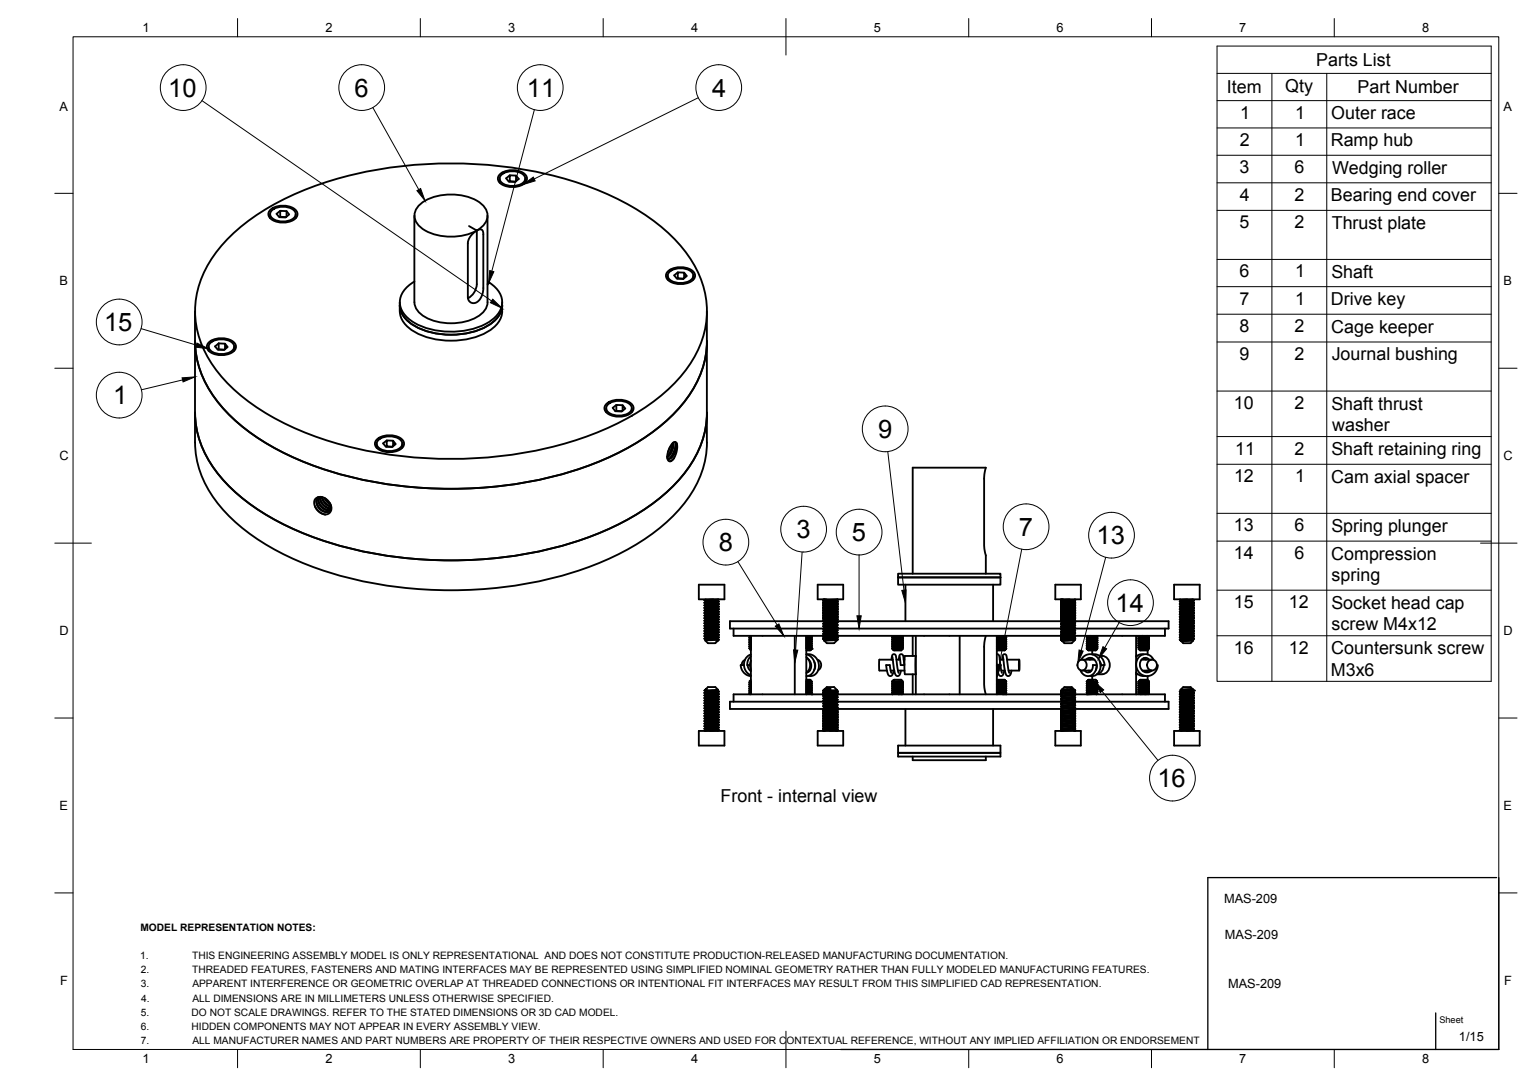
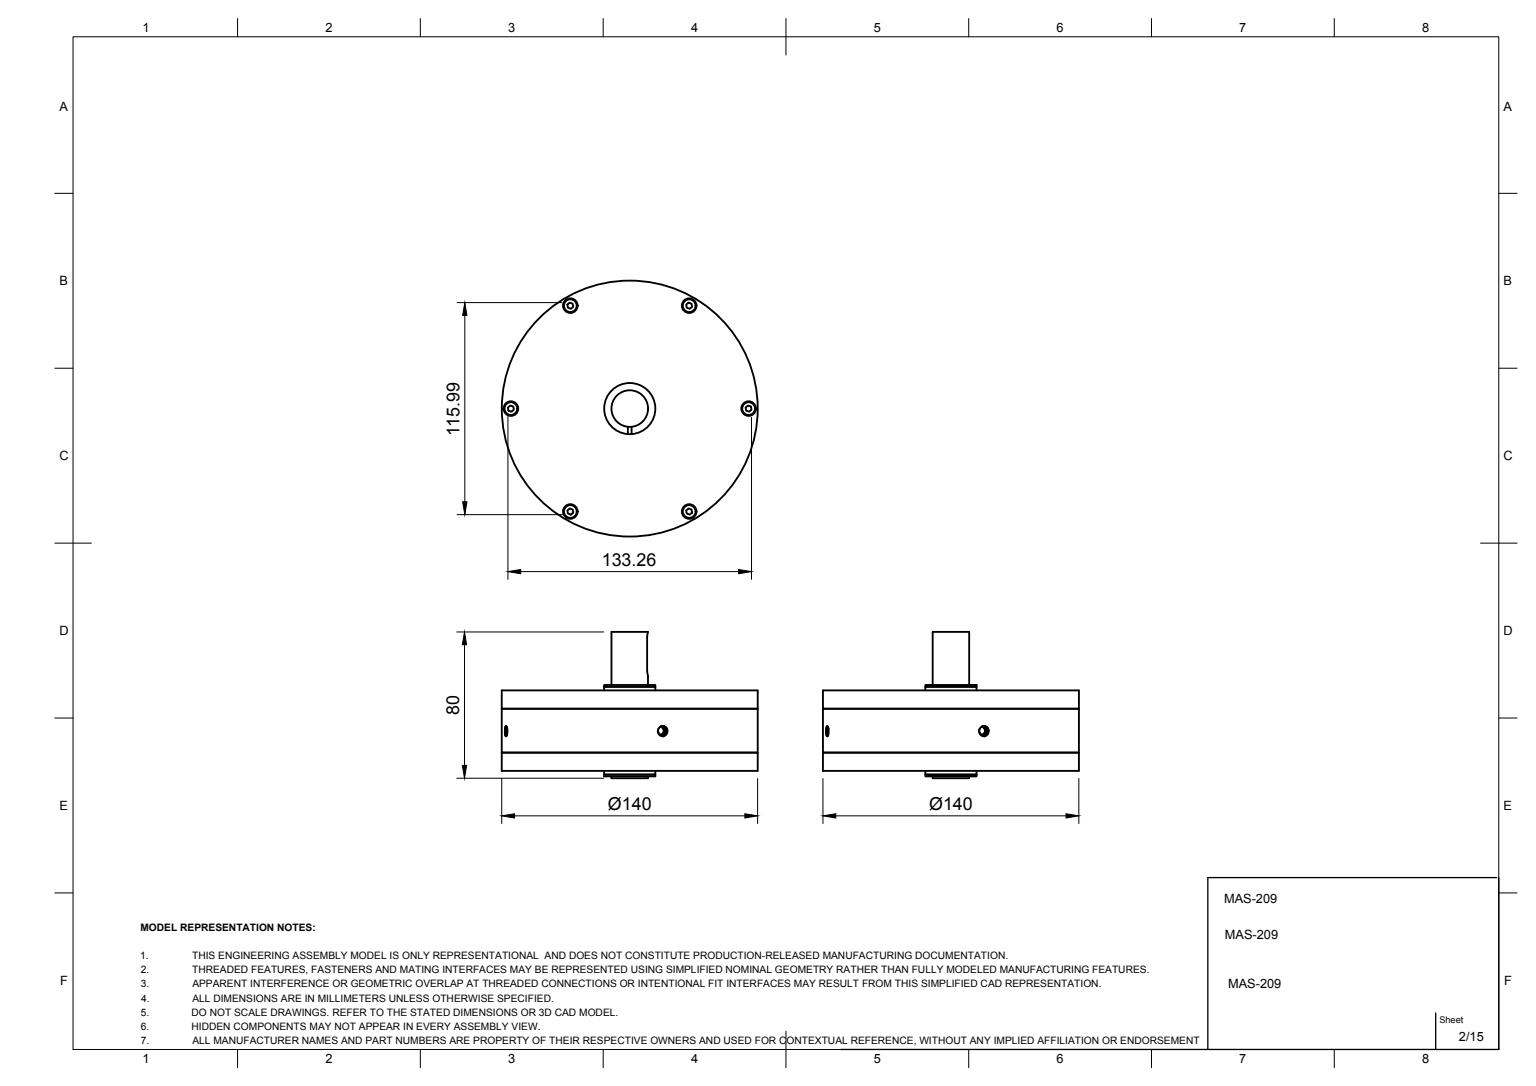
ISO-10303-21;
HEADER;
/* Generated by software containing ST-Developer
 * from STEP Tools, Inc. (www.steptools.com) 
 */

FILE_DESCRIPTION(
/* description */ ('Independent bearing-supported roller-ramp one-way clutch. Six logarit
hmic ramps with plain solid rollers, sprung guided plungers, native Co
il variants, removable shared keepers, rounded parallel key, shaft wit
h complete retaining lips, bronze journal/thrust support and bolted co
vers. Native rotor, roller planar/spin and plunger joints permit manua
l geometric engaged/released inspection. Automatic frictional torque s
witching/contact dynamics are not simulated; no capacity, hardness, fi
t, lubrication, speed, force or life rating. External input driver/cou
pling/anchors outside assembly.'),
/* implementation_level */ '2;1');

FILE_NAME(
/* name */ 'MAS-209.step',
/* time_stamp */ '2026-11-08T07:04:38-08:00',
/* author */ (''),
/* organization */ (''),
/* preprocessor_version */ 'ST-DEVELOPER v20.2',
/* originating_system */ 'Autodesk Translation Framework v15.17.0.0',
/* authorisation */ '');

FILE_SCHEMA (('AUTOMOTIVE_DESIGN { 1 0 10303 214 3 1 1 }'));
ENDSEC;

DATA;
#10=MECHANICAL_DESIGN_GEOMETRIC_PRESENTATION_REPRESENTATION('',(#300,#301,
#302,#303,#304,#305,#306,#307,#308,#309,#310,#311,#312,#313,#314,#315),
#99526);
#11=ITEM_DEFINED_TRANSFORMATION($,$,#18464,#19740);
#12=ITEM_DEFINED_TRANSFORMATION($,$,#18965,#19741);
#13=ITEM_DEFINED_TRANSFORMATION($,$,#19489,#19742);
#14=ITEM_DEFINED_TRANSFORMATION($,$,#19495,#19743);
#15=ITEM_DEFINED_TRANSFORMATION($,$,#19546,#19744);
#16=ITEM_DEFINED_TRANSFORMATION($,$,#19430,#19745);
#17=ITEM_DEFINED_TRANSFORMATION($,$,#19478,#19746);
#18=ITEM_DEFINED_TRANSFORMATION($,$,#19555,#19747);
#19=ITEM_DEFINED_TRANSFORMATION($,$,#19594,#19748);
#20=ITEM_DEFINED_TRANSFORMATION($,$,#19489,#19749);
#21=ITEM_DEFINED_TRANSFORMATION($,$,#19489,#19750);
#22=ITEM_DEFINED_TRANSFORMATION($,$,#19489,#19751);
#23=ITEM_DEFINED_TRANSFORMATION($,$,#19489,#19752);
#24=ITEM_DEFINED_TRANSFORMATION($,$,#19489,#19753);
#25=ITEM_DEFINED_TRANSFORMATION($,$,#19495,#19754);
#26=ITEM_DEFINED_TRANSFORMATION($,$,#19546,#19755);
#27=ITEM_DEFINED_TRANSFORMATION($,$,#19555,#19756);
#28=ITEM_DEFINED_TRANSFORMATION($,$,#19612,#19757);
#29=ITEM_DEFINED_TRANSFORMATION($,$,#19594,#19758);
#30=ITEM_DEFINED_TRANSFORMATION($,$,#19621,#19759);
#31=ITEM_DEFINED_TRANSFORMATION($,$,#19603,#19760);
#32=ITEM_DEFINED_TRANSFORMATION($,$,#19632,#19761);
#33=ITEM_DEFINED_TRANSFORMATION($,$,#19642,#19762);
#34=ITEM_DEFINED_TRANSFORMATION($,$,#19612,#19763);
#35=ITEM_DEFINED_TRANSFORMATION($,$,#19621,#19764);
#36=ITEM_DEFINED_TRANSFORMATION($,$,#19632,#19765);
#37=ITEM_DEFINED_TRANSFORMATION($,$,#19632,#19766);
#38=ITEM_DEFINED_TRANSFORMATION($,$,#19632,#19767);
#39=ITEM_DEFINED_TRANSFORMATION($,$,#19632,#19768);
#40=ITEM_DEFINED_TRANSFORMATION($,$,#19632,#19769);
#41=ITEM_DEFINED_TRANSFORMATION($,$,#19647,#19770);
#42=ITEM_DEFINED_TRANSFORMATION($,$,#19701,#19771);
#43=ITEM_DEFINED_TRANSFORMATION($,$,#19642,#19772);
#44=ITEM_DEFINED_TRANSFORMATION($,$,#19642,#19773);
#45=ITEM_DEFINED_TRANSFORMATION($,$,#19642,#19774);
#46=ITEM_DEFINED_TRANSFORMATION($,$,#19642,#19775);
#47=ITEM_DEFINED_TRANSFORMATION($,$,#19642,#19776);
#48=ITEM_DEFINED_TRANSFORMATION($,$,#19647,#19777);
#49=ITEM_DEFINED_TRANSFORMATION($,$,#19647,#19778);
#50=ITEM_DEFINED_TRANSFORMATION($,$,#19647,#19779);
#51=ITEM_DEFINED_TRANSFORMATION($,$,#19647,#19780);
#52=ITEM_DEFINED_TRANSFORMATION($,$,#19647,#19781);
#53=ITEM_DEFINED_TRANSFORMATION($,$,#19647,#19782);
#54=ITEM_DEFINED_TRANSFORMATION($,$,#19647,#19783);
#55=ITEM_DEFINED_TRANSFORMATION($,$,#19647,#19784);
#56=ITEM_DEFINED_TRANSFORMATION($,$,#19647,#19785);
#57=ITEM_DEFINED_TRANSFORMATION($,$,#19647,#19786);
#58=ITEM_DEFINED_TRANSFORMATION($,$,#19647,#19787);
#59=ITEM_DEFINED_TRANSFORMATION($,$,#19701,#19788);
#60=ITEM_DEFINED_TRANSFORMATION($,$,#19701,#19789);
#61=ITEM_DEFINED_TRANSFORMATION($,$,#19701,#19790);
#62=ITEM_DEFINED_TRANSFORMATION($,$,#19701,#19791);
#63=ITEM_DEFINED_TRANSFORMATION($,$,#19701,#19792);
#64=ITEM_DEFINED_TRANSFORMATION($,$,#19701,#19793);
#65=ITEM_DEFINED_TRANSFORMATION($,$,#19701,#19794);
#66=ITEM_DEFINED_TRANSFORMATION($,$,#19701,#19795);
#67=ITEM_DEFINED_TRANSFORMATION($,$,#19701,#19796);
#68=ITEM_DEFINED_TRANSFORMATION($,$,#19701,#19797);
#69=ITEM_DEFINED_TRANSFORMATION($,$,#19701,#19798);
#70=(
REPRESENTATION_RELATIONSHIP($,$,#99625,#99624)
REPRESENTATION_RELATIONSHIP_WITH_TRANSFORMATION(#11)
SHAPE_REPRESENTATION_RELATIONSHIP()
);
#71=(
REPRESENTATION_RELATIONSHIP($,$,#99626,#99624)
REPRESENTATION_RELATIONSHIP_WITH_TRANSFORMATION(#12)
SHAPE_REPRESENTATION_RELATIONSHIP()
);
#72=(
REPRESENTATION_RELATIONSHIP($,$,#99629,#99624)
REPRESENTATION_RELATIONSHIP_WITH_TRANSFORMATION(#13)
SHAPE_REPRESENTATION_RELATIONSHIP()
);
#73=(
REPRESENTATION_RELATIONSHIP($,$,#99630,#99624)
REPRESENTATION_RELATIONSHIP_WITH_TRANSFORMATION(#14)
SHAPE_REPRESENTATION_RELATIONSHIP()
);
#74=(
REPRESENTATION_RELATIONSHIP($,$,#99631,#99624)
REPRESENTATION_RELATIONSHIP_WITH_TRANSFORMATION(#15)
SHAPE_REPRESENTATION_RELATIONSHIP()
);
#75=(
REPRESENTATION_RELATIONSHIP($,$,#99627,#99624)
REPRESENTATION_RELATIONSHIP_WITH_TRANSFORMATION(#16)
SHAPE_REPRESENTATION_RELATIONSHIP()
);
#76=(
REPRESENTATION_RELATIONSHIP($,$,#99628,#99624)
REPRESENTATION_RELATIONSHIP_WITH_TRANSFORMATION(#17)
SHAPE_REPRESENTATION_RELATIONSHIP()
);
#77=(
REPRESENTATION_RELATIONSHIP($,$,#99632,#99624)
REPRESENTATION_RELATIONSHIP_WITH_TRANSFORMATION(#18)
SHAPE_REPRESENTATION_RELATIONSHIP()
);
#78=(
REPRESENTATION_RELATIONSHIP($,$,#99633,#99624)
REPRESENTATION_RELATIONSHIP_WITH_TRANSFORMATION(#19)
SHAPE_REPRESENTATION_RELATIONSHIP()
);
#79=(
REPRESENTATION_RELATIONSHIP($,$,#99629,#99624)
REPRESENTATION_RELATIONSHIP_WITH_TRANSFORMATION(#20)
SHAPE_REPRESENTATION_RELATIONSHIP()
);
#80=(
REPRESENTATION_RELATIONSHIP($,$,#99629,#99624)
REPRESENTATION_RELATIONSHIP_WITH_TRANSFORMATION(#21)
SHAPE_REPRESENTATION_RELATIONSHIP()
);
#81=(
REPRESENTATION_RELATIONSHIP($,$,#99629,#99624)
REPRESENTATION_RELATIONSHIP_WITH_TRANSFORMATION(#22)
SHAPE_REPRESENTATION_RELATIONSHIP()
);
#82=(
REPRESENTATION_RELATIONSHIP($,$,#99629,#99624)
REPRESENTATION_RELATIONSHIP_WITH_TRANSFORMATION(#23)
SHAPE_REPRESENTATION_RELATIONSHIP()
);
#83=(
REPRESENTATION_RELATIONSHIP($,$,#99629,#99624)
REPRESENTATION_RELATIONSHIP_WITH_TRANSFORMATION(#24)
SHAPE_REPRESENTATION_RELATIONSHIP()
);
#84=(
REPRESENTATION_RELATIONSHIP($,$,#99630,#99624)
REPRESENTATION_RELATIONSHIP_WITH_TRANSFORMATION(#25)
SHAPE_REPRESENTATION_RELATIONSHIP()
);
#85=(
REPRESENTATION_RELATIONSHIP($,$,#99631,#99624)
REPRESENTATION_RELATIONSHIP_WITH_TRANSFORMATION(#26)
SHAPE_REPRESENTATION_RELATIONSHIP()
);
#86=(
REPRESENTATION_RELATIONSHIP($,$,#99632,#99624)
REPRESENTATION_RELATIONSHIP_WITH_TRANSFORMATION(#27)
SHAPE_REPRESENTATION_RELATIONSHIP()
);
#87=(
REPRESENTATION_RELATIONSHIP($,$,#99635,#99624)
REPRESENTATION_RELATIONSHIP_WITH_TRANSFORMATION(#28)
SHAPE_REPRESENTATION_RELATIONSHIP()
);
#88=(
REPRESENTATION_RELATIONSHIP($,$,#99633,#99624)
REPRESENTATION_RELATIONSHIP_WITH_TRANSFORMATION(#29)
SHAPE_REPRESENTATION_RELATIONSHIP()
);
#89=(
REPRESENTATION_RELATIONSHIP($,$,#99636,#99624)
REPRESENTATION_RELATIONSHIP_WITH_TRANSFORMATION(#30)
SHAPE_REPRESENTATION_RELATIONSHIP()
);
#90=(
REPRESENTATION_RELATIONSHIP($,$,#99634,#99624)
REPRESENTATION_RELATIONSHIP_WITH_TRANSFORMATION(#31)
SHAPE_REPRESENTATION_RELATIONSHIP()
);
#91=(
REPRESENTATION_RELATIONSHIP($,$,#99637,#99624)
REPRESENTATION_RELATIONSHIP_WITH_TRANSFORMATION(#32)
SHAPE_REPRESENTATION_RELATIONSHIP()
);
#92=(
REPRESENTATION_RELATIONSHIP($,$,#99638,#99624)
REPRESENTATION_RELATIONSHIP_WITH_TRANSFORMATION(#33)
SHAPE_REPRESENTATION_RELATIONSHIP()
);
#93=(
REPRESENTATION_RELATIONSHIP($,$,#99635,#99624)
REPRESENTATION_RELATIONSHIP_WITH_TRANSFORMATION(#34)
SHAPE_REPRESENTATION_RELATIONSHIP()
);
#94=(
REPRESENTATION_RELATIONSHIP($,$,#99636,#99624)
REPRESENTATION_RELATIONSHIP_WITH_TRANSFORMATION(#35)
SHAPE_REPRESENTATION_RELATIONSHIP()
);
#95=(
REPRESENTATION_RELATIONSHIP($,$,#99637,#99624)
REPRESENTATION_RELATIONSHIP_WITH_TRANSFORMATION(#36)
SHAPE_REPRESENTATION_RELATIONSHIP()
);
#96=(
REPRESENTATION_RELATIONSHIP($,$,#99637,#99624)
REPRESENTATION_RELATIONSHIP_WITH_TRANSFORMATION(#37)
SHAPE_REPRESENTATION_RELATIONSHIP()
);
#97=(
REPRESENTATION_RELATIONSHIP($,$,#99637,#99624)
REPRESENTATION_RELATIONSHIP_WITH_TRANSFORMATION(#38)
SHAPE_REPRESENTATION_RELATIONSHIP()
);
#98=(
REPRESENTATION_RELATIONSHIP($,$,#99637,#99624)
REPRESENTATION_RELATIONSHIP_WITH_TRANSFORMATION(#39)
SHAPE_REPRESENTATION_RELATIONSHIP()
);
#99=(
REPRESENTATION_RELATIONSHIP($,$,#99637,#99624)
REPRESENTATION_RELATIONSHIP_WITH_TRANSFORMATION(#40)
SHAPE_REPRESENTATION_RELATIONSHIP()
);
#100=(
REPRESENTATION_RELATIONSHIP($,$,#99639,#99624)
REPRESENTATION_RELATIONSHIP_WITH_TRANSFORMATION(#41)
SHAPE_REPRESENTATION_RELATIONSHIP()
);
#101=(
REPRESENTATION_RELATIONSHIP($,$,#99640,#99624)
REPRESENTATION_RELATIONSHIP_WITH_TRANSFORMATION(#42)
SHAPE_REPRESENTATION_RELATIONSHIP()
);
#102=(
REPRESENTATION_RELATIONSHIP($,$,#99638,#99624)
REPRESENTATION_RELATIONSHIP_WITH_TRANSFORMATION(#43)
SHAPE_REPRESENTATION_RELATIONSHIP()
);
#103=(
REPRESENTATION_RELATIONSHIP($,$,#99638,#99624)
REPRESENTATION_RELATIONSHIP_WITH_TRANSFORMATION(#44)
SHAPE_REPRESENTATION_RELATIONSHIP()
);
#104=(
REPRESENTATION_RELATIONSHIP($,$,#99638,#99624)
REPRESENTATION_RELATIONSHIP_WITH_TRANSFORMATION(#45)
SHAPE_REPRESENTATION_RELATIONSHIP()
);
#105=(
REPRESENTATION_RELATIONSHIP($,$,#99638,#99624)
REPRESENTATION_RELATIONSHIP_WITH_TRANSFORMATION(#46)
SHAPE_REPRESENTATION_RELATIONSHIP()
);
#106=(
REPRESENTATION_RELATIONSHIP($,$,#99638,#99624)
REPRESENTATION_RELATIONSHIP_WITH_TRANSFORMATION(#47)
SHAPE_REPRESENTATION_RELATIONSHIP()
);
#107=(
REPRESENTATION_RELATIONSHIP($,$,#99639,#99624)
REPRESENTATION_RELATIONSHIP_WITH_TRANSFORMATION(#48)
SHAPE_REPRESENTATION_RELATIONSHIP()
);
#108=(
REPRESENTATION_RELATIONSHIP($,$,#99639,#99624)
REPRESENTATION_RELATIONSHIP_WITH_TRANSFORMATION(#49)
SHAPE_REPRESENTATION_RELATIONSHIP()
);
#109=(
REPRESENTATION_RELATIONSHIP($,$,#99639,#99624)
REPRESENTATION_RELATIONSHIP_WITH_TRANSFORMATION(#50)
SHAPE_REPRESENTATION_RELATIONSHIP()
);
#110=(
REPRESENTATION_RELATIONSHIP($,$,#99639,#99624)
REPRESENTATION_RELATIONSHIP_WITH_TRANSFORMATION(#51)
SHAPE_REPRESENTATION_RELATIONSHIP()
);
#111=(
REPRESENTATION_RELATIONSHIP($,$,#99639,#99624)
REPRESENTATION_RELATIONSHIP_WITH_TRANSFORMATION(#52)
SHAPE_REPRESENTATION_RELATIONSHIP()
);
#112=(
REPRESENTATION_RELATIONSHIP($,$,#99639,#99624)
REPRESENTATION_RELATIONSHIP_WITH_TRANSFORMATION(#53)
SHAPE_REPRESENTATION_RELATIONSHIP()
);
#113=(
REPRESENTATION_RELATIONSHIP($,$,#99639,#99624)
REPRESENTATION_RELATIONSHIP_WITH_TRANSFORMATION(#54)
SHAPE_REPRESENTATION_RELATIONSHIP()
);
#114=(
REPRESENTATION_RELATIONSHIP($,$,#99639,#99624)
REPRESENTATION_RELATIONSHIP_WITH_TRANSFORMATION(#55)
SHAPE_REPRESENTATION_RELATIONSHIP()
);
#115=(
REPRESENTATION_RELATIONSHIP($,$,#99639,#99624)
REPRESENTATION_RELATIONSHIP_WITH_TRANSFORMATION(#56)
SHAPE_REPRESENTATION_RELATIONSHIP()
);
#116=(
REPRESENTATION_RELATIONSHIP($,$,#99639,#99624)
REPRESENTATION_RELATIONSHIP_WITH_TRANSFORMATION(#57)
SHAPE_REPRESENTATION_RELATIONSHIP()
);
#117=(
REPRESENTATION_RELATIONSHIP($,$,#99639,#99624)
REPRESENTATION_RELATIONSHIP_WITH_TRANSFORMATION(#58)
SHAPE_REPRESENTATION_RELATIONSHIP()
);
#118=(
REPRESENTATION_RELATIONSHIP($,$,#99640,#99624)
REPRESENTATION_RELATIONSHIP_WITH_TRANSFORMATION(#59)
SHAPE_REPRESENTATION_RELATIONSHIP()
);
#119=(
REPRESENTATION_RELATIONSHIP($,$,#99640,#99624)
REPRESENTATION_RELATIONSHIP_WITH_TRANSFORMATION(#60)
SHAPE_REPRESENTATION_RELATIONSHIP()
);
#120=(
REPRESENTATION_RELATIONSHIP($,$,#99640,#99624)
REPRESENTATION_RELATIONSHIP_WITH_TRANSFORMATION(#61)
SHAPE_REPRESENTATION_RELATIONSHIP()
);
#121=(
REPRESENTATION_RELATIONSHIP($,$,#99640,#99624)
REPRESENTATION_RELATIONSHIP_WITH_TRANSFORMATION(#62)
SHAPE_REPRESENTATION_RELATIONSHIP()
);
#122=(
REPRESENTATION_RELATIONSHIP($,$,#99640,#99624)
REPRESENTATION_RELATIONSHIP_WITH_TRANSFORMATION(#63)
SHAPE_REPRESENTATION_RELATIONSHIP()
);
#123=(
REPRESENTATION_RELATIONSHIP($,$,#99640,#99624)
REPRESENTATION_RELATIONSHIP_WITH_TRANSFORMATION(#64)
SHAPE_REPRESENTATION_RELATIONSHIP()
);
#124=(
REPRESENTATION_RELATIONSHIP($,$,#99640,#99624)
REPRESENTATION_RELATIONSHIP_WITH_TRANSFORMATION(#65)
SHAPE_REPRESENTATION_RELATIONSHIP()
);
#125=(
REPRESENTATION_RELATIONSHIP($,$,#99640,#99624)
REPRESENTATION_RELATIONSHIP_WITH_TRANSFORMATION(#66)
SHAPE_REPRESENTATION_RELATIONSHIP()
);
#126=(
REPRESENTATION_RELATIONSHIP($,$,#99640,#99624)
REPRESENTATION_RELATIONSHIP_WITH_TRANSFORMATION(#67)
SHAPE_REPRESENTATION_RELATIONSHIP()
);
#127=(
REPRESENTATION_RELATIONSHIP($,$,#99640,#99624)
REPRESENTATION_RELATIONSHIP_WITH_TRANSFORMATION(#68)
SHAPE_REPRESENTATION_RELATIONSHIP()
);
#128=(
REPRESENTATION_RELATIONSHIP($,$,#99640,#99624)
REPRESENTATION_RELATIONSHIP_WITH_TRANSFORMATION(#69)
SHAPE_REPRESENTATION_RELATIONSHIP()
);
#129=CONTEXT_DEPENDENT_SHAPE_REPRESENTATION(#70,#99565);
#130=CONTEXT_DEPENDENT_SHAPE_REPRESENTATION(#71,#99566);
#131=CONTEXT_DEPENDENT_SHAPE_REPRESENTATION(#72,#99567);
#132=CONTEXT_DEPENDENT_SHAPE_REPRESENTATION(#73,#99568);
#133=CONTEXT_DEPENDENT_SHAPE_REPRESENTATION(#74,#99569);
#134=CONTEXT_DEPENDENT_SHAPE_REPRESENTATION(#75,#99570);
#135=CONTEXT_DEPENDENT_SHAPE_REPRESENTATION(#76,#99571);
#136=CONTEXT_DEPENDENT_SHAPE_REPRESENTATION(#77,#99572);
#137=CONTEXT_DEPENDENT_SHAPE_REPRESENTATION(#78,#99573);
#138=CONTEXT_DEPENDENT_SHAPE_REPRESENTATION(#79,#99574);
#139=CONTEXT_DEPENDENT_SHAPE_REPRESENTATION(#80,#99575);
#140=CONTEXT_DEPENDENT_SHAPE_REPRESENTATION(#81,#99576);
#141=CONTEXT_DEPENDENT_SHAPE_REPRESENTATION(#82,#99577);
#142=CONTEXT_DEPENDENT_SHAPE_REPRESENTATION(#83,#99578);
#143=CONTEXT_DEPENDENT_SHAPE_REPRESENTATION(#84,#99579);
#144=CONTEXT_DEPENDENT_SHAPE_REPRESENTATION(#85,#99580);
#145=CONTEXT_DEPENDENT_SHAPE_REPRESENTATION(#86,#99581);
#146=CONTEXT_DEPENDENT_SHAPE_REPRESENTATION(#87,#99582);
#147=CONTEXT_DEPENDENT_SHAPE_REPRESENTATION(#88,#99583);
#148=CONTEXT_DEPENDENT_SHAPE_REPRESENTATION(#89,#99584);
#149=CONTEXT_DEPENDENT_SHAPE_REPRESENTATION(#90,#99585);
#150=CONTEXT_DEPENDENT_SHAPE_REPRESENTATION(#91,#99586);
#151=CONTEXT_DEPENDENT_SHAPE_REPRESENTATION(#92,#99587);
#152=CONTEXT_DEPENDENT_SHAPE_REPRESENTATION(#93,#99588);
#153=CONTEXT_DEPENDENT_SHAPE_REPRESENTATION(#94,#99589);
#154=CONTEXT_DEPENDENT_SHAPE_REPRESENTATION(#95,#99590);
#155=CONTEXT_DEPENDENT_SHAPE_REPRESENTATION(#96,#99591);
#156=CONTEXT_DEPENDENT_SHAPE_REPRESENTATION(#97,#99592);
#157=CONTEXT_DEPENDENT_SHAPE_REPRESENTATION(#98,#99593);
#158=CONTEXT_DEPENDENT_SHAPE_REPRESENTATION(#99,#99594);
#159=CONTEXT_DEPENDENT_SHAPE_REPRESENTATION(#100,#99595);
#160=CONTEXT_DEPENDENT_SHAPE_REPRESENTATION(#101,#99596);
#161=CONTEXT_DEPENDENT_SHAPE_REPRESENTATION(#102,#99597);
#162=CONTEXT_DEPENDENT_SHAPE_REPRESENTATION(#103,#99598);
#163=CONTEXT_DEPENDENT_SHAPE_REPRESENTATION(#104,#99599);
#164=CONTEXT_DEPENDENT_SHAPE_REPRESENTATION(#105,#99600);
#165=CONTEXT_DEPENDENT_SHAPE_REPRESENTATION(#106,#99601);
#166=CONTEXT_DEPENDENT_SHAPE_REPRESENTATION(#107,#99602);
#167=CONTEXT_DEPENDENT_SHAPE_REPRESENTATION(#108,#99603);
#168=CONTEXT_DEPENDENT_SHAPE_REPRESENTATION(#109,#99604);
#169=CONTEXT_DEPENDENT_SHAPE_REPRESENTATION(#110,#99605);
#170=CONTEXT_DEPENDENT_SHAPE_REPRESENTATION(#111,#99606);
#171=CONTEXT_DEPENDENT_SHAPE_REPRESENTATION(#112,#99607);
#172=CONTEXT_DEPENDENT_SHAPE_REPRESENTATION(#113,#99608);
#173=CONTEXT_DEPENDENT_SHAPE_REPRESENTATION(#114,#99609);
#174=CONTEXT_DEPENDENT_SHAPE_REPRESENTATION(#115,#99610);
#175=CONTEXT_DEPENDENT_SHAPE_REPRESENTATION(#116,#99611);
#176=CONTEXT_DEPENDENT_SHAPE_REPRESENTATION(#117,#99612);
#177=CONTEXT_DEPENDENT_SHAPE_REPRESENTATION(#118,#99613);
#178=CONTEXT_DEPENDENT_SHAPE_REPRESENTATION(#119,#99614);
#179=CONTEXT_DEPENDENT_SHAPE_REPRESENTATION(#120,#99615);
#180=CONTEXT_DEPENDENT_SHAPE_REPRESENTATION(#121,#99616);
#181=CONTEXT_DEPENDENT_SHAPE_REPRESENTATION(#122,#99617);
#182=CONTEXT_DEPENDENT_SHAPE_REPRESENTATION(#123,#99618);
#183=CONTEXT_DEPENDENT_SHAPE_REPRESENTATION(#124,#99619);
#184=CONTEXT_DEPENDENT_SHAPE_REPRESENTATION(#125,#99620);
#185=CONTEXT_DEPENDENT_SHAPE_REPRESENTATION(#126,#99621);
#186=CONTEXT_DEPENDENT_SHAPE_REPRESENTATION(#127,#99622);
#187=CONTEXT_DEPENDENT_SHAPE_REPRESENTATION(#128,#99623);
#188=NEXT_ASSEMBLY_USAGE_OCCURRENCE('Outer race:1','Outer race:1',
'Outer race:1',#99642,#99643,'Outer race:1');
#189=NEXT_ASSEMBLY_USAGE_OCCURRENCE('Ramp hub:1','Ramp hub:1',
'Ramp hub:1',#99642,#99644,'Ramp hub:1');
#190=NEXT_ASSEMBLY_USAGE_OCCURRENCE('Wedging roller:1',
'Wedging roller:1','Wedging roller:1',#99642,#99647,'Wedging roller:1');
#191=NEXT_ASSEMBLY_USAGE_OCCURRENCE('Bearing end cover:1',
'Bearing end cover:1','Bearing end cover:1',#99642,#99648,
'Bearing end cover:1');
#192=NEXT_ASSEMBLY_USAGE_OCCURRENCE('Thrust plate:1','Thrust plate:1',
'Thrust plate:1',#99642,#99649,'Thrust plate:1');
#193=NEXT_ASSEMBLY_USAGE_OCCURRENCE('Shaft:1','Shaft:1','Shaft:1',#99642,
#99645,'Shaft:1');
#194=NEXT_ASSEMBLY_USAGE_OCCURRENCE('Drive key:1','Drive key:1',
'Drive key:1',#99642,#99646,'Drive key:1');
#195=NEXT_ASSEMBLY_USAGE_OCCURRENCE('Cage keeper:1','Cage keeper:1',
'Cage keeper:1',#99642,#99650,'Cage keeper:1');
#196=NEXT_ASSEMBLY_USAGE_OCCURRENCE('Journal bushing:1',
'Journal bushing:1','Journal bushing:1',#99642,#99651,
'Journal bushing:1');
#197=NEXT_ASSEMBLY_USAGE_OCCURRENCE('Wedging roller:2',
'Wedging roller:2','Wedging roller:2',#99642,#99647,'Wedging roller:2');
#198=NEXT_ASSEMBLY_USAGE_OCCURRENCE('Wedging roller:3',
'Wedging roller:3','Wedging roller:3',#99642,#99647,'Wedging roller:3');
#199=NEXT_ASSEMBLY_USAGE_OCCURRENCE('Wedging roller:4',
'Wedging roller:4','Wedging roller:4',#99642,#99647,'Wedging roller:4');
#200=NEXT_ASSEMBLY_USAGE_OCCURRENCE('Wedging roller:5',
'Wedging roller:5','Wedging roller:5',#99642,#99647,'Wedging roller:5');
#201=NEXT_ASSEMBLY_USAGE_OCCURRENCE('Wedging roller:6',
'Wedging roller:6','Wedging roller:6',#99642,#99647,'Wedging roller:6');
#202=NEXT_ASSEMBLY_USAGE_OCCURRENCE('Bearing end cover:2',
'Bearing end cover:2','Bearing end cover:2',#99642,#99648,
'Bearing end cover:2');
#203=NEXT_ASSEMBLY_USAGE_OCCURRENCE('Thrust plate:2','Thrust plate:2',
'Thrust plate:2',#99642,#99649,'Thrust plate:2');
#204=NEXT_ASSEMBLY_USAGE_OCCURRENCE('Cage keeper:2','Cage keeper:2',
'Cage keeper:2',#99642,#99650,'Cage keeper:2');
#205=NEXT_ASSEMBLY_USAGE_OCCURRENCE('Shaft thrust washer:1',
'Shaft thrust washer:1','Shaft thrust washer:1',#99642,#99653,
'Shaft thrust washer:1');
#206=NEXT_ASSEMBLY_USAGE_OCCURRENCE('Journal bushing:2',
'Journal bushing:2','Journal bushing:2',#99642,#99651,
'Journal bushing:2');
#207=NEXT_ASSEMBLY_USAGE_OCCURRENCE('Shaft retaining ring:1',
'Shaft retaining ring:1','Shaft retaining ring:1',#99642,#99654,
'Shaft retaining ring:1');
#208=NEXT_ASSEMBLY_USAGE_OCCURRENCE('Cam axial spacer:1',
'Cam axial spacer:1','Cam axial spacer:1',#99642,#99652,
'Cam axial spacer:1');
#209=NEXT_ASSEMBLY_USAGE_OCCURRENCE('Spring plunger:1',
'Spring plunger:1','Spring plunger:1',#99642,#99655,'Spring plunger:1');
#210=NEXT_ASSEMBLY_USAGE_OCCURRENCE('Compression spring:1',
'Compression spring:1','Compression spring:1',#99642,#99656,
'Compression spring:1');
#211=NEXT_ASSEMBLY_USAGE_OCCURRENCE('Shaft thrust washer:2',
'Shaft thrust washer:2','Shaft thrust washer:2',#99642,#99653,
'Shaft thrust washer:2');
#212=NEXT_ASSEMBLY_USAGE_OCCURRENCE('Shaft retaining ring:2',
'Shaft retaining ring:2','Shaft retaining ring:2',#99642,#99654,
'Shaft retaining ring:2');
#213=NEXT_ASSEMBLY_USAGE_OCCURRENCE('Spring plunger:2',
'Spring plunger:2','Spring plunger:2',#99642,#99655,'Spring plunger:2');
#214=NEXT_ASSEMBLY_USAGE_OCCURRENCE('Spring plunger:3',
'Spring plunger:3','Spring plunger:3',#99642,#99655,'Spring plunger:3');
#215=NEXT_ASSEMBLY_USAGE_OCCURRENCE('Spring plunger:4',
'Spring plunger:4','Spring plunger:4',#99642,#99655,'Spring plunger:4');
#216=NEXT_ASSEMBLY_USAGE_OCCURRENCE('Spring plunger:5',
'Spring plunger:5','Spring plunger:5',#99642,#99655,'Spring plunger:5');
#217=NEXT_ASSEMBLY_USAGE_OCCURRENCE('Spring plunger:6',
'Spring plunger:6','Spring plunger:6',#99642,#99655,'Spring plunger:6');
#218=NEXT_ASSEMBLY_USAGE_OCCURRENCE('Socket head cap screw M4x12:1',
'Socket head cap screw M4x12:1','Socket head cap screw M4x12:1',#99642,
#99657,'Socket head cap screw M4x12:1');
#219=NEXT_ASSEMBLY_USAGE_OCCURRENCE('Countersunk screw M3x6:1',
'Countersunk screw M3x6:1','Countersunk screw M3x6:1',#99642,#99658,
'Countersunk screw M3x6:1');
#220=NEXT_ASSEMBLY_USAGE_OCCURRENCE('Compression spring:2',
'Compression spring:2','Compression spring:2',#99642,#99656,
'Compression spring:2');
#221=NEXT_ASSEMBLY_USAGE_OCCURRENCE('Compression spring:3',
'Compression spring:3','Compression spring:3',#99642,#99656,
'Compression spring:3');
#222=NEXT_ASSEMBLY_USAGE_OCCURRENCE('Compression spring:4',
'Compression spring:4','Compression spring:4',#99642,#99656,
'Compression spring:4');
#223=NEXT_ASSEMBLY_USAGE_OCCURRENCE('Compression spring:5',
'Compression spring:5','Compression spring:5',#99642,#99656,
'Compression spring:5');
#224=NEXT_ASSEMBLY_USAGE_OCCURRENCE('Compression spring:6',
'Compression spring:6','Compression spring:6',#99642,#99656,
'Compression spring:6');
#225=NEXT_ASSEMBLY_USAGE_OCCURRENCE('Socket head cap screw M4x12:2',
'Socket head cap screw M4x12:2','Socket head cap screw M4x12:2',#99642,
#99657,'Socket head cap screw M4x12:2');
#226=NEXT_ASSEMBLY_USAGE_OCCURRENCE('Socket head cap screw M4x12:3',
'Socket head cap screw M4x12:3','Socket head cap screw M4x12:3',#99642,
#99657,'Socket head cap screw M4x12:3');
#227=NEXT_ASSEMBLY_USAGE_OCCURRENCE('Socket head cap screw M4x12:4',
'Socket head cap screw M4x12:4','Socket head cap screw M4x12:4',#99642,
#99657,'Socket head cap screw M4x12:4');
#228=NEXT_ASSEMBLY_USAGE_OCCURRENCE('Socket head cap screw M4x12:5',
'Socket head cap screw M4x12:5','Socket head cap screw M4x12:5',#99642,
#99657,'Socket head cap screw M4x12:5');
#229=NEXT_ASSEMBLY_USAGE_OCCURRENCE('Socket head cap screw M4x12:6',
'Socket head cap screw M4x12:6','Socket head cap screw M4x12:6',#99642,
#99657,'Socket head cap screw M4x12:6');
#230=NEXT_ASSEMBLY_USAGE_OCCURRENCE('Socket head cap screw M4x12:7',
'Socket head cap screw M4x12:7','Socket head cap screw M4x12:7',#99642,
#99657,'Socket head cap screw M4x12:7');
#231=NEXT_ASSEMBLY_USAGE_OCCURRENCE('Socket head cap screw M4x12:8',
'Socket head cap screw M4x12:8','Socket head cap screw M4x12:8',#99642,
#99657,'Socket head cap screw M4x12:8');
#232=NEXT_ASSEMBLY_USAGE_OCCURRENCE('Socket head cap screw M4x12:9',
'Socket head cap screw M4x12:9','Socket head cap screw M4x12:9',#99642,
#99657,'Socket head cap screw M4x12:9');
#233=NEXT_ASSEMBLY_USAGE_OCCURRENCE('Socket head cap screw M4x12:10',
'Socket head cap screw M4x12:10','Socket head cap screw M4x12:10',#99642,
#99657,'Socket head cap screw M4x12:10');
#234=NEXT_ASSEMBLY_USAGE_OCCURRENCE('Socket head cap screw M4x12:11',
'Socket head cap screw M4x12:11','Socket head cap screw M4x12:11',#99642,
#99657,'Socket head cap screw M4x12:11');
#235=NEXT_ASSEMBLY_USAGE_OCCURRENCE('Socket head cap screw M4x12:12',
'Socket head cap screw M4x12:12','Socket head cap screw M4x12:12',#99642,
#99657,'Socket head cap screw M4x12:12');
#236=NEXT_ASSEMBLY_USAGE_OCCURRENCE('Countersunk screw M3x6:2',
'Countersunk screw M3x6:2','Countersunk screw M3x6:2',#99642,#99658,
'Countersunk screw M3x6:2');
#237=NEXT_ASSEMBLY_USAGE_OCCURRENCE('Countersunk screw M3x6:3',
'Countersunk screw M3x6:3','Countersunk screw M3x6:3',#99642,#99658,
'Countersunk screw M3x6:3');
#238=NEXT_ASSEMBLY_USAGE_OCCURRENCE('Countersunk screw M3x6:4',
'Countersunk screw M3x6:4','Countersunk screw M3x6:4',#99642,#99658,
'Countersunk screw M3x6:4');
#239=NEXT_ASSEMBLY_USAGE_OCCURRENCE('Countersunk screw M3x6:5',
'Countersunk screw M3x6:5','Countersunk screw M3x6:5',#99642,#99658,
'Countersunk screw M3x6:5');
#240=NEXT_ASSEMBLY_USAGE_OCCURRENCE('Countersunk screw M3x6:6',
'Countersunk screw M3x6:6','Countersunk screw M3x6:6',#99642,#99658,
'Countersunk screw M3x6:6');
#241=NEXT_ASSEMBLY_USAGE_OCCURRENCE('Countersunk screw M3x6:7',
'Countersunk screw M3x6:7','Countersunk screw M3x6:7',#99642,#99658,
'Countersunk screw M3x6:7');
#242=NEXT_ASSEMBLY_USAGE_OCCURRENCE('Countersunk screw M3x6:8',
'Countersunk screw M3x6:8','Countersunk screw M3x6:8',#99642,#99658,
'Countersunk screw M3x6:8');
#243=NEXT_ASSEMBLY_USAGE_OCCURRENCE('Countersunk screw M3x6:9',
'Countersunk screw M3x6:9','Countersunk screw M3x6:9',#99642,#99658,
'Countersunk screw M3x6:9');
#244=NEXT_ASSEMBLY_USAGE_OCCURRENCE('Countersunk screw M3x6:10',
'Countersunk screw M3x6:10','Countersunk screw M3x6:10',#99642,#99658,
'Countersunk screw M3x6:10');
#245=NEXT_ASSEMBLY_USAGE_OCCURRENCE('Countersunk screw M3x6:11',
'Countersunk screw M3x6:11','Countersunk screw M3x6:11',#99642,#99658,
'Countersunk screw M3x6:11');
#246=NEXT_ASSEMBLY_USAGE_OCCURRENCE('Countersunk screw M3x6:12',
'Countersunk screw M3x6:12','Countersunk screw M3x6:12',#99642,#99658,
'Countersunk screw M3x6:12');
#247=CONICAL_SURFACE('',#19556,2.5,0.785398163397448);
#248=CONICAL_SURFACE('',#19561,2.5,0.785398163397448);
#249=CONICAL_SURFACE('',#19566,2.5,0.785398163397448);
#250=CONICAL_SURFACE('',#19571,2.5,0.785398163397448);
#251=CONICAL_SURFACE('',#19576,2.5,0.785398163397448);
#252=CONICAL_SURFACE('',#19581,2.5,0.785398163397448);
#253=CONICAL_SURFACE('',#19682,1.5,0.785398163397449);
#254=CONICAL_SURFACE('',#19720,1.25,0.785398163397449);
#255=CONICAL_SURFACE('',#19738,2.25,0.785398163397448);
#256=(
BOUNDED_SURFACE()
B_SPLINE_SURFACE(5,1,((#70021,#70022),(#70023,#70024),(#70025,#70026),(#70027,
#70028),(#70029,#70030),(#70031,#70032),(#70033,#70034),(#70035,#70036),
(#70037,#70038),(#70039,#70040),(#70041,#70042),(#70043,#70044),(#70045,
#70046),(#70047,#70048),(#70049,#70050),(#70051,#70052),(#70053,#70054),
(#70055,#70056),(#70057,#70058),(#70059,#70060),(#70061,#70062),(#70063,
#70064),(#70065,#70066),(#70067,#70068),(#70069,#70070),(#70071,#70072),
(#70073,#70074),(#70075,#70076),(#70077,#70078),(#70079,#70080),(#70081,
#70082),(#70083,#70084),(#70085,#70086),(#70087,#70088),(#70089,#70090),
(#70091,#70092),(#70093,#70094),(#70095,#70096),(#70097,#70098),(#70099,
#70100),(#70101,#70102),(#70103,#70104),(#70105,#70106),(#70107,#70108),
(#70109,#70110),(#70111,#70112),(#70113,#70114),(#70115,#70116),(#70117,
#70118),(#70119,#70120),(#70121,#70122),(#70123,#70124),(#70125,#70126),
(#70127,#70128),(#70129,#70130),(#70131,#70132),(#70133,#70134),(#70135,
#70136),(#70137,#70138),(#70139,#70140),(#70141,#70142),(#70143,#70144),
(#70145,#70146),(#70147,#70148),(#70149,#70150),(#70151,#70152),(#70153,
#70154),(#70155,#70156),(#70157,#70158),(#70159,#70160),(#70161,#70162),
(#70163,#70164),(#70165,#70166),(#70167,#70168),(#70169,#70170),(#70171,
#70172),(#70173,#70174),(#70175,#70176),(#70177,#70178),(#70179,#70180),
(#70181,#70182),(#70183,#70184),(#70185,#70186),(#70187,#70188),(#70189,
#70190),(#70191,#70192),(#70193,#70194),(#70195,#70196),(#70197,#70198),
(#70199,#70200),(#70201,#70202),(#70203,#70204),(#70205,#70206),(#70207,
#70208),(#70209,#70210),(#70211,#70212),(#70213,#70214),(#70215,#70216),
(#70217,#70218),(#70219,#70220),(#70221,#70222),(#70223,#70224),(#70225,
#70226),(#70227,#70228),(#70229,#70230),(#70231,#70232),(#70233,#70234),
(#70235,#70236),(#70237,#70238),(#70239,#70240),(#70241,#70242),(#70243,
#70244),(#70245,#70246),(#70247,#70248),(#70249,#70250),(#70251,#70252),
(#70253,#70254),(#70255,#70256),(#70257,#70258),(#70259,#70260),(#70261,
#70262),(#70263,#70264),(#70265,#70266),(#70267,#70268),(#70269,#70270),
(#70271,#70272),(#70273,#70274),(#70275,#70276),(#70277,#70278),(#70279,
#70280),(#70281,#70282),(#70283,#70284),(#70285,#70286),(#70287,#70288),
(#70289,#70290),(#70291,#70292),(#70293,#70294),(#70295,#70296),(#70297,
#70298),(#70299,#70300),(#70301,#70302),(#70303,#70304),(#70305,#70306),
(#70307,#70308),(#70309,#70310),(#70311,#70312),(#70313,#70314),(#70315,
#70316),(#70317,#70318),(#70319,#70320),(#70321,#70322),(#70323,#70324),
(#70325,#70326),(#70327,#70328),(#70329,#70330),(#70331,#70332),(#70333,
#70334),(#70335,#70336),(#70337,#70338),(#70339,#70340),(#70341,#70342),
(#70343,#70344),(#70345,#70346),(#70347,#70348),(#70349,#70350),(#70351,
#70352),(#70353,#70354),(#70355,#70356),(#70357,#70358),(#70359,#70360),
(#70361,#70362),(#70363,#70364),(#70365,#70366),(#70367,#70368),(#70369,
#70370),(#70371,#70372),(#70373,#70374),(#70375,#70376),(#70377,#70378),
(#70379,#70380),(#70381,#70382),(#70383,#70384),(#70385,#70386),(#70387,
#70388),(#70389,#70390),(#70391,#70392),(#70393,#70394),(#70395,#70396),
(#70397,#70398),(#70399,#70400),(#70401,#70402),(#70403,#70404),(#70405,
#70406),(#70407,#70408),(#70409,#70410),(#70411,#70412),(#70413,#70414),
(#70415,#70416),(#70417,#70418),(#70419,#70420),(#70421,#70422),(#70423,
#70424),(#70425,#70426),(#70427,#70428),(#70429,#70430),(#70431,#70432),
(#70433,#70434),(#70435,#70436),(#70437,#70438),(#70439,#70440),(#70441,
#70442),(#70443,#70444),(#70445,#70446),(#70447,#70448),(#70449,#70450),
(#70451,#70452),(#70453,#70454),(#70455,#70456),(#70457,#70458),(#70459,
#70460),(#70461,#70462),(#70463,#70464),(#70465,#70466),(#70467,#70468),
(#70469,#70470),(#70471,#70472),(#70473,#70474),(#70475,#70476),(#70477,
#70478),(#70479,#70480),(#70481,#70482),(#70483,#70484),(#70485,#70486),
(#70487,#70488),(#70489,#70490),(#70491,#70492),(#70493,#70494),(#70495,
#70496),(#70497,#70498),(#70499,#70500),(#70501,#70502),(#70503,#70504),
(#70505,#70506),(#70507,#70508),(#70509,#70510),(#70511,#70512),(#70513,
#70514),(#70515,#70516),(#70517,#70518),(#70519,#70520),(#70521,#70522),
(#70523,#70524),(#70525,#70526),(#70527,#70528),(#70529,#70530),(#70531,
#70532),(#70533,#70534),(#70535,#70536),(#70537,#70538),(#70539,#70540),
(#70541,#70542),(#70543,#70544),(#70545,#70546),(#70547,#70548),(#70549,
#70550),(#70551,#70552),(#70553,#70554),(#70555,#70556),(#70557,#70558),
(#70559,#70560),(#70561,#70562),(#70563,#70564),(#70565,#70566),(#70567,
#70568),(#70569,#70570),(#70571,#70572),(#70573,#70574),(#70575,#70576),
(#70577,#70578),(#70579,#70580),(#70581,#70582),(#70583,#70584),(#70585,
#70586),(#70587,#70588),(#70589,#70590),(#70591,#70592),(#70593,#70594),
(#70595,#70596),(#70597,#70598),(#70599,#70600),(#70601,#70602),(#70603,
#70604),(#70605,#70606),(#70607,#70608),(#70609,#70610),(#70611,#70612),
(#70613,#70614),(#70615,#70616),(#70617,#70618),(#70619,#70620),(#70621,
#70622),(#70623,#70624),(#70625,#70626),(#70627,#70628),(#70629,#70630),
(#70631,#70632),(#70633,#70634),(#70635,#70636),(#70637,#70638),(#70639,
#70640),(#70641,#70642),(#70643,#70644),(#70645,#70646),(#70647,#70648),
(#70649,#70650),(#70651,#70652),(#70653,#70654),(#70655,#70656),(#70657,
#70658),(#70659,#70660),(#70661,#70662),(#70663,#70664),(#70665,#70666),
(#70667,#70668),(#70669,#70670),(#70671,#70672),(#70673,#70674),(#70675,
#70676),(#70677,#70678),(#70679,#70680),(#70681,#70682),(#70683,#70684),
(#70685,#70686),(#70687,#70688),(#70689,#70690),(#70691,#70692),(#70693,
#70694),(#70695,#70696),(#70697,#70698),(#70699,#70700),(#70701,#70702),
(#70703,#70704),(#70705,#70706),(#70707,#70708),(#70709,#70710),(#70711,
#70712),(#70713,#70714),(#70715,#70716),(#70717,#70718),(#70719,#70720),
(#70721,#70722),(#70723,#70724),(#70725,#70726),(#70727,#70728),(#70729,
#70730),(#70731,#70732),(#70733,#70734),(#70735,#70736),(#70737,#70738),
(#70739,#70740),(#70741,#70742),(#70743,#70744),(#70745,#70746),(#70747,
#70748),(#70749,#70750),(#70751,#70752),(#70753,#70754),(#70755,#70756),
(#70757,#70758),(#70759,#70760),(#70761,#70762),(#70763,#70764),(#70765,
#70766),(#70767,#70768),(#70769,#70770),(#70771,#70772),(#70773,#70774),
(#70775,#70776),(#70777,#70778),(#70779,#70780),(#70781,#70782),(#70783,
#70784),(#70785,#70786),(#70787,#70788),(#70789,#70790),(#70791,#70792),
(#70793,#70794),(#70795,#70796),(#70797,#70798),(#70799,#70800),(#70801,
#70802),(#70803,#70804),(#70805,#70806),(#70807,#70808),(#70809,#70810),
(#70811,#70812),(#70813,#70814),(#70815,#70816),(#70817,#70818),(#70819,
#70820),(#70821,#70822),(#70823,#70824),(#70825,#70826),(#70827,#70828),
(#70829,#70830),(#70831,#70832),(#70833,#70834),(#70835,#70836),(#70837,
#70838),(#70839,#70840),(#70841,#70842),(#70843,#70844),(#70845,#70846),
(#70847,#70848),(#70849,#70850),(#70851,#70852),(#70853,#70854),(#70855,
#70856),(#70857,#70858),(#70859,#70860),(#70861,#70862),(#70863,#70864),
(#70865,#70866),(#70867,#70868),(#70869,#70870),(#70871,#70872),(#70873,
#70874),(#70875,#70876),(#70877,#70878),(#70879,#70880),(#70881,#70882),
(#70883,#70884),(#70885,#70886),(#70887,#70888),(#70889,#70890),(#70891,
#70892),(#70893,#70894),(#70895,#70896),(#70897,#70898),(#70899,#70900),
(#70901,#70902),(#70903,#70904),(#70905,#70906),(#70907,#70908),(#70909,
#70910),(#70911,#70912),(#70913,#70914),(#70915,#70916),(#70917,#70918),
(#70919,#70920),(#70921,#70922),(#70923,#70924),(#70925,#70926),(#70927,
#70928),(#70929,#70930),(#70931,#70932),(#70933,#70934),(#70935,#70936),
(#70937,#70938),(#70939,#70940),(#70941,#70942),(#70943,#70944),(#70945,
#70946),(#70947,#70948),(#70949,#70950),(#70951,#70952),(#70953,#70954),
(#70955,#70956),(#70957,#70958),(#70959,#70960),(#70961,#70962),(#70963,
#70964),(#70965,#70966),(#70967,#70968),(#70969,#70970),(#70971,#70972),
(#70973,#70974),(#70975,#70976),(#70977,#70978),(#70979,#70980),(#70981,
#70982),(#70983,#70984),(#70985,#70986),(#70987,#70988),(#70989,#70990),
(#70991,#70992),(#70993,#70994),(#70995,#70996),(#70997,#70998),(#70999,
#71000),(#71001,#71002),(#71003,#71004),(#71005,#71006),(#71007,#71008),
(#71009,#71010),(#71011,#71012),(#71013,#71014),(#71015,#71016),(#71017,
#71018),(#71019,#71020),(#71021,#71022),(#71023,#71024),(#71025,#71026),
(#71027,#71028),(#71029,#71030),(#71031,#71032),(#71033,#71034),(#71035,
#71036),(#71037,#71038),(#71039,#71040),(#71041,#71042),(#71043,#71044),
(#71045,#71046),(#71047,#71048),(#71049,#71050),(#71051,#71052),(#71053,
#71054),(#71055,#71056),(#71057,#71058),(#71059,#71060),(#71061,#71062),
(#71063,#71064),(#71065,#71066),(#71067,#71068),(#71069,#71070),(#71071,
#71072),(#71073,#71074),(#71075,#71076),(#71077,#71078),(#71079,#71080),
(#71081,#71082),(#71083,#71084),(#71085,#71086),(#71087,#71088),(#71089,
#71090),(#71091,#71092),(#71093,#71094),(#71095,#71096),(#71097,#71098),
(#71099,#71100),(#71101,#71102),(#71103,#71104),(#71105,#71106),(#71107,
#71108),(#71109,#71110),(#71111,#71112),(#71113,#71114),(#71115,#71116),
(#71117,#71118),(#71119,#71120),(#71121,#71122),(#71123,#71124),(#71125,
#71126),(#71127,#71128),(#71129,#71130),(#71131,#71132),(#71133,#71134),
(#71135,#71136),(#71137,#71138),(#71139,#71140),(#71141,#71142),(#71143,
#71144),(#71145,#71146),(#71147,#71148),(#71149,#71150),(#71151,#71152),
(#71153,#71154),(#71155,#71156),(#71157,#71158),(#71159,#71160),(#71161,
#71162),(#71163,#71164),(#71165,#71166),(#71167,#71168),(#71169,#71170),
(#71171,#71172),(#71173,#71174),(#71175,#71176),(#71177,#71178),(#71179,
#71180),(#71181,#71182),(#71183,#71184),(#71185,#71186),(#71187,#71188),
(#71189,#71190),(#71191,#71192),(#71193,#71194),(#71195,#71196),(#71197,
#71198),(#71199,#71200),(#71201,#71202),(#71203,#71204),(#71205,#71206),
(#71207,#71208),(#71209,#71210),(#71211,#71212),(#71213,#71214),(#71215,
#71216),(#71217,#71218),(#71219,#71220),(#71221,#71222),(#71223,#71224),
(#71225,#71226),(#71227,#71228),(#71229,#71230),(#71231,#71232),(#71233,
#71234),(#71235,#71236),(#71237,#71238),(#71239,#71240),(#71241,#71242),
(#71243,#71244),(#71245,#71246),(#71247,#71248),(#71249,#71250),(#71251,
#71252),(#71253,#71254),(#71255,#71256),(#71257,#71258),(#71259,#71260),
(#71261,#71262),(#71263,#71264),(#71265,#71266),(#71267,#71268),(#71269,
#71270),(#71271,#71272),(#71273,#71274),(#71275,#71276),(#71277,#71278),
(#71279,#71280),(#71281,#71282),(#71283,#71284),(#71285,#71286),(#71287,
#71288),(#71289,#71290),(#71291,#71292),(#71293,#71294),(#71295,#71296),
(#71297,#71298),(#71299,#71300),(#71301,#71302),(#71303,#71304),(#71305,
#71306),(#71307,#71308),(#71309,#71310),(#71311,#71312),(#71313,#71314),
(#71315,#71316),(#71317,#71318),(#71319,#71320),(#71321,#71322),(#71323,
#71324),(#71325,#71326),(#71327,#71328),(#71329,#71330),(#71331,#71332),
(#71333,#71334),(#71335,#71336),(#71337,#71338),(#71339,#71340),(#71341,
#71342),(#71343,#71344),(#71345,#71346),(#71347,#71348),(#71349,#71350),
(#71351,#71352),(#71353,#71354),(#71355,#71356),(#71357,#71358),(#71359,
#71360),(#71361,#71362),(#71363,#71364),(#71365,#71366),(#71367,#71368),
(#71369,#71370),(#71371,#71372),(#71373,#71374),(#71375,#71376),(#71377,
#71378),(#71379,#71380),(#71381,#71382),(#71383,#71384),(#71385,#71386),
(#71387,#71388),(#71389,#71390),(#71391,#71392),(#71393,#71394),(#71395,
#71396),(#71397,#71398),(#71399,#71400),(#71401,#71402),(#71403,#71404),
(#71405,#71406),(#71407,#71408),(#71409,#71410),(#71411,#71412),(#71413,
#71414),(#71415,#71416),(#71417,#71418),(#71419,#71420),(#71421,#71422),
(#71423,#71424),(#71425,#71426),(#71427,#71428),(#71429,#71430),(#71431,
#71432),(#71433,#71434),(#71435,#71436),(#71437,#71438),(#71439,#71440),
(#71441,#71442),(#71443,#71444),(#71445,#71446),(#71447,#71448),(#71449,
#71450),(#71451,#71452),(#71453,#71454),(#71455,#71456),(#71457,#71458),
(#71459,#71460),(#71461,#71462),(#71463,#71464),(#71465,#71466),(#71467,
#71468),(#71469,#71470),(#71471,#71472),(#71473,#71474),(#71475,#71476),
(#71477,#71478),(#71479,#71480),(#71481,#71482),(#71483,#71484),(#71485,
#71486),(#71487,#71488),(#71489,#71490),(#71491,#71492),(#71493,#71494),
(#71495,#71496),(#71497,#71498),(#71499,#71500),(#71501,#71502),(#71503,
#71504),(#71505,#71506),(#71507,#71508),(#71509,#71510),(#71511,#71512),
(#71513,#71514),(#71515,#71516),(#71517,#71518),(#71519,#71520),(#71521,
#71522),(#71523,#71524),(#71525,#71526),(#71527,#71528),(#71529,#71530),
(#71531,#71532),(#71533,#71534),(#71535,#71536),(#71537,#71538),(#71539,
#71540),(#71541,#71542),(#71543,#71544),(#71545,#71546),(#71547,#71548),
(#71549,#71550),(#71551,#71552),(#71553,#71554),(#71555,#71556),(#71557,
#71558),(#71559,#71560),(#71561,#71562),(#71563,#71564),(#71565,#71566),
(#71567,#71568),(#71569,#71570),(#71571,#71572),(#71573,#71574),(#71575,
#71576),(#71577,#71578),(#71579,#71580),(#71581,#71582),(#71583,#71584),
(#71585,#71586),(#71587,#71588),(#71589,#71590),(#71591,#71592),(#71593,
#71594),(#71595,#71596),(#71597,#71598),(#71599,#71600),(#71601,#71602),
(#71603,#71604),(#71605,#71606),(#71607,#71608),(#71609,#71610),(#71611,
#71612),(#71613,#71614),(#71615,#71616),(#71617,#71618),(#71619,#71620),
(#71621,#71622),(#71623,#71624),(#71625,#71626),(#71627,#71628),(#71629,
#71630),(#71631,#71632),(#71633,#71634),(#71635,#71636),(#71637,#71638),
(#71639,#71640),(#71641,#71642),(#71643,#71644),(#71645,#71646),(#71647,
#71648),(#71649,#71650),(#71651,#71652),(#71653,#71654),(#71655,#71656),
(#71657,#71658),(#71659,#71660),(#71661,#71662),(#71663,#71664),(#71665,
#71666),(#71667,#71668),(#71669,#71670),(#71671,#71672),(#71673,#71674),
(#71675,#71676),(#71677,#71678),(#71679,#71680),(#71681,#71682),(#71683,
#71684),(#71685,#71686),(#71687,#71688),(#71689,#71690),(#71691,#71692),
(#71693,#71694),(#71695,#71696),(#71697,#71698),(#71699,#71700),(#71701,
#71702),(#71703,#71704),(#71705,#71706),(#71707,#71708),(#71709,#71710),
(#71711,#71712),(#71713,#71714),(#71715,#71716),(#71717,#71718),(#71719,
#71720),(#71721,#71722),(#71723,#71724),(#71725,#71726),(#71727,#71728),
(#71729,#71730),(#71731,#71732),(#71733,#71734),(#71735,#71736),(#71737,
#71738),(#71739,#71740),(#71741,#71742),(#71743,#71744),(#71745,#71746),
(#71747,#71748),(#71749,#71750),(#71751,#71752),(#71753,#71754),(#71755,
#71756),(#71757,#71758),(#71759,#71760),(#71761,#71762),(#71763,#71764),
(#71765,#71766),(#71767,#71768),(#71769,#71770),(#71771,#71772),(#71773,
#71774),(#71775,#71776),(#71777,#71778),(#71779,#71780),(#71781,#71782),
(#71783,#71784),(#71785,#71786),(#71787,#71788),(#71789,#71790),(#71791,
#71792),(#71793,#71794),(#71795,#71796),(#71797,#71798),(#71799,#71800),
(#71801,#71802),(#71803,#71804),(#71805,#71806),(#71807,#71808),(#71809,
#71810),(#71811,#71812),(#71813,#71814),(#71815,#71816),(#71817,#71818),
(#71819,#71820),(#71821,#71822),(#71823,#71824),(#71825,#71826),(#71827,
#71828),(#71829,#71830),(#71831,#71832),(#71833,#71834),(#71835,#71836),
(#71837,#71838),(#71839,#71840),(#71841,#71842),(#71843,#71844),(#71845,
#71846),(#71847,#71848),(#71849,#71850),(#71851,#71852),(#71853,#71854),
(#71855,#71856),(#71857,#71858),(#71859,#71860),(#71861,#71862),(#71863,
#71864),(#71865,#71866),(#71867,#71868),(#71869,#71870),(#71871,#71872),
(#71873,#71874),(#71875,#71876),(#71877,#71878),(#71879,#71880),(#71881,
#71882),(#71883,#71884),(#71885,#71886),(#71887,#71888),(#71889,#71890),
(#71891,#71892),(#71893,#71894),(#71895,#71896),(#71897,#71898),(#71899,
#71900),(#71901,#71902),(#71903,#71904),(#71905,#71906),(#71907,#71908),
(#71909,#71910),(#71911,#71912),(#71913,#71914),(#71915,#71916),(#71917,
#71918),(#71919,#71920),(#71921,#71922),(#71923,#71924),(#71925,#71926),
(#71927,#71928),(#71929,#71930),(#71931,#71932),(#71933,#71934),(#71935,
#71936),(#71937,#71938),(#71939,#71940),(#71941,#71942),(#71943,#71944),
(#71945,#71946),(#71947,#71948),(#71949,#71950),(#71951,#71952),(#71953,
#71954),(#71955,#71956),(#71957,#71958),(#71959,#71960),(#71961,#71962),
(#71963,#71964),(#71965,#71966),(#71967,#71968),(#71969,#71970),(#71971,
#71972),(#71973,#71974),(#71975,#71976),(#71977,#71978),(#71979,#71980),
(#71981,#71982),(#71983,#71984),(#71985,#71986),(#71987,#71988),(#71989,
#71990),(#71991,#71992),(#71993,#71994),(#71995,#71996),(#71997,#71998),
(#71999,#72000),(#72001,#72002),(#72003,#72004),(#72005,#72006),(#72007,
#72008),(#72009,#72010),(#72011,#72012),(#72013,#72014),(#72015,#72016),
(#72017,#72018),(#72019,#72020),(#72021,#72022),(#72023,#72024),(#72025,
#72026),(#72027,#72028),(#72029,#72030)),.UNSPECIFIED.,.F.,.F.,.F.)
B_SPLINE_SURFACE_WITH_KNOTS((6,1,1,1,1,1,1,1,1,1,1,1,1,1,1,1,1,1,1,1,1,
1,1,1,1,1,1,1,1,1,1,1,1,1,1,1,1,1,1,1,1,1,1,1,1,1,1,1,1,1,1,1,1,1,1,1,1,
1,1,1,1,1,1,1,1,1,1,1,1,1,1,1,1,1,1,1,1,1,1,1,1,1,1,1,1,1,1,1,1,1,1,1,1,
1,1,1,1,1,1,1,1,1,1,1,1,1,1,1,1,1,1,1,1,1,1,1,1,1,1,1,1,1,1,1,1,1,1,1,1,
1,1,1,1,1,1,1,1,1,1,1,1,1,1,1,1,1,1,1,1,1,1,1,1,1,1,1,1,1,1,1,1,1,1,1,1,
1,1,1,1,1,1,1,1,1,1,1,1,1,1,1,1,1,1,1,1,1,1,1,1,1,1,1,1,1,1,1,1,1,1,1,1,
1,1,1,1,1,1,1,1,1,1,1,1,1,1,1,1,1,1,1,1,1,1,1,1,1,1,1,1,1,1,1,1,1,1,1,1,
1,1,1,1,1,1,1,1,1,1,1,1,1,1,1,1,1,1,1,1,1,1,1,1,1,1,1,1,1,1,1,1,1,1,1,1,
1,1,1,1,1,1,1,1,1,1,1,1,1,1,1,1,1,1,1,1,1,1,1,1,1,1,1,1,1,1,1,1,1,1,1,1,
1,1,1,1,1,1,1,1,1,1,1,1,1,1,1,1,1,1,1,1,1,1,1,1,1,1,1,1,1,1,1,1,1,1,1,1,
1,1,1,1,1,1,1,1,1,1,1,1,1,1,1,1,1,1,1,1,1,1,1,1,1,1,1,1,1,1,1,1,1,1,1,1,
1,1,1,1,1,1,1,1,1,1,1,1,1,1,1,1,1,1,1,1,1,1,1,1,1,1,1,1,1,1,1,1,1,1,1,1,
1,1,1,1,1,1,1,1,1,1,1,1,1,1,1,1,1,1,1,1,1,1,1,1,1,1,1,1,1,1,1,1,1,1,1,1,
1,1,1,1,1,1,1,1,1,1,1,1,1,1,1,1,1,1,1,1,1,1,1,1,1,1,1,1,1,1,1,1,1,1,1,1,
1,1,1,1,1,1,1,1,1,1,1,1,1,1,1,1,1,1,1,1,1,1,1,1,1,1,1,1,1,1,1,1,1,1,1,1,
1,1,1,1,1,1,1,1,1,1,1,1,1,1,1,1,1,1,1,1,1,1,1,1,1,1,1,1,1,1,1,1,1,1,1,1,
1,1,1,1,1,1,1,1,1,1,1,1,1,1,1,1,1,1,1,1,1,1,1,1,1,1,1,1,1,1,1,1,1,1,1,1,
1,1,1,1,1,1,1,1,1,1,1,1,1,1,1,1,1,1,1,1,1,1,1,1,1,1,1,1,1,1,1,1,1,1,1,1,
1,1,1,1,1,1,1,1,1,1,1,1,1,1,1,1,1,1,1,1,1,1,1,1,1,1,1,1,1,1,1,1,1,1,1,1,
1,1,1,1,1,1,1,1,1,1,1,1,1,1,1,1,1,1,1,1,1,1,1,1,1,1,1,1,1,1,1,1,1,1,1,1,
1,1,1,1,1,1,1,1,1,1,1,1,1,1,1,1,1,1,1,1,1,1,1,1,1,1,1,1,1,1,1,1,1,1,1,1,
1,1,1,1,1,1,1,1,1,1,1,1,1,1,1,1,1,1,1,1,1,1,1,1,1,1,1,1,1,1,1,1,1,1,1,1,
1,1,1,1,1,1,1,1,1,1,1,1,1,1,1,1,1,1,1,1,1,1,1,1,1,1,1,1,1,1,1,1,1,1,1,1,
1,1,1,1,1,1,1,1,1,1,1,1,1,1,1,1,1,1,1,1,1,1,1,1,1,1,1,1,1,1,1,1,1,1,1,1,
1,1,1,1,1,1,1,1,1,1,1,1,1,1,1,1,1,1,1,1,1,1,1,1,1,1,1,1,1,1,1,1,1,1,1,1,
1,1,1,1,1,1,1,1,1,1,1,1,1,1,1,1,1,1,1,1,1,1,1,1,1,1,1,1,1,1,1,1,1,1,1,1,
1,1,1,1,1,1,1,1,1,1,1,1,1,1,1,1,1,1,1,1,1,1,1,1,1,1,1,1,1,1,1,1,1,1,1,1,
1,1,1,1,1,1,1,1,1,1,1,1,1,1,1,1,1,1,1,1,1,1,1,1,1,1,1,1,1,1,1,1,1,1,1,1,
1,1,1,1,1,1,1,6),(2,2),(-1.,-0.999000000000001,-0.998000000000001,-0.997000000000001,
-0.996000000000001,-0.995000000000001,-0.994000000000001,-0.993000000000001,
-0.992000000000001,-0.991000000000001,-0.990000000000001,-0.989000000000001,
-0.988000000000001,-0.987000000000001,-0.986000000000001,-0.985000000000001,
-0.984000000000001,-0.983000000000001,-0.982000000000001,-0.981000000000001,
-0.980000000000001,-0.979000000000001,-0.978000000000001,-0.977000000000001,
-0.976000000000001,-0.975000000000001,-0.974000000000001,-0.973000000000001,
-0.972000000000001,-0.971000000000001,-0.970000000000001,-0.969000000000001,
-0.968000000000001,-0.967000000000001,-0.966000000000001,-0.965000000000001,
-0.964000000000001,-0.963000000000001,-0.962000000000001,-0.961000000000001,
-0.960000000000001,-0.959000000000001,-0.958000000000001,-0.957000000000001,
-0.956000000000001,-0.955000000000001,-0.954000000000001,-0.953000000000001,
-0.952000000000001,-0.951000000000001,-0.950000000000001,-0.949000000000001,
-0.948000000000001,-0.947000000000001,-0.946000000000001,-0.945000000000001,
-0.944000000000001,-0.943000000000001,-0.942000000000001,-0.941000000000001,
-0.940000000000001,-0.939000000000001,-0.938000000000001,-0.937000000000001,
-0.936000000000001,-0.935000000000001,-0.934000000000001,-0.933000000000001,
-0.932000000000001,-0.931000000000001,-0.930000000000001,-0.929000000000001,
-0.928000000000001,-0.927000000000001,-0.926000000000001,-0.925000000000001,
-0.924000000000001,-0.923000000000001,-0.922000000000001,-0.921000000000001,
-0.920000000000001,-0.919000000000001,-0.918000000000001,-0.917000000000001,
-0.916000000000001,-0.915000000000001,-0.914000000000001,-0.913000000000001,
-0.912000000000001,-0.911000000000001,-0.910000000000001,-0.909000000000001,
-0.908000000000001,-0.907000000000001,-0.906000000000001,-0.905000000000001,
-0.904000000000001,-0.903000000000001,-0.902000000000001,-0.901000000000001,
-0.900000000000001,-0.899000000000001,-0.898000000000001,-0.897000000000001,
-0.896000000000001,-0.895000000000001,-0.894000000000001,-0.893000000000001,
-0.892000000000001,-0.891000000000001,-0.890000000000001,-0.889000000000001,
-0.888000000000001,-0.887000000000001,-0.886000000000001,-0.885000000000001,
-0.884000000000001,-0.883000000000001,-0.882000000000001,-0.881000000000001,
-0.880000000000001,-0.879000000000001,-0.878000000000001,-0.877000000000001,
-0.876000000000001,-0.875000000000001,-0.874000000000001,-0.873000000000001,
-0.872000000000001,-0.871000000000001,-0.870000000000001,-0.869000000000001,
-0.868000000000001,-0.867000000000001,-0.866000000000001,-0.865000000000001,
-0.864000000000001,-0.863000000000001,-0.862000000000001,-0.861000000000001,
-0.860000000000001,-0.859000000000001,-0.858000000000001,-0.857000000000001,
-0.856000000000001,-0.855000000000001,-0.854000000000001,-0.853000000000001,
-0.852000000000001,-0.851000000000001,-0.850000000000001,-0.849000000000001,
-0.848000000000001,-0.847000000000001,-0.846000000000001,-0.845000000000001,
-0.844000000000001,-0.843000000000001,-0.842000000000001,-0.841000000000001,
-0.840000000000001,-0.839000000000001,-0.838000000000001,-0.837000000000001,
-0.836000000000001,-0.835000000000001,-0.834000000000001,-0.833000000000001,
-0.832000000000001,-0.831000000000001,-0.830000000000001,-0.829000000000001,
-0.828000000000001,-0.827000000000001,-0.826000000000001,-0.825000000000001,
-0.824000000000001,-0.823000000000001,-0.822000000000001,-0.821000000000001,
-0.820000000000001,-0.819000000000001,-0.818000000000001,-0.817000000000001,
-0.816000000000001,-0.815000000000001,-0.814000000000001,-0.813000000000001,
-0.812000000000001,-0.811000000000001,-0.810000000000001,-0.809000000000001,
-0.808000000000001,-0.807000000000001,-0.806000000000001,-0.805000000000001,
-0.804000000000001,-0.803000000000001,-0.802000000000001,-0.801000000000001,
-0.800000000000001,-0.799000000000001,-0.798000000000001,-0.797000000000001,
-0.796000000000001,-0.795000000000001,-0.794000000000001,-0.793000000000001,
-0.792000000000001,-0.791000000000001,-0.790000000000001,-0.789000000000001,
-0.788000000000001,-0.787000000000001,-0.786000000000001,-0.785000000000001,
-0.784000000000001,-0.783000000000001,-0.782000000000001,-0.781000000000001,
-0.780000000000001,-0.779000000000001,-0.778000000000001,-0.777000000000001,
-0.776000000000001,-0.775000000000001,-0.774000000000001,-0.773000000000001,
-0.772000000000001,-0.771000000000001,-0.770000000000001,-0.769000000000001,
-0.768000000000001,-0.767000000000001,-0.766000000000001,-0.765000000000001,
-0.764000000000001,-0.763000000000001,-0.762000000000001,-0.761000000000001,
-0.760000000000001,-0.759000000000001,-0.758000000000001,-0.757000000000001,
-0.756000000000001,-0.755000000000001,-0.754000000000001,-0.753000000000001,
-0.752000000000001,-0.751000000000001,-0.750000000000001,-0.749000000000001,
-0.748000000000001,-0.747000000000001,-0.746000000000001,-0.745000000000001,
-0.744000000000001,-0.743000000000001,-0.742000000000001,-0.741000000000001,
-0.740000000000001,-0.739000000000001,-0.738000000000001,-0.737000000000001,
-0.736000000000001,-0.735000000000001,-0.734000000000001,-0.733000000000001,
-0.732000000000001,-0.731000000000001,-0.730000000000001,-0.729000000000001,
-0.728000000000001,-0.727000000000001,-0.726000000000001,-0.725000000000001,
-0.724000000000001,-0.723000000000001,-0.722000000000001,-0.721000000000001,
-0.720000000000001,-0.719000000000001,-0.718000000000001,-0.717000000000001,
-0.716000000000001,-0.715000000000001,-0.714000000000001,-0.713000000000001,
-0.712000000000001,-0.711000000000001,-0.710000000000001,-0.709000000000001,
-0.708000000000001,-0.707000000000001,-0.706000000000001,-0.705000000000001,
-0.704000000000001,-0.703000000000001,-0.702000000000001,-0.701000000000001,
-0.700000000000001,-0.699000000000001,-0.698000000000001,-0.697000000000001,
-0.696000000000001,-0.695000000000001,-0.694000000000001,-0.693000000000001,
-0.692000000000001,-0.691000000000001,-0.690000000000001,-0.689000000000001,
-0.688000000000001,-0.687,-0.686,-0.685,-0.684,-0.683,-0.682,-0.681,-0.68,
-0.679,-0.678,-0.677,-0.676,-0.675,-0.674,-0.673,-0.672,-0.671,-0.67,-0.669,
-0.668,-0.667,-0.666,-0.665,-0.664,-0.663,-0.662,-0.661,-0.66,-0.659,-0.658,
-0.657,-0.656,-0.655,-0.654,-0.653,-0.652,-0.651,-0.65,-0.649,-0.648,-0.647,
-0.646,-0.645,-0.644,-0.643,-0.642,-0.641,-0.64,-0.639,-0.638,-0.637,-0.636,
-0.635,-0.634,-0.633,-0.632,-0.631,-0.63,-0.629,-0.628,-0.627,-0.626,-0.625,
-0.624,-0.623,-0.622,-0.621,-0.62,-0.619,-0.618,-0.617,-0.616,-0.615,-0.614,
-0.613,-0.612,-0.611,-0.61,-0.609,-0.608,-0.607,-0.606,-0.605,-0.604,-0.603,
-0.602,-0.601,-0.6,-0.599,-0.598,-0.597,-0.596,-0.595,-0.594,-0.593,-0.592,
-0.591,-0.59,-0.589,-0.588,-0.587,-0.586,-0.585,-0.584,-0.583,-0.582,-0.581,
-0.58,-0.579,-0.578,-0.577,-0.576,-0.575,-0.574,-0.573,-0.572,-0.571,-0.57,
-0.569,-0.568,-0.567,-0.566,-0.565,-0.564,-0.563,-0.562,-0.561,-0.56,-0.559,
-0.558,-0.557,-0.556,-0.555,-0.554,-0.553,-0.552,-0.551,-0.55,-0.549,-0.548,
-0.547,-0.546,-0.545,-0.544,-0.543,-0.542,-0.541,-0.54,-0.539,-0.538,-0.537,
-0.536,-0.535,-0.534,-0.533,-0.532,-0.531,-0.53,-0.529,-0.528,-0.527,-0.526,
-0.525,-0.524,-0.523,-0.522,-0.521,-0.52,-0.519,-0.518,-0.517,-0.516,-0.515,
-0.514,-0.513,-0.512,-0.511,-0.51,-0.509,-0.508,-0.507,-0.506,-0.505,-0.504,
-0.503,-0.502,-0.501,-0.5,-0.499,-0.498,-0.497,-0.496,-0.495,-0.494,-0.493,
-0.492,-0.491,-0.49,-0.489,-0.488,-0.487,-0.486,-0.485,-0.484,-0.483,-0.482,
-0.481,-0.48,-0.479,-0.478,-0.477,-0.476,-0.475,-0.474,-0.473,-0.472,-0.471,
-0.47,-0.469,-0.468,-0.467,-0.466,-0.465,-0.464,-0.463,-0.462,-0.461,-0.46,
-0.459,-0.458,-0.457,-0.456,-0.455,-0.454,-0.453,-0.452,-0.451,-0.45,-0.449,
-0.448,-0.447,-0.446,-0.445,-0.444,-0.443,-0.442,-0.441,-0.44,-0.439,-0.438,
-0.437,-0.436,-0.435,-0.434,-0.433,-0.432,-0.431,-0.43,-0.429,-0.428,-0.427,
-0.426,-0.425,-0.424,-0.423,-0.422,-0.421,-0.42,-0.419,-0.418,-0.417,-0.416,
-0.415,-0.414,-0.413,-0.412,-0.411,-0.41,-0.409,-0.408,-0.407,-0.406,-0.405,
-0.404,-0.403,-0.402,-0.401,-0.4,-0.399,-0.398,-0.397,-0.396,-0.395,-0.394,
-0.393,-0.392,-0.391,-0.39,-0.389,-0.388,-0.387,-0.386,-0.385,-0.384,-0.383,
-0.382,-0.381,-0.38,-0.379,-0.378,-0.377,-0.376,-0.375,-0.374,-0.373,-0.372,
-0.371,-0.37,-0.369,-0.368,-0.367,-0.366,-0.365,-0.364,-0.363,-0.362,-0.361,
-0.36,-0.359,-0.358,-0.357,-0.356,-0.355,-0.354,-0.353,-0.352,-0.351,-0.35,
-0.349,-0.348,-0.347,-0.346,-0.345,-0.344,-0.343,-0.342,-0.341,-0.34,-0.339,
-0.338,-0.337,-0.336,-0.335,-0.334,-0.333,-0.332,-0.331,-0.33,-0.329,-0.328,
-0.327,-0.326,-0.325,-0.324,-0.323,-0.322,-0.321,-0.32,-0.319,-0.318,-0.317,
-0.316,-0.315,-0.314,-0.313,-0.312,-0.311,-0.31,-0.309,-0.308,-0.307,-0.306,
-0.305,-0.304,-0.303,-0.302,-0.301,-0.3,-0.299,-0.298,-0.297,-0.296,-0.295,
-0.294,-0.293,-0.292,-0.291,-0.29,-0.289,-0.288,-0.287,-0.286,-0.285,-0.284,
-0.283,-0.282,-0.281,-0.28,-0.279,-0.278,-0.277,-0.276,-0.275,-0.274,-0.273,
-0.272,-0.271,-0.27,-0.269,-0.268,-0.267,-0.266,-0.265,-0.264,-0.263,-0.262,
-0.261,-0.26,-0.259,-0.258,-0.257,-0.256,-0.255,-0.254,-0.253,-0.252,-0.251,
-0.25,-0.249,-0.248,-0.247,-0.246,-0.245,-0.244,-0.243,-0.242,-0.241,-0.24,
-0.239,-0.238,-0.237,-0.236,-0.235,-0.234,-0.233,-0.232,-0.231,-0.23,-0.229,
-0.228,-0.227,-0.226,-0.225,-0.224,-0.223,-0.222,-0.221,-0.22,-0.219,-0.218,
-0.217,-0.216,-0.215,-0.214,-0.213,-0.212,-0.211,-0.21,-0.209,-0.208,-0.207,
-0.206,-0.205,-0.204,-0.203,-0.202,-0.201,-0.2,-0.199,-0.198,-0.197,-0.196,
-0.195,-0.194,-0.193,-0.192,-0.191,-0.19,-0.189,-0.188,-0.187,-0.186,-0.185,
-0.184,-0.183,-0.182,-0.181,-0.18,-0.179,-0.178,-0.177,-0.176,-0.175,-0.174,
-0.173,-0.172,-0.171,-0.17,-0.169,-0.168,-0.167,-0.166,-0.165,-0.164,-0.163,
-0.162,-0.161,-0.16,-0.159,-0.158,-0.157,-0.156,-0.155,-0.154,-0.153,-0.152,
-0.151,-0.15,-0.149,-0.148,-0.147,-0.146,-0.145,-0.144,-0.143,-0.142,-0.141,
-0.14,-0.139,-0.138,-0.137,-0.136,-0.135,-0.134,-0.133,-0.132,-0.131,-0.13,
-0.129,-0.128,-0.127,-0.126,-0.125,-0.124,-0.123,-0.122,-0.121,-0.12,-0.119,
-0.118,-0.117,-0.116,-0.115,-0.114,-0.113,-0.112,-0.111,-0.11,-0.109,-0.108,
-0.107,-0.106,-0.105,-0.104,-0.103,-0.102,-0.101,-0.1,-0.0990000000000001,
-0.0980000000000001,-0.0970000000000001,-0.0960000000000001,-0.0950000000000001,
-0.0940000000000001,-0.0930000000000001,-0.0920000000000001,-0.0910000000000001,
-0.0900000000000001,-0.0890000000000001,-0.0880000000000001,-0.0870000000000001,
-0.0860000000000001,-0.0850000000000001,-0.0840000000000001,-0.0830000000000001,
-0.0820000000000001,-0.0810000000000001,-0.0800000000000001,-0.0790000000000001,
-0.0780000000000001,-0.0770000000000001,-0.0760000000000001,-0.0750000000000001,
-0.0740000000000001,-0.0730000000000001,-0.0720000000000001,-0.071,-0.07,
-0.069,-0.068,-0.067,-0.066,-0.065,-0.064,-0.063,-0.062,-0.061,-0.06,-0.059,
-0.058,-0.057,-0.056,-0.055,-0.054,-0.053,-0.052,-0.051,-0.05,-0.049,-0.048,
-0.047,-0.046,-0.045,-0.044,-0.043,-0.042,-0.041,-0.04,-0.039,-0.038,-0.037,
-0.036,-0.035,-0.034,-0.033,-0.032,-0.031,-0.03,-0.029,-0.028,-0.027,-0.026,
-0.025,-0.024,-0.023,-0.022,-0.021,-0.02,-0.019,-0.018,-0.017,-0.016,-0.015,
-0.014,-0.013,-0.012,-0.011,-0.01,-0.009,-0.008,-0.007,-0.006,-0.005,-0.004,
-0.003,-0.002,-0.001,0.),(0.,2.),.UNSPECIFIED.)
GEOMETRIC_REPRESENTATION_ITEM()
RATIONAL_B_SPLINE_SURFACE(((1.,1.),(1.,1.),(1.,1.),(1.,1.),(1.,1.),(1.,
1.),(1.,1.),(1.,1.),(1.,1.),(1.,1.),(1.,1.),(1.,1.),(1.,1.),(1.,1.),(1.,
1.),(1.,1.),(1.,1.),(1.,1.),(1.,1.),(1.,1.),(1.,1.),(1.,1.),(1.,1.),(1.,
1.),(1.,1.),(1.,1.),(1.,1.),(1.,1.),(1.,1.),(1.,1.),(1.,1.),(1.,1.),(1.,
1.),(1.,1.),(1.,1.),(1.,1.),(1.,1.),(1.,1.),(1.,1.),(1.,1.),(1.,1.),(1.,
1.),(1.,1.),(1.,1.),(1.,1.),(1.,1.),(1.,1.),(1.,1.),(1.,1.),(1.,1.),(1.,
1.),(1.,1.),(1.,1.),(1.,1.),(1.,1.),(1.,1.),(1.,1.),(1.,1.),(1.,1.),(1.,
1.),(1.,1.),(1.,1.),(1.,1.),(1.,1.),(1.,1.),(1.,1.),(1.,1.),(1.,1.),(1.,
1.),(1.,1.),(1.,1.),(1.,1.),(1.,1.),(1.,1.),(1.,1.),(1.,1.),(1.,1.),(1.,
1.),(1.,1.),(1.,1.),(1.,1.),(1.,1.),(1.,1.),(1.,1.),(1.,1.),(1.,1.),(1.,
1.),(1.,1.),(1.,1.),(1.,1.),(1.,1.),(1.,1.),(1.,1.),(1.,1.),(1.,1.),(1.,
1.),(1.,1.),(1.,1.),(1.,1.),(1.,1.),(1.,1.),(1.,1.),(1.,1.),(1.,1.),(1.,
1.),(1.,1.),(1.,1.),(1.,1.),(1.,1.),(1.,1.),(1.,1.),(1.,1.),(1.,1.),(1.,
1.),(1.,1.),(1.,1.),(1.,1.),(1.,1.),(1.,1.),(1.,1.),(1.,1.),(1.,1.),(1.,
1.),(1.,1.),(1.,1.),(1.,1.),(1.,1.),(1.,1.),(1.,1.),(1.,1.),(1.,1.),(1.,
1.),(1.,1.),(1.,1.),(1.,1.),(1.,1.),(1.,1.),(1.,1.),(1.,1.),(1.,1.),(1.,
1.),(1.,1.),(1.,1.),(1.,1.),(1.,1.),(1.,1.),(1.,1.),(1.,1.),(1.,1.),(1.,
1.),(1.,1.),(1.,1.),(1.,1.),(1.,1.),(1.,1.),(1.,1.),(1.,1.),(1.,1.),(1.,
1.),(1.,1.),(1.,1.),(1.,1.),(1.,1.),(1.,1.),(1.,1.),(1.,1.),(1.,1.),(1.,
1.),(1.,1.),(1.,1.),(1.,1.),(1.,1.),(1.,1.),(1.,1.),(1.,1.),(1.,1.),(1.,
1.),(1.,1.),(1.,1.),(1.,1.),(1.,1.),(1.,1.),(1.,1.),(1.,1.),(1.,1.),(1.,
1.),(1.,1.),(1.,1.),(1.,1.),(1.,1.),(1.,1.),(1.,1.),(1.,1.),(1.,1.),(1.,
1.),(1.,1.),(1.,1.),(1.,1.),(1.,1.),(1.,1.),(1.,1.),(1.,1.),(1.,1.),(1.,
1.),(1.,1.),(1.,1.),(1.,1.),(1.,1.),(1.,1.),(1.,1.),(1.,1.),(1.,1.),(1.,
1.),(1.,1.),(1.,1.),(1.,1.),(1.,1.),(1.,1.),(1.,1.),(1.,1.),(1.,1.),(1.,
1.),(1.,1.),(1.,1.),(1.,1.),(1.,1.),(1.,1.),(1.,1.),(1.,1.),(1.,1.),(1.,
1.),(1.,1.),(1.,1.),(1.,1.),(1.,1.),(1.,1.),(1.,1.),(1.,1.),(1.,1.),(1.,
1.),(1.,1.),(1.,1.),(1.,1.),(1.,1.),(1.,1.),(1.,1.),(1.,1.),(1.,1.),(1.,
1.),(1.,1.),(1.,1.),(1.,1.),(1.,1.),(1.,1.),(1.,1.),(1.,1.),(1.,1.),(1.,
1.),(1.,1.),(1.,1.),(1.,1.),(1.,1.),(1.,1.),(1.,1.),(1.,1.),(1.,1.),(1.,
1.),(1.,1.),(1.,1.),(1.,1.),(1.,1.),(1.,1.),(1.,1.),(1.,1.),(1.,1.),(1.,
1.),(1.,1.),(1.,1.),(1.,1.),(1.,1.),(1.,1.),(1.,1.),(1.,1.),(1.,1.),(1.,
1.),(1.,1.),(1.,1.),(1.,1.),(1.,1.),(1.,1.),(1.,1.),(1.,1.),(1.,1.),(1.,
1.),(1.,1.),(1.,1.),(1.,1.),(1.,1.),(1.,1.),(1.,1.),(1.,1.),(1.,1.),(1.,
1.),(1.,1.),(1.,1.),(1.,1.),(1.,1.),(1.,1.),(1.,1.),(1.,1.),(1.,1.),(1.,
1.),(1.,1.),(1.,1.),(1.,1.),(1.,1.),(1.,1.),(1.,1.),(1.,1.),(1.,1.),(1.,
1.),(1.,1.),(1.,1.),(1.,1.),(1.,1.),(1.,1.),(1.,1.),(1.,1.),(1.,1.),(1.,
1.),(1.,1.),(1.,1.),(1.,1.),(1.,1.),(1.,1.),(1.,1.),(1.,1.),(1.,1.),(1.,
1.),(1.,1.),(1.,1.),(1.,1.),(1.,1.),(1.,1.),(1.,1.),(1.,1.),(1.,1.),(1.,
1.),(1.,1.),(1.,1.),(1.,1.),(1.,1.),(1.,1.),(1.,1.),(1.,1.),(1.,1.),(1.,
1.),(1.,1.),(1.,1.),(1.,1.),(1.,1.),(1.,1.),(1.,1.),(1.,1.),(1.,1.),(1.,
1.),(1.,1.),(1.,1.),(1.,1.),(1.,1.),(1.,1.),(1.,1.),(1.,1.),(1.,1.),(1.,
1.),(1.,1.),(1.,1.),(1.,1.),(1.,1.),(1.,1.),(1.,1.),(1.,1.),(1.,1.),(1.,
1.),(1.,1.),(1.,1.),(1.,1.),(1.,1.),(1.,1.),(1.,1.),(1.,1.),(1.,1.),(1.,
1.),(1.,1.),(1.,1.),(1.,1.),(1.,1.),(1.,1.),(1.,1.),(1.,1.),(1.,1.),(1.,
1.),(1.,1.),(1.,1.),(1.,1.),(1.,1.),(1.,1.),(1.,1.),(1.,1.),(1.,1.),(1.,
1.),(1.,1.),(1.,1.),(1.,1.),(1.,1.),(1.,1.),(1.,1.),(1.,1.),(1.,1.),(1.,
1.),(1.,1.),(1.,1.),(1.,1.),(1.,1.),(1.,1.),(1.,1.),(1.,1.),(1.,1.),(1.,
1.),(1.,1.),(1.,1.),(1.,1.),(1.,1.),(1.,1.),(1.,1.),(1.,1.),(1.,1.),(1.,
1.),(1.,1.),(1.,1.),(1.,1.),(1.,1.),(1.,1.),(1.,1.),(1.,1.),(1.,1.),(1.,
1.),(1.,1.),(1.,1.),(1.,1.),(1.,1.),(1.,1.),(1.,1.),(1.,1.),(1.,1.),(1.,
1.),(1.,1.),(1.,1.),(1.,1.),(1.,1.),(1.,1.),(1.,1.),(1.,1.),(1.,1.),(1.,
1.),(1.,1.),(1.,1.),(1.,1.),(1.,1.),(1.,1.),(1.,1.),(1.,1.),(1.,1.),(1.,
1.),(1.,1.),(1.,1.),(1.,1.),(1.,1.),(1.,1.),(1.,1.),(1.,1.),(1.,1.),(1.,
1.),(1.,1.),(1.,1.),(1.,1.),(1.,1.),(1.,1.),(1.,1.),(1.,1.),(1.,1.),(1.,
1.),(1.,1.),(1.,1.),(1.,1.),(1.,1.),(1.,1.),(1.,1.),(1.,1.),(1.,1.),(1.,
1.),(1.,1.),(1.,1.),(1.,1.),(1.,1.),(1.,1.),(1.,1.),(1.,1.),(1.,1.),(1.,
1.),(1.,1.),(1.,1.),(1.,1.),(1.,1.),(1.,1.),(1.,1.),(1.,1.),(1.,1.),(1.,
1.),(1.,1.),(1.,1.),(1.,1.),(1.,1.),(1.,1.),(1.,1.),(1.,1.),(1.,1.),(1.,
1.),(1.,1.),(1.,1.),(1.,1.),(1.,1.),(1.,1.),(1.,1.),(1.,1.),(1.,1.),(1.,
1.),(1.,1.),(1.,1.),(1.,1.),(1.,1.),(1.,1.),(1.,1.),(1.,1.),(1.,1.),(1.,
1.),(1.,1.),(1.,1.),(1.,1.),(1.,1.),(1.,1.),(1.,1.),(1.,1.),(1.,1.),(1.,
1.),(1.,1.),(1.,1.),(1.,1.),(1.,1.),(1.,1.),(1.,1.),(1.,1.),(1.,1.),(1.,
1.),(1.,1.),(1.,1.),(1.,1.),(1.,1.),(1.,1.),(1.,1.),(1.,1.),(1.,1.),(1.,
1.),(1.,1.),(1.,1.),(1.,1.),(1.,1.),(1.,1.),(1.,1.),(1.,1.),(1.,1.),(1.,
1.),(1.,1.),(1.,1.),(1.,1.),(1.,1.),(1.,1.),(1.,1.),(1.,1.),(1.,1.),(1.,
1.),(1.,1.),(1.,1.),(1.,1.),(1.,1.),(1.,1.),(1.,1.),(1.,1.),(1.,1.),(1.,
1.),(1.,1.),(1.,1.),(1.,1.),(1.,1.),(1.,1.),(1.,1.),(1.,1.),(1.,1.),(1.,
1.),(1.,1.),(1.,1.),(1.,1.),(1.,1.),(1.,1.),(1.,1.),(1.,1.),(1.,1.),(1.,
1.),(1.,1.),(1.,1.),(1.,1.),(1.,1.),(1.,1.),(1.,1.),(1.,1.),(1.,1.),(1.,
1.),(1.,1.),(1.,1.),(1.,1.),(1.,1.),(1.,1.),(1.,1.),(1.,1.),(1.,1.),(1.,
1.),(1.,1.),(1.,1.),(1.,1.),(1.,1.),(1.,1.),(1.,1.),(1.,1.),(1.,1.),(1.,
1.),(1.,1.),(1.,1.),(1.,1.),(1.,1.),(1.,1.),(1.,1.),(1.,1.),(1.,1.),(1.,
1.),(1.,1.),(1.,1.),(1.,1.),(1.,1.),(1.,1.),(1.,1.),(1.,1.),(1.,1.),(1.,
1.),(1.,1.),(1.,1.),(1.,1.),(1.,1.),(1.,1.),(1.,1.),(1.,1.),(1.,1.),(1.,
1.),(1.,1.),(1.,1.),(1.,1.),(1.,1.),(1.,1.),(1.,1.),(1.,1.),(1.,1.),(1.,
1.),(1.,1.),(1.,1.),(1.,1.),(1.,1.),(1.,1.),(1.,1.),(1.,1.),(1.,1.),(1.,
1.),(1.,1.),(1.,1.),(1.,1.),(1.,1.),(1.,1.),(1.,1.),(1.,1.),(1.,1.),(1.,
1.),(1.,1.),(1.,1.),(1.,1.),(1.,1.),(1.,1.),(1.,1.),(1.,1.),(1.,1.),(1.,
1.),(1.,1.),(1.,1.),(1.,1.),(1.,1.),(1.,1.),(1.,1.),(1.,1.),(1.,1.),(1.,
1.),(1.,1.),(1.,1.),(1.,1.),(1.,1.),(1.,1.),(1.,1.),(1.,1.),(1.,1.),(1.,
1.),(1.,1.),(1.,1.),(1.,1.),(1.,1.),(1.,1.),(1.,1.),(1.,1.),(1.,1.),(1.,
1.),(1.,1.),(1.,1.),(1.,1.),(1.,1.),(1.,1.),(1.,1.),(1.,1.),(1.,1.),(1.,
1.),(1.,1.),(1.,1.),(1.,1.),(1.,1.),(1.,1.),(1.,1.),(1.,1.),(1.,1.),(1.,
1.),(1.,1.),(1.,1.),(1.,1.),(1.,1.),(1.,1.),(1.,1.),(1.,1.),(1.,1.),(1.,
1.),(1.,1.),(1.,1.),(1.,1.),(1.,1.),(1.,1.),(1.,1.),(1.,1.),(1.,1.),(1.,
1.),(1.,1.),(1.,1.),(1.,1.),(1.,1.),(1.,1.),(1.,1.),(1.,1.),(1.,1.),(1.,
1.),(1.,1.),(1.,1.),(1.,1.),(1.,1.),(1.,1.),(1.,1.),(1.,1.),(1.,1.),(1.,
1.),(1.,1.),(1.,1.),(1.,1.),(1.,1.),(1.,1.),(1.,1.),(1.,1.),(1.,1.),(1.,
1.),(1.,1.),(1.,1.),(1.,1.),(1.,1.),(1.,1.),(1.,1.),(1.,1.),(1.,1.),(1.,
1.),(1.,1.),(1.,1.),(1.,1.),(1.,1.),(1.,1.),(1.,1.),(1.,1.),(1.,1.),(1.,
1.),(1.,1.),(1.,1.),(1.,1.),(1.,1.),(1.,1.),(1.,1.),(1.,1.),(1.,1.),(1.,
1.),(1.,1.),(1.,1.),(1.,1.),(1.,1.),(1.,1.),(1.,1.),(1.,1.),(1.,1.),(1.,
1.),(1.,1.),(1.,1.),(1.,1.),(1.,1.),(1.,1.),(1.,1.),(1.,1.),(1.,1.),(1.,
1.),(1.,1.),(1.,1.),(1.,1.),(1.,1.),(1.,1.),(1.,1.),(1.,1.),(1.,1.),(1.,
1.),(1.,1.),(1.,1.),(1.,1.),(1.,1.),(1.,1.),(1.,1.),(1.,1.),(1.,1.),(1.,
1.),(1.,1.),(1.,1.),(1.,1.),(1.,1.),(1.,1.),(1.,1.),(1.,1.),(1.,1.),(1.,
1.),(1.,1.),(1.,1.),(1.,1.),(1.,1.),(1.,1.),(1.,1.),(1.,1.),(1.,1.),(1.,
1.),(1.,1.),(1.,1.),(1.,1.),(1.,1.),(1.,1.),(1.,1.),(1.,1.),(1.,1.),(1.,
1.),(1.,1.),(1.,1.),(1.,1.),(1.,1.),(1.,1.),(1.,1.),(1.,1.),(1.,1.),(1.,
1.),(1.,1.),(1.,1.),(1.,1.),(1.,1.),(1.,1.),(1.,1.),(1.,1.),(1.,1.),(1.,
1.),(1.,1.),(1.,1.),(1.,1.),(1.,1.),(1.,1.),(1.,1.),(1.,1.),(1.,1.),(1.,
1.),(1.,1.),(1.,1.),(1.,1.),(1.,1.),(1.,1.),(1.,1.),(1.,1.),(1.,1.),(1.,
1.),(1.,1.),(1.,1.),(1.,1.),(1.,1.),(1.,1.),(1.,1.),(1.,1.),(1.,1.),(1.,
1.),(1.,1.),(1.,1.),(1.,1.),(1.,1.),(1.,1.),(1.,1.),(1.,1.),(1.,1.),(1.,
1.),(1.,1.),(1.,1.),(1.,1.),(1.,1.),(1.,1.),(1.,1.),(1.,1.),(1.,1.),(1.,
1.),(1.,1.),(1.,1.),(1.,1.),(1.,1.),(1.,1.),(1.,1.),(1.,1.),(1.,1.),(1.,
1.),(1.,1.),(1.,1.),(1.,1.),(1.,1.),(1.,1.),(1.,1.),(1.,1.),(1.,1.),(1.,
1.),(1.,1.),(1.,1.),(1.,1.),(1.,1.),(1.,1.),(1.,1.),(1.,1.),(1.,1.),(1.,
1.),(1.,1.),(1.,1.),(1.,1.),(1.,1.),(1.,1.),(1.,1.),(1.,1.),(1.,1.),(1.,
1.),(1.,1.),(1.,1.),(1.,1.),(1.,1.),(1.,1.),(1.,1.),(1.,1.),(1.,1.),(1.,
1.),(1.,1.),(1.,1.),(1.,1.),(1.,1.),(1.,1.),(1.,1.),(1.,1.),(1.,1.),(1.,
1.)))
REPRESENTATION_ITEM('')
SURFACE()
);
#257=(
BOUNDED_SURFACE()
B_SPLINE_SURFACE(5,1,((#72061,#72062),(#72063,#72064),(#72065,#72066),(#72067,
#72068),(#72069,#72070),(#72071,#72072),(#72073,#72074),(#72075,#72076),
(#72077,#72078),(#72079,#72080),(#72081,#72082),(#72083,#72084),(#72085,
#72086),(#72087,#72088),(#72089,#72090),(#72091,#72092),(#72093,#72094),
(#72095,#72096),(#72097,#72098),(#72099,#72100),(#72101,#72102),(#72103,
#72104),(#72105,#72106),(#72107,#72108),(#72109,#72110),(#72111,#72112),
(#72113,#72114),(#72115,#72116),(#72117,#72118),(#72119,#72120),(#72121,
#72122),(#72123,#72124),(#72125,#72126),(#72127,#72128),(#72129,#72130),
(#72131,#72132),(#72133,#72134),(#72135,#72136),(#72137,#72138),(#72139,
#72140),(#72141,#72142),(#72143,#72144),(#72145,#72146),(#72147,#72148),
(#72149,#72150),(#72151,#72152),(#72153,#72154),(#72155,#72156),(#72157,
#72158),(#72159,#72160),(#72161,#72162),(#72163,#72164),(#72165,#72166),
(#72167,#72168),(#72169,#72170),(#72171,#72172),(#72173,#72174),(#72175,
#72176),(#72177,#72178),(#72179,#72180),(#72181,#72182),(#72183,#72184),
(#72185,#72186),(#72187,#72188),(#72189,#72190),(#72191,#72192),(#72193,
#72194),(#72195,#72196),(#72197,#72198),(#72199,#72200),(#72201,#72202),
(#72203,#72204),(#72205,#72206),(#72207,#72208),(#72209,#72210),(#72211,
#72212),(#72213,#72214),(#72215,#72216),(#72217,#72218),(#72219,#72220),
(#72221,#72222),(#72223,#72224),(#72225,#72226),(#72227,#72228),(#72229,
#72230),(#72231,#72232),(#72233,#72234),(#72235,#72236),(#72237,#72238),
(#72239,#72240),(#72241,#72242),(#72243,#72244),(#72245,#72246),(#72247,
#72248),(#72249,#72250),(#72251,#72252),(#72253,#72254),(#72255,#72256),
(#72257,#72258),(#72259,#72260),(#72261,#72262),(#72263,#72264),(#72265,
#72266),(#72267,#72268),(#72269,#72270),(#72271,#72272),(#72273,#72274),
(#72275,#72276),(#72277,#72278),(#72279,#72280),(#72281,#72282),(#72283,
#72284),(#72285,#72286),(#72287,#72288),(#72289,#72290),(#72291,#72292),
(#72293,#72294),(#72295,#72296),(#72297,#72298),(#72299,#72300),(#72301,
#72302),(#72303,#72304),(#72305,#72306),(#72307,#72308),(#72309,#72310),
(#72311,#72312),(#72313,#72314),(#72315,#72316),(#72317,#72318),(#72319,
#72320),(#72321,#72322),(#72323,#72324),(#72325,#72326),(#72327,#72328),
(#72329,#72330),(#72331,#72332),(#72333,#72334),(#72335,#72336),(#72337,
#72338),(#72339,#72340),(#72341,#72342),(#72343,#72344),(#72345,#72346),
(#72347,#72348),(#72349,#72350),(#72351,#72352),(#72353,#72354),(#72355,
#72356),(#72357,#72358),(#72359,#72360),(#72361,#72362),(#72363,#72364),
(#72365,#72366),(#72367,#72368),(#72369,#72370),(#72371,#72372),(#72373,
#72374),(#72375,#72376),(#72377,#72378),(#72379,#72380),(#72381,#72382),
(#72383,#72384),(#72385,#72386),(#72387,#72388),(#72389,#72390),(#72391,
#72392),(#72393,#72394),(#72395,#72396),(#72397,#72398),(#72399,#72400),
(#72401,#72402),(#72403,#72404),(#72405,#72406),(#72407,#72408),(#72409,
#72410),(#72411,#72412),(#72413,#72414),(#72415,#72416),(#72417,#72418),
(#72419,#72420),(#72421,#72422),(#72423,#72424),(#72425,#72426),(#72427,
#72428),(#72429,#72430),(#72431,#72432),(#72433,#72434),(#72435,#72436),
(#72437,#72438),(#72439,#72440),(#72441,#72442),(#72443,#72444),(#72445,
#72446),(#72447,#72448),(#72449,#72450),(#72451,#72452),(#72453,#72454),
(#72455,#72456),(#72457,#72458),(#72459,#72460),(#72461,#72462),(#72463,
#72464),(#72465,#72466),(#72467,#72468),(#72469,#72470),(#72471,#72472),
(#72473,#72474),(#72475,#72476),(#72477,#72478),(#72479,#72480),(#72481,
#72482),(#72483,#72484),(#72485,#72486),(#72487,#72488),(#72489,#72490),
(#72491,#72492),(#72493,#72494),(#72495,#72496),(#72497,#72498),(#72499,
#72500),(#72501,#72502),(#72503,#72504),(#72505,#72506),(#72507,#72508),
(#72509,#72510),(#72511,#72512),(#72513,#72514),(#72515,#72516),(#72517,
#72518),(#72519,#72520),(#72521,#72522),(#72523,#72524),(#72525,#72526),
(#72527,#72528),(#72529,#72530),(#72531,#72532),(#72533,#72534),(#72535,
#72536),(#72537,#72538),(#72539,#72540),(#72541,#72542),(#72543,#72544),
(#72545,#72546),(#72547,#72548),(#72549,#72550),(#72551,#72552),(#72553,
#72554),(#72555,#72556),(#72557,#72558),(#72559,#72560),(#72561,#72562),
(#72563,#72564),(#72565,#72566),(#72567,#72568),(#72569,#72570),(#72571,
#72572),(#72573,#72574),(#72575,#72576),(#72577,#72578),(#72579,#72580),
(#72581,#72582),(#72583,#72584),(#72585,#72586),(#72587,#72588),(#72589,
#72590),(#72591,#72592),(#72593,#72594),(#72595,#72596),(#72597,#72598),
(#72599,#72600),(#72601,#72602),(#72603,#72604),(#72605,#72606),(#72607,
#72608),(#72609,#72610),(#72611,#72612),(#72613,#72614),(#72615,#72616),
(#72617,#72618),(#72619,#72620),(#72621,#72622),(#72623,#72624),(#72625,
#72626),(#72627,#72628),(#72629,#72630),(#72631,#72632),(#72633,#72634),
(#72635,#72636),(#72637,#72638),(#72639,#72640),(#72641,#72642),(#72643,
#72644),(#72645,#72646),(#72647,#72648),(#72649,#72650),(#72651,#72652),
(#72653,#72654),(#72655,#72656),(#72657,#72658),(#72659,#72660),(#72661,
#72662),(#72663,#72664),(#72665,#72666),(#72667,#72668),(#72669,#72670),
(#72671,#72672),(#72673,#72674),(#72675,#72676),(#72677,#72678),(#72679,
#72680),(#72681,#72682),(#72683,#72684),(#72685,#72686),(#72687,#72688),
(#72689,#72690),(#72691,#72692),(#72693,#72694),(#72695,#72696),(#72697,
#72698),(#72699,#72700),(#72701,#72702),(#72703,#72704),(#72705,#72706),
(#72707,#72708),(#72709,#72710),(#72711,#72712),(#72713,#72714),(#72715,
#72716),(#72717,#72718),(#72719,#72720),(#72721,#72722),(#72723,#72724),
(#72725,#72726),(#72727,#72728),(#72729,#72730),(#72731,#72732),(#72733,
#72734),(#72735,#72736),(#72737,#72738),(#72739,#72740),(#72741,#72742),
(#72743,#72744),(#72745,#72746),(#72747,#72748),(#72749,#72750),(#72751,
#72752),(#72753,#72754),(#72755,#72756),(#72757,#72758),(#72759,#72760),
(#72761,#72762),(#72763,#72764),(#72765,#72766),(#72767,#72768),(#72769,
#72770),(#72771,#72772),(#72773,#72774),(#72775,#72776),(#72777,#72778),
(#72779,#72780),(#72781,#72782),(#72783,#72784),(#72785,#72786),(#72787,
#72788),(#72789,#72790),(#72791,#72792),(#72793,#72794),(#72795,#72796),
(#72797,#72798),(#72799,#72800),(#72801,#72802),(#72803,#72804),(#72805,
#72806),(#72807,#72808),(#72809,#72810),(#72811,#72812),(#72813,#72814),
(#72815,#72816),(#72817,#72818),(#72819,#72820),(#72821,#72822),(#72823,
#72824),(#72825,#72826),(#72827,#72828),(#72829,#72830),(#72831,#72832),
(#72833,#72834),(#72835,#72836),(#72837,#72838),(#72839,#72840),(#72841,
#72842),(#72843,#72844),(#72845,#72846),(#72847,#72848),(#72849,#72850),
(#72851,#72852),(#72853,#72854),(#72855,#72856),(#72857,#72858),(#72859,
#72860),(#72861,#72862),(#72863,#72864),(#72865,#72866),(#72867,#72868),
(#72869,#72870),(#72871,#72872),(#72873,#72874),(#72875,#72876),(#72877,
#72878),(#72879,#72880),(#72881,#72882),(#72883,#72884),(#72885,#72886),
(#72887,#72888),(#72889,#72890),(#72891,#72892),(#72893,#72894),(#72895,
#72896),(#72897,#72898),(#72899,#72900),(#72901,#72902),(#72903,#72904),
(#72905,#72906),(#72907,#72908),(#72909,#72910),(#72911,#72912),(#72913,
#72914),(#72915,#72916),(#72917,#72918),(#72919,#72920),(#72921,#72922),
(#72923,#72924),(#72925,#72926),(#72927,#72928),(#72929,#72930),(#72931,
#72932),(#72933,#72934),(#72935,#72936),(#72937,#72938),(#72939,#72940),
(#72941,#72942),(#72943,#72944),(#72945,#72946),(#72947,#72948),(#72949,
#72950),(#72951,#72952),(#72953,#72954),(#72955,#72956),(#72957,#72958),
(#72959,#72960),(#72961,#72962),(#72963,#72964),(#72965,#72966),(#72967,
#72968),(#72969,#72970),(#72971,#72972),(#72973,#72974),(#72975,#72976),
(#72977,#72978),(#72979,#72980),(#72981,#72982),(#72983,#72984),(#72985,
#72986),(#72987,#72988),(#72989,#72990),(#72991,#72992),(#72993,#72994),
(#72995,#72996),(#72997,#72998),(#72999,#73000),(#73001,#73002),(#73003,
#73004),(#73005,#73006),(#73007,#73008),(#73009,#73010),(#73011,#73012),
(#73013,#73014),(#73015,#73016),(#73017,#73018),(#73019,#73020),(#73021,
#73022),(#73023,#73024),(#73025,#73026),(#73027,#73028),(#73029,#73030),
(#73031,#73032),(#73033,#73034),(#73035,#73036),(#73037,#73038),(#73039,
#73040),(#73041,#73042),(#73043,#73044),(#73045,#73046),(#73047,#73048),
(#73049,#73050),(#73051,#73052),(#73053,#73054),(#73055,#73056),(#73057,
#73058),(#73059,#73060),(#73061,#73062),(#73063,#73064),(#73065,#73066),
(#73067,#73068),(#73069,#73070),(#73071,#73072),(#73073,#73074),(#73075,
#73076),(#73077,#73078),(#73079,#73080),(#73081,#73082),(#73083,#73084),
(#73085,#73086),(#73087,#73088),(#73089,#73090),(#73091,#73092),(#73093,
#73094),(#73095,#73096),(#73097,#73098),(#73099,#73100),(#73101,#73102),
(#73103,#73104),(#73105,#73106),(#73107,#73108),(#73109,#73110),(#73111,
#73112),(#73113,#73114),(#73115,#73116),(#73117,#73118),(#73119,#73120),
(#73121,#73122),(#73123,#73124),(#73125,#73126),(#73127,#73128),(#73129,
#73130),(#73131,#73132),(#73133,#73134),(#73135,#73136),(#73137,#73138),
(#73139,#73140),(#73141,#73142),(#73143,#73144),(#73145,#73146),(#73147,
#73148),(#73149,#73150),(#73151,#73152),(#73153,#73154),(#73155,#73156),
(#73157,#73158),(#73159,#73160),(#73161,#73162),(#73163,#73164),(#73165,
#73166),(#73167,#73168),(#73169,#73170),(#73171,#73172),(#73173,#73174),
(#73175,#73176),(#73177,#73178),(#73179,#73180),(#73181,#73182),(#73183,
#73184),(#73185,#73186),(#73187,#73188),(#73189,#73190),(#73191,#73192),
(#73193,#73194),(#73195,#73196),(#73197,#73198),(#73199,#73200),(#73201,
#73202),(#73203,#73204),(#73205,#73206),(#73207,#73208),(#73209,#73210),
(#73211,#73212),(#73213,#73214),(#73215,#73216),(#73217,#73218),(#73219,
#73220),(#73221,#73222),(#73223,#73224),(#73225,#73226),(#73227,#73228),
(#73229,#73230),(#73231,#73232),(#73233,#73234),(#73235,#73236),(#73237,
#73238),(#73239,#73240),(#73241,#73242),(#73243,#73244),(#73245,#73246),
(#73247,#73248),(#73249,#73250),(#73251,#73252),(#73253,#73254),(#73255,
#73256),(#73257,#73258),(#73259,#73260),(#73261,#73262),(#73263,#73264),
(#73265,#73266),(#73267,#73268),(#73269,#73270),(#73271,#73272),(#73273,
#73274),(#73275,#73276),(#73277,#73278),(#73279,#73280),(#73281,#73282),
(#73283,#73284),(#73285,#73286),(#73287,#73288),(#73289,#73290),(#73291,
#73292),(#73293,#73294),(#73295,#73296),(#73297,#73298),(#73299,#73300),
(#73301,#73302),(#73303,#73304),(#73305,#73306),(#73307,#73308),(#73309,
#73310),(#73311,#73312),(#73313,#73314),(#73315,#73316),(#73317,#73318),
(#73319,#73320),(#73321,#73322),(#73323,#73324),(#73325,#73326),(#73327,
#73328),(#73329,#73330),(#73331,#73332),(#73333,#73334),(#73335,#73336),
(#73337,#73338),(#73339,#73340),(#73341,#73342),(#73343,#73344),(#73345,
#73346),(#73347,#73348),(#73349,#73350),(#73351,#73352),(#73353,#73354),
(#73355,#73356),(#73357,#73358),(#73359,#73360),(#73361,#73362),(#73363,
#73364),(#73365,#73366),(#73367,#73368),(#73369,#73370),(#73371,#73372),
(#73373,#73374),(#73375,#73376),(#73377,#73378),(#73379,#73380),(#73381,
#73382),(#73383,#73384),(#73385,#73386),(#73387,#73388),(#73389,#73390),
(#73391,#73392),(#73393,#73394),(#73395,#73396),(#73397,#73398),(#73399,
#73400),(#73401,#73402),(#73403,#73404),(#73405,#73406),(#73407,#73408),
(#73409,#73410),(#73411,#73412),(#73413,#73414),(#73415,#73416),(#73417,
#73418),(#73419,#73420),(#73421,#73422),(#73423,#73424),(#73425,#73426),
(#73427,#73428),(#73429,#73430),(#73431,#73432),(#73433,#73434),(#73435,
#73436),(#73437,#73438),(#73439,#73440),(#73441,#73442),(#73443,#73444),
(#73445,#73446),(#73447,#73448),(#73449,#73450),(#73451,#73452),(#73453,
#73454),(#73455,#73456),(#73457,#73458),(#73459,#73460),(#73461,#73462),
(#73463,#73464),(#73465,#73466),(#73467,#73468),(#73469,#73470),(#73471,
#73472),(#73473,#73474),(#73475,#73476),(#73477,#73478),(#73479,#73480),
(#73481,#73482),(#73483,#73484),(#73485,#73486),(#73487,#73488),(#73489,
#73490),(#73491,#73492),(#73493,#73494),(#73495,#73496),(#73497,#73498),
(#73499,#73500),(#73501,#73502),(#73503,#73504),(#73505,#73506),(#73507,
#73508),(#73509,#73510),(#73511,#73512),(#73513,#73514),(#73515,#73516),
(#73517,#73518),(#73519,#73520),(#73521,#73522),(#73523,#73524),(#73525,
#73526),(#73527,#73528),(#73529,#73530),(#73531,#73532),(#73533,#73534),
(#73535,#73536),(#73537,#73538),(#73539,#73540),(#73541,#73542),(#73543,
#73544),(#73545,#73546),(#73547,#73548),(#73549,#73550),(#73551,#73552),
(#73553,#73554),(#73555,#73556),(#73557,#73558),(#73559,#73560),(#73561,
#73562),(#73563,#73564),(#73565,#73566),(#73567,#73568),(#73569,#73570),
(#73571,#73572),(#73573,#73574),(#73575,#73576),(#73577,#73578),(#73579,
#73580),(#73581,#73582),(#73583,#73584),(#73585,#73586),(#73587,#73588),
(#73589,#73590),(#73591,#73592),(#73593,#73594),(#73595,#73596),(#73597,
#73598),(#73599,#73600),(#73601,#73602),(#73603,#73604),(#73605,#73606),
(#73607,#73608),(#73609,#73610),(#73611,#73612),(#73613,#73614),(#73615,
#73616),(#73617,#73618),(#73619,#73620),(#73621,#73622),(#73623,#73624),
(#73625,#73626),(#73627,#73628),(#73629,#73630),(#73631,#73632),(#73633,
#73634),(#73635,#73636),(#73637,#73638),(#73639,#73640),(#73641,#73642),
(#73643,#73644),(#73645,#73646),(#73647,#73648),(#73649,#73650),(#73651,
#73652),(#73653,#73654),(#73655,#73656),(#73657,#73658),(#73659,#73660),
(#73661,#73662),(#73663,#73664),(#73665,#73666),(#73667,#73668),(#73669,
#73670),(#73671,#73672),(#73673,#73674),(#73675,#73676),(#73677,#73678),
(#73679,#73680),(#73681,#73682),(#73683,#73684),(#73685,#73686),(#73687,
#73688),(#73689,#73690),(#73691,#73692),(#73693,#73694),(#73695,#73696),
(#73697,#73698),(#73699,#73700),(#73701,#73702),(#73703,#73704),(#73705,
#73706),(#73707,#73708),(#73709,#73710),(#73711,#73712),(#73713,#73714),
(#73715,#73716),(#73717,#73718),(#73719,#73720),(#73721,#73722),(#73723,
#73724),(#73725,#73726),(#73727,#73728),(#73729,#73730),(#73731,#73732),
(#73733,#73734),(#73735,#73736),(#73737,#73738),(#73739,#73740),(#73741,
#73742),(#73743,#73744),(#73745,#73746),(#73747,#73748),(#73749,#73750),
(#73751,#73752),(#73753,#73754),(#73755,#73756),(#73757,#73758),(#73759,
#73760),(#73761,#73762),(#73763,#73764),(#73765,#73766),(#73767,#73768),
(#73769,#73770),(#73771,#73772),(#73773,#73774),(#73775,#73776),(#73777,
#73778),(#73779,#73780),(#73781,#73782),(#73783,#73784),(#73785,#73786),
(#73787,#73788),(#73789,#73790),(#73791,#73792),(#73793,#73794),(#73795,
#73796),(#73797,#73798),(#73799,#73800),(#73801,#73802),(#73803,#73804),
(#73805,#73806),(#73807,#73808),(#73809,#73810),(#73811,#73812),(#73813,
#73814),(#73815,#73816),(#73817,#73818),(#73819,#73820),(#73821,#73822),
(#73823,#73824),(#73825,#73826),(#73827,#73828),(#73829,#73830),(#73831,
#73832),(#73833,#73834),(#73835,#73836),(#73837,#73838),(#73839,#73840),
(#73841,#73842),(#73843,#73844),(#73845,#73846),(#73847,#73848),(#73849,
#73850),(#73851,#73852),(#73853,#73854),(#73855,#73856),(#73857,#73858),
(#73859,#73860),(#73861,#73862),(#73863,#73864),(#73865,#73866),(#73867,
#73868),(#73869,#73870),(#73871,#73872),(#73873,#73874),(#73875,#73876),
(#73877,#73878),(#73879,#73880),(#73881,#73882),(#73883,#73884),(#73885,
#73886),(#73887,#73888),(#73889,#73890),(#73891,#73892),(#73893,#73894),
(#73895,#73896),(#73897,#73898),(#73899,#73900),(#73901,#73902),(#73903,
#73904),(#73905,#73906),(#73907,#73908),(#73909,#73910),(#73911,#73912),
(#73913,#73914),(#73915,#73916),(#73917,#73918),(#73919,#73920),(#73921,
#73922),(#73923,#73924),(#73925,#73926),(#73927,#73928),(#73929,#73930),
(#73931,#73932),(#73933,#73934),(#73935,#73936),(#73937,#73938),(#73939,
#73940),(#73941,#73942),(#73943,#73944),(#73945,#73946),(#73947,#73948),
(#73949,#73950),(#73951,#73952),(#73953,#73954),(#73955,#73956),(#73957,
#73958),(#73959,#73960),(#73961,#73962),(#73963,#73964),(#73965,#73966),
(#73967,#73968),(#73969,#73970),(#73971,#73972),(#73973,#73974),(#73975,
#73976),(#73977,#73978),(#73979,#73980),(#73981,#73982),(#73983,#73984),
(#73985,#73986),(#73987,#73988),(#73989,#73990),(#73991,#73992),(#73993,
#73994),(#73995,#73996),(#73997,#73998),(#73999,#74000),(#74001,#74002),
(#74003,#74004),(#74005,#74006),(#74007,#74008),(#74009,#74010),(#74011,
#74012),(#74013,#74014),(#74015,#74016),(#74017,#74018),(#74019,#74020),
(#74021,#74022),(#74023,#74024),(#74025,#74026),(#74027,#74028),(#74029,
#74030),(#74031,#74032),(#74033,#74034),(#74035,#74036),(#74037,#74038),
(#74039,#74040),(#74041,#74042),(#74043,#74044),(#74045,#74046),(#74047,
#74048),(#74049,#74050),(#74051,#74052),(#74053,#74054),(#74055,#74056),
(#74057,#74058),(#74059,#74060),(#74061,#74062),(#74063,#74064),(#74065,
#74066),(#74067,#74068),(#74069,#74070)),.UNSPECIFIED.,.F.,.F.,.F.)
B_SPLINE_SURFACE_WITH_KNOTS((6,1,1,1,1,1,1,1,1,1,1,1,1,1,1,1,1,1,1,1,1,
1,1,1,1,1,1,1,1,1,1,1,1,1,1,1,1,1,1,1,1,1,1,1,1,1,1,1,1,1,1,1,1,1,1,1,1,
1,1,1,1,1,1,1,1,1,1,1,1,1,1,1,1,1,1,1,1,1,1,1,1,1,1,1,1,1,1,1,1,1,1,1,1,
1,1,1,1,1,1,1,1,1,1,1,1,1,1,1,1,1,1,1,1,1,1,1,1,1,1,1,1,1,1,1,1,1,1,1,1,
1,1,1,1,1,1,1,1,1,1,1,1,1,1,1,1,1,1,1,1,1,1,1,1,1,1,1,1,1,1,1,1,1,1,1,1,
1,1,1,1,1,1,1,1,1,1,1,1,1,1,1,1,1,1,1,1,1,1,1,1,1,1,1,1,1,1,1,1,1,1,1,1,
1,1,1,1,1,1,1,1,1,1,1,1,1,1,1,1,1,1,1,1,1,1,1,1,1,1,1,1,1,1,1,1,1,1,1,1,
1,1,1,1,1,1,1,1,1,1,1,1,1,1,1,1,1,1,1,1,1,1,1,1,1,1,1,1,1,1,1,1,1,1,1,1,
1,1,1,1,1,1,1,1,1,1,1,1,1,1,1,1,1,1,1,1,1,1,1,1,1,1,1,1,1,1,1,1,1,1,1,1,
1,1,1,1,1,1,1,1,1,1,1,1,1,1,1,1,1,1,1,1,1,1,1,1,1,1,1,1,1,1,1,1,1,1,1,1,
1,1,1,1,1,1,1,1,1,1,1,1,1,1,1,1,1,1,1,1,1,1,1,1,1,1,1,1,1,1,1,1,1,1,1,1,
1,1,1,1,1,1,1,1,1,1,1,1,1,1,1,1,1,1,1,1,1,1,1,1,1,1,1,1,1,1,1,1,1,1,1,1,
1,1,1,1,1,1,1,1,1,1,1,1,1,1,1,1,1,1,1,1,1,1,1,1,1,1,1,1,1,1,1,1,1,1,1,1,
1,1,1,1,1,1,1,1,1,1,1,1,1,1,1,1,1,1,1,1,1,1,1,1,1,1,1,1,1,1,1,1,1,1,1,1,
1,1,1,1,1,1,1,1,1,1,1,1,1,1,1,1,1,1,1,1,1,1,1,1,1,1,1,1,1,1,1,1,1,1,1,1,
1,1,1,1,1,1,1,1,1,1,1,1,1,1,1,1,1,1,1,1,1,1,1,1,1,1,1,1,1,1,1,1,1,1,1,1,
1,1,1,1,1,1,1,1,1,1,1,1,1,1,1,1,1,1,1,1,1,1,1,1,1,1,1,1,1,1,1,1,1,1,1,1,
1,1,1,1,1,1,1,1,1,1,1,1,1,1,1,1,1,1,1,1,1,1,1,1,1,1,1,1,1,1,1,1,1,1,1,1,
1,1,1,1,1,1,1,1,1,1,1,1,1,1,1,1,1,1,1,1,1,1,1,1,1,1,1,1,1,1,1,1,1,1,1,1,
1,1,1,1,1,1,1,1,1,1,1,1,1,1,1,1,1,1,1,1,1,1,1,1,1,1,1,1,1,1,1,1,1,1,1,1,
1,1,1,1,1,1,1,1,1,1,1,1,1,1,1,1,1,1,1,1,1,1,1,1,1,1,1,1,1,1,1,1,1,1,1,1,
1,1,1,1,1,1,1,1,1,1,1,1,1,1,1,1,1,1,1,1,1,1,1,1,1,1,1,1,1,1,1,1,1,1,1,1,
1,1,1,1,1,1,1,1,1,1,1,1,1,1,1,1,1,1,1,1,1,1,1,1,1,1,1,1,1,1,1,1,1,1,1,1,
1,1,1,1,1,1,1,1,1,1,1,1,1,1,1,1,1,1,1,1,1,1,1,1,1,1,1,1,1,1,1,1,1,1,1,1,
1,1,1,1,1,1,1,1,1,1,1,1,1,1,1,1,1,1,1,1,1,1,1,1,1,1,1,1,1,1,1,1,1,1,1,1,
1,1,1,1,1,1,1,1,1,1,1,1,1,1,1,1,1,1,1,1,1,1,1,1,1,1,1,1,1,1,1,1,1,1,1,1,
1,1,1,1,1,1,1,1,1,1,1,1,1,1,1,1,1,1,1,1,1,1,1,1,1,1,1,1,1,1,1,1,1,1,1,1,
1,1,1,1,1,1,1,1,1,1,1,1,1,1,1,1,1,1,1,1,1,1,1,1,1,1,1,1,1,1,1,1,1,1,1,1,
1,1,1,1,1,1,1,6),(2,2),(-1.,-0.999000000000001,-0.998000000000001,-0.997000000000001,
-0.996000000000001,-0.995000000000001,-0.994000000000001,-0.993000000000001,
-0.992000000000001,-0.991000000000001,-0.990000000000001,-0.989000000000001,
-0.988000000000001,-0.987000000000001,-0.986000000000001,-0.985000000000001,
-0.984000000000001,-0.983000000000001,-0.982000000000001,-0.981000000000001,
-0.980000000000001,-0.979000000000001,-0.978000000000001,-0.977000000000001,
-0.976000000000001,-0.975000000000001,-0.974000000000001,-0.973000000000001,
-0.972000000000001,-0.971000000000001,-0.970000000000001,-0.969000000000001,
-0.968000000000001,-0.967000000000001,-0.966000000000001,-0.965000000000001,
-0.964000000000001,-0.963000000000001,-0.962000000000001,-0.961000000000001,
-0.960000000000001,-0.959000000000001,-0.958000000000001,-0.957000000000001,
-0.956000000000001,-0.955000000000001,-0.954000000000001,-0.953000000000001,
-0.952000000000001,-0.951000000000001,-0.950000000000001,-0.949000000000001,
-0.948000000000001,-0.947000000000001,-0.946000000000001,-0.945000000000001,
-0.944000000000001,-0.943000000000001,-0.942000000000001,-0.941000000000001,
-0.940000000000001,-0.939000000000001,-0.938000000000001,-0.937000000000001,
-0.936000000000001,-0.935000000000001,-0.934000000000001,-0.933000000000001,
-0.932000000000001,-0.931000000000001,-0.930000000000001,-0.929000000000001,
-0.928000000000001,-0.927000000000001,-0.926000000000001,-0.925000000000001,
-0.924000000000001,-0.923000000000001,-0.922000000000001,-0.921000000000001,
-0.920000000000001,-0.919000000000001,-0.918000000000001,-0.917000000000001,
-0.916000000000001,-0.915000000000001,-0.914000000000001,-0.913000000000001,
-0.912000000000001,-0.911000000000001,-0.910000000000001,-0.909000000000001,
-0.908000000000001,-0.907000000000001,-0.906000000000001,-0.905000000000001,
-0.904000000000001,-0.903000000000001,-0.902000000000001,-0.901000000000001,
-0.900000000000001,-0.899000000000001,-0.898000000000001,-0.897000000000001,
-0.896000000000001,-0.895000000000001,-0.894000000000001,-0.893000000000001,
-0.892000000000001,-0.891000000000001,-0.890000000000001,-0.889000000000001,
-0.888000000000001,-0.887000000000001,-0.886000000000001,-0.885000000000001,
-0.884000000000001,-0.883000000000001,-0.882000000000001,-0.881000000000001,
-0.880000000000001,-0.879000000000001,-0.878000000000001,-0.877000000000001,
-0.876000000000001,-0.875000000000001,-0.874000000000001,-0.873000000000001,
-0.872000000000001,-0.871000000000001,-0.870000000000001,-0.869000000000001,
-0.868000000000001,-0.867000000000001,-0.866000000000001,-0.865000000000001,
-0.864000000000001,-0.863000000000001,-0.862000000000001,-0.861000000000001,
-0.860000000000001,-0.859000000000001,-0.858000000000001,-0.857000000000001,
-0.856000000000001,-0.855000000000001,-0.854000000000001,-0.853000000000001,
-0.852000000000001,-0.851000000000001,-0.850000000000001,-0.849000000000001,
-0.848000000000001,-0.847000000000001,-0.846000000000001,-0.845000000000001,
-0.844000000000001,-0.843000000000001,-0.842000000000001,-0.841000000000001,
-0.840000000000001,-0.839000000000001,-0.838000000000001,-0.837000000000001,
-0.836000000000001,-0.835000000000001,-0.834000000000001,-0.833000000000001,
-0.832000000000001,-0.831000000000001,-0.830000000000001,-0.829000000000001,
-0.828000000000001,-0.827000000000001,-0.826000000000001,-0.825000000000001,
-0.824000000000001,-0.823000000000001,-0.822000000000001,-0.821000000000001,
-0.820000000000001,-0.819000000000001,-0.818000000000001,-0.817000000000001,
-0.816000000000001,-0.815000000000001,-0.814000000000001,-0.813000000000001,
-0.812000000000001,-0.811000000000001,-0.810000000000001,-0.809000000000001,
-0.808000000000001,-0.807000000000001,-0.806000000000001,-0.805000000000001,
-0.804000000000001,-0.803000000000001,-0.802000000000001,-0.801000000000001,
-0.800000000000001,-0.799000000000001,-0.798000000000001,-0.797000000000001,
-0.796000000000001,-0.795000000000001,-0.794000000000001,-0.793000000000001,
-0.792000000000001,-0.791000000000001,-0.790000000000001,-0.789000000000001,
-0.788000000000001,-0.787000000000001,-0.786000000000001,-0.785000000000001,
-0.784000000000001,-0.783000000000001,-0.782000000000001,-0.781000000000001,
-0.780000000000001,-0.779000000000001,-0.778000000000001,-0.777000000000001,
-0.776000000000001,-0.775000000000001,-0.774000000000001,-0.773000000000001,
-0.772000000000001,-0.771000000000001,-0.770000000000001,-0.769000000000001,
-0.768000000000001,-0.767000000000001,-0.766000000000001,-0.765000000000001,
-0.764000000000001,-0.763000000000001,-0.762000000000001,-0.761000000000001,
-0.760000000000001,-0.759000000000001,-0.758000000000001,-0.757000000000001,
-0.756000000000001,-0.755000000000001,-0.754000000000001,-0.753000000000001,
-0.752000000000001,-0.751000000000001,-0.750000000000001,-0.749000000000001,
-0.748000000000001,-0.747000000000001,-0.746000000000001,-0.745000000000001,
-0.744000000000001,-0.743000000000001,-0.742000000000001,-0.741000000000001,
-0.740000000000001,-0.739000000000001,-0.738000000000001,-0.737000000000001,
-0.736000000000001,-0.735000000000001,-0.734000000000001,-0.733000000000001,
-0.732000000000001,-0.731000000000001,-0.730000000000001,-0.729000000000001,
-0.728000000000001,-0.727000000000001,-0.726000000000001,-0.725000000000001,
-0.724000000000001,-0.723000000000001,-0.722000000000001,-0.721000000000001,
-0.720000000000001,-0.719000000000001,-0.718000000000001,-0.717000000000001,
-0.716000000000001,-0.715000000000001,-0.714000000000001,-0.713000000000001,
-0.712000000000001,-0.711000000000001,-0.710000000000001,-0.709000000000001,
-0.708000000000001,-0.707000000000001,-0.706000000000001,-0.705000000000001,
-0.704000000000001,-0.703000000000001,-0.702000000000001,-0.701000000000001,
-0.700000000000001,-0.699000000000001,-0.698000000000001,-0.697000000000001,
-0.696000000000001,-0.695000000000001,-0.694000000000001,-0.693000000000001,
-0.692000000000001,-0.691000000000001,-0.690000000000001,-0.689000000000001,
-0.688000000000001,-0.687,-0.686,-0.685,-0.684,-0.683,-0.682,-0.681,-0.68,
-0.679,-0.678,-0.677,-0.676,-0.675,-0.674,-0.673,-0.672,-0.671,-0.67,-0.669,
-0.668,-0.667,-0.666,-0.665,-0.664,-0.663,-0.662,-0.661,-0.66,-0.659,-0.658,
-0.657,-0.656,-0.655,-0.654,-0.653,-0.652,-0.651,-0.65,-0.649,-0.648,-0.647,
-0.646,-0.645,-0.644,-0.643,-0.642,-0.641,-0.64,-0.639,-0.638,-0.637,-0.636,
-0.635,-0.634,-0.633,-0.632,-0.631,-0.63,-0.629,-0.628,-0.627,-0.626,-0.625,
-0.624,-0.623,-0.622,-0.621,-0.62,-0.619,-0.618,-0.617,-0.616,-0.615,-0.614,
-0.613,-0.612,-0.611,-0.61,-0.609,-0.608,-0.607,-0.606,-0.605,-0.604,-0.603,
-0.602,-0.601,-0.6,-0.599,-0.598,-0.597,-0.596,-0.595,-0.594,-0.593,-0.592,
-0.591,-0.59,-0.589,-0.588,-0.587,-0.586,-0.585,-0.584,-0.583,-0.582,-0.581,
-0.58,-0.579,-0.578,-0.577,-0.576,-0.575,-0.574,-0.573,-0.572,-0.571,-0.57,
-0.569,-0.568,-0.567,-0.566,-0.565,-0.564,-0.563,-0.562,-0.561,-0.56,-0.559,
-0.558,-0.557,-0.556,-0.555,-0.554,-0.553,-0.552,-0.551,-0.55,-0.549,-0.548,
-0.547,-0.546,-0.545,-0.544,-0.543,-0.542,-0.541,-0.54,-0.539,-0.538,-0.537,
-0.536,-0.535,-0.534,-0.533,-0.532,-0.531,-0.53,-0.529,-0.528,-0.527,-0.526,
-0.525,-0.524,-0.523,-0.522,-0.521,-0.52,-0.519,-0.518,-0.517,-0.516,-0.515,
-0.514,-0.513,-0.512,-0.511,-0.51,-0.509,-0.508,-0.507,-0.506,-0.505,-0.504,
-0.503,-0.502,-0.501,-0.5,-0.499,-0.498,-0.497,-0.496,-0.495,-0.494,-0.493,
-0.492,-0.491,-0.49,-0.489,-0.488,-0.487,-0.486,-0.485,-0.484,-0.483,-0.482,
-0.481,-0.48,-0.479,-0.478,-0.477,-0.476,-0.475,-0.474,-0.473,-0.472,-0.471,
-0.47,-0.469,-0.468,-0.467,-0.466,-0.465,-0.464,-0.463,-0.462,-0.461,-0.46,
-0.459,-0.458,-0.457,-0.456,-0.455,-0.454,-0.453,-0.452,-0.451,-0.45,-0.449,
-0.448,-0.447,-0.446,-0.445,-0.444,-0.443,-0.442,-0.441,-0.44,-0.439,-0.438,
-0.437,-0.436,-0.435,-0.434,-0.433,-0.432,-0.431,-0.43,-0.429,-0.428,-0.427,
-0.426,-0.425,-0.424,-0.423,-0.422,-0.421,-0.42,-0.419,-0.418,-0.417,-0.416,
-0.415,-0.414,-0.413,-0.412,-0.411,-0.41,-0.409,-0.408,-0.407,-0.406,-0.405,
-0.404,-0.403,-0.402,-0.401,-0.4,-0.399,-0.398,-0.397,-0.396,-0.395,-0.394,
-0.393,-0.392,-0.391,-0.39,-0.389,-0.388,-0.387,-0.386,-0.385,-0.384,-0.383,
-0.382,-0.381,-0.38,-0.379,-0.378,-0.377,-0.376,-0.375,-0.374,-0.373,-0.372,
-0.371,-0.37,-0.369,-0.368,-0.367,-0.366,-0.365,-0.364,-0.363,-0.362,-0.361,
-0.36,-0.359,-0.358,-0.357,-0.356,-0.355,-0.354,-0.353,-0.352,-0.351,-0.35,
-0.349,-0.348,-0.347,-0.346,-0.345,-0.344,-0.343,-0.342,-0.341,-0.34,-0.339,
-0.338,-0.337,-0.336,-0.335,-0.334,-0.333,-0.332,-0.331,-0.33,-0.329,-0.328,
-0.327,-0.326,-0.325,-0.324,-0.323,-0.322,-0.321,-0.32,-0.319,-0.318,-0.317,
-0.316,-0.315,-0.314,-0.313,-0.312,-0.311,-0.31,-0.309,-0.308,-0.307,-0.306,
-0.305,-0.304,-0.303,-0.302,-0.301,-0.3,-0.299,-0.298,-0.297,-0.296,-0.295,
-0.294,-0.293,-0.292,-0.291,-0.29,-0.289,-0.288,-0.287,-0.286,-0.285,-0.284,
-0.283,-0.282,-0.281,-0.28,-0.279,-0.278,-0.277,-0.276,-0.275,-0.274,-0.273,
-0.272,-0.271,-0.27,-0.269,-0.268,-0.267,-0.266,-0.265,-0.264,-0.263,-0.262,
-0.261,-0.26,-0.259,-0.258,-0.257,-0.256,-0.255,-0.254,-0.253,-0.252,-0.251,
-0.25,-0.249,-0.248,-0.247,-0.246,-0.245,-0.244,-0.243,-0.242,-0.241,-0.24,
-0.239,-0.238,-0.237,-0.236,-0.235,-0.234,-0.233,-0.232,-0.231,-0.23,-0.229,
-0.228,-0.227,-0.226,-0.225,-0.224,-0.223,-0.222,-0.221,-0.22,-0.219,-0.218,
-0.217,-0.216,-0.215,-0.214,-0.213,-0.212,-0.211,-0.21,-0.209,-0.208,-0.207,
-0.206,-0.205,-0.204,-0.203,-0.202,-0.201,-0.2,-0.199,-0.198,-0.197,-0.196,
-0.195,-0.194,-0.193,-0.192,-0.191,-0.19,-0.189,-0.188,-0.187,-0.186,-0.185,
-0.184,-0.183,-0.182,-0.181,-0.18,-0.179,-0.178,-0.177,-0.176,-0.175,-0.174,
-0.173,-0.172,-0.171,-0.17,-0.169,-0.168,-0.167,-0.166,-0.165,-0.164,-0.163,
-0.162,-0.161,-0.16,-0.159,-0.158,-0.157,-0.156,-0.155,-0.154,-0.153,-0.152,
-0.151,-0.15,-0.149,-0.148,-0.147,-0.146,-0.145,-0.144,-0.143,-0.142,-0.141,
-0.14,-0.139,-0.138,-0.137,-0.136,-0.135,-0.134,-0.133,-0.132,-0.131,-0.13,
-0.129,-0.128,-0.127,-0.126,-0.125,-0.124,-0.123,-0.122,-0.121,-0.12,-0.119,
-0.118,-0.117,-0.116,-0.115,-0.114,-0.113,-0.112,-0.111,-0.11,-0.109,-0.108,
-0.107,-0.106,-0.105,-0.104,-0.103,-0.102,-0.101,-0.1,-0.0990000000000001,
-0.0980000000000001,-0.0970000000000001,-0.0960000000000001,-0.0950000000000001,
-0.0940000000000001,-0.0930000000000001,-0.0920000000000001,-0.0910000000000001,
-0.0900000000000001,-0.0890000000000001,-0.0880000000000001,-0.0870000000000001,
-0.0860000000000001,-0.0850000000000001,-0.0840000000000001,-0.0830000000000001,
-0.0820000000000001,-0.0810000000000001,-0.0800000000000001,-0.0790000000000001,
-0.0780000000000001,-0.0770000000000001,-0.0760000000000001,-0.0750000000000001,
-0.0740000000000001,-0.0730000000000001,-0.0720000000000001,-0.071,-0.07,
-0.069,-0.068,-0.067,-0.066,-0.065,-0.064,-0.063,-0.062,-0.061,-0.06,-0.059,
-0.058,-0.057,-0.056,-0.055,-0.054,-0.053,-0.052,-0.051,-0.05,-0.049,-0.048,
-0.047,-0.046,-0.045,-0.044,-0.043,-0.042,-0.041,-0.04,-0.039,-0.038,-0.037,
-0.036,-0.035,-0.034,-0.033,-0.032,-0.031,-0.03,-0.029,-0.028,-0.027,-0.026,
-0.025,-0.024,-0.023,-0.022,-0.021,-0.02,-0.019,-0.018,-0.017,-0.016,-0.015,
-0.014,-0.013,-0.012,-0.011,-0.01,-0.009,-0.008,-0.007,-0.006,-0.005,-0.004,
-0.003,-0.002,-0.001,0.),(0.,2.),.UNSPECIFIED.)
GEOMETRIC_REPRESENTATION_ITEM()
RATIONAL_B_SPLINE_SURFACE(((1.,1.),(1.,1.),(1.,1.),(1.,1.),(1.,1.),(1.,
1.),(1.,1.),(1.,1.),(1.,1.),(1.,1.),(1.,1.),(1.,1.),(1.,1.),(1.,1.),(1.,
1.),(1.,1.),(1.,1.),(1.,1.),(1.,1.),(1.,1.),(1.,1.),(1.,1.),(1.,1.),(1.,
1.),(1.,1.),(1.,1.),(1.,1.),(1.,1.),(1.,1.),(1.,1.),(1.,1.),(1.,1.),(1.,
1.),(1.,1.),(1.,1.),(1.,1.),(1.,1.),(1.,1.),(1.,1.),(1.,1.),(1.,1.),(1.,
1.),(1.,1.),(1.,1.),(1.,1.),(1.,1.),(1.,1.),(1.,1.),(1.,1.),(1.,1.),(1.,
1.),(1.,1.),(1.,1.),(1.,1.),(1.,1.),(1.,1.),(1.,1.),(1.,1.),(1.,1.),(1.,
1.),(1.,1.),(1.,1.),(1.,1.),(1.,1.),(1.,1.),(1.,1.),(1.,1.),(1.,1.),(1.,
1.),(1.,1.),(1.,1.),(1.,1.),(1.,1.),(1.,1.),(1.,1.),(1.,1.),(1.,1.),(1.,
1.),(1.,1.),(1.,1.),(1.,1.),(1.,1.),(1.,1.),(1.,1.),(1.,1.),(1.,1.),(1.,
1.),(1.,1.),(1.,1.),(1.,1.),(1.,1.),(1.,1.),(1.,1.),(1.,1.),(1.,1.),(1.,
1.),(1.,1.),(1.,1.),(1.,1.),(1.,1.),(1.,1.),(1.,1.),(1.,1.),(1.,1.),(1.,
1.),(1.,1.),(1.,1.),(1.,1.),(1.,1.),(1.,1.),(1.,1.),(1.,1.),(1.,1.),(1.,
1.),(1.,1.),(1.,1.),(1.,1.),(1.,1.),(1.,1.),(1.,1.),(1.,1.),(1.,1.),(1.,
1.),(1.,1.),(1.,1.),(1.,1.),(1.,1.),(1.,1.),(1.,1.),(1.,1.),(1.,1.),(1.,
1.),(1.,1.),(1.,1.),(1.,1.),(1.,1.),(1.,1.),(1.,1.),(1.,1.),(1.,1.),(1.,
1.),(1.,1.),(1.,1.),(1.,1.),(1.,1.),(1.,1.),(1.,1.),(1.,1.),(1.,1.),(1.,
1.),(1.,1.),(1.,1.),(1.,1.),(1.,1.),(1.,1.),(1.,1.),(1.,1.),(1.,1.),(1.,
1.),(1.,1.),(1.,1.),(1.,1.),(1.,1.),(1.,1.),(1.,1.),(1.,1.),(1.,1.),(1.,
1.),(1.,1.),(1.,1.),(1.,1.),(1.,1.),(1.,1.),(1.,1.),(1.,1.),(1.,1.),(1.,
1.),(1.,1.),(1.,1.),(1.,1.),(1.,1.),(1.,1.),(1.,1.),(1.,1.),(1.,1.),(1.,
1.),(1.,1.),(1.,1.),(1.,1.),(1.,1.),(1.,1.),(1.,1.),(1.,1.),(1.,1.),(1.,
1.),(1.,1.),(1.,1.),(1.,1.),(1.,1.),(1.,1.),(1.,1.),(1.,1.),(1.,1.),(1.,
1.),(1.,1.),(1.,1.),(1.,1.),(1.,1.),(1.,1.),(1.,1.),(1.,1.),(1.,1.),(1.,
1.),(1.,1.),(1.,1.),(1.,1.),(1.,1.),(1.,1.),(1.,1.),(1.,1.),(1.,1.),(1.,
1.),(1.,1.),(1.,1.),(1.,1.),(1.,1.),(1.,1.),(1.,1.),(1.,1.),(1.,1.),(1.,
1.),(1.,1.),(1.,1.),(1.,1.),(1.,1.),(1.,1.),(1.,1.),(1.,1.),(1.,1.),(1.,
1.),(1.,1.),(1.,1.),(1.,1.),(1.,1.),(1.,1.),(1.,1.),(1.,1.),(1.,1.),(1.,
1.),(1.,1.),(1.,1.),(1.,1.),(1.,1.),(1.,1.),(1.,1.),(1.,1.),(1.,1.),(1.,
1.),(1.,1.),(1.,1.),(1.,1.),(1.,1.),(1.,1.),(1.,1.),(1.,1.),(1.,1.),(1.,
1.),(1.,1.),(1.,1.),(1.,1.),(1.,1.),(1.,1.),(1.,1.),(1.,1.),(1.,1.),(1.,
1.),(1.,1.),(1.,1.),(1.,1.),(1.,1.),(1.,1.),(1.,1.),(1.,1.),(1.,1.),(1.,
1.),(1.,1.),(1.,1.),(1.,1.),(1.,1.),(1.,1.),(1.,1.),(1.,1.),(1.,1.),(1.,
1.),(1.,1.),(1.,1.),(1.,1.),(1.,1.),(1.,1.),(1.,1.),(1.,1.),(1.,1.),(1.,
1.),(1.,1.),(1.,1.),(1.,1.),(1.,1.),(1.,1.),(1.,1.),(1.,1.),(1.,1.),(1.,
1.),(1.,1.),(1.,1.),(1.,1.),(1.,1.),(1.,1.),(1.,1.),(1.,1.),(1.,1.),(1.,
1.),(1.,1.),(1.,1.),(1.,1.),(1.,1.),(1.,1.),(1.,1.),(1.,1.),(1.,1.),(1.,
1.),(1.,1.),(1.,1.),(1.,1.),(1.,1.),(1.,1.),(1.,1.),(1.,1.),(1.,1.),(1.,
1.),(1.,1.),(1.,1.),(1.,1.),(1.,1.),(1.,1.),(1.,1.),(1.,1.),(1.,1.),(1.,
1.),(1.,1.),(1.,1.),(1.,1.),(1.,1.),(1.,1.),(1.,1.),(1.,1.),(1.,1.),(1.,
1.),(1.,1.),(1.,1.),(1.,1.),(1.,1.),(1.,1.),(1.,1.),(1.,1.),(1.,1.),(1.,
1.),(1.,1.),(1.,1.),(1.,1.),(1.,1.),(1.,1.),(1.,1.),(1.,1.),(1.,1.),(1.,
1.),(1.,1.),(1.,1.),(1.,1.),(1.,1.),(1.,1.),(1.,1.),(1.,1.),(1.,1.),(1.,
1.),(1.,1.),(1.,1.),(1.,1.),(1.,1.),(1.,1.),(1.,1.),(1.,1.),(1.,1.),(1.,
1.),(1.,1.),(1.,1.),(1.,1.),(1.,1.),(1.,1.),(1.,1.),(1.,1.),(1.,1.),(1.,
1.),(1.,1.),(1.,1.),(1.,1.),(1.,1.),(1.,1.),(1.,1.),(1.,1.),(1.,1.),(1.,
1.),(1.,1.),(1.,1.),(1.,1.),(1.,1.),(1.,1.),(1.,1.),(1.,1.),(1.,1.),(1.,
1.),(1.,1.),(1.,1.),(1.,1.),(1.,1.),(1.,1.),(1.,1.),(1.,1.),(1.,1.),(1.,
1.),(1.,1.),(1.,1.),(1.,1.),(1.,1.),(1.,1.),(1.,1.),(1.,1.),(1.,1.),(1.,
1.),(1.,1.),(1.,1.),(1.,1.),(1.,1.),(1.,1.),(1.,1.),(1.,1.),(1.,1.),(1.,
1.),(1.,1.),(1.,1.),(1.,1.),(1.,1.),(1.,1.),(1.,1.),(1.,1.),(1.,1.),(1.,
1.),(1.,1.),(1.,1.),(1.,1.),(1.,1.),(1.,1.),(1.,1.),(1.,1.),(1.,1.),(1.,
1.),(1.,1.),(1.,1.),(1.,1.),(1.,1.),(1.,1.),(1.,1.),(1.,1.),(1.,1.),(1.,
1.),(1.,1.),(1.,1.),(1.,1.),(1.,1.),(1.,1.),(1.,1.),(1.,1.),(1.,1.),(1.,
1.),(1.,1.),(1.,1.),(1.,1.),(1.,1.),(1.,1.),(1.,1.),(1.,1.),(1.,1.),(1.,
1.),(1.,1.),(1.,1.),(1.,1.),(1.,1.),(1.,1.),(1.,1.),(1.,1.),(1.,1.),(1.,
1.),(1.,1.),(1.,1.),(1.,1.),(1.,1.),(1.,1.),(1.,1.),(1.,1.),(1.,1.),(1.,
1.),(1.,1.),(1.,1.),(1.,1.),(1.,1.),(1.,1.),(1.,1.),(1.,1.),(1.,1.),(1.,
1.),(1.,1.),(1.,1.),(1.,1.),(1.,1.),(1.,1.),(1.,1.),(1.,1.),(1.,1.),(1.,
1.),(1.,1.),(1.,1.),(1.,1.),(1.,1.),(1.,1.),(1.,1.),(1.,1.),(1.,1.),(1.,
1.),(1.,1.),(1.,1.),(1.,1.),(1.,1.),(1.,1.),(1.,1.),(1.,1.),(1.,1.),(1.,
1.),(1.,1.),(1.,1.),(1.,1.),(1.,1.),(1.,1.),(1.,1.),(1.,1.),(1.,1.),(1.,
1.),(1.,1.),(1.,1.),(1.,1.),(1.,1.),(1.,1.),(1.,1.),(1.,1.),(1.,1.),(1.,
1.),(1.,1.),(1.,1.),(1.,1.),(1.,1.),(1.,1.),(1.,1.),(1.,1.),(1.,1.),(1.,
1.),(1.,1.),(1.,1.),(1.,1.),(1.,1.),(1.,1.),(1.,1.),(1.,1.),(1.,1.),(1.,
1.),(1.,1.),(1.,1.),(1.,1.),(1.,1.),(1.,1.),(1.,1.),(1.,1.),(1.,1.),(1.,
1.),(1.,1.),(1.,1.),(1.,1.),(1.,1.),(1.,1.),(1.,1.),(1.,1.),(1.,1.),(1.,
1.),(1.,1.),(1.,1.),(1.,1.),(1.,1.),(1.,1.),(1.,1.),(1.,1.),(1.,1.),(1.,
1.),(1.,1.),(1.,1.),(1.,1.),(1.,1.),(1.,1.),(1.,1.),(1.,1.),(1.,1.),(1.,
1.),(1.,1.),(1.,1.),(1.,1.),(1.,1.),(1.,1.),(1.,1.),(1.,1.),(1.,1.),(1.,
1.),(1.,1.),(1.,1.),(1.,1.),(1.,1.),(1.,1.),(1.,1.),(1.,1.),(1.,1.),(1.,
1.),(1.,1.),(1.,1.),(1.,1.),(1.,1.),(1.,1.),(1.,1.),(1.,1.),(1.,1.),(1.,
1.),(1.,1.),(1.,1.),(1.,1.),(1.,1.),(1.,1.),(1.,1.),(1.,1.),(1.,1.),(1.,
1.),(1.,1.),(1.,1.),(1.,1.),(1.,1.),(1.,1.),(1.,1.),(1.,1.),(1.,1.),(1.,
1.),(1.,1.),(1.,1.),(1.,1.),(1.,1.),(1.,1.),(1.,1.),(1.,1.),(1.,1.),(1.,
1.),(1.,1.),(1.,1.),(1.,1.),(1.,1.),(1.,1.),(1.,1.),(1.,1.),(1.,1.),(1.,
1.),(1.,1.),(1.,1.),(1.,1.),(1.,1.),(1.,1.),(1.,1.),(1.,1.),(1.,1.),(1.,
1.),(1.,1.),(1.,1.),(1.,1.),(1.,1.),(1.,1.),(1.,1.),(1.,1.),(1.,1.),(1.,
1.),(1.,1.),(1.,1.),(1.,1.),(1.,1.),(1.,1.),(1.,1.),(1.,1.),(1.,1.),(1.,
1.),(1.,1.),(1.,1.),(1.,1.),(1.,1.),(1.,1.),(1.,1.),(1.,1.),(1.,1.),(1.,
1.),(1.,1.),(1.,1.),(1.,1.),(1.,1.),(1.,1.),(1.,1.),(1.,1.),(1.,1.),(1.,
1.),(1.,1.),(1.,1.),(1.,1.),(1.,1.),(1.,1.),(1.,1.),(1.,1.),(1.,1.),(1.,
1.),(1.,1.),(1.,1.),(1.,1.),(1.,1.),(1.,1.),(1.,1.),(1.,1.),(1.,1.),(1.,
1.),(1.,1.),(1.,1.),(1.,1.),(1.,1.),(1.,1.),(1.,1.),(1.,1.),(1.,1.),(1.,
1.),(1.,1.),(1.,1.),(1.,1.),(1.,1.),(1.,1.),(1.,1.),(1.,1.),(1.,1.),(1.,
1.),(1.,1.),(1.,1.),(1.,1.),(1.,1.),(1.,1.),(1.,1.),(1.,1.),(1.,1.),(1.,
1.),(1.,1.),(1.,1.),(1.,1.),(1.,1.),(1.,1.),(1.,1.),(1.,1.),(1.,1.),(1.,
1.),(1.,1.),(1.,1.),(1.,1.),(1.,1.),(1.,1.),(1.,1.),(1.,1.),(1.,1.),(1.,
1.),(1.,1.),(1.,1.),(1.,1.),(1.,1.),(1.,1.),(1.,1.),(1.,1.),(1.,1.),(1.,
1.),(1.,1.),(1.,1.),(1.,1.),(1.,1.),(1.,1.),(1.,1.),(1.,1.),(1.,1.),(1.,
1.),(1.,1.),(1.,1.),(1.,1.),(1.,1.),(1.,1.),(1.,1.),(1.,1.),(1.,1.),(1.,
1.),(1.,1.),(1.,1.),(1.,1.),(1.,1.),(1.,1.),(1.,1.),(1.,1.),(1.,1.),(1.,
1.),(1.,1.),(1.,1.),(1.,1.),(1.,1.),(1.,1.),(1.,1.),(1.,1.),(1.,1.),(1.,
1.),(1.,1.),(1.,1.),(1.,1.),(1.,1.),(1.,1.),(1.,1.),(1.,1.),(1.,1.),(1.,
1.),(1.,1.),(1.,1.),(1.,1.),(1.,1.),(1.,1.),(1.,1.),(1.,1.),(1.,1.),(1.,
1.),(1.,1.),(1.,1.),(1.,1.),(1.,1.),(1.,1.),(1.,1.),(1.,1.),(1.,1.),(1.,
1.),(1.,1.),(1.,1.),(1.,1.),(1.,1.),(1.,1.),(1.,1.),(1.,1.),(1.,1.),(1.,
1.),(1.,1.),(1.,1.),(1.,1.),(1.,1.),(1.,1.),(1.,1.),(1.,1.),(1.,1.),(1.,
1.),(1.,1.),(1.,1.),(1.,1.),(1.,1.),(1.,1.),(1.,1.),(1.,1.),(1.,1.),(1.,
1.),(1.,1.),(1.,1.),(1.,1.),(1.,1.),(1.,1.),(1.,1.),(1.,1.),(1.,1.),(1.,
1.),(1.,1.),(1.,1.),(1.,1.),(1.,1.),(1.,1.),(1.,1.),(1.,1.),(1.,1.),(1.,
1.),(1.,1.),(1.,1.),(1.,1.),(1.,1.),(1.,1.),(1.,1.),(1.,1.),(1.,1.),(1.,
1.),(1.,1.),(1.,1.),(1.,1.),(1.,1.),(1.,1.),(1.,1.),(1.,1.),(1.,1.),(1.,
1.),(1.,1.),(1.,1.),(1.,1.),(1.,1.),(1.,1.),(1.,1.),(1.,1.),(1.,1.),(1.,
1.),(1.,1.),(1.,1.),(1.,1.),(1.,1.),(1.,1.),(1.,1.),(1.,1.),(1.,1.),(1.,
1.),(1.,1.),(1.,1.),(1.,1.),(1.,1.),(1.,1.),(1.,1.),(1.,1.),(1.,1.),(1.,
1.),(1.,1.),(1.,1.),(1.,1.),(1.,1.),(1.,1.),(1.,1.),(1.,1.),(1.,1.),(1.,
1.),(1.,1.),(1.,1.),(1.,1.),(1.,1.),(1.,1.),(1.,1.),(1.,1.),(1.,1.),(1.,
1.),(1.,1.),(1.,1.),(1.,1.),(1.,1.),(1.,1.),(1.,1.),(1.,1.),(1.,1.),(1.,
1.),(1.,1.),(1.,1.),(1.,1.),(1.,1.),(1.,1.),(1.,1.),(1.,1.),(1.,1.),(1.,
1.),(1.,1.),(1.,1.),(1.,1.),(1.,1.),(1.,1.),(1.,1.),(1.,1.),(1.,1.),(1.,
1.),(1.,1.),(1.,1.),(1.,1.),(1.,1.),(1.,1.),(1.,1.),(1.,1.),(1.,1.),(1.,
1.)))
REPRESENTATION_ITEM('')
SURFACE()
);
#258=(
BOUNDED_SURFACE()
B_SPLINE_SURFACE(5,1,((#74101,#74102),(#74103,#74104),(#74105,#74106),(#74107,
#74108),(#74109,#74110),(#74111,#74112),(#74113,#74114),(#74115,#74116),
(#74117,#74118),(#74119,#74120),(#74121,#74122),(#74123,#74124),(#74125,
#74126),(#74127,#74128),(#74129,#74130),(#74131,#74132),(#74133,#74134),
(#74135,#74136),(#74137,#74138),(#74139,#74140),(#74141,#74142),(#74143,
#74144),(#74145,#74146),(#74147,#74148),(#74149,#74150),(#74151,#74152),
(#74153,#74154),(#74155,#74156),(#74157,#74158),(#74159,#74160),(#74161,
#74162),(#74163,#74164),(#74165,#74166),(#74167,#74168),(#74169,#74170),
(#74171,#74172),(#74173,#74174),(#74175,#74176),(#74177,#74178),(#74179,
#74180),(#74181,#74182),(#74183,#74184),(#74185,#74186),(#74187,#74188),
(#74189,#74190),(#74191,#74192),(#74193,#74194),(#74195,#74196),(#74197,
#74198),(#74199,#74200),(#74201,#74202),(#74203,#74204),(#74205,#74206),
(#74207,#74208),(#74209,#74210),(#74211,#74212),(#74213,#74214),(#74215,
#74216),(#74217,#74218),(#74219,#74220),(#74221,#74222),(#74223,#74224),
(#74225,#74226),(#74227,#74228),(#74229,#74230),(#74231,#74232),(#74233,
#74234),(#74235,#74236),(#74237,#74238),(#74239,#74240),(#74241,#74242),
(#74243,#74244),(#74245,#74246),(#74247,#74248),(#74249,#74250),(#74251,
#74252),(#74253,#74254),(#74255,#74256),(#74257,#74258),(#74259,#74260),
(#74261,#74262),(#74263,#74264),(#74265,#74266),(#74267,#74268),(#74269,
#74270),(#74271,#74272),(#74273,#74274),(#74275,#74276),(#74277,#74278),
(#74279,#74280),(#74281,#74282),(#74283,#74284),(#74285,#74286),(#74287,
#74288),(#74289,#74290),(#74291,#74292),(#74293,#74294),(#74295,#74296),
(#74297,#74298),(#74299,#74300),(#74301,#74302),(#74303,#74304),(#74305,
#74306),(#74307,#74308),(#74309,#74310),(#74311,#74312),(#74313,#74314),
(#74315,#74316),(#74317,#74318),(#74319,#74320),(#74321,#74322),(#74323,
#74324),(#74325,#74326),(#74327,#74328),(#74329,#74330),(#74331,#74332),
(#74333,#74334),(#74335,#74336),(#74337,#74338),(#74339,#74340),(#74341,
#74342),(#74343,#74344),(#74345,#74346),(#74347,#74348),(#74349,#74350),
(#74351,#74352),(#74353,#74354),(#74355,#74356),(#74357,#74358),(#74359,
#74360),(#74361,#74362),(#74363,#74364),(#74365,#74366),(#74367,#74368),
(#74369,#74370),(#74371,#74372),(#74373,#74374),(#74375,#74376),(#74377,
#74378),(#74379,#74380),(#74381,#74382),(#74383,#74384),(#74385,#74386),
(#74387,#74388),(#74389,#74390),(#74391,#74392),(#74393,#74394),(#74395,
#74396),(#74397,#74398),(#74399,#74400),(#74401,#74402),(#74403,#74404),
(#74405,#74406),(#74407,#74408),(#74409,#74410),(#74411,#74412),(#74413,
#74414),(#74415,#74416),(#74417,#74418),(#74419,#74420),(#74421,#74422),
(#74423,#74424),(#74425,#74426),(#74427,#74428),(#74429,#74430),(#74431,
#74432),(#74433,#74434),(#74435,#74436),(#74437,#74438),(#74439,#74440),
(#74441,#74442),(#74443,#74444),(#74445,#74446),(#74447,#74448),(#74449,
#74450),(#74451,#74452),(#74453,#74454),(#74455,#74456),(#74457,#74458),
(#74459,#74460),(#74461,#74462),(#74463,#74464),(#74465,#74466),(#74467,
#74468),(#74469,#74470),(#74471,#74472),(#74473,#74474),(#74475,#74476),
(#74477,#74478),(#74479,#74480),(#74481,#74482),(#74483,#74484),(#74485,
#74486),(#74487,#74488),(#74489,#74490),(#74491,#74492),(#74493,#74494),
(#74495,#74496),(#74497,#74498),(#74499,#74500),(#74501,#74502),(#74503,
#74504),(#74505,#74506),(#74507,#74508),(#74509,#74510),(#74511,#74512),
(#74513,#74514),(#74515,#74516),(#74517,#74518),(#74519,#74520),(#74521,
#74522),(#74523,#74524),(#74525,#74526),(#74527,#74528),(#74529,#74530),
(#74531,#74532),(#74533,#74534),(#74535,#74536),(#74537,#74538),(#74539,
#74540),(#74541,#74542),(#74543,#74544),(#74545,#74546),(#74547,#74548),
(#74549,#74550),(#74551,#74552),(#74553,#74554),(#74555,#74556),(#74557,
#74558),(#74559,#74560),(#74561,#74562),(#74563,#74564),(#74565,#74566),
(#74567,#74568),(#74569,#74570),(#74571,#74572),(#74573,#74574),(#74575,
#74576),(#74577,#74578),(#74579,#74580),(#74581,#74582),(#74583,#74584),
(#74585,#74586),(#74587,#74588),(#74589,#74590),(#74591,#74592),(#74593,
#74594),(#74595,#74596),(#74597,#74598),(#74599,#74600),(#74601,#74602),
(#74603,#74604),(#74605,#74606),(#74607,#74608),(#74609,#74610),(#74611,
#74612),(#74613,#74614),(#74615,#74616),(#74617,#74618),(#74619,#74620),
(#74621,#74622),(#74623,#74624),(#74625,#74626),(#74627,#74628),(#74629,
#74630),(#74631,#74632),(#74633,#74634),(#74635,#74636),(#74637,#74638),
(#74639,#74640),(#74641,#74642),(#74643,#74644),(#74645,#74646),(#74647,
#74648),(#74649,#74650),(#74651,#74652),(#74653,#74654),(#74655,#74656),
(#74657,#74658),(#74659,#74660),(#74661,#74662),(#74663,#74664),(#74665,
#74666),(#74667,#74668),(#74669,#74670),(#74671,#74672),(#74673,#74674),
(#74675,#74676),(#74677,#74678),(#74679,#74680),(#74681,#74682),(#74683,
#74684),(#74685,#74686),(#74687,#74688),(#74689,#74690),(#74691,#74692),
(#74693,#74694),(#74695,#74696),(#74697,#74698),(#74699,#74700),(#74701,
#74702),(#74703,#74704),(#74705,#74706),(#74707,#74708),(#74709,#74710),
(#74711,#74712),(#74713,#74714),(#74715,#74716),(#74717,#74718),(#74719,
#74720),(#74721,#74722),(#74723,#74724),(#74725,#74726),(#74727,#74728),
(#74729,#74730),(#74731,#74732),(#74733,#74734),(#74735,#74736),(#74737,
#74738),(#74739,#74740),(#74741,#74742),(#74743,#74744),(#74745,#74746),
(#74747,#74748),(#74749,#74750),(#74751,#74752),(#74753,#74754),(#74755,
#74756),(#74757,#74758),(#74759,#74760),(#74761,#74762),(#74763,#74764),
(#74765,#74766),(#74767,#74768),(#74769,#74770),(#74771,#74772),(#74773,
#74774),(#74775,#74776),(#74777,#74778),(#74779,#74780),(#74781,#74782),
(#74783,#74784),(#74785,#74786),(#74787,#74788),(#74789,#74790),(#74791,
#74792),(#74793,#74794),(#74795,#74796),(#74797,#74798),(#74799,#74800),
(#74801,#74802),(#74803,#74804),(#74805,#74806),(#74807,#74808),(#74809,
#74810),(#74811,#74812),(#74813,#74814),(#74815,#74816),(#74817,#74818),
(#74819,#74820),(#74821,#74822),(#74823,#74824),(#74825,#74826),(#74827,
#74828),(#74829,#74830),(#74831,#74832),(#74833,#74834),(#74835,#74836),
(#74837,#74838),(#74839,#74840),(#74841,#74842),(#74843,#74844),(#74845,
#74846),(#74847,#74848),(#74849,#74850),(#74851,#74852),(#74853,#74854),
(#74855,#74856),(#74857,#74858),(#74859,#74860),(#74861,#74862),(#74863,
#74864),(#74865,#74866),(#74867,#74868),(#74869,#74870),(#74871,#74872),
(#74873,#74874),(#74875,#74876),(#74877,#74878),(#74879,#74880),(#74881,
#74882),(#74883,#74884),(#74885,#74886),(#74887,#74888),(#74889,#74890),
(#74891,#74892),(#74893,#74894),(#74895,#74896),(#74897,#74898),(#74899,
#74900),(#74901,#74902),(#74903,#74904),(#74905,#74906),(#74907,#74908),
(#74909,#74910),(#74911,#74912),(#74913,#74914),(#74915,#74916),(#74917,
#74918),(#74919,#74920),(#74921,#74922),(#74923,#74924),(#74925,#74926),
(#74927,#74928),(#74929,#74930),(#74931,#74932),(#74933,#74934),(#74935,
#74936),(#74937,#74938),(#74939,#74940),(#74941,#74942),(#74943,#74944),
(#74945,#74946),(#74947,#74948),(#74949,#74950),(#74951,#74952),(#74953,
#74954),(#74955,#74956),(#74957,#74958),(#74959,#74960),(#74961,#74962),
(#74963,#74964),(#74965,#74966),(#74967,#74968),(#74969,#74970),(#74971,
#74972),(#74973,#74974),(#74975,#74976),(#74977,#74978),(#74979,#74980),
(#74981,#74982),(#74983,#74984),(#74985,#74986),(#74987,#74988),(#74989,
#74990),(#74991,#74992),(#74993,#74994),(#74995,#74996),(#74997,#74998),
(#74999,#75000),(#75001,#75002),(#75003,#75004),(#75005,#75006),(#75007,
#75008),(#75009,#75010),(#75011,#75012),(#75013,#75014),(#75015,#75016),
(#75017,#75018),(#75019,#75020),(#75021,#75022),(#75023,#75024),(#75025,
#75026),(#75027,#75028),(#75029,#75030),(#75031,#75032),(#75033,#75034),
(#75035,#75036),(#75037,#75038),(#75039,#75040),(#75041,#75042),(#75043,
#75044),(#75045,#75046),(#75047,#75048),(#75049,#75050),(#75051,#75052),
(#75053,#75054),(#75055,#75056),(#75057,#75058),(#75059,#75060),(#75061,
#75062),(#75063,#75064),(#75065,#75066),(#75067,#75068),(#75069,#75070),
(#75071,#75072),(#75073,#75074),(#75075,#75076),(#75077,#75078),(#75079,
#75080),(#75081,#75082),(#75083,#75084),(#75085,#75086),(#75087,#75088),
(#75089,#75090),(#75091,#75092),(#75093,#75094),(#75095,#75096),(#75097,
#75098),(#75099,#75100),(#75101,#75102),(#75103,#75104),(#75105,#75106),
(#75107,#75108),(#75109,#75110),(#75111,#75112),(#75113,#75114),(#75115,
#75116),(#75117,#75118),(#75119,#75120),(#75121,#75122),(#75123,#75124),
(#75125,#75126),(#75127,#75128),(#75129,#75130),(#75131,#75132),(#75133,
#75134),(#75135,#75136),(#75137,#75138),(#75139,#75140),(#75141,#75142),
(#75143,#75144),(#75145,#75146),(#75147,#75148),(#75149,#75150),(#75151,
#75152),(#75153,#75154),(#75155,#75156),(#75157,#75158),(#75159,#75160),
(#75161,#75162),(#75163,#75164),(#75165,#75166),(#75167,#75168),(#75169,
#75170),(#75171,#75172),(#75173,#75174),(#75175,#75176),(#75177,#75178),
(#75179,#75180),(#75181,#75182),(#75183,#75184),(#75185,#75186),(#75187,
#75188),(#75189,#75190),(#75191,#75192),(#75193,#75194),(#75195,#75196),
(#75197,#75198),(#75199,#75200),(#75201,#75202),(#75203,#75204),(#75205,
#75206),(#75207,#75208),(#75209,#75210),(#75211,#75212),(#75213,#75214),
(#75215,#75216),(#75217,#75218),(#75219,#75220),(#75221,#75222),(#75223,
#75224),(#75225,#75226),(#75227,#75228),(#75229,#75230),(#75231,#75232),
(#75233,#75234),(#75235,#75236),(#75237,#75238),(#75239,#75240),(#75241,
#75242),(#75243,#75244),(#75245,#75246),(#75247,#75248),(#75249,#75250),
(#75251,#75252),(#75253,#75254),(#75255,#75256),(#75257,#75258),(#75259,
#75260),(#75261,#75262),(#75263,#75264),(#75265,#75266),(#75267,#75268),
(#75269,#75270),(#75271,#75272),(#75273,#75274),(#75275,#75276),(#75277,
#75278),(#75279,#75280),(#75281,#75282),(#75283,#75284),(#75285,#75286),
(#75287,#75288),(#75289,#75290),(#75291,#75292),(#75293,#75294),(#75295,
#75296),(#75297,#75298),(#75299,#75300),(#75301,#75302),(#75303,#75304),
(#75305,#75306),(#75307,#75308),(#75309,#75310),(#75311,#75312),(#75313,
#75314),(#75315,#75316),(#75317,#75318),(#75319,#75320),(#75321,#75322),
(#75323,#75324),(#75325,#75326),(#75327,#75328),(#75329,#75330),(#75331,
#75332),(#75333,#75334),(#75335,#75336),(#75337,#75338),(#75339,#75340),
(#75341,#75342),(#75343,#75344),(#75345,#75346),(#75347,#75348),(#75349,
#75350),(#75351,#75352),(#75353,#75354),(#75355,#75356),(#75357,#75358),
(#75359,#75360),(#75361,#75362),(#75363,#75364),(#75365,#75366),(#75367,
#75368),(#75369,#75370),(#75371,#75372),(#75373,#75374),(#75375,#75376),
(#75377,#75378),(#75379,#75380),(#75381,#75382),(#75383,#75384),(#75385,
#75386),(#75387,#75388),(#75389,#75390),(#75391,#75392),(#75393,#75394),
(#75395,#75396),(#75397,#75398),(#75399,#75400),(#75401,#75402),(#75403,
#75404),(#75405,#75406),(#75407,#75408),(#75409,#75410),(#75411,#75412),
(#75413,#75414),(#75415,#75416),(#75417,#75418),(#75419,#75420),(#75421,
#75422),(#75423,#75424),(#75425,#75426),(#75427,#75428),(#75429,#75430),
(#75431,#75432),(#75433,#75434),(#75435,#75436),(#75437,#75438),(#75439,
#75440),(#75441,#75442),(#75443,#75444),(#75445,#75446),(#75447,#75448),
(#75449,#75450),(#75451,#75452),(#75453,#75454),(#75455,#75456),(#75457,
#75458),(#75459,#75460),(#75461,#75462),(#75463,#75464),(#75465,#75466),
(#75467,#75468),(#75469,#75470),(#75471,#75472),(#75473,#75474),(#75475,
#75476),(#75477,#75478),(#75479,#75480),(#75481,#75482),(#75483,#75484),
(#75485,#75486),(#75487,#75488),(#75489,#75490),(#75491,#75492),(#75493,
#75494),(#75495,#75496),(#75497,#75498),(#75499,#75500),(#75501,#75502),
(#75503,#75504),(#75505,#75506),(#75507,#75508),(#75509,#75510),(#75511,
#75512),(#75513,#75514),(#75515,#75516),(#75517,#75518),(#75519,#75520),
(#75521,#75522),(#75523,#75524),(#75525,#75526),(#75527,#75528),(#75529,
#75530),(#75531,#75532),(#75533,#75534),(#75535,#75536),(#75537,#75538),
(#75539,#75540),(#75541,#75542),(#75543,#75544),(#75545,#75546),(#75547,
#75548),(#75549,#75550),(#75551,#75552),(#75553,#75554),(#75555,#75556),
(#75557,#75558),(#75559,#75560),(#75561,#75562),(#75563,#75564),(#75565,
#75566),(#75567,#75568),(#75569,#75570),(#75571,#75572),(#75573,#75574),
(#75575,#75576),(#75577,#75578),(#75579,#75580),(#75581,#75582),(#75583,
#75584),(#75585,#75586),(#75587,#75588),(#75589,#75590),(#75591,#75592),
(#75593,#75594),(#75595,#75596),(#75597,#75598),(#75599,#75600),(#75601,
#75602),(#75603,#75604),(#75605,#75606),(#75607,#75608),(#75609,#75610),
(#75611,#75612),(#75613,#75614),(#75615,#75616),(#75617,#75618),(#75619,
#75620),(#75621,#75622),(#75623,#75624),(#75625,#75626),(#75627,#75628),
(#75629,#75630),(#75631,#75632),(#75633,#75634),(#75635,#75636),(#75637,
#75638),(#75639,#75640),(#75641,#75642),(#75643,#75644),(#75645,#75646),
(#75647,#75648),(#75649,#75650),(#75651,#75652),(#75653,#75654),(#75655,
#75656),(#75657,#75658),(#75659,#75660),(#75661,#75662),(#75663,#75664),
(#75665,#75666),(#75667,#75668),(#75669,#75670),(#75671,#75672),(#75673,
#75674),(#75675,#75676),(#75677,#75678),(#75679,#75680),(#75681,#75682),
(#75683,#75684),(#75685,#75686),(#75687,#75688),(#75689,#75690),(#75691,
#75692),(#75693,#75694),(#75695,#75696),(#75697,#75698),(#75699,#75700),
(#75701,#75702),(#75703,#75704),(#75705,#75706),(#75707,#75708),(#75709,
#75710),(#75711,#75712),(#75713,#75714),(#75715,#75716),(#75717,#75718),
(#75719,#75720),(#75721,#75722),(#75723,#75724),(#75725,#75726),(#75727,
#75728),(#75729,#75730),(#75731,#75732),(#75733,#75734),(#75735,#75736),
(#75737,#75738),(#75739,#75740),(#75741,#75742),(#75743,#75744),(#75745,
#75746),(#75747,#75748),(#75749,#75750),(#75751,#75752),(#75753,#75754),
(#75755,#75756),(#75757,#75758),(#75759,#75760),(#75761,#75762),(#75763,
#75764),(#75765,#75766),(#75767,#75768),(#75769,#75770),(#75771,#75772),
(#75773,#75774),(#75775,#75776),(#75777,#75778),(#75779,#75780),(#75781,
#75782),(#75783,#75784),(#75785,#75786),(#75787,#75788),(#75789,#75790),
(#75791,#75792),(#75793,#75794),(#75795,#75796),(#75797,#75798),(#75799,
#75800),(#75801,#75802),(#75803,#75804),(#75805,#75806),(#75807,#75808),
(#75809,#75810),(#75811,#75812),(#75813,#75814),(#75815,#75816),(#75817,
#75818),(#75819,#75820),(#75821,#75822),(#75823,#75824),(#75825,#75826),
(#75827,#75828),(#75829,#75830),(#75831,#75832),(#75833,#75834),(#75835,
#75836),(#75837,#75838),(#75839,#75840),(#75841,#75842),(#75843,#75844),
(#75845,#75846),(#75847,#75848),(#75849,#75850),(#75851,#75852),(#75853,
#75854),(#75855,#75856),(#75857,#75858),(#75859,#75860),(#75861,#75862),
(#75863,#75864),(#75865,#75866),(#75867,#75868),(#75869,#75870),(#75871,
#75872),(#75873,#75874),(#75875,#75876),(#75877,#75878),(#75879,#75880),
(#75881,#75882),(#75883,#75884),(#75885,#75886),(#75887,#75888),(#75889,
#75890),(#75891,#75892),(#75893,#75894),(#75895,#75896),(#75897,#75898),
(#75899,#75900),(#75901,#75902),(#75903,#75904),(#75905,#75906),(#75907,
#75908),(#75909,#75910),(#75911,#75912),(#75913,#75914),(#75915,#75916),
(#75917,#75918),(#75919,#75920),(#75921,#75922),(#75923,#75924),(#75925,
#75926),(#75927,#75928),(#75929,#75930),(#75931,#75932),(#75933,#75934),
(#75935,#75936),(#75937,#75938),(#75939,#75940),(#75941,#75942),(#75943,
#75944),(#75945,#75946),(#75947,#75948),(#75949,#75950),(#75951,#75952),
(#75953,#75954),(#75955,#75956),(#75957,#75958),(#75959,#75960),(#75961,
#75962),(#75963,#75964),(#75965,#75966),(#75967,#75968),(#75969,#75970),
(#75971,#75972),(#75973,#75974),(#75975,#75976),(#75977,#75978),(#75979,
#75980),(#75981,#75982),(#75983,#75984),(#75985,#75986),(#75987,#75988),
(#75989,#75990),(#75991,#75992),(#75993,#75994),(#75995,#75996),(#75997,
#75998),(#75999,#76000),(#76001,#76002),(#76003,#76004),(#76005,#76006),
(#76007,#76008),(#76009,#76010),(#76011,#76012),(#76013,#76014),(#76015,
#76016),(#76017,#76018),(#76019,#76020),(#76021,#76022),(#76023,#76024),
(#76025,#76026),(#76027,#76028),(#76029,#76030),(#76031,#76032),(#76033,
#76034),(#76035,#76036),(#76037,#76038),(#76039,#76040),(#76041,#76042),
(#76043,#76044),(#76045,#76046),(#76047,#76048),(#76049,#76050),(#76051,
#76052),(#76053,#76054),(#76055,#76056),(#76057,#76058),(#76059,#76060),
(#76061,#76062),(#76063,#76064),(#76065,#76066),(#76067,#76068),(#76069,
#76070),(#76071,#76072),(#76073,#76074),(#76075,#76076),(#76077,#76078),
(#76079,#76080),(#76081,#76082),(#76083,#76084),(#76085,#76086),(#76087,
#76088),(#76089,#76090),(#76091,#76092),(#76093,#76094),(#76095,#76096),
(#76097,#76098),(#76099,#76100),(#76101,#76102),(#76103,#76104),(#76105,
#76106),(#76107,#76108),(#76109,#76110)),.UNSPECIFIED.,.F.,.F.,.F.)
B_SPLINE_SURFACE_WITH_KNOTS((6,1,1,1,1,1,1,1,1,1,1,1,1,1,1,1,1,1,1,1,1,
1,1,1,1,1,1,1,1,1,1,1,1,1,1,1,1,1,1,1,1,1,1,1,1,1,1,1,1,1,1,1,1,1,1,1,1,
1,1,1,1,1,1,1,1,1,1,1,1,1,1,1,1,1,1,1,1,1,1,1,1,1,1,1,1,1,1,1,1,1,1,1,1,
1,1,1,1,1,1,1,1,1,1,1,1,1,1,1,1,1,1,1,1,1,1,1,1,1,1,1,1,1,1,1,1,1,1,1,1,
1,1,1,1,1,1,1,1,1,1,1,1,1,1,1,1,1,1,1,1,1,1,1,1,1,1,1,1,1,1,1,1,1,1,1,1,
1,1,1,1,1,1,1,1,1,1,1,1,1,1,1,1,1,1,1,1,1,1,1,1,1,1,1,1,1,1,1,1,1,1,1,1,
1,1,1,1,1,1,1,1,1,1,1,1,1,1,1,1,1,1,1,1,1,1,1,1,1,1,1,1,1,1,1,1,1,1,1,1,
1,1,1,1,1,1,1,1,1,1,1,1,1,1,1,1,1,1,1,1,1,1,1,1,1,1,1,1,1,1,1,1,1,1,1,1,
1,1,1,1,1,1,1,1,1,1,1,1,1,1,1,1,1,1,1,1,1,1,1,1,1,1,1,1,1,1,1,1,1,1,1,1,
1,1,1,1,1,1,1,1,1,1,1,1,1,1,1,1,1,1,1,1,1,1,1,1,1,1,1,1,1,1,1,1,1,1,1,1,
1,1,1,1,1,1,1,1,1,1,1,1,1,1,1,1,1,1,1,1,1,1,1,1,1,1,1,1,1,1,1,1,1,1,1,1,
1,1,1,1,1,1,1,1,1,1,1,1,1,1,1,1,1,1,1,1,1,1,1,1,1,1,1,1,1,1,1,1,1,1,1,1,
1,1,1,1,1,1,1,1,1,1,1,1,1,1,1,1,1,1,1,1,1,1,1,1,1,1,1,1,1,1,1,1,1,1,1,1,
1,1,1,1,1,1,1,1,1,1,1,1,1,1,1,1,1,1,1,1,1,1,1,1,1,1,1,1,1,1,1,1,1,1,1,1,
1,1,1,1,1,1,1,1,1,1,1,1,1,1,1,1,1,1,1,1,1,1,1,1,1,1,1,1,1,1,1,1,1,1,1,1,
1,1,1,1,1,1,1,1,1,1,1,1,1,1,1,1,1,1,1,1,1,1,1,1,1,1,1,1,1,1,1,1,1,1,1,1,
1,1,1,1,1,1,1,1,1,1,1,1,1,1,1,1,1,1,1,1,1,1,1,1,1,1,1,1,1,1,1,1,1,1,1,1,
1,1,1,1,1,1,1,1,1,1,1,1,1,1,1,1,1,1,1,1,1,1,1,1,1,1,1,1,1,1,1,1,1,1,1,1,
1,1,1,1,1,1,1,1,1,1,1,1,1,1,1,1,1,1,1,1,1,1,1,1,1,1,1,1,1,1,1,1,1,1,1,1,
1,1,1,1,1,1,1,1,1,1,1,1,1,1,1,1,1,1,1,1,1,1,1,1,1,1,1,1,1,1,1,1,1,1,1,1,
1,1,1,1,1,1,1,1,1,1,1,1,1,1,1,1,1,1,1,1,1,1,1,1,1,1,1,1,1,1,1,1,1,1,1,1,
1,1,1,1,1,1,1,1,1,1,1,1,1,1,1,1,1,1,1,1,1,1,1,1,1,1,1,1,1,1,1,1,1,1,1,1,
1,1,1,1,1,1,1,1,1,1,1,1,1,1,1,1,1,1,1,1,1,1,1,1,1,1,1,1,1,1,1,1,1,1,1,1,
1,1,1,1,1,1,1,1,1,1,1,1,1,1,1,1,1,1,1,1,1,1,1,1,1,1,1,1,1,1,1,1,1,1,1,1,
1,1,1,1,1,1,1,1,1,1,1,1,1,1,1,1,1,1,1,1,1,1,1,1,1,1,1,1,1,1,1,1,1,1,1,1,
1,1,1,1,1,1,1,1,1,1,1,1,1,1,1,1,1,1,1,1,1,1,1,1,1,1,1,1,1,1,1,1,1,1,1,1,
1,1,1,1,1,1,1,1,1,1,1,1,1,1,1,1,1,1,1,1,1,1,1,1,1,1,1,1,1,1,1,1,1,1,1,1,
1,1,1,1,1,1,1,1,1,1,1,1,1,1,1,1,1,1,1,1,1,1,1,1,1,1,1,1,1,1,1,1,1,1,1,1,
1,1,1,1,1,1,1,6),(2,2),(-1.,-0.999000000000001,-0.998000000000001,-0.997000000000001,
-0.996000000000001,-0.995000000000001,-0.994000000000001,-0.993000000000001,
-0.992000000000001,-0.991000000000001,-0.990000000000001,-0.989000000000001,
-0.988000000000001,-0.987000000000001,-0.986000000000001,-0.985000000000001,
-0.984000000000001,-0.983000000000001,-0.982000000000001,-0.981000000000001,
-0.980000000000001,-0.979000000000001,-0.978000000000001,-0.977000000000001,
-0.976000000000001,-0.975000000000001,-0.974000000000001,-0.973000000000001,
-0.972000000000001,-0.971000000000001,-0.970000000000001,-0.969000000000001,
-0.968000000000001,-0.967000000000001,-0.966000000000001,-0.965000000000001,
-0.964000000000001,-0.963000000000001,-0.962000000000001,-0.961000000000001,
-0.960000000000001,-0.959000000000001,-0.958000000000001,-0.957000000000001,
-0.956000000000001,-0.955000000000001,-0.954000000000001,-0.953000000000001,
-0.952000000000001,-0.951000000000001,-0.950000000000001,-0.949000000000001,
-0.948000000000001,-0.947000000000001,-0.946000000000001,-0.945000000000001,
-0.944000000000001,-0.943000000000001,-0.942000000000001,-0.941000000000001,
-0.940000000000001,-0.939000000000001,-0.938000000000001,-0.937000000000001,
-0.936000000000001,-0.935000000000001,-0.934000000000001,-0.933000000000001,
-0.932000000000001,-0.931000000000001,-0.930000000000001,-0.929000000000001,
-0.928000000000001,-0.927000000000001,-0.926000000000001,-0.925000000000001,
-0.924000000000001,-0.923000000000001,-0.922000000000001,-0.921000000000001,
-0.920000000000001,-0.919000000000001,-0.918000000000001,-0.917000000000001,
-0.916000000000001,-0.915000000000001,-0.914000000000001,-0.913000000000001,
-0.912000000000001,-0.911000000000001,-0.910000000000001,-0.909000000000001,
-0.908000000000001,-0.907000000000001,-0.906000000000001,-0.905000000000001,
-0.904000000000001,-0.903000000000001,-0.902000000000001,-0.901000000000001,
-0.900000000000001,-0.899000000000001,-0.898000000000001,-0.897000000000001,
-0.896000000000001,-0.895000000000001,-0.894000000000001,-0.893000000000001,
-0.892000000000001,-0.891000000000001,-0.890000000000001,-0.889000000000001,
-0.888000000000001,-0.887000000000001,-0.886000000000001,-0.885000000000001,
-0.884000000000001,-0.883000000000001,-0.882000000000001,-0.881000000000001,
-0.880000000000001,-0.879000000000001,-0.878000000000001,-0.877000000000001,
-0.876000000000001,-0.875000000000001,-0.874000000000001,-0.873000000000001,
-0.872000000000001,-0.871000000000001,-0.870000000000001,-0.869000000000001,
-0.868000000000001,-0.867000000000001,-0.866000000000001,-0.865000000000001,
-0.864000000000001,-0.863000000000001,-0.862000000000001,-0.861000000000001,
-0.860000000000001,-0.859000000000001,-0.858000000000001,-0.857000000000001,
-0.856000000000001,-0.855000000000001,-0.854000000000001,-0.853000000000001,
-0.852000000000001,-0.851000000000001,-0.850000000000001,-0.849000000000001,
-0.848000000000001,-0.847000000000001,-0.846000000000001,-0.845000000000001,
-0.844000000000001,-0.843000000000001,-0.842000000000001,-0.841000000000001,
-0.840000000000001,-0.839000000000001,-0.838000000000001,-0.837000000000001,
-0.836000000000001,-0.835000000000001,-0.834000000000001,-0.833000000000001,
-0.832000000000001,-0.831000000000001,-0.830000000000001,-0.829000000000001,
-0.828000000000001,-0.827000000000001,-0.826000000000001,-0.825000000000001,
-0.824000000000001,-0.823000000000001,-0.822000000000001,-0.821000000000001,
-0.820000000000001,-0.819000000000001,-0.818000000000001,-0.817000000000001,
-0.816000000000001,-0.815000000000001,-0.814000000000001,-0.813000000000001,
-0.812000000000001,-0.811000000000001,-0.810000000000001,-0.809000000000001,
-0.808000000000001,-0.807000000000001,-0.806000000000001,-0.805000000000001,
-0.804000000000001,-0.803000000000001,-0.802000000000001,-0.801000000000001,
-0.800000000000001,-0.799000000000001,-0.798000000000001,-0.797000000000001,
-0.796000000000001,-0.795000000000001,-0.794000000000001,-0.793000000000001,
-0.792000000000001,-0.791000000000001,-0.790000000000001,-0.789000000000001,
-0.788000000000001,-0.787000000000001,-0.786000000000001,-0.785000000000001,
-0.784000000000001,-0.783000000000001,-0.782000000000001,-0.781000000000001,
-0.780000000000001,-0.779000000000001,-0.778000000000001,-0.777000000000001,
-0.776000000000001,-0.775000000000001,-0.774000000000001,-0.773000000000001,
-0.772000000000001,-0.771000000000001,-0.770000000000001,-0.769000000000001,
-0.768000000000001,-0.767000000000001,-0.766000000000001,-0.765000000000001,
-0.764000000000001,-0.763000000000001,-0.762000000000001,-0.761000000000001,
-0.760000000000001,-0.759000000000001,-0.758000000000001,-0.757000000000001,
-0.756000000000001,-0.755000000000001,-0.754000000000001,-0.753000000000001,
-0.752000000000001,-0.751000000000001,-0.750000000000001,-0.749000000000001,
-0.748000000000001,-0.747000000000001,-0.746000000000001,-0.745000000000001,
-0.744000000000001,-0.743000000000001,-0.742000000000001,-0.741000000000001,
-0.740000000000001,-0.739000000000001,-0.738000000000001,-0.737000000000001,
-0.736000000000001,-0.735000000000001,-0.734000000000001,-0.733000000000001,
-0.732000000000001,-0.731000000000001,-0.730000000000001,-0.729000000000001,
-0.728000000000001,-0.727000000000001,-0.726000000000001,-0.725000000000001,
-0.724000000000001,-0.723000000000001,-0.722000000000001,-0.721000000000001,
-0.720000000000001,-0.719000000000001,-0.718000000000001,-0.717000000000001,
-0.716000000000001,-0.715000000000001,-0.714000000000001,-0.713000000000001,
-0.712000000000001,-0.711000000000001,-0.710000000000001,-0.709000000000001,
-0.708000000000001,-0.707000000000001,-0.706000000000001,-0.705000000000001,
-0.704000000000001,-0.703000000000001,-0.702000000000001,-0.701000000000001,
-0.700000000000001,-0.699000000000001,-0.698000000000001,-0.697000000000001,
-0.696000000000001,-0.695000000000001,-0.694000000000001,-0.693000000000001,
-0.692000000000001,-0.691000000000001,-0.690000000000001,-0.689000000000001,
-0.688000000000001,-0.687,-0.686,-0.685,-0.684,-0.683,-0.682,-0.681,-0.68,
-0.679,-0.678,-0.677,-0.676,-0.675,-0.674,-0.673,-0.672,-0.671,-0.67,-0.669,
-0.668,-0.667,-0.666,-0.665,-0.664,-0.663,-0.662,-0.661,-0.66,-0.659,-0.658,
-0.657,-0.656,-0.655,-0.654,-0.653,-0.652,-0.651,-0.65,-0.649,-0.648,-0.647,
-0.646,-0.645,-0.644,-0.643,-0.642,-0.641,-0.64,-0.639,-0.638,-0.637,-0.636,
-0.635,-0.634,-0.633,-0.632,-0.631,-0.63,-0.629,-0.628,-0.627,-0.626,-0.625,
-0.624,-0.623,-0.622,-0.621,-0.62,-0.619,-0.618,-0.617,-0.616,-0.615,-0.614,
-0.613,-0.612,-0.611,-0.61,-0.609,-0.608,-0.607,-0.606,-0.605,-0.604,-0.603,
-0.602,-0.601,-0.6,-0.599,-0.598,-0.597,-0.596,-0.595,-0.594,-0.593,-0.592,
-0.591,-0.59,-0.589,-0.588,-0.587,-0.586,-0.585,-0.584,-0.583,-0.582,-0.581,
-0.58,-0.579,-0.578,-0.577,-0.576,-0.575,-0.574,-0.573,-0.572,-0.571,-0.57,
-0.569,-0.568,-0.567,-0.566,-0.565,-0.564,-0.563,-0.562,-0.561,-0.56,-0.559,
-0.558,-0.557,-0.556,-0.555,-0.554,-0.553,-0.552,-0.551,-0.55,-0.549,-0.548,
-0.547,-0.546,-0.545,-0.544,-0.543,-0.542,-0.541,-0.54,-0.539,-0.538,-0.537,
-0.536,-0.535,-0.534,-0.533,-0.532,-0.531,-0.53,-0.529,-0.528,-0.527,-0.526,
-0.525,-0.524,-0.523,-0.522,-0.521,-0.52,-0.519,-0.518,-0.517,-0.516,-0.515,
-0.514,-0.513,-0.512,-0.511,-0.51,-0.509,-0.508,-0.507,-0.506,-0.505,-0.504,
-0.503,-0.502,-0.501,-0.5,-0.499,-0.498,-0.497,-0.496,-0.495,-0.494,-0.493,
-0.492,-0.491,-0.49,-0.489,-0.488,-0.487,-0.486,-0.485,-0.484,-0.483,-0.482,
-0.481,-0.48,-0.479,-0.478,-0.477,-0.476,-0.475,-0.474,-0.473,-0.472,-0.471,
-0.47,-0.469,-0.468,-0.467,-0.466,-0.465,-0.464,-0.463,-0.462,-0.461,-0.46,
-0.459,-0.458,-0.457,-0.456,-0.455,-0.454,-0.453,-0.452,-0.451,-0.45,-0.449,
-0.448,-0.447,-0.446,-0.445,-0.444,-0.443,-0.442,-0.441,-0.44,-0.439,-0.438,
-0.437,-0.436,-0.435,-0.434,-0.433,-0.432,-0.431,-0.43,-0.429,-0.428,-0.427,
-0.426,-0.425,-0.424,-0.423,-0.422,-0.421,-0.42,-0.419,-0.418,-0.417,-0.416,
-0.415,-0.414,-0.413,-0.412,-0.411,-0.41,-0.409,-0.408,-0.407,-0.406,-0.405,
-0.404,-0.403,-0.402,-0.401,-0.4,-0.399,-0.398,-0.397,-0.396,-0.395,-0.394,
-0.393,-0.392,-0.391,-0.39,-0.389,-0.388,-0.387,-0.386,-0.385,-0.384,-0.383,
-0.382,-0.381,-0.38,-0.379,-0.378,-0.377,-0.376,-0.375,-0.374,-0.373,-0.372,
-0.371,-0.37,-0.369,-0.368,-0.367,-0.366,-0.365,-0.364,-0.363,-0.362,-0.361,
-0.36,-0.359,-0.358,-0.357,-0.356,-0.355,-0.354,-0.353,-0.352,-0.351,-0.35,
-0.349,-0.348,-0.347,-0.346,-0.345,-0.344,-0.343,-0.342,-0.341,-0.34,-0.339,
-0.338,-0.337,-0.336,-0.335,-0.334,-0.333,-0.332,-0.331,-0.33,-0.329,-0.328,
-0.327,-0.326,-0.325,-0.324,-0.323,-0.322,-0.321,-0.32,-0.319,-0.318,-0.317,
-0.316,-0.315,-0.314,-0.313,-0.312,-0.311,-0.31,-0.309,-0.308,-0.307,-0.306,
-0.305,-0.304,-0.303,-0.302,-0.301,-0.3,-0.299,-0.298,-0.297,-0.296,-0.295,
-0.294,-0.293,-0.292,-0.291,-0.29,-0.289,-0.288,-0.287,-0.286,-0.285,-0.284,
-0.283,-0.282,-0.281,-0.28,-0.279,-0.278,-0.277,-0.276,-0.275,-0.274,-0.273,
-0.272,-0.271,-0.27,-0.269,-0.268,-0.267,-0.266,-0.265,-0.264,-0.263,-0.262,
-0.261,-0.26,-0.259,-0.258,-0.257,-0.256,-0.255,-0.254,-0.253,-0.252,-0.251,
-0.25,-0.249,-0.248,-0.247,-0.246,-0.245,-0.244,-0.243,-0.242,-0.241,-0.24,
-0.239,-0.238,-0.237,-0.236,-0.235,-0.234,-0.233,-0.232,-0.231,-0.23,-0.229,
-0.228,-0.227,-0.226,-0.225,-0.224,-0.223,-0.222,-0.221,-0.22,-0.219,-0.218,
-0.217,-0.216,-0.215,-0.214,-0.213,-0.212,-0.211,-0.21,-0.209,-0.208,-0.207,
-0.206,-0.205,-0.204,-0.203,-0.202,-0.201,-0.2,-0.199,-0.198,-0.197,-0.196,
-0.195,-0.194,-0.193,-0.192,-0.191,-0.19,-0.189,-0.188,-0.187,-0.186,-0.185,
-0.184,-0.183,-0.182,-0.181,-0.18,-0.179,-0.178,-0.177,-0.176,-0.175,-0.174,
-0.173,-0.172,-0.171,-0.17,-0.169,-0.168,-0.167,-0.166,-0.165,-0.164,-0.163,
-0.162,-0.161,-0.16,-0.159,-0.158,-0.157,-0.156,-0.155,-0.154,-0.153,-0.152,
-0.151,-0.15,-0.149,-0.148,-0.147,-0.146,-0.145,-0.144,-0.143,-0.142,-0.141,
-0.14,-0.139,-0.138,-0.137,-0.136,-0.135,-0.134,-0.133,-0.132,-0.131,-0.13,
-0.129,-0.128,-0.127,-0.126,-0.125,-0.124,-0.123,-0.122,-0.121,-0.12,-0.119,
-0.118,-0.117,-0.116,-0.115,-0.114,-0.113,-0.112,-0.111,-0.11,-0.109,-0.108,
-0.107,-0.106,-0.105,-0.104,-0.103,-0.102,-0.101,-0.1,-0.0990000000000001,
-0.0980000000000001,-0.0970000000000001,-0.0960000000000001,-0.0950000000000001,
-0.0940000000000001,-0.0930000000000001,-0.0920000000000001,-0.0910000000000001,
-0.0900000000000001,-0.0890000000000001,-0.0880000000000001,-0.0870000000000001,
-0.0860000000000001,-0.0850000000000001,-0.0840000000000001,-0.0830000000000001,
-0.0820000000000001,-0.0810000000000001,-0.0800000000000001,-0.0790000000000001,
-0.0780000000000001,-0.0770000000000001,-0.0760000000000001,-0.0750000000000001,
-0.0740000000000001,-0.0730000000000001,-0.0720000000000001,-0.071,-0.07,
-0.069,-0.068,-0.067,-0.066,-0.065,-0.064,-0.063,-0.062,-0.061,-0.06,-0.059,
-0.058,-0.057,-0.056,-0.055,-0.054,-0.053,-0.052,-0.051,-0.05,-0.049,-0.048,
-0.047,-0.046,-0.045,-0.044,-0.043,-0.042,-0.041,-0.04,-0.039,-0.038,-0.037,
-0.036,-0.035,-0.034,-0.033,-0.032,-0.031,-0.03,-0.029,-0.028,-0.027,-0.026,
-0.025,-0.024,-0.023,-0.022,-0.021,-0.02,-0.019,-0.018,-0.017,-0.016,-0.015,
-0.014,-0.013,-0.012,-0.011,-0.01,-0.009,-0.008,-0.007,-0.006,-0.005,-0.004,
-0.003,-0.002,-0.001,0.),(0.,2.),.UNSPECIFIED.)
GEOMETRIC_REPRESENTATION_ITEM()
RATIONAL_B_SPLINE_SURFACE(((1.,1.),(1.,1.),(1.,1.),(1.,1.),(1.,1.),(1.,
1.),(1.,1.),(1.,1.),(1.,1.),(1.,1.),(1.,1.),(1.,1.),(1.,1.),(1.,1.),(1.,
1.),(1.,1.),(1.,1.),(1.,1.),(1.,1.),(1.,1.),(1.,1.),(1.,1.),(1.,1.),(1.,
1.),(1.,1.),(1.,1.),(1.,1.),(1.,1.),(1.,1.),(1.,1.),(1.,1.),(1.,1.),(1.,
1.),(1.,1.),(1.,1.),(1.,1.),(1.,1.),(1.,1.),(1.,1.),(1.,1.),(1.,1.),(1.,
1.),(1.,1.),(1.,1.),(1.,1.),(1.,1.),(1.,1.),(1.,1.),(1.,1.),(1.,1.),(1.,
1.),(1.,1.),(1.,1.),(1.,1.),(1.,1.),(1.,1.),(1.,1.),(1.,1.),(1.,1.),(1.,
1.),(1.,1.),(1.,1.),(1.,1.),(1.,1.),(1.,1.),(1.,1.),(1.,1.),(1.,1.),(1.,
1.),(1.,1.),(1.,1.),(1.,1.),(1.,1.),(1.,1.),(1.,1.),(1.,1.),(1.,1.),(1.,
1.),(1.,1.),(1.,1.),(1.,1.),(1.,1.),(1.,1.),(1.,1.),(1.,1.),(1.,1.),(1.,
1.),(1.,1.),(1.,1.),(1.,1.),(1.,1.),(1.,1.),(1.,1.),(1.,1.),(1.,1.),(1.,
1.),(1.,1.),(1.,1.),(1.,1.),(1.,1.),(1.,1.),(1.,1.),(1.,1.),(1.,1.),(1.,
1.),(1.,1.),(1.,1.),(1.,1.),(1.,1.),(1.,1.),(1.,1.),(1.,1.),(1.,1.),(1.,
1.),(1.,1.),(1.,1.),(1.,1.),(1.,1.),(1.,1.),(1.,1.),(1.,1.),(1.,1.),(1.,
1.),(1.,1.),(1.,1.),(1.,1.),(1.,1.),(1.,1.),(1.,1.),(1.,1.),(1.,1.),(1.,
1.),(1.,1.),(1.,1.),(1.,1.),(1.,1.),(1.,1.),(1.,1.),(1.,1.),(1.,1.),(1.,
1.),(1.,1.),(1.,1.),(1.,1.),(1.,1.),(1.,1.),(1.,1.),(1.,1.),(1.,1.),(1.,
1.),(1.,1.),(1.,1.),(1.,1.),(1.,1.),(1.,1.),(1.,1.),(1.,1.),(1.,1.),(1.,
1.),(1.,1.),(1.,1.),(1.,1.),(1.,1.),(1.,1.),(1.,1.),(1.,1.),(1.,1.),(1.,
1.),(1.,1.),(1.,1.),(1.,1.),(1.,1.),(1.,1.),(1.,1.),(1.,1.),(1.,1.),(1.,
1.),(1.,1.),(1.,1.),(1.,1.),(1.,1.),(1.,1.),(1.,1.),(1.,1.),(1.,1.),(1.,
1.),(1.,1.),(1.,1.),(1.,1.),(1.,1.),(1.,1.),(1.,1.),(1.,1.),(1.,1.),(1.,
1.),(1.,1.),(1.,1.),(1.,1.),(1.,1.),(1.,1.),(1.,1.),(1.,1.),(1.,1.),(1.,
1.),(1.,1.),(1.,1.),(1.,1.),(1.,1.),(1.,1.),(1.,1.),(1.,1.),(1.,1.),(1.,
1.),(1.,1.),(1.,1.),(1.,1.),(1.,1.),(1.,1.),(1.,1.),(1.,1.),(1.,1.),(1.,
1.),(1.,1.),(1.,1.),(1.,1.),(1.,1.),(1.,1.),(1.,1.),(1.,1.),(1.,1.),(1.,
1.),(1.,1.),(1.,1.),(1.,1.),(1.,1.),(1.,1.),(1.,1.),(1.,1.),(1.,1.),(1.,
1.),(1.,1.),(1.,1.),(1.,1.),(1.,1.),(1.,1.),(1.,1.),(1.,1.),(1.,1.),(1.,
1.),(1.,1.),(1.,1.),(1.,1.),(1.,1.),(1.,1.),(1.,1.),(1.,1.),(1.,1.),(1.,
1.),(1.,1.),(1.,1.),(1.,1.),(1.,1.),(1.,1.),(1.,1.),(1.,1.),(1.,1.),(1.,
1.),(1.,1.),(1.,1.),(1.,1.),(1.,1.),(1.,1.),(1.,1.),(1.,1.),(1.,1.),(1.,
1.),(1.,1.),(1.,1.),(1.,1.),(1.,1.),(1.,1.),(1.,1.),(1.,1.),(1.,1.),(1.,
1.),(1.,1.),(1.,1.),(1.,1.),(1.,1.),(1.,1.),(1.,1.),(1.,1.),(1.,1.),(1.,
1.),(1.,1.),(1.,1.),(1.,1.),(1.,1.),(1.,1.),(1.,1.),(1.,1.),(1.,1.),(1.,
1.),(1.,1.),(1.,1.),(1.,1.),(1.,1.),(1.,1.),(1.,1.),(1.,1.),(1.,1.),(1.,
1.),(1.,1.),(1.,1.),(1.,1.),(1.,1.),(1.,1.),(1.,1.),(1.,1.),(1.,1.),(1.,
1.),(1.,1.),(1.,1.),(1.,1.),(1.,1.),(1.,1.),(1.,1.),(1.,1.),(1.,1.),(1.,
1.),(1.,1.),(1.,1.),(1.,1.),(1.,1.),(1.,1.),(1.,1.),(1.,1.),(1.,1.),(1.,
1.),(1.,1.),(1.,1.),(1.,1.),(1.,1.),(1.,1.),(1.,1.),(1.,1.),(1.,1.),(1.,
1.),(1.,1.),(1.,1.),(1.,1.),(1.,1.),(1.,1.),(1.,1.),(1.,1.),(1.,1.),(1.,
1.),(1.,1.),(1.,1.),(1.,1.),(1.,1.),(1.,1.),(1.,1.),(1.,1.),(1.,1.),(1.,
1.),(1.,1.),(1.,1.),(1.,1.),(1.,1.),(1.,1.),(1.,1.),(1.,1.),(1.,1.),(1.,
1.),(1.,1.),(1.,1.),(1.,1.),(1.,1.),(1.,1.),(1.,1.),(1.,1.),(1.,1.),(1.,
1.),(1.,1.),(1.,1.),(1.,1.),(1.,1.),(1.,1.),(1.,1.),(1.,1.),(1.,1.),(1.,
1.),(1.,1.),(1.,1.),(1.,1.),(1.,1.),(1.,1.),(1.,1.),(1.,1.),(1.,1.),(1.,
1.),(1.,1.),(1.,1.),(1.,1.),(1.,1.),(1.,1.),(1.,1.),(1.,1.),(1.,1.),(1.,
1.),(1.,1.),(1.,1.),(1.,1.),(1.,1.),(1.,1.),(1.,1.),(1.,1.),(1.,1.),(1.,
1.),(1.,1.),(1.,1.),(1.,1.),(1.,1.),(1.,1.),(1.,1.),(1.,1.),(1.,1.),(1.,
1.),(1.,1.),(1.,1.),(1.,1.),(1.,1.),(1.,1.),(1.,1.),(1.,1.),(1.,1.),(1.,
1.),(1.,1.),(1.,1.),(1.,1.),(1.,1.),(1.,1.),(1.,1.),(1.,1.),(1.,1.),(1.,
1.),(1.,1.),(1.,1.),(1.,1.),(1.,1.),(1.,1.),(1.,1.),(1.,1.),(1.,1.),(1.,
1.),(1.,1.),(1.,1.),(1.,1.),(1.,1.),(1.,1.),(1.,1.),(1.,1.),(1.,1.),(1.,
1.),(1.,1.),(1.,1.),(1.,1.),(1.,1.),(1.,1.),(1.,1.),(1.,1.),(1.,1.),(1.,
1.),(1.,1.),(1.,1.),(1.,1.),(1.,1.),(1.,1.),(1.,1.),(1.,1.),(1.,1.),(1.,
1.),(1.,1.),(1.,1.),(1.,1.),(1.,1.),(1.,1.),(1.,1.),(1.,1.),(1.,1.),(1.,
1.),(1.,1.),(1.,1.),(1.,1.),(1.,1.),(1.,1.),(1.,1.),(1.,1.),(1.,1.),(1.,
1.),(1.,1.),(1.,1.),(1.,1.),(1.,1.),(1.,1.),(1.,1.),(1.,1.),(1.,1.),(1.,
1.),(1.,1.),(1.,1.),(1.,1.),(1.,1.),(1.,1.),(1.,1.),(1.,1.),(1.,1.),(1.,
1.),(1.,1.),(1.,1.),(1.,1.),(1.,1.),(1.,1.),(1.,1.),(1.,1.),(1.,1.),(1.,
1.),(1.,1.),(1.,1.),(1.,1.),(1.,1.),(1.,1.),(1.,1.),(1.,1.),(1.,1.),(1.,
1.),(1.,1.),(1.,1.),(1.,1.),(1.,1.),(1.,1.),(1.,1.),(1.,1.),(1.,1.),(1.,
1.),(1.,1.),(1.,1.),(1.,1.),(1.,1.),(1.,1.),(1.,1.),(1.,1.),(1.,1.),(1.,
1.),(1.,1.),(1.,1.),(1.,1.),(1.,1.),(1.,1.),(1.,1.),(1.,1.),(1.,1.),(1.,
1.),(1.,1.),(1.,1.),(1.,1.),(1.,1.),(1.,1.),(1.,1.),(1.,1.),(1.,1.),(1.,
1.),(1.,1.),(1.,1.),(1.,1.),(1.,1.),(1.,1.),(1.,1.),(1.,1.),(1.,1.),(1.,
1.),(1.,1.),(1.,1.),(1.,1.),(1.,1.),(1.,1.),(1.,1.),(1.,1.),(1.,1.),(1.,
1.),(1.,1.),(1.,1.),(1.,1.),(1.,1.),(1.,1.),(1.,1.),(1.,1.),(1.,1.),(1.,
1.),(1.,1.),(1.,1.),(1.,1.),(1.,1.),(1.,1.),(1.,1.),(1.,1.),(1.,1.),(1.,
1.),(1.,1.),(1.,1.),(1.,1.),(1.,1.),(1.,1.),(1.,1.),(1.,1.),(1.,1.),(1.,
1.),(1.,1.),(1.,1.),(1.,1.),(1.,1.),(1.,1.),(1.,1.),(1.,1.),(1.,1.),(1.,
1.),(1.,1.),(1.,1.),(1.,1.),(1.,1.),(1.,1.),(1.,1.),(1.,1.),(1.,1.),(1.,
1.),(1.,1.),(1.,1.),(1.,1.),(1.,1.),(1.,1.),(1.,1.),(1.,1.),(1.,1.),(1.,
1.),(1.,1.),(1.,1.),(1.,1.),(1.,1.),(1.,1.),(1.,1.),(1.,1.),(1.,1.),(1.,
1.),(1.,1.),(1.,1.),(1.,1.),(1.,1.),(1.,1.),(1.,1.),(1.,1.),(1.,1.),(1.,
1.),(1.,1.),(1.,1.),(1.,1.),(1.,1.),(1.,1.),(1.,1.),(1.,1.),(1.,1.),(1.,
1.),(1.,1.),(1.,1.),(1.,1.),(1.,1.),(1.,1.),(1.,1.),(1.,1.),(1.,1.),(1.,
1.),(1.,1.),(1.,1.),(1.,1.),(1.,1.),(1.,1.),(1.,1.),(1.,1.),(1.,1.),(1.,
1.),(1.,1.),(1.,1.),(1.,1.),(1.,1.),(1.,1.),(1.,1.),(1.,1.),(1.,1.),(1.,
1.),(1.,1.),(1.,1.),(1.,1.),(1.,1.),(1.,1.),(1.,1.),(1.,1.),(1.,1.),(1.,
1.),(1.,1.),(1.,1.),(1.,1.),(1.,1.),(1.,1.),(1.,1.),(1.,1.),(1.,1.),(1.,
1.),(1.,1.),(1.,1.),(1.,1.),(1.,1.),(1.,1.),(1.,1.),(1.,1.),(1.,1.),(1.,
1.),(1.,1.),(1.,1.),(1.,1.),(1.,1.),(1.,1.),(1.,1.),(1.,1.),(1.,1.),(1.,
1.),(1.,1.),(1.,1.),(1.,1.),(1.,1.),(1.,1.),(1.,1.),(1.,1.),(1.,1.),(1.,
1.),(1.,1.),(1.,1.),(1.,1.),(1.,1.),(1.,1.),(1.,1.),(1.,1.),(1.,1.),(1.,
1.),(1.,1.),(1.,1.),(1.,1.),(1.,1.),(1.,1.),(1.,1.),(1.,1.),(1.,1.),(1.,
1.),(1.,1.),(1.,1.),(1.,1.),(1.,1.),(1.,1.),(1.,1.),(1.,1.),(1.,1.),(1.,
1.),(1.,1.),(1.,1.),(1.,1.),(1.,1.),(1.,1.),(1.,1.),(1.,1.),(1.,1.),(1.,
1.),(1.,1.),(1.,1.),(1.,1.),(1.,1.),(1.,1.),(1.,1.),(1.,1.),(1.,1.),(1.,
1.),(1.,1.),(1.,1.),(1.,1.),(1.,1.),(1.,1.),(1.,1.),(1.,1.),(1.,1.),(1.,
1.),(1.,1.),(1.,1.),(1.,1.),(1.,1.),(1.,1.),(1.,1.),(1.,1.),(1.,1.),(1.,
1.),(1.,1.),(1.,1.),(1.,1.),(1.,1.),(1.,1.),(1.,1.),(1.,1.),(1.,1.),(1.,
1.),(1.,1.),(1.,1.),(1.,1.),(1.,1.),(1.,1.),(1.,1.),(1.,1.),(1.,1.),(1.,
1.),(1.,1.),(1.,1.),(1.,1.),(1.,1.),(1.,1.),(1.,1.),(1.,1.),(1.,1.),(1.,
1.),(1.,1.),(1.,1.),(1.,1.),(1.,1.),(1.,1.),(1.,1.),(1.,1.),(1.,1.),(1.,
1.),(1.,1.),(1.,1.),(1.,1.),(1.,1.),(1.,1.),(1.,1.),(1.,1.),(1.,1.),(1.,
1.),(1.,1.),(1.,1.),(1.,1.),(1.,1.),(1.,1.),(1.,1.),(1.,1.),(1.,1.),(1.,
1.),(1.,1.),(1.,1.),(1.,1.),(1.,1.),(1.,1.),(1.,1.),(1.,1.),(1.,1.),(1.,
1.),(1.,1.),(1.,1.),(1.,1.),(1.,1.),(1.,1.),(1.,1.),(1.,1.),(1.,1.),(1.,
1.),(1.,1.),(1.,1.),(1.,1.),(1.,1.),(1.,1.),(1.,1.),(1.,1.),(1.,1.),(1.,
1.),(1.,1.),(1.,1.),(1.,1.),(1.,1.),(1.,1.),(1.,1.),(1.,1.),(1.,1.),(1.,
1.),(1.,1.),(1.,1.),(1.,1.),(1.,1.),(1.,1.),(1.,1.),(1.,1.),(1.,1.),(1.,
1.),(1.,1.),(1.,1.),(1.,1.),(1.,1.),(1.,1.),(1.,1.),(1.,1.),(1.,1.),(1.,
1.),(1.,1.),(1.,1.),(1.,1.),(1.,1.),(1.,1.),(1.,1.),(1.,1.),(1.,1.),(1.,
1.),(1.,1.),(1.,1.),(1.,1.),(1.,1.),(1.,1.),(1.,1.),(1.,1.),(1.,1.),(1.,
1.),(1.,1.),(1.,1.),(1.,1.),(1.,1.),(1.,1.),(1.,1.),(1.,1.),(1.,1.),(1.,
1.),(1.,1.),(1.,1.),(1.,1.),(1.,1.),(1.,1.),(1.,1.),(1.,1.),(1.,1.),(1.,
1.),(1.,1.),(1.,1.),(1.,1.),(1.,1.),(1.,1.),(1.,1.),(1.,1.),(1.,1.),(1.,
1.),(1.,1.),(1.,1.),(1.,1.),(1.,1.),(1.,1.),(1.,1.),(1.,1.),(1.,1.),(1.,
1.),(1.,1.),(1.,1.),(1.,1.),(1.,1.),(1.,1.),(1.,1.),(1.,1.),(1.,1.),(1.,
1.),(1.,1.),(1.,1.),(1.,1.),(1.,1.),(1.,1.),(1.,1.),(1.,1.),(1.,1.),(1.,
1.),(1.,1.),(1.,1.),(1.,1.),(1.,1.),(1.,1.),(1.,1.),(1.,1.),(1.,1.),(1.,
1.),(1.,1.),(1.,1.),(1.,1.),(1.,1.),(1.,1.),(1.,1.),(1.,1.),(1.,1.),(1.,
1.)))
REPRESENTATION_ITEM('')
SURFACE()
);
#259=(
BOUNDED_SURFACE()
B_SPLINE_SURFACE(5,1,((#76117,#76118),(#76119,#76120),(#76121,#76122),(#76123,
#76124),(#76125,#76126),(#76127,#76128),(#76129,#76130),(#76131,#76132),
(#76133,#76134),(#76135,#76136),(#76137,#76138),(#76139,#76140),(#76141,
#76142),(#76143,#76144),(#76145,#76146),(#76147,#76148),(#76149,#76150),
(#76151,#76152),(#76153,#76154),(#76155,#76156),(#76157,#76158),(#76159,
#76160),(#76161,#76162),(#76163,#76164),(#76165,#76166),(#76167,#76168),
(#76169,#76170),(#76171,#76172),(#76173,#76174),(#76175,#76176),(#76177,
#76178),(#76179,#76180),(#76181,#76182),(#76183,#76184),(#76185,#76186),
(#76187,#76188),(#76189,#76190),(#76191,#76192),(#76193,#76194),(#76195,
#76196),(#76197,#76198),(#76199,#76200),(#76201,#76202),(#76203,#76204),
(#76205,#76206),(#76207,#76208),(#76209,#76210),(#76211,#76212),(#76213,
#76214),(#76215,#76216),(#76217,#76218),(#76219,#76220),(#76221,#76222),
(#76223,#76224),(#76225,#76226),(#76227,#76228),(#76229,#76230),(#76231,
#76232),(#76233,#76234),(#76235,#76236),(#76237,#76238),(#76239,#76240),
(#76241,#76242),(#76243,#76244),(#76245,#76246),(#76247,#76248),(#76249,
#76250),(#76251,#76252),(#76253,#76254),(#76255,#76256),(#76257,#76258),
(#76259,#76260),(#76261,#76262),(#76263,#76264),(#76265,#76266),(#76267,
#76268),(#76269,#76270),(#76271,#76272),(#76273,#76274),(#76275,#76276),
(#76277,#76278),(#76279,#76280),(#76281,#76282),(#76283,#76284),(#76285,
#76286),(#76287,#76288),(#76289,#76290),(#76291,#76292),(#76293,#76294),
(#76295,#76296),(#76297,#76298),(#76299,#76300),(#76301,#76302),(#76303,
#76304),(#76305,#76306),(#76307,#76308),(#76309,#76310),(#76311,#76312),
(#76313,#76314),(#76315,#76316),(#76317,#76318),(#76319,#76320),(#76321,
#76322),(#76323,#76324),(#76325,#76326),(#76327,#76328),(#76329,#76330),
(#76331,#76332),(#76333,#76334),(#76335,#76336),(#76337,#76338),(#76339,
#76340),(#76341,#76342),(#76343,#76344),(#76345,#76346),(#76347,#76348),
(#76349,#76350),(#76351,#76352),(#76353,#76354),(#76355,#76356),(#76357,
#76358),(#76359,#76360),(#76361,#76362),(#76363,#76364),(#76365,#76366),
(#76367,#76368),(#76369,#76370),(#76371,#76372),(#76373,#76374),(#76375,
#76376),(#76377,#76378),(#76379,#76380),(#76381,#76382),(#76383,#76384),
(#76385,#76386),(#76387,#76388),(#76389,#76390),(#76391,#76392),(#76393,
#76394),(#76395,#76396),(#76397,#76398),(#76399,#76400),(#76401,#76402),
(#76403,#76404),(#76405,#76406),(#76407,#76408),(#76409,#76410),(#76411,
#76412),(#76413,#76414),(#76415,#76416),(#76417,#76418),(#76419,#76420),
(#76421,#76422),(#76423,#76424),(#76425,#76426),(#76427,#76428),(#76429,
#76430),(#76431,#76432),(#76433,#76434),(#76435,#76436),(#76437,#76438),
(#76439,#76440),(#76441,#76442),(#76443,#76444),(#76445,#76446),(#76447,
#76448),(#76449,#76450),(#76451,#76452),(#76453,#76454),(#76455,#76456),
(#76457,#76458),(#76459,#76460),(#76461,#76462),(#76463,#76464),(#76465,
#76466),(#76467,#76468),(#76469,#76470),(#76471,#76472),(#76473,#76474),
(#76475,#76476),(#76477,#76478),(#76479,#76480),(#76481,#76482),(#76483,
#76484),(#76485,#76486),(#76487,#76488),(#76489,#76490),(#76491,#76492),
(#76493,#76494),(#76495,#76496),(#76497,#76498),(#76499,#76500),(#76501,
#76502),(#76503,#76504),(#76505,#76506),(#76507,#76508),(#76509,#76510),
(#76511,#76512),(#76513,#76514),(#76515,#76516),(#76517,#76518),(#76519,
#76520),(#76521,#76522),(#76523,#76524),(#76525,#76526),(#76527,#76528),
(#76529,#76530),(#76531,#76532),(#76533,#76534),(#76535,#76536),(#76537,
#76538),(#76539,#76540),(#76541,#76542),(#76543,#76544),(#76545,#76546),
(#76547,#76548),(#76549,#76550),(#76551,#76552),(#76553,#76554),(#76555,
#76556),(#76557,#76558),(#76559,#76560),(#76561,#76562),(#76563,#76564),
(#76565,#76566),(#76567,#76568),(#76569,#76570),(#76571,#76572),(#76573,
#76574),(#76575,#76576),(#76577,#76578),(#76579,#76580),(#76581,#76582),
(#76583,#76584),(#76585,#76586),(#76587,#76588),(#76589,#76590),(#76591,
#76592),(#76593,#76594),(#76595,#76596),(#76597,#76598),(#76599,#76600),
(#76601,#76602),(#76603,#76604),(#76605,#76606),(#76607,#76608),(#76609,
#76610),(#76611,#76612),(#76613,#76614),(#76615,#76616),(#76617,#76618),
(#76619,#76620),(#76621,#76622),(#76623,#76624),(#76625,#76626),(#76627,
#76628),(#76629,#76630),(#76631,#76632),(#76633,#76634),(#76635,#76636),
(#76637,#76638),(#76639,#76640),(#76641,#76642),(#76643,#76644),(#76645,
#76646),(#76647,#76648),(#76649,#76650),(#76651,#76652),(#76653,#76654),
(#76655,#76656),(#76657,#76658),(#76659,#76660),(#76661,#76662),(#76663,
#76664),(#76665,#76666),(#76667,#76668),(#76669,#76670),(#76671,#76672),
(#76673,#76674),(#76675,#76676),(#76677,#76678),(#76679,#76680),(#76681,
#76682),(#76683,#76684),(#76685,#76686),(#76687,#76688),(#76689,#76690),
(#76691,#76692),(#76693,#76694),(#76695,#76696),(#76697,#76698),(#76699,
#76700),(#76701,#76702),(#76703,#76704),(#76705,#76706),(#76707,#76708),
(#76709,#76710),(#76711,#76712),(#76713,#76714),(#76715,#76716),(#76717,
#76718),(#76719,#76720),(#76721,#76722),(#76723,#76724),(#76725,#76726),
(#76727,#76728),(#76729,#76730),(#76731,#76732),(#76733,#76734),(#76735,
#76736),(#76737,#76738),(#76739,#76740),(#76741,#76742),(#76743,#76744),
(#76745,#76746),(#76747,#76748),(#76749,#76750),(#76751,#76752),(#76753,
#76754),(#76755,#76756),(#76757,#76758),(#76759,#76760),(#76761,#76762),
(#76763,#76764),(#76765,#76766),(#76767,#76768),(#76769,#76770),(#76771,
#76772),(#76773,#76774),(#76775,#76776),(#76777,#76778),(#76779,#76780),
(#76781,#76782),(#76783,#76784),(#76785,#76786),(#76787,#76788),(#76789,
#76790),(#76791,#76792),(#76793,#76794),(#76795,#76796),(#76797,#76798),
(#76799,#76800),(#76801,#76802),(#76803,#76804),(#76805,#76806),(#76807,
#76808),(#76809,#76810),(#76811,#76812),(#76813,#76814),(#76815,#76816),
(#76817,#76818),(#76819,#76820),(#76821,#76822),(#76823,#76824),(#76825,
#76826),(#76827,#76828),(#76829,#76830),(#76831,#76832),(#76833,#76834),
(#76835,#76836),(#76837,#76838),(#76839,#76840),(#76841,#76842),(#76843,
#76844),(#76845,#76846),(#76847,#76848),(#76849,#76850),(#76851,#76852),
(#76853,#76854),(#76855,#76856),(#76857,#76858),(#76859,#76860),(#76861,
#76862),(#76863,#76864),(#76865,#76866),(#76867,#76868),(#76869,#76870),
(#76871,#76872),(#76873,#76874),(#76875,#76876),(#76877,#76878),(#76879,
#76880),(#76881,#76882),(#76883,#76884),(#76885,#76886),(#76887,#76888),
(#76889,#76890),(#76891,#76892),(#76893,#76894),(#76895,#76896),(#76897,
#76898),(#76899,#76900),(#76901,#76902),(#76903,#76904),(#76905,#76906),
(#76907,#76908),(#76909,#76910),(#76911,#76912),(#76913,#76914),(#76915,
#76916),(#76917,#76918),(#76919,#76920),(#76921,#76922),(#76923,#76924),
(#76925,#76926),(#76927,#76928),(#76929,#76930),(#76931,#76932),(#76933,
#76934),(#76935,#76936),(#76937,#76938),(#76939,#76940),(#76941,#76942),
(#76943,#76944),(#76945,#76946),(#76947,#76948),(#76949,#76950),(#76951,
#76952),(#76953,#76954),(#76955,#76956),(#76957,#76958),(#76959,#76960),
(#76961,#76962),(#76963,#76964),(#76965,#76966),(#76967,#76968),(#76969,
#76970),(#76971,#76972),(#76973,#76974),(#76975,#76976),(#76977,#76978),
(#76979,#76980),(#76981,#76982),(#76983,#76984),(#76985,#76986),(#76987,
#76988),(#76989,#76990),(#76991,#76992),(#76993,#76994),(#76995,#76996),
(#76997,#76998),(#76999,#77000),(#77001,#77002),(#77003,#77004),(#77005,
#77006),(#77007,#77008),(#77009,#77010),(#77011,#77012),(#77013,#77014),
(#77015,#77016),(#77017,#77018),(#77019,#77020),(#77021,#77022),(#77023,
#77024),(#77025,#77026),(#77027,#77028),(#77029,#77030),(#77031,#77032),
(#77033,#77034),(#77035,#77036),(#77037,#77038),(#77039,#77040),(#77041,
#77042),(#77043,#77044),(#77045,#77046),(#77047,#77048),(#77049,#77050),
(#77051,#77052),(#77053,#77054),(#77055,#77056),(#77057,#77058),(#77059,
#77060),(#77061,#77062),(#77063,#77064),(#77065,#77066),(#77067,#77068),
(#77069,#77070),(#77071,#77072),(#77073,#77074),(#77075,#77076),(#77077,
#77078),(#77079,#77080),(#77081,#77082),(#77083,#77084),(#77085,#77086),
(#77087,#77088),(#77089,#77090),(#77091,#77092),(#77093,#77094),(#77095,
#77096),(#77097,#77098),(#77099,#77100),(#77101,#77102),(#77103,#77104),
(#77105,#77106),(#77107,#77108),(#77109,#77110),(#77111,#77112),(#77113,
#77114),(#77115,#77116),(#77117,#77118),(#77119,#77120),(#77121,#77122),
(#77123,#77124),(#77125,#77126),(#77127,#77128),(#77129,#77130),(#77131,
#77132),(#77133,#77134),(#77135,#77136),(#77137,#77138),(#77139,#77140),
(#77141,#77142),(#77143,#77144),(#77145,#77146),(#77147,#77148),(#77149,
#77150),(#77151,#77152),(#77153,#77154),(#77155,#77156),(#77157,#77158),
(#77159,#77160),(#77161,#77162),(#77163,#77164),(#77165,#77166),(#77167,
#77168),(#77169,#77170),(#77171,#77172),(#77173,#77174),(#77175,#77176),
(#77177,#77178),(#77179,#77180),(#77181,#77182),(#77183,#77184),(#77185,
#77186),(#77187,#77188),(#77189,#77190),(#77191,#77192),(#77193,#77194),
(#77195,#77196),(#77197,#77198),(#77199,#77200),(#77201,#77202),(#77203,
#77204),(#77205,#77206),(#77207,#77208),(#77209,#77210),(#77211,#77212),
(#77213,#77214),(#77215,#77216),(#77217,#77218),(#77219,#77220),(#77221,
#77222),(#77223,#77224),(#77225,#77226),(#77227,#77228),(#77229,#77230),
(#77231,#77232),(#77233,#77234),(#77235,#77236),(#77237,#77238),(#77239,
#77240),(#77241,#77242),(#77243,#77244),(#77245,#77246),(#77247,#77248),
(#77249,#77250),(#77251,#77252),(#77253,#77254),(#77255,#77256),(#77257,
#77258),(#77259,#77260),(#77261,#77262),(#77263,#77264),(#77265,#77266),
(#77267,#77268),(#77269,#77270),(#77271,#77272),(#77273,#77274),(#77275,
#77276),(#77277,#77278),(#77279,#77280),(#77281,#77282),(#77283,#77284),
(#77285,#77286),(#77287,#77288),(#77289,#77290),(#77291,#77292),(#77293,
#77294),(#77295,#77296),(#77297,#77298),(#77299,#77300),(#77301,#77302),
(#77303,#77304),(#77305,#77306),(#77307,#77308),(#77309,#77310),(#77311,
#77312),(#77313,#77314),(#77315,#77316),(#77317,#77318),(#77319,#77320),
(#77321,#77322),(#77323,#77324),(#77325,#77326),(#77327,#77328),(#77329,
#77330),(#77331,#77332),(#77333,#77334),(#77335,#77336),(#77337,#77338),
(#77339,#77340),(#77341,#77342),(#77343,#77344),(#77345,#77346),(#77347,
#77348),(#77349,#77350),(#77351,#77352),(#77353,#77354),(#77355,#77356),
(#77357,#77358),(#77359,#77360),(#77361,#77362),(#77363,#77364),(#77365,
#77366),(#77367,#77368),(#77369,#77370),(#77371,#77372),(#77373,#77374),
(#77375,#77376),(#77377,#77378),(#77379,#77380),(#77381,#77382),(#77383,
#77384),(#77385,#77386),(#77387,#77388),(#77389,#77390),(#77391,#77392),
(#77393,#77394),(#77395,#77396),(#77397,#77398),(#77399,#77400),(#77401,
#77402),(#77403,#77404),(#77405,#77406),(#77407,#77408),(#77409,#77410),
(#77411,#77412),(#77413,#77414),(#77415,#77416),(#77417,#77418),(#77419,
#77420),(#77421,#77422),(#77423,#77424),(#77425,#77426),(#77427,#77428),
(#77429,#77430),(#77431,#77432),(#77433,#77434),(#77435,#77436),(#77437,
#77438),(#77439,#77440),(#77441,#77442),(#77443,#77444),(#77445,#77446),
(#77447,#77448),(#77449,#77450),(#77451,#77452),(#77453,#77454),(#77455,
#77456),(#77457,#77458),(#77459,#77460),(#77461,#77462),(#77463,#77464),
(#77465,#77466),(#77467,#77468),(#77469,#77470),(#77471,#77472),(#77473,
#77474),(#77475,#77476),(#77477,#77478),(#77479,#77480),(#77481,#77482),
(#77483,#77484),(#77485,#77486),(#77487,#77488),(#77489,#77490),(#77491,
#77492),(#77493,#77494),(#77495,#77496),(#77497,#77498),(#77499,#77500),
(#77501,#77502),(#77503,#77504),(#77505,#77506),(#77507,#77508),(#77509,
#77510),(#77511,#77512),(#77513,#77514),(#77515,#77516),(#77517,#77518),
(#77519,#77520),(#77521,#77522),(#77523,#77524),(#77525,#77526),(#77527,
#77528),(#77529,#77530),(#77531,#77532),(#77533,#77534),(#77535,#77536),
(#77537,#77538),(#77539,#77540),(#77541,#77542),(#77543,#77544),(#77545,
#77546),(#77547,#77548),(#77549,#77550),(#77551,#77552),(#77553,#77554),
(#77555,#77556),(#77557,#77558),(#77559,#77560),(#77561,#77562),(#77563,
#77564),(#77565,#77566),(#77567,#77568),(#77569,#77570),(#77571,#77572),
(#77573,#77574),(#77575,#77576),(#77577,#77578),(#77579,#77580),(#77581,
#77582),(#77583,#77584),(#77585,#77586),(#77587,#77588),(#77589,#77590),
(#77591,#77592),(#77593,#77594),(#77595,#77596),(#77597,#77598),(#77599,
#77600),(#77601,#77602),(#77603,#77604),(#77605,#77606),(#77607,#77608),
(#77609,#77610),(#77611,#77612),(#77613,#77614),(#77615,#77616),(#77617,
#77618),(#77619,#77620),(#77621,#77622),(#77623,#77624),(#77625,#77626),
(#77627,#77628),(#77629,#77630),(#77631,#77632),(#77633,#77634),(#77635,
#77636),(#77637,#77638),(#77639,#77640),(#77641,#77642),(#77643,#77644),
(#77645,#77646),(#77647,#77648),(#77649,#77650),(#77651,#77652),(#77653,
#77654),(#77655,#77656),(#77657,#77658),(#77659,#77660),(#77661,#77662),
(#77663,#77664),(#77665,#77666),(#77667,#77668),(#77669,#77670),(#77671,
#77672),(#77673,#77674),(#77675,#77676),(#77677,#77678),(#77679,#77680),
(#77681,#77682),(#77683,#77684),(#77685,#77686),(#77687,#77688),(#77689,
#77690),(#77691,#77692),(#77693,#77694),(#77695,#77696),(#77697,#77698),
(#77699,#77700),(#77701,#77702),(#77703,#77704),(#77705,#77706),(#77707,
#77708),(#77709,#77710),(#77711,#77712),(#77713,#77714),(#77715,#77716),
(#77717,#77718),(#77719,#77720),(#77721,#77722),(#77723,#77724),(#77725,
#77726),(#77727,#77728),(#77729,#77730),(#77731,#77732),(#77733,#77734),
(#77735,#77736),(#77737,#77738),(#77739,#77740),(#77741,#77742),(#77743,
#77744),(#77745,#77746),(#77747,#77748),(#77749,#77750),(#77751,#77752),
(#77753,#77754),(#77755,#77756),(#77757,#77758),(#77759,#77760),(#77761,
#77762),(#77763,#77764),(#77765,#77766),(#77767,#77768),(#77769,#77770),
(#77771,#77772),(#77773,#77774),(#77775,#77776),(#77777,#77778),(#77779,
#77780),(#77781,#77782),(#77783,#77784),(#77785,#77786),(#77787,#77788),
(#77789,#77790),(#77791,#77792),(#77793,#77794),(#77795,#77796),(#77797,
#77798),(#77799,#77800),(#77801,#77802),(#77803,#77804),(#77805,#77806),
(#77807,#77808),(#77809,#77810),(#77811,#77812),(#77813,#77814),(#77815,
#77816),(#77817,#77818),(#77819,#77820),(#77821,#77822),(#77823,#77824),
(#77825,#77826),(#77827,#77828),(#77829,#77830),(#77831,#77832),(#77833,
#77834),(#77835,#77836),(#77837,#77838),(#77839,#77840),(#77841,#77842),
(#77843,#77844),(#77845,#77846),(#77847,#77848),(#77849,#77850),(#77851,
#77852),(#77853,#77854),(#77855,#77856),(#77857,#77858),(#77859,#77860),
(#77861,#77862),(#77863,#77864),(#77865,#77866),(#77867,#77868),(#77869,
#77870),(#77871,#77872),(#77873,#77874),(#77875,#77876),(#77877,#77878),
(#77879,#77880),(#77881,#77882),(#77883,#77884),(#77885,#77886),(#77887,
#77888),(#77889,#77890),(#77891,#77892),(#77893,#77894),(#77895,#77896),
(#77897,#77898),(#77899,#77900),(#77901,#77902),(#77903,#77904),(#77905,
#77906),(#77907,#77908),(#77909,#77910),(#77911,#77912),(#77913,#77914),
(#77915,#77916),(#77917,#77918),(#77919,#77920),(#77921,#77922),(#77923,
#77924),(#77925,#77926),(#77927,#77928),(#77929,#77930),(#77931,#77932),
(#77933,#77934),(#77935,#77936),(#77937,#77938),(#77939,#77940),(#77941,
#77942),(#77943,#77944),(#77945,#77946),(#77947,#77948),(#77949,#77950),
(#77951,#77952),(#77953,#77954),(#77955,#77956),(#77957,#77958),(#77959,
#77960),(#77961,#77962),(#77963,#77964),(#77965,#77966),(#77967,#77968),
(#77969,#77970),(#77971,#77972),(#77973,#77974),(#77975,#77976),(#77977,
#77978),(#77979,#77980),(#77981,#77982),(#77983,#77984),(#77985,#77986),
(#77987,#77988),(#77989,#77990),(#77991,#77992),(#77993,#77994),(#77995,
#77996),(#77997,#77998),(#77999,#78000),(#78001,#78002),(#78003,#78004),
(#78005,#78006),(#78007,#78008),(#78009,#78010),(#78011,#78012),(#78013,
#78014),(#78015,#78016),(#78017,#78018),(#78019,#78020),(#78021,#78022),
(#78023,#78024),(#78025,#78026),(#78027,#78028),(#78029,#78030),(#78031,
#78032),(#78033,#78034),(#78035,#78036),(#78037,#78038),(#78039,#78040),
(#78041,#78042),(#78043,#78044),(#78045,#78046),(#78047,#78048),(#78049,
#78050),(#78051,#78052),(#78053,#78054),(#78055,#78056),(#78057,#78058),
(#78059,#78060),(#78061,#78062),(#78063,#78064),(#78065,#78066),(#78067,
#78068),(#78069,#78070),(#78071,#78072),(#78073,#78074),(#78075,#78076),
(#78077,#78078),(#78079,#78080),(#78081,#78082),(#78083,#78084),(#78085,
#78086),(#78087,#78088),(#78089,#78090),(#78091,#78092),(#78093,#78094),
(#78095,#78096),(#78097,#78098),(#78099,#78100),(#78101,#78102),(#78103,
#78104),(#78105,#78106),(#78107,#78108),(#78109,#78110),(#78111,#78112),
(#78113,#78114),(#78115,#78116),(#78117,#78118),(#78119,#78120),(#78121,
#78122),(#78123,#78124),(#78125,#78126)),.UNSPECIFIED.,.F.,.F.,.F.)
B_SPLINE_SURFACE_WITH_KNOTS((6,1,1,1,1,1,1,1,1,1,1,1,1,1,1,1,1,1,1,1,1,
1,1,1,1,1,1,1,1,1,1,1,1,1,1,1,1,1,1,1,1,1,1,1,1,1,1,1,1,1,1,1,1,1,1,1,1,
1,1,1,1,1,1,1,1,1,1,1,1,1,1,1,1,1,1,1,1,1,1,1,1,1,1,1,1,1,1,1,1,1,1,1,1,
1,1,1,1,1,1,1,1,1,1,1,1,1,1,1,1,1,1,1,1,1,1,1,1,1,1,1,1,1,1,1,1,1,1,1,1,
1,1,1,1,1,1,1,1,1,1,1,1,1,1,1,1,1,1,1,1,1,1,1,1,1,1,1,1,1,1,1,1,1,1,1,1,
1,1,1,1,1,1,1,1,1,1,1,1,1,1,1,1,1,1,1,1,1,1,1,1,1,1,1,1,1,1,1,1,1,1,1,1,
1,1,1,1,1,1,1,1,1,1,1,1,1,1,1,1,1,1,1,1,1,1,1,1,1,1,1,1,1,1,1,1,1,1,1,1,
1,1,1,1,1,1,1,1,1,1,1,1,1,1,1,1,1,1,1,1,1,1,1,1,1,1,1,1,1,1,1,1,1,1,1,1,
1,1,1,1,1,1,1,1,1,1,1,1,1,1,1,1,1,1,1,1,1,1,1,1,1,1,1,1,1,1,1,1,1,1,1,1,
1,1,1,1,1,1,1,1,1,1,1,1,1,1,1,1,1,1,1,1,1,1,1,1,1,1,1,1,1,1,1,1,1,1,1,1,
1,1,1,1,1,1,1,1,1,1,1,1,1,1,1,1,1,1,1,1,1,1,1,1,1,1,1,1,1,1,1,1,1,1,1,1,
1,1,1,1,1,1,1,1,1,1,1,1,1,1,1,1,1,1,1,1,1,1,1,1,1,1,1,1,1,1,1,1,1,1,1,1,
1,1,1,1,1,1,1,1,1,1,1,1,1,1,1,1,1,1,1,1,1,1,1,1,1,1,1,1,1,1,1,1,1,1,1,1,
1,1,1,1,1,1,1,1,1,1,1,1,1,1,1,1,1,1,1,1,1,1,1,1,1,1,1,1,1,1,1,1,1,1,1,1,
1,1,1,1,1,1,1,1,1,1,1,1,1,1,1,1,1,1,1,1,1,1,1,1,1,1,1,1,1,1,1,1,1,1,1,1,
1,1,1,1,1,1,1,1,1,1,1,1,1,1,1,1,1,1,1,1,1,1,1,1,1,1,1,1,1,1,1,1,1,1,1,1,
1,1,1,1,1,1,1,1,1,1,1,1,1,1,1,1,1,1,1,1,1,1,1,1,1,1,1,1,1,1,1,1,1,1,1,1,
1,1,1,1,1,1,1,1,1,1,1,1,1,1,1,1,1,1,1,1,1,1,1,1,1,1,1,1,1,1,1,1,1,1,1,1,
1,1,1,1,1,1,1,1,1,1,1,1,1,1,1,1,1,1,1,1,1,1,1,1,1,1,1,1,1,1,1,1,1,1,1,1,
1,1,1,1,1,1,1,1,1,1,1,1,1,1,1,1,1,1,1,1,1,1,1,1,1,1,1,1,1,1,1,1,1,1,1,1,
1,1,1,1,1,1,1,1,1,1,1,1,1,1,1,1,1,1,1,1,1,1,1,1,1,1,1,1,1,1,1,1,1,1,1,1,
1,1,1,1,1,1,1,1,1,1,1,1,1,1,1,1,1,1,1,1,1,1,1,1,1,1,1,1,1,1,1,1,1,1,1,1,
1,1,1,1,1,1,1,1,1,1,1,1,1,1,1,1,1,1,1,1,1,1,1,1,1,1,1,1,1,1,1,1,1,1,1,1,
1,1,1,1,1,1,1,1,1,1,1,1,1,1,1,1,1,1,1,1,1,1,1,1,1,1,1,1,1,1,1,1,1,1,1,1,
1,1,1,1,1,1,1,1,1,1,1,1,1,1,1,1,1,1,1,1,1,1,1,1,1,1,1,1,1,1,1,1,1,1,1,1,
1,1,1,1,1,1,1,1,1,1,1,1,1,1,1,1,1,1,1,1,1,1,1,1,1,1,1,1,1,1,1,1,1,1,1,1,
1,1,1,1,1,1,1,1,1,1,1,1,1,1,1,1,1,1,1,1,1,1,1,1,1,1,1,1,1,1,1,1,1,1,1,1,
1,1,1,1,1,1,1,1,1,1,1,1,1,1,1,1,1,1,1,1,1,1,1,1,1,1,1,1,1,1,1,1,1,1,1,1,
1,1,1,1,1,1,1,6),(2,2),(-1.,-0.999000000000001,-0.998000000000001,-0.997000000000001,
-0.996000000000001,-0.995000000000001,-0.994000000000001,-0.993000000000001,
-0.992000000000001,-0.991000000000001,-0.990000000000001,-0.989000000000001,
-0.988000000000001,-0.987000000000001,-0.986000000000001,-0.985000000000001,
-0.984000000000001,-0.983000000000001,-0.982000000000001,-0.981000000000001,
-0.980000000000001,-0.979000000000001,-0.978000000000001,-0.977000000000001,
-0.976000000000001,-0.975000000000001,-0.974000000000001,-0.973000000000001,
-0.972000000000001,-0.971000000000001,-0.970000000000001,-0.969000000000001,
-0.968000000000001,-0.967000000000001,-0.966000000000001,-0.965000000000001,
-0.964000000000001,-0.963000000000001,-0.962000000000001,-0.961000000000001,
-0.960000000000001,-0.959000000000001,-0.958000000000001,-0.957000000000001,
-0.956000000000001,-0.955000000000001,-0.954000000000001,-0.953000000000001,
-0.952000000000001,-0.951000000000001,-0.950000000000001,-0.949000000000001,
-0.948000000000001,-0.947000000000001,-0.946000000000001,-0.945000000000001,
-0.944000000000001,-0.943000000000001,-0.942000000000001,-0.941000000000001,
-0.940000000000001,-0.939000000000001,-0.938000000000001,-0.937000000000001,
-0.936000000000001,-0.935000000000001,-0.934000000000001,-0.933000000000001,
-0.932000000000001,-0.931000000000001,-0.930000000000001,-0.929000000000001,
-0.928000000000001,-0.927000000000001,-0.926000000000001,-0.925000000000001,
-0.924000000000001,-0.923000000000001,-0.922000000000001,-0.921000000000001,
-0.920000000000001,-0.919000000000001,-0.918000000000001,-0.917000000000001,
-0.916000000000001,-0.915000000000001,-0.914000000000001,-0.913000000000001,
-0.912000000000001,-0.911000000000001,-0.910000000000001,-0.909000000000001,
-0.908000000000001,-0.907000000000001,-0.906000000000001,-0.905000000000001,
-0.904000000000001,-0.903000000000001,-0.902000000000001,-0.901000000000001,
-0.900000000000001,-0.899000000000001,-0.898000000000001,-0.897000000000001,
-0.896000000000001,-0.895000000000001,-0.894000000000001,-0.893000000000001,
-0.892000000000001,-0.891000000000001,-0.890000000000001,-0.889000000000001,
-0.888000000000001,-0.887000000000001,-0.886000000000001,-0.885000000000001,
-0.884000000000001,-0.883000000000001,-0.882000000000001,-0.881000000000001,
-0.880000000000001,-0.879000000000001,-0.878000000000001,-0.877000000000001,
-0.876000000000001,-0.875000000000001,-0.874000000000001,-0.873000000000001,
-0.872000000000001,-0.871000000000001,-0.870000000000001,-0.869000000000001,
-0.868000000000001,-0.867000000000001,-0.866000000000001,-0.865000000000001,
-0.864000000000001,-0.863000000000001,-0.862000000000001,-0.861000000000001,
-0.860000000000001,-0.859000000000001,-0.858000000000001,-0.857000000000001,
-0.856000000000001,-0.855000000000001,-0.854000000000001,-0.853000000000001,
-0.852000000000001,-0.851000000000001,-0.850000000000001,-0.849000000000001,
-0.848000000000001,-0.847000000000001,-0.846000000000001,-0.845000000000001,
-0.844000000000001,-0.843000000000001,-0.842000000000001,-0.841000000000001,
-0.840000000000001,-0.839000000000001,-0.838000000000001,-0.837000000000001,
-0.836000000000001,-0.835000000000001,-0.834000000000001,-0.833000000000001,
-0.832000000000001,-0.831000000000001,-0.830000000000001,-0.829000000000001,
-0.828000000000001,-0.827000000000001,-0.826000000000001,-0.825000000000001,
-0.824000000000001,-0.823000000000001,-0.822000000000001,-0.821000000000001,
-0.820000000000001,-0.819000000000001,-0.818000000000001,-0.817000000000001,
-0.816000000000001,-0.815000000000001,-0.814000000000001,-0.813000000000001,
-0.812000000000001,-0.811000000000001,-0.810000000000001,-0.809000000000001,
-0.808000000000001,-0.807000000000001,-0.806000000000001,-0.805000000000001,
-0.804000000000001,-0.803000000000001,-0.802000000000001,-0.801000000000001,
-0.800000000000001,-0.799000000000001,-0.798000000000001,-0.797000000000001,
-0.796000000000001,-0.795000000000001,-0.794000000000001,-0.793000000000001,
-0.792000000000001,-0.791000000000001,-0.790000000000001,-0.789000000000001,
-0.788000000000001,-0.787000000000001,-0.786000000000001,-0.785000000000001,
-0.784000000000001,-0.783000000000001,-0.782000000000001,-0.781000000000001,
-0.780000000000001,-0.779000000000001,-0.778000000000001,-0.777000000000001,
-0.776000000000001,-0.775000000000001,-0.774000000000001,-0.773000000000001,
-0.772000000000001,-0.771000000000001,-0.770000000000001,-0.769000000000001,
-0.768000000000001,-0.767000000000001,-0.766000000000001,-0.765000000000001,
-0.764000000000001,-0.763000000000001,-0.762000000000001,-0.761000000000001,
-0.760000000000001,-0.759000000000001,-0.758000000000001,-0.757000000000001,
-0.756000000000001,-0.755000000000001,-0.754000000000001,-0.753000000000001,
-0.752000000000001,-0.751000000000001,-0.750000000000001,-0.749000000000001,
-0.748000000000001,-0.747000000000001,-0.746000000000001,-0.745000000000001,
-0.744000000000001,-0.743000000000001,-0.742000000000001,-0.741000000000001,
-0.740000000000001,-0.739000000000001,-0.738000000000001,-0.737000000000001,
-0.736000000000001,-0.735000000000001,-0.734000000000001,-0.733000000000001,
-0.732000000000001,-0.731000000000001,-0.730000000000001,-0.729000000000001,
-0.728000000000001,-0.727000000000001,-0.726000000000001,-0.725000000000001,
-0.724000000000001,-0.723000000000001,-0.722000000000001,-0.721000000000001,
-0.720000000000001,-0.719000000000001,-0.718000000000001,-0.717000000000001,
-0.716000000000001,-0.715000000000001,-0.714000000000001,-0.713000000000001,
-0.712000000000001,-0.711000000000001,-0.710000000000001,-0.709000000000001,
-0.708000000000001,-0.707000000000001,-0.706000000000001,-0.705000000000001,
-0.704000000000001,-0.703000000000001,-0.702000000000001,-0.701000000000001,
-0.700000000000001,-0.699000000000001,-0.698000000000001,-0.697000000000001,
-0.696000000000001,-0.695000000000001,-0.694000000000001,-0.693000000000001,
-0.692000000000001,-0.691000000000001,-0.690000000000001,-0.689000000000001,
-0.688000000000001,-0.687,-0.686,-0.685,-0.684,-0.683,-0.682,-0.681,-0.68,
-0.679,-0.678,-0.677,-0.676,-0.675,-0.674,-0.673,-0.672,-0.671,-0.67,-0.669,
-0.668,-0.667,-0.666,-0.665,-0.664,-0.663,-0.662,-0.661,-0.66,-0.659,-0.658,
-0.657,-0.656,-0.655,-0.654,-0.653,-0.652,-0.651,-0.65,-0.649,-0.648,-0.647,
-0.646,-0.645,-0.644,-0.643,-0.642,-0.641,-0.64,-0.639,-0.638,-0.637,-0.636,
-0.635,-0.634,-0.633,-0.632,-0.631,-0.63,-0.629,-0.628,-0.627,-0.626,-0.625,
-0.624,-0.623,-0.622,-0.621,-0.62,-0.619,-0.618,-0.617,-0.616,-0.615,-0.614,
-0.613,-0.612,-0.611,-0.61,-0.609,-0.608,-0.607,-0.606,-0.605,-0.604,-0.603,
-0.602,-0.601,-0.6,-0.599,-0.598,-0.597,-0.596,-0.595,-0.594,-0.593,-0.592,
-0.591,-0.59,-0.589,-0.588,-0.587,-0.586,-0.585,-0.584,-0.583,-0.582,-0.581,
-0.58,-0.579,-0.578,-0.577,-0.576,-0.575,-0.574,-0.573,-0.572,-0.571,-0.57,
-0.569,-0.568,-0.567,-0.566,-0.565,-0.564,-0.563,-0.562,-0.561,-0.56,-0.559,
-0.558,-0.557,-0.556,-0.555,-0.554,-0.553,-0.552,-0.551,-0.55,-0.549,-0.548,
-0.547,-0.546,-0.545,-0.544,-0.543,-0.542,-0.541,-0.54,-0.539,-0.538,-0.537,
-0.536,-0.535,-0.534,-0.533,-0.532,-0.531,-0.53,-0.529,-0.528,-0.527,-0.526,
-0.525,-0.524,-0.523,-0.522,-0.521,-0.52,-0.519,-0.518,-0.517,-0.516,-0.515,
-0.514,-0.513,-0.512,-0.511,-0.51,-0.509,-0.508,-0.507,-0.506,-0.505,-0.504,
-0.503,-0.502,-0.501,-0.5,-0.499,-0.498,-0.497,-0.496,-0.495,-0.494,-0.493,
-0.492,-0.491,-0.49,-0.489,-0.488,-0.487,-0.486,-0.485,-0.484,-0.483,-0.482,
-0.481,-0.48,-0.479,-0.478,-0.477,-0.476,-0.475,-0.474,-0.473,-0.472,-0.471,
-0.47,-0.469,-0.468,-0.467,-0.466,-0.465,-0.464,-0.463,-0.462,-0.461,-0.46,
-0.459,-0.458,-0.457,-0.456,-0.455,-0.454,-0.453,-0.452,-0.451,-0.45,-0.449,
-0.448,-0.447,-0.446,-0.445,-0.444,-0.443,-0.442,-0.441,-0.44,-0.439,-0.438,
-0.437,-0.436,-0.435,-0.434,-0.433,-0.432,-0.431,-0.43,-0.429,-0.428,-0.427,
-0.426,-0.425,-0.424,-0.423,-0.422,-0.421,-0.42,-0.419,-0.418,-0.417,-0.416,
-0.415,-0.414,-0.413,-0.412,-0.411,-0.41,-0.409,-0.408,-0.407,-0.406,-0.405,
-0.404,-0.403,-0.402,-0.401,-0.4,-0.399,-0.398,-0.397,-0.396,-0.395,-0.394,
-0.393,-0.392,-0.391,-0.39,-0.389,-0.388,-0.387,-0.386,-0.385,-0.384,-0.383,
-0.382,-0.381,-0.38,-0.379,-0.378,-0.377,-0.376,-0.375,-0.374,-0.373,-0.372,
-0.371,-0.37,-0.369,-0.368,-0.367,-0.366,-0.365,-0.364,-0.363,-0.362,-0.361,
-0.36,-0.359,-0.358,-0.357,-0.356,-0.355,-0.354,-0.353,-0.352,-0.351,-0.35,
-0.349,-0.348,-0.347,-0.346,-0.345,-0.344,-0.343,-0.342,-0.341,-0.34,-0.339,
-0.338,-0.337,-0.336,-0.335,-0.334,-0.333,-0.332,-0.331,-0.33,-0.329,-0.328,
-0.327,-0.326,-0.325,-0.324,-0.323,-0.322,-0.321,-0.32,-0.319,-0.318,-0.317,
-0.316,-0.315,-0.314,-0.313,-0.312,-0.311,-0.31,-0.309,-0.308,-0.307,-0.306,
-0.305,-0.304,-0.303,-0.302,-0.301,-0.3,-0.299,-0.298,-0.297,-0.296,-0.295,
-0.294,-0.293,-0.292,-0.291,-0.29,-0.289,-0.288,-0.287,-0.286,-0.285,-0.284,
-0.283,-0.282,-0.281,-0.28,-0.279,-0.278,-0.277,-0.276,-0.275,-0.274,-0.273,
-0.272,-0.271,-0.27,-0.269,-0.268,-0.267,-0.266,-0.265,-0.264,-0.263,-0.262,
-0.261,-0.26,-0.259,-0.258,-0.257,-0.256,-0.255,-0.254,-0.253,-0.252,-0.251,
-0.25,-0.249,-0.248,-0.247,-0.246,-0.245,-0.244,-0.243,-0.242,-0.241,-0.24,
-0.239,-0.238,-0.237,-0.236,-0.235,-0.234,-0.233,-0.232,-0.231,-0.23,-0.229,
-0.228,-0.227,-0.226,-0.225,-0.224,-0.223,-0.222,-0.221,-0.22,-0.219,-0.218,
-0.217,-0.216,-0.215,-0.214,-0.213,-0.212,-0.211,-0.21,-0.209,-0.208,-0.207,
-0.206,-0.205,-0.204,-0.203,-0.202,-0.201,-0.2,-0.199,-0.198,-0.197,-0.196,
-0.195,-0.194,-0.193,-0.192,-0.191,-0.19,-0.189,-0.188,-0.187,-0.186,-0.185,
-0.184,-0.183,-0.182,-0.181,-0.18,-0.179,-0.178,-0.177,-0.176,-0.175,-0.174,
-0.173,-0.172,-0.171,-0.17,-0.169,-0.168,-0.167,-0.166,-0.165,-0.164,-0.163,
-0.162,-0.161,-0.16,-0.159,-0.158,-0.157,-0.156,-0.155,-0.154,-0.153,-0.152,
-0.151,-0.15,-0.149,-0.148,-0.147,-0.146,-0.145,-0.144,-0.143,-0.142,-0.141,
-0.14,-0.139,-0.138,-0.137,-0.136,-0.135,-0.134,-0.133,-0.132,-0.131,-0.13,
-0.129,-0.128,-0.127,-0.126,-0.125,-0.124,-0.123,-0.122,-0.121,-0.12,-0.119,
-0.118,-0.117,-0.116,-0.115,-0.114,-0.113,-0.112,-0.111,-0.11,-0.109,-0.108,
-0.107,-0.106,-0.105,-0.104,-0.103,-0.102,-0.101,-0.1,-0.0990000000000001,
-0.0980000000000001,-0.0970000000000001,-0.0960000000000001,-0.0950000000000001,
-0.0940000000000001,-0.0930000000000001,-0.0920000000000001,-0.0910000000000001,
-0.0900000000000001,-0.0890000000000001,-0.0880000000000001,-0.0870000000000001,
-0.0860000000000001,-0.0850000000000001,-0.0840000000000001,-0.0830000000000001,
-0.0820000000000001,-0.0810000000000001,-0.0800000000000001,-0.0790000000000001,
-0.0780000000000001,-0.0770000000000001,-0.0760000000000001,-0.0750000000000001,
-0.0740000000000001,-0.0730000000000001,-0.0720000000000001,-0.071,-0.07,
-0.069,-0.068,-0.067,-0.066,-0.065,-0.064,-0.063,-0.062,-0.061,-0.06,-0.059,
-0.058,-0.057,-0.056,-0.055,-0.054,-0.053,-0.052,-0.051,-0.05,-0.049,-0.048,
-0.047,-0.046,-0.045,-0.044,-0.043,-0.042,-0.041,-0.04,-0.039,-0.038,-0.037,
-0.036,-0.035,-0.034,-0.033,-0.032,-0.031,-0.03,-0.029,-0.028,-0.027,-0.026,
-0.025,-0.024,-0.023,-0.022,-0.021,-0.02,-0.019,-0.018,-0.017,-0.016,-0.015,
-0.014,-0.013,-0.012,-0.011,-0.01,-0.009,-0.008,-0.007,-0.006,-0.005,-0.004,
-0.003,-0.002,-0.001,0.),(0.,2.),.UNSPECIFIED.)
GEOMETRIC_REPRESENTATION_ITEM()
RATIONAL_B_SPLINE_SURFACE(((1.,1.),(1.,1.),(1.,1.),(1.,1.),(1.,1.),(1.,
1.),(1.,1.),(1.,1.),(1.,1.),(1.,1.),(1.,1.),(1.,1.),(1.,1.),(1.,1.),(1.,
1.),(1.,1.),(1.,1.),(1.,1.),(1.,1.),(1.,1.),(1.,1.),(1.,1.),(1.,1.),(1.,
1.),(1.,1.),(1.,1.),(1.,1.),(1.,1.),(1.,1.),(1.,1.),(1.,1.),(1.,1.),(1.,
1.),(1.,1.),(1.,1.),(1.,1.),(1.,1.),(1.,1.),(1.,1.),(1.,1.),(1.,1.),(1.,
1.),(1.,1.),(1.,1.),(1.,1.),(1.,1.),(1.,1.),(1.,1.),(1.,1.),(1.,1.),(1.,
1.),(1.,1.),(1.,1.),(1.,1.),(1.,1.),(1.,1.),(1.,1.),(1.,1.),(1.,1.),(1.,
1.),(1.,1.),(1.,1.),(1.,1.),(1.,1.),(1.,1.),(1.,1.),(1.,1.),(1.,1.),(1.,
1.),(1.,1.),(1.,1.),(1.,1.),(1.,1.),(1.,1.),(1.,1.),(1.,1.),(1.,1.),(1.,
1.),(1.,1.),(1.,1.),(1.,1.),(1.,1.),(1.,1.),(1.,1.),(1.,1.),(1.,1.),(1.,
1.),(1.,1.),(1.,1.),(1.,1.),(1.,1.),(1.,1.),(1.,1.),(1.,1.),(1.,1.),(1.,
1.),(1.,1.),(1.,1.),(1.,1.),(1.,1.),(1.,1.),(1.,1.),(1.,1.),(1.,1.),(1.,
1.),(1.,1.),(1.,1.),(1.,1.),(1.,1.),(1.,1.),(1.,1.),(1.,1.),(1.,1.),(1.,
1.),(1.,1.),(1.,1.),(1.,1.),(1.,1.),(1.,1.),(1.,1.),(1.,1.),(1.,1.),(1.,
1.),(1.,1.),(1.,1.),(1.,1.),(1.,1.),(1.,1.),(1.,1.),(1.,1.),(1.,1.),(1.,
1.),(1.,1.),(1.,1.),(1.,1.),(1.,1.),(1.,1.),(1.,1.),(1.,1.),(1.,1.),(1.,
1.),(1.,1.),(1.,1.),(1.,1.),(1.,1.),(1.,1.),(1.,1.),(1.,1.),(1.,1.),(1.,
1.),(1.,1.),(1.,1.),(1.,1.),(1.,1.),(1.,1.),(1.,1.),(1.,1.),(1.,1.),(1.,
1.),(1.,1.),(1.,1.),(1.,1.),(1.,1.),(1.,1.),(1.,1.),(1.,1.),(1.,1.),(1.,
1.),(1.,1.),(1.,1.),(1.,1.),(1.,1.),(1.,1.),(1.,1.),(1.,1.),(1.,1.),(1.,
1.),(1.,1.),(1.,1.),(1.,1.),(1.,1.),(1.,1.),(1.,1.),(1.,1.),(1.,1.),(1.,
1.),(1.,1.),(1.,1.),(1.,1.),(1.,1.),(1.,1.),(1.,1.),(1.,1.),(1.,1.),(1.,
1.),(1.,1.),(1.,1.),(1.,1.),(1.,1.),(1.,1.),(1.,1.),(1.,1.),(1.,1.),(1.,
1.),(1.,1.),(1.,1.),(1.,1.),(1.,1.),(1.,1.),(1.,1.),(1.,1.),(1.,1.),(1.,
1.),(1.,1.),(1.,1.),(1.,1.),(1.,1.),(1.,1.),(1.,1.),(1.,1.),(1.,1.),(1.,
1.),(1.,1.),(1.,1.),(1.,1.),(1.,1.),(1.,1.),(1.,1.),(1.,1.),(1.,1.),(1.,
1.),(1.,1.),(1.,1.),(1.,1.),(1.,1.),(1.,1.),(1.,1.),(1.,1.),(1.,1.),(1.,
1.),(1.,1.),(1.,1.),(1.,1.),(1.,1.),(1.,1.),(1.,1.),(1.,1.),(1.,1.),(1.,
1.),(1.,1.),(1.,1.),(1.,1.),(1.,1.),(1.,1.),(1.,1.),(1.,1.),(1.,1.),(1.,
1.),(1.,1.),(1.,1.),(1.,1.),(1.,1.),(1.,1.),(1.,1.),(1.,1.),(1.,1.),(1.,
1.),(1.,1.),(1.,1.),(1.,1.),(1.,1.),(1.,1.),(1.,1.),(1.,1.),(1.,1.),(1.,
1.),(1.,1.),(1.,1.),(1.,1.),(1.,1.),(1.,1.),(1.,1.),(1.,1.),(1.,1.),(1.,
1.),(1.,1.),(1.,1.),(1.,1.),(1.,1.),(1.,1.),(1.,1.),(1.,1.),(1.,1.),(1.,
1.),(1.,1.),(1.,1.),(1.,1.),(1.,1.),(1.,1.),(1.,1.),(1.,1.),(1.,1.),(1.,
1.),(1.,1.),(1.,1.),(1.,1.),(1.,1.),(1.,1.),(1.,1.),(1.,1.),(1.,1.),(1.,
1.),(1.,1.),(1.,1.),(1.,1.),(1.,1.),(1.,1.),(1.,1.),(1.,1.),(1.,1.),(1.,
1.),(1.,1.),(1.,1.),(1.,1.),(1.,1.),(1.,1.),(1.,1.),(1.,1.),(1.,1.),(1.,
1.),(1.,1.),(1.,1.),(1.,1.),(1.,1.),(1.,1.),(1.,1.),(1.,1.),(1.,1.),(1.,
1.),(1.,1.),(1.,1.),(1.,1.),(1.,1.),(1.,1.),(1.,1.),(1.,1.),(1.,1.),(1.,
1.),(1.,1.),(1.,1.),(1.,1.),(1.,1.),(1.,1.),(1.,1.),(1.,1.),(1.,1.),(1.,
1.),(1.,1.),(1.,1.),(1.,1.),(1.,1.),(1.,1.),(1.,1.),(1.,1.),(1.,1.),(1.,
1.),(1.,1.),(1.,1.),(1.,1.),(1.,1.),(1.,1.),(1.,1.),(1.,1.),(1.,1.),(1.,
1.),(1.,1.),(1.,1.),(1.,1.),(1.,1.),(1.,1.),(1.,1.),(1.,1.),(1.,1.),(1.,
1.),(1.,1.),(1.,1.),(1.,1.),(1.,1.),(1.,1.),(1.,1.),(1.,1.),(1.,1.),(1.,
1.),(1.,1.),(1.,1.),(1.,1.),(1.,1.),(1.,1.),(1.,1.),(1.,1.),(1.,1.),(1.,
1.),(1.,1.),(1.,1.),(1.,1.),(1.,1.),(1.,1.),(1.,1.),(1.,1.),(1.,1.),(1.,
1.),(1.,1.),(1.,1.),(1.,1.),(1.,1.),(1.,1.),(1.,1.),(1.,1.),(1.,1.),(1.,
1.),(1.,1.),(1.,1.),(1.,1.),(1.,1.),(1.,1.),(1.,1.),(1.,1.),(1.,1.),(1.,
1.),(1.,1.),(1.,1.),(1.,1.),(1.,1.),(1.,1.),(1.,1.),(1.,1.),(1.,1.),(1.,
1.),(1.,1.),(1.,1.),(1.,1.),(1.,1.),(1.,1.),(1.,1.),(1.,1.),(1.,1.),(1.,
1.),(1.,1.),(1.,1.),(1.,1.),(1.,1.),(1.,1.),(1.,1.),(1.,1.),(1.,1.),(1.,
1.),(1.,1.),(1.,1.),(1.,1.),(1.,1.),(1.,1.),(1.,1.),(1.,1.),(1.,1.),(1.,
1.),(1.,1.),(1.,1.),(1.,1.),(1.,1.),(1.,1.),(1.,1.),(1.,1.),(1.,1.),(1.,
1.),(1.,1.),(1.,1.),(1.,1.),(1.,1.),(1.,1.),(1.,1.),(1.,1.),(1.,1.),(1.,
1.),(1.,1.),(1.,1.),(1.,1.),(1.,1.),(1.,1.),(1.,1.),(1.,1.),(1.,1.),(1.,
1.),(1.,1.),(1.,1.),(1.,1.),(1.,1.),(1.,1.),(1.,1.),(1.,1.),(1.,1.),(1.,
1.),(1.,1.),(1.,1.),(1.,1.),(1.,1.),(1.,1.),(1.,1.),(1.,1.),(1.,1.),(1.,
1.),(1.,1.),(1.,1.),(1.,1.),(1.,1.),(1.,1.),(1.,1.),(1.,1.),(1.,1.),(1.,
1.),(1.,1.),(1.,1.),(1.,1.),(1.,1.),(1.,1.),(1.,1.),(1.,1.),(1.,1.),(1.,
1.),(1.,1.),(1.,1.),(1.,1.),(1.,1.),(1.,1.),(1.,1.),(1.,1.),(1.,1.),(1.,
1.),(1.,1.),(1.,1.),(1.,1.),(1.,1.),(1.,1.),(1.,1.),(1.,1.),(1.,1.),(1.,
1.),(1.,1.),(1.,1.),(1.,1.),(1.,1.),(1.,1.),(1.,1.),(1.,1.),(1.,1.),(1.,
1.),(1.,1.),(1.,1.),(1.,1.),(1.,1.),(1.,1.),(1.,1.),(1.,1.),(1.,1.),(1.,
1.),(1.,1.),(1.,1.),(1.,1.),(1.,1.),(1.,1.),(1.,1.),(1.,1.),(1.,1.),(1.,
1.),(1.,1.),(1.,1.),(1.,1.),(1.,1.),(1.,1.),(1.,1.),(1.,1.),(1.,1.),(1.,
1.),(1.,1.),(1.,1.),(1.,1.),(1.,1.),(1.,1.),(1.,1.),(1.,1.),(1.,1.),(1.,
1.),(1.,1.),(1.,1.),(1.,1.),(1.,1.),(1.,1.),(1.,1.),(1.,1.),(1.,1.),(1.,
1.),(1.,1.),(1.,1.),(1.,1.),(1.,1.),(1.,1.),(1.,1.),(1.,1.),(1.,1.),(1.,
1.),(1.,1.),(1.,1.),(1.,1.),(1.,1.),(1.,1.),(1.,1.),(1.,1.),(1.,1.),(1.,
1.),(1.,1.),(1.,1.),(1.,1.),(1.,1.),(1.,1.),(1.,1.),(1.,1.),(1.,1.),(1.,
1.),(1.,1.),(1.,1.),(1.,1.),(1.,1.),(1.,1.),(1.,1.),(1.,1.),(1.,1.),(1.,
1.),(1.,1.),(1.,1.),(1.,1.),(1.,1.),(1.,1.),(1.,1.),(1.,1.),(1.,1.),(1.,
1.),(1.,1.),(1.,1.),(1.,1.),(1.,1.),(1.,1.),(1.,1.),(1.,1.),(1.,1.),(1.,
1.),(1.,1.),(1.,1.),(1.,1.),(1.,1.),(1.,1.),(1.,1.),(1.,1.),(1.,1.),(1.,
1.),(1.,1.),(1.,1.),(1.,1.),(1.,1.),(1.,1.),(1.,1.),(1.,1.),(1.,1.),(1.,
1.),(1.,1.),(1.,1.),(1.,1.),(1.,1.),(1.,1.),(1.,1.),(1.,1.),(1.,1.),(1.,
1.),(1.,1.),(1.,1.),(1.,1.),(1.,1.),(1.,1.),(1.,1.),(1.,1.),(1.,1.),(1.,
1.),(1.,1.),(1.,1.),(1.,1.),(1.,1.),(1.,1.),(1.,1.),(1.,1.),(1.,1.),(1.,
1.),(1.,1.),(1.,1.),(1.,1.),(1.,1.),(1.,1.),(1.,1.),(1.,1.),(1.,1.),(1.,
1.),(1.,1.),(1.,1.),(1.,1.),(1.,1.),(1.,1.),(1.,1.),(1.,1.),(1.,1.),(1.,
1.),(1.,1.),(1.,1.),(1.,1.),(1.,1.),(1.,1.),(1.,1.),(1.,1.),(1.,1.),(1.,
1.),(1.,1.),(1.,1.),(1.,1.),(1.,1.),(1.,1.),(1.,1.),(1.,1.),(1.,1.),(1.,
1.),(1.,1.),(1.,1.),(1.,1.),(1.,1.),(1.,1.),(1.,1.),(1.,1.),(1.,1.),(1.,
1.),(1.,1.),(1.,1.),(1.,1.),(1.,1.),(1.,1.),(1.,1.),(1.,1.),(1.,1.),(1.,
1.),(1.,1.),(1.,1.),(1.,1.),(1.,1.),(1.,1.),(1.,1.),(1.,1.),(1.,1.),(1.,
1.),(1.,1.),(1.,1.),(1.,1.),(1.,1.),(1.,1.),(1.,1.),(1.,1.),(1.,1.),(1.,
1.),(1.,1.),(1.,1.),(1.,1.),(1.,1.),(1.,1.),(1.,1.),(1.,1.),(1.,1.),(1.,
1.),(1.,1.),(1.,1.),(1.,1.),(1.,1.),(1.,1.),(1.,1.),(1.,1.),(1.,1.),(1.,
1.),(1.,1.),(1.,1.),(1.,1.),(1.,1.),(1.,1.),(1.,1.),(1.,1.),(1.,1.),(1.,
1.),(1.,1.),(1.,1.),(1.,1.),(1.,1.),(1.,1.),(1.,1.),(1.,1.),(1.,1.),(1.,
1.),(1.,1.),(1.,1.),(1.,1.),(1.,1.),(1.,1.),(1.,1.),(1.,1.),(1.,1.),(1.,
1.),(1.,1.),(1.,1.),(1.,1.),(1.,1.),(1.,1.),(1.,1.),(1.,1.),(1.,1.),(1.,
1.),(1.,1.),(1.,1.),(1.,1.),(1.,1.),(1.,1.),(1.,1.),(1.,1.),(1.,1.),(1.,
1.),(1.,1.),(1.,1.),(1.,1.),(1.,1.),(1.,1.),(1.,1.),(1.,1.),(1.,1.),(1.,
1.),(1.,1.),(1.,1.),(1.,1.),(1.,1.),(1.,1.),(1.,1.),(1.,1.),(1.,1.),(1.,
1.),(1.,1.),(1.,1.),(1.,1.),(1.,1.),(1.,1.),(1.,1.),(1.,1.),(1.,1.),(1.,
1.),(1.,1.),(1.,1.),(1.,1.),(1.,1.),(1.,1.),(1.,1.),(1.,1.),(1.,1.),(1.,
1.),(1.,1.),(1.,1.),(1.,1.),(1.,1.),(1.,1.),(1.,1.),(1.,1.),(1.,1.),(1.,
1.),(1.,1.),(1.,1.),(1.,1.),(1.,1.),(1.,1.),(1.,1.),(1.,1.),(1.,1.),(1.,
1.),(1.,1.),(1.,1.),(1.,1.),(1.,1.),(1.,1.),(1.,1.),(1.,1.),(1.,1.),(1.,
1.),(1.,1.),(1.,1.),(1.,1.),(1.,1.),(1.,1.),(1.,1.),(1.,1.),(1.,1.),(1.,
1.),(1.,1.),(1.,1.),(1.,1.),(1.,1.),(1.,1.),(1.,1.),(1.,1.),(1.,1.),(1.,
1.),(1.,1.),(1.,1.),(1.,1.),(1.,1.),(1.,1.),(1.,1.),(1.,1.),(1.,1.),(1.,
1.),(1.,1.),(1.,1.),(1.,1.),(1.,1.),(1.,1.),(1.,1.),(1.,1.),(1.,1.),(1.,
1.),(1.,1.),(1.,1.),(1.,1.),(1.,1.),(1.,1.),(1.,1.),(1.,1.),(1.,1.),(1.,
1.),(1.,1.),(1.,1.),(1.,1.),(1.,1.),(1.,1.),(1.,1.),(1.,1.),(1.,1.),(1.,
1.),(1.,1.),(1.,1.),(1.,1.),(1.,1.),(1.,1.),(1.,1.),(1.,1.),(1.,1.),(1.,
1.),(1.,1.),(1.,1.),(1.,1.),(1.,1.),(1.,1.),(1.,1.),(1.,1.),(1.,1.),(1.,
1.),(1.,1.),(1.,1.),(1.,1.),(1.,1.),(1.,1.),(1.,1.),(1.,1.),(1.,1.),(1.,
1.),(1.,1.),(1.,1.),(1.,1.),(1.,1.),(1.,1.),(1.,1.),(1.,1.),(1.,1.),(1.,
1.),(1.,1.),(1.,1.),(1.,1.),(1.,1.),(1.,1.),(1.,1.),(1.,1.),(1.,1.),(1.,
1.),(1.,1.),(1.,1.),(1.,1.),(1.,1.),(1.,1.),(1.,1.),(1.,1.),(1.,1.),(1.,
1.)))
REPRESENTATION_ITEM('')
SURFACE()
);
#260=(
BOUNDED_SURFACE()
B_SPLINE_SURFACE(5,1,((#78157,#78158),(#78159,#78160),(#78161,#78162),(#78163,
#78164),(#78165,#78166),(#78167,#78168),(#78169,#78170),(#78171,#78172),
(#78173,#78174),(#78175,#78176),(#78177,#78178),(#78179,#78180),(#78181,
#78182),(#78183,#78184),(#78185,#78186),(#78187,#78188),(#78189,#78190),
(#78191,#78192),(#78193,#78194),(#78195,#78196),(#78197,#78198),(#78199,
#78200),(#78201,#78202),(#78203,#78204),(#78205,#78206),(#78207,#78208),
(#78209,#78210),(#78211,#78212),(#78213,#78214),(#78215,#78216),(#78217,
#78218),(#78219,#78220),(#78221,#78222),(#78223,#78224),(#78225,#78226),
(#78227,#78228),(#78229,#78230),(#78231,#78232),(#78233,#78234),(#78235,
#78236),(#78237,#78238),(#78239,#78240),(#78241,#78242),(#78243,#78244),
(#78245,#78246),(#78247,#78248),(#78249,#78250),(#78251,#78252),(#78253,
#78254),(#78255,#78256),(#78257,#78258),(#78259,#78260),(#78261,#78262),
(#78263,#78264),(#78265,#78266),(#78267,#78268),(#78269,#78270),(#78271,
#78272),(#78273,#78274),(#78275,#78276),(#78277,#78278),(#78279,#78280),
(#78281,#78282),(#78283,#78284),(#78285,#78286),(#78287,#78288),(#78289,
#78290),(#78291,#78292),(#78293,#78294),(#78295,#78296),(#78297,#78298),
(#78299,#78300),(#78301,#78302),(#78303,#78304),(#78305,#78306),(#78307,
#78308),(#78309,#78310),(#78311,#78312),(#78313,#78314),(#78315,#78316),
(#78317,#78318),(#78319,#78320),(#78321,#78322),(#78323,#78324),(#78325,
#78326),(#78327,#78328),(#78329,#78330),(#78331,#78332),(#78333,#78334),
(#78335,#78336),(#78337,#78338),(#78339,#78340),(#78341,#78342),(#78343,
#78344),(#78345,#78346),(#78347,#78348),(#78349,#78350),(#78351,#78352),
(#78353,#78354),(#78355,#78356),(#78357,#78358),(#78359,#78360),(#78361,
#78362),(#78363,#78364),(#78365,#78366),(#78367,#78368),(#78369,#78370),
(#78371,#78372),(#78373,#78374),(#78375,#78376),(#78377,#78378),(#78379,
#78380),(#78381,#78382),(#78383,#78384),(#78385,#78386),(#78387,#78388),
(#78389,#78390),(#78391,#78392),(#78393,#78394),(#78395,#78396),(#78397,
#78398),(#78399,#78400),(#78401,#78402),(#78403,#78404),(#78405,#78406),
(#78407,#78408),(#78409,#78410),(#78411,#78412),(#78413,#78414),(#78415,
#78416),(#78417,#78418),(#78419,#78420),(#78421,#78422),(#78423,#78424),
(#78425,#78426),(#78427,#78428),(#78429,#78430),(#78431,#78432),(#78433,
#78434),(#78435,#78436),(#78437,#78438),(#78439,#78440),(#78441,#78442),
(#78443,#78444),(#78445,#78446),(#78447,#78448),(#78449,#78450),(#78451,
#78452),(#78453,#78454),(#78455,#78456),(#78457,#78458),(#78459,#78460),
(#78461,#78462),(#78463,#78464),(#78465,#78466),(#78467,#78468),(#78469,
#78470),(#78471,#78472),(#78473,#78474),(#78475,#78476),(#78477,#78478),
(#78479,#78480),(#78481,#78482),(#78483,#78484),(#78485,#78486),(#78487,
#78488),(#78489,#78490),(#78491,#78492),(#78493,#78494),(#78495,#78496),
(#78497,#78498),(#78499,#78500),(#78501,#78502),(#78503,#78504),(#78505,
#78506),(#78507,#78508),(#78509,#78510),(#78511,#78512),(#78513,#78514),
(#78515,#78516),(#78517,#78518),(#78519,#78520),(#78521,#78522),(#78523,
#78524),(#78525,#78526),(#78527,#78528),(#78529,#78530),(#78531,#78532),
(#78533,#78534),(#78535,#78536),(#78537,#78538),(#78539,#78540),(#78541,
#78542),(#78543,#78544),(#78545,#78546),(#78547,#78548),(#78549,#78550),
(#78551,#78552),(#78553,#78554),(#78555,#78556),(#78557,#78558),(#78559,
#78560),(#78561,#78562),(#78563,#78564),(#78565,#78566),(#78567,#78568),
(#78569,#78570),(#78571,#78572),(#78573,#78574),(#78575,#78576),(#78577,
#78578),(#78579,#78580),(#78581,#78582),(#78583,#78584),(#78585,#78586),
(#78587,#78588),(#78589,#78590),(#78591,#78592),(#78593,#78594),(#78595,
#78596),(#78597,#78598),(#78599,#78600),(#78601,#78602),(#78603,#78604),
(#78605,#78606),(#78607,#78608),(#78609,#78610),(#78611,#78612),(#78613,
#78614),(#78615,#78616),(#78617,#78618),(#78619,#78620),(#78621,#78622),
(#78623,#78624),(#78625,#78626),(#78627,#78628),(#78629,#78630),(#78631,
#78632),(#78633,#78634),(#78635,#78636),(#78637,#78638),(#78639,#78640),
(#78641,#78642),(#78643,#78644),(#78645,#78646),(#78647,#78648),(#78649,
#78650),(#78651,#78652),(#78653,#78654),(#78655,#78656),(#78657,#78658),
(#78659,#78660),(#78661,#78662),(#78663,#78664),(#78665,#78666),(#78667,
#78668),(#78669,#78670),(#78671,#78672),(#78673,#78674),(#78675,#78676),
(#78677,#78678),(#78679,#78680),(#78681,#78682),(#78683,#78684),(#78685,
#78686),(#78687,#78688),(#78689,#78690),(#78691,#78692),(#78693,#78694),
(#78695,#78696),(#78697,#78698),(#78699,#78700),(#78701,#78702),(#78703,
#78704),(#78705,#78706),(#78707,#78708),(#78709,#78710),(#78711,#78712),
(#78713,#78714),(#78715,#78716),(#78717,#78718),(#78719,#78720),(#78721,
#78722),(#78723,#78724),(#78725,#78726),(#78727,#78728),(#78729,#78730),
(#78731,#78732),(#78733,#78734),(#78735,#78736),(#78737,#78738),(#78739,
#78740),(#78741,#78742),(#78743,#78744),(#78745,#78746),(#78747,#78748),
(#78749,#78750),(#78751,#78752),(#78753,#78754),(#78755,#78756),(#78757,
#78758),(#78759,#78760),(#78761,#78762),(#78763,#78764),(#78765,#78766),
(#78767,#78768),(#78769,#78770),(#78771,#78772),(#78773,#78774),(#78775,
#78776),(#78777,#78778),(#78779,#78780),(#78781,#78782),(#78783,#78784),
(#78785,#78786),(#78787,#78788),(#78789,#78790),(#78791,#78792),(#78793,
#78794),(#78795,#78796),(#78797,#78798),(#78799,#78800),(#78801,#78802),
(#78803,#78804),(#78805,#78806),(#78807,#78808),(#78809,#78810),(#78811,
#78812),(#78813,#78814),(#78815,#78816),(#78817,#78818),(#78819,#78820),
(#78821,#78822),(#78823,#78824),(#78825,#78826),(#78827,#78828),(#78829,
#78830),(#78831,#78832),(#78833,#78834),(#78835,#78836),(#78837,#78838),
(#78839,#78840),(#78841,#78842),(#78843,#78844),(#78845,#78846),(#78847,
#78848),(#78849,#78850),(#78851,#78852),(#78853,#78854),(#78855,#78856),
(#78857,#78858),(#78859,#78860),(#78861,#78862),(#78863,#78864),(#78865,
#78866),(#78867,#78868),(#78869,#78870),(#78871,#78872),(#78873,#78874),
(#78875,#78876),(#78877,#78878),(#78879,#78880),(#78881,#78882),(#78883,
#78884),(#78885,#78886),(#78887,#78888),(#78889,#78890),(#78891,#78892),
(#78893,#78894),(#78895,#78896),(#78897,#78898),(#78899,#78900),(#78901,
#78902),(#78903,#78904),(#78905,#78906),(#78907,#78908),(#78909,#78910),
(#78911,#78912),(#78913,#78914),(#78915,#78916),(#78917,#78918),(#78919,
#78920),(#78921,#78922),(#78923,#78924),(#78925,#78926),(#78927,#78928),
(#78929,#78930),(#78931,#78932),(#78933,#78934),(#78935,#78936),(#78937,
#78938),(#78939,#78940),(#78941,#78942),(#78943,#78944),(#78945,#78946),
(#78947,#78948),(#78949,#78950),(#78951,#78952),(#78953,#78954),(#78955,
#78956),(#78957,#78958),(#78959,#78960),(#78961,#78962),(#78963,#78964),
(#78965,#78966),(#78967,#78968),(#78969,#78970),(#78971,#78972),(#78973,
#78974),(#78975,#78976),(#78977,#78978),(#78979,#78980),(#78981,#78982),
(#78983,#78984),(#78985,#78986),(#78987,#78988),(#78989,#78990),(#78991,
#78992),(#78993,#78994),(#78995,#78996),(#78997,#78998),(#78999,#79000),
(#79001,#79002),(#79003,#79004),(#79005,#79006),(#79007,#79008),(#79009,
#79010),(#79011,#79012),(#79013,#79014),(#79015,#79016),(#79017,#79018),
(#79019,#79020),(#79021,#79022),(#79023,#79024),(#79025,#79026),(#79027,
#79028),(#79029,#79030),(#79031,#79032),(#79033,#79034),(#79035,#79036),
(#79037,#79038),(#79039,#79040),(#79041,#79042),(#79043,#79044),(#79045,
#79046),(#79047,#79048),(#79049,#79050),(#79051,#79052),(#79053,#79054),
(#79055,#79056),(#79057,#79058),(#79059,#79060),(#79061,#79062),(#79063,
#79064),(#79065,#79066),(#79067,#79068),(#79069,#79070),(#79071,#79072),
(#79073,#79074),(#79075,#79076),(#79077,#79078),(#79079,#79080),(#79081,
#79082),(#79083,#79084),(#79085,#79086),(#79087,#79088),(#79089,#79090),
(#79091,#79092),(#79093,#79094),(#79095,#79096),(#79097,#79098),(#79099,
#79100),(#79101,#79102),(#79103,#79104),(#79105,#79106),(#79107,#79108),
(#79109,#79110),(#79111,#79112),(#79113,#79114),(#79115,#79116),(#79117,
#79118),(#79119,#79120),(#79121,#79122),(#79123,#79124),(#79125,#79126),
(#79127,#79128),(#79129,#79130),(#79131,#79132),(#79133,#79134),(#79135,
#79136),(#79137,#79138),(#79139,#79140),(#79141,#79142),(#79143,#79144),
(#79145,#79146),(#79147,#79148),(#79149,#79150),(#79151,#79152),(#79153,
#79154),(#79155,#79156),(#79157,#79158),(#79159,#79160),(#79161,#79162),
(#79163,#79164),(#79165,#79166),(#79167,#79168),(#79169,#79170),(#79171,
#79172),(#79173,#79174),(#79175,#79176),(#79177,#79178),(#79179,#79180),
(#79181,#79182),(#79183,#79184),(#79185,#79186),(#79187,#79188),(#79189,
#79190),(#79191,#79192),(#79193,#79194),(#79195,#79196),(#79197,#79198),
(#79199,#79200),(#79201,#79202),(#79203,#79204),(#79205,#79206),(#79207,
#79208),(#79209,#79210),(#79211,#79212),(#79213,#79214),(#79215,#79216),
(#79217,#79218),(#79219,#79220),(#79221,#79222),(#79223,#79224),(#79225,
#79226),(#79227,#79228),(#79229,#79230),(#79231,#79232),(#79233,#79234),
(#79235,#79236),(#79237,#79238),(#79239,#79240),(#79241,#79242),(#79243,
#79244),(#79245,#79246),(#79247,#79248),(#79249,#79250),(#79251,#79252),
(#79253,#79254),(#79255,#79256),(#79257,#79258),(#79259,#79260),(#79261,
#79262),(#79263,#79264),(#79265,#79266),(#79267,#79268),(#79269,#79270),
(#79271,#79272),(#79273,#79274),(#79275,#79276),(#79277,#79278),(#79279,
#79280),(#79281,#79282),(#79283,#79284),(#79285,#79286),(#79287,#79288),
(#79289,#79290),(#79291,#79292),(#79293,#79294),(#79295,#79296),(#79297,
#79298),(#79299,#79300),(#79301,#79302),(#79303,#79304),(#79305,#79306),
(#79307,#79308),(#79309,#79310),(#79311,#79312),(#79313,#79314),(#79315,
#79316),(#79317,#79318),(#79319,#79320),(#79321,#79322),(#79323,#79324),
(#79325,#79326),(#79327,#79328),(#79329,#79330),(#79331,#79332),(#79333,
#79334),(#79335,#79336),(#79337,#79338),(#79339,#79340),(#79341,#79342),
(#79343,#79344),(#79345,#79346),(#79347,#79348),(#79349,#79350),(#79351,
#79352),(#79353,#79354),(#79355,#79356),(#79357,#79358),(#79359,#79360),
(#79361,#79362),(#79363,#79364),(#79365,#79366),(#79367,#79368),(#79369,
#79370),(#79371,#79372),(#79373,#79374),(#79375,#79376),(#79377,#79378),
(#79379,#79380),(#79381,#79382),(#79383,#79384),(#79385,#79386),(#79387,
#79388),(#79389,#79390),(#79391,#79392),(#79393,#79394),(#79395,#79396),
(#79397,#79398),(#79399,#79400),(#79401,#79402),(#79403,#79404),(#79405,
#79406),(#79407,#79408),(#79409,#79410),(#79411,#79412),(#79413,#79414),
(#79415,#79416),(#79417,#79418),(#79419,#79420),(#79421,#79422),(#79423,
#79424),(#79425,#79426),(#79427,#79428),(#79429,#79430),(#79431,#79432),
(#79433,#79434),(#79435,#79436),(#79437,#79438),(#79439,#79440),(#79441,
#79442),(#79443,#79444),(#79445,#79446),(#79447,#79448),(#79449,#79450),
(#79451,#79452),(#79453,#79454),(#79455,#79456),(#79457,#79458),(#79459,
#79460),(#79461,#79462),(#79463,#79464),(#79465,#79466),(#79467,#79468),
(#79469,#79470),(#79471,#79472),(#79473,#79474),(#79475,#79476),(#79477,
#79478),(#79479,#79480),(#79481,#79482),(#79483,#79484),(#79485,#79486),
(#79487,#79488),(#79489,#79490),(#79491,#79492),(#79493,#79494),(#79495,
#79496),(#79497,#79498),(#79499,#79500),(#79501,#79502),(#79503,#79504),
(#79505,#79506),(#79507,#79508),(#79509,#79510),(#79511,#79512),(#79513,
#79514),(#79515,#79516),(#79517,#79518),(#79519,#79520),(#79521,#79522),
(#79523,#79524),(#79525,#79526),(#79527,#79528),(#79529,#79530),(#79531,
#79532),(#79533,#79534),(#79535,#79536),(#79537,#79538),(#79539,#79540),
(#79541,#79542),(#79543,#79544),(#79545,#79546),(#79547,#79548),(#79549,
#79550),(#79551,#79552),(#79553,#79554),(#79555,#79556),(#79557,#79558),
(#79559,#79560),(#79561,#79562),(#79563,#79564),(#79565,#79566),(#79567,
#79568),(#79569,#79570),(#79571,#79572),(#79573,#79574),(#79575,#79576),
(#79577,#79578),(#79579,#79580),(#79581,#79582),(#79583,#79584),(#79585,
#79586),(#79587,#79588),(#79589,#79590),(#79591,#79592),(#79593,#79594),
(#79595,#79596),(#79597,#79598),(#79599,#79600),(#79601,#79602),(#79603,
#79604),(#79605,#79606),(#79607,#79608),(#79609,#79610),(#79611,#79612),
(#79613,#79614),(#79615,#79616),(#79617,#79618),(#79619,#79620),(#79621,
#79622),(#79623,#79624),(#79625,#79626),(#79627,#79628),(#79629,#79630),
(#79631,#79632),(#79633,#79634),(#79635,#79636),(#79637,#79638),(#79639,
#79640),(#79641,#79642),(#79643,#79644),(#79645,#79646),(#79647,#79648),
(#79649,#79650),(#79651,#79652),(#79653,#79654),(#79655,#79656),(#79657,
#79658),(#79659,#79660),(#79661,#79662),(#79663,#79664),(#79665,#79666),
(#79667,#79668),(#79669,#79670),(#79671,#79672),(#79673,#79674),(#79675,
#79676),(#79677,#79678),(#79679,#79680),(#79681,#79682),(#79683,#79684),
(#79685,#79686),(#79687,#79688),(#79689,#79690),(#79691,#79692),(#79693,
#79694),(#79695,#79696),(#79697,#79698),(#79699,#79700),(#79701,#79702),
(#79703,#79704),(#79705,#79706),(#79707,#79708),(#79709,#79710),(#79711,
#79712),(#79713,#79714),(#79715,#79716),(#79717,#79718),(#79719,#79720),
(#79721,#79722),(#79723,#79724),(#79725,#79726),(#79727,#79728),(#79729,
#79730),(#79731,#79732),(#79733,#79734),(#79735,#79736),(#79737,#79738),
(#79739,#79740),(#79741,#79742),(#79743,#79744),(#79745,#79746),(#79747,
#79748),(#79749,#79750),(#79751,#79752),(#79753,#79754),(#79755,#79756),
(#79757,#79758),(#79759,#79760),(#79761,#79762),(#79763,#79764),(#79765,
#79766),(#79767,#79768),(#79769,#79770),(#79771,#79772),(#79773,#79774),
(#79775,#79776),(#79777,#79778),(#79779,#79780),(#79781,#79782),(#79783,
#79784),(#79785,#79786),(#79787,#79788),(#79789,#79790),(#79791,#79792),
(#79793,#79794),(#79795,#79796),(#79797,#79798),(#79799,#79800),(#79801,
#79802),(#79803,#79804),(#79805,#79806),(#79807,#79808),(#79809,#79810),
(#79811,#79812),(#79813,#79814),(#79815,#79816),(#79817,#79818),(#79819,
#79820),(#79821,#79822),(#79823,#79824),(#79825,#79826),(#79827,#79828),
(#79829,#79830),(#79831,#79832),(#79833,#79834),(#79835,#79836),(#79837,
#79838),(#79839,#79840),(#79841,#79842),(#79843,#79844),(#79845,#79846),
(#79847,#79848),(#79849,#79850),(#79851,#79852),(#79853,#79854),(#79855,
#79856),(#79857,#79858),(#79859,#79860),(#79861,#79862),(#79863,#79864),
(#79865,#79866),(#79867,#79868),(#79869,#79870),(#79871,#79872),(#79873,
#79874),(#79875,#79876),(#79877,#79878),(#79879,#79880),(#79881,#79882),
(#79883,#79884),(#79885,#79886),(#79887,#79888),(#79889,#79890),(#79891,
#79892),(#79893,#79894),(#79895,#79896),(#79897,#79898),(#79899,#79900),
(#79901,#79902),(#79903,#79904),(#79905,#79906),(#79907,#79908),(#79909,
#79910),(#79911,#79912),(#79913,#79914),(#79915,#79916),(#79917,#79918),
(#79919,#79920),(#79921,#79922),(#79923,#79924),(#79925,#79926),(#79927,
#79928),(#79929,#79930),(#79931,#79932),(#79933,#79934),(#79935,#79936),
(#79937,#79938),(#79939,#79940),(#79941,#79942),(#79943,#79944),(#79945,
#79946),(#79947,#79948),(#79949,#79950),(#79951,#79952),(#79953,#79954),
(#79955,#79956),(#79957,#79958),(#79959,#79960),(#79961,#79962),(#79963,
#79964),(#79965,#79966),(#79967,#79968),(#79969,#79970),(#79971,#79972),
(#79973,#79974),(#79975,#79976),(#79977,#79978),(#79979,#79980),(#79981,
#79982),(#79983,#79984),(#79985,#79986),(#79987,#79988),(#79989,#79990),
(#79991,#79992),(#79993,#79994),(#79995,#79996),(#79997,#79998),(#79999,
#80000),(#80001,#80002),(#80003,#80004),(#80005,#80006),(#80007,#80008),
(#80009,#80010),(#80011,#80012),(#80013,#80014),(#80015,#80016),(#80017,
#80018),(#80019,#80020),(#80021,#80022),(#80023,#80024),(#80025,#80026),
(#80027,#80028),(#80029,#80030),(#80031,#80032),(#80033,#80034),(#80035,
#80036),(#80037,#80038),(#80039,#80040),(#80041,#80042),(#80043,#80044),
(#80045,#80046),(#80047,#80048),(#80049,#80050),(#80051,#80052),(#80053,
#80054),(#80055,#80056),(#80057,#80058),(#80059,#80060),(#80061,#80062),
(#80063,#80064),(#80065,#80066),(#80067,#80068),(#80069,#80070),(#80071,
#80072),(#80073,#80074),(#80075,#80076),(#80077,#80078),(#80079,#80080),
(#80081,#80082),(#80083,#80084),(#80085,#80086),(#80087,#80088),(#80089,
#80090),(#80091,#80092),(#80093,#80094),(#80095,#80096),(#80097,#80098),
(#80099,#80100),(#80101,#80102),(#80103,#80104),(#80105,#80106),(#80107,
#80108),(#80109,#80110),(#80111,#80112),(#80113,#80114),(#80115,#80116),
(#80117,#80118),(#80119,#80120),(#80121,#80122),(#80123,#80124),(#80125,
#80126),(#80127,#80128),(#80129,#80130),(#80131,#80132),(#80133,#80134),
(#80135,#80136),(#80137,#80138),(#80139,#80140),(#80141,#80142),(#80143,
#80144),(#80145,#80146),(#80147,#80148),(#80149,#80150),(#80151,#80152),
(#80153,#80154),(#80155,#80156),(#80157,#80158),(#80159,#80160),(#80161,
#80162),(#80163,#80164),(#80165,#80166)),.UNSPECIFIED.,.F.,.F.,.F.)
B_SPLINE_SURFACE_WITH_KNOTS((6,1,1,1,1,1,1,1,1,1,1,1,1,1,1,1,1,1,1,1,1,
1,1,1,1,1,1,1,1,1,1,1,1,1,1,1,1,1,1,1,1,1,1,1,1,1,1,1,1,1,1,1,1,1,1,1,1,
1,1,1,1,1,1,1,1,1,1,1,1,1,1,1,1,1,1,1,1,1,1,1,1,1,1,1,1,1,1,1,1,1,1,1,1,
1,1,1,1,1,1,1,1,1,1,1,1,1,1,1,1,1,1,1,1,1,1,1,1,1,1,1,1,1,1,1,1,1,1,1,1,
1,1,1,1,1,1,1,1,1,1,1,1,1,1,1,1,1,1,1,1,1,1,1,1,1,1,1,1,1,1,1,1,1,1,1,1,
1,1,1,1,1,1,1,1,1,1,1,1,1,1,1,1,1,1,1,1,1,1,1,1,1,1,1,1,1,1,1,1,1,1,1,1,
1,1,1,1,1,1,1,1,1,1,1,1,1,1,1,1,1,1,1,1,1,1,1,1,1,1,1,1,1,1,1,1,1,1,1,1,
1,1,1,1,1,1,1,1,1,1,1,1,1,1,1,1,1,1,1,1,1,1,1,1,1,1,1,1,1,1,1,1,1,1,1,1,
1,1,1,1,1,1,1,1,1,1,1,1,1,1,1,1,1,1,1,1,1,1,1,1,1,1,1,1,1,1,1,1,1,1,1,1,
1,1,1,1,1,1,1,1,1,1,1,1,1,1,1,1,1,1,1,1,1,1,1,1,1,1,1,1,1,1,1,1,1,1,1,1,
1,1,1,1,1,1,1,1,1,1,1,1,1,1,1,1,1,1,1,1,1,1,1,1,1,1,1,1,1,1,1,1,1,1,1,1,
1,1,1,1,1,1,1,1,1,1,1,1,1,1,1,1,1,1,1,1,1,1,1,1,1,1,1,1,1,1,1,1,1,1,1,1,
1,1,1,1,1,1,1,1,1,1,1,1,1,1,1,1,1,1,1,1,1,1,1,1,1,1,1,1,1,1,1,1,1,1,1,1,
1,1,1,1,1,1,1,1,1,1,1,1,1,1,1,1,1,1,1,1,1,1,1,1,1,1,1,1,1,1,1,1,1,1,1,1,
1,1,1,1,1,1,1,1,1,1,1,1,1,1,1,1,1,1,1,1,1,1,1,1,1,1,1,1,1,1,1,1,1,1,1,1,
1,1,1,1,1,1,1,1,1,1,1,1,1,1,1,1,1,1,1,1,1,1,1,1,1,1,1,1,1,1,1,1,1,1,1,1,
1,1,1,1,1,1,1,1,1,1,1,1,1,1,1,1,1,1,1,1,1,1,1,1,1,1,1,1,1,1,1,1,1,1,1,1,
1,1,1,1,1,1,1,1,1,1,1,1,1,1,1,1,1,1,1,1,1,1,1,1,1,1,1,1,1,1,1,1,1,1,1,1,
1,1,1,1,1,1,1,1,1,1,1,1,1,1,1,1,1,1,1,1,1,1,1,1,1,1,1,1,1,1,1,1,1,1,1,1,
1,1,1,1,1,1,1,1,1,1,1,1,1,1,1,1,1,1,1,1,1,1,1,1,1,1,1,1,1,1,1,1,1,1,1,1,
1,1,1,1,1,1,1,1,1,1,1,1,1,1,1,1,1,1,1,1,1,1,1,1,1,1,1,1,1,1,1,1,1,1,1,1,
1,1,1,1,1,1,1,1,1,1,1,1,1,1,1,1,1,1,1,1,1,1,1,1,1,1,1,1,1,1,1,1,1,1,1,1,
1,1,1,1,1,1,1,1,1,1,1,1,1,1,1,1,1,1,1,1,1,1,1,1,1,1,1,1,1,1,1,1,1,1,1,1,
1,1,1,1,1,1,1,1,1,1,1,1,1,1,1,1,1,1,1,1,1,1,1,1,1,1,1,1,1,1,1,1,1,1,1,1,
1,1,1,1,1,1,1,1,1,1,1,1,1,1,1,1,1,1,1,1,1,1,1,1,1,1,1,1,1,1,1,1,1,1,1,1,
1,1,1,1,1,1,1,1,1,1,1,1,1,1,1,1,1,1,1,1,1,1,1,1,1,1,1,1,1,1,1,1,1,1,1,1,
1,1,1,1,1,1,1,1,1,1,1,1,1,1,1,1,1,1,1,1,1,1,1,1,1,1,1,1,1,1,1,1,1,1,1,1,
1,1,1,1,1,1,1,1,1,1,1,1,1,1,1,1,1,1,1,1,1,1,1,1,1,1,1,1,1,1,1,1,1,1,1,1,
1,1,1,1,1,1,1,6),(2,2),(-1.,-0.999000000000001,-0.998000000000001,-0.997000000000001,
-0.996000000000001,-0.995000000000001,-0.994000000000001,-0.993000000000001,
-0.992000000000001,-0.991000000000001,-0.990000000000001,-0.989000000000001,
-0.988000000000001,-0.987000000000001,-0.986000000000001,-0.985000000000001,
-0.984000000000001,-0.983000000000001,-0.982000000000001,-0.981000000000001,
-0.980000000000001,-0.979000000000001,-0.978000000000001,-0.977000000000001,
-0.976000000000001,-0.975000000000001,-0.974000000000001,-0.973000000000001,
-0.972000000000001,-0.971000000000001,-0.970000000000001,-0.969000000000001,
-0.968000000000001,-0.967000000000001,-0.966000000000001,-0.965000000000001,
-0.964000000000001,-0.963000000000001,-0.962000000000001,-0.961000000000001,
-0.960000000000001,-0.959000000000001,-0.958000000000001,-0.957000000000001,
-0.956000000000001,-0.955000000000001,-0.954000000000001,-0.953000000000001,
-0.952000000000001,-0.951000000000001,-0.950000000000001,-0.949000000000001,
-0.948000000000001,-0.947000000000001,-0.946000000000001,-0.945000000000001,
-0.944000000000001,-0.943000000000001,-0.942000000000001,-0.941000000000001,
-0.940000000000001,-0.939000000000001,-0.938000000000001,-0.937000000000001,
-0.936000000000001,-0.935000000000001,-0.934000000000001,-0.933000000000001,
-0.932000000000001,-0.931000000000001,-0.930000000000001,-0.929000000000001,
-0.928000000000001,-0.927000000000001,-0.926000000000001,-0.925000000000001,
-0.924000000000001,-0.923000000000001,-0.922000000000001,-0.921000000000001,
-0.920000000000001,-0.919000000000001,-0.918000000000001,-0.917000000000001,
-0.916000000000001,-0.915000000000001,-0.914000000000001,-0.913000000000001,
-0.912000000000001,-0.911000000000001,-0.910000000000001,-0.909000000000001,
-0.908000000000001,-0.907000000000001,-0.906000000000001,-0.905000000000001,
-0.904000000000001,-0.903000000000001,-0.902000000000001,-0.901000000000001,
-0.900000000000001,-0.899000000000001,-0.898000000000001,-0.897000000000001,
-0.896000000000001,-0.895000000000001,-0.894000000000001,-0.893000000000001,
-0.892000000000001,-0.891000000000001,-0.890000000000001,-0.889000000000001,
-0.888000000000001,-0.887000000000001,-0.886000000000001,-0.885000000000001,
-0.884000000000001,-0.883000000000001,-0.882000000000001,-0.881000000000001,
-0.880000000000001,-0.879000000000001,-0.878000000000001,-0.877000000000001,
-0.876000000000001,-0.875000000000001,-0.874000000000001,-0.873000000000001,
-0.872000000000001,-0.871000000000001,-0.870000000000001,-0.869000000000001,
-0.868000000000001,-0.867000000000001,-0.866000000000001,-0.865000000000001,
-0.864000000000001,-0.863000000000001,-0.862000000000001,-0.861000000000001,
-0.860000000000001,-0.859000000000001,-0.858000000000001,-0.857000000000001,
-0.856000000000001,-0.855000000000001,-0.854000000000001,-0.853000000000001,
-0.852000000000001,-0.851000000000001,-0.850000000000001,-0.849000000000001,
-0.848000000000001,-0.847000000000001,-0.846000000000001,-0.845000000000001,
-0.844000000000001,-0.843000000000001,-0.842000000000001,-0.841000000000001,
-0.840000000000001,-0.839000000000001,-0.838000000000001,-0.837000000000001,
-0.836000000000001,-0.835000000000001,-0.834000000000001,-0.833000000000001,
-0.832000000000001,-0.831000000000001,-0.830000000000001,-0.829000000000001,
-0.828000000000001,-0.827000000000001,-0.826000000000001,-0.825000000000001,
-0.824000000000001,-0.823000000000001,-0.822000000000001,-0.821000000000001,
-0.820000000000001,-0.819000000000001,-0.818000000000001,-0.817000000000001,
-0.816000000000001,-0.815000000000001,-0.814000000000001,-0.813000000000001,
-0.812000000000001,-0.811000000000001,-0.810000000000001,-0.809000000000001,
-0.808000000000001,-0.807000000000001,-0.806000000000001,-0.805000000000001,
-0.804000000000001,-0.803000000000001,-0.802000000000001,-0.801000000000001,
-0.800000000000001,-0.799000000000001,-0.798000000000001,-0.797000000000001,
-0.796000000000001,-0.795000000000001,-0.794000000000001,-0.793000000000001,
-0.792000000000001,-0.791000000000001,-0.790000000000001,-0.789000000000001,
-0.788000000000001,-0.787000000000001,-0.786000000000001,-0.785000000000001,
-0.784000000000001,-0.783000000000001,-0.782000000000001,-0.781000000000001,
-0.780000000000001,-0.779000000000001,-0.778000000000001,-0.777000000000001,
-0.776000000000001,-0.775000000000001,-0.774000000000001,-0.773000000000001,
-0.772000000000001,-0.771000000000001,-0.770000000000001,-0.769000000000001,
-0.768000000000001,-0.767000000000001,-0.766000000000001,-0.765000000000001,
-0.764000000000001,-0.763000000000001,-0.762000000000001,-0.761000000000001,
-0.760000000000001,-0.759000000000001,-0.758000000000001,-0.757000000000001,
-0.756000000000001,-0.755000000000001,-0.754000000000001,-0.753000000000001,
-0.752000000000001,-0.751000000000001,-0.750000000000001,-0.749000000000001,
-0.748000000000001,-0.747000000000001,-0.746000000000001,-0.745000000000001,
-0.744000000000001,-0.743000000000001,-0.742000000000001,-0.741000000000001,
-0.740000000000001,-0.739000000000001,-0.738000000000001,-0.737000000000001,
-0.736000000000001,-0.735000000000001,-0.734000000000001,-0.733000000000001,
-0.732000000000001,-0.731000000000001,-0.730000000000001,-0.729000000000001,
-0.728000000000001,-0.727000000000001,-0.726000000000001,-0.725000000000001,
-0.724000000000001,-0.723000000000001,-0.722000000000001,-0.721000000000001,
-0.720000000000001,-0.719000000000001,-0.718000000000001,-0.717000000000001,
-0.716000000000001,-0.715000000000001,-0.714000000000001,-0.713000000000001,
-0.712000000000001,-0.711000000000001,-0.710000000000001,-0.709000000000001,
-0.708000000000001,-0.707000000000001,-0.706000000000001,-0.705000000000001,
-0.704000000000001,-0.703000000000001,-0.702000000000001,-0.701000000000001,
-0.700000000000001,-0.699000000000001,-0.698000000000001,-0.697000000000001,
-0.696000000000001,-0.695000000000001,-0.694000000000001,-0.693000000000001,
-0.692000000000001,-0.691000000000001,-0.690000000000001,-0.689000000000001,
-0.688000000000001,-0.687,-0.686,-0.685,-0.684,-0.683,-0.682,-0.681,-0.68,
-0.679,-0.678,-0.677,-0.676,-0.675,-0.674,-0.673,-0.672,-0.671,-0.67,-0.669,
-0.668,-0.667,-0.666,-0.665,-0.664,-0.663,-0.662,-0.661,-0.66,-0.659,-0.658,
-0.657,-0.656,-0.655,-0.654,-0.653,-0.652,-0.651,-0.65,-0.649,-0.648,-0.647,
-0.646,-0.645,-0.644,-0.643,-0.642,-0.641,-0.64,-0.639,-0.638,-0.637,-0.636,
-0.635,-0.634,-0.633,-0.632,-0.631,-0.63,-0.629,-0.628,-0.627,-0.626,-0.625,
-0.624,-0.623,-0.622,-0.621,-0.62,-0.619,-0.618,-0.617,-0.616,-0.615,-0.614,
-0.613,-0.612,-0.611,-0.61,-0.609,-0.608,-0.607,-0.606,-0.605,-0.604,-0.603,
-0.602,-0.601,-0.6,-0.599,-0.598,-0.597,-0.596,-0.595,-0.594,-0.593,-0.592,
-0.591,-0.59,-0.589,-0.588,-0.587,-0.586,-0.585,-0.584,-0.583,-0.582,-0.581,
-0.58,-0.579,-0.578,-0.577,-0.576,-0.575,-0.574,-0.573,-0.572,-0.571,-0.57,
-0.569,-0.568,-0.567,-0.566,-0.565,-0.564,-0.563,-0.562,-0.561,-0.56,-0.559,
-0.558,-0.557,-0.556,-0.555,-0.554,-0.553,-0.552,-0.551,-0.55,-0.549,-0.548,
-0.547,-0.546,-0.545,-0.544,-0.543,-0.542,-0.541,-0.54,-0.539,-0.538,-0.537,
-0.536,-0.535,-0.534,-0.533,-0.532,-0.531,-0.53,-0.529,-0.528,-0.527,-0.526,
-0.525,-0.524,-0.523,-0.522,-0.521,-0.52,-0.519,-0.518,-0.517,-0.516,-0.515,
-0.514,-0.513,-0.512,-0.511,-0.51,-0.509,-0.508,-0.507,-0.506,-0.505,-0.504,
-0.503,-0.502,-0.501,-0.5,-0.499,-0.498,-0.497,-0.496,-0.495,-0.494,-0.493,
-0.492,-0.491,-0.49,-0.489,-0.488,-0.487,-0.486,-0.485,-0.484,-0.483,-0.482,
-0.481,-0.48,-0.479,-0.478,-0.477,-0.476,-0.475,-0.474,-0.473,-0.472,-0.471,
-0.47,-0.469,-0.468,-0.467,-0.466,-0.465,-0.464,-0.463,-0.462,-0.461,-0.46,
-0.459,-0.458,-0.457,-0.456,-0.455,-0.454,-0.453,-0.452,-0.451,-0.45,-0.449,
-0.448,-0.447,-0.446,-0.445,-0.444,-0.443,-0.442,-0.441,-0.44,-0.439,-0.438,
-0.437,-0.436,-0.435,-0.434,-0.433,-0.432,-0.431,-0.43,-0.429,-0.428,-0.427,
-0.426,-0.425,-0.424,-0.423,-0.422,-0.421,-0.42,-0.419,-0.418,-0.417,-0.416,
-0.415,-0.414,-0.413,-0.412,-0.411,-0.41,-0.409,-0.408,-0.407,-0.406,-0.405,
-0.404,-0.403,-0.402,-0.401,-0.4,-0.399,-0.398,-0.397,-0.396,-0.395,-0.394,
-0.393,-0.392,-0.391,-0.39,-0.389,-0.388,-0.387,-0.386,-0.385,-0.384,-0.383,
-0.382,-0.381,-0.38,-0.379,-0.378,-0.377,-0.376,-0.375,-0.374,-0.373,-0.372,
-0.371,-0.37,-0.369,-0.368,-0.367,-0.366,-0.365,-0.364,-0.363,-0.362,-0.361,
-0.36,-0.359,-0.358,-0.357,-0.356,-0.355,-0.354,-0.353,-0.352,-0.351,-0.35,
-0.349,-0.348,-0.347,-0.346,-0.345,-0.344,-0.343,-0.342,-0.341,-0.34,-0.339,
-0.338,-0.337,-0.336,-0.335,-0.334,-0.333,-0.332,-0.331,-0.33,-0.329,-0.328,
-0.327,-0.326,-0.325,-0.324,-0.323,-0.322,-0.321,-0.32,-0.319,-0.318,-0.317,
-0.316,-0.315,-0.314,-0.313,-0.312,-0.311,-0.31,-0.309,-0.308,-0.307,-0.306,
-0.305,-0.304,-0.303,-0.302,-0.301,-0.3,-0.299,-0.298,-0.297,-0.296,-0.295,
-0.294,-0.293,-0.292,-0.291,-0.29,-0.289,-0.288,-0.287,-0.286,-0.285,-0.284,
-0.283,-0.282,-0.281,-0.28,-0.279,-0.278,-0.277,-0.276,-0.275,-0.274,-0.273,
-0.272,-0.271,-0.27,-0.269,-0.268,-0.267,-0.266,-0.265,-0.264,-0.263,-0.262,
-0.261,-0.26,-0.259,-0.258,-0.257,-0.256,-0.255,-0.254,-0.253,-0.252,-0.251,
-0.25,-0.249,-0.248,-0.247,-0.246,-0.245,-0.244,-0.243,-0.242,-0.241,-0.24,
-0.239,-0.238,-0.237,-0.236,-0.235,-0.234,-0.233,-0.232,-0.231,-0.23,-0.229,
-0.228,-0.227,-0.226,-0.225,-0.224,-0.223,-0.222,-0.221,-0.22,-0.219,-0.218,
-0.217,-0.216,-0.215,-0.214,-0.213,-0.212,-0.211,-0.21,-0.209,-0.208,-0.207,
-0.206,-0.205,-0.204,-0.203,-0.202,-0.201,-0.2,-0.199,-0.198,-0.197,-0.196,
-0.195,-0.194,-0.193,-0.192,-0.191,-0.19,-0.189,-0.188,-0.187,-0.186,-0.185,
-0.184,-0.183,-0.182,-0.181,-0.18,-0.179,-0.178,-0.177,-0.176,-0.175,-0.174,
-0.173,-0.172,-0.171,-0.17,-0.169,-0.168,-0.167,-0.166,-0.165,-0.164,-0.163,
-0.162,-0.161,-0.16,-0.159,-0.158,-0.157,-0.156,-0.155,-0.154,-0.153,-0.152,
-0.151,-0.15,-0.149,-0.148,-0.147,-0.146,-0.145,-0.144,-0.143,-0.142,-0.141,
-0.14,-0.139,-0.138,-0.137,-0.136,-0.135,-0.134,-0.133,-0.132,-0.131,-0.13,
-0.129,-0.128,-0.127,-0.126,-0.125,-0.124,-0.123,-0.122,-0.121,-0.12,-0.119,
-0.118,-0.117,-0.116,-0.115,-0.114,-0.113,-0.112,-0.111,-0.11,-0.109,-0.108,
-0.107,-0.106,-0.105,-0.104,-0.103,-0.102,-0.101,-0.1,-0.0990000000000001,
-0.0980000000000001,-0.0970000000000001,-0.0960000000000001,-0.0950000000000001,
-0.0940000000000001,-0.0930000000000001,-0.0920000000000001,-0.0910000000000001,
-0.0900000000000001,-0.0890000000000001,-0.0880000000000001,-0.0870000000000001,
-0.0860000000000001,-0.0850000000000001,-0.0840000000000001,-0.0830000000000001,
-0.0820000000000001,-0.0810000000000001,-0.0800000000000001,-0.0790000000000001,
-0.0780000000000001,-0.0770000000000001,-0.0760000000000001,-0.0750000000000001,
-0.0740000000000001,-0.0730000000000001,-0.0720000000000001,-0.071,-0.07,
-0.069,-0.068,-0.067,-0.066,-0.065,-0.064,-0.063,-0.062,-0.061,-0.06,-0.059,
-0.058,-0.057,-0.056,-0.055,-0.054,-0.053,-0.052,-0.051,-0.05,-0.049,-0.048,
-0.047,-0.046,-0.045,-0.044,-0.043,-0.042,-0.041,-0.04,-0.039,-0.038,-0.037,
-0.036,-0.035,-0.034,-0.033,-0.032,-0.031,-0.03,-0.029,-0.028,-0.027,-0.026,
-0.025,-0.024,-0.023,-0.022,-0.021,-0.02,-0.019,-0.018,-0.017,-0.016,-0.015,
-0.014,-0.013,-0.012,-0.011,-0.01,-0.009,-0.008,-0.007,-0.006,-0.005,-0.004,
-0.003,-0.002,-0.001,0.),(0.,2.),.UNSPECIFIED.)
GEOMETRIC_REPRESENTATION_ITEM()
RATIONAL_B_SPLINE_SURFACE(((1.,1.),(1.,1.),(1.,1.),(1.,1.),(1.,1.),(1.,
1.),(1.,1.),(1.,1.),(1.,1.),(1.,1.),(1.,1.),(1.,1.),(1.,1.),(1.,1.),(1.,
1.),(1.,1.),(1.,1.),(1.,1.),(1.,1.),(1.,1.),(1.,1.),(1.,1.),(1.,1.),(1.,
1.),(1.,1.),(1.,1.),(1.,1.),(1.,1.),(1.,1.),(1.,1.),(1.,1.),(1.,1.),(1.,
1.),(1.,1.),(1.,1.),(1.,1.),(1.,1.),(1.,1.),(1.,1.),(1.,1.),(1.,1.),(1.,
1.),(1.,1.),(1.,1.),(1.,1.),(1.,1.),(1.,1.),(1.,1.),(1.,1.),(1.,1.),(1.,
1.),(1.,1.),(1.,1.),(1.,1.),(1.,1.),(1.,1.),(1.,1.),(1.,1.),(1.,1.),(1.,
1.),(1.,1.),(1.,1.),(1.,1.),(1.,1.),(1.,1.),(1.,1.),(1.,1.),(1.,1.),(1.,
1.),(1.,1.),(1.,1.),(1.,1.),(1.,1.),(1.,1.),(1.,1.),(1.,1.),(1.,1.),(1.,
1.),(1.,1.),(1.,1.),(1.,1.),(1.,1.),(1.,1.),(1.,1.),(1.,1.),(1.,1.),(1.,
1.),(1.,1.),(1.,1.),(1.,1.),(1.,1.),(1.,1.),(1.,1.),(1.,1.),(1.,1.),(1.,
1.),(1.,1.),(1.,1.),(1.,1.),(1.,1.),(1.,1.),(1.,1.),(1.,1.),(1.,1.),(1.,
1.),(1.,1.),(1.,1.),(1.,1.),(1.,1.),(1.,1.),(1.,1.),(1.,1.),(1.,1.),(1.,
1.),(1.,1.),(1.,1.),(1.,1.),(1.,1.),(1.,1.),(1.,1.),(1.,1.),(1.,1.),(1.,
1.),(1.,1.),(1.,1.),(1.,1.),(1.,1.),(1.,1.),(1.,1.),(1.,1.),(1.,1.),(1.,
1.),(1.,1.),(1.,1.),(1.,1.),(1.,1.),(1.,1.),(1.,1.),(1.,1.),(1.,1.),(1.,
1.),(1.,1.),(1.,1.),(1.,1.),(1.,1.),(1.,1.),(1.,1.),(1.,1.),(1.,1.),(1.,
1.),(1.,1.),(1.,1.),(1.,1.),(1.,1.),(1.,1.),(1.,1.),(1.,1.),(1.,1.),(1.,
1.),(1.,1.),(1.,1.),(1.,1.),(1.,1.),(1.,1.),(1.,1.),(1.,1.),(1.,1.),(1.,
1.),(1.,1.),(1.,1.),(1.,1.),(1.,1.),(1.,1.),(1.,1.),(1.,1.),(1.,1.),(1.,
1.),(1.,1.),(1.,1.),(1.,1.),(1.,1.),(1.,1.),(1.,1.),(1.,1.),(1.,1.),(1.,
1.),(1.,1.),(1.,1.),(1.,1.),(1.,1.),(1.,1.),(1.,1.),(1.,1.),(1.,1.),(1.,
1.),(1.,1.),(1.,1.),(1.,1.),(1.,1.),(1.,1.),(1.,1.),(1.,1.),(1.,1.),(1.,
1.),(1.,1.),(1.,1.),(1.,1.),(1.,1.),(1.,1.),(1.,1.),(1.,1.),(1.,1.),(1.,
1.),(1.,1.),(1.,1.),(1.,1.),(1.,1.),(1.,1.),(1.,1.),(1.,1.),(1.,1.),(1.,
1.),(1.,1.),(1.,1.),(1.,1.),(1.,1.),(1.,1.),(1.,1.),(1.,1.),(1.,1.),(1.,
1.),(1.,1.),(1.,1.),(1.,1.),(1.,1.),(1.,1.),(1.,1.),(1.,1.),(1.,1.),(1.,
1.),(1.,1.),(1.,1.),(1.,1.),(1.,1.),(1.,1.),(1.,1.),(1.,1.),(1.,1.),(1.,
1.),(1.,1.),(1.,1.),(1.,1.),(1.,1.),(1.,1.),(1.,1.),(1.,1.),(1.,1.),(1.,
1.),(1.,1.),(1.,1.),(1.,1.),(1.,1.),(1.,1.),(1.,1.),(1.,1.),(1.,1.),(1.,
1.),(1.,1.),(1.,1.),(1.,1.),(1.,1.),(1.,1.),(1.,1.),(1.,1.),(1.,1.),(1.,
1.),(1.,1.),(1.,1.),(1.,1.),(1.,1.),(1.,1.),(1.,1.),(1.,1.),(1.,1.),(1.,
1.),(1.,1.),(1.,1.),(1.,1.),(1.,1.),(1.,1.),(1.,1.),(1.,1.),(1.,1.),(1.,
1.),(1.,1.),(1.,1.),(1.,1.),(1.,1.),(1.,1.),(1.,1.),(1.,1.),(1.,1.),(1.,
1.),(1.,1.),(1.,1.),(1.,1.),(1.,1.),(1.,1.),(1.,1.),(1.,1.),(1.,1.),(1.,
1.),(1.,1.),(1.,1.),(1.,1.),(1.,1.),(1.,1.),(1.,1.),(1.,1.),(1.,1.),(1.,
1.),(1.,1.),(1.,1.),(1.,1.),(1.,1.),(1.,1.),(1.,1.),(1.,1.),(1.,1.),(1.,
1.),(1.,1.),(1.,1.),(1.,1.),(1.,1.),(1.,1.),(1.,1.),(1.,1.),(1.,1.),(1.,
1.),(1.,1.),(1.,1.),(1.,1.),(1.,1.),(1.,1.),(1.,1.),(1.,1.),(1.,1.),(1.,
1.),(1.,1.),(1.,1.),(1.,1.),(1.,1.),(1.,1.),(1.,1.),(1.,1.),(1.,1.),(1.,
1.),(1.,1.),(1.,1.),(1.,1.),(1.,1.),(1.,1.),(1.,1.),(1.,1.),(1.,1.),(1.,
1.),(1.,1.),(1.,1.),(1.,1.),(1.,1.),(1.,1.),(1.,1.),(1.,1.),(1.,1.),(1.,
1.),(1.,1.),(1.,1.),(1.,1.),(1.,1.),(1.,1.),(1.,1.),(1.,1.),(1.,1.),(1.,
1.),(1.,1.),(1.,1.),(1.,1.),(1.,1.),(1.,1.),(1.,1.),(1.,1.),(1.,1.),(1.,
1.),(1.,1.),(1.,1.),(1.,1.),(1.,1.),(1.,1.),(1.,1.),(1.,1.),(1.,1.),(1.,
1.),(1.,1.),(1.,1.),(1.,1.),(1.,1.),(1.,1.),(1.,1.),(1.,1.),(1.,1.),(1.,
1.),(1.,1.),(1.,1.),(1.,1.),(1.,1.),(1.,1.),(1.,1.),(1.,1.),(1.,1.),(1.,
1.),(1.,1.),(1.,1.),(1.,1.),(1.,1.),(1.,1.),(1.,1.),(1.,1.),(1.,1.),(1.,
1.),(1.,1.),(1.,1.),(1.,1.),(1.,1.),(1.,1.),(1.,1.),(1.,1.),(1.,1.),(1.,
1.),(1.,1.),(1.,1.),(1.,1.),(1.,1.),(1.,1.),(1.,1.),(1.,1.),(1.,1.),(1.,
1.),(1.,1.),(1.,1.),(1.,1.),(1.,1.),(1.,1.),(1.,1.),(1.,1.),(1.,1.),(1.,
1.),(1.,1.),(1.,1.),(1.,1.),(1.,1.),(1.,1.),(1.,1.),(1.,1.),(1.,1.),(1.,
1.),(1.,1.),(1.,1.),(1.,1.),(1.,1.),(1.,1.),(1.,1.),(1.,1.),(1.,1.),(1.,
1.),(1.,1.),(1.,1.),(1.,1.),(1.,1.),(1.,1.),(1.,1.),(1.,1.),(1.,1.),(1.,
1.),(1.,1.),(1.,1.),(1.,1.),(1.,1.),(1.,1.),(1.,1.),(1.,1.),(1.,1.),(1.,
1.),(1.,1.),(1.,1.),(1.,1.),(1.,1.),(1.,1.),(1.,1.),(1.,1.),(1.,1.),(1.,
1.),(1.,1.),(1.,1.),(1.,1.),(1.,1.),(1.,1.),(1.,1.),(1.,1.),(1.,1.),(1.,
1.),(1.,1.),(1.,1.),(1.,1.),(1.,1.),(1.,1.),(1.,1.),(1.,1.),(1.,1.),(1.,
1.),(1.,1.),(1.,1.),(1.,1.),(1.,1.),(1.,1.),(1.,1.),(1.,1.),(1.,1.),(1.,
1.),(1.,1.),(1.,1.),(1.,1.),(1.,1.),(1.,1.),(1.,1.),(1.,1.),(1.,1.),(1.,
1.),(1.,1.),(1.,1.),(1.,1.),(1.,1.),(1.,1.),(1.,1.),(1.,1.),(1.,1.),(1.,
1.),(1.,1.),(1.,1.),(1.,1.),(1.,1.),(1.,1.),(1.,1.),(1.,1.),(1.,1.),(1.,
1.),(1.,1.),(1.,1.),(1.,1.),(1.,1.),(1.,1.),(1.,1.),(1.,1.),(1.,1.),(1.,
1.),(1.,1.),(1.,1.),(1.,1.),(1.,1.),(1.,1.),(1.,1.),(1.,1.),(1.,1.),(1.,
1.),(1.,1.),(1.,1.),(1.,1.),(1.,1.),(1.,1.),(1.,1.),(1.,1.),(1.,1.),(1.,
1.),(1.,1.),(1.,1.),(1.,1.),(1.,1.),(1.,1.),(1.,1.),(1.,1.),(1.,1.),(1.,
1.),(1.,1.),(1.,1.),(1.,1.),(1.,1.),(1.,1.),(1.,1.),(1.,1.),(1.,1.),(1.,
1.),(1.,1.),(1.,1.),(1.,1.),(1.,1.),(1.,1.),(1.,1.),(1.,1.),(1.,1.),(1.,
1.),(1.,1.),(1.,1.),(1.,1.),(1.,1.),(1.,1.),(1.,1.),(1.,1.),(1.,1.),(1.,
1.),(1.,1.),(1.,1.),(1.,1.),(1.,1.),(1.,1.),(1.,1.),(1.,1.),(1.,1.),(1.,
1.),(1.,1.),(1.,1.),(1.,1.),(1.,1.),(1.,1.),(1.,1.),(1.,1.),(1.,1.),(1.,
1.),(1.,1.),(1.,1.),(1.,1.),(1.,1.),(1.,1.),(1.,1.),(1.,1.),(1.,1.),(1.,
1.),(1.,1.),(1.,1.),(1.,1.),(1.,1.),(1.,1.),(1.,1.),(1.,1.),(1.,1.),(1.,
1.),(1.,1.),(1.,1.),(1.,1.),(1.,1.),(1.,1.),(1.,1.),(1.,1.),(1.,1.),(1.,
1.),(1.,1.),(1.,1.),(1.,1.),(1.,1.),(1.,1.),(1.,1.),(1.,1.),(1.,1.),(1.,
1.),(1.,1.),(1.,1.),(1.,1.),(1.,1.),(1.,1.),(1.,1.),(1.,1.),(1.,1.),(1.,
1.),(1.,1.),(1.,1.),(1.,1.),(1.,1.),(1.,1.),(1.,1.),(1.,1.),(1.,1.),(1.,
1.),(1.,1.),(1.,1.),(1.,1.),(1.,1.),(1.,1.),(1.,1.),(1.,1.),(1.,1.),(1.,
1.),(1.,1.),(1.,1.),(1.,1.),(1.,1.),(1.,1.),(1.,1.),(1.,1.),(1.,1.),(1.,
1.),(1.,1.),(1.,1.),(1.,1.),(1.,1.),(1.,1.),(1.,1.),(1.,1.),(1.,1.),(1.,
1.),(1.,1.),(1.,1.),(1.,1.),(1.,1.),(1.,1.),(1.,1.),(1.,1.),(1.,1.),(1.,
1.),(1.,1.),(1.,1.),(1.,1.),(1.,1.),(1.,1.),(1.,1.),(1.,1.),(1.,1.),(1.,
1.),(1.,1.),(1.,1.),(1.,1.),(1.,1.),(1.,1.),(1.,1.),(1.,1.),(1.,1.),(1.,
1.),(1.,1.),(1.,1.),(1.,1.),(1.,1.),(1.,1.),(1.,1.),(1.,1.),(1.,1.),(1.,
1.),(1.,1.),(1.,1.),(1.,1.),(1.,1.),(1.,1.),(1.,1.),(1.,1.),(1.,1.),(1.,
1.),(1.,1.),(1.,1.),(1.,1.),(1.,1.),(1.,1.),(1.,1.),(1.,1.),(1.,1.),(1.,
1.),(1.,1.),(1.,1.),(1.,1.),(1.,1.),(1.,1.),(1.,1.),(1.,1.),(1.,1.),(1.,
1.),(1.,1.),(1.,1.),(1.,1.),(1.,1.),(1.,1.),(1.,1.),(1.,1.),(1.,1.),(1.,
1.),(1.,1.),(1.,1.),(1.,1.),(1.,1.),(1.,1.),(1.,1.),(1.,1.),(1.,1.),(1.,
1.),(1.,1.),(1.,1.),(1.,1.),(1.,1.),(1.,1.),(1.,1.),(1.,1.),(1.,1.),(1.,
1.),(1.,1.),(1.,1.),(1.,1.),(1.,1.),(1.,1.),(1.,1.),(1.,1.),(1.,1.),(1.,
1.),(1.,1.),(1.,1.),(1.,1.),(1.,1.),(1.,1.),(1.,1.),(1.,1.),(1.,1.),(1.,
1.),(1.,1.),(1.,1.),(1.,1.),(1.,1.),(1.,1.),(1.,1.),(1.,1.),(1.,1.),(1.,
1.),(1.,1.),(1.,1.),(1.,1.),(1.,1.),(1.,1.),(1.,1.),(1.,1.),(1.,1.),(1.,
1.),(1.,1.),(1.,1.),(1.,1.),(1.,1.),(1.,1.),(1.,1.),(1.,1.),(1.,1.),(1.,
1.),(1.,1.),(1.,1.),(1.,1.),(1.,1.),(1.,1.),(1.,1.),(1.,1.),(1.,1.),(1.,
1.),(1.,1.),(1.,1.),(1.,1.),(1.,1.),(1.,1.),(1.,1.),(1.,1.),(1.,1.),(1.,
1.),(1.,1.),(1.,1.),(1.,1.),(1.,1.),(1.,1.),(1.,1.),(1.,1.),(1.,1.),(1.,
1.),(1.,1.),(1.,1.),(1.,1.),(1.,1.),(1.,1.),(1.,1.),(1.,1.),(1.,1.),(1.,
1.),(1.,1.),(1.,1.),(1.,1.),(1.,1.),(1.,1.),(1.,1.),(1.,1.),(1.,1.),(1.,
1.),(1.,1.),(1.,1.),(1.,1.),(1.,1.),(1.,1.),(1.,1.),(1.,1.),(1.,1.),(1.,
1.),(1.,1.),(1.,1.),(1.,1.),(1.,1.),(1.,1.),(1.,1.),(1.,1.),(1.,1.),(1.,
1.),(1.,1.),(1.,1.),(1.,1.),(1.,1.),(1.,1.),(1.,1.),(1.,1.),(1.,1.),(1.,
1.),(1.,1.),(1.,1.),(1.,1.),(1.,1.),(1.,1.),(1.,1.),(1.,1.),(1.,1.),(1.,
1.),(1.,1.),(1.,1.),(1.,1.),(1.,1.),(1.,1.),(1.,1.),(1.,1.),(1.,1.),(1.,
1.),(1.,1.),(1.,1.),(1.,1.),(1.,1.),(1.,1.),(1.,1.),(1.,1.),(1.,1.),(1.,
1.),(1.,1.),(1.,1.),(1.,1.),(1.,1.),(1.,1.),(1.,1.),(1.,1.),(1.,1.),(1.,
1.),(1.,1.),(1.,1.),(1.,1.),(1.,1.),(1.,1.),(1.,1.),(1.,1.),(1.,1.),(1.,
1.),(1.,1.),(1.,1.),(1.,1.),(1.,1.),(1.,1.),(1.,1.),(1.,1.),(1.,1.),(1.,
1.),(1.,1.),(1.,1.),(1.,1.),(1.,1.),(1.,1.),(1.,1.),(1.,1.),(1.,1.),(1.,
1.),(1.,1.),(1.,1.),(1.,1.),(1.,1.),(1.,1.),(1.,1.),(1.,1.),(1.,1.),(1.,
1.),(1.,1.),(1.,1.),(1.,1.),(1.,1.),(1.,1.),(1.,1.),(1.,1.),(1.,1.),(1.,
1.)))
REPRESENTATION_ITEM('')
SURFACE()
);
#261=(
BOUNDED_SURFACE()
B_SPLINE_SURFACE(5,1,((#80173,#80174),(#80175,#80176),(#80177,#80178),(#80179,
#80180),(#80181,#80182),(#80183,#80184),(#80185,#80186),(#80187,#80188),
(#80189,#80190),(#80191,#80192),(#80193,#80194),(#80195,#80196),(#80197,
#80198),(#80199,#80200),(#80201,#80202),(#80203,#80204),(#80205,#80206),
(#80207,#80208),(#80209,#80210),(#80211,#80212),(#80213,#80214),(#80215,
#80216),(#80217,#80218),(#80219,#80220),(#80221,#80222),(#80223,#80224),
(#80225,#80226),(#80227,#80228),(#80229,#80230),(#80231,#80232),(#80233,
#80234),(#80235,#80236),(#80237,#80238),(#80239,#80240),(#80241,#80242),
(#80243,#80244),(#80245,#80246),(#80247,#80248),(#80249,#80250),(#80251,
#80252),(#80253,#80254),(#80255,#80256),(#80257,#80258),(#80259,#80260),
(#80261,#80262),(#80263,#80264),(#80265,#80266),(#80267,#80268),(#80269,
#80270),(#80271,#80272),(#80273,#80274),(#80275,#80276),(#80277,#80278),
(#80279,#80280),(#80281,#80282),(#80283,#80284),(#80285,#80286),(#80287,
#80288),(#80289,#80290),(#80291,#80292),(#80293,#80294),(#80295,#80296),
(#80297,#80298),(#80299,#80300),(#80301,#80302),(#80303,#80304),(#80305,
#80306),(#80307,#80308),(#80309,#80310),(#80311,#80312),(#80313,#80314),
(#80315,#80316),(#80317,#80318),(#80319,#80320),(#80321,#80322),(#80323,
#80324),(#80325,#80326),(#80327,#80328),(#80329,#80330),(#80331,#80332),
(#80333,#80334),(#80335,#80336),(#80337,#80338),(#80339,#80340),(#80341,
#80342),(#80343,#80344),(#80345,#80346),(#80347,#80348),(#80349,#80350),
(#80351,#80352),(#80353,#80354),(#80355,#80356),(#80357,#80358),(#80359,
#80360),(#80361,#80362),(#80363,#80364),(#80365,#80366),(#80367,#80368),
(#80369,#80370),(#80371,#80372),(#80373,#80374),(#80375,#80376),(#80377,
#80378),(#80379,#80380),(#80381,#80382),(#80383,#80384),(#80385,#80386),
(#80387,#80388),(#80389,#80390),(#80391,#80392),(#80393,#80394),(#80395,
#80396),(#80397,#80398),(#80399,#80400),(#80401,#80402),(#80403,#80404),
(#80405,#80406),(#80407,#80408),(#80409,#80410),(#80411,#80412),(#80413,
#80414),(#80415,#80416),(#80417,#80418),(#80419,#80420),(#80421,#80422),
(#80423,#80424),(#80425,#80426),(#80427,#80428),(#80429,#80430),(#80431,
#80432),(#80433,#80434),(#80435,#80436),(#80437,#80438),(#80439,#80440),
(#80441,#80442),(#80443,#80444),(#80445,#80446),(#80447,#80448),(#80449,
#80450),(#80451,#80452),(#80453,#80454),(#80455,#80456),(#80457,#80458),
(#80459,#80460),(#80461,#80462),(#80463,#80464),(#80465,#80466),(#80467,
#80468),(#80469,#80470),(#80471,#80472),(#80473,#80474),(#80475,#80476),
(#80477,#80478),(#80479,#80480),(#80481,#80482),(#80483,#80484),(#80485,
#80486),(#80487,#80488),(#80489,#80490),(#80491,#80492),(#80493,#80494),
(#80495,#80496),(#80497,#80498),(#80499,#80500),(#80501,#80502),(#80503,
#80504),(#80505,#80506),(#80507,#80508),(#80509,#80510),(#80511,#80512),
(#80513,#80514),(#80515,#80516),(#80517,#80518),(#80519,#80520),(#80521,
#80522),(#80523,#80524),(#80525,#80526),(#80527,#80528),(#80529,#80530),
(#80531,#80532),(#80533,#80534),(#80535,#80536),(#80537,#80538),(#80539,
#80540),(#80541,#80542),(#80543,#80544),(#80545,#80546),(#80547,#80548),
(#80549,#80550),(#80551,#80552),(#80553,#80554),(#80555,#80556),(#80557,
#80558),(#80559,#80560),(#80561,#80562),(#80563,#80564),(#80565,#80566),
(#80567,#80568),(#80569,#80570),(#80571,#80572),(#80573,#80574),(#80575,
#80576),(#80577,#80578),(#80579,#80580),(#80581,#80582),(#80583,#80584),
(#80585,#80586),(#80587,#80588),(#80589,#80590),(#80591,#80592),(#80593,
#80594),(#80595,#80596),(#80597,#80598),(#80599,#80600),(#80601,#80602),
(#80603,#80604),(#80605,#80606),(#80607,#80608),(#80609,#80610),(#80611,
#80612),(#80613,#80614),(#80615,#80616),(#80617,#80618),(#80619,#80620),
(#80621,#80622),(#80623,#80624),(#80625,#80626),(#80627,#80628),(#80629,
#80630),(#80631,#80632),(#80633,#80634),(#80635,#80636),(#80637,#80638),
(#80639,#80640),(#80641,#80642),(#80643,#80644),(#80645,#80646),(#80647,
#80648),(#80649,#80650),(#80651,#80652),(#80653,#80654),(#80655,#80656),
(#80657,#80658),(#80659,#80660),(#80661,#80662),(#80663,#80664),(#80665,
#80666),(#80667,#80668),(#80669,#80670),(#80671,#80672),(#80673,#80674),
(#80675,#80676),(#80677,#80678),(#80679,#80680),(#80681,#80682),(#80683,
#80684),(#80685,#80686),(#80687,#80688),(#80689,#80690),(#80691,#80692),
(#80693,#80694),(#80695,#80696),(#80697,#80698),(#80699,#80700),(#80701,
#80702),(#80703,#80704),(#80705,#80706),(#80707,#80708),(#80709,#80710),
(#80711,#80712),(#80713,#80714),(#80715,#80716),(#80717,#80718),(#80719,
#80720),(#80721,#80722),(#80723,#80724),(#80725,#80726),(#80727,#80728),
(#80729,#80730),(#80731,#80732),(#80733,#80734),(#80735,#80736),(#80737,
#80738),(#80739,#80740),(#80741,#80742),(#80743,#80744),(#80745,#80746),
(#80747,#80748),(#80749,#80750),(#80751,#80752),(#80753,#80754),(#80755,
#80756),(#80757,#80758),(#80759,#80760),(#80761,#80762),(#80763,#80764),
(#80765,#80766),(#80767,#80768),(#80769,#80770),(#80771,#80772),(#80773,
#80774),(#80775,#80776),(#80777,#80778),(#80779,#80780),(#80781,#80782),
(#80783,#80784),(#80785,#80786),(#80787,#80788),(#80789,#80790),(#80791,
#80792),(#80793,#80794),(#80795,#80796),(#80797,#80798),(#80799,#80800),
(#80801,#80802),(#80803,#80804),(#80805,#80806),(#80807,#80808),(#80809,
#80810),(#80811,#80812),(#80813,#80814),(#80815,#80816),(#80817,#80818),
(#80819,#80820),(#80821,#80822),(#80823,#80824),(#80825,#80826),(#80827,
#80828),(#80829,#80830),(#80831,#80832),(#80833,#80834),(#80835,#80836),
(#80837,#80838),(#80839,#80840),(#80841,#80842),(#80843,#80844),(#80845,
#80846),(#80847,#80848),(#80849,#80850),(#80851,#80852),(#80853,#80854),
(#80855,#80856),(#80857,#80858),(#80859,#80860),(#80861,#80862),(#80863,
#80864),(#80865,#80866),(#80867,#80868),(#80869,#80870),(#80871,#80872),
(#80873,#80874),(#80875,#80876),(#80877,#80878),(#80879,#80880),(#80881,
#80882),(#80883,#80884),(#80885,#80886),(#80887,#80888),(#80889,#80890),
(#80891,#80892),(#80893,#80894),(#80895,#80896),(#80897,#80898),(#80899,
#80900),(#80901,#80902),(#80903,#80904),(#80905,#80906),(#80907,#80908),
(#80909,#80910),(#80911,#80912),(#80913,#80914),(#80915,#80916),(#80917,
#80918),(#80919,#80920),(#80921,#80922),(#80923,#80924),(#80925,#80926),
(#80927,#80928),(#80929,#80930),(#80931,#80932),(#80933,#80934),(#80935,
#80936),(#80937,#80938),(#80939,#80940),(#80941,#80942),(#80943,#80944),
(#80945,#80946),(#80947,#80948),(#80949,#80950),(#80951,#80952),(#80953,
#80954),(#80955,#80956),(#80957,#80958),(#80959,#80960),(#80961,#80962),
(#80963,#80964),(#80965,#80966),(#80967,#80968),(#80969,#80970),(#80971,
#80972),(#80973,#80974),(#80975,#80976),(#80977,#80978),(#80979,#80980),
(#80981,#80982),(#80983,#80984),(#80985,#80986),(#80987,#80988),(#80989,
#80990),(#80991,#80992),(#80993,#80994),(#80995,#80996),(#80997,#80998),
(#80999,#81000),(#81001,#81002),(#81003,#81004),(#81005,#81006),(#81007,
#81008),(#81009,#81010),(#81011,#81012),(#81013,#81014),(#81015,#81016),
(#81017,#81018),(#81019,#81020),(#81021,#81022),(#81023,#81024),(#81025,
#81026),(#81027,#81028),(#81029,#81030),(#81031,#81032),(#81033,#81034),
(#81035,#81036),(#81037,#81038),(#81039,#81040),(#81041,#81042),(#81043,
#81044),(#81045,#81046),(#81047,#81048),(#81049,#81050),(#81051,#81052),
(#81053,#81054),(#81055,#81056),(#81057,#81058),(#81059,#81060),(#81061,
#81062),(#81063,#81064),(#81065,#81066),(#81067,#81068),(#81069,#81070),
(#81071,#81072),(#81073,#81074),(#81075,#81076),(#81077,#81078),(#81079,
#81080),(#81081,#81082),(#81083,#81084),(#81085,#81086),(#81087,#81088),
(#81089,#81090),(#81091,#81092),(#81093,#81094),(#81095,#81096),(#81097,
#81098),(#81099,#81100),(#81101,#81102),(#81103,#81104),(#81105,#81106),
(#81107,#81108),(#81109,#81110),(#81111,#81112),(#81113,#81114),(#81115,
#81116),(#81117,#81118),(#81119,#81120),(#81121,#81122),(#81123,#81124),
(#81125,#81126),(#81127,#81128),(#81129,#81130),(#81131,#81132),(#81133,
#81134),(#81135,#81136),(#81137,#81138),(#81139,#81140),(#81141,#81142),
(#81143,#81144),(#81145,#81146),(#81147,#81148),(#81149,#81150),(#81151,
#81152),(#81153,#81154),(#81155,#81156),(#81157,#81158),(#81159,#81160),
(#81161,#81162),(#81163,#81164),(#81165,#81166),(#81167,#81168),(#81169,
#81170),(#81171,#81172),(#81173,#81174),(#81175,#81176),(#81177,#81178),
(#81179,#81180),(#81181,#81182),(#81183,#81184),(#81185,#81186),(#81187,
#81188),(#81189,#81190),(#81191,#81192),(#81193,#81194),(#81195,#81196),
(#81197,#81198),(#81199,#81200),(#81201,#81202),(#81203,#81204),(#81205,
#81206),(#81207,#81208),(#81209,#81210),(#81211,#81212),(#81213,#81214),
(#81215,#81216),(#81217,#81218),(#81219,#81220),(#81221,#81222),(#81223,
#81224),(#81225,#81226),(#81227,#81228),(#81229,#81230),(#81231,#81232),
(#81233,#81234),(#81235,#81236),(#81237,#81238),(#81239,#81240),(#81241,
#81242),(#81243,#81244),(#81245,#81246),(#81247,#81248),(#81249,#81250),
(#81251,#81252),(#81253,#81254),(#81255,#81256),(#81257,#81258),(#81259,
#81260),(#81261,#81262),(#81263,#81264),(#81265,#81266),(#81267,#81268),
(#81269,#81270),(#81271,#81272),(#81273,#81274),(#81275,#81276),(#81277,
#81278),(#81279,#81280),(#81281,#81282),(#81283,#81284),(#81285,#81286),
(#81287,#81288),(#81289,#81290),(#81291,#81292),(#81293,#81294),(#81295,
#81296),(#81297,#81298),(#81299,#81300),(#81301,#81302),(#81303,#81304),
(#81305,#81306),(#81307,#81308),(#81309,#81310),(#81311,#81312),(#81313,
#81314),(#81315,#81316),(#81317,#81318),(#81319,#81320),(#81321,#81322),
(#81323,#81324),(#81325,#81326),(#81327,#81328),(#81329,#81330),(#81331,
#81332),(#81333,#81334),(#81335,#81336),(#81337,#81338),(#81339,#81340),
(#81341,#81342),(#81343,#81344),(#81345,#81346),(#81347,#81348),(#81349,
#81350),(#81351,#81352),(#81353,#81354),(#81355,#81356),(#81357,#81358),
(#81359,#81360),(#81361,#81362),(#81363,#81364),(#81365,#81366),(#81367,
#81368),(#81369,#81370),(#81371,#81372),(#81373,#81374),(#81375,#81376),
(#81377,#81378),(#81379,#81380),(#81381,#81382),(#81383,#81384),(#81385,
#81386),(#81387,#81388),(#81389,#81390),(#81391,#81392),(#81393,#81394),
(#81395,#81396),(#81397,#81398),(#81399,#81400),(#81401,#81402),(#81403,
#81404),(#81405,#81406),(#81407,#81408),(#81409,#81410),(#81411,#81412),
(#81413,#81414),(#81415,#81416),(#81417,#81418),(#81419,#81420),(#81421,
#81422),(#81423,#81424),(#81425,#81426),(#81427,#81428),(#81429,#81430),
(#81431,#81432),(#81433,#81434),(#81435,#81436),(#81437,#81438),(#81439,
#81440),(#81441,#81442),(#81443,#81444),(#81445,#81446),(#81447,#81448),
(#81449,#81450),(#81451,#81452),(#81453,#81454),(#81455,#81456),(#81457,
#81458),(#81459,#81460),(#81461,#81462),(#81463,#81464),(#81465,#81466),
(#81467,#81468),(#81469,#81470),(#81471,#81472),(#81473,#81474),(#81475,
#81476),(#81477,#81478),(#81479,#81480),(#81481,#81482),(#81483,#81484),
(#81485,#81486),(#81487,#81488),(#81489,#81490),(#81491,#81492),(#81493,
#81494),(#81495,#81496),(#81497,#81498),(#81499,#81500),(#81501,#81502),
(#81503,#81504),(#81505,#81506),(#81507,#81508),(#81509,#81510),(#81511,
#81512),(#81513,#81514),(#81515,#81516),(#81517,#81518),(#81519,#81520),
(#81521,#81522),(#81523,#81524),(#81525,#81526),(#81527,#81528),(#81529,
#81530),(#81531,#81532),(#81533,#81534),(#81535,#81536),(#81537,#81538),
(#81539,#81540),(#81541,#81542),(#81543,#81544),(#81545,#81546),(#81547,
#81548),(#81549,#81550),(#81551,#81552),(#81553,#81554),(#81555,#81556),
(#81557,#81558),(#81559,#81560),(#81561,#81562),(#81563,#81564),(#81565,
#81566),(#81567,#81568),(#81569,#81570),(#81571,#81572),(#81573,#81574),
(#81575,#81576),(#81577,#81578),(#81579,#81580),(#81581,#81582),(#81583,
#81584),(#81585,#81586),(#81587,#81588),(#81589,#81590),(#81591,#81592),
(#81593,#81594),(#81595,#81596),(#81597,#81598),(#81599,#81600),(#81601,
#81602),(#81603,#81604),(#81605,#81606),(#81607,#81608),(#81609,#81610),
(#81611,#81612),(#81613,#81614),(#81615,#81616),(#81617,#81618),(#81619,
#81620),(#81621,#81622),(#81623,#81624),(#81625,#81626),(#81627,#81628),
(#81629,#81630),(#81631,#81632),(#81633,#81634),(#81635,#81636),(#81637,
#81638),(#81639,#81640),(#81641,#81642),(#81643,#81644),(#81645,#81646),
(#81647,#81648),(#81649,#81650),(#81651,#81652),(#81653,#81654),(#81655,
#81656),(#81657,#81658),(#81659,#81660),(#81661,#81662),(#81663,#81664),
(#81665,#81666),(#81667,#81668),(#81669,#81670),(#81671,#81672),(#81673,
#81674),(#81675,#81676),(#81677,#81678),(#81679,#81680),(#81681,#81682),
(#81683,#81684),(#81685,#81686),(#81687,#81688),(#81689,#81690),(#81691,
#81692),(#81693,#81694),(#81695,#81696),(#81697,#81698),(#81699,#81700),
(#81701,#81702),(#81703,#81704),(#81705,#81706),(#81707,#81708),(#81709,
#81710),(#81711,#81712),(#81713,#81714),(#81715,#81716),(#81717,#81718),
(#81719,#81720),(#81721,#81722),(#81723,#81724),(#81725,#81726),(#81727,
#81728),(#81729,#81730),(#81731,#81732),(#81733,#81734),(#81735,#81736),
(#81737,#81738),(#81739,#81740),(#81741,#81742),(#81743,#81744),(#81745,
#81746),(#81747,#81748),(#81749,#81750),(#81751,#81752),(#81753,#81754),
(#81755,#81756),(#81757,#81758),(#81759,#81760),(#81761,#81762),(#81763,
#81764),(#81765,#81766),(#81767,#81768),(#81769,#81770),(#81771,#81772),
(#81773,#81774),(#81775,#81776),(#81777,#81778),(#81779,#81780),(#81781,
#81782),(#81783,#81784),(#81785,#81786),(#81787,#81788),(#81789,#81790),
(#81791,#81792),(#81793,#81794),(#81795,#81796),(#81797,#81798),(#81799,
#81800),(#81801,#81802),(#81803,#81804),(#81805,#81806),(#81807,#81808),
(#81809,#81810),(#81811,#81812),(#81813,#81814),(#81815,#81816),(#81817,
#81818),(#81819,#81820),(#81821,#81822),(#81823,#81824),(#81825,#81826),
(#81827,#81828),(#81829,#81830),(#81831,#81832),(#81833,#81834),(#81835,
#81836),(#81837,#81838),(#81839,#81840),(#81841,#81842),(#81843,#81844),
(#81845,#81846),(#81847,#81848),(#81849,#81850),(#81851,#81852),(#81853,
#81854),(#81855,#81856),(#81857,#81858),(#81859,#81860),(#81861,#81862),
(#81863,#81864),(#81865,#81866),(#81867,#81868),(#81869,#81870),(#81871,
#81872),(#81873,#81874),(#81875,#81876),(#81877,#81878),(#81879,#81880),
(#81881,#81882),(#81883,#81884),(#81885,#81886),(#81887,#81888),(#81889,
#81890),(#81891,#81892),(#81893,#81894),(#81895,#81896),(#81897,#81898),
(#81899,#81900),(#81901,#81902),(#81903,#81904),(#81905,#81906),(#81907,
#81908),(#81909,#81910),(#81911,#81912),(#81913,#81914),(#81915,#81916),
(#81917,#81918),(#81919,#81920),(#81921,#81922),(#81923,#81924),(#81925,
#81926),(#81927,#81928),(#81929,#81930),(#81931,#81932),(#81933,#81934),
(#81935,#81936),(#81937,#81938),(#81939,#81940),(#81941,#81942),(#81943,
#81944),(#81945,#81946),(#81947,#81948),(#81949,#81950),(#81951,#81952),
(#81953,#81954),(#81955,#81956),(#81957,#81958),(#81959,#81960),(#81961,
#81962),(#81963,#81964),(#81965,#81966),(#81967,#81968),(#81969,#81970),
(#81971,#81972),(#81973,#81974),(#81975,#81976),(#81977,#81978),(#81979,
#81980),(#81981,#81982),(#81983,#81984),(#81985,#81986),(#81987,#81988),
(#81989,#81990),(#81991,#81992),(#81993,#81994),(#81995,#81996),(#81997,
#81998),(#81999,#82000),(#82001,#82002),(#82003,#82004),(#82005,#82006),
(#82007,#82008),(#82009,#82010),(#82011,#82012),(#82013,#82014),(#82015,
#82016),(#82017,#82018),(#82019,#82020),(#82021,#82022),(#82023,#82024),
(#82025,#82026),(#82027,#82028),(#82029,#82030),(#82031,#82032),(#82033,
#82034),(#82035,#82036),(#82037,#82038),(#82039,#82040),(#82041,#82042),
(#82043,#82044),(#82045,#82046),(#82047,#82048),(#82049,#82050),(#82051,
#82052),(#82053,#82054),(#82055,#82056),(#82057,#82058),(#82059,#82060),
(#82061,#82062),(#82063,#82064),(#82065,#82066),(#82067,#82068),(#82069,
#82070),(#82071,#82072),(#82073,#82074),(#82075,#82076),(#82077,#82078),
(#82079,#82080),(#82081,#82082),(#82083,#82084),(#82085,#82086),(#82087,
#82088),(#82089,#82090),(#82091,#82092),(#82093,#82094),(#82095,#82096),
(#82097,#82098),(#82099,#82100),(#82101,#82102),(#82103,#82104),(#82105,
#82106),(#82107,#82108),(#82109,#82110),(#82111,#82112),(#82113,#82114),
(#82115,#82116),(#82117,#82118),(#82119,#82120),(#82121,#82122),(#82123,
#82124),(#82125,#82126),(#82127,#82128),(#82129,#82130),(#82131,#82132),
(#82133,#82134),(#82135,#82136),(#82137,#82138),(#82139,#82140),(#82141,
#82142),(#82143,#82144),(#82145,#82146),(#82147,#82148),(#82149,#82150),
(#82151,#82152),(#82153,#82154),(#82155,#82156),(#82157,#82158),(#82159,
#82160),(#82161,#82162),(#82163,#82164),(#82165,#82166),(#82167,#82168),
(#82169,#82170),(#82171,#82172),(#82173,#82174),(#82175,#82176),(#82177,
#82178),(#82179,#82180),(#82181,#82182)),.UNSPECIFIED.,.F.,.F.,.F.)
B_SPLINE_SURFACE_WITH_KNOTS((6,1,1,1,1,1,1,1,1,1,1,1,1,1,1,1,1,1,1,1,1,
1,1,1,1,1,1,1,1,1,1,1,1,1,1,1,1,1,1,1,1,1,1,1,1,1,1,1,1,1,1,1,1,1,1,1,1,
1,1,1,1,1,1,1,1,1,1,1,1,1,1,1,1,1,1,1,1,1,1,1,1,1,1,1,1,1,1,1,1,1,1,1,1,
1,1,1,1,1,1,1,1,1,1,1,1,1,1,1,1,1,1,1,1,1,1,1,1,1,1,1,1,1,1,1,1,1,1,1,1,
1,1,1,1,1,1,1,1,1,1,1,1,1,1,1,1,1,1,1,1,1,1,1,1,1,1,1,1,1,1,1,1,1,1,1,1,
1,1,1,1,1,1,1,1,1,1,1,1,1,1,1,1,1,1,1,1,1,1,1,1,1,1,1,1,1,1,1,1,1,1,1,1,
1,1,1,1,1,1,1,1,1,1,1,1,1,1,1,1,1,1,1,1,1,1,1,1,1,1,1,1,1,1,1,1,1,1,1,1,
1,1,1,1,1,1,1,1,1,1,1,1,1,1,1,1,1,1,1,1,1,1,1,1,1,1,1,1,1,1,1,1,1,1,1,1,
1,1,1,1,1,1,1,1,1,1,1,1,1,1,1,1,1,1,1,1,1,1,1,1,1,1,1,1,1,1,1,1,1,1,1,1,
1,1,1,1,1,1,1,1,1,1,1,1,1,1,1,1,1,1,1,1,1,1,1,1,1,1,1,1,1,1,1,1,1,1,1,1,
1,1,1,1,1,1,1,1,1,1,1,1,1,1,1,1,1,1,1,1,1,1,1,1,1,1,1,1,1,1,1,1,1,1,1,1,
1,1,1,1,1,1,1,1,1,1,1,1,1,1,1,1,1,1,1,1,1,1,1,1,1,1,1,1,1,1,1,1,1,1,1,1,
1,1,1,1,1,1,1,1,1,1,1,1,1,1,1,1,1,1,1,1,1,1,1,1,1,1,1,1,1,1,1,1,1,1,1,1,
1,1,1,1,1,1,1,1,1,1,1,1,1,1,1,1,1,1,1,1,1,1,1,1,1,1,1,1,1,1,1,1,1,1,1,1,
1,1,1,1,1,1,1,1,1,1,1,1,1,1,1,1,1,1,1,1,1,1,1,1,1,1,1,1,1,1,1,1,1,1,1,1,
1,1,1,1,1,1,1,1,1,1,1,1,1,1,1,1,1,1,1,1,1,1,1,1,1,1,1,1,1,1,1,1,1,1,1,1,
1,1,1,1,1,1,1,1,1,1,1,1,1,1,1,1,1,1,1,1,1,1,1,1,1,1,1,1,1,1,1,1,1,1,1,1,
1,1,1,1,1,1,1,1,1,1,1,1,1,1,1,1,1,1,1,1,1,1,1,1,1,1,1,1,1,1,1,1,1,1,1,1,
1,1,1,1,1,1,1,1,1,1,1,1,1,1,1,1,1,1,1,1,1,1,1,1,1,1,1,1,1,1,1,1,1,1,1,1,
1,1,1,1,1,1,1,1,1,1,1,1,1,1,1,1,1,1,1,1,1,1,1,1,1,1,1,1,1,1,1,1,1,1,1,1,
1,1,1,1,1,1,1,1,1,1,1,1,1,1,1,1,1,1,1,1,1,1,1,1,1,1,1,1,1,1,1,1,1,1,1,1,
1,1,1,1,1,1,1,1,1,1,1,1,1,1,1,1,1,1,1,1,1,1,1,1,1,1,1,1,1,1,1,1,1,1,1,1,
1,1,1,1,1,1,1,1,1,1,1,1,1,1,1,1,1,1,1,1,1,1,1,1,1,1,1,1,1,1,1,1,1,1,1,1,
1,1,1,1,1,1,1,1,1,1,1,1,1,1,1,1,1,1,1,1,1,1,1,1,1,1,1,1,1,1,1,1,1,1,1,1,
1,1,1,1,1,1,1,1,1,1,1,1,1,1,1,1,1,1,1,1,1,1,1,1,1,1,1,1,1,1,1,1,1,1,1,1,
1,1,1,1,1,1,1,1,1,1,1,1,1,1,1,1,1,1,1,1,1,1,1,1,1,1,1,1,1,1,1,1,1,1,1,1,
1,1,1,1,1,1,1,1,1,1,1,1,1,1,1,1,1,1,1,1,1,1,1,1,1,1,1,1,1,1,1,1,1,1,1,1,
1,1,1,1,1,1,1,1,1,1,1,1,1,1,1,1,1,1,1,1,1,1,1,1,1,1,1,1,1,1,1,1,1,1,1,1,
1,1,1,1,1,1,1,6),(2,2),(-1.,-0.999000000000001,-0.998000000000001,-0.997000000000001,
-0.996000000000001,-0.995000000000001,-0.994000000000001,-0.993000000000001,
-0.992000000000001,-0.991000000000001,-0.990000000000001,-0.989000000000001,
-0.988000000000001,-0.987000000000001,-0.986000000000001,-0.985000000000001,
-0.984000000000001,-0.983000000000001,-0.982000000000001,-0.981000000000001,
-0.980000000000001,-0.979000000000001,-0.978000000000001,-0.977000000000001,
-0.976000000000001,-0.975000000000001,-0.974000000000001,-0.973000000000001,
-0.972000000000001,-0.971000000000001,-0.970000000000001,-0.969000000000001,
-0.968000000000001,-0.967000000000001,-0.966000000000001,-0.965000000000001,
-0.964000000000001,-0.963000000000001,-0.962000000000001,-0.961000000000001,
-0.960000000000001,-0.959000000000001,-0.958000000000001,-0.957000000000001,
-0.956000000000001,-0.955000000000001,-0.954000000000001,-0.953000000000001,
-0.952000000000001,-0.951000000000001,-0.950000000000001,-0.949000000000001,
-0.948000000000001,-0.947000000000001,-0.946000000000001,-0.945000000000001,
-0.944000000000001,-0.943000000000001,-0.942000000000001,-0.941000000000001,
-0.940000000000001,-0.939000000000001,-0.938000000000001,-0.937000000000001,
-0.936000000000001,-0.935000000000001,-0.934000000000001,-0.933000000000001,
-0.932000000000001,-0.931000000000001,-0.930000000000001,-0.929000000000001,
-0.928000000000001,-0.927000000000001,-0.926000000000001,-0.925000000000001,
-0.924000000000001,-0.923000000000001,-0.922000000000001,-0.921000000000001,
-0.920000000000001,-0.919000000000001,-0.918000000000001,-0.917000000000001,
-0.916000000000001,-0.915000000000001,-0.914000000000001,-0.913000000000001,
-0.912000000000001,-0.911000000000001,-0.910000000000001,-0.909000000000001,
-0.908000000000001,-0.907000000000001,-0.906000000000001,-0.905000000000001,
-0.904000000000001,-0.903000000000001,-0.902000000000001,-0.901000000000001,
-0.900000000000001,-0.899000000000001,-0.898000000000001,-0.897000000000001,
-0.896000000000001,-0.895000000000001,-0.894000000000001,-0.893000000000001,
-0.892000000000001,-0.891000000000001,-0.890000000000001,-0.889000000000001,
-0.888000000000001,-0.887000000000001,-0.886000000000001,-0.885000000000001,
-0.884000000000001,-0.883000000000001,-0.882000000000001,-0.881000000000001,
-0.880000000000001,-0.879000000000001,-0.878000000000001,-0.877000000000001,
-0.876000000000001,-0.875000000000001,-0.874000000000001,-0.873000000000001,
-0.872000000000001,-0.871000000000001,-0.870000000000001,-0.869000000000001,
-0.868000000000001,-0.867000000000001,-0.866000000000001,-0.865000000000001,
-0.864000000000001,-0.863000000000001,-0.862000000000001,-0.861000000000001,
-0.860000000000001,-0.859000000000001,-0.858000000000001,-0.857000000000001,
-0.856000000000001,-0.855000000000001,-0.854000000000001,-0.853000000000001,
-0.852000000000001,-0.851000000000001,-0.850000000000001,-0.849000000000001,
-0.848000000000001,-0.847000000000001,-0.846000000000001,-0.845000000000001,
-0.844000000000001,-0.843000000000001,-0.842000000000001,-0.841000000000001,
-0.840000000000001,-0.839000000000001,-0.838000000000001,-0.837000000000001,
-0.836000000000001,-0.835000000000001,-0.834000000000001,-0.833000000000001,
-0.832000000000001,-0.831000000000001,-0.830000000000001,-0.829000000000001,
-0.828000000000001,-0.827000000000001,-0.826000000000001,-0.825000000000001,
-0.824000000000001,-0.823000000000001,-0.822000000000001,-0.821000000000001,
-0.820000000000001,-0.819000000000001,-0.818000000000001,-0.817000000000001,
-0.816000000000001,-0.815000000000001,-0.814000000000001,-0.813000000000001,
-0.812000000000001,-0.811000000000001,-0.810000000000001,-0.809000000000001,
-0.808000000000001,-0.807000000000001,-0.806000000000001,-0.805000000000001,
-0.804000000000001,-0.803000000000001,-0.802000000000001,-0.801000000000001,
-0.800000000000001,-0.799000000000001,-0.798000000000001,-0.797000000000001,
-0.796000000000001,-0.795000000000001,-0.794000000000001,-0.793000000000001,
-0.792000000000001,-0.791000000000001,-0.790000000000001,-0.789000000000001,
-0.788000000000001,-0.787000000000001,-0.786000000000001,-0.785000000000001,
-0.784000000000001,-0.783000000000001,-0.782000000000001,-0.781000000000001,
-0.780000000000001,-0.779000000000001,-0.778000000000001,-0.777000000000001,
-0.776000000000001,-0.775000000000001,-0.774000000000001,-0.773000000000001,
-0.772000000000001,-0.771000000000001,-0.770000000000001,-0.769000000000001,
-0.768000000000001,-0.767000000000001,-0.766000000000001,-0.765000000000001,
-0.764000000000001,-0.763000000000001,-0.762000000000001,-0.761000000000001,
-0.760000000000001,-0.759000000000001,-0.758000000000001,-0.757000000000001,
-0.756000000000001,-0.755000000000001,-0.754000000000001,-0.753000000000001,
-0.752000000000001,-0.751000000000001,-0.750000000000001,-0.749000000000001,
-0.748000000000001,-0.747000000000001,-0.746000000000001,-0.745000000000001,
-0.744000000000001,-0.743000000000001,-0.742000000000001,-0.741000000000001,
-0.740000000000001,-0.739000000000001,-0.738000000000001,-0.737000000000001,
-0.736000000000001,-0.735000000000001,-0.734000000000001,-0.733000000000001,
-0.732000000000001,-0.731000000000001,-0.730000000000001,-0.729000000000001,
-0.728000000000001,-0.727000000000001,-0.726000000000001,-0.725000000000001,
-0.724000000000001,-0.723000000000001,-0.722000000000001,-0.721000000000001,
-0.720000000000001,-0.719000000000001,-0.718000000000001,-0.717000000000001,
-0.716000000000001,-0.715000000000001,-0.714000000000001,-0.713000000000001,
-0.712000000000001,-0.711000000000001,-0.710000000000001,-0.709000000000001,
-0.708000000000001,-0.707000000000001,-0.706000000000001,-0.705000000000001,
-0.704000000000001,-0.703000000000001,-0.702000000000001,-0.701000000000001,
-0.700000000000001,-0.699000000000001,-0.698000000000001,-0.697000000000001,
-0.696000000000001,-0.695000000000001,-0.694000000000001,-0.693000000000001,
-0.692000000000001,-0.691000000000001,-0.690000000000001,-0.689000000000001,
-0.688000000000001,-0.687,-0.686,-0.685,-0.684,-0.683,-0.682,-0.681,-0.68,
-0.679,-0.678,-0.677,-0.676,-0.675,-0.674,-0.673,-0.672,-0.671,-0.67,-0.669,
-0.668,-0.667,-0.666,-0.665,-0.664,-0.663,-0.662,-0.661,-0.66,-0.659,-0.658,
-0.657,-0.656,-0.655,-0.654,-0.653,-0.652,-0.651,-0.65,-0.649,-0.648,-0.647,
-0.646,-0.645,-0.644,-0.643,-0.642,-0.641,-0.64,-0.639,-0.638,-0.637,-0.636,
-0.635,-0.634,-0.633,-0.632,-0.631,-0.63,-0.629,-0.628,-0.627,-0.626,-0.625,
-0.624,-0.623,-0.622,-0.621,-0.62,-0.619,-0.618,-0.617,-0.616,-0.615,-0.614,
-0.613,-0.612,-0.611,-0.61,-0.609,-0.608,-0.607,-0.606,-0.605,-0.604,-0.603,
-0.602,-0.601,-0.6,-0.599,-0.598,-0.597,-0.596,-0.595,-0.594,-0.593,-0.592,
-0.591,-0.59,-0.589,-0.588,-0.587,-0.586,-0.585,-0.584,-0.583,-0.582,-0.581,
-0.58,-0.579,-0.578,-0.577,-0.576,-0.575,-0.574,-0.573,-0.572,-0.571,-0.57,
-0.569,-0.568,-0.567,-0.566,-0.565,-0.564,-0.563,-0.562,-0.561,-0.56,-0.559,
-0.558,-0.557,-0.556,-0.555,-0.554,-0.553,-0.552,-0.551,-0.55,-0.549,-0.548,
-0.547,-0.546,-0.545,-0.544,-0.543,-0.542,-0.541,-0.54,-0.539,-0.538,-0.537,
-0.536,-0.535,-0.534,-0.533,-0.532,-0.531,-0.53,-0.529,-0.528,-0.527,-0.526,
-0.525,-0.524,-0.523,-0.522,-0.521,-0.52,-0.519,-0.518,-0.517,-0.516,-0.515,
-0.514,-0.513,-0.512,-0.511,-0.51,-0.509,-0.508,-0.507,-0.506,-0.505,-0.504,
-0.503,-0.502,-0.501,-0.5,-0.499,-0.498,-0.497,-0.496,-0.495,-0.494,-0.493,
-0.492,-0.491,-0.49,-0.489,-0.488,-0.487,-0.486,-0.485,-0.484,-0.483,-0.482,
-0.481,-0.48,-0.479,-0.478,-0.477,-0.476,-0.475,-0.474,-0.473,-0.472,-0.471,
-0.47,-0.469,-0.468,-0.467,-0.466,-0.465,-0.464,-0.463,-0.462,-0.461,-0.46,
-0.459,-0.458,-0.457,-0.456,-0.455,-0.454,-0.453,-0.452,-0.451,-0.45,-0.449,
-0.448,-0.447,-0.446,-0.445,-0.444,-0.443,-0.442,-0.441,-0.44,-0.439,-0.438,
-0.437,-0.436,-0.435,-0.434,-0.433,-0.432,-0.431,-0.43,-0.429,-0.428,-0.427,
-0.426,-0.425,-0.424,-0.423,-0.422,-0.421,-0.42,-0.419,-0.418,-0.417,-0.416,
-0.415,-0.414,-0.413,-0.412,-0.411,-0.41,-0.409,-0.408,-0.407,-0.406,-0.405,
-0.404,-0.403,-0.402,-0.401,-0.4,-0.399,-0.398,-0.397,-0.396,-0.395,-0.394,
-0.393,-0.392,-0.391,-0.39,-0.389,-0.388,-0.387,-0.386,-0.385,-0.384,-0.383,
-0.382,-0.381,-0.38,-0.379,-0.378,-0.377,-0.376,-0.375,-0.374,-0.373,-0.372,
-0.371,-0.37,-0.369,-0.368,-0.367,-0.366,-0.365,-0.364,-0.363,-0.362,-0.361,
-0.36,-0.359,-0.358,-0.357,-0.356,-0.355,-0.354,-0.353,-0.352,-0.351,-0.35,
-0.349,-0.348,-0.347,-0.346,-0.345,-0.344,-0.343,-0.342,-0.341,-0.34,-0.339,
-0.338,-0.337,-0.336,-0.335,-0.334,-0.333,-0.332,-0.331,-0.33,-0.329,-0.328,
-0.327,-0.326,-0.325,-0.324,-0.323,-0.322,-0.321,-0.32,-0.319,-0.318,-0.317,
-0.316,-0.315,-0.314,-0.313,-0.312,-0.311,-0.31,-0.309,-0.308,-0.307,-0.306,
-0.305,-0.304,-0.303,-0.302,-0.301,-0.3,-0.299,-0.298,-0.297,-0.296,-0.295,
-0.294,-0.293,-0.292,-0.291,-0.29,-0.289,-0.288,-0.287,-0.286,-0.285,-0.284,
-0.283,-0.282,-0.281,-0.28,-0.279,-0.278,-0.277,-0.276,-0.275,-0.274,-0.273,
-0.272,-0.271,-0.27,-0.269,-0.268,-0.267,-0.266,-0.265,-0.264,-0.263,-0.262,
-0.261,-0.26,-0.259,-0.258,-0.257,-0.256,-0.255,-0.254,-0.253,-0.252,-0.251,
-0.25,-0.249,-0.248,-0.247,-0.246,-0.245,-0.244,-0.243,-0.242,-0.241,-0.24,
-0.239,-0.238,-0.237,-0.236,-0.235,-0.234,-0.233,-0.232,-0.231,-0.23,-0.229,
-0.228,-0.227,-0.226,-0.225,-0.224,-0.223,-0.222,-0.221,-0.22,-0.219,-0.218,
-0.217,-0.216,-0.215,-0.214,-0.213,-0.212,-0.211,-0.21,-0.209,-0.208,-0.207,
-0.206,-0.205,-0.204,-0.203,-0.202,-0.201,-0.2,-0.199,-0.198,-0.197,-0.196,
-0.195,-0.194,-0.193,-0.192,-0.191,-0.19,-0.189,-0.188,-0.187,-0.186,-0.185,
-0.184,-0.183,-0.182,-0.181,-0.18,-0.179,-0.178,-0.177,-0.176,-0.175,-0.174,
-0.173,-0.172,-0.171,-0.17,-0.169,-0.168,-0.167,-0.166,-0.165,-0.164,-0.163,
-0.162,-0.161,-0.16,-0.159,-0.158,-0.157,-0.156,-0.155,-0.154,-0.153,-0.152,
-0.151,-0.15,-0.149,-0.148,-0.147,-0.146,-0.145,-0.144,-0.143,-0.142,-0.141,
-0.14,-0.139,-0.138,-0.137,-0.136,-0.135,-0.134,-0.133,-0.132,-0.131,-0.13,
-0.129,-0.128,-0.127,-0.126,-0.125,-0.124,-0.123,-0.122,-0.121,-0.12,-0.119,
-0.118,-0.117,-0.116,-0.115,-0.114,-0.113,-0.112,-0.111,-0.11,-0.109,-0.108,
-0.107,-0.106,-0.105,-0.104,-0.103,-0.102,-0.101,-0.1,-0.0990000000000001,
-0.0980000000000001,-0.0970000000000001,-0.0960000000000001,-0.0950000000000001,
-0.0940000000000001,-0.0930000000000001,-0.0920000000000001,-0.0910000000000001,
-0.0900000000000001,-0.0890000000000001,-0.0880000000000001,-0.0870000000000001,
-0.0860000000000001,-0.0850000000000001,-0.0840000000000001,-0.0830000000000001,
-0.0820000000000001,-0.0810000000000001,-0.0800000000000001,-0.0790000000000001,
-0.0780000000000001,-0.0770000000000001,-0.0760000000000001,-0.0750000000000001,
-0.0740000000000001,-0.0730000000000001,-0.0720000000000001,-0.071,-0.07,
-0.069,-0.068,-0.067,-0.066,-0.065,-0.064,-0.063,-0.062,-0.061,-0.06,-0.059,
-0.058,-0.057,-0.056,-0.055,-0.054,-0.053,-0.052,-0.051,-0.05,-0.049,-0.048,
-0.047,-0.046,-0.045,-0.044,-0.043,-0.042,-0.041,-0.04,-0.039,-0.038,-0.037,
-0.036,-0.035,-0.034,-0.033,-0.032,-0.031,-0.03,-0.029,-0.028,-0.027,-0.026,
-0.025,-0.024,-0.023,-0.022,-0.021,-0.02,-0.019,-0.018,-0.017,-0.016,-0.015,
-0.014,-0.013,-0.012,-0.011,-0.01,-0.009,-0.008,-0.007,-0.006,-0.005,-0.004,
-0.003,-0.002,-0.001,0.),(0.,2.),.UNSPECIFIED.)
GEOMETRIC_REPRESENTATION_ITEM()
RATIONAL_B_SPLINE_SURFACE(((1.,1.),(1.,1.),(1.,1.),(1.,1.),(1.,1.),(1.,
1.),(1.,1.),(1.,1.),(1.,1.),(1.,1.),(1.,1.),(1.,1.),(1.,1.),(1.,1.),(1.,
1.),(1.,1.),(1.,1.),(1.,1.),(1.,1.),(1.,1.),(1.,1.),(1.,1.),(1.,1.),(1.,
1.),(1.,1.),(1.,1.),(1.,1.),(1.,1.),(1.,1.),(1.,1.),(1.,1.),(1.,1.),(1.,
1.),(1.,1.),(1.,1.),(1.,1.),(1.,1.),(1.,1.),(1.,1.),(1.,1.),(1.,1.),(1.,
1.),(1.,1.),(1.,1.),(1.,1.),(1.,1.),(1.,1.),(1.,1.),(1.,1.),(1.,1.),(1.,
1.),(1.,1.),(1.,1.),(1.,1.),(1.,1.),(1.,1.),(1.,1.),(1.,1.),(1.,1.),(1.,
1.),(1.,1.),(1.,1.),(1.,1.),(1.,1.),(1.,1.),(1.,1.),(1.,1.),(1.,1.),(1.,
1.),(1.,1.),(1.,1.),(1.,1.),(1.,1.),(1.,1.),(1.,1.),(1.,1.),(1.,1.),(1.,
1.),(1.,1.),(1.,1.),(1.,1.),(1.,1.),(1.,1.),(1.,1.),(1.,1.),(1.,1.),(1.,
1.),(1.,1.),(1.,1.),(1.,1.),(1.,1.),(1.,1.),(1.,1.),(1.,1.),(1.,1.),(1.,
1.),(1.,1.),(1.,1.),(1.,1.),(1.,1.),(1.,1.),(1.,1.),(1.,1.),(1.,1.),(1.,
1.),(1.,1.),(1.,1.),(1.,1.),(1.,1.),(1.,1.),(1.,1.),(1.,1.),(1.,1.),(1.,
1.),(1.,1.),(1.,1.),(1.,1.),(1.,1.),(1.,1.),(1.,1.),(1.,1.),(1.,1.),(1.,
1.),(1.,1.),(1.,1.),(1.,1.),(1.,1.),(1.,1.),(1.,1.),(1.,1.),(1.,1.),(1.,
1.),(1.,1.),(1.,1.),(1.,1.),(1.,1.),(1.,1.),(1.,1.),(1.,1.),(1.,1.),(1.,
1.),(1.,1.),(1.,1.),(1.,1.),(1.,1.),(1.,1.),(1.,1.),(1.,1.),(1.,1.),(1.,
1.),(1.,1.),(1.,1.),(1.,1.),(1.,1.),(1.,1.),(1.,1.),(1.,1.),(1.,1.),(1.,
1.),(1.,1.),(1.,1.),(1.,1.),(1.,1.),(1.,1.),(1.,1.),(1.,1.),(1.,1.),(1.,
1.),(1.,1.),(1.,1.),(1.,1.),(1.,1.),(1.,1.),(1.,1.),(1.,1.),(1.,1.),(1.,
1.),(1.,1.),(1.,1.),(1.,1.),(1.,1.),(1.,1.),(1.,1.),(1.,1.),(1.,1.),(1.,
1.),(1.,1.),(1.,1.),(1.,1.),(1.,1.),(1.,1.),(1.,1.),(1.,1.),(1.,1.),(1.,
1.),(1.,1.),(1.,1.),(1.,1.),(1.,1.),(1.,1.),(1.,1.),(1.,1.),(1.,1.),(1.,
1.),(1.,1.),(1.,1.),(1.,1.),(1.,1.),(1.,1.),(1.,1.),(1.,1.),(1.,1.),(1.,
1.),(1.,1.),(1.,1.),(1.,1.),(1.,1.),(1.,1.),(1.,1.),(1.,1.),(1.,1.),(1.,
1.),(1.,1.),(1.,1.),(1.,1.),(1.,1.),(1.,1.),(1.,1.),(1.,1.),(1.,1.),(1.,
1.),(1.,1.),(1.,1.),(1.,1.),(1.,1.),(1.,1.),(1.,1.),(1.,1.),(1.,1.),(1.,
1.),(1.,1.),(1.,1.),(1.,1.),(1.,1.),(1.,1.),(1.,1.),(1.,1.),(1.,1.),(1.,
1.),(1.,1.),(1.,1.),(1.,1.),(1.,1.),(1.,1.),(1.,1.),(1.,1.),(1.,1.),(1.,
1.),(1.,1.),(1.,1.),(1.,1.),(1.,1.),(1.,1.),(1.,1.),(1.,1.),(1.,1.),(1.,
1.),(1.,1.),(1.,1.),(1.,1.),(1.,1.),(1.,1.),(1.,1.),(1.,1.),(1.,1.),(1.,
1.),(1.,1.),(1.,1.),(1.,1.),(1.,1.),(1.,1.),(1.,1.),(1.,1.),(1.,1.),(1.,
1.),(1.,1.),(1.,1.),(1.,1.),(1.,1.),(1.,1.),(1.,1.),(1.,1.),(1.,1.),(1.,
1.),(1.,1.),(1.,1.),(1.,1.),(1.,1.),(1.,1.),(1.,1.),(1.,1.),(1.,1.),(1.,
1.),(1.,1.),(1.,1.),(1.,1.),(1.,1.),(1.,1.),(1.,1.),(1.,1.),(1.,1.),(1.,
1.),(1.,1.),(1.,1.),(1.,1.),(1.,1.),(1.,1.),(1.,1.),(1.,1.),(1.,1.),(1.,
1.),(1.,1.),(1.,1.),(1.,1.),(1.,1.),(1.,1.),(1.,1.),(1.,1.),(1.,1.),(1.,
1.),(1.,1.),(1.,1.),(1.,1.),(1.,1.),(1.,1.),(1.,1.),(1.,1.),(1.,1.),(1.,
1.),(1.,1.),(1.,1.),(1.,1.),(1.,1.),(1.,1.),(1.,1.),(1.,1.),(1.,1.),(1.,
1.),(1.,1.),(1.,1.),(1.,1.),(1.,1.),(1.,1.),(1.,1.),(1.,1.),(1.,1.),(1.,
1.),(1.,1.),(1.,1.),(1.,1.),(1.,1.),(1.,1.),(1.,1.),(1.,1.),(1.,1.),(1.,
1.),(1.,1.),(1.,1.),(1.,1.),(1.,1.),(1.,1.),(1.,1.),(1.,1.),(1.,1.),(1.,
1.),(1.,1.),(1.,1.),(1.,1.),(1.,1.),(1.,1.),(1.,1.),(1.,1.),(1.,1.),(1.,
1.),(1.,1.),(1.,1.),(1.,1.),(1.,1.),(1.,1.),(1.,1.),(1.,1.),(1.,1.),(1.,
1.),(1.,1.),(1.,1.),(1.,1.),(1.,1.),(1.,1.),(1.,1.),(1.,1.),(1.,1.),(1.,
1.),(1.,1.),(1.,1.),(1.,1.),(1.,1.),(1.,1.),(1.,1.),(1.,1.),(1.,1.),(1.,
1.),(1.,1.),(1.,1.),(1.,1.),(1.,1.),(1.,1.),(1.,1.),(1.,1.),(1.,1.),(1.,
1.),(1.,1.),(1.,1.),(1.,1.),(1.,1.),(1.,1.),(1.,1.),(1.,1.),(1.,1.),(1.,
1.),(1.,1.),(1.,1.),(1.,1.),(1.,1.),(1.,1.),(1.,1.),(1.,1.),(1.,1.),(1.,
1.),(1.,1.),(1.,1.),(1.,1.),(1.,1.),(1.,1.),(1.,1.),(1.,1.),(1.,1.),(1.,
1.),(1.,1.),(1.,1.),(1.,1.),(1.,1.),(1.,1.),(1.,1.),(1.,1.),(1.,1.),(1.,
1.),(1.,1.),(1.,1.),(1.,1.),(1.,1.),(1.,1.),(1.,1.),(1.,1.),(1.,1.),(1.,
1.),(1.,1.),(1.,1.),(1.,1.),(1.,1.),(1.,1.),(1.,1.),(1.,1.),(1.,1.),(1.,
1.),(1.,1.),(1.,1.),(1.,1.),(1.,1.),(1.,1.),(1.,1.),(1.,1.),(1.,1.),(1.,
1.),(1.,1.),(1.,1.),(1.,1.),(1.,1.),(1.,1.),(1.,1.),(1.,1.),(1.,1.),(1.,
1.),(1.,1.),(1.,1.),(1.,1.),(1.,1.),(1.,1.),(1.,1.),(1.,1.),(1.,1.),(1.,
1.),(1.,1.),(1.,1.),(1.,1.),(1.,1.),(1.,1.),(1.,1.),(1.,1.),(1.,1.),(1.,
1.),(1.,1.),(1.,1.),(1.,1.),(1.,1.),(1.,1.),(1.,1.),(1.,1.),(1.,1.),(1.,
1.),(1.,1.),(1.,1.),(1.,1.),(1.,1.),(1.,1.),(1.,1.),(1.,1.),(1.,1.),(1.,
1.),(1.,1.),(1.,1.),(1.,1.),(1.,1.),(1.,1.),(1.,1.),(1.,1.),(1.,1.),(1.,
1.),(1.,1.),(1.,1.),(1.,1.),(1.,1.),(1.,1.),(1.,1.),(1.,1.),(1.,1.),(1.,
1.),(1.,1.),(1.,1.),(1.,1.),(1.,1.),(1.,1.),(1.,1.),(1.,1.),(1.,1.),(1.,
1.),(1.,1.),(1.,1.),(1.,1.),(1.,1.),(1.,1.),(1.,1.),(1.,1.),(1.,1.),(1.,
1.),(1.,1.),(1.,1.),(1.,1.),(1.,1.),(1.,1.),(1.,1.),(1.,1.),(1.,1.),(1.,
1.),(1.,1.),(1.,1.),(1.,1.),(1.,1.),(1.,1.),(1.,1.),(1.,1.),(1.,1.),(1.,
1.),(1.,1.),(1.,1.),(1.,1.),(1.,1.),(1.,1.),(1.,1.),(1.,1.),(1.,1.),(1.,
1.),(1.,1.),(1.,1.),(1.,1.),(1.,1.),(1.,1.),(1.,1.),(1.,1.),(1.,1.),(1.,
1.),(1.,1.),(1.,1.),(1.,1.),(1.,1.),(1.,1.),(1.,1.),(1.,1.),(1.,1.),(1.,
1.),(1.,1.),(1.,1.),(1.,1.),(1.,1.),(1.,1.),(1.,1.),(1.,1.),(1.,1.),(1.,
1.),(1.,1.),(1.,1.),(1.,1.),(1.,1.),(1.,1.),(1.,1.),(1.,1.),(1.,1.),(1.,
1.),(1.,1.),(1.,1.),(1.,1.),(1.,1.),(1.,1.),(1.,1.),(1.,1.),(1.,1.),(1.,
1.),(1.,1.),(1.,1.),(1.,1.),(1.,1.),(1.,1.),(1.,1.),(1.,1.),(1.,1.),(1.,
1.),(1.,1.),(1.,1.),(1.,1.),(1.,1.),(1.,1.),(1.,1.),(1.,1.),(1.,1.),(1.,
1.),(1.,1.),(1.,1.),(1.,1.),(1.,1.),(1.,1.),(1.,1.),(1.,1.),(1.,1.),(1.,
1.),(1.,1.),(1.,1.),(1.,1.),(1.,1.),(1.,1.),(1.,1.),(1.,1.),(1.,1.),(1.,
1.),(1.,1.),(1.,1.),(1.,1.),(1.,1.),(1.,1.),(1.,1.),(1.,1.),(1.,1.),(1.,
1.),(1.,1.),(1.,1.),(1.,1.),(1.,1.),(1.,1.),(1.,1.),(1.,1.),(1.,1.),(1.,
1.),(1.,1.),(1.,1.),(1.,1.),(1.,1.),(1.,1.),(1.,1.),(1.,1.),(1.,1.),(1.,
1.),(1.,1.),(1.,1.),(1.,1.),(1.,1.),(1.,1.),(1.,1.),(1.,1.),(1.,1.),(1.,
1.),(1.,1.),(1.,1.),(1.,1.),(1.,1.),(1.,1.),(1.,1.),(1.,1.),(1.,1.),(1.,
1.),(1.,1.),(1.,1.),(1.,1.),(1.,1.),(1.,1.),(1.,1.),(1.,1.),(1.,1.),(1.,
1.),(1.,1.),(1.,1.),(1.,1.),(1.,1.),(1.,1.),(1.,1.),(1.,1.),(1.,1.),(1.,
1.),(1.,1.),(1.,1.),(1.,1.),(1.,1.),(1.,1.),(1.,1.),(1.,1.),(1.,1.),(1.,
1.),(1.,1.),(1.,1.),(1.,1.),(1.,1.),(1.,1.),(1.,1.),(1.,1.),(1.,1.),(1.,
1.),(1.,1.),(1.,1.),(1.,1.),(1.,1.),(1.,1.),(1.,1.),(1.,1.),(1.,1.),(1.,
1.),(1.,1.),(1.,1.),(1.,1.),(1.,1.),(1.,1.),(1.,1.),(1.,1.),(1.,1.),(1.,
1.),(1.,1.),(1.,1.),(1.,1.),(1.,1.),(1.,1.),(1.,1.),(1.,1.),(1.,1.),(1.,
1.),(1.,1.),(1.,1.),(1.,1.),(1.,1.),(1.,1.),(1.,1.),(1.,1.),(1.,1.),(1.,
1.),(1.,1.),(1.,1.),(1.,1.),(1.,1.),(1.,1.),(1.,1.),(1.,1.),(1.,1.),(1.,
1.),(1.,1.),(1.,1.),(1.,1.),(1.,1.),(1.,1.),(1.,1.),(1.,1.),(1.,1.),(1.,
1.),(1.,1.),(1.,1.),(1.,1.),(1.,1.),(1.,1.),(1.,1.),(1.,1.),(1.,1.),(1.,
1.),(1.,1.),(1.,1.),(1.,1.),(1.,1.),(1.,1.),(1.,1.),(1.,1.),(1.,1.),(1.,
1.),(1.,1.),(1.,1.),(1.,1.),(1.,1.),(1.,1.),(1.,1.),(1.,1.),(1.,1.),(1.,
1.),(1.,1.),(1.,1.),(1.,1.),(1.,1.),(1.,1.),(1.,1.),(1.,1.),(1.,1.),(1.,
1.),(1.,1.),(1.,1.),(1.,1.),(1.,1.),(1.,1.),(1.,1.),(1.,1.),(1.,1.),(1.,
1.),(1.,1.),(1.,1.),(1.,1.),(1.,1.),(1.,1.),(1.,1.),(1.,1.),(1.,1.),(1.,
1.),(1.,1.),(1.,1.),(1.,1.),(1.,1.),(1.,1.),(1.,1.),(1.,1.),(1.,1.),(1.,
1.),(1.,1.),(1.,1.),(1.,1.),(1.,1.),(1.,1.),(1.,1.),(1.,1.),(1.,1.),(1.,
1.),(1.,1.),(1.,1.),(1.,1.),(1.,1.),(1.,1.),(1.,1.),(1.,1.),(1.,1.),(1.,
1.),(1.,1.),(1.,1.),(1.,1.),(1.,1.),(1.,1.),(1.,1.),(1.,1.),(1.,1.),(1.,
1.),(1.,1.),(1.,1.),(1.,1.),(1.,1.),(1.,1.),(1.,1.),(1.,1.),(1.,1.),(1.,
1.),(1.,1.),(1.,1.),(1.,1.),(1.,1.),(1.,1.),(1.,1.),(1.,1.),(1.,1.),(1.,
1.),(1.,1.),(1.,1.),(1.,1.),(1.,1.),(1.,1.),(1.,1.),(1.,1.),(1.,1.),(1.,
1.),(1.,1.),(1.,1.),(1.,1.),(1.,1.),(1.,1.),(1.,1.),(1.,1.),(1.,1.),(1.,
1.),(1.,1.),(1.,1.),(1.,1.),(1.,1.),(1.,1.),(1.,1.),(1.,1.),(1.,1.),(1.,
1.),(1.,1.),(1.,1.),(1.,1.),(1.,1.),(1.,1.),(1.,1.),(1.,1.),(1.,1.),(1.,
1.),(1.,1.),(1.,1.),(1.,1.),(1.,1.),(1.,1.),(1.,1.),(1.,1.),(1.,1.),(1.,
1.),(1.,1.),(1.,1.),(1.,1.),(1.,1.),(1.,1.),(1.,1.),(1.,1.),(1.,1.),(1.,
1.),(1.,1.),(1.,1.),(1.,1.),(1.,1.),(1.,1.),(1.,1.),(1.,1.),(1.,1.),(1.,
1.),(1.,1.),(1.,1.),(1.,1.),(1.,1.),(1.,1.),(1.,1.),(1.,1.),(1.,1.),(1.,
1.),(1.,1.),(1.,1.),(1.,1.),(1.,1.),(1.,1.),(1.,1.),(1.,1.),(1.,1.),(1.,
1.),(1.,1.),(1.,1.),(1.,1.),(1.,1.),(1.,1.),(1.,1.),(1.,1.),(1.,1.),(1.,
1.)))
REPRESENTATION_ITEM('')
SURFACE()
);
#262=(
BOUNDED_SURFACE()
B_SPLINE_SURFACE(5,1,((#82213,#82214),(#82215,#82216),(#82217,#82218),(#82219,
#82220),(#82221,#82222),(#82223,#82224),(#82225,#82226),(#82227,#82228),
(#82229,#82230),(#82231,#82232),(#82233,#82234),(#82235,#82236),(#82237,
#82238),(#82239,#82240),(#82241,#82242),(#82243,#82244),(#82245,#82246),
(#82247,#82248),(#82249,#82250),(#82251,#82252),(#82253,#82254),(#82255,
#82256),(#82257,#82258),(#82259,#82260),(#82261,#82262),(#82263,#82264),
(#82265,#82266),(#82267,#82268),(#82269,#82270),(#82271,#82272),(#82273,
#82274),(#82275,#82276),(#82277,#82278),(#82279,#82280),(#82281,#82282),
(#82283,#82284),(#82285,#82286),(#82287,#82288),(#82289,#82290),(#82291,
#82292),(#82293,#82294),(#82295,#82296),(#82297,#82298),(#82299,#82300),
(#82301,#82302),(#82303,#82304),(#82305,#82306),(#82307,#82308),(#82309,
#82310),(#82311,#82312),(#82313,#82314),(#82315,#82316),(#82317,#82318),
(#82319,#82320),(#82321,#82322),(#82323,#82324),(#82325,#82326),(#82327,
#82328),(#82329,#82330),(#82331,#82332),(#82333,#82334),(#82335,#82336),
(#82337,#82338),(#82339,#82340),(#82341,#82342),(#82343,#82344),(#82345,
#82346),(#82347,#82348),(#82349,#82350),(#82351,#82352),(#82353,#82354),
(#82355,#82356),(#82357,#82358),(#82359,#82360),(#82361,#82362),(#82363,
#82364),(#82365,#82366),(#82367,#82368),(#82369,#82370),(#82371,#82372),
(#82373,#82374),(#82375,#82376),(#82377,#82378),(#82379,#82380),(#82381,
#82382),(#82383,#82384),(#82385,#82386),(#82387,#82388),(#82389,#82390),
(#82391,#82392),(#82393,#82394),(#82395,#82396),(#82397,#82398),(#82399,
#82400),(#82401,#82402),(#82403,#82404),(#82405,#82406),(#82407,#82408),
(#82409,#82410),(#82411,#82412),(#82413,#82414),(#82415,#82416),(#82417,
#82418),(#82419,#82420),(#82421,#82422),(#82423,#82424),(#82425,#82426),
(#82427,#82428),(#82429,#82430),(#82431,#82432),(#82433,#82434),(#82435,
#82436),(#82437,#82438),(#82439,#82440),(#82441,#82442),(#82443,#82444),
(#82445,#82446),(#82447,#82448),(#82449,#82450),(#82451,#82452),(#82453,
#82454),(#82455,#82456),(#82457,#82458),(#82459,#82460),(#82461,#82462),
(#82463,#82464),(#82465,#82466),(#82467,#82468),(#82469,#82470),(#82471,
#82472),(#82473,#82474),(#82475,#82476),(#82477,#82478),(#82479,#82480),
(#82481,#82482),(#82483,#82484),(#82485,#82486),(#82487,#82488),(#82489,
#82490),(#82491,#82492),(#82493,#82494),(#82495,#82496),(#82497,#82498),
(#82499,#82500),(#82501,#82502),(#82503,#82504),(#82505,#82506),(#82507,
#82508),(#82509,#82510),(#82511,#82512),(#82513,#82514),(#82515,#82516),
(#82517,#82518),(#82519,#82520),(#82521,#82522),(#82523,#82524),(#82525,
#82526),(#82527,#82528),(#82529,#82530),(#82531,#82532),(#82533,#82534),
(#82535,#82536),(#82537,#82538),(#82539,#82540),(#82541,#82542),(#82543,
#82544),(#82545,#82546),(#82547,#82548),(#82549,#82550),(#82551,#82552),
(#82553,#82554),(#82555,#82556),(#82557,#82558),(#82559,#82560),(#82561,
#82562),(#82563,#82564),(#82565,#82566),(#82567,#82568),(#82569,#82570),
(#82571,#82572),(#82573,#82574),(#82575,#82576),(#82577,#82578),(#82579,
#82580),(#82581,#82582),(#82583,#82584),(#82585,#82586),(#82587,#82588),
(#82589,#82590),(#82591,#82592),(#82593,#82594),(#82595,#82596),(#82597,
#82598),(#82599,#82600),(#82601,#82602),(#82603,#82604),(#82605,#82606),
(#82607,#82608),(#82609,#82610),(#82611,#82612),(#82613,#82614),(#82615,
#82616),(#82617,#82618),(#82619,#82620),(#82621,#82622),(#82623,#82624),
(#82625,#82626),(#82627,#82628),(#82629,#82630),(#82631,#82632),(#82633,
#82634),(#82635,#82636),(#82637,#82638),(#82639,#82640),(#82641,#82642),
(#82643,#82644),(#82645,#82646),(#82647,#82648),(#82649,#82650),(#82651,
#82652),(#82653,#82654),(#82655,#82656),(#82657,#82658),(#82659,#82660),
(#82661,#82662),(#82663,#82664),(#82665,#82666),(#82667,#82668),(#82669,
#82670),(#82671,#82672),(#82673,#82674),(#82675,#82676),(#82677,#82678),
(#82679,#82680),(#82681,#82682),(#82683,#82684),(#82685,#82686),(#82687,
#82688),(#82689,#82690),(#82691,#82692),(#82693,#82694),(#82695,#82696),
(#82697,#82698),(#82699,#82700),(#82701,#82702),(#82703,#82704),(#82705,
#82706),(#82707,#82708),(#82709,#82710),(#82711,#82712),(#82713,#82714),
(#82715,#82716),(#82717,#82718),(#82719,#82720),(#82721,#82722),(#82723,
#82724),(#82725,#82726),(#82727,#82728),(#82729,#82730),(#82731,#82732),
(#82733,#82734),(#82735,#82736),(#82737,#82738),(#82739,#82740),(#82741,
#82742),(#82743,#82744),(#82745,#82746),(#82747,#82748),(#82749,#82750),
(#82751,#82752),(#82753,#82754),(#82755,#82756),(#82757,#82758),(#82759,
#82760),(#82761,#82762),(#82763,#82764),(#82765,#82766),(#82767,#82768),
(#82769,#82770),(#82771,#82772),(#82773,#82774),(#82775,#82776),(#82777,
#82778),(#82779,#82780),(#82781,#82782),(#82783,#82784),(#82785,#82786),
(#82787,#82788),(#82789,#82790),(#82791,#82792),(#82793,#82794),(#82795,
#82796),(#82797,#82798),(#82799,#82800),(#82801,#82802),(#82803,#82804),
(#82805,#82806),(#82807,#82808),(#82809,#82810),(#82811,#82812),(#82813,
#82814),(#82815,#82816),(#82817,#82818),(#82819,#82820),(#82821,#82822),
(#82823,#82824),(#82825,#82826),(#82827,#82828),(#82829,#82830),(#82831,
#82832),(#82833,#82834),(#82835,#82836),(#82837,#82838),(#82839,#82840),
(#82841,#82842),(#82843,#82844),(#82845,#82846),(#82847,#82848),(#82849,
#82850),(#82851,#82852),(#82853,#82854),(#82855,#82856),(#82857,#82858),
(#82859,#82860),(#82861,#82862),(#82863,#82864),(#82865,#82866),(#82867,
#82868),(#82869,#82870),(#82871,#82872),(#82873,#82874),(#82875,#82876),
(#82877,#82878),(#82879,#82880),(#82881,#82882),(#82883,#82884),(#82885,
#82886),(#82887,#82888),(#82889,#82890),(#82891,#82892),(#82893,#82894),
(#82895,#82896),(#82897,#82898),(#82899,#82900),(#82901,#82902),(#82903,
#82904),(#82905,#82906),(#82907,#82908),(#82909,#82910),(#82911,#82912),
(#82913,#82914),(#82915,#82916),(#82917,#82918),(#82919,#82920),(#82921,
#82922),(#82923,#82924),(#82925,#82926),(#82927,#82928),(#82929,#82930),
(#82931,#82932),(#82933,#82934),(#82935,#82936),(#82937,#82938),(#82939,
#82940),(#82941,#82942),(#82943,#82944),(#82945,#82946),(#82947,#82948),
(#82949,#82950),(#82951,#82952),(#82953,#82954),(#82955,#82956),(#82957,
#82958),(#82959,#82960),(#82961,#82962),(#82963,#82964),(#82965,#82966),
(#82967,#82968),(#82969,#82970),(#82971,#82972),(#82973,#82974),(#82975,
#82976),(#82977,#82978),(#82979,#82980),(#82981,#82982),(#82983,#82984),
(#82985,#82986),(#82987,#82988),(#82989,#82990),(#82991,#82992),(#82993,
#82994),(#82995,#82996),(#82997,#82998),(#82999,#83000),(#83001,#83002),
(#83003,#83004),(#83005,#83006),(#83007,#83008),(#83009,#83010),(#83011,
#83012),(#83013,#83014),(#83015,#83016),(#83017,#83018),(#83019,#83020),
(#83021,#83022),(#83023,#83024),(#83025,#83026),(#83027,#83028),(#83029,
#83030),(#83031,#83032),(#83033,#83034),(#83035,#83036),(#83037,#83038),
(#83039,#83040),(#83041,#83042),(#83043,#83044),(#83045,#83046),(#83047,
#83048),(#83049,#83050),(#83051,#83052),(#83053,#83054),(#83055,#83056),
(#83057,#83058),(#83059,#83060),(#83061,#83062),(#83063,#83064),(#83065,
#83066),(#83067,#83068),(#83069,#83070),(#83071,#83072),(#83073,#83074),
(#83075,#83076),(#83077,#83078),(#83079,#83080),(#83081,#83082),(#83083,
#83084),(#83085,#83086),(#83087,#83088),(#83089,#83090),(#83091,#83092),
(#83093,#83094),(#83095,#83096),(#83097,#83098),(#83099,#83100),(#83101,
#83102),(#83103,#83104),(#83105,#83106),(#83107,#83108),(#83109,#83110),
(#83111,#83112),(#83113,#83114),(#83115,#83116),(#83117,#83118),(#83119,
#83120),(#83121,#83122),(#83123,#83124),(#83125,#83126),(#83127,#83128),
(#83129,#83130),(#83131,#83132),(#83133,#83134),(#83135,#83136),(#83137,
#83138),(#83139,#83140),(#83141,#83142),(#83143,#83144),(#83145,#83146),
(#83147,#83148),(#83149,#83150),(#83151,#83152),(#83153,#83154),(#83155,
#83156),(#83157,#83158),(#83159,#83160),(#83161,#83162),(#83163,#83164),
(#83165,#83166),(#83167,#83168),(#83169,#83170),(#83171,#83172),(#83173,
#83174),(#83175,#83176),(#83177,#83178),(#83179,#83180),(#83181,#83182),
(#83183,#83184),(#83185,#83186),(#83187,#83188),(#83189,#83190),(#83191,
#83192),(#83193,#83194),(#83195,#83196),(#83197,#83198),(#83199,#83200),
(#83201,#83202),(#83203,#83204),(#83205,#83206),(#83207,#83208),(#83209,
#83210),(#83211,#83212),(#83213,#83214),(#83215,#83216),(#83217,#83218),
(#83219,#83220),(#83221,#83222),(#83223,#83224),(#83225,#83226),(#83227,
#83228),(#83229,#83230),(#83231,#83232),(#83233,#83234),(#83235,#83236),
(#83237,#83238),(#83239,#83240),(#83241,#83242),(#83243,#83244),(#83245,
#83246),(#83247,#83248),(#83249,#83250),(#83251,#83252),(#83253,#83254),
(#83255,#83256),(#83257,#83258),(#83259,#83260),(#83261,#83262),(#83263,
#83264),(#83265,#83266),(#83267,#83268),(#83269,#83270),(#83271,#83272),
(#83273,#83274),(#83275,#83276),(#83277,#83278),(#83279,#83280),(#83281,
#83282),(#83283,#83284),(#83285,#83286),(#83287,#83288),(#83289,#83290),
(#83291,#83292),(#83293,#83294),(#83295,#83296),(#83297,#83298),(#83299,
#83300),(#83301,#83302),(#83303,#83304),(#83305,#83306),(#83307,#83308),
(#83309,#83310),(#83311,#83312),(#83313,#83314),(#83315,#83316),(#83317,
#83318),(#83319,#83320),(#83321,#83322),(#83323,#83324),(#83325,#83326),
(#83327,#83328),(#83329,#83330),(#83331,#83332),(#83333,#83334),(#83335,
#83336),(#83337,#83338),(#83339,#83340),(#83341,#83342),(#83343,#83344),
(#83345,#83346),(#83347,#83348),(#83349,#83350),(#83351,#83352),(#83353,
#83354),(#83355,#83356),(#83357,#83358),(#83359,#83360),(#83361,#83362),
(#83363,#83364),(#83365,#83366),(#83367,#83368),(#83369,#83370),(#83371,
#83372),(#83373,#83374),(#83375,#83376),(#83377,#83378),(#83379,#83380),
(#83381,#83382),(#83383,#83384),(#83385,#83386),(#83387,#83388),(#83389,
#83390),(#83391,#83392),(#83393,#83394),(#83395,#83396),(#83397,#83398),
(#83399,#83400),(#83401,#83402),(#83403,#83404),(#83405,#83406),(#83407,
#83408),(#83409,#83410),(#83411,#83412),(#83413,#83414),(#83415,#83416),
(#83417,#83418),(#83419,#83420),(#83421,#83422),(#83423,#83424),(#83425,
#83426),(#83427,#83428),(#83429,#83430),(#83431,#83432),(#83433,#83434),
(#83435,#83436),(#83437,#83438),(#83439,#83440),(#83441,#83442),(#83443,
#83444),(#83445,#83446),(#83447,#83448),(#83449,#83450),(#83451,#83452),
(#83453,#83454),(#83455,#83456),(#83457,#83458),(#83459,#83460),(#83461,
#83462),(#83463,#83464),(#83465,#83466),(#83467,#83468),(#83469,#83470),
(#83471,#83472),(#83473,#83474),(#83475,#83476),(#83477,#83478),(#83479,
#83480),(#83481,#83482),(#83483,#83484),(#83485,#83486),(#83487,#83488),
(#83489,#83490),(#83491,#83492),(#83493,#83494),(#83495,#83496),(#83497,
#83498),(#83499,#83500),(#83501,#83502),(#83503,#83504),(#83505,#83506),
(#83507,#83508),(#83509,#83510),(#83511,#83512),(#83513,#83514),(#83515,
#83516),(#83517,#83518),(#83519,#83520),(#83521,#83522),(#83523,#83524),
(#83525,#83526),(#83527,#83528),(#83529,#83530),(#83531,#83532),(#83533,
#83534),(#83535,#83536),(#83537,#83538),(#83539,#83540),(#83541,#83542),
(#83543,#83544),(#83545,#83546),(#83547,#83548),(#83549,#83550),(#83551,
#83552),(#83553,#83554),(#83555,#83556),(#83557,#83558),(#83559,#83560),
(#83561,#83562),(#83563,#83564),(#83565,#83566),(#83567,#83568),(#83569,
#83570),(#83571,#83572),(#83573,#83574),(#83575,#83576),(#83577,#83578),
(#83579,#83580),(#83581,#83582),(#83583,#83584),(#83585,#83586),(#83587,
#83588),(#83589,#83590),(#83591,#83592),(#83593,#83594),(#83595,#83596),
(#83597,#83598),(#83599,#83600),(#83601,#83602),(#83603,#83604),(#83605,
#83606),(#83607,#83608),(#83609,#83610),(#83611,#83612),(#83613,#83614),
(#83615,#83616),(#83617,#83618),(#83619,#83620),(#83621,#83622),(#83623,
#83624),(#83625,#83626),(#83627,#83628),(#83629,#83630),(#83631,#83632),
(#83633,#83634),(#83635,#83636),(#83637,#83638),(#83639,#83640),(#83641,
#83642),(#83643,#83644),(#83645,#83646),(#83647,#83648),(#83649,#83650),
(#83651,#83652),(#83653,#83654),(#83655,#83656),(#83657,#83658),(#83659,
#83660),(#83661,#83662),(#83663,#83664),(#83665,#83666),(#83667,#83668),
(#83669,#83670),(#83671,#83672),(#83673,#83674),(#83675,#83676),(#83677,
#83678),(#83679,#83680),(#83681,#83682),(#83683,#83684),(#83685,#83686),
(#83687,#83688),(#83689,#83690),(#83691,#83692),(#83693,#83694),(#83695,
#83696),(#83697,#83698),(#83699,#83700),(#83701,#83702),(#83703,#83704),
(#83705,#83706),(#83707,#83708),(#83709,#83710),(#83711,#83712),(#83713,
#83714),(#83715,#83716),(#83717,#83718),(#83719,#83720),(#83721,#83722),
(#83723,#83724),(#83725,#83726),(#83727,#83728),(#83729,#83730),(#83731,
#83732),(#83733,#83734),(#83735,#83736),(#83737,#83738),(#83739,#83740),
(#83741,#83742),(#83743,#83744),(#83745,#83746),(#83747,#83748),(#83749,
#83750),(#83751,#83752),(#83753,#83754),(#83755,#83756),(#83757,#83758),
(#83759,#83760),(#83761,#83762),(#83763,#83764),(#83765,#83766),(#83767,
#83768),(#83769,#83770),(#83771,#83772),(#83773,#83774),(#83775,#83776),
(#83777,#83778),(#83779,#83780),(#83781,#83782),(#83783,#83784),(#83785,
#83786),(#83787,#83788),(#83789,#83790),(#83791,#83792),(#83793,#83794),
(#83795,#83796),(#83797,#83798),(#83799,#83800),(#83801,#83802),(#83803,
#83804),(#83805,#83806),(#83807,#83808),(#83809,#83810),(#83811,#83812),
(#83813,#83814),(#83815,#83816),(#83817,#83818),(#83819,#83820),(#83821,
#83822),(#83823,#83824),(#83825,#83826),(#83827,#83828),(#83829,#83830),
(#83831,#83832),(#83833,#83834),(#83835,#83836),(#83837,#83838),(#83839,
#83840),(#83841,#83842),(#83843,#83844),(#83845,#83846),(#83847,#83848),
(#83849,#83850),(#83851,#83852),(#83853,#83854),(#83855,#83856),(#83857,
#83858),(#83859,#83860),(#83861,#83862),(#83863,#83864),(#83865,#83866),
(#83867,#83868),(#83869,#83870),(#83871,#83872),(#83873,#83874),(#83875,
#83876),(#83877,#83878),(#83879,#83880),(#83881,#83882),(#83883,#83884),
(#83885,#83886),(#83887,#83888),(#83889,#83890),(#83891,#83892),(#83893,
#83894),(#83895,#83896),(#83897,#83898),(#83899,#83900),(#83901,#83902),
(#83903,#83904),(#83905,#83906),(#83907,#83908),(#83909,#83910),(#83911,
#83912),(#83913,#83914),(#83915,#83916),(#83917,#83918),(#83919,#83920),
(#83921,#83922),(#83923,#83924),(#83925,#83926),(#83927,#83928),(#83929,
#83930),(#83931,#83932),(#83933,#83934),(#83935,#83936),(#83937,#83938),
(#83939,#83940),(#83941,#83942),(#83943,#83944),(#83945,#83946),(#83947,
#83948),(#83949,#83950),(#83951,#83952),(#83953,#83954),(#83955,#83956),
(#83957,#83958),(#83959,#83960),(#83961,#83962),(#83963,#83964),(#83965,
#83966),(#83967,#83968),(#83969,#83970),(#83971,#83972),(#83973,#83974),
(#83975,#83976),(#83977,#83978),(#83979,#83980),(#83981,#83982),(#83983,
#83984),(#83985,#83986),(#83987,#83988),(#83989,#83990),(#83991,#83992),
(#83993,#83994),(#83995,#83996),(#83997,#83998),(#83999,#84000),(#84001,
#84002),(#84003,#84004),(#84005,#84006),(#84007,#84008),(#84009,#84010),
(#84011,#84012),(#84013,#84014),(#84015,#84016),(#84017,#84018),(#84019,
#84020),(#84021,#84022),(#84023,#84024),(#84025,#84026),(#84027,#84028),
(#84029,#84030),(#84031,#84032),(#84033,#84034),(#84035,#84036),(#84037,
#84038),(#84039,#84040),(#84041,#84042),(#84043,#84044),(#84045,#84046),
(#84047,#84048),(#84049,#84050),(#84051,#84052),(#84053,#84054),(#84055,
#84056),(#84057,#84058),(#84059,#84060),(#84061,#84062),(#84063,#84064),
(#84065,#84066),(#84067,#84068),(#84069,#84070),(#84071,#84072),(#84073,
#84074),(#84075,#84076),(#84077,#84078),(#84079,#84080),(#84081,#84082),
(#84083,#84084),(#84085,#84086),(#84087,#84088),(#84089,#84090),(#84091,
#84092),(#84093,#84094),(#84095,#84096),(#84097,#84098),(#84099,#84100),
(#84101,#84102),(#84103,#84104),(#84105,#84106),(#84107,#84108),(#84109,
#84110),(#84111,#84112),(#84113,#84114),(#84115,#84116),(#84117,#84118),
(#84119,#84120),(#84121,#84122),(#84123,#84124),(#84125,#84126),(#84127,
#84128),(#84129,#84130),(#84131,#84132),(#84133,#84134),(#84135,#84136),
(#84137,#84138),(#84139,#84140),(#84141,#84142),(#84143,#84144),(#84145,
#84146),(#84147,#84148),(#84149,#84150),(#84151,#84152),(#84153,#84154),
(#84155,#84156),(#84157,#84158),(#84159,#84160),(#84161,#84162),(#84163,
#84164),(#84165,#84166),(#84167,#84168),(#84169,#84170),(#84171,#84172),
(#84173,#84174),(#84175,#84176),(#84177,#84178),(#84179,#84180),(#84181,
#84182),(#84183,#84184),(#84185,#84186),(#84187,#84188),(#84189,#84190),
(#84191,#84192),(#84193,#84194),(#84195,#84196),(#84197,#84198),(#84199,
#84200),(#84201,#84202),(#84203,#84204),(#84205,#84206),(#84207,#84208),
(#84209,#84210),(#84211,#84212),(#84213,#84214),(#84215,#84216),(#84217,
#84218),(#84219,#84220),(#84221,#84222)),.UNSPECIFIED.,.F.,.F.,.F.)
B_SPLINE_SURFACE_WITH_KNOTS((6,1,1,1,1,1,1,1,1,1,1,1,1,1,1,1,1,1,1,1,1,
1,1,1,1,1,1,1,1,1,1,1,1,1,1,1,1,1,1,1,1,1,1,1,1,1,1,1,1,1,1,1,1,1,1,1,1,
1,1,1,1,1,1,1,1,1,1,1,1,1,1,1,1,1,1,1,1,1,1,1,1,1,1,1,1,1,1,1,1,1,1,1,1,
1,1,1,1,1,1,1,1,1,1,1,1,1,1,1,1,1,1,1,1,1,1,1,1,1,1,1,1,1,1,1,1,1,1,1,1,
1,1,1,1,1,1,1,1,1,1,1,1,1,1,1,1,1,1,1,1,1,1,1,1,1,1,1,1,1,1,1,1,1,1,1,1,
1,1,1,1,1,1,1,1,1,1,1,1,1,1,1,1,1,1,1,1,1,1,1,1,1,1,1,1,1,1,1,1,1,1,1,1,
1,1,1,1,1,1,1,1,1,1,1,1,1,1,1,1,1,1,1,1,1,1,1,1,1,1,1,1,1,1,1,1,1,1,1,1,
1,1,1,1,1,1,1,1,1,1,1,1,1,1,1,1,1,1,1,1,1,1,1,1,1,1,1,1,1,1,1,1,1,1,1,1,
1,1,1,1,1,1,1,1,1,1,1,1,1,1,1,1,1,1,1,1,1,1,1,1,1,1,1,1,1,1,1,1,1,1,1,1,
1,1,1,1,1,1,1,1,1,1,1,1,1,1,1,1,1,1,1,1,1,1,1,1,1,1,1,1,1,1,1,1,1,1,1,1,
1,1,1,1,1,1,1,1,1,1,1,1,1,1,1,1,1,1,1,1,1,1,1,1,1,1,1,1,1,1,1,1,1,1,1,1,
1,1,1,1,1,1,1,1,1,1,1,1,1,1,1,1,1,1,1,1,1,1,1,1,1,1,1,1,1,1,1,1,1,1,1,1,
1,1,1,1,1,1,1,1,1,1,1,1,1,1,1,1,1,1,1,1,1,1,1,1,1,1,1,1,1,1,1,1,1,1,1,1,
1,1,1,1,1,1,1,1,1,1,1,1,1,1,1,1,1,1,1,1,1,1,1,1,1,1,1,1,1,1,1,1,1,1,1,1,
1,1,1,1,1,1,1,1,1,1,1,1,1,1,1,1,1,1,1,1,1,1,1,1,1,1,1,1,1,1,1,1,1,1,1,1,
1,1,1,1,1,1,1,1,1,1,1,1,1,1,1,1,1,1,1,1,1,1,1,1,1,1,1,1,1,1,1,1,1,1,1,1,
1,1,1,1,1,1,1,1,1,1,1,1,1,1,1,1,1,1,1,1,1,1,1,1,1,1,1,1,1,1,1,1,1,1,1,1,
1,1,1,1,1,1,1,1,1,1,1,1,1,1,1,1,1,1,1,1,1,1,1,1,1,1,1,1,1,1,1,1,1,1,1,1,
1,1,1,1,1,1,1,1,1,1,1,1,1,1,1,1,1,1,1,1,1,1,1,1,1,1,1,1,1,1,1,1,1,1,1,1,
1,1,1,1,1,1,1,1,1,1,1,1,1,1,1,1,1,1,1,1,1,1,1,1,1,1,1,1,1,1,1,1,1,1,1,1,
1,1,1,1,1,1,1,1,1,1,1,1,1,1,1,1,1,1,1,1,1,1,1,1,1,1,1,1,1,1,1,1,1,1,1,1,
1,1,1,1,1,1,1,1,1,1,1,1,1,1,1,1,1,1,1,1,1,1,1,1,1,1,1,1,1,1,1,1,1,1,1,1,
1,1,1,1,1,1,1,1,1,1,1,1,1,1,1,1,1,1,1,1,1,1,1,1,1,1,1,1,1,1,1,1,1,1,1,1,
1,1,1,1,1,1,1,1,1,1,1,1,1,1,1,1,1,1,1,1,1,1,1,1,1,1,1,1,1,1,1,1,1,1,1,1,
1,1,1,1,1,1,1,1,1,1,1,1,1,1,1,1,1,1,1,1,1,1,1,1,1,1,1,1,1,1,1,1,1,1,1,1,
1,1,1,1,1,1,1,1,1,1,1,1,1,1,1,1,1,1,1,1,1,1,1,1,1,1,1,1,1,1,1,1,1,1,1,1,
1,1,1,1,1,1,1,1,1,1,1,1,1,1,1,1,1,1,1,1,1,1,1,1,1,1,1,1,1,1,1,1,1,1,1,1,
1,1,1,1,1,1,1,1,1,1,1,1,1,1,1,1,1,1,1,1,1,1,1,1,1,1,1,1,1,1,1,1,1,1,1,1,
1,1,1,1,1,1,1,6),(2,2),(-1.,-0.999000000000001,-0.998000000000001,-0.997000000000001,
-0.996000000000001,-0.995000000000001,-0.994000000000001,-0.993000000000001,
-0.992000000000001,-0.991000000000001,-0.990000000000001,-0.989000000000001,
-0.988000000000001,-0.987000000000001,-0.986000000000001,-0.985000000000001,
-0.984000000000001,-0.983000000000001,-0.982000000000001,-0.981000000000001,
-0.980000000000001,-0.979000000000001,-0.978000000000001,-0.977000000000001,
-0.976000000000001,-0.975000000000001,-0.974000000000001,-0.973000000000001,
-0.972000000000001,-0.971000000000001,-0.970000000000001,-0.969000000000001,
-0.968000000000001,-0.967000000000001,-0.966000000000001,-0.965000000000001,
-0.964000000000001,-0.963000000000001,-0.962000000000001,-0.961000000000001,
-0.960000000000001,-0.959000000000001,-0.958000000000001,-0.957000000000001,
-0.956000000000001,-0.955000000000001,-0.954000000000001,-0.953000000000001,
-0.952000000000001,-0.951000000000001,-0.950000000000001,-0.949000000000001,
-0.948000000000001,-0.947000000000001,-0.946000000000001,-0.945000000000001,
-0.944000000000001,-0.943000000000001,-0.942000000000001,-0.941000000000001,
-0.940000000000001,-0.939000000000001,-0.938000000000001,-0.937000000000001,
-0.936000000000001,-0.935000000000001,-0.934000000000001,-0.933000000000001,
-0.932000000000001,-0.931000000000001,-0.930000000000001,-0.929000000000001,
-0.928000000000001,-0.927000000000001,-0.926000000000001,-0.925000000000001,
-0.924000000000001,-0.923000000000001,-0.922000000000001,-0.921000000000001,
-0.920000000000001,-0.919000000000001,-0.918000000000001,-0.917000000000001,
-0.916000000000001,-0.915000000000001,-0.914000000000001,-0.913000000000001,
-0.912000000000001,-0.911000000000001,-0.910000000000001,-0.909000000000001,
-0.908000000000001,-0.907000000000001,-0.906000000000001,-0.905000000000001,
-0.904000000000001,-0.903000000000001,-0.902000000000001,-0.901000000000001,
-0.900000000000001,-0.899000000000001,-0.898000000000001,-0.897000000000001,
-0.896000000000001,-0.895000000000001,-0.894000000000001,-0.893000000000001,
-0.892000000000001,-0.891000000000001,-0.890000000000001,-0.889000000000001,
-0.888000000000001,-0.887000000000001,-0.886000000000001,-0.885000000000001,
-0.884000000000001,-0.883000000000001,-0.882000000000001,-0.881000000000001,
-0.880000000000001,-0.879000000000001,-0.878000000000001,-0.877000000000001,
-0.876000000000001,-0.875000000000001,-0.874000000000001,-0.873000000000001,
-0.872000000000001,-0.871000000000001,-0.870000000000001,-0.869000000000001,
-0.868000000000001,-0.867000000000001,-0.866000000000001,-0.865000000000001,
-0.864000000000001,-0.863000000000001,-0.862000000000001,-0.861000000000001,
-0.860000000000001,-0.859000000000001,-0.858000000000001,-0.857000000000001,
-0.856000000000001,-0.855000000000001,-0.854000000000001,-0.853000000000001,
-0.852000000000001,-0.851000000000001,-0.850000000000001,-0.849000000000001,
-0.848000000000001,-0.847000000000001,-0.846000000000001,-0.845000000000001,
-0.844000000000001,-0.843000000000001,-0.842000000000001,-0.841000000000001,
-0.840000000000001,-0.839000000000001,-0.838000000000001,-0.837000000000001,
-0.836000000000001,-0.835000000000001,-0.834000000000001,-0.833000000000001,
-0.832000000000001,-0.831000000000001,-0.830000000000001,-0.829000000000001,
-0.828000000000001,-0.827000000000001,-0.826000000000001,-0.825000000000001,
-0.824000000000001,-0.823000000000001,-0.822000000000001,-0.821000000000001,
-0.820000000000001,-0.819000000000001,-0.818000000000001,-0.817000000000001,
-0.816000000000001,-0.815000000000001,-0.814000000000001,-0.813000000000001,
-0.812000000000001,-0.811000000000001,-0.810000000000001,-0.809000000000001,
-0.808000000000001,-0.807000000000001,-0.806000000000001,-0.805000000000001,
-0.804000000000001,-0.803000000000001,-0.802000000000001,-0.801000000000001,
-0.800000000000001,-0.799000000000001,-0.798000000000001,-0.797000000000001,
-0.796000000000001,-0.795000000000001,-0.794000000000001,-0.793000000000001,
-0.792000000000001,-0.791000000000001,-0.790000000000001,-0.789000000000001,
-0.788000000000001,-0.787000000000001,-0.786000000000001,-0.785000000000001,
-0.784000000000001,-0.783000000000001,-0.782000000000001,-0.781000000000001,
-0.780000000000001,-0.779000000000001,-0.778000000000001,-0.777000000000001,
-0.776000000000001,-0.775000000000001,-0.774000000000001,-0.773000000000001,
-0.772000000000001,-0.771000000000001,-0.770000000000001,-0.769000000000001,
-0.768000000000001,-0.767000000000001,-0.766000000000001,-0.765000000000001,
-0.764000000000001,-0.763000000000001,-0.762000000000001,-0.761000000000001,
-0.760000000000001,-0.759000000000001,-0.758000000000001,-0.757000000000001,
-0.756000000000001,-0.755000000000001,-0.754000000000001,-0.753000000000001,
-0.752000000000001,-0.751000000000001,-0.750000000000001,-0.749000000000001,
-0.748000000000001,-0.747000000000001,-0.746000000000001,-0.745000000000001,
-0.744000000000001,-0.743000000000001,-0.742000000000001,-0.741000000000001,
-0.740000000000001,-0.739000000000001,-0.738000000000001,-0.737000000000001,
-0.736000000000001,-0.735000000000001,-0.734000000000001,-0.733000000000001,
-0.732000000000001,-0.731000000000001,-0.730000000000001,-0.729000000000001,
-0.728000000000001,-0.727000000000001,-0.726000000000001,-0.725000000000001,
-0.724000000000001,-0.723000000000001,-0.722000000000001,-0.721000000000001,
-0.720000000000001,-0.719000000000001,-0.718000000000001,-0.717000000000001,
-0.716000000000001,-0.715000000000001,-0.714000000000001,-0.713000000000001,
-0.712000000000001,-0.711000000000001,-0.710000000000001,-0.709000000000001,
-0.708000000000001,-0.707000000000001,-0.706000000000001,-0.705000000000001,
-0.704000000000001,-0.703000000000001,-0.702000000000001,-0.701000000000001,
-0.700000000000001,-0.699000000000001,-0.698000000000001,-0.697000000000001,
-0.696000000000001,-0.695000000000001,-0.694000000000001,-0.693000000000001,
-0.692000000000001,-0.691000000000001,-0.690000000000001,-0.689000000000001,
-0.688000000000001,-0.687,-0.686,-0.685,-0.684,-0.683,-0.682,-0.681,-0.68,
-0.679,-0.678,-0.677,-0.676,-0.675,-0.674,-0.673,-0.672,-0.671,-0.67,-0.669,
-0.668,-0.667,-0.666,-0.665,-0.664,-0.663,-0.662,-0.661,-0.66,-0.659,-0.658,
-0.657,-0.656,-0.655,-0.654,-0.653,-0.652,-0.651,-0.65,-0.649,-0.648,-0.647,
-0.646,-0.645,-0.644,-0.643,-0.642,-0.641,-0.64,-0.639,-0.638,-0.637,-0.636,
-0.635,-0.634,-0.633,-0.632,-0.631,-0.63,-0.629,-0.628,-0.627,-0.626,-0.625,
-0.624,-0.623,-0.622,-0.621,-0.62,-0.619,-0.618,-0.617,-0.616,-0.615,-0.614,
-0.613,-0.612,-0.611,-0.61,-0.609,-0.608,-0.607,-0.606,-0.605,-0.604,-0.603,
-0.602,-0.601,-0.6,-0.599,-0.598,-0.597,-0.596,-0.595,-0.594,-0.593,-0.592,
-0.591,-0.59,-0.589,-0.588,-0.587,-0.586,-0.585,-0.584,-0.583,-0.582,-0.581,
-0.58,-0.579,-0.578,-0.577,-0.576,-0.575,-0.574,-0.573,-0.572,-0.571,-0.57,
-0.569,-0.568,-0.567,-0.566,-0.565,-0.564,-0.563,-0.562,-0.561,-0.56,-0.559,
-0.558,-0.557,-0.556,-0.555,-0.554,-0.553,-0.552,-0.551,-0.55,-0.549,-0.548,
-0.547,-0.546,-0.545,-0.544,-0.543,-0.542,-0.541,-0.54,-0.539,-0.538,-0.537,
-0.536,-0.535,-0.534,-0.533,-0.532,-0.531,-0.53,-0.529,-0.528,-0.527,-0.526,
-0.525,-0.524,-0.523,-0.522,-0.521,-0.52,-0.519,-0.518,-0.517,-0.516,-0.515,
-0.514,-0.513,-0.512,-0.511,-0.51,-0.509,-0.508,-0.507,-0.506,-0.505,-0.504,
-0.503,-0.502,-0.501,-0.5,-0.499,-0.498,-0.497,-0.496,-0.495,-0.494,-0.493,
-0.492,-0.491,-0.49,-0.489,-0.488,-0.487,-0.486,-0.485,-0.484,-0.483,-0.482,
-0.481,-0.48,-0.479,-0.478,-0.477,-0.476,-0.475,-0.474,-0.473,-0.472,-0.471,
-0.47,-0.469,-0.468,-0.467,-0.466,-0.465,-0.464,-0.463,-0.462,-0.461,-0.46,
-0.459,-0.458,-0.457,-0.456,-0.455,-0.454,-0.453,-0.452,-0.451,-0.45,-0.449,
-0.448,-0.447,-0.446,-0.445,-0.444,-0.443,-0.442,-0.441,-0.44,-0.439,-0.438,
-0.437,-0.436,-0.435,-0.434,-0.433,-0.432,-0.431,-0.43,-0.429,-0.428,-0.427,
-0.426,-0.425,-0.424,-0.423,-0.422,-0.421,-0.42,-0.419,-0.418,-0.417,-0.416,
-0.415,-0.414,-0.413,-0.412,-0.411,-0.41,-0.409,-0.408,-0.407,-0.406,-0.405,
-0.404,-0.403,-0.402,-0.401,-0.4,-0.399,-0.398,-0.397,-0.396,-0.395,-0.394,
-0.393,-0.392,-0.391,-0.39,-0.389,-0.388,-0.387,-0.386,-0.385,-0.384,-0.383,
-0.382,-0.381,-0.38,-0.379,-0.378,-0.377,-0.376,-0.375,-0.374,-0.373,-0.372,
-0.371,-0.37,-0.369,-0.368,-0.367,-0.366,-0.365,-0.364,-0.363,-0.362,-0.361,
-0.36,-0.359,-0.358,-0.357,-0.356,-0.355,-0.354,-0.353,-0.352,-0.351,-0.35,
-0.349,-0.348,-0.347,-0.346,-0.345,-0.344,-0.343,-0.342,-0.341,-0.34,-0.339,
-0.338,-0.337,-0.336,-0.335,-0.334,-0.333,-0.332,-0.331,-0.33,-0.329,-0.328,
-0.327,-0.326,-0.325,-0.324,-0.323,-0.322,-0.321,-0.32,-0.319,-0.318,-0.317,
-0.316,-0.315,-0.314,-0.313,-0.312,-0.311,-0.31,-0.309,-0.308,-0.307,-0.306,
-0.305,-0.304,-0.303,-0.302,-0.301,-0.3,-0.299,-0.298,-0.297,-0.296,-0.295,
-0.294,-0.293,-0.292,-0.291,-0.29,-0.289,-0.288,-0.287,-0.286,-0.285,-0.284,
-0.283,-0.282,-0.281,-0.28,-0.279,-0.278,-0.277,-0.276,-0.275,-0.274,-0.273,
-0.272,-0.271,-0.27,-0.269,-0.268,-0.267,-0.266,-0.265,-0.264,-0.263,-0.262,
-0.261,-0.26,-0.259,-0.258,-0.257,-0.256,-0.255,-0.254,-0.253,-0.252,-0.251,
-0.25,-0.249,-0.248,-0.247,-0.246,-0.245,-0.244,-0.243,-0.242,-0.241,-0.24,
-0.239,-0.238,-0.237,-0.236,-0.235,-0.234,-0.233,-0.232,-0.231,-0.23,-0.229,
-0.228,-0.227,-0.226,-0.225,-0.224,-0.223,-0.222,-0.221,-0.22,-0.219,-0.218,
-0.217,-0.216,-0.215,-0.214,-0.213,-0.212,-0.211,-0.21,-0.209,-0.208,-0.207,
-0.206,-0.205,-0.204,-0.203,-0.202,-0.201,-0.2,-0.199,-0.198,-0.197,-0.196,
-0.195,-0.194,-0.193,-0.192,-0.191,-0.19,-0.189,-0.188,-0.187,-0.186,-0.185,
-0.184,-0.183,-0.182,-0.181,-0.18,-0.179,-0.178,-0.177,-0.176,-0.175,-0.174,
-0.173,-0.172,-0.171,-0.17,-0.169,-0.168,-0.167,-0.166,-0.165,-0.164,-0.163,
-0.162,-0.161,-0.16,-0.159,-0.158,-0.157,-0.156,-0.155,-0.154,-0.153,-0.152,
-0.151,-0.15,-0.149,-0.148,-0.147,-0.146,-0.145,-0.144,-0.143,-0.142,-0.141,
-0.14,-0.139,-0.138,-0.137,-0.136,-0.135,-0.134,-0.133,-0.132,-0.131,-0.13,
-0.129,-0.128,-0.127,-0.126,-0.125,-0.124,-0.123,-0.122,-0.121,-0.12,-0.119,
-0.118,-0.117,-0.116,-0.115,-0.114,-0.113,-0.112,-0.111,-0.11,-0.109,-0.108,
-0.107,-0.106,-0.105,-0.104,-0.103,-0.102,-0.101,-0.1,-0.0990000000000001,
-0.0980000000000001,-0.0970000000000001,-0.0960000000000001,-0.0950000000000001,
-0.0940000000000001,-0.0930000000000001,-0.0920000000000001,-0.0910000000000001,
-0.0900000000000001,-0.0890000000000001,-0.0880000000000001,-0.0870000000000001,
-0.0860000000000001,-0.0850000000000001,-0.0840000000000001,-0.0830000000000001,
-0.0820000000000001,-0.0810000000000001,-0.0800000000000001,-0.0790000000000001,
-0.0780000000000001,-0.0770000000000001,-0.0760000000000001,-0.0750000000000001,
-0.0740000000000001,-0.0730000000000001,-0.0720000000000001,-0.071,-0.07,
-0.069,-0.068,-0.067,-0.066,-0.065,-0.064,-0.063,-0.062,-0.061,-0.06,-0.059,
-0.058,-0.057,-0.056,-0.055,-0.054,-0.053,-0.052,-0.051,-0.05,-0.049,-0.048,
-0.047,-0.046,-0.045,-0.044,-0.043,-0.042,-0.041,-0.04,-0.039,-0.038,-0.037,
-0.036,-0.035,-0.034,-0.033,-0.032,-0.031,-0.03,-0.029,-0.028,-0.027,-0.026,
-0.025,-0.024,-0.023,-0.022,-0.021,-0.02,-0.019,-0.018,-0.017,-0.016,-0.015,
-0.014,-0.013,-0.012,-0.011,-0.01,-0.009,-0.008,-0.007,-0.006,-0.005,-0.004,
-0.003,-0.002,-0.001,0.),(0.,2.),.UNSPECIFIED.)
GEOMETRIC_REPRESENTATION_ITEM()
RATIONAL_B_SPLINE_SURFACE(((1.,1.),(1.,1.),(1.,1.),(1.,1.),(1.,1.),(1.,
1.),(1.,1.),(1.,1.),(1.,1.),(1.,1.),(1.,1.),(1.,1.),(1.,1.),(1.,1.),(1.,
1.),(1.,1.),(1.,1.),(1.,1.),(1.,1.),(1.,1.),(1.,1.),(1.,1.),(1.,1.),(1.,
1.),(1.,1.),(1.,1.),(1.,1.),(1.,1.),(1.,1.),(1.,1.),(1.,1.),(1.,1.),(1.,
1.),(1.,1.),(1.,1.),(1.,1.),(1.,1.),(1.,1.),(1.,1.),(1.,1.),(1.,1.),(1.,
1.),(1.,1.),(1.,1.),(1.,1.),(1.,1.),(1.,1.),(1.,1.),(1.,1.),(1.,1.),(1.,
1.),(1.,1.),(1.,1.),(1.,1.),(1.,1.),(1.,1.),(1.,1.),(1.,1.),(1.,1.),(1.,
1.),(1.,1.),(1.,1.),(1.,1.),(1.,1.),(1.,1.),(1.,1.),(1.,1.),(1.,1.),(1.,
1.),(1.,1.),(1.,1.),(1.,1.),(1.,1.),(1.,1.),(1.,1.),(1.,1.),(1.,1.),(1.,
1.),(1.,1.),(1.,1.),(1.,1.),(1.,1.),(1.,1.),(1.,1.),(1.,1.),(1.,1.),(1.,
1.),(1.,1.),(1.,1.),(1.,1.),(1.,1.),(1.,1.),(1.,1.),(1.,1.),(1.,1.),(1.,
1.),(1.,1.),(1.,1.),(1.,1.),(1.,1.),(1.,1.),(1.,1.),(1.,1.),(1.,1.),(1.,
1.),(1.,1.),(1.,1.),(1.,1.),(1.,1.),(1.,1.),(1.,1.),(1.,1.),(1.,1.),(1.,
1.),(1.,1.),(1.,1.),(1.,1.),(1.,1.),(1.,1.),(1.,1.),(1.,1.),(1.,1.),(1.,
1.),(1.,1.),(1.,1.),(1.,1.),(1.,1.),(1.,1.),(1.,1.),(1.,1.),(1.,1.),(1.,
1.),(1.,1.),(1.,1.),(1.,1.),(1.,1.),(1.,1.),(1.,1.),(1.,1.),(1.,1.),(1.,
1.),(1.,1.),(1.,1.),(1.,1.),(1.,1.),(1.,1.),(1.,1.),(1.,1.),(1.,1.),(1.,
1.),(1.,1.),(1.,1.),(1.,1.),(1.,1.),(1.,1.),(1.,1.),(1.,1.),(1.,1.),(1.,
1.),(1.,1.),(1.,1.),(1.,1.),(1.,1.),(1.,1.),(1.,1.),(1.,1.),(1.,1.),(1.,
1.),(1.,1.),(1.,1.),(1.,1.),(1.,1.),(1.,1.),(1.,1.),(1.,1.),(1.,1.),(1.,
1.),(1.,1.),(1.,1.),(1.,1.),(1.,1.),(1.,1.),(1.,1.),(1.,1.),(1.,1.),(1.,
1.),(1.,1.),(1.,1.),(1.,1.),(1.,1.),(1.,1.),(1.,1.),(1.,1.),(1.,1.),(1.,
1.),(1.,1.),(1.,1.),(1.,1.),(1.,1.),(1.,1.),(1.,1.),(1.,1.),(1.,1.),(1.,
1.),(1.,1.),(1.,1.),(1.,1.),(1.,1.),(1.,1.),(1.,1.),(1.,1.),(1.,1.),(1.,
1.),(1.,1.),(1.,1.),(1.,1.),(1.,1.),(1.,1.),(1.,1.),(1.,1.),(1.,1.),(1.,
1.),(1.,1.),(1.,1.),(1.,1.),(1.,1.),(1.,1.),(1.,1.),(1.,1.),(1.,1.),(1.,
1.),(1.,1.),(1.,1.),(1.,1.),(1.,1.),(1.,1.),(1.,1.),(1.,1.),(1.,1.),(1.,
1.),(1.,1.),(1.,1.),(1.,1.),(1.,1.),(1.,1.),(1.,1.),(1.,1.),(1.,1.),(1.,
1.),(1.,1.),(1.,1.),(1.,1.),(1.,1.),(1.,1.),(1.,1.),(1.,1.),(1.,1.),(1.,
1.),(1.,1.),(1.,1.),(1.,1.),(1.,1.),(1.,1.),(1.,1.),(1.,1.),(1.,1.),(1.,
1.),(1.,1.),(1.,1.),(1.,1.),(1.,1.),(1.,1.),(1.,1.),(1.,1.),(1.,1.),(1.,
1.),(1.,1.),(1.,1.),(1.,1.),(1.,1.),(1.,1.),(1.,1.),(1.,1.),(1.,1.),(1.,
1.),(1.,1.),(1.,1.),(1.,1.),(1.,1.),(1.,1.),(1.,1.),(1.,1.),(1.,1.),(1.,
1.),(1.,1.),(1.,1.),(1.,1.),(1.,1.),(1.,1.),(1.,1.),(1.,1.),(1.,1.),(1.,
1.),(1.,1.),(1.,1.),(1.,1.),(1.,1.),(1.,1.),(1.,1.),(1.,1.),(1.,1.),(1.,
1.),(1.,1.),(1.,1.),(1.,1.),(1.,1.),(1.,1.),(1.,1.),(1.,1.),(1.,1.),(1.,
1.),(1.,1.),(1.,1.),(1.,1.),(1.,1.),(1.,1.),(1.,1.),(1.,1.),(1.,1.),(1.,
1.),(1.,1.),(1.,1.),(1.,1.),(1.,1.),(1.,1.),(1.,1.),(1.,1.),(1.,1.),(1.,
1.),(1.,1.),(1.,1.),(1.,1.),(1.,1.),(1.,1.),(1.,1.),(1.,1.),(1.,1.),(1.,
1.),(1.,1.),(1.,1.),(1.,1.),(1.,1.),(1.,1.),(1.,1.),(1.,1.),(1.,1.),(1.,
1.),(1.,1.),(1.,1.),(1.,1.),(1.,1.),(1.,1.),(1.,1.),(1.,1.),(1.,1.),(1.,
1.),(1.,1.),(1.,1.),(1.,1.),(1.,1.),(1.,1.),(1.,1.),(1.,1.),(1.,1.),(1.,
1.),(1.,1.),(1.,1.),(1.,1.),(1.,1.),(1.,1.),(1.,1.),(1.,1.),(1.,1.),(1.,
1.),(1.,1.),(1.,1.),(1.,1.),(1.,1.),(1.,1.),(1.,1.),(1.,1.),(1.,1.),(1.,
1.),(1.,1.),(1.,1.),(1.,1.),(1.,1.),(1.,1.),(1.,1.),(1.,1.),(1.,1.),(1.,
1.),(1.,1.),(1.,1.),(1.,1.),(1.,1.),(1.,1.),(1.,1.),(1.,1.),(1.,1.),(1.,
1.),(1.,1.),(1.,1.),(1.,1.),(1.,1.),(1.,1.),(1.,1.),(1.,1.),(1.,1.),(1.,
1.),(1.,1.),(1.,1.),(1.,1.),(1.,1.),(1.,1.),(1.,1.),(1.,1.),(1.,1.),(1.,
1.),(1.,1.),(1.,1.),(1.,1.),(1.,1.),(1.,1.),(1.,1.),(1.,1.),(1.,1.),(1.,
1.),(1.,1.),(1.,1.),(1.,1.),(1.,1.),(1.,1.),(1.,1.),(1.,1.),(1.,1.),(1.,
1.),(1.,1.),(1.,1.),(1.,1.),(1.,1.),(1.,1.),(1.,1.),(1.,1.),(1.,1.),(1.,
1.),(1.,1.),(1.,1.),(1.,1.),(1.,1.),(1.,1.),(1.,1.),(1.,1.),(1.,1.),(1.,
1.),(1.,1.),(1.,1.),(1.,1.),(1.,1.),(1.,1.),(1.,1.),(1.,1.),(1.,1.),(1.,
1.),(1.,1.),(1.,1.),(1.,1.),(1.,1.),(1.,1.),(1.,1.),(1.,1.),(1.,1.),(1.,
1.),(1.,1.),(1.,1.),(1.,1.),(1.,1.),(1.,1.),(1.,1.),(1.,1.),(1.,1.),(1.,
1.),(1.,1.),(1.,1.),(1.,1.),(1.,1.),(1.,1.),(1.,1.),(1.,1.),(1.,1.),(1.,
1.),(1.,1.),(1.,1.),(1.,1.),(1.,1.),(1.,1.),(1.,1.),(1.,1.),(1.,1.),(1.,
1.),(1.,1.),(1.,1.),(1.,1.),(1.,1.),(1.,1.),(1.,1.),(1.,1.),(1.,1.),(1.,
1.),(1.,1.),(1.,1.),(1.,1.),(1.,1.),(1.,1.),(1.,1.),(1.,1.),(1.,1.),(1.,
1.),(1.,1.),(1.,1.),(1.,1.),(1.,1.),(1.,1.),(1.,1.),(1.,1.),(1.,1.),(1.,
1.),(1.,1.),(1.,1.),(1.,1.),(1.,1.),(1.,1.),(1.,1.),(1.,1.),(1.,1.),(1.,
1.),(1.,1.),(1.,1.),(1.,1.),(1.,1.),(1.,1.),(1.,1.),(1.,1.),(1.,1.),(1.,
1.),(1.,1.),(1.,1.),(1.,1.),(1.,1.),(1.,1.),(1.,1.),(1.,1.),(1.,1.),(1.,
1.),(1.,1.),(1.,1.),(1.,1.),(1.,1.),(1.,1.),(1.,1.),(1.,1.),(1.,1.),(1.,
1.),(1.,1.),(1.,1.),(1.,1.),(1.,1.),(1.,1.),(1.,1.),(1.,1.),(1.,1.),(1.,
1.),(1.,1.),(1.,1.),(1.,1.),(1.,1.),(1.,1.),(1.,1.),(1.,1.),(1.,1.),(1.,
1.),(1.,1.),(1.,1.),(1.,1.),(1.,1.),(1.,1.),(1.,1.),(1.,1.),(1.,1.),(1.,
1.),(1.,1.),(1.,1.),(1.,1.),(1.,1.),(1.,1.),(1.,1.),(1.,1.),(1.,1.),(1.,
1.),(1.,1.),(1.,1.),(1.,1.),(1.,1.),(1.,1.),(1.,1.),(1.,1.),(1.,1.),(1.,
1.),(1.,1.),(1.,1.),(1.,1.),(1.,1.),(1.,1.),(1.,1.),(1.,1.),(1.,1.),(1.,
1.),(1.,1.),(1.,1.),(1.,1.),(1.,1.),(1.,1.),(1.,1.),(1.,1.),(1.,1.),(1.,
1.),(1.,1.),(1.,1.),(1.,1.),(1.,1.),(1.,1.),(1.,1.),(1.,1.),(1.,1.),(1.,
1.),(1.,1.),(1.,1.),(1.,1.),(1.,1.),(1.,1.),(1.,1.),(1.,1.),(1.,1.),(1.,
1.),(1.,1.),(1.,1.),(1.,1.),(1.,1.),(1.,1.),(1.,1.),(1.,1.),(1.,1.),(1.,
1.),(1.,1.),(1.,1.),(1.,1.),(1.,1.),(1.,1.),(1.,1.),(1.,1.),(1.,1.),(1.,
1.),(1.,1.),(1.,1.),(1.,1.),(1.,1.),(1.,1.),(1.,1.),(1.,1.),(1.,1.),(1.,
1.),(1.,1.),(1.,1.),(1.,1.),(1.,1.),(1.,1.),(1.,1.),(1.,1.),(1.,1.),(1.,
1.),(1.,1.),(1.,1.),(1.,1.),(1.,1.),(1.,1.),(1.,1.),(1.,1.),(1.,1.),(1.,
1.),(1.,1.),(1.,1.),(1.,1.),(1.,1.),(1.,1.),(1.,1.),(1.,1.),(1.,1.),(1.,
1.),(1.,1.),(1.,1.),(1.,1.),(1.,1.),(1.,1.),(1.,1.),(1.,1.),(1.,1.),(1.,
1.),(1.,1.),(1.,1.),(1.,1.),(1.,1.),(1.,1.),(1.,1.),(1.,1.),(1.,1.),(1.,
1.),(1.,1.),(1.,1.),(1.,1.),(1.,1.),(1.,1.),(1.,1.),(1.,1.),(1.,1.),(1.,
1.),(1.,1.),(1.,1.),(1.,1.),(1.,1.),(1.,1.),(1.,1.),(1.,1.),(1.,1.),(1.,
1.),(1.,1.),(1.,1.),(1.,1.),(1.,1.),(1.,1.),(1.,1.),(1.,1.),(1.,1.),(1.,
1.),(1.,1.),(1.,1.),(1.,1.),(1.,1.),(1.,1.),(1.,1.),(1.,1.),(1.,1.),(1.,
1.),(1.,1.),(1.,1.),(1.,1.),(1.,1.),(1.,1.),(1.,1.),(1.,1.),(1.,1.),(1.,
1.),(1.,1.),(1.,1.),(1.,1.),(1.,1.),(1.,1.),(1.,1.),(1.,1.),(1.,1.),(1.,
1.),(1.,1.),(1.,1.),(1.,1.),(1.,1.),(1.,1.),(1.,1.),(1.,1.),(1.,1.),(1.,
1.),(1.,1.),(1.,1.),(1.,1.),(1.,1.),(1.,1.),(1.,1.),(1.,1.),(1.,1.),(1.,
1.),(1.,1.),(1.,1.),(1.,1.),(1.,1.),(1.,1.),(1.,1.),(1.,1.),(1.,1.),(1.,
1.),(1.,1.),(1.,1.),(1.,1.),(1.,1.),(1.,1.),(1.,1.),(1.,1.),(1.,1.),(1.,
1.),(1.,1.),(1.,1.),(1.,1.),(1.,1.),(1.,1.),(1.,1.),(1.,1.),(1.,1.),(1.,
1.),(1.,1.),(1.,1.),(1.,1.),(1.,1.),(1.,1.),(1.,1.),(1.,1.),(1.,1.),(1.,
1.),(1.,1.),(1.,1.),(1.,1.),(1.,1.),(1.,1.),(1.,1.),(1.,1.),(1.,1.),(1.,
1.),(1.,1.),(1.,1.),(1.,1.),(1.,1.),(1.,1.),(1.,1.),(1.,1.),(1.,1.),(1.,
1.),(1.,1.),(1.,1.),(1.,1.),(1.,1.),(1.,1.),(1.,1.),(1.,1.),(1.,1.),(1.,
1.),(1.,1.),(1.,1.),(1.,1.),(1.,1.),(1.,1.),(1.,1.),(1.,1.),(1.,1.),(1.,
1.),(1.,1.),(1.,1.),(1.,1.),(1.,1.),(1.,1.),(1.,1.),(1.,1.),(1.,1.),(1.,
1.),(1.,1.),(1.,1.),(1.,1.),(1.,1.),(1.,1.),(1.,1.),(1.,1.),(1.,1.),(1.,
1.),(1.,1.),(1.,1.),(1.,1.),(1.,1.),(1.,1.),(1.,1.),(1.,1.),(1.,1.),(1.,
1.),(1.,1.),(1.,1.),(1.,1.),(1.,1.),(1.,1.),(1.,1.),(1.,1.),(1.,1.),(1.,
1.),(1.,1.),(1.,1.),(1.,1.),(1.,1.),(1.,1.),(1.,1.),(1.,1.),(1.,1.),(1.,
1.),(1.,1.),(1.,1.),(1.,1.),(1.,1.),(1.,1.),(1.,1.),(1.,1.),(1.,1.),(1.,
1.),(1.,1.),(1.,1.),(1.,1.),(1.,1.),(1.,1.),(1.,1.),(1.,1.),(1.,1.),(1.,
1.),(1.,1.),(1.,1.),(1.,1.),(1.,1.),(1.,1.),(1.,1.),(1.,1.),(1.,1.),(1.,
1.),(1.,1.),(1.,1.),(1.,1.),(1.,1.),(1.,1.),(1.,1.),(1.,1.),(1.,1.),(1.,
1.),(1.,1.),(1.,1.),(1.,1.),(1.,1.),(1.,1.),(1.,1.),(1.,1.),(1.,1.),(1.,
1.),(1.,1.),(1.,1.),(1.,1.),(1.,1.),(1.,1.),(1.,1.),(1.,1.),(1.,1.),(1.,
1.),(1.,1.),(1.,1.),(1.,1.),(1.,1.),(1.,1.),(1.,1.),(1.,1.),(1.,1.),(1.,
1.),(1.,1.),(1.,1.),(1.,1.),(1.,1.),(1.,1.),(1.,1.),(1.,1.),(1.,1.),(1.,
1.),(1.,1.),(1.,1.),(1.,1.),(1.,1.),(1.,1.),(1.,1.),(1.,1.),(1.,1.),(1.,
1.),(1.,1.),(1.,1.),(1.,1.),(1.,1.),(1.,1.),(1.,1.),(1.,1.),(1.,1.),(1.,
1.)))
REPRESENTATION_ITEM('')
SURFACE()
);
#263=(
BOUNDED_SURFACE()
B_SPLINE_SURFACE(5,1,((#84229,#84230),(#84231,#84232),(#84233,#84234),(#84235,
#84236),(#84237,#84238),(#84239,#84240),(#84241,#84242),(#84243,#84244),
(#84245,#84246),(#84247,#84248),(#84249,#84250),(#84251,#84252),(#84253,
#84254),(#84255,#84256),(#84257,#84258),(#84259,#84260),(#84261,#84262),
(#84263,#84264),(#84265,#84266),(#84267,#84268),(#84269,#84270),(#84271,
#84272),(#84273,#84274),(#84275,#84276),(#84277,#84278),(#84279,#84280),
(#84281,#84282),(#84283,#84284),(#84285,#84286),(#84287,#84288),(#84289,
#84290),(#84291,#84292),(#84293,#84294),(#84295,#84296),(#84297,#84298),
(#84299,#84300),(#84301,#84302),(#84303,#84304),(#84305,#84306),(#84307,
#84308),(#84309,#84310),(#84311,#84312),(#84313,#84314),(#84315,#84316),
(#84317,#84318),(#84319,#84320),(#84321,#84322),(#84323,#84324),(#84325,
#84326),(#84327,#84328),(#84329,#84330),(#84331,#84332),(#84333,#84334),
(#84335,#84336),(#84337,#84338),(#84339,#84340),(#84341,#84342),(#84343,
#84344),(#84345,#84346),(#84347,#84348),(#84349,#84350),(#84351,#84352),
(#84353,#84354),(#84355,#84356),(#84357,#84358),(#84359,#84360),(#84361,
#84362),(#84363,#84364),(#84365,#84366),(#84367,#84368),(#84369,#84370),
(#84371,#84372),(#84373,#84374),(#84375,#84376),(#84377,#84378),(#84379,
#84380),(#84381,#84382),(#84383,#84384),(#84385,#84386),(#84387,#84388),
(#84389,#84390),(#84391,#84392),(#84393,#84394),(#84395,#84396),(#84397,
#84398),(#84399,#84400),(#84401,#84402),(#84403,#84404),(#84405,#84406),
(#84407,#84408),(#84409,#84410),(#84411,#84412),(#84413,#84414),(#84415,
#84416),(#84417,#84418),(#84419,#84420),(#84421,#84422),(#84423,#84424),
(#84425,#84426),(#84427,#84428),(#84429,#84430),(#84431,#84432),(#84433,
#84434),(#84435,#84436),(#84437,#84438),(#84439,#84440),(#84441,#84442),
(#84443,#84444),(#84445,#84446),(#84447,#84448),(#84449,#84450),(#84451,
#84452),(#84453,#84454),(#84455,#84456),(#84457,#84458),(#84459,#84460),
(#84461,#84462),(#84463,#84464),(#84465,#84466),(#84467,#84468),(#84469,
#84470),(#84471,#84472),(#84473,#84474),(#84475,#84476),(#84477,#84478),
(#84479,#84480),(#84481,#84482),(#84483,#84484),(#84485,#84486),(#84487,
#84488),(#84489,#84490),(#84491,#84492),(#84493,#84494),(#84495,#84496),
(#84497,#84498),(#84499,#84500),(#84501,#84502),(#84503,#84504),(#84505,
#84506),(#84507,#84508),(#84509,#84510),(#84511,#84512),(#84513,#84514),
(#84515,#84516),(#84517,#84518),(#84519,#84520),(#84521,#84522),(#84523,
#84524),(#84525,#84526),(#84527,#84528),(#84529,#84530),(#84531,#84532),
(#84533,#84534),(#84535,#84536),(#84537,#84538),(#84539,#84540),(#84541,
#84542),(#84543,#84544),(#84545,#84546),(#84547,#84548),(#84549,#84550),
(#84551,#84552),(#84553,#84554),(#84555,#84556),(#84557,#84558),(#84559,
#84560),(#84561,#84562),(#84563,#84564),(#84565,#84566),(#84567,#84568),
(#84569,#84570),(#84571,#84572),(#84573,#84574),(#84575,#84576),(#84577,
#84578),(#84579,#84580),(#84581,#84582),(#84583,#84584),(#84585,#84586),
(#84587,#84588),(#84589,#84590),(#84591,#84592),(#84593,#84594),(#84595,
#84596),(#84597,#84598),(#84599,#84600),(#84601,#84602),(#84603,#84604),
(#84605,#84606),(#84607,#84608),(#84609,#84610),(#84611,#84612),(#84613,
#84614),(#84615,#84616),(#84617,#84618),(#84619,#84620),(#84621,#84622),
(#84623,#84624),(#84625,#84626),(#84627,#84628),(#84629,#84630),(#84631,
#84632),(#84633,#84634),(#84635,#84636),(#84637,#84638),(#84639,#84640),
(#84641,#84642),(#84643,#84644),(#84645,#84646),(#84647,#84648),(#84649,
#84650),(#84651,#84652),(#84653,#84654),(#84655,#84656),(#84657,#84658),
(#84659,#84660),(#84661,#84662),(#84663,#84664),(#84665,#84666),(#84667,
#84668),(#84669,#84670),(#84671,#84672),(#84673,#84674),(#84675,#84676),
(#84677,#84678),(#84679,#84680),(#84681,#84682),(#84683,#84684),(#84685,
#84686),(#84687,#84688),(#84689,#84690),(#84691,#84692),(#84693,#84694),
(#84695,#84696),(#84697,#84698),(#84699,#84700),(#84701,#84702),(#84703,
#84704),(#84705,#84706),(#84707,#84708),(#84709,#84710),(#84711,#84712),
(#84713,#84714),(#84715,#84716),(#84717,#84718),(#84719,#84720),(#84721,
#84722),(#84723,#84724),(#84725,#84726),(#84727,#84728),(#84729,#84730),
(#84731,#84732),(#84733,#84734),(#84735,#84736),(#84737,#84738),(#84739,
#84740),(#84741,#84742),(#84743,#84744),(#84745,#84746),(#84747,#84748),
(#84749,#84750),(#84751,#84752),(#84753,#84754),(#84755,#84756),(#84757,
#84758),(#84759,#84760),(#84761,#84762),(#84763,#84764),(#84765,#84766),
(#84767,#84768),(#84769,#84770),(#84771,#84772),(#84773,#84774),(#84775,
#84776),(#84777,#84778),(#84779,#84780),(#84781,#84782),(#84783,#84784),
(#84785,#84786),(#84787,#84788),(#84789,#84790),(#84791,#84792),(#84793,
#84794),(#84795,#84796),(#84797,#84798),(#84799,#84800),(#84801,#84802),
(#84803,#84804),(#84805,#84806),(#84807,#84808),(#84809,#84810),(#84811,
#84812),(#84813,#84814),(#84815,#84816),(#84817,#84818),(#84819,#84820),
(#84821,#84822),(#84823,#84824),(#84825,#84826),(#84827,#84828),(#84829,
#84830),(#84831,#84832),(#84833,#84834),(#84835,#84836),(#84837,#84838),
(#84839,#84840),(#84841,#84842),(#84843,#84844),(#84845,#84846),(#84847,
#84848),(#84849,#84850),(#84851,#84852),(#84853,#84854),(#84855,#84856),
(#84857,#84858),(#84859,#84860),(#84861,#84862),(#84863,#84864),(#84865,
#84866),(#84867,#84868),(#84869,#84870),(#84871,#84872),(#84873,#84874),
(#84875,#84876),(#84877,#84878),(#84879,#84880),(#84881,#84882),(#84883,
#84884),(#84885,#84886),(#84887,#84888),(#84889,#84890),(#84891,#84892),
(#84893,#84894),(#84895,#84896),(#84897,#84898),(#84899,#84900),(#84901,
#84902),(#84903,#84904),(#84905,#84906),(#84907,#84908),(#84909,#84910),
(#84911,#84912),(#84913,#84914),(#84915,#84916),(#84917,#84918),(#84919,
#84920),(#84921,#84922),(#84923,#84924),(#84925,#84926),(#84927,#84928),
(#84929,#84930),(#84931,#84932),(#84933,#84934),(#84935,#84936),(#84937,
#84938),(#84939,#84940),(#84941,#84942),(#84943,#84944),(#84945,#84946),
(#84947,#84948),(#84949,#84950),(#84951,#84952),(#84953,#84954),(#84955,
#84956),(#84957,#84958),(#84959,#84960),(#84961,#84962),(#84963,#84964),
(#84965,#84966),(#84967,#84968),(#84969,#84970),(#84971,#84972),(#84973,
#84974),(#84975,#84976),(#84977,#84978),(#84979,#84980),(#84981,#84982),
(#84983,#84984),(#84985,#84986),(#84987,#84988),(#84989,#84990),(#84991,
#84992),(#84993,#84994),(#84995,#84996),(#84997,#84998),(#84999,#85000),
(#85001,#85002),(#85003,#85004),(#85005,#85006),(#85007,#85008),(#85009,
#85010),(#85011,#85012),(#85013,#85014),(#85015,#85016),(#85017,#85018),
(#85019,#85020),(#85021,#85022),(#85023,#85024),(#85025,#85026),(#85027,
#85028),(#85029,#85030),(#85031,#85032),(#85033,#85034),(#85035,#85036),
(#85037,#85038),(#85039,#85040),(#85041,#85042),(#85043,#85044),(#85045,
#85046),(#85047,#85048),(#85049,#85050),(#85051,#85052),(#85053,#85054),
(#85055,#85056),(#85057,#85058),(#85059,#85060),(#85061,#85062),(#85063,
#85064),(#85065,#85066),(#85067,#85068),(#85069,#85070),(#85071,#85072),
(#85073,#85074),(#85075,#85076),(#85077,#85078),(#85079,#85080),(#85081,
#85082),(#85083,#85084),(#85085,#85086),(#85087,#85088),(#85089,#85090),
(#85091,#85092),(#85093,#85094),(#85095,#85096),(#85097,#85098),(#85099,
#85100),(#85101,#85102),(#85103,#85104),(#85105,#85106),(#85107,#85108),
(#85109,#85110),(#85111,#85112),(#85113,#85114),(#85115,#85116),(#85117,
#85118),(#85119,#85120),(#85121,#85122),(#85123,#85124),(#85125,#85126),
(#85127,#85128),(#85129,#85130),(#85131,#85132),(#85133,#85134),(#85135,
#85136),(#85137,#85138),(#85139,#85140),(#85141,#85142),(#85143,#85144),
(#85145,#85146),(#85147,#85148),(#85149,#85150),(#85151,#85152),(#85153,
#85154),(#85155,#85156),(#85157,#85158),(#85159,#85160),(#85161,#85162),
(#85163,#85164),(#85165,#85166),(#85167,#85168),(#85169,#85170),(#85171,
#85172),(#85173,#85174),(#85175,#85176),(#85177,#85178),(#85179,#85180),
(#85181,#85182),(#85183,#85184),(#85185,#85186),(#85187,#85188),(#85189,
#85190),(#85191,#85192),(#85193,#85194),(#85195,#85196),(#85197,#85198),
(#85199,#85200),(#85201,#85202),(#85203,#85204),(#85205,#85206),(#85207,
#85208),(#85209,#85210),(#85211,#85212),(#85213,#85214),(#85215,#85216),
(#85217,#85218),(#85219,#85220),(#85221,#85222),(#85223,#85224),(#85225,
#85226),(#85227,#85228),(#85229,#85230),(#85231,#85232),(#85233,#85234),
(#85235,#85236),(#85237,#85238),(#85239,#85240),(#85241,#85242),(#85243,
#85244),(#85245,#85246),(#85247,#85248),(#85249,#85250),(#85251,#85252),
(#85253,#85254),(#85255,#85256),(#85257,#85258),(#85259,#85260),(#85261,
#85262),(#85263,#85264),(#85265,#85266),(#85267,#85268),(#85269,#85270),
(#85271,#85272),(#85273,#85274),(#85275,#85276),(#85277,#85278),(#85279,
#85280),(#85281,#85282),(#85283,#85284),(#85285,#85286),(#85287,#85288),
(#85289,#85290),(#85291,#85292),(#85293,#85294),(#85295,#85296),(#85297,
#85298),(#85299,#85300),(#85301,#85302),(#85303,#85304),(#85305,#85306),
(#85307,#85308),(#85309,#85310),(#85311,#85312),(#85313,#85314),(#85315,
#85316),(#85317,#85318),(#85319,#85320),(#85321,#85322),(#85323,#85324),
(#85325,#85326),(#85327,#85328),(#85329,#85330),(#85331,#85332),(#85333,
#85334),(#85335,#85336),(#85337,#85338),(#85339,#85340),(#85341,#85342),
(#85343,#85344),(#85345,#85346),(#85347,#85348),(#85349,#85350),(#85351,
#85352),(#85353,#85354),(#85355,#85356),(#85357,#85358),(#85359,#85360),
(#85361,#85362),(#85363,#85364),(#85365,#85366),(#85367,#85368),(#85369,
#85370),(#85371,#85372),(#85373,#85374),(#85375,#85376),(#85377,#85378),
(#85379,#85380),(#85381,#85382),(#85383,#85384),(#85385,#85386),(#85387,
#85388),(#85389,#85390),(#85391,#85392),(#85393,#85394),(#85395,#85396),
(#85397,#85398),(#85399,#85400),(#85401,#85402),(#85403,#85404),(#85405,
#85406),(#85407,#85408),(#85409,#85410),(#85411,#85412),(#85413,#85414),
(#85415,#85416),(#85417,#85418),(#85419,#85420),(#85421,#85422),(#85423,
#85424),(#85425,#85426),(#85427,#85428),(#85429,#85430),(#85431,#85432),
(#85433,#85434),(#85435,#85436),(#85437,#85438),(#85439,#85440),(#85441,
#85442),(#85443,#85444),(#85445,#85446),(#85447,#85448),(#85449,#85450),
(#85451,#85452),(#85453,#85454),(#85455,#85456),(#85457,#85458),(#85459,
#85460),(#85461,#85462),(#85463,#85464),(#85465,#85466),(#85467,#85468),
(#85469,#85470),(#85471,#85472),(#85473,#85474),(#85475,#85476),(#85477,
#85478),(#85479,#85480),(#85481,#85482),(#85483,#85484),(#85485,#85486),
(#85487,#85488),(#85489,#85490),(#85491,#85492),(#85493,#85494),(#85495,
#85496),(#85497,#85498),(#85499,#85500),(#85501,#85502),(#85503,#85504),
(#85505,#85506),(#85507,#85508),(#85509,#85510),(#85511,#85512),(#85513,
#85514),(#85515,#85516),(#85517,#85518),(#85519,#85520),(#85521,#85522),
(#85523,#85524),(#85525,#85526),(#85527,#85528),(#85529,#85530),(#85531,
#85532),(#85533,#85534),(#85535,#85536),(#85537,#85538),(#85539,#85540),
(#85541,#85542),(#85543,#85544),(#85545,#85546),(#85547,#85548),(#85549,
#85550),(#85551,#85552),(#85553,#85554),(#85555,#85556),(#85557,#85558),
(#85559,#85560),(#85561,#85562),(#85563,#85564),(#85565,#85566),(#85567,
#85568),(#85569,#85570),(#85571,#85572),(#85573,#85574),(#85575,#85576),
(#85577,#85578),(#85579,#85580),(#85581,#85582),(#85583,#85584),(#85585,
#85586),(#85587,#85588),(#85589,#85590),(#85591,#85592),(#85593,#85594),
(#85595,#85596),(#85597,#85598),(#85599,#85600),(#85601,#85602),(#85603,
#85604),(#85605,#85606),(#85607,#85608),(#85609,#85610),(#85611,#85612),
(#85613,#85614),(#85615,#85616),(#85617,#85618),(#85619,#85620),(#85621,
#85622),(#85623,#85624),(#85625,#85626),(#85627,#85628),(#85629,#85630),
(#85631,#85632),(#85633,#85634),(#85635,#85636),(#85637,#85638),(#85639,
#85640),(#85641,#85642),(#85643,#85644),(#85645,#85646),(#85647,#85648),
(#85649,#85650),(#85651,#85652),(#85653,#85654),(#85655,#85656),(#85657,
#85658),(#85659,#85660),(#85661,#85662),(#85663,#85664),(#85665,#85666),
(#85667,#85668),(#85669,#85670),(#85671,#85672),(#85673,#85674),(#85675,
#85676),(#85677,#85678),(#85679,#85680),(#85681,#85682),(#85683,#85684),
(#85685,#85686),(#85687,#85688),(#85689,#85690),(#85691,#85692),(#85693,
#85694),(#85695,#85696),(#85697,#85698),(#85699,#85700),(#85701,#85702),
(#85703,#85704),(#85705,#85706),(#85707,#85708),(#85709,#85710),(#85711,
#85712),(#85713,#85714),(#85715,#85716),(#85717,#85718),(#85719,#85720),
(#85721,#85722),(#85723,#85724),(#85725,#85726),(#85727,#85728),(#85729,
#85730),(#85731,#85732),(#85733,#85734),(#85735,#85736),(#85737,#85738),
(#85739,#85740),(#85741,#85742),(#85743,#85744),(#85745,#85746),(#85747,
#85748),(#85749,#85750),(#85751,#85752),(#85753,#85754),(#85755,#85756),
(#85757,#85758),(#85759,#85760),(#85761,#85762),(#85763,#85764),(#85765,
#85766),(#85767,#85768),(#85769,#85770),(#85771,#85772),(#85773,#85774),
(#85775,#85776),(#85777,#85778),(#85779,#85780),(#85781,#85782),(#85783,
#85784),(#85785,#85786),(#85787,#85788),(#85789,#85790),(#85791,#85792),
(#85793,#85794),(#85795,#85796),(#85797,#85798),(#85799,#85800),(#85801,
#85802),(#85803,#85804),(#85805,#85806),(#85807,#85808),(#85809,#85810),
(#85811,#85812),(#85813,#85814),(#85815,#85816),(#85817,#85818),(#85819,
#85820),(#85821,#85822),(#85823,#85824),(#85825,#85826),(#85827,#85828),
(#85829,#85830),(#85831,#85832),(#85833,#85834),(#85835,#85836),(#85837,
#85838),(#85839,#85840),(#85841,#85842),(#85843,#85844),(#85845,#85846),
(#85847,#85848),(#85849,#85850),(#85851,#85852),(#85853,#85854),(#85855,
#85856),(#85857,#85858),(#85859,#85860),(#85861,#85862),(#85863,#85864),
(#85865,#85866),(#85867,#85868),(#85869,#85870),(#85871,#85872),(#85873,
#85874),(#85875,#85876),(#85877,#85878),(#85879,#85880),(#85881,#85882),
(#85883,#85884),(#85885,#85886),(#85887,#85888),(#85889,#85890),(#85891,
#85892),(#85893,#85894),(#85895,#85896),(#85897,#85898),(#85899,#85900),
(#85901,#85902),(#85903,#85904),(#85905,#85906),(#85907,#85908),(#85909,
#85910),(#85911,#85912),(#85913,#85914),(#85915,#85916),(#85917,#85918),
(#85919,#85920),(#85921,#85922),(#85923,#85924),(#85925,#85926),(#85927,
#85928),(#85929,#85930),(#85931,#85932),(#85933,#85934),(#85935,#85936),
(#85937,#85938),(#85939,#85940),(#85941,#85942),(#85943,#85944),(#85945,
#85946),(#85947,#85948),(#85949,#85950),(#85951,#85952),(#85953,#85954),
(#85955,#85956),(#85957,#85958),(#85959,#85960),(#85961,#85962),(#85963,
#85964),(#85965,#85966),(#85967,#85968),(#85969,#85970),(#85971,#85972),
(#85973,#85974),(#85975,#85976),(#85977,#85978),(#85979,#85980),(#85981,
#85982),(#85983,#85984),(#85985,#85986),(#85987,#85988),(#85989,#85990),
(#85991,#85992),(#85993,#85994),(#85995,#85996),(#85997,#85998),(#85999,
#86000),(#86001,#86002),(#86003,#86004),(#86005,#86006),(#86007,#86008),
(#86009,#86010),(#86011,#86012),(#86013,#86014),(#86015,#86016),(#86017,
#86018),(#86019,#86020),(#86021,#86022),(#86023,#86024),(#86025,#86026),
(#86027,#86028),(#86029,#86030),(#86031,#86032),(#86033,#86034),(#86035,
#86036),(#86037,#86038),(#86039,#86040),(#86041,#86042),(#86043,#86044),
(#86045,#86046),(#86047,#86048),(#86049,#86050),(#86051,#86052),(#86053,
#86054),(#86055,#86056),(#86057,#86058),(#86059,#86060),(#86061,#86062),
(#86063,#86064),(#86065,#86066),(#86067,#86068),(#86069,#86070),(#86071,
#86072),(#86073,#86074),(#86075,#86076),(#86077,#86078),(#86079,#86080),
(#86081,#86082),(#86083,#86084),(#86085,#86086),(#86087,#86088),(#86089,
#86090),(#86091,#86092),(#86093,#86094),(#86095,#86096),(#86097,#86098),
(#86099,#86100),(#86101,#86102),(#86103,#86104),(#86105,#86106),(#86107,
#86108),(#86109,#86110),(#86111,#86112),(#86113,#86114),(#86115,#86116),
(#86117,#86118),(#86119,#86120),(#86121,#86122),(#86123,#86124),(#86125,
#86126),(#86127,#86128),(#86129,#86130),(#86131,#86132),(#86133,#86134),
(#86135,#86136),(#86137,#86138),(#86139,#86140),(#86141,#86142),(#86143,
#86144),(#86145,#86146),(#86147,#86148),(#86149,#86150),(#86151,#86152),
(#86153,#86154),(#86155,#86156),(#86157,#86158),(#86159,#86160),(#86161,
#86162),(#86163,#86164),(#86165,#86166),(#86167,#86168),(#86169,#86170),
(#86171,#86172),(#86173,#86174),(#86175,#86176),(#86177,#86178),(#86179,
#86180),(#86181,#86182),(#86183,#86184),(#86185,#86186),(#86187,#86188),
(#86189,#86190),(#86191,#86192),(#86193,#86194),(#86195,#86196),(#86197,
#86198),(#86199,#86200),(#86201,#86202),(#86203,#86204),(#86205,#86206),
(#86207,#86208),(#86209,#86210),(#86211,#86212),(#86213,#86214),(#86215,
#86216),(#86217,#86218),(#86219,#86220),(#86221,#86222),(#86223,#86224),
(#86225,#86226),(#86227,#86228),(#86229,#86230),(#86231,#86232),(#86233,
#86234),(#86235,#86236),(#86237,#86238)),.UNSPECIFIED.,.F.,.F.,.F.)
B_SPLINE_SURFACE_WITH_KNOTS((6,1,1,1,1,1,1,1,1,1,1,1,1,1,1,1,1,1,1,1,1,
1,1,1,1,1,1,1,1,1,1,1,1,1,1,1,1,1,1,1,1,1,1,1,1,1,1,1,1,1,1,1,1,1,1,1,1,
1,1,1,1,1,1,1,1,1,1,1,1,1,1,1,1,1,1,1,1,1,1,1,1,1,1,1,1,1,1,1,1,1,1,1,1,
1,1,1,1,1,1,1,1,1,1,1,1,1,1,1,1,1,1,1,1,1,1,1,1,1,1,1,1,1,1,1,1,1,1,1,1,
1,1,1,1,1,1,1,1,1,1,1,1,1,1,1,1,1,1,1,1,1,1,1,1,1,1,1,1,1,1,1,1,1,1,1,1,
1,1,1,1,1,1,1,1,1,1,1,1,1,1,1,1,1,1,1,1,1,1,1,1,1,1,1,1,1,1,1,1,1,1,1,1,
1,1,1,1,1,1,1,1,1,1,1,1,1,1,1,1,1,1,1,1,1,1,1,1,1,1,1,1,1,1,1,1,1,1,1,1,
1,1,1,1,1,1,1,1,1,1,1,1,1,1,1,1,1,1,1,1,1,1,1,1,1,1,1,1,1,1,1,1,1,1,1,1,
1,1,1,1,1,1,1,1,1,1,1,1,1,1,1,1,1,1,1,1,1,1,1,1,1,1,1,1,1,1,1,1,1,1,1,1,
1,1,1,1,1,1,1,1,1,1,1,1,1,1,1,1,1,1,1,1,1,1,1,1,1,1,1,1,1,1,1,1,1,1,1,1,
1,1,1,1,1,1,1,1,1,1,1,1,1,1,1,1,1,1,1,1,1,1,1,1,1,1,1,1,1,1,1,1,1,1,1,1,
1,1,1,1,1,1,1,1,1,1,1,1,1,1,1,1,1,1,1,1,1,1,1,1,1,1,1,1,1,1,1,1,1,1,1,1,
1,1,1,1,1,1,1,1,1,1,1,1,1,1,1,1,1,1,1,1,1,1,1,1,1,1,1,1,1,1,1,1,1,1,1,1,
1,1,1,1,1,1,1,1,1,1,1,1,1,1,1,1,1,1,1,1,1,1,1,1,1,1,1,1,1,1,1,1,1,1,1,1,
1,1,1,1,1,1,1,1,1,1,1,1,1,1,1,1,1,1,1,1,1,1,1,1,1,1,1,1,1,1,1,1,1,1,1,1,
1,1,1,1,1,1,1,1,1,1,1,1,1,1,1,1,1,1,1,1,1,1,1,1,1,1,1,1,1,1,1,1,1,1,1,1,
1,1,1,1,1,1,1,1,1,1,1,1,1,1,1,1,1,1,1,1,1,1,1,1,1,1,1,1,1,1,1,1,1,1,1,1,
1,1,1,1,1,1,1,1,1,1,1,1,1,1,1,1,1,1,1,1,1,1,1,1,1,1,1,1,1,1,1,1,1,1,1,1,
1,1,1,1,1,1,1,1,1,1,1,1,1,1,1,1,1,1,1,1,1,1,1,1,1,1,1,1,1,1,1,1,1,1,1,1,
1,1,1,1,1,1,1,1,1,1,1,1,1,1,1,1,1,1,1,1,1,1,1,1,1,1,1,1,1,1,1,1,1,1,1,1,
1,1,1,1,1,1,1,1,1,1,1,1,1,1,1,1,1,1,1,1,1,1,1,1,1,1,1,1,1,1,1,1,1,1,1,1,
1,1,1,1,1,1,1,1,1,1,1,1,1,1,1,1,1,1,1,1,1,1,1,1,1,1,1,1,1,1,1,1,1,1,1,1,
1,1,1,1,1,1,1,1,1,1,1,1,1,1,1,1,1,1,1,1,1,1,1,1,1,1,1,1,1,1,1,1,1,1,1,1,
1,1,1,1,1,1,1,1,1,1,1,1,1,1,1,1,1,1,1,1,1,1,1,1,1,1,1,1,1,1,1,1,1,1,1,1,
1,1,1,1,1,1,1,1,1,1,1,1,1,1,1,1,1,1,1,1,1,1,1,1,1,1,1,1,1,1,1,1,1,1,1,1,
1,1,1,1,1,1,1,1,1,1,1,1,1,1,1,1,1,1,1,1,1,1,1,1,1,1,1,1,1,1,1,1,1,1,1,1,
1,1,1,1,1,1,1,1,1,1,1,1,1,1,1,1,1,1,1,1,1,1,1,1,1,1,1,1,1,1,1,1,1,1,1,1,
1,1,1,1,1,1,1,1,1,1,1,1,1,1,1,1,1,1,1,1,1,1,1,1,1,1,1,1,1,1,1,1,1,1,1,1,
1,1,1,1,1,1,1,6),(2,2),(-1.,-0.999000000000001,-0.998000000000001,-0.997000000000001,
-0.996000000000001,-0.995000000000001,-0.994000000000001,-0.993000000000001,
-0.992000000000001,-0.991000000000001,-0.990000000000001,-0.989000000000001,
-0.988000000000001,-0.987000000000001,-0.986000000000001,-0.985000000000001,
-0.984000000000001,-0.983000000000001,-0.982000000000001,-0.981000000000001,
-0.980000000000001,-0.979000000000001,-0.978000000000001,-0.977000000000001,
-0.976000000000001,-0.975000000000001,-0.974000000000001,-0.973000000000001,
-0.972000000000001,-0.971000000000001,-0.970000000000001,-0.969000000000001,
-0.968000000000001,-0.967000000000001,-0.966000000000001,-0.965000000000001,
-0.964000000000001,-0.963000000000001,-0.962000000000001,-0.961000000000001,
-0.960000000000001,-0.959000000000001,-0.958000000000001,-0.957000000000001,
-0.956000000000001,-0.955000000000001,-0.954000000000001,-0.953000000000001,
-0.952000000000001,-0.951000000000001,-0.950000000000001,-0.949000000000001,
-0.948000000000001,-0.947000000000001,-0.946000000000001,-0.945000000000001,
-0.944000000000001,-0.943000000000001,-0.942000000000001,-0.941000000000001,
-0.940000000000001,-0.939000000000001,-0.938000000000001,-0.937000000000001,
-0.936000000000001,-0.935000000000001,-0.934000000000001,-0.933000000000001,
-0.932000000000001,-0.931000000000001,-0.930000000000001,-0.929000000000001,
-0.928000000000001,-0.927000000000001,-0.926000000000001,-0.925000000000001,
-0.924000000000001,-0.923000000000001,-0.922000000000001,-0.921000000000001,
-0.920000000000001,-0.919000000000001,-0.918000000000001,-0.917000000000001,
-0.916000000000001,-0.915000000000001,-0.914000000000001,-0.913000000000001,
-0.912000000000001,-0.911000000000001,-0.910000000000001,-0.909000000000001,
-0.908000000000001,-0.907000000000001,-0.906000000000001,-0.905000000000001,
-0.904000000000001,-0.903000000000001,-0.902000000000001,-0.901000000000001,
-0.900000000000001,-0.899000000000001,-0.898000000000001,-0.897000000000001,
-0.896000000000001,-0.895000000000001,-0.894000000000001,-0.893000000000001,
-0.892000000000001,-0.891000000000001,-0.890000000000001,-0.889000000000001,
-0.888000000000001,-0.887000000000001,-0.886000000000001,-0.885000000000001,
-0.884000000000001,-0.883000000000001,-0.882000000000001,-0.881000000000001,
-0.880000000000001,-0.879000000000001,-0.878000000000001,-0.877000000000001,
-0.876000000000001,-0.875000000000001,-0.874000000000001,-0.873000000000001,
-0.872000000000001,-0.871000000000001,-0.870000000000001,-0.869000000000001,
-0.868000000000001,-0.867000000000001,-0.866000000000001,-0.865000000000001,
-0.864000000000001,-0.863000000000001,-0.862000000000001,-0.861000000000001,
-0.860000000000001,-0.859000000000001,-0.858000000000001,-0.857000000000001,
-0.856000000000001,-0.855000000000001,-0.854000000000001,-0.853000000000001,
-0.852000000000001,-0.851000000000001,-0.850000000000001,-0.849000000000001,
-0.848000000000001,-0.847000000000001,-0.846000000000001,-0.845000000000001,
-0.844000000000001,-0.843000000000001,-0.842000000000001,-0.841000000000001,
-0.840000000000001,-0.839000000000001,-0.838000000000001,-0.837000000000001,
-0.836000000000001,-0.835000000000001,-0.834000000000001,-0.833000000000001,
-0.832000000000001,-0.831000000000001,-0.830000000000001,-0.829000000000001,
-0.828000000000001,-0.827000000000001,-0.826000000000001,-0.825000000000001,
-0.824000000000001,-0.823000000000001,-0.822000000000001,-0.821000000000001,
-0.820000000000001,-0.819000000000001,-0.818000000000001,-0.817000000000001,
-0.816000000000001,-0.815000000000001,-0.814000000000001,-0.813000000000001,
-0.812000000000001,-0.811000000000001,-0.810000000000001,-0.809000000000001,
-0.808000000000001,-0.807000000000001,-0.806000000000001,-0.805000000000001,
-0.804000000000001,-0.803000000000001,-0.802000000000001,-0.801000000000001,
-0.800000000000001,-0.799000000000001,-0.798000000000001,-0.797000000000001,
-0.796000000000001,-0.795000000000001,-0.794000000000001,-0.793000000000001,
-0.792000000000001,-0.791000000000001,-0.790000000000001,-0.789000000000001,
-0.788000000000001,-0.787000000000001,-0.786000000000001,-0.785000000000001,
-0.784000000000001,-0.783000000000001,-0.782000000000001,-0.781000000000001,
-0.780000000000001,-0.779000000000001,-0.778000000000001,-0.777000000000001,
-0.776000000000001,-0.775000000000001,-0.774000000000001,-0.773000000000001,
-0.772000000000001,-0.771000000000001,-0.770000000000001,-0.769000000000001,
-0.768000000000001,-0.767000000000001,-0.766000000000001,-0.765000000000001,
-0.764000000000001,-0.763000000000001,-0.762000000000001,-0.761000000000001,
-0.760000000000001,-0.759000000000001,-0.758000000000001,-0.757000000000001,
-0.756000000000001,-0.755000000000001,-0.754000000000001,-0.753000000000001,
-0.752000000000001,-0.751000000000001,-0.750000000000001,-0.749000000000001,
-0.748000000000001,-0.747000000000001,-0.746000000000001,-0.745000000000001,
-0.744000000000001,-0.743000000000001,-0.742000000000001,-0.741000000000001,
-0.740000000000001,-0.739000000000001,-0.738000000000001,-0.737000000000001,
-0.736000000000001,-0.735000000000001,-0.734000000000001,-0.733000000000001,
-0.732000000000001,-0.731000000000001,-0.730000000000001,-0.729000000000001,
-0.728000000000001,-0.727000000000001,-0.726000000000001,-0.725000000000001,
-0.724000000000001,-0.723000000000001,-0.722000000000001,-0.721000000000001,
-0.720000000000001,-0.719000000000001,-0.718000000000001,-0.717000000000001,
-0.716000000000001,-0.715000000000001,-0.714000000000001,-0.713000000000001,
-0.712000000000001,-0.711000000000001,-0.710000000000001,-0.709000000000001,
-0.708000000000001,-0.707000000000001,-0.706000000000001,-0.705000000000001,
-0.704000000000001,-0.703000000000001,-0.702000000000001,-0.701000000000001,
-0.700000000000001,-0.699000000000001,-0.698000000000001,-0.697000000000001,
-0.696000000000001,-0.695000000000001,-0.694000000000001,-0.693000000000001,
-0.692000000000001,-0.691000000000001,-0.690000000000001,-0.689000000000001,
-0.688000000000001,-0.687,-0.686,-0.685,-0.684,-0.683,-0.682,-0.681,-0.68,
-0.679,-0.678,-0.677,-0.676,-0.675,-0.674,-0.673,-0.672,-0.671,-0.67,-0.669,
-0.668,-0.667,-0.666,-0.665,-0.664,-0.663,-0.662,-0.661,-0.66,-0.659,-0.658,
-0.657,-0.656,-0.655,-0.654,-0.653,-0.652,-0.651,-0.65,-0.649,-0.648,-0.647,
-0.646,-0.645,-0.644,-0.643,-0.642,-0.641,-0.64,-0.639,-0.638,-0.637,-0.636,
-0.635,-0.634,-0.633,-0.632,-0.631,-0.63,-0.629,-0.628,-0.627,-0.626,-0.625,
-0.624,-0.623,-0.622,-0.621,-0.62,-0.619,-0.618,-0.617,-0.616,-0.615,-0.614,
-0.613,-0.612,-0.611,-0.61,-0.609,-0.608,-0.607,-0.606,-0.605,-0.604,-0.603,
-0.602,-0.601,-0.6,-0.599,-0.598,-0.597,-0.596,-0.595,-0.594,-0.593,-0.592,
-0.591,-0.59,-0.589,-0.588,-0.587,-0.586,-0.585,-0.584,-0.583,-0.582,-0.581,
-0.58,-0.579,-0.578,-0.577,-0.576,-0.575,-0.574,-0.573,-0.572,-0.571,-0.57,
-0.569,-0.568,-0.567,-0.566,-0.565,-0.564,-0.563,-0.562,-0.561,-0.56,-0.559,
-0.558,-0.557,-0.556,-0.555,-0.554,-0.553,-0.552,-0.551,-0.55,-0.549,-0.548,
-0.547,-0.546,-0.545,-0.544,-0.543,-0.542,-0.541,-0.54,-0.539,-0.538,-0.537,
-0.536,-0.535,-0.534,-0.533,-0.532,-0.531,-0.53,-0.529,-0.528,-0.527,-0.526,
-0.525,-0.524,-0.523,-0.522,-0.521,-0.52,-0.519,-0.518,-0.517,-0.516,-0.515,
-0.514,-0.513,-0.512,-0.511,-0.51,-0.509,-0.508,-0.507,-0.506,-0.505,-0.504,
-0.503,-0.502,-0.501,-0.5,-0.499,-0.498,-0.497,-0.496,-0.495,-0.494,-0.493,
-0.492,-0.491,-0.49,-0.489,-0.488,-0.487,-0.486,-0.485,-0.484,-0.483,-0.482,
-0.481,-0.48,-0.479,-0.478,-0.477,-0.476,-0.475,-0.474,-0.473,-0.472,-0.471,
-0.47,-0.469,-0.468,-0.467,-0.466,-0.465,-0.464,-0.463,-0.462,-0.461,-0.46,
-0.459,-0.458,-0.457,-0.456,-0.455,-0.454,-0.453,-0.452,-0.451,-0.45,-0.449,
-0.448,-0.447,-0.446,-0.445,-0.444,-0.443,-0.442,-0.441,-0.44,-0.439,-0.438,
-0.437,-0.436,-0.435,-0.434,-0.433,-0.432,-0.431,-0.43,-0.429,-0.428,-0.427,
-0.426,-0.425,-0.424,-0.423,-0.422,-0.421,-0.42,-0.419,-0.418,-0.417,-0.416,
-0.415,-0.414,-0.413,-0.412,-0.411,-0.41,-0.409,-0.408,-0.407,-0.406,-0.405,
-0.404,-0.403,-0.402,-0.401,-0.4,-0.399,-0.398,-0.397,-0.396,-0.395,-0.394,
-0.393,-0.392,-0.391,-0.39,-0.389,-0.388,-0.387,-0.386,-0.385,-0.384,-0.383,
-0.382,-0.381,-0.38,-0.379,-0.378,-0.377,-0.376,-0.375,-0.374,-0.373,-0.372,
-0.371,-0.37,-0.369,-0.368,-0.367,-0.366,-0.365,-0.364,-0.363,-0.362,-0.361,
-0.36,-0.359,-0.358,-0.357,-0.356,-0.355,-0.354,-0.353,-0.352,-0.351,-0.35,
-0.349,-0.348,-0.347,-0.346,-0.345,-0.344,-0.343,-0.342,-0.341,-0.34,-0.339,
-0.338,-0.337,-0.336,-0.335,-0.334,-0.333,-0.332,-0.331,-0.33,-0.329,-0.328,
-0.327,-0.326,-0.325,-0.324,-0.323,-0.322,-0.321,-0.32,-0.319,-0.318,-0.317,
-0.316,-0.315,-0.314,-0.313,-0.312,-0.311,-0.31,-0.309,-0.308,-0.307,-0.306,
-0.305,-0.304,-0.303,-0.302,-0.301,-0.3,-0.299,-0.298,-0.297,-0.296,-0.295,
-0.294,-0.293,-0.292,-0.291,-0.29,-0.289,-0.288,-0.287,-0.286,-0.285,-0.284,
-0.283,-0.282,-0.281,-0.28,-0.279,-0.278,-0.277,-0.276,-0.275,-0.274,-0.273,
-0.272,-0.271,-0.27,-0.269,-0.268,-0.267,-0.266,-0.265,-0.264,-0.263,-0.262,
-0.261,-0.26,-0.259,-0.258,-0.257,-0.256,-0.255,-0.254,-0.253,-0.252,-0.251,
-0.25,-0.249,-0.248,-0.247,-0.246,-0.245,-0.244,-0.243,-0.242,-0.241,-0.24,
-0.239,-0.238,-0.237,-0.236,-0.235,-0.234,-0.233,-0.232,-0.231,-0.23,-0.229,
-0.228,-0.227,-0.226,-0.225,-0.224,-0.223,-0.222,-0.221,-0.22,-0.219,-0.218,
-0.217,-0.216,-0.215,-0.214,-0.213,-0.212,-0.211,-0.21,-0.209,-0.208,-0.207,
-0.206,-0.205,-0.204,-0.203,-0.202,-0.201,-0.2,-0.199,-0.198,-0.197,-0.196,
-0.195,-0.194,-0.193,-0.192,-0.191,-0.19,-0.189,-0.188,-0.187,-0.186,-0.185,
-0.184,-0.183,-0.182,-0.181,-0.18,-0.179,-0.178,-0.177,-0.176,-0.175,-0.174,
-0.173,-0.172,-0.171,-0.17,-0.169,-0.168,-0.167,-0.166,-0.165,-0.164,-0.163,
-0.162,-0.161,-0.16,-0.159,-0.158,-0.157,-0.156,-0.155,-0.154,-0.153,-0.152,
-0.151,-0.15,-0.149,-0.148,-0.147,-0.146,-0.145,-0.144,-0.143,-0.142,-0.141,
-0.14,-0.139,-0.138,-0.137,-0.136,-0.135,-0.134,-0.133,-0.132,-0.131,-0.13,
-0.129,-0.128,-0.127,-0.126,-0.125,-0.124,-0.123,-0.122,-0.121,-0.12,-0.119,
-0.118,-0.117,-0.116,-0.115,-0.114,-0.113,-0.112,-0.111,-0.11,-0.109,-0.108,
-0.107,-0.106,-0.105,-0.104,-0.103,-0.102,-0.101,-0.1,-0.0990000000000001,
-0.0980000000000001,-0.0970000000000001,-0.0960000000000001,-0.0950000000000001,
-0.0940000000000001,-0.0930000000000001,-0.0920000000000001,-0.0910000000000001,
-0.0900000000000001,-0.0890000000000001,-0.0880000000000001,-0.0870000000000001,
-0.0860000000000001,-0.0850000000000001,-0.0840000000000001,-0.0830000000000001,
-0.0820000000000001,-0.0810000000000001,-0.0800000000000001,-0.0790000000000001,
-0.0780000000000001,-0.0770000000000001,-0.0760000000000001,-0.0750000000000001,
-0.0740000000000001,-0.0730000000000001,-0.0720000000000001,-0.071,-0.07,
-0.069,-0.068,-0.067,-0.066,-0.065,-0.064,-0.063,-0.062,-0.061,-0.06,-0.059,
-0.058,-0.057,-0.056,-0.055,-0.054,-0.053,-0.052,-0.051,-0.05,-0.049,-0.048,
-0.047,-0.046,-0.045,-0.044,-0.043,-0.042,-0.041,-0.04,-0.039,-0.038,-0.037,
-0.036,-0.035,-0.034,-0.033,-0.032,-0.031,-0.03,-0.029,-0.028,-0.027,-0.026,
-0.025,-0.024,-0.023,-0.022,-0.021,-0.02,-0.019,-0.018,-0.017,-0.016,-0.015,
-0.014,-0.013,-0.012,-0.011,-0.01,-0.009,-0.008,-0.007,-0.006,-0.005,-0.004,
-0.003,-0.002,-0.001,0.),(0.,2.),.UNSPECIFIED.)
GEOMETRIC_REPRESENTATION_ITEM()
RATIONAL_B_SPLINE_SURFACE(((1.,1.),(1.,1.),(1.,1.),(1.,1.),(1.,1.),(1.,
1.),(1.,1.),(1.,1.),(1.,1.),(1.,1.),(1.,1.),(1.,1.),(1.,1.),(1.,1.),(1.,
1.),(1.,1.),(1.,1.),(1.,1.),(1.,1.),(1.,1.),(1.,1.),(1.,1.),(1.,1.),(1.,
1.),(1.,1.),(1.,1.),(1.,1.),(1.,1.),(1.,1.),(1.,1.),(1.,1.),(1.,1.),(1.,
1.),(1.,1.),(1.,1.),(1.,1.),(1.,1.),(1.,1.),(1.,1.),(1.,1.),(1.,1.),(1.,
1.),(1.,1.),(1.,1.),(1.,1.),(1.,1.),(1.,1.),(1.,1.),(1.,1.),(1.,1.),(1.,
1.),(1.,1.),(1.,1.),(1.,1.),(1.,1.),(1.,1.),(1.,1.),(1.,1.),(1.,1.),(1.,
1.),(1.,1.),(1.,1.),(1.,1.),(1.,1.),(1.,1.),(1.,1.),(1.,1.),(1.,1.),(1.,
1.),(1.,1.),(1.,1.),(1.,1.),(1.,1.),(1.,1.),(1.,1.),(1.,1.),(1.,1.),(1.,
1.),(1.,1.),(1.,1.),(1.,1.),(1.,1.),(1.,1.),(1.,1.),(1.,1.),(1.,1.),(1.,
1.),(1.,1.),(1.,1.),(1.,1.),(1.,1.),(1.,1.),(1.,1.),(1.,1.),(1.,1.),(1.,
1.),(1.,1.),(1.,1.),(1.,1.),(1.,1.),(1.,1.),(1.,1.),(1.,1.),(1.,1.),(1.,
1.),(1.,1.),(1.,1.),(1.,1.),(1.,1.),(1.,1.),(1.,1.),(1.,1.),(1.,1.),(1.,
1.),(1.,1.),(1.,1.),(1.,1.),(1.,1.),(1.,1.),(1.,1.),(1.,1.),(1.,1.),(1.,
1.),(1.,1.),(1.,1.),(1.,1.),(1.,1.),(1.,1.),(1.,1.),(1.,1.),(1.,1.),(1.,
1.),(1.,1.),(1.,1.),(1.,1.),(1.,1.),(1.,1.),(1.,1.),(1.,1.),(1.,1.),(1.,
1.),(1.,1.),(1.,1.),(1.,1.),(1.,1.),(1.,1.),(1.,1.),(1.,1.),(1.,1.),(1.,
1.),(1.,1.),(1.,1.),(1.,1.),(1.,1.),(1.,1.),(1.,1.),(1.,1.),(1.,1.),(1.,
1.),(1.,1.),(1.,1.),(1.,1.),(1.,1.),(1.,1.),(1.,1.),(1.,1.),(1.,1.),(1.,
1.),(1.,1.),(1.,1.),(1.,1.),(1.,1.),(1.,1.),(1.,1.),(1.,1.),(1.,1.),(1.,
1.),(1.,1.),(1.,1.),(1.,1.),(1.,1.),(1.,1.),(1.,1.),(1.,1.),(1.,1.),(1.,
1.),(1.,1.),(1.,1.),(1.,1.),(1.,1.),(1.,1.),(1.,1.),(1.,1.),(1.,1.),(1.,
1.),(1.,1.),(1.,1.),(1.,1.),(1.,1.),(1.,1.),(1.,1.),(1.,1.),(1.,1.),(1.,
1.),(1.,1.),(1.,1.),(1.,1.),(1.,1.),(1.,1.),(1.,1.),(1.,1.),(1.,1.),(1.,
1.),(1.,1.),(1.,1.),(1.,1.),(1.,1.),(1.,1.),(1.,1.),(1.,1.),(1.,1.),(1.,
1.),(1.,1.),(1.,1.),(1.,1.),(1.,1.),(1.,1.),(1.,1.),(1.,1.),(1.,1.),(1.,
1.),(1.,1.),(1.,1.),(1.,1.),(1.,1.),(1.,1.),(1.,1.),(1.,1.),(1.,1.),(1.,
1.),(1.,1.),(1.,1.),(1.,1.),(1.,1.),(1.,1.),(1.,1.),(1.,1.),(1.,1.),(1.,
1.),(1.,1.),(1.,1.),(1.,1.),(1.,1.),(1.,1.),(1.,1.),(1.,1.),(1.,1.),(1.,
1.),(1.,1.),(1.,1.),(1.,1.),(1.,1.),(1.,1.),(1.,1.),(1.,1.),(1.,1.),(1.,
1.),(1.,1.),(1.,1.),(1.,1.),(1.,1.),(1.,1.),(1.,1.),(1.,1.),(1.,1.),(1.,
1.),(1.,1.),(1.,1.),(1.,1.),(1.,1.),(1.,1.),(1.,1.),(1.,1.),(1.,1.),(1.,
1.),(1.,1.),(1.,1.),(1.,1.),(1.,1.),(1.,1.),(1.,1.),(1.,1.),(1.,1.),(1.,
1.),(1.,1.),(1.,1.),(1.,1.),(1.,1.),(1.,1.),(1.,1.),(1.,1.),(1.,1.),(1.,
1.),(1.,1.),(1.,1.),(1.,1.),(1.,1.),(1.,1.),(1.,1.),(1.,1.),(1.,1.),(1.,
1.),(1.,1.),(1.,1.),(1.,1.),(1.,1.),(1.,1.),(1.,1.),(1.,1.),(1.,1.),(1.,
1.),(1.,1.),(1.,1.),(1.,1.),(1.,1.),(1.,1.),(1.,1.),(1.,1.),(1.,1.),(1.,
1.),(1.,1.),(1.,1.),(1.,1.),(1.,1.),(1.,1.),(1.,1.),(1.,1.),(1.,1.),(1.,
1.),(1.,1.),(1.,1.),(1.,1.),(1.,1.),(1.,1.),(1.,1.),(1.,1.),(1.,1.),(1.,
1.),(1.,1.),(1.,1.),(1.,1.),(1.,1.),(1.,1.),(1.,1.),(1.,1.),(1.,1.),(1.,
1.),(1.,1.),(1.,1.),(1.,1.),(1.,1.),(1.,1.),(1.,1.),(1.,1.),(1.,1.),(1.,
1.),(1.,1.),(1.,1.),(1.,1.),(1.,1.),(1.,1.),(1.,1.),(1.,1.),(1.,1.),(1.,
1.),(1.,1.),(1.,1.),(1.,1.),(1.,1.),(1.,1.),(1.,1.),(1.,1.),(1.,1.),(1.,
1.),(1.,1.),(1.,1.),(1.,1.),(1.,1.),(1.,1.),(1.,1.),(1.,1.),(1.,1.),(1.,
1.),(1.,1.),(1.,1.),(1.,1.),(1.,1.),(1.,1.),(1.,1.),(1.,1.),(1.,1.),(1.,
1.),(1.,1.),(1.,1.),(1.,1.),(1.,1.),(1.,1.),(1.,1.),(1.,1.),(1.,1.),(1.,
1.),(1.,1.),(1.,1.),(1.,1.),(1.,1.),(1.,1.),(1.,1.),(1.,1.),(1.,1.),(1.,
1.),(1.,1.),(1.,1.),(1.,1.),(1.,1.),(1.,1.),(1.,1.),(1.,1.),(1.,1.),(1.,
1.),(1.,1.),(1.,1.),(1.,1.),(1.,1.),(1.,1.),(1.,1.),(1.,1.),(1.,1.),(1.,
1.),(1.,1.),(1.,1.),(1.,1.),(1.,1.),(1.,1.),(1.,1.),(1.,1.),(1.,1.),(1.,
1.),(1.,1.),(1.,1.),(1.,1.),(1.,1.),(1.,1.),(1.,1.),(1.,1.),(1.,1.),(1.,
1.),(1.,1.),(1.,1.),(1.,1.),(1.,1.),(1.,1.),(1.,1.),(1.,1.),(1.,1.),(1.,
1.),(1.,1.),(1.,1.),(1.,1.),(1.,1.),(1.,1.),(1.,1.),(1.,1.),(1.,1.),(1.,
1.),(1.,1.),(1.,1.),(1.,1.),(1.,1.),(1.,1.),(1.,1.),(1.,1.),(1.,1.),(1.,
1.),(1.,1.),(1.,1.),(1.,1.),(1.,1.),(1.,1.),(1.,1.),(1.,1.),(1.,1.),(1.,
1.),(1.,1.),(1.,1.),(1.,1.),(1.,1.),(1.,1.),(1.,1.),(1.,1.),(1.,1.),(1.,
1.),(1.,1.),(1.,1.),(1.,1.),(1.,1.),(1.,1.),(1.,1.),(1.,1.),(1.,1.),(1.,
1.),(1.,1.),(1.,1.),(1.,1.),(1.,1.),(1.,1.),(1.,1.),(1.,1.),(1.,1.),(1.,
1.),(1.,1.),(1.,1.),(1.,1.),(1.,1.),(1.,1.),(1.,1.),(1.,1.),(1.,1.),(1.,
1.),(1.,1.),(1.,1.),(1.,1.),(1.,1.),(1.,1.),(1.,1.),(1.,1.),(1.,1.),(1.,
1.),(1.,1.),(1.,1.),(1.,1.),(1.,1.),(1.,1.),(1.,1.),(1.,1.),(1.,1.),(1.,
1.),(1.,1.),(1.,1.),(1.,1.),(1.,1.),(1.,1.),(1.,1.),(1.,1.),(1.,1.),(1.,
1.),(1.,1.),(1.,1.),(1.,1.),(1.,1.),(1.,1.),(1.,1.),(1.,1.),(1.,1.),(1.,
1.),(1.,1.),(1.,1.),(1.,1.),(1.,1.),(1.,1.),(1.,1.),(1.,1.),(1.,1.),(1.,
1.),(1.,1.),(1.,1.),(1.,1.),(1.,1.),(1.,1.),(1.,1.),(1.,1.),(1.,1.),(1.,
1.),(1.,1.),(1.,1.),(1.,1.),(1.,1.),(1.,1.),(1.,1.),(1.,1.),(1.,1.),(1.,
1.),(1.,1.),(1.,1.),(1.,1.),(1.,1.),(1.,1.),(1.,1.),(1.,1.),(1.,1.),(1.,
1.),(1.,1.),(1.,1.),(1.,1.),(1.,1.),(1.,1.),(1.,1.),(1.,1.),(1.,1.),(1.,
1.),(1.,1.),(1.,1.),(1.,1.),(1.,1.),(1.,1.),(1.,1.),(1.,1.),(1.,1.),(1.,
1.),(1.,1.),(1.,1.),(1.,1.),(1.,1.),(1.,1.),(1.,1.),(1.,1.),(1.,1.),(1.,
1.),(1.,1.),(1.,1.),(1.,1.),(1.,1.),(1.,1.),(1.,1.),(1.,1.),(1.,1.),(1.,
1.),(1.,1.),(1.,1.),(1.,1.),(1.,1.),(1.,1.),(1.,1.),(1.,1.),(1.,1.),(1.,
1.),(1.,1.),(1.,1.),(1.,1.),(1.,1.),(1.,1.),(1.,1.),(1.,1.),(1.,1.),(1.,
1.),(1.,1.),(1.,1.),(1.,1.),(1.,1.),(1.,1.),(1.,1.),(1.,1.),(1.,1.),(1.,
1.),(1.,1.),(1.,1.),(1.,1.),(1.,1.),(1.,1.),(1.,1.),(1.,1.),(1.,1.),(1.,
1.),(1.,1.),(1.,1.),(1.,1.),(1.,1.),(1.,1.),(1.,1.),(1.,1.),(1.,1.),(1.,
1.),(1.,1.),(1.,1.),(1.,1.),(1.,1.),(1.,1.),(1.,1.),(1.,1.),(1.,1.),(1.,
1.),(1.,1.),(1.,1.),(1.,1.),(1.,1.),(1.,1.),(1.,1.),(1.,1.),(1.,1.),(1.,
1.),(1.,1.),(1.,1.),(1.,1.),(1.,1.),(1.,1.),(1.,1.),(1.,1.),(1.,1.),(1.,
1.),(1.,1.),(1.,1.),(1.,1.),(1.,1.),(1.,1.),(1.,1.),(1.,1.),(1.,1.),(1.,
1.),(1.,1.),(1.,1.),(1.,1.),(1.,1.),(1.,1.),(1.,1.),(1.,1.),(1.,1.),(1.,
1.),(1.,1.),(1.,1.),(1.,1.),(1.,1.),(1.,1.),(1.,1.),(1.,1.),(1.,1.),(1.,
1.),(1.,1.),(1.,1.),(1.,1.),(1.,1.),(1.,1.),(1.,1.),(1.,1.),(1.,1.),(1.,
1.),(1.,1.),(1.,1.),(1.,1.),(1.,1.),(1.,1.),(1.,1.),(1.,1.),(1.,1.),(1.,
1.),(1.,1.),(1.,1.),(1.,1.),(1.,1.),(1.,1.),(1.,1.),(1.,1.),(1.,1.),(1.,
1.),(1.,1.),(1.,1.),(1.,1.),(1.,1.),(1.,1.),(1.,1.),(1.,1.),(1.,1.),(1.,
1.),(1.,1.),(1.,1.),(1.,1.),(1.,1.),(1.,1.),(1.,1.),(1.,1.),(1.,1.),(1.,
1.),(1.,1.),(1.,1.),(1.,1.),(1.,1.),(1.,1.),(1.,1.),(1.,1.),(1.,1.),(1.,
1.),(1.,1.),(1.,1.),(1.,1.),(1.,1.),(1.,1.),(1.,1.),(1.,1.),(1.,1.),(1.,
1.),(1.,1.),(1.,1.),(1.,1.),(1.,1.),(1.,1.),(1.,1.),(1.,1.),(1.,1.),(1.,
1.),(1.,1.),(1.,1.),(1.,1.),(1.,1.),(1.,1.),(1.,1.),(1.,1.),(1.,1.),(1.,
1.),(1.,1.),(1.,1.),(1.,1.),(1.,1.),(1.,1.),(1.,1.),(1.,1.),(1.,1.),(1.,
1.),(1.,1.),(1.,1.),(1.,1.),(1.,1.),(1.,1.),(1.,1.),(1.,1.),(1.,1.),(1.,
1.),(1.,1.),(1.,1.),(1.,1.),(1.,1.),(1.,1.),(1.,1.),(1.,1.),(1.,1.),(1.,
1.),(1.,1.),(1.,1.),(1.,1.),(1.,1.),(1.,1.),(1.,1.),(1.,1.),(1.,1.),(1.,
1.),(1.,1.),(1.,1.),(1.,1.),(1.,1.),(1.,1.),(1.,1.),(1.,1.),(1.,1.),(1.,
1.),(1.,1.),(1.,1.),(1.,1.),(1.,1.),(1.,1.),(1.,1.),(1.,1.),(1.,1.),(1.,
1.),(1.,1.),(1.,1.),(1.,1.),(1.,1.),(1.,1.),(1.,1.),(1.,1.),(1.,1.),(1.,
1.),(1.,1.),(1.,1.),(1.,1.),(1.,1.),(1.,1.),(1.,1.),(1.,1.),(1.,1.),(1.,
1.),(1.,1.),(1.,1.),(1.,1.),(1.,1.),(1.,1.),(1.,1.),(1.,1.),(1.,1.),(1.,
1.),(1.,1.),(1.,1.),(1.,1.),(1.,1.),(1.,1.),(1.,1.),(1.,1.),(1.,1.),(1.,
1.),(1.,1.),(1.,1.),(1.,1.),(1.,1.),(1.,1.),(1.,1.),(1.,1.),(1.,1.),(1.,
1.),(1.,1.),(1.,1.),(1.,1.),(1.,1.),(1.,1.),(1.,1.),(1.,1.),(1.,1.),(1.,
1.),(1.,1.),(1.,1.),(1.,1.),(1.,1.),(1.,1.),(1.,1.),(1.,1.),(1.,1.),(1.,
1.),(1.,1.),(1.,1.),(1.,1.),(1.,1.),(1.,1.),(1.,1.),(1.,1.),(1.,1.),(1.,
1.),(1.,1.),(1.,1.),(1.,1.),(1.,1.),(1.,1.),(1.,1.),(1.,1.),(1.,1.),(1.,
1.),(1.,1.),(1.,1.),(1.,1.),(1.,1.),(1.,1.),(1.,1.),(1.,1.),(1.,1.),(1.,
1.),(1.,1.),(1.,1.),(1.,1.),(1.,1.),(1.,1.),(1.,1.),(1.,1.),(1.,1.),(1.,
1.),(1.,1.),(1.,1.),(1.,1.),(1.,1.),(1.,1.),(1.,1.),(1.,1.),(1.,1.),(1.,
1.),(1.,1.),(1.,1.),(1.,1.),(1.,1.),(1.,1.),(1.,1.),(1.,1.),(1.,1.),(1.,
1.),(1.,1.),(1.,1.),(1.,1.),(1.,1.),(1.,1.),(1.,1.),(1.,1.),(1.,1.),(1.,
1.),(1.,1.),(1.,1.),(1.,1.),(1.,1.),(1.,1.),(1.,1.),(1.,1.),(1.,1.),(1.,
1.)))
REPRESENTATION_ITEM('')
SURFACE()
);
#264=(
BOUNDED_SURFACE()
B_SPLINE_SURFACE(5,1,((#86297,#86298),(#86299,#86300),(#86301,#86302),(#86303,
#86304),(#86305,#86306),(#86307,#86308),(#86309,#86310),(#86311,#86312),
(#86313,#86314),(#86315,#86316),(#86317,#86318),(#86319,#86320),(#86321,
#86322),(#86323,#86324),(#86325,#86326),(#86327,#86328),(#86329,#86330),
(#86331,#86332),(#86333,#86334),(#86335,#86336),(#86337,#86338),(#86339,
#86340),(#86341,#86342),(#86343,#86344),(#86345,#86346),(#86347,#86348),
(#86349,#86350),(#86351,#86352),(#86353,#86354),(#86355,#86356),(#86357,
#86358),(#86359,#86360),(#86361,#86362),(#86363,#86364),(#86365,#86366),
(#86367,#86368),(#86369,#86370),(#86371,#86372),(#86373,#86374),(#86375,
#86376),(#86377,#86378),(#86379,#86380),(#86381,#86382),(#86383,#86384),
(#86385,#86386),(#86387,#86388),(#86389,#86390),(#86391,#86392),(#86393,
#86394),(#86395,#86396),(#86397,#86398),(#86399,#86400),(#86401,#86402),
(#86403,#86404),(#86405,#86406),(#86407,#86408),(#86409,#86410),(#86411,
#86412),(#86413,#86414),(#86415,#86416),(#86417,#86418),(#86419,#86420),
(#86421,#86422),(#86423,#86424),(#86425,#86426),(#86427,#86428),(#86429,
#86430),(#86431,#86432),(#86433,#86434),(#86435,#86436),(#86437,#86438),
(#86439,#86440),(#86441,#86442),(#86443,#86444),(#86445,#86446),(#86447,
#86448),(#86449,#86450),(#86451,#86452),(#86453,#86454),(#86455,#86456),
(#86457,#86458),(#86459,#86460),(#86461,#86462),(#86463,#86464),(#86465,
#86466),(#86467,#86468),(#86469,#86470),(#86471,#86472),(#86473,#86474),
(#86475,#86476),(#86477,#86478),(#86479,#86480),(#86481,#86482),(#86483,
#86484),(#86485,#86486),(#86487,#86488),(#86489,#86490),(#86491,#86492),
(#86493,#86494),(#86495,#86496),(#86497,#86498),(#86499,#86500),(#86501,
#86502),(#86503,#86504),(#86505,#86506),(#86507,#86508),(#86509,#86510),
(#86511,#86512),(#86513,#86514),(#86515,#86516),(#86517,#86518),(#86519,
#86520),(#86521,#86522),(#86523,#86524),(#86525,#86526),(#86527,#86528),
(#86529,#86530),(#86531,#86532),(#86533,#86534),(#86535,#86536),(#86537,
#86538),(#86539,#86540),(#86541,#86542),(#86543,#86544),(#86545,#86546),
(#86547,#86548),(#86549,#86550),(#86551,#86552),(#86553,#86554),(#86555,
#86556),(#86557,#86558),(#86559,#86560),(#86561,#86562),(#86563,#86564),
(#86565,#86566),(#86567,#86568),(#86569,#86570),(#86571,#86572),(#86573,
#86574),(#86575,#86576),(#86577,#86578),(#86579,#86580),(#86581,#86582),
(#86583,#86584),(#86585,#86586),(#86587,#86588),(#86589,#86590),(#86591,
#86592),(#86593,#86594),(#86595,#86596),(#86597,#86598),(#86599,#86600),
(#86601,#86602),(#86603,#86604),(#86605,#86606),(#86607,#86608),(#86609,
#86610),(#86611,#86612),(#86613,#86614),(#86615,#86616),(#86617,#86618),
(#86619,#86620),(#86621,#86622),(#86623,#86624),(#86625,#86626),(#86627,
#86628),(#86629,#86630),(#86631,#86632),(#86633,#86634),(#86635,#86636),
(#86637,#86638),(#86639,#86640),(#86641,#86642),(#86643,#86644),(#86645,
#86646),(#86647,#86648),(#86649,#86650),(#86651,#86652),(#86653,#86654),
(#86655,#86656),(#86657,#86658),(#86659,#86660),(#86661,#86662),(#86663,
#86664),(#86665,#86666),(#86667,#86668),(#86669,#86670),(#86671,#86672),
(#86673,#86674),(#86675,#86676),(#86677,#86678),(#86679,#86680),(#86681,
#86682),(#86683,#86684),(#86685,#86686),(#86687,#86688),(#86689,#86690),
(#86691,#86692),(#86693,#86694),(#86695,#86696),(#86697,#86698),(#86699,
#86700),(#86701,#86702),(#86703,#86704),(#86705,#86706),(#86707,#86708),
(#86709,#86710),(#86711,#86712),(#86713,#86714),(#86715,#86716),(#86717,
#86718),(#86719,#86720),(#86721,#86722),(#86723,#86724),(#86725,#86726),
(#86727,#86728),(#86729,#86730),(#86731,#86732),(#86733,#86734),(#86735,
#86736),(#86737,#86738),(#86739,#86740),(#86741,#86742),(#86743,#86744),
(#86745,#86746),(#86747,#86748),(#86749,#86750),(#86751,#86752),(#86753,
#86754),(#86755,#86756),(#86757,#86758),(#86759,#86760),(#86761,#86762),
(#86763,#86764),(#86765,#86766),(#86767,#86768),(#86769,#86770),(#86771,
#86772),(#86773,#86774),(#86775,#86776),(#86777,#86778),(#86779,#86780),
(#86781,#86782),(#86783,#86784),(#86785,#86786),(#86787,#86788),(#86789,
#86790),(#86791,#86792),(#86793,#86794),(#86795,#86796),(#86797,#86798),
(#86799,#86800),(#86801,#86802),(#86803,#86804),(#86805,#86806),(#86807,
#86808),(#86809,#86810),(#86811,#86812),(#86813,#86814),(#86815,#86816),
(#86817,#86818),(#86819,#86820),(#86821,#86822),(#86823,#86824),(#86825,
#86826),(#86827,#86828),(#86829,#86830),(#86831,#86832),(#86833,#86834),
(#86835,#86836),(#86837,#86838),(#86839,#86840),(#86841,#86842),(#86843,
#86844),(#86845,#86846),(#86847,#86848),(#86849,#86850),(#86851,#86852),
(#86853,#86854),(#86855,#86856),(#86857,#86858),(#86859,#86860),(#86861,
#86862),(#86863,#86864),(#86865,#86866),(#86867,#86868),(#86869,#86870),
(#86871,#86872),(#86873,#86874),(#86875,#86876),(#86877,#86878),(#86879,
#86880),(#86881,#86882),(#86883,#86884),(#86885,#86886),(#86887,#86888),
(#86889,#86890),(#86891,#86892),(#86893,#86894),(#86895,#86896),(#86897,
#86898),(#86899,#86900),(#86901,#86902),(#86903,#86904),(#86905,#86906),
(#86907,#86908),(#86909,#86910),(#86911,#86912),(#86913,#86914),(#86915,
#86916),(#86917,#86918),(#86919,#86920),(#86921,#86922),(#86923,#86924),
(#86925,#86926),(#86927,#86928),(#86929,#86930),(#86931,#86932),(#86933,
#86934),(#86935,#86936),(#86937,#86938),(#86939,#86940),(#86941,#86942),
(#86943,#86944),(#86945,#86946),(#86947,#86948),(#86949,#86950),(#86951,
#86952),(#86953,#86954),(#86955,#86956),(#86957,#86958),(#86959,#86960),
(#86961,#86962),(#86963,#86964),(#86965,#86966),(#86967,#86968),(#86969,
#86970),(#86971,#86972),(#86973,#86974),(#86975,#86976),(#86977,#86978),
(#86979,#86980),(#86981,#86982),(#86983,#86984),(#86985,#86986),(#86987,
#86988),(#86989,#86990),(#86991,#86992),(#86993,#86994),(#86995,#86996),
(#86997,#86998),(#86999,#87000),(#87001,#87002),(#87003,#87004),(#87005,
#87006),(#87007,#87008),(#87009,#87010),(#87011,#87012),(#87013,#87014),
(#87015,#87016),(#87017,#87018),(#87019,#87020),(#87021,#87022),(#87023,
#87024),(#87025,#87026),(#87027,#87028),(#87029,#87030),(#87031,#87032),
(#87033,#87034),(#87035,#87036),(#87037,#87038),(#87039,#87040),(#87041,
#87042),(#87043,#87044),(#87045,#87046),(#87047,#87048),(#87049,#87050),
(#87051,#87052),(#87053,#87054),(#87055,#87056),(#87057,#87058),(#87059,
#87060),(#87061,#87062),(#87063,#87064),(#87065,#87066),(#87067,#87068),
(#87069,#87070),(#87071,#87072),(#87073,#87074),(#87075,#87076),(#87077,
#87078),(#87079,#87080),(#87081,#87082),(#87083,#87084),(#87085,#87086),
(#87087,#87088),(#87089,#87090),(#87091,#87092),(#87093,#87094),(#87095,
#87096),(#87097,#87098),(#87099,#87100),(#87101,#87102),(#87103,#87104),
(#87105,#87106),(#87107,#87108),(#87109,#87110),(#87111,#87112),(#87113,
#87114),(#87115,#87116),(#87117,#87118),(#87119,#87120),(#87121,#87122),
(#87123,#87124),(#87125,#87126),(#87127,#87128),(#87129,#87130),(#87131,
#87132),(#87133,#87134),(#87135,#87136),(#87137,#87138),(#87139,#87140),
(#87141,#87142),(#87143,#87144),(#87145,#87146),(#87147,#87148),(#87149,
#87150),(#87151,#87152),(#87153,#87154),(#87155,#87156),(#87157,#87158),
(#87159,#87160),(#87161,#87162),(#87163,#87164),(#87165,#87166),(#87167,
#87168),(#87169,#87170),(#87171,#87172),(#87173,#87174),(#87175,#87176),
(#87177,#87178),(#87179,#87180),(#87181,#87182),(#87183,#87184),(#87185,
#87186),(#87187,#87188),(#87189,#87190),(#87191,#87192),(#87193,#87194),
(#87195,#87196),(#87197,#87198),(#87199,#87200),(#87201,#87202),(#87203,
#87204),(#87205,#87206),(#87207,#87208),(#87209,#87210),(#87211,#87212),
(#87213,#87214),(#87215,#87216),(#87217,#87218),(#87219,#87220),(#87221,
#87222),(#87223,#87224),(#87225,#87226),(#87227,#87228),(#87229,#87230),
(#87231,#87232),(#87233,#87234),(#87235,#87236),(#87237,#87238),(#87239,
#87240),(#87241,#87242),(#87243,#87244),(#87245,#87246),(#87247,#87248),
(#87249,#87250),(#87251,#87252),(#87253,#87254),(#87255,#87256),(#87257,
#87258),(#87259,#87260),(#87261,#87262),(#87263,#87264),(#87265,#87266),
(#87267,#87268),(#87269,#87270),(#87271,#87272),(#87273,#87274),(#87275,
#87276),(#87277,#87278),(#87279,#87280),(#87281,#87282),(#87283,#87284),
(#87285,#87286),(#87287,#87288),(#87289,#87290),(#87291,#87292),(#87293,
#87294),(#87295,#87296),(#87297,#87298),(#87299,#87300),(#87301,#87302),
(#87303,#87304),(#87305,#87306),(#87307,#87308),(#87309,#87310),(#87311,
#87312),(#87313,#87314),(#87315,#87316),(#87317,#87318),(#87319,#87320),
(#87321,#87322),(#87323,#87324),(#87325,#87326),(#87327,#87328),(#87329,
#87330),(#87331,#87332),(#87333,#87334),(#87335,#87336),(#87337,#87338),
(#87339,#87340),(#87341,#87342),(#87343,#87344),(#87345,#87346),(#87347,
#87348),(#87349,#87350),(#87351,#87352),(#87353,#87354),(#87355,#87356),
(#87357,#87358),(#87359,#87360),(#87361,#87362),(#87363,#87364),(#87365,
#87366),(#87367,#87368),(#87369,#87370),(#87371,#87372),(#87373,#87374),
(#87375,#87376),(#87377,#87378),(#87379,#87380),(#87381,#87382),(#87383,
#87384),(#87385,#87386),(#87387,#87388),(#87389,#87390),(#87391,#87392),
(#87393,#87394),(#87395,#87396),(#87397,#87398),(#87399,#87400),(#87401,
#87402),(#87403,#87404),(#87405,#87406),(#87407,#87408),(#87409,#87410),
(#87411,#87412),(#87413,#87414),(#87415,#87416),(#87417,#87418),(#87419,
#87420),(#87421,#87422),(#87423,#87424),(#87425,#87426),(#87427,#87428),
(#87429,#87430),(#87431,#87432),(#87433,#87434),(#87435,#87436),(#87437,
#87438),(#87439,#87440),(#87441,#87442),(#87443,#87444),(#87445,#87446),
(#87447,#87448),(#87449,#87450),(#87451,#87452),(#87453,#87454),(#87455,
#87456),(#87457,#87458),(#87459,#87460),(#87461,#87462),(#87463,#87464),
(#87465,#87466),(#87467,#87468),(#87469,#87470),(#87471,#87472),(#87473,
#87474),(#87475,#87476),(#87477,#87478),(#87479,#87480),(#87481,#87482),
(#87483,#87484),(#87485,#87486),(#87487,#87488),(#87489,#87490),(#87491,
#87492),(#87493,#87494),(#87495,#87496),(#87497,#87498),(#87499,#87500),
(#87501,#87502),(#87503,#87504),(#87505,#87506),(#87507,#87508),(#87509,
#87510),(#87511,#87512),(#87513,#87514),(#87515,#87516),(#87517,#87518),
(#87519,#87520),(#87521,#87522),(#87523,#87524),(#87525,#87526),(#87527,
#87528),(#87529,#87530),(#87531,#87532),(#87533,#87534),(#87535,#87536),
(#87537,#87538),(#87539,#87540),(#87541,#87542),(#87543,#87544),(#87545,
#87546),(#87547,#87548),(#87549,#87550),(#87551,#87552),(#87553,#87554),
(#87555,#87556),(#87557,#87558),(#87559,#87560),(#87561,#87562),(#87563,
#87564),(#87565,#87566),(#87567,#87568),(#87569,#87570),(#87571,#87572),
(#87573,#87574),(#87575,#87576),(#87577,#87578),(#87579,#87580),(#87581,
#87582),(#87583,#87584),(#87585,#87586),(#87587,#87588),(#87589,#87590),
(#87591,#87592),(#87593,#87594),(#87595,#87596),(#87597,#87598),(#87599,
#87600),(#87601,#87602),(#87603,#87604),(#87605,#87606),(#87607,#87608),
(#87609,#87610),(#87611,#87612),(#87613,#87614),(#87615,#87616),(#87617,
#87618),(#87619,#87620),(#87621,#87622),(#87623,#87624),(#87625,#87626),
(#87627,#87628),(#87629,#87630),(#87631,#87632),(#87633,#87634),(#87635,
#87636),(#87637,#87638),(#87639,#87640),(#87641,#87642),(#87643,#87644),
(#87645,#87646),(#87647,#87648),(#87649,#87650),(#87651,#87652),(#87653,
#87654),(#87655,#87656),(#87657,#87658),(#87659,#87660),(#87661,#87662),
(#87663,#87664),(#87665,#87666),(#87667,#87668),(#87669,#87670),(#87671,
#87672),(#87673,#87674),(#87675,#87676),(#87677,#87678),(#87679,#87680),
(#87681,#87682),(#87683,#87684),(#87685,#87686),(#87687,#87688),(#87689,
#87690),(#87691,#87692),(#87693,#87694),(#87695,#87696),(#87697,#87698),
(#87699,#87700),(#87701,#87702),(#87703,#87704),(#87705,#87706),(#87707,
#87708),(#87709,#87710),(#87711,#87712),(#87713,#87714),(#87715,#87716),
(#87717,#87718),(#87719,#87720),(#87721,#87722),(#87723,#87724),(#87725,
#87726),(#87727,#87728),(#87729,#87730),(#87731,#87732),(#87733,#87734),
(#87735,#87736),(#87737,#87738),(#87739,#87740),(#87741,#87742),(#87743,
#87744),(#87745,#87746),(#87747,#87748),(#87749,#87750),(#87751,#87752),
(#87753,#87754),(#87755,#87756),(#87757,#87758),(#87759,#87760),(#87761,
#87762),(#87763,#87764),(#87765,#87766),(#87767,#87768),(#87769,#87770),
(#87771,#87772),(#87773,#87774),(#87775,#87776),(#87777,#87778),(#87779,
#87780),(#87781,#87782),(#87783,#87784),(#87785,#87786),(#87787,#87788),
(#87789,#87790),(#87791,#87792),(#87793,#87794),(#87795,#87796),(#87797,
#87798),(#87799,#87800),(#87801,#87802),(#87803,#87804),(#87805,#87806),
(#87807,#87808),(#87809,#87810),(#87811,#87812),(#87813,#87814),(#87815,
#87816),(#87817,#87818),(#87819,#87820),(#87821,#87822),(#87823,#87824),
(#87825,#87826),(#87827,#87828),(#87829,#87830),(#87831,#87832),(#87833,
#87834),(#87835,#87836),(#87837,#87838),(#87839,#87840),(#87841,#87842),
(#87843,#87844),(#87845,#87846),(#87847,#87848),(#87849,#87850),(#87851,
#87852),(#87853,#87854),(#87855,#87856),(#87857,#87858),(#87859,#87860),
(#87861,#87862),(#87863,#87864),(#87865,#87866),(#87867,#87868),(#87869,
#87870),(#87871,#87872),(#87873,#87874),(#87875,#87876),(#87877,#87878),
(#87879,#87880),(#87881,#87882),(#87883,#87884),(#87885,#87886),(#87887,
#87888),(#87889,#87890),(#87891,#87892),(#87893,#87894),(#87895,#87896),
(#87897,#87898),(#87899,#87900),(#87901,#87902),(#87903,#87904),(#87905,
#87906),(#87907,#87908),(#87909,#87910),(#87911,#87912),(#87913,#87914),
(#87915,#87916),(#87917,#87918),(#87919,#87920),(#87921,#87922),(#87923,
#87924),(#87925,#87926),(#87927,#87928),(#87929,#87930),(#87931,#87932),
(#87933,#87934),(#87935,#87936),(#87937,#87938),(#87939,#87940),(#87941,
#87942),(#87943,#87944),(#87945,#87946),(#87947,#87948),(#87949,#87950),
(#87951,#87952),(#87953,#87954),(#87955,#87956),(#87957,#87958),(#87959,
#87960),(#87961,#87962),(#87963,#87964),(#87965,#87966),(#87967,#87968),
(#87969,#87970),(#87971,#87972),(#87973,#87974),(#87975,#87976),(#87977,
#87978),(#87979,#87980),(#87981,#87982),(#87983,#87984),(#87985,#87986),
(#87987,#87988),(#87989,#87990),(#87991,#87992),(#87993,#87994),(#87995,
#87996),(#87997,#87998),(#87999,#88000),(#88001,#88002),(#88003,#88004),
(#88005,#88006),(#88007,#88008),(#88009,#88010),(#88011,#88012),(#88013,
#88014),(#88015,#88016),(#88017,#88018),(#88019,#88020),(#88021,#88022),
(#88023,#88024),(#88025,#88026),(#88027,#88028),(#88029,#88030),(#88031,
#88032),(#88033,#88034),(#88035,#88036),(#88037,#88038),(#88039,#88040),
(#88041,#88042),(#88043,#88044),(#88045,#88046),(#88047,#88048),(#88049,
#88050),(#88051,#88052),(#88053,#88054),(#88055,#88056),(#88057,#88058),
(#88059,#88060),(#88061,#88062),(#88063,#88064),(#88065,#88066),(#88067,
#88068),(#88069,#88070),(#88071,#88072),(#88073,#88074),(#88075,#88076),
(#88077,#88078),(#88079,#88080),(#88081,#88082),(#88083,#88084),(#88085,
#88086),(#88087,#88088),(#88089,#88090),(#88091,#88092),(#88093,#88094),
(#88095,#88096),(#88097,#88098),(#88099,#88100),(#88101,#88102),(#88103,
#88104),(#88105,#88106),(#88107,#88108),(#88109,#88110),(#88111,#88112),
(#88113,#88114),(#88115,#88116),(#88117,#88118),(#88119,#88120),(#88121,
#88122),(#88123,#88124),(#88125,#88126),(#88127,#88128),(#88129,#88130),
(#88131,#88132),(#88133,#88134),(#88135,#88136),(#88137,#88138),(#88139,
#88140),(#88141,#88142),(#88143,#88144),(#88145,#88146),(#88147,#88148),
(#88149,#88150),(#88151,#88152),(#88153,#88154),(#88155,#88156),(#88157,
#88158),(#88159,#88160),(#88161,#88162),(#88163,#88164),(#88165,#88166),
(#88167,#88168),(#88169,#88170),(#88171,#88172),(#88173,#88174),(#88175,
#88176),(#88177,#88178),(#88179,#88180),(#88181,#88182),(#88183,#88184),
(#88185,#88186),(#88187,#88188),(#88189,#88190),(#88191,#88192),(#88193,
#88194),(#88195,#88196),(#88197,#88198),(#88199,#88200),(#88201,#88202),
(#88203,#88204),(#88205,#88206),(#88207,#88208),(#88209,#88210),(#88211,
#88212),(#88213,#88214),(#88215,#88216),(#88217,#88218),(#88219,#88220),
(#88221,#88222),(#88223,#88224),(#88225,#88226),(#88227,#88228),(#88229,
#88230),(#88231,#88232),(#88233,#88234),(#88235,#88236),(#88237,#88238),
(#88239,#88240),(#88241,#88242),(#88243,#88244),(#88245,#88246),(#88247,
#88248),(#88249,#88250),(#88251,#88252),(#88253,#88254),(#88255,#88256),
(#88257,#88258),(#88259,#88260),(#88261,#88262),(#88263,#88264),(#88265,
#88266),(#88267,#88268),(#88269,#88270),(#88271,#88272),(#88273,#88274),
(#88275,#88276),(#88277,#88278),(#88279,#88280),(#88281,#88282),(#88283,
#88284),(#88285,#88286),(#88287,#88288),(#88289,#88290),(#88291,#88292),
(#88293,#88294),(#88295,#88296),(#88297,#88298),(#88299,#88300),(#88301,
#88302),(#88303,#88304),(#88305,#88306)),.UNSPECIFIED.,.F.,.F.,.F.)
B_SPLINE_SURFACE_WITH_KNOTS((6,1,1,1,1,1,1,1,1,1,1,1,1,1,1,1,1,1,1,1,1,
1,1,1,1,1,1,1,1,1,1,1,1,1,1,1,1,1,1,1,1,1,1,1,1,1,1,1,1,1,1,1,1,1,1,1,1,
1,1,1,1,1,1,1,1,1,1,1,1,1,1,1,1,1,1,1,1,1,1,1,1,1,1,1,1,1,1,1,1,1,1,1,1,
1,1,1,1,1,1,1,1,1,1,1,1,1,1,1,1,1,1,1,1,1,1,1,1,1,1,1,1,1,1,1,1,1,1,1,1,
1,1,1,1,1,1,1,1,1,1,1,1,1,1,1,1,1,1,1,1,1,1,1,1,1,1,1,1,1,1,1,1,1,1,1,1,
1,1,1,1,1,1,1,1,1,1,1,1,1,1,1,1,1,1,1,1,1,1,1,1,1,1,1,1,1,1,1,1,1,1,1,1,
1,1,1,1,1,1,1,1,1,1,1,1,1,1,1,1,1,1,1,1,1,1,1,1,1,1,1,1,1,1,1,1,1,1,1,1,
1,1,1,1,1,1,1,1,1,1,1,1,1,1,1,1,1,1,1,1,1,1,1,1,1,1,1,1,1,1,1,1,1,1,1,1,
1,1,1,1,1,1,1,1,1,1,1,1,1,1,1,1,1,1,1,1,1,1,1,1,1,1,1,1,1,1,1,1,1,1,1,1,
1,1,1,1,1,1,1,1,1,1,1,1,1,1,1,1,1,1,1,1,1,1,1,1,1,1,1,1,1,1,1,1,1,1,1,1,
1,1,1,1,1,1,1,1,1,1,1,1,1,1,1,1,1,1,1,1,1,1,1,1,1,1,1,1,1,1,1,1,1,1,1,1,
1,1,1,1,1,1,1,1,1,1,1,1,1,1,1,1,1,1,1,1,1,1,1,1,1,1,1,1,1,1,1,1,1,1,1,1,
1,1,1,1,1,1,1,1,1,1,1,1,1,1,1,1,1,1,1,1,1,1,1,1,1,1,1,1,1,1,1,1,1,1,1,1,
1,1,1,1,1,1,1,1,1,1,1,1,1,1,1,1,1,1,1,1,1,1,1,1,1,1,1,1,1,1,1,1,1,1,1,1,
1,1,1,1,1,1,1,1,1,1,1,1,1,1,1,1,1,1,1,1,1,1,1,1,1,1,1,1,1,1,1,1,1,1,1,1,
1,1,1,1,1,1,1,1,1,1,1,1,1,1,1,1,1,1,1,1,1,1,1,1,1,1,1,1,1,1,1,1,1,1,1,1,
1,1,1,1,1,1,1,1,1,1,1,1,1,1,1,1,1,1,1,1,1,1,1,1,1,1,1,1,1,1,1,1,1,1,1,1,
1,1,1,1,1,1,1,1,1,1,1,1,1,1,1,1,1,1,1,1,1,1,1,1,1,1,1,1,1,1,1,1,1,1,1,1,
1,1,1,1,1,1,1,1,1,1,1,1,1,1,1,1,1,1,1,1,1,1,1,1,1,1,1,1,1,1,1,1,1,1,1,1,
1,1,1,1,1,1,1,1,1,1,1,1,1,1,1,1,1,1,1,1,1,1,1,1,1,1,1,1,1,1,1,1,1,1,1,1,
1,1,1,1,1,1,1,1,1,1,1,1,1,1,1,1,1,1,1,1,1,1,1,1,1,1,1,1,1,1,1,1,1,1,1,1,
1,1,1,1,1,1,1,1,1,1,1,1,1,1,1,1,1,1,1,1,1,1,1,1,1,1,1,1,1,1,1,1,1,1,1,1,
1,1,1,1,1,1,1,1,1,1,1,1,1,1,1,1,1,1,1,1,1,1,1,1,1,1,1,1,1,1,1,1,1,1,1,1,
1,1,1,1,1,1,1,1,1,1,1,1,1,1,1,1,1,1,1,1,1,1,1,1,1,1,1,1,1,1,1,1,1,1,1,1,
1,1,1,1,1,1,1,1,1,1,1,1,1,1,1,1,1,1,1,1,1,1,1,1,1,1,1,1,1,1,1,1,1,1,1,1,
1,1,1,1,1,1,1,1,1,1,1,1,1,1,1,1,1,1,1,1,1,1,1,1,1,1,1,1,1,1,1,1,1,1,1,1,
1,1,1,1,1,1,1,1,1,1,1,1,1,1,1,1,1,1,1,1,1,1,1,1,1,1,1,1,1,1,1,1,1,1,1,1,
1,1,1,1,1,1,1,1,1,1,1,1,1,1,1,1,1,1,1,1,1,1,1,1,1,1,1,1,1,1,1,1,1,1,1,1,
1,1,1,1,1,1,1,6),(2,2),(-1.,-0.999000000000001,-0.998000000000001,-0.997000000000001,
-0.996000000000001,-0.995000000000001,-0.994000000000001,-0.993000000000001,
-0.992000000000001,-0.991000000000001,-0.990000000000001,-0.989000000000001,
-0.988000000000001,-0.987000000000001,-0.986000000000001,-0.985000000000001,
-0.984000000000001,-0.983000000000001,-0.982000000000001,-0.981000000000001,
-0.980000000000001,-0.979000000000001,-0.978000000000001,-0.977000000000001,
-0.976000000000001,-0.975000000000001,-0.974000000000001,-0.973000000000001,
-0.972000000000001,-0.971000000000001,-0.970000000000001,-0.969000000000001,
-0.968000000000001,-0.967000000000001,-0.966000000000001,-0.965000000000001,
-0.964000000000001,-0.963000000000001,-0.962000000000001,-0.961000000000001,
-0.960000000000001,-0.959000000000001,-0.958000000000001,-0.957000000000001,
-0.956000000000001,-0.955000000000001,-0.954000000000001,-0.953000000000001,
-0.952000000000001,-0.951000000000001,-0.950000000000001,-0.949000000000001,
-0.948000000000001,-0.947000000000001,-0.946000000000001,-0.945000000000001,
-0.944000000000001,-0.943000000000001,-0.942000000000001,-0.941000000000001,
-0.940000000000001,-0.939000000000001,-0.938000000000001,-0.937000000000001,
-0.936000000000001,-0.935000000000001,-0.934000000000001,-0.933000000000001,
-0.932000000000001,-0.931000000000001,-0.930000000000001,-0.929000000000001,
-0.928000000000001,-0.927000000000001,-0.926000000000001,-0.925000000000001,
-0.924000000000001,-0.923000000000001,-0.922000000000001,-0.921000000000001,
-0.920000000000001,-0.919000000000001,-0.918000000000001,-0.917000000000001,
-0.916000000000001,-0.915000000000001,-0.914000000000001,-0.913000000000001,
-0.912000000000001,-0.911000000000001,-0.910000000000001,-0.909000000000001,
-0.908000000000001,-0.907000000000001,-0.906000000000001,-0.905000000000001,
-0.904000000000001,-0.903000000000001,-0.902000000000001,-0.901000000000001,
-0.900000000000001,-0.899000000000001,-0.898000000000001,-0.897000000000001,
-0.896000000000001,-0.895000000000001,-0.894000000000001,-0.893000000000001,
-0.892000000000001,-0.891000000000001,-0.890000000000001,-0.889000000000001,
-0.888000000000001,-0.887000000000001,-0.886000000000001,-0.885000000000001,
-0.884000000000001,-0.883000000000001,-0.882000000000001,-0.881000000000001,
-0.880000000000001,-0.879000000000001,-0.878000000000001,-0.877000000000001,
-0.876000000000001,-0.875000000000001,-0.874000000000001,-0.873000000000001,
-0.872000000000001,-0.871000000000001,-0.870000000000001,-0.869000000000001,
-0.868000000000001,-0.867000000000001,-0.866000000000001,-0.865000000000001,
-0.864000000000001,-0.863000000000001,-0.862000000000001,-0.861000000000001,
-0.860000000000001,-0.859000000000001,-0.858000000000001,-0.857000000000001,
-0.856000000000001,-0.855000000000001,-0.854000000000001,-0.853000000000001,
-0.852000000000001,-0.851000000000001,-0.850000000000001,-0.849000000000001,
-0.848000000000001,-0.847000000000001,-0.846000000000001,-0.845000000000001,
-0.844000000000001,-0.843000000000001,-0.842000000000001,-0.841000000000001,
-0.840000000000001,-0.839000000000001,-0.838000000000001,-0.837000000000001,
-0.836000000000001,-0.835000000000001,-0.834000000000001,-0.833000000000001,
-0.832000000000001,-0.831000000000001,-0.830000000000001,-0.829000000000001,
-0.828000000000001,-0.827000000000001,-0.826000000000001,-0.825000000000001,
-0.824000000000001,-0.823000000000001,-0.822000000000001,-0.821000000000001,
-0.820000000000001,-0.819000000000001,-0.818000000000001,-0.817000000000001,
-0.816000000000001,-0.815000000000001,-0.814000000000001,-0.813000000000001,
-0.812000000000001,-0.811000000000001,-0.810000000000001,-0.809000000000001,
-0.808000000000001,-0.807000000000001,-0.806000000000001,-0.805000000000001,
-0.804000000000001,-0.803000000000001,-0.802000000000001,-0.801000000000001,
-0.800000000000001,-0.799000000000001,-0.798000000000001,-0.797000000000001,
-0.796000000000001,-0.795000000000001,-0.794000000000001,-0.793000000000001,
-0.792000000000001,-0.791000000000001,-0.790000000000001,-0.789000000000001,
-0.788000000000001,-0.787000000000001,-0.786000000000001,-0.785000000000001,
-0.784000000000001,-0.783000000000001,-0.782000000000001,-0.781000000000001,
-0.780000000000001,-0.779000000000001,-0.778000000000001,-0.777000000000001,
-0.776000000000001,-0.775000000000001,-0.774000000000001,-0.773000000000001,
-0.772000000000001,-0.771000000000001,-0.770000000000001,-0.769000000000001,
-0.768000000000001,-0.767000000000001,-0.766000000000001,-0.765000000000001,
-0.764000000000001,-0.763000000000001,-0.762000000000001,-0.761000000000001,
-0.760000000000001,-0.759000000000001,-0.758000000000001,-0.757000000000001,
-0.756000000000001,-0.755000000000001,-0.754000000000001,-0.753000000000001,
-0.752000000000001,-0.751000000000001,-0.750000000000001,-0.749000000000001,
-0.748000000000001,-0.747000000000001,-0.746000000000001,-0.745000000000001,
-0.744000000000001,-0.743000000000001,-0.742000000000001,-0.741000000000001,
-0.740000000000001,-0.739000000000001,-0.738000000000001,-0.737000000000001,
-0.736000000000001,-0.735000000000001,-0.734000000000001,-0.733000000000001,
-0.732000000000001,-0.731000000000001,-0.730000000000001,-0.729000000000001,
-0.728000000000001,-0.727000000000001,-0.726000000000001,-0.725000000000001,
-0.724000000000001,-0.723000000000001,-0.722000000000001,-0.721000000000001,
-0.720000000000001,-0.719000000000001,-0.718000000000001,-0.717000000000001,
-0.716000000000001,-0.715000000000001,-0.714000000000001,-0.713000000000001,
-0.712000000000001,-0.711000000000001,-0.710000000000001,-0.709000000000001,
-0.708000000000001,-0.707000000000001,-0.706000000000001,-0.705000000000001,
-0.704000000000001,-0.703000000000001,-0.702000000000001,-0.701000000000001,
-0.700000000000001,-0.699000000000001,-0.698000000000001,-0.697000000000001,
-0.696000000000001,-0.695000000000001,-0.694000000000001,-0.693000000000001,
-0.692000000000001,-0.691000000000001,-0.690000000000001,-0.689000000000001,
-0.688000000000001,-0.687,-0.686,-0.685,-0.684,-0.683,-0.682,-0.681,-0.68,
-0.679,-0.678,-0.677,-0.676,-0.675,-0.674,-0.673,-0.672,-0.671,-0.67,-0.669,
-0.668,-0.667,-0.666,-0.665,-0.664,-0.663,-0.662,-0.661,-0.66,-0.659,-0.658,
-0.657,-0.656,-0.655,-0.654,-0.653,-0.652,-0.651,-0.65,-0.649,-0.648,-0.647,
-0.646,-0.645,-0.644,-0.643,-0.642,-0.641,-0.64,-0.639,-0.638,-0.637,-0.636,
-0.635,-0.634,-0.633,-0.632,-0.631,-0.63,-0.629,-0.628,-0.627,-0.626,-0.625,
-0.624,-0.623,-0.622,-0.621,-0.62,-0.619,-0.618,-0.617,-0.616,-0.615,-0.614,
-0.613,-0.612,-0.611,-0.61,-0.609,-0.608,-0.607,-0.606,-0.605,-0.604,-0.603,
-0.602,-0.601,-0.6,-0.599,-0.598,-0.597,-0.596,-0.595,-0.594,-0.593,-0.592,
-0.591,-0.59,-0.589,-0.588,-0.587,-0.586,-0.585,-0.584,-0.583,-0.582,-0.581,
-0.58,-0.579,-0.578,-0.577,-0.576,-0.575,-0.574,-0.573,-0.572,-0.571,-0.57,
-0.569,-0.568,-0.567,-0.566,-0.565,-0.564,-0.563,-0.562,-0.561,-0.56,-0.559,
-0.558,-0.557,-0.556,-0.555,-0.554,-0.553,-0.552,-0.551,-0.55,-0.549,-0.548,
-0.547,-0.546,-0.545,-0.544,-0.543,-0.542,-0.541,-0.54,-0.539,-0.538,-0.537,
-0.536,-0.535,-0.534,-0.533,-0.532,-0.531,-0.53,-0.529,-0.528,-0.527,-0.526,
-0.525,-0.524,-0.523,-0.522,-0.521,-0.52,-0.519,-0.518,-0.517,-0.516,-0.515,
-0.514,-0.513,-0.512,-0.511,-0.51,-0.509,-0.508,-0.507,-0.506,-0.505,-0.504,
-0.503,-0.502,-0.501,-0.5,-0.499,-0.498,-0.497,-0.496,-0.495,-0.494,-0.493,
-0.492,-0.491,-0.49,-0.489,-0.488,-0.487,-0.486,-0.485,-0.484,-0.483,-0.482,
-0.481,-0.48,-0.479,-0.478,-0.477,-0.476,-0.475,-0.474,-0.473,-0.472,-0.471,
-0.47,-0.469,-0.468,-0.467,-0.466,-0.465,-0.464,-0.463,-0.462,-0.461,-0.46,
-0.459,-0.458,-0.457,-0.456,-0.455,-0.454,-0.453,-0.452,-0.451,-0.45,-0.449,
-0.448,-0.447,-0.446,-0.445,-0.444,-0.443,-0.442,-0.441,-0.44,-0.439,-0.438,
-0.437,-0.436,-0.435,-0.434,-0.433,-0.432,-0.431,-0.43,-0.429,-0.428,-0.427,
-0.426,-0.425,-0.424,-0.423,-0.422,-0.421,-0.42,-0.419,-0.418,-0.417,-0.416,
-0.415,-0.414,-0.413,-0.412,-0.411,-0.41,-0.409,-0.408,-0.407,-0.406,-0.405,
-0.404,-0.403,-0.402,-0.401,-0.4,-0.399,-0.398,-0.397,-0.396,-0.395,-0.394,
-0.393,-0.392,-0.391,-0.39,-0.389,-0.388,-0.387,-0.386,-0.385,-0.384,-0.383,
-0.382,-0.381,-0.38,-0.379,-0.378,-0.377,-0.376,-0.375,-0.374,-0.373,-0.372,
-0.371,-0.37,-0.369,-0.368,-0.367,-0.366,-0.365,-0.364,-0.363,-0.362,-0.361,
-0.36,-0.359,-0.358,-0.357,-0.356,-0.355,-0.354,-0.353,-0.352,-0.351,-0.35,
-0.349,-0.348,-0.347,-0.346,-0.345,-0.344,-0.343,-0.342,-0.341,-0.34,-0.339,
-0.338,-0.337,-0.336,-0.335,-0.334,-0.333,-0.332,-0.331,-0.33,-0.329,-0.328,
-0.327,-0.326,-0.325,-0.324,-0.323,-0.322,-0.321,-0.32,-0.319,-0.318,-0.317,
-0.316,-0.315,-0.314,-0.313,-0.312,-0.311,-0.31,-0.309,-0.308,-0.307,-0.306,
-0.305,-0.304,-0.303,-0.302,-0.301,-0.3,-0.299,-0.298,-0.297,-0.296,-0.295,
-0.294,-0.293,-0.292,-0.291,-0.29,-0.289,-0.288,-0.287,-0.286,-0.285,-0.284,
-0.283,-0.282,-0.281,-0.28,-0.279,-0.278,-0.277,-0.276,-0.275,-0.274,-0.273,
-0.272,-0.271,-0.27,-0.269,-0.268,-0.267,-0.266,-0.265,-0.264,-0.263,-0.262,
-0.261,-0.26,-0.259,-0.258,-0.257,-0.256,-0.255,-0.254,-0.253,-0.252,-0.251,
-0.25,-0.249,-0.248,-0.247,-0.246,-0.245,-0.244,-0.243,-0.242,-0.241,-0.24,
-0.239,-0.238,-0.237,-0.236,-0.235,-0.234,-0.233,-0.232,-0.231,-0.23,-0.229,
-0.228,-0.227,-0.226,-0.225,-0.224,-0.223,-0.222,-0.221,-0.22,-0.219,-0.218,
-0.217,-0.216,-0.215,-0.214,-0.213,-0.212,-0.211,-0.21,-0.209,-0.208,-0.207,
-0.206,-0.205,-0.204,-0.203,-0.202,-0.201,-0.2,-0.199,-0.198,-0.197,-0.196,
-0.195,-0.194,-0.193,-0.192,-0.191,-0.19,-0.189,-0.188,-0.187,-0.186,-0.185,
-0.184,-0.183,-0.182,-0.181,-0.18,-0.179,-0.178,-0.177,-0.176,-0.175,-0.174,
-0.173,-0.172,-0.171,-0.17,-0.169,-0.168,-0.167,-0.166,-0.165,-0.164,-0.163,
-0.162,-0.161,-0.16,-0.159,-0.158,-0.157,-0.156,-0.155,-0.154,-0.153,-0.152,
-0.151,-0.15,-0.149,-0.148,-0.147,-0.146,-0.145,-0.144,-0.143,-0.142,-0.141,
-0.14,-0.139,-0.138,-0.137,-0.136,-0.135,-0.134,-0.133,-0.132,-0.131,-0.13,
-0.129,-0.128,-0.127,-0.126,-0.125,-0.124,-0.123,-0.122,-0.121,-0.12,-0.119,
-0.118,-0.117,-0.116,-0.115,-0.114,-0.113,-0.112,-0.111,-0.11,-0.109,-0.108,
-0.107,-0.106,-0.105,-0.104,-0.103,-0.102,-0.101,-0.1,-0.0990000000000001,
-0.0980000000000001,-0.0970000000000001,-0.0960000000000001,-0.0950000000000001,
-0.0940000000000001,-0.0930000000000001,-0.0920000000000001,-0.0910000000000001,
-0.0900000000000001,-0.0890000000000001,-0.0880000000000001,-0.0870000000000001,
-0.0860000000000001,-0.0850000000000001,-0.0840000000000001,-0.0830000000000001,
-0.0820000000000001,-0.0810000000000001,-0.0800000000000001,-0.0790000000000001,
-0.0780000000000001,-0.0770000000000001,-0.0760000000000001,-0.0750000000000001,
-0.0740000000000001,-0.0730000000000001,-0.0720000000000001,-0.071,-0.07,
-0.069,-0.068,-0.067,-0.066,-0.065,-0.064,-0.063,-0.062,-0.061,-0.06,-0.059,
-0.058,-0.057,-0.056,-0.055,-0.054,-0.053,-0.052,-0.051,-0.05,-0.049,-0.048,
-0.047,-0.046,-0.045,-0.044,-0.043,-0.042,-0.041,-0.04,-0.039,-0.038,-0.037,
-0.036,-0.035,-0.034,-0.033,-0.032,-0.031,-0.03,-0.029,-0.028,-0.027,-0.026,
-0.025,-0.024,-0.023,-0.022,-0.021,-0.02,-0.019,-0.018,-0.017,-0.016,-0.015,
-0.014,-0.013,-0.012,-0.011,-0.01,-0.009,-0.008,-0.007,-0.006,-0.005,-0.004,
-0.003,-0.002,-0.001,0.),(0.,2.),.UNSPECIFIED.)
GEOMETRIC_REPRESENTATION_ITEM()
RATIONAL_B_SPLINE_SURFACE(((1.,1.),(1.,1.),(1.,1.),(1.,1.),(1.,1.),(1.,
1.),(1.,1.),(1.,1.),(1.,1.),(1.,1.),(1.,1.),(1.,1.),(1.,1.),(1.,1.),(1.,
1.),(1.,1.),(1.,1.),(1.,1.),(1.,1.),(1.,1.),(1.,1.),(1.,1.),(1.,1.),(1.,
1.),(1.,1.),(1.,1.),(1.,1.),(1.,1.),(1.,1.),(1.,1.),(1.,1.),(1.,1.),(1.,
1.),(1.,1.),(1.,1.),(1.,1.),(1.,1.),(1.,1.),(1.,1.),(1.,1.),(1.,1.),(1.,
1.),(1.,1.),(1.,1.),(1.,1.),(1.,1.),(1.,1.),(1.,1.),(1.,1.),(1.,1.),(1.,
1.),(1.,1.),(1.,1.),(1.,1.),(1.,1.),(1.,1.),(1.,1.),(1.,1.),(1.,1.),(1.,
1.),(1.,1.),(1.,1.),(1.,1.),(1.,1.),(1.,1.),(1.,1.),(1.,1.),(1.,1.),(1.,
1.),(1.,1.),(1.,1.),(1.,1.),(1.,1.),(1.,1.),(1.,1.),(1.,1.),(1.,1.),(1.,
1.),(1.,1.),(1.,1.),(1.,1.),(1.,1.),(1.,1.),(1.,1.),(1.,1.),(1.,1.),(1.,
1.),(1.,1.),(1.,1.),(1.,1.),(1.,1.),(1.,1.),(1.,1.),(1.,1.),(1.,1.),(1.,
1.),(1.,1.),(1.,1.),(1.,1.),(1.,1.),(1.,1.),(1.,1.),(1.,1.),(1.,1.),(1.,
1.),(1.,1.),(1.,1.),(1.,1.),(1.,1.),(1.,1.),(1.,1.),(1.,1.),(1.,1.),(1.,
1.),(1.,1.),(1.,1.),(1.,1.),(1.,1.),(1.,1.),(1.,1.),(1.,1.),(1.,1.),(1.,
1.),(1.,1.),(1.,1.),(1.,1.),(1.,1.),(1.,1.),(1.,1.),(1.,1.),(1.,1.),(1.,
1.),(1.,1.),(1.,1.),(1.,1.),(1.,1.),(1.,1.),(1.,1.),(1.,1.),(1.,1.),(1.,
1.),(1.,1.),(1.,1.),(1.,1.),(1.,1.),(1.,1.),(1.,1.),(1.,1.),(1.,1.),(1.,
1.),(1.,1.),(1.,1.),(1.,1.),(1.,1.),(1.,1.),(1.,1.),(1.,1.),(1.,1.),(1.,
1.),(1.,1.),(1.,1.),(1.,1.),(1.,1.),(1.,1.),(1.,1.),(1.,1.),(1.,1.),(1.,
1.),(1.,1.),(1.,1.),(1.,1.),(1.,1.),(1.,1.),(1.,1.),(1.,1.),(1.,1.),(1.,
1.),(1.,1.),(1.,1.),(1.,1.),(1.,1.),(1.,1.),(1.,1.),(1.,1.),(1.,1.),(1.,
1.),(1.,1.),(1.,1.),(1.,1.),(1.,1.),(1.,1.),(1.,1.),(1.,1.),(1.,1.),(1.,
1.),(1.,1.),(1.,1.),(1.,1.),(1.,1.),(1.,1.),(1.,1.),(1.,1.),(1.,1.),(1.,
1.),(1.,1.),(1.,1.),(1.,1.),(1.,1.),(1.,1.),(1.,1.),(1.,1.),(1.,1.),(1.,
1.),(1.,1.),(1.,1.),(1.,1.),(1.,1.),(1.,1.),(1.,1.),(1.,1.),(1.,1.),(1.,
1.),(1.,1.),(1.,1.),(1.,1.),(1.,1.),(1.,1.),(1.,1.),(1.,1.),(1.,1.),(1.,
1.),(1.,1.),(1.,1.),(1.,1.),(1.,1.),(1.,1.),(1.,1.),(1.,1.),(1.,1.),(1.,
1.),(1.,1.),(1.,1.),(1.,1.),(1.,1.),(1.,1.),(1.,1.),(1.,1.),(1.,1.),(1.,
1.),(1.,1.),(1.,1.),(1.,1.),(1.,1.),(1.,1.),(1.,1.),(1.,1.),(1.,1.),(1.,
1.),(1.,1.),(1.,1.),(1.,1.),(1.,1.),(1.,1.),(1.,1.),(1.,1.),(1.,1.),(1.,
1.),(1.,1.),(1.,1.),(1.,1.),(1.,1.),(1.,1.),(1.,1.),(1.,1.),(1.,1.),(1.,
1.),(1.,1.),(1.,1.),(1.,1.),(1.,1.),(1.,1.),(1.,1.),(1.,1.),(1.,1.),(1.,
1.),(1.,1.),(1.,1.),(1.,1.),(1.,1.),(1.,1.),(1.,1.),(1.,1.),(1.,1.),(1.,
1.),(1.,1.),(1.,1.),(1.,1.),(1.,1.),(1.,1.),(1.,1.),(1.,1.),(1.,1.),(1.,
1.),(1.,1.),(1.,1.),(1.,1.),(1.,1.),(1.,1.),(1.,1.),(1.,1.),(1.,1.),(1.,
1.),(1.,1.),(1.,1.),(1.,1.),(1.,1.),(1.,1.),(1.,1.),(1.,1.),(1.,1.),(1.,
1.),(1.,1.),(1.,1.),(1.,1.),(1.,1.),(1.,1.),(1.,1.),(1.,1.),(1.,1.),(1.,
1.),(1.,1.),(1.,1.),(1.,1.),(1.,1.),(1.,1.),(1.,1.),(1.,1.),(1.,1.),(1.,
1.),(1.,1.),(1.,1.),(1.,1.),(1.,1.),(1.,1.),(1.,1.),(1.,1.),(1.,1.),(1.,
1.),(1.,1.),(1.,1.),(1.,1.),(1.,1.),(1.,1.),(1.,1.),(1.,1.),(1.,1.),(1.,
1.),(1.,1.),(1.,1.),(1.,1.),(1.,1.),(1.,1.),(1.,1.),(1.,1.),(1.,1.),(1.,
1.),(1.,1.),(1.,1.),(1.,1.),(1.,1.),(1.,1.),(1.,1.),(1.,1.),(1.,1.),(1.,
1.),(1.,1.),(1.,1.),(1.,1.),(1.,1.),(1.,1.),(1.,1.),(1.,1.),(1.,1.),(1.,
1.),(1.,1.),(1.,1.),(1.,1.),(1.,1.),(1.,1.),(1.,1.),(1.,1.),(1.,1.),(1.,
1.),(1.,1.),(1.,1.),(1.,1.),(1.,1.),(1.,1.),(1.,1.),(1.,1.),(1.,1.),(1.,
1.),(1.,1.),(1.,1.),(1.,1.),(1.,1.),(1.,1.),(1.,1.),(1.,1.),(1.,1.),(1.,
1.),(1.,1.),(1.,1.),(1.,1.),(1.,1.),(1.,1.),(1.,1.),(1.,1.),(1.,1.),(1.,
1.),(1.,1.),(1.,1.),(1.,1.),(1.,1.),(1.,1.),(1.,1.),(1.,1.),(1.,1.),(1.,
1.),(1.,1.),(1.,1.),(1.,1.),(1.,1.),(1.,1.),(1.,1.),(1.,1.),(1.,1.),(1.,
1.),(1.,1.),(1.,1.),(1.,1.),(1.,1.),(1.,1.),(1.,1.),(1.,1.),(1.,1.),(1.,
1.),(1.,1.),(1.,1.),(1.,1.),(1.,1.),(1.,1.),(1.,1.),(1.,1.),(1.,1.),(1.,
1.),(1.,1.),(1.,1.),(1.,1.),(1.,1.),(1.,1.),(1.,1.),(1.,1.),(1.,1.),(1.,
1.),(1.,1.),(1.,1.),(1.,1.),(1.,1.),(1.,1.),(1.,1.),(1.,1.),(1.,1.),(1.,
1.),(1.,1.),(1.,1.),(1.,1.),(1.,1.),(1.,1.),(1.,1.),(1.,1.),(1.,1.),(1.,
1.),(1.,1.),(1.,1.),(1.,1.),(1.,1.),(1.,1.),(1.,1.),(1.,1.),(1.,1.),(1.,
1.),(1.,1.),(1.,1.),(1.,1.),(1.,1.),(1.,1.),(1.,1.),(1.,1.),(1.,1.),(1.,
1.),(1.,1.),(1.,1.),(1.,1.),(1.,1.),(1.,1.),(1.,1.),(1.,1.),(1.,1.),(1.,
1.),(1.,1.),(1.,1.),(1.,1.),(1.,1.),(1.,1.),(1.,1.),(1.,1.),(1.,1.),(1.,
1.),(1.,1.),(1.,1.),(1.,1.),(1.,1.),(1.,1.),(1.,1.),(1.,1.),(1.,1.),(1.,
1.),(1.,1.),(1.,1.),(1.,1.),(1.,1.),(1.,1.),(1.,1.),(1.,1.),(1.,1.),(1.,
1.),(1.,1.),(1.,1.),(1.,1.),(1.,1.),(1.,1.),(1.,1.),(1.,1.),(1.,1.),(1.,
1.),(1.,1.),(1.,1.),(1.,1.),(1.,1.),(1.,1.),(1.,1.),(1.,1.),(1.,1.),(1.,
1.),(1.,1.),(1.,1.),(1.,1.),(1.,1.),(1.,1.),(1.,1.),(1.,1.),(1.,1.),(1.,
1.),(1.,1.),(1.,1.),(1.,1.),(1.,1.),(1.,1.),(1.,1.),(1.,1.),(1.,1.),(1.,
1.),(1.,1.),(1.,1.),(1.,1.),(1.,1.),(1.,1.),(1.,1.),(1.,1.),(1.,1.),(1.,
1.),(1.,1.),(1.,1.),(1.,1.),(1.,1.),(1.,1.),(1.,1.),(1.,1.),(1.,1.),(1.,
1.),(1.,1.),(1.,1.),(1.,1.),(1.,1.),(1.,1.),(1.,1.),(1.,1.),(1.,1.),(1.,
1.),(1.,1.),(1.,1.),(1.,1.),(1.,1.),(1.,1.),(1.,1.),(1.,1.),(1.,1.),(1.,
1.),(1.,1.),(1.,1.),(1.,1.),(1.,1.),(1.,1.),(1.,1.),(1.,1.),(1.,1.),(1.,
1.),(1.,1.),(1.,1.),(1.,1.),(1.,1.),(1.,1.),(1.,1.),(1.,1.),(1.,1.),(1.,
1.),(1.,1.),(1.,1.),(1.,1.),(1.,1.),(1.,1.),(1.,1.),(1.,1.),(1.,1.),(1.,
1.),(1.,1.),(1.,1.),(1.,1.),(1.,1.),(1.,1.),(1.,1.),(1.,1.),(1.,1.),(1.,
1.),(1.,1.),(1.,1.),(1.,1.),(1.,1.),(1.,1.),(1.,1.),(1.,1.),(1.,1.),(1.,
1.),(1.,1.),(1.,1.),(1.,1.),(1.,1.),(1.,1.),(1.,1.),(1.,1.),(1.,1.),(1.,
1.),(1.,1.),(1.,1.),(1.,1.),(1.,1.),(1.,1.),(1.,1.),(1.,1.),(1.,1.),(1.,
1.),(1.,1.),(1.,1.),(1.,1.),(1.,1.),(1.,1.),(1.,1.),(1.,1.),(1.,1.),(1.,
1.),(1.,1.),(1.,1.),(1.,1.),(1.,1.),(1.,1.),(1.,1.),(1.,1.),(1.,1.),(1.,
1.),(1.,1.),(1.,1.),(1.,1.),(1.,1.),(1.,1.),(1.,1.),(1.,1.),(1.,1.),(1.,
1.),(1.,1.),(1.,1.),(1.,1.),(1.,1.),(1.,1.),(1.,1.),(1.,1.),(1.,1.),(1.,
1.),(1.,1.),(1.,1.),(1.,1.),(1.,1.),(1.,1.),(1.,1.),(1.,1.),(1.,1.),(1.,
1.),(1.,1.),(1.,1.),(1.,1.),(1.,1.),(1.,1.),(1.,1.),(1.,1.),(1.,1.),(1.,
1.),(1.,1.),(1.,1.),(1.,1.),(1.,1.),(1.,1.),(1.,1.),(1.,1.),(1.,1.),(1.,
1.),(1.,1.),(1.,1.),(1.,1.),(1.,1.),(1.,1.),(1.,1.),(1.,1.),(1.,1.),(1.,
1.),(1.,1.),(1.,1.),(1.,1.),(1.,1.),(1.,1.),(1.,1.),(1.,1.),(1.,1.),(1.,
1.),(1.,1.),(1.,1.),(1.,1.),(1.,1.),(1.,1.),(1.,1.),(1.,1.),(1.,1.),(1.,
1.),(1.,1.),(1.,1.),(1.,1.),(1.,1.),(1.,1.),(1.,1.),(1.,1.),(1.,1.),(1.,
1.),(1.,1.),(1.,1.),(1.,1.),(1.,1.),(1.,1.),(1.,1.),(1.,1.),(1.,1.),(1.,
1.),(1.,1.),(1.,1.),(1.,1.),(1.,1.),(1.,1.),(1.,1.),(1.,1.),(1.,1.),(1.,
1.),(1.,1.),(1.,1.),(1.,1.),(1.,1.),(1.,1.),(1.,1.),(1.,1.),(1.,1.),(1.,
1.),(1.,1.),(1.,1.),(1.,1.),(1.,1.),(1.,1.),(1.,1.),(1.,1.),(1.,1.),(1.,
1.),(1.,1.),(1.,1.),(1.,1.),(1.,1.),(1.,1.),(1.,1.),(1.,1.),(1.,1.),(1.,
1.),(1.,1.),(1.,1.),(1.,1.),(1.,1.),(1.,1.),(1.,1.),(1.,1.),(1.,1.),(1.,
1.),(1.,1.),(1.,1.),(1.,1.),(1.,1.),(1.,1.),(1.,1.),(1.,1.),(1.,1.),(1.,
1.),(1.,1.),(1.,1.),(1.,1.),(1.,1.),(1.,1.),(1.,1.),(1.,1.),(1.,1.),(1.,
1.),(1.,1.),(1.,1.),(1.,1.),(1.,1.),(1.,1.),(1.,1.),(1.,1.),(1.,1.),(1.,
1.),(1.,1.),(1.,1.),(1.,1.),(1.,1.),(1.,1.),(1.,1.),(1.,1.),(1.,1.),(1.,
1.),(1.,1.),(1.,1.),(1.,1.),(1.,1.),(1.,1.),(1.,1.),(1.,1.),(1.,1.),(1.,
1.),(1.,1.),(1.,1.),(1.,1.),(1.,1.),(1.,1.),(1.,1.),(1.,1.),(1.,1.),(1.,
1.),(1.,1.),(1.,1.),(1.,1.),(1.,1.),(1.,1.),(1.,1.),(1.,1.),(1.,1.),(1.,
1.),(1.,1.),(1.,1.),(1.,1.),(1.,1.),(1.,1.),(1.,1.),(1.,1.),(1.,1.),(1.,
1.),(1.,1.),(1.,1.),(1.,1.),(1.,1.),(1.,1.),(1.,1.),(1.,1.),(1.,1.),(1.,
1.),(1.,1.),(1.,1.),(1.,1.),(1.,1.),(1.,1.),(1.,1.),(1.,1.),(1.,1.),(1.,
1.),(1.,1.),(1.,1.),(1.,1.),(1.,1.),(1.,1.),(1.,1.),(1.,1.),(1.,1.),(1.,
1.),(1.,1.),(1.,1.),(1.,1.),(1.,1.),(1.,1.),(1.,1.),(1.,1.),(1.,1.),(1.,
1.),(1.,1.),(1.,1.),(1.,1.),(1.,1.),(1.,1.),(1.,1.),(1.,1.),(1.,1.),(1.,
1.),(1.,1.),(1.,1.),(1.,1.),(1.,1.),(1.,1.),(1.,1.),(1.,1.),(1.,1.),(1.,
1.),(1.,1.),(1.,1.),(1.,1.),(1.,1.),(1.,1.),(1.,1.),(1.,1.),(1.,1.),(1.,
1.),(1.,1.),(1.,1.),(1.,1.),(1.,1.),(1.,1.),(1.,1.),(1.,1.),(1.,1.),(1.,
1.),(1.,1.),(1.,1.),(1.,1.),(1.,1.),(1.,1.),(1.,1.),(1.,1.),(1.,1.),(1.,
1.),(1.,1.),(1.,1.),(1.,1.),(1.,1.),(1.,1.),(1.,1.),(1.,1.),(1.,1.),(1.,
1.),(1.,1.),(1.,1.),(1.,1.),(1.,1.),(1.,1.),(1.,1.),(1.,1.),(1.,1.),(1.,
1.),(1.,1.),(1.,1.),(1.,1.),(1.,1.),(1.,1.),(1.,1.),(1.,1.),(1.,1.),(1.,
1.)))
REPRESENTATION_ITEM('')
SURFACE()
);
#265=(
BOUNDED_SURFACE()
B_SPLINE_SURFACE(5,1,((#88405,#88406),(#88407,#88408),(#88409,#88410),(#88411,
#88412),(#88413,#88414),(#88415,#88416),(#88417,#88418),(#88419,#88420),
(#88421,#88422),(#88423,#88424),(#88425,#88426),(#88427,#88428),(#88429,
#88430),(#88431,#88432),(#88433,#88434),(#88435,#88436),(#88437,#88438),
(#88439,#88440),(#88441,#88442),(#88443,#88444),(#88445,#88446),(#88447,
#88448),(#88449,#88450),(#88451,#88452),(#88453,#88454),(#88455,#88456),
(#88457,#88458),(#88459,#88460),(#88461,#88462),(#88463,#88464),(#88465,
#88466),(#88467,#88468),(#88469,#88470),(#88471,#88472),(#88473,#88474),
(#88475,#88476),(#88477,#88478),(#88479,#88480),(#88481,#88482),(#88483,
#88484),(#88485,#88486),(#88487,#88488),(#88489,#88490),(#88491,#88492),
(#88493,#88494),(#88495,#88496),(#88497,#88498),(#88499,#88500),(#88501,
#88502),(#88503,#88504),(#88505,#88506),(#88507,#88508),(#88509,#88510),
(#88511,#88512),(#88513,#88514),(#88515,#88516),(#88517,#88518),(#88519,
#88520),(#88521,#88522),(#88523,#88524),(#88525,#88526),(#88527,#88528),
(#88529,#88530),(#88531,#88532),(#88533,#88534),(#88535,#88536),(#88537,
#88538),(#88539,#88540),(#88541,#88542),(#88543,#88544),(#88545,#88546),
(#88547,#88548),(#88549,#88550),(#88551,#88552),(#88553,#88554),(#88555,
#88556),(#88557,#88558),(#88559,#88560),(#88561,#88562),(#88563,#88564),
(#88565,#88566),(#88567,#88568),(#88569,#88570),(#88571,#88572),(#88573,
#88574),(#88575,#88576),(#88577,#88578),(#88579,#88580),(#88581,#88582),
(#88583,#88584),(#88585,#88586),(#88587,#88588),(#88589,#88590),(#88591,
#88592),(#88593,#88594),(#88595,#88596),(#88597,#88598),(#88599,#88600),
(#88601,#88602),(#88603,#88604),(#88605,#88606),(#88607,#88608),(#88609,
#88610),(#88611,#88612),(#88613,#88614),(#88615,#88616),(#88617,#88618),
(#88619,#88620),(#88621,#88622),(#88623,#88624),(#88625,#88626),(#88627,
#88628),(#88629,#88630),(#88631,#88632),(#88633,#88634),(#88635,#88636),
(#88637,#88638),(#88639,#88640),(#88641,#88642),(#88643,#88644),(#88645,
#88646),(#88647,#88648),(#88649,#88650),(#88651,#88652),(#88653,#88654),
(#88655,#88656),(#88657,#88658),(#88659,#88660),(#88661,#88662),(#88663,
#88664),(#88665,#88666),(#88667,#88668),(#88669,#88670),(#88671,#88672),
(#88673,#88674),(#88675,#88676),(#88677,#88678),(#88679,#88680),(#88681,
#88682),(#88683,#88684),(#88685,#88686),(#88687,#88688),(#88689,#88690),
(#88691,#88692),(#88693,#88694),(#88695,#88696),(#88697,#88698),(#88699,
#88700),(#88701,#88702),(#88703,#88704),(#88705,#88706),(#88707,#88708),
(#88709,#88710),(#88711,#88712),(#88713,#88714),(#88715,#88716),(#88717,
#88718),(#88719,#88720),(#88721,#88722),(#88723,#88724),(#88725,#88726),
(#88727,#88728),(#88729,#88730),(#88731,#88732),(#88733,#88734),(#88735,
#88736),(#88737,#88738),(#88739,#88740),(#88741,#88742),(#88743,#88744),
(#88745,#88746),(#88747,#88748),(#88749,#88750),(#88751,#88752),(#88753,
#88754),(#88755,#88756),(#88757,#88758),(#88759,#88760),(#88761,#88762),
(#88763,#88764),(#88765,#88766),(#88767,#88768),(#88769,#88770),(#88771,
#88772),(#88773,#88774),(#88775,#88776),(#88777,#88778),(#88779,#88780),
(#88781,#88782),(#88783,#88784),(#88785,#88786),(#88787,#88788),(#88789,
#88790),(#88791,#88792),(#88793,#88794),(#88795,#88796),(#88797,#88798),
(#88799,#88800),(#88801,#88802),(#88803,#88804),(#88805,#88806),(#88807,
#88808),(#88809,#88810),(#88811,#88812),(#88813,#88814),(#88815,#88816),
(#88817,#88818),(#88819,#88820),(#88821,#88822),(#88823,#88824),(#88825,
#88826),(#88827,#88828),(#88829,#88830),(#88831,#88832),(#88833,#88834),
(#88835,#88836),(#88837,#88838),(#88839,#88840),(#88841,#88842),(#88843,
#88844),(#88845,#88846),(#88847,#88848),(#88849,#88850),(#88851,#88852),
(#88853,#88854),(#88855,#88856),(#88857,#88858),(#88859,#88860),(#88861,
#88862),(#88863,#88864),(#88865,#88866),(#88867,#88868),(#88869,#88870),
(#88871,#88872),(#88873,#88874),(#88875,#88876),(#88877,#88878),(#88879,
#88880),(#88881,#88882),(#88883,#88884),(#88885,#88886),(#88887,#88888),
(#88889,#88890),(#88891,#88892),(#88893,#88894),(#88895,#88896),(#88897,
#88898),(#88899,#88900),(#88901,#88902),(#88903,#88904),(#88905,#88906),
(#88907,#88908),(#88909,#88910),(#88911,#88912),(#88913,#88914),(#88915,
#88916),(#88917,#88918),(#88919,#88920),(#88921,#88922),(#88923,#88924),
(#88925,#88926),(#88927,#88928),(#88929,#88930),(#88931,#88932),(#88933,
#88934),(#88935,#88936),(#88937,#88938),(#88939,#88940),(#88941,#88942),
(#88943,#88944),(#88945,#88946),(#88947,#88948),(#88949,#88950),(#88951,
#88952),(#88953,#88954),(#88955,#88956),(#88957,#88958),(#88959,#88960),
(#88961,#88962),(#88963,#88964),(#88965,#88966),(#88967,#88968),(#88969,
#88970),(#88971,#88972),(#88973,#88974),(#88975,#88976),(#88977,#88978),
(#88979,#88980),(#88981,#88982),(#88983,#88984),(#88985,#88986),(#88987,
#88988),(#88989,#88990),(#88991,#88992),(#88993,#88994),(#88995,#88996),
(#88997,#88998),(#88999,#89000),(#89001,#89002),(#89003,#89004),(#89005,
#89006),(#89007,#89008),(#89009,#89010),(#89011,#89012),(#89013,#89014),
(#89015,#89016),(#89017,#89018),(#89019,#89020),(#89021,#89022),(#89023,
#89024),(#89025,#89026),(#89027,#89028),(#89029,#89030),(#89031,#89032),
(#89033,#89034),(#89035,#89036),(#89037,#89038),(#89039,#89040),(#89041,
#89042),(#89043,#89044),(#89045,#89046),(#89047,#89048),(#89049,#89050),
(#89051,#89052),(#89053,#89054),(#89055,#89056),(#89057,#89058),(#89059,
#89060),(#89061,#89062),(#89063,#89064),(#89065,#89066),(#89067,#89068),
(#89069,#89070),(#89071,#89072),(#89073,#89074),(#89075,#89076),(#89077,
#89078),(#89079,#89080),(#89081,#89082),(#89083,#89084),(#89085,#89086),
(#89087,#89088),(#89089,#89090),(#89091,#89092),(#89093,#89094),(#89095,
#89096),(#89097,#89098),(#89099,#89100),(#89101,#89102),(#89103,#89104),
(#89105,#89106),(#89107,#89108),(#89109,#89110),(#89111,#89112),(#89113,
#89114),(#89115,#89116),(#89117,#89118),(#89119,#89120),(#89121,#89122),
(#89123,#89124),(#89125,#89126),(#89127,#89128),(#89129,#89130),(#89131,
#89132),(#89133,#89134),(#89135,#89136),(#89137,#89138),(#89139,#89140),
(#89141,#89142),(#89143,#89144),(#89145,#89146),(#89147,#89148),(#89149,
#89150),(#89151,#89152),(#89153,#89154),(#89155,#89156),(#89157,#89158),
(#89159,#89160),(#89161,#89162),(#89163,#89164),(#89165,#89166),(#89167,
#89168),(#89169,#89170),(#89171,#89172),(#89173,#89174),(#89175,#89176),
(#89177,#89178),(#89179,#89180),(#89181,#89182),(#89183,#89184),(#89185,
#89186),(#89187,#89188),(#89189,#89190),(#89191,#89192),(#89193,#89194),
(#89195,#89196),(#89197,#89198),(#89199,#89200),(#89201,#89202),(#89203,
#89204),(#89205,#89206),(#89207,#89208),(#89209,#89210),(#89211,#89212),
(#89213,#89214),(#89215,#89216),(#89217,#89218),(#89219,#89220),(#89221,
#89222),(#89223,#89224),(#89225,#89226),(#89227,#89228),(#89229,#89230),
(#89231,#89232),(#89233,#89234),(#89235,#89236),(#89237,#89238),(#89239,
#89240),(#89241,#89242),(#89243,#89244),(#89245,#89246),(#89247,#89248),
(#89249,#89250),(#89251,#89252),(#89253,#89254),(#89255,#89256),(#89257,
#89258),(#89259,#89260),(#89261,#89262),(#89263,#89264),(#89265,#89266),
(#89267,#89268),(#89269,#89270),(#89271,#89272),(#89273,#89274),(#89275,
#89276),(#89277,#89278),(#89279,#89280),(#89281,#89282),(#89283,#89284),
(#89285,#89286),(#89287,#89288),(#89289,#89290),(#89291,#89292),(#89293,
#89294),(#89295,#89296),(#89297,#89298),(#89299,#89300),(#89301,#89302),
(#89303,#89304),(#89305,#89306),(#89307,#89308),(#89309,#89310),(#89311,
#89312),(#89313,#89314),(#89315,#89316),(#89317,#89318),(#89319,#89320),
(#89321,#89322),(#89323,#89324),(#89325,#89326),(#89327,#89328),(#89329,
#89330),(#89331,#89332),(#89333,#89334),(#89335,#89336),(#89337,#89338),
(#89339,#89340),(#89341,#89342),(#89343,#89344),(#89345,#89346),(#89347,
#89348),(#89349,#89350),(#89351,#89352),(#89353,#89354),(#89355,#89356),
(#89357,#89358),(#89359,#89360),(#89361,#89362),(#89363,#89364),(#89365,
#89366),(#89367,#89368),(#89369,#89370),(#89371,#89372),(#89373,#89374),
(#89375,#89376),(#89377,#89378),(#89379,#89380),(#89381,#89382),(#89383,
#89384),(#89385,#89386),(#89387,#89388),(#89389,#89390),(#89391,#89392),
(#89393,#89394),(#89395,#89396),(#89397,#89398),(#89399,#89400),(#89401,
#89402),(#89403,#89404),(#89405,#89406),(#89407,#89408),(#89409,#89410),
(#89411,#89412),(#89413,#89414),(#89415,#89416),(#89417,#89418),(#89419,
#89420),(#89421,#89422),(#89423,#89424),(#89425,#89426),(#89427,#89428),
(#89429,#89430),(#89431,#89432),(#89433,#89434),(#89435,#89436),(#89437,
#89438),(#89439,#89440),(#89441,#89442),(#89443,#89444),(#89445,#89446),
(#89447,#89448),(#89449,#89450),(#89451,#89452),(#89453,#89454),(#89455,
#89456),(#89457,#89458),(#89459,#89460),(#89461,#89462),(#89463,#89464),
(#89465,#89466),(#89467,#89468),(#89469,#89470),(#89471,#89472),(#89473,
#89474),(#89475,#89476),(#89477,#89478),(#89479,#89480),(#89481,#89482),
(#89483,#89484),(#89485,#89486),(#89487,#89488),(#89489,#89490),(#89491,
#89492),(#89493,#89494),(#89495,#89496),(#89497,#89498),(#89499,#89500),
(#89501,#89502),(#89503,#89504),(#89505,#89506),(#89507,#89508),(#89509,
#89510),(#89511,#89512),(#89513,#89514),(#89515,#89516),(#89517,#89518),
(#89519,#89520),(#89521,#89522),(#89523,#89524),(#89525,#89526),(#89527,
#89528),(#89529,#89530),(#89531,#89532),(#89533,#89534),(#89535,#89536),
(#89537,#89538),(#89539,#89540),(#89541,#89542),(#89543,#89544),(#89545,
#89546),(#89547,#89548),(#89549,#89550),(#89551,#89552),(#89553,#89554),
(#89555,#89556),(#89557,#89558),(#89559,#89560),(#89561,#89562),(#89563,
#89564),(#89565,#89566),(#89567,#89568),(#89569,#89570),(#89571,#89572),
(#89573,#89574),(#89575,#89576),(#89577,#89578),(#89579,#89580),(#89581,
#89582),(#89583,#89584),(#89585,#89586),(#89587,#89588),(#89589,#89590),
(#89591,#89592),(#89593,#89594),(#89595,#89596),(#89597,#89598),(#89599,
#89600),(#89601,#89602),(#89603,#89604),(#89605,#89606),(#89607,#89608),
(#89609,#89610),(#89611,#89612),(#89613,#89614),(#89615,#89616),(#89617,
#89618),(#89619,#89620),(#89621,#89622),(#89623,#89624),(#89625,#89626),
(#89627,#89628),(#89629,#89630),(#89631,#89632),(#89633,#89634),(#89635,
#89636),(#89637,#89638),(#89639,#89640),(#89641,#89642),(#89643,#89644),
(#89645,#89646),(#89647,#89648),(#89649,#89650),(#89651,#89652),(#89653,
#89654),(#89655,#89656),(#89657,#89658),(#89659,#89660),(#89661,#89662),
(#89663,#89664),(#89665,#89666),(#89667,#89668),(#89669,#89670),(#89671,
#89672),(#89673,#89674),(#89675,#89676),(#89677,#89678),(#89679,#89680),
(#89681,#89682),(#89683,#89684),(#89685,#89686),(#89687,#89688),(#89689,
#89690),(#89691,#89692),(#89693,#89694),(#89695,#89696),(#89697,#89698),
(#89699,#89700),(#89701,#89702),(#89703,#89704),(#89705,#89706),(#89707,
#89708),(#89709,#89710),(#89711,#89712),(#89713,#89714),(#89715,#89716),
(#89717,#89718),(#89719,#89720),(#89721,#89722),(#89723,#89724),(#89725,
#89726),(#89727,#89728),(#89729,#89730),(#89731,#89732),(#89733,#89734),
(#89735,#89736),(#89737,#89738),(#89739,#89740),(#89741,#89742),(#89743,
#89744),(#89745,#89746),(#89747,#89748),(#89749,#89750),(#89751,#89752),
(#89753,#89754),(#89755,#89756),(#89757,#89758),(#89759,#89760),(#89761,
#89762),(#89763,#89764),(#89765,#89766),(#89767,#89768),(#89769,#89770),
(#89771,#89772),(#89773,#89774),(#89775,#89776),(#89777,#89778),(#89779,
#89780),(#89781,#89782),(#89783,#89784),(#89785,#89786),(#89787,#89788),
(#89789,#89790),(#89791,#89792),(#89793,#89794),(#89795,#89796),(#89797,
#89798),(#89799,#89800),(#89801,#89802),(#89803,#89804),(#89805,#89806),
(#89807,#89808),(#89809,#89810),(#89811,#89812),(#89813,#89814),(#89815,
#89816),(#89817,#89818),(#89819,#89820),(#89821,#89822),(#89823,#89824),
(#89825,#89826),(#89827,#89828),(#89829,#89830),(#89831,#89832),(#89833,
#89834),(#89835,#89836),(#89837,#89838),(#89839,#89840),(#89841,#89842),
(#89843,#89844),(#89845,#89846),(#89847,#89848),(#89849,#89850),(#89851,
#89852),(#89853,#89854),(#89855,#89856),(#89857,#89858),(#89859,#89860),
(#89861,#89862),(#89863,#89864),(#89865,#89866),(#89867,#89868),(#89869,
#89870),(#89871,#89872),(#89873,#89874),(#89875,#89876),(#89877,#89878),
(#89879,#89880),(#89881,#89882),(#89883,#89884),(#89885,#89886),(#89887,
#89888),(#89889,#89890),(#89891,#89892),(#89893,#89894),(#89895,#89896),
(#89897,#89898),(#89899,#89900),(#89901,#89902),(#89903,#89904),(#89905,
#89906),(#89907,#89908),(#89909,#89910),(#89911,#89912),(#89913,#89914),
(#89915,#89916),(#89917,#89918),(#89919,#89920),(#89921,#89922),(#89923,
#89924),(#89925,#89926),(#89927,#89928),(#89929,#89930),(#89931,#89932),
(#89933,#89934),(#89935,#89936),(#89937,#89938),(#89939,#89940),(#89941,
#89942),(#89943,#89944),(#89945,#89946),(#89947,#89948),(#89949,#89950),
(#89951,#89952),(#89953,#89954),(#89955,#89956),(#89957,#89958),(#89959,
#89960),(#89961,#89962),(#89963,#89964),(#89965,#89966),(#89967,#89968),
(#89969,#89970),(#89971,#89972),(#89973,#89974),(#89975,#89976),(#89977,
#89978),(#89979,#89980),(#89981,#89982),(#89983,#89984),(#89985,#89986),
(#89987,#89988),(#89989,#89990),(#89991,#89992),(#89993,#89994),(#89995,
#89996),(#89997,#89998),(#89999,#90000),(#90001,#90002),(#90003,#90004),
(#90005,#90006),(#90007,#90008),(#90009,#90010),(#90011,#90012),(#90013,
#90014),(#90015,#90016),(#90017,#90018),(#90019,#90020),(#90021,#90022),
(#90023,#90024),(#90025,#90026),(#90027,#90028),(#90029,#90030),(#90031,
#90032),(#90033,#90034),(#90035,#90036),(#90037,#90038),(#90039,#90040),
(#90041,#90042),(#90043,#90044),(#90045,#90046),(#90047,#90048),(#90049,
#90050),(#90051,#90052),(#90053,#90054),(#90055,#90056),(#90057,#90058),
(#90059,#90060),(#90061,#90062),(#90063,#90064),(#90065,#90066),(#90067,
#90068),(#90069,#90070),(#90071,#90072),(#90073,#90074),(#90075,#90076),
(#90077,#90078),(#90079,#90080),(#90081,#90082),(#90083,#90084),(#90085,
#90086),(#90087,#90088),(#90089,#90090),(#90091,#90092),(#90093,#90094),
(#90095,#90096),(#90097,#90098),(#90099,#90100),(#90101,#90102),(#90103,
#90104),(#90105,#90106),(#90107,#90108),(#90109,#90110),(#90111,#90112),
(#90113,#90114),(#90115,#90116),(#90117,#90118),(#90119,#90120),(#90121,
#90122),(#90123,#90124),(#90125,#90126),(#90127,#90128),(#90129,#90130),
(#90131,#90132),(#90133,#90134),(#90135,#90136),(#90137,#90138),(#90139,
#90140),(#90141,#90142),(#90143,#90144),(#90145,#90146),(#90147,#90148),
(#90149,#90150),(#90151,#90152),(#90153,#90154),(#90155,#90156),(#90157,
#90158),(#90159,#90160),(#90161,#90162),(#90163,#90164),(#90165,#90166),
(#90167,#90168),(#90169,#90170),(#90171,#90172),(#90173,#90174),(#90175,
#90176),(#90177,#90178),(#90179,#90180),(#90181,#90182),(#90183,#90184),
(#90185,#90186),(#90187,#90188),(#90189,#90190),(#90191,#90192),(#90193,
#90194),(#90195,#90196),(#90197,#90198),(#90199,#90200),(#90201,#90202),
(#90203,#90204),(#90205,#90206),(#90207,#90208),(#90209,#90210),(#90211,
#90212),(#90213,#90214),(#90215,#90216),(#90217,#90218),(#90219,#90220),
(#90221,#90222),(#90223,#90224),(#90225,#90226),(#90227,#90228),(#90229,
#90230),(#90231,#90232),(#90233,#90234),(#90235,#90236),(#90237,#90238),
(#90239,#90240),(#90241,#90242),(#90243,#90244),(#90245,#90246),(#90247,
#90248),(#90249,#90250),(#90251,#90252),(#90253,#90254),(#90255,#90256),
(#90257,#90258),(#90259,#90260),(#90261,#90262),(#90263,#90264),(#90265,
#90266),(#90267,#90268),(#90269,#90270),(#90271,#90272),(#90273,#90274),
(#90275,#90276),(#90277,#90278),(#90279,#90280),(#90281,#90282),(#90283,
#90284),(#90285,#90286),(#90287,#90288),(#90289,#90290),(#90291,#90292),
(#90293,#90294),(#90295,#90296),(#90297,#90298),(#90299,#90300),(#90301,
#90302),(#90303,#90304),(#90305,#90306),(#90307,#90308),(#90309,#90310),
(#90311,#90312),(#90313,#90314),(#90315,#90316),(#90317,#90318),(#90319,
#90320),(#90321,#90322),(#90323,#90324),(#90325,#90326),(#90327,#90328),
(#90329,#90330),(#90331,#90332),(#90333,#90334),(#90335,#90336),(#90337,
#90338),(#90339,#90340),(#90341,#90342),(#90343,#90344),(#90345,#90346),
(#90347,#90348),(#90349,#90350),(#90351,#90352),(#90353,#90354),(#90355,
#90356),(#90357,#90358),(#90359,#90360),(#90361,#90362),(#90363,#90364),
(#90365,#90366),(#90367,#90368),(#90369,#90370),(#90371,#90372),(#90373,
#90374),(#90375,#90376),(#90377,#90378),(#90379,#90380),(#90381,#90382),
(#90383,#90384),(#90385,#90386),(#90387,#90388),(#90389,#90390),(#90391,
#90392),(#90393,#90394),(#90395,#90396),(#90397,#90398),(#90399,#90400),
(#90401,#90402),(#90403,#90404),(#90405,#90406),(#90407,#90408),(#90409,
#90410),(#90411,#90412),(#90413,#90414)),.UNSPECIFIED.,.F.,.F.,.F.)
B_SPLINE_SURFACE_WITH_KNOTS((6,1,1,1,1,1,1,1,1,1,1,1,1,1,1,1,1,1,1,1,1,
1,1,1,1,1,1,1,1,1,1,1,1,1,1,1,1,1,1,1,1,1,1,1,1,1,1,1,1,1,1,1,1,1,1,1,1,
1,1,1,1,1,1,1,1,1,1,1,1,1,1,1,1,1,1,1,1,1,1,1,1,1,1,1,1,1,1,1,1,1,1,1,1,
1,1,1,1,1,1,1,1,1,1,1,1,1,1,1,1,1,1,1,1,1,1,1,1,1,1,1,1,1,1,1,1,1,1,1,1,
1,1,1,1,1,1,1,1,1,1,1,1,1,1,1,1,1,1,1,1,1,1,1,1,1,1,1,1,1,1,1,1,1,1,1,1,
1,1,1,1,1,1,1,1,1,1,1,1,1,1,1,1,1,1,1,1,1,1,1,1,1,1,1,1,1,1,1,1,1,1,1,1,
1,1,1,1,1,1,1,1,1,1,1,1,1,1,1,1,1,1,1,1,1,1,1,1,1,1,1,1,1,1,1,1,1,1,1,1,
1,1,1,1,1,1,1,1,1,1,1,1,1,1,1,1,1,1,1,1,1,1,1,1,1,1,1,1,1,1,1,1,1,1,1,1,
1,1,1,1,1,1,1,1,1,1,1,1,1,1,1,1,1,1,1,1,1,1,1,1,1,1,1,1,1,1,1,1,1,1,1,1,
1,1,1,1,1,1,1,1,1,1,1,1,1,1,1,1,1,1,1,1,1,1,1,1,1,1,1,1,1,1,1,1,1,1,1,1,
1,1,1,1,1,1,1,1,1,1,1,1,1,1,1,1,1,1,1,1,1,1,1,1,1,1,1,1,1,1,1,1,1,1,1,1,
1,1,1,1,1,1,1,1,1,1,1,1,1,1,1,1,1,1,1,1,1,1,1,1,1,1,1,1,1,1,1,1,1,1,1,1,
1,1,1,1,1,1,1,1,1,1,1,1,1,1,1,1,1,1,1,1,1,1,1,1,1,1,1,1,1,1,1,1,1,1,1,1,
1,1,1,1,1,1,1,1,1,1,1,1,1,1,1,1,1,1,1,1,1,1,1,1,1,1,1,1,1,1,1,1,1,1,1,1,
1,1,1,1,1,1,1,1,1,1,1,1,1,1,1,1,1,1,1,1,1,1,1,1,1,1,1,1,1,1,1,1,1,1,1,1,
1,1,1,1,1,1,1,1,1,1,1,1,1,1,1,1,1,1,1,1,1,1,1,1,1,1,1,1,1,1,1,1,1,1,1,1,
1,1,1,1,1,1,1,1,1,1,1,1,1,1,1,1,1,1,1,1,1,1,1,1,1,1,1,1,1,1,1,1,1,1,1,1,
1,1,1,1,1,1,1,1,1,1,1,1,1,1,1,1,1,1,1,1,1,1,1,1,1,1,1,1,1,1,1,1,1,1,1,1,
1,1,1,1,1,1,1,1,1,1,1,1,1,1,1,1,1,1,1,1,1,1,1,1,1,1,1,1,1,1,1,1,1,1,1,1,
1,1,1,1,1,1,1,1,1,1,1,1,1,1,1,1,1,1,1,1,1,1,1,1,1,1,1,1,1,1,1,1,1,1,1,1,
1,1,1,1,1,1,1,1,1,1,1,1,1,1,1,1,1,1,1,1,1,1,1,1,1,1,1,1,1,1,1,1,1,1,1,1,
1,1,1,1,1,1,1,1,1,1,1,1,1,1,1,1,1,1,1,1,1,1,1,1,1,1,1,1,1,1,1,1,1,1,1,1,
1,1,1,1,1,1,1,1,1,1,1,1,1,1,1,1,1,1,1,1,1,1,1,1,1,1,1,1,1,1,1,1,1,1,1,1,
1,1,1,1,1,1,1,1,1,1,1,1,1,1,1,1,1,1,1,1,1,1,1,1,1,1,1,1,1,1,1,1,1,1,1,1,
1,1,1,1,1,1,1,1,1,1,1,1,1,1,1,1,1,1,1,1,1,1,1,1,1,1,1,1,1,1,1,1,1,1,1,1,
1,1,1,1,1,1,1,1,1,1,1,1,1,1,1,1,1,1,1,1,1,1,1,1,1,1,1,1,1,1,1,1,1,1,1,1,
1,1,1,1,1,1,1,1,1,1,1,1,1,1,1,1,1,1,1,1,1,1,1,1,1,1,1,1,1,1,1,1,1,1,1,1,
1,1,1,1,1,1,1,1,1,1,1,1,1,1,1,1,1,1,1,1,1,1,1,1,1,1,1,1,1,1,1,1,1,1,1,1,
1,1,1,1,1,1,1,6),(2,2),(-1.,-0.999000000000001,-0.998000000000001,-0.997000000000001,
-0.996000000000001,-0.995000000000001,-0.994000000000001,-0.993000000000001,
-0.992000000000001,-0.991000000000001,-0.990000000000001,-0.989000000000001,
-0.988000000000001,-0.987000000000001,-0.986000000000001,-0.985000000000001,
-0.984000000000001,-0.983000000000001,-0.982000000000001,-0.981000000000001,
-0.980000000000001,-0.979000000000001,-0.978000000000001,-0.977000000000001,
-0.976000000000001,-0.975000000000001,-0.974000000000001,-0.973000000000001,
-0.972000000000001,-0.971000000000001,-0.970000000000001,-0.969000000000001,
-0.968000000000001,-0.967000000000001,-0.966000000000001,-0.965000000000001,
-0.964000000000001,-0.963000000000001,-0.962000000000001,-0.961000000000001,
-0.960000000000001,-0.959000000000001,-0.958000000000001,-0.957000000000001,
-0.956000000000001,-0.955000000000001,-0.954000000000001,-0.953000000000001,
-0.952000000000001,-0.951000000000001,-0.950000000000001,-0.949000000000001,
-0.948000000000001,-0.947000000000001,-0.946000000000001,-0.945000000000001,
-0.944000000000001,-0.943000000000001,-0.942000000000001,-0.941000000000001,
-0.940000000000001,-0.939000000000001,-0.938000000000001,-0.937000000000001,
-0.936000000000001,-0.935000000000001,-0.934000000000001,-0.933000000000001,
-0.932000000000001,-0.931000000000001,-0.930000000000001,-0.929000000000001,
-0.928000000000001,-0.927000000000001,-0.926000000000001,-0.925000000000001,
-0.924000000000001,-0.923000000000001,-0.922000000000001,-0.921000000000001,
-0.920000000000001,-0.919000000000001,-0.918000000000001,-0.917000000000001,
-0.916000000000001,-0.915000000000001,-0.914000000000001,-0.913000000000001,
-0.912000000000001,-0.911000000000001,-0.910000000000001,-0.909000000000001,
-0.908000000000001,-0.907000000000001,-0.906000000000001,-0.905000000000001,
-0.904000000000001,-0.903000000000001,-0.902000000000001,-0.901000000000001,
-0.900000000000001,-0.899000000000001,-0.898000000000001,-0.897000000000001,
-0.896000000000001,-0.895000000000001,-0.894000000000001,-0.893000000000001,
-0.892000000000001,-0.891000000000001,-0.890000000000001,-0.889000000000001,
-0.888000000000001,-0.887000000000001,-0.886000000000001,-0.885000000000001,
-0.884000000000001,-0.883000000000001,-0.882000000000001,-0.881000000000001,
-0.880000000000001,-0.879000000000001,-0.878000000000001,-0.877000000000001,
-0.876000000000001,-0.875000000000001,-0.874000000000001,-0.873000000000001,
-0.872000000000001,-0.871000000000001,-0.870000000000001,-0.869000000000001,
-0.868000000000001,-0.867000000000001,-0.866000000000001,-0.865000000000001,
-0.864000000000001,-0.863000000000001,-0.862000000000001,-0.861000000000001,
-0.860000000000001,-0.859000000000001,-0.858000000000001,-0.857000000000001,
-0.856000000000001,-0.855000000000001,-0.854000000000001,-0.853000000000001,
-0.852000000000001,-0.851000000000001,-0.850000000000001,-0.849000000000001,
-0.848000000000001,-0.847000000000001,-0.846000000000001,-0.845000000000001,
-0.844000000000001,-0.843000000000001,-0.842000000000001,-0.841000000000001,
-0.840000000000001,-0.839000000000001,-0.838000000000001,-0.837000000000001,
-0.836000000000001,-0.835000000000001,-0.834000000000001,-0.833000000000001,
-0.832000000000001,-0.831000000000001,-0.830000000000001,-0.829000000000001,
-0.828000000000001,-0.827000000000001,-0.826000000000001,-0.825000000000001,
-0.824000000000001,-0.823000000000001,-0.822000000000001,-0.821000000000001,
-0.820000000000001,-0.819000000000001,-0.818000000000001,-0.817000000000001,
-0.816000000000001,-0.815000000000001,-0.814000000000001,-0.813000000000001,
-0.812000000000001,-0.811000000000001,-0.810000000000001,-0.809000000000001,
-0.808000000000001,-0.807000000000001,-0.806000000000001,-0.805000000000001,
-0.804000000000001,-0.803000000000001,-0.802000000000001,-0.801000000000001,
-0.800000000000001,-0.799000000000001,-0.798000000000001,-0.797000000000001,
-0.796000000000001,-0.795000000000001,-0.794000000000001,-0.793000000000001,
-0.792000000000001,-0.791000000000001,-0.790000000000001,-0.789000000000001,
-0.788000000000001,-0.787000000000001,-0.786000000000001,-0.785000000000001,
-0.784000000000001,-0.783000000000001,-0.782000000000001,-0.781000000000001,
-0.780000000000001,-0.779000000000001,-0.778000000000001,-0.777000000000001,
-0.776000000000001,-0.775000000000001,-0.774000000000001,-0.773000000000001,
-0.772000000000001,-0.771000000000001,-0.770000000000001,-0.769000000000001,
-0.768000000000001,-0.767000000000001,-0.766000000000001,-0.765000000000001,
-0.764000000000001,-0.763000000000001,-0.762000000000001,-0.761000000000001,
-0.760000000000001,-0.759000000000001,-0.758000000000001,-0.757000000000001,
-0.756000000000001,-0.755000000000001,-0.754000000000001,-0.753000000000001,
-0.752000000000001,-0.751000000000001,-0.750000000000001,-0.749000000000001,
-0.748000000000001,-0.747000000000001,-0.746000000000001,-0.745000000000001,
-0.744000000000001,-0.743000000000001,-0.742000000000001,-0.741000000000001,
-0.740000000000001,-0.739000000000001,-0.738000000000001,-0.737000000000001,
-0.736000000000001,-0.735000000000001,-0.734000000000001,-0.733000000000001,
-0.732000000000001,-0.731000000000001,-0.730000000000001,-0.729000000000001,
-0.728000000000001,-0.727000000000001,-0.726000000000001,-0.725000000000001,
-0.724000000000001,-0.723000000000001,-0.722000000000001,-0.721000000000001,
-0.720000000000001,-0.719000000000001,-0.718000000000001,-0.717000000000001,
-0.716000000000001,-0.715000000000001,-0.714000000000001,-0.713000000000001,
-0.712000000000001,-0.711000000000001,-0.710000000000001,-0.709000000000001,
-0.708000000000001,-0.707000000000001,-0.706000000000001,-0.705000000000001,
-0.704000000000001,-0.703000000000001,-0.702000000000001,-0.701000000000001,
-0.700000000000001,-0.699000000000001,-0.698000000000001,-0.697000000000001,
-0.696000000000001,-0.695000000000001,-0.694000000000001,-0.693000000000001,
-0.692000000000001,-0.691000000000001,-0.690000000000001,-0.689000000000001,
-0.688000000000001,-0.687,-0.686,-0.685,-0.684,-0.683,-0.682,-0.681,-0.68,
-0.679,-0.678,-0.677,-0.676,-0.675,-0.674,-0.673,-0.672,-0.671,-0.67,-0.669,
-0.668,-0.667,-0.666,-0.665,-0.664,-0.663,-0.662,-0.661,-0.66,-0.659,-0.658,
-0.657,-0.656,-0.655,-0.654,-0.653,-0.652,-0.651,-0.65,-0.649,-0.648,-0.647,
-0.646,-0.645,-0.644,-0.643,-0.642,-0.641,-0.64,-0.639,-0.638,-0.637,-0.636,
-0.635,-0.634,-0.633,-0.632,-0.631,-0.63,-0.629,-0.628,-0.627,-0.626,-0.625,
-0.624,-0.623,-0.622,-0.621,-0.62,-0.619,-0.618,-0.617,-0.616,-0.615,-0.614,
-0.613,-0.612,-0.611,-0.61,-0.609,-0.608,-0.607,-0.606,-0.605,-0.604,-0.603,
-0.602,-0.601,-0.6,-0.599,-0.598,-0.597,-0.596,-0.595,-0.594,-0.593,-0.592,
-0.591,-0.59,-0.589,-0.588,-0.587,-0.586,-0.585,-0.584,-0.583,-0.582,-0.581,
-0.58,-0.579,-0.578,-0.577,-0.576,-0.575,-0.574,-0.573,-0.572,-0.571,-0.57,
-0.569,-0.568,-0.567,-0.566,-0.565,-0.564,-0.563,-0.562,-0.561,-0.56,-0.559,
-0.558,-0.557,-0.556,-0.555,-0.554,-0.553,-0.552,-0.551,-0.55,-0.549,-0.548,
-0.547,-0.546,-0.545,-0.544,-0.543,-0.542,-0.541,-0.54,-0.539,-0.538,-0.537,
-0.536,-0.535,-0.534,-0.533,-0.532,-0.531,-0.53,-0.529,-0.528,-0.527,-0.526,
-0.525,-0.524,-0.523,-0.522,-0.521,-0.52,-0.519,-0.518,-0.517,-0.516,-0.515,
-0.514,-0.513,-0.512,-0.511,-0.51,-0.509,-0.508,-0.507,-0.506,-0.505,-0.504,
-0.503,-0.502,-0.501,-0.5,-0.499,-0.498,-0.497,-0.496,-0.495,-0.494,-0.493,
-0.492,-0.491,-0.49,-0.489,-0.488,-0.487,-0.486,-0.485,-0.484,-0.483,-0.482,
-0.481,-0.48,-0.479,-0.478,-0.477,-0.476,-0.475,-0.474,-0.473,-0.472,-0.471,
-0.47,-0.469,-0.468,-0.467,-0.466,-0.465,-0.464,-0.463,-0.462,-0.461,-0.46,
-0.459,-0.458,-0.457,-0.456,-0.455,-0.454,-0.453,-0.452,-0.451,-0.45,-0.449,
-0.448,-0.447,-0.446,-0.445,-0.444,-0.443,-0.442,-0.441,-0.44,-0.439,-0.438,
-0.437,-0.436,-0.435,-0.434,-0.433,-0.432,-0.431,-0.43,-0.429,-0.428,-0.427,
-0.426,-0.425,-0.424,-0.423,-0.422,-0.421,-0.42,-0.419,-0.418,-0.417,-0.416,
-0.415,-0.414,-0.413,-0.412,-0.411,-0.41,-0.409,-0.408,-0.407,-0.406,-0.405,
-0.404,-0.403,-0.402,-0.401,-0.4,-0.399,-0.398,-0.397,-0.396,-0.395,-0.394,
-0.393,-0.392,-0.391,-0.39,-0.389,-0.388,-0.387,-0.386,-0.385,-0.384,-0.383,
-0.382,-0.381,-0.38,-0.379,-0.378,-0.377,-0.376,-0.375,-0.374,-0.373,-0.372,
-0.371,-0.37,-0.369,-0.368,-0.367,-0.366,-0.365,-0.364,-0.363,-0.362,-0.361,
-0.36,-0.359,-0.358,-0.357,-0.356,-0.355,-0.354,-0.353,-0.352,-0.351,-0.35,
-0.349,-0.348,-0.347,-0.346,-0.345,-0.344,-0.343,-0.342,-0.341,-0.34,-0.339,
-0.338,-0.337,-0.336,-0.335,-0.334,-0.333,-0.332,-0.331,-0.33,-0.329,-0.328,
-0.327,-0.326,-0.325,-0.324,-0.323,-0.322,-0.321,-0.32,-0.319,-0.318,-0.317,
-0.316,-0.315,-0.314,-0.313,-0.312,-0.311,-0.31,-0.309,-0.308,-0.307,-0.306,
-0.305,-0.304,-0.303,-0.302,-0.301,-0.3,-0.299,-0.298,-0.297,-0.296,-0.295,
-0.294,-0.293,-0.292,-0.291,-0.29,-0.289,-0.288,-0.287,-0.286,-0.285,-0.284,
-0.283,-0.282,-0.281,-0.28,-0.279,-0.278,-0.277,-0.276,-0.275,-0.274,-0.273,
-0.272,-0.271,-0.27,-0.269,-0.268,-0.267,-0.266,-0.265,-0.264,-0.263,-0.262,
-0.261,-0.26,-0.259,-0.258,-0.257,-0.256,-0.255,-0.254,-0.253,-0.252,-0.251,
-0.25,-0.249,-0.248,-0.247,-0.246,-0.245,-0.244,-0.243,-0.242,-0.241,-0.24,
-0.239,-0.238,-0.237,-0.236,-0.235,-0.234,-0.233,-0.232,-0.231,-0.23,-0.229,
-0.228,-0.227,-0.226,-0.225,-0.224,-0.223,-0.222,-0.221,-0.22,-0.219,-0.218,
-0.217,-0.216,-0.215,-0.214,-0.213,-0.212,-0.211,-0.21,-0.209,-0.208,-0.207,
-0.206,-0.205,-0.204,-0.203,-0.202,-0.201,-0.2,-0.199,-0.198,-0.197,-0.196,
-0.195,-0.194,-0.193,-0.192,-0.191,-0.19,-0.189,-0.188,-0.187,-0.186,-0.185,
-0.184,-0.183,-0.182,-0.181,-0.18,-0.179,-0.178,-0.177,-0.176,-0.175,-0.174,
-0.173,-0.172,-0.171,-0.17,-0.169,-0.168,-0.167,-0.166,-0.165,-0.164,-0.163,
-0.162,-0.161,-0.16,-0.159,-0.158,-0.157,-0.156,-0.155,-0.154,-0.153,-0.152,
-0.151,-0.15,-0.149,-0.148,-0.147,-0.146,-0.145,-0.144,-0.143,-0.142,-0.141,
-0.14,-0.139,-0.138,-0.137,-0.136,-0.135,-0.134,-0.133,-0.132,-0.131,-0.13,
-0.129,-0.128,-0.127,-0.126,-0.125,-0.124,-0.123,-0.122,-0.121,-0.12,-0.119,
-0.118,-0.117,-0.116,-0.115,-0.114,-0.113,-0.112,-0.111,-0.11,-0.109,-0.108,
-0.107,-0.106,-0.105,-0.104,-0.103,-0.102,-0.101,-0.1,-0.0990000000000001,
-0.0980000000000001,-0.0970000000000001,-0.0960000000000001,-0.0950000000000001,
-0.0940000000000001,-0.0930000000000001,-0.0920000000000001,-0.0910000000000001,
-0.0900000000000001,-0.0890000000000001,-0.0880000000000001,-0.0870000000000001,
-0.0860000000000001,-0.0850000000000001,-0.0840000000000001,-0.0830000000000001,
-0.0820000000000001,-0.0810000000000001,-0.0800000000000001,-0.0790000000000001,
-0.0780000000000001,-0.0770000000000001,-0.0760000000000001,-0.0750000000000001,
-0.0740000000000001,-0.0730000000000001,-0.0720000000000001,-0.071,-0.07,
-0.069,-0.068,-0.067,-0.066,-0.065,-0.064,-0.063,-0.062,-0.061,-0.06,-0.059,
-0.058,-0.057,-0.056,-0.055,-0.054,-0.053,-0.052,-0.051,-0.05,-0.049,-0.048,
-0.047,-0.046,-0.045,-0.044,-0.043,-0.042,-0.041,-0.04,-0.039,-0.038,-0.037,
-0.036,-0.035,-0.034,-0.033,-0.032,-0.031,-0.03,-0.029,-0.028,-0.027,-0.026,
-0.025,-0.024,-0.023,-0.022,-0.021,-0.02,-0.019,-0.018,-0.017,-0.016,-0.015,
-0.014,-0.013,-0.012,-0.011,-0.01,-0.009,-0.008,-0.007,-0.006,-0.005,-0.004,
-0.003,-0.002,-0.001,0.),(0.,2.),.UNSPECIFIED.)
GEOMETRIC_REPRESENTATION_ITEM()
RATIONAL_B_SPLINE_SURFACE(((1.,1.),(1.,1.),(1.,1.),(1.,1.),(1.,1.),(1.,
1.),(1.,1.),(1.,1.),(1.,1.),(1.,1.),(1.,1.),(1.,1.),(1.,1.),(1.,1.),(1.,
1.),(1.,1.),(1.,1.),(1.,1.),(1.,1.),(1.,1.),(1.,1.),(1.,1.),(1.,1.),(1.,
1.),(1.,1.),(1.,1.),(1.,1.),(1.,1.),(1.,1.),(1.,1.),(1.,1.),(1.,1.),(1.,
1.),(1.,1.),(1.,1.),(1.,1.),(1.,1.),(1.,1.),(1.,1.),(1.,1.),(1.,1.),(1.,
1.),(1.,1.),(1.,1.),(1.,1.),(1.,1.),(1.,1.),(1.,1.),(1.,1.),(1.,1.),(1.,
1.),(1.,1.),(1.,1.),(1.,1.),(1.,1.),(1.,1.),(1.,1.),(1.,1.),(1.,1.),(1.,
1.),(1.,1.),(1.,1.),(1.,1.),(1.,1.),(1.,1.),(1.,1.),(1.,1.),(1.,1.),(1.,
1.),(1.,1.),(1.,1.),(1.,1.),(1.,1.),(1.,1.),(1.,1.),(1.,1.),(1.,1.),(1.,
1.),(1.,1.),(1.,1.),(1.,1.),(1.,1.),(1.,1.),(1.,1.),(1.,1.),(1.,1.),(1.,
1.),(1.,1.),(1.,1.),(1.,1.),(1.,1.),(1.,1.),(1.,1.),(1.,1.),(1.,1.),(1.,
1.),(1.,1.),(1.,1.),(1.,1.),(1.,1.),(1.,1.),(1.,1.),(1.,1.),(1.,1.),(1.,
1.),(1.,1.),(1.,1.),(1.,1.),(1.,1.),(1.,1.),(1.,1.),(1.,1.),(1.,1.),(1.,
1.),(1.,1.),(1.,1.),(1.,1.),(1.,1.),(1.,1.),(1.,1.),(1.,1.),(1.,1.),(1.,
1.),(1.,1.),(1.,1.),(1.,1.),(1.,1.),(1.,1.),(1.,1.),(1.,1.),(1.,1.),(1.,
1.),(1.,1.),(1.,1.),(1.,1.),(1.,1.),(1.,1.),(1.,1.),(1.,1.),(1.,1.),(1.,
1.),(1.,1.),(1.,1.),(1.,1.),(1.,1.),(1.,1.),(1.,1.),(1.,1.),(1.,1.),(1.,
1.),(1.,1.),(1.,1.),(1.,1.),(1.,1.),(1.,1.),(1.,1.),(1.,1.),(1.,1.),(1.,
1.),(1.,1.),(1.,1.),(1.,1.),(1.,1.),(1.,1.),(1.,1.),(1.,1.),(1.,1.),(1.,
1.),(1.,1.),(1.,1.),(1.,1.),(1.,1.),(1.,1.),(1.,1.),(1.,1.),(1.,1.),(1.,
1.),(1.,1.),(1.,1.),(1.,1.),(1.,1.),(1.,1.),(1.,1.),(1.,1.),(1.,1.),(1.,
1.),(1.,1.),(1.,1.),(1.,1.),(1.,1.),(1.,1.),(1.,1.),(1.,1.),(1.,1.),(1.,
1.),(1.,1.),(1.,1.),(1.,1.),(1.,1.),(1.,1.),(1.,1.),(1.,1.),(1.,1.),(1.,
1.),(1.,1.),(1.,1.),(1.,1.),(1.,1.),(1.,1.),(1.,1.),(1.,1.),(1.,1.),(1.,
1.),(1.,1.),(1.,1.),(1.,1.),(1.,1.),(1.,1.),(1.,1.),(1.,1.),(1.,1.),(1.,
1.),(1.,1.),(1.,1.),(1.,1.),(1.,1.),(1.,1.),(1.,1.),(1.,1.),(1.,1.),(1.,
1.),(1.,1.),(1.,1.),(1.,1.),(1.,1.),(1.,1.),(1.,1.),(1.,1.),(1.,1.),(1.,
1.),(1.,1.),(1.,1.),(1.,1.),(1.,1.),(1.,1.),(1.,1.),(1.,1.),(1.,1.),(1.,
1.),(1.,1.),(1.,1.),(1.,1.),(1.,1.),(1.,1.),(1.,1.),(1.,1.),(1.,1.),(1.,
1.),(1.,1.),(1.,1.),(1.,1.),(1.,1.),(1.,1.),(1.,1.),(1.,1.),(1.,1.),(1.,
1.),(1.,1.),(1.,1.),(1.,1.),(1.,1.),(1.,1.),(1.,1.),(1.,1.),(1.,1.),(1.,
1.),(1.,1.),(1.,1.),(1.,1.),(1.,1.),(1.,1.),(1.,1.),(1.,1.),(1.,1.),(1.,
1.),(1.,1.),(1.,1.),(1.,1.),(1.,1.),(1.,1.),(1.,1.),(1.,1.),(1.,1.),(1.,
1.),(1.,1.),(1.,1.),(1.,1.),(1.,1.),(1.,1.),(1.,1.),(1.,1.),(1.,1.),(1.,
1.),(1.,1.),(1.,1.),(1.,1.),(1.,1.),(1.,1.),(1.,1.),(1.,1.),(1.,1.),(1.,
1.),(1.,1.),(1.,1.),(1.,1.),(1.,1.),(1.,1.),(1.,1.),(1.,1.),(1.,1.),(1.,
1.),(1.,1.),(1.,1.),(1.,1.),(1.,1.),(1.,1.),(1.,1.),(1.,1.),(1.,1.),(1.,
1.),(1.,1.),(1.,1.),(1.,1.),(1.,1.),(1.,1.),(1.,1.),(1.,1.),(1.,1.),(1.,
1.),(1.,1.),(1.,1.),(1.,1.),(1.,1.),(1.,1.),(1.,1.),(1.,1.),(1.,1.),(1.,
1.),(1.,1.),(1.,1.),(1.,1.),(1.,1.),(1.,1.),(1.,1.),(1.,1.),(1.,1.),(1.,
1.),(1.,1.),(1.,1.),(1.,1.),(1.,1.),(1.,1.),(1.,1.),(1.,1.),(1.,1.),(1.,
1.),(1.,1.),(1.,1.),(1.,1.),(1.,1.),(1.,1.),(1.,1.),(1.,1.),(1.,1.),(1.,
1.),(1.,1.),(1.,1.),(1.,1.),(1.,1.),(1.,1.),(1.,1.),(1.,1.),(1.,1.),(1.,
1.),(1.,1.),(1.,1.),(1.,1.),(1.,1.),(1.,1.),(1.,1.),(1.,1.),(1.,1.),(1.,
1.),(1.,1.),(1.,1.),(1.,1.),(1.,1.),(1.,1.),(1.,1.),(1.,1.),(1.,1.),(1.,
1.),(1.,1.),(1.,1.),(1.,1.),(1.,1.),(1.,1.),(1.,1.),(1.,1.),(1.,1.),(1.,
1.),(1.,1.),(1.,1.),(1.,1.),(1.,1.),(1.,1.),(1.,1.),(1.,1.),(1.,1.),(1.,
1.),(1.,1.),(1.,1.),(1.,1.),(1.,1.),(1.,1.),(1.,1.),(1.,1.),(1.,1.),(1.,
1.),(1.,1.),(1.,1.),(1.,1.),(1.,1.),(1.,1.),(1.,1.),(1.,1.),(1.,1.),(1.,
1.),(1.,1.),(1.,1.),(1.,1.),(1.,1.),(1.,1.),(1.,1.),(1.,1.),(1.,1.),(1.,
1.),(1.,1.),(1.,1.),(1.,1.),(1.,1.),(1.,1.),(1.,1.),(1.,1.),(1.,1.),(1.,
1.),(1.,1.),(1.,1.),(1.,1.),(1.,1.),(1.,1.),(1.,1.),(1.,1.),(1.,1.),(1.,
1.),(1.,1.),(1.,1.),(1.,1.),(1.,1.),(1.,1.),(1.,1.),(1.,1.),(1.,1.),(1.,
1.),(1.,1.),(1.,1.),(1.,1.),(1.,1.),(1.,1.),(1.,1.),(1.,1.),(1.,1.),(1.,
1.),(1.,1.),(1.,1.),(1.,1.),(1.,1.),(1.,1.),(1.,1.),(1.,1.),(1.,1.),(1.,
1.),(1.,1.),(1.,1.),(1.,1.),(1.,1.),(1.,1.),(1.,1.),(1.,1.),(1.,1.),(1.,
1.),(1.,1.),(1.,1.),(1.,1.),(1.,1.),(1.,1.),(1.,1.),(1.,1.),(1.,1.),(1.,
1.),(1.,1.),(1.,1.),(1.,1.),(1.,1.),(1.,1.),(1.,1.),(1.,1.),(1.,1.),(1.,
1.),(1.,1.),(1.,1.),(1.,1.),(1.,1.),(1.,1.),(1.,1.),(1.,1.),(1.,1.),(1.,
1.),(1.,1.),(1.,1.),(1.,1.),(1.,1.),(1.,1.),(1.,1.),(1.,1.),(1.,1.),(1.,
1.),(1.,1.),(1.,1.),(1.,1.),(1.,1.),(1.,1.),(1.,1.),(1.,1.),(1.,1.),(1.,
1.),(1.,1.),(1.,1.),(1.,1.),(1.,1.),(1.,1.),(1.,1.),(1.,1.),(1.,1.),(1.,
1.),(1.,1.),(1.,1.),(1.,1.),(1.,1.),(1.,1.),(1.,1.),(1.,1.),(1.,1.),(1.,
1.),(1.,1.),(1.,1.),(1.,1.),(1.,1.),(1.,1.),(1.,1.),(1.,1.),(1.,1.),(1.,
1.),(1.,1.),(1.,1.),(1.,1.),(1.,1.),(1.,1.),(1.,1.),(1.,1.),(1.,1.),(1.,
1.),(1.,1.),(1.,1.),(1.,1.),(1.,1.),(1.,1.),(1.,1.),(1.,1.),(1.,1.),(1.,
1.),(1.,1.),(1.,1.),(1.,1.),(1.,1.),(1.,1.),(1.,1.),(1.,1.),(1.,1.),(1.,
1.),(1.,1.),(1.,1.),(1.,1.),(1.,1.),(1.,1.),(1.,1.),(1.,1.),(1.,1.),(1.,
1.),(1.,1.),(1.,1.),(1.,1.),(1.,1.),(1.,1.),(1.,1.),(1.,1.),(1.,1.),(1.,
1.),(1.,1.),(1.,1.),(1.,1.),(1.,1.),(1.,1.),(1.,1.),(1.,1.),(1.,1.),(1.,
1.),(1.,1.),(1.,1.),(1.,1.),(1.,1.),(1.,1.),(1.,1.),(1.,1.),(1.,1.),(1.,
1.),(1.,1.),(1.,1.),(1.,1.),(1.,1.),(1.,1.),(1.,1.),(1.,1.),(1.,1.),(1.,
1.),(1.,1.),(1.,1.),(1.,1.),(1.,1.),(1.,1.),(1.,1.),(1.,1.),(1.,1.),(1.,
1.),(1.,1.),(1.,1.),(1.,1.),(1.,1.),(1.,1.),(1.,1.),(1.,1.),(1.,1.),(1.,
1.),(1.,1.),(1.,1.),(1.,1.),(1.,1.),(1.,1.),(1.,1.),(1.,1.),(1.,1.),(1.,
1.),(1.,1.),(1.,1.),(1.,1.),(1.,1.),(1.,1.),(1.,1.),(1.,1.),(1.,1.),(1.,
1.),(1.,1.),(1.,1.),(1.,1.),(1.,1.),(1.,1.),(1.,1.),(1.,1.),(1.,1.),(1.,
1.),(1.,1.),(1.,1.),(1.,1.),(1.,1.),(1.,1.),(1.,1.),(1.,1.),(1.,1.),(1.,
1.),(1.,1.),(1.,1.),(1.,1.),(1.,1.),(1.,1.),(1.,1.),(1.,1.),(1.,1.),(1.,
1.),(1.,1.),(1.,1.),(1.,1.),(1.,1.),(1.,1.),(1.,1.),(1.,1.),(1.,1.),(1.,
1.),(1.,1.),(1.,1.),(1.,1.),(1.,1.),(1.,1.),(1.,1.),(1.,1.),(1.,1.),(1.,
1.),(1.,1.),(1.,1.),(1.,1.),(1.,1.),(1.,1.),(1.,1.),(1.,1.),(1.,1.),(1.,
1.),(1.,1.),(1.,1.),(1.,1.),(1.,1.),(1.,1.),(1.,1.),(1.,1.),(1.,1.),(1.,
1.),(1.,1.),(1.,1.),(1.,1.),(1.,1.),(1.,1.),(1.,1.),(1.,1.),(1.,1.),(1.,
1.),(1.,1.),(1.,1.),(1.,1.),(1.,1.),(1.,1.),(1.,1.),(1.,1.),(1.,1.),(1.,
1.),(1.,1.),(1.,1.),(1.,1.),(1.,1.),(1.,1.),(1.,1.),(1.,1.),(1.,1.),(1.,
1.),(1.,1.),(1.,1.),(1.,1.),(1.,1.),(1.,1.),(1.,1.),(1.,1.),(1.,1.),(1.,
1.),(1.,1.),(1.,1.),(1.,1.),(1.,1.),(1.,1.),(1.,1.),(1.,1.),(1.,1.),(1.,
1.),(1.,1.),(1.,1.),(1.,1.),(1.,1.),(1.,1.),(1.,1.),(1.,1.),(1.,1.),(1.,
1.),(1.,1.),(1.,1.),(1.,1.),(1.,1.),(1.,1.),(1.,1.),(1.,1.),(1.,1.),(1.,
1.),(1.,1.),(1.,1.),(1.,1.),(1.,1.),(1.,1.),(1.,1.),(1.,1.),(1.,1.),(1.,
1.),(1.,1.),(1.,1.),(1.,1.),(1.,1.),(1.,1.),(1.,1.),(1.,1.),(1.,1.),(1.,
1.),(1.,1.),(1.,1.),(1.,1.),(1.,1.),(1.,1.),(1.,1.),(1.,1.),(1.,1.),(1.,
1.),(1.,1.),(1.,1.),(1.,1.),(1.,1.),(1.,1.),(1.,1.),(1.,1.),(1.,1.),(1.,
1.),(1.,1.),(1.,1.),(1.,1.),(1.,1.),(1.,1.),(1.,1.),(1.,1.),(1.,1.),(1.,
1.),(1.,1.),(1.,1.),(1.,1.),(1.,1.),(1.,1.),(1.,1.),(1.,1.),(1.,1.),(1.,
1.),(1.,1.),(1.,1.),(1.,1.),(1.,1.),(1.,1.),(1.,1.),(1.,1.),(1.,1.),(1.,
1.),(1.,1.),(1.,1.),(1.,1.),(1.,1.),(1.,1.),(1.,1.),(1.,1.),(1.,1.),(1.,
1.),(1.,1.),(1.,1.),(1.,1.),(1.,1.),(1.,1.),(1.,1.),(1.,1.),(1.,1.),(1.,
1.),(1.,1.),(1.,1.),(1.,1.),(1.,1.),(1.,1.),(1.,1.),(1.,1.),(1.,1.),(1.,
1.),(1.,1.),(1.,1.),(1.,1.),(1.,1.),(1.,1.),(1.,1.),(1.,1.),(1.,1.),(1.,
1.),(1.,1.),(1.,1.),(1.,1.),(1.,1.),(1.,1.),(1.,1.),(1.,1.),(1.,1.),(1.,
1.),(1.,1.),(1.,1.),(1.,1.),(1.,1.),(1.,1.),(1.,1.),(1.,1.),(1.,1.),(1.,
1.),(1.,1.),(1.,1.),(1.,1.),(1.,1.),(1.,1.),(1.,1.),(1.,1.),(1.,1.),(1.,
1.),(1.,1.),(1.,1.),(1.,1.),(1.,1.),(1.,1.),(1.,1.),(1.,1.),(1.,1.),(1.,
1.),(1.,1.),(1.,1.),(1.,1.),(1.,1.),(1.,1.),(1.,1.),(1.,1.),(1.,1.),(1.,
1.),(1.,1.),(1.,1.),(1.,1.),(1.,1.),(1.,1.),(1.,1.),(1.,1.),(1.,1.),(1.,
1.),(1.,1.),(1.,1.),(1.,1.),(1.,1.),(1.,1.),(1.,1.),(1.,1.),(1.,1.),(1.,
1.),(1.,1.),(1.,1.),(1.,1.),(1.,1.),(1.,1.),(1.,1.),(1.,1.),(1.,1.),(1.,
1.),(1.,1.),(1.,1.),(1.,1.),(1.,1.),(1.,1.),(1.,1.),(1.,1.),(1.,1.),(1.,
1.),(1.,1.),(1.,1.),(1.,1.),(1.,1.),(1.,1.),(1.,1.),(1.,1.),(1.,1.),(1.,
1.),(1.,1.),(1.,1.),(1.,1.),(1.,1.),(1.,1.),(1.,1.),(1.,1.),(1.,1.),(1.,
1.)))
REPRESENTATION_ITEM('')
SURFACE()
);
#266=(
BOUNDED_SURFACE()
B_SPLINE_SURFACE(5,1,((#90421,#90422),(#90423,#90424),(#90425,#90426),(#90427,
#90428),(#90429,#90430),(#90431,#90432),(#90433,#90434),(#90435,#90436),
(#90437,#90438),(#90439,#90440),(#90441,#90442),(#90443,#90444),(#90445,
#90446),(#90447,#90448),(#90449,#90450),(#90451,#90452),(#90453,#90454),
(#90455,#90456),(#90457,#90458),(#90459,#90460),(#90461,#90462),(#90463,
#90464),(#90465,#90466),(#90467,#90468),(#90469,#90470),(#90471,#90472),
(#90473,#90474),(#90475,#90476),(#90477,#90478),(#90479,#90480),(#90481,
#90482),(#90483,#90484),(#90485,#90486),(#90487,#90488),(#90489,#90490),
(#90491,#90492),(#90493,#90494),(#90495,#90496),(#90497,#90498),(#90499,
#90500),(#90501,#90502),(#90503,#90504),(#90505,#90506),(#90507,#90508),
(#90509,#90510),(#90511,#90512),(#90513,#90514),(#90515,#90516),(#90517,
#90518),(#90519,#90520),(#90521,#90522),(#90523,#90524),(#90525,#90526),
(#90527,#90528),(#90529,#90530),(#90531,#90532),(#90533,#90534),(#90535,
#90536),(#90537,#90538),(#90539,#90540),(#90541,#90542),(#90543,#90544),
(#90545,#90546),(#90547,#90548),(#90549,#90550),(#90551,#90552),(#90553,
#90554),(#90555,#90556),(#90557,#90558),(#90559,#90560),(#90561,#90562),
(#90563,#90564),(#90565,#90566),(#90567,#90568),(#90569,#90570),(#90571,
#90572),(#90573,#90574),(#90575,#90576),(#90577,#90578),(#90579,#90580),
(#90581,#90582),(#90583,#90584),(#90585,#90586),(#90587,#90588),(#90589,
#90590),(#90591,#90592),(#90593,#90594),(#90595,#90596),(#90597,#90598),
(#90599,#90600),(#90601,#90602),(#90603,#90604),(#90605,#90606),(#90607,
#90608),(#90609,#90610),(#90611,#90612),(#90613,#90614),(#90615,#90616),
(#90617,#90618),(#90619,#90620),(#90621,#90622),(#90623,#90624),(#90625,
#90626),(#90627,#90628),(#90629,#90630),(#90631,#90632),(#90633,#90634),
(#90635,#90636),(#90637,#90638),(#90639,#90640),(#90641,#90642),(#90643,
#90644),(#90645,#90646),(#90647,#90648),(#90649,#90650),(#90651,#90652),
(#90653,#90654),(#90655,#90656),(#90657,#90658),(#90659,#90660),(#90661,
#90662),(#90663,#90664),(#90665,#90666),(#90667,#90668),(#90669,#90670),
(#90671,#90672),(#90673,#90674),(#90675,#90676),(#90677,#90678),(#90679,
#90680),(#90681,#90682),(#90683,#90684),(#90685,#90686),(#90687,#90688),
(#90689,#90690),(#90691,#90692),(#90693,#90694),(#90695,#90696),(#90697,
#90698),(#90699,#90700),(#90701,#90702),(#90703,#90704),(#90705,#90706),
(#90707,#90708),(#90709,#90710),(#90711,#90712),(#90713,#90714),(#90715,
#90716),(#90717,#90718),(#90719,#90720),(#90721,#90722),(#90723,#90724),
(#90725,#90726),(#90727,#90728),(#90729,#90730),(#90731,#90732),(#90733,
#90734),(#90735,#90736),(#90737,#90738),(#90739,#90740),(#90741,#90742),
(#90743,#90744),(#90745,#90746),(#90747,#90748),(#90749,#90750),(#90751,
#90752),(#90753,#90754),(#90755,#90756),(#90757,#90758),(#90759,#90760),
(#90761,#90762),(#90763,#90764),(#90765,#90766),(#90767,#90768),(#90769,
#90770),(#90771,#90772),(#90773,#90774),(#90775,#90776),(#90777,#90778),
(#90779,#90780),(#90781,#90782),(#90783,#90784),(#90785,#90786),(#90787,
#90788),(#90789,#90790),(#90791,#90792),(#90793,#90794),(#90795,#90796),
(#90797,#90798),(#90799,#90800),(#90801,#90802),(#90803,#90804),(#90805,
#90806),(#90807,#90808),(#90809,#90810),(#90811,#90812),(#90813,#90814),
(#90815,#90816),(#90817,#90818),(#90819,#90820),(#90821,#90822),(#90823,
#90824),(#90825,#90826),(#90827,#90828),(#90829,#90830),(#90831,#90832),
(#90833,#90834),(#90835,#90836),(#90837,#90838),(#90839,#90840),(#90841,
#90842),(#90843,#90844),(#90845,#90846),(#90847,#90848),(#90849,#90850),
(#90851,#90852),(#90853,#90854),(#90855,#90856),(#90857,#90858),(#90859,
#90860),(#90861,#90862),(#90863,#90864),(#90865,#90866),(#90867,#90868),
(#90869,#90870),(#90871,#90872),(#90873,#90874),(#90875,#90876),(#90877,
#90878),(#90879,#90880),(#90881,#90882),(#90883,#90884),(#90885,#90886),
(#90887,#90888),(#90889,#90890),(#90891,#90892),(#90893,#90894),(#90895,
#90896),(#90897,#90898),(#90899,#90900),(#90901,#90902),(#90903,#90904),
(#90905,#90906),(#90907,#90908),(#90909,#90910),(#90911,#90912),(#90913,
#90914),(#90915,#90916),(#90917,#90918),(#90919,#90920),(#90921,#90922),
(#90923,#90924),(#90925,#90926),(#90927,#90928),(#90929,#90930),(#90931,
#90932),(#90933,#90934),(#90935,#90936),(#90937,#90938),(#90939,#90940),
(#90941,#90942),(#90943,#90944),(#90945,#90946),(#90947,#90948),(#90949,
#90950),(#90951,#90952),(#90953,#90954),(#90955,#90956),(#90957,#90958),
(#90959,#90960),(#90961,#90962),(#90963,#90964),(#90965,#90966),(#90967,
#90968),(#90969,#90970),(#90971,#90972),(#90973,#90974),(#90975,#90976),
(#90977,#90978),(#90979,#90980),(#90981,#90982),(#90983,#90984),(#90985,
#90986),(#90987,#90988),(#90989,#90990),(#90991,#90992),(#90993,#90994),
(#90995,#90996),(#90997,#90998),(#90999,#91000),(#91001,#91002),(#91003,
#91004),(#91005,#91006),(#91007,#91008),(#91009,#91010),(#91011,#91012),
(#91013,#91014),(#91015,#91016),(#91017,#91018),(#91019,#91020),(#91021,
#91022),(#91023,#91024),(#91025,#91026),(#91027,#91028),(#91029,#91030),
(#91031,#91032),(#91033,#91034),(#91035,#91036),(#91037,#91038),(#91039,
#91040),(#91041,#91042),(#91043,#91044),(#91045,#91046),(#91047,#91048),
(#91049,#91050),(#91051,#91052),(#91053,#91054),(#91055,#91056),(#91057,
#91058),(#91059,#91060),(#91061,#91062),(#91063,#91064),(#91065,#91066),
(#91067,#91068),(#91069,#91070),(#91071,#91072),(#91073,#91074),(#91075,
#91076),(#91077,#91078),(#91079,#91080),(#91081,#91082),(#91083,#91084),
(#91085,#91086),(#91087,#91088),(#91089,#91090),(#91091,#91092),(#91093,
#91094),(#91095,#91096),(#91097,#91098),(#91099,#91100),(#91101,#91102),
(#91103,#91104),(#91105,#91106),(#91107,#91108),(#91109,#91110),(#91111,
#91112),(#91113,#91114),(#91115,#91116),(#91117,#91118),(#91119,#91120),
(#91121,#91122),(#91123,#91124),(#91125,#91126),(#91127,#91128),(#91129,
#91130),(#91131,#91132),(#91133,#91134),(#91135,#91136),(#91137,#91138),
(#91139,#91140),(#91141,#91142),(#91143,#91144),(#91145,#91146),(#91147,
#91148),(#91149,#91150),(#91151,#91152),(#91153,#91154),(#91155,#91156),
(#91157,#91158),(#91159,#91160),(#91161,#91162),(#91163,#91164),(#91165,
#91166),(#91167,#91168),(#91169,#91170),(#91171,#91172),(#91173,#91174),
(#91175,#91176),(#91177,#91178),(#91179,#91180),(#91181,#91182),(#91183,
#91184),(#91185,#91186),(#91187,#91188),(#91189,#91190),(#91191,#91192),
(#91193,#91194),(#91195,#91196),(#91197,#91198),(#91199,#91200),(#91201,
#91202),(#91203,#91204),(#91205,#91206),(#91207,#91208),(#91209,#91210),
(#91211,#91212),(#91213,#91214),(#91215,#91216),(#91217,#91218),(#91219,
#91220),(#91221,#91222),(#91223,#91224),(#91225,#91226),(#91227,#91228),
(#91229,#91230),(#91231,#91232),(#91233,#91234),(#91235,#91236),(#91237,
#91238),(#91239,#91240),(#91241,#91242),(#91243,#91244),(#91245,#91246),
(#91247,#91248),(#91249,#91250),(#91251,#91252),(#91253,#91254),(#91255,
#91256),(#91257,#91258),(#91259,#91260),(#91261,#91262),(#91263,#91264),
(#91265,#91266),(#91267,#91268),(#91269,#91270),(#91271,#91272),(#91273,
#91274),(#91275,#91276),(#91277,#91278),(#91279,#91280),(#91281,#91282),
(#91283,#91284),(#91285,#91286),(#91287,#91288),(#91289,#91290),(#91291,
#91292),(#91293,#91294),(#91295,#91296),(#91297,#91298),(#91299,#91300),
(#91301,#91302),(#91303,#91304),(#91305,#91306),(#91307,#91308),(#91309,
#91310),(#91311,#91312),(#91313,#91314),(#91315,#91316),(#91317,#91318),
(#91319,#91320),(#91321,#91322),(#91323,#91324),(#91325,#91326),(#91327,
#91328),(#91329,#91330),(#91331,#91332),(#91333,#91334),(#91335,#91336),
(#91337,#91338),(#91339,#91340),(#91341,#91342),(#91343,#91344),(#91345,
#91346),(#91347,#91348),(#91349,#91350),(#91351,#91352),(#91353,#91354),
(#91355,#91356),(#91357,#91358),(#91359,#91360),(#91361,#91362),(#91363,
#91364),(#91365,#91366),(#91367,#91368),(#91369,#91370),(#91371,#91372),
(#91373,#91374),(#91375,#91376),(#91377,#91378),(#91379,#91380),(#91381,
#91382),(#91383,#91384),(#91385,#91386),(#91387,#91388),(#91389,#91390),
(#91391,#91392),(#91393,#91394),(#91395,#91396),(#91397,#91398),(#91399,
#91400),(#91401,#91402),(#91403,#91404),(#91405,#91406),(#91407,#91408),
(#91409,#91410),(#91411,#91412),(#91413,#91414),(#91415,#91416),(#91417,
#91418),(#91419,#91420),(#91421,#91422),(#91423,#91424),(#91425,#91426),
(#91427,#91428),(#91429,#91430),(#91431,#91432),(#91433,#91434),(#91435,
#91436),(#91437,#91438),(#91439,#91440),(#91441,#91442),(#91443,#91444),
(#91445,#91446),(#91447,#91448),(#91449,#91450),(#91451,#91452),(#91453,
#91454),(#91455,#91456),(#91457,#91458),(#91459,#91460),(#91461,#91462),
(#91463,#91464),(#91465,#91466),(#91467,#91468),(#91469,#91470),(#91471,
#91472),(#91473,#91474),(#91475,#91476),(#91477,#91478),(#91479,#91480),
(#91481,#91482),(#91483,#91484),(#91485,#91486),(#91487,#91488),(#91489,
#91490),(#91491,#91492),(#91493,#91494),(#91495,#91496),(#91497,#91498),
(#91499,#91500),(#91501,#91502),(#91503,#91504),(#91505,#91506),(#91507,
#91508),(#91509,#91510),(#91511,#91512),(#91513,#91514),(#91515,#91516),
(#91517,#91518),(#91519,#91520),(#91521,#91522),(#91523,#91524),(#91525,
#91526),(#91527,#91528),(#91529,#91530),(#91531,#91532),(#91533,#91534),
(#91535,#91536),(#91537,#91538),(#91539,#91540),(#91541,#91542),(#91543,
#91544),(#91545,#91546),(#91547,#91548),(#91549,#91550),(#91551,#91552),
(#91553,#91554),(#91555,#91556),(#91557,#91558),(#91559,#91560),(#91561,
#91562),(#91563,#91564),(#91565,#91566),(#91567,#91568),(#91569,#91570),
(#91571,#91572),(#91573,#91574),(#91575,#91576),(#91577,#91578),(#91579,
#91580),(#91581,#91582),(#91583,#91584),(#91585,#91586),(#91587,#91588),
(#91589,#91590),(#91591,#91592),(#91593,#91594),(#91595,#91596),(#91597,
#91598),(#91599,#91600),(#91601,#91602),(#91603,#91604),(#91605,#91606),
(#91607,#91608),(#91609,#91610),(#91611,#91612),(#91613,#91614),(#91615,
#91616),(#91617,#91618),(#91619,#91620),(#91621,#91622),(#91623,#91624),
(#91625,#91626),(#91627,#91628),(#91629,#91630),(#91631,#91632),(#91633,
#91634),(#91635,#91636),(#91637,#91638),(#91639,#91640),(#91641,#91642),
(#91643,#91644),(#91645,#91646),(#91647,#91648),(#91649,#91650),(#91651,
#91652),(#91653,#91654),(#91655,#91656),(#91657,#91658),(#91659,#91660),
(#91661,#91662),(#91663,#91664),(#91665,#91666),(#91667,#91668),(#91669,
#91670),(#91671,#91672),(#91673,#91674),(#91675,#91676),(#91677,#91678),
(#91679,#91680),(#91681,#91682),(#91683,#91684),(#91685,#91686),(#91687,
#91688),(#91689,#91690),(#91691,#91692),(#91693,#91694),(#91695,#91696),
(#91697,#91698),(#91699,#91700),(#91701,#91702),(#91703,#91704),(#91705,
#91706),(#91707,#91708),(#91709,#91710),(#91711,#91712),(#91713,#91714),
(#91715,#91716),(#91717,#91718),(#91719,#91720),(#91721,#91722),(#91723,
#91724),(#91725,#91726),(#91727,#91728),(#91729,#91730),(#91731,#91732),
(#91733,#91734),(#91735,#91736),(#91737,#91738),(#91739,#91740),(#91741,
#91742),(#91743,#91744),(#91745,#91746),(#91747,#91748),(#91749,#91750),
(#91751,#91752),(#91753,#91754),(#91755,#91756),(#91757,#91758),(#91759,
#91760),(#91761,#91762),(#91763,#91764),(#91765,#91766),(#91767,#91768),
(#91769,#91770),(#91771,#91772),(#91773,#91774),(#91775,#91776),(#91777,
#91778),(#91779,#91780),(#91781,#91782),(#91783,#91784),(#91785,#91786),
(#91787,#91788),(#91789,#91790),(#91791,#91792),(#91793,#91794),(#91795,
#91796),(#91797,#91798),(#91799,#91800),(#91801,#91802),(#91803,#91804),
(#91805,#91806),(#91807,#91808),(#91809,#91810),(#91811,#91812),(#91813,
#91814),(#91815,#91816),(#91817,#91818),(#91819,#91820),(#91821,#91822),
(#91823,#91824),(#91825,#91826),(#91827,#91828),(#91829,#91830),(#91831,
#91832),(#91833,#91834),(#91835,#91836),(#91837,#91838),(#91839,#91840),
(#91841,#91842),(#91843,#91844),(#91845,#91846),(#91847,#91848),(#91849,
#91850),(#91851,#91852),(#91853,#91854),(#91855,#91856),(#91857,#91858),
(#91859,#91860),(#91861,#91862),(#91863,#91864),(#91865,#91866),(#91867,
#91868),(#91869,#91870),(#91871,#91872),(#91873,#91874),(#91875,#91876),
(#91877,#91878),(#91879,#91880),(#91881,#91882),(#91883,#91884),(#91885,
#91886),(#91887,#91888),(#91889,#91890),(#91891,#91892),(#91893,#91894),
(#91895,#91896),(#91897,#91898),(#91899,#91900),(#91901,#91902),(#91903,
#91904),(#91905,#91906),(#91907,#91908),(#91909,#91910),(#91911,#91912),
(#91913,#91914),(#91915,#91916),(#91917,#91918),(#91919,#91920),(#91921,
#91922),(#91923,#91924),(#91925,#91926),(#91927,#91928),(#91929,#91930),
(#91931,#91932),(#91933,#91934),(#91935,#91936),(#91937,#91938),(#91939,
#91940),(#91941,#91942),(#91943,#91944),(#91945,#91946),(#91947,#91948),
(#91949,#91950),(#91951,#91952),(#91953,#91954),(#91955,#91956),(#91957,
#91958),(#91959,#91960),(#91961,#91962),(#91963,#91964),(#91965,#91966),
(#91967,#91968),(#91969,#91970),(#91971,#91972),(#91973,#91974),(#91975,
#91976),(#91977,#91978),(#91979,#91980),(#91981,#91982),(#91983,#91984),
(#91985,#91986),(#91987,#91988),(#91989,#91990),(#91991,#91992),(#91993,
#91994),(#91995,#91996),(#91997,#91998),(#91999,#92000),(#92001,#92002),
(#92003,#92004),(#92005,#92006),(#92007,#92008),(#92009,#92010),(#92011,
#92012),(#92013,#92014),(#92015,#92016),(#92017,#92018),(#92019,#92020),
(#92021,#92022),(#92023,#92024),(#92025,#92026),(#92027,#92028),(#92029,
#92030),(#92031,#92032),(#92033,#92034),(#92035,#92036),(#92037,#92038),
(#92039,#92040),(#92041,#92042),(#92043,#92044),(#92045,#92046),(#92047,
#92048),(#92049,#92050),(#92051,#92052),(#92053,#92054),(#92055,#92056),
(#92057,#92058),(#92059,#92060),(#92061,#92062),(#92063,#92064),(#92065,
#92066),(#92067,#92068),(#92069,#92070),(#92071,#92072),(#92073,#92074),
(#92075,#92076),(#92077,#92078),(#92079,#92080),(#92081,#92082),(#92083,
#92084),(#92085,#92086),(#92087,#92088),(#92089,#92090),(#92091,#92092),
(#92093,#92094),(#92095,#92096),(#92097,#92098),(#92099,#92100),(#92101,
#92102),(#92103,#92104),(#92105,#92106),(#92107,#92108),(#92109,#92110),
(#92111,#92112),(#92113,#92114),(#92115,#92116),(#92117,#92118),(#92119,
#92120),(#92121,#92122),(#92123,#92124),(#92125,#92126),(#92127,#92128),
(#92129,#92130),(#92131,#92132),(#92133,#92134),(#92135,#92136),(#92137,
#92138),(#92139,#92140),(#92141,#92142),(#92143,#92144),(#92145,#92146),
(#92147,#92148),(#92149,#92150),(#92151,#92152),(#92153,#92154),(#92155,
#92156),(#92157,#92158),(#92159,#92160),(#92161,#92162),(#92163,#92164),
(#92165,#92166),(#92167,#92168),(#92169,#92170),(#92171,#92172),(#92173,
#92174),(#92175,#92176),(#92177,#92178),(#92179,#92180),(#92181,#92182),
(#92183,#92184),(#92185,#92186),(#92187,#92188),(#92189,#92190),(#92191,
#92192),(#92193,#92194),(#92195,#92196),(#92197,#92198),(#92199,#92200),
(#92201,#92202),(#92203,#92204),(#92205,#92206),(#92207,#92208),(#92209,
#92210),(#92211,#92212),(#92213,#92214),(#92215,#92216),(#92217,#92218),
(#92219,#92220),(#92221,#92222),(#92223,#92224),(#92225,#92226),(#92227,
#92228),(#92229,#92230),(#92231,#92232),(#92233,#92234),(#92235,#92236),
(#92237,#92238),(#92239,#92240),(#92241,#92242),(#92243,#92244),(#92245,
#92246),(#92247,#92248),(#92249,#92250),(#92251,#92252),(#92253,#92254),
(#92255,#92256),(#92257,#92258),(#92259,#92260),(#92261,#92262),(#92263,
#92264),(#92265,#92266),(#92267,#92268),(#92269,#92270),(#92271,#92272),
(#92273,#92274),(#92275,#92276),(#92277,#92278),(#92279,#92280),(#92281,
#92282),(#92283,#92284),(#92285,#92286),(#92287,#92288),(#92289,#92290),
(#92291,#92292),(#92293,#92294),(#92295,#92296),(#92297,#92298),(#92299,
#92300),(#92301,#92302),(#92303,#92304),(#92305,#92306),(#92307,#92308),
(#92309,#92310),(#92311,#92312),(#92313,#92314),(#92315,#92316),(#92317,
#92318),(#92319,#92320),(#92321,#92322),(#92323,#92324),(#92325,#92326),
(#92327,#92328),(#92329,#92330),(#92331,#92332),(#92333,#92334),(#92335,
#92336),(#92337,#92338),(#92339,#92340),(#92341,#92342),(#92343,#92344),
(#92345,#92346),(#92347,#92348),(#92349,#92350),(#92351,#92352),(#92353,
#92354),(#92355,#92356),(#92357,#92358),(#92359,#92360),(#92361,#92362),
(#92363,#92364),(#92365,#92366),(#92367,#92368),(#92369,#92370),(#92371,
#92372),(#92373,#92374),(#92375,#92376),(#92377,#92378),(#92379,#92380),
(#92381,#92382),(#92383,#92384),(#92385,#92386),(#92387,#92388),(#92389,
#92390),(#92391,#92392),(#92393,#92394),(#92395,#92396),(#92397,#92398),
(#92399,#92400),(#92401,#92402),(#92403,#92404),(#92405,#92406),(#92407,
#92408),(#92409,#92410),(#92411,#92412),(#92413,#92414),(#92415,#92416),
(#92417,#92418),(#92419,#92420),(#92421,#92422),(#92423,#92424),(#92425,
#92426),(#92427,#92428),(#92429,#92430)),.UNSPECIFIED.,.F.,.F.,.F.)
B_SPLINE_SURFACE_WITH_KNOTS((6,1,1,1,1,1,1,1,1,1,1,1,1,1,1,1,1,1,1,1,1,
1,1,1,1,1,1,1,1,1,1,1,1,1,1,1,1,1,1,1,1,1,1,1,1,1,1,1,1,1,1,1,1,1,1,1,1,
1,1,1,1,1,1,1,1,1,1,1,1,1,1,1,1,1,1,1,1,1,1,1,1,1,1,1,1,1,1,1,1,1,1,1,1,
1,1,1,1,1,1,1,1,1,1,1,1,1,1,1,1,1,1,1,1,1,1,1,1,1,1,1,1,1,1,1,1,1,1,1,1,
1,1,1,1,1,1,1,1,1,1,1,1,1,1,1,1,1,1,1,1,1,1,1,1,1,1,1,1,1,1,1,1,1,1,1,1,
1,1,1,1,1,1,1,1,1,1,1,1,1,1,1,1,1,1,1,1,1,1,1,1,1,1,1,1,1,1,1,1,1,1,1,1,
1,1,1,1,1,1,1,1,1,1,1,1,1,1,1,1,1,1,1,1,1,1,1,1,1,1,1,1,1,1,1,1,1,1,1,1,
1,1,1,1,1,1,1,1,1,1,1,1,1,1,1,1,1,1,1,1,1,1,1,1,1,1,1,1,1,1,1,1,1,1,1,1,
1,1,1,1,1,1,1,1,1,1,1,1,1,1,1,1,1,1,1,1,1,1,1,1,1,1,1,1,1,1,1,1,1,1,1,1,
1,1,1,1,1,1,1,1,1,1,1,1,1,1,1,1,1,1,1,1,1,1,1,1,1,1,1,1,1,1,1,1,1,1,1,1,
1,1,1,1,1,1,1,1,1,1,1,1,1,1,1,1,1,1,1,1,1,1,1,1,1,1,1,1,1,1,1,1,1,1,1,1,
1,1,1,1,1,1,1,1,1,1,1,1,1,1,1,1,1,1,1,1,1,1,1,1,1,1,1,1,1,1,1,1,1,1,1,1,
1,1,1,1,1,1,1,1,1,1,1,1,1,1,1,1,1,1,1,1,1,1,1,1,1,1,1,1,1,1,1,1,1,1,1,1,
1,1,1,1,1,1,1,1,1,1,1,1,1,1,1,1,1,1,1,1,1,1,1,1,1,1,1,1,1,1,1,1,1,1,1,1,
1,1,1,1,1,1,1,1,1,1,1,1,1,1,1,1,1,1,1,1,1,1,1,1,1,1,1,1,1,1,1,1,1,1,1,1,
1,1,1,1,1,1,1,1,1,1,1,1,1,1,1,1,1,1,1,1,1,1,1,1,1,1,1,1,1,1,1,1,1,1,1,1,
1,1,1,1,1,1,1,1,1,1,1,1,1,1,1,1,1,1,1,1,1,1,1,1,1,1,1,1,1,1,1,1,1,1,1,1,
1,1,1,1,1,1,1,1,1,1,1,1,1,1,1,1,1,1,1,1,1,1,1,1,1,1,1,1,1,1,1,1,1,1,1,1,
1,1,1,1,1,1,1,1,1,1,1,1,1,1,1,1,1,1,1,1,1,1,1,1,1,1,1,1,1,1,1,1,1,1,1,1,
1,1,1,1,1,1,1,1,1,1,1,1,1,1,1,1,1,1,1,1,1,1,1,1,1,1,1,1,1,1,1,1,1,1,1,1,
1,1,1,1,1,1,1,1,1,1,1,1,1,1,1,1,1,1,1,1,1,1,1,1,1,1,1,1,1,1,1,1,1,1,1,1,
1,1,1,1,1,1,1,1,1,1,1,1,1,1,1,1,1,1,1,1,1,1,1,1,1,1,1,1,1,1,1,1,1,1,1,1,
1,1,1,1,1,1,1,1,1,1,1,1,1,1,1,1,1,1,1,1,1,1,1,1,1,1,1,1,1,1,1,1,1,1,1,1,
1,1,1,1,1,1,1,1,1,1,1,1,1,1,1,1,1,1,1,1,1,1,1,1,1,1,1,1,1,1,1,1,1,1,1,1,
1,1,1,1,1,1,1,1,1,1,1,1,1,1,1,1,1,1,1,1,1,1,1,1,1,1,1,1,1,1,1,1,1,1,1,1,
1,1,1,1,1,1,1,1,1,1,1,1,1,1,1,1,1,1,1,1,1,1,1,1,1,1,1,1,1,1,1,1,1,1,1,1,
1,1,1,1,1,1,1,1,1,1,1,1,1,1,1,1,1,1,1,1,1,1,1,1,1,1,1,1,1,1,1,1,1,1,1,1,
1,1,1,1,1,1,1,1,1,1,1,1,1,1,1,1,1,1,1,1,1,1,1,1,1,1,1,1,1,1,1,1,1,1,1,1,
1,1,1,1,1,1,1,6),(2,2),(-1.,-0.999000000000001,-0.998000000000001,-0.997000000000001,
-0.996000000000001,-0.995000000000001,-0.994000000000001,-0.993000000000001,
-0.992000000000001,-0.991000000000001,-0.990000000000001,-0.989000000000001,
-0.988000000000001,-0.987000000000001,-0.986000000000001,-0.985000000000001,
-0.984000000000001,-0.983000000000001,-0.982000000000001,-0.981000000000001,
-0.980000000000001,-0.979000000000001,-0.978000000000001,-0.977000000000001,
-0.976000000000001,-0.975000000000001,-0.974000000000001,-0.973000000000001,
-0.972000000000001,-0.971000000000001,-0.970000000000001,-0.969000000000001,
-0.968000000000001,-0.967000000000001,-0.966000000000001,-0.965000000000001,
-0.964000000000001,-0.963000000000001,-0.962000000000001,-0.961000000000001,
-0.960000000000001,-0.959000000000001,-0.958000000000001,-0.957000000000001,
-0.956000000000001,-0.955000000000001,-0.954000000000001,-0.953000000000001,
-0.952000000000001,-0.951000000000001,-0.950000000000001,-0.949000000000001,
-0.948000000000001,-0.947000000000001,-0.946000000000001,-0.945000000000001,
-0.944000000000001,-0.943000000000001,-0.942000000000001,-0.941000000000001,
-0.940000000000001,-0.939000000000001,-0.938000000000001,-0.937000000000001,
-0.936000000000001,-0.935000000000001,-0.934000000000001,-0.933000000000001,
-0.932000000000001,-0.931000000000001,-0.930000000000001,-0.929000000000001,
-0.928000000000001,-0.927000000000001,-0.926000000000001,-0.925000000000001,
-0.924000000000001,-0.923000000000001,-0.922000000000001,-0.921000000000001,
-0.920000000000001,-0.919000000000001,-0.918000000000001,-0.917000000000001,
-0.916000000000001,-0.915000000000001,-0.914000000000001,-0.913000000000001,
-0.912000000000001,-0.911000000000001,-0.910000000000001,-0.909000000000001,
-0.908000000000001,-0.907000000000001,-0.906000000000001,-0.905000000000001,
-0.904000000000001,-0.903000000000001,-0.902000000000001,-0.901000000000001,
-0.900000000000001,-0.899000000000001,-0.898000000000001,-0.897000000000001,
-0.896000000000001,-0.895000000000001,-0.894000000000001,-0.893000000000001,
-0.892000000000001,-0.891000000000001,-0.890000000000001,-0.889000000000001,
-0.888000000000001,-0.887000000000001,-0.886000000000001,-0.885000000000001,
-0.884000000000001,-0.883000000000001,-0.882000000000001,-0.881000000000001,
-0.880000000000001,-0.879000000000001,-0.878000000000001,-0.877000000000001,
-0.876000000000001,-0.875000000000001,-0.874000000000001,-0.873000000000001,
-0.872000000000001,-0.871000000000001,-0.870000000000001,-0.869000000000001,
-0.868000000000001,-0.867000000000001,-0.866000000000001,-0.865000000000001,
-0.864000000000001,-0.863000000000001,-0.862000000000001,-0.861000000000001,
-0.860000000000001,-0.859000000000001,-0.858000000000001,-0.857000000000001,
-0.856000000000001,-0.855000000000001,-0.854000000000001,-0.853000000000001,
-0.852000000000001,-0.851000000000001,-0.850000000000001,-0.849000000000001,
-0.848000000000001,-0.847000000000001,-0.846000000000001,-0.845000000000001,
-0.844000000000001,-0.843000000000001,-0.842000000000001,-0.841000000000001,
-0.840000000000001,-0.839000000000001,-0.838000000000001,-0.837000000000001,
-0.836000000000001,-0.835000000000001,-0.834000000000001,-0.833000000000001,
-0.832000000000001,-0.831000000000001,-0.830000000000001,-0.829000000000001,
-0.828000000000001,-0.827000000000001,-0.826000000000001,-0.825000000000001,
-0.824000000000001,-0.823000000000001,-0.822000000000001,-0.821000000000001,
-0.820000000000001,-0.819000000000001,-0.818000000000001,-0.817000000000001,
-0.816000000000001,-0.815000000000001,-0.814000000000001,-0.813000000000001,
-0.812000000000001,-0.811000000000001,-0.810000000000001,-0.809000000000001,
-0.808000000000001,-0.807000000000001,-0.806000000000001,-0.805000000000001,
-0.804000000000001,-0.803000000000001,-0.802000000000001,-0.801000000000001,
-0.800000000000001,-0.799000000000001,-0.798000000000001,-0.797000000000001,
-0.796000000000001,-0.795000000000001,-0.794000000000001,-0.793000000000001,
-0.792000000000001,-0.791000000000001,-0.790000000000001,-0.789000000000001,
-0.788000000000001,-0.787000000000001,-0.786000000000001,-0.785000000000001,
-0.784000000000001,-0.783000000000001,-0.782000000000001,-0.781000000000001,
-0.780000000000001,-0.779000000000001,-0.778000000000001,-0.777000000000001,
-0.776000000000001,-0.775000000000001,-0.774000000000001,-0.773000000000001,
-0.772000000000001,-0.771000000000001,-0.770000000000001,-0.769000000000001,
-0.768000000000001,-0.767000000000001,-0.766000000000001,-0.765000000000001,
-0.764000000000001,-0.763000000000001,-0.762000000000001,-0.761000000000001,
-0.760000000000001,-0.759000000000001,-0.758000000000001,-0.757000000000001,
-0.756000000000001,-0.755000000000001,-0.754000000000001,-0.753000000000001,
-0.752000000000001,-0.751000000000001,-0.750000000000001,-0.749000000000001,
-0.748000000000001,-0.747000000000001,-0.746000000000001,-0.745000000000001,
-0.744000000000001,-0.743000000000001,-0.742000000000001,-0.741000000000001,
-0.740000000000001,-0.739000000000001,-0.738000000000001,-0.737000000000001,
-0.736000000000001,-0.735000000000001,-0.734000000000001,-0.733000000000001,
-0.732000000000001,-0.731000000000001,-0.730000000000001,-0.729000000000001,
-0.728000000000001,-0.727000000000001,-0.726000000000001,-0.725000000000001,
-0.724000000000001,-0.723000000000001,-0.722000000000001,-0.721000000000001,
-0.720000000000001,-0.719000000000001,-0.718000000000001,-0.717000000000001,
-0.716000000000001,-0.715000000000001,-0.714000000000001,-0.713000000000001,
-0.712000000000001,-0.711000000000001,-0.710000000000001,-0.709000000000001,
-0.708000000000001,-0.707000000000001,-0.706000000000001,-0.705000000000001,
-0.704000000000001,-0.703000000000001,-0.702000000000001,-0.701000000000001,
-0.700000000000001,-0.699000000000001,-0.698000000000001,-0.697000000000001,
-0.696000000000001,-0.695000000000001,-0.694000000000001,-0.693000000000001,
-0.692000000000001,-0.691000000000001,-0.690000000000001,-0.689000000000001,
-0.688000000000001,-0.687,-0.686,-0.685,-0.684,-0.683,-0.682,-0.681,-0.68,
-0.679,-0.678,-0.677,-0.676,-0.675,-0.674,-0.673,-0.672,-0.671,-0.67,-0.669,
-0.668,-0.667,-0.666,-0.665,-0.664,-0.663,-0.662,-0.661,-0.66,-0.659,-0.658,
-0.657,-0.656,-0.655,-0.654,-0.653,-0.652,-0.651,-0.65,-0.649,-0.648,-0.647,
-0.646,-0.645,-0.644,-0.643,-0.642,-0.641,-0.64,-0.639,-0.638,-0.637,-0.636,
-0.635,-0.634,-0.633,-0.632,-0.631,-0.63,-0.629,-0.628,-0.627,-0.626,-0.625,
-0.624,-0.623,-0.622,-0.621,-0.62,-0.619,-0.618,-0.617,-0.616,-0.615,-0.614,
-0.613,-0.612,-0.611,-0.61,-0.609,-0.608,-0.607,-0.606,-0.605,-0.604,-0.603,
-0.602,-0.601,-0.6,-0.599,-0.598,-0.597,-0.596,-0.595,-0.594,-0.593,-0.592,
-0.591,-0.59,-0.589,-0.588,-0.587,-0.586,-0.585,-0.584,-0.583,-0.582,-0.581,
-0.58,-0.579,-0.578,-0.577,-0.576,-0.575,-0.574,-0.573,-0.572,-0.571,-0.57,
-0.569,-0.568,-0.567,-0.566,-0.565,-0.564,-0.563,-0.562,-0.561,-0.56,-0.559,
-0.558,-0.557,-0.556,-0.555,-0.554,-0.553,-0.552,-0.551,-0.55,-0.549,-0.548,
-0.547,-0.546,-0.545,-0.544,-0.543,-0.542,-0.541,-0.54,-0.539,-0.538,-0.537,
-0.536,-0.535,-0.534,-0.533,-0.532,-0.531,-0.53,-0.529,-0.528,-0.527,-0.526,
-0.525,-0.524,-0.523,-0.522,-0.521,-0.52,-0.519,-0.518,-0.517,-0.516,-0.515,
-0.514,-0.513,-0.512,-0.511,-0.51,-0.509,-0.508,-0.507,-0.506,-0.505,-0.504,
-0.503,-0.502,-0.501,-0.5,-0.499,-0.498,-0.497,-0.496,-0.495,-0.494,-0.493,
-0.492,-0.491,-0.49,-0.489,-0.488,-0.487,-0.486,-0.485,-0.484,-0.483,-0.482,
-0.481,-0.48,-0.479,-0.478,-0.477,-0.476,-0.475,-0.474,-0.473,-0.472,-0.471,
-0.47,-0.469,-0.468,-0.467,-0.466,-0.465,-0.464,-0.463,-0.462,-0.461,-0.46,
-0.459,-0.458,-0.457,-0.456,-0.455,-0.454,-0.453,-0.452,-0.451,-0.45,-0.449,
-0.448,-0.447,-0.446,-0.445,-0.444,-0.443,-0.442,-0.441,-0.44,-0.439,-0.438,
-0.437,-0.436,-0.435,-0.434,-0.433,-0.432,-0.431,-0.43,-0.429,-0.428,-0.427,
-0.426,-0.425,-0.424,-0.423,-0.422,-0.421,-0.42,-0.419,-0.418,-0.417,-0.416,
-0.415,-0.414,-0.413,-0.412,-0.411,-0.41,-0.409,-0.408,-0.407,-0.406,-0.405,
-0.404,-0.403,-0.402,-0.401,-0.4,-0.399,-0.398,-0.397,-0.396,-0.395,-0.394,
-0.393,-0.392,-0.391,-0.39,-0.389,-0.388,-0.387,-0.386,-0.385,-0.384,-0.383,
-0.382,-0.381,-0.38,-0.379,-0.378,-0.377,-0.376,-0.375,-0.374,-0.373,-0.372,
-0.371,-0.37,-0.369,-0.368,-0.367,-0.366,-0.365,-0.364,-0.363,-0.362,-0.361,
-0.36,-0.359,-0.358,-0.357,-0.356,-0.355,-0.354,-0.353,-0.352,-0.351,-0.35,
-0.349,-0.348,-0.347,-0.346,-0.345,-0.344,-0.343,-0.342,-0.341,-0.34,-0.339,
-0.338,-0.337,-0.336,-0.335,-0.334,-0.333,-0.332,-0.331,-0.33,-0.329,-0.328,
-0.327,-0.326,-0.325,-0.324,-0.323,-0.322,-0.321,-0.32,-0.319,-0.318,-0.317,
-0.316,-0.315,-0.314,-0.313,-0.312,-0.311,-0.31,-0.309,-0.308,-0.307,-0.306,
-0.305,-0.304,-0.303,-0.302,-0.301,-0.3,-0.299,-0.298,-0.297,-0.296,-0.295,
-0.294,-0.293,-0.292,-0.291,-0.29,-0.289,-0.288,-0.287,-0.286,-0.285,-0.284,
-0.283,-0.282,-0.281,-0.28,-0.279,-0.278,-0.277,-0.276,-0.275,-0.274,-0.273,
-0.272,-0.271,-0.27,-0.269,-0.268,-0.267,-0.266,-0.265,-0.264,-0.263,-0.262,
-0.261,-0.26,-0.259,-0.258,-0.257,-0.256,-0.255,-0.254,-0.253,-0.252,-0.251,
-0.25,-0.249,-0.248,-0.247,-0.246,-0.245,-0.244,-0.243,-0.242,-0.241,-0.24,
-0.239,-0.238,-0.237,-0.236,-0.235,-0.234,-0.233,-0.232,-0.231,-0.23,-0.229,
-0.228,-0.227,-0.226,-0.225,-0.224,-0.223,-0.222,-0.221,-0.22,-0.219,-0.218,
-0.217,-0.216,-0.215,-0.214,-0.213,-0.212,-0.211,-0.21,-0.209,-0.208,-0.207,
-0.206,-0.205,-0.204,-0.203,-0.202,-0.201,-0.2,-0.199,-0.198,-0.197,-0.196,
-0.195,-0.194,-0.193,-0.192,-0.191,-0.19,-0.189,-0.188,-0.187,-0.186,-0.185,
-0.184,-0.183,-0.182,-0.181,-0.18,-0.179,-0.178,-0.177,-0.176,-0.175,-0.174,
-0.173,-0.172,-0.171,-0.17,-0.169,-0.168,-0.167,-0.166,-0.165,-0.164,-0.163,
-0.162,-0.161,-0.16,-0.159,-0.158,-0.157,-0.156,-0.155,-0.154,-0.153,-0.152,
-0.151,-0.15,-0.149,-0.148,-0.147,-0.146,-0.145,-0.144,-0.143,-0.142,-0.141,
-0.14,-0.139,-0.138,-0.137,-0.136,-0.135,-0.134,-0.133,-0.132,-0.131,-0.13,
-0.129,-0.128,-0.127,-0.126,-0.125,-0.124,-0.123,-0.122,-0.121,-0.12,-0.119,
-0.118,-0.117,-0.116,-0.115,-0.114,-0.113,-0.112,-0.111,-0.11,-0.109,-0.108,
-0.107,-0.106,-0.105,-0.104,-0.103,-0.102,-0.101,-0.1,-0.0990000000000001,
-0.0980000000000001,-0.0970000000000001,-0.0960000000000001,-0.0950000000000001,
-0.0940000000000001,-0.0930000000000001,-0.0920000000000001,-0.0910000000000001,
-0.0900000000000001,-0.0890000000000001,-0.0880000000000001,-0.0870000000000001,
-0.0860000000000001,-0.0850000000000001,-0.0840000000000001,-0.0830000000000001,
-0.0820000000000001,-0.0810000000000001,-0.0800000000000001,-0.0790000000000001,
-0.0780000000000001,-0.0770000000000001,-0.0760000000000001,-0.0750000000000001,
-0.0740000000000001,-0.0730000000000001,-0.0720000000000001,-0.071,-0.07,
-0.069,-0.068,-0.067,-0.066,-0.065,-0.064,-0.063,-0.062,-0.061,-0.06,-0.059,
-0.058,-0.057,-0.056,-0.055,-0.054,-0.053,-0.052,-0.051,-0.05,-0.049,-0.048,
-0.047,-0.046,-0.045,-0.044,-0.043,-0.042,-0.041,-0.04,-0.039,-0.038,-0.037,
-0.036,-0.035,-0.034,-0.033,-0.032,-0.031,-0.03,-0.029,-0.028,-0.027,-0.026,
-0.025,-0.024,-0.023,-0.022,-0.021,-0.02,-0.019,-0.018,-0.017,-0.016,-0.015,
-0.014,-0.013,-0.012,-0.011,-0.01,-0.009,-0.008,-0.007,-0.006,-0.005,-0.004,
-0.003,-0.002,-0.001,0.),(0.,2.),.UNSPECIFIED.)
GEOMETRIC_REPRESENTATION_ITEM()
RATIONAL_B_SPLINE_SURFACE(((1.,1.),(1.,1.),(1.,1.),(1.,1.),(1.,1.),(1.,
1.),(1.,1.),(1.,1.),(1.,1.),(1.,1.),(1.,1.),(1.,1.),(1.,1.),(1.,1.),(1.,
1.),(1.,1.),(1.,1.),(1.,1.),(1.,1.),(1.,1.),(1.,1.),(1.,1.),(1.,1.),(1.,
1.),(1.,1.),(1.,1.),(1.,1.),(1.,1.),(1.,1.),(1.,1.),(1.,1.),(1.,1.),(1.,
1.),(1.,1.),(1.,1.),(1.,1.),(1.,1.),(1.,1.),(1.,1.),(1.,1.),(1.,1.),(1.,
1.),(1.,1.),(1.,1.),(1.,1.),(1.,1.),(1.,1.),(1.,1.),(1.,1.),(1.,1.),(1.,
1.),(1.,1.),(1.,1.),(1.,1.),(1.,1.),(1.,1.),(1.,1.),(1.,1.),(1.,1.),(1.,
1.),(1.,1.),(1.,1.),(1.,1.),(1.,1.),(1.,1.),(1.,1.),(1.,1.),(1.,1.),(1.,
1.),(1.,1.),(1.,1.),(1.,1.),(1.,1.),(1.,1.),(1.,1.),(1.,1.),(1.,1.),(1.,
1.),(1.,1.),(1.,1.),(1.,1.),(1.,1.),(1.,1.),(1.,1.),(1.,1.),(1.,1.),(1.,
1.),(1.,1.),(1.,1.),(1.,1.),(1.,1.),(1.,1.),(1.,1.),(1.,1.),(1.,1.),(1.,
1.),(1.,1.),(1.,1.),(1.,1.),(1.,1.),(1.,1.),(1.,1.),(1.,1.),(1.,1.),(1.,
1.),(1.,1.),(1.,1.),(1.,1.),(1.,1.),(1.,1.),(1.,1.),(1.,1.),(1.,1.),(1.,
1.),(1.,1.),(1.,1.),(1.,1.),(1.,1.),(1.,1.),(1.,1.),(1.,1.),(1.,1.),(1.,
1.),(1.,1.),(1.,1.),(1.,1.),(1.,1.),(1.,1.),(1.,1.),(1.,1.),(1.,1.),(1.,
1.),(1.,1.),(1.,1.),(1.,1.),(1.,1.),(1.,1.),(1.,1.),(1.,1.),(1.,1.),(1.,
1.),(1.,1.),(1.,1.),(1.,1.),(1.,1.),(1.,1.),(1.,1.),(1.,1.),(1.,1.),(1.,
1.),(1.,1.),(1.,1.),(1.,1.),(1.,1.),(1.,1.),(1.,1.),(1.,1.),(1.,1.),(1.,
1.),(1.,1.),(1.,1.),(1.,1.),(1.,1.),(1.,1.),(1.,1.),(1.,1.),(1.,1.),(1.,
1.),(1.,1.),(1.,1.),(1.,1.),(1.,1.),(1.,1.),(1.,1.),(1.,1.),(1.,1.),(1.,
1.),(1.,1.),(1.,1.),(1.,1.),(1.,1.),(1.,1.),(1.,1.),(1.,1.),(1.,1.),(1.,
1.),(1.,1.),(1.,1.),(1.,1.),(1.,1.),(1.,1.),(1.,1.),(1.,1.),(1.,1.),(1.,
1.),(1.,1.),(1.,1.),(1.,1.),(1.,1.),(1.,1.),(1.,1.),(1.,1.),(1.,1.),(1.,
1.),(1.,1.),(1.,1.),(1.,1.),(1.,1.),(1.,1.),(1.,1.),(1.,1.),(1.,1.),(1.,
1.),(1.,1.),(1.,1.),(1.,1.),(1.,1.),(1.,1.),(1.,1.),(1.,1.),(1.,1.),(1.,
1.),(1.,1.),(1.,1.),(1.,1.),(1.,1.),(1.,1.),(1.,1.),(1.,1.),(1.,1.),(1.,
1.),(1.,1.),(1.,1.),(1.,1.),(1.,1.),(1.,1.),(1.,1.),(1.,1.),(1.,1.),(1.,
1.),(1.,1.),(1.,1.),(1.,1.),(1.,1.),(1.,1.),(1.,1.),(1.,1.),(1.,1.),(1.,
1.),(1.,1.),(1.,1.),(1.,1.),(1.,1.),(1.,1.),(1.,1.),(1.,1.),(1.,1.),(1.,
1.),(1.,1.),(1.,1.),(1.,1.),(1.,1.),(1.,1.),(1.,1.),(1.,1.),(1.,1.),(1.,
1.),(1.,1.),(1.,1.),(1.,1.),(1.,1.),(1.,1.),(1.,1.),(1.,1.),(1.,1.),(1.,
1.),(1.,1.),(1.,1.),(1.,1.),(1.,1.),(1.,1.),(1.,1.),(1.,1.),(1.,1.),(1.,
1.),(1.,1.),(1.,1.),(1.,1.),(1.,1.),(1.,1.),(1.,1.),(1.,1.),(1.,1.),(1.,
1.),(1.,1.),(1.,1.),(1.,1.),(1.,1.),(1.,1.),(1.,1.),(1.,1.),(1.,1.),(1.,
1.),(1.,1.),(1.,1.),(1.,1.),(1.,1.),(1.,1.),(1.,1.),(1.,1.),(1.,1.),(1.,
1.),(1.,1.),(1.,1.),(1.,1.),(1.,1.),(1.,1.),(1.,1.),(1.,1.),(1.,1.),(1.,
1.),(1.,1.),(1.,1.),(1.,1.),(1.,1.),(1.,1.),(1.,1.),(1.,1.),(1.,1.),(1.,
1.),(1.,1.),(1.,1.),(1.,1.),(1.,1.),(1.,1.),(1.,1.),(1.,1.),(1.,1.),(1.,
1.),(1.,1.),(1.,1.),(1.,1.),(1.,1.),(1.,1.),(1.,1.),(1.,1.),(1.,1.),(1.,
1.),(1.,1.),(1.,1.),(1.,1.),(1.,1.),(1.,1.),(1.,1.),(1.,1.),(1.,1.),(1.,
1.),(1.,1.),(1.,1.),(1.,1.),(1.,1.),(1.,1.),(1.,1.),(1.,1.),(1.,1.),(1.,
1.),(1.,1.),(1.,1.),(1.,1.),(1.,1.),(1.,1.),(1.,1.),(1.,1.),(1.,1.),(1.,
1.),(1.,1.),(1.,1.),(1.,1.),(1.,1.),(1.,1.),(1.,1.),(1.,1.),(1.,1.),(1.,
1.),(1.,1.),(1.,1.),(1.,1.),(1.,1.),(1.,1.),(1.,1.),(1.,1.),(1.,1.),(1.,
1.),(1.,1.),(1.,1.),(1.,1.),(1.,1.),(1.,1.),(1.,1.),(1.,1.),(1.,1.),(1.,
1.),(1.,1.),(1.,1.),(1.,1.),(1.,1.),(1.,1.),(1.,1.),(1.,1.),(1.,1.),(1.,
1.),(1.,1.),(1.,1.),(1.,1.),(1.,1.),(1.,1.),(1.,1.),(1.,1.),(1.,1.),(1.,
1.),(1.,1.),(1.,1.),(1.,1.),(1.,1.),(1.,1.),(1.,1.),(1.,1.),(1.,1.),(1.,
1.),(1.,1.),(1.,1.),(1.,1.),(1.,1.),(1.,1.),(1.,1.),(1.,1.),(1.,1.),(1.,
1.),(1.,1.),(1.,1.),(1.,1.),(1.,1.),(1.,1.),(1.,1.),(1.,1.),(1.,1.),(1.,
1.),(1.,1.),(1.,1.),(1.,1.),(1.,1.),(1.,1.),(1.,1.),(1.,1.),(1.,1.),(1.,
1.),(1.,1.),(1.,1.),(1.,1.),(1.,1.),(1.,1.),(1.,1.),(1.,1.),(1.,1.),(1.,
1.),(1.,1.),(1.,1.),(1.,1.),(1.,1.),(1.,1.),(1.,1.),(1.,1.),(1.,1.),(1.,
1.),(1.,1.),(1.,1.),(1.,1.),(1.,1.),(1.,1.),(1.,1.),(1.,1.),(1.,1.),(1.,
1.),(1.,1.),(1.,1.),(1.,1.),(1.,1.),(1.,1.),(1.,1.),(1.,1.),(1.,1.),(1.,
1.),(1.,1.),(1.,1.),(1.,1.),(1.,1.),(1.,1.),(1.,1.),(1.,1.),(1.,1.),(1.,
1.),(1.,1.),(1.,1.),(1.,1.),(1.,1.),(1.,1.),(1.,1.),(1.,1.),(1.,1.),(1.,
1.),(1.,1.),(1.,1.),(1.,1.),(1.,1.),(1.,1.),(1.,1.),(1.,1.),(1.,1.),(1.,
1.),(1.,1.),(1.,1.),(1.,1.),(1.,1.),(1.,1.),(1.,1.),(1.,1.),(1.,1.),(1.,
1.),(1.,1.),(1.,1.),(1.,1.),(1.,1.),(1.,1.),(1.,1.),(1.,1.),(1.,1.),(1.,
1.),(1.,1.),(1.,1.),(1.,1.),(1.,1.),(1.,1.),(1.,1.),(1.,1.),(1.,1.),(1.,
1.),(1.,1.),(1.,1.),(1.,1.),(1.,1.),(1.,1.),(1.,1.),(1.,1.),(1.,1.),(1.,
1.),(1.,1.),(1.,1.),(1.,1.),(1.,1.),(1.,1.),(1.,1.),(1.,1.),(1.,1.),(1.,
1.),(1.,1.),(1.,1.),(1.,1.),(1.,1.),(1.,1.),(1.,1.),(1.,1.),(1.,1.),(1.,
1.),(1.,1.),(1.,1.),(1.,1.),(1.,1.),(1.,1.),(1.,1.),(1.,1.),(1.,1.),(1.,
1.),(1.,1.),(1.,1.),(1.,1.),(1.,1.),(1.,1.),(1.,1.),(1.,1.),(1.,1.),(1.,
1.),(1.,1.),(1.,1.),(1.,1.),(1.,1.),(1.,1.),(1.,1.),(1.,1.),(1.,1.),(1.,
1.),(1.,1.),(1.,1.),(1.,1.),(1.,1.),(1.,1.),(1.,1.),(1.,1.),(1.,1.),(1.,
1.),(1.,1.),(1.,1.),(1.,1.),(1.,1.),(1.,1.),(1.,1.),(1.,1.),(1.,1.),(1.,
1.),(1.,1.),(1.,1.),(1.,1.),(1.,1.),(1.,1.),(1.,1.),(1.,1.),(1.,1.),(1.,
1.),(1.,1.),(1.,1.),(1.,1.),(1.,1.),(1.,1.),(1.,1.),(1.,1.),(1.,1.),(1.,
1.),(1.,1.),(1.,1.),(1.,1.),(1.,1.),(1.,1.),(1.,1.),(1.,1.),(1.,1.),(1.,
1.),(1.,1.),(1.,1.),(1.,1.),(1.,1.),(1.,1.),(1.,1.),(1.,1.),(1.,1.),(1.,
1.),(1.,1.),(1.,1.),(1.,1.),(1.,1.),(1.,1.),(1.,1.),(1.,1.),(1.,1.),(1.,
1.),(1.,1.),(1.,1.),(1.,1.),(1.,1.),(1.,1.),(1.,1.),(1.,1.),(1.,1.),(1.,
1.),(1.,1.),(1.,1.),(1.,1.),(1.,1.),(1.,1.),(1.,1.),(1.,1.),(1.,1.),(1.,
1.),(1.,1.),(1.,1.),(1.,1.),(1.,1.),(1.,1.),(1.,1.),(1.,1.),(1.,1.),(1.,
1.),(1.,1.),(1.,1.),(1.,1.),(1.,1.),(1.,1.),(1.,1.),(1.,1.),(1.,1.),(1.,
1.),(1.,1.),(1.,1.),(1.,1.),(1.,1.),(1.,1.),(1.,1.),(1.,1.),(1.,1.),(1.,
1.),(1.,1.),(1.,1.),(1.,1.),(1.,1.),(1.,1.),(1.,1.),(1.,1.),(1.,1.),(1.,
1.),(1.,1.),(1.,1.),(1.,1.),(1.,1.),(1.,1.),(1.,1.),(1.,1.),(1.,1.),(1.,
1.),(1.,1.),(1.,1.),(1.,1.),(1.,1.),(1.,1.),(1.,1.),(1.,1.),(1.,1.),(1.,
1.),(1.,1.),(1.,1.),(1.,1.),(1.,1.),(1.,1.),(1.,1.),(1.,1.),(1.,1.),(1.,
1.),(1.,1.),(1.,1.),(1.,1.),(1.,1.),(1.,1.),(1.,1.),(1.,1.),(1.,1.),(1.,
1.),(1.,1.),(1.,1.),(1.,1.),(1.,1.),(1.,1.),(1.,1.),(1.,1.),(1.,1.),(1.,
1.),(1.,1.),(1.,1.),(1.,1.),(1.,1.),(1.,1.),(1.,1.),(1.,1.),(1.,1.),(1.,
1.),(1.,1.),(1.,1.),(1.,1.),(1.,1.),(1.,1.),(1.,1.),(1.,1.),(1.,1.),(1.,
1.),(1.,1.),(1.,1.),(1.,1.),(1.,1.),(1.,1.),(1.,1.),(1.,1.),(1.,1.),(1.,
1.),(1.,1.),(1.,1.),(1.,1.),(1.,1.),(1.,1.),(1.,1.),(1.,1.),(1.,1.),(1.,
1.),(1.,1.),(1.,1.),(1.,1.),(1.,1.),(1.,1.),(1.,1.),(1.,1.),(1.,1.),(1.,
1.),(1.,1.),(1.,1.),(1.,1.),(1.,1.),(1.,1.),(1.,1.),(1.,1.),(1.,1.),(1.,
1.),(1.,1.),(1.,1.),(1.,1.),(1.,1.),(1.,1.),(1.,1.),(1.,1.),(1.,1.),(1.,
1.),(1.,1.),(1.,1.),(1.,1.),(1.,1.),(1.,1.),(1.,1.),(1.,1.),(1.,1.),(1.,
1.),(1.,1.),(1.,1.),(1.,1.),(1.,1.),(1.,1.),(1.,1.),(1.,1.),(1.,1.),(1.,
1.),(1.,1.),(1.,1.),(1.,1.),(1.,1.),(1.,1.),(1.,1.),(1.,1.),(1.,1.),(1.,
1.),(1.,1.),(1.,1.),(1.,1.),(1.,1.),(1.,1.),(1.,1.),(1.,1.),(1.,1.),(1.,
1.),(1.,1.),(1.,1.),(1.,1.),(1.,1.),(1.,1.),(1.,1.),(1.,1.),(1.,1.),(1.,
1.),(1.,1.),(1.,1.),(1.,1.),(1.,1.),(1.,1.),(1.,1.),(1.,1.),(1.,1.),(1.,
1.),(1.,1.),(1.,1.),(1.,1.),(1.,1.),(1.,1.),(1.,1.),(1.,1.),(1.,1.),(1.,
1.),(1.,1.),(1.,1.),(1.,1.),(1.,1.),(1.,1.),(1.,1.),(1.,1.),(1.,1.),(1.,
1.),(1.,1.),(1.,1.),(1.,1.),(1.,1.),(1.,1.),(1.,1.),(1.,1.),(1.,1.),(1.,
1.),(1.,1.),(1.,1.),(1.,1.),(1.,1.),(1.,1.),(1.,1.),(1.,1.),(1.,1.),(1.,
1.),(1.,1.),(1.,1.),(1.,1.),(1.,1.),(1.,1.),(1.,1.),(1.,1.),(1.,1.),(1.,
1.),(1.,1.),(1.,1.),(1.,1.),(1.,1.),(1.,1.),(1.,1.),(1.,1.),(1.,1.),(1.,
1.),(1.,1.),(1.,1.),(1.,1.),(1.,1.),(1.,1.),(1.,1.),(1.,1.),(1.,1.),(1.,
1.),(1.,1.),(1.,1.),(1.,1.),(1.,1.),(1.,1.),(1.,1.),(1.,1.),(1.,1.),(1.,
1.),(1.,1.),(1.,1.),(1.,1.),(1.,1.),(1.,1.),(1.,1.),(1.,1.),(1.,1.),(1.,
1.),(1.,1.),(1.,1.),(1.,1.),(1.,1.),(1.,1.),(1.,1.),(1.,1.),(1.,1.),(1.,
1.),(1.,1.),(1.,1.),(1.,1.),(1.,1.),(1.,1.),(1.,1.),(1.,1.),(1.,1.),(1.,
1.),(1.,1.),(1.,1.),(1.,1.),(1.,1.),(1.,1.),(1.,1.),(1.,1.),(1.,1.),(1.,
1.),(1.,1.),(1.,1.),(1.,1.),(1.,1.),(1.,1.),(1.,1.),(1.,1.),(1.,1.),(1.,
1.),(1.,1.),(1.,1.),(1.,1.),(1.,1.),(1.,1.),(1.,1.),(1.,1.),(1.,1.),(1.,
1.)))
REPRESENTATION_ITEM('')
SURFACE()
);
#267=(
BOUNDED_SURFACE()
B_SPLINE_SURFACE(5,1,((#92433,#92434),(#92435,#92436),(#92437,#92438),(#92439,
#92440),(#92441,#92442),(#92443,#92444),(#92445,#92446),(#92447,#92448),
(#92449,#92450),(#92451,#92452),(#92453,#92454),(#92455,#92456),(#92457,
#92458),(#92459,#92460),(#92461,#92462),(#92463,#92464),(#92465,#92466),
(#92467,#92468),(#92469,#92470),(#92471,#92472),(#92473,#92474),(#92475,
#92476),(#92477,#92478),(#92479,#92480),(#92481,#92482),(#92483,#92484),
(#92485,#92486),(#92487,#92488),(#92489,#92490),(#92491,#92492),(#92493,
#92494),(#92495,#92496),(#92497,#92498),(#92499,#92500),(#92501,#92502),
(#92503,#92504),(#92505,#92506),(#92507,#92508),(#92509,#92510),(#92511,
#92512),(#92513,#92514),(#92515,#92516),(#92517,#92518),(#92519,#92520),
(#92521,#92522),(#92523,#92524),(#92525,#92526),(#92527,#92528),(#92529,
#92530),(#92531,#92532),(#92533,#92534),(#92535,#92536),(#92537,#92538),
(#92539,#92540),(#92541,#92542),(#92543,#92544),(#92545,#92546),(#92547,
#92548),(#92549,#92550),(#92551,#92552),(#92553,#92554),(#92555,#92556),
(#92557,#92558),(#92559,#92560),(#92561,#92562),(#92563,#92564),(#92565,
#92566),(#92567,#92568),(#92569,#92570),(#92571,#92572),(#92573,#92574),
(#92575,#92576),(#92577,#92578),(#92579,#92580),(#92581,#92582),(#92583,
#92584),(#92585,#92586),(#92587,#92588),(#92589,#92590),(#92591,#92592),
(#92593,#92594),(#92595,#92596),(#92597,#92598),(#92599,#92600),(#92601,
#92602),(#92603,#92604),(#92605,#92606),(#92607,#92608),(#92609,#92610),
(#92611,#92612),(#92613,#92614),(#92615,#92616),(#92617,#92618),(#92619,
#92620),(#92621,#92622),(#92623,#92624),(#92625,#92626),(#92627,#92628),
(#92629,#92630),(#92631,#92632),(#92633,#92634),(#92635,#92636),(#92637,
#92638),(#92639,#92640),(#92641,#92642),(#92643,#92644),(#92645,#92646),
(#92647,#92648),(#92649,#92650),(#92651,#92652),(#92653,#92654),(#92655,
#92656),(#92657,#92658),(#92659,#92660),(#92661,#92662),(#92663,#92664),
(#92665,#92666),(#92667,#92668),(#92669,#92670),(#92671,#92672),(#92673,
#92674),(#92675,#92676),(#92677,#92678),(#92679,#92680),(#92681,#92682),
(#92683,#92684),(#92685,#92686),(#92687,#92688),(#92689,#92690),(#92691,
#92692),(#92693,#92694),(#92695,#92696),(#92697,#92698),(#92699,#92700),
(#92701,#92702),(#92703,#92704),(#92705,#92706),(#92707,#92708),(#92709,
#92710),(#92711,#92712),(#92713,#92714),(#92715,#92716),(#92717,#92718),
(#92719,#92720),(#92721,#92722),(#92723,#92724),(#92725,#92726),(#92727,
#92728),(#92729,#92730),(#92731,#92732),(#92733,#92734),(#92735,#92736),
(#92737,#92738),(#92739,#92740),(#92741,#92742),(#92743,#92744),(#92745,
#92746),(#92747,#92748),(#92749,#92750),(#92751,#92752),(#92753,#92754),
(#92755,#92756),(#92757,#92758),(#92759,#92760),(#92761,#92762),(#92763,
#92764),(#92765,#92766),(#92767,#92768),(#92769,#92770),(#92771,#92772),
(#92773,#92774),(#92775,#92776),(#92777,#92778),(#92779,#92780),(#92781,
#92782),(#92783,#92784),(#92785,#92786),(#92787,#92788),(#92789,#92790),
(#92791,#92792),(#92793,#92794),(#92795,#92796),(#92797,#92798),(#92799,
#92800),(#92801,#92802),(#92803,#92804),(#92805,#92806),(#92807,#92808),
(#92809,#92810),(#92811,#92812),(#92813,#92814),(#92815,#92816),(#92817,
#92818),(#92819,#92820),(#92821,#92822),(#92823,#92824),(#92825,#92826),
(#92827,#92828),(#92829,#92830),(#92831,#92832),(#92833,#92834),(#92835,
#92836),(#92837,#92838),(#92839,#92840),(#92841,#92842),(#92843,#92844),
(#92845,#92846),(#92847,#92848),(#92849,#92850),(#92851,#92852),(#92853,
#92854),(#92855,#92856),(#92857,#92858),(#92859,#92860),(#92861,#92862),
(#92863,#92864),(#92865,#92866),(#92867,#92868),(#92869,#92870),(#92871,
#92872),(#92873,#92874),(#92875,#92876),(#92877,#92878),(#92879,#92880),
(#92881,#92882),(#92883,#92884),(#92885,#92886),(#92887,#92888),(#92889,
#92890),(#92891,#92892),(#92893,#92894),(#92895,#92896),(#92897,#92898),
(#92899,#92900),(#92901,#92902),(#92903,#92904),(#92905,#92906),(#92907,
#92908),(#92909,#92910),(#92911,#92912),(#92913,#92914),(#92915,#92916),
(#92917,#92918),(#92919,#92920),(#92921,#92922),(#92923,#92924),(#92925,
#92926),(#92927,#92928),(#92929,#92930),(#92931,#92932),(#92933,#92934),
(#92935,#92936),(#92937,#92938),(#92939,#92940),(#92941,#92942),(#92943,
#92944),(#92945,#92946),(#92947,#92948),(#92949,#92950),(#92951,#92952),
(#92953,#92954),(#92955,#92956),(#92957,#92958),(#92959,#92960),(#92961,
#92962),(#92963,#92964),(#92965,#92966),(#92967,#92968),(#92969,#92970),
(#92971,#92972),(#92973,#92974),(#92975,#92976),(#92977,#92978),(#92979,
#92980),(#92981,#92982),(#92983,#92984),(#92985,#92986),(#92987,#92988),
(#92989,#92990),(#92991,#92992),(#92993,#92994),(#92995,#92996),(#92997,
#92998),(#92999,#93000),(#93001,#93002),(#93003,#93004),(#93005,#93006),
(#93007,#93008),(#93009,#93010),(#93011,#93012),(#93013,#93014),(#93015,
#93016),(#93017,#93018),(#93019,#93020),(#93021,#93022),(#93023,#93024),
(#93025,#93026),(#93027,#93028),(#93029,#93030),(#93031,#93032),(#93033,
#93034),(#93035,#93036),(#93037,#93038),(#93039,#93040),(#93041,#93042),
(#93043,#93044),(#93045,#93046),(#93047,#93048),(#93049,#93050),(#93051,
#93052),(#93053,#93054),(#93055,#93056),(#93057,#93058),(#93059,#93060),
(#93061,#93062),(#93063,#93064),(#93065,#93066),(#93067,#93068),(#93069,
#93070),(#93071,#93072),(#93073,#93074),(#93075,#93076),(#93077,#93078),
(#93079,#93080),(#93081,#93082),(#93083,#93084),(#93085,#93086),(#93087,
#93088),(#93089,#93090),(#93091,#93092),(#93093,#93094),(#93095,#93096),
(#93097,#93098),(#93099,#93100),(#93101,#93102),(#93103,#93104),(#93105,
#93106),(#93107,#93108),(#93109,#93110),(#93111,#93112),(#93113,#93114),
(#93115,#93116),(#93117,#93118),(#93119,#93120),(#93121,#93122),(#93123,
#93124),(#93125,#93126),(#93127,#93128),(#93129,#93130),(#93131,#93132),
(#93133,#93134),(#93135,#93136),(#93137,#93138),(#93139,#93140),(#93141,
#93142),(#93143,#93144),(#93145,#93146),(#93147,#93148),(#93149,#93150),
(#93151,#93152),(#93153,#93154),(#93155,#93156),(#93157,#93158),(#93159,
#93160),(#93161,#93162),(#93163,#93164),(#93165,#93166),(#93167,#93168),
(#93169,#93170),(#93171,#93172),(#93173,#93174),(#93175,#93176),(#93177,
#93178),(#93179,#93180),(#93181,#93182),(#93183,#93184),(#93185,#93186),
(#93187,#93188),(#93189,#93190),(#93191,#93192),(#93193,#93194),(#93195,
#93196),(#93197,#93198),(#93199,#93200),(#93201,#93202),(#93203,#93204),
(#93205,#93206),(#93207,#93208),(#93209,#93210),(#93211,#93212),(#93213,
#93214),(#93215,#93216),(#93217,#93218),(#93219,#93220),(#93221,#93222),
(#93223,#93224),(#93225,#93226),(#93227,#93228),(#93229,#93230),(#93231,
#93232),(#93233,#93234),(#93235,#93236),(#93237,#93238),(#93239,#93240),
(#93241,#93242),(#93243,#93244),(#93245,#93246),(#93247,#93248),(#93249,
#93250),(#93251,#93252),(#93253,#93254),(#93255,#93256),(#93257,#93258),
(#93259,#93260),(#93261,#93262),(#93263,#93264),(#93265,#93266),(#93267,
#93268),(#93269,#93270),(#93271,#93272),(#93273,#93274),(#93275,#93276),
(#93277,#93278),(#93279,#93280),(#93281,#93282),(#93283,#93284),(#93285,
#93286),(#93287,#93288),(#93289,#93290),(#93291,#93292),(#93293,#93294),
(#93295,#93296),(#93297,#93298),(#93299,#93300),(#93301,#93302),(#93303,
#93304),(#93305,#93306),(#93307,#93308),(#93309,#93310),(#93311,#93312),
(#93313,#93314),(#93315,#93316),(#93317,#93318),(#93319,#93320),(#93321,
#93322),(#93323,#93324),(#93325,#93326),(#93327,#93328),(#93329,#93330),
(#93331,#93332),(#93333,#93334),(#93335,#93336),(#93337,#93338),(#93339,
#93340),(#93341,#93342),(#93343,#93344),(#93345,#93346),(#93347,#93348),
(#93349,#93350),(#93351,#93352),(#93353,#93354),(#93355,#93356),(#93357,
#93358),(#93359,#93360),(#93361,#93362),(#93363,#93364),(#93365,#93366),
(#93367,#93368),(#93369,#93370),(#93371,#93372),(#93373,#93374),(#93375,
#93376),(#93377,#93378),(#93379,#93380),(#93381,#93382),(#93383,#93384),
(#93385,#93386),(#93387,#93388),(#93389,#93390),(#93391,#93392),(#93393,
#93394),(#93395,#93396),(#93397,#93398),(#93399,#93400),(#93401,#93402),
(#93403,#93404),(#93405,#93406),(#93407,#93408),(#93409,#93410),(#93411,
#93412),(#93413,#93414),(#93415,#93416),(#93417,#93418),(#93419,#93420),
(#93421,#93422),(#93423,#93424),(#93425,#93426),(#93427,#93428),(#93429,
#93430),(#93431,#93432),(#93433,#93434),(#93435,#93436),(#93437,#93438),
(#93439,#93440),(#93441,#93442),(#93443,#93444),(#93445,#93446),(#93447,
#93448),(#93449,#93450),(#93451,#93452),(#93453,#93454),(#93455,#93456),
(#93457,#93458),(#93459,#93460),(#93461,#93462),(#93463,#93464),(#93465,
#93466),(#93467,#93468),(#93469,#93470),(#93471,#93472),(#93473,#93474),
(#93475,#93476),(#93477,#93478),(#93479,#93480),(#93481,#93482),(#93483,
#93484),(#93485,#93486),(#93487,#93488),(#93489,#93490),(#93491,#93492),
(#93493,#93494),(#93495,#93496),(#93497,#93498),(#93499,#93500),(#93501,
#93502),(#93503,#93504),(#93505,#93506),(#93507,#93508),(#93509,#93510),
(#93511,#93512),(#93513,#93514),(#93515,#93516),(#93517,#93518),(#93519,
#93520),(#93521,#93522),(#93523,#93524),(#93525,#93526),(#93527,#93528),
(#93529,#93530),(#93531,#93532),(#93533,#93534),(#93535,#93536),(#93537,
#93538),(#93539,#93540),(#93541,#93542),(#93543,#93544),(#93545,#93546),
(#93547,#93548),(#93549,#93550),(#93551,#93552),(#93553,#93554),(#93555,
#93556),(#93557,#93558),(#93559,#93560),(#93561,#93562),(#93563,#93564),
(#93565,#93566),(#93567,#93568),(#93569,#93570),(#93571,#93572),(#93573,
#93574),(#93575,#93576),(#93577,#93578),(#93579,#93580),(#93581,#93582),
(#93583,#93584),(#93585,#93586),(#93587,#93588),(#93589,#93590),(#93591,
#93592),(#93593,#93594),(#93595,#93596),(#93597,#93598),(#93599,#93600),
(#93601,#93602),(#93603,#93604),(#93605,#93606),(#93607,#93608),(#93609,
#93610),(#93611,#93612),(#93613,#93614),(#93615,#93616),(#93617,#93618),
(#93619,#93620),(#93621,#93622),(#93623,#93624),(#93625,#93626),(#93627,
#93628),(#93629,#93630),(#93631,#93632),(#93633,#93634),(#93635,#93636),
(#93637,#93638),(#93639,#93640),(#93641,#93642),(#93643,#93644),(#93645,
#93646),(#93647,#93648),(#93649,#93650),(#93651,#93652),(#93653,#93654),
(#93655,#93656),(#93657,#93658),(#93659,#93660),(#93661,#93662),(#93663,
#93664),(#93665,#93666),(#93667,#93668),(#93669,#93670),(#93671,#93672),
(#93673,#93674),(#93675,#93676),(#93677,#93678),(#93679,#93680),(#93681,
#93682),(#93683,#93684),(#93685,#93686),(#93687,#93688),(#93689,#93690),
(#93691,#93692),(#93693,#93694),(#93695,#93696),(#93697,#93698),(#93699,
#93700),(#93701,#93702),(#93703,#93704),(#93705,#93706),(#93707,#93708),
(#93709,#93710),(#93711,#93712),(#93713,#93714),(#93715,#93716),(#93717,
#93718),(#93719,#93720),(#93721,#93722),(#93723,#93724),(#93725,#93726),
(#93727,#93728),(#93729,#93730),(#93731,#93732),(#93733,#93734),(#93735,
#93736),(#93737,#93738),(#93739,#93740),(#93741,#93742),(#93743,#93744),
(#93745,#93746),(#93747,#93748),(#93749,#93750),(#93751,#93752),(#93753,
#93754),(#93755,#93756),(#93757,#93758),(#93759,#93760),(#93761,#93762),
(#93763,#93764),(#93765,#93766),(#93767,#93768),(#93769,#93770),(#93771,
#93772),(#93773,#93774),(#93775,#93776),(#93777,#93778),(#93779,#93780),
(#93781,#93782),(#93783,#93784),(#93785,#93786),(#93787,#93788),(#93789,
#93790),(#93791,#93792),(#93793,#93794),(#93795,#93796),(#93797,#93798),
(#93799,#93800),(#93801,#93802),(#93803,#93804),(#93805,#93806),(#93807,
#93808),(#93809,#93810),(#93811,#93812),(#93813,#93814),(#93815,#93816),
(#93817,#93818),(#93819,#93820),(#93821,#93822),(#93823,#93824),(#93825,
#93826),(#93827,#93828),(#93829,#93830),(#93831,#93832),(#93833,#93834),
(#93835,#93836),(#93837,#93838),(#93839,#93840),(#93841,#93842),(#93843,
#93844),(#93845,#93846),(#93847,#93848),(#93849,#93850),(#93851,#93852),
(#93853,#93854),(#93855,#93856),(#93857,#93858),(#93859,#93860),(#93861,
#93862),(#93863,#93864),(#93865,#93866),(#93867,#93868),(#93869,#93870),
(#93871,#93872),(#93873,#93874),(#93875,#93876),(#93877,#93878),(#93879,
#93880),(#93881,#93882),(#93883,#93884),(#93885,#93886),(#93887,#93888),
(#93889,#93890),(#93891,#93892),(#93893,#93894),(#93895,#93896),(#93897,
#93898),(#93899,#93900),(#93901,#93902),(#93903,#93904),(#93905,#93906),
(#93907,#93908),(#93909,#93910),(#93911,#93912),(#93913,#93914),(#93915,
#93916),(#93917,#93918),(#93919,#93920),(#93921,#93922),(#93923,#93924),
(#93925,#93926),(#93927,#93928),(#93929,#93930),(#93931,#93932),(#93933,
#93934),(#93935,#93936),(#93937,#93938),(#93939,#93940),(#93941,#93942),
(#93943,#93944),(#93945,#93946),(#93947,#93948),(#93949,#93950),(#93951,
#93952),(#93953,#93954),(#93955,#93956),(#93957,#93958),(#93959,#93960),
(#93961,#93962),(#93963,#93964),(#93965,#93966),(#93967,#93968),(#93969,
#93970),(#93971,#93972),(#93973,#93974),(#93975,#93976),(#93977,#93978),
(#93979,#93980),(#93981,#93982),(#93983,#93984),(#93985,#93986),(#93987,
#93988),(#93989,#93990),(#93991,#93992),(#93993,#93994),(#93995,#93996),
(#93997,#93998),(#93999,#94000),(#94001,#94002),(#94003,#94004),(#94005,
#94006),(#94007,#94008),(#94009,#94010),(#94011,#94012),(#94013,#94014),
(#94015,#94016),(#94017,#94018),(#94019,#94020),(#94021,#94022),(#94023,
#94024),(#94025,#94026),(#94027,#94028),(#94029,#94030),(#94031,#94032),
(#94033,#94034),(#94035,#94036),(#94037,#94038),(#94039,#94040),(#94041,
#94042),(#94043,#94044),(#94045,#94046),(#94047,#94048),(#94049,#94050),
(#94051,#94052),(#94053,#94054),(#94055,#94056),(#94057,#94058),(#94059,
#94060),(#94061,#94062),(#94063,#94064),(#94065,#94066),(#94067,#94068),
(#94069,#94070),(#94071,#94072),(#94073,#94074),(#94075,#94076),(#94077,
#94078),(#94079,#94080),(#94081,#94082),(#94083,#94084),(#94085,#94086),
(#94087,#94088),(#94089,#94090),(#94091,#94092),(#94093,#94094),(#94095,
#94096),(#94097,#94098),(#94099,#94100),(#94101,#94102),(#94103,#94104),
(#94105,#94106),(#94107,#94108),(#94109,#94110),(#94111,#94112),(#94113,
#94114),(#94115,#94116),(#94117,#94118),(#94119,#94120),(#94121,#94122),
(#94123,#94124),(#94125,#94126),(#94127,#94128),(#94129,#94130),(#94131,
#94132),(#94133,#94134),(#94135,#94136),(#94137,#94138),(#94139,#94140),
(#94141,#94142),(#94143,#94144),(#94145,#94146),(#94147,#94148),(#94149,
#94150),(#94151,#94152),(#94153,#94154),(#94155,#94156),(#94157,#94158),
(#94159,#94160),(#94161,#94162),(#94163,#94164),(#94165,#94166),(#94167,
#94168),(#94169,#94170),(#94171,#94172),(#94173,#94174),(#94175,#94176),
(#94177,#94178),(#94179,#94180),(#94181,#94182),(#94183,#94184),(#94185,
#94186),(#94187,#94188),(#94189,#94190),(#94191,#94192),(#94193,#94194),
(#94195,#94196),(#94197,#94198),(#94199,#94200),(#94201,#94202),(#94203,
#94204),(#94205,#94206),(#94207,#94208),(#94209,#94210),(#94211,#94212),
(#94213,#94214),(#94215,#94216),(#94217,#94218),(#94219,#94220),(#94221,
#94222),(#94223,#94224),(#94225,#94226),(#94227,#94228),(#94229,#94230),
(#94231,#94232),(#94233,#94234),(#94235,#94236),(#94237,#94238),(#94239,
#94240),(#94241,#94242),(#94243,#94244),(#94245,#94246),(#94247,#94248),
(#94249,#94250),(#94251,#94252),(#94253,#94254),(#94255,#94256),(#94257,
#94258),(#94259,#94260),(#94261,#94262),(#94263,#94264),(#94265,#94266),
(#94267,#94268),(#94269,#94270),(#94271,#94272),(#94273,#94274),(#94275,
#94276),(#94277,#94278),(#94279,#94280),(#94281,#94282),(#94283,#94284),
(#94285,#94286),(#94287,#94288),(#94289,#94290),(#94291,#94292),(#94293,
#94294),(#94295,#94296),(#94297,#94298),(#94299,#94300),(#94301,#94302),
(#94303,#94304),(#94305,#94306),(#94307,#94308),(#94309,#94310),(#94311,
#94312),(#94313,#94314),(#94315,#94316),(#94317,#94318),(#94319,#94320),
(#94321,#94322),(#94323,#94324),(#94325,#94326),(#94327,#94328),(#94329,
#94330),(#94331,#94332),(#94333,#94334),(#94335,#94336),(#94337,#94338),
(#94339,#94340),(#94341,#94342),(#94343,#94344),(#94345,#94346),(#94347,
#94348),(#94349,#94350),(#94351,#94352),(#94353,#94354),(#94355,#94356),
(#94357,#94358),(#94359,#94360),(#94361,#94362),(#94363,#94364),(#94365,
#94366),(#94367,#94368),(#94369,#94370),(#94371,#94372),(#94373,#94374),
(#94375,#94376),(#94377,#94378),(#94379,#94380),(#94381,#94382),(#94383,
#94384),(#94385,#94386),(#94387,#94388),(#94389,#94390),(#94391,#94392),
(#94393,#94394),(#94395,#94396),(#94397,#94398),(#94399,#94400),(#94401,
#94402),(#94403,#94404),(#94405,#94406),(#94407,#94408),(#94409,#94410),
(#94411,#94412),(#94413,#94414),(#94415,#94416),(#94417,#94418),(#94419,
#94420),(#94421,#94422),(#94423,#94424),(#94425,#94426),(#94427,#94428),
(#94429,#94430),(#94431,#94432),(#94433,#94434),(#94435,#94436),(#94437,
#94438),(#94439,#94440),(#94441,#94442)),.UNSPECIFIED.,.F.,.F.,.F.)
B_SPLINE_SURFACE_WITH_KNOTS((6,1,1,1,1,1,1,1,1,1,1,1,1,1,1,1,1,1,1,1,1,
1,1,1,1,1,1,1,1,1,1,1,1,1,1,1,1,1,1,1,1,1,1,1,1,1,1,1,1,1,1,1,1,1,1,1,1,
1,1,1,1,1,1,1,1,1,1,1,1,1,1,1,1,1,1,1,1,1,1,1,1,1,1,1,1,1,1,1,1,1,1,1,1,
1,1,1,1,1,1,1,1,1,1,1,1,1,1,1,1,1,1,1,1,1,1,1,1,1,1,1,1,1,1,1,1,1,1,1,1,
1,1,1,1,1,1,1,1,1,1,1,1,1,1,1,1,1,1,1,1,1,1,1,1,1,1,1,1,1,1,1,1,1,1,1,1,
1,1,1,1,1,1,1,1,1,1,1,1,1,1,1,1,1,1,1,1,1,1,1,1,1,1,1,1,1,1,1,1,1,1,1,1,
1,1,1,1,1,1,1,1,1,1,1,1,1,1,1,1,1,1,1,1,1,1,1,1,1,1,1,1,1,1,1,1,1,1,1,1,
1,1,1,1,1,1,1,1,1,1,1,1,1,1,1,1,1,1,1,1,1,1,1,1,1,1,1,1,1,1,1,1,1,1,1,1,
1,1,1,1,1,1,1,1,1,1,1,1,1,1,1,1,1,1,1,1,1,1,1,1,1,1,1,1,1,1,1,1,1,1,1,1,
1,1,1,1,1,1,1,1,1,1,1,1,1,1,1,1,1,1,1,1,1,1,1,1,1,1,1,1,1,1,1,1,1,1,1,1,
1,1,1,1,1,1,1,1,1,1,1,1,1,1,1,1,1,1,1,1,1,1,1,1,1,1,1,1,1,1,1,1,1,1,1,1,
1,1,1,1,1,1,1,1,1,1,1,1,1,1,1,1,1,1,1,1,1,1,1,1,1,1,1,1,1,1,1,1,1,1,1,1,
1,1,1,1,1,1,1,1,1,1,1,1,1,1,1,1,1,1,1,1,1,1,1,1,1,1,1,1,1,1,1,1,1,1,1,1,
1,1,1,1,1,1,1,1,1,1,1,1,1,1,1,1,1,1,1,1,1,1,1,1,1,1,1,1,1,1,1,1,1,1,1,1,
1,1,1,1,1,1,1,1,1,1,1,1,1,1,1,1,1,1,1,1,1,1,1,1,1,1,1,1,1,1,1,1,1,1,1,1,
1,1,1,1,1,1,1,1,1,1,1,1,1,1,1,1,1,1,1,1,1,1,1,1,1,1,1,1,1,1,1,1,1,1,1,1,
1,1,1,1,1,1,1,1,1,1,1,1,1,1,1,1,1,1,1,1,1,1,1,1,1,1,1,1,1,1,1,1,1,1,1,1,
1,1,1,1,1,1,1,1,1,1,1,1,1,1,1,1,1,1,1,1,1,1,1,1,1,1,1,1,1,1,1,1,1,1,1,1,
1,1,1,1,1,1,1,1,1,1,1,1,1,1,1,1,1,1,1,1,1,1,1,1,1,1,1,1,1,1,1,1,1,1,1,1,
1,1,1,1,1,1,1,1,1,1,1,1,1,1,1,1,1,1,1,1,1,1,1,1,1,1,1,1,1,1,1,1,1,1,1,1,
1,1,1,1,1,1,1,1,1,1,1,1,1,1,1,1,1,1,1,1,1,1,1,1,1,1,1,1,1,1,1,1,1,1,1,1,
1,1,1,1,1,1,1,1,1,1,1,1,1,1,1,1,1,1,1,1,1,1,1,1,1,1,1,1,1,1,1,1,1,1,1,1,
1,1,1,1,1,1,1,1,1,1,1,1,1,1,1,1,1,1,1,1,1,1,1,1,1,1,1,1,1,1,1,1,1,1,1,1,
1,1,1,1,1,1,1,1,1,1,1,1,1,1,1,1,1,1,1,1,1,1,1,1,1,1,1,1,1,1,1,1,1,1,1,1,
1,1,1,1,1,1,1,1,1,1,1,1,1,1,1,1,1,1,1,1,1,1,1,1,1,1,1,1,1,1,1,1,1,1,1,1,
1,1,1,1,1,1,1,1,1,1,1,1,1,1,1,1,1,1,1,1,1,1,1,1,1,1,1,1,1,1,1,1,1,1,1,1,
1,1,1,1,1,1,1,1,1,1,1,1,1,1,1,1,1,1,1,1,1,1,1,1,1,1,1,1,1,1,1,1,1,1,1,1,
1,1,1,1,1,1,1,1,1,1,1,1,1,1,1,1,1,1,1,1,1,1,1,1,1,1,1,1,1,1,1,1,1,1,1,1,
1,1,1,1,1,1,1,6),(2,2),(-1.,-0.999000000000001,-0.998000000000001,-0.997000000000001,
-0.996000000000001,-0.995000000000001,-0.994000000000001,-0.993000000000001,
-0.992000000000001,-0.991000000000001,-0.990000000000001,-0.989000000000001,
-0.988000000000001,-0.987000000000001,-0.986000000000001,-0.985000000000001,
-0.984000000000001,-0.983000000000001,-0.982000000000001,-0.981000000000001,
-0.980000000000001,-0.979000000000001,-0.978000000000001,-0.977000000000001,
-0.976000000000001,-0.975000000000001,-0.974000000000001,-0.973000000000001,
-0.972000000000001,-0.971000000000001,-0.970000000000001,-0.969000000000001,
-0.968000000000001,-0.967000000000001,-0.966000000000001,-0.965000000000001,
-0.964000000000001,-0.963000000000001,-0.962000000000001,-0.961000000000001,
-0.960000000000001,-0.959000000000001,-0.958000000000001,-0.957000000000001,
-0.956000000000001,-0.955000000000001,-0.954000000000001,-0.953000000000001,
-0.952000000000001,-0.951000000000001,-0.950000000000001,-0.949000000000001,
-0.948000000000001,-0.947000000000001,-0.946000000000001,-0.945000000000001,
-0.944000000000001,-0.943000000000001,-0.942000000000001,-0.941000000000001,
-0.940000000000001,-0.939000000000001,-0.938000000000001,-0.937000000000001,
-0.936000000000001,-0.935000000000001,-0.934000000000001,-0.933000000000001,
-0.932000000000001,-0.931000000000001,-0.930000000000001,-0.929000000000001,
-0.928000000000001,-0.927000000000001,-0.926000000000001,-0.925000000000001,
-0.924000000000001,-0.923000000000001,-0.922000000000001,-0.921000000000001,
-0.920000000000001,-0.919000000000001,-0.918000000000001,-0.917000000000001,
-0.916000000000001,-0.915000000000001,-0.914000000000001,-0.913000000000001,
-0.912000000000001,-0.911000000000001,-0.910000000000001,-0.909000000000001,
-0.908000000000001,-0.907000000000001,-0.906000000000001,-0.905000000000001,
-0.904000000000001,-0.903000000000001,-0.902000000000001,-0.901000000000001,
-0.900000000000001,-0.899000000000001,-0.898000000000001,-0.897000000000001,
-0.896000000000001,-0.895000000000001,-0.894000000000001,-0.893000000000001,
-0.892000000000001,-0.891000000000001,-0.890000000000001,-0.889000000000001,
-0.888000000000001,-0.887000000000001,-0.886000000000001,-0.885000000000001,
-0.884000000000001,-0.883000000000001,-0.882000000000001,-0.881000000000001,
-0.880000000000001,-0.879000000000001,-0.878000000000001,-0.877000000000001,
-0.876000000000001,-0.875000000000001,-0.874000000000001,-0.873000000000001,
-0.872000000000001,-0.871000000000001,-0.870000000000001,-0.869000000000001,
-0.868000000000001,-0.867000000000001,-0.866000000000001,-0.865000000000001,
-0.864000000000001,-0.863000000000001,-0.862000000000001,-0.861000000000001,
-0.860000000000001,-0.859000000000001,-0.858000000000001,-0.857000000000001,
-0.856000000000001,-0.855000000000001,-0.854000000000001,-0.853000000000001,
-0.852000000000001,-0.851000000000001,-0.850000000000001,-0.849000000000001,
-0.848000000000001,-0.847000000000001,-0.846000000000001,-0.845000000000001,
-0.844000000000001,-0.843000000000001,-0.842000000000001,-0.841000000000001,
-0.840000000000001,-0.839000000000001,-0.838000000000001,-0.837000000000001,
-0.836000000000001,-0.835000000000001,-0.834000000000001,-0.833000000000001,
-0.832000000000001,-0.831000000000001,-0.830000000000001,-0.829000000000001,
-0.828000000000001,-0.827000000000001,-0.826000000000001,-0.825000000000001,
-0.824000000000001,-0.823000000000001,-0.822000000000001,-0.821000000000001,
-0.820000000000001,-0.819000000000001,-0.818000000000001,-0.817000000000001,
-0.816000000000001,-0.815000000000001,-0.814000000000001,-0.813000000000001,
-0.812000000000001,-0.811000000000001,-0.810000000000001,-0.809000000000001,
-0.808000000000001,-0.807000000000001,-0.806000000000001,-0.805000000000001,
-0.804000000000001,-0.803000000000001,-0.802000000000001,-0.801000000000001,
-0.800000000000001,-0.799000000000001,-0.798000000000001,-0.797000000000001,
-0.796000000000001,-0.795000000000001,-0.794000000000001,-0.793000000000001,
-0.792000000000001,-0.791000000000001,-0.790000000000001,-0.789000000000001,
-0.788000000000001,-0.787000000000001,-0.786000000000001,-0.785000000000001,
-0.784000000000001,-0.783000000000001,-0.782000000000001,-0.781000000000001,
-0.780000000000001,-0.779000000000001,-0.778000000000001,-0.777000000000001,
-0.776000000000001,-0.775000000000001,-0.774000000000001,-0.773000000000001,
-0.772000000000001,-0.771000000000001,-0.770000000000001,-0.769000000000001,
-0.768000000000001,-0.767000000000001,-0.766000000000001,-0.765000000000001,
-0.764000000000001,-0.763000000000001,-0.762000000000001,-0.761000000000001,
-0.760000000000001,-0.759000000000001,-0.758000000000001,-0.757000000000001,
-0.756000000000001,-0.755000000000001,-0.754000000000001,-0.753000000000001,
-0.752000000000001,-0.751000000000001,-0.750000000000001,-0.749000000000001,
-0.748000000000001,-0.747000000000001,-0.746000000000001,-0.745000000000001,
-0.744000000000001,-0.743000000000001,-0.742000000000001,-0.741000000000001,
-0.740000000000001,-0.739000000000001,-0.738000000000001,-0.737000000000001,
-0.736000000000001,-0.735000000000001,-0.734000000000001,-0.733000000000001,
-0.732000000000001,-0.731000000000001,-0.730000000000001,-0.729000000000001,
-0.728000000000001,-0.727000000000001,-0.726000000000001,-0.725000000000001,
-0.724000000000001,-0.723000000000001,-0.722000000000001,-0.721000000000001,
-0.720000000000001,-0.719000000000001,-0.718000000000001,-0.717000000000001,
-0.716000000000001,-0.715000000000001,-0.714000000000001,-0.713000000000001,
-0.712000000000001,-0.711000000000001,-0.710000000000001,-0.709000000000001,
-0.708000000000001,-0.707000000000001,-0.706000000000001,-0.705000000000001,
-0.704000000000001,-0.703000000000001,-0.702000000000001,-0.701000000000001,
-0.700000000000001,-0.699000000000001,-0.698000000000001,-0.697000000000001,
-0.696000000000001,-0.695000000000001,-0.694000000000001,-0.693000000000001,
-0.692000000000001,-0.691000000000001,-0.690000000000001,-0.689000000000001,
-0.688000000000001,-0.687,-0.686,-0.685,-0.684,-0.683,-0.682,-0.681,-0.68,
-0.679,-0.678,-0.677,-0.676,-0.675,-0.674,-0.673,-0.672,-0.671,-0.67,-0.669,
-0.668,-0.667,-0.666,-0.665,-0.664,-0.663,-0.662,-0.661,-0.66,-0.659,-0.658,
-0.657,-0.656,-0.655,-0.654,-0.653,-0.652,-0.651,-0.65,-0.649,-0.648,-0.647,
-0.646,-0.645,-0.644,-0.643,-0.642,-0.641,-0.64,-0.639,-0.638,-0.637,-0.636,
-0.635,-0.634,-0.633,-0.632,-0.631,-0.63,-0.629,-0.628,-0.627,-0.626,-0.625,
-0.624,-0.623,-0.622,-0.621,-0.62,-0.619,-0.618,-0.617,-0.616,-0.615,-0.614,
-0.613,-0.612,-0.611,-0.61,-0.609,-0.608,-0.607,-0.606,-0.605,-0.604,-0.603,
-0.602,-0.601,-0.6,-0.599,-0.598,-0.597,-0.596,-0.595,-0.594,-0.593,-0.592,
-0.591,-0.59,-0.589,-0.588,-0.587,-0.586,-0.585,-0.584,-0.583,-0.582,-0.581,
-0.58,-0.579,-0.578,-0.577,-0.576,-0.575,-0.574,-0.573,-0.572,-0.571,-0.57,
-0.569,-0.568,-0.567,-0.566,-0.565,-0.564,-0.563,-0.562,-0.561,-0.56,-0.559,
-0.558,-0.557,-0.556,-0.555,-0.554,-0.553,-0.552,-0.551,-0.55,-0.549,-0.548,
-0.547,-0.546,-0.545,-0.544,-0.543,-0.542,-0.541,-0.54,-0.539,-0.538,-0.537,
-0.536,-0.535,-0.534,-0.533,-0.532,-0.531,-0.53,-0.529,-0.528,-0.527,-0.526,
-0.525,-0.524,-0.523,-0.522,-0.521,-0.52,-0.519,-0.518,-0.517,-0.516,-0.515,
-0.514,-0.513,-0.512,-0.511,-0.51,-0.509,-0.508,-0.507,-0.506,-0.505,-0.504,
-0.503,-0.502,-0.501,-0.5,-0.499,-0.498,-0.497,-0.496,-0.495,-0.494,-0.493,
-0.492,-0.491,-0.49,-0.489,-0.488,-0.487,-0.486,-0.485,-0.484,-0.483,-0.482,
-0.481,-0.48,-0.479,-0.478,-0.477,-0.476,-0.475,-0.474,-0.473,-0.472,-0.471,
-0.47,-0.469,-0.468,-0.467,-0.466,-0.465,-0.464,-0.463,-0.462,-0.461,-0.46,
-0.459,-0.458,-0.457,-0.456,-0.455,-0.454,-0.453,-0.452,-0.451,-0.45,-0.449,
-0.448,-0.447,-0.446,-0.445,-0.444,-0.443,-0.442,-0.441,-0.44,-0.439,-0.438,
-0.437,-0.436,-0.435,-0.434,-0.433,-0.432,-0.431,-0.43,-0.429,-0.428,-0.427,
-0.426,-0.425,-0.424,-0.423,-0.422,-0.421,-0.42,-0.419,-0.418,-0.417,-0.416,
-0.415,-0.414,-0.413,-0.412,-0.411,-0.41,-0.409,-0.408,-0.407,-0.406,-0.405,
-0.404,-0.403,-0.402,-0.401,-0.4,-0.399,-0.398,-0.397,-0.396,-0.395,-0.394,
-0.393,-0.392,-0.391,-0.39,-0.389,-0.388,-0.387,-0.386,-0.385,-0.384,-0.383,
-0.382,-0.381,-0.38,-0.379,-0.378,-0.377,-0.376,-0.375,-0.374,-0.373,-0.372,
-0.371,-0.37,-0.369,-0.368,-0.367,-0.366,-0.365,-0.364,-0.363,-0.362,-0.361,
-0.36,-0.359,-0.358,-0.357,-0.356,-0.355,-0.354,-0.353,-0.352,-0.351,-0.35,
-0.349,-0.348,-0.347,-0.346,-0.345,-0.344,-0.343,-0.342,-0.341,-0.34,-0.339,
-0.338,-0.337,-0.336,-0.335,-0.334,-0.333,-0.332,-0.331,-0.33,-0.329,-0.328,
-0.327,-0.326,-0.325,-0.324,-0.323,-0.322,-0.321,-0.32,-0.319,-0.318,-0.317,
-0.316,-0.315,-0.314,-0.313,-0.312,-0.311,-0.31,-0.309,-0.308,-0.307,-0.306,
-0.305,-0.304,-0.303,-0.302,-0.301,-0.3,-0.299,-0.298,-0.297,-0.296,-0.295,
-0.294,-0.293,-0.292,-0.291,-0.29,-0.289,-0.288,-0.287,-0.286,-0.285,-0.284,
-0.283,-0.282,-0.281,-0.28,-0.279,-0.278,-0.277,-0.276,-0.275,-0.274,-0.273,
-0.272,-0.271,-0.27,-0.269,-0.268,-0.267,-0.266,-0.265,-0.264,-0.263,-0.262,
-0.261,-0.26,-0.259,-0.258,-0.257,-0.256,-0.255,-0.254,-0.253,-0.252,-0.251,
-0.25,-0.249,-0.248,-0.247,-0.246,-0.245,-0.244,-0.243,-0.242,-0.241,-0.24,
-0.239,-0.238,-0.237,-0.236,-0.235,-0.234,-0.233,-0.232,-0.231,-0.23,-0.229,
-0.228,-0.227,-0.226,-0.225,-0.224,-0.223,-0.222,-0.221,-0.22,-0.219,-0.218,
-0.217,-0.216,-0.215,-0.214,-0.213,-0.212,-0.211,-0.21,-0.209,-0.208,-0.207,
-0.206,-0.205,-0.204,-0.203,-0.202,-0.201,-0.2,-0.199,-0.198,-0.197,-0.196,
-0.195,-0.194,-0.193,-0.192,-0.191,-0.19,-0.189,-0.188,-0.187,-0.186,-0.185,
-0.184,-0.183,-0.182,-0.181,-0.18,-0.179,-0.178,-0.177,-0.176,-0.175,-0.174,
-0.173,-0.172,-0.171,-0.17,-0.169,-0.168,-0.167,-0.166,-0.165,-0.164,-0.163,
-0.162,-0.161,-0.16,-0.159,-0.158,-0.157,-0.156,-0.155,-0.154,-0.153,-0.152,
-0.151,-0.15,-0.149,-0.148,-0.147,-0.146,-0.145,-0.144,-0.143,-0.142,-0.141,
-0.14,-0.139,-0.138,-0.137,-0.136,-0.135,-0.134,-0.133,-0.132,-0.131,-0.13,
-0.129,-0.128,-0.127,-0.126,-0.125,-0.124,-0.123,-0.122,-0.121,-0.12,-0.119,
-0.118,-0.117,-0.116,-0.115,-0.114,-0.113,-0.112,-0.111,-0.11,-0.109,-0.108,
-0.107,-0.106,-0.105,-0.104,-0.103,-0.102,-0.101,-0.1,-0.0990000000000001,
-0.0980000000000001,-0.0970000000000001,-0.0960000000000001,-0.0950000000000001,
-0.0940000000000001,-0.0930000000000001,-0.0920000000000001,-0.0910000000000001,
-0.0900000000000001,-0.0890000000000001,-0.0880000000000001,-0.0870000000000001,
-0.0860000000000001,-0.0850000000000001,-0.0840000000000001,-0.0830000000000001,
-0.0820000000000001,-0.0810000000000001,-0.0800000000000001,-0.0790000000000001,
-0.0780000000000001,-0.0770000000000001,-0.0760000000000001,-0.0750000000000001,
-0.0740000000000001,-0.0730000000000001,-0.0720000000000001,-0.071,-0.07,
-0.069,-0.068,-0.067,-0.066,-0.065,-0.064,-0.063,-0.062,-0.061,-0.06,-0.059,
-0.058,-0.057,-0.056,-0.055,-0.054,-0.053,-0.052,-0.051,-0.05,-0.049,-0.048,
-0.047,-0.046,-0.045,-0.044,-0.043,-0.042,-0.041,-0.04,-0.039,-0.038,-0.037,
-0.036,-0.035,-0.034,-0.033,-0.032,-0.031,-0.03,-0.029,-0.028,-0.027,-0.026,
-0.025,-0.024,-0.023,-0.022,-0.021,-0.02,-0.019,-0.018,-0.017,-0.016,-0.015,
-0.014,-0.013,-0.012,-0.011,-0.01,-0.009,-0.008,-0.007,-0.006,-0.005,-0.004,
-0.003,-0.002,-0.001,0.),(0.,2.),.UNSPECIFIED.)
GEOMETRIC_REPRESENTATION_ITEM()
RATIONAL_B_SPLINE_SURFACE(((1.,1.),(1.,1.),(1.,1.),(1.,1.),(1.,1.),(1.,
1.),(1.,1.),(1.,1.),(1.,1.),(1.,1.),(1.,1.),(1.,1.),(1.,1.),(1.,1.),(1.,
1.),(1.,1.),(1.,1.),(1.,1.),(1.,1.),(1.,1.),(1.,1.),(1.,1.),(1.,1.),(1.,
1.),(1.,1.),(1.,1.),(1.,1.),(1.,1.),(1.,1.),(1.,1.),(1.,1.),(1.,1.),(1.,
1.),(1.,1.),(1.,1.),(1.,1.),(1.,1.),(1.,1.),(1.,1.),(1.,1.),(1.,1.),(1.,
1.),(1.,1.),(1.,1.),(1.,1.),(1.,1.),(1.,1.),(1.,1.),(1.,1.),(1.,1.),(1.,
1.),(1.,1.),(1.,1.),(1.,1.),(1.,1.),(1.,1.),(1.,1.),(1.,1.),(1.,1.),(1.,
1.),(1.,1.),(1.,1.),(1.,1.),(1.,1.),(1.,1.),(1.,1.),(1.,1.),(1.,1.),(1.,
1.),(1.,1.),(1.,1.),(1.,1.),(1.,1.),(1.,1.),(1.,1.),(1.,1.),(1.,1.),(1.,
1.),(1.,1.),(1.,1.),(1.,1.),(1.,1.),(1.,1.),(1.,1.),(1.,1.),(1.,1.),(1.,
1.),(1.,1.),(1.,1.),(1.,1.),(1.,1.),(1.,1.),(1.,1.),(1.,1.),(1.,1.),(1.,
1.),(1.,1.),(1.,1.),(1.,1.),(1.,1.),(1.,1.),(1.,1.),(1.,1.),(1.,1.),(1.,
1.),(1.,1.),(1.,1.),(1.,1.),(1.,1.),(1.,1.),(1.,1.),(1.,1.),(1.,1.),(1.,
1.),(1.,1.),(1.,1.),(1.,1.),(1.,1.),(1.,1.),(1.,1.),(1.,1.),(1.,1.),(1.,
1.),(1.,1.),(1.,1.),(1.,1.),(1.,1.),(1.,1.),(1.,1.),(1.,1.),(1.,1.),(1.,
1.),(1.,1.),(1.,1.),(1.,1.),(1.,1.),(1.,1.),(1.,1.),(1.,1.),(1.,1.),(1.,
1.),(1.,1.),(1.,1.),(1.,1.),(1.,1.),(1.,1.),(1.,1.),(1.,1.),(1.,1.),(1.,
1.),(1.,1.),(1.,1.),(1.,1.),(1.,1.),(1.,1.),(1.,1.),(1.,1.),(1.,1.),(1.,
1.),(1.,1.),(1.,1.),(1.,1.),(1.,1.),(1.,1.),(1.,1.),(1.,1.),(1.,1.),(1.,
1.),(1.,1.),(1.,1.),(1.,1.),(1.,1.),(1.,1.),(1.,1.),(1.,1.),(1.,1.),(1.,
1.),(1.,1.),(1.,1.),(1.,1.),(1.,1.),(1.,1.),(1.,1.),(1.,1.),(1.,1.),(1.,
1.),(1.,1.),(1.,1.),(1.,1.),(1.,1.),(1.,1.),(1.,1.),(1.,1.),(1.,1.),(1.,
1.),(1.,1.),(1.,1.),(1.,1.),(1.,1.),(1.,1.),(1.,1.),(1.,1.),(1.,1.),(1.,
1.),(1.,1.),(1.,1.),(1.,1.),(1.,1.),(1.,1.),(1.,1.),(1.,1.),(1.,1.),(1.,
1.),(1.,1.),(1.,1.),(1.,1.),(1.,1.),(1.,1.),(1.,1.),(1.,1.),(1.,1.),(1.,
1.),(1.,1.),(1.,1.),(1.,1.),(1.,1.),(1.,1.),(1.,1.),(1.,1.),(1.,1.),(1.,
1.),(1.,1.),(1.,1.),(1.,1.),(1.,1.),(1.,1.),(1.,1.),(1.,1.),(1.,1.),(1.,
1.),(1.,1.),(1.,1.),(1.,1.),(1.,1.),(1.,1.),(1.,1.),(1.,1.),(1.,1.),(1.,
1.),(1.,1.),(1.,1.),(1.,1.),(1.,1.),(1.,1.),(1.,1.),(1.,1.),(1.,1.),(1.,
1.),(1.,1.),(1.,1.),(1.,1.),(1.,1.),(1.,1.),(1.,1.),(1.,1.),(1.,1.),(1.,
1.),(1.,1.),(1.,1.),(1.,1.),(1.,1.),(1.,1.),(1.,1.),(1.,1.),(1.,1.),(1.,
1.),(1.,1.),(1.,1.),(1.,1.),(1.,1.),(1.,1.),(1.,1.),(1.,1.),(1.,1.),(1.,
1.),(1.,1.),(1.,1.),(1.,1.),(1.,1.),(1.,1.),(1.,1.),(1.,1.),(1.,1.),(1.,
1.),(1.,1.),(1.,1.),(1.,1.),(1.,1.),(1.,1.),(1.,1.),(1.,1.),(1.,1.),(1.,
1.),(1.,1.),(1.,1.),(1.,1.),(1.,1.),(1.,1.),(1.,1.),(1.,1.),(1.,1.),(1.,
1.),(1.,1.),(1.,1.),(1.,1.),(1.,1.),(1.,1.),(1.,1.),(1.,1.),(1.,1.),(1.,
1.),(1.,1.),(1.,1.),(1.,1.),(1.,1.),(1.,1.),(1.,1.),(1.,1.),(1.,1.),(1.,
1.),(1.,1.),(1.,1.),(1.,1.),(1.,1.),(1.,1.),(1.,1.),(1.,1.),(1.,1.),(1.,
1.),(1.,1.),(1.,1.),(1.,1.),(1.,1.),(1.,1.),(1.,1.),(1.,1.),(1.,1.),(1.,
1.),(1.,1.),(1.,1.),(1.,1.),(1.,1.),(1.,1.),(1.,1.),(1.,1.),(1.,1.),(1.,
1.),(1.,1.),(1.,1.),(1.,1.),(1.,1.),(1.,1.),(1.,1.),(1.,1.),(1.,1.),(1.,
1.),(1.,1.),(1.,1.),(1.,1.),(1.,1.),(1.,1.),(1.,1.),(1.,1.),(1.,1.),(1.,
1.),(1.,1.),(1.,1.),(1.,1.),(1.,1.),(1.,1.),(1.,1.),(1.,1.),(1.,1.),(1.,
1.),(1.,1.),(1.,1.),(1.,1.),(1.,1.),(1.,1.),(1.,1.),(1.,1.),(1.,1.),(1.,
1.),(1.,1.),(1.,1.),(1.,1.),(1.,1.),(1.,1.),(1.,1.),(1.,1.),(1.,1.),(1.,
1.),(1.,1.),(1.,1.),(1.,1.),(1.,1.),(1.,1.),(1.,1.),(1.,1.),(1.,1.),(1.,
1.),(1.,1.),(1.,1.),(1.,1.),(1.,1.),(1.,1.),(1.,1.),(1.,1.),(1.,1.),(1.,
1.),(1.,1.),(1.,1.),(1.,1.),(1.,1.),(1.,1.),(1.,1.),(1.,1.),(1.,1.),(1.,
1.),(1.,1.),(1.,1.),(1.,1.),(1.,1.),(1.,1.),(1.,1.),(1.,1.),(1.,1.),(1.,
1.),(1.,1.),(1.,1.),(1.,1.),(1.,1.),(1.,1.),(1.,1.),(1.,1.),(1.,1.),(1.,
1.),(1.,1.),(1.,1.),(1.,1.),(1.,1.),(1.,1.),(1.,1.),(1.,1.),(1.,1.),(1.,
1.),(1.,1.),(1.,1.),(1.,1.),(1.,1.),(1.,1.),(1.,1.),(1.,1.),(1.,1.),(1.,
1.),(1.,1.),(1.,1.),(1.,1.),(1.,1.),(1.,1.),(1.,1.),(1.,1.),(1.,1.),(1.,
1.),(1.,1.),(1.,1.),(1.,1.),(1.,1.),(1.,1.),(1.,1.),(1.,1.),(1.,1.),(1.,
1.),(1.,1.),(1.,1.),(1.,1.),(1.,1.),(1.,1.),(1.,1.),(1.,1.),(1.,1.),(1.,
1.),(1.,1.),(1.,1.),(1.,1.),(1.,1.),(1.,1.),(1.,1.),(1.,1.),(1.,1.),(1.,
1.),(1.,1.),(1.,1.),(1.,1.),(1.,1.),(1.,1.),(1.,1.),(1.,1.),(1.,1.),(1.,
1.),(1.,1.),(1.,1.),(1.,1.),(1.,1.),(1.,1.),(1.,1.),(1.,1.),(1.,1.),(1.,
1.),(1.,1.),(1.,1.),(1.,1.),(1.,1.),(1.,1.),(1.,1.),(1.,1.),(1.,1.),(1.,
1.),(1.,1.),(1.,1.),(1.,1.),(1.,1.),(1.,1.),(1.,1.),(1.,1.),(1.,1.),(1.,
1.),(1.,1.),(1.,1.),(1.,1.),(1.,1.),(1.,1.),(1.,1.),(1.,1.),(1.,1.),(1.,
1.),(1.,1.),(1.,1.),(1.,1.),(1.,1.),(1.,1.),(1.,1.),(1.,1.),(1.,1.),(1.,
1.),(1.,1.),(1.,1.),(1.,1.),(1.,1.),(1.,1.),(1.,1.),(1.,1.),(1.,1.),(1.,
1.),(1.,1.),(1.,1.),(1.,1.),(1.,1.),(1.,1.),(1.,1.),(1.,1.),(1.,1.),(1.,
1.),(1.,1.),(1.,1.),(1.,1.),(1.,1.),(1.,1.),(1.,1.),(1.,1.),(1.,1.),(1.,
1.),(1.,1.),(1.,1.),(1.,1.),(1.,1.),(1.,1.),(1.,1.),(1.,1.),(1.,1.),(1.,
1.),(1.,1.),(1.,1.),(1.,1.),(1.,1.),(1.,1.),(1.,1.),(1.,1.),(1.,1.),(1.,
1.),(1.,1.),(1.,1.),(1.,1.),(1.,1.),(1.,1.),(1.,1.),(1.,1.),(1.,1.),(1.,
1.),(1.,1.),(1.,1.),(1.,1.),(1.,1.),(1.,1.),(1.,1.),(1.,1.),(1.,1.),(1.,
1.),(1.,1.),(1.,1.),(1.,1.),(1.,1.),(1.,1.),(1.,1.),(1.,1.),(1.,1.),(1.,
1.),(1.,1.),(1.,1.),(1.,1.),(1.,1.),(1.,1.),(1.,1.),(1.,1.),(1.,1.),(1.,
1.),(1.,1.),(1.,1.),(1.,1.),(1.,1.),(1.,1.),(1.,1.),(1.,1.),(1.,1.),(1.,
1.),(1.,1.),(1.,1.),(1.,1.),(1.,1.),(1.,1.),(1.,1.),(1.,1.),(1.,1.),(1.,
1.),(1.,1.),(1.,1.),(1.,1.),(1.,1.),(1.,1.),(1.,1.),(1.,1.),(1.,1.),(1.,
1.),(1.,1.),(1.,1.),(1.,1.),(1.,1.),(1.,1.),(1.,1.),(1.,1.),(1.,1.),(1.,
1.),(1.,1.),(1.,1.),(1.,1.),(1.,1.),(1.,1.),(1.,1.),(1.,1.),(1.,1.),(1.,
1.),(1.,1.),(1.,1.),(1.,1.),(1.,1.),(1.,1.),(1.,1.),(1.,1.),(1.,1.),(1.,
1.),(1.,1.),(1.,1.),(1.,1.),(1.,1.),(1.,1.),(1.,1.),(1.,1.),(1.,1.),(1.,
1.),(1.,1.),(1.,1.),(1.,1.),(1.,1.),(1.,1.),(1.,1.),(1.,1.),(1.,1.),(1.,
1.),(1.,1.),(1.,1.),(1.,1.),(1.,1.),(1.,1.),(1.,1.),(1.,1.),(1.,1.),(1.,
1.),(1.,1.),(1.,1.),(1.,1.),(1.,1.),(1.,1.),(1.,1.),(1.,1.),(1.,1.),(1.,
1.),(1.,1.),(1.,1.),(1.,1.),(1.,1.),(1.,1.),(1.,1.),(1.,1.),(1.,1.),(1.,
1.),(1.,1.),(1.,1.),(1.,1.),(1.,1.),(1.,1.),(1.,1.),(1.,1.),(1.,1.),(1.,
1.),(1.,1.),(1.,1.),(1.,1.),(1.,1.),(1.,1.),(1.,1.),(1.,1.),(1.,1.),(1.,
1.),(1.,1.),(1.,1.),(1.,1.),(1.,1.),(1.,1.),(1.,1.),(1.,1.),(1.,1.),(1.,
1.),(1.,1.),(1.,1.),(1.,1.),(1.,1.),(1.,1.),(1.,1.),(1.,1.),(1.,1.),(1.,
1.),(1.,1.),(1.,1.),(1.,1.),(1.,1.),(1.,1.),(1.,1.),(1.,1.),(1.,1.),(1.,
1.),(1.,1.),(1.,1.),(1.,1.),(1.,1.),(1.,1.),(1.,1.),(1.,1.),(1.,1.),(1.,
1.),(1.,1.),(1.,1.),(1.,1.),(1.,1.),(1.,1.),(1.,1.),(1.,1.),(1.,1.),(1.,
1.),(1.,1.),(1.,1.),(1.,1.),(1.,1.),(1.,1.),(1.,1.),(1.,1.),(1.,1.),(1.,
1.),(1.,1.),(1.,1.),(1.,1.),(1.,1.),(1.,1.),(1.,1.),(1.,1.),(1.,1.),(1.,
1.),(1.,1.),(1.,1.),(1.,1.),(1.,1.),(1.,1.),(1.,1.),(1.,1.),(1.,1.),(1.,
1.),(1.,1.),(1.,1.),(1.,1.),(1.,1.),(1.,1.),(1.,1.),(1.,1.),(1.,1.),(1.,
1.),(1.,1.),(1.,1.),(1.,1.),(1.,1.),(1.,1.),(1.,1.),(1.,1.),(1.,1.),(1.,
1.),(1.,1.),(1.,1.),(1.,1.),(1.,1.),(1.,1.),(1.,1.),(1.,1.),(1.,1.),(1.,
1.),(1.,1.),(1.,1.),(1.,1.),(1.,1.),(1.,1.),(1.,1.),(1.,1.),(1.,1.),(1.,
1.),(1.,1.),(1.,1.),(1.,1.),(1.,1.),(1.,1.),(1.,1.),(1.,1.),(1.,1.),(1.,
1.),(1.,1.),(1.,1.),(1.,1.),(1.,1.),(1.,1.),(1.,1.),(1.,1.),(1.,1.),(1.,
1.),(1.,1.),(1.,1.),(1.,1.),(1.,1.),(1.,1.),(1.,1.),(1.,1.),(1.,1.),(1.,
1.),(1.,1.),(1.,1.),(1.,1.),(1.,1.),(1.,1.),(1.,1.),(1.,1.),(1.,1.),(1.,
1.),(1.,1.),(1.,1.),(1.,1.),(1.,1.),(1.,1.),(1.,1.),(1.,1.),(1.,1.),(1.,
1.),(1.,1.),(1.,1.),(1.,1.),(1.,1.),(1.,1.),(1.,1.),(1.,1.),(1.,1.),(1.,
1.),(1.,1.),(1.,1.),(1.,1.),(1.,1.),(1.,1.),(1.,1.),(1.,1.),(1.,1.),(1.,
1.),(1.,1.),(1.,1.),(1.,1.),(1.,1.),(1.,1.),(1.,1.),(1.,1.),(1.,1.),(1.,
1.),(1.,1.),(1.,1.),(1.,1.),(1.,1.),(1.,1.),(1.,1.),(1.,1.),(1.,1.),(1.,
1.),(1.,1.),(1.,1.),(1.,1.),(1.,1.),(1.,1.),(1.,1.),(1.,1.),(1.,1.),(1.,
1.),(1.,1.),(1.,1.),(1.,1.),(1.,1.),(1.,1.),(1.,1.),(1.,1.),(1.,1.),(1.,
1.),(1.,1.),(1.,1.),(1.,1.),(1.,1.),(1.,1.),(1.,1.),(1.,1.),(1.,1.),(1.,
1.),(1.,1.),(1.,1.),(1.,1.),(1.,1.),(1.,1.),(1.,1.),(1.,1.),(1.,1.),(1.,
1.),(1.,1.),(1.,1.),(1.,1.),(1.,1.),(1.,1.),(1.,1.),(1.,1.),(1.,1.),(1.,
1.),(1.,1.),(1.,1.),(1.,1.),(1.,1.),(1.,1.),(1.,1.),(1.,1.),(1.,1.),(1.,
1.),(1.,1.),(1.,1.),(1.,1.),(1.,1.),(1.,1.),(1.,1.),(1.,1.),(1.,1.),(1.,
1.)))
REPRESENTATION_ITEM('')
SURFACE()
);
#268=SHAPE_REPRESENTATION_RELATIONSHIP('SRR','None',#99625,#284);
#269=SHAPE_REPRESENTATION_RELATIONSHIP('SRR','None',#99626,#285);
#270=SHAPE_REPRESENTATION_RELATIONSHIP('SRR','None',#99627,#286);
#271=SHAPE_REPRESENTATION_RELATIONSHIP('SRR','None',#99628,#287);
#272=SHAPE_REPRESENTATION_RELATIONSHIP('SRR','None',#99629,#288);
#273=SHAPE_REPRESENTATION_RELATIONSHIP('SRR','None',#99630,#289);
#274=SHAPE_REPRESENTATION_RELATIONSHIP('SRR','None',#99631,#290);
#275=SHAPE_REPRESENTATION_RELATIONSHIP('SRR','None',#99632,#291);
#276=SHAPE_REPRESENTATION_RELATIONSHIP('SRR','None',#99633,#292);
#277=SHAPE_REPRESENTATION_RELATIONSHIP('SRR','None',#99634,#293);
#278=SHAPE_REPRESENTATION_RELATIONSHIP('SRR','None',#99635,#294);
#279=SHAPE_REPRESENTATION_RELATIONSHIP('SRR','None',#99636,#295);
#280=SHAPE_REPRESENTATION_RELATIONSHIP('SRR','None',#99637,#296);
#281=SHAPE_REPRESENTATION_RELATIONSHIP('SRR','None',#99638,#297);
#282=SHAPE_REPRESENTATION_RELATIONSHIP('SRR','None',#99639,#298);
#283=SHAPE_REPRESENTATION_RELATIONSHIP('SRR','None',#99640,#299);
#284=ADVANCED_BREP_SHAPE_REPRESENTATION('',(#316),#99510);
#285=ADVANCED_BREP_SHAPE_REPRESENTATION('',(#317),#99511);
#286=ADVANCED_BREP_SHAPE_REPRESENTATION('',(#318),#99512);
#287=ADVANCED_BREP_SHAPE_REPRESENTATION('',(#319),#99513);
#288=ADVANCED_BREP_SHAPE_REPRESENTATION('',(#320),#99514);
#289=ADVANCED_BREP_SHAPE_REPRESENTATION('',(#321),#99515);
#290=ADVANCED_BREP_SHAPE_REPRESENTATION('',(#322),#99516);
#291=ADVANCED_BREP_SHAPE_REPRESENTATION('',(#323),#99517);
#292=ADVANCED_BREP_SHAPE_REPRESENTATION('',(#324),#99518);
#293=ADVANCED_BREP_SHAPE_REPRESENTATION('',(#325),#99519);
#294=ADVANCED_BREP_SHAPE_REPRESENTATION('',(#326),#99520);
#295=ADVANCED_BREP_SHAPE_REPRESENTATION('',(#327),#99521);
#296=ADVANCED_BREP_SHAPE_REPRESENTATION('',(#328),#99522);
#297=ADVANCED_BREP_SHAPE_REPRESENTATION('',(#329),#99523);
#298=ADVANCED_BREP_SHAPE_REPRESENTATION('',(#330),#99524);
#299=ADVANCED_BREP_SHAPE_REPRESENTATION('',(#331),#99525);
#300=STYLED_ITEM('',(#99714),#316);
#301=STYLED_ITEM('',(#99715),#317);
#302=STYLED_ITEM('',(#99716),#318);
#303=STYLED_ITEM('',(#99717),#319);
#304=STYLED_ITEM('',(#99718),#320);
#305=STYLED_ITEM('',(#99719),#321);
#306=STYLED_ITEM('',(#99717),#322);
#307=STYLED_ITEM('',(#99715),#323);
#308=STYLED_ITEM('',(#99720),#324);
#309=STYLED_ITEM('',(#99721),#325);
#310=STYLED_ITEM('',(#99717),#326);
#311=STYLED_ITEM('',(#99722),#327);
#312=STYLED_ITEM('',(#99723),#328);
#313=STYLED_ITEM('',(#99724),#329);
#314=STYLED_ITEM('',(#99722),#330);
#315=STYLED_ITEM('',(#99725),#331);
#316=MANIFOLD_SOLID_BREP('Body1',#18270);
#317=MANIFOLD_SOLID_BREP('Gear blank',#18271);
#318=MANIFOLD_SOLID_BREP('Body1',#18272);
#319=MANIFOLD_SOLID_BREP('Body1',#18273);
#320=MANIFOLD_SOLID_BREP('Body1',#18274);
#321=MANIFOLD_SOLID_BREP('Body1',#18275);
#322=MANIFOLD_SOLID_BREP('Body1',#18276);
#323=MANIFOLD_SOLID_BREP('Body1',#18277);
#324=MANIFOLD_SOLID_BREP('Body1',#18278);
#325=MANIFOLD_SOLID_BREP('Body1',#18279);
#326=MANIFOLD_SOLID_BREP('Body1',#18280);
#327=MANIFOLD_SOLID_BREP('Body1',#18281);
#328=MANIFOLD_SOLID_BREP('Body1',#18282);
#329=MANIFOLD_SOLID_BREP('Body1',#18283);
#330=MANIFOLD_SOLID_BREP('Body1',#18284);
#331=MANIFOLD_SOLID_BREP('Body1',#18285);
#332=FACE_BOUND('',#2130,.T.);
#333=FACE_BOUND('',#2131,.T.);
#334=FACE_BOUND('',#2132,.T.);
#335=FACE_BOUND('',#2133,.T.);
#336=FACE_BOUND('',#2135,.T.);
#337=FACE_BOUND('',#2136,.T.);
#338=FACE_BOUND('',#2137,.T.);
#339=FACE_BOUND('',#2138,.T.);
#340=FACE_BOUND('',#2139,.T.);
#341=FACE_BOUND('',#2140,.T.);
#342=FACE_BOUND('',#2141,.T.);
#343=FACE_BOUND('',#2143,.T.);
#344=FACE_BOUND('',#2144,.T.);
#345=FACE_BOUND('',#2145,.T.);
#346=FACE_BOUND('',#2146,.T.);
#347=FACE_BOUND('',#2147,.T.);
#348=FACE_BOUND('',#2148,.T.);
#349=FACE_BOUND('',#2149,.T.);
#350=FACE_BOUND('',#2346,.T.);
#351=FACE_BOUND('',#2347,.T.);
#352=FACE_BOUND('',#2348,.T.);
#353=FACE_BOUND('',#2349,.T.);
#354=FACE_BOUND('',#2350,.T.);
#355=FACE_BOUND('',#2351,.T.);
#356=FACE_BOUND('',#2352,.T.);
#357=FACE_BOUND('',#2439,.T.);
#358=FACE_BOUND('',#2441,.T.);
#359=FACE_BOUND('',#2444,.T.);
#360=FACE_BOUND('',#2446,.T.);
#361=FACE_BOUND('',#2449,.T.);
#362=FACE_BOUND('',#2451,.T.);
#363=FACE_BOUND('',#2454,.T.);
#364=FACE_BOUND('',#2456,.T.);
#365=FACE_BOUND('',#2459,.T.);
#366=FACE_BOUND('',#2461,.T.);
#367=FACE_BOUND('',#2464,.T.);
#368=FACE_BOUND('',#2466,.T.);
#369=FACE_BOUND('',#2469,.T.);
#370=FACE_BOUND('',#2472,.T.);
#371=FACE_BOUND('',#2474,.T.);
#372=FACE_BOUND('',#2477,.T.);
#373=FACE_BOUND('',#2480,.T.);
#374=FACE_BOUND('',#2483,.T.);
#375=FACE_BOUND('',#2486,.T.);
#376=FACE_BOUND('',#2489,.T.);
#377=FACE_BOUND('',#2493,.T.);
#378=FACE_BOUND('',#2496,.T.);
#379=FACE_BOUND('',#2507,.T.);
#380=FACE_BOUND('',#2510,.T.);
#381=FACE_BOUND('',#2522,.T.);
#382=FACE_BOUND('',#2523,.T.);
#383=FACE_BOUND('',#2524,.T.);
#384=FACE_BOUND('',#2525,.T.);
#385=FACE_BOUND('',#2526,.T.);
#386=FACE_BOUND('',#2527,.T.);
#387=FACE_BOUND('',#2528,.T.);
#388=FACE_BOUND('',#2557,.T.);
#389=FACE_BOUND('',#2559,.T.);
#390=FACE_BOUND('',#2562,.T.);
#391=FACE_BOUND('',#2564,.T.);
#392=FACE_BOUND('',#2567,.T.);
#393=FACE_BOUND('',#2569,.T.);
#394=FACE_BOUND('',#2584,.T.);
#395=FACE_BOUND('',#2588,.T.);
#396=FACE_BOUND('',#2592,.T.);
#397=FACE_BOUND('',#2596,.T.);
#398=FACE_BOUND('',#2600,.T.);
#399=FACE_BOUND('',#2604,.T.);
#400=FACE_BOUND('',#2610,.T.);
#401=FACE_BOUND('',#2611,.T.);
#402=FACE_BOUND('',#2612,.T.);
#403=FACE_BOUND('',#2613,.T.);
#404=FACE_BOUND('',#2614,.T.);
#405=FACE_BOUND('',#2615,.T.);
#406=FACE_BOUND('',#2616,.T.);
#407=FACE_BOUND('',#2618,.T.);
#408=FACE_BOUND('',#2619,.T.);
#409=FACE_BOUND('',#2620,.T.);
#410=FACE_BOUND('',#2621,.T.);
#411=FACE_BOUND('',#2622,.T.);
#412=FACE_BOUND('',#2623,.T.);
#413=FACE_BOUND('',#2624,.T.);
#414=FACE_BOUND('',#2628,.T.);
#415=FACE_BOUND('',#2630,.T.);
#416=FACE_BOUND('',#2646,.T.);
#417=FACE_BOUND('',#2647,.T.);
#418=FACE_BOUND('',#2648,.T.);
#419=FACE_BOUND('',#2649,.T.);
#420=FACE_BOUND('',#2650,.T.);
#421=FACE_BOUND('',#2651,.T.);
#422=FACE_BOUND('',#2652,.T.);
#423=FACE_BOUND('',#2654,.T.);
#424=FACE_BOUND('',#2655,.T.);
#425=FACE_BOUND('',#2656,.T.);
#426=FACE_BOUND('',#2657,.T.);
#427=FACE_BOUND('',#2658,.T.);
#428=FACE_BOUND('',#2659,.T.);
#429=FACE_BOUND('',#2660,.T.);
#430=FACE_BOUND('',#2664,.T.);
#431=FACE_BOUND('',#2666,.T.);
#432=FACE_BOUND('',#2670,.T.);
#433=FACE_BOUND('',#2672,.T.);
#434=FACE_BOUND('',#2676,.T.);
#435=FACE_BOUND('',#2678,.T.);
#436=FACE_BOUND('',#2686,.T.);
#437=FACE_BOUND('',#2739,.T.);
#438=FACE_BOUND('',#2742,.T.);
#439=FACE_BOUND('',#2774,.T.);
#440=PLANE('',#18901);
#441=PLANE('',#18903);
#442=PLANE('',#18905);
#443=PLANE('',#18908);
#444=PLANE('',#18909);
#445=PLANE('',#18912);
#446=PLANE('',#18915);
#447=PLANE('',#18918);
#448=PLANE('',#18921);
#449=PLANE('',#18924);
#450=PLANE('',#18925);
#451=PLANE('',#18926);
#452=PLANE('',#18927);
#453=PLANE('',#18928);
#454=PLANE('',#18929);
#455=PLANE('',#18932);
#456=PLANE('',#18935);
#457=PLANE('',#18938);
#458=PLANE('',#18941);
#459=PLANE('',#18944);
#460=PLANE('',#18945);
#461=PLANE('',#18946);
#462=PLANE('',#18947);
#463=PLANE('',#18948);
#464=PLANE('',#18949);
#465=PLANE('',#18952);
#466=PLANE('',#18953);
#467=PLANE('',#18956);
#468=PLANE('',#18963);
#469=PLANE('',#18964);
#470=PLANE('',#19254);
#471=PLANE('',#19255);
#472=PLANE('',#19256);
#473=PLANE('',#19257);
#474=PLANE('',#19271);
#475=PLANE('',#19274);
#476=PLANE('',#19277);
#477=PLANE('',#19280);
#478=PLANE('',#19283);
#479=PLANE('',#19286);
#480=PLANE('',#19287);
#481=PLANE('',#19288);
#482=PLANE('',#19289);
#483=PLANE('',#19290);
#484=PLANE('',#19291);
#485=PLANE('',#19292);
#486=PLANE('',#19293);
#487=PLANE('',#19294);
#488=PLANE('',#19295);
#489=PLANE('',#19296);
#490=PLANE('',#19299);
#491=PLANE('',#19302);
#492=PLANE('',#19305);
#493=PLANE('',#19308);
#494=PLANE('',#19311);
#495=PLANE('',#19312);
#496=PLANE('',#19313);
#497=PLANE('',#19314);
#498=PLANE('',#19315);
#499=PLANE('',#19316);
#500=PLANE('',#19317);
#501=PLANE('',#19318);
#502=PLANE('',#19319);
#503=PLANE('',#19320);
#504=PLANE('',#19321);
#505=PLANE('',#19324);
#506=PLANE('',#19325);
#507=PLANE('',#19326);
#508=PLANE('',#19329);
#509=PLANE('',#19330);
#510=PLANE('',#19337);
#511=PLANE('',#19344);
#512=PLANE('',#19351);
#513=PLANE('',#19358);
#514=PLANE('',#19365);
#515=PLANE('',#19372);
#516=PLANE('',#19373);
#517=PLANE('',#19374);
#518=PLANE('',#19375);
#519=PLANE('',#19376);
#520=PLANE('',#19377);
#521=PLANE('',#19378);
#522=PLANE('',#19379);
#523=PLANE('',#19380);
#524=PLANE('',#19381);
#525=PLANE('',#19382);
#526=PLANE('',#19383);
#527=PLANE('',#19384);
#528=PLANE('',#19385);
#529=PLANE('',#19386);
#530=PLANE('',#19387);
#531=PLANE('',#19388);
#532=PLANE('',#19389);
#533=PLANE('',#19390);
#534=PLANE('',#19391);
#535=PLANE('',#19392);
#536=PLANE('',#19393);
#537=PLANE('',#19394);
#538=PLANE('',#19395);
#539=PLANE('',#19396);
#540=PLANE('',#19401);
#541=PLANE('',#19406);
#542=PLANE('',#19411);
#543=PLANE('',#19412);
#544=PLANE('',#19420);
#545=PLANE('',#19423);
#546=PLANE('',#19426);
#547=PLANE('',#19435);
#548=PLANE('',#19438);
#549=PLANE('',#19439);
#550=PLANE('',#19446);
#551=PLANE('',#19449);
#552=PLANE('',#19450);
#553=PLANE('',#19458);
#554=PLANE('',#19459);
#555=PLANE('',#19463);
#556=PLANE('',#19465);
#557=PLANE('',#19469);
#558=PLANE('',#19471);
#559=PLANE('',#19476);
#560=PLANE('',#19477);
#561=PLANE('',#19479);
#562=PLANE('',#19483);
#563=PLANE('',#19487);
#564=PLANE('',#19488);
#565=PLANE('',#19493);
#566=PLANE('',#19494);
#567=PLANE('',#19496);
#568=PLANE('',#19503);
#569=PLANE('',#19510);
#570=PLANE('',#19517);
#571=PLANE('',#19524);
#572=PLANE('',#19531);
#573=PLANE('',#19544);
#574=PLANE('',#19545);
#575=PLANE('',#19553);
#576=PLANE('',#19554);
#577=PLANE('',#19592);
#578=PLANE('',#19593);
#579=PLANE('',#19601);
#580=PLANE('',#19602);
#581=PLANE('',#19610);
#582=PLANE('',#19611);
#583=PLANE('',#19619);
#584=PLANE('',#19620);
#585=PLANE('',#19622);
#586=PLANE('',#19623);
#587=PLANE('',#19624);
#588=PLANE('',#19631);
#589=PLANE('',#19633);
#590=PLANE('',#19638);
#591=PLANE('',#19641);
#592=PLANE('',#19645);
#593=PLANE('',#19646);
#594=PLANE('',#19688);
#595=PLANE('',#19689);
#596=PLANE('',#19690);
#597=PLANE('',#19691);
#598=PLANE('',#19692);
#599=PLANE('',#19693);
#600=PLANE('',#19694);
#601=PLANE('',#19695);
#602=PLANE('',#19699);
#603=PLANE('',#19700);
#604=PLANE('',#19725);
#605=PLANE('',#19726);
#606=PLANE('',#19727);
#607=PLANE('',#19728);
#608=PLANE('',#19729);
#609=PLANE('',#19730);
#610=PLANE('',#19731);
#611=PLANE('',#19732);
#612=PLANE('',#19736);
#613=PLANE('',#19739);
#614=B_SPLINE_SURFACE_WITH_KNOTS('',3,3,((#36513,#36514,#36515,#36516,#36517,
#36518,#36519,#36520,#36521,#36522,#36523,#36524,#36525,#36526,#36527,#36528,
#36529,#36530,#36531,#36532,#36533,#36534,#36535,#36536,#36537,#36538,#36539,
#36540,#36541,#36542,#36543,#36544,#36545,#36546,#36547,#36548,#36549,#36550,
#36551,#36552,#36553,#36554,#36555,#36556,#36557,#36558,#36559,#36560,#36561,
#36562,#36563,#36564,#36565,#36566,#36567,#36568),(#36569,#36570,#36571,
#36572,#36573,#36574,#36575,#36576,#36577,#36578,#36579,#36580,#36581,#36582,
#36583,#36584,#36585,#36586,#36587,#36588,#36589,#36590,#36591,#36592,#36593,
#36594,#36595,#36596,#36597,#36598,#36599,#36600,#36601,#36602,#36603,#36604,
#36605,#36606,#36607,#36608,#36609,#36610,#36611,#36612,#36613,#36614,#36615,
#36616,#36617,#36618,#36619,#36620,#36621,#36622,#36623,#36624),(#36625,
#36626,#36627,#36628,#36629,#36630,#36631,#36632,#36633,#36634,#36635,#36636,
#36637,#36638,#36639,#36640,#36641,#36642,#36643,#36644,#36645,#36646,#36647,
#36648,#36649,#36650,#36651,#36652,#36653,#36654,#36655,#36656,#36657,#36658,
#36659,#36660,#36661,#36662,#36663,#36664,#36665,#36666,#36667,#36668,#36669,
#36670,#36671,#36672,#36673,#36674,#36675,#36676,#36677,#36678,#36679,#36680),
(#36681,#36682,#36683,#36684,#36685,#36686,#36687,#36688,#36689,#36690,
#36691,#36692,#36693,#36694,#36695,#36696,#36697,#36698,#36699,#36700,#36701,
#36702,#36703,#36704,#36705,#36706,#36707,#36708,#36709,#36710,#36711,#36712,
#36713,#36714,#36715,#36716,#36717,#36718,#36719,#36720,#36721,#36722,#36723,
#36724,#36725,#36726,#36727,#36728,#36729,#36730,#36731,#36732,#36733,#36734,
#36735,#36736)),.UNSPECIFIED.,.F.,.F.,.F.,(4,4),(4,1,1,1,1,1,1,1,1,1,1,
1,1,1,1,1,1,1,1,1,1,1,1,1,1,1,1,1,1,1,1,1,1,1,1,1,1,1,1,1,1,1,1,1,1,1,1,
1,1,1,1,1,1,4),(0.,0.0642013499338865),(12.0817516052311,13.0640094280149,
14.0462672507987,15.0285250735825,16.0107828963664,16.9930407191502,17.975298541934,
18.9575563647178,19.9398141875016,20.9220720102854,21.9043298330692,22.886587655853,
23.8688454786368,24.8511033014206,25.8333611242044,26.8156189469882,27.797876769772,
28.7801345925559,29.7623924153397,30.7446502381235,31.7269080609073,32.7091658836911,
33.6914237064749,34.6736815292587,35.6559393520425,36.6381971748263,37.6204549976101,
38.6027128203939,39.5849706431777,40.5672284659615,41.5494862887453,42.5317441115292,
43.514001934313,44.4962597570968,45.4785175798806,46.4607754026644,47.4430332254482,
48.425291048232,49.4075488710158,50.3898066937996,51.3720645165834,52.3543223393672,
53.336580162151,54.3188379849348,55.3010958077186,56.2833536305025,57.2656114532863,
58.2478692760701,59.2301270988539,60.2123849216377,61.1946427444215,62.1769005672053,
63.1591583899891,64.1414162127729),.UNSPECIFIED.);
#615=B_SPLINE_SURFACE_WITH_KNOTS('',3,3,((#36890,#36891,#36892,#36893,#36894,
#36895,#36896,#36897,#36898,#36899,#36900,#36901,#36902,#36903,#36904,#36905,
#36906,#36907,#36908,#36909,#36910,#36911,#36912,#36913,#36914,#36915,#36916,
#36917,#36918,#36919,#36920,#36921,#36922,#36923,#36924,#36925,#36926,#36927,
#36928,#36929,#36930,#36931,#36932,#36933,#36934,#36935,#36936,#36937,#36938,
#36939,#36940,#36941,#36942,#36943,#36944,#36945),(#36946,#36947,#36948,
#36949,#36950,#36951,#36952,#36953,#36954,#36955,#36956,#36957,#36958,#36959,
#36960,#36961,#36962,#36963,#36964,#36965,#36966,#36967,#36968,#36969,#36970,
#36971,#36972,#36973,#36974,#36975,#36976,#36977,#36978,#36979,#36980,#36981,
#36982,#36983,#36984,#36985,#36986,#36987,#36988,#36989,#36990,#36991,#36992,
#36993,#36994,#36995,#36996,#36997,#36998,#36999,#37000,#37001),(#37002,
#37003,#37004,#37005,#37006,#37007,#37008,#37009,#37010,#37011,#37012,#37013,
#37014,#37015,#37016,#37017,#37018,#37019,#37020,#37021,#37022,#37023,#37024,
#37025,#37026,#37027,#37028,#37029,#37030,#37031,#37032,#37033,#37034,#37035,
#37036,#37037,#37038,#37039,#37040,#37041,#37042,#37043,#37044,#37045,#37046,
#37047,#37048,#37049,#37050,#37051,#37052,#37053,#37054,#37055,#37056,#37057),
(#37058,#37059,#37060,#37061,#37062,#37063,#37064,#37065,#37066,#37067,
#37068,#37069,#37070,#37071,#37072,#37073,#37074,#37075,#37076,#37077,#37078,
#37079,#37080,#37081,#37082,#37083,#37084,#37085,#37086,#37087,#37088,#37089,
#37090,#37091,#37092,#37093,#37094,#37095,#37096,#37097,#37098,#37099,#37100,
#37101,#37102,#37103,#37104,#37105,#37106,#37107,#37108,#37109,#37110,#37111,
#37112,#37113)),.UNSPECIFIED.,.F.,.F.,.F.,(4,4),(4,1,1,1,1,1,1,1,1,1,1,
1,1,1,1,1,1,1,1,1,1,1,1,1,1,1,1,1,1,1,1,1,1,1,1,1,1,1,1,1,1,1,1,1,1,1,1,
1,1,1,1,1,1,4),(0.,0.0642013499338865),(14.4348810643014,15.4206536381342,
16.4064262119669,17.3921987857997,18.3779713596324,19.3637439334652,20.3495165072979,
21.3352890811306,22.3210616549634,23.3068342287961,24.2926068026289,25.2783793764616,
26.2641519502944,27.2499245241271,28.2356970979599,29.2214696717926,30.2072422456253,
31.1930148194581,32.1787873932908,33.1645599671236,34.1503325409563,35.1361051147891,
36.1218776886218,37.1076502624546,38.0934228362873,39.07919541012,40.0649679839528,
41.0507405577855,42.0365131316183,43.022285705451,44.0080582792838,44.9938308531165,
45.9796034269493,46.965376000782,47.9511485746147,48.9369211484475,49.9226937222802,
50.908466296113,51.8942388699457,52.8800114437785,53.8657840176112,54.851556591444,
55.8373291652767,56.8231017391094,57.8088743129422,58.7946468867749,59.7804194606077,
60.7661920344404,61.7519646082732,62.7377371821059,63.7235097559387,64.7092823297714,
65.6950549036041,66.6808274774369),.UNSPECIFIED.);
#616=B_SPLINE_SURFACE_WITH_KNOTS('',3,3,((#37247,#37248,#37249,#37250,#37251,
#37252,#37253,#37254,#37255,#37256,#37257,#37258,#37259,#37260,#37261,#37262,
#37263,#37264,#37265,#37266,#37267,#37268,#37269,#37270,#37271,#37272,#37273,
#37274,#37275,#37276,#37277,#37278,#37279,#37280,#37281,#37282,#37283,#37284,
#37285,#37286,#37287,#37288,#37289,#37290,#37291,#37292,#37293,#37294,#37295,
#37296,#37297,#37298,#37299,#37300,#37301,#37302),(#37303,#37304,#37305,
#37306,#37307,#37308,#37309,#37310,#37311,#37312,#37313,#37314,#37315,#37316,
#37317,#37318,#37319,#37320,#37321,#37322,#37323,#37324,#37325,#37326,#37327,
#37328,#37329,#37330,#37331,#37332,#37333,#37334,#37335,#37336,#37337,#37338,
#37339,#37340,#37341,#37342,#37343,#37344,#37345,#37346,#37347,#37348,#37349,
#37350,#37351,#37352,#37353,#37354,#37355,#37356,#37357,#37358),(#37359,
#37360,#37361,#37362,#37363,#37364,#37365,#37366,#37367,#37368,#37369,#37370,
#37371,#37372,#37373,#37374,#37375,#37376,#37377,#37378,#37379,#37380,#37381,
#37382,#37383,#37384,#37385,#37386,#37387,#37388,#37389,#37390,#37391,#37392,
#37393,#37394,#37395,#37396,#37397,#37398,#37399,#37400,#37401,#37402,#37403,
#37404,#37405,#37406,#37407,#37408,#37409,#37410,#37411,#37412,#37413,#37414),
(#37415,#37416,#37417,#37418,#37419,#37420,#37421,#37422,#37423,#37424,
#37425,#37426,#37427,#37428,#37429,#37430,#37431,#37432,#37433,#37434,#37435,
#37436,#37437,#37438,#37439,#37440,#37441,#37442,#37443,#37444,#37445,#37446,
#37447,#37448,#37449,#37450,#37451,#37452,#37453,#37454,#37455,#37456,#37457,
#37458,#37459,#37460,#37461,#37462,#37463,#37464,#37465,#37466,#37467,#37468,
#37469,#37470)),.UNSPECIFIED.,.F.,.F.,.F.,(4,4),(4,1,1,1,1,1,1,1,1,1,1,
1,1,1,1,1,1,1,1,1,1,1,1,1,1,1,1,1,1,1,1,1,1,1,1,1,1,1,1,1,1,1,1,1,1,1,1,
1,1,1,1,1,1,4),(0.,0.0642013499338865),(12.0817516052313,13.0640094280151,
14.046267250799,15.0285250735828,16.0107828963666,16.9930407191504,17.9752985419342,
18.957556364718,19.9398141875018,20.9220720102856,21.9043298330694,22.8865876558532,
23.868845478637,24.8511033014208,25.8333611242046,26.8156189469884,27.7978767697722,
28.780134592556,29.7623924153398,30.7446502381237,31.7269080609075,32.7091658836913,
33.6914237064751,34.6736815292589,35.6559393520427,36.6381971748265,37.6204549976103,
38.6027128203941,39.5849706431779,40.5672284659617,41.5494862887455,42.5317441115293,
43.5140019343131,44.4962597570969,45.4785175798807,46.4607754026645,47.4430332254484,
48.4252910482322,49.407548871016,50.3898066937998,51.3720645165836,52.3543223393674,
53.3365801621512,54.318837984935,55.3010958077188,56.2833536305026,57.2656114532864,
58.2478692760702,59.230127098854,60.2123849216378,61.1946427444216,62.1769005672054,
63.1591583899892,64.1414162127731),.UNSPECIFIED.);
#617=B_SPLINE_SURFACE_WITH_KNOTS('',3,3,((#37624,#37625,#37626,#37627,#37628,
#37629,#37630,#37631,#37632,#37633,#37634,#37635,#37636,#37637,#37638,#37639,
#37640,#37641,#37642,#37643,#37644,#37645,#37646,#37647,#37648,#37649,#37650,
#37651,#37652,#37653,#37654,#37655,#37656,#37657,#37658,#37659,#37660,#37661,
#37662,#37663,#37664,#37665,#37666,#37667,#37668,#37669,#37670,#37671,#37672,
#37673,#37674,#37675,#37676,#37677,#37678,#37679),(#37680,#37681,#37682,
#37683,#37684,#37685,#37686,#37687,#37688,#37689,#37690,#37691,#37692,#37693,
#37694,#37695,#37696,#37697,#37698,#37699,#37700,#37701,#37702,#37703,#37704,
#37705,#37706,#37707,#37708,#37709,#37710,#37711,#37712,#37713,#37714,#37715,
#37716,#37717,#37718,#37719,#37720,#37721,#37722,#37723,#37724,#37725,#37726,
#37727,#37728,#37729,#37730,#37731,#37732,#37733,#37734,#37735),(#37736,
#37737,#37738,#37739,#37740,#37741,#37742,#37743,#37744,#37745,#37746,#37747,
#37748,#37749,#37750,#37751,#37752,#37753,#37754,#37755,#37756,#37757,#37758,
#37759,#37760,#37761,#37762,#37763,#37764,#37765,#37766,#37767,#37768,#37769,
#37770,#37771,#37772,#37773,#37774,#37775,#37776,#37777,#37778,#37779,#37780,
#37781,#37782,#37783,#37784,#37785,#37786,#37787,#37788,#37789,#37790,#37791),
(#37792,#37793,#37794,#37795,#37796,#37797,#37798,#37799,#37800,#37801,
#37802,#37803,#37804,#37805,#37806,#37807,#37808,#37809,#37810,#37811,#37812,
#37813,#37814,#37815,#37816,#37817,#37818,#37819,#37820,#37821,#37822,#37823,
#37824,#37825,#37826,#37827,#37828,#37829,#37830,#37831,#37832,#37833,#37834,
#37835,#37836,#37837,#37838,#37839,#37840,#37841,#37842,#37843,#37844,#37845,
#37846,#37847)),.UNSPECIFIED.,.F.,.F.,.F.,(4,4),(4,1,1,1,1,1,1,1,1,1,1,
1,1,1,1,1,1,1,1,1,1,1,1,1,1,1,1,1,1,1,1,1,1,1,1,1,1,1,1,1,1,1,1,1,1,1,1,
1,1,1,1,1,1,4),(0.,0.0642013499338865),(14.4348810643015,15.4206536381343,
16.406426211967,17.3921987857997,18.3779713596325,19.3637439334652,20.349516507298,
21.3352890811307,22.3210616549635,23.3068342287962,24.292606802629,25.2783793764617,
26.2641519502944,27.2499245241272,28.2356970979599,29.2214696717927,30.2072422456254,
31.1930148194582,32.1787873932909,33.1645599671237,34.1503325409564,35.1361051147891,
36.1218776886219,37.1076502624546,38.0934228362874,39.0791954101201,40.0649679839529,
41.0507405577856,42.0365131316183,43.0222857054511,44.0080582792838,44.9938308531166,
45.9796034269493,46.9653760007821,47.9511485746148,48.9369211484476,49.9226937222803,
50.908466296113,51.8942388699458,52.8800114437785,53.8657840176113,54.851556591444,
55.8373291652768,56.8231017391095,57.8088743129423,58.794646886775,59.7804194606078,
60.7661920344405,61.7519646082732,62.737737182106,63.7235097559387,64.7092823297715,
65.6950549036042,66.680827477437),.UNSPECIFIED.);
#618=B_SPLINE_SURFACE_WITH_KNOTS('',3,3,((#37981,#37982,#37983,#37984,#37985,
#37986,#37987,#37988,#37989,#37990,#37991,#37992,#37993,#37994,#37995,#37996,
#37997,#37998,#37999,#38000,#38001,#38002,#38003,#38004,#38005,#38006,#38007,
#38008,#38009,#38010,#38011,#38012,#38013,#38014,#38015,#38016,#38017,#38018,
#38019,#38020,#38021,#38022,#38023,#38024,#38025,#38026,#38027,#38028,#38029,
#38030,#38031,#38032,#38033,#38034,#38035,#38036),(#38037,#38038,#38039,
#38040,#38041,#38042,#38043,#38044,#38045,#38046,#38047,#38048,#38049,#38050,
#38051,#38052,#38053,#38054,#38055,#38056,#38057,#38058,#38059,#38060,#38061,
#38062,#38063,#38064,#38065,#38066,#38067,#38068,#38069,#38070,#38071,#38072,
#38073,#38074,#38075,#38076,#38077,#38078,#38079,#38080,#38081,#38082,#38083,
#38084,#38085,#38086,#38087,#38088,#38089,#38090,#38091,#38092),(#38093,
#38094,#38095,#38096,#38097,#38098,#38099,#38100,#38101,#38102,#38103,#38104,
#38105,#38106,#38107,#38108,#38109,#38110,#38111,#38112,#38113,#38114,#38115,
#38116,#38117,#38118,#38119,#38120,#38121,#38122,#38123,#38124,#38125,#38126,
#38127,#38128,#38129,#38130,#38131,#38132,#38133,#38134,#38135,#38136,#38137,
#38138,#38139,#38140,#38141,#38142,#38143,#38144,#38145,#38146,#38147,#38148),
(#38149,#38150,#38151,#38152,#38153,#38154,#38155,#38156,#38157,#38158,
#38159,#38160,#38161,#38162,#38163,#38164,#38165,#38166,#38167,#38168,#38169,
#38170,#38171,#38172,#38173,#38174,#38175,#38176,#38177,#38178,#38179,#38180,
#38181,#38182,#38183,#38184,#38185,#38186,#38187,#38188,#38189,#38190,#38191,
#38192,#38193,#38194,#38195,#38196,#38197,#38198,#38199,#38200,#38201,#38202,
#38203,#38204)),.UNSPECIFIED.,.F.,.F.,.F.,(4,4),(4,1,1,1,1,1,1,1,1,1,1,
1,1,1,1,1,1,1,1,1,1,1,1,1,1,1,1,1,1,1,1,1,1,1,1,1,1,1,1,1,1,1,1,1,1,1,1,
1,1,1,1,1,1,4),(0.,0.0642013499338865),(12.0817516052311,13.0640094280149,
14.0462672507987,15.0285250735825,16.0107828963663,16.9930407191502,17.975298541934,
18.9575563647178,19.9398141875016,20.9220720102854,21.9043298330692,22.886587655853,
23.8688454786368,24.8511033014206,25.8333611242044,26.8156189469882,27.797876769772,
28.7801345925558,29.7623924153396,30.7446502381234,31.7269080609072,32.709165883691,
33.6914237064749,34.6736815292587,35.6559393520425,36.6381971748263,37.6204549976101,
38.6027128203939,39.5849706431777,40.5672284659615,41.5494862887453,42.5317441115291,
43.5140019343129,44.4962597570967,45.4785175798805,46.4607754026643,47.4430332254481,
48.4252910482319,49.4075488710157,50.3898066937996,51.3720645165834,52.3543223393672,
53.336580162151,54.3188379849348,55.3010958077186,56.2833536305024,57.2656114532862,
58.24786927607,59.2301270988538,60.2123849216376,61.1946427444214,62.1769005672052,
63.159158389989,64.1414162127728),.UNSPECIFIED.);
#619=B_SPLINE_SURFACE_WITH_KNOTS('',3,3,((#38358,#38359,#38360,#38361,#38362,
#38363,#38364,#38365,#38366,#38367,#38368,#38369,#38370,#38371,#38372,#38373,
#38374,#38375,#38376,#38377,#38378,#38379,#38380,#38381,#38382,#38383,#38384,
#38385,#38386,#38387,#38388,#38389,#38390,#38391,#38392,#38393,#38394,#38395,
#38396,#38397,#38398,#38399,#38400,#38401,#38402,#38403,#38404,#38405,#38406,
#38407,#38408,#38409,#38410,#38411,#38412,#38413),(#38414,#38415,#38416,
#38417,#38418,#38419,#38420,#38421,#38422,#38423,#38424,#38425,#38426,#38427,
#38428,#38429,#38430,#38431,#38432,#38433,#38434,#38435,#38436,#38437,#38438,
#38439,#38440,#38441,#38442,#38443,#38444,#38445,#38446,#38447,#38448,#38449,
#38450,#38451,#38452,#38453,#38454,#38455,#38456,#38457,#38458,#38459,#38460,
#38461,#38462,#38463,#38464,#38465,#38466,#38467,#38468,#38469),(#38470,
#38471,#38472,#38473,#38474,#38475,#38476,#38477,#38478,#38479,#38480,#38481,
#38482,#38483,#38484,#38485,#38486,#38487,#38488,#38489,#38490,#38491,#38492,
#38493,#38494,#38495,#38496,#38497,#38498,#38499,#38500,#38501,#38502,#38503,
#38504,#38505,#38506,#38507,#38508,#38509,#38510,#38511,#38512,#38513,#38514,
#38515,#38516,#38517,#38518,#38519,#38520,#38521,#38522,#38523,#38524,#38525),
(#38526,#38527,#38528,#38529,#38530,#38531,#38532,#38533,#38534,#38535,
#38536,#38537,#38538,#38539,#38540,#38541,#38542,#38543,#38544,#38545,#38546,
#38547,#38548,#38549,#38550,#38551,#38552,#38553,#38554,#38555,#38556,#38557,
#38558,#38559,#38560,#38561,#38562,#38563,#38564,#38565,#38566,#38567,#38568,
#38569,#38570,#38571,#38572,#38573,#38574,#38575,#38576,#38577,#38578,#38579,
#38580,#38581)),.UNSPECIFIED.,.F.,.F.,.F.,(4,4),(4,1,1,1,1,1,1,1,1,1,1,
1,1,1,1,1,1,1,1,1,1,1,1,1,1,1,1,1,1,1,1,1,1,1,1,1,1,1,1,1,1,1,1,1,1,1,1,
1,1,1,1,1,1,4),(0.,0.0642013499338865),(14.4348810643012,15.420653638134,
16.4064262119667,17.3921987857995,18.3779713596322,19.363743933465,20.3495165072977,
21.3352890811305,22.3210616549632,23.3068342287959,24.2926068026287,25.2783793764614,
26.2641519502942,27.2499245241269,28.2356970979597,29.2214696717924,30.2072422456252,
31.1930148194579,32.1787873932907,33.1645599671234,34.1503325409562,35.1361051147889,
36.1218776886216,37.1076502624544,38.0934228362871,39.0791954101199,40.0649679839526,
41.0507405577854,42.0365131316181,43.0222857054509,44.0080582792836,44.9938308531164,
45.9796034269491,46.9653760007819,47.9511485746146,48.9369211484474,49.9226937222801,
50.9084662961128,51.8942388699456,52.8800114437783,53.8657840176111,54.8515565914438,
55.8373291652766,56.8231017391093,57.8088743129421,58.7946468867748,59.7804194606076,
60.7661920344403,61.751964608273,62.7377371821058,63.7235097559385,64.7092823297713,
65.695054903604,66.6808274774368),.UNSPECIFIED.);
#620=B_SPLINE_SURFACE_WITH_KNOTS('',3,3,((#38721,#38722,#38723,#38724,#38725,
#38726,#38727,#38728,#38729,#38730,#38731,#38732,#38733,#38734,#38735,#38736,
#38737,#38738,#38739,#38740,#38741,#38742,#38743,#38744,#38745,#38746,#38747,
#38748,#38749,#38750,#38751,#38752,#38753,#38754,#38755,#38756,#38757,#38758,
#38759,#38760,#38761,#38762,#38763,#38764,#38765,#38766,#38767,#38768,#38769,
#38770,#38771,#38772,#38773,#38774,#38775,#38776),(#38777,#38778,#38779,
#38780,#38781,#38782,#38783,#38784,#38785,#38786,#38787,#38788,#38789,#38790,
#38791,#38792,#38793,#38794,#38795,#38796,#38797,#38798,#38799,#38800,#38801,
#38802,#38803,#38804,#38805,#38806,#38807,#38808,#38809,#38810,#38811,#38812,
#38813,#38814,#38815,#38816,#38817,#38818,#38819,#38820,#38821,#38822,#38823,
#38824,#38825,#38826,#38827,#38828,#38829,#38830,#38831,#38832),(#38833,
#38834,#38835,#38836,#38837,#38838,#38839,#38840,#38841,#38842,#38843,#38844,
#38845,#38846,#38847,#38848,#38849,#38850,#38851,#38852,#38853,#38854,#38855,
#38856,#38857,#38858,#38859,#38860,#38861,#38862,#38863,#38864,#38865,#38866,
#38867,#38868,#38869,#38870,#38871,#38872,#38873,#38874,#38875,#38876,#38877,
#38878,#38879,#38880,#38881,#38882,#38883,#38884,#38885,#38886,#38887,#38888),
(#38889,#38890,#38891,#38892,#38893,#38894,#38895,#38896,#38897,#38898,
#38899,#38900,#38901,#38902,#38903,#38904,#38905,#38906,#38907,#38908,#38909,
#38910,#38911,#38912,#38913,#38914,#38915,#38916,#38917,#38918,#38919,#38920,
#38921,#38922,#38923,#38924,#38925,#38926,#38927,#38928,#38929,#38930,#38931,
#38932,#38933,#38934,#38935,#38936,#38937,#38938,#38939,#38940,#38941,#38942,
#38943,#38944)),.UNSPECIFIED.,.F.,.F.,.F.,(4,4),(4,1,1,1,1,1,1,1,1,1,1,
1,1,1,1,1,1,1,1,1,1,1,1,1,1,1,1,1,1,1,1,1,1,1,1,1,1,1,1,1,1,1,1,1,1,1,1,
1,1,1,1,1,1,4),(0.,0.0642013499338865),(12.0817516052311,13.0640094280149,
14.0462672507987,15.0285250735825,16.0107828963663,16.9930407191501,17.9752985419339,
18.9575563647177,19.9398141875016,20.9220720102854,21.9043298330692,22.886587655853,
23.8688454786368,24.8511033014206,25.8333611242044,26.8156189469882,27.797876769772,
28.7801345925558,29.7623924153396,30.7446502381234,31.7269080609072,32.709165883691,
33.6914237064748,34.6736815292587,35.6559393520425,36.6381971748263,37.6204549976101,
38.6027128203939,39.5849706431777,40.5672284659615,41.5494862887453,42.5317441115291,
43.5140019343129,44.4962597570967,45.4785175798805,46.4607754026643,47.4430332254481,
48.4252910482319,49.4075488710157,50.3898066937995,51.3720645165834,52.3543223393672,
53.336580162151,54.3188379849348,55.3010958077186,56.2833536305024,57.2656114532862,
58.24786927607,59.2301270988538,60.2123849216376,61.1946427444214,62.1769005672052,
63.159158389989,64.1414162127728),.UNSPECIFIED.);
#621=B_SPLINE_SURFACE_WITH_KNOTS('',3,3,((#39098,#39099,#39100,#39101,#39102,
#39103,#39104,#39105,#39106,#39107,#39108,#39109,#39110,#39111,#39112,#39113,
#39114,#39115,#39116,#39117,#39118,#39119,#39120,#39121,#39122,#39123,#39124,
#39125,#39126,#39127,#39128,#39129,#39130,#39131,#39132,#39133,#39134,#39135,
#39136,#39137,#39138,#39139,#39140,#39141,#39142,#39143,#39144,#39145,#39146,
#39147,#39148,#39149,#39150,#39151,#39152,#39153),(#39154,#39155,#39156,
#39157,#39158,#39159,#39160,#39161,#39162,#39163,#39164,#39165,#39166,#39167,
#39168,#39169,#39170,#39171,#39172,#39173,#39174,#39175,#39176,#39177,#39178,
#39179,#39180,#39181,#39182,#39183,#39184,#39185,#39186,#39187,#39188,#39189,
#39190,#39191,#39192,#39193,#39194,#39195,#39196,#39197,#39198,#39199,#39200,
#39201,#39202,#39203,#39204,#39205,#39206,#39207,#39208,#39209),(#39210,
#39211,#39212,#39213,#39214,#39215,#39216,#39217,#39218,#39219,#39220,#39221,
#39222,#39223,#39224,#39225,#39226,#39227,#39228,#39229,#39230,#39231,#39232,
#39233,#39234,#39235,#39236,#39237,#39238,#39239,#39240,#39241,#39242,#39243,
#39244,#39245,#39246,#39247,#39248,#39249,#39250,#39251,#39252,#39253,#39254,
#39255,#39256,#39257,#39258,#39259,#39260,#39261,#39262,#39263,#39264,#39265),
(#39266,#39267,#39268,#39269,#39270,#39271,#39272,#39273,#39274,#39275,
#39276,#39277,#39278,#39279,#39280,#39281,#39282,#39283,#39284,#39285,#39286,
#39287,#39288,#39289,#39290,#39291,#39292,#39293,#39294,#39295,#39296,#39297,
#39298,#39299,#39300,#39301,#39302,#39303,#39304,#39305,#39306,#39307,#39308,
#39309,#39310,#39311,#39312,#39313,#39314,#39315,#39316,#39317,#39318,#39319,
#39320,#39321)),.UNSPECIFIED.,.F.,.F.,.F.,(4,4),(4,1,1,1,1,1,1,1,1,1,1,
1,1,1,1,1,1,1,1,1,1,1,1,1,1,1,1,1,1,1,1,1,1,1,1,1,1,1,1,1,1,1,1,1,1,1,1,
1,1,1,1,1,1,4),(0.,0.0642013499338865),(14.4348810643014,15.4206536381342,
16.4064262119669,17.3921987857997,18.3779713596324,19.3637439334652,20.3495165072979,
21.3352890811306,22.3210616549634,23.3068342287961,24.2926068026289,25.2783793764616,
26.2641519502944,27.2499245241271,28.2356970979599,29.2214696717926,30.2072422456253,
31.1930148194581,32.1787873932908,33.1645599671236,34.1503325409563,35.1361051147891,
36.1218776886218,37.1076502624545,38.0934228362873,39.07919541012,40.0649679839528,
41.0507405577855,42.0365131316183,43.022285705451,44.0080582792838,44.9938308531165,
45.9796034269492,46.965376000782,47.9511485746147,48.9369211484475,49.9226937222802,
50.908466296113,51.8942388699457,52.8800114437785,53.8657840176112,54.8515565914439,
55.8373291652767,56.8231017391094,57.8088743129422,58.7946468867749,59.7804194606077,
60.7661920344404,61.7519646082732,62.7377371821059,63.7235097559386,64.7092823297714,
65.6950549036041,66.6808274774369),.UNSPECIFIED.);
#622=B_SPLINE_SURFACE_WITH_KNOTS('',3,3,((#39653,#39654,#39655,#39656,#39657,
#39658,#39659,#39660,#39661,#39662,#39663,#39664,#39665,#39666,#39667,#39668,
#39669,#39670,#39671,#39672,#39673,#39674,#39675,#39676,#39677,#39678,#39679,
#39680,#39681,#39682,#39683,#39684,#39685,#39686,#39687,#39688,#39689,#39690,
#39691,#39692,#39693,#39694,#39695,#39696,#39697,#39698,#39699,#39700,#39701,
#39702,#39703,#39704,#39705,#39706,#39707,#39708,#39709,#39710,#39711,#39712,
#39713,#39714,#39715,#39716,#39717,#39718,#39719,#39720,#39721,#39722,#39723,
#39724,#39725,#39726,#39727,#39728,#39729,#39730,#39731,#39732,#39733,#39734,
#39735,#39736,#39737,#39738),(#39739,#39740,#39741,#39742,#39743,#39744,
#39745,#39746,#39747,#39748,#39749,#39750,#39751,#39752,#39753,#39754,#39755,
#39756,#39757,#39758,#39759,#39760,#39761,#39762,#39763,#39764,#39765,#39766,
#39767,#39768,#39769,#39770,#39771,#39772,#39773,#39774,#39775,#39776,#39777,
#39778,#39779,#39780,#39781,#39782,#39783,#39784,#39785,#39786,#39787,#39788,
#39789,#39790,#39791,#39792,#39793,#39794,#39795,#39796,#39797,#39798,#39799,
#39800,#39801,#39802,#39803,#39804,#39805,#39806,#39807,#39808,#39809,#39810,
#39811,#39812,#39813,#39814,#39815,#39816,#39817,#39818,#39819,#39820,#39821,
#39822,#39823,#39824),(#39825,#39826,#39827,#39828,#39829,#39830,#39831,
#39832,#39833,#39834,#39835,#39836,#39837,#39838,#39839,#39840,#39841,#39842,
#39843,#39844,#39845,#39846,#39847,#39848,#39849,#39850,#39851,#39852,#39853,
#39854,#39855,#39856,#39857,#39858,#39859,#39860,#39861,#39862,#39863,#39864,
#39865,#39866,#39867,#39868,#39869,#39870,#39871,#39872,#39873,#39874,#39875,
#39876,#39877,#39878,#39879,#39880,#39881,#39882,#39883,#39884,#39885,#39886,
#39887,#39888,#39889,#39890,#39891,#39892,#39893,#39894,#39895,#39896,#39897,
#39898,#39899,#39900,#39901,#39902,#39903,#39904,#39905,#39906,#39907,#39908,
#39909,#39910),(#39911,#39912,#39913,#39914,#39915,#39916,#39917,#39918,
#39919,#39920,#39921,#39922,#39923,#39924,#39925,#39926,#39927,#39928,#39929,
#39930,#39931,#39932,#39933,#39934,#39935,#39936,#39937,#39938,#39939,#39940,
#39941,#39942,#39943,#39944,#39945,#39946,#39947,#39948,#39949,#39950,#39951,
#39952,#39953,#39954,#39955,#39956,#39957,#39958,#39959,#39960,#39961,#39962,
#39963,#39964,#39965,#39966,#39967,#39968,#39969,#39970,#39971,#39972,#39973,
#39974,#39975,#39976,#39977,#39978,#39979,#39980,#39981,#39982,#39983,#39984,
#39985,#39986,#39987,#39988,#39989,#39990,#39991,#39992,#39993,#39994,#39995,
#39996)),.UNSPECIFIED.,.F.,.F.,.F.,(4,4),(4,1,1,1,1,1,1,1,1,1,1,1,1,1,1,
1,1,1,1,1,1,1,1,1,1,1,1,1,1,1,1,1,1,1,1,1,1,1,1,1,1,1,1,1,1,1,1,1,1,1,1,
1,1,1,1,1,1,1,1,1,1,1,1,1,1,1,1,1,1,1,1,1,1,1,1,1,1,1,1,1,1,1,1,4),(0.,
0.0448889834294934),(11.8615800042567,12.8591513772396,13.8567227502225,
14.8542941232055,15.8518654961884,16.8494368691713,17.8470082421543,18.8445796151372,
19.8421509881201,20.8397223611031,21.837293734086,22.8348651070689,23.8324364800519,
24.8300078530348,25.8275792260177,26.8251505990007,27.8227219719836,28.8202933449665,
29.8178647179495,30.8154360909324,31.8130074639153,32.8105788368983,33.8081502098812,
34.8057215828641,35.803292955847,36.80086432883,37.7984357018129,38.7960070747958,
39.7935784477788,40.7911498207617,41.7887211937446,42.7862925667276,43.7838639397105,
44.7814353126934,45.7790066856764,46.7765780586593,47.7741494316422,48.7717208046252,
49.7692921776081,50.766863550591,51.764434923574,52.7620062965569,53.7595776695398,
54.7571490425228,55.7547204155057,56.7522917884886,57.7498631614716,58.7474345344545,
59.7450059074374,60.7425772804204,61.7401486534033,62.7377200263862,63.7352913993692,
64.7328627723521,65.730434145335,66.728005518318,67.7255768913009,68.7231482642838,
69.7207196372668,70.7182910102497,71.7158623832326,72.7134337562156,73.7110051291985,
74.7085765021814,75.7061478751643,76.7037192481473,77.7012906211302,78.6988619941132,
79.6964333670961,80.694004740079,81.691576113062,82.6891474860449,83.6867188590278,
84.6842902320108,85.6818616049937,86.6794329779766,87.6770043509595,88.6745757239425,
89.6721470969254,90.6697184699083,91.6672898428913,92.6648612158742,93.6624325888571,
94.6600039618401),.UNSPECIFIED.);
#623=B_SPLINE_SURFACE_WITH_KNOTS('',3,3,((#40104,#40105,#40106,#40107,#40108,
#40109,#40110,#40111,#40112,#40113,#40114,#40115,#40116,#40117,#40118,#40119,
#40120,#40121,#40122,#40123,#40124,#40125,#40126,#40127,#40128,#40129,#40130,
#40131,#40132,#40133,#40134,#40135,#40136,#40137,#40138,#40139,#40140,#40141,
#40142,#40143,#40144,#40145,#40146,#40147,#40148,#40149,#40150,#40151,#40152,
#40153,#40154,#40155,#40156,#40157,#40158,#40159,#40160,#40161,#40162,#40163,
#40164,#40165,#40166,#40167,#40168,#40169,#40170,#40171,#40172,#40173,#40174,
#40175,#40176,#40177,#40178,#40179,#40180,#40181,#40182,#40183,#40184,#40185,
#40186,#40187,#40188,#40189),(#40190,#40191,#40192,#40193,#40194,#40195,
#40196,#40197,#40198,#40199,#40200,#40201,#40202,#40203,#40204,#40205,#40206,
#40207,#40208,#40209,#40210,#40211,#40212,#40213,#40214,#40215,#40216,#40217,
#40218,#40219,#40220,#40221,#40222,#40223,#40224,#40225,#40226,#40227,#40228,
#40229,#40230,#40231,#40232,#40233,#40234,#40235,#40236,#40237,#40238,#40239,
#40240,#40241,#40242,#40243,#40244,#40245,#40246,#40247,#40248,#40249,#40250,
#40251,#40252,#40253,#40254,#40255,#40256,#40257,#40258,#40259,#40260,#40261,
#40262,#40263,#40264,#40265,#40266,#40267,#40268,#40269,#40270,#40271,#40272,
#40273,#40274,#40275),(#40276,#40277,#40278,#40279,#40280,#40281,#40282,
#40283,#40284,#40285,#40286,#40287,#40288,#40289,#40290,#40291,#40292,#40293,
#40294,#40295,#40296,#40297,#40298,#40299,#40300,#40301,#40302,#40303,#40304,
#40305,#40306,#40307,#40308,#40309,#40310,#40311,#40312,#40313,#40314,#40315,
#40316,#40317,#40318,#40319,#40320,#40321,#40322,#40323,#40324,#40325,#40326,
#40327,#40328,#40329,#40330,#40331,#40332,#40333,#40334,#40335,#40336,#40337,
#40338,#40339,#40340,#40341,#40342,#40343,#40344,#40345,#40346,#40347,#40348,
#40349,#40350,#40351,#40352,#40353,#40354,#40355,#40356,#40357,#40358,#40359,
#40360,#40361),(#40362,#40363,#40364,#40365,#40366,#40367,#40368,#40369,
#40370,#40371,#40372,#40373,#40374,#40375,#40376,#40377,#40378,#40379,#40380,
#40381,#40382,#40383,#40384,#40385,#40386,#40387,#40388,#40389,#40390,#40391,
#40392,#40393,#40394,#40395,#40396,#40397,#40398,#40399,#40400,#40401,#40402,
#40403,#40404,#40405,#40406,#40407,#40408,#40409,#40410,#40411,#40412,#40413,
#40414,#40415,#40416,#40417,#40418,#40419,#40420,#40421,#40422,#40423,#40424,
#40425,#40426,#40427,#40428,#40429,#40430,#40431,#40432,#40433,#40434,#40435,
#40436,#40437,#40438,#40439,#40440,#40441,#40442,#40443,#40444,#40445,#40446,
#40447)),.UNSPECIFIED.,.F.,.F.,.F.,(4,4),(4,1,1,1,1,1,1,1,1,1,1,1,1,1,1,
1,1,1,1,1,1,1,1,1,1,1,1,1,1,1,1,1,1,1,1,1,1,1,1,1,1,1,1,1,1,1,1,1,1,1,1,
1,1,1,1,1,1,1,1,1,1,1,1,1,1,1,1,1,1,1,1,1,1,1,1,1,1,1,1,1,1,1,1,4),(0.,
0.0448889834294934),(14.3981410127769,15.3957123857598,16.3932837587428,
17.3908551317257,18.3884265047086,19.3859978776916,20.3835692506745,21.3811406236574,
22.3787119966404,23.3762833696233,24.3738547426062,25.3714261155892,26.3689974885721,
27.366568861555,28.364140234538,29.3617116075209,30.3592829805038,31.3568543534868,
32.3544257264697,33.3519970994526,34.3495684724356,35.3471398454185,36.3447112184014,
37.3422825913844,38.3398539643673,39.3374253373502,40.3349967103332,41.3325680833161,
42.330139456299,43.327710829282,44.3252822022649,45.3228535752478,46.3204249482308,
47.3179963212137,48.3155676941966,49.3131390671795,50.3107104401625,51.3082818131454,
52.3058531861283,53.3034245591113,54.3009959320942,55.2985673050771,56.2961386780601,
57.293710051043,58.2912814240259,59.2888527970089,60.2864241699918,61.2839955429747,
62.2815669159577,63.2791382889406,64.2767096619235,65.2742810349065,66.2718524078894,
67.2694237808723,68.2669951538553,69.2645665268382,70.2621378998211,71.2597092728041,
72.257280645787,73.2548520187699,74.2524233917529,75.2499947647358,76.2475661377187,
77.2451375107017,78.2427088836846,79.2402802566675,80.2378516296505,81.2354230026334,
82.2329943756163,83.2305657485992,84.2281371215822,85.2257084945651,86.2232798675481,
87.220851240531,88.2184226135139,89.2159939864968,90.2135653594798,91.2111367324627,
92.2087081054457,93.2062794784286,94.2038508514115,95.2014222243944,96.1989935973774,
97.1965649703603),.UNSPECIFIED.);
#624=B_SPLINE_SURFACE_WITH_KNOTS('',3,3,((#40752,#40753,#40754,#40755,#40756,
#40757,#40758,#40759,#40760,#40761,#40762,#40763,#40764,#40765,#40766,#40767,
#40768,#40769,#40770,#40771,#40772,#40773,#40774,#40775,#40776,#40777,#40778,
#40779,#40780,#40781,#40782,#40783,#40784,#40785,#40786,#40787,#40788,#40789,
#40790,#40791,#40792,#40793,#40794,#40795,#40796,#40797,#40798,#40799,#40800,
#40801,#40802,#40803,#40804,#40805,#40806,#40807,#40808,#40809,#40810,#40811,
#40812,#40813,#40814,#40815,#40816,#40817,#40818,#40819,#40820,#40821,#40822,
#40823,#40824,#40825,#40826,#40827,#40828,#40829,#40830,#40831,#40832,#40833,
#40834,#40835,#40836,#40837),(#40838,#40839,#40840,#40841,#40842,#40843,
#40844,#40845,#40846,#40847,#40848,#40849,#40850,#40851,#40852,#40853,#40854,
#40855,#40856,#40857,#40858,#40859,#40860,#40861,#40862,#40863,#40864,#40865,
#40866,#40867,#40868,#40869,#40870,#40871,#40872,#40873,#40874,#40875,#40876,
#40877,#40878,#40879,#40880,#40881,#40882,#40883,#40884,#40885,#40886,#40887,
#40888,#40889,#40890,#40891,#40892,#40893,#40894,#40895,#40896,#40897,#40898,
#40899,#40900,#40901,#40902,#40903,#40904,#40905,#40906,#40907,#40908,#40909,
#40910,#40911,#40912,#40913,#40914,#40915,#40916,#40917,#40918,#40919,#40920,
#40921,#40922,#40923),(#40924,#40925,#40926,#40927,#40928,#40929,#40930,
#40931,#40932,#40933,#40934,#40935,#40936,#40937,#40938,#40939,#40940,#40941,
#40942,#40943,#40944,#40945,#40946,#40947,#40948,#40949,#40950,#40951,#40952,
#40953,#40954,#40955,#40956,#40957,#40958,#40959,#40960,#40961,#40962,#40963,
#40964,#40965,#40966,#40967,#40968,#40969,#40970,#40971,#40972,#40973,#40974,
#40975,#40976,#40977,#40978,#40979,#40980,#40981,#40982,#40983,#40984,#40985,
#40986,#40987,#40988,#40989,#40990,#40991,#40992,#40993,#40994,#40995,#40996,
#40997,#40998,#40999,#41000,#41001,#41002,#41003,#41004,#41005,#41006,#41007,
#41008,#41009),(#41010,#41011,#41012,#41013,#41014,#41015,#41016,#41017,
#41018,#41019,#41020,#41021,#41022,#41023,#41024,#41025,#41026,#41027,#41028,
#41029,#41030,#41031,#41032,#41033,#41034,#41035,#41036,#41037,#41038,#41039,
#41040,#41041,#41042,#41043,#41044,#41045,#41046,#41047,#41048,#41049,#41050,
#41051,#41052,#41053,#41054,#41055,#41056,#41057,#41058,#41059,#41060,#41061,
#41062,#41063,#41064,#41065,#41066,#41067,#41068,#41069,#41070,#41071,#41072,
#41073,#41074,#41075,#41076,#41077,#41078,#41079,#41080,#41081,#41082,#41083,
#41084,#41085,#41086,#41087,#41088,#41089,#41090,#41091,#41092,#41093,#41094,
#41095)),.UNSPECIFIED.,.F.,.F.,.F.,(4,4),(4,1,1,1,1,1,1,1,1,1,1,1,1,1,1,
1,1,1,1,1,1,1,1,1,1,1,1,1,1,1,1,1,1,1,1,1,1,1,1,1,1,1,1,1,1,1,1,1,1,1,1,
1,1,1,1,1,1,1,1,1,1,1,1,1,1,1,1,1,1,1,1,1,1,1,1,1,1,1,1,1,1,1,1,4),(0.,
0.0448889834294934),(11.8615800042567,12.8591513772396,13.8567227502225,
14.8542941232055,15.8518654961884,16.8494368691713,17.8470082421543,18.8445796151372,
19.8421509881201,20.8397223611031,21.837293734086,22.8348651070689,23.8324364800519,
24.8300078530348,25.8275792260177,26.8251505990007,27.8227219719836,28.8202933449665,
29.8178647179495,30.8154360909324,31.8130074639153,32.8105788368983,33.8081502098812,
34.8057215828641,35.803292955847,36.80086432883,37.7984357018129,38.7960070747959,
39.7935784477788,40.7911498207617,41.7887211937446,42.7862925667276,43.7838639397105,
44.7814353126934,45.7790066856764,46.7765780586593,47.7741494316422,48.7717208046252,
49.7692921776081,50.766863550591,51.764434923574,52.7620062965569,53.7595776695398,
54.7571490425228,55.7547204155057,56.7522917884886,57.7498631614716,58.7474345344545,
59.7450059074374,60.7425772804204,61.7401486534033,62.7377200263862,63.7352913993692,
64.7328627723521,65.730434145335,66.728005518318,67.7255768913009,68.7231482642838,
69.7207196372668,70.7182910102497,71.7158623832326,72.7134337562156,73.7110051291985,
74.7085765021814,75.7061478751644,76.7037192481473,77.7012906211302,78.6988619941132,
79.6964333670961,80.694004740079,81.691576113062,82.6891474860449,83.6867188590278,
84.6842902320108,85.6818616049937,86.6794329779766,87.6770043509595,88.6745757239425,
89.6721470969254,90.6697184699083,91.6672898428913,92.6648612158742,93.6624325888571,
94.6600039618401),.UNSPECIFIED.);
#625=B_SPLINE_SURFACE_WITH_KNOTS('',3,3,((#41203,#41204,#41205,#41206,#41207,
#41208,#41209,#41210,#41211,#41212,#41213,#41214,#41215,#41216,#41217,#41218,
#41219,#41220,#41221,#41222,#41223,#41224,#41225,#41226,#41227,#41228,#41229,
#41230,#41231,#41232,#41233,#41234,#41235,#41236,#41237,#41238,#41239,#41240,
#41241,#41242,#41243,#41244,#41245,#41246,#41247,#41248,#41249,#41250,#41251,
#41252,#41253,#41254,#41255,#41256,#41257,#41258,#41259,#41260,#41261,#41262,
#41263,#41264,#41265,#41266,#41267,#41268,#41269,#41270,#41271,#41272,#41273,
#41274,#41275,#41276,#41277,#41278,#41279,#41280,#41281,#41282,#41283,#41284,
#41285,#41286,#41287,#41288),(#41289,#41290,#41291,#41292,#41293,#41294,
#41295,#41296,#41297,#41298,#41299,#41300,#41301,#41302,#41303,#41304,#41305,
#41306,#41307,#41308,#41309,#41310,#41311,#41312,#41313,#41314,#41315,#41316,
#41317,#41318,#41319,#41320,#41321,#41322,#41323,#41324,#41325,#41326,#41327,
#41328,#41329,#41330,#41331,#41332,#41333,#41334,#41335,#41336,#41337,#41338,
#41339,#41340,#41341,#41342,#41343,#41344,#41345,#41346,#41347,#41348,#41349,
#41350,#41351,#41352,#41353,#41354,#41355,#41356,#41357,#41358,#41359,#41360,
#41361,#41362,#41363,#41364,#41365,#41366,#41367,#41368,#41369,#41370,#41371,
#41372,#41373,#41374),(#41375,#41376,#41377,#41378,#41379,#41380,#41381,
#41382,#41383,#41384,#41385,#41386,#41387,#41388,#41389,#41390,#41391,#41392,
#41393,#41394,#41395,#41396,#41397,#41398,#41399,#41400,#41401,#41402,#41403,
#41404,#41405,#41406,#41407,#41408,#41409,#41410,#41411,#41412,#41413,#41414,
#41415,#41416,#41417,#41418,#41419,#41420,#41421,#41422,#41423,#41424,#41425,
#41426,#41427,#41428,#41429,#41430,#41431,#41432,#41433,#41434,#41435,#41436,
#41437,#41438,#41439,#41440,#41441,#41442,#41443,#41444,#41445,#41446,#41447,
#41448,#41449,#41450,#41451,#41452,#41453,#41454,#41455,#41456,#41457,#41458,
#41459,#41460),(#41461,#41462,#41463,#41464,#41465,#41466,#41467,#41468,
#41469,#41470,#41471,#41472,#41473,#41474,#41475,#41476,#41477,#41478,#41479,
#41480,#41481,#41482,#41483,#41484,#41485,#41486,#41487,#41488,#41489,#41490,
#41491,#41492,#41493,#41494,#41495,#41496,#41497,#41498,#41499,#41500,#41501,
#41502,#41503,#41504,#41505,#41506,#41507,#41508,#41509,#41510,#41511,#41512,
#41513,#41514,#41515,#41516,#41517,#41518,#41519,#41520,#41521,#41522,#41523,
#41524,#41525,#41526,#41527,#41528,#41529,#41530,#41531,#41532,#41533,#41534,
#41535,#41536,#41537,#41538,#41539,#41540,#41541,#41542,#41543,#41544,#41545,
#41546)),.UNSPECIFIED.,.F.,.F.,.F.,(4,4),(4,1,1,1,1,1,1,1,1,1,1,1,1,1,1,
1,1,1,1,1,1,1,1,1,1,1,1,1,1,1,1,1,1,1,1,1,1,1,1,1,1,1,1,1,1,1,1,1,1,1,1,
1,1,1,1,1,1,1,1,1,1,1,1,1,1,1,1,1,1,1,1,1,1,1,1,1,1,1,1,1,1,1,1,4),(0.,
0.0448889834294934),(14.3981410127769,15.3957123857599,16.3932837587428,
17.3908551317257,18.3884265047086,19.3859978776916,20.3835692506745,21.3811406236574,
22.3787119966404,23.3762833696233,24.3738547426062,25.3714261155892,26.3689974885721,
27.366568861555,28.364140234538,29.3617116075209,30.3592829805038,31.3568543534868,
32.3544257264697,33.3519970994526,34.3495684724356,35.3471398454185,36.3447112184014,
37.3422825913844,38.3398539643673,39.3374253373502,40.3349967103332,41.3325680833161,
42.330139456299,43.327710829282,44.3252822022649,45.3228535752478,46.3204249482308,
47.3179963212137,48.3155676941966,49.3131390671796,50.3107104401625,51.3082818131454,
52.3058531861284,53.3034245591113,54.3009959320942,55.2985673050772,56.2961386780601,
57.293710051043,58.291281424026,59.2888527970089,60.2864241699918,61.2839955429748,
62.2815669159577,63.2791382889406,64.2767096619235,65.2742810349065,66.2718524078894,
67.2694237808723,68.2669951538553,69.2645665268382,70.2621378998211,71.2597092728041,
72.257280645787,73.25485201877,74.2524233917529,75.2499947647358,76.2475661377187,
77.2451375107017,78.2427088836846,79.2402802566675,80.2378516296505,81.2354230026334,
82.2329943756163,83.2305657485993,84.2281371215822,85.2257084945651,86.2232798675481,
87.220851240531,88.2184226135139,89.2159939864969,90.2135653594798,91.2111367324627,
92.2087081054457,93.2062794784286,94.2038508514115,95.2014222243945,96.1989935973774,
97.1965649703603),.UNSPECIFIED.);
#626=B_SPLINE_SURFACE_WITH_KNOTS('',3,3,((#41851,#41852,#41853,#41854,#41855,
#41856,#41857,#41858,#41859,#41860,#41861,#41862,#41863,#41864,#41865,#41866,
#41867,#41868,#41869,#41870,#41871,#41872,#41873,#41874,#41875,#41876,#41877,
#41878,#41879,#41880,#41881,#41882,#41883,#41884,#41885,#41886,#41887,#41888,
#41889,#41890,#41891,#41892,#41893,#41894,#41895,#41896,#41897,#41898,#41899,
#41900,#41901,#41902,#41903,#41904,#41905,#41906,#41907,#41908,#41909,#41910,
#41911,#41912,#41913,#41914,#41915,#41916,#41917,#41918,#41919,#41920,#41921,
#41922,#41923,#41924,#41925,#41926,#41927,#41928,#41929,#41930,#41931,#41932,
#41933,#41934,#41935,#41936),(#41937,#41938,#41939,#41940,#41941,#41942,
#41943,#41944,#41945,#41946,#41947,#41948,#41949,#41950,#41951,#41952,#41953,
#41954,#41955,#41956,#41957,#41958,#41959,#41960,#41961,#41962,#41963,#41964,
#41965,#41966,#41967,#41968,#41969,#41970,#41971,#41972,#41973,#41974,#41975,
#41976,#41977,#41978,#41979,#41980,#41981,#41982,#41983,#41984,#41985,#41986,
#41987,#41988,#41989,#41990,#41991,#41992,#41993,#41994,#41995,#41996,#41997,
#41998,#41999,#42000,#42001,#42002,#42003,#42004,#42005,#42006,#42007,#42008,
#42009,#42010,#42011,#42012,#42013,#42014,#42015,#42016,#42017,#42018,#42019,
#42020,#42021,#42022),(#42023,#42024,#42025,#42026,#42027,#42028,#42029,
#42030,#42031,#42032,#42033,#42034,#42035,#42036,#42037,#42038,#42039,#42040,
#42041,#42042,#42043,#42044,#42045,#42046,#42047,#42048,#42049,#42050,#42051,
#42052,#42053,#42054,#42055,#42056,#42057,#42058,#42059,#42060,#42061,#42062,
#42063,#42064,#42065,#42066,#42067,#42068,#42069,#42070,#42071,#42072,#42073,
#42074,#42075,#42076,#42077,#42078,#42079,#42080,#42081,#42082,#42083,#42084,
#42085,#42086,#42087,#42088,#42089,#42090,#42091,#42092,#42093,#42094,#42095,
#42096,#42097,#42098,#42099,#42100,#42101,#42102,#42103,#42104,#42105,#42106,
#42107,#42108),(#42109,#42110,#42111,#42112,#42113,#42114,#42115,#42116,
#42117,#42118,#42119,#42120,#42121,#42122,#42123,#42124,#42125,#42126,#42127,
#42128,#42129,#42130,#42131,#42132,#42133,#42134,#42135,#42136,#42137,#42138,
#42139,#42140,#42141,#42142,#42143,#42144,#42145,#42146,#42147,#42148,#42149,
#42150,#42151,#42152,#42153,#42154,#42155,#42156,#42157,#42158,#42159,#42160,
#42161,#42162,#42163,#42164,#42165,#42166,#42167,#42168,#42169,#42170,#42171,
#42172,#42173,#42174,#42175,#42176,#42177,#42178,#42179,#42180,#42181,#42182,
#42183,#42184,#42185,#42186,#42187,#42188,#42189,#42190,#42191,#42192,#42193,
#42194)),.UNSPECIFIED.,.F.,.F.,.F.,(4,4),(4,1,1,1,1,1,1,1,1,1,1,1,1,1,1,
1,1,1,1,1,1,1,1,1,1,1,1,1,1,1,1,1,1,1,1,1,1,1,1,1,1,1,1,1,1,1,1,1,1,1,1,
1,1,1,1,1,1,1,1,1,1,1,1,1,1,1,1,1,1,1,1,1,1,1,1,1,1,1,1,1,1,1,1,4),(0.,
0.0448889834294934),(11.8615800042567,12.8591513772396,13.8567227502225,
14.8542941232055,15.8518654961884,16.8494368691713,17.8470082421543,18.8445796151372,
19.8421509881201,20.8397223611031,21.837293734086,22.8348651070689,23.8324364800519,
24.8300078530348,25.8275792260177,26.8251505990007,27.8227219719836,28.8202933449665,
29.8178647179495,30.8154360909324,31.8130074639153,32.8105788368983,33.8081502098812,
34.8057215828641,35.8032929558471,36.80086432883,37.7984357018129,38.7960070747959,
39.7935784477788,40.7911498207617,41.7887211937447,42.7862925667276,43.7838639397105,
44.7814353126935,45.7790066856764,46.7765780586593,47.7741494316423,48.7717208046252,
49.7692921776081,50.7668635505911,51.764434923574,52.7620062965569,53.7595776695399,
54.7571490425228,55.7547204155057,56.7522917884886,57.7498631614716,58.7474345344545,
59.7450059074374,60.7425772804204,61.7401486534033,62.7377200263862,63.7352913993692,
64.7328627723521,65.730434145335,66.728005518318,67.7255768913009,68.7231482642838,
69.7207196372668,70.7182910102497,71.7158623832326,72.7134337562156,73.7110051291985,
74.7085765021814,75.7061478751644,76.7037192481473,77.7012906211302,78.6988619941132,
79.6964333670961,80.694004740079,81.691576113062,82.6891474860449,83.6867188590278,
84.6842902320108,85.6818616049937,86.6794329779766,87.6770043509596,88.6745757239425,
89.6721470969254,90.6697184699084,91.6672898428913,92.6648612158742,93.6624325888572,
94.6600039618401),.UNSPECIFIED.);
#627=B_SPLINE_SURFACE_WITH_KNOTS('',3,3,((#42302,#42303,#42304,#42305,#42306,
#42307,#42308,#42309,#42310,#42311,#42312,#42313,#42314,#42315,#42316,#42317,
#42318,#42319,#42320,#42321,#42322,#42323,#42324,#42325,#42326,#42327,#42328,
#42329,#42330,#42331,#42332,#42333,#42334,#42335,#42336,#42337,#42338,#42339,
#42340,#42341,#42342,#42343,#42344,#42345,#42346,#42347,#42348,#42349,#42350,
#42351,#42352,#42353,#42354,#42355,#42356,#42357,#42358,#42359,#42360,#42361,
#42362,#42363,#42364,#42365,#42366,#42367,#42368,#42369,#42370,#42371,#42372,
#42373,#42374,#42375,#42376,#42377,#42378,#42379,#42380,#42381,#42382,#42383,
#42384,#42385,#42386,#42387),(#42388,#42389,#42390,#42391,#42392,#42393,
#42394,#42395,#42396,#42397,#42398,#42399,#42400,#42401,#42402,#42403,#42404,
#42405,#42406,#42407,#42408,#42409,#42410,#42411,#42412,#42413,#42414,#42415,
#42416,#42417,#42418,#42419,#42420,#42421,#42422,#42423,#42424,#42425,#42426,
#42427,#42428,#42429,#42430,#42431,#42432,#42433,#42434,#42435,#42436,#42437,
#42438,#42439,#42440,#42441,#42442,#42443,#42444,#42445,#42446,#42447,#42448,
#42449,#42450,#42451,#42452,#42453,#42454,#42455,#42456,#42457,#42458,#42459,
#42460,#42461,#42462,#42463,#42464,#42465,#42466,#42467,#42468,#42469,#42470,
#42471,#42472,#42473),(#42474,#42475,#42476,#42477,#42478,#42479,#42480,
#42481,#42482,#42483,#42484,#42485,#42486,#42487,#42488,#42489,#42490,#42491,
#42492,#42493,#42494,#42495,#42496,#42497,#42498,#42499,#42500,#42501,#42502,
#42503,#42504,#42505,#42506,#42507,#42508,#42509,#42510,#42511,#42512,#42513,
#42514,#42515,#42516,#42517,#42518,#42519,#42520,#42521,#42522,#42523,#42524,
#42525,#42526,#42527,#42528,#42529,#42530,#42531,#42532,#42533,#42534,#42535,
#42536,#42537,#42538,#42539,#42540,#42541,#42542,#42543,#42544,#42545,#42546,
#42547,#42548,#42549,#42550,#42551,#42552,#42553,#42554,#42555,#42556,#42557,
#42558,#42559),(#42560,#42561,#42562,#42563,#42564,#42565,#42566,#42567,
#42568,#42569,#42570,#42571,#42572,#42573,#42574,#42575,#42576,#42577,#42578,
#42579,#42580,#42581,#42582,#42583,#42584,#42585,#42586,#42587,#42588,#42589,
#42590,#42591,#42592,#42593,#42594,#42595,#42596,#42597,#42598,#42599,#42600,
#42601,#42602,#42603,#42604,#42605,#42606,#42607,#42608,#42609,#42610,#42611,
#42612,#42613,#42614,#42615,#42616,#42617,#42618,#42619,#42620,#42621,#42622,
#42623,#42624,#42625,#42626,#42627,#42628,#42629,#42630,#42631,#42632,#42633,
#42634,#42635,#42636,#42637,#42638,#42639,#42640,#42641,#42642,#42643,#42644,
#42645)),.UNSPECIFIED.,.F.,.F.,.F.,(4,4),(4,1,1,1,1,1,1,1,1,1,1,1,1,1,1,
1,1,1,1,1,1,1,1,1,1,1,1,1,1,1,1,1,1,1,1,1,1,1,1,1,1,1,1,1,1,1,1,1,1,1,1,
1,1,1,1,1,1,1,1,1,1,1,1,1,1,1,1,1,1,1,1,1,1,1,1,1,1,1,1,1,1,1,1,4),(0.,
0.0448889834294934),(14.3981410127769,15.3957123857599,16.3932837587428,
17.3908551317257,18.3884265047087,19.3859978776916,20.3835692506745,21.3811406236575,
22.3787119966404,23.3762833696233,24.3738547426063,25.3714261155892,26.3689974885721,
27.3665688615551,28.364140234538,29.3617116075209,30.3592829805038,31.3568543534868,
32.3544257264697,33.3519970994526,34.3495684724356,35.3471398454185,36.3447112184014,
37.3422825913844,38.3398539643673,39.3374253373502,40.3349967103332,41.3325680833161,
42.330139456299,43.327710829282,44.3252822022649,45.3228535752478,46.3204249482308,
47.3179963212137,48.3155676941966,49.3131390671796,50.3107104401625,51.3082818131454,
52.3058531861284,53.3034245591113,54.3009959320942,55.2985673050772,56.2961386780601,
57.293710051043,58.291281424026,59.2888527970089,60.2864241699918,61.2839955429748,
62.2815669159577,63.2791382889406,64.2767096619236,65.2742810349065,66.2718524078894,
67.2694237808724,68.2669951538553,69.2645665268382,70.2621378998212,71.2597092728041,
72.257280645787,73.25485201877,74.2524233917529,75.2499947647358,76.2475661377187,
77.2451375107017,78.2427088836846,79.2402802566675,80.2378516296505,81.2354230026334,
82.2329943756163,83.2305657485993,84.2281371215822,85.2257084945651,86.2232798675481,
87.220851240531,88.2184226135139,89.2159939864969,90.2135653594798,91.2111367324627,
92.2087081054457,93.2062794784286,94.2038508514115,95.2014222243945,96.1989935973774,
97.1965649703603),.UNSPECIFIED.);
#628=B_SPLINE_SURFACE_WITH_KNOTS('',3,3,((#42950,#42951,#42952,#42953,#42954,
#42955,#42956,#42957,#42958,#42959,#42960,#42961,#42962,#42963,#42964,#42965,
#42966,#42967,#42968,#42969,#42970,#42971,#42972,#42973,#42974,#42975,#42976,
#42977,#42978,#42979,#42980,#42981,#42982,#42983,#42984,#42985,#42986,#42987,
#42988,#42989,#42990,#42991,#42992,#42993,#42994,#42995,#42996,#42997,#42998,
#42999,#43000,#43001,#43002,#43003,#43004,#43005,#43006,#43007,#43008,#43009,
#43010,#43011,#43012,#43013,#43014,#43015,#43016,#43017,#43018,#43019,#43020,
#43021,#43022,#43023,#43024,#43025,#43026,#43027,#43028,#43029,#43030,#43031,
#43032,#43033,#43034,#43035),(#43036,#43037,#43038,#43039,#43040,#43041,
#43042,#43043,#43044,#43045,#43046,#43047,#43048,#43049,#43050,#43051,#43052,
#43053,#43054,#43055,#43056,#43057,#43058,#43059,#43060,#43061,#43062,#43063,
#43064,#43065,#43066,#43067,#43068,#43069,#43070,#43071,#43072,#43073,#43074,
#43075,#43076,#43077,#43078,#43079,#43080,#43081,#43082,#43083,#43084,#43085,
#43086,#43087,#43088,#43089,#43090,#43091,#43092,#43093,#43094,#43095,#43096,
#43097,#43098,#43099,#43100,#43101,#43102,#43103,#43104,#43105,#43106,#43107,
#43108,#43109,#43110,#43111,#43112,#43113,#43114,#43115,#43116,#43117,#43118,
#43119,#43120,#43121),(#43122,#43123,#43124,#43125,#43126,#43127,#43128,
#43129,#43130,#43131,#43132,#43133,#43134,#43135,#43136,#43137,#43138,#43139,
#43140,#43141,#43142,#43143,#43144,#43145,#43146,#43147,#43148,#43149,#43150,
#43151,#43152,#43153,#43154,#43155,#43156,#43157,#43158,#43159,#43160,#43161,
#43162,#43163,#43164,#43165,#43166,#43167,#43168,#43169,#43170,#43171,#43172,
#43173,#43174,#43175,#43176,#43177,#43178,#43179,#43180,#43181,#43182,#43183,
#43184,#43185,#43186,#43187,#43188,#43189,#43190,#43191,#43192,#43193,#43194,
#43195,#43196,#43197,#43198,#43199,#43200,#43201,#43202,#43203,#43204,#43205,
#43206,#43207),(#43208,#43209,#43210,#43211,#43212,#43213,#43214,#43215,
#43216,#43217,#43218,#43219,#43220,#43221,#43222,#43223,#43224,#43225,#43226,
#43227,#43228,#43229,#43230,#43231,#43232,#43233,#43234,#43235,#43236,#43237,
#43238,#43239,#43240,#43241,#43242,#43243,#43244,#43245,#43246,#43247,#43248,
#43249,#43250,#43251,#43252,#43253,#43254,#43255,#43256,#43257,#43258,#43259,
#43260,#43261,#43262,#43263,#43264,#43265,#43266,#43267,#43268,#43269,#43270,
#43271,#43272,#43273,#43274,#43275,#43276,#43277,#43278,#43279,#43280,#43281,
#43282,#43283,#43284,#43285,#43286,#43287,#43288,#43289,#43290,#43291,#43292,
#43293)),.UNSPECIFIED.,.F.,.F.,.F.,(4,4),(4,1,1,1,1,1,1,1,1,1,1,1,1,1,1,
1,1,1,1,1,1,1,1,1,1,1,1,1,1,1,1,1,1,1,1,1,1,1,1,1,1,1,1,1,1,1,1,1,1,1,1,
1,1,1,1,1,1,1,1,1,1,1,1,1,1,1,1,1,1,1,1,1,1,1,1,1,1,1,1,1,1,1,1,4),(0.,
0.0448889834294934),(11.8615800042567,12.8591513772396,13.8567227502225,
14.8542941232055,15.8518654961884,16.8494368691713,17.8470082421543,18.8445796151372,
19.8421509881201,20.8397223611031,21.837293734086,22.8348651070689,23.8324364800519,
24.8300078530348,25.8275792260177,26.8251505990007,27.8227219719836,28.8202933449665,
29.8178647179495,30.8154360909324,31.8130074639153,32.8105788368983,33.8081502098812,
34.8057215828641,35.8032929558471,36.80086432883,37.7984357018129,38.7960070747959,
39.7935784477788,40.7911498207617,41.7887211937447,42.7862925667276,43.7838639397105,
44.7814353126935,45.7790066856764,46.7765780586593,47.7741494316423,48.7717208046252,
49.7692921776081,50.7668635505911,51.764434923574,52.7620062965569,53.7595776695399,
54.7571490425228,55.7547204155057,56.7522917884886,57.7498631614716,58.7474345344545,
59.7450059074374,60.7425772804204,61.7401486534033,62.7377200263862,63.7352913993692,
64.7328627723521,65.730434145335,66.728005518318,67.7255768913009,68.7231482642838,
69.7207196372668,70.7182910102497,71.7158623832326,72.7134337562156,73.7110051291985,
74.7085765021814,75.7061478751644,76.7037192481473,77.7012906211302,78.6988619941132,
79.6964333670961,80.694004740079,81.691576113062,82.6891474860449,83.6867188590278,
84.6842902320108,85.6818616049937,86.6794329779766,87.6770043509596,88.6745757239425,
89.6721470969254,90.6697184699084,91.6672898428913,92.6648612158742,93.6624325888572,
94.6600039618401),.UNSPECIFIED.);
#629=B_SPLINE_SURFACE_WITH_KNOTS('',3,3,((#43401,#43402,#43403,#43404,#43405,
#43406,#43407,#43408,#43409,#43410,#43411,#43412,#43413,#43414,#43415,#43416,
#43417,#43418,#43419,#43420,#43421,#43422,#43423,#43424,#43425,#43426,#43427,
#43428,#43429,#43430,#43431,#43432,#43433,#43434,#43435,#43436,#43437,#43438,
#43439,#43440,#43441,#43442,#43443,#43444,#43445,#43446,#43447,#43448,#43449,
#43450,#43451,#43452,#43453,#43454,#43455,#43456,#43457,#43458,#43459,#43460,
#43461,#43462,#43463,#43464,#43465,#43466,#43467,#43468,#43469,#43470,#43471,
#43472,#43473,#43474,#43475,#43476,#43477,#43478,#43479,#43480,#43481,#43482,
#43483,#43484,#43485,#43486),(#43487,#43488,#43489,#43490,#43491,#43492,
#43493,#43494,#43495,#43496,#43497,#43498,#43499,#43500,#43501,#43502,#43503,
#43504,#43505,#43506,#43507,#43508,#43509,#43510,#43511,#43512,#43513,#43514,
#43515,#43516,#43517,#43518,#43519,#43520,#43521,#43522,#43523,#43524,#43525,
#43526,#43527,#43528,#43529,#43530,#43531,#43532,#43533,#43534,#43535,#43536,
#43537,#43538,#43539,#43540,#43541,#43542,#43543,#43544,#43545,#43546,#43547,
#43548,#43549,#43550,#43551,#43552,#43553,#43554,#43555,#43556,#43557,#43558,
#43559,#43560,#43561,#43562,#43563,#43564,#43565,#43566,#43567,#43568,#43569,
#43570,#43571,#43572),(#43573,#43574,#43575,#43576,#43577,#43578,#43579,
#43580,#43581,#43582,#43583,#43584,#43585,#43586,#43587,#43588,#43589,#43590,
#43591,#43592,#43593,#43594,#43595,#43596,#43597,#43598,#43599,#43600,#43601,
#43602,#43603,#43604,#43605,#43606,#43607,#43608,#43609,#43610,#43611,#43612,
#43613,#43614,#43615,#43616,#43617,#43618,#43619,#43620,#43621,#43622,#43623,
#43624,#43625,#43626,#43627,#43628,#43629,#43630,#43631,#43632,#43633,#43634,
#43635,#43636,#43637,#43638,#43639,#43640,#43641,#43642,#43643,#43644,#43645,
#43646,#43647,#43648,#43649,#43650,#43651,#43652,#43653,#43654,#43655,#43656,
#43657,#43658),(#43659,#43660,#43661,#43662,#43663,#43664,#43665,#43666,
#43667,#43668,#43669,#43670,#43671,#43672,#43673,#43674,#43675,#43676,#43677,
#43678,#43679,#43680,#43681,#43682,#43683,#43684,#43685,#43686,#43687,#43688,
#43689,#43690,#43691,#43692,#43693,#43694,#43695,#43696,#43697,#43698,#43699,
#43700,#43701,#43702,#43703,#43704,#43705,#43706,#43707,#43708,#43709,#43710,
#43711,#43712,#43713,#43714,#43715,#43716,#43717,#43718,#43719,#43720,#43721,
#43722,#43723,#43724,#43725,#43726,#43727,#43728,#43729,#43730,#43731,#43732,
#43733,#43734,#43735,#43736,#43737,#43738,#43739,#43740,#43741,#43742,#43743,
#43744)),.UNSPECIFIED.,.F.,.F.,.F.,(4,4),(4,1,1,1,1,1,1,1,1,1,1,1,1,1,1,
1,1,1,1,1,1,1,1,1,1,1,1,1,1,1,1,1,1,1,1,1,1,1,1,1,1,1,1,1,1,1,1,1,1,1,1,
1,1,1,1,1,1,1,1,1,1,1,1,1,1,1,1,1,1,1,1,1,1,1,1,1,1,1,1,1,1,1,1,4),(0.,
0.0448889834294934),(14.3981410127769,15.3957123857599,16.3932837587428,
17.3908551317257,18.3884265047087,19.3859978776916,20.3835692506745,21.3811406236575,
22.3787119966404,23.3762833696233,24.3738547426063,25.3714261155892,26.3689974885721,
27.3665688615551,28.364140234538,29.3617116075209,30.3592829805038,31.3568543534868,
32.3544257264697,33.3519970994526,34.3495684724356,35.3471398454185,36.3447112184014,
37.3422825913844,38.3398539643673,39.3374253373502,40.3349967103332,41.3325680833161,
42.330139456299,43.327710829282,44.3252822022649,45.3228535752478,46.3204249482308,
47.3179963212137,48.3155676941966,49.3131390671796,50.3107104401625,51.3082818131454,
52.3058531861284,53.3034245591113,54.3009959320942,55.2985673050772,56.2961386780601,
57.293710051043,58.291281424026,59.2888527970089,60.2864241699918,61.2839955429748,
62.2815669159577,63.2791382889406,64.2767096619236,65.2742810349065,66.2718524078894,
67.2694237808724,68.2669951538553,69.2645665268382,70.2621378998212,71.2597092728041,
72.257280645787,73.25485201877,74.2524233917529,75.2499947647358,76.2475661377187,
77.2451375107017,78.2427088836846,79.2402802566675,80.2378516296505,81.2354230026334,
82.2329943756163,83.2305657485993,84.2281371215822,85.2257084945651,86.2232798675481,
87.220851240531,88.2184226135139,89.2159939864969,90.2135653594798,91.2111367324627,
92.2087081054457,93.2062794784286,94.2038508514115,95.2014222243945,96.1989935973774,
97.1965649703603),.UNSPECIFIED.);
#630=B_SPLINE_SURFACE_WITH_KNOTS('',3,3,((#44049,#44050,#44051,#44052,#44053,
#44054,#44055,#44056,#44057,#44058,#44059,#44060,#44061,#44062,#44063,#44064,
#44065,#44066,#44067,#44068,#44069,#44070,#44071,#44072,#44073,#44074,#44075,
#44076,#44077,#44078,#44079,#44080,#44081,#44082,#44083,#44084,#44085,#44086,
#44087,#44088,#44089,#44090,#44091,#44092,#44093,#44094,#44095,#44096,#44097,
#44098,#44099,#44100,#44101,#44102,#44103,#44104,#44105,#44106,#44107,#44108,
#44109,#44110,#44111,#44112,#44113,#44114,#44115,#44116,#44117,#44118,#44119,
#44120,#44121,#44122,#44123,#44124,#44125,#44126,#44127,#44128,#44129,#44130,
#44131,#44132,#44133,#44134),(#44135,#44136,#44137,#44138,#44139,#44140,
#44141,#44142,#44143,#44144,#44145,#44146,#44147,#44148,#44149,#44150,#44151,
#44152,#44153,#44154,#44155,#44156,#44157,#44158,#44159,#44160,#44161,#44162,
#44163,#44164,#44165,#44166,#44167,#44168,#44169,#44170,#44171,#44172,#44173,
#44174,#44175,#44176,#44177,#44178,#44179,#44180,#44181,#44182,#44183,#44184,
#44185,#44186,#44187,#44188,#44189,#44190,#44191,#44192,#44193,#44194,#44195,
#44196,#44197,#44198,#44199,#44200,#44201,#44202,#44203,#44204,#44205,#44206,
#44207,#44208,#44209,#44210,#44211,#44212,#44213,#44214,#44215,#44216,#44217,
#44218,#44219,#44220),(#44221,#44222,#44223,#44224,#44225,#44226,#44227,
#44228,#44229,#44230,#44231,#44232,#44233,#44234,#44235,#44236,#44237,#44238,
#44239,#44240,#44241,#44242,#44243,#44244,#44245,#44246,#44247,#44248,#44249,
#44250,#44251,#44252,#44253,#44254,#44255,#44256,#44257,#44258,#44259,#44260,
#44261,#44262,#44263,#44264,#44265,#44266,#44267,#44268,#44269,#44270,#44271,
#44272,#44273,#44274,#44275,#44276,#44277,#44278,#44279,#44280,#44281,#44282,
#44283,#44284,#44285,#44286,#44287,#44288,#44289,#44290,#44291,#44292,#44293,
#44294,#44295,#44296,#44297,#44298,#44299,#44300,#44301,#44302,#44303,#44304,
#44305,#44306),(#44307,#44308,#44309,#44310,#44311,#44312,#44313,#44314,
#44315,#44316,#44317,#44318,#44319,#44320,#44321,#44322,#44323,#44324,#44325,
#44326,#44327,#44328,#44329,#44330,#44331,#44332,#44333,#44334,#44335,#44336,
#44337,#44338,#44339,#44340,#44341,#44342,#44343,#44344,#44345,#44346,#44347,
#44348,#44349,#44350,#44351,#44352,#44353,#44354,#44355,#44356,#44357,#44358,
#44359,#44360,#44361,#44362,#44363,#44364,#44365,#44366,#44367,#44368,#44369,
#44370,#44371,#44372,#44373,#44374,#44375,#44376,#44377,#44378,#44379,#44380,
#44381,#44382,#44383,#44384,#44385,#44386,#44387,#44388,#44389,#44390,#44391,
#44392)),.UNSPECIFIED.,.F.,.F.,.F.,(4,4),(4,1,1,1,1,1,1,1,1,1,1,1,1,1,1,
1,1,1,1,1,1,1,1,1,1,1,1,1,1,1,1,1,1,1,1,1,1,1,1,1,1,1,1,1,1,1,1,1,1,1,1,
1,1,1,1,1,1,1,1,1,1,1,1,1,1,1,1,1,1,1,1,1,1,1,1,1,1,1,1,1,1,1,1,4),(0.,
0.0448889834294934),(11.8615800042567,12.8591513772396,13.8567227502225,
14.8542941232055,15.8518654961884,16.8494368691713,17.8470082421543,18.8445796151372,
19.8421509881201,20.8397223611031,21.837293734086,22.8348651070689,23.8324364800519,
24.8300078530348,25.8275792260177,26.8251505990007,27.8227219719836,28.8202933449665,
29.8178647179495,30.8154360909324,31.8130074639153,32.8105788368983,33.8081502098812,
34.8057215828641,35.8032929558471,36.80086432883,37.7984357018129,38.7960070747959,
39.7935784477788,40.7911498207617,41.7887211937447,42.7862925667276,43.7838639397105,
44.7814353126935,45.7790066856764,46.7765780586593,47.7741494316423,48.7717208046252,
49.7692921776081,50.7668635505911,51.764434923574,52.7620062965569,53.7595776695399,
54.7571490425228,55.7547204155057,56.7522917884886,57.7498631614716,58.7474345344545,
59.7450059074374,60.7425772804204,61.7401486534033,62.7377200263862,63.7352913993692,
64.7328627723521,65.7304341453351,66.728005518318,67.7255768913009,68.7231482642839,
69.7207196372668,70.7182910102497,71.7158623832326,72.7134337562156,73.7110051291985,
74.7085765021814,75.7061478751644,76.7037192481473,77.7012906211302,78.6988619941132,
79.6964333670961,80.694004740079,81.691576113062,82.6891474860449,83.6867188590278,
84.6842902320108,85.6818616049937,86.6794329779766,87.6770043509596,88.6745757239425,
89.6721470969254,90.6697184699084,91.6672898428913,92.6648612158742,93.6624325888572,
94.6600039618401),.UNSPECIFIED.);
#631=B_SPLINE_SURFACE_WITH_KNOTS('',3,3,((#44500,#44501,#44502,#44503,#44504,
#44505,#44506,#44507,#44508,#44509,#44510,#44511,#44512,#44513,#44514,#44515,
#44516,#44517,#44518,#44519,#44520,#44521,#44522,#44523,#44524,#44525,#44526,
#44527,#44528,#44529,#44530,#44531,#44532,#44533,#44534,#44535,#44536,#44537,
#44538,#44539,#44540,#44541,#44542,#44543,#44544,#44545,#44546,#44547,#44548,
#44549,#44550,#44551,#44552,#44553,#44554,#44555,#44556,#44557,#44558,#44559,
#44560,#44561,#44562,#44563,#44564,#44565,#44566,#44567,#44568,#44569,#44570,
#44571,#44572,#44573,#44574,#44575,#44576,#44577,#44578,#44579,#44580,#44581,
#44582,#44583,#44584,#44585),(#44586,#44587,#44588,#44589,#44590,#44591,
#44592,#44593,#44594,#44595,#44596,#44597,#44598,#44599,#44600,#44601,#44602,
#44603,#44604,#44605,#44606,#44607,#44608,#44609,#44610,#44611,#44612,#44613,
#44614,#44615,#44616,#44617,#44618,#44619,#44620,#44621,#44622,#44623,#44624,
#44625,#44626,#44627,#44628,#44629,#44630,#44631,#44632,#44633,#44634,#44635,
#44636,#44637,#44638,#44639,#44640,#44641,#44642,#44643,#44644,#44645,#44646,
#44647,#44648,#44649,#44650,#44651,#44652,#44653,#44654,#44655,#44656,#44657,
#44658,#44659,#44660,#44661,#44662,#44663,#44664,#44665,#44666,#44667,#44668,
#44669,#44670,#44671),(#44672,#44673,#44674,#44675,#44676,#44677,#44678,
#44679,#44680,#44681,#44682,#44683,#44684,#44685,#44686,#44687,#44688,#44689,
#44690,#44691,#44692,#44693,#44694,#44695,#44696,#44697,#44698,#44699,#44700,
#44701,#44702,#44703,#44704,#44705,#44706,#44707,#44708,#44709,#44710,#44711,
#44712,#44713,#44714,#44715,#44716,#44717,#44718,#44719,#44720,#44721,#44722,
#44723,#44724,#44725,#44726,#44727,#44728,#44729,#44730,#44731,#44732,#44733,
#44734,#44735,#44736,#44737,#44738,#44739,#44740,#44741,#44742,#44743,#44744,
#44745,#44746,#44747,#44748,#44749,#44750,#44751,#44752,#44753,#44754,#44755,
#44756,#44757),(#44758,#44759,#44760,#44761,#44762,#44763,#44764,#44765,
#44766,#44767,#44768,#44769,#44770,#44771,#44772,#44773,#44774,#44775,#44776,
#44777,#44778,#44779,#44780,#44781,#44782,#44783,#44784,#44785,#44786,#44787,
#44788,#44789,#44790,#44791,#44792,#44793,#44794,#44795,#44796,#44797,#44798,
#44799,#44800,#44801,#44802,#44803,#44804,#44805,#44806,#44807,#44808,#44809,
#44810,#44811,#44812,#44813,#44814,#44815,#44816,#44817,#44818,#44819,#44820,
#44821,#44822,#44823,#44824,#44825,#44826,#44827,#44828,#44829,#44830,#44831,
#44832,#44833,#44834,#44835,#44836,#44837,#44838,#44839,#44840,#44841,#44842,
#44843)),.UNSPECIFIED.,.F.,.F.,.F.,(4,4),(4,1,1,1,1,1,1,1,1,1,1,1,1,1,1,
1,1,1,1,1,1,1,1,1,1,1,1,1,1,1,1,1,1,1,1,1,1,1,1,1,1,1,1,1,1,1,1,1,1,1,1,
1,1,1,1,1,1,1,1,1,1,1,1,1,1,1,1,1,1,1,1,1,1,1,1,1,1,1,1,1,1,1,1,4),(0.,
0.0448889834294934),(14.3981410127769,15.3957123857599,16.3932837587428,
17.3908551317257,18.3884265047087,19.3859978776916,20.3835692506745,21.3811406236575,
22.3787119966404,23.3762833696233,24.3738547426063,25.3714261155892,26.3689974885721,
27.3665688615551,28.364140234538,29.3617116075209,30.3592829805038,31.3568543534868,
32.3544257264697,33.3519970994526,34.3495684724356,35.3471398454185,36.3447112184014,
37.3422825913844,38.3398539643673,39.3374253373502,40.3349967103332,41.3325680833161,
42.330139456299,43.327710829282,44.3252822022649,45.3228535752478,46.3204249482308,
47.3179963212137,48.3155676941966,49.3131390671796,50.3107104401625,51.3082818131454,
52.3058531861284,53.3034245591113,54.3009959320942,55.2985673050772,56.2961386780601,
57.293710051043,58.291281424026,59.2888527970089,60.2864241699918,61.2839955429748,
62.2815669159577,63.2791382889406,64.2767096619236,65.2742810349065,66.2718524078894,
67.2694237808724,68.2669951538553,69.2645665268382,70.2621378998212,71.2597092728041,
72.257280645787,73.25485201877,74.2524233917529,75.2499947647358,76.2475661377187,
77.2451375107017,78.2427088836846,79.2402802566675,80.2378516296505,81.2354230026334,
82.2329943756163,83.2305657485993,84.2281371215822,85.2257084945651,86.2232798675481,
87.220851240531,88.2184226135139,89.2159939864969,90.2135653594798,91.2111367324627,
92.2087081054457,93.2062794784286,94.2038508514115,95.2014222243945,96.1989935973774,
97.1965649703603),.UNSPECIFIED.);
#632=B_SPLINE_SURFACE_WITH_KNOTS('',3,3,((#45153,#45154,#45155,#45156,#45157,
#45158,#45159,#45160,#45161,#45162,#45163,#45164,#45165,#45166,#45167,#45168,
#45169,#45170,#45171,#45172,#45173,#45174,#45175,#45176,#45177,#45178,#45179,
#45180,#45181,#45182,#45183,#45184,#45185,#45186,#45187,#45188,#45189,#45190,
#45191,#45192,#45193,#45194,#45195,#45196,#45197,#45198,#45199,#45200,#45201,
#45202,#45203,#45204,#45205,#45206,#45207,#45208,#45209,#45210,#45211,#45212,
#45213,#45214,#45215,#45216,#45217,#45218,#45219,#45220,#45221,#45222,#45223,
#45224,#45225,#45226,#45227,#45228,#45229,#45230,#45231,#45232,#45233,#45234,
#45235,#45236,#45237,#45238),(#45239,#45240,#45241,#45242,#45243,#45244,
#45245,#45246,#45247,#45248,#45249,#45250,#45251,#45252,#45253,#45254,#45255,
#45256,#45257,#45258,#45259,#45260,#45261,#45262,#45263,#45264,#45265,#45266,
#45267,#45268,#45269,#45270,#45271,#45272,#45273,#45274,#45275,#45276,#45277,
#45278,#45279,#45280,#45281,#45282,#45283,#45284,#45285,#45286,#45287,#45288,
#45289,#45290,#45291,#45292,#45293,#45294,#45295,#45296,#45297,#45298,#45299,
#45300,#45301,#45302,#45303,#45304,#45305,#45306,#45307,#45308,#45309,#45310,
#45311,#45312,#45313,#45314,#45315,#45316,#45317,#45318,#45319,#45320,#45321,
#45322,#45323,#45324),(#45325,#45326,#45327,#45328,#45329,#45330,#45331,
#45332,#45333,#45334,#45335,#45336,#45337,#45338,#45339,#45340,#45341,#45342,
#45343,#45344,#45345,#45346,#45347,#45348,#45349,#45350,#45351,#45352,#45353,
#45354,#45355,#45356,#45357,#45358,#45359,#45360,#45361,#45362,#45363,#45364,
#45365,#45366,#45367,#45368,#45369,#45370,#45371,#45372,#45373,#45374,#45375,
#45376,#45377,#45378,#45379,#45380,#45381,#45382,#45383,#45384,#45385,#45386,
#45387,#45388,#45389,#45390,#45391,#45392,#45393,#45394,#45395,#45396,#45397,
#45398,#45399,#45400,#45401,#45402,#45403,#45404,#45405,#45406,#45407,#45408,
#45409,#45410),(#45411,#45412,#45413,#45414,#45415,#45416,#45417,#45418,
#45419,#45420,#45421,#45422,#45423,#45424,#45425,#45426,#45427,#45428,#45429,
#45430,#45431,#45432,#45433,#45434,#45435,#45436,#45437,#45438,#45439,#45440,
#45441,#45442,#45443,#45444,#45445,#45446,#45447,#45448,#45449,#45450,#45451,
#45452,#45453,#45454,#45455,#45456,#45457,#45458,#45459,#45460,#45461,#45462,
#45463,#45464,#45465,#45466,#45467,#45468,#45469,#45470,#45471,#45472,#45473,
#45474,#45475,#45476,#45477,#45478,#45479,#45480,#45481,#45482,#45483,#45484,
#45485,#45486,#45487,#45488,#45489,#45490,#45491,#45492,#45493,#45494,#45495,
#45496)),.UNSPECIFIED.,.F.,.F.,.F.,(4,4),(4,1,1,1,1,1,1,1,1,1,1,1,1,1,1,
1,1,1,1,1,1,1,1,1,1,1,1,1,1,1,1,1,1,1,1,1,1,1,1,1,1,1,1,1,1,1,1,1,1,1,1,
1,1,1,1,1,1,1,1,1,1,1,1,1,1,1,1,1,1,1,1,1,1,1,1,1,1,1,1,1,1,1,1,4),(0.,
0.0448889834294934),(11.8615800042566,12.8591513772395,13.8567227502225,
14.8542941232054,15.8518654961883,16.8494368691713,17.8470082421542,18.8445796151371,
19.8421509881201,20.839722361103,21.8372937340859,22.8348651070689,23.8324364800518,
24.8300078530347,25.8275792260177,26.8251505990006,27.8227219719835,28.8202933449665,
29.8178647179494,30.8154360909323,31.8130074639152,32.8105788368982,33.8081502098811,
34.805721582864,35.803292955847,36.8008643288299,37.7984357018128,38.7960070747958,
39.7935784477787,40.7911498207616,41.7887211937446,42.7862925667275,43.7838639397104,
44.7814353126934,45.7790066856763,46.7765780586592,47.7741494316422,48.7717208046251,
49.769292177608,50.766863550591,51.7644349235739,52.7620062965568,53.7595776695398,
54.7571490425227,55.7547204155056,56.7522917884886,57.7498631614715,58.7474345344544,
59.7450059074374,60.7425772804203,61.7401486534032,62.7377200263862,63.7352913993691,
64.732862772352,65.730434145335,66.7280055183179,67.7255768913008,68.7231482642838,
69.7207196372667,70.7182910102496,71.7158623832325,72.7134337562155,73.7110051291984,
74.7085765021813,75.7061478751643,76.7037192481472,77.7012906211301,78.6988619941131,
79.696433367096,80.6940047400789,81.6915761130619,82.6891474860448,83.6867188590277,
84.6842902320107,85.6818616049936,86.6794329779765,87.6770043509595,88.6745757239424,
89.6721470969253,90.6697184699083,91.6672898428912,92.6648612158741,93.6624325888571,
94.66000396184),.UNSPECIFIED.);
#633=B_SPLINE_SURFACE_WITH_KNOTS('',3,3,((#45604,#45605,#45606,#45607,#45608,
#45609,#45610,#45611,#45612,#45613,#45614,#45615,#45616,#45617,#45618,#45619,
#45620,#45621,#45622,#45623,#45624,#45625,#45626,#45627,#45628,#45629,#45630,
#45631,#45632,#45633,#45634,#45635,#45636,#45637,#45638,#45639,#45640,#45641,
#45642,#45643,#45644,#45645,#45646,#45647,#45648,#45649,#45650,#45651,#45652,
#45653,#45654,#45655,#45656,#45657,#45658,#45659,#45660,#45661,#45662,#45663,
#45664,#45665,#45666,#45667,#45668,#45669,#45670,#45671,#45672,#45673,#45674,
#45675,#45676,#45677,#45678,#45679,#45680,#45681,#45682,#45683,#45684,#45685,
#45686,#45687,#45688,#45689),(#45690,#45691,#45692,#45693,#45694,#45695,
#45696,#45697,#45698,#45699,#45700,#45701,#45702,#45703,#45704,#45705,#45706,
#45707,#45708,#45709,#45710,#45711,#45712,#45713,#45714,#45715,#45716,#45717,
#45718,#45719,#45720,#45721,#45722,#45723,#45724,#45725,#45726,#45727,#45728,
#45729,#45730,#45731,#45732,#45733,#45734,#45735,#45736,#45737,#45738,#45739,
#45740,#45741,#45742,#45743,#45744,#45745,#45746,#45747,#45748,#45749,#45750,
#45751,#45752,#45753,#45754,#45755,#45756,#45757,#45758,#45759,#45760,#45761,
#45762,#45763,#45764,#45765,#45766,#45767,#45768,#45769,#45770,#45771,#45772,
#45773,#45774,#45775),(#45776,#45777,#45778,#45779,#45780,#45781,#45782,
#45783,#45784,#45785,#45786,#45787,#45788,#45789,#45790,#45791,#45792,#45793,
#45794,#45795,#45796,#45797,#45798,#45799,#45800,#45801,#45802,#45803,#45804,
#45805,#45806,#45807,#45808,#45809,#45810,#45811,#45812,#45813,#45814,#45815,
#45816,#45817,#45818,#45819,#45820,#45821,#45822,#45823,#45824,#45825,#45826,
#45827,#45828,#45829,#45830,#45831,#45832,#45833,#45834,#45835,#45836,#45837,
#45838,#45839,#45840,#45841,#45842,#45843,#45844,#45845,#45846,#45847,#45848,
#45849,#45850,#45851,#45852,#45853,#45854,#45855,#45856,#45857,#45858,#45859,
#45860,#45861),(#45862,#45863,#45864,#45865,#45866,#45867,#45868,#45869,
#45870,#45871,#45872,#45873,#45874,#45875,#45876,#45877,#45878,#45879,#45880,
#45881,#45882,#45883,#45884,#45885,#45886,#45887,#45888,#45889,#45890,#45891,
#45892,#45893,#45894,#45895,#45896,#45897,#45898,#45899,#45900,#45901,#45902,
#45903,#45904,#45905,#45906,#45907,#45908,#45909,#45910,#45911,#45912,#45913,
#45914,#45915,#45916,#45917,#45918,#45919,#45920,#45921,#45922,#45923,#45924,
#45925,#45926,#45927,#45928,#45929,#45930,#45931,#45932,#45933,#45934,#45935,
#45936,#45937,#45938,#45939,#45940,#45941,#45942,#45943,#45944,#45945,#45946,
#45947)),.UNSPECIFIED.,.F.,.F.,.F.,(4,4),(4,1,1,1,1,1,1,1,1,1,1,1,1,1,1,
1,1,1,1,1,1,1,1,1,1,1,1,1,1,1,1,1,1,1,1,1,1,1,1,1,1,1,1,1,1,1,1,1,1,1,1,
1,1,1,1,1,1,1,1,1,1,1,1,1,1,1,1,1,1,1,1,1,1,1,1,1,1,1,1,1,1,1,1,4),(0.,
0.0448889834294934),(14.3981410127769,15.3957123857598,16.3932837587427,
17.3908551317257,18.3884265047086,19.3859978776915,20.3835692506745,21.3811406236574,
22.3787119966403,23.3762833696233,24.3738547426062,25.3714261155891,26.3689974885721,
27.366568861555,28.3641402345379,29.3617116075208,30.3592829805038,31.3568543534867,
32.3544257264696,33.3519970994526,34.3495684724355,35.3471398454184,36.3447112184014,
37.3422825913843,38.3398539643672,39.3374253373502,40.3349967103331,41.332568083316,
42.330139456299,43.3277108292819,44.3252822022648,45.3228535752478,46.3204249482307,
47.3179963212136,48.3155676941966,49.3131390671795,50.3107104401624,51.3082818131454,
52.3058531861283,53.3034245591112,54.3009959320942,55.2985673050771,56.29613867806,
57.293710051043,58.2912814240259,59.2888527970088,60.2864241699918,61.2839955429747,
62.2815669159576,63.2791382889406,64.2767096619235,65.2742810349064,66.2718524078894,
67.2694237808723,68.2669951538552,69.2645665268382,70.2621378998211,71.259709272804,
72.2572806457869,73.2548520187699,74.2524233917528,75.2499947647357,76.2475661377187,
77.2451375107016,78.2427088836845,79.2402802566675,80.2378516296504,81.2354230026333,
82.2329943756163,83.2305657485992,84.2281371215821,85.2257084945651,86.223279867548,
87.2208512405309,88.2184226135139,89.2159939864968,90.2135653594797,91.2111367324627,
92.2087081054456,93.2062794784285,94.2038508514115,95.2014222243944,96.1989935973773,
97.1965649703603),.UNSPECIFIED.);
#634=B_SPLINE_SURFACE_WITH_KNOTS('',3,3,((#46252,#46253,#46254,#46255,#46256,
#46257,#46258,#46259,#46260,#46261,#46262,#46263,#46264,#46265,#46266,#46267,
#46268,#46269,#46270,#46271,#46272,#46273,#46274,#46275,#46276,#46277,#46278,
#46279,#46280,#46281,#46282,#46283,#46284,#46285,#46286,#46287,#46288,#46289,
#46290,#46291,#46292,#46293,#46294,#46295,#46296,#46297,#46298,#46299,#46300,
#46301,#46302,#46303,#46304,#46305,#46306,#46307,#46308,#46309,#46310,#46311,
#46312,#46313,#46314,#46315,#46316,#46317,#46318,#46319,#46320,#46321,#46322,
#46323,#46324,#46325,#46326,#46327,#46328,#46329,#46330,#46331,#46332,#46333,
#46334,#46335,#46336,#46337),(#46338,#46339,#46340,#46341,#46342,#46343,
#46344,#46345,#46346,#46347,#46348,#46349,#46350,#46351,#46352,#46353,#46354,
#46355,#46356,#46357,#46358,#46359,#46360,#46361,#46362,#46363,#46364,#46365,
#46366,#46367,#46368,#46369,#46370,#46371,#46372,#46373,#46374,#46375,#46376,
#46377,#46378,#46379,#46380,#46381,#46382,#46383,#46384,#46385,#46386,#46387,
#46388,#46389,#46390,#46391,#46392,#46393,#46394,#46395,#46396,#46397,#46398,
#46399,#46400,#46401,#46402,#46403,#46404,#46405,#46406,#46407,#46408,#46409,
#46410,#46411,#46412,#46413,#46414,#46415,#46416,#46417,#46418,#46419,#46420,
#46421,#46422,#46423),(#46424,#46425,#46426,#46427,#46428,#46429,#46430,
#46431,#46432,#46433,#46434,#46435,#46436,#46437,#46438,#46439,#46440,#46441,
#46442,#46443,#46444,#46445,#46446,#46447,#46448,#46449,#46450,#46451,#46452,
#46453,#46454,#46455,#46456,#46457,#46458,#46459,#46460,#46461,#46462,#46463,
#46464,#46465,#46466,#46467,#46468,#46469,#46470,#46471,#46472,#46473,#46474,
#46475,#46476,#46477,#46478,#46479,#46480,#46481,#46482,#46483,#46484,#46485,
#46486,#46487,#46488,#46489,#46490,#46491,#46492,#46493,#46494,#46495,#46496,
#46497,#46498,#46499,#46500,#46501,#46502,#46503,#46504,#46505,#46506,#46507,
#46508,#46509),(#46510,#46511,#46512,#46513,#46514,#46515,#46516,#46517,
#46518,#46519,#46520,#46521,#46522,#46523,#46524,#46525,#46526,#46527,#46528,
#46529,#46530,#46531,#46532,#46533,#46534,#46535,#46536,#46537,#46538,#46539,
#46540,#46541,#46542,#46543,#46544,#46545,#46546,#46547,#46548,#46549,#46550,
#46551,#46552,#46553,#46554,#46555,#46556,#46557,#46558,#46559,#46560,#46561,
#46562,#46563,#46564,#46565,#46566,#46567,#46568,#46569,#46570,#46571,#46572,
#46573,#46574,#46575,#46576,#46577,#46578,#46579,#46580,#46581,#46582,#46583,
#46584,#46585,#46586,#46587,#46588,#46589,#46590,#46591,#46592,#46593,#46594,
#46595)),.UNSPECIFIED.,.F.,.F.,.F.,(4,4),(4,1,1,1,1,1,1,1,1,1,1,1,1,1,1,
1,1,1,1,1,1,1,1,1,1,1,1,1,1,1,1,1,1,1,1,1,1,1,1,1,1,1,1,1,1,1,1,1,1,1,1,
1,1,1,1,1,1,1,1,1,1,1,1,1,1,1,1,1,1,1,1,1,1,1,1,1,1,1,1,1,1,1,1,4),(0.,
0.0448889834294934),(11.8615800042566,12.8591513772395,13.8567227502225,
14.8542941232054,15.8518654961883,16.8494368691713,17.8470082421542,18.8445796151371,
19.8421509881201,20.839722361103,21.8372937340859,22.8348651070689,23.8324364800518,
24.8300078530347,25.8275792260177,26.8251505990006,27.8227219719835,28.8202933449665,
29.8178647179494,30.8154360909323,31.8130074639152,32.8105788368982,33.8081502098811,
34.805721582864,35.803292955847,36.8008643288299,37.7984357018128,38.7960070747958,
39.7935784477787,40.7911498207616,41.7887211937446,42.7862925667275,43.7838639397104,
44.7814353126934,45.7790066856763,46.7765780586592,47.7741494316422,48.7717208046251,
49.769292177608,50.766863550591,51.7644349235739,52.7620062965568,53.7595776695398,
54.7571490425227,55.7547204155056,56.7522917884886,57.7498631614715,58.7474345344544,
59.7450059074374,60.7425772804203,61.7401486534032,62.7377200263862,63.7352913993691,
64.732862772352,65.730434145335,66.7280055183179,67.7255768913008,68.7231482642838,
69.7207196372667,70.7182910102496,71.7158623832325,72.7134337562155,73.7110051291984,
74.7085765021813,75.7061478751643,76.7037192481472,77.7012906211301,78.6988619941131,
79.696433367096,80.6940047400789,81.6915761130619,82.6891474860448,83.6867188590277,
84.6842902320107,85.6818616049936,86.6794329779765,87.6770043509595,88.6745757239424,
89.6721470969253,90.6697184699083,91.6672898428912,92.6648612158741,93.6624325888571,
94.66000396184),.UNSPECIFIED.);
#635=B_SPLINE_SURFACE_WITH_KNOTS('',3,3,((#46703,#46704,#46705,#46706,#46707,
#46708,#46709,#46710,#46711,#46712,#46713,#46714,#46715,#46716,#46717,#46718,
#46719,#46720,#46721,#46722,#46723,#46724,#46725,#46726,#46727,#46728,#46729,
#46730,#46731,#46732,#46733,#46734,#46735,#46736,#46737,#46738,#46739,#46740,
#46741,#46742,#46743,#46744,#46745,#46746,#46747,#46748,#46749,#46750,#46751,
#46752,#46753,#46754,#46755,#46756,#46757,#46758,#46759,#46760,#46761,#46762,
#46763,#46764,#46765,#46766,#46767,#46768,#46769,#46770,#46771,#46772,#46773,
#46774,#46775,#46776,#46777,#46778,#46779,#46780,#46781,#46782,#46783,#46784,
#46785,#46786,#46787,#46788),(#46789,#46790,#46791,#46792,#46793,#46794,
#46795,#46796,#46797,#46798,#46799,#46800,#46801,#46802,#46803,#46804,#46805,
#46806,#46807,#46808,#46809,#46810,#46811,#46812,#46813,#46814,#46815,#46816,
#46817,#46818,#46819,#46820,#46821,#46822,#46823,#46824,#46825,#46826,#46827,
#46828,#46829,#46830,#46831,#46832,#46833,#46834,#46835,#46836,#46837,#46838,
#46839,#46840,#46841,#46842,#46843,#46844,#46845,#46846,#46847,#46848,#46849,
#46850,#46851,#46852,#46853,#46854,#46855,#46856,#46857,#46858,#46859,#46860,
#46861,#46862,#46863,#46864,#46865,#46866,#46867,#46868,#46869,#46870,#46871,
#46872,#46873,#46874),(#46875,#46876,#46877,#46878,#46879,#46880,#46881,
#46882,#46883,#46884,#46885,#46886,#46887,#46888,#46889,#46890,#46891,#46892,
#46893,#46894,#46895,#46896,#46897,#46898,#46899,#46900,#46901,#46902,#46903,
#46904,#46905,#46906,#46907,#46908,#46909,#46910,#46911,#46912,#46913,#46914,
#46915,#46916,#46917,#46918,#46919,#46920,#46921,#46922,#46923,#46924,#46925,
#46926,#46927,#46928,#46929,#46930,#46931,#46932,#46933,#46934,#46935,#46936,
#46937,#46938,#46939,#46940,#46941,#46942,#46943,#46944,#46945,#46946,#46947,
#46948,#46949,#46950,#46951,#46952,#46953,#46954,#46955,#46956,#46957,#46958,
#46959,#46960),(#46961,#46962,#46963,#46964,#46965,#46966,#46967,#46968,
#46969,#46970,#46971,#46972,#46973,#46974,#46975,#46976,#46977,#46978,#46979,
#46980,#46981,#46982,#46983,#46984,#46985,#46986,#46987,#46988,#46989,#46990,
#46991,#46992,#46993,#46994,#46995,#46996,#46997,#46998,#46999,#47000,#47001,
#47002,#47003,#47004,#47005,#47006,#47007,#47008,#47009,#47010,#47011,#47012,
#47013,#47014,#47015,#47016,#47017,#47018,#47019,#47020,#47021,#47022,#47023,
#47024,#47025,#47026,#47027,#47028,#47029,#47030,#47031,#47032,#47033,#47034,
#47035,#47036,#47037,#47038,#47039,#47040,#47041,#47042,#47043,#47044,#47045,
#47046)),.UNSPECIFIED.,.F.,.F.,.F.,(4,4),(4,1,1,1,1,1,1,1,1,1,1,1,1,1,1,
1,1,1,1,1,1,1,1,1,1,1,1,1,1,1,1,1,1,1,1,1,1,1,1,1,1,1,1,1,1,1,1,1,1,1,1,
1,1,1,1,1,1,1,1,1,1,1,1,1,1,1,1,1,1,1,1,1,1,1,1,1,1,1,1,1,1,1,1,4),(0.,
0.0448889834294934),(14.3981410127769,15.3957123857598,16.3932837587427,
17.3908551317257,18.3884265047086,19.3859978776915,20.3835692506745,21.3811406236574,
22.3787119966403,23.3762833696233,24.3738547426062,25.3714261155891,26.3689974885721,
27.366568861555,28.3641402345379,29.3617116075209,30.3592829805038,31.3568543534867,
32.3544257264696,33.3519970994526,34.3495684724355,35.3471398454184,36.3447112184014,
37.3422825913843,38.3398539643673,39.3374253373502,40.3349967103331,41.332568083316,
42.330139456299,43.3277108292819,44.3252822022648,45.3228535752478,46.3204249482307,
47.3179963212136,48.3155676941966,49.3131390671795,50.3107104401624,51.3082818131454,
52.3058531861283,53.3034245591112,54.3009959320942,55.2985673050771,56.29613867806,
57.293710051043,58.2912814240259,59.2888527970088,60.2864241699918,61.2839955429747,
62.2815669159576,63.2791382889406,64.2767096619235,65.2742810349064,66.2718524078894,
67.2694237808723,68.2669951538552,69.2645665268382,70.2621378998211,71.259709272804,
72.2572806457869,73.2548520187699,74.2524233917528,75.2499947647357,76.2475661377187,
77.2451375107016,78.2427088836845,79.2402802566675,80.2378516296504,81.2354230026333,
82.2329943756163,83.2305657485992,84.2281371215821,85.2257084945651,86.223279867548,
87.2208512405309,88.2184226135139,89.2159939864968,90.2135653594797,91.2111367324627,
92.2087081054456,93.2062794784285,94.2038508514115,95.2014222243944,96.1989935973773,
97.1965649703603),.UNSPECIFIED.);
#636=B_SPLINE_SURFACE_WITH_KNOTS('',3,3,((#47351,#47352,#47353,#47354,#47355,
#47356,#47357,#47358,#47359,#47360,#47361,#47362,#47363,#47364,#47365,#47366,
#47367,#47368,#47369,#47370,#47371,#47372,#47373,#47374,#47375,#47376,#47377,
#47378,#47379,#47380,#47381,#47382,#47383,#47384,#47385,#47386,#47387,#47388,
#47389,#47390,#47391,#47392,#47393,#47394,#47395,#47396,#47397,#47398,#47399,
#47400,#47401,#47402,#47403,#47404,#47405,#47406,#47407,#47408,#47409,#47410,
#47411,#47412,#47413,#47414,#47415,#47416,#47417,#47418,#47419,#47420,#47421,
#47422,#47423,#47424,#47425,#47426,#47427,#47428,#47429,#47430,#47431,#47432,
#47433,#47434,#47435,#47436),(#47437,#47438,#47439,#47440,#47441,#47442,
#47443,#47444,#47445,#47446,#47447,#47448,#47449,#47450,#47451,#47452,#47453,
#47454,#47455,#47456,#47457,#47458,#47459,#47460,#47461,#47462,#47463,#47464,
#47465,#47466,#47467,#47468,#47469,#47470,#47471,#47472,#47473,#47474,#47475,
#47476,#47477,#47478,#47479,#47480,#47481,#47482,#47483,#47484,#47485,#47486,
#47487,#47488,#47489,#47490,#47491,#47492,#47493,#47494,#47495,#47496,#47497,
#47498,#47499,#47500,#47501,#47502,#47503,#47504,#47505,#47506,#47507,#47508,
#47509,#47510,#47511,#47512,#47513,#47514,#47515,#47516,#47517,#47518,#47519,
#47520,#47521,#47522),(#47523,#47524,#47525,#47526,#47527,#47528,#47529,
#47530,#47531,#47532,#47533,#47534,#47535,#47536,#47537,#47538,#47539,#47540,
#47541,#47542,#47543,#47544,#47545,#47546,#47547,#47548,#47549,#47550,#47551,
#47552,#47553,#47554,#47555,#47556,#47557,#47558,#47559,#47560,#47561,#47562,
#47563,#47564,#47565,#47566,#47567,#47568,#47569,#47570,#47571,#47572,#47573,
#47574,#47575,#47576,#47577,#47578,#47579,#47580,#47581,#47582,#47583,#47584,
#47585,#47586,#47587,#47588,#47589,#47590,#47591,#47592,#47593,#47594,#47595,
#47596,#47597,#47598,#47599,#47600,#47601,#47602,#47603,#47604,#47605,#47606,
#47607,#47608),(#47609,#47610,#47611,#47612,#47613,#47614,#47615,#47616,
#47617,#47618,#47619,#47620,#47621,#47622,#47623,#47624,#47625,#47626,#47627,
#47628,#47629,#47630,#47631,#47632,#47633,#47634,#47635,#47636,#47637,#47638,
#47639,#47640,#47641,#47642,#47643,#47644,#47645,#47646,#47647,#47648,#47649,
#47650,#47651,#47652,#47653,#47654,#47655,#47656,#47657,#47658,#47659,#47660,
#47661,#47662,#47663,#47664,#47665,#47666,#47667,#47668,#47669,#47670,#47671,
#47672,#47673,#47674,#47675,#47676,#47677,#47678,#47679,#47680,#47681,#47682,
#47683,#47684,#47685,#47686,#47687,#47688,#47689,#47690,#47691,#47692,#47693,
#47694)),.UNSPECIFIED.,.F.,.F.,.F.,(4,4),(4,1,1,1,1,1,1,1,1,1,1,1,1,1,1,
1,1,1,1,1,1,1,1,1,1,1,1,1,1,1,1,1,1,1,1,1,1,1,1,1,1,1,1,1,1,1,1,1,1,1,1,
1,1,1,1,1,1,1,1,1,1,1,1,1,1,1,1,1,1,1,1,1,1,1,1,1,1,1,1,1,1,1,1,4),(0.,
0.0448889834294935),(11.8615800042566,12.8591513772396,13.8567227502225,
14.8542941232054,15.8518654961884,16.8494368691713,17.8470082421542,18.8445796151372,
19.8421509881201,20.839722361103,21.837293734086,22.8348651070689,23.8324364800518,
24.8300078530348,25.8275792260177,26.8251505990006,27.8227219719836,28.8202933449665,
29.8178647179494,30.8154360909324,31.8130074639153,32.8105788368982,33.8081502098811,
34.8057215828641,35.803292955847,36.80086432883,37.7984357018129,38.7960070747958,
39.7935784477787,40.7911498207617,41.7887211937446,42.7862925667275,43.7838639397105,
44.7814353126934,45.7790066856763,46.7765780586593,47.7741494316422,48.7717208046251,
49.7692921776081,50.766863550591,51.7644349235739,52.7620062965569,53.7595776695398,
54.7571490425227,55.7547204155057,56.7522917884886,57.7498631614715,58.7474345344545,
59.7450059074374,60.7425772804203,61.7401486534033,62.7377200263862,63.7352913993691,
64.7328627723521,65.730434145335,66.7280055183179,67.7255768913009,68.7231482642838,
69.7207196372667,70.7182910102497,71.7158623832326,72.7134337562155,73.7110051291985,
74.7085765021814,75.7061478751643,76.7037192481473,77.7012906211302,78.6988619941131,
79.696433367096,80.694004740079,81.6915761130619,82.6891474860448,83.6867188590278,
84.6842902320107,85.6818616049936,86.6794329779766,87.6770043509595,88.6745757239424,
89.6721470969254,90.6697184699083,91.6672898428912,92.6648612158742,93.6624325888571,
94.66000396184),.UNSPECIFIED.);
#637=B_SPLINE_SURFACE_WITH_KNOTS('',3,3,((#47802,#47803,#47804,#47805,#47806,
#47807,#47808,#47809,#47810,#47811,#47812,#47813,#47814,#47815,#47816,#47817,
#47818,#47819,#47820,#47821,#47822,#47823,#47824,#47825,#47826,#47827,#47828,
#47829,#47830,#47831,#47832,#47833,#47834,#47835,#47836,#47837,#47838,#47839,
#47840,#47841,#47842,#47843,#47844,#47845,#47846,#47847,#47848,#47849,#47850,
#47851,#47852,#47853,#47854,#47855,#47856,#47857,#47858,#47859,#47860,#47861,
#47862,#47863,#47864,#47865,#47866,#47867,#47868,#47869,#47870,#47871,#47872,
#47873,#47874,#47875,#47876,#47877,#47878,#47879,#47880,#47881,#47882,#47883,
#47884,#47885,#47886,#47887),(#47888,#47889,#47890,#47891,#47892,#47893,
#47894,#47895,#47896,#47897,#47898,#47899,#47900,#47901,#47902,#47903,#47904,
#47905,#47906,#47907,#47908,#47909,#47910,#47911,#47912,#47913,#47914,#47915,
#47916,#47917,#47918,#47919,#47920,#47921,#47922,#47923,#47924,#47925,#47926,
#47927,#47928,#47929,#47930,#47931,#47932,#47933,#47934,#47935,#47936,#47937,
#47938,#47939,#47940,#47941,#47942,#47943,#47944,#47945,#47946,#47947,#47948,
#47949,#47950,#47951,#47952,#47953,#47954,#47955,#47956,#47957,#47958,#47959,
#47960,#47961,#47962,#47963,#47964,#47965,#47966,#47967,#47968,#47969,#47970,
#47971,#47972,#47973),(#47974,#47975,#47976,#47977,#47978,#47979,#47980,
#47981,#47982,#47983,#47984,#47985,#47986,#47987,#47988,#47989,#47990,#47991,
#47992,#47993,#47994,#47995,#47996,#47997,#47998,#47999,#48000,#48001,#48002,
#48003,#48004,#48005,#48006,#48007,#48008,#48009,#48010,#48011,#48012,#48013,
#48014,#48015,#48016,#48017,#48018,#48019,#48020,#48021,#48022,#48023,#48024,
#48025,#48026,#48027,#48028,#48029,#48030,#48031,#48032,#48033,#48034,#48035,
#48036,#48037,#48038,#48039,#48040,#48041,#48042,#48043,#48044,#48045,#48046,
#48047,#48048,#48049,#48050,#48051,#48052,#48053,#48054,#48055,#48056,#48057,
#48058,#48059),(#48060,#48061,#48062,#48063,#48064,#48065,#48066,#48067,
#48068,#48069,#48070,#48071,#48072,#48073,#48074,#48075,#48076,#48077,#48078,
#48079,#48080,#48081,#48082,#48083,#48084,#48085,#48086,#48087,#48088,#48089,
#48090,#48091,#48092,#48093,#48094,#48095,#48096,#48097,#48098,#48099,#48100,
#48101,#48102,#48103,#48104,#48105,#48106,#48107,#48108,#48109,#48110,#48111,
#48112,#48113,#48114,#48115,#48116,#48117,#48118,#48119,#48120,#48121,#48122,
#48123,#48124,#48125,#48126,#48127,#48128,#48129,#48130,#48131,#48132,#48133,
#48134,#48135,#48136,#48137,#48138,#48139,#48140,#48141,#48142,#48143,#48144,
#48145)),.UNSPECIFIED.,.F.,.F.,.F.,(4,4),(4,1,1,1,1,1,1,1,1,1,1,1,1,1,1,
1,1,1,1,1,1,1,1,1,1,1,1,1,1,1,1,1,1,1,1,1,1,1,1,1,1,1,1,1,1,1,1,1,1,1,1,
1,1,1,1,1,1,1,1,1,1,1,1,1,1,1,1,1,1,1,1,1,1,1,1,1,1,1,1,1,1,1,1,4),(0.,
0.0448889834294935),(14.3981410127769,15.3957123857598,16.3932837587428,
17.3908551317257,18.3884265047086,19.3859978776916,20.3835692506745,21.3811406236574,
22.3787119966404,23.3762833696233,24.3738547426062,25.3714261155892,26.3689974885721,
27.366568861555,28.364140234538,29.3617116075209,30.3592829805038,31.3568543534868,
32.3544257264697,33.3519970994526,34.3495684724355,35.3471398454185,36.3447112184014,
37.3422825913843,38.3398539643673,39.3374253373502,40.3349967103332,41.3325680833161,
42.330139456299,43.3277108292819,44.3252822022649,45.3228535752478,46.3204249482307,
47.3179963212137,48.3155676941966,49.3131390671795,50.3107104401625,51.3082818131454,
52.3058531861283,53.3034245591113,54.3009959320942,55.2985673050771,56.2961386780601,
57.293710051043,58.2912814240259,59.2888527970089,60.2864241699918,61.2839955429747,
62.2815669159577,63.2791382889406,64.2767096619235,65.2742810349065,66.2718524078894,
67.2694237808723,68.2669951538553,69.2645665268382,70.2621378998211,71.2597092728041,
72.257280645787,73.2548520187699,74.2524233917529,75.2499947647358,76.2475661377187,
77.2451375107017,78.2427088836846,79.2402802566675,80.2378516296505,81.2354230026334,
82.2329943756163,83.2305657485992,84.2281371215822,85.2257084945651,86.223279867548,
87.220851240531,88.2184226135139,89.2159939864968,90.2135653594798,91.2111367324627,
92.2087081054456,93.2062794784286,94.2038508514115,95.2014222243944,96.1989935973774,
97.1965649703603),.UNSPECIFIED.);
#638=B_SPLINE_SURFACE_WITH_KNOTS('',3,3,((#48450,#48451,#48452,#48453,#48454,
#48455,#48456,#48457,#48458,#48459,#48460,#48461,#48462,#48463,#48464,#48465,
#48466,#48467,#48468,#48469,#48470,#48471,#48472,#48473,#48474,#48475,#48476,
#48477,#48478,#48479,#48480,#48481,#48482,#48483,#48484,#48485,#48486,#48487,
#48488,#48489,#48490,#48491,#48492,#48493,#48494,#48495,#48496,#48497,#48498,
#48499,#48500,#48501,#48502,#48503,#48504,#48505,#48506,#48507,#48508,#48509,
#48510,#48511,#48512,#48513,#48514,#48515,#48516,#48517,#48518,#48519,#48520,
#48521,#48522,#48523,#48524,#48525,#48526,#48527,#48528,#48529,#48530,#48531,
#48532,#48533,#48534,#48535),(#48536,#48537,#48538,#48539,#48540,#48541,
#48542,#48543,#48544,#48545,#48546,#48547,#48548,#48549,#48550,#48551,#48552,
#48553,#48554,#48555,#48556,#48557,#48558,#48559,#48560,#48561,#48562,#48563,
#48564,#48565,#48566,#48567,#48568,#48569,#48570,#48571,#48572,#48573,#48574,
#48575,#48576,#48577,#48578,#48579,#48580,#48581,#48582,#48583,#48584,#48585,
#48586,#48587,#48588,#48589,#48590,#48591,#48592,#48593,#48594,#48595,#48596,
#48597,#48598,#48599,#48600,#48601,#48602,#48603,#48604,#48605,#48606,#48607,
#48608,#48609,#48610,#48611,#48612,#48613,#48614,#48615,#48616,#48617,#48618,
#48619,#48620,#48621),(#48622,#48623,#48624,#48625,#48626,#48627,#48628,
#48629,#48630,#48631,#48632,#48633,#48634,#48635,#48636,#48637,#48638,#48639,
#48640,#48641,#48642,#48643,#48644,#48645,#48646,#48647,#48648,#48649,#48650,
#48651,#48652,#48653,#48654,#48655,#48656,#48657,#48658,#48659,#48660,#48661,
#48662,#48663,#48664,#48665,#48666,#48667,#48668,#48669,#48670,#48671,#48672,
#48673,#48674,#48675,#48676,#48677,#48678,#48679,#48680,#48681,#48682,#48683,
#48684,#48685,#48686,#48687,#48688,#48689,#48690,#48691,#48692,#48693,#48694,
#48695,#48696,#48697,#48698,#48699,#48700,#48701,#48702,#48703,#48704,#48705,
#48706,#48707),(#48708,#48709,#48710,#48711,#48712,#48713,#48714,#48715,
#48716,#48717,#48718,#48719,#48720,#48721,#48722,#48723,#48724,#48725,#48726,
#48727,#48728,#48729,#48730,#48731,#48732,#48733,#48734,#48735,#48736,#48737,
#48738,#48739,#48740,#48741,#48742,#48743,#48744,#48745,#48746,#48747,#48748,
#48749,#48750,#48751,#48752,#48753,#48754,#48755,#48756,#48757,#48758,#48759,
#48760,#48761,#48762,#48763,#48764,#48765,#48766,#48767,#48768,#48769,#48770,
#48771,#48772,#48773,#48774,#48775,#48776,#48777,#48778,#48779,#48780,#48781,
#48782,#48783,#48784,#48785,#48786,#48787,#48788,#48789,#48790,#48791,#48792,
#48793)),.UNSPECIFIED.,.F.,.F.,.F.,(4,4),(4,1,1,1,1,1,1,1,1,1,1,1,1,1,1,
1,1,1,1,1,1,1,1,1,1,1,1,1,1,1,1,1,1,1,1,1,1,1,1,1,1,1,1,1,1,1,1,1,1,1,1,
1,1,1,1,1,1,1,1,1,1,1,1,1,1,1,1,1,1,1,1,1,1,1,1,1,1,1,1,1,1,1,1,4),(0.,
0.0448889834294934),(11.8615800042566,12.8591513772395,13.8567227502225,
14.8542941232054,15.8518654961883,16.8494368691713,17.8470082421542,18.8445796151371,
19.8421509881201,20.839722361103,21.8372937340859,22.8348651070689,23.8324364800518,
24.8300078530347,25.8275792260177,26.8251505990006,27.8227219719835,28.8202933449664,
29.8178647179494,30.8154360909323,31.8130074639152,32.8105788368982,33.8081502098811,
34.805721582864,35.803292955847,36.8008643288299,37.7984357018128,38.7960070747958,
39.7935784477787,40.7911498207616,41.7887211937446,42.7862925667275,43.7838639397104,
44.7814353126934,45.7790066856763,46.7765780586592,47.7741494316422,48.7717208046251,
49.769292177608,50.766863550591,51.7644349235739,52.7620062965568,53.7595776695398,
54.7571490425227,55.7547204155056,56.7522917884886,57.7498631614715,58.7474345344544,
59.7450059074374,60.7425772804203,61.7401486534032,62.7377200263862,63.7352913993691,
64.732862772352,65.730434145335,66.7280055183179,67.7255768913008,68.7231482642838,
69.7207196372667,70.7182910102496,71.7158623832325,72.7134337562155,73.7110051291984,
74.7085765021813,75.7061478751643,76.7037192481472,77.7012906211301,78.6988619941131,
79.696433367096,80.6940047400789,81.6915761130619,82.6891474860448,83.6867188590277,
84.6842902320107,85.6818616049936,86.6794329779765,87.6770043509595,88.6745757239424,
89.6721470969253,90.6697184699083,91.6672898428912,92.6648612158741,93.6624325888571,
94.66000396184),.UNSPECIFIED.);
#639=B_SPLINE_SURFACE_WITH_KNOTS('',3,3,((#48901,#48902,#48903,#48904,#48905,
#48906,#48907,#48908,#48909,#48910,#48911,#48912,#48913,#48914,#48915,#48916,
#48917,#48918,#48919,#48920,#48921,#48922,#48923,#48924,#48925,#48926,#48927,
#48928,#48929,#48930,#48931,#48932,#48933,#48934,#48935,#48936,#48937,#48938,
#48939,#48940,#48941,#48942,#48943,#48944,#48945,#48946,#48947,#48948,#48949,
#48950,#48951,#48952,#48953,#48954,#48955,#48956,#48957,#48958,#48959,#48960,
#48961,#48962,#48963,#48964,#48965,#48966,#48967,#48968,#48969,#48970,#48971,
#48972,#48973,#48974,#48975,#48976,#48977,#48978,#48979,#48980,#48981,#48982,
#48983,#48984,#48985,#48986),(#48987,#48988,#48989,#48990,#48991,#48992,
#48993,#48994,#48995,#48996,#48997,#48998,#48999,#49000,#49001,#49002,#49003,
#49004,#49005,#49006,#49007,#49008,#49009,#49010,#49011,#49012,#49013,#49014,
#49015,#49016,#49017,#49018,#49019,#49020,#49021,#49022,#49023,#49024,#49025,
#49026,#49027,#49028,#49029,#49030,#49031,#49032,#49033,#49034,#49035,#49036,
#49037,#49038,#49039,#49040,#49041,#49042,#49043,#49044,#49045,#49046,#49047,
#49048,#49049,#49050,#49051,#49052,#49053,#49054,#49055,#49056,#49057,#49058,
#49059,#49060,#49061,#49062,#49063,#49064,#49065,#49066,#49067,#49068,#49069,
#49070,#49071,#49072),(#49073,#49074,#49075,#49076,#49077,#49078,#49079,
#49080,#49081,#49082,#49083,#49084,#49085,#49086,#49087,#49088,#49089,#49090,
#49091,#49092,#49093,#49094,#49095,#49096,#49097,#49098,#49099,#49100,#49101,
#49102,#49103,#49104,#49105,#49106,#49107,#49108,#49109,#49110,#49111,#49112,
#49113,#49114,#49115,#49116,#49117,#49118,#49119,#49120,#49121,#49122,#49123,
#49124,#49125,#49126,#49127,#49128,#49129,#49130,#49131,#49132,#49133,#49134,
#49135,#49136,#49137,#49138,#49139,#49140,#49141,#49142,#49143,#49144,#49145,
#49146,#49147,#49148,#49149,#49150,#49151,#49152,#49153,#49154,#49155,#49156,
#49157,#49158),(#49159,#49160,#49161,#49162,#49163,#49164,#49165,#49166,
#49167,#49168,#49169,#49170,#49171,#49172,#49173,#49174,#49175,#49176,#49177,
#49178,#49179,#49180,#49181,#49182,#49183,#49184,#49185,#49186,#49187,#49188,
#49189,#49190,#49191,#49192,#49193,#49194,#49195,#49196,#49197,#49198,#49199,
#49200,#49201,#49202,#49203,#49204,#49205,#49206,#49207,#49208,#49209,#49210,
#49211,#49212,#49213,#49214,#49215,#49216,#49217,#49218,#49219,#49220,#49221,
#49222,#49223,#49224,#49225,#49226,#49227,#49228,#49229,#49230,#49231,#49232,
#49233,#49234,#49235,#49236,#49237,#49238,#49239,#49240,#49241,#49242,#49243,
#49244)),.UNSPECIFIED.,.F.,.F.,.F.,(4,4),(4,1,1,1,1,1,1,1,1,1,1,1,1,1,1,
1,1,1,1,1,1,1,1,1,1,1,1,1,1,1,1,1,1,1,1,1,1,1,1,1,1,1,1,1,1,1,1,1,1,1,1,
1,1,1,1,1,1,1,1,1,1,1,1,1,1,1,1,1,1,1,1,1,1,1,1,1,1,1,1,1,1,1,1,4),(0.,
0.0448889834294934),(14.3981410127769,15.3957123857598,16.3932837587427,
17.3908551317257,18.3884265047086,19.3859978776915,20.3835692506745,21.3811406236574,
22.3787119966403,23.3762833696233,24.3738547426062,25.3714261155891,26.3689974885721,
27.366568861555,28.3641402345379,29.3617116075209,30.3592829805038,31.3568543534867,
32.3544257264696,33.3519970994526,34.3495684724355,35.3471398454184,36.3447112184014,
37.3422825913843,38.3398539643673,39.3374253373502,40.3349967103331,41.332568083316,
42.330139456299,43.3277108292819,44.3252822022648,45.3228535752478,46.3204249482307,
47.3179963212136,48.3155676941966,49.3131390671795,50.3107104401624,51.3082818131454,
52.3058531861283,53.3034245591112,54.3009959320942,55.2985673050771,56.29613867806,
57.293710051043,58.2912814240259,59.2888527970088,60.2864241699918,61.2839955429747,
62.2815669159576,63.2791382889406,64.2767096619235,65.2742810349064,66.2718524078894,
67.2694237808723,68.2669951538552,69.2645665268382,70.2621378998211,71.259709272804,
72.2572806457869,73.2548520187699,74.2524233917528,75.2499947647357,76.2475661377187,
77.2451375107016,78.2427088836845,79.2402802566675,80.2378516296504,81.2354230026333,
82.2329943756163,83.2305657485992,84.2281371215821,85.2257084945651,86.223279867548,
87.2208512405309,88.2184226135139,89.2159939864968,90.2135653594797,91.2111367324627,
92.2087081054456,93.2062794784285,94.2038508514115,95.2014222243944,96.1989935973773,
97.1965649703603),.UNSPECIFIED.);
#640=B_SPLINE_SURFACE_WITH_KNOTS('',3,3,((#49549,#49550,#49551,#49552,#49553,
#49554,#49555,#49556,#49557,#49558,#49559,#49560,#49561,#49562,#49563,#49564,
#49565,#49566,#49567,#49568,#49569,#49570,#49571,#49572,#49573,#49574,#49575,
#49576,#49577,#49578,#49579,#49580,#49581,#49582,#49583,#49584,#49585,#49586,
#49587,#49588,#49589,#49590,#49591,#49592,#49593,#49594,#49595,#49596,#49597,
#49598,#49599,#49600,#49601,#49602,#49603,#49604,#49605,#49606,#49607,#49608,
#49609,#49610,#49611,#49612,#49613,#49614,#49615,#49616,#49617,#49618,#49619,
#49620,#49621,#49622,#49623,#49624,#49625,#49626,#49627,#49628,#49629,#49630,
#49631,#49632,#49633,#49634),(#49635,#49636,#49637,#49638,#49639,#49640,
#49641,#49642,#49643,#49644,#49645,#49646,#49647,#49648,#49649,#49650,#49651,
#49652,#49653,#49654,#49655,#49656,#49657,#49658,#49659,#49660,#49661,#49662,
#49663,#49664,#49665,#49666,#49667,#49668,#49669,#49670,#49671,#49672,#49673,
#49674,#49675,#49676,#49677,#49678,#49679,#49680,#49681,#49682,#49683,#49684,
#49685,#49686,#49687,#49688,#49689,#49690,#49691,#49692,#49693,#49694,#49695,
#49696,#49697,#49698,#49699,#49700,#49701,#49702,#49703,#49704,#49705,#49706,
#49707,#49708,#49709,#49710,#49711,#49712,#49713,#49714,#49715,#49716,#49717,
#49718,#49719,#49720),(#49721,#49722,#49723,#49724,#49725,#49726,#49727,
#49728,#49729,#49730,#49731,#49732,#49733,#49734,#49735,#49736,#49737,#49738,
#49739,#49740,#49741,#49742,#49743,#49744,#49745,#49746,#49747,#49748,#49749,
#49750,#49751,#49752,#49753,#49754,#49755,#49756,#49757,#49758,#49759,#49760,
#49761,#49762,#49763,#49764,#49765,#49766,#49767,#49768,#49769,#49770,#49771,
#49772,#49773,#49774,#49775,#49776,#49777,#49778,#49779,#49780,#49781,#49782,
#49783,#49784,#49785,#49786,#49787,#49788,#49789,#49790,#49791,#49792,#49793,
#49794,#49795,#49796,#49797,#49798,#49799,#49800,#49801,#49802,#49803,#49804,
#49805,#49806),(#49807,#49808,#49809,#49810,#49811,#49812,#49813,#49814,
#49815,#49816,#49817,#49818,#49819,#49820,#49821,#49822,#49823,#49824,#49825,
#49826,#49827,#49828,#49829,#49830,#49831,#49832,#49833,#49834,#49835,#49836,
#49837,#49838,#49839,#49840,#49841,#49842,#49843,#49844,#49845,#49846,#49847,
#49848,#49849,#49850,#49851,#49852,#49853,#49854,#49855,#49856,#49857,#49858,
#49859,#49860,#49861,#49862,#49863,#49864,#49865,#49866,#49867,#49868,#49869,
#49870,#49871,#49872,#49873,#49874,#49875,#49876,#49877,#49878,#49879,#49880,
#49881,#49882,#49883,#49884,#49885,#49886,#49887,#49888,#49889,#49890,#49891,
#49892)),.UNSPECIFIED.,.F.,.F.,.F.,(4,4),(4,1,1,1,1,1,1,1,1,1,1,1,1,1,1,
1,1,1,1,1,1,1,1,1,1,1,1,1,1,1,1,1,1,1,1,1,1,1,1,1,1,1,1,1,1,1,1,1,1,1,1,
1,1,1,1,1,1,1,1,1,1,1,1,1,1,1,1,1,1,1,1,1,1,1,1,1,1,1,1,1,1,1,1,4),(0.,
0.0448889834294934),(11.8615800042566,12.8591513772395,13.8567227502225,
14.8542941232054,15.8518654961883,16.8494368691713,17.8470082421542,18.8445796151371,
19.8421509881201,20.839722361103,21.8372937340859,22.8348651070689,23.8324364800518,
24.8300078530347,25.8275792260177,26.8251505990006,27.8227219719835,28.8202933449665,
29.8178647179494,30.8154360909323,31.8130074639152,32.8105788368982,33.8081502098811,
34.805721582864,35.803292955847,36.8008643288299,37.7984357018128,38.7960070747958,
39.7935784477787,40.7911498207616,41.7887211937446,42.7862925667275,43.7838639397104,
44.7814353126934,45.7790066856763,46.7765780586592,47.7741494316422,48.7717208046251,
49.769292177608,50.766863550591,51.7644349235739,52.7620062965568,53.7595776695398,
54.7571490425227,55.7547204155056,56.7522917884886,57.7498631614715,58.7474345344544,
59.7450059074374,60.7425772804203,61.7401486534032,62.7377200263862,63.7352913993691,
64.732862772352,65.730434145335,66.7280055183179,67.7255768913008,68.7231482642838,
69.7207196372667,70.7182910102496,71.7158623832325,72.7134337562155,73.7110051291984,
74.7085765021813,75.7061478751643,76.7037192481472,77.7012906211301,78.6988619941131,
79.696433367096,80.6940047400789,81.6915761130619,82.6891474860448,83.6867188590277,
84.6842902320107,85.6818616049936,86.6794329779765,87.6770043509595,88.6745757239424,
89.6721470969253,90.6697184699083,91.6672898428912,92.6648612158741,93.6624325888571,
94.66000396184),.UNSPECIFIED.);
#641=B_SPLINE_SURFACE_WITH_KNOTS('',3,3,((#50000,#50001,#50002,#50003,#50004,
#50005,#50006,#50007,#50008,#50009,#50010,#50011,#50012,#50013,#50014,#50015,
#50016,#50017,#50018,#50019,#50020,#50021,#50022,#50023,#50024,#50025,#50026,
#50027,#50028,#50029,#50030,#50031,#50032,#50033,#50034,#50035,#50036,#50037,
#50038,#50039,#50040,#50041,#50042,#50043,#50044,#50045,#50046,#50047,#50048,
#50049,#50050,#50051,#50052,#50053,#50054,#50055,#50056,#50057,#50058,#50059,
#50060,#50061,#50062,#50063,#50064,#50065,#50066,#50067,#50068,#50069,#50070,
#50071,#50072,#50073,#50074,#50075,#50076,#50077,#50078,#50079,#50080,#50081,
#50082,#50083,#50084,#50085),(#50086,#50087,#50088,#50089,#50090,#50091,
#50092,#50093,#50094,#50095,#50096,#50097,#50098,#50099,#50100,#50101,#50102,
#50103,#50104,#50105,#50106,#50107,#50108,#50109,#50110,#50111,#50112,#50113,
#50114,#50115,#50116,#50117,#50118,#50119,#50120,#50121,#50122,#50123,#50124,
#50125,#50126,#50127,#50128,#50129,#50130,#50131,#50132,#50133,#50134,#50135,
#50136,#50137,#50138,#50139,#50140,#50141,#50142,#50143,#50144,#50145,#50146,
#50147,#50148,#50149,#50150,#50151,#50152,#50153,#50154,#50155,#50156,#50157,
#50158,#50159,#50160,#50161,#50162,#50163,#50164,#50165,#50166,#50167,#50168,
#50169,#50170,#50171),(#50172,#50173,#50174,#50175,#50176,#50177,#50178,
#50179,#50180,#50181,#50182,#50183,#50184,#50185,#50186,#50187,#50188,#50189,
#50190,#50191,#50192,#50193,#50194,#50195,#50196,#50197,#50198,#50199,#50200,
#50201,#50202,#50203,#50204,#50205,#50206,#50207,#50208,#50209,#50210,#50211,
#50212,#50213,#50214,#50215,#50216,#50217,#50218,#50219,#50220,#50221,#50222,
#50223,#50224,#50225,#50226,#50227,#50228,#50229,#50230,#50231,#50232,#50233,
#50234,#50235,#50236,#50237,#50238,#50239,#50240,#50241,#50242,#50243,#50244,
#50245,#50246,#50247,#50248,#50249,#50250,#50251,#50252,#50253,#50254,#50255,
#50256,#50257),(#50258,#50259,#50260,#50261,#50262,#50263,#50264,#50265,
#50266,#50267,#50268,#50269,#50270,#50271,#50272,#50273,#50274,#50275,#50276,
#50277,#50278,#50279,#50280,#50281,#50282,#50283,#50284,#50285,#50286,#50287,
#50288,#50289,#50290,#50291,#50292,#50293,#50294,#50295,#50296,#50297,#50298,
#50299,#50300,#50301,#50302,#50303,#50304,#50305,#50306,#50307,#50308,#50309,
#50310,#50311,#50312,#50313,#50314,#50315,#50316,#50317,#50318,#50319,#50320,
#50321,#50322,#50323,#50324,#50325,#50326,#50327,#50328,#50329,#50330,#50331,
#50332,#50333,#50334,#50335,#50336,#50337,#50338,#50339,#50340,#50341,#50342,
#50343)),.UNSPECIFIED.,.F.,.F.,.F.,(4,4),(4,1,1,1,1,1,1,1,1,1,1,1,1,1,1,
1,1,1,1,1,1,1,1,1,1,1,1,1,1,1,1,1,1,1,1,1,1,1,1,1,1,1,1,1,1,1,1,1,1,1,1,
1,1,1,1,1,1,1,1,1,1,1,1,1,1,1,1,1,1,1,1,1,1,1,1,1,1,1,1,1,1,1,1,4),(0.,
0.0448889834294934),(14.3981410127769,15.3957123857598,16.3932837587427,
17.3908551317257,18.3884265047086,19.3859978776915,20.3835692506745,21.3811406236574,
22.3787119966403,23.3762833696233,24.3738547426062,25.3714261155891,26.3689974885721,
27.366568861555,28.3641402345379,29.3617116075209,30.3592829805038,31.3568543534867,
32.3544257264696,33.3519970994526,34.3495684724355,35.3471398454184,36.3447112184014,
37.3422825913843,38.3398539643672,39.3374253373502,40.3349967103331,41.332568083316,
42.330139456299,43.3277108292819,44.3252822022648,45.3228535752478,46.3204249482307,
47.3179963212136,48.3155676941966,49.3131390671795,50.3107104401624,51.3082818131454,
52.3058531861283,53.3034245591112,54.3009959320942,55.2985673050771,56.29613867806,
57.293710051043,58.2912814240259,59.2888527970088,60.2864241699918,61.2839955429747,
62.2815669159576,63.2791382889406,64.2767096619235,65.2742810349064,66.2718524078894,
67.2694237808723,68.2669951538552,69.2645665268382,70.2621378998211,71.259709272804,
72.2572806457869,73.2548520187699,74.2524233917528,75.2499947647357,76.2475661377187,
77.2451375107016,78.2427088836845,79.2402802566675,80.2378516296504,81.2354230026333,
82.2329943756163,83.2305657485992,84.2281371215821,85.2257084945651,86.223279867548,
87.2208512405309,88.2184226135139,89.2159939864968,90.2135653594797,91.2111367324627,
92.2087081054456,93.2062794784285,94.2038508514115,95.2014222243944,96.1989935973773,
97.1965649703603),.UNSPECIFIED.);
#642=B_SPLINE_SURFACE_WITH_KNOTS('',3,3,((#50653,#50654,#50655,#50656,#50657,
#50658,#50659,#50660,#50661,#50662,#50663,#50664,#50665,#50666,#50667,#50668,
#50669,#50670,#50671,#50672,#50673,#50674,#50675,#50676,#50677,#50678,#50679,
#50680,#50681,#50682,#50683,#50684,#50685,#50686,#50687,#50688,#50689,#50690,
#50691,#50692,#50693,#50694,#50695,#50696,#50697,#50698,#50699,#50700,#50701,
#50702,#50703,#50704,#50705,#50706,#50707,#50708,#50709,#50710,#50711,#50712,
#50713,#50714,#50715,#50716,#50717,#50718,#50719,#50720,#50721,#50722,#50723,
#50724,#50725,#50726,#50727,#50728,#50729,#50730,#50731,#50732,#50733,#50734,
#50735,#50736,#50737,#50738),(#50739,#50740,#50741,#50742,#50743,#50744,
#50745,#50746,#50747,#50748,#50749,#50750,#50751,#50752,#50753,#50754,#50755,
#50756,#50757,#50758,#50759,#50760,#50761,#50762,#50763,#50764,#50765,#50766,
#50767,#50768,#50769,#50770,#50771,#50772,#50773,#50774,#50775,#50776,#50777,
#50778,#50779,#50780,#50781,#50782,#50783,#50784,#50785,#50786,#50787,#50788,
#50789,#50790,#50791,#50792,#50793,#50794,#50795,#50796,#50797,#50798,#50799,
#50800,#50801,#50802,#50803,#50804,#50805,#50806,#50807,#50808,#50809,#50810,
#50811,#50812,#50813,#50814,#50815,#50816,#50817,#50818,#50819,#50820,#50821,
#50822,#50823,#50824),(#50825,#50826,#50827,#50828,#50829,#50830,#50831,
#50832,#50833,#50834,#50835,#50836,#50837,#50838,#50839,#50840,#50841,#50842,
#50843,#50844,#50845,#50846,#50847,#50848,#50849,#50850,#50851,#50852,#50853,
#50854,#50855,#50856,#50857,#50858,#50859,#50860,#50861,#50862,#50863,#50864,
#50865,#50866,#50867,#50868,#50869,#50870,#50871,#50872,#50873,#50874,#50875,
#50876,#50877,#50878,#50879,#50880,#50881,#50882,#50883,#50884,#50885,#50886,
#50887,#50888,#50889,#50890,#50891,#50892,#50893,#50894,#50895,#50896,#50897,
#50898,#50899,#50900,#50901,#50902,#50903,#50904,#50905,#50906,#50907,#50908,
#50909,#50910),(#50911,#50912,#50913,#50914,#50915,#50916,#50917,#50918,
#50919,#50920,#50921,#50922,#50923,#50924,#50925,#50926,#50927,#50928,#50929,
#50930,#50931,#50932,#50933,#50934,#50935,#50936,#50937,#50938,#50939,#50940,
#50941,#50942,#50943,#50944,#50945,#50946,#50947,#50948,#50949,#50950,#50951,
#50952,#50953,#50954,#50955,#50956,#50957,#50958,#50959,#50960,#50961,#50962,
#50963,#50964,#50965,#50966,#50967,#50968,#50969,#50970,#50971,#50972,#50973,
#50974,#50975,#50976,#50977,#50978,#50979,#50980,#50981,#50982,#50983,#50984,
#50985,#50986,#50987,#50988,#50989,#50990,#50991,#50992,#50993,#50994,#50995,
#50996)),.UNSPECIFIED.,.F.,.F.,.F.,(4,4),(4,1,1,1,1,1,1,1,1,1,1,1,1,1,1,
1,1,1,1,1,1,1,1,1,1,1,1,1,1,1,1,1,1,1,1,1,1,1,1,1,1,1,1,1,1,1,1,1,1,1,1,
1,1,1,1,1,1,1,1,1,1,1,1,1,1,1,1,1,1,1,1,1,1,1,1,1,1,1,1,1,1,1,1,4),(0.,
0.0448889834294934),(11.8615800042567,12.8591513772396,13.8567227502225,
14.8542941232055,15.8518654961884,16.8494368691713,17.8470082421543,18.8445796151372,
19.8421509881201,20.8397223611031,21.837293734086,22.8348651070689,23.8324364800519,
24.8300078530348,25.8275792260177,26.8251505990007,27.8227219719836,28.8202933449665,
29.8178647179495,30.8154360909324,31.8130074639153,32.8105788368983,33.8081502098812,
34.8057215828641,35.8032929558471,36.80086432883,37.7984357018129,38.7960070747959,
39.7935784477788,40.7911498207617,41.7887211937447,42.7862925667276,43.7838639397105,
44.7814353126935,45.7790066856764,46.7765780586593,47.7741494316423,48.7717208046252,
49.7692921776081,50.7668635505911,51.764434923574,52.7620062965569,53.7595776695399,
54.7571490425228,55.7547204155057,56.7522917884886,57.7498631614716,58.7474345344545,
59.7450059074374,60.7425772804204,61.7401486534033,62.7377200263862,63.7352913993692,
64.7328627723521,65.730434145335,66.728005518318,67.7255768913009,68.7231482642838,
69.7207196372668,70.7182910102497,71.7158623832326,72.7134337562156,73.7110051291985,
74.7085765021814,75.7061478751644,76.7037192481473,77.7012906211302,78.6988619941132,
79.6964333670961,80.694004740079,81.691576113062,82.6891474860449,83.6867188590278,
84.6842902320108,85.6818616049937,86.6794329779766,87.6770043509596,88.6745757239425,
89.6721470969254,90.6697184699084,91.6672898428913,92.6648612158742,93.6624325888572,
94.6600039618401),.UNSPECIFIED.);
#643=B_SPLINE_SURFACE_WITH_KNOTS('',3,3,((#51104,#51105,#51106,#51107,#51108,
#51109,#51110,#51111,#51112,#51113,#51114,#51115,#51116,#51117,#51118,#51119,
#51120,#51121,#51122,#51123,#51124,#51125,#51126,#51127,#51128,#51129,#51130,
#51131,#51132,#51133,#51134,#51135,#51136,#51137,#51138,#51139,#51140,#51141,
#51142,#51143,#51144,#51145,#51146,#51147,#51148,#51149,#51150,#51151,#51152,
#51153,#51154,#51155,#51156,#51157,#51158,#51159,#51160,#51161,#51162,#51163,
#51164,#51165,#51166,#51167,#51168,#51169,#51170,#51171,#51172,#51173,#51174,
#51175,#51176,#51177,#51178,#51179,#51180,#51181,#51182,#51183,#51184,#51185,
#51186,#51187,#51188,#51189),(#51190,#51191,#51192,#51193,#51194,#51195,
#51196,#51197,#51198,#51199,#51200,#51201,#51202,#51203,#51204,#51205,#51206,
#51207,#51208,#51209,#51210,#51211,#51212,#51213,#51214,#51215,#51216,#51217,
#51218,#51219,#51220,#51221,#51222,#51223,#51224,#51225,#51226,#51227,#51228,
#51229,#51230,#51231,#51232,#51233,#51234,#51235,#51236,#51237,#51238,#51239,
#51240,#51241,#51242,#51243,#51244,#51245,#51246,#51247,#51248,#51249,#51250,
#51251,#51252,#51253,#51254,#51255,#51256,#51257,#51258,#51259,#51260,#51261,
#51262,#51263,#51264,#51265,#51266,#51267,#51268,#51269,#51270,#51271,#51272,
#51273,#51274,#51275),(#51276,#51277,#51278,#51279,#51280,#51281,#51282,
#51283,#51284,#51285,#51286,#51287,#51288,#51289,#51290,#51291,#51292,#51293,
#51294,#51295,#51296,#51297,#51298,#51299,#51300,#51301,#51302,#51303,#51304,
#51305,#51306,#51307,#51308,#51309,#51310,#51311,#51312,#51313,#51314,#51315,
#51316,#51317,#51318,#51319,#51320,#51321,#51322,#51323,#51324,#51325,#51326,
#51327,#51328,#51329,#51330,#51331,#51332,#51333,#51334,#51335,#51336,#51337,
#51338,#51339,#51340,#51341,#51342,#51343,#51344,#51345,#51346,#51347,#51348,
#51349,#51350,#51351,#51352,#51353,#51354,#51355,#51356,#51357,#51358,#51359,
#51360,#51361),(#51362,#51363,#51364,#51365,#51366,#51367,#51368,#51369,
#51370,#51371,#51372,#51373,#51374,#51375,#51376,#51377,#51378,#51379,#51380,
#51381,#51382,#51383,#51384,#51385,#51386,#51387,#51388,#51389,#51390,#51391,
#51392,#51393,#51394,#51395,#51396,#51397,#51398,#51399,#51400,#51401,#51402,
#51403,#51404,#51405,#51406,#51407,#51408,#51409,#51410,#51411,#51412,#51413,
#51414,#51415,#51416,#51417,#51418,#51419,#51420,#51421,#51422,#51423,#51424,
#51425,#51426,#51427,#51428,#51429,#51430,#51431,#51432,#51433,#51434,#51435,
#51436,#51437,#51438,#51439,#51440,#51441,#51442,#51443,#51444,#51445,#51446,
#51447)),.UNSPECIFIED.,.F.,.F.,.F.,(4,4),(4,1,1,1,1,1,1,1,1,1,1,1,1,1,1,
1,1,1,1,1,1,1,1,1,1,1,1,1,1,1,1,1,1,1,1,1,1,1,1,1,1,1,1,1,1,1,1,1,1,1,1,
1,1,1,1,1,1,1,1,1,1,1,1,1,1,1,1,1,1,1,1,1,1,1,1,1,1,1,1,1,1,1,1,4),(0.,
0.0448889834294934),(14.3981410127769,15.3957123857599,16.3932837587428,
17.3908551317257,18.3884265047087,19.3859978776916,20.3835692506745,21.3811406236575,
22.3787119966404,23.3762833696233,24.3738547426063,25.3714261155892,26.3689974885721,
27.3665688615551,28.364140234538,29.3617116075209,30.3592829805038,31.3568543534868,
32.3544257264697,33.3519970994526,34.3495684724356,35.3471398454185,36.3447112184014,
37.3422825913844,38.3398539643673,39.3374253373502,40.3349967103332,41.3325680833161,
42.330139456299,43.327710829282,44.3252822022649,45.3228535752478,46.3204249482308,
47.3179963212137,48.3155676941966,49.3131390671796,50.3107104401625,51.3082818131454,
52.3058531861284,53.3034245591113,54.3009959320942,55.2985673050772,56.2961386780601,
57.293710051043,58.291281424026,59.2888527970089,60.2864241699918,61.2839955429748,
62.2815669159577,63.2791382889406,64.2767096619236,65.2742810349065,66.2718524078894,
67.2694237808724,68.2669951538553,69.2645665268382,70.2621378998212,71.2597092728041,
72.257280645787,73.25485201877,74.2524233917529,75.2499947647358,76.2475661377187,
77.2451375107017,78.2427088836846,79.2402802566675,80.2378516296505,81.2354230026334,
82.2329943756163,83.2305657485993,84.2281371215822,85.2257084945651,86.2232798675481,
87.220851240531,88.2184226135139,89.2159939864969,90.2135653594798,91.2111367324627,
92.2087081054457,93.2062794784286,94.2038508514115,95.2014222243945,96.1989935973774,
97.1965649703603),.UNSPECIFIED.);
#644=B_SPLINE_SURFACE_WITH_KNOTS('',3,3,((#51753,#51754,#51755,#51756,#51757,
#51758,#51759,#51760,#51761,#51762,#51763,#51764,#51765,#51766,#51767,#51768,
#51769,#51770,#51771,#51772,#51773,#51774,#51775,#51776,#51777,#51778,#51779,
#51780,#51781,#51782,#51783,#51784,#51785,#51786,#51787,#51788,#51789,#51790,
#51791,#51792,#51793,#51794,#51795,#51796,#51797,#51798,#51799,#51800,#51801,
#51802,#51803,#51804,#51805,#51806,#51807,#51808,#51809,#51810,#51811,#51812,
#51813,#51814,#51815,#51816,#51817,#51818,#51819,#51820,#51821,#51822,#51823,
#51824,#51825,#51826,#51827,#51828,#51829,#51830,#51831,#51832,#51833,#51834,
#51835,#51836,#51837,#51838),(#51839,#51840,#51841,#51842,#51843,#51844,
#51845,#51846,#51847,#51848,#51849,#51850,#51851,#51852,#51853,#51854,#51855,
#51856,#51857,#51858,#51859,#51860,#51861,#51862,#51863,#51864,#51865,#51866,
#51867,#51868,#51869,#51870,#51871,#51872,#51873,#51874,#51875,#51876,#51877,
#51878,#51879,#51880,#51881,#51882,#51883,#51884,#51885,#51886,#51887,#51888,
#51889,#51890,#51891,#51892,#51893,#51894,#51895,#51896,#51897,#51898,#51899,
#51900,#51901,#51902,#51903,#51904,#51905,#51906,#51907,#51908,#51909,#51910,
#51911,#51912,#51913,#51914,#51915,#51916,#51917,#51918,#51919,#51920,#51921,
#51922,#51923,#51924),(#51925,#51926,#51927,#51928,#51929,#51930,#51931,
#51932,#51933,#51934,#51935,#51936,#51937,#51938,#51939,#51940,#51941,#51942,
#51943,#51944,#51945,#51946,#51947,#51948,#51949,#51950,#51951,#51952,#51953,
#51954,#51955,#51956,#51957,#51958,#51959,#51960,#51961,#51962,#51963,#51964,
#51965,#51966,#51967,#51968,#51969,#51970,#51971,#51972,#51973,#51974,#51975,
#51976,#51977,#51978,#51979,#51980,#51981,#51982,#51983,#51984,#51985,#51986,
#51987,#51988,#51989,#51990,#51991,#51992,#51993,#51994,#51995,#51996,#51997,
#51998,#51999,#52000,#52001,#52002,#52003,#52004,#52005,#52006,#52007,#52008,
#52009,#52010),(#52011,#52012,#52013,#52014,#52015,#52016,#52017,#52018,
#52019,#52020,#52021,#52022,#52023,#52024,#52025,#52026,#52027,#52028,#52029,
#52030,#52031,#52032,#52033,#52034,#52035,#52036,#52037,#52038,#52039,#52040,
#52041,#52042,#52043,#52044,#52045,#52046,#52047,#52048,#52049,#52050,#52051,
#52052,#52053,#52054,#52055,#52056,#52057,#52058,#52059,#52060,#52061,#52062,
#52063,#52064,#52065,#52066,#52067,#52068,#52069,#52070,#52071,#52072,#52073,
#52074,#52075,#52076,#52077,#52078,#52079,#52080,#52081,#52082,#52083,#52084,
#52085,#52086,#52087,#52088,#52089,#52090,#52091,#52092,#52093,#52094,#52095,
#52096)),.UNSPECIFIED.,.F.,.F.,.F.,(4,4),(4,1,1,1,1,1,1,1,1,1,1,1,1,1,1,
1,1,1,1,1,1,1,1,1,1,1,1,1,1,1,1,1,1,1,1,1,1,1,1,1,1,1,1,1,1,1,1,1,1,1,1,
1,1,1,1,1,1,1,1,1,1,1,1,1,1,1,1,1,1,1,1,1,1,1,1,1,1,1,1,1,1,1,1,4),(0.,
0.0448889834294935),(11.8615800042566,12.8591513772396,13.8567227502225,
14.8542941232054,15.8518654961884,16.8494368691713,17.8470082421542,18.8445796151372,
19.8421509881201,20.839722361103,21.837293734086,22.8348651070689,23.8324364800518,
24.8300078530348,25.8275792260177,26.8251505990006,27.8227219719836,28.8202933449665,
29.8178647179494,30.8154360909324,31.8130074639153,32.8105788368982,33.8081502098811,
34.8057215828641,35.803292955847,36.80086432883,37.7984357018129,38.7960070747958,
39.7935784477787,40.7911498207617,41.7887211937446,42.7862925667275,43.7838639397105,
44.7814353126934,45.7790066856763,46.7765780586593,47.7741494316422,48.7717208046251,
49.7692921776081,50.766863550591,51.7644349235739,52.7620062965569,53.7595776695398,
54.7571490425227,55.7547204155057,56.7522917884886,57.7498631614715,58.7474345344545,
59.7450059074374,60.7425772804203,61.7401486534033,62.7377200263862,63.7352913993691,
64.7328627723521,65.730434145335,66.7280055183179,67.7255768913009,68.7231482642838,
69.7207196372667,70.7182910102497,71.7158623832326,72.7134337562155,73.7110051291985,
74.7085765021814,75.7061478751643,76.7037192481473,77.7012906211302,78.6988619941131,
79.696433367096,80.694004740079,81.6915761130619,82.6891474860448,83.6867188590278,
84.6842902320107,85.6818616049936,86.6794329779766,87.6770043509595,88.6745757239424,
89.6721470969254,90.6697184699083,91.6672898428912,92.6648612158742,93.6624325888571,
94.66000396184),.UNSPECIFIED.);
#645=B_SPLINE_SURFACE_WITH_KNOTS('',3,3,((#52204,#52205,#52206,#52207,#52208,
#52209,#52210,#52211,#52212,#52213,#52214,#52215,#52216,#52217,#52218,#52219,
#52220,#52221,#52222,#52223,#52224,#52225,#52226,#52227,#52228,#52229,#52230,
#52231,#52232,#52233,#52234,#52235,#52236,#52237,#52238,#52239,#52240,#52241,
#52242,#52243,#52244,#52245,#52246,#52247,#52248,#52249,#52250,#52251,#52252,
#52253,#52254,#52255,#52256,#52257,#52258,#52259,#52260,#52261,#52262,#52263,
#52264,#52265,#52266,#52267,#52268,#52269,#52270,#52271,#52272,#52273,#52274,
#52275,#52276,#52277,#52278,#52279,#52280,#52281,#52282,#52283,#52284,#52285,
#52286,#52287,#52288,#52289),(#52290,#52291,#52292,#52293,#52294,#52295,
#52296,#52297,#52298,#52299,#52300,#52301,#52302,#52303,#52304,#52305,#52306,
#52307,#52308,#52309,#52310,#52311,#52312,#52313,#52314,#52315,#52316,#52317,
#52318,#52319,#52320,#52321,#52322,#52323,#52324,#52325,#52326,#52327,#52328,
#52329,#52330,#52331,#52332,#52333,#52334,#52335,#52336,#52337,#52338,#52339,
#52340,#52341,#52342,#52343,#52344,#52345,#52346,#52347,#52348,#52349,#52350,
#52351,#52352,#52353,#52354,#52355,#52356,#52357,#52358,#52359,#52360,#52361,
#52362,#52363,#52364,#52365,#52366,#52367,#52368,#52369,#52370,#52371,#52372,
#52373,#52374,#52375),(#52376,#52377,#52378,#52379,#52380,#52381,#52382,
#52383,#52384,#52385,#52386,#52387,#52388,#52389,#52390,#52391,#52392,#52393,
#52394,#52395,#52396,#52397,#52398,#52399,#52400,#52401,#52402,#52403,#52404,
#52405,#52406,#52407,#52408,#52409,#52410,#52411,#52412,#52413,#52414,#52415,
#52416,#52417,#52418,#52419,#52420,#52421,#52422,#52423,#52424,#52425,#52426,
#52427,#52428,#52429,#52430,#52431,#52432,#52433,#52434,#52435,#52436,#52437,
#52438,#52439,#52440,#52441,#52442,#52443,#52444,#52445,#52446,#52447,#52448,
#52449,#52450,#52451,#52452,#52453,#52454,#52455,#52456,#52457,#52458,#52459,
#52460,#52461),(#52462,#52463,#52464,#52465,#52466,#52467,#52468,#52469,
#52470,#52471,#52472,#52473,#52474,#52475,#52476,#52477,#52478,#52479,#52480,
#52481,#52482,#52483,#52484,#52485,#52486,#52487,#52488,#52489,#52490,#52491,
#52492,#52493,#52494,#52495,#52496,#52497,#52498,#52499,#52500,#52501,#52502,
#52503,#52504,#52505,#52506,#52507,#52508,#52509,#52510,#52511,#52512,#52513,
#52514,#52515,#52516,#52517,#52518,#52519,#52520,#52521,#52522,#52523,#52524,
#52525,#52526,#52527,#52528,#52529,#52530,#52531,#52532,#52533,#52534,#52535,
#52536,#52537,#52538,#52539,#52540,#52541,#52542,#52543,#52544,#52545,#52546,
#52547)),.UNSPECIFIED.,.F.,.F.,.F.,(4,4),(4,1,1,1,1,1,1,1,1,1,1,1,1,1,1,
1,1,1,1,1,1,1,1,1,1,1,1,1,1,1,1,1,1,1,1,1,1,1,1,1,1,1,1,1,1,1,1,1,1,1,1,
1,1,1,1,1,1,1,1,1,1,1,1,1,1,1,1,1,1,1,1,1,1,1,1,1,1,1,1,1,1,1,1,4),(0.,
0.0448889834294935),(14.3981410127769,15.3957123857598,16.3932837587428,
17.3908551317257,18.3884265047086,19.3859978776916,20.3835692506745,21.3811406236574,
22.3787119966404,23.3762833696233,24.3738547426062,25.3714261155892,26.3689974885721,
27.366568861555,28.364140234538,29.3617116075209,30.3592829805038,31.3568543534868,
32.3544257264697,33.3519970994526,34.3495684724355,35.3471398454185,36.3447112184014,
37.3422825913843,38.3398539643673,39.3374253373502,40.3349967103332,41.3325680833161,
42.330139456299,43.3277108292819,44.3252822022649,45.3228535752478,46.3204249482307,
47.3179963212137,48.3155676941966,49.3131390671795,50.3107104401625,51.3082818131454,
52.3058531861283,53.3034245591113,54.3009959320942,55.2985673050771,56.2961386780601,
57.293710051043,58.2912814240259,59.2888527970089,60.2864241699918,61.2839955429747,
62.2815669159577,63.2791382889406,64.2767096619235,65.2742810349065,66.2718524078894,
67.2694237808723,68.2669951538553,69.2645665268382,70.2621378998211,71.2597092728041,
72.257280645787,73.2548520187699,74.2524233917529,75.2499947647358,76.2475661377187,
77.2451375107017,78.2427088836846,79.2402802566675,80.2378516296505,81.2354230026334,
82.2329943756163,83.2305657485992,84.2281371215822,85.2257084945651,86.223279867548,
87.220851240531,88.2184226135139,89.2159939864968,90.2135653594798,91.2111367324627,
92.2087081054456,93.2062794784286,94.2038508514115,95.2014222243944,96.1989935973774,
97.1965649703603),.UNSPECIFIED.);
#646=B_SPLINE_SURFACE_WITH_KNOTS('',3,3,((#60804,#60805,#60806,#60807,#60808,
#60809,#60810,#60811,#60812,#60813,#60814,#60815,#60816,#60817,#60818,#60819,
#60820,#60821,#60822,#60823,#60824,#60825,#60826,#60827,#60828,#60829,#60830,
#60831,#60832,#60833,#60834,#60835,#60836,#60837,#60838,#60839,#60840,#60841,
#60842,#60843,#60844,#60845,#60846,#60847,#60848,#60849,#60850,#60851,#60852,
#60853,#60854,#60855,#60856,#60857,#60858,#60859),(#60860,#60861,#60862,
#60863,#60864,#60865,#60866,#60867,#60868,#60869,#60870,#60871,#60872,#60873,
#60874,#60875,#60876,#60877,#60878,#60879,#60880,#60881,#60882,#60883,#60884,
#60885,#60886,#60887,#60888,#60889,#60890,#60891,#60892,#60893,#60894,#60895,
#60896,#60897,#60898,#60899,#60900,#60901,#60902,#60903,#60904,#60905,#60906,
#60907,#60908,#60909,#60910,#60911,#60912,#60913,#60914,#60915),(#60916,
#60917,#60918,#60919,#60920,#60921,#60922,#60923,#60924,#60925,#60926,#60927,
#60928,#60929,#60930,#60931,#60932,#60933,#60934,#60935,#60936,#60937,#60938,
#60939,#60940,#60941,#60942,#60943,#60944,#60945,#60946,#60947,#60948,#60949,
#60950,#60951,#60952,#60953,#60954,#60955,#60956,#60957,#60958,#60959,#60960,
#60961,#60962,#60963,#60964,#60965,#60966,#60967,#60968,#60969,#60970,#60971),
(#60972,#60973,#60974,#60975,#60976,#60977,#60978,#60979,#60980,#60981,
#60982,#60983,#60984,#60985,#60986,#60987,#60988,#60989,#60990,#60991,#60992,
#60993,#60994,#60995,#60996,#60997,#60998,#60999,#61000,#61001,#61002,#61003,
#61004,#61005,#61006,#61007,#61008,#61009,#61010,#61011,#61012,#61013,#61014,
#61015,#61016,#61017,#61018,#61019,#61020,#61021,#61022,#61023,#61024,#61025,
#61026,#61027)),.UNSPECIFIED.,.F.,.F.,.F.,(4,4),(4,1,1,1,1,1,1,1,1,1,1,
1,1,1,1,1,1,1,1,1,1,1,1,1,1,1,1,1,1,1,1,1,1,1,1,1,1,1,1,1,1,1,1,1,1,1,1,
1,1,1,1,1,1,4),(0.,0.0321584099938623),(11.8553612635793,12.8418906022434,
13.8284199409074,14.8149492795714,15.8014786182354,16.7880079568995,17.7745372955635,
18.7610666342275,19.7475959728916,20.7341253115556,21.7206546502196,22.7071839888837,
23.6937133275477,24.6802426662117,25.6667720048757,26.6533013435398,27.6398306822038,
28.6263600208678,29.6128893595319,30.5994186981959,31.5859480368599,32.572477375524,
33.559006714188,34.545536052852,35.5320653915161,36.5185947301801,37.5051240688441,
38.4916534075081,39.4781827461722,40.4647120848362,41.4512414235002,42.4377707621643,
43.4243001008283,44.4108294394923,45.3973587781564,46.3838881168204,47.3704174554844,
48.3569467941485,49.3434761328125,50.3300054714765,51.3165348101405,52.3030641488046,
53.2895934874686,54.2761228261326,55.2626521647967,56.2491815034607,57.2357108421247,
58.2222401807888,59.2087695194528,60.1952988581168,61.1818281967808,62.1683575354449,
63.1548868741089,64.1414162127729),.UNSPECIFIED.);
#647=B_SPLINE_SURFACE_WITH_KNOTS('',3,3,((#61135,#61136,#61137,#61138,#61139,
#61140,#61141,#61142,#61143,#61144,#61145,#61146,#61147,#61148,#61149,#61150,
#61151,#61152,#61153,#61154,#61155,#61156,#61157,#61158,#61159,#61160,#61161,
#61162,#61163,#61164,#61165,#61166,#61167,#61168,#61169,#61170,#61171,#61172,
#61173,#61174,#61175,#61176,#61177,#61178,#61179,#61180,#61181,#61182,#61183,
#61184,#61185,#61186,#61187,#61188,#61189,#61190),(#61191,#61192,#61193,
#61194,#61195,#61196,#61197,#61198,#61199,#61200,#61201,#61202,#61203,#61204,
#61205,#61206,#61207,#61208,#61209,#61210,#61211,#61212,#61213,#61214,#61215,
#61216,#61217,#61218,#61219,#61220,#61221,#61222,#61223,#61224,#61225,#61226,
#61227,#61228,#61229,#61230,#61231,#61232,#61233,#61234,#61235,#61236,#61237,
#61238,#61239,#61240,#61241,#61242,#61243,#61244,#61245,#61246),(#61247,
#61248,#61249,#61250,#61251,#61252,#61253,#61254,#61255,#61256,#61257,#61258,
#61259,#61260,#61261,#61262,#61263,#61264,#61265,#61266,#61267,#61268,#61269,
#61270,#61271,#61272,#61273,#61274,#61275,#61276,#61277,#61278,#61279,#61280,
#61281,#61282,#61283,#61284,#61285,#61286,#61287,#61288,#61289,#61290,#61291,
#61292,#61293,#61294,#61295,#61296,#61297,#61298,#61299,#61300,#61301,#61302),
(#61303,#61304,#61305,#61306,#61307,#61308,#61309,#61310,#61311,#61312,
#61313,#61314,#61315,#61316,#61317,#61318,#61319,#61320,#61321,#61322,#61323,
#61324,#61325,#61326,#61327,#61328,#61329,#61330,#61331,#61332,#61333,#61334,
#61335,#61336,#61337,#61338,#61339,#61340,#61341,#61342,#61343,#61344,#61345,
#61346,#61347,#61348,#61349,#61350,#61351,#61352,#61353,#61354,#61355,#61356,
#61357,#61358)),.UNSPECIFIED.,.F.,.F.,.F.,(4,4),(4,1,1,1,1,1,1,1,1,1,1,
1,1,1,1,1,1,1,1,1,1,1,1,1,1,1,1,1,1,1,1,1,1,1,1,1,1,1,1,1,1,1,1,1,1,1,1,
1,1,1,1,1,1,4),(0.,0.0321584099938623),(14.3984001269718,15.3849294656359,
16.3714588042999,17.3579881429639,18.3445174816279,19.331046820292,20.317576158956,
21.30410549762,22.2906348362841,23.2771641749481,24.2636935136121,25.2502228522762,
26.2367521909402,27.2232815296042,28.2098108682683,29.1963402069323,30.1828695455963,
31.1693988842603,32.1559282229244,33.1424575615884,34.1289869002524,35.1155162389165,
36.1020455775805,37.0885749162445,38.0751042549086,39.0616335935726,40.0481629322366,
41.0346922709007,42.0212216095647,43.0077509482287,43.9942802868927,44.9808096255568,
45.9673389642208,46.9538683028848,47.9403976415489,48.9269269802129,49.9134563188769,
50.899985657541,51.886514996205,52.873044334869,53.8595736735331,54.8461030121971,
55.8326323508611,56.8191616895252,57.8056910281892,58.7922203668532,59.7787497055172,
60.7652790441813,61.7518083828453,62.7383377215093,63.7248670601734,64.7113963988374,
65.6979257375014,66.6844550761655),.UNSPECIFIED.);
#648=B_SPLINE_SURFACE_WITH_KNOTS('',3,3,((#61645,#61646,#61647,#61648,#61649,
#61650,#61651,#61652,#61653,#61654,#61655,#61656,#61657,#61658,#61659,#61660,
#61661,#61662,#61663,#61664,#61665,#61666,#61667,#61668,#61669,#61670,#61671,
#61672,#61673,#61674,#61675,#61676,#61677,#61678,#61679,#61680,#61681,#61682,
#61683,#61684,#61685,#61686,#61687,#61688,#61689,#61690,#61691,#61692,#61693,
#61694,#61695,#61696,#61697,#61698,#61699,#61700),(#61701,#61702,#61703,
#61704,#61705,#61706,#61707,#61708,#61709,#61710,#61711,#61712,#61713,#61714,
#61715,#61716,#61717,#61718,#61719,#61720,#61721,#61722,#61723,#61724,#61725,
#61726,#61727,#61728,#61729,#61730,#61731,#61732,#61733,#61734,#61735,#61736,
#61737,#61738,#61739,#61740,#61741,#61742,#61743,#61744,#61745,#61746,#61747,
#61748,#61749,#61750,#61751,#61752,#61753,#61754,#61755,#61756),(#61757,
#61758,#61759,#61760,#61761,#61762,#61763,#61764,#61765,#61766,#61767,#61768,
#61769,#61770,#61771,#61772,#61773,#61774,#61775,#61776,#61777,#61778,#61779,
#61780,#61781,#61782,#61783,#61784,#61785,#61786,#61787,#61788,#61789,#61790,
#61791,#61792,#61793,#61794,#61795,#61796,#61797,#61798,#61799,#61800,#61801,
#61802,#61803,#61804,#61805,#61806,#61807,#61808,#61809,#61810,#61811,#61812),
(#61813,#61814,#61815,#61816,#61817,#61818,#61819,#61820,#61821,#61822,
#61823,#61824,#61825,#61826,#61827,#61828,#61829,#61830,#61831,#61832,#61833,
#61834,#61835,#61836,#61837,#61838,#61839,#61840,#61841,#61842,#61843,#61844,
#61845,#61846,#61847,#61848,#61849,#61850,#61851,#61852,#61853,#61854,#61855,
#61856,#61857,#61858,#61859,#61860,#61861,#61862,#61863,#61864,#61865,#61866,
#61867,#61868)),.UNSPECIFIED.,.F.,.F.,.F.,(4,4),(4,1,1,1,1,1,1,1,1,1,1,
1,1,1,1,1,1,1,1,1,1,1,1,1,1,1,1,1,1,1,1,1,1,1,1,1,1,1,1,1,1,1,1,1,1,1,1,
1,1,1,1,1,1,4),(0.,0.0321584099938627),(11.8553612635793,12.8418906022434,
13.8284199409074,14.8149492795714,15.8014786182355,16.7880079568995,17.7745372955635,
18.7610666342275,19.7475959728916,20.7341253115556,21.7206546502196,22.7071839888837,
23.6937133275477,24.6802426662117,25.6667720048758,26.6533013435398,27.6398306822038,
28.6263600208679,29.6128893595319,30.5994186981959,31.5859480368599,32.572477375524,
33.559006714188,34.545536052852,35.5320653915161,36.5185947301801,37.5051240688441,
38.4916534075082,39.4781827461722,40.4647120848362,41.4512414235002,42.4377707621643,
43.4243001008283,44.4108294394923,45.3973587781564,46.3838881168204,47.3704174554844,
48.3569467941485,49.3434761328125,50.3300054714765,51.3165348101406,52.3030641488046,
53.2895934874686,54.2761228261326,55.2626521647967,56.2491815034607,57.2357108421247,
58.2222401807888,59.2087695194528,60.1952988581168,61.1818281967809,62.1683575354449,
63.1548868741089,64.141416212773),.UNSPECIFIED.);
#649=B_SPLINE_SURFACE_WITH_KNOTS('',3,3,((#61976,#61977,#61978,#61979,#61980,
#61981,#61982,#61983,#61984,#61985,#61986,#61987,#61988,#61989,#61990,#61991,
#61992,#61993,#61994,#61995,#61996,#61997,#61998,#61999,#62000,#62001,#62002,
#62003,#62004,#62005,#62006,#62007,#62008,#62009,#62010,#62011,#62012,#62013,
#62014,#62015,#62016,#62017,#62018,#62019,#62020,#62021,#62022,#62023,#62024,
#62025,#62026,#62027,#62028,#62029,#62030,#62031),(#62032,#62033,#62034,
#62035,#62036,#62037,#62038,#62039,#62040,#62041,#62042,#62043,#62044,#62045,
#62046,#62047,#62048,#62049,#62050,#62051,#62052,#62053,#62054,#62055,#62056,
#62057,#62058,#62059,#62060,#62061,#62062,#62063,#62064,#62065,#62066,#62067,
#62068,#62069,#62070,#62071,#62072,#62073,#62074,#62075,#62076,#62077,#62078,
#62079,#62080,#62081,#62082,#62083,#62084,#62085,#62086,#62087),(#62088,
#62089,#62090,#62091,#62092,#62093,#62094,#62095,#62096,#62097,#62098,#62099,
#62100,#62101,#62102,#62103,#62104,#62105,#62106,#62107,#62108,#62109,#62110,
#62111,#62112,#62113,#62114,#62115,#62116,#62117,#62118,#62119,#62120,#62121,
#62122,#62123,#62124,#62125,#62126,#62127,#62128,#62129,#62130,#62131,#62132,
#62133,#62134,#62135,#62136,#62137,#62138,#62139,#62140,#62141,#62142,#62143),
(#62144,#62145,#62146,#62147,#62148,#62149,#62150,#62151,#62152,#62153,
#62154,#62155,#62156,#62157,#62158,#62159,#62160,#62161,#62162,#62163,#62164,
#62165,#62166,#62167,#62168,#62169,#62170,#62171,#62172,#62173,#62174,#62175,
#62176,#62177,#62178,#62179,#62180,#62181,#62182,#62183,#62184,#62185,#62186,
#62187,#62188,#62189,#62190,#62191,#62192,#62193,#62194,#62195,#62196,#62197,
#62198,#62199)),.UNSPECIFIED.,.F.,.F.,.F.,(4,4),(4,1,1,1,1,1,1,1,1,1,1,
1,1,1,1,1,1,1,1,1,1,1,1,1,1,1,1,1,1,1,1,1,1,1,1,1,1,1,1,1,1,1,1,1,1,1,1,
1,1,1,1,1,1,4),(0.,0.0321584099938627),(14.3984001269718,15.3849294656359,
16.3714588042999,17.3579881429639,18.344517481628,19.331046820292,20.317576158956,
21.3041054976201,22.2906348362841,23.2771641749481,24.2636935136121,25.2502228522762,
26.2367521909402,27.2232815296042,28.2098108682683,29.1963402069323,30.1828695455963,
31.1693988842604,32.1559282229244,33.1424575615884,34.1289869002525,35.1155162389165,
36.1020455775805,37.0885749162445,38.0751042549086,39.0616335935726,40.0481629322366,
41.0346922709007,42.0212216095647,43.0077509482287,43.9942802868928,44.9808096255568,
45.9673389642208,46.9538683028849,47.9403976415489,48.9269269802129,49.9134563188769,
50.899985657541,51.886514996205,52.873044334869,53.8595736735331,54.8461030121971,
55.8326323508611,56.8191616895252,57.8056910281892,58.7922203668532,59.7787497055173,
60.7652790441813,61.7518083828453,62.7383377215094,63.7248670601734,64.7113963988374,
65.6979257375014,66.6844550761655),.UNSPECIFIED.);
#650=B_SPLINE_SURFACE_WITH_KNOTS('',3,3,((#62486,#62487,#62488,#62489,#62490,
#62491,#62492,#62493,#62494,#62495,#62496,#62497,#62498,#62499,#62500,#62501,
#62502,#62503,#62504,#62505,#62506,#62507,#62508,#62509,#62510,#62511,#62512,
#62513,#62514,#62515,#62516,#62517,#62518,#62519,#62520,#62521,#62522,#62523,
#62524,#62525,#62526,#62527,#62528,#62529,#62530,#62531,#62532,#62533,#62534,
#62535,#62536,#62537,#62538,#62539,#62540,#62541),(#62542,#62543,#62544,
#62545,#62546,#62547,#62548,#62549,#62550,#62551,#62552,#62553,#62554,#62555,
#62556,#62557,#62558,#62559,#62560,#62561,#62562,#62563,#62564,#62565,#62566,
#62567,#62568,#62569,#62570,#62571,#62572,#62573,#62574,#62575,#62576,#62577,
#62578,#62579,#62580,#62581,#62582,#62583,#62584,#62585,#62586,#62587,#62588,
#62589,#62590,#62591,#62592,#62593,#62594,#62595,#62596,#62597),(#62598,
#62599,#62600,#62601,#62602,#62603,#62604,#62605,#62606,#62607,#62608,#62609,
#62610,#62611,#62612,#62613,#62614,#62615,#62616,#62617,#62618,#62619,#62620,
#62621,#62622,#62623,#62624,#62625,#62626,#62627,#62628,#62629,#62630,#62631,
#62632,#62633,#62634,#62635,#62636,#62637,#62638,#62639,#62640,#62641,#62642,
#62643,#62644,#62645,#62646,#62647,#62648,#62649,#62650,#62651,#62652,#62653),
(#62654,#62655,#62656,#62657,#62658,#62659,#62660,#62661,#62662,#62663,
#62664,#62665,#62666,#62667,#62668,#62669,#62670,#62671,#62672,#62673,#62674,
#62675,#62676,#62677,#62678,#62679,#62680,#62681,#62682,#62683,#62684,#62685,
#62686,#62687,#62688,#62689,#62690,#62691,#62692,#62693,#62694,#62695,#62696,
#62697,#62698,#62699,#62700,#62701,#62702,#62703,#62704,#62705,#62706,#62707,
#62708,#62709)),.UNSPECIFIED.,.F.,.F.,.F.,(4,4),(4,1,1,1,1,1,1,1,1,1,1,
1,1,1,1,1,1,1,1,1,1,1,1,1,1,1,1,1,1,1,1,1,1,1,1,1,1,1,1,1,1,1,1,1,1,1,1,
1,1,1,1,1,1,4),(0.,0.0321584099938621),(11.8553612635793,12.8418906022434,
13.8284199409074,14.8149492795714,15.8014786182354,16.7880079568995,17.7745372955635,
18.7610666342275,19.7475959728916,20.7341253115556,21.7206546502196,22.7071839888837,
23.6937133275477,24.6802426662117,25.6667720048758,26.6533013435398,27.6398306822038,
28.6263600208678,29.6128893595319,30.5994186981959,31.5859480368599,32.572477375524,
33.559006714188,34.545536052852,35.5320653915161,36.5185947301801,37.5051240688441,
38.4916534075081,39.4781827461722,40.4647120848362,41.4512414235002,42.4377707621643,
43.4243001008283,44.4108294394923,45.3973587781564,46.3838881168204,47.3704174554844,
48.3569467941485,49.3434761328125,50.3300054714765,51.3165348101405,52.3030641488046,
53.2895934874686,54.2761228261326,55.2626521647967,56.2491815034607,57.2357108421247,
58.2222401807888,59.2087695194528,60.1952988581168,61.1818281967808,62.1683575354449,
63.1548868741089,64.1414162127729),.UNSPECIFIED.);
#651=B_SPLINE_SURFACE_WITH_KNOTS('',3,3,((#62817,#62818,#62819,#62820,#62821,
#62822,#62823,#62824,#62825,#62826,#62827,#62828,#62829,#62830,#62831,#62832,
#62833,#62834,#62835,#62836,#62837,#62838,#62839,#62840,#62841,#62842,#62843,
#62844,#62845,#62846,#62847,#62848,#62849,#62850,#62851,#62852,#62853,#62854,
#62855,#62856,#62857,#62858,#62859,#62860,#62861,#62862,#62863,#62864,#62865,
#62866,#62867,#62868,#62869,#62870,#62871,#62872),(#62873,#62874,#62875,
#62876,#62877,#62878,#62879,#62880,#62881,#62882,#62883,#62884,#62885,#62886,
#62887,#62888,#62889,#62890,#62891,#62892,#62893,#62894,#62895,#62896,#62897,
#62898,#62899,#62900,#62901,#62902,#62903,#62904,#62905,#62906,#62907,#62908,
#62909,#62910,#62911,#62912,#62913,#62914,#62915,#62916,#62917,#62918,#62919,
#62920,#62921,#62922,#62923,#62924,#62925,#62926,#62927,#62928),(#62929,
#62930,#62931,#62932,#62933,#62934,#62935,#62936,#62937,#62938,#62939,#62940,
#62941,#62942,#62943,#62944,#62945,#62946,#62947,#62948,#62949,#62950,#62951,
#62952,#62953,#62954,#62955,#62956,#62957,#62958,#62959,#62960,#62961,#62962,
#62963,#62964,#62965,#62966,#62967,#62968,#62969,#62970,#62971,#62972,#62973,
#62974,#62975,#62976,#62977,#62978,#62979,#62980,#62981,#62982,#62983,#62984),
(#62985,#62986,#62987,#62988,#62989,#62990,#62991,#62992,#62993,#62994,
#62995,#62996,#62997,#62998,#62999,#63000,#63001,#63002,#63003,#63004,#63005,
#63006,#63007,#63008,#63009,#63010,#63011,#63012,#63013,#63014,#63015,#63016,
#63017,#63018,#63019,#63020,#63021,#63022,#63023,#63024,#63025,#63026,#63027,
#63028,#63029,#63030,#63031,#63032,#63033,#63034,#63035,#63036,#63037,#63038,
#63039,#63040)),.UNSPECIFIED.,.F.,.F.,.F.,(4,4),(4,1,1,1,1,1,1,1,1,1,1,
1,1,1,1,1,1,1,1,1,1,1,1,1,1,1,1,1,1,1,1,1,1,1,1,1,1,1,1,1,1,1,1,1,1,1,1,
1,1,1,1,1,1,4),(0.,0.0321584099938621),(14.3984001269718,15.3849294656359,
16.3714588042999,17.3579881429639,18.3445174816279,19.331046820292,20.317576158956,
21.30410549762,22.2906348362841,23.2771641749481,24.2636935136121,25.2502228522762,
26.2367521909402,27.2232815296042,28.2098108682683,29.1963402069323,30.1828695455963,
31.1693988842603,32.1559282229244,33.1424575615884,34.1289869002524,35.1155162389165,
36.1020455775805,37.0885749162445,38.0751042549086,39.0616335935726,40.0481629322366,
41.0346922709007,42.0212216095647,43.0077509482287,43.9942802868928,44.9808096255568,
45.9673389642208,46.9538683028848,47.9403976415489,48.9269269802129,49.9134563188769,
50.899985657541,51.886514996205,52.873044334869,53.8595736735331,54.8461030121971,
55.8326323508611,56.8191616895252,57.8056910281892,58.7922203668532,59.7787497055172,
60.7652790441813,61.7518083828453,62.7383377215093,63.7248670601734,64.7113963988374,
65.6979257375014,66.6844550761655),.UNSPECIFIED.);
#652=B_SPLINE_SURFACE_WITH_KNOTS('',3,3,((#63327,#63328,#63329,#63330,#63331,
#63332,#63333,#63334,#63335,#63336,#63337,#63338,#63339,#63340,#63341,#63342,
#63343,#63344,#63345,#63346,#63347,#63348,#63349,#63350,#63351,#63352,#63353,
#63354,#63355,#63356,#63357,#63358,#63359,#63360,#63361,#63362,#63363,#63364,
#63365,#63366,#63367,#63368,#63369,#63370,#63371,#63372,#63373,#63374,#63375,
#63376,#63377,#63378,#63379,#63380,#63381,#63382),(#63383,#63384,#63385,
#63386,#63387,#63388,#63389,#63390,#63391,#63392,#63393,#63394,#63395,#63396,
#63397,#63398,#63399,#63400,#63401,#63402,#63403,#63404,#63405,#63406,#63407,
#63408,#63409,#63410,#63411,#63412,#63413,#63414,#63415,#63416,#63417,#63418,
#63419,#63420,#63421,#63422,#63423,#63424,#63425,#63426,#63427,#63428,#63429,
#63430,#63431,#63432,#63433,#63434,#63435,#63436,#63437,#63438),(#63439,
#63440,#63441,#63442,#63443,#63444,#63445,#63446,#63447,#63448,#63449,#63450,
#63451,#63452,#63453,#63454,#63455,#63456,#63457,#63458,#63459,#63460,#63461,
#63462,#63463,#63464,#63465,#63466,#63467,#63468,#63469,#63470,#63471,#63472,
#63473,#63474,#63475,#63476,#63477,#63478,#63479,#63480,#63481,#63482,#63483,
#63484,#63485,#63486,#63487,#63488,#63489,#63490,#63491,#63492,#63493,#63494),
(#63495,#63496,#63497,#63498,#63499,#63500,#63501,#63502,#63503,#63504,
#63505,#63506,#63507,#63508,#63509,#63510,#63511,#63512,#63513,#63514,#63515,
#63516,#63517,#63518,#63519,#63520,#63521,#63522,#63523,#63524,#63525,#63526,
#63527,#63528,#63529,#63530,#63531,#63532,#63533,#63534,#63535,#63536,#63537,
#63538,#63539,#63540,#63541,#63542,#63543,#63544,#63545,#63546,#63547,#63548,
#63549,#63550)),.UNSPECIFIED.,.F.,.F.,.F.,(4,4),(4,1,1,1,1,1,1,1,1,1,1,
1,1,1,1,1,1,1,1,1,1,1,1,1,1,1,1,1,1,1,1,1,1,1,1,1,1,1,1,1,1,1,1,1,1,1,1,
1,1,1,1,1,1,4),(0.,0.0321584099938623),(11.8553612635793,12.8418906022434,
13.8284199409074,14.8149492795714,15.8014786182354,16.7880079568995,17.7745372955635,
18.7610666342275,19.7475959728916,20.7341253115556,21.7206546502196,22.7071839888837,
23.6937133275477,24.6802426662117,25.6667720048757,26.6533013435398,27.6398306822038,
28.6263600208678,29.6128893595319,30.5994186981959,31.5859480368599,32.572477375524,
33.559006714188,34.545536052852,35.5320653915161,36.5185947301801,37.5051240688441,
38.4916534075081,39.4781827461722,40.4647120848362,41.4512414235002,42.4377707621643,
43.4243001008283,44.4108294394923,45.3973587781564,46.3838881168204,47.3704174554844,
48.3569467941485,49.3434761328125,50.3300054714765,51.3165348101405,52.3030641488046,
53.2895934874686,54.2761228261326,55.2626521647967,56.2491815034607,57.2357108421247,
58.2222401807888,59.2087695194528,60.1952988581168,61.1818281967808,62.1683575354449,
63.1548868741089,64.1414162127729),.UNSPECIFIED.);
#653=B_SPLINE_SURFACE_WITH_KNOTS('',3,3,((#63658,#63659,#63660,#63661,#63662,
#63663,#63664,#63665,#63666,#63667,#63668,#63669,#63670,#63671,#63672,#63673,
#63674,#63675,#63676,#63677,#63678,#63679,#63680,#63681,#63682,#63683,#63684,
#63685,#63686,#63687,#63688,#63689,#63690,#63691,#63692,#63693,#63694,#63695,
#63696,#63697,#63698,#63699,#63700,#63701,#63702,#63703,#63704,#63705,#63706,
#63707,#63708,#63709,#63710,#63711,#63712,#63713),(#63714,#63715,#63716,
#63717,#63718,#63719,#63720,#63721,#63722,#63723,#63724,#63725,#63726,#63727,
#63728,#63729,#63730,#63731,#63732,#63733,#63734,#63735,#63736,#63737,#63738,
#63739,#63740,#63741,#63742,#63743,#63744,#63745,#63746,#63747,#63748,#63749,
#63750,#63751,#63752,#63753,#63754,#63755,#63756,#63757,#63758,#63759,#63760,
#63761,#63762,#63763,#63764,#63765,#63766,#63767,#63768,#63769),(#63770,
#63771,#63772,#63773,#63774,#63775,#63776,#63777,#63778,#63779,#63780,#63781,
#63782,#63783,#63784,#63785,#63786,#63787,#63788,#63789,#63790,#63791,#63792,
#63793,#63794,#63795,#63796,#63797,#63798,#63799,#63800,#63801,#63802,#63803,
#63804,#63805,#63806,#63807,#63808,#63809,#63810,#63811,#63812,#63813,#63814,
#63815,#63816,#63817,#63818,#63819,#63820,#63821,#63822,#63823,#63824,#63825),
(#63826,#63827,#63828,#63829,#63830,#63831,#63832,#63833,#63834,#63835,
#63836,#63837,#63838,#63839,#63840,#63841,#63842,#63843,#63844,#63845,#63846,
#63847,#63848,#63849,#63850,#63851,#63852,#63853,#63854,#63855,#63856,#63857,
#63858,#63859,#63860,#63861,#63862,#63863,#63864,#63865,#63866,#63867,#63868,
#63869,#63870,#63871,#63872,#63873,#63874,#63875,#63876,#63877,#63878,#63879,
#63880,#63881)),.UNSPECIFIED.,.F.,.F.,.F.,(4,4),(4,1,1,1,1,1,1,1,1,1,1,
1,1,1,1,1,1,1,1,1,1,1,1,1,1,1,1,1,1,1,1,1,1,1,1,1,1,1,1,1,1,1,1,1,1,1,1,
1,1,1,1,1,1,4),(0.,0.0321584099938623),(14.3984001269718,15.3849294656359,
16.3714588042999,17.3579881429639,18.3445174816279,19.331046820292,20.317576158956,
21.30410549762,22.2906348362841,23.2771641749481,24.2636935136121,25.2502228522762,
26.2367521909402,27.2232815296042,28.2098108682683,29.1963402069323,30.1828695455963,
31.1693988842603,32.1559282229244,33.1424575615884,34.1289869002524,35.1155162389165,
36.1020455775805,37.0885749162445,38.0751042549086,39.0616335935726,40.0481629322366,
41.0346922709007,42.0212216095647,43.0077509482287,43.9942802868928,44.9808096255568,
45.9673389642208,46.9538683028848,47.9403976415489,48.9269269802129,49.9134563188769,
50.899985657541,51.886514996205,52.873044334869,53.8595736735331,54.8461030121971,
55.8326323508611,56.8191616895252,57.8056910281892,58.7922203668532,59.7787497055172,
60.7652790441813,61.7518083828453,62.7383377215093,63.7248670601734,64.7113963988374,
65.6979257375014,66.6844550761655),.UNSPECIFIED.);
#654=B_SPLINE_SURFACE_WITH_KNOTS('',3,3,((#64168,#64169,#64170,#64171,#64172,
#64173,#64174,#64175,#64176,#64177,#64178,#64179,#64180,#64181,#64182,#64183,
#64184,#64185,#64186,#64187,#64188,#64189,#64190,#64191,#64192,#64193,#64194,
#64195,#64196,#64197,#64198,#64199,#64200,#64201,#64202,#64203,#64204,#64205,
#64206,#64207,#64208,#64209,#64210,#64211,#64212,#64213,#64214,#64215,#64216,
#64217,#64218,#64219,#64220,#64221,#64222,#64223),(#64224,#64225,#64226,
#64227,#64228,#64229,#64230,#64231,#64232,#64233,#64234,#64235,#64236,#64237,
#64238,#64239,#64240,#64241,#64242,#64243,#64244,#64245,#64246,#64247,#64248,
#64249,#64250,#64251,#64252,#64253,#64254,#64255,#64256,#64257,#64258,#64259,
#64260,#64261,#64262,#64263,#64264,#64265,#64266,#64267,#64268,#64269,#64270,
#64271,#64272,#64273,#64274,#64275,#64276,#64277,#64278,#64279),(#64280,
#64281,#64282,#64283,#64284,#64285,#64286,#64287,#64288,#64289,#64290,#64291,
#64292,#64293,#64294,#64295,#64296,#64297,#64298,#64299,#64300,#64301,#64302,
#64303,#64304,#64305,#64306,#64307,#64308,#64309,#64310,#64311,#64312,#64313,
#64314,#64315,#64316,#64317,#64318,#64319,#64320,#64321,#64322,#64323,#64324,
#64325,#64326,#64327,#64328,#64329,#64330,#64331,#64332,#64333,#64334,#64335),
(#64336,#64337,#64338,#64339,#64340,#64341,#64342,#64343,#64344,#64345,
#64346,#64347,#64348,#64349,#64350,#64351,#64352,#64353,#64354,#64355,#64356,
#64357,#64358,#64359,#64360,#64361,#64362,#64363,#64364,#64365,#64366,#64367,
#64368,#64369,#64370,#64371,#64372,#64373,#64374,#64375,#64376,#64377,#64378,
#64379,#64380,#64381,#64382,#64383,#64384,#64385,#64386,#64387,#64388,#64389,
#64390,#64391)),.UNSPECIFIED.,.F.,.F.,.F.,(4,4),(4,1,1,1,1,1,1,1,1,1,1,
1,1,1,1,1,1,1,1,1,1,1,1,1,1,1,1,1,1,1,1,1,1,1,1,1,1,1,1,1,1,1,1,1,1,1,1,
1,1,1,1,1,1,4),(0.,0.0321584099938627),(11.8553612635793,12.8418906022434,
13.8284199409074,14.8149492795714,15.8014786182355,16.7880079568995,17.7745372955635,
18.7610666342275,19.7475959728916,20.7341253115556,21.7206546502196,22.7071839888837,
23.6937133275477,24.6802426662117,25.6667720048758,26.6533013435398,27.6398306822038,
28.6263600208678,29.6128893595319,30.5994186981959,31.5859480368599,32.572477375524,
33.559006714188,34.545536052852,35.5320653915161,36.5185947301801,37.5051240688441,
38.4916534075082,39.4781827461722,40.4647120848362,41.4512414235002,42.4377707621643,
43.4243001008283,44.4108294394923,45.3973587781564,46.3838881168204,47.3704174554844,
48.3569467941485,49.3434761328125,50.3300054714765,51.3165348101406,52.3030641488046,
53.2895934874686,54.2761228261326,55.2626521647967,56.2491815034607,57.2357108421247,
58.2222401807888,59.2087695194528,60.1952988581168,61.1818281967809,62.1683575354449,
63.1548868741089,64.1414162127729),.UNSPECIFIED.);
#655=B_SPLINE_SURFACE_WITH_KNOTS('',3,3,((#64499,#64500,#64501,#64502,#64503,
#64504,#64505,#64506,#64507,#64508,#64509,#64510,#64511,#64512,#64513,#64514,
#64515,#64516,#64517,#64518,#64519,#64520,#64521,#64522,#64523,#64524,#64525,
#64526,#64527,#64528,#64529,#64530,#64531,#64532,#64533,#64534,#64535,#64536,
#64537,#64538,#64539,#64540,#64541,#64542,#64543,#64544,#64545,#64546,#64547,
#64548,#64549,#64550,#64551,#64552,#64553,#64554),(#64555,#64556,#64557,
#64558,#64559,#64560,#64561,#64562,#64563,#64564,#64565,#64566,#64567,#64568,
#64569,#64570,#64571,#64572,#64573,#64574,#64575,#64576,#64577,#64578,#64579,
#64580,#64581,#64582,#64583,#64584,#64585,#64586,#64587,#64588,#64589,#64590,
#64591,#64592,#64593,#64594,#64595,#64596,#64597,#64598,#64599,#64600,#64601,
#64602,#64603,#64604,#64605,#64606,#64607,#64608,#64609,#64610),(#64611,
#64612,#64613,#64614,#64615,#64616,#64617,#64618,#64619,#64620,#64621,#64622,
#64623,#64624,#64625,#64626,#64627,#64628,#64629,#64630,#64631,#64632,#64633,
#64634,#64635,#64636,#64637,#64638,#64639,#64640,#64641,#64642,#64643,#64644,
#64645,#64646,#64647,#64648,#64649,#64650,#64651,#64652,#64653,#64654,#64655,
#64656,#64657,#64658,#64659,#64660,#64661,#64662,#64663,#64664,#64665,#64666),
(#64667,#64668,#64669,#64670,#64671,#64672,#64673,#64674,#64675,#64676,
#64677,#64678,#64679,#64680,#64681,#64682,#64683,#64684,#64685,#64686,#64687,
#64688,#64689,#64690,#64691,#64692,#64693,#64694,#64695,#64696,#64697,#64698,
#64699,#64700,#64701,#64702,#64703,#64704,#64705,#64706,#64707,#64708,#64709,
#64710,#64711,#64712,#64713,#64714,#64715,#64716,#64717,#64718,#64719,#64720,
#64721,#64722)),.UNSPECIFIED.,.F.,.F.,.F.,(4,4),(4,1,1,1,1,1,1,1,1,1,1,
1,1,1,1,1,1,1,1,1,1,1,1,1,1,1,1,1,1,1,1,1,1,1,1,1,1,1,1,1,1,1,1,1,1,1,1,
1,1,1,1,1,1,4),(0.,0.0321584099938627),(14.3984001269718,15.3849294656359,
16.3714588042999,17.3579881429639,18.344517481628,19.331046820292,20.317576158956,
21.30410549762,22.2906348362841,23.2771641749481,24.2636935136121,25.2502228522762,
26.2367521909402,27.2232815296042,28.2098108682683,29.1963402069323,30.1828695455963,
31.1693988842604,32.1559282229244,33.1424575615884,34.1289869002524,35.1155162389165,
36.1020455775805,37.0885749162445,38.0751042549086,39.0616335935726,40.0481629322366,
41.0346922709007,42.0212216095647,43.0077509482287,43.9942802868928,44.9808096255568,
45.9673389642208,46.9538683028848,47.9403976415489,48.9269269802129,49.9134563188769,
50.899985657541,51.886514996205,52.873044334869,53.8595736735331,54.8461030121971,
55.8326323508611,56.8191616895252,57.8056910281892,58.7922203668532,59.7787497055172,
60.7652790441813,61.7518083828453,62.7383377215093,63.7248670601734,64.7113963988374,
65.6979257375014,66.6844550761655),.UNSPECIFIED.);
#656=B_SPLINE_SURFACE_WITH_KNOTS('',3,3,((#65029,#65030,#65031,#65032,#65033,
#65034,#65035,#65036,#65037,#65038,#65039,#65040,#65041,#65042,#65043,#65044,
#65045,#65046,#65047,#65048,#65049,#65050,#65051,#65052,#65053,#65054,#65055,
#65056,#65057,#65058,#65059,#65060,#65061,#65062,#65063,#65064,#65065,#65066,
#65067,#65068,#65069,#65070,#65071,#65072,#65073,#65074,#65075,#65076,#65077,
#65078,#65079,#65080,#65081,#65082,#65083,#65084),(#65085,#65086,#65087,
#65088,#65089,#65090,#65091,#65092,#65093,#65094,#65095,#65096,#65097,#65098,
#65099,#65100,#65101,#65102,#65103,#65104,#65105,#65106,#65107,#65108,#65109,
#65110,#65111,#65112,#65113,#65114,#65115,#65116,#65117,#65118,#65119,#65120,
#65121,#65122,#65123,#65124,#65125,#65126,#65127,#65128,#65129,#65130,#65131,
#65132,#65133,#65134,#65135,#65136,#65137,#65138,#65139,#65140),(#65141,
#65142,#65143,#65144,#65145,#65146,#65147,#65148,#65149,#65150,#65151,#65152,
#65153,#65154,#65155,#65156,#65157,#65158,#65159,#65160,#65161,#65162,#65163,
#65164,#65165,#65166,#65167,#65168,#65169,#65170,#65171,#65172,#65173,#65174,
#65175,#65176,#65177,#65178,#65179,#65180,#65181,#65182,#65183,#65184,#65185,
#65186,#65187,#65188,#65189,#65190,#65191,#65192,#65193,#65194,#65195,#65196),
(#65197,#65198,#65199,#65200,#65201,#65202,#65203,#65204,#65205,#65206,
#65207,#65208,#65209,#65210,#65211,#65212,#65213,#65214,#65215,#65216,#65217,
#65218,#65219,#65220,#65221,#65222,#65223,#65224,#65225,#65226,#65227,#65228,
#65229,#65230,#65231,#65232,#65233,#65234,#65235,#65236,#65237,#65238,#65239,
#65240,#65241,#65242,#65243,#65244,#65245,#65246,#65247,#65248,#65249,#65250,
#65251,#65252)),.UNSPECIFIED.,.F.,.F.,.F.,(4,4),(4,1,1,1,1,1,1,1,1,1,1,
1,1,1,1,1,1,1,1,1,1,1,1,1,1,1,1,1,1,1,1,1,1,1,1,1,1,1,1,1,1,1,1,1,1,1,1,
1,1,1,1,1,1,4),(0.,0.032158409993862),(11.8553612635794,12.8418906022434,
13.8284199409074,14.8149492795714,15.8014786182355,16.7880079568995,17.7745372955635,
18.7610666342276,19.7475959728916,20.7341253115556,21.7206546502197,22.7071839888837,
23.6937133275477,24.6802426662118,25.6667720048758,26.6533013435398,27.6398306822038,
28.6263600208679,29.6128893595319,30.5994186981959,31.58594803686,32.572477375524,
33.559006714188,34.5455360528521,35.5320653915161,36.5185947301801,37.5051240688441,
38.4916534075082,39.4781827461722,40.4647120848362,41.4512414235003,42.4377707621643,
43.4243001008283,44.4108294394924,45.3973587781564,46.3838881168204,47.3704174554844,
48.3569467941485,49.3434761328125,50.3300054714765,51.3165348101406,52.3030641488046,
53.2895934874686,54.2761228261327,55.2626521647967,56.2491815034607,57.2357108421248,
58.2222401807888,59.2087695194528,60.1952988581168,61.1818281967809,62.1683575354449,
63.1548868741089,64.141416212773),.UNSPECIFIED.);
#657=B_SPLINE_SURFACE_WITH_KNOTS('',3,3,((#65278,#65279,#65280,#65281,#65282,
#65283,#65284,#65285,#65286,#65287,#65288,#65289,#65290,#65291,#65292,#65293,
#65294,#65295,#65296,#65297,#65298,#65299,#65300,#65301,#65302,#65303,#65304,
#65305,#65306,#65307,#65308,#65309,#65310,#65311,#65312,#65313,#65314,#65315,
#65316,#65317,#65318,#65319,#65320,#65321,#65322,#65323,#65324,#65325,#65326,
#65327,#65328,#65329,#65330,#65331,#65332,#65333),(#65334,#65335,#65336,
#65337,#65338,#65339,#65340,#65341,#65342,#65343,#65344,#65345,#65346,#65347,
#65348,#65349,#65350,#65351,#65352,#65353,#65354,#65355,#65356,#65357,#65358,
#65359,#65360,#65361,#65362,#65363,#65364,#65365,#65366,#65367,#65368,#65369,
#65370,#65371,#65372,#65373,#65374,#65375,#65376,#65377,#65378,#65379,#65380,
#65381,#65382,#65383,#65384,#65385,#65386,#65387,#65388,#65389),(#65390,
#65391,#65392,#65393,#65394,#65395,#65396,#65397,#65398,#65399,#65400,#65401,
#65402,#65403,#65404,#65405,#65406,#65407,#65408,#65409,#65410,#65411,#65412,
#65413,#65414,#65415,#65416,#65417,#65418,#65419,#65420,#65421,#65422,#65423,
#65424,#65425,#65426,#65427,#65428,#65429,#65430,#65431,#65432,#65433,#65434,
#65435,#65436,#65437,#65438,#65439,#65440,#65441,#65442,#65443,#65444,#65445),
(#65446,#65447,#65448,#65449,#65450,#65451,#65452,#65453,#65454,#65455,
#65456,#65457,#65458,#65459,#65460,#65461,#65462,#65463,#65464,#65465,#65466,
#65467,#65468,#65469,#65470,#65471,#65472,#65473,#65474,#65475,#65476,#65477,
#65478,#65479,#65480,#65481,#65482,#65483,#65484,#65485,#65486,#65487,#65488,
#65489,#65490,#65491,#65492,#65493,#65494,#65495,#65496,#65497,#65498,#65499,
#65500,#65501)),.UNSPECIFIED.,.F.,.F.,.F.,(4,4),(4,1,1,1,1,1,1,1,1,1,1,
1,1,1,1,1,1,1,1,1,1,1,1,1,1,1,1,1,1,1,1,1,1,1,1,1,1,1,1,1,1,1,1,1,1,1,1,
1,1,1,1,1,1,4),(0.,0.032158409993862),(14.3984001269719,15.3849294656359,
16.3714588042999,17.357988142964,18.344517481628,19.331046820292,20.317576158956,
21.3041054976201,22.2906348362841,23.2771641749481,24.2636935136122,25.2502228522762,
26.2367521909402,27.2232815296043,28.2098108682683,29.1963402069323,30.1828695455963,
31.1693988842604,32.1559282229244,33.1424575615884,34.1289869002525,35.1155162389165,
36.1020455775805,37.0885749162446,38.0751042549086,39.0616335935726,40.0481629322367,
41.0346922709007,42.0212216095647,43.0077509482287,43.9942802868928,44.9808096255568,
45.9673389642208,46.9538683028849,47.9403976415489,48.9269269802129,49.913456318877,
50.899985657541,51.886514996205,52.873044334869,53.8595736735331,54.8461030121971,
55.8326323508611,56.8191616895252,57.8056910281892,58.7922203668532,59.7787497055173,
60.7652790441813,61.7518083828453,62.7383377215094,63.7248670601734,64.7113963988374,
65.6979257375014,66.6844550761655),.UNSPECIFIED.);
#658=B_SPLINE_SURFACE_WITH_KNOTS('',3,3,((#65709,#65710,#65711,#65712,#65713,
#65714,#65715,#65716,#65717,#65718,#65719,#65720,#65721,#65722,#65723,#65724,
#65725,#65726,#65727,#65728,#65729,#65730,#65731,#65732,#65733,#65734,#65735,
#65736,#65737,#65738,#65739,#65740,#65741,#65742,#65743,#65744,#65745,#65746,
#65747,#65748,#65749,#65750,#65751,#65752,#65753,#65754,#65755,#65756,#65757,
#65758,#65759,#65760,#65761,#65762,#65763,#65764),(#65765,#65766,#65767,
#65768,#65769,#65770,#65771,#65772,#65773,#65774,#65775,#65776,#65777,#65778,
#65779,#65780,#65781,#65782,#65783,#65784,#65785,#65786,#65787,#65788,#65789,
#65790,#65791,#65792,#65793,#65794,#65795,#65796,#65797,#65798,#65799,#65800,
#65801,#65802,#65803,#65804,#65805,#65806,#65807,#65808,#65809,#65810,#65811,
#65812,#65813,#65814,#65815,#65816,#65817,#65818,#65819,#65820),(#65821,
#65822,#65823,#65824,#65825,#65826,#65827,#65828,#65829,#65830,#65831,#65832,
#65833,#65834,#65835,#65836,#65837,#65838,#65839,#65840,#65841,#65842,#65843,
#65844,#65845,#65846,#65847,#65848,#65849,#65850,#65851,#65852,#65853,#65854,
#65855,#65856,#65857,#65858,#65859,#65860,#65861,#65862,#65863,#65864,#65865,
#65866,#65867,#65868,#65869,#65870,#65871,#65872,#65873,#65874,#65875,#65876),
(#65877,#65878,#65879,#65880,#65881,#65882,#65883,#65884,#65885,#65886,
#65887,#65888,#65889,#65890,#65891,#65892,#65893,#65894,#65895,#65896,#65897,
#65898,#65899,#65900,#65901,#65902,#65903,#65904,#65905,#65906,#65907,#65908,
#65909,#65910,#65911,#65912,#65913,#65914,#65915,#65916,#65917,#65918,#65919,
#65920,#65921,#65922,#65923,#65924,#65925,#65926,#65927,#65928,#65929,#65930,
#65931,#65932)),.UNSPECIFIED.,.F.,.F.,.F.,(4,4),(4,1,1,1,1,1,1,1,1,1,1,
1,1,1,1,1,1,1,1,1,1,1,1,1,1,1,1,1,1,1,1,1,1,1,1,1,1,1,1,1,1,1,1,1,1,1,1,
1,1,1,1,1,1,4),(0.,0.0321584099938627),(11.8553612635794,12.8418906022434,
13.8284199409074,14.8149492795714,15.8014786182355,16.7880079568995,17.7745372955635,
18.7610666342276,19.7475959728916,20.7341253115556,21.7206546502197,22.7071839888837,
23.6937133275477,24.6802426662118,25.6667720048758,26.6533013435398,27.6398306822038,
28.6263600208679,29.6128893595319,30.5994186981959,31.58594803686,32.572477375524,
33.559006714188,34.5455360528521,35.5320653915161,36.5185947301801,37.5051240688441,
38.4916534075082,39.4781827461722,40.4647120848362,41.4512414235003,42.4377707621643,
43.4243001008283,44.4108294394924,45.3973587781564,46.3838881168204,47.3704174554844,
48.3569467941485,49.3434761328125,50.3300054714765,51.3165348101406,52.3030641488046,
53.2895934874686,54.2761228261327,55.2626521647967,56.2491815034607,57.2357108421248,
58.2222401807888,59.2087695194528,60.1952988581168,61.1818281967809,62.1683575354449,
63.1548868741089,64.141416212773),.UNSPECIFIED.);
#659=B_SPLINE_SURFACE_WITH_KNOTS('',3,3,((#65958,#65959,#65960,#65961,#65962,
#65963,#65964,#65965,#65966,#65967,#65968,#65969,#65970,#65971,#65972,#65973,
#65974,#65975,#65976,#65977,#65978,#65979,#65980,#65981,#65982,#65983,#65984,
#65985,#65986,#65987,#65988,#65989,#65990,#65991,#65992,#65993,#65994,#65995,
#65996,#65997,#65998,#65999,#66000,#66001,#66002,#66003,#66004,#66005,#66006,
#66007,#66008,#66009,#66010,#66011,#66012,#66013),(#66014,#66015,#66016,
#66017,#66018,#66019,#66020,#66021,#66022,#66023,#66024,#66025,#66026,#66027,
#66028,#66029,#66030,#66031,#66032,#66033,#66034,#66035,#66036,#66037,#66038,
#66039,#66040,#66041,#66042,#66043,#66044,#66045,#66046,#66047,#66048,#66049,
#66050,#66051,#66052,#66053,#66054,#66055,#66056,#66057,#66058,#66059,#66060,
#66061,#66062,#66063,#66064,#66065,#66066,#66067,#66068,#66069),(#66070,
#66071,#66072,#66073,#66074,#66075,#66076,#66077,#66078,#66079,#66080,#66081,
#66082,#66083,#66084,#66085,#66086,#66087,#66088,#66089,#66090,#66091,#66092,
#66093,#66094,#66095,#66096,#66097,#66098,#66099,#66100,#66101,#66102,#66103,
#66104,#66105,#66106,#66107,#66108,#66109,#66110,#66111,#66112,#66113,#66114,
#66115,#66116,#66117,#66118,#66119,#66120,#66121,#66122,#66123,#66124,#66125),
(#66126,#66127,#66128,#66129,#66130,#66131,#66132,#66133,#66134,#66135,
#66136,#66137,#66138,#66139,#66140,#66141,#66142,#66143,#66144,#66145,#66146,
#66147,#66148,#66149,#66150,#66151,#66152,#66153,#66154,#66155,#66156,#66157,
#66158,#66159,#66160,#66161,#66162,#66163,#66164,#66165,#66166,#66167,#66168,
#66169,#66170,#66171,#66172,#66173,#66174,#66175,#66176,#66177,#66178,#66179,
#66180,#66181)),.UNSPECIFIED.,.F.,.F.,.F.,(4,4),(4,1,1,1,1,1,1,1,1,1,1,
1,1,1,1,1,1,1,1,1,1,1,1,1,1,1,1,1,1,1,1,1,1,1,1,1,1,1,1,1,1,1,1,1,1,1,1,
1,1,1,1,1,1,4),(0.,0.0321584099938627),(14.3984001269719,15.3849294656359,
16.3714588042999,17.357988142964,18.344517481628,19.331046820292,20.317576158956,
21.3041054976201,22.2906348362841,23.2771641749481,24.2636935136122,25.2502228522762,
26.2367521909402,27.2232815296043,28.2098108682683,29.1963402069323,30.1828695455963,
31.1693988842604,32.1559282229244,33.1424575615884,34.1289869002525,35.1155162389165,
36.1020455775805,37.0885749162446,38.0751042549086,39.0616335935726,40.0481629322367,
41.0346922709007,42.0212216095647,43.0077509482287,43.9942802868928,44.9808096255568,
45.9673389642208,46.9538683028849,47.9403976415489,48.9269269802129,49.913456318877,
50.899985657541,51.886514996205,52.873044334869,53.8595736735331,54.8461030121971,
55.8326323508611,56.8191616895252,57.8056910281892,58.7922203668532,59.7787497055173,
60.7652790441813,61.7518083828453,62.7383377215094,63.7248670601734,64.7113963988374,
65.6979257375014,66.6844550761655),.UNSPECIFIED.);
#660=B_SPLINE_SURFACE_WITH_KNOTS('',3,3,((#66389,#66390,#66391,#66392,#66393,
#66394,#66395,#66396,#66397,#66398,#66399,#66400,#66401,#66402,#66403,#66404,
#66405,#66406,#66407,#66408,#66409,#66410,#66411,#66412,#66413,#66414,#66415,
#66416,#66417,#66418,#66419,#66420,#66421,#66422,#66423,#66424,#66425,#66426,
#66427,#66428,#66429,#66430,#66431,#66432,#66433,#66434,#66435,#66436,#66437,
#66438,#66439,#66440,#66441,#66442,#66443,#66444),(#66445,#66446,#66447,
#66448,#66449,#66450,#66451,#66452,#66453,#66454,#66455,#66456,#66457,#66458,
#66459,#66460,#66461,#66462,#66463,#66464,#66465,#66466,#66467,#66468,#66469,
#66470,#66471,#66472,#66473,#66474,#66475,#66476,#66477,#66478,#66479,#66480,
#66481,#66482,#66483,#66484,#66485,#66486,#66487,#66488,#66489,#66490,#66491,
#66492,#66493,#66494,#66495,#66496,#66497,#66498,#66499,#66500),(#66501,
#66502,#66503,#66504,#66505,#66506,#66507,#66508,#66509,#66510,#66511,#66512,
#66513,#66514,#66515,#66516,#66517,#66518,#66519,#66520,#66521,#66522,#66523,
#66524,#66525,#66526,#66527,#66528,#66529,#66530,#66531,#66532,#66533,#66534,
#66535,#66536,#66537,#66538,#66539,#66540,#66541,#66542,#66543,#66544,#66545,
#66546,#66547,#66548,#66549,#66550,#66551,#66552,#66553,#66554,#66555,#66556),
(#66557,#66558,#66559,#66560,#66561,#66562,#66563,#66564,#66565,#66566,
#66567,#66568,#66569,#66570,#66571,#66572,#66573,#66574,#66575,#66576,#66577,
#66578,#66579,#66580,#66581,#66582,#66583,#66584,#66585,#66586,#66587,#66588,
#66589,#66590,#66591,#66592,#66593,#66594,#66595,#66596,#66597,#66598,#66599,
#66600,#66601,#66602,#66603,#66604,#66605,#66606,#66607,#66608,#66609,#66610,
#66611,#66612)),.UNSPECIFIED.,.F.,.F.,.F.,(4,4),(4,1,1,1,1,1,1,1,1,1,1,
1,1,1,1,1,1,1,1,1,1,1,1,1,1,1,1,1,1,1,1,1,1,1,1,1,1,1,1,1,1,1,1,1,1,1,1,
1,1,1,1,1,1,4),(0.,0.0321584099938621),(11.8553612635794,12.8418906022434,
13.8284199409074,14.8149492795714,15.8014786182355,16.7880079568995,17.7745372955635,
18.7610666342276,19.7475959728916,20.7341253115556,21.7206546502197,22.7071839888837,
23.6937133275477,24.6802426662117,25.6667720048758,26.6533013435398,27.6398306822038,
28.6263600208679,29.6128893595319,30.5994186981959,31.58594803686,32.572477375524,
33.559006714188,34.5455360528521,35.5320653915161,36.5185947301801,37.5051240688441,
38.4916534075082,39.4781827461722,40.4647120848362,41.4512414235003,42.4377707621643,
43.4243001008283,44.4108294394924,45.3973587781564,46.3838881168204,47.3704174554844,
48.3569467941485,49.3434761328125,50.3300054714765,51.3165348101406,52.3030641488046,
53.2895934874686,54.2761228261327,55.2626521647967,56.2491815034607,57.2357108421247,
58.2222401807888,59.2087695194528,60.1952988581168,61.1818281967809,62.1683575354449,
63.1548868741089,64.141416212773),.UNSPECIFIED.);
#661=B_SPLINE_SURFACE_WITH_KNOTS('',3,3,((#66638,#66639,#66640,#66641,#66642,
#66643,#66644,#66645,#66646,#66647,#66648,#66649,#66650,#66651,#66652,#66653,
#66654,#66655,#66656,#66657,#66658,#66659,#66660,#66661,#66662,#66663,#66664,
#66665,#66666,#66667,#66668,#66669,#66670,#66671,#66672,#66673,#66674,#66675,
#66676,#66677,#66678,#66679,#66680,#66681,#66682,#66683,#66684,#66685,#66686,
#66687,#66688,#66689,#66690,#66691,#66692,#66693),(#66694,#66695,#66696,
#66697,#66698,#66699,#66700,#66701,#66702,#66703,#66704,#66705,#66706,#66707,
#66708,#66709,#66710,#66711,#66712,#66713,#66714,#66715,#66716,#66717,#66718,
#66719,#66720,#66721,#66722,#66723,#66724,#66725,#66726,#66727,#66728,#66729,
#66730,#66731,#66732,#66733,#66734,#66735,#66736,#66737,#66738,#66739,#66740,
#66741,#66742,#66743,#66744,#66745,#66746,#66747,#66748,#66749),(#66750,
#66751,#66752,#66753,#66754,#66755,#66756,#66757,#66758,#66759,#66760,#66761,
#66762,#66763,#66764,#66765,#66766,#66767,#66768,#66769,#66770,#66771,#66772,
#66773,#66774,#66775,#66776,#66777,#66778,#66779,#66780,#66781,#66782,#66783,
#66784,#66785,#66786,#66787,#66788,#66789,#66790,#66791,#66792,#66793,#66794,
#66795,#66796,#66797,#66798,#66799,#66800,#66801,#66802,#66803,#66804,#66805),
(#66806,#66807,#66808,#66809,#66810,#66811,#66812,#66813,#66814,#66815,
#66816,#66817,#66818,#66819,#66820,#66821,#66822,#66823,#66824,#66825,#66826,
#66827,#66828,#66829,#66830,#66831,#66832,#66833,#66834,#66835,#66836,#66837,
#66838,#66839,#66840,#66841,#66842,#66843,#66844,#66845,#66846,#66847,#66848,
#66849,#66850,#66851,#66852,#66853,#66854,#66855,#66856,#66857,#66858,#66859,
#66860,#66861)),.UNSPECIFIED.,.F.,.F.,.F.,(4,4),(4,1,1,1,1,1,1,1,1,1,1,
1,1,1,1,1,1,1,1,1,1,1,1,1,1,1,1,1,1,1,1,1,1,1,1,1,1,1,1,1,1,1,1,1,1,1,1,
1,1,1,1,1,1,4),(0.,0.0321584099938621),(14.3984001269719,15.3849294656359,
16.3714588042999,17.357988142964,18.344517481628,19.331046820292,20.317576158956,
21.3041054976201,22.2906348362841,23.2771641749481,24.2636935136122,25.2502228522762,
26.2367521909402,27.2232815296043,28.2098108682683,29.1963402069323,30.1828695455963,
31.1693988842604,32.1559282229244,33.1424575615884,34.1289869002525,35.1155162389165,
36.1020455775805,37.0885749162446,38.0751042549086,39.0616335935726,40.0481629322367,
41.0346922709007,42.0212216095647,43.0077509482287,43.9942802868928,44.9808096255568,
45.9673389642208,46.9538683028849,47.9403976415489,48.9269269802129,49.913456318877,
50.899985657541,51.886514996205,52.873044334869,53.8595736735331,54.8461030121971,
55.8326323508611,56.8191616895252,57.8056910281892,58.7922203668532,59.7787497055173,
60.7652790441813,61.7518083828453,62.7383377215094,63.7248670601734,64.7113963988374,
65.6979257375014,66.6844550761655),.UNSPECIFIED.);
#662=B_SPLINE_SURFACE_WITH_KNOTS('',3,3,((#67069,#67070,#67071,#67072,#67073,
#67074,#67075,#67076,#67077,#67078,#67079,#67080,#67081,#67082,#67083,#67084,
#67085,#67086,#67087,#67088,#67089,#67090,#67091,#67092,#67093,#67094,#67095,
#67096,#67097,#67098,#67099,#67100,#67101,#67102,#67103,#67104,#67105,#67106,
#67107,#67108,#67109,#67110,#67111,#67112,#67113,#67114,#67115,#67116,#67117,
#67118,#67119,#67120,#67121,#67122,#67123,#67124),(#67125,#67126,#67127,
#67128,#67129,#67130,#67131,#67132,#67133,#67134,#67135,#67136,#67137,#67138,
#67139,#67140,#67141,#67142,#67143,#67144,#67145,#67146,#67147,#67148,#67149,
#67150,#67151,#67152,#67153,#67154,#67155,#67156,#67157,#67158,#67159,#67160,
#67161,#67162,#67163,#67164,#67165,#67166,#67167,#67168,#67169,#67170,#67171,
#67172,#67173,#67174,#67175,#67176,#67177,#67178,#67179,#67180),(#67181,
#67182,#67183,#67184,#67185,#67186,#67187,#67188,#67189,#67190,#67191,#67192,
#67193,#67194,#67195,#67196,#67197,#67198,#67199,#67200,#67201,#67202,#67203,
#67204,#67205,#67206,#67207,#67208,#67209,#67210,#67211,#67212,#67213,#67214,
#67215,#67216,#67217,#67218,#67219,#67220,#67221,#67222,#67223,#67224,#67225,
#67226,#67227,#67228,#67229,#67230,#67231,#67232,#67233,#67234,#67235,#67236),
(#67237,#67238,#67239,#67240,#67241,#67242,#67243,#67244,#67245,#67246,
#67247,#67248,#67249,#67250,#67251,#67252,#67253,#67254,#67255,#67256,#67257,
#67258,#67259,#67260,#67261,#67262,#67263,#67264,#67265,#67266,#67267,#67268,
#67269,#67270,#67271,#67272,#67273,#67274,#67275,#67276,#67277,#67278,#67279,
#67280,#67281,#67282,#67283,#67284,#67285,#67286,#67287,#67288,#67289,#67290,
#67291,#67292)),.UNSPECIFIED.,.F.,.F.,.F.,(4,4),(4,1,1,1,1,1,1,1,1,1,1,
1,1,1,1,1,1,1,1,1,1,1,1,1,1,1,1,1,1,1,1,1,1,1,1,1,1,1,1,1,1,1,1,1,1,1,1,
1,1,1,1,1,1,4),(0.,0.032158409993862),(11.8553612635794,12.8418906022434,
13.8284199409074,14.8149492795714,15.8014786182355,16.7880079568995,17.7745372955635,
18.7610666342276,19.7475959728916,20.7341253115556,21.7206546502197,22.7071839888837,
23.6937133275477,24.6802426662118,25.6667720048758,26.6533013435398,27.6398306822039,
28.6263600208679,29.6128893595319,30.5994186981959,31.58594803686,32.572477375524,
33.559006714188,34.5455360528521,35.5320653915161,36.5185947301801,37.5051240688442,
38.4916534075082,39.4781827461722,40.4647120848363,41.4512414235003,42.4377707621643,
43.4243001008283,44.4108294394924,45.3973587781564,46.3838881168204,47.3704174554845,
48.3569467941485,49.3434761328125,50.3300054714766,51.3165348101406,52.3030641488046,
53.2895934874687,54.2761228261327,55.2626521647967,56.2491815034607,57.2357108421248,
58.2222401807888,59.2087695194528,60.1952988581169,61.1818281967809,62.1683575354449,
63.154886874109,64.141416212773),.UNSPECIFIED.);
#663=B_SPLINE_SURFACE_WITH_KNOTS('',3,3,((#67318,#67319,#67320,#67321,#67322,
#67323,#67324,#67325,#67326,#67327,#67328,#67329,#67330,#67331,#67332,#67333,
#67334,#67335,#67336,#67337,#67338,#67339,#67340,#67341,#67342,#67343,#67344,
#67345,#67346,#67347,#67348,#67349,#67350,#67351,#67352,#67353,#67354,#67355,
#67356,#67357,#67358,#67359,#67360,#67361,#67362,#67363,#67364,#67365,#67366,
#67367,#67368,#67369,#67370,#67371,#67372,#67373),(#67374,#67375,#67376,
#67377,#67378,#67379,#67380,#67381,#67382,#67383,#67384,#67385,#67386,#67387,
#67388,#67389,#67390,#67391,#67392,#67393,#67394,#67395,#67396,#67397,#67398,
#67399,#67400,#67401,#67402,#67403,#67404,#67405,#67406,#67407,#67408,#67409,
#67410,#67411,#67412,#67413,#67414,#67415,#67416,#67417,#67418,#67419,#67420,
#67421,#67422,#67423,#67424,#67425,#67426,#67427,#67428,#67429),(#67430,
#67431,#67432,#67433,#67434,#67435,#67436,#67437,#67438,#67439,#67440,#67441,
#67442,#67443,#67444,#67445,#67446,#67447,#67448,#67449,#67450,#67451,#67452,
#67453,#67454,#67455,#67456,#67457,#67458,#67459,#67460,#67461,#67462,#67463,
#67464,#67465,#67466,#67467,#67468,#67469,#67470,#67471,#67472,#67473,#67474,
#67475,#67476,#67477,#67478,#67479,#67480,#67481,#67482,#67483,#67484,#67485),
(#67486,#67487,#67488,#67489,#67490,#67491,#67492,#67493,#67494,#67495,
#67496,#67497,#67498,#67499,#67500,#67501,#67502,#67503,#67504,#67505,#67506,
#67507,#67508,#67509,#67510,#67511,#67512,#67513,#67514,#67515,#67516,#67517,
#67518,#67519,#67520,#67521,#67522,#67523,#67524,#67525,#67526,#67527,#67528,
#67529,#67530,#67531,#67532,#67533,#67534,#67535,#67536,#67537,#67538,#67539,
#67540,#67541)),.UNSPECIFIED.,.F.,.F.,.F.,(4,4),(4,1,1,1,1,1,1,1,1,1,1,
1,1,1,1,1,1,1,1,1,1,1,1,1,1,1,1,1,1,1,1,1,1,1,1,1,1,1,1,1,1,1,1,1,1,1,1,
1,1,1,1,1,1,4),(0.,0.032158409993862),(14.3984001269719,15.3849294656359,
16.3714588042999,17.357988142964,18.344517481628,19.331046820292,20.317576158956,
21.3041054976201,22.2906348362841,23.2771641749481,24.2636935136122,25.2502228522762,
26.2367521909402,27.2232815296043,28.2098108682683,29.1963402069323,30.1828695455964,
31.1693988842604,32.1559282229244,33.1424575615884,34.1289869002525,35.1155162389165,
36.1020455775805,37.0885749162446,38.0751042549086,39.0616335935726,40.0481629322367,
41.0346922709007,42.0212216095647,43.0077509482288,43.9942802868928,44.9808096255568,
45.9673389642208,46.9538683028849,47.9403976415489,48.9269269802129,49.913456318877,
50.899985657541,51.886514996205,52.8730443348691,53.8595736735331,54.8461030121971,
55.8326323508612,56.8191616895252,57.8056910281892,58.7922203668532,59.7787497055173,
60.7652790441813,61.7518083828453,62.7383377215094,63.7248670601734,64.7113963988374,
65.6979257375015,66.6844550761655),.UNSPECIFIED.);
#664=B_SPLINE_SURFACE_WITH_KNOTS('',3,3,((#67749,#67750,#67751,#67752,#67753,
#67754,#67755,#67756,#67757,#67758,#67759,#67760,#67761,#67762,#67763,#67764,
#67765,#67766,#67767,#67768,#67769,#67770,#67771,#67772,#67773,#67774,#67775,
#67776,#67777,#67778,#67779,#67780,#67781,#67782,#67783,#67784,#67785,#67786,
#67787,#67788,#67789,#67790,#67791,#67792,#67793,#67794,#67795,#67796,#67797,
#67798,#67799,#67800,#67801,#67802,#67803,#67804),(#67805,#67806,#67807,
#67808,#67809,#67810,#67811,#67812,#67813,#67814,#67815,#67816,#67817,#67818,
#67819,#67820,#67821,#67822,#67823,#67824,#67825,#67826,#67827,#67828,#67829,
#67830,#67831,#67832,#67833,#67834,#67835,#67836,#67837,#67838,#67839,#67840,
#67841,#67842,#67843,#67844,#67845,#67846,#67847,#67848,#67849,#67850,#67851,
#67852,#67853,#67854,#67855,#67856,#67857,#67858,#67859,#67860),(#67861,
#67862,#67863,#67864,#67865,#67866,#67867,#67868,#67869,#67870,#67871,#67872,
#67873,#67874,#67875,#67876,#67877,#67878,#67879,#67880,#67881,#67882,#67883,
#67884,#67885,#67886,#67887,#67888,#67889,#67890,#67891,#67892,#67893,#67894,
#67895,#67896,#67897,#67898,#67899,#67900,#67901,#67902,#67903,#67904,#67905,
#67906,#67907,#67908,#67909,#67910,#67911,#67912,#67913,#67914,#67915,#67916),
(#67917,#67918,#67919,#67920,#67921,#67922,#67923,#67924,#67925,#67926,
#67927,#67928,#67929,#67930,#67931,#67932,#67933,#67934,#67935,#67936,#67937,
#67938,#67939,#67940,#67941,#67942,#67943,#67944,#67945,#67946,#67947,#67948,
#67949,#67950,#67951,#67952,#67953,#67954,#67955,#67956,#67957,#67958,#67959,
#67960,#67961,#67962,#67963,#67964,#67965,#67966,#67967,#67968,#67969,#67970,
#67971,#67972)),.UNSPECIFIED.,.F.,.F.,.F.,(4,4),(4,1,1,1,1,1,1,1,1,1,1,
1,1,1,1,1,1,1,1,1,1,1,1,1,1,1,1,1,1,1,1,1,1,1,1,1,1,1,1,1,1,1,1,1,1,1,1,
1,1,1,1,1,1,4),(0.,0.0321584099938627),(11.8553612635793,12.8418906022434,
13.8284199409074,14.8149492795714,15.8014786182354,16.7880079568995,17.7745372955635,
18.7610666342275,19.7475959728916,20.7341253115556,21.7206546502196,22.7071839888837,
23.6937133275477,24.6802426662117,25.6667720048758,26.6533013435398,27.6398306822038,
28.6263600208678,29.6128893595319,30.5994186981959,31.5859480368599,32.572477375524,
33.559006714188,34.545536052852,35.5320653915161,36.5185947301801,37.5051240688441,
38.4916534075082,39.4781827461722,40.4647120848362,41.4512414235002,42.4377707621643,
43.4243001008283,44.4108294394923,45.3973587781564,46.3838881168204,47.3704174554844,
48.3569467941485,49.3434761328125,50.3300054714765,51.3165348101405,52.3030641488046,
53.2895934874686,54.2761228261326,55.2626521647967,56.2491815034607,57.2357108421247,
58.2222401807888,59.2087695194528,60.1952988581168,61.1818281967808,62.1683575354449,
63.1548868741089,64.1414162127729),.UNSPECIFIED.);
#665=B_SPLINE_SURFACE_WITH_KNOTS('',3,3,((#67998,#67999,#68000,#68001,#68002,
#68003,#68004,#68005,#68006,#68007,#68008,#68009,#68010,#68011,#68012,#68013,
#68014,#68015,#68016,#68017,#68018,#68019,#68020,#68021,#68022,#68023,#68024,
#68025,#68026,#68027,#68028,#68029,#68030,#68031,#68032,#68033,#68034,#68035,
#68036,#68037,#68038,#68039,#68040,#68041,#68042,#68043,#68044,#68045,#68046,
#68047,#68048,#68049,#68050,#68051,#68052,#68053),(#68054,#68055,#68056,
#68057,#68058,#68059,#68060,#68061,#68062,#68063,#68064,#68065,#68066,#68067,
#68068,#68069,#68070,#68071,#68072,#68073,#68074,#68075,#68076,#68077,#68078,
#68079,#68080,#68081,#68082,#68083,#68084,#68085,#68086,#68087,#68088,#68089,
#68090,#68091,#68092,#68093,#68094,#68095,#68096,#68097,#68098,#68099,#68100,
#68101,#68102,#68103,#68104,#68105,#68106,#68107,#68108,#68109),(#68110,
#68111,#68112,#68113,#68114,#68115,#68116,#68117,#68118,#68119,#68120,#68121,
#68122,#68123,#68124,#68125,#68126,#68127,#68128,#68129,#68130,#68131,#68132,
#68133,#68134,#68135,#68136,#68137,#68138,#68139,#68140,#68141,#68142,#68143,
#68144,#68145,#68146,#68147,#68148,#68149,#68150,#68151,#68152,#68153,#68154,
#68155,#68156,#68157,#68158,#68159,#68160,#68161,#68162,#68163,#68164,#68165),
(#68166,#68167,#68168,#68169,#68170,#68171,#68172,#68173,#68174,#68175,
#68176,#68177,#68178,#68179,#68180,#68181,#68182,#68183,#68184,#68185,#68186,
#68187,#68188,#68189,#68190,#68191,#68192,#68193,#68194,#68195,#68196,#68197,
#68198,#68199,#68200,#68201,#68202,#68203,#68204,#68205,#68206,#68207,#68208,
#68209,#68210,#68211,#68212,#68213,#68214,#68215,#68216,#68217,#68218,#68219,
#68220,#68221)),.UNSPECIFIED.,.F.,.F.,.F.,(4,4),(4,1,1,1,1,1,1,1,1,1,1,
1,1,1,1,1,1,1,1,1,1,1,1,1,1,1,1,1,1,1,1,1,1,1,1,1,1,1,1,1,1,1,1,1,1,1,1,
1,1,1,1,1,1,4),(0.,0.0321584099938627),(14.3984001269718,15.3849294656359,
16.3714588042999,17.3579881429639,18.344517481628,19.331046820292,20.317576158956,
21.30410549762,22.2906348362841,23.2771641749481,24.2636935136121,25.2502228522762,
26.2367521909402,27.2232815296042,28.2098108682683,29.1963402069323,30.1828695455963,
31.1693988842603,32.1559282229244,33.1424575615884,34.1289869002524,35.1155162389165,
36.1020455775805,37.0885749162445,38.0751042549086,39.0616335935726,40.0481629322366,
41.0346922709006,42.0212216095647,43.0077509482287,43.9942802868927,44.9808096255568,
45.9673389642208,46.9538683028848,47.9403976415489,48.9269269802129,49.9134563188769,
50.899985657541,51.886514996205,52.873044334869,53.859573673533,54.8461030121971,
55.8326323508611,56.8191616895251,57.8056910281892,58.7922203668532,59.7787497055172,
60.7652790441813,61.7518083828453,62.7383377215093,63.7248670601733,64.7113963988374,
65.6979257375014,66.6844550761654),.UNSPECIFIED.);
#666=B_SPLINE_SURFACE_WITH_KNOTS('',3,3,((#68449,#68450,#68451,#68452,#68453,
#68454,#68455,#68456,#68457,#68458,#68459,#68460,#68461,#68462,#68463,#68464,
#68465,#68466,#68467,#68468,#68469,#68470,#68471,#68472,#68473,#68474,#68475,
#68476,#68477,#68478,#68479,#68480,#68481,#68482,#68483,#68484,#68485,#68486,
#68487,#68488,#68489,#68490,#68491,#68492,#68493,#68494,#68495,#68496,#68497,
#68498,#68499,#68500,#68501,#68502,#68503,#68504),(#68505,#68506,#68507,
#68508,#68509,#68510,#68511,#68512,#68513,#68514,#68515,#68516,#68517,#68518,
#68519,#68520,#68521,#68522,#68523,#68524,#68525,#68526,#68527,#68528,#68529,
#68530,#68531,#68532,#68533,#68534,#68535,#68536,#68537,#68538,#68539,#68540,
#68541,#68542,#68543,#68544,#68545,#68546,#68547,#68548,#68549,#68550,#68551,
#68552,#68553,#68554,#68555,#68556,#68557,#68558,#68559,#68560),(#68561,
#68562,#68563,#68564,#68565,#68566,#68567,#68568,#68569,#68570,#68571,#68572,
#68573,#68574,#68575,#68576,#68577,#68578,#68579,#68580,#68581,#68582,#68583,
#68584,#68585,#68586,#68587,#68588,#68589,#68590,#68591,#68592,#68593,#68594,
#68595,#68596,#68597,#68598,#68599,#68600,#68601,#68602,#68603,#68604,#68605,
#68606,#68607,#68608,#68609,#68610,#68611,#68612,#68613,#68614,#68615,#68616),
(#68617,#68618,#68619,#68620,#68621,#68622,#68623,#68624,#68625,#68626,
#68627,#68628,#68629,#68630,#68631,#68632,#68633,#68634,#68635,#68636,#68637,
#68638,#68639,#68640,#68641,#68642,#68643,#68644,#68645,#68646,#68647,#68648,
#68649,#68650,#68651,#68652,#68653,#68654,#68655,#68656,#68657,#68658,#68659,
#68660,#68661,#68662,#68663,#68664,#68665,#68666,#68667,#68668,#68669,#68670,
#68671,#68672)),.UNSPECIFIED.,.F.,.F.,.F.,(4,4),(4,1,1,1,1,1,1,1,1,1,1,
1,1,1,1,1,1,1,1,1,1,1,1,1,1,1,1,1,1,1,1,1,1,1,1,1,1,1,1,1,1,1,1,1,1,1,1,
1,1,1,1,1,1,4),(0.,0.0321584099938621),(11.8553612635793,12.8418906022434,
13.8284199409074,14.8149492795714,15.8014786182355,16.7880079568995,17.7745372955635,
18.7610666342275,19.7475959728916,20.7341253115556,21.7206546502196,22.7071839888837,
23.6937133275477,24.6802426662117,25.6667720048758,26.6533013435398,27.6398306822038,
28.6263600208679,29.6128893595319,30.5994186981959,31.5859480368599,32.572477375524,
33.559006714188,34.545536052852,35.5320653915161,36.5185947301801,37.5051240688441,
38.4916534075082,39.4781827461722,40.4647120848362,41.4512414235002,42.4377707621643,
43.4243001008283,44.4108294394923,45.3973587781564,46.3838881168204,47.3704174554844,
48.3569467941485,49.3434761328125,50.3300054714765,51.3165348101406,52.3030641488046,
53.2895934874686,54.2761228261326,55.2626521647967,56.2491815034607,57.2357108421247,
58.2222401807888,59.2087695194528,60.1952988581168,61.1818281967809,62.1683575354449,
63.1548868741089,64.141416212773),.UNSPECIFIED.);
#667=B_SPLINE_SURFACE_WITH_KNOTS('',3,3,((#68780,#68781,#68782,#68783,#68784,
#68785,#68786,#68787,#68788,#68789,#68790,#68791,#68792,#68793,#68794,#68795,
#68796,#68797,#68798,#68799,#68800,#68801,#68802,#68803,#68804,#68805,#68806,
#68807,#68808,#68809,#68810,#68811,#68812,#68813,#68814,#68815,#68816,#68817,
#68818,#68819,#68820,#68821,#68822,#68823,#68824,#68825,#68826,#68827,#68828,
#68829,#68830,#68831,#68832,#68833,#68834,#68835),(#68836,#68837,#68838,
#68839,#68840,#68841,#68842,#68843,#68844,#68845,#68846,#68847,#68848,#68849,
#68850,#68851,#68852,#68853,#68854,#68855,#68856,#68857,#68858,#68859,#68860,
#68861,#68862,#68863,#68864,#68865,#68866,#68867,#68868,#68869,#68870,#68871,
#68872,#68873,#68874,#68875,#68876,#68877,#68878,#68879,#68880,#68881,#68882,
#68883,#68884,#68885,#68886,#68887,#68888,#68889,#68890,#68891),(#68892,
#68893,#68894,#68895,#68896,#68897,#68898,#68899,#68900,#68901,#68902,#68903,
#68904,#68905,#68906,#68907,#68908,#68909,#68910,#68911,#68912,#68913,#68914,
#68915,#68916,#68917,#68918,#68919,#68920,#68921,#68922,#68923,#68924,#68925,
#68926,#68927,#68928,#68929,#68930,#68931,#68932,#68933,#68934,#68935,#68936,
#68937,#68938,#68939,#68940,#68941,#68942,#68943,#68944,#68945,#68946,#68947),
(#68948,#68949,#68950,#68951,#68952,#68953,#68954,#68955,#68956,#68957,
#68958,#68959,#68960,#68961,#68962,#68963,#68964,#68965,#68966,#68967,#68968,
#68969,#68970,#68971,#68972,#68973,#68974,#68975,#68976,#68977,#68978,#68979,
#68980,#68981,#68982,#68983,#68984,#68985,#68986,#68987,#68988,#68989,#68990,
#68991,#68992,#68993,#68994,#68995,#68996,#68997,#68998,#68999,#69000,#69001,
#69002,#69003)),.UNSPECIFIED.,.F.,.F.,.F.,(4,4),(4,1,1,1,1,1,1,1,1,1,1,
1,1,1,1,1,1,1,1,1,1,1,1,1,1,1,1,1,1,1,1,1,1,1,1,1,1,1,1,1,1,1,1,1,1,1,1,
1,1,1,1,1,1,4),(0.,0.0321584099938621),(14.3984001269718,15.3849294656359,
16.3714588042999,17.3579881429639,18.344517481628,19.331046820292,20.317576158956,
21.3041054976201,22.2906348362841,23.2771641749481,24.2636935136121,25.2502228522762,
26.2367521909402,27.2232815296042,28.2098108682683,29.1963402069323,30.1828695455963,
31.1693988842604,32.1559282229244,33.1424575615884,34.1289869002525,35.1155162389165,
36.1020455775805,37.0885749162445,38.0751042549086,39.0616335935726,40.0481629322366,
41.0346922709007,42.0212216095647,43.0077509482287,43.9942802868928,44.9808096255568,
45.9673389642208,46.9538683028849,47.9403976415489,48.9269269802129,49.9134563188769,
50.899985657541,51.886514996205,52.873044334869,53.8595736735331,54.8461030121971,
55.8326323508611,56.8191616895252,57.8056910281892,58.7922203668532,59.7787497055173,
60.7652790441813,61.7518083828453,62.7383377215094,63.7248670601734,64.7113963988374,
65.6979257375014,66.6844550761655),.UNSPECIFIED.);
#668=B_SPLINE_SURFACE_WITH_KNOTS('',3,3,((#69294,#69295,#69296,#69297,#69298,
#69299,#69300,#69301,#69302,#69303,#69304,#69305,#69306,#69307,#69308,#69309,
#69310,#69311,#69312,#69313,#69314,#69315,#69316,#69317,#69318,#69319,#69320,
#69321,#69322,#69323,#69324,#69325,#69326,#69327,#69328,#69329,#69330,#69331,
#69332,#69333,#69334,#69335,#69336,#69337,#69338,#69339,#69340,#69341,#69342,
#69343,#69344,#69345,#69346,#69347,#69348,#69349),(#69350,#69351,#69352,
#69353,#69354,#69355,#69356,#69357,#69358,#69359,#69360,#69361,#69362,#69363,
#69364,#69365,#69366,#69367,#69368,#69369,#69370,#69371,#69372,#69373,#69374,
#69375,#69376,#69377,#69378,#69379,#69380,#69381,#69382,#69383,#69384,#69385,
#69386,#69387,#69388,#69389,#69390,#69391,#69392,#69393,#69394,#69395,#69396,
#69397,#69398,#69399,#69400,#69401,#69402,#69403,#69404,#69405),(#69406,
#69407,#69408,#69409,#69410,#69411,#69412,#69413,#69414,#69415,#69416,#69417,
#69418,#69419,#69420,#69421,#69422,#69423,#69424,#69425,#69426,#69427,#69428,
#69429,#69430,#69431,#69432,#69433,#69434,#69435,#69436,#69437,#69438,#69439,
#69440,#69441,#69442,#69443,#69444,#69445,#69446,#69447,#69448,#69449,#69450,
#69451,#69452,#69453,#69454,#69455,#69456,#69457,#69458,#69459,#69460,#69461),
(#69462,#69463,#69464,#69465,#69466,#69467,#69468,#69469,#69470,#69471,
#69472,#69473,#69474,#69475,#69476,#69477,#69478,#69479,#69480,#69481,#69482,
#69483,#69484,#69485,#69486,#69487,#69488,#69489,#69490,#69491,#69492,#69493,
#69494,#69495,#69496,#69497,#69498,#69499,#69500,#69501,#69502,#69503,#69504,
#69505,#69506,#69507,#69508,#69509,#69510,#69511,#69512,#69513,#69514,#69515,
#69516,#69517)),.UNSPECIFIED.,.F.,.F.,.F.,(4,4),(4,1,1,1,1,1,1,1,1,1,1,
1,1,1,1,1,1,1,1,1,1,1,1,1,1,1,1,1,1,1,1,1,1,1,1,1,1,1,1,1,1,1,1,1,1,1,1,
1,1,1,1,1,1,4),(0.,0.0321584099938621),(11.8553612635794,12.8418906022434,
13.8284199409074,14.8149492795714,15.8014786182355,16.7880079568995,17.7745372955635,
18.7610666342276,19.7475959728916,20.7341253115556,21.7206546502197,22.7071839888837,
23.6937133275477,24.6802426662117,25.6667720048758,26.6533013435398,27.6398306822038,
28.6263600208679,29.6128893595319,30.5994186981959,31.58594803686,32.572477375524,
33.559006714188,34.5455360528521,35.5320653915161,36.5185947301801,37.5051240688441,
38.4916534075082,39.4781827461722,40.4647120848362,41.4512414235003,42.4377707621643,
43.4243001008283,44.4108294394924,45.3973587781564,46.3838881168204,47.3704174554844,
48.3569467941485,49.3434761328125,50.3300054714765,51.3165348101406,52.3030641488046,
53.2895934874686,54.2761228261327,55.2626521647967,56.2491815034607,57.2357108421248,
58.2222401807888,59.2087695194528,60.1952988581168,61.1818281967809,62.1683575354449,
63.1548868741089,64.141416212773),.UNSPECIFIED.);
#669=B_SPLINE_SURFACE_WITH_KNOTS('',3,3,((#69543,#69544,#69545,#69546,#69547,
#69548,#69549,#69550,#69551,#69552,#69553,#69554,#69555,#69556,#69557,#69558,
#69559,#69560,#69561,#69562,#69563,#69564,#69565,#69566,#69567,#69568,#69569,
#69570,#69571,#69572,#69573,#69574,#69575,#69576,#69577,#69578,#69579,#69580,
#69581,#69582,#69583,#69584,#69585,#69586,#69587,#69588,#69589,#69590,#69591,
#69592,#69593,#69594,#69595,#69596,#69597,#69598),(#69599,#69600,#69601,
#69602,#69603,#69604,#69605,#69606,#69607,#69608,#69609,#69610,#69611,#69612,
#69613,#69614,#69615,#69616,#69617,#69618,#69619,#69620,#69621,#69622,#69623,
#69624,#69625,#69626,#69627,#69628,#69629,#69630,#69631,#69632,#69633,#69634,
#69635,#69636,#69637,#69638,#69639,#69640,#69641,#69642,#69643,#69644,#69645,
#69646,#69647,#69648,#69649,#69650,#69651,#69652,#69653,#69654),(#69655,
#69656,#69657,#69658,#69659,#69660,#69661,#69662,#69663,#69664,#69665,#69666,
#69667,#69668,#69669,#69670,#69671,#69672,#69673,#69674,#69675,#69676,#69677,
#69678,#69679,#69680,#69681,#69682,#69683,#69684,#69685,#69686,#69687,#69688,
#69689,#69690,#69691,#69692,#69693,#69694,#69695,#69696,#69697,#69698,#69699,
#69700,#69701,#69702,#69703,#69704,#69705,#69706,#69707,#69708,#69709,#69710),
(#69711,#69712,#69713,#69714,#69715,#69716,#69717,#69718,#69719,#69720,
#69721,#69722,#69723,#69724,#69725,#69726,#69727,#69728,#69729,#69730,#69731,
#69732,#69733,#69734,#69735,#69736,#69737,#69738,#69739,#69740,#69741,#69742,
#69743,#69744,#69745,#69746,#69747,#69748,#69749,#69750,#69751,#69752,#69753,
#69754,#69755,#69756,#69757,#69758,#69759,#69760,#69761,#69762,#69763,#69764,
#69765,#69766)),.UNSPECIFIED.,.F.,.F.,.F.,(4,4),(4,1,1,1,1,1,1,1,1,1,1,
1,1,1,1,1,1,1,1,1,1,1,1,1,1,1,1,1,1,1,1,1,1,1,1,1,1,1,1,1,1,1,1,1,1,1,1,
1,1,1,1,1,1,4),(0.,0.0321584099938621),(14.3984001269719,15.3849294656359,
16.3714588042999,17.357988142964,18.344517481628,19.331046820292,20.317576158956,
21.3041054976201,22.2906348362841,23.2771641749481,24.2636935136122,25.2502228522762,
26.2367521909402,27.2232815296043,28.2098108682683,29.1963402069323,30.1828695455963,
31.1693988842604,32.1559282229244,33.1424575615884,34.1289869002525,35.1155162389165,
36.1020455775805,37.0885749162446,38.0751042549086,39.0616335935726,40.0481629322367,
41.0346922709007,42.0212216095647,43.0077509482287,43.9942802868928,44.9808096255568,
45.9673389642208,46.9538683028849,47.9403976415489,48.9269269802129,49.913456318877,
50.899985657541,51.886514996205,52.873044334869,53.8595736735331,54.8461030121971,
55.8326323508611,56.8191616895252,57.8056910281892,58.7922203668532,59.7787497055172,
60.7652790441813,61.7518083828453,62.7383377215093,63.7248670601734,64.7113963988374,
65.6979257375014,66.6844550761655),.UNSPECIFIED.);
#670=B_SPLINE_SURFACE_WITH_KNOTS('',3,3,((#94938,#94939,#94940,#94941,#94942,
#94943,#94944,#94945,#94946,#94947,#94948,#94949,#94950,#94951,#94952,#94953,
#94954,#94955,#94956,#94957,#94958,#94959,#94960,#94961,#94962,#94963,#94964,
#94965,#94966),(#94967,#94968,#94969,#94970,#94971,#94972,#94973,#94974,
#94975,#94976,#94977,#94978,#94979,#94980,#94981,#94982,#94983,#94984,#94985,
#94986,#94987,#94988,#94989,#94990,#94991,#94992,#94993,#94994,#94995),
(#94996,#94997,#94998,#94999,#95000,#95001,#95002,#95003,#95004,#95005,
#95006,#95007,#95008,#95009,#95010,#95011,#95012,#95013,#95014,#95015,#95016,
#95017,#95018,#95019,#95020,#95021,#95022,#95023,#95024),(#95025,#95026,
#95027,#95028,#95029,#95030,#95031,#95032,#95033,#95034,#95035,#95036,#95037,
#95038,#95039,#95040,#95041,#95042,#95043,#95044,#95045,#95046,#95047,#95048,
#95049,#95050,#95051,#95052,#95053),(#95054,#95055,#95056,#95057,#95058,
#95059,#95060,#95061,#95062,#95063,#95064,#95065,#95066,#95067,#95068,#95069,
#95070,#95071,#95072,#95073,#95074,#95075,#95076,#95077,#95078,#95079,#95080,
#95081,#95082),(#95083,#95084,#95085,#95086,#95087,#95088,#95089,#95090,
#95091,#95092,#95093,#95094,#95095,#95096,#95097,#95098,#95099,#95100,#95101,
#95102,#95103,#95104,#95105,#95106,#95107,#95108,#95109,#95110,#95111),
(#95112,#95113,#95114,#95115,#95116,#95117,#95118,#95119,#95120,#95121,
#95122,#95123,#95124,#95125,#95126,#95127,#95128,#95129,#95130,#95131,#95132,
#95133,#95134,#95135,#95136,#95137,#95138,#95139,#95140),(#95141,#95142,
#95143,#95144,#95145,#95146,#95147,#95148,#95149,#95150,#95151,#95152,#95153,
#95154,#95155,#95156,#95157,#95158,#95159,#95160,#95161,#95162,#95163,#95164,
#95165,#95166,#95167,#95168,#95169),(#95170,#95171,#95172,#95173,#95174,
#95175,#95176,#95177,#95178,#95179,#95180,#95181,#95182,#95183,#95184,#95185,
#95186,#95187,#95188,#95189,#95190,#95191,#95192,#95193,#95194,#95195,#95196,
#95197,#95198),(#95199,#95200,#95201,#95202,#95203,#95204,#95205,#95206,
#95207,#95208,#95209,#95210,#95211,#95212,#95213,#95214,#95215,#95216,#95217,
#95218,#95219,#95220,#95221,#95222,#95223,#95224,#95225,#95226,#95227)),
 .UNSPECIFIED.,.T.,.F.,.F.,(4,1,1,1,1,1,1,4),(4,1,1,1,1,1,1,1,1,1,1,1,1,
1,1,1,1,1,1,1,1,1,1,1,1,1,4),(-3.14159265358979,-2.24399475256414,-1.34639685153848,
-0.448798950512828,0.448798950512828,1.34639685153848,2.24399475256414,
3.14159265358979),(0.,0.483321946706122,0.966643893412244,1.44996584011837,
1.93328778682449,2.41660973353061,2.89993168023673,3.38325362694285,3.86657557364898,
4.3498975203551,4.83321946706122,5.31654141376734,5.79986336047346,6.28318530717959,
6.76650725388571,7.24982920059183,7.73315114729795,8.21647309400407,8.6997950407102,
9.18311698741632,9.66643893412244,10.1497608808286,10.6330828275347,11.1164047742408,
11.5997267209469,12.083048667653,12.5663706143592),.UNSPECIFIED.);
#671=B_SPLINE_SURFACE_WITH_KNOTS('',3,3,((#96718,#96719,#96720,#96721,#96722,
#96723,#96724,#96725,#96726,#96727,#96728,#96729,#96730,#96731,#96732,#96733,
#96734,#96735,#96736,#96737,#96738,#96739,#96740,#96741,#96742,#96743,#96744,
#96745,#96746,#96747,#96748,#96749,#96750,#96751,#96752,#96753,#96754,#96755,
#96756,#96757,#96758,#96759,#96760,#96761,#96762,#96763,#96764,#96765,#96766,
#96767,#96768,#96769,#96770,#96771,#96772,#96773,#96774,#96775,#96776,#96777,
#96778,#96779,#96780,#96781,#96782,#96783,#96784,#96785,#96786,#96787,#96788,
#96789,#96790,#96791,#96792,#96793,#96794,#96795,#96796,#96797,#96798,#96799,
#96800,#96801,#96802,#96803,#96804,#96805,#96806,#96807,#96808,#96809,#96810,
#96811,#96812,#96813,#96814,#96815,#96816,#96817,#96818,#96819,#96820,#96821,
#96822,#96823),(#96824,#96825,#96826,#96827,#96828,#96829,#96830,#96831,
#96832,#96833,#96834,#96835,#96836,#96837,#96838,#96839,#96840,#96841,#96842,
#96843,#96844,#96845,#96846,#96847,#96848,#96849,#96850,#96851,#96852,#96853,
#96854,#96855,#96856,#96857,#96858,#96859,#96860,#96861,#96862,#96863,#96864,
#96865,#96866,#96867,#96868,#96869,#96870,#96871,#96872,#96873,#96874,#96875,
#96876,#96877,#96878,#96879,#96880,#96881,#96882,#96883,#96884,#96885,#96886,
#96887,#96888,#96889,#96890,#96891,#96892,#96893,#96894,#96895,#96896,#96897,
#96898,#96899,#96900,#96901,#96902,#96903,#96904,#96905,#96906,#96907,#96908,
#96909,#96910,#96911,#96912,#96913,#96914,#96915,#96916,#96917,#96918,#96919,
#96920,#96921,#96922,#96923,#96924,#96925,#96926,#96927,#96928,#96929),
(#96930,#96931,#96932,#96933,#96934,#96935,#96936,#96937,#96938,#96939,
#96940,#96941,#96942,#96943,#96944,#96945,#96946,#96947,#96948,#96949,#96950,
#96951,#96952,#96953,#96954,#96955,#96956,#96957,#96958,#96959,#96960,#96961,
#96962,#96963,#96964,#96965,#96966,#96967,#96968,#96969,#96970,#96971,#96972,
#96973,#96974,#96975,#96976,#96977,#96978,#96979,#96980,#96981,#96982,#96983,
#96984,#96985,#96986,#96987,#96988,#96989,#96990,#96991,#96992,#96993,#96994,
#96995,#96996,#96997,#96998,#96999,#97000,#97001,#97002,#97003,#97004,#97005,
#97006,#97007,#97008,#97009,#97010,#97011,#97012,#97013,#97014,#97015,#97016,
#97017,#97018,#97019,#97020,#97021,#97022,#97023,#97024,#97025,#97026,#97027,
#97028,#97029,#97030,#97031,#97032,#97033,#97034,#97035),(#97036,#97037,
#97038,#97039,#97040,#97041,#97042,#97043,#97044,#97045,#97046,#97047,#97048,
#97049,#97050,#97051,#97052,#97053,#97054,#97055,#97056,#97057,#97058,#97059,
#97060,#97061,#97062,#97063,#97064,#97065,#97066,#97067,#97068,#97069,#97070,
#97071,#97072,#97073,#97074,#97075,#97076,#97077,#97078,#97079,#97080,#97081,
#97082,#97083,#97084,#97085,#97086,#97087,#97088,#97089,#97090,#97091,#97092,
#97093,#97094,#97095,#97096,#97097,#97098,#97099,#97100,#97101,#97102,#97103,
#97104,#97105,#97106,#97107,#97108,#97109,#97110,#97111,#97112,#97113,#97114,
#97115,#97116,#97117,#97118,#97119,#97120,#97121,#97122,#97123,#97124,#97125,
#97126,#97127,#97128,#97129,#97130,#97131,#97132,#97133,#97134,#97135,#97136,
#97137,#97138,#97139,#97140,#97141)),.UNSPECIFIED.,.F.,.F.,.F.,(4,4),(4,
1,1,1,1,1,1,1,1,1,1,1,1,1,1,1,1,1,1,1,1,1,1,1,1,1,1,1,1,1,1,1,1,1,1,1,1,
1,1,1,1,1,1,1,1,1,1,1,1,1,1,1,1,1,1,1,1,1,1,1,1,1,1,1,1,1,1,1,1,1,1,1,1,
1,1,1,1,1,1,1,1,1,1,1,1,1,1,1,1,1,1,1,1,1,1,1,1,1,1,1,1,1,1,4),(0.,0.0460148164544132),
(11.6154215191105,12.6127573616628,13.610093204215,14.6074290467673,15.6047648893195,
16.6021007318718,17.599436574424,18.5967724169762,19.5941082595285,20.5914441020807,
21.588779944633,22.5861157871852,23.5834516297375,24.5807874722897,25.5781233148419,
26.5754591573942,27.5727949999464,28.5701308424987,29.5674666850509,30.5648025276032,
31.5621383701554,32.5594742127077,33.5568100552599,34.5541458978121,35.5514817403644,
36.5488175829166,37.5461534254689,38.5434892680211,39.5408251105734,40.5381609531256,
41.5354967956779,42.5328326382301,43.5301684807823,44.5275043233346,45.5248401658868,
46.5221760084391,47.5195118509913,48.5168476935436,49.5141835360958,50.5115193786481,
51.5088552212003,52.5061910637525,53.5035269063048,54.500862748857,55.4981985914093,
56.4955344339615,57.4928702765138,58.490206119066,59.4875419616182,60.4848778041705,
61.4822136467227,62.479549489275,63.4768853318272,64.4742211743795,65.4715570169317,
66.468892859484,67.4662287020362,68.4635645445884,69.4609003871407,70.4582362296929,
71.4555720722452,72.4529079147974,73.4502437573497,74.4475795999019,75.4449154424541,
76.4422512850064,77.4395871275586,78.4369229701109,79.4342588126631,80.4315946552154,
81.4289304977676,82.4262663403199,83.4236021828721,84.4209380254243,85.4182738679766,
86.4156097105288,87.4129455530811,88.4102813956333,89.4076172381856,90.4049530807378,
91.4022889232901,92.3996247658423,93.3969606083945,94.3942964509468,95.391632293499,
96.3889681360513,97.3863039786035,98.3836398211558,99.380975663708,100.37831150626,
101.375647348812,102.372983191365,103.370319033917,104.367654876469,105.364990719021,
106.362326561574,107.359662404126,108.356998246678,109.35433408923,110.351669931783,
111.349005774335,112.346341616887,113.343677459439,114.341013301992),
 .UNSPECIFIED.);
#672=B_SPLINE_SURFACE_WITH_KNOTS('',3,3,((#97261,#97262,#97263,#97264,#97265,
#97266,#97267,#97268,#97269,#97270,#97271,#97272,#97273,#97274,#97275,#97276,
#97277,#97278,#97279,#97280,#97281,#97282,#97283,#97284,#97285,#97286,#97287,
#97288,#97289,#97290,#97291,#97292,#97293,#97294,#97295,#97296,#97297,#97298,
#97299,#97300,#97301,#97302,#97303,#97304,#97305,#97306,#97307,#97308,#97309,
#97310,#97311,#97312,#97313,#97314,#97315,#97316,#97317,#97318,#97319,#97320,
#97321,#97322,#97323,#97324,#97325,#97326,#97327,#97328,#97329,#97330,#97331,
#97332,#97333,#97334,#97335,#97336,#97337,#97338,#97339,#97340,#97341,#97342,
#97343,#97344,#97345,#97346,#97347,#97348,#97349,#97350,#97351,#97352,#97353,
#97354,#97355,#97356,#97357,#97358,#97359,#97360,#97361,#97362,#97363,#97364,
#97365,#97366,#97367,#97368),(#97369,#97370,#97371,#97372,#97373,#97374,
#97375,#97376,#97377,#97378,#97379,#97380,#97381,#97382,#97383,#97384,#97385,
#97386,#97387,#97388,#97389,#97390,#97391,#97392,#97393,#97394,#97395,#97396,
#97397,#97398,#97399,#97400,#97401,#97402,#97403,#97404,#97405,#97406,#97407,
#97408,#97409,#97410,#97411,#97412,#97413,#97414,#97415,#97416,#97417,#97418,
#97419,#97420,#97421,#97422,#97423,#97424,#97425,#97426,#97427,#97428,#97429,
#97430,#97431,#97432,#97433,#97434,#97435,#97436,#97437,#97438,#97439,#97440,
#97441,#97442,#97443,#97444,#97445,#97446,#97447,#97448,#97449,#97450,#97451,
#97452,#97453,#97454,#97455,#97456,#97457,#97458,#97459,#97460,#97461,#97462,
#97463,#97464,#97465,#97466,#97467,#97468,#97469,#97470,#97471,#97472,#97473,
#97474,#97475,#97476),(#97477,#97478,#97479,#97480,#97481,#97482,#97483,
#97484,#97485,#97486,#97487,#97488,#97489,#97490,#97491,#97492,#97493,#97494,
#97495,#97496,#97497,#97498,#97499,#97500,#97501,#97502,#97503,#97504,#97505,
#97506,#97507,#97508,#97509,#97510,#97511,#97512,#97513,#97514,#97515,#97516,
#97517,#97518,#97519,#97520,#97521,#97522,#97523,#97524,#97525,#97526,#97527,
#97528,#97529,#97530,#97531,#97532,#97533,#97534,#97535,#97536,#97537,#97538,
#97539,#97540,#97541,#97542,#97543,#97544,#97545,#97546,#97547,#97548,#97549,
#97550,#97551,#97552,#97553,#97554,#97555,#97556,#97557,#97558,#97559,#97560,
#97561,#97562,#97563,#97564,#97565,#97566,#97567,#97568,#97569,#97570,#97571,
#97572,#97573,#97574,#97575,#97576,#97577,#97578,#97579,#97580,#97581,#97582,
#97583,#97584),(#97585,#97586,#97587,#97588,#97589,#97590,#97591,#97592,
#97593,#97594,#97595,#97596,#97597,#97598,#97599,#97600,#97601,#97602,#97603,
#97604,#97605,#97606,#97607,#97608,#97609,#97610,#97611,#97612,#97613,#97614,
#97615,#97616,#97617,#97618,#97619,#97620,#97621,#97622,#97623,#97624,#97625,
#97626,#97627,#97628,#97629,#97630,#97631,#97632,#97633,#97634,#97635,#97636,
#97637,#97638,#97639,#97640,#97641,#97642,#97643,#97644,#97645,#97646,#97647,
#97648,#97649,#97650,#97651,#97652,#97653,#97654,#97655,#97656,#97657,#97658,
#97659,#97660,#97661,#97662,#97663,#97664,#97665,#97666,#97667,#97668,#97669,
#97670,#97671,#97672,#97673,#97674,#97675,#97676,#97677,#97678,#97679,#97680,
#97681,#97682,#97683,#97684,#97685,#97686,#97687,#97688,#97689,#97690,#97691,
#97692)),.UNSPECIFIED.,.F.,.F.,.F.,(4,4),(4,1,1,1,1,1,1,1,1,1,1,1,1,1,1,
1,1,1,1,1,1,1,1,1,1,1,1,1,1,1,1,1,1,1,1,1,1,1,1,1,1,1,1,1,1,1,1,1,1,1,1,
1,1,1,1,1,1,1,1,1,1,1,1,1,1,1,1,1,1,1,1,1,1,1,1,1,1,1,1,1,1,1,1,1,1,1,1,
1,1,1,1,1,1,1,1,1,1,1,1,1,1,1,1,1,1,4),(0.,0.0460148164544132),(8.31058692273969,
9.30859389336977,10.3066008639999,11.30460783463,12.30261480526,13.3006217758901,
14.2986287465202,15.2966357171503,16.2946426877804,17.2926496584105,18.2906566290406,
19.2886635996707,20.2866705703008,21.2846775409308,22.2826845115609,23.280691482191,
24.2786984528211,25.2767054234512,26.2747123940813,27.2727193647114,28.2707263353415,
29.2687333059716,30.2667402766016,31.2647472472317,32.2627542178618,33.2607611884919,
34.258768159122,35.2567751297521,36.2547821003822,37.2527890710123,38.2507960416424,
39.2488030122724,40.2468099829025,41.2448169535326,42.2428239241627,43.2408308947928,
44.2388378654229,45.236844836053,46.2348518066831,47.2328587773132,48.2308657479432,
49.2288727185733,50.2268796892034,51.2248866598335,52.2228936304636,53.2209006010937,
54.2189075717238,55.2169145423539,56.214921512984,57.212928483614,58.2109354542441,
59.2089424248742,60.2069493955043,61.2049563661344,62.2029633367645,63.2009703073946,
64.1989772780247,65.1969842486548,66.1949912192848,67.1929981899149,68.191005160545,
69.1890121311751,70.1870191018052,71.1850260724353,72.1830330430654,73.1810400136955,
74.1790469843256,75.1770539549557,76.1750609255857,77.1730678962158,78.1710748668459,
79.169081837476,80.1670888081061,81.1650957787362,82.1631027493663,83.1611097199964,
84.1591166906264,85.1571236612565,86.1551306318866,87.1531376025167,88.1511445731468,
89.1491515437769,90.147158514407,91.1451654850371,92.1431724556672,93.1411794262973,
94.1391863969273,95.1371933675574,96.1352003381875,97.1332073088176,98.1312142794477,
99.1292212500778,100.127228220708,101.125235191338,102.123242161968,103.121249132598,
104.119256103228,105.117263073858,106.115270044488,107.113277015118,108.111283985749,
109.109290956379,110.107297927009,111.105304897639,112.103311868269,113.101318838899),
 .UNSPECIFIED.);
#673=B_SPLINE_SURFACE_WITH_KNOTS('',3,3,((#98697,#98698,#98699,#98700,#98701,
#98702,#98703,#98704,#98705,#98706,#98707,#98708,#98709,#98710,#98711,#98712,
#98713,#98714,#98715,#98716,#98717,#98718,#98719,#98720,#98721,#98722,#98723,
#98724,#98725,#98726,#98727,#98728,#98729,#98730,#98731,#98732,#98733,#98734,
#98735,#98736,#98737,#98738,#98739,#98740,#98741,#98742,#98743,#98744,#98745,
#98746,#98747,#98748,#98749,#98750,#98751,#98752,#98753),(#98754,#98755,
#98756,#98757,#98758,#98759,#98760,#98761,#98762,#98763,#98764,#98765,#98766,
#98767,#98768,#98769,#98770,#98771,#98772,#98773,#98774,#98775,#98776,#98777,
#98778,#98779,#98780,#98781,#98782,#98783,#98784,#98785,#98786,#98787,#98788,
#98789,#98790,#98791,#98792,#98793,#98794,#98795,#98796,#98797,#98798,#98799,
#98800,#98801,#98802,#98803,#98804,#98805,#98806,#98807,#98808,#98809,#98810),
(#98811,#98812,#98813,#98814,#98815,#98816,#98817,#98818,#98819,#98820,
#98821,#98822,#98823,#98824,#98825,#98826,#98827,#98828,#98829,#98830,#98831,
#98832,#98833,#98834,#98835,#98836,#98837,#98838,#98839,#98840,#98841,#98842,
#98843,#98844,#98845,#98846,#98847,#98848,#98849,#98850,#98851,#98852,#98853,
#98854,#98855,#98856,#98857,#98858,#98859,#98860,#98861,#98862,#98863,#98864,
#98865,#98866,#98867),(#98868,#98869,#98870,#98871,#98872,#98873,#98874,
#98875,#98876,#98877,#98878,#98879,#98880,#98881,#98882,#98883,#98884,#98885,
#98886,#98887,#98888,#98889,#98890,#98891,#98892,#98893,#98894,#98895,#98896,
#98897,#98898,#98899,#98900,#98901,#98902,#98903,#98904,#98905,#98906,#98907,
#98908,#98909,#98910,#98911,#98912,#98913,#98914,#98915,#98916,#98917,#98918,
#98919,#98920,#98921,#98922,#98923,#98924)),.UNSPECIFIED.,.F.,.F.,.F.,(4,
4),(4,1,1,1,1,1,1,1,1,1,1,1,1,1,1,1,1,1,1,1,1,1,1,1,1,1,1,1,1,1,1,1,1,1,
1,1,1,1,1,1,1,1,1,1,1,1,1,1,1,1,1,1,1,1,4),(0.,0.0329955678841871),(11.6159397475004,
12.6132790597317,13.610618371963,14.6079576841943,15.6052969964256,16.6026363086569,
17.5999756208882,18.5973149331195,19.5946542453507,20.591993557582,21.5893328698133,
22.5866721820446,23.5840114942759,24.5813508065072,25.5786901187385,26.5760294309698,
27.5733687432011,28.5707080554324,29.5680473676637,30.565386679895,31.5627259921263,
32.5600653043576,33.5574046165888,34.5547439288201,35.5520832410514,36.5494225532827,
37.546761865514,38.5441011777453,39.5414404899766,40.5387798022079,41.5361191144392,
42.5334584266705,43.5307977389018,44.5281370511331,45.5254763633644,46.5228156755957,
47.520154987827,48.5174943000582,49.5148336122895,50.5121729245208,51.5095122367521,
52.5068515489834,53.5041908612147,54.501530173446,55.4988694856773,56.4962087979086,
57.4935481101399,58.4908874223712,59.4882267346025,60.4855660468338,61.4829053590651,
62.4802446712963,63.4775839835276,64.4749232957589,65.4722626079902),
 .UNSPECIFIED.);
#674=B_SPLINE_SURFACE_WITH_KNOTS('',3,3,((#99081,#99082,#99083,#99084,#99085,
#99086,#99087,#99088,#99089,#99090,#99091,#99092,#99093,#99094,#99095,#99096,
#99097,#99098,#99099,#99100,#99101,#99102,#99103,#99104,#99105,#99106,#99107,
#99108,#99109,#99110,#99111,#99112,#99113,#99114,#99115,#99116,#99117,#99118,
#99119,#99120,#99121,#99122,#99123,#99124,#99125,#99126,#99127,#99128,#99129,
#99130,#99131,#99132,#99133,#99134,#99135,#99136,#99137,#99138,#99139),
(#99140,#99141,#99142,#99143,#99144,#99145,#99146,#99147,#99148,#99149,
#99150,#99151,#99152,#99153,#99154,#99155,#99156,#99157,#99158,#99159,#99160,
#99161,#99162,#99163,#99164,#99165,#99166,#99167,#99168,#99169,#99170,#99171,
#99172,#99173,#99174,#99175,#99176,#99177,#99178,#99179,#99180,#99181,#99182,
#99183,#99184,#99185,#99186,#99187,#99188,#99189,#99190,#99191,#99192,#99193,
#99194,#99195,#99196,#99197,#99198),(#99199,#99200,#99201,#99202,#99203,
#99204,#99205,#99206,#99207,#99208,#99209,#99210,#99211,#99212,#99213,#99214,
#99215,#99216,#99217,#99218,#99219,#99220,#99221,#99222,#99223,#99224,#99225,
#99226,#99227,#99228,#99229,#99230,#99231,#99232,#99233,#99234,#99235,#99236,
#99237,#99238,#99239,#99240,#99241,#99242,#99243,#99244,#99245,#99246,#99247,
#99248,#99249,#99250,#99251,#99252,#99253,#99254,#99255,#99256,#99257),
(#99258,#99259,#99260,#99261,#99262,#99263,#99264,#99265,#99266,#99267,
#99268,#99269,#99270,#99271,#99272,#99273,#99274,#99275,#99276,#99277,#99278,
#99279,#99280,#99281,#99282,#99283,#99284,#99285,#99286,#99287,#99288,#99289,
#99290,#99291,#99292,#99293,#99294,#99295,#99296,#99297,#99298,#99299,#99300,
#99301,#99302,#99303,#99304,#99305,#99306,#99307,#99308,#99309,#99310,#99311,
#99312,#99313,#99314,#99315,#99316)),.UNSPECIFIED.,.F.,.F.,.F.,(4,4),(4,
1,1,1,1,1,1,1,1,1,1,1,1,1,1,1,1,1,1,1,1,1,1,1,1,1,1,1,1,1,1,1,1,1,1,1,1,
1,1,1,1,1,1,1,1,1,1,1,1,1,1,1,1,1,1,1,4),(0.,0.0329955678841871),(8.30203615430837,
9.30077714598354,10.2995181376587,11.2982591293339,12.2970001210091,13.2957411126842,
14.2944821043594,15.2932230960346,16.2919640877097,17.2907050793849,18.2894460710601,
19.2881870627352,20.2869280544104,21.2856690460856,22.2844100377608,23.2831510294359,
24.2818920211111,25.2806330127863,26.2793740044614,27.2781149961366,28.2768559878118,
29.2755969794869,30.2743379711621,31.2730789628373,32.2718199545125,33.2705609461876,
34.2693019378628,35.268042929538,36.2667839212131,37.2655249128883,38.2642659045635,
39.2630068962386,40.2617478879138,41.260488879589,42.2592298712642,43.2579708629393,
44.2567118546145,45.2554528462897,46.2541938379648,47.25293482964,48.2516758213152,
49.2504168129903,50.2491578046655,51.2478987963407,52.2466397880159,53.245380779691,
54.2441217713662,55.2428627630414,56.2416037547165,57.2403447463917,58.2390857380669,
59.237826729742,60.2365677214172,61.2353087130924,62.2340497047676,63.2327906964427,
64.2315316881179),.UNSPECIFIED.);
#675=FACE_OUTER_BOUND('',#1672,.T.);
#676=FACE_OUTER_BOUND('',#1673,.T.);
#677=FACE_OUTER_BOUND('',#1674,.T.);
#678=FACE_OUTER_BOUND('',#1675,.T.);
#679=FACE_OUTER_BOUND('',#1676,.T.);
#680=FACE_OUTER_BOUND('',#1677,.T.);
#681=FACE_OUTER_BOUND('',#1678,.T.);
#682=FACE_OUTER_BOUND('',#1679,.T.);
#683=FACE_OUTER_BOUND('',#1680,.T.);
#684=FACE_OUTER_BOUND('',#1681,.T.);
#685=FACE_OUTER_BOUND('',#1682,.T.);
#686=FACE_OUTER_BOUND('',#1683,.T.);
#687=FACE_OUTER_BOUND('',#1684,.T.);
#688=FACE_OUTER_BOUND('',#1685,.T.);
#689=FACE_OUTER_BOUND('',#1686,.T.);
#690=FACE_OUTER_BOUND('',#1687,.T.);
#691=FACE_OUTER_BOUND('',#1688,.T.);
#692=FACE_OUTER_BOUND('',#1689,.T.);
#693=FACE_OUTER_BOUND('',#1690,.T.);
#694=FACE_OUTER_BOUND('',#1691,.T.);
#695=FACE_OUTER_BOUND('',#1692,.T.);
#696=FACE_OUTER_BOUND('',#1693,.T.);
#697=FACE_OUTER_BOUND('',#1694,.T.);
#698=FACE_OUTER_BOUND('',#1695,.T.);
#699=FACE_OUTER_BOUND('',#1696,.T.);
#700=FACE_OUTER_BOUND('',#1697,.T.);
#701=FACE_OUTER_BOUND('',#1698,.T.);
#702=FACE_OUTER_BOUND('',#1699,.T.);
#703=FACE_OUTER_BOUND('',#1700,.T.);
#704=FACE_OUTER_BOUND('',#1701,.T.);
#705=FACE_OUTER_BOUND('',#1702,.T.);
#706=FACE_OUTER_BOUND('',#1703,.T.);
#707=FACE_OUTER_BOUND('',#1704,.T.);
#708=FACE_OUTER_BOUND('',#1705,.T.);
#709=FACE_OUTER_BOUND('',#1706,.T.);
#710=FACE_OUTER_BOUND('',#1707,.T.);
#711=FACE_OUTER_BOUND('',#1708,.T.);
#712=FACE_OUTER_BOUND('',#1709,.T.);
#713=FACE_OUTER_BOUND('',#1710,.T.);
#714=FACE_OUTER_BOUND('',#1711,.T.);
#715=FACE_OUTER_BOUND('',#1712,.T.);
#716=FACE_OUTER_BOUND('',#1713,.T.);
#717=FACE_OUTER_BOUND('',#1714,.T.);
#718=FACE_OUTER_BOUND('',#1715,.T.);
#719=FACE_OUTER_BOUND('',#1716,.T.);
#720=FACE_OUTER_BOUND('',#1717,.T.);
#721=FACE_OUTER_BOUND('',#1718,.T.);
#722=FACE_OUTER_BOUND('',#1719,.T.);
#723=FACE_OUTER_BOUND('',#1720,.T.);
#724=FACE_OUTER_BOUND('',#1721,.T.);
#725=FACE_OUTER_BOUND('',#1722,.T.);
#726=FACE_OUTER_BOUND('',#1723,.T.);
#727=FACE_OUTER_BOUND('',#1724,.T.);
#728=FACE_OUTER_BOUND('',#1725,.T.);
#729=FACE_OUTER_BOUND('',#1726,.T.);
#730=FACE_OUTER_BOUND('',#1727,.T.);
#731=FACE_OUTER_BOUND('',#1728,.T.);
#732=FACE_OUTER_BOUND('',#1729,.T.);
#733=FACE_OUTER_BOUND('',#1730,.T.);
#734=FACE_OUTER_BOUND('',#1731,.T.);
#735=FACE_OUTER_BOUND('',#1732,.T.);
#736=FACE_OUTER_BOUND('',#1733,.T.);
#737=FACE_OUTER_BOUND('',#1734,.T.);
#738=FACE_OUTER_BOUND('',#1735,.T.);
#739=FACE_OUTER_BOUND('',#1736,.T.);
#740=FACE_OUTER_BOUND('',#1737,.T.);
#741=FACE_OUTER_BOUND('',#1738,.T.);
#742=FACE_OUTER_BOUND('',#1739,.T.);
#743=FACE_OUTER_BOUND('',#1740,.T.);
#744=FACE_OUTER_BOUND('',#1741,.T.);
#745=FACE_OUTER_BOUND('',#1742,.T.);
#746=FACE_OUTER_BOUND('',#1743,.T.);
#747=FACE_OUTER_BOUND('',#1744,.T.);
#748=FACE_OUTER_BOUND('',#1745,.T.);
#749=FACE_OUTER_BOUND('',#1746,.T.);
#750=FACE_OUTER_BOUND('',#1747,.T.);
#751=FACE_OUTER_BOUND('',#1748,.T.);
#752=FACE_OUTER_BOUND('',#1749,.T.);
#753=FACE_OUTER_BOUND('',#1750,.T.);
#754=FACE_OUTER_BOUND('',#1751,.T.);
#755=FACE_OUTER_BOUND('',#1752,.T.);
#756=FACE_OUTER_BOUND('',#1753,.T.);
#757=FACE_OUTER_BOUND('',#1754,.T.);
#758=FACE_OUTER_BOUND('',#1755,.T.);
#759=FACE_OUTER_BOUND('',#1756,.T.);
#760=FACE_OUTER_BOUND('',#1757,.T.);
#761=FACE_OUTER_BOUND('',#1758,.T.);
#762=FACE_OUTER_BOUND('',#1759,.T.);
#763=FACE_OUTER_BOUND('',#1760,.T.);
#764=FACE_OUTER_BOUND('',#1761,.T.);
#765=FACE_OUTER_BOUND('',#1762,.T.);
#766=FACE_OUTER_BOUND('',#1763,.T.);
#767=FACE_OUTER_BOUND('',#1764,.T.);
#768=FACE_OUTER_BOUND('',#1765,.T.);
#769=FACE_OUTER_BOUND('',#1766,.T.);
#770=FACE_OUTER_BOUND('',#1767,.T.);
#771=FACE_OUTER_BOUND('',#1768,.T.);
#772=FACE_OUTER_BOUND('',#1769,.T.);
#773=FACE_OUTER_BOUND('',#1770,.T.);
#774=FACE_OUTER_BOUND('',#1771,.T.);
#775=FACE_OUTER_BOUND('',#1772,.T.);
#776=FACE_OUTER_BOUND('',#1773,.T.);
#777=FACE_OUTER_BOUND('',#1774,.T.);
#778=FACE_OUTER_BOUND('',#1775,.T.);
#779=FACE_OUTER_BOUND('',#1776,.T.);
#780=FACE_OUTER_BOUND('',#1777,.T.);
#781=FACE_OUTER_BOUND('',#1778,.T.);
#782=FACE_OUTER_BOUND('',#1779,.T.);
#783=FACE_OUTER_BOUND('',#1780,.T.);
#784=FACE_OUTER_BOUND('',#1781,.T.);
#785=FACE_OUTER_BOUND('',#1782,.T.);
#786=FACE_OUTER_BOUND('',#1783,.T.);
#787=FACE_OUTER_BOUND('',#1784,.T.);
#788=FACE_OUTER_BOUND('',#1785,.T.);
#789=FACE_OUTER_BOUND('',#1786,.T.);
#790=FACE_OUTER_BOUND('',#1787,.T.);
#791=FACE_OUTER_BOUND('',#1788,.T.);
#792=FACE_OUTER_BOUND('',#1789,.T.);
#793=FACE_OUTER_BOUND('',#1790,.T.);
#794=FACE_OUTER_BOUND('',#1791,.T.);
#795=FACE_OUTER_BOUND('',#1792,.T.);
#796=FACE_OUTER_BOUND('',#1793,.T.);
#797=FACE_OUTER_BOUND('',#1794,.T.);
#798=FACE_OUTER_BOUND('',#1795,.T.);
#799=FACE_OUTER_BOUND('',#1796,.T.);
#800=FACE_OUTER_BOUND('',#1797,.T.);
#801=FACE_OUTER_BOUND('',#1798,.T.);
#802=FACE_OUTER_BOUND('',#1799,.T.);
#803=FACE_OUTER_BOUND('',#1800,.T.);
#804=FACE_OUTER_BOUND('',#1801,.T.);
#805=FACE_OUTER_BOUND('',#1802,.T.);
#806=FACE_OUTER_BOUND('',#1803,.T.);
#807=FACE_OUTER_BOUND('',#1804,.T.);
#808=FACE_OUTER_BOUND('',#1805,.T.);
#809=FACE_OUTER_BOUND('',#1806,.T.);
#810=FACE_OUTER_BOUND('',#1807,.T.);
#811=FACE_OUTER_BOUND('',#1808,.T.);
#812=FACE_OUTER_BOUND('',#1809,.T.);
#813=FACE_OUTER_BOUND('',#1810,.T.);
#814=FACE_OUTER_BOUND('',#1811,.T.);
#815=FACE_OUTER_BOUND('',#1812,.T.);
#816=FACE_OUTER_BOUND('',#1813,.T.);
#817=FACE_OUTER_BOUND('',#1814,.T.);
#818=FACE_OUTER_BOUND('',#1815,.T.);
#819=FACE_OUTER_BOUND('',#1816,.T.);
#820=FACE_OUTER_BOUND('',#1817,.T.);
#821=FACE_OUTER_BOUND('',#1818,.T.);
#822=FACE_OUTER_BOUND('',#1819,.T.);
#823=FACE_OUTER_BOUND('',#1820,.T.);
#824=FACE_OUTER_BOUND('',#1821,.T.);
#825=FACE_OUTER_BOUND('',#1822,.T.);
#826=FACE_OUTER_BOUND('',#1823,.T.);
#827=FACE_OUTER_BOUND('',#1824,.T.);
#828=FACE_OUTER_BOUND('',#1825,.T.);
#829=FACE_OUTER_BOUND('',#1826,.T.);
#830=FACE_OUTER_BOUND('',#1827,.T.);
#831=FACE_OUTER_BOUND('',#1828,.T.);
#832=FACE_OUTER_BOUND('',#1829,.T.);
#833=FACE_OUTER_BOUND('',#1830,.T.);
#834=FACE_OUTER_BOUND('',#1831,.T.);
#835=FACE_OUTER_BOUND('',#1832,.T.);
#836=FACE_OUTER_BOUND('',#1833,.T.);
#837=FACE_OUTER_BOUND('',#1834,.T.);
#838=FACE_OUTER_BOUND('',#1835,.T.);
#839=FACE_OUTER_BOUND('',#1836,.T.);
#840=FACE_OUTER_BOUND('',#1837,.T.);
#841=FACE_OUTER_BOUND('',#1838,.T.);
#842=FACE_OUTER_BOUND('',#1839,.T.);
#843=FACE_OUTER_BOUND('',#1840,.T.);
#844=FACE_OUTER_BOUND('',#1841,.T.);
#845=FACE_OUTER_BOUND('',#1842,.T.);
#846=FACE_OUTER_BOUND('',#1843,.T.);
#847=FACE_OUTER_BOUND('',#1844,.T.);
#848=FACE_OUTER_BOUND('',#1845,.T.);
#849=FACE_OUTER_BOUND('',#1846,.T.);
#850=FACE_OUTER_BOUND('',#1847,.T.);
#851=FACE_OUTER_BOUND('',#1848,.T.);
#852=FACE_OUTER_BOUND('',#1849,.T.);
#853=FACE_OUTER_BOUND('',#1850,.T.);
#854=FACE_OUTER_BOUND('',#1851,.T.);
#855=FACE_OUTER_BOUND('',#1852,.T.);
#856=FACE_OUTER_BOUND('',#1853,.T.);
#857=FACE_OUTER_BOUND('',#1854,.T.);
#858=FACE_OUTER_BOUND('',#1855,.T.);
#859=FACE_OUTER_BOUND('',#1856,.T.);
#860=FACE_OUTER_BOUND('',#1857,.T.);
#861=FACE_OUTER_BOUND('',#1858,.T.);
#862=FACE_OUTER_BOUND('',#1859,.T.);
#863=FACE_OUTER_BOUND('',#1860,.T.);
#864=FACE_OUTER_BOUND('',#1861,.T.);
#865=FACE_OUTER_BOUND('',#1862,.T.);
#866=FACE_OUTER_BOUND('',#1863,.T.);
#867=FACE_OUTER_BOUND('',#1864,.T.);
#868=FACE_OUTER_BOUND('',#1865,.T.);
#869=FACE_OUTER_BOUND('',#1866,.T.);
#870=FACE_OUTER_BOUND('',#1867,.T.);
#871=FACE_OUTER_BOUND('',#1868,.T.);
#872=FACE_OUTER_BOUND('',#1869,.T.);
#873=FACE_OUTER_BOUND('',#1870,.T.);
#874=FACE_OUTER_BOUND('',#1871,.T.);
#875=FACE_OUTER_BOUND('',#1872,.T.);
#876=FACE_OUTER_BOUND('',#1873,.T.);
#877=FACE_OUTER_BOUND('',#1874,.T.);
#878=FACE_OUTER_BOUND('',#1875,.T.);
#879=FACE_OUTER_BOUND('',#1876,.T.);
#880=FACE_OUTER_BOUND('',#1877,.T.);
#881=FACE_OUTER_BOUND('',#1878,.T.);
#882=FACE_OUTER_BOUND('',#1879,.T.);
#883=FACE_OUTER_BOUND('',#1880,.T.);
#884=FACE_OUTER_BOUND('',#1881,.T.);
#885=FACE_OUTER_BOUND('',#1882,.T.);
#886=FACE_OUTER_BOUND('',#1883,.T.);
#887=FACE_OUTER_BOUND('',#1884,.T.);
#888=FACE_OUTER_BOUND('',#1885,.T.);
#889=FACE_OUTER_BOUND('',#1886,.T.);
#890=FACE_OUTER_BOUND('',#1887,.T.);
#891=FACE_OUTER_BOUND('',#1888,.T.);
#892=FACE_OUTER_BOUND('',#1889,.T.);
#893=FACE_OUTER_BOUND('',#1890,.T.);
#894=FACE_OUTER_BOUND('',#1891,.T.);
#895=FACE_OUTER_BOUND('',#1892,.T.);
#896=FACE_OUTER_BOUND('',#1893,.T.);
#897=FACE_OUTER_BOUND('',#1894,.T.);
#898=FACE_OUTER_BOUND('',#1895,.T.);
#899=FACE_OUTER_BOUND('',#1896,.T.);
#900=FACE_OUTER_BOUND('',#1897,.T.);
#901=FACE_OUTER_BOUND('',#1898,.T.);
#902=FACE_OUTER_BOUND('',#1899,.T.);
#903=FACE_OUTER_BOUND('',#1900,.T.);
#904=FACE_OUTER_BOUND('',#1901,.T.);
#905=FACE_OUTER_BOUND('',#1902,.T.);
#906=FACE_OUTER_BOUND('',#1903,.T.);
#907=FACE_OUTER_BOUND('',#1904,.T.);
#908=FACE_OUTER_BOUND('',#1905,.T.);
#909=FACE_OUTER_BOUND('',#1906,.T.);
#910=FACE_OUTER_BOUND('',#1907,.T.);
#911=FACE_OUTER_BOUND('',#1908,.T.);
#912=FACE_OUTER_BOUND('',#1909,.T.);
#913=FACE_OUTER_BOUND('',#1910,.T.);
#914=FACE_OUTER_BOUND('',#1911,.T.);
#915=FACE_OUTER_BOUND('',#1912,.T.);
#916=FACE_OUTER_BOUND('',#1913,.T.);
#917=FACE_OUTER_BOUND('',#1914,.T.);
#918=FACE_OUTER_BOUND('',#1915,.T.);
#919=FACE_OUTER_BOUND('',#1916,.T.);
#920=FACE_OUTER_BOUND('',#1917,.T.);
#921=FACE_OUTER_BOUND('',#1918,.T.);
#922=FACE_OUTER_BOUND('',#1919,.T.);
#923=FACE_OUTER_BOUND('',#1920,.T.);
#924=FACE_OUTER_BOUND('',#1921,.T.);
#925=FACE_OUTER_BOUND('',#1922,.T.);
#926=FACE_OUTER_BOUND('',#1923,.T.);
#927=FACE_OUTER_BOUND('',#1924,.T.);
#928=FACE_OUTER_BOUND('',#1925,.T.);
#929=FACE_OUTER_BOUND('',#1926,.T.);
#930=FACE_OUTER_BOUND('',#1927,.T.);
#931=FACE_OUTER_BOUND('',#1928,.T.);
#932=FACE_OUTER_BOUND('',#1929,.T.);
#933=FACE_OUTER_BOUND('',#1930,.T.);
#934=FACE_OUTER_BOUND('',#1931,.T.);
#935=FACE_OUTER_BOUND('',#1932,.T.);
#936=FACE_OUTER_BOUND('',#1933,.T.);
#937=FACE_OUTER_BOUND('',#1934,.T.);
#938=FACE_OUTER_BOUND('',#1935,.T.);
#939=FACE_OUTER_BOUND('',#1936,.T.);
#940=FACE_OUTER_BOUND('',#1937,.T.);
#941=FACE_OUTER_BOUND('',#1938,.T.);
#942=FACE_OUTER_BOUND('',#1939,.T.);
#943=FACE_OUTER_BOUND('',#1940,.T.);
#944=FACE_OUTER_BOUND('',#1941,.T.);
#945=FACE_OUTER_BOUND('',#1942,.T.);
#946=FACE_OUTER_BOUND('',#1943,.T.);
#947=FACE_OUTER_BOUND('',#1944,.T.);
#948=FACE_OUTER_BOUND('',#1945,.T.);
#949=FACE_OUTER_BOUND('',#1946,.T.);
#950=FACE_OUTER_BOUND('',#1947,.T.);
#951=FACE_OUTER_BOUND('',#1948,.T.);
#952=FACE_OUTER_BOUND('',#1949,.T.);
#953=FACE_OUTER_BOUND('',#1950,.T.);
#954=FACE_OUTER_BOUND('',#1951,.T.);
#955=FACE_OUTER_BOUND('',#1952,.T.);
#956=FACE_OUTER_BOUND('',#1953,.T.);
#957=FACE_OUTER_BOUND('',#1954,.T.);
#958=FACE_OUTER_BOUND('',#1955,.T.);
#959=FACE_OUTER_BOUND('',#1956,.T.);
#960=FACE_OUTER_BOUND('',#1957,.T.);
#961=FACE_OUTER_BOUND('',#1958,.T.);
#962=FACE_OUTER_BOUND('',#1959,.T.);
#963=FACE_OUTER_BOUND('',#1960,.T.);
#964=FACE_OUTER_BOUND('',#1961,.T.);
#965=FACE_OUTER_BOUND('',#1962,.T.);
#966=FACE_OUTER_BOUND('',#1963,.T.);
#967=FACE_OUTER_BOUND('',#1964,.T.);
#968=FACE_OUTER_BOUND('',#1965,.T.);
#969=FACE_OUTER_BOUND('',#1966,.T.);
#970=FACE_OUTER_BOUND('',#1967,.T.);
#971=FACE_OUTER_BOUND('',#1968,.T.);
#972=FACE_OUTER_BOUND('',#1969,.T.);
#973=FACE_OUTER_BOUND('',#1970,.T.);
#974=FACE_OUTER_BOUND('',#1971,.T.);
#975=FACE_OUTER_BOUND('',#1972,.T.);
#976=FACE_OUTER_BOUND('',#1973,.T.);
#977=FACE_OUTER_BOUND('',#1974,.T.);
#978=FACE_OUTER_BOUND('',#1975,.T.);
#979=FACE_OUTER_BOUND('',#1976,.T.);
#980=FACE_OUTER_BOUND('',#1977,.T.);
#981=FACE_OUTER_BOUND('',#1978,.T.);
#982=FACE_OUTER_BOUND('',#1979,.T.);
#983=FACE_OUTER_BOUND('',#1980,.T.);
#984=FACE_OUTER_BOUND('',#1981,.T.);
#985=FACE_OUTER_BOUND('',#1982,.T.);
#986=FACE_OUTER_BOUND('',#1983,.T.);
#987=FACE_OUTER_BOUND('',#1984,.T.);
#988=FACE_OUTER_BOUND('',#1985,.T.);
#989=FACE_OUTER_BOUND('',#1986,.T.);
#990=FACE_OUTER_BOUND('',#1987,.T.);
#991=FACE_OUTER_BOUND('',#1988,.T.);
#992=FACE_OUTER_BOUND('',#1989,.T.);
#993=FACE_OUTER_BOUND('',#1990,.T.);
#994=FACE_OUTER_BOUND('',#1991,.T.);
#995=FACE_OUTER_BOUND('',#1992,.T.);
#996=FACE_OUTER_BOUND('',#1993,.T.);
#997=FACE_OUTER_BOUND('',#1994,.T.);
#998=FACE_OUTER_BOUND('',#1995,.T.);
#999=FACE_OUTER_BOUND('',#1996,.T.);
#1000=FACE_OUTER_BOUND('',#1997,.T.);
#1001=FACE_OUTER_BOUND('',#1998,.T.);
#1002=FACE_OUTER_BOUND('',#1999,.T.);
#1003=FACE_OUTER_BOUND('',#2000,.T.);
#1004=FACE_OUTER_BOUND('',#2001,.T.);
#1005=FACE_OUTER_BOUND('',#2002,.T.);
#1006=FACE_OUTER_BOUND('',#2003,.T.);
#1007=FACE_OUTER_BOUND('',#2004,.T.);
#1008=FACE_OUTER_BOUND('',#2005,.T.);
#1009=FACE_OUTER_BOUND('',#2006,.T.);
#1010=FACE_OUTER_BOUND('',#2007,.T.);
#1011=FACE_OUTER_BOUND('',#2008,.T.);
#1012=FACE_OUTER_BOUND('',#2009,.T.);
#1013=FACE_OUTER_BOUND('',#2010,.T.);
#1014=FACE_OUTER_BOUND('',#2011,.T.);
#1015=FACE_OUTER_BOUND('',#2012,.T.);
#1016=FACE_OUTER_BOUND('',#2013,.T.);
#1017=FACE_OUTER_BOUND('',#2014,.T.);
#1018=FACE_OUTER_BOUND('',#2015,.T.);
#1019=FACE_OUTER_BOUND('',#2016,.T.);
#1020=FACE_OUTER_BOUND('',#2017,.T.);
#1021=FACE_OUTER_BOUND('',#2018,.T.);
#1022=FACE_OUTER_BOUND('',#2019,.T.);
#1023=FACE_OUTER_BOUND('',#2020,.T.);
#1024=FACE_OUTER_BOUND('',#2021,.T.);
#1025=FACE_OUTER_BOUND('',#2022,.T.);
#1026=FACE_OUTER_BOUND('',#2023,.T.);
#1027=FACE_OUTER_BOUND('',#2024,.T.);
#1028=FACE_OUTER_BOUND('',#2025,.T.);
#1029=FACE_OUTER_BOUND('',#2026,.T.);
#1030=FACE_OUTER_BOUND('',#2027,.T.);
#1031=FACE_OUTER_BOUND('',#2028,.T.);
#1032=FACE_OUTER_BOUND('',#2029,.T.);
#1033=FACE_OUTER_BOUND('',#2030,.T.);
#1034=FACE_OUTER_BOUND('',#2031,.T.);
#1035=FACE_OUTER_BOUND('',#2032,.T.);
#1036=FACE_OUTER_BOUND('',#2033,.T.);
#1037=FACE_OUTER_BOUND('',#2034,.T.);
#1038=FACE_OUTER_BOUND('',#2035,.T.);
#1039=FACE_OUTER_BOUND('',#2036,.T.);
#1040=FACE_OUTER_BOUND('',#2037,.T.);
#1041=FACE_OUTER_BOUND('',#2038,.T.);
#1042=FACE_OUTER_BOUND('',#2039,.T.);
#1043=FACE_OUTER_BOUND('',#2040,.T.);
#1044=FACE_OUTER_BOUND('',#2041,.T.);
#1045=FACE_OUTER_BOUND('',#2042,.T.);
#1046=FACE_OUTER_BOUND('',#2043,.T.);
#1047=FACE_OUTER_BOUND('',#2044,.T.);
#1048=FACE_OUTER_BOUND('',#2045,.T.);
#1049=FACE_OUTER_BOUND('',#2046,.T.);
#1050=FACE_OUTER_BOUND('',#2047,.T.);
#1051=FACE_OUTER_BOUND('',#2048,.T.);
#1052=FACE_OUTER_BOUND('',#2049,.T.);
#1053=FACE_OUTER_BOUND('',#2050,.T.);
#1054=FACE_OUTER_BOUND('',#2051,.T.);
#1055=FACE_OUTER_BOUND('',#2052,.T.);
#1056=FACE_OUTER_BOUND('',#2053,.T.);
#1057=FACE_OUTER_BOUND('',#2054,.T.);
#1058=FACE_OUTER_BOUND('',#2055,.T.);
#1059=FACE_OUTER_BOUND('',#2056,.T.);
#1060=FACE_OUTER_BOUND('',#2057,.T.);
#1061=FACE_OUTER_BOUND('',#2058,.T.);
#1062=FACE_OUTER_BOUND('',#2059,.T.);
#1063=FACE_OUTER_BOUND('',#2060,.T.);
#1064=FACE_OUTER_BOUND('',#2061,.T.);
#1065=FACE_OUTER_BOUND('',#2062,.T.);
#1066=FACE_OUTER_BOUND('',#2063,.T.);
#1067=FACE_OUTER_BOUND('',#2064,.T.);
#1068=FACE_OUTER_BOUND('',#2065,.T.);
#1069=FACE_OUTER_BOUND('',#2066,.T.);
#1070=FACE_OUTER_BOUND('',#2067,.T.);
#1071=FACE_OUTER_BOUND('',#2068,.T.);
#1072=FACE_OUTER_BOUND('',#2069,.T.);
#1073=FACE_OUTER_BOUND('',#2070,.T.);
#1074=FACE_OUTER_BOUND('',#2071,.T.);
#1075=FACE_OUTER_BOUND('',#2072,.T.);
#1076=FACE_OUTER_BOUND('',#2073,.T.);
#1077=FACE_OUTER_BOUND('',#2074,.T.);
#1078=FACE_OUTER_BOUND('',#2075,.T.);
#1079=FACE_OUTER_BOUND('',#2076,.T.);
#1080=FACE_OUTER_BOUND('',#2077,.T.);
#1081=FACE_OUTER_BOUND('',#2078,.T.);
#1082=FACE_OUTER_BOUND('',#2079,.T.);
#1083=FACE_OUTER_BOUND('',#2080,.T.);
#1084=FACE_OUTER_BOUND('',#2081,.T.);
#1085=FACE_OUTER_BOUND('',#2082,.T.);
#1086=FACE_OUTER_BOUND('',#2083,.T.);
#1087=FACE_OUTER_BOUND('',#2084,.T.);
#1088=FACE_OUTER_BOUND('',#2085,.T.);
#1089=FACE_OUTER_BOUND('',#2086,.T.);
#1090=FACE_OUTER_BOUND('',#2087,.T.);
#1091=FACE_OUTER_BOUND('',#2088,.T.);
#1092=FACE_OUTER_BOUND('',#2089,.T.);
#1093=FACE_OUTER_BOUND('',#2090,.T.);
#1094=FACE_OUTER_BOUND('',#2091,.T.);
#1095=FACE_OUTER_BOUND('',#2092,.T.);
#1096=FACE_OUTER_BOUND('',#2093,.T.);
#1097=FACE_OUTER_BOUND('',#2094,.T.);
#1098=FACE_OUTER_BOUND('',#2095,.T.);
#1099=FACE_OUTER_BOUND('',#2096,.T.);
#1100=FACE_OUTER_BOUND('',#2097,.T.);
#1101=FACE_OUTER_BOUND('',#2098,.T.);
#1102=FACE_OUTER_BOUND('',#2099,.T.);
#1103=FACE_OUTER_BOUND('',#2100,.T.);
#1104=FACE_OUTER_BOUND('',#2101,.T.);
#1105=FACE_OUTER_BOUND('',#2102,.T.);
#1106=FACE_OUTER_BOUND('',#2103,.T.);
#1107=FACE_OUTER_BOUND('',#2104,.T.);
#1108=FACE_OUTER_BOUND('',#2105,.T.);
#1109=FACE_OUTER_BOUND('',#2106,.T.);
#1110=FACE_OUTER_BOUND('',#2107,.T.);
#1111=FACE_OUTER_BOUND('',#2108,.T.);
#1112=FACE_OUTER_BOUND('',#2109,.T.);
#1113=FACE_OUTER_BOUND('',#2110,.T.);
#1114=FACE_OUTER_BOUND('',#2111,.T.);
#1115=FACE_OUTER_BOUND('',#2112,.T.);
#1116=FACE_OUTER_BOUND('',#2113,.T.);
#1117=FACE_OUTER_BOUND('',#2114,.T.);
#1118=FACE_OUTER_BOUND('',#2115,.T.);
#1119=FACE_OUTER_BOUND('',#2116,.T.);
#1120=FACE_OUTER_BOUND('',#2117,.T.);
#1121=FACE_OUTER_BOUND('',#2118,.T.);
#1122=FACE_OUTER_BOUND('',#2119,.T.);
#1123=FACE_OUTER_BOUND('',#2120,.T.);
#1124=FACE_OUTER_BOUND('',#2121,.T.);
#1125=FACE_OUTER_BOUND('',#2122,.T.);
#1126=FACE_OUTER_BOUND('',#2123,.T.);
#1127=FACE_OUTER_BOUND('',#2124,.T.);
#1128=FACE_OUTER_BOUND('',#2125,.T.);
#1129=FACE_OUTER_BOUND('',#2126,.T.);
#1130=FACE_OUTER_BOUND('',#2127,.T.);
#1131=FACE_OUTER_BOUND('',#2128,.T.);
#1132=FACE_OUTER_BOUND('',#2129,.T.);
#1133=FACE_OUTER_BOUND('',#2134,.T.);
#1134=FACE_OUTER_BOUND('',#2142,.T.);
#1135=FACE_OUTER_BOUND('',#2150,.T.);
#1136=FACE_OUTER_BOUND('',#2151,.T.);
#1137=FACE_OUTER_BOUND('',#2152,.T.);
#1138=FACE_OUTER_BOUND('',#2153,.T.);
#1139=FACE_OUTER_BOUND('',#2154,.T.);
#1140=FACE_OUTER_BOUND('',#2155,.T.);
#1141=FACE_OUTER_BOUND('',#2156,.T.);
#1142=FACE_OUTER_BOUND('',#2157,.T.);
#1143=FACE_OUTER_BOUND('',#2158,.T.);
#1144=FACE_OUTER_BOUND('',#2159,.T.);
#1145=FACE_OUTER_BOUND('',#2160,.T.);
#1146=FACE_OUTER_BOUND('',#2161,.T.);
#1147=FACE_OUTER_BOUND('',#2162,.T.);
#1148=FACE_OUTER_BOUND('',#2163,.T.);
#1149=FACE_OUTER_BOUND('',#2164,.T.);
#1150=FACE_OUTER_BOUND('',#2165,.T.);
#1151=FACE_OUTER_BOUND('',#2166,.T.);
#1152=FACE_OUTER_BOUND('',#2167,.T.);
#1153=FACE_OUTER_BOUND('',#2168,.T.);
#1154=FACE_OUTER_BOUND('',#2169,.T.);
#1155=FACE_OUTER_BOUND('',#2170,.T.);
#1156=FACE_OUTER_BOUND('',#2171,.T.);
#1157=FACE_OUTER_BOUND('',#2172,.T.);
#1158=FACE_OUTER_BOUND('',#2173,.T.);
#1159=FACE_OUTER_BOUND('',#2174,.T.);
#1160=FACE_OUTER_BOUND('',#2175,.T.);
#1161=FACE_OUTER_BOUND('',#2176,.T.);
#1162=FACE_OUTER_BOUND('',#2177,.T.);
#1163=FACE_OUTER_BOUND('',#2178,.T.);
#1164=FACE_OUTER_BOUND('',#2179,.T.);
#1165=FACE_OUTER_BOUND('',#2180,.T.);
#1166=FACE_OUTER_BOUND('',#2181,.T.);
#1167=FACE_OUTER_BOUND('',#2182,.T.);
#1168=FACE_OUTER_BOUND('',#2183,.T.);
#1169=FACE_OUTER_BOUND('',#2184,.T.);
#1170=FACE_OUTER_BOUND('',#2185,.T.);
#1171=FACE_OUTER_BOUND('',#2186,.T.);
#1172=FACE_OUTER_BOUND('',#2187,.T.);
#1173=FACE_OUTER_BOUND('',#2188,.T.);
#1174=FACE_OUTER_BOUND('',#2189,.T.);
#1175=FACE_OUTER_BOUND('',#2190,.T.);
#1176=FACE_OUTER_BOUND('',#2191,.T.);
#1177=FACE_OUTER_BOUND('',#2192,.T.);
#1178=FACE_OUTER_BOUND('',#2193,.T.);
#1179=FACE_OUTER_BOUND('',#2194,.T.);
#1180=FACE_OUTER_BOUND('',#2195,.T.);
#1181=FACE_OUTER_BOUND('',#2196,.T.);
#1182=FACE_OUTER_BOUND('',#2197,.T.);
#1183=FACE_OUTER_BOUND('',#2198,.T.);
#1184=FACE_OUTER_BOUND('',#2199,.T.);
#1185=FACE_OUTER_BOUND('',#2200,.T.);
#1186=FACE_OUTER_BOUND('',#2201,.T.);
#1187=FACE_OUTER_BOUND('',#2202,.T.);
#1188=FACE_OUTER_BOUND('',#2203,.T.);
#1189=FACE_OUTER_BOUND('',#2204,.T.);
#1190=FACE_OUTER_BOUND('',#2205,.T.);
#1191=FACE_OUTER_BOUND('',#2206,.T.);
#1192=FACE_OUTER_BOUND('',#2207,.T.);
#1193=FACE_OUTER_BOUND('',#2208,.T.);
#1194=FACE_OUTER_BOUND('',#2209,.T.);
#1195=FACE_OUTER_BOUND('',#2210,.T.);
#1196=FACE_OUTER_BOUND('',#2211,.T.);
#1197=FACE_OUTER_BOUND('',#2212,.T.);
#1198=FACE_OUTER_BOUND('',#2213,.T.);
#1199=FACE_OUTER_BOUND('',#2214,.T.);
#1200=FACE_OUTER_BOUND('',#2215,.T.);
#1201=FACE_OUTER_BOUND('',#2216,.T.);
#1202=FACE_OUTER_BOUND('',#2217,.T.);
#1203=FACE_OUTER_BOUND('',#2218,.T.);
#1204=FACE_OUTER_BOUND('',#2219,.T.);
#1205=FACE_OUTER_BOUND('',#2220,.T.);
#1206=FACE_OUTER_BOUND('',#2221,.T.);
#1207=FACE_OUTER_BOUND('',#2222,.T.);
#1208=FACE_OUTER_BOUND('',#2223,.T.);
#1209=FACE_OUTER_BOUND('',#2224,.T.);
#1210=FACE_OUTER_BOUND('',#2225,.T.);
#1211=FACE_OUTER_BOUND('',#2226,.T.);
#1212=FACE_OUTER_BOUND('',#2227,.T.);
#1213=FACE_OUTER_BOUND('',#2228,.T.);
#1214=FACE_OUTER_BOUND('',#2229,.T.);
#1215=FACE_OUTER_BOUND('',#2230,.T.);
#1216=FACE_OUTER_BOUND('',#2231,.T.);
#1217=FACE_OUTER_BOUND('',#2232,.T.);
#1218=FACE_OUTER_BOUND('',#2233,.T.);
#1219=FACE_OUTER_BOUND('',#2234,.T.);
#1220=FACE_OUTER_BOUND('',#2235,.T.);
#1221=FACE_OUTER_BOUND('',#2236,.T.);
#1222=FACE_OUTER_BOUND('',#2237,.T.);
#1223=FACE_OUTER_BOUND('',#2238,.T.);
#1224=FACE_OUTER_BOUND('',#2239,.T.);
#1225=FACE_OUTER_BOUND('',#2240,.T.);
#1226=FACE_OUTER_BOUND('',#2241,.T.);
#1227=FACE_OUTER_BOUND('',#2242,.T.);
#1228=FACE_OUTER_BOUND('',#2243,.T.);
#1229=FACE_OUTER_BOUND('',#2244,.T.);
#1230=FACE_OUTER_BOUND('',#2245,.T.);
#1231=FACE_OUTER_BOUND('',#2246,.T.);
#1232=FACE_OUTER_BOUND('',#2247,.T.);
#1233=FACE_OUTER_BOUND('',#2248,.T.);
#1234=FACE_OUTER_BOUND('',#2249,.T.);
#1235=FACE_OUTER_BOUND('',#2250,.T.);
#1236=FACE_OUTER_BOUND('',#2251,.T.);
#1237=FACE_OUTER_BOUND('',#2252,.T.);
#1238=FACE_OUTER_BOUND('',#2253,.T.);
#1239=FACE_OUTER_BOUND('',#2254,.T.);
#1240=FACE_OUTER_BOUND('',#2255,.T.);
#1241=FACE_OUTER_BOUND('',#2256,.T.);
#1242=FACE_OUTER_BOUND('',#2257,.T.);
#1243=FACE_OUTER_BOUND('',#2258,.T.);
#1244=FACE_OUTER_BOUND('',#2259,.T.);
#1245=FACE_OUTER_BOUND('',#2260,.T.);
#1246=FACE_OUTER_BOUND('',#2261,.T.);
#1247=FACE_OUTER_BOUND('',#2262,.T.);
#1248=FACE_OUTER_BOUND('',#2263,.T.);
#1249=FACE_OUTER_BOUND('',#2264,.T.);
#1250=FACE_OUTER_BOUND('',#2265,.T.);
#1251=FACE_OUTER_BOUND('',#2266,.T.);
#1252=FACE_OUTER_BOUND('',#2267,.T.);
#1253=FACE_OUTER_BOUND('',#2268,.T.);
#1254=FACE_OUTER_BOUND('',#2269,.T.);
#1255=FACE_OUTER_BOUND('',#2270,.T.);
#1256=FACE_OUTER_BOUND('',#2271,.T.);
#1257=FACE_OUTER_BOUND('',#2272,.T.);
#1258=FACE_OUTER_BOUND('',#2273,.T.);
#1259=FACE_OUTER_BOUND('',#2274,.T.);
#1260=FACE_OUTER_BOUND('',#2275,.T.);
#1261=FACE_OUTER_BOUND('',#2276,.T.);
#1262=FACE_OUTER_BOUND('',#2277,.T.);
#1263=FACE_OUTER_BOUND('',#2278,.T.);
#1264=FACE_OUTER_BOUND('',#2279,.T.);
#1265=FACE_OUTER_BOUND('',#2280,.T.);
#1266=FACE_OUTER_BOUND('',#2281,.T.);
#1267=FACE_OUTER_BOUND('',#2282,.T.);
#1268=FACE_OUTER_BOUND('',#2283,.T.);
#1269=FACE_OUTER_BOUND('',#2284,.T.);
#1270=FACE_OUTER_BOUND('',#2285,.T.);
#1271=FACE_OUTER_BOUND('',#2286,.T.);
#1272=FACE_OUTER_BOUND('',#2287,.T.);
#1273=FACE_OUTER_BOUND('',#2288,.T.);
#1274=FACE_OUTER_BOUND('',#2289,.T.);
#1275=FACE_OUTER_BOUND('',#2290,.T.);
#1276=FACE_OUTER_BOUND('',#2291,.T.);
#1277=FACE_OUTER_BOUND('',#2292,.T.);
#1278=FACE_OUTER_BOUND('',#2293,.T.);
#1279=FACE_OUTER_BOUND('',#2294,.T.);
#1280=FACE_OUTER_BOUND('',#2295,.T.);
#1281=FACE_OUTER_BOUND('',#2296,.T.);
#1282=FACE_OUTER_BOUND('',#2297,.T.);
#1283=FACE_OUTER_BOUND('',#2298,.T.);
#1284=FACE_OUTER_BOUND('',#2299,.T.);
#1285=FACE_OUTER_BOUND('',#2300,.T.);
#1286=FACE_OUTER_BOUND('',#2301,.T.);
#1287=FACE_OUTER_BOUND('',#2302,.T.);
#1288=FACE_OUTER_BOUND('',#2303,.T.);
#1289=FACE_OUTER_BOUND('',#2304,.T.);
#1290=FACE_OUTER_BOUND('',#2305,.T.);
#1291=FACE_OUTER_BOUND('',#2306,.T.);
#1292=FACE_OUTER_BOUND('',#2307,.T.);
#1293=FACE_OUTER_BOUND('',#2308,.T.);
#1294=FACE_OUTER_BOUND('',#2309,.T.);
#1295=FACE_OUTER_BOUND('',#2310,.T.);
#1296=FACE_OUTER_BOUND('',#2311,.T.);
#1297=FACE_OUTER_BOUND('',#2312,.T.);
#1298=FACE_OUTER_BOUND('',#2313,.T.);
#1299=FACE_OUTER_BOUND('',#2314,.T.);
#1300=FACE_OUTER_BOUND('',#2315,.T.);
#1301=FACE_OUTER_BOUND('',#2316,.T.);
#1302=FACE_OUTER_BOUND('',#2317,.T.);
#1303=FACE_OUTER_BOUND('',#2318,.T.);
#1304=FACE_OUTER_BOUND('',#2319,.T.);
#1305=FACE_OUTER_BOUND('',#2320,.T.);
#1306=FACE_OUTER_BOUND('',#2321,.T.);
#1307=FACE_OUTER_BOUND('',#2322,.T.);
#1308=FACE_OUTER_BOUND('',#2323,.T.);
#1309=FACE_OUTER_BOUND('',#2324,.T.);
#1310=FACE_OUTER_BOUND('',#2325,.T.);
#1311=FACE_OUTER_BOUND('',#2326,.T.);
#1312=FACE_OUTER_BOUND('',#2327,.T.);
#1313=FACE_OUTER_BOUND('',#2328,.T.);
#1314=FACE_OUTER_BOUND('',#2329,.T.);
#1315=FACE_OUTER_BOUND('',#2330,.T.);
#1316=FACE_OUTER_BOUND('',#2331,.T.);
#1317=FACE_OUTER_BOUND('',#2332,.T.);
#1318=FACE_OUTER_BOUND('',#2333,.T.);
#1319=FACE_OUTER_BOUND('',#2334,.T.);
#1320=FACE_OUTER_BOUND('',#2335,.T.);
#1321=FACE_OUTER_BOUND('',#2336,.T.);
#1322=FACE_OUTER_BOUND('',#2337,.T.);
#1323=FACE_OUTER_BOUND('',#2338,.T.);
#1324=FACE_OUTER_BOUND('',#2339,.T.);
#1325=FACE_OUTER_BOUND('',#2340,.T.);
#1326=FACE_OUTER_BOUND('',#2341,.T.);
#1327=FACE_OUTER_BOUND('',#2342,.T.);
#1328=FACE_OUTER_BOUND('',#2343,.T.);
#1329=FACE_OUTER_BOUND('',#2344,.T.);
#1330=FACE_OUTER_BOUND('',#2345,.T.);
#1331=FACE_OUTER_BOUND('',#2353,.T.);
#1332=FACE_OUTER_BOUND('',#2354,.T.);
#1333=FACE_OUTER_BOUND('',#2355,.T.);
#1334=FACE_OUTER_BOUND('',#2356,.T.);
#1335=FACE_OUTER_BOUND('',#2357,.T.);
#1336=FACE_OUTER_BOUND('',#2358,.T.);
#1337=FACE_OUTER_BOUND('',#2359,.T.);
#1338=FACE_OUTER_BOUND('',#2360,.T.);
#1339=FACE_OUTER_BOUND('',#2361,.T.);
#1340=FACE_OUTER_BOUND('',#2362,.T.);
#1341=FACE_OUTER_BOUND('',#2363,.T.);
#1342=FACE_OUTER_BOUND('',#2364,.T.);
#1343=FACE_OUTER_BOUND('',#2365,.T.);
#1344=FACE_OUTER_BOUND('',#2366,.T.);
#1345=FACE_OUTER_BOUND('',#2367,.T.);
#1346=FACE_OUTER_BOUND('',#2368,.T.);
#1347=FACE_OUTER_BOUND('',#2369,.T.);
#1348=FACE_OUTER_BOUND('',#2370,.T.);
#1349=FACE_OUTER_BOUND('',#2371,.T.);
#1350=FACE_OUTER_BOUND('',#2372,.T.);
#1351=FACE_OUTER_BOUND('',#2373,.T.);
#1352=FACE_OUTER_BOUND('',#2374,.T.);
#1353=FACE_OUTER_BOUND('',#2375,.T.);
#1354=FACE_OUTER_BOUND('',#2376,.T.);
#1355=FACE_OUTER_BOUND('',#2377,.T.);
#1356=FACE_OUTER_BOUND('',#2378,.T.);
#1357=FACE_OUTER_BOUND('',#2379,.T.);
#1358=FACE_OUTER_BOUND('',#2380,.T.);
#1359=FACE_OUTER_BOUND('',#2381,.T.);
#1360=FACE_OUTER_BOUND('',#2382,.T.);
#1361=FACE_OUTER_BOUND('',#2383,.T.);
#1362=FACE_OUTER_BOUND('',#2384,.T.);
#1363=FACE_OUTER_BOUND('',#2385,.T.);
#1364=FACE_OUTER_BOUND('',#2386,.T.);
#1365=FACE_OUTER_BOUND('',#2387,.T.);
#1366=FACE_OUTER_BOUND('',#2388,.T.);
#1367=FACE_OUTER_BOUND('',#2389,.T.);
#1368=FACE_OUTER_BOUND('',#2390,.T.);
#1369=FACE_OUTER_BOUND('',#2391,.T.);
#1370=FACE_OUTER_BOUND('',#2392,.T.);
#1371=FACE_OUTER_BOUND('',#2393,.T.);
#1372=FACE_OUTER_BOUND('',#2394,.T.);
#1373=FACE_OUTER_BOUND('',#2395,.T.);
#1374=FACE_OUTER_BOUND('',#2396,.T.);
#1375=FACE_OUTER_BOUND('',#2397,.T.);
#1376=FACE_OUTER_BOUND('',#2398,.T.);
#1377=FACE_OUTER_BOUND('',#2399,.T.);
#1378=FACE_OUTER_BOUND('',#2400,.T.);
#1379=FACE_OUTER_BOUND('',#2401,.T.);
#1380=FACE_OUTER_BOUND('',#2402,.T.);
#1381=FACE_OUTER_BOUND('',#2403,.T.);
#1382=FACE_OUTER_BOUND('',#2404,.T.);
#1383=FACE_OUTER_BOUND('',#2405,.T.);
#1384=FACE_OUTER_BOUND('',#2406,.T.);
#1385=FACE_OUTER_BOUND('',#2407,.T.);
#1386=FACE_OUTER_BOUND('',#2408,.T.);
#1387=FACE_OUTER_BOUND('',#2409,.T.);
#1388=FACE_OUTER_BOUND('',#2410,.T.);
#1389=FACE_OUTER_BOUND('',#2411,.T.);
#1390=FACE_OUTER_BOUND('',#2412,.T.);
#1391=FACE_OUTER_BOUND('',#2413,.T.);
#1392=FACE_OUTER_BOUND('',#2414,.T.);
#1393=FACE_OUTER_BOUND('',#2415,.T.);
#1394=FACE_OUTER_BOUND('',#2416,.T.);
#1395=FACE_OUTER_BOUND('',#2417,.T.);
#1396=FACE_OUTER_BOUND('',#2418,.T.);
#1397=FACE_OUTER_BOUND('',#2419,.T.);
#1398=FACE_OUTER_BOUND('',#2420,.T.);
#1399=FACE_OUTER_BOUND('',#2421,.T.);
#1400=FACE_OUTER_BOUND('',#2422,.T.);
#1401=FACE_OUTER_BOUND('',#2423,.T.);
#1402=FACE_OUTER_BOUND('',#2424,.T.);
#1403=FACE_OUTER_BOUND('',#2425,.T.);
#1404=FACE_OUTER_BOUND('',#2426,.T.);
#1405=FACE_OUTER_BOUND('',#2427,.T.);
#1406=FACE_OUTER_BOUND('',#2428,.T.);
#1407=FACE_OUTER_BOUND('',#2429,.T.);
#1408=FACE_OUTER_BOUND('',#2430,.T.);
#1409=FACE_OUTER_BOUND('',#2431,.T.);
#1410=FACE_OUTER_BOUND('',#2432,.T.);
#1411=FACE_OUTER_BOUND('',#2433,.T.);
#1412=FACE_OUTER_BOUND('',#2434,.T.);
#1413=FACE_OUTER_BOUND('',#2435,.T.);
#1414=FACE_OUTER_BOUND('',#2436,.T.);
#1415=FACE_OUTER_BOUND('',#2437,.T.);
#1416=FACE_OUTER_BOUND('',#2438,.T.);
#1417=FACE_OUTER_BOUND('',#2440,.T.);
#1418=FACE_OUTER_BOUND('',#2442,.T.);
#1419=FACE_OUTER_BOUND('',#2443,.T.);
#1420=FACE_OUTER_BOUND('',#2445,.T.);
#1421=FACE_OUTER_BOUND('',#2447,.T.);
#1422=FACE_OUTER_BOUND('',#2448,.T.);
#1423=FACE_OUTER_BOUND('',#2450,.T.);
#1424=FACE_OUTER_BOUND('',#2452,.T.);
#1425=FACE_OUTER_BOUND('',#2453,.T.);
#1426=FACE_OUTER_BOUND('',#2455,.T.);
#1427=FACE_OUTER_BOUND('',#2457,.T.);
#1428=FACE_OUTER_BOUND('',#2458,.T.);
#1429=FACE_OUTER_BOUND('',#2460,.T.);
#1430=FACE_OUTER_BOUND('',#2462,.T.);
#1431=FACE_OUTER_BOUND('',#2463,.T.);
#1432=FACE_OUTER_BOUND('',#2465,.T.);
#1433=FACE_OUTER_BOUND('',#2467,.T.);
#1434=FACE_OUTER_BOUND('',#2468,.T.);
#1435=FACE_OUTER_BOUND('',#2470,.T.);
#1436=FACE_OUTER_BOUND('',#2471,.T.);
#1437=FACE_OUTER_BOUND('',#2473,.T.);
#1438=FACE_OUTER_BOUND('',#2475,.T.);
#1439=FACE_OUTER_BOUND('',#2476,.T.);
#1440=FACE_OUTER_BOUND('',#2478,.T.);
#1441=FACE_OUTER_BOUND('',#2479,.T.);
#1442=FACE_OUTER_BOUND('',#2481,.T.);
#1443=FACE_OUTER_BOUND('',#2482,.T.);
#1444=FACE_OUTER_BOUND('',#2484,.T.);
#1445=FACE_OUTER_BOUND('',#2485,.T.);
#1446=FACE_OUTER_BOUND('',#2487,.T.);
#1447=FACE_OUTER_BOUND('',#2488,.T.);
#1448=FACE_OUTER_BOUND('',#2490,.T.);
#1449=FACE_OUTER_BOUND('',#2491,.T.);
#1450=FACE_OUTER_BOUND('',#2492,.T.);
#1451=FACE_OUTER_BOUND('',#2494,.T.);
#1452=FACE_OUTER_BOUND('',#2495,.T.);
#1453=FACE_OUTER_BOUND('',#2497,.T.);
#1454=FACE_OUTER_BOUND('',#2498,.T.);
#1455=FACE_OUTER_BOUND('',#2499,.T.);
#1456=FACE_OUTER_BOUND('',#2500,.T.);
#1457=FACE_OUTER_BOUND('',#2501,.T.);
#1458=FACE_OUTER_BOUND('',#2502,.T.);
#1459=FACE_OUTER_BOUND('',#2503,.T.);
#1460=FACE_OUTER_BOUND('',#2504,.T.);
#1461=FACE_OUTER_BOUND('',#2505,.T.);
#1462=FACE_OUTER_BOUND('',#2506,.T.);
#1463=FACE_OUTER_BOUND('',#2508,.T.);
#1464=FACE_OUTER_BOUND('',#2509,.T.);
#1465=FACE_OUTER_BOUND('',#2511,.T.);
#1466=FACE_OUTER_BOUND('',#2512,.T.);
#1467=FACE_OUTER_BOUND('',#2513,.T.);
#1468=FACE_OUTER_BOUND('',#2514,.T.);
#1469=FACE_OUTER_BOUND('',#2515,.T.);
#1470=FACE_OUTER_BOUND('',#2516,.T.);
#1471=FACE_OUTER_BOUND('',#2517,.T.);
#1472=FACE_OUTER_BOUND('',#2518,.T.);
#1473=FACE_OUTER_BOUND('',#2519,.T.);
#1474=FACE_OUTER_BOUND('',#2520,.T.);
#1475=FACE_OUTER_BOUND('',#2521,.T.);
#1476=FACE_OUTER_BOUND('',#2529,.T.);
#1477=FACE_OUTER_BOUND('',#2530,.T.);
#1478=FACE_OUTER_BOUND('',#2531,.T.);
#1479=FACE_OUTER_BOUND('',#2532,.T.);
#1480=FACE_OUTER_BOUND('',#2533,.T.);
#1481=FACE_OUTER_BOUND('',#2534,.T.);
#1482=FACE_OUTER_BOUND('',#2535,.T.);
#1483=FACE_OUTER_BOUND('',#2536,.T.);
#1484=FACE_OUTER_BOUND('',#2537,.T.);
#1485=FACE_OUTER_BOUND('',#2538,.T.);
#1486=FACE_OUTER_BOUND('',#2539,.T.);
#1487=FACE_OUTER_BOUND('',#2540,.T.);
#1488=FACE_OUTER_BOUND('',#2541,.T.);
#1489=FACE_OUTER_BOUND('',#2542,.T.);
#1490=FACE_OUTER_BOUND('',#2543,.T.);
#1491=FACE_OUTER_BOUND('',#2544,.T.);
#1492=FACE_OUTER_BOUND('',#2545,.T.);
#1493=FACE_OUTER_BOUND('',#2546,.T.);
#1494=FACE_OUTER_BOUND('',#2547,.T.);
#1495=FACE_OUTER_BOUND('',#2548,.T.);
#1496=FACE_OUTER_BOUND('',#2549,.T.);
#1497=FACE_OUTER_BOUND('',#2550,.T.);
#1498=FACE_OUTER_BOUND('',#2551,.T.);
#1499=FACE_OUTER_BOUND('',#2552,.T.);
#1500=FACE_OUTER_BOUND('',#2553,.T.);
#1501=FACE_OUTER_BOUND('',#2554,.T.);
#1502=FACE_OUTER_BOUND('',#2555,.T.);
#1503=FACE_OUTER_BOUND('',#2556,.T.);
#1504=FACE_OUTER_BOUND('',#2558,.T.);
#1505=FACE_OUTER_BOUND('',#2560,.T.);
#1506=FACE_OUTER_BOUND('',#2561,.T.);
#1507=FACE_OUTER_BOUND('',#2563,.T.);
#1508=FACE_OUTER_BOUND('',#2565,.T.);
#1509=FACE_OUTER_BOUND('',#2566,.T.);
#1510=FACE_OUTER_BOUND('',#2568,.T.);
#1511=FACE_OUTER_BOUND('',#2570,.T.);
#1512=FACE_OUTER_BOUND('',#2571,.T.);
#1513=FACE_OUTER_BOUND('',#2572,.T.);
#1514=FACE_OUTER_BOUND('',#2573,.T.);
#1515=FACE_OUTER_BOUND('',#2574,.T.);
#1516=FACE_OUTER_BOUND('',#2575,.T.);
#1517=FACE_OUTER_BOUND('',#2576,.T.);
#1518=FACE_OUTER_BOUND('',#2577,.T.);
#1519=FACE_OUTER_BOUND('',#2578,.T.);
#1520=FACE_OUTER_BOUND('',#2579,.T.);
#1521=FACE_OUTER_BOUND('',#2580,.T.);
#1522=FACE_OUTER_BOUND('',#2581,.T.);
#1523=FACE_OUTER_BOUND('',#2582,.T.);
#1524=FACE_OUTER_BOUND('',#2583,.T.);
#1525=FACE_OUTER_BOUND('',#2585,.T.);
#1526=FACE_OUTER_BOUND('',#2586,.T.);
#1527=FACE_OUTER_BOUND('',#2587,.T.);
#1528=FACE_OUTER_BOUND('',#2589,.T.);
#1529=FACE_OUTER_BOUND('',#2590,.T.);
#1530=FACE_OUTER_BOUND('',#2591,.T.);
#1531=FACE_OUTER_BOUND('',#2593,.T.);
#1532=FACE_OUTER_BOUND('',#2594,.T.);
#1533=FACE_OUTER_BOUND('',#2595,.T.);
#1534=FACE_OUTER_BOUND('',#2597,.T.);
#1535=FACE_OUTER_BOUND('',#2598,.T.);
#1536=FACE_OUTER_BOUND('',#2599,.T.);
#1537=FACE_OUTER_BOUND('',#2601,.T.);
#1538=FACE_OUTER_BOUND('',#2602,.T.);
#1539=FACE_OUTER_BOUND('',#2603,.T.);
#1540=FACE_OUTER_BOUND('',#2605,.T.);
#1541=FACE_OUTER_BOUND('',#2606,.T.);
#1542=FACE_OUTER_BOUND('',#2607,.T.);
#1543=FACE_OUTER_BOUND('',#2608,.T.);
#1544=FACE_OUTER_BOUND('',#2609,.T.);
#1545=FACE_OUTER_BOUND('',#2617,.T.);
#1546=FACE_OUTER_BOUND('',#2625,.T.);
#1547=FACE_OUTER_BOUND('',#2626,.T.);
#1548=FACE_OUTER_BOUND('',#2627,.T.);
#1549=FACE_OUTER_BOUND('',#2629,.T.);
#1550=FACE_OUTER_BOUND('',#2631,.T.);
#1551=FACE_OUTER_BOUND('',#2632,.T.);
#1552=FACE_OUTER_BOUND('',#2633,.T.);
#1553=FACE_OUTER_BOUND('',#2634,.T.);
#1554=FACE_OUTER_BOUND('',#2635,.T.);
#1555=FACE_OUTER_BOUND('',#2636,.T.);
#1556=FACE_OUTER_BOUND('',#2637,.T.);
#1557=FACE_OUTER_BOUND('',#2638,.T.);
#1558=FACE_OUTER_BOUND('',#2639,.T.);
#1559=FACE_OUTER_BOUND('',#2640,.T.);
#1560=FACE_OUTER_BOUND('',#2641,.T.);
#1561=FACE_OUTER_BOUND('',#2642,.T.);
#1562=FACE_OUTER_BOUND('',#2643,.T.);
#1563=FACE_OUTER_BOUND('',#2644,.T.);
#1564=FACE_OUTER_BOUND('',#2645,.T.);
#1565=FACE_OUTER_BOUND('',#2653,.T.);
#1566=FACE_OUTER_BOUND('',#2661,.T.);
#1567=FACE_OUTER_BOUND('',#2662,.T.);
#1568=FACE_OUTER_BOUND('',#2663,.T.);
#1569=FACE_OUTER_BOUND('',#2665,.T.);
#1570=FACE_OUTER_BOUND('',#2667,.T.);
#1571=FACE_OUTER_BOUND('',#2668,.T.);
#1572=FACE_OUTER_BOUND('',#2669,.T.);
#1573=FACE_OUTER_BOUND('',#2671,.T.);
#1574=FACE_OUTER_BOUND('',#2673,.T.);
#1575=FACE_OUTER_BOUND('',#2674,.T.);
#1576=FACE_OUTER_BOUND('',#2675,.T.);
#1577=FACE_OUTER_BOUND('',#2677,.T.);
#1578=FACE_OUTER_BOUND('',#2679,.T.);
#1579=FACE_OUTER_BOUND('',#2680,.T.);
#1580=FACE_OUTER_BOUND('',#2681,.T.);
#1581=FACE_OUTER_BOUND('',#2682,.T.);
#1582=FACE_OUTER_BOUND('',#2683,.T.);
#1583=FACE_OUTER_BOUND('',#2684,.T.);
#1584=FACE_OUTER_BOUND('',#2685,.T.);
#1585=FACE_OUTER_BOUND('',#2687,.T.);
#1586=FACE_OUTER_BOUND('',#2688,.T.);
#1587=FACE_OUTER_BOUND('',#2689,.T.);
#1588=FACE_OUTER_BOUND('',#2690,.T.);
#1589=FACE_OUTER_BOUND('',#2691,.T.);
#1590=FACE_OUTER_BOUND('',#2692,.T.);
#1591=FACE_OUTER_BOUND('',#2693,.T.);
#1592=FACE_OUTER_BOUND('',#2694,.T.);
#1593=FACE_OUTER_BOUND('',#2695,.T.);
#1594=FACE_OUTER_BOUND('',#2696,.T.);
#1595=FACE_OUTER_BOUND('',#2697,.T.);
#1596=FACE_OUTER_BOUND('',#2698,.T.);
#1597=FACE_OUTER_BOUND('',#2699,.T.);
#1598=FACE_OUTER_BOUND('',#2700,.T.);
#1599=FACE_OUTER_BOUND('',#2701,.T.);
#1600=FACE_OUTER_BOUND('',#2702,.T.);
#1601=FACE_OUTER_BOUND('',#2703,.T.);
#1602=FACE_OUTER_BOUND('',#2704,.T.);
#1603=FACE_OUTER_BOUND('',#2705,.T.);
#1604=FACE_OUTER_BOUND('',#2706,.T.);
#1605=FACE_OUTER_BOUND('',#2707,.T.);
#1606=FACE_OUTER_BOUND('',#2708,.T.);
#1607=FACE_OUTER_BOUND('',#2709,.T.);
#1608=FACE_OUTER_BOUND('',#2710,.T.);
#1609=FACE_OUTER_BOUND('',#2711,.T.);
#1610=FACE_OUTER_BOUND('',#2712,.T.);
#1611=FACE_OUTER_BOUND('',#2713,.T.);
#1612=FACE_OUTER_BOUND('',#2714,.T.);
#1613=FACE_OUTER_BOUND('',#2715,.T.);
#1614=FACE_OUTER_BOUND('',#2716,.T.);
#1615=FACE_OUTER_BOUND('',#2717,.T.);
#1616=FACE_OUTER_BOUND('',#2718,.T.);
#1617=FACE_OUTER_BOUND('',#2719,.T.);
#1618=FACE_OUTER_BOUND('',#2720,.T.);
#1619=FACE_OUTER_BOUND('',#2721,.T.);
#1620=FACE_OUTER_BOUND('',#2722,.T.);
#1621=FACE_OUTER_BOUND('',#2723,.T.);
#1622=FACE_OUTER_BOUND('',#2724,.T.);
#1623=FACE_OUTER_BOUND('',#2725,.T.);
#1624=FACE_OUTER_BOUND('',#2726,.T.);
#1625=FACE_OUTER_BOUND('',#2727,.T.);
#1626=FACE_OUTER_BOUND('',#2728,.T.);
#1627=FACE_OUTER_BOUND('',#2729,.T.);
#1628=FACE_OUTER_BOUND('',#2730,.T.);
#1629=FACE_OUTER_BOUND('',#2731,.T.);
#1630=FACE_OUTER_BOUND('',#2732,.T.);
#1631=FACE_OUTER_BOUND('',#2733,.T.);
#1632=FACE_OUTER_BOUND('',#2734,.T.);
#1633=FACE_OUTER_BOUND('',#2735,.T.);
#1634=FACE_OUTER_BOUND('',#2736,.T.);
#1635=FACE_OUTER_BOUND('',#2737,.T.);
#1636=FACE_OUTER_BOUND('',#2738,.T.);
#1637=FACE_OUTER_BOUND('',#2740,.T.);
#1638=FACE_OUTER_BOUND('',#2741,.T.);
#1639=FACE_OUTER_BOUND('',#2743,.T.);
#1640=FACE_OUTER_BOUND('',#2744,.T.);
#1641=FACE_OUTER_BOUND('',#2745,.T.);
#1642=FACE_OUTER_BOUND('',#2746,.T.);
#1643=FACE_OUTER_BOUND('',#2747,.T.);
#1644=FACE_OUTER_BOUND('',#2748,.T.);
#1645=FACE_OUTER_BOUND('',#2749,.T.);
#1646=FACE_OUTER_BOUND('',#2750,.T.);
#1647=FACE_OUTER_BOUND('',#2751,.T.);
#1648=FACE_OUTER_BOUND('',#2752,.T.);
#1649=FACE_OUTER_BOUND('',#2753,.T.);
#1650=FACE_OUTER_BOUND('',#2754,.T.);
#1651=FACE_OUTER_BOUND('',#2755,.T.);
#1652=FACE_OUTER_BOUND('',#2756,.T.);
#1653=FACE_OUTER_BOUND('',#2757,.T.);
#1654=FACE_OUTER_BOUND('',#2758,.T.);
#1655=FACE_OUTER_BOUND('',#2759,.T.);
#1656=FACE_OUTER_BOUND('',#2760,.T.);
#1657=FACE_OUTER_BOUND('',#2761,.T.);
#1658=FACE_OUTER_BOUND('',#2762,.T.);
#1659=FACE_OUTER_BOUND('',#2763,.T.);
#1660=FACE_OUTER_BOUND('',#2764,.T.);
#1661=FACE_OUTER_BOUND('',#2765,.T.);
#1662=FACE_OUTER_BOUND('',#2766,.T.);
#1663=FACE_OUTER_BOUND('',#2767,.T.);
#1664=FACE_OUTER_BOUND('',#2768,.T.);
#1665=FACE_OUTER_BOUND('',#2769,.T.);
#1666=FACE_OUTER_BOUND('',#2770,.T.);
#1667=FACE_OUTER_BOUND('',#2771,.T.);
#1668=FACE_OUTER_BOUND('',#2772,.T.);
#1669=FACE_OUTER_BOUND('',#2773,.T.);
#1670=FACE_OUTER_BOUND('',#2775,.T.);
#1671=FACE_OUTER_BOUND('',#2776,.T.);
#1672=EDGE_LOOP('',(#11018,#11019,#11020,#11021,#11022,#11023,#11024,#11025));
#1673=EDGE_LOOP('',(#11026,#11027,#11028,#11029));
#1674=EDGE_LOOP('',(#11030,#11031,#11032,#11033));
#1675=EDGE_LOOP('',(#11034,#11035,#11036,#11037));
#1676=EDGE_LOOP('',(#11038,#11039,#11040,#11041));
#1677=EDGE_LOOP('',(#11042,#11043,#11044,#11045));
#1678=EDGE_LOOP('',(#11046,#11047,#11048,#11049));
#1679=EDGE_LOOP('',(#11050,#11051,#11052,#11053));
#1680=EDGE_LOOP('',(#11054,#11055,#11056,#11057));
#1681=EDGE_LOOP('',(#11058,#11059,#11060,#11061));
#1682=EDGE_LOOP('',(#11062,#11063,#11064,#11065));
#1683=EDGE_LOOP('',(#11066,#11067,#11068,#11069));
#1684=EDGE_LOOP('',(#11070,#11071,#11072,#11073));
#1685=EDGE_LOOP('',(#11074,#11075,#11076,#11077));
#1686=EDGE_LOOP('',(#11078,#11079,#11080,#11081));
#1687=EDGE_LOOP('',(#11082,#11083,#11084,#11085));
#1688=EDGE_LOOP('',(#11086,#11087,#11088,#11089));
#1689=EDGE_LOOP('',(#11090,#11091,#11092,#11093));
#1690=EDGE_LOOP('',(#11094,#11095,#11096,#11097));
#1691=EDGE_LOOP('',(#11098,#11099,#11100,#11101));
#1692=EDGE_LOOP('',(#11102,#11103,#11104,#11105));
#1693=EDGE_LOOP('',(#11106,#11107,#11108,#11109));
#1694=EDGE_LOOP('',(#11110,#11111,#11112,#11113));
#1695=EDGE_LOOP('',(#11114,#11115,#11116,#11117));
#1696=EDGE_LOOP('',(#11118,#11119,#11120,#11121));
#1697=EDGE_LOOP('',(#11122,#11123,#11124,#11125,#11126,#11127,#11128,#11129));
#1698=EDGE_LOOP('',(#11130,#11131,#11132,#11133));
#1699=EDGE_LOOP('',(#11134,#11135,#11136,#11137));
#1700=EDGE_LOOP('',(#11138,#11139,#11140,#11141));
#1701=EDGE_LOOP('',(#11142,#11143,#11144,#11145));
#1702=EDGE_LOOP('',(#11146,#11147,#11148,#11149));
#1703=EDGE_LOOP('',(#11150,#11151,#11152,#11153));
#1704=EDGE_LOOP('',(#11154,#11155,#11156,#11157));
#1705=EDGE_LOOP('',(#11158,#11159,#11160,#11161));
#1706=EDGE_LOOP('',(#11162,#11163,#11164,#11165));
#1707=EDGE_LOOP('',(#11166,#11167,#11168,#11169));
#1708=EDGE_LOOP('',(#11170,#11171,#11172,#11173));
#1709=EDGE_LOOP('',(#11174,#11175,#11176,#11177));
#1710=EDGE_LOOP('',(#11178,#11179,#11180,#11181));
#1711=EDGE_LOOP('',(#11182,#11183,#11184,#11185));
#1712=EDGE_LOOP('',(#11186,#11187,#11188,#11189));
#1713=EDGE_LOOP('',(#11190,#11191,#11192,#11193));
#1714=EDGE_LOOP('',(#11194,#11195,#11196,#11197));
#1715=EDGE_LOOP('',(#11198,#11199,#11200,#11201));
#1716=EDGE_LOOP('',(#11202,#11203,#11204,#11205));
#1717=EDGE_LOOP('',(#11206,#11207,#11208,#11209));
#1718=EDGE_LOOP('',(#11210,#11211,#11212,#11213));
#1719=EDGE_LOOP('',(#11214,#11215,#11216,#11217));
#1720=EDGE_LOOP('',(#11218,#11219,#11220,#11221));
#1721=EDGE_LOOP('',(#11222,#11223,#11224,#11225));
#1722=EDGE_LOOP('',(#11226,#11227,#11228,#11229,#11230,#11231,#11232,#11233));
#1723=EDGE_LOOP('',(#11234,#11235,#11236,#11237));
#1724=EDGE_LOOP('',(#11238,#11239,#11240,#11241));
#1725=EDGE_LOOP('',(#11242,#11243,#11244,#11245));
#1726=EDGE_LOOP('',(#11246,#11247,#11248,#11249));
#1727=EDGE_LOOP('',(#11250,#11251,#11252,#11253));
#1728=EDGE_LOOP('',(#11254,#11255,#11256,#11257));
#1729=EDGE_LOOP('',(#11258,#11259,#11260,#11261));
#1730=EDGE_LOOP('',(#11262,#11263,#11264,#11265));
#1731=EDGE_LOOP('',(#11266,#11267,#11268,#11269));
#1732=EDGE_LOOP('',(#11270,#11271,#11272,#11273));
#1733=EDGE_LOOP('',(#11274,#11275,#11276,#11277));
#1734=EDGE_LOOP('',(#11278,#11279,#11280,#11281));
#1735=EDGE_LOOP('',(#11282,#11283,#11284,#11285));
#1736=EDGE_LOOP('',(#11286,#11287,#11288,#11289));
#1737=EDGE_LOOP('',(#11290,#11291,#11292,#11293));
#1738=EDGE_LOOP('',(#11294,#11295,#11296,#11297));
#1739=EDGE_LOOP('',(#11298,#11299,#11300,#11301));
#1740=EDGE_LOOP('',(#11302,#11303,#11304,#11305));
#1741=EDGE_LOOP('',(#11306,#11307,#11308,#11309));
#1742=EDGE_LOOP('',(#11310,#11311,#11312,#11313));
#1743=EDGE_LOOP('',(#11314,#11315,#11316,#11317));
#1744=EDGE_LOOP('',(#11318,#11319,#11320,#11321));
#1745=EDGE_LOOP('',(#11322,#11323,#11324,#11325));
#1746=EDGE_LOOP('',(#11326,#11327,#11328,#11329));
#1747=EDGE_LOOP('',(#11330,#11331,#11332,#11333,#11334,#11335,#11336,#11337));
#1748=EDGE_LOOP('',(#11338,#11339,#11340,#11341));
#1749=EDGE_LOOP('',(#11342,#11343,#11344,#11345));
#1750=EDGE_LOOP('',(#11346,#11347,#11348,#11349));
#1751=EDGE_LOOP('',(#11350,#11351,#11352,#11353));
#1752=EDGE_LOOP('',(#11354,#11355,#11356,#11357));
#1753=EDGE_LOOP('',(#11358,#11359,#11360,#11361));
#1754=EDGE_LOOP('',(#11362,#11363,#11364,#11365));
#1755=EDGE_LOOP('',(#11366,#11367,#11368,#11369));
#1756=EDGE_LOOP('',(#11370,#11371,#11372,#11373));
#1757=EDGE_LOOP('',(#11374,#11375,#11376,#11377));
#1758=EDGE_LOOP('',(#11378,#11379,#11380,#11381));
#1759=EDGE_LOOP('',(#11382,#11383,#11384,#11385));
#1760=EDGE_LOOP('',(#11386,#11387,#11388,#11389));
#1761=EDGE_LOOP('',(#11390,#11391,#11392,#11393));
#1762=EDGE_LOOP('',(#11394,#11395,#11396,#11397));
#1763=EDGE_LOOP('',(#11398,#11399,#11400,#11401));
#1764=EDGE_LOOP('',(#11402,#11403,#11404,#11405));
#1765=EDGE_LOOP('',(#11406,#11407,#11408,#11409));
#1766=EDGE_LOOP('',(#11410,#11411,#11412,#11413));
#1767=EDGE_LOOP('',(#11414,#11415,#11416,#11417));
#1768=EDGE_LOOP('',(#11418,#11419,#11420,#11421));
#1769=EDGE_LOOP('',(#11422,#11423,#11424,#11425));
#1770=EDGE_LOOP('',(#11426,#11427,#11428,#11429));
#1771=EDGE_LOOP('',(#11430,#11431,#11432,#11433));
#1772=EDGE_LOOP('',(#11434,#11435,#11436,#11437,#11438,#11439,#11440,#11441));
#1773=EDGE_LOOP('',(#11442,#11443,#11444,#11445));
#1774=EDGE_LOOP('',(#11446,#11447,#11448,#11449));
#1775=EDGE_LOOP('',(#11450,#11451,#11452,#11453));
#1776=EDGE_LOOP('',(#11454,#11455,#11456,#11457));
#1777=EDGE_LOOP('',(#11458,#11459,#11460,#11461));
#1778=EDGE_LOOP('',(#11462,#11463,#11464,#11465));
#1779=EDGE_LOOP('',(#11466,#11467,#11468,#11469));
#1780=EDGE_LOOP('',(#11470,#11471,#11472,#11473));
#1781=EDGE_LOOP('',(#11474,#11475,#11476,#11477));
#1782=EDGE_LOOP('',(#11478,#11479,#11480,#11481));
#1783=EDGE_LOOP('',(#11482,#11483,#11484,#11485));
#1784=EDGE_LOOP('',(#11486,#11487,#11488,#11489));
#1785=EDGE_LOOP('',(#11490,#11491,#11492,#11493));
#1786=EDGE_LOOP('',(#11494,#11495,#11496,#11497));
#1787=EDGE_LOOP('',(#11498,#11499,#11500,#11501));
#1788=EDGE_LOOP('',(#11502,#11503,#11504,#11505));
#1789=EDGE_LOOP('',(#11506,#11507,#11508,#11509));
#1790=EDGE_LOOP('',(#11510,#11511,#11512,#11513));
#1791=EDGE_LOOP('',(#11514,#11515,#11516,#11517));
#1792=EDGE_LOOP('',(#11518,#11519,#11520,#11521));
#1793=EDGE_LOOP('',(#11522,#11523,#11524,#11525));
#1794=EDGE_LOOP('',(#11526,#11527,#11528,#11529));
#1795=EDGE_LOOP('',(#11530,#11531,#11532,#11533));
#1796=EDGE_LOOP('',(#11534,#11535,#11536,#11537));
#1797=EDGE_LOOP('',(#11538,#11539,#11540,#11541,#11542,#11543,#11544,#11545));
#1798=EDGE_LOOP('',(#11546,#11547,#11548,#11549));
#1799=EDGE_LOOP('',(#11550,#11551,#11552,#11553));
#1800=EDGE_LOOP('',(#11554,#11555,#11556,#11557));
#1801=EDGE_LOOP('',(#11558,#11559,#11560,#11561));
#1802=EDGE_LOOP('',(#11562,#11563,#11564,#11565));
#1803=EDGE_LOOP('',(#11566,#11567,#11568,#11569));
#1804=EDGE_LOOP('',(#11570,#11571,#11572,#11573));
#1805=EDGE_LOOP('',(#11574,#11575,#11576,#11577));
#1806=EDGE_LOOP('',(#11578,#11579,#11580,#11581));
#1807=EDGE_LOOP('',(#11582,#11583,#11584,#11585));
#1808=EDGE_LOOP('',(#11586,#11587,#11588,#11589));
#1809=EDGE_LOOP('',(#11590,#11591,#11592,#11593));
#1810=EDGE_LOOP('',(#11594,#11595,#11596,#11597));
#1811=EDGE_LOOP('',(#11598,#11599,#11600,#11601));
#1812=EDGE_LOOP('',(#11602,#11603,#11604,#11605));
#1813=EDGE_LOOP('',(#11606,#11607,#11608,#11609));
#1814=EDGE_LOOP('',(#11610,#11611,#11612,#11613));
#1815=EDGE_LOOP('',(#11614,#11615,#11616,#11617));
#1816=EDGE_LOOP('',(#11618,#11619,#11620,#11621));
#1817=EDGE_LOOP('',(#11622,#11623,#11624,#11625));
#1818=EDGE_LOOP('',(#11626,#11627,#11628,#11629));
#1819=EDGE_LOOP('',(#11630,#11631,#11632,#11633));
#1820=EDGE_LOOP('',(#11634,#11635,#11636,#11637));
#1821=EDGE_LOOP('',(#11638,#11639,#11640,#11641));
#1822=EDGE_LOOP('',(#11642,#11643,#11644,#11645,#11646,#11647,#11648,#11649));
#1823=EDGE_LOOP('',(#11650,#11651,#11652,#11653));
#1824=EDGE_LOOP('',(#11654,#11655,#11656,#11657));
#1825=EDGE_LOOP('',(#11658,#11659,#11660,#11661));
#1826=EDGE_LOOP('',(#11662,#11663,#11664,#11665));
#1827=EDGE_LOOP('',(#11666,#11667,#11668,#11669));
#1828=EDGE_LOOP('',(#11670,#11671,#11672,#11673));
#1829=EDGE_LOOP('',(#11674,#11675,#11676,#11677));
#1830=EDGE_LOOP('',(#11678,#11679,#11680,#11681));
#1831=EDGE_LOOP('',(#11682,#11683,#11684,#11685));
#1832=EDGE_LOOP('',(#11686,#11687,#11688,#11689));
#1833=EDGE_LOOP('',(#11690,#11691,#11692,#11693));
#1834=EDGE_LOOP('',(#11694,#11695,#11696,#11697));
#1835=EDGE_LOOP('',(#11698,#11699,#11700,#11701));
#1836=EDGE_LOOP('',(#11702,#11703,#11704,#11705));
#1837=EDGE_LOOP('',(#11706,#11707,#11708,#11709));
#1838=EDGE_LOOP('',(#11710,#11711,#11712,#11713));
#1839=EDGE_LOOP('',(#11714,#11715,#11716,#11717));
#1840=EDGE_LOOP('',(#11718,#11719,#11720,#11721));
#1841=EDGE_LOOP('',(#11722,#11723,#11724,#11725));
#1842=EDGE_LOOP('',(#11726,#11727,#11728,#11729));
#1843=EDGE_LOOP('',(#11730,#11731,#11732,#11733));
#1844=EDGE_LOOP('',(#11734,#11735,#11736,#11737));
#1845=EDGE_LOOP('',(#11738,#11739,#11740,#11741));
#1846=EDGE_LOOP('',(#11742,#11743,#11744,#11745));
#1847=EDGE_LOOP('',(#11746,#11747,#11748,#11749,#11750,#11751,#11752,#11753));
#1848=EDGE_LOOP('',(#11754,#11755,#11756,#11757));
#1849=EDGE_LOOP('',(#11758,#11759,#11760,#11761));
#1850=EDGE_LOOP('',(#11762,#11763,#11764,#11765));
#1851=EDGE_LOOP('',(#11766,#11767,#11768,#11769));
#1852=EDGE_LOOP('',(#11770,#11771,#11772,#11773));
#1853=EDGE_LOOP('',(#11774,#11775,#11776,#11777));
#1854=EDGE_LOOP('',(#11778,#11779,#11780,#11781));
#1855=EDGE_LOOP('',(#11782,#11783,#11784,#11785));
#1856=EDGE_LOOP('',(#11786,#11787,#11788,#11789));
#1857=EDGE_LOOP('',(#11790,#11791,#11792,#11793));
#1858=EDGE_LOOP('',(#11794,#11795,#11796,#11797));
#1859=EDGE_LOOP('',(#11798,#11799,#11800,#11801));
#1860=EDGE_LOOP('',(#11802,#11803,#11804,#11805));
#1861=EDGE_LOOP('',(#11806,#11807,#11808,#11809));
#1862=EDGE_LOOP('',(#11810,#11811,#11812,#11813));
#1863=EDGE_LOOP('',(#11814,#11815,#11816,#11817));
#1864=EDGE_LOOP('',(#11818,#11819,#11820,#11821));
#1865=EDGE_LOOP('',(#11822,#11823,#11824,#11825));
#1866=EDGE_LOOP('',(#11826,#11827,#11828,#11829));
#1867=EDGE_LOOP('',(#11830,#11831,#11832,#11833));
#1868=EDGE_LOOP('',(#11834,#11835,#11836,#11837));
#1869=EDGE_LOOP('',(#11838,#11839,#11840,#11841));
#1870=EDGE_LOOP('',(#11842,#11843,#11844,#11845));
#1871=EDGE_LOOP('',(#11846,#11847,#11848,#11849));
#1872=EDGE_LOOP('',(#11850,#11851,#11852,#11853,#11854,#11855,#11856,#11857));
#1873=EDGE_LOOP('',(#11858,#11859,#11860,#11861));
#1874=EDGE_LOOP('',(#11862,#11863,#11864,#11865));
#1875=EDGE_LOOP('',(#11866,#11867,#11868,#11869));
#1876=EDGE_LOOP('',(#11870,#11871,#11872,#11873));
#1877=EDGE_LOOP('',(#11874,#11875,#11876,#11877));
#1878=EDGE_LOOP('',(#11878,#11879,#11880,#11881));
#1879=EDGE_LOOP('',(#11882,#11883,#11884,#11885));
#1880=EDGE_LOOP('',(#11886,#11887,#11888,#11889));
#1881=EDGE_LOOP('',(#11890,#11891,#11892,#11893));
#1882=EDGE_LOOP('',(#11894,#11895,#11896,#11897));
#1883=EDGE_LOOP('',(#11898,#11899,#11900,#11901));
#1884=EDGE_LOOP('',(#11902,#11903,#11904,#11905));
#1885=EDGE_LOOP('',(#11906,#11907,#11908,#11909));
#1886=EDGE_LOOP('',(#11910,#11911,#11912,#11913));
#1887=EDGE_LOOP('',(#11914,#11915,#11916,#11917));
#1888=EDGE_LOOP('',(#11918,#11919,#11920,#11921));
#1889=EDGE_LOOP('',(#11922,#11923,#11924,#11925));
#1890=EDGE_LOOP('',(#11926,#11927,#11928,#11929));
#1891=EDGE_LOOP('',(#11930,#11931,#11932,#11933));
#1892=EDGE_LOOP('',(#11934,#11935,#11936,#11937));
#1893=EDGE_LOOP('',(#11938,#11939,#11940,#11941));
#1894=EDGE_LOOP('',(#11942,#11943,#11944,#11945));
#1895=EDGE_LOOP('',(#11946,#11947,#11948,#11949));
#1896=EDGE_LOOP('',(#11950,#11951,#11952,#11953));
#1897=EDGE_LOOP('',(#11954,#11955,#11956,#11957,#11958,#11959,#11960,#11961));
#1898=EDGE_LOOP('',(#11962,#11963,#11964,#11965));
#1899=EDGE_LOOP('',(#11966,#11967,#11968,#11969));
#1900=EDGE_LOOP('',(#11970,#11971,#11972,#11973));
#1901=EDGE_LOOP('',(#11974,#11975,#11976,#11977));
#1902=EDGE_LOOP('',(#11978,#11979,#11980,#11981));
#1903=EDGE_LOOP('',(#11982,#11983,#11984,#11985));
#1904=EDGE_LOOP('',(#11986,#11987,#11988,#11989));
#1905=EDGE_LOOP('',(#11990,#11991,#11992,#11993));
#1906=EDGE_LOOP('',(#11994,#11995,#11996,#11997));
#1907=EDGE_LOOP('',(#11998,#11999,#12000,#12001));
#1908=EDGE_LOOP('',(#12002,#12003,#12004,#12005));
#1909=EDGE_LOOP('',(#12006,#12007,#12008,#12009));
#1910=EDGE_LOOP('',(#12010,#12011,#12012,#12013));
#1911=EDGE_LOOP('',(#12014,#12015,#12016,#12017));
#1912=EDGE_LOOP('',(#12018,#12019,#12020,#12021));
#1913=EDGE_LOOP('',(#12022,#12023,#12024,#12025));
#1914=EDGE_LOOP('',(#12026,#12027,#12028,#12029));
#1915=EDGE_LOOP('',(#12030,#12031,#12032,#12033));
#1916=EDGE_LOOP('',(#12034,#12035,#12036,#12037));
#1917=EDGE_LOOP('',(#12038,#12039,#12040,#12041));
#1918=EDGE_LOOP('',(#12042,#12043,#12044,#12045));
#1919=EDGE_LOOP('',(#12046,#12047,#12048,#12049));
#1920=EDGE_LOOP('',(#12050,#12051,#12052,#12053));
#1921=EDGE_LOOP('',(#12054,#12055,#12056,#12057));
#1922=EDGE_LOOP('',(#12058,#12059,#12060,#12061,#12062,#12063,#12064,#12065));
#1923=EDGE_LOOP('',(#12066,#12067,#12068,#12069));
#1924=EDGE_LOOP('',(#12070,#12071,#12072,#12073));
#1925=EDGE_LOOP('',(#12074,#12075,#12076,#12077));
#1926=EDGE_LOOP('',(#12078,#12079,#12080,#12081));
#1927=EDGE_LOOP('',(#12082,#12083,#12084,#12085));
#1928=EDGE_LOOP('',(#12086,#12087,#12088,#12089));
#1929=EDGE_LOOP('',(#12090,#12091,#12092,#12093));
#1930=EDGE_LOOP('',(#12094,#12095,#12096,#12097));
#1931=EDGE_LOOP('',(#12098,#12099,#12100,#12101));
#1932=EDGE_LOOP('',(#12102,#12103,#12104,#12105));
#1933=EDGE_LOOP('',(#12106,#12107,#12108,#12109));
#1934=EDGE_LOOP('',(#12110,#12111,#12112,#12113));
#1935=EDGE_LOOP('',(#12114,#12115,#12116,#12117));
#1936=EDGE_LOOP('',(#12118,#12119,#12120,#12121));
#1937=EDGE_LOOP('',(#12122,#12123,#12124,#12125));
#1938=EDGE_LOOP('',(#12126,#12127,#12128,#12129));
#1939=EDGE_LOOP('',(#12130,#12131,#12132,#12133));
#1940=EDGE_LOOP('',(#12134,#12135,#12136,#12137));
#1941=EDGE_LOOP('',(#12138,#12139,#12140,#12141));
#1942=EDGE_LOOP('',(#12142,#12143,#12144,#12145));
#1943=EDGE_LOOP('',(#12146,#12147,#12148,#12149));
#1944=EDGE_LOOP('',(#12150,#12151,#12152,#12153));
#1945=EDGE_LOOP('',(#12154,#12155,#12156,#12157));
#1946=EDGE_LOOP('',(#12158,#12159,#12160,#12161));
#1947=EDGE_LOOP('',(#12162,#12163,#12164,#12165,#12166,#12167,#12168,#12169));
#1948=EDGE_LOOP('',(#12170,#12171,#12172,#12173));
#1949=EDGE_LOOP('',(#12174,#12175,#12176,#12177));
#1950=EDGE_LOOP('',(#12178,#12179,#12180,#12181));
#1951=EDGE_LOOP('',(#12182,#12183,#12184,#12185));
#1952=EDGE_LOOP('',(#12186,#12187,#12188,#12189));
#1953=EDGE_LOOP('',(#12190,#12191,#12192,#12193));
#1954=EDGE_LOOP('',(#12194,#12195,#12196,#12197));
#1955=EDGE_LOOP('',(#12198,#12199,#12200,#12201));
#1956=EDGE_LOOP('',(#12202,#12203,#12204,#12205));
#1957=EDGE_LOOP('',(#12206,#12207,#12208,#12209));
#1958=EDGE_LOOP('',(#12210,#12211,#12212,#12213));
#1959=EDGE_LOOP('',(#12214,#12215,#12216,#12217));
#1960=EDGE_LOOP('',(#12218,#12219,#12220,#12221));
#1961=EDGE_LOOP('',(#12222,#12223,#12224,#12225));
#1962=EDGE_LOOP('',(#12226,#12227,#12228,#12229));
#1963=EDGE_LOOP('',(#12230,#12231,#12232,#12233));
#1964=EDGE_LOOP('',(#12234,#12235,#12236,#12237));
#1965=EDGE_LOOP('',(#12238,#12239,#12240,#12241));
#1966=EDGE_LOOP('',(#12242,#12243,#12244,#12245));
#1967=EDGE_LOOP('',(#12246,#12247,#12248,#12249));
#1968=EDGE_LOOP('',(#12250,#12251,#12252,#12253));
#1969=EDGE_LOOP('',(#12254,#12255,#12256,#12257));
#1970=EDGE_LOOP('',(#12258,#12259,#12260,#12261));
#1971=EDGE_LOOP('',(#12262,#12263,#12264,#12265));
#1972=EDGE_LOOP('',(#12266,#12267,#12268,#12269));
#1973=EDGE_LOOP('',(#12270,#12271,#12272,#12273));
#1974=EDGE_LOOP('',(#12274,#12275,#12276,#12277));
#1975=EDGE_LOOP('',(#12278,#12279,#12280,#12281));
#1976=EDGE_LOOP('',(#12282,#12283,#12284,#12285));
#1977=EDGE_LOOP('',(#12286,#12287,#12288,#12289));
#1978=EDGE_LOOP('',(#12290,#12291,#12292,#12293));
#1979=EDGE_LOOP('',(#12294,#12295,#12296,#12297));
#1980=EDGE_LOOP('',(#12298,#12299,#12300,#12301));
#1981=EDGE_LOOP('',(#12302,#12303,#12304,#12305));
#1982=EDGE_LOOP('',(#12306,#12307,#12308,#12309));
#1983=EDGE_LOOP('',(#12310,#12311,#12312,#12313));
#1984=EDGE_LOOP('',(#12314,#12315,#12316,#12317));
#1985=EDGE_LOOP('',(#12318,#12319,#12320,#12321));
#1986=EDGE_LOOP('',(#12322,#12323,#12324,#12325));
#1987=EDGE_LOOP('',(#12326,#12327,#12328,#12329,#12330));
#1988=EDGE_LOOP('',(#12331,#12332,#12333,#12334));
#1989=EDGE_LOOP('',(#12335,#12336,#12337,#12338));
#1990=EDGE_LOOP('',(#12339,#12340,#12341,#12342));
#1991=EDGE_LOOP('',(#12343,#12344,#12345,#12346));
#1992=EDGE_LOOP('',(#12347,#12348,#12349,#12350));
#1993=EDGE_LOOP('',(#12351,#12352,#12353,#12354));
#1994=EDGE_LOOP('',(#12355,#12356,#12357,#12358));
#1995=EDGE_LOOP('',(#12359,#12360,#12361,#12362));
#1996=EDGE_LOOP('',(#12363,#12364,#12365,#12366));
#1997=EDGE_LOOP('',(#12367,#12368,#12369,#12370));
#1998=EDGE_LOOP('',(#12371,#12372,#12373,#12374));
#1999=EDGE_LOOP('',(#12375,#12376,#12377,#12378));
#2000=EDGE_LOOP('',(#12379,#12380,#12381,#12382));
#2001=EDGE_LOOP('',(#12383,#12384,#12385,#12386));
#2002=EDGE_LOOP('',(#12387,#12388,#12389,#12390));
#2003=EDGE_LOOP('',(#12391,#12392,#12393,#12394));
#2004=EDGE_LOOP('',(#12395,#12396,#12397,#12398));
#2005=EDGE_LOOP('',(#12399,#12400,#12401,#12402));
#2006=EDGE_LOOP('',(#12403,#12404,#12405,#12406));
#2007=EDGE_LOOP('',(#12407,#12408,#12409,#12410));
#2008=EDGE_LOOP('',(#12411,#12412,#12413,#12414));
#2009=EDGE_LOOP('',(#12415,#12416,#12417,#12418));
#2010=EDGE_LOOP('',(#12419,#12420,#12421,#12422));
#2011=EDGE_LOOP('',(#12423,#12424,#12425,#12426));
#2012=EDGE_LOOP('',(#12427,#12428,#12429,#12430));
#2013=EDGE_LOOP('',(#12431,#12432,#12433,#12434));
#2014=EDGE_LOOP('',(#12435,#12436,#12437,#12438));
#2015=EDGE_LOOP('',(#12439,#12440,#12441,#12442));
#2016=EDGE_LOOP('',(#12443,#12444,#12445,#12446));
#2017=EDGE_LOOP('',(#12447,#12448,#12449,#12450));
#2018=EDGE_LOOP('',(#12451,#12452,#12453,#12454));
#2019=EDGE_LOOP('',(#12455,#12456,#12457,#12458,#12459));
#2020=EDGE_LOOP('',(#12460,#12461,#12462,#12463));
#2021=EDGE_LOOP('',(#12464,#12465,#12466,#12467));
#2022=EDGE_LOOP('',(#12468,#12469,#12470,#12471));
#2023=EDGE_LOOP('',(#12472,#12473,#12474,#12475));
#2024=EDGE_LOOP('',(#12476,#12477,#12478,#12479));
#2025=EDGE_LOOP('',(#12480,#12481,#12482,#12483));
#2026=EDGE_LOOP('',(#12484,#12485,#12486,#12487));
#2027=EDGE_LOOP('',(#12488,#12489,#12490,#12491,#12492));
#2028=EDGE_LOOP('',(#12493,#12494,#12495,#12496));
#2029=EDGE_LOOP('',(#12497,#12498,#12499,#12500));
#2030=EDGE_LOOP('',(#12501,#12502,#12503,#12504));
#2031=EDGE_LOOP('',(#12505,#12506,#12507,#12508));
#2032=EDGE_LOOP('',(#12509,#12510,#12511,#12512));
#2033=EDGE_LOOP('',(#12513,#12514,#12515,#12516));
#2034=EDGE_LOOP('',(#12517,#12518,#12519,#12520));
#2035=EDGE_LOOP('',(#12521,#12522,#12523,#12524,#12525));
#2036=EDGE_LOOP('',(#12526,#12527,#12528,#12529,#12530,#12531,#12532,#12533,
#12534,#12535,#12536,#12537,#12538,#12539,#12540,#12541,#12542,#12543,#12544,
#12545));
#2037=EDGE_LOOP('',(#12546,#12547,#12548,#12549));
#2038=EDGE_LOOP('',(#12550,#12551,#12552,#12553,#12554,#12555,#12556,#12557,
#12558,#12559,#12560,#12561,#12562,#12563,#12564,#12565,#12566,#12567,#12568,
#12569));
#2039=EDGE_LOOP('',(#12570,#12571,#12572,#12573,#12574,#12575,#12576,#12577,
#12578,#12579,#12580,#12581,#12582,#12583,#12584,#12585,#12586,#12587,#12588,
#12589));
#2040=EDGE_LOOP('',(#12590,#12591,#12592,#12593));
#2041=EDGE_LOOP('',(#12594,#12595,#12596,#12597,#12598,#12599,#12600,#12601,
#12602,#12603,#12604,#12605,#12606,#12607,#12608,#12609,#12610,#12611,#12612,
#12613));
#2042=EDGE_LOOP('',(#12614,#12615,#12616,#12617,#12618,#12619,#12620,#12621,
#12622,#12623,#12624,#12625,#12626,#12627,#12628,#12629,#12630,#12631,#12632,
#12633));
#2043=EDGE_LOOP('',(#12634,#12635,#12636,#12637));
#2044=EDGE_LOOP('',(#12638,#12639,#12640,#12641,#12642,#12643,#12644,#12645,
#12646,#12647,#12648,#12649,#12650,#12651,#12652,#12653,#12654,#12655,#12656,
#12657));
#2045=EDGE_LOOP('',(#12658,#12659,#12660,#12661));
#2046=EDGE_LOOP('',(#12662,#12663,#12664,#12665));
#2047=EDGE_LOOP('',(#12666,#12667,#12668,#12669));
#2048=EDGE_LOOP('',(#12670,#12671,#12672,#12673));
#2049=EDGE_LOOP('',(#12674,#12675,#12676,#12677));
#2050=EDGE_LOOP('',(#12678,#12679,#12680,#12681));
#2051=EDGE_LOOP('',(#12682,#12683,#12684,#12685,#12686,#12687,#12688,#12689,
#12690,#12691,#12692,#12693,#12694,#12695,#12696,#12697,#12698,#12699,#12700,
#12701));
#2052=EDGE_LOOP('',(#12702,#12703,#12704,#12705));
#2053=EDGE_LOOP('',(#12706,#12707,#12708,#12709,#12710,#12711,#12712,#12713,
#12714,#12715,#12716,#12717,#12718,#12719,#12720,#12721,#12722,#12723,#12724,
#12725));
#2054=EDGE_LOOP('',(#12726,#12727,#12728,#12729));
#2055=EDGE_LOOP('',(#12730,#12731,#12732,#12733));
#2056=EDGE_LOOP('',(#12734,#12735,#12736,#12737));
#2057=EDGE_LOOP('',(#12738,#12739,#12740,#12741));
#2058=EDGE_LOOP('',(#12742,#12743,#12744,#12745,#12746,#12747,#12748,#12749,
#12750,#12751,#12752,#12753,#12754,#12755,#12756,#12757,#12758,#12759,#12760,
#12761,#12762,#12763,#12764,#12765,#12766,#12767,#12768,#12769,#12770,#12771));
#2059=EDGE_LOOP('',(#12772,#12773,#12774,#12775,#12776,#12777,#12778,#12779,
#12780,#12781,#12782,#12783,#12784,#12785,#12786,#12787,#12788,#12789,#12790,
#12791,#12792,#12793,#12794,#12795,#12796,#12797,#12798,#12799,#12800));
#2060=EDGE_LOOP('',(#12801,#12802,#12803,#12804));
#2061=EDGE_LOOP('',(#12805,#12806,#12807,#12808));
#2062=EDGE_LOOP('',(#12809,#12810,#12811,#12812));
#2063=EDGE_LOOP('',(#12813,#12814,#12815,#12816,#12817,#12818,#12819,#12820,
#12821,#12822,#12823,#12824,#12825,#12826,#12827,#12828,#12829,#12830,#12831,
#12832,#12833,#12834,#12835,#12836,#12837,#12838,#12839,#12840,#12841,#12842));
#2064=EDGE_LOOP('',(#12843,#12844,#12845,#12846,#12847,#12848,#12849,#12850,
#12851,#12852,#12853,#12854,#12855,#12856,#12857,#12858,#12859,#12860,#12861,
#12862,#12863,#12864,#12865,#12866,#12867,#12868,#12869,#12870,#12871));
#2065=EDGE_LOOP('',(#12872,#12873,#12874,#12875));
#2066=EDGE_LOOP('',(#12876,#12877,#12878,#12879));
#2067=EDGE_LOOP('',(#12880,#12881,#12882,#12883));
#2068=EDGE_LOOP('',(#12884,#12885,#12886,#12887,#12888,#12889,#12890,#12891,
#12892,#12893,#12894,#12895,#12896,#12897,#12898,#12899,#12900,#12901,#12902,
#12903,#12904,#12905,#12906,#12907,#12908,#12909,#12910,#12911,#12912,#12913));
#2069=EDGE_LOOP('',(#12914,#12915,#12916,#12917,#12918,#12919,#12920,#12921,
#12922,#12923,#12924,#12925,#12926,#12927,#12928,#12929,#12930,#12931,#12932,
#12933,#12934,#12935,#12936,#12937,#12938,#12939,#12940,#12941,#12942));
#2070=EDGE_LOOP('',(#12943,#12944,#12945,#12946));
#2071=EDGE_LOOP('',(#12947,#12948,#12949,#12950));
#2072=EDGE_LOOP('',(#12951,#12952,#12953,#12954));
#2073=EDGE_LOOP('',(#12955,#12956,#12957,#12958,#12959,#12960,#12961,#12962,
#12963,#12964,#12965,#12966,#12967,#12968,#12969,#12970,#12971,#12972,#12973,
#12974,#12975,#12976,#12977,#12978,#12979,#12980,#12981,#12982,#12983,#12984));
#2074=EDGE_LOOP('',(#12985,#12986,#12987,#12988,#12989,#12990,#12991,#12992,
#12993,#12994,#12995,#12996,#12997,#12998,#12999,#13000,#13001,#13002,#13003,
#13004,#13005,#13006,#13007,#13008,#13009,#13010,#13011,#13012,#13013));
#2075=EDGE_LOOP('',(#13014,#13015,#13016,#13017));
#2076=EDGE_LOOP('',(#13018,#13019,#13020,#13021));
#2077=EDGE_LOOP('',(#13022,#13023,#13024,#13025));
#2078=EDGE_LOOP('',(#13026,#13027,#13028,#13029,#13030,#13031,#13032,#13033,
#13034,#13035,#13036,#13037,#13038,#13039,#13040,#13041,#13042,#13043,#13044,
#13045,#13046,#13047,#13048,#13049,#13050,#13051,#13052,#13053,#13054,#13055));
#2079=EDGE_LOOP('',(#13056,#13057,#13058,#13059,#13060,#13061,#13062,#13063,
#13064,#13065,#13066,#13067,#13068,#13069,#13070,#13071,#13072,#13073,#13074,
#13075,#13076,#13077,#13078,#13079,#13080,#13081,#13082,#13083,#13084));
#2080=EDGE_LOOP('',(#13085,#13086,#13087,#13088));
#2081=EDGE_LOOP('',(#13089));
#2082=EDGE_LOOP('',(#13090));
#2083=EDGE_LOOP('',(#13091));
#2084=EDGE_LOOP('',(#13092));
#2085=EDGE_LOOP('',(#13093));
#2086=EDGE_LOOP('',(#13094,#13095,#13096,#13097));
#2087=EDGE_LOOP('',(#13098,#13099,#13100,#13101));
#2088=EDGE_LOOP('',(#13102,#13103,#13104,#13105,#13106,#13107,#13108,#13109,
#13110,#13111,#13112,#13113,#13114,#13115,#13116,#13117,#13118,#13119,#13120,
#13121,#13122,#13123,#13124,#13125,#13126,#13127,#13128,#13129,#13130,#13131));
#2089=EDGE_LOOP('',(#13132,#13133,#13134,#13135,#13136,#13137,#13138,#13139,
#13140,#13141,#13142,#13143,#13144,#13145,#13146,#13147,#13148,#13149,#13150,
#13151,#13152,#13153,#13154,#13155,#13156,#13157,#13158,#13159,#13160));
#2090=EDGE_LOOP('',(#13161,#13162,#13163,#13164));
#2091=EDGE_LOOP('',(#13165,#13166,#13167,#13168));
#2092=EDGE_LOOP('',(#13169,#13170,#13171,#13172));
#2093=EDGE_LOOP('',(#13173,#13174,#13175,#13176,#13177,#13178,#13179,#13180,
#13181,#13182,#13183,#13184,#13185,#13186,#13187,#13188,#13189,#13190,#13191,
#13192,#13193,#13194,#13195,#13196,#13197,#13198,#13199,#13200,#13201,#13202));
#2094=EDGE_LOOP('',(#13203,#13204,#13205,#13206,#13207,#13208,#13209,#13210,
#13211,#13212,#13213,#13214,#13215,#13216,#13217,#13218,#13219,#13220,#13221,
#13222,#13223,#13224,#13225,#13226,#13227,#13228,#13229,#13230,#13231));
#2095=EDGE_LOOP('',(#13232,#13233,#13234,#13235));
#2096=EDGE_LOOP('',(#13236,#13237,#13238,#13239));
#2097=EDGE_LOOP('',(#13240,#13241,#13242,#13243));
#2098=EDGE_LOOP('',(#13244,#13245,#13246,#13247,#13248,#13249,#13250,#13251,
#13252,#13253,#13254,#13255,#13256,#13257,#13258,#13259,#13260,#13261,#13262,
#13263,#13264,#13265,#13266,#13267,#13268,#13269,#13270,#13271,#13272,#13273));
#2099=EDGE_LOOP('',(#13274,#13275,#13276,#13277,#13278,#13279,#13280,#13281,
#13282,#13283,#13284,#13285,#13286,#13287,#13288,#13289,#13290,#13291,#13292,
#13293,#13294,#13295,#13296,#13297,#13298,#13299,#13300,#13301,#13302));
#2100=EDGE_LOOP('',(#13303,#13304,#13305,#13306));
#2101=EDGE_LOOP('',(#13307,#13308,#13309,#13310));
#2102=EDGE_LOOP('',(#13311,#13312,#13313,#13314));
#2103=EDGE_LOOP('',(#13315,#13316,#13317,#13318,#13319,#13320,#13321,#13322,
#13323,#13324,#13325,#13326,#13327,#13328,#13329,#13330,#13331,#13332,#13333,
#13334,#13335,#13336,#13337,#13338,#13339,#13340,#13341,#13342,#13343,#13344));
#2104=EDGE_LOOP('',(#13345,#13346,#13347,#13348,#13349,#13350,#13351,#13352,
#13353,#13354,#13355,#13356,#13357,#13358,#13359,#13360,#13361,#13362,#13363,
#13364,#13365,#13366,#13367,#13368,#13369,#13370,#13371,#13372,#13373));
#2105=EDGE_LOOP('',(#13374,#13375,#13376,#13377));
#2106=EDGE_LOOP('',(#13378,#13379,#13380,#13381));
#2107=EDGE_LOOP('',(#13382,#13383,#13384,#13385));
#2108=EDGE_LOOP('',(#13386,#13387,#13388,#13389,#13390,#13391,#13392,#13393,
#13394,#13395,#13396,#13397,#13398,#13399,#13400,#13401,#13402,#13403,#13404,
#13405,#13406,#13407,#13408,#13409,#13410,#13411,#13412,#13413,#13414,#13415));
#2109=EDGE_LOOP('',(#13416,#13417,#13418,#13419,#13420,#13421,#13422,#13423,
#13424,#13425,#13426,#13427,#13428,#13429,#13430,#13431,#13432,#13433,#13434,
#13435,#13436,#13437,#13438,#13439,#13440,#13441,#13442,#13443,#13444));
#2110=EDGE_LOOP('',(#13445,#13446,#13447,#13448));
#2111=EDGE_LOOP('',(#13449));
#2112=EDGE_LOOP('',(#13450));
#2113=EDGE_LOOP('',(#13451));
#2114=EDGE_LOOP('',(#13452));
#2115=EDGE_LOOP('',(#13453));
#2116=EDGE_LOOP('',(#13454,#13455,#13456,#13457));
#2117=EDGE_LOOP('',(#13458,#13459,#13460,#13461));
#2118=EDGE_LOOP('',(#13462,#13463,#13464,#13465,#13466,#13467,#13468,#13469,
#13470,#13471,#13472,#13473,#13474,#13475,#13476,#13477,#13478,#13479,#13480,
#13481,#13482,#13483,#13484,#13485,#13486,#13487,#13488,#13489,#13490,#13491));
#2119=EDGE_LOOP('',(#13492,#13493,#13494,#13495,#13496,#13497,#13498,#13499,
#13500,#13501,#13502,#13503,#13504,#13505,#13506,#13507,#13508,#13509,#13510,
#13511,#13512,#13513,#13514,#13515,#13516,#13517,#13518,#13519,#13520));
#2120=EDGE_LOOP('',(#13521,#13522,#13523,#13524));
#2121=EDGE_LOOP('',(#13525));
#2122=EDGE_LOOP('',(#13526,#13527,#13528,#13529));
#2123=EDGE_LOOP('',(#13530,#13531,#13532,#13533));
#2124=EDGE_LOOP('',(#13534,#13535,#13536,#13537,#13538,#13539,#13540,#13541,
#13542,#13543,#13544,#13545,#13546,#13547,#13548,#13549,#13550,#13551,#13552,
#13553,#13554,#13555,#13556,#13557,#13558,#13559,#13560,#13561,#13562,#13563));
#2125=EDGE_LOOP('',(#13564,#13565,#13566,#13567,#13568,#13569,#13570,#13571,
#13572,#13573,#13574,#13575,#13576,#13577,#13578,#13579,#13580,#13581,#13582,
#13583,#13584,#13585,#13586,#13587,#13588,#13589,#13590,#13591,#13592));
#2126=EDGE_LOOP('',(#13593,#13594,#13595,#13596));
#2127=EDGE_LOOP('',(#13597));
#2128=EDGE_LOOP('',(#13598,#13599,#13600,#13601));
#2129=EDGE_LOOP('',(#13602,#13603,#13604,#13605));
#2130=EDGE_LOOP('',(#13606,#13607,#13608,#13609,#13610));
#2131=EDGE_LOOP('',(#13611,#13612,#13613,#13614,#13615));
#2132=EDGE_LOOP('',(#13616,#13617,#13618,#13619,#13620));
#2133=EDGE_LOOP('',(#13621,#13622,#13623,#13624,#13625));
#2134=EDGE_LOOP('',(#13626));
#2135=EDGE_LOOP('',(#13627,#13628,#13629,#13630));
#2136=EDGE_LOOP('',(#13631,#13632,#13633,#13634));
#2137=EDGE_LOOP('',(#13635,#13636,#13637,#13638));
#2138=EDGE_LOOP('',(#13639,#13640,#13641,#13642));
#2139=EDGE_LOOP('',(#13643,#13644,#13645,#13646));
#2140=EDGE_LOOP('',(#13647));
#2141=EDGE_LOOP('',(#13648,#13649,#13650,#13651));
#2142=EDGE_LOOP('',(#13652));
#2143=EDGE_LOOP('',(#13653,#13654,#13655,#13656));
#2144=EDGE_LOOP('',(#13657,#13658,#13659,#13660));
#2145=EDGE_LOOP('',(#13661,#13662,#13663,#13664));
#2146=EDGE_LOOP('',(#13665,#13666,#13667,#13668));
#2147=EDGE_LOOP('',(#13669,#13670,#13671,#13672));
#2148=EDGE_LOOP('',(#13673));
#2149=EDGE_LOOP('',(#13674,#13675,#13676,#13677));
#2150=EDGE_LOOP('',(#13678,#13679,#13680,#13681,#13682,#13683,#13684,#13685,
#13686,#13687));
#2151=EDGE_LOOP('',(#13688,#13689,#13690,#13691));
#2152=EDGE_LOOP('',(#13692,#13693,#13694,#13695));
#2153=EDGE_LOOP('',(#13696,#13697,#13698,#13699));
#2154=EDGE_LOOP('',(#13700,#13701,#13702,#13703));
#2155=EDGE_LOOP('',(#13704,#13705,#13706,#13707));
#2156=EDGE_LOOP('',(#13708,#13709,#13710,#13711));
#2157=EDGE_LOOP('',(#13712,#13713,#13714,#13715));
#2158=EDGE_LOOP('',(#13716,#13717,#13718,#13719));
#2159=EDGE_LOOP('',(#13720,#13721,#13722,#13723));
#2160=EDGE_LOOP('',(#13724,#13725,#13726,#13727));
#2161=EDGE_LOOP('',(#13728,#13729,#13730,#13731));
#2162=EDGE_LOOP('',(#13732,#13733,#13734,#13735));
#2163=EDGE_LOOP('',(#13736,#13737,#13738,#13739));
#2164=EDGE_LOOP('',(#13740,#13741,#13742,#13743));
#2165=EDGE_LOOP('',(#13744,#13745,#13746,#13747));
#2166=EDGE_LOOP('',(#13748,#13749,#13750,#13751,#13752,#13753,#13754,#13755,
#13756,#13757));
#2167=EDGE_LOOP('',(#13758,#13759,#13760,#13761));
#2168=EDGE_LOOP('',(#13762,#13763,#13764,#13765));
#2169=EDGE_LOOP('',(#13766,#13767,#13768,#13769));
#2170=EDGE_LOOP('',(#13770,#13771,#13772,#13773));
#2171=EDGE_LOOP('',(#13774,#13775,#13776,#13777));
#2172=EDGE_LOOP('',(#13778,#13779,#13780,#13781));
#2173=EDGE_LOOP('',(#13782,#13783,#13784,#13785));
#2174=EDGE_LOOP('',(#13786,#13787,#13788,#13789));
#2175=EDGE_LOOP('',(#13790,#13791,#13792,#13793));
#2176=EDGE_LOOP('',(#13794,#13795,#13796,#13797));
#2177=EDGE_LOOP('',(#13798,#13799,#13800,#13801));
#2178=EDGE_LOOP('',(#13802,#13803,#13804,#13805));
#2179=EDGE_LOOP('',(#13806,#13807,#13808,#13809));
#2180=EDGE_LOOP('',(#13810,#13811,#13812,#13813));
#2181=EDGE_LOOP('',(#13814,#13815,#13816,#13817));
#2182=EDGE_LOOP('',(#13818,#13819,#13820,#13821,#13822,#13823,#13824,#13825,
#13826,#13827));
#2183=EDGE_LOOP('',(#13828,#13829,#13830,#13831));
#2184=EDGE_LOOP('',(#13832,#13833,#13834,#13835));
#2185=EDGE_LOOP('',(#13836,#13837,#13838,#13839));
#2186=EDGE_LOOP('',(#13840,#13841,#13842,#13843));
#2187=EDGE_LOOP('',(#13844,#13845,#13846,#13847));
#2188=EDGE_LOOP('',(#13848,#13849,#13850,#13851));
#2189=EDGE_LOOP('',(#13852,#13853,#13854,#13855));
#2190=EDGE_LOOP('',(#13856,#13857,#13858,#13859));
#2191=EDGE_LOOP('',(#13860,#13861,#13862,#13863));
#2192=EDGE_LOOP('',(#13864,#13865,#13866,#13867));
#2193=EDGE_LOOP('',(#13868,#13869,#13870,#13871));
#2194=EDGE_LOOP('',(#13872,#13873,#13874,#13875));
#2195=EDGE_LOOP('',(#13876,#13877,#13878,#13879));
#2196=EDGE_LOOP('',(#13880,#13881,#13882,#13883));
#2197=EDGE_LOOP('',(#13884,#13885,#13886,#13887));
#2198=EDGE_LOOP('',(#13888,#13889,#13890,#13891,#13892,#13893,#13894,#13895,
#13896,#13897));
#2199=EDGE_LOOP('',(#13898,#13899,#13900,#13901));
#2200=EDGE_LOOP('',(#13902,#13903,#13904,#13905));
#2201=EDGE_LOOP('',(#13906,#13907,#13908,#13909));
#2202=EDGE_LOOP('',(#13910,#13911,#13912,#13913));
#2203=EDGE_LOOP('',(#13914,#13915,#13916,#13917));
#2204=EDGE_LOOP('',(#13918,#13919,#13920,#13921));
#2205=EDGE_LOOP('',(#13922,#13923,#13924,#13925));
#2206=EDGE_LOOP('',(#13926,#13927,#13928,#13929));
#2207=EDGE_LOOP('',(#13930,#13931,#13932,#13933));
#2208=EDGE_LOOP('',(#13934,#13935,#13936,#13937));
#2209=EDGE_LOOP('',(#13938,#13939,#13940,#13941));
#2210=EDGE_LOOP('',(#13942,#13943,#13944,#13945));
#2211=EDGE_LOOP('',(#13946,#13947,#13948,#13949));
#2212=EDGE_LOOP('',(#13950,#13951,#13952,#13953));
#2213=EDGE_LOOP('',(#13954,#13955,#13956,#13957));
#2214=EDGE_LOOP('',(#13958,#13959,#13960,#13961,#13962,#13963,#13964,#13965,
#13966,#13967));
#2215=EDGE_LOOP('',(#13968,#13969,#13970,#13971));
#2216=EDGE_LOOP('',(#13972,#13973,#13974,#13975));
#2217=EDGE_LOOP('',(#13976,#13977,#13978,#13979));
#2218=EDGE_LOOP('',(#13980,#13981,#13982,#13983));
#2219=EDGE_LOOP('',(#13984,#13985,#13986,#13987));
#2220=EDGE_LOOP('',(#13988,#13989,#13990,#13991));
#2221=EDGE_LOOP('',(#13992,#13993,#13994,#13995));
#2222=EDGE_LOOP('',(#13996,#13997,#13998,#13999));
#2223=EDGE_LOOP('',(#14000,#14001,#14002,#14003));
#2224=EDGE_LOOP('',(#14004,#14005,#14006,#14007));
#2225=EDGE_LOOP('',(#14008,#14009,#14010,#14011));
#2226=EDGE_LOOP('',(#14012,#14013,#14014,#14015));
#2227=EDGE_LOOP('',(#14016,#14017,#14018,#14019));
#2228=EDGE_LOOP('',(#14020,#14021,#14022,#14023));
#2229=EDGE_LOOP('',(#14024,#14025,#14026,#14027));
#2230=EDGE_LOOP('',(#14028,#14029,#14030,#14031,#14032,#14033,#14034,#14035,
#14036,#14037));
#2231=EDGE_LOOP('',(#14038,#14039,#14040,#14041));
#2232=EDGE_LOOP('',(#14042,#14043,#14044,#14045));
#2233=EDGE_LOOP('',(#14046,#14047,#14048,#14049));
#2234=EDGE_LOOP('',(#14050,#14051,#14052,#14053));
#2235=EDGE_LOOP('',(#14054,#14055,#14056,#14057));
#2236=EDGE_LOOP('',(#14058,#14059,#14060,#14061));
#2237=EDGE_LOOP('',(#14062,#14063,#14064,#14065));
#2238=EDGE_LOOP('',(#14066,#14067,#14068,#14069));
#2239=EDGE_LOOP('',(#14070,#14071,#14072,#14073));
#2240=EDGE_LOOP('',(#14074,#14075,#14076,#14077));
#2241=EDGE_LOOP('',(#14078,#14079,#14080,#14081));
#2242=EDGE_LOOP('',(#14082,#14083,#14084,#14085));
#2243=EDGE_LOOP('',(#14086,#14087,#14088,#14089));
#2244=EDGE_LOOP('',(#14090,#14091,#14092,#14093));
#2245=EDGE_LOOP('',(#14094,#14095,#14096,#14097));
#2246=EDGE_LOOP('',(#14098,#14099,#14100,#14101,#14102,#14103,#14104,#14105,
#14106,#14107));
#2247=EDGE_LOOP('',(#14108,#14109,#14110,#14111));
#2248=EDGE_LOOP('',(#14112,#14113,#14114,#14115));
#2249=EDGE_LOOP('',(#14116,#14117,#14118,#14119));
#2250=EDGE_LOOP('',(#14120,#14121,#14122,#14123));
#2251=EDGE_LOOP('',(#14124,#14125,#14126,#14127));
#2252=EDGE_LOOP('',(#14128,#14129,#14130,#14131));
#2253=EDGE_LOOP('',(#14132,#14133,#14134,#14135));
#2254=EDGE_LOOP('',(#14136,#14137,#14138,#14139));
#2255=EDGE_LOOP('',(#14140,#14141,#14142,#14143));
#2256=EDGE_LOOP('',(#14144,#14145,#14146,#14147));
#2257=EDGE_LOOP('',(#14148,#14149,#14150,#14151));
#2258=EDGE_LOOP('',(#14152,#14153,#14154,#14155));
#2259=EDGE_LOOP('',(#14156,#14157,#14158,#14159));
#2260=EDGE_LOOP('',(#14160,#14161,#14162,#14163));
#2261=EDGE_LOOP('',(#14164,#14165,#14166,#14167));
#2262=EDGE_LOOP('',(#14168,#14169,#14170,#14171,#14172,#14173,#14174,#14175,
#14176,#14177));
#2263=EDGE_LOOP('',(#14178,#14179,#14180,#14181));
#2264=EDGE_LOOP('',(#14182,#14183,#14184,#14185));
#2265=EDGE_LOOP('',(#14186,#14187,#14188,#14189));
#2266=EDGE_LOOP('',(#14190,#14191,#14192,#14193));
#2267=EDGE_LOOP('',(#14194,#14195,#14196,#14197));
#2268=EDGE_LOOP('',(#14198,#14199,#14200,#14201));
#2269=EDGE_LOOP('',(#14202,#14203,#14204,#14205));
#2270=EDGE_LOOP('',(#14206,#14207,#14208,#14209));
#2271=EDGE_LOOP('',(#14210,#14211,#14212,#14213));
#2272=EDGE_LOOP('',(#14214,#14215,#14216,#14217));
#2273=EDGE_LOOP('',(#14218,#14219,#14220,#14221));
#2274=EDGE_LOOP('',(#14222,#14223,#14224,#14225));
#2275=EDGE_LOOP('',(#14226,#14227,#14228,#14229));
#2276=EDGE_LOOP('',(#14230,#14231,#14232,#14233));
#2277=EDGE_LOOP('',(#14234,#14235,#14236,#14237));
#2278=EDGE_LOOP('',(#14238,#14239,#14240,#14241,#14242,#14243,#14244,#14245,
#14246,#14247));
#2279=EDGE_LOOP('',(#14248,#14249,#14250,#14251));
#2280=EDGE_LOOP('',(#14252,#14253,#14254,#14255));
#2281=EDGE_LOOP('',(#14256,#14257,#14258,#14259));
#2282=EDGE_LOOP('',(#14260,#14261,#14262,#14263));
#2283=EDGE_LOOP('',(#14264,#14265,#14266,#14267));
#2284=EDGE_LOOP('',(#14268,#14269,#14270,#14271));
#2285=EDGE_LOOP('',(#14272,#14273,#14274,#14275));
#2286=EDGE_LOOP('',(#14276,#14277,#14278,#14279));
#2287=EDGE_LOOP('',(#14280,#14281,#14282,#14283));
#2288=EDGE_LOOP('',(#14284,#14285,#14286,#14287));
#2289=EDGE_LOOP('',(#14288,#14289,#14290,#14291));
#2290=EDGE_LOOP('',(#14292,#14293,#14294,#14295));
#2291=EDGE_LOOP('',(#14296,#14297,#14298,#14299));
#2292=EDGE_LOOP('',(#14300,#14301,#14302,#14303));
#2293=EDGE_LOOP('',(#14304,#14305,#14306,#14307));
#2294=EDGE_LOOP('',(#14308,#14309,#14310,#14311,#14312,#14313,#14314,#14315,
#14316,#14317));
#2295=EDGE_LOOP('',(#14318,#14319,#14320,#14321));
#2296=EDGE_LOOP('',(#14322,#14323,#14324,#14325));
#2297=EDGE_LOOP('',(#14326,#14327,#14328,#14329));
#2298=EDGE_LOOP('',(#14330,#14331,#14332,#14333));
#2299=EDGE_LOOP('',(#14334,#14335,#14336,#14337));
#2300=EDGE_LOOP('',(#14338,#14339,#14340,#14341));
#2301=EDGE_LOOP('',(#14342,#14343,#14344,#14345));
#2302=EDGE_LOOP('',(#14346,#14347,#14348,#14349));
#2303=EDGE_LOOP('',(#14350,#14351,#14352,#14353));
#2304=EDGE_LOOP('',(#14354,#14355,#14356,#14357));
#2305=EDGE_LOOP('',(#14358,#14359,#14360,#14361));
#2306=EDGE_LOOP('',(#14362,#14363,#14364,#14365));
#2307=EDGE_LOOP('',(#14366,#14367,#14368,#14369));
#2308=EDGE_LOOP('',(#14370,#14371,#14372,#14373));
#2309=EDGE_LOOP('',(#14374,#14375,#14376,#14377));
#2310=EDGE_LOOP('',(#14378,#14379,#14380,#14381,#14382,#14383,#14384,#14385,
#14386,#14387));
#2311=EDGE_LOOP('',(#14388,#14389,#14390,#14391));
#2312=EDGE_LOOP('',(#14392,#14393,#14394,#14395));
#2313=EDGE_LOOP('',(#14396,#14397,#14398,#14399));
#2314=EDGE_LOOP('',(#14400,#14401,#14402,#14403));
#2315=EDGE_LOOP('',(#14404,#14405,#14406,#14407));
#2316=EDGE_LOOP('',(#14408,#14409,#14410,#14411));
#2317=EDGE_LOOP('',(#14412,#14413,#14414,#14415));
#2318=EDGE_LOOP('',(#14416,#14417,#14418,#14419));
#2319=EDGE_LOOP('',(#14420,#14421,#14422,#14423));
#2320=EDGE_LOOP('',(#14424,#14425,#14426,#14427));
#2321=EDGE_LOOP('',(#14428,#14429,#14430,#14431));
#2322=EDGE_LOOP('',(#14432,#14433,#14434,#14435));
#2323=EDGE_LOOP('',(#14436,#14437,#14438,#14439));
#2324=EDGE_LOOP('',(#14440,#14441,#14442,#14443));
#2325=EDGE_LOOP('',(#14444,#14445,#14446,#14447));
#2326=EDGE_LOOP('',(#14448,#14449,#14450,#14451,#14452,#14453,#14454,#14455,
#14456,#14457));
#2327=EDGE_LOOP('',(#14458,#14459,#14460,#14461));
#2328=EDGE_LOOP('',(#14462,#14463,#14464,#14465));
#2329=EDGE_LOOP('',(#14466,#14467,#14468,#14469));
#2330=EDGE_LOOP('',(#14470,#14471,#14472,#14473));
#2331=EDGE_LOOP('',(#14474,#14475,#14476,#14477));
#2332=EDGE_LOOP('',(#14478,#14479,#14480,#14481));
#2333=EDGE_LOOP('',(#14482,#14483,#14484,#14485));
#2334=EDGE_LOOP('',(#14486,#14487,#14488,#14489));
#2335=EDGE_LOOP('',(#14490,#14491,#14492,#14493));
#2336=EDGE_LOOP('',(#14494,#14495,#14496,#14497));
#2337=EDGE_LOOP('',(#14498,#14499,#14500,#14501));
#2338=EDGE_LOOP('',(#14502,#14503,#14504,#14505));
#2339=EDGE_LOOP('',(#14506,#14507,#14508,#14509));
#2340=EDGE_LOOP('',(#14510,#14511,#14512,#14513));
#2341=EDGE_LOOP('',(#14514,#14515,#14516,#14517));
#2342=EDGE_LOOP('',(#14518,#14519,#14520,#14521));
#2343=EDGE_LOOP('',(#14522,#14523,#14524,#14525));
#2344=EDGE_LOOP('',(#14526,#14527,#14528,#14529));
#2345=EDGE_LOOP('',(#14530,#14531,#14532,#14533,#14534,#14535,#14536,#14537,
#14538,#14539,#14540,#14541,#14542,#14543,#14544,#14545,#14546,#14547,#14548,
#14549,#14550,#14551,#14552,#14553,#14554,#14555,#14556,#14557,#14558,#14559,
#14560,#14561,#14562,#14563,#14564,#14565,#14566,#14567,#14568,#14569,#14570,
#14571,#14572,#14573,#14574,#14575,#14576,#14577,#14578,#14579,#14580,#14581,
#14582,#14583));
#2346=EDGE_LOOP('',(#14584,#14585,#14586,#14587));
#2347=EDGE_LOOP('',(#14588,#14589,#14590,#14591));
#2348=EDGE_LOOP('',(#14592,#14593,#14594,#14595));
#2349=EDGE_LOOP('',(#14596,#14597,#14598,#14599));
#2350=EDGE_LOOP('',(#14600,#14601,#14602,#14603));
#2351=EDGE_LOOP('',(#14604,#14605,#14606,#14607));
#2352=EDGE_LOOP('',(#14608,#14609,#14610,#14611));
#2353=EDGE_LOOP('',(#14612,#14613,#14614,#14615,#14616));
#2354=EDGE_LOOP('',(#14617,#14618,#14619,#14620));
#2355=EDGE_LOOP('',(#14621,#14622,#14623,#14624,#14625,#14626,#14627,#14628,
#14629,#14630,#14631,#14632,#14633,#14634,#14635,#14636,#14637,#14638,#14639,
#14640));
#2356=EDGE_LOOP('',(#14641,#14642,#14643,#14644,#14645,#14646,#14647,#14648,
#14649,#14650,#14651,#14652,#14653,#14654,#14655,#14656,#14657,#14658,#14659,
#14660));
#2357=EDGE_LOOP('',(#14661,#14662,#14663,#14664));
#2358=EDGE_LOOP('',(#14665,#14666,#14667,#14668,#14669));
#2359=EDGE_LOOP('',(#14670,#14671,#14672,#14673));
#2360=EDGE_LOOP('',(#14674,#14675,#14676,#14677,#14678,#14679,#14680,#14681,
#14682,#14683,#14684,#14685,#14686,#14687,#14688,#14689,#14690,#14691,#14692,
#14693));
#2361=EDGE_LOOP('',(#14694,#14695,#14696,#14697,#14698,#14699,#14700,#14701,
#14702,#14703,#14704,#14705,#14706,#14707,#14708,#14709,#14710,#14711,#14712,
#14713));
#2362=EDGE_LOOP('',(#14714,#14715,#14716,#14717));
#2363=EDGE_LOOP('',(#14718,#14719,#14720,#14721,#14722));
#2364=EDGE_LOOP('',(#14723,#14724,#14725,#14726));
#2365=EDGE_LOOP('',(#14727,#14728,#14729,#14730,#14731,#14732,#14733,#14734,
#14735,#14736,#14737,#14738,#14739,#14740,#14741,#14742,#14743,#14744,#14745,
#14746));
#2366=EDGE_LOOP('',(#14747,#14748,#14749,#14750,#14751,#14752,#14753,#14754,
#14755,#14756,#14757,#14758,#14759,#14760,#14761,#14762,#14763,#14764,#14765,
#14766));
#2367=EDGE_LOOP('',(#14767,#14768,#14769,#14770));
#2368=EDGE_LOOP('',(#14771,#14772,#14773,#14774,#14775));
#2369=EDGE_LOOP('',(#14776,#14777,#14778,#14779));
#2370=EDGE_LOOP('',(#14780,#14781,#14782,#14783,#14784,#14785,#14786,#14787,
#14788,#14789,#14790,#14791,#14792,#14793,#14794,#14795,#14796,#14797,#14798,
#14799));
#2371=EDGE_LOOP('',(#14800,#14801,#14802,#14803,#14804,#14805,#14806,#14807,
#14808,#14809,#14810,#14811,#14812,#14813,#14814,#14815,#14816,#14817,#14818,
#14819));
#2372=EDGE_LOOP('',(#14820,#14821,#14822,#14823));
#2373=EDGE_LOOP('',(#14824,#14825,#14826,#14827,#14828));
#2374=EDGE_LOOP('',(#14829,#14830,#14831,#14832));
#2375=EDGE_LOOP('',(#14833,#14834,#14835,#14836,#14837,#14838,#14839,#14840,
#14841,#14842,#14843,#14844,#14845,#14846,#14847,#14848,#14849,#14850,#14851,
#14852));
#2376=EDGE_LOOP('',(#14853,#14854,#14855,#14856,#14857,#14858,#14859,#14860,
#14861,#14862,#14863,#14864,#14865,#14866,#14867,#14868,#14869,#14870,#14871,
#14872));
#2377=EDGE_LOOP('',(#14873,#14874,#14875,#14876));
#2378=EDGE_LOOP('',(#14877,#14878,#14879));
#2379=EDGE_LOOP('',(#14880,#14881));
#2380=EDGE_LOOP('',(#14882,#14883,#14884));
#2381=EDGE_LOOP('',(#14885,#14886));
#2382=EDGE_LOOP('',(#14887,#14888,#14889));
#2383=EDGE_LOOP('',(#14890,#14891));
#2384=EDGE_LOOP('',(#14892,#14893,#14894));
#2385=EDGE_LOOP('',(#14895,#14896));
#2386=EDGE_LOOP('',(#14897,#14898,#14899));
#2387=EDGE_LOOP('',(#14900,#14901));
#2388=EDGE_LOOP('',(#14902,#14903,#14904,#14905,#14906));
#2389=EDGE_LOOP('',(#14907,#14908,#14909,#14910));
#2390=EDGE_LOOP('',(#14911,#14912,#14913,#14914,#14915,#14916,#14917,#14918,
#14919,#14920,#14921,#14922,#14923,#14924,#14925,#14926,#14927,#14928,#14929,
#14930));
#2391=EDGE_LOOP('',(#14931,#14932,#14933,#14934,#14935,#14936,#14937,#14938,
#14939,#14940,#14941,#14942,#14943,#14944,#14945,#14946,#14947,#14948,#14949,
#14950));
#2392=EDGE_LOOP('',(#14951,#14952,#14953,#14954));
#2393=EDGE_LOOP('',(#14955,#14956,#14957,#14958,#14959));
#2394=EDGE_LOOP('',(#14960,#14961,#14962,#14963));
#2395=EDGE_LOOP('',(#14964,#14965,#14966,#14967,#14968,#14969,#14970,#14971,
#14972,#14973,#14974,#14975,#14976,#14977,#14978,#14979,#14980,#14981,#14982,
#14983));
#2396=EDGE_LOOP('',(#14984,#14985,#14986,#14987,#14988,#14989,#14990,#14991,
#14992,#14993,#14994,#14995,#14996,#14997,#14998,#14999,#15000,#15001,#15002,
#15003));
#2397=EDGE_LOOP('',(#15004,#15005,#15006,#15007));
#2398=EDGE_LOOP('',(#15008,#15009,#15010,#15011,#15012));
#2399=EDGE_LOOP('',(#15013,#15014,#15015,#15016));
#2400=EDGE_LOOP('',(#15017,#15018,#15019,#15020,#15021,#15022,#15023,#15024,
#15025,#15026,#15027,#15028,#15029,#15030,#15031,#15032,#15033,#15034,#15035,
#15036));
#2401=EDGE_LOOP('',(#15037,#15038,#15039,#15040,#15041,#15042,#15043,#15044,
#15045,#15046,#15047,#15048,#15049,#15050,#15051,#15052,#15053,#15054,#15055,
#15056));
#2402=EDGE_LOOP('',(#15057,#15058,#15059,#15060));
#2403=EDGE_LOOP('',(#15061,#15062,#15063,#15064,#15065));
#2404=EDGE_LOOP('',(#15066,#15067,#15068,#15069));
#2405=EDGE_LOOP('',(#15070,#15071,#15072,#15073,#15074,#15075,#15076,#15077,
#15078,#15079,#15080,#15081,#15082,#15083,#15084,#15085,#15086,#15087,#15088,
#15089));
#2406=EDGE_LOOP('',(#15090,#15091,#15092,#15093,#15094,#15095,#15096,#15097,
#15098,#15099,#15100,#15101,#15102,#15103,#15104,#15105,#15106,#15107,#15108,
#15109));
#2407=EDGE_LOOP('',(#15110,#15111,#15112,#15113));
#2408=EDGE_LOOP('',(#15114,#15115,#15116,#15117,#15118));
#2409=EDGE_LOOP('',(#15119,#15120,#15121,#15122));
#2410=EDGE_LOOP('',(#15123,#15124,#15125,#15126,#15127,#15128,#15129,#15130,
#15131,#15132,#15133,#15134,#15135,#15136,#15137,#15138,#15139,#15140,#15141,
#15142));
#2411=EDGE_LOOP('',(#15143,#15144,#15145,#15146,#15147,#15148,#15149,#15150,
#15151,#15152,#15153,#15154,#15155,#15156,#15157,#15158,#15159,#15160,#15161,
#15162));
#2412=EDGE_LOOP('',(#15163,#15164,#15165,#15166));
#2413=EDGE_LOOP('',(#15167,#15168,#15169));
#2414=EDGE_LOOP('',(#15170,#15171));
#2415=EDGE_LOOP('',(#15172,#15173,#15174));
#2416=EDGE_LOOP('',(#15175,#15176));
#2417=EDGE_LOOP('',(#15177,#15178,#15179));
#2418=EDGE_LOOP('',(#15180,#15181));
#2419=EDGE_LOOP('',(#15182,#15183,#15184));
#2420=EDGE_LOOP('',(#15185,#15186));
#2421=EDGE_LOOP('',(#15187,#15188,#15189));
#2422=EDGE_LOOP('',(#15190,#15191));
#2423=EDGE_LOOP('',(#15192,#15193,#15194,#15195,#15196));
#2424=EDGE_LOOP('',(#15197,#15198,#15199,#15200));
#2425=EDGE_LOOP('',(#15201,#15202,#15203,#15204,#15205,#15206,#15207,#15208,
#15209,#15210,#15211,#15212,#15213,#15214,#15215,#15216,#15217,#15218,#15219,
#15220));
#2426=EDGE_LOOP('',(#15221,#15222,#15223,#15224,#15225,#15226,#15227,#15228,
#15229,#15230,#15231,#15232,#15233,#15234,#15235,#15236,#15237,#15238,#15239,
#15240));
#2427=EDGE_LOOP('',(#15241,#15242,#15243,#15244));
#2428=EDGE_LOOP('',(#15245,#15246,#15247));
#2429=EDGE_LOOP('',(#15248,#15249));
#2430=EDGE_LOOP('',(#15250,#15251,#15252,#15253,#15254));
#2431=EDGE_LOOP('',(#15255,#15256,#15257,#15258));
#2432=EDGE_LOOP('',(#15259,#15260,#15261,#15262,#15263,#15264,#15265,#15266,
#15267,#15268,#15269,#15270,#15271,#15272,#15273,#15274,#15275,#15276,#15277,
#15278));
#2433=EDGE_LOOP('',(#15279,#15280,#15281,#15282,#15283,#15284,#15285,#15286,
#15287,#15288,#15289,#15290,#15291,#15292,#15293,#15294,#15295,#15296,#15297,
#15298));
#2434=EDGE_LOOP('',(#15299,#15300,#15301,#15302));
#2435=EDGE_LOOP('',(#15303,#15304,#15305));
#2436=EDGE_LOOP('',(#15306,#15307));
#2437=EDGE_LOOP('',(#15308,#15309,#15310,#15311));
#2438=EDGE_LOOP('',(#15312,#15313,#15314,#15315,#15316,#15317,#15318,#15319));
#2439=EDGE_LOOP('',(#15320,#15321));
#2440=EDGE_LOOP('',(#15322));
#2441=EDGE_LOOP('',(#15323));
#2442=EDGE_LOOP('',(#15324,#15325,#15326,#15327));
#2443=EDGE_LOOP('',(#15328,#15329,#15330,#15331,#15332,#15333,#15334,#15335));
#2444=EDGE_LOOP('',(#15336,#15337));
#2445=EDGE_LOOP('',(#15338));
#2446=EDGE_LOOP('',(#15339));
#2447=EDGE_LOOP('',(#15340,#15341,#15342,#15343));
#2448=EDGE_LOOP('',(#15344,#15345,#15346,#15347,#15348,#15349,#15350,#15351));
#2449=EDGE_LOOP('',(#15352,#15353));
#2450=EDGE_LOOP('',(#15354));
#2451=EDGE_LOOP('',(#15355));
#2452=EDGE_LOOP('',(#15356,#15357,#15358,#15359));
#2453=EDGE_LOOP('',(#15360,#15361,#15362,#15363,#15364,#15365,#15366,#15367));
#2454=EDGE_LOOP('',(#15368,#15369));
#2455=EDGE_LOOP('',(#15370));
#2456=EDGE_LOOP('',(#15371));
#2457=EDGE_LOOP('',(#15372,#15373,#15374,#15375));
#2458=EDGE_LOOP('',(#15376,#15377,#15378,#15379,#15380,#15381,#15382,#15383));
#2459=EDGE_LOOP('',(#15384,#15385));
#2460=EDGE_LOOP('',(#15386));
#2461=EDGE_LOOP('',(#15387));
#2462=EDGE_LOOP('',(#15388,#15389,#15390,#15391));
#2463=EDGE_LOOP('',(#15392,#15393,#15394,#15395,#15396,#15397,#15398,#15399));
#2464=EDGE_LOOP('',(#15400,#15401));
#2465=EDGE_LOOP('',(#15402));
#2466=EDGE_LOOP('',(#15403));
#2467=EDGE_LOOP('',(#15404,#15405,#15406,#15407));
#2468=EDGE_LOOP('',(#15408,#15409,#15410,#15411));
#2469=EDGE_LOOP('',(#15412));
#2470=EDGE_LOOP('',(#15413,#15414,#15415,#15416));
#2471=EDGE_LOOP('',(#15417,#15418,#15419,#15420));
#2472=EDGE_LOOP('',(#15421));
#2473=EDGE_LOOP('',(#15422,#15423,#15424,#15425));
#2474=EDGE_LOOP('',(#15426));
#2475=EDGE_LOOP('',(#15427,#15428,#15429,#15430));
#2476=EDGE_LOOP('',(#15431,#15432,#15433,#15434));
#2477=EDGE_LOOP('',(#15435));
#2478=EDGE_LOOP('',(#15436,#15437,#15438,#15439));
#2479=EDGE_LOOP('',(#15440,#15441,#15442,#15443));
#2480=EDGE_LOOP('',(#15444));
#2481=EDGE_LOOP('',(#15445,#15446,#15447,#15448));
#2482=EDGE_LOOP('',(#15449,#15450,#15451,#15452));
#2483=EDGE_LOOP('',(#15453));
#2484=EDGE_LOOP('',(#15454,#15455,#15456,#15457));
#2485=EDGE_LOOP('',(#15458,#15459,#15460,#15461));
#2486=EDGE_LOOP('',(#15462));
#2487=EDGE_LOOP('',(#15463,#15464,#15465,#15466));
#2488=EDGE_LOOP('',(#15467,#15468,#15469,#15470));
#2489=EDGE_LOOP('',(#15471));
#2490=EDGE_LOOP('',(#15472,#15473,#15474,#15475));
#2491=EDGE_LOOP('',(#15476,#15477,#15478,#15479));
#2492=EDGE_LOOP('',(#15480,#15481,#15482,#15483));
#2493=EDGE_LOOP('',(#15484));
#2494=EDGE_LOOP('',(#15485,#15486,#15487,#15488));
#2495=EDGE_LOOP('',(#15489,#15490,#15491,#15492));
#2496=EDGE_LOOP('',(#15493));
#2497=EDGE_LOOP('',(#15494,#15495,#15496,#15497));
#2498=EDGE_LOOP('',(#15498,#15499,#15500,#15501));
#2499=EDGE_LOOP('',(#15502,#15503,#15504,#15505));
#2500=EDGE_LOOP('',(#15506,#15507,#15508,#15509));
#2501=EDGE_LOOP('',(#15510,#15511,#15512,#15513));
#2502=EDGE_LOOP('',(#15514,#15515,#15516,#15517));
#2503=EDGE_LOOP('',(#15518,#15519,#15520,#15521));
#2504=EDGE_LOOP('',(#15522,#15523,#15524,#15525));
#2505=EDGE_LOOP('',(#15526,#15527,#15528,#15529));
#2506=EDGE_LOOP('',(#15530,#15531,#15532,#15533));
#2507=EDGE_LOOP('',(#15534));
#2508=EDGE_LOOP('',(#15535,#15536,#15537,#15538));
#2509=EDGE_LOOP('',(#15539,#15540,#15541,#15542));
#2510=EDGE_LOOP('',(#15543));
#2511=EDGE_LOOP('',(#15544,#15545,#15546,#15547));
#2512=EDGE_LOOP('',(#15548,#15549,#15550,#15551));
#2513=EDGE_LOOP('',(#15552,#15553,#15554,#15555));
#2514=EDGE_LOOP('',(#15556,#15557,#15558,#15559));
#2515=EDGE_LOOP('',(#15560,#15561,#15562,#15563));
#2516=EDGE_LOOP('',(#15564,#15565,#15566,#15567));
#2517=EDGE_LOOP('',(#15568,#15569,#15570,#15571));
#2518=EDGE_LOOP('',(#15572,#15573,#15574,#15575));
#2519=EDGE_LOOP('',(#15576,#15577,#15578,#15579));
#2520=EDGE_LOOP('',(#15580,#15581,#15582,#15583));
#2521=EDGE_LOOP('',(#15584,#15585,#15586,#15587,#15588,#15589,#15590,#15591,
#15592,#15593,#15594,#15595,#15596,#15597,#15598,#15599,#15600,#15601,#15602,
#15603,#15604,#15605,#15606,#15607,#15608,#15609,#15610,#15611,#15612,#15613,
#15614,#15615,#15616,#15617,#15618,#15619,#15620,#15621,#15622,#15623,#15624,
#15625,#15626,#15627,#15628,#15629,#15630,#15631,#15632,#15633,#15634,#15635,
#15636,#15637));
#2522=EDGE_LOOP('',(#15638,#15639,#15640,#15641));
#2523=EDGE_LOOP('',(#15642,#15643,#15644,#15645));
#2524=EDGE_LOOP('',(#15646,#15647,#15648,#15649));
#2525=EDGE_LOOP('',(#15650,#15651,#15652,#15653));
#2526=EDGE_LOOP('',(#15654,#15655,#15656,#15657));
#2527=EDGE_LOOP('',(#15658,#15659,#15660,#15661));
#2528=EDGE_LOOP('',(#15662,#15663,#15664,#15665));
#2529=EDGE_LOOP('',(#15666,#15667,#15668,#15669));
#2530=EDGE_LOOP('',(#15670,#15671,#15672,#15673));
#2531=EDGE_LOOP('',(#15674,#15675,#15676,#15677));
#2532=EDGE_LOOP('',(#15678,#15679,#15680,#15681));
#2533=EDGE_LOOP('',(#15682,#15683,#15684,#15685));
#2534=EDGE_LOOP('',(#15686,#15687,#15688,#15689));
#2535=EDGE_LOOP('',(#15690,#15691,#15692,#15693));
#2536=EDGE_LOOP('',(#15694,#15695,#15696,#15697));
#2537=EDGE_LOOP('',(#15698,#15699,#15700,#15701));
#2538=EDGE_LOOP('',(#15702,#15703,#15704,#15705));
#2539=EDGE_LOOP('',(#15706,#15707,#15708,#15709));
#2540=EDGE_LOOP('',(#15710,#15711,#15712,#15713));
#2541=EDGE_LOOP('',(#15714,#15715,#15716,#15717));
#2542=EDGE_LOOP('',(#15718,#15719,#15720,#15721));
#2543=EDGE_LOOP('',(#15722,#15723,#15724,#15725));
#2544=EDGE_LOOP('',(#15726,#15727,#15728,#15729));
#2545=EDGE_LOOP('',(#15730,#15731,#15732,#15733));
#2546=EDGE_LOOP('',(#15734,#15735,#15736,#15737));
#2547=EDGE_LOOP('',(#15738,#15739,#15740,#15741,#15742));
#2548=EDGE_LOOP('',(#15743,#15744,#15745,#15746,#15747,#15748,#15749,#15750,
#15751,#15752));
#2549=EDGE_LOOP('',(#15753,#15754,#15755,#15756));
#2550=EDGE_LOOP('',(#15757,#15758,#15759,#15760));
#2551=EDGE_LOOP('',(#15761,#15762,#15763,#15764,#15765));
#2552=EDGE_LOOP('',(#15766,#15767,#15768,#15769));
#2553=EDGE_LOOP('',(#15770,#15771,#15772,#15773));
#2554=EDGE_LOOP('',(#15774,#15775,#15776,#15777,#15778,#15779,#15780,#15781,
#15782,#15783));
#2555=EDGE_LOOP('',(#15784,#15785,#15786,#15787));
#2556=EDGE_LOOP('',(#15788));
#2557=EDGE_LOOP('',(#15789));
#2558=EDGE_LOOP('',(#15790));
#2559=EDGE_LOOP('',(#15791));
#2560=EDGE_LOOP('',(#15792,#15793,#15794,#15795));
#2561=EDGE_LOOP('',(#15796));
#2562=EDGE_LOOP('',(#15797));
#2563=EDGE_LOOP('',(#15798));
#2564=EDGE_LOOP('',(#15799));
#2565=EDGE_LOOP('',(#15800,#15801,#15802,#15803));
#2566=EDGE_LOOP('',(#15804));
#2567=EDGE_LOOP('',(#15805,#15806));
#2568=EDGE_LOOP('',(#15807));
#2569=EDGE_LOOP('',(#15808));
#2570=EDGE_LOOP('',(#15809,#15810,#15811,#15812));
#2571=EDGE_LOOP('',(#15813,#15814,#15815,#15816));
#2572=EDGE_LOOP('',(#15817,#15818,#15819,#15820));
#2573=EDGE_LOOP('',(#15821));
#2574=EDGE_LOOP('',(#15822,#15823,#15824,#15825));
#2575=EDGE_LOOP('',(#15826,#15827,#15828,#15829));
#2576=EDGE_LOOP('',(#15830,#15831,#15832,#15833));
#2577=EDGE_LOOP('',(#15834,#15835,#15836,#15837));
#2578=EDGE_LOOP('',(#15838,#15839,#15840,#15841));
#2579=EDGE_LOOP('',(#15842,#15843,#15844,#15845));
#2580=EDGE_LOOP('',(#15846,#15847,#15848,#15849));
#2581=EDGE_LOOP('',(#15850));
#2582=EDGE_LOOP('',(#15851));
#2583=EDGE_LOOP('',(#15852));
#2584=EDGE_LOOP('',(#15853));
#2585=EDGE_LOOP('',(#15854,#15855,#15856,#15857));
#2586=EDGE_LOOP('',(#15858,#15859,#15860,#15861));
#2587=EDGE_LOOP('',(#15862));
#2588=EDGE_LOOP('',(#15863));
#2589=EDGE_LOOP('',(#15864,#15865,#15866,#15867));
#2590=EDGE_LOOP('',(#15868,#15869,#15870,#15871));
#2591=EDGE_LOOP('',(#15872));
#2592=EDGE_LOOP('',(#15873));
#2593=EDGE_LOOP('',(#15874,#15875,#15876,#15877));
#2594=EDGE_LOOP('',(#15878,#15879,#15880,#15881));
#2595=EDGE_LOOP('',(#15882));
#2596=EDGE_LOOP('',(#15883));
#2597=EDGE_LOOP('',(#15884,#15885,#15886,#15887));
#2598=EDGE_LOOP('',(#15888,#15889,#15890,#15891));
#2599=EDGE_LOOP('',(#15892));
#2600=EDGE_LOOP('',(#15893));
#2601=EDGE_LOOP('',(#15894,#15895,#15896,#15897));
#2602=EDGE_LOOP('',(#15898,#15899,#15900,#15901));
#2603=EDGE_LOOP('',(#15902));
#2604=EDGE_LOOP('',(#15903));
#2605=EDGE_LOOP('',(#15904,#15905,#15906,#15907));
#2606=EDGE_LOOP('',(#15908,#15909,#15910,#15911));
#2607=EDGE_LOOP('',(#15912,#15913,#15914,#15915));
#2608=EDGE_LOOP('',(#15916,#15917,#15918,#15919));
#2609=EDGE_LOOP('',(#15920));
#2610=EDGE_LOOP('',(#15921));
#2611=EDGE_LOOP('',(#15922));
#2612=EDGE_LOOP('',(#15923));
#2613=EDGE_LOOP('',(#15924));
#2614=EDGE_LOOP('',(#15925));
#2615=EDGE_LOOP('',(#15926));
#2616=EDGE_LOOP('',(#15927));
#2617=EDGE_LOOP('',(#15928));
#2618=EDGE_LOOP('',(#15929));
#2619=EDGE_LOOP('',(#15930));
#2620=EDGE_LOOP('',(#15931));
#2621=EDGE_LOOP('',(#15932));
#2622=EDGE_LOOP('',(#15933));
#2623=EDGE_LOOP('',(#15934));
#2624=EDGE_LOOP('',(#15935));
#2625=EDGE_LOOP('',(#15936,#15937,#15938,#15939));
#2626=EDGE_LOOP('',(#15940,#15941,#15942,#15943));
#2627=EDGE_LOOP('',(#15944));
#2628=EDGE_LOOP('',(#15945));
#2629=EDGE_LOOP('',(#15946));
#2630=EDGE_LOOP('',(#15947));
#2631=EDGE_LOOP('',(#15948,#15949,#15950,#15951));
#2632=EDGE_LOOP('',(#15952,#15953,#15954,#15955));
#2633=EDGE_LOOP('',(#15956,#15957,#15958,#15959));
#2634=EDGE_LOOP('',(#15960,#15961,#15962,#15963));
#2635=EDGE_LOOP('',(#15964,#15965,#15966,#15967));
#2636=EDGE_LOOP('',(#15968,#15969,#15970,#15971));
#2637=EDGE_LOOP('',(#15972,#15973,#15974,#15975));
#2638=EDGE_LOOP('',(#15976,#15977,#15978,#15979));
#2639=EDGE_LOOP('',(#15980,#15981,#15982,#15983));
#2640=EDGE_LOOP('',(#15984,#15985,#15986,#15987));
#2641=EDGE_LOOP('',(#15988,#15989,#15990,#15991));
#2642=EDGE_LOOP('',(#15992,#15993,#15994,#15995));
#2643=EDGE_LOOP('',(#15996,#15997,#15998,#15999));
#2644=EDGE_LOOP('',(#16000,#16001,#16002,#16003));
#2645=EDGE_LOOP('',(#16004));
#2646=EDGE_LOOP('',(#16005));
#2647=EDGE_LOOP('',(#16006));
#2648=EDGE_LOOP('',(#16007));
#2649=EDGE_LOOP('',(#16008));
#2650=EDGE_LOOP('',(#16009));
#2651=EDGE_LOOP('',(#16010));
#2652=EDGE_LOOP('',(#16011));
#2653=EDGE_LOOP('',(#16012));
#2654=EDGE_LOOP('',(#16013));
#2655=EDGE_LOOP('',(#16014));
#2656=EDGE_LOOP('',(#16015));
#2657=EDGE_LOOP('',(#16016));
#2658=EDGE_LOOP('',(#16017));
#2659=EDGE_LOOP('',(#16018));
#2660=EDGE_LOOP('',(#16019));
#2661=EDGE_LOOP('',(#16020,#16021,#16022,#16023));
#2662=EDGE_LOOP('',(#16024,#16025,#16026,#16027));
#2663=EDGE_LOOP('',(#16028));
#2664=EDGE_LOOP('',(#16029));
#2665=EDGE_LOOP('',(#16030));
#2666=EDGE_LOOP('',(#16031));
#2667=EDGE_LOOP('',(#16032,#16033,#16034,#16035));
#2668=EDGE_LOOP('',(#16036,#16037,#16038,#16039));
#2669=EDGE_LOOP('',(#16040));
#2670=EDGE_LOOP('',(#16041));
#2671=EDGE_LOOP('',(#16042));
#2672=EDGE_LOOP('',(#16043));
#2673=EDGE_LOOP('',(#16044,#16045,#16046,#16047));
#2674=EDGE_LOOP('',(#16048,#16049,#16050,#16051));
#2675=EDGE_LOOP('',(#16052));
#2676=EDGE_LOOP('',(#16053));
#2677=EDGE_LOOP('',(#16054));
#2678=EDGE_LOOP('',(#16055));
#2679=EDGE_LOOP('',(#16056,#16057,#16058,#16059));
#2680=EDGE_LOOP('',(#16060,#16061,#16062,#16063));
#2681=EDGE_LOOP('',(#16064,#16065,#16066,#16067));
#2682=EDGE_LOOP('',(#16068,#16069,#16070,#16071));
#2683=EDGE_LOOP('',(#16072,#16073,#16074,#16075));
#2684=EDGE_LOOP('',(#16076,#16077,#16078,#16079));
#2685=EDGE_LOOP('',(#16080));
#2686=EDGE_LOOP('',(#16081));
#2687=EDGE_LOOP('',(#16082,#16083,#16084,#16085));
#2688=EDGE_LOOP('',(#16086));
#2689=EDGE_LOOP('',(#16087,#16088,#16089,#16090));
#2690=EDGE_LOOP('',(#16091));
#2691=EDGE_LOOP('',(#16092,#16093,#16094,#16095));
#2692=EDGE_LOOP('',(#16096));
#2693=EDGE_LOOP('',(#16097));
#2694=EDGE_LOOP('',(#16098,#16099,#16100,#16101));
#2695=EDGE_LOOP('',(#16102,#16103,#16104,#16105));
#2696=EDGE_LOOP('',(#16106,#16107,#16108,#16109));
#2697=EDGE_LOOP('',(#16110,#16111,#16112,#16113));
#2698=EDGE_LOOP('',(#16114,#16115,#16116,#16117));
#2699=EDGE_LOOP('',(#16118,#16119,#16120,#16121));
#2700=EDGE_LOOP('',(#16122,#16123,#16124,#16125));
#2701=EDGE_LOOP('',(#16126,#16127,#16128,#16129));
#2702=EDGE_LOOP('',(#16130,#16131,#16132,#16133));
#2703=EDGE_LOOP('',(#16134,#16135,#16136,#16137));
#2704=EDGE_LOOP('',(#16138,#16139,#16140,#16141));
#2705=EDGE_LOOP('',(#16142,#16143,#16144,#16145));
#2706=EDGE_LOOP('',(#16146,#16147,#16148,#16149));
#2707=EDGE_LOOP('',(#16150,#16151,#16152,#16153));
#2708=EDGE_LOOP('',(#16154,#16155,#16156,#16157));
#2709=EDGE_LOOP('',(#16158,#16159,#16160,#16161));
#2710=EDGE_LOOP('',(#16162,#16163,#16164,#16165));
#2711=EDGE_LOOP('',(#16166,#16167,#16168,#16169));
#2712=EDGE_LOOP('',(#16170,#16171,#16172,#16173));
#2713=EDGE_LOOP('',(#16174,#16175,#16176,#16177));
#2714=EDGE_LOOP('',(#16178,#16179,#16180,#16181));
#2715=EDGE_LOOP('',(#16182,#16183,#16184,#16185));
#2716=EDGE_LOOP('',(#16186,#16187,#16188,#16189));
#2717=EDGE_LOOP('',(#16190,#16191,#16192,#16193));
#2718=EDGE_LOOP('',(#16194,#16195,#16196,#16197));
#2719=EDGE_LOOP('',(#16198,#16199,#16200,#16201));
#2720=EDGE_LOOP('',(#16202,#16203,#16204,#16205));
#2721=EDGE_LOOP('',(#16206,#16207,#16208,#16209));
#2722=EDGE_LOOP('',(#16210,#16211,#16212,#16213));
#2723=EDGE_LOOP('',(#16214,#16215,#16216,#16217));
#2724=EDGE_LOOP('',(#16218,#16219,#16220,#16221));
#2725=EDGE_LOOP('',(#16222,#16223,#16224,#16225));
#2726=EDGE_LOOP('',(#16226,#16227,#16228,#16229,#16230,#16231,#16232,#16233));
#2727=EDGE_LOOP('',(#16234,#16235,#16236,#16237,#16238,#16239,#16240,#16241,
#16242,#16243,#16244,#16245,#16246,#16247,#16248,#16249,#16250,#16251,#16252,
#16253,#16254,#16255,#16256,#16257,#16258,#16259,#16260,#16261,#16262,#16263,
#16264,#16265,#16266,#16267,#16268,#16269));
#2728=EDGE_LOOP('',(#16270,#16271,#16272,#16273));
#2729=EDGE_LOOP('',(#16274,#16275,#16276,#16277,#16278,#16279,#16280,#16281,
#16282,#16283,#16284,#16285,#16286,#16287,#16288,#16289,#16290,#16291,#16292,
#16293,#16294,#16295,#16296,#16297,#16298,#16299,#16300,#16301,#16302,#16303,
#16304,#16305,#16306,#16307,#16308,#16309,#16310));
#2730=EDGE_LOOP('',(#16311,#16312,#16313,#16314));
#2731=EDGE_LOOP('',(#16315,#16316,#16317,#16318));
#2732=EDGE_LOOP('',(#16319,#16320,#16321,#16322));
#2733=EDGE_LOOP('',(#16323,#16324,#16325,#16326));
#2734=EDGE_LOOP('',(#16327,#16328,#16329,#16330));
#2735=EDGE_LOOP('',(#16331,#16332,#16333,#16334));
#2736=EDGE_LOOP('',(#16335,#16336,#16337,#16338));
#2737=EDGE_LOOP('',(#16339,#16340,#16341,#16342,#16343,#16344));
#2738=EDGE_LOOP('',(#16345));
#2739=EDGE_LOOP('',(#16346,#16347,#16348,#16349));
#2740=EDGE_LOOP('',(#16350,#16351,#16352,#16353));
#2741=EDGE_LOOP('',(#16354));
#2742=EDGE_LOOP('',(#16355,#16356,#16357,#16358,#16359,#16360));
#2743=EDGE_LOOP('',(#16361));
#2744=EDGE_LOOP('',(#16362,#16363,#16364,#16365));
#2745=EDGE_LOOP('',(#16366,#16367,#16368,#16369));
#2746=EDGE_LOOP('',(#16370,#16371,#16372,#16373));
#2747=EDGE_LOOP('',(#16374,#16375,#16376,#16377));
#2748=EDGE_LOOP('',(#16378,#16379,#16380,#16381));
#2749=EDGE_LOOP('',(#16382,#16383,#16384,#16385));
#2750=EDGE_LOOP('',(#16386,#16387,#16388,#16389));
#2751=EDGE_LOOP('',(#16390,#16391,#16392,#16393));
#2752=EDGE_LOOP('',(#16394,#16395,#16396,#16397));
#2753=EDGE_LOOP('',(#16398,#16399,#16400,#16401));
#2754=EDGE_LOOP('',(#16402,#16403,#16404,#16405));
#2755=EDGE_LOOP('',(#16406,#16407,#16408,#16409));
#2756=EDGE_LOOP('',(#16410,#16411,#16412,#16413));
#2757=EDGE_LOOP('',(#16414,#16415,#16416,#16417));
#2758=EDGE_LOOP('',(#16418,#16419,#16420,#16421));
#2759=EDGE_LOOP('',(#16422,#16423,#16424,#16425));
#2760=EDGE_LOOP('',(#16426,#16427,#16428,#16429,#16430,#16431,#16432,#16433));
#2761=EDGE_LOOP('',(#16434,#16435,#16436,#16437,#16438,#16439,#16440,#16441,
#16442,#16443,#16444,#16445,#16446,#16447,#16448,#16449,#16450,#16451,#16452,
#16453));
#2762=EDGE_LOOP('',(#16454,#16455,#16456,#16457));
#2763=EDGE_LOOP('',(#16458,#16459,#16460,#16461));
#2764=EDGE_LOOP('',(#16462,#16463,#16464,#16465));
#2765=EDGE_LOOP('',(#16466,#16467,#16468,#16469));
#2766=EDGE_LOOP('',(#16470,#16471,#16472,#16473));
#2767=EDGE_LOOP('',(#16474,#16475,#16476,#16477));
#2768=EDGE_LOOP('',(#16478,#16479,#16480,#16481));
#2769=EDGE_LOOP('',(#16482,#16483,#16484,#16485,#16486,#16487));
#2770=EDGE_LOOP('',(#16488,#16489,#16490,#16491,#16492,#16493,#16494,#16495,
#16496,#16497,#16498,#16499,#16500,#16501,#16502,#16503,#16504,#16505,#16506,
#16507,#16508));
#2771=EDGE_LOOP('',(#16509,#16510,#16511,#16512,#16513));
#2772=EDGE_LOOP('',(#16514,#16515,#16516,#16517));
#2773=EDGE_LOOP('',(#16518));
#2774=EDGE_LOOP('',(#16519,#16520,#16521,#16522,#16523,#16524));
#2775=EDGE_LOOP('',(#16525,#16526,#16527,#16528,#16529,#16530));
#2776=EDGE_LOOP('',(#16531));
#2777=CIRCLE('',#18466,1.666);
#2778=CIRCLE('',#18467,1.666);
#2779=CIRCLE('',#18479,1.666);
#2780=CIRCLE('',#18481,2.05475);
#2781=CIRCLE('',#18494,2.05475);
#2782=CIRCLE('',#18496,1.666);
#2783=CIRCLE('',#18497,1.666);
#2784=CIRCLE('',#18509,1.666);
#2785=CIRCLE('',#18511,2.05475);
#2786=CIRCLE('',#18524,2.05475);
#2787=CIRCLE('',#18526,1.666);
#2788=CIRCLE('',#18527,1.666);
#2789=CIRCLE('',#18539,1.666);
#2790=CIRCLE('',#18541,2.05475);
#2791=CIRCLE('',#18554,2.05475);
#2792=CIRCLE('',#18556,1.666);
#2793=CIRCLE('',#18557,1.666);
#2794=CIRCLE('',#18569,1.666);
#2795=CIRCLE('',#18571,2.05474999999998);
#2796=CIRCLE('',#18584,2.05474999999998);
#2797=CIRCLE('',#18586,1.666);
#2798=CIRCLE('',#18587,1.666);
#2799=CIRCLE('',#18599,1.666);
#2800=CIRCLE('',#18601,2.05475);
#2801=CIRCLE('',#18614,2.05475);
#2802=CIRCLE('',#18616,1.666);
#2803=CIRCLE('',#18617,1.666);
#2804=CIRCLE('',#18629,1.666);
#2805=CIRCLE('',#18631,2.05474999999998);
#2806=CIRCLE('',#18644,2.05474999999998);
#2807=CIRCLE('',#18646,1.666);
#2808=CIRCLE('',#18647,1.666);
#2809=CIRCLE('',#18659,1.666);
#2810=CIRCLE('',#18661,2.05474999999998);
#2811=CIRCLE('',#18674,2.05474999999998);
#2812=CIRCLE('',#18676,1.666);
#2813=CIRCLE('',#18677,1.666);
#2814=CIRCLE('',#18689,1.666);
#2815=CIRCLE('',#18691,2.05475000000002);
#2816=CIRCLE('',#18704,2.05475000000002);
#2817=CIRCLE('',#18706,1.666);
#2818=CIRCLE('',#18707,1.666);
#2819=CIRCLE('',#18719,1.666);
#2820=CIRCLE('',#18721,2.05474999999998);
#2821=CIRCLE('',#18734,2.05474999999998);
#2822=CIRCLE('',#18736,1.666);
#2823=CIRCLE('',#18737,1.666);
#2824=CIRCLE('',#18749,1.666);
#2825=CIRCLE('',#18751,2.05475);
#2826=CIRCLE('',#18764,2.05475);
#2827=CIRCLE('',#18766,1.666);
#2828=CIRCLE('',#18767,1.666);
#2829=CIRCLE('',#18779,1.666);
#2830=CIRCLE('',#18781,2.05474999999999);
#2831=CIRCLE('',#18794,2.05474999999999);
#2832=CIRCLE('',#18796,1.666);
#2833=CIRCLE('',#18797,1.666);
#2834=CIRCLE('',#18809,1.666);
#2835=CIRCLE('',#18811,2.05475);
#2836=CIRCLE('',#18824,2.05475);
#2837=CIRCLE('',#18826,2.5175);
#2838=CIRCLE('',#18835,3.07350000000007);
#2839=CIRCLE('',#18844,2.5175);
#2840=CIRCLE('',#18853,2.5175);
#2841=CIRCLE('',#18862,2.5175);
#2842=CIRCLE('',#18871,3.07350000000007);
#2843=CIRCLE('',#18880,3.07350000000007);
#2844=CIRCLE('',#18889,3.07350000000007);
#2845=CIRCLE('',#18958,60.);
#2846=CIRCLE('',#18959,60.);
#2847=CIRCLE('',#18961,70.);
#2848=CIRCLE('',#18962,70.);
#2849=CIRCLE('',#18967,1.2645);
#2850=CIRCLE('',#18968,1.2645);
#2851=CIRCLE('',#18969,1.2645);
#2852=CIRCLE('',#18970,1.2645);
#2853=CIRCLE('',#18971,1.2645);
#2854=CIRCLE('',#18979,1.2645);
#2855=CIRCLE('',#18981,1.543);
#2856=CIRCLE('',#18989,1.543);
#2857=CIRCLE('',#18991,1.2645);
#2858=CIRCLE('',#18992,1.2645);
#2859=CIRCLE('',#18993,1.2645);
#2860=CIRCLE('',#18994,1.2645);
#2861=CIRCLE('',#18995,1.2645);
#2862=CIRCLE('',#19003,1.2645);
#2863=CIRCLE('',#19005,1.54299999999999);
#2864=CIRCLE('',#19013,1.54299999999999);
#2865=CIRCLE('',#19015,1.2645);
#2866=CIRCLE('',#19016,1.2645);
#2867=CIRCLE('',#19017,1.2645);
#2868=CIRCLE('',#19018,1.2645);
#2869=CIRCLE('',#19019,1.2645);
#2870=CIRCLE('',#19027,1.2645);
#2871=CIRCLE('',#19029,1.543);
#2872=CIRCLE('',#19037,1.543);
#2873=CIRCLE('',#19039,1.2645);
#2874=CIRCLE('',#19040,1.2645);
#2875=CIRCLE('',#19041,1.2645);
#2876=CIRCLE('',#19042,1.2645);
#2877=CIRCLE('',#19043,1.2645);
#2878=CIRCLE('',#19051,1.2645);
#2879=CIRCLE('',#19053,1.543);
#2880=CIRCLE('',#19061,1.543);
#2881=CIRCLE('',#19063,1.2645);
#2882=CIRCLE('',#19064,1.2645);
#2883=CIRCLE('',#19065,1.2645);
#2884=CIRCLE('',#19066,1.2645);
#2885=CIRCLE('',#19067,1.2645);
#2886=CIRCLE('',#19075,1.2645);
#2887=CIRCLE('',#19077,1.54300000000001);
#2888=CIRCLE('',#19085,1.54300000000001);
#2889=CIRCLE('',#19087,1.2645);
#2890=CIRCLE('',#19088,1.2645);
#2891=CIRCLE('',#19089,1.2645);
#2892=CIRCLE('',#19090,1.2645);
#2893=CIRCLE('',#19091,1.2645);
#2894=CIRCLE('',#19099,1.2645);
#2895=CIRCLE('',#19101,1.54300000000001);
#2896=CIRCLE('',#19109,1.54300000000001);
#2897=CIRCLE('',#19111,1.2645);
#2898=CIRCLE('',#19112,1.2645);
#2899=CIRCLE('',#19113,1.2645);
#2900=CIRCLE('',#19114,1.2645);
#2901=CIRCLE('',#19115,1.2645);
#2902=CIRCLE('',#19123,1.2645);
#2903=CIRCLE('',#19125,1.543);
#2904=CIRCLE('',#19133,1.543);
#2905=CIRCLE('',#19135,1.2645);
#2906=CIRCLE('',#19136,1.2645);
#2907=CIRCLE('',#19137,1.2645);
#2908=CIRCLE('',#19138,1.2645);
#2909=CIRCLE('',#19139,1.2645);
#2910=CIRCLE('',#19147,1.2645);
#2911=CIRCLE('',#19149,1.54300000000001);
#2912=CIRCLE('',#19157,1.54300000000001);
#2913=CIRCLE('',#19159,1.2645);
#2914=CIRCLE('',#19160,1.2645);
#2915=CIRCLE('',#19161,1.2645);
#2916=CIRCLE('',#19162,1.2645);
#2917=CIRCLE('',#19163,1.2645);
#2918=CIRCLE('',#19171,1.2645);
#2919=CIRCLE('',#19173,1.54300000000001);
#2920=CIRCLE('',#19181,1.54300000000001);
#2921=CIRCLE('',#19183,1.2645);
#2922=CIRCLE('',#19184,1.2645);
#2923=CIRCLE('',#19185,1.2645);
#2924=CIRCLE('',#19186,1.2645);
#2925=CIRCLE('',#19187,1.2645);
#2926=CIRCLE('',#19195,1.2645);
#2927=CIRCLE('',#19197,1.543);
#2928=CIRCLE('',#19205,1.543);
#2929=CIRCLE('',#19207,1.2645);
#2930=CIRCLE('',#19208,1.2645);
#2931=CIRCLE('',#19209,1.2645);
#2932=CIRCLE('',#19210,1.2645);
#2933=CIRCLE('',#19211,1.2645);
#2934=CIRCLE('',#19219,1.2645);
#2935=CIRCLE('',#19221,1.54299999999999);
#2936=CIRCLE('',#19229,1.54299999999999);
#2937=CIRCLE('',#19231,1.2645);
#2938=CIRCLE('',#19232,1.2645);
#2939=CIRCLE('',#19233,1.2645);
#2940=CIRCLE('',#19234,1.2645);
#2941=CIRCLE('',#19235,1.2645);
#2942=CIRCLE('',#19243,1.2645);
#2943=CIRCLE('',#19245,1.543);
#2944=CIRCLE('',#19253,1.543);
#2945=CIRCLE('',#19258,1.);
#2946=CIRCLE('',#19259,45.9999999999998);
#2947=CIRCLE('',#19260,1.);
#2948=CIRCLE('',#19261,45.9999999999998);
#2949=CIRCLE('',#19262,1.);
#2950=CIRCLE('',#19263,45.9999999999998);
#2951=CIRCLE('',#19264,1.);
#2952=CIRCLE('',#19265,45.9999999999998);
#2953=CIRCLE('',#19266,1.);
#2954=CIRCLE('',#19267,45.9999999999998);
#2955=CIRCLE('',#19268,1.);
#2956=CIRCLE('',#19269,45.9999999999998);
#2957=CIRCLE('',#19270,10.);
#2958=CIRCLE('',#19332,1.5);
#2959=CIRCLE('',#19333,1.5);
#2960=CIRCLE('',#19335,3.);
#2961=CIRCLE('',#19336,3.);
#2962=CIRCLE('',#19339,1.5);
#2963=CIRCLE('',#19340,1.5);
#2964=CIRCLE('',#19342,3.);
#2965=CIRCLE('',#19343,3.);
#2966=CIRCLE('',#19346,1.5);
#2967=CIRCLE('',#19347,1.5);
#2968=CIRCLE('',#19349,3.);
#2969=CIRCLE('',#19350,3.);
#2970=CIRCLE('',#19353,1.5);
#2971=CIRCLE('',#19354,1.5);
#2972=CIRCLE('',#19356,3.);
#2973=CIRCLE('',#19357,3.);
#2974=CIRCLE('',#19360,1.5);
#2975=CIRCLE('',#19361,1.5);
#2976=CIRCLE('',#19363,3.);
#2977=CIRCLE('',#19364,3.);
#2978=CIRCLE('',#19367,1.5);
#2979=CIRCLE('',#19368,1.5);
#2980=CIRCLE('',#19370,3.);
#2981=CIRCLE('',#19371,3.);
#2982=CIRCLE('',#19398,45.9999999999998);
#2983=CIRCLE('',#19400,1.);
#2984=CIRCLE('',#19403,45.9999999999998);
#2985=CIRCLE('',#19405,1.);
#2986=CIRCLE('',#19408,45.9999999999998);
#2987=CIRCLE('',#19410,1.);
#2988=CIRCLE('',#19413,45.9999999999998);
#2989=CIRCLE('',#19414,1.);
#2990=CIRCLE('',#19415,45.9999999999998);
#2991=CIRCLE('',#19416,1.);
#2992=CIRCLE('',#19417,45.9999999999998);
#2993=CIRCLE('',#19418,1.);
#2994=CIRCLE('',#19419,10.);
#2995=CIRCLE('',#19432,3.);
#2996=CIRCLE('',#19434,3.);
#2997=CIRCLE('',#19437,3.);
#2998=CIRCLE('',#19441,10.);
#2999=CIRCLE('',#19442,10.);
#3000=CIRCLE('',#19443,10.);
#3001=CIRCLE('',#19445,3.);
#3002=CIRCLE('',#19448,3.);
#3003=CIRCLE('',#19452,10.);
#3004=CIRCLE('',#19453,10.);
#3005=CIRCLE('',#19454,10.);
#3006=CIRCLE('',#19456,9.);
#3007=CIRCLE('',#19457,9.);
#3008=CIRCLE('',#19461,9.);
#3009=CIRCLE('',#19462,9.);
#3010=CIRCLE('',#19464,10.);
#3011=CIRCLE('',#19466,10.);
#3012=CIRCLE('',#19468,10.);
#3013=CIRCLE('',#19470,12.);
#3014=CIRCLE('',#19472,12.);
#3015=CIRCLE('',#19475,10.);
#3016=CIRCLE('',#19481,3.);
#3017=CIRCLE('',#19482,3.);
#3018=CIRCLE('',#19485,3.);
#3019=CIRCLE('',#19486,3.);
#3020=CIRCLE('',#19491,6.);
#3021=CIRCLE('',#19492,6.);
#3022=CIRCLE('',#19497,4.);
#3023=CIRCLE('',#19498,2.5);
#3024=CIRCLE('',#19500,4.);
#3025=CIRCLE('',#19502,2.5);
#3026=CIRCLE('',#19504,4.);
#3027=CIRCLE('',#19505,2.5);
#3028=CIRCLE('',#19507,4.);
#3029=CIRCLE('',#19509,2.5);
#3030=CIRCLE('',#19511,4.);
#3031=CIRCLE('',#19512,2.5);
#3032=CIRCLE('',#19514,4.);
#3033=CIRCLE('',#19516,2.5);
#3034=CIRCLE('',#19518,4.);
#3035=CIRCLE('',#19519,2.5);
#3036=CIRCLE('',#19521,4.);
#3037=CIRCLE('',#19523,2.5);
#3038=CIRCLE('',#19525,4.);
#3039=CIRCLE('',#19526,2.5);
#3040=CIRCLE('',#19528,4.);
#3041=CIRCLE('',#19530,2.5);
#3042=CIRCLE('',#19532,4.);
#3043=CIRCLE('',#19533,2.5);
#3044=CIRCLE('',#19535,4.);
#3045=CIRCLE('',#19537,2.5);
#3046=CIRCLE('',#19539,12.);
#3047=CIRCLE('',#19540,12.);
#3048=CIRCLE('',#19542,70.);
#3049=CIRCLE('',#19543,70.);
#3050=CIRCLE('',#19548,12.);
#3051=CIRCLE('',#19549,12.);
#3052=CIRCLE('',#19551,60.);
#3053=CIRCLE('',#19552,60.);
#3054=CIRCLE('',#19557,3.);
#3055=CIRCLE('',#19558,2.);
#3056=CIRCLE('',#19560,2.);
#3057=CIRCLE('',#19562,3.);
#3058=CIRCLE('',#19563,2.);
#3059=CIRCLE('',#19565,2.);
#3060=CIRCLE('',#19567,3.);
#3061=CIRCLE('',#19568,2.);
#3062=CIRCLE('',#19570,2.);
#3063=CIRCLE('',#19572,3.);
#3064=CIRCLE('',#19573,2.);
#3065=CIRCLE('',#19575,2.);
#3066=CIRCLE('',#19577,3.);
#3067=CIRCLE('',#19578,2.);
#3068=CIRCLE('',#19580,2.);
#3069=CIRCLE('',#19582,3.);
#3070=CIRCLE('',#19583,2.);
#3071=CIRCLE('',#19585,2.);
#3072=CIRCLE('',#19587,50.);
#3073=CIRCLE('',#19588,50.);
#3074=CIRCLE('',#19590,59.);
#3075=CIRCLE('',#19591,59.);
#3076=CIRCLE('',#19596,10.);
#3077=CIRCLE('',#19597,10.);
#3078=CIRCLE('',#19599,12.);
#3079=CIRCLE('',#19600,12.);
#3080=CIRCLE('',#19605,10.);
#3081=CIRCLE('',#19606,10.);
#3082=CIRCLE('',#19608,12.);
#3083=CIRCLE('',#19609,12.);
#3084=CIRCLE('',#19614,10.);
#3085=CIRCLE('',#19615,10.);
#3086=CIRCLE('',#19617,14.);
#3087=CIRCLE('',#19618,14.);
#3088=CIRCLE('',#19625,14.);
#3089=CIRCLE('',#19626,9.);
#3090=CIRCLE('',#19628,9.);
#3091=CIRCLE('',#19630,14.);
#3092=CIRCLE('',#19634,2.5);
#3093=CIRCLE('',#19635,1.5);
#3094=CIRCLE('',#19637,2.5);
#3095=CIRCLE('',#19640,1.5);
#3096=CIRCLE('',#19643,0.5);
#3097=CIRCLE('',#19644,0.5);
#3098=CIRCLE('',#19649,1.954);
#3099=CIRCLE('',#19666,1.5555);
#3100=CIRCLE('',#19683,1.954);
#3101=CIRCLE('',#19684,1.);
#3102=CIRCLE('',#19686,1.5555);
#3103=CIRCLE('',#19696,3.5);
#3104=CIRCLE('',#19698,3.5);
#3105=CIRCLE('',#19703,1.4635);
#3106=CIRCLE('',#19712,1.17775);
#3107=CIRCLE('',#19721,1.4635);
#3108=CIRCLE('',#19722,0.999999999999998);
#3109=CIRCLE('',#19724,1.17775);
#3110=CIRCLE('',#19733,1.4635);
#3111=CIRCLE('',#19734,1.4635);
#3112=CIRCLE('',#19737,3.);
#3113=B_SPLINE_CURVE_WITH_KNOTS('',3,(#23382,#23383,#23384,#23385,#23386,
#23387,#23388,#23389,#23390,#23391,#23392,#23393,#23394,#23395,#23396,#23397,
#23398,#23399,#23400,#23401,#23402,#23403),.UNSPECIFIED.,.F.,.F.,(4,3,3,
3,3,3,3,4),(76.708045941327,76.8129957196858,77.8105670926687,78.8081384656517,
79.8057098386346,80.8032812116175,81.8008525846005,82.7984239575834),
 .UNSPECIFIED.);
#3114=B_SPLINE_CURVE_WITH_KNOTS('',3,(#23407,#23408,#23409,#23410,#23411,
#23412,#23413),.UNSPECIFIED.,.F.,.F.,(4,3,4),(-80.7838110923089,-79.8057098386346,
-79.2446069498474),.UNSPECIFIED.);
#3115=B_SPLINE_CURVE_WITH_KNOTS('',3,(#23417,#23418,#23419,#23420,#23421,
#23422,#23423,#23424,#23425,#23426,#23427,#23428,#23429,#23430,#23431,#23432,
#23433,#23434,#23435,#23436,#23437,#23438),.UNSPECIFIED.,.F.,.F.,(4,3,3,
3,3,3,3,4),(-79.2446069498474,-78.8081384656517,-77.8105670926687,-76.8129957196858,
-75.8154243467029,-74.8178529737199,-73.820281600737,-72.9614216426678),
 .UNSPECIFIED.);
#3116=B_SPLINE_CURVE_WITH_KNOTS('',3,(#23443,#23444,#23445,#23446,#23447,
#23448,#23449,#23450,#23451,#23452,#23453,#23454,#23455,#23456,#23457,#23458,
#23459,#23460,#23461,#23462,#23463,#23464),.UNSPECIFIED.,.F.,.F.,(4,3,3,
3,3,3,3,4),(70.4248606341474,70.8275674817882,71.8251388547711,72.8227102277541,
73.820281600737,74.8178529737199,75.8154243467029,76.708045941327),
 .UNSPECIFIED.);
#3117=B_SPLINE_CURVE_WITH_KNOTS('',3,(#23465,#23466,#23467,#23468,#23469,
#23470,#23471,#23472,#23473,#23474,#23475,#23476,#23477,#23478,#23479,#23480,
#23481,#23482,#23483,#23484,#23485,#23486,#23487,#23488,#23489),
 .UNSPECIFIED.,.F.,.F.,(4,3,3,3,3,3,3,3,4),(-72.9614216426678,-72.8227102277541,
-71.8251388547712,-70.8275674817882,-69.8299961088053,-68.8324247358223,
-67.8348533628394,-66.8372819898565,-66.6782363354882),.UNSPECIFIED.);
#3118=B_SPLINE_CURVE_WITH_KNOTS('',3,(#23494,#23495,#23496,#23497,#23498,
#23499,#23500,#23501,#23502,#23503,#23504,#23505,#23506,#23507,#23508,#23509,
#23510,#23511,#23512,#23513,#23514,#23515),.UNSPECIFIED.,.F.,.F.,(4,3,3,
3,3,3,3,4),(64.1416753269678,64.8421392438906,65.8397106168735,66.8372819898565,
67.8348533628394,68.8324247358223,69.8299961088053,70.4248606341474),
 .UNSPECIFIED.);
#3119=B_SPLINE_CURVE_WITH_KNOTS('',3,(#23516,#23517,#23518,#23519,#23520,
#23521,#23522,#23523,#23524,#23525,#23526,#23527,#23528,#23529,#23530,#23531,
#23532,#23533,#23534,#23535,#23536,#23537),.UNSPECIFIED.,.F.,.F.,(4,3,3,
3,3,3,3,4),(-66.6782363354882,-65.8397106168735,-64.8421392438906,-63.8445678709077,
-62.8469964979248,-61.8494251249418,-60.8518537519589,-60.3950510283086),
 .UNSPECIFIED.);
#3120=B_SPLINE_CURVE_WITH_KNOTS('',3,(#23542,#23543,#23544,#23545,#23546,
#23547,#23548,#23549,#23550,#23551,#23552,#23553,#23554,#23555,#23556,#23557,
#23558,#23559,#23560,#23561,#23562,#23563),.UNSPECIFIED.,.F.,.F.,(4,3,3,
3,3,3,3,4),(57.8584900197882,58.856711005993,59.854282378976,60.8518537519589,
61.8494251249418,62.8469964979247,63.8445678709077,64.1416753269678),
 .UNSPECIFIED.);
#3121=B_SPLINE_CURVE_WITH_KNOTS('',3,(#23564,#23565,#23566,#23567,#23568,
#23569,#23570,#23571,#23572,#23573,#23574,#23575,#23576,#23577,#23578,#23579,
#23580,#23581,#23582,#23583,#23584,#23585),.UNSPECIFIED.,.F.,.F.,(4,3,3,
3,3,3,3,4),(-60.3950510283086,-59.854282378976,-58.856711005993,-57.8591396330101,
-56.8615682600271,-55.8639968870442,-54.8664255140613,-54.111865721129),
 .UNSPECIFIED.);
#3122=B_SPLINE_CURVE_WITH_KNOTS('',3,(#23590,#23591,#23592,#23593,#23594,
#23595,#23596,#23597,#23598,#23599,#23600,#23601,#23602,#23603,#23604,#23605,
#23606,#23607,#23608,#23609,#23610,#23611),.UNSPECIFIED.,.F.,.F.,(4,3,3,
3,3,3,3,4),(51.5753047126087,51.8737113951125,52.8712827680954,53.8688541410784,
54.8664255140613,55.8639968870442,56.8615682600272,57.8584900197882),
 .UNSPECIFIED.);
#3123=B_SPLINE_CURVE_WITH_KNOTS('',3,(#23612,#23613,#23614,#23615,#23616,
#23617,#23618,#23619,#23620,#23621,#23622,#23623,#23624,#23625,#23626,#23627,
#23628,#23629,#23630,#23631,#23632,#23633,#23634,#23635,#23636),
 .UNSPECIFIED.,.F.,.F.,(4,3,3,3,3,3,3,3,4),(-54.111865721129,-53.8688541410783,
-52.8712827680954,-51.8737113951125,-50.8761400221296,-49.8785686491466,
-48.8809972761637,-47.8834259031808,-47.8286804139494),.UNSPECIFIED.);
#3124=B_SPLINE_CURVE_WITH_KNOTS('',3,(#23641,#23642,#23643,#23644,#23645,
#23646,#23647,#23648,#23649,#23650,#23651,#23652,#23653,#23654,#23655,#23656,
#23657,#23658,#23659,#23660,#23661,#23662),.UNSPECIFIED.,.F.,.F.,(4,3,3,
3,3,3,3,4),(45.2921194054291,45.8882831572149,46.8858545301978,47.8834259031808,
48.8809972761637,49.8785686491466,50.8761400221296,51.5753047126087),
 .UNSPECIFIED.);
#3125=B_SPLINE_CURVE_WITH_KNOTS('',3,(#23663,#23664,#23665,#23666,#23667,
#23668,#23669,#23670,#23671,#23672,#23673,#23674,#23675,#23676,#23677,#23678,
#23679,#23680,#23681,#23682,#23683,#23684),.UNSPECIFIED.,.F.,.F.,(4,3,3,
3,3,3,3,4),(-47.8286804139494,-46.8858545301978,-45.8882831572149,-44.890711784232,
-43.893140411249,-42.8955690382661,-41.8979976652832,-41.5454951067698),
 .UNSPECIFIED.);
#3126=B_SPLINE_CURVE_WITH_KNOTS('',3,(#23689,#23690,#23691,#23692,#23693,
#23694,#23695,#23696,#23697,#23698,#23699,#23700,#23701,#23702,#23703,#23704,
#23705,#23706,#23707,#23708,#23709,#23710),.UNSPECIFIED.,.F.,.F.,(4,3,3,
3,3,3,3,4),(39.0089340982495,39.9028549193173,40.9004262923002,41.8979976652832,
42.8955690382661,43.893140411249,44.890711784232,45.2921194054291),
 .UNSPECIFIED.);
#3127=B_SPLINE_CURVE_WITH_KNOTS('',3,(#23711,#23712,#23713,#23714,#23715,
#23716,#23717,#23718,#23719,#23720,#23721,#23722,#23723,#23724,#23725,#23726,
#23727,#23728,#23729,#23730,#23731,#23732),.UNSPECIFIED.,.F.,.F.,(4,3,3,
3,3,3,3,4),(-41.5454951067698,-40.9004262923002,-39.9028549193173,-38.9052835463344,
-37.9077121733514,-36.9101408003685,-35.9125694273856,-35.2623097995902),
 .UNSPECIFIED.);
#3128=B_SPLINE_CURVE_WITH_KNOTS('',3,(#23737,#23738,#23739,#23740,#23741,
#23742,#23743,#23744,#23745,#23746,#23747,#23748,#23749,#23750,#23751,#23752,
#23753,#23754,#23755,#23756,#23757,#23758,#23759,#23760,#23761),
 .UNSPECIFIED.,.F.,.F.,(4,3,3,3,3,3,3,3,4),(32.7257487910699,32.9198553084368,
33.9174266814197,34.9149980544026,35.9125694273856,36.9101408003685,37.9077121733514,
38.9052835463344,39.0089340982495),.UNSPECIFIED.);
#3129=B_SPLINE_CURVE_WITH_KNOTS('',3,(#23762,#23763,#23764,#23765,#23766,
#23767,#23768,#23769,#23770,#23771,#23772,#23773,#23774,#23775,#23776,#23777,
#23778,#23779,#23780,#23781,#23782,#23783),.UNSPECIFIED.,.F.,.F.,(4,3,3,
3,3,3,3,4),(-35.2623097995902,-34.9149980544026,-33.9174266814197,-32.9198553084368,
-31.9222839354538,-30.9247125624709,-29.927141189488,-28.9791244924106),
 .UNSPECIFIED.);
#3130=B_SPLINE_CURVE_WITH_KNOTS('',3,(#23788,#23789,#23790,#23791,#23792,
#23793,#23794,#23795,#23796,#23797,#23798,#23799,#23800,#23801,#23802,#23803,
#23804,#23805,#23806,#23807,#23808,#23809),.UNSPECIFIED.,.F.,.F.,(4,3,3,
3,3,3,3,4),(26.4425634838903,26.9344270705392,27.9319984435221,28.929569816505,
29.927141189488,30.9247125624709,31.9222839354538,32.7257487910699),
 .UNSPECIFIED.);
#3131=B_SPLINE_CURVE_WITH_KNOTS('',3,(#23810,#23811,#23812,#23813,#23814,
#23815,#23816,#23817,#23818,#23819,#23820,#23821,#23822,#23823,#23824,#23825,
#23826,#23827,#23828,#23829,#23830,#23831,#23832,#23833,#23834),
 .UNSPECIFIED.,.F.,.F.,(4,3,3,3,3,3,3,3,4),(-28.9791244924106,-28.929569816505,
-27.9319984435221,-26.9344270705392,-25.9368556975563,-24.9392843245733,
-23.9417129515904,-22.9441415786074,-22.695939185231),.UNSPECIFIED.);
#3132=B_SPLINE_CURVE_WITH_KNOTS('',3,(#23839,#23840,#23841,#23842,#23843,
#23844,#23845,#23846,#23847,#23848,#23849,#23850,#23851,#23852,#23853,#23854,
#23855,#23856,#23857,#23858,#23859,#23860),.UNSPECIFIED.,.F.,.F.,(4,3,3,
3,3,3,3,4),(20.1593781767107,20.9489988326416,21.9465702056245,22.9441415786074,
23.9417129515904,24.9392843245733,25.9368556975563,26.4425634838903),
 .UNSPECIFIED.);
#3133=B_SPLINE_CURVE_WITH_KNOTS('',3,(#23861,#23862,#23863,#23864,#23865,
#23866,#23867,#23868,#23869,#23870,#23871,#23872,#23873,#23874,#23875,#23876,
#23877,#23878,#23879,#23880,#23881,#23882),.UNSPECIFIED.,.F.,.F.,(4,3,3,
3,3,3,3,4),(-22.695939185231,-21.9465702056245,-20.9489988326416,-19.9514274596586,
-18.9538560866757,-17.9562847136928,-16.9587133407099,-16.4127538780514),
 .UNSPECIFIED.);
#3134=B_SPLINE_CURVE_WITH_KNOTS('',3,(#23887,#23888,#23889,#23890,#23891,
#23892,#23893,#23894,#23895,#23896,#23897,#23898,#23899,#23900,#23901,#23902,
#23903,#23904,#23905,#23906,#23907,#23908,#23909,#23910,#23911),
 .UNSPECIFIED.,.F.,.F.,(4,3,3,3,3,3,3,3,4),(13.8761928695311,13.9659992217611,
14.963570594744,15.9611419677269,16.9587133407099,17.9562847136928,18.9538560866757,
19.9514274596586,20.1593781767107),.UNSPECIFIED.);
#3135=B_SPLINE_CURVE_WITH_KNOTS('',3,(#23912,#23913,#23914,#23915,#23916,
#23917,#23918,#23919,#23920,#23921,#23922,#23923,#23924,#23925,#23926,#23927,
#23928,#23929,#23930,#23931,#23932,#23933),.UNSPECIFIED.,.F.,.F.,(4,3,3,
3,3,3,3,4),(-16.4127538780514,-15.9611419677269,-14.963570594744,-13.9659992217611,
-12.9684278487781,-11.9708564757952,-10.9732851028123,-10.1295685708719),
 .UNSPECIFIED.);
#3136=B_SPLINE_CURVE_WITH_KNOTS('',3,(#23939,#23940,#23941,#23942,#23943,
#23944,#23945,#23946,#23947,#23948,#23949,#23950,#23951),.UNSPECIFIED.,
 .F.,.F.,(4,3,3,3,4),(-3.84638326369226,-2.9927141189488,-1.99514274596587,
-0.997571372982933,0.),.UNSPECIFIED.);
#3137=B_SPLINE_CURVE_WITH_KNOTS('',3,(#23954,#23955,#23956,#23957,#23958,
#23959,#23960,#23961,#23962,#23963,#23964,#23965,#23966,#23967,#23968,#23969,
#23970,#23971,#23972),.UNSPECIFIED.,.F.,.F.,(4,3,3,3,3,3,4),(2.01461286527445,
2.9927141189488,3.99028549193173,4.98785686491466,5.9854282378976,6.98299961088053,
7.59300756235153),.UNSPECIFIED.);
#3138=B_SPLINE_CURVE_WITH_KNOTS('',3,(#23978,#23979,#23980,#23981,#23982,
#23983,#23984),.UNSPECIFIED.,.F.,.F.,(4,1,1,1,4),(91.106186954104,91.6672898428912,
92.6648612158742,93.6624325888571,94.66000396184),.UNSPECIFIED.);
#3139=B_SPLINE_CURVE_WITH_KNOTS('',3,(#23987,#23988,#23989,#23990,#23991,
#23992,#23993,#23994),.UNSPECIFIED.,.F.,.F.,(4,1,1,1,1,4),(91.106186954104,
91.2111367324627,92.2087081054456,93.2062794784286,94.2038508514115,95.1819521050858),
 .UNSPECIFIED.);
#3140=B_SPLINE_CURVE_WITH_KNOTS('',3,(#23999,#24000,#24001,#24002,#24003,
#24004,#24005,#24006,#24007,#24008),.UNSPECIFIED.,.F.,.F.,(4,1,1,1,1,1,
1,4),(84.8230016469244,85.6818616049936,86.6794329779766,87.6770043509595,
88.6745757239424,89.6721470969254,90.6697184699083,91.106186954104),
 .UNSPECIFIED.);
#3141=B_SPLINE_CURVE_WITH_KNOTS('',3,(#24009,#24010,#24011,#24012,#24013,
#24014,#24015,#24016,#24017,#24018),.UNSPECIFIED.,.F.,.F.,(4,1,1,1,1,1,
1,4),(84.8230016469244,85.2257084945651,86.223279867548,87.220851240531,
88.2184226135139,89.2159939864968,90.2135653594798,91.106186954104),
 .UNSPECIFIED.);
#3142=B_SPLINE_CURVE_WITH_KNOTS('',3,(#24023,#24024,#24025,#24026,#24027,
#24028,#24029,#24030,#24031,#24032,#24033),.UNSPECIFIED.,.F.,.F.,(4,1,1,
1,1,1,1,1,4),(78.5398163397448,78.6988619941131,79.696433367096,80.694004740079,
81.6915761130619,82.6891474860448,83.6867188590278,84.6842902320107,84.8230016469244),
 .UNSPECIFIED.);
#3143=B_SPLINE_CURVE_WITH_KNOTS('',3,(#24034,#24035,#24036,#24037,#24038,
#24039,#24040,#24041,#24042,#24043),.UNSPECIFIED.,.F.,.F.,(4,1,1,1,1,1,
1,4),(78.5398163397448,79.2402802566675,80.2378516296505,81.2354230026334,
82.2329943756163,83.2305657485992,84.2281371215822,84.8230016469244),
 .UNSPECIFIED.);
#3144=B_SPLINE_CURVE_WITH_KNOTS('',3,(#24048,#24049,#24050,#24051,#24052,
#24053,#24054,#24055,#24056,#24057),.UNSPECIFIED.,.F.,.F.,(4,1,1,1,1,1,
1,4),(72.2566310325652,72.7134337562155,73.7110051291985,74.7085765021814,
75.7061478751643,76.7037192481473,77.7012906211302,78.5398163397448),
 .UNSPECIFIED.);
#3145=B_SPLINE_CURVE_WITH_KNOTS('',3,(#24058,#24059,#24060,#24061,#24062,
#24063,#24064,#24065,#24066,#24067,#24068),.UNSPECIFIED.,.F.,.F.,(4,1,1,
1,1,1,1,1,4),(72.2566310325652,72.257280645787,73.2548520187699,74.2524233917529,
75.2499947647358,76.2475661377187,77.2451375107017,78.2427088836846,78.5398163397448),
 .UNSPECIFIED.);
#3146=B_SPLINE_CURVE_WITH_KNOTS('',3,(#24073,#24074,#24075,#24076,#24077,
#24078,#24079,#24080,#24081,#24082),.UNSPECIFIED.,.F.,.F.,(4,1,1,1,1,1,
1,4),(65.9734457253856,66.7280055183179,67.7255768913009,68.7231482642838,
69.7207196372667,70.7182910102497,71.7158623832326,72.2566310325652),
 .UNSPECIFIED.);
#3147=B_SPLINE_CURVE_WITH_KNOTS('',3,(#24083,#24084,#24085,#24086,#24087,
#24088,#24089,#24090,#24091,#24092),.UNSPECIFIED.,.F.,.F.,(4,1,1,1,1,1,
1,4),(65.9734457253856,66.2718524078894,67.2694237808723,68.2669951538553,
69.2645665268382,70.2621378998211,71.2597092728041,72.2566310325652),
 .UNSPECIFIED.);
#3148=B_SPLINE_CURVE_WITH_KNOTS('',3,(#24097,#24098,#24099,#24100,#24101,
#24102,#24103,#24104,#24105,#24106,#24107),.UNSPECIFIED.,.F.,.F.,(4,1,1,
1,1,1,1,1,4),(59.690260418206,59.7450059074374,60.7425772804203,61.7401486534033,
62.7377200263862,63.7352913993691,64.7328627723521,65.730434145335,65.9734457253856),
 .UNSPECIFIED.);
#3149=B_SPLINE_CURVE_WITH_KNOTS('',3,(#24108,#24109,#24110,#24111,#24112,
#24113,#24114,#24115,#24116,#24117),.UNSPECIFIED.,.F.,.F.,(4,1,1,1,1,1,
1,4),(59.690260418206,60.2864241699918,61.2839955429747,62.2815669159577,
63.2791382889406,64.2767096619235,65.2742810349065,65.9734457253856),
 .UNSPECIFIED.);
#3150=B_SPLINE_CURVE_WITH_KNOTS('',3,(#24122,#24123,#24124,#24125,#24126,
#24127,#24128,#24129,#24130,#24131),.UNSPECIFIED.,.F.,.F.,(4,1,1,1,1,1,
1,4),(53.4070751110264,53.7595776695398,54.7571490425227,55.7547204155057,
56.7522917884886,57.7498631614715,58.7474345344545,59.690260418206),
 .UNSPECIFIED.);
#3151=B_SPLINE_CURVE_WITH_KNOTS('',3,(#24132,#24133,#24134,#24135,#24136,
#24137,#24138,#24139,#24140,#24141),.UNSPECIFIED.,.F.,.F.,(4,1,1,1,1,1,
1,4),(53.4070751110264,54.3009959320942,55.2985673050771,56.2961386780601,
57.293710051043,58.2912814240259,59.2888527970089,59.690260418206),
 .UNSPECIFIED.);
#3152=B_SPLINE_CURVE_WITH_KNOTS('',3,(#24146,#24147,#24148,#24149,#24150,
#24151,#24152,#24153,#24154,#24155),.UNSPECIFIED.,.F.,.F.,(4,1,1,1,1,1,
1,4),(47.1238898038468,47.7741494316422,48.7717208046251,49.7692921776081,
50.766863550591,51.7644349235739,52.7620062965569,53.4070751110264),
 .UNSPECIFIED.);
#3153=B_SPLINE_CURVE_WITH_KNOTS('',3,(#24156,#24157,#24158,#24159,#24160,
#24161,#24162,#24163,#24164,#24165,#24166),.UNSPECIFIED.,.F.,.F.,(4,1,1,
1,1,1,1,1,4),(47.1238898038468,47.3179963212137,48.3155676941966,49.3131390671795,
50.3107104401625,51.3082818131454,52.3058531861283,53.3034245591113,53.4070751110264),
 .UNSPECIFIED.);
#3154=B_SPLINE_CURVE_WITH_KNOTS('',3,(#24171,#24172,#24173,#24174,#24175,
#24176,#24177,#24178,#24179,#24180),.UNSPECIFIED.,.F.,.F.,(4,1,1,1,1,1,
1,4),(40.8407044966673,41.7887211937446,42.7862925667275,43.7838639397105,
44.7814353126934,45.7790066856763,46.7765780586593,47.1238898038468),
 .UNSPECIFIED.);
#3155=B_SPLINE_CURVE_WITH_KNOTS('',3,(#24181,#24182,#24183,#24184,#24185,
#24186,#24187,#24188,#24189,#24190),.UNSPECIFIED.,.F.,.F.,(4,1,1,1,1,1,
1,4),(40.8407044966673,41.3325680833161,42.330139456299,43.3277108292819,
44.3252822022649,45.3228535752478,46.3204249482307,47.1238898038468),
 .UNSPECIFIED.);
#3156=B_SPLINE_CURVE_WITH_KNOTS('',3,(#24195,#24196,#24197,#24198,#24199,
#24200,#24201,#24202,#24203,#24204,#24205),.UNSPECIFIED.,.F.,.F.,(4,1,1,
1,1,1,1,1,4),(34.5575191894876,34.8057215828641,35.803292955847,36.80086432883,
37.7984357018129,38.7960070747958,39.7935784477787,40.7911498207617,40.8407044966673),
 .UNSPECIFIED.);
#3157=B_SPLINE_CURVE_WITH_KNOTS('',3,(#24206,#24207,#24208,#24209,#24210,
#24211,#24212,#24213,#24214,#24215),.UNSPECIFIED.,.F.,.F.,(4,1,1,1,1,1,
1,4),(34.5575191894876,35.3471398454185,36.3447112184014,37.3422825913843,
38.3398539643673,39.3374253373502,40.3349967103332,40.8407044966673),
 .UNSPECIFIED.);
#3158=B_SPLINE_CURVE_WITH_KNOTS('',3,(#24220,#24221,#24222,#24223,#24224,
#24225,#24226,#24227,#24228,#24229),.UNSPECIFIED.,.F.,.F.,(4,1,1,1,1,1,
1,4),(28.2743338823081,28.8202933449665,29.8178647179494,30.8154360909324,
31.8130074639153,32.8105788368982,33.8081502098811,34.5575191894876),
 .UNSPECIFIED.);
#3159=B_SPLINE_CURVE_WITH_KNOTS('',3,(#24230,#24231,#24232,#24233,#24234,
#24235,#24236,#24237,#24238,#24239,#24240),.UNSPECIFIED.,.F.,.F.,(4,1,1,
1,1,1,1,1,4),(28.2743338823081,28.364140234538,29.3617116075209,30.3592829805038,
31.3568543534868,32.3544257264697,33.3519970994526,34.3495684724355,34.5575191894876),
 .UNSPECIFIED.);
#3160=B_SPLINE_CURVE_WITH_KNOTS('',3,(#24245,#24246,#24247,#24248,#24249,
#24250,#24251,#24252,#24253,#24254),.UNSPECIFIED.,.F.,.F.,(4,1,1,1,1,1,
1,4),(21.9911485751285,22.8348651070689,23.8324364800518,24.8300078530348,
25.8275792260177,26.8251505990006,27.8227219719836,28.2743338823081),
 .UNSPECIFIED.);
#3161=B_SPLINE_CURVE_WITH_KNOTS('',3,(#24255,#24256,#24257,#24258,#24259,
#24260,#24261,#24262,#24263,#24264),.UNSPECIFIED.,.F.,.F.,(4,1,1,1,1,1,
1,4),(21.9911485751285,22.3787119966404,23.3762833696233,24.3738547426062,
25.3714261155892,26.3689974885721,27.366568861555,28.2743338823081),
 .UNSPECIFIED.);
#3162=B_SPLINE_CURVE_WITH_KNOTS('',3,(#24270,#24271,#24272,#24273,#24274),
 .UNSPECIFIED.,.F.,.F.,(4,1,4),(14.3981410127769,15.3957123857598,15.7079632679489),
 .UNSPECIFIED.);
#3163=B_SPLINE_CURVE_WITH_KNOTS('',3,(#24277,#24278,#24279,#24280,#24281),
 .UNSPECIFIED.,.F.,.F.,(4,1,4),(13.8761928695311,14.8542941232054,15.7079632679489),
 .UNSPECIFIED.);
#3164=B_SPLINE_CURVE_WITH_KNOTS('',3,(#24287,#24288,#24289,#24290,#24291,
#24292,#24293,#24294,#24295,#24296,#24297,#24298,#24299,#24300,#24301,#24302,
#24303,#24304,#24305,#24306,#24307,#24308),.UNSPECIFIED.,.F.,.F.,(4,3,3,
3,3,3,3,4),(76.708045941327,76.8129957196858,77.8105670926687,78.8081384656517,
79.8057098386346,80.8032812116175,81.8008525846005,82.7984239575834),
 .UNSPECIFIED.);
#3165=B_SPLINE_CURVE_WITH_KNOTS('',3,(#24312,#24313,#24314,#24315,#24316,
#24317,#24318),.UNSPECIFIED.,.F.,.F.,(4,3,4),(-80.783811092309,-79.8057098386346,
-79.2446069498473),.UNSPECIFIED.);
#3166=B_SPLINE_CURVE_WITH_KNOTS('',3,(#24322,#24323,#24324,#24325,#24326,
#24327,#24328,#24329,#24330,#24331,#24332,#24333,#24334,#24335,#24336,#24337,
#24338,#24339,#24340,#24341,#24342,#24343),.UNSPECIFIED.,.F.,.F.,(4,3,3,
3,3,3,3,4),(-79.2446069498473,-78.8081384656517,-77.8105670926687,-76.8129957196858,
-75.8154243467029,-74.81785297372,-73.820281600737,-72.9614216426677),
 .UNSPECIFIED.);
#3167=B_SPLINE_CURVE_WITH_KNOTS('',3,(#24348,#24349,#24350,#24351,#24352,
#24353,#24354,#24355,#24356,#24357,#24358,#24359,#24360,#24361,#24362,#24363,
#24364,#24365,#24366,#24367,#24368,#24369),.UNSPECIFIED.,.F.,.F.,(4,3,3,
3,3,3,3,4),(70.4248606341474,70.8275674817882,71.8251388547712,72.8227102277541,
73.820281600737,74.81785297372,75.8154243467029,76.708045941327),
 .UNSPECIFIED.);
#3168=B_SPLINE_CURVE_WITH_KNOTS('',3,(#24370,#24371,#24372,#24373,#24374,
#24375,#24376,#24377,#24378,#24379,#24380,#24381,#24382,#24383,#24384,#24385,
#24386,#24387,#24388,#24389,#24390,#24391,#24392,#24393,#24394),
 .UNSPECIFIED.,.F.,.F.,(4,3,3,3,3,3,3,3,4),(-72.9614216426677,-72.8227102277541,
-71.8251388547712,-70.8275674817882,-69.8299961088053,-68.8324247358224,
-67.8348533628394,-66.8372819898565,-66.6782363354881),.UNSPECIFIED.);
#3169=B_SPLINE_CURVE_WITH_KNOTS('',3,(#24399,#24400,#24401,#24402,#24403,
#24404,#24405,#24406,#24407,#24408,#24409,#24410,#24411,#24412,#24413,#24414,
#24415,#24416,#24417,#24418,#24419,#24420),.UNSPECIFIED.,.F.,.F.,(4,3,3,
3,3,3,3,4),(64.1416753269678,64.8421392438906,65.8397106168735,66.8372819898565,
67.8348533628394,68.8324247358223,69.8299961088053,70.4248606341474),
 .UNSPECIFIED.);
#3170=B_SPLINE_CURVE_WITH_KNOTS('',3,(#24421,#24422,#24423,#24424,#24425,
#24426,#24427,#24428,#24429,#24430,#24431,#24432,#24433,#24434,#24435,#24436,
#24437,#24438,#24439,#24440,#24441,#24442),.UNSPECIFIED.,.F.,.F.,(4,3,3,
3,3,3,3,4),(-66.6782363354881,-65.8397106168736,-64.8421392438906,-63.8445678709077,
-62.8469964979248,-61.8494251249418,-60.8518537519589,-60.3950510283085),
 .UNSPECIFIED.);
#3171=B_SPLINE_CURVE_WITH_KNOTS('',3,(#24447,#24448,#24449,#24450,#24451,
#24452,#24453,#24454,#24455,#24456,#24457,#24458,#24459,#24460,#24461,#24462,
#24463,#24464,#24465,#24466,#24467,#24468),.UNSPECIFIED.,.F.,.F.,(4,3,3,
3,3,3,3,4),(57.8584900197882,58.856711005993,59.854282378976,60.8518537519589,
61.8494251249418,62.8469964979248,63.8445678709077,64.1416753269678),
 .UNSPECIFIED.);
#3172=B_SPLINE_CURVE_WITH_KNOTS('',3,(#24469,#24470,#24471,#24472,#24473,
#24474,#24475,#24476,#24477,#24478,#24479,#24480,#24481,#24482,#24483,#24484,
#24485,#24486,#24487,#24488,#24489,#24490),.UNSPECIFIED.,.F.,.F.,(4,3,3,
3,3,3,3,4),(-60.3950510283085,-59.854282378976,-58.856711005993,-57.8591396330101,
-56.8615682600271,-55.8639968870442,-54.8664255140613,-54.111865721129),
 .UNSPECIFIED.);
#3173=B_SPLINE_CURVE_WITH_KNOTS('',3,(#24495,#24496,#24497,#24498,#24499,
#24500,#24501,#24502,#24503,#24504,#24505,#24506,#24507,#24508,#24509,#24510,
#24511,#24512,#24513,#24514,#24515,#24516),.UNSPECIFIED.,.F.,.F.,(4,3,3,
3,3,3,3,4),(51.5753047126087,51.8737113951125,52.8712827680954,53.8688541410784,
54.8664255140613,55.8639968870442,56.8615682600272,57.8584900197882),
 .UNSPECIFIED.);
#3174=B_SPLINE_CURVE_WITH_KNOTS('',3,(#24517,#24518,#24519,#24520,#24521,
#24522,#24523,#24524,#24525,#24526,#24527,#24528,#24529,#24530,#24531,#24532,
#24533,#24534,#24535,#24536,#24537,#24538,#24539,#24540,#24541),
 .UNSPECIFIED.,.F.,.F.,(4,3,3,3,3,3,3,3,4),(-54.111865721129,-53.8688541410784,
-52.8712827680954,-51.8737113951125,-50.8761400221296,-49.8785686491466,
-48.8809972761637,-47.8834259031808,-47.8286804139494),.UNSPECIFIED.);
#3175=B_SPLINE_CURVE_WITH_KNOTS('',3,(#24546,#24547,#24548,#24549,#24550,
#24551,#24552,#24553,#24554,#24555,#24556,#24557,#24558,#24559,#24560,#24561,
#24562,#24563,#24564,#24565,#24566,#24567),.UNSPECIFIED.,.F.,.F.,(4,3,3,
3,3,3,3,4),(45.2921194054291,45.8882831572149,46.8858545301978,47.8834259031808,
48.8809972761637,49.8785686491466,50.8761400221296,51.5753047126087),
 .UNSPECIFIED.);
#3176=B_SPLINE_CURVE_WITH_KNOTS('',3,(#24568,#24569,#24570,#24571,#24572,
#24573,#24574,#24575,#24576,#24577,#24578,#24579,#24580,#24581,#24582,#24583,
#24584,#24585,#24586,#24587,#24588,#24589),.UNSPECIFIED.,.F.,.F.,(4,3,3,
3,3,3,3,4),(-47.8286804139494,-46.8858545301978,-45.8882831572149,-44.890711784232,
-43.893140411249,-42.8955690382661,-41.8979976652832,-41.5454951067698),
 .UNSPECIFIED.);
#3177=B_SPLINE_CURVE_WITH_KNOTS('',3,(#24594,#24595,#24596,#24597,#24598,
#24599,#24600,#24601,#24602,#24603,#24604,#24605,#24606,#24607,#24608,#24609,
#24610,#24611,#24612,#24613,#24614,#24615),.UNSPECIFIED.,.F.,.F.,(4,3,3,
3,3,3,3,4),(39.0089340982495,39.9028549193173,40.9004262923002,41.8979976652832,
42.8955690382661,43.893140411249,44.890711784232,45.2921194054291),
 .UNSPECIFIED.);
#3178=B_SPLINE_CURVE_WITH_KNOTS('',3,(#24616,#24617,#24618,#24619,#24620,
#24621,#24622,#24623,#24624,#24625,#24626,#24627,#24628,#24629,#24630,#24631,
#24632,#24633,#24634,#24635,#24636,#24637),.UNSPECIFIED.,.F.,.F.,(4,3,3,
3,3,3,3,4),(-41.5454951067698,-40.9004262923002,-39.9028549193173,-38.9052835463344,
-37.9077121733514,-36.9101408003685,-35.9125694273856,-35.2623097995902),
 .UNSPECIFIED.);
#3179=B_SPLINE_CURVE_WITH_KNOTS('',3,(#24642,#24643,#24644,#24645,#24646,
#24647,#24648,#24649,#24650,#24651,#24652,#24653,#24654,#24655,#24656,#24657,
#24658,#24659,#24660,#24661,#24662,#24663,#24664,#24665,#24666),
 .UNSPECIFIED.,.F.,.F.,(4,3,3,3,3,3,3,3,4),(32.7257487910699,32.9198553084368,
33.9174266814197,34.9149980544026,35.9125694273856,36.9101408003685,37.9077121733514,
38.9052835463344,39.0089340982495),.UNSPECIFIED.);
#3180=B_SPLINE_CURVE_WITH_KNOTS('',3,(#24667,#24668,#24669,#24670,#24671,
#24672,#24673,#24674,#24675,#24676,#24677,#24678,#24679,#24680,#24681,#24682,
#24683,#24684,#24685,#24686,#24687,#24688),.UNSPECIFIED.,.F.,.F.,(4,3,3,
3,3,3,3,4),(-35.2623097995902,-34.9149980544027,-33.9174266814197,-32.9198553084368,
-31.9222839354538,-30.9247125624709,-29.927141189488,-28.9791244924106),
 .UNSPECIFIED.);
#3181=B_SPLINE_CURVE_WITH_KNOTS('',3,(#24693,#24694,#24695,#24696,#24697,
#24698,#24699,#24700,#24701,#24702,#24703,#24704,#24705,#24706,#24707,#24708,
#24709,#24710,#24711,#24712,#24713,#24714),.UNSPECIFIED.,.F.,.F.,(4,3,3,
3,3,3,3,4),(26.4425634838903,26.9344270705392,27.9319984435221,28.929569816505,
29.927141189488,30.9247125624709,31.9222839354538,32.7257487910699),
 .UNSPECIFIED.);
#3182=B_SPLINE_CURVE_WITH_KNOTS('',3,(#24715,#24716,#24717,#24718,#24719,
#24720,#24721,#24722,#24723,#24724,#24725,#24726,#24727,#24728,#24729,#24730,
#24731,#24732,#24733,#24734,#24735,#24736,#24737,#24738,#24739),
 .UNSPECIFIED.,.F.,.F.,(4,3,3,3,3,3,3,3,4),(-28.9791244924106,-28.929569816505,
-27.9319984435221,-26.9344270705392,-25.9368556975562,-24.9392843245733,
-23.9417129515904,-22.9441415786075,-22.695939185231),.UNSPECIFIED.);
#3183=B_SPLINE_CURVE_WITH_KNOTS('',3,(#24744,#24745,#24746,#24747,#24748,
#24749,#24750,#24751,#24752,#24753,#24754,#24755,#24756,#24757,#24758,#24759,
#24760,#24761,#24762,#24763,#24764,#24765),.UNSPECIFIED.,.F.,.F.,(4,3,3,
3,3,3,3,4),(20.1593781767107,20.9489988326416,21.9465702056245,22.9441415786075,
23.9417129515904,24.9392843245733,25.9368556975563,26.4425634838903),
 .UNSPECIFIED.);
#3184=B_SPLINE_CURVE_WITH_KNOTS('',3,(#24766,#24767,#24768,#24769,#24770,
#24771,#24772,#24773,#24774,#24775,#24776,#24777,#24778,#24779,#24780,#24781,
#24782,#24783,#24784,#24785,#24786,#24787),.UNSPECIFIED.,.F.,.F.,(4,3,3,
3,3,3,3,4),(-22.695939185231,-21.9465702056245,-20.9489988326416,-19.9514274596587,
-18.9538560866757,-17.9562847136928,-16.9587133407099,-16.4127538780514),
 .UNSPECIFIED.);
#3185=B_SPLINE_CURVE_WITH_KNOTS('',3,(#24792,#24793,#24794,#24795,#24796,
#24797,#24798,#24799,#24800,#24801,#24802,#24803,#24804,#24805,#24806,#24807,
#24808,#24809,#24810,#24811,#24812,#24813,#24814,#24815,#24816),
 .UNSPECIFIED.,.F.,.F.,(4,3,3,3,3,3,3,3,4),(13.8761928695311,13.9659992217611,
14.963570594744,15.9611419677269,16.9587133407099,17.9562847136928,18.9538560866757,
19.9514274596586,20.1593781767107),.UNSPECIFIED.);
#3186=B_SPLINE_CURVE_WITH_KNOTS('',3,(#24817,#24818,#24819,#24820,#24821,
#24822,#24823,#24824,#24825,#24826,#24827,#24828,#24829,#24830,#24831,#24832,
#24833,#24834,#24835,#24836,#24837,#24838),.UNSPECIFIED.,.F.,.F.,(4,3,3,
3,3,3,3,4),(-16.4127538780514,-15.9611419677269,-14.963570594744,-13.9659992217611,
-12.9684278487781,-11.9708564757952,-10.9732851028123,-10.1295685708718),
 .UNSPECIFIED.);
#3187=B_SPLINE_CURVE_WITH_KNOTS('',3,(#24844,#24845,#24846,#24847,#24848,
#24849,#24850,#24851,#24852,#24853,#24854,#24855,#24856),.UNSPECIFIED.,
 .F.,.F.,(4,3,3,3,4),(-3.84638326369223,-2.9927141189488,-1.99514274596586,
-0.997571372982929,0.),.UNSPECIFIED.);
#3188=B_SPLINE_CURVE_WITH_KNOTS('',3,(#24859,#24860,#24861,#24862,#24863,
#24864,#24865,#24866,#24867,#24868,#24869,#24870,#24871,#24872,#24873,#24874,
#24875,#24876,#24877),.UNSPECIFIED.,.F.,.F.,(4,3,3,3,3,3,4),(2.01461286527443,
2.9927141189488,3.99028549193173,4.98785686491467,5.9854282378976,6.98299961088053,
7.59300756235153),.UNSPECIFIED.);
#3189=B_SPLINE_CURVE_WITH_KNOTS('',3,(#24883,#24884,#24885,#24886,#24887,
#24888,#24889),.UNSPECIFIED.,.F.,.F.,(4,1,1,1,4),(91.106186954104,91.6672898428913,
92.6648612158742,93.6624325888572,94.6600039618401),.UNSPECIFIED.);
#3190=B_SPLINE_CURVE_WITH_KNOTS('',3,(#24892,#24893,#24894,#24895,#24896,
#24897,#24898,#24899),.UNSPECIFIED.,.F.,.F.,(4,1,1,1,1,4),(91.106186954104,
91.2111367324627,92.2087081054457,93.2062794784286,94.2038508514115,95.1819521050859),
 .UNSPECIFIED.);
#3191=B_SPLINE_CURVE_WITH_KNOTS('',3,(#24904,#24905,#24906,#24907,#24908,
#24909,#24910,#24911,#24912,#24913),.UNSPECIFIED.,.F.,.F.,(4,1,1,1,1,1,
1,4),(84.8230016469244,85.6818616049937,86.6794329779766,87.6770043509596,
88.6745757239425,89.6721470969254,90.6697184699084,91.106186954104),
 .UNSPECIFIED.);
#3192=B_SPLINE_CURVE_WITH_KNOTS('',3,(#24914,#24915,#24916,#24917,#24918,
#24919,#24920,#24921,#24922,#24923),.UNSPECIFIED.,.F.,.F.,(4,1,1,1,1,1,
1,4),(84.8230016469244,85.2257084945651,86.2232798675481,87.220851240531,
88.2184226135139,89.2159939864969,90.2135653594798,91.106186954104),
 .UNSPECIFIED.);
#3193=B_SPLINE_CURVE_WITH_KNOTS('',3,(#24928,#24929,#24930,#24931,#24932,
#24933,#24934,#24935,#24936,#24937,#24938),.UNSPECIFIED.,.F.,.F.,(4,1,1,
1,1,1,1,1,4),(78.5398163397448,78.6988619941132,79.6964333670961,80.694004740079,
81.691576113062,82.6891474860449,83.6867188590278,84.6842902320108,84.8230016469244),
 .UNSPECIFIED.);
#3194=B_SPLINE_CURVE_WITH_KNOTS('',3,(#24939,#24940,#24941,#24942,#24943,
#24944,#24945,#24946,#24947,#24948),.UNSPECIFIED.,.F.,.F.,(4,1,1,1,1,1,
1,4),(78.5398163397448,79.2402802566675,80.2378516296505,81.2354230026334,
82.2329943756163,83.2305657485993,84.2281371215822,84.8230016469244),
 .UNSPECIFIED.);
#3195=B_SPLINE_CURVE_WITH_KNOTS('',3,(#24953,#24954,#24955,#24956,#24957,
#24958,#24959,#24960,#24961,#24962),.UNSPECIFIED.,.F.,.F.,(4,1,1,1,1,1,
1,4),(72.2566310325652,72.7134337562156,73.7110051291985,74.7085765021814,
75.7061478751644,76.7037192481473,77.7012906211302,78.5398163397448),
 .UNSPECIFIED.);
#3196=B_SPLINE_CURVE_WITH_KNOTS('',3,(#24963,#24964,#24965,#24966,#24967,
#24968,#24969,#24970,#24971,#24972,#24973),.UNSPECIFIED.,.F.,.F.,(4,1,1,
1,1,1,1,1,4),(72.2566310325652,72.257280645787,73.25485201877,74.2524233917529,
75.2499947647358,76.2475661377187,77.2451375107017,78.2427088836846,78.5398163397448),
 .UNSPECIFIED.);
#3197=B_SPLINE_CURVE_WITH_KNOTS('',3,(#24978,#24979,#24980,#24981,#24982,
#24983,#24984,#24985,#24986,#24987),.UNSPECIFIED.,.F.,.F.,(4,1,1,1,1,1,
1,4),(65.9734457253856,66.728005518318,67.7255768913009,68.7231482642838,
69.7207196372668,70.7182910102497,71.7158623832326,72.2566310325652),
 .UNSPECIFIED.);
#3198=B_SPLINE_CURVE_WITH_KNOTS('',3,(#24988,#24989,#24990,#24991,#24992,
#24993,#24994,#24995,#24996,#24997),.UNSPECIFIED.,.F.,.F.,(4,1,1,1,1,1,
1,4),(65.9734457253856,66.2718524078894,67.2694237808724,68.2669951538553,
69.2645665268382,70.2621378998212,71.2597092728041,72.2566310325652),
 .UNSPECIFIED.);
#3199=B_SPLINE_CURVE_WITH_KNOTS('',3,(#25002,#25003,#25004,#25005,#25006,
#25007,#25008,#25009,#25010,#25011,#25012),.UNSPECIFIED.,.F.,.F.,(4,1,1,
1,1,1,1,1,4),(59.690260418206,59.7450059074374,60.7425772804204,61.7401486534033,
62.7377200263862,63.7352913993692,64.7328627723521,65.730434145335,65.9734457253856),
 .UNSPECIFIED.);
#3200=B_SPLINE_CURVE_WITH_KNOTS('',3,(#25013,#25014,#25015,#25016,#25017,
#25018,#25019,#25020,#25021,#25022),.UNSPECIFIED.,.F.,.F.,(4,1,1,1,1,1,
1,4),(59.690260418206,60.2864241699918,61.2839955429748,62.2815669159577,
63.2791382889406,64.2767096619236,65.2742810349065,65.9734457253856),
 .UNSPECIFIED.);
#3201=B_SPLINE_CURVE_WITH_KNOTS('',3,(#25027,#25028,#25029,#25030,#25031,
#25032,#25033,#25034,#25035,#25036),.UNSPECIFIED.,.F.,.F.,(4,1,1,1,1,1,
1,4),(53.4070751110264,53.7595776695399,54.7571490425228,55.7547204155057,
56.7522917884886,57.7498631614716,58.7474345344545,59.690260418206),
 .UNSPECIFIED.);
#3202=B_SPLINE_CURVE_WITH_KNOTS('',3,(#25037,#25038,#25039,#25040,#25041,
#25042,#25043,#25044,#25045,#25046),.UNSPECIFIED.,.F.,.F.,(4,1,1,1,1,1,
1,4),(53.4070751110264,54.3009959320942,55.2985673050772,56.2961386780601,
57.293710051043,58.291281424026,59.2888527970089,59.690260418206),
 .UNSPECIFIED.);
#3203=B_SPLINE_CURVE_WITH_KNOTS('',3,(#25051,#25052,#25053,#25054,#25055,
#25056,#25057,#25058,#25059,#25060),.UNSPECIFIED.,.F.,.F.,(4,1,1,1,1,1,
1,4),(47.1238898038468,47.7741494316423,48.7717208046252,49.7692921776081,
50.7668635505911,51.764434923574,52.7620062965569,53.4070751110264),
 .UNSPECIFIED.);
#3204=B_SPLINE_CURVE_WITH_KNOTS('',3,(#25061,#25062,#25063,#25064,#25065,
#25066,#25067,#25068,#25069,#25070,#25071),.UNSPECIFIED.,.F.,.F.,(4,1,1,
1,1,1,1,1,4),(47.1238898038468,47.3179963212137,48.3155676941966,49.3131390671796,
50.3107104401625,51.3082818131454,52.3058531861284,53.3034245591113,53.4070751110264),
 .UNSPECIFIED.);
#3205=B_SPLINE_CURVE_WITH_KNOTS('',3,(#25076,#25077,#25078,#25079,#25080,
#25081,#25082,#25083,#25084,#25085),.UNSPECIFIED.,.F.,.F.,(4,1,1,1,1,1,
1,4),(40.8407044966673,41.7887211937447,42.7862925667276,43.7838639397105,
44.7814353126935,45.7790066856764,46.7765780586593,47.1238898038468),
 .UNSPECIFIED.);
#3206=B_SPLINE_CURVE_WITH_KNOTS('',3,(#25086,#25087,#25088,#25089,#25090,
#25091,#25092,#25093,#25094,#25095),.UNSPECIFIED.,.F.,.F.,(4,1,1,1,1,1,
1,4),(40.8407044966673,41.3325680833161,42.330139456299,43.327710829282,
44.3252822022649,45.3228535752478,46.3204249482308,47.1238898038468),
 .UNSPECIFIED.);
#3207=B_SPLINE_CURVE_WITH_KNOTS('',3,(#25100,#25101,#25102,#25103,#25104,
#25105,#25106,#25107,#25108,#25109,#25110),.UNSPECIFIED.,.F.,.F.,(4,1,1,
1,1,1,1,1,4),(34.5575191894876,34.8057215828641,35.8032929558471,36.80086432883,
37.7984357018129,38.7960070747959,39.7935784477788,40.7911498207617,40.8407044966673),
 .UNSPECIFIED.);
#3208=B_SPLINE_CURVE_WITH_KNOTS('',3,(#25111,#25112,#25113,#25114,#25115,
#25116,#25117,#25118,#25119,#25120),.UNSPECIFIED.,.F.,.F.,(4,1,1,1,1,1,
1,4),(34.5575191894876,35.3471398454185,36.3447112184014,37.3422825913844,
38.3398539643673,39.3374253373502,40.3349967103332,40.8407044966673),
 .UNSPECIFIED.);
#3209=B_SPLINE_CURVE_WITH_KNOTS('',3,(#25125,#25126,#25127,#25128,#25129,
#25130,#25131,#25132,#25133,#25134),.UNSPECIFIED.,.F.,.F.,(4,1,1,1,1,1,
1,4),(28.2743338823081,28.8202933449665,29.8178647179495,30.8154360909324,
31.8130074639153,32.8105788368983,33.8081502098812,34.5575191894876),
 .UNSPECIFIED.);
#3210=B_SPLINE_CURVE_WITH_KNOTS('',3,(#25135,#25136,#25137,#25138,#25139,
#25140,#25141,#25142,#25143,#25144,#25145),.UNSPECIFIED.,.F.,.F.,(4,1,1,
1,1,1,1,1,4),(28.2743338823081,28.364140234538,29.3617116075209,30.3592829805038,
31.3568543534868,32.3544257264697,33.3519970994526,34.3495684724356,34.5575191894876),
 .UNSPECIFIED.);
#3211=B_SPLINE_CURVE_WITH_KNOTS('',3,(#25150,#25151,#25152,#25153,#25154,
#25155,#25156,#25157,#25158,#25159),.UNSPECIFIED.,.F.,.F.,(4,1,1,1,1,1,
1,4),(21.9911485751285,22.8348651070689,23.8324364800519,24.8300078530348,
25.8275792260177,26.8251505990007,27.8227219719836,28.2743338823081),
 .UNSPECIFIED.);
#3212=B_SPLINE_CURVE_WITH_KNOTS('',3,(#25160,#25161,#25162,#25163,#25164,
#25165,#25166,#25167,#25168,#25169),.UNSPECIFIED.,.F.,.F.,(4,1,1,1,1,1,
1,4),(21.9911485751285,22.3787119966404,23.3762833696233,24.3738547426063,
25.3714261155892,26.3689974885721,27.3665688615551,28.2743338823081),
 .UNSPECIFIED.);
#3213=B_SPLINE_CURVE_WITH_KNOTS('',3,(#25175,#25176,#25177,#25178,#25179),
 .UNSPECIFIED.,.F.,.F.,(4,1,4),(14.3981410127769,15.3957123857599,15.7079632679489),
 .UNSPECIFIED.);
#3214=B_SPLINE_CURVE_WITH_KNOTS('',3,(#25182,#25183,#25184,#25185,#25186),
 .UNSPECIFIED.,.F.,.F.,(4,1,4),(13.8761928695311,14.8542941232055,15.7079632679489),
 .UNSPECIFIED.);
#3215=B_SPLINE_CURVE_WITH_KNOTS('',3,(#25192,#25193,#25194,#25195,#25196,
#25197,#25198,#25199,#25200,#25201,#25202,#25203,#25204,#25205,#25206,#25207,
#25208,#25209,#25210,#25211,#25212,#25213),.UNSPECIFIED.,.F.,.F.,(4,3,3,
3,3,3,3,4),(76.7080459413271,76.8129957196858,77.8105670926687,78.8081384656517,
79.8057098386346,80.8032812116175,81.8008525846005,82.7984239575834),
 .UNSPECIFIED.);
#3216=B_SPLINE_CURVE_WITH_KNOTS('',3,(#25217,#25218,#25219,#25220,#25221,
#25222,#25223),.UNSPECIFIED.,.F.,.F.,(4,3,4),(-80.783811092309,-79.8057098386346,
-79.2446069498474),.UNSPECIFIED.);
#3217=B_SPLINE_CURVE_WITH_KNOTS('',3,(#25227,#25228,#25229,#25230,#25231,
#25232,#25233,#25234,#25235,#25236,#25237,#25238,#25239,#25240,#25241,#25242,
#25243,#25244,#25245,#25246,#25247,#25248),.UNSPECIFIED.,.F.,.F.,(4,3,3,
3,3,3,3,4),(-79.2446069498474,-78.8081384656517,-77.8105670926687,-76.8129957196858,
-75.8154243467029,-74.8178529737199,-73.820281600737,-72.9614216426678),
 .UNSPECIFIED.);
#3218=B_SPLINE_CURVE_WITH_KNOTS('',3,(#25253,#25254,#25255,#25256,#25257,
#25258,#25259,#25260,#25261,#25262,#25263,#25264,#25265,#25266,#25267,#25268,
#25269,#25270,#25271,#25272,#25273,#25274),.UNSPECIFIED.,.F.,.F.,(4,3,3,
3,3,3,3,4),(70.4248606341475,70.8275674817882,71.8251388547711,72.8227102277541,
73.820281600737,74.8178529737199,75.8154243467029,76.7080459413271),
 .UNSPECIFIED.);
#3219=B_SPLINE_CURVE_WITH_KNOTS('',3,(#25275,#25276,#25277,#25278,#25279,
#25280,#25281,#25282,#25283,#25284,#25285,#25286,#25287,#25288,#25289,#25290,
#25291,#25292,#25293,#25294,#25295,#25296,#25297,#25298,#25299),
 .UNSPECIFIED.,.F.,.F.,(4,3,3,3,3,3,3,3,4),(-72.9614216426678,-72.8227102277541,
-71.8251388547711,-70.8275674817882,-69.8299961088053,-68.8324247358223,
-67.8348533628394,-66.8372819898565,-66.6782363354882),.UNSPECIFIED.);
#3220=B_SPLINE_CURVE_WITH_KNOTS('',3,(#25304,#25305,#25306,#25307,#25308,
#25309,#25310,#25311,#25312,#25313,#25314,#25315,#25316,#25317,#25318,#25319,
#25320,#25321,#25322,#25323,#25324,#25325),.UNSPECIFIED.,.F.,.F.,(4,3,3,
3,3,3,3,4),(64.1416753269679,64.8421392438906,65.8397106168735,66.8372819898565,
67.8348533628394,68.8324247358223,69.8299961088053,70.4248606341475),
 .UNSPECIFIED.);
#3221=B_SPLINE_CURVE_WITH_KNOTS('',3,(#25326,#25327,#25328,#25329,#25330,
#25331,#25332,#25333,#25334,#25335,#25336,#25337,#25338,#25339,#25340,#25341,
#25342,#25343,#25344,#25345,#25346,#25347),.UNSPECIFIED.,.F.,.F.,(4,3,3,
3,3,3,3,4),(-66.6782363354882,-65.8397106168736,-64.8421392438906,-63.8445678709077,
-62.8469964979247,-61.8494251249418,-60.8518537519589,-60.3950510283086),
 .UNSPECIFIED.);
#3222=B_SPLINE_CURVE_WITH_KNOTS('',3,(#25352,#25353,#25354,#25355,#25356,
#25357,#25358,#25359,#25360,#25361,#25362,#25363,#25364,#25365,#25366,#25367,
#25368,#25369,#25370,#25371,#25372,#25373),.UNSPECIFIED.,.F.,.F.,(4,3,3,
3,3,3,3,4),(57.8584900197883,58.856711005993,59.854282378976,60.8518537519589,
61.8494251249418,62.8469964979248,63.8445678709077,64.1416753269679),
 .UNSPECIFIED.);
#3223=B_SPLINE_CURVE_WITH_KNOTS('',3,(#25374,#25375,#25376,#25377,#25378,
#25379,#25380,#25381,#25382,#25383,#25384,#25385,#25386,#25387,#25388,#25389,
#25390,#25391,#25392,#25393,#25394,#25395),.UNSPECIFIED.,.F.,.F.,(4,3,3,
3,3,3,3,4),(-60.3950510283086,-59.854282378976,-58.856711005993,-57.8591396330101,
-56.8615682600272,-55.8639968870442,-54.8664255140613,-54.111865721129),
 .UNSPECIFIED.);
#3224=B_SPLINE_CURVE_WITH_KNOTS('',3,(#25400,#25401,#25402,#25403,#25404,
#25405,#25406,#25407,#25408,#25409,#25410,#25411,#25412,#25413,#25414,#25415,
#25416,#25417,#25418,#25419,#25420,#25421),.UNSPECIFIED.,.F.,.F.,(4,3,3,
3,3,3,3,4),(51.5753047126087,51.8737113951125,52.8712827680954,53.8688541410784,
54.8664255140613,55.8639968870442,56.8615682600272,57.8584900197883),
 .UNSPECIFIED.);
#3225=B_SPLINE_CURVE_WITH_KNOTS('',3,(#25422,#25423,#25424,#25425,#25426,
#25427,#25428,#25429,#25430,#25431,#25432,#25433,#25434,#25435,#25436,#25437,
#25438,#25439,#25440,#25441,#25442,#25443,#25444,#25445,#25446),
 .UNSPECIFIED.,.F.,.F.,(4,3,3,3,3,3,3,3,4),(-54.111865721129,-53.8688541410784,
-52.8712827680954,-51.8737113951125,-50.8761400221296,-49.8785686491466,
-48.8809972761637,-47.8834259031808,-47.8286804139494),.UNSPECIFIED.);
#3226=B_SPLINE_CURVE_WITH_KNOTS('',3,(#25451,#25452,#25453,#25454,#25455,
#25456,#25457,#25458,#25459,#25460,#25461,#25462,#25463,#25464,#25465,#25466,
#25467,#25468,#25469,#25470,#25471,#25472),.UNSPECIFIED.,.F.,.F.,(4,3,3,
3,3,3,3,4),(45.2921194054291,45.8882831572149,46.8858545301978,47.8834259031808,
48.8809972761637,49.8785686491466,50.8761400221296,51.5753047126087),
 .UNSPECIFIED.);
#3227=B_SPLINE_CURVE_WITH_KNOTS('',3,(#25473,#25474,#25475,#25476,#25477,
#25478,#25479,#25480,#25481,#25482,#25483,#25484,#25485,#25486,#25487,#25488,
#25489,#25490,#25491,#25492,#25493,#25494),.UNSPECIFIED.,.F.,.F.,(4,3,3,
3,3,3,3,4),(-47.8286804139494,-46.8858545301978,-45.8882831572149,-44.890711784232,
-43.893140411249,-42.8955690382661,-41.8979976652832,-41.5454951067698),
 .UNSPECIFIED.);
#3228=B_SPLINE_CURVE_WITH_KNOTS('',3,(#25499,#25500,#25501,#25502,#25503,
#25504,#25505,#25506,#25507,#25508,#25509,#25510,#25511,#25512,#25513,#25514,
#25515,#25516,#25517,#25518,#25519,#25520),.UNSPECIFIED.,.F.,.F.,(4,3,3,
3,3,3,3,4),(39.0089340982495,39.9028549193173,40.9004262923002,41.8979976652832,
42.8955690382661,43.893140411249,44.890711784232,45.2921194054291),
 .UNSPECIFIED.);
#3229=B_SPLINE_CURVE_WITH_KNOTS('',3,(#25521,#25522,#25523,#25524,#25525,
#25526,#25527,#25528,#25529,#25530,#25531,#25532,#25533,#25534,#25535,#25536,
#25537,#25538,#25539,#25540,#25541,#25542),.UNSPECIFIED.,.F.,.F.,(4,3,3,
3,3,3,3,4),(-41.5454951067698,-40.9004262923002,-39.9028549193173,-38.9052835463344,
-37.9077121733514,-36.9101408003685,-35.9125694273856,-35.2623097995902),
 .UNSPECIFIED.);
#3230=B_SPLINE_CURVE_WITH_KNOTS('',3,(#25547,#25548,#25549,#25550,#25551,
#25552,#25553,#25554,#25555,#25556,#25557,#25558,#25559,#25560,#25561,#25562,
#25563,#25564,#25565,#25566,#25567,#25568,#25569,#25570,#25571),
 .UNSPECIFIED.,.F.,.F.,(4,3,3,3,3,3,3,3,4),(32.7257487910699,32.9198553084368,
33.9174266814197,34.9149980544026,35.9125694273856,36.9101408003685,37.9077121733514,
38.9052835463344,39.0089340982495),.UNSPECIFIED.);
#3231=B_SPLINE_CURVE_WITH_KNOTS('',3,(#25572,#25573,#25574,#25575,#25576,
#25577,#25578,#25579,#25580,#25581,#25582,#25583,#25584,#25585,#25586,#25587,
#25588,#25589,#25590,#25591,#25592,#25593),.UNSPECIFIED.,.F.,.F.,(4,3,3,
3,3,3,3,4),(-35.2623097995902,-34.9149980544026,-33.9174266814197,-32.9198553084368,
-31.9222839354538,-30.9247125624709,-29.927141189488,-28.9791244924107),
 .UNSPECIFIED.);
#3232=B_SPLINE_CURVE_WITH_KNOTS('',3,(#25598,#25599,#25600,#25601,#25602,
#25603,#25604,#25605,#25606,#25607,#25608,#25609,#25610,#25611,#25612,#25613,
#25614,#25615,#25616,#25617,#25618,#25619),.UNSPECIFIED.,.F.,.F.,(4,3,3,
3,3,3,3,4),(26.4425634838903,26.9344270705392,27.9319984435221,28.9295698165051,
29.927141189488,30.9247125624709,31.9222839354538,32.7257487910699),
 .UNSPECIFIED.);
#3233=B_SPLINE_CURVE_WITH_KNOTS('',3,(#25620,#25621,#25622,#25623,#25624,
#25625,#25626,#25627,#25628,#25629,#25630,#25631,#25632,#25633,#25634,#25635,
#25636,#25637,#25638,#25639,#25640,#25641,#25642,#25643,#25644),
 .UNSPECIFIED.,.F.,.F.,(4,3,3,3,3,3,3,3,4),(-28.9791244924107,-28.929569816505,
-27.9319984435221,-26.9344270705392,-25.9368556975563,-24.9392843245733,
-23.9417129515904,-22.9441415786074,-22.6959391852311),.UNSPECIFIED.);
#3234=B_SPLINE_CURVE_WITH_KNOTS('',3,(#25649,#25650,#25651,#25652,#25653,
#25654,#25655,#25656,#25657,#25658,#25659,#25660,#25661,#25662,#25663,#25664,
#25665,#25666,#25667,#25668,#25669,#25670),.UNSPECIFIED.,.F.,.F.,(4,3,3,
3,3,3,3,4),(20.1593781767108,20.9489988326416,21.9465702056245,22.9441415786075,
23.9417129515904,24.9392843245733,25.9368556975563,26.4425634838903),
 .UNSPECIFIED.);
#3235=B_SPLINE_CURVE_WITH_KNOTS('',3,(#25671,#25672,#25673,#25674,#25675,
#25676,#25677,#25678,#25679,#25680,#25681,#25682,#25683,#25684,#25685,#25686,
#25687,#25688,#25689,#25690,#25691,#25692),.UNSPECIFIED.,.F.,.F.,(4,3,3,
3,3,3,3,4),(-22.6959391852311,-21.9465702056245,-20.9489988326416,-19.9514274596586,
-18.9538560866757,-17.9562847136928,-16.9587133407099,-16.4127538780515),
 .UNSPECIFIED.);
#3236=B_SPLINE_CURVE_WITH_KNOTS('',3,(#25697,#25698,#25699,#25700,#25701,
#25702,#25703,#25704,#25705,#25706,#25707,#25708,#25709,#25710,#25711,#25712,
#25713,#25714,#25715,#25716,#25717,#25718,#25719,#25720,#25721),
 .UNSPECIFIED.,.F.,.F.,(4,3,3,3,3,3,3,3,4),(13.8761928695312,13.9659992217611,
14.963570594744,15.9611419677269,16.9587133407099,17.9562847136928,18.9538560866757,
19.9514274596587,20.1593781767108),.UNSPECIFIED.);
#3237=B_SPLINE_CURVE_WITH_KNOTS('',3,(#25722,#25723,#25724,#25725,#25726,
#25727,#25728,#25729,#25730,#25731,#25732,#25733,#25734,#25735,#25736,#25737,
#25738,#25739,#25740,#25741,#25742,#25743),.UNSPECIFIED.,.F.,.F.,(4,3,3,
3,3,3,3,4),(-16.4127538780515,-15.9611419677269,-14.963570594744,-13.9659992217611,
-12.9684278487781,-11.9708564757952,-10.9732851028123,-10.1295685708719),
 .UNSPECIFIED.);
#3238=B_SPLINE_CURVE_WITH_KNOTS('',3,(#25749,#25750,#25751,#25752,#25753,
#25754,#25755,#25756,#25757,#25758,#25759,#25760,#25761),.UNSPECIFIED.,
 .F.,.F.,(4,3,3,3,4),(-3.8463832636923,-2.9927141189488,-1.99514274596586,
-0.997571372982932,0.),.UNSPECIFIED.);
#3239=B_SPLINE_CURVE_WITH_KNOTS('',3,(#25764,#25765,#25766,#25767,#25768,
#25769,#25770,#25771,#25772,#25773,#25774,#25775,#25776,#25777,#25778,#25779,
#25780,#25781,#25782),.UNSPECIFIED.,.F.,.F.,(4,3,3,3,3,3,4),(2.01461286527445,
2.9927141189488,3.99028549193173,4.98785686491466,5.98542823789759,6.98299961088053,
7.59300756235161),.UNSPECIFIED.);
#3240=B_SPLINE_CURVE_WITH_KNOTS('',3,(#25788,#25789,#25790,#25791,#25792,
#25793,#25794),.UNSPECIFIED.,.F.,.F.,(4,1,1,1,4),(91.106186954104,91.6672898428912,
92.6648612158741,93.6624325888571,94.66000396184),.UNSPECIFIED.);
#3241=B_SPLINE_CURVE_WITH_KNOTS('',3,(#25797,#25798,#25799,#25800,#25801,
#25802,#25803,#25804),.UNSPECIFIED.,.F.,.F.,(4,1,1,1,1,4),(91.106186954104,
91.2111367324627,92.2087081054456,93.2062794784285,94.2038508514115,95.1819521050858),
 .UNSPECIFIED.);
#3242=B_SPLINE_CURVE_WITH_KNOTS('',3,(#25809,#25810,#25811,#25812,#25813,
#25814,#25815,#25816,#25817,#25818),.UNSPECIFIED.,.F.,.F.,(4,1,1,1,1,1,
1,4),(84.8230016469244,85.6818616049936,86.6794329779765,87.6770043509595,
88.6745757239424,89.6721470969253,90.6697184699083,91.106186954104),
 .UNSPECIFIED.);
#3243=B_SPLINE_CURVE_WITH_KNOTS('',3,(#25819,#25820,#25821,#25822,#25823,
#25824,#25825,#25826,#25827,#25828),.UNSPECIFIED.,.F.,.F.,(4,1,1,1,1,1,
1,4),(84.8230016469244,85.2257084945651,86.223279867548,87.2208512405309,
88.2184226135139,89.2159939864968,90.2135653594797,91.106186954104),
 .UNSPECIFIED.);
#3244=B_SPLINE_CURVE_WITH_KNOTS('',3,(#25833,#25834,#25835,#25836,#25837,
#25838,#25839,#25840,#25841,#25842,#25843),.UNSPECIFIED.,.F.,.F.,(4,1,1,
1,1,1,1,1,4),(78.5398163397448,78.6988619941131,79.696433367096,80.6940047400789,
81.6915761130619,82.6891474860448,83.6867188590277,84.6842902320107,84.8230016469244),
 .UNSPECIFIED.);
#3245=B_SPLINE_CURVE_WITH_KNOTS('',3,(#25844,#25845,#25846,#25847,#25848,
#25849,#25850,#25851,#25852,#25853),.UNSPECIFIED.,.F.,.F.,(4,1,1,1,1,1,
1,4),(78.5398163397448,79.2402802566675,80.2378516296504,81.2354230026333,
82.2329943756163,83.2305657485992,84.2281371215821,84.8230016469244),
 .UNSPECIFIED.);
#3246=B_SPLINE_CURVE_WITH_KNOTS('',3,(#25858,#25859,#25860,#25861,#25862,
#25863,#25864,#25865,#25866,#25867),.UNSPECIFIED.,.F.,.F.,(4,1,1,1,1,1,
1,4),(72.2566310325652,72.7134337562155,73.7110051291984,74.7085765021813,
75.7061478751643,76.7037192481472,77.7012906211301,78.5398163397448),
 .UNSPECIFIED.);
#3247=B_SPLINE_CURVE_WITH_KNOTS('',3,(#25868,#25869,#25870,#25871,#25872,
#25873,#25874,#25875,#25876,#25877,#25878),.UNSPECIFIED.,.F.,.F.,(4,1,1,
1,1,1,1,1,4),(72.2566310325652,72.2572806457869,73.2548520187699,74.2524233917528,
75.2499947647357,76.2475661377187,77.2451375107016,78.2427088836845,78.5398163397448),
 .UNSPECIFIED.);
#3248=B_SPLINE_CURVE_WITH_KNOTS('',3,(#25883,#25884,#25885,#25886,#25887,
#25888,#25889,#25890,#25891,#25892),.UNSPECIFIED.,.F.,.F.,(4,1,1,1,1,1,
1,4),(65.9734457253856,66.7280055183179,67.7255768913008,68.7231482642838,
69.7207196372667,70.7182910102496,71.7158623832325,72.2566310325652),
 .UNSPECIFIED.);
#3249=B_SPLINE_CURVE_WITH_KNOTS('',3,(#25893,#25894,#25895,#25896,#25897,
#25898,#25899,#25900,#25901,#25902),.UNSPECIFIED.,.F.,.F.,(4,1,1,1,1,1,
1,4),(65.9734457253856,66.2718524078894,67.2694237808723,68.2669951538552,
69.2645665268382,70.2621378998211,71.259709272804,72.2566310325652),
 .UNSPECIFIED.);
#3250=B_SPLINE_CURVE_WITH_KNOTS('',3,(#25907,#25908,#25909,#25910,#25911,
#25912,#25913,#25914,#25915,#25916,#25917),.UNSPECIFIED.,.F.,.F.,(4,1,1,
1,1,1,1,1,4),(59.690260418206,59.7450059074374,60.7425772804203,61.7401486534032,
62.7377200263862,63.7352913993691,64.732862772352,65.730434145335,65.9734457253856),
 .UNSPECIFIED.);
#3251=B_SPLINE_CURVE_WITH_KNOTS('',3,(#25918,#25919,#25920,#25921,#25922,
#25923,#25924,#25925,#25926,#25927),.UNSPECIFIED.,.F.,.F.,(4,1,1,1,1,1,
1,4),(59.690260418206,60.2864241699918,61.2839955429747,62.2815669159576,
63.2791382889406,64.2767096619235,65.2742810349064,65.9734457253856),
 .UNSPECIFIED.);
#3252=B_SPLINE_CURVE_WITH_KNOTS('',3,(#25932,#25933,#25934,#25935,#25936,
#25937,#25938,#25939,#25940,#25941),.UNSPECIFIED.,.F.,.F.,(4,1,1,1,1,1,
1,4),(53.4070751110264,53.7595776695398,54.7571490425227,55.7547204155056,
56.7522917884886,57.7498631614715,58.7474345344544,59.690260418206),
 .UNSPECIFIED.);
#3253=B_SPLINE_CURVE_WITH_KNOTS('',3,(#25942,#25943,#25944,#25945,#25946,
#25947,#25948,#25949,#25950,#25951),.UNSPECIFIED.,.F.,.F.,(4,1,1,1,1,1,
1,4),(53.4070751110264,54.3009959320942,55.2985673050771,56.29613867806,
57.293710051043,58.2912814240259,59.2888527970088,59.690260418206),
 .UNSPECIFIED.);
#3254=B_SPLINE_CURVE_WITH_KNOTS('',3,(#25956,#25957,#25958,#25959,#25960,
#25961,#25962,#25963,#25964,#25965),.UNSPECIFIED.,.F.,.F.,(4,1,1,1,1,1,
1,4),(47.1238898038468,47.7741494316422,48.7717208046251,49.769292177608,
50.766863550591,51.7644349235739,52.7620062965568,53.4070751110264),
 .UNSPECIFIED.);
#3255=B_SPLINE_CURVE_WITH_KNOTS('',3,(#25966,#25967,#25968,#25969,#25970,
#25971,#25972,#25973,#25974,#25975,#25976),.UNSPECIFIED.,.F.,.F.,(4,1,1,
1,1,1,1,1,4),(47.1238898038468,47.3179963212136,48.3155676941966,49.3131390671795,
50.3107104401624,51.3082818131454,52.3058531861283,53.3034245591112,53.4070751110264),
 .UNSPECIFIED.);
#3256=B_SPLINE_CURVE_WITH_KNOTS('',3,(#25981,#25982,#25983,#25984,#25985,
#25986,#25987,#25988,#25989,#25990),.UNSPECIFIED.,.F.,.F.,(4,1,1,1,1,1,
1,4),(40.8407044966673,41.7887211937446,42.7862925667275,43.7838639397104,
44.7814353126934,45.7790066856763,46.7765780586592,47.1238898038468),
 .UNSPECIFIED.);
#3257=B_SPLINE_CURVE_WITH_KNOTS('',3,(#25991,#25992,#25993,#25994,#25995,
#25996,#25997,#25998,#25999,#26000),.UNSPECIFIED.,.F.,.F.,(4,1,1,1,1,1,
1,4),(40.8407044966673,41.332568083316,42.330139456299,43.3277108292819,
44.3252822022648,45.3228535752478,46.3204249482307,47.1238898038468),
 .UNSPECIFIED.);
#3258=B_SPLINE_CURVE_WITH_KNOTS('',3,(#26005,#26006,#26007,#26008,#26009,
#26010,#26011,#26012,#26013,#26014,#26015),.UNSPECIFIED.,.F.,.F.,(4,1,1,
1,1,1,1,1,4),(34.5575191894876,34.805721582864,35.803292955847,36.8008643288299,
37.7984357018128,38.7960070747958,39.7935784477787,40.7911498207616,40.8407044966673),
 .UNSPECIFIED.);
#3259=B_SPLINE_CURVE_WITH_KNOTS('',3,(#26016,#26017,#26018,#26019,#26020,
#26021,#26022,#26023,#26024,#26025),.UNSPECIFIED.,.F.,.F.,(4,1,1,1,1,1,
1,4),(34.5575191894876,35.3471398454184,36.3447112184014,37.3422825913843,
38.3398539643672,39.3374253373502,40.3349967103331,40.8407044966673),
 .UNSPECIFIED.);
#3260=B_SPLINE_CURVE_WITH_KNOTS('',3,(#26030,#26031,#26032,#26033,#26034,
#26035,#26036,#26037,#26038,#26039),.UNSPECIFIED.,.F.,.F.,(4,1,1,1,1,1,
1,4),(28.2743338823081,28.8202933449665,29.8178647179494,30.8154360909323,
31.8130074639152,32.8105788368982,33.8081502098811,34.5575191894876),
 .UNSPECIFIED.);
#3261=B_SPLINE_CURVE_WITH_KNOTS('',3,(#26040,#26041,#26042,#26043,#26044,
#26045,#26046,#26047,#26048,#26049,#26050),.UNSPECIFIED.,.F.,.F.,(4,1,1,
1,1,1,1,1,4),(28.2743338823081,28.3641402345379,29.3617116075209,30.3592829805038,
31.3568543534867,32.3544257264696,33.3519970994526,34.3495684724355,34.5575191894876),
 .UNSPECIFIED.);
#3262=B_SPLINE_CURVE_WITH_KNOTS('',3,(#26055,#26056,#26057,#26058,#26059,
#26060,#26061,#26062,#26063,#26064),.UNSPECIFIED.,.F.,.F.,(4,1,1,1,1,1,
1,4),(21.9911485751285,22.8348651070689,23.8324364800518,24.8300078530347,
25.8275792260177,26.8251505990006,27.8227219719835,28.2743338823081),
 .UNSPECIFIED.);
#3263=B_SPLINE_CURVE_WITH_KNOTS('',3,(#26065,#26066,#26067,#26068,#26069,
#26070,#26071,#26072,#26073,#26074),.UNSPECIFIED.,.F.,.F.,(4,1,1,1,1,1,
1,4),(21.9911485751285,22.3787119966403,23.3762833696233,24.3738547426062,
25.3714261155891,26.3689974885721,27.366568861555,28.2743338823081),
 .UNSPECIFIED.);
#3264=B_SPLINE_CURVE_WITH_KNOTS('',3,(#26080,#26081,#26082,#26083,#26084),
 .UNSPECIFIED.,.F.,.F.,(4,1,4),(14.3981410127769,15.3957123857598,15.7079632679489),
 .UNSPECIFIED.);
#3265=B_SPLINE_CURVE_WITH_KNOTS('',3,(#26087,#26088,#26089,#26090,#26091),
 .UNSPECIFIED.,.F.,.F.,(4,1,4),(13.8761928695311,14.8542941232054,15.7079632679489),
 .UNSPECIFIED.);
#3266=B_SPLINE_CURVE_WITH_KNOTS('',3,(#26097,#26098,#26099,#26100,#26101,
#26102,#26103,#26104,#26105,#26106,#26107,#26108,#26109,#26110,#26111,#26112,
#26113,#26114,#26115,#26116,#26117,#26118),.UNSPECIFIED.,.F.,.F.,(4,3,3,
3,3,3,3,4),(76.7080459413271,76.8129957196858,77.8105670926687,78.8081384656517,
79.8057098386346,80.8032812116175,81.8008525846005,82.7984239575834),
 .UNSPECIFIED.);
#3267=B_SPLINE_CURVE_WITH_KNOTS('',3,(#26122,#26123,#26124,#26125,#26126,
#26127,#26128),.UNSPECIFIED.,.F.,.F.,(4,3,4),(-80.783811092309,-79.8057098386346,
-79.2446069498474),.UNSPECIFIED.);
#3268=B_SPLINE_CURVE_WITH_KNOTS('',3,(#26132,#26133,#26134,#26135,#26136,
#26137,#26138,#26139,#26140,#26141,#26142,#26143,#26144,#26145,#26146,#26147,
#26148,#26149,#26150,#26151,#26152,#26153),.UNSPECIFIED.,.F.,.F.,(4,3,3,
3,3,3,3,4),(-79.2446069498474,-78.8081384656517,-77.8105670926687,-76.8129957196858,
-75.8154243467029,-74.8178529737199,-73.820281600737,-72.9614216426678),
 .UNSPECIFIED.);
#3269=B_SPLINE_CURVE_WITH_KNOTS('',3,(#26158,#26159,#26160,#26161,#26162,
#26163,#26164,#26165,#26166,#26167,#26168,#26169,#26170,#26171,#26172,#26173,
#26174,#26175,#26176,#26177,#26178,#26179),.UNSPECIFIED.,.F.,.F.,(4,3,3,
3,3,3,3,4),(70.4248606341475,70.8275674817882,71.8251388547711,72.8227102277541,
73.820281600737,74.81785297372,75.8154243467029,76.7080459413271),
 .UNSPECIFIED.);
#3270=B_SPLINE_CURVE_WITH_KNOTS('',3,(#26180,#26181,#26182,#26183,#26184,
#26185,#26186,#26187,#26188,#26189,#26190,#26191,#26192,#26193,#26194,#26195,
#26196,#26197,#26198,#26199,#26200,#26201,#26202,#26203,#26204),
 .UNSPECIFIED.,.F.,.F.,(4,3,3,3,3,3,3,3,4),(-72.9614216426678,-72.8227102277541,
-71.8251388547711,-70.8275674817882,-69.8299961088053,-68.8324247358223,
-67.8348533628394,-66.8372819898565,-66.6782363354882),.UNSPECIFIED.);
#3271=B_SPLINE_CURVE_WITH_KNOTS('',3,(#26209,#26210,#26211,#26212,#26213,
#26214,#26215,#26216,#26217,#26218,#26219,#26220,#26221,#26222,#26223,#26224,
#26225,#26226,#26227,#26228,#26229,#26230),.UNSPECIFIED.,.F.,.F.,(4,3,3,
3,3,3,3,4),(64.1416753269679,64.8421392438906,65.8397106168735,66.8372819898565,
67.8348533628394,68.8324247358223,69.8299961088053,70.4248606341475),
 .UNSPECIFIED.);
#3272=B_SPLINE_CURVE_WITH_KNOTS('',3,(#26231,#26232,#26233,#26234,#26235,
#26236,#26237,#26238,#26239,#26240,#26241,#26242,#26243,#26244,#26245,#26246,
#26247,#26248,#26249,#26250,#26251,#26252),.UNSPECIFIED.,.F.,.F.,(4,3,3,
3,3,3,3,4),(-66.6782363354882,-65.8397106168736,-64.8421392438906,-63.8445678709077,
-62.8469964979248,-61.8494251249418,-60.8518537519589,-60.3950510283086),
 .UNSPECIFIED.);
#3273=B_SPLINE_CURVE_WITH_KNOTS('',3,(#26257,#26258,#26259,#26260,#26261,
#26262,#26263,#26264,#26265,#26266,#26267,#26268,#26269,#26270,#26271,#26272,
#26273,#26274,#26275,#26276,#26277,#26278),.UNSPECIFIED.,.F.,.F.,(4,3,3,
3,3,3,3,4),(57.8584900197883,58.856711005993,59.854282378976,60.8518537519589,
61.8494251249418,62.8469964979247,63.8445678709077,64.1416753269679),
 .UNSPECIFIED.);
#3274=B_SPLINE_CURVE_WITH_KNOTS('',3,(#26279,#26280,#26281,#26282,#26283,
#26284,#26285,#26286,#26287,#26288,#26289,#26290,#26291,#26292,#26293,#26294,
#26295,#26296,#26297,#26298,#26299,#26300),.UNSPECIFIED.,.F.,.F.,(4,3,3,
3,3,3,3,4),(-60.3950510283086,-59.854282378976,-58.856711005993,-57.8591396330101,
-56.8615682600272,-55.8639968870442,-54.8664255140613,-54.111865721129),
 .UNSPECIFIED.);
#3275=B_SPLINE_CURVE_WITH_KNOTS('',3,(#26305,#26306,#26307,#26308,#26309,
#26310,#26311,#26312,#26313,#26314,#26315,#26316,#26317,#26318,#26319,#26320,
#26321,#26322,#26323,#26324,#26325,#26326),.UNSPECIFIED.,.F.,.F.,(4,3,3,
3,3,3,3,4),(51.5753047126087,51.8737113951125,52.8712827680954,53.8688541410784,
54.8664255140613,55.8639968870442,56.8615682600272,57.8584900197883),
 .UNSPECIFIED.);
#3276=B_SPLINE_CURVE_WITH_KNOTS('',3,(#26327,#26328,#26329,#26330,#26331,
#26332,#26333,#26334,#26335,#26336,#26337,#26338,#26339,#26340,#26341,#26342,
#26343,#26344,#26345,#26346,#26347,#26348,#26349,#26350,#26351),
 .UNSPECIFIED.,.F.,.F.,(4,3,3,3,3,3,3,3,4),(-54.111865721129,-53.8688541410784,
-52.8712827680954,-51.8737113951125,-50.8761400221296,-49.8785686491466,
-48.8809972761637,-47.8834259031808,-47.8286804139494),.UNSPECIFIED.);
#3277=B_SPLINE_CURVE_WITH_KNOTS('',3,(#26356,#26357,#26358,#26359,#26360,
#26361,#26362,#26363,#26364,#26365,#26366,#26367,#26368,#26369,#26370,#26371,
#26372,#26373,#26374,#26375,#26376,#26377),.UNSPECIFIED.,.F.,.F.,(4,3,3,
3,3,3,3,4),(45.2921194054291,45.8882831572149,46.8858545301978,47.8834259031808,
48.8809972761637,49.8785686491466,50.8761400221296,51.5753047126087),
 .UNSPECIFIED.);
#3278=B_SPLINE_CURVE_WITH_KNOTS('',3,(#26378,#26379,#26380,#26381,#26382,
#26383,#26384,#26385,#26386,#26387,#26388,#26389,#26390,#26391,#26392,#26393,
#26394,#26395,#26396,#26397,#26398,#26399),.UNSPECIFIED.,.F.,.F.,(4,3,3,
3,3,3,3,4),(-47.8286804139494,-46.8858545301978,-45.8882831572149,-44.890711784232,
-43.893140411249,-42.8955690382661,-41.8979976652832,-41.5454951067698),
 .UNSPECIFIED.);
#3279=B_SPLINE_CURVE_WITH_KNOTS('',3,(#26404,#26405,#26406,#26407,#26408,
#26409,#26410,#26411,#26412,#26413,#26414,#26415,#26416,#26417,#26418,#26419,
#26420,#26421,#26422,#26423,#26424,#26425),.UNSPECIFIED.,.F.,.F.,(4,3,3,
3,3,3,3,4),(39.0089340982495,39.9028549193173,40.9004262923002,41.8979976652832,
42.8955690382661,43.893140411249,44.890711784232,45.2921194054291),
 .UNSPECIFIED.);
#3280=B_SPLINE_CURVE_WITH_KNOTS('',3,(#26426,#26427,#26428,#26429,#26430,
#26431,#26432,#26433,#26434,#26435,#26436,#26437,#26438,#26439,#26440,#26441,
#26442,#26443,#26444,#26445,#26446,#26447),.UNSPECIFIED.,.F.,.F.,(4,3,3,
3,3,3,3,4),(-41.5454951067698,-40.9004262923002,-39.9028549193173,-38.9052835463344,
-37.9077121733514,-36.9101408003685,-35.9125694273856,-35.2623097995902),
 .UNSPECIFIED.);
#3281=B_SPLINE_CURVE_WITH_KNOTS('',3,(#26452,#26453,#26454,#26455,#26456,
#26457,#26458,#26459,#26460,#26461,#26462,#26463,#26464,#26465,#26466,#26467,
#26468,#26469,#26470,#26471,#26472,#26473,#26474,#26475,#26476),
 .UNSPECIFIED.,.F.,.F.,(4,3,3,3,3,3,3,3,4),(32.7257487910699,32.9198553084368,
33.9174266814197,34.9149980544026,35.9125694273856,36.9101408003685,37.9077121733514,
38.9052835463344,39.0089340982495),.UNSPECIFIED.);
#3282=B_SPLINE_CURVE_WITH_KNOTS('',3,(#26477,#26478,#26479,#26480,#26481,
#26482,#26483,#26484,#26485,#26486,#26487,#26488,#26489,#26490,#26491,#26492,
#26493,#26494,#26495,#26496,#26497,#26498),.UNSPECIFIED.,.F.,.F.,(4,3,3,
3,3,3,3,4),(-35.2623097995902,-34.9149980544026,-33.9174266814197,-32.9198553084368,
-31.9222839354538,-30.9247125624709,-29.927141189488,-28.9791244924107),
 .UNSPECIFIED.);
#3283=B_SPLINE_CURVE_WITH_KNOTS('',3,(#26503,#26504,#26505,#26506,#26507,
#26508,#26509,#26510,#26511,#26512,#26513,#26514,#26515,#26516,#26517,#26518,
#26519,#26520,#26521,#26522,#26523,#26524),.UNSPECIFIED.,.F.,.F.,(4,3,3,
3,3,3,3,4),(26.4425634838903,26.9344270705392,27.9319984435221,28.929569816505,
29.927141189488,30.9247125624709,31.9222839354538,32.7257487910699),
 .UNSPECIFIED.);
#3284=B_SPLINE_CURVE_WITH_KNOTS('',3,(#26525,#26526,#26527,#26528,#26529,
#26530,#26531,#26532,#26533,#26534,#26535,#26536,#26537,#26538,#26539,#26540,
#26541,#26542,#26543,#26544,#26545,#26546,#26547,#26548,#26549),
 .UNSPECIFIED.,.F.,.F.,(4,3,3,3,3,3,3,3,4),(-28.9791244924107,-28.929569816505,
-27.9319984435221,-26.9344270705392,-25.9368556975563,-24.9392843245733,
-23.9417129515904,-22.9441415786074,-22.6959391852311),.UNSPECIFIED.);
#3285=B_SPLINE_CURVE_WITH_KNOTS('',3,(#26554,#26555,#26556,#26557,#26558,
#26559,#26560,#26561,#26562,#26563,#26564,#26565,#26566,#26567,#26568,#26569,
#26570,#26571,#26572,#26573,#26574,#26575),.UNSPECIFIED.,.F.,.F.,(4,3,3,
3,3,3,3,4),(20.1593781767108,20.9489988326416,21.9465702056245,22.9441415786074,
23.9417129515904,24.9392843245733,25.9368556975562,26.4425634838903),
 .UNSPECIFIED.);
#3286=B_SPLINE_CURVE_WITH_KNOTS('',3,(#26576,#26577,#26578,#26579,#26580,
#26581,#26582,#26583,#26584,#26585,#26586,#26587,#26588,#26589,#26590,#26591,
#26592,#26593,#26594,#26595,#26596,#26597),.UNSPECIFIED.,.F.,.F.,(4,3,3,
3,3,3,3,4),(-22.6959391852311,-21.9465702056245,-20.9489988326416,-19.9514274596586,
-18.9538560866757,-17.9562847136928,-16.9587133407099,-16.4127538780515),
 .UNSPECIFIED.);
#3287=B_SPLINE_CURVE_WITH_KNOTS('',3,(#26602,#26603,#26604,#26605,#26606,
#26607,#26608,#26609,#26610,#26611,#26612,#26613,#26614,#26615,#26616,#26617,
#26618,#26619,#26620,#26621,#26622,#26623,#26624,#26625,#26626),
 .UNSPECIFIED.,.F.,.F.,(4,3,3,3,3,3,3,3,4),(13.8761928695312,13.9659992217611,
14.963570594744,15.9611419677269,16.9587133407099,17.9562847136928,18.9538560866757,
19.9514274596587,20.1593781767108),.UNSPECIFIED.);
#3288=B_SPLINE_CURVE_WITH_KNOTS('',3,(#26627,#26628,#26629,#26630,#26631,
#26632,#26633,#26634,#26635,#26636,#26637,#26638,#26639,#26640,#26641,#26642,
#26643,#26644,#26645,#26646,#26647,#26648),.UNSPECIFIED.,.F.,.F.,(4,3,3,
3,3,3,3,4),(-16.4127538780515,-15.9611419677269,-14.963570594744,-13.9659992217611,
-12.9684278487781,-11.9708564757952,-10.9732851028123,-10.1295685708719),
 .UNSPECIFIED.);
#3289=B_SPLINE_CURVE_WITH_KNOTS('',3,(#26654,#26655,#26656,#26657,#26658,
#26659,#26660,#26661,#26662,#26663,#26664,#26665,#26666),.UNSPECIFIED.,
 .F.,.F.,(4,3,3,3,4),(-3.8463832636923,-2.99271411894879,-1.99514274596586,
-0.997571372982931,0.),.UNSPECIFIED.);
#3290=B_SPLINE_CURVE_WITH_KNOTS('',3,(#26669,#26670,#26671,#26672,#26673,
#26674,#26675,#26676,#26677,#26678,#26679,#26680,#26681,#26682,#26683,#26684,
#26685,#26686,#26687),.UNSPECIFIED.,.F.,.F.,(4,3,3,3,3,3,4),(2.01461286527429,
2.99271411894879,3.99028549193173,4.98785686491466,5.9854282378976,6.98299961088053,
7.59300756235157),.UNSPECIFIED.);
#3291=B_SPLINE_CURVE_WITH_KNOTS('',3,(#26693,#26694,#26695,#26696,#26697,
#26698,#26699),.UNSPECIFIED.,.F.,.F.,(4,1,1,1,4),(91.106186954104,91.6672898428912,
92.6648612158741,93.6624325888571,94.66000396184),.UNSPECIFIED.);
#3292=B_SPLINE_CURVE_WITH_KNOTS('',3,(#26702,#26703,#26704,#26705,#26706,
#26707,#26708,#26709),.UNSPECIFIED.,.F.,.F.,(4,1,1,1,1,4),(91.106186954104,
91.2111367324627,92.2087081054456,93.2062794784285,94.2038508514115,95.1819521050858),
 .UNSPECIFIED.);
#3293=B_SPLINE_CURVE_WITH_KNOTS('',3,(#26714,#26715,#26716,#26717,#26718,
#26719,#26720,#26721,#26722,#26723),.UNSPECIFIED.,.F.,.F.,(4,1,1,1,1,1,
1,4),(84.8230016469244,85.6818616049936,86.6794329779765,87.6770043509595,
88.6745757239424,89.6721470969253,90.6697184699083,91.106186954104),
 .UNSPECIFIED.);
#3294=B_SPLINE_CURVE_WITH_KNOTS('',3,(#26724,#26725,#26726,#26727,#26728,
#26729,#26730,#26731,#26732,#26733),.UNSPECIFIED.,.F.,.F.,(4,1,1,1,1,1,
1,4),(84.8230016469244,85.2257084945651,86.223279867548,87.2208512405309,
88.2184226135139,89.2159939864968,90.2135653594797,91.106186954104),
 .UNSPECIFIED.);
#3295=B_SPLINE_CURVE_WITH_KNOTS('',3,(#26738,#26739,#26740,#26741,#26742,
#26743,#26744,#26745,#26746,#26747,#26748),.UNSPECIFIED.,.F.,.F.,(4,1,1,
1,1,1,1,1,4),(78.5398163397448,78.6988619941131,79.696433367096,80.6940047400789,
81.6915761130619,82.6891474860448,83.6867188590277,84.6842902320107,84.8230016469244),
 .UNSPECIFIED.);
#3296=B_SPLINE_CURVE_WITH_KNOTS('',3,(#26749,#26750,#26751,#26752,#26753,
#26754,#26755,#26756,#26757,#26758),.UNSPECIFIED.,.F.,.F.,(4,1,1,1,1,1,
1,4),(78.5398163397448,79.2402802566675,80.2378516296504,81.2354230026333,
82.2329943756163,83.2305657485992,84.2281371215821,84.8230016469244),
 .UNSPECIFIED.);
#3297=B_SPLINE_CURVE_WITH_KNOTS('',3,(#26763,#26764,#26765,#26766,#26767,
#26768,#26769,#26770,#26771,#26772),.UNSPECIFIED.,.F.,.F.,(4,1,1,1,1,1,
1,4),(72.2566310325652,72.7134337562155,73.7110051291984,74.7085765021813,
75.7061478751643,76.7037192481472,77.7012906211301,78.5398163397448),
 .UNSPECIFIED.);
#3298=B_SPLINE_CURVE_WITH_KNOTS('',3,(#26773,#26774,#26775,#26776,#26777,
#26778,#26779,#26780,#26781,#26782,#26783),.UNSPECIFIED.,.F.,.F.,(4,1,1,
1,1,1,1,1,4),(72.2566310325652,72.2572806457869,73.2548520187699,74.2524233917528,
75.2499947647357,76.2475661377187,77.2451375107016,78.2427088836845,78.5398163397448),
 .UNSPECIFIED.);
#3299=B_SPLINE_CURVE_WITH_KNOTS('',3,(#26788,#26789,#26790,#26791,#26792,
#26793,#26794,#26795,#26796,#26797),.UNSPECIFIED.,.F.,.F.,(4,1,1,1,1,1,
1,4),(65.9734457253856,66.7280055183179,67.7255768913008,68.7231482642838,
69.7207196372667,70.7182910102496,71.7158623832325,72.2566310325652),
 .UNSPECIFIED.);
#3300=B_SPLINE_CURVE_WITH_KNOTS('',3,(#26798,#26799,#26800,#26801,#26802,
#26803,#26804,#26805,#26806,#26807),.UNSPECIFIED.,.F.,.F.,(4,1,1,1,1,1,
1,4),(65.9734457253856,66.2718524078894,67.2694237808723,68.2669951538552,
69.2645665268382,70.2621378998211,71.259709272804,72.2566310325652),
 .UNSPECIFIED.);
#3301=B_SPLINE_CURVE_WITH_KNOTS('',3,(#26812,#26813,#26814,#26815,#26816,
#26817,#26818,#26819,#26820,#26821,#26822),.UNSPECIFIED.,.F.,.F.,(4,1,1,
1,1,1,1,1,4),(59.690260418206,59.7450059074374,60.7425772804203,61.7401486534032,
62.7377200263862,63.7352913993691,64.732862772352,65.730434145335,65.9734457253856),
 .UNSPECIFIED.);
#3302=B_SPLINE_CURVE_WITH_KNOTS('',3,(#26823,#26824,#26825,#26826,#26827,
#26828,#26829,#26830,#26831,#26832),.UNSPECIFIED.,.F.,.F.,(4,1,1,1,1,1,
1,4),(59.690260418206,60.2864241699918,61.2839955429747,62.2815669159576,
63.2791382889406,64.2767096619235,65.2742810349064,65.9734457253856),
 .UNSPECIFIED.);
#3303=B_SPLINE_CURVE_WITH_KNOTS('',3,(#26837,#26838,#26839,#26840,#26841,
#26842,#26843,#26844,#26845,#26846),.UNSPECIFIED.,.F.,.F.,(4,1,1,1,1,1,
1,4),(53.4070751110264,53.7595776695398,54.7571490425227,55.7547204155056,
56.7522917884886,57.7498631614715,58.7474345344544,59.690260418206),
 .UNSPECIFIED.);
#3304=B_SPLINE_CURVE_WITH_KNOTS('',3,(#26847,#26848,#26849,#26850,#26851,
#26852,#26853,#26854,#26855,#26856),.UNSPECIFIED.,.F.,.F.,(4,1,1,1,1,1,
1,4),(53.4070751110264,54.3009959320942,55.2985673050771,56.29613867806,
57.293710051043,58.2912814240259,59.2888527970088,59.690260418206),
 .UNSPECIFIED.);
#3305=B_SPLINE_CURVE_WITH_KNOTS('',3,(#26861,#26862,#26863,#26864,#26865,
#26866,#26867,#26868,#26869,#26870),.UNSPECIFIED.,.F.,.F.,(4,1,1,1,1,1,
1,4),(47.1238898038469,47.7741494316422,48.7717208046251,49.769292177608,
50.766863550591,51.7644349235739,52.7620062965568,53.4070751110264),
 .UNSPECIFIED.);
#3306=B_SPLINE_CURVE_WITH_KNOTS('',3,(#26871,#26872,#26873,#26874,#26875,
#26876,#26877,#26878,#26879,#26880,#26881),.UNSPECIFIED.,.F.,.F.,(4,1,1,
1,1,1,1,1,4),(47.1238898038468,47.3179963212136,48.3155676941966,49.3131390671795,
50.3107104401624,51.3082818131454,52.3058531861283,53.3034245591112,53.4070751110264),
 .UNSPECIFIED.);
#3307=B_SPLINE_CURVE_WITH_KNOTS('',3,(#26886,#26887,#26888,#26889,#26890,
#26891,#26892,#26893,#26894,#26895),.UNSPECIFIED.,.F.,.F.,(4,1,1,1,1,1,
1,4),(40.8407044966673,41.7887211937446,42.7862925667275,43.7838639397104,
44.7814353126934,45.7790066856763,46.7765780586592,47.1238898038469),
 .UNSPECIFIED.);
#3308=B_SPLINE_CURVE_WITH_KNOTS('',3,(#26896,#26897,#26898,#26899,#26900,
#26901,#26902,#26903,#26904,#26905),.UNSPECIFIED.,.F.,.F.,(4,1,1,1,1,1,
1,4),(40.8407044966673,41.332568083316,42.330139456299,43.3277108292819,
44.3252822022648,45.3228535752478,46.3204249482307,47.1238898038468),
 .UNSPECIFIED.);
#3309=B_SPLINE_CURVE_WITH_KNOTS('',3,(#26910,#26911,#26912,#26913,#26914,
#26915,#26916,#26917,#26918,#26919,#26920),.UNSPECIFIED.,.F.,.F.,(4,1,1,
1,1,1,1,1,4),(34.5575191894877,34.805721582864,35.803292955847,36.8008643288299,
37.7984357018128,38.7960070747958,39.7935784477787,40.7911498207616,40.8407044966673),
 .UNSPECIFIED.);
#3310=B_SPLINE_CURVE_WITH_KNOTS('',3,(#26921,#26922,#26923,#26924,#26925,
#26926,#26927,#26928,#26929,#26930),.UNSPECIFIED.,.F.,.F.,(4,1,1,1,1,1,
1,4),(34.5575191894876,35.3471398454184,36.3447112184014,37.3422825913843,
38.3398539643673,39.3374253373502,40.3349967103331,40.8407044966673),
 .UNSPECIFIED.);
#3311=B_SPLINE_CURVE_WITH_KNOTS('',3,(#26935,#26936,#26937,#26938,#26939,
#26940,#26941,#26942,#26943,#26944),.UNSPECIFIED.,.F.,.F.,(4,1,1,1,1,1,
1,4),(28.2743338823081,28.8202933449664,29.8178647179494,30.8154360909323,
31.8130074639152,32.8105788368982,33.8081502098811,34.5575191894877),
 .UNSPECIFIED.);
#3312=B_SPLINE_CURVE_WITH_KNOTS('',3,(#26945,#26946,#26947,#26948,#26949,
#26950,#26951,#26952,#26953,#26954,#26955),.UNSPECIFIED.,.F.,.F.,(4,1,1,
1,1,1,1,1,4),(28.2743338823081,28.3641402345379,29.3617116075209,30.3592829805038,
31.3568543534867,32.3544257264696,33.3519970994526,34.3495684724355,34.5575191894876),
 .UNSPECIFIED.);
#3313=B_SPLINE_CURVE_WITH_KNOTS('',3,(#26960,#26961,#26962,#26963,#26964,
#26965,#26966,#26967,#26968,#26969),.UNSPECIFIED.,.F.,.F.,(4,1,1,1,1,1,
1,4),(21.9911485751285,22.8348651070689,23.8324364800518,24.8300078530347,
25.8275792260177,26.8251505990006,27.8227219719835,28.2743338823081),
 .UNSPECIFIED.);
#3314=B_SPLINE_CURVE_WITH_KNOTS('',3,(#26970,#26971,#26972,#26973,#26974,
#26975,#26976,#26977,#26978,#26979),.UNSPECIFIED.,.F.,.F.,(4,1,1,1,1,1,
1,4),(21.9911485751285,22.3787119966403,23.3762833696233,24.3738547426062,
25.3714261155891,26.3689974885721,27.366568861555,28.2743338823081),
 .UNSPECIFIED.);
#3315=B_SPLINE_CURVE_WITH_KNOTS('',3,(#26985,#26986,#26987,#26988,#26989),
 .UNSPECIFIED.,.F.,.F.,(4,1,4),(14.3981410127769,15.3957123857598,15.7079632679489),
 .UNSPECIFIED.);
#3316=B_SPLINE_CURVE_WITH_KNOTS('',3,(#26992,#26993,#26994,#26995,#26996),
 .UNSPECIFIED.,.F.,.F.,(4,1,4),(13.8761928695311,14.8542941232054,15.7079632679489),
 .UNSPECIFIED.);
#3317=B_SPLINE_CURVE_WITH_KNOTS('',3,(#27002,#27003,#27004,#27005,#27006,
#27007,#27008,#27009,#27010,#27011,#27012,#27013,#27014,#27015,#27016,#27017,
#27018,#27019,#27020,#27021,#27022,#27023),.UNSPECIFIED.,.F.,.F.,(4,3,3,
3,3,3,3,4),(76.708045941327,76.8129957196858,77.8105670926687,78.8081384656517,
79.8057098386346,80.8032812116175,81.8008525846005,82.7984239575834),
 .UNSPECIFIED.);
#3318=B_SPLINE_CURVE_WITH_KNOTS('',3,(#27027,#27028,#27029,#27030,#27031,
#27032,#27033),.UNSPECIFIED.,.F.,.F.,(4,3,4),(-80.7838110923089,-79.8057098386346,
-79.2446069498474),.UNSPECIFIED.);
#3319=B_SPLINE_CURVE_WITH_KNOTS('',3,(#27037,#27038,#27039,#27040,#27041,
#27042,#27043,#27044,#27045,#27046,#27047,#27048,#27049,#27050,#27051,#27052,
#27053,#27054,#27055,#27056,#27057,#27058),.UNSPECIFIED.,.F.,.F.,(4,3,3,
3,3,3,3,4),(-79.2446069498474,-78.8081384656517,-77.8105670926687,-76.8129957196858,
-75.8154243467029,-74.8178529737199,-73.820281600737,-72.9614216426678),
 .UNSPECIFIED.);
#3320=B_SPLINE_CURVE_WITH_KNOTS('',3,(#27063,#27064,#27065,#27066,#27067,
#27068,#27069,#27070,#27071,#27072,#27073,#27074,#27075,#27076,#27077,#27078,
#27079,#27080,#27081,#27082,#27083,#27084),.UNSPECIFIED.,.F.,.F.,(4,3,3,
3,3,3,3,4),(70.4248606341474,70.8275674817882,71.8251388547711,72.8227102277541,
73.820281600737,74.8178529737199,75.8154243467029,76.708045941327),
 .UNSPECIFIED.);
#3321=B_SPLINE_CURVE_WITH_KNOTS('',3,(#27085,#27086,#27087,#27088,#27089,
#27090,#27091,#27092,#27093,#27094,#27095,#27096,#27097,#27098,#27099,#27100,
#27101,#27102,#27103,#27104,#27105,#27106,#27107,#27108,#27109),
 .UNSPECIFIED.,.F.,.F.,(4,3,3,3,3,3,3,3,4),(-72.9614216426678,-72.8227102277541,
-71.8251388547712,-70.8275674817882,-69.8299961088053,-68.8324247358223,
-67.8348533628394,-66.8372819898565,-66.6782363354882),.UNSPECIFIED.);
#3322=B_SPLINE_CURVE_WITH_KNOTS('',3,(#27114,#27115,#27116,#27117,#27118,
#27119,#27120,#27121,#27122,#27123,#27124,#27125,#27126,#27127,#27128,#27129,
#27130,#27131,#27132,#27133,#27134,#27135),.UNSPECIFIED.,.F.,.F.,(4,3,3,
3,3,3,3,4),(64.1416753269678,64.8421392438906,65.8397106168735,66.8372819898565,
67.8348533628394,68.8324247358223,69.8299961088053,70.4248606341474),
 .UNSPECIFIED.);
#3323=B_SPLINE_CURVE_WITH_KNOTS('',3,(#27136,#27137,#27138,#27139,#27140,
#27141,#27142,#27143,#27144,#27145,#27146,#27147,#27148,#27149,#27150,#27151,
#27152,#27153,#27154,#27155,#27156,#27157),.UNSPECIFIED.,.F.,.F.,(4,3,3,
3,3,3,3,4),(-66.6782363354882,-65.8397106168735,-64.8421392438906,-63.8445678709077,
-62.8469964979248,-61.8494251249418,-60.8518537519589,-60.3950510283086),
 .UNSPECIFIED.);
#3324=B_SPLINE_CURVE_WITH_KNOTS('',3,(#27162,#27163,#27164,#27165,#27166,
#27167,#27168,#27169,#27170,#27171,#27172,#27173,#27174,#27175,#27176,#27177,
#27178,#27179,#27180,#27181,#27182,#27183),.UNSPECIFIED.,.F.,.F.,(4,3,3,
3,3,3,3,4),(57.8584900197882,58.856711005993,59.854282378976,60.8518537519589,
61.8494251249418,62.8469964979247,63.8445678709077,64.1416753269678),
 .UNSPECIFIED.);
#3325=B_SPLINE_CURVE_WITH_KNOTS('',3,(#27184,#27185,#27186,#27187,#27188,
#27189,#27190,#27191,#27192,#27193,#27194,#27195,#27196,#27197,#27198,#27199,
#27200,#27201,#27202,#27203,#27204,#27205),.UNSPECIFIED.,.F.,.F.,(4,3,3,
3,3,3,3,4),(-60.3950510283086,-59.854282378976,-58.856711005993,-57.8591396330101,
-56.8615682600271,-55.8639968870442,-54.8664255140613,-54.111865721129),
 .UNSPECIFIED.);
#3326=B_SPLINE_CURVE_WITH_KNOTS('',3,(#27210,#27211,#27212,#27213,#27214,
#27215,#27216,#27217,#27218,#27219,#27220,#27221,#27222,#27223,#27224,#27225,
#27226,#27227,#27228,#27229,#27230,#27231),.UNSPECIFIED.,.F.,.F.,(4,3,3,
3,3,3,3,4),(51.5753047126087,51.8737113951125,52.8712827680954,53.8688541410784,
54.8664255140613,55.8639968870442,56.8615682600272,57.8584900197882),
 .UNSPECIFIED.);
#3327=B_SPLINE_CURVE_WITH_KNOTS('',3,(#27232,#27233,#27234,#27235,#27236,
#27237,#27238,#27239,#27240,#27241,#27242,#27243,#27244,#27245,#27246,#27247,
#27248,#27249,#27250,#27251,#27252,#27253,#27254,#27255,#27256),
 .UNSPECIFIED.,.F.,.F.,(4,3,3,3,3,3,3,3,4),(-54.111865721129,-53.8688541410783,
-52.8712827680954,-51.8737113951125,-50.8761400221296,-49.8785686491466,
-48.8809972761637,-47.8834259031808,-47.8286804139494),.UNSPECIFIED.);
#3328=B_SPLINE_CURVE_WITH_KNOTS('',3,(#27261,#27262,#27263,#27264,#27265,
#27266,#27267,#27268,#27269,#27270,#27271,#27272,#27273,#27274,#27275,#27276,
#27277,#27278,#27279,#27280,#27281,#27282),.UNSPECIFIED.,.F.,.F.,(4,3,3,
3,3,3,3,4),(45.2921194054291,45.8882831572149,46.8858545301978,47.8834259031808,
48.8809972761637,49.8785686491466,50.8761400221296,51.5753047126087),
 .UNSPECIFIED.);
#3329=B_SPLINE_CURVE_WITH_KNOTS('',3,(#27283,#27284,#27285,#27286,#27287,
#27288,#27289,#27290,#27291,#27292,#27293,#27294,#27295,#27296,#27297,#27298,
#27299,#27300,#27301,#27302,#27303,#27304),.UNSPECIFIED.,.F.,.F.,(4,3,3,
3,3,3,3,4),(-47.8286804139494,-46.8858545301978,-45.8882831572149,-44.890711784232,
-43.893140411249,-42.8955690382661,-41.8979976652832,-41.5454951067698),
 .UNSPECIFIED.);
#3330=B_SPLINE_CURVE_WITH_KNOTS('',3,(#27309,#27310,#27311,#27312,#27313,
#27314,#27315,#27316,#27317,#27318,#27319,#27320,#27321,#27322,#27323,#27324,
#27325,#27326,#27327,#27328,#27329,#27330),.UNSPECIFIED.,.F.,.F.,(4,3,3,
3,3,3,3,4),(39.0089340982495,39.9028549193173,40.9004262923002,41.8979976652832,
42.8955690382661,43.893140411249,44.890711784232,45.2921194054291),
 .UNSPECIFIED.);
#3331=B_SPLINE_CURVE_WITH_KNOTS('',3,(#27331,#27332,#27333,#27334,#27335,
#27336,#27337,#27338,#27339,#27340,#27341,#27342,#27343,#27344,#27345,#27346,
#27347,#27348,#27349,#27350,#27351,#27352),.UNSPECIFIED.,.F.,.F.,(4,3,3,
3,3,3,3,4),(-41.5454951067698,-40.9004262923002,-39.9028549193173,-38.9052835463344,
-37.9077121733514,-36.9101408003685,-35.9125694273856,-35.2623097995902),
 .UNSPECIFIED.);
#3332=B_SPLINE_CURVE_WITH_KNOTS('',3,(#27357,#27358,#27359,#27360,#27361,
#27362,#27363,#27364,#27365,#27366,#27367,#27368,#27369,#27370,#27371,#27372,
#27373,#27374,#27375,#27376,#27377,#27378,#27379,#27380,#27381),
 .UNSPECIFIED.,.F.,.F.,(4,3,3,3,3,3,3,3,4),(32.7257487910699,32.9198553084368,
33.9174266814197,34.9149980544026,35.9125694273856,36.9101408003685,37.9077121733514,
38.9052835463344,39.0089340982495),.UNSPECIFIED.);
#3333=B_SPLINE_CURVE_WITH_KNOTS('',3,(#27382,#27383,#27384,#27385,#27386,
#27387,#27388,#27389,#27390,#27391,#27392,#27393,#27394,#27395,#27396,#27397,
#27398,#27399,#27400,#27401,#27402,#27403),.UNSPECIFIED.,.F.,.F.,(4,3,3,
3,3,3,3,4),(-35.2623097995902,-34.9149980544026,-33.9174266814197,-32.9198553084368,
-31.9222839354538,-30.9247125624709,-29.927141189488,-28.9791244924106),
 .UNSPECIFIED.);
#3334=B_SPLINE_CURVE_WITH_KNOTS('',3,(#27408,#27409,#27410,#27411,#27412,
#27413,#27414,#27415,#27416,#27417,#27418,#27419,#27420,#27421,#27422,#27423,
#27424,#27425,#27426,#27427,#27428,#27429),.UNSPECIFIED.,.F.,.F.,(4,3,3,
3,3,3,3,4),(26.4425634838903,26.9344270705392,27.9319984435221,28.929569816505,
29.927141189488,30.9247125624709,31.9222839354538,32.7257487910699),
 .UNSPECIFIED.);
#3335=B_SPLINE_CURVE_WITH_KNOTS('',3,(#27430,#27431,#27432,#27433,#27434,
#27435,#27436,#27437,#27438,#27439,#27440,#27441,#27442,#27443,#27444,#27445,
#27446,#27447,#27448,#27449,#27450,#27451,#27452,#27453,#27454),
 .UNSPECIFIED.,.F.,.F.,(4,3,3,3,3,3,3,3,4),(-28.9791244924106,-28.929569816505,
-27.9319984435221,-26.9344270705392,-25.9368556975563,-24.9392843245733,
-23.9417129515904,-22.9441415786074,-22.695939185231),.UNSPECIFIED.);
#3336=B_SPLINE_CURVE_WITH_KNOTS('',3,(#27459,#27460,#27461,#27462,#27463,
#27464,#27465,#27466,#27467,#27468,#27469,#27470,#27471,#27472,#27473,#27474,
#27475,#27476,#27477,#27478,#27479,#27480),.UNSPECIFIED.,.F.,.F.,(4,3,3,
3,3,3,3,4),(20.1593781767107,20.9489988326416,21.9465702056245,22.9441415786074,
23.9417129515904,24.9392843245733,25.9368556975563,26.4425634838903),
 .UNSPECIFIED.);
#3337=B_SPLINE_CURVE_WITH_KNOTS('',3,(#27481,#27482,#27483,#27484,#27485,
#27486,#27487,#27488,#27489,#27490,#27491,#27492,#27493,#27494,#27495,#27496,
#27497,#27498,#27499,#27500,#27501,#27502),.UNSPECIFIED.,.F.,.F.,(4,3,3,
3,3,3,3,4),(-22.695939185231,-21.9465702056245,-20.9489988326416,-19.9514274596586,
-18.9538560866757,-17.9562847136928,-16.9587133407099,-16.4127538780514),
 .UNSPECIFIED.);
#3338=B_SPLINE_CURVE_WITH_KNOTS('',3,(#27507,#27508,#27509,#27510,#27511,
#27512,#27513,#27514,#27515,#27516,#27517,#27518,#27519,#27520,#27521,#27522,
#27523,#27524,#27525,#27526,#27527,#27528,#27529,#27530,#27531),
 .UNSPECIFIED.,.F.,.F.,(4,3,3,3,3,3,3,3,4),(13.8761928695311,13.9659992217611,
14.963570594744,15.9611419677269,16.9587133407099,17.9562847136928,18.9538560866757,
19.9514274596586,20.1593781767107),.UNSPECIFIED.);
#3339=B_SPLINE_CURVE_WITH_KNOTS('',3,(#27532,#27533,#27534,#27535,#27536,
#27537,#27538,#27539,#27540,#27541,#27542,#27543,#27544,#27545,#27546,#27547,
#27548,#27549,#27550,#27551,#27552,#27553),.UNSPECIFIED.,.F.,.F.,(4,3,3,
3,3,3,3,4),(-16.4127538780514,-15.9611419677269,-14.963570594744,-13.9659992217611,
-12.9684278487781,-11.9708564757952,-10.9732851028123,-10.1295685708719),
 .UNSPECIFIED.);
#3340=B_SPLINE_CURVE_WITH_KNOTS('',3,(#27559,#27560,#27561,#27562,#27563,
#27564,#27565,#27566,#27567,#27568,#27569,#27570,#27571),.UNSPECIFIED.,
 .F.,.F.,(4,3,3,3,4),(-3.84638326369226,-2.9927141189488,-1.99514274596587,
-0.997571372982933,0.),.UNSPECIFIED.);
#3341=B_SPLINE_CURVE_WITH_KNOTS('',3,(#27574,#27575,#27576,#27577,#27578,
#27579,#27580,#27581,#27582,#27583,#27584,#27585,#27586,#27587,#27588,#27589,
#27590,#27591,#27592),.UNSPECIFIED.,.F.,.F.,(4,3,3,3,3,3,4),(2.01461286527445,
2.9927141189488,3.99028549193173,4.98785686491466,5.9854282378976,6.98299961088053,
7.59300756235153),.UNSPECIFIED.);
#3342=B_SPLINE_CURVE_WITH_KNOTS('',3,(#27598,#27599,#27600,#27601,#27602,
#27603,#27604),.UNSPECIFIED.,.F.,.F.,(4,1,1,1,4),(91.106186954104,91.6672898428912,
92.6648612158742,93.6624325888571,94.66000396184),.UNSPECIFIED.);
#3343=B_SPLINE_CURVE_WITH_KNOTS('',3,(#27607,#27608,#27609,#27610,#27611,
#27612,#27613,#27614),.UNSPECIFIED.,.F.,.F.,(4,1,1,1,1,4),(91.106186954104,
91.2111367324627,92.2087081054456,93.2062794784286,94.2038508514115,95.1819521050858),
 .UNSPECIFIED.);
#3344=B_SPLINE_CURVE_WITH_KNOTS('',3,(#27619,#27620,#27621,#27622,#27623,
#27624,#27625,#27626,#27627,#27628),.UNSPECIFIED.,.F.,.F.,(4,1,1,1,1,1,
1,4),(84.8230016469244,85.6818616049936,86.6794329779766,87.6770043509595,
88.6745757239424,89.6721470969254,90.6697184699083,91.106186954104),
 .UNSPECIFIED.);
#3345=B_SPLINE_CURVE_WITH_KNOTS('',3,(#27629,#27630,#27631,#27632,#27633,
#27634,#27635,#27636,#27637,#27638),.UNSPECIFIED.,.F.,.F.,(4,1,1,1,1,1,
1,4),(84.8230016469244,85.2257084945651,86.223279867548,87.220851240531,
88.2184226135139,89.2159939864968,90.2135653594798,91.106186954104),
 .UNSPECIFIED.);
#3346=B_SPLINE_CURVE_WITH_KNOTS('',3,(#27643,#27644,#27645,#27646,#27647,
#27648,#27649,#27650,#27651,#27652,#27653),.UNSPECIFIED.,.F.,.F.,(4,1,1,
1,1,1,1,1,4),(78.5398163397448,78.6988619941131,79.696433367096,80.694004740079,
81.6915761130619,82.6891474860448,83.6867188590278,84.6842902320107,84.8230016469244),
 .UNSPECIFIED.);
#3347=B_SPLINE_CURVE_WITH_KNOTS('',3,(#27654,#27655,#27656,#27657,#27658,
#27659,#27660,#27661,#27662,#27663),.UNSPECIFIED.,.F.,.F.,(4,1,1,1,1,1,
1,4),(78.5398163397448,79.2402802566675,80.2378516296505,81.2354230026334,
82.2329943756163,83.2305657485992,84.2281371215822,84.8230016469244),
 .UNSPECIFIED.);
#3348=B_SPLINE_CURVE_WITH_KNOTS('',3,(#27668,#27669,#27670,#27671,#27672,
#27673,#27674,#27675,#27676,#27677),.UNSPECIFIED.,.F.,.F.,(4,1,1,1,1,1,
1,4),(72.2566310325652,72.7134337562155,73.7110051291985,74.7085765021814,
75.7061478751643,76.7037192481473,77.7012906211302,78.5398163397448),
 .UNSPECIFIED.);
#3349=B_SPLINE_CURVE_WITH_KNOTS('',3,(#27678,#27679,#27680,#27681,#27682,
#27683,#27684,#27685,#27686,#27687,#27688),.UNSPECIFIED.,.F.,.F.,(4,1,1,
1,1,1,1,1,4),(72.2566310325652,72.257280645787,73.2548520187699,74.2524233917529,
75.2499947647358,76.2475661377187,77.2451375107017,78.2427088836846,78.5398163397448),
 .UNSPECIFIED.);
#3350=B_SPLINE_CURVE_WITH_KNOTS('',3,(#27693,#27694,#27695,#27696,#27697,
#27698,#27699,#27700,#27701,#27702),.UNSPECIFIED.,.F.,.F.,(4,1,1,1,1,1,
1,4),(65.9734457253856,66.7280055183179,67.7255768913009,68.7231482642838,
69.7207196372667,70.7182910102497,71.7158623832326,72.2566310325652),
 .UNSPECIFIED.);
#3351=B_SPLINE_CURVE_WITH_KNOTS('',3,(#27703,#27704,#27705,#27706,#27707,
#27708,#27709,#27710,#27711,#27712),.UNSPECIFIED.,.F.,.F.,(4,1,1,1,1,1,
1,4),(65.9734457253856,66.2718524078894,67.2694237808723,68.2669951538553,
69.2645665268382,70.2621378998211,71.2597092728041,72.2566310325652),
 .UNSPECIFIED.);
#3352=B_SPLINE_CURVE_WITH_KNOTS('',3,(#27717,#27718,#27719,#27720,#27721,
#27722,#27723,#27724,#27725,#27726,#27727),.UNSPECIFIED.,.F.,.F.,(4,1,1,
1,1,1,1,1,4),(59.690260418206,59.7450059074374,60.7425772804203,61.7401486534033,
62.7377200263862,63.7352913993691,64.7328627723521,65.730434145335,65.9734457253856),
 .UNSPECIFIED.);
#3353=B_SPLINE_CURVE_WITH_KNOTS('',3,(#27728,#27729,#27730,#27731,#27732,
#27733,#27734,#27735,#27736,#27737),.UNSPECIFIED.,.F.,.F.,(4,1,1,1,1,1,
1,4),(59.690260418206,60.2864241699918,61.2839955429747,62.2815669159577,
63.2791382889406,64.2767096619235,65.2742810349065,65.9734457253856),
 .UNSPECIFIED.);
#3354=B_SPLINE_CURVE_WITH_KNOTS('',3,(#27742,#27743,#27744,#27745,#27746,
#27747,#27748,#27749,#27750,#27751),.UNSPECIFIED.,.F.,.F.,(4,1,1,1,1,1,
1,4),(53.4070751110264,53.7595776695398,54.7571490425227,55.7547204155057,
56.7522917884886,57.7498631614715,58.7474345344545,59.690260418206),
 .UNSPECIFIED.);
#3355=B_SPLINE_CURVE_WITH_KNOTS('',3,(#27752,#27753,#27754,#27755,#27756,
#27757,#27758,#27759,#27760,#27761),.UNSPECIFIED.,.F.,.F.,(4,1,1,1,1,1,
1,4),(53.4070751110264,54.3009959320942,55.2985673050771,56.2961386780601,
57.293710051043,58.2912814240259,59.2888527970089,59.690260418206),
 .UNSPECIFIED.);
#3356=B_SPLINE_CURVE_WITH_KNOTS('',3,(#27766,#27767,#27768,#27769,#27770,
#27771,#27772,#27773,#27774,#27775),.UNSPECIFIED.,.F.,.F.,(4,1,1,1,1,1,
1,4),(47.1238898038468,47.7741494316422,48.7717208046251,49.7692921776081,
50.766863550591,51.7644349235739,52.7620062965569,53.4070751110264),
 .UNSPECIFIED.);
#3357=B_SPLINE_CURVE_WITH_KNOTS('',3,(#27776,#27777,#27778,#27779,#27780,
#27781,#27782,#27783,#27784,#27785,#27786),.UNSPECIFIED.,.F.,.F.,(4,1,1,
1,1,1,1,1,4),(47.1238898038468,47.3179963212137,48.3155676941966,49.3131390671795,
50.3107104401625,51.3082818131454,52.3058531861283,53.3034245591113,53.4070751110264),
 .UNSPECIFIED.);
#3358=B_SPLINE_CURVE_WITH_KNOTS('',3,(#27791,#27792,#27793,#27794,#27795,
#27796,#27797,#27798,#27799,#27800),.UNSPECIFIED.,.F.,.F.,(4,1,1,1,1,1,
1,4),(40.8407044966673,41.7887211937446,42.7862925667275,43.7838639397105,
44.7814353126934,45.7790066856763,46.7765780586593,47.1238898038468),
 .UNSPECIFIED.);
#3359=B_SPLINE_CURVE_WITH_KNOTS('',3,(#27801,#27802,#27803,#27804,#27805,
#27806,#27807,#27808,#27809,#27810),.UNSPECIFIED.,.F.,.F.,(4,1,1,1,1,1,
1,4),(40.8407044966673,41.3325680833161,42.330139456299,43.3277108292819,
44.3252822022649,45.3228535752478,46.3204249482307,47.1238898038468),
 .UNSPECIFIED.);
#3360=B_SPLINE_CURVE_WITH_KNOTS('',3,(#27815,#27816,#27817,#27818,#27819,
#27820,#27821,#27822,#27823,#27824,#27825),.UNSPECIFIED.,.F.,.F.,(4,1,1,
1,1,1,1,1,4),(34.5575191894876,34.8057215828641,35.803292955847,36.80086432883,
37.7984357018129,38.7960070747958,39.7935784477787,40.7911498207617,40.8407044966673),
 .UNSPECIFIED.);
#3361=B_SPLINE_CURVE_WITH_KNOTS('',3,(#27826,#27827,#27828,#27829,#27830,
#27831,#27832,#27833,#27834,#27835),.UNSPECIFIED.,.F.,.F.,(4,1,1,1,1,1,
1,4),(34.5575191894876,35.3471398454185,36.3447112184014,37.3422825913843,
38.3398539643673,39.3374253373502,40.3349967103332,40.8407044966673),
 .UNSPECIFIED.);
#3362=B_SPLINE_CURVE_WITH_KNOTS('',3,(#27840,#27841,#27842,#27843,#27844,
#27845,#27846,#27847,#27848,#27849),.UNSPECIFIED.,.F.,.F.,(4,1,1,1,1,1,
1,4),(28.2743338823081,28.8202933449665,29.8178647179494,30.8154360909324,
31.8130074639153,32.8105788368982,33.8081502098811,34.5575191894876),
 .UNSPECIFIED.);
#3363=B_SPLINE_CURVE_WITH_KNOTS('',3,(#27850,#27851,#27852,#27853,#27854,
#27855,#27856,#27857,#27858,#27859,#27860),.UNSPECIFIED.,.F.,.F.,(4,1,1,
1,1,1,1,1,4),(28.2743338823081,28.364140234538,29.3617116075209,30.3592829805038,
31.3568543534868,32.3544257264697,33.3519970994526,34.3495684724355,34.5575191894876),
 .UNSPECIFIED.);
#3364=B_SPLINE_CURVE_WITH_KNOTS('',3,(#27865,#27866,#27867,#27868,#27869,
#27870,#27871,#27872,#27873,#27874),.UNSPECIFIED.,.F.,.F.,(4,1,1,1,1,1,
1,4),(21.9911485751285,22.8348651070689,23.8324364800518,24.8300078530348,
25.8275792260177,26.8251505990006,27.8227219719836,28.2743338823081),
 .UNSPECIFIED.);
#3365=B_SPLINE_CURVE_WITH_KNOTS('',3,(#27875,#27876,#27877,#27878,#27879,
#27880,#27881,#27882,#27883,#27884),.UNSPECIFIED.,.F.,.F.,(4,1,1,1,1,1,
1,4),(21.9911485751285,22.3787119966404,23.3762833696233,24.3738547426062,
25.3714261155892,26.3689974885721,27.366568861555,28.2743338823081),
 .UNSPECIFIED.);
#3366=B_SPLINE_CURVE_WITH_KNOTS('',3,(#27890,#27891,#27892,#27893,#27894),
 .UNSPECIFIED.,.F.,.F.,(4,1,4),(14.3981410127769,15.3957123857598,15.7079632679489),
 .UNSPECIFIED.);
#3367=B_SPLINE_CURVE_WITH_KNOTS('',3,(#27897,#27898,#27899,#27900,#27901),
 .UNSPECIFIED.,.F.,.F.,(4,1,4),(13.8761928695311,14.8542941232054,15.7079632679489),
 .UNSPECIFIED.);
#3368=B_SPLINE_CURVE_WITH_KNOTS('',3,(#27907,#27908,#27909,#27910,#27911,
#27912,#27913,#27914,#27915,#27916,#27917,#27918,#27919,#27920,#27921,#27922,
#27923,#27924,#27925,#27926,#27927,#27928),.UNSPECIFIED.,.F.,.F.,(4,3,3,
3,3,3,3,4),(76.7080459413271,76.8129957196858,77.8105670926687,78.8081384656517,
79.8057098386346,80.8032812116175,81.8008525846005,82.7984239575834),
 .UNSPECIFIED.);
#3369=B_SPLINE_CURVE_WITH_KNOTS('',3,(#27932,#27933,#27934,#27935,#27936,
#27937,#27938),.UNSPECIFIED.,.F.,.F.,(4,3,4),(-80.7838110923091,-79.8057098386346,
-79.2446069498474),.UNSPECIFIED.);
#3370=B_SPLINE_CURVE_WITH_KNOTS('',3,(#27942,#27943,#27944,#27945,#27946,
#27947,#27948,#27949,#27950,#27951,#27952,#27953,#27954,#27955,#27956,#27957,
#27958,#27959,#27960,#27961,#27962,#27963),.UNSPECIFIED.,.F.,.F.,(4,3,3,
3,3,3,3,4),(-79.2446069498474,-78.8081384656517,-77.8105670926687,-76.8129957196858,
-75.8154243467029,-74.8178529737199,-73.820281600737,-72.9614216426678),
 .UNSPECIFIED.);
#3371=B_SPLINE_CURVE_WITH_KNOTS('',3,(#27968,#27969,#27970,#27971,#27972,
#27973,#27974,#27975,#27976,#27977,#27978,#27979,#27980,#27981,#27982,#27983,
#27984,#27985,#27986,#27987,#27988,#27989),.UNSPECIFIED.,.F.,.F.,(4,3,3,
3,3,3,3,4),(70.4248606341475,70.8275674817882,71.8251388547711,72.8227102277541,
73.820281600737,74.8178529737199,75.8154243467029,76.7080459413271),
 .UNSPECIFIED.);
#3372=B_SPLINE_CURVE_WITH_KNOTS('',3,(#27990,#27991,#27992,#27993,#27994,
#27995,#27996,#27997,#27998,#27999,#28000,#28001,#28002,#28003,#28004,#28005,
#28006,#28007,#28008,#28009,#28010,#28011,#28012,#28013,#28014),
 .UNSPECIFIED.,.F.,.F.,(4,3,3,3,3,3,3,3,4),(-72.9614216426678,-72.8227102277541,
-71.8251388547711,-70.8275674817882,-69.8299961088053,-68.8324247358223,
-67.8348533628394,-66.8372819898565,-66.6782363354882),.UNSPECIFIED.);
#3373=B_SPLINE_CURVE_WITH_KNOTS('',3,(#28019,#28020,#28021,#28022,#28023,
#28024,#28025,#28026,#28027,#28028,#28029,#28030,#28031,#28032,#28033,#28034,
#28035,#28036,#28037,#28038,#28039,#28040),.UNSPECIFIED.,.F.,.F.,(4,3,3,
3,3,3,3,4),(64.1416753269679,64.8421392438906,65.8397106168735,66.8372819898565,
67.8348533628394,68.8324247358223,69.8299961088053,70.4248606341475),
 .UNSPECIFIED.);
#3374=B_SPLINE_CURVE_WITH_KNOTS('',3,(#28041,#28042,#28043,#28044,#28045,
#28046,#28047,#28048,#28049,#28050,#28051,#28052,#28053,#28054,#28055,#28056,
#28057,#28058,#28059,#28060,#28061,#28062),.UNSPECIFIED.,.F.,.F.,(4,3,3,
3,3,3,3,4),(-66.6782363354882,-65.8397106168736,-64.8421392438906,-63.8445678709077,
-62.8469964979247,-61.8494251249418,-60.8518537519589,-60.3950510283086),
 .UNSPECIFIED.);
#3375=B_SPLINE_CURVE_WITH_KNOTS('',3,(#28067,#28068,#28069,#28070,#28071,
#28072,#28073,#28074,#28075,#28076,#28077,#28078,#28079,#28080,#28081,#28082,
#28083,#28084,#28085,#28086,#28087,#28088),.UNSPECIFIED.,.F.,.F.,(4,3,3,
3,3,3,3,4),(57.8584900197883,58.856711005993,59.854282378976,60.8518537519589,
61.8494251249418,62.8469964979247,63.8445678709077,64.1416753269679),
 .UNSPECIFIED.);
#3376=B_SPLINE_CURVE_WITH_KNOTS('',3,(#28089,#28090,#28091,#28092,#28093,
#28094,#28095,#28096,#28097,#28098,#28099,#28100,#28101,#28102,#28103,#28104,
#28105,#28106,#28107,#28108,#28109,#28110),.UNSPECIFIED.,.F.,.F.,(4,3,3,
3,3,3,3,4),(-60.3950510283086,-59.854282378976,-58.856711005993,-57.8591396330101,
-56.8615682600272,-55.8639968870442,-54.8664255140613,-54.111865721129),
 .UNSPECIFIED.);
#3377=B_SPLINE_CURVE_WITH_KNOTS('',3,(#28115,#28116,#28117,#28118,#28119,
#28120,#28121,#28122,#28123,#28124,#28125,#28126,#28127,#28128,#28129,#28130,
#28131,#28132,#28133,#28134,#28135,#28136),.UNSPECIFIED.,.F.,.F.,(4,3,3,
3,3,3,3,4),(51.5753047126087,51.8737113951125,52.8712827680954,53.8688541410784,
54.8664255140613,55.8639968870442,56.8615682600272,57.8584900197883),
 .UNSPECIFIED.);
#3378=B_SPLINE_CURVE_WITH_KNOTS('',3,(#28137,#28138,#28139,#28140,#28141,
#28142,#28143,#28144,#28145,#28146,#28147,#28148,#28149,#28150,#28151,#28152,
#28153,#28154,#28155,#28156,#28157,#28158,#28159,#28160,#28161),
 .UNSPECIFIED.,.F.,.F.,(4,3,3,3,3,3,3,3,4),(-54.111865721129,-53.8688541410784,
-52.8712827680954,-51.8737113951125,-50.8761400221296,-49.8785686491466,
-48.8809972761637,-47.8834259031808,-47.8286804139494),.UNSPECIFIED.);
#3379=B_SPLINE_CURVE_WITH_KNOTS('',3,(#28166,#28167,#28168,#28169,#28170,
#28171,#28172,#28173,#28174,#28175,#28176,#28177,#28178,#28179,#28180,#28181,
#28182,#28183,#28184,#28185,#28186,#28187),.UNSPECIFIED.,.F.,.F.,(4,3,3,
3,3,3,3,4),(45.2921194054291,45.8882831572149,46.8858545301978,47.8834259031808,
48.8809972761637,49.8785686491466,50.8761400221296,51.5753047126087),
 .UNSPECIFIED.);
#3380=B_SPLINE_CURVE_WITH_KNOTS('',3,(#28188,#28189,#28190,#28191,#28192,
#28193,#28194,#28195,#28196,#28197,#28198,#28199,#28200,#28201,#28202,#28203,
#28204,#28205,#28206,#28207,#28208,#28209),.UNSPECIFIED.,.F.,.F.,(4,3,3,
3,3,3,3,4),(-47.8286804139494,-46.8858545301978,-45.8882831572149,-44.890711784232,
-43.893140411249,-42.8955690382661,-41.8979976652832,-41.5454951067698),
 .UNSPECIFIED.);
#3381=B_SPLINE_CURVE_WITH_KNOTS('',3,(#28214,#28215,#28216,#28217,#28218,
#28219,#28220,#28221,#28222,#28223,#28224,#28225,#28226,#28227,#28228,#28229,
#28230,#28231,#28232,#28233,#28234,#28235),.UNSPECIFIED.,.F.,.F.,(4,3,3,
3,3,3,3,4),(39.0089340982495,39.9028549193173,40.9004262923002,41.8979976652832,
42.8955690382661,43.893140411249,44.890711784232,45.2921194054291),
 .UNSPECIFIED.);
#3382=B_SPLINE_CURVE_WITH_KNOTS('',3,(#28236,#28237,#28238,#28239,#28240,
#28241,#28242,#28243,#28244,#28245,#28246,#28247,#28248,#28249,#28250,#28251,
#28252,#28253,#28254,#28255,#28256,#28257),.UNSPECIFIED.,.F.,.F.,(4,3,3,
3,3,3,3,4),(-41.5454951067698,-40.9004262923002,-39.9028549193173,-38.9052835463344,
-37.9077121733514,-36.9101408003685,-35.9125694273856,-35.2623097995902),
 .UNSPECIFIED.);
#3383=B_SPLINE_CURVE_WITH_KNOTS('',3,(#28262,#28263,#28264,#28265,#28266,
#28267,#28268,#28269,#28270,#28271,#28272,#28273,#28274,#28275,#28276,#28277,
#28278,#28279,#28280,#28281,#28282,#28283,#28284,#28285,#28286),
 .UNSPECIFIED.,.F.,.F.,(4,3,3,3,3,3,3,3,4),(32.7257487910699,32.9198553084368,
33.9174266814197,34.9149980544026,35.9125694273856,36.9101408003685,37.9077121733514,
38.9052835463344,39.0089340982495),.UNSPECIFIED.);
#3384=B_SPLINE_CURVE_WITH_KNOTS('',3,(#28287,#28288,#28289,#28290,#28291,
#28292,#28293,#28294,#28295,#28296,#28297,#28298,#28299,#28300,#28301,#28302,
#28303,#28304,#28305,#28306,#28307,#28308),.UNSPECIFIED.,.F.,.F.,(4,3,3,
3,3,3,3,4),(-35.2623097995902,-34.9149980544026,-33.9174266814197,-32.9198553084368,
-31.9222839354538,-30.9247125624709,-29.927141189488,-28.9791244924107),
 .UNSPECIFIED.);
#3385=B_SPLINE_CURVE_WITH_KNOTS('',3,(#28313,#28314,#28315,#28316,#28317,
#28318,#28319,#28320,#28321,#28322,#28323,#28324,#28325,#28326,#28327,#28328,
#28329,#28330,#28331,#28332,#28333,#28334),.UNSPECIFIED.,.F.,.F.,(4,3,3,
3,3,3,3,4),(26.4425634838903,26.9344270705392,27.9319984435221,28.9295698165051,
29.927141189488,30.9247125624709,31.9222839354538,32.7257487910699),
 .UNSPECIFIED.);
#3386=B_SPLINE_CURVE_WITH_KNOTS('',3,(#28335,#28336,#28337,#28338,#28339,
#28340,#28341,#28342,#28343,#28344,#28345,#28346,#28347,#28348,#28349,#28350,
#28351,#28352,#28353,#28354,#28355,#28356,#28357,#28358,#28359),
 .UNSPECIFIED.,.F.,.F.,(4,3,3,3,3,3,3,3,4),(-28.9791244924107,-28.929569816505,
-27.9319984435221,-26.9344270705392,-25.9368556975563,-24.9392843245733,
-23.9417129515904,-22.9441415786074,-22.6959391852311),.UNSPECIFIED.);
#3387=B_SPLINE_CURVE_WITH_KNOTS('',3,(#28364,#28365,#28366,#28367,#28368,
#28369,#28370,#28371,#28372,#28373,#28374,#28375,#28376,#28377,#28378,#28379,
#28380,#28381,#28382,#28383,#28384,#28385),.UNSPECIFIED.,.F.,.F.,(4,3,3,
3,3,3,3,4),(20.1593781767108,20.9489988326416,21.9465702056245,22.9441415786075,
23.9417129515904,24.9392843245733,25.9368556975563,26.4425634838903),
 .UNSPECIFIED.);
#3388=B_SPLINE_CURVE_WITH_KNOTS('',3,(#28386,#28387,#28388,#28389,#28390,
#28391,#28392,#28393,#28394,#28395,#28396,#28397,#28398,#28399,#28400,#28401,
#28402,#28403,#28404,#28405,#28406,#28407),.UNSPECIFIED.,.F.,.F.,(4,3,3,
3,3,3,3,4),(-22.6959391852311,-21.9465702056245,-20.9489988326416,-19.9514274596586,
-18.9538560866757,-17.9562847136928,-16.9587133407099,-16.4127538780515),
 .UNSPECIFIED.);
#3389=B_SPLINE_CURVE_WITH_KNOTS('',3,(#28412,#28413,#28414,#28415,#28416,
#28417,#28418,#28419,#28420,#28421,#28422,#28423,#28424,#28425,#28426,#28427,
#28428,#28429,#28430,#28431,#28432,#28433,#28434,#28435,#28436),
 .UNSPECIFIED.,.F.,.F.,(4,3,3,3,3,3,3,3,4),(13.8761928695312,13.9659992217611,
14.963570594744,15.9611419677269,16.9587133407099,17.9562847136928,18.9538560866757,
19.9514274596587,20.1593781767108),.UNSPECIFIED.);
#3390=B_SPLINE_CURVE_WITH_KNOTS('',3,(#28437,#28438,#28439,#28440,#28441,
#28442,#28443,#28444,#28445,#28446,#28447,#28448,#28449,#28450,#28451,#28452,
#28453,#28454,#28455,#28456,#28457,#28458),.UNSPECIFIED.,.F.,.F.,(4,3,3,
3,3,3,3,4),(-16.4127538780515,-15.9611419677269,-14.963570594744,-13.9659992217611,
-12.9684278487781,-11.9708564757952,-10.9732851028123,-10.1295685708719),
 .UNSPECIFIED.);
#3391=B_SPLINE_CURVE_WITH_KNOTS('',3,(#28464,#28465,#28466,#28467,#28468,
#28469,#28470,#28471,#28472,#28473,#28474,#28475,#28476),.UNSPECIFIED.,
 .F.,.F.,(4,3,3,3,4),(-3.8463832636923,-2.9927141189488,-1.99514274596586,
-0.997571372982932,0.),.UNSPECIFIED.);
#3392=B_SPLINE_CURVE_WITH_KNOTS('',3,(#28479,#28480,#28481,#28482,#28483,
#28484,#28485,#28486,#28487,#28488,#28489,#28490,#28491,#28492,#28493,#28494,
#28495,#28496,#28497),.UNSPECIFIED.,.F.,.F.,(4,3,3,3,3,3,4),(2.01461286527437,
2.9927141189488,3.99028549193173,4.98785686491466,5.9854282378976,6.98299961088053,
7.59300756235157),.UNSPECIFIED.);
#3393=B_SPLINE_CURVE_WITH_KNOTS('',3,(#28503,#28504,#28505,#28506,#28507,
#28508,#28509),.UNSPECIFIED.,.F.,.F.,(4,1,1,1,4),(91.106186954104,91.6672898428912,
92.6648612158741,93.6624325888571,94.66000396184),.UNSPECIFIED.);
#3394=B_SPLINE_CURVE_WITH_KNOTS('',3,(#28512,#28513,#28514,#28515,#28516,
#28517,#28518,#28519),.UNSPECIFIED.,.F.,.F.,(4,1,1,1,1,4),(91.106186954104,
91.2111367324627,92.2087081054456,93.2062794784285,94.2038508514115,95.1819521050858),
 .UNSPECIFIED.);
#3395=B_SPLINE_CURVE_WITH_KNOTS('',3,(#28524,#28525,#28526,#28527,#28528,
#28529,#28530,#28531,#28532,#28533),.UNSPECIFIED.,.F.,.F.,(4,1,1,1,1,1,
1,4),(84.8230016469244,85.6818616049936,86.6794329779765,87.6770043509595,
88.6745757239424,89.6721470969253,90.6697184699083,91.106186954104),
 .UNSPECIFIED.);
#3396=B_SPLINE_CURVE_WITH_KNOTS('',3,(#28534,#28535,#28536,#28537,#28538,
#28539,#28540,#28541,#28542,#28543),.UNSPECIFIED.,.F.,.F.,(4,1,1,1,1,1,
1,4),(84.8230016469244,85.2257084945651,86.223279867548,87.2208512405309,
88.2184226135139,89.2159939864968,90.2135653594797,91.106186954104),
 .UNSPECIFIED.);
#3397=B_SPLINE_CURVE_WITH_KNOTS('',3,(#28548,#28549,#28550,#28551,#28552,
#28553,#28554,#28555,#28556,#28557,#28558),.UNSPECIFIED.,.F.,.F.,(4,1,1,
1,1,1,1,1,4),(78.5398163397448,78.6988619941131,79.696433367096,80.6940047400789,
81.6915761130619,82.6891474860448,83.6867188590277,84.6842902320107,84.8230016469244),
 .UNSPECIFIED.);
#3398=B_SPLINE_CURVE_WITH_KNOTS('',3,(#28559,#28560,#28561,#28562,#28563,
#28564,#28565,#28566,#28567,#28568),.UNSPECIFIED.,.F.,.F.,(4,1,1,1,1,1,
1,4),(78.5398163397448,79.2402802566675,80.2378516296504,81.2354230026333,
82.2329943756163,83.2305657485992,84.2281371215821,84.8230016469244),
 .UNSPECIFIED.);
#3399=B_SPLINE_CURVE_WITH_KNOTS('',3,(#28573,#28574,#28575,#28576,#28577,
#28578,#28579,#28580,#28581,#28582),.UNSPECIFIED.,.F.,.F.,(4,1,1,1,1,1,
1,4),(72.2566310325652,72.7134337562155,73.7110051291984,74.7085765021813,
75.7061478751643,76.7037192481472,77.7012906211301,78.5398163397448),
 .UNSPECIFIED.);
#3400=B_SPLINE_CURVE_WITH_KNOTS('',3,(#28583,#28584,#28585,#28586,#28587,
#28588,#28589,#28590,#28591,#28592,#28593),.UNSPECIFIED.,.F.,.F.,(4,1,1,
1,1,1,1,1,4),(72.2566310325652,72.2572806457869,73.2548520187699,74.2524233917528,
75.2499947647357,76.2475661377187,77.2451375107016,78.2427088836845,78.5398163397448),
 .UNSPECIFIED.);
#3401=B_SPLINE_CURVE_WITH_KNOTS('',3,(#28598,#28599,#28600,#28601,#28602,
#28603,#28604,#28605,#28606,#28607),.UNSPECIFIED.,.F.,.F.,(4,1,1,1,1,1,
1,4),(65.9734457253856,66.7280055183179,67.7255768913008,68.7231482642838,
69.7207196372667,70.7182910102496,71.7158623832325,72.2566310325652),
 .UNSPECIFIED.);
#3402=B_SPLINE_CURVE_WITH_KNOTS('',3,(#28608,#28609,#28610,#28611,#28612,
#28613,#28614,#28615,#28616,#28617),.UNSPECIFIED.,.F.,.F.,(4,1,1,1,1,1,
1,4),(65.9734457253856,66.2718524078894,67.2694237808723,68.2669951538552,
69.2645665268382,70.2621378998211,71.259709272804,72.2566310325652),
 .UNSPECIFIED.);
#3403=B_SPLINE_CURVE_WITH_KNOTS('',3,(#28622,#28623,#28624,#28625,#28626,
#28627,#28628,#28629,#28630,#28631,#28632),.UNSPECIFIED.,.F.,.F.,(4,1,1,
1,1,1,1,1,4),(59.690260418206,59.7450059074374,60.7425772804203,61.7401486534032,
62.7377200263862,63.7352913993691,64.732862772352,65.730434145335,65.9734457253856),
 .UNSPECIFIED.);
#3404=B_SPLINE_CURVE_WITH_KNOTS('',3,(#28633,#28634,#28635,#28636,#28637,
#28638,#28639,#28640,#28641,#28642),.UNSPECIFIED.,.F.,.F.,(4,1,1,1,1,1,
1,4),(59.690260418206,60.2864241699918,61.2839955429747,62.2815669159576,
63.2791382889406,64.2767096619235,65.2742810349064,65.9734457253856),
 .UNSPECIFIED.);
#3405=B_SPLINE_CURVE_WITH_KNOTS('',3,(#28647,#28648,#28649,#28650,#28651,
#28652,#28653,#28654,#28655,#28656),.UNSPECIFIED.,.F.,.F.,(4,1,1,1,1,1,
1,4),(53.4070751110264,53.7595776695398,54.7571490425227,55.7547204155056,
56.7522917884886,57.7498631614715,58.7474345344544,59.690260418206),
 .UNSPECIFIED.);
#3406=B_SPLINE_CURVE_WITH_KNOTS('',3,(#28657,#28658,#28659,#28660,#28661,
#28662,#28663,#28664,#28665,#28666),.UNSPECIFIED.,.F.,.F.,(4,1,1,1,1,1,
1,4),(53.4070751110264,54.3009959320942,55.2985673050771,56.29613867806,
57.293710051043,58.2912814240259,59.2888527970088,59.690260418206),
 .UNSPECIFIED.);
#3407=B_SPLINE_CURVE_WITH_KNOTS('',3,(#28671,#28672,#28673,#28674,#28675,
#28676,#28677,#28678,#28679,#28680),.UNSPECIFIED.,.F.,.F.,(4,1,1,1,1,1,
1,4),(47.1238898038469,47.7741494316422,48.7717208046251,49.769292177608,
50.766863550591,51.7644349235739,52.7620062965568,53.4070751110264),
 .UNSPECIFIED.);
#3408=B_SPLINE_CURVE_WITH_KNOTS('',3,(#28681,#28682,#28683,#28684,#28685,
#28686,#28687,#28688,#28689,#28690,#28691),.UNSPECIFIED.,.F.,.F.,(4,1,1,
1,1,1,1,1,4),(47.1238898038468,47.3179963212136,48.3155676941966,49.3131390671795,
50.3107104401624,51.3082818131454,52.3058531861283,53.3034245591112,53.4070751110264),
 .UNSPECIFIED.);
#3409=B_SPLINE_CURVE_WITH_KNOTS('',3,(#28696,#28697,#28698,#28699,#28700,
#28701,#28702,#28703,#28704,#28705),.UNSPECIFIED.,.F.,.F.,(4,1,1,1,1,1,
1,4),(40.8407044966673,41.7887211937446,42.7862925667275,43.7838639397104,
44.7814353126934,45.7790066856763,46.7765780586592,47.1238898038469),
 .UNSPECIFIED.);
#3410=B_SPLINE_CURVE_WITH_KNOTS('',3,(#28706,#28707,#28708,#28709,#28710,
#28711,#28712,#28713,#28714,#28715),.UNSPECIFIED.,.F.,.F.,(4,1,1,1,1,1,
1,4),(40.8407044966673,41.332568083316,42.330139456299,43.3277108292819,
44.3252822022648,45.3228535752478,46.3204249482307,47.1238898038468),
 .UNSPECIFIED.);
#3411=B_SPLINE_CURVE_WITH_KNOTS('',3,(#28720,#28721,#28722,#28723,#28724,
#28725,#28726,#28727,#28728,#28729,#28730),.UNSPECIFIED.,.F.,.F.,(4,1,1,
1,1,1,1,1,4),(34.5575191894877,34.805721582864,35.803292955847,36.8008643288299,
37.7984357018128,38.7960070747958,39.7935784477787,40.7911498207616,40.8407044966673),
 .UNSPECIFIED.);
#3412=B_SPLINE_CURVE_WITH_KNOTS('',3,(#28731,#28732,#28733,#28734,#28735,
#28736,#28737,#28738,#28739,#28740),.UNSPECIFIED.,.F.,.F.,(4,1,1,1,1,1,
1,4),(34.5575191894876,35.3471398454184,36.3447112184014,37.3422825913843,
38.3398539643673,39.3374253373502,40.3349967103331,40.8407044966673),
 .UNSPECIFIED.);
#3413=B_SPLINE_CURVE_WITH_KNOTS('',3,(#28745,#28746,#28747,#28748,#28749,
#28750,#28751,#28752,#28753,#28754),.UNSPECIFIED.,.F.,.F.,(4,1,1,1,1,1,
1,4),(28.2743338823081,28.8202933449665,29.8178647179494,30.8154360909323,
31.8130074639152,32.8105788368982,33.8081502098811,34.5575191894877),
 .UNSPECIFIED.);
#3414=B_SPLINE_CURVE_WITH_KNOTS('',3,(#28755,#28756,#28757,#28758,#28759,
#28760,#28761,#28762,#28763,#28764,#28765),.UNSPECIFIED.,.F.,.F.,(4,1,1,
1,1,1,1,1,4),(28.2743338823081,28.3641402345379,29.3617116075209,30.3592829805038,
31.3568543534867,32.3544257264696,33.3519970994526,34.3495684724355,34.5575191894876),
 .UNSPECIFIED.);
#3415=B_SPLINE_CURVE_WITH_KNOTS('',3,(#28770,#28771,#28772,#28773,#28774,
#28775,#28776,#28777,#28778,#28779),.UNSPECIFIED.,.F.,.F.,(4,1,1,1,1,1,
1,4),(21.9911485751285,22.8348651070689,23.8324364800518,24.8300078530347,
25.8275792260177,26.8251505990006,27.8227219719835,28.2743338823081),
 .UNSPECIFIED.);
#3416=B_SPLINE_CURVE_WITH_KNOTS('',3,(#28780,#28781,#28782,#28783,#28784,
#28785,#28786,#28787,#28788,#28789),.UNSPECIFIED.,.F.,.F.,(4,1,1,1,1,1,
1,4),(21.9911485751285,22.3787119966403,23.3762833696233,24.3738547426062,
25.3714261155891,26.3689974885721,27.366568861555,28.2743338823081),
 .UNSPECIFIED.);
#3417=B_SPLINE_CURVE_WITH_KNOTS('',3,(#28795,#28796,#28797,#28798,#28799),
 .UNSPECIFIED.,.F.,.F.,(4,1,4),(14.3981410127769,15.3957123857598,15.7079632679489),
 .UNSPECIFIED.);
#3418=B_SPLINE_CURVE_WITH_KNOTS('',3,(#28802,#28803,#28804,#28805,#28806),
 .UNSPECIFIED.,.F.,.F.,(4,1,4),(13.8761928695311,14.8542941232054,15.7079632679489),
 .UNSPECIFIED.);
#3419=B_SPLINE_CURVE_WITH_KNOTS('',3,(#28812,#28813,#28814,#28815,#28816,
#28817,#28818,#28819,#28820,#28821,#28822,#28823,#28824,#28825,#28826,#28827,
#28828,#28829,#28830,#28831,#28832,#28833),.UNSPECIFIED.,.F.,.F.,(4,3,3,
3,3,3,3,4),(76.7080459413271,76.8129957196858,77.8105670926687,78.8081384656517,
79.8057098386346,80.8032812116175,81.8008525846005,82.7984239575834),
 .UNSPECIFIED.);
#3420=B_SPLINE_CURVE_WITH_KNOTS('',3,(#28837,#28838,#28839,#28840,#28841,
#28842,#28843),.UNSPECIFIED.,.F.,.F.,(4,3,4),(-80.783811092309,-79.8057098386346,
-79.2446069498474),.UNSPECIFIED.);
#3421=B_SPLINE_CURVE_WITH_KNOTS('',3,(#28847,#28848,#28849,#28850,#28851,
#28852,#28853,#28854,#28855,#28856,#28857,#28858,#28859,#28860,#28861,#28862,
#28863,#28864,#28865,#28866,#28867,#28868),.UNSPECIFIED.,.F.,.F.,(4,3,3,
3,3,3,3,4),(-79.2446069498474,-78.8081384656517,-77.8105670926687,-76.8129957196858,
-75.8154243467029,-74.8178529737199,-73.820281600737,-72.9614216426678),
 .UNSPECIFIED.);
#3422=B_SPLINE_CURVE_WITH_KNOTS('',3,(#28873,#28874,#28875,#28876,#28877,
#28878,#28879,#28880,#28881,#28882,#28883,#28884,#28885,#28886,#28887,#28888,
#28889,#28890,#28891,#28892,#28893,#28894),.UNSPECIFIED.,.F.,.F.,(4,3,3,
3,3,3,3,4),(70.4248606341475,70.8275674817882,71.8251388547711,72.8227102277541,
73.820281600737,74.81785297372,75.8154243467029,76.7080459413271),
 .UNSPECIFIED.);
#3423=B_SPLINE_CURVE_WITH_KNOTS('',3,(#28895,#28896,#28897,#28898,#28899,
#28900,#28901,#28902,#28903,#28904,#28905,#28906,#28907,#28908,#28909,#28910,
#28911,#28912,#28913,#28914,#28915,#28916,#28917,#28918,#28919),
 .UNSPECIFIED.,.F.,.F.,(4,3,3,3,3,3,3,3,4),(-72.9614216426678,-72.8227102277541,
-71.8251388547711,-70.8275674817882,-69.8299961088053,-68.8324247358223,
-67.8348533628394,-66.8372819898565,-66.6782363354882),.UNSPECIFIED.);
#3424=B_SPLINE_CURVE_WITH_KNOTS('',3,(#28924,#28925,#28926,#28927,#28928,
#28929,#28930,#28931,#28932,#28933,#28934,#28935,#28936,#28937,#28938,#28939,
#28940,#28941,#28942,#28943,#28944,#28945),.UNSPECIFIED.,.F.,.F.,(4,3,3,
3,3,3,3,4),(64.1416753269679,64.8421392438906,65.8397106168735,66.8372819898565,
67.8348533628394,68.8324247358223,69.8299961088053,70.4248606341475),
 .UNSPECIFIED.);
#3425=B_SPLINE_CURVE_WITH_KNOTS('',3,(#28946,#28947,#28948,#28949,#28950,
#28951,#28952,#28953,#28954,#28955,#28956,#28957,#28958,#28959,#28960,#28961,
#28962,#28963,#28964,#28965,#28966,#28967),.UNSPECIFIED.,.F.,.F.,(4,3,3,
3,3,3,3,4),(-66.6782363354882,-65.8397106168736,-64.8421392438906,-63.8445678709077,
-62.8469964979247,-61.8494251249418,-60.8518537519589,-60.3950510283086),
 .UNSPECIFIED.);
#3426=B_SPLINE_CURVE_WITH_KNOTS('',3,(#28972,#28973,#28974,#28975,#28976,
#28977,#28978,#28979,#28980,#28981,#28982,#28983,#28984,#28985,#28986,#28987,
#28988,#28989,#28990,#28991,#28992,#28993),.UNSPECIFIED.,.F.,.F.,(4,3,3,
3,3,3,3,4),(57.8584900197883,58.856711005993,59.854282378976,60.8518537519589,
61.8494251249418,62.8469964979247,63.8445678709077,64.1416753269679),
 .UNSPECIFIED.);
#3427=B_SPLINE_CURVE_WITH_KNOTS('',3,(#28994,#28995,#28996,#28997,#28998,
#28999,#29000,#29001,#29002,#29003,#29004,#29005,#29006,#29007,#29008,#29009,
#29010,#29011,#29012,#29013,#29014,#29015),.UNSPECIFIED.,.F.,.F.,(4,3,3,
3,3,3,3,4),(-60.3950510283086,-59.854282378976,-58.856711005993,-57.8591396330101,
-56.8615682600271,-55.8639968870442,-54.8664255140613,-54.111865721129),
 .UNSPECIFIED.);
#3428=B_SPLINE_CURVE_WITH_KNOTS('',3,(#29020,#29021,#29022,#29023,#29024,
#29025,#29026,#29027,#29028,#29029,#29030,#29031,#29032,#29033,#29034,#29035,
#29036,#29037,#29038,#29039,#29040,#29041),.UNSPECIFIED.,.F.,.F.,(4,3,3,
3,3,3,3,4),(51.5753047126087,51.8737113951125,52.8712827680954,53.8688541410784,
54.8664255140613,55.8639968870442,56.8615682600272,57.8584900197883),
 .UNSPECIFIED.);
#3429=B_SPLINE_CURVE_WITH_KNOTS('',3,(#29042,#29043,#29044,#29045,#29046,
#29047,#29048,#29049,#29050,#29051,#29052,#29053,#29054,#29055,#29056,#29057,
#29058,#29059,#29060,#29061,#29062,#29063,#29064,#29065,#29066),
 .UNSPECIFIED.,.F.,.F.,(4,3,3,3,3,3,3,3,4),(-54.111865721129,-53.8688541410784,
-52.8712827680954,-51.8737113951125,-50.8761400221296,-49.8785686491466,
-48.8809972761637,-47.8834259031808,-47.8286804139494),.UNSPECIFIED.);
#3430=B_SPLINE_CURVE_WITH_KNOTS('',3,(#29071,#29072,#29073,#29074,#29075,
#29076,#29077,#29078,#29079,#29080,#29081,#29082,#29083,#29084,#29085,#29086,
#29087,#29088,#29089,#29090,#29091,#29092),.UNSPECIFIED.,.F.,.F.,(4,3,3,
3,3,3,3,4),(45.2921194054291,45.8882831572149,46.8858545301978,47.8834259031808,
48.8809972761637,49.8785686491466,50.8761400221296,51.5753047126087),
 .UNSPECIFIED.);
#3431=B_SPLINE_CURVE_WITH_KNOTS('',3,(#29093,#29094,#29095,#29096,#29097,
#29098,#29099,#29100,#29101,#29102,#29103,#29104,#29105,#29106,#29107,#29108,
#29109,#29110,#29111,#29112,#29113,#29114),.UNSPECIFIED.,.F.,.F.,(4,3,3,
3,3,3,3,4),(-47.8286804139494,-46.8858545301978,-45.8882831572149,-44.890711784232,
-43.893140411249,-42.8955690382661,-41.8979976652832,-41.5454951067698),
 .UNSPECIFIED.);
#3432=B_SPLINE_CURVE_WITH_KNOTS('',3,(#29119,#29120,#29121,#29122,#29123,
#29124,#29125,#29126,#29127,#29128,#29129,#29130,#29131,#29132,#29133,#29134,
#29135,#29136,#29137,#29138,#29139,#29140),.UNSPECIFIED.,.F.,.F.,(4,3,3,
3,3,3,3,4),(39.0089340982495,39.9028549193173,40.9004262923002,41.8979976652832,
42.8955690382661,43.893140411249,44.890711784232,45.2921194054291),
 .UNSPECIFIED.);
#3433=B_SPLINE_CURVE_WITH_KNOTS('',3,(#29141,#29142,#29143,#29144,#29145,
#29146,#29147,#29148,#29149,#29150,#29151,#29152,#29153,#29154,#29155,#29156,
#29157,#29158,#29159,#29160,#29161,#29162),.UNSPECIFIED.,.F.,.F.,(4,3,3,
3,3,3,3,4),(-41.5454951067698,-40.9004262923002,-39.9028549193173,-38.9052835463344,
-37.9077121733514,-36.9101408003685,-35.9125694273856,-35.2623097995902),
 .UNSPECIFIED.);
#3434=B_SPLINE_CURVE_WITH_KNOTS('',3,(#29167,#29168,#29169,#29170,#29171,
#29172,#29173,#29174,#29175,#29176,#29177,#29178,#29179,#29180,#29181,#29182,
#29183,#29184,#29185,#29186,#29187,#29188,#29189,#29190,#29191),
 .UNSPECIFIED.,.F.,.F.,(4,3,3,3,3,3,3,3,4),(32.7257487910699,32.9198553084368,
33.9174266814197,34.9149980544026,35.9125694273856,36.9101408003685,37.9077121733514,
38.9052835463344,39.0089340982495),.UNSPECIFIED.);
#3435=B_SPLINE_CURVE_WITH_KNOTS('',3,(#29192,#29193,#29194,#29195,#29196,
#29197,#29198,#29199,#29200,#29201,#29202,#29203,#29204,#29205,#29206,#29207,
#29208,#29209,#29210,#29211,#29212,#29213),.UNSPECIFIED.,.F.,.F.,(4,3,3,
3,3,3,3,4),(-35.2623097995902,-34.9149980544026,-33.9174266814197,-32.9198553084368,
-31.9222839354538,-30.9247125624709,-29.927141189488,-28.9791244924106),
 .UNSPECIFIED.);
#3436=B_SPLINE_CURVE_WITH_KNOTS('',3,(#29218,#29219,#29220,#29221,#29222,
#29223,#29224,#29225,#29226,#29227,#29228,#29229,#29230,#29231,#29232,#29233,
#29234,#29235,#29236,#29237,#29238,#29239),.UNSPECIFIED.,.F.,.F.,(4,3,3,
3,3,3,3,4),(26.4425634838903,26.9344270705392,27.9319984435221,28.929569816505,
29.927141189488,30.9247125624709,31.9222839354538,32.7257487910699),
 .UNSPECIFIED.);
#3437=B_SPLINE_CURVE_WITH_KNOTS('',3,(#29240,#29241,#29242,#29243,#29244,
#29245,#29246,#29247,#29248,#29249,#29250,#29251,#29252,#29253,#29254,#29255,
#29256,#29257,#29258,#29259,#29260,#29261,#29262,#29263,#29264),
 .UNSPECIFIED.,.F.,.F.,(4,3,3,3,3,3,3,3,4),(-28.9791244924106,-28.929569816505,
-27.9319984435221,-26.9344270705392,-25.9368556975562,-24.9392843245733,
-23.9417129515904,-22.9441415786074,-22.6959391852311),.UNSPECIFIED.);
#3438=B_SPLINE_CURVE_WITH_KNOTS('',3,(#29269,#29270,#29271,#29272,#29273,
#29274,#29275,#29276,#29277,#29278,#29279,#29280,#29281,#29282,#29283,#29284,
#29285,#29286,#29287,#29288,#29289,#29290),.UNSPECIFIED.,.F.,.F.,(4,3,3,
3,3,3,3,4),(20.1593781767108,20.9489988326416,21.9465702056245,22.9441415786074,
23.9417129515904,24.9392843245733,25.9368556975562,26.4425634838903),
 .UNSPECIFIED.);
#3439=B_SPLINE_CURVE_WITH_KNOTS('',3,(#29291,#29292,#29293,#29294,#29295,
#29296,#29297,#29298,#29299,#29300,#29301,#29302,#29303,#29304,#29305,#29306,
#29307,#29308,#29309,#29310,#29311,#29312),.UNSPECIFIED.,.F.,.F.,(4,3,3,
3,3,3,3,4),(-22.6959391852311,-21.9465702056245,-20.9489988326416,-19.9514274596586,
-18.9538560866757,-17.9562847136928,-16.9587133407098,-16.4127538780515),
 .UNSPECIFIED.);
#3440=B_SPLINE_CURVE_WITH_KNOTS('',3,(#29317,#29318,#29319,#29320,#29321,
#29322,#29323,#29324,#29325,#29326,#29327,#29328,#29329,#29330,#29331,#29332,
#29333,#29334,#29335,#29336,#29337,#29338,#29339,#29340,#29341),
 .UNSPECIFIED.,.F.,.F.,(4,3,3,3,3,3,3,3,4),(13.8761928695311,13.9659992217611,
14.963570594744,15.9611419677269,16.9587133407098,17.9562847136928,18.9538560866757,
19.9514274596586,20.1593781767108),.UNSPECIFIED.);
#3441=B_SPLINE_CURVE_WITH_KNOTS('',3,(#29342,#29343,#29344,#29345,#29346,
#29347,#29348,#29349,#29350,#29351,#29352,#29353,#29354,#29355,#29356,#29357,
#29358,#29359,#29360,#29361,#29362,#29363),.UNSPECIFIED.,.F.,.F.,(4,3,3,
3,3,3,3,4),(-16.4127538780515,-15.9611419677269,-14.963570594744,-13.9659992217611,
-12.9684278487781,-11.9708564757952,-10.9732851028123,-10.1295685708719),
 .UNSPECIFIED.);
#3442=B_SPLINE_CURVE_WITH_KNOTS('',3,(#29369,#29370,#29371,#29372,#29373,
#29374,#29375,#29376,#29377,#29378,#29379,#29380,#29381),.UNSPECIFIED.,
 .F.,.F.,(4,3,3,3,4),(-3.8463832636923,-2.99271411894879,-1.99514274596586,
-0.997571372982927,0.),.UNSPECIFIED.);
#3443=B_SPLINE_CURVE_WITH_KNOTS('',3,(#29384,#29385,#29386,#29387,#29388,
#29389,#29390,#29391,#29392,#29393,#29394,#29395,#29396,#29397,#29398,#29399,
#29400,#29401,#29402),.UNSPECIFIED.,.F.,.F.,(4,3,3,3,3,3,4),(2.01461286527433,
2.9927141189488,3.99028549193173,4.98785686491466,5.98542823789759,6.98299961088052,
7.59300756235157),.UNSPECIFIED.);
#3444=B_SPLINE_CURVE_WITH_KNOTS('',3,(#29408,#29409,#29410,#29411,#29412,
#29413,#29414),.UNSPECIFIED.,.F.,.F.,(4,1,1,1,4),(91.106186954104,91.6672898428912,
92.6648612158741,93.6624325888571,94.66000396184),.UNSPECIFIED.);
#3445=B_SPLINE_CURVE_WITH_KNOTS('',3,(#29417,#29418,#29419,#29420,#29421,
#29422,#29423,#29424),.UNSPECIFIED.,.F.,.F.,(4,1,1,1,1,4),(91.106186954104,
91.2111367324627,92.2087081054456,93.2062794784285,94.2038508514115,95.1819521050858),
 .UNSPECIFIED.);
#3446=B_SPLINE_CURVE_WITH_KNOTS('',3,(#29429,#29430,#29431,#29432,#29433,
#29434,#29435,#29436,#29437,#29438),.UNSPECIFIED.,.F.,.F.,(4,1,1,1,1,1,
1,4),(84.8230016469244,85.6818616049936,86.6794329779765,87.6770043509595,
88.6745757239424,89.6721470969253,90.6697184699083,91.106186954104),
 .UNSPECIFIED.);
#3447=B_SPLINE_CURVE_WITH_KNOTS('',3,(#29439,#29440,#29441,#29442,#29443,
#29444,#29445,#29446,#29447,#29448),.UNSPECIFIED.,.F.,.F.,(4,1,1,1,1,1,
1,4),(84.8230016469244,85.2257084945651,86.223279867548,87.2208512405309,
88.2184226135139,89.2159939864968,90.2135653594797,91.106186954104),
 .UNSPECIFIED.);
#3448=B_SPLINE_CURVE_WITH_KNOTS('',3,(#29453,#29454,#29455,#29456,#29457,
#29458,#29459,#29460,#29461,#29462,#29463),.UNSPECIFIED.,.F.,.F.,(4,1,1,
1,1,1,1,1,4),(78.5398163397448,78.6988619941131,79.696433367096,80.6940047400789,
81.6915761130619,82.6891474860448,83.6867188590277,84.6842902320107,84.8230016469244),
 .UNSPECIFIED.);
#3449=B_SPLINE_CURVE_WITH_KNOTS('',3,(#29464,#29465,#29466,#29467,#29468,
#29469,#29470,#29471,#29472,#29473),.UNSPECIFIED.,.F.,.F.,(4,1,1,1,1,1,
1,4),(78.5398163397448,79.2402802566675,80.2378516296504,81.2354230026333,
82.2329943756163,83.2305657485992,84.2281371215821,84.8230016469244),
 .UNSPECIFIED.);
#3450=B_SPLINE_CURVE_WITH_KNOTS('',3,(#29478,#29479,#29480,#29481,#29482,
#29483,#29484,#29485,#29486,#29487),.UNSPECIFIED.,.F.,.F.,(4,1,1,1,1,1,
1,4),(72.2566310325652,72.7134337562155,73.7110051291984,74.7085765021813,
75.7061478751643,76.7037192481472,77.7012906211301,78.5398163397448),
 .UNSPECIFIED.);
#3451=B_SPLINE_CURVE_WITH_KNOTS('',3,(#29488,#29489,#29490,#29491,#29492,
#29493,#29494,#29495,#29496,#29497,#29498),.UNSPECIFIED.,.F.,.F.,(4,1,1,
1,1,1,1,1,4),(72.2566310325652,72.2572806457869,73.2548520187699,74.2524233917528,
75.2499947647357,76.2475661377187,77.2451375107016,78.2427088836845,78.5398163397448),
 .UNSPECIFIED.);
#3452=B_SPLINE_CURVE_WITH_KNOTS('',3,(#29503,#29504,#29505,#29506,#29507,
#29508,#29509,#29510,#29511,#29512),.UNSPECIFIED.,.F.,.F.,(4,1,1,1,1,1,
1,4),(65.9734457253856,66.7280055183179,67.7255768913008,68.7231482642838,
69.7207196372667,70.7182910102496,71.7158623832325,72.2566310325652),
 .UNSPECIFIED.);
#3453=B_SPLINE_CURVE_WITH_KNOTS('',3,(#29513,#29514,#29515,#29516,#29517,
#29518,#29519,#29520,#29521,#29522),.UNSPECIFIED.,.F.,.F.,(4,1,1,1,1,1,
1,4),(65.9734457253856,66.2718524078894,67.2694237808723,68.2669951538552,
69.2645665268382,70.2621378998211,71.259709272804,72.2566310325652),
 .UNSPECIFIED.);
#3454=B_SPLINE_CURVE_WITH_KNOTS('',3,(#29527,#29528,#29529,#29530,#29531,
#29532,#29533,#29534,#29535,#29536,#29537),.UNSPECIFIED.,.F.,.F.,(4,1,1,
1,1,1,1,1,4),(59.690260418206,59.7450059074374,60.7425772804203,61.7401486534032,
62.7377200263862,63.7352913993691,64.732862772352,65.730434145335,65.9734457253856),
 .UNSPECIFIED.);
#3455=B_SPLINE_CURVE_WITH_KNOTS('',3,(#29538,#29539,#29540,#29541,#29542,
#29543,#29544,#29545,#29546,#29547),.UNSPECIFIED.,.F.,.F.,(4,1,1,1,1,1,
1,4),(59.690260418206,60.2864241699918,61.2839955429747,62.2815669159576,
63.2791382889406,64.2767096619235,65.2742810349064,65.9734457253856),
 .UNSPECIFIED.);
#3456=B_SPLINE_CURVE_WITH_KNOTS('',3,(#29552,#29553,#29554,#29555,#29556,
#29557,#29558,#29559,#29560,#29561),.UNSPECIFIED.,.F.,.F.,(4,1,1,1,1,1,
1,4),(53.4070751110265,53.7595776695398,54.7571490425227,55.7547204155056,
56.7522917884886,57.7498631614715,58.7474345344544,59.690260418206),
 .UNSPECIFIED.);
#3457=B_SPLINE_CURVE_WITH_KNOTS('',3,(#29562,#29563,#29564,#29565,#29566,
#29567,#29568,#29569,#29570,#29571),.UNSPECIFIED.,.F.,.F.,(4,1,1,1,1,1,
1,4),(53.4070751110264,54.3009959320942,55.2985673050771,56.29613867806,
57.293710051043,58.2912814240259,59.2888527970088,59.690260418206),
 .UNSPECIFIED.);
#3458=B_SPLINE_CURVE_WITH_KNOTS('',3,(#29576,#29577,#29578,#29579,#29580,
#29581,#29582,#29583,#29584,#29585),.UNSPECIFIED.,.F.,.F.,(4,1,1,1,1,1,
1,4),(47.1238898038469,47.7741494316422,48.7717208046251,49.769292177608,
50.766863550591,51.7644349235739,52.7620062965568,53.4070751110265),
 .UNSPECIFIED.);
#3459=B_SPLINE_CURVE_WITH_KNOTS('',3,(#29586,#29587,#29588,#29589,#29590,
#29591,#29592,#29593,#29594,#29595,#29596),.UNSPECIFIED.,.F.,.F.,(4,1,1,
1,1,1,1,1,4),(47.1238898038468,47.3179963212136,48.3155676941966,49.3131390671795,
50.3107104401624,51.3082818131454,52.3058531861283,53.3034245591112,53.4070751110264),
 .UNSPECIFIED.);
#3460=B_SPLINE_CURVE_WITH_KNOTS('',3,(#29601,#29602,#29603,#29604,#29605,
#29606,#29607,#29608,#29609,#29610),.UNSPECIFIED.,.F.,.F.,(4,1,1,1,1,1,
1,4),(40.8407044966673,41.7887211937446,42.7862925667275,43.7838639397104,
44.7814353126934,45.7790066856763,46.7765780586592,47.1238898038469),
 .UNSPECIFIED.);
#3461=B_SPLINE_CURVE_WITH_KNOTS('',3,(#29611,#29612,#29613,#29614,#29615,
#29616,#29617,#29618,#29619,#29620),.UNSPECIFIED.,.F.,.F.,(4,1,1,1,1,1,
1,4),(40.8407044966673,41.332568083316,42.330139456299,43.3277108292819,
44.3252822022648,45.3228535752478,46.3204249482307,47.1238898038468),
 .UNSPECIFIED.);
#3462=B_SPLINE_CURVE_WITH_KNOTS('',3,(#29625,#29626,#29627,#29628,#29629,
#29630,#29631,#29632,#29633,#29634,#29635),.UNSPECIFIED.,.F.,.F.,(4,1,1,
1,1,1,1,1,4),(34.5575191894877,34.805721582864,35.803292955847,36.8008643288299,
37.7984357018128,38.7960070747958,39.7935784477787,40.7911498207616,40.8407044966673),
 .UNSPECIFIED.);
#3463=B_SPLINE_CURVE_WITH_KNOTS('',3,(#29636,#29637,#29638,#29639,#29640,
#29641,#29642,#29643,#29644,#29645),.UNSPECIFIED.,.F.,.F.,(4,1,1,1,1,1,
1,4),(34.5575191894876,35.3471398454184,36.3447112184014,37.3422825913843,
38.3398539643672,39.3374253373502,40.3349967103331,40.8407044966673),
 .UNSPECIFIED.);
#3464=B_SPLINE_CURVE_WITH_KNOTS('',3,(#29650,#29651,#29652,#29653,#29654,
#29655,#29656,#29657,#29658,#29659),.UNSPECIFIED.,.F.,.F.,(4,1,1,1,1,1,
1,4),(28.2743338823081,28.8202933449665,29.8178647179494,30.8154360909323,
31.8130074639152,32.8105788368982,33.8081502098811,34.5575191894877),
 .UNSPECIFIED.);
#3465=B_SPLINE_CURVE_WITH_KNOTS('',3,(#29660,#29661,#29662,#29663,#29664,
#29665,#29666,#29667,#29668,#29669,#29670),.UNSPECIFIED.,.F.,.F.,(4,1,1,
1,1,1,1,1,4),(28.2743338823081,28.3641402345379,29.3617116075208,30.3592829805038,
31.3568543534867,32.3544257264696,33.3519970994526,34.3495684724355,34.5575191894876),
 .UNSPECIFIED.);
#3466=B_SPLINE_CURVE_WITH_KNOTS('',3,(#29675,#29676,#29677,#29678,#29679,
#29680,#29681,#29682,#29683,#29684),.UNSPECIFIED.,.F.,.F.,(4,1,1,1,1,1,
1,4),(21.9911485751285,22.8348651070689,23.8324364800518,24.8300078530347,
25.8275792260177,26.8251505990006,27.8227219719835,28.2743338823081),
 .UNSPECIFIED.);
#3467=B_SPLINE_CURVE_WITH_KNOTS('',3,(#29685,#29686,#29687,#29688,#29689,
#29690,#29691,#29692,#29693,#29694),.UNSPECIFIED.,.F.,.F.,(4,1,1,1,1,1,
1,4),(21.9911485751285,22.3787119966403,23.3762833696233,24.3738547426062,
25.3714261155891,26.3689974885721,27.366568861555,28.2743338823081),
 .UNSPECIFIED.);
#3468=B_SPLINE_CURVE_WITH_KNOTS('',3,(#29700,#29701,#29702,#29703,#29704),
 .UNSPECIFIED.,.F.,.F.,(4,1,4),(14.3981410127769,15.3957123857598,15.7079632679489),
 .UNSPECIFIED.);
#3469=B_SPLINE_CURVE_WITH_KNOTS('',3,(#29707,#29708,#29709,#29710,#29711),
 .UNSPECIFIED.,.F.,.F.,(4,1,4),(13.8761928695311,14.8542941232054,15.7079632679489),
 .UNSPECIFIED.);
#3470=B_SPLINE_CURVE_WITH_KNOTS('',3,(#29717,#29718,#29719,#29720,#29721,
#29722,#29723,#29724,#29725,#29726,#29727,#29728,#29729,#29730,#29731,#29732,
#29733,#29734,#29735,#29736,#29737,#29738),.UNSPECIFIED.,.F.,.F.,(4,3,3,
3,3,3,3,4),(76.708045941327,76.8129957196858,77.8105670926687,78.8081384656517,
79.8057098386346,80.8032812116175,81.8008525846005,82.7984239575834),
 .UNSPECIFIED.);
#3471=B_SPLINE_CURVE_WITH_KNOTS('',3,(#29742,#29743,#29744,#29745,#29746,
#29747,#29748),.UNSPECIFIED.,.F.,.F.,(4,3,4),(-80.7838110923089,-79.8057098386346,
-79.2446069498473),.UNSPECIFIED.);
#3472=B_SPLINE_CURVE_WITH_KNOTS('',3,(#29752,#29753,#29754,#29755,#29756,
#29757,#29758,#29759,#29760,#29761,#29762,#29763,#29764,#29765,#29766,#29767,
#29768,#29769,#29770,#29771,#29772,#29773),.UNSPECIFIED.,.F.,.F.,(4,3,3,
3,3,3,3,4),(-79.2446069498473,-78.8081384656517,-77.8105670926687,-76.8129957196858,
-75.8154243467029,-74.81785297372,-73.820281600737,-72.9614216426677),
 .UNSPECIFIED.);
#3473=B_SPLINE_CURVE_WITH_KNOTS('',3,(#29778,#29779,#29780,#29781,#29782,
#29783,#29784,#29785,#29786,#29787,#29788,#29789,#29790,#29791,#29792,#29793,
#29794,#29795,#29796,#29797,#29798,#29799),.UNSPECIFIED.,.F.,.F.,(4,3,3,
3,3,3,3,4),(70.4248606341474,70.8275674817882,71.8251388547712,72.8227102277541,
73.820281600737,74.81785297372,75.8154243467029,76.708045941327),
 .UNSPECIFIED.);
#3474=B_SPLINE_CURVE_WITH_KNOTS('',3,(#29800,#29801,#29802,#29803,#29804,
#29805,#29806,#29807,#29808,#29809,#29810,#29811,#29812,#29813,#29814,#29815,
#29816,#29817,#29818,#29819,#29820,#29821,#29822,#29823,#29824),
 .UNSPECIFIED.,.F.,.F.,(4,3,3,3,3,3,3,3,4),(-72.9614216426677,-72.8227102277541,
-71.8251388547711,-70.8275674817882,-69.8299961088053,-68.8324247358223,
-67.8348533628394,-66.8372819898565,-66.6782363354881),.UNSPECIFIED.);
#3475=B_SPLINE_CURVE_WITH_KNOTS('',3,(#29829,#29830,#29831,#29832,#29833,
#29834,#29835,#29836,#29837,#29838,#29839,#29840,#29841,#29842,#29843,#29844,
#29845,#29846,#29847,#29848,#29849,#29850),.UNSPECIFIED.,.F.,.F.,(4,3,3,
3,3,3,3,4),(64.1416753269678,64.8421392438906,65.8397106168735,66.8372819898565,
67.8348533628394,68.8324247358223,69.8299961088053,70.4248606341474),
 .UNSPECIFIED.);
#3476=B_SPLINE_CURVE_WITH_KNOTS('',3,(#29851,#29852,#29853,#29854,#29855,
#29856,#29857,#29858,#29859,#29860,#29861,#29862,#29863,#29864,#29865,#29866,
#29867,#29868,#29869,#29870,#29871,#29872),.UNSPECIFIED.,.F.,.F.,(4,3,3,
3,3,3,3,4),(-66.6782363354881,-65.8397106168735,-64.8421392438906,-63.8445678709077,
-62.8469964979248,-61.8494251249418,-60.8518537519589,-60.3950510283085),
 .UNSPECIFIED.);
#3477=B_SPLINE_CURVE_WITH_KNOTS('',3,(#29877,#29878,#29879,#29880,#29881,
#29882,#29883,#29884,#29885,#29886,#29887,#29888,#29889,#29890,#29891,#29892,
#29893,#29894,#29895,#29896,#29897,#29898),.UNSPECIFIED.,.F.,.F.,(4,3,3,
3,3,3,3,4),(57.8584900197882,58.856711005993,59.854282378976,60.8518537519589,
61.8494251249418,62.8469964979248,63.8445678709077,64.1416753269678),
 .UNSPECIFIED.);
#3478=B_SPLINE_CURVE_WITH_KNOTS('',3,(#29899,#29900,#29901,#29902,#29903,
#29904,#29905,#29906,#29907,#29908,#29909,#29910,#29911,#29912,#29913,#29914,
#29915,#29916,#29917,#29918,#29919,#29920),.UNSPECIFIED.,.F.,.F.,(4,3,3,
3,3,3,3,4),(-60.3950510283085,-59.854282378976,-58.856711005993,-57.8591396330101,
-56.8615682600272,-55.8639968870442,-54.8664255140613,-54.111865721129),
 .UNSPECIFIED.);
#3479=B_SPLINE_CURVE_WITH_KNOTS('',3,(#29925,#29926,#29927,#29928,#29929,
#29930,#29931,#29932,#29933,#29934,#29935,#29936,#29937,#29938,#29939,#29940,
#29941,#29942,#29943,#29944,#29945,#29946),.UNSPECIFIED.,.F.,.F.,(4,3,3,
3,3,3,3,4),(51.5753047126087,51.8737113951125,52.8712827680954,53.8688541410784,
54.8664255140613,55.8639968870442,56.8615682600272,57.8584900197882),
 .UNSPECIFIED.);
#3480=B_SPLINE_CURVE_WITH_KNOTS('',3,(#29947,#29948,#29949,#29950,#29951,
#29952,#29953,#29954,#29955,#29956,#29957,#29958,#29959,#29960,#29961,#29962,
#29963,#29964,#29965,#29966,#29967,#29968,#29969,#29970,#29971),
 .UNSPECIFIED.,.F.,.F.,(4,3,3,3,3,3,3,3,4),(-54.111865721129,-53.8688541410784,
-52.8712827680954,-51.8737113951125,-50.8761400221296,-49.8785686491466,
-48.8809972761637,-47.8834259031808,-47.8286804139494),.UNSPECIFIED.);
#3481=B_SPLINE_CURVE_WITH_KNOTS('',3,(#29976,#29977,#29978,#29979,#29980,
#29981,#29982,#29983,#29984,#29985,#29986,#29987,#29988,#29989,#29990,#29991,
#29992,#29993,#29994,#29995,#29996,#29997),.UNSPECIFIED.,.F.,.F.,(4,3,3,
3,3,3,3,4),(45.2921194054291,45.8882831572149,46.8858545301978,47.8834259031808,
48.8809972761637,49.8785686491466,50.8761400221296,51.5753047126087),
 .UNSPECIFIED.);
#3482=B_SPLINE_CURVE_WITH_KNOTS('',3,(#29998,#29999,#30000,#30001,#30002,
#30003,#30004,#30005,#30006,#30007,#30008,#30009,#30010,#30011,#30012,#30013,
#30014,#30015,#30016,#30017,#30018,#30019),.UNSPECIFIED.,.F.,.F.,(4,3,3,
3,3,3,3,4),(-47.8286804139494,-46.8858545301978,-45.8882831572149,-44.890711784232,
-43.893140411249,-42.8955690382661,-41.8979976652832,-41.5454951067698),
 .UNSPECIFIED.);
#3483=B_SPLINE_CURVE_WITH_KNOTS('',3,(#30024,#30025,#30026,#30027,#30028,
#30029,#30030,#30031,#30032,#30033,#30034,#30035,#30036,#30037,#30038,#30039,
#30040,#30041,#30042,#30043,#30044,#30045),.UNSPECIFIED.,.F.,.F.,(4,3,3,
3,3,3,3,4),(39.0089340982495,39.9028549193173,40.9004262923002,41.8979976652832,
42.8955690382661,43.893140411249,44.890711784232,45.2921194054291),
 .UNSPECIFIED.);
#3484=B_SPLINE_CURVE_WITH_KNOTS('',3,(#30046,#30047,#30048,#30049,#30050,
#30051,#30052,#30053,#30054,#30055,#30056,#30057,#30058,#30059,#30060,#30061,
#30062,#30063,#30064,#30065,#30066,#30067),.UNSPECIFIED.,.F.,.F.,(4,3,3,
3,3,3,3,4),(-41.5454951067698,-40.9004262923002,-39.9028549193173,-38.9052835463344,
-37.9077121733514,-36.9101408003685,-35.9125694273856,-35.2623097995902),
 .UNSPECIFIED.);
#3485=B_SPLINE_CURVE_WITH_KNOTS('',3,(#30072,#30073,#30074,#30075,#30076,
#30077,#30078,#30079,#30080,#30081,#30082,#30083,#30084,#30085,#30086,#30087,
#30088,#30089,#30090,#30091,#30092,#30093,#30094,#30095,#30096),
 .UNSPECIFIED.,.F.,.F.,(4,3,3,3,3,3,3,3,4),(32.7257487910699,32.9198553084368,
33.9174266814197,34.9149980544026,35.9125694273856,36.9101408003685,37.9077121733514,
38.9052835463344,39.0089340982495),.UNSPECIFIED.);
#3486=B_SPLINE_CURVE_WITH_KNOTS('',3,(#30097,#30098,#30099,#30100,#30101,
#30102,#30103,#30104,#30105,#30106,#30107,#30108,#30109,#30110,#30111,#30112,
#30113,#30114,#30115,#30116,#30117,#30118),.UNSPECIFIED.,.F.,.F.,(4,3,3,
3,3,3,3,4),(-35.2623097995902,-34.9149980544027,-33.9174266814197,-32.9198553084368,
-31.9222839354539,-30.9247125624709,-29.927141189488,-28.9791244924106),
 .UNSPECIFIED.);
#3487=B_SPLINE_CURVE_WITH_KNOTS('',3,(#30123,#30124,#30125,#30126,#30127,
#30128,#30129,#30130,#30131,#30132,#30133,#30134,#30135,#30136,#30137,#30138,
#30139,#30140,#30141,#30142,#30143,#30144),.UNSPECIFIED.,.F.,.F.,(4,3,3,
3,3,3,3,4),(26.4425634838903,26.9344270705392,27.9319984435221,28.929569816505,
29.927141189488,30.9247125624709,31.9222839354538,32.7257487910699),
 .UNSPECIFIED.);
#3488=B_SPLINE_CURVE_WITH_KNOTS('',3,(#30145,#30146,#30147,#30148,#30149,
#30150,#30151,#30152,#30153,#30154,#30155,#30156,#30157,#30158,#30159,#30160,
#30161,#30162,#30163,#30164,#30165,#30166,#30167,#30168,#30169),
 .UNSPECIFIED.,.F.,.F.,(4,3,3,3,3,3,3,3,4),(-28.9791244924106,-28.9295698165051,
-27.9319984435221,-26.9344270705392,-25.9368556975562,-24.9392843245733,
-23.9417129515904,-22.9441415786075,-22.695939185231),.UNSPECIFIED.);
#3489=B_SPLINE_CURVE_WITH_KNOTS('',3,(#30174,#30175,#30176,#30177,#30178,
#30179,#30180,#30181,#30182,#30183,#30184,#30185,#30186,#30187,#30188,#30189,
#30190,#30191,#30192,#30193,#30194,#30195),.UNSPECIFIED.,.F.,.F.,(4,3,3,
3,3,3,3,4),(20.1593781767107,20.9489988326416,21.9465702056245,22.9441415786074,
23.9417129515904,24.9392843245733,25.9368556975562,26.4425634838903),
 .UNSPECIFIED.);
#3490=B_SPLINE_CURVE_WITH_KNOTS('',3,(#30196,#30197,#30198,#30199,#30200,
#30201,#30202,#30203,#30204,#30205,#30206,#30207,#30208,#30209,#30210,#30211,
#30212,#30213,#30214,#30215,#30216,#30217),.UNSPECIFIED.,.F.,.F.,(4,3,3,
3,3,3,3,4),(-22.695939185231,-21.9465702056245,-20.9489988326416,-19.9514274596587,
-18.9538560866757,-17.9562847136928,-16.9587133407099,-16.4127538780514),
 .UNSPECIFIED.);
#3491=B_SPLINE_CURVE_WITH_KNOTS('',3,(#30222,#30223,#30224,#30225,#30226,
#30227,#30228,#30229,#30230,#30231,#30232,#30233,#30234,#30235,#30236,#30237,
#30238,#30239,#30240,#30241,#30242,#30243,#30244,#30245,#30246),
 .UNSPECIFIED.,.F.,.F.,(4,3,3,3,3,3,3,3,4),(13.8761928695311,13.9659992217611,
14.963570594744,15.9611419677269,16.9587133407099,17.9562847136928,18.9538560866757,
19.9514274596586,20.1593781767107),.UNSPECIFIED.);
#3492=B_SPLINE_CURVE_WITH_KNOTS('',3,(#30247,#30248,#30249,#30250,#30251,
#30252,#30253,#30254,#30255,#30256,#30257,#30258,#30259,#30260,#30261,#30262,
#30263,#30264,#30265,#30266,#30267,#30268),.UNSPECIFIED.,.F.,.F.,(4,3,3,
3,3,3,3,4),(-16.4127538780514,-15.9611419677269,-14.963570594744,-13.9659992217611,
-12.9684278487781,-11.9708564757952,-10.9732851028123,-10.1295685708718),
 .UNSPECIFIED.);
#3493=B_SPLINE_CURVE_WITH_KNOTS('',3,(#30274,#30275,#30276,#30277,#30278,
#30279,#30280,#30281,#30282,#30283,#30284,#30285,#30286),.UNSPECIFIED.,
 .F.,.F.,(4,3,3,3,4),(-3.84638326369223,-2.9927141189488,-1.99514274596587,
-0.997571372982933,0.),.UNSPECIFIED.);
#3494=B_SPLINE_CURVE_WITH_KNOTS('',3,(#30289,#30290,#30291,#30292,#30293,
#30294,#30295,#30296,#30297,#30298,#30299,#30300,#30301,#30302,#30303,#30304,
#30305,#30306,#30307),.UNSPECIFIED.,.F.,.F.,(4,3,3,3,3,3,4),(2.01461286527451,
2.9927141189488,3.99028549193173,4.98785686491466,5.98542823789759,6.98299961088052,
7.59300756235153),.UNSPECIFIED.);
#3495=B_SPLINE_CURVE_WITH_KNOTS('',3,(#30313,#30314,#30315,#30316,#30317,
#30318,#30319),.UNSPECIFIED.,.F.,.F.,(4,1,1,1,4),(91.106186954104,91.6672898428913,
92.6648612158742,93.6624325888572,94.6600039618401),.UNSPECIFIED.);
#3496=B_SPLINE_CURVE_WITH_KNOTS('',3,(#30322,#30323,#30324,#30325,#30326,
#30327,#30328,#30329),.UNSPECIFIED.,.F.,.F.,(4,1,1,1,1,4),(91.106186954104,
91.2111367324627,92.2087081054457,93.2062794784286,94.2038508514115,95.1819521050859),
 .UNSPECIFIED.);
#3497=B_SPLINE_CURVE_WITH_KNOTS('',3,(#30334,#30335,#30336,#30337,#30338,
#30339,#30340,#30341,#30342,#30343),.UNSPECIFIED.,.F.,.F.,(4,1,1,1,1,1,
1,4),(84.8230016469244,85.6818616049937,86.6794329779766,87.6770043509596,
88.6745757239425,89.6721470969254,90.6697184699084,91.106186954104),
 .UNSPECIFIED.);
#3498=B_SPLINE_CURVE_WITH_KNOTS('',3,(#30344,#30345,#30346,#30347,#30348,
#30349,#30350,#30351,#30352,#30353),.UNSPECIFIED.,.F.,.F.,(4,1,1,1,1,1,
1,4),(84.8230016469244,85.2257084945651,86.2232798675481,87.220851240531,
88.2184226135139,89.2159939864969,90.2135653594798,91.106186954104),
 .UNSPECIFIED.);
#3499=B_SPLINE_CURVE_WITH_KNOTS('',3,(#30358,#30359,#30360,#30361,#30362,
#30363,#30364,#30365,#30366,#30367,#30368),.UNSPECIFIED.,.F.,.F.,(4,1,1,
1,1,1,1,1,4),(78.5398163397448,78.6988619941132,79.6964333670961,80.694004740079,
81.691576113062,82.6891474860449,83.6867188590278,84.6842902320108,84.8230016469244),
 .UNSPECIFIED.);
#3500=B_SPLINE_CURVE_WITH_KNOTS('',3,(#30369,#30370,#30371,#30372,#30373,
#30374,#30375,#30376,#30377,#30378),.UNSPECIFIED.,.F.,.F.,(4,1,1,1,1,1,
1,4),(78.5398163397448,79.2402802566675,80.2378516296505,81.2354230026334,
82.2329943756163,83.2305657485993,84.2281371215822,84.8230016469244),
 .UNSPECIFIED.);
#3501=B_SPLINE_CURVE_WITH_KNOTS('',3,(#30383,#30384,#30385,#30386,#30387,
#30388,#30389,#30390,#30391,#30392),.UNSPECIFIED.,.F.,.F.,(4,1,1,1,1,1,
1,4),(72.2566310325652,72.7134337562156,73.7110051291985,74.7085765021814,
75.7061478751644,76.7037192481473,77.7012906211302,78.5398163397448),
 .UNSPECIFIED.);
#3502=B_SPLINE_CURVE_WITH_KNOTS('',3,(#30393,#30394,#30395,#30396,#30397,
#30398,#30399,#30400,#30401,#30402,#30403),.UNSPECIFIED.,.F.,.F.,(4,1,1,
1,1,1,1,1,4),(72.2566310325652,72.257280645787,73.25485201877,74.2524233917529,
75.2499947647358,76.2475661377187,77.2451375107017,78.2427088836846,78.5398163397448),
 .UNSPECIFIED.);
#3503=B_SPLINE_CURVE_WITH_KNOTS('',3,(#30408,#30409,#30410,#30411,#30412,
#30413,#30414,#30415,#30416,#30417),.UNSPECIFIED.,.F.,.F.,(4,1,1,1,1,1,
1,4),(65.9734457253856,66.728005518318,67.7255768913009,68.7231482642839,
69.7207196372668,70.7182910102497,71.7158623832326,72.2566310325652),
 .UNSPECIFIED.);
#3504=B_SPLINE_CURVE_WITH_KNOTS('',3,(#30418,#30419,#30420,#30421,#30422,
#30423,#30424,#30425,#30426,#30427),.UNSPECIFIED.,.F.,.F.,(4,1,1,1,1,1,
1,4),(65.9734457253856,66.2718524078894,67.2694237808724,68.2669951538553,
69.2645665268382,70.2621378998212,71.2597092728041,72.2566310325652),
 .UNSPECIFIED.);
#3505=B_SPLINE_CURVE_WITH_KNOTS('',3,(#30432,#30433,#30434,#30435,#30436,
#30437,#30438,#30439,#30440,#30441,#30442),.UNSPECIFIED.,.F.,.F.,(4,1,1,
1,1,1,1,1,4),(59.690260418206,59.7450059074374,60.7425772804204,61.7401486534033,
62.7377200263862,63.7352913993692,64.7328627723521,65.7304341453351,65.9734457253856),
 .UNSPECIFIED.);
#3506=B_SPLINE_CURVE_WITH_KNOTS('',3,(#30443,#30444,#30445,#30446,#30447,
#30448,#30449,#30450,#30451,#30452),.UNSPECIFIED.,.F.,.F.,(4,1,1,1,1,1,
1,4),(59.690260418206,60.2864241699918,61.2839955429748,62.2815669159577,
63.2791382889406,64.2767096619236,65.2742810349065,65.9734457253856),
 .UNSPECIFIED.);
#3507=B_SPLINE_CURVE_WITH_KNOTS('',3,(#30457,#30458,#30459,#30460,#30461,
#30462,#30463,#30464,#30465,#30466),.UNSPECIFIED.,.F.,.F.,(4,1,1,1,1,1,
1,4),(53.4070751110264,53.7595776695399,54.7571490425228,55.7547204155057,
56.7522917884886,57.7498631614716,58.7474345344545,59.690260418206),
 .UNSPECIFIED.);
#3508=B_SPLINE_CURVE_WITH_KNOTS('',3,(#30467,#30468,#30469,#30470,#30471,
#30472,#30473,#30474,#30475,#30476),.UNSPECIFIED.,.F.,.F.,(4,1,1,1,1,1,
1,4),(53.4070751110264,54.3009959320942,55.2985673050772,56.2961386780601,
57.293710051043,58.291281424026,59.2888527970089,59.690260418206),
 .UNSPECIFIED.);
#3509=B_SPLINE_CURVE_WITH_KNOTS('',3,(#30481,#30482,#30483,#30484,#30485,
#30486,#30487,#30488,#30489,#30490),.UNSPECIFIED.,.F.,.F.,(4,1,1,1,1,1,
1,4),(47.1238898038468,47.7741494316423,48.7717208046252,49.7692921776081,
50.7668635505911,51.764434923574,52.7620062965569,53.4070751110264),
 .UNSPECIFIED.);
#3510=B_SPLINE_CURVE_WITH_KNOTS('',3,(#30491,#30492,#30493,#30494,#30495,
#30496,#30497,#30498,#30499,#30500,#30501),.UNSPECIFIED.,.F.,.F.,(4,1,1,
1,1,1,1,1,4),(47.1238898038468,47.3179963212137,48.3155676941966,49.3131390671796,
50.3107104401625,51.3082818131454,52.3058531861284,53.3034245591113,53.4070751110264),
 .UNSPECIFIED.);
#3511=B_SPLINE_CURVE_WITH_KNOTS('',3,(#30506,#30507,#30508,#30509,#30510,
#30511,#30512,#30513,#30514,#30515),.UNSPECIFIED.,.F.,.F.,(4,1,1,1,1,1,
1,4),(40.8407044966672,41.7887211937447,42.7862925667276,43.7838639397105,
44.7814353126935,45.7790066856764,46.7765780586593,47.1238898038468),
 .UNSPECIFIED.);
#3512=B_SPLINE_CURVE_WITH_KNOTS('',3,(#30516,#30517,#30518,#30519,#30520,
#30521,#30522,#30523,#30524,#30525),.UNSPECIFIED.,.F.,.F.,(4,1,1,1,1,1,
1,4),(40.8407044966673,41.3325680833161,42.330139456299,43.327710829282,
44.3252822022649,45.3228535752478,46.3204249482308,47.1238898038468),
 .UNSPECIFIED.);
#3513=B_SPLINE_CURVE_WITH_KNOTS('',3,(#30530,#30531,#30532,#30533,#30534,
#30535,#30536,#30537,#30538,#30539,#30540),.UNSPECIFIED.,.F.,.F.,(4,1,1,
1,1,1,1,1,4),(34.5575191894876,34.8057215828641,35.8032929558471,36.80086432883,
37.7984357018129,38.7960070747959,39.7935784477788,40.7911498207617,40.8407044966672),
 .UNSPECIFIED.);
#3514=B_SPLINE_CURVE_WITH_KNOTS('',3,(#30541,#30542,#30543,#30544,#30545,
#30546,#30547,#30548,#30549,#30550),.UNSPECIFIED.,.F.,.F.,(4,1,1,1,1,1,
1,4),(34.5575191894876,35.3471398454185,36.3447112184014,37.3422825913844,
38.3398539643673,39.3374253373502,40.3349967103332,40.8407044966673),
 .UNSPECIFIED.);
#3515=B_SPLINE_CURVE_WITH_KNOTS('',3,(#30555,#30556,#30557,#30558,#30559,
#30560,#30561,#30562,#30563,#30564),.UNSPECIFIED.,.F.,.F.,(4,1,1,1,1,1,
1,4),(28.2743338823081,28.8202933449665,29.8178647179495,30.8154360909324,
31.8130074639153,32.8105788368983,33.8081502098812,34.5575191894876),
 .UNSPECIFIED.);
#3516=B_SPLINE_CURVE_WITH_KNOTS('',3,(#30565,#30566,#30567,#30568,#30569,
#30570,#30571,#30572,#30573,#30574,#30575),.UNSPECIFIED.,.F.,.F.,(4,1,1,
1,1,1,1,1,4),(28.2743338823081,28.364140234538,29.3617116075209,30.3592829805038,
31.3568543534868,32.3544257264697,33.3519970994526,34.3495684724356,34.5575191894876),
 .UNSPECIFIED.);
#3517=B_SPLINE_CURVE_WITH_KNOTS('',3,(#30580,#30581,#30582,#30583,#30584,
#30585,#30586,#30587,#30588,#30589),.UNSPECIFIED.,.F.,.F.,(4,1,1,1,1,1,
1,4),(21.9911485751285,22.8348651070689,23.8324364800519,24.8300078530348,
25.8275792260177,26.8251505990007,27.8227219719836,28.2743338823081),
 .UNSPECIFIED.);
#3518=B_SPLINE_CURVE_WITH_KNOTS('',3,(#30590,#30591,#30592,#30593,#30594,
#30595,#30596,#30597,#30598,#30599),.UNSPECIFIED.,.F.,.F.,(4,1,1,1,1,1,
1,4),(21.9911485751285,22.3787119966404,23.3762833696233,24.3738547426063,
25.3714261155892,26.3689974885721,27.3665688615551,28.2743338823081),
 .UNSPECIFIED.);
#3519=B_SPLINE_CURVE_WITH_KNOTS('',3,(#30605,#30606,#30607,#30608,#30609),
 .UNSPECIFIED.,.F.,.F.,(4,1,4),(14.3981410127769,15.3957123857599,15.7079632679489),
 .UNSPECIFIED.);
#3520=B_SPLINE_CURVE_WITH_KNOTS('',3,(#30612,#30613,#30614,#30615,#30616),
 .UNSPECIFIED.,.F.,.F.,(4,1,4),(13.8761928695311,14.8542941232055,15.7079632679489),
 .UNSPECIFIED.);
#3521=B_SPLINE_CURVE_WITH_KNOTS('',3,(#30622,#30623,#30624,#30625,#30626,
#30627,#30628,#30629,#30630,#30631,#30632,#30633,#30634,#30635,#30636,#30637,
#30638,#30639,#30640,#30641,#30642,#30643),.UNSPECIFIED.,.F.,.F.,(4,3,3,
3,3,3,3,4),(76.708045941327,76.8129957196858,77.8105670926687,78.8081384656517,
79.8057098386346,80.8032812116175,81.8008525846005,82.7984239575834),
 .UNSPECIFIED.);
#3522=B_SPLINE_CURVE_WITH_KNOTS('',3,(#30647,#30648,#30649,#30650,#30651,
#30652,#30653),.UNSPECIFIED.,.F.,.F.,(4,3,4),(-80.7838110923091,-79.8057098386346,
-79.2446069498473),.UNSPECIFIED.);
#3523=B_SPLINE_CURVE_WITH_KNOTS('',3,(#30657,#30658,#30659,#30660,#30661,
#30662,#30663,#30664,#30665,#30666,#30667,#30668,#30669,#30670,#30671,#30672,
#30673,#30674,#30675,#30676,#30677,#30678),.UNSPECIFIED.,.F.,.F.,(4,3,3,
3,3,3,3,4),(-79.2446069498473,-78.8081384656517,-77.8105670926688,-76.8129957196858,
-75.8154243467029,-74.81785297372,-73.820281600737,-72.9614216426677),
 .UNSPECIFIED.);
#3524=B_SPLINE_CURVE_WITH_KNOTS('',3,(#30683,#30684,#30685,#30686,#30687,
#30688,#30689,#30690,#30691,#30692,#30693,#30694,#30695,#30696,#30697,#30698,
#30699,#30700,#30701,#30702,#30703,#30704),.UNSPECIFIED.,.F.,.F.,(4,3,3,
3,3,3,3,4),(70.4248606341474,70.8275674817882,71.8251388547712,72.8227102277541,
73.820281600737,74.81785297372,75.8154243467029,76.708045941327),
 .UNSPECIFIED.);
#3525=B_SPLINE_CURVE_WITH_KNOTS('',3,(#30705,#30706,#30707,#30708,#30709,
#30710,#30711,#30712,#30713,#30714,#30715,#30716,#30717,#30718,#30719,#30720,
#30721,#30722,#30723,#30724,#30725,#30726,#30727,#30728,#30729),
 .UNSPECIFIED.,.F.,.F.,(4,3,3,3,3,3,3,3,4),(-72.9614216426677,-72.8227102277541,
-71.8251388547712,-70.8275674817882,-69.8299961088053,-68.8324247358224,
-67.8348533628394,-66.8372819898565,-66.6782363354882),.UNSPECIFIED.);
#3526=B_SPLINE_CURVE_WITH_KNOTS('',3,(#30734,#30735,#30736,#30737,#30738,
#30739,#30740,#30741,#30742,#30743,#30744,#30745,#30746,#30747,#30748,#30749,
#30750,#30751,#30752,#30753,#30754,#30755),.UNSPECIFIED.,.F.,.F.,(4,3,3,
3,3,3,3,4),(64.1416753269678,64.8421392438906,65.8397106168735,66.8372819898565,
67.8348533628394,68.8324247358223,69.8299961088053,70.4248606341474),
 .UNSPECIFIED.);
#3527=B_SPLINE_CURVE_WITH_KNOTS('',3,(#30756,#30757,#30758,#30759,#30760,
#30761,#30762,#30763,#30764,#30765,#30766,#30767,#30768,#30769,#30770,#30771,
#30772,#30773,#30774,#30775,#30776,#30777),.UNSPECIFIED.,.F.,.F.,(4,3,3,
3,3,3,3,4),(-66.6782363354882,-65.8397106168736,-64.8421392438906,-63.8445678709077,
-62.8469964979248,-61.8494251249418,-60.8518537519589,-60.3950510283086),
 .UNSPECIFIED.);
#3528=B_SPLINE_CURVE_WITH_KNOTS('',3,(#30782,#30783,#30784,#30785,#30786,
#30787,#30788,#30789,#30790,#30791,#30792,#30793,#30794,#30795,#30796,#30797,
#30798,#30799,#30800,#30801,#30802,#30803),.UNSPECIFIED.,.F.,.F.,(4,3,3,
3,3,3,3,4),(57.8584900197882,58.856711005993,59.854282378976,60.8518537519589,
61.8494251249418,62.8469964979248,63.8445678709077,64.1416753269678),
 .UNSPECIFIED.);
#3529=B_SPLINE_CURVE_WITH_KNOTS('',3,(#30804,#30805,#30806,#30807,#30808,
#30809,#30810,#30811,#30812,#30813,#30814,#30815,#30816,#30817,#30818,#30819,
#30820,#30821,#30822,#30823,#30824,#30825),.UNSPECIFIED.,.F.,.F.,(4,3,3,
3,3,3,3,4),(-60.3950510283086,-59.854282378976,-58.856711005993,-57.8591396330101,
-56.8615682600272,-55.8639968870442,-54.8664255140613,-54.111865721129),
 .UNSPECIFIED.);
#3530=B_SPLINE_CURVE_WITH_KNOTS('',3,(#30830,#30831,#30832,#30833,#30834,
#30835,#30836,#30837,#30838,#30839,#30840,#30841,#30842,#30843,#30844,#30845,
#30846,#30847,#30848,#30849,#30850,#30851),.UNSPECIFIED.,.F.,.F.,(4,3,3,
3,3,3,3,4),(51.5753047126087,51.8737113951125,52.8712827680954,53.8688541410784,
54.8664255140613,55.8639968870442,56.8615682600272,57.8584900197882),
 .UNSPECIFIED.);
#3531=B_SPLINE_CURVE_WITH_KNOTS('',3,(#30852,#30853,#30854,#30855,#30856,
#30857,#30858,#30859,#30860,#30861,#30862,#30863,#30864,#30865,#30866,#30867,
#30868,#30869,#30870,#30871,#30872,#30873,#30874,#30875,#30876),
 .UNSPECIFIED.,.F.,.F.,(4,3,3,3,3,3,3,3,4),(-54.111865721129,-53.8688541410784,
-52.8712827680954,-51.8737113951125,-50.8761400221296,-49.8785686491466,
-48.8809972761637,-47.8834259031808,-47.8286804139494),.UNSPECIFIED.);
#3532=B_SPLINE_CURVE_WITH_KNOTS('',3,(#30881,#30882,#30883,#30884,#30885,
#30886,#30887,#30888,#30889,#30890,#30891,#30892,#30893,#30894,#30895,#30896,
#30897,#30898,#30899,#30900,#30901,#30902),.UNSPECIFIED.,.F.,.F.,(4,3,3,
3,3,3,3,4),(45.2921194054291,45.8882831572149,46.8858545301978,47.8834259031808,
48.8809972761637,49.8785686491466,50.8761400221296,51.5753047126087),
 .UNSPECIFIED.);
#3533=B_SPLINE_CURVE_WITH_KNOTS('',3,(#30903,#30904,#30905,#30906,#30907,
#30908,#30909,#30910,#30911,#30912,#30913,#30914,#30915,#30916,#30917,#30918,
#30919,#30920,#30921,#30922,#30923,#30924),.UNSPECIFIED.,.F.,.F.,(4,3,3,
3,3,3,3,4),(-47.8286804139494,-46.8858545301978,-45.8882831572149,-44.890711784232,
-43.893140411249,-42.8955690382661,-41.8979976652832,-41.5454951067698),
 .UNSPECIFIED.);
#3534=B_SPLINE_CURVE_WITH_KNOTS('',3,(#30929,#30930,#30931,#30932,#30933,
#30934,#30935,#30936,#30937,#30938,#30939,#30940,#30941,#30942,#30943,#30944,
#30945,#30946,#30947,#30948,#30949,#30950),.UNSPECIFIED.,.F.,.F.,(4,3,3,
3,3,3,3,4),(39.0089340982495,39.9028549193173,40.9004262923002,41.8979976652832,
42.8955690382661,43.893140411249,44.890711784232,45.2921194054291),
 .UNSPECIFIED.);
#3535=B_SPLINE_CURVE_WITH_KNOTS('',3,(#30951,#30952,#30953,#30954,#30955,
#30956,#30957,#30958,#30959,#30960,#30961,#30962,#30963,#30964,#30965,#30966,
#30967,#30968,#30969,#30970,#30971,#30972),.UNSPECIFIED.,.F.,.F.,(4,3,3,
3,3,3,3,4),(-41.5454951067698,-40.9004262923002,-39.9028549193173,-38.9052835463344,
-37.9077121733514,-36.9101408003685,-35.9125694273856,-35.2623097995902),
 .UNSPECIFIED.);
#3536=B_SPLINE_CURVE_WITH_KNOTS('',3,(#30977,#30978,#30979,#30980,#30981,
#30982,#30983,#30984,#30985,#30986,#30987,#30988,#30989,#30990,#30991,#30992,
#30993,#30994,#30995,#30996,#30997,#30998,#30999,#31000,#31001),
 .UNSPECIFIED.,.F.,.F.,(4,3,3,3,3,3,3,3,4),(32.7257487910699,32.9198553084368,
33.9174266814197,34.9149980544026,35.9125694273856,36.9101408003685,37.9077121733514,
38.9052835463344,39.0089340982495),.UNSPECIFIED.);
#3537=B_SPLINE_CURVE_WITH_KNOTS('',3,(#31002,#31003,#31004,#31005,#31006,
#31007,#31008,#31009,#31010,#31011,#31012,#31013,#31014,#31015,#31016,#31017,
#31018,#31019,#31020,#31021,#31022,#31023),.UNSPECIFIED.,.F.,.F.,(4,3,3,
3,3,3,3,4),(-35.2623097995902,-34.9149980544027,-33.9174266814197,-32.9198553084368,
-31.9222839354538,-30.9247125624709,-29.927141189488,-28.9791244924106),
 .UNSPECIFIED.);
#3538=B_SPLINE_CURVE_WITH_KNOTS('',3,(#31028,#31029,#31030,#31031,#31032,
#31033,#31034,#31035,#31036,#31037,#31038,#31039,#31040,#31041,#31042,#31043,
#31044,#31045,#31046,#31047,#31048,#31049),.UNSPECIFIED.,.F.,.F.,(4,3,3,
3,3,3,3,4),(26.4425634838903,26.9344270705392,27.9319984435221,28.929569816505,
29.927141189488,30.9247125624709,31.9222839354538,32.7257487910699),
 .UNSPECIFIED.);
#3539=B_SPLINE_CURVE_WITH_KNOTS('',3,(#31050,#31051,#31052,#31053,#31054,
#31055,#31056,#31057,#31058,#31059,#31060,#31061,#31062,#31063,#31064,#31065,
#31066,#31067,#31068,#31069,#31070,#31071,#31072,#31073,#31074),
 .UNSPECIFIED.,.F.,.F.,(4,3,3,3,3,3,3,3,4),(-28.9791244924106,-28.9295698165051,
-27.9319984435221,-26.9344270705392,-25.9368556975562,-24.9392843245733,
-23.9417129515904,-22.9441415786074,-22.695939185231),.UNSPECIFIED.);
#3540=B_SPLINE_CURVE_WITH_KNOTS('',3,(#31079,#31080,#31081,#31082,#31083,
#31084,#31085,#31086,#31087,#31088,#31089,#31090,#31091,#31092,#31093,#31094,
#31095,#31096,#31097,#31098,#31099,#31100),.UNSPECIFIED.,.F.,.F.,(4,3,3,
3,3,3,3,4),(20.1593781767107,20.9489988326416,21.9465702056245,22.9441415786075,
23.9417129515904,24.9392843245733,25.9368556975563,26.4425634838903),
 .UNSPECIFIED.);
#3541=B_SPLINE_CURVE_WITH_KNOTS('',3,(#31101,#31102,#31103,#31104,#31105,
#31106,#31107,#31108,#31109,#31110,#31111,#31112,#31113,#31114,#31115,#31116,
#31117,#31118,#31119,#31120,#31121,#31122),.UNSPECIFIED.,.F.,.F.,(4,3,3,
3,3,3,3,4),(-22.695939185231,-21.9465702056245,-20.9489988326416,-19.9514274596586,
-18.9538560866757,-17.9562847136928,-16.9587133407099,-16.4127538780514),
 .UNSPECIFIED.);
#3542=B_SPLINE_CURVE_WITH_KNOTS('',3,(#31127,#31128,#31129,#31130,#31131,
#31132,#31133,#31134,#31135,#31136,#31137,#31138,#31139,#31140,#31141,#31142,
#31143,#31144,#31145,#31146,#31147,#31148,#31149,#31150,#31151),
 .UNSPECIFIED.,.F.,.F.,(4,3,3,3,3,3,3,3,4),(13.8761928695311,13.9659992217611,
14.963570594744,15.9611419677269,16.9587133407099,17.9562847136928,18.9538560866757,
19.9514274596586,20.1593781767107),.UNSPECIFIED.);
#3543=B_SPLINE_CURVE_WITH_KNOTS('',3,(#31152,#31153,#31154,#31155,#31156,
#31157,#31158,#31159,#31160,#31161,#31162,#31163,#31164,#31165,#31166,#31167,
#31168,#31169,#31170,#31171,#31172,#31173),.UNSPECIFIED.,.F.,.F.,(4,3,3,
3,3,3,3,4),(-16.4127538780514,-15.9611419677269,-14.963570594744,-13.9659992217611,
-12.9684278487781,-11.9708564757952,-10.9732851028123,-10.1295685708718),
 .UNSPECIFIED.);
#3544=B_SPLINE_CURVE_WITH_KNOTS('',3,(#31179,#31180,#31181,#31182,#31183,
#31184,#31185,#31186,#31187,#31188,#31189,#31190,#31191),.UNSPECIFIED.,
 .F.,.F.,(4,3,3,3,4),(-3.84638326369224,-2.9927141189488,-1.99514274596586,
-0.997571372982933,0.),.UNSPECIFIED.);
#3545=B_SPLINE_CURVE_WITH_KNOTS('',3,(#31194,#31195,#31196,#31197,#31198,
#31199,#31200,#31201,#31202,#31203,#31204,#31205,#31206,#31207,#31208,#31209,
#31210,#31211,#31212),.UNSPECIFIED.,.F.,.F.,(4,3,3,3,3,3,4),(2.01461286527433,
2.9927141189488,3.99028549193173,4.98785686491466,5.9854282378976,6.98299961088053,
7.59300756235153),.UNSPECIFIED.);
#3546=B_SPLINE_CURVE_WITH_KNOTS('',3,(#31218,#31219,#31220,#31221,#31222,
#31223,#31224),.UNSPECIFIED.,.F.,.F.,(4,1,1,1,4),(91.106186954104,91.6672898428913,
92.6648612158742,93.6624325888572,94.6600039618401),.UNSPECIFIED.);
#3547=B_SPLINE_CURVE_WITH_KNOTS('',3,(#31227,#31228,#31229,#31230,#31231,
#31232,#31233,#31234),.UNSPECIFIED.,.F.,.F.,(4,1,1,1,1,4),(91.106186954104,
91.2111367324627,92.2087081054457,93.2062794784286,94.2038508514115,95.1819521050859),
 .UNSPECIFIED.);
#3548=B_SPLINE_CURVE_WITH_KNOTS('',3,(#31239,#31240,#31241,#31242,#31243,
#31244,#31245,#31246,#31247,#31248),.UNSPECIFIED.,.F.,.F.,(4,1,1,1,1,1,
1,4),(84.8230016469244,85.6818616049937,86.6794329779766,87.6770043509596,
88.6745757239425,89.6721470969254,90.6697184699084,91.106186954104),
 .UNSPECIFIED.);
#3549=B_SPLINE_CURVE_WITH_KNOTS('',3,(#31249,#31250,#31251,#31252,#31253,
#31254,#31255,#31256,#31257,#31258),.UNSPECIFIED.,.F.,.F.,(4,1,1,1,1,1,
1,4),(84.8230016469244,85.2257084945651,86.2232798675481,87.220851240531,
88.2184226135139,89.2159939864969,90.2135653594798,91.106186954104),
 .UNSPECIFIED.);
#3550=B_SPLINE_CURVE_WITH_KNOTS('',3,(#31263,#31264,#31265,#31266,#31267,
#31268,#31269,#31270,#31271,#31272,#31273),.UNSPECIFIED.,.F.,.F.,(4,1,1,
1,1,1,1,1,4),(78.5398163397448,78.6988619941132,79.6964333670961,80.694004740079,
81.691576113062,82.6891474860449,83.6867188590278,84.6842902320108,84.8230016469244),
 .UNSPECIFIED.);
#3551=B_SPLINE_CURVE_WITH_KNOTS('',3,(#31274,#31275,#31276,#31277,#31278,
#31279,#31280,#31281,#31282,#31283),.UNSPECIFIED.,.F.,.F.,(4,1,1,1,1,1,
1,4),(78.5398163397448,79.2402802566675,80.2378516296505,81.2354230026334,
82.2329943756163,83.2305657485993,84.2281371215822,84.8230016469244),
 .UNSPECIFIED.);
#3552=B_SPLINE_CURVE_WITH_KNOTS('',3,(#31288,#31289,#31290,#31291,#31292,
#31293,#31294,#31295,#31296,#31297),.UNSPECIFIED.,.F.,.F.,(4,1,1,1,1,1,
1,4),(72.2566310325652,72.7134337562156,73.7110051291985,74.7085765021814,
75.7061478751644,76.7037192481473,77.7012906211302,78.5398163397448),
 .UNSPECIFIED.);
#3553=B_SPLINE_CURVE_WITH_KNOTS('',3,(#31298,#31299,#31300,#31301,#31302,
#31303,#31304,#31305,#31306,#31307,#31308),.UNSPECIFIED.,.F.,.F.,(4,1,1,
1,1,1,1,1,4),(72.2566310325652,72.257280645787,73.25485201877,74.2524233917529,
75.2499947647358,76.2475661377187,77.2451375107017,78.2427088836846,78.5398163397448),
 .UNSPECIFIED.);
#3554=B_SPLINE_CURVE_WITH_KNOTS('',3,(#31313,#31314,#31315,#31316,#31317,
#31318,#31319,#31320,#31321,#31322),.UNSPECIFIED.,.F.,.F.,(4,1,1,1,1,1,
1,4),(65.9734457253856,66.728005518318,67.7255768913009,68.7231482642838,
69.7207196372668,70.7182910102497,71.7158623832326,72.2566310325652),
 .UNSPECIFIED.);
#3555=B_SPLINE_CURVE_WITH_KNOTS('',3,(#31323,#31324,#31325,#31326,#31327,
#31328,#31329,#31330,#31331,#31332),.UNSPECIFIED.,.F.,.F.,(4,1,1,1,1,1,
1,4),(65.9734457253856,66.2718524078894,67.2694237808724,68.2669951538553,
69.2645665268382,70.2621378998212,71.2597092728041,72.2566310325652),
 .UNSPECIFIED.);
#3556=B_SPLINE_CURVE_WITH_KNOTS('',3,(#31337,#31338,#31339,#31340,#31341,
#31342,#31343,#31344,#31345,#31346,#31347),.UNSPECIFIED.,.F.,.F.,(4,1,1,
1,1,1,1,1,4),(59.690260418206,59.7450059074374,60.7425772804204,61.7401486534033,
62.7377200263862,63.7352913993692,64.7328627723521,65.730434145335,65.9734457253856),
 .UNSPECIFIED.);
#3557=B_SPLINE_CURVE_WITH_KNOTS('',3,(#31348,#31349,#31350,#31351,#31352,
#31353,#31354,#31355,#31356,#31357),.UNSPECIFIED.,.F.,.F.,(4,1,1,1,1,1,
1,4),(59.690260418206,60.2864241699918,61.2839955429748,62.2815669159577,
63.2791382889406,64.2767096619236,65.2742810349065,65.9734457253856),
 .UNSPECIFIED.);
#3558=B_SPLINE_CURVE_WITH_KNOTS('',3,(#31362,#31363,#31364,#31365,#31366,
#31367,#31368,#31369,#31370,#31371),.UNSPECIFIED.,.F.,.F.,(4,1,1,1,1,1,
1,4),(53.4070751110264,53.7595776695399,54.7571490425228,55.7547204155057,
56.7522917884886,57.7498631614716,58.7474345344545,59.690260418206),
 .UNSPECIFIED.);
#3559=B_SPLINE_CURVE_WITH_KNOTS('',3,(#31372,#31373,#31374,#31375,#31376,
#31377,#31378,#31379,#31380,#31381),.UNSPECIFIED.,.F.,.F.,(4,1,1,1,1,1,
1,4),(53.4070751110265,54.3009959320942,55.2985673050772,56.2961386780601,
57.293710051043,58.291281424026,59.2888527970089,59.690260418206),
 .UNSPECIFIED.);
#3560=B_SPLINE_CURVE_WITH_KNOTS('',3,(#31386,#31387,#31388,#31389,#31390,
#31391,#31392,#31393,#31394,#31395),.UNSPECIFIED.,.F.,.F.,(4,1,1,1,1,1,
1,4),(47.1238898038468,47.7741494316423,48.7717208046252,49.7692921776081,
50.7668635505911,51.764434923574,52.7620062965569,53.4070751110264),
 .UNSPECIFIED.);
#3561=B_SPLINE_CURVE_WITH_KNOTS('',3,(#31396,#31397,#31398,#31399,#31400,
#31401,#31402,#31403,#31404,#31405,#31406),.UNSPECIFIED.,.F.,.F.,(4,1,1,
1,1,1,1,1,4),(47.1238898038469,47.3179963212137,48.3155676941966,49.3131390671796,
50.3107104401625,51.3082818131454,52.3058531861284,53.3034245591113,53.4070751110265),
 .UNSPECIFIED.);
#3562=B_SPLINE_CURVE_WITH_KNOTS('',3,(#31411,#31412,#31413,#31414,#31415,
#31416,#31417,#31418,#31419,#31420),.UNSPECIFIED.,.F.,.F.,(4,1,1,1,1,1,
1,4),(40.8407044966673,41.7887211937447,42.7862925667276,43.7838639397105,
44.7814353126935,45.7790066856764,46.7765780586593,47.1238898038468),
 .UNSPECIFIED.);
#3563=B_SPLINE_CURVE_WITH_KNOTS('',3,(#31421,#31422,#31423,#31424,#31425,
#31426,#31427,#31428,#31429,#31430),.UNSPECIFIED.,.F.,.F.,(4,1,1,1,1,1,
1,4),(40.8407044966673,41.3325680833161,42.330139456299,43.327710829282,
44.3252822022649,45.3228535752478,46.3204249482308,47.1238898038469),
 .UNSPECIFIED.);
#3564=B_SPLINE_CURVE_WITH_KNOTS('',3,(#31435,#31436,#31437,#31438,#31439,
#31440,#31441,#31442,#31443,#31444,#31445),.UNSPECIFIED.,.F.,.F.,(4,1,1,
1,1,1,1,1,4),(34.5575191894876,34.8057215828641,35.8032929558471,36.80086432883,
37.7984357018129,38.7960070747959,39.7935784477788,40.7911498207617,40.8407044966673),
 .UNSPECIFIED.);
#3565=B_SPLINE_CURVE_WITH_KNOTS('',3,(#31446,#31447,#31448,#31449,#31450,
#31451,#31452,#31453,#31454,#31455),.UNSPECIFIED.,.F.,.F.,(4,1,1,1,1,1,
1,4),(34.5575191894877,35.3471398454185,36.3447112184014,37.3422825913844,
38.3398539643673,39.3374253373502,40.3349967103332,40.8407044966673),
 .UNSPECIFIED.);
#3566=B_SPLINE_CURVE_WITH_KNOTS('',3,(#31460,#31461,#31462,#31463,#31464,
#31465,#31466,#31467,#31468,#31469),.UNSPECIFIED.,.F.,.F.,(4,1,1,1,1,1,
1,4),(28.2743338823081,28.8202933449665,29.8178647179495,30.8154360909324,
31.8130074639153,32.8105788368983,33.8081502098812,34.5575191894876),
 .UNSPECIFIED.);
#3567=B_SPLINE_CURVE_WITH_KNOTS('',3,(#31470,#31471,#31472,#31473,#31474,
#31475,#31476,#31477,#31478,#31479,#31480),.UNSPECIFIED.,.F.,.F.,(4,1,1,
1,1,1,1,1,4),(28.2743338823081,28.364140234538,29.3617116075209,30.3592829805038,
31.3568543534868,32.3544257264697,33.3519970994526,34.3495684724356,34.5575191894877),
 .UNSPECIFIED.);
#3568=B_SPLINE_CURVE_WITH_KNOTS('',3,(#31485,#31486,#31487,#31488,#31489,
#31490,#31491,#31492,#31493,#31494),.UNSPECIFIED.,.F.,.F.,(4,1,1,1,1,1,
1,4),(21.9911485751285,22.8348651070689,23.8324364800519,24.8300078530348,
25.8275792260177,26.8251505990007,27.8227219719836,28.2743338823081),
 .UNSPECIFIED.);
#3569=B_SPLINE_CURVE_WITH_KNOTS('',3,(#31495,#31496,#31497,#31498,#31499,
#31500,#31501,#31502,#31503,#31504),.UNSPECIFIED.,.F.,.F.,(4,1,1,1,1,1,
1,4),(21.9911485751285,22.3787119966404,23.3762833696233,24.3738547426063,
25.3714261155892,26.3689974885721,27.3665688615551,28.2743338823081),
 .UNSPECIFIED.);
#3570=B_SPLINE_CURVE_WITH_KNOTS('',3,(#31510,#31511,#31512,#31513,#31514),
 .UNSPECIFIED.,.F.,.F.,(4,1,4),(14.3981410127769,15.3957123857599,15.7079632679489),
 .UNSPECIFIED.);
#3571=B_SPLINE_CURVE_WITH_KNOTS('',3,(#31517,#31518,#31519,#31520,#31521),
 .UNSPECIFIED.,.F.,.F.,(4,1,4),(13.8761928695311,14.8542941232055,15.7079632679489),
 .UNSPECIFIED.);
#3572=B_SPLINE_CURVE_WITH_KNOTS('',3,(#31527,#31528,#31529,#31530,#31531,
#31532,#31533,#31534,#31535,#31536,#31537,#31538,#31539,#31540,#31541,#31542,
#31543,#31544,#31545,#31546,#31547,#31548),.UNSPECIFIED.,.F.,.F.,(4,3,3,
3,3,3,3,4),(76.708045941327,76.8129957196858,77.8105670926687,78.8081384656517,
79.8057098386346,80.8032812116175,81.8008525846005,82.7984239575834),
 .UNSPECIFIED.);
#3573=B_SPLINE_CURVE_WITH_KNOTS('',3,(#31552,#31553,#31554,#31555,#31556,
#31557,#31558),.UNSPECIFIED.,.F.,.F.,(4,3,4),(-80.783811092309,-79.8057098386346,
-79.2446069498473),.UNSPECIFIED.);
#3574=B_SPLINE_CURVE_WITH_KNOTS('',3,(#31562,#31563,#31564,#31565,#31566,
#31567,#31568,#31569,#31570,#31571,#31572,#31573,#31574,#31575,#31576,#31577,
#31578,#31579,#31580,#31581,#31582,#31583),.UNSPECIFIED.,.F.,.F.,(4,3,3,
3,3,3,3,4),(-79.2446069498473,-78.8081384656517,-77.8105670926687,-76.8129957196858,
-75.8154243467029,-74.81785297372,-73.820281600737,-72.9614216426677),
 .UNSPECIFIED.);
#3575=B_SPLINE_CURVE_WITH_KNOTS('',3,(#31588,#31589,#31590,#31591,#31592,
#31593,#31594,#31595,#31596,#31597,#31598,#31599,#31600,#31601,#31602,#31603,
#31604,#31605,#31606,#31607,#31608,#31609),.UNSPECIFIED.,.F.,.F.,(4,3,3,
3,3,3,3,4),(70.4248606341474,70.8275674817882,71.8251388547712,72.8227102277541,
73.820281600737,74.81785297372,75.8154243467029,76.708045941327),
 .UNSPECIFIED.);
#3576=B_SPLINE_CURVE_WITH_KNOTS('',3,(#31610,#31611,#31612,#31613,#31614,
#31615,#31616,#31617,#31618,#31619,#31620,#31621,#31622,#31623,#31624,#31625,
#31626,#31627,#31628,#31629,#31630,#31631,#31632,#31633,#31634),
 .UNSPECIFIED.,.F.,.F.,(4,3,3,3,3,3,3,3,4),(-72.9614216426677,-72.8227102277541,
-71.8251388547712,-70.8275674817882,-69.8299961088053,-68.8324247358224,
-67.8348533628394,-66.8372819898565,-66.6782363354881),.UNSPECIFIED.);
#3577=B_SPLINE_CURVE_WITH_KNOTS('',3,(#31639,#31640,#31641,#31642,#31643,
#31644,#31645,#31646,#31647,#31648,#31649,#31650,#31651,#31652,#31653,#31654,
#31655,#31656,#31657,#31658,#31659,#31660),.UNSPECIFIED.,.F.,.F.,(4,3,3,
3,3,3,3,4),(64.1416753269678,64.8421392438906,65.8397106168735,66.8372819898565,
67.8348533628394,68.8324247358223,69.8299961088053,70.4248606341474),
 .UNSPECIFIED.);
#3578=B_SPLINE_CURVE_WITH_KNOTS('',3,(#31661,#31662,#31663,#31664,#31665,
#31666,#31667,#31668,#31669,#31670,#31671,#31672,#31673,#31674,#31675,#31676,
#31677,#31678,#31679,#31680,#31681,#31682),.UNSPECIFIED.,.F.,.F.,(4,3,3,
3,3,3,3,4),(-66.6782363354881,-65.8397106168736,-64.8421392438906,-63.8445678709077,
-62.8469964979248,-61.8494251249418,-60.8518537519589,-60.3950510283085),
 .UNSPECIFIED.);
#3579=B_SPLINE_CURVE_WITH_KNOTS('',3,(#31687,#31688,#31689,#31690,#31691,
#31692,#31693,#31694,#31695,#31696,#31697,#31698,#31699,#31700,#31701,#31702,
#31703,#31704,#31705,#31706,#31707,#31708),.UNSPECIFIED.,.F.,.F.,(4,3,3,
3,3,3,3,4),(57.8584900197882,58.856711005993,59.854282378976,60.8518537519589,
61.8494251249418,62.8469964979248,63.8445678709077,64.1416753269678),
 .UNSPECIFIED.);
#3580=B_SPLINE_CURVE_WITH_KNOTS('',3,(#31709,#31710,#31711,#31712,#31713,
#31714,#31715,#31716,#31717,#31718,#31719,#31720,#31721,#31722,#31723,#31724,
#31725,#31726,#31727,#31728,#31729,#31730),.UNSPECIFIED.,.F.,.F.,(4,3,3,
3,3,3,3,4),(-60.3950510283085,-59.854282378976,-58.856711005993,-57.8591396330101,
-56.8615682600271,-55.8639968870442,-54.8664255140613,-54.111865721129),
 .UNSPECIFIED.);
#3581=B_SPLINE_CURVE_WITH_KNOTS('',3,(#31735,#31736,#31737,#31738,#31739,
#31740,#31741,#31742,#31743,#31744,#31745,#31746,#31747,#31748,#31749,#31750,
#31751,#31752,#31753,#31754,#31755,#31756),.UNSPECIFIED.,.F.,.F.,(4,3,3,
3,3,3,3,4),(51.5753047126087,51.8737113951125,52.8712827680954,53.8688541410784,
54.8664255140613,55.8639968870442,56.8615682600272,57.8584900197882),
 .UNSPECIFIED.);
#3582=B_SPLINE_CURVE_WITH_KNOTS('',3,(#31757,#31758,#31759,#31760,#31761,
#31762,#31763,#31764,#31765,#31766,#31767,#31768,#31769,#31770,#31771,#31772,
#31773,#31774,#31775,#31776,#31777,#31778,#31779,#31780,#31781),
 .UNSPECIFIED.,.F.,.F.,(4,3,3,3,3,3,3,3,4),(-54.111865721129,-53.8688541410784,
-52.8712827680954,-51.8737113951125,-50.8761400221296,-49.8785686491466,
-48.8809972761637,-47.8834259031808,-47.8286804139494),.UNSPECIFIED.);
#3583=B_SPLINE_CURVE_WITH_KNOTS('',3,(#31786,#31787,#31788,#31789,#31790,
#31791,#31792,#31793,#31794,#31795,#31796,#31797,#31798,#31799,#31800,#31801,
#31802,#31803,#31804,#31805,#31806,#31807),.UNSPECIFIED.,.F.,.F.,(4,3,3,
3,3,3,3,4),(45.2921194054291,45.8882831572149,46.8858545301978,47.8834259031808,
48.8809972761637,49.8785686491466,50.8761400221296,51.5753047126087),
 .UNSPECIFIED.);
#3584=B_SPLINE_CURVE_WITH_KNOTS('',3,(#31808,#31809,#31810,#31811,#31812,
#31813,#31814,#31815,#31816,#31817,#31818,#31819,#31820,#31821,#31822,#31823,
#31824,#31825,#31826,#31827,#31828,#31829),.UNSPECIFIED.,.F.,.F.,(4,3,3,
3,3,3,3,4),(-47.8286804139494,-46.8858545301978,-45.8882831572149,-44.890711784232,
-43.893140411249,-42.8955690382661,-41.8979976652832,-41.5454951067698),
 .UNSPECIFIED.);
#3585=B_SPLINE_CURVE_WITH_KNOTS('',3,(#31834,#31835,#31836,#31837,#31838,
#31839,#31840,#31841,#31842,#31843,#31844,#31845,#31846,#31847,#31848,#31849,
#31850,#31851,#31852,#31853,#31854,#31855),.UNSPECIFIED.,.F.,.F.,(4,3,3,
3,3,3,3,4),(39.0089340982495,39.9028549193173,40.9004262923002,41.8979976652832,
42.8955690382661,43.893140411249,44.890711784232,45.2921194054291),
 .UNSPECIFIED.);
#3586=B_SPLINE_CURVE_WITH_KNOTS('',3,(#31856,#31857,#31858,#31859,#31860,
#31861,#31862,#31863,#31864,#31865,#31866,#31867,#31868,#31869,#31870,#31871,
#31872,#31873,#31874,#31875,#31876,#31877),.UNSPECIFIED.,.F.,.F.,(4,3,3,
3,3,3,3,4),(-41.5454951067698,-40.9004262923002,-39.9028549193173,-38.9052835463344,
-37.9077121733514,-36.9101408003685,-35.9125694273856,-35.2623097995902),
 .UNSPECIFIED.);
#3587=B_SPLINE_CURVE_WITH_KNOTS('',3,(#31882,#31883,#31884,#31885,#31886,
#31887,#31888,#31889,#31890,#31891,#31892,#31893,#31894,#31895,#31896,#31897,
#31898,#31899,#31900,#31901,#31902,#31903,#31904,#31905,#31906),
 .UNSPECIFIED.,.F.,.F.,(4,3,3,3,3,3,3,3,4),(32.7257487910699,32.9198553084368,
33.9174266814197,34.9149980544026,35.9125694273856,36.9101408003685,37.9077121733514,
38.9052835463344,39.0089340982495),.UNSPECIFIED.);
#3588=B_SPLINE_CURVE_WITH_KNOTS('',3,(#31907,#31908,#31909,#31910,#31911,
#31912,#31913,#31914,#31915,#31916,#31917,#31918,#31919,#31920,#31921,#31922,
#31923,#31924,#31925,#31926,#31927,#31928),.UNSPECIFIED.,.F.,.F.,(4,3,3,
3,3,3,3,4),(-35.2623097995902,-34.9149980544027,-33.9174266814197,-32.9198553084368,
-31.9222839354538,-30.9247125624709,-29.927141189488,-28.9791244924106),
 .UNSPECIFIED.);
#3589=B_SPLINE_CURVE_WITH_KNOTS('',3,(#31933,#31934,#31935,#31936,#31937,
#31938,#31939,#31940,#31941,#31942,#31943,#31944,#31945,#31946,#31947,#31948,
#31949,#31950,#31951,#31952,#31953,#31954),.UNSPECIFIED.,.F.,.F.,(4,3,3,
3,3,3,3,4),(26.4425634838903,26.9344270705392,27.9319984435221,28.929569816505,
29.927141189488,30.9247125624709,31.9222839354538,32.7257487910699),
 .UNSPECIFIED.);
#3590=B_SPLINE_CURVE_WITH_KNOTS('',3,(#31955,#31956,#31957,#31958,#31959,
#31960,#31961,#31962,#31963,#31964,#31965,#31966,#31967,#31968,#31969,#31970,
#31971,#31972,#31973,#31974,#31975,#31976,#31977,#31978,#31979),
 .UNSPECIFIED.,.F.,.F.,(4,3,3,3,3,3,3,3,4),(-28.9791244924106,-28.929569816505,
-27.9319984435221,-26.9344270705392,-25.9368556975562,-24.9392843245733,
-23.9417129515904,-22.9441415786075,-22.695939185231),.UNSPECIFIED.);
#3591=B_SPLINE_CURVE_WITH_KNOTS('',3,(#31984,#31985,#31986,#31987,#31988,
#31989,#31990,#31991,#31992,#31993,#31994,#31995,#31996,#31997,#31998,#31999,
#32000,#32001,#32002,#32003,#32004,#32005),.UNSPECIFIED.,.F.,.F.,(4,3,3,
3,3,3,3,4),(20.1593781767107,20.9489988326416,21.9465702056245,22.9441415786074,
23.9417129515904,24.9392843245733,25.9368556975562,26.4425634838903),
 .UNSPECIFIED.);
#3592=B_SPLINE_CURVE_WITH_KNOTS('',3,(#32006,#32007,#32008,#32009,#32010,
#32011,#32012,#32013,#32014,#32015,#32016,#32017,#32018,#32019,#32020,#32021,
#32022,#32023,#32024,#32025,#32026,#32027),.UNSPECIFIED.,.F.,.F.,(4,3,3,
3,3,3,3,4),(-22.695939185231,-21.9465702056245,-20.9489988326416,-19.9514274596587,
-18.9538560866757,-17.9562847136928,-16.9587133407099,-16.4127538780514),
 .UNSPECIFIED.);
#3593=B_SPLINE_CURVE_WITH_KNOTS('',3,(#32032,#32033,#32034,#32035,#32036,
#32037,#32038,#32039,#32040,#32041,#32042,#32043,#32044,#32045,#32046,#32047,
#32048,#32049,#32050,#32051,#32052,#32053,#32054,#32055,#32056),
 .UNSPECIFIED.,.F.,.F.,(4,3,3,3,3,3,3,3,4),(13.8761928695311,13.9659992217611,
14.963570594744,15.9611419677269,16.9587133407099,17.9562847136928,18.9538560866757,
19.9514274596586,20.1593781767107),.UNSPECIFIED.);
#3594=B_SPLINE_CURVE_WITH_KNOTS('',3,(#32057,#32058,#32059,#32060,#32061,
#32062,#32063,#32064,#32065,#32066,#32067,#32068,#32069,#32070,#32071,#32072,
#32073,#32074,#32075,#32076,#32077,#32078),.UNSPECIFIED.,.F.,.F.,(4,3,3,
3,3,3,3,4),(-16.4127538780514,-15.9611419677269,-14.963570594744,-13.9659992217611,
-12.9684278487781,-11.9708564757952,-10.9732851028123,-10.1295685708718),
 .UNSPECIFIED.);
#3595=B_SPLINE_CURVE_WITH_KNOTS('',3,(#32084,#32085,#32086,#32087,#32088,
#32089,#32090,#32091,#32092,#32093,#32094,#32095,#32096),.UNSPECIFIED.,
 .F.,.F.,(4,3,3,3,4),(-3.84638326369223,-2.9927141189488,-1.99514274596586,
-0.997571372982929,0.),.UNSPECIFIED.);
#3596=B_SPLINE_CURVE_WITH_KNOTS('',3,(#32099,#32100,#32101,#32102,#32103,
#32104,#32105,#32106,#32107,#32108,#32109,#32110,#32111,#32112,#32113,#32114,
#32115,#32116,#32117),.UNSPECIFIED.,.F.,.F.,(4,3,3,3,3,3,4),(2.01461286527443,
2.9927141189488,3.99028549193173,4.98785686491467,5.9854282378976,6.98299961088053,
7.59300756235153),.UNSPECIFIED.);
#3597=B_SPLINE_CURVE_WITH_KNOTS('',3,(#32123,#32124,#32125,#32126,#32127,
#32128,#32129),.UNSPECIFIED.,.F.,.F.,(4,1,1,1,4),(91.106186954104,91.6672898428913,
92.6648612158742,93.6624325888572,94.6600039618401),.UNSPECIFIED.);
#3598=B_SPLINE_CURVE_WITH_KNOTS('',3,(#32132,#32133,#32134,#32135,#32136,
#32137,#32138,#32139),.UNSPECIFIED.,.F.,.F.,(4,1,1,1,1,4),(91.106186954104,
91.2111367324627,92.2087081054457,93.2062794784286,94.2038508514115,95.1819521050859),
 .UNSPECIFIED.);
#3599=B_SPLINE_CURVE_WITH_KNOTS('',3,(#32144,#32145,#32146,#32147,#32148,
#32149,#32150,#32151,#32152,#32153),.UNSPECIFIED.,.F.,.F.,(4,1,1,1,1,1,
1,4),(84.8230016469244,85.6818616049937,86.6794329779766,87.6770043509596,
88.6745757239425,89.6721470969254,90.6697184699084,91.106186954104),
 .UNSPECIFIED.);
#3600=B_SPLINE_CURVE_WITH_KNOTS('',3,(#32154,#32155,#32156,#32157,#32158,
#32159,#32160,#32161,#32162,#32163),.UNSPECIFIED.,.F.,.F.,(4,1,1,1,1,1,
1,4),(84.8230016469244,85.2257084945651,86.2232798675481,87.220851240531,
88.2184226135139,89.2159939864969,90.2135653594798,91.106186954104),
 .UNSPECIFIED.);
#3601=B_SPLINE_CURVE_WITH_KNOTS('',3,(#32168,#32169,#32170,#32171,#32172,
#32173,#32174,#32175,#32176,#32177,#32178),.UNSPECIFIED.,.F.,.F.,(4,1,1,
1,1,1,1,1,4),(78.5398163397448,78.6988619941132,79.6964333670961,80.694004740079,
81.691576113062,82.6891474860449,83.6867188590278,84.6842902320108,84.8230016469244),
 .UNSPECIFIED.);
#3602=B_SPLINE_CURVE_WITH_KNOTS('',3,(#32179,#32180,#32181,#32182,#32183,
#32184,#32185,#32186,#32187,#32188),.UNSPECIFIED.,.F.,.F.,(4,1,1,1,1,1,
1,4),(78.5398163397448,79.2402802566675,80.2378516296505,81.2354230026334,
82.2329943756163,83.2305657485993,84.2281371215822,84.8230016469244),
 .UNSPECIFIED.);
#3603=B_SPLINE_CURVE_WITH_KNOTS('',3,(#32193,#32194,#32195,#32196,#32197,
#32198,#32199,#32200,#32201,#32202),.UNSPECIFIED.,.F.,.F.,(4,1,1,1,1,1,
1,4),(72.2566310325652,72.7134337562156,73.7110051291985,74.7085765021814,
75.7061478751644,76.7037192481473,77.7012906211302,78.5398163397448),
 .UNSPECIFIED.);
#3604=B_SPLINE_CURVE_WITH_KNOTS('',3,(#32203,#32204,#32205,#32206,#32207,
#32208,#32209,#32210,#32211,#32212,#32213),.UNSPECIFIED.,.F.,.F.,(4,1,1,
1,1,1,1,1,4),(72.2566310325652,72.257280645787,73.25485201877,74.2524233917529,
75.2499947647358,76.2475661377187,77.2451375107017,78.2427088836846,78.5398163397448),
 .UNSPECIFIED.);
#3605=B_SPLINE_CURVE_WITH_KNOTS('',3,(#32218,#32219,#32220,#32221,#32222,
#32223,#32224,#32225,#32226,#32227),.UNSPECIFIED.,.F.,.F.,(4,1,1,1,1,1,
1,4),(65.9734457253856,66.728005518318,67.7255768913009,68.7231482642838,
69.7207196372668,70.7182910102497,71.7158623832326,72.2566310325652),
 .UNSPECIFIED.);
#3606=B_SPLINE_CURVE_WITH_KNOTS('',3,(#32228,#32229,#32230,#32231,#32232,
#32233,#32234,#32235,#32236,#32237),.UNSPECIFIED.,.F.,.F.,(4,1,1,1,1,1,
1,4),(65.9734457253856,66.2718524078894,67.2694237808724,68.2669951538553,
69.2645665268382,70.2621378998212,71.2597092728041,72.2566310325652),
 .UNSPECIFIED.);
#3607=B_SPLINE_CURVE_WITH_KNOTS('',3,(#32242,#32243,#32244,#32245,#32246,
#32247,#32248,#32249,#32250,#32251,#32252),.UNSPECIFIED.,.F.,.F.,(4,1,1,
1,1,1,1,1,4),(59.690260418206,59.7450059074374,60.7425772804204,61.7401486534033,
62.7377200263862,63.7352913993692,64.7328627723521,65.730434145335,65.9734457253856),
 .UNSPECIFIED.);
#3608=B_SPLINE_CURVE_WITH_KNOTS('',3,(#32253,#32254,#32255,#32256,#32257,
#32258,#32259,#32260,#32261,#32262),.UNSPECIFIED.,.F.,.F.,(4,1,1,1,1,1,
1,4),(59.690260418206,60.2864241699918,61.2839955429748,62.2815669159577,
63.2791382889406,64.2767096619236,65.2742810349065,65.9734457253856),
 .UNSPECIFIED.);
#3609=B_SPLINE_CURVE_WITH_KNOTS('',3,(#32267,#32268,#32269,#32270,#32271,
#32272,#32273,#32274,#32275,#32276),.UNSPECIFIED.,.F.,.F.,(4,1,1,1,1,1,
1,4),(53.4070751110264,53.7595776695399,54.7571490425228,55.7547204155057,
56.7522917884886,57.7498631614716,58.7474345344545,59.690260418206),
 .UNSPECIFIED.);
#3610=B_SPLINE_CURVE_WITH_KNOTS('',3,(#32277,#32278,#32279,#32280,#32281,
#32282,#32283,#32284,#32285,#32286),.UNSPECIFIED.,.F.,.F.,(4,1,1,1,1,1,
1,4),(53.4070751110264,54.3009959320942,55.2985673050772,56.2961386780601,
57.293710051043,58.291281424026,59.2888527970089,59.690260418206),
 .UNSPECIFIED.);
#3611=B_SPLINE_CURVE_WITH_KNOTS('',3,(#32291,#32292,#32293,#32294,#32295,
#32296,#32297,#32298,#32299,#32300),.UNSPECIFIED.,.F.,.F.,(4,1,1,1,1,1,
1,4),(47.1238898038468,47.7741494316423,48.7717208046252,49.7692921776081,
50.7668635505911,51.764434923574,52.7620062965569,53.4070751110264),
 .UNSPECIFIED.);
#3612=B_SPLINE_CURVE_WITH_KNOTS('',3,(#32301,#32302,#32303,#32304,#32305,
#32306,#32307,#32308,#32309,#32310,#32311),.UNSPECIFIED.,.F.,.F.,(4,1,1,
1,1,1,1,1,4),(47.1238898038468,47.3179963212137,48.3155676941966,49.3131390671796,
50.3107104401625,51.3082818131454,52.3058531861284,53.3034245591113,53.4070751110264),
 .UNSPECIFIED.);
#3613=B_SPLINE_CURVE_WITH_KNOTS('',3,(#32316,#32317,#32318,#32319,#32320,
#32321,#32322,#32323,#32324,#32325),.UNSPECIFIED.,.F.,.F.,(4,1,1,1,1,1,
1,4),(40.8407044966673,41.7887211937447,42.7862925667276,43.7838639397105,
44.7814353126935,45.7790066856764,46.7765780586593,47.1238898038468),
 .UNSPECIFIED.);
#3614=B_SPLINE_CURVE_WITH_KNOTS('',3,(#32326,#32327,#32328,#32329,#32330,
#32331,#32332,#32333,#32334,#32335),.UNSPECIFIED.,.F.,.F.,(4,1,1,1,1,1,
1,4),(40.8407044966673,41.3325680833161,42.330139456299,43.327710829282,
44.3252822022649,45.3228535752478,46.3204249482308,47.1238898038468),
 .UNSPECIFIED.);
#3615=B_SPLINE_CURVE_WITH_KNOTS('',3,(#32340,#32341,#32342,#32343,#32344,
#32345,#32346,#32347,#32348,#32349,#32350),.UNSPECIFIED.,.F.,.F.,(4,1,1,
1,1,1,1,1,4),(34.5575191894876,34.8057215828641,35.8032929558471,36.80086432883,
37.7984357018129,38.7960070747959,39.7935784477788,40.7911498207617,40.8407044966673),
 .UNSPECIFIED.);
#3616=B_SPLINE_CURVE_WITH_KNOTS('',3,(#32351,#32352,#32353,#32354,#32355,
#32356,#32357,#32358,#32359,#32360),.UNSPECIFIED.,.F.,.F.,(4,1,1,1,1,1,
1,4),(34.5575191894876,35.3471398454185,36.3447112184014,37.3422825913844,
38.3398539643673,39.3374253373502,40.3349967103332,40.8407044966673),
 .UNSPECIFIED.);
#3617=B_SPLINE_CURVE_WITH_KNOTS('',3,(#32365,#32366,#32367,#32368,#32369,
#32370,#32371,#32372,#32373,#32374),.UNSPECIFIED.,.F.,.F.,(4,1,1,1,1,1,
1,4),(28.2743338823081,28.8202933449665,29.8178647179495,30.8154360909324,
31.8130074639153,32.8105788368983,33.8081502098812,34.5575191894876),
 .UNSPECIFIED.);
#3618=B_SPLINE_CURVE_WITH_KNOTS('',3,(#32375,#32376,#32377,#32378,#32379,
#32380,#32381,#32382,#32383,#32384,#32385),.UNSPECIFIED.,.F.,.F.,(4,1,1,
1,1,1,1,1,4),(28.2743338823081,28.364140234538,29.3617116075209,30.3592829805038,
31.3568543534868,32.3544257264697,33.3519970994526,34.3495684724356,34.5575191894876),
 .UNSPECIFIED.);
#3619=B_SPLINE_CURVE_WITH_KNOTS('',3,(#32390,#32391,#32392,#32393,#32394,
#32395,#32396,#32397,#32398,#32399),.UNSPECIFIED.,.F.,.F.,(4,1,1,1,1,1,
1,4),(21.9911485751285,22.8348651070689,23.8324364800519,24.8300078530348,
25.8275792260177,26.8251505990007,27.8227219719836,28.2743338823081),
 .UNSPECIFIED.);
#3620=B_SPLINE_CURVE_WITH_KNOTS('',3,(#32400,#32401,#32402,#32403,#32404,
#32405,#32406,#32407,#32408,#32409),.UNSPECIFIED.,.F.,.F.,(4,1,1,1,1,1,
1,4),(21.9911485751285,22.3787119966404,23.3762833696233,24.3738547426063,
25.3714261155892,26.3689974885721,27.3665688615551,28.2743338823081),
 .UNSPECIFIED.);
#3621=B_SPLINE_CURVE_WITH_KNOTS('',3,(#32415,#32416,#32417,#32418,#32419),
 .UNSPECIFIED.,.F.,.F.,(4,1,4),(14.3981410127769,15.3957123857599,15.7079632679489),
 .UNSPECIFIED.);
#3622=B_SPLINE_CURVE_WITH_KNOTS('',3,(#32422,#32423,#32424,#32425,#32426),
 .UNSPECIFIED.,.F.,.F.,(4,1,4),(13.8761928695311,14.8542941232055,15.7079632679489),
 .UNSPECIFIED.);
#3623=B_SPLINE_CURVE_WITH_KNOTS('',3,(#32432,#32433,#32434,#32435,#32436,
#32437,#32438,#32439,#32440,#32441,#32442,#32443,#32444,#32445,#32446,#32447,
#32448,#32449,#32450,#32451,#32452,#32453),.UNSPECIFIED.,.F.,.F.,(4,3,3,
3,3,3,3,4),(76.708045941327,76.8129957196858,77.8105670926687,78.8081384656517,
79.8057098386346,80.8032812116175,81.8008525846005,82.7984239575834),
 .UNSPECIFIED.);
#3624=B_SPLINE_CURVE_WITH_KNOTS('',3,(#32457,#32458,#32459,#32460,#32461,
#32462,#32463),.UNSPECIFIED.,.F.,.F.,(4,3,4),(-80.783811092309,-79.8057098386346,
-79.2446069498473),.UNSPECIFIED.);
#3625=B_SPLINE_CURVE_WITH_KNOTS('',3,(#32467,#32468,#32469,#32470,#32471,
#32472,#32473,#32474,#32475,#32476,#32477,#32478,#32479,#32480,#32481,#32482,
#32483,#32484,#32485,#32486,#32487,#32488),.UNSPECIFIED.,.F.,.F.,(4,3,3,
3,3,3,3,4),(-79.2446069498473,-78.8081384656517,-77.8105670926687,-76.8129957196858,
-75.8154243467029,-74.81785297372,-73.820281600737,-72.9614216426677),
 .UNSPECIFIED.);
#3626=B_SPLINE_CURVE_WITH_KNOTS('',3,(#32493,#32494,#32495,#32496,#32497,
#32498,#32499,#32500,#32501,#32502,#32503,#32504,#32505,#32506,#32507,#32508,
#32509,#32510,#32511,#32512,#32513,#32514),.UNSPECIFIED.,.F.,.F.,(4,3,3,
3,3,3,3,4),(70.4248606341474,70.8275674817882,71.8251388547712,72.8227102277541,
73.820281600737,74.81785297372,75.8154243467029,76.708045941327),
 .UNSPECIFIED.);
#3627=B_SPLINE_CURVE_WITH_KNOTS('',3,(#32515,#32516,#32517,#32518,#32519,
#32520,#32521,#32522,#32523,#32524,#32525,#32526,#32527,#32528,#32529,#32530,
#32531,#32532,#32533,#32534,#32535,#32536,#32537,#32538,#32539),
 .UNSPECIFIED.,.F.,.F.,(4,3,3,3,3,3,3,3,4),(-72.9614216426677,-72.8227102277541,
-71.8251388547712,-70.8275674817882,-69.8299961088053,-68.8324247358224,
-67.8348533628394,-66.8372819898565,-66.6782363354882),.UNSPECIFIED.);
#3628=B_SPLINE_CURVE_WITH_KNOTS('',3,(#32544,#32545,#32546,#32547,#32548,
#32549,#32550,#32551,#32552,#32553,#32554,#32555,#32556,#32557,#32558,#32559,
#32560,#32561,#32562,#32563,#32564,#32565),.UNSPECIFIED.,.F.,.F.,(4,3,3,
3,3,3,3,4),(64.1416753269678,64.8421392438906,65.8397106168736,66.8372819898565,
67.8348533628394,68.8324247358224,69.8299961088053,70.4248606341474),
 .UNSPECIFIED.);
#3629=B_SPLINE_CURVE_WITH_KNOTS('',3,(#32566,#32567,#32568,#32569,#32570,
#32571,#32572,#32573,#32574,#32575,#32576,#32577,#32578,#32579,#32580,#32581,
#32582,#32583,#32584,#32585,#32586,#32587),.UNSPECIFIED.,.F.,.F.,(4,3,3,
3,3,3,3,4),(-66.6782363354882,-65.8397106168736,-64.8421392438906,-63.8445678709077,
-62.8469964979248,-61.8494251249418,-60.8518537519589,-60.3950510283085),
 .UNSPECIFIED.);
#3630=B_SPLINE_CURVE_WITH_KNOTS('',3,(#32592,#32593,#32594,#32595,#32596,
#32597,#32598,#32599,#32600,#32601,#32602,#32603,#32604,#32605,#32606,#32607,
#32608,#32609,#32610,#32611,#32612,#32613),.UNSPECIFIED.,.F.,.F.,(4,3,3,
3,3,3,3,4),(57.8584900197882,58.856711005993,59.854282378976,60.8518537519589,
61.8494251249418,62.8469964979248,63.8445678709077,64.1416753269678),
 .UNSPECIFIED.);
#3631=B_SPLINE_CURVE_WITH_KNOTS('',3,(#32614,#32615,#32616,#32617,#32618,
#32619,#32620,#32621,#32622,#32623,#32624,#32625,#32626,#32627,#32628,#32629,
#32630,#32631,#32632,#32633,#32634,#32635),.UNSPECIFIED.,.F.,.F.,(4,3,3,
3,3,3,3,4),(-60.3950510283085,-59.854282378976,-58.856711005993,-57.8591396330101,
-56.8615682600272,-55.8639968870442,-54.8664255140613,-54.111865721129),
 .UNSPECIFIED.);
#3632=B_SPLINE_CURVE_WITH_KNOTS('',3,(#32640,#32641,#32642,#32643,#32644,
#32645,#32646,#32647,#32648,#32649,#32650,#32651,#32652,#32653,#32654,#32655,
#32656,#32657,#32658,#32659,#32660,#32661),.UNSPECIFIED.,.F.,.F.,(4,3,3,
3,3,3,3,4),(51.5753047126086,51.8737113951125,52.8712827680954,53.8688541410784,
54.8664255140613,55.8639968870442,56.8615682600272,57.8584900197882),
 .UNSPECIFIED.);
#3633=B_SPLINE_CURVE_WITH_KNOTS('',3,(#32662,#32663,#32664,#32665,#32666,
#32667,#32668,#32669,#32670,#32671,#32672,#32673,#32674,#32675,#32676,#32677,
#32678,#32679,#32680,#32681,#32682,#32683,#32684,#32685,#32686),
 .UNSPECIFIED.,.F.,.F.,(4,3,3,3,3,3,3,3,4),(-54.111865721129,-53.8688541410784,
-52.8712827680954,-51.8737113951125,-50.8761400221296,-49.8785686491466,
-48.8809972761637,-47.8834259031808,-47.8286804139494),.UNSPECIFIED.);
#3634=B_SPLINE_CURVE_WITH_KNOTS('',3,(#32691,#32692,#32693,#32694,#32695,
#32696,#32697,#32698,#32699,#32700,#32701,#32702,#32703,#32704,#32705,#32706,
#32707,#32708,#32709,#32710,#32711,#32712),.UNSPECIFIED.,.F.,.F.,(4,3,3,
3,3,3,3,4),(45.2921194054291,45.8882831572149,46.8858545301978,47.8834259031808,
48.8809972761637,49.8785686491466,50.8761400221296,51.5753047126086),
 .UNSPECIFIED.);
#3635=B_SPLINE_CURVE_WITH_KNOTS('',3,(#32713,#32714,#32715,#32716,#32717,
#32718,#32719,#32720,#32721,#32722,#32723,#32724,#32725,#32726,#32727,#32728,
#32729,#32730,#32731,#32732,#32733,#32734),.UNSPECIFIED.,.F.,.F.,(4,3,3,
3,3,3,3,4),(-47.8286804139494,-46.8858545301978,-45.8882831572149,-44.890711784232,
-43.893140411249,-42.8955690382661,-41.8979976652832,-41.5454951067698),
 .UNSPECIFIED.);
#3636=B_SPLINE_CURVE_WITH_KNOTS('',3,(#32739,#32740,#32741,#32742,#32743,
#32744,#32745,#32746,#32747,#32748,#32749,#32750,#32751,#32752,#32753,#32754,
#32755,#32756,#32757,#32758,#32759,#32760),.UNSPECIFIED.,.F.,.F.,(4,3,3,
3,3,3,3,4),(39.0089340982495,39.9028549193173,40.9004262923002,41.8979976652832,
42.8955690382661,43.893140411249,44.890711784232,45.2921194054291),
 .UNSPECIFIED.);
#3637=B_SPLINE_CURVE_WITH_KNOTS('',3,(#32761,#32762,#32763,#32764,#32765,
#32766,#32767,#32768,#32769,#32770,#32771,#32772,#32773,#32774,#32775,#32776,
#32777,#32778,#32779,#32780,#32781,#32782),.UNSPECIFIED.,.F.,.F.,(4,3,3,
3,3,3,3,4),(-41.5454951067698,-40.9004262923002,-39.9028549193173,-38.9052835463344,
-37.9077121733514,-36.9101408003685,-35.9125694273856,-35.2623097995902),
 .UNSPECIFIED.);
#3638=B_SPLINE_CURVE_WITH_KNOTS('',3,(#32787,#32788,#32789,#32790,#32791,
#32792,#32793,#32794,#32795,#32796,#32797,#32798,#32799,#32800,#32801,#32802,
#32803,#32804,#32805,#32806,#32807,#32808,#32809,#32810,#32811),
 .UNSPECIFIED.,.F.,.F.,(4,3,3,3,3,3,3,3,4),(32.7257487910699,32.9198553084368,
33.9174266814197,34.9149980544027,35.9125694273856,36.9101408003685,37.9077121733514,
38.9052835463344,39.0089340982495),.UNSPECIFIED.);
#3639=B_SPLINE_CURVE_WITH_KNOTS('',3,(#32812,#32813,#32814,#32815,#32816,
#32817,#32818,#32819,#32820,#32821,#32822,#32823,#32824,#32825,#32826,#32827,
#32828,#32829,#32830,#32831,#32832,#32833),.UNSPECIFIED.,.F.,.F.,(4,3,3,
3,3,3,3,4),(-35.2623097995902,-34.9149980544026,-33.9174266814197,-32.9198553084368,
-31.9222839354538,-30.9247125624709,-29.927141189488,-28.9791244924106),
 .UNSPECIFIED.);
#3640=B_SPLINE_CURVE_WITH_KNOTS('',3,(#32838,#32839,#32840,#32841,#32842,
#32843,#32844,#32845,#32846,#32847,#32848,#32849,#32850,#32851,#32852,#32853,
#32854,#32855,#32856,#32857,#32858,#32859),.UNSPECIFIED.,.F.,.F.,(4,3,3,
3,3,3,3,4),(26.4425634838903,26.9344270705392,27.9319984435221,28.9295698165051,
29.927141189488,30.9247125624709,31.9222839354539,32.7257487910699),
 .UNSPECIFIED.);
#3641=B_SPLINE_CURVE_WITH_KNOTS('',3,(#32860,#32861,#32862,#32863,#32864,
#32865,#32866,#32867,#32868,#32869,#32870,#32871,#32872,#32873,#32874,#32875,
#32876,#32877,#32878,#32879,#32880,#32881,#32882,#32883,#32884),
 .UNSPECIFIED.,.F.,.F.,(4,3,3,3,3,3,3,3,4),(-28.9791244924106,-28.9295698165051,
-27.9319984435221,-26.9344270705392,-25.9368556975562,-24.9392843245733,
-23.9417129515904,-22.9441415786074,-22.695939185231),.UNSPECIFIED.);
#3642=B_SPLINE_CURVE_WITH_KNOTS('',3,(#32889,#32890,#32891,#32892,#32893,
#32894,#32895,#32896,#32897,#32898,#32899,#32900,#32901,#32902,#32903,#32904,
#32905,#32906,#32907,#32908,#32909,#32910),.UNSPECIFIED.,.F.,.F.,(4,3,3,
3,3,3,3,4),(20.1593781767107,20.9489988326416,21.9465702056245,22.9441415786075,
23.9417129515904,24.9392843245733,25.9368556975563,26.4425634838903),
 .UNSPECIFIED.);
#3643=B_SPLINE_CURVE_WITH_KNOTS('',3,(#32911,#32912,#32913,#32914,#32915,
#32916,#32917,#32918,#32919,#32920,#32921,#32922,#32923,#32924,#32925,#32926,
#32927,#32928,#32929,#32930,#32931,#32932),.UNSPECIFIED.,.F.,.F.,(4,3,3,
3,3,3,3,4),(-22.695939185231,-21.9465702056245,-20.9489988326416,-19.9514274596587,
-18.9538560866757,-17.9562847136928,-16.9587133407099,-16.4127538780514),
 .UNSPECIFIED.);
#3644=B_SPLINE_CURVE_WITH_KNOTS('',3,(#32937,#32938,#32939,#32940,#32941,
#32942,#32943,#32944,#32945,#32946,#32947,#32948,#32949,#32950,#32951,#32952,
#32953,#32954,#32955,#32956,#32957,#32958,#32959,#32960,#32961),
 .UNSPECIFIED.,.F.,.F.,(4,3,3,3,3,3,3,3,4),(13.8761928695311,13.9659992217611,
14.963570594744,15.9611419677269,16.9587133407099,17.9562847136928,18.9538560866757,
19.9514274596587,20.1593781767107),.UNSPECIFIED.);
#3645=B_SPLINE_CURVE_WITH_KNOTS('',3,(#32962,#32963,#32964,#32965,#32966,
#32967,#32968,#32969,#32970,#32971,#32972,#32973,#32974,#32975,#32976,#32977,
#32978,#32979,#32980,#32981,#32982,#32983),.UNSPECIFIED.,.F.,.F.,(4,3,3,
3,3,3,3,4),(-16.4127538780514,-15.9611419677269,-14.963570594744,-13.9659992217611,
-12.9684278487781,-11.9708564757952,-10.9732851028123,-10.1295685708718),
 .UNSPECIFIED.);
#3646=B_SPLINE_CURVE_WITH_KNOTS('',3,(#32989,#32990,#32991,#32992,#32993,
#32994,#32995,#32996,#32997,#32998,#32999,#33000,#33001),.UNSPECIFIED.,
 .F.,.F.,(4,3,3,3,4),(-3.84638326369223,-2.9927141189488,-1.99514274596586,
-0.997571372982932,0.),.UNSPECIFIED.);
#3647=B_SPLINE_CURVE_WITH_KNOTS('',3,(#33004,#33005,#33006,#33007,#33008,
#33009,#33010,#33011,#33012,#33013,#33014,#33015,#33016,#33017,#33018,#33019,
#33020,#33021,#33022),.UNSPECIFIED.,.F.,.F.,(4,3,3,3,3,3,4),(2.01461286527439,
2.9927141189488,3.99028549193173,4.98785686491467,5.9854282378976,6.98299961088053,
7.59300756235152),.UNSPECIFIED.);
#3648=B_SPLINE_CURVE_WITH_KNOTS('',3,(#33028,#33029,#33030,#33031,#33032,
#33033,#33034),.UNSPECIFIED.,.F.,.F.,(4,1,1,1,4),(91.106186954104,91.6672898428913,
92.6648612158742,93.6624325888571,94.6600039618401),.UNSPECIFIED.);
#3649=B_SPLINE_CURVE_WITH_KNOTS('',3,(#33037,#33038,#33039,#33040,#33041,
#33042,#33043,#33044),.UNSPECIFIED.,.F.,.F.,(4,1,1,1,1,4),(91.106186954104,
91.2111367324627,92.2087081054457,93.2062794784286,94.2038508514115,95.1819521050859),
 .UNSPECIFIED.);
#3650=B_SPLINE_CURVE_WITH_KNOTS('',3,(#33049,#33050,#33051,#33052,#33053,
#33054,#33055,#33056,#33057,#33058),.UNSPECIFIED.,.F.,.F.,(4,1,1,1,1,1,
1,4),(84.8230016469244,85.6818616049937,86.6794329779766,87.6770043509595,
88.6745757239425,89.6721470969254,90.6697184699083,91.106186954104),
 .UNSPECIFIED.);
#3651=B_SPLINE_CURVE_WITH_KNOTS('',3,(#33059,#33060,#33061,#33062,#33063,
#33064,#33065,#33066,#33067,#33068),.UNSPECIFIED.,.F.,.F.,(4,1,1,1,1,1,
1,4),(84.8230016469244,85.2257084945651,86.2232798675481,87.220851240531,
88.2184226135139,89.2159939864969,90.2135653594798,91.106186954104),
 .UNSPECIFIED.);
#3652=B_SPLINE_CURVE_WITH_KNOTS('',3,(#33073,#33074,#33075,#33076,#33077,
#33078,#33079,#33080,#33081,#33082,#33083),.UNSPECIFIED.,.F.,.F.,(4,1,1,
1,1,1,1,1,4),(78.5398163397448,78.6988619941132,79.6964333670961,80.694004740079,
81.691576113062,82.6891474860449,83.6867188590278,84.6842902320108,84.8230016469244),
 .UNSPECIFIED.);
#3653=B_SPLINE_CURVE_WITH_KNOTS('',3,(#33084,#33085,#33086,#33087,#33088,
#33089,#33090,#33091,#33092,#33093),.UNSPECIFIED.,.F.,.F.,(4,1,1,1,1,1,
1,4),(78.5398163397448,79.2402802566675,80.2378516296505,81.2354230026334,
82.2329943756163,83.2305657485993,84.2281371215822,84.8230016469244),
 .UNSPECIFIED.);
#3654=B_SPLINE_CURVE_WITH_KNOTS('',3,(#33098,#33099,#33100,#33101,#33102,
#33103,#33104,#33105,#33106,#33107),.UNSPECIFIED.,.F.,.F.,(4,1,1,1,1,1,
1,4),(72.2566310325652,72.7134337562156,73.7110051291985,74.7085765021814,
75.7061478751644,76.7037192481473,77.7012906211302,78.5398163397448),
 .UNSPECIFIED.);
#3655=B_SPLINE_CURVE_WITH_KNOTS('',3,(#33108,#33109,#33110,#33111,#33112,
#33113,#33114,#33115,#33116,#33117,#33118),.UNSPECIFIED.,.F.,.F.,(4,1,1,
1,1,1,1,1,4),(72.2566310325652,72.257280645787,73.25485201877,74.2524233917529,
75.2499947647358,76.2475661377187,77.2451375107017,78.2427088836846,78.5398163397448),
 .UNSPECIFIED.);
#3656=B_SPLINE_CURVE_WITH_KNOTS('',3,(#33123,#33124,#33125,#33126,#33127,
#33128,#33129,#33130,#33131,#33132),.UNSPECIFIED.,.F.,.F.,(4,1,1,1,1,1,
1,4),(65.9734457253856,66.728005518318,67.7255768913009,68.7231482642838,
69.7207196372668,70.7182910102497,71.7158623832326,72.2566310325652),
 .UNSPECIFIED.);
#3657=B_SPLINE_CURVE_WITH_KNOTS('',3,(#33133,#33134,#33135,#33136,#33137,
#33138,#33139,#33140,#33141,#33142),.UNSPECIFIED.,.F.,.F.,(4,1,1,1,1,1,
1,4),(65.9734457253856,66.2718524078894,67.2694237808723,68.2669951538553,
69.2645665268382,70.2621378998211,71.2597092728041,72.2566310325652),
 .UNSPECIFIED.);
#3658=B_SPLINE_CURVE_WITH_KNOTS('',3,(#33147,#33148,#33149,#33150,#33151,
#33152,#33153,#33154,#33155,#33156,#33157),.UNSPECIFIED.,.F.,.F.,(4,1,1,
1,1,1,1,1,4),(59.690260418206,59.7450059074374,60.7425772804204,61.7401486534033,
62.7377200263862,63.7352913993692,64.7328627723521,65.730434145335,65.9734457253856),
 .UNSPECIFIED.);
#3659=B_SPLINE_CURVE_WITH_KNOTS('',3,(#33158,#33159,#33160,#33161,#33162,
#33163,#33164,#33165,#33166,#33167),.UNSPECIFIED.,.F.,.F.,(4,1,1,1,1,1,
1,4),(59.690260418206,60.2864241699918,61.2839955429748,62.2815669159577,
63.2791382889406,64.2767096619235,65.2742810349065,65.9734457253856),
 .UNSPECIFIED.);
#3660=B_SPLINE_CURVE_WITH_KNOTS('',3,(#33172,#33173,#33174,#33175,#33176,
#33177,#33178,#33179,#33180,#33181),.UNSPECIFIED.,.F.,.F.,(4,1,1,1,1,1,
1,4),(53.4070751110265,53.7595776695398,54.7571490425228,55.7547204155057,
56.7522917884886,57.7498631614716,58.7474345344545,59.690260418206),
 .UNSPECIFIED.);
#3661=B_SPLINE_CURVE_WITH_KNOTS('',3,(#33182,#33183,#33184,#33185,#33186,
#33187,#33188,#33189,#33190,#33191),.UNSPECIFIED.,.F.,.F.,(4,1,1,1,1,1,
1,4),(53.4070751110264,54.3009959320942,55.2985673050772,56.2961386780601,
57.293710051043,58.291281424026,59.2888527970089,59.690260418206),
 .UNSPECIFIED.);
#3662=B_SPLINE_CURVE_WITH_KNOTS('',3,(#33196,#33197,#33198,#33199,#33200,
#33201,#33202,#33203,#33204,#33205),.UNSPECIFIED.,.F.,.F.,(4,1,1,1,1,1,
1,4),(47.1238898038469,47.7741494316422,48.7717208046252,49.7692921776081,
50.766863550591,51.764434923574,52.7620062965569,53.4070751110265),
 .UNSPECIFIED.);
#3663=B_SPLINE_CURVE_WITH_KNOTS('',3,(#33206,#33207,#33208,#33209,#33210,
#33211,#33212,#33213,#33214,#33215,#33216),.UNSPECIFIED.,.F.,.F.,(4,1,1,
1,1,1,1,1,4),(47.1238898038468,47.3179963212137,48.3155676941966,49.3131390671796,
50.3107104401625,51.3082818131454,52.3058531861284,53.3034245591113,53.4070751110264),
 .UNSPECIFIED.);
#3664=B_SPLINE_CURVE_WITH_KNOTS('',3,(#33221,#33222,#33223,#33224,#33225,
#33226,#33227,#33228,#33229,#33230),.UNSPECIFIED.,.F.,.F.,(4,1,1,1,1,1,
1,4),(40.8407044966673,41.7887211937446,42.7862925667276,43.7838639397105,
44.7814353126934,45.7790066856764,46.7765780586593,47.1238898038469),
 .UNSPECIFIED.);
#3665=B_SPLINE_CURVE_WITH_KNOTS('',3,(#33231,#33232,#33233,#33234,#33235,
#33236,#33237,#33238,#33239,#33240),.UNSPECIFIED.,.F.,.F.,(4,1,1,1,1,1,
1,4),(40.8407044966673,41.3325680833161,42.330139456299,43.327710829282,
44.3252822022649,45.3228535752478,46.3204249482308,47.1238898038468),
 .UNSPECIFIED.);
#3666=B_SPLINE_CURVE_WITH_KNOTS('',3,(#33245,#33246,#33247,#33248,#33249,
#33250,#33251,#33252,#33253,#33254,#33255),.UNSPECIFIED.,.F.,.F.,(4,1,1,
1,1,1,1,1,4),(34.5575191894877,34.8057215828641,35.803292955847,36.80086432883,
37.7984357018129,38.7960070747959,39.7935784477788,40.7911498207617,40.8407044966673),
 .UNSPECIFIED.);
#3667=B_SPLINE_CURVE_WITH_KNOTS('',3,(#33256,#33257,#33258,#33259,#33260,
#33261,#33262,#33263,#33264,#33265),.UNSPECIFIED.,.F.,.F.,(4,1,1,1,1,1,
1,4),(34.5575191894876,35.3471398454185,36.3447112184014,37.3422825913844,
38.3398539643673,39.3374253373502,40.3349967103332,40.8407044966673),
 .UNSPECIFIED.);
#3668=B_SPLINE_CURVE_WITH_KNOTS('',3,(#33270,#33271,#33272,#33273,#33274,
#33275,#33276,#33277,#33278,#33279),.UNSPECIFIED.,.F.,.F.,(4,1,1,1,1,1,
1,4),(28.2743338823081,28.8202933449665,29.8178647179495,30.8154360909324,
31.8130074639153,32.8105788368983,33.8081502098812,34.5575191894877),
 .UNSPECIFIED.);
#3669=B_SPLINE_CURVE_WITH_KNOTS('',3,(#33280,#33281,#33282,#33283,#33284,
#33285,#33286,#33287,#33288,#33289,#33290),.UNSPECIFIED.,.F.,.F.,(4,1,1,
1,1,1,1,1,4),(28.2743338823081,28.364140234538,29.3617116075209,30.3592829805038,
31.3568543534868,32.3544257264697,33.3519970994526,34.3495684724356,34.5575191894876),
 .UNSPECIFIED.);
#3670=B_SPLINE_CURVE_WITH_KNOTS('',3,(#33295,#33296,#33297,#33298,#33299,
#33300,#33301,#33302,#33303,#33304),.UNSPECIFIED.,.F.,.F.,(4,1,1,1,1,1,
1,4),(21.9911485751285,22.8348651070689,23.8324364800519,24.8300078530348,
25.8275792260177,26.8251505990007,27.8227219719836,28.2743338823081),
 .UNSPECIFIED.);
#3671=B_SPLINE_CURVE_WITH_KNOTS('',3,(#33305,#33306,#33307,#33308,#33309,
#33310,#33311,#33312,#33313,#33314),.UNSPECIFIED.,.F.,.F.,(4,1,1,1,1,1,
1,4),(21.9911485751285,22.3787119966404,23.3762833696233,24.3738547426062,
25.3714261155892,26.3689974885721,27.366568861555,28.2743338823081),
 .UNSPECIFIED.);
#3672=B_SPLINE_CURVE_WITH_KNOTS('',3,(#33320,#33321,#33322,#33323,#33324),
 .UNSPECIFIED.,.F.,.F.,(4,1,4),(14.3981410127769,15.3957123857599,15.7079632679489),
 .UNSPECIFIED.);
#3673=B_SPLINE_CURVE_WITH_KNOTS('',3,(#33327,#33328,#33329,#33330,#33331),
 .UNSPECIFIED.,.F.,.F.,(4,1,4),(13.8761928695311,14.8542941232055,15.7079632679489),
 .UNSPECIFIED.);
#3674=B_SPLINE_CURVE_WITH_KNOTS('',3,(#33337,#33338,#33339,#33340,#33341,
#33342,#33343,#33344,#33345,#33346,#33347,#33348,#33349,#33350,#33351,#33352,
#33353,#33354,#33355,#33356,#33357,#33358),.UNSPECIFIED.,.F.,.F.,(4,3,3,
3,3,3,3,4),(76.708045941327,76.8129957196858,77.8105670926687,78.8081384656517,
79.8057098386346,80.8032812116175,81.8008525846005,82.7984239575834),
 .UNSPECIFIED.);
#3675=B_SPLINE_CURVE_WITH_KNOTS('',3,(#33362,#33363,#33364,#33365,#33366,
#33367,#33368),.UNSPECIFIED.,.F.,.F.,(4,3,4),(-80.783811092309,-79.8057098386346,
-79.2446069498473),.UNSPECIFIED.);
#3676=B_SPLINE_CURVE_WITH_KNOTS('',3,(#33372,#33373,#33374,#33375,#33376,
#33377,#33378,#33379,#33380,#33381,#33382,#33383,#33384,#33385,#33386,#33387,
#33388,#33389,#33390,#33391,#33392,#33393),.UNSPECIFIED.,.F.,.F.,(4,3,3,
3,3,3,3,4),(-79.2446069498473,-78.8081384656517,-77.8105670926688,-76.8129957196858,
-75.8154243467029,-74.81785297372,-73.820281600737,-72.9614216426677),
 .UNSPECIFIED.);
#3677=B_SPLINE_CURVE_WITH_KNOTS('',3,(#33398,#33399,#33400,#33401,#33402,
#33403,#33404,#33405,#33406,#33407,#33408,#33409,#33410,#33411,#33412,#33413,
#33414,#33415,#33416,#33417,#33418,#33419),.UNSPECIFIED.,.F.,.F.,(4,3,3,
3,3,3,3,4),(70.4248606341474,70.8275674817882,71.8251388547711,72.8227102277541,
73.820281600737,74.8178529737199,75.8154243467029,76.708045941327),
 .UNSPECIFIED.);
#3678=B_SPLINE_CURVE_WITH_KNOTS('',3,(#33420,#33421,#33422,#33423,#33424,
#33425,#33426,#33427,#33428,#33429,#33430,#33431,#33432,#33433,#33434,#33435,
#33436,#33437,#33438,#33439,#33440,#33441,#33442,#33443,#33444),
 .UNSPECIFIED.,.F.,.F.,(4,3,3,3,3,3,3,3,4),(-72.9614216426677,-72.8227102277541,
-71.8251388547712,-70.8275674817882,-69.8299961088053,-68.8324247358224,
-67.8348533628394,-66.8372819898565,-66.6782363354882),.UNSPECIFIED.);
#3679=B_SPLINE_CURVE_WITH_KNOTS('',3,(#33449,#33450,#33451,#33452,#33453,
#33454,#33455,#33456,#33457,#33458,#33459,#33460,#33461,#33462,#33463,#33464,
#33465,#33466,#33467,#33468,#33469,#33470),.UNSPECIFIED.,.F.,.F.,(4,3,3,
3,3,3,3,4),(64.1416753269678,64.8421392438906,65.8397106168736,66.8372819898565,
67.8348533628394,68.8324247358223,69.8299961088053,70.4248606341474),
 .UNSPECIFIED.);
#3680=B_SPLINE_CURVE_WITH_KNOTS('',3,(#33471,#33472,#33473,#33474,#33475,
#33476,#33477,#33478,#33479,#33480,#33481,#33482,#33483,#33484,#33485,#33486,
#33487,#33488,#33489,#33490,#33491,#33492),.UNSPECIFIED.,.F.,.F.,(4,3,3,
3,3,3,3,4),(-66.6782363354882,-65.8397106168736,-64.8421392438906,-63.8445678709077,
-62.8469964979248,-61.8494251249418,-60.8518537519589,-60.3950510283085),
 .UNSPECIFIED.);
#3681=B_SPLINE_CURVE_WITH_KNOTS('',3,(#33497,#33498,#33499,#33500,#33501,
#33502,#33503,#33504,#33505,#33506,#33507,#33508,#33509,#33510,#33511,#33512,
#33513,#33514,#33515,#33516,#33517,#33518),.UNSPECIFIED.,.F.,.F.,(4,3,3,
3,3,3,3,4),(57.8584900197882,58.856711005993,59.854282378976,60.8518537519589,
61.8494251249418,62.8469964979247,63.8445678709077,64.1416753269678),
 .UNSPECIFIED.);
#3682=B_SPLINE_CURVE_WITH_KNOTS('',3,(#33519,#33520,#33521,#33522,#33523,
#33524,#33525,#33526,#33527,#33528,#33529,#33530,#33531,#33532,#33533,#33534,
#33535,#33536,#33537,#33538,#33539,#33540),.UNSPECIFIED.,.F.,.F.,(4,3,3,
3,3,3,3,4),(-60.3950510283085,-59.854282378976,-58.856711005993,-57.8591396330101,
-56.8615682600272,-55.8639968870442,-54.8664255140613,-54.111865721129),
 .UNSPECIFIED.);
#3683=B_SPLINE_CURVE_WITH_KNOTS('',3,(#33545,#33546,#33547,#33548,#33549,
#33550,#33551,#33552,#33553,#33554,#33555,#33556,#33557,#33558,#33559,#33560,
#33561,#33562,#33563,#33564,#33565,#33566),.UNSPECIFIED.,.F.,.F.,(4,3,3,
3,3,3,3,4),(51.5753047126087,51.8737113951125,52.8712827680954,53.8688541410784,
54.8664255140613,55.8639968870442,56.8615682600272,57.8584900197882),
 .UNSPECIFIED.);
#3684=B_SPLINE_CURVE_WITH_KNOTS('',3,(#33567,#33568,#33569,#33570,#33571,
#33572,#33573,#33574,#33575,#33576,#33577,#33578,#33579,#33580,#33581,#33582,
#33583,#33584,#33585,#33586,#33587,#33588,#33589,#33590,#33591),
 .UNSPECIFIED.,.F.,.F.,(4,3,3,3,3,3,3,3,4),(-54.111865721129,-53.8688541410784,
-52.8712827680954,-51.8737113951125,-50.8761400221296,-49.8785686491466,
-48.8809972761637,-47.8834259031808,-47.8286804139494),.UNSPECIFIED.);
#3685=B_SPLINE_CURVE_WITH_KNOTS('',3,(#33596,#33597,#33598,#33599,#33600,
#33601,#33602,#33603,#33604,#33605,#33606,#33607,#33608,#33609,#33610,#33611,
#33612,#33613,#33614,#33615,#33616,#33617),.UNSPECIFIED.,.F.,.F.,(4,3,3,
3,3,3,3,4),(45.2921194054291,45.8882831572149,46.8858545301978,47.8834259031808,
48.8809972761637,49.8785686491466,50.8761400221295,51.5753047126087),
 .UNSPECIFIED.);
#3686=B_SPLINE_CURVE_WITH_KNOTS('',3,(#33618,#33619,#33620,#33621,#33622,
#33623,#33624,#33625,#33626,#33627,#33628,#33629,#33630,#33631,#33632,#33633,
#33634,#33635,#33636,#33637,#33638,#33639),.UNSPECIFIED.,.F.,.F.,(4,3,3,
3,3,3,3,4),(-47.8286804139494,-46.8858545301978,-45.8882831572149,-44.890711784232,
-43.893140411249,-42.8955690382661,-41.8979976652832,-41.5454951067698),
 .UNSPECIFIED.);
#3687=B_SPLINE_CURVE_WITH_KNOTS('',3,(#33644,#33645,#33646,#33647,#33648,
#33649,#33650,#33651,#33652,#33653,#33654,#33655,#33656,#33657,#33658,#33659,
#33660,#33661,#33662,#33663,#33664,#33665),.UNSPECIFIED.,.F.,.F.,(4,3,3,
3,3,3,3,4),(39.0089340982495,39.9028549193173,40.9004262923002,41.8979976652832,
42.8955690382661,43.893140411249,44.890711784232,45.2921194054291),
 .UNSPECIFIED.);
#3688=B_SPLINE_CURVE_WITH_KNOTS('',3,(#33666,#33667,#33668,#33669,#33670,
#33671,#33672,#33673,#33674,#33675,#33676,#33677,#33678,#33679,#33680,#33681,
#33682,#33683,#33684,#33685,#33686,#33687),.UNSPECIFIED.,.F.,.F.,(4,3,3,
3,3,3,3,4),(-41.5454951067698,-40.9004262923002,-39.9028549193173,-38.9052835463344,
-37.9077121733514,-36.9101408003685,-35.9125694273856,-35.2623097995902),
 .UNSPECIFIED.);
#3689=B_SPLINE_CURVE_WITH_KNOTS('',3,(#33692,#33693,#33694,#33695,#33696,
#33697,#33698,#33699,#33700,#33701,#33702,#33703,#33704,#33705,#33706,#33707,
#33708,#33709,#33710,#33711,#33712,#33713,#33714,#33715,#33716),
 .UNSPECIFIED.,.F.,.F.,(4,3,3,3,3,3,3,3,4),(32.7257487910699,32.9198553084368,
33.9174266814197,34.9149980544026,35.9125694273856,36.9101408003685,37.9077121733514,
38.9052835463344,39.0089340982495),.UNSPECIFIED.);
#3690=B_SPLINE_CURVE_WITH_KNOTS('',3,(#33717,#33718,#33719,#33720,#33721,
#33722,#33723,#33724,#33725,#33726,#33727,#33728,#33729,#33730,#33731,#33732,
#33733,#33734,#33735,#33736,#33737,#33738),.UNSPECIFIED.,.F.,.F.,(4,3,3,
3,3,3,3,4),(-35.2623097995902,-34.9149980544027,-33.9174266814197,-32.9198553084368,
-31.9222839354538,-30.9247125624709,-29.927141189488,-28.9791244924106),
 .UNSPECIFIED.);
#3691=B_SPLINE_CURVE_WITH_KNOTS('',3,(#33743,#33744,#33745,#33746,#33747,
#33748,#33749,#33750,#33751,#33752,#33753,#33754,#33755,#33756,#33757,#33758,
#33759,#33760,#33761,#33762,#33763,#33764),.UNSPECIFIED.,.F.,.F.,(4,3,3,
3,3,3,3,4),(26.4425634838903,26.9344270705392,27.9319984435221,28.929569816505,
29.927141189488,30.9247125624709,31.9222839354538,32.7257487910699),
 .UNSPECIFIED.);
#3692=B_SPLINE_CURVE_WITH_KNOTS('',3,(#33765,#33766,#33767,#33768,#33769,
#33770,#33771,#33772,#33773,#33774,#33775,#33776,#33777,#33778,#33779,#33780,
#33781,#33782,#33783,#33784,#33785,#33786,#33787,#33788,#33789),
 .UNSPECIFIED.,.F.,.F.,(4,3,3,3,3,3,3,3,4),(-28.9791244924106,-28.929569816505,
-27.9319984435221,-26.9344270705392,-25.9368556975563,-24.9392843245733,
-23.9417129515904,-22.9441415786075,-22.695939185231),.UNSPECIFIED.);
#3693=B_SPLINE_CURVE_WITH_KNOTS('',3,(#33794,#33795,#33796,#33797,#33798,
#33799,#33800,#33801,#33802,#33803,#33804,#33805,#33806,#33807,#33808,#33809,
#33810,#33811,#33812,#33813,#33814,#33815),.UNSPECIFIED.,.F.,.F.,(4,3,3,
3,3,3,3,4),(20.1593781767107,20.9489988326416,21.9465702056245,22.9441415786075,
23.9417129515904,24.9392843245733,25.9368556975563,26.4425634838903),
 .UNSPECIFIED.);
#3694=B_SPLINE_CURVE_WITH_KNOTS('',3,(#33816,#33817,#33818,#33819,#33820,
#33821,#33822,#33823,#33824,#33825,#33826,#33827,#33828,#33829,#33830,#33831,
#33832,#33833,#33834,#33835,#33836,#33837),.UNSPECIFIED.,.F.,.F.,(4,3,3,
3,3,3,3,4),(-22.695939185231,-21.9465702056245,-20.9489988326416,-19.9514274596587,
-18.9538560866757,-17.9562847136928,-16.9587133407099,-16.4127538780514),
 .UNSPECIFIED.);
#3695=B_SPLINE_CURVE_WITH_KNOTS('',3,(#33842,#33843,#33844,#33845,#33846,
#33847,#33848,#33849,#33850,#33851,#33852,#33853,#33854,#33855,#33856,#33857,
#33858,#33859,#33860,#33861,#33862,#33863,#33864,#33865,#33866),
 .UNSPECIFIED.,.F.,.F.,(4,3,3,3,3,3,3,3,4),(13.8761928695311,13.9659992217611,
14.963570594744,15.9611419677269,16.9587133407099,17.9562847136928,18.9538560866757,
19.9514274596586,20.1593781767107),.UNSPECIFIED.);
#3696=B_SPLINE_CURVE_WITH_KNOTS('',3,(#33867,#33868,#33869,#33870,#33871,
#33872,#33873,#33874,#33875,#33876,#33877,#33878,#33879,#33880,#33881,#33882,
#33883,#33884,#33885,#33886,#33887,#33888),.UNSPECIFIED.,.F.,.F.,(4,3,3,
3,3,3,3,4),(-16.4127538780514,-15.9611419677269,-14.963570594744,-13.9659992217611,
-12.9684278487781,-11.9708564757952,-10.9732851028123,-10.1295685708718),
 .UNSPECIFIED.);
#3697=B_SPLINE_CURVE_WITH_KNOTS('',3,(#33894,#33895,#33896,#33897,#33898,
#33899,#33900,#33901,#33902,#33903,#33904,#33905,#33906),.UNSPECIFIED.,
 .F.,.F.,(4,3,3,3,4),(-3.84638326369224,-2.9927141189488,-1.99514274596586,
-0.997571372982931,0.),.UNSPECIFIED.);
#3698=B_SPLINE_CURVE_WITH_KNOTS('',3,(#33909,#33910,#33911,#33912,#33913,
#33914,#33915,#33916,#33917,#33918,#33919,#33920,#33921,#33922,#33923,#33924,
#33925,#33926,#33927),.UNSPECIFIED.,.F.,.F.,(4,3,3,3,3,3,4),(2.01461286527446,
2.99271411894879,3.99028549193172,4.98785686491466,5.98542823789759,6.98299961088052,
7.59300756235153),.UNSPECIFIED.);
#3699=B_SPLINE_CURVE_WITH_KNOTS('',3,(#33933,#33934,#33935,#33936,#33937,
#33938,#33939),.UNSPECIFIED.,.F.,.F.,(4,1,1,1,4),(91.106186954104,91.6672898428913,
92.6648612158742,93.6624325888571,94.6600039618401),.UNSPECIFIED.);
#3700=B_SPLINE_CURVE_WITH_KNOTS('',3,(#33942,#33943,#33944,#33945,#33946,
#33947,#33948,#33949),.UNSPECIFIED.,.F.,.F.,(4,1,1,1,1,4),(91.106186954104,
91.2111367324627,92.2087081054457,93.2062794784286,94.2038508514115,95.1819521050859),
 .UNSPECIFIED.);
#3701=B_SPLINE_CURVE_WITH_KNOTS('',3,(#33954,#33955,#33956,#33957,#33958,
#33959,#33960,#33961,#33962,#33963),.UNSPECIFIED.,.F.,.F.,(4,1,1,1,1,1,
1,4),(84.8230016469244,85.6818616049937,86.6794329779766,87.6770043509595,
88.6745757239425,89.6721470969254,90.6697184699083,91.106186954104),
 .UNSPECIFIED.);
#3702=B_SPLINE_CURVE_WITH_KNOTS('',3,(#33964,#33965,#33966,#33967,#33968,
#33969,#33970,#33971,#33972,#33973),.UNSPECIFIED.,.F.,.F.,(4,1,1,1,1,1,
1,4),(84.8230016469244,85.2257084945651,86.2232798675481,87.220851240531,
88.2184226135139,89.2159939864968,90.2135653594798,91.106186954104),
 .UNSPECIFIED.);
#3703=B_SPLINE_CURVE_WITH_KNOTS('',3,(#33978,#33979,#33980,#33981,#33982,
#33983,#33984,#33985,#33986,#33987,#33988),.UNSPECIFIED.,.F.,.F.,(4,1,1,
1,1,1,1,1,4),(78.5398163397448,78.6988619941132,79.6964333670961,80.694004740079,
81.691576113062,82.6891474860449,83.6867188590278,84.6842902320108,84.8230016469244),
 .UNSPECIFIED.);
#3704=B_SPLINE_CURVE_WITH_KNOTS('',3,(#33989,#33990,#33991,#33992,#33993,
#33994,#33995,#33996,#33997,#33998),.UNSPECIFIED.,.F.,.F.,(4,1,1,1,1,1,
1,4),(78.5398163397448,79.2402802566675,80.2378516296505,81.2354230026334,
82.2329943756163,83.2305657485992,84.2281371215822,84.8230016469244),
 .UNSPECIFIED.);
#3705=B_SPLINE_CURVE_WITH_KNOTS('',3,(#34003,#34004,#34005,#34006,#34007,
#34008,#34009,#34010,#34011,#34012),.UNSPECIFIED.,.F.,.F.,(4,1,1,1,1,1,
1,4),(72.2566310325652,72.7134337562156,73.7110051291985,74.7085765021814,
75.7061478751643,76.7037192481473,77.7012906211302,78.5398163397448),
 .UNSPECIFIED.);
#3706=B_SPLINE_CURVE_WITH_KNOTS('',3,(#34013,#34014,#34015,#34016,#34017,
#34018,#34019,#34020,#34021,#34022,#34023),.UNSPECIFIED.,.F.,.F.,(4,1,1,
1,1,1,1,1,4),(72.2566310325652,72.257280645787,73.2548520187699,74.2524233917529,
75.2499947647358,76.2475661377187,77.2451375107017,78.2427088836846,78.5398163397448),
 .UNSPECIFIED.);
#3707=B_SPLINE_CURVE_WITH_KNOTS('',3,(#34028,#34029,#34030,#34031,#34032,
#34033,#34034,#34035,#34036,#34037),.UNSPECIFIED.,.F.,.F.,(4,1,1,1,1,1,
1,4),(65.9734457253856,66.728005518318,67.7255768913009,68.7231482642838,
69.7207196372668,70.7182910102497,71.7158623832326,72.2566310325652),
 .UNSPECIFIED.);
#3708=B_SPLINE_CURVE_WITH_KNOTS('',3,(#34038,#34039,#34040,#34041,#34042,
#34043,#34044,#34045,#34046,#34047),.UNSPECIFIED.,.F.,.F.,(4,1,1,1,1,1,
1,4),(65.9734457253856,66.2718524078894,67.2694237808723,68.2669951538553,
69.2645665268382,70.2621378998211,71.2597092728041,72.2566310325652),
 .UNSPECIFIED.);
#3709=B_SPLINE_CURVE_WITH_KNOTS('',3,(#34052,#34053,#34054,#34055,#34056,
#34057,#34058,#34059,#34060,#34061,#34062),.UNSPECIFIED.,.F.,.F.,(4,1,1,
1,1,1,1,1,4),(59.690260418206,59.7450059074374,60.7425772804204,61.7401486534033,
62.7377200263862,63.7352913993692,64.7328627723521,65.730434145335,65.9734457253856),
 .UNSPECIFIED.);
#3710=B_SPLINE_CURVE_WITH_KNOTS('',3,(#34063,#34064,#34065,#34066,#34067,
#34068,#34069,#34070,#34071,#34072),.UNSPECIFIED.,.F.,.F.,(4,1,1,1,1,1,
1,4),(59.690260418206,60.2864241699918,61.2839955429747,62.2815669159577,
63.2791382889406,64.2767096619235,65.2742810349065,65.9734457253856),
 .UNSPECIFIED.);
#3711=B_SPLINE_CURVE_WITH_KNOTS('',3,(#34077,#34078,#34079,#34080,#34081,
#34082,#34083,#34084,#34085,#34086),.UNSPECIFIED.,.F.,.F.,(4,1,1,1,1,1,
1,4),(53.4070751110265,53.7595776695398,54.7571490425228,55.7547204155057,
56.7522917884886,57.7498631614716,58.7474345344545,59.690260418206),
 .UNSPECIFIED.);
#3712=B_SPLINE_CURVE_WITH_KNOTS('',3,(#34087,#34088,#34089,#34090,#34091,
#34092,#34093,#34094,#34095,#34096),.UNSPECIFIED.,.F.,.F.,(4,1,1,1,1,1,
1,4),(53.4070751110264,54.3009959320942,55.2985673050771,56.2961386780601,
57.293710051043,58.2912814240259,59.2888527970089,59.690260418206),
 .UNSPECIFIED.);
#3713=B_SPLINE_CURVE_WITH_KNOTS('',3,(#34101,#34102,#34103,#34104,#34105,
#34106,#34107,#34108,#34109,#34110),.UNSPECIFIED.,.F.,.F.,(4,1,1,1,1,1,
1,4),(47.1238898038469,47.7741494316422,48.7717208046252,49.7692921776081,
50.766863550591,51.764434923574,52.7620062965569,53.4070751110265),
 .UNSPECIFIED.);
#3714=B_SPLINE_CURVE_WITH_KNOTS('',3,(#34111,#34112,#34113,#34114,#34115,
#34116,#34117,#34118,#34119,#34120,#34121),.UNSPECIFIED.,.F.,.F.,(4,1,1,
1,1,1,1,1,4),(47.1238898038468,47.3179963212137,48.3155676941966,49.3131390671795,
50.3107104401625,51.3082818131454,52.3058531861283,53.3034245591113,53.4070751110264),
 .UNSPECIFIED.);
#3715=B_SPLINE_CURVE_WITH_KNOTS('',3,(#34126,#34127,#34128,#34129,#34130,
#34131,#34132,#34133,#34134,#34135),.UNSPECIFIED.,.F.,.F.,(4,1,1,1,1,1,
1,4),(40.8407044966673,41.7887211937446,42.7862925667276,43.7838639397105,
44.7814353126934,45.7790066856764,46.7765780586593,47.1238898038469),
 .UNSPECIFIED.);
#3716=B_SPLINE_CURVE_WITH_KNOTS('',3,(#34136,#34137,#34138,#34139,#34140,
#34141,#34142,#34143,#34144,#34145),.UNSPECIFIED.,.F.,.F.,(4,1,1,1,1,1,
1,4),(40.8407044966673,41.3325680833161,42.330139456299,43.327710829282,
44.3252822022649,45.3228535752478,46.3204249482308,47.1238898038468),
 .UNSPECIFIED.);
#3717=B_SPLINE_CURVE_WITH_KNOTS('',3,(#34150,#34151,#34152,#34153,#34154,
#34155,#34156,#34157,#34158,#34159,#34160),.UNSPECIFIED.,.F.,.F.,(4,1,1,
1,1,1,1,1,4),(34.5575191894877,34.8057215828641,35.803292955847,36.80086432883,
37.7984357018129,38.7960070747958,39.7935784477788,40.7911498207617,40.8407044966673),
 .UNSPECIFIED.);
#3718=B_SPLINE_CURVE_WITH_KNOTS('',3,(#34161,#34162,#34163,#34164,#34165,
#34166,#34167,#34168,#34169,#34170),.UNSPECIFIED.,.F.,.F.,(4,1,1,1,1,1,
1,4),(34.5575191894876,35.3471398454185,36.3447112184014,37.3422825913844,
38.3398539643673,39.3374253373502,40.3349967103332,40.8407044966673),
 .UNSPECIFIED.);
#3719=B_SPLINE_CURVE_WITH_KNOTS('',3,(#34175,#34176,#34177,#34178,#34179,
#34180,#34181,#34182,#34183,#34184),.UNSPECIFIED.,.F.,.F.,(4,1,1,1,1,1,
1,4),(28.2743338823081,28.8202933449665,29.8178647179495,30.8154360909324,
31.8130074639153,32.8105788368983,33.8081502098812,34.5575191894877),
 .UNSPECIFIED.);
#3720=B_SPLINE_CURVE_WITH_KNOTS('',3,(#34185,#34186,#34187,#34188,#34189,
#34190,#34191,#34192,#34193,#34194,#34195),.UNSPECIFIED.,.F.,.F.,(4,1,1,
1,1,1,1,1,4),(28.2743338823081,28.364140234538,29.3617116075209,30.3592829805038,
31.3568543534868,32.3544257264697,33.3519970994526,34.3495684724356,34.5575191894876),
 .UNSPECIFIED.);
#3721=B_SPLINE_CURVE_WITH_KNOTS('',3,(#34200,#34201,#34202,#34203,#34204,
#34205,#34206,#34207,#34208,#34209),.UNSPECIFIED.,.F.,.F.,(4,1,1,1,1,1,
1,4),(21.9911485751285,22.8348651070689,23.8324364800519,24.8300078530348,
25.8275792260177,26.8251505990007,27.8227219719836,28.2743338823081),
 .UNSPECIFIED.);
#3722=B_SPLINE_CURVE_WITH_KNOTS('',3,(#34210,#34211,#34212,#34213,#34214,
#34215,#34216,#34217,#34218,#34219),.UNSPECIFIED.,.F.,.F.,(4,1,1,1,1,1,
1,4),(21.9911485751285,22.3787119966404,23.3762833696233,24.3738547426062,
25.3714261155892,26.3689974885721,27.366568861555,28.2743338823081),
 .UNSPECIFIED.);
#3723=B_SPLINE_CURVE_WITH_KNOTS('',3,(#34225,#34226,#34227,#34228,#34229),
 .UNSPECIFIED.,.F.,.F.,(4,1,4),(14.3981410127769,15.3957123857598,15.7079632679489),
 .UNSPECIFIED.);
#3724=B_SPLINE_CURVE_WITH_KNOTS('',3,(#34232,#34233,#34234,#34235,#34236),
 .UNSPECIFIED.,.F.,.F.,(4,1,4),(13.8761928695311,14.8542941232055,15.7079632679489),
 .UNSPECIFIED.);
#3725=B_SPLINE_CURVE_WITH_KNOTS('',3,(#34242,#34243,#34244,#34245),
 .UNSPECIFIED.,.F.,.F.,(4,4),(51.5750455984138,52.2824273504651),
 .UNSPECIFIED.);
#3726=B_SPLINE_CURVE_WITH_KNOTS('',3,(#34248,#34249,#34250,#34251,#34252,
#34253,#34254,#34255,#34256,#34257),.UNSPECIFIED.,.F.,.F.,(4,3,3,4),(-50.2654824574366,
-49.3356538821136,-48.3533960593298,-47.8312715558982),.UNSPECIFIED.);
#3727=B_SPLINE_CURVE_WITH_KNOTS('',3,(#34262,#34263,#34264,#34265,#34266,
#34267,#34268,#34269,#34270,#34271,#34272,#34273,#34274,#34275,#34276,#34277,
#34278,#34279,#34280,#34281,#34282,#34283,#34284,#34285,#34286),
 .UNSPECIFIED.,.F.,.F.,(4,3,3,3,3,3,3,3,4),(45.2918602912342,45.3820193336359,
46.3677919074686,47.3535644813014,48.3393370551341,49.3251096289668,50.3108822027996,
51.2966547766323,51.5750455984138),.UNSPECIFIED.);
#3728=B_SPLINE_CURVE_WITH_KNOTS('',3,(#34287,#34288,#34289,#34290,#34291,
#34292,#34293,#34294,#34295,#34296,#34297,#34298,#34299,#34300,#34301,#34302,
#34303,#34304,#34305,#34306,#34307,#34308),.UNSPECIFIED.,.F.,.F.,(4,3,3,
3,3,3,3,4),(-47.8312715558982,-47.371138236546,-46.3888804137622,-45.4066225909784,
-44.4243647681946,-43.4421069454108,-42.459849122627,-41.5480862487186),
 .UNSPECIFIED.);
#3729=B_SPLINE_CURVE_WITH_KNOTS('',3,(#34313,#34314,#34315,#34316,#34317,
#34318,#34319,#34320,#34321,#34322,#34323,#34324,#34325,#34326,#34327,#34328,
#34329,#34330,#34331,#34332,#34333,#34334),.UNSPECIFIED.,.F.,.F.,(4,3,3,
3,3,3,3,4),(39.0086749840547,39.4673838906394,40.4531564644721,41.4389290383049,
42.4247016121376,43.4104741859704,44.3962467598031,45.2918602912342),
 .UNSPECIFIED.);
#3730=B_SPLINE_CURVE_WITH_KNOTS('',3,(#34335,#34336,#34337,#34338,#34339,
#34340,#34341,#34342,#34343,#34344,#34345,#34346,#34347,#34348,#34349,#34350,
#34351,#34352,#34353,#34354,#34355,#34356,#34357,#34358,#34359),
 .UNSPECIFIED.,.F.,.F.,(4,3,3,3,3,3,3,3,4),(-41.5480862487186,-41.4775912998432,
-40.4953334770593,-39.5130756542755,-38.5308178314917,-37.5485600087079,
-36.5663021859241,-35.5840443631403,-35.264900941539),.UNSPECIFIED.);
#3731=B_SPLINE_CURVE_WITH_KNOTS('',3,(#34364,#34365,#34366,#34367,#34368,
#34369,#34370,#34371,#34372,#34373,#34374,#34375,#34376,#34377,#34378,#34379,
#34380,#34381,#34382,#34383,#34384,#34385),.UNSPECIFIED.,.F.,.F.,(4,3,3,
3,3,3,3,4),(32.7254896768751,33.5527484476429,34.5385210214757,35.5242935953084,
36.5100661691412,37.4958387429739,38.4816113168067,39.0086749840547),
 .UNSPECIFIED.);
#3732=B_SPLINE_CURVE_WITH_KNOTS('',3,(#34386,#34387,#34388,#34389,#34390,
#34391,#34392,#34393,#34394,#34395,#34396,#34397,#34398,#34399,#34400,#34401,
#34402,#34403,#34404,#34405,#34406,#34407),.UNSPECIFIED.,.F.,.F.,(4,3,3,
3,3,3,3,4),(-35.264900941539,-34.6017865403565,-33.6195287175727,-32.6372708947889,
-31.6550130720051,-30.6727552492213,-29.6904974264375,-28.9817156343594),
 .UNSPECIFIED.);
#3733=B_SPLINE_CURVE_WITH_KNOTS('',3,(#34412,#34413,#34414,#34415,#34416,
#34417,#34418,#34419,#34420,#34421,#34422,#34423,#34424,#34425,#34426,#34427,
#34428,#34429,#34430,#34431,#34432,#34433,#34434,#34435,#34436),
 .UNSPECIFIED.,.F.,.F.,(4,3,3,3,3,3,3,3,4),(26.4423043696954,26.6523404308137,
27.6381130046465,28.6238855784792,29.609658152312,30.5954307261447,31.5812032999775,
32.5669758738102,32.7254896768751),.UNSPECIFIED.);
#3734=B_SPLINE_CURVE_WITH_KNOTS('',3,(#34437,#34438,#34439,#34440,#34441,
#34442,#34443,#34444,#34445,#34446,#34447,#34448,#34449,#34450,#34451,#34452,
#34453,#34454,#34455,#34456,#34457,#34458,#34459,#34460,#34461),
 .UNSPECIFIED.,.F.,.F.,(4,3,3,3,3,3,3,3,4),(-28.9817156343594,-28.7082396036537,
-27.7259817808699,-26.7437239580861,-25.7614661353022,-24.7792083125184,
-23.7969504897346,-22.8146926669508,-22.6985303271799),.UNSPECIFIED.);
#3735=B_SPLINE_CURVE_WITH_KNOTS('',3,(#34466,#34467,#34468,#34469,#34470,
#34471,#34472,#34473,#34474,#34475,#34476,#34477,#34478,#34479,#34480,#34481,
#34482,#34483,#34484,#34485,#34486,#34487),.UNSPECIFIED.,.F.,.F.,(4,3,3,
3,3,3,3,4),(20.1591190625158,20.7377049878173,21.72347756165,22.7092501354828,
23.6950227093155,24.6807952831482,25.666567856981,26.4423043696954),
 .UNSPECIFIED.);
#3736=B_SPLINE_CURVE_WITH_KNOTS('',3,(#34488,#34489,#34490,#34491,#34492,
#34493,#34494,#34495,#34496,#34497,#34498,#34499,#34500,#34501,#34502,#34503,
#34504,#34505,#34506,#34507,#34508,#34509),.UNSPECIFIED.,.F.,.F.,(4,3,3,
3,3,3,3,4),(-22.6985303271799,-21.832434844167,-20.8501770213832,-19.8679191985994,
-18.8856613758156,-17.9034035530318,-16.921145730248,-16.4153450200003),
 .UNSPECIFIED.);
#3737=B_SPLINE_CURVE_WITH_KNOTS('',3,(#34514,#34515,#34516,#34517,#34518,
#34519,#34520,#34521,#34522,#34523,#34524,#34525,#34526,#34527,#34528,#34529,
#34530,#34531,#34532,#34533,#34534,#34535),.UNSPECIFIED.,.F.,.F.,(4,3,3,
3,3,3,3,4),(13.8759337553363,14.8230695448208,15.8088421186535,16.7946146924863,
17.780387266319,18.7661598401518,19.7519324139845,20.1591190625158),
 .UNSPECIFIED.);
#3738=B_SPLINE_CURVE_WITH_KNOTS('',3,(#34536,#34537,#34538,#34539,#34540,
#34541,#34542,#34543,#34544,#34545,#34546,#34547,#34548,#34549,#34550,#34551,
#34552,#34553,#34554,#34555,#34556,#34557),.UNSPECIFIED.,.F.,.F.,(4,3,3,
3,3,3,3,4),(-16.4153450200003,-15.9388879074642,-14.9566300846804,-13.9743722618966,
-12.9921144391128,-12.009856616329,-11.0275987935451,-10.1321597128207),
 .UNSPECIFIED.);
#3739=B_SPLINE_CURVE_WITH_KNOTS('',3,(#34563,#34564,#34565,#34566,#34567,
#34568,#34569,#34570,#34571,#34572,#34573,#34574,#34575),.UNSPECIFIED.,
 .F.,.F.,(4,3,3,3,4),(-3.84897440564113,-3.1695362112747,-2.18727838849089,
-1.20502056570709,-0.222762742923284),.UNSPECIFIED.);
#3740=B_SPLINE_CURVE_WITH_KNOTS('',3,(#34577,#34578,#34579,#34580,#34581,
#34582,#34583,#34584,#34585,#34586,#34587,#34588),.UNSPECIFIED.,.F.,.F.,
(4,2,2,2,2,4),(0.202168863441191,0.284518942728512,0.37935858673359,0.474198230738669,
0.569037874743748,0.642071595472288),.UNSPECIFIED.);
#3741=B_SPLINE_CURVE_WITH_KNOTS('',3,(#34589,#34590,#34591,#34592,#34593,
#34594,#34595,#34596,#34597,#34598,#34599,#34600,#34601,#34602,#34603,#34604,
#34605,#34606,#34607),.UNSPECIFIED.,.F.,.F.,(4,3,3,3,3,3,4),(2.14497997264822,
2.99379865882787,3.97957123266061,4.96534380649336,5.9511163803261,6.93688895415885,
7.5927484481567),.UNSPECIFIED.);
#3742=B_SPLINE_CURVE_WITH_KNOTS('',3,(#34613,#34614,#34615,#34616,#34617,
#34618,#34619,#34620),.UNSPECIFIED.,.F.,.F.,(4,1,1,1,1,4),(59.6902604182061,
60.2123849216376,61.1946427444214,62.1769005672052,63.159158389989,64.1414162127728),
 .UNSPECIFIED.);
#3743=B_SPLINE_CURVE_WITH_KNOTS('',3,(#34623,#34624,#34625,#34626,#34627,
#34628,#34629,#34630,#34631),.UNSPECIFIED.,.F.,.F.,(4,1,1,1,1,1,4),(59.6902604182061,
59.7804194606077,60.7661920344404,61.7519646082732,62.7377371821059,63.7235097559386,
64.6638825844084),.UNSPECIFIED.);
#3744=B_SPLINE_CURVE_WITH_KNOTS('',3,(#34636,#34637,#34638,#34639,#34640,
#34641,#34642,#34643,#34644,#34645),.UNSPECIFIED.,.F.,.F.,(4,1,1,1,1,1,
1,4),(53.4070751110265,54.3188379849348,55.3010958077186,56.2833536305024,
57.2656114532862,58.24786927607,59.2301270988538,59.6902604182061),
 .UNSPECIFIED.);
#3745=B_SPLINE_CURVE_WITH_KNOTS('',3,(#34646,#34647,#34648,#34649,#34650,
#34651,#34652,#34653,#34654,#34655),.UNSPECIFIED.,.F.,.F.,(4,1,1,1,1,1,
1,4),(53.4070751110265,53.8657840176112,54.8515565914439,55.8373291652767,
56.8231017391094,57.8088743129422,58.7946468867749,59.6902604182061),
 .UNSPECIFIED.);
#3746=B_SPLINE_CURVE_WITH_KNOTS('',3,(#34660,#34661,#34662,#34663,#34664,
#34665,#34666,#34667,#34668,#34669,#34670),.UNSPECIFIED.,.F.,.F.,(4,1,1,
1,1,1,1,1,4),(47.1238898038469,47.4430332254481,48.4252910482319,49.4075488710157,
50.3898066937995,51.3720645165834,52.3543223393672,53.336580162151,53.4070751110265),
 .UNSPECIFIED.);
#3747=B_SPLINE_CURVE_WITH_KNOTS('',3,(#34671,#34672,#34673,#34674,#34675,
#34676,#34677,#34678,#34679,#34680),.UNSPECIFIED.,.F.,.F.,(4,1,1,1,1,1,
1,4),(47.1238898038469,47.9511485746147,48.9369211484475,49.9226937222802,
50.908466296113,51.8942388699457,52.8800114437785,53.4070751110265),
 .UNSPECIFIED.);
#3748=B_SPLINE_CURVE_WITH_KNOTS('',3,(#34685,#34686,#34687,#34688,#34689,
#34690,#34691,#34692,#34693,#34694),.UNSPECIFIED.,.F.,.F.,(4,1,1,1,1,1,
1,4),(40.8407044966673,41.5494862887453,42.5317441115291,43.5140019343129,
44.4962597570967,45.4785175798805,46.4607754026643,47.1238898038469),
 .UNSPECIFIED.);
#3749=B_SPLINE_CURVE_WITH_KNOTS('',3,(#34695,#34696,#34697,#34698,#34699,
#34700,#34701,#34702,#34703,#34704,#34705),.UNSPECIFIED.,.F.,.F.,(4,1,1,
1,1,1,1,1,4),(40.8407044966673,41.0507405577855,42.0365131316183,43.022285705451,
44.0080582792838,44.9938308531165,45.9796034269492,46.965376000782,47.1238898038469),
 .UNSPECIFIED.);
#3750=B_SPLINE_CURVE_WITH_KNOTS('',3,(#34710,#34711,#34712,#34713,#34714,
#34715,#34716,#34717,#34718,#34719,#34720),.UNSPECIFIED.,.F.,.F.,(4,1,1,
1,1,1,1,1,4),(34.5575191894877,34.6736815292587,35.6559393520425,36.6381971748263,
37.6204549976101,38.6027128203939,39.5849706431777,40.5672284659615,40.8407044966673),
 .UNSPECIFIED.);
#3751=B_SPLINE_CURVE_WITH_KNOTS('',3,(#34721,#34722,#34723,#34724,#34725,
#34726,#34727,#34728,#34729,#34730),.UNSPECIFIED.,.F.,.F.,(4,1,1,1,1,1,
1,4),(34.5575191894877,35.1361051147891,36.1218776886218,37.1076502624545,
38.0934228362873,39.07919541012,40.0649679839528,40.8407044966673),
 .UNSPECIFIED.);
#3752=B_SPLINE_CURVE_WITH_KNOTS('',3,(#34735,#34736,#34737,#34738,#34739,
#34740,#34741,#34742,#34743,#34744),.UNSPECIFIED.,.F.,.F.,(4,1,1,1,1,1,
1,4),(28.2743338823081,28.7801345925558,29.7623924153396,30.7446502381234,
31.7269080609072,32.709165883691,33.6914237064748,34.5575191894877),
 .UNSPECIFIED.);
#3753=B_SPLINE_CURVE_WITH_KNOTS('',3,(#34745,#34746,#34747,#34748,#34749,
#34750,#34751,#34752,#34753,#34754),.UNSPECIFIED.,.F.,.F.,(4,1,1,1,1,1,
1,4),(28.2743338823081,29.2214696717926,30.2072422456253,31.1930148194581,
32.1787873932908,33.1645599671236,34.1503325409563,34.5575191894877),
 .UNSPECIFIED.);
#3754=B_SPLINE_CURVE_WITH_KNOTS('',3,(#34759,#34760,#34761,#34762,#34763,
#34764,#34765,#34766,#34767,#34768),.UNSPECIFIED.,.F.,.F.,(4,1,1,1,1,1,
1,4),(21.9911485751285,22.886587655853,23.8688454786368,24.8511033014206,
25.8333611242044,26.8156189469882,27.797876769772,28.2743338823081),
 .UNSPECIFIED.);
#3755=B_SPLINE_CURVE_WITH_KNOTS('',3,(#34769,#34770,#34771,#34772,#34773,
#34774,#34775,#34776,#34777,#34778,#34779),.UNSPECIFIED.,.F.,.F.,(4,1,1,
1,1,1,1,1,4),(21.9911485751285,22.3210616549634,23.3068342287961,24.2926068026289,
25.2783793764616,26.2641519502944,27.2499245241271,28.2356970979599,28.2743338823081),
 .UNSPECIFIED.);
#3756=B_SPLINE_CURVE_WITH_KNOTS('',3,(#34785,#34786,#34787,#34788,#34789),
 .UNSPECIFIED.,.F.,.F.,(4,1,4),(14.4348810643014,15.4206536381342,15.7079632679489),
 .UNSPECIFIED.);
#3757=B_SPLINE_CURVE_WITH_KNOTS('',3,(#34791,#34792,#34793,#34794),
 .UNSPECIFIED.,.F.,.F.,(4,4),(1.38948745034524,1.47775448763834),
 .UNSPECIFIED.);
#3758=B_SPLINE_CURVE_WITH_KNOTS('',3,(#34796,#34797,#34798,#34799),
 .UNSPECIFIED.,.F.,.F.,(4,4),(1.3186667718152,1.38948745034524),
 .UNSPECIFIED.);
#3759=B_SPLINE_CURVE_WITH_KNOTS('',3,(#34800,#34801,#34802,#34803,#34804,
#34805),.UNSPECIFIED.,.F.,.F.,(4,1,1,4),(13.8994448374521,14.0462672507987,
15.0285250735825,15.7079632679489),.UNSPECIFIED.);
#3760=B_SPLINE_CURVE_WITH_KNOTS('',3,(#34811,#34812,#34813,#34814),
 .UNSPECIFIED.,.F.,.F.,(4,4),(51.5750455984139,52.282427350465),
 .UNSPECIFIED.);
#3761=B_SPLINE_CURVE_WITH_KNOTS('',3,(#34817,#34818,#34819,#34820,#34821,
#34822,#34823,#34824,#34825,#34826),.UNSPECIFIED.,.F.,.F.,(4,3,3,4),(-50.2654824574365,
-49.3356538821136,-48.3533960593298,-47.8312715558982),.UNSPECIFIED.);
#3762=B_SPLINE_CURVE_WITH_KNOTS('',3,(#34831,#34832,#34833,#34834,#34835,
#34836,#34837,#34838,#34839,#34840,#34841,#34842,#34843,#34844,#34845,#34846,
#34847,#34848,#34849,#34850,#34851,#34852,#34853,#34854,#34855),
 .UNSPECIFIED.,.F.,.F.,(4,3,3,3,3,3,3,3,4),(45.2918602912343,45.3820193336358,
46.3677919074686,47.3535644813013,48.3393370551341,49.3251096289668,50.3108822027995,
51.2966547766323,51.5750455984139),.UNSPECIFIED.);
#3763=B_SPLINE_CURVE_WITH_KNOTS('',3,(#34856,#34857,#34858,#34859,#34860,
#34861,#34862,#34863,#34864,#34865,#34866,#34867,#34868,#34869,#34870,#34871,
#34872,#34873,#34874,#34875,#34876,#34877),.UNSPECIFIED.,.F.,.F.,(4,3,3,
3,3,3,3,4),(-47.8312715558982,-47.371138236546,-46.3888804137622,-45.4066225909784,
-44.4243647681946,-43.4421069454107,-42.459849122627,-41.5480862487186),
 .UNSPECIFIED.);
#3764=B_SPLINE_CURVE_WITH_KNOTS('',3,(#34882,#34883,#34884,#34885,#34886,
#34887,#34888,#34889,#34890,#34891,#34892,#34893,#34894,#34895,#34896,#34897,
#34898,#34899,#34900,#34901,#34902,#34903),.UNSPECIFIED.,.F.,.F.,(4,3,3,
3,3,3,3,4),(39.0086749840547,39.4673838906393,40.4531564644721,41.4389290383048,
42.4247016121376,43.4104741859703,44.3962467598031,45.2918602912343),
 .UNSPECIFIED.);
#3765=B_SPLINE_CURVE_WITH_KNOTS('',3,(#34904,#34905,#34906,#34907,#34908,
#34909,#34910,#34911,#34912,#34913,#34914,#34915,#34916,#34917,#34918,#34919,
#34920,#34921,#34922,#34923,#34924,#34925,#34926,#34927,#34928),
 .UNSPECIFIED.,.F.,.F.,(4,3,3,3,3,3,3,3,4),(-41.5480862487186,-41.4775912998431,
-40.4953334770593,-39.5130756542755,-38.5308178314917,-37.5485600087079,
-36.5663021859241,-35.5840443631403,-35.264900941539),.UNSPECIFIED.);
#3766=B_SPLINE_CURVE_WITH_KNOTS('',3,(#34933,#34934,#34935,#34936,#34937,
#34938,#34939,#34940,#34941,#34942,#34943,#34944,#34945,#34946,#34947,#34948,
#34949,#34950,#34951,#34952,#34953,#34954),.UNSPECIFIED.,.F.,.F.,(4,3,3,
3,3,3,3,4),(32.7254896768751,33.5527484476429,34.5385210214756,35.5242935953084,
36.5100661691411,37.4958387429738,38.4816113168066,39.0086749840547),
 .UNSPECIFIED.);
#3767=B_SPLINE_CURVE_WITH_KNOTS('',3,(#34955,#34956,#34957,#34958,#34959,
#34960,#34961,#34962,#34963,#34964,#34965,#34966,#34967,#34968,#34969,#34970,
#34971,#34972,#34973,#34974,#34975,#34976),.UNSPECIFIED.,.F.,.F.,(4,3,3,
3,3,3,3,4),(-35.264900941539,-34.6017865403565,-33.6195287175727,-32.6372708947889,
-31.6550130720051,-30.6727552492213,-29.6904974264375,-28.9817156343594),
 .UNSPECIFIED.);
#3768=B_SPLINE_CURVE_WITH_KNOTS('',3,(#34981,#34982,#34983,#34984,#34985,
#34986,#34987,#34988,#34989,#34990,#34991,#34992,#34993,#34994,#34995,#34996,
#34997,#34998,#34999,#35000,#35001,#35002,#35003,#35004,#35005),
 .UNSPECIFIED.,.F.,.F.,(4,3,3,3,3,3,3,3,4),(26.4423043696955,26.6523404308136,
27.6381130046464,28.6238855784791,29.6096581523119,30.5954307261446,31.5812032999774,
32.5669758738101,32.7254896768751),.UNSPECIFIED.);
#3769=B_SPLINE_CURVE_WITH_KNOTS('',3,(#35006,#35007,#35008,#35009,#35010,
#35011,#35012,#35013,#35014,#35015,#35016,#35017,#35018,#35019,#35020,#35021,
#35022,#35023,#35024,#35025,#35026,#35027,#35028,#35029,#35030),
 .UNSPECIFIED.,.F.,.F.,(4,3,3,3,3,3,3,3,4),(-28.9817156343594,-28.7082396036537,
-27.7259817808699,-26.7437239580861,-25.7614661353022,-24.7792083125184,
-23.7969504897346,-22.8146926669508,-22.6985303271799),.UNSPECIFIED.);
#3770=B_SPLINE_CURVE_WITH_KNOTS('',3,(#35035,#35036,#35037,#35038,#35039,
#35040,#35041,#35042,#35043,#35044,#35045,#35046,#35047,#35048,#35049,#35050,
#35051,#35052,#35053,#35054,#35055,#35056),.UNSPECIFIED.,.F.,.F.,(4,3,3,
3,3,3,3,4),(20.1591190625159,20.7377049878172,21.7234775616499,22.7092501354827,
23.6950227093154,24.6807952831481,25.6665678569809,26.4423043696955),
 .UNSPECIFIED.);
#3771=B_SPLINE_CURVE_WITH_KNOTS('',3,(#35057,#35058,#35059,#35060,#35061,
#35062,#35063,#35064,#35065,#35066,#35067,#35068,#35069,#35070,#35071,#35072,
#35073,#35074,#35075,#35076,#35077,#35078),.UNSPECIFIED.,.F.,.F.,(4,3,3,
3,3,3,3,4),(-22.6985303271799,-21.832434844167,-20.8501770213832,-19.8679191985994,
-18.8856613758156,-17.9034035530318,-16.921145730248,-16.4153450200003),
 .UNSPECIFIED.);
#3772=B_SPLINE_CURVE_WITH_KNOTS('',3,(#35083,#35084,#35085,#35086,#35087,
#35088,#35089,#35090,#35091,#35092,#35093,#35094,#35095,#35096,#35097,#35098,
#35099,#35100,#35101,#35102,#35103,#35104),.UNSPECIFIED.,.F.,.F.,(4,3,3,
3,3,3,3,4),(13.8759337553364,14.8230695448207,15.8088421186534,16.7946146924862,
17.7803872663189,18.7661598401517,19.7519324139844,20.1591190625159),
 .UNSPECIFIED.);
#3773=B_SPLINE_CURVE_WITH_KNOTS('',3,(#35105,#35106,#35107,#35108,#35109,
#35110,#35111,#35112,#35113,#35114,#35115,#35116,#35117,#35118,#35119,#35120,
#35121,#35122,#35123,#35124,#35125,#35126),.UNSPECIFIED.,.F.,.F.,(4,3,3,
3,3,3,3,4),(-16.4153450200003,-15.9388879074642,-14.9566300846804,-13.9743722618966,
-12.9921144391128,-12.009856616329,-11.0275987935452,-10.1321597128207),
 .UNSPECIFIED.);
#3774=B_SPLINE_CURVE_WITH_KNOTS('',3,(#35132,#35133,#35134,#35135,#35136,
#35137,#35138,#35139,#35140,#35141,#35142,#35143,#35144),.UNSPECIFIED.,
 .F.,.F.,(4,3,3,3,4),(-3.84897440564107,-3.16953621127471,-2.1872783884909,
-1.20502056570709,-0.222762742923288),.UNSPECIFIED.);
#3775=B_SPLINE_CURVE_WITH_KNOTS('',3,(#35146,#35147,#35148,#35149,#35150,
#35151,#35152,#35153,#35154,#35155,#35156,#35157),.UNSPECIFIED.,.F.,.F.,
(4,2,2,2,2,4),(0.202168863441159,0.284518942728512,0.379358586733591,0.474198230738669,
0.569037874743748,0.642071595472281),.UNSPECIFIED.);
#3776=B_SPLINE_CURVE_WITH_KNOTS('',3,(#35158,#35159,#35160,#35161,#35162,
#35163,#35164,#35165,#35166,#35167,#35168,#35169,#35170,#35171,#35172,#35173,
#35174,#35175,#35176),.UNSPECIFIED.,.F.,.F.,(4,3,3,3,3,3,4),(2.14497997264816,
2.99379865882773,3.97957123266047,4.96534380649322,5.95111638032597,6.93688895415871,
7.59274844815675),.UNSPECIFIED.);
#3777=B_SPLINE_CURVE_WITH_KNOTS('',3,(#35182,#35183,#35184,#35185),
 .UNSPECIFIED.,.F.,.F.,(4,4),(51.5750455984139,52.2824273504652),
 .UNSPECIFIED.);
#3778=B_SPLINE_CURVE_WITH_KNOTS('',3,(#35188,#35189,#35190,#35191,#35192,
#35193,#35194,#35195,#35196,#35197),.UNSPECIFIED.,.F.,.F.,(4,3,3,4),(-50.2654824574367,
-49.3356538821138,-48.35339605933,-47.8312715558982),.UNSPECIFIED.);
#3779=B_SPLINE_CURVE_WITH_KNOTS('',3,(#35202,#35203,#35204,#35205,#35206,
#35207,#35208,#35209,#35210,#35211,#35212,#35213,#35214,#35215,#35216,#35217,
#35218,#35219,#35220,#35221,#35222,#35223,#35224,#35225,#35226),
 .UNSPECIFIED.,.F.,.F.,(4,3,3,3,3,3,3,3,4),(45.2918602912343,45.382019333636,
46.3677919074688,47.3535644813015,48.3393370551343,49.325109628967,50.3108822027997,
51.2966547766325,51.5750455984139),.UNSPECIFIED.);
#3780=B_SPLINE_CURVE_WITH_KNOTS('',3,(#35227,#35228,#35229,#35230,#35231,
#35232,#35233,#35234,#35235,#35236,#35237,#35238,#35239,#35240,#35241,#35242,
#35243,#35244,#35245,#35246,#35247,#35248),.UNSPECIFIED.,.F.,.F.,(4,3,3,
3,3,3,3,4),(-47.8312715558982,-47.3711382365462,-46.3888804137624,-45.4066225909786,
-44.4243647681948,-43.442106945411,-42.4598491226272,-41.5480862487186),
 .UNSPECIFIED.);
#3781=B_SPLINE_CURVE_WITH_KNOTS('',3,(#35253,#35254,#35255,#35256,#35257,
#35258,#35259,#35260,#35261,#35262,#35263,#35264,#35265,#35266,#35267,#35268,
#35269,#35270,#35271,#35272,#35273,#35274),.UNSPECIFIED.,.F.,.F.,(4,3,3,
3,3,3,3,4),(39.0086749840547,39.4673838906396,40.4531564644723,41.438929038305,
42.4247016121378,43.4104741859705,44.3962467598033,45.2918602912343),
 .UNSPECIFIED.);
#3782=B_SPLINE_CURVE_WITH_KNOTS('',3,(#35275,#35276,#35277,#35278,#35279,
#35280,#35281,#35282,#35283,#35284,#35285,#35286,#35287,#35288,#35289,#35290,
#35291,#35292,#35293,#35294,#35295,#35296,#35297,#35298,#35299),
 .UNSPECIFIED.,.F.,.F.,(4,3,3,3,3,3,3,3,4),(-41.5480862487186,-41.4775912998434,
-40.4953334770596,-39.5130756542758,-38.5308178314919,-37.5485600087081,
-36.5663021859243,-35.5840443631405,-35.264900941539),.UNSPECIFIED.);
#3783=B_SPLINE_CURVE_WITH_KNOTS('',3,(#35304,#35305,#35306,#35307,#35308,
#35309,#35310,#35311,#35312,#35313,#35314,#35315,#35316,#35317,#35318,#35319,
#35320,#35321,#35322,#35323,#35324,#35325),.UNSPECIFIED.,.F.,.F.,(4,3,3,
3,3,3,3,4),(32.7254896768751,33.5527484476431,34.5385210214758,35.5242935953086,
36.5100661691413,37.4958387429741,38.4816113168068,39.0086749840547),
 .UNSPECIFIED.);
#3784=B_SPLINE_CURVE_WITH_KNOTS('',3,(#35326,#35327,#35328,#35329,#35330,
#35331,#35332,#35333,#35334,#35335,#35336,#35337,#35338,#35339,#35340,#35341,
#35342,#35343,#35344,#35345,#35346,#35347),.UNSPECIFIED.,.F.,.F.,(4,3,3,
3,3,3,3,4),(-35.264900941539,-34.6017865403567,-33.6195287175729,-32.6372708947891,
-31.6550130720053,-30.6727552492215,-29.6904974264377,-28.9817156343594),
 .UNSPECIFIED.);
#3785=B_SPLINE_CURVE_WITH_KNOTS('',3,(#35352,#35353,#35354,#35355,#35356,
#35357,#35358,#35359,#35360,#35361,#35362,#35363,#35364,#35365,#35366,#35367,
#35368,#35369,#35370,#35371,#35372,#35373,#35374,#35375,#35376),
 .UNSPECIFIED.,.F.,.F.,(4,3,3,3,3,3,3,3,4),(26.4423043696955,26.6523404308139,
27.6381130046466,28.6238855784794,29.6096581523121,30.5954307261449,31.5812032999776,
32.5669758738103,32.7254896768751),.UNSPECIFIED.);
#3786=B_SPLINE_CURVE_WITH_KNOTS('',3,(#35377,#35378,#35379,#35380,#35381,
#35382,#35383,#35384,#35385,#35386,#35387,#35388,#35389,#35390,#35391,#35392,
#35393,#35394,#35395,#35396,#35397,#35398,#35399,#35400,#35401),
 .UNSPECIFIED.,.F.,.F.,(4,3,3,3,3,3,3,3,4),(-28.9817156343594,-28.7082396036539,
-27.7259817808701,-26.7437239580863,-25.7614661353025,-24.7792083125187,
-23.7969504897349,-22.8146926669511,-22.6985303271798),.UNSPECIFIED.);
#3787=B_SPLINE_CURVE_WITH_KNOTS('',3,(#35406,#35407,#35408,#35409,#35410,
#35411,#35412,#35413,#35414,#35415,#35416,#35417,#35418,#35419,#35420,#35421,
#35422,#35423,#35424,#35425,#35426,#35427),.UNSPECIFIED.,.F.,.F.,(4,3,3,
3,3,3,3,4),(20.1591190625159,20.7377049878174,21.7234775616502,22.7092501354829,
23.6950227093156,24.6807952831484,25.6665678569811,26.4423043696955),
 .UNSPECIFIED.);
#3788=B_SPLINE_CURVE_WITH_KNOTS('',3,(#35428,#35429,#35430,#35431,#35432,
#35433,#35434,#35435,#35436,#35437,#35438,#35439,#35440,#35441,#35442,#35443,
#35444,#35445,#35446,#35447,#35448,#35449),.UNSPECIFIED.,.F.,.F.,(4,3,3,
3,3,3,3,4),(-22.6985303271798,-21.8324348441672,-20.8501770213834,-19.8679191985996,
-18.8856613758158,-17.903403553032,-16.9211457302482,-16.4153450200003),
 .UNSPECIFIED.);
#3789=B_SPLINE_CURVE_WITH_KNOTS('',3,(#35454,#35455,#35456,#35457,#35458,
#35459,#35460,#35461,#35462,#35463,#35464,#35465,#35466,#35467,#35468,#35469,
#35470,#35471,#35472,#35473,#35474,#35475),.UNSPECIFIED.,.F.,.F.,(4,3,3,
3,3,3,3,4),(13.8759337553364,14.8230695448209,15.8088421186537,16.7946146924864,
17.7803872663192,18.7661598401519,19.7519324139847,20.1591190625159),
 .UNSPECIFIED.);
#3790=B_SPLINE_CURVE_WITH_KNOTS('',3,(#35476,#35477,#35478,#35479,#35480,
#35481,#35482,#35483,#35484,#35485,#35486,#35487,#35488,#35489,#35490,#35491,
#35492,#35493,#35494,#35495,#35496,#35497),.UNSPECIFIED.,.F.,.F.,(4,3,3,
3,3,3,3,4),(-16.4153450200003,-15.9388879074644,-14.9566300846806,-13.9743722618968,
-12.992114439113,-12.0098566163292,-11.0275987935454,-10.1321597128207),
 .UNSPECIFIED.);
#3791=B_SPLINE_CURVE_WITH_KNOTS('',3,(#35503,#35504,#35505,#35506,#35507,
#35508,#35509,#35510,#35511,#35512,#35513,#35514,#35515),.UNSPECIFIED.,
 .F.,.F.,(4,3,3,3,4),(-3.84897440564108,-3.16953621127493,-2.18727838849113,
-1.20502056570732,-0.222762742923517),.UNSPECIFIED.);
#3792=B_SPLINE_CURVE_WITH_KNOTS('',3,(#35517,#35518,#35519,#35520,#35521,
#35522,#35523,#35524,#35525,#35526,#35527,#35528),.UNSPECIFIED.,.F.,.F.,
(4,2,2,2,2,4),(0.202168863441204,0.284518942728512,0.379358586733591,0.474198230738669,
0.569037874743748,0.64207159547233),.UNSPECIFIED.);
#3793=B_SPLINE_CURVE_WITH_KNOTS('',3,(#35529,#35530,#35531,#35532,#35533,
#35534,#35535,#35536,#35537,#35538,#35539,#35540,#35541,#35542,#35543,#35544,
#35545,#35546,#35547),.UNSPECIFIED.,.F.,.F.,(4,3,3,3,3,3,4),(2.14497997264827,
2.99379865882801,3.97957123266076,4.9653438064935,5.95111638032624,6.93688895415899,
7.59274844815675),.UNSPECIFIED.);
#3794=B_SPLINE_CURVE_WITH_KNOTS('',3,(#35553,#35554,#35555,#35556),
 .UNSPECIFIED.,.F.,.F.,(4,4),(51.5750455984139,52.2824273504652),
 .UNSPECIFIED.);
#3795=B_SPLINE_CURVE_WITH_KNOTS('',3,(#35559,#35560,#35561,#35562,#35563,
#35564,#35565,#35566,#35567,#35568),.UNSPECIFIED.,.F.,.F.,(4,3,3,4),(-50.2654824574367,
-49.3356538821137,-48.3533960593299,-47.8312715558983),.UNSPECIFIED.);
#3796=B_SPLINE_CURVE_WITH_KNOTS('',3,(#35573,#35574,#35575,#35576,#35577,
#35578,#35579,#35580,#35581,#35582,#35583,#35584,#35585,#35586,#35587,#35588,
#35589,#35590,#35591,#35592,#35593,#35594,#35595,#35596,#35597),
 .UNSPECIFIED.,.F.,.F.,(4,3,3,3,3,3,3,3,4),(45.2918602912343,45.382019333636,
46.3677919074687,47.3535644813014,48.3393370551342,49.3251096289669,50.3108822027997,
51.2966547766324,51.5750455984139),.UNSPECIFIED.);
#3797=B_SPLINE_CURVE_WITH_KNOTS('',3,(#35598,#35599,#35600,#35601,#35602,
#35603,#35604,#35605,#35606,#35607,#35608,#35609,#35610,#35611,#35612,#35613,
#35614,#35615,#35616,#35617,#35618,#35619),.UNSPECIFIED.,.F.,.F.,(4,3,3,
3,3,3,3,4),(-47.8312715558983,-47.3711382365461,-46.3888804137623,-45.4066225909785,
-44.4243647681947,-43.4421069454109,-42.4598491226271,-41.5480862487187),
 .UNSPECIFIED.);
#3798=B_SPLINE_CURVE_WITH_KNOTS('',3,(#35624,#35625,#35626,#35627,#35628,
#35629,#35630,#35631,#35632,#35633,#35634,#35635,#35636,#35637,#35638,#35639,
#35640,#35641,#35642,#35643,#35644,#35645),.UNSPECIFIED.,.F.,.F.,(4,3,3,
3,3,3,3,4),(39.0086749840547,39.4673838906395,40.4531564644722,41.438929038305,
42.4247016121377,43.4104741859705,44.3962467598032,45.2918602912343),
 .UNSPECIFIED.);
#3799=B_SPLINE_CURVE_WITH_KNOTS('',3,(#35646,#35647,#35648,#35649,#35650,
#35651,#35652,#35653,#35654,#35655,#35656,#35657,#35658,#35659,#35660,#35661,
#35662,#35663,#35664,#35665,#35666,#35667,#35668,#35669,#35670),
 .UNSPECIFIED.,.F.,.F.,(4,3,3,3,3,3,3,3,4),(-41.5480862487187,-41.4775912998433,
-40.4953334770595,-39.5130756542757,-38.5308178314919,-37.5485600087081,
-36.5663021859243,-35.5840443631405,-35.2649009415391),.UNSPECIFIED.);
#3800=B_SPLINE_CURVE_WITH_KNOTS('',3,(#35675,#35676,#35677,#35678,#35679,
#35680,#35681,#35682,#35683,#35684,#35685,#35686,#35687,#35688,#35689,#35690,
#35691,#35692,#35693,#35694,#35695,#35696),.UNSPECIFIED.,.F.,.F.,(4,3,3,
3,3,3,3,4),(32.7254896768751,33.552748447643,34.5385210214758,35.5242935953085,
36.5100661691413,37.495838742974,38.4816113168067,39.0086749840547),
 .UNSPECIFIED.);
#3801=B_SPLINE_CURVE_WITH_KNOTS('',3,(#35697,#35698,#35699,#35700,#35701,
#35702,#35703,#35704,#35705,#35706,#35707,#35708,#35709,#35710,#35711,#35712,
#35713,#35714,#35715,#35716,#35717,#35718),.UNSPECIFIED.,.F.,.F.,(4,3,3,
3,3,3,3,4),(-35.2649009415391,-34.6017865403566,-33.6195287175728,-32.637270894789,
-31.6550130720052,-30.6727552492214,-29.6904974264376,-28.9817156343595),
 .UNSPECIFIED.);
#3802=B_SPLINE_CURVE_WITH_KNOTS('',3,(#35723,#35724,#35725,#35726,#35727,
#35728,#35729,#35730,#35731,#35732,#35733,#35734,#35735,#35736,#35737,#35738,
#35739,#35740,#35741,#35742,#35743,#35744,#35745,#35746,#35747),
 .UNSPECIFIED.,.F.,.F.,(4,3,3,3,3,3,3,3,4),(26.4423043696955,26.6523404308138,
27.6381130046466,28.6238855784793,29.609658152312,30.5954307261448,31.5812032999775,
32.5669758738103,32.7254896768751),.UNSPECIFIED.);
#3803=B_SPLINE_CURVE_WITH_KNOTS('',3,(#35748,#35749,#35750,#35751,#35752,
#35753,#35754,#35755,#35756,#35757,#35758,#35759,#35760,#35761,#35762,#35763,
#35764,#35765,#35766,#35767,#35768,#35769,#35770,#35771,#35772),
 .UNSPECIFIED.,.F.,.F.,(4,3,3,3,3,3,3,3,4),(-28.9817156343595,-28.7082396036538,
-27.72598178087,-26.7437239580862,-25.7614661353024,-24.7792083125186,-23.7969504897348,
-22.814692666951,-22.6985303271799),.UNSPECIFIED.);
#3804=B_SPLINE_CURVE_WITH_KNOTS('',3,(#35777,#35778,#35779,#35780,#35781,
#35782,#35783,#35784,#35785,#35786,#35787,#35788,#35789,#35790,#35791,#35792,
#35793,#35794,#35795,#35796,#35797,#35798),.UNSPECIFIED.,.F.,.F.,(4,3,3,
3,3,3,3,4),(20.159119062516,20.7377049878173,21.7234775616501,22.7092501354828,
23.6950227093156,24.6807952831483,25.6665678569811,26.4423043696955),
 .UNSPECIFIED.);
#3805=B_SPLINE_CURVE_WITH_KNOTS('',3,(#35799,#35800,#35801,#35802,#35803,
#35804,#35805,#35806,#35807,#35808,#35809,#35810,#35811,#35812,#35813,#35814,
#35815,#35816,#35817,#35818,#35819,#35820),.UNSPECIFIED.,.F.,.F.,(4,3,3,
3,3,3,3,4),(-22.6985303271799,-21.8324348441671,-20.8501770213833,-19.8679191985995,
-18.8856613758157,-17.9034035530319,-16.9211457302481,-16.4153450200003),
 .UNSPECIFIED.);
#3806=B_SPLINE_CURVE_WITH_KNOTS('',3,(#35825,#35826,#35827,#35828,#35829,
#35830,#35831,#35832,#35833,#35834,#35835,#35836,#35837,#35838,#35839,#35840,
#35841,#35842,#35843,#35844,#35845,#35846),.UNSPECIFIED.,.F.,.F.,(4,3,3,
3,3,3,3,4),(13.8759337553364,14.8230695448209,15.8088421186536,16.7946146924864,
17.7803872663191,18.7661598401519,19.7519324139846,20.159119062516),
 .UNSPECIFIED.);
#3807=B_SPLINE_CURVE_WITH_KNOTS('',3,(#35847,#35848,#35849,#35850,#35851,
#35852,#35853,#35854,#35855,#35856,#35857,#35858,#35859,#35860,#35861,#35862,
#35863,#35864,#35865,#35866,#35867,#35868),.UNSPECIFIED.,.F.,.F.,(4,3,3,
3,3,3,3,4),(-16.4153450200003,-15.9388879074643,-14.9566300846805,-13.9743722618967,
-12.9921144391129,-12.0098566163291,-11.0275987935453,-10.1321597128208),
 .UNSPECIFIED.);
#3808=B_SPLINE_CURVE_WITH_KNOTS('',3,(#35874,#35875,#35876,#35877,#35878,
#35879,#35880,#35881,#35882,#35883,#35884,#35885,#35886),.UNSPECIFIED.,
 .F.,.F.,(4,3,3,3,4),(-3.84897440564119,-3.16953621127481,-2.187278388491,
-1.2050205657072,-0.22276274292349),.UNSPECIFIED.);
#3809=B_SPLINE_CURVE_WITH_KNOTS('',3,(#35888,#35889,#35890,#35891,#35892,
#35893,#35894,#35895,#35896,#35897,#35898,#35899),.UNSPECIFIED.,.F.,.F.,
(4,2,2,2,2,4),(0.202168863441194,0.284518942728512,0.379358586733591,0.474198230738669,
0.569037874743748,0.642071595472304),.UNSPECIFIED.);
#3810=B_SPLINE_CURVE_WITH_KNOTS('',3,(#35900,#35901,#35902,#35903,#35904,
#35905,#35906,#35907,#35908,#35909,#35910,#35911,#35912,#35913,#35914,#35915,
#35916,#35917,#35918),.UNSPECIFIED.,.F.,.F.,(4,3,3,3,3,3,4),(2.14497997264832,
2.99379865882794,3.97957123266068,4.96534380649343,5.95111638032618,6.93688895415892,
7.59274844815675),.UNSPECIFIED.);
#3811=B_SPLINE_CURVE_WITH_KNOTS('',3,(#35924,#35925,#35926,#35927,#35928,
#35929,#35930,#35931),.UNSPECIFIED.,.F.,.F.,(4,1,1,1,1,4),(59.690260418206,
60.2123849216376,61.1946427444214,62.1769005672052,63.159158389989,64.1414162127728),
 .UNSPECIFIED.);
#3812=B_SPLINE_CURVE_WITH_KNOTS('',3,(#35934,#35935,#35936,#35937,#35938,
#35939,#35940,#35941,#35942),.UNSPECIFIED.,.F.,.F.,(4,1,1,1,1,1,4),(59.6902604182061,
59.7804194606076,60.7661920344403,61.751964608273,62.7377371821058,63.7235097559385,
64.6638825844083),.UNSPECIFIED.);
#3813=B_SPLINE_CURVE_WITH_KNOTS('',3,(#35947,#35948,#35949,#35950,#35951,
#35952,#35953,#35954,#35955,#35956),.UNSPECIFIED.,.F.,.F.,(4,1,1,1,1,1,
1,4),(53.4070751110265,54.3188379849348,55.3010958077186,56.2833536305024,
57.2656114532862,58.24786927607,59.2301270988538,59.690260418206),
 .UNSPECIFIED.);
#3814=B_SPLINE_CURVE_WITH_KNOTS('',3,(#35957,#35958,#35959,#35960,#35961,
#35962,#35963,#35964,#35965,#35966),.UNSPECIFIED.,.F.,.F.,(4,1,1,1,1,1,
1,4),(53.4070751110265,53.8657840176111,54.8515565914438,55.8373291652766,
56.8231017391093,57.8088743129421,58.7946468867748,59.6902604182061),
 .UNSPECIFIED.);
#3815=B_SPLINE_CURVE_WITH_KNOTS('',3,(#35971,#35972,#35973,#35974,#35975,
#35976,#35977,#35978,#35979,#35980,#35981),.UNSPECIFIED.,.F.,.F.,(4,1,1,
1,1,1,1,1,4),(47.1238898038469,47.4430332254481,48.4252910482319,49.4075488710157,
50.3898066937996,51.3720645165834,52.3543223393672,53.336580162151,53.4070751110265),
 .UNSPECIFIED.);
#3816=B_SPLINE_CURVE_WITH_KNOTS('',3,(#35982,#35983,#35984,#35985,#35986,
#35987,#35988,#35989,#35990,#35991),.UNSPECIFIED.,.F.,.F.,(4,1,1,1,1,1,
1,4),(47.1238898038469,47.9511485746146,48.9369211484474,49.9226937222801,
50.9084662961128,51.8942388699456,52.8800114437783,53.4070751110265),
 .UNSPECIFIED.);
#3817=B_SPLINE_CURVE_WITH_KNOTS('',3,(#35996,#35997,#35998,#35999,#36000,
#36001,#36002,#36003,#36004,#36005),.UNSPECIFIED.,.F.,.F.,(4,1,1,1,1,1,
1,4),(40.8407044966673,41.5494862887453,42.5317441115291,43.5140019343129,
44.4962597570967,45.4785175798805,46.4607754026643,47.1238898038469),
 .UNSPECIFIED.);
#3818=B_SPLINE_CURVE_WITH_KNOTS('',3,(#36006,#36007,#36008,#36009,#36010,
#36011,#36012,#36013,#36014,#36015,#36016),.UNSPECIFIED.,.F.,.F.,(4,1,1,
1,1,1,1,1,4),(40.8407044966673,41.0507405577854,42.0365131316181,43.0222857054509,
44.0080582792836,44.9938308531164,45.9796034269491,46.9653760007819,47.1238898038469),
 .UNSPECIFIED.);
#3819=B_SPLINE_CURVE_WITH_KNOTS('',3,(#36021,#36022,#36023,#36024,#36025,
#36026,#36027,#36028,#36029,#36030,#36031),.UNSPECIFIED.,.F.,.F.,(4,1,1,
1,1,1,1,1,4),(34.5575191894877,34.6736815292587,35.6559393520425,36.6381971748263,
37.6204549976101,38.6027128203939,39.5849706431777,40.5672284659615,40.8407044966673),
 .UNSPECIFIED.);
#3820=B_SPLINE_CURVE_WITH_KNOTS('',3,(#36032,#36033,#36034,#36035,#36036,
#36037,#36038,#36039,#36040,#36041),.UNSPECIFIED.,.F.,.F.,(4,1,1,1,1,1,
1,4),(34.5575191894877,35.1361051147889,36.1218776886216,37.1076502624544,
38.0934228362871,39.0791954101199,40.0649679839526,40.8407044966673),
 .UNSPECIFIED.);
#3821=B_SPLINE_CURVE_WITH_KNOTS('',3,(#36046,#36047,#36048,#36049,#36050,
#36051,#36052,#36053,#36054,#36055),.UNSPECIFIED.,.F.,.F.,(4,1,1,1,1,1,
1,4),(28.2743338823081,28.7801345925558,29.7623924153396,30.7446502381234,
31.7269080609072,32.709165883691,33.6914237064749,34.5575191894877),
 .UNSPECIFIED.);
#3822=B_SPLINE_CURVE_WITH_KNOTS('',3,(#36056,#36057,#36058,#36059,#36060,
#36061,#36062,#36063,#36064,#36065),.UNSPECIFIED.,.F.,.F.,(4,1,1,1,1,1,
1,4),(28.2743338823082,29.2214696717924,30.2072422456252,31.1930148194579,
32.1787873932907,33.1645599671234,34.1503325409562,34.5575191894877),
 .UNSPECIFIED.);
#3823=B_SPLINE_CURVE_WITH_KNOTS('',3,(#36070,#36071,#36072,#36073,#36074,
#36075,#36076,#36077,#36078,#36079),.UNSPECIFIED.,.F.,.F.,(4,1,1,1,1,1,
1,4),(21.9911485751285,22.886587655853,23.8688454786368,24.8511033014206,
25.8333611242044,26.8156189469882,27.797876769772,28.2743338823081),
 .UNSPECIFIED.);
#3824=B_SPLINE_CURVE_WITH_KNOTS('',3,(#36080,#36081,#36082,#36083,#36084,
#36085,#36086,#36087,#36088,#36089,#36090),.UNSPECIFIED.,.F.,.F.,(4,1,1,
1,1,1,1,1,4),(21.9911485751285,22.3210616549632,23.3068342287959,24.2926068026287,
25.2783793764614,26.2641519502942,27.2499245241269,28.2356970979597,28.2743338823082),
 .UNSPECIFIED.);
#3825=B_SPLINE_CURVE_WITH_KNOTS('',3,(#36096,#36097,#36098,#36099,#36100),
 .UNSPECIFIED.,.F.,.F.,(4,1,4),(14.4348810643012,15.420653638134,15.7079632679489),
 .UNSPECIFIED.);
#3826=B_SPLINE_CURVE_WITH_KNOTS('',3,(#36102,#36103,#36104,#36105),
 .UNSPECIFIED.,.F.,.F.,(4,4),(1.38948745034524,1.47775448763829),
 .UNSPECIFIED.);
#3827=B_SPLINE_CURVE_WITH_KNOTS('',3,(#36107,#36108,#36109,#36110),
 .UNSPECIFIED.,.F.,.F.,(4,4),(1.31866677181519,1.38948745034524),
 .UNSPECIFIED.);
#3828=B_SPLINE_CURVE_WITH_KNOTS('',3,(#36111,#36112,#36113,#36114,#36115,
#36116),.UNSPECIFIED.,.F.,.F.,(4,1,1,4),(13.8994448374521,14.0462672507987,
15.0285250735825,15.7079632679489),.UNSPECIFIED.);
#3829=B_SPLINE_CURVE_WITH_KNOTS('',3,(#36122,#36123,#36124,#36125,#36126,
#36127,#36128,#36129),.UNSPECIFIED.,.F.,.F.,(4,1,1,1,1,4),(59.690260418206,
60.2123849216378,61.1946427444216,62.1769005672054,63.1591583899892,64.1414162127731),
 .UNSPECIFIED.);
#3830=B_SPLINE_CURVE_WITH_KNOTS('',3,(#36132,#36133,#36134,#36135,#36136,
#36137,#36138,#36139,#36140),.UNSPECIFIED.,.F.,.F.,(4,1,1,1,1,1,4),(59.6902604182061,
59.7804194606078,60.7661920344405,61.7519646082732,62.737737182106,63.7235097559387,
64.6638825844085),.UNSPECIFIED.);
#3831=B_SPLINE_CURVE_WITH_KNOTS('',3,(#36145,#36146,#36147,#36148,#36149,
#36150,#36151,#36152,#36153,#36154),.UNSPECIFIED.,.F.,.F.,(4,1,1,1,1,1,
1,4),(53.4070751110265,54.318837984935,55.3010958077188,56.2833536305026,
57.2656114532864,58.2478692760702,59.230127098854,59.690260418206),
 .UNSPECIFIED.);
#3832=B_SPLINE_CURVE_WITH_KNOTS('',3,(#36155,#36156,#36157,#36158,#36159,
#36160,#36161,#36162,#36163,#36164),.UNSPECIFIED.,.F.,.F.,(4,1,1,1,1,1,
1,4),(53.4070751110265,53.8657840176113,54.851556591444,55.8373291652768,
56.8231017391095,57.8088743129423,58.794646886775,59.6902604182061),
 .UNSPECIFIED.);
#3833=B_SPLINE_CURVE_WITH_KNOTS('',3,(#36169,#36170,#36171,#36172,#36173,
#36174,#36175,#36176,#36177,#36178,#36179),.UNSPECIFIED.,.F.,.F.,(4,1,1,
1,1,1,1,1,4),(47.1238898038469,47.4430332254484,48.4252910482322,49.407548871016,
50.3898066937998,51.3720645165836,52.3543223393674,53.3365801621512,53.4070751110265),
 .UNSPECIFIED.);
#3834=B_SPLINE_CURVE_WITH_KNOTS('',3,(#36180,#36181,#36182,#36183,#36184,
#36185,#36186,#36187,#36188,#36189),.UNSPECIFIED.,.F.,.F.,(4,1,1,1,1,1,
1,4),(47.1238898038469,47.9511485746148,48.9369211484476,49.9226937222803,
50.908466296113,51.8942388699458,52.8800114437785,53.4070751110265),
 .UNSPECIFIED.);
#3835=B_SPLINE_CURVE_WITH_KNOTS('',3,(#36194,#36195,#36196,#36197,#36198,
#36199,#36200,#36201,#36202,#36203),.UNSPECIFIED.,.F.,.F.,(4,1,1,1,1,1,
1,4),(40.8407044966673,41.5494862887455,42.5317441115293,43.5140019343131,
44.4962597570969,45.4785175798807,46.4607754026645,47.1238898038469),
 .UNSPECIFIED.);
#3836=B_SPLINE_CURVE_WITH_KNOTS('',3,(#36204,#36205,#36206,#36207,#36208,
#36209,#36210,#36211,#36212,#36213,#36214),.UNSPECIFIED.,.F.,.F.,(4,1,1,
1,1,1,1,1,4),(40.8407044966673,41.0507405577856,42.0365131316183,43.0222857054511,
44.0080582792838,44.9938308531166,45.9796034269493,46.9653760007821,47.1238898038469),
 .UNSPECIFIED.);
#3837=B_SPLINE_CURVE_WITH_KNOTS('',3,(#36219,#36220,#36221,#36222,#36223,
#36224,#36225,#36226,#36227,#36228,#36229),.UNSPECIFIED.,.F.,.F.,(4,1,1,
1,1,1,1,1,4),(34.5575191894877,34.6736815292589,35.6559393520427,36.6381971748265,
37.6204549976103,38.6027128203941,39.5849706431779,40.5672284659617,40.8407044966673),
 .UNSPECIFIED.);
#3838=B_SPLINE_CURVE_WITH_KNOTS('',3,(#36230,#36231,#36232,#36233,#36234,
#36235,#36236,#36237,#36238,#36239),.UNSPECIFIED.,.F.,.F.,(4,1,1,1,1,1,
1,4),(34.5575191894877,35.1361051147891,36.1218776886219,37.1076502624546,
38.0934228362874,39.0791954101201,40.0649679839529,40.8407044966673),
 .UNSPECIFIED.);
#3839=B_SPLINE_CURVE_WITH_KNOTS('',3,(#36244,#36245,#36246,#36247,#36248,
#36249,#36250,#36251,#36252,#36253),.UNSPECIFIED.,.F.,.F.,(4,1,1,1,1,1,
1,4),(28.2743338823081,28.780134592556,29.7623924153398,30.7446502381237,
31.7269080609075,32.7091658836913,33.6914237064751,34.5575191894877),
 .UNSPECIFIED.);
#3840=B_SPLINE_CURVE_WITH_KNOTS('',3,(#36254,#36255,#36256,#36257,#36258,
#36259,#36260,#36261,#36262,#36263),.UNSPECIFIED.,.F.,.F.,(4,1,1,1,1,1,
1,4),(28.2743338823081,29.2214696717927,30.2072422456254,31.1930148194582,
32.1787873932909,33.1645599671237,34.1503325409564,34.5575191894877),
 .UNSPECIFIED.);
#3841=B_SPLINE_CURVE_WITH_KNOTS('',3,(#36268,#36269,#36270,#36271,#36272,
#36273,#36274,#36275,#36276,#36277),.UNSPECIFIED.,.F.,.F.,(4,1,1,1,1,1,
1,4),(21.9911485751285,22.8865876558532,23.868845478637,24.8511033014208,
25.8333611242046,26.8156189469884,27.7978767697722,28.2743338823081),
 .UNSPECIFIED.);
#3842=B_SPLINE_CURVE_WITH_KNOTS('',3,(#36278,#36279,#36280,#36281,#36282,
#36283,#36284,#36285,#36286,#36287,#36288),.UNSPECIFIED.,.F.,.F.,(4,1,1,
1,1,1,1,1,4),(21.9911485751285,22.3210616549635,23.3068342287962,24.292606802629,
25.2783793764617,26.2641519502944,27.2499245241272,28.2356970979599,28.2743338823081),
 .UNSPECIFIED.);
#3843=B_SPLINE_CURVE_WITH_KNOTS('',3,(#36294,#36295,#36296,#36297,#36298),
 .UNSPECIFIED.,.F.,.F.,(4,1,4),(14.4348810643015,15.4206536381343,15.7079632679489),
 .UNSPECIFIED.);
#3844=B_SPLINE_CURVE_WITH_KNOTS('',3,(#36300,#36301,#36302,#36303),
 .UNSPECIFIED.,.F.,.F.,(4,4),(1.38948745034523,1.47775448763837),
 .UNSPECIFIED.);
#3845=B_SPLINE_CURVE_WITH_KNOTS('',3,(#36305,#36306,#36307,#36308),
 .UNSPECIFIED.,.F.,.F.,(4,4),(1.31866677181523,1.38948745034523),
 .UNSPECIFIED.);
#3846=B_SPLINE_CURVE_WITH_KNOTS('',3,(#36309,#36310,#36311,#36312,#36313,
#36314),.UNSPECIFIED.,.F.,.F.,(4,1,1,4),(13.8994448374522,14.046267250799,
15.0285250735828,15.7079632679489),.UNSPECIFIED.);
#3847=B_SPLINE_CURVE_WITH_KNOTS('',3,(#36320,#36321,#36322,#36323,#36324,
#36325,#36326,#36327),.UNSPECIFIED.,.F.,.F.,(4,1,1,1,1,4),(59.690260418206,
60.2123849216377,61.1946427444215,62.1769005672053,63.1591583899891,64.1414162127729),
 .UNSPECIFIED.);
#3848=B_SPLINE_CURVE_WITH_KNOTS('',3,(#36330,#36331,#36332,#36333,#36334,
#36335,#36336,#36337,#36338),.UNSPECIFIED.,.F.,.F.,(4,1,1,1,1,1,4),(59.690260418206,
59.7804194606077,60.7661920344404,61.7519646082732,62.7377371821059,63.7235097559387,
64.6638825844084),.UNSPECIFIED.);
#3849=B_SPLINE_CURVE_WITH_KNOTS('',3,(#36343,#36344,#36345,#36346,#36347,
#36348,#36349,#36350,#36351,#36352),.UNSPECIFIED.,.F.,.F.,(4,1,1,1,1,1,
1,4),(53.4070751110265,54.3188379849348,55.3010958077186,56.2833536305025,
57.2656114532863,58.2478692760701,59.2301270988539,59.690260418206),
 .UNSPECIFIED.);
#3850=B_SPLINE_CURVE_WITH_KNOTS('',3,(#36353,#36354,#36355,#36356,#36357,
#36358,#36359,#36360,#36361,#36362),.UNSPECIFIED.,.F.,.F.,(4,1,1,1,1,1,
1,4),(53.4070751110265,53.8657840176112,54.851556591444,55.8373291652767,
56.8231017391094,57.8088743129422,58.7946468867749,59.690260418206),
 .UNSPECIFIED.);
#3851=B_SPLINE_CURVE_WITH_KNOTS('',3,(#36367,#36368,#36369,#36370,#36371,
#36372,#36373,#36374,#36375,#36376,#36377),.UNSPECIFIED.,.F.,.F.,(4,1,1,
1,1,1,1,1,4),(47.1238898038469,47.4430332254482,48.425291048232,49.4075488710158,
50.3898066937996,51.3720645165834,52.3543223393672,53.336580162151,53.4070751110265),
 .UNSPECIFIED.);
#3852=B_SPLINE_CURVE_WITH_KNOTS('',3,(#36378,#36379,#36380,#36381,#36382,
#36383,#36384,#36385,#36386,#36387),.UNSPECIFIED.,.F.,.F.,(4,1,1,1,1,1,
1,4),(47.1238898038469,47.9511485746147,48.9369211484475,49.9226937222802,
50.908466296113,51.8942388699457,52.8800114437785,53.4070751110265),
 .UNSPECIFIED.);
#3853=B_SPLINE_CURVE_WITH_KNOTS('',3,(#36392,#36393,#36394,#36395,#36396,
#36397,#36398,#36399,#36400,#36401),.UNSPECIFIED.,.F.,.F.,(4,1,1,1,1,1,
1,4),(40.8407044966673,41.5494862887453,42.5317441115292,43.514001934313,
44.4962597570968,45.4785175798806,46.4607754026644,47.1238898038469),
 .UNSPECIFIED.);
#3854=B_SPLINE_CURVE_WITH_KNOTS('',3,(#36402,#36403,#36404,#36405,#36406,
#36407,#36408,#36409,#36410,#36411,#36412),.UNSPECIFIED.,.F.,.F.,(4,1,1,
1,1,1,1,1,4),(40.8407044966673,41.0507405577855,42.0365131316183,43.022285705451,
44.0080582792838,44.9938308531165,45.9796034269493,46.965376000782,47.1238898038469),
 .UNSPECIFIED.);
#3855=B_SPLINE_CURVE_WITH_KNOTS('',3,(#36417,#36418,#36419,#36420,#36421,
#36422,#36423,#36424,#36425,#36426,#36427),.UNSPECIFIED.,.F.,.F.,(4,1,1,
1,1,1,1,1,4),(34.5575191894877,34.6736815292587,35.6559393520425,36.6381971748263,
37.6204549976101,38.6027128203939,39.5849706431777,40.5672284659615,40.8407044966673),
 .UNSPECIFIED.);
#3856=B_SPLINE_CURVE_WITH_KNOTS('',3,(#36428,#36429,#36430,#36431,#36432,
#36433,#36434,#36435,#36436,#36437),.UNSPECIFIED.,.F.,.F.,(4,1,1,1,1,1,
1,4),(34.5575191894877,35.1361051147891,36.1218776886218,37.1076502624546,
38.0934228362873,39.07919541012,40.0649679839528,40.8407044966673),
 .UNSPECIFIED.);
#3857=B_SPLINE_CURVE_WITH_KNOTS('',3,(#36442,#36443,#36444,#36445,#36446,
#36447,#36448,#36449,#36450,#36451),.UNSPECIFIED.,.F.,.F.,(4,1,1,1,1,1,
1,4),(28.2743338823081,28.7801345925559,29.7623924153397,30.7446502381235,
31.7269080609073,32.7091658836911,33.6914237064749,34.5575191894877),
 .UNSPECIFIED.);
#3858=B_SPLINE_CURVE_WITH_KNOTS('',3,(#36452,#36453,#36454,#36455,#36456,
#36457,#36458,#36459,#36460,#36461),.UNSPECIFIED.,.F.,.F.,(4,1,1,1,1,1,
1,4),(28.2743338823081,29.2214696717926,30.2072422456253,31.1930148194581,
32.1787873932908,33.1645599671236,34.1503325409563,34.5575191894877),
 .UNSPECIFIED.);
#3859=B_SPLINE_CURVE_WITH_KNOTS('',3,(#36466,#36467,#36468,#36469,#36470,
#36471,#36472,#36473,#36474,#36475),.UNSPECIFIED.,.F.,.F.,(4,1,1,1,1,1,
1,4),(21.9911485751285,22.886587655853,23.8688454786368,24.8511033014206,
25.8333611242044,26.8156189469882,27.797876769772,28.2743338823081),
 .UNSPECIFIED.);
#3860=B_SPLINE_CURVE_WITH_KNOTS('',3,(#36476,#36477,#36478,#36479,#36480,
#36481,#36482,#36483,#36484,#36485,#36486),.UNSPECIFIED.,.F.,.F.,(4,1,1,
1,1,1,1,1,4),(21.9911485751285,22.3210616549634,23.3068342287961,24.2926068026289,
25.2783793764616,26.2641519502944,27.2499245241271,28.2356970979599,28.2743338823081),
 .UNSPECIFIED.);
#3861=B_SPLINE_CURVE_WITH_KNOTS('',3,(#36492,#36493,#36494,#36495,#36496),
 .UNSPECIFIED.,.F.,.F.,(4,1,4),(14.4348810643014,15.4206536381342,15.7079632679489),
 .UNSPECIFIED.);
#3862=B_SPLINE_CURVE_WITH_KNOTS('',3,(#36498,#36499,#36500,#36501),
 .UNSPECIFIED.,.F.,.F.,(4,4),(1.38948745034523,1.47775448763834),
 .UNSPECIFIED.);
#3863=B_SPLINE_CURVE_WITH_KNOTS('',3,(#36503,#36504,#36505,#36506),
 .UNSPECIFIED.,.F.,.F.,(4,4),(1.31866677181519,1.38948745034523),
 .UNSPECIFIED.);
#3864=B_SPLINE_CURVE_WITH_KNOTS('',3,(#36507,#36508,#36509,#36510,#36511,
#36512),.UNSPECIFIED.,.F.,.F.,(4,1,1,4),(13.8994448374521,14.0462672507987,
15.0285250735825,15.7079632679489),.UNSPECIFIED.);
#3865=B_SPLINE_CURVE_WITH_KNOTS('',3,(#36737,#36738,#36739,#36740,#36741,
#36742,#36743,#36744,#36745,#36746,#36747,#36748),.UNSPECIFIED.,.F.,.F.,
(4,2,2,2,2,4),(0.,0.0939720040697306,0.191040004611618,0.294727654301763,
0.396757250727393,0.506753893125291),.UNSPECIFIED.);
#3866=B_SPLINE_CURVE_WITH_KNOTS('',3,(#36749,#36750,#36751,#36752,#36753,
#36754,#36755,#36756,#36757,#36758,#36759,#36760,#36761,#36762,#36763,#36764,
#36765,#36766,#36767,#36768,#36769,#36770,#36771,#36772,#36773),
 .UNSPECIFIED.,.F.,.F.,(4,3,3,3,3,3,3,3,4),(-10.1321597128208,-10.0453409707615,
-9.06308314797765,-8.08082532519384,-7.09856750241004,-6.11630967962623,
-5.13405185684243,-4.15179403405862,-3.84897440564119),.UNSPECIFIED.);
#3867=B_SPLINE_CURVE_WITH_KNOTS('',3,(#36774,#36775,#36776,#36777,#36778,
#36779,#36780,#36781,#36782,#36783,#36784,#36785,#36786,#36787,#36788,#36789,
#36790,#36791,#36792,#36793,#36794,#36795,#36796,#36797,#36798,#36799,#36800,
#36801,#36802,#36803,#36804,#36805,#36806,#36807,#36808,#36809,#36810,#36811,
#36812,#36813,#36814,#36815,#36816,#36817,#36818,#36819,#36820,#36821,#36822,
#36823,#36824,#36825,#36826,#36827,#36828,#36829,#36830,#36831,#36832,#36833,
#36834,#36835,#36836,#36837,#36838,#36839,#36840,#36841,#36842,#36843,#36844,
#36845,#36846,#36847,#36848,#36849,#36850,#36851,#36852,#36853,#36854,#36855,
#36856,#36857,#36858,#36859,#36860,#36861,#36862,#36863,#36864,#36865,#36866,
#36867),.UNSPECIFIED.,.F.,.F.,(4,3,3,3,3,3,3,3,3,3,3,3,3,3,3,3,3,3,3,3,
3,3,3,3,3,3,3,3,3,3,3,4),(-0.566847306048089,-0.536661395473507,-0.506059016755951,
-0.497326650809489,-0.490463963747992,-0.460323979286527,-0.437444973964932,
-0.425645739517285,-0.420672568156472,-0.391255347604605,-0.362370453937528,
-0.334033562322262,-0.319848155920138,-0.313024468520039,-0.308668713479008,
-0.280666905255211,-0.277291936713766,-0.248847901203608,-0.219408150886093,
-0.20505599758711,-0.200814316443281,-0.172984028418683,-0.14523356468346,
-0.11796097413067,-0.104882089697273,-0.100481501514816,-0.0962956903621217,
-0.0696281223924694,-0.0434020873669322,-0.0179348500541518,-0.0133298986634882,
0.),.UNSPECIFIED.);
#3868=B_SPLINE_CURVE_WITH_KNOTS('',3,(#36868,#36869,#36870,#36871,#36872,
#36873,#36874,#36875,#36876,#36877,#36878),.UNSPECIFIED.,.F.,.F.,(4,1,1,
1,1,1,1,1,4),(15.7079632679489,16.0107828963664,16.9930407191502,17.975298541934,
18.9575563647178,19.9398141875016,20.9220720102854,21.9043298330692,21.9911485751285),
 .UNSPECIFIED.);
#3869=B_SPLINE_CURVE_WITH_KNOTS('',3,(#36880,#36881,#36882,#36883,#36884,
#36885,#36886,#36887,#36888,#36889),.UNSPECIFIED.,.F.,.F.,(4,1,1,1,1,1,
1,4),(15.7079632679489,16.4064262119669,17.3921987857997,18.3779713596324,
19.3637439334652,20.3495165072979,21.3352890811306,21.9911485751285),
 .UNSPECIFIED.);
#3870=B_SPLINE_CURVE_WITH_KNOTS('',3,(#37114,#37115,#37116,#37117,#37118,
#37119,#37120,#37121,#37122,#37123,#37124,#37125,#37126,#37127),
 .UNSPECIFIED.,.F.,.F.,(4,2,2,2,2,2,4),(0.,0.122341475621437,0.233773139394309,
0.328065713266122,0.418619986828863,0.511091556851628,0.605234881207264),
 .UNSPECIFIED.);
#3871=B_SPLINE_CURVE_WITH_KNOTS('',3,(#37128,#37129,#37130,#37131,#37132,
#37133,#37134,#37135,#37136,#37137,#37138,#37139,#37140,#37141,#37142,#37143,
#37144,#37145,#37146,#37147,#37148,#37149,#37150,#37151,#37152,#37153,#37154,
#37155,#37156,#37157,#37158,#37159,#37160,#37161,#37162,#37163,#37164,#37165,
#37166,#37167,#37168,#37169,#37170,#37171,#37172,#37173,#37174,#37175,#37176,
#37177,#37178,#37179,#37180,#37181,#37182,#37183,#37184,#37185,#37186,#37187,
#37188,#37189,#37190,#37191,#37192,#37193,#37194,#37195,#37196,#37197,#37198,
#37199,#37200,#37201,#37202,#37203,#37204,#37205,#37206,#37207,#37208,#37209,
#37210,#37211,#37212,#37213,#37214,#37215,#37216,#37217,#37218,#37219,#37220,
#37221),.UNSPECIFIED.,.F.,.F.,(4,3,3,3,3,3,3,3,3,3,3,3,3,3,3,3,3,3,3,3,
3,3,3,3,3,3,3,3,3,3,3,4),(-0.569248610399481,-0.543568168745277,-0.517260903357168,
-0.510376876051222,-0.504799164129705,-0.477737437228182,-0.456135094562755,
-0.449160314492888,-0.442513472342989,-0.414784053155389,-0.386626551258596,
-0.358686347322027,-0.345244434467712,-0.34080557042231,-0.33631776891126,
-0.30739232536096,-0.30491869590477,-0.277130714479983,-0.248706827603265,
-0.233107805251665,-0.228466848903046,-0.199477467537415,-0.169916466664947,
-0.14012139652544,-0.124355841110362,-0.118742223062163,-0.114429203491767,
-0.083895606230837,-0.0533233406469446,-0.0233305921302133,-0.0139969532048209,
0.),.UNSPECIFIED.);
#3872=B_SPLINE_CURVE_WITH_KNOTS('',3,(#37222,#37223,#37224,#37225,#37226,
#37227,#37228,#37229,#37230,#37231,#37232,#37233,#37234,#37235,#37236,#37237,
#37238,#37239,#37240,#37241,#37242,#37243,#37244,#37245,#37246),
 .UNSPECIFIED.,.F.,.F.,(4,3,3,3,3,3,3,3,4),(7.59274844815675,7.92266152799166,
8.90843410182441,9.89420667565716,10.8799792494899,11.8657518233226,12.8515243971554,
13.8372969709881,13.8759337553364),.UNSPECIFIED.);
#3873=B_SPLINE_CURVE_WITH_KNOTS('',3,(#37471,#37472,#37473,#37474,#37475,
#37476,#37477,#37478,#37479,#37480,#37481,#37482),.UNSPECIFIED.,.F.,.F.,
(4,2,2,2,2,4),(0.,0.0939720040697043,0.191040004611567,0.294727654301641,
0.396757250727202,0.506753893125061),.UNSPECIFIED.);
#3874=B_SPLINE_CURVE_WITH_KNOTS('',3,(#37483,#37484,#37485,#37486,#37487,
#37488,#37489,#37490,#37491,#37492,#37493,#37494,#37495,#37496,#37497,#37498,
#37499,#37500,#37501,#37502,#37503,#37504,#37505,#37506,#37507),
 .UNSPECIFIED.,.F.,.F.,(4,3,3,3,3,3,3,3,4),(-10.1321597128207,-10.0453409707616,
-9.06308314797777,-8.08082532519396,-7.09856750241015,-6.11630967962635,
-5.13405185684255,-4.15179403405874,-3.84897440564108),.UNSPECIFIED.);
#3875=B_SPLINE_CURVE_WITH_KNOTS('',3,(#37508,#37509,#37510,#37511,#37512,
#37513,#37514,#37515,#37516,#37517,#37518,#37519,#37520,#37521,#37522,#37523,
#37524,#37525,#37526,#37527,#37528,#37529,#37530,#37531,#37532,#37533,#37534,
#37535,#37536,#37537,#37538,#37539,#37540,#37541,#37542,#37543,#37544,#37545,
#37546,#37547,#37548,#37549,#37550,#37551,#37552,#37553,#37554,#37555,#37556,
#37557,#37558,#37559,#37560,#37561,#37562,#37563,#37564,#37565,#37566,#37567,
#37568,#37569,#37570,#37571,#37572,#37573,#37574,#37575,#37576,#37577,#37578,
#37579,#37580,#37581,#37582,#37583,#37584,#37585,#37586,#37587,#37588,#37589,
#37590,#37591,#37592,#37593,#37594,#37595,#37596,#37597,#37598,#37599,#37600,
#37601),.UNSPECIFIED.,.F.,.F.,(4,3,3,3,3,3,3,3,3,3,3,3,3,3,3,3,3,3,3,3,
3,3,3,3,3,3,3,3,3,3,3,4),(-0.566847306048109,-0.536661395468383,-0.506059016754568,
-0.497326650805892,-0.490463963797695,-0.460323979336568,-0.437444974008718,
-0.425645739590181,-0.420672568143048,-0.391255347593568,-0.362370453926602,
-0.334033562313392,-0.319848155913487,-0.313024468510124,-0.308668713420628,
-0.280666905198208,-0.277291936713773,-0.248847901202399,-0.219408150885036,
-0.205055997585609,-0.200814316430888,-0.172984028406577,-0.145233564671321,
-0.117960974121696,-0.104882089689421,-0.100481501534044,-0.0962956903887221,
-0.0696281224182907,-0.04340208739252,-0.0179348500828051,-0.0133298986634936,
0.),.UNSPECIFIED.);
#3876=B_SPLINE_CURVE_WITH_KNOTS('',3,(#37602,#37603,#37604,#37605,#37606,
#37607,#37608,#37609,#37610,#37611,#37612),.UNSPECIFIED.,.F.,.F.,(4,1,1,
1,1,1,1,1,4),(15.7079632679489,16.0107828963666,16.9930407191504,17.9752985419342,
18.957556364718,19.9398141875018,20.9220720102856,21.9043298330694,21.9911485751285),
 .UNSPECIFIED.);
#3877=B_SPLINE_CURVE_WITH_KNOTS('',3,(#37614,#37615,#37616,#37617,#37618,
#37619,#37620,#37621,#37622,#37623),.UNSPECIFIED.,.F.,.F.,(4,1,1,1,1,1,
1,4),(15.7079632679489,16.406426211967,17.3921987857997,18.3779713596325,
19.3637439334652,20.349516507298,21.3352890811307,21.9911485751285),
 .UNSPECIFIED.);
#3878=B_SPLINE_CURVE_WITH_KNOTS('',3,(#37848,#37849,#37850,#37851,#37852,
#37853,#37854,#37855,#37856,#37857,#37858,#37859,#37860,#37861),
 .UNSPECIFIED.,.F.,.F.,(4,2,2,2,2,2,4),(0.,0.12234147562142,0.233773139394286,
0.328065713266116,0.418619986828843,0.511091556851594,0.605234881207211),
 .UNSPECIFIED.);
#3879=B_SPLINE_CURVE_WITH_KNOTS('',3,(#37862,#37863,#37864,#37865,#37866,
#37867,#37868,#37869,#37870,#37871,#37872,#37873,#37874,#37875,#37876,#37877,
#37878,#37879,#37880,#37881,#37882,#37883,#37884,#37885,#37886,#37887,#37888,
#37889,#37890,#37891,#37892,#37893,#37894,#37895,#37896,#37897,#37898,#37899,
#37900,#37901,#37902,#37903,#37904,#37905,#37906,#37907,#37908,#37909,#37910,
#37911,#37912,#37913,#37914,#37915,#37916,#37917,#37918,#37919,#37920,#37921,
#37922,#37923,#37924,#37925,#37926,#37927,#37928,#37929,#37930,#37931,#37932,
#37933,#37934,#37935,#37936,#37937,#37938,#37939,#37940,#37941,#37942,#37943,
#37944,#37945,#37946,#37947,#37948,#37949,#37950,#37951,#37952,#37953,#37954,
#37955),.UNSPECIFIED.,.F.,.F.,(4,3,3,3,3,3,3,3,3,3,3,3,3,3,3,3,3,3,3,3,
3,3,3,3,3,3,3,3,3,3,3,4),(-0.569248610399453,-0.543568168745332,-0.517260903359189,
-0.510376876055068,-0.504799164150761,-0.477737437250597,-0.456135094582367,
-0.44916031457044,-0.442513472333628,-0.414784053145682,-0.386626551248794,
-0.358686347310781,-0.345244434459274,-0.340805570317779,-0.336317768890034,
-0.307392325339199,-0.304918695904753,-0.277130714478965,-0.248706827603545,
-0.233107805253122,-0.228466848911822,-0.199477467538772,-0.169916466667501,
-0.140121396526104,-0.124355841110945,-0.118742223070016,-0.114429203500742,
-0.0838956062406663,-0.0533233406584259,-0.023330592138883,-0.013996953204826,
0.),.UNSPECIFIED.);
#3880=B_SPLINE_CURVE_WITH_KNOTS('',3,(#37956,#37957,#37958,#37959,#37960,
#37961,#37962,#37963,#37964,#37965,#37966,#37967,#37968,#37969,#37970,#37971,
#37972,#37973,#37974,#37975,#37976,#37977,#37978,#37979,#37980),
 .UNSPECIFIED.,.F.,.F.,(4,3,3,3,3,3,3,3,4),(7.59274844815675,7.92266152799173,
8.90843410182448,9.89420667565722,10.87997924949,11.8657518233227,12.8515243971555,
13.8372969709882,13.8759337553364),.UNSPECIFIED.);
#3881=B_SPLINE_CURVE_WITH_KNOTS('',3,(#38205,#38206,#38207,#38208,#38209,
#38210,#38211,#38212,#38213,#38214,#38215,#38216),.UNSPECIFIED.,.F.,.F.,
(4,2,2,2,2,4),(0.,0.09397200406971,0.191040004611562,0.294727654301647,
0.396757250727143,0.506753893124957),.UNSPECIFIED.);
#3882=B_SPLINE_CURVE_WITH_KNOTS('',3,(#38217,#38218,#38219,#38220,#38221,
#38222,#38223,#38224,#38225,#38226,#38227,#38228,#38229,#38230,#38231,#38232,
#38233,#38234,#38235,#38236,#38237,#38238,#38239,#38240,#38241),
 .UNSPECIFIED.,.F.,.F.,(4,3,3,3,3,3,3,3,4),(-10.1321597128207,-10.0453409707614,
-9.06308314797754,-8.08082532519374,-7.09856750240993,-6.11630967962613,
-5.13405185684232,-4.15179403405851,-3.84897440564107),.UNSPECIFIED.);
#3883=B_SPLINE_CURVE_WITH_KNOTS('',3,(#38242,#38243,#38244,#38245,#38246,
#38247,#38248,#38249,#38250,#38251,#38252,#38253,#38254,#38255,#38256,#38257,
#38258,#38259,#38260,#38261,#38262,#38263,#38264,#38265,#38266,#38267,#38268,
#38269,#38270,#38271,#38272,#38273,#38274,#38275,#38276,#38277,#38278,#38279,
#38280,#38281,#38282,#38283,#38284,#38285,#38286,#38287,#38288,#38289,#38290,
#38291,#38292,#38293,#38294,#38295,#38296,#38297,#38298,#38299,#38300,#38301,
#38302,#38303,#38304,#38305,#38306,#38307,#38308,#38309,#38310,#38311,#38312,
#38313,#38314,#38315,#38316,#38317,#38318,#38319,#38320,#38321,#38322,#38323,
#38324,#38325,#38326,#38327,#38328,#38329,#38330,#38331,#38332,#38333,#38334,
#38335),.UNSPECIFIED.,.F.,.F.,(4,3,3,3,3,3,3,3,3,3,3,3,3,3,3,3,3,3,3,3,
3,3,3,3,3,3,3,3,3,3,3,4),(-0.566847306048032,-0.536661395466917,-0.506059016751992,
-0.497326650803245,-0.490463963758655,-0.460323979298246,-0.437444973975183,
-0.425645739534236,-0.420672568143549,-0.391255347592175,-0.362370453925434,
-0.33403356230877,-0.319848155910013,-0.313024468504981,-0.308668713474399,
-0.280666905255003,-0.277291936713742,-0.248847901201056,-0.219408150883858,
-0.205055997583148,-0.20081431637463,-0.172984028349664,-0.145233564613907,
-0.117960974064228,-0.104882089639133,-0.100481501504229,-0.0962956903645289,
-0.0696281223931707,-0.0434020873672608,-0.0179348500541578,-0.0133298986634736,
0.),.UNSPECIFIED.);
#3884=B_SPLINE_CURVE_WITH_KNOTS('',3,(#38336,#38337,#38338,#38339,#38340,
#38341,#38342,#38343,#38344,#38345,#38346),.UNSPECIFIED.,.F.,.F.,(4,1,1,
1,1,1,1,1,4),(15.7079632679489,16.0107828963663,16.9930407191502,17.975298541934,
18.9575563647178,19.9398141875016,20.9220720102854,21.9043298330692,21.9911485751285),
 .UNSPECIFIED.);
#3885=B_SPLINE_CURVE_WITH_KNOTS('',3,(#38348,#38349,#38350,#38351,#38352,
#38353,#38354,#38355,#38356,#38357),.UNSPECIFIED.,.F.,.F.,(4,1,1,1,1,1,
1,4),(15.7079632679489,16.4064262119667,17.3921987857995,18.3779713596322,
19.363743933465,20.3495165072977,21.3352890811305,21.9911485751285),
 .UNSPECIFIED.);
#3886=B_SPLINE_CURVE_WITH_KNOTS('',3,(#38582,#38583,#38584,#38585,#38586,
#38587,#38588,#38589,#38590,#38591,#38592,#38593,#38594,#38595),
 .UNSPECIFIED.,.F.,.F.,(4,2,2,2,2,2,4),(0.,0.122341475621424,0.233773139394306,
0.328065713266132,0.41861998682885,0.511091556851618,0.605234881207287),
 .UNSPECIFIED.);
#3887=B_SPLINE_CURVE_WITH_KNOTS('',3,(#38596,#38597,#38598,#38599,#38600,
#38601,#38602,#38603,#38604,#38605,#38606,#38607,#38608,#38609,#38610,#38611,
#38612,#38613,#38614,#38615,#38616,#38617,#38618,#38619,#38620,#38621,#38622,
#38623,#38624,#38625,#38626,#38627,#38628,#38629,#38630,#38631,#38632,#38633,
#38634,#38635,#38636,#38637,#38638,#38639,#38640,#38641,#38642,#38643,#38644,
#38645,#38646,#38647,#38648,#38649,#38650,#38651,#38652,#38653,#38654,#38655,
#38656,#38657,#38658,#38659,#38660,#38661,#38662,#38663,#38664,#38665,#38666,
#38667,#38668,#38669,#38670,#38671,#38672,#38673,#38674,#38675,#38676,#38677,
#38678,#38679,#38680,#38681,#38682,#38683,#38684,#38685,#38686,#38687,#38688,
#38689),.UNSPECIFIED.,.F.,.F.,(4,3,3,3,3,3,3,3,3,3,3,3,3,3,3,3,3,3,3,3,
3,3,3,3,3,3,3,3,3,3,3,4),(-0.569248610399429,-0.543568168745069,-0.517260903354712,
-0.510376876043647,-0.504799164152385,-0.477737437252708,-0.456135094584214,
-0.449160314584278,-0.44251347235757,-0.414784053166835,-0.386626551270024,
-0.358686347331947,-0.345244434475149,-0.340805570470318,-0.336317768921927,
-0.307392325367316,-0.304918695904754,-0.277130714480542,-0.248706827608405,
-0.233107805261332,-0.2284668489227,-0.199477467554332,-0.169916466682518,
-0.140121396541974,-0.12435584112483,-0.118742223078146,-0.114429203510237,
-0.0838956062485887,-0.0533233406698207,-0.0233305921507268,-0.0139969532048219,
0.),.UNSPECIFIED.);
#3888=B_SPLINE_CURVE_WITH_KNOTS('',3,(#38690,#38691,#38692,#38693,#38694,
#38695,#38696,#38697,#38698,#38699,#38700,#38701,#38702,#38703,#38704,#38705,
#38706,#38707,#38708,#38709,#38710,#38711,#38712,#38713,#38714),
 .UNSPECIFIED.,.F.,.F.,(4,3,3,3,3,3,3,3,4),(7.59274844815675,7.92266152799146,
8.90843410182421,9.89420667565695,10.8799792494897,11.8657518233224,12.8515243971552,
13.8372969709879,13.8759337553364),.UNSPECIFIED.);
#3889=B_SPLINE_CURVE_WITH_KNOTS('',3,(#38945,#38946,#38947,#38948,#38949,
#38950,#38951,#38952,#38953,#38954,#38955,#38956),.UNSPECIFIED.,.F.,.F.,
(4,2,2,2,2,4),(0.,0.0939720040697054,0.191040004611548,0.294727654301647,
0.396757250727165,0.50675389312503),.UNSPECIFIED.);
#3890=B_SPLINE_CURVE_WITH_KNOTS('',3,(#38957,#38958,#38959,#38960,#38961,
#38962,#38963,#38964,#38965,#38966,#38967,#38968,#38969,#38970,#38971,#38972,
#38973,#38974,#38975,#38976,#38977,#38978,#38979,#38980,#38981),
 .UNSPECIFIED.,.F.,.F.,(4,3,3,3,3,3,3,3,4),(-10.1321597128207,-10.0453409707613,
-9.06308314797754,-8.08082532519373,-7.09856750240993,-6.11630967962612,
-5.13405185684231,-4.15179403405851,-3.84897440564113),.UNSPECIFIED.);
#3891=B_SPLINE_CURVE_WITH_KNOTS('',3,(#38982,#38983,#38984,#38985,#38986,
#38987,#38988,#38989,#38990,#38991,#38992,#38993,#38994,#38995,#38996,#38997,
#38998,#38999,#39000,#39001,#39002,#39003,#39004,#39005,#39006,#39007,#39008,
#39009,#39010,#39011,#39012,#39013,#39014,#39015,#39016,#39017,#39018,#39019,
#39020,#39021,#39022,#39023,#39024,#39025,#39026,#39027,#39028,#39029,#39030,
#39031,#39032,#39033,#39034,#39035,#39036,#39037,#39038,#39039,#39040,#39041,
#39042,#39043,#39044,#39045,#39046,#39047,#39048,#39049,#39050,#39051,#39052,
#39053,#39054,#39055,#39056,#39057,#39058,#39059,#39060,#39061,#39062,#39063,
#39064,#39065,#39066,#39067,#39068,#39069,#39070,#39071,#39072,#39073,#39074,
#39075),.UNSPECIFIED.,.F.,.F.,(4,3,3,3,3,3,3,3,3,3,3,3,3,3,3,3,3,3,3,3,
3,3,3,3,3,3,3,3,3,3,3,4),(-0.566847306048062,-0.53666139547184,-0.506059016754063,
-0.49732665080814,-0.490463963821467,-0.460323979361128,-0.437444974030206,
-0.425645739625527,-0.42067256805228,-0.391255347501007,-0.362370453835405,
-0.334033562222944,-0.319848155845646,-0.313024468412086,-0.30866871342461,
-0.280666905204325,-0.277291936713753,-0.248847901203833,-0.21940815088629,
-0.205055997588386,-0.200814316362458,-0.17298402833657,-0.145233564602108,
-0.117960974053518,-0.104882089629765,-0.100481501481134,-0.0962956902597121,
-0.0696281222892088,-0.043402087264509,-0.0179348499542768,-0.0133298986634882,
0.),.UNSPECIFIED.);
#3892=B_SPLINE_CURVE_WITH_KNOTS('',3,(#39076,#39077,#39078,#39079,#39080,
#39081,#39082,#39083,#39084,#39085,#39086),.UNSPECIFIED.,.F.,.F.,(4,1,1,
1,1,1,1,1,4),(15.7079632679489,16.0107828963663,16.9930407191501,17.9752985419339,
18.9575563647177,19.9398141875016,20.9220720102854,21.9043298330692,21.9911485751285),
 .UNSPECIFIED.);
#3893=B_SPLINE_CURVE_WITH_KNOTS('',3,(#39088,#39089,#39090,#39091,#39092,
#39093,#39094,#39095,#39096,#39097),.UNSPECIFIED.,.F.,.F.,(4,1,1,1,1,1,
1,4),(15.7079632679489,16.4064262119669,17.3921987857997,18.3779713596324,
19.3637439334652,20.3495165072979,21.3352890811306,21.9911485751285),
 .UNSPECIFIED.);
#3894=B_SPLINE_CURVE_WITH_KNOTS('',3,(#39322,#39323,#39324,#39325,#39326,
#39327,#39328,#39329,#39330,#39331,#39332,#39333,#39334,#39335),
 .UNSPECIFIED.,.F.,.F.,(4,2,2,2,2,2,4),(0.,0.122341475621436,0.233773139394342,
0.328065713266181,0.418619986828953,0.511091556851744,0.605234881207393),
 .UNSPECIFIED.);
#3895=B_SPLINE_CURVE_WITH_KNOTS('',3,(#39336,#39337,#39338,#39339,#39340,
#39341,#39342,#39343,#39344,#39345,#39346,#39347,#39348,#39349,#39350,#39351,
#39352,#39353,#39354,#39355,#39356,#39357,#39358,#39359,#39360,#39361,#39362,
#39363,#39364,#39365,#39366,#39367,#39368,#39369,#39370,#39371,#39372,#39373,
#39374,#39375,#39376,#39377,#39378,#39379,#39380,#39381,#39382,#39383,#39384,
#39385,#39386,#39387,#39388,#39389,#39390,#39391,#39392,#39393,#39394,#39395,
#39396,#39397,#39398,#39399,#39400,#39401,#39402,#39403,#39404,#39405,#39406,
#39407,#39408,#39409,#39410,#39411,#39412,#39413,#39414,#39415,#39416,#39417,
#39418,#39419,#39420,#39421,#39422,#39423,#39424,#39425,#39426,#39427,#39428,
#39429),.UNSPECIFIED.,.F.,.F.,(4,3,3,3,3,3,3,3,3,3,3,3,3,3,3,3,3,3,3,3,
3,3,3,3,3,3,3,3,3,3,3,4),(-0.56924861039948,-0.543568168743065,-0.517260903356135,
-0.51037687605013,-0.504799164228155,-0.477737437329509,-0.456135094651419,
-0.449160314870292,-0.442513472316536,-0.414784053132704,-0.386626551235781,
-0.358686347299406,-0.345244434450751,-0.340805570359703,-0.336317768898936,
-0.307392325353166,-0.304918695904789,-0.277130714479285,-0.248706827607001,
-0.233107805259422,-0.228466848824526,-0.199477467452263,-0.169916466577901,
-0.140121396437131,-0.124355841033094,-0.118742223014663,-0.114429203367402,
-0.0838956061053275,-0.0533233405264678,-0.02333059201217,-0.0139969532048341,
0.),.UNSPECIFIED.);
#3896=B_SPLINE_CURVE_WITH_KNOTS('',3,(#39430,#39431,#39432,#39433,#39434,
#39435,#39436,#39437,#39438,#39439,#39440,#39441,#39442,#39443,#39444,#39445,
#39446,#39447,#39448,#39449,#39450,#39451,#39452,#39453,#39454),
 .UNSPECIFIED.,.F.,.F.,(4,3,3,3,3,3,3,3,4),(7.5927484481567,7.92266152799159,
8.90843410182433,9.89420667565708,10.8799792494898,11.8657518233226,12.8515243971553,
13.8372969709881,13.8759337553363),.UNSPECIFIED.);
#3897=B_SPLINE_CURVE_WITH_KNOTS('',3,(#39458,#39459,#39460,#39461,#39462,
#39463,#39464,#39465,#39466,#39467,#39468,#39469,#39470,#39471,#39472,#39473,
#39474,#39475,#39476,#39477,#39478,#39479,#39480,#39481,#39482,#39483,#39484,
#39485,#39486,#39487,#39488,#39489,#39490,#39491,#39492,#39493,#39494,#39495,
#39496,#39497,#39498,#39499,#39500,#39501,#39502,#39503,#39504,#39505,#39506,
#39507,#39508,#39509,#39510,#39511,#39512,#39513,#39514,#39515,#39516,#39517,
#39518,#39519,#39520,#39521,#39522,#39523,#39524,#39525,#39526,#39527,#39528,
#39529,#39530,#39531,#39532,#39533,#39534,#39535,#39536,#39537,#39538,#39539,
#39540,#39541,#39542,#39543,#39544,#39545),.UNSPECIFIED.,.F.,.F.,(4,3,3,
3,3,3,3,3,3,3,3,3,3,3,3,3,3,3,3,3,3,3,3,3,3,3,3,3,3,4),(-0.378621596831439,
-0.359797351563908,-0.34785658095904,-0.339691168491925,-0.33536812849937,
-0.31549598337044,-0.301162672408894,-0.29722662849187,-0.293222646083178,
-0.272820189148395,-0.252122545583708,-0.239299283107299,-0.228793967352159,
-0.22450143777299,-0.203196862142534,-0.200829495678071,-0.180342172305092,
-0.158301477242566,-0.154267258991073,-0.150798053974315,-0.129414619358608,
-0.107580334749735,-0.0856137297500737,-0.0801849312914882,-0.075938243267924,
-0.0533906056048975,-0.0308184408529723,-0.00876003301059033,-0.00401661180488397,
0.),.UNSPECIFIED.);
#3898=B_SPLINE_CURVE_WITH_KNOTS('',3,(#39546,#39547,#39548,#39549,#39550,
#39551,#39552,#39553,#39554,#39555,#39556,#39557,#39558,#39559,#39560,#39561,
#39562,#39563,#39564,#39565,#39566,#39567,#39568,#39569,#39570,#39571,#39572,
#39573,#39574,#39575,#39576,#39577,#39578,#39579,#39580,#39581,#39582,#39583,
#39584,#39585,#39586,#39587,#39588,#39589,#39590,#39591,#39592,#39593,#39594,
#39595,#39596,#39597,#39598,#39599,#39600,#39601,#39602,#39603,#39604,#39605,
#39606,#39607,#39608,#39609,#39610,#39611,#39612,#39613,#39614,#39615,#39616,
#39617,#39618,#39619,#39620,#39621,#39622,#39623,#39624,#39625,#39626,#39627,
#39628,#39629,#39630),.UNSPECIFIED.,.F.,.F.,(4,3,3,3,3,3,3,3,3,3,3,3,3,
3,3,3,3,3,3,3,3,3,3,3,3,3,3,3,4),(-0.376940817211618,-0.354634182890013,
-0.332911763637628,-0.328063423851266,-0.305814805697609,-0.290194808594274,
-0.284256159181052,-0.27860087990661,-0.256917704097231,-0.23570018939777,
-0.214948003756356,-0.208204616608779,-0.204400619135709,-0.183824594219919,
-0.180854828870929,-0.159872080701967,-0.140296871743027,-0.135976593191014,
-0.1325994058261,-0.112140134041277,-0.0917753374355066,-0.0718467835548272,
-0.0676478648747052,-0.0636677276964501,-0.0441097307614711,-0.0249236995043246,
-0.00636086853661492,-0.00327040903044951,0.),.UNSPECIFIED.);
#3899=B_SPLINE_CURVE_WITH_KNOTS('',3,(#39632,#39633,#39634,#39635,#39636,
#39637,#39638,#39639,#39640,#39641,#39642),.UNSPECIFIED.,.F.,.F.,(4,1,1,
1,1,1,1,1,4),(15.7079632679489,15.8518654961884,16.8494368691713,17.8470082421543,
18.8445796151372,19.8421509881201,20.8397223611031,21.837293734086,21.9911485751285),
 .UNSPECIFIED.);
#3900=B_SPLINE_CURVE_WITH_KNOTS('',3,(#39643,#39644,#39645,#39646,#39647,
#39648,#39649,#39650,#39651,#39652),.UNSPECIFIED.,.F.,.F.,(4,1,1,1,1,1,
1,4),(15.7079632679489,16.3932837587428,17.3908551317257,18.3884265047086,
19.3859978776916,20.3835692506745,21.3811406236574,21.9911485751285),
 .UNSPECIFIED.);
#3901=B_SPLINE_CURVE_WITH_KNOTS('',3,(#39997,#39998,#39999,#40000,#40001,
#40002,#40003,#40004,#40005,#40006,#40007,#40008,#40009,#40010,#40011,#40012,
#40013,#40014,#40015,#40016,#40017,#40018,#40019,#40020,#40021,#40022,#40023,
#40024,#40025,#40026,#40027,#40028,#40029,#40030,#40031,#40032,#40033,#40034,
#40035,#40036,#40037,#40038,#40039,#40040,#40041,#40042,#40043,#40044,#40045,
#40046,#40047,#40048,#40049,#40050,#40051,#40052,#40053,#40054,#40055,#40056,
#40057,#40058,#40059,#40060,#40061,#40062,#40063,#40064,#40065,#40066,#40067,
#40068,#40069,#40070,#40071,#40072,#40073,#40074,#40075,#40076,#40077,#40078),
 .UNSPECIFIED.,.F.,.F.,(4,3,3,3,3,3,3,3,3,3,3,3,3,3,3,3,3,3,3,3,3,3,3,3,
3,3,3,4),(0.,0.0185976526102971,0.038423603067765,0.0557713097180495,0.0644755844468549,
0.068451628882596,0.0885059681202624,0.108915976702059,0.125988296594055,
0.133854408336341,0.137287722938539,0.15836259811627,0.177205256270041,
0.197733028930863,0.205653066409013,0.20912748618408,0.230133047566578,
0.251625243351313,0.268069199559052,0.278304581266316,0.284046628828574,
0.306315638091715,0.322971918689363,0.328167813305499,0.333183176091069,
0.355704559012681,0.372940760482309,0.376940817211655),.UNSPECIFIED.);
#3902=B_SPLINE_CURVE_WITH_KNOTS('',3,(#40079,#40080,#40081,#40082,#40083,
#40084,#40085,#40086,#40087,#40088,#40089,#40090,#40091,#40092,#40093,#40094,
#40095,#40096,#40097,#40098,#40099,#40100,#40101,#40102,#40103),
 .UNSPECIFIED.,.F.,.F.,(4,3,3,3,3,3,3,3,4),(-10.1295685708718,-9.97571372982932,
-8.97814235684639,-7.98057098386346,-6.98299961088053,-5.9854282378976,
-4.98785686491466,-3.99028549193173,-3.84638326369224),.UNSPECIFIED.);
#3903=B_SPLINE_CURVE_WITH_KNOTS('',3,(#40448,#40449,#40450,#40451,#40452,
#40453,#40454,#40455,#40456,#40457,#40458,#40459,#40460,#40461,#40462,#40463,
#40464,#40465,#40466,#40467,#40468,#40469),.UNSPECIFIED.,.F.,.F.,(4,3,3,
3,3,3,3,4),(7.59300756235153,7.98057098386346,8.97814235684639,9.97571372982932,
10.9732851028123,11.9708564757952,12.9684278487781,13.8761928695311),
 .UNSPECIFIED.);
#3904=B_SPLINE_CURVE_WITH_KNOTS('',3,(#40470,#40471,#40472,#40473,#40474,
#40475,#40476,#40477,#40478,#40479,#40480,#40481,#40482,#40483,#40484,#40485,
#40486,#40487,#40488,#40489,#40490,#40491,#40492,#40493,#40494,#40495,#40496,
#40497,#40498,#40499,#40500,#40501,#40502,#40503,#40504,#40505,#40506,#40507,
#40508,#40509,#40510,#40511,#40512,#40513,#40514,#40515,#40516,#40517,#40518,
#40519,#40520,#40521,#40522,#40523,#40524,#40525,#40526,#40527,#40528,#40529,
#40530,#40531,#40532,#40533,#40534,#40535,#40536,#40537,#40538,#40539,#40540,
#40541,#40542,#40543,#40544,#40545,#40546,#40547,#40548,#40549,#40550,#40551,
#40552,#40553,#40554),.UNSPECIFIED.,.F.,.F.,(4,3,3,3,3,3,3,3,3,3,3,3,3,
3,3,3,3,3,3,3,3,3,3,3,3,3,3,3,4),(0.,0.0219662478558776,0.0445437519028764,
0.0636212321933215,0.07209685366591,0.0767538544095747,0.0810484322391913,
0.102995052369132,0.124771335602438,0.142869400258438,0.150423566581854,
0.153920154512486,0.157567047704503,0.178337711801077,0.197163594226437,
0.219435545910495,0.224339035444425,0.229398553889566,0.250063614193726,
0.270724500169195,0.285678958575898,0.296896594122732,0.30062412117991,
0.320396425756097,0.334309228897919,0.338775005408962,0.357799813892921,
0.375339207698899,0.378621596831459),.UNSPECIFIED.);
#3905=B_SPLINE_CURVE_WITH_KNOTS('',3,(#40557,#40558,#40559,#40560,#40561,
#40562,#40563,#40564,#40565,#40566,#40567,#40568,#40569,#40570,#40571,#40572,
#40573,#40574,#40575,#40576,#40577,#40578,#40579,#40580,#40581,#40582,#40583,
#40584,#40585,#40586,#40587,#40588,#40589,#40590,#40591,#40592,#40593,#40594,
#40595,#40596,#40597,#40598,#40599,#40600,#40601,#40602,#40603,#40604,#40605,
#40606,#40607,#40608,#40609,#40610,#40611,#40612,#40613,#40614,#40615,#40616,
#40617,#40618,#40619,#40620,#40621,#40622,#40623,#40624,#40625,#40626,#40627,
#40628,#40629,#40630,#40631,#40632,#40633,#40634,#40635,#40636,#40637,#40638,
#40639,#40640,#40641,#40642,#40643,#40644),.UNSPECIFIED.,.F.,.F.,(4,3,3,
3,3,3,3,3,3,3,3,3,3,3,3,3,3,3,3,3,3,3,3,3,3,3,3,3,3,4),(-0.378621596831376,
-0.359797363526263,-0.347856611388035,-0.339691444400771,-0.335368277656519,
-0.315496143991729,-0.301162812952519,-0.297226950788673,-0.293222691569,
-0.272820243253334,-0.252122598473177,-0.239299322774394,-0.228794025865611,
-0.22450145691891,-0.203196880773058,-0.200829495678047,-0.180342164145179,
-0.158301470102644,-0.154267209525513,-0.150798043946759,-0.129414602665861,
-0.107580315103531,-0.0856137100538687,-0.0801848970193141,-0.0759382309635091,
-0.0533905919171353,-0.0308184274161136,-0.00876001820599945,-0.00401661180489279,
0.),.UNSPECIFIED.);
#3906=B_SPLINE_CURVE_WITH_KNOTS('',3,(#40645,#40646,#40647,#40648,#40649,
#40650,#40651,#40652,#40653,#40654,#40655,#40656,#40657,#40658,#40659,#40660,
#40661,#40662,#40663,#40664,#40665,#40666,#40667,#40668,#40669,#40670,#40671,
#40672,#40673,#40674,#40675,#40676,#40677,#40678,#40679,#40680,#40681,#40682,
#40683,#40684,#40685,#40686,#40687,#40688,#40689,#40690,#40691,#40692,#40693,
#40694,#40695,#40696,#40697,#40698,#40699,#40700,#40701,#40702,#40703,#40704,
#40705,#40706,#40707,#40708,#40709,#40710,#40711,#40712,#40713,#40714,#40715,
#40716,#40717,#40718,#40719,#40720,#40721,#40722,#40723,#40724,#40725,#40726,
#40727,#40728,#40729),.UNSPECIFIED.,.F.,.F.,(4,3,3,3,3,3,3,3,3,3,3,3,3,
3,3,3,3,3,3,3,3,3,3,3,3,3,3,3,4),(-0.376940817211658,-0.354634181776293,
-0.332911762663124,-0.32806342264117,-0.305814804501951,-0.290194807548075,
-0.28425615687011,-0.278600880008221,-0.256917704384274,-0.235700190161406,
-0.214948004827601,-0.20820461591444,-0.204400619278192,-0.183824594824418,
-0.180854828870941,-0.159872080703541,-0.140296871744405,-0.135976593972186,
-0.132599406442617,-0.112140134586177,-0.0917753381175245,-0.0718467848499371,
-0.0676478684587749,-0.063667728849533,-0.0441097322463572,-0.0249237017162217,
-0.00636087194527781,-0.00327040903045192,0.),.UNSPECIFIED.);
#3907=B_SPLINE_CURVE_WITH_KNOTS('',3,(#40731,#40732,#40733,#40734,#40735,
#40736,#40737,#40738,#40739,#40740,#40741),.UNSPECIFIED.,.F.,.F.,(4,1,1,
1,1,1,1,1,4),(15.7079632679489,15.8518654961884,16.8494368691713,17.8470082421543,
18.8445796151372,19.8421509881201,20.8397223611031,21.837293734086,21.9911485751285),
 .UNSPECIFIED.);
#3908=B_SPLINE_CURVE_WITH_KNOTS('',3,(#40742,#40743,#40744,#40745,#40746,
#40747,#40748,#40749,#40750,#40751),.UNSPECIFIED.,.F.,.F.,(4,1,1,1,1,1,
1,4),(15.7079632679489,16.3932837587428,17.3908551317257,18.3884265047086,
19.3859978776916,20.3835692506745,21.3811406236574,21.9911485751285),
 .UNSPECIFIED.);
#3909=B_SPLINE_CURVE_WITH_KNOTS('',3,(#41096,#41097,#41098,#41099,#41100,
#41101,#41102,#41103,#41104,#41105,#41106,#41107,#41108,#41109,#41110,#41111,
#41112,#41113,#41114,#41115,#41116,#41117,#41118,#41119,#41120,#41121,#41122,
#41123,#41124,#41125,#41126,#41127,#41128,#41129,#41130,#41131,#41132,#41133,
#41134,#41135,#41136,#41137,#41138,#41139,#41140,#41141,#41142,#41143,#41144,
#41145,#41146,#41147,#41148,#41149,#41150,#41151,#41152,#41153,#41154,#41155,
#41156,#41157,#41158,#41159,#41160,#41161,#41162,#41163,#41164,#41165,#41166,
#41167,#41168,#41169,#41170,#41171,#41172,#41173,#41174,#41175,#41176,#41177),
 .UNSPECIFIED.,.F.,.F.,(4,3,3,3,3,3,3,3,3,3,3,3,3,3,3,3,3,3,3,3,3,3,3,3,
3,3,3,4),(0.,0.0185976544397309,0.0384236046685196,0.0557713111187097,0.0644755868718208,
0.0684516295212589,0.088505970063774,0.10891597920695,0.125988298472723,
0.133854411295539,0.137287724515988,0.158362599521173,0.17720525627004,
0.197733028011595,0.205653065916169,0.209127485831402,0.230133046133618,
0.251625241350057,0.26806920002886,0.278304582355908,0.284046628542303,
0.306315637737753,0.322971918423894,0.328167812754554,0.333183175813273,
0.35570455874239,0.372940760482319,0.376940817211663),.UNSPECIFIED.);
#3910=B_SPLINE_CURVE_WITH_KNOTS('',3,(#41178,#41179,#41180,#41181,#41182,
#41183,#41184,#41185,#41186,#41187,#41188,#41189,#41190,#41191,#41192,#41193,
#41194,#41195,#41196,#41197,#41198,#41199,#41200,#41201,#41202),
 .UNSPECIFIED.,.F.,.F.,(4,3,3,3,3,3,3,3,4),(-10.1295685708718,-9.97571372982932,
-8.97814235684639,-7.98057098386346,-6.98299961088053,-5.98542823789759,
-4.98785686491466,-3.99028549193173,-3.84638326369223),.UNSPECIFIED.);
#3911=B_SPLINE_CURVE_WITH_KNOTS('',3,(#41547,#41548,#41549,#41550,#41551,
#41552,#41553,#41554,#41555,#41556,#41557,#41558,#41559,#41560,#41561,#41562,
#41563,#41564,#41565,#41566,#41567,#41568),.UNSPECIFIED.,.F.,.F.,(4,3,3,
3,3,3,3,4),(7.59300756235152,7.98057098386347,8.97814235684639,9.97571372982933,
10.9732851028123,11.9708564757952,12.9684278487781,13.8761928695311),
 .UNSPECIFIED.);
#3912=B_SPLINE_CURVE_WITH_KNOTS('',3,(#41569,#41570,#41571,#41572,#41573,
#41574,#41575,#41576,#41577,#41578,#41579,#41580,#41581,#41582,#41583,#41584,
#41585,#41586,#41587,#41588,#41589,#41590,#41591,#41592,#41593,#41594,#41595,
#41596,#41597,#41598,#41599,#41600,#41601,#41602,#41603,#41604,#41605,#41606,
#41607,#41608,#41609,#41610,#41611,#41612,#41613,#41614,#41615,#41616,#41617,
#41618,#41619,#41620,#41621,#41622,#41623,#41624,#41625,#41626,#41627,#41628,
#41629,#41630,#41631,#41632,#41633,#41634,#41635,#41636,#41637,#41638,#41639,
#41640,#41641,#41642,#41643,#41644,#41645,#41646,#41647,#41648,#41649,#41650,
#41651,#41652,#41653),.UNSPECIFIED.,.F.,.F.,(4,3,3,3,3,3,3,3,3,3,3,3,3,
3,3,3,3,3,3,3,3,3,3,3,3,3,3,3,4),(0.,0.0219662374681043,0.0445437405167695,
0.0636212222304769,0.0720968506878746,0.076753848109775,0.0810484305510295,
0.102995050890004,0.12477133726383,0.14286940150448,0.150423566044572,0.153920151202922,
0.157567046659697,0.178337713883236,0.197163594226428,0.219435545910486,
0.224339036280714,0.229398553932371,0.250063613828033,0.270724500179063,
0.28567896807331,0.296896610194788,0.300624125785386,0.320396434080511,
0.334309242700404,0.338775018539486,0.357799832913783,0.375339207698892,
0.378621596831452),.UNSPECIFIED.);
#3913=B_SPLINE_CURVE_WITH_KNOTS('',3,(#41656,#41657,#41658,#41659,#41660,
#41661,#41662,#41663,#41664,#41665,#41666,#41667,#41668,#41669,#41670,#41671,
#41672,#41673,#41674,#41675,#41676,#41677,#41678,#41679,#41680,#41681,#41682,
#41683,#41684,#41685,#41686,#41687,#41688,#41689,#41690,#41691,#41692,#41693,
#41694,#41695,#41696,#41697,#41698,#41699,#41700,#41701,#41702,#41703,#41704,
#41705,#41706,#41707,#41708,#41709,#41710,#41711,#41712,#41713,#41714,#41715,
#41716,#41717,#41718,#41719,#41720,#41721,#41722,#41723,#41724,#41725,#41726,
#41727,#41728,#41729,#41730,#41731,#41732,#41733,#41734,#41735,#41736,#41737,
#41738,#41739,#41740,#41741,#41742,#41743),.UNSPECIFIED.,.F.,.F.,(4,3,3,
3,3,3,3,3,3,3,3,3,3,3,3,3,3,3,3,3,3,3,3,3,3,3,3,3,3,4),(-0.378621596831417,
-0.359796324497287,-0.347853968212287,-0.339667381014858,-0.335354793046504,
-0.315481654145321,-0.301150134336916,-0.297197750169864,-0.293218427785562,
-0.272815226606713,-0.25211769236358,-0.239295643192204,-0.228788599050033,
-0.224499673213218,-0.203195145604267,-0.200829495678076,-0.180342878343926,
-0.158302095026546,-0.154271536503135,-0.150798918827255,-0.129416060220185,
-0.107582030156302,-0.085615429447784,-0.0801878898688665,-0.0759393010019052,
-0.0533917820942347,-0.0308195963821799,-0.00876131063080365,-0.00401661180488985,
0.),.UNSPECIFIED.);
#3914=B_SPLINE_CURVE_WITH_KNOTS('',3,(#41744,#41745,#41746,#41747,#41748,
#41749,#41750,#41751,#41752,#41753,#41754,#41755,#41756,#41757,#41758,#41759,
#41760,#41761,#41762,#41763,#41764,#41765,#41766,#41767,#41768,#41769,#41770,
#41771,#41772,#41773,#41774,#41775,#41776,#41777,#41778,#41779,#41780,#41781,
#41782,#41783,#41784,#41785,#41786,#41787,#41788,#41789,#41790,#41791,#41792,
#41793,#41794,#41795,#41796,#41797,#41798,#41799,#41800,#41801,#41802,#41803,
#41804,#41805,#41806,#41807,#41808,#41809,#41810,#41811,#41812,#41813,#41814,
#41815,#41816,#41817,#41818,#41819,#41820,#41821,#41822,#41823,#41824,#41825,
#41826,#41827,#41828),.UNSPECIFIED.,.F.,.F.,(4,3,3,3,3,3,3,3,3,3,3,3,3,
3,3,3,3,3,3,3,3,3,3,3,3,3,3,3,4),(-0.376940817211595,-0.354633525341539,
-0.332911188282713,-0.328062756081701,-0.305814149652336,-0.29019423455466,
-0.284254884688389,-0.278600964735507,-0.256917900776687,-0.235700669545305,
-0.214948669523327,-0.208204193208427,-0.204400682428168,-0.183824932405233,
-0.180854828870931,-0.15987208389359,-0.140296874535698,-0.135977073921547,
-0.132599774501717,-0.112140461891992,-0.0917757502446185,-0.0718475645954736,
-0.0676500217282804,-0.0636684046323996,-0.044110611854005,-0.0249250199568782,
-0.0063629054909037,-0.00327040903044969,0.),.UNSPECIFIED.);
#3915=B_SPLINE_CURVE_WITH_KNOTS('',3,(#41830,#41831,#41832,#41833,#41834,
#41835,#41836,#41837,#41838,#41839,#41840),.UNSPECIFIED.,.F.,.F.,(4,1,1,
1,1,1,1,1,4),(15.7079632679489,15.8518654961884,16.8494368691713,17.8470082421543,
18.8445796151372,19.8421509881201,20.8397223611031,21.837293734086,21.9911485751285),
 .UNSPECIFIED.);
#3916=B_SPLINE_CURVE_WITH_KNOTS('',3,(#41841,#41842,#41843,#41844,#41845,
#41846,#41847,#41848,#41849,#41850),.UNSPECIFIED.,.F.,.F.,(4,1,1,1,1,1,
1,4),(15.7079632679489,16.3932837587428,17.3908551317257,18.3884265047087,
19.3859978776916,20.3835692506745,21.3811406236575,21.9911485751285),
 .UNSPECIFIED.);
#3917=B_SPLINE_CURVE_WITH_KNOTS('',3,(#42195,#42196,#42197,#42198,#42199,
#42200,#42201,#42202,#42203,#42204,#42205,#42206,#42207,#42208,#42209,#42210,
#42211,#42212,#42213,#42214,#42215,#42216,#42217,#42218,#42219,#42220,#42221,
#42222,#42223,#42224,#42225,#42226,#42227,#42228,#42229,#42230,#42231,#42232,
#42233,#42234,#42235,#42236,#42237,#42238,#42239,#42240,#42241,#42242,#42243,
#42244,#42245,#42246,#42247,#42248,#42249,#42250,#42251,#42252,#42253,#42254,
#42255,#42256,#42257,#42258,#42259,#42260,#42261,#42262,#42263,#42264,#42265,
#42266,#42267,#42268,#42269,#42270,#42271,#42272,#42273,#42274,#42275,#42276),
 .UNSPECIFIED.,.F.,.F.,(4,3,3,3,3,3,3,3,3,3,3,3,3,3,3,3,3,3,3,3,3,3,3,3,
3,3,3,4),(0.,0.0185987341991705,0.0384245494580317,0.0557721378095353,0.0644770178564968,
0.0684520053950054,0.0885071145915648,0.108917452402041,0.125989403369046,
0.133856151023374,0.137288655787116,0.158363425172233,0.17720525627006,
0.197732482353245,0.205652770441454,0.209127273143543,0.230132191377097,
0.251624049744365,0.268069475041104,0.27830521821788,0.284046462285339,
0.306315432124743,0.322971764214144,0.328167478822272,0.333183009449727,
0.355704395480073,0.372940760482347,0.376940817211692),.UNSPECIFIED.);
#3918=B_SPLINE_CURVE_WITH_KNOTS('',3,(#42277,#42278,#42279,#42280,#42281,
#42282,#42283,#42284,#42285,#42286,#42287,#42288,#42289,#42290,#42291,#42292,
#42293,#42294,#42295,#42296,#42297,#42298,#42299,#42300,#42301),
 .UNSPECIFIED.,.F.,.F.,(4,3,3,3,3,3,3,3,4),(-10.1295685708718,-9.97571372982932,
-8.97814235684639,-7.98057098386346,-6.98299961088053,-5.98542823789759,
-4.98785686491466,-3.99028549193173,-3.84638326369223),.UNSPECIFIED.);
#3919=B_SPLINE_CURVE_WITH_KNOTS('',3,(#42646,#42647,#42648,#42649,#42650,
#42651,#42652,#42653,#42654,#42655,#42656,#42657,#42658,#42659,#42660,#42661,
#42662,#42663,#42664,#42665,#42666,#42667),.UNSPECIFIED.,.F.,.F.,(4,3,3,
3,3,3,3,4),(7.59300756235153,7.98057098386347,8.9781423568464,9.97571372982933,
10.9732851028123,11.9708564757952,12.9684278487781,13.8761928695311),
 .UNSPECIFIED.);
#3920=B_SPLINE_CURVE_WITH_KNOTS('',3,(#42668,#42669,#42670,#42671,#42672,
#42673,#42674,#42675,#42676,#42677,#42678,#42679,#42680,#42681,#42682,#42683,
#42684,#42685,#42686,#42687,#42688,#42689,#42690,#42691,#42692,#42693,#42694,
#42695,#42696,#42697,#42698,#42699,#42700,#42701,#42702,#42703,#42704,#42705,
#42706,#42707,#42708,#42709,#42710,#42711,#42712,#42713,#42714,#42715,#42716,
#42717,#42718,#42719,#42720,#42721,#42722,#42723,#42724,#42725,#42726,#42727,
#42728,#42729,#42730,#42731,#42732,#42733,#42734,#42735,#42736,#42737,#42738,
#42739,#42740,#42741,#42742,#42743,#42744,#42745,#42746,#42747,#42748,#42749,
#42750,#42751,#42752),.UNSPECIFIED.,.F.,.F.,(4,3,3,3,3,3,3,3,3,3,3,3,3,
3,3,3,3,3,3,3,3,3,3,3,3,3,3,3,4),(0.,0.0219671392711931,0.0445447270616514,
0.0636220854572485,0.0720971088191602,0.0767543937612894,0.0810485771086071,
0.102995177264468,0.124771188719879,0.142869290096516,0.150423609225613,
0.15392042550993,0.157567134754784,0.178337528535704,0.197163594226428,
0.219435545910483,0.224338960691668,0.229398550509701,0.250063644964382,
0.27072449500928,0.285678123754087,0.296895177895067,0.300623717144677,
0.320395694438786,0.334308019634333,0.338773858976101,0.35779815161244,
0.375339207698864,0.378621596831424),.UNSPECIFIED.);
#3921=B_SPLINE_CURVE_WITH_KNOTS('',3,(#42755,#42756,#42757,#42758,#42759,
#42760,#42761,#42762,#42763,#42764,#42765,#42766,#42767,#42768,#42769,#42770,
#42771,#42772,#42773,#42774,#42775,#42776,#42777,#42778,#42779,#42780,#42781,
#42782,#42783,#42784,#42785,#42786,#42787,#42788,#42789,#42790,#42791,#42792,
#42793,#42794,#42795,#42796,#42797,#42798,#42799,#42800,#42801,#42802,#42803,
#42804,#42805,#42806,#42807,#42808,#42809,#42810,#42811,#42812,#42813,#42814,
#42815,#42816,#42817,#42818,#42819,#42820,#42821,#42822,#42823,#42824,#42825,
#42826,#42827,#42828,#42829,#42830,#42831,#42832,#42833,#42834,#42835,#42836,
#42837,#42838,#42839,#42840,#42841,#42842),.UNSPECIFIED.,.F.,.F.,(4,3,3,
3,3,3,3,3,3,3,3,3,3,3,3,3,3,3,3,3,3,3,3,3,3,3,3,3,3,4),(-0.378621596831428,
-0.359797351570199,-0.347856580972857,-0.339691168602623,-0.335368128537906,
-0.315495983408754,-0.301162672442419,-0.297226628519414,-0.293222646087005,
-0.272820189154467,-0.25212254559016,-0.239299283112138,-0.228793967359004,
-0.224501437751794,-0.203196862127902,-0.200829495678073,-0.180342172303858,
-0.158301477241488,-0.154267258837984,-0.150798053944791,-0.129414619327559,
-0.107580334717304,-0.0856137297167705,-0.0801849312391385,-0.07593824324878,
-0.0533906055818233,-0.0308184408320373,-0.00876003298857159,-0.00401661180489581,
0.),.UNSPECIFIED.);
#3922=B_SPLINE_CURVE_WITH_KNOTS('',3,(#42843,#42844,#42845,#42846,#42847,
#42848,#42849,#42850,#42851,#42852,#42853,#42854,#42855,#42856,#42857,#42858,
#42859,#42860,#42861,#42862,#42863,#42864,#42865,#42866,#42867,#42868,#42869,
#42870,#42871,#42872,#42873,#42874,#42875,#42876,#42877,#42878,#42879,#42880,
#42881,#42882,#42883,#42884,#42885,#42886,#42887,#42888,#42889,#42890,#42891,
#42892,#42893,#42894,#42895,#42896,#42897,#42898,#42899,#42900,#42901,#42902,
#42903,#42904,#42905,#42906,#42907,#42908,#42909,#42910,#42911,#42912,#42913,
#42914,#42915,#42916,#42917,#42918,#42919,#42920,#42921,#42922,#42923,#42924,
#42925,#42926,#42927),.UNSPECIFIED.,.F.,.F.,(4,3,3,3,3,3,3,3,3,3,3,3,3,
3,3,3,3,3,3,3,3,3,3,3,3,3,3,3,4),(-0.376940817211567,-0.354634182893048,
-0.332911763640281,-0.328063423788498,-0.30581480563381,-0.290194808538448,
-0.284256159068131,-0.2786008798737,-0.256917704060186,-0.235700189361117,
-0.214948003718043,-0.208204616625186,-0.204400619173506,-0.183824594259318,
-0.180854828870914,-0.15987208070365,-0.1402968717445,-0.135976593196673,
-0.132599405819727,-0.112140134034935,-0.091775337431271,-0.0718467835475,
-0.0676478648567277,-0.0636677277271933,-0.0441097307912725,-0.0249236995322422,
-0.00636086856298682,-0.0032704090304496,0.),.UNSPECIFIED.);
#3923=B_SPLINE_CURVE_WITH_KNOTS('',3,(#42929,#42930,#42931,#42932,#42933,
#42934,#42935,#42936,#42937,#42938,#42939),.UNSPECIFIED.,.F.,.F.,(4,1,1,
1,1,1,1,1,4),(15.7079632679489,15.8518654961884,16.8494368691713,17.8470082421543,
18.8445796151372,19.8421509881201,20.8397223611031,21.837293734086,21.9911485751285),
 .UNSPECIFIED.);
#3924=B_SPLINE_CURVE_WITH_KNOTS('',3,(#42940,#42941,#42942,#42943,#42944,
#42945,#42946,#42947,#42948,#42949),.UNSPECIFIED.,.F.,.F.,(4,1,1,1,1,1,
1,4),(15.7079632679489,16.3932837587428,17.3908551317257,18.3884265047087,
19.3859978776916,20.3835692506745,21.3811406236575,21.9911485751285),
 .UNSPECIFIED.);
#3925=B_SPLINE_CURVE_WITH_KNOTS('',3,(#43294,#43295,#43296,#43297,#43298,
#43299,#43300,#43301,#43302,#43303,#43304,#43305,#43306,#43307,#43308,#43309,
#43310,#43311,#43312,#43313,#43314,#43315,#43316,#43317,#43318,#43319,#43320,
#43321,#43322,#43323,#43324,#43325,#43326,#43327,#43328,#43329,#43330,#43331,
#43332,#43333,#43334,#43335,#43336,#43337,#43338,#43339,#43340,#43341,#43342,
#43343,#43344,#43345,#43346,#43347,#43348,#43349,#43350,#43351,#43352,#43353,
#43354,#43355,#43356,#43357,#43358,#43359,#43360,#43361,#43362,#43363,#43364,
#43365,#43366,#43367,#43368,#43369,#43370,#43371,#43372,#43373,#43374,#43375),
 .UNSPECIFIED.,.F.,.F.,(4,3,3,3,3,3,3,3,3,3,3,3,3,3,3,3,3,3,3,3,3,3,3,3,
3,3,3,4),(0.,0.0185976526101627,0.038423603067645,0.055771309717942,0.0644755844464768,
0.0684516288828876,0.0885059681204507,0.108915976701888,0.125988296593921,
0.133854408336107,0.137287722941701,0.158362598119627,0.177205256270021,
0.197733028930412,0.205653066408773,0.209127486181638,0.230133047564113,
0.251625243348866,0.268069199560575,0.278304581270923,0.284046628826471,
0.306315638089425,0.322971918687632,0.32816781331511,0.333183176093119,
0.355704559014731,0.372940760482252,0.376940817211595),.UNSPECIFIED.);
#3926=B_SPLINE_CURVE_WITH_KNOTS('',3,(#43376,#43377,#43378,#43379,#43380,
#43381,#43382,#43383,#43384,#43385,#43386,#43387,#43388,#43389,#43390,#43391,
#43392,#43393,#43394,#43395,#43396,#43397,#43398,#43399,#43400),
 .UNSPECIFIED.,.F.,.F.,(4,3,3,3,3,3,3,3,4),(-10.1295685708718,-9.97571372982933,
-8.9781423568464,-7.98057098386346,-6.98299961088053,-5.9854282378976,-4.98785686491467,
-3.99028549193173,-3.84638326369224),.UNSPECIFIED.);
#3927=B_SPLINE_CURVE_WITH_KNOTS('',3,(#43745,#43746,#43747,#43748,#43749,
#43750,#43751,#43752,#43753,#43754,#43755,#43756,#43757,#43758,#43759,#43760,
#43761,#43762,#43763,#43764,#43765,#43766),.UNSPECIFIED.,.F.,.F.,(4,3,3,
3,3,3,3,4),(7.59300756235153,7.98057098386347,8.9781423568464,9.97571372982933,
10.9732851028123,11.9708564757952,12.9684278487781,13.8761928695311),
 .UNSPECIFIED.);
#3928=B_SPLINE_CURVE_WITH_KNOTS('',3,(#43767,#43768,#43769,#43770,#43771,
#43772,#43773,#43774,#43775,#43776,#43777,#43778,#43779,#43780,#43781,#43782,
#43783,#43784,#43785,#43786,#43787,#43788,#43789,#43790,#43791,#43792,#43793,
#43794,#43795,#43796,#43797,#43798,#43799,#43800,#43801,#43802,#43803,#43804,
#43805,#43806,#43807,#43808,#43809,#43810,#43811,#43812,#43813,#43814,#43815,
#43816,#43817,#43818,#43819,#43820,#43821,#43822,#43823,#43824,#43825,#43826,
#43827,#43828,#43829,#43830,#43831,#43832,#43833,#43834,#43835,#43836,#43837,
#43838,#43839,#43840,#43841,#43842,#43843,#43844,#43845,#43846,#43847,#43848,
#43849,#43850,#43851),.UNSPECIFIED.,.F.,.F.,(4,3,3,3,3,3,3,3,3,3,3,3,3,
3,3,3,3,3,3,3,3,3,3,3,3,3,3,3,4),(0.,0.021966247856033,0.0445437519030381,
0.063621232193463,0.0720968536658468,0.0767538544094051,0.0810484322397289,
0.102995052369737,0.124771335603005,0.142869400258863,0.150423566582265,
0.153920154508921,0.157567047703951,0.178337711800534,0.197163594226437,
0.219435545910494,0.224339035444409,0.229398553891155,0.250063614195313,
0.270724500170669,0.285678958579524,0.296896594129061,0.300624121181404,
0.320396425757778,0.334309228900126,0.338775005400257,0.357799813884156,
0.37533920769889,0.378621596831449),.UNSPECIFIED.);
#3929=B_SPLINE_CURVE_WITH_KNOTS('',3,(#43854,#43855,#43856,#43857,#43858,
#43859,#43860,#43861,#43862,#43863,#43864,#43865,#43866,#43867,#43868,#43869,
#43870,#43871,#43872,#43873,#43874,#43875,#43876,#43877,#43878,#43879,#43880,
#43881,#43882,#43883,#43884,#43885,#43886,#43887,#43888,#43889,#43890,#43891,
#43892,#43893,#43894,#43895,#43896,#43897,#43898,#43899,#43900,#43901,#43902,
#43903,#43904,#43905,#43906,#43907,#43908,#43909,#43910,#43911,#43912,#43913,
#43914,#43915,#43916,#43917,#43918,#43919,#43920,#43921,#43922,#43923,#43924,
#43925,#43926,#43927,#43928,#43929,#43930,#43931,#43932,#43933,#43934,#43935,
#43936,#43937,#43938,#43939,#43940,#43941),.UNSPECIFIED.,.F.,.F.,(4,3,3,
3,3,3,3,3,3,3,3,3,3,3,3,3,3,3,3,3,3,3,3,3,3,3,3,3,3,4),(-0.378621596831424,
-0.359797363524264,-0.34785661137902,-0.339691444332018,-0.335368277601998,
-0.315496143936723,-0.301162812904392,-0.297226950674736,-0.293222691552817,
-0.272820243231133,-0.252122598450948,-0.23929932275773,-0.228794025841657,
-0.224501456899104,-0.203196880753619,-0.200829495678077,-0.180342164145496,
-0.158301470102921,-0.154267209386573,-0.150798043919975,-0.129414602637409,
-0.107580315073585,-0.085613710021042,-0.0801848969680599,-0.075938230951137,
-0.0533905919055191,-0.0308184274067072,-0.00876001819588422,-0.00401661180489569,
0.),.UNSPECIFIED.);
#3930=B_SPLINE_CURVE_WITH_KNOTS('',3,(#43942,#43943,#43944,#43945,#43946,
#43947,#43948,#43949,#43950,#43951,#43952,#43953,#43954,#43955,#43956,#43957,
#43958,#43959,#43960,#43961,#43962,#43963,#43964,#43965,#43966,#43967,#43968,
#43969,#43970,#43971,#43972,#43973,#43974,#43975,#43976,#43977,#43978,#43979,
#43980,#43981,#43982,#43983,#43984,#43985,#43986,#43987,#43988,#43989,#43990,
#43991,#43992,#43993,#43994,#43995,#43996,#43997,#43998,#43999,#44000,#44001,
#44002,#44003,#44004,#44005,#44006,#44007,#44008,#44009,#44010,#44011,#44012,
#44013,#44014,#44015,#44016,#44017,#44018,#44019,#44020,#44021,#44022,#44023,
#44024,#44025,#44026),.UNSPECIFIED.,.F.,.F.,(4,3,3,3,3,3,3,3,3,3,3,3,3,
3,3,3,3,3,3,3,3,3,3,3,3,3,3,3,4),(-0.376940817211591,-0.354634181778186,
-0.332911762664777,-0.328063422667595,-0.305814804529428,-0.290194807572113,
-0.284256156918697,-0.278600880016598,-0.256917704389392,-0.235700190166293,
-0.214948004837694,-0.208204615907423,-0.204400619237651,-0.183824594781149,
-0.180854828870913,-0.15987208070781,-0.14029687174814,-0.135976593989551,
-0.13259940641991,-0.112140134563278,-0.0917753380936809,-0.0718467848234281,
-0.0676478683961129,-0.0636677288398687,-0.0441097322383243,-0.0249237017087955,
-0.0063608719337389,-0.00327040903045198,0.),.UNSPECIFIED.);
#3931=B_SPLINE_CURVE_WITH_KNOTS('',3,(#44028,#44029,#44030,#44031,#44032,
#44033,#44034,#44035,#44036,#44037,#44038),.UNSPECIFIED.,.F.,.F.,(4,1,1,
1,1,1,1,1,4),(15.7079632679489,15.8518654961884,16.8494368691713,17.8470082421543,
18.8445796151372,19.8421509881201,20.8397223611031,21.837293734086,21.9911485751285),
 .UNSPECIFIED.);
#3932=B_SPLINE_CURVE_WITH_KNOTS('',3,(#44039,#44040,#44041,#44042,#44043,
#44044,#44045,#44046,#44047,#44048),.UNSPECIFIED.,.F.,.F.,(4,1,1,1,1,1,
1,4),(15.7079632679489,16.3932837587428,17.3908551317257,18.3884265047087,
19.3859978776916,20.3835692506745,21.3811406236575,21.9911485751285),
 .UNSPECIFIED.);
#3933=B_SPLINE_CURVE_WITH_KNOTS('',3,(#44393,#44394,#44395,#44396,#44397,
#44398,#44399,#44400,#44401,#44402,#44403,#44404,#44405,#44406,#44407,#44408,
#44409,#44410,#44411,#44412,#44413,#44414,#44415,#44416,#44417,#44418,#44419,
#44420,#44421,#44422,#44423,#44424,#44425,#44426,#44427,#44428,#44429,#44430,
#44431,#44432,#44433,#44434,#44435,#44436,#44437,#44438,#44439,#44440,#44441,
#44442,#44443,#44444,#44445,#44446,#44447,#44448,#44449,#44450,#44451,#44452,
#44453,#44454,#44455,#44456,#44457,#44458,#44459,#44460,#44461,#44462,#44463,
#44464,#44465,#44466,#44467,#44468,#44469,#44470,#44471,#44472,#44473,#44474),
 .UNSPECIFIED.,.F.,.F.,(4,3,3,3,3,3,3,3,3,3,3,3,3,3,3,3,3,3,3,3,3,3,3,3,
3,3,3,4),(0.,0.0185976544398407,0.0384236046686153,0.0557713111187932,0.0644755868719157,
0.0684516295230809,0.0885059700661988,0.108915979209154,0.125988298474375,
0.133854411297929,0.137287724526441,0.158362599531486,0.177205256270038,
0.197733028011421,0.205653065916,0.20912748582868,0.230133046130665,0.251625241346934,
0.268069200030553,0.278304582359924,0.28404662854489,0.306315637741208,
0.322971918426484,0.328167812746273,0.333183175811798,0.355704558740549,
0.372940760482311,0.376940817211655),.UNSPECIFIED.);
#3934=B_SPLINE_CURVE_WITH_KNOTS('',3,(#44475,#44476,#44477,#44478,#44479,
#44480,#44481,#44482,#44483,#44484,#44485,#44486,#44487,#44488,#44489,#44490,
#44491,#44492,#44493,#44494,#44495,#44496,#44497,#44498,#44499),
 .UNSPECIFIED.,.F.,.F.,(4,3,3,3,3,3,3,3,4),(-10.1295685708718,-9.97571372982933,
-8.9781423568464,-7.98057098386346,-6.98299961088053,-5.9854282378976,-4.98785686491467,
-3.99028549193173,-3.84638326369223),.UNSPECIFIED.);
#3935=B_SPLINE_CURVE_WITH_KNOTS('',3,(#44844,#44845,#44846,#44847,#44848,
#44849,#44850,#44851,#44852,#44853,#44854,#44855,#44856,#44857,#44858,#44859,
#44860,#44861,#44862,#44863,#44864,#44865),.UNSPECIFIED.,.F.,.F.,(4,3,3,
3,3,3,3,4),(7.59300756235153,7.98057098386346,8.97814235684639,9.97571372982932,
10.9732851028123,11.9708564757952,12.9684278487781,13.8761928695311),
 .UNSPECIFIED.);
#3936=B_SPLINE_CURVE_WITH_KNOTS('',3,(#44866,#44867,#44868,#44869,#44870,
#44871,#44872,#44873,#44874,#44875,#44876,#44877,#44878,#44879,#44880,#44881,
#44882,#44883,#44884,#44885,#44886,#44887,#44888,#44889,#44890,#44891,#44892,
#44893,#44894,#44895,#44896,#44897,#44898,#44899,#44900,#44901,#44902,#44903,
#44904,#44905,#44906,#44907,#44908,#44909,#44910,#44911,#44912,#44913,#44914,
#44915,#44916,#44917,#44918,#44919,#44920,#44921,#44922,#44923,#44924,#44925,
#44926,#44927,#44928,#44929,#44930,#44931,#44932,#44933,#44934,#44935,#44936,
#44937,#44938,#44939,#44940,#44941,#44942,#44943,#44944,#44945,#44946,#44947,
#44948,#44949,#44950),.UNSPECIFIED.,.F.,.F.,(4,3,3,3,3,3,3,3,3,3,3,3,3,
3,3,3,3,3,3,3,3,3,3,3,3,3,3,3,4),(0.,0.0219662374680391,0.0445437405167158,
0.0636212222304308,0.0720968506878779,0.0767538481096382,0.081048430551138,
0.102995050890364,0.124771337264665,0.142869401505108,0.150423566045082,
0.153920151218966,0.157567046662202,0.178337713885749,0.197163594226436,
0.219435545910489,0.224339036280642,0.229398553932292,0.250063613827866,
0.270724500178625,0.285678968070037,0.296896610190914,0.30062412578472,
0.320396434080142,0.334309242699549,0.338775018538281,0.357799832912367,
0.375339207698863,0.378621596831421),.UNSPECIFIED.);
#3937=B_SPLINE_CURVE_WITH_KNOTS('',3,(#44958,#44959,#44960,#44961,#44962,
#44963,#44964,#44965,#44966,#44967,#44968,#44969,#44970,#44971,#44972,#44973,
#44974,#44975,#44976,#44977,#44978,#44979,#44980,#44981,#44982,#44983,#44984,
#44985,#44986,#44987,#44988,#44989,#44990,#44991,#44992,#44993,#44994,#44995,
#44996,#44997,#44998,#44999,#45000,#45001,#45002,#45003,#45004,#45005,#45006,
#45007,#45008,#45009,#45010,#45011,#45012,#45013,#45014,#45015,#45016,#45017,
#45018,#45019,#45020,#45021,#45022,#45023,#45024,#45025,#45026,#45027,#45028,
#45029,#45030,#45031,#45032,#45033,#45034,#45035,#45036,#45037,#45038,#45039,
#45040,#45041,#45042,#45043,#45044,#45045),.UNSPECIFIED.,.F.,.F.,(4,3,3,
3,3,3,3,3,3,3,3,3,3,3,3,3,3,3,3,3,3,3,3,3,3,3,3,3,3,4),(-0.378621596831482,
-0.359797939671017,-0.347858077335423,-0.339704706610793,-0.33537529913106,
-0.315503714728244,-0.301169437346976,-0.297242106085975,-0.293224790533046,
-0.27282275550358,-0.252125053752483,-0.239301164233888,-0.22879674266649,
-0.224502344128615,-0.203197744285114,-0.200829495678103,-0.180341772881595,
-0.158301127747009,-0.154264834760236,-0.150797561842571,-0.12941380077193,
-0.107579371162969,-0.0856127635779262,-0.0801832505987719,-0.0759376400558302,
-0.0533899343754914,-0.0308177819508918,-0.008759308379451,-0.00401661180490152,
0.),.UNSPECIFIED.);
#3938=B_SPLINE_CURVE_WITH_KNOTS('',3,(#45046,#45047,#45048,#45049,#45050,
#45051,#45052,#45053,#45054,#45055,#45056,#45057,#45058,#45059,#45060,#45061,
#45062,#45063,#45064,#45065,#45066,#45067,#45068,#45069,#45070,#45071,#45072,
#45073,#45074,#45075,#45076,#45077,#45078,#45079,#45080,#45081,#45082,#45083,
#45084,#45085,#45086,#45087,#45088,#45089,#45090,#45091,#45092,#45093,#45094,
#45095,#45096,#45097,#45098,#45099,#45100,#45101,#45102,#45103,#45104,#45105,
#45106,#45107,#45108,#45109,#45110,#45111,#45112,#45113,#45114,#45115,#45116,
#45117,#45118,#45119,#45120,#45121,#45122,#45123,#45124,#45125,#45126,#45127,
#45128,#45129,#45130),.UNSPECIFIED.,.F.,.F.,(4,3,3,3,3,3,3,3,3,3,3,3,3,
3,3,3,3,3,3,3,3,3,3,3,3,3,3,3,4),(-0.376940817211645,-0.354634583492538,
-0.332912114164838,-0.328063830062097,-0.305815206809885,-0.290195159567516,
-0.284256938553548,-0.278600828101315,-0.25691758637424,-0.23569990131557,
-0.214947604399832,-0.208204874074823,-0.204400580937649,-0.183824390832658,
-0.180854828870938,-0.159872079452346,-0.14029687064961,-0.135976312797154,
-0.132599190254655,-0.112139944657484,-0.0917751008216024,-0.0718463313280328,
-0.067646608948578,-0.0636673307706993,-0.044109215855187,-0.0249229264978586,
-0.00635967183413765,-0.0032704090304543,0.),.UNSPECIFIED.);
#3939=B_SPLINE_CURVE_WITH_KNOTS('',3,(#45132,#45133,#45134,#45135,#45136,
#45137,#45138,#45139,#45140,#45141,#45142),.UNSPECIFIED.,.F.,.F.,(4,1,1,
1,1,1,1,1,4),(15.7079632679489,15.8518654961883,16.8494368691713,17.8470082421542,
18.8445796151371,19.8421509881201,20.839722361103,21.8372937340859,21.9911485751285),
 .UNSPECIFIED.);
#3940=B_SPLINE_CURVE_WITH_KNOTS('',3,(#45143,#45144,#45145,#45146,#45147,
#45148,#45149,#45150,#45151,#45152),.UNSPECIFIED.,.F.,.F.,(4,1,1,1,1,1,
1,4),(15.7079632679489,16.3932837587427,17.3908551317257,18.3884265047086,
19.3859978776915,20.3835692506745,21.3811406236574,21.9911485751285),
 .UNSPECIFIED.);
#3941=B_SPLINE_CURVE_WITH_KNOTS('',3,(#45497,#45498,#45499,#45500,#45501,
#45502,#45503,#45504,#45505,#45506,#45507,#45508,#45509,#45510,#45511,#45512,
#45513,#45514,#45515,#45516,#45517,#45518,#45519,#45520,#45521,#45522,#45523,
#45524,#45525,#45526,#45527,#45528,#45529,#45530,#45531,#45532,#45533,#45534,
#45535,#45536,#45537,#45538,#45539,#45540,#45541,#45542,#45543,#45544,#45545,
#45546,#45547,#45548,#45549,#45550,#45551,#45552,#45553,#45554,#45555,#45556,
#45557,#45558,#45559,#45560,#45561,#45562,#45563,#45564,#45565,#45566,#45567,
#45568,#45569,#45570,#45571,#45572,#45573,#45574,#45575,#45576,#45577,#45578),
 .UNSPECIFIED.,.F.,.F.,(4,3,3,3,3,3,3,3,3,3,3,3,3,3,3,3,3,3,3,3,3,3,3,3,
3,3,3,4),(0.,0.0185969955131322,0.0384230281077451,0.0557708066280314,0.0644747133135174,
0.0684514005852745,0.0885052705827287,0.108915076403666,0.125987621370258,
0.133853344527305,0.137287156143503,0.158362091944416,0.177205256270036,
0.19773335754956,0.205653241463164,0.20912761153043,0.230133559208142,0.251625958497864,
0.268069030050869,0.27830418763456,0.284046730395759,0.306315763835364,
0.322972012997098,0.328168014027546,0.333183276135758,0.355704655810399,
0.372940760482301,0.376940817211646),.UNSPECIFIED.);
#3942=B_SPLINE_CURVE_WITH_KNOTS('',3,(#45579,#45580,#45581,#45582,#45583,
#45584,#45585,#45586,#45587,#45588,#45589,#45590,#45591,#45592,#45593,#45594,
#45595,#45596,#45597,#45598,#45599,#45600,#45601,#45602,#45603),
 .UNSPECIFIED.,.F.,.F.,(4,3,3,3,3,3,3,3,4),(-10.1295685708719,-9.97571372982932,
-8.97814235684639,-7.98057098386345,-6.98299961088052,-5.98542823789759,
-4.98785686491465,-3.99028549193172,-3.8463832636923),.UNSPECIFIED.);
#3943=B_SPLINE_CURVE_WITH_KNOTS('',3,(#45948,#45949,#45950,#45951,#45952,
#45953,#45954,#45955,#45956,#45957,#45958,#45959,#45960,#45961,#45962,#45963,
#45964,#45965,#45966,#45967,#45968,#45969),.UNSPECIFIED.,.F.,.F.,(4,3,3,
3,3,3,3,4),(7.59300756235157,7.98057098386346,8.97814235684639,9.97571372982932,
10.9732851028123,11.9708564757952,12.9684278487781,13.8761928695311),
 .UNSPECIFIED.);
#3944=B_SPLINE_CURVE_WITH_KNOTS('',3,(#45970,#45971,#45972,#45973,#45974,
#45975,#45976,#45977,#45978,#45979,#45980,#45981,#45982,#45983,#45984,#45985,
#45986,#45987,#45988,#45989,#45990,#45991,#45992,#45993,#45994,#45995,#45996,
#45997,#45998,#45999,#46000,#46001,#46002,#46003,#46004,#46005,#46006,#46007,
#46008,#46009,#46010,#46011,#46012,#46013,#46014,#46015,#46016,#46017,#46018,
#46019,#46020,#46021,#46022,#46023,#46024,#46025,#46026,#46027,#46028,#46029,
#46030,#46031,#46032,#46033,#46034,#46035,#46036,#46037,#46038,#46039,#46040,
#46041,#46042,#46043,#46044,#46045,#46046,#46047,#46048,#46049,#46050,#46051,
#46052,#46053,#46054),.UNSPECIFIED.,.F.,.F.,(4,3,3,3,3,3,3,3,3,3,3,3,3,
3,3,3,3,3,3,3,3,3,3,3,3,3,3,3,4),(0.,0.0219657370419595,0.0445431913692733,
0.0636207417264163,0.072096707092799,0.0767535441972317,0.0810483489290845,
0.102994978685481,0.124771415616641,0.142869460269085,0.150423538874486,
0.153919987844215,0.157566995524998,0.178337812740353,0.197163594226417,
0.219435545910471,0.224339075599447,0.229398555825431,0.250063595737514,
0.270724499006124,0.285679418592838,0.296897371656218,0.300624344614772,
0.320396829483506,0.334309899382154,0.338775644838224,0.357800739663862,
0.37533920769885,0.37862159683141),.UNSPECIFIED.);
#3945=B_SPLINE_CURVE_WITH_KNOTS('',3,(#46057,#46058,#46059,#46060,#46061,
#46062,#46063,#46064,#46065,#46066,#46067,#46068,#46069,#46070,#46071,#46072,
#46073,#46074,#46075,#46076,#46077,#46078,#46079,#46080,#46081,#46082,#46083,
#46084,#46085,#46086,#46087,#46088,#46089,#46090,#46091,#46092,#46093,#46094,
#46095,#46096,#46097,#46098,#46099,#46100,#46101,#46102,#46103,#46104,#46105,
#46106,#46107,#46108,#46109,#46110,#46111,#46112,#46113,#46114,#46115,#46116,
#46117,#46118,#46119,#46120,#46121,#46122,#46123,#46124,#46125,#46126,#46127,
#46128,#46129,#46130,#46131,#46132,#46133,#46134,#46135,#46136,#46137,#46138,
#46139,#46140,#46141,#46142,#46143,#46144),.UNSPECIFIED.,.F.,.F.,(4,3,3,
3,3,3,3,3,3,3,3,3,3,3,3,3,3,3,3,3,3,3,3,3,3,3,3,3,3,4),(-0.378621596831388,
-0.359797936891699,-0.347858070259707,-0.339704642744632,-0.335375265981626,
-0.315503678944408,-0.301169406036115,-0.297242034708142,-0.293224780830876,
-0.272822743809878,-0.252125042326135,-0.239301155664117,-0.228796730020428,
-0.224502340033354,-0.203197740293726,-0.200829495678066,-0.180341774760636,
-0.158301129391169,-0.15426484634161,-0.150797564195065,-0.129413804659794,
-0.107579375734867,-0.0856127681572894,-0.0801832585579418,-0.075937642934926,
-0.0533899375766034,-0.030817785094969,-0.00875931182590463,-0.0040166118048955,
0.),.UNSPECIFIED.);
#3946=B_SPLINE_CURVE_WITH_KNOTS('',3,(#46145,#46146,#46147,#46148,#46149,
#46150,#46151,#46152,#46153,#46154,#46155,#46156,#46157,#46158,#46159,#46160,
#46161,#46162,#46163,#46164,#46165,#46166,#46167,#46168,#46169,#46170,#46171,
#46172,#46173,#46174,#46175,#46176,#46177,#46178,#46179,#46180,#46181,#46182,
#46183,#46184,#46185,#46186,#46187,#46188,#46189,#46190,#46191,#46192,#46193,
#46194,#46195,#46196,#46197,#46198,#46199,#46200,#46201,#46202,#46203,#46204,
#46205,#46206,#46207,#46208,#46209,#46210,#46211,#46212,#46213,#46214,#46215,
#46216,#46217,#46218,#46219,#46220,#46221,#46222,#46223,#46224,#46225,#46226,
#46227,#46228,#46229),.UNSPECIFIED.,.F.,.F.,(4,3,3,3,3,3,3,3,3,3,3,3,3,
3,3,3,3,3,3,3,3,3,3,3,3,3,3,3,4),(-0.376940817211649,-0.354634582184037,
-0.332912113019899,-0.328063828659571,-0.305815205420689,-0.29019515835197,
-0.284256935866937,-0.27860082826073,-0.256917586745712,-0.235699902239903,
-0.214947605686915,-0.208204873234999,-0.2044005811046,-0.183824391534274,
-0.180854828870936,-0.159872079459671,-0.140296870656019,-0.135976313715434,
-0.132599191025858,-0.112139945341909,-0.0917751016524139,-0.0718463328503837,
-0.0676466131531402,-0.063667332080833,-0.0441092175415555,-0.0249229290113584,
-0.00635967571411871,-0.003270409030452,0.),.UNSPECIFIED.);
#3947=B_SPLINE_CURVE_WITH_KNOTS('',3,(#46231,#46232,#46233,#46234,#46235,
#46236,#46237,#46238,#46239,#46240,#46241),.UNSPECIFIED.,.F.,.F.,(4,1,1,
1,1,1,1,1,4),(15.7079632679489,15.8518654961883,16.8494368691713,17.8470082421542,
18.8445796151371,19.8421509881201,20.839722361103,21.8372937340859,21.9911485751285),
 .UNSPECIFIED.);
#3948=B_SPLINE_CURVE_WITH_KNOTS('',3,(#46242,#46243,#46244,#46245,#46246,
#46247,#46248,#46249,#46250,#46251),.UNSPECIFIED.,.F.,.F.,(4,1,1,1,1,1,
1,4),(15.7079632679489,16.3932837587427,17.3908551317257,18.3884265047086,
19.3859978776915,20.3835692506745,21.3811406236574,21.9911485751285),
 .UNSPECIFIED.);
#3949=B_SPLINE_CURVE_WITH_KNOTS('',3,(#46596,#46597,#46598,#46599,#46600,
#46601,#46602,#46603,#46604,#46605,#46606,#46607,#46608,#46609,#46610,#46611,
#46612,#46613,#46614,#46615,#46616,#46617,#46618,#46619,#46620,#46621,#46622,
#46623,#46624,#46625,#46626,#46627,#46628,#46629,#46630,#46631,#46632,#46633,
#46634,#46635,#46636,#46637,#46638,#46639,#46640,#46641,#46642,#46643,#46644,
#46645,#46646,#46647,#46648,#46649,#46650,#46651,#46652,#46653,#46654,#46655,
#46656,#46657,#46658,#46659,#46660,#46661,#46662,#46663,#46664,#46665,#46666,
#46667,#46668,#46669,#46670,#46671,#46672,#46673,#46674,#46675,#46676,#46677),
 .UNSPECIFIED.,.F.,.F.,(4,3,3,3,3,3,3,3,3,3,3,3,3,3,3,3,3,3,3,3,3,3,3,3,
3,3,3,4),(0.,0.0185969976548629,0.0384230299817592,0.0557708082677935,0.0644747161532653,
0.0684514013184625,0.0885052728468933,0.108915079332587,0.125987623566949,
0.133853347989331,0.137287157984682,0.158362093592479,0.177205256270033,
0.197733356483111,0.205653240898836,0.209127611126219,0.230133557550482,
0.251625956178859,0.26806903060611,0.278304188926851,0.28404673006319,0.30631576342394,
0.322972012688533,0.328168013360337,0.33318327580766,0.35570465549395,0.372940760482311,
0.376940817211655),.UNSPECIFIED.);
#3950=B_SPLINE_CURVE_WITH_KNOTS('',3,(#46678,#46679,#46680,#46681,#46682,
#46683,#46684,#46685,#46686,#46687,#46688,#46689,#46690,#46691,#46692,#46693,
#46694,#46695,#46696,#46697,#46698,#46699,#46700,#46701,#46702),
 .UNSPECIFIED.,.F.,.F.,(4,3,3,3,3,3,3,3,4),(-10.1295685708719,-9.97571372982933,
-8.97814235684639,-7.98057098386346,-6.98299961088053,-5.9854282378976,
-4.98785686491466,-3.99028549193173,-3.8463832636923),.UNSPECIFIED.);
#3951=B_SPLINE_CURVE_WITH_KNOTS('',3,(#47047,#47048,#47049,#47050,#47051,
#47052,#47053,#47054,#47055,#47056,#47057,#47058,#47059,#47060,#47061,#47062,
#47063,#47064,#47065,#47066,#47067,#47068),.UNSPECIFIED.,.F.,.F.,(4,3,3,
3,3,3,3,4),(7.59300756235157,7.98057098386346,8.97814235684639,9.97571372982933,
10.9732851028123,11.9708564757952,12.9684278487781,13.8761928695312),
 .UNSPECIFIED.);
#3952=B_SPLINE_CURVE_WITH_KNOTS('',3,(#47069,#47070,#47071,#47072,#47073,
#47074,#47075,#47076,#47077,#47078,#47079,#47080,#47081,#47082,#47083,#47084,
#47085,#47086,#47087,#47088,#47089,#47090,#47091,#47092,#47093,#47094,#47095,
#47096,#47097,#47098,#47099,#47100,#47101,#47102,#47103,#47104,#47105,#47106,
#47107,#47108,#47109,#47110,#47111,#47112,#47113,#47114,#47115,#47116,#47117,
#47118,#47119,#47120,#47121,#47122,#47123,#47124,#47125,#47126,#47127,#47128,
#47129,#47130,#47131,#47132,#47133,#47134,#47135,#47136,#47137,#47138,#47139,
#47140,#47141,#47142,#47143,#47144,#47145,#47146,#47147,#47148,#47149,#47150,
#47151,#47152,#47153),.UNSPECIFIED.,.F.,.F.,(4,3,3,3,3,3,3,3,3,3,3,3,3,
3,3,3,3,3,3,3,3,3,3,3,3,3,3,3,4),(0.,0.021965739453955,0.0445431940190658,
0.0636207440449849,0.0720967077854655,0.0767535456635768,0.0810483493206851,
0.102994979034739,0.124771415243574,0.142869459989285,0.150423539009583,
0.1539199886521,0.157566995775498,0.178337812271127,0.197163594226419,0.219435545910471,
0.2243390754146,0.229398555820982,0.250063595830876,0.270724499023616,0.285679416466335,
0.296897368065093,0.300624343578509,0.320396827608135,0.334309896261688,
0.338775641864317,0.357800735353592,0.37533920769884,0.378621596831401),
 .UNSPECIFIED.);
#3953=B_SPLINE_CURVE_WITH_KNOTS('',3,(#47156,#47157,#47158,#47159,#47160,
#47161,#47162,#47163,#47164,#47165,#47166,#47167,#47168,#47169,#47170,#47171,
#47172,#47173,#47174,#47175,#47176,#47177,#47178,#47179,#47180,#47181,#47182,
#47183,#47184,#47185,#47186,#47187,#47188,#47189,#47190,#47191,#47192,#47193,
#47194,#47195,#47196,#47197,#47198,#47199,#47200,#47201,#47202,#47203,#47204,
#47205,#47206,#47207,#47208,#47209,#47210,#47211,#47212,#47213,#47214,#47215,
#47216,#47217,#47218,#47219,#47220,#47221,#47222,#47223,#47224,#47225,#47226,
#47227,#47228,#47229,#47230,#47231,#47232,#47233,#47234,#47235,#47236,#47237,
#47238,#47239,#47240,#47241,#47242,#47243),.UNSPECIFIED.,.F.,.F.,(4,3,3,
3,3,3,3,3,3,3,3,3,3,3,3,3,3,3,3,3,3,3,3,3,3,3,3,3,3,4),(-0.378621596831452,
-0.359796964371007,-0.347855595893935,-0.3396822224573,-0.335363223682036,
-0.315490706099021,-0.301158054796405,-0.297216022503385,-0.293221129613966,
-0.272818393289542,-0.252120789784161,-0.239297966257643,-0.22879202499115,
-0.224500801126252,-0.203196242755057,-0.200829495678088,-0.18034243723251,
-0.158301709054058,-0.154268865136119,-0.150798379245078,-0.129415160921567,
-0.10758097209064,-0.0856143687498464,-0.0801860432915195,-0.0759386414271447,
-0.0533910485483734,-0.0308188758174934,-0.00876051290910059,-0.0040166118048957,
0.),.UNSPECIFIED.);
#3954=B_SPLINE_CURVE_WITH_KNOTS('',3,(#47244,#47245,#47246,#47247,#47248,
#47249,#47250,#47251,#47252,#47253,#47254,#47255,#47256,#47257,#47258,#47259,
#47260,#47261,#47262,#47263,#47264,#47265,#47266,#47267,#47268,#47269,#47270,
#47271,#47272,#47273,#47274,#47275,#47276,#47277,#47278,#47279,#47280,#47281,
#47282,#47283,#47284,#47285,#47286,#47287,#47288,#47289,#47290,#47291,#47292,
#47293,#47294,#47295,#47296,#47297,#47298,#47299,#47300,#47301,#47302,#47303,
#47304,#47305,#47306,#47307,#47308,#47309,#47310,#47311,#47312,#47313,#47314,
#47315,#47316,#47317,#47318,#47319,#47320,#47321,#47322,#47323,#47324,#47325,
#47326,#47327,#47328),.UNSPECIFIED.,.F.,.F.,(4,3,3,3,3,3,3,3,3,3,3,3,3,
3,3,3,3,3,3,3,3,3,3,3,3,3,3,3,4),(-0.376940817211631,-0.35463396460261,
-0.332911572636152,-0.328063202289398,-0.305814587568867,-0.290194617731627,
-0.28425573539935,-0.278600908076312,-0.2569177688984,-0.235700347785391,
-0.214948223363317,-0.208204476166349,-0.20440064004034,-0.183824705876023,
-0.180854828870946,-0.159872081610939,-0.140296872538378,-0.13597675000539,
-0.132599526202686,-0.112140240570565,-0.0917754711453113,-0.0718470375330435,
-0.0676485678532571,-0.0636679489962621,-0.0441100183864258,-0.0249241308188154,
-0.0063615348116712,-0.00327040903045197,0.),.UNSPECIFIED.);
#3955=B_SPLINE_CURVE_WITH_KNOTS('',3,(#47330,#47331,#47332,#47333,#47334,
#47335,#47336,#47337,#47338,#47339,#47340),.UNSPECIFIED.,.F.,.F.,(4,1,1,
1,1,1,1,1,4),(15.7079632679489,15.8518654961884,16.8494368691713,17.8470082421542,
18.8445796151372,19.8421509881201,20.839722361103,21.837293734086,21.9911485751285),
 .UNSPECIFIED.);
#3956=B_SPLINE_CURVE_WITH_KNOTS('',3,(#47341,#47342,#47343,#47344,#47345,
#47346,#47347,#47348,#47349,#47350),.UNSPECIFIED.,.F.,.F.,(4,1,1,1,1,1,
1,4),(15.7079632679489,16.3932837587428,17.3908551317257,18.3884265047086,
19.3859978776916,20.3835692506745,21.3811406236574,21.9911485751285),
 .UNSPECIFIED.);
#3957=B_SPLINE_CURVE_WITH_KNOTS('',3,(#47695,#47696,#47697,#47698,#47699,
#47700,#47701,#47702,#47703,#47704,#47705,#47706,#47707,#47708,#47709,#47710,
#47711,#47712,#47713,#47714,#47715,#47716,#47717,#47718,#47719,#47720,#47721,
#47722,#47723,#47724,#47725,#47726,#47727,#47728,#47729,#47730,#47731,#47732,
#47733,#47734,#47735,#47736,#47737,#47738,#47739,#47740,#47741,#47742,#47743,
#47744,#47745,#47746,#47747,#47748,#47749,#47750,#47751,#47752,#47753,#47754,
#47755,#47756,#47757,#47758,#47759,#47760,#47761,#47762,#47763,#47764,#47765,
#47766,#47767,#47768,#47769,#47770,#47771,#47772,#47773,#47774,#47775,#47776),
 .UNSPECIFIED.,.F.,.F.,(4,3,3,3,3,3,3,3,3,3,3,3,3,3,3,3,3,3,3,3,3,3,3,3,
3,3,3,4),(0.,0.0185980112514911,0.038423916878807,0.0557715843027085,0.0644760598123438,
0.0684517536303943,0.0885063485075443,0.10891646687441,0.125988664223312,
0.133854987331634,0.137288032273647,0.158362873189272,0.177205256270019,
0.197732848455495,0.20565296933075,0.209127416437683,0.230132765546023,
0.251624849770108,0.268069291425062,0.278304794066786,0.28404657349794,
0.306315569631616,0.322971867344282,0.328167702944214,0.333183121096512,
0.35570450535538,0.372940760482276,0.37694081721162),.UNSPECIFIED.);
#3958=B_SPLINE_CURVE_WITH_KNOTS('',3,(#47777,#47778,#47779,#47780,#47781,
#47782,#47783,#47784,#47785,#47786,#47787,#47788,#47789,#47790,#47791,#47792,
#47793,#47794,#47795,#47796,#47797,#47798,#47799,#47800,#47801),
 .UNSPECIFIED.,.F.,.F.,(4,3,3,3,3,3,3,3,4),(-10.1295685708719,-9.97571372982933,
-8.97814235684639,-7.98057098386346,-6.98299961088053,-5.9854282378976,
-4.98785686491466,-3.99028549193173,-3.84638326369226),.UNSPECIFIED.);
#3959=B_SPLINE_CURVE_WITH_KNOTS('',3,(#48146,#48147,#48148,#48149,#48150,
#48151,#48152,#48153,#48154,#48155,#48156,#48157,#48158,#48159,#48160,#48161,
#48162,#48163,#48164,#48165,#48166,#48167),.UNSPECIFIED.,.F.,.F.,(4,3,3,
3,3,3,3,4),(7.59300756235153,7.98057098386346,8.97814235684639,9.97571372982933,
10.9732851028123,11.9708564757952,12.9684278487781,13.8761928695311),
 .UNSPECIFIED.);
#3960=B_SPLINE_CURVE_WITH_KNOTS('',3,(#48168,#48169,#48170,#48171,#48172,
#48173,#48174,#48175,#48176,#48177,#48178,#48179,#48180,#48181,#48182,#48183,
#48184,#48185,#48186,#48187,#48188,#48189,#48190,#48191,#48192,#48193,#48194,
#48195,#48196,#48197,#48198,#48199,#48200,#48201,#48202,#48203,#48204,#48205,
#48206,#48207,#48208,#48209,#48210,#48211,#48212,#48213,#48214,#48215,#48216,
#48217,#48218,#48219,#48220,#48221,#48222,#48223,#48224,#48225,#48226,#48227,
#48228,#48229,#48230,#48231,#48232,#48233,#48234,#48235,#48236,#48237,#48238,
#48239,#48240,#48241,#48242,#48243,#48244,#48245,#48246,#48247,#48248,#48249,
#48250,#48251,#48252),.UNSPECIFIED.,.F.,.F.,(4,3,3,3,3,3,3,3,3,3,3,3,3,
3,3,3,3,3,3,3,3,3,3,3,3,3,3,3,4),(0.,0.0219665840178867,0.0445441200922607,
0.0636215543590298,0.0720969499798807,0.0767540580968768,0.0810484869492208,
0.102995100015702,0.124771281281709,0.142869359517885,0.150423583504265,
0.153920259627952,0.157567081121822,0.178337643732188,0.197163594226413,
0.21943554591047,0.224339007945502,0.229398552615548,0.250063626007469,
0.270724499289659,0.285678648504219,0.296896068874714,0.300623970906574,
0.320396153948268,0.334308778690984,0.338774577578954,0.357799193940268,
0.375339207698864,0.378621596831425),.UNSPECIFIED.);
#3961=B_SPLINE_CURVE_WITH_KNOTS('',3,(#48255,#48256,#48257,#48258,#48259,
#48260,#48261,#48262,#48263,#48264,#48265,#48266,#48267,#48268,#48269,#48270,
#48271,#48272,#48273,#48274,#48275,#48276,#48277,#48278,#48279,#48280,#48281,
#48282,#48283,#48284,#48285,#48286,#48287,#48288,#48289,#48290,#48291,#48292,
#48293,#48294,#48295,#48296,#48297,#48298,#48299,#48300,#48301,#48302,#48303,
#48304,#48305,#48306,#48307,#48308,#48309,#48310,#48311,#48312,#48313,#48314,
#48315,#48316,#48317,#48318,#48319,#48320,#48321,#48322,#48323,#48324,#48325,
#48326,#48327,#48328,#48329,#48330,#48331,#48332,#48333,#48334,#48335,#48336,
#48337,#48338,#48339,#48340,#48341,#48342),.UNSPECIFIED.,.F.,.F.,(4,3,3,
3,3,3,3,3,3,3,3,3,3,3,3,3,3,3,3,3,3,3,3,3,3,3,3,3,3,4),(-0.378621596831355,
-0.359797939668059,-0.347858077317233,-0.339704706466932,-0.335375299042539,
-0.315503714637518,-0.301169437267586,-0.297242105936665,-0.293224790512653,
-0.272822755477615,-0.252125053726975,-0.239301164214745,-0.228796742638415,
-0.224502344135147,-0.203197744287783,-0.200829495678057,-0.180341772881768,
-0.158301127747159,-0.154264834896697,-0.150797561869219,-0.129413800799564,
-0.107579371191749,-0.0856127636019974,-0.080183250637186,-0.0759376400731541,
-0.0533899343934191,-0.0308177819684862,-0.00875930839909695,-0.00401661180489583,
0.),.UNSPECIFIED.);
#3962=B_SPLINE_CURVE_WITH_KNOTS('',3,(#48343,#48344,#48345,#48346,#48347,
#48348,#48349,#48350,#48351,#48352,#48353,#48354,#48355,#48356,#48357,#48358,
#48359,#48360,#48361,#48362,#48363,#48364,#48365,#48366,#48367,#48368,#48369,
#48370,#48371,#48372,#48373,#48374,#48375,#48376,#48377,#48378,#48379,#48380,
#48381,#48382,#48383,#48384,#48385,#48386,#48387,#48388,#48389,#48390,#48391,
#48392,#48393,#48394,#48395,#48396,#48397,#48398,#48399,#48400,#48401,#48402,
#48403,#48404,#48405,#48406,#48407,#48408,#48409,#48410,#48411,#48412,#48413,
#48414,#48415,#48416,#48417,#48418,#48419,#48420,#48421,#48422,#48423,#48424,
#48425,#48426,#48427),.UNSPECIFIED.,.F.,.F.,(4,3,3,3,3,3,3,3,3,3,3,3,3,
3,3,3,3,3,3,3,3,3,3,3,3,3,3,3,4),(-0.376940817211684,-0.35463458349161,
-0.332912114164028,-0.328063829993201,-0.305815206742055,-0.290195159508168,
-0.284256938433436,-0.278600828085135,-0.256917586360118,-0.23569990130069,
-0.214947604386309,-0.208204874079122,-0.204400580976051,-0.183824390870239,
-0.180854828870958,-0.159872079452921,-0.140296870650113,-0.135976312799136,
-0.132599190292493,-0.112139944695331,-0.091775100858925,-0.0718463313651108,
-0.0676466090368204,-0.0636673307830578,-0.0441092158685665,-0.0249229265103377,
-0.00635967184351045,-0.00327040903045443,0.),.UNSPECIFIED.);
#3963=B_SPLINE_CURVE_WITH_KNOTS('',3,(#48429,#48430,#48431,#48432,#48433,
#48434,#48435,#48436,#48437,#48438,#48439),.UNSPECIFIED.,.F.,.F.,(4,1,1,
1,1,1,1,1,4),(15.7079632679489,15.8518654961883,16.8494368691713,17.8470082421542,
18.8445796151371,19.8421509881201,20.839722361103,21.8372937340859,21.9911485751285),
 .UNSPECIFIED.);
#3964=B_SPLINE_CURVE_WITH_KNOTS('',3,(#48440,#48441,#48442,#48443,#48444,
#48445,#48446,#48447,#48448,#48449),.UNSPECIFIED.,.F.,.F.,(4,1,1,1,1,1,
1,4),(15.7079632679489,16.3932837587427,17.3908551317257,18.3884265047086,
19.3859978776915,20.3835692506745,21.3811406236574,21.9911485751285),
 .UNSPECIFIED.);
#3965=B_SPLINE_CURVE_WITH_KNOTS('',3,(#48794,#48795,#48796,#48797,#48798,
#48799,#48800,#48801,#48802,#48803,#48804,#48805,#48806,#48807,#48808,#48809,
#48810,#48811,#48812,#48813,#48814,#48815,#48816,#48817,#48818,#48819,#48820,
#48821,#48822,#48823,#48824,#48825,#48826,#48827,#48828,#48829,#48830,#48831,
#48832,#48833,#48834,#48835,#48836,#48837,#48838,#48839,#48840,#48841,#48842,
#48843,#48844,#48845,#48846,#48847,#48848,#48849,#48850,#48851,#48852,#48853,
#48854,#48855,#48856,#48857,#48858,#48859,#48860,#48861,#48862,#48863,#48864,
#48865,#48866,#48867,#48868,#48869,#48870,#48871,#48872,#48873,#48874,#48875),
 .UNSPECIFIED.,.F.,.F.,(4,3,3,3,3,3,3,3,3,3,3,3,3,3,3,3,3,3,3,3,3,3,3,3,
3,3,3,4),(0.,0.018596995512751,0.0384230281074114,0.0557708066277392,0.0644747133130811,
0.0684514005740294,0.088505270571274,0.108915076392686,0.125987621362023,
0.133853344514643,0.137287156136604,0.158362091937476,0.177205256270034,
0.197733357549519,0.205653241463143,0.209127611534079,0.230133559211876,
0.251625958501743,0.268069030048616,0.278304187628649,0.284046730391058,
0.306315763830865,0.322972012993724,0.328168014023333,0.33318327613479,
0.355704655809054,0.3729407604823,0.376940817211644),.UNSPECIFIED.);
#3966=B_SPLINE_CURVE_WITH_KNOTS('',3,(#48876,#48877,#48878,#48879,#48880,
#48881,#48882,#48883,#48884,#48885,#48886,#48887,#48888,#48889,#48890,#48891,
#48892,#48893,#48894,#48895,#48896,#48897,#48898,#48899,#48900),
 .UNSPECIFIED.,.F.,.F.,(4,3,3,3,3,3,3,3,4),(-10.1295685708719,-9.97571372982932,
-8.97814235684639,-7.98057098386345,-6.98299961088052,-5.98542823789759,
-4.98785686491466,-3.99028549193172,-3.8463832636923),.UNSPECIFIED.);
#3967=B_SPLINE_CURVE_WITH_KNOTS('',3,(#49245,#49246,#49247,#49248,#49249,
#49250,#49251,#49252,#49253,#49254,#49255,#49256,#49257,#49258,#49259,#49260,
#49261,#49262,#49263,#49264,#49265,#49266),.UNSPECIFIED.,.F.,.F.,(4,3,3,
3,3,3,3,4),(7.59300756235157,7.98057098386346,8.97814235684639,9.97571372982933,
10.9732851028123,11.9708564757952,12.9684278487781,13.8761928695312),
 .UNSPECIFIED.);
#3968=B_SPLINE_CURVE_WITH_KNOTS('',3,(#49267,#49268,#49269,#49270,#49271,
#49272,#49273,#49274,#49275,#49276,#49277,#49278,#49279,#49280,#49281,#49282,
#49283,#49284,#49285,#49286,#49287,#49288,#49289,#49290,#49291,#49292,#49293,
#49294,#49295,#49296,#49297,#49298,#49299,#49300,#49301,#49302,#49303,#49304,
#49305,#49306,#49307,#49308,#49309,#49310,#49311,#49312,#49313,#49314,#49315,
#49316,#49317,#49318,#49319,#49320,#49321,#49322,#49323,#49324,#49325,#49326,
#49327,#49328,#49329,#49330,#49331,#49332,#49333,#49334,#49335,#49336,#49337,
#49338,#49339,#49340,#49341,#49342,#49343,#49344,#49345,#49346,#49347,#49348,
#49349,#49350,#49351),.UNSPECIFIED.,.F.,.F.,(4,3,3,3,3,3,3,3,3,3,3,3,3,
3,3,3,3,3,3,3,3,3,3,3,3,3,3,3,4),(0.,0.0219657370421621,0.0445431913694635,
0.0636207417265848,0.0720967070927941,0.0767535441972933,0.0810483489287806,
0.10299497868505,0.124771415616059,0.142869460268653,0.15042353887417,0.15391998785172,
0.157566995526094,0.17833781274149,0.197163594226434,0.219435545910493,
0.224339075599542,0.229398555827627,0.250063595739872,0.270724499008654,
0.285679418600401,0.296897371668684,0.300624344617424,0.320396829485849,
0.334309899384856,0.338775644842177,0.357800739667655,0.375339207698901,
0.378621596831463),.UNSPECIFIED.);
#3969=B_SPLINE_CURVE_WITH_KNOTS('',3,(#49354,#49355,#49356,#49357,#49358,
#49359,#49360,#49361,#49362,#49363,#49364,#49365,#49366,#49367,#49368,#49369,
#49370,#49371,#49372,#49373,#49374,#49375,#49376,#49377,#49378,#49379,#49380,
#49381,#49382,#49383,#49384,#49385,#49386,#49387,#49388,#49389,#49390,#49391,
#49392,#49393,#49394,#49395,#49396,#49397,#49398,#49399,#49400,#49401,#49402,
#49403,#49404,#49405,#49406,#49407,#49408,#49409,#49410,#49411,#49412,#49413,
#49414,#49415,#49416,#49417,#49418,#49419,#49420,#49421,#49422,#49423,#49424,
#49425,#49426,#49427,#49428,#49429,#49430,#49431,#49432,#49433,#49434,#49435,
#49436,#49437,#49438,#49439,#49440,#49441),.UNSPECIFIED.,.F.,.F.,(4,3,3,
3,3,3,3,3,3,3,3,3,3,3,3,3,3,3,3,3,3,3,3,3,3,3,3,3,3,4),(-0.378621596831419,
-0.359797936894149,-0.347858070276125,-0.339704642905692,-0.335375266132442,
-0.315503679098809,-0.301169406171218,-0.297242034943752,-0.293224780862376,
-0.272822743843532,-0.252125042359958,-0.239301155689489,-0.228796730058329,
-0.224502340016174,-0.203197740281884,-0.200829495678081,-0.180341774760402,
-0.158301129390964,-0.154264846295692,-0.150797564186461,-0.129413804651141,
-0.107579375726104,-0.085612768153713,-0.0801832585527506,-0.0759376429114784,
-0.0533899375499779,-0.0308177850670804,-0.0087593118006187,-0.0040166118048958,
0.),.UNSPECIFIED.);
#3970=B_SPLINE_CURVE_WITH_KNOTS('',3,(#49442,#49443,#49444,#49445,#49446,
#49447,#49448,#49449,#49450,#49451,#49452,#49453,#49454,#49455,#49456,#49457,
#49458,#49459,#49460,#49461,#49462,#49463,#49464,#49465,#49466,#49467,#49468,
#49469,#49470,#49471,#49472,#49473,#49474,#49475,#49476,#49477,#49478,#49479,
#49480,#49481,#49482,#49483,#49484,#49485,#49486,#49487,#49488,#49489,#49490,
#49491,#49492,#49493,#49494,#49495,#49496,#49497,#49498,#49499,#49500,#49501,
#49502,#49503,#49504,#49505,#49506,#49507,#49508,#49509,#49510,#49511,#49512,
#49513,#49514,#49515,#49516,#49517,#49518,#49519,#49520,#49521,#49522,#49523,
#49524,#49525,#49526),.UNSPECIFIED.,.F.,.F.,(4,3,3,3,3,3,3,3,3,3,3,3,3,
3,3,3,3,3,3,3,3,3,3,3,3,3,3,3,4),(-0.376940817211647,-0.354634582187994,
-0.332912113023362,-0.328063828673689,-0.305815205437262,-0.290195158366472,
-0.284256935896806,-0.2786008282367,-0.256917586723634,-0.235699902217931,
-0.214947605661536,-0.208204873247512,-0.204400581023048,-0.183824391454496,
-0.180854828870938,-0.159872079456263,-0.140296870653037,-0.135976313701251,
-0.132599190986633,-0.112139945302261,-0.0917751016125585,-0.0718463328109456,
-0.0676466130607016,-0.0636673320630382,-0.0441092175240187,-0.0249229289937617,
-0.00635967569699575,-0.00327040903045435,0.),.UNSPECIFIED.);
#3971=B_SPLINE_CURVE_WITH_KNOTS('',3,(#49528,#49529,#49530,#49531,#49532,
#49533,#49534,#49535,#49536,#49537,#49538),.UNSPECIFIED.,.F.,.F.,(4,1,1,
1,1,1,1,1,4),(15.7079632679489,15.8518654961883,16.8494368691713,17.8470082421542,
18.8445796151371,19.8421509881201,20.839722361103,21.8372937340859,21.9911485751285),
 .UNSPECIFIED.);
#3972=B_SPLINE_CURVE_WITH_KNOTS('',3,(#49539,#49540,#49541,#49542,#49543,
#49544,#49545,#49546,#49547,#49548),.UNSPECIFIED.,.F.,.F.,(4,1,1,1,1,1,
1,4),(15.7079632679489,16.3932837587427,17.3908551317257,18.3884265047086,
19.3859978776915,20.3835692506745,21.3811406236574,21.9911485751285),
 .UNSPECIFIED.);
#3973=B_SPLINE_CURVE_WITH_KNOTS('',3,(#49893,#49894,#49895,#49896,#49897,
#49898,#49899,#49900,#49901,#49902,#49903,#49904,#49905,#49906,#49907,#49908,
#49909,#49910,#49911,#49912,#49913,#49914,#49915,#49916,#49917,#49918,#49919,
#49920,#49921,#49922,#49923,#49924,#49925,#49926,#49927,#49928,#49929,#49930,
#49931,#49932,#49933,#49934,#49935,#49936,#49937,#49938,#49939,#49940,#49941,
#49942,#49943,#49944,#49945,#49946,#49947,#49948,#49949,#49950,#49951,#49952,
#49953,#49954,#49955,#49956,#49957,#49958,#49959,#49960,#49961,#49962,#49963,
#49964,#49965,#49966,#49967,#49968,#49969,#49970,#49971,#49972,#49973,#49974),
 .UNSPECIFIED.,.F.,.F.,(4,3,3,3,3,3,3,3,3,3,3,3,3,3,3,3,3,3,3,3,3,3,3,3,
3,3,3,4),(0.,0.0185969976546447,0.0384230299815686,0.0557708082676271,0.0644747161530116,
0.0684514013219826,0.0885052728499997,0.108915079335808,0.125987623569365,
0.133853347992972,0.13728715798927,0.158362093597067,0.177205256270036,
0.197733356483041,0.205653240898805,0.209127611124312,0.23013355754844,
0.251625956176866,0.268069030607125,0.278304188929636,0.284046730059679,
0.306315763420324,0.322972012685815,0.328168013379916,0.333183275811836,
0.355704655498454,0.372940760482288,0.376940817211632),.UNSPECIFIED.);
#3974=B_SPLINE_CURVE_WITH_KNOTS('',3,(#49975,#49976,#49977,#49978,#49979,
#49980,#49981,#49982,#49983,#49984,#49985,#49986,#49987,#49988,#49989,#49990,
#49991,#49992,#49993,#49994,#49995,#49996,#49997,#49998,#49999),
 .UNSPECIFIED.,.F.,.F.,(4,3,3,3,3,3,3,3,4),(-10.1295685708719,-9.97571372982932,
-8.97814235684639,-7.98057098386346,-6.98299961088053,-5.9854282378976,
-4.98785686491466,-3.99028549193173,-3.8463832636923),.UNSPECIFIED.);
#3975=B_SPLINE_CURVE_WITH_KNOTS('',3,(#50344,#50345,#50346,#50347,#50348,
#50349,#50350,#50351,#50352,#50353,#50354,#50355,#50356,#50357,#50358,#50359,
#50360,#50361,#50362,#50363,#50364,#50365),.UNSPECIFIED.,.F.,.F.,(4,3,3,
3,3,3,3,4),(7.59300756235161,7.98057098386346,8.97814235684639,9.97571372982932,
10.9732851028123,11.9708564757952,12.9684278487781,13.8761928695312),
 .UNSPECIFIED.);
#3976=B_SPLINE_CURVE_WITH_KNOTS('',3,(#50366,#50367,#50368,#50369,#50370,
#50371,#50372,#50373,#50374,#50375,#50376,#50377,#50378,#50379,#50380,#50381,
#50382,#50383,#50384,#50385,#50386,#50387,#50388,#50389,#50390,#50391,#50392,
#50393,#50394,#50395,#50396,#50397,#50398,#50399,#50400,#50401,#50402,#50403,
#50404,#50405,#50406,#50407,#50408,#50409,#50410,#50411,#50412,#50413,#50414,
#50415,#50416,#50417,#50418,#50419,#50420,#50421,#50422,#50423,#50424,#50425,
#50426,#50427,#50428,#50429,#50430,#50431,#50432,#50433,#50434,#50435,#50436,
#50437,#50438,#50439,#50440,#50441,#50442,#50443,#50444,#50445,#50446,#50447,
#50448,#50449,#50450),.UNSPECIFIED.,.F.,.F.,(4,3,3,3,3,3,3,3,3,3,3,3,3,
3,3,3,3,3,3,3,3,3,3,3,3,3,3,3,4),(0.,0.0219657394536776,0.0445431940187976,
0.0636207440447494,0.0720967077855105,0.0767535456638122,0.0810483493275398,
0.102994979041479,0.124771415249923,0.142869459994045,0.150423539013126,
0.153919988666253,0.15756699577772,0.178337812273338,0.197163594226412,
0.219435545910467,0.224339075414555,0.229398555814321,0.250063595824097,
0.270724499016863,0.285679416448513,0.296897368037468,0.300624343572328,
0.320396827601905,0.334309896252106,0.338775641841365,0.357800735330979,
0.375339207698853,0.378621596831413),.UNSPECIFIED.);
#3977=B_SPLINE_CURVE_WITH_KNOTS('',3,(#50458,#50459,#50460,#50461,#50462,
#50463,#50464,#50465,#50466,#50467,#50468,#50469,#50470,#50471,#50472,#50473,
#50474,#50475,#50476,#50477,#50478,#50479,#50480,#50481,#50482,#50483,#50484,
#50485,#50486,#50487,#50488,#50489,#50490,#50491,#50492,#50493,#50494,#50495,
#50496,#50497,#50498,#50499,#50500,#50501,#50502,#50503,#50504,#50505,#50506,
#50507,#50508,#50509,#50510,#50511,#50512,#50513,#50514,#50515,#50516,#50517,
#50518,#50519,#50520,#50521,#50522,#50523,#50524,#50525,#50526,#50527,#50528,
#50529,#50530,#50531,#50532,#50533,#50534,#50535,#50536,#50537,#50538,#50539,
#50540,#50541,#50542,#50543,#50544,#50545),.UNSPECIFIED.,.F.,.F.,(4,3,3,
3,3,3,3,3,3,3,3,3,3,3,3,3,3,3,3,3,3,3,3,3,3,3,3,3,3,4),(-0.378621596831417,
-0.359796324497933,-0.347853968215386,-0.339667381051392,-0.33535479313986,
-0.315481654241569,-0.301150134421133,-0.297197750394092,-0.293218427819012,
-0.272815226641669,-0.252117692398167,-0.239295643218144,-0.228788599088732,
-0.224499673218097,-0.203195145608534,-0.200829495678077,-0.18034287834285,
-0.158302095025605,-0.154271536511048,-0.150798918828779,-0.129416060221611,
-0.107582030158341,-0.0856154294482134,-0.0801878898697612,-0.0759393010155595,
-0.0533917821073025,-0.0308195963955261,-0.00876131064632734,-0.00401661180488987,
0.),.UNSPECIFIED.);
#3978=B_SPLINE_CURVE_WITH_KNOTS('',3,(#50546,#50547,#50548,#50549,#50550,
#50551,#50552,#50553,#50554,#50555,#50556,#50557,#50558,#50559,#50560,#50561,
#50562,#50563,#50564,#50565,#50566,#50567,#50568,#50569,#50570,#50571,#50572,
#50573,#50574,#50575,#50576,#50577,#50578,#50579,#50580,#50581,#50582,#50583,
#50584,#50585,#50586,#50587,#50588,#50589,#50590,#50591,#50592,#50593,#50594,
#50595,#50596,#50597,#50598,#50599,#50600,#50601,#50602,#50603,#50604,#50605,
#50606,#50607,#50608,#50609,#50610,#50611,#50612,#50613,#50614,#50615,#50616,
#50617,#50618,#50619,#50620,#50621,#50622,#50623,#50624,#50625,#50626,#50627,
#50628,#50629,#50630),.UNSPECIFIED.,.F.,.F.,(4,3,3,3,3,3,3,3,3,3,3,3,3,
3,3,3,3,3,3,3,3,3,3,3,3,3,3,3,4),(-0.376940817211599,-0.354633525341571,
-0.332911188282741,-0.328062756116004,-0.305814149686869,-0.290194234584877,
-0.284254884750481,-0.278600964800113,-0.256917900841735,-0.235700669608916,
-0.214948669584839,-0.208204193177863,-0.204400682430755,-0.18382493241094,
-0.180854828870933,-0.159872083890278,-0.1402968745328,-0.135977073907336,
-0.132599774507536,-0.112140461897276,-0.0917757502511294,-0.0718475646021411,
-0.0676500217440913,-0.0636684046549802,-0.044110611876292,-0.0249250199794228,
-0.00636290551127469,-0.00327040903045178,0.),.UNSPECIFIED.);
#3979=B_SPLINE_CURVE_WITH_KNOTS('',3,(#50632,#50633,#50634,#50635,#50636,
#50637,#50638,#50639,#50640,#50641,#50642),.UNSPECIFIED.,.F.,.F.,(4,1,1,
1,1,1,1,1,4),(15.7079632679489,15.8518654961884,16.8494368691713,17.8470082421543,
18.8445796151372,19.8421509881201,20.8397223611031,21.837293734086,21.9911485751285),
 .UNSPECIFIED.);
#3980=B_SPLINE_CURVE_WITH_KNOTS('',3,(#50643,#50644,#50645,#50646,#50647,
#50648,#50649,#50650,#50651,#50652),.UNSPECIFIED.,.F.,.F.,(4,1,1,1,1,1,
1,4),(15.7079632679489,16.3932837587428,17.3908551317257,18.3884265047087,
19.3859978776916,20.3835692506745,21.3811406236575,21.9911485751285),
 .UNSPECIFIED.);
#3981=B_SPLINE_CURVE_WITH_KNOTS('',3,(#50997,#50998,#50999,#51000,#51001,
#51002,#51003,#51004,#51005,#51006,#51007,#51008,#51009,#51010,#51011,#51012,
#51013,#51014,#51015,#51016,#51017,#51018,#51019,#51020,#51021,#51022,#51023,
#51024,#51025,#51026,#51027,#51028,#51029,#51030,#51031,#51032,#51033,#51034,
#51035,#51036,#51037,#51038,#51039,#51040,#51041,#51042,#51043,#51044,#51045,
#51046,#51047,#51048,#51049,#51050,#51051,#51052,#51053,#51054,#51055,#51056,
#51057,#51058,#51059,#51060,#51061,#51062,#51063,#51064,#51065,#51066,#51067,
#51068,#51069,#51070,#51071,#51072,#51073,#51074,#51075,#51076,#51077,#51078),
 .UNSPECIFIED.,.F.,.F.,(4,3,3,3,3,3,3,3,3,3,3,3,3,3,3,3,3,3,3,3,3,3,3,3,
3,3,3,4),(0.,0.0185987341995647,0.0384245494583765,0.0557721378098369,0.0644770178569765,
0.068452005390303,0.0885071145869722,0.108917452397134,0.125989403365366,
0.133856151017707,0.137288655783233,0.15836342516836,0.177205256270059,
0.197732482353179,0.20565277044136,0.209127273146685,0.230132191380251,
0.251624049747522,0.268069475039372,0.27830521821265,0.284046462288397,
0.306315432127717,0.322971764216374,0.328167478835643,0.333183009452404,
0.355704395482805,0.372940760482345,0.37694081721169),.UNSPECIFIED.);
#3982=B_SPLINE_CURVE_WITH_KNOTS('',3,(#51079,#51080,#51081,#51082,#51083,
#51084,#51085,#51086,#51087,#51088,#51089,#51090,#51091,#51092,#51093,#51094,
#51095,#51096,#51097,#51098,#51099,#51100,#51101,#51102,#51103),
 .UNSPECIFIED.,.F.,.F.,(4,3,3,3,3,3,3,3,4),(-10.1295685708718,-9.97571372982932,
-8.97814235684639,-7.98057098386346,-6.98299961088053,-5.98542823789759,
-4.98785686491466,-3.99028549193173,-3.84638326369223),.UNSPECIFIED.);
#3983=B_SPLINE_CURVE_WITH_KNOTS('',3,(#51448,#51449,#51450,#51451,#51452,
#51453,#51454,#51455,#51456,#51457,#51458,#51459,#51460,#51461,#51462,#51463,
#51464,#51465,#51466,#51467,#51468,#51469),.UNSPECIFIED.,.F.,.F.,(4,3,3,
3,3,3,3,4),(7.59300756235153,7.98057098386347,8.9781423568464,9.97571372982933,
10.9732851028123,11.9708564757952,12.9684278487781,13.8761928695311),
 .UNSPECIFIED.);
#3984=B_SPLINE_CURVE_WITH_KNOTS('',3,(#51470,#51471,#51472,#51473,#51474,
#51475,#51476,#51477,#51478,#51479,#51480,#51481,#51482,#51483,#51484,#51485,
#51486,#51487,#51488,#51489,#51490,#51491,#51492,#51493,#51494,#51495,#51496,
#51497,#51498,#51499,#51500,#51501,#51502,#51503,#51504,#51505,#51506,#51507,
#51508,#51509,#51510,#51511,#51512,#51513,#51514,#51515,#51516,#51517,#51518,
#51519,#51520,#51521,#51522,#51523,#51524,#51525,#51526,#51527,#51528,#51529,
#51530,#51531,#51532,#51533,#51534,#51535,#51536,#51537,#51538,#51539,#51540,
#51541,#51542,#51543,#51544,#51545,#51546,#51547,#51548,#51549,#51550,#51551,
#51552,#51553,#51554),.UNSPECIFIED.,.F.,.F.,(4,3,3,3,3,3,3,3,3,3,3,3,3,
3,3,3,3,3,3,3,3,3,3,3,3,3,3,3,4),(0.,0.0219671392710627,0.0445447270614996,
0.0636220854571156,0.0720971088190858,0.0767543937611971,0.0810485771087931,
0.102995177264397,0.12477118871929,0.142869290096075,0.150423609225186,
0.153920425498144,0.15756713475292,0.178337528533867,0.197163594226427,
0.219435545910481,0.224338960691702,0.229398550502591,0.250063644957184,
0.270724495002125,0.2856781237343,0.296895177864656,0.300623717137974,0.32039569443208,
0.334308019624689,0.338773858972783,0.357798151609198,0.37533920769886,
0.37862159683142),.UNSPECIFIED.);
#3985=B_SPLINE_CURVE_WITH_KNOTS('',3,(#51558,#51559,#51560,#51561,#51562,
#51563,#51564,#51565,#51566,#51567,#51568,#51569,#51570,#51571,#51572,#51573,
#51574,#51575,#51576,#51577,#51578,#51579,#51580,#51581,#51582,#51583,#51584,
#51585,#51586,#51587,#51588,#51589,#51590,#51591,#51592,#51593,#51594,#51595,
#51596,#51597,#51598,#51599,#51600,#51601,#51602,#51603,#51604,#51605,#51606,
#51607,#51608,#51609,#51610,#51611,#51612,#51613,#51614,#51615,#51616,#51617,
#51618,#51619,#51620,#51621,#51622,#51623,#51624,#51625,#51626,#51627,#51628,
#51629,#51630,#51631,#51632,#51633,#51634,#51635,#51636,#51637,#51638,#51639,
#51640,#51641,#51642,#51643,#51644,#51645),.UNSPECIFIED.,.F.,.F.,(4,3,3,
3,3,3,3,3,3,3,3,3,3,3,3,3,3,3,3,3,3,3,3,3,3,3,3,3,3,4),(-0.378621596831453,
-0.359796964367516,-0.34785559588844,-0.339682222403536,-0.335363223677477,
-0.31549070609328,-0.301158054791382,-0.297216022364776,-0.29322112959255,
-0.272818393264414,-0.252120789758935,-0.239297966238724,-0.228792024964215,
-0.224500801096337,-0.203196242733446,-0.200829495678093,-0.180342437231382,
-0.158301709053072,-0.15426886502637,-0.150798379224116,-0.129415160899972,
-0.10758097206945,-0.0856143687245085,-0.080186043251393,-0.0759386413924393,
-0.053391048511125,-0.0308188757754254,-0.00876051286996735,-0.00401661180489571,
0.),.UNSPECIFIED.);
#3986=B_SPLINE_CURVE_WITH_KNOTS('',3,(#51646,#51647,#51648,#51649,#51650,
#51651,#51652,#51653,#51654,#51655,#51656,#51657,#51658,#51659,#51660,#51661,
#51662,#51663,#51664,#51665,#51666,#51667,#51668,#51669,#51670,#51671,#51672,
#51673,#51674,#51675,#51676,#51677,#51678,#51679,#51680,#51681,#51682,#51683,
#51684,#51685,#51686,#51687,#51688,#51689,#51690,#51691,#51692,#51693,#51694,
#51695,#51696,#51697,#51698,#51699,#51700,#51701,#51702,#51703,#51704,#51705,
#51706,#51707,#51708,#51709,#51710,#51711,#51712,#51713,#51714,#51715,#51716,
#51717,#51718,#51719,#51720,#51721,#51722,#51723,#51724,#51725,#51726,#51727,
#51728,#51729,#51730),.UNSPECIFIED.,.F.,.F.,(4,3,3,3,3,3,3,3,3,3,3,3,3,
3,3,3,3,3,3,3,3,3,3,3,3,3,3,3,4),(-0.376940817211633,-0.354633964602481,
-0.332911572636038,-0.328063202247457,-0.305814587526729,-0.290194617694755,
-0.284255735322417,-0.278600908077479,-0.256917768897898,-0.235700347784253,
-0.214948223366311,-0.208204476162521,-0.204400640110824,-0.183824705944621,
-0.180854828870941,-0.159872081610359,-0.140296872537871,-0.13597675000398,
-0.132599526175717,-0.112140240543943,-0.0917754711192709,-0.0718470375036391,
-0.0676485677836509,-0.0636679489822672,-0.0441100183726961,-0.0249241308057409,
-0.00636153480048415,-0.00327040903045198,0.),.UNSPECIFIED.);
#3987=B_SPLINE_CURVE_WITH_KNOTS('',3,(#51732,#51733,#51734,#51735,#51736,
#51737,#51738,#51739,#51740,#51741,#51742),.UNSPECIFIED.,.F.,.F.,(4,1,1,
1,1,1,1,1,4),(15.7079632679489,15.8518654961884,16.8494368691713,17.8470082421542,
18.8445796151372,19.8421509881201,20.839722361103,21.837293734086,21.9911485751285),
 .UNSPECIFIED.);
#3988=B_SPLINE_CURVE_WITH_KNOTS('',3,(#51743,#51744,#51745,#51746,#51747,
#51748,#51749,#51750,#51751,#51752),.UNSPECIFIED.,.F.,.F.,(4,1,1,1,1,1,
1,4),(15.7079632679489,16.3932837587428,17.3908551317257,18.3884265047086,
19.3859978776916,20.3835692506745,21.3811406236574,21.9911485751285),
 .UNSPECIFIED.);
#3989=B_SPLINE_CURVE_WITH_KNOTS('',3,(#52097,#52098,#52099,#52100,#52101,
#52102,#52103,#52104,#52105,#52106,#52107,#52108,#52109,#52110,#52111,#52112,
#52113,#52114,#52115,#52116,#52117,#52118,#52119,#52120,#52121,#52122,#52123,
#52124,#52125,#52126,#52127,#52128,#52129,#52130,#52131,#52132,#52133,#52134,
#52135,#52136,#52137,#52138,#52139,#52140,#52141,#52142,#52143,#52144,#52145,
#52146,#52147,#52148,#52149,#52150,#52151,#52152,#52153,#52154,#52155,#52156,
#52157,#52158,#52159,#52160,#52161,#52162,#52163,#52164,#52165,#52166,#52167,
#52168,#52169,#52170,#52171,#52172,#52173,#52174,#52175,#52176,#52177,#52178),
 .UNSPECIFIED.,.F.,.F.,(4,3,3,3,3,3,3,3,3,3,3,3,3,3,3,3,3,3,3,3,3,3,3,3,
3,3,3,4),(0.,0.0185980112512777,0.0384239168786204,0.0557715843025452,0.0644760598120422,
0.0684517536273742,0.0885063485050852,0.108916466871302,0.125988664220981,
0.133854987328047,0.137288032277356,0.158362873192896,0.177205256270019,
0.197732848455459,0.205652969330799,0.209127416443499,0.230132765552162,
0.251624849776322,0.268069291421993,0.278304794057273,0.284046573502879,
0.306315569636911,0.322971867348254,0.328167702950825,0.333183121098172,
0.355704505357051,0.372940760482282,0.376940817211626),.UNSPECIFIED.);
#3990=B_SPLINE_CURVE_WITH_KNOTS('',3,(#52179,#52180,#52181,#52182,#52183,
#52184,#52185,#52186,#52187,#52188,#52189,#52190,#52191,#52192,#52193,#52194,
#52195,#52196,#52197,#52198,#52199,#52200,#52201,#52202,#52203),
 .UNSPECIFIED.,.F.,.F.,(4,3,3,3,3,3,3,3,4),(-10.1295685708719,-9.97571372982933,
-8.97814235684639,-7.98057098386346,-6.98299961088053,-5.9854282378976,
-4.98785686491466,-3.99028549193173,-3.84638326369226),.UNSPECIFIED.);
#3991=B_SPLINE_CURVE_WITH_KNOTS('',3,(#52548,#52549,#52550,#52551,#52552,
#52553,#52554,#52555,#52556,#52557,#52558,#52559,#52560,#52561,#52562,#52563,
#52564,#52565,#52566,#52567,#52568,#52569),.UNSPECIFIED.,.F.,.F.,(4,3,3,
3,3,3,3,4),(7.59300756235153,7.98057098386346,8.97814235684639,9.97571372982933,
10.9732851028123,11.9708564757952,12.9684278487781,13.8761928695311),
 .UNSPECIFIED.);
#3992=B_SPLINE_CURVE_WITH_KNOTS('',3,(#52570,#52571,#52572,#52573,#52574,
#52575,#52576,#52577,#52578,#52579,#52580,#52581,#52582,#52583,#52584,#52585,
#52586,#52587,#52588,#52589,#52590,#52591,#52592,#52593,#52594,#52595,#52596,
#52597,#52598,#52599,#52600,#52601,#52602,#52603,#52604,#52605,#52606,#52607,
#52608,#52609,#52610,#52611,#52612,#52613,#52614,#52615,#52616,#52617,#52618,
#52619,#52620,#52621,#52622,#52623,#52624,#52625,#52626,#52627,#52628,#52629,
#52630,#52631,#52632,#52633,#52634,#52635,#52636,#52637,#52638,#52639,#52640,
#52641,#52642,#52643,#52644,#52645,#52646,#52647,#52648,#52649,#52650,#52651,
#52652,#52653,#52654),.UNSPECIFIED.,.F.,.F.,(4,3,3,3,3,3,3,3,3,3,3,3,3,
3,3,3,3,3,3,3,3,3,3,3,3,3,3,3,4),(0.,0.0219665840177821,0.0445441200922931,
0.0636215543590582,0.0720969499799132,0.0767540580968699,0.0810484869491109,
0.102995100015314,0.12477128128117,0.142869359517481,0.150423583503905,
0.153920259630152,0.157567081122177,0.178337643732528,0.197163594226414,
0.219435545910471,0.224339007945445,0.229398552617908,0.250063626009798,
0.270724499291964,0.285678648510981,0.296896068885296,0.300623970908951,
0.320396153950705,0.334308778694922,0.338774577569346,0.357799193930767,
0.375339207698866,0.378621596831428),.UNSPECIFIED.);
#3993=B_SPLINE_CURVE_WITH_KNOTS('',3,(#52677,#52678,#52679,#52680),
 .UNSPECIFIED.,.F.,.F.,(4,4),(51.5750455984138,52.2860549491936),
 .UNSPECIFIED.);
#3994=B_SPLINE_CURVE_WITH_KNOTS('',3,(#52692,#52693,#52694,#52695,#52696,
#52697,#52698,#52699,#52700,#52701),.UNSPECIFIED.,.F.,.F.,(4,3,3,4),(-50.2654824574367,
-49.3264669332015,-48.3399375945375,-47.8348991546267),.UNSPECIFIED.);
#3995=B_SPLINE_CURVE_WITH_KNOTS('',3,(#52706,#52707,#52708,#52709,#52710,
#52711,#52712,#52713,#52714,#52715,#52716,#52717,#52718,#52719,#52720,#52721,
#52722,#52723,#52724,#52725,#52726,#52727,#52728,#52729,#52730),
 .UNSPECIFIED.,.F.,.F.,(4,3,3,3,3,3,3,3,4),(45.2918602912342,45.3803495785454,
46.3668789172094,47.3534082558734,48.3399375945375,49.3264669332015,50.3129962718655,
51.2995256105296,51.5750455984138),.UNSPECIFIED.);
#3996=B_SPLINE_CURVE_WITH_KNOTS('',3,(#52731,#52732,#52733,#52734,#52735,
#52736,#52737,#52738,#52739,#52740,#52741,#52742,#52743,#52744,#52745,#52746,
#52747,#52748,#52749,#52750,#52751,#52752),.UNSPECIFIED.,.F.,.F.,(4,3,3,
3,3,3,3,4),(-47.8348991546267,-47.3534082558735,-46.3668789172094,-45.3803495785454,
-44.3938202398814,-43.4072909012173,-42.4207615625533,-41.5517138474471),
 .UNSPECIFIED.);
#3997=B_SPLINE_CURVE_WITH_KNOTS('',3,(#52757,#52758,#52759,#52760,#52761,
#52762,#52763,#52764,#52765,#52766,#52767,#52768,#52769,#52770,#52771,#52772,
#52773,#52774,#52775,#52776,#52777,#52778),.UNSPECIFIED.,.F.,.F.,(4,3,3,
3,3,3,3,4),(39.0086749840546,39.4611735465612,40.4477028852252,41.4342322238893,
42.4207615625533,43.4072909012173,44.3938202398814,45.2918602912342),
 .UNSPECIFIED.);
#3998=B_SPLINE_CURVE_WITH_KNOTS('',3,(#52779,#52780,#52781,#52782,#52783,
#52784,#52785,#52786,#52787,#52788,#52789,#52790,#52791,#52792,#52793,#52794,
#52795,#52796,#52797,#52798,#52799,#52800,#52801,#52802,#52803),
 .UNSPECIFIED.,.F.,.F.,(4,3,3,3,3,3,3,3,4),(-41.5517138474471,-41.4342322238893,
-40.4477028852252,-39.4611735465612,-38.4746442078972,-37.4881148692332,
-36.5015855305691,-35.5150561919051,-35.2685285402675),.UNSPECIFIED.);
#3999=B_SPLINE_CURVE_WITH_KNOTS('',3,(#52808,#52809,#52810,#52811,#52812,
#52813,#52814,#52815,#52816,#52817,#52818,#52819,#52820,#52821,#52822,#52823,
#52824,#52825,#52826,#52827,#52828,#52829),.UNSPECIFIED.,.F.,.F.,(4,3,3,
3,3,3,3,4),(32.725489676875,33.541997514577,34.5285268532411,35.5150561919051,
36.5015855305691,37.4881148692331,38.4746442078972,39.0086749840546),
 .UNSPECIFIED.);
#4000=B_SPLINE_CURVE_WITH_KNOTS('',3,(#52830,#52831,#52832,#52833,#52834,
#52835,#52836,#52837,#52838,#52839,#52840,#52841,#52842,#52843,#52844,#52845,
#52846,#52847,#52848,#52849,#52850,#52851),.UNSPECIFIED.,.F.,.F.,(4,3,3,
3,3,3,3,4),(-35.2685285402675,-34.5285268532411,-33.541997514577,-32.555468175913,
-31.568938837249,-30.5824094985849,-29.5958801599209,-28.9853432330879),
 .UNSPECIFIED.);
#4001=B_SPLINE_CURVE_WITH_KNOTS('',3,(#52856,#52857,#52858,#52859,#52860,
#52861,#52862,#52863,#52864,#52865,#52866,#52867,#52868,#52869,#52870,#52871,
#52872,#52873,#52874,#52875,#52876,#52877,#52878,#52879,#52880),
 .UNSPECIFIED.,.F.,.F.,(4,3,3,3,3,3,3,3,4),(26.4423043696954,26.6362921439288,
27.6228214825928,28.6093508212569,29.5958801599209,30.5824094985849,31.568938837249,
32.555468175913,32.725489676875),.UNSPECIFIED.);
#4002=B_SPLINE_CURVE_WITH_KNOTS('',3,(#52881,#52882,#52883,#52884,#52885,
#52886,#52887,#52888,#52889,#52890,#52891,#52892,#52893,#52894,#52895,#52896,
#52897,#52898,#52899,#52900,#52901,#52902),.UNSPECIFIED.,.F.,.F.,(4,3,3,
3,3,3,3,4),(-28.9853432330879,-28.6093508212569,-27.6228214825929,-26.6362921439288,
-25.6497628052648,-24.6632334666008,-23.6767041279367,-22.7021579259083),
 .UNSPECIFIED.);
#4003=B_SPLINE_CURVE_WITH_KNOTS('',3,(#52907,#52908,#52909,#52910,#52911,
#52912,#52913,#52914,#52915,#52916,#52917,#52918,#52919,#52920,#52921,#52922,
#52923,#52924,#52925,#52926,#52927,#52928),.UNSPECIFIED.,.F.,.F.,(4,3,3,
3,3,3,3,4),(20.1591190625158,20.7171161119446,21.7036454506087,22.6901747892727,
23.6767041279367,24.6632334666008,25.6497628052648,26.4423043696954),
 .UNSPECIFIED.);
#4004=B_SPLINE_CURVE_WITH_KNOTS('',3,(#52929,#52930,#52931,#52932,#52933,
#52934,#52935,#52936,#52937,#52938,#52939,#52940,#52941,#52942,#52943,#52944,
#52945,#52946,#52947,#52948,#52949,#52950,#52951,#52952,#52953),
 .UNSPECIFIED.,.F.,.F.,(4,3,3,3,3,3,3,3,4),(-22.7021579259083,-22.6901747892727,
-21.7036454506087,-20.7171161119446,-19.7305867732806,-18.7440574346166,
-17.7575280959525,-16.7709987572885,-16.4189726187288),.UNSPECIFIED.);
#4005=B_SPLINE_CURVE_WITH_KNOTS('',3,(#52958,#52959,#52960,#52961,#52962,
#52963,#52964,#52965,#52966,#52967,#52968,#52969,#52970,#52971,#52972,#52973,
#52974,#52975,#52976,#52977,#52978,#52979),.UNSPECIFIED.,.F.,.F.,(4,3,3,
3,3,3,3,4),(13.8759337553362,14.7979400799604,15.7844694186245,16.7709987572885,
17.7575280959525,18.7440574346166,19.7305867732806,20.1591190625158),
 .UNSPECIFIED.);
#4006=B_SPLINE_CURVE_WITH_KNOTS('',3,(#52980,#52981,#52982,#52983,#52984,
#52985,#52986,#52987,#52988,#52989,#52990,#52991,#52992,#52993,#52994,#52995,
#52996,#52997,#52998,#52999,#53000,#53001),.UNSPECIFIED.,.F.,.F.,(4,3,3,
3,3,3,3,4),(-16.4189726187288,-15.7844694186245,-14.7979400799605,-13.8114107412964,
-12.8248814026324,-11.8383520639684,-10.8518227253043,-10.1357873115492),
 .UNSPECIFIED.);
#4007=B_SPLINE_CURVE_WITH_KNOTS('',3,(#53007,#53008,#53009,#53010,#53011,
#53012,#53013,#53014,#53015,#53016,#53017,#53018,#53019),.UNSPECIFIED.,
 .F.,.F.,(4,3,3,3,4),(-3.85260200436958,-2.95958801599209,-1.97305867732806,
-0.986529338664031,0.),.UNSPECIFIED.);
#4008=B_SPLINE_CURVE_WITH_KNOTS('',3,(#53022,#53023,#53024,#53025,#53026,
#53027,#53028,#53029,#53030,#53031,#53032,#53033,#53034,#53035,#53036,#53037,
#53038,#53039,#53040),.UNSPECIFIED.,.F.,.F.,(4,3,3,3,3,3,4),(2.02057249175696,
2.95958801599209,3.94611735465612,4.93264669332015,5.91917603198418,6.90570537064821,
7.59274844815664),.UNSPECIFIED.);
#4009=B_SPLINE_CURVE_WITH_KNOTS('',3,(#53046,#53047,#53048,#53049,#53050,
#53051,#53052,#53053),.UNSPECIFIED.,.F.,.F.,(4,1,1,1,1,4),(59.6902604182061,
60.1952988581168,61.1818281967809,62.1683575354449,63.1548868741089,64.141416212773),
 .UNSPECIFIED.);
#4010=B_SPLINE_CURVE_WITH_KNOTS('',3,(#53056,#53057,#53058,#53059,#53060,
#53061,#53062,#53063,#53064),.UNSPECIFIED.,.F.,.F.,(4,1,1,1,1,1,4),(59.6902604182061,
59.7787497055172,60.7652790441813,61.7518083828453,62.7383377215093,63.7248670601734,
64.6638825844085),.UNSPECIFIED.);
#4011=B_SPLINE_CURVE_WITH_KNOTS('',3,(#53069,#53070,#53071,#53072,#53073,
#53074,#53075,#53076,#53077,#53078),.UNSPECIFIED.,.F.,.F.,(4,1,1,1,1,1,
1,4),(53.4070751110265,54.2761228261327,55.2626521647967,56.2491815034607,
57.2357108421248,58.2222401807888,59.2087695194528,59.6902604182061),
 .UNSPECIFIED.);
#4012=B_SPLINE_CURVE_WITH_KNOTS('',3,(#53079,#53080,#53081,#53082,#53083,
#53084,#53085,#53086,#53087,#53088),.UNSPECIFIED.,.F.,.F.,(4,1,1,1,1,1,
1,4),(53.4070751110265,53.8595736735331,54.8461030121971,55.8326323508611,
56.8191616895252,57.8056910281892,58.7922203668532,59.6902604182061),
 .UNSPECIFIED.);
#4013=B_SPLINE_CURVE_WITH_KNOTS('',3,(#53093,#53094,#53095,#53096,#53097,
#53098,#53099,#53100,#53101,#53102,#53103),.UNSPECIFIED.,.F.,.F.,(4,1,1,
1,1,1,1,1,4),(47.1238898038469,47.3704174554844,48.3569467941485,49.3434761328125,
50.3300054714765,51.3165348101406,52.3030641488046,53.2895934874686,53.4070751110265),
 .UNSPECIFIED.);
#4014=B_SPLINE_CURVE_WITH_KNOTS('',3,(#53104,#53105,#53106,#53107,#53108,
#53109,#53110,#53111,#53112,#53113),.UNSPECIFIED.,.F.,.F.,(4,1,1,1,1,1,
1,4),(47.1238898038469,47.9403976415489,48.9269269802129,49.913456318877,
50.899985657541,51.886514996205,52.873044334869,53.4070751110265),
 .UNSPECIFIED.);
#4015=B_SPLINE_CURVE_WITH_KNOTS('',3,(#53118,#53119,#53120,#53121,#53122,
#53123,#53124,#53125,#53126,#53127),.UNSPECIFIED.,.F.,.F.,(4,1,1,1,1,1,
1,4),(40.8407044966673,41.4512414235003,42.4377707621643,43.4243001008283,
44.4108294394924,45.3973587781564,46.3838881168204,47.1238898038469),
 .UNSPECIFIED.);
#4016=B_SPLINE_CURVE_WITH_KNOTS('',3,(#53128,#53129,#53130,#53131,#53132,
#53133,#53134,#53135,#53136,#53137,#53138),.UNSPECIFIED.,.F.,.F.,(4,1,1,
1,1,1,1,1,4),(40.8407044966673,41.0346922709007,42.0212216095647,43.0077509482287,
43.9942802868928,44.9808096255568,45.9673389642208,46.9538683028849,47.1238898038469),
 .UNSPECIFIED.);
#4017=B_SPLINE_CURVE_WITH_KNOTS('',3,(#53143,#53144,#53145,#53146,#53147,
#53148,#53149,#53150,#53151,#53152),.UNSPECIFIED.,.F.,.F.,(4,1,1,1,1,1,
1,4),(34.5575191894877,35.5320653915161,36.5185947301801,37.5051240688441,
38.4916534075082,39.4781827461722,40.4647120848362,40.8407044966673),
 .UNSPECIFIED.);
#4018=B_SPLINE_CURVE_WITH_KNOTS('',3,(#53153,#53154,#53155,#53156,#53157,
#53158,#53159,#53160,#53161,#53162),.UNSPECIFIED.,.F.,.F.,(4,1,1,1,1,1,
1,4),(34.5575191894877,35.1155162389165,36.1020455775805,37.0885749162446,
38.0751042549086,39.0616335935726,40.0481629322367,40.8407044966673),
 .UNSPECIFIED.);
#4019=B_SPLINE_CURVE_WITH_KNOTS('',3,(#53167,#53168,#53169,#53170,#53171,
#53172,#53173,#53174,#53175,#53176,#53177),.UNSPECIFIED.,.F.,.F.,(4,1,1,
1,1,1,1,1,4),(28.2743338823081,28.6263600208679,29.6128893595319,30.5994186981959,
31.58594803686,32.572477375524,33.559006714188,34.5455360528521,34.5575191894877),
 .UNSPECIFIED.);
#4020=B_SPLINE_CURVE_WITH_KNOTS('',3,(#53178,#53179,#53180,#53181,#53182,
#53183,#53184,#53185,#53186,#53187),.UNSPECIFIED.,.F.,.F.,(4,1,1,1,1,1,
1,4),(28.2743338823081,29.1963402069323,30.1828695455963,31.1693988842604,
32.1559282229244,33.1424575615884,34.1289869002525,34.5575191894877),
 .UNSPECIFIED.);
#4021=B_SPLINE_CURVE_WITH_KNOTS('',3,(#53192,#53193,#53194,#53195,#53196,
#53197,#53198,#53199,#53200,#53201),.UNSPECIFIED.,.F.,.F.,(4,1,1,1,1,1,
1,4),(21.9911485751285,22.7071839888837,23.6937133275477,24.6802426662117,
25.6667720048758,26.6533013435398,27.6398306822038,28.2743338823081),
 .UNSPECIFIED.);
#4022=B_SPLINE_CURVE_WITH_KNOTS('',3,(#53202,#53203,#53204,#53205,#53206,
#53207,#53208,#53209,#53210,#53211,#53212),.UNSPECIFIED.,.F.,.F.,(4,1,1,
1,1,1,1,1,4),(21.9911485751285,22.2906348362841,23.2771641749481,24.2636935136122,
25.2502228522762,26.2367521909402,27.2232815296043,28.2098108682683,28.2743338823081),
 .UNSPECIFIED.);
#4023=B_SPLINE_CURVE_WITH_KNOTS('',3,(#53218,#53219,#53220,#53221,#53222),
 .UNSPECIFIED.,.F.,.F.,(4,1,4),(14.3984001269719,15.3849294656359,15.7079632679489),
 .UNSPECIFIED.);
#4024=B_SPLINE_CURVE_WITH_KNOTS('',3,(#53225,#53226,#53227,#53228,#53229),
 .UNSPECIFIED.,.F.,.F.,(4,1,4),(13.8759337553363,14.8149492795714,15.7079632679489),
 .UNSPECIFIED.);
#4025=B_SPLINE_CURVE_WITH_KNOTS('',3,(#53235,#53236,#53237,#53238),
 .UNSPECIFIED.,.F.,.F.,(4,4),(51.5750455984138,52.2860549491937),
 .UNSPECIFIED.);
#4026=B_SPLINE_CURVE_WITH_KNOTS('',3,(#53250,#53251,#53252,#53253,#53254,
#53255,#53256,#53257,#53258,#53259),.UNSPECIFIED.,.F.,.F.,(4,3,3,4),(-50.2654824574367,
-49.3264669332015,-48.3399375945375,-47.8348991546267),.UNSPECIFIED.);
#4027=B_SPLINE_CURVE_WITH_KNOTS('',3,(#53264,#53265,#53266,#53267,#53268,
#53269,#53270,#53271,#53272,#53273,#53274,#53275,#53276,#53277,#53278,#53279,
#53280,#53281,#53282,#53283,#53284,#53285,#53286,#53287,#53288),
 .UNSPECIFIED.,.F.,.F.,(4,3,3,3,3,3,3,3,4),(45.2918602912342,45.3803495785454,
46.3668789172095,47.3534082558735,48.3399375945375,49.3264669332015,50.3129962718656,
51.2995256105296,51.5750455984138),.UNSPECIFIED.);
#4028=B_SPLINE_CURVE_WITH_KNOTS('',3,(#53289,#53290,#53291,#53292,#53293,
#53294,#53295,#53296,#53297,#53298,#53299,#53300,#53301,#53302,#53303,#53304,
#53305,#53306,#53307,#53308,#53309,#53310),.UNSPECIFIED.,.F.,.F.,(4,3,3,
3,3,3,3,4),(-47.8348991546267,-47.3534082558735,-46.3668789172094,-45.3803495785454,
-44.3938202398814,-43.4072909012173,-42.4207615625533,-41.5517138474471),
 .UNSPECIFIED.);
#4029=B_SPLINE_CURVE_WITH_KNOTS('',3,(#53315,#53316,#53317,#53318,#53319,
#53320,#53321,#53322,#53323,#53324,#53325,#53326,#53327,#53328,#53329,#53330,
#53331,#53332,#53333,#53334,#53335,#53336),.UNSPECIFIED.,.F.,.F.,(4,3,3,
3,3,3,3,4),(39.0086749840546,39.4611735465612,40.4477028852253,41.4342322238893,
42.4207615625533,43.4072909012174,44.3938202398814,45.2918602912342),
 .UNSPECIFIED.);
#4030=B_SPLINE_CURVE_WITH_KNOTS('',3,(#53337,#53338,#53339,#53340,#53341,
#53342,#53343,#53344,#53345,#53346,#53347,#53348,#53349,#53350,#53351,#53352,
#53353,#53354,#53355,#53356,#53357,#53358,#53359,#53360,#53361),
 .UNSPECIFIED.,.F.,.F.,(4,3,3,3,3,3,3,3,4),(-41.5517138474471,-41.4342322238893,
-40.4477028852253,-39.4611735465612,-38.4746442078972,-37.4881148692332,
-36.5015855305691,-35.5150561919051,-35.2685285402676),.UNSPECIFIED.);
#4031=B_SPLINE_CURVE_WITH_KNOTS('',3,(#53366,#53367,#53368,#53369,#53370,
#53371,#53372,#53373,#53374,#53375,#53376,#53377,#53378,#53379,#53380,#53381,
#53382,#53383,#53384,#53385,#53386,#53387),.UNSPECIFIED.,.F.,.F.,(4,3,3,
3,3,3,3,4),(32.725489676875,33.541997514577,34.5285268532411,35.5150561919051,
36.5015855305691,37.4881148692332,38.4746442078972,39.0086749840546),
 .UNSPECIFIED.);
#4032=B_SPLINE_CURVE_WITH_KNOTS('',3,(#53388,#53389,#53390,#53391,#53392,
#53393,#53394,#53395,#53396,#53397,#53398,#53399,#53400,#53401,#53402,#53403,
#53404,#53405,#53406,#53407,#53408,#53409),.UNSPECIFIED.,.F.,.F.,(4,3,3,
3,3,3,3,4),(-35.2685285402676,-34.5285268532411,-33.541997514577,-32.555468175913,
-31.568938837249,-30.5824094985849,-29.5958801599209,-28.985343233088),
 .UNSPECIFIED.);
#4033=B_SPLINE_CURVE_WITH_KNOTS('',3,(#53414,#53415,#53416,#53417,#53418,
#53419,#53420,#53421,#53422,#53423,#53424,#53425,#53426,#53427,#53428,#53429,
#53430,#53431,#53432,#53433,#53434,#53435,#53436,#53437,#53438),
 .UNSPECIFIED.,.F.,.F.,(4,3,3,3,3,3,3,3,4),(26.4423043696954,26.6362921439288,
27.6228214825929,28.6093508212569,29.5958801599209,30.582409498585,31.568938837249,
32.555468175913,32.725489676875),.UNSPECIFIED.);
#4034=B_SPLINE_CURVE_WITH_KNOTS('',3,(#53439,#53440,#53441,#53442,#53443,
#53444,#53445,#53446,#53447,#53448,#53449,#53450,#53451,#53452,#53453,#53454,
#53455,#53456,#53457,#53458,#53459,#53460),.UNSPECIFIED.,.F.,.F.,(4,3,3,
3,3,3,3,4),(-28.985343233088,-28.6093508212569,-27.6228214825929,-26.6362921439288,
-25.6497628052648,-24.6632334666008,-23.6767041279367,-22.7021579259084),
 .UNSPECIFIED.);
#4035=B_SPLINE_CURVE_WITH_KNOTS('',3,(#53465,#53466,#53467,#53468,#53469,
#53470,#53471,#53472,#53473,#53474,#53475,#53476,#53477,#53478,#53479,#53480,
#53481,#53482,#53483,#53484,#53485,#53486),.UNSPECIFIED.,.F.,.F.,(4,3,3,
3,3,3,3,4),(20.1591190625159,20.7171161119446,21.7036454506087,22.6901747892727,
23.6767041279367,24.6632334666008,25.6497628052648,26.4423043696954),
 .UNSPECIFIED.);
#4036=B_SPLINE_CURVE_WITH_KNOTS('',3,(#53487,#53488,#53489,#53490,#53491,
#53492,#53493,#53494,#53495,#53496,#53497,#53498,#53499,#53500,#53501,#53502,
#53503,#53504,#53505,#53506,#53507,#53508,#53509,#53510,#53511),
 .UNSPECIFIED.,.F.,.F.,(4,3,3,3,3,3,3,3,4),(-22.7021579259084,-22.6901747892727,
-21.7036454506087,-20.7171161119446,-19.7305867732806,-18.7440574346166,
-17.7575280959526,-16.7709987572885,-16.4189726187288),.UNSPECIFIED.);
#4037=B_SPLINE_CURVE_WITH_KNOTS('',3,(#53516,#53517,#53518,#53519,#53520,
#53521,#53522,#53523,#53524,#53525,#53526,#53527,#53528,#53529,#53530,#53531,
#53532,#53533,#53534,#53535,#53536,#53537),.UNSPECIFIED.,.F.,.F.,(4,3,3,
3,3,3,3,4),(13.8759337553363,14.7979400799605,15.7844694186245,16.7709987572885,
17.7575280959526,18.7440574346166,19.7305867732806,20.1591190625159),
 .UNSPECIFIED.);
#4038=B_SPLINE_CURVE_WITH_KNOTS('',3,(#53538,#53539,#53540,#53541,#53542,
#53543,#53544,#53545,#53546,#53547,#53548,#53549,#53550,#53551,#53552,#53553,
#53554,#53555,#53556,#53557,#53558,#53559),.UNSPECIFIED.,.F.,.F.,(4,3,3,
3,3,3,3,4),(-16.4189726187288,-15.7844694186245,-14.7979400799605,-13.8114107412964,
-12.8248814026324,-11.8383520639684,-10.8518227253043,-10.1357873115492),
 .UNSPECIFIED.);
#4039=B_SPLINE_CURVE_WITH_KNOTS('',3,(#53565,#53566,#53567,#53568,#53569,
#53570,#53571,#53572,#53573,#53574,#53575,#53576,#53577),.UNSPECIFIED.,
 .F.,.F.,(4,3,3,3,4),(-3.85260200436962,-2.9595880159921,-1.97305867732806,
-0.986529338664032,0.),.UNSPECIFIED.);
#4040=B_SPLINE_CURVE_WITH_KNOTS('',3,(#53580,#53581,#53582,#53583,#53584,
#53585,#53586,#53587,#53588,#53589,#53590,#53591,#53592,#53593,#53594,#53595,
#53596,#53597,#53598),.UNSPECIFIED.,.F.,.F.,(4,3,3,3,3,3,4),(2.02057249175687,
2.95958801599209,3.94611735465612,4.93264669332016,5.91917603198419,6.90570537064822,
7.59274844815668),.UNSPECIFIED.);
#4041=B_SPLINE_CURVE_WITH_KNOTS('',3,(#53604,#53605,#53606,#53607,#53608,
#53609,#53610,#53611),.UNSPECIFIED.,.F.,.F.,(4,1,1,1,1,4),(59.6902604182061,
60.1952988581168,61.1818281967809,62.1683575354449,63.1548868741089,64.141416212773),
 .UNSPECIFIED.);
#4042=B_SPLINE_CURVE_WITH_KNOTS('',3,(#53614,#53615,#53616,#53617,#53618,
#53619,#53620,#53621,#53622),.UNSPECIFIED.,.F.,.F.,(4,1,1,1,1,1,4),(59.6902604182061,
59.7787497055173,60.7652790441813,61.7518083828453,62.7383377215094,63.7248670601734,
64.6638825844085),.UNSPECIFIED.);
#4043=B_SPLINE_CURVE_WITH_KNOTS('',3,(#53627,#53628,#53629,#53630,#53631,
#53632,#53633,#53634,#53635,#53636),.UNSPECIFIED.,.F.,.F.,(4,1,1,1,1,1,
1,4),(53.4070751110265,54.2761228261326,55.2626521647967,56.2491815034607,
57.2357108421247,58.2222401807888,59.2087695194528,59.6902604182061),
 .UNSPECIFIED.);
#4044=B_SPLINE_CURVE_WITH_KNOTS('',3,(#53637,#53638,#53639,#53640,#53641,
#53642,#53643,#53644,#53645,#53646),.UNSPECIFIED.,.F.,.F.,(4,1,1,1,1,1,
1,4),(53.4070751110265,53.8595736735331,54.8461030121971,55.8326323508611,
56.8191616895252,57.8056910281892,58.7922203668532,59.6902604182061),
 .UNSPECIFIED.);
#4045=B_SPLINE_CURVE_WITH_KNOTS('',3,(#53651,#53652,#53653,#53654,#53655,
#53656,#53657,#53658,#53659,#53660,#53661),.UNSPECIFIED.,.F.,.F.,(4,1,1,
1,1,1,1,1,4),(47.1238898038469,47.3704174554844,48.3569467941485,49.3434761328125,
50.3300054714765,51.3165348101406,52.3030641488046,53.2895934874686,53.4070751110265),
 .UNSPECIFIED.);
#4046=B_SPLINE_CURVE_WITH_KNOTS('',3,(#53662,#53663,#53664,#53665,#53666,
#53667,#53668,#53669,#53670,#53671),.UNSPECIFIED.,.F.,.F.,(4,1,1,1,1,1,
1,4),(47.1238898038469,47.9403976415489,48.9269269802129,49.9134563188769,
50.899985657541,51.886514996205,52.873044334869,53.4070751110265),
 .UNSPECIFIED.);
#4047=B_SPLINE_CURVE_WITH_KNOTS('',3,(#53676,#53677,#53678,#53679,#53680,
#53681,#53682,#53683,#53684,#53685),.UNSPECIFIED.,.F.,.F.,(4,1,1,1,1,1,
1,4),(40.8407044966673,41.4512414235002,42.4377707621643,43.4243001008283,
44.4108294394923,45.3973587781564,46.3838881168204,47.1238898038469),
 .UNSPECIFIED.);
#4048=B_SPLINE_CURVE_WITH_KNOTS('',3,(#53686,#53687,#53688,#53689,#53690,
#53691,#53692,#53693,#53694,#53695,#53696),.UNSPECIFIED.,.F.,.F.,(4,1,1,
1,1,1,1,1,4),(40.8407044966673,41.0346922709007,42.0212216095647,43.0077509482287,
43.9942802868928,44.9808096255568,45.9673389642208,46.9538683028849,47.1238898038469),
 .UNSPECIFIED.);
#4049=B_SPLINE_CURVE_WITH_KNOTS('',3,(#53701,#53702,#53703,#53704,#53705,
#53706,#53707,#53708,#53709,#53710),.UNSPECIFIED.,.F.,.F.,(4,1,1,1,1,1,
1,4),(34.5575191894877,35.5320653915161,36.5185947301801,37.5051240688441,
38.4916534075082,39.4781827461722,40.4647120848362,40.8407044966673),
 .UNSPECIFIED.);
#4050=B_SPLINE_CURVE_WITH_KNOTS('',3,(#53711,#53712,#53713,#53714,#53715,
#53716,#53717,#53718,#53719,#53720),.UNSPECIFIED.,.F.,.F.,(4,1,1,1,1,1,
1,4),(34.5575191894877,35.1155162389165,36.1020455775805,37.0885749162445,
38.0751042549086,39.0616335935726,40.0481629322366,40.8407044966673),
 .UNSPECIFIED.);
#4051=B_SPLINE_CURVE_WITH_KNOTS('',3,(#53725,#53726,#53727,#53728,#53729,
#53730,#53731,#53732,#53733,#53734,#53735),.UNSPECIFIED.,.F.,.F.,(4,1,1,
1,1,1,1,1,4),(28.2743338823081,28.6263600208679,29.6128893595319,30.5994186981959,
31.5859480368599,32.572477375524,33.559006714188,34.545536052852,34.5575191894877),
 .UNSPECIFIED.);
#4052=B_SPLINE_CURVE_WITH_KNOTS('',3,(#53736,#53737,#53738,#53739,#53740,
#53741,#53742,#53743,#53744,#53745),.UNSPECIFIED.,.F.,.F.,(4,1,1,1,1,1,
1,4),(28.2743338823081,29.1963402069323,30.1828695455963,31.1693988842604,
32.1559282229244,33.1424575615884,34.1289869002525,34.5575191894877),
 .UNSPECIFIED.);
#4053=B_SPLINE_CURVE_WITH_KNOTS('',3,(#53750,#53751,#53752,#53753,#53754,
#53755,#53756,#53757,#53758,#53759),.UNSPECIFIED.,.F.,.F.,(4,1,1,1,1,1,
1,4),(21.9911485751285,22.7071839888837,23.6937133275477,24.6802426662117,
25.6667720048758,26.6533013435398,27.6398306822038,28.2743338823081),
 .UNSPECIFIED.);
#4054=B_SPLINE_CURVE_WITH_KNOTS('',3,(#53760,#53761,#53762,#53763,#53764,
#53765,#53766,#53767,#53768,#53769,#53770),.UNSPECIFIED.,.F.,.F.,(4,1,1,
1,1,1,1,1,4),(21.9911485751285,22.2906348362841,23.2771641749481,24.2636935136121,
25.2502228522762,26.2367521909402,27.2232815296042,28.2098108682683,28.2743338823081),
 .UNSPECIFIED.);
#4055=B_SPLINE_CURVE_WITH_KNOTS('',3,(#53776,#53777,#53778,#53779,#53780),
 .UNSPECIFIED.,.F.,.F.,(4,1,4),(14.3984001269718,15.3849294656359,15.7079632679489),
 .UNSPECIFIED.);
#4056=B_SPLINE_CURVE_WITH_KNOTS('',3,(#53783,#53784,#53785,#53786,#53787),
 .UNSPECIFIED.,.F.,.F.,(4,1,4),(13.8759337553363,14.8149492795714,15.7079632679489),
 .UNSPECIFIED.);
#4057=B_SPLINE_CURVE_WITH_KNOTS('',3,(#53793,#53794,#53795,#53796),
 .UNSPECIFIED.,.F.,.F.,(4,4),(51.5750455984138,52.2860549491936),
 .UNSPECIFIED.);
#4058=B_SPLINE_CURVE_WITH_KNOTS('',3,(#53808,#53809,#53810,#53811,#53812,
#53813,#53814,#53815,#53816,#53817),.UNSPECIFIED.,.F.,.F.,(4,3,3,4),(-50.2654824574367,
-49.3264669332015,-48.3399375945375,-47.8348991546267),.UNSPECIFIED.);
#4059=B_SPLINE_CURVE_WITH_KNOTS('',3,(#53822,#53823,#53824,#53825,#53826,
#53827,#53828,#53829,#53830,#53831,#53832,#53833,#53834,#53835,#53836,#53837,
#53838,#53839,#53840,#53841,#53842,#53843,#53844,#53845,#53846),
 .UNSPECIFIED.,.F.,.F.,(4,3,3,3,3,3,3,3,4),(45.2918602912342,45.3803495785454,
46.3668789172094,47.3534082558735,48.3399375945375,49.3264669332015,50.3129962718655,
51.2995256105296,51.5750455984138),.UNSPECIFIED.);
#4060=B_SPLINE_CURVE_WITH_KNOTS('',3,(#53847,#53848,#53849,#53850,#53851,
#53852,#53853,#53854,#53855,#53856,#53857,#53858,#53859,#53860,#53861,#53862,
#53863,#53864,#53865,#53866,#53867,#53868),.UNSPECIFIED.,.F.,.F.,(4,3,3,
3,3,3,3,4),(-47.8348991546267,-47.3534082558735,-46.3668789172094,-45.3803495785454,
-44.3938202398814,-43.4072909012173,-42.4207615625533,-41.5517138474471),
 .UNSPECIFIED.);
#4061=B_SPLINE_CURVE_WITH_KNOTS('',3,(#53873,#53874,#53875,#53876,#53877,
#53878,#53879,#53880,#53881,#53882,#53883,#53884,#53885,#53886,#53887,#53888,
#53889,#53890,#53891,#53892,#53893,#53894),.UNSPECIFIED.,.F.,.F.,(4,3,3,
3,3,3,3,4),(39.0086749840546,39.4611735465612,40.4477028852252,41.4342322238893,
42.4207615625533,43.4072909012173,44.3938202398814,45.2918602912342),
 .UNSPECIFIED.);
#4062=B_SPLINE_CURVE_WITH_KNOTS('',3,(#53895,#53896,#53897,#53898,#53899,
#53900,#53901,#53902,#53903,#53904,#53905,#53906,#53907,#53908,#53909,#53910,
#53911,#53912,#53913,#53914,#53915,#53916,#53917,#53918,#53919),
 .UNSPECIFIED.,.F.,.F.,(4,3,3,3,3,3,3,3,4),(-41.5517138474471,-41.4342322238893,
-40.4477028852252,-39.4611735465612,-38.4746442078972,-37.4881148692332,
-36.5015855305691,-35.5150561919051,-35.2685285402675),.UNSPECIFIED.);
#4063=B_SPLINE_CURVE_WITH_KNOTS('',3,(#53924,#53925,#53926,#53927,#53928,
#53929,#53930,#53931,#53932,#53933,#53934,#53935,#53936,#53937,#53938,#53939,
#53940,#53941,#53942,#53943,#53944,#53945),.UNSPECIFIED.,.F.,.F.,(4,3,3,
3,3,3,3,4),(32.725489676875,33.541997514577,34.5285268532411,35.5150561919051,
36.5015855305691,37.4881148692332,38.4746442078972,39.0086749840546),
 .UNSPECIFIED.);
#4064=B_SPLINE_CURVE_WITH_KNOTS('',3,(#53946,#53947,#53948,#53949,#53950,
#53951,#53952,#53953,#53954,#53955,#53956,#53957,#53958,#53959,#53960,#53961,
#53962,#53963,#53964,#53965,#53966,#53967),.UNSPECIFIED.,.F.,.F.,(4,3,3,
3,3,3,3,4),(-35.2685285402675,-34.5285268532411,-33.541997514577,-32.555468175913,
-31.568938837249,-30.582409498585,-29.5958801599209,-28.9853432330879),
 .UNSPECIFIED.);
#4065=B_SPLINE_CURVE_WITH_KNOTS('',3,(#53972,#53973,#53974,#53975,#53976,
#53977,#53978,#53979,#53980,#53981,#53982,#53983,#53984,#53985,#53986,#53987,
#53988,#53989,#53990,#53991,#53992,#53993,#53994,#53995,#53996),
 .UNSPECIFIED.,.F.,.F.,(4,3,3,3,3,3,3,3,4),(26.4423043696954,26.6362921439288,
27.6228214825928,28.6093508212569,29.5958801599209,30.5824094985849,31.568938837249,
32.555468175913,32.725489676875),.UNSPECIFIED.);
#4066=B_SPLINE_CURVE_WITH_KNOTS('',3,(#53997,#53998,#53999,#54000,#54001,
#54002,#54003,#54004,#54005,#54006,#54007,#54008,#54009,#54010,#54011,#54012,
#54013,#54014,#54015,#54016,#54017,#54018),.UNSPECIFIED.,.F.,.F.,(4,3,3,
3,3,3,3,4),(-28.9853432330879,-28.6093508212569,-27.6228214825929,-26.6362921439288,
-25.6497628052648,-24.6632334666008,-23.6767041279367,-22.7021579259084),
 .UNSPECIFIED.);
#4067=B_SPLINE_CURVE_WITH_KNOTS('',3,(#54023,#54024,#54025,#54026,#54027,
#54028,#54029,#54030,#54031,#54032,#54033,#54034,#54035,#54036,#54037,#54038,
#54039,#54040,#54041,#54042,#54043,#54044),.UNSPECIFIED.,.F.,.F.,(4,3,3,
3,3,3,3,4),(20.1591190625158,20.7171161119446,21.7036454506087,22.6901747892727,
23.6767041279367,24.6632334666008,25.6497628052648,26.4423043696954),
 .UNSPECIFIED.);
#4068=B_SPLINE_CURVE_WITH_KNOTS('',3,(#54045,#54046,#54047,#54048,#54049,
#54050,#54051,#54052,#54053,#54054,#54055,#54056,#54057,#54058,#54059,#54060,
#54061,#54062,#54063,#54064,#54065,#54066,#54067,#54068,#54069),
 .UNSPECIFIED.,.F.,.F.,(4,3,3,3,3,3,3,3,4),(-22.7021579259084,-22.6901747892727,
-21.7036454506087,-20.7171161119446,-19.7305867732806,-18.7440574346166,
-17.7575280959525,-16.7709987572885,-16.4189726187288),.UNSPECIFIED.);
#4069=B_SPLINE_CURVE_WITH_KNOTS('',3,(#54074,#54075,#54076,#54077,#54078,
#54079,#54080,#54081,#54082,#54083,#54084,#54085,#54086,#54087,#54088,#54089,
#54090,#54091,#54092,#54093,#54094,#54095),.UNSPECIFIED.,.F.,.F.,(4,3,3,
3,3,3,3,4),(13.8759337553362,14.7979400799604,15.7844694186245,16.7709987572885,
17.7575280959525,18.7440574346166,19.7305867732806,20.1591190625158),
 .UNSPECIFIED.);
#4070=B_SPLINE_CURVE_WITH_KNOTS('',3,(#54096,#54097,#54098,#54099,#54100,
#54101,#54102,#54103,#54104,#54105,#54106,#54107,#54108,#54109,#54110,#54111,
#54112,#54113,#54114,#54115,#54116,#54117),.UNSPECIFIED.,.F.,.F.,(4,3,3,
3,3,3,3,4),(-16.4189726187288,-15.7844694186245,-14.7979400799605,-13.8114107412964,
-12.8248814026324,-11.8383520639684,-10.8518227253043,-10.1357873115492),
 .UNSPECIFIED.);
#4071=B_SPLINE_CURVE_WITH_KNOTS('',3,(#54123,#54124,#54125,#54126,#54127,
#54128,#54129,#54130,#54131,#54132,#54133,#54134,#54135),.UNSPECIFIED.,
 .F.,.F.,(4,3,3,3,4),(-3.85260200436958,-2.95958801599209,-1.97305867732806,
-0.986529338664032,0.),.UNSPECIFIED.);
#4072=B_SPLINE_CURVE_WITH_KNOTS('',3,(#54138,#54139,#54140,#54141,#54142,
#54143,#54144,#54145,#54146,#54147,#54148,#54149,#54150,#54151,#54152,#54153,
#54154,#54155,#54156),.UNSPECIFIED.,.F.,.F.,(4,3,3,3,3,3,4),(2.02057249175685,
2.95958801599209,3.94611735465612,4.93264669332016,5.91917603198418,6.90570537064822,
7.59274844815664),.UNSPECIFIED.);
#4073=B_SPLINE_CURVE_WITH_KNOTS('',3,(#54162,#54163,#54164,#54165,#54166,
#54167,#54168,#54169),.UNSPECIFIED.,.F.,.F.,(4,1,1,1,1,4),(59.6902604182061,
60.1952988581168,61.1818281967808,62.1683575354449,63.1548868741089,64.1414162127729),
 .UNSPECIFIED.);
#4074=B_SPLINE_CURVE_WITH_KNOTS('',3,(#54172,#54173,#54174,#54175,#54176,
#54177,#54178,#54179,#54180),.UNSPECIFIED.,.F.,.F.,(4,1,1,1,1,1,4),(59.6902604182061,
59.7787497055172,60.7652790441813,61.7518083828453,62.7383377215093,63.7248670601733,
64.6638825844085),.UNSPECIFIED.);
#4075=B_SPLINE_CURVE_WITH_KNOTS('',3,(#54185,#54186,#54187,#54188,#54189,
#54190,#54191,#54192,#54193,#54194),.UNSPECIFIED.,.F.,.F.,(4,1,1,1,1,1,
1,4),(53.4070751110265,54.2761228261326,55.2626521647967,56.2491815034607,
57.2357108421247,58.2222401807888,59.2087695194528,59.6902604182061),
 .UNSPECIFIED.);
#4076=B_SPLINE_CURVE_WITH_KNOTS('',3,(#54195,#54196,#54197,#54198,#54199,
#54200,#54201,#54202,#54203,#54204),.UNSPECIFIED.,.F.,.F.,(4,1,1,1,1,1,
1,4),(53.4070751110265,53.859573673533,54.8461030121971,55.8326323508611,
56.8191616895251,57.8056910281892,58.7922203668532,59.6902604182061),
 .UNSPECIFIED.);
#4077=B_SPLINE_CURVE_WITH_KNOTS('',3,(#54209,#54210,#54211,#54212,#54213,
#54214,#54215,#54216,#54217,#54218,#54219),.UNSPECIFIED.,.F.,.F.,(4,1,1,
1,1,1,1,1,4),(47.1238898038469,47.3704174554844,48.3569467941485,49.3434761328125,
50.3300054714765,51.3165348101405,52.3030641488046,53.2895934874686,53.4070751110265),
 .UNSPECIFIED.);
#4078=B_SPLINE_CURVE_WITH_KNOTS('',3,(#54220,#54221,#54222,#54223,#54224,
#54225,#54226,#54227,#54228,#54229),.UNSPECIFIED.,.F.,.F.,(4,1,1,1,1,1,
1,4),(47.1238898038469,47.9403976415489,48.9269269802129,49.9134563188769,
50.899985657541,51.886514996205,52.873044334869,53.4070751110265),
 .UNSPECIFIED.);
#4079=B_SPLINE_CURVE_WITH_KNOTS('',3,(#54234,#54235,#54236,#54237,#54238,
#54239,#54240,#54241,#54242,#54243),.UNSPECIFIED.,.F.,.F.,(4,1,1,1,1,1,
1,4),(40.8407044966673,41.4512414235002,42.4377707621643,43.4243001008283,
44.4108294394923,45.3973587781564,46.3838881168204,47.1238898038469),
 .UNSPECIFIED.);
#4080=B_SPLINE_CURVE_WITH_KNOTS('',3,(#54244,#54245,#54246,#54247,#54248,
#54249,#54250,#54251,#54252,#54253,#54254),.UNSPECIFIED.,.F.,.F.,(4,1,1,
1,1,1,1,1,4),(40.8407044966673,41.0346922709006,42.0212216095647,43.0077509482287,
43.9942802868927,44.9808096255568,45.9673389642208,46.9538683028848,47.1238898038469),
 .UNSPECIFIED.);
#4081=B_SPLINE_CURVE_WITH_KNOTS('',3,(#54259,#54260,#54261,#54262,#54263,
#54264,#54265,#54266,#54267,#54268),.UNSPECIFIED.,.F.,.F.,(4,1,1,1,1,1,
1,4),(34.5575191894877,35.5320653915161,36.5185947301801,37.5051240688441,
38.4916534075082,39.4781827461722,40.4647120848362,40.8407044966673),
 .UNSPECIFIED.);
#4082=B_SPLINE_CURVE_WITH_KNOTS('',3,(#54269,#54270,#54271,#54272,#54273,
#54274,#54275,#54276,#54277,#54278),.UNSPECIFIED.,.F.,.F.,(4,1,1,1,1,1,
1,4),(34.5575191894877,35.1155162389165,36.1020455775805,37.0885749162445,
38.0751042549086,39.0616335935726,40.0481629322366,40.8407044966673),
 .UNSPECIFIED.);
#4083=B_SPLINE_CURVE_WITH_KNOTS('',3,(#54283,#54284,#54285,#54286,#54287,
#54288,#54289,#54290,#54291,#54292,#54293),.UNSPECIFIED.,.F.,.F.,(4,1,1,
1,1,1,1,1,4),(28.2743338823081,28.6263600208678,29.6128893595319,30.5994186981959,
31.5859480368599,32.572477375524,33.559006714188,34.545536052852,34.5575191894877),
 .UNSPECIFIED.);
#4084=B_SPLINE_CURVE_WITH_KNOTS('',3,(#54294,#54295,#54296,#54297,#54298,
#54299,#54300,#54301,#54302,#54303),.UNSPECIFIED.,.F.,.F.,(4,1,1,1,1,1,
1,4),(28.2743338823081,29.1963402069323,30.1828695455963,31.1693988842603,
32.1559282229244,33.1424575615884,34.1289869002524,34.5575191894877),
 .UNSPECIFIED.);
#4085=B_SPLINE_CURVE_WITH_KNOTS('',3,(#54308,#54309,#54310,#54311,#54312,
#54313,#54314,#54315,#54316,#54317),.UNSPECIFIED.,.F.,.F.,(4,1,1,1,1,1,
1,4),(21.9911485751285,22.7071839888837,23.6937133275477,24.6802426662117,
25.6667720048758,26.6533013435398,27.6398306822038,28.2743338823081),
 .UNSPECIFIED.);
#4086=B_SPLINE_CURVE_WITH_KNOTS('',3,(#54318,#54319,#54320,#54321,#54322,
#54323,#54324,#54325,#54326,#54327,#54328),.UNSPECIFIED.,.F.,.F.,(4,1,1,
1,1,1,1,1,4),(21.9911485751285,22.2906348362841,23.2771641749481,24.2636935136121,
25.2502228522762,26.2367521909402,27.2232815296042,28.2098108682683,28.2743338823081),
 .UNSPECIFIED.);
#4087=B_SPLINE_CURVE_WITH_KNOTS('',3,(#54334,#54335,#54336,#54337,#54338),
 .UNSPECIFIED.,.F.,.F.,(4,1,4),(14.3984001269718,15.3849294656359,15.7079632679489),
 .UNSPECIFIED.);
#4088=B_SPLINE_CURVE_WITH_KNOTS('',3,(#54341,#54342,#54343,#54344,#54345),
 .UNSPECIFIED.,.F.,.F.,(4,1,4),(13.8759337553363,14.8149492795714,15.7079632679489),
 .UNSPECIFIED.);
#4089=B_SPLINE_CURVE_WITH_KNOTS('',3,(#54351,#54352,#54353,#54354),
 .UNSPECIFIED.,.F.,.F.,(4,4),(51.5750455984138,52.2860549491936),
 .UNSPECIFIED.);
#4090=B_SPLINE_CURVE_WITH_KNOTS('',3,(#54366,#54367,#54368,#54369,#54370,
#54371,#54372,#54373,#54374,#54375),.UNSPECIFIED.,.F.,.F.,(4,3,3,4),(-50.2654824574367,
-49.3264669332015,-48.3399375945375,-47.8348991546267),.UNSPECIFIED.);
#4091=B_SPLINE_CURVE_WITH_KNOTS('',3,(#54380,#54381,#54382,#54383,#54384,
#54385,#54386,#54387,#54388,#54389,#54390,#54391,#54392,#54393,#54394,#54395,
#54396,#54397,#54398,#54399,#54400,#54401,#54402,#54403,#54404),
 .UNSPECIFIED.,.F.,.F.,(4,3,3,3,3,3,3,3,4),(45.2918602912342,45.3803495785454,
46.3668789172094,47.3534082558735,48.3399375945375,49.3264669332015,50.3129962718656,
51.2995256105296,51.5750455984138),.UNSPECIFIED.);
#4092=B_SPLINE_CURVE_WITH_KNOTS('',3,(#54405,#54406,#54407,#54408,#54409,
#54410,#54411,#54412,#54413,#54414,#54415,#54416,#54417,#54418,#54419,#54420,
#54421,#54422,#54423,#54424,#54425,#54426),.UNSPECIFIED.,.F.,.F.,(4,3,3,
3,3,3,3,4),(-47.8348991546267,-47.3534082558735,-46.3668789172095,-45.3803495785454,
-44.3938202398814,-43.4072909012174,-42.4207615625533,-41.5517138474471),
 .UNSPECIFIED.);
#4093=B_SPLINE_CURVE_WITH_KNOTS('',3,(#54431,#54432,#54433,#54434,#54435,
#54436,#54437,#54438,#54439,#54440,#54441,#54442,#54443,#54444,#54445,#54446,
#54447,#54448,#54449,#54450,#54451,#54452),.UNSPECIFIED.,.F.,.F.,(4,3,3,
3,3,3,3,4),(39.0086749840546,39.4611735465612,40.4477028852253,41.4342322238893,
42.4207615625533,43.4072909012174,44.3938202398814,45.2918602912342),
 .UNSPECIFIED.);
#4094=B_SPLINE_CURVE_WITH_KNOTS('',3,(#54453,#54454,#54455,#54456,#54457,
#54458,#54459,#54460,#54461,#54462,#54463,#54464,#54465,#54466,#54467,#54468,
#54469,#54470,#54471,#54472,#54473,#54474,#54475,#54476,#54477),
 .UNSPECIFIED.,.F.,.F.,(4,3,3,3,3,3,3,3,4),(-41.5517138474471,-41.4342322238893,
-40.4477028852253,-39.4611735465612,-38.4746442078972,-37.4881148692332,
-36.5015855305691,-35.5150561919051,-35.2685285402675),.UNSPECIFIED.);
#4095=B_SPLINE_CURVE_WITH_KNOTS('',3,(#54482,#54483,#54484,#54485,#54486,
#54487,#54488,#54489,#54490,#54491,#54492,#54493,#54494,#54495,#54496,#54497,
#54498,#54499,#54500,#54501,#54502,#54503),.UNSPECIFIED.,.F.,.F.,(4,3,3,
3,3,3,3,4),(32.725489676875,33.541997514577,34.5285268532411,35.5150561919051,
36.5015855305691,37.4881148692332,38.4746442078972,39.0086749840546),
 .UNSPECIFIED.);
#4096=B_SPLINE_CURVE_WITH_KNOTS('',3,(#54504,#54505,#54506,#54507,#54508,
#54509,#54510,#54511,#54512,#54513,#54514,#54515,#54516,#54517,#54518,#54519,
#54520,#54521,#54522,#54523,#54524,#54525),.UNSPECIFIED.,.F.,.F.,(4,3,3,
3,3,3,3,4),(-35.2685285402675,-34.5285268532411,-33.541997514577,-32.555468175913,
-31.568938837249,-30.582409498585,-29.5958801599209,-28.9853432330879),
 .UNSPECIFIED.);
#4097=B_SPLINE_CURVE_WITH_KNOTS('',3,(#54530,#54531,#54532,#54533,#54534,
#54535,#54536,#54537,#54538,#54539,#54540,#54541,#54542,#54543,#54544,#54545,
#54546,#54547,#54548,#54549,#54550,#54551,#54552,#54553,#54554),
 .UNSPECIFIED.,.F.,.F.,(4,3,3,3,3,3,3,3,4),(26.4423043696954,26.6362921439288,
27.6228214825929,28.6093508212569,29.5958801599209,30.582409498585,31.568938837249,
32.555468175913,32.725489676875),.UNSPECIFIED.);
#4098=B_SPLINE_CURVE_WITH_KNOTS('',3,(#54555,#54556,#54557,#54558,#54559,
#54560,#54561,#54562,#54563,#54564,#54565,#54566,#54567,#54568,#54569,#54570,
#54571,#54572,#54573,#54574,#54575,#54576),.UNSPECIFIED.,.F.,.F.,(4,3,3,
3,3,3,3,4),(-28.9853432330879,-28.6093508212569,-27.6228214825929,-26.6362921439288,
-25.6497628052648,-24.6632334666008,-23.6767041279367,-22.7021579259083),
 .UNSPECIFIED.);
#4099=B_SPLINE_CURVE_WITH_KNOTS('',3,(#54581,#54582,#54583,#54584,#54585,
#54586,#54587,#54588,#54589,#54590,#54591,#54592,#54593,#54594,#54595,#54596,
#54597,#54598,#54599,#54600,#54601,#54602),.UNSPECIFIED.,.F.,.F.,(4,3,3,
3,3,3,3,4),(20.1591190625158,20.7171161119446,21.7036454506087,22.6901747892727,
23.6767041279367,24.6632334666008,25.6497628052648,26.4423043696954),
 .UNSPECIFIED.);
#4100=B_SPLINE_CURVE_WITH_KNOTS('',3,(#54603,#54604,#54605,#54606,#54607,
#54608,#54609,#54610,#54611,#54612,#54613,#54614,#54615,#54616,#54617,#54618,
#54619,#54620,#54621,#54622,#54623,#54624,#54625,#54626,#54627),
 .UNSPECIFIED.,.F.,.F.,(4,3,3,3,3,3,3,3,4),(-22.7021579259083,-22.6901747892727,
-21.7036454506087,-20.7171161119447,-19.7305867732806,-18.7440574346166,
-17.7575280959526,-16.7709987572885,-16.4189726187287),.UNSPECIFIED.);
#4101=B_SPLINE_CURVE_WITH_KNOTS('',3,(#54632,#54633,#54634,#54635,#54636,
#54637,#54638,#54639,#54640,#54641,#54642,#54643,#54644,#54645,#54646,#54647,
#54648,#54649,#54650,#54651,#54652,#54653),.UNSPECIFIED.,.F.,.F.,(4,3,3,
3,3,3,3,4),(13.8759337553362,14.7979400799605,15.7844694186245,16.7709987572885,
17.7575280959526,18.7440574346166,19.7305867732806,20.1591190625158),
 .UNSPECIFIED.);
#4102=B_SPLINE_CURVE_WITH_KNOTS('',3,(#54654,#54655,#54656,#54657,#54658,
#54659,#54660,#54661,#54662,#54663,#54664,#54665,#54666,#54667,#54668,#54669,
#54670,#54671,#54672,#54673,#54674,#54675),.UNSPECIFIED.,.F.,.F.,(4,3,3,
3,3,3,3,4),(-16.4189726187287,-15.7844694186245,-14.7979400799605,-13.8114107412964,
-12.8248814026324,-11.8383520639684,-10.8518227253043,-10.1357873115491),
 .UNSPECIFIED.);
#4103=B_SPLINE_CURVE_WITH_KNOTS('',3,(#54681,#54682,#54683,#54684,#54685,
#54686,#54687,#54688,#54689,#54690,#54691,#54692,#54693),.UNSPECIFIED.,
 .F.,.F.,(4,3,3,3,4),(-3.85260200436958,-2.95958801599209,-1.97305867732806,
-0.986529338664031,0.),.UNSPECIFIED.);
#4104=B_SPLINE_CURVE_WITH_KNOTS('',3,(#54696,#54697,#54698,#54699,#54700,
#54701,#54702,#54703,#54704,#54705,#54706,#54707,#54708,#54709,#54710,#54711,
#54712,#54713,#54714),.UNSPECIFIED.,.F.,.F.,(4,3,3,3,3,3,4),(2.02057249175696,
2.95958801599209,3.94611735465612,4.93264669332015,5.91917603198418,6.90570537064821,
7.59274844815661),.UNSPECIFIED.);
#4105=B_SPLINE_CURVE_WITH_KNOTS('',3,(#54720,#54721,#54722,#54723,#54724,
#54725,#54726,#54727),.UNSPECIFIED.,.F.,.F.,(4,1,1,1,1,4),(59.6902604182061,
60.1952988581169,61.1818281967809,62.1683575354449,63.154886874109,64.141416212773),
 .UNSPECIFIED.);
#4106=B_SPLINE_CURVE_WITH_KNOTS('',3,(#54730,#54731,#54732,#54733,#54734,
#54735,#54736,#54737,#54738),.UNSPECIFIED.,.F.,.F.,(4,1,1,1,1,1,4),(59.6902604182061,
59.7787497055173,60.7652790441813,61.7518083828453,62.7383377215094,63.7248670601734,
64.6638825844086),.UNSPECIFIED.);
#4107=B_SPLINE_CURVE_WITH_KNOTS('',3,(#54743,#54744,#54745,#54746,#54747,
#54748,#54749,#54750,#54751,#54752),.UNSPECIFIED.,.F.,.F.,(4,1,1,1,1,1,
1,4),(53.4070751110265,54.2761228261327,55.2626521647967,56.2491815034607,
57.2357108421248,58.2222401807888,59.2087695194528,59.6902604182061),
 .UNSPECIFIED.);
#4108=B_SPLINE_CURVE_WITH_KNOTS('',3,(#54753,#54754,#54755,#54756,#54757,
#54758,#54759,#54760,#54761,#54762),.UNSPECIFIED.,.F.,.F.,(4,1,1,1,1,1,
1,4),(53.4070751110265,53.8595736735331,54.8461030121971,55.8326323508612,
56.8191616895252,57.8056910281892,58.7922203668532,59.6902604182061),
 .UNSPECIFIED.);
#4109=B_SPLINE_CURVE_WITH_KNOTS('',3,(#54767,#54768,#54769,#54770,#54771,
#54772,#54773,#54774,#54775,#54776,#54777),.UNSPECIFIED.,.F.,.F.,(4,1,1,
1,1,1,1,1,4),(47.1238898038469,47.3704174554845,48.3569467941485,49.3434761328125,
50.3300054714766,51.3165348101406,52.3030641488046,53.2895934874687,53.4070751110265),
 .UNSPECIFIED.);
#4110=B_SPLINE_CURVE_WITH_KNOTS('',3,(#54778,#54779,#54780,#54781,#54782,
#54783,#54784,#54785,#54786,#54787),.UNSPECIFIED.,.F.,.F.,(4,1,1,1,1,1,
1,4),(47.1238898038469,47.9403976415489,48.9269269802129,49.913456318877,
50.899985657541,51.886514996205,52.8730443348691,53.4070751110265),
 .UNSPECIFIED.);
#4111=B_SPLINE_CURVE_WITH_KNOTS('',3,(#54792,#54793,#54794,#54795,#54796,
#54797,#54798,#54799,#54800,#54801),.UNSPECIFIED.,.F.,.F.,(4,1,1,1,1,1,
1,4),(40.8407044966673,41.4512414235003,42.4377707621643,43.4243001008283,
44.4108294394924,45.3973587781564,46.3838881168204,47.1238898038469),
 .UNSPECIFIED.);
#4112=B_SPLINE_CURVE_WITH_KNOTS('',3,(#54802,#54803,#54804,#54805,#54806,
#54807,#54808,#54809,#54810,#54811,#54812),.UNSPECIFIED.,.F.,.F.,(4,1,1,
1,1,1,1,1,4),(40.8407044966673,41.0346922709007,42.0212216095647,43.0077509482288,
43.9942802868928,44.9808096255568,45.9673389642208,46.9538683028849,47.1238898038469),
 .UNSPECIFIED.);
#4113=B_SPLINE_CURVE_WITH_KNOTS('',3,(#54817,#54818,#54819,#54820,#54821,
#54822,#54823,#54824,#54825,#54826),.UNSPECIFIED.,.F.,.F.,(4,1,1,1,1,1,
1,4),(34.5575191894877,35.5320653915161,36.5185947301801,37.5051240688442,
38.4916534075082,39.4781827461722,40.4647120848363,40.8407044966673),
 .UNSPECIFIED.);
#4114=B_SPLINE_CURVE_WITH_KNOTS('',3,(#54827,#54828,#54829,#54830,#54831,
#54832,#54833,#54834,#54835,#54836),.UNSPECIFIED.,.F.,.F.,(4,1,1,1,1,1,
1,4),(34.5575191894877,35.1155162389165,36.1020455775805,37.0885749162446,
38.0751042549086,39.0616335935726,40.0481629322367,40.8407044966673),
 .UNSPECIFIED.);
#4115=B_SPLINE_CURVE_WITH_KNOTS('',3,(#54841,#54842,#54843,#54844,#54845,
#54846,#54847,#54848,#54849,#54850,#54851),.UNSPECIFIED.,.F.,.F.,(4,1,1,
1,1,1,1,1,4),(28.2743338823081,28.6263600208679,29.6128893595319,30.5994186981959,
31.58594803686,32.572477375524,33.559006714188,34.5455360528521,34.5575191894877),
 .UNSPECIFIED.);
#4116=B_SPLINE_CURVE_WITH_KNOTS('',3,(#54852,#54853,#54854,#54855,#54856,
#54857,#54858,#54859,#54860,#54861),.UNSPECIFIED.,.F.,.F.,(4,1,1,1,1,1,
1,4),(28.2743338823081,29.1963402069323,30.1828695455964,31.1693988842604,
32.1559282229244,33.1424575615884,34.1289869002525,34.5575191894877),
 .UNSPECIFIED.);
#4117=B_SPLINE_CURVE_WITH_KNOTS('',3,(#54866,#54867,#54868,#54869,#54870,
#54871,#54872,#54873,#54874,#54875),.UNSPECIFIED.,.F.,.F.,(4,1,1,1,1,1,
1,4),(21.9911485751285,22.7071839888837,23.6937133275477,24.6802426662118,
25.6667720048758,26.6533013435398,27.6398306822039,28.2743338823081),
 .UNSPECIFIED.);
#4118=B_SPLINE_CURVE_WITH_KNOTS('',3,(#54876,#54877,#54878,#54879,#54880,
#54881,#54882,#54883,#54884,#54885,#54886),.UNSPECIFIED.,.F.,.F.,(4,1,1,
1,1,1,1,1,4),(21.9911485751285,22.2906348362841,23.2771641749481,24.2636935136122,
25.2502228522762,26.2367521909402,27.2232815296043,28.2098108682683,28.2743338823081),
 .UNSPECIFIED.);
#4119=B_SPLINE_CURVE_WITH_KNOTS('',3,(#54892,#54893,#54894,#54895,#54896),
 .UNSPECIFIED.,.F.,.F.,(4,1,4),(14.3984001269719,15.3849294656359,15.7079632679489),
 .UNSPECIFIED.);
#4120=B_SPLINE_CURVE_WITH_KNOTS('',3,(#54899,#54900,#54901,#54902,#54903),
 .UNSPECIFIED.,.F.,.F.,(4,1,4),(13.8759337553363,14.8149492795714,15.7079632679489),
 .UNSPECIFIED.);
#4121=B_SPLINE_CURVE_WITH_KNOTS('',3,(#54909,#54910,#54911,#54912),
 .UNSPECIFIED.,.F.,.F.,(4,4),(51.5750455984138,52.2860549491936),
 .UNSPECIFIED.);
#4122=B_SPLINE_CURVE_WITH_KNOTS('',3,(#54924,#54925,#54926,#54927,#54928,
#54929,#54930,#54931,#54932,#54933),.UNSPECIFIED.,.F.,.F.,(4,3,3,4),(-50.2654824574366,
-49.3264669332015,-48.3399375945375,-47.8348991546267),.UNSPECIFIED.);
#4123=B_SPLINE_CURVE_WITH_KNOTS('',3,(#54938,#54939,#54940,#54941,#54942,
#54943,#54944,#54945,#54946,#54947,#54948,#54949,#54950,#54951,#54952,#54953,
#54954,#54955,#54956,#54957,#54958,#54959,#54960,#54961,#54962),
 .UNSPECIFIED.,.F.,.F.,(4,3,3,3,3,3,3,3,4),(45.2918602912342,45.3803495785454,
46.3668789172094,47.3534082558735,48.3399375945375,49.3264669332015,50.3129962718656,
51.2995256105296,51.5750455984138),.UNSPECIFIED.);
#4124=B_SPLINE_CURVE_WITH_KNOTS('',3,(#54963,#54964,#54965,#54966,#54967,
#54968,#54969,#54970,#54971,#54972,#54973,#54974,#54975,#54976,#54977,#54978,
#54979,#54980,#54981,#54982,#54983,#54984),.UNSPECIFIED.,.F.,.F.,(4,3,3,
3,3,3,3,4),(-47.8348991546267,-47.3534082558735,-46.3668789172094,-45.3803495785454,
-44.3938202398814,-43.4072909012173,-42.4207615625533,-41.5517138474471),
 .UNSPECIFIED.);
#4125=B_SPLINE_CURVE_WITH_KNOTS('',3,(#54989,#54990,#54991,#54992,#54993,
#54994,#54995,#54996,#54997,#54998,#54999,#55000,#55001,#55002,#55003,#55004,
#55005,#55006,#55007,#55008,#55009,#55010),.UNSPECIFIED.,.F.,.F.,(4,3,3,
3,3,3,3,4),(39.0086749840546,39.4611735465612,40.4477028852253,41.4342322238893,
42.4207615625533,43.4072909012173,44.3938202398814,45.2918602912342),
 .UNSPECIFIED.);
#4126=B_SPLINE_CURVE_WITH_KNOTS('',3,(#55011,#55012,#55013,#55014,#55015,
#55016,#55017,#55018,#55019,#55020,#55021,#55022,#55023,#55024,#55025,#55026,
#55027,#55028,#55029,#55030,#55031,#55032,#55033,#55034,#55035),
 .UNSPECIFIED.,.F.,.F.,(4,3,3,3,3,3,3,3,4),(-41.5517138474471,-41.4342322238893,
-40.4477028852253,-39.4611735465612,-38.4746442078972,-37.4881148692332,
-36.5015855305691,-35.5150561919051,-35.2685285402675),.UNSPECIFIED.);
#4127=B_SPLINE_CURVE_WITH_KNOTS('',3,(#55040,#55041,#55042,#55043,#55044,
#55045,#55046,#55047,#55048,#55049,#55050,#55051,#55052,#55053,#55054,#55055,
#55056,#55057,#55058,#55059,#55060,#55061),.UNSPECIFIED.,.F.,.F.,(4,3,3,
3,3,3,3,4),(32.725489676875,33.541997514577,34.5285268532411,35.5150561919051,
36.5015855305691,37.4881148692332,38.4746442078972,39.0086749840546),
 .UNSPECIFIED.);
#4128=B_SPLINE_CURVE_WITH_KNOTS('',3,(#55062,#55063,#55064,#55065,#55066,
#55067,#55068,#55069,#55070,#55071,#55072,#55073,#55074,#55075,#55076,#55077,
#55078,#55079,#55080,#55081,#55082,#55083),.UNSPECIFIED.,.F.,.F.,(4,3,3,
3,3,3,3,4),(-35.2685285402675,-34.5285268532411,-33.541997514577,-32.555468175913,
-31.568938837249,-30.5824094985849,-29.5958801599209,-28.9853432330879),
 .UNSPECIFIED.);
#4129=B_SPLINE_CURVE_WITH_KNOTS('',3,(#55088,#55089,#55090,#55091,#55092,
#55093,#55094,#55095,#55096,#55097,#55098,#55099,#55100,#55101,#55102,#55103,
#55104,#55105,#55106,#55107,#55108,#55109,#55110,#55111,#55112),
 .UNSPECIFIED.,.F.,.F.,(4,3,3,3,3,3,3,3,4),(26.4423043696954,26.6362921439288,
27.6228214825929,28.6093508212569,29.5958801599209,30.5824094985849,31.568938837249,
32.555468175913,32.725489676875),.UNSPECIFIED.);
#4130=B_SPLINE_CURVE_WITH_KNOTS('',3,(#55113,#55114,#55115,#55116,#55117,
#55118,#55119,#55120,#55121,#55122,#55123,#55124,#55125,#55126,#55127,#55128,
#55129,#55130,#55131,#55132,#55133,#55134),.UNSPECIFIED.,.F.,.F.,(4,3,3,
3,3,3,3,4),(-28.9853432330879,-28.6093508212569,-27.6228214825929,-26.6362921439288,
-25.6497628052648,-24.6632334666008,-23.6767041279367,-22.7021579259084),
 .UNSPECIFIED.);
#4131=B_SPLINE_CURVE_WITH_KNOTS('',3,(#55139,#55140,#55141,#55142,#55143,
#55144,#55145,#55146,#55147,#55148,#55149,#55150,#55151,#55152,#55153,#55154,
#55155,#55156,#55157,#55158,#55159,#55160),.UNSPECIFIED.,.F.,.F.,(4,3,3,
3,3,3,3,4),(20.1591190625158,20.7171161119446,21.7036454506087,22.6901747892727,
23.6767041279367,24.6632334666008,25.6497628052648,26.4423043696954),
 .UNSPECIFIED.);
#4132=B_SPLINE_CURVE_WITH_KNOTS('',3,(#55161,#55162,#55163,#55164,#55165,
#55166,#55167,#55168,#55169,#55170,#55171,#55172,#55173,#55174,#55175,#55176,
#55177,#55178,#55179,#55180,#55181,#55182,#55183,#55184,#55185),
 .UNSPECIFIED.,.F.,.F.,(4,3,3,3,3,3,3,3,4),(-22.7021579259084,-22.6901747892727,
-21.7036454506087,-20.7171161119446,-19.7305867732806,-18.7440574346166,
-17.7575280959525,-16.7709987572885,-16.4189726187288),.UNSPECIFIED.);
#4133=B_SPLINE_CURVE_WITH_KNOTS('',3,(#55190,#55191,#55192,#55193,#55194,
#55195,#55196,#55197,#55198,#55199,#55200,#55201,#55202,#55203,#55204,#55205,
#55206,#55207,#55208,#55209,#55210,#55211),.UNSPECIFIED.,.F.,.F.,(4,3,3,
3,3,3,3,4),(13.8759337553362,14.7979400799605,15.7844694186245,16.7709987572885,
17.7575280959526,18.7440574346166,19.7305867732806,20.1591190625158),
 .UNSPECIFIED.);
#4134=B_SPLINE_CURVE_WITH_KNOTS('',3,(#55212,#55213,#55214,#55215,#55216,
#55217,#55218,#55219,#55220,#55221,#55222,#55223,#55224,#55225,#55226,#55227,
#55228,#55229,#55230,#55231,#55232,#55233),.UNSPECIFIED.,.F.,.F.,(4,3,3,
3,3,3,3,4),(-16.4189726187288,-15.7844694186245,-14.7979400799605,-13.8114107412964,
-12.8248814026324,-11.8383520639684,-10.8518227253043,-10.1357873115492),
 .UNSPECIFIED.);
#4135=B_SPLINE_CURVE_WITH_KNOTS('',3,(#55239,#55240,#55241,#55242,#55243,
#55244,#55245,#55246,#55247,#55248,#55249,#55250,#55251),.UNSPECIFIED.,
 .F.,.F.,(4,3,3,3,4),(-3.85260200436961,-2.95958801599209,-1.97305867732806,
-0.986529338664032,0.),.UNSPECIFIED.);
#4136=B_SPLINE_CURVE_WITH_KNOTS('',3,(#55254,#55255,#55256,#55257,#55258,
#55259,#55260,#55261,#55262,#55263,#55264,#55265,#55266,#55267,#55268,#55269,
#55270,#55271,#55272),.UNSPECIFIED.,.F.,.F.,(4,3,3,3,3,3,4),(2.02057249175701,
2.9595880159921,3.94611735465613,4.93264669332016,5.91917603198419,6.90570537064822,
7.59274844815664),.UNSPECIFIED.);
#4137=B_SPLINE_CURVE_WITH_KNOTS('',3,(#55278,#55279,#55280,#55281,#55282,
#55283,#55284,#55285),.UNSPECIFIED.,.F.,.F.,(4,1,1,1,1,4),(59.6902604182061,
60.1952988581168,61.1818281967809,62.1683575354449,63.1548868741089,64.141416212773),
 .UNSPECIFIED.);
#4138=B_SPLINE_CURVE_WITH_KNOTS('',3,(#55288,#55289,#55290,#55291,#55292,
#55293,#55294,#55295,#55296),.UNSPECIFIED.,.F.,.F.,(4,1,1,1,1,1,4),(59.6902604182061,
59.7787497055173,60.7652790441813,61.7518083828453,62.7383377215094,63.7248670601734,
64.6638825844085),.UNSPECIFIED.);
#4139=B_SPLINE_CURVE_WITH_KNOTS('',3,(#55301,#55302,#55303,#55304,#55305,
#55306,#55307,#55308,#55309,#55310),.UNSPECIFIED.,.F.,.F.,(4,1,1,1,1,1,
1,4),(53.4070751110265,54.2761228261327,55.2626521647967,56.2491815034607,
57.2357108421247,58.2222401807888,59.2087695194528,59.6902604182061),
 .UNSPECIFIED.);
#4140=B_SPLINE_CURVE_WITH_KNOTS('',3,(#55311,#55312,#55313,#55314,#55315,
#55316,#55317,#55318,#55319,#55320),.UNSPECIFIED.,.F.,.F.,(4,1,1,1,1,1,
1,4),(53.4070751110265,53.8595736735331,54.8461030121971,55.8326323508611,
56.8191616895252,57.8056910281892,58.7922203668532,59.6902604182061),
 .UNSPECIFIED.);
#4141=B_SPLINE_CURVE_WITH_KNOTS('',3,(#55325,#55326,#55327,#55328,#55329,
#55330,#55331,#55332,#55333,#55334,#55335),.UNSPECIFIED.,.F.,.F.,(4,1,1,
1,1,1,1,1,4),(47.1238898038469,47.3704174554844,48.3569467941485,49.3434761328125,
50.3300054714765,51.3165348101406,52.3030641488046,53.2895934874686,53.4070751110265),
 .UNSPECIFIED.);
#4142=B_SPLINE_CURVE_WITH_KNOTS('',3,(#55336,#55337,#55338,#55339,#55340,
#55341,#55342,#55343,#55344,#55345),.UNSPECIFIED.,.F.,.F.,(4,1,1,1,1,1,
1,4),(47.1238898038469,47.9403976415489,48.9269269802129,49.913456318877,
50.899985657541,51.886514996205,52.873044334869,53.4070751110265),
 .UNSPECIFIED.);
#4143=B_SPLINE_CURVE_WITH_KNOTS('',3,(#55350,#55351,#55352,#55353,#55354,
#55355,#55356,#55357,#55358,#55359),.UNSPECIFIED.,.F.,.F.,(4,1,1,1,1,1,
1,4),(40.8407044966673,41.4512414235003,42.4377707621643,43.4243001008283,
44.4108294394924,45.3973587781564,46.3838881168204,47.1238898038469),
 .UNSPECIFIED.);
#4144=B_SPLINE_CURVE_WITH_KNOTS('',3,(#55360,#55361,#55362,#55363,#55364,
#55365,#55366,#55367,#55368,#55369,#55370),.UNSPECIFIED.,.F.,.F.,(4,1,1,
1,1,1,1,1,4),(40.8407044966673,41.0346922709007,42.0212216095647,43.0077509482287,
43.9942802868928,44.9808096255568,45.9673389642208,46.9538683028849,47.1238898038469),
 .UNSPECIFIED.);
#4145=B_SPLINE_CURVE_WITH_KNOTS('',3,(#55375,#55376,#55377,#55378,#55379,
#55380,#55381,#55382,#55383,#55384),.UNSPECIFIED.,.F.,.F.,(4,1,1,1,1,1,
1,4),(34.5575191894877,35.5320653915161,36.5185947301801,37.5051240688441,
38.4916534075082,39.4781827461722,40.4647120848362,40.8407044966673),
 .UNSPECIFIED.);
#4146=B_SPLINE_CURVE_WITH_KNOTS('',3,(#55385,#55386,#55387,#55388,#55389,
#55390,#55391,#55392,#55393,#55394),.UNSPECIFIED.,.F.,.F.,(4,1,1,1,1,1,
1,4),(34.5575191894877,35.1155162389165,36.1020455775805,37.0885749162446,
38.0751042549086,39.0616335935726,40.0481629322367,40.8407044966673),
 .UNSPECIFIED.);
#4147=B_SPLINE_CURVE_WITH_KNOTS('',3,(#55399,#55400,#55401,#55402,#55403,
#55404,#55405,#55406,#55407,#55408,#55409),.UNSPECIFIED.,.F.,.F.,(4,1,1,
1,1,1,1,1,4),(28.2743338823081,28.6263600208679,29.6128893595319,30.5994186981959,
31.58594803686,32.572477375524,33.559006714188,34.5455360528521,34.5575191894877),
 .UNSPECIFIED.);
#4148=B_SPLINE_CURVE_WITH_KNOTS('',3,(#55410,#55411,#55412,#55413,#55414,
#55415,#55416,#55417,#55418,#55419),.UNSPECIFIED.,.F.,.F.,(4,1,1,1,1,1,
1,4),(28.2743338823081,29.1963402069323,30.1828695455963,31.1693988842604,
32.1559282229244,33.1424575615884,34.1289869002525,34.5575191894877),
 .UNSPECIFIED.);
#4149=B_SPLINE_CURVE_WITH_KNOTS('',3,(#55424,#55425,#55426,#55427,#55428,
#55429,#55430,#55431,#55432,#55433),.UNSPECIFIED.,.F.,.F.,(4,1,1,1,1,1,
1,4),(21.9911485751285,22.7071839888837,23.6937133275477,24.6802426662117,
25.6667720048758,26.6533013435398,27.6398306822038,28.2743338823081),
 .UNSPECIFIED.);
#4150=B_SPLINE_CURVE_WITH_KNOTS('',3,(#55434,#55435,#55436,#55437,#55438,
#55439,#55440,#55441,#55442,#55443,#55444),.UNSPECIFIED.,.F.,.F.,(4,1,1,
1,1,1,1,1,4),(21.9911485751285,22.2906348362841,23.2771641749481,24.2636935136122,
25.2502228522762,26.2367521909402,27.2232815296043,28.2098108682683,28.2743338823081),
 .UNSPECIFIED.);
#4151=B_SPLINE_CURVE_WITH_KNOTS('',3,(#55450,#55451,#55452,#55453,#55454),
 .UNSPECIFIED.,.F.,.F.,(4,1,4),(14.3984001269719,15.3849294656359,15.7079632679489),
 .UNSPECIFIED.);
#4152=B_SPLINE_CURVE_WITH_KNOTS('',3,(#55457,#55458,#55459,#55460,#55461),
 .UNSPECIFIED.,.F.,.F.,(4,1,4),(13.8759337553363,14.8149492795714,15.7079632679489),
 .UNSPECIFIED.);
#4153=B_SPLINE_CURVE_WITH_KNOTS('',3,(#55467,#55468,#55469,#55470),
 .UNSPECIFIED.,.F.,.F.,(4,4),(51.5750455984138,52.2860549491936),
 .UNSPECIFIED.);
#4154=B_SPLINE_CURVE_WITH_KNOTS('',3,(#55482,#55483,#55484,#55485,#55486,
#55487,#55488,#55489,#55490,#55491),.UNSPECIFIED.,.F.,.F.,(4,3,3,4),(-50.2654824574366,
-49.3264669332015,-48.3399375945375,-47.8348991546267),.UNSPECIFIED.);
#4155=B_SPLINE_CURVE_WITH_KNOTS('',3,(#55496,#55497,#55498,#55499,#55500,
#55501,#55502,#55503,#55504,#55505,#55506,#55507,#55508,#55509,#55510,#55511,
#55512,#55513,#55514,#55515,#55516,#55517,#55518,#55519,#55520),
 .UNSPECIFIED.,.F.,.F.,(4,3,3,3,3,3,3,3,4),(45.2918602912342,45.3803495785454,
46.3668789172094,47.3534082558735,48.3399375945375,49.3264669332015,50.3129962718656,
51.2995256105296,51.5750455984138),.UNSPECIFIED.);
#4156=B_SPLINE_CURVE_WITH_KNOTS('',3,(#55521,#55522,#55523,#55524,#55525,
#55526,#55527,#55528,#55529,#55530,#55531,#55532,#55533,#55534,#55535,#55536,
#55537,#55538,#55539,#55540,#55541,#55542),.UNSPECIFIED.,.F.,.F.,(4,3,3,
3,3,3,3,4),(-47.8348991546267,-47.3534082558735,-46.3668789172094,-45.3803495785454,
-44.3938202398814,-43.4072909012173,-42.4207615625533,-41.5517138474471),
 .UNSPECIFIED.);
#4157=B_SPLINE_CURVE_WITH_KNOTS('',3,(#55547,#55548,#55549,#55550,#55551,
#55552,#55553,#55554,#55555,#55556,#55557,#55558,#55559,#55560,#55561,#55562,
#55563,#55564,#55565,#55566,#55567,#55568),.UNSPECIFIED.,.F.,.F.,(4,3,3,
3,3,3,3,4),(39.0086749840546,39.4611735465612,40.4477028852253,41.4342322238893,
42.4207615625533,43.4072909012173,44.3938202398814,45.2918602912342),
 .UNSPECIFIED.);
#4158=B_SPLINE_CURVE_WITH_KNOTS('',3,(#55569,#55570,#55571,#55572,#55573,
#55574,#55575,#55576,#55577,#55578,#55579,#55580,#55581,#55582,#55583,#55584,
#55585,#55586,#55587,#55588,#55589,#55590,#55591,#55592,#55593),
 .UNSPECIFIED.,.F.,.F.,(4,3,3,3,3,3,3,3,4),(-41.5517138474471,-41.4342322238893,
-40.4477028852252,-39.4611735465612,-38.4746442078972,-37.4881148692332,
-36.5015855305691,-35.5150561919051,-35.2685285402675),.UNSPECIFIED.);
#4159=B_SPLINE_CURVE_WITH_KNOTS('',3,(#55598,#55599,#55600,#55601,#55602,
#55603,#55604,#55605,#55606,#55607,#55608,#55609,#55610,#55611,#55612,#55613,
#55614,#55615,#55616,#55617,#55618,#55619),.UNSPECIFIED.,.F.,.F.,(4,3,3,
3,3,3,3,4),(32.725489676875,33.541997514577,34.5285268532411,35.5150561919051,
36.5015855305691,37.4881148692332,38.4746442078972,39.0086749840546),
 .UNSPECIFIED.);
#4160=B_SPLINE_CURVE_WITH_KNOTS('',3,(#55620,#55621,#55622,#55623,#55624,
#55625,#55626,#55627,#55628,#55629,#55630,#55631,#55632,#55633,#55634,#55635,
#55636,#55637,#55638,#55639,#55640,#55641),.UNSPECIFIED.,.F.,.F.,(4,3,3,
3,3,3,3,4),(-35.2685285402675,-34.5285268532411,-33.541997514577,-32.555468175913,
-31.568938837249,-30.5824094985849,-29.5958801599209,-28.9853432330879),
 .UNSPECIFIED.);
#4161=B_SPLINE_CURVE_WITH_KNOTS('',3,(#55646,#55647,#55648,#55649,#55650,
#55651,#55652,#55653,#55654,#55655,#55656,#55657,#55658,#55659,#55660,#55661,
#55662,#55663,#55664,#55665,#55666,#55667,#55668,#55669,#55670),
 .UNSPECIFIED.,.F.,.F.,(4,3,3,3,3,3,3,3,4),(26.4423043696954,26.6362921439288,
27.6228214825929,28.6093508212569,29.5958801599209,30.582409498585,31.568938837249,
32.555468175913,32.725489676875),.UNSPECIFIED.);
#4162=B_SPLINE_CURVE_WITH_KNOTS('',3,(#55671,#55672,#55673,#55674,#55675,
#55676,#55677,#55678,#55679,#55680,#55681,#55682,#55683,#55684,#55685,#55686,
#55687,#55688,#55689,#55690,#55691,#55692),.UNSPECIFIED.,.F.,.F.,(4,3,3,
3,3,3,3,4),(-28.9853432330879,-28.6093508212569,-27.6228214825929,-26.6362921439288,
-25.6497628052648,-24.6632334666008,-23.6767041279367,-22.7021579259083),
 .UNSPECIFIED.);
#4163=B_SPLINE_CURVE_WITH_KNOTS('',3,(#55697,#55698,#55699,#55700,#55701,
#55702,#55703,#55704,#55705,#55706,#55707,#55708,#55709,#55710,#55711,#55712,
#55713,#55714,#55715,#55716,#55717,#55718),.UNSPECIFIED.,.F.,.F.,(4,3,3,
3,3,3,3,4),(20.1591190625158,20.7171161119446,21.7036454506087,22.6901747892727,
23.6767041279367,24.6632334666008,25.6497628052648,26.4423043696954),
 .UNSPECIFIED.);
#4164=B_SPLINE_CURVE_WITH_KNOTS('',3,(#55719,#55720,#55721,#55722,#55723,
#55724,#55725,#55726,#55727,#55728,#55729,#55730,#55731,#55732,#55733,#55734,
#55735,#55736,#55737,#55738,#55739,#55740,#55741,#55742,#55743),
 .UNSPECIFIED.,.F.,.F.,(4,3,3,3,3,3,3,3,4),(-22.7021579259083,-22.6901747892727,
-21.7036454506087,-20.7171161119446,-19.7305867732806,-18.7440574346166,
-17.7575280959526,-16.7709987572885,-16.4189726187288),.UNSPECIFIED.);
#4165=B_SPLINE_CURVE_WITH_KNOTS('',3,(#55748,#55749,#55750,#55751,#55752,
#55753,#55754,#55755,#55756,#55757,#55758,#55759,#55760,#55761,#55762,#55763,
#55764,#55765,#55766,#55767,#55768,#55769),.UNSPECIFIED.,.F.,.F.,(4,3,3,
3,3,3,3,4),(13.8759337553362,14.7979400799605,15.7844694186245,16.7709987572885,
17.7575280959525,18.7440574346166,19.7305867732806,20.1591190625158),
 .UNSPECIFIED.);
#4166=B_SPLINE_CURVE_WITH_KNOTS('',3,(#55770,#55771,#55772,#55773,#55774,
#55775,#55776,#55777,#55778,#55779,#55780,#55781,#55782,#55783,#55784,#55785,
#55786,#55787,#55788,#55789,#55790,#55791),.UNSPECIFIED.,.F.,.F.,(4,3,3,
3,3,3,3,4),(-16.4189726187288,-15.7844694186245,-14.7979400799605,-13.8114107412964,
-12.8248814026324,-11.8383520639684,-10.8518227253043,-10.1357873115492),
 .UNSPECIFIED.);
#4167=B_SPLINE_CURVE_WITH_KNOTS('',3,(#55797,#55798,#55799,#55800,#55801,
#55802,#55803,#55804,#55805,#55806,#55807,#55808,#55809),.UNSPECIFIED.,
 .F.,.F.,(4,3,3,3,4),(-3.85260200436958,-2.95958801599209,-1.97305867732806,
-0.986529338664032,0.),.UNSPECIFIED.);
#4168=B_SPLINE_CURVE_WITH_KNOTS('',3,(#55812,#55813,#55814,#55815,#55816,
#55817,#55818,#55819,#55820,#55821,#55822,#55823,#55824,#55825,#55826,#55827,
#55828,#55829,#55830),.UNSPECIFIED.,.F.,.F.,(4,3,3,3,3,3,4),(2.02057249175696,
2.95958801599209,3.94611735465612,4.93264669332015,5.91917603198418,6.90570537064821,
7.59274844815664),.UNSPECIFIED.);
#4169=B_SPLINE_CURVE_WITH_KNOTS('',3,(#55836,#55837,#55838,#55839,#55840,
#55841,#55842,#55843),.UNSPECIFIED.,.F.,.F.,(4,1,1,1,1,4),(59.6902604182061,
60.1952988581168,61.1818281967809,62.1683575354449,63.1548868741089,64.141416212773),
 .UNSPECIFIED.);
#4170=B_SPLINE_CURVE_WITH_KNOTS('',3,(#55846,#55847,#55848,#55849,#55850,
#55851,#55852,#55853,#55854),.UNSPECIFIED.,.F.,.F.,(4,1,1,1,1,1,4),(59.6902604182061,
59.7787497055173,60.7652790441813,61.7518083828453,62.7383377215094,63.7248670601734,
64.6638825844085),.UNSPECIFIED.);
#4171=B_SPLINE_CURVE_WITH_KNOTS('',3,(#55859,#55860,#55861,#55862,#55863,
#55864,#55865,#55866,#55867,#55868),.UNSPECIFIED.,.F.,.F.,(4,1,1,1,1,1,
1,4),(53.4070751110265,54.2761228261327,55.2626521647967,56.2491815034607,
57.2357108421248,58.2222401807888,59.2087695194528,59.6902604182061),
 .UNSPECIFIED.);
#4172=B_SPLINE_CURVE_WITH_KNOTS('',3,(#55869,#55870,#55871,#55872,#55873,
#55874,#55875,#55876,#55877,#55878),.UNSPECIFIED.,.F.,.F.,(4,1,1,1,1,1,
1,4),(53.4070751110265,53.8595736735331,54.8461030121971,55.8326323508611,
56.8191616895252,57.8056910281892,58.7922203668532,59.6902604182061),
 .UNSPECIFIED.);
#4173=B_SPLINE_CURVE_WITH_KNOTS('',3,(#55883,#55884,#55885,#55886,#55887,
#55888,#55889,#55890,#55891,#55892,#55893),.UNSPECIFIED.,.F.,.F.,(4,1,1,
1,1,1,1,1,4),(47.1238898038469,47.3704174554844,48.3569467941485,49.3434761328125,
50.3300054714765,51.3165348101406,52.3030641488046,53.2895934874686,53.4070751110265),
 .UNSPECIFIED.);
#4174=B_SPLINE_CURVE_WITH_KNOTS('',3,(#55894,#55895,#55896,#55897,#55898,
#55899,#55900,#55901,#55902,#55903),.UNSPECIFIED.,.F.,.F.,(4,1,1,1,1,1,
1,4),(47.1238898038469,47.9403976415489,48.9269269802129,49.913456318877,
50.899985657541,51.886514996205,52.873044334869,53.4070751110265),
 .UNSPECIFIED.);
#4175=B_SPLINE_CURVE_WITH_KNOTS('',3,(#55908,#55909,#55910,#55911,#55912,
#55913,#55914,#55915,#55916,#55917),.UNSPECIFIED.,.F.,.F.,(4,1,1,1,1,1,
1,4),(40.8407044966673,41.4512414235003,42.4377707621643,43.4243001008283,
44.4108294394924,45.3973587781564,46.3838881168204,47.1238898038469),
 .UNSPECIFIED.);
#4176=B_SPLINE_CURVE_WITH_KNOTS('',3,(#55918,#55919,#55920,#55921,#55922,
#55923,#55924,#55925,#55926,#55927,#55928),.UNSPECIFIED.,.F.,.F.,(4,1,1,
1,1,1,1,1,4),(40.8407044966673,41.0346922709007,42.0212216095647,43.0077509482287,
43.9942802868928,44.9808096255568,45.9673389642208,46.9538683028849,47.1238898038469),
 .UNSPECIFIED.);
#4177=B_SPLINE_CURVE_WITH_KNOTS('',3,(#55933,#55934,#55935,#55936,#55937,
#55938,#55939,#55940,#55941,#55942),.UNSPECIFIED.,.F.,.F.,(4,1,1,1,1,1,
1,4),(34.5575191894877,35.5320653915161,36.5185947301801,37.5051240688441,
38.4916534075082,39.4781827461722,40.4647120848362,40.8407044966673),
 .UNSPECIFIED.);
#4178=B_SPLINE_CURVE_WITH_KNOTS('',3,(#55943,#55944,#55945,#55946,#55947,
#55948,#55949,#55950,#55951,#55952),.UNSPECIFIED.,.F.,.F.,(4,1,1,1,1,1,
1,4),(34.5575191894877,35.1155162389165,36.1020455775805,37.0885749162446,
38.0751042549086,39.0616335935726,40.0481629322367,40.8407044966673),
 .UNSPECIFIED.);
#4179=B_SPLINE_CURVE_WITH_KNOTS('',3,(#55957,#55958,#55959,#55960,#55961,
#55962,#55963,#55964,#55965,#55966,#55967),.UNSPECIFIED.,.F.,.F.,(4,1,1,
1,1,1,1,1,4),(28.2743338823081,28.6263600208679,29.6128893595319,30.5994186981959,
31.58594803686,32.572477375524,33.559006714188,34.5455360528521,34.5575191894877),
 .UNSPECIFIED.);
#4180=B_SPLINE_CURVE_WITH_KNOTS('',3,(#55968,#55969,#55970,#55971,#55972,
#55973,#55974,#55975,#55976,#55977),.UNSPECIFIED.,.F.,.F.,(4,1,1,1,1,1,
1,4),(28.2743338823081,29.1963402069323,30.1828695455963,31.1693988842604,
32.1559282229244,33.1424575615884,34.1289869002525,34.5575191894877),
 .UNSPECIFIED.);
#4181=B_SPLINE_CURVE_WITH_KNOTS('',3,(#55982,#55983,#55984,#55985,#55986,
#55987,#55988,#55989,#55990,#55991),.UNSPECIFIED.,.F.,.F.,(4,1,1,1,1,1,
1,4),(21.9911485751285,22.7071839888837,23.6937133275477,24.6802426662118,
25.6667720048758,26.6533013435398,27.6398306822038,28.2743338823081),
 .UNSPECIFIED.);
#4182=B_SPLINE_CURVE_WITH_KNOTS('',3,(#55992,#55993,#55994,#55995,#55996,
#55997,#55998,#55999,#56000,#56001,#56002),.UNSPECIFIED.,.F.,.F.,(4,1,1,
1,1,1,1,1,4),(21.9911485751285,22.2906348362841,23.2771641749481,24.2636935136122,
25.2502228522762,26.2367521909402,27.2232815296043,28.2098108682683,28.2743338823081),
 .UNSPECIFIED.);
#4183=B_SPLINE_CURVE_WITH_KNOTS('',3,(#56008,#56009,#56010,#56011,#56012),
 .UNSPECIFIED.,.F.,.F.,(4,1,4),(14.3984001269719,15.3849294656359,15.7079632679489),
 .UNSPECIFIED.);
#4184=B_SPLINE_CURVE_WITH_KNOTS('',3,(#56015,#56016,#56017,#56018,#56019),
 .UNSPECIFIED.,.F.,.F.,(4,1,4),(13.8759337553363,14.8149492795714,15.7079632679489),
 .UNSPECIFIED.);
#4185=B_SPLINE_CURVE_WITH_KNOTS('',3,(#56025,#56026,#56027,#56028),
 .UNSPECIFIED.,.F.,.F.,(4,4),(51.5750455984138,52.2860549491936),
 .UNSPECIFIED.);
#4186=B_SPLINE_CURVE_WITH_KNOTS('',3,(#56040,#56041,#56042,#56043,#56044,
#56045,#56046,#56047,#56048,#56049),.UNSPECIFIED.,.F.,.F.,(4,3,3,4),(-50.2654824574367,
-49.3264669332015,-48.3399375945375,-47.8348991546267),.UNSPECIFIED.);
#4187=B_SPLINE_CURVE_WITH_KNOTS('',3,(#56054,#56055,#56056,#56057,#56058,
#56059,#56060,#56061,#56062,#56063,#56064,#56065,#56066,#56067,#56068,#56069,
#56070,#56071,#56072,#56073,#56074,#56075,#56076,#56077,#56078),
 .UNSPECIFIED.,.F.,.F.,(4,3,3,3,3,3,3,3,4),(45.2918602912342,45.3803495785454,
46.3668789172094,47.3534082558735,48.3399375945375,49.3264669332015,50.3129962718656,
51.2995256105296,51.5750455984138),.UNSPECIFIED.);
#4188=B_SPLINE_CURVE_WITH_KNOTS('',3,(#56079,#56080,#56081,#56082,#56083,
#56084,#56085,#56086,#56087,#56088,#56089,#56090,#56091,#56092,#56093,#56094,
#56095,#56096,#56097,#56098,#56099,#56100),.UNSPECIFIED.,.F.,.F.,(4,3,3,
3,3,3,3,4),(-47.8348991546267,-47.3534082558735,-46.3668789172094,-45.3803495785454,
-44.3938202398814,-43.4072909012173,-42.4207615625533,-41.5517138474471),
 .UNSPECIFIED.);
#4189=B_SPLINE_CURVE_WITH_KNOTS('',3,(#56105,#56106,#56107,#56108,#56109,
#56110,#56111,#56112,#56113,#56114,#56115,#56116,#56117,#56118,#56119,#56120,
#56121,#56122,#56123,#56124,#56125,#56126),.UNSPECIFIED.,.F.,.F.,(4,3,3,
3,3,3,3,4),(39.0086749840546,39.4611735465612,40.4477028852253,41.4342322238893,
42.4207615625533,43.4072909012173,44.3938202398814,45.2918602912342),
 .UNSPECIFIED.);
#4190=B_SPLINE_CURVE_WITH_KNOTS('',3,(#56127,#56128,#56129,#56130,#56131,
#56132,#56133,#56134,#56135,#56136,#56137,#56138,#56139,#56140,#56141,#56142,
#56143,#56144,#56145,#56146,#56147,#56148,#56149,#56150,#56151),
 .UNSPECIFIED.,.F.,.F.,(4,3,3,3,3,3,3,3,4),(-41.5517138474471,-41.4342322238893,
-40.4477028852252,-39.4611735465612,-38.4746442078972,-37.4881148692332,
-36.5015855305691,-35.5150561919051,-35.2685285402675),.UNSPECIFIED.);
#4191=B_SPLINE_CURVE_WITH_KNOTS('',3,(#56156,#56157,#56158,#56159,#56160,
#56161,#56162,#56163,#56164,#56165,#56166,#56167,#56168,#56169,#56170,#56171,
#56172,#56173,#56174,#56175,#56176,#56177),.UNSPECIFIED.,.F.,.F.,(4,3,3,
3,3,3,3,4),(32.725489676875,33.541997514577,34.5285268532411,35.5150561919051,
36.5015855305691,37.4881148692332,38.4746442078972,39.0086749840546),
 .UNSPECIFIED.);
#4192=B_SPLINE_CURVE_WITH_KNOTS('',3,(#56178,#56179,#56180,#56181,#56182,
#56183,#56184,#56185,#56186,#56187,#56188,#56189,#56190,#56191,#56192,#56193,
#56194,#56195,#56196,#56197,#56198,#56199),.UNSPECIFIED.,.F.,.F.,(4,3,3,
3,3,3,3,4),(-35.2685285402675,-34.5285268532411,-33.541997514577,-32.555468175913,
-31.568938837249,-30.5824094985849,-29.5958801599209,-28.9853432330879),
 .UNSPECIFIED.);
#4193=B_SPLINE_CURVE_WITH_KNOTS('',3,(#56204,#56205,#56206,#56207,#56208,
#56209,#56210,#56211,#56212,#56213,#56214,#56215,#56216,#56217,#56218,#56219,
#56220,#56221,#56222,#56223,#56224,#56225,#56226,#56227,#56228),
 .UNSPECIFIED.,.F.,.F.,(4,3,3,3,3,3,3,3,4),(26.4423043696954,26.6362921439288,
27.6228214825929,28.6093508212569,29.5958801599209,30.582409498585,31.568938837249,
32.555468175913,32.725489676875),.UNSPECIFIED.);
#4194=B_SPLINE_CURVE_WITH_KNOTS('',3,(#56229,#56230,#56231,#56232,#56233,
#56234,#56235,#56236,#56237,#56238,#56239,#56240,#56241,#56242,#56243,#56244,
#56245,#56246,#56247,#56248,#56249,#56250),.UNSPECIFIED.,.F.,.F.,(4,3,3,
3,3,3,3,4),(-28.9853432330879,-28.6093508212569,-27.6228214825929,-26.6362921439288,
-25.6497628052648,-24.6632334666008,-23.6767041279367,-22.7021579259083),
 .UNSPECIFIED.);
#4195=B_SPLINE_CURVE_WITH_KNOTS('',3,(#56255,#56256,#56257,#56258,#56259,
#56260,#56261,#56262,#56263,#56264,#56265,#56266,#56267,#56268,#56269,#56270,
#56271,#56272,#56273,#56274,#56275,#56276),.UNSPECIFIED.,.F.,.F.,(4,3,3,
3,3,3,3,4),(20.1591190625158,20.7171161119446,21.7036454506087,22.6901747892727,
23.6767041279367,24.6632334666008,25.6497628052648,26.4423043696954),
 .UNSPECIFIED.);
#4196=B_SPLINE_CURVE_WITH_KNOTS('',3,(#56277,#56278,#56279,#56280,#56281,
#56282,#56283,#56284,#56285,#56286,#56287,#56288,#56289,#56290,#56291,#56292,
#56293,#56294,#56295,#56296,#56297,#56298,#56299,#56300,#56301),
 .UNSPECIFIED.,.F.,.F.,(4,3,3,3,3,3,3,3,4),(-22.7021579259083,-22.6901747892727,
-21.7036454506087,-20.7171161119446,-19.7305867732806,-18.7440574346166,
-17.7575280959525,-16.7709987572885,-16.4189726187287),.UNSPECIFIED.);
#4197=B_SPLINE_CURVE_WITH_KNOTS('',3,(#56306,#56307,#56308,#56309,#56310,
#56311,#56312,#56313,#56314,#56315,#56316,#56317,#56318,#56319,#56320,#56321,
#56322,#56323,#56324,#56325,#56326,#56327),.UNSPECIFIED.,.F.,.F.,(4,3,3,
3,3,3,3,4),(13.8759337553362,14.7979400799605,15.7844694186245,16.7709987572885,
17.7575280959525,18.7440574346166,19.7305867732806,20.1591190625158),
 .UNSPECIFIED.);
#4198=B_SPLINE_CURVE_WITH_KNOTS('',3,(#56328,#56329,#56330,#56331,#56332,
#56333,#56334,#56335,#56336,#56337,#56338,#56339,#56340,#56341,#56342,#56343,
#56344,#56345,#56346,#56347,#56348,#56349),.UNSPECIFIED.,.F.,.F.,(4,3,3,
3,3,3,3,4),(-16.4189726187287,-15.7844694186245,-14.7979400799605,-13.8114107412964,
-12.8248814026324,-11.8383520639684,-10.8518227253043,-10.1357873115492),
 .UNSPECIFIED.);
#4199=B_SPLINE_CURVE_WITH_KNOTS('',3,(#56355,#56356,#56357,#56358,#56359,
#56360,#56361,#56362,#56363,#56364,#56365,#56366,#56367),.UNSPECIFIED.,
 .F.,.F.,(4,3,3,3,4),(-3.85260200436958,-2.95958801599209,-1.97305867732806,
-0.986529338664031,0.),.UNSPECIFIED.);
#4200=B_SPLINE_CURVE_WITH_KNOTS('',3,(#56370,#56371,#56372,#56373,#56374,
#56375,#56376,#56377,#56378,#56379,#56380,#56381,#56382,#56383,#56384,#56385,
#56386,#56387,#56388),.UNSPECIFIED.,.F.,.F.,(4,3,3,3,3,3,4),(2.02057249175696,
2.95958801599209,3.94611735465612,4.93264669332015,5.91917603198419,6.90570537064821,
7.59274844815664),.UNSPECIFIED.);
#4201=B_SPLINE_CURVE_WITH_KNOTS('',3,(#56394,#56395,#56396,#56397,#56398,
#56399,#56400,#56401),.UNSPECIFIED.,.F.,.F.,(4,1,1,1,1,4),(59.6902604182061,
60.1952988581168,61.1818281967809,62.1683575354449,63.1548868741089,64.141416212773),
 .UNSPECIFIED.);
#4202=B_SPLINE_CURVE_WITH_KNOTS('',3,(#56404,#56405,#56406,#56407,#56408,
#56409,#56410,#56411,#56412),.UNSPECIFIED.,.F.,.F.,(4,1,1,1,1,1,4),(59.6902604182061,
59.7787497055173,60.7652790441813,61.7518083828453,62.7383377215094,63.7248670601734,
64.6638825844085),.UNSPECIFIED.);
#4203=B_SPLINE_CURVE_WITH_KNOTS('',3,(#56417,#56418,#56419,#56420,#56421,
#56422,#56423,#56424,#56425,#56426),.UNSPECIFIED.,.F.,.F.,(4,1,1,1,1,1,
1,4),(53.4070751110265,54.2761228261327,55.2626521647967,56.2491815034607,
57.2357108421248,58.2222401807888,59.2087695194528,59.6902604182061),
 .UNSPECIFIED.);
#4204=B_SPLINE_CURVE_WITH_KNOTS('',3,(#56427,#56428,#56429,#56430,#56431,
#56432,#56433,#56434,#56435,#56436),.UNSPECIFIED.,.F.,.F.,(4,1,1,1,1,1,
1,4),(53.4070751110265,53.8595736735331,54.8461030121971,55.8326323508611,
56.8191616895252,57.8056910281892,58.7922203668532,59.6902604182061),
 .UNSPECIFIED.);
#4205=B_SPLINE_CURVE_WITH_KNOTS('',3,(#56441,#56442,#56443,#56444,#56445,
#56446,#56447,#56448,#56449,#56450,#56451),.UNSPECIFIED.,.F.,.F.,(4,1,1,
1,1,1,1,1,4),(47.1238898038469,47.3704174554844,48.3569467941485,49.3434761328125,
50.3300054714765,51.3165348101406,52.3030641488046,53.2895934874686,53.4070751110265),
 .UNSPECIFIED.);
#4206=B_SPLINE_CURVE_WITH_KNOTS('',3,(#56452,#56453,#56454,#56455,#56456,
#56457,#56458,#56459,#56460,#56461),.UNSPECIFIED.,.F.,.F.,(4,1,1,1,1,1,
1,4),(47.1238898038469,47.9403976415489,48.9269269802129,49.913456318877,
50.899985657541,51.886514996205,52.873044334869,53.4070751110265),
 .UNSPECIFIED.);
#4207=B_SPLINE_CURVE_WITH_KNOTS('',3,(#56466,#56467,#56468,#56469,#56470,
#56471,#56472,#56473,#56474,#56475),.UNSPECIFIED.,.F.,.F.,(4,1,1,1,1,1,
1,4),(40.8407044966673,41.4512414235003,42.4377707621643,43.4243001008283,
44.4108294394924,45.3973587781564,46.3838881168204,47.1238898038469),
 .UNSPECIFIED.);
#4208=B_SPLINE_CURVE_WITH_KNOTS('',3,(#56476,#56477,#56478,#56479,#56480,
#56481,#56482,#56483,#56484,#56485,#56486),.UNSPECIFIED.,.F.,.F.,(4,1,1,
1,1,1,1,1,4),(40.8407044966673,41.0346922709007,42.0212216095647,43.0077509482287,
43.9942802868928,44.9808096255568,45.9673389642208,46.9538683028849,47.1238898038469),
 .UNSPECIFIED.);
#4209=B_SPLINE_CURVE_WITH_KNOTS('',3,(#56491,#56492,#56493,#56494,#56495,
#56496,#56497,#56498,#56499,#56500),.UNSPECIFIED.,.F.,.F.,(4,1,1,1,1,1,
1,4),(34.5575191894877,35.5320653915161,36.5185947301801,37.5051240688441,
38.4916534075082,39.4781827461722,40.4647120848362,40.8407044966673),
 .UNSPECIFIED.);
#4210=B_SPLINE_CURVE_WITH_KNOTS('',3,(#56501,#56502,#56503,#56504,#56505,
#56506,#56507,#56508,#56509,#56510),.UNSPECIFIED.,.F.,.F.,(4,1,1,1,1,1,
1,4),(34.5575191894877,35.1155162389165,36.1020455775805,37.0885749162446,
38.0751042549086,39.0616335935726,40.0481629322367,40.8407044966673),
 .UNSPECIFIED.);
#4211=B_SPLINE_CURVE_WITH_KNOTS('',3,(#56515,#56516,#56517,#56518,#56519,
#56520,#56521,#56522,#56523,#56524,#56525),.UNSPECIFIED.,.F.,.F.,(4,1,1,
1,1,1,1,1,4),(28.2743338823081,28.6263600208679,29.6128893595319,30.5994186981959,
31.58594803686,32.572477375524,33.559006714188,34.5455360528521,34.5575191894877),
 .UNSPECIFIED.);
#4212=B_SPLINE_CURVE_WITH_KNOTS('',3,(#56526,#56527,#56528,#56529,#56530,
#56531,#56532,#56533,#56534,#56535),.UNSPECIFIED.,.F.,.F.,(4,1,1,1,1,1,
1,4),(28.2743338823081,29.1963402069323,30.1828695455963,31.1693988842604,
32.1559282229244,33.1424575615884,34.1289869002525,34.5575191894877),
 .UNSPECIFIED.);
#4213=B_SPLINE_CURVE_WITH_KNOTS('',3,(#56540,#56541,#56542,#56543,#56544,
#56545,#56546,#56547,#56548,#56549),.UNSPECIFIED.,.F.,.F.,(4,1,1,1,1,1,
1,4),(21.9911485751285,22.7071839888837,23.6937133275477,24.6802426662118,
25.6667720048758,26.6533013435398,27.6398306822038,28.2743338823081),
 .UNSPECIFIED.);
#4214=B_SPLINE_CURVE_WITH_KNOTS('',3,(#56550,#56551,#56552,#56553,#56554,
#56555,#56556,#56557,#56558,#56559,#56560),.UNSPECIFIED.,.F.,.F.,(4,1,1,
1,1,1,1,1,4),(21.9911485751285,22.2906348362841,23.2771641749481,24.2636935136122,
25.2502228522762,26.2367521909402,27.2232815296043,28.2098108682683,28.2743338823081),
 .UNSPECIFIED.);
#4215=B_SPLINE_CURVE_WITH_KNOTS('',3,(#56566,#56567,#56568,#56569,#56570),
 .UNSPECIFIED.,.F.,.F.,(4,1,4),(14.3984001269719,15.3849294656359,15.7079632679489),
 .UNSPECIFIED.);
#4216=B_SPLINE_CURVE_WITH_KNOTS('',3,(#56573,#56574,#56575,#56576,#56577),
 .UNSPECIFIED.,.F.,.F.,(4,1,4),(13.8759337553363,14.8149492795714,15.7079632679489),
 .UNSPECIFIED.);
#4217=B_SPLINE_CURVE_WITH_KNOTS('',3,(#56583,#56584,#56585,#56586),
 .UNSPECIFIED.,.F.,.F.,(4,4),(51.5750455984138,52.2860549491936),
 .UNSPECIFIED.);
#4218=B_SPLINE_CURVE_WITH_KNOTS('',3,(#56598,#56599,#56600,#56601,#56602,
#56603,#56604,#56605,#56606,#56607),.UNSPECIFIED.,.F.,.F.,(4,3,3,4),(-50.2654824574367,
-49.3264669332015,-48.3399375945375,-47.8348991546267),.UNSPECIFIED.);
#4219=B_SPLINE_CURVE_WITH_KNOTS('',3,(#56612,#56613,#56614,#56615,#56616,
#56617,#56618,#56619,#56620,#56621,#56622,#56623,#56624,#56625,#56626,#56627,
#56628,#56629,#56630,#56631,#56632,#56633,#56634,#56635,#56636),
 .UNSPECIFIED.,.F.,.F.,(4,3,3,3,3,3,3,3,4),(45.2918602912342,45.3803495785454,
46.3668789172094,47.3534082558735,48.3399375945375,49.3264669332015,50.3129962718656,
51.2995256105296,51.5750455984138),.UNSPECIFIED.);
#4220=B_SPLINE_CURVE_WITH_KNOTS('',3,(#56637,#56638,#56639,#56640,#56641,
#56642,#56643,#56644,#56645,#56646,#56647,#56648,#56649,#56650,#56651,#56652,
#56653,#56654,#56655,#56656,#56657,#56658),.UNSPECIFIED.,.F.,.F.,(4,3,3,
3,3,3,3,4),(-47.8348991546267,-47.3534082558735,-46.3668789172094,-45.3803495785454,
-44.3938202398814,-43.4072909012174,-42.4207615625533,-41.5517138474471),
 .UNSPECIFIED.);
#4221=B_SPLINE_CURVE_WITH_KNOTS('',3,(#56663,#56664,#56665,#56666,#56667,
#56668,#56669,#56670,#56671,#56672,#56673,#56674,#56675,#56676,#56677,#56678,
#56679,#56680,#56681,#56682,#56683,#56684),.UNSPECIFIED.,.F.,.F.,(4,3,3,
3,3,3,3,4),(39.0086749840546,39.4611735465612,40.4477028852253,41.4342322238893,
42.4207615625533,43.4072909012174,44.3938202398814,45.2918602912342),
 .UNSPECIFIED.);
#4222=B_SPLINE_CURVE_WITH_KNOTS('',3,(#56685,#56686,#56687,#56688,#56689,
#56690,#56691,#56692,#56693,#56694,#56695,#56696,#56697,#56698,#56699,#56700,
#56701,#56702,#56703,#56704,#56705,#56706,#56707,#56708,#56709),
 .UNSPECIFIED.,.F.,.F.,(4,3,3,3,3,3,3,3,4),(-41.5517138474471,-41.4342322238893,
-40.4477028852253,-39.4611735465612,-38.4746442078972,-37.4881148692332,
-36.5015855305691,-35.5150561919051,-35.2685285402676),.UNSPECIFIED.);
#4223=B_SPLINE_CURVE_WITH_KNOTS('',3,(#56714,#56715,#56716,#56717,#56718,
#56719,#56720,#56721,#56722,#56723,#56724,#56725,#56726,#56727,#56728,#56729,
#56730,#56731,#56732,#56733,#56734,#56735),.UNSPECIFIED.,.F.,.F.,(4,3,3,
3,3,3,3,4),(32.725489676875,33.541997514577,34.5285268532411,35.5150561919051,
36.5015855305691,37.4881148692332,38.4746442078972,39.0086749840546),
 .UNSPECIFIED.);
#4224=B_SPLINE_CURVE_WITH_KNOTS('',3,(#56736,#56737,#56738,#56739,#56740,
#56741,#56742,#56743,#56744,#56745,#56746,#56747,#56748,#56749,#56750,#56751,
#56752,#56753,#56754,#56755,#56756,#56757),.UNSPECIFIED.,.F.,.F.,(4,3,3,
3,3,3,3,4),(-35.2685285402676,-34.5285268532411,-33.541997514577,-32.555468175913,
-31.568938837249,-30.5824094985849,-29.5958801599209,-28.985343233088),
 .UNSPECIFIED.);
#4225=B_SPLINE_CURVE_WITH_KNOTS('',3,(#56762,#56763,#56764,#56765,#56766,
#56767,#56768,#56769,#56770,#56771,#56772,#56773,#56774,#56775,#56776,#56777,
#56778,#56779,#56780,#56781,#56782,#56783,#56784,#56785,#56786),
 .UNSPECIFIED.,.F.,.F.,(4,3,3,3,3,3,3,3,4),(26.4423043696954,26.6362921439288,
27.6228214825929,28.6093508212569,29.5958801599209,30.582409498585,31.568938837249,
32.555468175913,32.725489676875),.UNSPECIFIED.);
#4226=B_SPLINE_CURVE_WITH_KNOTS('',3,(#56787,#56788,#56789,#56790,#56791,
#56792,#56793,#56794,#56795,#56796,#56797,#56798,#56799,#56800,#56801,#56802,
#56803,#56804,#56805,#56806,#56807,#56808),.UNSPECIFIED.,.F.,.F.,(4,3,3,
3,3,3,3,4),(-28.985343233088,-28.6093508212569,-27.6228214825929,-26.6362921439288,
-25.6497628052648,-24.6632334666008,-23.6767041279367,-22.7021579259084),
 .UNSPECIFIED.);
#4227=B_SPLINE_CURVE_WITH_KNOTS('',3,(#56813,#56814,#56815,#56816,#56817,
#56818,#56819,#56820,#56821,#56822,#56823,#56824,#56825,#56826,#56827,#56828,
#56829,#56830,#56831,#56832,#56833,#56834),.UNSPECIFIED.,.F.,.F.,(4,3,3,
3,3,3,3,4),(20.1591190625159,20.7171161119446,21.7036454506087,22.6901747892727,
23.6767041279367,24.6632334666008,25.6497628052648,26.4423043696954),
 .UNSPECIFIED.);
#4228=B_SPLINE_CURVE_WITH_KNOTS('',3,(#56835,#56836,#56837,#56838,#56839,
#56840,#56841,#56842,#56843,#56844,#56845,#56846,#56847,#56848,#56849,#56850,
#56851,#56852,#56853,#56854,#56855,#56856,#56857,#56858,#56859),
 .UNSPECIFIED.,.F.,.F.,(4,3,3,3,3,3,3,3,4),(-22.7021579259084,-22.6901747892727,
-21.7036454506087,-20.7171161119446,-19.7305867732806,-18.7440574346166,
-17.7575280959526,-16.7709987572885,-16.4189726187288),.UNSPECIFIED.);
#4229=B_SPLINE_CURVE_WITH_KNOTS('',3,(#56864,#56865,#56866,#56867,#56868,
#56869,#56870,#56871,#56872,#56873,#56874,#56875,#56876,#56877,#56878,#56879,
#56880,#56881,#56882,#56883,#56884,#56885),.UNSPECIFIED.,.F.,.F.,(4,3,3,
3,3,3,3,4),(13.8759337553363,14.7979400799605,15.7844694186245,16.7709987572885,
17.7575280959526,18.7440574346166,19.7305867732806,20.1591190625159),
 .UNSPECIFIED.);
#4230=B_SPLINE_CURVE_WITH_KNOTS('',3,(#56886,#56887,#56888,#56889,#56890,
#56891,#56892,#56893,#56894,#56895,#56896,#56897,#56898,#56899,#56900,#56901,
#56902,#56903,#56904,#56905,#56906,#56907),.UNSPECIFIED.,.F.,.F.,(4,3,3,
3,3,3,3,4),(-16.4189726187288,-15.7844694186245,-14.7979400799605,-13.8114107412964,
-12.8248814026324,-11.8383520639684,-10.8518227253043,-10.1357873115492),
 .UNSPECIFIED.);
#4231=B_SPLINE_CURVE_WITH_KNOTS('',3,(#56913,#56914,#56915,#56916,#56917,
#56918,#56919,#56920,#56921,#56922,#56923,#56924,#56925),.UNSPECIFIED.,
 .F.,.F.,(4,3,3,3,4),(-3.85260200436962,-2.95958801599209,-1.97305867732806,
-0.986529338664032,0.),.UNSPECIFIED.);
#4232=B_SPLINE_CURVE_WITH_KNOTS('',3,(#56928,#56929,#56930,#56931,#56932,
#56933,#56934,#56935,#56936,#56937,#56938,#56939,#56940,#56941,#56942,#56943,
#56944,#56945,#56946),.UNSPECIFIED.,.F.,.F.,(4,3,3,3,3,3,4),(2.02057249175696,
2.95958801599209,3.94611735465612,4.93264669332015,5.91917603198418,6.90570537064821,
7.59274844815668),.UNSPECIFIED.);
#4233=B_SPLINE_CURVE_WITH_KNOTS('',3,(#56952,#56953,#56954,#56955,#56956,
#56957,#56958,#56959),.UNSPECIFIED.,.F.,.F.,(4,1,1,1,1,4),(59.6902604182061,
60.1952988581168,61.1818281967809,62.1683575354449,63.1548868741089,64.1414162127729),
 .UNSPECIFIED.);
#4234=B_SPLINE_CURVE_WITH_KNOTS('',3,(#56962,#56963,#56964,#56965,#56966,
#56967,#56968,#56969,#56970),.UNSPECIFIED.,.F.,.F.,(4,1,1,1,1,1,4),(59.6902604182061,
59.7787497055172,60.7652790441813,61.7518083828453,62.7383377215093,63.7248670601734,
64.6638825844085),.UNSPECIFIED.);
#4235=B_SPLINE_CURVE_WITH_KNOTS('',3,(#56975,#56976,#56977,#56978,#56979,
#56980,#56981,#56982,#56983,#56984),.UNSPECIFIED.,.F.,.F.,(4,1,1,1,1,1,
1,4),(53.4070751110265,54.2761228261326,55.2626521647967,56.2491815034607,
57.2357108421247,58.2222401807888,59.2087695194528,59.6902604182061),
 .UNSPECIFIED.);
#4236=B_SPLINE_CURVE_WITH_KNOTS('',3,(#56985,#56986,#56987,#56988,#56989,
#56990,#56991,#56992,#56993,#56994),.UNSPECIFIED.,.F.,.F.,(4,1,1,1,1,1,
1,4),(53.4070751110265,53.8595736735331,54.8461030121971,55.8326323508611,
56.8191616895252,57.8056910281892,58.7922203668532,59.6902604182061),
 .UNSPECIFIED.);
#4237=B_SPLINE_CURVE_WITH_KNOTS('',3,(#56999,#57000,#57001,#57002,#57003,
#57004,#57005,#57006,#57007,#57008,#57009),.UNSPECIFIED.,.F.,.F.,(4,1,1,
1,1,1,1,1,4),(47.1238898038469,47.3704174554844,48.3569467941485,49.3434761328125,
50.3300054714765,51.3165348101406,52.3030641488046,53.2895934874686,53.4070751110265),
 .UNSPECIFIED.);
#4238=B_SPLINE_CURVE_WITH_KNOTS('',3,(#57010,#57011,#57012,#57013,#57014,
#57015,#57016,#57017,#57018,#57019),.UNSPECIFIED.,.F.,.F.,(4,1,1,1,1,1,
1,4),(47.1238898038469,47.9403976415489,48.9269269802129,49.9134563188769,
50.899985657541,51.886514996205,52.873044334869,53.4070751110265),
 .UNSPECIFIED.);
#4239=B_SPLINE_CURVE_WITH_KNOTS('',3,(#57024,#57025,#57026,#57027,#57028,
#57029,#57030,#57031,#57032,#57033),.UNSPECIFIED.,.F.,.F.,(4,1,1,1,1,1,
1,4),(40.8407044966673,41.4512414235002,42.4377707621643,43.4243001008283,
44.4108294394923,45.3973587781564,46.3838881168204,47.1238898038469),
 .UNSPECIFIED.);
#4240=B_SPLINE_CURVE_WITH_KNOTS('',3,(#57034,#57035,#57036,#57037,#57038,
#57039,#57040,#57041,#57042,#57043,#57044),.UNSPECIFIED.,.F.,.F.,(4,1,1,
1,1,1,1,1,4),(40.8407044966673,41.0346922709007,42.0212216095647,43.0077509482287,
43.9942802868928,44.9808096255568,45.9673389642208,46.9538683028848,47.1238898038469),
 .UNSPECIFIED.);
#4241=B_SPLINE_CURVE_WITH_KNOTS('',3,(#57049,#57050,#57051,#57052,#57053,
#57054,#57055,#57056,#57057,#57058),.UNSPECIFIED.,.F.,.F.,(4,1,1,1,1,1,
1,4),(34.5575191894877,35.5320653915161,36.5185947301801,37.5051240688441,
38.4916534075082,39.4781827461722,40.4647120848362,40.8407044966673),
 .UNSPECIFIED.);
#4242=B_SPLINE_CURVE_WITH_KNOTS('',3,(#57059,#57060,#57061,#57062,#57063,
#57064,#57065,#57066,#57067,#57068),.UNSPECIFIED.,.F.,.F.,(4,1,1,1,1,1,
1,4),(34.5575191894877,35.1155162389165,36.1020455775805,37.0885749162445,
38.0751042549086,39.0616335935726,40.0481629322366,40.8407044966673),
 .UNSPECIFIED.);
#4243=B_SPLINE_CURVE_WITH_KNOTS('',3,(#57073,#57074,#57075,#57076,#57077,
#57078,#57079,#57080,#57081,#57082,#57083),.UNSPECIFIED.,.F.,.F.,(4,1,1,
1,1,1,1,1,4),(28.2743338823081,28.6263600208678,29.6128893595319,30.5994186981959,
31.5859480368599,32.572477375524,33.559006714188,34.545536052852,34.5575191894877),
 .UNSPECIFIED.);
#4244=B_SPLINE_CURVE_WITH_KNOTS('',3,(#57084,#57085,#57086,#57087,#57088,
#57089,#57090,#57091,#57092,#57093),.UNSPECIFIED.,.F.,.F.,(4,1,1,1,1,1,
1,4),(28.2743338823081,29.1963402069323,30.1828695455963,31.1693988842604,
32.1559282229244,33.1424575615884,34.1289869002524,34.5575191894877),
 .UNSPECIFIED.);
#4245=B_SPLINE_CURVE_WITH_KNOTS('',3,(#57098,#57099,#57100,#57101,#57102,
#57103,#57104,#57105,#57106,#57107),.UNSPECIFIED.,.F.,.F.,(4,1,1,1,1,1,
1,4),(21.9911485751285,22.7071839888837,23.6937133275477,24.6802426662117,
25.6667720048758,26.6533013435398,27.6398306822038,28.2743338823081),
 .UNSPECIFIED.);
#4246=B_SPLINE_CURVE_WITH_KNOTS('',3,(#57108,#57109,#57110,#57111,#57112,
#57113,#57114,#57115,#57116,#57117,#57118),.UNSPECIFIED.,.F.,.F.,(4,1,1,
1,1,1,1,1,4),(21.9911485751285,22.2906348362841,23.2771641749481,24.2636935136121,
25.2502228522762,26.2367521909402,27.2232815296042,28.2098108682683,28.2743338823081),
 .UNSPECIFIED.);
#4247=B_SPLINE_CURVE_WITH_KNOTS('',3,(#57124,#57125,#57126,#57127,#57128),
 .UNSPECIFIED.,.F.,.F.,(4,1,4),(14.3984001269718,15.3849294656359,15.7079632679489),
 .UNSPECIFIED.);
#4248=B_SPLINE_CURVE_WITH_KNOTS('',3,(#57131,#57132,#57133,#57134,#57135),
 .UNSPECIFIED.,.F.,.F.,(4,1,4),(13.8759337553363,14.8149492795714,15.7079632679489),
 .UNSPECIFIED.);
#4249=B_SPLINE_CURVE_WITH_KNOTS('',3,(#57141,#57142,#57143,#57144),
 .UNSPECIFIED.,.F.,.F.,(4,4),(51.5750455984138,52.2860549491936),
 .UNSPECIFIED.);
#4250=B_SPLINE_CURVE_WITH_KNOTS('',3,(#57156,#57157,#57158,#57159,#57160,
#57161,#57162,#57163,#57164,#57165),.UNSPECIFIED.,.F.,.F.,(4,3,3,4),(-50.2654824574366,
-49.3264669332015,-48.3399375945375,-47.8348991546267),.UNSPECIFIED.);
#4251=B_SPLINE_CURVE_WITH_KNOTS('',3,(#57170,#57171,#57172,#57173,#57174,
#57175,#57176,#57177,#57178,#57179,#57180,#57181,#57182,#57183,#57184,#57185,
#57186,#57187,#57188,#57189,#57190,#57191,#57192,#57193,#57194),
 .UNSPECIFIED.,.F.,.F.,(4,3,3,3,3,3,3,3,4),(45.2918602912342,45.3803495785454,
46.3668789172095,47.3534082558735,48.3399375945375,49.3264669332015,50.3129962718656,
51.2995256105296,51.5750455984138),.UNSPECIFIED.);
#4252=B_SPLINE_CURVE_WITH_KNOTS('',3,(#57195,#57196,#57197,#57198,#57199,
#57200,#57201,#57202,#57203,#57204,#57205,#57206,#57207,#57208,#57209,#57210,
#57211,#57212,#57213,#57214,#57215,#57216),.UNSPECIFIED.,.F.,.F.,(4,3,3,
3,3,3,3,4),(-47.8348991546267,-47.3534082558735,-46.3668789172094,-45.3803495785454,
-44.3938202398814,-43.4072909012173,-42.4207615625533,-41.5517138474471),
 .UNSPECIFIED.);
#4253=B_SPLINE_CURVE_WITH_KNOTS('',3,(#57221,#57222,#57223,#57224,#57225,
#57226,#57227,#57228,#57229,#57230,#57231,#57232,#57233,#57234,#57235,#57236,
#57237,#57238,#57239,#57240,#57241,#57242),.UNSPECIFIED.,.F.,.F.,(4,3,3,
3,3,3,3,4),(39.0086749840546,39.4611735465612,40.4477028852253,41.4342322238893,
42.4207615625533,43.4072909012174,44.3938202398814,45.2918602912342),
 .UNSPECIFIED.);
#4254=B_SPLINE_CURVE_WITH_KNOTS('',3,(#57243,#57244,#57245,#57246,#57247,
#57248,#57249,#57250,#57251,#57252,#57253,#57254,#57255,#57256,#57257,#57258,
#57259,#57260,#57261,#57262,#57263,#57264,#57265,#57266,#57267),
 .UNSPECIFIED.,.F.,.F.,(4,3,3,3,3,3,3,3,4),(-41.5517138474471,-41.4342322238893,
-40.4477028852252,-39.4611735465612,-38.4746442078972,-37.4881148692332,
-36.5015855305691,-35.5150561919051,-35.2685285402676),.UNSPECIFIED.);
#4255=B_SPLINE_CURVE_WITH_KNOTS('',3,(#57272,#57273,#57274,#57275,#57276,
#57277,#57278,#57279,#57280,#57281,#57282,#57283,#57284,#57285,#57286,#57287,
#57288,#57289,#57290,#57291,#57292,#57293),.UNSPECIFIED.,.F.,.F.,(4,3,3,
3,3,3,3,4),(32.725489676875,33.541997514577,34.5285268532411,35.5150561919051,
36.5015855305691,37.4881148692332,38.4746442078972,39.0086749840546),
 .UNSPECIFIED.);
#4256=B_SPLINE_CURVE_WITH_KNOTS('',3,(#57294,#57295,#57296,#57297,#57298,
#57299,#57300,#57301,#57302,#57303,#57304,#57305,#57306,#57307,#57308,#57309,
#57310,#57311,#57312,#57313,#57314,#57315),.UNSPECIFIED.,.F.,.F.,(4,3,3,
3,3,3,3,4),(-35.2685285402676,-34.5285268532411,-33.541997514577,-32.555468175913,
-31.568938837249,-30.5824094985849,-29.5958801599209,-28.985343233088),
 .UNSPECIFIED.);
#4257=B_SPLINE_CURVE_WITH_KNOTS('',3,(#57320,#57321,#57322,#57323,#57324,
#57325,#57326,#57327,#57328,#57329,#57330,#57331,#57332,#57333,#57334,#57335,
#57336,#57337,#57338,#57339,#57340,#57341,#57342,#57343,#57344),
 .UNSPECIFIED.,.F.,.F.,(4,3,3,3,3,3,3,3,4),(26.4423043696954,26.6362921439288,
27.6228214825929,28.6093508212569,29.5958801599209,30.582409498585,31.568938837249,
32.555468175913,32.725489676875),.UNSPECIFIED.);
#4258=B_SPLINE_CURVE_WITH_KNOTS('',3,(#57345,#57346,#57347,#57348,#57349,
#57350,#57351,#57352,#57353,#57354,#57355,#57356,#57357,#57358,#57359,#57360,
#57361,#57362,#57363,#57364,#57365,#57366),.UNSPECIFIED.,.F.,.F.,(4,3,3,
3,3,3,3,4),(-28.985343233088,-28.6093508212569,-27.6228214825929,-26.6362921439288,
-25.6497628052648,-24.6632334666008,-23.6767041279367,-22.7021579259084),
 .UNSPECIFIED.);
#4259=B_SPLINE_CURVE_WITH_KNOTS('',3,(#57371,#57372,#57373,#57374,#57375,
#57376,#57377,#57378,#57379,#57380,#57381,#57382,#57383,#57384,#57385,#57386,
#57387,#57388,#57389,#57390,#57391,#57392),.UNSPECIFIED.,.F.,.F.,(4,3,3,
3,3,3,3,4),(20.1591190625158,20.7171161119446,21.7036454506087,22.6901747892727,
23.6767041279367,24.6632334666008,25.6497628052648,26.4423043696954),
 .UNSPECIFIED.);
#4260=B_SPLINE_CURVE_WITH_KNOTS('',3,(#57393,#57394,#57395,#57396,#57397,
#57398,#57399,#57400,#57401,#57402,#57403,#57404,#57405,#57406,#57407,#57408,
#57409,#57410,#57411,#57412,#57413,#57414,#57415,#57416,#57417),
 .UNSPECIFIED.,.F.,.F.,(4,3,3,3,3,3,3,3,4),(-22.7021579259084,-22.6901747892727,
-21.7036454506087,-20.7171161119446,-19.7305867732806,-18.7440574346166,
-17.7575280959526,-16.7709987572885,-16.4189726187288),.UNSPECIFIED.);
#4261=B_SPLINE_CURVE_WITH_KNOTS('',3,(#57422,#57423,#57424,#57425,#57426,
#57427,#57428,#57429,#57430,#57431,#57432,#57433,#57434,#57435,#57436,#57437,
#57438,#57439,#57440,#57441,#57442,#57443),.UNSPECIFIED.,.F.,.F.,(4,3,3,
3,3,3,3,4),(13.8759337553363,14.7979400799605,15.7844694186245,16.7709987572885,
17.7575280959526,18.7440574346166,19.7305867732806,20.1591190625158),
 .UNSPECIFIED.);
#4262=B_SPLINE_CURVE_WITH_KNOTS('',3,(#57444,#57445,#57446,#57447,#57448,
#57449,#57450,#57451,#57452,#57453,#57454,#57455,#57456,#57457,#57458,#57459,
#57460,#57461,#57462,#57463,#57464,#57465),.UNSPECIFIED.,.F.,.F.,(4,3,3,
3,3,3,3,4),(-16.4189726187288,-15.7844694186245,-14.7979400799605,-13.8114107412964,
-12.8248814026324,-11.8383520639684,-10.8518227253043,-10.1357873115492),
 .UNSPECIFIED.);
#4263=B_SPLINE_CURVE_WITH_KNOTS('',3,(#57471,#57472,#57473,#57474,#57475,
#57476,#57477,#57478,#57479,#57480,#57481,#57482,#57483),.UNSPECIFIED.,
 .F.,.F.,(4,3,3,3,4),(-3.85260200436961,-2.95958801599209,-1.97305867732806,
-0.98652933866403,0.),.UNSPECIFIED.);
#4264=B_SPLINE_CURVE_WITH_KNOTS('',3,(#57486,#57487,#57488,#57489,#57490,
#57491,#57492,#57493,#57494,#57495,#57496,#57497,#57498,#57499,#57500,#57501,
#57502,#57503,#57504),.UNSPECIFIED.,.F.,.F.,(4,3,3,3,3,3,4),(2.020572491757,
2.95958801599209,3.94611735465612,4.93264669332015,5.91917603198419,6.90570537064822,
7.59274844815667),.UNSPECIFIED.);
#4265=B_SPLINE_CURVE_WITH_KNOTS('',3,(#57510,#57511,#57512,#57513,#57514,
#57515,#57516,#57517),.UNSPECIFIED.,.F.,.F.,(4,1,1,1,1,4),(59.6902604182061,
60.1952988581168,61.1818281967808,62.1683575354449,63.1548868741089,64.1414162127729),
 .UNSPECIFIED.);
#4266=B_SPLINE_CURVE_WITH_KNOTS('',3,(#57520,#57521,#57522,#57523,#57524,
#57525,#57526,#57527,#57528),.UNSPECIFIED.,.F.,.F.,(4,1,1,1,1,1,4),(59.6902604182061,
59.7787497055172,60.7652790441813,61.7518083828453,62.7383377215093,63.7248670601734,
64.6638825844085),.UNSPECIFIED.);
#4267=B_SPLINE_CURVE_WITH_KNOTS('',3,(#57533,#57534,#57535,#57536,#57537,
#57538,#57539,#57540,#57541,#57542),.UNSPECIFIED.,.F.,.F.,(4,1,1,1,1,1,
1,4),(53.4070751110265,54.2761228261326,55.2626521647967,56.2491815034607,
57.2357108421247,58.2222401807888,59.2087695194528,59.6902604182061),
 .UNSPECIFIED.);
#4268=B_SPLINE_CURVE_WITH_KNOTS('',3,(#57543,#57544,#57545,#57546,#57547,
#57548,#57549,#57550,#57551,#57552),.UNSPECIFIED.,.F.,.F.,(4,1,1,1,1,1,
1,4),(53.4070751110265,53.8595736735331,54.8461030121971,55.8326323508611,
56.8191616895252,57.8056910281892,58.7922203668532,59.6902604182061),
 .UNSPECIFIED.);
#4269=B_SPLINE_CURVE_WITH_KNOTS('',3,(#57557,#57558,#57559,#57560,#57561,
#57562,#57563,#57564,#57565,#57566,#57567),.UNSPECIFIED.,.F.,.F.,(4,1,1,
1,1,1,1,1,4),(47.1238898038469,47.3704174554844,48.3569467941485,49.3434761328125,
50.3300054714765,51.3165348101405,52.3030641488046,53.2895934874686,53.4070751110265),
 .UNSPECIFIED.);
#4270=B_SPLINE_CURVE_WITH_KNOTS('',3,(#57568,#57569,#57570,#57571,#57572,
#57573,#57574,#57575,#57576,#57577),.UNSPECIFIED.,.F.,.F.,(4,1,1,1,1,1,
1,4),(47.1238898038469,47.9403976415489,48.9269269802129,49.9134563188769,
50.899985657541,51.886514996205,52.873044334869,53.4070751110265),
 .UNSPECIFIED.);
#4271=B_SPLINE_CURVE_WITH_KNOTS('',3,(#57582,#57583,#57584,#57585,#57586,
#57587,#57588,#57589,#57590,#57591),.UNSPECIFIED.,.F.,.F.,(4,1,1,1,1,1,
1,4),(40.8407044966673,41.4512414235002,42.4377707621643,43.4243001008283,
44.4108294394923,45.3973587781564,46.3838881168204,47.1238898038469),
 .UNSPECIFIED.);
#4272=B_SPLINE_CURVE_WITH_KNOTS('',3,(#57592,#57593,#57594,#57595,#57596,
#57597,#57598,#57599,#57600,#57601,#57602),.UNSPECIFIED.,.F.,.F.,(4,1,1,
1,1,1,1,1,4),(40.8407044966673,41.0346922709007,42.0212216095647,43.0077509482287,
43.9942802868928,44.9808096255568,45.9673389642208,46.9538683028848,47.1238898038469),
 .UNSPECIFIED.);
#4273=B_SPLINE_CURVE_WITH_KNOTS('',3,(#57607,#57608,#57609,#57610,#57611,
#57612,#57613,#57614,#57615,#57616),.UNSPECIFIED.,.F.,.F.,(4,1,1,1,1,1,
1,4),(34.5575191894877,35.5320653915161,36.5185947301801,37.5051240688441,
38.4916534075081,39.4781827461722,40.4647120848362,40.8407044966673),
 .UNSPECIFIED.);
#4274=B_SPLINE_CURVE_WITH_KNOTS('',3,(#57617,#57618,#57619,#57620,#57621,
#57622,#57623,#57624,#57625,#57626),.UNSPECIFIED.,.F.,.F.,(4,1,1,1,1,1,
1,4),(34.5575191894877,35.1155162389165,36.1020455775805,37.0885749162445,
38.0751042549086,39.0616335935726,40.0481629322366,40.8407044966673),
 .UNSPECIFIED.);
#4275=B_SPLINE_CURVE_WITH_KNOTS('',3,(#57631,#57632,#57633,#57634,#57635,
#57636,#57637,#57638,#57639,#57640,#57641),.UNSPECIFIED.,.F.,.F.,(4,1,1,
1,1,1,1,1,4),(28.2743338823081,28.6263600208678,29.6128893595319,30.5994186981959,
31.5859480368599,32.572477375524,33.559006714188,34.545536052852,34.5575191894877),
 .UNSPECIFIED.);
#4276=B_SPLINE_CURVE_WITH_KNOTS('',3,(#57642,#57643,#57644,#57645,#57646,
#57647,#57648,#57649,#57650,#57651),.UNSPECIFIED.,.F.,.F.,(4,1,1,1,1,1,
1,4),(28.2743338823081,29.1963402069323,30.1828695455963,31.1693988842603,
32.1559282229244,33.1424575615884,34.1289869002524,34.5575191894877),
 .UNSPECIFIED.);
#4277=B_SPLINE_CURVE_WITH_KNOTS('',3,(#57656,#57657,#57658,#57659,#57660,
#57661,#57662,#57663,#57664,#57665),.UNSPECIFIED.,.F.,.F.,(4,1,1,1,1,1,
1,4),(21.9911485751285,22.7071839888837,23.6937133275477,24.6802426662117,
25.6667720048757,26.6533013435398,27.6398306822038,28.2743338823081),
 .UNSPECIFIED.);
#4278=B_SPLINE_CURVE_WITH_KNOTS('',3,(#57666,#57667,#57668,#57669,#57670,
#57671,#57672,#57673,#57674,#57675,#57676),.UNSPECIFIED.,.F.,.F.,(4,1,1,
1,1,1,1,1,4),(21.9911485751285,22.2906348362841,23.2771641749481,24.2636935136121,
25.2502228522762,26.2367521909402,27.2232815296042,28.2098108682683,28.2743338823081),
 .UNSPECIFIED.);
#4279=B_SPLINE_CURVE_WITH_KNOTS('',3,(#57682,#57683,#57684,#57685,#57686),
 .UNSPECIFIED.,.F.,.F.,(4,1,4),(14.3984001269718,15.3849294656359,15.7079632679489),
 .UNSPECIFIED.);
#4280=B_SPLINE_CURVE_WITH_KNOTS('',3,(#57689,#57690,#57691,#57692,#57693),
 .UNSPECIFIED.,.F.,.F.,(4,1,4),(13.8759337553362,14.8149492795714,15.7079632679489),
 .UNSPECIFIED.);
#4281=B_SPLINE_CURVE_WITH_KNOTS('',3,(#57699,#57700,#57701,#57702),
 .UNSPECIFIED.,.F.,.F.,(4,4),(51.5750455984138,52.2860549491937),
 .UNSPECIFIED.);
#4282=B_SPLINE_CURVE_WITH_KNOTS('',3,(#57714,#57715,#57716,#57717,#57718,
#57719,#57720,#57721,#57722,#57723),.UNSPECIFIED.,.F.,.F.,(4,3,3,4),(-50.2654824574367,
-49.3264669332015,-48.3399375945375,-47.8348991546267),.UNSPECIFIED.);
#4283=B_SPLINE_CURVE_WITH_KNOTS('',3,(#57728,#57729,#57730,#57731,#57732,
#57733,#57734,#57735,#57736,#57737,#57738,#57739,#57740,#57741,#57742,#57743,
#57744,#57745,#57746,#57747,#57748,#57749,#57750,#57751,#57752),
 .UNSPECIFIED.,.F.,.F.,(4,3,3,3,3,3,3,3,4),(45.2918602912342,45.3803495785454,
46.3668789172095,47.3534082558735,48.3399375945375,49.3264669332015,50.3129962718656,
51.2995256105296,51.5750455984138),.UNSPECIFIED.);
#4284=B_SPLINE_CURVE_WITH_KNOTS('',3,(#57753,#57754,#57755,#57756,#57757,
#57758,#57759,#57760,#57761,#57762,#57763,#57764,#57765,#57766,#57767,#57768,
#57769,#57770,#57771,#57772,#57773,#57774),.UNSPECIFIED.,.F.,.F.,(4,3,3,
3,3,3,3,4),(-47.8348991546267,-47.3534082558735,-46.3668789172094,-45.3803495785454,
-44.3938202398814,-43.4072909012173,-42.4207615625533,-41.5517138474471),
 .UNSPECIFIED.);
#4285=B_SPLINE_CURVE_WITH_KNOTS('',3,(#57779,#57780,#57781,#57782,#57783,
#57784,#57785,#57786,#57787,#57788,#57789,#57790,#57791,#57792,#57793,#57794,
#57795,#57796,#57797,#57798,#57799,#57800),.UNSPECIFIED.,.F.,.F.,(4,3,3,
3,3,3,3,4),(39.0086749840546,39.4611735465612,40.4477028852253,41.4342322238893,
42.4207615625533,43.4072909012174,44.3938202398814,45.2918602912342),
 .UNSPECIFIED.);
#4286=B_SPLINE_CURVE_WITH_KNOTS('',3,(#57801,#57802,#57803,#57804,#57805,
#57806,#57807,#57808,#57809,#57810,#57811,#57812,#57813,#57814,#57815,#57816,
#57817,#57818,#57819,#57820,#57821,#57822,#57823,#57824,#57825),
 .UNSPECIFIED.,.F.,.F.,(4,3,3,3,3,3,3,3,4),(-41.5517138474471,-41.4342322238893,
-40.4477028852252,-39.4611735465612,-38.4746442078972,-37.4881148692332,
-36.5015855305691,-35.5150561919051,-35.2685285402675),.UNSPECIFIED.);
#4287=B_SPLINE_CURVE_WITH_KNOTS('',3,(#57830,#57831,#57832,#57833,#57834,
#57835,#57836,#57837,#57838,#57839,#57840,#57841,#57842,#57843,#57844,#57845,
#57846,#57847,#57848,#57849,#57850,#57851),.UNSPECIFIED.,.F.,.F.,(4,3,3,
3,3,3,3,4),(32.725489676875,33.541997514577,34.5285268532411,35.5150561919051,
36.5015855305691,37.4881148692332,38.4746442078972,39.0086749840546),
 .UNSPECIFIED.);
#4288=B_SPLINE_CURVE_WITH_KNOTS('',3,(#57852,#57853,#57854,#57855,#57856,
#57857,#57858,#57859,#57860,#57861,#57862,#57863,#57864,#57865,#57866,#57867,
#57868,#57869,#57870,#57871,#57872,#57873),.UNSPECIFIED.,.F.,.F.,(4,3,3,
3,3,3,3,4),(-35.2685285402675,-34.5285268532411,-33.541997514577,-32.555468175913,
-31.568938837249,-30.5824094985849,-29.5958801599209,-28.985343233088),
 .UNSPECIFIED.);
#4289=B_SPLINE_CURVE_WITH_KNOTS('',3,(#57878,#57879,#57880,#57881,#57882,
#57883,#57884,#57885,#57886,#57887,#57888,#57889,#57890,#57891,#57892,#57893,
#57894,#57895,#57896,#57897,#57898,#57899,#57900,#57901,#57902),
 .UNSPECIFIED.,.F.,.F.,(4,3,3,3,3,3,3,3,4),(26.4423043696954,26.6362921439288,
27.6228214825929,28.6093508212569,29.5958801599209,30.582409498585,31.568938837249,
32.555468175913,32.725489676875),.UNSPECIFIED.);
#4290=B_SPLINE_CURVE_WITH_KNOTS('',3,(#57903,#57904,#57905,#57906,#57907,
#57908,#57909,#57910,#57911,#57912,#57913,#57914,#57915,#57916,#57917,#57918,
#57919,#57920,#57921,#57922,#57923,#57924),.UNSPECIFIED.,.F.,.F.,(4,3,3,
3,3,3,3,4),(-28.985343233088,-28.6093508212569,-27.6228214825929,-26.6362921439288,
-25.6497628052648,-24.6632334666008,-23.6767041279367,-22.7021579259084),
 .UNSPECIFIED.);
#4291=B_SPLINE_CURVE_WITH_KNOTS('',3,(#57929,#57930,#57931,#57932,#57933,
#57934,#57935,#57936,#57937,#57938,#57939,#57940,#57941,#57942,#57943,#57944,
#57945,#57946,#57947,#57948,#57949,#57950),.UNSPECIFIED.,.F.,.F.,(4,3,3,
3,3,3,3,4),(20.1591190625159,20.7171161119446,21.7036454506087,22.6901747892727,
23.6767041279367,24.6632334666008,25.6497628052648,26.4423043696954),
 .UNSPECIFIED.);
#4292=B_SPLINE_CURVE_WITH_KNOTS('',3,(#57951,#57952,#57953,#57954,#57955,
#57956,#57957,#57958,#57959,#57960,#57961,#57962,#57963,#57964,#57965,#57966,
#57967,#57968,#57969,#57970,#57971,#57972,#57973,#57974,#57975),
 .UNSPECIFIED.,.F.,.F.,(4,3,3,3,3,3,3,3,4),(-22.7021579259084,-22.6901747892727,
-21.7036454506087,-20.7171161119446,-19.7305867732806,-18.7440574346166,
-17.7575280959525,-16.7709987572885,-16.4189726187288),.UNSPECIFIED.);
#4293=B_SPLINE_CURVE_WITH_KNOTS('',3,(#57980,#57981,#57982,#57983,#57984,
#57985,#57986,#57987,#57988,#57989,#57990,#57991,#57992,#57993,#57994,#57995,
#57996,#57997,#57998,#57999,#58000,#58001),.UNSPECIFIED.,.F.,.F.,(4,3,3,
3,3,3,3,4),(13.8759337553363,14.7979400799605,15.7844694186245,16.7709987572885,
17.7575280959526,18.7440574346166,19.7305867732806,20.1591190625159),
 .UNSPECIFIED.);
#4294=B_SPLINE_CURVE_WITH_KNOTS('',3,(#58002,#58003,#58004,#58005,#58006,
#58007,#58008,#58009,#58010,#58011,#58012,#58013,#58014,#58015,#58016,#58017,
#58018,#58019,#58020,#58021,#58022,#58023),.UNSPECIFIED.,.F.,.F.,(4,3,3,
3,3,3,3,4),(-16.4189726187288,-15.7844694186245,-14.7979400799605,-13.8114107412964,
-12.8248814026324,-11.8383520639684,-10.8518227253043,-10.1357873115492),
 .UNSPECIFIED.);
#4295=B_SPLINE_CURVE_WITH_KNOTS('',3,(#58029,#58030,#58031,#58032,#58033,
#58034,#58035,#58036,#58037,#58038,#58039,#58040,#58041),.UNSPECIFIED.,
 .F.,.F.,(4,3,3,3,4),(-3.85260200436961,-2.95958801599209,-1.97305867732806,
-0.986529338664033,0.),.UNSPECIFIED.);
#4296=B_SPLINE_CURVE_WITH_KNOTS('',3,(#58044,#58045,#58046,#58047,#58048,
#58049,#58050,#58051,#58052,#58053,#58054,#58055,#58056,#58057,#58058,#58059,
#58060,#58061,#58062),.UNSPECIFIED.,.F.,.F.,(4,3,3,3,3,3,4),(2.02057249175696,
2.95958801599209,3.94611735465612,4.93264669332015,5.91917603198419,6.90570537064821,
7.59274844815668),.UNSPECIFIED.);
#4297=B_SPLINE_CURVE_WITH_KNOTS('',3,(#58068,#58069,#58070,#58071,#58072,
#58073,#58074,#58075),.UNSPECIFIED.,.F.,.F.,(4,1,1,1,1,4),(59.6902604182061,
60.1952988581168,61.1818281967808,62.1683575354449,63.1548868741089,64.1414162127729),
 .UNSPECIFIED.);
#4298=B_SPLINE_CURVE_WITH_KNOTS('',3,(#58078,#58079,#58080,#58081,#58082,
#58083,#58084,#58085,#58086),.UNSPECIFIED.,.F.,.F.,(4,1,1,1,1,1,4),(59.6902604182061,
59.7787497055172,60.7652790441813,61.7518083828453,62.7383377215093,63.7248670601734,
64.6638825844085),.UNSPECIFIED.);
#4299=B_SPLINE_CURVE_WITH_KNOTS('',3,(#58091,#58092,#58093,#58094,#58095,
#58096,#58097,#58098,#58099,#58100),.UNSPECIFIED.,.F.,.F.,(4,1,1,1,1,1,
1,4),(53.4070751110265,54.2761228261326,55.2626521647967,56.2491815034607,
57.2357108421247,58.2222401807888,59.2087695194528,59.6902604182061),
 .UNSPECIFIED.);
#4300=B_SPLINE_CURVE_WITH_KNOTS('',3,(#58101,#58102,#58103,#58104,#58105,
#58106,#58107,#58108,#58109,#58110),.UNSPECIFIED.,.F.,.F.,(4,1,1,1,1,1,
1,4),(53.4070751110265,53.8595736735331,54.8461030121971,55.8326323508611,
56.8191616895252,57.8056910281892,58.7922203668532,59.6902604182061),
 .UNSPECIFIED.);
#4301=B_SPLINE_CURVE_WITH_KNOTS('',3,(#58115,#58116,#58117,#58118,#58119,
#58120,#58121,#58122,#58123,#58124,#58125),.UNSPECIFIED.,.F.,.F.,(4,1,1,
1,1,1,1,1,4),(47.1238898038469,47.3704174554844,48.3569467941485,49.3434761328125,
50.3300054714765,51.3165348101405,52.3030641488046,53.2895934874686,53.4070751110265),
 .UNSPECIFIED.);
#4302=B_SPLINE_CURVE_WITH_KNOTS('',3,(#58126,#58127,#58128,#58129,#58130,
#58131,#58132,#58133,#58134,#58135),.UNSPECIFIED.,.F.,.F.,(4,1,1,1,1,1,
1,4),(47.1238898038469,47.9403976415489,48.9269269802129,49.9134563188769,
50.899985657541,51.886514996205,52.873044334869,53.4070751110265),
 .UNSPECIFIED.);
#4303=B_SPLINE_CURVE_WITH_KNOTS('',3,(#58140,#58141,#58142,#58143,#58144,
#58145,#58146,#58147,#58148,#58149),.UNSPECIFIED.,.F.,.F.,(4,1,1,1,1,1,
1,4),(40.8407044966673,41.4512414235002,42.4377707621643,43.4243001008283,
44.4108294394923,45.3973587781564,46.3838881168204,47.1238898038469),
 .UNSPECIFIED.);
#4304=B_SPLINE_CURVE_WITH_KNOTS('',3,(#58150,#58151,#58152,#58153,#58154,
#58155,#58156,#58157,#58158,#58159,#58160),.UNSPECIFIED.,.F.,.F.,(4,1,1,
1,1,1,1,1,4),(40.8407044966673,41.0346922709007,42.0212216095647,43.0077509482287,
43.9942802868928,44.9808096255568,45.9673389642208,46.9538683028848,47.1238898038469),
 .UNSPECIFIED.);
#4305=B_SPLINE_CURVE_WITH_KNOTS('',3,(#58165,#58166,#58167,#58168,#58169,
#58170,#58171,#58172,#58173,#58174),.UNSPECIFIED.,.F.,.F.,(4,1,1,1,1,1,
1,4),(34.5575191894877,35.5320653915161,36.5185947301801,37.5051240688441,
38.4916534075081,39.4781827461722,40.4647120848362,40.8407044966673),
 .UNSPECIFIED.);
#4306=B_SPLINE_CURVE_WITH_KNOTS('',3,(#58175,#58176,#58177,#58178,#58179,
#58180,#58181,#58182,#58183,#58184),.UNSPECIFIED.,.F.,.F.,(4,1,1,1,1,1,
1,4),(34.5575191894877,35.1155162389165,36.1020455775805,37.0885749162445,
38.0751042549086,39.0616335935726,40.0481629322366,40.8407044966673),
 .UNSPECIFIED.);
#4307=B_SPLINE_CURVE_WITH_KNOTS('',3,(#58189,#58190,#58191,#58192,#58193,
#58194,#58195,#58196,#58197,#58198,#58199),.UNSPECIFIED.,.F.,.F.,(4,1,1,
1,1,1,1,1,4),(28.2743338823081,28.6263600208678,29.6128893595319,30.5994186981959,
31.5859480368599,32.572477375524,33.559006714188,34.545536052852,34.5575191894877),
 .UNSPECIFIED.);
#4308=B_SPLINE_CURVE_WITH_KNOTS('',3,(#58200,#58201,#58202,#58203,#58204,
#58205,#58206,#58207,#58208,#58209),.UNSPECIFIED.,.F.,.F.,(4,1,1,1,1,1,
1,4),(28.2743338823081,29.1963402069323,30.1828695455963,31.1693988842603,
32.1559282229244,33.1424575615884,34.1289869002524,34.5575191894877),
 .UNSPECIFIED.);
#4309=B_SPLINE_CURVE_WITH_KNOTS('',3,(#58214,#58215,#58216,#58217,#58218,
#58219,#58220,#58221,#58222,#58223),.UNSPECIFIED.,.F.,.F.,(4,1,1,1,1,1,
1,4),(21.9911485751285,22.7071839888837,23.6937133275477,24.6802426662117,
25.6667720048758,26.6533013435398,27.6398306822038,28.2743338823081),
 .UNSPECIFIED.);
#4310=B_SPLINE_CURVE_WITH_KNOTS('',3,(#58224,#58225,#58226,#58227,#58228,
#58229,#58230,#58231,#58232,#58233,#58234),.UNSPECIFIED.,.F.,.F.,(4,1,1,
1,1,1,1,1,4),(21.9911485751285,22.2906348362841,23.2771641749481,24.2636935136121,
25.2502228522762,26.2367521909402,27.2232815296042,28.2098108682683,28.2743338823081),
 .UNSPECIFIED.);
#4311=B_SPLINE_CURVE_WITH_KNOTS('',3,(#58240,#58241,#58242,#58243,#58244),
 .UNSPECIFIED.,.F.,.F.,(4,1,4),(14.3984001269718,15.3849294656359,15.7079632679489),
 .UNSPECIFIED.);
#4312=B_SPLINE_CURVE_WITH_KNOTS('',3,(#58247,#58248,#58249,#58250,#58251),
 .UNSPECIFIED.,.F.,.F.,(4,1,4),(13.8759337553362,14.8149492795714,15.7079632679489),
 .UNSPECIFIED.);
#4313=B_SPLINE_CURVE_WITH_KNOTS('',3,(#58257,#58258,#58259,#58260),
 .UNSPECIFIED.,.F.,.F.,(4,4),(51.5750455984138,52.2860549491937),
 .UNSPECIFIED.);
#4314=B_SPLINE_CURVE_WITH_KNOTS('',3,(#58272,#58273,#58274,#58275,#58276,
#58277,#58278,#58279,#58280,#58281),.UNSPECIFIED.,.F.,.F.,(4,3,3,4),(-50.2654824574368,
-49.3264669332015,-48.3399375945375,-47.8348991546267),.UNSPECIFIED.);
#4315=B_SPLINE_CURVE_WITH_KNOTS('',3,(#58286,#58287,#58288,#58289,#58290,
#58291,#58292,#58293,#58294,#58295,#58296,#58297,#58298,#58299,#58300,#58301,
#58302,#58303,#58304,#58305,#58306,#58307,#58308,#58309,#58310),
 .UNSPECIFIED.,.F.,.F.,(4,3,3,3,3,3,3,3,4),(45.2918602912342,45.3803495785454,
46.3668789172095,47.3534082558735,48.3399375945375,49.3264669332015,50.3129962718656,
51.2995256105296,51.5750455984138),.UNSPECIFIED.);
#4316=B_SPLINE_CURVE_WITH_KNOTS('',3,(#58311,#58312,#58313,#58314,#58315,
#58316,#58317,#58318,#58319,#58320,#58321,#58322,#58323,#58324,#58325,#58326,
#58327,#58328,#58329,#58330,#58331,#58332),.UNSPECIFIED.,.F.,.F.,(4,3,3,
3,3,3,3,4),(-47.8348991546267,-47.3534082558735,-46.3668789172094,-45.3803495785454,
-44.3938202398814,-43.4072909012173,-42.4207615625533,-41.5517138474471),
 .UNSPECIFIED.);
#4317=B_SPLINE_CURVE_WITH_KNOTS('',3,(#58337,#58338,#58339,#58340,#58341,
#58342,#58343,#58344,#58345,#58346,#58347,#58348,#58349,#58350,#58351,#58352,
#58353,#58354,#58355,#58356,#58357,#58358),.UNSPECIFIED.,.F.,.F.,(4,3,3,
3,3,3,3,4),(39.0086749840546,39.4611735465612,40.4477028852253,41.4342322238893,
42.4207615625533,43.4072909012174,44.3938202398814,45.2918602912342),
 .UNSPECIFIED.);
#4318=B_SPLINE_CURVE_WITH_KNOTS('',3,(#58359,#58360,#58361,#58362,#58363,
#58364,#58365,#58366,#58367,#58368,#58369,#58370,#58371,#58372,#58373,#58374,
#58375,#58376,#58377,#58378,#58379,#58380,#58381,#58382,#58383),
 .UNSPECIFIED.,.F.,.F.,(4,3,3,3,3,3,3,3,4),(-41.5517138474471,-41.4342322238893,
-40.4477028852253,-39.4611735465612,-38.4746442078972,-37.4881148692332,
-36.5015855305691,-35.5150561919051,-35.2685285402676),.UNSPECIFIED.);
#4319=B_SPLINE_CURVE_WITH_KNOTS('',3,(#58388,#58389,#58390,#58391,#58392,
#58393,#58394,#58395,#58396,#58397,#58398,#58399,#58400,#58401,#58402,#58403,
#58404,#58405,#58406,#58407,#58408,#58409),.UNSPECIFIED.,.F.,.F.,(4,3,3,
3,3,3,3,4),(32.725489676875,33.541997514577,34.5285268532411,35.5150561919051,
36.5015855305691,37.4881148692332,38.4746442078972,39.0086749840546),
 .UNSPECIFIED.);
#4320=B_SPLINE_CURVE_WITH_KNOTS('',3,(#58410,#58411,#58412,#58413,#58414,
#58415,#58416,#58417,#58418,#58419,#58420,#58421,#58422,#58423,#58424,#58425,
#58426,#58427,#58428,#58429,#58430,#58431),.UNSPECIFIED.,.F.,.F.,(4,3,3,
3,3,3,3,4),(-35.2685285402676,-34.5285268532411,-33.541997514577,-32.555468175913,
-31.568938837249,-30.5824094985849,-29.5958801599209,-28.985343233088),
 .UNSPECIFIED.);
#4321=B_SPLINE_CURVE_WITH_KNOTS('',3,(#58436,#58437,#58438,#58439,#58440,
#58441,#58442,#58443,#58444,#58445,#58446,#58447,#58448,#58449,#58450,#58451,
#58452,#58453,#58454,#58455,#58456,#58457,#58458,#58459,#58460),
 .UNSPECIFIED.,.F.,.F.,(4,3,3,3,3,3,3,3,4),(26.4423043696954,26.6362921439288,
27.6228214825929,28.6093508212569,29.5958801599209,30.582409498585,31.568938837249,
32.555468175913,32.725489676875),.UNSPECIFIED.);
#4322=B_SPLINE_CURVE_WITH_KNOTS('',3,(#58461,#58462,#58463,#58464,#58465,
#58466,#58467,#58468,#58469,#58470,#58471,#58472,#58473,#58474,#58475,#58476,
#58477,#58478,#58479,#58480,#58481,#58482),.UNSPECIFIED.,.F.,.F.,(4,3,3,
3,3,3,3,4),(-28.985343233088,-28.6093508212569,-27.6228214825929,-26.6362921439288,
-25.6497628052648,-24.6632334666008,-23.6767041279367,-22.7021579259084),
 .UNSPECIFIED.);
#4323=B_SPLINE_CURVE_WITH_KNOTS('',3,(#58487,#58488,#58489,#58490,#58491,
#58492,#58493,#58494,#58495,#58496,#58497,#58498,#58499,#58500,#58501,#58502,
#58503,#58504,#58505,#58506,#58507,#58508),.UNSPECIFIED.,.F.,.F.,(4,3,3,
3,3,3,3,4),(20.1591190625159,20.7171161119446,21.7036454506087,22.6901747892727,
23.6767041279367,24.6632334666008,25.6497628052648,26.4423043696954),
 .UNSPECIFIED.);
#4324=B_SPLINE_CURVE_WITH_KNOTS('',3,(#58509,#58510,#58511,#58512,#58513,
#58514,#58515,#58516,#58517,#58518,#58519,#58520,#58521,#58522,#58523,#58524,
#58525,#58526,#58527,#58528,#58529,#58530,#58531,#58532,#58533),
 .UNSPECIFIED.,.F.,.F.,(4,3,3,3,3,3,3,3,4),(-22.7021579259084,-22.6901747892727,
-21.7036454506087,-20.7171161119446,-19.7305867732806,-18.7440574346166,
-17.7575280959526,-16.7709987572885,-16.4189726187288),.UNSPECIFIED.);
#4325=B_SPLINE_CURVE_WITH_KNOTS('',3,(#58538,#58539,#58540,#58541,#58542,
#58543,#58544,#58545,#58546,#58547,#58548,#58549,#58550,#58551,#58552,#58553,
#58554,#58555,#58556,#58557,#58558,#58559),.UNSPECIFIED.,.F.,.F.,(4,3,3,
3,3,3,3,4),(13.8759337553363,14.7979400799605,15.7844694186245,16.7709987572885,
17.7575280959526,18.7440574346166,19.7305867732806,20.1591190625159),
 .UNSPECIFIED.);
#4326=B_SPLINE_CURVE_WITH_KNOTS('',3,(#58560,#58561,#58562,#58563,#58564,
#58565,#58566,#58567,#58568,#58569,#58570,#58571,#58572,#58573,#58574,#58575,
#58576,#58577,#58578,#58579,#58580,#58581),.UNSPECIFIED.,.F.,.F.,(4,3,3,
3,3,3,3,4),(-16.4189726187288,-15.7844694186245,-14.7979400799605,-13.8114107412964,
-12.8248814026324,-11.8383520639684,-10.8518227253043,-10.1357873115492),
 .UNSPECIFIED.);
#4327=B_SPLINE_CURVE_WITH_KNOTS('',3,(#58587,#58588,#58589,#58590,#58591,
#58592,#58593,#58594,#58595,#58596,#58597,#58598,#58599),.UNSPECIFIED.,
 .F.,.F.,(4,3,3,3,4),(-3.85260200436962,-2.95958801599209,-1.97305867732806,
-0.986529338664033,0.),.UNSPECIFIED.);
#4328=B_SPLINE_CURVE_WITH_KNOTS('',3,(#58602,#58603,#58604,#58605,#58606,
#58607,#58608,#58609,#58610,#58611,#58612,#58613,#58614,#58615,#58616,#58617,
#58618,#58619,#58620),.UNSPECIFIED.,.F.,.F.,(4,3,3,3,3,3,4),(2.02057249175683,
2.95958801599209,3.94611735465612,4.93264669332015,5.91917603198419,6.90570537064822,
7.59274844815668),.UNSPECIFIED.);
#4329=B_SPLINE_CURVE_WITH_KNOTS('',3,(#58626,#58627,#58628,#58629,#58630,
#58631,#58632,#58633),.UNSPECIFIED.,.F.,.F.,(4,1,1,1,1,4),(59.6902604182061,
60.1952988581168,61.1818281967809,62.1683575354449,63.1548868741089,64.141416212773),
 .UNSPECIFIED.);
#4330=B_SPLINE_CURVE_WITH_KNOTS('',3,(#58636,#58637,#58638,#58639,#58640,
#58641,#58642,#58643,#58644),.UNSPECIFIED.,.F.,.F.,(4,1,1,1,1,1,4),(59.6902604182061,
59.7787497055173,60.7652790441813,61.7518083828453,62.7383377215094,63.7248670601734,
64.6638825844085),.UNSPECIFIED.);
#4331=B_SPLINE_CURVE_WITH_KNOTS('',3,(#58649,#58650,#58651,#58652,#58653,
#58654,#58655,#58656,#58657,#58658),.UNSPECIFIED.,.F.,.F.,(4,1,1,1,1,1,
1,4),(53.4070751110265,54.2761228261326,55.2626521647967,56.2491815034607,
57.2357108421247,58.2222401807888,59.2087695194528,59.6902604182061),
 .UNSPECIFIED.);
#4332=B_SPLINE_CURVE_WITH_KNOTS('',3,(#58659,#58660,#58661,#58662,#58663,
#58664,#58665,#58666,#58667,#58668),.UNSPECIFIED.,.F.,.F.,(4,1,1,1,1,1,
1,4),(53.4070751110265,53.8595736735331,54.8461030121971,55.8326323508611,
56.8191616895252,57.8056910281892,58.7922203668532,59.6902604182061),
 .UNSPECIFIED.);
#4333=B_SPLINE_CURVE_WITH_KNOTS('',3,(#58673,#58674,#58675,#58676,#58677,
#58678,#58679,#58680,#58681,#58682,#58683),.UNSPECIFIED.,.F.,.F.,(4,1,1,
1,1,1,1,1,4),(47.1238898038469,47.3704174554844,48.3569467941485,49.3434761328125,
50.3300054714765,51.3165348101406,52.3030641488046,53.2895934874686,53.4070751110265),
 .UNSPECIFIED.);
#4334=B_SPLINE_CURVE_WITH_KNOTS('',3,(#58684,#58685,#58686,#58687,#58688,
#58689,#58690,#58691,#58692,#58693),.UNSPECIFIED.,.F.,.F.,(4,1,1,1,1,1,
1,4),(47.1238898038469,47.9403976415489,48.9269269802129,49.9134563188769,
50.899985657541,51.886514996205,52.873044334869,53.4070751110265),
 .UNSPECIFIED.);
#4335=B_SPLINE_CURVE_WITH_KNOTS('',3,(#58698,#58699,#58700,#58701,#58702,
#58703,#58704,#58705,#58706,#58707),.UNSPECIFIED.,.F.,.F.,(4,1,1,1,1,1,
1,4),(40.8407044966673,41.4512414235002,42.4377707621643,43.4243001008283,
44.4108294394923,45.3973587781564,46.3838881168204,47.1238898038469),
 .UNSPECIFIED.);
#4336=B_SPLINE_CURVE_WITH_KNOTS('',3,(#58708,#58709,#58710,#58711,#58712,
#58713,#58714,#58715,#58716,#58717,#58718),.UNSPECIFIED.,.F.,.F.,(4,1,1,
1,1,1,1,1,4),(40.8407044966673,41.0346922709007,42.0212216095647,43.0077509482287,
43.9942802868928,44.9808096255568,45.9673389642208,46.9538683028849,47.1238898038469),
 .UNSPECIFIED.);
#4337=B_SPLINE_CURVE_WITH_KNOTS('',3,(#58723,#58724,#58725,#58726,#58727,
#58728,#58729,#58730,#58731,#58732),.UNSPECIFIED.,.F.,.F.,(4,1,1,1,1,1,
1,4),(34.5575191894877,35.5320653915161,36.5185947301801,37.5051240688441,
38.4916534075082,39.4781827461722,40.4647120848362,40.8407044966673),
 .UNSPECIFIED.);
#4338=B_SPLINE_CURVE_WITH_KNOTS('',3,(#58733,#58734,#58735,#58736,#58737,
#58738,#58739,#58740,#58741,#58742),.UNSPECIFIED.,.F.,.F.,(4,1,1,1,1,1,
1,4),(34.5575191894877,35.1155162389165,36.1020455775805,37.0885749162445,
38.0751042549086,39.0616335935726,40.0481629322366,40.8407044966673),
 .UNSPECIFIED.);
#4339=B_SPLINE_CURVE_WITH_KNOTS('',3,(#58747,#58748,#58749,#58750,#58751,
#58752,#58753,#58754,#58755,#58756,#58757),.UNSPECIFIED.,.F.,.F.,(4,1,1,
1,1,1,1,1,4),(28.2743338823081,28.6263600208679,29.6128893595319,30.5994186981959,
31.5859480368599,32.572477375524,33.559006714188,34.545536052852,34.5575191894877),
 .UNSPECIFIED.);
#4340=B_SPLINE_CURVE_WITH_KNOTS('',3,(#58758,#58759,#58760,#58761,#58762,
#58763,#58764,#58765,#58766,#58767),.UNSPECIFIED.,.F.,.F.,(4,1,1,1,1,1,
1,4),(28.2743338823081,29.1963402069323,30.1828695455963,31.1693988842604,
32.1559282229244,33.1424575615884,34.1289869002525,34.5575191894877),
 .UNSPECIFIED.);
#4341=B_SPLINE_CURVE_WITH_KNOTS('',3,(#58772,#58773,#58774,#58775,#58776,
#58777,#58778,#58779,#58780,#58781),.UNSPECIFIED.,.F.,.F.,(4,1,1,1,1,1,
1,4),(21.9911485751285,22.7071839888837,23.6937133275477,24.6802426662117,
25.6667720048758,26.6533013435398,27.6398306822038,28.2743338823081),
 .UNSPECIFIED.);
#4342=B_SPLINE_CURVE_WITH_KNOTS('',3,(#58782,#58783,#58784,#58785,#58786,
#58787,#58788,#58789,#58790,#58791,#58792),.UNSPECIFIED.,.F.,.F.,(4,1,1,
1,1,1,1,1,4),(21.9911485751285,22.2906348362841,23.2771641749481,24.2636935136121,
25.2502228522762,26.2367521909402,27.2232815296042,28.2098108682683,28.2743338823081),
 .UNSPECIFIED.);
#4343=B_SPLINE_CURVE_WITH_KNOTS('',3,(#58798,#58799,#58800,#58801,#58802),
 .UNSPECIFIED.,.F.,.F.,(4,1,4),(14.3984001269718,15.3849294656359,15.7079632679489),
 .UNSPECIFIED.);
#4344=B_SPLINE_CURVE_WITH_KNOTS('',3,(#58805,#58806,#58807,#58808,#58809),
 .UNSPECIFIED.,.F.,.F.,(4,1,4),(13.8759337553363,14.8149492795714,15.7079632679489),
 .UNSPECIFIED.);
#4345=B_SPLINE_CURVE_WITH_KNOTS('',3,(#58815,#58816,#58817,#58818),
 .UNSPECIFIED.,.F.,.F.,(4,4),(51.5750455984138,52.2860549491937),
 .UNSPECIFIED.);
#4346=B_SPLINE_CURVE_WITH_KNOTS('',3,(#58830,#58831,#58832,#58833,#58834,
#58835,#58836,#58837,#58838,#58839),.UNSPECIFIED.,.F.,.F.,(4,3,3,4),(-50.2654824574367,
-49.3264669332015,-48.3399375945375,-47.8348991546267),.UNSPECIFIED.);
#4347=B_SPLINE_CURVE_WITH_KNOTS('',3,(#58844,#58845,#58846,#58847,#58848,
#58849,#58850,#58851,#58852,#58853,#58854,#58855,#58856,#58857,#58858,#58859,
#58860,#58861,#58862,#58863,#58864,#58865,#58866,#58867,#58868),
 .UNSPECIFIED.,.F.,.F.,(4,3,3,3,3,3,3,3,4),(45.2918602912342,45.3803495785454,
46.3668789172095,47.3534082558735,48.3399375945375,49.3264669332015,50.3129962718656,
51.2995256105296,51.5750455984138),.UNSPECIFIED.);
#4348=B_SPLINE_CURVE_WITH_KNOTS('',3,(#58869,#58870,#58871,#58872,#58873,
#58874,#58875,#58876,#58877,#58878,#58879,#58880,#58881,#58882,#58883,#58884,
#58885,#58886,#58887,#58888,#58889,#58890),.UNSPECIFIED.,.F.,.F.,(4,3,3,
3,3,3,3,4),(-47.8348991546267,-47.3534082558735,-46.3668789172094,-45.3803495785454,
-44.3938202398814,-43.4072909012173,-42.4207615625533,-41.5517138474471),
 .UNSPECIFIED.);
#4349=B_SPLINE_CURVE_WITH_KNOTS('',3,(#58895,#58896,#58897,#58898,#58899,
#58900,#58901,#58902,#58903,#58904,#58905,#58906,#58907,#58908,#58909,#58910,
#58911,#58912,#58913,#58914,#58915,#58916),.UNSPECIFIED.,.F.,.F.,(4,3,3,
3,3,3,3,4),(39.0086749840546,39.4611735465612,40.4477028852253,41.4342322238893,
42.4207615625533,43.4072909012174,44.3938202398814,45.2918602912342),
 .UNSPECIFIED.);
#4350=B_SPLINE_CURVE_WITH_KNOTS('',3,(#58917,#58918,#58919,#58920,#58921,
#58922,#58923,#58924,#58925,#58926,#58927,#58928,#58929,#58930,#58931,#58932,
#58933,#58934,#58935,#58936,#58937,#58938,#58939,#58940,#58941),
 .UNSPECIFIED.,.F.,.F.,(4,3,3,3,3,3,3,3,4),(-41.5517138474471,-41.4342322238893,
-40.4477028852252,-39.4611735465612,-38.4746442078972,-37.4881148692332,
-36.5015855305691,-35.5150561919051,-35.2685285402676),.UNSPECIFIED.);
#4351=B_SPLINE_CURVE_WITH_KNOTS('',3,(#58946,#58947,#58948,#58949,#58950,
#58951,#58952,#58953,#58954,#58955,#58956,#58957,#58958,#58959,#58960,#58961,
#58962,#58963,#58964,#58965,#58966,#58967),.UNSPECIFIED.,.F.,.F.,(4,3,3,
3,3,3,3,4),(32.725489676875,33.5419975145771,34.5285268532411,35.5150561919051,
36.5015855305692,37.4881148692332,38.4746442078972,39.0086749840546),
 .UNSPECIFIED.);
#4352=B_SPLINE_CURVE_WITH_KNOTS('',3,(#58968,#58969,#58970,#58971,#58972,
#58973,#58974,#58975,#58976,#58977,#58978,#58979,#58980,#58981,#58982,#58983,
#58984,#58985,#58986,#58987,#58988,#58989),.UNSPECIFIED.,.F.,.F.,(4,3,3,
3,3,3,3,4),(-35.2685285402676,-34.5285268532411,-33.541997514577,-32.555468175913,
-31.568938837249,-30.5824094985849,-29.5958801599209,-28.985343233088),
 .UNSPECIFIED.);
#4353=B_SPLINE_CURVE_WITH_KNOTS('',3,(#58994,#58995,#58996,#58997,#58998,
#58999,#59000,#59001,#59002,#59003,#59004,#59005,#59006,#59007,#59008,#59009,
#59010,#59011,#59012,#59013,#59014,#59015,#59016,#59017,#59018),
 .UNSPECIFIED.,.F.,.F.,(4,3,3,3,3,3,3,3,4),(26.4423043696954,26.6362921439288,
27.6228214825929,28.6093508212569,29.5958801599209,30.582409498585,31.568938837249,
32.555468175913,32.725489676875),.UNSPECIFIED.);
#4354=B_SPLINE_CURVE_WITH_KNOTS('',3,(#59019,#59020,#59021,#59022,#59023,
#59024,#59025,#59026,#59027,#59028,#59029,#59030,#59031,#59032,#59033,#59034,
#59035,#59036,#59037,#59038,#59039,#59040),.UNSPECIFIED.,.F.,.F.,(4,3,3,
3,3,3,3,4),(-28.985343233088,-28.6093508212569,-27.6228214825929,-26.6362921439288,
-25.6497628052648,-24.6632334666008,-23.6767041279367,-22.7021579259084),
 .UNSPECIFIED.);
#4355=B_SPLINE_CURVE_WITH_KNOTS('',3,(#59045,#59046,#59047,#59048,#59049,
#59050,#59051,#59052,#59053,#59054,#59055,#59056,#59057,#59058,#59059,#59060,
#59061,#59062,#59063,#59064,#59065,#59066),.UNSPECIFIED.,.F.,.F.,(4,3,3,
3,3,3,3,4),(20.1591190625159,20.7171161119447,21.7036454506087,22.6901747892727,
23.6767041279367,24.6632334666008,25.6497628052648,26.4423043696954),
 .UNSPECIFIED.);
#4356=B_SPLINE_CURVE_WITH_KNOTS('',3,(#59067,#59068,#59069,#59070,#59071,
#59072,#59073,#59074,#59075,#59076,#59077,#59078,#59079,#59080,#59081,#59082,
#59083,#59084,#59085,#59086,#59087,#59088,#59089,#59090,#59091),
 .UNSPECIFIED.,.F.,.F.,(4,3,3,3,3,3,3,3,4),(-22.7021579259084,-22.6901747892727,
-21.7036454506087,-20.7171161119446,-19.7305867732806,-18.7440574346166,
-17.7575280959525,-16.7709987572885,-16.4189726187288),.UNSPECIFIED.);
#4357=B_SPLINE_CURVE_WITH_KNOTS('',3,(#59096,#59097,#59098,#59099,#59100,
#59101,#59102,#59103,#59104,#59105,#59106,#59107,#59108,#59109,#59110,#59111,
#59112,#59113,#59114,#59115,#59116,#59117),.UNSPECIFIED.,.F.,.F.,(4,3,3,
3,3,3,3,4),(13.8759337553363,14.7979400799605,15.7844694186245,16.7709987572885,
17.7575280959526,18.7440574346166,19.7305867732806,20.1591190625159),
 .UNSPECIFIED.);
#4358=B_SPLINE_CURVE_WITH_KNOTS('',3,(#59118,#59119,#59120,#59121,#59122,
#59123,#59124,#59125,#59126,#59127,#59128,#59129,#59130,#59131,#59132,#59133,
#59134,#59135,#59136,#59137,#59138,#59139),.UNSPECIFIED.,.F.,.F.,(4,3,3,
3,3,3,3,4),(-16.4189726187288,-15.7844694186245,-14.7979400799605,-13.8114107412964,
-12.8248814026324,-11.8383520639684,-10.8518227253043,-10.1357873115492),
 .UNSPECIFIED.);
#4359=B_SPLINE_CURVE_WITH_KNOTS('',3,(#59145,#59146,#59147,#59148,#59149,
#59150,#59151,#59152,#59153,#59154,#59155,#59156,#59157),.UNSPECIFIED.,
 .F.,.F.,(4,3,3,3,4),(-3.85260200436961,-2.95958801599209,-1.97305867732806,
-0.986529338664031,0.),.UNSPECIFIED.);
#4360=B_SPLINE_CURVE_WITH_KNOTS('',3,(#59160,#59161,#59162,#59163,#59164,
#59165,#59166,#59167,#59168,#59169,#59170,#59171,#59172,#59173,#59174,#59175,
#59176,#59177,#59178),.UNSPECIFIED.,.F.,.F.,(4,3,3,3,3,3,4),(2.02057249175691,
2.95958801599209,3.94611735465613,4.93264669332016,5.91917603198419,6.90570537064822,
7.59274844815668),.UNSPECIFIED.);
#4361=B_SPLINE_CURVE_WITH_KNOTS('',3,(#59184,#59185,#59186,#59187,#59188,
#59189,#59190,#59191),.UNSPECIFIED.,.F.,.F.,(4,1,1,1,1,4),(59.6902604182061,
60.1952988581168,61.1818281967808,62.1683575354449,63.1548868741089,64.1414162127729),
 .UNSPECIFIED.);
#4362=B_SPLINE_CURVE_WITH_KNOTS('',3,(#59194,#59195,#59196,#59197,#59198,
#59199,#59200,#59201,#59202),.UNSPECIFIED.,.F.,.F.,(4,1,1,1,1,1,4),(59.6902604182061,
59.7787497055172,60.7652790441813,61.7518083828453,62.7383377215093,63.7248670601734,
64.6638825844085),.UNSPECIFIED.);
#4363=B_SPLINE_CURVE_WITH_KNOTS('',3,(#59207,#59208,#59209,#59210,#59211,
#59212,#59213,#59214,#59215,#59216),.UNSPECIFIED.,.F.,.F.,(4,1,1,1,1,1,
1,4),(53.4070751110265,54.2761228261326,55.2626521647967,56.2491815034607,
57.2357108421247,58.2222401807888,59.2087695194528,59.6902604182061),
 .UNSPECIFIED.);
#4364=B_SPLINE_CURVE_WITH_KNOTS('',3,(#59217,#59218,#59219,#59220,#59221,
#59222,#59223,#59224,#59225,#59226),.UNSPECIFIED.,.F.,.F.,(4,1,1,1,1,1,
1,4),(53.4070751110265,53.8595736735331,54.8461030121971,55.8326323508611,
56.8191616895252,57.8056910281892,58.7922203668532,59.6902604182061),
 .UNSPECIFIED.);
#4365=B_SPLINE_CURVE_WITH_KNOTS('',3,(#59231,#59232,#59233,#59234,#59235,
#59236,#59237,#59238,#59239,#59240,#59241),.UNSPECIFIED.,.F.,.F.,(4,1,1,
1,1,1,1,1,4),(47.1238898038469,47.3704174554844,48.3569467941485,49.3434761328125,
50.3300054714765,51.3165348101405,52.3030641488046,53.2895934874686,53.4070751110265),
 .UNSPECIFIED.);
#4366=B_SPLINE_CURVE_WITH_KNOTS('',3,(#59242,#59243,#59244,#59245,#59246,
#59247,#59248,#59249,#59250,#59251),.UNSPECIFIED.,.F.,.F.,(4,1,1,1,1,1,
1,4),(47.1238898038469,47.9403976415489,48.9269269802129,49.9134563188769,
50.899985657541,51.886514996205,52.873044334869,53.4070751110265),
 .UNSPECIFIED.);
#4367=B_SPLINE_CURVE_WITH_KNOTS('',3,(#59256,#59257,#59258,#59259,#59260,
#59261,#59262,#59263,#59264,#59265),.UNSPECIFIED.,.F.,.F.,(4,1,1,1,1,1,
1,4),(40.8407044966673,41.4512414235002,42.4377707621643,43.4243001008283,
44.4108294394923,45.3973587781564,46.3838881168204,47.1238898038469),
 .UNSPECIFIED.);
#4368=B_SPLINE_CURVE_WITH_KNOTS('',3,(#59266,#59267,#59268,#59269,#59270,
#59271,#59272,#59273,#59274,#59275,#59276),.UNSPECIFIED.,.F.,.F.,(4,1,1,
1,1,1,1,1,4),(40.8407044966673,41.0346922709007,42.0212216095647,43.0077509482287,
43.9942802868927,44.9808096255568,45.9673389642208,46.9538683028848,47.1238898038469),
 .UNSPECIFIED.);
#4369=B_SPLINE_CURVE_WITH_KNOTS('',3,(#59281,#59282,#59283,#59284,#59285,
#59286,#59287,#59288,#59289,#59290),.UNSPECIFIED.,.F.,.F.,(4,1,1,1,1,1,
1,4),(34.5575191894877,35.5320653915161,36.5185947301801,37.5051240688441,
38.4916534075081,39.4781827461722,40.4647120848362,40.8407044966673),
 .UNSPECIFIED.);
#4370=B_SPLINE_CURVE_WITH_KNOTS('',3,(#59291,#59292,#59293,#59294,#59295,
#59296,#59297,#59298,#59299,#59300),.UNSPECIFIED.,.F.,.F.,(4,1,1,1,1,1,
1,4),(34.5575191894877,35.1155162389165,36.1020455775805,37.0885749162445,
38.0751042549086,39.0616335935726,40.0481629322366,40.8407044966673),
 .UNSPECIFIED.);
#4371=B_SPLINE_CURVE_WITH_KNOTS('',3,(#59305,#59306,#59307,#59308,#59309,
#59310,#59311,#59312,#59313,#59314,#59315),.UNSPECIFIED.,.F.,.F.,(4,1,1,
1,1,1,1,1,4),(28.2743338823081,28.6263600208678,29.6128893595319,30.5994186981959,
31.5859480368599,32.572477375524,33.559006714188,34.545536052852,34.5575191894877),
 .UNSPECIFIED.);
#4372=B_SPLINE_CURVE_WITH_KNOTS('',3,(#59316,#59317,#59318,#59319,#59320,
#59321,#59322,#59323,#59324,#59325),.UNSPECIFIED.,.F.,.F.,(4,1,1,1,1,1,
1,4),(28.2743338823081,29.1963402069323,30.1828695455963,31.1693988842603,
32.1559282229244,33.1424575615884,34.1289869002524,34.5575191894877),
 .UNSPECIFIED.);
#4373=B_SPLINE_CURVE_WITH_KNOTS('',3,(#59330,#59331,#59332,#59333,#59334,
#59335,#59336,#59337,#59338,#59339),.UNSPECIFIED.,.F.,.F.,(4,1,1,1,1,1,
1,4),(21.9911485751285,22.7071839888837,23.6937133275477,24.6802426662117,
25.6667720048757,26.6533013435398,27.6398306822038,28.2743338823081),
 .UNSPECIFIED.);
#4374=B_SPLINE_CURVE_WITH_KNOTS('',3,(#59340,#59341,#59342,#59343,#59344,
#59345,#59346,#59347,#59348,#59349,#59350),.UNSPECIFIED.,.F.,.F.,(4,1,1,
1,1,1,1,1,4),(21.9911485751285,22.2906348362841,23.2771641749481,24.2636935136121,
25.2502228522762,26.2367521909402,27.2232815296042,28.2098108682683,28.2743338823081),
 .UNSPECIFIED.);
#4375=B_SPLINE_CURVE_WITH_KNOTS('',3,(#59356,#59357,#59358,#59359,#59360),
 .UNSPECIFIED.,.F.,.F.,(4,1,4),(14.3984001269718,15.3849294656359,15.7079632679489),
 .UNSPECIFIED.);
#4376=B_SPLINE_CURVE_WITH_KNOTS('',3,(#59363,#59364,#59365,#59366,#59367),
 .UNSPECIFIED.,.F.,.F.,(4,1,4),(13.8759337553362,14.8149492795714,15.7079632679489),
 .UNSPECIFIED.);
#4377=B_SPLINE_CURVE_WITH_KNOTS('',3,(#59392,#59393,#59394,#59395,#59396,
#59397,#59398,#59399,#59400,#59401,#59402,#59403,#59404,#59405,#59406,#59407,
#59408,#59409,#59410,#59411,#59412,#59413,#59414,#59415,#59416,#59417,#59418,
#59419),.UNSPECIFIED.,.F.,.F.,(4,3,3,3,3,3,3,3,3,4),(-3.3351277338005,-3.21581204732697,
-2.97127448377657,-2.7269541692994,-2.48284991968139,-2.23896215435049,
-1.99538742760096,-1.75200286037067,-1.50889051064716,-1.38513595606351),
 .UNSPECIFIED.);
#4378=B_SPLINE_CURVE_WITH_KNOTS('',3,(#59427,#59428,#59429,#59430),
 .UNSPECIFIED.,.F.,.F.,(4,4),(-0.742759490140667,0.),.UNSPECIFIED.);
#4379=B_SPLINE_CURVE_WITH_KNOTS('',3,(#59440,#59441,#59442,#59443,#59444,
#59445,#59446,#59447,#59448,#59449,#59450,#59451,#59452,#59453,#59454,#59455,
#59456,#59457,#59458,#59459,#59460,#59461,#59462,#59463,#59464,#59465,#59466,
#59467),.UNSPECIFIED.,.F.,.F.,(4,3,3,3,3,3,3,3,3,4),(-3.33512774168352,
-3.21581203937105,-2.9712743901168,-2.72695409823512,-2.48284967780954,
-2.23896138594529,-1.99538662077021,-1.75200218102298,-1.50888981531756,
-1.38513595694967),.UNSPECIFIED.);
#4380=B_SPLINE_CURVE_WITH_KNOTS('',3,(#59475,#59476,#59477,#59478),
 .UNSPECIFIED.,.F.,.F.,(4,4),(-0.742759490382603,0.),.UNSPECIFIED.);
#4381=B_SPLINE_CURVE_WITH_KNOTS('',3,(#59488,#59489,#59490,#59491,#59492,
#59493,#59494,#59495,#59496,#59497,#59498,#59499,#59500,#59501,#59502,#59503,
#59504,#59505,#59506,#59507,#59508,#59509,#59510,#59511,#59512,#59513,#59514,
#59515),.UNSPECIFIED.,.F.,.F.,(4,3,3,3,3,3,3,3,3,4),(-3.33512773971227,
-3.21581201970404,-2.97127437729292,-2.72695395668863,-2.48284982134185,
-2.23896171731076,-1.99538699487002,-1.75200192521914,-1.50888988861517,
-1.38513595702442),.UNSPECIFIED.);
#4382=B_SPLINE_CURVE_WITH_KNOTS('',3,(#59523,#59524,#59525,#59526),
 .UNSPECIFIED.,.F.,.F.,(4,4),(-0.742759490770743,0.),.UNSPECIFIED.);
#4383=B_SPLINE_CURVE_WITH_KNOTS('',3,(#59536,#59537,#59538,#59539,#59540,
#59541),.UNSPECIFIED.,.F.,.F.,(4,2,4),(-3.33512774197138,-1.65413782257416,
-1.38513595763138),.UNSPECIFIED.);
#4384=B_SPLINE_CURVE_WITH_KNOTS('',3,(#59549,#59550,#59551,#59552),
 .UNSPECIFIED.,.F.,.F.,(4,4),(-0.742759491009937,0.),.UNSPECIFIED.);
#4385=B_SPLINE_CURVE_WITH_KNOTS('',3,(#59562,#59563,#59564,#59565,#59566,
#59567,#59568,#59569,#59570,#59571,#59572,#59573,#59574,#59575,#59576,#59577,
#59578,#59579,#59580,#59581,#59582,#59583,#59584,#59585,#59586,#59587,#59588,
#59589),.UNSPECIFIED.,.F.,.F.,(4,3,3,3,3,3,3,3,3,4),(-3.33512774327252,
-3.21581188244371,-2.97127402802938,-2.72695367771143,-2.48284924184614,
-2.23896121967729,-1.99538649326093,-1.75200210679088,-1.50888993573079,
-1.38513595840749),.UNSPECIFIED.);
#4386=B_SPLINE_CURVE_WITH_KNOTS('',3,(#59597,#59598,#59599,#59600),
 .UNSPECIFIED.,.F.,.F.,(4,4),(-0.742759490516493,0.),.UNSPECIFIED.);
#4387=B_SPLINE_CURVE_WITH_KNOTS('',3,(#59610,#59611,#59612,#59613,#59614,
#59615,#59616,#59617,#59618,#59619,#59620,#59621,#59622,#59623,#59624,#59625,
#59626,#59627,#59628,#59629,#59630,#59631,#59632,#59633,#59634,#59635,#59636,
#59637),.UNSPECIFIED.,.F.,.F.,(4,3,3,3,3,3,3,3,3,4),(-3.33512774337593,
-3.21581201730802,-2.97127431262814,-2.72695414046584,-2.48285027782337,
-2.2389618830467,-1.99538715953051,-1.7520020612767,-1.5088900089662,-1.38513595750991),
 .UNSPECIFIED.);
#4388=B_SPLINE_CURVE_WITH_KNOTS('',3,(#59645,#59646,#59647,#59648),
 .UNSPECIFIED.,.F.,.F.,(4,4),(-0.742759490399252,0.),.UNSPECIFIED.);
#4389=B_SPLINE_CURVE_WITH_KNOTS('',3,(#59656,#59657,#59658,#59659,#59660,
#59661,#59662,#59663,#59664,#59665,#59666,#59667,#59668,#59669,#59670,#59671,
#59672,#59673,#59674,#59675,#59676,#59677,#59678,#59679,#59680,#59681,#59682,
#59683,#59684,#59685,#59686,#59687,#59688,#59689,#59690,#59691,#59692,#59693,
#59694,#59695,#59696,#59697,#59698,#59699,#59700,#59701,#59702,#59703,#59704,
#59705,#59706,#59707,#59708,#59709,#59710,#59711,#59712,#59713,#59714,#59715,
#59716,#59717,#59718,#59719,#59720,#59721,#59722,#59723,#59724,#59725,#59726,
#59727,#59728,#59729,#59730,#59731,#59732,#59733,#59734),.UNSPECIFIED.,
 .F.,.F.,(4,3,3,3,3,3,3,3,3,3,3,3,3,3,3,3,3,3,3,3,3,3,3,3,3,3,4),(0.,0.0183455177171488,
0.0365842194687939,0.0503567097523435,0.0575063938651825,0.0612717135192181,
0.0790233191281566,0.096412403715043,0.10900033822058,0.115579427932303,
0.11863915864875,0.13548956751629,0.14676414173719,0.163451454243383,0.168605352621408,
0.173128046239674,0.189898672554047,0.206649133260606,0.217355581880073,
0.222872485157851,0.226199941445228,0.2422909706325,0.252395568311884,0.256090122700147,
0.271598926188493,0.280262641786736,0.286347380332249),.UNSPECIFIED.);
#4390=B_SPLINE_CURVE_WITH_KNOTS('',3,(#59735,#59736,#59737,#59738,#59739,
#59740,#59741,#59742,#59743,#59744,#59745,#59746,#59747,#59748,#59749,#59750,
#59751,#59752,#59753,#59754,#59755,#59756,#59757,#59758,#59759,#59760,#59761,
#59762,#59763,#59764,#59765,#59766,#59767,#59768,#59769,#59770,#59771,#59772,
#59773,#59774,#59775,#59776,#59777,#59778,#59779,#59780,#59781,#59782,#59783,
#59784,#59785,#59786,#59787,#59788,#59789,#59790,#59791,#59792,#59793,#59794,
#59795,#59796,#59797,#59798,#59799,#59800,#59801,#59802,#59803,#59804,#59805,
#59806,#59807,#59808,#59809,#59810,#59811,#59812,#59813,#59814,#59815,#59816),
 .UNSPECIFIED.,.F.,.F.,(4,3,3,3,3,3,3,3,3,3,3,3,3,3,3,3,3,3,3,3,3,3,3,3,
3,3,3,4),(0.,0.0151376945523622,0.0309539555233482,0.0436386424985849,0.049000547090806,
0.0520439606424598,0.0683447111906178,0.0849441791722525,0.0968159972104999,
0.101863070537586,0.10487005785608,0.121945783028775,0.132431451325242,
0.149057557666816,0.154031803331322,0.158630806444058,0.175669023659517,
0.193110008838669,0.203698775422856,0.209528903797298,0.213039490372793,
0.231030287351627,0.242727750891762,0.247562329943512,0.251101657049746,
0.269297746623456,0.277820141512166,0.285142803995177),.UNSPECIFIED.);
#4391=B_SPLINE_CURVE_WITH_KNOTS('',3,(#59818,#59819,#59820,#59821,#59822,
#59823,#59824,#59825,#59826,#59827,#59828,#59829,#59830,#59831,#59832,#59833,
#59834,#59835,#59836,#59837,#59838,#59839,#59840,#59841,#59842,#59843,#59844,
#59845,#59846,#59847,#59848,#59849,#59850,#59851,#59852,#59853,#59854,#59855,
#59856,#59857,#59858,#59859,#59860,#59861,#59862,#59863,#59864,#59865,#59866,
#59867,#59868,#59869,#59870,#59871,#59872,#59873,#59874,#59875,#59876,#59877,
#59878,#59879,#59880,#59881,#59882,#59883,#59884,#59885,#59886,#59887,#59888,
#59889,#59890,#59891,#59892,#59893,#59894,#59895,#59896),.UNSPECIFIED.,
 .F.,.F.,(4,3,3,3,3,3,3,3,3,3,3,3,3,3,3,3,3,3,3,3,3,3,3,3,3,3,4),(0.,0.0183455177171464,
0.0365842202218134,0.0503567104112331,0.0575063958814502,0.0612717147976262,
0.0790233202990436,0.096412400821268,0.109000336050244,0.115579427690159,
0.11863915902179,0.135489564068242,0.146764141737171,0.163451454243363,
0.168605347203144,0.173128047807504,0.189898674519216,0.206649134734921,
0.217355586796981,0.222872485969177,0.226199940772131,0.24229096629471,
0.252395560905716,0.256090108931784,0.271598906474471,0.280262641786705,
0.286347380332217),.UNSPECIFIED.);
#4392=B_SPLINE_CURVE_WITH_KNOTS('',3,(#59897,#59898,#59899,#59900,#59901,
#59902,#59903,#59904,#59905,#59906,#59907,#59908,#59909,#59910,#59911,#59912,
#59913,#59914,#59915,#59916,#59917,#59918,#59919,#59920,#59921,#59922,#59923,
#59924,#59925,#59926,#59927,#59928,#59929,#59930,#59931,#59932,#59933,#59934,
#59935,#59936,#59937,#59938,#59939,#59940,#59941,#59942,#59943,#59944,#59945,
#59946,#59947,#59948,#59949,#59950,#59951,#59952,#59953,#59954,#59955,#59956,
#59957,#59958,#59959,#59960,#59961,#59962,#59963,#59964,#59965,#59966,#59967,
#59968,#59969,#59970,#59971,#59972,#59973,#59974,#59975,#59976,#59977,#59978),
 .UNSPECIFIED.,.F.,.F.,(4,3,3,3,3,3,3,3,3,3,3,3,3,3,3,3,3,3,3,3,3,3,3,3,
3,3,3,4),(0.,0.0151377073331275,0.0309539773939491,0.0436386616353583,0.049000603702908,
0.0520439678481244,0.068344727340715,0.0849441979341871,0.0968160112819461,
0.101863110224252,0.104870125248596,0.121945848980836,0.132431451325223,
0.149057551294161,0.154031802130475,0.158630806791255,0.175669017059408,
0.193109999022821,0.203698766833983,0.209528894188178,0.213039481192876,
0.231030277572612,0.242727743557488,0.24756230355572,0.251101629527168,
0.26929771945885,0.277820141512119,0.285142803995128),.UNSPECIFIED.);
#4393=B_SPLINE_CURVE_WITH_KNOTS('',3,(#59979,#59980,#59981,#59982,#59983,
#59984,#59985,#59986,#59987,#59988,#59989,#59990,#59991,#59992,#59993,#59994,
#59995,#59996,#59997,#59998,#59999,#60000,#60001,#60002,#60003,#60004,#60005,
#60006,#60007,#60008,#60009,#60010,#60011,#60012,#60013,#60014,#60015,#60016,
#60017,#60018,#60019,#60020,#60021,#60022,#60023,#60024,#60025,#60026,#60027,
#60028,#60029,#60030,#60031,#60032,#60033,#60034,#60035,#60036,#60037,#60038,
#60039,#60040,#60041,#60042,#60043,#60044,#60045,#60046,#60047,#60048,#60049,
#60050,#60051,#60052,#60053,#60054,#60055,#60056,#60057),.UNSPECIFIED.,
 .F.,.F.,(4,3,3,3,3,3,3,3,3,3,3,3,3,3,3,3,3,3,3,3,3,3,3,3,3,3,4),(0.,0.0183455177171491,
0.0365841943725053,0.0503566877930912,0.0575063272586958,0.0612716713524759,
0.0790232799247667,0.0964124964716688,0.10900040778805,0.115579434178192,
0.118639143887527,0.135489676819533,0.146764141737193,0.163451454243384,
0.168605528191993,0.173127995302464,0.189898608413707,0.206649084167343,
0.217355422796664,0.222872458887097,0.226199963177961,0.24229110995885,
0.252395806920558,0.256090567682751,0.27159956261746,0.280262641786727,
0.28634738033224),.UNSPECIFIED.);
#4394=B_SPLINE_CURVE_WITH_KNOTS('',3,(#60058,#60059,#60060,#60061,#60062,
#60063,#60064,#60065,#60066,#60067,#60068,#60069,#60070,#60071,#60072,#60073,
#60074,#60075,#60076,#60077,#60078,#60079,#60080,#60081,#60082,#60083,#60084,
#60085,#60086,#60087,#60088,#60089,#60090,#60091,#60092,#60093,#60094,#60095,
#60096,#60097,#60098,#60099,#60100,#60101,#60102,#60103,#60104,#60105,#60106,
#60107,#60108,#60109,#60110,#60111,#60112,#60113,#60114,#60115,#60116,#60117,
#60118,#60119,#60120,#60121,#60122,#60123,#60124,#60125,#60126,#60127,#60128,
#60129,#60130,#60131,#60132,#60133,#60134,#60135,#60136,#60137,#60138,#60139),
 .UNSPECIFIED.,.F.,.F.,(4,3,3,3,3,3,3,3,3,3,3,3,3,3,3,3,3,3,3,3,3,3,3,3,
3,3,3,4),(0.,0.0151372184044385,0.0309531403735887,0.043637929242543,0.0489984376247301,
0.0520436975026237,0.0683441145647309,0.0849434845410623,0.0968154762371025,
0.10186160092259,0.10486756751019,0.121943345305763,0.132431451325223,0.149057794056237,
0.154031847028422,0.158630793802344,0.175669268709996,0.193110373371059,
0.203699094388695,0.209529259612817,0.213039830397245,0.231030649717207,
0.242728022665942,0.247563307937232,0.251102678589767,0.269298754560415,
0.277820141512145,0.285142803995156),.UNSPECIFIED.);
#4395=B_SPLINE_CURVE_WITH_KNOTS('',3,(#60140,#60141,#60142,#60143,#60144,
#60145,#60146,#60147,#60148,#60149,#60150,#60151,#60152,#60153,#60154,#60155,
#60156,#60157,#60158,#60159,#60160,#60161,#60162,#60163,#60164,#60165,#60166,
#60167,#60168,#60169,#60170,#60171,#60172,#60173,#60174,#60175,#60176,#60177,
#60178,#60179,#60180,#60181,#60182,#60183,#60184,#60185,#60186,#60187,#60188,
#60189,#60190,#60191,#60192,#60193,#60194,#60195,#60196,#60197,#60198,#60199,
#60200,#60201,#60202,#60203,#60204,#60205,#60206,#60207,#60208,#60209,#60210,
#60211,#60212,#60213,#60214,#60215,#60216,#60217,#60218),.UNSPECIFIED.,
 .F.,.F.,(4,3,3,3,3,3,3,3,3,3,3,3,3,3,3,3,3,3,3,3,3,3,3,3,3,3,4),(0.,0.0183455177171496,
0.0365842194687423,0.0503567097522991,0.0575063938651049,0.0612717135166192,
0.0790233191256915,0.0964124037125833,0.109000338218737,0.115579427930349,
0.118639158644869,0.13548956751248,0.146764141737196,0.163451454243393,
0.16860535262136,0.173128046238754,0.189898672553141,0.206649133259799,
0.21735558187922,0.222872485156807,0.226199941447941,0.242290970635022,
0.252395568315028,0.256090122699954,0.271598926188319,0.280262641786767,
0.286347380332284),.UNSPECIFIED.);
#4396=B_SPLINE_CURVE_WITH_KNOTS('',3,(#60219,#60220,#60221,#60222,#60223,
#60224,#60225,#60226,#60227,#60228,#60229,#60230,#60231,#60232,#60233,#60234,
#60235,#60236,#60237,#60238,#60239,#60240,#60241,#60242,#60243,#60244,#60245,
#60246,#60247,#60248,#60249,#60250,#60251,#60252,#60253,#60254,#60255,#60256,
#60257,#60258,#60259,#60260,#60261,#60262,#60263,#60264,#60265,#60266,#60267,
#60268,#60269,#60270,#60271,#60272,#60273,#60274,#60275,#60276,#60277,#60278,
#60279,#60280,#60281,#60282,#60283,#60284,#60285,#60286,#60287,#60288,#60289,
#60290,#60291,#60292,#60293,#60294,#60295,#60296,#60297,#60298,#60299,#60300),
 .UNSPECIFIED.,.F.,.F.,(4,3,3,3,3,3,3,3,3,3,3,3,3,3,3,3,3,3,3,3,3,3,3,3,
3,3,3,4),(0.,0.015137694552346,0.0309539555233422,0.0436386424985786,0.0490005470908032,
0.052043960644431,0.068344711192548,0.0849441791741085,0.0968159972118898,
0.101863070541411,0.104870057863348,0.121945783035943,0.132431451325233,
0.149057557666585,0.154031803331171,0.158630806444046,0.175669023659537,
0.193110008838639,0.203698775422825,0.209528903797183,0.213039490371705,
0.231030287350353,0.242727750890797,0.24756232993717,0.251101657039408,
0.26929774661335,0.277820141512129,0.285142803995137),.UNSPECIFIED.);
#4397=B_SPLINE_CURVE_WITH_KNOTS('',3,(#60301,#60302,#60303,#60304,#60305,
#60306,#60307,#60308,#60309,#60310,#60311,#60312,#60313,#60314,#60315,#60316,
#60317,#60318,#60319,#60320,#60321,#60322,#60323,#60324,#60325,#60326,#60327,
#60328,#60329,#60330,#60331,#60332,#60333,#60334,#60335,#60336,#60337,#60338,
#60339,#60340,#60341,#60342,#60343,#60344,#60345,#60346,#60347,#60348,#60349,
#60350,#60351,#60352,#60353,#60354,#60355,#60356,#60357,#60358,#60359,#60360,
#60361,#60362,#60363,#60364,#60365,#60366,#60367,#60368,#60369,#60370,#60371,
#60372,#60373,#60374,#60375,#60376,#60377,#60378,#60379),.UNSPECIFIED.,
 .F.,.F.,(4,3,3,3,3,3,3,3,3,3,3,3,3,3,3,3,3,3,3,3,3,3,3,3,3,3,4),(0.,0.0183455177171492,
0.0365842202217887,0.0503567104112144,0.0575063958813968,0.0612717147969415,
0.0790233202984323,0.0964124008207027,0.109000336049826,0.115579427689752,
0.118639159024108,0.135489564070542,0.146764141737194,0.163451454243389,
0.168605347203302,0.173128047809237,0.189898674521018,0.206649134736986,
0.217355586794765,0.222872485965579,0.226199940772176,0.242290966294427,
0.252395560905467,0.256090108929053,0.271598906471585,0.280262641786756,
0.286347380332274),.UNSPECIFIED.);
#4398=B_SPLINE_CURVE_WITH_KNOTS('',3,(#60380,#60381,#60382,#60383,#60384,
#60385,#60386,#60387,#60388,#60389,#60390,#60391,#60392,#60393,#60394,#60395,
#60396,#60397,#60398,#60399,#60400,#60401,#60402,#60403,#60404,#60405,#60406,
#60407,#60408,#60409,#60410,#60411,#60412,#60413,#60414,#60415,#60416,#60417,
#60418,#60419,#60420,#60421,#60422,#60423,#60424,#60425,#60426,#60427,#60428,
#60429,#60430,#60431,#60432,#60433,#60434,#60435,#60436,#60437,#60438,#60439,
#60440,#60441,#60442,#60443,#60444,#60445,#60446,#60447,#60448,#60449,#60450,
#60451,#60452,#60453,#60454,#60455,#60456,#60457,#60458,#60459,#60460,#60461),
 .UNSPECIFIED.,.F.,.F.,(4,3,3,3,3,3,3,3,3,3,3,3,3,3,3,3,3,3,3,3,3,3,3,3,
3,3,3,4),(0.,0.0151377073334981,0.0309539773942999,0.0436386616356645,0.0490006037038296,
0.0520439678487852,0.0683447273416009,0.0849441979349755,0.0968160112825359,
0.101863110225754,0.104870125256082,0.121945848988211,0.132431451325217,
0.149057551294131,0.154031802130417,0.158630806785895,0.1756690170539,0.193109999017219,
0.203698766829082,0.209528894184026,0.213039481197191,0.231030277576794,
0.242727743560627,0.247562303564317,0.251101629536978,0.269297719468806,
0.277820141512128,0.285142803995138),.UNSPECIFIED.);
#4399=B_SPLINE_CURVE_WITH_KNOTS('',3,(#60462,#60463,#60464,#60465,#60466,
#60467,#60468,#60469,#60470,#60471,#60472,#60473,#60474,#60475,#60476,#60477,
#60478,#60479,#60480,#60481,#60482,#60483,#60484,#60485,#60486,#60487,#60488,
#60489,#60490,#60491,#60492,#60493,#60494,#60495,#60496,#60497,#60498,#60499,
#60500,#60501,#60502,#60503,#60504,#60505,#60506,#60507,#60508,#60509,#60510,
#60511,#60512,#60513,#60514,#60515,#60516,#60517,#60518,#60519,#60520,#60521,
#60522,#60523,#60524,#60525,#60526,#60527,#60528,#60529,#60530,#60531,#60532,
#60533,#60534,#60535,#60536,#60537,#60538,#60539,#60540),.UNSPECIFIED.,
 .F.,.F.,(4,3,3,3,3,3,3,3,3,3,3,3,3,3,3,3,3,3,3,3,3,3,3,3,3,3,4),(0.,0.018345517717149,
0.0365841943724813,0.0503566877930701,0.057506327258564,0.0612716713518624,
0.079023279923942,0.0964124964708253,0.109000407787417,0.115579434177528,
0.118639143891469,0.135489676823446,0.146764141737192,0.163451454243385,
0.168605528191884,0.173127995305518,0.189898608416791,0.206649084170442,
0.21735542279444,0.222872458884167,0.226199963170307,0.242291109951151,
0.252395806910312,0.256090567650659,0.271599562585826,0.280262641786738,
0.286347380332254),.UNSPECIFIED.);
#4400=B_SPLINE_CURVE_WITH_KNOTS('',3,(#60541,#60542,#60543,#60544,#60545,
#60546,#60547,#60548,#60549,#60550,#60551,#60552,#60553,#60554,#60555,#60556,
#60557,#60558,#60559,#60560,#60561,#60562,#60563,#60564,#60565,#60566,#60567,
#60568,#60569,#60570,#60571,#60572,#60573,#60574,#60575,#60576,#60577,#60578,
#60579,#60580,#60581,#60582,#60583,#60584,#60585,#60586,#60587,#60588,#60589,
#60590,#60591,#60592,#60593,#60594,#60595,#60596,#60597,#60598,#60599,#60600,
#60601,#60602,#60603,#60604,#60605,#60606,#60607,#60608,#60609,#60610,#60611,
#60612,#60613,#60614,#60615,#60616,#60617,#60618,#60619,#60620,#60621,#60622),
 .UNSPECIFIED.,.F.,.F.,(4,3,3,3,3,3,3,3,3,3,3,3,3,3,3,3,3,3,3,3,3,3,3,3,
3,3,3,4),(0.,0.0151372184042629,0.0309531403734452,0.0436379292424174,0.0489984376244327,
0.0520436974965136,0.068344114558214,0.0849434845342685,0.0968154762320069,
0.101861600908548,0.104867567483352,0.121943345279016,0.132431451325222,
0.149057794056487,0.15403184702849,0.158630793803121,0.175669268710828,
0.193110373371818,0.203699094389356,0.209529259613411,0.213039830390277,
0.23103064971016,0.242728022660651,0.247563307922767,0.251102678572032,
0.26929875454266,0.277820141512126,0.285142803995136),.UNSPECIFIED.);
#4401=B_SPLINE_CURVE_WITH_KNOTS('',3,(#60624,#60625,#60626,#60627,#60628,
#60629,#60630,#60631,#60632,#60633,#60634,#60635,#60636,#60637,#60638,#60639,
#60640,#60641,#60642,#60643,#60644,#60645,#60646,#60647,#60648,#60649,#60650,
#60651,#60652,#60653,#60654,#60655,#60656,#60657,#60658,#60659,#60660,#60661,
#60662,#60663,#60664,#60665,#60666,#60667,#60668,#60669,#60670,#60671,#60672,
#60673,#60674,#60675,#60676,#60677,#60678,#60679,#60680,#60681,#60682,#60683,
#60684,#60685,#60686,#60687,#60688,#60689,#60690,#60691,#60692,#60693,#60694,
#60695,#60696,#60697,#60698,#60699,#60700,#60701,#60702,#60703,#60704,#60705),
 .UNSPECIFIED.,.F.,.F.,(4,3,3,3,3,3,3,3,3,3,3,3,3,3,3,3,3,3,3,3,3,3,3,3,
3,3,3,4),(-0.286347380332265,-0.271025621689181,-0.2607001267017,-0.255933999919549,
-0.251928786217061,-0.235739770681133,-0.229543552625755,-0.225090694889911,
-0.221644284966547,-0.204610638152085,-0.187823738644011,-0.179057759822907,
-0.17435510384889,-0.171011960015997,-0.168068908456346,-0.153509697708698,
-0.136938545278062,-0.120740430888098,-0.116772838424861,-0.113777170632241,
-0.0964534278367324,-0.0787580645164197,-0.0609069559269026,-0.0568632900112524,
-0.0386443178831796,-0.0205854755521028,-0.00735363015835137,0.),
 .UNSPECIFIED.);
#4402=B_SPLINE_CURVE_WITH_KNOTS('',3,(#60706,#60707,#60708,#60709,#60710,
#60711,#60712,#60713,#60714,#60715,#60716,#60717,#60718,#60719,#60720,#60721,
#60722,#60723,#60724,#60725,#60726,#60727,#60728,#60729,#60730,#60731,#60732,
#60733,#60734,#60735,#60736,#60737,#60738,#60739,#60740,#60741,#60742,#60743,
#60744,#60745,#60746,#60747,#60748,#60749,#60750,#60751,#60752,#60753,#60754,
#60755,#60756,#60757,#60758,#60759,#60760,#60761,#60762,#60763,#60764,#60765,
#60766,#60767,#60768,#60769,#60770,#60771,#60772,#60773,#60774,#60775,#60776,
#60777,#60778,#60779,#60780,#60781),.UNSPECIFIED.,.F.,.F.,(4,3,3,3,3,3,
3,3,3,3,3,3,3,3,3,3,3,3,3,3,3,3,3,3,3,4),(-0.285142803995153,-0.266893522635859,
-0.249971640311975,-0.245887155067402,-0.227911309461469,-0.216815964918886,
-0.213019369676792,-0.209467693445812,-0.19188790836456,-0.174756961586316,
-0.165469070515125,-0.157741742341544,-0.154438844453031,-0.139148553120806,
-0.122062040548429,-0.107562425207839,-0.103576093458224,-0.100472602942305,
-0.0838658643924183,-0.067352053952836,-0.0520303199205553,-0.0480946799675465,
-0.0321859944606069,-0.0168167950639115,-0.00606511782371307,0.),
 .UNSPECIFIED.);
#4403=B_SPLINE_CURVE_WITH_KNOTS('',3,(#60783,#60784,#60785,#60786,#60787,
#60788,#60789,#60790,#60791,#60792,#60793),.UNSPECIFIED.,.F.,.F.,(4,1,1,
1,1,1,1,1,4),(15.7079632679489,15.8014786182354,16.7880079568995,17.7745372955635,
18.7610666342275,19.7475959728916,20.7341253115556,21.7206546502196,21.9911485751285),
 .UNSPECIFIED.);
#4404=B_SPLINE_CURVE_WITH_KNOTS('',3,(#60794,#60795,#60796,#60797,#60798,
#60799,#60800,#60801,#60802,#60803),.UNSPECIFIED.,.F.,.F.,(4,1,1,1,1,1,
1,4),(15.7079632679489,16.3714588042999,17.3579881429639,18.3445174816279,
19.331046820292,20.317576158956,21.30410549762,21.9911485751285),
 .UNSPECIFIED.);
#4405=B_SPLINE_CURVE_WITH_KNOTS('',3,(#61028,#61029,#61030,#61031,#61032,
#61033,#61034,#61035,#61036,#61037,#61038,#61039,#61040,#61041,#61042,#61043,
#61044,#61045,#61046,#61047,#61048,#61049,#61050,#61051,#61052,#61053,#61054,
#61055,#61056,#61057,#61058,#61059,#61060,#61061,#61062,#61063,#61064,#61065,
#61066,#61067,#61068,#61069,#61070,#61071,#61072,#61073,#61074,#61075,#61076,
#61077,#61078,#61079,#61080,#61081,#61082,#61083,#61084,#61085,#61086,#61087,
#61088,#61089,#61090,#61091,#61092,#61093,#61094,#61095,#61096,#61097,#61098,
#61099,#61100,#61101,#61102,#61103,#61104,#61105,#61106,#61107,#61108,#61109),
 .UNSPECIFIED.,.F.,.F.,(4,3,3,3,3,3,3,3,3,3,3,3,3,3,3,3,3,3,3,3,3,3,3,3,
3,3,3,4),(0.,0.015137799248671,0.0309541346648961,0.0436387992474388,0.0490010108224065,
0.0520440199058781,0.0683448437142619,0.0849443330626919,0.0968161126283283,
0.101863396045917,0.104870610850094,0.121946324179646,0.132431451325237,
0.149057505425983,0.154031793452878,0.158630809285983,0.175668969545569,
0.193109928370158,0.203698705012908,0.209528824985022,0.213039415113619,
0.231030207185071,0.242727690766841,0.247562113630917,0.251101431476904,
0.269297523974363,0.277820141512152,0.285142803995165),.UNSPECIFIED.);
#4406=B_SPLINE_CURVE_WITH_KNOTS('',3,(#61110,#61111,#61112,#61113,#61114,
#61115,#61116,#61117,#61118,#61119,#61120,#61121,#61122,#61123,#61124,#61125,
#61126,#61127,#61128,#61129,#61130,#61131,#61132,#61133,#61134),
 .UNSPECIFIED.,.F.,.F.,(4,3,3,3,3,3,3,3,4),(-10.1357873115492,-9.86529338664031,
-8.87876404797627,-7.89223470931224,-6.90570537064822,-5.91917603198418,
-4.93264669332015,-3.94611735465612,-3.85260200436961),.UNSPECIFIED.);
#4407=B_SPLINE_CURVE_WITH_KNOTS('',3,(#61359,#61360,#61361,#61362,#61363,
#61364,#61365,#61366,#61367,#61368,#61369,#61370,#61371,#61372,#61373,#61374,
#61375,#61376,#61377,#61378,#61379,#61380,#61381,#61382,#61383),
 .UNSPECIFIED.,.F.,.F.,(4,3,3,3,3,3,3,3,4),(7.59274844815668,7.89223470931225,
8.87876404797628,9.86529338664031,10.8518227253043,11.8383520639684,12.8248814026324,
13.8114107412964,13.8759337553363),.UNSPECIFIED.);
#4408=B_SPLINE_CURVE_WITH_KNOTS('',3,(#61384,#61385,#61386,#61387,#61388,
#61389,#61390,#61391,#61392,#61393,#61394,#61395,#61396,#61397,#61398,#61399,
#61400,#61401,#61402,#61403,#61404,#61405,#61406,#61407,#61408,#61409,#61410,
#61411,#61412,#61413,#61414,#61415,#61416,#61417,#61418,#61419,#61420,#61421,
#61422,#61423,#61424,#61425,#61426,#61427,#61428,#61429,#61430,#61431,#61432,
#61433,#61434,#61435,#61436,#61437,#61438,#61439,#61440,#61441,#61442,#61443,
#61444,#61445,#61446,#61447,#61448,#61449,#61450,#61451,#61452,#61453,#61454,
#61455,#61456,#61457,#61458,#61459,#61460,#61461,#61462),.UNSPECIFIED.,
 .F.,.F.,(4,3,3,3,3,3,3,3,3,3,3,3,3,3,3,3,3,3,3,3,3,3,3,3,3,3,4),(0.,0.0183455177171469,
0.0365842224515149,0.0503567123622224,0.0575064018579709,0.0612717186027069,
0.0790233237781577,0.0964123922275627,0.109000329604966,0.115579426964778,
0.118639160106121,0.135489553802985,0.146764141737175,0.16345145424337,
0.16860533110635,0.173128052468331,0.189898680357127,0.206649139105657,
0.217355601404692,0.2228724883745,0.226199938776673,0.242290953398615,0.252395538894453,
0.256090068020206,0.271598847885511,0.280262641786736,0.286347380332253),
 .UNSPECIFIED.);
#4409=B_SPLINE_CURVE_WITH_KNOTS('',3,(#61465,#61466,#61467,#61468,#61469,
#61470,#61471,#61472,#61473,#61474,#61475,#61476,#61477,#61478,#61479,#61480,
#61481,#61482,#61483,#61484,#61485,#61486,#61487,#61488,#61489,#61490,#61491,
#61492,#61493,#61494,#61495,#61496,#61497,#61498,#61499,#61500,#61501,#61502,
#61503,#61504,#61505,#61506,#61507,#61508,#61509,#61510,#61511,#61512,#61513,
#61514,#61515,#61516,#61517,#61518,#61519,#61520,#61521,#61522,#61523,#61524,
#61525,#61526,#61527,#61528,#61529,#61530,#61531,#61532,#61533,#61534,#61535,
#61536,#61537,#61538,#61539,#61540,#61541,#61542,#61543,#61544,#61545,#61546),
 .UNSPECIFIED.,.F.,.F.,(4,3,3,3,3,3,3,3,3,3,3,3,3,3,3,3,3,3,3,3,3,3,3,3,
3,3,3,4),(-0.286347380332235,-0.271025121721878,-0.260698471407634,-0.255927424635191,
-0.251928101931866,-0.235738748722702,-0.229541533305995,-0.225083562731207,
-0.221641685050275,-0.204608688214882,-0.187821861453013,-0.179056467789758,
-0.17435297386637,-0.171008268443927,-0.168068104867454,-0.153509697708701,
-0.136938887237132,-0.120740730102284,-0.116774494101265,-0.113778981555512,
-0.0964555421171121,-0.0787603000996159,-0.0609086326142997,-0.0568635712073007,
-0.0386446475024485,-0.0205858121909903,-0.00735363015835102,0.),
 .UNSPECIFIED.);
#4410=B_SPLINE_CURVE_WITH_KNOTS('',3,(#61547,#61548,#61549,#61550,#61551,
#61552,#61553,#61554,#61555,#61556,#61557,#61558,#61559,#61560,#61561,#61562,
#61563,#61564,#61565,#61566,#61567,#61568,#61569,#61570,#61571,#61572,#61573,
#61574,#61575,#61576,#61577,#61578,#61579,#61580,#61581,#61582,#61583,#61584,
#61585,#61586,#61587,#61588,#61589,#61590,#61591,#61592,#61593,#61594,#61595,
#61596,#61597,#61598,#61599,#61600,#61601,#61602,#61603,#61604,#61605,#61606,
#61607,#61608,#61609,#61610,#61611,#61612,#61613,#61614,#61615,#61616,#61617,
#61618,#61619,#61620,#61621,#61622),.UNSPECIFIED.,.F.,.F.,(4,3,3,3,3,3,
3,3,3,3,3,3,3,3,3,3,3,3,3,3,3,3,3,3,3,4),(-0.285142803995111,-0.266893522635822,
-0.249971476962298,-0.24588710473722,-0.22791128063125,-0.216815939692444,
-0.213019163167601,-0.209467643672605,-0.191887871034653,-0.174757065702234,
-0.165469235776541,-0.157741962735036,-0.154438808545209,-0.139148553120797,
-0.122062022789849,-0.107562409669082,-0.103576180068673,-0.100472613982929,
-0.0838658564336281,-0.0673520878880563,-0.0520303453719698,-0.0480947095105707,
-0.0321861105599142,-0.0168171759222756,-0.0060651178237103,0.),
 .UNSPECIFIED.);
#4411=B_SPLINE_CURVE_WITH_KNOTS('',3,(#61624,#61625,#61626,#61627,#61628,
#61629,#61630,#61631,#61632,#61633,#61634),.UNSPECIFIED.,.F.,.F.,(4,1,1,
1,1,1,1,1,4),(15.7079632679489,15.8014786182355,16.7880079568995,17.7745372955635,
18.7610666342275,19.7475959728916,20.7341253115556,21.7206546502196,21.9911485751285),
 .UNSPECIFIED.);
#4412=B_SPLINE_CURVE_WITH_KNOTS('',3,(#61635,#61636,#61637,#61638,#61639,
#61640,#61641,#61642,#61643,#61644),.UNSPECIFIED.,.F.,.F.,(4,1,1,1,1,1,
1,4),(15.7079632679489,16.3714588042999,17.3579881429639,18.344517481628,
19.331046820292,20.317576158956,21.3041054976201,21.9911485751285),
 .UNSPECIFIED.);
#4413=B_SPLINE_CURVE_WITH_KNOTS('',3,(#61869,#61870,#61871,#61872,#61873,
#61874,#61875,#61876,#61877,#61878,#61879,#61880,#61881,#61882,#61883,#61884,
#61885,#61886,#61887,#61888,#61889,#61890,#61891,#61892,#61893,#61894,#61895,
#61896,#61897,#61898,#61899,#61900,#61901,#61902,#61903,#61904,#61905,#61906,
#61907,#61908,#61909,#61910,#61911,#61912,#61913,#61914,#61915,#61916,#61917,
#61918,#61919,#61920,#61921,#61922,#61923,#61924,#61925,#61926,#61927,#61928,
#61929,#61930,#61931,#61932,#61933,#61934,#61935,#61936,#61937,#61938,#61939,
#61940,#61941,#61942,#61943,#61944,#61945,#61946,#61947,#61948,#61949,#61950),
 .UNSPECIFIED.,.F.,.F.,(4,3,3,3,3,3,3,3,3,3,3,3,3,3,3,3,3,3,3,3,3,3,3,3,
3,3,3,4),(0.,0.0151383248854633,0.0309550335466972,0.0436395857690147,0.0490033384906151,
0.0520443250916062,0.0683455163450802,0.084945111984634,0.0968166968197849,
0.101865043241974,0.10487341705618,0.121949069466398,0.132431451325238,
0.14905724175649,0.154031742415311,0.158630823850449,0.17566869659654,0.193109522683113,
0.203698350036742,0.209528426219277,0.213039034676904,0.231029802154963,
0.242727386994258,0.247561020935096,0.251100294233131,0.269296401038409,
0.277820141512142,0.285142803995154),.UNSPECIFIED.);
#4414=B_SPLINE_CURVE_WITH_KNOTS('',3,(#61951,#61952,#61953,#61954,#61955,
#61956,#61957,#61958,#61959,#61960,#61961,#61962,#61963,#61964,#61965,#61966,
#61967,#61968,#61969,#61970,#61971,#61972,#61973,#61974,#61975),
 .UNSPECIFIED.,.F.,.F.,(4,3,3,3,3,3,3,3,4),(-10.1357873115492,-9.86529338664031,
-8.87876404797628,-7.89223470931225,-6.90570537064822,-5.91917603198419,
-4.93264669332016,-3.94611735465612,-3.85260200436962),.UNSPECIFIED.);
#4415=B_SPLINE_CURVE_WITH_KNOTS('',3,(#62200,#62201,#62202,#62203,#62204,
#62205,#62206,#62207,#62208,#62209,#62210,#62211,#62212,#62213,#62214,#62215,
#62216,#62217,#62218,#62219,#62220,#62221,#62222,#62223,#62224),
 .UNSPECIFIED.,.F.,.F.,(4,3,3,3,3,3,3,3,4),(7.59274844815668,7.89223470931225,
8.87876404797628,9.86529338664031,10.8518227253043,11.8383520639684,12.8248814026324,
13.8114107412964,13.8759337553363),.UNSPECIFIED.);
#4416=B_SPLINE_CURVE_WITH_KNOTS('',3,(#62225,#62226,#62227,#62228,#62229,
#62230,#62231,#62232,#62233,#62234,#62235,#62236,#62237,#62238,#62239,#62240,
#62241,#62242,#62243,#62244,#62245,#62246,#62247,#62248,#62249,#62250,#62251,
#62252,#62253,#62254,#62255,#62256,#62257,#62258,#62259,#62260,#62261,#62262,
#62263,#62264,#62265,#62266,#62267,#62268,#62269,#62270,#62271,#62272,#62273,
#62274,#62275,#62276,#62277,#62278,#62279,#62280,#62281,#62282,#62283,#62284,
#62285,#62286,#62287,#62288,#62289,#62290,#62291,#62292,#62293,#62294,#62295,
#62296,#62297,#62298,#62299,#62300,#62301,#62302,#62303),.UNSPECIFIED.,
 .F.,.F.,(4,3,3,3,3,3,3,3,3,3,3,3,3,3,3,3,3,3,3,3,3,3,3,3,3,3,4),(0.,0.0183455177171484,
0.0365842486584377,0.0503567352932813,0.057506472843321,0.0612717639518736,
0.0790233645150093,0.096412286696173,0.109000250456427,0.115579416228416,
0.118639170027439,0.135489426230602,0.146764141737187,0.163451454243377,
0.16860513566105,0.173128108917708,0.189898750695883,0.20664919054828,0.217355779107483,
0.22287251764273,0.226199914557468,0.242290795343361,0.252395270027202,
0.256089569829458,0.271598133490708,0.280262641786704,0.28634738033222),
 .UNSPECIFIED.);
#4417=B_SPLINE_CURVE_WITH_KNOTS('',3,(#62306,#62307,#62308,#62309,#62310,
#62311,#62312,#62313,#62314,#62315,#62316,#62317,#62318,#62319,#62320,#62321,
#62322,#62323,#62324,#62325,#62326,#62327,#62328,#62329,#62330,#62331,#62332,
#62333,#62334,#62335,#62336,#62337,#62338,#62339,#62340,#62341,#62342,#62343,
#62344,#62345,#62346,#62347,#62348,#62349,#62350,#62351,#62352,#62353,#62354,
#62355,#62356,#62357,#62358,#62359,#62360,#62361,#62362,#62363,#62364,#62365,
#62366,#62367,#62368,#62369,#62370,#62371,#62372,#62373,#62374,#62375,#62376,
#62377,#62378,#62379,#62380,#62381,#62382,#62383,#62384,#62385,#62386,#62387),
 .UNSPECIFIED.,.F.,.F.,(4,3,3,3,3,3,3,3,3,3,3,3,3,3,3,3,3,3,3,3,3,3,3,3,
3,3,3,4),(-0.28634738033221,-0.271025134810133,-0.260698514729526,-0.255927597095004,
-0.251928120084434,-0.235738775707159,-0.229541586612368,-0.225083751275628,
-0.221641755210153,-0.204608740834787,-0.187821912129427,-0.179056502768601,
-0.174353031512105,-0.17100836839964,-0.168068126672392,-0.153509697708691,
-0.136938878241907,-0.120740722231463,-0.116774450513702,-0.113778933952734,
-0.0964554865389578,-0.078760241337473,-0.0609085885426931,-0.0568635638370591,
-0.0386446388676857,-0.0205858033551501,-0.00735363015835327,0.),
 .UNSPECIFIED.);
#4418=B_SPLINE_CURVE_WITH_KNOTS('',3,(#62388,#62389,#62390,#62391,#62392,
#62393,#62394,#62395,#62396,#62397,#62398,#62399,#62400,#62401,#62402,#62403,
#62404,#62405,#62406,#62407,#62408,#62409,#62410,#62411,#62412,#62413,#62414,
#62415,#62416,#62417,#62418,#62419,#62420,#62421,#62422,#62423,#62424,#62425,
#62426,#62427,#62428,#62429,#62430,#62431,#62432,#62433,#62434,#62435,#62436,
#62437,#62438,#62439,#62440,#62441,#62442,#62443,#62444,#62445,#62446,#62447,
#62448,#62449,#62450,#62451,#62452,#62453,#62454,#62455,#62456,#62457,#62458,
#62459,#62460,#62461,#62462,#62463),.UNSPECIFIED.,.F.,.F.,(4,3,3,3,3,3,
3,3,3,3,3,3,3,3,3,3,3,3,3,3,3,3,3,3,3,4),(-0.285142803995119,-0.266893522635827,
-0.249971481821918,-0.245887106233145,-0.227911281467346,-0.216815940424025,
-0.213019169001087,-0.209467645119212,-0.191887872119604,-0.174757062554003,
-0.165469230791568,-0.157741956071688,-0.154438809614972,-0.139148553120781,
-0.122062023309062,-0.107562410123394,-0.10357617742568,-0.100472613627008,
-0.0838658566323333,-0.0673520867984852,-0.0520303445547921,-0.048094708626416,
-0.0321861070442482,-0.0168171644241619,-0.00606511782371298,0.),
 .UNSPECIFIED.);
#4419=B_SPLINE_CURVE_WITH_KNOTS('',3,(#62465,#62466,#62467,#62468,#62469,
#62470,#62471,#62472,#62473,#62474,#62475),.UNSPECIFIED.,.F.,.F.,(4,1,1,
1,1,1,1,1,4),(15.7079632679489,15.8014786182354,16.7880079568995,17.7745372955635,
18.7610666342275,19.7475959728916,20.7341253115556,21.7206546502196,21.9911485751285),
 .UNSPECIFIED.);
#4420=B_SPLINE_CURVE_WITH_KNOTS('',3,(#62476,#62477,#62478,#62479,#62480,
#62481,#62482,#62483,#62484,#62485),.UNSPECIFIED.,.F.,.F.,(4,1,1,1,1,1,
1,4),(15.7079632679489,16.3714588042999,17.3579881429639,18.3445174816279,
19.331046820292,20.317576158956,21.30410549762,21.9911485751285),
 .UNSPECIFIED.);
#4421=B_SPLINE_CURVE_WITH_KNOTS('',3,(#62710,#62711,#62712,#62713,#62714,
#62715,#62716,#62717,#62718,#62719,#62720,#62721,#62722,#62723,#62724,#62725,
#62726,#62727,#62728,#62729,#62730,#62731,#62732,#62733,#62734,#62735,#62736,
#62737,#62738,#62739,#62740,#62741,#62742,#62743,#62744,#62745,#62746,#62747,
#62748,#62749,#62750,#62751,#62752,#62753,#62754,#62755,#62756,#62757,#62758,
#62759,#62760,#62761,#62762,#62763,#62764,#62765,#62766,#62767,#62768,#62769,
#62770,#62771,#62772,#62773,#62774,#62775,#62776,#62777,#62778,#62779,#62780,
#62781,#62782,#62783,#62784,#62785,#62786,#62787,#62788,#62789,#62790,#62791),
 .UNSPECIFIED.,.F.,.F.,(4,3,3,3,3,3,3,3,3,3,3,3,3,3,3,3,3,3,3,3,3,3,3,3,
3,3,3,4),(0.,0.0151383092199202,0.030955006769346,0.0436395623388301,0.0490032691308595,
0.0520443158127519,0.0683454961235161,0.0849450886188161,0.0968166792954167,
0.101864993838732,0.104873332695592,0.121948986956247,0.132431451325219,
0.149057249647569,0.154031743970792,0.15863082340794,0.17566870475993,0.193109534812356,
0.203698360649826,0.209528438175835,0.213039046070598,0.231029814280384,
0.242727396088317,0.247561053645041,0.251100328226373,0.269296434614431,
0.277820141512116,0.285142803995131),.UNSPECIFIED.);
#4422=B_SPLINE_CURVE_WITH_KNOTS('',3,(#62792,#62793,#62794,#62795,#62796,
#62797,#62798,#62799,#62800,#62801,#62802,#62803,#62804,#62805,#62806,#62807,
#62808,#62809,#62810,#62811,#62812,#62813,#62814,#62815,#62816),
 .UNSPECIFIED.,.F.,.F.,(4,3,3,3,3,3,3,3,4),(-10.1357873115492,-9.8652933866403,
-8.87876404797628,-7.89223470931224,-6.90570537064822,-5.91917603198418,
-4.93264669332016,-3.94611735465612,-3.85260200436961),.UNSPECIFIED.);
#4423=B_SPLINE_CURVE_WITH_KNOTS('',3,(#63041,#63042,#63043,#63044,#63045,
#63046,#63047,#63048,#63049,#63050,#63051,#63052,#63053,#63054,#63055,#63056,
#63057,#63058,#63059,#63060,#63061,#63062,#63063,#63064,#63065),
 .UNSPECIFIED.,.F.,.F.,(4,3,3,3,3,3,3,3,4),(7.59274844815668,7.89223470931225,
8.87876404797628,9.86529338664031,10.8518227253043,11.8383520639684,12.8248814026324,
13.8114107412964,13.8759337553363),.UNSPECIFIED.);
#4424=B_SPLINE_CURVE_WITH_KNOTS('',3,(#63066,#63067,#63068,#63069,#63070,
#63071,#63072,#63073,#63074,#63075,#63076,#63077,#63078,#63079,#63080,#63081,
#63082,#63083,#63084,#63085,#63086,#63087,#63088,#63089,#63090,#63091,#63092,
#63093,#63094,#63095,#63096,#63097,#63098,#63099,#63100,#63101,#63102,#63103,
#63104,#63105,#63106,#63107,#63108,#63109,#63110,#63111,#63112,#63113,#63114,
#63115,#63116,#63117,#63118,#63119,#63120,#63121,#63122,#63123,#63124,#63125,
#63126,#63127,#63128,#63129,#63130,#63131,#63132,#63133,#63134,#63135,#63136,
#63137,#63138,#63139,#63140,#63141,#63142,#63143,#63144),.UNSPECIFIED.,
 .F.,.F.,(4,3,3,3,3,3,3,3,3,3,3,3,3,3,3,3,3,3,3,3,3,3,3,3,3,3,4),(0.,0.0183455177171501,
0.0365842479880188,0.0503567347066666,0.0575064710097809,0.06127176277414,
0.0790233634744086,0.096412289501403,0.109000252560352,0.115579416554078,
0.118639169840573,0.135489429658593,0.146764141737201,0.163451454243393,
0.168605140810027,0.173128107436249,0.189898748857662,0.2066491892331,0.217355774416626,
0.222872516868838,0.226199915188627,0.242290799535295,0.25239527713926,
0.25608958297081,0.27159815236556,0.280262641786741,0.286347380332253),
 .UNSPECIFIED.);
#4425=B_SPLINE_CURVE_WITH_KNOTS('',3,(#63147,#63148,#63149,#63150,#63151,
#63152,#63153,#63154,#63155,#63156,#63157,#63158,#63159,#63160,#63161,#63162,
#63163,#63164,#63165,#63166,#63167,#63168,#63169,#63170,#63171,#63172,#63173,
#63174,#63175,#63176,#63177,#63178,#63179,#63180,#63181,#63182,#63183,#63184,
#63185,#63186,#63187,#63188,#63189,#63190,#63191,#63192,#63193,#63194,#63195,
#63196,#63197,#63198,#63199,#63200,#63201,#63202,#63203,#63204,#63205,#63206,
#63207,#63208,#63209,#63210,#63211,#63212,#63213,#63214,#63215,#63216,#63217,
#63218,#63219,#63220,#63221,#63222,#63223,#63224,#63225,#63226,#63227,#63228),
 .UNSPECIFIED.,.F.,.F.,(4,3,3,3,3,3,3,3,3,3,3,3,3,3,3,3,3,3,3,3,3,3,3,3,
3,3,3,4),(-0.286347380332241,-0.271025621689686,-0.260700126708286,-0.255933999923882,
-0.251928786217571,-0.235739770682513,-0.229543552627355,-0.225090694895415,
-0.221644284962138,-0.204610638148777,-0.187823738640676,-0.179057759820386,
-0.174355103845197,-0.171011959994442,-0.168068908451443,-0.153509697708694,
-0.136938545278193,-0.120740430888213,-0.116772838423195,-0.113777170653691,
-0.0964534278594871,-0.0787580645389843,-0.0609069559438266,-0.0568632900412494,
-0.0386443179131428,-0.0205854755819572,-0.00735363015835342,0.),
 .UNSPECIFIED.);
#4426=B_SPLINE_CURVE_WITH_KNOTS('',3,(#63229,#63230,#63231,#63232,#63233,
#63234,#63235,#63236,#63237,#63238,#63239,#63240,#63241,#63242,#63243,#63244,
#63245,#63246,#63247,#63248,#63249,#63250,#63251,#63252,#63253,#63254,#63255,
#63256,#63257,#63258,#63259,#63260,#63261,#63262,#63263,#63264,#63265,#63266,
#63267,#63268,#63269,#63270,#63271,#63272,#63273,#63274,#63275,#63276,#63277,
#63278,#63279,#63280,#63281,#63282,#63283,#63284,#63285,#63286,#63287,#63288,
#63289,#63290,#63291,#63292,#63293,#63294,#63295,#63296,#63297,#63298,#63299,
#63300,#63301,#63302,#63303,#63304),.UNSPECIFIED.,.F.,.F.,(4,3,3,3,3,3,
3,3,3,3,3,3,3,3,3,3,3,3,3,3,3,3,3,3,3,4),(-0.285142803995115,-0.266893522635823,
-0.249971640312005,-0.245887155062476,-0.227911309456783,-0.216815964914783,
-0.213019369681369,-0.209467693446233,-0.191887908364871,-0.174756961587167,
-0.165469070516051,-0.157741742342989,-0.15443884445219,-0.139148553120784,
-0.122062040548301,-0.107562425207727,-0.103576093457847,-0.100472602972665,
-0.0838658644229591,-0.0673520539817759,-0.0520303199422602,-0.0480946799671829,
-0.0321859944606137,-0.0168167950638599,-0.00606511782371299,0.),
 .UNSPECIFIED.);
#4427=B_SPLINE_CURVE_WITH_KNOTS('',3,(#63306,#63307,#63308,#63309,#63310,
#63311,#63312,#63313,#63314,#63315,#63316),.UNSPECIFIED.,.F.,.F.,(4,1,1,
1,1,1,1,1,4),(15.7079632679489,15.8014786182354,16.7880079568995,17.7745372955635,
18.7610666342275,19.7475959728916,20.7341253115556,21.7206546502196,21.9911485751285),
 .UNSPECIFIED.);
#4428=B_SPLINE_CURVE_WITH_KNOTS('',3,(#63317,#63318,#63319,#63320,#63321,
#63322,#63323,#63324,#63325,#63326),.UNSPECIFIED.,.F.,.F.,(4,1,1,1,1,1,
1,4),(15.7079632679489,16.3714588042999,17.3579881429639,18.3445174816279,
19.331046820292,20.317576158956,21.30410549762,21.9911485751285),
 .UNSPECIFIED.);
#4429=B_SPLINE_CURVE_WITH_KNOTS('',3,(#63551,#63552,#63553,#63554,#63555,
#63556,#63557,#63558,#63559,#63560,#63561,#63562,#63563,#63564,#63565,#63566,
#63567,#63568,#63569,#63570,#63571,#63572,#63573,#63574,#63575,#63576,#63577,
#63578,#63579,#63580,#63581,#63582,#63583,#63584,#63585,#63586,#63587,#63588,
#63589,#63590,#63591,#63592,#63593,#63594,#63595,#63596,#63597,#63598,#63599,
#63600,#63601,#63602,#63603,#63604,#63605,#63606,#63607,#63608,#63609,#63610,
#63611,#63612,#63613,#63614,#63615,#63616,#63617,#63618,#63619,#63620,#63621,
#63622,#63623,#63624,#63625,#63626,#63627,#63628,#63629,#63630,#63631,#63632),
 .UNSPECIFIED.,.F.,.F.,(4,3,3,3,3,3,3,3,3,3,3,3,3,3,3,3,3,3,3,3,3,3,3,3,
3,3,3,4),(0.,0.0151377992486527,0.0309541346648382,0.0436387992473864,0.049001010822214,
0.0520440199057219,0.0683448437138882,0.084944333062083,0.0968161126278682,
0.101863396044648,0.104870610854465,0.121946324184151,0.132431451325224,
0.149057505426147,0.154031793452874,0.158630809283319,0.175668969542699,
0.193109928367254,0.203698705010364,0.209528824983296,0.213039415112694,
0.231030207184506,0.242727690766411,0.247562113622632,0.251101431476124,
0.269297523973198,0.277820141512129,0.28514280399514),.UNSPECIFIED.);
#4430=B_SPLINE_CURVE_WITH_KNOTS('',3,(#63633,#63634,#63635,#63636,#63637,
#63638,#63639,#63640,#63641,#63642,#63643,#63644,#63645,#63646,#63647,#63648,
#63649,#63650,#63651,#63652,#63653,#63654,#63655,#63656,#63657),
 .UNSPECIFIED.,.F.,.F.,(4,3,3,3,3,3,3,3,4),(-10.1357873115492,-9.86529338664031,
-8.87876404797628,-7.89223470931225,-6.90570537064822,-5.91917603198419,
-4.93264669332015,-3.94611735465612,-3.85260200436961),.UNSPECIFIED.);
#4431=B_SPLINE_CURVE_WITH_KNOTS('',3,(#63882,#63883,#63884,#63885,#63886,
#63887,#63888,#63889,#63890,#63891,#63892,#63893,#63894,#63895,#63896,#63897,
#63898,#63899,#63900,#63901,#63902,#63903,#63904,#63905,#63906),
 .UNSPECIFIED.,.F.,.F.,(4,3,3,3,3,3,3,3,4),(7.59274844815667,7.89223470931225,
8.87876404797628,9.86529338664031,10.8518227253043,11.8383520639684,12.8248814026324,
13.8114107412964,13.8759337553363),.UNSPECIFIED.);
#4432=B_SPLINE_CURVE_WITH_KNOTS('',3,(#63907,#63908,#63909,#63910,#63911,
#63912,#63913,#63914,#63915,#63916,#63917,#63918,#63919,#63920,#63921,#63922,
#63923,#63924,#63925,#63926,#63927,#63928,#63929,#63930,#63931,#63932,#63933,
#63934,#63935,#63936,#63937,#63938,#63939,#63940,#63941,#63942,#63943,#63944,
#63945,#63946,#63947,#63948,#63949,#63950,#63951,#63952,#63953,#63954,#63955,
#63956,#63957,#63958,#63959,#63960,#63961,#63962,#63963,#63964,#63965,#63966,
#63967,#63968,#63969,#63970,#63971,#63972,#63973,#63974,#63975,#63976,#63977,
#63978,#63979,#63980,#63981,#63982,#63983,#63984,#63985),.UNSPECIFIED.,
 .F.,.F.,(4,3,3,3,3,3,3,3,3,3,3,3,3,3,3,3,3,3,3,3,3,3,3,3,3,3,4),(0.,0.0183455177171494,
0.0365842224514134,0.0503567123621361,0.0575064018577643,0.0612717186008677,
0.0790233237763444,0.096412392225862,0.109000329603695,0.115579426963446,
0.118639160101204,0.135489553798197,0.146764141737195,0.163451454243386,
0.168605331106135,0.173128052469876,0.189898680358684,0.206649139107136,
0.217355601404959,0.222872488375841,0.22619993877691,0.242290953399338,
0.252395538895798,0.256090068005537,0.271598847870641,0.280262641786722,
0.286347380332235),.UNSPECIFIED.);
#4433=B_SPLINE_CURVE_WITH_KNOTS('',3,(#63988,#63989,#63990,#63991,#63992,
#63993,#63994,#63995,#63996,#63997,#63998,#63999,#64000,#64001,#64002,#64003,
#64004,#64005,#64006,#64007,#64008,#64009,#64010,#64011,#64012,#64013,#64014,
#64015,#64016,#64017,#64018,#64019,#64020,#64021,#64022,#64023,#64024,#64025,
#64026,#64027,#64028,#64029,#64030,#64031,#64032,#64033,#64034,#64035,#64036,
#64037,#64038,#64039,#64040,#64041,#64042,#64043,#64044,#64045,#64046,#64047,
#64048,#64049,#64050,#64051,#64052,#64053,#64054,#64055,#64056,#64057,#64058,
#64059,#64060,#64061,#64062,#64063,#64064,#64065,#64066,#64067,#64068,#64069),
 .UNSPECIFIED.,.F.,.F.,(4,3,3,3,3,3,3,3,3,3,3,3,3,3,3,3,3,3,3,3,3,3,3,3,
3,3,3,4),(-0.286347380332241,-0.271025121721634,-0.260698471406766,-0.255927424639791,
-0.251928101932755,-0.235738748723829,-0.229541533307826,-0.225083562737093,
-0.22164168507229,-0.20460868823139,-0.187821861469231,-0.179056467802176,
-0.174352973887146,-0.171008268495978,-0.168068104878629,-0.153509697708687,
-0.136938887238054,-0.120740730103091,-0.116774494105204,-0.113778981547202,
-0.0964555421096816,-0.0787603000911127,-0.0609086326079217,-0.0568635712110021,
-0.0386446475073598,-0.0205858121953219,-0.00735363015834877,0.),
 .UNSPECIFIED.);
#4434=B_SPLINE_CURVE_WITH_KNOTS('',3,(#64070,#64071,#64072,#64073,#64074,
#64075,#64076,#64077,#64078,#64079,#64080,#64081,#64082,#64083,#64084,#64085,
#64086,#64087,#64088,#64089,#64090,#64091,#64092,#64093,#64094,#64095,#64096,
#64097,#64098,#64099,#64100,#64101,#64102,#64103,#64104,#64105,#64106,#64107,
#64108,#64109,#64110,#64111,#64112,#64113,#64114,#64115,#64116,#64117,#64118,
#64119,#64120,#64121,#64122,#64123,#64124,#64125,#64126,#64127,#64128,#64129,
#64130,#64131,#64132,#64133,#64134,#64135,#64136,#64137,#64138,#64139,#64140,
#64141,#64142,#64143,#64144,#64145),.UNSPECIFIED.,.F.,.F.,(4,3,3,3,3,3,
3,3,3,3,3,3,3,3,3,3,3,3,3,3,3,3,3,3,3,4),(-0.285142803995177,-0.266893522635881,
-0.24997147696309,-0.245887104754832,-0.227911280648222,-0.216815939707296,
-0.213019163245401,-0.209467643680815,-0.191887871040814,-0.174757065708801,
-0.16546923578312,-0.157741962744139,-0.154438808517409,-0.13914855312081,
-0.122062022789569,-0.107562409668837,-0.103576180068357,-0.100472613959823,
-0.0838658564094648,-0.0673520878642787,-0.0520303453541372,-0.0480947095174562,
-0.0321861105661567,-0.0168171759288923,-0.00606511782371295,0.),
 .UNSPECIFIED.);
#4435=B_SPLINE_CURVE_WITH_KNOTS('',3,(#64147,#64148,#64149,#64150,#64151,
#64152,#64153,#64154,#64155,#64156,#64157),.UNSPECIFIED.,.F.,.F.,(4,1,1,
1,1,1,1,1,4),(15.7079632679489,15.8014786182355,16.7880079568995,17.7745372955635,
18.7610666342275,19.7475959728916,20.7341253115556,21.7206546502196,21.9911485751285),
 .UNSPECIFIED.);
#4436=B_SPLINE_CURVE_WITH_KNOTS('',3,(#64158,#64159,#64160,#64161,#64162,
#64163,#64164,#64165,#64166,#64167),.UNSPECIFIED.,.F.,.F.,(4,1,1,1,1,1,
1,4),(15.7079632679489,16.3714588042999,17.3579881429639,18.344517481628,
19.331046820292,20.317576158956,21.30410549762,21.9911485751285),
 .UNSPECIFIED.);
#4437=B_SPLINE_CURVE_WITH_KNOTS('',3,(#64392,#64393,#64394,#64395,#64396,
#64397,#64398,#64399,#64400,#64401,#64402,#64403,#64404,#64405,#64406,#64407,
#64408,#64409,#64410,#64411,#64412,#64413,#64414,#64415,#64416,#64417,#64418,
#64419,#64420,#64421,#64422,#64423,#64424,#64425,#64426,#64427,#64428,#64429,
#64430,#64431,#64432,#64433,#64434,#64435,#64436,#64437,#64438,#64439,#64440,
#64441,#64442,#64443,#64444,#64445,#64446,#64447,#64448,#64449,#64450,#64451,
#64452,#64453,#64454,#64455,#64456,#64457,#64458,#64459,#64460,#64461,#64462,
#64463,#64464,#64465,#64466,#64467,#64468,#64469,#64470,#64471,#64472,#64473),
 .UNSPECIFIED.,.F.,.F.,(4,3,3,3,3,3,3,3,3,3,3,3,3,3,3,3,3,3,3,3,3,3,3,3,
3,3,3,4),(0.,0.0151383248856871,0.0309550335469064,0.0436395857691952,0.0490033384910799,
0.0520443250910099,0.0683455163444214,0.0849451119840661,0.0968166968193539,
0.101865043240895,0.104873417046857,0.121949069457094,0.132431451325217,
0.149057241756068,0.154031742415278,0.15863082385134,0.175668696597353,
0.193109522683886,0.203698350037412,0.209528426219566,0.213039034673188,
0.231029802151329,0.24272738699152,0.247561020928704,0.251100294224577,
0.269296401030219,0.277820141512092,0.285142803995105),.UNSPECIFIED.);
#4438=B_SPLINE_CURVE_WITH_KNOTS('',3,(#64474,#64475,#64476,#64477,#64478,
#64479,#64480,#64481,#64482,#64483,#64484,#64485,#64486,#64487,#64488,#64489,
#64490,#64491,#64492,#64493,#64494,#64495,#64496,#64497,#64498),
 .UNSPECIFIED.,.F.,.F.,(4,3,3,3,3,3,3,3,4),(-10.1357873115492,-9.86529338664031,
-8.87876404797628,-7.89223470931225,-6.90570537064822,-5.91917603198419,
-4.93264669332015,-3.94611735465612,-3.85260200436962),.UNSPECIFIED.);
#4439=B_SPLINE_CURVE_WITH_KNOTS('',3,(#64723,#64724,#64725,#64726,#64727,
#64728,#64729,#64730,#64731,#64732,#64733,#64734,#64735,#64736,#64737,#64738,
#64739,#64740,#64741,#64742,#64743,#64744,#64745,#64746,#64747),
 .UNSPECIFIED.,.F.,.F.,(4,3,3,3,3,3,3,3,4),(7.59274844815668,7.89223470931224,
8.87876404797627,9.8652933866403,10.8518227253043,11.8383520639684,12.8248814026324,
13.8114107412964,13.8759337553363),.UNSPECIFIED.);
#4440=B_SPLINE_CURVE_WITH_KNOTS('',3,(#64748,#64749,#64750,#64751,#64752,
#64753,#64754,#64755,#64756,#64757,#64758,#64759,#64760,#64761,#64762,#64763,
#64764,#64765,#64766,#64767,#64768,#64769,#64770,#64771,#64772,#64773,#64774,
#64775,#64776,#64777,#64778,#64779,#64780,#64781,#64782,#64783,#64784,#64785,
#64786,#64787,#64788,#64789,#64790,#64791,#64792,#64793,#64794,#64795,#64796,
#64797,#64798,#64799,#64800,#64801,#64802,#64803,#64804,#64805,#64806,#64807,
#64808,#64809,#64810,#64811,#64812,#64813,#64814,#64815,#64816,#64817,#64818,
#64819,#64820,#64821,#64822,#64823,#64824,#64825,#64826),.UNSPECIFIED.,
 .F.,.F.,(4,3,3,3,3,3,3,3,3,3,3,3,3,3,3,3,3,3,3,3,3,3,3,3,3,3,4),(0.,0.0183455177171494,
0.0365842486584371,0.0503567352932819,0.0575064728432776,0.0612717639547951,
0.0790233645178617,0.0964122866988397,0.109000250458429,0.115579416230427,
0.118639170032811,0.135489426235933,0.146764141737196,0.163451454243387,
0.168605135661181,0.173128108919256,0.189898750697359,0.206649190549959,
0.217355779106873,0.222872517642441,0.22619991455212,0.242290795338002,
0.2523952700195,0.256089569811339,0.271598133473104,0.280262641786723,0.286347380332239),
 .UNSPECIFIED.);
#4441=B_SPLINE_CURVE_WITH_KNOTS('',3,(#64849,#64850,#64851,#64852,#64853,
#64854,#64855,#64856,#64857,#64858,#64859,#64860,#64861,#64862,#64863,#64864,
#64865,#64866,#64867,#64868,#64869,#64870,#64871,#64872,#64873,#64874,#64875,
#64876,#64877,#64878,#64879,#64880,#64881,#64882,#64883,#64884,#64885,#64886,
#64887,#64888,#64889,#64890,#64891,#64892,#64893,#64894,#64895,#64896,#64897,
#64898,#64899,#64900,#64901,#64902,#64903,#64904,#64905,#64906,#64907,#64908,
#64909,#64910,#64911,#64912,#64913,#64914,#64915,#64916,#64917,#64918,#64919,
#64920,#64921,#64922,#64923,#64924,#64925,#64926,#64927,#64928,#64929,#64930),
 .UNSPECIFIED.,.F.,.F.,(4,3,3,3,3,3,3,3,3,3,3,3,3,3,3,3,3,3,3,3,3,3,3,3,
3,3,3,4),(-0.286347380332242,-0.271026132708159,-0.26070181912171,-0.255940688203078,
-0.251929465810934,-0.235740795969021,-0.229545579465539,-0.225097832776575,
-0.221646776596611,-0.204612506874632,-0.187825536148012,-0.179058989177513,
-0.17435713213233,-0.17101547339657,-0.168069670163224,-0.153509697708693,
-0.136938199431907,-0.120740128272712,-0.116771166875623,-0.113775334580713,
-0.096451284491223,-0.0787557978507567,-0.0609052559276548,-0.0568630026035331,
-0.0386439810009667,-0.0205851328894473,-0.00735363015834924,0.),
 .UNSPECIFIED.);
#4442=B_SPLINE_CURVE_WITH_KNOTS('',3,(#64931,#64932,#64933,#64934,#64935,
#64936,#64937,#64938,#64939,#64940,#64941,#64942,#64943,#64944,#64945,#64946,
#64947,#64948,#64949,#64950,#64951,#64952,#64953,#64954,#64955,#64956,#64957,
#64958,#64959,#64960,#64961,#64962,#64963,#64964,#64965,#64966,#64967,#64968,
#64969,#64970,#64971,#64972,#64973,#64974,#64975,#64976,#64977,#64978,#64979,
#64980,#64981,#64982,#64983,#64984,#64985,#64986,#64987,#64988,#64989,#64990,
#64991,#64992,#64993,#64994,#64995,#64996,#64997,#64998,#64999,#65000,#65001,
#65002,#65003,#65004,#65005,#65006),.UNSPECIFIED.,.F.,.F.,(4,3,3,3,3,3,
3,3,3,3,3,3,3,3,3,3,3,3,3,3,3,3,3,3,3,4),(-0.285142803995146,-0.266893522635853,
-0.249971821339198,-0.245887210812531,-0.227911342993235,-0.216815994259181,
-0.21301961305492,-0.209467750298075,-0.191887951003757,-0.174756849434581,
-0.165468891951558,-0.157741505410476,-0.1544388836839,-0.139148553120802,
-0.122062060978925,-0.107562443084524,-0.103576002803389,-0.10047259097034,
-0.0838658743207705,-0.0673520207865497,-0.0520302950458412,-0.0480946476761015,
-0.0321858707120756,-0.0168163861623916,-0.00606511782371579,0.),
 .UNSPECIFIED.);
#4443=B_SPLINE_CURVE_WITH_KNOTS('',3,(#65008,#65009,#65010,#65011,#65012,
#65013,#65014,#65015,#65016,#65017,#65018),.UNSPECIFIED.,.F.,.F.,(4,1,1,
1,1,1,1,1,4),(15.7079632679489,15.8014786182355,16.7880079568995,17.7745372955635,
18.7610666342276,19.7475959728916,20.7341253115556,21.7206546502197,21.9911485751285),
 .UNSPECIFIED.);
#4444=B_SPLINE_CURVE_WITH_KNOTS('',3,(#65019,#65020,#65021,#65022,#65023,
#65024,#65025,#65026,#65027,#65028),.UNSPECIFIED.,.F.,.F.,(4,1,1,1,1,1,
1,4),(15.7079632679489,16.3714588042999,17.357988142964,18.344517481628,
19.331046820292,20.317576158956,21.3041054976201,21.9911485751285),
 .UNSPECIFIED.);
#4445=B_SPLINE_CURVE_WITH_KNOTS('',3,(#65253,#65254,#65255,#65256,#65257,
#65258,#65259,#65260,#65261,#65262,#65263,#65264,#65265,#65266,#65267,#65268,
#65269,#65270,#65271,#65272,#65273,#65274,#65275,#65276,#65277),
 .UNSPECIFIED.,.F.,.F.,(4,3,3,3,3,3,3,3,4),(-10.1357873115492,-9.8652933866403,
-8.87876404797628,-7.89223470931225,-6.90570537064821,-5.91917603198418,
-4.93264669332015,-3.94611735465612,-3.85260200436958),.UNSPECIFIED.);
#4446=B_SPLINE_CURVE_WITH_KNOTS('',3,(#65502,#65503,#65504,#65505,#65506,
#65507,#65508,#65509,#65510,#65511,#65512,#65513,#65514,#65515,#65516,#65517,
#65518,#65519,#65520,#65521,#65522,#65523,#65524,#65525,#65526),
 .UNSPECIFIED.,.F.,.F.,(4,3,3,3,3,3,3,3,4),(7.59274844815664,7.89223470931225,
8.87876404797627,9.86529338664031,10.8518227253043,11.8383520639684,12.8248814026324,
13.8114107412964,13.8759337553362),.UNSPECIFIED.);
#4447=B_SPLINE_CURVE_WITH_KNOTS('',3,(#65529,#65530,#65531,#65532,#65533,
#65534,#65535,#65536,#65537,#65538,#65539,#65540,#65541,#65542,#65543,#65544,
#65545,#65546,#65547,#65548,#65549,#65550,#65551,#65552,#65553,#65554,#65555,
#65556,#65557,#65558,#65559,#65560,#65561,#65562,#65563,#65564,#65565,#65566,
#65567,#65568,#65569,#65570,#65571,#65572,#65573,#65574,#65575,#65576,#65577,
#65578,#65579,#65580,#65581,#65582,#65583,#65584,#65585,#65586,#65587,#65588,
#65589,#65590,#65591,#65592,#65593,#65594,#65595,#65596,#65597,#65598,#65599,
#65600,#65601,#65602,#65603,#65604,#65605,#65606,#65607,#65608,#65609,#65610),
 .UNSPECIFIED.,.F.,.F.,(4,3,3,3,3,3,3,3,3,3,3,3,3,3,3,3,3,3,3,3,3,3,3,3,
3,3,3,4),(-0.286347380332275,-0.27102566316108,-0.260700264038628,-0.255934543840492,
-0.251928842105127,-0.235739854602674,-0.229543718486113,-0.225091279778216,
-0.221644493299042,-0.204610794401459,-0.187823888995587,-0.179057862959692,
-0.174355273945332,-0.171012254723885,-0.168068972461,-0.153509697708709,
-0.136938517071018,-0.120740406206935,-0.116772701979239,-0.113777021075996,
-0.0964532532380554,-0.0787578798842962,-0.0609068174528094,-0.056863266677987,
-0.0386442905322982,-0.0205854476800074,-0.00735363015834906,0.),
 .UNSPECIFIED.);
#4448=B_SPLINE_CURVE_WITH_KNOTS('',3,(#65611,#65612,#65613,#65614,#65615,
#65616,#65617,#65618,#65619,#65620,#65621,#65622,#65623,#65624,#65625,#65626,
#65627,#65628,#65629,#65630,#65631,#65632,#65633,#65634,#65635,#65636,#65637,
#65638,#65639,#65640,#65641,#65642,#65643,#65644,#65645,#65646,#65647,#65648,
#65649,#65650,#65651,#65652,#65653,#65654,#65655,#65656,#65657,#65658,#65659,
#65660,#65661,#65662,#65663,#65664,#65665,#65666,#65667,#65668,#65669,#65670,
#65671,#65672,#65673,#65674,#65675,#65676,#65677,#65678,#65679,#65680,#65681,
#65682,#65683,#65684,#65685,#65686),.UNSPECIFIED.,.F.,.F.,(4,3,3,3,3,3,
3,3,3,3,3,3,3,3,3,3,3,3,3,3,3,3,3,3,3,4),(-0.285142803995182,-0.266893522635886,
-0.249971668921242,-0.245887163875788,-0.227911314645579,-0.216815969454983,
-0.213019407143944,-0.209467702314156,-0.19188791501582,-0.174756943635084,
-0.165469041972909,-0.157741704382841,-0.154438850672044,-0.139148553120812,
-0.122062043724214,-0.107562427986652,-0.103576078755324,-0.100472601057323,
-0.0838658659084289,-0.0673520484249552,-0.0520303157746454,-0.0480946748254668,
-0.0321859745524222,-0.0168167295122947,-0.00606511782371583,0.),
 .UNSPECIFIED.);
#4449=B_SPLINE_CURVE_WITH_KNOTS('',3,(#65688,#65689,#65690,#65691,#65692,
#65693,#65694,#65695,#65696,#65697,#65698),.UNSPECIFIED.,.F.,.F.,(4,1,1,
1,1,1,1,1,4),(15.7079632679489,15.8014786182355,16.7880079568995,17.7745372955635,
18.7610666342276,19.7475959728916,20.7341253115556,21.7206546502197,21.9911485751285),
 .UNSPECIFIED.);
#4450=B_SPLINE_CURVE_WITH_KNOTS('',3,(#65699,#65700,#65701,#65702,#65703,
#65704,#65705,#65706,#65707,#65708),.UNSPECIFIED.,.F.,.F.,(4,1,1,1,1,1,
1,4),(15.7079632679489,16.3714588042999,17.357988142964,18.344517481628,
19.331046820292,20.317576158956,21.3041054976201,21.9911485751285),
 .UNSPECIFIED.);
#4451=B_SPLINE_CURVE_WITH_KNOTS('',3,(#65933,#65934,#65935,#65936,#65937,
#65938,#65939,#65940,#65941,#65942,#65943,#65944,#65945,#65946,#65947,#65948,
#65949,#65950,#65951,#65952,#65953,#65954,#65955,#65956,#65957),
 .UNSPECIFIED.,.F.,.F.,(4,3,3,3,3,3,3,3,4),(-10.1357873115492,-9.86529338664031,
-8.87876404797628,-7.89223470931225,-6.90570537064822,-5.91917603198419,
-4.93264669332016,-3.94611735465613,-3.85260200436958),.UNSPECIFIED.);
#4452=B_SPLINE_CURVE_WITH_KNOTS('',3,(#66182,#66183,#66184,#66185,#66186,
#66187,#66188,#66189,#66190,#66191,#66192,#66193,#66194,#66195,#66196,#66197,
#66198,#66199,#66200,#66201,#66202,#66203,#66204,#66205,#66206),
 .UNSPECIFIED.,.F.,.F.,(4,3,3,3,3,3,3,3,4),(7.59274844815664,7.89223470931224,
8.87876404797627,9.86529338664031,10.8518227253043,11.8383520639684,12.8248814026324,
13.8114107412964,13.8759337553362),.UNSPECIFIED.);
#4453=B_SPLINE_CURVE_WITH_KNOTS('',3,(#66209,#66210,#66211,#66212,#66213,
#66214,#66215,#66216,#66217,#66218,#66219,#66220,#66221,#66222,#66223,#66224,
#66225,#66226,#66227,#66228,#66229,#66230,#66231,#66232,#66233,#66234,#66235,
#66236,#66237,#66238,#66239,#66240,#66241,#66242,#66243,#66244,#66245,#66246,
#66247,#66248,#66249,#66250,#66251,#66252,#66253,#66254,#66255,#66256,#66257,
#66258,#66259,#66260,#66261,#66262,#66263,#66264,#66265,#66266,#66267,#66268,
#66269,#66270,#66271,#66272,#66273,#66274,#66275,#66276,#66277,#66278,#66279,
#66280,#66281,#66282,#66283,#66284,#66285,#66286,#66287,#66288,#66289,#66290),
 .UNSPECIFIED.,.F.,.F.,(4,3,3,3,3,3,3,3,3,3,3,3,3,3,3,3,3,3,3,3,3,3,3,3,
3,3,3,4),(-0.286347380332252,-0.271025677132851,-0.260700310300518,-0.25593472713892,
-0.251928860913337,-0.235739882855375,-0.229543774327833,-0.225091476664371,
-0.221644563262721,-0.204610846874213,-0.18782393948616,-0.179057897584765,
-0.174355331052151,-0.171012353638296,-0.168068993938383,-0.15350969770869,
-0.136938507575371,-0.120740397898244,-0.116772656051337,-0.113776970697825,
-0.0964531944270655,-0.0787578176938258,-0.0609067708099572,-0.0568632588365736,
-0.0386442813392898,-0.020585438313091,-0.0073536301583514,0.),
 .UNSPECIFIED.);
#4454=B_SPLINE_CURVE_WITH_KNOTS('',3,(#66291,#66292,#66293,#66294,#66295,
#66296,#66297,#66298,#66299,#66300,#66301,#66302,#66303,#66304,#66305,#66306,
#66307,#66308,#66309,#66310,#66311,#66312,#66313,#66314,#66315,#66316,#66317,
#66318,#66319,#66320,#66321,#66322,#66323,#66324,#66325,#66326,#66327,#66328,
#66329,#66330,#66331,#66332,#66333,#66334,#66335,#66336,#66337,#66338,#66339,
#66340,#66341,#66342,#66343,#66344,#66345,#66346,#66347,#66348,#66349,#66350,
#66351,#66352,#66353,#66354,#66355,#66356,#66357,#66358,#66359,#66360,#66361,
#66362,#66363,#66364,#66365,#66366),.UNSPECIFIED.,.F.,.F.,(4,3,3,3,3,3,
3,3,3,3,3,3,3,3,3,3,3,3,3,3,3,3,3,3,3,4),(-0.285142803995135,-0.266893522635843,
-0.24997167290136,-0.245887165108436,-0.227911315377379,-0.216815970095306,
-0.213019412325979,-0.20946770354527,-0.191887915939152,-0.174756941140708,
-0.165469038008051,-0.157741699112297,-0.154438851562339,-0.139148553120795,
-0.122062044167205,-0.107562428374269,-0.10357607672048,-0.100472600788513,
-0.083865866115183,-0.0673520476568359,-0.0520303151985547,-0.0480946741162576,
-0.0321859717979194,-0.0168167204262572,-0.00606511782371128,0.),
 .UNSPECIFIED.);
#4455=B_SPLINE_CURVE_WITH_KNOTS('',3,(#66368,#66369,#66370,#66371,#66372,
#66373,#66374,#66375,#66376,#66377,#66378),.UNSPECIFIED.,.F.,.F.,(4,1,1,
1,1,1,1,1,4),(15.7079632679489,15.8014786182355,16.7880079568995,17.7745372955635,
18.7610666342276,19.7475959728916,20.7341253115556,21.7206546502197,21.9911485751285),
 .UNSPECIFIED.);
#4456=B_SPLINE_CURVE_WITH_KNOTS('',3,(#66379,#66380,#66381,#66382,#66383,
#66384,#66385,#66386,#66387,#66388),.UNSPECIFIED.,.F.,.F.,(4,1,1,1,1,1,
1,4),(15.7079632679489,16.3714588042999,17.357988142964,18.344517481628,
19.331046820292,20.317576158956,21.3041054976201,21.9911485751285),
 .UNSPECIFIED.);
#4457=B_SPLINE_CURVE_WITH_KNOTS('',3,(#66613,#66614,#66615,#66616,#66617,
#66618,#66619,#66620,#66621,#66622,#66623,#66624,#66625,#66626,#66627,#66628,
#66629,#66630,#66631,#66632,#66633,#66634,#66635,#66636,#66637),
 .UNSPECIFIED.,.F.,.F.,(4,3,3,3,3,3,3,3,4),(-10.1357873115492,-9.86529338664031,
-8.87876404797628,-7.89223470931225,-6.90570537064822,-5.91917603198419,
-4.93264669332016,-3.94611735465613,-3.85260200436961),.UNSPECIFIED.);
#4458=B_SPLINE_CURVE_WITH_KNOTS('',3,(#66862,#66863,#66864,#66865,#66866,
#66867,#66868,#66869,#66870,#66871,#66872,#66873,#66874,#66875,#66876,#66877,
#66878,#66879,#66880,#66881,#66882,#66883,#66884,#66885,#66886),
 .UNSPECIFIED.,.F.,.F.,(4,3,3,3,3,3,3,3,4),(7.59274844815664,7.89223470931225,
8.87876404797628,9.86529338664032,10.8518227253043,11.8383520639684,12.8248814026324,
13.8114107412964,13.8759337553362),.UNSPECIFIED.);
#4459=B_SPLINE_CURVE_WITH_KNOTS('',3,(#66889,#66890,#66891,#66892,#66893,
#66894,#66895,#66896,#66897,#66898,#66899,#66900,#66901,#66902,#66903,#66904,
#66905,#66906,#66907,#66908,#66909,#66910,#66911,#66912,#66913,#66914,#66915,
#66916,#66917,#66918,#66919,#66920,#66921,#66922,#66923,#66924,#66925,#66926,
#66927,#66928,#66929,#66930,#66931,#66932,#66933,#66934,#66935,#66936,#66937,
#66938,#66939,#66940,#66941,#66942,#66943,#66944,#66945,#66946,#66947,#66948,
#66949,#66950,#66951,#66952,#66953,#66954,#66955,#66956,#66957,#66958,#66959,
#66960,#66961,#66962,#66963,#66964,#66965,#66966,#66967,#66968,#66969,#66970),
 .UNSPECIFIED.,.F.,.F.,(4,3,3,3,3,3,3,3,3,3,3,3,3,3,3,3,3,3,3,3,3,3,3,3,
3,3,3,4),(-0.286347380332231,-0.271026132710428,-0.260701819128595,-0.255940688215407,
-0.251929465812578,-0.235740795970596,-0.229545579468544,-0.225097832787767,
-0.221646776634828,-0.204612506903293,-0.187825536176126,-0.179058989199214,
-0.174357132167787,-0.171015473459643,-0.168069670176233,-0.153509697708689,
-0.136938199431204,-0.120740128272097,-0.116771166870588,-0.11377533457899,
-0.0964512844881509,-0.0787557978480441,-0.0609052559256208,-0.0568630026064093,
-0.0386439810009145,-0.0205851328893904,-0.00735363015835105,0.),
 .UNSPECIFIED.);
#4460=B_SPLINE_CURVE_WITH_KNOTS('',3,(#66971,#66972,#66973,#66974,#66975,
#66976,#66977,#66978,#66979,#66980,#66981,#66982,#66983,#66984,#66985,#66986,
#66987,#66988,#66989,#66990,#66991,#66992,#66993,#66994,#66995,#66996,#66997,
#66998,#66999,#67000,#67001,#67002,#67003,#67004,#67005,#67006,#67007,#67008,
#67009,#67010,#67011,#67012,#67013,#67014,#67015,#67016,#67017,#67018,#67019,
#67020,#67021,#67022,#67023,#67024,#67025,#67026,#67027,#67028,#67029,#67030,
#67031,#67032,#67033,#67034,#67035,#67036,#67037,#67038,#67039,#67040,#67041,
#67042,#67043,#67044,#67045,#67046),.UNSPECIFIED.,.F.,.F.,(4,3,3,3,3,3,
3,3,3,3,3,3,3,3,3,3,3,3,3,3,3,3,3,3,3,4),(-0.285142803995179,-0.266893522635882,
-0.249971821340761,-0.245887210846563,-0.227911343027248,-0.216815994288942,
-0.213019613595473,-0.209467750355521,-0.191887951046842,-0.174756849476473,
-0.165468891994637,-0.157741505469733,-0.154438883651103,-0.139148553120804,
-0.122062060979163,-0.107562443084732,-0.103576002803925,-0.100472590970432,
-0.0838658743199319,-0.0673520207859246,-0.0520302950453719,-0.0480946476698915,
-0.0321858707070638,-0.0168163861575255,-0.00606511782371399,0.),
 .UNSPECIFIED.);
#4461=B_SPLINE_CURVE_WITH_KNOTS('',3,(#67048,#67049,#67050,#67051,#67052,
#67053,#67054,#67055,#67056,#67057,#67058),.UNSPECIFIED.,.F.,.F.,(4,1,1,
1,1,1,1,1,4),(15.7079632679489,15.8014786182355,16.7880079568995,17.7745372955635,
18.7610666342276,19.7475959728916,20.7341253115556,21.7206546502197,21.9911485751285),
 .UNSPECIFIED.);
#4462=B_SPLINE_CURVE_WITH_KNOTS('',3,(#67059,#67060,#67061,#67062,#67063,
#67064,#67065,#67066,#67067,#67068),.UNSPECIFIED.,.F.,.F.,(4,1,1,1,1,1,
1,4),(15.7079632679489,16.3714588042999,17.357988142964,18.344517481628,
19.331046820292,20.317576158956,21.3041054976201,21.9911485751285),
 .UNSPECIFIED.);
#4463=B_SPLINE_CURVE_WITH_KNOTS('',3,(#67293,#67294,#67295,#67296,#67297,
#67298,#67299,#67300,#67301,#67302,#67303,#67304,#67305,#67306,#67307,#67308,
#67309,#67310,#67311,#67312,#67313,#67314,#67315,#67316,#67317),
 .UNSPECIFIED.,.F.,.F.,(4,3,3,3,3,3,3,3,4),(-10.1357873115491,-9.86529338664031,
-8.87876404797628,-7.89223470931225,-6.90570537064822,-5.91917603198419,
-4.93264669332015,-3.94611735465612,-3.85260200436958),.UNSPECIFIED.);
#4464=B_SPLINE_CURVE_WITH_KNOTS('',3,(#67542,#67543,#67544,#67545,#67546,
#67547,#67548,#67549,#67550,#67551,#67552,#67553,#67554,#67555,#67556,#67557,
#67558,#67559,#67560,#67561,#67562,#67563,#67564,#67565,#67566),
 .UNSPECIFIED.,.F.,.F.,(4,3,3,3,3,3,3,3,4),(7.59274844815661,7.89223470931225,
8.87876404797628,9.86529338664031,10.8518227253043,11.8383520639684,12.8248814026324,
13.8114107412964,13.8759337553362),.UNSPECIFIED.);
#4465=B_SPLINE_CURVE_WITH_KNOTS('',3,(#67569,#67570,#67571,#67572,#67573,
#67574,#67575,#67576,#67577,#67578,#67579,#67580,#67581,#67582,#67583,#67584,
#67585,#67586,#67587,#67588,#67589,#67590,#67591,#67592,#67593,#67594,#67595,
#67596,#67597,#67598,#67599,#67600,#67601,#67602,#67603,#67604,#67605,#67606,
#67607,#67608,#67609,#67610,#67611,#67612,#67613,#67614,#67615,#67616,#67617,
#67618,#67619,#67620,#67621,#67622,#67623,#67624,#67625,#67626,#67627,#67628,
#67629,#67630,#67631,#67632,#67633,#67634,#67635,#67636,#67637,#67638,#67639,
#67640,#67641,#67642,#67643,#67644,#67645,#67646,#67647,#67648,#67649,#67650),
 .UNSPECIFIED.,.F.,.F.,(4,3,3,3,3,3,3,3,3,3,3,3,3,3,3,3,3,3,3,3,3,3,3,3,
3,3,3,4),(-0.28634738033223,-0.271025663162511,-0.260700264029441,-0.25593454384516,
-0.251928842104989,-0.235739854602305,-0.229543718489692,-0.225091279789565,
-0.22164449331224,-0.204610794411351,-0.187823889005095,-0.17905786296708,
-0.174355273957306,-0.171012254735667,-0.168068972463406,-0.153509697708683,
-0.136938517070056,-0.120740406206092,-0.116772701974538,-0.113777021063045,
-0.0964532532245246,-0.0787578798704614,-0.0609068174424322,-0.0568632666880998,
-0.0386442905433222,-0.020585447690582,-0.00735363015834469,0.),
 .UNSPECIFIED.);
#4466=B_SPLINE_CURVE_WITH_KNOTS('',3,(#67651,#67652,#67653,#67654,#67655,
#67656,#67657,#67658,#67659,#67660,#67661,#67662,#67663,#67664,#67665,#67666,
#67667,#67668,#67669,#67670,#67671,#67672,#67673,#67674,#67675,#67676,#67677,
#67678,#67679,#67680,#67681,#67682,#67683,#67684,#67685,#67686,#67687,#67688,
#67689,#67690,#67691,#67692,#67693,#67694,#67695,#67696,#67697,#67698,#67699,
#67700,#67701,#67702,#67703,#67704,#67705,#67706,#67707,#67708,#67709,#67710,
#67711,#67712,#67713,#67714,#67715,#67716,#67717,#67718,#67719,#67720,#67721,
#67722,#67723,#67724,#67725,#67726),.UNSPECIFIED.,.F.,.F.,(4,3,3,3,3,3,
3,3,3,3,3,3,3,3,3,3,3,3,3,3,3,3,3,3,3,4),(-0.285142803995139,-0.266893522635845,
-0.24997166892056,-0.245887163874206,-0.227911314643986,-0.216815969453587,
-0.213019407093492,-0.209467702309002,-0.191887915011948,-0.174756943631577,
-0.165469041969139,-0.157741704377863,-0.154438850709308,-0.139148553120788,
-0.122062043723843,-0.107562427986327,-0.103576078754398,-0.100472601051161,
-0.0838658659032878,-0.0673520484187001,-0.0520303157699535,-0.0480946748290876,
-0.0321859745551226,-0.0168167295145933,-0.00606511782371382,0.),
 .UNSPECIFIED.);
#4467=B_SPLINE_CURVE_WITH_KNOTS('',3,(#67728,#67729,#67730,#67731,#67732,
#67733,#67734,#67735,#67736,#67737,#67738),.UNSPECIFIED.,.F.,.F.,(4,1,1,
1,1,1,1,1,4),(15.7079632679489,15.8014786182354,16.7880079568995,17.7745372955635,
18.7610666342275,19.7475959728916,20.7341253115556,21.7206546502196,21.9911485751285),
 .UNSPECIFIED.);
#4468=B_SPLINE_CURVE_WITH_KNOTS('',3,(#67739,#67740,#67741,#67742,#67743,
#67744,#67745,#67746,#67747,#67748),.UNSPECIFIED.,.F.,.F.,(4,1,1,1,1,1,
1,4),(15.7079632679489,16.3714588042999,17.3579881429639,18.344517481628,
19.331046820292,20.317576158956,21.30410549762,21.9911485751285),
 .UNSPECIFIED.);
#4469=B_SPLINE_CURVE_WITH_KNOTS('',3,(#67973,#67974,#67975,#67976,#67977,
#67978,#67979,#67980,#67981,#67982,#67983,#67984,#67985,#67986,#67987,#67988,
#67989,#67990,#67991,#67992,#67993,#67994,#67995,#67996,#67997),
 .UNSPECIFIED.,.F.,.F.,(4,3,3,3,3,3,3,3,4),(-10.1357873115492,-9.86529338664031,
-8.87876404797628,-7.89223470931225,-6.90570537064822,-5.91917603198418,
-4.93264669332015,-3.94611735465612,-3.85260200436958),.UNSPECIFIED.);
#4470=B_SPLINE_CURVE_WITH_KNOTS('',3,(#68222,#68223,#68224,#68225,#68226,
#68227,#68228,#68229,#68230,#68231,#68232,#68233,#68234,#68235,#68236,#68237,
#68238,#68239,#68240,#68241,#68242,#68243,#68244,#68245,#68246),
 .UNSPECIFIED.,.F.,.F.,(4,3,3,3,3,3,3,3,4),(7.59274844815664,7.89223470931224,
8.87876404797627,9.86529338664031,10.8518227253043,11.8383520639684,12.8248814026324,
13.8114107412964,13.8759337553362),.UNSPECIFIED.);
#4471=B_SPLINE_CURVE_WITH_KNOTS('',3,(#68269,#68270,#68271,#68272,#68273,
#68274,#68275,#68276,#68277,#68278,#68279,#68280,#68281,#68282,#68283,#68284,
#68285,#68286,#68287,#68288,#68289,#68290,#68291,#68292,#68293,#68294,#68295,
#68296,#68297,#68298,#68299,#68300,#68301,#68302,#68303,#68304,#68305,#68306,
#68307,#68308,#68309,#68310,#68311,#68312,#68313,#68314,#68315,#68316,#68317,
#68318,#68319,#68320,#68321,#68322,#68323,#68324,#68325,#68326,#68327,#68328,
#68329,#68330,#68331,#68332,#68333,#68334,#68335,#68336,#68337,#68338,#68339,
#68340,#68341,#68342,#68343,#68344,#68345,#68346,#68347,#68348,#68349,#68350),
 .UNSPECIFIED.,.F.,.F.,(4,3,3,3,3,3,3,3,3,3,3,3,3,3,3,3,3,3,3,3,3,3,3,3,
3,3,3,4),(-0.286347380332213,-0.271025134809031,-0.260698514723011,-0.255927597151592,
-0.251928120089878,-0.23573877571394,-0.229541586624538,-0.225083751316981,
-0.22164175520813,-0.204608740833268,-0.18782191212788,-0.179056502767314,
-0.17435303150997,-0.171008368415998,-0.168068126675904,-0.153509697708681,
-0.136938878241049,-0.120740722230713,-0.116774450511282,-0.113778933942795,
-0.0964554865286861,-0.0787602413272305,-0.0609085885350118,-0.0568635638522563,
-0.0386446388833524,-0.0205858033701879,-0.00735363015835568,0.),
 .UNSPECIFIED.);
#4472=B_SPLINE_CURVE_WITH_KNOTS('',3,(#68351,#68352,#68353,#68354,#68355,
#68356,#68357,#68358,#68359,#68360,#68361,#68362,#68363,#68364,#68365,#68366,
#68367,#68368,#68369,#68370,#68371,#68372,#68373,#68374,#68375,#68376,#68377,
#68378,#68379,#68380,#68381,#68382,#68383,#68384,#68385,#68386,#68387,#68388,
#68389,#68390,#68391,#68392,#68393,#68394,#68395,#68396,#68397,#68398,#68399,
#68400,#68401,#68402,#68403,#68404,#68405,#68406,#68407,#68408,#68409,#68410,
#68411,#68412,#68413,#68414,#68415,#68416,#68417,#68418,#68419,#68420,#68421,
#68422,#68423,#68424,#68425,#68426),.UNSPECIFIED.,.F.,.F.,(4,3,3,3,3,3,
3,3,3,3,3,3,3,3,3,3,3,3,3,3,3,3,3,3,3,4),(-0.285142803995108,-0.266893522635817,
-0.24997148182261,-0.245887106228687,-0.227911281463377,-0.216815940420553,
-0.21301916907798,-0.209467645127105,-0.191887872125524,-0.174757062559625,
-0.165469230797229,-0.157741956079593,-0.154438809603899,-0.13914855312078,
-0.122062023308955,-0.107562410123299,-0.103576177425209,-0.100472613628106,
-0.0838658566327193,-0.0673520867998959,-0.0520303445558493,-0.0480947086188938,
-0.0321861070361084,-0.016817164416105,-0.00606511782370935,0.),
 .UNSPECIFIED.);
#4473=B_SPLINE_CURVE_WITH_KNOTS('',3,(#68428,#68429,#68430,#68431,#68432,
#68433,#68434,#68435,#68436,#68437,#68438),.UNSPECIFIED.,.F.,.F.,(4,1,1,
1,1,1,1,1,4),(15.7079632679489,15.8014786182355,16.7880079568995,17.7745372955635,
18.7610666342275,19.7475959728916,20.7341253115556,21.7206546502196,21.9911485751285),
 .UNSPECIFIED.);
#4474=B_SPLINE_CURVE_WITH_KNOTS('',3,(#68439,#68440,#68441,#68442,#68443,
#68444,#68445,#68446,#68447,#68448),.UNSPECIFIED.,.F.,.F.,(4,1,1,1,1,1,
1,4),(15.7079632679489,16.3714588042999,17.3579881429639,18.344517481628,
19.331046820292,20.317576158956,21.3041054976201,21.9911485751285),
 .UNSPECIFIED.);
#4475=B_SPLINE_CURVE_WITH_KNOTS('',3,(#68673,#68674,#68675,#68676,#68677,
#68678,#68679,#68680,#68681,#68682,#68683,#68684,#68685,#68686,#68687,#68688,
#68689,#68690,#68691,#68692,#68693,#68694,#68695,#68696,#68697,#68698,#68699,
#68700,#68701,#68702,#68703,#68704,#68705,#68706,#68707,#68708,#68709,#68710,
#68711,#68712,#68713,#68714,#68715,#68716,#68717,#68718,#68719,#68720,#68721,
#68722,#68723,#68724,#68725,#68726,#68727,#68728,#68729,#68730,#68731,#68732,
#68733,#68734,#68735,#68736,#68737,#68738,#68739,#68740,#68741,#68742,#68743,
#68744,#68745,#68746,#68747,#68748,#68749,#68750,#68751,#68752,#68753,#68754),
 .UNSPECIFIED.,.F.,.F.,(4,3,3,3,3,3,3,3,3,3,3,3,3,3,3,3,3,3,3,3,3,3,3,3,
3,3,3,4),(0.,0.0151383092197915,0.0309550067692597,0.043639562338757,0.0490032691307438,
0.0520443158185715,0.0683454961299883,0.0849450886251988,0.0968166793002086,
0.101864993851806,0.10487333271342,0.121948986974184,0.132431451325238,
0.149057249647502,0.154031743970893,0.158630823409783,0.175668704761865,
0.193109534814407,0.203698360651626,0.209528438177436,0.213039046077353,
0.231029814287289,0.242727396093505,0.247561053661448,0.251100328242942,
0.269296434630926,0.277820141512155,0.285142803995171),.UNSPECIFIED.);
#4476=B_SPLINE_CURVE_WITH_KNOTS('',3,(#68755,#68756,#68757,#68758,#68759,
#68760,#68761,#68762,#68763,#68764,#68765,#68766,#68767,#68768,#68769,#68770,
#68771,#68772,#68773,#68774,#68775,#68776,#68777,#68778,#68779),
 .UNSPECIFIED.,.F.,.F.,(4,3,3,3,3,3,3,3,4),(-10.1357873115492,-9.86529338664031,
-8.87876404797628,-7.89223470931225,-6.90570537064822,-5.91917603198418,
-4.93264669332016,-3.94611735465613,-3.85260200436962),.UNSPECIFIED.);
#4477=B_SPLINE_CURVE_WITH_KNOTS('',3,(#69004,#69005,#69006,#69007,#69008,
#69009,#69010,#69011,#69012,#69013,#69014,#69015,#69016,#69017,#69018,#69019,
#69020,#69021,#69022,#69023,#69024,#69025,#69026,#69027,#69028),
 .UNSPECIFIED.,.F.,.F.,(4,3,3,3,3,3,3,3,4),(7.59274844815668,7.89223470931225,
8.87876404797628,9.86529338664031,10.8518227253043,11.8383520639684,12.8248814026324,
13.8114107412964,13.8759337553363),.UNSPECIFIED.);
#4478=B_SPLINE_CURVE_WITH_KNOTS('',3,(#69029,#69030,#69031,#69032,#69033,
#69034,#69035,#69036,#69037,#69038,#69039,#69040,#69041,#69042,#69043,#69044,
#69045,#69046,#69047,#69048,#69049,#69050,#69051,#69052,#69053,#69054,#69055,
#69056,#69057,#69058,#69059,#69060,#69061,#69062,#69063,#69064,#69065,#69066,
#69067,#69068,#69069,#69070,#69071,#69072,#69073,#69074,#69075,#69076,#69077,
#69078,#69079,#69080,#69081,#69082,#69083,#69084,#69085,#69086,#69087,#69088,
#69089,#69090,#69091,#69092,#69093,#69094,#69095,#69096,#69097,#69098,#69099,
#69100,#69101,#69102,#69103,#69104,#69105,#69106,#69107),.UNSPECIFIED.,
 .F.,.F.,(4,3,3,3,3,3,3,3,3,3,3,3,3,3,3,3,3,3,3,3,3,3,3,3,3,3,4),(0.,0.0183455177171492,
0.0365842479880597,0.0503567347067014,0.0575064710097589,0.0612717627824107,
0.0790233634825616,0.09641228950938,0.109000252566333,0.115579416560097,
0.118639169849882,0.13548942966781,0.146764141737194,0.163451454243388,
0.168605140809902,0.173128107433064,0.189898748854532,0.206649189230336,
0.217355774416694,0.222872516867536,0.226199915190878,0.242290799536828,
0.252395277141555,0.256089582974829,0.271598152369448,0.280262641786752,
0.286347380332268),.UNSPECIFIED.);
#4479=B_SPLINE_CURVE_WITH_KNOTS('',3,(#69114,#69115,#69116,#69117,#69118,
#69119,#69120,#69121,#69122,#69123,#69124,#69125,#69126,#69127,#69128,#69129,
#69130,#69131,#69132,#69133,#69134,#69135,#69136,#69137,#69138,#69139,#69140,
#69141,#69142,#69143,#69144,#69145,#69146,#69147,#69148,#69149,#69150,#69151,
#69152,#69153,#69154,#69155,#69156,#69157,#69158,#69159,#69160,#69161,#69162,
#69163,#69164,#69165,#69166,#69167,#69168,#69169,#69170,#69171,#69172,#69173,
#69174,#69175,#69176,#69177,#69178,#69179,#69180,#69181,#69182,#69183,#69184,
#69185,#69186,#69187,#69188,#69189,#69190,#69191,#69192,#69193,#69194,#69195),
 .UNSPECIFIED.,.F.,.F.,(4,3,3,3,3,3,3,3,3,3,3,3,3,3,3,3,3,3,3,3,3,3,3,3,
3,3,3,4),(-0.286347380332246,-0.271025677130926,-0.260700310292963,-0.255934727086495,
-0.25192886090893,-0.235739882849757,-0.229543774316331,-0.225091476626096,
-0.221644563245787,-0.204610846861512,-0.187823939473357,-0.179057897575031,
-0.174355331036021,-0.171012353628943,-0.168068993936419,-0.153509697708686,
-0.136938507575535,-0.120740397898387,-0.116772656048653,-0.113776970694075,
-0.0964531944223393,-0.0787578176889207,-0.0609067708062778,-0.0568632588541979,
-0.0386442813548163,-0.0205854383279417,-0.00735363015834907,0.),
 .UNSPECIFIED.);
#4480=B_SPLINE_CURVE_WITH_KNOTS('',3,(#69196,#69197,#69198,#69199,#69200,
#69201,#69202,#69203,#69204,#69205,#69206,#69207,#69208,#69209,#69210,#69211,
#69212,#69213,#69214,#69215,#69216,#69217,#69218,#69219,#69220,#69221,#69222,
#69223,#69224,#69225,#69226,#69227,#69228,#69229,#69230,#69231,#69232,#69233,
#69234,#69235,#69236,#69237,#69238,#69239,#69240,#69241,#69242,#69243,#69244,
#69245,#69246,#69247,#69248,#69249,#69250,#69251,#69252,#69253,#69254,#69255,
#69256,#69257,#69258,#69259,#69260,#69261,#69262,#69263,#69264,#69265,#69266,
#69267,#69268,#69269,#69270,#69271),.UNSPECIFIED.,.F.,.F.,(4,3,3,3,3,3,
3,3,3,3,3,3,3,3,3,3,3,3,3,3,3,3,3,3,3,4),(-0.285142803995095,-0.266893522635806,
-0.24997167290184,-0.245887165090684,-0.227911315359866,-0.21681597007998,
-0.213019412352564,-0.209467703547662,-0.191887915940942,-0.174756941142404,
-0.165469038009959,-0.157741699115177,-0.15443885155403,-0.139148553120782,
-0.122062044167413,-0.10756242837445,-0.103576076720583,-0.100472600797313,
-0.0838658661242367,-0.0673520476672987,-0.0520303152064016,-0.0480946741240866,
-0.0321859718066127,-0.016816720434557,-0.00606511782371032,0.),
 .UNSPECIFIED.);
#4481=B_SPLINE_CURVE_WITH_KNOTS('',3,(#69273,#69274,#69275,#69276,#69277,
#69278,#69279,#69280,#69281,#69282,#69283),.UNSPECIFIED.,.F.,.F.,(4,1,1,
1,1,1,1,1,4),(15.7079632679489,15.8014786182355,16.7880079568995,17.7745372955635,
18.7610666342276,19.7475959728916,20.7341253115556,21.7206546502197,21.9911485751285),
 .UNSPECIFIED.);
#4482=B_SPLINE_CURVE_WITH_KNOTS('',3,(#69284,#69285,#69286,#69287,#69288,
#69289,#69290,#69291,#69292,#69293),.UNSPECIFIED.,.F.,.F.,(4,1,1,1,1,1,
1,4),(15.7079632679489,16.3714588042999,17.357988142964,18.344517481628,
19.331046820292,20.317576158956,21.3041054976201,21.9911485751285),
 .UNSPECIFIED.);
#4483=B_SPLINE_CURVE_WITH_KNOTS('',3,(#69518,#69519,#69520,#69521,#69522,
#69523,#69524,#69525,#69526,#69527,#69528,#69529,#69530,#69531,#69532,#69533,
#69534,#69535,#69536,#69537,#69538,#69539,#69540,#69541,#69542),
 .UNSPECIFIED.,.F.,.F.,(4,3,3,3,3,3,3,3,4),(-10.1357873115492,-9.8652933866403,
-8.87876404797628,-7.89223470931224,-6.90570537064821,-5.91917603198418,
-4.93264669332015,-3.94611735465612,-3.85260200436958),.UNSPECIFIED.);
#4484=B_SPLINE_CURVE_WITH_KNOTS('',3,(#69767,#69768,#69769,#69770,#69771,
#69772,#69773,#69774,#69775,#69776,#69777,#69778,#69779,#69780,#69781,#69782,
#69783,#69784,#69785,#69786,#69787,#69788,#69789,#69790,#69791),
 .UNSPECIFIED.,.F.,.F.,(4,3,3,3,3,3,3,3,4),(7.59274844815664,7.89223470931223,
8.87876404797627,9.8652933866403,10.8518227253043,11.8383520639684,12.8248814026324,
13.8114107412964,13.8759337553362),.UNSPECIFIED.);
#4485=B_SPLINE_CURVE_WITH_KNOTS('',3,(#69883,#69884,#69885,#69886,#69887,
#69888),.UNSPECIFIED.,.F.,.F.,(4,2,4),(-1.6,-0.8,0.),.UNSPECIFIED.);
#4486=B_SPLINE_CURVE_WITH_KNOTS('',3,(#69894,#69895,#69896,#69897,#69898,
#69899),.UNSPECIFIED.,.F.,.F.,(4,2,4),(-1.6,-0.8,0.),.UNSPECIFIED.);
#4487=B_SPLINE_CURVE_WITH_KNOTS('',3,(#69911,#69912,#69913,#69914,#69915,
#69916),.UNSPECIFIED.,.F.,.F.,(4,2,4),(-1.6,-0.8,0.),.UNSPECIFIED.);
#4488=B_SPLINE_CURVE_WITH_KNOTS('',3,(#69930,#69931,#69932,#69933,#69934,
#69935),.UNSPECIFIED.,.F.,.F.,(4,2,4),(-1.6,-0.8,0.),.UNSPECIFIED.);
#4489=B_SPLINE_CURVE_WITH_KNOTS('',3,(#69939,#69940,#69941,#69942,#69943,
#69944),.UNSPECIFIED.,.F.,.F.,(4,2,4),(-1.6,-0.8,0.),.UNSPECIFIED.);
#4490=B_SPLINE_CURVE_WITH_KNOTS('',3,(#69958,#69959,#69960,#69961,#69962,
#69963),.UNSPECIFIED.,.F.,.F.,(4,2,4),(-1.6,-0.8,0.),.UNSPECIFIED.);
#4491=B_SPLINE_CURVE_WITH_KNOTS('',3,(#69967,#69968,#69969,#69970,#69971,
#69972),.UNSPECIFIED.,.F.,.F.,(4,2,4),(-1.6,-0.8,0.),.UNSPECIFIED.);
#4492=B_SPLINE_CURVE_WITH_KNOTS('',3,(#69986,#69987,#69988,#69989,#69990,
#69991),.UNSPECIFIED.,.F.,.F.,(4,2,4),(-1.6,-0.8,0.),.UNSPECIFIED.);
#4493=B_SPLINE_CURVE_WITH_KNOTS('',3,(#69995,#69996,#69997,#69998,#69999,
#70000),.UNSPECIFIED.,.F.,.F.,(4,2,4),(-1.6,-0.8,0.),.UNSPECIFIED.);
#4494=B_SPLINE_CURVE_WITH_KNOTS('',3,(#70006,#70007,#70008,#70009,#70010,
#70011),.UNSPECIFIED.,.F.,.F.,(4,2,4),(-1.6,-0.8,0.),.UNSPECIFIED.);
#4495=B_SPLINE_CURVE_WITH_KNOTS('',3,(#72032,#72033,#72034,#72035,#72036,
#72037,#72038,#72039,#72040,#72041,#72042,#72043,#72044,#72045,#72046,#72047,
#72048,#72049,#72050,#72051,#72052,#72053,#72054,#72055,#72056,#72057,#72058,
#72059),.UNSPECIFIED.,.F.,.F.,(4,3,3,3,3,3,3,3,3,4),(-1.95245002670228,
-1.7083937733645,-1.4646957205336,-1.22078701844286,-0.97666712493882,-0.732202856815818,
-0.487562123458939,-0.24378106172947,-0.0832160650278452,0.),
 .UNSPECIFIED.);
#4496=B_SPLINE_CURVE_WITH_KNOTS('',3,(#74072,#74073,#74074,#74075,#74076,
#74077,#74078,#74079,#74080,#74081,#74082,#74083,#74084,#74085,#74086,#74087,
#74088,#74089,#74090,#74091,#74092,#74093,#74094,#74095,#74096,#74097,#74098,
#74099),.UNSPECIFIED.,.F.,.F.,(4,3,3,3,3,3,3,3,3,4),(-1.95245002774481,
-1.70839377427671,-1.46469569943071,-1.22078743097454,-0.976667451078158,
-0.732203245920036,-0.487562280383025,-0.243781140191512,-0.0832160609216453,
0.),.UNSPECIFIED.);
#4497=B_SPLINE_CURVE_WITH_KNOTS('',3,(#76113,#76114,#76115,#76116),
 .UNSPECIFIED.,.F.,.F.,(4,4),(-3.33933214605564,-2.59563630155322),
 .UNSPECIFIED.);
#4498=B_SPLINE_CURVE_WITH_KNOTS('',3,(#78128,#78129,#78130,#78131,#78132,
#78133,#78134,#78135,#78136,#78137,#78138,#78139,#78140,#78141,#78142,#78143,
#78144,#78145,#78146,#78147,#78148,#78149,#78150,#78151,#78152,#78153,#78154,
#78155),.UNSPECIFIED.,.F.,.F.,(4,3,3,3,3,3,3,3,3,4),(-1.95245003576054,
-1.70839378129047,-1.46469576962979,-1.22078693523904,-0.976667204248944,
-0.732202830545938,-0.487562139320946,-0.243781069660473,-0.0832159489912239,
0.),.UNSPECIFIED.);
#4499=B_SPLINE_CURVE_WITH_KNOTS('',3,(#80169,#80170,#80171,#80172),
 .UNSPECIFIED.,.F.,.F.,(4,4),(-3.3393321613758,-2.59563631294433),
 .UNSPECIFIED.);
#4500=B_SPLINE_CURVE_WITH_KNOTS('',3,(#82184,#82185,#82186,#82187,#82188,
#82189,#82190,#82191,#82192,#82193,#82194,#82195,#82196,#82197,#82198,#82199,
#82200,#82201,#82202,#82203,#82204,#82205,#82206,#82207,#82208,#82209,#82210,
#82211),.UNSPECIFIED.,.F.,.F.,(4,3,3,3,3,3,3,3,3,4),(-1.95245002395252,
-1.70839377095845,-1.46469574316389,-1.22078724480627,-0.97666698126864,
-0.732202626712538,-0.487561565272828,-0.243780782636414,-0.083215645232922,
0.),.UNSPECIFIED.);
#4501=B_SPLINE_CURVE_WITH_KNOTS('',3,(#84225,#84226,#84227,#84228),
 .UNSPECIFIED.,.F.,.F.,(4,4),(-3.33933214077653,-2.59563629688202),
 .UNSPECIFIED.);
#4502=B_SPLINE_CURVE_WITH_KNOTS('',3,(#86240,#86241,#86242,#86243,#86244,
#86245,#86246,#86247,#86248,#86249,#86250,#86251,#86252,#86253,#86254,#86255,
#86256,#86257,#86258,#86259,#86260,#86261,#86262,#86263,#86264,#86265,#86266,
#86267),.UNSPECIFIED.,.F.,.F.,(4,3,3,3,3,3,3,3,3,4),(-1.95245003704233,
-1.70839378241204,-1.46469565989463,-1.22078739198828,-0.97666741362503,
-0.732203206774895,-0.487562540884707,-0.243781270442354,-0.0832161724652675,
0.),.UNSPECIFIED.);
#4503=B_SPLINE_CURVE_WITH_KNOTS('',3,(#86271,#86272,#86273,#86274,#86275,
#86276),.UNSPECIFIED.,.F.,.F.,(4,2,4),(-1.6,-0.8,0.),.UNSPECIFIED.);
#4504=B_SPLINE_CURVE_WITH_KNOTS('',3,(#86282,#86283,#86284,#86285,#86286,
#86287),.UNSPECIFIED.,.F.,.F.,(4,2,4),(-1.6,-0.8,0.),.UNSPECIFIED.);
#4505=B_SPLINE_CURVE_WITH_KNOTS('',3,(#88308,#88309,#88310,#88311,#88312,
#88313,#88314,#88315,#88316,#88317,#88318,#88319,#88320,#88321,#88322,#88323,
#88324,#88325,#88326,#88327,#88328,#88329,#88330,#88331,#88332,#88333,#88334,
#88335),.UNSPECIFIED.,.F.,.F.,(4,3,3,3,3,3,3,3,3,4),(-1.95245003867437,
-1.70839378384007,-1.46469580928766,-1.22078735724755,-0.976667179798372,
-0.732202890769605,-0.487561952370783,-0.243780976185391,-0.0832159842231958,
0.),.UNSPECIFIED.);
#4506=B_SPLINE_CURVE_WITH_KNOTS('',3,(#88369,#88370,#88371,#88372),
 .UNSPECIFIED.,.F.,.F.,(4,4),(-3.3393321486059,-2.59563630156681),
 .UNSPECIFIED.);
#4507=B_SPLINE_CURVE_WITH_KNOTS('',3,(#88379,#88380,#88381,#88382),
 .UNSPECIFIED.,.F.,.F.,(4,4),(-3.33933216373174,-2.59563631465892),
 .UNSPECIFIED.);
#4508=B_SPLINE_CURVE_WITH_KNOTS('',3,(#88389,#88390,#88391,#88392),
 .UNSPECIFIED.,.F.,.F.,(4,4),(-3.33933216499304,-2.59563631632113),
 .UNSPECIFIED.);
#4509=B_SPLINE_CURVE_WITH_KNOTS('',3,(#94457,#94458,#94459,#94460,#94461,
#94462,#94463,#94464,#94465,#94466),.UNSPECIFIED.,.F.,.F.,(4,2,2,2,4),(-0.455064911568751,
-0.34131563198115,-0.227566352393549,-0.113783176196775,0.),
 .UNSPECIFIED.);
#4510=B_SPLINE_CURVE_WITH_KNOTS('',3,(#94469,#94470,#94471,#94472,#94473,
#94474,#94475,#94476,#94477,#94478),.UNSPECIFIED.,.F.,.F.,(4,2,2,2,4),(-0.910129823137502,
-0.796346646940727,-0.682563470743952,-0.568814191156351,-0.455064911568751),
 .UNSPECIFIED.);
#4511=B_SPLINE_CURVE_WITH_KNOTS('',3,(#94491,#94492,#94493,#94494,#94495,
#94496,#94497,#94498,#94499,#94500,#94501,#94502,#94503,#94504,#94505,#94506,
#94507,#94508),.UNSPECIFIED.,.F.,.F.,(4,2,2,2,2,2,2,2,4),(0.,0.113783176196775,
0.227566352393549,0.34131563198115,0.455064911568751,0.568814191156351,
0.682563470743952,0.796346646940727,0.910129823137502),.UNSPECIFIED.);
#4512=B_SPLINE_CURVE_WITH_KNOTS('',3,(#94526,#94527,#94528,#94529,#94530,
#94531,#94532,#94533,#94534,#94535,#94536,#94537,#94538,#94539,#94540,#94541,
#94542,#94543),.UNSPECIFIED.,.F.,.F.,(4,2,2,2,2,2,2,2,4),(-0.910129823137503,
-0.796346646940728,-0.682563470743953,-0.568814191156352,-0.455064911568751,
-0.341315631981151,-0.22756635239355,-0.113783176196775,0.),
 .UNSPECIFIED.);
#4513=B_SPLINE_CURVE_WITH_KNOTS('',3,(#94558,#94559,#94560,#94561,#94562,
#94563,#94564,#94565,#94566,#94567),.UNSPECIFIED.,.F.,.F.,(4,2,2,2,4),(0.455064911568751,
0.568814191156352,0.682563470743953,0.796346646940727,0.910129823137502),
 .UNSPECIFIED.);
#4514=B_SPLINE_CURVE_WITH_KNOTS('',3,(#94568,#94569,#94570,#94571,#94572,
#94573,#94574,#94575,#94576,#94577),.UNSPECIFIED.,.F.,.F.,(4,2,2,2,4),(0.,
0.113783176196775,0.22756635239355,0.341315631981151,0.455064911568751),
 .UNSPECIFIED.);
#4515=B_SPLINE_CURVE_WITH_KNOTS('',3,(#95231,#95232,#95233,#95234,#95235,
#95236,#95237,#95238,#95239,#95240,#95241,#95242,#95243,#95244,#95245,#95246,
#95247,#95248,#95249,#95250,#95251,#95252,#95253,#95254,#95255,#95256,#95257,
#95258,#95259),.UNSPECIFIED.,.F.,.F.,(4,1,1,1,1,1,1,1,1,1,1,1,1,1,1,1,1,
1,1,1,1,1,1,1,1,1,4),(0.,0.483321946706122,0.966643893412244,1.44996584011837,
1.93328778682449,2.41660973353061,2.89993168023673,3.38325362694285,3.86657557364898,
4.3498975203551,4.83321946706122,5.31654141376734,5.79986336047346,6.28318530717959,
6.76650725388571,7.24982920059183,7.73315114729795,8.21647309400407,8.6997950407102,
9.18311698741632,9.66643893412244,10.1497608808286,10.6330828275347,11.1164047742408,
11.5997267209469,12.083048667653,12.5663706143592),.UNSPECIFIED.);
#4516=B_SPLINE_CURVE_WITH_KNOTS('',3,(#95269,#95270,#95271,#95272,#95273,
#95274,#95275,#95276,#95277,#95278),.UNSPECIFIED.,.F.,.F.,(4,3,3,4),(-4.09254174883833,
-3.98934337020898,-2.99200752765673,-2.06514013327813),.UNSPECIFIED.);
#4517=B_SPLINE_CURVE_WITH_KNOTS('',3,(#95281,#95282,#95283,#95284,#95285,
#95286,#95287),.UNSPECIFIED.,.F.,.F.,(4,3,4),(0.,0.998006970630082,1.11419103802948),
 .UNSPECIFIED.);
#4518=B_SPLINE_CURVE_WITH_KNOTS('',3,(#95292,#95293,#95294,#95295,#95296,
#95297,#95298,#95299,#95300,#95301,#95302,#95303,#95304,#95305,#95306,#95307,
#95308,#95309,#95310,#95311,#95312,#95313),.UNSPECIFIED.,.F.,.F.,(4,3,3,
3,3,3,3,4),(-10.3757270560179,-9.97335842552244,-8.9760225829702,-7.97868674041795,
-6.9813508978657,-5.98401505531347,-4.98667921276122,-4.09254174883833),
 .UNSPECIFIED.);
#4519=B_SPLINE_CURVE_WITH_KNOTS('',3,(#95314,#95315,#95316,#95317,#95318,
#95319,#95320,#95321,#95322,#95323,#95324,#95325,#95326,#95327,#95328,#95329,
#95330,#95331,#95332,#95333,#95334,#95335),.UNSPECIFIED.,.F.,.F.,(4,3,3,
3,3,3,3,4),(1.11419103802948,1.99601394126018,2.99402091189026,3.99202788252035,
4.99003485315045,5.98804182378054,6.98604879441062,7.39737634520907),
 .UNSPECIFIED.);
#4520=B_SPLINE_CURVE_WITH_KNOTS('',3,(#95340,#95341,#95342,#95343,#95344,
#95345,#95346,#95347,#95348,#95349,#95350,#95351,#95352,#95353,#95354,#95355,
#95356,#95357,#95358,#95359,#95360,#95361),.UNSPECIFIED.,.F.,.F.,(4,3,3,
3,3,3,3,4),(-16.6589123631975,-15.9573734808359,-14.9600376382837,-13.9627017957314,
-12.9653659531792,-11.9680301106269,-10.9706942680747,-10.3757270560179),
 .UNSPECIFIED.);
#4521=B_SPLINE_CURVE_WITH_KNOTS('',3,(#95362,#95363,#95364,#95365,#95366,
#95367,#95368,#95369,#95370,#95371,#95372,#95373,#95374,#95375,#95376,#95377,
#95378,#95379,#95380,#95381,#95382,#95383),.UNSPECIFIED.,.F.,.F.,(4,3,3,
3,3,3,3,4),(7.39737634520907,7.98405576504071,8.9820627356708,9.98006970630089,
10.978076676931,11.9760836475611,12.9740906181912,13.6805616523887),
 .UNSPECIFIED.);
#4522=B_SPLINE_CURVE_WITH_KNOTS('',3,(#95388,#95389,#95390,#95391,#95392,
#95393,#95394,#95395,#95396,#95397,#95398,#95399,#95400,#95401,#95402,#95403,
#95404,#95405,#95406,#95407,#95408,#95409,#95410,#95411,#95412),
 .UNSPECIFIED.,.F.,.F.,(4,3,3,3,3,3,3,3,4),(-22.9420976703771,-22.9387243787016,
-21.9413885361494,-20.9440526935971,-19.9467168510449,-18.9493810084926,
-17.9520451659404,-16.9547093233881,-16.6589123631975),.UNSPECIFIED.);
#4523=B_SPLINE_CURVE_WITH_KNOTS('',3,(#95413,#95414,#95415,#95416,#95417,
#95418,#95419,#95420,#95421,#95422,#95423,#95424,#95425,#95426,#95427,#95428,
#95429,#95430,#95431,#95432,#95433,#95434,#95435,#95436,#95437),
 .UNSPECIFIED.,.F.,.F.,(4,3,3,3,3,3,3,3,4),(13.6805616523887,13.9720975888212,
14.9701045594513,15.9681115300814,16.9661185007115,17.9641254713416,18.9621324419717,
19.9601394126018,19.9637469595682),.UNSPECIFIED.);
#4524=B_SPLINE_CURVE_WITH_KNOTS('',3,(#95442,#95443,#95444,#95445,#95446,
#95447,#95448,#95449,#95450,#95451,#95452,#95453,#95454,#95455,#95456,#95457,
#95458,#95459,#95460,#95461,#95462,#95463),.UNSPECIFIED.,.F.,.F.,(4,3,3,
3,3,3,3,4),(-29.2252829775567,-28.9227394340151,-27.9254035914628,-26.9280677489106,
-25.9307319063583,-24.9333960638061,-23.9360602212539,-22.9420976703771),
 .UNSPECIFIED.);
#4525=B_SPLINE_CURVE_WITH_KNOTS('',3,(#95464,#95465,#95466,#95467,#95468,
#95469,#95470,#95471,#95472,#95473,#95474,#95475,#95476,#95477,#95478,#95479,
#95480,#95481,#95482,#95483,#95484,#95485),.UNSPECIFIED.,.F.,.F.,(4,3,3,
3,3,3,3,4),(19.9637469595682,20.9581463832319,21.956153353862,22.954160324492,
23.9521672951221,24.9501742657522,25.9481812363823,26.2469322667478),
 .UNSPECIFIED.);
#4526=B_SPLINE_CURVE_WITH_KNOTS('',3,(#95490,#95491,#95492,#95493,#95494,
#95495,#95496,#95497,#95498,#95499,#95500,#95501,#95502,#95503,#95504,#95505,
#95506,#95507,#95508,#95509,#95510,#95511),.UNSPECIFIED.,.F.,.F.,(4,3,3,
3,3,3,3,4),(-35.5084682847363,-34.9067544893285,-33.9094186467763,-32.9120828042241,
-31.9147469616718,-30.9174111191196,-29.9200752765673,-29.2252829775567),
 .UNSPECIFIED.);
#4527=B_SPLINE_CURVE_WITH_KNOTS('',3,(#95512,#95513,#95514,#95515,#95516,
#95517,#95518,#95519,#95520,#95521,#95522,#95523,#95524,#95525,#95526,#95527,
#95528,#95529,#95530,#95531,#95532,#95533),.UNSPECIFIED.,.F.,.F.,(4,3,3,
3,3,3,3,4),(26.2469322667478,26.9461882070124,27.9441951776425,28.9422021482726,
29.9402091189027,30.9382160895327,31.9362230601628,32.5301175739274),
 .UNSPECIFIED.);
#4528=B_SPLINE_CURVE_WITH_KNOTS('',3,(#95538,#95539,#95540,#95541,#95542,
#95543,#95544,#95545,#95546,#95547,#95548,#95549,#95550,#95551,#95552,#95553,
#95554,#95555,#95556,#95557,#95558,#95559),.UNSPECIFIED.,.F.,.F.,(4,3,3,
3,3,3,3,4),(-41.7916535919159,-40.890769544642,-39.8934337020898,-38.8960978595375,
-37.8987620169853,-36.901426174433,-35.9040903318808,-35.5084682847363),
 .UNSPECIFIED.);
#4529=B_SPLINE_CURVE_WITH_KNOTS('',3,(#95560,#95561,#95562,#95563,#95564,
#95565,#95566,#95567,#95568,#95569,#95570,#95571,#95572,#95573,#95574,#95575,
#95576,#95577,#95578,#95579,#95580,#95581),.UNSPECIFIED.,.F.,.F.,(4,3,3,
3,3,3,3,4),(32.5301175739274,32.9342300307929,33.932237001423,34.9302439720531,
35.9282509426832,36.9262579133133,37.9242648839434,38.813302881107),
 .UNSPECIFIED.);
#4530=B_SPLINE_CURVE_WITH_KNOTS('',3,(#95586,#95587,#95588,#95589,#95590,
#95591,#95592,#95593,#95594,#95595,#95596,#95597,#95598,#95599,#95600,#95601,
#95602,#95603,#95604,#95605,#95606,#95607,#95608,#95609,#95610),
 .UNSPECIFIED.,.F.,.F.,(4,3,3,3,3,3,3,3,4),(-48.0748388990955,-47.8721204425077,
-46.8747845999555,-45.8774487574032,-44.880112914851,-43.8827770722987,
-42.8854412297465,-41.8881053871943,-41.7916535919159),.UNSPECIFIED.);
#4531=B_SPLINE_CURVE_WITH_KNOTS('',3,(#95611,#95612,#95613,#95614,#95615,
#95616,#95617,#95618,#95619,#95620,#95621,#95622,#95623,#95624,#95625,#95626,
#95627,#95628,#95629,#95630,#95631,#95632,#95633,#95634,#95635),
 .UNSPECIFIED.,.F.,.F.,(4,3,3,3,3,3,3,3,4),(38.813302881107,38.9222718545735,
39.9202788252036,40.9182857958337,41.9162927664637,42.9142997370938,43.9123067077239,
44.910313678354,45.0964881882866),.UNSPECIFIED.);
#4532=B_SPLINE_CURVE_WITH_KNOTS('',3,(#95640,#95641,#95642,#95643,#95644,
#95645,#95646,#95647,#95648,#95649,#95650,#95651,#95652,#95653,#95654,#95655,
#95656,#95657,#95658,#95659,#95660,#95661),.UNSPECIFIED.,.F.,.F.,(4,3,3,
3,3,3,3,4),(-54.3580242062751,-53.8561354978212,-52.8587996552689,-51.8614638127167,
-50.8641279701645,-49.8667921276122,-48.86945628506,-48.0748388990955),
 .UNSPECIFIED.);
#4533=B_SPLINE_CURVE_WITH_KNOTS('',3,(#95662,#95663,#95664,#95665,#95666,
#95667,#95668,#95669,#95670,#95671,#95672,#95673,#95674,#95675,#95676,#95677,
#95678,#95679,#95680,#95681,#95682,#95683),.UNSPECIFIED.,.F.,.F.,(4,3,3,
3,3,3,3,4),(45.0964881882866,45.9083206489841,46.9063276196142,47.9043345902443,
48.9023415608744,49.9003485315045,50.8983555021345,51.3796734954662),
 .UNSPECIFIED.);
#4534=B_SPLINE_CURVE_WITH_KNOTS('',3,(#95688,#95689,#95690,#95691,#95692,
#95693,#95694,#95695,#95696,#95697,#95698,#95699,#95700,#95701,#95702,#95703,
#95704,#95705,#95706,#95707,#95708,#95709),.UNSPECIFIED.,.F.,.F.,(4,3,3,
3,3,3,3,4),(-60.6412095134546,-59.8401505531347,-58.8428147105824,-57.8454788680302,
-56.8481430254779,-55.8508071829257,-54.8534713403734,-54.3580242062751),
 .UNSPECIFIED.);
#4535=B_SPLINE_CURVE_WITH_KNOTS('',3,(#95710,#95711,#95712,#95713,#95714,
#95715,#95716,#95717,#95718,#95719,#95720,#95721,#95722,#95723,#95724,#95725,
#95726,#95727,#95728,#95729,#95730,#95731),.UNSPECIFIED.,.F.,.F.,(4,3,3,
3,3,3,3,4),(51.3796734954662,51.8963624727646,52.8943694433947,53.8923764140248,
54.8903833846549,55.888390355285,56.8863973259151,57.6628588026458),
 .UNSPECIFIED.);
#4536=B_SPLINE_CURVE_WITH_KNOTS('',3,(#95736,#95737,#95738,#95739,#95740,
#95741,#95742,#95743,#95744,#95745,#95746,#95747,#95748,#95749,#95750,#95751,
#95752,#95753,#95754,#95755,#95756,#95757,#95758,#95759,#95760),
 .UNSPECIFIED.,.F.,.F.,(4,3,3,3,3,3,3,3,4),(-66.9243948206342,-66.8215014510004,
-65.8241656084481,-64.8268297658959,-63.8294939233436,-62.8321580807914,
-61.8348222382391,-60.8374863956869,-60.6412095134546),.UNSPECIFIED.);
#4537=B_SPLINE_CURVE_WITH_KNOTS('',3,(#95761,#95762,#95763,#95764,#95765,
#95766,#95767,#95768,#95769,#95770,#95771,#95772,#95773,#95774,#95775,#95776,
#95777,#95778,#95779,#95780,#95781,#95782,#95783,#95784,#95785),
 .UNSPECIFIED.,.F.,.F.,(4,3,3,3,3,3,3,3,4),(57.6628588026458,57.8844042965452,
58.8824112671752,59.8804182378054,60.8784252084354,61.8764321790655,62.8744391496956,
63.8724461203257,63.9460441098254),.UNSPECIFIED.);
#4538=B_SPLINE_CURVE_WITH_KNOTS('',3,(#95790,#95791,#95792,#95793,#95794,
#95795,#95796,#95797,#95798,#95799,#95800,#95801,#95802,#95803,#95804,#95805,
#95806,#95807,#95808,#95809,#95810,#95811),.UNSPECIFIED.,.F.,.F.,(4,3,3,
3,3,3,3,4),(-73.2075801278138,-72.8055165063138,-71.8081806637616,-70.8108448212093,
-69.8135089786571,-68.8161731361048,-67.8188372935526,-66.9243948206342),
 .UNSPECIFIED.);
#4539=B_SPLINE_CURVE_WITH_KNOTS('',3,(#95812,#95813,#95814,#95815,#95816,
#95817,#95818,#95819,#95820,#95821,#95822,#95823,#95824,#95825,#95826,#95827,
#95828,#95829,#95830,#95831,#95832,#95833),.UNSPECIFIED.,.F.,.F.,(4,3,3,
3,3,3,3,4),(63.9460441098254,64.8704530909558,65.8684600615859,66.866467032216,
67.8644740028461,68.8624809734761,69.8604879441062,70.229229417005),
 .UNSPECIFIED.);
#4540=B_SPLINE_CURVE_WITH_KNOTS('',3,(#95838,#95839,#95840,#95841,#95842,
#95843,#95844,#95845,#95846,#95847,#95848,#95849,#95850,#95851,#95852,#95853,
#95854,#95855,#95856,#95857,#95858,#95859),.UNSPECIFIED.,.F.,.F.,(4,3,3,
3,3,3,3,4),(-79.4907654349934,-78.7895315616273,-77.792195719075,-76.7948598765228,
-75.7975240339705,-74.8001881914183,-73.802852348866,-73.2075801278138),
 .UNSPECIFIED.);
#4541=B_SPLINE_CURVE_WITH_KNOTS('',3,(#95860,#95861,#95862,#95863,#95864,
#95865,#95866,#95867,#95868,#95869,#95870,#95871,#95872,#95873,#95874,#95875,
#95876,#95877,#95878,#95879,#95880,#95881),.UNSPECIFIED.,.F.,.F.,(4,3,3,
3,3,3,3,4),(70.229229417005,70.8584949147363,71.8565018853664,72.8545088559965,
73.8525158266266,74.8505227972567,75.8485297678868,76.5124147241846),
 .UNSPECIFIED.);
#4542=B_SPLINE_CURVE_WITH_KNOTS('',3,(#95886,#95887,#95888,#95889,#95890,
#95891,#95892,#95893,#95894,#95895,#95896,#95897,#95898,#95899,#95900,#95901,
#95902,#95903,#95904,#95905,#95906,#95907,#95908,#95909,#95910),
 .UNSPECIFIED.,.F.,.F.,(4,3,3,3,3,3,3,3,4),(-85.773950742173,-85.770882459493,
-84.7735466169407,-83.7762107743885,-82.7788749318363,-81.781539089284,
-80.7842032467318,-79.7868674041795,-79.4907654349934),.UNSPECIFIED.);
#4543=B_SPLINE_CURVE_WITH_KNOTS('',3,(#95911,#95912,#95913,#95914,#95915,
#95916,#95917,#95918,#95919,#95920,#95921,#95922,#95923,#95924,#95925,#95926,
#95927,#95928,#95929,#95930,#95931,#95932),.UNSPECIFIED.,.F.,.F.,(4,3,3,
3,3,3,3,4),(76.5124147241846,76.8465367385169,77.8445437091469,78.842550679777,
79.8405576504071,80.8385646210372,81.8365715916673,82.7956000313642),
 .UNSPECIFIED.);
#4544=B_SPLINE_CURVE_WITH_KNOTS('',3,(#95937,#95938,#95939,#95940,#95941,
#95942,#95943,#95944,#95945,#95946,#95947,#95948,#95949,#95950,#95951,#95952,
#95953,#95954,#95955,#95956,#95957,#95958),.UNSPECIFIED.,.F.,.F.,(4,3,3,
3,3,3,3,4),(-92.0571360493526,-91.7548975148065,-90.7575616722542,-89.760225829702,
-88.7628899871497,-87.7655541445975,-86.7682183020452,-85.773950742173),
 .UNSPECIFIED.);
#4545=B_SPLINE_CURVE_WITH_KNOTS('',3,(#95959,#95960,#95961,#95962,#95963,
#95964,#95965,#95966,#95967,#95968,#95969,#95970,#95971,#95972,#95973,#95974,
#95975,#95976,#95977,#95978,#95979,#95980,#95981,#95982,#95983),
 .UNSPECIFIED.,.F.,.F.,(4,3,3,3,3,3,3,3,4),(82.7956000313642,82.8345785622974,
83.8325855329275,84.8305925035576,85.8285994741877,86.8266064448178,87.8246134154479,
88.822620386078,89.0787853385438),.UNSPECIFIED.);
#4546=B_SPLINE_CURVE_WITH_KNOTS('',3,(#95988,#95989,#95990,#95991,#95992,
#95993,#95994,#95995,#95996,#95997,#95998,#95999,#96000,#96001,#96002,#96003,
#96004,#96005,#96006,#96007,#96008,#96009),.UNSPECIFIED.,.F.,.F.,(4,3,3,
3,3,3,3,4),(-98.3403213565322,-97.7389125701199,-96.7415767275677,-95.7442408850154,
-94.7469050424632,-93.7495691999109,-92.7522333573587,-92.0571360493526),
 .UNSPECIFIED.);
#4547=B_SPLINE_CURVE_WITH_KNOTS('',3,(#96010,#96011,#96012,#96013,#96014,
#96015,#96016,#96017,#96018,#96019,#96020,#96021,#96022,#96023,#96024,#96025,
#96026,#96027,#96028,#96029,#96030,#96031),.UNSPECIFIED.,.F.,.F.,(4,3,3,
3,3,3,3,4),(89.0787853385438,89.820627356708,90.8186343273381,91.8166412979682,
92.8146482685983,93.8126552392284,94.8106622098585,95.3619706457233),
 .UNSPECIFIED.);
#4548=B_SPLINE_CURVE_WITH_KNOTS('',3,(#96037,#96038,#96039,#96040,#96041,
#96042,#96043,#96044),.UNSPECIFIED.,.F.,.F.,(4,1,1,1,1,4),(109.955742875643,
110.351669931783,111.349005774335,112.346341616887,113.343677459439,114.341013301992),
 .UNSPECIFIED.);
#4549=B_SPLINE_CURVE_WITH_KNOTS('',3,(#96047,#96048,#96049,#96050,#96051,
#96052,#96053),.UNSPECIFIED.,.F.,.F.,(4,1,1,1,4),(109.955742875643,110.107297927009,
111.105304897639,112.103311868269,113.101318838899),.UNSPECIFIED.);
#4550=B_SPLINE_CURVE_WITH_KNOTS('',3,(#96058,#96059,#96060,#96061,#96062,
#96063,#96064,#96065,#96066,#96067),.UNSPECIFIED.,.F.,.F.,(4,1,1,1,1,1,
1,4),(103.672557568463,104.367654876469,105.364990719021,106.362326561574,
107.359662404126,108.356998246678,109.35433408923,109.955742875643),
 .UNSPECIFIED.);
#4551=B_SPLINE_CURVE_WITH_KNOTS('',3,(#96068,#96069,#96070,#96071,#96072,
#96073,#96074,#96075,#96076,#96077),.UNSPECIFIED.,.F.,.F.,(4,1,1,1,1,1,
1,4),(103.672557568463,104.119256103228,105.117263073858,106.115270044488,
107.113277015118,108.111283985749,109.109290956379,109.955742875643),
 .UNSPECIFIED.);
#4552=B_SPLINE_CURVE_WITH_KNOTS('',3,(#96082,#96083,#96084,#96085,#96086,
#96087,#96088,#96089,#96090,#96091),.UNSPECIFIED.,.F.,.F.,(4,1,1,1,1,1,
1,4),(97.3893722612836,98.3836398211558,99.380975663708,100.37831150626,
101.375647348812,102.372983191365,103.370319033917,103.672557568463),
 .UNSPECIFIED.);
#4553=B_SPLINE_CURVE_WITH_KNOTS('',3,(#96092,#96093,#96094,#96095,#96096,
#96097,#96098,#96099,#96100,#96101),.UNSPECIFIED.,.F.,.F.,(4,1,1,1,1,1,
1,4),(97.3893722612836,98.1312142794477,99.1292212500778,100.127228220708,
101.125235191338,102.123242161968,103.121249132598,103.672557568463),
 .UNSPECIFIED.);
#4554=B_SPLINE_CURVE_WITH_KNOTS('',3,(#96106,#96107,#96108,#96109,#96110,
#96111,#96112,#96113,#96114,#96115,#96116),.UNSPECIFIED.,.F.,.F.,(4,1,1,
1,1,1,1,1,4),(91.106186954104,91.4022889232901,92.3996247658423,93.3969606083945,
94.3942964509468,95.391632293499,96.3889681360513,97.3863039786035,97.3893722612836),
 .UNSPECIFIED.);
#4555=B_SPLINE_CURVE_WITH_KNOTS('',3,(#96117,#96118,#96119,#96120,#96121,
#96122,#96123,#96124,#96125,#96126,#96127),.UNSPECIFIED.,.F.,.F.,(4,1,1,
1,1,1,1,1,4),(91.106186954104,91.1451654850371,92.1431724556672,93.1411794262973,
94.1391863969273,95.1371933675574,96.1352003381875,97.1332073088176,97.3893722612836),
 .UNSPECIFIED.);
#4556=B_SPLINE_CURVE_WITH_KNOTS('',3,(#96132,#96133,#96134,#96135,#96136,
#96137,#96138,#96139,#96140,#96141),.UNSPECIFIED.,.F.,.F.,(4,1,1,1,1,1,
1,4),(84.8230016469244,85.4182738679766,86.4156097105288,87.4129455530811,
88.4102813956333,89.4076172381856,90.4049530807378,91.106186954104),
 .UNSPECIFIED.);
#4557=B_SPLINE_CURVE_WITH_KNOTS('',3,(#96142,#96143,#96144,#96145,#96146,
#96147,#96148,#96149,#96150,#96151),.UNSPECIFIED.,.F.,.F.,(4,1,1,1,1,1,
1,4),(84.8230016469244,85.1571236612565,86.1551306318866,87.1531376025167,
88.1511445731468,89.1491515437769,90.147158514407,91.106186954104),
 .UNSPECIFIED.);
#4558=B_SPLINE_CURVE_WITH_KNOTS('',3,(#96156,#96157,#96158,#96159,#96160,
#96161,#96162,#96163,#96164,#96165),.UNSPECIFIED.,.F.,.F.,(4,1,1,1,1,1,
1,4),(78.5398163397448,79.4342588126631,80.4315946552154,81.4289304977676,
82.4262663403199,83.4236021828721,84.4209380254243,84.8230016469244),
 .UNSPECIFIED.);
#4559=B_SPLINE_CURVE_WITH_KNOTS('',3,(#96166,#96167,#96168,#96169,#96170,
#96171,#96172,#96173,#96174,#96175),.UNSPECIFIED.,.F.,.F.,(4,1,1,1,1,1,
1,4),(78.5398163397448,79.169081837476,80.1670888081061,81.1650957787362,
82.1631027493663,83.1611097199964,84.1591166906264,84.8230016469244),
 .UNSPECIFIED.);
#4560=B_SPLINE_CURVE_WITH_KNOTS('',3,(#96180,#96181,#96182,#96183,#96184,
#96185,#96186,#96187,#96188,#96189,#96190),.UNSPECIFIED.,.F.,.F.,(4,1,1,
1,1,1,1,1,4),(72.2566310325652,72.4529079147974,73.4502437573497,74.4475795999019,
75.4449154424541,76.4422512850064,77.4395871275586,78.4369229701109,78.5398163397448),
 .UNSPECIFIED.);
#4561=B_SPLINE_CURVE_WITH_KNOTS('',3,(#96191,#96192,#96193,#96194,#96195,
#96196,#96197,#96198,#96199,#96200),.UNSPECIFIED.,.F.,.F.,(4,1,1,1,1,1,
1,4),(72.2566310325652,73.1810400136955,74.1790469843256,75.1770539549557,
76.1750609255857,77.1730678962158,78.1710748668459,78.5398163397448),
 .UNSPECIFIED.);
#4562=B_SPLINE_CURVE_WITH_KNOTS('',3,(#96205,#96206,#96207,#96208,#96209,
#96210,#96211,#96212,#96213,#96214),.UNSPECIFIED.,.F.,.F.,(4,1,1,1,1,1,
1,4),(65.9734457253856,66.468892859484,67.4662287020362,68.4635645445884,
69.4609003871407,70.4582362296929,71.4555720722452,72.2566310325652),
 .UNSPECIFIED.);
#4563=B_SPLINE_CURVE_WITH_KNOTS('',3,(#96215,#96216,#96217,#96218,#96219,
#96220,#96221,#96222,#96223,#96224,#96225),.UNSPECIFIED.,.F.,.F.,(4,1,1,
1,1,1,1,1,4),(65.9734457253856,66.1949912192848,67.1929981899149,68.191005160545,
69.1890121311751,70.1870191018052,71.1850260724353,72.1830330430654,72.2566310325652),
 .UNSPECIFIED.);
#4564=B_SPLINE_CURVE_WITH_KNOTS('',3,(#96230,#96231,#96232,#96233,#96234,
#96235,#96236,#96237,#96238,#96239),.UNSPECIFIED.,.F.,.F.,(4,1,1,1,1,1,
1,4),(59.690260418206,60.4848778041705,61.4822136467227,62.479549489275,
63.4768853318272,64.4742211743795,65.4715570169317,65.9734457253856),
 .UNSPECIFIED.);
#4565=B_SPLINE_CURVE_WITH_KNOTS('',3,(#96240,#96241,#96242,#96243,#96244,
#96245,#96246,#96247,#96248,#96249),.UNSPECIFIED.,.F.,.F.,(4,1,1,1,1,1,
1,4),(59.690260418206,60.2069493955043,61.2049563661344,62.2029633367645,
63.2009703073946,64.1989772780247,65.1969842486548,65.9734457253856),
 .UNSPECIFIED.);
#4566=B_SPLINE_CURVE_WITH_KNOTS('',3,(#96254,#96255,#96256,#96257,#96258,
#96259,#96260,#96261,#96262,#96263,#96264),.UNSPECIFIED.,.F.,.F.,(4,1,1,
1,1,1,1,1,4),(53.4070751110265,53.5035269063048,54.500862748857,55.4981985914093,
56.4955344339615,57.4928702765138,58.490206119066,59.4875419616182,59.690260418206),
 .UNSPECIFIED.);
#4567=B_SPLINE_CURVE_WITH_KNOTS('',3,(#96265,#96266,#96267,#96268,#96269,
#96270,#96271,#96272,#96273,#96274),.UNSPECIFIED.,.F.,.F.,(4,1,1,1,1,1,
1,4),(53.4070751110264,54.2189075717238,55.2169145423539,56.214921512984,
57.212928483614,58.2109354542441,59.2089424248742,59.690260418206),
 .UNSPECIFIED.);
#4568=B_SPLINE_CURVE_WITH_KNOTS('',3,(#96279,#96280,#96281,#96282,#96283,
#96284,#96285,#96286,#96287,#96288),.UNSPECIFIED.,.F.,.F.,(4,1,1,1,1,1,
1,4),(47.1238898038469,47.5195118509913,48.5168476935436,49.5141835360958,
50.5115193786481,51.5088552212003,52.5061910637525,53.4070751110265),
 .UNSPECIFIED.);
#4569=B_SPLINE_CURVE_WITH_KNOTS('',3,(#96289,#96290,#96291,#96292,#96293,
#96294,#96295,#96296,#96297,#96298,#96299),.UNSPECIFIED.,.F.,.F.,(4,1,1,
1,1,1,1,1,4),(47.1238898038468,47.2328587773132,48.2308657479432,49.2288727185733,
50.2268796892034,51.2248866598335,52.2228936304636,53.2209006010937,53.4070751110264),
 .UNSPECIFIED.);
#4570=B_SPLINE_CURVE_WITH_KNOTS('',3,(#96304,#96305,#96306,#96307,#96308,
#96309,#96310,#96311,#96312,#96313),.UNSPECIFIED.,.F.,.F.,(4,1,1,1,1,1,
1,4),(40.8407044966673,41.5354967956779,42.5328326382301,43.5301684807823,
44.5275043233346,45.5248401658868,46.5221760084391,47.1238898038469),
 .UNSPECIFIED.);
#4571=B_SPLINE_CURVE_WITH_KNOTS('',3,(#96314,#96315,#96316,#96317,#96318,
#96319,#96320,#96321,#96322,#96323),.UNSPECIFIED.,.F.,.F.,(4,1,1,1,1,1,
1,4),(40.8407044966672,41.2448169535326,42.2428239241627,43.2408308947928,
44.2388378654229,45.236844836053,46.2348518066831,47.1238898038468),
 .UNSPECIFIED.);
#4572=B_SPLINE_CURVE_WITH_KNOTS('',3,(#96328,#96329,#96330,#96331,#96332,
#96333,#96334,#96335,#96336,#96337),.UNSPECIFIED.,.F.,.F.,(4,1,1,1,1,1,
1,4),(34.5575191894877,35.5514817403644,36.5488175829166,37.5461534254689,
38.5434892680211,39.5408251105734,40.5381609531256,40.8407044966673),
 .UNSPECIFIED.);
#4573=B_SPLINE_CURVE_WITH_KNOTS('',3,(#96338,#96339,#96340,#96341,#96342,
#96343,#96344,#96345,#96346,#96347),.UNSPECIFIED.,.F.,.F.,(4,1,1,1,1,1,
1,4),(34.5575191894876,35.2567751297521,36.2547821003822,37.2527890710123,
38.2507960416424,39.2488030122724,40.2468099829025,40.8407044966672),
 .UNSPECIFIED.);
#4574=B_SPLINE_CURVE_WITH_KNOTS('',3,(#96352,#96353,#96354,#96355,#96356,
#96357,#96358,#96359,#96360,#96361,#96362),.UNSPECIFIED.,.F.,.F.,(4,1,1,
1,1,1,1,1,4),(28.2743338823081,28.5701308424987,29.5674666850509,30.5648025276032,
31.5621383701554,32.5594742127077,33.5568100552599,34.5541458978121,34.5575191894877),
 .UNSPECIFIED.);
#4575=B_SPLINE_CURVE_WITH_KNOTS('',3,(#96363,#96364,#96365,#96366,#96367,
#96368,#96369,#96370,#96371,#96372),.UNSPECIFIED.,.F.,.F.,(4,1,1,1,1,1,
1,4),(28.274333882308,29.2687333059716,30.2667402766016,31.2647472472317,
32.2627542178618,33.2607611884919,34.258768159122,34.5575191894876),
 .UNSPECIFIED.);
#4576=B_SPLINE_CURVE_WITH_KNOTS('',3,(#96377,#96378,#96379,#96380,#96381,
#96382,#96383,#96384,#96385,#96386),.UNSPECIFIED.,.F.,.F.,(4,1,1,1,1,1,
1,4),(21.9911485751285,22.5861157871852,23.5834516297375,24.5807874722897,
25.5781233148419,26.5754591573942,27.5727949999464,28.2743338823081),
 .UNSPECIFIED.);
#4577=B_SPLINE_CURVE_WITH_KNOTS('',3,(#96387,#96388,#96389,#96390,#96391,
#96392,#96393,#96394,#96395,#96396,#96397),.UNSPECIFIED.,.F.,.F.,(4,1,1,
1,1,1,1,1,4),(21.9911485751285,22.2826845115609,23.280691482191,24.2786984528211,
25.2767054234512,26.2747123940813,27.2727193647114,28.2707263353415,28.274333882308),
 .UNSPECIFIED.);
#4578=B_SPLINE_CURVE_WITH_KNOTS('',3,(#96402,#96403,#96404,#96405,#96406,
#96407,#96408,#96409,#96410,#96411),.UNSPECIFIED.,.F.,.F.,(4,1,1,1,1,1,
1,4),(15.7079632679489,16.6021007318718,17.599436574424,18.5967724169762,
19.5941082595285,20.5914441020807,21.588779944633,21.9911485751285),
 .UNSPECIFIED.);
#4579=B_SPLINE_CURVE_WITH_KNOTS('',3,(#96412,#96413,#96414,#96415,#96416,
#96417,#96418,#96419,#96420,#96421),.UNSPECIFIED.,.F.,.F.,(4,1,1,1,1,1,
1,4),(15.7079632679489,16.2946426877804,17.2926496584105,18.2906566290406,
19.2886635996707,20.2866705703008,21.2846775409308,21.9911485751285),
 .UNSPECIFIED.);
#4580=B_SPLINE_CURVE_WITH_KNOTS('',3,(#96424,#96425,#96426,#96427,#96428,
#96429,#96430,#96431,#96432,#96433,#96434,#96435,#96436,#96437,#96438,#96439,
#96440,#96441,#96442,#96443,#96444,#96445,#96446,#96447,#96448,#96449,#96450,
#96451,#96452,#96453,#96454,#96455,#96456,#96457,#96458,#96459,#96460,#96461,
#96462,#96463,#96464,#96465,#96466,#96467,#96468,#96469,#96470,#96471,#96472,
#96473,#96474,#96475,#96476,#96477,#96478,#96479,#96480,#96481,#96482,#96483,
#96484,#96485,#96486,#96487,#96488,#96489,#96490,#96491,#96492,#96493,#96494,
#96495,#96496,#96497,#96498,#96499,#96500,#96501,#96502,#96503,#96504,#96505,
#96506,#96507,#96508,#96509,#96510,#96511,#96512,#96513,#96514,#96515,#96516,
#96517,#96518,#96519,#96520,#96521,#96522,#96523,#96524,#96525,#96526,#96527,
#96528,#96529,#96530,#96531,#96532,#96533,#96534,#96535,#96536,#96537,#96538,
#96539,#96540,#96541,#96542,#96543,#96544,#96545,#96546,#96547,#96548,#96549,
#96550),.UNSPECIFIED.,.F.,.F.,(4,3,3,3,3,3,3,3,3,3,3,3,3,3,3,3,3,3,3,3,
3,3,3,3,3,3,3,3,3,3,3,3,3,3,3,3,3,3,3,3,3,3,4),(-0.996917990983956,-0.978871588953361,
-0.96111138213616,-0.951572166884024,-0.94788730271085,-0.928958746515757,
-0.909876465942473,-0.904936500084987,-0.901848009849201,-0.882541837721487,
-0.863353532865677,-0.850071733640713,-0.842096384739765,-0.838733342910066,
-0.836789934415749,-0.818254783653573,-0.798902591036692,-0.782735584954257,
-0.778204258927876,-0.774298497031817,-0.75473106557298,-0.734923369072796,
-0.7185841623989,-0.712646708603056,-0.709110058221935,-0.689189804001172,
-0.669566542377212,-0.649891129487148,-0.644972000047888,-0.641670824784499,
-0.621885476350888,-0.601705353300825,-0.588427767916722,-0.579820295317846,
-0.575107459303169,-0.554609906499435,-0.53420632583291,-0.514845498030454,
-0.510394870356688,-0.506773348856668,-0.495484670227998,-0.475532816008266,
-0.468408511919796),.UNSPECIFIED.);
#4581=B_SPLINE_CURVE_WITH_KNOTS('',3,(#96552,#96553,#96554,#96555,#96556,
#96557,#96558,#96559,#96560,#96561,#96562,#96563,#96564,#96565,#96566,#96567,
#96568,#96569,#96570,#96571,#96572,#96573,#96574,#96575,#96576,#96577,#96578,
#96579,#96580,#96581,#96582,#96583,#96584,#96585,#96586,#96587,#96588,#96589,
#96590,#96591,#96592,#96593,#96594,#96595,#96596,#96597,#96598,#96599,#96600,
#96601,#96602,#96603,#96604,#96605,#96606,#96607,#96608,#96609),
 .UNSPECIFIED.,.F.,.F.,(4,3,3,3,3,3,3,3,3,3,3,3,3,3,3,3,3,3,3,4),(-0.271362855059921,
-0.249815156703991,-0.228817954605844,-0.214757059032555,-0.202695986178297,
-0.199258382274391,-0.179079040584676,-0.172574372312687,-0.151002575773601,
-0.132127253801901,-0.128545223737615,-0.108660382312346,-0.0889046320299183,
-0.0695673553379917,-0.0643976613730527,-0.0611873083345303,-0.0424332578302701,
-0.0240014673407122,-0.00610701619818059,0.),.UNSPECIFIED.);
#4582=B_SPLINE_CURVE_WITH_KNOTS('',3,(#96612,#96613,#96614,#96615,#96616,
#96617,#96618,#96619,#96620,#96621,#96622,#96623,#96624,#96625,#96626,#96627,
#96628,#96629,#96630,#96631,#96632,#96633,#96634,#96635,#96636,#96637,#96638,
#96639,#96640,#96641,#96642,#96643,#96644,#96645,#96646,#96647,#96648,#96649,
#96650,#96651,#96652,#96653,#96654,#96655,#96656,#96657,#96658,#96659,#96660,
#96661,#96662,#96663,#96664,#96665,#96666,#96667,#96668,#96669,#96670,#96671,
#96672,#96673,#96674,#96675,#96676,#96677,#96678,#96679,#96680,#96681,#96682,
#96683,#96684,#96685,#96686,#96687,#96688,#96689,#96690,#96691,#96692,#96693,
#96694,#96695,#96696,#96697,#96698,#96699,#96700,#96701,#96702,#96703,#96704,
#96705,#96706,#96707,#96708,#96709,#96710,#96711,#96712,#96713,#96714),
 .UNSPECIFIED.,.F.,.F.,(4,3,3,3,3,3,3,3,3,3,3,3,3,3,3,3,3,3,3,3,3,3,3,3,
3,3,3,3,3,3,3,3,3,3,4),(-0.468408511919796,-0.449159592277506,-0.442679572366002,
-0.439139523917826,-0.418501747794262,-0.397540534942074,-0.376759689901926,
-0.369408338867191,-0.366188435771172,-0.344993296658329,-0.324164935680159,
-0.314417154781481,-0.302674036643168,-0.298303152413865,-0.294792657786698,
-0.273759483634418,-0.252453791079512,-0.23671297526563,-0.228622459040654,
-0.22484613779528,-0.221071692886511,-0.199520974492535,-0.177947952659577,
-0.156760757052952,-0.151824997028116,-0.148277425274246,-0.12652726456846,
-0.105236270462937,-0.0835127492652271,-0.0784406535722348,-0.0733870619889256,
-0.0516031153801045,-0.029512914496819,-0.0074997402847098,0.),
 .UNSPECIFIED.);
#4583=B_SPLINE_CURVE_WITH_KNOTS('',3,(#97143,#97144,#97145,#97146,#97147,
#97148,#97149,#97150),.UNSPECIFIED.,.F.,.F.,(4,1,1,1,1,4),(11.6154215191105,
12.6127573616628,13.610093204215,14.6074290467673,15.6047648893195,15.7079632679489),
 .UNSPECIFIED.);
#4584=B_SPLINE_CURVE_WITH_KNOTS('',3,(#97151,#97152,#97153,#97154,#97155,
#97156,#97157,#97158,#97159,#97160,#97161,#97162,#97163,#97164,#97165,#97166,
#97167,#97168,#97169,#97170,#97171,#97172,#97173,#97174,#97175,#97176,#97177,
#97178,#97179,#97180,#97181,#97182,#97183,#97184,#97185,#97186,#97187,#97188,
#97189,#97190,#97191,#97192,#97193,#97194,#97195,#97196,#97197,#97198,#97199,
#97200,#97201,#97202,#97203,#97204,#97205,#97206,#97207,#97208,#97209,#97210,
#97211,#97212,#97213,#97214,#97215,#97216,#97217,#97218,#97219,#97220,#97221,
#97222,#97223,#97224,#97225,#97226,#97227,#97228,#97229,#97230,#97231,#97232,
#97233,#97234,#97235),.UNSPECIFIED.,.F.,.F.,(4,3,3,3,3,3,3,3,3,3,3,3,3,
3,3,3,3,3,3,3,3,3,3,3,3,3,3,3,4),(-0.364629307890661,-0.350885759085945,
-0.329296488089375,-0.318978386270927,-0.313741431878983,-0.309365163672801,
-0.288042901568511,-0.272809238661881,-0.264006177467146,-0.26029818106468,
-0.239567096461013,-0.219346880276472,-0.206053559786221,-0.194876880502573,
-0.191399047668888,-0.171813366976952,-0.166173598315468,-0.145401898526034,
-0.126706873608775,-0.123379860192083,-0.103925496661725,-0.0845481894111439,
-0.065567586070534,-0.0621782887363481,-0.05894467115978,-0.0403543924373443,
-0.0220984153978596,-0.00442511140790438,0.),.UNSPECIFIED.);
#4585=B_SPLINE_CURVE_WITH_KNOTS('',3,(#97236,#97237,#97238,#97239,#97240,
#97241,#97242,#97243,#97244,#97245,#97246,#97247,#97248),.UNSPECIFIED.,
 .F.,.F.,(4,3,3,3,4),(-101.213804280572,-100.730920097777,-99.7335842552244,
-98.7362484126722,-98.3403213565322),.UNSPECIFIED.);
#4586=B_SPLINE_CURVE_WITH_KNOTS('',3,(#97251,#97252,#97253,#97254,#97255,
#97256,#97257,#97258,#97259),.UNSPECIFIED.,.F.,.F.,(4,1,1,1,1,1,4),(10.3757270560178,
11.30460783463,12.30261480526,13.3006217758901,14.2986287465202,15.2966357171503,
15.7079632679489),.UNSPECIFIED.);
#4587=B_SPLINE_CURVE_WITH_KNOTS('',3,(#97693,#97694,#97695,#97696,#97697,
#97698,#97699,#97700,#97701,#97702,#97703,#97704,#97705,#97706,#97707,#97708),
 .UNSPECIFIED.,.F.,.F.,(4,3,3,3,3,4),(95.3619706457233,95.8086691804886,
96.8066761511186,97.8046831217487,98.8026900923788,99.1486641472938),
 .UNSPECIFIED.);
#4588=B_SPLINE_CURVE_WITH_KNOTS('',3,(#97709,#97710,#97711,#97712,#97713,
#97714,#97715,#97716,#97717,#97718,#97719,#97720,#97721,#97722,#97723,#97724,
#97725,#97726,#97727,#97728,#97729,#97730,#97731,#97732,#97733,#97734,#97735,
#97736,#97737,#97738,#97739,#97740,#97741,#97742,#97743,#97744,#97745,#97746,
#97747,#97748,#97749,#97750,#97751,#97752,#97753,#97754,#97755,#97756,#97757,
#97758,#97759,#97760,#97761,#97762,#97763,#97764,#97765,#97766,#97767,#97768,
#97769,#97770,#97771,#97772,#97773,#97774,#97775,#97776,#97777,#97778,#97779,
#97780,#97781,#97782,#97783,#97784,#97785,#97786,#97787,#97788,#97789,#97790,
#97791,#97792,#97793),.UNSPECIFIED.,.F.,.F.,(4,3,3,3,3,3,3,3,3,3,3,3,3,
3,3,3,3,3,3,3,3,3,3,3,3,3,3,3,4),(-0.366397579005845,-0.355461226466819,
-0.337490969642209,-0.327214164040339,-0.321649482146298,-0.302840833811487,
-0.288386907394637,-0.281257238921911,-0.277593927902022,-0.258153123971634,
-0.238335729520815,-0.225554152759783,-0.218411056976172,-0.214856426708649,
-0.194426531587897,-0.187209422476688,-0.167504451243421,-0.156894426252658,
-0.149523127563347,-0.145921626399787,-0.125494957624892,-0.104619107174947,
-0.0835512936559854,-0.0752831225832569,-0.0721648689176682,-0.0505208253811386,
-0.028827309118007,-0.00759789023731293,0.),.UNSPECIFIED.);
#4589=B_SPLINE_CURVE_WITH_KNOTS('',3,(#97847,#97848,#97849,#97850,#97851,
#97852,#97853,#97854,#97855,#97856),.UNSPECIFIED.,.F.,.F.,(4,3,3,4),(-4.09202352044853,
-3.98935724892517,-2.99201793669388,-2.07317267331972),.UNSPECIFIED.);
#4590=B_SPLINE_CURVE_WITH_KNOTS('',3,(#97859,#97860,#97861,#97862,#97863,
#97864,#97865),.UNSPECIFIED.,.F.,.F.,(4,3,4),(0.,0.998740991675169,1.12274180646096),
 .UNSPECIFIED.);
#4591=B_SPLINE_CURVE_WITH_KNOTS('',3,(#97870,#97871,#97872,#97873,#97874,
#97875,#97876,#97877,#97878,#97879,#97880,#97881,#97882,#97883,#97884,#97885,
#97886,#97887,#97888,#97889,#97890,#97891),.UNSPECIFIED.,.F.,.F.,(4,3,3,
3,3,3,3,4),(-10.3752088276281,-9.97339312231293,-8.97605381008164,-7.97871449785035,
-6.98137518561906,-5.98403587338776,-4.98669656115647,-4.09202352044853),
 .UNSPECIFIED.);
#4592=B_SPLINE_CURVE_WITH_KNOTS('',3,(#97892,#97893,#97894,#97895,#97896,
#97897,#97898,#97899,#97900,#97901,#97902,#97903,#97904,#97905,#97906,#97907,
#97908,#97909,#97910,#97911,#97912,#97913),.UNSPECIFIED.,.F.,.F.,(4,3,3,
3,3,3,3,4),(1.12274180646096,1.99748198335034,2.99622297502551,3.99496396670068,
4.99370495837585,5.99244595005102,6.99118694172619,7.40592711364054),
 .UNSPECIFIED.);
#4593=B_SPLINE_CURVE_WITH_KNOTS('',3,(#97918,#97919,#97920,#97921,#97922,
#97923,#97924,#97925,#97926,#97927,#97928,#97929,#97930,#97931,#97932,#97933,
#97934,#97935,#97936,#97937,#97938,#97939),.UNSPECIFIED.,.F.,.F.,(4,3,3,
3,3,3,3,4),(-16.6583941348077,-15.9574289957007,-14.9600896834694,-13.9627503712381,
-12.9654110590068,-11.9680717467755,-10.9707324345442,-10.3752088276281),
 .UNSPECIFIED.);
#4594=B_SPLINE_CURVE_WITH_KNOTS('',3,(#97940,#97941,#97942,#97943,#97944,
#97945,#97946,#97947,#97948,#97949,#97950,#97951,#97952,#97953,#97954,#97955,
#97956,#97957,#97958,#97959,#97960,#97961),.UNSPECIFIED.,.F.,.F.,(4,3,3,
3,3,3,3,4),(7.40592711364054,7.98992793340136,8.98866892507653,9.9874099167517,
10.9861509084269,11.984891900102,12.9836328917772,13.6891124208201),
 .UNSPECIFIED.);
#4595=B_SPLINE_CURVE_WITH_KNOTS('',3,(#97966,#97967,#97968,#97969,#97970,
#97971,#97972,#97973,#97974,#97975,#97976,#97977,#97978,#97979,#97980,#97981,
#97982,#97983,#97984,#97985,#97986,#97987),.UNSPECIFIED.,.F.,.F.,(4,3,3,
3,3,3,3,4),(-22.9415794419873,-21.9414648690884,-20.9441255568571,-19.9467862446259,
-18.9494469323946,-17.9521076201633,-16.954768307932,-16.6583941348077),
 .UNSPECIFIED.);
#4596=B_SPLINE_CURVE_WITH_KNOTS('',3,(#97988,#97989,#97990,#97991,#97992,
#97993,#97994,#97995,#97996,#97997,#97998,#97999,#98000,#98001,#98002,#98003,
#98004,#98005,#98006,#98007,#98008,#98009),.UNSPECIFIED.,.F.,.F.,(4,3,3,
3,3,3,3,4),(13.6891124208201,13.9823738834524,14.9811148751276,15.9798558668027,
16.9785968584779,17.9773378501531,18.9760788418282,19.9722977279997),
 .UNSPECIFIED.);
#4597=B_SPLINE_CURVE_WITH_KNOTS('',3,(#98014,#98015,#98016,#98017,#98018,
#98019,#98020,#98021,#98022,#98023,#98024,#98025,#98026,#98027,#98028,#98029,
#98030,#98031,#98032,#98033,#98034,#98035),.UNSPECIFIED.,.F.,.F.,(4,3,3,
3,3,3,3,4),(-29.2247647491669,-28.9228400547075,-27.9255007424762,-26.9281614302449,
-25.9308221180136,-24.9334828057823,-23.936143493551,-22.9415794419873),
 .UNSPECIFIED.);
#4598=B_SPLINE_CURVE_WITH_KNOTS('',3,(#98036,#98037,#98038,#98039,#98040,
#98041,#98042,#98043,#98044,#98045,#98046,#98047,#98048,#98049,#98050,#98051,
#98052,#98053,#98054,#98055,#98056,#98057),.UNSPECIFIED.,.F.,.F.,(4,3,3,
3,3,3,3,4),(19.9722977279997,20.9735608251786,21.9723018168537,22.9710428085289,
23.9697838002041,24.9685247918793,25.9672657835544,26.2554830351793),
 .UNSPECIFIED.);
#4599=B_SPLINE_CURVE_WITH_KNOTS('',3,(#98062,#98063,#98064,#98065,#98066,
#98067,#98068,#98069,#98070,#98071,#98072,#98073,#98074,#98075,#98076,#98077,
#98078,#98079,#98080,#98081,#98082,#98083),.UNSPECIFIED.,.F.,.F.,(4,3,3,
3,3,3,3,4),(-35.5079500563465,-34.9068759280953,-33.909536615864,-32.9121973036327,
-31.9148579914014,-30.9175186791701,-29.9201793669388,-29.2247647491669),
 .UNSPECIFIED.);
#4600=B_SPLINE_CURVE_WITH_KNOTS('',3,(#98084,#98085,#98086,#98087,#98088,
#98089,#98090,#98091,#98092,#98093,#98094,#98095,#98096,#98097,#98098,#98099,
#98100,#98101,#98102,#98103,#98104,#98105),.UNSPECIFIED.,.F.,.F.,(4,3,3,
3,3,3,3,4),(26.2554830351793,26.9660067752296,27.9647477669048,28.9634887585799,
29.9622297502551,30.9609707419303,31.9597117336054,32.5386683423589),
 .UNSPECIFIED.);
#4601=B_SPLINE_CURVE_WITH_KNOTS('',3,(#98110,#98111,#98112,#98113,#98114,
#98115,#98116,#98117,#98118,#98119,#98120,#98121,#98122,#98123,#98124,#98125,
#98126,#98127,#98128,#98129,#98130,#98131),.UNSPECIFIED.,.F.,.F.,(4,3,3,
3,3,3,3,4),(-41.791135363526,-40.890911801483,-39.8935724892517,-38.8962331770204,
-37.8988938647891,-36.9015545525578,-35.9042152403266,-35.5079500563465),
 .UNSPECIFIED.);
#4602=B_SPLINE_CURVE_WITH_KNOTS('',3,(#98132,#98133,#98134,#98135,#98136,
#98137,#98138,#98139,#98140,#98141,#98142,#98143,#98144,#98145,#98146,#98147,
#98148,#98149,#98150,#98151,#98152,#98153),.UNSPECIFIED.,.F.,.F.,(4,3,3,
3,3,3,3,4),(32.5386683423589,32.9584527252806,33.9571937169558,34.955934708631,
35.9546757003061,36.9534166919813,37.9521576836565,38.8218536495385),
 .UNSPECIFIED.);
#4603=B_SPLINE_CURVE_WITH_KNOTS('',3,(#98158,#98159,#98160,#98161,#98162,
#98163,#98164,#98165,#98166,#98167,#98168,#98169,#98170,#98171,#98172,#98173,
#98174,#98175,#98176,#98177,#98178,#98179,#98180,#98181,#98182),
 .UNSPECIFIED.,.F.,.F.,(4,3,3,3,3,3,3,3,4),(-48.0743206707056,-47.8722869871021,
-46.8749476748708,-45.8776083626395,-44.8802690504082,-43.8829297381769,
-42.8855904259456,-41.8882511137143,-41.791135363526),.UNSPECIFIED.);
#4604=B_SPLINE_CURVE_WITH_KNOTS('',3,(#98183,#98184,#98185,#98186,#98187,
#98188,#98189,#98190,#98191,#98192,#98193,#98194,#98195,#98196,#98197,#98198,
#98199,#98200,#98201,#98202,#98203,#98204,#98205,#98206,#98207),
 .UNSPECIFIED.,.F.,.F.,(4,3,3,3,3,3,3,3,4),(38.8218536495385,38.9508986753316,
39.9496396670068,40.948380658682,41.9471216503571,42.9458626420323,43.9446036337075,
44.9433446253827,45.1050389567181),.UNSPECIFIED.);
#4605=B_SPLINE_CURVE_WITH_KNOTS('',3,(#98213,#98214,#98215,#98216,#98217,
#98218,#98219,#98220,#98221),.UNSPECIFIED.,.F.,.F.,(4,1,1,1,1,1,4),(59.6902604182061,
60.4855660468338,61.4829053590651,62.4802446712963,63.4775839835276,64.4749232957589,
65.4722626079902),.UNSPECIFIED.);
#4606=B_SPLINE_CURVE_WITH_KNOTS('',3,(#98224,#98225,#98226,#98227,#98228,
#98229,#98230,#98231),.UNSPECIFIED.,.F.,.F.,(4,1,1,1,1,4),(59.6902604182061,
60.2365677214172,61.2353087130924,62.2340497047676,63.2327906964427,64.2315316881179),
 .UNSPECIFIED.);
#4607=B_SPLINE_CURVE_WITH_KNOTS('',3,(#98236,#98237,#98238,#98239,#98240,
#98241,#98242,#98243,#98244,#98245,#98246),.UNSPECIFIED.,.F.,.F.,(4,1,1,
1,1,1,1,1,4),(53.4070751110265,53.5041908612147,54.501530173446,55.4988694856773,
56.4962087979086,57.4935481101399,58.4908874223712,59.4882267346025,59.6902604182061),
 .UNSPECIFIED.);
#4608=B_SPLINE_CURVE_WITH_KNOTS('',3,(#98247,#98248,#98249,#98250,#98251,
#98252,#98253,#98254,#98255,#98256),.UNSPECIFIED.,.F.,.F.,(4,1,1,1,1,1,
1,4),(53.4070751110265,54.2441217713662,55.2428627630414,56.2416037547165,
57.2403447463917,58.2390857380669,59.237826729742,59.6902604182061),
 .UNSPECIFIED.);
#4609=B_SPLINE_CURVE_WITH_KNOTS('',3,(#98261,#98262,#98263,#98264,#98265,
#98266,#98267,#98268,#98269,#98270),.UNSPECIFIED.,.F.,.F.,(4,1,1,1,1,1,
1,4),(47.1238898038469,47.520154987827,48.5174943000582,49.5148336122895,
50.5121729245208,51.5095122367521,52.5068515489834,53.4070751110265),
 .UNSPECIFIED.);
#4610=B_SPLINE_CURVE_WITH_KNOTS('',3,(#98271,#98272,#98273,#98274,#98275,
#98276,#98277,#98278,#98279,#98280,#98281),.UNSPECIFIED.,.F.,.F.,(4,1,1,
1,1,1,1,1,4),(47.1238898038469,47.25293482964,48.2516758213152,49.2504168129903,
50.2491578046655,51.2478987963407,52.2466397880159,53.245380779691,53.4070751110265),
 .UNSPECIFIED.);
#4611=B_SPLINE_CURVE_WITH_KNOTS('',3,(#98286,#98287,#98288,#98289,#98290,
#98291,#98292,#98293,#98294,#98295),.UNSPECIFIED.,.F.,.F.,(4,1,1,1,1,1,
1,4),(40.8407044966673,41.5361191144392,42.5334584266705,43.5307977389018,
44.5281370511331,45.5254763633644,46.5228156755957,47.1238898038469),
 .UNSPECIFIED.);
#4612=B_SPLINE_CURVE_WITH_KNOTS('',3,(#98296,#98297,#98298,#98299,#98300,
#98301,#98302,#98303,#98304,#98305),.UNSPECIFIED.,.F.,.F.,(4,1,1,1,1,1,
1,4),(40.8407044966673,41.260488879589,42.2592298712642,43.2579708629393,
44.2567118546145,45.2554528462897,46.2541938379648,47.1238898038469),
 .UNSPECIFIED.);
#4613=B_SPLINE_CURVE_WITH_KNOTS('',3,(#98310,#98311,#98312,#98313,#98314,
#98315,#98316,#98317,#98318,#98319),.UNSPECIFIED.,.F.,.F.,(4,1,1,1,1,1,
1,4),(34.5575191894877,35.5520832410514,36.5494225532827,37.546761865514,
38.5441011777453,39.5414404899766,40.5387798022079,40.8407044966673),
 .UNSPECIFIED.);
#4614=B_SPLINE_CURVE_WITH_KNOTS('',3,(#98320,#98321,#98322,#98323,#98324,
#98325,#98326,#98327,#98328,#98329),.UNSPECIFIED.,.F.,.F.,(4,1,1,1,1,1,
1,4),(34.5575191894877,35.268042929538,36.2667839212131,37.2655249128883,
38.2642659045635,39.2630068962386,40.2617478879138,40.8407044966673),
 .UNSPECIFIED.);
#4615=B_SPLINE_CURVE_WITH_KNOTS('',3,(#98334,#98335,#98336,#98337,#98338,
#98339,#98340,#98341,#98342,#98343,#98344),.UNSPECIFIED.,.F.,.F.,(4,1,1,
1,1,1,1,1,4),(28.2743338823081,28.5707080554324,29.5680473676637,30.565386679895,
31.5627259921263,32.5600653043576,33.5574046165888,34.5547439288201,34.5575191894877),
 .UNSPECIFIED.);
#4616=B_SPLINE_CURVE_WITH_KNOTS('',3,(#98345,#98346,#98347,#98348,#98349,
#98350,#98351,#98352,#98353,#98354,#98355),.UNSPECIFIED.,.F.,.F.,(4,1,1,
1,1,1,1,1,4),(28.2743338823081,28.2768559878118,29.2755969794869,30.2743379711621,
31.2730789628373,32.2718199545125,33.2705609461876,34.2693019378628,34.5575191894877),
 .UNSPECIFIED.);
#4617=B_SPLINE_CURVE_WITH_KNOTS('',3,(#98360,#98361,#98362,#98363,#98364,
#98365,#98366,#98367,#98368,#98369),.UNSPECIFIED.,.F.,.F.,(4,1,1,1,1,1,
1,4),(21.9911485751285,22.5866721820446,23.5840114942759,24.5813508065072,
25.5786901187385,26.5760294309698,27.5733687432011,28.2743338823081),
 .UNSPECIFIED.);
#4618=B_SPLINE_CURVE_WITH_KNOTS('',3,(#98370,#98371,#98372,#98373,#98374,
#98375,#98376,#98377,#98378,#98379),.UNSPECIFIED.,.F.,.F.,(4,1,1,1,1,1,
1,4),(21.9911485751285,22.2844100377608,23.2831510294359,24.2818920211111,
25.2806330127863,26.2793740044614,27.2781149961366,28.2743338823081),
 .UNSPECIFIED.);
#4619=B_SPLINE_CURVE_WITH_KNOTS('',3,(#98384,#98385,#98386,#98387,#98388,
#98389,#98390,#98391,#98392,#98393),.UNSPECIFIED.,.F.,.F.,(4,1,1,1,1,1,
1,4),(15.7079632679489,16.6026363086569,17.5999756208882,18.5973149331195,
19.5946542453507,20.591993557582,21.5893328698133,21.9911485751285),
 .UNSPECIFIED.);
#4620=B_SPLINE_CURVE_WITH_KNOTS('',3,(#98394,#98395,#98396,#98397,#98398,
#98399,#98400,#98401,#98402,#98403),.UNSPECIFIED.,.F.,.F.,(4,1,1,1,1,1,
1,4),(15.7079632679489,16.2919640877097,17.2907050793849,18.2894460710601,
19.2881870627352,20.2869280544104,21.2856690460856,21.9911485751285),
 .UNSPECIFIED.);
#4621=B_SPLINE_CURVE_WITH_KNOTS('',3,(#98406,#98407,#98408,#98409,#98410,
#98411,#98412,#98413,#98414,#98415,#98416,#98417,#98418,#98419,#98420,#98421,
#98422,#98423,#98424,#98425,#98426,#98427,#98428,#98429,#98430,#98431,#98432,
#98433,#98434,#98435,#98436,#98437,#98438,#98439,#98440,#98441,#98442,#98443,
#98444,#98445,#98446,#98447,#98448,#98449,#98450,#98451,#98452,#98453,#98454,
#98455,#98456,#98457,#98458,#98459,#98460,#98461,#98462,#98463,#98464,#98465,
#98466,#98467,#98468,#98469,#98470,#98471,#98472,#98473,#98474,#98475,#98476,
#98477,#98478,#98479,#98480,#98481,#98482,#98483,#98484,#98485,#98486,#98487,
#98488,#98489,#98490,#98491,#98492,#98493,#98494,#98495,#98496,#98497,#98498,
#98499,#98500,#98501,#98502,#98503,#98504,#98505,#98506,#98507,#98508,#98509,
#98510,#98511,#98512,#98513,#98514,#98515,#98516,#98517,#98518,#98519,#98520,
#98521,#98522,#98523,#98524,#98525,#98526,#98527,#98528,#98529,#98530,#98531,
#98532,#98533,#98534,#98535,#98536,#98537,#98538,#98539,#98540,#98541,#98542,
#98543,#98544,#98545,#98546,#98547,#98548,#98549,#98550,#98551,#98552,#98553,
#98554,#98555,#98556,#98557,#98558,#98559,#98560,#98561,#98562,#98563,#98564,
#98565,#98566,#98567,#98568,#98569,#98570,#98571,#98572,#98573,#98574,#98575,
#98576,#98577,#98578,#98579,#98580,#98581,#98582,#98583,#98584,#98585,#98586,
#98587,#98588,#98589),.UNSPECIFIED.,.F.,.F.,(4,3,3,3,3,3,3,3,3,3,3,3,3,
3,3,3,3,3,3,3,3,3,3,3,3,3,3,3,3,3,3,3,3,3,3,3,3,3,3,3,3,3,3,3,3,3,3,3,3,
3,3,3,3,3,3,3,3,3,3,3,3,4),(-0.753008129282157,-0.73786527623977,-0.724615279827681,
-0.717098895378918,-0.713787159730779,-0.698410405843186,-0.682933186955955,
-0.679855182994275,-0.664200486121929,-0.648032895532493,-0.639949100237776,
-0.635216460798448,-0.632188335448626,-0.631865304943058,-0.61690168950646,
-0.601227264223793,-0.589281754696583,-0.585169909644513,-0.581926626388212,
-0.566053286590164,-0.550081089144897,-0.538976613860202,-0.534874931105234,
-0.531662796183257,-0.515550254278411,-0.505663188006116,-0.489273050645826,
-0.485270605061208,-0.482408633379521,-0.466387560157893,-0.450041076803483,
-0.440603703343523,-0.433818542109577,-0.430853819905116,-0.414279731357498,
-0.397826739572435,-0.386184414348117,-0.382110700287907,-0.379222591070396,
-0.3745420891238,-0.358536027981697,-0.343522511777778,-0.33597373730796,
-0.331449848714152,-0.327650568312031,-0.31091799154362,-0.293972525585514,
-0.280086368776722,-0.276804967864447,-0.27376471063138,-0.256096304490863,
-0.239324632856325,-0.238427898350346,-0.228865409785226,-0.224320857142883,
-0.220678125153778,-0.203840509088529,-0.186665330500045,-0.174296660164717,
-0.169386715434793,-0.1662786999892,-0.161927989829389),.UNSPECIFIED.);
#4622=B_SPLINE_CURVE_WITH_KNOTS('',3,(#98591,#98592,#98593,#98594,#98595,
#98596,#98597,#98598,#98599,#98600,#98601,#98602,#98603,#98604,#98605,#98606,
#98607,#98608,#98609,#98610,#98611,#98612,#98613,#98614,#98615,#98616,#98617,
#98618,#98619,#98620,#98621,#98622,#98623,#98624,#98625,#98626,#98627,#98628,
#98629,#98630,#98631,#98632,#98633,#98634,#98635,#98636,#98637,#98638,#98639,
#98640,#98641,#98642,#98643,#98644,#98645,#98646,#98647,#98648,#98649,#98650,
#98651),.UNSPECIFIED.,.F.,.F.,(4,3,3,3,3,3,3,3,3,3,3,3,3,3,3,3,3,3,3,3,
4),(-0.204609524178332,-0.187229444739388,-0.170308057115437,-0.160178775707448,
-0.152889242910402,-0.149873358866868,-0.133572111564231,-0.129790931483479,
-0.113567065048044,-0.105824638338513,-0.0991132485902469,-0.0961971109838234,
-0.0801003606559814,-0.0641272763676895,-0.0555369672079658,-0.0490619748994989,
-0.0460483768969834,-0.0308260628889665,-0.0154130314444832,-0.000938554365243004,
0.),.UNSPECIFIED.);
#4623=B_SPLINE_CURVE_WITH_KNOTS('',3,(#98654,#98655,#98656,#98657,#98658,
#98659,#98660,#98661,#98662,#98663,#98664,#98665,#98666,#98667,#98668,#98669,
#98670,#98671,#98672,#98673,#98674,#98675,#98676,#98677,#98678,#98679,#98680,
#98681,#98682,#98683,#98684,#98685,#98686,#98687,#98688,#98689,#98690,#98691,
#98692,#98693),.UNSPECIFIED.,.F.,.F.,(4,3,3,3,3,3,3,3,3,3,3,3,3,4),(-0.161927989829389,
-0.14445211284144,-0.127148387454473,-0.119019661086295,-0.114739079705313,
-0.110791737995318,-0.0974340408014069,-0.0803127274975295,-0.0628060442148566,
-0.0579606305293774,-0.0547831112214332,-0.0372028960526897,-0.0186014480263448,
0.),.UNSPECIFIED.);
#4624=B_SPLINE_CURVE_WITH_KNOTS('',3,(#98926,#98927,#98928,#98929,#98930,
#98931,#98932,#98933),.UNSPECIFIED.,.F.,.F.,(4,1,1,1,1,4),(11.6159397475004,
12.6132790597317,13.610618371963,14.6079576841943,15.6052969964256,15.7079632679489),
 .UNSPECIFIED.);
#4625=B_SPLINE_CURVE_WITH_KNOTS('',3,(#98934,#98935,#98936,#98937,#98938,
#98939,#98940,#98941,#98942,#98943,#98944,#98945,#98946,#98947,#98948,#98949,
#98950,#98951,#98952,#98953,#98954,#98955,#98956,#98957,#98958,#98959,#98960,
#98961,#98962,#98963,#98964,#98965,#98966,#98967,#98968,#98969,#98970,#98971,
#98972,#98973,#98974,#98975,#98976,#98977,#98978,#98979,#98980,#98981,#98982,
#98983,#98984,#98985,#98986,#98987,#98988,#98989,#98990,#98991,#98992,#98993,
#98994,#98995,#98996,#98997,#98998,#98999,#99000,#99001,#99002,#99003,#99004,
#99005,#99006,#99007,#99008,#99009,#99010,#99011,#99012,#99013,#99014,#99015),
 .UNSPECIFIED.,.F.,.F.,(4,3,3,3,3,3,3,3,3,3,3,3,3,3,3,3,3,3,3,3,3,3,3,3,
3,3,3,4),(-0.275362278356883,-0.263900331993925,-0.246578497995159,-0.237038384704303,
-0.233158136947895,-0.215956509362073,-0.204627653192289,-0.199386939936824,
-0.195964342542413,-0.179215296048088,-0.162902384492512,-0.153508203370335,
-0.148362000491666,-0.144152894533275,-0.128300920501684,-0.125325660003802,
-0.108643799301575,-0.101041482676622,-0.0956984034813221,-0.0926133309948634,
-0.0768446933414484,-0.0611549478274358,-0.0532963163041718,-0.0475064809797105,
-0.0447082261449061,-0.0296004251347768,-0.0148002125673884,0.),
 .UNSPECIFIED.);
#4626=B_SPLINE_CURVE_WITH_KNOTS('',3,(#99016,#99017,#99018,#99019,#99020,
#99021,#99022,#99023,#99024,#99025,#99026,#99027,#99028,#99029,#99030,#99031),
 .UNSPECIFIED.,.F.,.F.,(4,3,3,3,3,4),(-52.3386551307564,-51.8616442360272,
-50.8643049237959,-49.8669656115647,-48.8696262993334,-48.0743206707056),
 .UNSPECIFIED.);
#4627=B_SPLINE_CURVE_WITH_KNOTS('',3,(#99034,#99035,#99036,#99037,#99038,
#99039,#99040,#99041,#99042),.UNSPECIFIED.,.F.,.F.,(4,1,1,1,1,1,4),(10.3752088276281,
11.2982591293339,12.2970001210091,13.2957411126842,14.2944821043594,15.2932230960346,
15.7079632679489),.UNSPECIFIED.);
#4628=B_SPLINE_CURVE_WITH_KNOTS('',3,(#99317,#99318,#99319,#99320,#99321,
#99322,#99323,#99324,#99325,#99326,#99327,#99328,#99329,#99330,#99331,#99332,
#99333,#99334,#99335),.UNSPECIFIED.,.F.,.F.,(4,3,3,3,3,3,4),(45.1050389567181,
45.9420856170578,46.940826608733,47.9395676004082,48.9383085920833,49.9370495837585,
50.2654824574366),.UNSPECIFIED.);
#4629=B_SPLINE_CURVE_WITH_KNOTS('',3,(#99336,#99337,#99338,#99339,#99340,
#99341,#99342,#99343,#99344,#99345,#99346,#99347,#99348,#99349,#99350,#99351,
#99352,#99353,#99354,#99355,#99356,#99357,#99358,#99359,#99360,#99361,#99362,
#99363,#99364,#99365,#99366,#99367,#99368,#99369,#99370,#99371,#99372,#99373,
#99374,#99375,#99376,#99377,#99378,#99379,#99380,#99381,#99382,#99383,#99384,
#99385,#99386,#99387,#99388,#99389,#99390,#99391,#99392,#99393,#99394,#99395,
#99396,#99397,#99398,#99399,#99400,#99401,#99402,#99403,#99404,#99405,#99406,
#99407,#99408,#99409,#99410,#99411,#99412,#99413,#99414,#99415,#99416,#99417,
#99418,#99419,#99420),.UNSPECIFIED.,.F.,.F.,(4,3,3,3,3,3,3,3,3,3,3,3,3,
3,3,3,3,3,3,3,3,3,3,3,3,3,3,3,4),(-0.276631791712721,-0.267572232012667,
-0.252957312390642,-0.247122920332528,-0.24209048560573,-0.22681681001417,
-0.216036201245221,-0.21183998522367,-0.208623843551383,-0.192852303440504,
-0.176802879296701,-0.16774514443817,-0.162460607960523,-0.15957229971733,
-0.143044531332662,-0.140571939862575,-0.124627165055967,-0.116201869211177,
-0.111145681876705,-0.108000260957167,-0.0914514087508209,-0.0745399955216332,
-0.0650233471421523,-0.0590680435779011,-0.0560616749739794,-0.0530529570050865,
-0.0355838889451872,-0.0177919444725936,0.),.UNSPECIFIED.);
#4630=LINE('',#23380,#5534);
#4631=LINE('',#23415,#5535);
#4632=LINE('',#23442,#5536);
#4633=LINE('',#23493,#5537);
#4634=LINE('',#23541,#5538);
#4635=LINE('',#23589,#5539);
#4636=LINE('',#23640,#5540);
#4637=LINE('',#23688,#5541);
#4638=LINE('',#23736,#5542);
#4639=LINE('',#23787,#5543);
#4640=LINE('',#23838,#5544);
#4641=LINE('',#23886,#5545);
#4642=LINE('',#23937,#5546);
#4643=LINE('',#23976,#5547);
#4644=LINE('',#23998,#5548);
#4645=LINE('',#24022,#5549);
#4646=LINE('',#24047,#5550);
#4647=LINE('',#24072,#5551);
#4648=LINE('',#24096,#5552);
#4649=LINE('',#24121,#5553);
#4650=LINE('',#24145,#5554);
#4651=LINE('',#24170,#5555);
#4652=LINE('',#24194,#5556);
#4653=LINE('',#24219,#5557);
#4654=LINE('',#24244,#5558);
#4655=LINE('',#24268,#5559);
#4656=LINE('',#24285,#5560);
#4657=LINE('',#24320,#5561);
#4658=LINE('',#24347,#5562);
#4659=LINE('',#24398,#5563);
#4660=LINE('',#24446,#5564);
#4661=LINE('',#24494,#5565);
#4662=LINE('',#24545,#5566);
#4663=LINE('',#24593,#5567);
#4664=LINE('',#24641,#5568);
#4665=LINE('',#24692,#5569);
#4666=LINE('',#24743,#5570);
#4667=LINE('',#24791,#5571);
#4668=LINE('',#24842,#5572);
#4669=LINE('',#24881,#5573);
#4670=LINE('',#24903,#5574);
#4671=LINE('',#24927,#5575);
#4672=LINE('',#24952,#5576);
#4673=LINE('',#24977,#5577);
#4674=LINE('',#25001,#5578);
#4675=LINE('',#25026,#5579);
#4676=LINE('',#25050,#5580);
#4677=LINE('',#25075,#5581);
#4678=LINE('',#25099,#5582);
#4679=LINE('',#25124,#5583);
#4680=LINE('',#25149,#5584);
#4681=LINE('',#25173,#5585);
#4682=LINE('',#25190,#5586);
#4683=LINE('',#25225,#5587);
#4684=LINE('',#25252,#5588);
#4685=LINE('',#25303,#5589);
#4686=LINE('',#25351,#5590);
#4687=LINE('',#25399,#5591);
#4688=LINE('',#25450,#5592);
#4689=LINE('',#25498,#5593);
#4690=LINE('',#25546,#5594);
#4691=LINE('',#25597,#5595);
#4692=LINE('',#25648,#5596);
#4693=LINE('',#25696,#5597);
#4694=LINE('',#25747,#5598);
#4695=LINE('',#25786,#5599);
#4696=LINE('',#25808,#5600);
#4697=LINE('',#25832,#5601);
#4698=LINE('',#25857,#5602);
#4699=LINE('',#25882,#5603);
#4700=LINE('',#25906,#5604);
#4701=LINE('',#25931,#5605);
#4702=LINE('',#25955,#5606);
#4703=LINE('',#25980,#5607);
#4704=LINE('',#26004,#5608);
#4705=LINE('',#26029,#5609);
#4706=LINE('',#26054,#5610);
#4707=LINE('',#26078,#5611);
#4708=LINE('',#26095,#5612);
#4709=LINE('',#26130,#5613);
#4710=LINE('',#26157,#5614);
#4711=LINE('',#26208,#5615);
#4712=LINE('',#26256,#5616);
#4713=LINE('',#26304,#5617);
#4714=LINE('',#26355,#5618);
#4715=LINE('',#26403,#5619);
#4716=LINE('',#26451,#5620);
#4717=LINE('',#26502,#5621);
#4718=LINE('',#26553,#5622);
#4719=LINE('',#26601,#5623);
#4720=LINE('',#26652,#5624);
#4721=LINE('',#26691,#5625);
#4722=LINE('',#26713,#5626);
#4723=LINE('',#26737,#5627);
#4724=LINE('',#26762,#5628);
#4725=LINE('',#26787,#5629);
#4726=LINE('',#26811,#5630);
#4727=LINE('',#26836,#5631);
#4728=LINE('',#26860,#5632);
#4729=LINE('',#26885,#5633);
#4730=LINE('',#26909,#5634);
#4731=LINE('',#26934,#5635);
#4732=LINE('',#26959,#5636);
#4733=LINE('',#26983,#5637);
#4734=LINE('',#27000,#5638);
#4735=LINE('',#27035,#5639);
#4736=LINE('',#27062,#5640);
#4737=LINE('',#27113,#5641);
#4738=LINE('',#27161,#5642);
#4739=LINE('',#27209,#5643);
#4740=LINE('',#27260,#5644);
#4741=LINE('',#27308,#5645);
#4742=LINE('',#27356,#5646);
#4743=LINE('',#27407,#5647);
#4744=LINE('',#27458,#5648);
#4745=LINE('',#27506,#5649);
#4746=LINE('',#27557,#5650);
#4747=LINE('',#27596,#5651);
#4748=LINE('',#27618,#5652);
#4749=LINE('',#27642,#5653);
#4750=LINE('',#27667,#5654);
#4751=LINE('',#27692,#5655);
#4752=LINE('',#27716,#5656);
#4753=LINE('',#27741,#5657);
#4754=LINE('',#27765,#5658);
#4755=LINE('',#27790,#5659);
#4756=LINE('',#27814,#5660);
#4757=LINE('',#27839,#5661);
#4758=LINE('',#27864,#5662);
#4759=LINE('',#27888,#5663);
#4760=LINE('',#27905,#5664);
#4761=LINE('',#27940,#5665);
#4762=LINE('',#27967,#5666);
#4763=LINE('',#28018,#5667);
#4764=LINE('',#28066,#5668);
#4765=LINE('',#28114,#5669);
#4766=LINE('',#28165,#5670);
#4767=LINE('',#28213,#5671);
#4768=LINE('',#28261,#5672);
#4769=LINE('',#28312,#5673);
#4770=LINE('',#28363,#5674);
#4771=LINE('',#28411,#5675);
#4772=LINE('',#28462,#5676);
#4773=LINE('',#28501,#5677);
#4774=LINE('',#28523,#5678);
#4775=LINE('',#28547,#5679);
#4776=LINE('',#28572,#5680);
#4777=LINE('',#28597,#5681);
#4778=LINE('',#28621,#5682);
#4779=LINE('',#28646,#5683);
#4780=LINE('',#28670,#5684);
#4781=LINE('',#28695,#5685);
#4782=LINE('',#28719,#5686);
#4783=LINE('',#28744,#5687);
#4784=LINE('',#28769,#5688);
#4785=LINE('',#28793,#5689);
#4786=LINE('',#28810,#5690);
#4787=LINE('',#28845,#5691);
#4788=LINE('',#28872,#5692);
#4789=LINE('',#28923,#5693);
#4790=LINE('',#28971,#5694);
#4791=LINE('',#29019,#5695);
#4792=LINE('',#29070,#5696);
#4793=LINE('',#29118,#5697);
#4794=LINE('',#29166,#5698);
#4795=LINE('',#29217,#5699);
#4796=LINE('',#29268,#5700);
#4797=LINE('',#29316,#5701);
#4798=LINE('',#29367,#5702);
#4799=LINE('',#29406,#5703);
#4800=LINE('',#29428,#5704);
#4801=LINE('',#29452,#5705);
#4802=LINE('',#29477,#5706);
#4803=LINE('',#29502,#5707);
#4804=LINE('',#29526,#5708);
#4805=LINE('',#29551,#5709);
#4806=LINE('',#29575,#5710);
#4807=LINE('',#29600,#5711);
#4808=LINE('',#29624,#5712);
#4809=LINE('',#29649,#5713);
#4810=LINE('',#29674,#5714);
#4811=LINE('',#29698,#5715);
#4812=LINE('',#29715,#5716);
#4813=LINE('',#29750,#5717);
#4814=LINE('',#29777,#5718);
#4815=LINE('',#29828,#5719);
#4816=LINE('',#29876,#5720);
#4817=LINE('',#29924,#5721);
#4818=LINE('',#29975,#5722);
#4819=LINE('',#30023,#5723);
#4820=LINE('',#30071,#5724);
#4821=LINE('',#30122,#5725);
#4822=LINE('',#30173,#5726);
#4823=LINE('',#30221,#5727);
#4824=LINE('',#30272,#5728);
#4825=LINE('',#30311,#5729);
#4826=LINE('',#30333,#5730);
#4827=LINE('',#30357,#5731);
#4828=LINE('',#30382,#5732);
#4829=LINE('',#30407,#5733);
#4830=LINE('',#30431,#5734);
#4831=LINE('',#30456,#5735);
#4832=LINE('',#30480,#5736);
#4833=LINE('',#30505,#5737);
#4834=LINE('',#30529,#5738);
#4835=LINE('',#30554,#5739);
#4836=LINE('',#30579,#5740);
#4837=LINE('',#30603,#5741);
#4838=LINE('',#30620,#5742);
#4839=LINE('',#30655,#5743);
#4840=LINE('',#30682,#5744);
#4841=LINE('',#30733,#5745);
#4842=LINE('',#30781,#5746);
#4843=LINE('',#30829,#5747);
#4844=LINE('',#30880,#5748);
#4845=LINE('',#30928,#5749);
#4846=LINE('',#30976,#5750);
#4847=LINE('',#31027,#5751);
#4848=LINE('',#31078,#5752);
#4849=LINE('',#31126,#5753);
#4850=LINE('',#31177,#5754);
#4851=LINE('',#31216,#5755);
#4852=LINE('',#31238,#5756);
#4853=LINE('',#31262,#5757);
#4854=LINE('',#31287,#5758);
#4855=LINE('',#31312,#5759);
#4856=LINE('',#31336,#5760);
#4857=LINE('',#31361,#5761);
#4858=LINE('',#31385,#5762);
#4859=LINE('',#31410,#5763);
#4860=LINE('',#31434,#5764);
#4861=LINE('',#31459,#5765);
#4862=LINE('',#31484,#5766);
#4863=LINE('',#31508,#5767);
#4864=LINE('',#31525,#5768);
#4865=LINE('',#31560,#5769);
#4866=LINE('',#31587,#5770);
#4867=LINE('',#31638,#5771);
#4868=LINE('',#31686,#5772);
#4869=LINE('',#31734,#5773);
#4870=LINE('',#31785,#5774);
#4871=LINE('',#31833,#5775);
#4872=LINE('',#31881,#5776);
#4873=LINE('',#31932,#5777);
#4874=LINE('',#31983,#5778);
#4875=LINE('',#32031,#5779);
#4876=LINE('',#32082,#5780);
#4877=LINE('',#32121,#5781);
#4878=LINE('',#32143,#5782);
#4879=LINE('',#32167,#5783);
#4880=LINE('',#32192,#5784);
#4881=LINE('',#32217,#5785);
#4882=LINE('',#32241,#5786);
#4883=LINE('',#32266,#5787);
#4884=LINE('',#32290,#5788);
#4885=LINE('',#32315,#5789);
#4886=LINE('',#32339,#5790);
#4887=LINE('',#32364,#5791);
#4888=LINE('',#32389,#5792);
#4889=LINE('',#32413,#5793);
#4890=LINE('',#32430,#5794);
#4891=LINE('',#32465,#5795);
#4892=LINE('',#32492,#5796);
#4893=LINE('',#32543,#5797);
#4894=LINE('',#32591,#5798);
#4895=LINE('',#32639,#5799);
#4896=LINE('',#32690,#5800);
#4897=LINE('',#32738,#5801);
#4898=LINE('',#32786,#5802);
#4899=LINE('',#32837,#5803);
#4900=LINE('',#32888,#5804);
#4901=LINE('',#32936,#5805);
#4902=LINE('',#32987,#5806);
#4903=LINE('',#33026,#5807);
#4904=LINE('',#33048,#5808);
#4905=LINE('',#33072,#5809);
#4906=LINE('',#33097,#5810);
#4907=LINE('',#33122,#5811);
#4908=LINE('',#33146,#5812);
#4909=LINE('',#33171,#5813);
#4910=LINE('',#33195,#5814);
#4911=LINE('',#33220,#5815);
#4912=LINE('',#33244,#5816);
#4913=LINE('',#33269,#5817);
#4914=LINE('',#33294,#5818);
#4915=LINE('',#33318,#5819);
#4916=LINE('',#33335,#5820);
#4917=LINE('',#33370,#5821);
#4918=LINE('',#33397,#5822);
#4919=LINE('',#33448,#5823);
#4920=LINE('',#33496,#5824);
#4921=LINE('',#33544,#5825);
#4922=LINE('',#33595,#5826);
#4923=LINE('',#33643,#5827);
#4924=LINE('',#33691,#5828);
#4925=LINE('',#33742,#5829);
#4926=LINE('',#33793,#5830);
#4927=LINE('',#33841,#5831);
#4928=LINE('',#33892,#5832);
#4929=LINE('',#33931,#5833);
#4930=LINE('',#33953,#5834);
#4931=LINE('',#33977,#5835);
#4932=LINE('',#34002,#5836);
#4933=LINE('',#34027,#5837);
#4934=LINE('',#34051,#5838);
#4935=LINE('',#34076,#5839);
#4936=LINE('',#34100,#5840);
#4937=LINE('',#34125,#5841);
#4938=LINE('',#34149,#5842);
#4939=LINE('',#34174,#5843);
#4940=LINE('',#34199,#5844);
#4941=LINE('',#34223,#5845);
#4942=LINE('',#34240,#5846);
#4943=LINE('',#34261,#5847);
#4944=LINE('',#34312,#5848);
#4945=LINE('',#34363,#5849);
#4946=LINE('',#34411,#5850);
#4947=LINE('',#34465,#5851);
#4948=LINE('',#34513,#5852);
#4949=LINE('',#34561,#5853);
#4950=LINE('',#34611,#5854);
#4951=LINE('',#34635,#5855);
#4952=LINE('',#34659,#5856);
#4953=LINE('',#34684,#5857);
#4954=LINE('',#34709,#5858);
#4955=LINE('',#34734,#5859);
#4956=LINE('',#34758,#5860);
#4957=LINE('',#34783,#5861);
#4958=LINE('',#34809,#5862);
#4959=LINE('',#34830,#5863);
#4960=LINE('',#34881,#5864);
#4961=LINE('',#34932,#5865);
#4962=LINE('',#34980,#5866);
#4963=LINE('',#35034,#5867);
#4964=LINE('',#35082,#5868);
#4965=LINE('',#35130,#5869);
#4966=LINE('',#35180,#5870);
#4967=LINE('',#35201,#5871);
#4968=LINE('',#35252,#5872);
#4969=LINE('',#35303,#5873);
#4970=LINE('',#35351,#5874);
#4971=LINE('',#35405,#5875);
#4972=LINE('',#35453,#5876);
#4973=LINE('',#35501,#5877);
#4974=LINE('',#35551,#5878);
#4975=LINE('',#35572,#5879);
#4976=LINE('',#35623,#5880);
#4977=LINE('',#35674,#5881);
#4978=LINE('',#35722,#5882);
#4979=LINE('',#35776,#5883);
#4980=LINE('',#35824,#5884);
#4981=LINE('',#35872,#5885);
#4982=LINE('',#35922,#5886);
#4983=LINE('',#35946,#5887);
#4984=LINE('',#35970,#5888);
#4985=LINE('',#35995,#5889);
#4986=LINE('',#36020,#5890);
#4987=LINE('',#36045,#5891);
#4988=LINE('',#36069,#5892);
#4989=LINE('',#36094,#5893);
#4990=LINE('',#36120,#5894);
#4991=LINE('',#36144,#5895);
#4992=LINE('',#36168,#5896);
#4993=LINE('',#36193,#5897);
#4994=LINE('',#36218,#5898);
#4995=LINE('',#36243,#5899);
#4996=LINE('',#36267,#5900);
#4997=LINE('',#36292,#5901);
#4998=LINE('',#36318,#5902);
#4999=LINE('',#36342,#5903);
#5000=LINE('',#36366,#5904);
#5001=LINE('',#36391,#5905);
#5002=LINE('',#36416,#5906);
#5003=LINE('',#36441,#5907);
#5004=LINE('',#36465,#5908);
#5005=LINE('',#36490,#5909);
#5006=LINE('',#52661,#5910);
#5007=LINE('',#52667,#5911);
#5008=LINE('',#52675,#5912);
#5009=LINE('',#52684,#5913);
#5010=LINE('',#52705,#5914);
#5011=LINE('',#52756,#5915);
#5012=LINE('',#52807,#5916);
#5013=LINE('',#52855,#5917);
#5014=LINE('',#52906,#5918);
#5015=LINE('',#52957,#5919);
#5016=LINE('',#53005,#5920);
#5017=LINE('',#53044,#5921);
#5018=LINE('',#53068,#5922);
#5019=LINE('',#53092,#5923);
#5020=LINE('',#53117,#5924);
#5021=LINE('',#53142,#5925);
#5022=LINE('',#53166,#5926);
#5023=LINE('',#53191,#5927);
#5024=LINE('',#53216,#5928);
#5025=LINE('',#53233,#5929);
#5026=LINE('',#53242,#5930);
#5027=LINE('',#53263,#5931);
#5028=LINE('',#53314,#5932);
#5029=LINE('',#53365,#5933);
#5030=LINE('',#53413,#5934);
#5031=LINE('',#53464,#5935);
#5032=LINE('',#53515,#5936);
#5033=LINE('',#53563,#5937);
#5034=LINE('',#53602,#5938);
#5035=LINE('',#53626,#5939);
#5036=LINE('',#53650,#5940);
#5037=LINE('',#53675,#5941);
#5038=LINE('',#53700,#5942);
#5039=LINE('',#53724,#5943);
#5040=LINE('',#53749,#5944);
#5041=LINE('',#53774,#5945);
#5042=LINE('',#53791,#5946);
#5043=LINE('',#53800,#5947);
#5044=LINE('',#53821,#5948);
#5045=LINE('',#53872,#5949);
#5046=LINE('',#53923,#5950);
#5047=LINE('',#53971,#5951);
#5048=LINE('',#54022,#5952);
#5049=LINE('',#54073,#5953);
#5050=LINE('',#54121,#5954);
#5051=LINE('',#54160,#5955);
#5052=LINE('',#54184,#5956);
#5053=LINE('',#54208,#5957);
#5054=LINE('',#54233,#5958);
#5055=LINE('',#54258,#5959);
#5056=LINE('',#54282,#5960);
#5057=LINE('',#54307,#5961);
#5058=LINE('',#54332,#5962);
#5059=LINE('',#54349,#5963);
#5060=LINE('',#54358,#5964);
#5061=LINE('',#54379,#5965);
#5062=LINE('',#54430,#5966);
#5063=LINE('',#54481,#5967);
#5064=LINE('',#54529,#5968);
#5065=LINE('',#54580,#5969);
#5066=LINE('',#54631,#5970);
#5067=LINE('',#54679,#5971);
#5068=LINE('',#54718,#5972);
#5069=LINE('',#54742,#5973);
#5070=LINE('',#54766,#5974);
#5071=LINE('',#54791,#5975);
#5072=LINE('',#54816,#5976);
#5073=LINE('',#54840,#5977);
#5074=LINE('',#54865,#5978);
#5075=LINE('',#54890,#5979);
#5076=LINE('',#54907,#5980);
#5077=LINE('',#54916,#5981);
#5078=LINE('',#54937,#5982);
#5079=LINE('',#54988,#5983);
#5080=LINE('',#55039,#5984);
#5081=LINE('',#55087,#5985);
#5082=LINE('',#55138,#5986);
#5083=LINE('',#55189,#5987);
#5084=LINE('',#55237,#5988);
#5085=LINE('',#55276,#5989);
#5086=LINE('',#55300,#5990);
#5087=LINE('',#55324,#5991);
#5088=LINE('',#55349,#5992);
#5089=LINE('',#55374,#5993);
#5090=LINE('',#55398,#5994);
#5091=LINE('',#55423,#5995);
#5092=LINE('',#55448,#5996);
#5093=LINE('',#55465,#5997);
#5094=LINE('',#55474,#5998);
#5095=LINE('',#55495,#5999);
#5096=LINE('',#55546,#6000);
#5097=LINE('',#55597,#6001);
#5098=LINE('',#55645,#6002);
#5099=LINE('',#55696,#6003);
#5100=LINE('',#55747,#6004);
#5101=LINE('',#55795,#6005);
#5102=LINE('',#55834,#6006);
#5103=LINE('',#55858,#6007);
#5104=LINE('',#55882,#6008);
#5105=LINE('',#55907,#6009);
#5106=LINE('',#55932,#6010);
#5107=LINE('',#55956,#6011);
#5108=LINE('',#55981,#6012);
#5109=LINE('',#56006,#6013);
#5110=LINE('',#56023,#6014);
#5111=LINE('',#56032,#6015);
#5112=LINE('',#56053,#6016);
#5113=LINE('',#56104,#6017);
#5114=LINE('',#56155,#6018);
#5115=LINE('',#56203,#6019);
#5116=LINE('',#56254,#6020);
#5117=LINE('',#56305,#6021);
#5118=LINE('',#56353,#6022);
#5119=LINE('',#56392,#6023);
#5120=LINE('',#56416,#6024);
#5121=LINE('',#56440,#6025);
#5122=LINE('',#56465,#6026);
#5123=LINE('',#56490,#6027);
#5124=LINE('',#56514,#6028);
#5125=LINE('',#56539,#6029);
#5126=LINE('',#56564,#6030);
#5127=LINE('',#56581,#6031);
#5128=LINE('',#56590,#6032);
#5129=LINE('',#56611,#6033);
#5130=LINE('',#56662,#6034);
#5131=LINE('',#56713,#6035);
#5132=LINE('',#56761,#6036);
#5133=LINE('',#56812,#6037);
#5134=LINE('',#56863,#6038);
#5135=LINE('',#56911,#6039);
#5136=LINE('',#56950,#6040);
#5137=LINE('',#56974,#6041);
#5138=LINE('',#56998,#6042);
#5139=LINE('',#57023,#6043);
#5140=LINE('',#57048,#6044);
#5141=LINE('',#57072,#6045);
#5142=LINE('',#57097,#6046);
#5143=LINE('',#57122,#6047);
#5144=LINE('',#57139,#6048);
#5145=LINE('',#57148,#6049);
#5146=LINE('',#57169,#6050);
#5147=LINE('',#57220,#6051);
#5148=LINE('',#57271,#6052);
#5149=LINE('',#57319,#6053);
#5150=LINE('',#57370,#6054);
#5151=LINE('',#57421,#6055);
#5152=LINE('',#57469,#6056);
#5153=LINE('',#57508,#6057);
#5154=LINE('',#57532,#6058);
#5155=LINE('',#57556,#6059);
#5156=LINE('',#57581,#6060);
#5157=LINE('',#57606,#6061);
#5158=LINE('',#57630,#6062);
#5159=LINE('',#57655,#6063);
#5160=LINE('',#57680,#6064);
#5161=LINE('',#57697,#6065);
#5162=LINE('',#57706,#6066);
#5163=LINE('',#57727,#6067);
#5164=LINE('',#57778,#6068);
#5165=LINE('',#57829,#6069);
#5166=LINE('',#57877,#6070);
#5167=LINE('',#57928,#6071);
#5168=LINE('',#57979,#6072);
#5169=LINE('',#58027,#6073);
#5170=LINE('',#58066,#6074);
#5171=LINE('',#58090,#6075);
#5172=LINE('',#58114,#6076);
#5173=LINE('',#58139,#6077);
#5174=LINE('',#58164,#6078);
#5175=LINE('',#58188,#6079);
#5176=LINE('',#58213,#6080);
#5177=LINE('',#58238,#6081);
#5178=LINE('',#58255,#6082);
#5179=LINE('',#58264,#6083);
#5180=LINE('',#58285,#6084);
#5181=LINE('',#58336,#6085);
#5182=LINE('',#58387,#6086);
#5183=LINE('',#58435,#6087);
#5184=LINE('',#58486,#6088);
#5185=LINE('',#58537,#6089);
#5186=LINE('',#58585,#6090);
#5187=LINE('',#58624,#6091);
#5188=LINE('',#58648,#6092);
#5189=LINE('',#58672,#6093);
#5190=LINE('',#58697,#6094);
#5191=LINE('',#58722,#6095);
#5192=LINE('',#58746,#6096);
#5193=LINE('',#58771,#6097);
#5194=LINE('',#58796,#6098);
#5195=LINE('',#58813,#6099);
#5196=LINE('',#58822,#6100);
#5197=LINE('',#58843,#6101);
#5198=LINE('',#58894,#6102);
#5199=LINE('',#58945,#6103);
#5200=LINE('',#58993,#6104);
#5201=LINE('',#59044,#6105);
#5202=LINE('',#59095,#6106);
#5203=LINE('',#59143,#6107);
#5204=LINE('',#59182,#6108);
#5205=LINE('',#59206,#6109);
#5206=LINE('',#59230,#6110);
#5207=LINE('',#59255,#6111);
#5208=LINE('',#59280,#6112);
#5209=LINE('',#59304,#6113);
#5210=LINE('',#59329,#6114);
#5211=LINE('',#59354,#6115);
#5212=LINE('',#59371,#6116);
#5213=LINE('',#59373,#6117);
#5214=LINE('',#59375,#6118);
#5215=LINE('',#59376,#6119);
#5216=LINE('',#59379,#6120);
#5217=LINE('',#59381,#6121);
#5218=LINE('',#59382,#6122);
#5219=LINE('',#59386,#6123);
#5220=LINE('',#59387,#6124);
#5221=LINE('',#59388,#6125);
#5222=LINE('',#59421,#6126);
#5223=LINE('',#59432,#6127);
#5224=LINE('',#59434,#6128);
#5225=LINE('',#59436,#6129);
#5226=LINE('',#59438,#6130);
#5227=LINE('',#59469,#6131);
#5228=LINE('',#59480,#6132);
#5229=LINE('',#59482,#6133);
#5230=LINE('',#59484,#6134);
#5231=LINE('',#59486,#6135);
#5232=LINE('',#59517,#6136);
#5233=LINE('',#59528,#6137);
#5234=LINE('',#59530,#6138);
#5235=LINE('',#59532,#6139);
#5236=LINE('',#59534,#6140);
#5237=LINE('',#59543,#6141);
#5238=LINE('',#59554,#6142);
#5239=LINE('',#59556,#6143);
#5240=LINE('',#59558,#6144);
#5241=LINE('',#59560,#6145);
#5242=LINE('',#59591,#6146);
#5243=LINE('',#59602,#6147);
#5244=LINE('',#59604,#6148);
#5245=LINE('',#59606,#6149);
#5246=LINE('',#59608,#6150);
#5247=LINE('',#59639,#6151);
#5248=LINE('',#59650,#6152);
#5249=LINE('',#59652,#6153);
#5250=LINE('',#59654,#6154);
#5251=LINE('',#59655,#6155);
#5252=LINE('',#64829,#6156);
#5253=LINE('',#64831,#6157);
#5254=LINE('',#64833,#6158);
#5255=LINE('',#64835,#6159);
#5256=LINE('',#64837,#6160);
#5257=LINE('',#64839,#6161);
#5258=LINE('',#64841,#6162);
#5259=LINE('',#64843,#6163);
#5260=LINE('',#64845,#6164);
#5261=LINE('',#64847,#6165);
#5262=LINE('',#68249,#6166);
#5263=LINE('',#68251,#6167);
#5264=LINE('',#68253,#6168);
#5265=LINE('',#68255,#6169);
#5266=LINE('',#68257,#6170);
#5267=LINE('',#68259,#6171);
#5268=LINE('',#68261,#6172);
#5269=LINE('',#68263,#6173);
#5270=LINE('',#68265,#6174);
#5271=LINE('',#68267,#6175);
#5272=LINE('',#69110,#6176);
#5273=LINE('',#69112,#6177);
#5274=LINE('',#69794,#6178);
#5275=LINE('',#69796,#6179);
#5276=LINE('',#69801,#6180);
#5277=LINE('',#69806,#6181);
#5278=LINE('',#69808,#6182);
#5279=LINE('',#69815,#6183);
#5280=LINE('',#69820,#6184);
#5281=LINE('',#69822,#6185);
#5282=LINE('',#69829,#6186);
#5283=LINE('',#69834,#6187);
#5284=LINE('',#69836,#6188);
#5285=LINE('',#69843,#6189);
#5286=LINE('',#69848,#6190);
#5287=LINE('',#69850,#6191);
#5288=LINE('',#69857,#6192);
#5289=LINE('',#69862,#6193);
#5290=LINE('',#69864,#6194);
#5291=LINE('',#69871,#6195);
#5292=LINE('',#69876,#6196);
#5293=LINE('',#69878,#6197);
#5294=LINE('',#69890,#6198);
#5295=LINE('',#69891,#6199);
#5296=LINE('',#69901,#6200);
#5297=LINE('',#69902,#6201);
#5298=LINE('',#69905,#6202);
#5299=LINE('',#69906,#6203);
#5300=LINE('',#69908,#6204);
#5301=LINE('',#69918,#6205);
#5302=LINE('',#69919,#6206);
#5303=LINE('',#69922,#6207);
#5304=LINE('',#69923,#6208);
#5305=LINE('',#69926,#6209);
#5306=LINE('',#69927,#6210);
#5307=LINE('',#69936,#6211);
#5308=LINE('',#69946,#6212);
#5309=LINE('',#69947,#6213);
#5310=LINE('',#69950,#6214);
#5311=LINE('',#69951,#6215);
#5312=LINE('',#69954,#6216);
#5313=LINE('',#69955,#6217);
#5314=LINE('',#69964,#6218);
#5315=LINE('',#69974,#6219);
#5316=LINE('',#69975,#6220);
#5317=LINE('',#69978,#6221);
#5318=LINE('',#69979,#6222);
#5319=LINE('',#69982,#6223);
#5320=LINE('',#69983,#6224);
#5321=LINE('',#69992,#6225);
#5322=LINE('',#70002,#6226);
#5323=LINE('',#70003,#6227);
#5324=LINE('',#70013,#6228);
#5325=LINE('',#70014,#6229);
#5326=LINE('',#70017,#6230);
#5327=LINE('',#70018,#6231);
#5328=LINE('',#70020,#6232);
#5329=LINE('',#72060,#6233);
#5330=LINE('',#74100,#6234);
#5331=LINE('',#76112,#6235);
#5332=LINE('',#78156,#6236);
#5333=LINE('',#80168,#6237);
#5334=LINE('',#82212,#6238);
#5335=LINE('',#84224,#6239);
#5336=LINE('',#86268,#6240);
#5337=LINE('',#86278,#6241);
#5338=LINE('',#86279,#6242);
#5339=LINE('',#86289,#6243);
#5340=LINE('',#86290,#6244);
#5341=LINE('',#86293,#6245);
#5342=LINE('',#86294,#6246);
#5343=LINE('',#86296,#6247);
#5344=LINE('',#88336,#6248);
#5345=LINE('',#88339,#6249);
#5346=LINE('',#88343,#6250);
#5347=LINE('',#88346,#6251);
#5348=LINE('',#88349,#6252);
#5349=LINE('',#88353,#6253);
#5350=LINE('',#88356,#6254);
#5351=LINE('',#88359,#6255);
#5352=LINE('',#88363,#6256);
#5353=LINE('',#88366,#6257);
#5354=LINE('',#88377,#6258);
#5355=LINE('',#88387,#6259);
#5356=LINE('',#88397,#6260);
#5357=LINE('',#88400,#6261);
#5358=LINE('',#88402,#6262);
#5359=LINE('',#88404,#6263);
#5360=LINE('',#90416,#6264);
#5361=LINE('',#90418,#6265);
#5362=LINE('',#90420,#6266);
#5363=LINE('',#92432,#6267);
#5364=LINE('',#94443,#6268);
#5365=LINE('',#94445,#6269);
#5366=LINE('',#94452,#6270);
#5367=LINE('',#94456,#6271);
#5368=LINE('',#94480,#6272);
#5369=LINE('',#94482,#6273);
#5370=LINE('',#94485,#6274);
#5371=LINE('',#94487,#6275);
#5372=LINE('',#94488,#6276);
#5373=LINE('',#94511,#6277);
#5374=LINE('',#94513,#6278);
#5375=LINE('',#94514,#6279);
#5376=LINE('',#94521,#6280);
#5377=LINE('',#94545,#6281);
#5378=LINE('',#94548,#6282);
#5379=LINE('',#94551,#6283);
#5380=LINE('',#94553,#6284);
#5381=LINE('',#94554,#6285);
#5382=LINE('',#94580,#6286);
#5383=LINE('',#94582,#6287);
#5384=LINE('',#94583,#6288);
#5385=LINE('',#94589,#6289);
#5386=LINE('',#94596,#6290);
#5387=LINE('',#94604,#6291);
#5388=LINE('',#94615,#6292);
#5389=LINE('',#94623,#6293);
#5390=LINE('',#94626,#6294);
#5391=LINE('',#94634,#6295);
#5392=LINE('',#94636,#6296);
#5393=LINE('',#94638,#6297);
#5394=LINE('',#94639,#6298);
#5395=LINE('',#94645,#6299);
#5396=LINE('',#94648,#6300);
#5397=LINE('',#94650,#6301);
#5398=LINE('',#94651,#6302);
#5399=LINE('',#94662,#6303);
#5400=LINE('',#94675,#6304);
#5401=LINE('',#94678,#6305);
#5402=LINE('',#94688,#6306);
#5403=LINE('',#94691,#6307);
#5404=LINE('',#94701,#6308);
#5405=LINE('',#94704,#6309);
#5406=LINE('',#94714,#6310);
#5407=LINE('',#94717,#6311);
#5408=LINE('',#94727,#6312);
#5409=LINE('',#94730,#6313);
#5410=LINE('',#94740,#6314);
#5411=LINE('',#94743,#6315);
#5412=LINE('',#94749,#6316);
#5413=LINE('',#94755,#6317);
#5414=LINE('',#94764,#6318);
#5415=LINE('',#94770,#6319);
#5416=LINE('',#94779,#6320);
#5417=LINE('',#94783,#6321);
#5418=LINE('',#94789,#6322);
#5419=LINE('',#94793,#6323);
#5420=LINE('',#94799,#6324);
#5421=LINE('',#94803,#6325);
#5422=LINE('',#94809,#6326);
#5423=LINE('',#94813,#6327);
#5424=LINE('',#94819,#6328);
#5425=LINE('',#94823,#6329);
#5426=LINE('',#94829,#6330);
#5427=LINE('',#94833,#6331);
#5428=LINE('',#94839,#6332);
#5429=LINE('',#94845,#6333);
#5430=LINE('',#94854,#6334);
#5431=LINE('',#94860,#6335);
#5432=LINE('',#94869,#6336);
#5433=LINE('',#94875,#6337);
#5434=LINE('',#94884,#6338);
#5435=LINE('',#94890,#6339);
#5436=LINE('',#94898,#6340);
#5437=LINE('',#94900,#6341);
#5438=LINE('',#94902,#6342);
#5439=LINE('',#94903,#6343);
#5440=LINE('',#94907,#6344);
#5441=LINE('',#94909,#6345);
#5442=LINE('',#94911,#6346);
#5443=LINE('',#94912,#6347);
#5444=LINE('',#94930,#6348);
#5445=LINE('',#94934,#6349);
#5446=LINE('',#95267,#6350);
#5447=LINE('',#95291,#6351);
#5448=LINE('',#95339,#6352);
#5449=LINE('',#95387,#6353);
#5450=LINE('',#95441,#6354);
#5451=LINE('',#95489,#6355);
#5452=LINE('',#95537,#6356);
#5453=LINE('',#95585,#6357);
#5454=LINE('',#95639,#6358);
#5455=LINE('',#95687,#6359);
#5456=LINE('',#95735,#6360);
#5457=LINE('',#95789,#6361);
#5458=LINE('',#95837,#6362);
#5459=LINE('',#95885,#6363);
#5460=LINE('',#95936,#6364);
#5461=LINE('',#95987,#6365);
#5462=LINE('',#96035,#6366);
#5463=LINE('',#96057,#6367);
#5464=LINE('',#96081,#6368);
#5465=LINE('',#96105,#6369);
#5466=LINE('',#96131,#6370);
#5467=LINE('',#96155,#6371);
#5468=LINE('',#96179,#6372);
#5469=LINE('',#96204,#6373);
#5470=LINE('',#96229,#6374);
#5471=LINE('',#96253,#6375);
#5472=LINE('',#96278,#6376);
#5473=LINE('',#96303,#6377);
#5474=LINE('',#96327,#6378);
#5475=LINE('',#96351,#6379);
#5476=LINE('',#96376,#6380);
#5477=LINE('',#96401,#6381);
#5478=LINE('',#96716,#6382);
#5479=LINE('',#97798,#6383);
#5480=LINE('',#97800,#6384);
#5481=LINE('',#97802,#6385);
#5482=LINE('',#97803,#6386);
#5483=LINE('',#97806,#6387);
#5484=LINE('',#97808,#6388);
#5485=LINE('',#97809,#6389);
#5486=LINE('',#97812,#6390);
#5487=LINE('',#97814,#6391);
#5488=LINE('',#97815,#6392);
#5489=LINE('',#97818,#6393);
#5490=LINE('',#97820,#6394);
#5491=LINE('',#97821,#6395);
#5492=LINE('',#97824,#6396);
#5493=LINE('',#97826,#6397);
#5494=LINE('',#97827,#6398);
#5495=LINE('',#97829,#6399);
#5496=LINE('',#97830,#6400);
#5497=LINE('',#97837,#6401);
#5498=LINE('',#97845,#6402);
#5499=LINE('',#97869,#6403);
#5500=LINE('',#97917,#6404);
#5501=LINE('',#97965,#6405);
#5502=LINE('',#98013,#6406);
#5503=LINE('',#98061,#6407);
#5504=LINE('',#98109,#6408);
#5505=LINE('',#98157,#6409);
#5506=LINE('',#98211,#6410);
#5507=LINE('',#98235,#6411);
#5508=LINE('',#98260,#6412);
#5509=LINE('',#98285,#6413);
#5510=LINE('',#98309,#6414);
#5511=LINE('',#98333,#6415);
#5512=LINE('',#98359,#6416);
#5513=LINE('',#98383,#6417);
#5514=LINE('',#98695,#6418);
#5515=LINE('',#99047,#6419);
#5516=LINE('',#99049,#6420);
#5517=LINE('',#99051,#6421);
#5518=LINE('',#99052,#6422);
#5519=LINE('',#99055,#6423);
#5520=LINE('',#99057,#6424);
#5521=LINE('',#99058,#6425);
#5522=LINE('',#99061,#6426);
#5523=LINE('',#99063,#6427);
#5524=LINE('',#99064,#6428);
#5525=LINE('',#99067,#6429);
#5526=LINE('',#99069,#6430);
#5527=LINE('',#99070,#6431);
#5528=LINE('',#99073,#6432);
#5529=LINE('',#99075,#6433);
#5530=LINE('',#99076,#6434);
#5531=LINE('',#99078,#6435);
#5532=LINE('',#99079,#6436);
#5533=LINE('',#99430,#6437);
#5534=VECTOR('',#19805,2.);
#5535=VECTOR('',#19808,2.);
#5536=VECTOR('',#19813,2.);
#5537=VECTOR('',#19816,2.);
#5538=VECTOR('',#19819,2.);
#5539=VECTOR('',#19822,2.);
#5540=VECTOR('',#19825,2.);
#5541=VECTOR('',#19828,2.);
#5542=VECTOR('',#19831,2.);
#5543=VECTOR('',#19834,2.);
#5544=VECTOR('',#19837,2.);
#5545=VECTOR('',#19840,2.);
#5546=VECTOR('',#19843,2.);
#5547=VECTOR('',#19848,2.05475);
#5548=VECTOR('',#19853,2.05475);
#5549=VECTOR('',#19856,2.05475);
#5550=VECTOR('',#19859,2.05475);
#5551=VECTOR('',#19862,2.05475);
#5552=VECTOR('',#19865,2.05475);
#5553=VECTOR('',#19868,2.05475);
#5554=VECTOR('',#19871,2.05475);
#5555=VECTOR('',#19874,2.05475);
#5556=VECTOR('',#19877,2.05475);
#5557=VECTOR('',#19880,2.05475);
#5558=VECTOR('',#19883,2.05475);
#5559=VECTOR('',#19886,2.05475);
#5560=VECTOR('',#19891,2.);
#5561=VECTOR('',#19894,2.);
#5562=VECTOR('',#19899,2.);
#5563=VECTOR('',#19902,2.);
#5564=VECTOR('',#19905,2.);
#5565=VECTOR('',#19908,2.);
#5566=VECTOR('',#19911,2.);
#5567=VECTOR('',#19914,2.);
#5568=VECTOR('',#19917,2.);
#5569=VECTOR('',#19920,2.);
#5570=VECTOR('',#19923,2.);
#5571=VECTOR('',#19926,2.);
#5572=VECTOR('',#19929,2.);
#5573=VECTOR('',#19934,2.05475);
#5574=VECTOR('',#19939,2.05475);
#5575=VECTOR('',#19942,2.05475);
#5576=VECTOR('',#19945,2.05475);
#5577=VECTOR('',#19948,2.05475);
#5578=VECTOR('',#19951,2.05475);
#5579=VECTOR('',#19954,2.05475);
#5580=VECTOR('',#19957,2.05475);
#5581=VECTOR('',#19960,2.05475);
#5582=VECTOR('',#19963,2.05475);
#5583=VECTOR('',#19966,2.05475);
#5584=VECTOR('',#19969,2.05475);
#5585=VECTOR('',#19972,2.05475);
#5586=VECTOR('',#19977,2.);
#5587=VECTOR('',#19980,2.);
#5588=VECTOR('',#19985,2.);
#5589=VECTOR('',#19988,2.);
#5590=VECTOR('',#19991,2.);
#5591=VECTOR('',#19994,2.);
#5592=VECTOR('',#19997,2.);
#5593=VECTOR('',#20000,2.);
#5594=VECTOR('',#20003,2.);
#5595=VECTOR('',#20006,2.);
#5596=VECTOR('',#20009,2.);
#5597=VECTOR('',#20012,2.);
#5598=VECTOR('',#20015,2.);
#5599=VECTOR('',#20020,2.05475);
#5600=VECTOR('',#20025,2.05475);
#5601=VECTOR('',#20028,2.05475);
#5602=VECTOR('',#20031,2.05475);
#5603=VECTOR('',#20034,2.05475);
#5604=VECTOR('',#20037,2.05475);
#5605=VECTOR('',#20040,2.05475);
#5606=VECTOR('',#20043,2.05475);
#5607=VECTOR('',#20046,2.05475);
#5608=VECTOR('',#20049,2.05475);
#5609=VECTOR('',#20052,2.05475);
#5610=VECTOR('',#20055,2.05475);
#5611=VECTOR('',#20058,2.05475);
#5612=VECTOR('',#20063,2.);
#5613=VECTOR('',#20066,2.);
#5614=VECTOR('',#20071,2.);
#5615=VECTOR('',#20074,2.);
#5616=VECTOR('',#20077,2.);
#5617=VECTOR('',#20080,2.);
#5618=VECTOR('',#20083,2.);
#5619=VECTOR('',#20086,2.);
#5620=VECTOR('',#20089,2.);
#5621=VECTOR('',#20092,2.);
#5622=VECTOR('',#20095,2.);
#5623=VECTOR('',#20098,2.);
#5624=VECTOR('',#20101,2.);
#5625=VECTOR('',#20106,2.05474999999998);
#5626=VECTOR('',#20111,2.05474999999998);
#5627=VECTOR('',#20114,2.05474999999998);
#5628=VECTOR('',#20117,2.05474999999998);
#5629=VECTOR('',#20120,2.05474999999998);
#5630=VECTOR('',#20123,2.05474999999998);
#5631=VECTOR('',#20126,2.05474999999998);
#5632=VECTOR('',#20129,2.05474999999998);
#5633=VECTOR('',#20132,2.05474999999998);
#5634=VECTOR('',#20135,2.05474999999998);
#5635=VECTOR('',#20138,2.05474999999998);
#5636=VECTOR('',#20141,2.05474999999998);
#5637=VECTOR('',#20144,2.05474999999998);
#5638=VECTOR('',#20149,2.);
#5639=VECTOR('',#20152,2.);
#5640=VECTOR('',#20157,2.);
#5641=VECTOR('',#20160,2.);
#5642=VECTOR('',#20163,2.);
#5643=VECTOR('',#20166,2.);
#5644=VECTOR('',#20169,2.);
#5645=VECTOR('',#20172,2.);
#5646=VECTOR('',#20175,2.);
#5647=VECTOR('',#20178,2.);
#5648=VECTOR('',#20181,2.);
#5649=VECTOR('',#20184,2.);
#5650=VECTOR('',#20187,2.);
#5651=VECTOR('',#20192,2.05475);
#5652=VECTOR('',#20197,2.05475);
#5653=VECTOR('',#20200,2.05475);
#5654=VECTOR('',#20203,2.05475);
#5655=VECTOR('',#20206,2.05475);
#5656=VECTOR('',#20209,2.05475);
#5657=VECTOR('',#20212,2.05475);
#5658=VECTOR('',#20215,2.05475);
#5659=VECTOR('',#20218,2.05475);
#5660=VECTOR('',#20221,2.05475);
#5661=VECTOR('',#20224,2.05475);
#5662=VECTOR('',#20227,2.05475);
#5663=VECTOR('',#20230,2.05475);
#5664=VECTOR('',#20235,2.);
#5665=VECTOR('',#20238,2.);
#5666=VECTOR('',#20243,2.);
#5667=VECTOR('',#20246,2.);
#5668=VECTOR('',#20249,2.);
#5669=VECTOR('',#20252,2.);
#5670=VECTOR('',#20255,2.);
#5671=VECTOR('',#20258,2.);
#5672=VECTOR('',#20261,2.);
#5673=VECTOR('',#20264,2.);
#5674=VECTOR('',#20267,2.);
#5675=VECTOR('',#20270,2.);
#5676=VECTOR('',#20273,2.);
#5677=VECTOR('',#20278,2.05474999999998);
#5678=VECTOR('',#20283,2.05474999999998);
#5679=VECTOR('',#20286,2.05474999999998);
#5680=VECTOR('',#20289,2.05474999999998);
#5681=VECTOR('',#20292,2.05474999999998);
#5682=VECTOR('',#20295,2.05474999999998);
#5683=VECTOR('',#20298,2.05474999999998);
#5684=VECTOR('',#20301,2.05474999999998);
#5685=VECTOR('',#20304,2.05474999999998);
#5686=VECTOR('',#20307,2.05474999999998);
#5687=VECTOR('',#20310,2.05474999999998);
#5688=VECTOR('',#20313,2.05474999999998);
#5689=VECTOR('',#20316,2.05474999999998);
#5690=VECTOR('',#20321,2.);
#5691=VECTOR('',#20324,2.);
#5692=VECTOR('',#20329,2.);
#5693=VECTOR('',#20332,2.);
#5694=VECTOR('',#20335,2.);
#5695=VECTOR('',#20338,2.);
#5696=VECTOR('',#20341,2.);
#5697=VECTOR('',#20344,2.);
#5698=VECTOR('',#20347,2.);
#5699=VECTOR('',#20350,2.);
#5700=VECTOR('',#20353,2.);
#5701=VECTOR('',#20356,2.);
#5702=VECTOR('',#20359,2.);
#5703=VECTOR('',#20364,2.05474999999998);
#5704=VECTOR('',#20369,2.05474999999998);
#5705=VECTOR('',#20372,2.05474999999998);
#5706=VECTOR('',#20375,2.05474999999998);
#5707=VECTOR('',#20378,2.05474999999998);
#5708=VECTOR('',#20381,2.05474999999998);
#5709=VECTOR('',#20384,2.05474999999998);
#5710=VECTOR('',#20387,2.05474999999998);
#5711=VECTOR('',#20390,2.05474999999998);
#5712=VECTOR('',#20393,2.05474999999998);
#5713=VECTOR('',#20396,2.05474999999998);
#5714=VECTOR('',#20399,2.05474999999998);
#5715=VECTOR('',#20402,2.05474999999998);
#5716=VECTOR('',#20407,2.);
#5717=VECTOR('',#20410,2.);
#5718=VECTOR('',#20415,2.);
#5719=VECTOR('',#20418,2.);
#5720=VECTOR('',#20421,2.);
#5721=VECTOR('',#20424,2.);
#5722=VECTOR('',#20427,2.);
#5723=VECTOR('',#20430,2.);
#5724=VECTOR('',#20433,2.);
#5725=VECTOR('',#20436,2.);
#5726=VECTOR('',#20439,2.);
#5727=VECTOR('',#20442,2.);
#5728=VECTOR('',#20445,2.);
#5729=VECTOR('',#20450,2.05475000000002);
#5730=VECTOR('',#20455,2.05475000000002);
#5731=VECTOR('',#20458,2.05475000000002);
#5732=VECTOR('',#20461,2.05475000000002);
#5733=VECTOR('',#20464,2.05475000000002);
#5734=VECTOR('',#20467,2.05475000000002);
#5735=VECTOR('',#20470,2.05475000000002);
#5736=VECTOR('',#20473,2.05475000000002);
#5737=VECTOR('',#20476,2.05475000000002);
#5738=VECTOR('',#20479,2.05475000000002);
#5739=VECTOR('',#20482,2.05475000000002);
#5740=VECTOR('',#20485,2.05475000000002);
#5741=VECTOR('',#20488,2.05475000000002);
#5742=VECTOR('',#20493,2.);
#5743=VECTOR('',#20496,2.);
#5744=VECTOR('',#20501,2.);
#5745=VECTOR('',#20504,2.);
#5746=VECTOR('',#20507,2.);
#5747=VECTOR('',#20510,2.);
#5748=VECTOR('',#20513,2.);
#5749=VECTOR('',#20516,2.);
#5750=VECTOR('',#20519,2.);
#5751=VECTOR('',#20522,2.);
#5752=VECTOR('',#20525,2.);
#5753=VECTOR('',#20528,2.);
#5754=VECTOR('',#20531,2.);
#5755=VECTOR('',#20536,2.05474999999998);
#5756=VECTOR('',#20541,2.05474999999998);
#5757=VECTOR('',#20544,2.05474999999998);
#5758=VECTOR('',#20547,2.05474999999998);
#5759=VECTOR('',#20550,2.05474999999998);
#5760=VECTOR('',#20553,2.05474999999998);
#5761=VECTOR('',#20556,2.05474999999998);
#5762=VECTOR('',#20559,2.05474999999998);
#5763=VECTOR('',#20562,2.05474999999998);
#5764=VECTOR('',#20565,2.05474999999998);
#5765=VECTOR('',#20568,2.05474999999998);
#5766=VECTOR('',#20571,2.05474999999998);
#5767=VECTOR('',#20574,2.05474999999998);
#5768=VECTOR('',#20579,2.);
#5769=VECTOR('',#20582,2.);
#5770=VECTOR('',#20587,2.);
#5771=VECTOR('',#20590,2.);
#5772=VECTOR('',#20593,2.);
#5773=VECTOR('',#20596,2.);
#5774=VECTOR('',#20599,2.);
#5775=VECTOR('',#20602,2.);
#5776=VECTOR('',#20605,2.);
#5777=VECTOR('',#20608,2.);
#5778=VECTOR('',#20611,2.);
#5779=VECTOR('',#20614,2.);
#5780=VECTOR('',#20617,2.);
#5781=VECTOR('',#20622,2.05475);
#5782=VECTOR('',#20627,2.05475);
#5783=VECTOR('',#20630,2.05475);
#5784=VECTOR('',#20633,2.05475);
#5785=VECTOR('',#20636,2.05475);
#5786=VECTOR('',#20639,2.05475);
#5787=VECTOR('',#20642,2.05475);
#5788=VECTOR('',#20645,2.05475);
#5789=VECTOR('',#20648,2.05475);
#5790=VECTOR('',#20651,2.05475);
#5791=VECTOR('',#20654,2.05475);
#5792=VECTOR('',#20657,2.05475);
#5793=VECTOR('',#20660,2.05475);
#5794=VECTOR('',#20665,2.);
#5795=VECTOR('',#20668,2.);
#5796=VECTOR('',#20673,2.);
#5797=VECTOR('',#20676,2.);
#5798=VECTOR('',#20679,2.);
#5799=VECTOR('',#20682,2.);
#5800=VECTOR('',#20685,2.);
#5801=VECTOR('',#20688,2.);
#5802=VECTOR('',#20691,2.);
#5803=VECTOR('',#20694,2.);
#5804=VECTOR('',#20697,2.);
#5805=VECTOR('',#20700,2.);
#5806=VECTOR('',#20703,2.);
#5807=VECTOR('',#20708,2.05474999999999);
#5808=VECTOR('',#20713,2.05474999999999);
#5809=VECTOR('',#20716,2.05474999999999);
#5810=VECTOR('',#20719,2.05474999999999);
#5811=VECTOR('',#20722,2.05474999999999);
#5812=VECTOR('',#20725,2.05474999999999);
#5813=VECTOR('',#20728,2.05474999999999);
#5814=VECTOR('',#20731,2.05474999999999);
#5815=VECTOR('',#20734,2.05474999999999);
#5816=VECTOR('',#20737,2.05474999999999);
#5817=VECTOR('',#20740,2.05474999999999);
#5818=VECTOR('',#20743,2.05474999999999);
#5819=VECTOR('',#20746,2.05474999999999);
#5820=VECTOR('',#20751,2.);
#5821=VECTOR('',#20754,2.);
#5822=VECTOR('',#20759,2.);
#5823=VECTOR('',#20762,2.);
#5824=VECTOR('',#20765,2.);
#5825=VECTOR('',#20768,2.);
#5826=VECTOR('',#20771,2.);
#5827=VECTOR('',#20774,2.);
#5828=VECTOR('',#20777,2.);
#5829=VECTOR('',#20780,2.);
#5830=VECTOR('',#20783,2.);
#5831=VECTOR('',#20786,2.);
#5832=VECTOR('',#20789,2.);
#5833=VECTOR('',#20794,2.05475);
#5834=VECTOR('',#20799,2.05475);
#5835=VECTOR('',#20802,2.05475);
#5836=VECTOR('',#20805,2.05475);
#5837=VECTOR('',#20808,2.05475);
#5838=VECTOR('',#20811,2.05475);
#5839=VECTOR('',#20814,2.05475);
#5840=VECTOR('',#20817,2.05475);
#5841=VECTOR('',#20820,2.05475);
#5842=VECTOR('',#20823,2.05475);
#5843=VECTOR('',#20826,2.05475);
#5844=VECTOR('',#20829,2.05475);
#5845=VECTOR('',#20832,2.05475);
#5846=VECTOR('',#20837,3.);
#5847=VECTOR('',#20842,3.);
#5848=VECTOR('',#20845,3.);
#5849=VECTOR('',#20848,3.);
#5850=VECTOR('',#20851,3.);
#5851=VECTOR('',#20854,3.);
#5852=VECTOR('',#20857,3.);
#5853=VECTOR('',#20860,3.);
#5854=VECTOR('',#20863,3.07350000000001);
#5855=VECTOR('',#20868,3.07350000000001);
#5856=VECTOR('',#20871,3.07350000000001);
#5857=VECTOR('',#20874,3.07350000000001);
#5858=VECTOR('',#20877,3.07350000000001);
#5859=VECTOR('',#20880,3.07350000000001);
#5860=VECTOR('',#20883,3.07350000000001);
#5861=VECTOR('',#20886,3.07350000000001);
#5862=VECTOR('',#20889,3.);
#5863=VECTOR('',#20894,3.);
#5864=VECTOR('',#20897,3.);
#5865=VECTOR('',#20900,3.);
#5866=VECTOR('',#20903,3.);
#5867=VECTOR('',#20906,3.);
#5868=VECTOR('',#20909,3.);
#5869=VECTOR('',#20912,3.);
#5870=VECTOR('',#20915,3.);
#5871=VECTOR('',#20920,3.);
#5872=VECTOR('',#20923,3.);
#5873=VECTOR('',#20926,3.);
#5874=VECTOR('',#20929,3.);
#5875=VECTOR('',#20932,3.);
#5876=VECTOR('',#20935,3.);
#5877=VECTOR('',#20938,3.);
#5878=VECTOR('',#20941,3.);
#5879=VECTOR('',#20946,3.);
#5880=VECTOR('',#20949,3.);
#5881=VECTOR('',#20952,3.);
#5882=VECTOR('',#20955,3.);
#5883=VECTOR('',#20958,3.);
#5884=VECTOR('',#20961,3.);
#5885=VECTOR('',#20964,3.);
#5886=VECTOR('',#20967,3.07350000000001);
#5887=VECTOR('',#20972,3.07350000000001);
#5888=VECTOR('',#20975,3.07350000000001);
#5889=VECTOR('',#20978,3.07350000000001);
#5890=VECTOR('',#20981,3.07350000000001);
#5891=VECTOR('',#20984,3.07350000000001);
#5892=VECTOR('',#20987,3.07350000000001);
#5893=VECTOR('',#20990,3.07350000000001);
#5894=VECTOR('',#20993,3.0735);
#5895=VECTOR('',#20998,3.0735);
#5896=VECTOR('',#21001,3.0735);
#5897=VECTOR('',#21004,3.0735);
#5898=VECTOR('',#21007,3.0735);
#5899=VECTOR('',#21010,3.0735);
#5900=VECTOR('',#21013,3.0735);
#5901=VECTOR('',#21016,3.0735);
#5902=VECTOR('',#21019,3.0735);
#5903=VECTOR('',#21024,3.0735);
#5904=VECTOR('',#21027,3.0735);
#5905=VECTOR('',#21030,3.0735);
#5906=VECTOR('',#21033,3.0735);
#5907=VECTOR('',#21036,3.0735);
#5908=VECTOR('',#21039,3.0735);
#5909=VECTOR('',#21042,3.0735);
#5910=VECTOR('',#21167,60.);
#5911=VECTOR('',#21174,70.);
#5912=VECTOR('',#21185,1.5);
#5913=VECTOR('',#21188,1.5);
#5914=VECTOR('',#21199,1.5);
#5915=VECTOR('',#21202,1.5);
#5916=VECTOR('',#21205,1.5);
#5917=VECTOR('',#21208,1.5);
#5918=VECTOR('',#21211,1.5);
#5919=VECTOR('',#21214,1.5);
#5920=VECTOR('',#21217,1.5);
#5921=VECTOR('',#21222,1.543);
#5922=VECTOR('',#21227,1.543);
#5923=VECTOR('',#21230,1.543);
#5924=VECTOR('',#21233,1.543);
#5925=VECTOR('',#21236,1.543);
#5926=VECTOR('',#21239,1.543);
#5927=VECTOR('',#21242,1.543);
#5928=VECTOR('',#21245,1.543);
#5929=VECTOR('',#21250,1.5);
#5930=VECTOR('',#21253,1.5);
#5931=VECTOR('',#21264,1.5);
#5932=VECTOR('',#21267,1.5);
#5933=VECTOR('',#21270,1.5);
#5934=VECTOR('',#21273,1.5);
#5935=VECTOR('',#21276,1.5);
#5936=VECTOR('',#21279,1.5);
#5937=VECTOR('',#21282,1.5);
#5938=VECTOR('',#21287,1.54299999999999);
#5939=VECTOR('',#21292,1.54299999999999);
#5940=VECTOR('',#21295,1.54299999999999);
#5941=VECTOR('',#21298,1.54299999999999);
#5942=VECTOR('',#21301,1.54299999999999);
#5943=VECTOR('',#21304,1.54299999999999);
#5944=VECTOR('',#21307,1.54299999999999);
#5945=VECTOR('',#21310,1.54299999999999);
#5946=VECTOR('',#21315,1.5);
#5947=VECTOR('',#21318,1.5);
#5948=VECTOR('',#21329,1.5);
#5949=VECTOR('',#21332,1.5);
#5950=VECTOR('',#21335,1.5);
#5951=VECTOR('',#21338,1.5);
#5952=VECTOR('',#21341,1.5);
#5953=VECTOR('',#21344,1.5);
#5954=VECTOR('',#21347,1.5);
#5955=VECTOR('',#21352,1.543);
#5956=VECTOR('',#21357,1.543);
#5957=VECTOR('',#21360,1.543);
#5958=VECTOR('',#21363,1.543);
#5959=VECTOR('',#21366,1.543);
#5960=VECTOR('',#21369,1.543);
#5961=VECTOR('',#21372,1.543);
#5962=VECTOR('',#21375,1.543);
#5963=VECTOR('',#21380,1.5);
#5964=VECTOR('',#21383,1.5);
#5965=VECTOR('',#21394,1.5);
#5966=VECTOR('',#21397,1.5);
#5967=VECTOR('',#21400,1.5);
#5968=VECTOR('',#21403,1.5);
#5969=VECTOR('',#21406,1.5);
#5970=VECTOR('',#21409,1.5);
#5971=VECTOR('',#21412,1.5);
#5972=VECTOR('',#21417,1.543);
#5973=VECTOR('',#21422,1.543);
#5974=VECTOR('',#21425,1.543);
#5975=VECTOR('',#21428,1.543);
#5976=VECTOR('',#21431,1.543);
#5977=VECTOR('',#21434,1.543);
#5978=VECTOR('',#21437,1.543);
#5979=VECTOR('',#21440,1.543);
#5980=VECTOR('',#21445,1.5);
#5981=VECTOR('',#21448,1.5);
#5982=VECTOR('',#21459,1.5);
#5983=VECTOR('',#21462,1.5);
#5984=VECTOR('',#21465,1.5);
#5985=VECTOR('',#21468,1.5);
#5986=VECTOR('',#21471,1.5);
#5987=VECTOR('',#21474,1.5);
#5988=VECTOR('',#21477,1.5);
#5989=VECTOR('',#21482,1.54300000000001);
#5990=VECTOR('',#21487,1.54300000000001);
#5991=VECTOR('',#21490,1.54300000000001);
#5992=VECTOR('',#21493,1.54300000000001);
#5993=VECTOR('',#21496,1.54300000000001);
#5994=VECTOR('',#21499,1.54300000000001);
#5995=VECTOR('',#21502,1.54300000000001);
#5996=VECTOR('',#21505,1.54300000000001);
#5997=VECTOR('',#21510,1.5);
#5998=VECTOR('',#21513,1.5);
#5999=VECTOR('',#21524,1.5);
#6000=VECTOR('',#21527,1.5);
#6001=VECTOR('',#21530,1.5);
#6002=VECTOR('',#21533,1.5);
#6003=VECTOR('',#21536,1.5);
#6004=VECTOR('',#21539,1.5);
#6005=VECTOR('',#21542,1.5);
#6006=VECTOR('',#21547,1.54300000000001);
#6007=VECTOR('',#21552,1.54300000000001);
#6008=VECTOR('',#21555,1.54300000000001);
#6009=VECTOR('',#21558,1.54300000000001);
#6010=VECTOR('',#21561,1.54300000000001);
#6011=VECTOR('',#21564,1.54300000000001);
#6012=VECTOR('',#21567,1.54300000000001);
#6013=VECTOR('',#21570,1.54300000000001);
#6014=VECTOR('',#21575,1.5);
#6015=VECTOR('',#21578,1.5);
#6016=VECTOR('',#21589,1.5);
#6017=VECTOR('',#21592,1.5);
#6018=VECTOR('',#21595,1.5);
#6019=VECTOR('',#21598,1.5);
#6020=VECTOR('',#21601,1.5);
#6021=VECTOR('',#21604,1.5);
#6022=VECTOR('',#21607,1.5);
#6023=VECTOR('',#21612,1.543);
#6024=VECTOR('',#21617,1.543);
#6025=VECTOR('',#21620,1.543);
#6026=VECTOR('',#21623,1.543);
#6027=VECTOR('',#21626,1.543);
#6028=VECTOR('',#21629,1.543);
#6029=VECTOR('',#21632,1.543);
#6030=VECTOR('',#21635,1.543);
#6031=VECTOR('',#21640,1.5);
#6032=VECTOR('',#21643,1.5);
#6033=VECTOR('',#21654,1.5);
#6034=VECTOR('',#21657,1.5);
#6035=VECTOR('',#21660,1.5);
#6036=VECTOR('',#21663,1.5);
#6037=VECTOR('',#21666,1.5);
#6038=VECTOR('',#21669,1.5);
#6039=VECTOR('',#21672,1.5);
#6040=VECTOR('',#21677,1.54300000000001);
#6041=VECTOR('',#21682,1.54300000000001);
#6042=VECTOR('',#21685,1.54300000000001);
#6043=VECTOR('',#21688,1.54300000000001);
#6044=VECTOR('',#21691,1.54300000000001);
#6045=VECTOR('',#21694,1.54300000000001);
#6046=VECTOR('',#21697,1.54300000000001);
#6047=VECTOR('',#21700,1.54300000000001);
#6048=VECTOR('',#21705,1.5);
#6049=VECTOR('',#21708,1.5);
#6050=VECTOR('',#21719,1.5);
#6051=VECTOR('',#21722,1.5);
#6052=VECTOR('',#21725,1.5);
#6053=VECTOR('',#21728,1.5);
#6054=VECTOR('',#21731,1.5);
#6055=VECTOR('',#21734,1.5);
#6056=VECTOR('',#21737,1.5);
#6057=VECTOR('',#21742,1.54300000000001);
#6058=VECTOR('',#21747,1.54300000000001);
#6059=VECTOR('',#21750,1.54300000000001);
#6060=VECTOR('',#21753,1.54300000000001);
#6061=VECTOR('',#21756,1.54300000000001);
#6062=VECTOR('',#21759,1.54300000000001);
#6063=VECTOR('',#21762,1.54300000000001);
#6064=VECTOR('',#21765,1.54300000000001);
#6065=VECTOR('',#21770,1.5);
#6066=VECTOR('',#21773,1.5);
#6067=VECTOR('',#21784,1.5);
#6068=VECTOR('',#21787,1.5);
#6069=VECTOR('',#21790,1.5);
#6070=VECTOR('',#21793,1.5);
#6071=VECTOR('',#21796,1.5);
#6072=VECTOR('',#21799,1.5);
#6073=VECTOR('',#21802,1.5);
#6074=VECTOR('',#21807,1.543);
#6075=VECTOR('',#21812,1.543);
#6076=VECTOR('',#21815,1.543);
#6077=VECTOR('',#21818,1.543);
#6078=VECTOR('',#21821,1.543);
#6079=VECTOR('',#21824,1.543);
#6080=VECTOR('',#21827,1.543);
#6081=VECTOR('',#21830,1.543);
#6082=VECTOR('',#21835,1.5);
#6083=VECTOR('',#21838,1.5);
#6084=VECTOR('',#21849,1.5);
#6085=VECTOR('',#21852,1.5);
#6086=VECTOR('',#21855,1.5);
#6087=VECTOR('',#21858,1.5);
#6088=VECTOR('',#21861,1.5);
#6089=VECTOR('',#21864,1.5);
#6090=VECTOR('',#21867,1.5);
#6091=VECTOR('',#21872,1.54299999999999);
#6092=VECTOR('',#21877,1.54299999999999);
#6093=VECTOR('',#21880,1.54299999999999);
#6094=VECTOR('',#21883,1.54299999999999);
#6095=VECTOR('',#21886,1.54299999999999);
#6096=VECTOR('',#21889,1.54299999999999);
#6097=VECTOR('',#21892,1.54299999999999);
#6098=VECTOR('',#21895,1.54299999999999);
#6099=VECTOR('',#21900,1.5);
#6100=VECTOR('',#21903,1.5);
#6101=VECTOR('',#21914,1.5);
#6102=VECTOR('',#21917,1.5);
#6103=VECTOR('',#21920,1.5);
#6104=VECTOR('',#21923,1.5);
#6105=VECTOR('',#21926,1.5);
#6106=VECTOR('',#21929,1.5);
#6107=VECTOR('',#21932,1.5);
#6108=VECTOR('',#21937,1.543);
#6109=VECTOR('',#21942,1.543);
#6110=VECTOR('',#21945,1.543);
#6111=VECTOR('',#21948,1.543);
#6112=VECTOR('',#21951,1.543);
#6113=VECTOR('',#21954,1.543);
#6114=VECTOR('',#21957,1.543);
#6115=VECTOR('',#21960,1.543);
#6116=VECTOR('',#21965,10.);
#6117=VECTOR('',#21966,10.);
#6118=VECTOR('',#21967,10.);
#6119=VECTOR('',#21968,10.);
#6120=VECTOR('',#21971,10.);
#6121=VECTOR('',#21972,10.);
#6122=VECTOR('',#21973,10.);
#6123=VECTOR('',#21976,10.);
#6124=VECTOR('',#21977,10.);
#6125=VECTOR('',#21978,10.);
#6126=VECTOR('',#21981,10.);
#6127=VECTOR('',#21986,10.);
#6128=VECTOR('',#21987,10.);
#6129=VECTOR('',#21988,10.);
#6130=VECTOR('',#21989,10.);
#6131=VECTOR('',#21990,10.);
#6132=VECTOR('',#21995,10.);
#6133=VECTOR('',#21996,10.);
#6134=VECTOR('',#21997,10.);
#6135=VECTOR('',#21998,10.);
#6136=VECTOR('',#21999,10.);
#6137=VECTOR('',#22004,10.);
#6138=VECTOR('',#22005,10.);
#6139=VECTOR('',#22006,10.);
#6140=VECTOR('',#22007,10.);
#6141=VECTOR('',#22008,10.);
#6142=VECTOR('',#22013,10.);
#6143=VECTOR('',#22014,10.);
#6144=VECTOR('',#22015,10.);
#6145=VECTOR('',#22016,10.);
#6146=VECTOR('',#22017,10.);
#6147=VECTOR('',#22022,10.);
#6148=VECTOR('',#22023,10.);
#6149=VECTOR('',#22024,10.);
#6150=VECTOR('',#22025,10.);
#6151=VECTOR('',#22026,10.);
#6152=VECTOR('',#22031,10.);
#6153=VECTOR('',#22032,10.);
#6154=VECTOR('',#22033,10.);
#6155=VECTOR('',#22034,10.);
#6156=VECTOR('',#22069,10.);
#6157=VECTOR('',#22072,10.);
#6158=VECTOR('',#22075,10.);
#6159=VECTOR('',#22078,10.);
#6160=VECTOR('',#22081,10.);
#6161=VECTOR('',#22084,10.);
#6162=VECTOR('',#22087,10.);
#6163=VECTOR('',#22090,10.);
#6164=VECTOR('',#22093,10.);
#6165=VECTOR('',#22096,10.);
#6166=VECTOR('',#22129,10.);
#6167=VECTOR('',#22132,10.);
#6168=VECTOR('',#22135,10.);
#6169=VECTOR('',#22138,10.);
#6170=VECTOR('',#22141,10.);
#6171=VECTOR('',#22144,10.);
#6172=VECTOR('',#22147,10.);
#6173=VECTOR('',#22150,10.);
#6174=VECTOR('',#22153,10.);
#6175=VECTOR('',#22156,10.);
#6176=VECTOR('',#22165,10.);
#6177=VECTOR('',#22168,10.);
#6178=VECTOR('',#22177,10.);
#6179=VECTOR('',#22180,10.);
#6180=VECTOR('',#22185,1.5);
#6181=VECTOR('',#22192,3.);
#6182=VECTOR('',#22193,3.);
#6183=VECTOR('',#22202,1.5);
#6184=VECTOR('',#22209,3.);
#6185=VECTOR('',#22210,3.);
#6186=VECTOR('',#22219,1.5);
#6187=VECTOR('',#22226,3.);
#6188=VECTOR('',#22227,3.);
#6189=VECTOR('',#22236,1.5);
#6190=VECTOR('',#22243,3.);
#6191=VECTOR('',#22244,3.);
#6192=VECTOR('',#22253,1.5);
#6193=VECTOR('',#22260,3.);
#6194=VECTOR('',#22261,3.);
#6195=VECTOR('',#22270,1.5);
#6196=VECTOR('',#22277,3.);
#6197=VECTOR('',#22278,3.);
#6198=VECTOR('',#22285,10.);
#6199=VECTOR('',#22286,10.);
#6200=VECTOR('',#22289,10.);
#6201=VECTOR('',#22290,10.);
#6202=VECTOR('',#22293,10.);
#6203=VECTOR('',#22294,10.);
#6204=VECTOR('',#22297,10.);
#6205=VECTOR('',#22300,10.);
#6206=VECTOR('',#22301,10.);
#6207=VECTOR('',#22304,10.);
#6208=VECTOR('',#22305,10.);
#6209=VECTOR('',#22308,10.);
#6210=VECTOR('',#22309,10.);
#6211=VECTOR('',#22312,10.);
#6212=VECTOR('',#22315,10.);
#6213=VECTOR('',#22316,10.);
#6214=VECTOR('',#22319,10.);
#6215=VECTOR('',#22320,10.);
#6216=VECTOR('',#22323,10.);
#6217=VECTOR('',#22324,10.);
#6218=VECTOR('',#22327,10.);
#6219=VECTOR('',#22330,10.);
#6220=VECTOR('',#22331,10.);
#6221=VECTOR('',#22334,10.);
#6222=VECTOR('',#22335,10.);
#6223=VECTOR('',#22338,10.);
#6224=VECTOR('',#22339,10.);
#6225=VECTOR('',#22342,10.);
#6226=VECTOR('',#22345,10.);
#6227=VECTOR('',#22346,10.);
#6228=VECTOR('',#22349,10.);
#6229=VECTOR('',#22350,10.);
#6230=VECTOR('',#22353,10.);
#6231=VECTOR('',#22354,10.);
#6232=VECTOR('',#22357,10.);
#6233=VECTOR('',#22358,10.);
#6234=VECTOR('',#22359,10.);
#6235=VECTOR('',#22360,10.);
#6236=VECTOR('',#22361,10.);
#6237=VECTOR('',#22362,10.);
#6238=VECTOR('',#22363,10.);
#6239=VECTOR('',#22364,10.);
#6240=VECTOR('',#22365,10.);
#6241=VECTOR('',#22368,10.);
#6242=VECTOR('',#22369,10.);
#6243=VECTOR('',#22372,10.);
#6244=VECTOR('',#22373,10.);
#6245=VECTOR('',#22376,10.);
#6246=VECTOR('',#22377,10.);
#6247=VECTOR('',#22380,10.);
#6248=VECTOR('',#22381,10.);
#6249=VECTOR('',#22384,10.);
#6250=VECTOR('',#22389,10.);
#6251=VECTOR('',#22394,10.);
#6252=VECTOR('',#22397,10.);
#6253=VECTOR('',#22402,10.);
#6254=VECTOR('',#22407,10.);
#6255=VECTOR('',#22410,10.);
#6256=VECTOR('',#22415,10.);
#6257=VECTOR('',#22420,10.);
#6258=VECTOR('',#22427,10.);
#6259=VECTOR('',#22432,10.);
#6260=VECTOR('',#22437,10.);
#6261=VECTOR('',#22442,10.);
#6262=VECTOR('',#22445,10.);
#6263=VECTOR('',#22448,10.);
#6264=VECTOR('',#22451,10.);
#6265=VECTOR('',#22454,10.);
#6266=VECTOR('',#22457,10.);
#6267=VECTOR('',#22460,10.);
#6268=VECTOR('',#22461,10.);
#6269=VECTOR('',#22464,10.);
#6270=VECTOR('',#22473,10.);
#6271=VECTOR('',#22476,10.);
#6272=VECTOR('',#22479,10.);
#6273=VECTOR('',#22482,10.);
#6274=VECTOR('',#22485,10.);
#6275=VECTOR('',#22486,10.);
#6276=VECTOR('',#22487,10.);
#6277=VECTOR('',#22492,10.);
#6278=VECTOR('',#22495,10.);
#6279=VECTOR('',#22496,10.);
#6280=VECTOR('',#22505,10.);
#6281=VECTOR('',#22510,10.);
#6282=VECTOR('',#22513,10.);
#6283=VECTOR('',#22516,10.);
#6284=VECTOR('',#22517,10.);
#6285=VECTOR('',#22518,10.);
#6286=VECTOR('',#22523,10.);
#6287=VECTOR('',#22526,10.);
#6288=VECTOR('',#22527,10.);
#6289=VECTOR('',#22534,10.);
#6290=VECTOR('',#22543,9.);
#6291=VECTOR('',#22554,9.);
#6292=VECTOR('',#22569,10.);
#6293=VECTOR('',#22580,12.);
#6294=VECTOR('',#22583,10.);
#6295=VECTOR('',#22594,10.);
#6296=VECTOR('',#22595,10.);
#6297=VECTOR('',#22596,10.);
#6298=VECTOR('',#22597,10.);
#6299=VECTOR('',#22604,10.);
#6300=VECTOR('',#22607,10.);
#6301=VECTOR('',#22608,10.);
#6302=VECTOR('',#22609,10.);
#6303=VECTOR('',#22626,6.);
#6304=VECTOR('',#22645,4.);
#6305=VECTOR('',#22648,2.5);
#6306=VECTOR('',#22661,4.);
#6307=VECTOR('',#22664,2.5);
#6308=VECTOR('',#22677,4.);
#6309=VECTOR('',#22680,2.5);
#6310=VECTOR('',#22693,4.);
#6311=VECTOR('',#22696,2.5);
#6312=VECTOR('',#22709,4.);
#6313=VECTOR('',#22712,2.5);
#6314=VECTOR('',#22725,4.);
#6315=VECTOR('',#22728,2.5);
#6316=VECTOR('',#22735,12.);
#6317=VECTOR('',#22742,70.);
#6318=VECTOR('',#22755,12.);
#6319=VECTOR('',#22762,60.);
#6320=VECTOR('',#22775,2.5);
#6321=VECTOR('',#22780,2.);
#6322=VECTOR('',#22787,2.5);
#6323=VECTOR('',#22792,2.);
#6324=VECTOR('',#22799,2.5);
#6325=VECTOR('',#22804,2.);
#6326=VECTOR('',#22811,2.5);
#6327=VECTOR('',#22816,2.);
#6328=VECTOR('',#22823,2.5);
#6329=VECTOR('',#22828,2.);
#6330=VECTOR('',#22835,2.5);
#6331=VECTOR('',#22840,2.);
#6332=VECTOR('',#22847,50.);
#6333=VECTOR('',#22854,59.);
#6334=VECTOR('',#22867,10.);
#6335=VECTOR('',#22874,12.);
#6336=VECTOR('',#22887,10.);
#6337=VECTOR('',#22894,12.);
#6338=VECTOR('',#22907,10.);
#6339=VECTOR('',#22914,14.);
#6340=VECTOR('',#22925,10.);
#6341=VECTOR('',#22926,10.);
#6342=VECTOR('',#22927,10.);
#6343=VECTOR('',#22928,10.);
#6344=VECTOR('',#22931,10.);
#6345=VECTOR('',#22932,10.);
#6346=VECTOR('',#22933,10.);
#6347=VECTOR('',#22934,10.);
#6348=VECTOR('',#22963,2.5);
#6349=VECTOR('',#22968,1.5);
#6350=VECTOR('',#22987,2.);
#6351=VECTOR('',#22992,2.);
#6352=VECTOR('',#22995,2.);
#6353=VECTOR('',#22998,2.);
#6354=VECTOR('',#23001,2.);
#6355=VECTOR('',#23004,2.);
#6356=VECTOR('',#23007,2.);
#6357=VECTOR('',#23010,2.);
#6358=VECTOR('',#23013,2.);
#6359=VECTOR('',#23016,2.);
#6360=VECTOR('',#23019,2.);
#6361=VECTOR('',#23022,2.);
#6362=VECTOR('',#23025,2.);
#6363=VECTOR('',#23028,2.);
#6364=VECTOR('',#23031,2.);
#6365=VECTOR('',#23034,2.);
#6366=VECTOR('',#23037,1.5555);
#6367=VECTOR('',#23042,1.5555);
#6368=VECTOR('',#23045,1.5555);
#6369=VECTOR('',#23048,1.5555);
#6370=VECTOR('',#23051,1.5555);
#6371=VECTOR('',#23054,1.5555);
#6372=VECTOR('',#23057,1.5555);
#6373=VECTOR('',#23060,1.5555);
#6374=VECTOR('',#23063,1.5555);
#6375=VECTOR('',#23066,1.5555);
#6376=VECTOR('',#23069,1.5555);
#6377=VECTOR('',#23072,1.5555);
#6378=VECTOR('',#23075,1.5555);
#6379=VECTOR('',#23078,1.5555);
#6380=VECTOR('',#23081,1.5555);
#6381=VECTOR('',#23084,1.5555);
#6382=VECTOR('',#23089,1.5);
#6383=VECTOR('',#23100,10.);
#6384=VECTOR('',#23101,10.);
#6385=VECTOR('',#23102,10.);
#6386=VECTOR('',#23103,10.);
#6387=VECTOR('',#23106,10.);
#6388=VECTOR('',#23107,10.);
#6389=VECTOR('',#23108,10.);
#6390=VECTOR('',#23111,10.);
#6391=VECTOR('',#23112,10.);
#6392=VECTOR('',#23113,10.);
#6393=VECTOR('',#23116,10.);
#6394=VECTOR('',#23117,10.);
#6395=VECTOR('',#23118,10.);
#6396=VECTOR('',#23121,10.);
#6397=VECTOR('',#23122,10.);
#6398=VECTOR('',#23123,10.);
#6399=VECTOR('',#23126,10.);
#6400=VECTOR('',#23127,10.);
#6401=VECTOR('',#23136,3.5);
#6402=VECTOR('',#23147,1.5);
#6403=VECTOR('',#23152,1.5);
#6404=VECTOR('',#23155,1.5);
#6405=VECTOR('',#23158,1.5);
#6406=VECTOR('',#23161,1.5);
#6407=VECTOR('',#23164,1.5);
#6408=VECTOR('',#23167,1.5);
#6409=VECTOR('',#23170,1.5);
#6410=VECTOR('',#23173,1.17775);
#6411=VECTOR('',#23178,1.17775);
#6412=VECTOR('',#23181,1.17775);
#6413=VECTOR('',#23184,1.17775);
#6414=VECTOR('',#23187,1.17775);
#6415=VECTOR('',#23190,1.17775);
#6416=VECTOR('',#23193,1.17775);
#6417=VECTOR('',#23196,1.17775);
#6418=VECTOR('',#23201,1.25);
#6419=VECTOR('',#23210,10.);
#6420=VECTOR('',#23211,10.);
#6421=VECTOR('',#23212,10.);
#6422=VECTOR('',#23213,10.);
#6423=VECTOR('',#23216,10.);
#6424=VECTOR('',#23217,10.);
#6425=VECTOR('',#23218,10.);
#6426=VECTOR('',#23221,10.);
#6427=VECTOR('',#23222,10.);
#6428=VECTOR('',#23223,10.);
#6429=VECTOR('',#23226,10.);
#6430=VECTOR('',#23227,10.);
#6431=VECTOR('',#23228,10.);
#6432=VECTOR('',#23231,10.);
#6433=VECTOR('',#23232,10.);
#6434=VECTOR('',#23233,10.);
#6435=VECTOR('',#23236,10.);
#6436=VECTOR('',#23237,10.);
#6437=VECTOR('',#23254,2.25);
#6438=VERTEX_POINT('',#23378);
#6439=VERTEX_POINT('',#23379);
#6440=VERTEX_POINT('',#23381);
#6441=VERTEX_POINT('',#23404);
#6442=VERTEX_POINT('',#23406);
#6443=VERTEX_POINT('',#23414);
#6444=VERTEX_POINT('',#23440);
#6445=VERTEX_POINT('',#23441);
#6446=VERTEX_POINT('',#23491);
#6447=VERTEX_POINT('',#23492);
#6448=VERTEX_POINT('',#23539);
#6449=VERTEX_POINT('',#23540);
#6450=VERTEX_POINT('',#23587);
#6451=VERTEX_POINT('',#23588);
#6452=VERTEX_POINT('',#23638);
#6453=VERTEX_POINT('',#23639);
#6454=VERTEX_POINT('',#23686);
#6455=VERTEX_POINT('',#23687);
#6456=VERTEX_POINT('',#23734);
#6457=VERTEX_POINT('',#23735);
#6458=VERTEX_POINT('',#23785);
#6459=VERTEX_POINT('',#23786);
#6460=VERTEX_POINT('',#23836);
#6461=VERTEX_POINT('',#23837);
#6462=VERTEX_POINT('',#23884);
#6463=VERTEX_POINT('',#23885);
#6464=VERTEX_POINT('',#23935);
#6465=VERTEX_POINT('',#23936);
#6466=VERTEX_POINT('',#23938);
#6467=VERTEX_POINT('',#23952);
#6468=VERTEX_POINT('',#23974);
#6469=VERTEX_POINT('',#23975);
#6470=VERTEX_POINT('',#23977);
#6471=VERTEX_POINT('',#23985);
#6472=VERTEX_POINT('',#23996);
#6473=VERTEX_POINT('',#23997);
#6474=VERTEX_POINT('',#24020);
#6475=VERTEX_POINT('',#24021);
#6476=VERTEX_POINT('',#24045);
#6477=VERTEX_POINT('',#24046);
#6478=VERTEX_POINT('',#24070);
#6479=VERTEX_POINT('',#24071);
#6480=VERTEX_POINT('',#24094);
#6481=VERTEX_POINT('',#24095);
#6482=VERTEX_POINT('',#24119);
#6483=VERTEX_POINT('',#24120);
#6484=VERTEX_POINT('',#24143);
#6485=VERTEX_POINT('',#24144);
#6486=VERTEX_POINT('',#24168);
#6487=VERTEX_POINT('',#24169);
#6488=VERTEX_POINT('',#24192);
#6489=VERTEX_POINT('',#24193);
#6490=VERTEX_POINT('',#24217);
#6491=VERTEX_POINT('',#24218);
#6492=VERTEX_POINT('',#24242);
#6493=VERTEX_POINT('',#24243);
#6494=VERTEX_POINT('',#24266);
#6495=VERTEX_POINT('',#24267);
#6496=VERTEX_POINT('',#24269);
#6497=VERTEX_POINT('',#24275);
#6498=VERTEX_POINT('',#24283);
#6499=VERTEX_POINT('',#24284);
#6500=VERTEX_POINT('',#24286);
#6501=VERTEX_POINT('',#24309);
#6502=VERTEX_POINT('',#24311);
#6503=VERTEX_POINT('',#24319);
#6504=VERTEX_POINT('',#24345);
#6505=VERTEX_POINT('',#24346);
#6506=VERTEX_POINT('',#24396);
#6507=VERTEX_POINT('',#24397);
#6508=VERTEX_POINT('',#24444);
#6509=VERTEX_POINT('',#24445);
#6510=VERTEX_POINT('',#24492);
#6511=VERTEX_POINT('',#24493);
#6512=VERTEX_POINT('',#24543);
#6513=VERTEX_POINT('',#24544);
#6514=VERTEX_POINT('',#24591);
#6515=VERTEX_POINT('',#24592);
#6516=VERTEX_POINT('',#24639);
#6517=VERTEX_POINT('',#24640);
#6518=VERTEX_POINT('',#24690);
#6519=VERTEX_POINT('',#24691);
#6520=VERTEX_POINT('',#24741);
#6521=VERTEX_POINT('',#24742);
#6522=VERTEX_POINT('',#24789);
#6523=VERTEX_POINT('',#24790);
#6524=VERTEX_POINT('',#24840);
#6525=VERTEX_POINT('',#24841);
#6526=VERTEX_POINT('',#24843);
#6527=VERTEX_POINT('',#24857);
#6528=VERTEX_POINT('',#24879);
#6529=VERTEX_POINT('',#24880);
#6530=VERTEX_POINT('',#24882);
#6531=VERTEX_POINT('',#24890);
#6532=VERTEX_POINT('',#24901);
#6533=VERTEX_POINT('',#24902);
#6534=VERTEX_POINT('',#24925);
#6535=VERTEX_POINT('',#24926);
#6536=VERTEX_POINT('',#24950);
#6537=VERTEX_POINT('',#24951);
#6538=VERTEX_POINT('',#24975);
#6539=VERTEX_POINT('',#24976);
#6540=VERTEX_POINT('',#24999);
#6541=VERTEX_POINT('',#25000);
#6542=VERTEX_POINT('',#25024);
#6543=VERTEX_POINT('',#25025);
#6544=VERTEX_POINT('',#25048);
#6545=VERTEX_POINT('',#25049);
#6546=VERTEX_POINT('',#25073);
#6547=VERTEX_POINT('',#25074);
#6548=VERTEX_POINT('',#25097);
#6549=VERTEX_POINT('',#25098);
#6550=VERTEX_POINT('',#25122);
#6551=VERTEX_POINT('',#25123);
#6552=VERTEX_POINT('',#25147);
#6553=VERTEX_POINT('',#25148);
#6554=VERTEX_POINT('',#25171);
#6555=VERTEX_POINT('',#25172);
#6556=VERTEX_POINT('',#25174);
#6557=VERTEX_POINT('',#25180);
#6558=VERTEX_POINT('',#25188);
#6559=VERTEX_POINT('',#25189);
#6560=VERTEX_POINT('',#25191);
#6561=VERTEX_POINT('',#25214);
#6562=VERTEX_POINT('',#25216);
#6563=VERTEX_POINT('',#25224);
#6564=VERTEX_POINT('',#25250);
#6565=VERTEX_POINT('',#25251);
#6566=VERTEX_POINT('',#25301);
#6567=VERTEX_POINT('',#25302);
#6568=VERTEX_POINT('',#25349);
#6569=VERTEX_POINT('',#25350);
#6570=VERTEX_POINT('',#25397);
#6571=VERTEX_POINT('',#25398);
#6572=VERTEX_POINT('',#25448);
#6573=VERTEX_POINT('',#25449);
#6574=VERTEX_POINT('',#25496);
#6575=VERTEX_POINT('',#25497);
#6576=VERTEX_POINT('',#25544);
#6577=VERTEX_POINT('',#25545);
#6578=VERTEX_POINT('',#25595);
#6579=VERTEX_POINT('',#25596);
#6580=VERTEX_POINT('',#25646);
#6581=VERTEX_POINT('',#25647);
#6582=VERTEX_POINT('',#25694);
#6583=VERTEX_POINT('',#25695);
#6584=VERTEX_POINT('',#25745);
#6585=VERTEX_POINT('',#25746);
#6586=VERTEX_POINT('',#25748);
#6587=VERTEX_POINT('',#25762);
#6588=VERTEX_POINT('',#25784);
#6589=VERTEX_POINT('',#25785);
#6590=VERTEX_POINT('',#25787);
#6591=VERTEX_POINT('',#25795);
#6592=VERTEX_POINT('',#25806);
#6593=VERTEX_POINT('',#25807);
#6594=VERTEX_POINT('',#25830);
#6595=VERTEX_POINT('',#25831);
#6596=VERTEX_POINT('',#25855);
#6597=VERTEX_POINT('',#25856);
#6598=VERTEX_POINT('',#25880);
#6599=VERTEX_POINT('',#25881);
#6600=VERTEX_POINT('',#25904);
#6601=VERTEX_POINT('',#25905);
#6602=VERTEX_POINT('',#25929);
#6603=VERTEX_POINT('',#25930);
#6604=VERTEX_POINT('',#25953);
#6605=VERTEX_POINT('',#25954);
#6606=VERTEX_POINT('',#25978);
#6607=VERTEX_POINT('',#25979);
#6608=VERTEX_POINT('',#26002);
#6609=VERTEX_POINT('',#26003);
#6610=VERTEX_POINT('',#26027);
#6611=VERTEX_POINT('',#26028);
#6612=VERTEX_POINT('',#26052);
#6613=VERTEX_POINT('',#26053);
#6614=VERTEX_POINT('',#26076);
#6615=VERTEX_POINT('',#26077);
#6616=VERTEX_POINT('',#26079);
#6617=VERTEX_POINT('',#26085);
#6618=VERTEX_POINT('',#26093);
#6619=VERTEX_POINT('',#26094);
#6620=VERTEX_POINT('',#26096);
#6621=VERTEX_POINT('',#26119);
#6622=VERTEX_POINT('',#26121);
#6623=VERTEX_POINT('',#26129);
#6624=VERTEX_POINT('',#26155);
#6625=VERTEX_POINT('',#26156);
#6626=VERTEX_POINT('',#26206);
#6627=VERTEX_POINT('',#26207);
#6628=VERTEX_POINT('',#26254);
#6629=VERTEX_POINT('',#26255);
#6630=VERTEX_POINT('',#26302);
#6631=VERTEX_POINT('',#26303);
#6632=VERTEX_POINT('',#26353);
#6633=VERTEX_POINT('',#26354);
#6634=VERTEX_POINT('',#26401);
#6635=VERTEX_POINT('',#26402);
#6636=VERTEX_POINT('',#26449);
#6637=VERTEX_POINT('',#26450);
#6638=VERTEX_POINT('',#26500);
#6639=VERTEX_POINT('',#26501);
#6640=VERTEX_POINT('',#26551);
#6641=VERTEX_POINT('',#26552);
#6642=VERTEX_POINT('',#26599);
#6643=VERTEX_POINT('',#26600);
#6644=VERTEX_POINT('',#26650);
#6645=VERTEX_POINT('',#26651);
#6646=VERTEX_POINT('',#26653);
#6647=VERTEX_POINT('',#26667);
#6648=VERTEX_POINT('',#26689);
#6649=VERTEX_POINT('',#26690);
#6650=VERTEX_POINT('',#26692);
#6651=VERTEX_POINT('',#26700);
#6652=VERTEX_POINT('',#26711);
#6653=VERTEX_POINT('',#26712);
#6654=VERTEX_POINT('',#26735);
#6655=VERTEX_POINT('',#26736);
#6656=VERTEX_POINT('',#26760);
#6657=VERTEX_POINT('',#26761);
#6658=VERTEX_POINT('',#26785);
#6659=VERTEX_POINT('',#26786);
#6660=VERTEX_POINT('',#26809);
#6661=VERTEX_POINT('',#26810);
#6662=VERTEX_POINT('',#26834);
#6663=VERTEX_POINT('',#26835);
#6664=VERTEX_POINT('',#26858);
#6665=VERTEX_POINT('',#26859);
#6666=VERTEX_POINT('',#26883);
#6667=VERTEX_POINT('',#26884);
#6668=VERTEX_POINT('',#26907);
#6669=VERTEX_POINT('',#26908);
#6670=VERTEX_POINT('',#26932);
#6671=VERTEX_POINT('',#26933);
#6672=VERTEX_POINT('',#26957);
#6673=VERTEX_POINT('',#26958);
#6674=VERTEX_POINT('',#26981);
#6675=VERTEX_POINT('',#26982);
#6676=VERTEX_POINT('',#26984);
#6677=VERTEX_POINT('',#26990);
#6678=VERTEX_POINT('',#26998);
#6679=VERTEX_POINT('',#26999);
#6680=VERTEX_POINT('',#27001);
#6681=VERTEX_POINT('',#27024);
#6682=VERTEX_POINT('',#27026);
#6683=VERTEX_POINT('',#27034);
#6684=VERTEX_POINT('',#27060);
#6685=VERTEX_POINT('',#27061);
#6686=VERTEX_POINT('',#27111);
#6687=VERTEX_POINT('',#27112);
#6688=VERTEX_POINT('',#27159);
#6689=VERTEX_POINT('',#27160);
#6690=VERTEX_POINT('',#27207);
#6691=VERTEX_POINT('',#27208);
#6692=VERTEX_POINT('',#27258);
#6693=VERTEX_POINT('',#27259);
#6694=VERTEX_POINT('',#27306);
#6695=VERTEX_POINT('',#27307);
#6696=VERTEX_POINT('',#27354);
#6697=VERTEX_POINT('',#27355);
#6698=VERTEX_POINT('',#27405);
#6699=VERTEX_POINT('',#27406);
#6700=VERTEX_POINT('',#27456);
#6701=VERTEX_POINT('',#27457);
#6702=VERTEX_POINT('',#27504);
#6703=VERTEX_POINT('',#27505);
#6704=VERTEX_POINT('',#27555);
#6705=VERTEX_POINT('',#27556);
#6706=VERTEX_POINT('',#27558);
#6707=VERTEX_POINT('',#27572);
#6708=VERTEX_POINT('',#27594);
#6709=VERTEX_POINT('',#27595);
#6710=VERTEX_POINT('',#27597);
#6711=VERTEX_POINT('',#27605);
#6712=VERTEX_POINT('',#27616);
#6713=VERTEX_POINT('',#27617);
#6714=VERTEX_POINT('',#27640);
#6715=VERTEX_POINT('',#27641);
#6716=VERTEX_POINT('',#27665);
#6717=VERTEX_POINT('',#27666);
#6718=VERTEX_POINT('',#27690);
#6719=VERTEX_POINT('',#27691);
#6720=VERTEX_POINT('',#27714);
#6721=VERTEX_POINT('',#27715);
#6722=VERTEX_POINT('',#27739);
#6723=VERTEX_POINT('',#27740);
#6724=VERTEX_POINT('',#27763);
#6725=VERTEX_POINT('',#27764);
#6726=VERTEX_POINT('',#27788);
#6727=VERTEX_POINT('',#27789);
#6728=VERTEX_POINT('',#27812);
#6729=VERTEX_POINT('',#27813);
#6730=VERTEX_POINT('',#27837);
#6731=VERTEX_POINT('',#27838);
#6732=VERTEX_POINT('',#27862);
#6733=VERTEX_POINT('',#27863);
#6734=VERTEX_POINT('',#27886);
#6735=VERTEX_POINT('',#27887);
#6736=VERTEX_POINT('',#27889);
#6737=VERTEX_POINT('',#27895);
#6738=VERTEX_POINT('',#27903);
#6739=VERTEX_POINT('',#27904);
#6740=VERTEX_POINT('',#27906);
#6741=VERTEX_POINT('',#27929);
#6742=VERTEX_POINT('',#27931);
#6743=VERTEX_POINT('',#27939);
#6744=VERTEX_POINT('',#27965);
#6745=VERTEX_POINT('',#27966);
#6746=VERTEX_POINT('',#28016);
#6747=VERTEX_POINT('',#28017);
#6748=VERTEX_POINT('',#28064);
#6749=VERTEX_POINT('',#28065);
#6750=VERTEX_POINT('',#28112);
#6751=VERTEX_POINT('',#28113);
#6752=VERTEX_POINT('',#28163);
#6753=VERTEX_POINT('',#28164);
#6754=VERTEX_POINT('',#28211);
#6755=VERTEX_POINT('',#28212);
#6756=VERTEX_POINT('',#28259);
#6757=VERTEX_POINT('',#28260);
#6758=VERTEX_POINT('',#28310);
#6759=VERTEX_POINT('',#28311);
#6760=VERTEX_POINT('',#28361);
#6761=VERTEX_POINT('',#28362);
#6762=VERTEX_POINT('',#28409);
#6763=VERTEX_POINT('',#28410);
#6764=VERTEX_POINT('',#28460);
#6765=VERTEX_POINT('',#28461);
#6766=VERTEX_POINT('',#28463);
#6767=VERTEX_POINT('',#28477);
#6768=VERTEX_POINT('',#28499);
#6769=VERTEX_POINT('',#28500);
#6770=VERTEX_POINT('',#28502);
#6771=VERTEX_POINT('',#28510);
#6772=VERTEX_POINT('',#28521);
#6773=VERTEX_POINT('',#28522);
#6774=VERTEX_POINT('',#28545);
#6775=VERTEX_POINT('',#28546);
#6776=VERTEX_POINT('',#28570);
#6777=VERTEX_POINT('',#28571);
#6778=VERTEX_POINT('',#28595);
#6779=VERTEX_POINT('',#28596);
#6780=VERTEX_POINT('',#28619);
#6781=VERTEX_POINT('',#28620);
#6782=VERTEX_POINT('',#28644);
#6783=VERTEX_POINT('',#28645);
#6784=VERTEX_POINT('',#28668);
#6785=VERTEX_POINT('',#28669);
#6786=VERTEX_POINT('',#28693);
#6787=VERTEX_POINT('',#28694);
#6788=VERTEX_POINT('',#28717);
#6789=VERTEX_POINT('',#28718);
#6790=VERTEX_POINT('',#28742);
#6791=VERTEX_POINT('',#28743);
#6792=VERTEX_POINT('',#28767);
#6793=VERTEX_POINT('',#28768);
#6794=VERTEX_POINT('',#28791);
#6795=VERTEX_POINT('',#28792);
#6796=VERTEX_POINT('',#28794);
#6797=VERTEX_POINT('',#28800);
#6798=VERTEX_POINT('',#28808);
#6799=VERTEX_POINT('',#28809);
#6800=VERTEX_POINT('',#28811);
#6801=VERTEX_POINT('',#28834);
#6802=VERTEX_POINT('',#28836);
#6803=VERTEX_POINT('',#28844);
#6804=VERTEX_POINT('',#28870);
#6805=VERTEX_POINT('',#28871);
#6806=VERTEX_POINT('',#28921);
#6807=VERTEX_POINT('',#28922);
#6808=VERTEX_POINT('',#28969);
#6809=VERTEX_POINT('',#28970);
#6810=VERTEX_POINT('',#29017);
#6811=VERTEX_POINT('',#29018);
#6812=VERTEX_POINT('',#29068);
#6813=VERTEX_POINT('',#29069);
#6814=VERTEX_POINT('',#29116);
#6815=VERTEX_POINT('',#29117);
#6816=VERTEX_POINT('',#29164);
#6817=VERTEX_POINT('',#29165);
#6818=VERTEX_POINT('',#29215);
#6819=VERTEX_POINT('',#29216);
#6820=VERTEX_POINT('',#29266);
#6821=VERTEX_POINT('',#29267);
#6822=VERTEX_POINT('',#29314);
#6823=VERTEX_POINT('',#29315);
#6824=VERTEX_POINT('',#29365);
#6825=VERTEX_POINT('',#29366);
#6826=VERTEX_POINT('',#29368);
#6827=VERTEX_POINT('',#29382);
#6828=VERTEX_POINT('',#29404);
#6829=VERTEX_POINT('',#29405);
#6830=VERTEX_POINT('',#29407);
#6831=VERTEX_POINT('',#29415);
#6832=VERTEX_POINT('',#29426);
#6833=VERTEX_POINT('',#29427);
#6834=VERTEX_POINT('',#29450);
#6835=VERTEX_POINT('',#29451);
#6836=VERTEX_POINT('',#29475);
#6837=VERTEX_POINT('',#29476);
#6838=VERTEX_POINT('',#29500);
#6839=VERTEX_POINT('',#29501);
#6840=VERTEX_POINT('',#29524);
#6841=VERTEX_POINT('',#29525);
#6842=VERTEX_POINT('',#29549);
#6843=VERTEX_POINT('',#29550);
#6844=VERTEX_POINT('',#29573);
#6845=VERTEX_POINT('',#29574);
#6846=VERTEX_POINT('',#29598);
#6847=VERTEX_POINT('',#29599);
#6848=VERTEX_POINT('',#29622);
#6849=VERTEX_POINT('',#29623);
#6850=VERTEX_POINT('',#29647);
#6851=VERTEX_POINT('',#29648);
#6852=VERTEX_POINT('',#29672);
#6853=VERTEX_POINT('',#29673);
#6854=VERTEX_POINT('',#29696);
#6855=VERTEX_POINT('',#29697);
#6856=VERTEX_POINT('',#29699);
#6857=VERTEX_POINT('',#29705);
#6858=VERTEX_POINT('',#29713);
#6859=VERTEX_POINT('',#29714);
#6860=VERTEX_POINT('',#29716);
#6861=VERTEX_POINT('',#29739);
#6862=VERTEX_POINT('',#29741);
#6863=VERTEX_POINT('',#29749);
#6864=VERTEX_POINT('',#29775);
#6865=VERTEX_POINT('',#29776);
#6866=VERTEX_POINT('',#29826);
#6867=VERTEX_POINT('',#29827);
#6868=VERTEX_POINT('',#29874);
#6869=VERTEX_POINT('',#29875);
#6870=VERTEX_POINT('',#29922);
#6871=VERTEX_POINT('',#29923);
#6872=VERTEX_POINT('',#29973);
#6873=VERTEX_POINT('',#29974);
#6874=VERTEX_POINT('',#30021);
#6875=VERTEX_POINT('',#30022);
#6876=VERTEX_POINT('',#30069);
#6877=VERTEX_POINT('',#30070);
#6878=VERTEX_POINT('',#30120);
#6879=VERTEX_POINT('',#30121);
#6880=VERTEX_POINT('',#30171);
#6881=VERTEX_POINT('',#30172);
#6882=VERTEX_POINT('',#30219);
#6883=VERTEX_POINT('',#30220);
#6884=VERTEX_POINT('',#30270);
#6885=VERTEX_POINT('',#30271);
#6886=VERTEX_POINT('',#30273);
#6887=VERTEX_POINT('',#30287);
#6888=VERTEX_POINT('',#30309);
#6889=VERTEX_POINT('',#30310);
#6890=VERTEX_POINT('',#30312);
#6891=VERTEX_POINT('',#30320);
#6892=VERTEX_POINT('',#30331);
#6893=VERTEX_POINT('',#30332);
#6894=VERTEX_POINT('',#30355);
#6895=VERTEX_POINT('',#30356);
#6896=VERTEX_POINT('',#30380);
#6897=VERTEX_POINT('',#30381);
#6898=VERTEX_POINT('',#30405);
#6899=VERTEX_POINT('',#30406);
#6900=VERTEX_POINT('',#30429);
#6901=VERTEX_POINT('',#30430);
#6902=VERTEX_POINT('',#30454);
#6903=VERTEX_POINT('',#30455);
#6904=VERTEX_POINT('',#30478);
#6905=VERTEX_POINT('',#30479);
#6906=VERTEX_POINT('',#30503);
#6907=VERTEX_POINT('',#30504);
#6908=VERTEX_POINT('',#30527);
#6909=VERTEX_POINT('',#30528);
#6910=VERTEX_POINT('',#30552);
#6911=VERTEX_POINT('',#30553);
#6912=VERTEX_POINT('',#30577);
#6913=VERTEX_POINT('',#30578);
#6914=VERTEX_POINT('',#30601);
#6915=VERTEX_POINT('',#30602);
#6916=VERTEX_POINT('',#30604);
#6917=VERTEX_POINT('',#30610);
#6918=VERTEX_POINT('',#30618);
#6919=VERTEX_POINT('',#30619);
#6920=VERTEX_POINT('',#30621);
#6921=VERTEX_POINT('',#30644);
#6922=VERTEX_POINT('',#30646);
#6923=VERTEX_POINT('',#30654);
#6924=VERTEX_POINT('',#30680);
#6925=VERTEX_POINT('',#30681);
#6926=VERTEX_POINT('',#30731);
#6927=VERTEX_POINT('',#30732);
#6928=VERTEX_POINT('',#30779);
#6929=VERTEX_POINT('',#30780);
#6930=VERTEX_POINT('',#30827);
#6931=VERTEX_POINT('',#30828);
#6932=VERTEX_POINT('',#30878);
#6933=VERTEX_POINT('',#30879);
#6934=VERTEX_POINT('',#30926);
#6935=VERTEX_POINT('',#30927);
#6936=VERTEX_POINT('',#30974);
#6937=VERTEX_POINT('',#30975);
#6938=VERTEX_POINT('',#31025);
#6939=VERTEX_POINT('',#31026);
#6940=VERTEX_POINT('',#31076);
#6941=VERTEX_POINT('',#31077);
#6942=VERTEX_POINT('',#31124);
#6943=VERTEX_POINT('',#31125);
#6944=VERTEX_POINT('',#31175);
#6945=VERTEX_POINT('',#31176);
#6946=VERTEX_POINT('',#31178);
#6947=VERTEX_POINT('',#31192);
#6948=VERTEX_POINT('',#31214);
#6949=VERTEX_POINT('',#31215);
#6950=VERTEX_POINT('',#31217);
#6951=VERTEX_POINT('',#31225);
#6952=VERTEX_POINT('',#31236);
#6953=VERTEX_POINT('',#31237);
#6954=VERTEX_POINT('',#31260);
#6955=VERTEX_POINT('',#31261);
#6956=VERTEX_POINT('',#31285);
#6957=VERTEX_POINT('',#31286);
#6958=VERTEX_POINT('',#31310);
#6959=VERTEX_POINT('',#31311);
#6960=VERTEX_POINT('',#31334);
#6961=VERTEX_POINT('',#31335);
#6962=VERTEX_POINT('',#31359);
#6963=VERTEX_POINT('',#31360);
#6964=VERTEX_POINT('',#31383);
#6965=VERTEX_POINT('',#31384);
#6966=VERTEX_POINT('',#31408);
#6967=VERTEX_POINT('',#31409);
#6968=VERTEX_POINT('',#31432);
#6969=VERTEX_POINT('',#31433);
#6970=VERTEX_POINT('',#31457);
#6971=VERTEX_POINT('',#31458);
#6972=VERTEX_POINT('',#31482);
#6973=VERTEX_POINT('',#31483);
#6974=VERTEX_POINT('',#31506);
#6975=VERTEX_POINT('',#31507);
#6976=VERTEX_POINT('',#31509);
#6977=VERTEX_POINT('',#31515);
#6978=VERTEX_POINT('',#31523);
#6979=VERTEX_POINT('',#31524);
#6980=VERTEX_POINT('',#31526);
#6981=VERTEX_POINT('',#31549);
#6982=VERTEX_POINT('',#31551);
#6983=VERTEX_POINT('',#31559);
#6984=VERTEX_POINT('',#31585);
#6985=VERTEX_POINT('',#31586);
#6986=VERTEX_POINT('',#31636);
#6987=VERTEX_POINT('',#31637);
#6988=VERTEX_POINT('',#31684);
#6989=VERTEX_POINT('',#31685);
#6990=VERTEX_POINT('',#31732);
#6991=VERTEX_POINT('',#31733);
#6992=VERTEX_POINT('',#31783);
#6993=VERTEX_POINT('',#31784);
#6994=VERTEX_POINT('',#31831);
#6995=VERTEX_POINT('',#31832);
#6996=VERTEX_POINT('',#31879);
#6997=VERTEX_POINT('',#31880);
#6998=VERTEX_POINT('',#31930);
#6999=VERTEX_POINT('',#31931);
#7000=VERTEX_POINT('',#31981);
#7001=VERTEX_POINT('',#31982);
#7002=VERTEX_POINT('',#32029);
#7003=VERTEX_POINT('',#32030);
#7004=VERTEX_POINT('',#32080);
#7005=VERTEX_POINT('',#32081);
#7006=VERTEX_POINT('',#32083);
#7007=VERTEX_POINT('',#32097);
#7008=VERTEX_POINT('',#32119);
#7009=VERTEX_POINT('',#32120);
#7010=VERTEX_POINT('',#32122);
#7011=VERTEX_POINT('',#32130);
#7012=VERTEX_POINT('',#32141);
#7013=VERTEX_POINT('',#32142);
#7014=VERTEX_POINT('',#32165);
#7015=VERTEX_POINT('',#32166);
#7016=VERTEX_POINT('',#32190);
#7017=VERTEX_POINT('',#32191);
#7018=VERTEX_POINT('',#32215);
#7019=VERTEX_POINT('',#32216);
#7020=VERTEX_POINT('',#32239);
#7021=VERTEX_POINT('',#32240);
#7022=VERTEX_POINT('',#32264);
#7023=VERTEX_POINT('',#32265);
#7024=VERTEX_POINT('',#32288);
#7025=VERTEX_POINT('',#32289);
#7026=VERTEX_POINT('',#32313);
#7027=VERTEX_POINT('',#32314);
#7028=VERTEX_POINT('',#32337);
#7029=VERTEX_POINT('',#32338);
#7030=VERTEX_POINT('',#32362);
#7031=VERTEX_POINT('',#32363);
#7032=VERTEX_POINT('',#32387);
#7033=VERTEX_POINT('',#32388);
#7034=VERTEX_POINT('',#32411);
#7035=VERTEX_POINT('',#32412);
#7036=VERTEX_POINT('',#32414);
#7037=VERTEX_POINT('',#32420);
#7038=VERTEX_POINT('',#32428);
#7039=VERTEX_POINT('',#32429);
#7040=VERTEX_POINT('',#32431);
#7041=VERTEX_POINT('',#32454);
#7042=VERTEX_POINT('',#32456);
#7043=VERTEX_POINT('',#32464);
#7044=VERTEX_POINT('',#32490);
#7045=VERTEX_POINT('',#32491);
#7046=VERTEX_POINT('',#32541);
#7047=VERTEX_POINT('',#32542);
#7048=VERTEX_POINT('',#32589);
#7049=VERTEX_POINT('',#32590);
#7050=VERTEX_POINT('',#32637);
#7051=VERTEX_POINT('',#32638);
#7052=VERTEX_POINT('',#32688);
#7053=VERTEX_POINT('',#32689);
#7054=VERTEX_POINT('',#32736);
#7055=VERTEX_POINT('',#32737);
#7056=VERTEX_POINT('',#32784);
#7057=VERTEX_POINT('',#32785);
#7058=VERTEX_POINT('',#32835);
#7059=VERTEX_POINT('',#32836);
#7060=VERTEX_POINT('',#32886);
#7061=VERTEX_POINT('',#32887);
#7062=VERTEX_POINT('',#32934);
#7063=VERTEX_POINT('',#32935);
#7064=VERTEX_POINT('',#32985);
#7065=VERTEX_POINT('',#32986);
#7066=VERTEX_POINT('',#32988);
#7067=VERTEX_POINT('',#33002);
#7068=VERTEX_POINT('',#33024);
#7069=VERTEX_POINT('',#33025);
#7070=VERTEX_POINT('',#33027);
#7071=VERTEX_POINT('',#33035);
#7072=VERTEX_POINT('',#33046);
#7073=VERTEX_POINT('',#33047);
#7074=VERTEX_POINT('',#33070);
#7075=VERTEX_POINT('',#33071);
#7076=VERTEX_POINT('',#33095);
#7077=VERTEX_POINT('',#33096);
#7078=VERTEX_POINT('',#33120);
#7079=VERTEX_POINT('',#33121);
#7080=VERTEX_POINT('',#33144);
#7081=VERTEX_POINT('',#33145);
#7082=VERTEX_POINT('',#33169);
#7083=VERTEX_POINT('',#33170);
#7084=VERTEX_POINT('',#33193);
#7085=VERTEX_POINT('',#33194);
#7086=VERTEX_POINT('',#33218);
#7087=VERTEX_POINT('',#33219);
#7088=VERTEX_POINT('',#33242);
#7089=VERTEX_POINT('',#33243);
#7090=VERTEX_POINT('',#33267);
#7091=VERTEX_POINT('',#33268);
#7092=VERTEX_POINT('',#33292);
#7093=VERTEX_POINT('',#33293);
#7094=VERTEX_POINT('',#33316);
#7095=VERTEX_POINT('',#33317);
#7096=VERTEX_POINT('',#33319);
#7097=VERTEX_POINT('',#33325);
#7098=VERTEX_POINT('',#33333);
#7099=VERTEX_POINT('',#33334);
#7100=VERTEX_POINT('',#33336);
#7101=VERTEX_POINT('',#33359);
#7102=VERTEX_POINT('',#33361);
#7103=VERTEX_POINT('',#33369);
#7104=VERTEX_POINT('',#33395);
#7105=VERTEX_POINT('',#33396);
#7106=VERTEX_POINT('',#33446);
#7107=VERTEX_POINT('',#33447);
#7108=VERTEX_POINT('',#33494);
#7109=VERTEX_POINT('',#33495);
#7110=VERTEX_POINT('',#33542);
#7111=VERTEX_POINT('',#33543);
#7112=VERTEX_POINT('',#33593);
#7113=VERTEX_POINT('',#33594);
#7114=VERTEX_POINT('',#33641);
#7115=VERTEX_POINT('',#33642);
#7116=VERTEX_POINT('',#33689);
#7117=VERTEX_POINT('',#33690);
#7118=VERTEX_POINT('',#33740);
#7119=VERTEX_POINT('',#33741);
#7120=VERTEX_POINT('',#33791);
#7121=VERTEX_POINT('',#33792);
#7122=VERTEX_POINT('',#33839);
#7123=VERTEX_POINT('',#33840);
#7124=VERTEX_POINT('',#33890);
#7125=VERTEX_POINT('',#33891);
#7126=VERTEX_POINT('',#33893);
#7127=VERTEX_POINT('',#33907);
#7128=VERTEX_POINT('',#33929);
#7129=VERTEX_POINT('',#33930);
#7130=VERTEX_POINT('',#33932);
#7131=VERTEX_POINT('',#33940);
#7132=VERTEX_POINT('',#33951);
#7133=VERTEX_POINT('',#33952);
#7134=VERTEX_POINT('',#33975);
#7135=VERTEX_POINT('',#33976);
#7136=VERTEX_POINT('',#34000);
#7137=VERTEX_POINT('',#34001);
#7138=VERTEX_POINT('',#34025);
#7139=VERTEX_POINT('',#34026);
#7140=VERTEX_POINT('',#34049);
#7141=VERTEX_POINT('',#34050);
#7142=VERTEX_POINT('',#34074);
#7143=VERTEX_POINT('',#34075);
#7144=VERTEX_POINT('',#34098);
#7145=VERTEX_POINT('',#34099);
#7146=VERTEX_POINT('',#34123);
#7147=VERTEX_POINT('',#34124);
#7148=VERTEX_POINT('',#34147);
#7149=VERTEX_POINT('',#34148);
#7150=VERTEX_POINT('',#34172);
#7151=VERTEX_POINT('',#34173);
#7152=VERTEX_POINT('',#34197);
#7153=VERTEX_POINT('',#34198);
#7154=VERTEX_POINT('',#34221);
#7155=VERTEX_POINT('',#34222);
#7156=VERTEX_POINT('',#34224);
#7157=VERTEX_POINT('',#34230);
#7158=VERTEX_POINT('',#34238);
#7159=VERTEX_POINT('',#34239);
#7160=VERTEX_POINT('',#34241);
#7161=VERTEX_POINT('',#34246);
#7162=VERTEX_POINT('',#34259);
#7163=VERTEX_POINT('',#34260);
#7164=VERTEX_POINT('',#34310);
#7165=VERTEX_POINT('',#34311);
#7166=VERTEX_POINT('',#34361);
#7167=VERTEX_POINT('',#34362);
#7168=VERTEX_POINT('',#34409);
#7169=VERTEX_POINT('',#34410);
#7170=VERTEX_POINT('',#34463);
#7171=VERTEX_POINT('',#34464);
#7172=VERTEX_POINT('',#34511);
#7173=VERTEX_POINT('',#34512);
#7174=VERTEX_POINT('',#34559);
#7175=VERTEX_POINT('',#34560);
#7176=VERTEX_POINT('',#34562);
#7177=VERTEX_POINT('',#34576);
#7178=VERTEX_POINT('',#34609);
#7179=VERTEX_POINT('',#34610);
#7180=VERTEX_POINT('',#34612);
#7181=VERTEX_POINT('',#34621);
#7182=VERTEX_POINT('',#34633);
#7183=VERTEX_POINT('',#34634);
#7184=VERTEX_POINT('',#34657);
#7185=VERTEX_POINT('',#34658);
#7186=VERTEX_POINT('',#34682);
#7187=VERTEX_POINT('',#34683);
#7188=VERTEX_POINT('',#34707);
#7189=VERTEX_POINT('',#34708);
#7190=VERTEX_POINT('',#34732);
#7191=VERTEX_POINT('',#34733);
#7192=VERTEX_POINT('',#34756);
#7193=VERTEX_POINT('',#34757);
#7194=VERTEX_POINT('',#34781);
#7195=VERTEX_POINT('',#34782);
#7196=VERTEX_POINT('',#34784);
#7197=VERTEX_POINT('',#34790);
#7198=VERTEX_POINT('',#34795);
#7199=VERTEX_POINT('',#34807);
#7200=VERTEX_POINT('',#34808);
#7201=VERTEX_POINT('',#34810);
#7202=VERTEX_POINT('',#34815);
#7203=VERTEX_POINT('',#34828);
#7204=VERTEX_POINT('',#34829);
#7205=VERTEX_POINT('',#34879);
#7206=VERTEX_POINT('',#34880);
#7207=VERTEX_POINT('',#34930);
#7208=VERTEX_POINT('',#34931);
#7209=VERTEX_POINT('',#34978);
#7210=VERTEX_POINT('',#34979);
#7211=VERTEX_POINT('',#35032);
#7212=VERTEX_POINT('',#35033);
#7213=VERTEX_POINT('',#35080);
#7214=VERTEX_POINT('',#35081);
#7215=VERTEX_POINT('',#35128);
#7216=VERTEX_POINT('',#35129);
#7217=VERTEX_POINT('',#35131);
#7218=VERTEX_POINT('',#35145);
#7219=VERTEX_POINT('',#35178);
#7220=VERTEX_POINT('',#35179);
#7221=VERTEX_POINT('',#35181);
#7222=VERTEX_POINT('',#35186);
#7223=VERTEX_POINT('',#35199);
#7224=VERTEX_POINT('',#35200);
#7225=VERTEX_POINT('',#35250);
#7226=VERTEX_POINT('',#35251);
#7227=VERTEX_POINT('',#35301);
#7228=VERTEX_POINT('',#35302);
#7229=VERTEX_POINT('',#35349);
#7230=VERTEX_POINT('',#35350);
#7231=VERTEX_POINT('',#35403);
#7232=VERTEX_POINT('',#35404);
#7233=VERTEX_POINT('',#35451);
#7234=VERTEX_POINT('',#35452);
#7235=VERTEX_POINT('',#35499);
#7236=VERTEX_POINT('',#35500);
#7237=VERTEX_POINT('',#35502);
#7238=VERTEX_POINT('',#35516);
#7239=VERTEX_POINT('',#35549);
#7240=VERTEX_POINT('',#35550);
#7241=VERTEX_POINT('',#35552);
#7242=VERTEX_POINT('',#35557);
#7243=VERTEX_POINT('',#35570);
#7244=VERTEX_POINT('',#35571);
#7245=VERTEX_POINT('',#35621);
#7246=VERTEX_POINT('',#35622);
#7247=VERTEX_POINT('',#35672);
#7248=VERTEX_POINT('',#35673);
#7249=VERTEX_POINT('',#35720);
#7250=VERTEX_POINT('',#35721);
#7251=VERTEX_POINT('',#35774);
#7252=VERTEX_POINT('',#35775);
#7253=VERTEX_POINT('',#35822);
#7254=VERTEX_POINT('',#35823);
#7255=VERTEX_POINT('',#35870);
#7256=VERTEX_POINT('',#35871);
#7257=VERTEX_POINT('',#35873);
#7258=VERTEX_POINT('',#35887);
#7259=VERTEX_POINT('',#35920);
#7260=VERTEX_POINT('',#35921);
#7261=VERTEX_POINT('',#35923);
#7262=VERTEX_POINT('',#35932);
#7263=VERTEX_POINT('',#35944);
#7264=VERTEX_POINT('',#35945);
#7265=VERTEX_POINT('',#35968);
#7266=VERTEX_POINT('',#35969);
#7267=VERTEX_POINT('',#35993);
#7268=VERTEX_POINT('',#35994);
#7269=VERTEX_POINT('',#36018);
#7270=VERTEX_POINT('',#36019);
#7271=VERTEX_POINT('',#36043);
#7272=VERTEX_POINT('',#36044);
#7273=VERTEX_POINT('',#36067);
#7274=VERTEX_POINT('',#36068);
#7275=VERTEX_POINT('',#36092);
#7276=VERTEX_POINT('',#36093);
#7277=VERTEX_POINT('',#36095);
#7278=VERTEX_POINT('',#36101);
#7279=VERTEX_POINT('',#36106);
#7280=VERTEX_POINT('',#36118);
#7281=VERTEX_POINT('',#36119);
#7282=VERTEX_POINT('',#36121);
#7283=VERTEX_POINT('',#36130);
#7284=VERTEX_POINT('',#36142);
#7285=VERTEX_POINT('',#36143);
#7286=VERTEX_POINT('',#36166);
#7287=VERTEX_POINT('',#36167);
#7288=VERTEX_POINT('',#36191);
#7289=VERTEX_POINT('',#36192);
#7290=VERTEX_POINT('',#36216);
#7291=VERTEX_POINT('',#36217);
#7292=VERTEX_POINT('',#36241);
#7293=VERTEX_POINT('',#36242);
#7294=VERTEX_POINT('',#36265);
#7295=VERTEX_POINT('',#36266);
#7296=VERTEX_POINT('',#36290);
#7297=VERTEX_POINT('',#36291);
#7298=VERTEX_POINT('',#36293);
#7299=VERTEX_POINT('',#36299);
#7300=VERTEX_POINT('',#36304);
#7301=VERTEX_POINT('',#36316);
#7302=VERTEX_POINT('',#36317);
#7303=VERTEX_POINT('',#36319);
#7304=VERTEX_POINT('',#36328);
#7305=VERTEX_POINT('',#36340);
#7306=VERTEX_POINT('',#36341);
#7307=VERTEX_POINT('',#36364);
#7308=VERTEX_POINT('',#36365);
#7309=VERTEX_POINT('',#36389);
#7310=VERTEX_POINT('',#36390);
#7311=VERTEX_POINT('',#36414);
#7312=VERTEX_POINT('',#36415);
#7313=VERTEX_POINT('',#36439);
#7314=VERTEX_POINT('',#36440);
#7315=VERTEX_POINT('',#36463);
#7316=VERTEX_POINT('',#36464);
#7317=VERTEX_POINT('',#36488);
#7318=VERTEX_POINT('',#36489);
#7319=VERTEX_POINT('',#36491);
#7320=VERTEX_POINT('',#36497);
#7321=VERTEX_POINT('',#36502);
#7322=VERTEX_POINT('',#52658);
#7323=VERTEX_POINT('',#52660);
#7324=VERTEX_POINT('',#52664);
#7325=VERTEX_POINT('',#52666);
#7326=VERTEX_POINT('',#52673);
#7327=VERTEX_POINT('',#52674);
#7328=VERTEX_POINT('',#52676);
#7329=VERTEX_POINT('',#52681);
#7330=VERTEX_POINT('',#52683);
#7331=VERTEX_POINT('',#52685);
#7332=VERTEX_POINT('',#52687);
#7333=VERTEX_POINT('',#52690);
#7334=VERTEX_POINT('',#52703);
#7335=VERTEX_POINT('',#52704);
#7336=VERTEX_POINT('',#52754);
#7337=VERTEX_POINT('',#52755);
#7338=VERTEX_POINT('',#52805);
#7339=VERTEX_POINT('',#52806);
#7340=VERTEX_POINT('',#52853);
#7341=VERTEX_POINT('',#52854);
#7342=VERTEX_POINT('',#52904);
#7343=VERTEX_POINT('',#52905);
#7344=VERTEX_POINT('',#52955);
#7345=VERTEX_POINT('',#52956);
#7346=VERTEX_POINT('',#53003);
#7347=VERTEX_POINT('',#53004);
#7348=VERTEX_POINT('',#53006);
#7349=VERTEX_POINT('',#53020);
#7350=VERTEX_POINT('',#53042);
#7351=VERTEX_POINT('',#53043);
#7352=VERTEX_POINT('',#53045);
#7353=VERTEX_POINT('',#53054);
#7354=VERTEX_POINT('',#53066);
#7355=VERTEX_POINT('',#53067);
#7356=VERTEX_POINT('',#53090);
#7357=VERTEX_POINT('',#53091);
#7358=VERTEX_POINT('',#53115);
#7359=VERTEX_POINT('',#53116);
#7360=VERTEX_POINT('',#53140);
#7361=VERTEX_POINT('',#53141);
#7362=VERTEX_POINT('',#53164);
#7363=VERTEX_POINT('',#53165);
#7364=VERTEX_POINT('',#53189);
#7365=VERTEX_POINT('',#53190);
#7366=VERTEX_POINT('',#53214);
#7367=VERTEX_POINT('',#53215);
#7368=VERTEX_POINT('',#53217);
#7369=VERTEX_POINT('',#53223);
#7370=VERTEX_POINT('',#53231);
#7371=VERTEX_POINT('',#53232);
#7372=VERTEX_POINT('',#53234);
#7373=VERTEX_POINT('',#53239);
#7374=VERTEX_POINT('',#53241);
#7375=VERTEX_POINT('',#53243);
#7376=VERTEX_POINT('',#53245);
#7377=VERTEX_POINT('',#53248);
#7378=VERTEX_POINT('',#53261);
#7379=VERTEX_POINT('',#53262);
#7380=VERTEX_POINT('',#53312);
#7381=VERTEX_POINT('',#53313);
#7382=VERTEX_POINT('',#53363);
#7383=VERTEX_POINT('',#53364);
#7384=VERTEX_POINT('',#53411);
#7385=VERTEX_POINT('',#53412);
#7386=VERTEX_POINT('',#53462);
#7387=VERTEX_POINT('',#53463);
#7388=VERTEX_POINT('',#53513);
#7389=VERTEX_POINT('',#53514);
#7390=VERTEX_POINT('',#53561);
#7391=VERTEX_POINT('',#53562);
#7392=VERTEX_POINT('',#53564);
#7393=VERTEX_POINT('',#53578);
#7394=VERTEX_POINT('',#53600);
#7395=VERTEX_POINT('',#53601);
#7396=VERTEX_POINT('',#53603);
#7397=VERTEX_POINT('',#53612);
#7398=VERTEX_POINT('',#53624);
#7399=VERTEX_POINT('',#53625);
#7400=VERTEX_POINT('',#53648);
#7401=VERTEX_POINT('',#53649);
#7402=VERTEX_POINT('',#53673);
#7403=VERTEX_POINT('',#53674);
#7404=VERTEX_POINT('',#53698);
#7405=VERTEX_POINT('',#53699);
#7406=VERTEX_POINT('',#53722);
#7407=VERTEX_POINT('',#53723);
#7408=VERTEX_POINT('',#53747);
#7409=VERTEX_POINT('',#53748);
#7410=VERTEX_POINT('',#53772);
#7411=VERTEX_POINT('',#53773);
#7412=VERTEX_POINT('',#53775);
#7413=VERTEX_POINT('',#53781);
#7414=VERTEX_POINT('',#53789);
#7415=VERTEX_POINT('',#53790);
#7416=VERTEX_POINT('',#53792);
#7417=VERTEX_POINT('',#53797);
#7418=VERTEX_POINT('',#53799);
#7419=VERTEX_POINT('',#53801);
#7420=VERTEX_POINT('',#53803);
#7421=VERTEX_POINT('',#53806);
#7422=VERTEX_POINT('',#53819);
#7423=VERTEX_POINT('',#53820);
#7424=VERTEX_POINT('',#53870);
#7425=VERTEX_POINT('',#53871);
#7426=VERTEX_POINT('',#53921);
#7427=VERTEX_POINT('',#53922);
#7428=VERTEX_POINT('',#53969);
#7429=VERTEX_POINT('',#53970);
#7430=VERTEX_POINT('',#54020);
#7431=VERTEX_POINT('',#54021);
#7432=VERTEX_POINT('',#54071);
#7433=VERTEX_POINT('',#54072);
#7434=VERTEX_POINT('',#54119);
#7435=VERTEX_POINT('',#54120);
#7436=VERTEX_POINT('',#54122);
#7437=VERTEX_POINT('',#54136);
#7438=VERTEX_POINT('',#54158);
#7439=VERTEX_POINT('',#54159);
#7440=VERTEX_POINT('',#54161);
#7441=VERTEX_POINT('',#54170);
#7442=VERTEX_POINT('',#54182);
#7443=VERTEX_POINT('',#54183);
#7444=VERTEX_POINT('',#54206);
#7445=VERTEX_POINT('',#54207);
#7446=VERTEX_POINT('',#54231);
#7447=VERTEX_POINT('',#54232);
#7448=VERTEX_POINT('',#54256);
#7449=VERTEX_POINT('',#54257);
#7450=VERTEX_POINT('',#54280);
#7451=VERTEX_POINT('',#54281);
#7452=VERTEX_POINT('',#54305);
#7453=VERTEX_POINT('',#54306);
#7454=VERTEX_POINT('',#54330);
#7455=VERTEX_POINT('',#54331);
#7456=VERTEX_POINT('',#54333);
#7457=VERTEX_POINT('',#54339);
#7458=VERTEX_POINT('',#54347);
#7459=VERTEX_POINT('',#54348);
#7460=VERTEX_POINT('',#54350);
#7461=VERTEX_POINT('',#54355);
#7462=VERTEX_POINT('',#54357);
#7463=VERTEX_POINT('',#54359);
#7464=VERTEX_POINT('',#54361);
#7465=VERTEX_POINT('',#54364);
#7466=VERTEX_POINT('',#54377);
#7467=VERTEX_POINT('',#54378);
#7468=VERTEX_POINT('',#54428);
#7469=VERTEX_POINT('',#54429);
#7470=VERTEX_POINT('',#54479);
#7471=VERTEX_POINT('',#54480);
#7472=VERTEX_POINT('',#54527);
#7473=VERTEX_POINT('',#54528);
#7474=VERTEX_POINT('',#54578);
#7475=VERTEX_POINT('',#54579);
#7476=VERTEX_POINT('',#54629);
#7477=VERTEX_POINT('',#54630);
#7478=VERTEX_POINT('',#54677);
#7479=VERTEX_POINT('',#54678);
#7480=VERTEX_POINT('',#54680);
#7481=VERTEX_POINT('',#54694);
#7482=VERTEX_POINT('',#54716);
#7483=VERTEX_POINT('',#54717);
#7484=VERTEX_POINT('',#54719);
#7485=VERTEX_POINT('',#54728);
#7486=VERTEX_POINT('',#54740);
#7487=VERTEX_POINT('',#54741);
#7488=VERTEX_POINT('',#54764);
#7489=VERTEX_POINT('',#54765);
#7490=VERTEX_POINT('',#54789);
#7491=VERTEX_POINT('',#54790);
#7492=VERTEX_POINT('',#54814);
#7493=VERTEX_POINT('',#54815);
#7494=VERTEX_POINT('',#54838);
#7495=VERTEX_POINT('',#54839);
#7496=VERTEX_POINT('',#54863);
#7497=VERTEX_POINT('',#54864);
#7498=VERTEX_POINT('',#54888);
#7499=VERTEX_POINT('',#54889);
#7500=VERTEX_POINT('',#54891);
#7501=VERTEX_POINT('',#54897);
#7502=VERTEX_POINT('',#54905);
#7503=VERTEX_POINT('',#54906);
#7504=VERTEX_POINT('',#54908);
#7505=VERTEX_POINT('',#54913);
#7506=VERTEX_POINT('',#54915);
#7507=VERTEX_POINT('',#54917);
#7508=VERTEX_POINT('',#54919);
#7509=VERTEX_POINT('',#54922);
#7510=VERTEX_POINT('',#54935);
#7511=VERTEX_POINT('',#54936);
#7512=VERTEX_POINT('',#54986);
#7513=VERTEX_POINT('',#54987);
#7514=VERTEX_POINT('',#55037);
#7515=VERTEX_POINT('',#55038);
#7516=VERTEX_POINT('',#55085);
#7517=VERTEX_POINT('',#55086);
#7518=VERTEX_POINT('',#55136);
#7519=VERTEX_POINT('',#55137);
#7520=VERTEX_POINT('',#55187);
#7521=VERTEX_POINT('',#55188);
#7522=VERTEX_POINT('',#55235);
#7523=VERTEX_POINT('',#55236);
#7524=VERTEX_POINT('',#55238);
#7525=VERTEX_POINT('',#55252);
#7526=VERTEX_POINT('',#55274);
#7527=VERTEX_POINT('',#55275);
#7528=VERTEX_POINT('',#55277);
#7529=VERTEX_POINT('',#55286);
#7530=VERTEX_POINT('',#55298);
#7531=VERTEX_POINT('',#55299);
#7532=VERTEX_POINT('',#55322);
#7533=VERTEX_POINT('',#55323);
#7534=VERTEX_POINT('',#55347);
#7535=VERTEX_POINT('',#55348);
#7536=VERTEX_POINT('',#55372);
#7537=VERTEX_POINT('',#55373);
#7538=VERTEX_POINT('',#55396);
#7539=VERTEX_POINT('',#55397);
#7540=VERTEX_POINT('',#55421);
#7541=VERTEX_POINT('',#55422);
#7542=VERTEX_POINT('',#55446);
#7543=VERTEX_POINT('',#55447);
#7544=VERTEX_POINT('',#55449);
#7545=VERTEX_POINT('',#55455);
#7546=VERTEX_POINT('',#55463);
#7547=VERTEX_POINT('',#55464);
#7548=VERTEX_POINT('',#55466);
#7549=VERTEX_POINT('',#55471);
#7550=VERTEX_POINT('',#55473);
#7551=VERTEX_POINT('',#55475);
#7552=VERTEX_POINT('',#55477);
#7553=VERTEX_POINT('',#55480);
#7554=VERTEX_POINT('',#55493);
#7555=VERTEX_POINT('',#55494);
#7556=VERTEX_POINT('',#55544);
#7557=VERTEX_POINT('',#55545);
#7558=VERTEX_POINT('',#55595);
#7559=VERTEX_POINT('',#55596);
#7560=VERTEX_POINT('',#55643);
#7561=VERTEX_POINT('',#55644);
#7562=VERTEX_POINT('',#55694);
#7563=VERTEX_POINT('',#55695);
#7564=VERTEX_POINT('',#55745);
#7565=VERTEX_POINT('',#55746);
#7566=VERTEX_POINT('',#55793);
#7567=VERTEX_POINT('',#55794);
#7568=VERTEX_POINT('',#55796);
#7569=VERTEX_POINT('',#55810);
#7570=VERTEX_POINT('',#55832);
#7571=VERTEX_POINT('',#55833);
#7572=VERTEX_POINT('',#55835);
#7573=VERTEX_POINT('',#55844);
#7574=VERTEX_POINT('',#55856);
#7575=VERTEX_POINT('',#55857);
#7576=VERTEX_POINT('',#55880);
#7577=VERTEX_POINT('',#55881);
#7578=VERTEX_POINT('',#55905);
#7579=VERTEX_POINT('',#55906);
#7580=VERTEX_POINT('',#55930);
#7581=VERTEX_POINT('',#55931);
#7582=VERTEX_POINT('',#55954);
#7583=VERTEX_POINT('',#55955);
#7584=VERTEX_POINT('',#55979);
#7585=VERTEX_POINT('',#55980);
#7586=VERTEX_POINT('',#56004);
#7587=VERTEX_POINT('',#56005);
#7588=VERTEX_POINT('',#56007);
#7589=VERTEX_POINT('',#56013);
#7590=VERTEX_POINT('',#56021);
#7591=VERTEX_POINT('',#56022);
#7592=VERTEX_POINT('',#56024);
#7593=VERTEX_POINT('',#56029);
#7594=VERTEX_POINT('',#56031);
#7595=VERTEX_POINT('',#56033);
#7596=VERTEX_POINT('',#56035);
#7597=VERTEX_POINT('',#56038);
#7598=VERTEX_POINT('',#56051);
#7599=VERTEX_POINT('',#56052);
#7600=VERTEX_POINT('',#56102);
#7601=VERTEX_POINT('',#56103);
#7602=VERTEX_POINT('',#56153);
#7603=VERTEX_POINT('',#56154);
#7604=VERTEX_POINT('',#56201);
#7605=VERTEX_POINT('',#56202);
#7606=VERTEX_POINT('',#56252);
#7607=VERTEX_POINT('',#56253);
#7608=VERTEX_POINT('',#56303);
#7609=VERTEX_POINT('',#56304);
#7610=VERTEX_POINT('',#56351);
#7611=VERTEX_POINT('',#56352);
#7612=VERTEX_POINT('',#56354);
#7613=VERTEX_POINT('',#56368);
#7614=VERTEX_POINT('',#56390);
#7615=VERTEX_POINT('',#56391);
#7616=VERTEX_POINT('',#56393);
#7617=VERTEX_POINT('',#56402);
#7618=VERTEX_POINT('',#56414);
#7619=VERTEX_POINT('',#56415);
#7620=VERTEX_POINT('',#56438);
#7621=VERTEX_POINT('',#56439);
#7622=VERTEX_POINT('',#56463);
#7623=VERTEX_POINT('',#56464);
#7624=VERTEX_POINT('',#56488);
#7625=VERTEX_POINT('',#56489);
#7626=VERTEX_POINT('',#56512);
#7627=VERTEX_POINT('',#56513);
#7628=VERTEX_POINT('',#56537);
#7629=VERTEX_POINT('',#56538);
#7630=VERTEX_POINT('',#56562);
#7631=VERTEX_POINT('',#56563);
#7632=VERTEX_POINT('',#56565);
#7633=VERTEX_POINT('',#56571);
#7634=VERTEX_POINT('',#56579);
#7635=VERTEX_POINT('',#56580);
#7636=VERTEX_POINT('',#56582);
#7637=VERTEX_POINT('',#56587);
#7638=VERTEX_POINT('',#56589);
#7639=VERTEX_POINT('',#56591);
#7640=VERTEX_POINT('',#56593);
#7641=VERTEX_POINT('',#56596);
#7642=VERTEX_POINT('',#56609);
#7643=VERTEX_POINT('',#56610);
#7644=VERTEX_POINT('',#56660);
#7645=VERTEX_POINT('',#56661);
#7646=VERTEX_POINT('',#56711);
#7647=VERTEX_POINT('',#56712);
#7648=VERTEX_POINT('',#56759);
#7649=VERTEX_POINT('',#56760);
#7650=VERTEX_POINT('',#56810);
#7651=VERTEX_POINT('',#56811);
#7652=VERTEX_POINT('',#56861);
#7653=VERTEX_POINT('',#56862);
#7654=VERTEX_POINT('',#56909);
#7655=VERTEX_POINT('',#56910);
#7656=VERTEX_POINT('',#56912);
#7657=VERTEX_POINT('',#56926);
#7658=VERTEX_POINT('',#56948);
#7659=VERTEX_POINT('',#56949);
#7660=VERTEX_POINT('',#56951);
#7661=VERTEX_POINT('',#56960);
#7662=VERTEX_POINT('',#56972);
#7663=VERTEX_POINT('',#56973);
#7664=VERTEX_POINT('',#56996);
#7665=VERTEX_POINT('',#56997);
#7666=VERTEX_POINT('',#57021);
#7667=VERTEX_POINT('',#57022);
#7668=VERTEX_POINT('',#57046);
#7669=VERTEX_POINT('',#57047);
#7670=VERTEX_POINT('',#57070);
#7671=VERTEX_POINT('',#57071);
#7672=VERTEX_POINT('',#57095);
#7673=VERTEX_POINT('',#57096);
#7674=VERTEX_POINT('',#57120);
#7675=VERTEX_POINT('',#57121);
#7676=VERTEX_POINT('',#57123);
#7677=VERTEX_POINT('',#57129);
#7678=VERTEX_POINT('',#57137);
#7679=VERTEX_POINT('',#57138);
#7680=VERTEX_POINT('',#57140);
#7681=VERTEX_POINT('',#57145);
#7682=VERTEX_POINT('',#57147);
#7683=VERTEX_POINT('',#57149);
#7684=VERTEX_POINT('',#57151);
#7685=VERTEX_POINT('',#57154);
#7686=VERTEX_POINT('',#57167);
#7687=VERTEX_POINT('',#57168);
#7688=VERTEX_POINT('',#57218);
#7689=VERTEX_POINT('',#57219);
#7690=VERTEX_POINT('',#57269);
#7691=VERTEX_POINT('',#57270);
#7692=VERTEX_POINT('',#57317);
#7693=VERTEX_POINT('',#57318);
#7694=VERTEX_POINT('',#57368);
#7695=VERTEX_POINT('',#57369);
#7696=VERTEX_POINT('',#57419);
#7697=VERTEX_POINT('',#57420);
#7698=VERTEX_POINT('',#57467);
#7699=VERTEX_POINT('',#57468);
#7700=VERTEX_POINT('',#57470);
#7701=VERTEX_POINT('',#57484);
#7702=VERTEX_POINT('',#57506);
#7703=VERTEX_POINT('',#57507);
#7704=VERTEX_POINT('',#57509);
#7705=VERTEX_POINT('',#57518);
#7706=VERTEX_POINT('',#57530);
#7707=VERTEX_POINT('',#57531);
#7708=VERTEX_POINT('',#57554);
#7709=VERTEX_POINT('',#57555);
#7710=VERTEX_POINT('',#57579);
#7711=VERTEX_POINT('',#57580);
#7712=VERTEX_POINT('',#57604);
#7713=VERTEX_POINT('',#57605);
#7714=VERTEX_POINT('',#57628);
#7715=VERTEX_POINT('',#57629);
#7716=VERTEX_POINT('',#57653);
#7717=VERTEX_POINT('',#57654);
#7718=VERTEX_POINT('',#57678);
#7719=VERTEX_POINT('',#57679);
#7720=VERTEX_POINT('',#57681);
#7721=VERTEX_POINT('',#57687);
#7722=VERTEX_POINT('',#57695);
#7723=VERTEX_POINT('',#57696);
#7724=VERTEX_POINT('',#57698);
#7725=VERTEX_POINT('',#57703);
#7726=VERTEX_POINT('',#57705);
#7727=VERTEX_POINT('',#57707);
#7728=VERTEX_POINT('',#57709);
#7729=VERTEX_POINT('',#57712);
#7730=VERTEX_POINT('',#57725);
#7731=VERTEX_POINT('',#57726);
#7732=VERTEX_POINT('',#57776);
#7733=VERTEX_POINT('',#57777);
#7734=VERTEX_POINT('',#57827);
#7735=VERTEX_POINT('',#57828);
#7736=VERTEX_POINT('',#57875);
#7737=VERTEX_POINT('',#57876);
#7738=VERTEX_POINT('',#57926);
#7739=VERTEX_POINT('',#57927);
#7740=VERTEX_POINT('',#57977);
#7741=VERTEX_POINT('',#57978);
#7742=VERTEX_POINT('',#58025);
#7743=VERTEX_POINT('',#58026);
#7744=VERTEX_POINT('',#58028);
#7745=VERTEX_POINT('',#58042);
#7746=VERTEX_POINT('',#58064);
#7747=VERTEX_POINT('',#58065);
#7748=VERTEX_POINT('',#58067);
#7749=VERTEX_POINT('',#58076);
#7750=VERTEX_POINT('',#58088);
#7751=VERTEX_POINT('',#58089);
#7752=VERTEX_POINT('',#58112);
#7753=VERTEX_POINT('',#58113);
#7754=VERTEX_POINT('',#58137);
#7755=VERTEX_POINT('',#58138);
#7756=VERTEX_POINT('',#58162);
#7757=VERTEX_POINT('',#58163);
#7758=VERTEX_POINT('',#58186);
#7759=VERTEX_POINT('',#58187);
#7760=VERTEX_POINT('',#58211);
#7761=VERTEX_POINT('',#58212);
#7762=VERTEX_POINT('',#58236);
#7763=VERTEX_POINT('',#58237);
#7764=VERTEX_POINT('',#58239);
#7765=VERTEX_POINT('',#58245);
#7766=VERTEX_POINT('',#58253);
#7767=VERTEX_POINT('',#58254);
#7768=VERTEX_POINT('',#58256);
#7769=VERTEX_POINT('',#58261);
#7770=VERTEX_POINT('',#58263);
#7771=VERTEX_POINT('',#58265);
#7772=VERTEX_POINT('',#58267);
#7773=VERTEX_POINT('',#58270);
#7774=VERTEX_POINT('',#58283);
#7775=VERTEX_POINT('',#58284);
#7776=VERTEX_POINT('',#58334);
#7777=VERTEX_POINT('',#58335);
#7778=VERTEX_POINT('',#58385);
#7779=VERTEX_POINT('',#58386);
#7780=VERTEX_POINT('',#58433);
#7781=VERTEX_POINT('',#58434);
#7782=VERTEX_POINT('',#58484);
#7783=VERTEX_POINT('',#58485);
#7784=VERTEX_POINT('',#58535);
#7785=VERTEX_POINT('',#58536);
#7786=VERTEX_POINT('',#58583);
#7787=VERTEX_POINT('',#58584);
#7788=VERTEX_POINT('',#58586);
#7789=VERTEX_POINT('',#58600);
#7790=VERTEX_POINT('',#58622);
#7791=VERTEX_POINT('',#58623);
#7792=VERTEX_POINT('',#58625);
#7793=VERTEX_POINT('',#58634);
#7794=VERTEX_POINT('',#58646);
#7795=VERTEX_POINT('',#58647);
#7796=VERTEX_POINT('',#58670);
#7797=VERTEX_POINT('',#58671);
#7798=VERTEX_POINT('',#58695);
#7799=VERTEX_POINT('',#58696);
#7800=VERTEX_POINT('',#58720);
#7801=VERTEX_POINT('',#58721);
#7802=VERTEX_POINT('',#58744);
#7803=VERTEX_POINT('',#58745);
#7804=VERTEX_POINT('',#58769);
#7805=VERTEX_POINT('',#58770);
#7806=VERTEX_POINT('',#58794);
#7807=VERTEX_POINT('',#58795);
#7808=VERTEX_POINT('',#58797);
#7809=VERTEX_POINT('',#58803);
#7810=VERTEX_POINT('',#58811);
#7811=VERTEX_POINT('',#58812);
#7812=VERTEX_POINT('',#58814);
#7813=VERTEX_POINT('',#58819);
#7814=VERTEX_POINT('',#58821);
#7815=VERTEX_POINT('',#58823);
#7816=VERTEX_POINT('',#58825);
#7817=VERTEX_POINT('',#58828);
#7818=VERTEX_POINT('',#58841);
#7819=VERTEX_POINT('',#58842);
#7820=VERTEX_POINT('',#58892);
#7821=VERTEX_POINT('',#58893);
#7822=VERTEX_POINT('',#58943);
#7823=VERTEX_POINT('',#58944);
#7824=VERTEX_POINT('',#58991);
#7825=VERTEX_POINT('',#58992);
#7826=VERTEX_POINT('',#59042);
#7827=VERTEX_POINT('',#59043);
#7828=VERTEX_POINT('',#59093);
#7829=VERTEX_POINT('',#59094);
#7830=VERTEX_POINT('',#59141);
#7831=VERTEX_POINT('',#59142);
#7832=VERTEX_POINT('',#59144);
#7833=VERTEX_POINT('',#59158);
#7834=VERTEX_POINT('',#59180);
#7835=VERTEX_POINT('',#59181);
#7836=VERTEX_POINT('',#59183);
#7837=VERTEX_POINT('',#59192);
#7838=VERTEX_POINT('',#59204);
#7839=VERTEX_POINT('',#59205);
#7840=VERTEX_POINT('',#59228);
#7841=VERTEX_POINT('',#59229);
#7842=VERTEX_POINT('',#59253);
#7843=VERTEX_POINT('',#59254);
#7844=VERTEX_POINT('',#59278);
#7845=VERTEX_POINT('',#59279);
#7846=VERTEX_POINT('',#59302);
#7847=VERTEX_POINT('',#59303);
#7848=VERTEX_POINT('',#59327);
#7849=VERTEX_POINT('',#59328);
#7850=VERTEX_POINT('',#59352);
#7851=VERTEX_POINT('',#59353);
#7852=VERTEX_POINT('',#59355);
#7853=VERTEX_POINT('',#59361);
#7854=VERTEX_POINT('',#59369);
#7855=VERTEX_POINT('',#59370);
#7856=VERTEX_POINT('',#59372);
#7857=VERTEX_POINT('',#59374);
#7858=VERTEX_POINT('',#59378);
#7859=VERTEX_POINT('',#59380);
#7860=VERTEX_POINT('',#59384);
#7861=VERTEX_POINT('',#59385);
#7862=VERTEX_POINT('',#59390);
#7863=VERTEX_POINT('',#59391);
#7864=VERTEX_POINT('',#59420);
#7865=VERTEX_POINT('',#59422);
#7866=VERTEX_POINT('',#59424);
#7867=VERTEX_POINT('',#59426);
#7868=VERTEX_POINT('',#59431);
#7869=VERTEX_POINT('',#59433);
#7870=VERTEX_POINT('',#59435);
#7871=VERTEX_POINT('',#59437);
#7872=VERTEX_POINT('',#59439);
#7873=VERTEX_POINT('',#59468);
#7874=VERTEX_POINT('',#59470);
#7875=VERTEX_POINT('',#59472);
#7876=VERTEX_POINT('',#59474);
#7877=VERTEX_POINT('',#59479);
#7878=VERTEX_POINT('',#59481);
#7879=VERTEX_POINT('',#59483);
#7880=VERTEX_POINT('',#59485);
#7881=VERTEX_POINT('',#59487);
#7882=VERTEX_POINT('',#59516);
#7883=VERTEX_POINT('',#59518);
#7884=VERTEX_POINT('',#59520);
#7885=VERTEX_POINT('',#59522);
#7886=VERTEX_POINT('',#59527);
#7887=VERTEX_POINT('',#59529);
#7888=VERTEX_POINT('',#59531);
#7889=VERTEX_POINT('',#59533);
#7890=VERTEX_POINT('',#59535);
#7891=VERTEX_POINT('',#59542);
#7892=VERTEX_POINT('',#59544);
#7893=VERTEX_POINT('',#59546);
#7894=VERTEX_POINT('',#59548);
#7895=VERTEX_POINT('',#59553);
#7896=VERTEX_POINT('',#59555);
#7897=VERTEX_POINT('',#59557);
#7898=VERTEX_POINT('',#59559);
#7899=VERTEX_POINT('',#59561);
#7900=VERTEX_POINT('',#59590);
#7901=VERTEX_POINT('',#59592);
#7902=VERTEX_POINT('',#59594);
#7903=VERTEX_POINT('',#59596);
#7904=VERTEX_POINT('',#59601);
#7905=VERTEX_POINT('',#59603);
#7906=VERTEX_POINT('',#59605);
#7907=VERTEX_POINT('',#59607);
#7908=VERTEX_POINT('',#59609);
#7909=VERTEX_POINT('',#59638);
#7910=VERTEX_POINT('',#59640);
#7911=VERTEX_POINT('',#59642);
#7912=VERTEX_POINT('',#59644);
#7913=VERTEX_POINT('',#59649);
#7914=VERTEX_POINT('',#59651);
#7915=VERTEX_POINT('',#59653);
#7916=VERTEX_POINT('',#69798);
#7917=VERTEX_POINT('',#69800);
#7918=VERTEX_POINT('',#69804);
#7919=VERTEX_POINT('',#69807);
#7920=VERTEX_POINT('',#69812);
#7921=VERTEX_POINT('',#69814);
#7922=VERTEX_POINT('',#69818);
#7923=VERTEX_POINT('',#69821);
#7924=VERTEX_POINT('',#69826);
#7925=VERTEX_POINT('',#69828);
#7926=VERTEX_POINT('',#69832);
#7927=VERTEX_POINT('',#69835);
#7928=VERTEX_POINT('',#69840);
#7929=VERTEX_POINT('',#69842);
#7930=VERTEX_POINT('',#69846);
#7931=VERTEX_POINT('',#69849);
#7932=VERTEX_POINT('',#69854);
#7933=VERTEX_POINT('',#69856);
#7934=VERTEX_POINT('',#69860);
#7935=VERTEX_POINT('',#69863);
#7936=VERTEX_POINT('',#69868);
#7937=VERTEX_POINT('',#69870);
#7938=VERTEX_POINT('',#69874);
#7939=VERTEX_POINT('',#69877);
#7940=VERTEX_POINT('',#69882);
#7941=VERTEX_POINT('',#69889);
#7942=VERTEX_POINT('',#69893);
#7943=VERTEX_POINT('',#69900);
#7944=VERTEX_POINT('',#69904);
#7945=VERTEX_POINT('',#69910);
#7946=VERTEX_POINT('',#69917);
#7947=VERTEX_POINT('',#69921);
#7948=VERTEX_POINT('',#69925);
#7949=VERTEX_POINT('',#69929);
#7950=VERTEX_POINT('',#69938);
#7951=VERTEX_POINT('',#69945);
#7952=VERTEX_POINT('',#69949);
#7953=VERTEX_POINT('',#69953);
#7954=VERTEX_POINT('',#69957);
#7955=VERTEX_POINT('',#69966);
#7956=VERTEX_POINT('',#69973);
#7957=VERTEX_POINT('',#69977);
#7958=VERTEX_POINT('',#69981);
#7959=VERTEX_POINT('',#69985);
#7960=VERTEX_POINT('',#69994);
#7961=VERTEX_POINT('',#70001);
#7962=VERTEX_POINT('',#70005);
#7963=VERTEX_POINT('',#70012);
#7964=VERTEX_POINT('',#70016);
#7965=VERTEX_POINT('',#72031);
#7966=VERTEX_POINT('',#74071);
#7967=VERTEX_POINT('',#76111);
#7968=VERTEX_POINT('',#78127);
#7969=VERTEX_POINT('',#80167);
#7970=VERTEX_POINT('',#82183);
#7971=VERTEX_POINT('',#84223);
#7972=VERTEX_POINT('',#86239);
#7973=VERTEX_POINT('',#86270);
#7974=VERTEX_POINT('',#86277);
#7975=VERTEX_POINT('',#86281);
#7976=VERTEX_POINT('',#86288);
#7977=VERTEX_POINT('',#86292);
#7978=VERTEX_POINT('',#88307);
#7979=VERTEX_POINT('',#88338);
#7980=VERTEX_POINT('',#88342);
#7981=VERTEX_POINT('',#88348);
#7982=VERTEX_POINT('',#88352);
#7983=VERTEX_POINT('',#88358);
#7984=VERTEX_POINT('',#88362);
#7985=VERTEX_POINT('',#88368);
#7986=VERTEX_POINT('',#88373);
#7987=VERTEX_POINT('',#88375);
#7988=VERTEX_POINT('',#88378);
#7989=VERTEX_POINT('',#88383);
#7990=VERTEX_POINT('',#88385);
#7991=VERTEX_POINT('',#88388);
#7992=VERTEX_POINT('',#88393);
#7993=VERTEX_POINT('',#88395);
#7994=VERTEX_POINT('',#94450);
#7995=VERTEX_POINT('',#94451);
#7996=VERTEX_POINT('',#94453);
#7997=VERTEX_POINT('',#94455);
#7998=VERTEX_POINT('',#94468);
#7999=VERTEX_POINT('',#94479);
#8000=VERTEX_POINT('',#94484);
#8001=VERTEX_POINT('',#94486);
#8002=VERTEX_POINT('',#94490);
#8003=VERTEX_POINT('',#94509);
#8004=VERTEX_POINT('',#94517);
#8005=VERTEX_POINT('',#94520);
#8006=VERTEX_POINT('',#94524);
#8007=VERTEX_POINT('',#94525);
#8008=VERTEX_POINT('',#94544);
#8009=VERTEX_POINT('',#94546);
#8010=VERTEX_POINT('',#94550);
#8011=VERTEX_POINT('',#94552);
#8012=VERTEX_POINT('',#94556);
#8013=VERTEX_POINT('',#94557);
#8014=VERTEX_POINT('',#94578);
#8015=VERTEX_POINT('',#94586);
#8016=VERTEX_POINT('',#94588);
#8017=VERTEX_POINT('',#94593);
#8018=VERTEX_POINT('',#94595);
#8019=VERTEX_POINT('',#94601);
#8020=VERTEX_POINT('',#94603);
#8021=VERTEX_POINT('',#94607);
#8022=VERTEX_POINT('',#94610);
#8023=VERTEX_POINT('',#94613);
#8024=VERTEX_POINT('',#94617);
#8025=VERTEX_POINT('',#94620);
#8026=VERTEX_POINT('',#94625);
#8027=VERTEX_POINT('',#94632);
#8028=VERTEX_POINT('',#94633);
#8029=VERTEX_POINT('',#94635);
#8030=VERTEX_POINT('',#94637);
#8031=VERTEX_POINT('',#94641);
#8032=VERTEX_POINT('',#94643);
#8033=VERTEX_POINT('',#94647);
#8034=VERTEX_POINT('',#94649);
#8035=VERTEX_POINT('',#94659);
#8036=VERTEX_POINT('',#94661);
#8037=VERTEX_POINT('',#94668);
#8038=VERTEX_POINT('',#94670);
#8039=VERTEX_POINT('',#94673);
#8040=VERTEX_POINT('',#94677);
#8041=VERTEX_POINT('',#94681);
#8042=VERTEX_POINT('',#94683);
#8043=VERTEX_POINT('',#94686);
#8044=VERTEX_POINT('',#94690);
#8045=VERTEX_POINT('',#94694);
#8046=VERTEX_POINT('',#94696);
#8047=VERTEX_POINT('',#94699);
#8048=VERTEX_POINT('',#94703);
#8049=VERTEX_POINT('',#94707);
#8050=VERTEX_POINT('',#94709);
#8051=VERTEX_POINT('',#94712);
#8052=VERTEX_POINT('',#94716);
#8053=VERTEX_POINT('',#94720);
#8054=VERTEX_POINT('',#94722);
#8055=VERTEX_POINT('',#94725);
#8056=VERTEX_POINT('',#94729);
#8057=VERTEX_POINT('',#94733);
#8058=VERTEX_POINT('',#94735);
#8059=VERTEX_POINT('',#94738);
#8060=VERTEX_POINT('',#94742);
#8061=VERTEX_POINT('',#94746);
#8062=VERTEX_POINT('',#94748);
#8063=VERTEX_POINT('',#94752);
#8064=VERTEX_POINT('',#94754);
#8065=VERTEX_POINT('',#94761);
#8066=VERTEX_POINT('',#94763);
#8067=VERTEX_POINT('',#94767);
#8068=VERTEX_POINT('',#94769);
#8069=VERTEX_POINT('',#94776);
#8070=VERTEX_POINT('',#94778);
#8071=VERTEX_POINT('',#94782);
#8072=VERTEX_POINT('',#94786);
#8073=VERTEX_POINT('',#94788);
#8074=VERTEX_POINT('',#94792);
#8075=VERTEX_POINT('',#94796);
#8076=VERTEX_POINT('',#94798);
#8077=VERTEX_POINT('',#94802);
#8078=VERTEX_POINT('',#94806);
#8079=VERTEX_POINT('',#94808);
#8080=VERTEX_POINT('',#94812);
#8081=VERTEX_POINT('',#94816);
#8082=VERTEX_POINT('',#94818);
#8083=VERTEX_POINT('',#94822);
#8084=VERTEX_POINT('',#94826);
#8085=VERTEX_POINT('',#94828);
#8086=VERTEX_POINT('',#94832);
#8087=VERTEX_POINT('',#94836);
#8088=VERTEX_POINT('',#94838);
#8089=VERTEX_POINT('',#94842);
#8090=VERTEX_POINT('',#94844);
#8091=VERTEX_POINT('',#94851);
#8092=VERTEX_POINT('',#94853);
#8093=VERTEX_POINT('',#94857);
#8094=VERTEX_POINT('',#94859);
#8095=VERTEX_POINT('',#94866);
#8096=VERTEX_POINT('',#94868);
#8097=VERTEX_POINT('',#94872);
#8098=VERTEX_POINT('',#94874);
#8099=VERTEX_POINT('',#94881);
#8100=VERTEX_POINT('',#94883);
#8101=VERTEX_POINT('',#94887);
#8102=VERTEX_POINT('',#94889);
#8103=VERTEX_POINT('',#94896);
#8104=VERTEX_POINT('',#94897);
#8105=VERTEX_POINT('',#94899);
#8106=VERTEX_POINT('',#94901);
#8107=VERTEX_POINT('',#94905);
#8108=VERTEX_POINT('',#94906);
#8109=VERTEX_POINT('',#94908);
#8110=VERTEX_POINT('',#94910);
#8111=VERTEX_POINT('',#94923);
#8112=VERTEX_POINT('',#94925);
#8113=VERTEX_POINT('',#94928);
#8114=VERTEX_POINT('',#94933);
#8115=VERTEX_POINT('',#95228);
#8116=VERTEX_POINT('',#95230);
#8117=VERTEX_POINT('',#95265);
#8118=VERTEX_POINT('',#95266);
#8119=VERTEX_POINT('',#95268);
#8120=VERTEX_POINT('',#95279);
#8121=VERTEX_POINT('',#95289);
#8122=VERTEX_POINT('',#95290);
#8123=VERTEX_POINT('',#95337);
#8124=VERTEX_POINT('',#95338);
#8125=VERTEX_POINT('',#95385);
#8126=VERTEX_POINT('',#95386);
#8127=VERTEX_POINT('',#95439);
#8128=VERTEX_POINT('',#95440);
#8129=VERTEX_POINT('',#95487);
#8130=VERTEX_POINT('',#95488);
#8131=VERTEX_POINT('',#95535);
#8132=VERTEX_POINT('',#95536);
#8133=VERTEX_POINT('',#95583);
#8134=VERTEX_POINT('',#95584);
#8135=VERTEX_POINT('',#95637);
#8136=VERTEX_POINT('',#95638);
#8137=VERTEX_POINT('',#95685);
#8138=VERTEX_POINT('',#95686);
#8139=VERTEX_POINT('',#95733);
#8140=VERTEX_POINT('',#95734);
#8141=VERTEX_POINT('',#95787);
#8142=VERTEX_POINT('',#95788);
#8143=VERTEX_POINT('',#95835);
#8144=VERTEX_POINT('',#95836);
#8145=VERTEX_POINT('',#95883);
#8146=VERTEX_POINT('',#95884);
#8147=VERTEX_POINT('',#95934);
#8148=VERTEX_POINT('',#95935);
#8149=VERTEX_POINT('',#95985);
#8150=VERTEX_POINT('',#95986);
#8151=VERTEX_POINT('',#96033);
#8152=VERTEX_POINT('',#96034);
#8153=VERTEX_POINT('',#96036);
#8154=VERTEX_POINT('',#96045);
#8155=VERTEX_POINT('',#96055);
#8156=VERTEX_POINT('',#96056);
#8157=VERTEX_POINT('',#96079);
#8158=VERTEX_POINT('',#96080);
#8159=VERTEX_POINT('',#96103);
#8160=VERTEX_POINT('',#96104);
#8161=VERTEX_POINT('',#96129);
#8162=VERTEX_POINT('',#96130);
#8163=VERTEX_POINT('',#96153);
#8164=VERTEX_POINT('',#96154);
#8165=VERTEX_POINT('',#96177);
#8166=VERTEX_POINT('',#96178);
#8167=VERTEX_POINT('',#96202);
#8168=VERTEX_POINT('',#96203);
#8169=VERTEX_POINT('',#96227);
#8170=VERTEX_POINT('',#96228);
#8171=VERTEX_POINT('',#96251);
#8172=VERTEX_POINT('',#96252);
#8173=VERTEX_POINT('',#96276);
#8174=VERTEX_POINT('',#96277);
#8175=VERTEX_POINT('',#96301);
#8176=VERTEX_POINT('',#96302);
#8177=VERTEX_POINT('',#96325);
#8178=VERTEX_POINT('',#96326);
#8179=VERTEX_POINT('',#96349);
#8180=VERTEX_POINT('',#96350);
#8181=VERTEX_POINT('',#96374);
#8182=VERTEX_POINT('',#96375);
#8183=VERTEX_POINT('',#96399);
#8184=VERTEX_POINT('',#96400);
#8185=VERTEX_POINT('',#96423);
#8186=VERTEX_POINT('',#96551);
#8187=VERTEX_POINT('',#96610);
#8188=VERTEX_POINT('',#96715);
#8189=VERTEX_POINT('',#97142);
#8190=VERTEX_POINT('',#97250);
#8191=VERTEX_POINT('',#97796);
#8192=VERTEX_POINT('',#97797);
#8193=VERTEX_POINT('',#97799);
#8194=VERTEX_POINT('',#97801);
#8195=VERTEX_POINT('',#97805);
#8196=VERTEX_POINT('',#97807);
#8197=VERTEX_POINT('',#97811);
#8198=VERTEX_POINT('',#97813);
#8199=VERTEX_POINT('',#97817);
#8200=VERTEX_POINT('',#97819);
#8201=VERTEX_POINT('',#97823);
#8202=VERTEX_POINT('',#97825);
#8203=VERTEX_POINT('',#97833);
#8204=VERTEX_POINT('',#97836);
#8205=VERTEX_POINT('',#97843);
#8206=VERTEX_POINT('',#97844);
#8207=VERTEX_POINT('',#97846);
#8208=VERTEX_POINT('',#97857);
#8209=VERTEX_POINT('',#97867);
#8210=VERTEX_POINT('',#97868);
#8211=VERTEX_POINT('',#97915);
#8212=VERTEX_POINT('',#97916);
#8213=VERTEX_POINT('',#97963);
#8214=VERTEX_POINT('',#97964);
#8215=VERTEX_POINT('',#98011);
#8216=VERTEX_POINT('',#98012);
#8217=VERTEX_POINT('',#98059);
#8218=VERTEX_POINT('',#98060);
#8219=VERTEX_POINT('',#98107);
#8220=VERTEX_POINT('',#98108);
#8221=VERTEX_POINT('',#98155);
#8222=VERTEX_POINT('',#98156);
#8223=VERTEX_POINT('',#98209);
#8224=VERTEX_POINT('',#98210);
#8225=VERTEX_POINT('',#98212);
#8226=VERTEX_POINT('',#98222);
#8227=VERTEX_POINT('',#98233);
#8228=VERTEX_POINT('',#98234);
#8229=VERTEX_POINT('',#98258);
#8230=VERTEX_POINT('',#98259);
#8231=VERTEX_POINT('',#98283);
#8232=VERTEX_POINT('',#98284);
#8233=VERTEX_POINT('',#98307);
#8234=VERTEX_POINT('',#98308);
#8235=VERTEX_POINT('',#98331);
#8236=VERTEX_POINT('',#98332);
#8237=VERTEX_POINT('',#98357);
#8238=VERTEX_POINT('',#98358);
#8239=VERTEX_POINT('',#98381);
#8240=VERTEX_POINT('',#98382);
#8241=VERTEX_POINT('',#98405);
#8242=VERTEX_POINT('',#98590);
#8243=VERTEX_POINT('',#98652);
#8244=VERTEX_POINT('',#98694);
#8245=VERTEX_POINT('',#98925);
#8246=VERTEX_POINT('',#99033);
#8247=VERTEX_POINT('',#99045);
#8248=VERTEX_POINT('',#99046);
#8249=VERTEX_POINT('',#99048);
#8250=VERTEX_POINT('',#99050);
#8251=VERTEX_POINT('',#99054);
#8252=VERTEX_POINT('',#99056);
#8253=VERTEX_POINT('',#99060);
#8254=VERTEX_POINT('',#99062);
#8255=VERTEX_POINT('',#99066);
#8256=VERTEX_POINT('',#99068);
#8257=VERTEX_POINT('',#99072);
#8258=VERTEX_POINT('',#99074);
#8259=VERTEX_POINT('',#99422);
#8260=VERTEX_POINT('',#99427);
#8261=EDGE_CURVE('',#6438,#6439,#4630,.T.);
#8262=EDGE_CURVE('',#6439,#6440,#3113,.T.);
#8263=EDGE_CURVE('',#6440,#6441,#2777,.T.);
#8264=EDGE_CURVE('',#6441,#6442,#3114,.T.);
#8265=EDGE_CURVE('',#6442,#6443,#4631,.T.);
#8266=EDGE_CURVE('',#6443,#6443,#2778,.F.);
#8267=EDGE_CURVE('',#6442,#6438,#3115,.T.);
#8268=EDGE_CURVE('',#6444,#6445,#4632,.T.);
#8269=EDGE_CURVE('',#6445,#6439,#3116,.T.);
#8270=EDGE_CURVE('',#6438,#6444,#3117,.T.);
#8271=EDGE_CURVE('',#6446,#6447,#4633,.T.);
#8272=EDGE_CURVE('',#6447,#6445,#3118,.T.);
#8273=EDGE_CURVE('',#6444,#6446,#3119,.T.);
#8274=EDGE_CURVE('',#6448,#6449,#4634,.T.);
#8275=EDGE_CURVE('',#6449,#6447,#3120,.T.);
#8276=EDGE_CURVE('',#6446,#6448,#3121,.T.);
#8277=EDGE_CURVE('',#6450,#6451,#4635,.T.);
#8278=EDGE_CURVE('',#6451,#6449,#3122,.T.);
#8279=EDGE_CURVE('',#6448,#6450,#3123,.T.);
#8280=EDGE_CURVE('',#6452,#6453,#4636,.T.);
#8281=EDGE_CURVE('',#6453,#6451,#3124,.T.);
#8282=EDGE_CURVE('',#6450,#6452,#3125,.T.);
#8283=EDGE_CURVE('',#6454,#6455,#4637,.T.);
#8284=EDGE_CURVE('',#6455,#6453,#3126,.T.);
#8285=EDGE_CURVE('',#6452,#6454,#3127,.T.);
#8286=EDGE_CURVE('',#6456,#6457,#4638,.T.);
#8287=EDGE_CURVE('',#6457,#6455,#3128,.T.);
#8288=EDGE_CURVE('',#6454,#6456,#3129,.T.);
#8289=EDGE_CURVE('',#6458,#6459,#4639,.T.);
#8290=EDGE_CURVE('',#6459,#6457,#3130,.T.);
#8291=EDGE_CURVE('',#6456,#6458,#3131,.T.);
#8292=EDGE_CURVE('',#6460,#6461,#4640,.T.);
#8293=EDGE_CURVE('',#6461,#6459,#3132,.T.);
#8294=EDGE_CURVE('',#6458,#6460,#3133,.T.);
#8295=EDGE_CURVE('',#6462,#6463,#4641,.T.);
#8296=EDGE_CURVE('',#6463,#6461,#3134,.T.);
#8297=EDGE_CURVE('',#6460,#6462,#3135,.T.);
#8298=EDGE_CURVE('',#6464,#6465,#4642,.T.);
#8299=EDGE_CURVE('',#6464,#6466,#3136,.T.);
#8300=EDGE_CURVE('',#6467,#6466,#2779,.T.);
#8301=EDGE_CURVE('',#6467,#6465,#3137,.T.);
#8302=EDGE_CURVE('',#6468,#6469,#4643,.T.);
#8303=EDGE_CURVE('',#6469,#6470,#3138,.T.);
#8304=EDGE_CURVE('',#6471,#6470,#2780,.T.);
#8305=EDGE_CURVE('',#6468,#6471,#3139,.T.);
#8306=EDGE_CURVE('',#6472,#6473,#4644,.T.);
#8307=EDGE_CURVE('',#6473,#6469,#3140,.T.);
#8308=EDGE_CURVE('',#6472,#6468,#3141,.T.);
#8309=EDGE_CURVE('',#6474,#6475,#4645,.T.);
#8310=EDGE_CURVE('',#6475,#6473,#3142,.T.);
#8311=EDGE_CURVE('',#6474,#6472,#3143,.T.);
#8312=EDGE_CURVE('',#6476,#6477,#4646,.T.);
#8313=EDGE_CURVE('',#6477,#6475,#3144,.T.);
#8314=EDGE_CURVE('',#6476,#6474,#3145,.T.);
#8315=EDGE_CURVE('',#6478,#6479,#4647,.T.);
#8316=EDGE_CURVE('',#6479,#6477,#3146,.T.);
#8317=EDGE_CURVE('',#6478,#6476,#3147,.T.);
#8318=EDGE_CURVE('',#6480,#6481,#4648,.T.);
#8319=EDGE_CURVE('',#6481,#6479,#3148,.T.);
#8320=EDGE_CURVE('',#6480,#6478,#3149,.T.);
#8321=EDGE_CURVE('',#6482,#6483,#4649,.T.);
#8322=EDGE_CURVE('',#6483,#6481,#3150,.T.);
#8323=EDGE_CURVE('',#6482,#6480,#3151,.T.);
#8324=EDGE_CURVE('',#6484,#6485,#4650,.T.);
#8325=EDGE_CURVE('',#6485,#6483,#3152,.T.);
#8326=EDGE_CURVE('',#6484,#6482,#3153,.T.);
#8327=EDGE_CURVE('',#6486,#6487,#4651,.T.);
#8328=EDGE_CURVE('',#6487,#6485,#3154,.T.);
#8329=EDGE_CURVE('',#6486,#6484,#3155,.T.);
#8330=EDGE_CURVE('',#6488,#6489,#4652,.T.);
#8331=EDGE_CURVE('',#6489,#6487,#3156,.T.);
#8332=EDGE_CURVE('',#6488,#6486,#3157,.T.);
#8333=EDGE_CURVE('',#6490,#6491,#4653,.T.);
#8334=EDGE_CURVE('',#6491,#6489,#3158,.T.);
#8335=EDGE_CURVE('',#6490,#6488,#3159,.T.);
#8336=EDGE_CURVE('',#6492,#6493,#4654,.T.);
#8337=EDGE_CURVE('',#6493,#6491,#3160,.T.);
#8338=EDGE_CURVE('',#6492,#6490,#3161,.T.);
#8339=EDGE_CURVE('',#6494,#6495,#4655,.T.);
#8340=EDGE_CURVE('',#6496,#6494,#3162,.T.);
#8341=EDGE_CURVE('',#6497,#6496,#2781,.T.);
#8342=EDGE_CURVE('',#6497,#6495,#3163,.T.);
#8343=EDGE_CURVE('',#6498,#6499,#4656,.T.);
#8344=EDGE_CURVE('',#6499,#6500,#3164,.T.);
#8345=EDGE_CURVE('',#6500,#6501,#2782,.T.);
#8346=EDGE_CURVE('',#6501,#6502,#3165,.T.);
#8347=EDGE_CURVE('',#6502,#6503,#4657,.T.);
#8348=EDGE_CURVE('',#6503,#6503,#2783,.F.);
#8349=EDGE_CURVE('',#6502,#6498,#3166,.T.);
#8350=EDGE_CURVE('',#6504,#6505,#4658,.T.);
#8351=EDGE_CURVE('',#6505,#6499,#3167,.T.);
#8352=EDGE_CURVE('',#6498,#6504,#3168,.T.);
#8353=EDGE_CURVE('',#6506,#6507,#4659,.T.);
#8354=EDGE_CURVE('',#6507,#6505,#3169,.T.);
#8355=EDGE_CURVE('',#6504,#6506,#3170,.T.);
#8356=EDGE_CURVE('',#6508,#6509,#4660,.T.);
#8357=EDGE_CURVE('',#6509,#6507,#3171,.T.);
#8358=EDGE_CURVE('',#6506,#6508,#3172,.T.);
#8359=EDGE_CURVE('',#6510,#6511,#4661,.T.);
#8360=EDGE_CURVE('',#6511,#6509,#3173,.T.);
#8361=EDGE_CURVE('',#6508,#6510,#3174,.T.);
#8362=EDGE_CURVE('',#6512,#6513,#4662,.T.);
#8363=EDGE_CURVE('',#6513,#6511,#3175,.T.);
#8364=EDGE_CURVE('',#6510,#6512,#3176,.T.);
#8365=EDGE_CURVE('',#6514,#6515,#4663,.T.);
#8366=EDGE_CURVE('',#6515,#6513,#3177,.T.);
#8367=EDGE_CURVE('',#6512,#6514,#3178,.T.);
#8368=EDGE_CURVE('',#6516,#6517,#4664,.T.);
#8369=EDGE_CURVE('',#6517,#6515,#3179,.T.);
#8370=EDGE_CURVE('',#6514,#6516,#3180,.T.);
#8371=EDGE_CURVE('',#6518,#6519,#4665,.T.);
#8372=EDGE_CURVE('',#6519,#6517,#3181,.T.);
#8373=EDGE_CURVE('',#6516,#6518,#3182,.T.);
#8374=EDGE_CURVE('',#6520,#6521,#4666,.T.);
#8375=EDGE_CURVE('',#6521,#6519,#3183,.T.);
#8376=EDGE_CURVE('',#6518,#6520,#3184,.T.);
#8377=EDGE_CURVE('',#6522,#6523,#4667,.T.);
#8378=EDGE_CURVE('',#6523,#6521,#3185,.T.);
#8379=EDGE_CURVE('',#6520,#6522,#3186,.T.);
#8380=EDGE_CURVE('',#6524,#6525,#4668,.T.);
#8381=EDGE_CURVE('',#6524,#6526,#3187,.T.);
#8382=EDGE_CURVE('',#6527,#6526,#2784,.F.);
#8383=EDGE_CURVE('',#6527,#6525,#3188,.T.);
#8384=EDGE_CURVE('',#6528,#6529,#4669,.T.);
#8385=EDGE_CURVE('',#6529,#6530,#3189,.T.);
#8386=EDGE_CURVE('',#6531,#6530,#2785,.T.);
#8387=EDGE_CURVE('',#6528,#6531,#3190,.T.);
#8388=EDGE_CURVE('',#6532,#6533,#4670,.T.);
#8389=EDGE_CURVE('',#6533,#6529,#3191,.T.);
#8390=EDGE_CURVE('',#6532,#6528,#3192,.T.);
#8391=EDGE_CURVE('',#6534,#6535,#4671,.T.);
#8392=EDGE_CURVE('',#6535,#6533,#3193,.T.);
#8393=EDGE_CURVE('',#6534,#6532,#3194,.T.);
#8394=EDGE_CURVE('',#6536,#6537,#4672,.T.);
#8395=EDGE_CURVE('',#6537,#6535,#3195,.T.);
#8396=EDGE_CURVE('',#6536,#6534,#3196,.T.);
#8397=EDGE_CURVE('',#6538,#6539,#4673,.T.);
#8398=EDGE_CURVE('',#6539,#6537,#3197,.T.);
#8399=EDGE_CURVE('',#6538,#6536,#3198,.T.);
#8400=EDGE_CURVE('',#6540,#6541,#4674,.T.);
#8401=EDGE_CURVE('',#6541,#6539,#3199,.T.);
#8402=EDGE_CURVE('',#6540,#6538,#3200,.T.);
#8403=EDGE_CURVE('',#6542,#6543,#4675,.T.);
#8404=EDGE_CURVE('',#6543,#6541,#3201,.T.);
#8405=EDGE_CURVE('',#6542,#6540,#3202,.T.);
#8406=EDGE_CURVE('',#6544,#6545,#4676,.T.);
#8407=EDGE_CURVE('',#6545,#6543,#3203,.T.);
#8408=EDGE_CURVE('',#6544,#6542,#3204,.T.);
#8409=EDGE_CURVE('',#6546,#6547,#4677,.T.);
#8410=EDGE_CURVE('',#6547,#6545,#3205,.T.);
#8411=EDGE_CURVE('',#6546,#6544,#3206,.T.);
#8412=EDGE_CURVE('',#6548,#6549,#4678,.T.);
#8413=EDGE_CURVE('',#6549,#6547,#3207,.T.);
#8414=EDGE_CURVE('',#6548,#6546,#3208,.T.);
#8415=EDGE_CURVE('',#6550,#6551,#4679,.T.);
#8416=EDGE_CURVE('',#6551,#6549,#3209,.T.);
#8417=EDGE_CURVE('',#6550,#6548,#3210,.T.);
#8418=EDGE_CURVE('',#6552,#6553,#4680,.T.);
#8419=EDGE_CURVE('',#6553,#6551,#3211,.T.);
#8420=EDGE_CURVE('',#6552,#6550,#3212,.T.);
#8421=EDGE_CURVE('',#6554,#6555,#4681,.T.);
#8422=EDGE_CURVE('',#6556,#6554,#3213,.T.);
#8423=EDGE_CURVE('',#6557,#6556,#2786,.T.);
#8424=EDGE_CURVE('',#6557,#6555,#3214,.T.);
#8425=EDGE_CURVE('',#6558,#6559,#4682,.T.);
#8426=EDGE_CURVE('',#6559,#6560,#3215,.T.);
#8427=EDGE_CURVE('',#6560,#6561,#2787,.T.);
#8428=EDGE_CURVE('',#6561,#6562,#3216,.T.);
#8429=EDGE_CURVE('',#6562,#6563,#4683,.T.);
#8430=EDGE_CURVE('',#6563,#6563,#2788,.F.);
#8431=EDGE_CURVE('',#6562,#6558,#3217,.T.);
#8432=EDGE_CURVE('',#6564,#6565,#4684,.T.);
#8433=EDGE_CURVE('',#6565,#6559,#3218,.T.);
#8434=EDGE_CURVE('',#6558,#6564,#3219,.T.);
#8435=EDGE_CURVE('',#6566,#6567,#4685,.T.);
#8436=EDGE_CURVE('',#6567,#6565,#3220,.T.);
#8437=EDGE_CURVE('',#6564,#6566,#3221,.T.);
#8438=EDGE_CURVE('',#6568,#6569,#4686,.T.);
#8439=EDGE_CURVE('',#6569,#6567,#3222,.T.);
#8440=EDGE_CURVE('',#6566,#6568,#3223,.T.);
#8441=EDGE_CURVE('',#6570,#6571,#4687,.T.);
#8442=EDGE_CURVE('',#6571,#6569,#3224,.T.);
#8443=EDGE_CURVE('',#6568,#6570,#3225,.T.);
#8444=EDGE_CURVE('',#6572,#6573,#4688,.T.);
#8445=EDGE_CURVE('',#6573,#6571,#3226,.T.);
#8446=EDGE_CURVE('',#6570,#6572,#3227,.T.);
#8447=EDGE_CURVE('',#6574,#6575,#4689,.T.);
#8448=EDGE_CURVE('',#6575,#6573,#3228,.T.);
#8449=EDGE_CURVE('',#6572,#6574,#3229,.T.);
#8450=EDGE_CURVE('',#6576,#6577,#4690,.T.);
#8451=EDGE_CURVE('',#6577,#6575,#3230,.T.);
#8452=EDGE_CURVE('',#6574,#6576,#3231,.T.);
#8453=EDGE_CURVE('',#6578,#6579,#4691,.T.);
#8454=EDGE_CURVE('',#6579,#6577,#3232,.T.);
#8455=EDGE_CURVE('',#6576,#6578,#3233,.T.);
#8456=EDGE_CURVE('',#6580,#6581,#4692,.T.);
#8457=EDGE_CURVE('',#6581,#6579,#3234,.T.);
#8458=EDGE_CURVE('',#6578,#6580,#3235,.T.);
#8459=EDGE_CURVE('',#6582,#6583,#4693,.T.);
#8460=EDGE_CURVE('',#6583,#6581,#3236,.T.);
#8461=EDGE_CURVE('',#6580,#6582,#3237,.T.);
#8462=EDGE_CURVE('',#6584,#6585,#4694,.T.);
#8463=EDGE_CURVE('',#6584,#6586,#3238,.T.);
#8464=EDGE_CURVE('',#6587,#6586,#2789,.T.);
#8465=EDGE_CURVE('',#6587,#6585,#3239,.T.);
#8466=EDGE_CURVE('',#6588,#6589,#4695,.T.);
#8467=EDGE_CURVE('',#6589,#6590,#3240,.T.);
#8468=EDGE_CURVE('',#6591,#6590,#2790,.T.);
#8469=EDGE_CURVE('',#6588,#6591,#3241,.T.);
#8470=EDGE_CURVE('',#6592,#6593,#4696,.T.);
#8471=EDGE_CURVE('',#6593,#6589,#3242,.T.);
#8472=EDGE_CURVE('',#6592,#6588,#3243,.T.);
#8473=EDGE_CURVE('',#6594,#6595,#4697,.T.);
#8474=EDGE_CURVE('',#6595,#6593,#3244,.T.);
#8475=EDGE_CURVE('',#6594,#6592,#3245,.T.);
#8476=EDGE_CURVE('',#6596,#6597,#4698,.T.);
#8477=EDGE_CURVE('',#6597,#6595,#3246,.T.);
#8478=EDGE_CURVE('',#6596,#6594,#3247,.T.);
#8479=EDGE_CURVE('',#6598,#6599,#4699,.T.);
#8480=EDGE_CURVE('',#6599,#6597,#3248,.T.);
#8481=EDGE_CURVE('',#6598,#6596,#3249,.T.);
#8482=EDGE_CURVE('',#6600,#6601,#4700,.T.);
#8483=EDGE_CURVE('',#6601,#6599,#3250,.T.);
#8484=EDGE_CURVE('',#6600,#6598,#3251,.T.);
#8485=EDGE_CURVE('',#6602,#6603,#4701,.T.);
#8486=EDGE_CURVE('',#6603,#6601,#3252,.T.);
#8487=EDGE_CURVE('',#6602,#6600,#3253,.T.);
#8488=EDGE_CURVE('',#6604,#6605,#4702,.T.);
#8489=EDGE_CURVE('',#6605,#6603,#3254,.T.);
#8490=EDGE_CURVE('',#6604,#6602,#3255,.T.);
#8491=EDGE_CURVE('',#6606,#6607,#4703,.T.);
#8492=EDGE_CURVE('',#6607,#6605,#3256,.T.);
#8493=EDGE_CURVE('',#6606,#6604,#3257,.T.);
#8494=EDGE_CURVE('',#6608,#6609,#4704,.T.);
#8495=EDGE_CURVE('',#6609,#6607,#3258,.T.);
#8496=EDGE_CURVE('',#6608,#6606,#3259,.T.);
#8497=EDGE_CURVE('',#6610,#6611,#4705,.T.);
#8498=EDGE_CURVE('',#6611,#6609,#3260,.T.);
#8499=EDGE_CURVE('',#6610,#6608,#3261,.T.);
#8500=EDGE_CURVE('',#6612,#6613,#4706,.T.);
#8501=EDGE_CURVE('',#6613,#6611,#3262,.T.);
#8502=EDGE_CURVE('',#6612,#6610,#3263,.T.);
#8503=EDGE_CURVE('',#6614,#6615,#4707,.T.);
#8504=EDGE_CURVE('',#6616,#6614,#3264,.T.);
#8505=EDGE_CURVE('',#6617,#6616,#2791,.T.);
#8506=EDGE_CURVE('',#6617,#6615,#3265,.T.);
#8507=EDGE_CURVE('',#6618,#6619,#4708,.T.);
#8508=EDGE_CURVE('',#6619,#6620,#3266,.T.);
#8509=EDGE_CURVE('',#6620,#6621,#2792,.T.);
#8510=EDGE_CURVE('',#6621,#6622,#3267,.T.);
#8511=EDGE_CURVE('',#6622,#6623,#4709,.T.);
#8512=EDGE_CURVE('',#6623,#6623,#2793,.F.);
#8513=EDGE_CURVE('',#6622,#6618,#3268,.T.);
#8514=EDGE_CURVE('',#6624,#6625,#4710,.T.);
#8515=EDGE_CURVE('',#6625,#6619,#3269,.T.);
#8516=EDGE_CURVE('',#6618,#6624,#3270,.T.);
#8517=EDGE_CURVE('',#6626,#6627,#4711,.T.);
#8518=EDGE_CURVE('',#6627,#6625,#3271,.T.);
#8519=EDGE_CURVE('',#6624,#6626,#3272,.T.);
#8520=EDGE_CURVE('',#6628,#6629,#4712,.T.);
#8521=EDGE_CURVE('',#6629,#6627,#3273,.T.);
#8522=EDGE_CURVE('',#6626,#6628,#3274,.T.);
#8523=EDGE_CURVE('',#6630,#6631,#4713,.T.);
#8524=EDGE_CURVE('',#6631,#6629,#3275,.T.);
#8525=EDGE_CURVE('',#6628,#6630,#3276,.T.);
#8526=EDGE_CURVE('',#6632,#6633,#4714,.T.);
#8527=EDGE_CURVE('',#6633,#6631,#3277,.T.);
#8528=EDGE_CURVE('',#6630,#6632,#3278,.T.);
#8529=EDGE_CURVE('',#6634,#6635,#4715,.T.);
#8530=EDGE_CURVE('',#6635,#6633,#3279,.T.);
#8531=EDGE_CURVE('',#6632,#6634,#3280,.T.);
#8532=EDGE_CURVE('',#6636,#6637,#4716,.T.);
#8533=EDGE_CURVE('',#6637,#6635,#3281,.T.);
#8534=EDGE_CURVE('',#6634,#6636,#3282,.T.);
#8535=EDGE_CURVE('',#6638,#6639,#4717,.T.);
#8536=EDGE_CURVE('',#6639,#6637,#3283,.T.);
#8537=EDGE_CURVE('',#6636,#6638,#3284,.T.);
#8538=EDGE_CURVE('',#6640,#6641,#4718,.T.);
#8539=EDGE_CURVE('',#6641,#6639,#3285,.T.);
#8540=EDGE_CURVE('',#6638,#6640,#3286,.T.);
#8541=EDGE_CURVE('',#6642,#6643,#4719,.T.);
#8542=EDGE_CURVE('',#6643,#6641,#3287,.T.);
#8543=EDGE_CURVE('',#6640,#6642,#3288,.T.);
#8544=EDGE_CURVE('',#6644,#6645,#4720,.T.);
#8545=EDGE_CURVE('',#6644,#6646,#3289,.T.);
#8546=EDGE_CURVE('',#6647,#6646,#2794,.T.);
#8547=EDGE_CURVE('',#6647,#6645,#3290,.T.);
#8548=EDGE_CURVE('',#6648,#6649,#4721,.T.);
#8549=EDGE_CURVE('',#6649,#6650,#3291,.T.);
#8550=EDGE_CURVE('',#6651,#6650,#2795,.T.);
#8551=EDGE_CURVE('',#6648,#6651,#3292,.T.);
#8552=EDGE_CURVE('',#6652,#6653,#4722,.T.);
#8553=EDGE_CURVE('',#6653,#6649,#3293,.T.);
#8554=EDGE_CURVE('',#6652,#6648,#3294,.T.);
#8555=EDGE_CURVE('',#6654,#6655,#4723,.T.);
#8556=EDGE_CURVE('',#6655,#6653,#3295,.T.);
#8557=EDGE_CURVE('',#6654,#6652,#3296,.T.);
#8558=EDGE_CURVE('',#6656,#6657,#4724,.T.);
#8559=EDGE_CURVE('',#6657,#6655,#3297,.T.);
#8560=EDGE_CURVE('',#6656,#6654,#3298,.T.);
#8561=EDGE_CURVE('',#6658,#6659,#4725,.T.);
#8562=EDGE_CURVE('',#6659,#6657,#3299,.T.);
#8563=EDGE_CURVE('',#6658,#6656,#3300,.T.);
#8564=EDGE_CURVE('',#6660,#6661,#4726,.T.);
#8565=EDGE_CURVE('',#6661,#6659,#3301,.T.);
#8566=EDGE_CURVE('',#6660,#6658,#3302,.T.);
#8567=EDGE_CURVE('',#6662,#6663,#4727,.T.);
#8568=EDGE_CURVE('',#6663,#6661,#3303,.T.);
#8569=EDGE_CURVE('',#6662,#6660,#3304,.T.);
#8570=EDGE_CURVE('',#6664,#6665,#4728,.T.);
#8571=EDGE_CURVE('',#6665,#6663,#3305,.T.);
#8572=EDGE_CURVE('',#6664,#6662,#3306,.T.);
#8573=EDGE_CURVE('',#6666,#6667,#4729,.T.);
#8574=EDGE_CURVE('',#6667,#6665,#3307,.T.);
#8575=EDGE_CURVE('',#6666,#6664,#3308,.T.);
#8576=EDGE_CURVE('',#6668,#6669,#4730,.T.);
#8577=EDGE_CURVE('',#6669,#6667,#3309,.T.);
#8578=EDGE_CURVE('',#6668,#6666,#3310,.T.);
#8579=EDGE_CURVE('',#6670,#6671,#4731,.T.);
#8580=EDGE_CURVE('',#6671,#6669,#3311,.T.);
#8581=EDGE_CURVE('',#6670,#6668,#3312,.T.);
#8582=EDGE_CURVE('',#6672,#6673,#4732,.T.);
#8583=EDGE_CURVE('',#6673,#6671,#3313,.T.);
#8584=EDGE_CURVE('',#6672,#6670,#3314,.T.);
#8585=EDGE_CURVE('',#6674,#6675,#4733,.T.);
#8586=EDGE_CURVE('',#6676,#6674,#3315,.T.);
#8587=EDGE_CURVE('',#6677,#6676,#2796,.T.);
#8588=EDGE_CURVE('',#6677,#6675,#3316,.T.);
#8589=EDGE_CURVE('',#6678,#6679,#4734,.T.);
#8590=EDGE_CURVE('',#6679,#6680,#3317,.T.);
#8591=EDGE_CURVE('',#6680,#6681,#2797,.T.);
#8592=EDGE_CURVE('',#6681,#6682,#3318,.T.);
#8593=EDGE_CURVE('',#6682,#6683,#4735,.T.);
#8594=EDGE_CURVE('',#6683,#6683,#2798,.F.);
#8595=EDGE_CURVE('',#6682,#6678,#3319,.T.);
#8596=EDGE_CURVE('',#6684,#6685,#4736,.T.);
#8597=EDGE_CURVE('',#6685,#6679,#3320,.T.);
#8598=EDGE_CURVE('',#6678,#6684,#3321,.T.);
#8599=EDGE_CURVE('',#6686,#6687,#4737,.T.);
#8600=EDGE_CURVE('',#6687,#6685,#3322,.T.);
#8601=EDGE_CURVE('',#6684,#6686,#3323,.T.);
#8602=EDGE_CURVE('',#6688,#6689,#4738,.T.);
#8603=EDGE_CURVE('',#6689,#6687,#3324,.T.);
#8604=EDGE_CURVE('',#6686,#6688,#3325,.T.);
#8605=EDGE_CURVE('',#6690,#6691,#4739,.T.);
#8606=EDGE_CURVE('',#6691,#6689,#3326,.T.);
#8607=EDGE_CURVE('',#6688,#6690,#3327,.T.);
#8608=EDGE_CURVE('',#6692,#6693,#4740,.T.);
#8609=EDGE_CURVE('',#6693,#6691,#3328,.T.);
#8610=EDGE_CURVE('',#6690,#6692,#3329,.T.);
#8611=EDGE_CURVE('',#6694,#6695,#4741,.T.);
#8612=EDGE_CURVE('',#6695,#6693,#3330,.T.);
#8613=EDGE_CURVE('',#6692,#6694,#3331,.T.);
#8614=EDGE_CURVE('',#6696,#6697,#4742,.T.);
#8615=EDGE_CURVE('',#6697,#6695,#3332,.T.);
#8616=EDGE_CURVE('',#6694,#6696,#3333,.T.);
#8617=EDGE_CURVE('',#6698,#6699,#4743,.T.);
#8618=EDGE_CURVE('',#6699,#6697,#3334,.T.);
#8619=EDGE_CURVE('',#6696,#6698,#3335,.T.);
#8620=EDGE_CURVE('',#6700,#6701,#4744,.T.);
#8621=EDGE_CURVE('',#6701,#6699,#3336,.T.);
#8622=EDGE_CURVE('',#6698,#6700,#3337,.T.);
#8623=EDGE_CURVE('',#6702,#6703,#4745,.T.);
#8624=EDGE_CURVE('',#6703,#6701,#3338,.T.);
#8625=EDGE_CURVE('',#6700,#6702,#3339,.T.);
#8626=EDGE_CURVE('',#6704,#6705,#4746,.T.);
#8627=EDGE_CURVE('',#6704,#6706,#3340,.T.);
#8628=EDGE_CURVE('',#6707,#6706,#2799,.T.);
#8629=EDGE_CURVE('',#6707,#6705,#3341,.T.);
#8630=EDGE_CURVE('',#6708,#6709,#4747,.T.);
#8631=EDGE_CURVE('',#6709,#6710,#3342,.T.);
#8632=EDGE_CURVE('',#6711,#6710,#2800,.T.);
#8633=EDGE_CURVE('',#6708,#6711,#3343,.T.);
#8634=EDGE_CURVE('',#6712,#6713,#4748,.T.);
#8635=EDGE_CURVE('',#6713,#6709,#3344,.T.);
#8636=EDGE_CURVE('',#6712,#6708,#3345,.T.);
#8637=EDGE_CURVE('',#6714,#6715,#4749,.T.);
#8638=EDGE_CURVE('',#6715,#6713,#3346,.T.);
#8639=EDGE_CURVE('',#6714,#6712,#3347,.T.);
#8640=EDGE_CURVE('',#6716,#6717,#4750,.T.);
#8641=EDGE_CURVE('',#6717,#6715,#3348,.T.);
#8642=EDGE_CURVE('',#6716,#6714,#3349,.T.);
#8643=EDGE_CURVE('',#6718,#6719,#4751,.T.);
#8644=EDGE_CURVE('',#6719,#6717,#3350,.T.);
#8645=EDGE_CURVE('',#6718,#6716,#3351,.T.);
#8646=EDGE_CURVE('',#6720,#6721,#4752,.T.);
#8647=EDGE_CURVE('',#6721,#6719,#3352,.T.);
#8648=EDGE_CURVE('',#6720,#6718,#3353,.T.);
#8649=EDGE_CURVE('',#6722,#6723,#4753,.T.);
#8650=EDGE_CURVE('',#6723,#6721,#3354,.T.);
#8651=EDGE_CURVE('',#6722,#6720,#3355,.T.);
#8652=EDGE_CURVE('',#6724,#6725,#4754,.T.);
#8653=EDGE_CURVE('',#6725,#6723,#3356,.T.);
#8654=EDGE_CURVE('',#6724,#6722,#3357,.T.);
#8655=EDGE_CURVE('',#6726,#6727,#4755,.T.);
#8656=EDGE_CURVE('',#6727,#6725,#3358,.T.);
#8657=EDGE_CURVE('',#6726,#6724,#3359,.T.);
#8658=EDGE_CURVE('',#6728,#6729,#4756,.T.);
#8659=EDGE_CURVE('',#6729,#6727,#3360,.T.);
#8660=EDGE_CURVE('',#6728,#6726,#3361,.T.);
#8661=EDGE_CURVE('',#6730,#6731,#4757,.T.);
#8662=EDGE_CURVE('',#6731,#6729,#3362,.T.);
#8663=EDGE_CURVE('',#6730,#6728,#3363,.T.);
#8664=EDGE_CURVE('',#6732,#6733,#4758,.T.);
#8665=EDGE_CURVE('',#6733,#6731,#3364,.T.);
#8666=EDGE_CURVE('',#6732,#6730,#3365,.T.);
#8667=EDGE_CURVE('',#6734,#6735,#4759,.T.);
#8668=EDGE_CURVE('',#6736,#6734,#3366,.T.);
#8669=EDGE_CURVE('',#6737,#6736,#2801,.T.);
#8670=EDGE_CURVE('',#6737,#6735,#3367,.T.);
#8671=EDGE_CURVE('',#6738,#6739,#4760,.T.);
#8672=EDGE_CURVE('',#6739,#6740,#3368,.T.);
#8673=EDGE_CURVE('',#6740,#6741,#2802,.T.);
#8674=EDGE_CURVE('',#6741,#6742,#3369,.T.);
#8675=EDGE_CURVE('',#6742,#6743,#4761,.T.);
#8676=EDGE_CURVE('',#6743,#6743,#2803,.F.);
#8677=EDGE_CURVE('',#6742,#6738,#3370,.T.);
#8678=EDGE_CURVE('',#6744,#6745,#4762,.T.);
#8679=EDGE_CURVE('',#6745,#6739,#3371,.T.);
#8680=EDGE_CURVE('',#6738,#6744,#3372,.T.);
#8681=EDGE_CURVE('',#6746,#6747,#4763,.T.);
#8682=EDGE_CURVE('',#6747,#6745,#3373,.T.);
#8683=EDGE_CURVE('',#6744,#6746,#3374,.T.);
#8684=EDGE_CURVE('',#6748,#6749,#4764,.T.);
#8685=EDGE_CURVE('',#6749,#6747,#3375,.T.);
#8686=EDGE_CURVE('',#6746,#6748,#3376,.T.);
#8687=EDGE_CURVE('',#6750,#6751,#4765,.T.);
#8688=EDGE_CURVE('',#6751,#6749,#3377,.T.);
#8689=EDGE_CURVE('',#6748,#6750,#3378,.T.);
#8690=EDGE_CURVE('',#6752,#6753,#4766,.T.);
#8691=EDGE_CURVE('',#6753,#6751,#3379,.T.);
#8692=EDGE_CURVE('',#6750,#6752,#3380,.T.);
#8693=EDGE_CURVE('',#6754,#6755,#4767,.T.);
#8694=EDGE_CURVE('',#6755,#6753,#3381,.T.);
#8695=EDGE_CURVE('',#6752,#6754,#3382,.T.);
#8696=EDGE_CURVE('',#6756,#6757,#4768,.T.);
#8697=EDGE_CURVE('',#6757,#6755,#3383,.T.);
#8698=EDGE_CURVE('',#6754,#6756,#3384,.T.);
#8699=EDGE_CURVE('',#6758,#6759,#4769,.T.);
#8700=EDGE_CURVE('',#6759,#6757,#3385,.T.);
#8701=EDGE_CURVE('',#6756,#6758,#3386,.T.);
#8702=EDGE_CURVE('',#6760,#6761,#4770,.T.);
#8703=EDGE_CURVE('',#6761,#6759,#3387,.T.);
#8704=EDGE_CURVE('',#6758,#6760,#3388,.T.);
#8705=EDGE_CURVE('',#6762,#6763,#4771,.T.);
#8706=EDGE_CURVE('',#6763,#6761,#3389,.T.);
#8707=EDGE_CURVE('',#6760,#6762,#3390,.T.);
#8708=EDGE_CURVE('',#6764,#6765,#4772,.T.);
#8709=EDGE_CURVE('',#6764,#6766,#3391,.T.);
#8710=EDGE_CURVE('',#6767,#6766,#2804,.T.);
#8711=EDGE_CURVE('',#6767,#6765,#3392,.T.);
#8712=EDGE_CURVE('',#6768,#6769,#4773,.T.);
#8713=EDGE_CURVE('',#6769,#6770,#3393,.T.);
#8714=EDGE_CURVE('',#6771,#6770,#2805,.T.);
#8715=EDGE_CURVE('',#6768,#6771,#3394,.T.);
#8716=EDGE_CURVE('',#6772,#6773,#4774,.T.);
#8717=EDGE_CURVE('',#6773,#6769,#3395,.T.);
#8718=EDGE_CURVE('',#6772,#6768,#3396,.T.);
#8719=EDGE_CURVE('',#6774,#6775,#4775,.T.);
#8720=EDGE_CURVE('',#6775,#6773,#3397,.T.);
#8721=EDGE_CURVE('',#6774,#6772,#3398,.T.);
#8722=EDGE_CURVE('',#6776,#6777,#4776,.T.);
#8723=EDGE_CURVE('',#6777,#6775,#3399,.T.);
#8724=EDGE_CURVE('',#6776,#6774,#3400,.T.);
#8725=EDGE_CURVE('',#6778,#6779,#4777,.T.);
#8726=EDGE_CURVE('',#6779,#6777,#3401,.T.);
#8727=EDGE_CURVE('',#6778,#6776,#3402,.T.);
#8728=EDGE_CURVE('',#6780,#6781,#4778,.T.);
#8729=EDGE_CURVE('',#6781,#6779,#3403,.T.);
#8730=EDGE_CURVE('',#6780,#6778,#3404,.T.);
#8731=EDGE_CURVE('',#6782,#6783,#4779,.T.);
#8732=EDGE_CURVE('',#6783,#6781,#3405,.T.);
#8733=EDGE_CURVE('',#6782,#6780,#3406,.T.);
#8734=EDGE_CURVE('',#6784,#6785,#4780,.T.);
#8735=EDGE_CURVE('',#6785,#6783,#3407,.T.);
#8736=EDGE_CURVE('',#6784,#6782,#3408,.T.);
#8737=EDGE_CURVE('',#6786,#6787,#4781,.T.);
#8738=EDGE_CURVE('',#6787,#6785,#3409,.T.);
#8739=EDGE_CURVE('',#6786,#6784,#3410,.T.);
#8740=EDGE_CURVE('',#6788,#6789,#4782,.T.);
#8741=EDGE_CURVE('',#6789,#6787,#3411,.T.);
#8742=EDGE_CURVE('',#6788,#6786,#3412,.T.);
#8743=EDGE_CURVE('',#6790,#6791,#4783,.T.);
#8744=EDGE_CURVE('',#6791,#6789,#3413,.T.);
#8745=EDGE_CURVE('',#6790,#6788,#3414,.T.);
#8746=EDGE_CURVE('',#6792,#6793,#4784,.T.);
#8747=EDGE_CURVE('',#6793,#6791,#3415,.T.);
#8748=EDGE_CURVE('',#6792,#6790,#3416,.T.);
#8749=EDGE_CURVE('',#6794,#6795,#4785,.T.);
#8750=EDGE_CURVE('',#6796,#6794,#3417,.T.);
#8751=EDGE_CURVE('',#6797,#6796,#2806,.T.);
#8752=EDGE_CURVE('',#6797,#6795,#3418,.T.);
#8753=EDGE_CURVE('',#6798,#6799,#4786,.T.);
#8754=EDGE_CURVE('',#6799,#6800,#3419,.T.);
#8755=EDGE_CURVE('',#6800,#6801,#2807,.T.);
#8756=EDGE_CURVE('',#6801,#6802,#3420,.T.);
#8757=EDGE_CURVE('',#6802,#6803,#4787,.T.);
#8758=EDGE_CURVE('',#6803,#6803,#2808,.F.);
#8759=EDGE_CURVE('',#6802,#6798,#3421,.T.);
#8760=EDGE_CURVE('',#6804,#6805,#4788,.T.);
#8761=EDGE_CURVE('',#6805,#6799,#3422,.T.);
#8762=EDGE_CURVE('',#6798,#6804,#3423,.T.);
#8763=EDGE_CURVE('',#6806,#6807,#4789,.T.);
#8764=EDGE_CURVE('',#6807,#6805,#3424,.T.);
#8765=EDGE_CURVE('',#6804,#6806,#3425,.T.);
#8766=EDGE_CURVE('',#6808,#6809,#4790,.T.);
#8767=EDGE_CURVE('',#6809,#6807,#3426,.T.);
#8768=EDGE_CURVE('',#6806,#6808,#3427,.T.);
#8769=EDGE_CURVE('',#6810,#6811,#4791,.T.);
#8770=EDGE_CURVE('',#6811,#6809,#3428,.T.);
#8771=EDGE_CURVE('',#6808,#6810,#3429,.T.);
#8772=EDGE_CURVE('',#6812,#6813,#4792,.T.);
#8773=EDGE_CURVE('',#6813,#6811,#3430,.T.);
#8774=EDGE_CURVE('',#6810,#6812,#3431,.T.);
#8775=EDGE_CURVE('',#6814,#6815,#4793,.T.);
#8776=EDGE_CURVE('',#6815,#6813,#3432,.T.);
#8777=EDGE_CURVE('',#6812,#6814,#3433,.T.);
#8778=EDGE_CURVE('',#6816,#6817,#4794,.T.);
#8779=EDGE_CURVE('',#6817,#6815,#3434,.T.);
#8780=EDGE_CURVE('',#6814,#6816,#3435,.T.);
#8781=EDGE_CURVE('',#6818,#6819,#4795,.T.);
#8782=EDGE_CURVE('',#6819,#6817,#3436,.T.);
#8783=EDGE_CURVE('',#6816,#6818,#3437,.T.);
#8784=EDGE_CURVE('',#6820,#6821,#4796,.T.);
#8785=EDGE_CURVE('',#6821,#6819,#3438,.T.);
#8786=EDGE_CURVE('',#6818,#6820,#3439,.T.);
#8787=EDGE_CURVE('',#6822,#6823,#4797,.T.);
#8788=EDGE_CURVE('',#6823,#6821,#3440,.T.);
#8789=EDGE_CURVE('',#6820,#6822,#3441,.T.);
#8790=EDGE_CURVE('',#6824,#6825,#4798,.T.);
#8791=EDGE_CURVE('',#6824,#6826,#3442,.T.);
#8792=EDGE_CURVE('',#6827,#6826,#2809,.T.);
#8793=EDGE_CURVE('',#6827,#6825,#3443,.T.);
#8794=EDGE_CURVE('',#6828,#6829,#4799,.T.);
#8795=EDGE_CURVE('',#6829,#6830,#3444,.T.);
#8796=EDGE_CURVE('',#6831,#6830,#2810,.T.);
#8797=EDGE_CURVE('',#6828,#6831,#3445,.T.);
#8798=EDGE_CURVE('',#6832,#6833,#4800,.T.);
#8799=EDGE_CURVE('',#6833,#6829,#3446,.T.);
#8800=EDGE_CURVE('',#6832,#6828,#3447,.T.);
#8801=EDGE_CURVE('',#6834,#6835,#4801,.T.);
#8802=EDGE_CURVE('',#6835,#6833,#3448,.T.);
#8803=EDGE_CURVE('',#6834,#6832,#3449,.T.);
#8804=EDGE_CURVE('',#6836,#6837,#4802,.T.);
#8805=EDGE_CURVE('',#6837,#6835,#3450,.T.);
#8806=EDGE_CURVE('',#6836,#6834,#3451,.T.);
#8807=EDGE_CURVE('',#6838,#6839,#4803,.T.);
#8808=EDGE_CURVE('',#6839,#6837,#3452,.T.);
#8809=EDGE_CURVE('',#6838,#6836,#3453,.T.);
#8810=EDGE_CURVE('',#6840,#6841,#4804,.T.);
#8811=EDGE_CURVE('',#6841,#6839,#3454,.T.);
#8812=EDGE_CURVE('',#6840,#6838,#3455,.T.);
#8813=EDGE_CURVE('',#6842,#6843,#4805,.T.);
#8814=EDGE_CURVE('',#6843,#6841,#3456,.T.);
#8815=EDGE_CURVE('',#6842,#6840,#3457,.T.);
#8816=EDGE_CURVE('',#6844,#6845,#4806,.T.);
#8817=EDGE_CURVE('',#6845,#6843,#3458,.T.);
#8818=EDGE_CURVE('',#6844,#6842,#3459,.T.);
#8819=EDGE_CURVE('',#6846,#6847,#4807,.T.);
#8820=EDGE_CURVE('',#6847,#6845,#3460,.T.);
#8821=EDGE_CURVE('',#6846,#6844,#3461,.T.);
#8822=EDGE_CURVE('',#6848,#6849,#4808,.T.);
#8823=EDGE_CURVE('',#6849,#6847,#3462,.T.);
#8824=EDGE_CURVE('',#6848,#6846,#3463,.T.);
#8825=EDGE_CURVE('',#6850,#6851,#4809,.T.);
#8826=EDGE_CURVE('',#6851,#6849,#3464,.T.);
#8827=EDGE_CURVE('',#6850,#6848,#3465,.T.);
#8828=EDGE_CURVE('',#6852,#6853,#4810,.T.);
#8829=EDGE_CURVE('',#6853,#6851,#3466,.T.);
#8830=EDGE_CURVE('',#6852,#6850,#3467,.T.);
#8831=EDGE_CURVE('',#6854,#6855,#4811,.T.);
#8832=EDGE_CURVE('',#6856,#6854,#3468,.T.);
#8833=EDGE_CURVE('',#6857,#6856,#2811,.T.);
#8834=EDGE_CURVE('',#6857,#6855,#3469,.T.);
#8835=EDGE_CURVE('',#6858,#6859,#4812,.T.);
#8836=EDGE_CURVE('',#6859,#6860,#3470,.T.);
#8837=EDGE_CURVE('',#6860,#6861,#2812,.T.);
#8838=EDGE_CURVE('',#6861,#6862,#3471,.T.);
#8839=EDGE_CURVE('',#6862,#6863,#4813,.T.);
#8840=EDGE_CURVE('',#6863,#6863,#2813,.F.);
#8841=EDGE_CURVE('',#6862,#6858,#3472,.T.);
#8842=EDGE_CURVE('',#6864,#6865,#4814,.T.);
#8843=EDGE_CURVE('',#6865,#6859,#3473,.T.);
#8844=EDGE_CURVE('',#6858,#6864,#3474,.T.);
#8845=EDGE_CURVE('',#6866,#6867,#4815,.T.);
#8846=EDGE_CURVE('',#6867,#6865,#3475,.T.);
#8847=EDGE_CURVE('',#6864,#6866,#3476,.T.);
#8848=EDGE_CURVE('',#6868,#6869,#4816,.T.);
#8849=EDGE_CURVE('',#6869,#6867,#3477,.T.);
#8850=EDGE_CURVE('',#6866,#6868,#3478,.T.);
#8851=EDGE_CURVE('',#6870,#6871,#4817,.T.);
#8852=EDGE_CURVE('',#6871,#6869,#3479,.T.);
#8853=EDGE_CURVE('',#6868,#6870,#3480,.T.);
#8854=EDGE_CURVE('',#6872,#6873,#4818,.T.);
#8855=EDGE_CURVE('',#6873,#6871,#3481,.T.);
#8856=EDGE_CURVE('',#6870,#6872,#3482,.T.);
#8857=EDGE_CURVE('',#6874,#6875,#4819,.T.);
#8858=EDGE_CURVE('',#6875,#6873,#3483,.T.);
#8859=EDGE_CURVE('',#6872,#6874,#3484,.T.);
#8860=EDGE_CURVE('',#6876,#6877,#4820,.T.);
#8861=EDGE_CURVE('',#6877,#6875,#3485,.T.);
#8862=EDGE_CURVE('',#6874,#6876,#3486,.T.);
#8863=EDGE_CURVE('',#6878,#6879,#4821,.T.);
#8864=EDGE_CURVE('',#6879,#6877,#3487,.T.);
#8865=EDGE_CURVE('',#6876,#6878,#3488,.T.);
#8866=EDGE_CURVE('',#6880,#6881,#4822,.T.);
#8867=EDGE_CURVE('',#6881,#6879,#3489,.T.);
#8868=EDGE_CURVE('',#6878,#6880,#3490,.T.);
#8869=EDGE_CURVE('',#6882,#6883,#4823,.T.);
#8870=EDGE_CURVE('',#6883,#6881,#3491,.T.);
#8871=EDGE_CURVE('',#6880,#6882,#3492,.T.);
#8872=EDGE_CURVE('',#6884,#6885,#4824,.T.);
#8873=EDGE_CURVE('',#6884,#6886,#3493,.T.);
#8874=EDGE_CURVE('',#6887,#6886,#2814,.F.);
#8875=EDGE_CURVE('',#6887,#6885,#3494,.T.);
#8876=EDGE_CURVE('',#6888,#6889,#4825,.T.);
#8877=EDGE_CURVE('',#6889,#6890,#3495,.T.);
#8878=EDGE_CURVE('',#6891,#6890,#2815,.T.);
#8879=EDGE_CURVE('',#6888,#6891,#3496,.T.);
#8880=EDGE_CURVE('',#6892,#6893,#4826,.T.);
#8881=EDGE_CURVE('',#6893,#6889,#3497,.T.);
#8882=EDGE_CURVE('',#6892,#6888,#3498,.T.);
#8883=EDGE_CURVE('',#6894,#6895,#4827,.T.);
#8884=EDGE_CURVE('',#6895,#6893,#3499,.T.);
#8885=EDGE_CURVE('',#6894,#6892,#3500,.T.);
#8886=EDGE_CURVE('',#6896,#6897,#4828,.T.);
#8887=EDGE_CURVE('',#6897,#6895,#3501,.T.);
#8888=EDGE_CURVE('',#6896,#6894,#3502,.T.);
#8889=EDGE_CURVE('',#6898,#6899,#4829,.T.);
#8890=EDGE_CURVE('',#6899,#6897,#3503,.T.);
#8891=EDGE_CURVE('',#6898,#6896,#3504,.T.);
#8892=EDGE_CURVE('',#6900,#6901,#4830,.T.);
#8893=EDGE_CURVE('',#6901,#6899,#3505,.T.);
#8894=EDGE_CURVE('',#6900,#6898,#3506,.T.);
#8895=EDGE_CURVE('',#6902,#6903,#4831,.T.);
#8896=EDGE_CURVE('',#6903,#6901,#3507,.T.);
#8897=EDGE_CURVE('',#6902,#6900,#3508,.T.);
#8898=EDGE_CURVE('',#6904,#6905,#4832,.T.);
#8899=EDGE_CURVE('',#6905,#6903,#3509,.T.);
#8900=EDGE_CURVE('',#6904,#6902,#3510,.T.);
#8901=EDGE_CURVE('',#6906,#6907,#4833,.T.);
#8902=EDGE_CURVE('',#6907,#6905,#3511,.T.);
#8903=EDGE_CURVE('',#6906,#6904,#3512,.T.);
#8904=EDGE_CURVE('',#6908,#6909,#4834,.T.);
#8905=EDGE_CURVE('',#6909,#6907,#3513,.T.);
#8906=EDGE_CURVE('',#6908,#6906,#3514,.T.);
#8907=EDGE_CURVE('',#6910,#6911,#4835,.T.);
#8908=EDGE_CURVE('',#6911,#6909,#3515,.T.);
#8909=EDGE_CURVE('',#6910,#6908,#3516,.T.);
#8910=EDGE_CURVE('',#6912,#6913,#4836,.T.);
#8911=EDGE_CURVE('',#6913,#6911,#3517,.T.);
#8912=EDGE_CURVE('',#6912,#6910,#3518,.T.);
#8913=EDGE_CURVE('',#6914,#6915,#4837,.T.);
#8914=EDGE_CURVE('',#6916,#6914,#3519,.T.);
#8915=EDGE_CURVE('',#6917,#6916,#2816,.T.);
#8916=EDGE_CURVE('',#6917,#6915,#3520,.T.);
#8917=EDGE_CURVE('',#6918,#6919,#4838,.T.);
#8918=EDGE_CURVE('',#6919,#6920,#3521,.T.);
#8919=EDGE_CURVE('',#6920,#6921,#2817,.T.);
#8920=EDGE_CURVE('',#6921,#6922,#3522,.T.);
#8921=EDGE_CURVE('',#6922,#6923,#4839,.T.);
#8922=EDGE_CURVE('',#6923,#6923,#2818,.F.);
#8923=EDGE_CURVE('',#6922,#6918,#3523,.T.);
#8924=EDGE_CURVE('',#6924,#6925,#4840,.T.);
#8925=EDGE_CURVE('',#6925,#6919,#3524,.T.);
#8926=EDGE_CURVE('',#6918,#6924,#3525,.T.);
#8927=EDGE_CURVE('',#6926,#6927,#4841,.T.);
#8928=EDGE_CURVE('',#6927,#6925,#3526,.T.);
#8929=EDGE_CURVE('',#6924,#6926,#3527,.T.);
#8930=EDGE_CURVE('',#6928,#6929,#4842,.T.);
#8931=EDGE_CURVE('',#6929,#6927,#3528,.T.);
#8932=EDGE_CURVE('',#6926,#6928,#3529,.T.);
#8933=EDGE_CURVE('',#6930,#6931,#4843,.T.);
#8934=EDGE_CURVE('',#6931,#6929,#3530,.T.);
#8935=EDGE_CURVE('',#6928,#6930,#3531,.T.);
#8936=EDGE_CURVE('',#6932,#6933,#4844,.T.);
#8937=EDGE_CURVE('',#6933,#6931,#3532,.T.);
#8938=EDGE_CURVE('',#6930,#6932,#3533,.T.);
#8939=EDGE_CURVE('',#6934,#6935,#4845,.T.);
#8940=EDGE_CURVE('',#6935,#6933,#3534,.T.);
#8941=EDGE_CURVE('',#6932,#6934,#3535,.T.);
#8942=EDGE_CURVE('',#6936,#6937,#4846,.T.);
#8943=EDGE_CURVE('',#6937,#6935,#3536,.T.);
#8944=EDGE_CURVE('',#6934,#6936,#3537,.T.);
#8945=EDGE_CURVE('',#6938,#6939,#4847,.T.);
#8946=EDGE_CURVE('',#6939,#6937,#3538,.T.);
#8947=EDGE_CURVE('',#6936,#6938,#3539,.T.);
#8948=EDGE_CURVE('',#6940,#6941,#4848,.T.);
#8949=EDGE_CURVE('',#6941,#6939,#3540,.T.);
#8950=EDGE_CURVE('',#6938,#6940,#3541,.T.);
#8951=EDGE_CURVE('',#6942,#6943,#4849,.T.);
#8952=EDGE_CURVE('',#6943,#6941,#3542,.T.);
#8953=EDGE_CURVE('',#6940,#6942,#3543,.T.);
#8954=EDGE_CURVE('',#6944,#6945,#4850,.T.);
#8955=EDGE_CURVE('',#6944,#6946,#3544,.T.);
#8956=EDGE_CURVE('',#6947,#6946,#2819,.F.);
#8957=EDGE_CURVE('',#6947,#6945,#3545,.T.);
#8958=EDGE_CURVE('',#6948,#6949,#4851,.T.);
#8959=EDGE_CURVE('',#6949,#6950,#3546,.T.);
#8960=EDGE_CURVE('',#6951,#6950,#2820,.T.);
#8961=EDGE_CURVE('',#6948,#6951,#3547,.T.);
#8962=EDGE_CURVE('',#6952,#6953,#4852,.T.);
#8963=EDGE_CURVE('',#6953,#6949,#3548,.T.);
#8964=EDGE_CURVE('',#6952,#6948,#3549,.T.);
#8965=EDGE_CURVE('',#6954,#6955,#4853,.T.);
#8966=EDGE_CURVE('',#6955,#6953,#3550,.T.);
#8967=EDGE_CURVE('',#6954,#6952,#3551,.T.);
#8968=EDGE_CURVE('',#6956,#6957,#4854,.T.);
#8969=EDGE_CURVE('',#6957,#6955,#3552,.T.);
#8970=EDGE_CURVE('',#6956,#6954,#3553,.T.);
#8971=EDGE_CURVE('',#6958,#6959,#4855,.T.);
#8972=EDGE_CURVE('',#6959,#6957,#3554,.T.);
#8973=EDGE_CURVE('',#6958,#6956,#3555,.T.);
#8974=EDGE_CURVE('',#6960,#6961,#4856,.T.);
#8975=EDGE_CURVE('',#6961,#6959,#3556,.T.);
#8976=EDGE_CURVE('',#6960,#6958,#3557,.T.);
#8977=EDGE_CURVE('',#6962,#6963,#4857,.T.);
#8978=EDGE_CURVE('',#6963,#6961,#3558,.T.);
#8979=EDGE_CURVE('',#6962,#6960,#3559,.T.);
#8980=EDGE_CURVE('',#6964,#6965,#4858,.T.);
#8981=EDGE_CURVE('',#6965,#6963,#3560,.T.);
#8982=EDGE_CURVE('',#6964,#6962,#3561,.T.);
#8983=EDGE_CURVE('',#6966,#6967,#4859,.T.);
#8984=EDGE_CURVE('',#6967,#6965,#3562,.T.);
#8985=EDGE_CURVE('',#6966,#6964,#3563,.T.);
#8986=EDGE_CURVE('',#6968,#6969,#4860,.T.);
#8987=EDGE_CURVE('',#6969,#6967,#3564,.T.);
#8988=EDGE_CURVE('',#6968,#6966,#3565,.T.);
#8989=EDGE_CURVE('',#6970,#6971,#4861,.T.);
#8990=EDGE_CURVE('',#6971,#6969,#3566,.T.);
#8991=EDGE_CURVE('',#6970,#6968,#3567,.T.);
#8992=EDGE_CURVE('',#6972,#6973,#4862,.T.);
#8993=EDGE_CURVE('',#6973,#6971,#3568,.T.);
#8994=EDGE_CURVE('',#6972,#6970,#3569,.T.);
#8995=EDGE_CURVE('',#6974,#6975,#4863,.T.);
#8996=EDGE_CURVE('',#6976,#6974,#3570,.T.);
#8997=EDGE_CURVE('',#6977,#6976,#2821,.T.);
#8998=EDGE_CURVE('',#6977,#6975,#3571,.T.);
#8999=EDGE_CURVE('',#6978,#6979,#4864,.T.);
#9000=EDGE_CURVE('',#6979,#6980,#3572,.T.);
#9001=EDGE_CURVE('',#6980,#6981,#2822,.T.);
#9002=EDGE_CURVE('',#6981,#6982,#3573,.T.);
#9003=EDGE_CURVE('',#6982,#6983,#4865,.T.);
#9004=EDGE_CURVE('',#6983,#6983,#2823,.F.);
#9005=EDGE_CURVE('',#6982,#6978,#3574,.T.);
#9006=EDGE_CURVE('',#6984,#6985,#4866,.T.);
#9007=EDGE_CURVE('',#6985,#6979,#3575,.T.);
#9008=EDGE_CURVE('',#6978,#6984,#3576,.T.);
#9009=EDGE_CURVE('',#6986,#6987,#4867,.T.);
#9010=EDGE_CURVE('',#6987,#6985,#3577,.T.);
#9011=EDGE_CURVE('',#6984,#6986,#3578,.T.);
#9012=EDGE_CURVE('',#6988,#6989,#4868,.T.);
#9013=EDGE_CURVE('',#6989,#6987,#3579,.T.);
#9014=EDGE_CURVE('',#6986,#6988,#3580,.T.);
#9015=EDGE_CURVE('',#6990,#6991,#4869,.T.);
#9016=EDGE_CURVE('',#6991,#6989,#3581,.T.);
#9017=EDGE_CURVE('',#6988,#6990,#3582,.T.);
#9018=EDGE_CURVE('',#6992,#6993,#4870,.T.);
#9019=EDGE_CURVE('',#6993,#6991,#3583,.T.);
#9020=EDGE_CURVE('',#6990,#6992,#3584,.T.);
#9021=EDGE_CURVE('',#6994,#6995,#4871,.T.);
#9022=EDGE_CURVE('',#6995,#6993,#3585,.T.);
#9023=EDGE_CURVE('',#6992,#6994,#3586,.T.);
#9024=EDGE_CURVE('',#6996,#6997,#4872,.T.);
#9025=EDGE_CURVE('',#6997,#6995,#3587,.T.);
#9026=EDGE_CURVE('',#6994,#6996,#3588,.T.);
#9027=EDGE_CURVE('',#6998,#6999,#4873,.T.);
#9028=EDGE_CURVE('',#6999,#6997,#3589,.T.);
#9029=EDGE_CURVE('',#6996,#6998,#3590,.T.);
#9030=EDGE_CURVE('',#7000,#7001,#4874,.T.);
#9031=EDGE_CURVE('',#7001,#6999,#3591,.T.);
#9032=EDGE_CURVE('',#6998,#7000,#3592,.T.);
#9033=EDGE_CURVE('',#7002,#7003,#4875,.T.);
#9034=EDGE_CURVE('',#7003,#7001,#3593,.T.);
#9035=EDGE_CURVE('',#7000,#7002,#3594,.T.);
#9036=EDGE_CURVE('',#7004,#7005,#4876,.T.);
#9037=EDGE_CURVE('',#7004,#7006,#3595,.T.);
#9038=EDGE_CURVE('',#7007,#7006,#2824,.F.);
#9039=EDGE_CURVE('',#7007,#7005,#3596,.T.);
#9040=EDGE_CURVE('',#7008,#7009,#4877,.T.);
#9041=EDGE_CURVE('',#7009,#7010,#3597,.T.);
#9042=EDGE_CURVE('',#7011,#7010,#2825,.T.);
#9043=EDGE_CURVE('',#7008,#7011,#3598,.T.);
#9044=EDGE_CURVE('',#7012,#7013,#4878,.T.);
#9045=EDGE_CURVE('',#7013,#7009,#3599,.T.);
#9046=EDGE_CURVE('',#7012,#7008,#3600,.T.);
#9047=EDGE_CURVE('',#7014,#7015,#4879,.T.);
#9048=EDGE_CURVE('',#7015,#7013,#3601,.T.);
#9049=EDGE_CURVE('',#7014,#7012,#3602,.T.);
#9050=EDGE_CURVE('',#7016,#7017,#4880,.T.);
#9051=EDGE_CURVE('',#7017,#7015,#3603,.T.);
#9052=EDGE_CURVE('',#7016,#7014,#3604,.T.);
#9053=EDGE_CURVE('',#7018,#7019,#4881,.T.);
#9054=EDGE_CURVE('',#7019,#7017,#3605,.T.);
#9055=EDGE_CURVE('',#7018,#7016,#3606,.T.);
#9056=EDGE_CURVE('',#7020,#7021,#4882,.T.);
#9057=EDGE_CURVE('',#7021,#7019,#3607,.T.);
#9058=EDGE_CURVE('',#7020,#7018,#3608,.T.);
#9059=EDGE_CURVE('',#7022,#7023,#4883,.T.);
#9060=EDGE_CURVE('',#7023,#7021,#3609,.T.);
#9061=EDGE_CURVE('',#7022,#7020,#3610,.T.);
#9062=EDGE_CURVE('',#7024,#7025,#4884,.T.);
#9063=EDGE_CURVE('',#7025,#7023,#3611,.T.);
#9064=EDGE_CURVE('',#7024,#7022,#3612,.T.);
#9065=EDGE_CURVE('',#7026,#7027,#4885,.T.);
#9066=EDGE_CURVE('',#7027,#7025,#3613,.T.);
#9067=EDGE_CURVE('',#7026,#7024,#3614,.T.);
#9068=EDGE_CURVE('',#7028,#7029,#4886,.T.);
#9069=EDGE_CURVE('',#7029,#7027,#3615,.T.);
#9070=EDGE_CURVE('',#7028,#7026,#3616,.T.);
#9071=EDGE_CURVE('',#7030,#7031,#4887,.T.);
#9072=EDGE_CURVE('',#7031,#7029,#3617,.T.);
#9073=EDGE_CURVE('',#7030,#7028,#3618,.T.);
#9074=EDGE_CURVE('',#7032,#7033,#4888,.T.);
#9075=EDGE_CURVE('',#7033,#7031,#3619,.T.);
#9076=EDGE_CURVE('',#7032,#7030,#3620,.T.);
#9077=EDGE_CURVE('',#7034,#7035,#4889,.T.);
#9078=EDGE_CURVE('',#7036,#7034,#3621,.T.);
#9079=EDGE_CURVE('',#7037,#7036,#2826,.T.);
#9080=EDGE_CURVE('',#7037,#7035,#3622,.T.);
#9081=EDGE_CURVE('',#7038,#7039,#4890,.T.);
#9082=EDGE_CURVE('',#7039,#7040,#3623,.T.);
#9083=EDGE_CURVE('',#7040,#7041,#2827,.T.);
#9084=EDGE_CURVE('',#7041,#7042,#3624,.T.);
#9085=EDGE_CURVE('',#7042,#7043,#4891,.T.);
#9086=EDGE_CURVE('',#7043,#7043,#2828,.F.);
#9087=EDGE_CURVE('',#7042,#7038,#3625,.T.);
#9088=EDGE_CURVE('',#7044,#7045,#4892,.T.);
#9089=EDGE_CURVE('',#7045,#7039,#3626,.T.);
#9090=EDGE_CURVE('',#7038,#7044,#3627,.T.);
#9091=EDGE_CURVE('',#7046,#7047,#4893,.T.);
#9092=EDGE_CURVE('',#7047,#7045,#3628,.T.);
#9093=EDGE_CURVE('',#7044,#7046,#3629,.T.);
#9094=EDGE_CURVE('',#7048,#7049,#4894,.T.);
#9095=EDGE_CURVE('',#7049,#7047,#3630,.T.);
#9096=EDGE_CURVE('',#7046,#7048,#3631,.T.);
#9097=EDGE_CURVE('',#7050,#7051,#4895,.T.);
#9098=EDGE_CURVE('',#7051,#7049,#3632,.T.);
#9099=EDGE_CURVE('',#7048,#7050,#3633,.T.);
#9100=EDGE_CURVE('',#7052,#7053,#4896,.T.);
#9101=EDGE_CURVE('',#7053,#7051,#3634,.T.);
#9102=EDGE_CURVE('',#7050,#7052,#3635,.T.);
#9103=EDGE_CURVE('',#7054,#7055,#4897,.T.);
#9104=EDGE_CURVE('',#7055,#7053,#3636,.T.);
#9105=EDGE_CURVE('',#7052,#7054,#3637,.T.);
#9106=EDGE_CURVE('',#7056,#7057,#4898,.T.);
#9107=EDGE_CURVE('',#7057,#7055,#3638,.T.);
#9108=EDGE_CURVE('',#7054,#7056,#3639,.T.);
#9109=EDGE_CURVE('',#7058,#7059,#4899,.T.);
#9110=EDGE_CURVE('',#7059,#7057,#3640,.T.);
#9111=EDGE_CURVE('',#7056,#7058,#3641,.T.);
#9112=EDGE_CURVE('',#7060,#7061,#4900,.T.);
#9113=EDGE_CURVE('',#7061,#7059,#3642,.T.);
#9114=EDGE_CURVE('',#7058,#7060,#3643,.T.);
#9115=EDGE_CURVE('',#7062,#7063,#4901,.T.);
#9116=EDGE_CURVE('',#7063,#7061,#3644,.T.);
#9117=EDGE_CURVE('',#7060,#7062,#3645,.T.);
#9118=EDGE_CURVE('',#7064,#7065,#4902,.T.);
#9119=EDGE_CURVE('',#7064,#7066,#3646,.T.);
#9120=EDGE_CURVE('',#7067,#7066,#2829,.F.);
#9121=EDGE_CURVE('',#7067,#7065,#3647,.T.);
#9122=EDGE_CURVE('',#7068,#7069,#4903,.T.);
#9123=EDGE_CURVE('',#7069,#7070,#3648,.T.);
#9124=EDGE_CURVE('',#7071,#7070,#2830,.T.);
#9125=EDGE_CURVE('',#7068,#7071,#3649,.T.);
#9126=EDGE_CURVE('',#7072,#7073,#4904,.T.);
#9127=EDGE_CURVE('',#7073,#7069,#3650,.T.);
#9128=EDGE_CURVE('',#7072,#7068,#3651,.T.);
#9129=EDGE_CURVE('',#7074,#7075,#4905,.T.);
#9130=EDGE_CURVE('',#7075,#7073,#3652,.T.);
#9131=EDGE_CURVE('',#7074,#7072,#3653,.T.);
#9132=EDGE_CURVE('',#7076,#7077,#4906,.T.);
#9133=EDGE_CURVE('',#7077,#7075,#3654,.T.);
#9134=EDGE_CURVE('',#7076,#7074,#3655,.T.);
#9135=EDGE_CURVE('',#7078,#7079,#4907,.T.);
#9136=EDGE_CURVE('',#7079,#7077,#3656,.T.);
#9137=EDGE_CURVE('',#7078,#7076,#3657,.T.);
#9138=EDGE_CURVE('',#7080,#7081,#4908,.T.);
#9139=EDGE_CURVE('',#7081,#7079,#3658,.T.);
#9140=EDGE_CURVE('',#7080,#7078,#3659,.T.);
#9141=EDGE_CURVE('',#7082,#7083,#4909,.T.);
#9142=EDGE_CURVE('',#7083,#7081,#3660,.T.);
#9143=EDGE_CURVE('',#7082,#7080,#3661,.T.);
#9144=EDGE_CURVE('',#7084,#7085,#4910,.T.);
#9145=EDGE_CURVE('',#7085,#7083,#3662,.T.);
#9146=EDGE_CURVE('',#7084,#7082,#3663,.T.);
#9147=EDGE_CURVE('',#7086,#7087,#4911,.T.);
#9148=EDGE_CURVE('',#7087,#7085,#3664,.T.);
#9149=EDGE_CURVE('',#7086,#7084,#3665,.T.);
#9150=EDGE_CURVE('',#7088,#7089,#4912,.T.);
#9151=EDGE_CURVE('',#7089,#7087,#3666,.T.);
#9152=EDGE_CURVE('',#7088,#7086,#3667,.T.);
#9153=EDGE_CURVE('',#7090,#7091,#4913,.T.);
#9154=EDGE_CURVE('',#7091,#7089,#3668,.T.);
#9155=EDGE_CURVE('',#7090,#7088,#3669,.T.);
#9156=EDGE_CURVE('',#7092,#7093,#4914,.T.);
#9157=EDGE_CURVE('',#7093,#7091,#3670,.T.);
#9158=EDGE_CURVE('',#7092,#7090,#3671,.T.);
#9159=EDGE_CURVE('',#7094,#7095,#4915,.T.);
#9160=EDGE_CURVE('',#7096,#7094,#3672,.T.);
#9161=EDGE_CURVE('',#7097,#7096,#2831,.T.);
#9162=EDGE_CURVE('',#7097,#7095,#3673,.T.);
#9163=EDGE_CURVE('',#7098,#7099,#4916,.T.);
#9164=EDGE_CURVE('',#7099,#7100,#3674,.T.);
#9165=EDGE_CURVE('',#7100,#7101,#2832,.T.);
#9166=EDGE_CURVE('',#7101,#7102,#3675,.T.);
#9167=EDGE_CURVE('',#7102,#7103,#4917,.T.);
#9168=EDGE_CURVE('',#7103,#7103,#2833,.F.);
#9169=EDGE_CURVE('',#7102,#7098,#3676,.T.);
#9170=EDGE_CURVE('',#7104,#7105,#4918,.T.);
#9171=EDGE_CURVE('',#7105,#7099,#3677,.T.);
#9172=EDGE_CURVE('',#7098,#7104,#3678,.T.);
#9173=EDGE_CURVE('',#7106,#7107,#4919,.T.);
#9174=EDGE_CURVE('',#7107,#7105,#3679,.T.);
#9175=EDGE_CURVE('',#7104,#7106,#3680,.T.);
#9176=EDGE_CURVE('',#7108,#7109,#4920,.T.);
#9177=EDGE_CURVE('',#7109,#7107,#3681,.T.);
#9178=EDGE_CURVE('',#7106,#7108,#3682,.T.);
#9179=EDGE_CURVE('',#7110,#7111,#4921,.T.);
#9180=EDGE_CURVE('',#7111,#7109,#3683,.T.);
#9181=EDGE_CURVE('',#7108,#7110,#3684,.T.);
#9182=EDGE_CURVE('',#7112,#7113,#4922,.T.);
#9183=EDGE_CURVE('',#7113,#7111,#3685,.T.);
#9184=EDGE_CURVE('',#7110,#7112,#3686,.T.);
#9185=EDGE_CURVE('',#7114,#7115,#4923,.T.);
#9186=EDGE_CURVE('',#7115,#7113,#3687,.T.);
#9187=EDGE_CURVE('',#7112,#7114,#3688,.T.);
#9188=EDGE_CURVE('',#7116,#7117,#4924,.T.);
#9189=EDGE_CURVE('',#7117,#7115,#3689,.T.);
#9190=EDGE_CURVE('',#7114,#7116,#3690,.T.);
#9191=EDGE_CURVE('',#7118,#7119,#4925,.T.);
#9192=EDGE_CURVE('',#7119,#7117,#3691,.T.);
#9193=EDGE_CURVE('',#7116,#7118,#3692,.T.);
#9194=EDGE_CURVE('',#7120,#7121,#4926,.T.);
#9195=EDGE_CURVE('',#7121,#7119,#3693,.T.);
#9196=EDGE_CURVE('',#7118,#7120,#3694,.T.);
#9197=EDGE_CURVE('',#7122,#7123,#4927,.T.);
#9198=EDGE_CURVE('',#7123,#7121,#3695,.T.);
#9199=EDGE_CURVE('',#7120,#7122,#3696,.T.);
#9200=EDGE_CURVE('',#7124,#7125,#4928,.T.);
#9201=EDGE_CURVE('',#7124,#7126,#3697,.T.);
#9202=EDGE_CURVE('',#7127,#7126,#2834,.F.);
#9203=EDGE_CURVE('',#7127,#7125,#3698,.T.);
#9204=EDGE_CURVE('',#7128,#7129,#4929,.T.);
#9205=EDGE_CURVE('',#7129,#7130,#3699,.T.);
#9206=EDGE_CURVE('',#7131,#7130,#2835,.T.);
#9207=EDGE_CURVE('',#7128,#7131,#3700,.T.);
#9208=EDGE_CURVE('',#7132,#7133,#4930,.T.);
#9209=EDGE_CURVE('',#7133,#7129,#3701,.T.);
#9210=EDGE_CURVE('',#7132,#7128,#3702,.T.);
#9211=EDGE_CURVE('',#7134,#7135,#4931,.T.);
#9212=EDGE_CURVE('',#7135,#7133,#3703,.T.);
#9213=EDGE_CURVE('',#7134,#7132,#3704,.T.);
#9214=EDGE_CURVE('',#7136,#7137,#4932,.T.);
#9215=EDGE_CURVE('',#7137,#7135,#3705,.T.);
#9216=EDGE_CURVE('',#7136,#7134,#3706,.T.);
#9217=EDGE_CURVE('',#7138,#7139,#4933,.T.);
#9218=EDGE_CURVE('',#7139,#7137,#3707,.T.);
#9219=EDGE_CURVE('',#7138,#7136,#3708,.T.);
#9220=EDGE_CURVE('',#7140,#7141,#4934,.T.);
#9221=EDGE_CURVE('',#7141,#7139,#3709,.T.);
#9222=EDGE_CURVE('',#7140,#7138,#3710,.T.);
#9223=EDGE_CURVE('',#7142,#7143,#4935,.T.);
#9224=EDGE_CURVE('',#7143,#7141,#3711,.T.);
#9225=EDGE_CURVE('',#7142,#7140,#3712,.T.);
#9226=EDGE_CURVE('',#7144,#7145,#4936,.T.);
#9227=EDGE_CURVE('',#7145,#7143,#3713,.T.);
#9228=EDGE_CURVE('',#7144,#7142,#3714,.T.);
#9229=EDGE_CURVE('',#7146,#7147,#4937,.T.);
#9230=EDGE_CURVE('',#7147,#7145,#3715,.T.);
#9231=EDGE_CURVE('',#7146,#7144,#3716,.T.);
#9232=EDGE_CURVE('',#7148,#7149,#4938,.T.);
#9233=EDGE_CURVE('',#7149,#7147,#3717,.T.);
#9234=EDGE_CURVE('',#7148,#7146,#3718,.T.);
#9235=EDGE_CURVE('',#7150,#7151,#4939,.T.);
#9236=EDGE_CURVE('',#7151,#7149,#3719,.T.);
#9237=EDGE_CURVE('',#7150,#7148,#3720,.T.);
#9238=EDGE_CURVE('',#7152,#7153,#4940,.T.);
#9239=EDGE_CURVE('',#7153,#7151,#3721,.T.);
#9240=EDGE_CURVE('',#7152,#7150,#3722,.T.);
#9241=EDGE_CURVE('',#7154,#7155,#4941,.T.);
#9242=EDGE_CURVE('',#7156,#7154,#3723,.T.);
#9243=EDGE_CURVE('',#7157,#7156,#2836,.T.);
#9244=EDGE_CURVE('',#7157,#7155,#3724,.T.);
#9245=EDGE_CURVE('',#7158,#7159,#4942,.T.);
#9246=EDGE_CURVE('',#7159,#7160,#3725,.T.);
#9247=EDGE_CURVE('',#7160,#7161,#2837,.F.);
#9248=EDGE_CURVE('',#7161,#7158,#3726,.T.);
#9249=EDGE_CURVE('',#7162,#7163,#4943,.T.);
#9250=EDGE_CURVE('',#7163,#7159,#3727,.T.);
#9251=EDGE_CURVE('',#7158,#7162,#3728,.T.);
#9252=EDGE_CURVE('',#7164,#7165,#4944,.T.);
#9253=EDGE_CURVE('',#7165,#7163,#3729,.T.);
#9254=EDGE_CURVE('',#7162,#7164,#3730,.T.);
#9255=EDGE_CURVE('',#7166,#7167,#4945,.T.);
#9256=EDGE_CURVE('',#7167,#7165,#3731,.T.);
#9257=EDGE_CURVE('',#7164,#7166,#3732,.T.);
#9258=EDGE_CURVE('',#7168,#7169,#4946,.T.);
#9259=EDGE_CURVE('',#7169,#7167,#3733,.T.);
#9260=EDGE_CURVE('',#7166,#7168,#3734,.T.);
#9261=EDGE_CURVE('',#7170,#7171,#4947,.T.);
#9262=EDGE_CURVE('',#7171,#7169,#3735,.T.);
#9263=EDGE_CURVE('',#7168,#7170,#3736,.T.);
#9264=EDGE_CURVE('',#7172,#7173,#4948,.T.);
#9265=EDGE_CURVE('',#7173,#7171,#3737,.T.);
#9266=EDGE_CURVE('',#7170,#7172,#3738,.T.);
#9267=EDGE_CURVE('',#7174,#7175,#4949,.T.);
#9268=EDGE_CURVE('',#7174,#7176,#3739,.T.);
#9269=EDGE_CURVE('',#7177,#7176,#3740,.T.);
#9270=EDGE_CURVE('',#7177,#7175,#3741,.T.);
#9271=EDGE_CURVE('',#7178,#7179,#4950,.T.);
#9272=EDGE_CURVE('',#7179,#7180,#3742,.T.);
#9273=EDGE_CURVE('',#7181,#7180,#2838,.T.);
#9274=EDGE_CURVE('',#7178,#7181,#3743,.T.);
#9275=EDGE_CURVE('',#7182,#7183,#4951,.T.);
#9276=EDGE_CURVE('',#7183,#7179,#3744,.T.);
#9277=EDGE_CURVE('',#7182,#7178,#3745,.T.);
#9278=EDGE_CURVE('',#7184,#7185,#4952,.T.);
#9279=EDGE_CURVE('',#7185,#7183,#3746,.T.);
#9280=EDGE_CURVE('',#7184,#7182,#3747,.T.);
#9281=EDGE_CURVE('',#7186,#7187,#4953,.T.);
#9282=EDGE_CURVE('',#7187,#7185,#3748,.T.);
#9283=EDGE_CURVE('',#7186,#7184,#3749,.T.);
#9284=EDGE_CURVE('',#7188,#7189,#4954,.T.);
#9285=EDGE_CURVE('',#7189,#7187,#3750,.T.);
#9286=EDGE_CURVE('',#7188,#7186,#3751,.T.);
#9287=EDGE_CURVE('',#7190,#7191,#4955,.T.);
#9288=EDGE_CURVE('',#7191,#7189,#3752,.T.);
#9289=EDGE_CURVE('',#7190,#7188,#3753,.T.);
#9290=EDGE_CURVE('',#7192,#7193,#4956,.T.);
#9291=EDGE_CURVE('',#7193,#7191,#3754,.T.);
#9292=EDGE_CURVE('',#7192,#7190,#3755,.T.);
#9293=EDGE_CURVE('',#7194,#7195,#4957,.T.);
#9294=EDGE_CURVE('',#7196,#7194,#3756,.T.);
#9295=EDGE_CURVE('',#7197,#7196,#3757,.T.);
#9296=EDGE_CURVE('',#7198,#7197,#3758,.T.);
#9297=EDGE_CURVE('',#7198,#7195,#3759,.T.);
#9298=EDGE_CURVE('',#7199,#7200,#4958,.T.);
#9299=EDGE_CURVE('',#7200,#7201,#3760,.T.);
#9300=EDGE_CURVE('',#7201,#7202,#2839,.F.);
#9301=EDGE_CURVE('',#7202,#7199,#3761,.T.);
#9302=EDGE_CURVE('',#7203,#7204,#4959,.T.);
#9303=EDGE_CURVE('',#7204,#7200,#3762,.T.);
#9304=EDGE_CURVE('',#7199,#7203,#3763,.T.);
#9305=EDGE_CURVE('',#7205,#7206,#4960,.T.);
#9306=EDGE_CURVE('',#7206,#7204,#3764,.T.);
#9307=EDGE_CURVE('',#7203,#7205,#3765,.T.);
#9308=EDGE_CURVE('',#7207,#7208,#4961,.T.);
#9309=EDGE_CURVE('',#7208,#7206,#3766,.T.);
#9310=EDGE_CURVE('',#7205,#7207,#3767,.T.);
#9311=EDGE_CURVE('',#7209,#7210,#4962,.T.);
#9312=EDGE_CURVE('',#7210,#7208,#3768,.T.);
#9313=EDGE_CURVE('',#7207,#7209,#3769,.T.);
#9314=EDGE_CURVE('',#7211,#7212,#4963,.T.);
#9315=EDGE_CURVE('',#7212,#7210,#3770,.T.);
#9316=EDGE_CURVE('',#7209,#7211,#3771,.T.);
#9317=EDGE_CURVE('',#7213,#7214,#4964,.T.);
#9318=EDGE_CURVE('',#7214,#7212,#3772,.T.);
#9319=EDGE_CURVE('',#7211,#7213,#3773,.T.);
#9320=EDGE_CURVE('',#7215,#7216,#4965,.T.);
#9321=EDGE_CURVE('',#7215,#7217,#3774,.T.);
#9322=EDGE_CURVE('',#7218,#7217,#3775,.T.);
#9323=EDGE_CURVE('',#7218,#7216,#3776,.T.);
#9324=EDGE_CURVE('',#7219,#7220,#4966,.T.);
#9325=EDGE_CURVE('',#7220,#7221,#3777,.T.);
#9326=EDGE_CURVE('',#7221,#7222,#2840,.F.);
#9327=EDGE_CURVE('',#7222,#7219,#3778,.T.);
#9328=EDGE_CURVE('',#7223,#7224,#4967,.T.);
#9329=EDGE_CURVE('',#7224,#7220,#3779,.T.);
#9330=EDGE_CURVE('',#7219,#7223,#3780,.T.);
#9331=EDGE_CURVE('',#7225,#7226,#4968,.T.);
#9332=EDGE_CURVE('',#7226,#7224,#3781,.T.);
#9333=EDGE_CURVE('',#7223,#7225,#3782,.T.);
#9334=EDGE_CURVE('',#7227,#7228,#4969,.T.);
#9335=EDGE_CURVE('',#7228,#7226,#3783,.T.);
#9336=EDGE_CURVE('',#7225,#7227,#3784,.T.);
#9337=EDGE_CURVE('',#7229,#7230,#4970,.T.);
#9338=EDGE_CURVE('',#7230,#7228,#3785,.T.);
#9339=EDGE_CURVE('',#7227,#7229,#3786,.T.);
#9340=EDGE_CURVE('',#7231,#7232,#4971,.T.);
#9341=EDGE_CURVE('',#7232,#7230,#3787,.T.);
#9342=EDGE_CURVE('',#7229,#7231,#3788,.T.);
#9343=EDGE_CURVE('',#7233,#7234,#4972,.T.);
#9344=EDGE_CURVE('',#7234,#7232,#3789,.T.);
#9345=EDGE_CURVE('',#7231,#7233,#3790,.T.);
#9346=EDGE_CURVE('',#7235,#7236,#4973,.T.);
#9347=EDGE_CURVE('',#7235,#7237,#3791,.T.);
#9348=EDGE_CURVE('',#7238,#7237,#3792,.T.);
#9349=EDGE_CURVE('',#7238,#7236,#3793,.T.);
#9350=EDGE_CURVE('',#7239,#7240,#4974,.T.);
#9351=EDGE_CURVE('',#7240,#7241,#3794,.T.);
#9352=EDGE_CURVE('',#7241,#7242,#2841,.F.);
#9353=EDGE_CURVE('',#7242,#7239,#3795,.T.);
#9354=EDGE_CURVE('',#7243,#7244,#4975,.T.);
#9355=EDGE_CURVE('',#7244,#7240,#3796,.T.);
#9356=EDGE_CURVE('',#7239,#7243,#3797,.T.);
#9357=EDGE_CURVE('',#7245,#7246,#4976,.T.);
#9358=EDGE_CURVE('',#7246,#7244,#3798,.T.);
#9359=EDGE_CURVE('',#7243,#7245,#3799,.T.);
#9360=EDGE_CURVE('',#7247,#7248,#4977,.T.);
#9361=EDGE_CURVE('',#7248,#7246,#3800,.T.);
#9362=EDGE_CURVE('',#7245,#7247,#3801,.T.);
#9363=EDGE_CURVE('',#7249,#7250,#4978,.T.);
#9364=EDGE_CURVE('',#7250,#7248,#3802,.T.);
#9365=EDGE_CURVE('',#7247,#7249,#3803,.T.);
#9366=EDGE_CURVE('',#7251,#7252,#4979,.T.);
#9367=EDGE_CURVE('',#7252,#7250,#3804,.T.);
#9368=EDGE_CURVE('',#7249,#7251,#3805,.T.);
#9369=EDGE_CURVE('',#7253,#7254,#4980,.T.);
#9370=EDGE_CURVE('',#7254,#7252,#3806,.T.);
#9371=EDGE_CURVE('',#7251,#7253,#3807,.T.);
#9372=EDGE_CURVE('',#7255,#7256,#4981,.T.);
#9373=EDGE_CURVE('',#7255,#7257,#3808,.T.);
#9374=EDGE_CURVE('',#7258,#7257,#3809,.T.);
#9375=EDGE_CURVE('',#7258,#7256,#3810,.T.);
#9376=EDGE_CURVE('',#7259,#7260,#4982,.T.);
#9377=EDGE_CURVE('',#7260,#7261,#3811,.T.);
#9378=EDGE_CURVE('',#7262,#7261,#2842,.T.);
#9379=EDGE_CURVE('',#7259,#7262,#3812,.T.);
#9380=EDGE_CURVE('',#7263,#7264,#4983,.T.);
#9381=EDGE_CURVE('',#7264,#7260,#3813,.T.);
#9382=EDGE_CURVE('',#7263,#7259,#3814,.T.);
#9383=EDGE_CURVE('',#7265,#7266,#4984,.T.);
#9384=EDGE_CURVE('',#7266,#7264,#3815,.T.);
#9385=EDGE_CURVE('',#7265,#7263,#3816,.T.);
#9386=EDGE_CURVE('',#7267,#7268,#4985,.T.);
#9387=EDGE_CURVE('',#7268,#7266,#3817,.T.);
#9388=EDGE_CURVE('',#7267,#7265,#3818,.T.);
#9389=EDGE_CURVE('',#7269,#7270,#4986,.T.);
#9390=EDGE_CURVE('',#7270,#7268,#3819,.T.);
#9391=EDGE_CURVE('',#7269,#7267,#3820,.T.);
#9392=EDGE_CURVE('',#7271,#7272,#4987,.T.);
#9393=EDGE_CURVE('',#7272,#7270,#3821,.T.);
#9394=EDGE_CURVE('',#7271,#7269,#3822,.T.);
#9395=EDGE_CURVE('',#7273,#7274,#4988,.T.);
#9396=EDGE_CURVE('',#7274,#7272,#3823,.T.);
#9397=EDGE_CURVE('',#7273,#7271,#3824,.T.);
#9398=EDGE_CURVE('',#7275,#7276,#4989,.T.);
#9399=EDGE_CURVE('',#7277,#7275,#3825,.T.);
#9400=EDGE_CURVE('',#7278,#7277,#3826,.T.);
#9401=EDGE_CURVE('',#7279,#7278,#3827,.T.);
#9402=EDGE_CURVE('',#7279,#7276,#3828,.T.);
#9403=EDGE_CURVE('',#7280,#7281,#4990,.T.);
#9404=EDGE_CURVE('',#7281,#7282,#3829,.T.);
#9405=EDGE_CURVE('',#7283,#7282,#2843,.T.);
#9406=EDGE_CURVE('',#7280,#7283,#3830,.T.);
#9407=EDGE_CURVE('',#7284,#7285,#4991,.T.);
#9408=EDGE_CURVE('',#7285,#7281,#3831,.T.);
#9409=EDGE_CURVE('',#7284,#7280,#3832,.T.);
#9410=EDGE_CURVE('',#7286,#7287,#4992,.T.);
#9411=EDGE_CURVE('',#7287,#7285,#3833,.T.);
#9412=EDGE_CURVE('',#7286,#7284,#3834,.T.);
#9413=EDGE_CURVE('',#7288,#7289,#4993,.T.);
#9414=EDGE_CURVE('',#7289,#7287,#3835,.T.);
#9415=EDGE_CURVE('',#7288,#7286,#3836,.T.);
#9416=EDGE_CURVE('',#7290,#7291,#4994,.T.);
#9417=EDGE_CURVE('',#7291,#7289,#3837,.T.);
#9418=EDGE_CURVE('',#7290,#7288,#3838,.T.);
#9419=EDGE_CURVE('',#7292,#7293,#4995,.T.);
#9420=EDGE_CURVE('',#7293,#7291,#3839,.T.);
#9421=EDGE_CURVE('',#7292,#7290,#3840,.T.);
#9422=EDGE_CURVE('',#7294,#7295,#4996,.T.);
#9423=EDGE_CURVE('',#7295,#7293,#3841,.T.);
#9424=EDGE_CURVE('',#7294,#7292,#3842,.T.);
#9425=EDGE_CURVE('',#7296,#7297,#4997,.T.);
#9426=EDGE_CURVE('',#7298,#7296,#3843,.T.);
#9427=EDGE_CURVE('',#7299,#7298,#3844,.T.);
#9428=EDGE_CURVE('',#7300,#7299,#3845,.T.);
#9429=EDGE_CURVE('',#7300,#7297,#3846,.T.);
#9430=EDGE_CURVE('',#7301,#7302,#4998,.T.);
#9431=EDGE_CURVE('',#7302,#7303,#3847,.T.);
#9432=EDGE_CURVE('',#7304,#7303,#2844,.T.);
#9433=EDGE_CURVE('',#7301,#7304,#3848,.T.);
#9434=EDGE_CURVE('',#7305,#7306,#4999,.T.);
#9435=EDGE_CURVE('',#7306,#7302,#3849,.T.);
#9436=EDGE_CURVE('',#7305,#7301,#3850,.T.);
#9437=EDGE_CURVE('',#7307,#7308,#5000,.T.);
#9438=EDGE_CURVE('',#7308,#7306,#3851,.T.);
#9439=EDGE_CURVE('',#7307,#7305,#3852,.T.);
#9440=EDGE_CURVE('',#7309,#7310,#5001,.T.);
#9441=EDGE_CURVE('',#7310,#7308,#3853,.T.);
#9442=EDGE_CURVE('',#7309,#7307,#3854,.T.);
#9443=EDGE_CURVE('',#7311,#7312,#5002,.T.);
#9444=EDGE_CURVE('',#7312,#7310,#3855,.T.);
#9445=EDGE_CURVE('',#7311,#7309,#3856,.T.);
#9446=EDGE_CURVE('',#7313,#7314,#5003,.T.);
#9447=EDGE_CURVE('',#7314,#7312,#3857,.T.);
#9448=EDGE_CURVE('',#7313,#7311,#3858,.T.);
#9449=EDGE_CURVE('',#7315,#7316,#5004,.T.);
#9450=EDGE_CURVE('',#7316,#7314,#3859,.T.);
#9451=EDGE_CURVE('',#7315,#7313,#3860,.T.);
#9452=EDGE_CURVE('',#7317,#7318,#5005,.T.);
#9453=EDGE_CURVE('',#7319,#7317,#3861,.T.);
#9454=EDGE_CURVE('',#7320,#7319,#3862,.T.);
#9455=EDGE_CURVE('',#7321,#7320,#3863,.T.);
#9456=EDGE_CURVE('',#7321,#7318,#3864,.T.);
#9457=EDGE_CURVE('',#7257,#7321,#3865,.T.);
#9458=EDGE_CURVE('',#7253,#7255,#3866,.T.);
#9459=EDGE_CURVE('',#7303,#7242,#3867,.T.);
#9460=EDGE_CURVE('',#7318,#7316,#3868,.T.);
#9461=EDGE_CURVE('',#7317,#7315,#3869,.T.);
#9462=EDGE_CURVE('',#7319,#7258,#3870,.T.);
#9463=EDGE_CURVE('',#7241,#7304,#3871,.T.);
#9464=EDGE_CURVE('',#7256,#7254,#3872,.T.);
#9465=EDGE_CURVE('',#7237,#7300,#3873,.T.);
#9466=EDGE_CURVE('',#7233,#7235,#3874,.T.);
#9467=EDGE_CURVE('',#7282,#7222,#3875,.T.);
#9468=EDGE_CURVE('',#7297,#7295,#3876,.T.);
#9469=EDGE_CURVE('',#7296,#7294,#3877,.T.);
#9470=EDGE_CURVE('',#7298,#7238,#3878,.T.);
#9471=EDGE_CURVE('',#7221,#7283,#3879,.T.);
#9472=EDGE_CURVE('',#7236,#7234,#3880,.T.);
#9473=EDGE_CURVE('',#7217,#7279,#3881,.T.);
#9474=EDGE_CURVE('',#7213,#7215,#3882,.T.);
#9475=EDGE_CURVE('',#7261,#7202,#3883,.T.);
#9476=EDGE_CURVE('',#7276,#7274,#3884,.T.);
#9477=EDGE_CURVE('',#7275,#7273,#3885,.T.);
#9478=EDGE_CURVE('',#7277,#7218,#3886,.T.);
#9479=EDGE_CURVE('',#7201,#7262,#3887,.T.);
#9480=EDGE_CURVE('',#7216,#7214,#3888,.T.);
#9481=EDGE_CURVE('',#7176,#7198,#3889,.T.);
#9482=EDGE_CURVE('',#7172,#7174,#3890,.T.);
#9483=EDGE_CURVE('',#7180,#7161,#3891,.T.);
#9484=EDGE_CURVE('',#7195,#7193,#3892,.T.);
#9485=EDGE_CURVE('',#7194,#7192,#3893,.T.);
#9486=EDGE_CURVE('',#7196,#7177,#3894,.T.);
#9487=EDGE_CURVE('',#7160,#7181,#3895,.T.);
#9488=EDGE_CURVE('',#7175,#7173,#3896,.T.);
#9489=EDGE_CURVE('',#7100,#7131,#3897,.T.);
#9490=EDGE_CURVE('',#7130,#7101,#3898,.T.);
#9491=EDGE_CURVE('',#7155,#7153,#3899,.T.);
#9492=EDGE_CURVE('',#7154,#7152,#3900,.T.);
#9493=EDGE_CURVE('',#7126,#7157,#3901,.T.);
#9494=EDGE_CURVE('',#7122,#7124,#3902,.T.);
#9495=EDGE_CURVE('',#7125,#7123,#3903,.T.);
#9496=EDGE_CURVE('',#7156,#7127,#3904,.T.);
#9497=EDGE_CURVE('',#7040,#7071,#3905,.T.);
#9498=EDGE_CURVE('',#7070,#7041,#3906,.T.);
#9499=EDGE_CURVE('',#7095,#7093,#3907,.T.);
#9500=EDGE_CURVE('',#7094,#7092,#3908,.T.);
#9501=EDGE_CURVE('',#7066,#7097,#3909,.T.);
#9502=EDGE_CURVE('',#7062,#7064,#3910,.T.);
#9503=EDGE_CURVE('',#7065,#7063,#3911,.T.);
#9504=EDGE_CURVE('',#7096,#7067,#3912,.T.);
#9505=EDGE_CURVE('',#6980,#7011,#3913,.T.);
#9506=EDGE_CURVE('',#7010,#6981,#3914,.T.);
#9507=EDGE_CURVE('',#7035,#7033,#3915,.T.);
#9508=EDGE_CURVE('',#7034,#7032,#3916,.T.);
#9509=EDGE_CURVE('',#7006,#7037,#3917,.T.);
#9510=EDGE_CURVE('',#7002,#7004,#3918,.T.);
#9511=EDGE_CURVE('',#7005,#7003,#3919,.T.);
#9512=EDGE_CURVE('',#7036,#7007,#3920,.T.);
#9513=EDGE_CURVE('',#6920,#6951,#3921,.T.);
#9514=EDGE_CURVE('',#6950,#6921,#3922,.T.);
#9515=EDGE_CURVE('',#6975,#6973,#3923,.T.);
#9516=EDGE_CURVE('',#6974,#6972,#3924,.T.);
#9517=EDGE_CURVE('',#6946,#6977,#3925,.T.);
#9518=EDGE_CURVE('',#6942,#6944,#3926,.T.);
#9519=EDGE_CURVE('',#6945,#6943,#3927,.T.);
#9520=EDGE_CURVE('',#6976,#6947,#3928,.T.);
#9521=EDGE_CURVE('',#6860,#6891,#3929,.T.);
#9522=EDGE_CURVE('',#6890,#6861,#3930,.T.);
#9523=EDGE_CURVE('',#6915,#6913,#3931,.T.);
#9524=EDGE_CURVE('',#6914,#6912,#3932,.T.);
#9525=EDGE_CURVE('',#6886,#6917,#3933,.T.);
#9526=EDGE_CURVE('',#6882,#6884,#3934,.T.);
#9527=EDGE_CURVE('',#6885,#6883,#3935,.T.);
#9528=EDGE_CURVE('',#6916,#6887,#3936,.T.);
#9529=EDGE_CURVE('',#6800,#6831,#3937,.T.);
#9530=EDGE_CURVE('',#6830,#6801,#3938,.T.);
#9531=EDGE_CURVE('',#6855,#6853,#3939,.T.);
#9532=EDGE_CURVE('',#6854,#6852,#3940,.T.);
#9533=EDGE_CURVE('',#6826,#6857,#3941,.T.);
#9534=EDGE_CURVE('',#6822,#6824,#3942,.T.);
#9535=EDGE_CURVE('',#6825,#6823,#3943,.T.);
#9536=EDGE_CURVE('',#6856,#6827,#3944,.T.);
#9537=EDGE_CURVE('',#6740,#6771,#3945,.T.);
#9538=EDGE_CURVE('',#6770,#6741,#3946,.T.);
#9539=EDGE_CURVE('',#6795,#6793,#3947,.T.);
#9540=EDGE_CURVE('',#6794,#6792,#3948,.T.);
#9541=EDGE_CURVE('',#6766,#6797,#3949,.T.);
#9542=EDGE_CURVE('',#6762,#6764,#3950,.T.);
#9543=EDGE_CURVE('',#6765,#6763,#3951,.T.);
#9544=EDGE_CURVE('',#6796,#6767,#3952,.T.);
#9545=EDGE_CURVE('',#6680,#6711,#3953,.T.);
#9546=EDGE_CURVE('',#6710,#6681,#3954,.T.);
#9547=EDGE_CURVE('',#6735,#6733,#3955,.T.);
#9548=EDGE_CURVE('',#6734,#6732,#3956,.T.);
#9549=EDGE_CURVE('',#6706,#6737,#3957,.T.);
#9550=EDGE_CURVE('',#6702,#6704,#3958,.T.);
#9551=EDGE_CURVE('',#6705,#6703,#3959,.T.);
#9552=EDGE_CURVE('',#6736,#6707,#3960,.T.);
#9553=EDGE_CURVE('',#6620,#6651,#3961,.T.);
#9554=EDGE_CURVE('',#6650,#6621,#3962,.T.);
#9555=EDGE_CURVE('',#6675,#6673,#3963,.T.);
#9556=EDGE_CURVE('',#6674,#6672,#3964,.T.);
#9557=EDGE_CURVE('',#6646,#6677,#3965,.T.);
#9558=EDGE_CURVE('',#6642,#6644,#3966,.T.);
#9559=EDGE_CURVE('',#6645,#6643,#3967,.T.);
#9560=EDGE_CURVE('',#6676,#6647,#3968,.T.);
#9561=EDGE_CURVE('',#6560,#6591,#3969,.T.);
#9562=EDGE_CURVE('',#6590,#6561,#3970,.T.);
#9563=EDGE_CURVE('',#6615,#6613,#3971,.T.);
#9564=EDGE_CURVE('',#6614,#6612,#3972,.T.);
#9565=EDGE_CURVE('',#6586,#6617,#3973,.T.);
#9566=EDGE_CURVE('',#6582,#6584,#3974,.T.);
#9567=EDGE_CURVE('',#6585,#6583,#3975,.T.);
#9568=EDGE_CURVE('',#6616,#6587,#3976,.T.);
#9569=EDGE_CURVE('',#6500,#6531,#3977,.T.);
#9570=EDGE_CURVE('',#6530,#6501,#3978,.T.);
#9571=EDGE_CURVE('',#6555,#6553,#3979,.T.);
#9572=EDGE_CURVE('',#6554,#6552,#3980,.T.);
#9573=EDGE_CURVE('',#6526,#6557,#3981,.T.);
#9574=EDGE_CURVE('',#6522,#6524,#3982,.T.);
#9575=EDGE_CURVE('',#6525,#6523,#3983,.T.);
#9576=EDGE_CURVE('',#6556,#6527,#3984,.T.);
#9577=EDGE_CURVE('',#6440,#6471,#3985,.T.);
#9578=EDGE_CURVE('',#6470,#6441,#3986,.T.);
#9579=EDGE_CURVE('',#6495,#6493,#3987,.T.);
#9580=EDGE_CURVE('',#6494,#6492,#3988,.T.);
#9581=EDGE_CURVE('',#6466,#6497,#3989,.T.);
#9582=EDGE_CURVE('',#6462,#6464,#3990,.T.);
#9583=EDGE_CURVE('',#6465,#6463,#3991,.T.);
#9584=EDGE_CURVE('',#6496,#6467,#3992,.T.);
#9585=EDGE_CURVE('',#7322,#7322,#2845,.T.);
#9586=EDGE_CURVE('',#7322,#7323,#5006,.T.);
#9587=EDGE_CURVE('',#7323,#7323,#2846,.T.);
#9588=EDGE_CURVE('',#7324,#7324,#2847,.T.);
#9589=EDGE_CURVE('',#7324,#7325,#5007,.T.);
#9590=EDGE_CURVE('',#7325,#7325,#2848,.T.);
#9591=EDGE_CURVE('',#7326,#7327,#5008,.T.);
#9592=EDGE_CURVE('',#7327,#7328,#3993,.T.);
#9593=EDGE_CURVE('',#7328,#7329,#2849,.T.);
#9594=EDGE_CURVE('',#7329,#7330,#5009,.T.);
#9595=EDGE_CURVE('',#7330,#7331,#2850,.F.);
#9596=EDGE_CURVE('',#7331,#7332,#2851,.F.);
#9597=EDGE_CURVE('',#7332,#7330,#2852,.F.);
#9598=EDGE_CURVE('',#7329,#7333,#2853,.T.);
#9599=EDGE_CURVE('',#7333,#7326,#3994,.T.);
#9600=EDGE_CURVE('',#7334,#7335,#5010,.T.);
#9601=EDGE_CURVE('',#7335,#7327,#3995,.T.);
#9602=EDGE_CURVE('',#7326,#7334,#3996,.T.);
#9603=EDGE_CURVE('',#7336,#7337,#5011,.T.);
#9604=EDGE_CURVE('',#7337,#7335,#3997,.T.);
#9605=EDGE_CURVE('',#7334,#7336,#3998,.T.);
#9606=EDGE_CURVE('',#7338,#7339,#5012,.T.);
#9607=EDGE_CURVE('',#7339,#7337,#3999,.T.);
#9608=EDGE_CURVE('',#7336,#7338,#4000,.T.);
#9609=EDGE_CURVE('',#7340,#7341,#5013,.T.);
#9610=EDGE_CURVE('',#7341,#7339,#4001,.T.);
#9611=EDGE_CURVE('',#7338,#7340,#4002,.T.);
#9612=EDGE_CURVE('',#7342,#7343,#5014,.T.);
#9613=EDGE_CURVE('',#7343,#7341,#4003,.T.);
#9614=EDGE_CURVE('',#7340,#7342,#4004,.T.);
#9615=EDGE_CURVE('',#7344,#7345,#5015,.T.);
#9616=EDGE_CURVE('',#7345,#7343,#4005,.T.);
#9617=EDGE_CURVE('',#7342,#7344,#4006,.T.);
#9618=EDGE_CURVE('',#7346,#7347,#5016,.T.);
#9619=EDGE_CURVE('',#7346,#7348,#4007,.T.);
#9620=EDGE_CURVE('',#7349,#7348,#2854,.F.);
#9621=EDGE_CURVE('',#7349,#7347,#4008,.T.);
#9622=EDGE_CURVE('',#7350,#7351,#5017,.T.);
#9623=EDGE_CURVE('',#7351,#7352,#4009,.T.);
#9624=EDGE_CURVE('',#7353,#7352,#2855,.T.);
#9625=EDGE_CURVE('',#7350,#7353,#4010,.T.);
#9626=EDGE_CURVE('',#7354,#7355,#5018,.T.);
#9627=EDGE_CURVE('',#7355,#7351,#4011,.T.);
#9628=EDGE_CURVE('',#7354,#7350,#4012,.T.);
#9629=EDGE_CURVE('',#7356,#7357,#5019,.T.);
#9630=EDGE_CURVE('',#7357,#7355,#4013,.T.);
#9631=EDGE_CURVE('',#7356,#7354,#4014,.T.);
#9632=EDGE_CURVE('',#7358,#7359,#5020,.T.);
#9633=EDGE_CURVE('',#7359,#7357,#4015,.T.);
#9634=EDGE_CURVE('',#7358,#7356,#4016,.T.);
#9635=EDGE_CURVE('',#7360,#7361,#5021,.T.);
#9636=EDGE_CURVE('',#7361,#7359,#4017,.T.);
#9637=EDGE_CURVE('',#7360,#7358,#4018,.T.);
#9638=EDGE_CURVE('',#7362,#7363,#5022,.T.);
#9639=EDGE_CURVE('',#7363,#7361,#4019,.T.);
#9640=EDGE_CURVE('',#7362,#7360,#4020,.T.);
#9641=EDGE_CURVE('',#7364,#7365,#5023,.T.);
#9642=EDGE_CURVE('',#7365,#7363,#4021,.T.);
#9643=EDGE_CURVE('',#7364,#7362,#4022,.T.);
#9644=EDGE_CURVE('',#7366,#7367,#5024,.T.);
#9645=EDGE_CURVE('',#7368,#7366,#4023,.T.);
#9646=EDGE_CURVE('',#7369,#7368,#2856,.T.);
#9647=EDGE_CURVE('',#7369,#7367,#4024,.T.);
#9648=EDGE_CURVE('',#7370,#7371,#5025,.T.);
#9649=EDGE_CURVE('',#7371,#7372,#4025,.T.);
#9650=EDGE_CURVE('',#7372,#7373,#2857,.T.);
#9651=EDGE_CURVE('',#7373,#7374,#5026,.T.);
#9652=EDGE_CURVE('',#7374,#7375,#2858,.F.);
#9653=EDGE_CURVE('',#7375,#7376,#2859,.F.);
#9654=EDGE_CURVE('',#7376,#7374,#2860,.F.);
#9655=EDGE_CURVE('',#7373,#7377,#2861,.T.);
#9656=EDGE_CURVE('',#7377,#7370,#4026,.T.);
#9657=EDGE_CURVE('',#7378,#7379,#5027,.T.);
#9658=EDGE_CURVE('',#7379,#7371,#4027,.T.);
#9659=EDGE_CURVE('',#7370,#7378,#4028,.T.);
#9660=EDGE_CURVE('',#7380,#7381,#5028,.T.);
#9661=EDGE_CURVE('',#7381,#7379,#4029,.T.);
#9662=EDGE_CURVE('',#7378,#7380,#4030,.T.);
#9663=EDGE_CURVE('',#7382,#7383,#5029,.T.);
#9664=EDGE_CURVE('',#7383,#7381,#4031,.T.);
#9665=EDGE_CURVE('',#7380,#7382,#4032,.T.);
#9666=EDGE_CURVE('',#7384,#7385,#5030,.T.);
#9667=EDGE_CURVE('',#7385,#7383,#4033,.T.);
#9668=EDGE_CURVE('',#7382,#7384,#4034,.T.);
#9669=EDGE_CURVE('',#7386,#7387,#5031,.T.);
#9670=EDGE_CURVE('',#7387,#7385,#4035,.T.);
#9671=EDGE_CURVE('',#7384,#7386,#4036,.T.);
#9672=EDGE_CURVE('',#7388,#7389,#5032,.T.);
#9673=EDGE_CURVE('',#7389,#7387,#4037,.T.);
#9674=EDGE_CURVE('',#7386,#7388,#4038,.T.);
#9675=EDGE_CURVE('',#7390,#7391,#5033,.T.);
#9676=EDGE_CURVE('',#7390,#7392,#4039,.T.);
#9677=EDGE_CURVE('',#7393,#7392,#2862,.F.);
#9678=EDGE_CURVE('',#7393,#7391,#4040,.T.);
#9679=EDGE_CURVE('',#7394,#7395,#5034,.T.);
#9680=EDGE_CURVE('',#7395,#7396,#4041,.T.);
#9681=EDGE_CURVE('',#7397,#7396,#2863,.T.);
#9682=EDGE_CURVE('',#7394,#7397,#4042,.T.);
#9683=EDGE_CURVE('',#7398,#7399,#5035,.T.);
#9684=EDGE_CURVE('',#7399,#7395,#4043,.T.);
#9685=EDGE_CURVE('',#7398,#7394,#4044,.T.);
#9686=EDGE_CURVE('',#7400,#7401,#5036,.T.);
#9687=EDGE_CURVE('',#7401,#7399,#4045,.T.);
#9688=EDGE_CURVE('',#7400,#7398,#4046,.T.);
#9689=EDGE_CURVE('',#7402,#7403,#5037,.T.);
#9690=EDGE_CURVE('',#7403,#7401,#4047,.T.);
#9691=EDGE_CURVE('',#7402,#7400,#4048,.T.);
#9692=EDGE_CURVE('',#7404,#7405,#5038,.T.);
#9693=EDGE_CURVE('',#7405,#7403,#4049,.T.);
#9694=EDGE_CURVE('',#7404,#7402,#4050,.T.);
#9695=EDGE_CURVE('',#7406,#7407,#5039,.T.);
#9696=EDGE_CURVE('',#7407,#7405,#4051,.T.);
#9697=EDGE_CURVE('',#7406,#7404,#4052,.T.);
#9698=EDGE_CURVE('',#7408,#7409,#5040,.T.);
#9699=EDGE_CURVE('',#7409,#7407,#4053,.T.);
#9700=EDGE_CURVE('',#7408,#7406,#4054,.T.);
#9701=EDGE_CURVE('',#7410,#7411,#5041,.T.);
#9702=EDGE_CURVE('',#7412,#7410,#4055,.T.);
#9703=EDGE_CURVE('',#7413,#7412,#2864,.T.);
#9704=EDGE_CURVE('',#7413,#7411,#4056,.T.);
#9705=EDGE_CURVE('',#7414,#7415,#5042,.T.);
#9706=EDGE_CURVE('',#7415,#7416,#4057,.T.);
#9707=EDGE_CURVE('',#7416,#7417,#2865,.T.);
#9708=EDGE_CURVE('',#7417,#7418,#5043,.T.);
#9709=EDGE_CURVE('',#7418,#7419,#2866,.F.);
#9710=EDGE_CURVE('',#7419,#7420,#2867,.F.);
#9711=EDGE_CURVE('',#7420,#7418,#2868,.F.);
#9712=EDGE_CURVE('',#7417,#7421,#2869,.T.);
#9713=EDGE_CURVE('',#7421,#7414,#4058,.T.);
#9714=EDGE_CURVE('',#7422,#7423,#5044,.T.);
#9715=EDGE_CURVE('',#7423,#7415,#4059,.T.);
#9716=EDGE_CURVE('',#7414,#7422,#4060,.T.);
#9717=EDGE_CURVE('',#7424,#7425,#5045,.T.);
#9718=EDGE_CURVE('',#7425,#7423,#4061,.T.);
#9719=EDGE_CURVE('',#7422,#7424,#4062,.T.);
#9720=EDGE_CURVE('',#7426,#7427,#5046,.T.);
#9721=EDGE_CURVE('',#7427,#7425,#4063,.T.);
#9722=EDGE_CURVE('',#7424,#7426,#4064,.T.);
#9723=EDGE_CURVE('',#7428,#7429,#5047,.T.);
#9724=EDGE_CURVE('',#7429,#7427,#4065,.T.);
#9725=EDGE_CURVE('',#7426,#7428,#4066,.T.);
#9726=EDGE_CURVE('',#7430,#7431,#5048,.T.);
#9727=EDGE_CURVE('',#7431,#7429,#4067,.T.);
#9728=EDGE_CURVE('',#7428,#7430,#4068,.T.);
#9729=EDGE_CURVE('',#7432,#7433,#5049,.T.);
#9730=EDGE_CURVE('',#7433,#7431,#4069,.T.);
#9731=EDGE_CURVE('',#7430,#7432,#4070,.T.);
#9732=EDGE_CURVE('',#7434,#7435,#5050,.T.);
#9733=EDGE_CURVE('',#7434,#7436,#4071,.T.);
#9734=EDGE_CURVE('',#7437,#7436,#2870,.F.);
#9735=EDGE_CURVE('',#7437,#7435,#4072,.T.);
#9736=EDGE_CURVE('',#7438,#7439,#5051,.T.);
#9737=EDGE_CURVE('',#7439,#7440,#4073,.T.);
#9738=EDGE_CURVE('',#7441,#7440,#2871,.T.);
#9739=EDGE_CURVE('',#7438,#7441,#4074,.T.);
#9740=EDGE_CURVE('',#7442,#7443,#5052,.T.);
#9741=EDGE_CURVE('',#7443,#7439,#4075,.T.);
#9742=EDGE_CURVE('',#7442,#7438,#4076,.T.);
#9743=EDGE_CURVE('',#7444,#7445,#5053,.T.);
#9744=EDGE_CURVE('',#7445,#7443,#4077,.T.);
#9745=EDGE_CURVE('',#7444,#7442,#4078,.T.);
#9746=EDGE_CURVE('',#7446,#7447,#5054,.T.);
#9747=EDGE_CURVE('',#7447,#7445,#4079,.T.);
#9748=EDGE_CURVE('',#7446,#7444,#4080,.T.);
#9749=EDGE_CURVE('',#7448,#7449,#5055,.T.);
#9750=EDGE_CURVE('',#7449,#7447,#4081,.T.);
#9751=EDGE_CURVE('',#7448,#7446,#4082,.T.);
#9752=EDGE_CURVE('',#7450,#7451,#5056,.T.);
#9753=EDGE_CURVE('',#7451,#7449,#4083,.T.);
#9754=EDGE_CURVE('',#7450,#7448,#4084,.T.);
#9755=EDGE_CURVE('',#7452,#7453,#5057,.T.);
#9756=EDGE_CURVE('',#7453,#7451,#4085,.T.);
#9757=EDGE_CURVE('',#7452,#7450,#4086,.T.);
#9758=EDGE_CURVE('',#7454,#7455,#5058,.T.);
#9759=EDGE_CURVE('',#7456,#7454,#4087,.T.);
#9760=EDGE_CURVE('',#7457,#7456,#2872,.T.);
#9761=EDGE_CURVE('',#7457,#7455,#4088,.T.);
#9762=EDGE_CURVE('',#7458,#7459,#5059,.T.);
#9763=EDGE_CURVE('',#7459,#7460,#4089,.T.);
#9764=EDGE_CURVE('',#7460,#7461,#2873,.T.);
#9765=EDGE_CURVE('',#7461,#7462,#5060,.T.);
#9766=EDGE_CURVE('',#7462,#7463,#2874,.F.);
#9767=EDGE_CURVE('',#7463,#7464,#2875,.F.);
#9768=EDGE_CURVE('',#7464,#7462,#2876,.F.);
#9769=EDGE_CURVE('',#7461,#7465,#2877,.T.);
#9770=EDGE_CURVE('',#7465,#7458,#4090,.T.);
#9771=EDGE_CURVE('',#7466,#7467,#5061,.T.);
#9772=EDGE_CURVE('',#7467,#7459,#4091,.T.);
#9773=EDGE_CURVE('',#7458,#7466,#4092,.T.);
#9774=EDGE_CURVE('',#7468,#7469,#5062,.T.);
#9775=EDGE_CURVE('',#7469,#7467,#4093,.T.);
#9776=EDGE_CURVE('',#7466,#7468,#4094,.T.);
#9777=EDGE_CURVE('',#7470,#7471,#5063,.T.);
#9778=EDGE_CURVE('',#7471,#7469,#4095,.T.);
#9779=EDGE_CURVE('',#7468,#7470,#4096,.T.);
#9780=EDGE_CURVE('',#7472,#7473,#5064,.T.);
#9781=EDGE_CURVE('',#7473,#7471,#4097,.T.);
#9782=EDGE_CURVE('',#7470,#7472,#4098,.T.);
#9783=EDGE_CURVE('',#7474,#7475,#5065,.T.);
#9784=EDGE_CURVE('',#7475,#7473,#4099,.T.);
#9785=EDGE_CURVE('',#7472,#7474,#4100,.T.);
#9786=EDGE_CURVE('',#7476,#7477,#5066,.T.);
#9787=EDGE_CURVE('',#7477,#7475,#4101,.T.);
#9788=EDGE_CURVE('',#7474,#7476,#4102,.T.);
#9789=EDGE_CURVE('',#7478,#7479,#5067,.T.);
#9790=EDGE_CURVE('',#7478,#7480,#4103,.T.);
#9791=EDGE_CURVE('',#7481,#7480,#2878,.F.);
#9792=EDGE_CURVE('',#7481,#7479,#4104,.T.);
#9793=EDGE_CURVE('',#7482,#7483,#5068,.T.);
#9794=EDGE_CURVE('',#7483,#7484,#4105,.T.);
#9795=EDGE_CURVE('',#7485,#7484,#2879,.T.);
#9796=EDGE_CURVE('',#7482,#7485,#4106,.T.);
#9797=EDGE_CURVE('',#7486,#7487,#5069,.T.);
#9798=EDGE_CURVE('',#7487,#7483,#4107,.T.);
#9799=EDGE_CURVE('',#7486,#7482,#4108,.T.);
#9800=EDGE_CURVE('',#7488,#7489,#5070,.T.);
#9801=EDGE_CURVE('',#7489,#7487,#4109,.T.);
#9802=EDGE_CURVE('',#7488,#7486,#4110,.T.);
#9803=EDGE_CURVE('',#7490,#7491,#5071,.T.);
#9804=EDGE_CURVE('',#7491,#7489,#4111,.T.);
#9805=EDGE_CURVE('',#7490,#7488,#4112,.T.);
#9806=EDGE_CURVE('',#7492,#7493,#5072,.T.);
#9807=EDGE_CURVE('',#7493,#7491,#4113,.T.);
#9808=EDGE_CURVE('',#7492,#7490,#4114,.T.);
#9809=EDGE_CURVE('',#7494,#7495,#5073,.T.);
#9810=EDGE_CURVE('',#7495,#7493,#4115,.T.);
#9811=EDGE_CURVE('',#7494,#7492,#4116,.T.);
#9812=EDGE_CURVE('',#7496,#7497,#5074,.T.);
#9813=EDGE_CURVE('',#7497,#7495,#4117,.T.);
#9814=EDGE_CURVE('',#7496,#7494,#4118,.T.);
#9815=EDGE_CURVE('',#7498,#7499,#5075,.T.);
#9816=EDGE_CURVE('',#7500,#7498,#4119,.T.);
#9817=EDGE_CURVE('',#7501,#7500,#2880,.T.);
#9818=EDGE_CURVE('',#7501,#7499,#4120,.T.);
#9819=EDGE_CURVE('',#7502,#7503,#5076,.T.);
#9820=EDGE_CURVE('',#7503,#7504,#4121,.T.);
#9821=EDGE_CURVE('',#7504,#7505,#2881,.T.);
#9822=EDGE_CURVE('',#7505,#7506,#5077,.T.);
#9823=EDGE_CURVE('',#7506,#7507,#2882,.F.);
#9824=EDGE_CURVE('',#7507,#7508,#2883,.F.);
#9825=EDGE_CURVE('',#7508,#7506,#2884,.F.);
#9826=EDGE_CURVE('',#7505,#7509,#2885,.T.);
#9827=EDGE_CURVE('',#7509,#7502,#4122,.T.);
#9828=EDGE_CURVE('',#7510,#7511,#5078,.T.);
#9829=EDGE_CURVE('',#7511,#7503,#4123,.T.);
#9830=EDGE_CURVE('',#7502,#7510,#4124,.T.);
#9831=EDGE_CURVE('',#7512,#7513,#5079,.T.);
#9832=EDGE_CURVE('',#7513,#7511,#4125,.T.);
#9833=EDGE_CURVE('',#7510,#7512,#4126,.T.);
#9834=EDGE_CURVE('',#7514,#7515,#5080,.T.);
#9835=EDGE_CURVE('',#7515,#7513,#4127,.T.);
#9836=EDGE_CURVE('',#7512,#7514,#4128,.T.);
#9837=EDGE_CURVE('',#7516,#7517,#5081,.T.);
#9838=EDGE_CURVE('',#7517,#7515,#4129,.T.);
#9839=EDGE_CURVE('',#7514,#7516,#4130,.T.);
#9840=EDGE_CURVE('',#7518,#7519,#5082,.T.);
#9841=EDGE_CURVE('',#7519,#7517,#4131,.T.);
#9842=EDGE_CURVE('',#7516,#7518,#4132,.T.);
#9843=EDGE_CURVE('',#7520,#7521,#5083,.T.);
#9844=EDGE_CURVE('',#7521,#7519,#4133,.T.);
#9845=EDGE_CURVE('',#7518,#7520,#4134,.T.);
#9846=EDGE_CURVE('',#7522,#7523,#5084,.T.);
#9847=EDGE_CURVE('',#7522,#7524,#4135,.T.);
#9848=EDGE_CURVE('',#7525,#7524,#2886,.F.);
#9849=EDGE_CURVE('',#7525,#7523,#4136,.T.);
#9850=EDGE_CURVE('',#7526,#7527,#5085,.T.);
#9851=EDGE_CURVE('',#7527,#7528,#4137,.T.);
#9852=EDGE_CURVE('',#7529,#7528,#2887,.T.);
#9853=EDGE_CURVE('',#7526,#7529,#4138,.T.);
#9854=EDGE_CURVE('',#7530,#7531,#5086,.T.);
#9855=EDGE_CURVE('',#7531,#7527,#4139,.T.);
#9856=EDGE_CURVE('',#7530,#7526,#4140,.T.);
#9857=EDGE_CURVE('',#7532,#7533,#5087,.T.);
#9858=EDGE_CURVE('',#7533,#7531,#4141,.T.);
#9859=EDGE_CURVE('',#7532,#7530,#4142,.T.);
#9860=EDGE_CURVE('',#7534,#7535,#5088,.T.);
#9861=EDGE_CURVE('',#7535,#7533,#4143,.T.);
#9862=EDGE_CURVE('',#7534,#7532,#4144,.T.);
#9863=EDGE_CURVE('',#7536,#7537,#5089,.T.);
#9864=EDGE_CURVE('',#7537,#7535,#4145,.T.);
#9865=EDGE_CURVE('',#7536,#7534,#4146,.T.);
#9866=EDGE_CURVE('',#7538,#7539,#5090,.T.);
#9867=EDGE_CURVE('',#7539,#7537,#4147,.T.);
#9868=EDGE_CURVE('',#7538,#7536,#4148,.T.);
#9869=EDGE_CURVE('',#7540,#7541,#5091,.T.);
#9870=EDGE_CURVE('',#7541,#7539,#4149,.T.);
#9871=EDGE_CURVE('',#7540,#7538,#4150,.T.);
#9872=EDGE_CURVE('',#7542,#7543,#5092,.T.);
#9873=EDGE_CURVE('',#7544,#7542,#4151,.T.);
#9874=EDGE_CURVE('',#7545,#7544,#2888,.T.);
#9875=EDGE_CURVE('',#7545,#7543,#4152,.T.);
#9876=EDGE_CURVE('',#7546,#7547,#5093,.T.);
#9877=EDGE_CURVE('',#7547,#7548,#4153,.T.);
#9878=EDGE_CURVE('',#7548,#7549,#2889,.T.);
#9879=EDGE_CURVE('',#7549,#7550,#5094,.T.);
#9880=EDGE_CURVE('',#7550,#7551,#2890,.F.);
#9881=EDGE_CURVE('',#7551,#7552,#2891,.F.);
#9882=EDGE_CURVE('',#7552,#7550,#2892,.F.);
#9883=EDGE_CURVE('',#7549,#7553,#2893,.T.);
#9884=EDGE_CURVE('',#7553,#7546,#4154,.T.);
#9885=EDGE_CURVE('',#7554,#7555,#5095,.T.);
#9886=EDGE_CURVE('',#7555,#7547,#4155,.T.);
#9887=EDGE_CURVE('',#7546,#7554,#4156,.T.);
#9888=EDGE_CURVE('',#7556,#7557,#5096,.T.);
#9889=EDGE_CURVE('',#7557,#7555,#4157,.T.);
#9890=EDGE_CURVE('',#7554,#7556,#4158,.T.);
#9891=EDGE_CURVE('',#7558,#7559,#5097,.T.);
#9892=EDGE_CURVE('',#7559,#7557,#4159,.T.);
#9893=EDGE_CURVE('',#7556,#7558,#4160,.T.);
#9894=EDGE_CURVE('',#7560,#7561,#5098,.T.);
#9895=EDGE_CURVE('',#7561,#7559,#4161,.T.);
#9896=EDGE_CURVE('',#7558,#7560,#4162,.T.);
#9897=EDGE_CURVE('',#7562,#7563,#5099,.T.);
#9898=EDGE_CURVE('',#7563,#7561,#4163,.T.);
#9899=EDGE_CURVE('',#7560,#7562,#4164,.T.);
#9900=EDGE_CURVE('',#7564,#7565,#5100,.T.);
#9901=EDGE_CURVE('',#7565,#7563,#4165,.T.);
#9902=EDGE_CURVE('',#7562,#7564,#4166,.T.);
#9903=EDGE_CURVE('',#7566,#7567,#5101,.T.);
#9904=EDGE_CURVE('',#7566,#7568,#4167,.T.);
#9905=EDGE_CURVE('',#7569,#7568,#2894,.F.);
#9906=EDGE_CURVE('',#7569,#7567,#4168,.T.);
#9907=EDGE_CURVE('',#7570,#7571,#5102,.T.);
#9908=EDGE_CURVE('',#7571,#7572,#4169,.T.);
#9909=EDGE_CURVE('',#7573,#7572,#2895,.T.);
#9910=EDGE_CURVE('',#7570,#7573,#4170,.T.);
#9911=EDGE_CURVE('',#7574,#7575,#5103,.T.);
#9912=EDGE_CURVE('',#7575,#7571,#4171,.T.);
#9913=EDGE_CURVE('',#7574,#7570,#4172,.T.);
#9914=EDGE_CURVE('',#7576,#7577,#5104,.T.);
#9915=EDGE_CURVE('',#7577,#7575,#4173,.T.);
#9916=EDGE_CURVE('',#7576,#7574,#4174,.T.);
#9917=EDGE_CURVE('',#7578,#7579,#5105,.T.);
#9918=EDGE_CURVE('',#7579,#7577,#4175,.T.);
#9919=EDGE_CURVE('',#7578,#7576,#4176,.T.);
#9920=EDGE_CURVE('',#7580,#7581,#5106,.T.);
#9921=EDGE_CURVE('',#7581,#7579,#4177,.T.);
#9922=EDGE_CURVE('',#7580,#7578,#4178,.T.);
#9923=EDGE_CURVE('',#7582,#7583,#5107,.T.);
#9924=EDGE_CURVE('',#7583,#7581,#4179,.T.);
#9925=EDGE_CURVE('',#7582,#7580,#4180,.T.);
#9926=EDGE_CURVE('',#7584,#7585,#5108,.T.);
#9927=EDGE_CURVE('',#7585,#7583,#4181,.T.);
#9928=EDGE_CURVE('',#7584,#7582,#4182,.T.);
#9929=EDGE_CURVE('',#7586,#7587,#5109,.T.);
#9930=EDGE_CURVE('',#7588,#7586,#4183,.T.);
#9931=EDGE_CURVE('',#7589,#7588,#2896,.T.);
#9932=EDGE_CURVE('',#7589,#7587,#4184,.T.);
#9933=EDGE_CURVE('',#7590,#7591,#5110,.T.);
#9934=EDGE_CURVE('',#7591,#7592,#4185,.T.);
#9935=EDGE_CURVE('',#7592,#7593,#2897,.T.);
#9936=EDGE_CURVE('',#7593,#7594,#5111,.T.);
#9937=EDGE_CURVE('',#7594,#7595,#2898,.F.);
#9938=EDGE_CURVE('',#7595,#7596,#2899,.F.);
#9939=EDGE_CURVE('',#7596,#7594,#2900,.F.);
#9940=EDGE_CURVE('',#7593,#7597,#2901,.T.);
#9941=EDGE_CURVE('',#7597,#7590,#4186,.T.);
#9942=EDGE_CURVE('',#7598,#7599,#5112,.T.);
#9943=EDGE_CURVE('',#7599,#7591,#4187,.T.);
#9944=EDGE_CURVE('',#7590,#7598,#4188,.T.);
#9945=EDGE_CURVE('',#7600,#7601,#5113,.T.);
#9946=EDGE_CURVE('',#7601,#7599,#4189,.T.);
#9947=EDGE_CURVE('',#7598,#7600,#4190,.T.);
#9948=EDGE_CURVE('',#7602,#7603,#5114,.T.);
#9949=EDGE_CURVE('',#7603,#7601,#4191,.T.);
#9950=EDGE_CURVE('',#7600,#7602,#4192,.T.);
#9951=EDGE_CURVE('',#7604,#7605,#5115,.T.);
#9952=EDGE_CURVE('',#7605,#7603,#4193,.T.);
#9953=EDGE_CURVE('',#7602,#7604,#4194,.T.);
#9954=EDGE_CURVE('',#7606,#7607,#5116,.T.);
#9955=EDGE_CURVE('',#7607,#7605,#4195,.T.);
#9956=EDGE_CURVE('',#7604,#7606,#4196,.T.);
#9957=EDGE_CURVE('',#7608,#7609,#5117,.T.);
#9958=EDGE_CURVE('',#7609,#7607,#4197,.T.);
#9959=EDGE_CURVE('',#7606,#7608,#4198,.T.);
#9960=EDGE_CURVE('',#7610,#7611,#5118,.T.);
#9961=EDGE_CURVE('',#7610,#7612,#4199,.T.);
#9962=EDGE_CURVE('',#7613,#7612,#2902,.F.);
#9963=EDGE_CURVE('',#7613,#7611,#4200,.T.);
#9964=EDGE_CURVE('',#7614,#7615,#5119,.T.);
#9965=EDGE_CURVE('',#7615,#7616,#4201,.T.);
#9966=EDGE_CURVE('',#7617,#7616,#2903,.T.);
#9967=EDGE_CURVE('',#7614,#7617,#4202,.T.);
#9968=EDGE_CURVE('',#7618,#7619,#5120,.T.);
#9969=EDGE_CURVE('',#7619,#7615,#4203,.T.);
#9970=EDGE_CURVE('',#7618,#7614,#4204,.T.);
#9971=EDGE_CURVE('',#7620,#7621,#5121,.T.);
#9972=EDGE_CURVE('',#7621,#7619,#4205,.T.);
#9973=EDGE_CURVE('',#7620,#7618,#4206,.T.);
#9974=EDGE_CURVE('',#7622,#7623,#5122,.T.);
#9975=EDGE_CURVE('',#7623,#7621,#4207,.T.);
#9976=EDGE_CURVE('',#7622,#7620,#4208,.T.);
#9977=EDGE_CURVE('',#7624,#7625,#5123,.T.);
#9978=EDGE_CURVE('',#7625,#7623,#4209,.T.);
#9979=EDGE_CURVE('',#7624,#7622,#4210,.T.);
#9980=EDGE_CURVE('',#7626,#7627,#5124,.T.);
#9981=EDGE_CURVE('',#7627,#7625,#4211,.T.);
#9982=EDGE_CURVE('',#7626,#7624,#4212,.T.);
#9983=EDGE_CURVE('',#7628,#7629,#5125,.T.);
#9984=EDGE_CURVE('',#7629,#7627,#4213,.T.);
#9985=EDGE_CURVE('',#7628,#7626,#4214,.T.);
#9986=EDGE_CURVE('',#7630,#7631,#5126,.T.);
#9987=EDGE_CURVE('',#7632,#7630,#4215,.T.);
#9988=EDGE_CURVE('',#7633,#7632,#2904,.T.);
#9989=EDGE_CURVE('',#7633,#7631,#4216,.T.);
#9990=EDGE_CURVE('',#7634,#7635,#5127,.T.);
#9991=EDGE_CURVE('',#7635,#7636,#4217,.T.);
#9992=EDGE_CURVE('',#7636,#7637,#2905,.T.);
#9993=EDGE_CURVE('',#7637,#7638,#5128,.T.);
#9994=EDGE_CURVE('',#7638,#7639,#2906,.F.);
#9995=EDGE_CURVE('',#7639,#7640,#2907,.F.);
#9996=EDGE_CURVE('',#7640,#7638,#2908,.F.);
#9997=EDGE_CURVE('',#7637,#7641,#2909,.T.);
#9998=EDGE_CURVE('',#7641,#7634,#4218,.T.);
#9999=EDGE_CURVE('',#7642,#7643,#5129,.T.);
#10000=EDGE_CURVE('',#7643,#7635,#4219,.T.);
#10001=EDGE_CURVE('',#7634,#7642,#4220,.T.);
#10002=EDGE_CURVE('',#7644,#7645,#5130,.T.);
#10003=EDGE_CURVE('',#7645,#7643,#4221,.T.);
#10004=EDGE_CURVE('',#7642,#7644,#4222,.T.);
#10005=EDGE_CURVE('',#7646,#7647,#5131,.T.);
#10006=EDGE_CURVE('',#7647,#7645,#4223,.T.);
#10007=EDGE_CURVE('',#7644,#7646,#4224,.T.);
#10008=EDGE_CURVE('',#7648,#7649,#5132,.T.);
#10009=EDGE_CURVE('',#7649,#7647,#4225,.T.);
#10010=EDGE_CURVE('',#7646,#7648,#4226,.T.);
#10011=EDGE_CURVE('',#7650,#7651,#5133,.T.);
#10012=EDGE_CURVE('',#7651,#7649,#4227,.T.);
#10013=EDGE_CURVE('',#7648,#7650,#4228,.T.);
#10014=EDGE_CURVE('',#7652,#7653,#5134,.T.);
#10015=EDGE_CURVE('',#7653,#7651,#4229,.T.);
#10016=EDGE_CURVE('',#7650,#7652,#4230,.T.);
#10017=EDGE_CURVE('',#7654,#7655,#5135,.T.);
#10018=EDGE_CURVE('',#7654,#7656,#4231,.T.);
#10019=EDGE_CURVE('',#7657,#7656,#2910,.F.);
#10020=EDGE_CURVE('',#7657,#7655,#4232,.T.);
#10021=EDGE_CURVE('',#7658,#7659,#5136,.T.);
#10022=EDGE_CURVE('',#7659,#7660,#4233,.T.);
#10023=EDGE_CURVE('',#7661,#7660,#2911,.T.);
#10024=EDGE_CURVE('',#7658,#7661,#4234,.T.);
#10025=EDGE_CURVE('',#7662,#7663,#5137,.T.);
#10026=EDGE_CURVE('',#7663,#7659,#4235,.T.);
#10027=EDGE_CURVE('',#7662,#7658,#4236,.T.);
#10028=EDGE_CURVE('',#7664,#7665,#5138,.T.);
#10029=EDGE_CURVE('',#7665,#7663,#4237,.T.);
#10030=EDGE_CURVE('',#7664,#7662,#4238,.T.);
#10031=EDGE_CURVE('',#7666,#7667,#5139,.T.);
#10032=EDGE_CURVE('',#7667,#7665,#4239,.T.);
#10033=EDGE_CURVE('',#7666,#7664,#4240,.T.);
#10034=EDGE_CURVE('',#7668,#7669,#5140,.T.);
#10035=EDGE_CURVE('',#7669,#7667,#4241,.T.);
#10036=EDGE_CURVE('',#7668,#7666,#4242,.T.);
#10037=EDGE_CURVE('',#7670,#7671,#5141,.T.);
#10038=EDGE_CURVE('',#7671,#7669,#4243,.T.);
#10039=EDGE_CURVE('',#7670,#7668,#4244,.T.);
#10040=EDGE_CURVE('',#7672,#7673,#5142,.T.);
#10041=EDGE_CURVE('',#7673,#7671,#4245,.T.);
#10042=EDGE_CURVE('',#7672,#7670,#4246,.T.);
#10043=EDGE_CURVE('',#7674,#7675,#5143,.T.);
#10044=EDGE_CURVE('',#7676,#7674,#4247,.T.);
#10045=EDGE_CURVE('',#7677,#7676,#2912,.T.);
#10046=EDGE_CURVE('',#7677,#7675,#4248,.T.);
#10047=EDGE_CURVE('',#7678,#7679,#5144,.T.);
#10048=EDGE_CURVE('',#7679,#7680,#4249,.T.);
#10049=EDGE_CURVE('',#7680,#7681,#2913,.T.);
#10050=EDGE_CURVE('',#7681,#7682,#5145,.T.);
#10051=EDGE_CURVE('',#7682,#7683,#2914,.F.);
#10052=EDGE_CURVE('',#7683,#7684,#2915,.F.);
#10053=EDGE_CURVE('',#7684,#7682,#2916,.F.);
#10054=EDGE_CURVE('',#7681,#7685,#2917,.T.);
#10055=EDGE_CURVE('',#7685,#7678,#4250,.T.);
#10056=EDGE_CURVE('',#7686,#7687,#5146,.T.);
#10057=EDGE_CURVE('',#7687,#7679,#4251,.T.);
#10058=EDGE_CURVE('',#7678,#7686,#4252,.T.);
#10059=EDGE_CURVE('',#7688,#7689,#5147,.T.);
#10060=EDGE_CURVE('',#7689,#7687,#4253,.T.);
#10061=EDGE_CURVE('',#7686,#7688,#4254,.T.);
#10062=EDGE_CURVE('',#7690,#7691,#5148,.T.);
#10063=EDGE_CURVE('',#7691,#7689,#4255,.T.);
#10064=EDGE_CURVE('',#7688,#7690,#4256,.T.);
#10065=EDGE_CURVE('',#7692,#7693,#5149,.T.);
#10066=EDGE_CURVE('',#7693,#7691,#4257,.T.);
#10067=EDGE_CURVE('',#7690,#7692,#4258,.T.);
#10068=EDGE_CURVE('',#7694,#7695,#5150,.T.);
#10069=EDGE_CURVE('',#7695,#7693,#4259,.T.);
#10070=EDGE_CURVE('',#7692,#7694,#4260,.T.);
#10071=EDGE_CURVE('',#7696,#7697,#5151,.T.);
#10072=EDGE_CURVE('',#7697,#7695,#4261,.T.);
#10073=EDGE_CURVE('',#7694,#7696,#4262,.T.);
#10074=EDGE_CURVE('',#7698,#7699,#5152,.T.);
#10075=EDGE_CURVE('',#7698,#7700,#4263,.T.);
#10076=EDGE_CURVE('',#7701,#7700,#2918,.F.);
#10077=EDGE_CURVE('',#7701,#7699,#4264,.T.);
#10078=EDGE_CURVE('',#7702,#7703,#5153,.T.);
#10079=EDGE_CURVE('',#7703,#7704,#4265,.T.);
#10080=EDGE_CURVE('',#7705,#7704,#2919,.T.);
#10081=EDGE_CURVE('',#7702,#7705,#4266,.T.);
#10082=EDGE_CURVE('',#7706,#7707,#5154,.T.);
#10083=EDGE_CURVE('',#7707,#7703,#4267,.T.);
#10084=EDGE_CURVE('',#7706,#7702,#4268,.T.);
#10085=EDGE_CURVE('',#7708,#7709,#5155,.T.);
#10086=EDGE_CURVE('',#7709,#7707,#4269,.T.);
#10087=EDGE_CURVE('',#7708,#7706,#4270,.T.);
#10088=EDGE_CURVE('',#7710,#7711,#5156,.T.);
#10089=EDGE_CURVE('',#7711,#7709,#4271,.T.);
#10090=EDGE_CURVE('',#7710,#7708,#4272,.T.);
#10091=EDGE_CURVE('',#7712,#7713,#5157,.T.);
#10092=EDGE_CURVE('',#7713,#7711,#4273,.T.);
#10093=EDGE_CURVE('',#7712,#7710,#4274,.T.);
#10094=EDGE_CURVE('',#7714,#7715,#5158,.T.);
#10095=EDGE_CURVE('',#7715,#7713,#4275,.T.);
#10096=EDGE_CURVE('',#7714,#7712,#4276,.T.);
#10097=EDGE_CURVE('',#7716,#7717,#5159,.T.);
#10098=EDGE_CURVE('',#7717,#7715,#4277,.T.);
#10099=EDGE_CURVE('',#7716,#7714,#4278,.T.);
#10100=EDGE_CURVE('',#7718,#7719,#5160,.T.);
#10101=EDGE_CURVE('',#7720,#7718,#4279,.T.);
#10102=EDGE_CURVE('',#7721,#7720,#2920,.T.);
#10103=EDGE_CURVE('',#7721,#7719,#4280,.T.);
#10104=EDGE_CURVE('',#7722,#7723,#5161,.T.);
#10105=EDGE_CURVE('',#7723,#7724,#4281,.T.);
#10106=EDGE_CURVE('',#7724,#7725,#2921,.T.);
#10107=EDGE_CURVE('',#7725,#7726,#5162,.T.);
#10108=EDGE_CURVE('',#7726,#7727,#2922,.F.);
#10109=EDGE_CURVE('',#7727,#7728,#2923,.F.);
#10110=EDGE_CURVE('',#7728,#7726,#2924,.F.);
#10111=EDGE_CURVE('',#7725,#7729,#2925,.T.);
#10112=EDGE_CURVE('',#7729,#7722,#4282,.T.);
#10113=EDGE_CURVE('',#7730,#7731,#5163,.T.);
#10114=EDGE_CURVE('',#7731,#7723,#4283,.T.);
#10115=EDGE_CURVE('',#7722,#7730,#4284,.T.);
#10116=EDGE_CURVE('',#7732,#7733,#5164,.T.);
#10117=EDGE_CURVE('',#7733,#7731,#4285,.T.);
#10118=EDGE_CURVE('',#7730,#7732,#4286,.T.);
#10119=EDGE_CURVE('',#7734,#7735,#5165,.T.);
#10120=EDGE_CURVE('',#7735,#7733,#4287,.T.);
#10121=EDGE_CURVE('',#7732,#7734,#4288,.T.);
#10122=EDGE_CURVE('',#7736,#7737,#5166,.T.);
#10123=EDGE_CURVE('',#7737,#7735,#4289,.T.);
#10124=EDGE_CURVE('',#7734,#7736,#4290,.T.);
#10125=EDGE_CURVE('',#7738,#7739,#5167,.T.);
#10126=EDGE_CURVE('',#7739,#7737,#4291,.T.);
#10127=EDGE_CURVE('',#7736,#7738,#4292,.T.);
#10128=EDGE_CURVE('',#7740,#7741,#5168,.T.);
#10129=EDGE_CURVE('',#7741,#7739,#4293,.T.);
#10130=EDGE_CURVE('',#7738,#7740,#4294,.T.);
#10131=EDGE_CURVE('',#7742,#7743,#5169,.T.);
#10132=EDGE_CURVE('',#7742,#7744,#4295,.T.);
#10133=EDGE_CURVE('',#7745,#7744,#2926,.F.);
#10134=EDGE_CURVE('',#7745,#7743,#4296,.T.);
#10135=EDGE_CURVE('',#7746,#7747,#5170,.T.);
#10136=EDGE_CURVE('',#7747,#7748,#4297,.T.);
#10137=EDGE_CURVE('',#7749,#7748,#2927,.T.);
#10138=EDGE_CURVE('',#7746,#7749,#4298,.T.);
#10139=EDGE_CURVE('',#7750,#7751,#5171,.T.);
#10140=EDGE_CURVE('',#7751,#7747,#4299,.T.);
#10141=EDGE_CURVE('',#7750,#7746,#4300,.T.);
#10142=EDGE_CURVE('',#7752,#7753,#5172,.T.);
#10143=EDGE_CURVE('',#7753,#7751,#4301,.T.);
#10144=EDGE_CURVE('',#7752,#7750,#4302,.T.);
#10145=EDGE_CURVE('',#7754,#7755,#5173,.T.);
#10146=EDGE_CURVE('',#7755,#7753,#4303,.T.);
#10147=EDGE_CURVE('',#7754,#7752,#4304,.T.);
#10148=EDGE_CURVE('',#7756,#7757,#5174,.T.);
#10149=EDGE_CURVE('',#7757,#7755,#4305,.T.);
#10150=EDGE_CURVE('',#7756,#7754,#4306,.T.);
#10151=EDGE_CURVE('',#7758,#7759,#5175,.T.);
#10152=EDGE_CURVE('',#7759,#7757,#4307,.T.);
#10153=EDGE_CURVE('',#7758,#7756,#4308,.T.);
#10154=EDGE_CURVE('',#7760,#7761,#5176,.T.);
#10155=EDGE_CURVE('',#7761,#7759,#4309,.T.);
#10156=EDGE_CURVE('',#7760,#7758,#4310,.T.);
#10157=EDGE_CURVE('',#7762,#7763,#5177,.T.);
#10158=EDGE_CURVE('',#7764,#7762,#4311,.T.);
#10159=EDGE_CURVE('',#7765,#7764,#2928,.T.);
#10160=EDGE_CURVE('',#7765,#7763,#4312,.T.);
#10161=EDGE_CURVE('',#7766,#7767,#5178,.T.);
#10162=EDGE_CURVE('',#7767,#7768,#4313,.T.);
#10163=EDGE_CURVE('',#7768,#7769,#2929,.T.);
#10164=EDGE_CURVE('',#7769,#7770,#5179,.T.);
#10165=EDGE_CURVE('',#7770,#7771,#2930,.F.);
#10166=EDGE_CURVE('',#7771,#7772,#2931,.F.);
#10167=EDGE_CURVE('',#7772,#7770,#2932,.F.);
#10168=EDGE_CURVE('',#7769,#7773,#2933,.T.);
#10169=EDGE_CURVE('',#7773,#7766,#4314,.T.);
#10170=EDGE_CURVE('',#7774,#7775,#5180,.T.);
#10171=EDGE_CURVE('',#7775,#7767,#4315,.T.);
#10172=EDGE_CURVE('',#7766,#7774,#4316,.T.);
#10173=EDGE_CURVE('',#7776,#7777,#5181,.T.);
#10174=EDGE_CURVE('',#7777,#7775,#4317,.T.);
#10175=EDGE_CURVE('',#7774,#7776,#4318,.T.);
#10176=EDGE_CURVE('',#7778,#7779,#5182,.T.);
#10177=EDGE_CURVE('',#7779,#7777,#4319,.T.);
#10178=EDGE_CURVE('',#7776,#7778,#4320,.T.);
#10179=EDGE_CURVE('',#7780,#7781,#5183,.T.);
#10180=EDGE_CURVE('',#7781,#7779,#4321,.T.);
#10181=EDGE_CURVE('',#7778,#7780,#4322,.T.);
#10182=EDGE_CURVE('',#7782,#7783,#5184,.T.);
#10183=EDGE_CURVE('',#7783,#7781,#4323,.T.);
#10184=EDGE_CURVE('',#7780,#7782,#4324,.T.);
#10185=EDGE_CURVE('',#7784,#7785,#5185,.T.);
#10186=EDGE_CURVE('',#7785,#7783,#4325,.T.);
#10187=EDGE_CURVE('',#7782,#7784,#4326,.T.);
#10188=EDGE_CURVE('',#7786,#7787,#5186,.T.);
#10189=EDGE_CURVE('',#7786,#7788,#4327,.T.);
#10190=EDGE_CURVE('',#7789,#7788,#2934,.F.);
#10191=EDGE_CURVE('',#7789,#7787,#4328,.T.);
#10192=EDGE_CURVE('',#7790,#7791,#5187,.T.);
#10193=EDGE_CURVE('',#7791,#7792,#4329,.T.);
#10194=EDGE_CURVE('',#7793,#7792,#2935,.T.);
#10195=EDGE_CURVE('',#7790,#7793,#4330,.T.);
#10196=EDGE_CURVE('',#7794,#7795,#5188,.T.);
#10197=EDGE_CURVE('',#7795,#7791,#4331,.T.);
#10198=EDGE_CURVE('',#7794,#7790,#4332,.T.);
#10199=EDGE_CURVE('',#7796,#7797,#5189,.T.);
#10200=EDGE_CURVE('',#7797,#7795,#4333,.T.);
#10201=EDGE_CURVE('',#7796,#7794,#4334,.T.);
#10202=EDGE_CURVE('',#7798,#7799,#5190,.T.);
#10203=EDGE_CURVE('',#7799,#7797,#4335,.T.);
#10204=EDGE_CURVE('',#7798,#7796,#4336,.T.);
#10205=EDGE_CURVE('',#7800,#7801,#5191,.T.);
#10206=EDGE_CURVE('',#7801,#7799,#4337,.T.);
#10207=EDGE_CURVE('',#7800,#7798,#4338,.T.);
#10208=EDGE_CURVE('',#7802,#7803,#5192,.T.);
#10209=EDGE_CURVE('',#7803,#7801,#4339,.T.);
#10210=EDGE_CURVE('',#7802,#7800,#4340,.T.);
#10211=EDGE_CURVE('',#7804,#7805,#5193,.T.);
#10212=EDGE_CURVE('',#7805,#7803,#4341,.T.);
#10213=EDGE_CURVE('',#7804,#7802,#4342,.T.);
#10214=EDGE_CURVE('',#7806,#7807,#5194,.T.);
#10215=EDGE_CURVE('',#7808,#7806,#4343,.T.);
#10216=EDGE_CURVE('',#7809,#7808,#2936,.T.);
#10217=EDGE_CURVE('',#7809,#7807,#4344,.T.);
#10218=EDGE_CURVE('',#7810,#7811,#5195,.T.);
#10219=EDGE_CURVE('',#7811,#7812,#4345,.T.);
#10220=EDGE_CURVE('',#7812,#7813,#2937,.T.);
#10221=EDGE_CURVE('',#7813,#7814,#5196,.T.);
#10222=EDGE_CURVE('',#7814,#7815,#2938,.F.);
#10223=EDGE_CURVE('',#7815,#7816,#2939,.F.);
#10224=EDGE_CURVE('',#7816,#7814,#2940,.F.);
#10225=EDGE_CURVE('',#7813,#7817,#2941,.T.);
#10226=EDGE_CURVE('',#7817,#7810,#4346,.T.);
#10227=EDGE_CURVE('',#7818,#7819,#5197,.T.);
#10228=EDGE_CURVE('',#7819,#7811,#4347,.T.);
#10229=EDGE_CURVE('',#7810,#7818,#4348,.T.);
#10230=EDGE_CURVE('',#7820,#7821,#5198,.T.);
#10231=EDGE_CURVE('',#7821,#7819,#4349,.T.);
#10232=EDGE_CURVE('',#7818,#7820,#4350,.T.);
#10233=EDGE_CURVE('',#7822,#7823,#5199,.T.);
#10234=EDGE_CURVE('',#7823,#7821,#4351,.T.);
#10235=EDGE_CURVE('',#7820,#7822,#4352,.T.);
#10236=EDGE_CURVE('',#7824,#7825,#5200,.T.);
#10237=EDGE_CURVE('',#7825,#7823,#4353,.T.);
#10238=EDGE_CURVE('',#7822,#7824,#4354,.T.);
#10239=EDGE_CURVE('',#7826,#7827,#5201,.T.);
#10240=EDGE_CURVE('',#7827,#7825,#4355,.T.);
#10241=EDGE_CURVE('',#7824,#7826,#4356,.T.);
#10242=EDGE_CURVE('',#7828,#7829,#5202,.T.);
#10243=EDGE_CURVE('',#7829,#7827,#4357,.T.);
#10244=EDGE_CURVE('',#7826,#7828,#4358,.T.);
#10245=EDGE_CURVE('',#7830,#7831,#5203,.T.);
#10246=EDGE_CURVE('',#7830,#7832,#4359,.T.);
#10247=EDGE_CURVE('',#7833,#7832,#2942,.F.);
#10248=EDGE_CURVE('',#7833,#7831,#4360,.T.);
#10249=EDGE_CURVE('',#7834,#7835,#5204,.T.);
#10250=EDGE_CURVE('',#7835,#7836,#4361,.T.);
#10251=EDGE_CURVE('',#7837,#7836,#2943,.T.);
#10252=EDGE_CURVE('',#7834,#7837,#4362,.T.);
#10253=EDGE_CURVE('',#7838,#7839,#5205,.T.);
#10254=EDGE_CURVE('',#7839,#7835,#4363,.T.);
#10255=EDGE_CURVE('',#7838,#7834,#4364,.T.);
#10256=EDGE_CURVE('',#7840,#7841,#5206,.T.);
#10257=EDGE_CURVE('',#7841,#7839,#4365,.T.);
#10258=EDGE_CURVE('',#7840,#7838,#4366,.T.);
#10259=EDGE_CURVE('',#7842,#7843,#5207,.T.);
#10260=EDGE_CURVE('',#7843,#7841,#4367,.T.);
#10261=EDGE_CURVE('',#7842,#7840,#4368,.T.);
#10262=EDGE_CURVE('',#7844,#7845,#5208,.T.);
#10263=EDGE_CURVE('',#7845,#7843,#4369,.T.);
#10264=EDGE_CURVE('',#7844,#7842,#4370,.T.);
#10265=EDGE_CURVE('',#7846,#7847,#5209,.T.);
#10266=EDGE_CURVE('',#7847,#7845,#4371,.T.);
#10267=EDGE_CURVE('',#7846,#7844,#4372,.T.);
#10268=EDGE_CURVE('',#7848,#7849,#5210,.T.);
#10269=EDGE_CURVE('',#7849,#7847,#4373,.T.);
#10270=EDGE_CURVE('',#7848,#7846,#4374,.T.);
#10271=EDGE_CURVE('',#7850,#7851,#5211,.T.);
#10272=EDGE_CURVE('',#7852,#7850,#4375,.T.);
#10273=EDGE_CURVE('',#7853,#7852,#2944,.T.);
#10274=EDGE_CURVE('',#7853,#7851,#4376,.T.);
#10275=EDGE_CURVE('',#7854,#7855,#5212,.T.);
#10276=EDGE_CURVE('',#7856,#7854,#5213,.T.);
#10277=EDGE_CURVE('',#7856,#7857,#5214,.T.);
#10278=EDGE_CURVE('',#7855,#7857,#5215,.T.);
#10279=EDGE_CURVE('',#7858,#7856,#5216,.T.);
#10280=EDGE_CURVE('',#7858,#7859,#5217,.T.);
#10281=EDGE_CURVE('',#7857,#7859,#5218,.T.);
#10282=EDGE_CURVE('',#7860,#7861,#5219,.T.);
#10283=EDGE_CURVE('',#7859,#7860,#5220,.T.);
#10284=EDGE_CURVE('',#7861,#7858,#5221,.T.);
#10285=EDGE_CURVE('',#7862,#7863,#4377,.T.);
#10286=EDGE_CURVE('',#7864,#7862,#5222,.T.);
#10287=EDGE_CURVE('',#7865,#7864,#2945,.T.);
#10288=EDGE_CURVE('',#7866,#7865,#2946,.T.);
#10289=EDGE_CURVE('',#7867,#7866,#4378,.T.);
#10290=EDGE_CURVE('',#7867,#7868,#5223,.T.);
#10291=EDGE_CURVE('',#7868,#7869,#5224,.T.);
#10292=EDGE_CURVE('',#7869,#7870,#5225,.T.);
#10293=EDGE_CURVE('',#7870,#7871,#5226,.T.);
#10294=EDGE_CURVE('',#7872,#7871,#4379,.T.);
#10295=EDGE_CURVE('',#7873,#7872,#5227,.T.);
#10296=EDGE_CURVE('',#7874,#7873,#2947,.T.);
#10297=EDGE_CURVE('',#7875,#7874,#2948,.T.);
#10298=EDGE_CURVE('',#7876,#7875,#4380,.T.);
#10299=EDGE_CURVE('',#7876,#7877,#5228,.T.);
#10300=EDGE_CURVE('',#7877,#7878,#5229,.T.);
#10301=EDGE_CURVE('',#7878,#7879,#5230,.T.);
#10302=EDGE_CURVE('',#7879,#7880,#5231,.T.);
#10303=EDGE_CURVE('',#7881,#7880,#4381,.T.);
#10304=EDGE_CURVE('',#7882,#7881,#5232,.T.);
#10305=EDGE_CURVE('',#7883,#7882,#2949,.T.);
#10306=EDGE_CURVE('',#7884,#7883,#2950,.T.);
#10307=EDGE_CURVE('',#7885,#7884,#4382,.T.);
#10308=EDGE_CURVE('',#7885,#7886,#5233,.T.);
#10309=EDGE_CURVE('',#7886,#7887,#5234,.T.);
#10310=EDGE_CURVE('',#7887,#7888,#5235,.T.);
#10311=EDGE_CURVE('',#7888,#7889,#5236,.T.);
#10312=EDGE_CURVE('',#7890,#7889,#4383,.T.);
#10313=EDGE_CURVE('',#7891,#7890,#5237,.T.);
#10314=EDGE_CURVE('',#7892,#7891,#2951,.T.);
#10315=EDGE_CURVE('',#7893,#7892,#2952,.T.);
#10316=EDGE_CURVE('',#7894,#7893,#4384,.T.);
#10317=EDGE_CURVE('',#7894,#7895,#5238,.T.);
#10318=EDGE_CURVE('',#7895,#7896,#5239,.T.);
#10319=EDGE_CURVE('',#7896,#7897,#5240,.T.);
#10320=EDGE_CURVE('',#7897,#7898,#5241,.T.);
#10321=EDGE_CURVE('',#7899,#7898,#4385,.T.);
#10322=EDGE_CURVE('',#7900,#7899,#5242,.T.);
#10323=EDGE_CURVE('',#7901,#7900,#2953,.T.);
#10324=EDGE_CURVE('',#7902,#7901,#2954,.T.);
#10325=EDGE_CURVE('',#7903,#7902,#4386,.T.);
#10326=EDGE_CURVE('',#7903,#7904,#5243,.T.);
#10327=EDGE_CURVE('',#7904,#7905,#5244,.T.);
#10328=EDGE_CURVE('',#7905,#7906,#5245,.T.);
#10329=EDGE_CURVE('',#7906,#7907,#5246,.T.);
#10330=EDGE_CURVE('',#7908,#7907,#4387,.T.);
#10331=EDGE_CURVE('',#7909,#7908,#5247,.T.);
#10332=EDGE_CURVE('',#7910,#7909,#2955,.T.);
#10333=EDGE_CURVE('',#7911,#7910,#2956,.T.);
#10334=EDGE_CURVE('',#7912,#7911,#4388,.T.);
#10335=EDGE_CURVE('',#7912,#7913,#5248,.T.);
#10336=EDGE_CURVE('',#7913,#7914,#5249,.T.);
#10337=EDGE_CURVE('',#7914,#7915,#5250,.T.);
#10338=EDGE_CURVE('',#7915,#7863,#5251,.T.);
#10339=EDGE_CURVE('',#7368,#7349,#4389,.T.);
#10340=EDGE_CURVE('',#7348,#7369,#4390,.T.);
#10341=EDGE_CURVE('',#7861,#7854,#2957,.T.);
#10342=EDGE_CURVE('',#7456,#7437,#4391,.T.);
#10343=EDGE_CURVE('',#7436,#7457,#4392,.T.);
#10344=EDGE_CURVE('',#7500,#7481,#4393,.T.);
#10345=EDGE_CURVE('',#7480,#7501,#4394,.T.);
#10346=EDGE_CURVE('',#7544,#7525,#4395,.T.);
#10347=EDGE_CURVE('',#7524,#7545,#4396,.T.);
#10348=EDGE_CURVE('',#7588,#7569,#4397,.T.);
#10349=EDGE_CURVE('',#7568,#7589,#4398,.T.);
#10350=EDGE_CURVE('',#7632,#7613,#4399,.T.);
#10351=EDGE_CURVE('',#7612,#7633,#4400,.T.);
#10352=EDGE_CURVE('',#7812,#7837,#4401,.T.);
#10353=EDGE_CURVE('',#7836,#7817,#4402,.T.);
#10354=EDGE_CURVE('',#7851,#7849,#4403,.T.);
#10355=EDGE_CURVE('',#7850,#7848,#4404,.T.);
#10356=EDGE_CURVE('',#7832,#7853,#4405,.T.);
#10357=EDGE_CURVE('',#7828,#7830,#4406,.T.);
#10358=EDGE_CURVE('',#7831,#7829,#4407,.T.);
#10359=EDGE_CURVE('',#7852,#7833,#4408,.T.);
#10360=EDGE_CURVE('',#7768,#7793,#4409,.T.);
#10361=EDGE_CURVE('',#7792,#7773,#4410,.T.);
#10362=EDGE_CURVE('',#7807,#7805,#4411,.T.);
#10363=EDGE_CURVE('',#7806,#7804,#4412,.T.);
#10364=EDGE_CURVE('',#7788,#7809,#4413,.T.);
#10365=EDGE_CURVE('',#7784,#7786,#4414,.T.);
#10366=EDGE_CURVE('',#7787,#7785,#4415,.T.);
#10367=EDGE_CURVE('',#7808,#7789,#4416,.T.);
#10368=EDGE_CURVE('',#7724,#7749,#4417,.T.);
#10369=EDGE_CURVE('',#7748,#7729,#4418,.T.);
#10370=EDGE_CURVE('',#7763,#7761,#4419,.T.);
#10371=EDGE_CURVE('',#7762,#7760,#4420,.T.);
#10372=EDGE_CURVE('',#7744,#7765,#4421,.T.);
#10373=EDGE_CURVE('',#7740,#7742,#4422,.T.);
#10374=EDGE_CURVE('',#7743,#7741,#4423,.T.);
#10375=EDGE_CURVE('',#7764,#7745,#4424,.T.);
#10376=EDGE_CURVE('',#7680,#7705,#4425,.T.);
#10377=EDGE_CURVE('',#7704,#7685,#4426,.T.);
#10378=EDGE_CURVE('',#7719,#7717,#4427,.T.);
#10379=EDGE_CURVE('',#7718,#7716,#4428,.T.);
#10380=EDGE_CURVE('',#7700,#7721,#4429,.T.);
#10381=EDGE_CURVE('',#7696,#7698,#4430,.T.);
#10382=EDGE_CURVE('',#7699,#7697,#4431,.T.);
#10383=EDGE_CURVE('',#7720,#7701,#4432,.T.);
#10384=EDGE_CURVE('',#7636,#7661,#4433,.T.);
#10385=EDGE_CURVE('',#7660,#7641,#4434,.T.);
#10386=EDGE_CURVE('',#7675,#7673,#4435,.T.);
#10387=EDGE_CURVE('',#7674,#7672,#4436,.T.);
#10388=EDGE_CURVE('',#7656,#7677,#4437,.T.);
#10389=EDGE_CURVE('',#7652,#7654,#4438,.T.);
#10390=EDGE_CURVE('',#7655,#7653,#4439,.T.);
#10391=EDGE_CURVE('',#7676,#7657,#4440,.T.);
#10392=EDGE_CURVE('',#7816,#7815,#5252,.T.);
#10393=EDGE_CURVE('',#7816,#7815,#5253,.T.);
#10394=EDGE_CURVE('',#7772,#7771,#5254,.T.);
#10395=EDGE_CURVE('',#7772,#7771,#5255,.T.);
#10396=EDGE_CURVE('',#7728,#7727,#5256,.T.);
#10397=EDGE_CURVE('',#7728,#7727,#5257,.T.);
#10398=EDGE_CURVE('',#7684,#7683,#5258,.T.);
#10399=EDGE_CURVE('',#7684,#7683,#5259,.T.);
#10400=EDGE_CURVE('',#7640,#7639,#5260,.T.);
#10401=EDGE_CURVE('',#7640,#7639,#5261,.T.);
#10402=EDGE_CURVE('',#7592,#7617,#4441,.T.);
#10403=EDGE_CURVE('',#7616,#7597,#4442,.T.);
#10404=EDGE_CURVE('',#7631,#7629,#4443,.T.);
#10405=EDGE_CURVE('',#7630,#7628,#4444,.T.);
#10406=EDGE_CURVE('',#7608,#7610,#4445,.T.);
#10407=EDGE_CURVE('',#7611,#7609,#4446,.T.);
#10408=EDGE_CURVE('',#7548,#7573,#4447,.T.);
#10409=EDGE_CURVE('',#7572,#7553,#4448,.T.);
#10410=EDGE_CURVE('',#7587,#7585,#4449,.T.);
#10411=EDGE_CURVE('',#7586,#7584,#4450,.T.);
#10412=EDGE_CURVE('',#7564,#7566,#4451,.T.);
#10413=EDGE_CURVE('',#7567,#7565,#4452,.T.);
#10414=EDGE_CURVE('',#7504,#7529,#4453,.T.);
#10415=EDGE_CURVE('',#7528,#7509,#4454,.T.);
#10416=EDGE_CURVE('',#7543,#7541,#4455,.T.);
#10417=EDGE_CURVE('',#7542,#7540,#4456,.T.);
#10418=EDGE_CURVE('',#7520,#7522,#4457,.T.);
#10419=EDGE_CURVE('',#7523,#7521,#4458,.T.);
#10420=EDGE_CURVE('',#7460,#7485,#4459,.T.);
#10421=EDGE_CURVE('',#7484,#7465,#4460,.T.);
#10422=EDGE_CURVE('',#7499,#7497,#4461,.T.);
#10423=EDGE_CURVE('',#7498,#7496,#4462,.T.);
#10424=EDGE_CURVE('',#7476,#7478,#4463,.T.);
#10425=EDGE_CURVE('',#7479,#7477,#4464,.T.);
#10426=EDGE_CURVE('',#7416,#7441,#4465,.T.);
#10427=EDGE_CURVE('',#7440,#7421,#4466,.T.);
#10428=EDGE_CURVE('',#7455,#7453,#4467,.T.);
#10429=EDGE_CURVE('',#7454,#7452,#4468,.T.);
#10430=EDGE_CURVE('',#7432,#7434,#4469,.T.);
#10431=EDGE_CURVE('',#7435,#7433,#4470,.T.);
#10432=EDGE_CURVE('',#7596,#7595,#5262,.T.);
#10433=EDGE_CURVE('',#7596,#7595,#5263,.T.);
#10434=EDGE_CURVE('',#7552,#7551,#5264,.T.);
#10435=EDGE_CURVE('',#7552,#7551,#5265,.T.);
#10436=EDGE_CURVE('',#7508,#7507,#5266,.T.);
#10437=EDGE_CURVE('',#7508,#7507,#5267,.T.);
#10438=EDGE_CURVE('',#7464,#7463,#5268,.T.);
#10439=EDGE_CURVE('',#7464,#7463,#5269,.T.);
#10440=EDGE_CURVE('',#7420,#7419,#5270,.T.);
#10441=EDGE_CURVE('',#7420,#7419,#5271,.T.);
#10442=EDGE_CURVE('',#7372,#7397,#4471,.T.);
#10443=EDGE_CURVE('',#7396,#7377,#4472,.T.);
#10444=EDGE_CURVE('',#7411,#7409,#4473,.T.);
#10445=EDGE_CURVE('',#7410,#7408,#4474,.T.);
#10446=EDGE_CURVE('',#7392,#7413,#4475,.T.);
#10447=EDGE_CURVE('',#7388,#7390,#4476,.T.);
#10448=EDGE_CURVE('',#7391,#7389,#4477,.T.);
#10449=EDGE_CURVE('',#7412,#7393,#4478,.T.);
#10450=EDGE_CURVE('',#7376,#7375,#5272,.T.);
#10451=EDGE_CURVE('',#7376,#7375,#5273,.T.);
#10452=EDGE_CURVE('',#7328,#7353,#4479,.T.);
#10453=EDGE_CURVE('',#7352,#7333,#4480,.T.);
#10454=EDGE_CURVE('',#7367,#7365,#4481,.T.);
#10455=EDGE_CURVE('',#7366,#7364,#4482,.T.);
#10456=EDGE_CURVE('',#7344,#7346,#4483,.T.);
#10457=EDGE_CURVE('',#7347,#7345,#4484,.T.);
#10458=EDGE_CURVE('',#7332,#7331,#5274,.T.);
#10459=EDGE_CURVE('',#7332,#7331,#5275,.T.);
#10460=EDGE_CURVE('',#7916,#7916,#2958,.T.);
#10461=EDGE_CURVE('',#7916,#7917,#5276,.T.);
#10462=EDGE_CURVE('',#7917,#7917,#2959,.T.);
#10463=EDGE_CURVE('',#7918,#7918,#2960,.T.);
#10464=EDGE_CURVE('',#7918,#7815,#5277,.T.);
#10465=EDGE_CURVE('',#7816,#7919,#5278,.T.);
#10466=EDGE_CURVE('',#7919,#7919,#2961,.T.);
#10467=EDGE_CURVE('',#7920,#7920,#2962,.T.);
#10468=EDGE_CURVE('',#7920,#7921,#5279,.T.);
#10469=EDGE_CURVE('',#7921,#7921,#2963,.T.);
#10470=EDGE_CURVE('',#7922,#7922,#2964,.T.);
#10471=EDGE_CURVE('',#7922,#7771,#5280,.T.);
#10472=EDGE_CURVE('',#7772,#7923,#5281,.T.);
#10473=EDGE_CURVE('',#7923,#7923,#2965,.T.);
#10474=EDGE_CURVE('',#7924,#7924,#2966,.T.);
#10475=EDGE_CURVE('',#7924,#7925,#5282,.T.);
#10476=EDGE_CURVE('',#7925,#7925,#2967,.T.);
#10477=EDGE_CURVE('',#7926,#7926,#2968,.T.);
#10478=EDGE_CURVE('',#7926,#7727,#5283,.T.);
#10479=EDGE_CURVE('',#7728,#7927,#5284,.T.);
#10480=EDGE_CURVE('',#7927,#7927,#2969,.T.);
#10481=EDGE_CURVE('',#7928,#7928,#2970,.T.);
#10482=EDGE_CURVE('',#7928,#7929,#5285,.T.);
#10483=EDGE_CURVE('',#7929,#7929,#2971,.T.);
#10484=EDGE_CURVE('',#7930,#7930,#2972,.T.);
#10485=EDGE_CURVE('',#7930,#7683,#5286,.T.);
#10486=EDGE_CURVE('',#7684,#7931,#5287,.T.);
#10487=EDGE_CURVE('',#7931,#7931,#2973,.T.);
#10488=EDGE_CURVE('',#7932,#7932,#2974,.T.);
#10489=EDGE_CURVE('',#7932,#7933,#5288,.T.);
#10490=EDGE_CURVE('',#7933,#7933,#2975,.T.);
#10491=EDGE_CURVE('',#7934,#7934,#2976,.T.);
#10492=EDGE_CURVE('',#7934,#7639,#5289,.T.);
#10493=EDGE_CURVE('',#7640,#7935,#5290,.T.);
#10494=EDGE_CURVE('',#7935,#7935,#2977,.T.);
#10495=EDGE_CURVE('',#7936,#7936,#2978,.T.);
#10496=EDGE_CURVE('',#7936,#7937,#5291,.T.);
#10497=EDGE_CURVE('',#7937,#7937,#2979,.T.);
#10498=EDGE_CURVE('',#7938,#7938,#2980,.T.);
#10499=EDGE_CURVE('',#7938,#7375,#5292,.T.);
#10500=EDGE_CURVE('',#7376,#7939,#5293,.T.);
#10501=EDGE_CURVE('',#7939,#7939,#2981,.T.);
#10502=EDGE_CURVE('',#7940,#7912,#4485,.T.);
#10503=EDGE_CURVE('',#7940,#7941,#5294,.T.);
#10504=EDGE_CURVE('',#7941,#7913,#5295,.T.);
#10505=EDGE_CURVE('',#7863,#7942,#4486,.T.);
#10506=EDGE_CURVE('',#7943,#7915,#5296,.T.);
#10507=EDGE_CURVE('',#7943,#7942,#5297,.T.);
#10508=EDGE_CURVE('',#7944,#7943,#5298,.T.);
#10509=EDGE_CURVE('',#7944,#7914,#5299,.T.);
#10510=EDGE_CURVE('',#7941,#7944,#5300,.T.);
#10511=EDGE_CURVE('',#7907,#7945,#4487,.T.);
#10512=EDGE_CURVE('',#7946,#7906,#5301,.T.);
#10513=EDGE_CURVE('',#7946,#7945,#5302,.T.);
#10514=EDGE_CURVE('',#7947,#7946,#5303,.T.);
#10515=EDGE_CURVE('',#7947,#7905,#5304,.T.);
#10516=EDGE_CURVE('',#7948,#7947,#5305,.T.);
#10517=EDGE_CURVE('',#7948,#7904,#5306,.T.);
#10518=EDGE_CURVE('',#7949,#7903,#4488,.T.);
#10519=EDGE_CURVE('',#7949,#7948,#5307,.T.);
#10520=EDGE_CURVE('',#7898,#7950,#4489,.T.);
#10521=EDGE_CURVE('',#7951,#7897,#5308,.T.);
#10522=EDGE_CURVE('',#7951,#7950,#5309,.T.);
#10523=EDGE_CURVE('',#7952,#7951,#5310,.T.);
#10524=EDGE_CURVE('',#7952,#7896,#5311,.T.);
#10525=EDGE_CURVE('',#7953,#7952,#5312,.T.);
#10526=EDGE_CURVE('',#7953,#7895,#5313,.T.);
#10527=EDGE_CURVE('',#7954,#7894,#4490,.T.);
#10528=EDGE_CURVE('',#7954,#7953,#5314,.T.);
#10529=EDGE_CURVE('',#7889,#7955,#4491,.T.);
#10530=EDGE_CURVE('',#7956,#7888,#5315,.T.);
#10531=EDGE_CURVE('',#7956,#7955,#5316,.T.);
#10532=EDGE_CURVE('',#7957,#7956,#5317,.T.);
#10533=EDGE_CURVE('',#7957,#7887,#5318,.T.);
#10534=EDGE_CURVE('',#7958,#7957,#5319,.T.);
#10535=EDGE_CURVE('',#7958,#7886,#5320,.T.);
#10536=EDGE_CURVE('',#7959,#7885,#4492,.T.);
#10537=EDGE_CURVE('',#7959,#7958,#5321,.T.);
#10538=EDGE_CURVE('',#7960,#7876,#4493,.T.);
#10539=EDGE_CURVE('',#7960,#7961,#5322,.T.);
#10540=EDGE_CURVE('',#7961,#7877,#5323,.T.);
#10541=EDGE_CURVE('',#7880,#7962,#4494,.T.);
#10542=EDGE_CURVE('',#7963,#7879,#5324,.T.);
#10543=EDGE_CURVE('',#7963,#7962,#5325,.T.);
#10544=EDGE_CURVE('',#7964,#7963,#5326,.T.);
#10545=EDGE_CURVE('',#7964,#7878,#5327,.T.);
#10546=EDGE_CURVE('',#7961,#7964,#5328,.T.);
#10547=EDGE_CURVE('',#7942,#7965,#4495,.T.);
#10548=EDGE_CURVE('',#7862,#7965,#5329,.T.);
#10549=EDGE_CURVE('',#7945,#7966,#4496,.T.);
#10550=EDGE_CURVE('',#7908,#7966,#5330,.T.);
#10551=EDGE_CURVE('',#7967,#7902,#5331,.T.);
#10552=EDGE_CURVE('',#7967,#7949,#4497,.T.);
#10553=EDGE_CURVE('',#7950,#7968,#4498,.T.);
#10554=EDGE_CURVE('',#7899,#7968,#5332,.T.);
#10555=EDGE_CURVE('',#7969,#7893,#5333,.T.);
#10556=EDGE_CURVE('',#7969,#7954,#4499,.T.);
#10557=EDGE_CURVE('',#7955,#7970,#4500,.T.);
#10558=EDGE_CURVE('',#7890,#7970,#5334,.T.);
#10559=EDGE_CURVE('',#7971,#7884,#5335,.T.);
#10560=EDGE_CURVE('',#7971,#7959,#4501,.T.);
#10561=EDGE_CURVE('',#7962,#7972,#4502,.T.);
#10562=EDGE_CURVE('',#7881,#7972,#5336,.T.);
#10563=EDGE_CURVE('',#7973,#7867,#4503,.T.);
#10564=EDGE_CURVE('',#7973,#7974,#5337,.T.);
#10565=EDGE_CURVE('',#7974,#7868,#5338,.T.);
#10566=EDGE_CURVE('',#7871,#7975,#4504,.T.);
#10567=EDGE_CURVE('',#7976,#7870,#5339,.T.);
#10568=EDGE_CURVE('',#7976,#7975,#5340,.T.);
#10569=EDGE_CURVE('',#7977,#7976,#5341,.T.);
#10570=EDGE_CURVE('',#7977,#7869,#5342,.T.);
#10571=EDGE_CURVE('',#7974,#7977,#5343,.T.);
#10572=EDGE_CURVE('',#7975,#7978,#4505,.T.);
#10573=EDGE_CURVE('',#7872,#7978,#5344,.T.);
#10574=EDGE_CURVE('',#7979,#7901,#5345,.T.);
#10575=EDGE_CURVE('',#7979,#7967,#2982,.T.);
#10576=EDGE_CURVE('',#7900,#7980,#5346,.T.);
#10577=EDGE_CURVE('',#7980,#7979,#2983,.T.);
#10578=EDGE_CURVE('',#7968,#7980,#5347,.T.);
#10579=EDGE_CURVE('',#7981,#7892,#5348,.T.);
#10580=EDGE_CURVE('',#7981,#7969,#2984,.T.);
#10581=EDGE_CURVE('',#7891,#7982,#5349,.T.);
#10582=EDGE_CURVE('',#7982,#7981,#2985,.T.);
#10583=EDGE_CURVE('',#7970,#7982,#5350,.T.);
#10584=EDGE_CURVE('',#7983,#7883,#5351,.T.);
#10585=EDGE_CURVE('',#7983,#7971,#2986,.T.);
#10586=EDGE_CURVE('',#7882,#7984,#5352,.T.);
#10587=EDGE_CURVE('',#7984,#7983,#2987,.T.);
#10588=EDGE_CURVE('',#7972,#7984,#5353,.T.);
#10589=EDGE_CURVE('',#7985,#7940,#4506,.T.);
#10590=EDGE_CURVE('',#7986,#7985,#2988,.T.);
#10591=EDGE_CURVE('',#7987,#7986,#2989,.T.);
#10592=EDGE_CURVE('',#7966,#7987,#5354,.T.);
#10593=EDGE_CURVE('',#7988,#7960,#4507,.T.);
#10594=EDGE_CURVE('',#7989,#7988,#2990,.T.);
#10595=EDGE_CURVE('',#7990,#7989,#2991,.T.);
#10596=EDGE_CURVE('',#7978,#7990,#5355,.T.);
#10597=EDGE_CURVE('',#7991,#7973,#4508,.T.);
#10598=EDGE_CURVE('',#7992,#7991,#2992,.T.);
#10599=EDGE_CURVE('',#7993,#7992,#2993,.T.);
#10600=EDGE_CURVE('',#7965,#7993,#5356,.T.);
#10601=EDGE_CURVE('',#7855,#7860,#2994,.T.);
#10602=EDGE_CURVE('',#7909,#7987,#5357,.T.);
#10603=EDGE_CURVE('',#7986,#7910,#5358,.T.);
#10604=EDGE_CURVE('',#7985,#7911,#5359,.T.);
#10605=EDGE_CURVE('',#7864,#7993,#5360,.T.);
#10606=EDGE_CURVE('',#7992,#7865,#5361,.T.);
#10607=EDGE_CURVE('',#7991,#7866,#5362,.T.);
#10608=EDGE_CURVE('',#7873,#7990,#5363,.T.);
#10609=EDGE_CURVE('',#7988,#7875,#5364,.T.);
#10610=EDGE_CURVE('',#7989,#7874,#5365,.T.);
#10611=EDGE_CURVE('',#7994,#7995,#5366,.T.);
#10612=EDGE_CURVE('',#7996,#7994,#2995,.T.);
#10613=EDGE_CURVE('',#7996,#7997,#5367,.T.);
#10614=EDGE_CURVE('',#7995,#7997,#4509,.T.);
#10615=EDGE_CURVE('',#7998,#7995,#4510,.T.);
#10616=EDGE_CURVE('',#7999,#7998,#5368,.T.);
#10617=EDGE_CURVE('',#7994,#7999,#2996,.T.);
#10618=EDGE_CURVE('',#7994,#7995,#5369,.T.);
#10619=EDGE_CURVE('',#7997,#8000,#5370,.T.);
#10620=EDGE_CURVE('',#7996,#8001,#5371,.T.);
#10621=EDGE_CURVE('',#8001,#8000,#5372,.T.);
#10622=EDGE_CURVE('',#8000,#8002,#4511,.T.);
#10623=EDGE_CURVE('',#8003,#8001,#2997,.T.);
#10624=EDGE_CURVE('',#8003,#8002,#5373,.T.);
#10625=EDGE_CURVE('',#8002,#7998,#5374,.T.);
#10626=EDGE_CURVE('',#8003,#7999,#5375,.T.);
#10627=EDGE_CURVE('',#7995,#8004,#2998,.T.);
#10628=EDGE_CURVE('',#8004,#7995,#2999,.T.);
#10629=EDGE_CURVE('',#8004,#8005,#5376,.T.);
#10630=EDGE_CURVE('',#8005,#8005,#3000,.T.);
#10631=EDGE_CURVE('',#8006,#8007,#4512,.T.);
#10632=EDGE_CURVE('',#8008,#8006,#5377,.T.);
#10633=EDGE_CURVE('',#8009,#8008,#3001,.T.);
#10634=EDGE_CURVE('',#8009,#8007,#5378,.T.);
#10635=EDGE_CURVE('',#8007,#8010,#5379,.T.);
#10636=EDGE_CURVE('',#8009,#8011,#5380,.T.);
#10637=EDGE_CURVE('',#8011,#8010,#5381,.T.);
#10638=EDGE_CURVE('',#8012,#8013,#4513,.T.);
#10639=EDGE_CURVE('',#8010,#8012,#4514,.T.);
#10640=EDGE_CURVE('',#8014,#8011,#3002,.T.);
#10641=EDGE_CURVE('',#8014,#8013,#5382,.T.);
#10642=EDGE_CURVE('',#8013,#8006,#5383,.T.);
#10643=EDGE_CURVE('',#8014,#8008,#5384,.T.);
#10644=EDGE_CURVE('',#8015,#8015,#3003,.T.);
#10645=EDGE_CURVE('',#8015,#8016,#5385,.T.);
#10646=EDGE_CURVE('',#8016,#8012,#3004,.T.);
#10647=EDGE_CURVE('',#8012,#8016,#3005,.T.);
#10648=EDGE_CURVE('',#8017,#8017,#3006,.T.);
#10649=EDGE_CURVE('',#8017,#8018,#5386,.T.);
#10650=EDGE_CURVE('',#8018,#8018,#3007,.T.);
#10651=EDGE_CURVE('',#8019,#8019,#3008,.T.);
#10652=EDGE_CURVE('',#8019,#8020,#5387,.T.);
#10653=EDGE_CURVE('',#8020,#8020,#3009,.T.);
#10654=EDGE_CURVE('',#8021,#8021,#3010,.T.);
#10655=EDGE_CURVE('',#8022,#8022,#3011,.T.);
#10656=EDGE_CURVE('',#8023,#8023,#3012,.T.);
#10657=EDGE_CURVE('',#8023,#8022,#5388,.T.);
#10658=EDGE_CURVE('',#8024,#8024,#3013,.T.);
#10659=EDGE_CURVE('',#8025,#8025,#3014,.T.);
#10660=EDGE_CURVE('',#8024,#8025,#5389,.T.);
#10661=EDGE_CURVE('',#8021,#8026,#5390,.T.);
#10662=EDGE_CURVE('',#8026,#8026,#3015,.T.);
#10663=EDGE_CURVE('',#8027,#8028,#5391,.T.);
#10664=EDGE_CURVE('',#8027,#8029,#5392,.T.);
#10665=EDGE_CURVE('',#8030,#8029,#5393,.T.);
#10666=EDGE_CURVE('',#8028,#8030,#5394,.T.);
#10667=EDGE_CURVE('',#8031,#8028,#3016,.T.);
#10668=EDGE_CURVE('',#8032,#8030,#3017,.T.);
#10669=EDGE_CURVE('',#8031,#8032,#5395,.T.);
#10670=EDGE_CURVE('',#8031,#8033,#5396,.T.);
#10671=EDGE_CURVE('',#8034,#8032,#5397,.T.);
#10672=EDGE_CURVE('',#8033,#8034,#5398,.T.);
#10673=EDGE_CURVE('',#8027,#8033,#3018,.T.);
#10674=EDGE_CURVE('',#8029,#8034,#3019,.T.);
#10675=EDGE_CURVE('',#8035,#8035,#3020,.T.);
#10676=EDGE_CURVE('',#8035,#8036,#5399,.T.);
#10677=EDGE_CURVE('',#8036,#8036,#3021,.T.);
#10678=EDGE_CURVE('',#8037,#8037,#3022,.T.);
#10679=EDGE_CURVE('',#8038,#8038,#3023,.T.);
#10680=EDGE_CURVE('',#8039,#8039,#3024,.T.);
#10681=EDGE_CURVE('',#8039,#8037,#5400,.T.);
#10682=EDGE_CURVE('',#8038,#8040,#5401,.T.);
#10683=EDGE_CURVE('',#8040,#8040,#3025,.T.);
#10684=EDGE_CURVE('',#8041,#8041,#3026,.T.);
#10685=EDGE_CURVE('',#8042,#8042,#3027,.T.);
#10686=EDGE_CURVE('',#8043,#8043,#3028,.T.);
#10687=EDGE_CURVE('',#8043,#8041,#5402,.T.);
#10688=EDGE_CURVE('',#8042,#8044,#5403,.T.);
#10689=EDGE_CURVE('',#8044,#8044,#3029,.T.);
#10690=EDGE_CURVE('',#8045,#8045,#3030,.T.);
#10691=EDGE_CURVE('',#8046,#8046,#3031,.T.);
#10692=EDGE_CURVE('',#8047,#8047,#3032,.T.);
#10693=EDGE_CURVE('',#8047,#8045,#5404,.T.);
#10694=EDGE_CURVE('',#8046,#8048,#5405,.T.);
#10695=EDGE_CURVE('',#8048,#8048,#3033,.T.);
#10696=EDGE_CURVE('',#8049,#8049,#3034,.T.);
#10697=EDGE_CURVE('',#8050,#8050,#3035,.T.);
#10698=EDGE_CURVE('',#8051,#8051,#3036,.T.);
#10699=EDGE_CURVE('',#8051,#8049,#5406,.T.);
#10700=EDGE_CURVE('',#8050,#8052,#5407,.T.);
#10701=EDGE_CURVE('',#8052,#8052,#3037,.T.);
#10702=EDGE_CURVE('',#8053,#8053,#3038,.T.);
#10703=EDGE_CURVE('',#8054,#8054,#3039,.T.);
#10704=EDGE_CURVE('',#8055,#8055,#3040,.T.);
#10705=EDGE_CURVE('',#8055,#8053,#5408,.T.);
#10706=EDGE_CURVE('',#8054,#8056,#5409,.T.);
#10707=EDGE_CURVE('',#8056,#8056,#3041,.T.);
#10708=EDGE_CURVE('',#8057,#8057,#3042,.T.);
#10709=EDGE_CURVE('',#8058,#8058,#3043,.T.);
#10710=EDGE_CURVE('',#8059,#8059,#3044,.T.);
#10711=EDGE_CURVE('',#8059,#8057,#5410,.T.);
#10712=EDGE_CURVE('',#8058,#8060,#5411,.T.);
#10713=EDGE_CURVE('',#8060,#8060,#3045,.T.);
#10714=EDGE_CURVE('',#8061,#8061,#3046,.T.);
#10715=EDGE_CURVE('',#8061,#8062,#5412,.T.);
#10716=EDGE_CURVE('',#8062,#8062,#3047,.T.);
#10717=EDGE_CURVE('',#8063,#8063,#3048,.T.);
#10718=EDGE_CURVE('',#8063,#8064,#5413,.T.);
#10719=EDGE_CURVE('',#8064,#8064,#3049,.T.);
#10720=EDGE_CURVE('',#8065,#8065,#3050,.T.);
#10721=EDGE_CURVE('',#8065,#8066,#5414,.T.);
#10722=EDGE_CURVE('',#8066,#8066,#3051,.T.);
#10723=EDGE_CURVE('',#8067,#8067,#3052,.T.);
#10724=EDGE_CURVE('',#8067,#8068,#5415,.T.);
#10725=EDGE_CURVE('',#8068,#8068,#3053,.T.);
#10726=EDGE_CURVE('',#8069,#8069,#3054,.T.);
#10727=EDGE_CURVE('',#8069,#8070,#5416,.T.);
#10728=EDGE_CURVE('',#8070,#8070,#3055,.T.);
#10729=EDGE_CURVE('',#8070,#8071,#5417,.T.);
#10730=EDGE_CURVE('',#8071,#8071,#3056,.T.);
#10731=EDGE_CURVE('',#8072,#8072,#3057,.T.);
#10732=EDGE_CURVE('',#8072,#8073,#5418,.T.);
#10733=EDGE_CURVE('',#8073,#8073,#3058,.T.);
#10734=EDGE_CURVE('',#8073,#8074,#5419,.T.);
#10735=EDGE_CURVE('',#8074,#8074,#3059,.T.);
#10736=EDGE_CURVE('',#8075,#8075,#3060,.T.);
#10737=EDGE_CURVE('',#8075,#8076,#5420,.T.);
#10738=EDGE_CURVE('',#8076,#8076,#3061,.T.);
#10739=EDGE_CURVE('',#8076,#8077,#5421,.T.);
#10740=EDGE_CURVE('',#8077,#8077,#3062,.T.);
#10741=EDGE_CURVE('',#8078,#8078,#3063,.T.);
#10742=EDGE_CURVE('',#8078,#8079,#5422,.T.);
#10743=EDGE_CURVE('',#8079,#8079,#3064,.T.);
#10744=EDGE_CURVE('',#8079,#8080,#5423,.T.);
#10745=EDGE_CURVE('',#8080,#8080,#3065,.T.);
#10746=EDGE_CURVE('',#8081,#8081,#3066,.T.);
#10747=EDGE_CURVE('',#8081,#8082,#5424,.T.);
#10748=EDGE_CURVE('',#8082,#8082,#3067,.T.);
#10749=EDGE_CURVE('',#8082,#8083,#5425,.T.);
#10750=EDGE_CURVE('',#8083,#8083,#3068,.T.);
#10751=EDGE_CURVE('',#8084,#8084,#3069,.T.);
#10752=EDGE_CURVE('',#8084,#8085,#5426,.T.);
#10753=EDGE_CURVE('',#8085,#8085,#3070,.T.);
#10754=EDGE_CURVE('',#8085,#8086,#5427,.T.);
#10755=EDGE_CURVE('',#8086,#8086,#3071,.T.);
#10756=EDGE_CURVE('',#8087,#8087,#3072,.T.);
#10757=EDGE_CURVE('',#8087,#8088,#5428,.T.);
#10758=EDGE_CURVE('',#8088,#8088,#3073,.T.);
#10759=EDGE_CURVE('',#8089,#8089,#3074,.T.);
#10760=EDGE_CURVE('',#8089,#8090,#5429,.T.);
#10761=EDGE_CURVE('',#8090,#8090,#3075,.T.);
#10762=EDGE_CURVE('',#8091,#8091,#3076,.T.);
#10763=EDGE_CURVE('',#8091,#8092,#5430,.T.);
#10764=EDGE_CURVE('',#8092,#8092,#3077,.T.);
#10765=EDGE_CURVE('',#8093,#8093,#3078,.T.);
#10766=EDGE_CURVE('',#8093,#8094,#5431,.T.);
#10767=EDGE_CURVE('',#8094,#8094,#3079,.T.);
#10768=EDGE_CURVE('',#8095,#8095,#3080,.T.);
#10769=EDGE_CURVE('',#8095,#8096,#5432,.T.);
#10770=EDGE_CURVE('',#8096,#8096,#3081,.T.);
#10771=EDGE_CURVE('',#8097,#8097,#3082,.T.);
#10772=EDGE_CURVE('',#8097,#8098,#5433,.T.);
#10773=EDGE_CURVE('',#8098,#8098,#3083,.T.);
#10774=EDGE_CURVE('',#8099,#8099,#3084,.T.);
#10775=EDGE_CURVE('',#8099,#8100,#5434,.T.);
#10776=EDGE_CURVE('',#8100,#8100,#3085,.T.);
#10777=EDGE_CURVE('',#8101,#8101,#3086,.T.);
#10778=EDGE_CURVE('',#8101,#8102,#5435,.T.);
#10779=EDGE_CURVE('',#8102,#8102,#3087,.T.);
#10780=EDGE_CURVE('',#8103,#8104,#5436,.T.);
#10781=EDGE_CURVE('',#8105,#8103,#5437,.T.);
#10782=EDGE_CURVE('',#8106,#8105,#5438,.T.);
#10783=EDGE_CURVE('',#8104,#8106,#5439,.T.);
#10784=EDGE_CURVE('',#8107,#8108,#5440,.T.);
#10785=EDGE_CURVE('',#8109,#8107,#5441,.T.);
#10786=EDGE_CURVE('',#8110,#8109,#5442,.T.);
#10787=EDGE_CURVE('',#8108,#8110,#5443,.T.);
#10788=EDGE_CURVE('',#8105,#8110,#3088,.T.);
#10789=EDGE_CURVE('',#8108,#8103,#3089,.T.);
#10790=EDGE_CURVE('',#8107,#8104,#3090,.T.);
#10791=EDGE_CURVE('',#8106,#8109,#3091,.T.);
#10792=EDGE_CURVE('',#8111,#8111,#3092,.T.);
#10793=EDGE_CURVE('',#8112,#8112,#3093,.T.);
#10794=EDGE_CURVE('',#8113,#8113,#3094,.T.);
#10795=EDGE_CURVE('',#8113,#8111,#5444,.T.);
#10796=EDGE_CURVE('',#8112,#8114,#5445,.T.);
#10797=EDGE_CURVE('',#8114,#8114,#3095,.T.);
#10798=EDGE_CURVE('',#8115,#8115,#3096,.T.);
#10799=EDGE_CURVE('',#8115,#8116,#4515,.T.);
#10800=EDGE_CURVE('',#8116,#8116,#3097,.T.);
#10801=EDGE_CURVE('',#8117,#8118,#5446,.T.);
#10802=EDGE_CURVE('',#8117,#8119,#4516,.T.);
#10803=EDGE_CURVE('',#8119,#8120,#3098,.F.);
#10804=EDGE_CURVE('',#8120,#8118,#4517,.T.);
#10805=EDGE_CURVE('',#8121,#8122,#5447,.T.);
#10806=EDGE_CURVE('',#8121,#8117,#4518,.T.);
#10807=EDGE_CURVE('',#8118,#8122,#4519,.T.);
#10808=EDGE_CURVE('',#8123,#8124,#5448,.T.);
#10809=EDGE_CURVE('',#8123,#8121,#4520,.T.);
#10810=EDGE_CURVE('',#8122,#8124,#4521,.T.);
#10811=EDGE_CURVE('',#8125,#8126,#5449,.T.);
#10812=EDGE_CURVE('',#8125,#8123,#4522,.T.);
#10813=EDGE_CURVE('',#8124,#8126,#4523,.T.);
#10814=EDGE_CURVE('',#8127,#8128,#5450,.T.);
#10815=EDGE_CURVE('',#8127,#8125,#4524,.T.);
#10816=EDGE_CURVE('',#8126,#8128,#4525,.T.);
#10817=EDGE_CURVE('',#8129,#8130,#5451,.T.);
#10818=EDGE_CURVE('',#8129,#8127,#4526,.T.);
#10819=EDGE_CURVE('',#8128,#8130,#4527,.T.);
#10820=EDGE_CURVE('',#8131,#8132,#5452,.T.);
#10821=EDGE_CURVE('',#8131,#8129,#4528,.T.);
#10822=EDGE_CURVE('',#8130,#8132,#4529,.T.);
#10823=EDGE_CURVE('',#8133,#8134,#5453,.T.);
#10824=EDGE_CURVE('',#8133,#8131,#4530,.T.);
#10825=EDGE_CURVE('',#8132,#8134,#4531,.T.);
#10826=EDGE_CURVE('',#8135,#8136,#5454,.T.);
#10827=EDGE_CURVE('',#8135,#8133,#4532,.T.);
#10828=EDGE_CURVE('',#8134,#8136,#4533,.T.);
#10829=EDGE_CURVE('',#8137,#8138,#5455,.T.);
#10830=EDGE_CURVE('',#8137,#8135,#4534,.T.);
#10831=EDGE_CURVE('',#8136,#8138,#4535,.T.);
#10832=EDGE_CURVE('',#8139,#8140,#5456,.T.);
#10833=EDGE_CURVE('',#8139,#8137,#4536,.T.);
#10834=EDGE_CURVE('',#8138,#8140,#4537,.T.);
#10835=EDGE_CURVE('',#8141,#8142,#5457,.T.);
#10836=EDGE_CURVE('',#8141,#8139,#4538,.T.);
#10837=EDGE_CURVE('',#8140,#8142,#4539,.T.);
#10838=EDGE_CURVE('',#8143,#8144,#5458,.T.);
#10839=EDGE_CURVE('',#8143,#8141,#4540,.T.);
#10840=EDGE_CURVE('',#8142,#8144,#4541,.T.);
#10841=EDGE_CURVE('',#8145,#8146,#5459,.T.);
#10842=EDGE_CURVE('',#8145,#8143,#4542,.T.);
#10843=EDGE_CURVE('',#8144,#8146,#4543,.T.);
#10844=EDGE_CURVE('',#8147,#8148,#5460,.T.);
#10845=EDGE_CURVE('',#8147,#8145,#4544,.T.);
#10846=EDGE_CURVE('',#8146,#8148,#4545,.T.);
#10847=EDGE_CURVE('',#8149,#8150,#5461,.T.);
#10848=EDGE_CURVE('',#8149,#8147,#4546,.T.);
#10849=EDGE_CURVE('',#8148,#8150,#4547,.T.);
#10850=EDGE_CURVE('',#8151,#8152,#5462,.T.);
#10851=EDGE_CURVE('',#8151,#8153,#4548,.T.);
#10852=EDGE_CURVE('',#8153,#8154,#3099,.T.);
#10853=EDGE_CURVE('',#8152,#8154,#4549,.T.);
#10854=EDGE_CURVE('',#8155,#8156,#5463,.T.);
#10855=EDGE_CURVE('',#8155,#8151,#4550,.T.);
#10856=EDGE_CURVE('',#8156,#8152,#4551,.T.);
#10857=EDGE_CURVE('',#8157,#8158,#5464,.T.);
#10858=EDGE_CURVE('',#8157,#8155,#4552,.T.);
#10859=EDGE_CURVE('',#8158,#8156,#4553,.T.);
#10860=EDGE_CURVE('',#8159,#8160,#5465,.T.);
#10861=EDGE_CURVE('',#8159,#8157,#4554,.T.);
#10862=EDGE_CURVE('',#8160,#8158,#4555,.T.);
#10863=EDGE_CURVE('',#8161,#8162,#5466,.T.);
#10864=EDGE_CURVE('',#8161,#8159,#4556,.T.);
#10865=EDGE_CURVE('',#8162,#8160,#4557,.T.);
#10866=EDGE_CURVE('',#8163,#8164,#5467,.T.);
#10867=EDGE_CURVE('',#8163,#8161,#4558,.T.);
#10868=EDGE_CURVE('',#8164,#8162,#4559,.T.);
#10869=EDGE_CURVE('',#8165,#8166,#5468,.T.);
#10870=EDGE_CURVE('',#8165,#8163,#4560,.T.);
#10871=EDGE_CURVE('',#8166,#8164,#4561,.T.);
#10872=EDGE_CURVE('',#8167,#8168,#5469,.T.);
#10873=EDGE_CURVE('',#8167,#8165,#4562,.T.);
#10874=EDGE_CURVE('',#8168,#8166,#4563,.T.);
#10875=EDGE_CURVE('',#8169,#8170,#5470,.T.);
#10876=EDGE_CURVE('',#8169,#8167,#4564,.T.);
#10877=EDGE_CURVE('',#8170,#8168,#4565,.T.);
#10878=EDGE_CURVE('',#8171,#8172,#5471,.T.);
#10879=EDGE_CURVE('',#8171,#8169,#4566,.T.);
#10880=EDGE_CURVE('',#8172,#8170,#4567,.T.);
#10881=EDGE_CURVE('',#8173,#8174,#5472,.T.);
#10882=EDGE_CURVE('',#8173,#8171,#4568,.T.);
#10883=EDGE_CURVE('',#8174,#8172,#4569,.T.);
#10884=EDGE_CURVE('',#8175,#8176,#5473,.T.);
#10885=EDGE_CURVE('',#8175,#8173,#4570,.T.);
#10886=EDGE_CURVE('',#8176,#8174,#4571,.T.);
#10887=EDGE_CURVE('',#8177,#8178,#5474,.T.);
#10888=EDGE_CURVE('',#8177,#8175,#4572,.T.);
#10889=EDGE_CURVE('',#8178,#8176,#4573,.T.);
#10890=EDGE_CURVE('',#8179,#8180,#5475,.T.);
#10891=EDGE_CURVE('',#8179,#8177,#4574,.T.);
#10892=EDGE_CURVE('',#8180,#8178,#4575,.T.);
#10893=EDGE_CURVE('',#8181,#8182,#5476,.T.);
#10894=EDGE_CURVE('',#8181,#8179,#4576,.T.);
#10895=EDGE_CURVE('',#8182,#8180,#4577,.T.);
#10896=EDGE_CURVE('',#8183,#8184,#5477,.T.);
#10897=EDGE_CURVE('',#8183,#8181,#4578,.T.);
#10898=EDGE_CURVE('',#8184,#8182,#4579,.T.);
#10899=EDGE_CURVE('',#8154,#8185,#4580,.T.);
#10900=EDGE_CURVE('',#8186,#8153,#4581,.T.);
#10901=EDGE_CURVE('',#8187,#8186,#3100,.T.);
#10902=EDGE_CURVE('',#8185,#8187,#4582,.T.);
#10903=EDGE_CURVE('',#8185,#8188,#5478,.T.);
#10904=EDGE_CURVE('',#8188,#8188,#3101,.T.);
#10905=EDGE_CURVE('',#8189,#8183,#4583,.T.);
#10906=EDGE_CURVE('',#8119,#8189,#4584,.T.);
#10907=EDGE_CURVE('',#8186,#8149,#4585,.T.);
#10908=EDGE_CURVE('',#8190,#8184,#4586,.T.);
#10909=EDGE_CURVE('',#8189,#8190,#3102,.T.);
#10910=EDGE_CURVE('',#8150,#8187,#4587,.T.);
#10911=EDGE_CURVE('',#8190,#8120,#4588,.T.);
#10912=EDGE_CURVE('',#8191,#8192,#5479,.T.);
#10913=EDGE_CURVE('',#8191,#8193,#5480,.T.);
#10914=EDGE_CURVE('',#8193,#8194,#5481,.T.);
#10915=EDGE_CURVE('',#8192,#8194,#5482,.T.);
#10916=EDGE_CURVE('',#8195,#8191,#5483,.T.);
#10917=EDGE_CURVE('',#8195,#8196,#5484,.T.);
#10918=EDGE_CURVE('',#8196,#8193,#5485,.T.);
#10919=EDGE_CURVE('',#8197,#8195,#5486,.T.);
#10920=EDGE_CURVE('',#8197,#8198,#5487,.T.);
#10921=EDGE_CURVE('',#8198,#8196,#5488,.T.);
#10922=EDGE_CURVE('',#8199,#8197,#5489,.T.);
#10923=EDGE_CURVE('',#8199,#8200,#5490,.T.);
#10924=EDGE_CURVE('',#8200,#8198,#5491,.T.);
#10925=EDGE_CURVE('',#8201,#8199,#5492,.T.);
#10926=EDGE_CURVE('',#8201,#8202,#5493,.T.);
#10927=EDGE_CURVE('',#8202,#8200,#5494,.T.);
#10928=EDGE_CURVE('',#8192,#8201,#5495,.T.);
#10929=EDGE_CURVE('',#8194,#8202,#5496,.T.);
#10930=EDGE_CURVE('',#8203,#8203,#3103,.T.);
#10931=EDGE_CURVE('',#8203,#8204,#5497,.T.);
#10932=EDGE_CURVE('',#8204,#8204,#3104,.T.);
#10933=EDGE_CURVE('',#8205,#8206,#5498,.T.);
#10934=EDGE_CURVE('',#8205,#8207,#4589,.T.);
#10935=EDGE_CURVE('',#8207,#8208,#3105,.F.);
#10936=EDGE_CURVE('',#8208,#8206,#4590,.T.);
#10937=EDGE_CURVE('',#8209,#8210,#5499,.T.);
#10938=EDGE_CURVE('',#8209,#8205,#4591,.T.);
#10939=EDGE_CURVE('',#8206,#8210,#4592,.T.);
#10940=EDGE_CURVE('',#8211,#8212,#5500,.T.);
#10941=EDGE_CURVE('',#8211,#8209,#4593,.T.);
#10942=EDGE_CURVE('',#8210,#8212,#4594,.T.);
#10943=EDGE_CURVE('',#8213,#8214,#5501,.T.);
#10944=EDGE_CURVE('',#8213,#8211,#4595,.T.);
#10945=EDGE_CURVE('',#8212,#8214,#4596,.T.);
#10946=EDGE_CURVE('',#8215,#8216,#5502,.T.);
#10947=EDGE_CURVE('',#8215,#8213,#4597,.T.);
#10948=EDGE_CURVE('',#8214,#8216,#4598,.T.);
#10949=EDGE_CURVE('',#8217,#8218,#5503,.T.);
#10950=EDGE_CURVE('',#8217,#8215,#4599,.T.);
#10951=EDGE_CURVE('',#8216,#8218,#4600,.T.);
#10952=EDGE_CURVE('',#8219,#8220,#5504,.T.);
#10953=EDGE_CURVE('',#8219,#8217,#4601,.T.);
#10954=EDGE_CURVE('',#8218,#8220,#4602,.T.);
#10955=EDGE_CURVE('',#8221,#8222,#5505,.T.);
#10956=EDGE_CURVE('',#8221,#8219,#4603,.T.);
#10957=EDGE_CURVE('',#8220,#8222,#4604,.T.);
#10958=EDGE_CURVE('',#8223,#8224,#5506,.T.);
#10959=EDGE_CURVE('',#8223,#8225,#4605,.T.);
#10960=EDGE_CURVE('',#8225,#8226,#3106,.T.);
#10961=EDGE_CURVE('',#8224,#8226,#4606,.T.);
#10962=EDGE_CURVE('',#8227,#8228,#5507,.T.);
#10963=EDGE_CURVE('',#8227,#8223,#4607,.T.);
#10964=EDGE_CURVE('',#8228,#8224,#4608,.T.);
#10965=EDGE_CURVE('',#8229,#8230,#5508,.T.);
#10966=EDGE_CURVE('',#8229,#8227,#4609,.T.);
#10967=EDGE_CURVE('',#8230,#8228,#4610,.T.);
#10968=EDGE_CURVE('',#8231,#8232,#5509,.T.);
#10969=EDGE_CURVE('',#8231,#8229,#4611,.T.);
#10970=EDGE_CURVE('',#8232,#8230,#4612,.T.);
#10971=EDGE_CURVE('',#8233,#8234,#5510,.T.);
#10972=EDGE_CURVE('',#8233,#8231,#4613,.T.);
#10973=EDGE_CURVE('',#8234,#8232,#4614,.T.);
#10974=EDGE_CURVE('',#8235,#8236,#5511,.T.);
#10975=EDGE_CURVE('',#8235,#8233,#4615,.T.);
#10976=EDGE_CURVE('',#8236,#8234,#4616,.T.);
#10977=EDGE_CURVE('',#8237,#8238,#5512,.T.);
#10978=EDGE_CURVE('',#8237,#8235,#4617,.T.);
#10979=EDGE_CURVE('',#8238,#8236,#4618,.T.);
#10980=EDGE_CURVE('',#8239,#8240,#5513,.T.);
#10981=EDGE_CURVE('',#8239,#8237,#4619,.T.);
#10982=EDGE_CURVE('',#8240,#8238,#4620,.T.);
#10983=EDGE_CURVE('',#8226,#8241,#4621,.T.);
#10984=EDGE_CURVE('',#8242,#8225,#4622,.T.);
#10985=EDGE_CURVE('',#8243,#8242,#3107,.T.);
#10986=EDGE_CURVE('',#8241,#8243,#4623,.T.);
#10987=EDGE_CURVE('',#8241,#8244,#5514,.T.);
#10988=EDGE_CURVE('',#8244,#8244,#3108,.T.);
#10989=EDGE_CURVE('',#8245,#8239,#4624,.T.);
#10990=EDGE_CURVE('',#8207,#8245,#4625,.T.);
#10991=EDGE_CURVE('',#8242,#8221,#4626,.T.);
#10992=EDGE_CURVE('',#8246,#8240,#4627,.T.);
#10993=EDGE_CURVE('',#8245,#8246,#3109,.T.);
#10994=EDGE_CURVE('',#8247,#8248,#5515,.T.);
#10995=EDGE_CURVE('',#8247,#8249,#5516,.T.);
#10996=EDGE_CURVE('',#8249,#8250,#5517,.T.);
#10997=EDGE_CURVE('',#8248,#8250,#5518,.T.);
#10998=EDGE_CURVE('',#8251,#8247,#5519,.T.);
#10999=EDGE_CURVE('',#8251,#8252,#5520,.T.);
#11000=EDGE_CURVE('',#8252,#8249,#5521,.T.);
#11001=EDGE_CURVE('',#8253,#8251,#5522,.T.);
#11002=EDGE_CURVE('',#8253,#8254,#5523,.T.);
#11003=EDGE_CURVE('',#8254,#8252,#5524,.T.);
#11004=EDGE_CURVE('',#8255,#8253,#5525,.T.);
#11005=EDGE_CURVE('',#8255,#8256,#5526,.T.);
#11006=EDGE_CURVE('',#8256,#8254,#5527,.T.);
#11007=EDGE_CURVE('',#8257,#8255,#5528,.T.);
#11008=EDGE_CURVE('',#8257,#8258,#5529,.T.);
#11009=EDGE_CURVE('',#8258,#8256,#5530,.T.);
#11010=EDGE_CURVE('',#8248,#8257,#5531,.T.);
#11011=EDGE_CURVE('',#8250,#8258,#5532,.T.);
#11012=EDGE_CURVE('',#8222,#8243,#4628,.T.);
#11013=EDGE_CURVE('',#8246,#8208,#4629,.T.);
#11014=EDGE_CURVE('',#8208,#8259,#3110,.F.);
#11015=EDGE_CURVE('',#8259,#8207,#3111,.F.);
#11016=EDGE_CURVE('',#8260,#8260,#3112,.T.);
#11017=EDGE_CURVE('',#8259,#8260,#5533,.T.);
#11018=ORIENTED_EDGE('',*,*,#8261,.T.);
#11019=ORIENTED_EDGE('',*,*,#8262,.T.);
#11020=ORIENTED_EDGE('',*,*,#8263,.T.);
#11021=ORIENTED_EDGE('',*,*,#8264,.T.);
#11022=ORIENTED_EDGE('',*,*,#8265,.T.);
#11023=ORIENTED_EDGE('',*,*,#8266,.T.);
#11024=ORIENTED_EDGE('',*,*,#8265,.F.);
#11025=ORIENTED_EDGE('',*,*,#8267,.T.);
#11026=ORIENTED_EDGE('',*,*,#8268,.T.);
#11027=ORIENTED_EDGE('',*,*,#8269,.T.);
#11028=ORIENTED_EDGE('',*,*,#8261,.F.);
#11029=ORIENTED_EDGE('',*,*,#8270,.T.);
#11030=ORIENTED_EDGE('',*,*,#8271,.T.);
#11031=ORIENTED_EDGE('',*,*,#8272,.T.);
#11032=ORIENTED_EDGE('',*,*,#8268,.F.);
#11033=ORIENTED_EDGE('',*,*,#8273,.T.);
#11034=ORIENTED_EDGE('',*,*,#8274,.T.);
#11035=ORIENTED_EDGE('',*,*,#8275,.T.);
#11036=ORIENTED_EDGE('',*,*,#8271,.F.);
#11037=ORIENTED_EDGE('',*,*,#8276,.T.);
#11038=ORIENTED_EDGE('',*,*,#8277,.T.);
#11039=ORIENTED_EDGE('',*,*,#8278,.T.);
#11040=ORIENTED_EDGE('',*,*,#8274,.F.);
#11041=ORIENTED_EDGE('',*,*,#8279,.T.);
#11042=ORIENTED_EDGE('',*,*,#8280,.T.);
#11043=ORIENTED_EDGE('',*,*,#8281,.T.);
#11044=ORIENTED_EDGE('',*,*,#8277,.F.);
#11045=ORIENTED_EDGE('',*,*,#8282,.T.);
#11046=ORIENTED_EDGE('',*,*,#8283,.T.);
#11047=ORIENTED_EDGE('',*,*,#8284,.T.);
#11048=ORIENTED_EDGE('',*,*,#8280,.F.);
#11049=ORIENTED_EDGE('',*,*,#8285,.T.);
#11050=ORIENTED_EDGE('',*,*,#8286,.T.);
#11051=ORIENTED_EDGE('',*,*,#8287,.T.);
#11052=ORIENTED_EDGE('',*,*,#8283,.F.);
#11053=ORIENTED_EDGE('',*,*,#8288,.T.);
#11054=ORIENTED_EDGE('',*,*,#8289,.T.);
#11055=ORIENTED_EDGE('',*,*,#8290,.T.);
#11056=ORIENTED_EDGE('',*,*,#8286,.F.);
#11057=ORIENTED_EDGE('',*,*,#8291,.T.);
#11058=ORIENTED_EDGE('',*,*,#8292,.T.);
#11059=ORIENTED_EDGE('',*,*,#8293,.T.);
#11060=ORIENTED_EDGE('',*,*,#8289,.F.);
#11061=ORIENTED_EDGE('',*,*,#8294,.T.);
#11062=ORIENTED_EDGE('',*,*,#8295,.T.);
#11063=ORIENTED_EDGE('',*,*,#8296,.T.);
#11064=ORIENTED_EDGE('',*,*,#8292,.F.);
#11065=ORIENTED_EDGE('',*,*,#8297,.T.);
#11066=ORIENTED_EDGE('',*,*,#8298,.F.);
#11067=ORIENTED_EDGE('',*,*,#8299,.T.);
#11068=ORIENTED_EDGE('',*,*,#8300,.F.);
#11069=ORIENTED_EDGE('',*,*,#8301,.T.);
#11070=ORIENTED_EDGE('',*,*,#8302,.T.);
#11071=ORIENTED_EDGE('',*,*,#8303,.T.);
#11072=ORIENTED_EDGE('',*,*,#8304,.F.);
#11073=ORIENTED_EDGE('',*,*,#8305,.F.);
#11074=ORIENTED_EDGE('',*,*,#8306,.T.);
#11075=ORIENTED_EDGE('',*,*,#8307,.T.);
#11076=ORIENTED_EDGE('',*,*,#8302,.F.);
#11077=ORIENTED_EDGE('',*,*,#8308,.F.);
#11078=ORIENTED_EDGE('',*,*,#8309,.T.);
#11079=ORIENTED_EDGE('',*,*,#8310,.T.);
#11080=ORIENTED_EDGE('',*,*,#8306,.F.);
#11081=ORIENTED_EDGE('',*,*,#8311,.F.);
#11082=ORIENTED_EDGE('',*,*,#8312,.T.);
#11083=ORIENTED_EDGE('',*,*,#8313,.T.);
#11084=ORIENTED_EDGE('',*,*,#8309,.F.);
#11085=ORIENTED_EDGE('',*,*,#8314,.F.);
#11086=ORIENTED_EDGE('',*,*,#8315,.T.);
#11087=ORIENTED_EDGE('',*,*,#8316,.T.);
#11088=ORIENTED_EDGE('',*,*,#8312,.F.);
#11089=ORIENTED_EDGE('',*,*,#8317,.F.);
#11090=ORIENTED_EDGE('',*,*,#8318,.T.);
#11091=ORIENTED_EDGE('',*,*,#8319,.T.);
#11092=ORIENTED_EDGE('',*,*,#8315,.F.);
#11093=ORIENTED_EDGE('',*,*,#8320,.F.);
#11094=ORIENTED_EDGE('',*,*,#8321,.T.);
#11095=ORIENTED_EDGE('',*,*,#8322,.T.);
#11096=ORIENTED_EDGE('',*,*,#8318,.F.);
#11097=ORIENTED_EDGE('',*,*,#8323,.F.);
#11098=ORIENTED_EDGE('',*,*,#8324,.T.);
#11099=ORIENTED_EDGE('',*,*,#8325,.T.);
#11100=ORIENTED_EDGE('',*,*,#8321,.F.);
#11101=ORIENTED_EDGE('',*,*,#8326,.F.);
#11102=ORIENTED_EDGE('',*,*,#8327,.T.);
#11103=ORIENTED_EDGE('',*,*,#8328,.T.);
#11104=ORIENTED_EDGE('',*,*,#8324,.F.);
#11105=ORIENTED_EDGE('',*,*,#8329,.F.);
#11106=ORIENTED_EDGE('',*,*,#8330,.T.);
#11107=ORIENTED_EDGE('',*,*,#8331,.T.);
#11108=ORIENTED_EDGE('',*,*,#8327,.F.);
#11109=ORIENTED_EDGE('',*,*,#8332,.F.);
#11110=ORIENTED_EDGE('',*,*,#8333,.T.);
#11111=ORIENTED_EDGE('',*,*,#8334,.T.);
#11112=ORIENTED_EDGE('',*,*,#8330,.F.);
#11113=ORIENTED_EDGE('',*,*,#8335,.F.);
#11114=ORIENTED_EDGE('',*,*,#8336,.T.);
#11115=ORIENTED_EDGE('',*,*,#8337,.T.);
#11116=ORIENTED_EDGE('',*,*,#8333,.F.);
#11117=ORIENTED_EDGE('',*,*,#8338,.F.);
#11118=ORIENTED_EDGE('',*,*,#8339,.F.);
#11119=ORIENTED_EDGE('',*,*,#8340,.F.);
#11120=ORIENTED_EDGE('',*,*,#8341,.F.);
#11121=ORIENTED_EDGE('',*,*,#8342,.T.);
#11122=ORIENTED_EDGE('',*,*,#8343,.T.);
#11123=ORIENTED_EDGE('',*,*,#8344,.T.);
#11124=ORIENTED_EDGE('',*,*,#8345,.T.);
#11125=ORIENTED_EDGE('',*,*,#8346,.T.);
#11126=ORIENTED_EDGE('',*,*,#8347,.T.);
#11127=ORIENTED_EDGE('',*,*,#8348,.T.);
#11128=ORIENTED_EDGE('',*,*,#8347,.F.);
#11129=ORIENTED_EDGE('',*,*,#8349,.T.);
#11130=ORIENTED_EDGE('',*,*,#8350,.T.);
#11131=ORIENTED_EDGE('',*,*,#8351,.T.);
#11132=ORIENTED_EDGE('',*,*,#8343,.F.);
#11133=ORIENTED_EDGE('',*,*,#8352,.T.);
#11134=ORIENTED_EDGE('',*,*,#8353,.T.);
#11135=ORIENTED_EDGE('',*,*,#8354,.T.);
#11136=ORIENTED_EDGE('',*,*,#8350,.F.);
#11137=ORIENTED_EDGE('',*,*,#8355,.T.);
#11138=ORIENTED_EDGE('',*,*,#8356,.T.);
#11139=ORIENTED_EDGE('',*,*,#8357,.T.);
#11140=ORIENTED_EDGE('',*,*,#8353,.F.);
#11141=ORIENTED_EDGE('',*,*,#8358,.T.);
#11142=ORIENTED_EDGE('',*,*,#8359,.T.);
#11143=ORIENTED_EDGE('',*,*,#8360,.T.);
#11144=ORIENTED_EDGE('',*,*,#8356,.F.);
#11145=ORIENTED_EDGE('',*,*,#8361,.T.);
#11146=ORIENTED_EDGE('',*,*,#8362,.T.);
#11147=ORIENTED_EDGE('',*,*,#8363,.T.);
#11148=ORIENTED_EDGE('',*,*,#8359,.F.);
#11149=ORIENTED_EDGE('',*,*,#8364,.T.);
#11150=ORIENTED_EDGE('',*,*,#8365,.T.);
#11151=ORIENTED_EDGE('',*,*,#8366,.T.);
#11152=ORIENTED_EDGE('',*,*,#8362,.F.);
#11153=ORIENTED_EDGE('',*,*,#8367,.T.);
#11154=ORIENTED_EDGE('',*,*,#8368,.T.);
#11155=ORIENTED_EDGE('',*,*,#8369,.T.);
#11156=ORIENTED_EDGE('',*,*,#8365,.F.);
#11157=ORIENTED_EDGE('',*,*,#8370,.T.);
#11158=ORIENTED_EDGE('',*,*,#8371,.T.);
#11159=ORIENTED_EDGE('',*,*,#8372,.T.);
#11160=ORIENTED_EDGE('',*,*,#8368,.F.);
#11161=ORIENTED_EDGE('',*,*,#8373,.T.);
#11162=ORIENTED_EDGE('',*,*,#8374,.T.);
#11163=ORIENTED_EDGE('',*,*,#8375,.T.);
#11164=ORIENTED_EDGE('',*,*,#8371,.F.);
#11165=ORIENTED_EDGE('',*,*,#8376,.T.);
#11166=ORIENTED_EDGE('',*,*,#8377,.T.);
#11167=ORIENTED_EDGE('',*,*,#8378,.T.);
#11168=ORIENTED_EDGE('',*,*,#8374,.F.);
#11169=ORIENTED_EDGE('',*,*,#8379,.T.);
#11170=ORIENTED_EDGE('',*,*,#8380,.F.);
#11171=ORIENTED_EDGE('',*,*,#8381,.T.);
#11172=ORIENTED_EDGE('',*,*,#8382,.F.);
#11173=ORIENTED_EDGE('',*,*,#8383,.T.);
#11174=ORIENTED_EDGE('',*,*,#8384,.T.);
#11175=ORIENTED_EDGE('',*,*,#8385,.T.);
#11176=ORIENTED_EDGE('',*,*,#8386,.F.);
#11177=ORIENTED_EDGE('',*,*,#8387,.F.);
#11178=ORIENTED_EDGE('',*,*,#8388,.T.);
#11179=ORIENTED_EDGE('',*,*,#8389,.T.);
#11180=ORIENTED_EDGE('',*,*,#8384,.F.);
#11181=ORIENTED_EDGE('',*,*,#8390,.F.);
#11182=ORIENTED_EDGE('',*,*,#8391,.T.);
#11183=ORIENTED_EDGE('',*,*,#8392,.T.);
#11184=ORIENTED_EDGE('',*,*,#8388,.F.);
#11185=ORIENTED_EDGE('',*,*,#8393,.F.);
#11186=ORIENTED_EDGE('',*,*,#8394,.T.);
#11187=ORIENTED_EDGE('',*,*,#8395,.T.);
#11188=ORIENTED_EDGE('',*,*,#8391,.F.);
#11189=ORIENTED_EDGE('',*,*,#8396,.F.);
#11190=ORIENTED_EDGE('',*,*,#8397,.T.);
#11191=ORIENTED_EDGE('',*,*,#8398,.T.);
#11192=ORIENTED_EDGE('',*,*,#8394,.F.);
#11193=ORIENTED_EDGE('',*,*,#8399,.F.);
#11194=ORIENTED_EDGE('',*,*,#8400,.T.);
#11195=ORIENTED_EDGE('',*,*,#8401,.T.);
#11196=ORIENTED_EDGE('',*,*,#8397,.F.);
#11197=ORIENTED_EDGE('',*,*,#8402,.F.);
#11198=ORIENTED_EDGE('',*,*,#8403,.T.);
#11199=ORIENTED_EDGE('',*,*,#8404,.T.);
#11200=ORIENTED_EDGE('',*,*,#8400,.F.);
#11201=ORIENTED_EDGE('',*,*,#8405,.F.);
#11202=ORIENTED_EDGE('',*,*,#8406,.T.);
#11203=ORIENTED_EDGE('',*,*,#8407,.T.);
#11204=ORIENTED_EDGE('',*,*,#8403,.F.);
#11205=ORIENTED_EDGE('',*,*,#8408,.F.);
#11206=ORIENTED_EDGE('',*,*,#8409,.T.);
#11207=ORIENTED_EDGE('',*,*,#8410,.T.);
#11208=ORIENTED_EDGE('',*,*,#8406,.F.);
#11209=ORIENTED_EDGE('',*,*,#8411,.F.);
#11210=ORIENTED_EDGE('',*,*,#8412,.T.);
#11211=ORIENTED_EDGE('',*,*,#8413,.T.);
#11212=ORIENTED_EDGE('',*,*,#8409,.F.);
#11213=ORIENTED_EDGE('',*,*,#8414,.F.);
#11214=ORIENTED_EDGE('',*,*,#8415,.T.);
#11215=ORIENTED_EDGE('',*,*,#8416,.T.);
#11216=ORIENTED_EDGE('',*,*,#8412,.F.);
#11217=ORIENTED_EDGE('',*,*,#8417,.F.);
#11218=ORIENTED_EDGE('',*,*,#8418,.T.);
#11219=ORIENTED_EDGE('',*,*,#8419,.T.);
#11220=ORIENTED_EDGE('',*,*,#8415,.F.);
#11221=ORIENTED_EDGE('',*,*,#8420,.F.);
#11222=ORIENTED_EDGE('',*,*,#8421,.F.);
#11223=ORIENTED_EDGE('',*,*,#8422,.F.);
#11224=ORIENTED_EDGE('',*,*,#8423,.F.);
#11225=ORIENTED_EDGE('',*,*,#8424,.T.);
#11226=ORIENTED_EDGE('',*,*,#8425,.T.);
#11227=ORIENTED_EDGE('',*,*,#8426,.T.);
#11228=ORIENTED_EDGE('',*,*,#8427,.T.);
#11229=ORIENTED_EDGE('',*,*,#8428,.T.);
#11230=ORIENTED_EDGE('',*,*,#8429,.T.);
#11231=ORIENTED_EDGE('',*,*,#8430,.T.);
#11232=ORIENTED_EDGE('',*,*,#8429,.F.);
#11233=ORIENTED_EDGE('',*,*,#8431,.T.);
#11234=ORIENTED_EDGE('',*,*,#8432,.T.);
#11235=ORIENTED_EDGE('',*,*,#8433,.T.);
#11236=ORIENTED_EDGE('',*,*,#8425,.F.);
#11237=ORIENTED_EDGE('',*,*,#8434,.T.);
#11238=ORIENTED_EDGE('',*,*,#8435,.T.);
#11239=ORIENTED_EDGE('',*,*,#8436,.T.);
#11240=ORIENTED_EDGE('',*,*,#8432,.F.);
#11241=ORIENTED_EDGE('',*,*,#8437,.T.);
#11242=ORIENTED_EDGE('',*,*,#8438,.T.);
#11243=ORIENTED_EDGE('',*,*,#8439,.T.);
#11244=ORIENTED_EDGE('',*,*,#8435,.F.);
#11245=ORIENTED_EDGE('',*,*,#8440,.T.);
#11246=ORIENTED_EDGE('',*,*,#8441,.T.);
#11247=ORIENTED_EDGE('',*,*,#8442,.T.);
#11248=ORIENTED_EDGE('',*,*,#8438,.F.);
#11249=ORIENTED_EDGE('',*,*,#8443,.T.);
#11250=ORIENTED_EDGE('',*,*,#8444,.T.);
#11251=ORIENTED_EDGE('',*,*,#8445,.T.);
#11252=ORIENTED_EDGE('',*,*,#8441,.F.);
#11253=ORIENTED_EDGE('',*,*,#8446,.T.);
#11254=ORIENTED_EDGE('',*,*,#8447,.T.);
#11255=ORIENTED_EDGE('',*,*,#8448,.T.);
#11256=ORIENTED_EDGE('',*,*,#8444,.F.);
#11257=ORIENTED_EDGE('',*,*,#8449,.T.);
#11258=ORIENTED_EDGE('',*,*,#8450,.T.);
#11259=ORIENTED_EDGE('',*,*,#8451,.T.);
#11260=ORIENTED_EDGE('',*,*,#8447,.F.);
#11261=ORIENTED_EDGE('',*,*,#8452,.T.);
#11262=ORIENTED_EDGE('',*,*,#8453,.T.);
#11263=ORIENTED_EDGE('',*,*,#8454,.T.);
#11264=ORIENTED_EDGE('',*,*,#8450,.F.);
#11265=ORIENTED_EDGE('',*,*,#8455,.T.);
#11266=ORIENTED_EDGE('',*,*,#8456,.T.);
#11267=ORIENTED_EDGE('',*,*,#8457,.T.);
#11268=ORIENTED_EDGE('',*,*,#8453,.F.);
#11269=ORIENTED_EDGE('',*,*,#8458,.T.);
#11270=ORIENTED_EDGE('',*,*,#8459,.T.);
#11271=ORIENTED_EDGE('',*,*,#8460,.T.);
#11272=ORIENTED_EDGE('',*,*,#8456,.F.);
#11273=ORIENTED_EDGE('',*,*,#8461,.T.);
#11274=ORIENTED_EDGE('',*,*,#8462,.F.);
#11275=ORIENTED_EDGE('',*,*,#8463,.T.);
#11276=ORIENTED_EDGE('',*,*,#8464,.F.);
#11277=ORIENTED_EDGE('',*,*,#8465,.T.);
#11278=ORIENTED_EDGE('',*,*,#8466,.T.);
#11279=ORIENTED_EDGE('',*,*,#8467,.T.);
#11280=ORIENTED_EDGE('',*,*,#8468,.F.);
#11281=ORIENTED_EDGE('',*,*,#8469,.F.);
#11282=ORIENTED_EDGE('',*,*,#8470,.T.);
#11283=ORIENTED_EDGE('',*,*,#8471,.T.);
#11284=ORIENTED_EDGE('',*,*,#8466,.F.);
#11285=ORIENTED_EDGE('',*,*,#8472,.F.);
#11286=ORIENTED_EDGE('',*,*,#8473,.T.);
#11287=ORIENTED_EDGE('',*,*,#8474,.T.);
#11288=ORIENTED_EDGE('',*,*,#8470,.F.);
#11289=ORIENTED_EDGE('',*,*,#8475,.F.);
#11290=ORIENTED_EDGE('',*,*,#8476,.T.);
#11291=ORIENTED_EDGE('',*,*,#8477,.T.);
#11292=ORIENTED_EDGE('',*,*,#8473,.F.);
#11293=ORIENTED_EDGE('',*,*,#8478,.F.);
#11294=ORIENTED_EDGE('',*,*,#8479,.T.);
#11295=ORIENTED_EDGE('',*,*,#8480,.T.);
#11296=ORIENTED_EDGE('',*,*,#8476,.F.);
#11297=ORIENTED_EDGE('',*,*,#8481,.F.);
#11298=ORIENTED_EDGE('',*,*,#8482,.T.);
#11299=ORIENTED_EDGE('',*,*,#8483,.T.);
#11300=ORIENTED_EDGE('',*,*,#8479,.F.);
#11301=ORIENTED_EDGE('',*,*,#8484,.F.);
#11302=ORIENTED_EDGE('',*,*,#8485,.T.);
#11303=ORIENTED_EDGE('',*,*,#8486,.T.);
#11304=ORIENTED_EDGE('',*,*,#8482,.F.);
#11305=ORIENTED_EDGE('',*,*,#8487,.F.);
#11306=ORIENTED_EDGE('',*,*,#8488,.T.);
#11307=ORIENTED_EDGE('',*,*,#8489,.T.);
#11308=ORIENTED_EDGE('',*,*,#8485,.F.);
#11309=ORIENTED_EDGE('',*,*,#8490,.F.);
#11310=ORIENTED_EDGE('',*,*,#8491,.T.);
#11311=ORIENTED_EDGE('',*,*,#8492,.T.);
#11312=ORIENTED_EDGE('',*,*,#8488,.F.);
#11313=ORIENTED_EDGE('',*,*,#8493,.F.);
#11314=ORIENTED_EDGE('',*,*,#8494,.T.);
#11315=ORIENTED_EDGE('',*,*,#8495,.T.);
#11316=ORIENTED_EDGE('',*,*,#8491,.F.);
#11317=ORIENTED_EDGE('',*,*,#8496,.F.);
#11318=ORIENTED_EDGE('',*,*,#8497,.T.);
#11319=ORIENTED_EDGE('',*,*,#8498,.T.);
#11320=ORIENTED_EDGE('',*,*,#8494,.F.);
#11321=ORIENTED_EDGE('',*,*,#8499,.F.);
#11322=ORIENTED_EDGE('',*,*,#8500,.T.);
#11323=ORIENTED_EDGE('',*,*,#8501,.T.);
#11324=ORIENTED_EDGE('',*,*,#8497,.F.);
#11325=ORIENTED_EDGE('',*,*,#8502,.F.);
#11326=ORIENTED_EDGE('',*,*,#8503,.F.);
#11327=ORIENTED_EDGE('',*,*,#8504,.F.);
#11328=ORIENTED_EDGE('',*,*,#8505,.F.);
#11329=ORIENTED_EDGE('',*,*,#8506,.T.);
#11330=ORIENTED_EDGE('',*,*,#8507,.T.);
#11331=ORIENTED_EDGE('',*,*,#8508,.T.);
#11332=ORIENTED_EDGE('',*,*,#8509,.T.);
#11333=ORIENTED_EDGE('',*,*,#8510,.T.);
#11334=ORIENTED_EDGE('',*,*,#8511,.T.);
#11335=ORIENTED_EDGE('',*,*,#8512,.T.);
#11336=ORIENTED_EDGE('',*,*,#8511,.F.);
#11337=ORIENTED_EDGE('',*,*,#8513,.T.);
#11338=ORIENTED_EDGE('',*,*,#8514,.T.);
#11339=ORIENTED_EDGE('',*,*,#8515,.T.);
#11340=ORIENTED_EDGE('',*,*,#8507,.F.);
#11341=ORIENTED_EDGE('',*,*,#8516,.T.);
#11342=ORIENTED_EDGE('',*,*,#8517,.T.);
#11343=ORIENTED_EDGE('',*,*,#8518,.T.);
#11344=ORIENTED_EDGE('',*,*,#8514,.F.);
#11345=ORIENTED_EDGE('',*,*,#8519,.T.);
#11346=ORIENTED_EDGE('',*,*,#8520,.T.);
#11347=ORIENTED_EDGE('',*,*,#8521,.T.);
#11348=ORIENTED_EDGE('',*,*,#8517,.F.);
#11349=ORIENTED_EDGE('',*,*,#8522,.T.);
#11350=ORIENTED_EDGE('',*,*,#8523,.T.);
#11351=ORIENTED_EDGE('',*,*,#8524,.T.);
#11352=ORIENTED_EDGE('',*,*,#8520,.F.);
#11353=ORIENTED_EDGE('',*,*,#8525,.T.);
#11354=ORIENTED_EDGE('',*,*,#8526,.T.);
#11355=ORIENTED_EDGE('',*,*,#8527,.T.);
#11356=ORIENTED_EDGE('',*,*,#8523,.F.);
#11357=ORIENTED_EDGE('',*,*,#8528,.T.);
#11358=ORIENTED_EDGE('',*,*,#8529,.T.);
#11359=ORIENTED_EDGE('',*,*,#8530,.T.);
#11360=ORIENTED_EDGE('',*,*,#8526,.F.);
#11361=ORIENTED_EDGE('',*,*,#8531,.T.);
#11362=ORIENTED_EDGE('',*,*,#8532,.T.);
#11363=ORIENTED_EDGE('',*,*,#8533,.T.);
#11364=ORIENTED_EDGE('',*,*,#8529,.F.);
#11365=ORIENTED_EDGE('',*,*,#8534,.T.);
#11366=ORIENTED_EDGE('',*,*,#8535,.T.);
#11367=ORIENTED_EDGE('',*,*,#8536,.T.);
#11368=ORIENTED_EDGE('',*,*,#8532,.F.);
#11369=ORIENTED_EDGE('',*,*,#8537,.T.);
#11370=ORIENTED_EDGE('',*,*,#8538,.T.);
#11371=ORIENTED_EDGE('',*,*,#8539,.T.);
#11372=ORIENTED_EDGE('',*,*,#8535,.F.);
#11373=ORIENTED_EDGE('',*,*,#8540,.T.);
#11374=ORIENTED_EDGE('',*,*,#8541,.T.);
#11375=ORIENTED_EDGE('',*,*,#8542,.T.);
#11376=ORIENTED_EDGE('',*,*,#8538,.F.);
#11377=ORIENTED_EDGE('',*,*,#8543,.T.);
#11378=ORIENTED_EDGE('',*,*,#8544,.F.);
#11379=ORIENTED_EDGE('',*,*,#8545,.T.);
#11380=ORIENTED_EDGE('',*,*,#8546,.F.);
#11381=ORIENTED_EDGE('',*,*,#8547,.T.);
#11382=ORIENTED_EDGE('',*,*,#8548,.T.);
#11383=ORIENTED_EDGE('',*,*,#8549,.T.);
#11384=ORIENTED_EDGE('',*,*,#8550,.F.);
#11385=ORIENTED_EDGE('',*,*,#8551,.F.);
#11386=ORIENTED_EDGE('',*,*,#8552,.T.);
#11387=ORIENTED_EDGE('',*,*,#8553,.T.);
#11388=ORIENTED_EDGE('',*,*,#8548,.F.);
#11389=ORIENTED_EDGE('',*,*,#8554,.F.);
#11390=ORIENTED_EDGE('',*,*,#8555,.T.);
#11391=ORIENTED_EDGE('',*,*,#8556,.T.);
#11392=ORIENTED_EDGE('',*,*,#8552,.F.);
#11393=ORIENTED_EDGE('',*,*,#8557,.F.);
#11394=ORIENTED_EDGE('',*,*,#8558,.T.);
#11395=ORIENTED_EDGE('',*,*,#8559,.T.);
#11396=ORIENTED_EDGE('',*,*,#8555,.F.);
#11397=ORIENTED_EDGE('',*,*,#8560,.F.);
#11398=ORIENTED_EDGE('',*,*,#8561,.T.);
#11399=ORIENTED_EDGE('',*,*,#8562,.T.);
#11400=ORIENTED_EDGE('',*,*,#8558,.F.);
#11401=ORIENTED_EDGE('',*,*,#8563,.F.);
#11402=ORIENTED_EDGE('',*,*,#8564,.T.);
#11403=ORIENTED_EDGE('',*,*,#8565,.T.);
#11404=ORIENTED_EDGE('',*,*,#8561,.F.);
#11405=ORIENTED_EDGE('',*,*,#8566,.F.);
#11406=ORIENTED_EDGE('',*,*,#8567,.T.);
#11407=ORIENTED_EDGE('',*,*,#8568,.T.);
#11408=ORIENTED_EDGE('',*,*,#8564,.F.);
#11409=ORIENTED_EDGE('',*,*,#8569,.F.);
#11410=ORIENTED_EDGE('',*,*,#8570,.T.);
#11411=ORIENTED_EDGE('',*,*,#8571,.T.);
#11412=ORIENTED_EDGE('',*,*,#8567,.F.);
#11413=ORIENTED_EDGE('',*,*,#8572,.F.);
#11414=ORIENTED_EDGE('',*,*,#8573,.T.);
#11415=ORIENTED_EDGE('',*,*,#8574,.T.);
#11416=ORIENTED_EDGE('',*,*,#8570,.F.);
#11417=ORIENTED_EDGE('',*,*,#8575,.F.);
#11418=ORIENTED_EDGE('',*,*,#8576,.T.);
#11419=ORIENTED_EDGE('',*,*,#8577,.T.);
#11420=ORIENTED_EDGE('',*,*,#8573,.F.);
#11421=ORIENTED_EDGE('',*,*,#8578,.F.);
#11422=ORIENTED_EDGE('',*,*,#8579,.T.);
#11423=ORIENTED_EDGE('',*,*,#8580,.T.);
#11424=ORIENTED_EDGE('',*,*,#8576,.F.);
#11425=ORIENTED_EDGE('',*,*,#8581,.F.);
#11426=ORIENTED_EDGE('',*,*,#8582,.T.);
#11427=ORIENTED_EDGE('',*,*,#8583,.T.);
#11428=ORIENTED_EDGE('',*,*,#8579,.F.);
#11429=ORIENTED_EDGE('',*,*,#8584,.F.);
#11430=ORIENTED_EDGE('',*,*,#8585,.F.);
#11431=ORIENTED_EDGE('',*,*,#8586,.F.);
#11432=ORIENTED_EDGE('',*,*,#8587,.F.);
#11433=ORIENTED_EDGE('',*,*,#8588,.T.);
#11434=ORIENTED_EDGE('',*,*,#8589,.T.);
#11435=ORIENTED_EDGE('',*,*,#8590,.T.);
#11436=ORIENTED_EDGE('',*,*,#8591,.T.);
#11437=ORIENTED_EDGE('',*,*,#8592,.T.);
#11438=ORIENTED_EDGE('',*,*,#8593,.T.);
#11439=ORIENTED_EDGE('',*,*,#8594,.T.);
#11440=ORIENTED_EDGE('',*,*,#8593,.F.);
#11441=ORIENTED_EDGE('',*,*,#8595,.T.);
#11442=ORIENTED_EDGE('',*,*,#8596,.T.);
#11443=ORIENTED_EDGE('',*,*,#8597,.T.);
#11444=ORIENTED_EDGE('',*,*,#8589,.F.);
#11445=ORIENTED_EDGE('',*,*,#8598,.T.);
#11446=ORIENTED_EDGE('',*,*,#8599,.T.);
#11447=ORIENTED_EDGE('',*,*,#8600,.T.);
#11448=ORIENTED_EDGE('',*,*,#8596,.F.);
#11449=ORIENTED_EDGE('',*,*,#8601,.T.);
#11450=ORIENTED_EDGE('',*,*,#8602,.T.);
#11451=ORIENTED_EDGE('',*,*,#8603,.T.);
#11452=ORIENTED_EDGE('',*,*,#8599,.F.);
#11453=ORIENTED_EDGE('',*,*,#8604,.T.);
#11454=ORIENTED_EDGE('',*,*,#8605,.T.);
#11455=ORIENTED_EDGE('',*,*,#8606,.T.);
#11456=ORIENTED_EDGE('',*,*,#8602,.F.);
#11457=ORIENTED_EDGE('',*,*,#8607,.T.);
#11458=ORIENTED_EDGE('',*,*,#8608,.T.);
#11459=ORIENTED_EDGE('',*,*,#8609,.T.);
#11460=ORIENTED_EDGE('',*,*,#8605,.F.);
#11461=ORIENTED_EDGE('',*,*,#8610,.T.);
#11462=ORIENTED_EDGE('',*,*,#8611,.T.);
#11463=ORIENTED_EDGE('',*,*,#8612,.T.);
#11464=ORIENTED_EDGE('',*,*,#8608,.F.);
#11465=ORIENTED_EDGE('',*,*,#8613,.T.);
#11466=ORIENTED_EDGE('',*,*,#8614,.T.);
#11467=ORIENTED_EDGE('',*,*,#8615,.T.);
#11468=ORIENTED_EDGE('',*,*,#8611,.F.);
#11469=ORIENTED_EDGE('',*,*,#8616,.T.);
#11470=ORIENTED_EDGE('',*,*,#8617,.T.);
#11471=ORIENTED_EDGE('',*,*,#8618,.T.);
#11472=ORIENTED_EDGE('',*,*,#8614,.F.);
#11473=ORIENTED_EDGE('',*,*,#8619,.T.);
#11474=ORIENTED_EDGE('',*,*,#8620,.T.);
#11475=ORIENTED_EDGE('',*,*,#8621,.T.);
#11476=ORIENTED_EDGE('',*,*,#8617,.F.);
#11477=ORIENTED_EDGE('',*,*,#8622,.T.);
#11478=ORIENTED_EDGE('',*,*,#8623,.T.);
#11479=ORIENTED_EDGE('',*,*,#8624,.T.);
#11480=ORIENTED_EDGE('',*,*,#8620,.F.);
#11481=ORIENTED_EDGE('',*,*,#8625,.T.);
#11482=ORIENTED_EDGE('',*,*,#8626,.F.);
#11483=ORIENTED_EDGE('',*,*,#8627,.T.);
#11484=ORIENTED_EDGE('',*,*,#8628,.F.);
#11485=ORIENTED_EDGE('',*,*,#8629,.T.);
#11486=ORIENTED_EDGE('',*,*,#8630,.T.);
#11487=ORIENTED_EDGE('',*,*,#8631,.T.);
#11488=ORIENTED_EDGE('',*,*,#8632,.F.);
#11489=ORIENTED_EDGE('',*,*,#8633,.F.);
#11490=ORIENTED_EDGE('',*,*,#8634,.T.);
#11491=ORIENTED_EDGE('',*,*,#8635,.T.);
#11492=ORIENTED_EDGE('',*,*,#8630,.F.);
#11493=ORIENTED_EDGE('',*,*,#8636,.F.);
#11494=ORIENTED_EDGE('',*,*,#8637,.T.);
#11495=ORIENTED_EDGE('',*,*,#8638,.T.);
#11496=ORIENTED_EDGE('',*,*,#8634,.F.);
#11497=ORIENTED_EDGE('',*,*,#8639,.F.);
#11498=ORIENTED_EDGE('',*,*,#8640,.T.);
#11499=ORIENTED_EDGE('',*,*,#8641,.T.);
#11500=ORIENTED_EDGE('',*,*,#8637,.F.);
#11501=ORIENTED_EDGE('',*,*,#8642,.F.);
#11502=ORIENTED_EDGE('',*,*,#8643,.T.);
#11503=ORIENTED_EDGE('',*,*,#8644,.T.);
#11504=ORIENTED_EDGE('',*,*,#8640,.F.);
#11505=ORIENTED_EDGE('',*,*,#8645,.F.);
#11506=ORIENTED_EDGE('',*,*,#8646,.T.);
#11507=ORIENTED_EDGE('',*,*,#8647,.T.);
#11508=ORIENTED_EDGE('',*,*,#8643,.F.);
#11509=ORIENTED_EDGE('',*,*,#8648,.F.);
#11510=ORIENTED_EDGE('',*,*,#8649,.T.);
#11511=ORIENTED_EDGE('',*,*,#8650,.T.);
#11512=ORIENTED_EDGE('',*,*,#8646,.F.);
#11513=ORIENTED_EDGE('',*,*,#8651,.F.);
#11514=ORIENTED_EDGE('',*,*,#8652,.T.);
#11515=ORIENTED_EDGE('',*,*,#8653,.T.);
#11516=ORIENTED_EDGE('',*,*,#8649,.F.);
#11517=ORIENTED_EDGE('',*,*,#8654,.F.);
#11518=ORIENTED_EDGE('',*,*,#8655,.T.);
#11519=ORIENTED_EDGE('',*,*,#8656,.T.);
#11520=ORIENTED_EDGE('',*,*,#8652,.F.);
#11521=ORIENTED_EDGE('',*,*,#8657,.F.);
#11522=ORIENTED_EDGE('',*,*,#8658,.T.);
#11523=ORIENTED_EDGE('',*,*,#8659,.T.);
#11524=ORIENTED_EDGE('',*,*,#8655,.F.);
#11525=ORIENTED_EDGE('',*,*,#8660,.F.);
#11526=ORIENTED_EDGE('',*,*,#8661,.T.);
#11527=ORIENTED_EDGE('',*,*,#8662,.T.);
#11528=ORIENTED_EDGE('',*,*,#8658,.F.);
#11529=ORIENTED_EDGE('',*,*,#8663,.F.);
#11530=ORIENTED_EDGE('',*,*,#8664,.T.);
#11531=ORIENTED_EDGE('',*,*,#8665,.T.);
#11532=ORIENTED_EDGE('',*,*,#8661,.F.);
#11533=ORIENTED_EDGE('',*,*,#8666,.F.);
#11534=ORIENTED_EDGE('',*,*,#8667,.F.);
#11535=ORIENTED_EDGE('',*,*,#8668,.F.);
#11536=ORIENTED_EDGE('',*,*,#8669,.F.);
#11537=ORIENTED_EDGE('',*,*,#8670,.T.);
#11538=ORIENTED_EDGE('',*,*,#8671,.T.);
#11539=ORIENTED_EDGE('',*,*,#8672,.T.);
#11540=ORIENTED_EDGE('',*,*,#8673,.T.);
#11541=ORIENTED_EDGE('',*,*,#8674,.T.);
#11542=ORIENTED_EDGE('',*,*,#8675,.T.);
#11543=ORIENTED_EDGE('',*,*,#8676,.T.);
#11544=ORIENTED_EDGE('',*,*,#8675,.F.);
#11545=ORIENTED_EDGE('',*,*,#8677,.T.);
#11546=ORIENTED_EDGE('',*,*,#8678,.T.);
#11547=ORIENTED_EDGE('',*,*,#8679,.T.);
#11548=ORIENTED_EDGE('',*,*,#8671,.F.);
#11549=ORIENTED_EDGE('',*,*,#8680,.T.);
#11550=ORIENTED_EDGE('',*,*,#8681,.T.);
#11551=ORIENTED_EDGE('',*,*,#8682,.T.);
#11552=ORIENTED_EDGE('',*,*,#8678,.F.);
#11553=ORIENTED_EDGE('',*,*,#8683,.T.);
#11554=ORIENTED_EDGE('',*,*,#8684,.T.);
#11555=ORIENTED_EDGE('',*,*,#8685,.T.);
#11556=ORIENTED_EDGE('',*,*,#8681,.F.);
#11557=ORIENTED_EDGE('',*,*,#8686,.T.);
#11558=ORIENTED_EDGE('',*,*,#8687,.T.);
#11559=ORIENTED_EDGE('',*,*,#8688,.T.);
#11560=ORIENTED_EDGE('',*,*,#8684,.F.);
#11561=ORIENTED_EDGE('',*,*,#8689,.T.);
#11562=ORIENTED_EDGE('',*,*,#8690,.T.);
#11563=ORIENTED_EDGE('',*,*,#8691,.T.);
#11564=ORIENTED_EDGE('',*,*,#8687,.F.);
#11565=ORIENTED_EDGE('',*,*,#8692,.T.);
#11566=ORIENTED_EDGE('',*,*,#8693,.T.);
#11567=ORIENTED_EDGE('',*,*,#8694,.T.);
#11568=ORIENTED_EDGE('',*,*,#8690,.F.);
#11569=ORIENTED_EDGE('',*,*,#8695,.T.);
#11570=ORIENTED_EDGE('',*,*,#8696,.T.);
#11571=ORIENTED_EDGE('',*,*,#8697,.T.);
#11572=ORIENTED_EDGE('',*,*,#8693,.F.);
#11573=ORIENTED_EDGE('',*,*,#8698,.T.);
#11574=ORIENTED_EDGE('',*,*,#8699,.T.);
#11575=ORIENTED_EDGE('',*,*,#8700,.T.);
#11576=ORIENTED_EDGE('',*,*,#8696,.F.);
#11577=ORIENTED_EDGE('',*,*,#8701,.T.);
#11578=ORIENTED_EDGE('',*,*,#8702,.T.);
#11579=ORIENTED_EDGE('',*,*,#8703,.T.);
#11580=ORIENTED_EDGE('',*,*,#8699,.F.);
#11581=ORIENTED_EDGE('',*,*,#8704,.T.);
#11582=ORIENTED_EDGE('',*,*,#8705,.T.);
#11583=ORIENTED_EDGE('',*,*,#8706,.T.);
#11584=ORIENTED_EDGE('',*,*,#8702,.F.);
#11585=ORIENTED_EDGE('',*,*,#8707,.T.);
#11586=ORIENTED_EDGE('',*,*,#8708,.F.);
#11587=ORIENTED_EDGE('',*,*,#8709,.T.);
#11588=ORIENTED_EDGE('',*,*,#8710,.F.);
#11589=ORIENTED_EDGE('',*,*,#8711,.T.);
#11590=ORIENTED_EDGE('',*,*,#8712,.T.);
#11591=ORIENTED_EDGE('',*,*,#8713,.T.);
#11592=ORIENTED_EDGE('',*,*,#8714,.F.);
#11593=ORIENTED_EDGE('',*,*,#8715,.F.);
#11594=ORIENTED_EDGE('',*,*,#8716,.T.);
#11595=ORIENTED_EDGE('',*,*,#8717,.T.);
#11596=ORIENTED_EDGE('',*,*,#8712,.F.);
#11597=ORIENTED_EDGE('',*,*,#8718,.F.);
#11598=ORIENTED_EDGE('',*,*,#8719,.T.);
#11599=ORIENTED_EDGE('',*,*,#8720,.T.);
#11600=ORIENTED_EDGE('',*,*,#8716,.F.);
#11601=ORIENTED_EDGE('',*,*,#8721,.F.);
#11602=ORIENTED_EDGE('',*,*,#8722,.T.);
#11603=ORIENTED_EDGE('',*,*,#8723,.T.);
#11604=ORIENTED_EDGE('',*,*,#8719,.F.);
#11605=ORIENTED_EDGE('',*,*,#8724,.F.);
#11606=ORIENTED_EDGE('',*,*,#8725,.T.);
#11607=ORIENTED_EDGE('',*,*,#8726,.T.);
#11608=ORIENTED_EDGE('',*,*,#8722,.F.);
#11609=ORIENTED_EDGE('',*,*,#8727,.F.);
#11610=ORIENTED_EDGE('',*,*,#8728,.T.);
#11611=ORIENTED_EDGE('',*,*,#8729,.T.);
#11612=ORIENTED_EDGE('',*,*,#8725,.F.);
#11613=ORIENTED_EDGE('',*,*,#8730,.F.);
#11614=ORIENTED_EDGE('',*,*,#8731,.T.);
#11615=ORIENTED_EDGE('',*,*,#8732,.T.);
#11616=ORIENTED_EDGE('',*,*,#8728,.F.);
#11617=ORIENTED_EDGE('',*,*,#8733,.F.);
#11618=ORIENTED_EDGE('',*,*,#8734,.T.);
#11619=ORIENTED_EDGE('',*,*,#8735,.T.);
#11620=ORIENTED_EDGE('',*,*,#8731,.F.);
#11621=ORIENTED_EDGE('',*,*,#8736,.F.);
#11622=ORIENTED_EDGE('',*,*,#8737,.T.);
#11623=ORIENTED_EDGE('',*,*,#8738,.T.);
#11624=ORIENTED_EDGE('',*,*,#8734,.F.);
#11625=ORIENTED_EDGE('',*,*,#8739,.F.);
#11626=ORIENTED_EDGE('',*,*,#8740,.T.);
#11627=ORIENTED_EDGE('',*,*,#8741,.T.);
#11628=ORIENTED_EDGE('',*,*,#8737,.F.);
#11629=ORIENTED_EDGE('',*,*,#8742,.F.);
#11630=ORIENTED_EDGE('',*,*,#8743,.T.);
#11631=ORIENTED_EDGE('',*,*,#8744,.T.);
#11632=ORIENTED_EDGE('',*,*,#8740,.F.);
#11633=ORIENTED_EDGE('',*,*,#8745,.F.);
#11634=ORIENTED_EDGE('',*,*,#8746,.T.);
#11635=ORIENTED_EDGE('',*,*,#8747,.T.);
#11636=ORIENTED_EDGE('',*,*,#8743,.F.);
#11637=ORIENTED_EDGE('',*,*,#8748,.F.);
#11638=ORIENTED_EDGE('',*,*,#8749,.F.);
#11639=ORIENTED_EDGE('',*,*,#8750,.F.);
#11640=ORIENTED_EDGE('',*,*,#8751,.F.);
#11641=ORIENTED_EDGE('',*,*,#8752,.T.);
#11642=ORIENTED_EDGE('',*,*,#8753,.T.);
#11643=ORIENTED_EDGE('',*,*,#8754,.T.);
#11644=ORIENTED_EDGE('',*,*,#8755,.T.);
#11645=ORIENTED_EDGE('',*,*,#8756,.T.);
#11646=ORIENTED_EDGE('',*,*,#8757,.T.);
#11647=ORIENTED_EDGE('',*,*,#8758,.T.);
#11648=ORIENTED_EDGE('',*,*,#8757,.F.);
#11649=ORIENTED_EDGE('',*,*,#8759,.T.);
#11650=ORIENTED_EDGE('',*,*,#8760,.T.);
#11651=ORIENTED_EDGE('',*,*,#8761,.T.);
#11652=ORIENTED_EDGE('',*,*,#8753,.F.);
#11653=ORIENTED_EDGE('',*,*,#8762,.T.);
#11654=ORIENTED_EDGE('',*,*,#8763,.T.);
#11655=ORIENTED_EDGE('',*,*,#8764,.T.);
#11656=ORIENTED_EDGE('',*,*,#8760,.F.);
#11657=ORIENTED_EDGE('',*,*,#8765,.T.);
#11658=ORIENTED_EDGE('',*,*,#8766,.T.);
#11659=ORIENTED_EDGE('',*,*,#8767,.T.);
#11660=ORIENTED_EDGE('',*,*,#8763,.F.);
#11661=ORIENTED_EDGE('',*,*,#8768,.T.);
#11662=ORIENTED_EDGE('',*,*,#8769,.T.);
#11663=ORIENTED_EDGE('',*,*,#8770,.T.);
#11664=ORIENTED_EDGE('',*,*,#8766,.F.);
#11665=ORIENTED_EDGE('',*,*,#8771,.T.);
#11666=ORIENTED_EDGE('',*,*,#8772,.T.);
#11667=ORIENTED_EDGE('',*,*,#8773,.T.);
#11668=ORIENTED_EDGE('',*,*,#8769,.F.);
#11669=ORIENTED_EDGE('',*,*,#8774,.T.);
#11670=ORIENTED_EDGE('',*,*,#8775,.T.);
#11671=ORIENTED_EDGE('',*,*,#8776,.T.);
#11672=ORIENTED_EDGE('',*,*,#8772,.F.);
#11673=ORIENTED_EDGE('',*,*,#8777,.T.);
#11674=ORIENTED_EDGE('',*,*,#8778,.T.);
#11675=ORIENTED_EDGE('',*,*,#8779,.T.);
#11676=ORIENTED_EDGE('',*,*,#8775,.F.);
#11677=ORIENTED_EDGE('',*,*,#8780,.T.);
#11678=ORIENTED_EDGE('',*,*,#8781,.T.);
#11679=ORIENTED_EDGE('',*,*,#8782,.T.);
#11680=ORIENTED_EDGE('',*,*,#8778,.F.);
#11681=ORIENTED_EDGE('',*,*,#8783,.T.);
#11682=ORIENTED_EDGE('',*,*,#8784,.T.);
#11683=ORIENTED_EDGE('',*,*,#8785,.T.);
#11684=ORIENTED_EDGE('',*,*,#8781,.F.);
#11685=ORIENTED_EDGE('',*,*,#8786,.T.);
#11686=ORIENTED_EDGE('',*,*,#8787,.T.);
#11687=ORIENTED_EDGE('',*,*,#8788,.T.);
#11688=ORIENTED_EDGE('',*,*,#8784,.F.);
#11689=ORIENTED_EDGE('',*,*,#8789,.T.);
#11690=ORIENTED_EDGE('',*,*,#8790,.F.);
#11691=ORIENTED_EDGE('',*,*,#8791,.T.);
#11692=ORIENTED_EDGE('',*,*,#8792,.F.);
#11693=ORIENTED_EDGE('',*,*,#8793,.T.);
#11694=ORIENTED_EDGE('',*,*,#8794,.T.);
#11695=ORIENTED_EDGE('',*,*,#8795,.T.);
#11696=ORIENTED_EDGE('',*,*,#8796,.F.);
#11697=ORIENTED_EDGE('',*,*,#8797,.F.);
#11698=ORIENTED_EDGE('',*,*,#8798,.T.);
#11699=ORIENTED_EDGE('',*,*,#8799,.T.);
#11700=ORIENTED_EDGE('',*,*,#8794,.F.);
#11701=ORIENTED_EDGE('',*,*,#8800,.F.);
#11702=ORIENTED_EDGE('',*,*,#8801,.T.);
#11703=ORIENTED_EDGE('',*,*,#8802,.T.);
#11704=ORIENTED_EDGE('',*,*,#8798,.F.);
#11705=ORIENTED_EDGE('',*,*,#8803,.F.);
#11706=ORIENTED_EDGE('',*,*,#8804,.T.);
#11707=ORIENTED_EDGE('',*,*,#8805,.T.);
#11708=ORIENTED_EDGE('',*,*,#8801,.F.);
#11709=ORIENTED_EDGE('',*,*,#8806,.F.);
#11710=ORIENTED_EDGE('',*,*,#8807,.T.);
#11711=ORIENTED_EDGE('',*,*,#8808,.T.);
#11712=ORIENTED_EDGE('',*,*,#8804,.F.);
#11713=ORIENTED_EDGE('',*,*,#8809,.F.);
#11714=ORIENTED_EDGE('',*,*,#8810,.T.);
#11715=ORIENTED_EDGE('',*,*,#8811,.T.);
#11716=ORIENTED_EDGE('',*,*,#8807,.F.);
#11717=ORIENTED_EDGE('',*,*,#8812,.F.);
#11718=ORIENTED_EDGE('',*,*,#8813,.T.);
#11719=ORIENTED_EDGE('',*,*,#8814,.T.);
#11720=ORIENTED_EDGE('',*,*,#8810,.F.);
#11721=ORIENTED_EDGE('',*,*,#8815,.F.);
#11722=ORIENTED_EDGE('',*,*,#8816,.T.);
#11723=ORIENTED_EDGE('',*,*,#8817,.T.);
#11724=ORIENTED_EDGE('',*,*,#8813,.F.);
#11725=ORIENTED_EDGE('',*,*,#8818,.F.);
#11726=ORIENTED_EDGE('',*,*,#8819,.T.);
#11727=ORIENTED_EDGE('',*,*,#8820,.T.);
#11728=ORIENTED_EDGE('',*,*,#8816,.F.);
#11729=ORIENTED_EDGE('',*,*,#8821,.F.);
#11730=ORIENTED_EDGE('',*,*,#8822,.T.);
#11731=ORIENTED_EDGE('',*,*,#8823,.T.);
#11732=ORIENTED_EDGE('',*,*,#8819,.F.);
#11733=ORIENTED_EDGE('',*,*,#8824,.F.);
#11734=ORIENTED_EDGE('',*,*,#8825,.T.);
#11735=ORIENTED_EDGE('',*,*,#8826,.T.);
#11736=ORIENTED_EDGE('',*,*,#8822,.F.);
#11737=ORIENTED_EDGE('',*,*,#8827,.F.);
#11738=ORIENTED_EDGE('',*,*,#8828,.T.);
#11739=ORIENTED_EDGE('',*,*,#8829,.T.);
#11740=ORIENTED_EDGE('',*,*,#8825,.F.);
#11741=ORIENTED_EDGE('',*,*,#8830,.F.);
#11742=ORIENTED_EDGE('',*,*,#8831,.F.);
#11743=ORIENTED_EDGE('',*,*,#8832,.F.);
#11744=ORIENTED_EDGE('',*,*,#8833,.F.);
#11745=ORIENTED_EDGE('',*,*,#8834,.T.);
#11746=ORIENTED_EDGE('',*,*,#8835,.T.);
#11747=ORIENTED_EDGE('',*,*,#8836,.T.);
#11748=ORIENTED_EDGE('',*,*,#8837,.T.);
#11749=ORIENTED_EDGE('',*,*,#8838,.T.);
#11750=ORIENTED_EDGE('',*,*,#8839,.T.);
#11751=ORIENTED_EDGE('',*,*,#8840,.T.);
#11752=ORIENTED_EDGE('',*,*,#8839,.F.);
#11753=ORIENTED_EDGE('',*,*,#8841,.T.);
#11754=ORIENTED_EDGE('',*,*,#8842,.T.);
#11755=ORIENTED_EDGE('',*,*,#8843,.T.);
#11756=ORIENTED_EDGE('',*,*,#8835,.F.);
#11757=ORIENTED_EDGE('',*,*,#8844,.T.);
#11758=ORIENTED_EDGE('',*,*,#8845,.T.);
#11759=ORIENTED_EDGE('',*,*,#8846,.T.);
#11760=ORIENTED_EDGE('',*,*,#8842,.F.);
#11761=ORIENTED_EDGE('',*,*,#8847,.T.);
#11762=ORIENTED_EDGE('',*,*,#8848,.T.);
#11763=ORIENTED_EDGE('',*,*,#8849,.T.);
#11764=ORIENTED_EDGE('',*,*,#8845,.F.);
#11765=ORIENTED_EDGE('',*,*,#8850,.T.);
#11766=ORIENTED_EDGE('',*,*,#8851,.T.);
#11767=ORIENTED_EDGE('',*,*,#8852,.T.);
#11768=ORIENTED_EDGE('',*,*,#8848,.F.);
#11769=ORIENTED_EDGE('',*,*,#8853,.T.);
#11770=ORIENTED_EDGE('',*,*,#8854,.T.);
#11771=ORIENTED_EDGE('',*,*,#8855,.T.);
#11772=ORIENTED_EDGE('',*,*,#8851,.F.);
#11773=ORIENTED_EDGE('',*,*,#8856,.T.);
#11774=ORIENTED_EDGE('',*,*,#8857,.T.);
#11775=ORIENTED_EDGE('',*,*,#8858,.T.);
#11776=ORIENTED_EDGE('',*,*,#8854,.F.);
#11777=ORIENTED_EDGE('',*,*,#8859,.T.);
#11778=ORIENTED_EDGE('',*,*,#8860,.T.);
#11779=ORIENTED_EDGE('',*,*,#8861,.T.);
#11780=ORIENTED_EDGE('',*,*,#8857,.F.);
#11781=ORIENTED_EDGE('',*,*,#8862,.T.);
#11782=ORIENTED_EDGE('',*,*,#8863,.T.);
#11783=ORIENTED_EDGE('',*,*,#8864,.T.);
#11784=ORIENTED_EDGE('',*,*,#8860,.F.);
#11785=ORIENTED_EDGE('',*,*,#8865,.T.);
#11786=ORIENTED_EDGE('',*,*,#8866,.T.);
#11787=ORIENTED_EDGE('',*,*,#8867,.T.);
#11788=ORIENTED_EDGE('',*,*,#8863,.F.);
#11789=ORIENTED_EDGE('',*,*,#8868,.T.);
#11790=ORIENTED_EDGE('',*,*,#8869,.T.);
#11791=ORIENTED_EDGE('',*,*,#8870,.T.);
#11792=ORIENTED_EDGE('',*,*,#8866,.F.);
#11793=ORIENTED_EDGE('',*,*,#8871,.T.);
#11794=ORIENTED_EDGE('',*,*,#8872,.F.);
#11795=ORIENTED_EDGE('',*,*,#8873,.T.);
#11796=ORIENTED_EDGE('',*,*,#8874,.F.);
#11797=ORIENTED_EDGE('',*,*,#8875,.T.);
#11798=ORIENTED_EDGE('',*,*,#8876,.T.);
#11799=ORIENTED_EDGE('',*,*,#8877,.T.);
#11800=ORIENTED_EDGE('',*,*,#8878,.F.);
#11801=ORIENTED_EDGE('',*,*,#8879,.F.);
#11802=ORIENTED_EDGE('',*,*,#8880,.T.);
#11803=ORIENTED_EDGE('',*,*,#8881,.T.);
#11804=ORIENTED_EDGE('',*,*,#8876,.F.);
#11805=ORIENTED_EDGE('',*,*,#8882,.F.);
#11806=ORIENTED_EDGE('',*,*,#8883,.T.);
#11807=ORIENTED_EDGE('',*,*,#8884,.T.);
#11808=ORIENTED_EDGE('',*,*,#8880,.F.);
#11809=ORIENTED_EDGE('',*,*,#8885,.F.);
#11810=ORIENTED_EDGE('',*,*,#8886,.T.);
#11811=ORIENTED_EDGE('',*,*,#8887,.T.);
#11812=ORIENTED_EDGE('',*,*,#8883,.F.);
#11813=ORIENTED_EDGE('',*,*,#8888,.F.);
#11814=ORIENTED_EDGE('',*,*,#8889,.T.);
#11815=ORIENTED_EDGE('',*,*,#8890,.T.);
#11816=ORIENTED_EDGE('',*,*,#8886,.F.);
#11817=ORIENTED_EDGE('',*,*,#8891,.F.);
#11818=ORIENTED_EDGE('',*,*,#8892,.T.);
#11819=ORIENTED_EDGE('',*,*,#8893,.T.);
#11820=ORIENTED_EDGE('',*,*,#8889,.F.);
#11821=ORIENTED_EDGE('',*,*,#8894,.F.);
#11822=ORIENTED_EDGE('',*,*,#8895,.T.);
#11823=ORIENTED_EDGE('',*,*,#8896,.T.);
#11824=ORIENTED_EDGE('',*,*,#8892,.F.);
#11825=ORIENTED_EDGE('',*,*,#8897,.F.);
#11826=ORIENTED_EDGE('',*,*,#8898,.T.);
#11827=ORIENTED_EDGE('',*,*,#8899,.T.);
#11828=ORIENTED_EDGE('',*,*,#8895,.F.);
#11829=ORIENTED_EDGE('',*,*,#8900,.F.);
#11830=ORIENTED_EDGE('',*,*,#8901,.T.);
#11831=ORIENTED_EDGE('',*,*,#8902,.T.);
#11832=ORIENTED_EDGE('',*,*,#8898,.F.);
#11833=ORIENTED_EDGE('',*,*,#8903,.F.);
#11834=ORIENTED_EDGE('',*,*,#8904,.T.);
#11835=ORIENTED_EDGE('',*,*,#8905,.T.);
#11836=ORIENTED_EDGE('',*,*,#8901,.F.);
#11837=ORIENTED_EDGE('',*,*,#8906,.F.);
#11838=ORIENTED_EDGE('',*,*,#8907,.T.);
#11839=ORIENTED_EDGE('',*,*,#8908,.T.);
#11840=ORIENTED_EDGE('',*,*,#8904,.F.);
#11841=ORIENTED_EDGE('',*,*,#8909,.F.);
#11842=ORIENTED_EDGE('',*,*,#8910,.T.);
#11843=ORIENTED_EDGE('',*,*,#8911,.T.);
#11844=ORIENTED_EDGE('',*,*,#8907,.F.);
#11845=ORIENTED_EDGE('',*,*,#8912,.F.);
#11846=ORIENTED_EDGE('',*,*,#8913,.F.);
#11847=ORIENTED_EDGE('',*,*,#8914,.F.);
#11848=ORIENTED_EDGE('',*,*,#8915,.F.);
#11849=ORIENTED_EDGE('',*,*,#8916,.T.);
#11850=ORIENTED_EDGE('',*,*,#8917,.T.);
#11851=ORIENTED_EDGE('',*,*,#8918,.T.);
#11852=ORIENTED_EDGE('',*,*,#8919,.T.);
#11853=ORIENTED_EDGE('',*,*,#8920,.T.);
#11854=ORIENTED_EDGE('',*,*,#8921,.T.);
#11855=ORIENTED_EDGE('',*,*,#8922,.T.);
#11856=ORIENTED_EDGE('',*,*,#8921,.F.);
#11857=ORIENTED_EDGE('',*,*,#8923,.T.);
#11858=ORIENTED_EDGE('',*,*,#8924,.T.);
#11859=ORIENTED_EDGE('',*,*,#8925,.T.);
#11860=ORIENTED_EDGE('',*,*,#8917,.F.);
#11861=ORIENTED_EDGE('',*,*,#8926,.T.);
#11862=ORIENTED_EDGE('',*,*,#8927,.T.);
#11863=ORIENTED_EDGE('',*,*,#8928,.T.);
#11864=ORIENTED_EDGE('',*,*,#8924,.F.);
#11865=ORIENTED_EDGE('',*,*,#8929,.T.);
#11866=ORIENTED_EDGE('',*,*,#8930,.T.);
#11867=ORIENTED_EDGE('',*,*,#8931,.T.);
#11868=ORIENTED_EDGE('',*,*,#8927,.F.);
#11869=ORIENTED_EDGE('',*,*,#8932,.T.);
#11870=ORIENTED_EDGE('',*,*,#8933,.T.);
#11871=ORIENTED_EDGE('',*,*,#8934,.T.);
#11872=ORIENTED_EDGE('',*,*,#8930,.F.);
#11873=ORIENTED_EDGE('',*,*,#8935,.T.);
#11874=ORIENTED_EDGE('',*,*,#8936,.T.);
#11875=ORIENTED_EDGE('',*,*,#8937,.T.);
#11876=ORIENTED_EDGE('',*,*,#8933,.F.);
#11877=ORIENTED_EDGE('',*,*,#8938,.T.);
#11878=ORIENTED_EDGE('',*,*,#8939,.T.);
#11879=ORIENTED_EDGE('',*,*,#8940,.T.);
#11880=ORIENTED_EDGE('',*,*,#8936,.F.);
#11881=ORIENTED_EDGE('',*,*,#8941,.T.);
#11882=ORIENTED_EDGE('',*,*,#8942,.T.);
#11883=ORIENTED_EDGE('',*,*,#8943,.T.);
#11884=ORIENTED_EDGE('',*,*,#8939,.F.);
#11885=ORIENTED_EDGE('',*,*,#8944,.T.);
#11886=ORIENTED_EDGE('',*,*,#8945,.T.);
#11887=ORIENTED_EDGE('',*,*,#8946,.T.);
#11888=ORIENTED_EDGE('',*,*,#8942,.F.);
#11889=ORIENTED_EDGE('',*,*,#8947,.T.);
#11890=ORIENTED_EDGE('',*,*,#8948,.T.);
#11891=ORIENTED_EDGE('',*,*,#8949,.T.);
#11892=ORIENTED_EDGE('',*,*,#8945,.F.);
#11893=ORIENTED_EDGE('',*,*,#8950,.T.);
#11894=ORIENTED_EDGE('',*,*,#8951,.T.);
#11895=ORIENTED_EDGE('',*,*,#8952,.T.);
#11896=ORIENTED_EDGE('',*,*,#8948,.F.);
#11897=ORIENTED_EDGE('',*,*,#8953,.T.);
#11898=ORIENTED_EDGE('',*,*,#8954,.F.);
#11899=ORIENTED_EDGE('',*,*,#8955,.T.);
#11900=ORIENTED_EDGE('',*,*,#8956,.F.);
#11901=ORIENTED_EDGE('',*,*,#8957,.T.);
#11902=ORIENTED_EDGE('',*,*,#8958,.T.);
#11903=ORIENTED_EDGE('',*,*,#8959,.T.);
#11904=ORIENTED_EDGE('',*,*,#8960,.F.);
#11905=ORIENTED_EDGE('',*,*,#8961,.F.);
#11906=ORIENTED_EDGE('',*,*,#8962,.T.);
#11907=ORIENTED_EDGE('',*,*,#8963,.T.);
#11908=ORIENTED_EDGE('',*,*,#8958,.F.);
#11909=ORIENTED_EDGE('',*,*,#8964,.F.);
#11910=ORIENTED_EDGE('',*,*,#8965,.T.);
#11911=ORIENTED_EDGE('',*,*,#8966,.T.);
#11912=ORIENTED_EDGE('',*,*,#8962,.F.);
#11913=ORIENTED_EDGE('',*,*,#8967,.F.);
#11914=ORIENTED_EDGE('',*,*,#8968,.T.);
#11915=ORIENTED_EDGE('',*,*,#8969,.T.);
#11916=ORIENTED_EDGE('',*,*,#8965,.F.);
#11917=ORIENTED_EDGE('',*,*,#8970,.F.);
#11918=ORIENTED_EDGE('',*,*,#8971,.T.);
#11919=ORIENTED_EDGE('',*,*,#8972,.T.);
#11920=ORIENTED_EDGE('',*,*,#8968,.F.);
#11921=ORIENTED_EDGE('',*,*,#8973,.F.);
#11922=ORIENTED_EDGE('',*,*,#8974,.T.);
#11923=ORIENTED_EDGE('',*,*,#8975,.T.);
#11924=ORIENTED_EDGE('',*,*,#8971,.F.);
#11925=ORIENTED_EDGE('',*,*,#8976,.F.);
#11926=ORIENTED_EDGE('',*,*,#8977,.T.);
#11927=ORIENTED_EDGE('',*,*,#8978,.T.);
#11928=ORIENTED_EDGE('',*,*,#8974,.F.);
#11929=ORIENTED_EDGE('',*,*,#8979,.F.);
#11930=ORIENTED_EDGE('',*,*,#8980,.T.);
#11931=ORIENTED_EDGE('',*,*,#8981,.T.);
#11932=ORIENTED_EDGE('',*,*,#8977,.F.);
#11933=ORIENTED_EDGE('',*,*,#8982,.F.);
#11934=ORIENTED_EDGE('',*,*,#8983,.T.);
#11935=ORIENTED_EDGE('',*,*,#8984,.T.);
#11936=ORIENTED_EDGE('',*,*,#8980,.F.);
#11937=ORIENTED_EDGE('',*,*,#8985,.F.);
#11938=ORIENTED_EDGE('',*,*,#8986,.T.);
#11939=ORIENTED_EDGE('',*,*,#8987,.T.);
#11940=ORIENTED_EDGE('',*,*,#8983,.F.);
#11941=ORIENTED_EDGE('',*,*,#8988,.F.);
#11942=ORIENTED_EDGE('',*,*,#8989,.T.);
#11943=ORIENTED_EDGE('',*,*,#8990,.T.);
#11944=ORIENTED_EDGE('',*,*,#8986,.F.);
#11945=ORIENTED_EDGE('',*,*,#8991,.F.);
#11946=ORIENTED_EDGE('',*,*,#8992,.T.);
#11947=ORIENTED_EDGE('',*,*,#8993,.T.);
#11948=ORIENTED_EDGE('',*,*,#8989,.F.);
#11949=ORIENTED_EDGE('',*,*,#8994,.F.);
#11950=ORIENTED_EDGE('',*,*,#8995,.F.);
#11951=ORIENTED_EDGE('',*,*,#8996,.F.);
#11952=ORIENTED_EDGE('',*,*,#8997,.F.);
#11953=ORIENTED_EDGE('',*,*,#8998,.T.);
#11954=ORIENTED_EDGE('',*,*,#8999,.T.);
#11955=ORIENTED_EDGE('',*,*,#9000,.T.);
#11956=ORIENTED_EDGE('',*,*,#9001,.T.);
#11957=ORIENTED_EDGE('',*,*,#9002,.T.);
#11958=ORIENTED_EDGE('',*,*,#9003,.T.);
#11959=ORIENTED_EDGE('',*,*,#9004,.T.);
#11960=ORIENTED_EDGE('',*,*,#9003,.F.);
#11961=ORIENTED_EDGE('',*,*,#9005,.T.);
#11962=ORIENTED_EDGE('',*,*,#9006,.T.);
#11963=ORIENTED_EDGE('',*,*,#9007,.T.);
#11964=ORIENTED_EDGE('',*,*,#8999,.F.);
#11965=ORIENTED_EDGE('',*,*,#9008,.T.);
#11966=ORIENTED_EDGE('',*,*,#9009,.T.);
#11967=ORIENTED_EDGE('',*,*,#9010,.T.);
#11968=ORIENTED_EDGE('',*,*,#9006,.F.);
#11969=ORIENTED_EDGE('',*,*,#9011,.T.);
#11970=ORIENTED_EDGE('',*,*,#9012,.T.);
#11971=ORIENTED_EDGE('',*,*,#9013,.T.);
#11972=ORIENTED_EDGE('',*,*,#9009,.F.);
#11973=ORIENTED_EDGE('',*,*,#9014,.T.);
#11974=ORIENTED_EDGE('',*,*,#9015,.T.);
#11975=ORIENTED_EDGE('',*,*,#9016,.T.);
#11976=ORIENTED_EDGE('',*,*,#9012,.F.);
#11977=ORIENTED_EDGE('',*,*,#9017,.T.);
#11978=ORIENTED_EDGE('',*,*,#9018,.T.);
#11979=ORIENTED_EDGE('',*,*,#9019,.T.);
#11980=ORIENTED_EDGE('',*,*,#9015,.F.);
#11981=ORIENTED_EDGE('',*,*,#9020,.T.);
#11982=ORIENTED_EDGE('',*,*,#9021,.T.);
#11983=ORIENTED_EDGE('',*,*,#9022,.T.);
#11984=ORIENTED_EDGE('',*,*,#9018,.F.);
#11985=ORIENTED_EDGE('',*,*,#9023,.T.);
#11986=ORIENTED_EDGE('',*,*,#9024,.T.);
#11987=ORIENTED_EDGE('',*,*,#9025,.T.);
#11988=ORIENTED_EDGE('',*,*,#9021,.F.);
#11989=ORIENTED_EDGE('',*,*,#9026,.T.);
#11990=ORIENTED_EDGE('',*,*,#9027,.T.);
#11991=ORIENTED_EDGE('',*,*,#9028,.T.);
#11992=ORIENTED_EDGE('',*,*,#9024,.F.);
#11993=ORIENTED_EDGE('',*,*,#9029,.T.);
#11994=ORIENTED_EDGE('',*,*,#9030,.T.);
#11995=ORIENTED_EDGE('',*,*,#9031,.T.);
#11996=ORIENTED_EDGE('',*,*,#9027,.F.);
#11997=ORIENTED_EDGE('',*,*,#9032,.T.);
#11998=ORIENTED_EDGE('',*,*,#9033,.T.);
#11999=ORIENTED_EDGE('',*,*,#9034,.T.);
#12000=ORIENTED_EDGE('',*,*,#9030,.F.);
#12001=ORIENTED_EDGE('',*,*,#9035,.T.);
#12002=ORIENTED_EDGE('',*,*,#9036,.F.);
#12003=ORIENTED_EDGE('',*,*,#9037,.T.);
#12004=ORIENTED_EDGE('',*,*,#9038,.F.);
#12005=ORIENTED_EDGE('',*,*,#9039,.T.);
#12006=ORIENTED_EDGE('',*,*,#9040,.T.);
#12007=ORIENTED_EDGE('',*,*,#9041,.T.);
#12008=ORIENTED_EDGE('',*,*,#9042,.F.);
#12009=ORIENTED_EDGE('',*,*,#9043,.F.);
#12010=ORIENTED_EDGE('',*,*,#9044,.T.);
#12011=ORIENTED_EDGE('',*,*,#9045,.T.);
#12012=ORIENTED_EDGE('',*,*,#9040,.F.);
#12013=ORIENTED_EDGE('',*,*,#9046,.F.);
#12014=ORIENTED_EDGE('',*,*,#9047,.T.);
#12015=ORIENTED_EDGE('',*,*,#9048,.T.);
#12016=ORIENTED_EDGE('',*,*,#9044,.F.);
#12017=ORIENTED_EDGE('',*,*,#9049,.F.);
#12018=ORIENTED_EDGE('',*,*,#9050,.T.);
#12019=ORIENTED_EDGE('',*,*,#9051,.T.);
#12020=ORIENTED_EDGE('',*,*,#9047,.F.);
#12021=ORIENTED_EDGE('',*,*,#9052,.F.);
#12022=ORIENTED_EDGE('',*,*,#9053,.T.);
#12023=ORIENTED_EDGE('',*,*,#9054,.T.);
#12024=ORIENTED_EDGE('',*,*,#9050,.F.);
#12025=ORIENTED_EDGE('',*,*,#9055,.F.);
#12026=ORIENTED_EDGE('',*,*,#9056,.T.);
#12027=ORIENTED_EDGE('',*,*,#9057,.T.);
#12028=ORIENTED_EDGE('',*,*,#9053,.F.);
#12029=ORIENTED_EDGE('',*,*,#9058,.F.);
#12030=ORIENTED_EDGE('',*,*,#9059,.T.);
#12031=ORIENTED_EDGE('',*,*,#9060,.T.);
#12032=ORIENTED_EDGE('',*,*,#9056,.F.);
#12033=ORIENTED_EDGE('',*,*,#9061,.F.);
#12034=ORIENTED_EDGE('',*,*,#9062,.T.);
#12035=ORIENTED_EDGE('',*,*,#9063,.T.);
#12036=ORIENTED_EDGE('',*,*,#9059,.F.);
#12037=ORIENTED_EDGE('',*,*,#9064,.F.);
#12038=ORIENTED_EDGE('',*,*,#9065,.T.);
#12039=ORIENTED_EDGE('',*,*,#9066,.T.);
#12040=ORIENTED_EDGE('',*,*,#9062,.F.);
#12041=ORIENTED_EDGE('',*,*,#9067,.F.);
#12042=ORIENTED_EDGE('',*,*,#9068,.T.);
#12043=ORIENTED_EDGE('',*,*,#9069,.T.);
#12044=ORIENTED_EDGE('',*,*,#9065,.F.);
#12045=ORIENTED_EDGE('',*,*,#9070,.F.);
#12046=ORIENTED_EDGE('',*,*,#9071,.T.);
#12047=ORIENTED_EDGE('',*,*,#9072,.T.);
#12048=ORIENTED_EDGE('',*,*,#9068,.F.);
#12049=ORIENTED_EDGE('',*,*,#9073,.F.);
#12050=ORIENTED_EDGE('',*,*,#9074,.T.);
#12051=ORIENTED_EDGE('',*,*,#9075,.T.);
#12052=ORIENTED_EDGE('',*,*,#9071,.F.);
#12053=ORIENTED_EDGE('',*,*,#9076,.F.);
#12054=ORIENTED_EDGE('',*,*,#9077,.F.);
#12055=ORIENTED_EDGE('',*,*,#9078,.F.);
#12056=ORIENTED_EDGE('',*,*,#9079,.F.);
#12057=ORIENTED_EDGE('',*,*,#9080,.T.);
#12058=ORIENTED_EDGE('',*,*,#9081,.T.);
#12059=ORIENTED_EDGE('',*,*,#9082,.T.);
#12060=ORIENTED_EDGE('',*,*,#9083,.T.);
#12061=ORIENTED_EDGE('',*,*,#9084,.T.);
#12062=ORIENTED_EDGE('',*,*,#9085,.T.);
#12063=ORIENTED_EDGE('',*,*,#9086,.T.);
#12064=ORIENTED_EDGE('',*,*,#9085,.F.);
#12065=ORIENTED_EDGE('',*,*,#9087,.T.);
#12066=ORIENTED_EDGE('',*,*,#9088,.T.);
#12067=ORIENTED_EDGE('',*,*,#9089,.T.);
#12068=ORIENTED_EDGE('',*,*,#9081,.F.);
#12069=ORIENTED_EDGE('',*,*,#9090,.T.);
#12070=ORIENTED_EDGE('',*,*,#9091,.T.);
#12071=ORIENTED_EDGE('',*,*,#9092,.T.);
#12072=ORIENTED_EDGE('',*,*,#9088,.F.);
#12073=ORIENTED_EDGE('',*,*,#9093,.T.);
#12074=ORIENTED_EDGE('',*,*,#9094,.T.);
#12075=ORIENTED_EDGE('',*,*,#9095,.T.);
#12076=ORIENTED_EDGE('',*,*,#9091,.F.);
#12077=ORIENTED_EDGE('',*,*,#9096,.T.);
#12078=ORIENTED_EDGE('',*,*,#9097,.T.);
#12079=ORIENTED_EDGE('',*,*,#9098,.T.);
#12080=ORIENTED_EDGE('',*,*,#9094,.F.);
#12081=ORIENTED_EDGE('',*,*,#9099,.T.);
#12082=ORIENTED_EDGE('',*,*,#9100,.T.);
#12083=ORIENTED_EDGE('',*,*,#9101,.T.);
#12084=ORIENTED_EDGE('',*,*,#9097,.F.);
#12085=ORIENTED_EDGE('',*,*,#9102,.T.);
#12086=ORIENTED_EDGE('',*,*,#9103,.T.);
#12087=ORIENTED_EDGE('',*,*,#9104,.T.);
#12088=ORIENTED_EDGE('',*,*,#9100,.F.);
#12089=ORIENTED_EDGE('',*,*,#9105,.T.);
#12090=ORIENTED_EDGE('',*,*,#9106,.T.);
#12091=ORIENTED_EDGE('',*,*,#9107,.T.);
#12092=ORIENTED_EDGE('',*,*,#9103,.F.);
#12093=ORIENTED_EDGE('',*,*,#9108,.T.);
#12094=ORIENTED_EDGE('',*,*,#9109,.T.);
#12095=ORIENTED_EDGE('',*,*,#9110,.T.);
#12096=ORIENTED_EDGE('',*,*,#9106,.F.);
#12097=ORIENTED_EDGE('',*,*,#9111,.T.);
#12098=ORIENTED_EDGE('',*,*,#9112,.T.);
#12099=ORIENTED_EDGE('',*,*,#9113,.T.);
#12100=ORIENTED_EDGE('',*,*,#9109,.F.);
#12101=ORIENTED_EDGE('',*,*,#9114,.T.);
#12102=ORIENTED_EDGE('',*,*,#9115,.T.);
#12103=ORIENTED_EDGE('',*,*,#9116,.T.);
#12104=ORIENTED_EDGE('',*,*,#9112,.F.);
#12105=ORIENTED_EDGE('',*,*,#9117,.T.);
#12106=ORIENTED_EDGE('',*,*,#9118,.F.);
#12107=ORIENTED_EDGE('',*,*,#9119,.T.);
#12108=ORIENTED_EDGE('',*,*,#9120,.F.);
#12109=ORIENTED_EDGE('',*,*,#9121,.T.);
#12110=ORIENTED_EDGE('',*,*,#9122,.T.);
#12111=ORIENTED_EDGE('',*,*,#9123,.T.);
#12112=ORIENTED_EDGE('',*,*,#9124,.F.);
#12113=ORIENTED_EDGE('',*,*,#9125,.F.);
#12114=ORIENTED_EDGE('',*,*,#9126,.T.);
#12115=ORIENTED_EDGE('',*,*,#9127,.T.);
#12116=ORIENTED_EDGE('',*,*,#9122,.F.);
#12117=ORIENTED_EDGE('',*,*,#9128,.F.);
#12118=ORIENTED_EDGE('',*,*,#9129,.T.);
#12119=ORIENTED_EDGE('',*,*,#9130,.T.);
#12120=ORIENTED_EDGE('',*,*,#9126,.F.);
#12121=ORIENTED_EDGE('',*,*,#9131,.F.);
#12122=ORIENTED_EDGE('',*,*,#9132,.T.);
#12123=ORIENTED_EDGE('',*,*,#9133,.T.);
#12124=ORIENTED_EDGE('',*,*,#9129,.F.);
#12125=ORIENTED_EDGE('',*,*,#9134,.F.);
#12126=ORIENTED_EDGE('',*,*,#9135,.T.);
#12127=ORIENTED_EDGE('',*,*,#9136,.T.);
#12128=ORIENTED_EDGE('',*,*,#9132,.F.);
#12129=ORIENTED_EDGE('',*,*,#9137,.F.);
#12130=ORIENTED_EDGE('',*,*,#9138,.T.);
#12131=ORIENTED_EDGE('',*,*,#9139,.T.);
#12132=ORIENTED_EDGE('',*,*,#9135,.F.);
#12133=ORIENTED_EDGE('',*,*,#9140,.F.);
#12134=ORIENTED_EDGE('',*,*,#9141,.T.);
#12135=ORIENTED_EDGE('',*,*,#9142,.T.);
#12136=ORIENTED_EDGE('',*,*,#9138,.F.);
#12137=ORIENTED_EDGE('',*,*,#9143,.F.);
#12138=ORIENTED_EDGE('',*,*,#9144,.T.);
#12139=ORIENTED_EDGE('',*,*,#9145,.T.);
#12140=ORIENTED_EDGE('',*,*,#9141,.F.);
#12141=ORIENTED_EDGE('',*,*,#9146,.F.);
#12142=ORIENTED_EDGE('',*,*,#9147,.T.);
#12143=ORIENTED_EDGE('',*,*,#9148,.T.);
#12144=ORIENTED_EDGE('',*,*,#9144,.F.);
#12145=ORIENTED_EDGE('',*,*,#9149,.F.);
#12146=ORIENTED_EDGE('',*,*,#9150,.T.);
#12147=ORIENTED_EDGE('',*,*,#9151,.T.);
#12148=ORIENTED_EDGE('',*,*,#9147,.F.);
#12149=ORIENTED_EDGE('',*,*,#9152,.F.);
#12150=ORIENTED_EDGE('',*,*,#9153,.T.);
#12151=ORIENTED_EDGE('',*,*,#9154,.T.);
#12152=ORIENTED_EDGE('',*,*,#9150,.F.);
#12153=ORIENTED_EDGE('',*,*,#9155,.F.);
#12154=ORIENTED_EDGE('',*,*,#9156,.T.);
#12155=ORIENTED_EDGE('',*,*,#9157,.T.);
#12156=ORIENTED_EDGE('',*,*,#9153,.F.);
#12157=ORIENTED_EDGE('',*,*,#9158,.F.);
#12158=ORIENTED_EDGE('',*,*,#9159,.F.);
#12159=ORIENTED_EDGE('',*,*,#9160,.F.);
#12160=ORIENTED_EDGE('',*,*,#9161,.F.);
#12161=ORIENTED_EDGE('',*,*,#9162,.T.);
#12162=ORIENTED_EDGE('',*,*,#9163,.T.);
#12163=ORIENTED_EDGE('',*,*,#9164,.T.);
#12164=ORIENTED_EDGE('',*,*,#9165,.T.);
#12165=ORIENTED_EDGE('',*,*,#9166,.T.);
#12166=ORIENTED_EDGE('',*,*,#9167,.T.);
#12167=ORIENTED_EDGE('',*,*,#9168,.T.);
#12168=ORIENTED_EDGE('',*,*,#9167,.F.);
#12169=ORIENTED_EDGE('',*,*,#9169,.T.);
#12170=ORIENTED_EDGE('',*,*,#9170,.T.);
#12171=ORIENTED_EDGE('',*,*,#9171,.T.);
#12172=ORIENTED_EDGE('',*,*,#9163,.F.);
#12173=ORIENTED_EDGE('',*,*,#9172,.T.);
#12174=ORIENTED_EDGE('',*,*,#9173,.T.);
#12175=ORIENTED_EDGE('',*,*,#9174,.T.);
#12176=ORIENTED_EDGE('',*,*,#9170,.F.);
#12177=ORIENTED_EDGE('',*,*,#9175,.T.);
#12178=ORIENTED_EDGE('',*,*,#9176,.T.);
#12179=ORIENTED_EDGE('',*,*,#9177,.T.);
#12180=ORIENTED_EDGE('',*,*,#9173,.F.);
#12181=ORIENTED_EDGE('',*,*,#9178,.T.);
#12182=ORIENTED_EDGE('',*,*,#9179,.T.);
#12183=ORIENTED_EDGE('',*,*,#9180,.T.);
#12184=ORIENTED_EDGE('',*,*,#9176,.F.);
#12185=ORIENTED_EDGE('',*,*,#9181,.T.);
#12186=ORIENTED_EDGE('',*,*,#9182,.T.);
#12187=ORIENTED_EDGE('',*,*,#9183,.T.);
#12188=ORIENTED_EDGE('',*,*,#9179,.F.);
#12189=ORIENTED_EDGE('',*,*,#9184,.T.);
#12190=ORIENTED_EDGE('',*,*,#9185,.T.);
#12191=ORIENTED_EDGE('',*,*,#9186,.T.);
#12192=ORIENTED_EDGE('',*,*,#9182,.F.);
#12193=ORIENTED_EDGE('',*,*,#9187,.T.);
#12194=ORIENTED_EDGE('',*,*,#9188,.T.);
#12195=ORIENTED_EDGE('',*,*,#9189,.T.);
#12196=ORIENTED_EDGE('',*,*,#9185,.F.);
#12197=ORIENTED_EDGE('',*,*,#9190,.T.);
#12198=ORIENTED_EDGE('',*,*,#9191,.T.);
#12199=ORIENTED_EDGE('',*,*,#9192,.T.);
#12200=ORIENTED_EDGE('',*,*,#9188,.F.);
#12201=ORIENTED_EDGE('',*,*,#9193,.T.);
#12202=ORIENTED_EDGE('',*,*,#9194,.T.);
#12203=ORIENTED_EDGE('',*,*,#9195,.T.);
#12204=ORIENTED_EDGE('',*,*,#9191,.F.);
#12205=ORIENTED_EDGE('',*,*,#9196,.T.);
#12206=ORIENTED_EDGE('',*,*,#9197,.T.);
#12207=ORIENTED_EDGE('',*,*,#9198,.T.);
#12208=ORIENTED_EDGE('',*,*,#9194,.F.);
#12209=ORIENTED_EDGE('',*,*,#9199,.T.);
#12210=ORIENTED_EDGE('',*,*,#9200,.F.);
#12211=ORIENTED_EDGE('',*,*,#9201,.T.);
#12212=ORIENTED_EDGE('',*,*,#9202,.F.);
#12213=ORIENTED_EDGE('',*,*,#9203,.T.);
#12214=ORIENTED_EDGE('',*,*,#9204,.T.);
#12215=ORIENTED_EDGE('',*,*,#9205,.T.);
#12216=ORIENTED_EDGE('',*,*,#9206,.F.);
#12217=ORIENTED_EDGE('',*,*,#9207,.F.);
#12218=ORIENTED_EDGE('',*,*,#9208,.T.);
#12219=ORIENTED_EDGE('',*,*,#9209,.T.);
#12220=ORIENTED_EDGE('',*,*,#9204,.F.);
#12221=ORIENTED_EDGE('',*,*,#9210,.F.);
#12222=ORIENTED_EDGE('',*,*,#9211,.T.);
#12223=ORIENTED_EDGE('',*,*,#9212,.T.);
#12224=ORIENTED_EDGE('',*,*,#9208,.F.);
#12225=ORIENTED_EDGE('',*,*,#9213,.F.);
#12226=ORIENTED_EDGE('',*,*,#9214,.T.);
#12227=ORIENTED_EDGE('',*,*,#9215,.T.);
#12228=ORIENTED_EDGE('',*,*,#9211,.F.);
#12229=ORIENTED_EDGE('',*,*,#9216,.F.);
#12230=ORIENTED_EDGE('',*,*,#9217,.T.);
#12231=ORIENTED_EDGE('',*,*,#9218,.T.);
#12232=ORIENTED_EDGE('',*,*,#9214,.F.);
#12233=ORIENTED_EDGE('',*,*,#9219,.F.);
#12234=ORIENTED_EDGE('',*,*,#9220,.T.);
#12235=ORIENTED_EDGE('',*,*,#9221,.T.);
#12236=ORIENTED_EDGE('',*,*,#9217,.F.);
#12237=ORIENTED_EDGE('',*,*,#9222,.F.);
#12238=ORIENTED_EDGE('',*,*,#9223,.T.);
#12239=ORIENTED_EDGE('',*,*,#9224,.T.);
#12240=ORIENTED_EDGE('',*,*,#9220,.F.);
#12241=ORIENTED_EDGE('',*,*,#9225,.F.);
#12242=ORIENTED_EDGE('',*,*,#9226,.T.);
#12243=ORIENTED_EDGE('',*,*,#9227,.T.);
#12244=ORIENTED_EDGE('',*,*,#9223,.F.);
#12245=ORIENTED_EDGE('',*,*,#9228,.F.);
#12246=ORIENTED_EDGE('',*,*,#9229,.T.);
#12247=ORIENTED_EDGE('',*,*,#9230,.T.);
#12248=ORIENTED_EDGE('',*,*,#9226,.F.);
#12249=ORIENTED_EDGE('',*,*,#9231,.F.);
#12250=ORIENTED_EDGE('',*,*,#9232,.T.);
#12251=ORIENTED_EDGE('',*,*,#9233,.T.);
#12252=ORIENTED_EDGE('',*,*,#9229,.F.);
#12253=ORIENTED_EDGE('',*,*,#9234,.F.);
#12254=ORIENTED_EDGE('',*,*,#9235,.T.);
#12255=ORIENTED_EDGE('',*,*,#9236,.T.);
#12256=ORIENTED_EDGE('',*,*,#9232,.F.);
#12257=ORIENTED_EDGE('',*,*,#9237,.F.);
#12258=ORIENTED_EDGE('',*,*,#9238,.T.);
#12259=ORIENTED_EDGE('',*,*,#9239,.T.);
#12260=ORIENTED_EDGE('',*,*,#9235,.F.);
#12261=ORIENTED_EDGE('',*,*,#9240,.F.);
#12262=ORIENTED_EDGE('',*,*,#9241,.F.);
#12263=ORIENTED_EDGE('',*,*,#9242,.F.);
#12264=ORIENTED_EDGE('',*,*,#9243,.F.);
#12265=ORIENTED_EDGE('',*,*,#9244,.T.);
#12266=ORIENTED_EDGE('',*,*,#9245,.T.);
#12267=ORIENTED_EDGE('',*,*,#9246,.T.);
#12268=ORIENTED_EDGE('',*,*,#9247,.T.);
#12269=ORIENTED_EDGE('',*,*,#9248,.T.);
#12270=ORIENTED_EDGE('',*,*,#9249,.T.);
#12271=ORIENTED_EDGE('',*,*,#9250,.T.);
#12272=ORIENTED_EDGE('',*,*,#9245,.F.);
#12273=ORIENTED_EDGE('',*,*,#9251,.T.);
#12274=ORIENTED_EDGE('',*,*,#9252,.T.);
#12275=ORIENTED_EDGE('',*,*,#9253,.T.);
#12276=ORIENTED_EDGE('',*,*,#9249,.F.);
#12277=ORIENTED_EDGE('',*,*,#9254,.T.);
#12278=ORIENTED_EDGE('',*,*,#9255,.T.);
#12279=ORIENTED_EDGE('',*,*,#9256,.T.);
#12280=ORIENTED_EDGE('',*,*,#9252,.F.);
#12281=ORIENTED_EDGE('',*,*,#9257,.T.);
#12282=ORIENTED_EDGE('',*,*,#9258,.T.);
#12283=ORIENTED_EDGE('',*,*,#9259,.T.);
#12284=ORIENTED_EDGE('',*,*,#9255,.F.);
#12285=ORIENTED_EDGE('',*,*,#9260,.T.);
#12286=ORIENTED_EDGE('',*,*,#9261,.T.);
#12287=ORIENTED_EDGE('',*,*,#9262,.T.);
#12288=ORIENTED_EDGE('',*,*,#9258,.F.);
#12289=ORIENTED_EDGE('',*,*,#9263,.T.);
#12290=ORIENTED_EDGE('',*,*,#9264,.T.);
#12291=ORIENTED_EDGE('',*,*,#9265,.T.);
#12292=ORIENTED_EDGE('',*,*,#9261,.F.);
#12293=ORIENTED_EDGE('',*,*,#9266,.T.);
#12294=ORIENTED_EDGE('',*,*,#9267,.F.);
#12295=ORIENTED_EDGE('',*,*,#9268,.T.);
#12296=ORIENTED_EDGE('',*,*,#9269,.F.);
#12297=ORIENTED_EDGE('',*,*,#9270,.T.);
#12298=ORIENTED_EDGE('',*,*,#9271,.T.);
#12299=ORIENTED_EDGE('',*,*,#9272,.T.);
#12300=ORIENTED_EDGE('',*,*,#9273,.F.);
#12301=ORIENTED_EDGE('',*,*,#9274,.F.);
#12302=ORIENTED_EDGE('',*,*,#9275,.T.);
#12303=ORIENTED_EDGE('',*,*,#9276,.T.);
#12304=ORIENTED_EDGE('',*,*,#9271,.F.);
#12305=ORIENTED_EDGE('',*,*,#9277,.F.);
#12306=ORIENTED_EDGE('',*,*,#9278,.T.);
#12307=ORIENTED_EDGE('',*,*,#9279,.T.);
#12308=ORIENTED_EDGE('',*,*,#9275,.F.);
#12309=ORIENTED_EDGE('',*,*,#9280,.F.);
#12310=ORIENTED_EDGE('',*,*,#9281,.T.);
#12311=ORIENTED_EDGE('',*,*,#9282,.T.);
#12312=ORIENTED_EDGE('',*,*,#9278,.F.);
#12313=ORIENTED_EDGE('',*,*,#9283,.F.);
#12314=ORIENTED_EDGE('',*,*,#9284,.T.);
#12315=ORIENTED_EDGE('',*,*,#9285,.T.);
#12316=ORIENTED_EDGE('',*,*,#9281,.F.);
#12317=ORIENTED_EDGE('',*,*,#9286,.F.);
#12318=ORIENTED_EDGE('',*,*,#9287,.T.);
#12319=ORIENTED_EDGE('',*,*,#9288,.T.);
#12320=ORIENTED_EDGE('',*,*,#9284,.F.);
#12321=ORIENTED_EDGE('',*,*,#9289,.F.);
#12322=ORIENTED_EDGE('',*,*,#9290,.T.);
#12323=ORIENTED_EDGE('',*,*,#9291,.T.);
#12324=ORIENTED_EDGE('',*,*,#9287,.F.);
#12325=ORIENTED_EDGE('',*,*,#9292,.F.);
#12326=ORIENTED_EDGE('',*,*,#9293,.F.);
#12327=ORIENTED_EDGE('',*,*,#9294,.F.);
#12328=ORIENTED_EDGE('',*,*,#9295,.F.);
#12329=ORIENTED_EDGE('',*,*,#9296,.F.);
#12330=ORIENTED_EDGE('',*,*,#9297,.T.);
#12331=ORIENTED_EDGE('',*,*,#9298,.T.);
#12332=ORIENTED_EDGE('',*,*,#9299,.T.);
#12333=ORIENTED_EDGE('',*,*,#9300,.T.);
#12334=ORIENTED_EDGE('',*,*,#9301,.T.);
#12335=ORIENTED_EDGE('',*,*,#9302,.T.);
#12336=ORIENTED_EDGE('',*,*,#9303,.T.);
#12337=ORIENTED_EDGE('',*,*,#9298,.F.);
#12338=ORIENTED_EDGE('',*,*,#9304,.T.);
#12339=ORIENTED_EDGE('',*,*,#9305,.T.);
#12340=ORIENTED_EDGE('',*,*,#9306,.T.);
#12341=ORIENTED_EDGE('',*,*,#9302,.F.);
#12342=ORIENTED_EDGE('',*,*,#9307,.T.);
#12343=ORIENTED_EDGE('',*,*,#9308,.T.);
#12344=ORIENTED_EDGE('',*,*,#9309,.T.);
#12345=ORIENTED_EDGE('',*,*,#9305,.F.);
#12346=ORIENTED_EDGE('',*,*,#9310,.T.);
#12347=ORIENTED_EDGE('',*,*,#9311,.T.);
#12348=ORIENTED_EDGE('',*,*,#9312,.T.);
#12349=ORIENTED_EDGE('',*,*,#9308,.F.);
#12350=ORIENTED_EDGE('',*,*,#9313,.T.);
#12351=ORIENTED_EDGE('',*,*,#9314,.T.);
#12352=ORIENTED_EDGE('',*,*,#9315,.T.);
#12353=ORIENTED_EDGE('',*,*,#9311,.F.);
#12354=ORIENTED_EDGE('',*,*,#9316,.T.);
#12355=ORIENTED_EDGE('',*,*,#9317,.T.);
#12356=ORIENTED_EDGE('',*,*,#9318,.T.);
#12357=ORIENTED_EDGE('',*,*,#9314,.F.);
#12358=ORIENTED_EDGE('',*,*,#9319,.T.);
#12359=ORIENTED_EDGE('',*,*,#9320,.F.);
#12360=ORIENTED_EDGE('',*,*,#9321,.T.);
#12361=ORIENTED_EDGE('',*,*,#9322,.F.);
#12362=ORIENTED_EDGE('',*,*,#9323,.T.);
#12363=ORIENTED_EDGE('',*,*,#9324,.T.);
#12364=ORIENTED_EDGE('',*,*,#9325,.T.);
#12365=ORIENTED_EDGE('',*,*,#9326,.T.);
#12366=ORIENTED_EDGE('',*,*,#9327,.T.);
#12367=ORIENTED_EDGE('',*,*,#9328,.T.);
#12368=ORIENTED_EDGE('',*,*,#9329,.T.);
#12369=ORIENTED_EDGE('',*,*,#9324,.F.);
#12370=ORIENTED_EDGE('',*,*,#9330,.T.);
#12371=ORIENTED_EDGE('',*,*,#9331,.T.);
#12372=ORIENTED_EDGE('',*,*,#9332,.T.);
#12373=ORIENTED_EDGE('',*,*,#9328,.F.);
#12374=ORIENTED_EDGE('',*,*,#9333,.T.);
#12375=ORIENTED_EDGE('',*,*,#9334,.T.);
#12376=ORIENTED_EDGE('',*,*,#9335,.T.);
#12377=ORIENTED_EDGE('',*,*,#9331,.F.);
#12378=ORIENTED_EDGE('',*,*,#9336,.T.);
#12379=ORIENTED_EDGE('',*,*,#9337,.T.);
#12380=ORIENTED_EDGE('',*,*,#9338,.T.);
#12381=ORIENTED_EDGE('',*,*,#9334,.F.);
#12382=ORIENTED_EDGE('',*,*,#9339,.T.);
#12383=ORIENTED_EDGE('',*,*,#9340,.T.);
#12384=ORIENTED_EDGE('',*,*,#9341,.T.);
#12385=ORIENTED_EDGE('',*,*,#9337,.F.);
#12386=ORIENTED_EDGE('',*,*,#9342,.T.);
#12387=ORIENTED_EDGE('',*,*,#9343,.T.);
#12388=ORIENTED_EDGE('',*,*,#9344,.T.);
#12389=ORIENTED_EDGE('',*,*,#9340,.F.);
#12390=ORIENTED_EDGE('',*,*,#9345,.T.);
#12391=ORIENTED_EDGE('',*,*,#9346,.F.);
#12392=ORIENTED_EDGE('',*,*,#9347,.T.);
#12393=ORIENTED_EDGE('',*,*,#9348,.F.);
#12394=ORIENTED_EDGE('',*,*,#9349,.T.);
#12395=ORIENTED_EDGE('',*,*,#9350,.T.);
#12396=ORIENTED_EDGE('',*,*,#9351,.T.);
#12397=ORIENTED_EDGE('',*,*,#9352,.T.);
#12398=ORIENTED_EDGE('',*,*,#9353,.T.);
#12399=ORIENTED_EDGE('',*,*,#9354,.T.);
#12400=ORIENTED_EDGE('',*,*,#9355,.T.);
#12401=ORIENTED_EDGE('',*,*,#9350,.F.);
#12402=ORIENTED_EDGE('',*,*,#9356,.T.);
#12403=ORIENTED_EDGE('',*,*,#9357,.T.);
#12404=ORIENTED_EDGE('',*,*,#9358,.T.);
#12405=ORIENTED_EDGE('',*,*,#9354,.F.);
#12406=ORIENTED_EDGE('',*,*,#9359,.T.);
#12407=ORIENTED_EDGE('',*,*,#9360,.T.);
#12408=ORIENTED_EDGE('',*,*,#9361,.T.);
#12409=ORIENTED_EDGE('',*,*,#9357,.F.);
#12410=ORIENTED_EDGE('',*,*,#9362,.T.);
#12411=ORIENTED_EDGE('',*,*,#9363,.T.);
#12412=ORIENTED_EDGE('',*,*,#9364,.T.);
#12413=ORIENTED_EDGE('',*,*,#9360,.F.);
#12414=ORIENTED_EDGE('',*,*,#9365,.T.);
#12415=ORIENTED_EDGE('',*,*,#9366,.T.);
#12416=ORIENTED_EDGE('',*,*,#9367,.T.);
#12417=ORIENTED_EDGE('',*,*,#9363,.F.);
#12418=ORIENTED_EDGE('',*,*,#9368,.T.);
#12419=ORIENTED_EDGE('',*,*,#9369,.T.);
#12420=ORIENTED_EDGE('',*,*,#9370,.T.);
#12421=ORIENTED_EDGE('',*,*,#9366,.F.);
#12422=ORIENTED_EDGE('',*,*,#9371,.T.);
#12423=ORIENTED_EDGE('',*,*,#9372,.F.);
#12424=ORIENTED_EDGE('',*,*,#9373,.T.);
#12425=ORIENTED_EDGE('',*,*,#9374,.F.);
#12426=ORIENTED_EDGE('',*,*,#9375,.T.);
#12427=ORIENTED_EDGE('',*,*,#9376,.T.);
#12428=ORIENTED_EDGE('',*,*,#9377,.T.);
#12429=ORIENTED_EDGE('',*,*,#9378,.F.);
#12430=ORIENTED_EDGE('',*,*,#9379,.F.);
#12431=ORIENTED_EDGE('',*,*,#9380,.T.);
#12432=ORIENTED_EDGE('',*,*,#9381,.T.);
#12433=ORIENTED_EDGE('',*,*,#9376,.F.);
#12434=ORIENTED_EDGE('',*,*,#9382,.F.);
#12435=ORIENTED_EDGE('',*,*,#9383,.T.);
#12436=ORIENTED_EDGE('',*,*,#9384,.T.);
#12437=ORIENTED_EDGE('',*,*,#9380,.F.);
#12438=ORIENTED_EDGE('',*,*,#9385,.F.);
#12439=ORIENTED_EDGE('',*,*,#9386,.T.);
#12440=ORIENTED_EDGE('',*,*,#9387,.T.);
#12441=ORIENTED_EDGE('',*,*,#9383,.F.);
#12442=ORIENTED_EDGE('',*,*,#9388,.F.);
#12443=ORIENTED_EDGE('',*,*,#9389,.T.);
#12444=ORIENTED_EDGE('',*,*,#9390,.T.);
#12445=ORIENTED_EDGE('',*,*,#9386,.F.);
#12446=ORIENTED_EDGE('',*,*,#9391,.F.);
#12447=ORIENTED_EDGE('',*,*,#9392,.T.);
#12448=ORIENTED_EDGE('',*,*,#9393,.T.);
#12449=ORIENTED_EDGE('',*,*,#9389,.F.);
#12450=ORIENTED_EDGE('',*,*,#9394,.F.);
#12451=ORIENTED_EDGE('',*,*,#9395,.T.);
#12452=ORIENTED_EDGE('',*,*,#9396,.T.);
#12453=ORIENTED_EDGE('',*,*,#9392,.F.);
#12454=ORIENTED_EDGE('',*,*,#9397,.F.);
#12455=ORIENTED_EDGE('',*,*,#9398,.F.);
#12456=ORIENTED_EDGE('',*,*,#9399,.F.);
#12457=ORIENTED_EDGE('',*,*,#9400,.F.);
#12458=ORIENTED_EDGE('',*,*,#9401,.F.);
#12459=ORIENTED_EDGE('',*,*,#9402,.T.);
#12460=ORIENTED_EDGE('',*,*,#9403,.T.);
#12461=ORIENTED_EDGE('',*,*,#9404,.T.);
#12462=ORIENTED_EDGE('',*,*,#9405,.F.);
#12463=ORIENTED_EDGE('',*,*,#9406,.F.);
#12464=ORIENTED_EDGE('',*,*,#9407,.T.);
#12465=ORIENTED_EDGE('',*,*,#9408,.T.);
#12466=ORIENTED_EDGE('',*,*,#9403,.F.);
#12467=ORIENTED_EDGE('',*,*,#9409,.F.);
#12468=ORIENTED_EDGE('',*,*,#9410,.T.);
#12469=ORIENTED_EDGE('',*,*,#9411,.T.);
#12470=ORIENTED_EDGE('',*,*,#9407,.F.);
#12471=ORIENTED_EDGE('',*,*,#9412,.F.);
#12472=ORIENTED_EDGE('',*,*,#9413,.T.);
#12473=ORIENTED_EDGE('',*,*,#9414,.T.);
#12474=ORIENTED_EDGE('',*,*,#9410,.F.);
#12475=ORIENTED_EDGE('',*,*,#9415,.F.);
#12476=ORIENTED_EDGE('',*,*,#9416,.T.);
#12477=ORIENTED_EDGE('',*,*,#9417,.T.);
#12478=ORIENTED_EDGE('',*,*,#9413,.F.);
#12479=ORIENTED_EDGE('',*,*,#9418,.F.);
#12480=ORIENTED_EDGE('',*,*,#9419,.T.);
#12481=ORIENTED_EDGE('',*,*,#9420,.T.);
#12482=ORIENTED_EDGE('',*,*,#9416,.F.);
#12483=ORIENTED_EDGE('',*,*,#9421,.F.);
#12484=ORIENTED_EDGE('',*,*,#9422,.T.);
#12485=ORIENTED_EDGE('',*,*,#9423,.T.);
#12486=ORIENTED_EDGE('',*,*,#9419,.F.);
#12487=ORIENTED_EDGE('',*,*,#9424,.F.);
#12488=ORIENTED_EDGE('',*,*,#9425,.F.);
#12489=ORIENTED_EDGE('',*,*,#9426,.F.);
#12490=ORIENTED_EDGE('',*,*,#9427,.F.);
#12491=ORIENTED_EDGE('',*,*,#9428,.F.);
#12492=ORIENTED_EDGE('',*,*,#9429,.T.);
#12493=ORIENTED_EDGE('',*,*,#9430,.T.);
#12494=ORIENTED_EDGE('',*,*,#9431,.T.);
#12495=ORIENTED_EDGE('',*,*,#9432,.F.);
#12496=ORIENTED_EDGE('',*,*,#9433,.F.);
#12497=ORIENTED_EDGE('',*,*,#9434,.T.);
#12498=ORIENTED_EDGE('',*,*,#9435,.T.);
#12499=ORIENTED_EDGE('',*,*,#9430,.F.);
#12500=ORIENTED_EDGE('',*,*,#9436,.F.);
#12501=ORIENTED_EDGE('',*,*,#9437,.T.);
#12502=ORIENTED_EDGE('',*,*,#9438,.T.);
#12503=ORIENTED_EDGE('',*,*,#9434,.F.);
#12504=ORIENTED_EDGE('',*,*,#9439,.F.);
#12505=ORIENTED_EDGE('',*,*,#9440,.T.);
#12506=ORIENTED_EDGE('',*,*,#9441,.T.);
#12507=ORIENTED_EDGE('',*,*,#9437,.F.);
#12508=ORIENTED_EDGE('',*,*,#9442,.F.);
#12509=ORIENTED_EDGE('',*,*,#9443,.T.);
#12510=ORIENTED_EDGE('',*,*,#9444,.T.);
#12511=ORIENTED_EDGE('',*,*,#9440,.F.);
#12512=ORIENTED_EDGE('',*,*,#9445,.F.);
#12513=ORIENTED_EDGE('',*,*,#9446,.T.);
#12514=ORIENTED_EDGE('',*,*,#9447,.T.);
#12515=ORIENTED_EDGE('',*,*,#9443,.F.);
#12516=ORIENTED_EDGE('',*,*,#9448,.F.);
#12517=ORIENTED_EDGE('',*,*,#9449,.T.);
#12518=ORIENTED_EDGE('',*,*,#9450,.T.);
#12519=ORIENTED_EDGE('',*,*,#9446,.F.);
#12520=ORIENTED_EDGE('',*,*,#9451,.F.);
#12521=ORIENTED_EDGE('',*,*,#9452,.F.);
#12522=ORIENTED_EDGE('',*,*,#9453,.F.);
#12523=ORIENTED_EDGE('',*,*,#9454,.F.);
#12524=ORIENTED_EDGE('',*,*,#9455,.F.);
#12525=ORIENTED_EDGE('',*,*,#9456,.T.);
#12526=ORIENTED_EDGE('',*,*,#9457,.F.);
#12527=ORIENTED_EDGE('',*,*,#9373,.F.);
#12528=ORIENTED_EDGE('',*,*,#9458,.F.);
#12529=ORIENTED_EDGE('',*,*,#9371,.F.);
#12530=ORIENTED_EDGE('',*,*,#9368,.F.);
#12531=ORIENTED_EDGE('',*,*,#9365,.F.);
#12532=ORIENTED_EDGE('',*,*,#9362,.F.);
#12533=ORIENTED_EDGE('',*,*,#9359,.F.);
#12534=ORIENTED_EDGE('',*,*,#9356,.F.);
#12535=ORIENTED_EDGE('',*,*,#9353,.F.);
#12536=ORIENTED_EDGE('',*,*,#9459,.F.);
#12537=ORIENTED_EDGE('',*,*,#9431,.F.);
#12538=ORIENTED_EDGE('',*,*,#9435,.F.);
#12539=ORIENTED_EDGE('',*,*,#9438,.F.);
#12540=ORIENTED_EDGE('',*,*,#9441,.F.);
#12541=ORIENTED_EDGE('',*,*,#9444,.F.);
#12542=ORIENTED_EDGE('',*,*,#9447,.F.);
#12543=ORIENTED_EDGE('',*,*,#9450,.F.);
#12544=ORIENTED_EDGE('',*,*,#9460,.F.);
#12545=ORIENTED_EDGE('',*,*,#9456,.F.);
#12546=ORIENTED_EDGE('',*,*,#9452,.T.);
#12547=ORIENTED_EDGE('',*,*,#9460,.T.);
#12548=ORIENTED_EDGE('',*,*,#9449,.F.);
#12549=ORIENTED_EDGE('',*,*,#9461,.F.);
#12550=ORIENTED_EDGE('',*,*,#9462,.F.);
#12551=ORIENTED_EDGE('',*,*,#9453,.T.);
#12552=ORIENTED_EDGE('',*,*,#9461,.T.);
#12553=ORIENTED_EDGE('',*,*,#9451,.T.);
#12554=ORIENTED_EDGE('',*,*,#9448,.T.);
#12555=ORIENTED_EDGE('',*,*,#9445,.T.);
#12556=ORIENTED_EDGE('',*,*,#9442,.T.);
#12557=ORIENTED_EDGE('',*,*,#9439,.T.);
#12558=ORIENTED_EDGE('',*,*,#9436,.T.);
#12559=ORIENTED_EDGE('',*,*,#9433,.T.);
#12560=ORIENTED_EDGE('',*,*,#9463,.F.);
#12561=ORIENTED_EDGE('',*,*,#9351,.F.);
#12562=ORIENTED_EDGE('',*,*,#9355,.F.);
#12563=ORIENTED_EDGE('',*,*,#9358,.F.);
#12564=ORIENTED_EDGE('',*,*,#9361,.F.);
#12565=ORIENTED_EDGE('',*,*,#9364,.F.);
#12566=ORIENTED_EDGE('',*,*,#9367,.F.);
#12567=ORIENTED_EDGE('',*,*,#9370,.F.);
#12568=ORIENTED_EDGE('',*,*,#9464,.F.);
#12569=ORIENTED_EDGE('',*,*,#9375,.F.);
#12570=ORIENTED_EDGE('',*,*,#9465,.F.);
#12571=ORIENTED_EDGE('',*,*,#9347,.F.);
#12572=ORIENTED_EDGE('',*,*,#9466,.F.);
#12573=ORIENTED_EDGE('',*,*,#9345,.F.);
#12574=ORIENTED_EDGE('',*,*,#9342,.F.);
#12575=ORIENTED_EDGE('',*,*,#9339,.F.);
#12576=ORIENTED_EDGE('',*,*,#9336,.F.);
#12577=ORIENTED_EDGE('',*,*,#9333,.F.);
#12578=ORIENTED_EDGE('',*,*,#9330,.F.);
#12579=ORIENTED_EDGE('',*,*,#9327,.F.);
#12580=ORIENTED_EDGE('',*,*,#9467,.F.);
#12581=ORIENTED_EDGE('',*,*,#9404,.F.);
#12582=ORIENTED_EDGE('',*,*,#9408,.F.);
#12583=ORIENTED_EDGE('',*,*,#9411,.F.);
#12584=ORIENTED_EDGE('',*,*,#9414,.F.);
#12585=ORIENTED_EDGE('',*,*,#9417,.F.);
#12586=ORIENTED_EDGE('',*,*,#9420,.F.);
#12587=ORIENTED_EDGE('',*,*,#9423,.F.);
#12588=ORIENTED_EDGE('',*,*,#9468,.F.);
#12589=ORIENTED_EDGE('',*,*,#9429,.F.);
#12590=ORIENTED_EDGE('',*,*,#9425,.T.);
#12591=ORIENTED_EDGE('',*,*,#9468,.T.);
#12592=ORIENTED_EDGE('',*,*,#9422,.F.);
#12593=ORIENTED_EDGE('',*,*,#9469,.F.);
#12594=ORIENTED_EDGE('',*,*,#9470,.F.);
#12595=ORIENTED_EDGE('',*,*,#9426,.T.);
#12596=ORIENTED_EDGE('',*,*,#9469,.T.);
#12597=ORIENTED_EDGE('',*,*,#9424,.T.);
#12598=ORIENTED_EDGE('',*,*,#9421,.T.);
#12599=ORIENTED_EDGE('',*,*,#9418,.T.);
#12600=ORIENTED_EDGE('',*,*,#9415,.T.);
#12601=ORIENTED_EDGE('',*,*,#9412,.T.);
#12602=ORIENTED_EDGE('',*,*,#9409,.T.);
#12603=ORIENTED_EDGE('',*,*,#9406,.T.);
#12604=ORIENTED_EDGE('',*,*,#9471,.F.);
#12605=ORIENTED_EDGE('',*,*,#9325,.F.);
#12606=ORIENTED_EDGE('',*,*,#9329,.F.);
#12607=ORIENTED_EDGE('',*,*,#9332,.F.);
#12608=ORIENTED_EDGE('',*,*,#9335,.F.);
#12609=ORIENTED_EDGE('',*,*,#9338,.F.);
#12610=ORIENTED_EDGE('',*,*,#9341,.F.);
#12611=ORIENTED_EDGE('',*,*,#9344,.F.);
#12612=ORIENTED_EDGE('',*,*,#9472,.F.);
#12613=ORIENTED_EDGE('',*,*,#9349,.F.);
#12614=ORIENTED_EDGE('',*,*,#9473,.F.);
#12615=ORIENTED_EDGE('',*,*,#9321,.F.);
#12616=ORIENTED_EDGE('',*,*,#9474,.F.);
#12617=ORIENTED_EDGE('',*,*,#9319,.F.);
#12618=ORIENTED_EDGE('',*,*,#9316,.F.);
#12619=ORIENTED_EDGE('',*,*,#9313,.F.);
#12620=ORIENTED_EDGE('',*,*,#9310,.F.);
#12621=ORIENTED_EDGE('',*,*,#9307,.F.);
#12622=ORIENTED_EDGE('',*,*,#9304,.F.);
#12623=ORIENTED_EDGE('',*,*,#9301,.F.);
#12624=ORIENTED_EDGE('',*,*,#9475,.F.);
#12625=ORIENTED_EDGE('',*,*,#9377,.F.);
#12626=ORIENTED_EDGE('',*,*,#9381,.F.);
#12627=ORIENTED_EDGE('',*,*,#9384,.F.);
#12628=ORIENTED_EDGE('',*,*,#9387,.F.);
#12629=ORIENTED_EDGE('',*,*,#9390,.F.);
#12630=ORIENTED_EDGE('',*,*,#9393,.F.);
#12631=ORIENTED_EDGE('',*,*,#9396,.F.);
#12632=ORIENTED_EDGE('',*,*,#9476,.F.);
#12633=ORIENTED_EDGE('',*,*,#9402,.F.);
#12634=ORIENTED_EDGE('',*,*,#9398,.T.);
#12635=ORIENTED_EDGE('',*,*,#9476,.T.);
#12636=ORIENTED_EDGE('',*,*,#9395,.F.);
#12637=ORIENTED_EDGE('',*,*,#9477,.F.);
#12638=ORIENTED_EDGE('',*,*,#9478,.F.);
#12639=ORIENTED_EDGE('',*,*,#9399,.T.);
#12640=ORIENTED_EDGE('',*,*,#9477,.T.);
#12641=ORIENTED_EDGE('',*,*,#9397,.T.);
#12642=ORIENTED_EDGE('',*,*,#9394,.T.);
#12643=ORIENTED_EDGE('',*,*,#9391,.T.);
#12644=ORIENTED_EDGE('',*,*,#9388,.T.);
#12645=ORIENTED_EDGE('',*,*,#9385,.T.);
#12646=ORIENTED_EDGE('',*,*,#9382,.T.);
#12647=ORIENTED_EDGE('',*,*,#9379,.T.);
#12648=ORIENTED_EDGE('',*,*,#9479,.F.);
#12649=ORIENTED_EDGE('',*,*,#9299,.F.);
#12650=ORIENTED_EDGE('',*,*,#9303,.F.);
#12651=ORIENTED_EDGE('',*,*,#9306,.F.);
#12652=ORIENTED_EDGE('',*,*,#9309,.F.);
#12653=ORIENTED_EDGE('',*,*,#9312,.F.);
#12654=ORIENTED_EDGE('',*,*,#9315,.F.);
#12655=ORIENTED_EDGE('',*,*,#9318,.F.);
#12656=ORIENTED_EDGE('',*,*,#9480,.F.);
#12657=ORIENTED_EDGE('',*,*,#9323,.F.);
#12658=ORIENTED_EDGE('',*,*,#9372,.T.);
#12659=ORIENTED_EDGE('',*,*,#9464,.T.);
#12660=ORIENTED_EDGE('',*,*,#9369,.F.);
#12661=ORIENTED_EDGE('',*,*,#9458,.T.);
#12662=ORIENTED_EDGE('',*,*,#9463,.T.);
#12663=ORIENTED_EDGE('',*,*,#9432,.T.);
#12664=ORIENTED_EDGE('',*,*,#9459,.T.);
#12665=ORIENTED_EDGE('',*,*,#9352,.F.);
#12666=ORIENTED_EDGE('',*,*,#9346,.T.);
#12667=ORIENTED_EDGE('',*,*,#9472,.T.);
#12668=ORIENTED_EDGE('',*,*,#9343,.F.);
#12669=ORIENTED_EDGE('',*,*,#9466,.T.);
#12670=ORIENTED_EDGE('',*,*,#9471,.T.);
#12671=ORIENTED_EDGE('',*,*,#9405,.T.);
#12672=ORIENTED_EDGE('',*,*,#9467,.T.);
#12673=ORIENTED_EDGE('',*,*,#9326,.F.);
#12674=ORIENTED_EDGE('',*,*,#9320,.T.);
#12675=ORIENTED_EDGE('',*,*,#9480,.T.);
#12676=ORIENTED_EDGE('',*,*,#9317,.F.);
#12677=ORIENTED_EDGE('',*,*,#9474,.T.);
#12678=ORIENTED_EDGE('',*,*,#9479,.T.);
#12679=ORIENTED_EDGE('',*,*,#9378,.T.);
#12680=ORIENTED_EDGE('',*,*,#9475,.T.);
#12681=ORIENTED_EDGE('',*,*,#9300,.F.);
#12682=ORIENTED_EDGE('',*,*,#9481,.F.);
#12683=ORIENTED_EDGE('',*,*,#9268,.F.);
#12684=ORIENTED_EDGE('',*,*,#9482,.F.);
#12685=ORIENTED_EDGE('',*,*,#9266,.F.);
#12686=ORIENTED_EDGE('',*,*,#9263,.F.);
#12687=ORIENTED_EDGE('',*,*,#9260,.F.);
#12688=ORIENTED_EDGE('',*,*,#9257,.F.);
#12689=ORIENTED_EDGE('',*,*,#9254,.F.);
#12690=ORIENTED_EDGE('',*,*,#9251,.F.);
#12691=ORIENTED_EDGE('',*,*,#9248,.F.);
#12692=ORIENTED_EDGE('',*,*,#9483,.F.);
#12693=ORIENTED_EDGE('',*,*,#9272,.F.);
#12694=ORIENTED_EDGE('',*,*,#9276,.F.);
#12695=ORIENTED_EDGE('',*,*,#9279,.F.);
#12696=ORIENTED_EDGE('',*,*,#9282,.F.);
#12697=ORIENTED_EDGE('',*,*,#9285,.F.);
#12698=ORIENTED_EDGE('',*,*,#9288,.F.);
#12699=ORIENTED_EDGE('',*,*,#9291,.F.);
#12700=ORIENTED_EDGE('',*,*,#9484,.F.);
#12701=ORIENTED_EDGE('',*,*,#9297,.F.);
#12702=ORIENTED_EDGE('',*,*,#9293,.T.);
#12703=ORIENTED_EDGE('',*,*,#9484,.T.);
#12704=ORIENTED_EDGE('',*,*,#9290,.F.);
#12705=ORIENTED_EDGE('',*,*,#9485,.F.);
#12706=ORIENTED_EDGE('',*,*,#9486,.F.);
#12707=ORIENTED_EDGE('',*,*,#9294,.T.);
#12708=ORIENTED_EDGE('',*,*,#9485,.T.);
#12709=ORIENTED_EDGE('',*,*,#9292,.T.);
#12710=ORIENTED_EDGE('',*,*,#9289,.T.);
#12711=ORIENTED_EDGE('',*,*,#9286,.T.);
#12712=ORIENTED_EDGE('',*,*,#9283,.T.);
#12713=ORIENTED_EDGE('',*,*,#9280,.T.);
#12714=ORIENTED_EDGE('',*,*,#9277,.T.);
#12715=ORIENTED_EDGE('',*,*,#9274,.T.);
#12716=ORIENTED_EDGE('',*,*,#9487,.F.);
#12717=ORIENTED_EDGE('',*,*,#9246,.F.);
#12718=ORIENTED_EDGE('',*,*,#9250,.F.);
#12719=ORIENTED_EDGE('',*,*,#9253,.F.);
#12720=ORIENTED_EDGE('',*,*,#9256,.F.);
#12721=ORIENTED_EDGE('',*,*,#9259,.F.);
#12722=ORIENTED_EDGE('',*,*,#9262,.F.);
#12723=ORIENTED_EDGE('',*,*,#9265,.F.);
#12724=ORIENTED_EDGE('',*,*,#9488,.F.);
#12725=ORIENTED_EDGE('',*,*,#9270,.F.);
#12726=ORIENTED_EDGE('',*,*,#9267,.T.);
#12727=ORIENTED_EDGE('',*,*,#9488,.T.);
#12728=ORIENTED_EDGE('',*,*,#9264,.F.);
#12729=ORIENTED_EDGE('',*,*,#9482,.T.);
#12730=ORIENTED_EDGE('',*,*,#9487,.T.);
#12731=ORIENTED_EDGE('',*,*,#9273,.T.);
#12732=ORIENTED_EDGE('',*,*,#9483,.T.);
#12733=ORIENTED_EDGE('',*,*,#9247,.F.);
#12734=ORIENTED_EDGE('',*,*,#9165,.F.);
#12735=ORIENTED_EDGE('',*,*,#9489,.T.);
#12736=ORIENTED_EDGE('',*,*,#9206,.T.);
#12737=ORIENTED_EDGE('',*,*,#9490,.T.);
#12738=ORIENTED_EDGE('',*,*,#9241,.T.);
#12739=ORIENTED_EDGE('',*,*,#9491,.T.);
#12740=ORIENTED_EDGE('',*,*,#9238,.F.);
#12741=ORIENTED_EDGE('',*,*,#9492,.F.);
#12742=ORIENTED_EDGE('',*,*,#9490,.F.);
#12743=ORIENTED_EDGE('',*,*,#9205,.F.);
#12744=ORIENTED_EDGE('',*,*,#9209,.F.);
#12745=ORIENTED_EDGE('',*,*,#9212,.F.);
#12746=ORIENTED_EDGE('',*,*,#9215,.F.);
#12747=ORIENTED_EDGE('',*,*,#9218,.F.);
#12748=ORIENTED_EDGE('',*,*,#9221,.F.);
#12749=ORIENTED_EDGE('',*,*,#9224,.F.);
#12750=ORIENTED_EDGE('',*,*,#9227,.F.);
#12751=ORIENTED_EDGE('',*,*,#9230,.F.);
#12752=ORIENTED_EDGE('',*,*,#9233,.F.);
#12753=ORIENTED_EDGE('',*,*,#9236,.F.);
#12754=ORIENTED_EDGE('',*,*,#9239,.F.);
#12755=ORIENTED_EDGE('',*,*,#9491,.F.);
#12756=ORIENTED_EDGE('',*,*,#9244,.F.);
#12757=ORIENTED_EDGE('',*,*,#9493,.F.);
#12758=ORIENTED_EDGE('',*,*,#9201,.F.);
#12759=ORIENTED_EDGE('',*,*,#9494,.F.);
#12760=ORIENTED_EDGE('',*,*,#9199,.F.);
#12761=ORIENTED_EDGE('',*,*,#9196,.F.);
#12762=ORIENTED_EDGE('',*,*,#9193,.F.);
#12763=ORIENTED_EDGE('',*,*,#9190,.F.);
#12764=ORIENTED_EDGE('',*,*,#9187,.F.);
#12765=ORIENTED_EDGE('',*,*,#9184,.F.);
#12766=ORIENTED_EDGE('',*,*,#9181,.F.);
#12767=ORIENTED_EDGE('',*,*,#9178,.F.);
#12768=ORIENTED_EDGE('',*,*,#9175,.F.);
#12769=ORIENTED_EDGE('',*,*,#9172,.F.);
#12770=ORIENTED_EDGE('',*,*,#9169,.F.);
#12771=ORIENTED_EDGE('',*,*,#9166,.F.);
#12772=ORIENTED_EDGE('',*,*,#9489,.F.);
#12773=ORIENTED_EDGE('',*,*,#9164,.F.);
#12774=ORIENTED_EDGE('',*,*,#9171,.F.);
#12775=ORIENTED_EDGE('',*,*,#9174,.F.);
#12776=ORIENTED_EDGE('',*,*,#9177,.F.);
#12777=ORIENTED_EDGE('',*,*,#9180,.F.);
#12778=ORIENTED_EDGE('',*,*,#9183,.F.);
#12779=ORIENTED_EDGE('',*,*,#9186,.F.);
#12780=ORIENTED_EDGE('',*,*,#9189,.F.);
#12781=ORIENTED_EDGE('',*,*,#9192,.F.);
#12782=ORIENTED_EDGE('',*,*,#9195,.F.);
#12783=ORIENTED_EDGE('',*,*,#9198,.F.);
#12784=ORIENTED_EDGE('',*,*,#9495,.F.);
#12785=ORIENTED_EDGE('',*,*,#9203,.F.);
#12786=ORIENTED_EDGE('',*,*,#9496,.F.);
#12787=ORIENTED_EDGE('',*,*,#9242,.T.);
#12788=ORIENTED_EDGE('',*,*,#9492,.T.);
#12789=ORIENTED_EDGE('',*,*,#9240,.T.);
#12790=ORIENTED_EDGE('',*,*,#9237,.T.);
#12791=ORIENTED_EDGE('',*,*,#9234,.T.);
#12792=ORIENTED_EDGE('',*,*,#9231,.T.);
#12793=ORIENTED_EDGE('',*,*,#9228,.T.);
#12794=ORIENTED_EDGE('',*,*,#9225,.T.);
#12795=ORIENTED_EDGE('',*,*,#9222,.T.);
#12796=ORIENTED_EDGE('',*,*,#9219,.T.);
#12797=ORIENTED_EDGE('',*,*,#9216,.T.);
#12798=ORIENTED_EDGE('',*,*,#9213,.T.);
#12799=ORIENTED_EDGE('',*,*,#9210,.T.);
#12800=ORIENTED_EDGE('',*,*,#9207,.T.);
#12801=ORIENTED_EDGE('',*,*,#9200,.T.);
#12802=ORIENTED_EDGE('',*,*,#9495,.T.);
#12803=ORIENTED_EDGE('',*,*,#9197,.F.);
#12804=ORIENTED_EDGE('',*,*,#9494,.T.);
#12805=ORIENTED_EDGE('',*,*,#9083,.F.);
#12806=ORIENTED_EDGE('',*,*,#9497,.T.);
#12807=ORIENTED_EDGE('',*,*,#9124,.T.);
#12808=ORIENTED_EDGE('',*,*,#9498,.T.);
#12809=ORIENTED_EDGE('',*,*,#9159,.T.);
#12810=ORIENTED_EDGE('',*,*,#9499,.T.);
#12811=ORIENTED_EDGE('',*,*,#9156,.F.);
#12812=ORIENTED_EDGE('',*,*,#9500,.F.);
#12813=ORIENTED_EDGE('',*,*,#9498,.F.);
#12814=ORIENTED_EDGE('',*,*,#9123,.F.);
#12815=ORIENTED_EDGE('',*,*,#9127,.F.);
#12816=ORIENTED_EDGE('',*,*,#9130,.F.);
#12817=ORIENTED_EDGE('',*,*,#9133,.F.);
#12818=ORIENTED_EDGE('',*,*,#9136,.F.);
#12819=ORIENTED_EDGE('',*,*,#9139,.F.);
#12820=ORIENTED_EDGE('',*,*,#9142,.F.);
#12821=ORIENTED_EDGE('',*,*,#9145,.F.);
#12822=ORIENTED_EDGE('',*,*,#9148,.F.);
#12823=ORIENTED_EDGE('',*,*,#9151,.F.);
#12824=ORIENTED_EDGE('',*,*,#9154,.F.);
#12825=ORIENTED_EDGE('',*,*,#9157,.F.);
#12826=ORIENTED_EDGE('',*,*,#9499,.F.);
#12827=ORIENTED_EDGE('',*,*,#9162,.F.);
#12828=ORIENTED_EDGE('',*,*,#9501,.F.);
#12829=ORIENTED_EDGE('',*,*,#9119,.F.);
#12830=ORIENTED_EDGE('',*,*,#9502,.F.);
#12831=ORIENTED_EDGE('',*,*,#9117,.F.);
#12832=ORIENTED_EDGE('',*,*,#9114,.F.);
#12833=ORIENTED_EDGE('',*,*,#9111,.F.);
#12834=ORIENTED_EDGE('',*,*,#9108,.F.);
#12835=ORIENTED_EDGE('',*,*,#9105,.F.);
#12836=ORIENTED_EDGE('',*,*,#9102,.F.);
#12837=ORIENTED_EDGE('',*,*,#9099,.F.);
#12838=ORIENTED_EDGE('',*,*,#9096,.F.);
#12839=ORIENTED_EDGE('',*,*,#9093,.F.);
#12840=ORIENTED_EDGE('',*,*,#9090,.F.);
#12841=ORIENTED_EDGE('',*,*,#9087,.F.);
#12842=ORIENTED_EDGE('',*,*,#9084,.F.);
#12843=ORIENTED_EDGE('',*,*,#9497,.F.);
#12844=ORIENTED_EDGE('',*,*,#9082,.F.);
#12845=ORIENTED_EDGE('',*,*,#9089,.F.);
#12846=ORIENTED_EDGE('',*,*,#9092,.F.);
#12847=ORIENTED_EDGE('',*,*,#9095,.F.);
#12848=ORIENTED_EDGE('',*,*,#9098,.F.);
#12849=ORIENTED_EDGE('',*,*,#9101,.F.);
#12850=ORIENTED_EDGE('',*,*,#9104,.F.);
#12851=ORIENTED_EDGE('',*,*,#9107,.F.);
#12852=ORIENTED_EDGE('',*,*,#9110,.F.);
#12853=ORIENTED_EDGE('',*,*,#9113,.F.);
#12854=ORIENTED_EDGE('',*,*,#9116,.F.);
#12855=ORIENTED_EDGE('',*,*,#9503,.F.);
#12856=ORIENTED_EDGE('',*,*,#9121,.F.);
#12857=ORIENTED_EDGE('',*,*,#9504,.F.);
#12858=ORIENTED_EDGE('',*,*,#9160,.T.);
#12859=ORIENTED_EDGE('',*,*,#9500,.T.);
#12860=ORIENTED_EDGE('',*,*,#9158,.T.);
#12861=ORIENTED_EDGE('',*,*,#9155,.T.);
#12862=ORIENTED_EDGE('',*,*,#9152,.T.);
#12863=ORIENTED_EDGE('',*,*,#9149,.T.);
#12864=ORIENTED_EDGE('',*,*,#9146,.T.);
#12865=ORIENTED_EDGE('',*,*,#9143,.T.);
#12866=ORIENTED_EDGE('',*,*,#9140,.T.);
#12867=ORIENTED_EDGE('',*,*,#9137,.T.);
#12868=ORIENTED_EDGE('',*,*,#9134,.T.);
#12869=ORIENTED_EDGE('',*,*,#9131,.T.);
#12870=ORIENTED_EDGE('',*,*,#9128,.T.);
#12871=ORIENTED_EDGE('',*,*,#9125,.T.);
#12872=ORIENTED_EDGE('',*,*,#9118,.T.);
#12873=ORIENTED_EDGE('',*,*,#9503,.T.);
#12874=ORIENTED_EDGE('',*,*,#9115,.F.);
#12875=ORIENTED_EDGE('',*,*,#9502,.T.);
#12876=ORIENTED_EDGE('',*,*,#9001,.F.);
#12877=ORIENTED_EDGE('',*,*,#9505,.T.);
#12878=ORIENTED_EDGE('',*,*,#9042,.T.);
#12879=ORIENTED_EDGE('',*,*,#9506,.T.);
#12880=ORIENTED_EDGE('',*,*,#9077,.T.);
#12881=ORIENTED_EDGE('',*,*,#9507,.T.);
#12882=ORIENTED_EDGE('',*,*,#9074,.F.);
#12883=ORIENTED_EDGE('',*,*,#9508,.F.);
#12884=ORIENTED_EDGE('',*,*,#9506,.F.);
#12885=ORIENTED_EDGE('',*,*,#9041,.F.);
#12886=ORIENTED_EDGE('',*,*,#9045,.F.);
#12887=ORIENTED_EDGE('',*,*,#9048,.F.);
#12888=ORIENTED_EDGE('',*,*,#9051,.F.);
#12889=ORIENTED_EDGE('',*,*,#9054,.F.);
#12890=ORIENTED_EDGE('',*,*,#9057,.F.);
#12891=ORIENTED_EDGE('',*,*,#9060,.F.);
#12892=ORIENTED_EDGE('',*,*,#9063,.F.);
#12893=ORIENTED_EDGE('',*,*,#9066,.F.);
#12894=ORIENTED_EDGE('',*,*,#9069,.F.);
#12895=ORIENTED_EDGE('',*,*,#9072,.F.);
#12896=ORIENTED_EDGE('',*,*,#9075,.F.);
#12897=ORIENTED_EDGE('',*,*,#9507,.F.);
#12898=ORIENTED_EDGE('',*,*,#9080,.F.);
#12899=ORIENTED_EDGE('',*,*,#9509,.F.);
#12900=ORIENTED_EDGE('',*,*,#9037,.F.);
#12901=ORIENTED_EDGE('',*,*,#9510,.F.);
#12902=ORIENTED_EDGE('',*,*,#9035,.F.);
#12903=ORIENTED_EDGE('',*,*,#9032,.F.);
#12904=ORIENTED_EDGE('',*,*,#9029,.F.);
#12905=ORIENTED_EDGE('',*,*,#9026,.F.);
#12906=ORIENTED_EDGE('',*,*,#9023,.F.);
#12907=ORIENTED_EDGE('',*,*,#9020,.F.);
#12908=ORIENTED_EDGE('',*,*,#9017,.F.);
#12909=ORIENTED_EDGE('',*,*,#9014,.F.);
#12910=ORIENTED_EDGE('',*,*,#9011,.F.);
#12911=ORIENTED_EDGE('',*,*,#9008,.F.);
#12912=ORIENTED_EDGE('',*,*,#9005,.F.);
#12913=ORIENTED_EDGE('',*,*,#9002,.F.);
#12914=ORIENTED_EDGE('',*,*,#9505,.F.);
#12915=ORIENTED_EDGE('',*,*,#9000,.F.);
#12916=ORIENTED_EDGE('',*,*,#9007,.F.);
#12917=ORIENTED_EDGE('',*,*,#9010,.F.);
#12918=ORIENTED_EDGE('',*,*,#9013,.F.);
#12919=ORIENTED_EDGE('',*,*,#9016,.F.);
#12920=ORIENTED_EDGE('',*,*,#9019,.F.);
#12921=ORIENTED_EDGE('',*,*,#9022,.F.);
#12922=ORIENTED_EDGE('',*,*,#9025,.F.);
#12923=ORIENTED_EDGE('',*,*,#9028,.F.);
#12924=ORIENTED_EDGE('',*,*,#9031,.F.);
#12925=ORIENTED_EDGE('',*,*,#9034,.F.);
#12926=ORIENTED_EDGE('',*,*,#9511,.F.);
#12927=ORIENTED_EDGE('',*,*,#9039,.F.);
#12928=ORIENTED_EDGE('',*,*,#9512,.F.);
#12929=ORIENTED_EDGE('',*,*,#9078,.T.);
#12930=ORIENTED_EDGE('',*,*,#9508,.T.);
#12931=ORIENTED_EDGE('',*,*,#9076,.T.);
#12932=ORIENTED_EDGE('',*,*,#9073,.T.);
#12933=ORIENTED_EDGE('',*,*,#9070,.T.);
#12934=ORIENTED_EDGE('',*,*,#9067,.T.);
#12935=ORIENTED_EDGE('',*,*,#9064,.T.);
#12936=ORIENTED_EDGE('',*,*,#9061,.T.);
#12937=ORIENTED_EDGE('',*,*,#9058,.T.);
#12938=ORIENTED_EDGE('',*,*,#9055,.T.);
#12939=ORIENTED_EDGE('',*,*,#9052,.T.);
#12940=ORIENTED_EDGE('',*,*,#9049,.T.);
#12941=ORIENTED_EDGE('',*,*,#9046,.T.);
#12942=ORIENTED_EDGE('',*,*,#9043,.T.);
#12943=ORIENTED_EDGE('',*,*,#9036,.T.);
#12944=ORIENTED_EDGE('',*,*,#9511,.T.);
#12945=ORIENTED_EDGE('',*,*,#9033,.F.);
#12946=ORIENTED_EDGE('',*,*,#9510,.T.);
#12947=ORIENTED_EDGE('',*,*,#8919,.F.);
#12948=ORIENTED_EDGE('',*,*,#9513,.T.);
#12949=ORIENTED_EDGE('',*,*,#8960,.T.);
#12950=ORIENTED_EDGE('',*,*,#9514,.T.);
#12951=ORIENTED_EDGE('',*,*,#8995,.T.);
#12952=ORIENTED_EDGE('',*,*,#9515,.T.);
#12953=ORIENTED_EDGE('',*,*,#8992,.F.);
#12954=ORIENTED_EDGE('',*,*,#9516,.F.);
#12955=ORIENTED_EDGE('',*,*,#9514,.F.);
#12956=ORIENTED_EDGE('',*,*,#8959,.F.);
#12957=ORIENTED_EDGE('',*,*,#8963,.F.);
#12958=ORIENTED_EDGE('',*,*,#8966,.F.);
#12959=ORIENTED_EDGE('',*,*,#8969,.F.);
#12960=ORIENTED_EDGE('',*,*,#8972,.F.);
#12961=ORIENTED_EDGE('',*,*,#8975,.F.);
#12962=ORIENTED_EDGE('',*,*,#8978,.F.);
#12963=ORIENTED_EDGE('',*,*,#8981,.F.);
#12964=ORIENTED_EDGE('',*,*,#8984,.F.);
#12965=ORIENTED_EDGE('',*,*,#8987,.F.);
#12966=ORIENTED_EDGE('',*,*,#8990,.F.);
#12967=ORIENTED_EDGE('',*,*,#8993,.F.);
#12968=ORIENTED_EDGE('',*,*,#9515,.F.);
#12969=ORIENTED_EDGE('',*,*,#8998,.F.);
#12970=ORIENTED_EDGE('',*,*,#9517,.F.);
#12971=ORIENTED_EDGE('',*,*,#8955,.F.);
#12972=ORIENTED_EDGE('',*,*,#9518,.F.);
#12973=ORIENTED_EDGE('',*,*,#8953,.F.);
#12974=ORIENTED_EDGE('',*,*,#8950,.F.);
#12975=ORIENTED_EDGE('',*,*,#8947,.F.);
#12976=ORIENTED_EDGE('',*,*,#8944,.F.);
#12977=ORIENTED_EDGE('',*,*,#8941,.F.);
#12978=ORIENTED_EDGE('',*,*,#8938,.F.);
#12979=ORIENTED_EDGE('',*,*,#8935,.F.);
#12980=ORIENTED_EDGE('',*,*,#8932,.F.);
#12981=ORIENTED_EDGE('',*,*,#8929,.F.);
#12982=ORIENTED_EDGE('',*,*,#8926,.F.);
#12983=ORIENTED_EDGE('',*,*,#8923,.F.);
#12984=ORIENTED_EDGE('',*,*,#8920,.F.);
#12985=ORIENTED_EDGE('',*,*,#9513,.F.);
#12986=ORIENTED_EDGE('',*,*,#8918,.F.);
#12987=ORIENTED_EDGE('',*,*,#8925,.F.);
#12988=ORIENTED_EDGE('',*,*,#8928,.F.);
#12989=ORIENTED_EDGE('',*,*,#8931,.F.);
#12990=ORIENTED_EDGE('',*,*,#8934,.F.);
#12991=ORIENTED_EDGE('',*,*,#8937,.F.);
#12992=ORIENTED_EDGE('',*,*,#8940,.F.);
#12993=ORIENTED_EDGE('',*,*,#8943,.F.);
#12994=ORIENTED_EDGE('',*,*,#8946,.F.);
#12995=ORIENTED_EDGE('',*,*,#8949,.F.);
#12996=ORIENTED_EDGE('',*,*,#8952,.F.);
#12997=ORIENTED_EDGE('',*,*,#9519,.F.);
#12998=ORIENTED_EDGE('',*,*,#8957,.F.);
#12999=ORIENTED_EDGE('',*,*,#9520,.F.);
#13000=ORIENTED_EDGE('',*,*,#8996,.T.);
#13001=ORIENTED_EDGE('',*,*,#9516,.T.);
#13002=ORIENTED_EDGE('',*,*,#8994,.T.);
#13003=ORIENTED_EDGE('',*,*,#8991,.T.);
#13004=ORIENTED_EDGE('',*,*,#8988,.T.);
#13005=ORIENTED_EDGE('',*,*,#8985,.T.);
#13006=ORIENTED_EDGE('',*,*,#8982,.T.);
#13007=ORIENTED_EDGE('',*,*,#8979,.T.);
#13008=ORIENTED_EDGE('',*,*,#8976,.T.);
#13009=ORIENTED_EDGE('',*,*,#8973,.T.);
#13010=ORIENTED_EDGE('',*,*,#8970,.T.);
#13011=ORIENTED_EDGE('',*,*,#8967,.T.);
#13012=ORIENTED_EDGE('',*,*,#8964,.T.);
#13013=ORIENTED_EDGE('',*,*,#8961,.T.);
#13014=ORIENTED_EDGE('',*,*,#8954,.T.);
#13015=ORIENTED_EDGE('',*,*,#9519,.T.);
#13016=ORIENTED_EDGE('',*,*,#8951,.F.);
#13017=ORIENTED_EDGE('',*,*,#9518,.T.);
#13018=ORIENTED_EDGE('',*,*,#8837,.F.);
#13019=ORIENTED_EDGE('',*,*,#9521,.T.);
#13020=ORIENTED_EDGE('',*,*,#8878,.T.);
#13021=ORIENTED_EDGE('',*,*,#9522,.T.);
#13022=ORIENTED_EDGE('',*,*,#8913,.T.);
#13023=ORIENTED_EDGE('',*,*,#9523,.T.);
#13024=ORIENTED_EDGE('',*,*,#8910,.F.);
#13025=ORIENTED_EDGE('',*,*,#9524,.F.);
#13026=ORIENTED_EDGE('',*,*,#9522,.F.);
#13027=ORIENTED_EDGE('',*,*,#8877,.F.);
#13028=ORIENTED_EDGE('',*,*,#8881,.F.);
#13029=ORIENTED_EDGE('',*,*,#8884,.F.);
#13030=ORIENTED_EDGE('',*,*,#8887,.F.);
#13031=ORIENTED_EDGE('',*,*,#8890,.F.);
#13032=ORIENTED_EDGE('',*,*,#8893,.F.);
#13033=ORIENTED_EDGE('',*,*,#8896,.F.);
#13034=ORIENTED_EDGE('',*,*,#8899,.F.);
#13035=ORIENTED_EDGE('',*,*,#8902,.F.);
#13036=ORIENTED_EDGE('',*,*,#8905,.F.);
#13037=ORIENTED_EDGE('',*,*,#8908,.F.);
#13038=ORIENTED_EDGE('',*,*,#8911,.F.);
#13039=ORIENTED_EDGE('',*,*,#9523,.F.);
#13040=ORIENTED_EDGE('',*,*,#8916,.F.);
#13041=ORIENTED_EDGE('',*,*,#9525,.F.);
#13042=ORIENTED_EDGE('',*,*,#8873,.F.);
#13043=ORIENTED_EDGE('',*,*,#9526,.F.);
#13044=ORIENTED_EDGE('',*,*,#8871,.F.);
#13045=ORIENTED_EDGE('',*,*,#8868,.F.);
#13046=ORIENTED_EDGE('',*,*,#8865,.F.);
#13047=ORIENTED_EDGE('',*,*,#8862,.F.);
#13048=ORIENTED_EDGE('',*,*,#8859,.F.);
#13049=ORIENTED_EDGE('',*,*,#8856,.F.);
#13050=ORIENTED_EDGE('',*,*,#8853,.F.);
#13051=ORIENTED_EDGE('',*,*,#8850,.F.);
#13052=ORIENTED_EDGE('',*,*,#8847,.F.);
#13053=ORIENTED_EDGE('',*,*,#8844,.F.);
#13054=ORIENTED_EDGE('',*,*,#8841,.F.);
#13055=ORIENTED_EDGE('',*,*,#8838,.F.);
#13056=ORIENTED_EDGE('',*,*,#9521,.F.);
#13057=ORIENTED_EDGE('',*,*,#8836,.F.);
#13058=ORIENTED_EDGE('',*,*,#8843,.F.);
#13059=ORIENTED_EDGE('',*,*,#8846,.F.);
#13060=ORIENTED_EDGE('',*,*,#8849,.F.);
#13061=ORIENTED_EDGE('',*,*,#8852,.F.);
#13062=ORIENTED_EDGE('',*,*,#8855,.F.);
#13063=ORIENTED_EDGE('',*,*,#8858,.F.);
#13064=ORIENTED_EDGE('',*,*,#8861,.F.);
#13065=ORIENTED_EDGE('',*,*,#8864,.F.);
#13066=ORIENTED_EDGE('',*,*,#8867,.F.);
#13067=ORIENTED_EDGE('',*,*,#8870,.F.);
#13068=ORIENTED_EDGE('',*,*,#9527,.F.);
#13069=ORIENTED_EDGE('',*,*,#8875,.F.);
#13070=ORIENTED_EDGE('',*,*,#9528,.F.);
#13071=ORIENTED_EDGE('',*,*,#8914,.T.);
#13072=ORIENTED_EDGE('',*,*,#9524,.T.);
#13073=ORIENTED_EDGE('',*,*,#8912,.T.);
#13074=ORIENTED_EDGE('',*,*,#8909,.T.);
#13075=ORIENTED_EDGE('',*,*,#8906,.T.);
#13076=ORIENTED_EDGE('',*,*,#8903,.T.);
#13077=ORIENTED_EDGE('',*,*,#8900,.T.);
#13078=ORIENTED_EDGE('',*,*,#8897,.T.);
#13079=ORIENTED_EDGE('',*,*,#8894,.T.);
#13080=ORIENTED_EDGE('',*,*,#8891,.T.);
#13081=ORIENTED_EDGE('',*,*,#8888,.T.);
#13082=ORIENTED_EDGE('',*,*,#8885,.T.);
#13083=ORIENTED_EDGE('',*,*,#8882,.T.);
#13084=ORIENTED_EDGE('',*,*,#8879,.T.);
#13085=ORIENTED_EDGE('',*,*,#8872,.T.);
#13086=ORIENTED_EDGE('',*,*,#9527,.T.);
#13087=ORIENTED_EDGE('',*,*,#8869,.F.);
#13088=ORIENTED_EDGE('',*,*,#9526,.T.);
#13089=ORIENTED_EDGE('',*,*,#9168,.F.);
#13090=ORIENTED_EDGE('',*,*,#9086,.F.);
#13091=ORIENTED_EDGE('',*,*,#9004,.F.);
#13092=ORIENTED_EDGE('',*,*,#8922,.F.);
#13093=ORIENTED_EDGE('',*,*,#8840,.F.);
#13094=ORIENTED_EDGE('',*,*,#8755,.F.);
#13095=ORIENTED_EDGE('',*,*,#9529,.T.);
#13096=ORIENTED_EDGE('',*,*,#8796,.T.);
#13097=ORIENTED_EDGE('',*,*,#9530,.T.);
#13098=ORIENTED_EDGE('',*,*,#8831,.T.);
#13099=ORIENTED_EDGE('',*,*,#9531,.T.);
#13100=ORIENTED_EDGE('',*,*,#8828,.F.);
#13101=ORIENTED_EDGE('',*,*,#9532,.F.);
#13102=ORIENTED_EDGE('',*,*,#9530,.F.);
#13103=ORIENTED_EDGE('',*,*,#8795,.F.);
#13104=ORIENTED_EDGE('',*,*,#8799,.F.);
#13105=ORIENTED_EDGE('',*,*,#8802,.F.);
#13106=ORIENTED_EDGE('',*,*,#8805,.F.);
#13107=ORIENTED_EDGE('',*,*,#8808,.F.);
#13108=ORIENTED_EDGE('',*,*,#8811,.F.);
#13109=ORIENTED_EDGE('',*,*,#8814,.F.);
#13110=ORIENTED_EDGE('',*,*,#8817,.F.);
#13111=ORIENTED_EDGE('',*,*,#8820,.F.);
#13112=ORIENTED_EDGE('',*,*,#8823,.F.);
#13113=ORIENTED_EDGE('',*,*,#8826,.F.);
#13114=ORIENTED_EDGE('',*,*,#8829,.F.);
#13115=ORIENTED_EDGE('',*,*,#9531,.F.);
#13116=ORIENTED_EDGE('',*,*,#8834,.F.);
#13117=ORIENTED_EDGE('',*,*,#9533,.F.);
#13118=ORIENTED_EDGE('',*,*,#8791,.F.);
#13119=ORIENTED_EDGE('',*,*,#9534,.F.);
#13120=ORIENTED_EDGE('',*,*,#8789,.F.);
#13121=ORIENTED_EDGE('',*,*,#8786,.F.);
#13122=ORIENTED_EDGE('',*,*,#8783,.F.);
#13123=ORIENTED_EDGE('',*,*,#8780,.F.);
#13124=ORIENTED_EDGE('',*,*,#8777,.F.);
#13125=ORIENTED_EDGE('',*,*,#8774,.F.);
#13126=ORIENTED_EDGE('',*,*,#8771,.F.);
#13127=ORIENTED_EDGE('',*,*,#8768,.F.);
#13128=ORIENTED_EDGE('',*,*,#8765,.F.);
#13129=ORIENTED_EDGE('',*,*,#8762,.F.);
#13130=ORIENTED_EDGE('',*,*,#8759,.F.);
#13131=ORIENTED_EDGE('',*,*,#8756,.F.);
#13132=ORIENTED_EDGE('',*,*,#9529,.F.);
#13133=ORIENTED_EDGE('',*,*,#8754,.F.);
#13134=ORIENTED_EDGE('',*,*,#8761,.F.);
#13135=ORIENTED_EDGE('',*,*,#8764,.F.);
#13136=ORIENTED_EDGE('',*,*,#8767,.F.);
#13137=ORIENTED_EDGE('',*,*,#8770,.F.);
#13138=ORIENTED_EDGE('',*,*,#8773,.F.);
#13139=ORIENTED_EDGE('',*,*,#8776,.F.);
#13140=ORIENTED_EDGE('',*,*,#8779,.F.);
#13141=ORIENTED_EDGE('',*,*,#8782,.F.);
#13142=ORIENTED_EDGE('',*,*,#8785,.F.);
#13143=ORIENTED_EDGE('',*,*,#8788,.F.);
#13144=ORIENTED_EDGE('',*,*,#9535,.F.);
#13145=ORIENTED_EDGE('',*,*,#8793,.F.);
#13146=ORIENTED_EDGE('',*,*,#9536,.F.);
#13147=ORIENTED_EDGE('',*,*,#8832,.T.);
#13148=ORIENTED_EDGE('',*,*,#9532,.T.);
#13149=ORIENTED_EDGE('',*,*,#8830,.T.);
#13150=ORIENTED_EDGE('',*,*,#8827,.T.);
#13151=ORIENTED_EDGE('',*,*,#8824,.T.);
#13152=ORIENTED_EDGE('',*,*,#8821,.T.);
#13153=ORIENTED_EDGE('',*,*,#8818,.T.);
#13154=ORIENTED_EDGE('',*,*,#8815,.T.);
#13155=ORIENTED_EDGE('',*,*,#8812,.T.);
#13156=ORIENTED_EDGE('',*,*,#8809,.T.);
#13157=ORIENTED_EDGE('',*,*,#8806,.T.);
#13158=ORIENTED_EDGE('',*,*,#8803,.T.);
#13159=ORIENTED_EDGE('',*,*,#8800,.T.);
#13160=ORIENTED_EDGE('',*,*,#8797,.T.);
#13161=ORIENTED_EDGE('',*,*,#8790,.T.);
#13162=ORIENTED_EDGE('',*,*,#9535,.T.);
#13163=ORIENTED_EDGE('',*,*,#8787,.F.);
#13164=ORIENTED_EDGE('',*,*,#9534,.T.);
#13165=ORIENTED_EDGE('',*,*,#8673,.F.);
#13166=ORIENTED_EDGE('',*,*,#9537,.T.);
#13167=ORIENTED_EDGE('',*,*,#8714,.T.);
#13168=ORIENTED_EDGE('',*,*,#9538,.T.);
#13169=ORIENTED_EDGE('',*,*,#8749,.T.);
#13170=ORIENTED_EDGE('',*,*,#9539,.T.);
#13171=ORIENTED_EDGE('',*,*,#8746,.F.);
#13172=ORIENTED_EDGE('',*,*,#9540,.F.);
#13173=ORIENTED_EDGE('',*,*,#9538,.F.);
#13174=ORIENTED_EDGE('',*,*,#8713,.F.);
#13175=ORIENTED_EDGE('',*,*,#8717,.F.);
#13176=ORIENTED_EDGE('',*,*,#8720,.F.);
#13177=ORIENTED_EDGE('',*,*,#8723,.F.);
#13178=ORIENTED_EDGE('',*,*,#8726,.F.);
#13179=ORIENTED_EDGE('',*,*,#8729,.F.);
#13180=ORIENTED_EDGE('',*,*,#8732,.F.);
#13181=ORIENTED_EDGE('',*,*,#8735,.F.);
#13182=ORIENTED_EDGE('',*,*,#8738,.F.);
#13183=ORIENTED_EDGE('',*,*,#8741,.F.);
#13184=ORIENTED_EDGE('',*,*,#8744,.F.);
#13185=ORIENTED_EDGE('',*,*,#8747,.F.);
#13186=ORIENTED_EDGE('',*,*,#9539,.F.);
#13187=ORIENTED_EDGE('',*,*,#8752,.F.);
#13188=ORIENTED_EDGE('',*,*,#9541,.F.);
#13189=ORIENTED_EDGE('',*,*,#8709,.F.);
#13190=ORIENTED_EDGE('',*,*,#9542,.F.);
#13191=ORIENTED_EDGE('',*,*,#8707,.F.);
#13192=ORIENTED_EDGE('',*,*,#8704,.F.);
#13193=ORIENTED_EDGE('',*,*,#8701,.F.);
#13194=ORIENTED_EDGE('',*,*,#8698,.F.);
#13195=ORIENTED_EDGE('',*,*,#8695,.F.);
#13196=ORIENTED_EDGE('',*,*,#8692,.F.);
#13197=ORIENTED_EDGE('',*,*,#8689,.F.);
#13198=ORIENTED_EDGE('',*,*,#8686,.F.);
#13199=ORIENTED_EDGE('',*,*,#8683,.F.);
#13200=ORIENTED_EDGE('',*,*,#8680,.F.);
#13201=ORIENTED_EDGE('',*,*,#8677,.F.);
#13202=ORIENTED_EDGE('',*,*,#8674,.F.);
#13203=ORIENTED_EDGE('',*,*,#9537,.F.);
#13204=ORIENTED_EDGE('',*,*,#8672,.F.);
#13205=ORIENTED_EDGE('',*,*,#8679,.F.);
#13206=ORIENTED_EDGE('',*,*,#8682,.F.);
#13207=ORIENTED_EDGE('',*,*,#8685,.F.);
#13208=ORIENTED_EDGE('',*,*,#8688,.F.);
#13209=ORIENTED_EDGE('',*,*,#8691,.F.);
#13210=ORIENTED_EDGE('',*,*,#8694,.F.);
#13211=ORIENTED_EDGE('',*,*,#8697,.F.);
#13212=ORIENTED_EDGE('',*,*,#8700,.F.);
#13213=ORIENTED_EDGE('',*,*,#8703,.F.);
#13214=ORIENTED_EDGE('',*,*,#8706,.F.);
#13215=ORIENTED_EDGE('',*,*,#9543,.F.);
#13216=ORIENTED_EDGE('',*,*,#8711,.F.);
#13217=ORIENTED_EDGE('',*,*,#9544,.F.);
#13218=ORIENTED_EDGE('',*,*,#8750,.T.);
#13219=ORIENTED_EDGE('',*,*,#9540,.T.);
#13220=ORIENTED_EDGE('',*,*,#8748,.T.);
#13221=ORIENTED_EDGE('',*,*,#8745,.T.);
#13222=ORIENTED_EDGE('',*,*,#8742,.T.);
#13223=ORIENTED_EDGE('',*,*,#8739,.T.);
#13224=ORIENTED_EDGE('',*,*,#8736,.T.);
#13225=ORIENTED_EDGE('',*,*,#8733,.T.);
#13226=ORIENTED_EDGE('',*,*,#8730,.T.);
#13227=ORIENTED_EDGE('',*,*,#8727,.T.);
#13228=ORIENTED_EDGE('',*,*,#8724,.T.);
#13229=ORIENTED_EDGE('',*,*,#8721,.T.);
#13230=ORIENTED_EDGE('',*,*,#8718,.T.);
#13231=ORIENTED_EDGE('',*,*,#8715,.T.);
#13232=ORIENTED_EDGE('',*,*,#8708,.T.);
#13233=ORIENTED_EDGE('',*,*,#9543,.T.);
#13234=ORIENTED_EDGE('',*,*,#8705,.F.);
#13235=ORIENTED_EDGE('',*,*,#9542,.T.);
#13236=ORIENTED_EDGE('',*,*,#8591,.F.);
#13237=ORIENTED_EDGE('',*,*,#9545,.T.);
#13238=ORIENTED_EDGE('',*,*,#8632,.T.);
#13239=ORIENTED_EDGE('',*,*,#9546,.T.);
#13240=ORIENTED_EDGE('',*,*,#8667,.T.);
#13241=ORIENTED_EDGE('',*,*,#9547,.T.);
#13242=ORIENTED_EDGE('',*,*,#8664,.F.);
#13243=ORIENTED_EDGE('',*,*,#9548,.F.);
#13244=ORIENTED_EDGE('',*,*,#9546,.F.);
#13245=ORIENTED_EDGE('',*,*,#8631,.F.);
#13246=ORIENTED_EDGE('',*,*,#8635,.F.);
#13247=ORIENTED_EDGE('',*,*,#8638,.F.);
#13248=ORIENTED_EDGE('',*,*,#8641,.F.);
#13249=ORIENTED_EDGE('',*,*,#8644,.F.);
#13250=ORIENTED_EDGE('',*,*,#8647,.F.);
#13251=ORIENTED_EDGE('',*,*,#8650,.F.);
#13252=ORIENTED_EDGE('',*,*,#8653,.F.);
#13253=ORIENTED_EDGE('',*,*,#8656,.F.);
#13254=ORIENTED_EDGE('',*,*,#8659,.F.);
#13255=ORIENTED_EDGE('',*,*,#8662,.F.);
#13256=ORIENTED_EDGE('',*,*,#8665,.F.);
#13257=ORIENTED_EDGE('',*,*,#9547,.F.);
#13258=ORIENTED_EDGE('',*,*,#8670,.F.);
#13259=ORIENTED_EDGE('',*,*,#9549,.F.);
#13260=ORIENTED_EDGE('',*,*,#8627,.F.);
#13261=ORIENTED_EDGE('',*,*,#9550,.F.);
#13262=ORIENTED_EDGE('',*,*,#8625,.F.);
#13263=ORIENTED_EDGE('',*,*,#8622,.F.);
#13264=ORIENTED_EDGE('',*,*,#8619,.F.);
#13265=ORIENTED_EDGE('',*,*,#8616,.F.);
#13266=ORIENTED_EDGE('',*,*,#8613,.F.);
#13267=ORIENTED_EDGE('',*,*,#8610,.F.);
#13268=ORIENTED_EDGE('',*,*,#8607,.F.);
#13269=ORIENTED_EDGE('',*,*,#8604,.F.);
#13270=ORIENTED_EDGE('',*,*,#8601,.F.);
#13271=ORIENTED_EDGE('',*,*,#8598,.F.);
#13272=ORIENTED_EDGE('',*,*,#8595,.F.);
#13273=ORIENTED_EDGE('',*,*,#8592,.F.);
#13274=ORIENTED_EDGE('',*,*,#9545,.F.);
#13275=ORIENTED_EDGE('',*,*,#8590,.F.);
#13276=ORIENTED_EDGE('',*,*,#8597,.F.);
#13277=ORIENTED_EDGE('',*,*,#8600,.F.);
#13278=ORIENTED_EDGE('',*,*,#8603,.F.);
#13279=ORIENTED_EDGE('',*,*,#8606,.F.);
#13280=ORIENTED_EDGE('',*,*,#8609,.F.);
#13281=ORIENTED_EDGE('',*,*,#8612,.F.);
#13282=ORIENTED_EDGE('',*,*,#8615,.F.);
#13283=ORIENTED_EDGE('',*,*,#8618,.F.);
#13284=ORIENTED_EDGE('',*,*,#8621,.F.);
#13285=ORIENTED_EDGE('',*,*,#8624,.F.);
#13286=ORIENTED_EDGE('',*,*,#9551,.F.);
#13287=ORIENTED_EDGE('',*,*,#8629,.F.);
#13288=ORIENTED_EDGE('',*,*,#9552,.F.);
#13289=ORIENTED_EDGE('',*,*,#8668,.T.);
#13290=ORIENTED_EDGE('',*,*,#9548,.T.);
#13291=ORIENTED_EDGE('',*,*,#8666,.T.);
#13292=ORIENTED_EDGE('',*,*,#8663,.T.);
#13293=ORIENTED_EDGE('',*,*,#8660,.T.);
#13294=ORIENTED_EDGE('',*,*,#8657,.T.);
#13295=ORIENTED_EDGE('',*,*,#8654,.T.);
#13296=ORIENTED_EDGE('',*,*,#8651,.T.);
#13297=ORIENTED_EDGE('',*,*,#8648,.T.);
#13298=ORIENTED_EDGE('',*,*,#8645,.T.);
#13299=ORIENTED_EDGE('',*,*,#8642,.T.);
#13300=ORIENTED_EDGE('',*,*,#8639,.T.);
#13301=ORIENTED_EDGE('',*,*,#8636,.T.);
#13302=ORIENTED_EDGE('',*,*,#8633,.T.);
#13303=ORIENTED_EDGE('',*,*,#8626,.T.);
#13304=ORIENTED_EDGE('',*,*,#9551,.T.);
#13305=ORIENTED_EDGE('',*,*,#8623,.F.);
#13306=ORIENTED_EDGE('',*,*,#9550,.T.);
#13307=ORIENTED_EDGE('',*,*,#8509,.F.);
#13308=ORIENTED_EDGE('',*,*,#9553,.T.);
#13309=ORIENTED_EDGE('',*,*,#8550,.T.);
#13310=ORIENTED_EDGE('',*,*,#9554,.T.);
#13311=ORIENTED_EDGE('',*,*,#8585,.T.);
#13312=ORIENTED_EDGE('',*,*,#9555,.T.);
#13313=ORIENTED_EDGE('',*,*,#8582,.F.);
#13314=ORIENTED_EDGE('',*,*,#9556,.F.);
#13315=ORIENTED_EDGE('',*,*,#9554,.F.);
#13316=ORIENTED_EDGE('',*,*,#8549,.F.);
#13317=ORIENTED_EDGE('',*,*,#8553,.F.);
#13318=ORIENTED_EDGE('',*,*,#8556,.F.);
#13319=ORIENTED_EDGE('',*,*,#8559,.F.);
#13320=ORIENTED_EDGE('',*,*,#8562,.F.);
#13321=ORIENTED_EDGE('',*,*,#8565,.F.);
#13322=ORIENTED_EDGE('',*,*,#8568,.F.);
#13323=ORIENTED_EDGE('',*,*,#8571,.F.);
#13324=ORIENTED_EDGE('',*,*,#8574,.F.);
#13325=ORIENTED_EDGE('',*,*,#8577,.F.);
#13326=ORIENTED_EDGE('',*,*,#8580,.F.);
#13327=ORIENTED_EDGE('',*,*,#8583,.F.);
#13328=ORIENTED_EDGE('',*,*,#9555,.F.);
#13329=ORIENTED_EDGE('',*,*,#8588,.F.);
#13330=ORIENTED_EDGE('',*,*,#9557,.F.);
#13331=ORIENTED_EDGE('',*,*,#8545,.F.);
#13332=ORIENTED_EDGE('',*,*,#9558,.F.);
#13333=ORIENTED_EDGE('',*,*,#8543,.F.);
#13334=ORIENTED_EDGE('',*,*,#8540,.F.);
#13335=ORIENTED_EDGE('',*,*,#8537,.F.);
#13336=ORIENTED_EDGE('',*,*,#8534,.F.);
#13337=ORIENTED_EDGE('',*,*,#8531,.F.);
#13338=ORIENTED_EDGE('',*,*,#8528,.F.);
#13339=ORIENTED_EDGE('',*,*,#8525,.F.);
#13340=ORIENTED_EDGE('',*,*,#8522,.F.);
#13341=ORIENTED_EDGE('',*,*,#8519,.F.);
#13342=ORIENTED_EDGE('',*,*,#8516,.F.);
#13343=ORIENTED_EDGE('',*,*,#8513,.F.);
#13344=ORIENTED_EDGE('',*,*,#8510,.F.);
#13345=ORIENTED_EDGE('',*,*,#9553,.F.);
#13346=ORIENTED_EDGE('',*,*,#8508,.F.);
#13347=ORIENTED_EDGE('',*,*,#8515,.F.);
#13348=ORIENTED_EDGE('',*,*,#8518,.F.);
#13349=ORIENTED_EDGE('',*,*,#8521,.F.);
#13350=ORIENTED_EDGE('',*,*,#8524,.F.);
#13351=ORIENTED_EDGE('',*,*,#8527,.F.);
#13352=ORIENTED_EDGE('',*,*,#8530,.F.);
#13353=ORIENTED_EDGE('',*,*,#8533,.F.);
#13354=ORIENTED_EDGE('',*,*,#8536,.F.);
#13355=ORIENTED_EDGE('',*,*,#8539,.F.);
#13356=ORIENTED_EDGE('',*,*,#8542,.F.);
#13357=ORIENTED_EDGE('',*,*,#9559,.F.);
#13358=ORIENTED_EDGE('',*,*,#8547,.F.);
#13359=ORIENTED_EDGE('',*,*,#9560,.F.);
#13360=ORIENTED_EDGE('',*,*,#8586,.T.);
#13361=ORIENTED_EDGE('',*,*,#9556,.T.);
#13362=ORIENTED_EDGE('',*,*,#8584,.T.);
#13363=ORIENTED_EDGE('',*,*,#8581,.T.);
#13364=ORIENTED_EDGE('',*,*,#8578,.T.);
#13365=ORIENTED_EDGE('',*,*,#8575,.T.);
#13366=ORIENTED_EDGE('',*,*,#8572,.T.);
#13367=ORIENTED_EDGE('',*,*,#8569,.T.);
#13368=ORIENTED_EDGE('',*,*,#8566,.T.);
#13369=ORIENTED_EDGE('',*,*,#8563,.T.);
#13370=ORIENTED_EDGE('',*,*,#8560,.T.);
#13371=ORIENTED_EDGE('',*,*,#8557,.T.);
#13372=ORIENTED_EDGE('',*,*,#8554,.T.);
#13373=ORIENTED_EDGE('',*,*,#8551,.T.);
#13374=ORIENTED_EDGE('',*,*,#8544,.T.);
#13375=ORIENTED_EDGE('',*,*,#9559,.T.);
#13376=ORIENTED_EDGE('',*,*,#8541,.F.);
#13377=ORIENTED_EDGE('',*,*,#9558,.T.);
#13378=ORIENTED_EDGE('',*,*,#8427,.F.);
#13379=ORIENTED_EDGE('',*,*,#9561,.T.);
#13380=ORIENTED_EDGE('',*,*,#8468,.T.);
#13381=ORIENTED_EDGE('',*,*,#9562,.T.);
#13382=ORIENTED_EDGE('',*,*,#8503,.T.);
#13383=ORIENTED_EDGE('',*,*,#9563,.T.);
#13384=ORIENTED_EDGE('',*,*,#8500,.F.);
#13385=ORIENTED_EDGE('',*,*,#9564,.F.);
#13386=ORIENTED_EDGE('',*,*,#9562,.F.);
#13387=ORIENTED_EDGE('',*,*,#8467,.F.);
#13388=ORIENTED_EDGE('',*,*,#8471,.F.);
#13389=ORIENTED_EDGE('',*,*,#8474,.F.);
#13390=ORIENTED_EDGE('',*,*,#8477,.F.);
#13391=ORIENTED_EDGE('',*,*,#8480,.F.);
#13392=ORIENTED_EDGE('',*,*,#8483,.F.);
#13393=ORIENTED_EDGE('',*,*,#8486,.F.);
#13394=ORIENTED_EDGE('',*,*,#8489,.F.);
#13395=ORIENTED_EDGE('',*,*,#8492,.F.);
#13396=ORIENTED_EDGE('',*,*,#8495,.F.);
#13397=ORIENTED_EDGE('',*,*,#8498,.F.);
#13398=ORIENTED_EDGE('',*,*,#8501,.F.);
#13399=ORIENTED_EDGE('',*,*,#9563,.F.);
#13400=ORIENTED_EDGE('',*,*,#8506,.F.);
#13401=ORIENTED_EDGE('',*,*,#9565,.F.);
#13402=ORIENTED_EDGE('',*,*,#8463,.F.);
#13403=ORIENTED_EDGE('',*,*,#9566,.F.);
#13404=ORIENTED_EDGE('',*,*,#8461,.F.);
#13405=ORIENTED_EDGE('',*,*,#8458,.F.);
#13406=ORIENTED_EDGE('',*,*,#8455,.F.);
#13407=ORIENTED_EDGE('',*,*,#8452,.F.);
#13408=ORIENTED_EDGE('',*,*,#8449,.F.);
#13409=ORIENTED_EDGE('',*,*,#8446,.F.);
#13410=ORIENTED_EDGE('',*,*,#8443,.F.);
#13411=ORIENTED_EDGE('',*,*,#8440,.F.);
#13412=ORIENTED_EDGE('',*,*,#8437,.F.);
#13413=ORIENTED_EDGE('',*,*,#8434,.F.);
#13414=ORIENTED_EDGE('',*,*,#8431,.F.);
#13415=ORIENTED_EDGE('',*,*,#8428,.F.);
#13416=ORIENTED_EDGE('',*,*,#9561,.F.);
#13417=ORIENTED_EDGE('',*,*,#8426,.F.);
#13418=ORIENTED_EDGE('',*,*,#8433,.F.);
#13419=ORIENTED_EDGE('',*,*,#8436,.F.);
#13420=ORIENTED_EDGE('',*,*,#8439,.F.);
#13421=ORIENTED_EDGE('',*,*,#8442,.F.);
#13422=ORIENTED_EDGE('',*,*,#8445,.F.);
#13423=ORIENTED_EDGE('',*,*,#8448,.F.);
#13424=ORIENTED_EDGE('',*,*,#8451,.F.);
#13425=ORIENTED_EDGE('',*,*,#8454,.F.);
#13426=ORIENTED_EDGE('',*,*,#8457,.F.);
#13427=ORIENTED_EDGE('',*,*,#8460,.F.);
#13428=ORIENTED_EDGE('',*,*,#9567,.F.);
#13429=ORIENTED_EDGE('',*,*,#8465,.F.);
#13430=ORIENTED_EDGE('',*,*,#9568,.F.);
#13431=ORIENTED_EDGE('',*,*,#8504,.T.);
#13432=ORIENTED_EDGE('',*,*,#9564,.T.);
#13433=ORIENTED_EDGE('',*,*,#8502,.T.);
#13434=ORIENTED_EDGE('',*,*,#8499,.T.);
#13435=ORIENTED_EDGE('',*,*,#8496,.T.);
#13436=ORIENTED_EDGE('',*,*,#8493,.T.);
#13437=ORIENTED_EDGE('',*,*,#8490,.T.);
#13438=ORIENTED_EDGE('',*,*,#8487,.T.);
#13439=ORIENTED_EDGE('',*,*,#8484,.T.);
#13440=ORIENTED_EDGE('',*,*,#8481,.T.);
#13441=ORIENTED_EDGE('',*,*,#8478,.T.);
#13442=ORIENTED_EDGE('',*,*,#8475,.T.);
#13443=ORIENTED_EDGE('',*,*,#8472,.T.);
#13444=ORIENTED_EDGE('',*,*,#8469,.T.);
#13445=ORIENTED_EDGE('',*,*,#8462,.T.);
#13446=ORIENTED_EDGE('',*,*,#9567,.T.);
#13447=ORIENTED_EDGE('',*,*,#8459,.F.);
#13448=ORIENTED_EDGE('',*,*,#9566,.T.);
#13449=ORIENTED_EDGE('',*,*,#8758,.F.);
#13450=ORIENTED_EDGE('',*,*,#8676,.F.);
#13451=ORIENTED_EDGE('',*,*,#8594,.F.);
#13452=ORIENTED_EDGE('',*,*,#8512,.F.);
#13453=ORIENTED_EDGE('',*,*,#8430,.F.);
#13454=ORIENTED_EDGE('',*,*,#8345,.F.);
#13455=ORIENTED_EDGE('',*,*,#9569,.T.);
#13456=ORIENTED_EDGE('',*,*,#8386,.T.);
#13457=ORIENTED_EDGE('',*,*,#9570,.T.);
#13458=ORIENTED_EDGE('',*,*,#8421,.T.);
#13459=ORIENTED_EDGE('',*,*,#9571,.T.);
#13460=ORIENTED_EDGE('',*,*,#8418,.F.);
#13461=ORIENTED_EDGE('',*,*,#9572,.F.);
#13462=ORIENTED_EDGE('',*,*,#9570,.F.);
#13463=ORIENTED_EDGE('',*,*,#8385,.F.);
#13464=ORIENTED_EDGE('',*,*,#8389,.F.);
#13465=ORIENTED_EDGE('',*,*,#8392,.F.);
#13466=ORIENTED_EDGE('',*,*,#8395,.F.);
#13467=ORIENTED_EDGE('',*,*,#8398,.F.);
#13468=ORIENTED_EDGE('',*,*,#8401,.F.);
#13469=ORIENTED_EDGE('',*,*,#8404,.F.);
#13470=ORIENTED_EDGE('',*,*,#8407,.F.);
#13471=ORIENTED_EDGE('',*,*,#8410,.F.);
#13472=ORIENTED_EDGE('',*,*,#8413,.F.);
#13473=ORIENTED_EDGE('',*,*,#8416,.F.);
#13474=ORIENTED_EDGE('',*,*,#8419,.F.);
#13475=ORIENTED_EDGE('',*,*,#9571,.F.);
#13476=ORIENTED_EDGE('',*,*,#8424,.F.);
#13477=ORIENTED_EDGE('',*,*,#9573,.F.);
#13478=ORIENTED_EDGE('',*,*,#8381,.F.);
#13479=ORIENTED_EDGE('',*,*,#9574,.F.);
#13480=ORIENTED_EDGE('',*,*,#8379,.F.);
#13481=ORIENTED_EDGE('',*,*,#8376,.F.);
#13482=ORIENTED_EDGE('',*,*,#8373,.F.);
#13483=ORIENTED_EDGE('',*,*,#8370,.F.);
#13484=ORIENTED_EDGE('',*,*,#8367,.F.);
#13485=ORIENTED_EDGE('',*,*,#8364,.F.);
#13486=ORIENTED_EDGE('',*,*,#8361,.F.);
#13487=ORIENTED_EDGE('',*,*,#8358,.F.);
#13488=ORIENTED_EDGE('',*,*,#8355,.F.);
#13489=ORIENTED_EDGE('',*,*,#8352,.F.);
#13490=ORIENTED_EDGE('',*,*,#8349,.F.);
#13491=ORIENTED_EDGE('',*,*,#8346,.F.);
#13492=ORIENTED_EDGE('',*,*,#9569,.F.);
#13493=ORIENTED_EDGE('',*,*,#8344,.F.);
#13494=ORIENTED_EDGE('',*,*,#8351,.F.);
#13495=ORIENTED_EDGE('',*,*,#8354,.F.);
#13496=ORIENTED_EDGE('',*,*,#8357,.F.);
#13497=ORIENTED_EDGE('',*,*,#8360,.F.);
#13498=ORIENTED_EDGE('',*,*,#8363,.F.);
#13499=ORIENTED_EDGE('',*,*,#8366,.F.);
#13500=ORIENTED_EDGE('',*,*,#8369,.F.);
#13501=ORIENTED_EDGE('',*,*,#8372,.F.);
#13502=ORIENTED_EDGE('',*,*,#8375,.F.);
#13503=ORIENTED_EDGE('',*,*,#8378,.F.);
#13504=ORIENTED_EDGE('',*,*,#9575,.F.);
#13505=ORIENTED_EDGE('',*,*,#8383,.F.);
#13506=ORIENTED_EDGE('',*,*,#9576,.F.);
#13507=ORIENTED_EDGE('',*,*,#8422,.T.);
#13508=ORIENTED_EDGE('',*,*,#9572,.T.);
#13509=ORIENTED_EDGE('',*,*,#8420,.T.);
#13510=ORIENTED_EDGE('',*,*,#8417,.T.);
#13511=ORIENTED_EDGE('',*,*,#8414,.T.);
#13512=ORIENTED_EDGE('',*,*,#8411,.T.);
#13513=ORIENTED_EDGE('',*,*,#8408,.T.);
#13514=ORIENTED_EDGE('',*,*,#8405,.T.);
#13515=ORIENTED_EDGE('',*,*,#8402,.T.);
#13516=ORIENTED_EDGE('',*,*,#8399,.T.);
#13517=ORIENTED_EDGE('',*,*,#8396,.T.);
#13518=ORIENTED_EDGE('',*,*,#8393,.T.);
#13519=ORIENTED_EDGE('',*,*,#8390,.T.);
#13520=ORIENTED_EDGE('',*,*,#8387,.T.);
#13521=ORIENTED_EDGE('',*,*,#8380,.T.);
#13522=ORIENTED_EDGE('',*,*,#9575,.T.);
#13523=ORIENTED_EDGE('',*,*,#8377,.F.);
#13524=ORIENTED_EDGE('',*,*,#9574,.T.);
#13525=ORIENTED_EDGE('',*,*,#8348,.F.);
#13526=ORIENTED_EDGE('',*,*,#8263,.F.);
#13527=ORIENTED_EDGE('',*,*,#9577,.T.);
#13528=ORIENTED_EDGE('',*,*,#8304,.T.);
#13529=ORIENTED_EDGE('',*,*,#9578,.T.);
#13530=ORIENTED_EDGE('',*,*,#8339,.T.);
#13531=ORIENTED_EDGE('',*,*,#9579,.T.);
#13532=ORIENTED_EDGE('',*,*,#8336,.F.);
#13533=ORIENTED_EDGE('',*,*,#9580,.F.);
#13534=ORIENTED_EDGE('',*,*,#9578,.F.);
#13535=ORIENTED_EDGE('',*,*,#8303,.F.);
#13536=ORIENTED_EDGE('',*,*,#8307,.F.);
#13537=ORIENTED_EDGE('',*,*,#8310,.F.);
#13538=ORIENTED_EDGE('',*,*,#8313,.F.);
#13539=ORIENTED_EDGE('',*,*,#8316,.F.);
#13540=ORIENTED_EDGE('',*,*,#8319,.F.);
#13541=ORIENTED_EDGE('',*,*,#8322,.F.);
#13542=ORIENTED_EDGE('',*,*,#8325,.F.);
#13543=ORIENTED_EDGE('',*,*,#8328,.F.);
#13544=ORIENTED_EDGE('',*,*,#8331,.F.);
#13545=ORIENTED_EDGE('',*,*,#8334,.F.);
#13546=ORIENTED_EDGE('',*,*,#8337,.F.);
#13547=ORIENTED_EDGE('',*,*,#9579,.F.);
#13548=ORIENTED_EDGE('',*,*,#8342,.F.);
#13549=ORIENTED_EDGE('',*,*,#9581,.F.);
#13550=ORIENTED_EDGE('',*,*,#8299,.F.);
#13551=ORIENTED_EDGE('',*,*,#9582,.F.);
#13552=ORIENTED_EDGE('',*,*,#8297,.F.);
#13553=ORIENTED_EDGE('',*,*,#8294,.F.);
#13554=ORIENTED_EDGE('',*,*,#8291,.F.);
#13555=ORIENTED_EDGE('',*,*,#8288,.F.);
#13556=ORIENTED_EDGE('',*,*,#8285,.F.);
#13557=ORIENTED_EDGE('',*,*,#8282,.F.);
#13558=ORIENTED_EDGE('',*,*,#8279,.F.);
#13559=ORIENTED_EDGE('',*,*,#8276,.F.);
#13560=ORIENTED_EDGE('',*,*,#8273,.F.);
#13561=ORIENTED_EDGE('',*,*,#8270,.F.);
#13562=ORIENTED_EDGE('',*,*,#8267,.F.);
#13563=ORIENTED_EDGE('',*,*,#8264,.F.);
#13564=ORIENTED_EDGE('',*,*,#9577,.F.);
#13565=ORIENTED_EDGE('',*,*,#8262,.F.);
#13566=ORIENTED_EDGE('',*,*,#8269,.F.);
#13567=ORIENTED_EDGE('',*,*,#8272,.F.);
#13568=ORIENTED_EDGE('',*,*,#8275,.F.);
#13569=ORIENTED_EDGE('',*,*,#8278,.F.);
#13570=ORIENTED_EDGE('',*,*,#8281,.F.);
#13571=ORIENTED_EDGE('',*,*,#8284,.F.);
#13572=ORIENTED_EDGE('',*,*,#8287,.F.);
#13573=ORIENTED_EDGE('',*,*,#8290,.F.);
#13574=ORIENTED_EDGE('',*,*,#8293,.F.);
#13575=ORIENTED_EDGE('',*,*,#8296,.F.);
#13576=ORIENTED_EDGE('',*,*,#9583,.F.);
#13577=ORIENTED_EDGE('',*,*,#8301,.F.);
#13578=ORIENTED_EDGE('',*,*,#9584,.F.);
#13579=ORIENTED_EDGE('',*,*,#8340,.T.);
#13580=ORIENTED_EDGE('',*,*,#9580,.T.);
#13581=ORIENTED_EDGE('',*,*,#8338,.T.);
#13582=ORIENTED_EDGE('',*,*,#8335,.T.);
#13583=ORIENTED_EDGE('',*,*,#8332,.T.);
#13584=ORIENTED_EDGE('',*,*,#8329,.T.);
#13585=ORIENTED_EDGE('',*,*,#8326,.T.);
#13586=ORIENTED_EDGE('',*,*,#8323,.T.);
#13587=ORIENTED_EDGE('',*,*,#8320,.T.);
#13588=ORIENTED_EDGE('',*,*,#8317,.T.);
#13589=ORIENTED_EDGE('',*,*,#8314,.T.);
#13590=ORIENTED_EDGE('',*,*,#8311,.T.);
#13591=ORIENTED_EDGE('',*,*,#8308,.T.);
#13592=ORIENTED_EDGE('',*,*,#8305,.T.);
#13593=ORIENTED_EDGE('',*,*,#8298,.T.);
#13594=ORIENTED_EDGE('',*,*,#9583,.T.);
#13595=ORIENTED_EDGE('',*,*,#8295,.F.);
#13596=ORIENTED_EDGE('',*,*,#9582,.T.);
#13597=ORIENTED_EDGE('',*,*,#8266,.F.);
#13598=ORIENTED_EDGE('',*,*,#9585,.F.);
#13599=ORIENTED_EDGE('',*,*,#9586,.T.);
#13600=ORIENTED_EDGE('',*,*,#9587,.T.);
#13601=ORIENTED_EDGE('',*,*,#9586,.F.);
#13602=ORIENTED_EDGE('',*,*,#9588,.F.);
#13603=ORIENTED_EDGE('',*,*,#9589,.T.);
#13604=ORIENTED_EDGE('',*,*,#9590,.T.);
#13605=ORIENTED_EDGE('',*,*,#9589,.F.);
#13606=ORIENTED_EDGE('',*,*,#9462,.T.);
#13607=ORIENTED_EDGE('',*,*,#9374,.T.);
#13608=ORIENTED_EDGE('',*,*,#9457,.T.);
#13609=ORIENTED_EDGE('',*,*,#9455,.T.);
#13610=ORIENTED_EDGE('',*,*,#9454,.T.);
#13611=ORIENTED_EDGE('',*,*,#9470,.T.);
#13612=ORIENTED_EDGE('',*,*,#9348,.T.);
#13613=ORIENTED_EDGE('',*,*,#9465,.T.);
#13614=ORIENTED_EDGE('',*,*,#9428,.T.);
#13615=ORIENTED_EDGE('',*,*,#9427,.T.);
#13616=ORIENTED_EDGE('',*,*,#9478,.T.);
#13617=ORIENTED_EDGE('',*,*,#9322,.T.);
#13618=ORIENTED_EDGE('',*,*,#9473,.T.);
#13619=ORIENTED_EDGE('',*,*,#9401,.T.);
#13620=ORIENTED_EDGE('',*,*,#9400,.T.);
#13621=ORIENTED_EDGE('',*,*,#9486,.T.);
#13622=ORIENTED_EDGE('',*,*,#9269,.T.);
#13623=ORIENTED_EDGE('',*,*,#9481,.T.);
#13624=ORIENTED_EDGE('',*,*,#9296,.T.);
#13625=ORIENTED_EDGE('',*,*,#9295,.T.);
#13626=ORIENTED_EDGE('',*,*,#9588,.T.);
#13627=ORIENTED_EDGE('',*,*,#9536,.T.);
#13628=ORIENTED_EDGE('',*,*,#8792,.T.);
#13629=ORIENTED_EDGE('',*,*,#9533,.T.);
#13630=ORIENTED_EDGE('',*,*,#8833,.T.);
#13631=ORIENTED_EDGE('',*,*,#9544,.T.);
#13632=ORIENTED_EDGE('',*,*,#8710,.T.);
#13633=ORIENTED_EDGE('',*,*,#9541,.T.);
#13634=ORIENTED_EDGE('',*,*,#8751,.T.);
#13635=ORIENTED_EDGE('',*,*,#9552,.T.);
#13636=ORIENTED_EDGE('',*,*,#8628,.T.);
#13637=ORIENTED_EDGE('',*,*,#9549,.T.);
#13638=ORIENTED_EDGE('',*,*,#8669,.T.);
#13639=ORIENTED_EDGE('',*,*,#9560,.T.);
#13640=ORIENTED_EDGE('',*,*,#8546,.T.);
#13641=ORIENTED_EDGE('',*,*,#9557,.T.);
#13642=ORIENTED_EDGE('',*,*,#8587,.T.);
#13643=ORIENTED_EDGE('',*,*,#9568,.T.);
#13644=ORIENTED_EDGE('',*,*,#8464,.T.);
#13645=ORIENTED_EDGE('',*,*,#9565,.T.);
#13646=ORIENTED_EDGE('',*,*,#8505,.T.);
#13647=ORIENTED_EDGE('',*,*,#9585,.T.);
#13648=ORIENTED_EDGE('',*,*,#9584,.T.);
#13649=ORIENTED_EDGE('',*,*,#8300,.T.);
#13650=ORIENTED_EDGE('',*,*,#9581,.T.);
#13651=ORIENTED_EDGE('',*,*,#8341,.T.);
#13652=ORIENTED_EDGE('',*,*,#9590,.F.);
#13653=ORIENTED_EDGE('',*,*,#9496,.T.);
#13654=ORIENTED_EDGE('',*,*,#9202,.T.);
#13655=ORIENTED_EDGE('',*,*,#9493,.T.);
#13656=ORIENTED_EDGE('',*,*,#9243,.T.);
#13657=ORIENTED_EDGE('',*,*,#9504,.T.);
#13658=ORIENTED_EDGE('',*,*,#9120,.T.);
#13659=ORIENTED_EDGE('',*,*,#9501,.T.);
#13660=ORIENTED_EDGE('',*,*,#9161,.T.);
#13661=ORIENTED_EDGE('',*,*,#9512,.T.);
#13662=ORIENTED_EDGE('',*,*,#9038,.T.);
#13663=ORIENTED_EDGE('',*,*,#9509,.T.);
#13664=ORIENTED_EDGE('',*,*,#9079,.T.);
#13665=ORIENTED_EDGE('',*,*,#9520,.T.);
#13666=ORIENTED_EDGE('',*,*,#8956,.T.);
#13667=ORIENTED_EDGE('',*,*,#9517,.T.);
#13668=ORIENTED_EDGE('',*,*,#8997,.T.);
#13669=ORIENTED_EDGE('',*,*,#9528,.T.);
#13670=ORIENTED_EDGE('',*,*,#8874,.T.);
#13671=ORIENTED_EDGE('',*,*,#9525,.T.);
#13672=ORIENTED_EDGE('',*,*,#8915,.T.);
#13673=ORIENTED_EDGE('',*,*,#9587,.F.);
#13674=ORIENTED_EDGE('',*,*,#9576,.T.);
#13675=ORIENTED_EDGE('',*,*,#8382,.T.);
#13676=ORIENTED_EDGE('',*,*,#9573,.T.);
#13677=ORIENTED_EDGE('',*,*,#8423,.T.);
#13678=ORIENTED_EDGE('',*,*,#9591,.T.);
#13679=ORIENTED_EDGE('',*,*,#9592,.T.);
#13680=ORIENTED_EDGE('',*,*,#9593,.T.);
#13681=ORIENTED_EDGE('',*,*,#9594,.T.);
#13682=ORIENTED_EDGE('',*,*,#9595,.T.);
#13683=ORIENTED_EDGE('',*,*,#9596,.T.);
#13684=ORIENTED_EDGE('',*,*,#9597,.T.);
#13685=ORIENTED_EDGE('',*,*,#9594,.F.);
#13686=ORIENTED_EDGE('',*,*,#9598,.T.);
#13687=ORIENTED_EDGE('',*,*,#9599,.T.);
#13688=ORIENTED_EDGE('',*,*,#9600,.T.);
#13689=ORIENTED_EDGE('',*,*,#9601,.T.);
#13690=ORIENTED_EDGE('',*,*,#9591,.F.);
#13691=ORIENTED_EDGE('',*,*,#9602,.T.);
#13692=ORIENTED_EDGE('',*,*,#9603,.T.);
#13693=ORIENTED_EDGE('',*,*,#9604,.T.);
#13694=ORIENTED_EDGE('',*,*,#9600,.F.);
#13695=ORIENTED_EDGE('',*,*,#9605,.T.);
#13696=ORIENTED_EDGE('',*,*,#9606,.T.);
#13697=ORIENTED_EDGE('',*,*,#9607,.T.);
#13698=ORIENTED_EDGE('',*,*,#9603,.F.);
#13699=ORIENTED_EDGE('',*,*,#9608,.T.);
#13700=ORIENTED_EDGE('',*,*,#9609,.T.);
#13701=ORIENTED_EDGE('',*,*,#9610,.T.);
#13702=ORIENTED_EDGE('',*,*,#9606,.F.);
#13703=ORIENTED_EDGE('',*,*,#9611,.T.);
#13704=ORIENTED_EDGE('',*,*,#9612,.T.);
#13705=ORIENTED_EDGE('',*,*,#9613,.T.);
#13706=ORIENTED_EDGE('',*,*,#9609,.F.);
#13707=ORIENTED_EDGE('',*,*,#9614,.T.);
#13708=ORIENTED_EDGE('',*,*,#9615,.T.);
#13709=ORIENTED_EDGE('',*,*,#9616,.T.);
#13710=ORIENTED_EDGE('',*,*,#9612,.F.);
#13711=ORIENTED_EDGE('',*,*,#9617,.T.);
#13712=ORIENTED_EDGE('',*,*,#9618,.F.);
#13713=ORIENTED_EDGE('',*,*,#9619,.T.);
#13714=ORIENTED_EDGE('',*,*,#9620,.F.);
#13715=ORIENTED_EDGE('',*,*,#9621,.T.);
#13716=ORIENTED_EDGE('',*,*,#9622,.T.);
#13717=ORIENTED_EDGE('',*,*,#9623,.T.);
#13718=ORIENTED_EDGE('',*,*,#9624,.F.);
#13719=ORIENTED_EDGE('',*,*,#9625,.F.);
#13720=ORIENTED_EDGE('',*,*,#9626,.T.);
#13721=ORIENTED_EDGE('',*,*,#9627,.T.);
#13722=ORIENTED_EDGE('',*,*,#9622,.F.);
#13723=ORIENTED_EDGE('',*,*,#9628,.F.);
#13724=ORIENTED_EDGE('',*,*,#9629,.T.);
#13725=ORIENTED_EDGE('',*,*,#9630,.T.);
#13726=ORIENTED_EDGE('',*,*,#9626,.F.);
#13727=ORIENTED_EDGE('',*,*,#9631,.F.);
#13728=ORIENTED_EDGE('',*,*,#9632,.T.);
#13729=ORIENTED_EDGE('',*,*,#9633,.T.);
#13730=ORIENTED_EDGE('',*,*,#9629,.F.);
#13731=ORIENTED_EDGE('',*,*,#9634,.F.);
#13732=ORIENTED_EDGE('',*,*,#9635,.T.);
#13733=ORIENTED_EDGE('',*,*,#9636,.T.);
#13734=ORIENTED_EDGE('',*,*,#9632,.F.);
#13735=ORIENTED_EDGE('',*,*,#9637,.F.);
#13736=ORIENTED_EDGE('',*,*,#9638,.T.);
#13737=ORIENTED_EDGE('',*,*,#9639,.T.);
#13738=ORIENTED_EDGE('',*,*,#9635,.F.);
#13739=ORIENTED_EDGE('',*,*,#9640,.F.);
#13740=ORIENTED_EDGE('',*,*,#9641,.T.);
#13741=ORIENTED_EDGE('',*,*,#9642,.T.);
#13742=ORIENTED_EDGE('',*,*,#9638,.F.);
#13743=ORIENTED_EDGE('',*,*,#9643,.F.);
#13744=ORIENTED_EDGE('',*,*,#9644,.F.);
#13745=ORIENTED_EDGE('',*,*,#9645,.F.);
#13746=ORIENTED_EDGE('',*,*,#9646,.F.);
#13747=ORIENTED_EDGE('',*,*,#9647,.T.);
#13748=ORIENTED_EDGE('',*,*,#9648,.T.);
#13749=ORIENTED_EDGE('',*,*,#9649,.T.);
#13750=ORIENTED_EDGE('',*,*,#9650,.T.);
#13751=ORIENTED_EDGE('',*,*,#9651,.T.);
#13752=ORIENTED_EDGE('',*,*,#9652,.T.);
#13753=ORIENTED_EDGE('',*,*,#9653,.T.);
#13754=ORIENTED_EDGE('',*,*,#9654,.T.);
#13755=ORIENTED_EDGE('',*,*,#9651,.F.);
#13756=ORIENTED_EDGE('',*,*,#9655,.T.);
#13757=ORIENTED_EDGE('',*,*,#9656,.T.);
#13758=ORIENTED_EDGE('',*,*,#9657,.T.);
#13759=ORIENTED_EDGE('',*,*,#9658,.T.);
#13760=ORIENTED_EDGE('',*,*,#9648,.F.);
#13761=ORIENTED_EDGE('',*,*,#9659,.T.);
#13762=ORIENTED_EDGE('',*,*,#9660,.T.);
#13763=ORIENTED_EDGE('',*,*,#9661,.T.);
#13764=ORIENTED_EDGE('',*,*,#9657,.F.);
#13765=ORIENTED_EDGE('',*,*,#9662,.T.);
#13766=ORIENTED_EDGE('',*,*,#9663,.T.);
#13767=ORIENTED_EDGE('',*,*,#9664,.T.);
#13768=ORIENTED_EDGE('',*,*,#9660,.F.);
#13769=ORIENTED_EDGE('',*,*,#9665,.T.);
#13770=ORIENTED_EDGE('',*,*,#9666,.T.);
#13771=ORIENTED_EDGE('',*,*,#9667,.T.);
#13772=ORIENTED_EDGE('',*,*,#9663,.F.);
#13773=ORIENTED_EDGE('',*,*,#9668,.T.);
#13774=ORIENTED_EDGE('',*,*,#9669,.T.);
#13775=ORIENTED_EDGE('',*,*,#9670,.T.);
#13776=ORIENTED_EDGE('',*,*,#9666,.F.);
#13777=ORIENTED_EDGE('',*,*,#9671,.T.);
#13778=ORIENTED_EDGE('',*,*,#9672,.T.);
#13779=ORIENTED_EDGE('',*,*,#9673,.T.);
#13780=ORIENTED_EDGE('',*,*,#9669,.F.);
#13781=ORIENTED_EDGE('',*,*,#9674,.T.);
#13782=ORIENTED_EDGE('',*,*,#9675,.F.);
#13783=ORIENTED_EDGE('',*,*,#9676,.T.);
#13784=ORIENTED_EDGE('',*,*,#9677,.F.);
#13785=ORIENTED_EDGE('',*,*,#9678,.T.);
#13786=ORIENTED_EDGE('',*,*,#9679,.T.);
#13787=ORIENTED_EDGE('',*,*,#9680,.T.);
#13788=ORIENTED_EDGE('',*,*,#9681,.F.);
#13789=ORIENTED_EDGE('',*,*,#9682,.F.);
#13790=ORIENTED_EDGE('',*,*,#9683,.T.);
#13791=ORIENTED_EDGE('',*,*,#9684,.T.);
#13792=ORIENTED_EDGE('',*,*,#9679,.F.);
#13793=ORIENTED_EDGE('',*,*,#9685,.F.);
#13794=ORIENTED_EDGE('',*,*,#9686,.T.);
#13795=ORIENTED_EDGE('',*,*,#9687,.T.);
#13796=ORIENTED_EDGE('',*,*,#9683,.F.);
#13797=ORIENTED_EDGE('',*,*,#9688,.F.);
#13798=ORIENTED_EDGE('',*,*,#9689,.T.);
#13799=ORIENTED_EDGE('',*,*,#9690,.T.);
#13800=ORIENTED_EDGE('',*,*,#9686,.F.);
#13801=ORIENTED_EDGE('',*,*,#9691,.F.);
#13802=ORIENTED_EDGE('',*,*,#9692,.T.);
#13803=ORIENTED_EDGE('',*,*,#9693,.T.);
#13804=ORIENTED_EDGE('',*,*,#9689,.F.);
#13805=ORIENTED_EDGE('',*,*,#9694,.F.);
#13806=ORIENTED_EDGE('',*,*,#9695,.T.);
#13807=ORIENTED_EDGE('',*,*,#9696,.T.);
#13808=ORIENTED_EDGE('',*,*,#9692,.F.);
#13809=ORIENTED_EDGE('',*,*,#9697,.F.);
#13810=ORIENTED_EDGE('',*,*,#9698,.T.);
#13811=ORIENTED_EDGE('',*,*,#9699,.T.);
#13812=ORIENTED_EDGE('',*,*,#9695,.F.);
#13813=ORIENTED_EDGE('',*,*,#9700,.F.);
#13814=ORIENTED_EDGE('',*,*,#9701,.F.);
#13815=ORIENTED_EDGE('',*,*,#9702,.F.);
#13816=ORIENTED_EDGE('',*,*,#9703,.F.);
#13817=ORIENTED_EDGE('',*,*,#9704,.T.);
#13818=ORIENTED_EDGE('',*,*,#9705,.T.);
#13819=ORIENTED_EDGE('',*,*,#9706,.T.);
#13820=ORIENTED_EDGE('',*,*,#9707,.T.);
#13821=ORIENTED_EDGE('',*,*,#9708,.T.);
#13822=ORIENTED_EDGE('',*,*,#9709,.T.);
#13823=ORIENTED_EDGE('',*,*,#9710,.T.);
#13824=ORIENTED_EDGE('',*,*,#9711,.T.);
#13825=ORIENTED_EDGE('',*,*,#9708,.F.);
#13826=ORIENTED_EDGE('',*,*,#9712,.T.);
#13827=ORIENTED_EDGE('',*,*,#9713,.T.);
#13828=ORIENTED_EDGE('',*,*,#9714,.T.);
#13829=ORIENTED_EDGE('',*,*,#9715,.T.);
#13830=ORIENTED_EDGE('',*,*,#9705,.F.);
#13831=ORIENTED_EDGE('',*,*,#9716,.T.);
#13832=ORIENTED_EDGE('',*,*,#9717,.T.);
#13833=ORIENTED_EDGE('',*,*,#9718,.T.);
#13834=ORIENTED_EDGE('',*,*,#9714,.F.);
#13835=ORIENTED_EDGE('',*,*,#9719,.T.);
#13836=ORIENTED_EDGE('',*,*,#9720,.T.);
#13837=ORIENTED_EDGE('',*,*,#9721,.T.);
#13838=ORIENTED_EDGE('',*,*,#9717,.F.);
#13839=ORIENTED_EDGE('',*,*,#9722,.T.);
#13840=ORIENTED_EDGE('',*,*,#9723,.T.);
#13841=ORIENTED_EDGE('',*,*,#9724,.T.);
#13842=ORIENTED_EDGE('',*,*,#9720,.F.);
#13843=ORIENTED_EDGE('',*,*,#9725,.T.);
#13844=ORIENTED_EDGE('',*,*,#9726,.T.);
#13845=ORIENTED_EDGE('',*,*,#9727,.T.);
#13846=ORIENTED_EDGE('',*,*,#9723,.F.);
#13847=ORIENTED_EDGE('',*,*,#9728,.T.);
#13848=ORIENTED_EDGE('',*,*,#9729,.T.);
#13849=ORIENTED_EDGE('',*,*,#9730,.T.);
#13850=ORIENTED_EDGE('',*,*,#9726,.F.);
#13851=ORIENTED_EDGE('',*,*,#9731,.T.);
#13852=ORIENTED_EDGE('',*,*,#9732,.F.);
#13853=ORIENTED_EDGE('',*,*,#9733,.T.);
#13854=ORIENTED_EDGE('',*,*,#9734,.F.);
#13855=ORIENTED_EDGE('',*,*,#9735,.T.);
#13856=ORIENTED_EDGE('',*,*,#9736,.T.);
#13857=ORIENTED_EDGE('',*,*,#9737,.T.);
#13858=ORIENTED_EDGE('',*,*,#9738,.F.);
#13859=ORIENTED_EDGE('',*,*,#9739,.F.);
#13860=ORIENTED_EDGE('',*,*,#9740,.T.);
#13861=ORIENTED_EDGE('',*,*,#9741,.T.);
#13862=ORIENTED_EDGE('',*,*,#9736,.F.);
#13863=ORIENTED_EDGE('',*,*,#9742,.F.);
#13864=ORIENTED_EDGE('',*,*,#9743,.T.);
#13865=ORIENTED_EDGE('',*,*,#9744,.T.);
#13866=ORIENTED_EDGE('',*,*,#9740,.F.);
#13867=ORIENTED_EDGE('',*,*,#9745,.F.);
#13868=ORIENTED_EDGE('',*,*,#9746,.T.);
#13869=ORIENTED_EDGE('',*,*,#9747,.T.);
#13870=ORIENTED_EDGE('',*,*,#9743,.F.);
#13871=ORIENTED_EDGE('',*,*,#9748,.F.);
#13872=ORIENTED_EDGE('',*,*,#9749,.T.);
#13873=ORIENTED_EDGE('',*,*,#9750,.T.);
#13874=ORIENTED_EDGE('',*,*,#9746,.F.);
#13875=ORIENTED_EDGE('',*,*,#9751,.F.);
#13876=ORIENTED_EDGE('',*,*,#9752,.T.);
#13877=ORIENTED_EDGE('',*,*,#9753,.T.);
#13878=ORIENTED_EDGE('',*,*,#9749,.F.);
#13879=ORIENTED_EDGE('',*,*,#9754,.F.);
#13880=ORIENTED_EDGE('',*,*,#9755,.T.);
#13881=ORIENTED_EDGE('',*,*,#9756,.T.);
#13882=ORIENTED_EDGE('',*,*,#9752,.F.);
#13883=ORIENTED_EDGE('',*,*,#9757,.F.);
#13884=ORIENTED_EDGE('',*,*,#9758,.F.);
#13885=ORIENTED_EDGE('',*,*,#9759,.F.);
#13886=ORIENTED_EDGE('',*,*,#9760,.F.);
#13887=ORIENTED_EDGE('',*,*,#9761,.T.);
#13888=ORIENTED_EDGE('',*,*,#9762,.T.);
#13889=ORIENTED_EDGE('',*,*,#9763,.T.);
#13890=ORIENTED_EDGE('',*,*,#9764,.T.);
#13891=ORIENTED_EDGE('',*,*,#9765,.T.);
#13892=ORIENTED_EDGE('',*,*,#9766,.T.);
#13893=ORIENTED_EDGE('',*,*,#9767,.T.);
#13894=ORIENTED_EDGE('',*,*,#9768,.T.);
#13895=ORIENTED_EDGE('',*,*,#9765,.F.);
#13896=ORIENTED_EDGE('',*,*,#9769,.T.);
#13897=ORIENTED_EDGE('',*,*,#9770,.T.);
#13898=ORIENTED_EDGE('',*,*,#9771,.T.);
#13899=ORIENTED_EDGE('',*,*,#9772,.T.);
#13900=ORIENTED_EDGE('',*,*,#9762,.F.);
#13901=ORIENTED_EDGE('',*,*,#9773,.T.);
#13902=ORIENTED_EDGE('',*,*,#9774,.T.);
#13903=ORIENTED_EDGE('',*,*,#9775,.T.);
#13904=ORIENTED_EDGE('',*,*,#9771,.F.);
#13905=ORIENTED_EDGE('',*,*,#9776,.T.);
#13906=ORIENTED_EDGE('',*,*,#9777,.T.);
#13907=ORIENTED_EDGE('',*,*,#9778,.T.);
#13908=ORIENTED_EDGE('',*,*,#9774,.F.);
#13909=ORIENTED_EDGE('',*,*,#9779,.T.);
#13910=ORIENTED_EDGE('',*,*,#9780,.T.);
#13911=ORIENTED_EDGE('',*,*,#9781,.T.);
#13912=ORIENTED_EDGE('',*,*,#9777,.F.);
#13913=ORIENTED_EDGE('',*,*,#9782,.T.);
#13914=ORIENTED_EDGE('',*,*,#9783,.T.);
#13915=ORIENTED_EDGE('',*,*,#9784,.T.);
#13916=ORIENTED_EDGE('',*,*,#9780,.F.);
#13917=ORIENTED_EDGE('',*,*,#9785,.T.);
#13918=ORIENTED_EDGE('',*,*,#9786,.T.);
#13919=ORIENTED_EDGE('',*,*,#9787,.T.);
#13920=ORIENTED_EDGE('',*,*,#9783,.F.);
#13921=ORIENTED_EDGE('',*,*,#9788,.T.);
#13922=ORIENTED_EDGE('',*,*,#9789,.F.);
#13923=ORIENTED_EDGE('',*,*,#9790,.T.);
#13924=ORIENTED_EDGE('',*,*,#9791,.F.);
#13925=ORIENTED_EDGE('',*,*,#9792,.T.);
#13926=ORIENTED_EDGE('',*,*,#9793,.T.);
#13927=ORIENTED_EDGE('',*,*,#9794,.T.);
#13928=ORIENTED_EDGE('',*,*,#9795,.F.);
#13929=ORIENTED_EDGE('',*,*,#9796,.F.);
#13930=ORIENTED_EDGE('',*,*,#9797,.T.);
#13931=ORIENTED_EDGE('',*,*,#9798,.T.);
#13932=ORIENTED_EDGE('',*,*,#9793,.F.);
#13933=ORIENTED_EDGE('',*,*,#9799,.F.);
#13934=ORIENTED_EDGE('',*,*,#9800,.T.);
#13935=ORIENTED_EDGE('',*,*,#9801,.T.);
#13936=ORIENTED_EDGE('',*,*,#9797,.F.);
#13937=ORIENTED_EDGE('',*,*,#9802,.F.);
#13938=ORIENTED_EDGE('',*,*,#9803,.T.);
#13939=ORIENTED_EDGE('',*,*,#9804,.T.);
#13940=ORIENTED_EDGE('',*,*,#9800,.F.);
#13941=ORIENTED_EDGE('',*,*,#9805,.F.);
#13942=ORIENTED_EDGE('',*,*,#9806,.T.);
#13943=ORIENTED_EDGE('',*,*,#9807,.T.);
#13944=ORIENTED_EDGE('',*,*,#9803,.F.);
#13945=ORIENTED_EDGE('',*,*,#9808,.F.);
#13946=ORIENTED_EDGE('',*,*,#9809,.T.);
#13947=ORIENTED_EDGE('',*,*,#9810,.T.);
#13948=ORIENTED_EDGE('',*,*,#9806,.F.);
#13949=ORIENTED_EDGE('',*,*,#9811,.F.);
#13950=ORIENTED_EDGE('',*,*,#9812,.T.);
#13951=ORIENTED_EDGE('',*,*,#9813,.T.);
#13952=ORIENTED_EDGE('',*,*,#9809,.F.);
#13953=ORIENTED_EDGE('',*,*,#9814,.F.);
#13954=ORIENTED_EDGE('',*,*,#9815,.F.);
#13955=ORIENTED_EDGE('',*,*,#9816,.F.);
#13956=ORIENTED_EDGE('',*,*,#9817,.F.);
#13957=ORIENTED_EDGE('',*,*,#9818,.T.);
#13958=ORIENTED_EDGE('',*,*,#9819,.T.);
#13959=ORIENTED_EDGE('',*,*,#9820,.T.);
#13960=ORIENTED_EDGE('',*,*,#9821,.T.);
#13961=ORIENTED_EDGE('',*,*,#9822,.T.);
#13962=ORIENTED_EDGE('',*,*,#9823,.T.);
#13963=ORIENTED_EDGE('',*,*,#9824,.T.);
#13964=ORIENTED_EDGE('',*,*,#9825,.T.);
#13965=ORIENTED_EDGE('',*,*,#9822,.F.);
#13966=ORIENTED_EDGE('',*,*,#9826,.T.);
#13967=ORIENTED_EDGE('',*,*,#9827,.T.);
#13968=ORIENTED_EDGE('',*,*,#9828,.T.);
#13969=ORIENTED_EDGE('',*,*,#9829,.T.);
#13970=ORIENTED_EDGE('',*,*,#9819,.F.);
#13971=ORIENTED_EDGE('',*,*,#9830,.T.);
#13972=ORIENTED_EDGE('',*,*,#9831,.T.);
#13973=ORIENTED_EDGE('',*,*,#9832,.T.);
#13974=ORIENTED_EDGE('',*,*,#9828,.F.);
#13975=ORIENTED_EDGE('',*,*,#9833,.T.);
#13976=ORIENTED_EDGE('',*,*,#9834,.T.);
#13977=ORIENTED_EDGE('',*,*,#9835,.T.);
#13978=ORIENTED_EDGE('',*,*,#9831,.F.);
#13979=ORIENTED_EDGE('',*,*,#9836,.T.);
#13980=ORIENTED_EDGE('',*,*,#9837,.T.);
#13981=ORIENTED_EDGE('',*,*,#9838,.T.);
#13982=ORIENTED_EDGE('',*,*,#9834,.F.);
#13983=ORIENTED_EDGE('',*,*,#9839,.T.);
#13984=ORIENTED_EDGE('',*,*,#9840,.T.);
#13985=ORIENTED_EDGE('',*,*,#9841,.T.);
#13986=ORIENTED_EDGE('',*,*,#9837,.F.);
#13987=ORIENTED_EDGE('',*,*,#9842,.T.);
#13988=ORIENTED_EDGE('',*,*,#9843,.T.);
#13989=ORIENTED_EDGE('',*,*,#9844,.T.);
#13990=ORIENTED_EDGE('',*,*,#9840,.F.);
#13991=ORIENTED_EDGE('',*,*,#9845,.T.);
#13992=ORIENTED_EDGE('',*,*,#9846,.F.);
#13993=ORIENTED_EDGE('',*,*,#9847,.T.);
#13994=ORIENTED_EDGE('',*,*,#9848,.F.);
#13995=ORIENTED_EDGE('',*,*,#9849,.T.);
#13996=ORIENTED_EDGE('',*,*,#9850,.T.);
#13997=ORIENTED_EDGE('',*,*,#9851,.T.);
#13998=ORIENTED_EDGE('',*,*,#9852,.F.);
#13999=ORIENTED_EDGE('',*,*,#9853,.F.);
#14000=ORIENTED_EDGE('',*,*,#9854,.T.);
#14001=ORIENTED_EDGE('',*,*,#9855,.T.);
#14002=ORIENTED_EDGE('',*,*,#9850,.F.);
#14003=ORIENTED_EDGE('',*,*,#9856,.F.);
#14004=ORIENTED_EDGE('',*,*,#9857,.T.);
#14005=ORIENTED_EDGE('',*,*,#9858,.T.);
#14006=ORIENTED_EDGE('',*,*,#9854,.F.);
#14007=ORIENTED_EDGE('',*,*,#9859,.F.);
#14008=ORIENTED_EDGE('',*,*,#9860,.T.);
#14009=ORIENTED_EDGE('',*,*,#9861,.T.);
#14010=ORIENTED_EDGE('',*,*,#9857,.F.);
#14011=ORIENTED_EDGE('',*,*,#9862,.F.);
#14012=ORIENTED_EDGE('',*,*,#9863,.T.);
#14013=ORIENTED_EDGE('',*,*,#9864,.T.);
#14014=ORIENTED_EDGE('',*,*,#9860,.F.);
#14015=ORIENTED_EDGE('',*,*,#9865,.F.);
#14016=ORIENTED_EDGE('',*,*,#9866,.T.);
#14017=ORIENTED_EDGE('',*,*,#9867,.T.);
#14018=ORIENTED_EDGE('',*,*,#9863,.F.);
#14019=ORIENTED_EDGE('',*,*,#9868,.F.);
#14020=ORIENTED_EDGE('',*,*,#9869,.T.);
#14021=ORIENTED_EDGE('',*,*,#9870,.T.);
#14022=ORIENTED_EDGE('',*,*,#9866,.F.);
#14023=ORIENTED_EDGE('',*,*,#9871,.F.);
#14024=ORIENTED_EDGE('',*,*,#9872,.F.);
#14025=ORIENTED_EDGE('',*,*,#9873,.F.);
#14026=ORIENTED_EDGE('',*,*,#9874,.F.);
#14027=ORIENTED_EDGE('',*,*,#9875,.T.);
#14028=ORIENTED_EDGE('',*,*,#9876,.T.);
#14029=ORIENTED_EDGE('',*,*,#9877,.T.);
#14030=ORIENTED_EDGE('',*,*,#9878,.T.);
#14031=ORIENTED_EDGE('',*,*,#9879,.T.);
#14032=ORIENTED_EDGE('',*,*,#9880,.T.);
#14033=ORIENTED_EDGE('',*,*,#9881,.T.);
#14034=ORIENTED_EDGE('',*,*,#9882,.T.);
#14035=ORIENTED_EDGE('',*,*,#9879,.F.);
#14036=ORIENTED_EDGE('',*,*,#9883,.T.);
#14037=ORIENTED_EDGE('',*,*,#9884,.T.);
#14038=ORIENTED_EDGE('',*,*,#9885,.T.);
#14039=ORIENTED_EDGE('',*,*,#9886,.T.);
#14040=ORIENTED_EDGE('',*,*,#9876,.F.);
#14041=ORIENTED_EDGE('',*,*,#9887,.T.);
#14042=ORIENTED_EDGE('',*,*,#9888,.T.);
#14043=ORIENTED_EDGE('',*,*,#9889,.T.);
#14044=ORIENTED_EDGE('',*,*,#9885,.F.);
#14045=ORIENTED_EDGE('',*,*,#9890,.T.);
#14046=ORIENTED_EDGE('',*,*,#9891,.T.);
#14047=ORIENTED_EDGE('',*,*,#9892,.T.);
#14048=ORIENTED_EDGE('',*,*,#9888,.F.);
#14049=ORIENTED_EDGE('',*,*,#9893,.T.);
#14050=ORIENTED_EDGE('',*,*,#9894,.T.);
#14051=ORIENTED_EDGE('',*,*,#9895,.T.);
#14052=ORIENTED_EDGE('',*,*,#9891,.F.);
#14053=ORIENTED_EDGE('',*,*,#9896,.T.);
#14054=ORIENTED_EDGE('',*,*,#9897,.T.);
#14055=ORIENTED_EDGE('',*,*,#9898,.T.);
#14056=ORIENTED_EDGE('',*,*,#9894,.F.);
#14057=ORIENTED_EDGE('',*,*,#9899,.T.);
#14058=ORIENTED_EDGE('',*,*,#9900,.T.);
#14059=ORIENTED_EDGE('',*,*,#9901,.T.);
#14060=ORIENTED_EDGE('',*,*,#9897,.F.);
#14061=ORIENTED_EDGE('',*,*,#9902,.T.);
#14062=ORIENTED_EDGE('',*,*,#9903,.F.);
#14063=ORIENTED_EDGE('',*,*,#9904,.T.);
#14064=ORIENTED_EDGE('',*,*,#9905,.F.);
#14065=ORIENTED_EDGE('',*,*,#9906,.T.);
#14066=ORIENTED_EDGE('',*,*,#9907,.T.);
#14067=ORIENTED_EDGE('',*,*,#9908,.T.);
#14068=ORIENTED_EDGE('',*,*,#9909,.F.);
#14069=ORIENTED_EDGE('',*,*,#9910,.F.);
#14070=ORIENTED_EDGE('',*,*,#9911,.T.);
#14071=ORIENTED_EDGE('',*,*,#9912,.T.);
#14072=ORIENTED_EDGE('',*,*,#9907,.F.);
#14073=ORIENTED_EDGE('',*,*,#9913,.F.);
#14074=ORIENTED_EDGE('',*,*,#9914,.T.);
#14075=ORIENTED_EDGE('',*,*,#9915,.T.);
#14076=ORIENTED_EDGE('',*,*,#9911,.F.);
#14077=ORIENTED_EDGE('',*,*,#9916,.F.);
#14078=ORIENTED_EDGE('',*,*,#9917,.T.);
#14079=ORIENTED_EDGE('',*,*,#9918,.T.);
#14080=ORIENTED_EDGE('',*,*,#9914,.F.);
#14081=ORIENTED_EDGE('',*,*,#9919,.F.);
#14082=ORIENTED_EDGE('',*,*,#9920,.T.);
#14083=ORIENTED_EDGE('',*,*,#9921,.T.);
#14084=ORIENTED_EDGE('',*,*,#9917,.F.);
#14085=ORIENTED_EDGE('',*,*,#9922,.F.);
#14086=ORIENTED_EDGE('',*,*,#9923,.T.);
#14087=ORIENTED_EDGE('',*,*,#9924,.T.);
#14088=ORIENTED_EDGE('',*,*,#9920,.F.);
#14089=ORIENTED_EDGE('',*,*,#9925,.F.);
#14090=ORIENTED_EDGE('',*,*,#9926,.T.);
#14091=ORIENTED_EDGE('',*,*,#9927,.T.);
#14092=ORIENTED_EDGE('',*,*,#9923,.F.);
#14093=ORIENTED_EDGE('',*,*,#9928,.F.);
#14094=ORIENTED_EDGE('',*,*,#9929,.F.);
#14095=ORIENTED_EDGE('',*,*,#9930,.F.);
#14096=ORIENTED_EDGE('',*,*,#9931,.F.);
#14097=ORIENTED_EDGE('',*,*,#9932,.T.);
#14098=ORIENTED_EDGE('',*,*,#9933,.T.);
#14099=ORIENTED_EDGE('',*,*,#9934,.T.);
#14100=ORIENTED_EDGE('',*,*,#9935,.T.);
#14101=ORIENTED_EDGE('',*,*,#9936,.T.);
#14102=ORIENTED_EDGE('',*,*,#9937,.T.);
#14103=ORIENTED_EDGE('',*,*,#9938,.T.);
#14104=ORIENTED_EDGE('',*,*,#9939,.T.);
#14105=ORIENTED_EDGE('',*,*,#9936,.F.);
#14106=ORIENTED_EDGE('',*,*,#9940,.T.);
#14107=ORIENTED_EDGE('',*,*,#9941,.T.);
#14108=ORIENTED_EDGE('',*,*,#9942,.T.);
#14109=ORIENTED_EDGE('',*,*,#9943,.T.);
#14110=ORIENTED_EDGE('',*,*,#9933,.F.);
#14111=ORIENTED_EDGE('',*,*,#9944,.T.);
#14112=ORIENTED_EDGE('',*,*,#9945,.T.);
#14113=ORIENTED_EDGE('',*,*,#9946,.T.);
#14114=ORIENTED_EDGE('',*,*,#9942,.F.);
#14115=ORIENTED_EDGE('',*,*,#9947,.T.);
#14116=ORIENTED_EDGE('',*,*,#9948,.T.);
#14117=ORIENTED_EDGE('',*,*,#9949,.T.);
#14118=ORIENTED_EDGE('',*,*,#9945,.F.);
#14119=ORIENTED_EDGE('',*,*,#9950,.T.);
#14120=ORIENTED_EDGE('',*,*,#9951,.T.);
#14121=ORIENTED_EDGE('',*,*,#9952,.T.);
#14122=ORIENTED_EDGE('',*,*,#9948,.F.);
#14123=ORIENTED_EDGE('',*,*,#9953,.T.);
#14124=ORIENTED_EDGE('',*,*,#9954,.T.);
#14125=ORIENTED_EDGE('',*,*,#9955,.T.);
#14126=ORIENTED_EDGE('',*,*,#9951,.F.);
#14127=ORIENTED_EDGE('',*,*,#9956,.T.);
#14128=ORIENTED_EDGE('',*,*,#9957,.T.);
#14129=ORIENTED_EDGE('',*,*,#9958,.T.);
#14130=ORIENTED_EDGE('',*,*,#9954,.F.);
#14131=ORIENTED_EDGE('',*,*,#9959,.T.);
#14132=ORIENTED_EDGE('',*,*,#9960,.F.);
#14133=ORIENTED_EDGE('',*,*,#9961,.T.);
#14134=ORIENTED_EDGE('',*,*,#9962,.F.);
#14135=ORIENTED_EDGE('',*,*,#9963,.T.);
#14136=ORIENTED_EDGE('',*,*,#9964,.T.);
#14137=ORIENTED_EDGE('',*,*,#9965,.T.);
#14138=ORIENTED_EDGE('',*,*,#9966,.F.);
#14139=ORIENTED_EDGE('',*,*,#9967,.F.);
#14140=ORIENTED_EDGE('',*,*,#9968,.T.);
#14141=ORIENTED_EDGE('',*,*,#9969,.T.);
#14142=ORIENTED_EDGE('',*,*,#9964,.F.);
#14143=ORIENTED_EDGE('',*,*,#9970,.F.);
#14144=ORIENTED_EDGE('',*,*,#9971,.T.);
#14145=ORIENTED_EDGE('',*,*,#9972,.T.);
#14146=ORIENTED_EDGE('',*,*,#9968,.F.);
#14147=ORIENTED_EDGE('',*,*,#9973,.F.);
#14148=ORIENTED_EDGE('',*,*,#9974,.T.);
#14149=ORIENTED_EDGE('',*,*,#9975,.T.);
#14150=ORIENTED_EDGE('',*,*,#9971,.F.);
#14151=ORIENTED_EDGE('',*,*,#9976,.F.);
#14152=ORIENTED_EDGE('',*,*,#9977,.T.);
#14153=ORIENTED_EDGE('',*,*,#9978,.T.);
#14154=ORIENTED_EDGE('',*,*,#9974,.F.);
#14155=ORIENTED_EDGE('',*,*,#9979,.F.);
#14156=ORIENTED_EDGE('',*,*,#9980,.T.);
#14157=ORIENTED_EDGE('',*,*,#9981,.T.);
#14158=ORIENTED_EDGE('',*,*,#9977,.F.);
#14159=ORIENTED_EDGE('',*,*,#9982,.F.);
#14160=ORIENTED_EDGE('',*,*,#9983,.T.);
#14161=ORIENTED_EDGE('',*,*,#9984,.T.);
#14162=ORIENTED_EDGE('',*,*,#9980,.F.);
#14163=ORIENTED_EDGE('',*,*,#9985,.F.);
#14164=ORIENTED_EDGE('',*,*,#9986,.F.);
#14165=ORIENTED_EDGE('',*,*,#9987,.F.);
#14166=ORIENTED_EDGE('',*,*,#9988,.F.);
#14167=ORIENTED_EDGE('',*,*,#9989,.T.);
#14168=ORIENTED_EDGE('',*,*,#9990,.T.);
#14169=ORIENTED_EDGE('',*,*,#9991,.T.);
#14170=ORIENTED_EDGE('',*,*,#9992,.T.);
#14171=ORIENTED_EDGE('',*,*,#9993,.T.);
#14172=ORIENTED_EDGE('',*,*,#9994,.T.);
#14173=ORIENTED_EDGE('',*,*,#9995,.T.);
#14174=ORIENTED_EDGE('',*,*,#9996,.T.);
#14175=ORIENTED_EDGE('',*,*,#9993,.F.);
#14176=ORIENTED_EDGE('',*,*,#9997,.T.);
#14177=ORIENTED_EDGE('',*,*,#9998,.T.);
#14178=ORIENTED_EDGE('',*,*,#9999,.T.);
#14179=ORIENTED_EDGE('',*,*,#10000,.T.);
#14180=ORIENTED_EDGE('',*,*,#9990,.F.);
#14181=ORIENTED_EDGE('',*,*,#10001,.T.);
#14182=ORIENTED_EDGE('',*,*,#10002,.T.);
#14183=ORIENTED_EDGE('',*,*,#10003,.T.);
#14184=ORIENTED_EDGE('',*,*,#9999,.F.);
#14185=ORIENTED_EDGE('',*,*,#10004,.T.);
#14186=ORIENTED_EDGE('',*,*,#10005,.T.);
#14187=ORIENTED_EDGE('',*,*,#10006,.T.);
#14188=ORIENTED_EDGE('',*,*,#10002,.F.);
#14189=ORIENTED_EDGE('',*,*,#10007,.T.);
#14190=ORIENTED_EDGE('',*,*,#10008,.T.);
#14191=ORIENTED_EDGE('',*,*,#10009,.T.);
#14192=ORIENTED_EDGE('',*,*,#10005,.F.);
#14193=ORIENTED_EDGE('',*,*,#10010,.T.);
#14194=ORIENTED_EDGE('',*,*,#10011,.T.);
#14195=ORIENTED_EDGE('',*,*,#10012,.T.);
#14196=ORIENTED_EDGE('',*,*,#10008,.F.);
#14197=ORIENTED_EDGE('',*,*,#10013,.T.);
#14198=ORIENTED_EDGE('',*,*,#10014,.T.);
#14199=ORIENTED_EDGE('',*,*,#10015,.T.);
#14200=ORIENTED_EDGE('',*,*,#10011,.F.);
#14201=ORIENTED_EDGE('',*,*,#10016,.T.);
#14202=ORIENTED_EDGE('',*,*,#10017,.F.);
#14203=ORIENTED_EDGE('',*,*,#10018,.T.);
#14204=ORIENTED_EDGE('',*,*,#10019,.F.);
#14205=ORIENTED_EDGE('',*,*,#10020,.T.);
#14206=ORIENTED_EDGE('',*,*,#10021,.T.);
#14207=ORIENTED_EDGE('',*,*,#10022,.T.);
#14208=ORIENTED_EDGE('',*,*,#10023,.F.);
#14209=ORIENTED_EDGE('',*,*,#10024,.F.);
#14210=ORIENTED_EDGE('',*,*,#10025,.T.);
#14211=ORIENTED_EDGE('',*,*,#10026,.T.);
#14212=ORIENTED_EDGE('',*,*,#10021,.F.);
#14213=ORIENTED_EDGE('',*,*,#10027,.F.);
#14214=ORIENTED_EDGE('',*,*,#10028,.T.);
#14215=ORIENTED_EDGE('',*,*,#10029,.T.);
#14216=ORIENTED_EDGE('',*,*,#10025,.F.);
#14217=ORIENTED_EDGE('',*,*,#10030,.F.);
#14218=ORIENTED_EDGE('',*,*,#10031,.T.);
#14219=ORIENTED_EDGE('',*,*,#10032,.T.);
#14220=ORIENTED_EDGE('',*,*,#10028,.F.);
#14221=ORIENTED_EDGE('',*,*,#10033,.F.);
#14222=ORIENTED_EDGE('',*,*,#10034,.T.);
#14223=ORIENTED_EDGE('',*,*,#10035,.T.);
#14224=ORIENTED_EDGE('',*,*,#10031,.F.);
#14225=ORIENTED_EDGE('',*,*,#10036,.F.);
#14226=ORIENTED_EDGE('',*,*,#10037,.T.);
#14227=ORIENTED_EDGE('',*,*,#10038,.T.);
#14228=ORIENTED_EDGE('',*,*,#10034,.F.);
#14229=ORIENTED_EDGE('',*,*,#10039,.F.);
#14230=ORIENTED_EDGE('',*,*,#10040,.T.);
#14231=ORIENTED_EDGE('',*,*,#10041,.T.);
#14232=ORIENTED_EDGE('',*,*,#10037,.F.);
#14233=ORIENTED_EDGE('',*,*,#10042,.F.);
#14234=ORIENTED_EDGE('',*,*,#10043,.F.);
#14235=ORIENTED_EDGE('',*,*,#10044,.F.);
#14236=ORIENTED_EDGE('',*,*,#10045,.F.);
#14237=ORIENTED_EDGE('',*,*,#10046,.T.);
#14238=ORIENTED_EDGE('',*,*,#10047,.T.);
#14239=ORIENTED_EDGE('',*,*,#10048,.T.);
#14240=ORIENTED_EDGE('',*,*,#10049,.T.);
#14241=ORIENTED_EDGE('',*,*,#10050,.T.);
#14242=ORIENTED_EDGE('',*,*,#10051,.T.);
#14243=ORIENTED_EDGE('',*,*,#10052,.T.);
#14244=ORIENTED_EDGE('',*,*,#10053,.T.);
#14245=ORIENTED_EDGE('',*,*,#10050,.F.);
#14246=ORIENTED_EDGE('',*,*,#10054,.T.);
#14247=ORIENTED_EDGE('',*,*,#10055,.T.);
#14248=ORIENTED_EDGE('',*,*,#10056,.T.);
#14249=ORIENTED_EDGE('',*,*,#10057,.T.);
#14250=ORIENTED_EDGE('',*,*,#10047,.F.);
#14251=ORIENTED_EDGE('',*,*,#10058,.T.);
#14252=ORIENTED_EDGE('',*,*,#10059,.T.);
#14253=ORIENTED_EDGE('',*,*,#10060,.T.);
#14254=ORIENTED_EDGE('',*,*,#10056,.F.);
#14255=ORIENTED_EDGE('',*,*,#10061,.T.);
#14256=ORIENTED_EDGE('',*,*,#10062,.T.);
#14257=ORIENTED_EDGE('',*,*,#10063,.T.);
#14258=ORIENTED_EDGE('',*,*,#10059,.F.);
#14259=ORIENTED_EDGE('',*,*,#10064,.T.);
#14260=ORIENTED_EDGE('',*,*,#10065,.T.);
#14261=ORIENTED_EDGE('',*,*,#10066,.T.);
#14262=ORIENTED_EDGE('',*,*,#10062,.F.);
#14263=ORIENTED_EDGE('',*,*,#10067,.T.);
#14264=ORIENTED_EDGE('',*,*,#10068,.T.);
#14265=ORIENTED_EDGE('',*,*,#10069,.T.);
#14266=ORIENTED_EDGE('',*,*,#10065,.F.);
#14267=ORIENTED_EDGE('',*,*,#10070,.T.);
#14268=ORIENTED_EDGE('',*,*,#10071,.T.);
#14269=ORIENTED_EDGE('',*,*,#10072,.T.);
#14270=ORIENTED_EDGE('',*,*,#10068,.F.);
#14271=ORIENTED_EDGE('',*,*,#10073,.T.);
#14272=ORIENTED_EDGE('',*,*,#10074,.F.);
#14273=ORIENTED_EDGE('',*,*,#10075,.T.);
#14274=ORIENTED_EDGE('',*,*,#10076,.F.);
#14275=ORIENTED_EDGE('',*,*,#10077,.T.);
#14276=ORIENTED_EDGE('',*,*,#10078,.T.);
#14277=ORIENTED_EDGE('',*,*,#10079,.T.);
#14278=ORIENTED_EDGE('',*,*,#10080,.F.);
#14279=ORIENTED_EDGE('',*,*,#10081,.F.);
#14280=ORIENTED_EDGE('',*,*,#10082,.T.);
#14281=ORIENTED_EDGE('',*,*,#10083,.T.);
#14282=ORIENTED_EDGE('',*,*,#10078,.F.);
#14283=ORIENTED_EDGE('',*,*,#10084,.F.);
#14284=ORIENTED_EDGE('',*,*,#10085,.T.);
#14285=ORIENTED_EDGE('',*,*,#10086,.T.);
#14286=ORIENTED_EDGE('',*,*,#10082,.F.);
#14287=ORIENTED_EDGE('',*,*,#10087,.F.);
#14288=ORIENTED_EDGE('',*,*,#10088,.T.);
#14289=ORIENTED_EDGE('',*,*,#10089,.T.);
#14290=ORIENTED_EDGE('',*,*,#10085,.F.);
#14291=ORIENTED_EDGE('',*,*,#10090,.F.);
#14292=ORIENTED_EDGE('',*,*,#10091,.T.);
#14293=ORIENTED_EDGE('',*,*,#10092,.T.);
#14294=ORIENTED_EDGE('',*,*,#10088,.F.);
#14295=ORIENTED_EDGE('',*,*,#10093,.F.);
#14296=ORIENTED_EDGE('',*,*,#10094,.T.);
#14297=ORIENTED_EDGE('',*,*,#10095,.T.);
#14298=ORIENTED_EDGE('',*,*,#10091,.F.);
#14299=ORIENTED_EDGE('',*,*,#10096,.F.);
#14300=ORIENTED_EDGE('',*,*,#10097,.T.);
#14301=ORIENTED_EDGE('',*,*,#10098,.T.);
#14302=ORIENTED_EDGE('',*,*,#10094,.F.);
#14303=ORIENTED_EDGE('',*,*,#10099,.F.);
#14304=ORIENTED_EDGE('',*,*,#10100,.F.);
#14305=ORIENTED_EDGE('',*,*,#10101,.F.);
#14306=ORIENTED_EDGE('',*,*,#10102,.F.);
#14307=ORIENTED_EDGE('',*,*,#10103,.T.);
#14308=ORIENTED_EDGE('',*,*,#10104,.T.);
#14309=ORIENTED_EDGE('',*,*,#10105,.T.);
#14310=ORIENTED_EDGE('',*,*,#10106,.T.);
#14311=ORIENTED_EDGE('',*,*,#10107,.T.);
#14312=ORIENTED_EDGE('',*,*,#10108,.T.);
#14313=ORIENTED_EDGE('',*,*,#10109,.T.);
#14314=ORIENTED_EDGE('',*,*,#10110,.T.);
#14315=ORIENTED_EDGE('',*,*,#10107,.F.);
#14316=ORIENTED_EDGE('',*,*,#10111,.T.);
#14317=ORIENTED_EDGE('',*,*,#10112,.T.);
#14318=ORIENTED_EDGE('',*,*,#10113,.T.);
#14319=ORIENTED_EDGE('',*,*,#10114,.T.);
#14320=ORIENTED_EDGE('',*,*,#10104,.F.);
#14321=ORIENTED_EDGE('',*,*,#10115,.T.);
#14322=ORIENTED_EDGE('',*,*,#10116,.T.);
#14323=ORIENTED_EDGE('',*,*,#10117,.T.);
#14324=ORIENTED_EDGE('',*,*,#10113,.F.);
#14325=ORIENTED_EDGE('',*,*,#10118,.T.);
#14326=ORIENTED_EDGE('',*,*,#10119,.T.);
#14327=ORIENTED_EDGE('',*,*,#10120,.T.);
#14328=ORIENTED_EDGE('',*,*,#10116,.F.);
#14329=ORIENTED_EDGE('',*,*,#10121,.T.);
#14330=ORIENTED_EDGE('',*,*,#10122,.T.);
#14331=ORIENTED_EDGE('',*,*,#10123,.T.);
#14332=ORIENTED_EDGE('',*,*,#10119,.F.);
#14333=ORIENTED_EDGE('',*,*,#10124,.T.);
#14334=ORIENTED_EDGE('',*,*,#10125,.T.);
#14335=ORIENTED_EDGE('',*,*,#10126,.T.);
#14336=ORIENTED_EDGE('',*,*,#10122,.F.);
#14337=ORIENTED_EDGE('',*,*,#10127,.T.);
#14338=ORIENTED_EDGE('',*,*,#10128,.T.);
#14339=ORIENTED_EDGE('',*,*,#10129,.T.);
#14340=ORIENTED_EDGE('',*,*,#10125,.F.);
#14341=ORIENTED_EDGE('',*,*,#10130,.T.);
#14342=ORIENTED_EDGE('',*,*,#10131,.F.);
#14343=ORIENTED_EDGE('',*,*,#10132,.T.);
#14344=ORIENTED_EDGE('',*,*,#10133,.F.);
#14345=ORIENTED_EDGE('',*,*,#10134,.T.);
#14346=ORIENTED_EDGE('',*,*,#10135,.T.);
#14347=ORIENTED_EDGE('',*,*,#10136,.T.);
#14348=ORIENTED_EDGE('',*,*,#10137,.F.);
#14349=ORIENTED_EDGE('',*,*,#10138,.F.);
#14350=ORIENTED_EDGE('',*,*,#10139,.T.);
#14351=ORIENTED_EDGE('',*,*,#10140,.T.);
#14352=ORIENTED_EDGE('',*,*,#10135,.F.);
#14353=ORIENTED_EDGE('',*,*,#10141,.F.);
#14354=ORIENTED_EDGE('',*,*,#10142,.T.);
#14355=ORIENTED_EDGE('',*,*,#10143,.T.);
#14356=ORIENTED_EDGE('',*,*,#10139,.F.);
#14357=ORIENTED_EDGE('',*,*,#10144,.F.);
#14358=ORIENTED_EDGE('',*,*,#10145,.T.);
#14359=ORIENTED_EDGE('',*,*,#10146,.T.);
#14360=ORIENTED_EDGE('',*,*,#10142,.F.);
#14361=ORIENTED_EDGE('',*,*,#10147,.F.);
#14362=ORIENTED_EDGE('',*,*,#10148,.T.);
#14363=ORIENTED_EDGE('',*,*,#10149,.T.);
#14364=ORIENTED_EDGE('',*,*,#10145,.F.);
#14365=ORIENTED_EDGE('',*,*,#10150,.F.);
#14366=ORIENTED_EDGE('',*,*,#10151,.T.);
#14367=ORIENTED_EDGE('',*,*,#10152,.T.);
#14368=ORIENTED_EDGE('',*,*,#10148,.F.);
#14369=ORIENTED_EDGE('',*,*,#10153,.F.);
#14370=ORIENTED_EDGE('',*,*,#10154,.T.);
#14371=ORIENTED_EDGE('',*,*,#10155,.T.);
#14372=ORIENTED_EDGE('',*,*,#10151,.F.);
#14373=ORIENTED_EDGE('',*,*,#10156,.F.);
#14374=ORIENTED_EDGE('',*,*,#10157,.F.);
#14375=ORIENTED_EDGE('',*,*,#10158,.F.);
#14376=ORIENTED_EDGE('',*,*,#10159,.F.);
#14377=ORIENTED_EDGE('',*,*,#10160,.T.);
#14378=ORIENTED_EDGE('',*,*,#10161,.T.);
#14379=ORIENTED_EDGE('',*,*,#10162,.T.);
#14380=ORIENTED_EDGE('',*,*,#10163,.T.);
#14381=ORIENTED_EDGE('',*,*,#10164,.T.);
#14382=ORIENTED_EDGE('',*,*,#10165,.T.);
#14383=ORIENTED_EDGE('',*,*,#10166,.T.);
#14384=ORIENTED_EDGE('',*,*,#10167,.T.);
#14385=ORIENTED_EDGE('',*,*,#10164,.F.);
#14386=ORIENTED_EDGE('',*,*,#10168,.T.);
#14387=ORIENTED_EDGE('',*,*,#10169,.T.);
#14388=ORIENTED_EDGE('',*,*,#10170,.T.);
#14389=ORIENTED_EDGE('',*,*,#10171,.T.);
#14390=ORIENTED_EDGE('',*,*,#10161,.F.);
#14391=ORIENTED_EDGE('',*,*,#10172,.T.);
#14392=ORIENTED_EDGE('',*,*,#10173,.T.);
#14393=ORIENTED_EDGE('',*,*,#10174,.T.);
#14394=ORIENTED_EDGE('',*,*,#10170,.F.);
#14395=ORIENTED_EDGE('',*,*,#10175,.T.);
#14396=ORIENTED_EDGE('',*,*,#10176,.T.);
#14397=ORIENTED_EDGE('',*,*,#10177,.T.);
#14398=ORIENTED_EDGE('',*,*,#10173,.F.);
#14399=ORIENTED_EDGE('',*,*,#10178,.T.);
#14400=ORIENTED_EDGE('',*,*,#10179,.T.);
#14401=ORIENTED_EDGE('',*,*,#10180,.T.);
#14402=ORIENTED_EDGE('',*,*,#10176,.F.);
#14403=ORIENTED_EDGE('',*,*,#10181,.T.);
#14404=ORIENTED_EDGE('',*,*,#10182,.T.);
#14405=ORIENTED_EDGE('',*,*,#10183,.T.);
#14406=ORIENTED_EDGE('',*,*,#10179,.F.);
#14407=ORIENTED_EDGE('',*,*,#10184,.T.);
#14408=ORIENTED_EDGE('',*,*,#10185,.T.);
#14409=ORIENTED_EDGE('',*,*,#10186,.T.);
#14410=ORIENTED_EDGE('',*,*,#10182,.F.);
#14411=ORIENTED_EDGE('',*,*,#10187,.T.);
#14412=ORIENTED_EDGE('',*,*,#10188,.F.);
#14413=ORIENTED_EDGE('',*,*,#10189,.T.);
#14414=ORIENTED_EDGE('',*,*,#10190,.F.);
#14415=ORIENTED_EDGE('',*,*,#10191,.T.);
#14416=ORIENTED_EDGE('',*,*,#10192,.T.);
#14417=ORIENTED_EDGE('',*,*,#10193,.T.);
#14418=ORIENTED_EDGE('',*,*,#10194,.F.);
#14419=ORIENTED_EDGE('',*,*,#10195,.F.);
#14420=ORIENTED_EDGE('',*,*,#10196,.T.);
#14421=ORIENTED_EDGE('',*,*,#10197,.T.);
#14422=ORIENTED_EDGE('',*,*,#10192,.F.);
#14423=ORIENTED_EDGE('',*,*,#10198,.F.);
#14424=ORIENTED_EDGE('',*,*,#10199,.T.);
#14425=ORIENTED_EDGE('',*,*,#10200,.T.);
#14426=ORIENTED_EDGE('',*,*,#10196,.F.);
#14427=ORIENTED_EDGE('',*,*,#10201,.F.);
#14428=ORIENTED_EDGE('',*,*,#10202,.T.);
#14429=ORIENTED_EDGE('',*,*,#10203,.T.);
#14430=ORIENTED_EDGE('',*,*,#10199,.F.);
#14431=ORIENTED_EDGE('',*,*,#10204,.F.);
#14432=ORIENTED_EDGE('',*,*,#10205,.T.);
#14433=ORIENTED_EDGE('',*,*,#10206,.T.);
#14434=ORIENTED_EDGE('',*,*,#10202,.F.);
#14435=ORIENTED_EDGE('',*,*,#10207,.F.);
#14436=ORIENTED_EDGE('',*,*,#10208,.T.);
#14437=ORIENTED_EDGE('',*,*,#10209,.T.);
#14438=ORIENTED_EDGE('',*,*,#10205,.F.);
#14439=ORIENTED_EDGE('',*,*,#10210,.F.);
#14440=ORIENTED_EDGE('',*,*,#10211,.T.);
#14441=ORIENTED_EDGE('',*,*,#10212,.T.);
#14442=ORIENTED_EDGE('',*,*,#10208,.F.);
#14443=ORIENTED_EDGE('',*,*,#10213,.F.);
#14444=ORIENTED_EDGE('',*,*,#10214,.F.);
#14445=ORIENTED_EDGE('',*,*,#10215,.F.);
#14446=ORIENTED_EDGE('',*,*,#10216,.F.);
#14447=ORIENTED_EDGE('',*,*,#10217,.T.);
#14448=ORIENTED_EDGE('',*,*,#10218,.T.);
#14449=ORIENTED_EDGE('',*,*,#10219,.T.);
#14450=ORIENTED_EDGE('',*,*,#10220,.T.);
#14451=ORIENTED_EDGE('',*,*,#10221,.T.);
#14452=ORIENTED_EDGE('',*,*,#10222,.T.);
#14453=ORIENTED_EDGE('',*,*,#10223,.T.);
#14454=ORIENTED_EDGE('',*,*,#10224,.T.);
#14455=ORIENTED_EDGE('',*,*,#10221,.F.);
#14456=ORIENTED_EDGE('',*,*,#10225,.T.);
#14457=ORIENTED_EDGE('',*,*,#10226,.T.);
#14458=ORIENTED_EDGE('',*,*,#10227,.T.);
#14459=ORIENTED_EDGE('',*,*,#10228,.T.);
#14460=ORIENTED_EDGE('',*,*,#10218,.F.);
#14461=ORIENTED_EDGE('',*,*,#10229,.T.);
#14462=ORIENTED_EDGE('',*,*,#10230,.T.);
#14463=ORIENTED_EDGE('',*,*,#10231,.T.);
#14464=ORIENTED_EDGE('',*,*,#10227,.F.);
#14465=ORIENTED_EDGE('',*,*,#10232,.T.);
#14466=ORIENTED_EDGE('',*,*,#10233,.T.);
#14467=ORIENTED_EDGE('',*,*,#10234,.T.);
#14468=ORIENTED_EDGE('',*,*,#10230,.F.);
#14469=ORIENTED_EDGE('',*,*,#10235,.T.);
#14470=ORIENTED_EDGE('',*,*,#10236,.T.);
#14471=ORIENTED_EDGE('',*,*,#10237,.T.);
#14472=ORIENTED_EDGE('',*,*,#10233,.F.);
#14473=ORIENTED_EDGE('',*,*,#10238,.T.);
#14474=ORIENTED_EDGE('',*,*,#10239,.T.);
#14475=ORIENTED_EDGE('',*,*,#10240,.T.);
#14476=ORIENTED_EDGE('',*,*,#10236,.F.);
#14477=ORIENTED_EDGE('',*,*,#10241,.T.);
#14478=ORIENTED_EDGE('',*,*,#10242,.T.);
#14479=ORIENTED_EDGE('',*,*,#10243,.T.);
#14480=ORIENTED_EDGE('',*,*,#10239,.F.);
#14481=ORIENTED_EDGE('',*,*,#10244,.T.);
#14482=ORIENTED_EDGE('',*,*,#10245,.F.);
#14483=ORIENTED_EDGE('',*,*,#10246,.T.);
#14484=ORIENTED_EDGE('',*,*,#10247,.F.);
#14485=ORIENTED_EDGE('',*,*,#10248,.T.);
#14486=ORIENTED_EDGE('',*,*,#10249,.T.);
#14487=ORIENTED_EDGE('',*,*,#10250,.T.);
#14488=ORIENTED_EDGE('',*,*,#10251,.F.);
#14489=ORIENTED_EDGE('',*,*,#10252,.F.);
#14490=ORIENTED_EDGE('',*,*,#10253,.T.);
#14491=ORIENTED_EDGE('',*,*,#10254,.T.);
#14492=ORIENTED_EDGE('',*,*,#10249,.F.);
#14493=ORIENTED_EDGE('',*,*,#10255,.F.);
#14494=ORIENTED_EDGE('',*,*,#10256,.T.);
#14495=ORIENTED_EDGE('',*,*,#10257,.T.);
#14496=ORIENTED_EDGE('',*,*,#10253,.F.);
#14497=ORIENTED_EDGE('',*,*,#10258,.F.);
#14498=ORIENTED_EDGE('',*,*,#10259,.T.);
#14499=ORIENTED_EDGE('',*,*,#10260,.T.);
#14500=ORIENTED_EDGE('',*,*,#10256,.F.);
#14501=ORIENTED_EDGE('',*,*,#10261,.F.);
#14502=ORIENTED_EDGE('',*,*,#10262,.T.);
#14503=ORIENTED_EDGE('',*,*,#10263,.T.);
#14504=ORIENTED_EDGE('',*,*,#10259,.F.);
#14505=ORIENTED_EDGE('',*,*,#10264,.F.);
#14506=ORIENTED_EDGE('',*,*,#10265,.T.);
#14507=ORIENTED_EDGE('',*,*,#10266,.T.);
#14508=ORIENTED_EDGE('',*,*,#10262,.F.);
#14509=ORIENTED_EDGE('',*,*,#10267,.F.);
#14510=ORIENTED_EDGE('',*,*,#10268,.T.);
#14511=ORIENTED_EDGE('',*,*,#10269,.T.);
#14512=ORIENTED_EDGE('',*,*,#10265,.F.);
#14513=ORIENTED_EDGE('',*,*,#10270,.F.);
#14514=ORIENTED_EDGE('',*,*,#10271,.F.);
#14515=ORIENTED_EDGE('',*,*,#10272,.F.);
#14516=ORIENTED_EDGE('',*,*,#10273,.F.);
#14517=ORIENTED_EDGE('',*,*,#10274,.T.);
#14518=ORIENTED_EDGE('',*,*,#10275,.F.);
#14519=ORIENTED_EDGE('',*,*,#10276,.F.);
#14520=ORIENTED_EDGE('',*,*,#10277,.T.);
#14521=ORIENTED_EDGE('',*,*,#10278,.F.);
#14522=ORIENTED_EDGE('',*,*,#10279,.F.);
#14523=ORIENTED_EDGE('',*,*,#10280,.T.);
#14524=ORIENTED_EDGE('',*,*,#10281,.F.);
#14525=ORIENTED_EDGE('',*,*,#10277,.F.);
#14526=ORIENTED_EDGE('',*,*,#10282,.F.);
#14527=ORIENTED_EDGE('',*,*,#10283,.F.);
#14528=ORIENTED_EDGE('',*,*,#10280,.F.);
#14529=ORIENTED_EDGE('',*,*,#10284,.F.);
#14530=ORIENTED_EDGE('',*,*,#10285,.F.);
#14531=ORIENTED_EDGE('',*,*,#10286,.F.);
#14532=ORIENTED_EDGE('',*,*,#10287,.F.);
#14533=ORIENTED_EDGE('',*,*,#10288,.F.);
#14534=ORIENTED_EDGE('',*,*,#10289,.F.);
#14535=ORIENTED_EDGE('',*,*,#10290,.T.);
#14536=ORIENTED_EDGE('',*,*,#10291,.T.);
#14537=ORIENTED_EDGE('',*,*,#10292,.T.);
#14538=ORIENTED_EDGE('',*,*,#10293,.T.);
#14539=ORIENTED_EDGE('',*,*,#10294,.F.);
#14540=ORIENTED_EDGE('',*,*,#10295,.F.);
#14541=ORIENTED_EDGE('',*,*,#10296,.F.);
#14542=ORIENTED_EDGE('',*,*,#10297,.F.);
#14543=ORIENTED_EDGE('',*,*,#10298,.F.);
#14544=ORIENTED_EDGE('',*,*,#10299,.T.);
#14545=ORIENTED_EDGE('',*,*,#10300,.T.);
#14546=ORIENTED_EDGE('',*,*,#10301,.T.);
#14547=ORIENTED_EDGE('',*,*,#10302,.T.);
#14548=ORIENTED_EDGE('',*,*,#10303,.F.);
#14549=ORIENTED_EDGE('',*,*,#10304,.F.);
#14550=ORIENTED_EDGE('',*,*,#10305,.F.);
#14551=ORIENTED_EDGE('',*,*,#10306,.F.);
#14552=ORIENTED_EDGE('',*,*,#10307,.F.);
#14553=ORIENTED_EDGE('',*,*,#10308,.T.);
#14554=ORIENTED_EDGE('',*,*,#10309,.T.);
#14555=ORIENTED_EDGE('',*,*,#10310,.T.);
#14556=ORIENTED_EDGE('',*,*,#10311,.T.);
#14557=ORIENTED_EDGE('',*,*,#10312,.F.);
#14558=ORIENTED_EDGE('',*,*,#10313,.F.);
#14559=ORIENTED_EDGE('',*,*,#10314,.F.);
#14560=ORIENTED_EDGE('',*,*,#10315,.F.);
#14561=ORIENTED_EDGE('',*,*,#10316,.F.);
#14562=ORIENTED_EDGE('',*,*,#10317,.T.);
#14563=ORIENTED_EDGE('',*,*,#10318,.T.);
#14564=ORIENTED_EDGE('',*,*,#10319,.T.);
#14565=ORIENTED_EDGE('',*,*,#10320,.T.);
#14566=ORIENTED_EDGE('',*,*,#10321,.F.);
#14567=ORIENTED_EDGE('',*,*,#10322,.F.);
#14568=ORIENTED_EDGE('',*,*,#10323,.F.);
#14569=ORIENTED_EDGE('',*,*,#10324,.F.);
#14570=ORIENTED_EDGE('',*,*,#10325,.F.);
#14571=ORIENTED_EDGE('',*,*,#10326,.T.);
#14572=ORIENTED_EDGE('',*,*,#10327,.T.);
#14573=ORIENTED_EDGE('',*,*,#10328,.T.);
#14574=ORIENTED_EDGE('',*,*,#10329,.T.);
#14575=ORIENTED_EDGE('',*,*,#10330,.F.);
#14576=ORIENTED_EDGE('',*,*,#10331,.F.);
#14577=ORIENTED_EDGE('',*,*,#10332,.F.);
#14578=ORIENTED_EDGE('',*,*,#10333,.F.);
#14579=ORIENTED_EDGE('',*,*,#10334,.F.);
#14580=ORIENTED_EDGE('',*,*,#10335,.T.);
#14581=ORIENTED_EDGE('',*,*,#10336,.T.);
#14582=ORIENTED_EDGE('',*,*,#10337,.T.);
#14583=ORIENTED_EDGE('',*,*,#10338,.T.);
#14584=ORIENTED_EDGE('',*,*,#10339,.T.);
#14585=ORIENTED_EDGE('',*,*,#9620,.T.);
#14586=ORIENTED_EDGE('',*,*,#10340,.T.);
#14587=ORIENTED_EDGE('',*,*,#9646,.T.);
#14588=ORIENTED_EDGE('',*,*,#10284,.T.);
#14589=ORIENTED_EDGE('',*,*,#10279,.T.);
#14590=ORIENTED_EDGE('',*,*,#10276,.T.);
#14591=ORIENTED_EDGE('',*,*,#10341,.F.);
#14592=ORIENTED_EDGE('',*,*,#10342,.T.);
#14593=ORIENTED_EDGE('',*,*,#9734,.T.);
#14594=ORIENTED_EDGE('',*,*,#10343,.T.);
#14595=ORIENTED_EDGE('',*,*,#9760,.T.);
#14596=ORIENTED_EDGE('',*,*,#10344,.T.);
#14597=ORIENTED_EDGE('',*,*,#9791,.T.);
#14598=ORIENTED_EDGE('',*,*,#10345,.T.);
#14599=ORIENTED_EDGE('',*,*,#9817,.T.);
#14600=ORIENTED_EDGE('',*,*,#10346,.T.);
#14601=ORIENTED_EDGE('',*,*,#9848,.T.);
#14602=ORIENTED_EDGE('',*,*,#10347,.T.);
#14603=ORIENTED_EDGE('',*,*,#9874,.T.);
#14604=ORIENTED_EDGE('',*,*,#10348,.T.);
#14605=ORIENTED_EDGE('',*,*,#9905,.T.);
#14606=ORIENTED_EDGE('',*,*,#10349,.T.);
#14607=ORIENTED_EDGE('',*,*,#9931,.T.);
#14608=ORIENTED_EDGE('',*,*,#10350,.T.);
#14609=ORIENTED_EDGE('',*,*,#9962,.T.);
#14610=ORIENTED_EDGE('',*,*,#10351,.T.);
#14611=ORIENTED_EDGE('',*,*,#9988,.T.);
#14612=ORIENTED_EDGE('',*,*,#10220,.F.);
#14613=ORIENTED_EDGE('',*,*,#10352,.T.);
#14614=ORIENTED_EDGE('',*,*,#10251,.T.);
#14615=ORIENTED_EDGE('',*,*,#10353,.T.);
#14616=ORIENTED_EDGE('',*,*,#10225,.F.);
#14617=ORIENTED_EDGE('',*,*,#10271,.T.);
#14618=ORIENTED_EDGE('',*,*,#10354,.T.);
#14619=ORIENTED_EDGE('',*,*,#10268,.F.);
#14620=ORIENTED_EDGE('',*,*,#10355,.F.);
#14621=ORIENTED_EDGE('',*,*,#10353,.F.);
#14622=ORIENTED_EDGE('',*,*,#10250,.F.);
#14623=ORIENTED_EDGE('',*,*,#10254,.F.);
#14624=ORIENTED_EDGE('',*,*,#10257,.F.);
#14625=ORIENTED_EDGE('',*,*,#10260,.F.);
#14626=ORIENTED_EDGE('',*,*,#10263,.F.);
#14627=ORIENTED_EDGE('',*,*,#10266,.F.);
#14628=ORIENTED_EDGE('',*,*,#10269,.F.);
#14629=ORIENTED_EDGE('',*,*,#10354,.F.);
#14630=ORIENTED_EDGE('',*,*,#10274,.F.);
#14631=ORIENTED_EDGE('',*,*,#10356,.F.);
#14632=ORIENTED_EDGE('',*,*,#10246,.F.);
#14633=ORIENTED_EDGE('',*,*,#10357,.F.);
#14634=ORIENTED_EDGE('',*,*,#10244,.F.);
#14635=ORIENTED_EDGE('',*,*,#10241,.F.);
#14636=ORIENTED_EDGE('',*,*,#10238,.F.);
#14637=ORIENTED_EDGE('',*,*,#10235,.F.);
#14638=ORIENTED_EDGE('',*,*,#10232,.F.);
#14639=ORIENTED_EDGE('',*,*,#10229,.F.);
#14640=ORIENTED_EDGE('',*,*,#10226,.F.);
#14641=ORIENTED_EDGE('',*,*,#10352,.F.);
#14642=ORIENTED_EDGE('',*,*,#10219,.F.);
#14643=ORIENTED_EDGE('',*,*,#10228,.F.);
#14644=ORIENTED_EDGE('',*,*,#10231,.F.);
#14645=ORIENTED_EDGE('',*,*,#10234,.F.);
#14646=ORIENTED_EDGE('',*,*,#10237,.F.);
#14647=ORIENTED_EDGE('',*,*,#10240,.F.);
#14648=ORIENTED_EDGE('',*,*,#10243,.F.);
#14649=ORIENTED_EDGE('',*,*,#10358,.F.);
#14650=ORIENTED_EDGE('',*,*,#10248,.F.);
#14651=ORIENTED_EDGE('',*,*,#10359,.F.);
#14652=ORIENTED_EDGE('',*,*,#10272,.T.);
#14653=ORIENTED_EDGE('',*,*,#10355,.T.);
#14654=ORIENTED_EDGE('',*,*,#10270,.T.);
#14655=ORIENTED_EDGE('',*,*,#10267,.T.);
#14656=ORIENTED_EDGE('',*,*,#10264,.T.);
#14657=ORIENTED_EDGE('',*,*,#10261,.T.);
#14658=ORIENTED_EDGE('',*,*,#10258,.T.);
#14659=ORIENTED_EDGE('',*,*,#10255,.T.);
#14660=ORIENTED_EDGE('',*,*,#10252,.T.);
#14661=ORIENTED_EDGE('',*,*,#10245,.T.);
#14662=ORIENTED_EDGE('',*,*,#10358,.T.);
#14663=ORIENTED_EDGE('',*,*,#10242,.F.);
#14664=ORIENTED_EDGE('',*,*,#10357,.T.);
#14665=ORIENTED_EDGE('',*,*,#10163,.F.);
#14666=ORIENTED_EDGE('',*,*,#10360,.T.);
#14667=ORIENTED_EDGE('',*,*,#10194,.T.);
#14668=ORIENTED_EDGE('',*,*,#10361,.T.);
#14669=ORIENTED_EDGE('',*,*,#10168,.F.);
#14670=ORIENTED_EDGE('',*,*,#10214,.T.);
#14671=ORIENTED_EDGE('',*,*,#10362,.T.);
#14672=ORIENTED_EDGE('',*,*,#10211,.F.);
#14673=ORIENTED_EDGE('',*,*,#10363,.F.);
#14674=ORIENTED_EDGE('',*,*,#10361,.F.);
#14675=ORIENTED_EDGE('',*,*,#10193,.F.);
#14676=ORIENTED_EDGE('',*,*,#10197,.F.);
#14677=ORIENTED_EDGE('',*,*,#10200,.F.);
#14678=ORIENTED_EDGE('',*,*,#10203,.F.);
#14679=ORIENTED_EDGE('',*,*,#10206,.F.);
#14680=ORIENTED_EDGE('',*,*,#10209,.F.);
#14681=ORIENTED_EDGE('',*,*,#10212,.F.);
#14682=ORIENTED_EDGE('',*,*,#10362,.F.);
#14683=ORIENTED_EDGE('',*,*,#10217,.F.);
#14684=ORIENTED_EDGE('',*,*,#10364,.F.);
#14685=ORIENTED_EDGE('',*,*,#10189,.F.);
#14686=ORIENTED_EDGE('',*,*,#10365,.F.);
#14687=ORIENTED_EDGE('',*,*,#10187,.F.);
#14688=ORIENTED_EDGE('',*,*,#10184,.F.);
#14689=ORIENTED_EDGE('',*,*,#10181,.F.);
#14690=ORIENTED_EDGE('',*,*,#10178,.F.);
#14691=ORIENTED_EDGE('',*,*,#10175,.F.);
#14692=ORIENTED_EDGE('',*,*,#10172,.F.);
#14693=ORIENTED_EDGE('',*,*,#10169,.F.);
#14694=ORIENTED_EDGE('',*,*,#10360,.F.);
#14695=ORIENTED_EDGE('',*,*,#10162,.F.);
#14696=ORIENTED_EDGE('',*,*,#10171,.F.);
#14697=ORIENTED_EDGE('',*,*,#10174,.F.);
#14698=ORIENTED_EDGE('',*,*,#10177,.F.);
#14699=ORIENTED_EDGE('',*,*,#10180,.F.);
#14700=ORIENTED_EDGE('',*,*,#10183,.F.);
#14701=ORIENTED_EDGE('',*,*,#10186,.F.);
#14702=ORIENTED_EDGE('',*,*,#10366,.F.);
#14703=ORIENTED_EDGE('',*,*,#10191,.F.);
#14704=ORIENTED_EDGE('',*,*,#10367,.F.);
#14705=ORIENTED_EDGE('',*,*,#10215,.T.);
#14706=ORIENTED_EDGE('',*,*,#10363,.T.);
#14707=ORIENTED_EDGE('',*,*,#10213,.T.);
#14708=ORIENTED_EDGE('',*,*,#10210,.T.);
#14709=ORIENTED_EDGE('',*,*,#10207,.T.);
#14710=ORIENTED_EDGE('',*,*,#10204,.T.);
#14711=ORIENTED_EDGE('',*,*,#10201,.T.);
#14712=ORIENTED_EDGE('',*,*,#10198,.T.);
#14713=ORIENTED_EDGE('',*,*,#10195,.T.);
#14714=ORIENTED_EDGE('',*,*,#10188,.T.);
#14715=ORIENTED_EDGE('',*,*,#10366,.T.);
#14716=ORIENTED_EDGE('',*,*,#10185,.F.);
#14717=ORIENTED_EDGE('',*,*,#10365,.T.);
#14718=ORIENTED_EDGE('',*,*,#10106,.F.);
#14719=ORIENTED_EDGE('',*,*,#10368,.T.);
#14720=ORIENTED_EDGE('',*,*,#10137,.T.);
#14721=ORIENTED_EDGE('',*,*,#10369,.T.);
#14722=ORIENTED_EDGE('',*,*,#10111,.F.);
#14723=ORIENTED_EDGE('',*,*,#10157,.T.);
#14724=ORIENTED_EDGE('',*,*,#10370,.T.);
#14725=ORIENTED_EDGE('',*,*,#10154,.F.);
#14726=ORIENTED_EDGE('',*,*,#10371,.F.);
#14727=ORIENTED_EDGE('',*,*,#10369,.F.);
#14728=ORIENTED_EDGE('',*,*,#10136,.F.);
#14729=ORIENTED_EDGE('',*,*,#10140,.F.);
#14730=ORIENTED_EDGE('',*,*,#10143,.F.);
#14731=ORIENTED_EDGE('',*,*,#10146,.F.);
#14732=ORIENTED_EDGE('',*,*,#10149,.F.);
#14733=ORIENTED_EDGE('',*,*,#10152,.F.);
#14734=ORIENTED_EDGE('',*,*,#10155,.F.);
#14735=ORIENTED_EDGE('',*,*,#10370,.F.);
#14736=ORIENTED_EDGE('',*,*,#10160,.F.);
#14737=ORIENTED_EDGE('',*,*,#10372,.F.);
#14738=ORIENTED_EDGE('',*,*,#10132,.F.);
#14739=ORIENTED_EDGE('',*,*,#10373,.F.);
#14740=ORIENTED_EDGE('',*,*,#10130,.F.);
#14741=ORIENTED_EDGE('',*,*,#10127,.F.);
#14742=ORIENTED_EDGE('',*,*,#10124,.F.);
#14743=ORIENTED_EDGE('',*,*,#10121,.F.);
#14744=ORIENTED_EDGE('',*,*,#10118,.F.);
#14745=ORIENTED_EDGE('',*,*,#10115,.F.);
#14746=ORIENTED_EDGE('',*,*,#10112,.F.);
#14747=ORIENTED_EDGE('',*,*,#10368,.F.);
#14748=ORIENTED_EDGE('',*,*,#10105,.F.);
#14749=ORIENTED_EDGE('',*,*,#10114,.F.);
#14750=ORIENTED_EDGE('',*,*,#10117,.F.);
#14751=ORIENTED_EDGE('',*,*,#10120,.F.);
#14752=ORIENTED_EDGE('',*,*,#10123,.F.);
#14753=ORIENTED_EDGE('',*,*,#10126,.F.);
#14754=ORIENTED_EDGE('',*,*,#10129,.F.);
#14755=ORIENTED_EDGE('',*,*,#10374,.F.);
#14756=ORIENTED_EDGE('',*,*,#10134,.F.);
#14757=ORIENTED_EDGE('',*,*,#10375,.F.);
#14758=ORIENTED_EDGE('',*,*,#10158,.T.);
#14759=ORIENTED_EDGE('',*,*,#10371,.T.);
#14760=ORIENTED_EDGE('',*,*,#10156,.T.);
#14761=ORIENTED_EDGE('',*,*,#10153,.T.);
#14762=ORIENTED_EDGE('',*,*,#10150,.T.);
#14763=ORIENTED_EDGE('',*,*,#10147,.T.);
#14764=ORIENTED_EDGE('',*,*,#10144,.T.);
#14765=ORIENTED_EDGE('',*,*,#10141,.T.);
#14766=ORIENTED_EDGE('',*,*,#10138,.T.);
#14767=ORIENTED_EDGE('',*,*,#10131,.T.);
#14768=ORIENTED_EDGE('',*,*,#10374,.T.);
#14769=ORIENTED_EDGE('',*,*,#10128,.F.);
#14770=ORIENTED_EDGE('',*,*,#10373,.T.);
#14771=ORIENTED_EDGE('',*,*,#10049,.F.);
#14772=ORIENTED_EDGE('',*,*,#10376,.T.);
#14773=ORIENTED_EDGE('',*,*,#10080,.T.);
#14774=ORIENTED_EDGE('',*,*,#10377,.T.);
#14775=ORIENTED_EDGE('',*,*,#10054,.F.);
#14776=ORIENTED_EDGE('',*,*,#10100,.T.);
#14777=ORIENTED_EDGE('',*,*,#10378,.T.);
#14778=ORIENTED_EDGE('',*,*,#10097,.F.);
#14779=ORIENTED_EDGE('',*,*,#10379,.F.);
#14780=ORIENTED_EDGE('',*,*,#10377,.F.);
#14781=ORIENTED_EDGE('',*,*,#10079,.F.);
#14782=ORIENTED_EDGE('',*,*,#10083,.F.);
#14783=ORIENTED_EDGE('',*,*,#10086,.F.);
#14784=ORIENTED_EDGE('',*,*,#10089,.F.);
#14785=ORIENTED_EDGE('',*,*,#10092,.F.);
#14786=ORIENTED_EDGE('',*,*,#10095,.F.);
#14787=ORIENTED_EDGE('',*,*,#10098,.F.);
#14788=ORIENTED_EDGE('',*,*,#10378,.F.);
#14789=ORIENTED_EDGE('',*,*,#10103,.F.);
#14790=ORIENTED_EDGE('',*,*,#10380,.F.);
#14791=ORIENTED_EDGE('',*,*,#10075,.F.);
#14792=ORIENTED_EDGE('',*,*,#10381,.F.);
#14793=ORIENTED_EDGE('',*,*,#10073,.F.);
#14794=ORIENTED_EDGE('',*,*,#10070,.F.);
#14795=ORIENTED_EDGE('',*,*,#10067,.F.);
#14796=ORIENTED_EDGE('',*,*,#10064,.F.);
#14797=ORIENTED_EDGE('',*,*,#10061,.F.);
#14798=ORIENTED_EDGE('',*,*,#10058,.F.);
#14799=ORIENTED_EDGE('',*,*,#10055,.F.);
#14800=ORIENTED_EDGE('',*,*,#10376,.F.);
#14801=ORIENTED_EDGE('',*,*,#10048,.F.);
#14802=ORIENTED_EDGE('',*,*,#10057,.F.);
#14803=ORIENTED_EDGE('',*,*,#10060,.F.);
#14804=ORIENTED_EDGE('',*,*,#10063,.F.);
#14805=ORIENTED_EDGE('',*,*,#10066,.F.);
#14806=ORIENTED_EDGE('',*,*,#10069,.F.);
#14807=ORIENTED_EDGE('',*,*,#10072,.F.);
#14808=ORIENTED_EDGE('',*,*,#10382,.F.);
#14809=ORIENTED_EDGE('',*,*,#10077,.F.);
#14810=ORIENTED_EDGE('',*,*,#10383,.F.);
#14811=ORIENTED_EDGE('',*,*,#10101,.T.);
#14812=ORIENTED_EDGE('',*,*,#10379,.T.);
#14813=ORIENTED_EDGE('',*,*,#10099,.T.);
#14814=ORIENTED_EDGE('',*,*,#10096,.T.);
#14815=ORIENTED_EDGE('',*,*,#10093,.T.);
#14816=ORIENTED_EDGE('',*,*,#10090,.T.);
#14817=ORIENTED_EDGE('',*,*,#10087,.T.);
#14818=ORIENTED_EDGE('',*,*,#10084,.T.);
#14819=ORIENTED_EDGE('',*,*,#10081,.T.);
#14820=ORIENTED_EDGE('',*,*,#10074,.T.);
#14821=ORIENTED_EDGE('',*,*,#10382,.T.);
#14822=ORIENTED_EDGE('',*,*,#10071,.F.);
#14823=ORIENTED_EDGE('',*,*,#10381,.T.);
#14824=ORIENTED_EDGE('',*,*,#9992,.F.);
#14825=ORIENTED_EDGE('',*,*,#10384,.T.);
#14826=ORIENTED_EDGE('',*,*,#10023,.T.);
#14827=ORIENTED_EDGE('',*,*,#10385,.T.);
#14828=ORIENTED_EDGE('',*,*,#9997,.F.);
#14829=ORIENTED_EDGE('',*,*,#10043,.T.);
#14830=ORIENTED_EDGE('',*,*,#10386,.T.);
#14831=ORIENTED_EDGE('',*,*,#10040,.F.);
#14832=ORIENTED_EDGE('',*,*,#10387,.F.);
#14833=ORIENTED_EDGE('',*,*,#10385,.F.);
#14834=ORIENTED_EDGE('',*,*,#10022,.F.);
#14835=ORIENTED_EDGE('',*,*,#10026,.F.);
#14836=ORIENTED_EDGE('',*,*,#10029,.F.);
#14837=ORIENTED_EDGE('',*,*,#10032,.F.);
#14838=ORIENTED_EDGE('',*,*,#10035,.F.);
#14839=ORIENTED_EDGE('',*,*,#10038,.F.);
#14840=ORIENTED_EDGE('',*,*,#10041,.F.);
#14841=ORIENTED_EDGE('',*,*,#10386,.F.);
#14842=ORIENTED_EDGE('',*,*,#10046,.F.);
#14843=ORIENTED_EDGE('',*,*,#10388,.F.);
#14844=ORIENTED_EDGE('',*,*,#10018,.F.);
#14845=ORIENTED_EDGE('',*,*,#10389,.F.);
#14846=ORIENTED_EDGE('',*,*,#10016,.F.);
#14847=ORIENTED_EDGE('',*,*,#10013,.F.);
#14848=ORIENTED_EDGE('',*,*,#10010,.F.);
#14849=ORIENTED_EDGE('',*,*,#10007,.F.);
#14850=ORIENTED_EDGE('',*,*,#10004,.F.);
#14851=ORIENTED_EDGE('',*,*,#10001,.F.);
#14852=ORIENTED_EDGE('',*,*,#9998,.F.);
#14853=ORIENTED_EDGE('',*,*,#10384,.F.);
#14854=ORIENTED_EDGE('',*,*,#9991,.F.);
#14855=ORIENTED_EDGE('',*,*,#10000,.F.);
#14856=ORIENTED_EDGE('',*,*,#10003,.F.);
#14857=ORIENTED_EDGE('',*,*,#10006,.F.);
#14858=ORIENTED_EDGE('',*,*,#10009,.F.);
#14859=ORIENTED_EDGE('',*,*,#10012,.F.);
#14860=ORIENTED_EDGE('',*,*,#10015,.F.);
#14861=ORIENTED_EDGE('',*,*,#10390,.F.);
#14862=ORIENTED_EDGE('',*,*,#10020,.F.);
#14863=ORIENTED_EDGE('',*,*,#10391,.F.);
#14864=ORIENTED_EDGE('',*,*,#10044,.T.);
#14865=ORIENTED_EDGE('',*,*,#10387,.T.);
#14866=ORIENTED_EDGE('',*,*,#10042,.T.);
#14867=ORIENTED_EDGE('',*,*,#10039,.T.);
#14868=ORIENTED_EDGE('',*,*,#10036,.T.);
#14869=ORIENTED_EDGE('',*,*,#10033,.T.);
#14870=ORIENTED_EDGE('',*,*,#10030,.T.);
#14871=ORIENTED_EDGE('',*,*,#10027,.T.);
#14872=ORIENTED_EDGE('',*,*,#10024,.T.);
#14873=ORIENTED_EDGE('',*,*,#10017,.T.);
#14874=ORIENTED_EDGE('',*,*,#10390,.T.);
#14875=ORIENTED_EDGE('',*,*,#10014,.F.);
#14876=ORIENTED_EDGE('',*,*,#10389,.T.);
#14877=ORIENTED_EDGE('',*,*,#10392,.T.);
#14878=ORIENTED_EDGE('',*,*,#10222,.F.);
#14879=ORIENTED_EDGE('',*,*,#10224,.F.);
#14880=ORIENTED_EDGE('',*,*,#10393,.F.);
#14881=ORIENTED_EDGE('',*,*,#10223,.F.);
#14882=ORIENTED_EDGE('',*,*,#10394,.T.);
#14883=ORIENTED_EDGE('',*,*,#10165,.F.);
#14884=ORIENTED_EDGE('',*,*,#10167,.F.);
#14885=ORIENTED_EDGE('',*,*,#10395,.F.);
#14886=ORIENTED_EDGE('',*,*,#10166,.F.);
#14887=ORIENTED_EDGE('',*,*,#10396,.T.);
#14888=ORIENTED_EDGE('',*,*,#10108,.F.);
#14889=ORIENTED_EDGE('',*,*,#10110,.F.);
#14890=ORIENTED_EDGE('',*,*,#10397,.F.);
#14891=ORIENTED_EDGE('',*,*,#10109,.F.);
#14892=ORIENTED_EDGE('',*,*,#10398,.T.);
#14893=ORIENTED_EDGE('',*,*,#10051,.F.);
#14894=ORIENTED_EDGE('',*,*,#10053,.F.);
#14895=ORIENTED_EDGE('',*,*,#10399,.F.);
#14896=ORIENTED_EDGE('',*,*,#10052,.F.);
#14897=ORIENTED_EDGE('',*,*,#10400,.T.);
#14898=ORIENTED_EDGE('',*,*,#9994,.F.);
#14899=ORIENTED_EDGE('',*,*,#9996,.F.);
#14900=ORIENTED_EDGE('',*,*,#10401,.F.);
#14901=ORIENTED_EDGE('',*,*,#9995,.F.);
#14902=ORIENTED_EDGE('',*,*,#9935,.F.);
#14903=ORIENTED_EDGE('',*,*,#10402,.T.);
#14904=ORIENTED_EDGE('',*,*,#9966,.T.);
#14905=ORIENTED_EDGE('',*,*,#10403,.T.);
#14906=ORIENTED_EDGE('',*,*,#9940,.F.);
#14907=ORIENTED_EDGE('',*,*,#9986,.T.);
#14908=ORIENTED_EDGE('',*,*,#10404,.T.);
#14909=ORIENTED_EDGE('',*,*,#9983,.F.);
#14910=ORIENTED_EDGE('',*,*,#10405,.F.);
#14911=ORIENTED_EDGE('',*,*,#10403,.F.);
#14912=ORIENTED_EDGE('',*,*,#9965,.F.);
#14913=ORIENTED_EDGE('',*,*,#9969,.F.);
#14914=ORIENTED_EDGE('',*,*,#9972,.F.);
#14915=ORIENTED_EDGE('',*,*,#9975,.F.);
#14916=ORIENTED_EDGE('',*,*,#9978,.F.);
#14917=ORIENTED_EDGE('',*,*,#9981,.F.);
#14918=ORIENTED_EDGE('',*,*,#9984,.F.);
#14919=ORIENTED_EDGE('',*,*,#10404,.F.);
#14920=ORIENTED_EDGE('',*,*,#9989,.F.);
#14921=ORIENTED_EDGE('',*,*,#10351,.F.);
#14922=ORIENTED_EDGE('',*,*,#9961,.F.);
#14923=ORIENTED_EDGE('',*,*,#10406,.F.);
#14924=ORIENTED_EDGE('',*,*,#9959,.F.);
#14925=ORIENTED_EDGE('',*,*,#9956,.F.);
#14926=ORIENTED_EDGE('',*,*,#9953,.F.);
#14927=ORIENTED_EDGE('',*,*,#9950,.F.);
#14928=ORIENTED_EDGE('',*,*,#9947,.F.);
#14929=ORIENTED_EDGE('',*,*,#9944,.F.);
#14930=ORIENTED_EDGE('',*,*,#9941,.F.);
#14931=ORIENTED_EDGE('',*,*,#10402,.F.);
#14932=ORIENTED_EDGE('',*,*,#9934,.F.);
#14933=ORIENTED_EDGE('',*,*,#9943,.F.);
#14934=ORIENTED_EDGE('',*,*,#9946,.F.);
#14935=ORIENTED_EDGE('',*,*,#9949,.F.);
#14936=ORIENTED_EDGE('',*,*,#9952,.F.);
#14937=ORIENTED_EDGE('',*,*,#9955,.F.);
#14938=ORIENTED_EDGE('',*,*,#9958,.F.);
#14939=ORIENTED_EDGE('',*,*,#10407,.F.);
#14940=ORIENTED_EDGE('',*,*,#9963,.F.);
#14941=ORIENTED_EDGE('',*,*,#10350,.F.);
#14942=ORIENTED_EDGE('',*,*,#9987,.T.);
#14943=ORIENTED_EDGE('',*,*,#10405,.T.);
#14944=ORIENTED_EDGE('',*,*,#9985,.T.);
#14945=ORIENTED_EDGE('',*,*,#9982,.T.);
#14946=ORIENTED_EDGE('',*,*,#9979,.T.);
#14947=ORIENTED_EDGE('',*,*,#9976,.T.);
#14948=ORIENTED_EDGE('',*,*,#9973,.T.);
#14949=ORIENTED_EDGE('',*,*,#9970,.T.);
#14950=ORIENTED_EDGE('',*,*,#9967,.T.);
#14951=ORIENTED_EDGE('',*,*,#9960,.T.);
#14952=ORIENTED_EDGE('',*,*,#10407,.T.);
#14953=ORIENTED_EDGE('',*,*,#9957,.F.);
#14954=ORIENTED_EDGE('',*,*,#10406,.T.);
#14955=ORIENTED_EDGE('',*,*,#9878,.F.);
#14956=ORIENTED_EDGE('',*,*,#10408,.T.);
#14957=ORIENTED_EDGE('',*,*,#9909,.T.);
#14958=ORIENTED_EDGE('',*,*,#10409,.T.);
#14959=ORIENTED_EDGE('',*,*,#9883,.F.);
#14960=ORIENTED_EDGE('',*,*,#9929,.T.);
#14961=ORIENTED_EDGE('',*,*,#10410,.T.);
#14962=ORIENTED_EDGE('',*,*,#9926,.F.);
#14963=ORIENTED_EDGE('',*,*,#10411,.F.);
#14964=ORIENTED_EDGE('',*,*,#10409,.F.);
#14965=ORIENTED_EDGE('',*,*,#9908,.F.);
#14966=ORIENTED_EDGE('',*,*,#9912,.F.);
#14967=ORIENTED_EDGE('',*,*,#9915,.F.);
#14968=ORIENTED_EDGE('',*,*,#9918,.F.);
#14969=ORIENTED_EDGE('',*,*,#9921,.F.);
#14970=ORIENTED_EDGE('',*,*,#9924,.F.);
#14971=ORIENTED_EDGE('',*,*,#9927,.F.);
#14972=ORIENTED_EDGE('',*,*,#10410,.F.);
#14973=ORIENTED_EDGE('',*,*,#9932,.F.);
#14974=ORIENTED_EDGE('',*,*,#10349,.F.);
#14975=ORIENTED_EDGE('',*,*,#9904,.F.);
#14976=ORIENTED_EDGE('',*,*,#10412,.F.);
#14977=ORIENTED_EDGE('',*,*,#9902,.F.);
#14978=ORIENTED_EDGE('',*,*,#9899,.F.);
#14979=ORIENTED_EDGE('',*,*,#9896,.F.);
#14980=ORIENTED_EDGE('',*,*,#9893,.F.);
#14981=ORIENTED_EDGE('',*,*,#9890,.F.);
#14982=ORIENTED_EDGE('',*,*,#9887,.F.);
#14983=ORIENTED_EDGE('',*,*,#9884,.F.);
#14984=ORIENTED_EDGE('',*,*,#10408,.F.);
#14985=ORIENTED_EDGE('',*,*,#9877,.F.);
#14986=ORIENTED_EDGE('',*,*,#9886,.F.);
#14987=ORIENTED_EDGE('',*,*,#9889,.F.);
#14988=ORIENTED_EDGE('',*,*,#9892,.F.);
#14989=ORIENTED_EDGE('',*,*,#9895,.F.);
#14990=ORIENTED_EDGE('',*,*,#9898,.F.);
#14991=ORIENTED_EDGE('',*,*,#9901,.F.);
#14992=ORIENTED_EDGE('',*,*,#10413,.F.);
#14993=ORIENTED_EDGE('',*,*,#9906,.F.);
#14994=ORIENTED_EDGE('',*,*,#10348,.F.);
#14995=ORIENTED_EDGE('',*,*,#9930,.T.);
#14996=ORIENTED_EDGE('',*,*,#10411,.T.);
#14997=ORIENTED_EDGE('',*,*,#9928,.T.);
#14998=ORIENTED_EDGE('',*,*,#9925,.T.);
#14999=ORIENTED_EDGE('',*,*,#9922,.T.);
#15000=ORIENTED_EDGE('',*,*,#9919,.T.);
#15001=ORIENTED_EDGE('',*,*,#9916,.T.);
#15002=ORIENTED_EDGE('',*,*,#9913,.T.);
#15003=ORIENTED_EDGE('',*,*,#9910,.T.);
#15004=ORIENTED_EDGE('',*,*,#9903,.T.);
#15005=ORIENTED_EDGE('',*,*,#10413,.T.);
#15006=ORIENTED_EDGE('',*,*,#9900,.F.);
#15007=ORIENTED_EDGE('',*,*,#10412,.T.);
#15008=ORIENTED_EDGE('',*,*,#9821,.F.);
#15009=ORIENTED_EDGE('',*,*,#10414,.T.);
#15010=ORIENTED_EDGE('',*,*,#9852,.T.);
#15011=ORIENTED_EDGE('',*,*,#10415,.T.);
#15012=ORIENTED_EDGE('',*,*,#9826,.F.);
#15013=ORIENTED_EDGE('',*,*,#9872,.T.);
#15014=ORIENTED_EDGE('',*,*,#10416,.T.);
#15015=ORIENTED_EDGE('',*,*,#9869,.F.);
#15016=ORIENTED_EDGE('',*,*,#10417,.F.);
#15017=ORIENTED_EDGE('',*,*,#10415,.F.);
#15018=ORIENTED_EDGE('',*,*,#9851,.F.);
#15019=ORIENTED_EDGE('',*,*,#9855,.F.);
#15020=ORIENTED_EDGE('',*,*,#9858,.F.);
#15021=ORIENTED_EDGE('',*,*,#9861,.F.);
#15022=ORIENTED_EDGE('',*,*,#9864,.F.);
#15023=ORIENTED_EDGE('',*,*,#9867,.F.);
#15024=ORIENTED_EDGE('',*,*,#9870,.F.);
#15025=ORIENTED_EDGE('',*,*,#10416,.F.);
#15026=ORIENTED_EDGE('',*,*,#9875,.F.);
#15027=ORIENTED_EDGE('',*,*,#10347,.F.);
#15028=ORIENTED_EDGE('',*,*,#9847,.F.);
#15029=ORIENTED_EDGE('',*,*,#10418,.F.);
#15030=ORIENTED_EDGE('',*,*,#9845,.F.);
#15031=ORIENTED_EDGE('',*,*,#9842,.F.);
#15032=ORIENTED_EDGE('',*,*,#9839,.F.);
#15033=ORIENTED_EDGE('',*,*,#9836,.F.);
#15034=ORIENTED_EDGE('',*,*,#9833,.F.);
#15035=ORIENTED_EDGE('',*,*,#9830,.F.);
#15036=ORIENTED_EDGE('',*,*,#9827,.F.);
#15037=ORIENTED_EDGE('',*,*,#10414,.F.);
#15038=ORIENTED_EDGE('',*,*,#9820,.F.);
#15039=ORIENTED_EDGE('',*,*,#9829,.F.);
#15040=ORIENTED_EDGE('',*,*,#9832,.F.);
#15041=ORIENTED_EDGE('',*,*,#9835,.F.);
#15042=ORIENTED_EDGE('',*,*,#9838,.F.);
#15043=ORIENTED_EDGE('',*,*,#9841,.F.);
#15044=ORIENTED_EDGE('',*,*,#9844,.F.);
#15045=ORIENTED_EDGE('',*,*,#10419,.F.);
#15046=ORIENTED_EDGE('',*,*,#9849,.F.);
#15047=ORIENTED_EDGE('',*,*,#10346,.F.);
#15048=ORIENTED_EDGE('',*,*,#9873,.T.);
#15049=ORIENTED_EDGE('',*,*,#10417,.T.);
#15050=ORIENTED_EDGE('',*,*,#9871,.T.);
#15051=ORIENTED_EDGE('',*,*,#9868,.T.);
#15052=ORIENTED_EDGE('',*,*,#9865,.T.);
#15053=ORIENTED_EDGE('',*,*,#9862,.T.);
#15054=ORIENTED_EDGE('',*,*,#9859,.T.);
#15055=ORIENTED_EDGE('',*,*,#9856,.T.);
#15056=ORIENTED_EDGE('',*,*,#9853,.T.);
#15057=ORIENTED_EDGE('',*,*,#9846,.T.);
#15058=ORIENTED_EDGE('',*,*,#10419,.T.);
#15059=ORIENTED_EDGE('',*,*,#9843,.F.);
#15060=ORIENTED_EDGE('',*,*,#10418,.T.);
#15061=ORIENTED_EDGE('',*,*,#9764,.F.);
#15062=ORIENTED_EDGE('',*,*,#10420,.T.);
#15063=ORIENTED_EDGE('',*,*,#9795,.T.);
#15064=ORIENTED_EDGE('',*,*,#10421,.T.);
#15065=ORIENTED_EDGE('',*,*,#9769,.F.);
#15066=ORIENTED_EDGE('',*,*,#9815,.T.);
#15067=ORIENTED_EDGE('',*,*,#10422,.T.);
#15068=ORIENTED_EDGE('',*,*,#9812,.F.);
#15069=ORIENTED_EDGE('',*,*,#10423,.F.);
#15070=ORIENTED_EDGE('',*,*,#10421,.F.);
#15071=ORIENTED_EDGE('',*,*,#9794,.F.);
#15072=ORIENTED_EDGE('',*,*,#9798,.F.);
#15073=ORIENTED_EDGE('',*,*,#9801,.F.);
#15074=ORIENTED_EDGE('',*,*,#9804,.F.);
#15075=ORIENTED_EDGE('',*,*,#9807,.F.);
#15076=ORIENTED_EDGE('',*,*,#9810,.F.);
#15077=ORIENTED_EDGE('',*,*,#9813,.F.);
#15078=ORIENTED_EDGE('',*,*,#10422,.F.);
#15079=ORIENTED_EDGE('',*,*,#9818,.F.);
#15080=ORIENTED_EDGE('',*,*,#10345,.F.);
#15081=ORIENTED_EDGE('',*,*,#9790,.F.);
#15082=ORIENTED_EDGE('',*,*,#10424,.F.);
#15083=ORIENTED_EDGE('',*,*,#9788,.F.);
#15084=ORIENTED_EDGE('',*,*,#9785,.F.);
#15085=ORIENTED_EDGE('',*,*,#9782,.F.);
#15086=ORIENTED_EDGE('',*,*,#9779,.F.);
#15087=ORIENTED_EDGE('',*,*,#9776,.F.);
#15088=ORIENTED_EDGE('',*,*,#9773,.F.);
#15089=ORIENTED_EDGE('',*,*,#9770,.F.);
#15090=ORIENTED_EDGE('',*,*,#10420,.F.);
#15091=ORIENTED_EDGE('',*,*,#9763,.F.);
#15092=ORIENTED_EDGE('',*,*,#9772,.F.);
#15093=ORIENTED_EDGE('',*,*,#9775,.F.);
#15094=ORIENTED_EDGE('',*,*,#9778,.F.);
#15095=ORIENTED_EDGE('',*,*,#9781,.F.);
#15096=ORIENTED_EDGE('',*,*,#9784,.F.);
#15097=ORIENTED_EDGE('',*,*,#9787,.F.);
#15098=ORIENTED_EDGE('',*,*,#10425,.F.);
#15099=ORIENTED_EDGE('',*,*,#9792,.F.);
#15100=ORIENTED_EDGE('',*,*,#10344,.F.);
#15101=ORIENTED_EDGE('',*,*,#9816,.T.);
#15102=ORIENTED_EDGE('',*,*,#10423,.T.);
#15103=ORIENTED_EDGE('',*,*,#9814,.T.);
#15104=ORIENTED_EDGE('',*,*,#9811,.T.);
#15105=ORIENTED_EDGE('',*,*,#9808,.T.);
#15106=ORIENTED_EDGE('',*,*,#9805,.T.);
#15107=ORIENTED_EDGE('',*,*,#9802,.T.);
#15108=ORIENTED_EDGE('',*,*,#9799,.T.);
#15109=ORIENTED_EDGE('',*,*,#9796,.T.);
#15110=ORIENTED_EDGE('',*,*,#9789,.T.);
#15111=ORIENTED_EDGE('',*,*,#10425,.T.);
#15112=ORIENTED_EDGE('',*,*,#9786,.F.);
#15113=ORIENTED_EDGE('',*,*,#10424,.T.);
#15114=ORIENTED_EDGE('',*,*,#9707,.F.);
#15115=ORIENTED_EDGE('',*,*,#10426,.T.);
#15116=ORIENTED_EDGE('',*,*,#9738,.T.);
#15117=ORIENTED_EDGE('',*,*,#10427,.T.);
#15118=ORIENTED_EDGE('',*,*,#9712,.F.);
#15119=ORIENTED_EDGE('',*,*,#9758,.T.);
#15120=ORIENTED_EDGE('',*,*,#10428,.T.);
#15121=ORIENTED_EDGE('',*,*,#9755,.F.);
#15122=ORIENTED_EDGE('',*,*,#10429,.F.);
#15123=ORIENTED_EDGE('',*,*,#10427,.F.);
#15124=ORIENTED_EDGE('',*,*,#9737,.F.);
#15125=ORIENTED_EDGE('',*,*,#9741,.F.);
#15126=ORIENTED_EDGE('',*,*,#9744,.F.);
#15127=ORIENTED_EDGE('',*,*,#9747,.F.);
#15128=ORIENTED_EDGE('',*,*,#9750,.F.);
#15129=ORIENTED_EDGE('',*,*,#9753,.F.);
#15130=ORIENTED_EDGE('',*,*,#9756,.F.);
#15131=ORIENTED_EDGE('',*,*,#10428,.F.);
#15132=ORIENTED_EDGE('',*,*,#9761,.F.);
#15133=ORIENTED_EDGE('',*,*,#10343,.F.);
#15134=ORIENTED_EDGE('',*,*,#9733,.F.);
#15135=ORIENTED_EDGE('',*,*,#10430,.F.);
#15136=ORIENTED_EDGE('',*,*,#9731,.F.);
#15137=ORIENTED_EDGE('',*,*,#9728,.F.);
#15138=ORIENTED_EDGE('',*,*,#9725,.F.);
#15139=ORIENTED_EDGE('',*,*,#9722,.F.);
#15140=ORIENTED_EDGE('',*,*,#9719,.F.);
#15141=ORIENTED_EDGE('',*,*,#9716,.F.);
#15142=ORIENTED_EDGE('',*,*,#9713,.F.);
#15143=ORIENTED_EDGE('',*,*,#10426,.F.);
#15144=ORIENTED_EDGE('',*,*,#9706,.F.);
#15145=ORIENTED_EDGE('',*,*,#9715,.F.);
#15146=ORIENTED_EDGE('',*,*,#9718,.F.);
#15147=ORIENTED_EDGE('',*,*,#9721,.F.);
#15148=ORIENTED_EDGE('',*,*,#9724,.F.);
#15149=ORIENTED_EDGE('',*,*,#9727,.F.);
#15150=ORIENTED_EDGE('',*,*,#9730,.F.);
#15151=ORIENTED_EDGE('',*,*,#10431,.F.);
#15152=ORIENTED_EDGE('',*,*,#9735,.F.);
#15153=ORIENTED_EDGE('',*,*,#10342,.F.);
#15154=ORIENTED_EDGE('',*,*,#9759,.T.);
#15155=ORIENTED_EDGE('',*,*,#10429,.T.);
#15156=ORIENTED_EDGE('',*,*,#9757,.T.);
#15157=ORIENTED_EDGE('',*,*,#9754,.T.);
#15158=ORIENTED_EDGE('',*,*,#9751,.T.);
#15159=ORIENTED_EDGE('',*,*,#9748,.T.);
#15160=ORIENTED_EDGE('',*,*,#9745,.T.);
#15161=ORIENTED_EDGE('',*,*,#9742,.T.);
#15162=ORIENTED_EDGE('',*,*,#9739,.T.);
#15163=ORIENTED_EDGE('',*,*,#9732,.T.);
#15164=ORIENTED_EDGE('',*,*,#10431,.T.);
#15165=ORIENTED_EDGE('',*,*,#9729,.F.);
#15166=ORIENTED_EDGE('',*,*,#10430,.T.);
#15167=ORIENTED_EDGE('',*,*,#10432,.T.);
#15168=ORIENTED_EDGE('',*,*,#9937,.F.);
#15169=ORIENTED_EDGE('',*,*,#9939,.F.);
#15170=ORIENTED_EDGE('',*,*,#10433,.F.);
#15171=ORIENTED_EDGE('',*,*,#9938,.F.);
#15172=ORIENTED_EDGE('',*,*,#10434,.T.);
#15173=ORIENTED_EDGE('',*,*,#9880,.F.);
#15174=ORIENTED_EDGE('',*,*,#9882,.F.);
#15175=ORIENTED_EDGE('',*,*,#10435,.F.);
#15176=ORIENTED_EDGE('',*,*,#9881,.F.);
#15177=ORIENTED_EDGE('',*,*,#10436,.T.);
#15178=ORIENTED_EDGE('',*,*,#9823,.F.);
#15179=ORIENTED_EDGE('',*,*,#9825,.F.);
#15180=ORIENTED_EDGE('',*,*,#10437,.F.);
#15181=ORIENTED_EDGE('',*,*,#9824,.F.);
#15182=ORIENTED_EDGE('',*,*,#10438,.T.);
#15183=ORIENTED_EDGE('',*,*,#9766,.F.);
#15184=ORIENTED_EDGE('',*,*,#9768,.F.);
#15185=ORIENTED_EDGE('',*,*,#10439,.F.);
#15186=ORIENTED_EDGE('',*,*,#9767,.F.);
#15187=ORIENTED_EDGE('',*,*,#10440,.T.);
#15188=ORIENTED_EDGE('',*,*,#9709,.F.);
#15189=ORIENTED_EDGE('',*,*,#9711,.F.);
#15190=ORIENTED_EDGE('',*,*,#10441,.F.);
#15191=ORIENTED_EDGE('',*,*,#9710,.F.);
#15192=ORIENTED_EDGE('',*,*,#9650,.F.);
#15193=ORIENTED_EDGE('',*,*,#10442,.T.);
#15194=ORIENTED_EDGE('',*,*,#9681,.T.);
#15195=ORIENTED_EDGE('',*,*,#10443,.T.);
#15196=ORIENTED_EDGE('',*,*,#9655,.F.);
#15197=ORIENTED_EDGE('',*,*,#9701,.T.);
#15198=ORIENTED_EDGE('',*,*,#10444,.T.);
#15199=ORIENTED_EDGE('',*,*,#9698,.F.);
#15200=ORIENTED_EDGE('',*,*,#10445,.F.);
#15201=ORIENTED_EDGE('',*,*,#10443,.F.);
#15202=ORIENTED_EDGE('',*,*,#9680,.F.);
#15203=ORIENTED_EDGE('',*,*,#9684,.F.);
#15204=ORIENTED_EDGE('',*,*,#9687,.F.);
#15205=ORIENTED_EDGE('',*,*,#9690,.F.);
#15206=ORIENTED_EDGE('',*,*,#9693,.F.);
#15207=ORIENTED_EDGE('',*,*,#9696,.F.);
#15208=ORIENTED_EDGE('',*,*,#9699,.F.);
#15209=ORIENTED_EDGE('',*,*,#10444,.F.);
#15210=ORIENTED_EDGE('',*,*,#9704,.F.);
#15211=ORIENTED_EDGE('',*,*,#10446,.F.);
#15212=ORIENTED_EDGE('',*,*,#9676,.F.);
#15213=ORIENTED_EDGE('',*,*,#10447,.F.);
#15214=ORIENTED_EDGE('',*,*,#9674,.F.);
#15215=ORIENTED_EDGE('',*,*,#9671,.F.);
#15216=ORIENTED_EDGE('',*,*,#9668,.F.);
#15217=ORIENTED_EDGE('',*,*,#9665,.F.);
#15218=ORIENTED_EDGE('',*,*,#9662,.F.);
#15219=ORIENTED_EDGE('',*,*,#9659,.F.);
#15220=ORIENTED_EDGE('',*,*,#9656,.F.);
#15221=ORIENTED_EDGE('',*,*,#10442,.F.);
#15222=ORIENTED_EDGE('',*,*,#9649,.F.);
#15223=ORIENTED_EDGE('',*,*,#9658,.F.);
#15224=ORIENTED_EDGE('',*,*,#9661,.F.);
#15225=ORIENTED_EDGE('',*,*,#9664,.F.);
#15226=ORIENTED_EDGE('',*,*,#9667,.F.);
#15227=ORIENTED_EDGE('',*,*,#9670,.F.);
#15228=ORIENTED_EDGE('',*,*,#9673,.F.);
#15229=ORIENTED_EDGE('',*,*,#10448,.F.);
#15230=ORIENTED_EDGE('',*,*,#9678,.F.);
#15231=ORIENTED_EDGE('',*,*,#10449,.F.);
#15232=ORIENTED_EDGE('',*,*,#9702,.T.);
#15233=ORIENTED_EDGE('',*,*,#10445,.T.);
#15234=ORIENTED_EDGE('',*,*,#9700,.T.);
#15235=ORIENTED_EDGE('',*,*,#9697,.T.);
#15236=ORIENTED_EDGE('',*,*,#9694,.T.);
#15237=ORIENTED_EDGE('',*,*,#9691,.T.);
#15238=ORIENTED_EDGE('',*,*,#9688,.T.);
#15239=ORIENTED_EDGE('',*,*,#9685,.T.);
#15240=ORIENTED_EDGE('',*,*,#9682,.T.);
#15241=ORIENTED_EDGE('',*,*,#9675,.T.);
#15242=ORIENTED_EDGE('',*,*,#10448,.T.);
#15243=ORIENTED_EDGE('',*,*,#9672,.F.);
#15244=ORIENTED_EDGE('',*,*,#10447,.T.);
#15245=ORIENTED_EDGE('',*,*,#10450,.T.);
#15246=ORIENTED_EDGE('',*,*,#9652,.F.);
#15247=ORIENTED_EDGE('',*,*,#9654,.F.);
#15248=ORIENTED_EDGE('',*,*,#10451,.F.);
#15249=ORIENTED_EDGE('',*,*,#9653,.F.);
#15250=ORIENTED_EDGE('',*,*,#9593,.F.);
#15251=ORIENTED_EDGE('',*,*,#10452,.T.);
#15252=ORIENTED_EDGE('',*,*,#9624,.T.);
#15253=ORIENTED_EDGE('',*,*,#10453,.T.);
#15254=ORIENTED_EDGE('',*,*,#9598,.F.);
#15255=ORIENTED_EDGE('',*,*,#9644,.T.);
#15256=ORIENTED_EDGE('',*,*,#10454,.T.);
#15257=ORIENTED_EDGE('',*,*,#9641,.F.);
#15258=ORIENTED_EDGE('',*,*,#10455,.F.);
#15259=ORIENTED_EDGE('',*,*,#10453,.F.);
#15260=ORIENTED_EDGE('',*,*,#9623,.F.);
#15261=ORIENTED_EDGE('',*,*,#9627,.F.);
#15262=ORIENTED_EDGE('',*,*,#9630,.F.);
#15263=ORIENTED_EDGE('',*,*,#9633,.F.);
#15264=ORIENTED_EDGE('',*,*,#9636,.F.);
#15265=ORIENTED_EDGE('',*,*,#9639,.F.);
#15266=ORIENTED_EDGE('',*,*,#9642,.F.);
#15267=ORIENTED_EDGE('',*,*,#10454,.F.);
#15268=ORIENTED_EDGE('',*,*,#9647,.F.);
#15269=ORIENTED_EDGE('',*,*,#10340,.F.);
#15270=ORIENTED_EDGE('',*,*,#9619,.F.);
#15271=ORIENTED_EDGE('',*,*,#10456,.F.);
#15272=ORIENTED_EDGE('',*,*,#9617,.F.);
#15273=ORIENTED_EDGE('',*,*,#9614,.F.);
#15274=ORIENTED_EDGE('',*,*,#9611,.F.);
#15275=ORIENTED_EDGE('',*,*,#9608,.F.);
#15276=ORIENTED_EDGE('',*,*,#9605,.F.);
#15277=ORIENTED_EDGE('',*,*,#9602,.F.);
#15278=ORIENTED_EDGE('',*,*,#9599,.F.);
#15279=ORIENTED_EDGE('',*,*,#10452,.F.);
#15280=ORIENTED_EDGE('',*,*,#9592,.F.);
#15281=ORIENTED_EDGE('',*,*,#9601,.F.);
#15282=ORIENTED_EDGE('',*,*,#9604,.F.);
#15283=ORIENTED_EDGE('',*,*,#9607,.F.);
#15284=ORIENTED_EDGE('',*,*,#9610,.F.);
#15285=ORIENTED_EDGE('',*,*,#9613,.F.);
#15286=ORIENTED_EDGE('',*,*,#9616,.F.);
#15287=ORIENTED_EDGE('',*,*,#10457,.F.);
#15288=ORIENTED_EDGE('',*,*,#9621,.F.);
#15289=ORIENTED_EDGE('',*,*,#10339,.F.);
#15290=ORIENTED_EDGE('',*,*,#9645,.T.);
#15291=ORIENTED_EDGE('',*,*,#10455,.T.);
#15292=ORIENTED_EDGE('',*,*,#9643,.T.);
#15293=ORIENTED_EDGE('',*,*,#9640,.T.);
#15294=ORIENTED_EDGE('',*,*,#9637,.T.);
#15295=ORIENTED_EDGE('',*,*,#9634,.T.);
#15296=ORIENTED_EDGE('',*,*,#9631,.T.);
#15297=ORIENTED_EDGE('',*,*,#9628,.T.);
#15298=ORIENTED_EDGE('',*,*,#9625,.T.);
#15299=ORIENTED_EDGE('',*,*,#9618,.T.);
#15300=ORIENTED_EDGE('',*,*,#10457,.T.);
#15301=ORIENTED_EDGE('',*,*,#9615,.F.);
#15302=ORIENTED_EDGE('',*,*,#10456,.T.);
#15303=ORIENTED_EDGE('',*,*,#10458,.T.);
#15304=ORIENTED_EDGE('',*,*,#9595,.F.);
#15305=ORIENTED_EDGE('',*,*,#9597,.F.);
#15306=ORIENTED_EDGE('',*,*,#10459,.F.);
#15307=ORIENTED_EDGE('',*,*,#9596,.F.);
#15308=ORIENTED_EDGE('',*,*,#10460,.F.);
#15309=ORIENTED_EDGE('',*,*,#10461,.T.);
#15310=ORIENTED_EDGE('',*,*,#10462,.F.);
#15311=ORIENTED_EDGE('',*,*,#10461,.F.);
#15312=ORIENTED_EDGE('',*,*,#10463,.F.);
#15313=ORIENTED_EDGE('',*,*,#10464,.T.);
#15314=ORIENTED_EDGE('',*,*,#10392,.F.);
#15315=ORIENTED_EDGE('',*,*,#10465,.T.);
#15316=ORIENTED_EDGE('',*,*,#10466,.T.);
#15317=ORIENTED_EDGE('',*,*,#10465,.F.);
#15318=ORIENTED_EDGE('',*,*,#10393,.T.);
#15319=ORIENTED_EDGE('',*,*,#10464,.F.);
#15320=ORIENTED_EDGE('',*,*,#10433,.T.);
#15321=ORIENTED_EDGE('',*,*,#10432,.F.);
#15322=ORIENTED_EDGE('',*,*,#10466,.F.);
#15323=ORIENTED_EDGE('',*,*,#10460,.T.);
#15324=ORIENTED_EDGE('',*,*,#10467,.F.);
#15325=ORIENTED_EDGE('',*,*,#10468,.T.);
#15326=ORIENTED_EDGE('',*,*,#10469,.F.);
#15327=ORIENTED_EDGE('',*,*,#10468,.F.);
#15328=ORIENTED_EDGE('',*,*,#10470,.F.);
#15329=ORIENTED_EDGE('',*,*,#10471,.T.);
#15330=ORIENTED_EDGE('',*,*,#10394,.F.);
#15331=ORIENTED_EDGE('',*,*,#10472,.T.);
#15332=ORIENTED_EDGE('',*,*,#10473,.T.);
#15333=ORIENTED_EDGE('',*,*,#10472,.F.);
#15334=ORIENTED_EDGE('',*,*,#10395,.T.);
#15335=ORIENTED_EDGE('',*,*,#10471,.F.);
#15336=ORIENTED_EDGE('',*,*,#10435,.T.);
#15337=ORIENTED_EDGE('',*,*,#10434,.F.);
#15338=ORIENTED_EDGE('',*,*,#10473,.F.);
#15339=ORIENTED_EDGE('',*,*,#10467,.T.);
#15340=ORIENTED_EDGE('',*,*,#10474,.F.);
#15341=ORIENTED_EDGE('',*,*,#10475,.T.);
#15342=ORIENTED_EDGE('',*,*,#10476,.F.);
#15343=ORIENTED_EDGE('',*,*,#10475,.F.);
#15344=ORIENTED_EDGE('',*,*,#10477,.F.);
#15345=ORIENTED_EDGE('',*,*,#10478,.T.);
#15346=ORIENTED_EDGE('',*,*,#10396,.F.);
#15347=ORIENTED_EDGE('',*,*,#10479,.T.);
#15348=ORIENTED_EDGE('',*,*,#10480,.T.);
#15349=ORIENTED_EDGE('',*,*,#10479,.F.);
#15350=ORIENTED_EDGE('',*,*,#10397,.T.);
#15351=ORIENTED_EDGE('',*,*,#10478,.F.);
#15352=ORIENTED_EDGE('',*,*,#10437,.T.);
#15353=ORIENTED_EDGE('',*,*,#10436,.F.);
#15354=ORIENTED_EDGE('',*,*,#10480,.F.);
#15355=ORIENTED_EDGE('',*,*,#10474,.T.);
#15356=ORIENTED_EDGE('',*,*,#10481,.F.);
#15357=ORIENTED_EDGE('',*,*,#10482,.T.);
#15358=ORIENTED_EDGE('',*,*,#10483,.F.);
#15359=ORIENTED_EDGE('',*,*,#10482,.F.);
#15360=ORIENTED_EDGE('',*,*,#10484,.F.);
#15361=ORIENTED_EDGE('',*,*,#10485,.T.);
#15362=ORIENTED_EDGE('',*,*,#10398,.F.);
#15363=ORIENTED_EDGE('',*,*,#10486,.T.);
#15364=ORIENTED_EDGE('',*,*,#10487,.T.);
#15365=ORIENTED_EDGE('',*,*,#10486,.F.);
#15366=ORIENTED_EDGE('',*,*,#10399,.T.);
#15367=ORIENTED_EDGE('',*,*,#10485,.F.);
#15368=ORIENTED_EDGE('',*,*,#10439,.T.);
#15369=ORIENTED_EDGE('',*,*,#10438,.F.);
#15370=ORIENTED_EDGE('',*,*,#10487,.F.);
#15371=ORIENTED_EDGE('',*,*,#10481,.T.);
#15372=ORIENTED_EDGE('',*,*,#10488,.F.);
#15373=ORIENTED_EDGE('',*,*,#10489,.T.);
#15374=ORIENTED_EDGE('',*,*,#10490,.F.);
#15375=ORIENTED_EDGE('',*,*,#10489,.F.);
#15376=ORIENTED_EDGE('',*,*,#10491,.F.);
#15377=ORIENTED_EDGE('',*,*,#10492,.T.);
#15378=ORIENTED_EDGE('',*,*,#10400,.F.);
#15379=ORIENTED_EDGE('',*,*,#10493,.T.);
#15380=ORIENTED_EDGE('',*,*,#10494,.T.);
#15381=ORIENTED_EDGE('',*,*,#10493,.F.);
#15382=ORIENTED_EDGE('',*,*,#10401,.T.);
#15383=ORIENTED_EDGE('',*,*,#10492,.F.);
#15384=ORIENTED_EDGE('',*,*,#10441,.T.);
#15385=ORIENTED_EDGE('',*,*,#10440,.F.);
#15386=ORIENTED_EDGE('',*,*,#10494,.F.);
#15387=ORIENTED_EDGE('',*,*,#10488,.T.);
#15388=ORIENTED_EDGE('',*,*,#10495,.F.);
#15389=ORIENTED_EDGE('',*,*,#10496,.T.);
#15390=ORIENTED_EDGE('',*,*,#10497,.F.);
#15391=ORIENTED_EDGE('',*,*,#10496,.F.);
#15392=ORIENTED_EDGE('',*,*,#10498,.F.);
#15393=ORIENTED_EDGE('',*,*,#10499,.T.);
#15394=ORIENTED_EDGE('',*,*,#10450,.F.);
#15395=ORIENTED_EDGE('',*,*,#10500,.T.);
#15396=ORIENTED_EDGE('',*,*,#10501,.T.);
#15397=ORIENTED_EDGE('',*,*,#10500,.F.);
#15398=ORIENTED_EDGE('',*,*,#10451,.T.);
#15399=ORIENTED_EDGE('',*,*,#10499,.F.);
#15400=ORIENTED_EDGE('',*,*,#10459,.T.);
#15401=ORIENTED_EDGE('',*,*,#10458,.F.);
#15402=ORIENTED_EDGE('',*,*,#10501,.F.);
#15403=ORIENTED_EDGE('',*,*,#10495,.T.);
#15404=ORIENTED_EDGE('',*,*,#10502,.F.);
#15405=ORIENTED_EDGE('',*,*,#10503,.T.);
#15406=ORIENTED_EDGE('',*,*,#10504,.T.);
#15407=ORIENTED_EDGE('',*,*,#10335,.F.);
#15408=ORIENTED_EDGE('',*,*,#10505,.F.);
#15409=ORIENTED_EDGE('',*,*,#10338,.F.);
#15410=ORIENTED_EDGE('',*,*,#10506,.F.);
#15411=ORIENTED_EDGE('',*,*,#10507,.T.);
#15412=ORIENTED_EDGE('',*,*,#10463,.T.);
#15413=ORIENTED_EDGE('',*,*,#10508,.T.);
#15414=ORIENTED_EDGE('',*,*,#10506,.T.);
#15415=ORIENTED_EDGE('',*,*,#10337,.F.);
#15416=ORIENTED_EDGE('',*,*,#10509,.F.);
#15417=ORIENTED_EDGE('',*,*,#10510,.T.);
#15418=ORIENTED_EDGE('',*,*,#10509,.T.);
#15419=ORIENTED_EDGE('',*,*,#10336,.F.);
#15420=ORIENTED_EDGE('',*,*,#10504,.F.);
#15421=ORIENTED_EDGE('',*,*,#10462,.T.);
#15422=ORIENTED_EDGE('',*,*,#10511,.F.);
#15423=ORIENTED_EDGE('',*,*,#10329,.F.);
#15424=ORIENTED_EDGE('',*,*,#10512,.F.);
#15425=ORIENTED_EDGE('',*,*,#10513,.T.);
#15426=ORIENTED_EDGE('',*,*,#10470,.T.);
#15427=ORIENTED_EDGE('',*,*,#10514,.T.);
#15428=ORIENTED_EDGE('',*,*,#10512,.T.);
#15429=ORIENTED_EDGE('',*,*,#10328,.F.);
#15430=ORIENTED_EDGE('',*,*,#10515,.F.);
#15431=ORIENTED_EDGE('',*,*,#10516,.T.);
#15432=ORIENTED_EDGE('',*,*,#10515,.T.);
#15433=ORIENTED_EDGE('',*,*,#10327,.F.);
#15434=ORIENTED_EDGE('',*,*,#10517,.F.);
#15435=ORIENTED_EDGE('',*,*,#10469,.T.);
#15436=ORIENTED_EDGE('',*,*,#10518,.F.);
#15437=ORIENTED_EDGE('',*,*,#10519,.T.);
#15438=ORIENTED_EDGE('',*,*,#10517,.T.);
#15439=ORIENTED_EDGE('',*,*,#10326,.F.);
#15440=ORIENTED_EDGE('',*,*,#10520,.F.);
#15441=ORIENTED_EDGE('',*,*,#10320,.F.);
#15442=ORIENTED_EDGE('',*,*,#10521,.F.);
#15443=ORIENTED_EDGE('',*,*,#10522,.T.);
#15444=ORIENTED_EDGE('',*,*,#10477,.T.);
#15445=ORIENTED_EDGE('',*,*,#10523,.T.);
#15446=ORIENTED_EDGE('',*,*,#10521,.T.);
#15447=ORIENTED_EDGE('',*,*,#10319,.F.);
#15448=ORIENTED_EDGE('',*,*,#10524,.F.);
#15449=ORIENTED_EDGE('',*,*,#10525,.T.);
#15450=ORIENTED_EDGE('',*,*,#10524,.T.);
#15451=ORIENTED_EDGE('',*,*,#10318,.F.);
#15452=ORIENTED_EDGE('',*,*,#10526,.F.);
#15453=ORIENTED_EDGE('',*,*,#10476,.T.);
#15454=ORIENTED_EDGE('',*,*,#10527,.F.);
#15455=ORIENTED_EDGE('',*,*,#10528,.T.);
#15456=ORIENTED_EDGE('',*,*,#10526,.T.);
#15457=ORIENTED_EDGE('',*,*,#10317,.F.);
#15458=ORIENTED_EDGE('',*,*,#10529,.F.);
#15459=ORIENTED_EDGE('',*,*,#10311,.F.);
#15460=ORIENTED_EDGE('',*,*,#10530,.F.);
#15461=ORIENTED_EDGE('',*,*,#10531,.T.);
#15462=ORIENTED_EDGE('',*,*,#10484,.T.);
#15463=ORIENTED_EDGE('',*,*,#10532,.T.);
#15464=ORIENTED_EDGE('',*,*,#10530,.T.);
#15465=ORIENTED_EDGE('',*,*,#10310,.F.);
#15466=ORIENTED_EDGE('',*,*,#10533,.F.);
#15467=ORIENTED_EDGE('',*,*,#10534,.T.);
#15468=ORIENTED_EDGE('',*,*,#10533,.T.);
#15469=ORIENTED_EDGE('',*,*,#10309,.F.);
#15470=ORIENTED_EDGE('',*,*,#10535,.F.);
#15471=ORIENTED_EDGE('',*,*,#10483,.T.);
#15472=ORIENTED_EDGE('',*,*,#10536,.F.);
#15473=ORIENTED_EDGE('',*,*,#10537,.T.);
#15474=ORIENTED_EDGE('',*,*,#10535,.T.);
#15475=ORIENTED_EDGE('',*,*,#10308,.F.);
#15476=ORIENTED_EDGE('',*,*,#10538,.F.);
#15477=ORIENTED_EDGE('',*,*,#10539,.T.);
#15478=ORIENTED_EDGE('',*,*,#10540,.T.);
#15479=ORIENTED_EDGE('',*,*,#10299,.F.);
#15480=ORIENTED_EDGE('',*,*,#10541,.F.);
#15481=ORIENTED_EDGE('',*,*,#10302,.F.);
#15482=ORIENTED_EDGE('',*,*,#10542,.F.);
#15483=ORIENTED_EDGE('',*,*,#10543,.T.);
#15484=ORIENTED_EDGE('',*,*,#10491,.T.);
#15485=ORIENTED_EDGE('',*,*,#10544,.T.);
#15486=ORIENTED_EDGE('',*,*,#10542,.T.);
#15487=ORIENTED_EDGE('',*,*,#10301,.F.);
#15488=ORIENTED_EDGE('',*,*,#10545,.F.);
#15489=ORIENTED_EDGE('',*,*,#10546,.T.);
#15490=ORIENTED_EDGE('',*,*,#10545,.T.);
#15491=ORIENTED_EDGE('',*,*,#10300,.F.);
#15492=ORIENTED_EDGE('',*,*,#10540,.F.);
#15493=ORIENTED_EDGE('',*,*,#10490,.T.);
#15494=ORIENTED_EDGE('',*,*,#10505,.T.);
#15495=ORIENTED_EDGE('',*,*,#10547,.T.);
#15496=ORIENTED_EDGE('',*,*,#10548,.F.);
#15497=ORIENTED_EDGE('',*,*,#10285,.T.);
#15498=ORIENTED_EDGE('',*,*,#10511,.T.);
#15499=ORIENTED_EDGE('',*,*,#10549,.T.);
#15500=ORIENTED_EDGE('',*,*,#10550,.F.);
#15501=ORIENTED_EDGE('',*,*,#10330,.T.);
#15502=ORIENTED_EDGE('',*,*,#10518,.T.);
#15503=ORIENTED_EDGE('',*,*,#10325,.T.);
#15504=ORIENTED_EDGE('',*,*,#10551,.F.);
#15505=ORIENTED_EDGE('',*,*,#10552,.T.);
#15506=ORIENTED_EDGE('',*,*,#10520,.T.);
#15507=ORIENTED_EDGE('',*,*,#10553,.T.);
#15508=ORIENTED_EDGE('',*,*,#10554,.F.);
#15509=ORIENTED_EDGE('',*,*,#10321,.T.);
#15510=ORIENTED_EDGE('',*,*,#10527,.T.);
#15511=ORIENTED_EDGE('',*,*,#10316,.T.);
#15512=ORIENTED_EDGE('',*,*,#10555,.F.);
#15513=ORIENTED_EDGE('',*,*,#10556,.T.);
#15514=ORIENTED_EDGE('',*,*,#10529,.T.);
#15515=ORIENTED_EDGE('',*,*,#10557,.T.);
#15516=ORIENTED_EDGE('',*,*,#10558,.F.);
#15517=ORIENTED_EDGE('',*,*,#10312,.T.);
#15518=ORIENTED_EDGE('',*,*,#10536,.T.);
#15519=ORIENTED_EDGE('',*,*,#10307,.T.);
#15520=ORIENTED_EDGE('',*,*,#10559,.F.);
#15521=ORIENTED_EDGE('',*,*,#10560,.T.);
#15522=ORIENTED_EDGE('',*,*,#10541,.T.);
#15523=ORIENTED_EDGE('',*,*,#10561,.T.);
#15524=ORIENTED_EDGE('',*,*,#10562,.F.);
#15525=ORIENTED_EDGE('',*,*,#10303,.T.);
#15526=ORIENTED_EDGE('',*,*,#10563,.F.);
#15527=ORIENTED_EDGE('',*,*,#10564,.T.);
#15528=ORIENTED_EDGE('',*,*,#10565,.T.);
#15529=ORIENTED_EDGE('',*,*,#10290,.F.);
#15530=ORIENTED_EDGE('',*,*,#10566,.F.);
#15531=ORIENTED_EDGE('',*,*,#10293,.F.);
#15532=ORIENTED_EDGE('',*,*,#10567,.F.);
#15533=ORIENTED_EDGE('',*,*,#10568,.T.);
#15534=ORIENTED_EDGE('',*,*,#10498,.T.);
#15535=ORIENTED_EDGE('',*,*,#10569,.T.);
#15536=ORIENTED_EDGE('',*,*,#10567,.T.);
#15537=ORIENTED_EDGE('',*,*,#10292,.F.);
#15538=ORIENTED_EDGE('',*,*,#10570,.F.);
#15539=ORIENTED_EDGE('',*,*,#10571,.T.);
#15540=ORIENTED_EDGE('',*,*,#10570,.T.);
#15541=ORIENTED_EDGE('',*,*,#10291,.F.);
#15542=ORIENTED_EDGE('',*,*,#10565,.F.);
#15543=ORIENTED_EDGE('',*,*,#10497,.T.);
#15544=ORIENTED_EDGE('',*,*,#10566,.T.);
#15545=ORIENTED_EDGE('',*,*,#10572,.T.);
#15546=ORIENTED_EDGE('',*,*,#10573,.F.);
#15547=ORIENTED_EDGE('',*,*,#10294,.T.);
#15548=ORIENTED_EDGE('',*,*,#10324,.T.);
#15549=ORIENTED_EDGE('',*,*,#10574,.F.);
#15550=ORIENTED_EDGE('',*,*,#10575,.T.);
#15551=ORIENTED_EDGE('',*,*,#10551,.T.);
#15552=ORIENTED_EDGE('',*,*,#10323,.T.);
#15553=ORIENTED_EDGE('',*,*,#10576,.T.);
#15554=ORIENTED_EDGE('',*,*,#10577,.T.);
#15555=ORIENTED_EDGE('',*,*,#10574,.T.);
#15556=ORIENTED_EDGE('',*,*,#10322,.T.);
#15557=ORIENTED_EDGE('',*,*,#10554,.T.);
#15558=ORIENTED_EDGE('',*,*,#10578,.T.);
#15559=ORIENTED_EDGE('',*,*,#10576,.F.);
#15560=ORIENTED_EDGE('',*,*,#10315,.T.);
#15561=ORIENTED_EDGE('',*,*,#10579,.F.);
#15562=ORIENTED_EDGE('',*,*,#10580,.T.);
#15563=ORIENTED_EDGE('',*,*,#10555,.T.);
#15564=ORIENTED_EDGE('',*,*,#10314,.T.);
#15565=ORIENTED_EDGE('',*,*,#10581,.T.);
#15566=ORIENTED_EDGE('',*,*,#10582,.T.);
#15567=ORIENTED_EDGE('',*,*,#10579,.T.);
#15568=ORIENTED_EDGE('',*,*,#10313,.T.);
#15569=ORIENTED_EDGE('',*,*,#10558,.T.);
#15570=ORIENTED_EDGE('',*,*,#10583,.T.);
#15571=ORIENTED_EDGE('',*,*,#10581,.F.);
#15572=ORIENTED_EDGE('',*,*,#10306,.T.);
#15573=ORIENTED_EDGE('',*,*,#10584,.F.);
#15574=ORIENTED_EDGE('',*,*,#10585,.T.);
#15575=ORIENTED_EDGE('',*,*,#10559,.T.);
#15576=ORIENTED_EDGE('',*,*,#10305,.T.);
#15577=ORIENTED_EDGE('',*,*,#10586,.T.);
#15578=ORIENTED_EDGE('',*,*,#10587,.T.);
#15579=ORIENTED_EDGE('',*,*,#10584,.T.);
#15580=ORIENTED_EDGE('',*,*,#10304,.T.);
#15581=ORIENTED_EDGE('',*,*,#10562,.T.);
#15582=ORIENTED_EDGE('',*,*,#10588,.T.);
#15583=ORIENTED_EDGE('',*,*,#10586,.F.);
#15584=ORIENTED_EDGE('',*,*,#10589,.F.);
#15585=ORIENTED_EDGE('',*,*,#10590,.F.);
#15586=ORIENTED_EDGE('',*,*,#10591,.F.);
#15587=ORIENTED_EDGE('',*,*,#10592,.F.);
#15588=ORIENTED_EDGE('',*,*,#10549,.F.);
#15589=ORIENTED_EDGE('',*,*,#10513,.F.);
#15590=ORIENTED_EDGE('',*,*,#10514,.F.);
#15591=ORIENTED_EDGE('',*,*,#10516,.F.);
#15592=ORIENTED_EDGE('',*,*,#10519,.F.);
#15593=ORIENTED_EDGE('',*,*,#10552,.F.);
#15594=ORIENTED_EDGE('',*,*,#10575,.F.);
#15595=ORIENTED_EDGE('',*,*,#10577,.F.);
#15596=ORIENTED_EDGE('',*,*,#10578,.F.);
#15597=ORIENTED_EDGE('',*,*,#10553,.F.);
#15598=ORIENTED_EDGE('',*,*,#10522,.F.);
#15599=ORIENTED_EDGE('',*,*,#10523,.F.);
#15600=ORIENTED_EDGE('',*,*,#10525,.F.);
#15601=ORIENTED_EDGE('',*,*,#10528,.F.);
#15602=ORIENTED_EDGE('',*,*,#10556,.F.);
#15603=ORIENTED_EDGE('',*,*,#10580,.F.);
#15604=ORIENTED_EDGE('',*,*,#10582,.F.);
#15605=ORIENTED_EDGE('',*,*,#10583,.F.);
#15606=ORIENTED_EDGE('',*,*,#10557,.F.);
#15607=ORIENTED_EDGE('',*,*,#10531,.F.);
#15608=ORIENTED_EDGE('',*,*,#10532,.F.);
#15609=ORIENTED_EDGE('',*,*,#10534,.F.);
#15610=ORIENTED_EDGE('',*,*,#10537,.F.);
#15611=ORIENTED_EDGE('',*,*,#10560,.F.);
#15612=ORIENTED_EDGE('',*,*,#10585,.F.);
#15613=ORIENTED_EDGE('',*,*,#10587,.F.);
#15614=ORIENTED_EDGE('',*,*,#10588,.F.);
#15615=ORIENTED_EDGE('',*,*,#10561,.F.);
#15616=ORIENTED_EDGE('',*,*,#10543,.F.);
#15617=ORIENTED_EDGE('',*,*,#10544,.F.);
#15618=ORIENTED_EDGE('',*,*,#10546,.F.);
#15619=ORIENTED_EDGE('',*,*,#10539,.F.);
#15620=ORIENTED_EDGE('',*,*,#10593,.F.);
#15621=ORIENTED_EDGE('',*,*,#10594,.F.);
#15622=ORIENTED_EDGE('',*,*,#10595,.F.);
#15623=ORIENTED_EDGE('',*,*,#10596,.F.);
#15624=ORIENTED_EDGE('',*,*,#10572,.F.);
#15625=ORIENTED_EDGE('',*,*,#10568,.F.);
#15626=ORIENTED_EDGE('',*,*,#10569,.F.);
#15627=ORIENTED_EDGE('',*,*,#10571,.F.);
#15628=ORIENTED_EDGE('',*,*,#10564,.F.);
#15629=ORIENTED_EDGE('',*,*,#10597,.F.);
#15630=ORIENTED_EDGE('',*,*,#10598,.F.);
#15631=ORIENTED_EDGE('',*,*,#10599,.F.);
#15632=ORIENTED_EDGE('',*,*,#10600,.F.);
#15633=ORIENTED_EDGE('',*,*,#10547,.F.);
#15634=ORIENTED_EDGE('',*,*,#10507,.F.);
#15635=ORIENTED_EDGE('',*,*,#10508,.F.);
#15636=ORIENTED_EDGE('',*,*,#10510,.F.);
#15637=ORIENTED_EDGE('',*,*,#10503,.F.);
#15638=ORIENTED_EDGE('',*,*,#10283,.T.);
#15639=ORIENTED_EDGE('',*,*,#10601,.F.);
#15640=ORIENTED_EDGE('',*,*,#10278,.T.);
#15641=ORIENTED_EDGE('',*,*,#10281,.T.);
#15642=ORIENTED_EDGE('',*,*,#10359,.T.);
#15643=ORIENTED_EDGE('',*,*,#10247,.T.);
#15644=ORIENTED_EDGE('',*,*,#10356,.T.);
#15645=ORIENTED_EDGE('',*,*,#10273,.T.);
#15646=ORIENTED_EDGE('',*,*,#10367,.T.);
#15647=ORIENTED_EDGE('',*,*,#10190,.T.);
#15648=ORIENTED_EDGE('',*,*,#10364,.T.);
#15649=ORIENTED_EDGE('',*,*,#10216,.T.);
#15650=ORIENTED_EDGE('',*,*,#10375,.T.);
#15651=ORIENTED_EDGE('',*,*,#10133,.T.);
#15652=ORIENTED_EDGE('',*,*,#10372,.T.);
#15653=ORIENTED_EDGE('',*,*,#10159,.T.);
#15654=ORIENTED_EDGE('',*,*,#10383,.T.);
#15655=ORIENTED_EDGE('',*,*,#10076,.T.);
#15656=ORIENTED_EDGE('',*,*,#10380,.T.);
#15657=ORIENTED_EDGE('',*,*,#10102,.T.);
#15658=ORIENTED_EDGE('',*,*,#10391,.T.);
#15659=ORIENTED_EDGE('',*,*,#10019,.T.);
#15660=ORIENTED_EDGE('',*,*,#10388,.T.);
#15661=ORIENTED_EDGE('',*,*,#10045,.T.);
#15662=ORIENTED_EDGE('',*,*,#10449,.T.);
#15663=ORIENTED_EDGE('',*,*,#9677,.T.);
#15664=ORIENTED_EDGE('',*,*,#10446,.T.);
#15665=ORIENTED_EDGE('',*,*,#9703,.T.);
#15666=ORIENTED_EDGE('',*,*,#10331,.T.);
#15667=ORIENTED_EDGE('',*,*,#10550,.T.);
#15668=ORIENTED_EDGE('',*,*,#10592,.T.);
#15669=ORIENTED_EDGE('',*,*,#10602,.F.);
#15670=ORIENTED_EDGE('',*,*,#10332,.T.);
#15671=ORIENTED_EDGE('',*,*,#10602,.T.);
#15672=ORIENTED_EDGE('',*,*,#10591,.T.);
#15673=ORIENTED_EDGE('',*,*,#10603,.T.);
#15674=ORIENTED_EDGE('',*,*,#10333,.T.);
#15675=ORIENTED_EDGE('',*,*,#10603,.F.);
#15676=ORIENTED_EDGE('',*,*,#10590,.T.);
#15677=ORIENTED_EDGE('',*,*,#10604,.T.);
#15678=ORIENTED_EDGE('',*,*,#10502,.T.);
#15679=ORIENTED_EDGE('',*,*,#10334,.T.);
#15680=ORIENTED_EDGE('',*,*,#10604,.F.);
#15681=ORIENTED_EDGE('',*,*,#10589,.T.);
#15682=ORIENTED_EDGE('',*,*,#10286,.T.);
#15683=ORIENTED_EDGE('',*,*,#10548,.T.);
#15684=ORIENTED_EDGE('',*,*,#10600,.T.);
#15685=ORIENTED_EDGE('',*,*,#10605,.F.);
#15686=ORIENTED_EDGE('',*,*,#10287,.T.);
#15687=ORIENTED_EDGE('',*,*,#10605,.T.);
#15688=ORIENTED_EDGE('',*,*,#10599,.T.);
#15689=ORIENTED_EDGE('',*,*,#10606,.T.);
#15690=ORIENTED_EDGE('',*,*,#10288,.T.);
#15691=ORIENTED_EDGE('',*,*,#10606,.F.);
#15692=ORIENTED_EDGE('',*,*,#10598,.T.);
#15693=ORIENTED_EDGE('',*,*,#10607,.T.);
#15694=ORIENTED_EDGE('',*,*,#10563,.T.);
#15695=ORIENTED_EDGE('',*,*,#10289,.T.);
#15696=ORIENTED_EDGE('',*,*,#10607,.F.);
#15697=ORIENTED_EDGE('',*,*,#10597,.T.);
#15698=ORIENTED_EDGE('',*,*,#10295,.T.);
#15699=ORIENTED_EDGE('',*,*,#10573,.T.);
#15700=ORIENTED_EDGE('',*,*,#10596,.T.);
#15701=ORIENTED_EDGE('',*,*,#10608,.F.);
#15702=ORIENTED_EDGE('',*,*,#10538,.T.);
#15703=ORIENTED_EDGE('',*,*,#10298,.T.);
#15704=ORIENTED_EDGE('',*,*,#10609,.F.);
#15705=ORIENTED_EDGE('',*,*,#10593,.T.);
#15706=ORIENTED_EDGE('',*,*,#10296,.T.);
#15707=ORIENTED_EDGE('',*,*,#10608,.T.);
#15708=ORIENTED_EDGE('',*,*,#10595,.T.);
#15709=ORIENTED_EDGE('',*,*,#10610,.T.);
#15710=ORIENTED_EDGE('',*,*,#10297,.T.);
#15711=ORIENTED_EDGE('',*,*,#10610,.F.);
#15712=ORIENTED_EDGE('',*,*,#10594,.T.);
#15713=ORIENTED_EDGE('',*,*,#10609,.T.);
#15714=ORIENTED_EDGE('',*,*,#10282,.T.);
#15715=ORIENTED_EDGE('',*,*,#10341,.T.);
#15716=ORIENTED_EDGE('',*,*,#10275,.T.);
#15717=ORIENTED_EDGE('',*,*,#10601,.T.);
#15718=ORIENTED_EDGE('',*,*,#10611,.F.);
#15719=ORIENTED_EDGE('',*,*,#10612,.F.);
#15720=ORIENTED_EDGE('',*,*,#10613,.T.);
#15721=ORIENTED_EDGE('',*,*,#10614,.F.);
#15722=ORIENTED_EDGE('',*,*,#10615,.F.);
#15723=ORIENTED_EDGE('',*,*,#10616,.F.);
#15724=ORIENTED_EDGE('',*,*,#10617,.F.);
#15725=ORIENTED_EDGE('',*,*,#10618,.T.);
#15726=ORIENTED_EDGE('',*,*,#10619,.F.);
#15727=ORIENTED_EDGE('',*,*,#10613,.F.);
#15728=ORIENTED_EDGE('',*,*,#10620,.T.);
#15729=ORIENTED_EDGE('',*,*,#10621,.T.);
#15730=ORIENTED_EDGE('',*,*,#10622,.F.);
#15731=ORIENTED_EDGE('',*,*,#10621,.F.);
#15732=ORIENTED_EDGE('',*,*,#10623,.F.);
#15733=ORIENTED_EDGE('',*,*,#10624,.T.);
#15734=ORIENTED_EDGE('',*,*,#10625,.F.);
#15735=ORIENTED_EDGE('',*,*,#10624,.F.);
#15736=ORIENTED_EDGE('',*,*,#10626,.T.);
#15737=ORIENTED_EDGE('',*,*,#10616,.T.);
#15738=ORIENTED_EDGE('',*,*,#10612,.T.);
#15739=ORIENTED_EDGE('',*,*,#10617,.T.);
#15740=ORIENTED_EDGE('',*,*,#10626,.F.);
#15741=ORIENTED_EDGE('',*,*,#10623,.T.);
#15742=ORIENTED_EDGE('',*,*,#10620,.F.);
#15743=ORIENTED_EDGE('',*,*,#10627,.F.);
#15744=ORIENTED_EDGE('',*,*,#10614,.T.);
#15745=ORIENTED_EDGE('',*,*,#10619,.T.);
#15746=ORIENTED_EDGE('',*,*,#10622,.T.);
#15747=ORIENTED_EDGE('',*,*,#10625,.T.);
#15748=ORIENTED_EDGE('',*,*,#10615,.T.);
#15749=ORIENTED_EDGE('',*,*,#10628,.F.);
#15750=ORIENTED_EDGE('',*,*,#10629,.T.);
#15751=ORIENTED_EDGE('',*,*,#10630,.T.);
#15752=ORIENTED_EDGE('',*,*,#10629,.F.);
#15753=ORIENTED_EDGE('',*,*,#10631,.F.);
#15754=ORIENTED_EDGE('',*,*,#10632,.F.);
#15755=ORIENTED_EDGE('',*,*,#10633,.F.);
#15756=ORIENTED_EDGE('',*,*,#10634,.T.);
#15757=ORIENTED_EDGE('',*,*,#10635,.F.);
#15758=ORIENTED_EDGE('',*,*,#10634,.F.);
#15759=ORIENTED_EDGE('',*,*,#10636,.T.);
#15760=ORIENTED_EDGE('',*,*,#10637,.T.);
#15761=ORIENTED_EDGE('',*,*,#10638,.F.);
#15762=ORIENTED_EDGE('',*,*,#10639,.F.);
#15763=ORIENTED_EDGE('',*,*,#10637,.F.);
#15764=ORIENTED_EDGE('',*,*,#10640,.F.);
#15765=ORIENTED_EDGE('',*,*,#10641,.T.);
#15766=ORIENTED_EDGE('',*,*,#10642,.F.);
#15767=ORIENTED_EDGE('',*,*,#10641,.F.);
#15768=ORIENTED_EDGE('',*,*,#10643,.T.);
#15769=ORIENTED_EDGE('',*,*,#10632,.T.);
#15770=ORIENTED_EDGE('',*,*,#10633,.T.);
#15771=ORIENTED_EDGE('',*,*,#10643,.F.);
#15772=ORIENTED_EDGE('',*,*,#10640,.T.);
#15773=ORIENTED_EDGE('',*,*,#10636,.F.);
#15774=ORIENTED_EDGE('',*,*,#10644,.T.);
#15775=ORIENTED_EDGE('',*,*,#10645,.T.);
#15776=ORIENTED_EDGE('',*,*,#10646,.T.);
#15777=ORIENTED_EDGE('',*,*,#10638,.T.);
#15778=ORIENTED_EDGE('',*,*,#10642,.T.);
#15779=ORIENTED_EDGE('',*,*,#10631,.T.);
#15780=ORIENTED_EDGE('',*,*,#10635,.T.);
#15781=ORIENTED_EDGE('',*,*,#10639,.T.);
#15782=ORIENTED_EDGE('',*,*,#10647,.T.);
#15783=ORIENTED_EDGE('',*,*,#10645,.F.);
#15784=ORIENTED_EDGE('',*,*,#10648,.T.);
#15785=ORIENTED_EDGE('',*,*,#10649,.T.);
#15786=ORIENTED_EDGE('',*,*,#10650,.F.);
#15787=ORIENTED_EDGE('',*,*,#10649,.F.);
#15788=ORIENTED_EDGE('',*,*,#10644,.F.);
#15789=ORIENTED_EDGE('',*,*,#10648,.F.);
#15790=ORIENTED_EDGE('',*,*,#10630,.F.);
#15791=ORIENTED_EDGE('',*,*,#10650,.T.);
#15792=ORIENTED_EDGE('',*,*,#10651,.T.);
#15793=ORIENTED_EDGE('',*,*,#10652,.T.);
#15794=ORIENTED_EDGE('',*,*,#10653,.F.);
#15795=ORIENTED_EDGE('',*,*,#10652,.F.);
#15796=ORIENTED_EDGE('',*,*,#10654,.F.);
#15797=ORIENTED_EDGE('',*,*,#10651,.F.);
#15798=ORIENTED_EDGE('',*,*,#10655,.F.);
#15799=ORIENTED_EDGE('',*,*,#10653,.T.);
#15800=ORIENTED_EDGE('',*,*,#10656,.T.);
#15801=ORIENTED_EDGE('',*,*,#10657,.T.);
#15802=ORIENTED_EDGE('',*,*,#10655,.T.);
#15803=ORIENTED_EDGE('',*,*,#10657,.F.);
#15804=ORIENTED_EDGE('',*,*,#10658,.T.);
#15805=ORIENTED_EDGE('',*,*,#10647,.F.);
#15806=ORIENTED_EDGE('',*,*,#10646,.F.);
#15807=ORIENTED_EDGE('',*,*,#10659,.F.);
#15808=ORIENTED_EDGE('',*,*,#10656,.F.);
#15809=ORIENTED_EDGE('',*,*,#10658,.F.);
#15810=ORIENTED_EDGE('',*,*,#10660,.T.);
#15811=ORIENTED_EDGE('',*,*,#10659,.T.);
#15812=ORIENTED_EDGE('',*,*,#10660,.F.);
#15813=ORIENTED_EDGE('',*,*,#10654,.T.);
#15814=ORIENTED_EDGE('',*,*,#10661,.T.);
#15815=ORIENTED_EDGE('',*,*,#10662,.T.);
#15816=ORIENTED_EDGE('',*,*,#10661,.F.);
#15817=ORIENTED_EDGE('',*,*,#10627,.T.);
#15818=ORIENTED_EDGE('',*,*,#10628,.T.);
#15819=ORIENTED_EDGE('',*,*,#10618,.F.);
#15820=ORIENTED_EDGE('',*,*,#10611,.T.);
#15821=ORIENTED_EDGE('',*,*,#10662,.F.);
#15822=ORIENTED_EDGE('',*,*,#10663,.F.);
#15823=ORIENTED_EDGE('',*,*,#10664,.T.);
#15824=ORIENTED_EDGE('',*,*,#10665,.F.);
#15825=ORIENTED_EDGE('',*,*,#10666,.F.);
#15826=ORIENTED_EDGE('',*,*,#10667,.T.);
#15827=ORIENTED_EDGE('',*,*,#10666,.T.);
#15828=ORIENTED_EDGE('',*,*,#10668,.F.);
#15829=ORIENTED_EDGE('',*,*,#10669,.F.);
#15830=ORIENTED_EDGE('',*,*,#10670,.F.);
#15831=ORIENTED_EDGE('',*,*,#10669,.T.);
#15832=ORIENTED_EDGE('',*,*,#10671,.F.);
#15833=ORIENTED_EDGE('',*,*,#10672,.F.);
#15834=ORIENTED_EDGE('',*,*,#10673,.T.);
#15835=ORIENTED_EDGE('',*,*,#10672,.T.);
#15836=ORIENTED_EDGE('',*,*,#10674,.F.);
#15837=ORIENTED_EDGE('',*,*,#10664,.F.);
#15838=ORIENTED_EDGE('',*,*,#10674,.T.);
#15839=ORIENTED_EDGE('',*,*,#10671,.T.);
#15840=ORIENTED_EDGE('',*,*,#10668,.T.);
#15841=ORIENTED_EDGE('',*,*,#10665,.T.);
#15842=ORIENTED_EDGE('',*,*,#10673,.F.);
#15843=ORIENTED_EDGE('',*,*,#10663,.T.);
#15844=ORIENTED_EDGE('',*,*,#10667,.F.);
#15845=ORIENTED_EDGE('',*,*,#10670,.T.);
#15846=ORIENTED_EDGE('',*,*,#10675,.F.);
#15847=ORIENTED_EDGE('',*,*,#10676,.T.);
#15848=ORIENTED_EDGE('',*,*,#10677,.T.);
#15849=ORIENTED_EDGE('',*,*,#10676,.F.);
#15850=ORIENTED_EDGE('',*,*,#10675,.T.);
#15851=ORIENTED_EDGE('',*,*,#10677,.F.);
#15852=ORIENTED_EDGE('',*,*,#10678,.F.);
#15853=ORIENTED_EDGE('',*,*,#10679,.T.);
#15854=ORIENTED_EDGE('',*,*,#10680,.F.);
#15855=ORIENTED_EDGE('',*,*,#10681,.T.);
#15856=ORIENTED_EDGE('',*,*,#10678,.T.);
#15857=ORIENTED_EDGE('',*,*,#10681,.F.);
#15858=ORIENTED_EDGE('',*,*,#10679,.F.);
#15859=ORIENTED_EDGE('',*,*,#10682,.T.);
#15860=ORIENTED_EDGE('',*,*,#10683,.F.);
#15861=ORIENTED_EDGE('',*,*,#10682,.F.);
#15862=ORIENTED_EDGE('',*,*,#10684,.F.);
#15863=ORIENTED_EDGE('',*,*,#10685,.T.);
#15864=ORIENTED_EDGE('',*,*,#10686,.F.);
#15865=ORIENTED_EDGE('',*,*,#10687,.T.);
#15866=ORIENTED_EDGE('',*,*,#10684,.T.);
#15867=ORIENTED_EDGE('',*,*,#10687,.F.);
#15868=ORIENTED_EDGE('',*,*,#10685,.F.);
#15869=ORIENTED_EDGE('',*,*,#10688,.T.);
#15870=ORIENTED_EDGE('',*,*,#10689,.F.);
#15871=ORIENTED_EDGE('',*,*,#10688,.F.);
#15872=ORIENTED_EDGE('',*,*,#10690,.F.);
#15873=ORIENTED_EDGE('',*,*,#10691,.T.);
#15874=ORIENTED_EDGE('',*,*,#10692,.F.);
#15875=ORIENTED_EDGE('',*,*,#10693,.T.);
#15876=ORIENTED_EDGE('',*,*,#10690,.T.);
#15877=ORIENTED_EDGE('',*,*,#10693,.F.);
#15878=ORIENTED_EDGE('',*,*,#10691,.F.);
#15879=ORIENTED_EDGE('',*,*,#10694,.T.);
#15880=ORIENTED_EDGE('',*,*,#10695,.F.);
#15881=ORIENTED_EDGE('',*,*,#10694,.F.);
#15882=ORIENTED_EDGE('',*,*,#10696,.F.);
#15883=ORIENTED_EDGE('',*,*,#10697,.T.);
#15884=ORIENTED_EDGE('',*,*,#10698,.F.);
#15885=ORIENTED_EDGE('',*,*,#10699,.T.);
#15886=ORIENTED_EDGE('',*,*,#10696,.T.);
#15887=ORIENTED_EDGE('',*,*,#10699,.F.);
#15888=ORIENTED_EDGE('',*,*,#10697,.F.);
#15889=ORIENTED_EDGE('',*,*,#10700,.T.);
#15890=ORIENTED_EDGE('',*,*,#10701,.F.);
#15891=ORIENTED_EDGE('',*,*,#10700,.F.);
#15892=ORIENTED_EDGE('',*,*,#10702,.F.);
#15893=ORIENTED_EDGE('',*,*,#10703,.T.);
#15894=ORIENTED_EDGE('',*,*,#10704,.F.);
#15895=ORIENTED_EDGE('',*,*,#10705,.T.);
#15896=ORIENTED_EDGE('',*,*,#10702,.T.);
#15897=ORIENTED_EDGE('',*,*,#10705,.F.);
#15898=ORIENTED_EDGE('',*,*,#10703,.F.);
#15899=ORIENTED_EDGE('',*,*,#10706,.T.);
#15900=ORIENTED_EDGE('',*,*,#10707,.F.);
#15901=ORIENTED_EDGE('',*,*,#10706,.F.);
#15902=ORIENTED_EDGE('',*,*,#10708,.F.);
#15903=ORIENTED_EDGE('',*,*,#10709,.T.);
#15904=ORIENTED_EDGE('',*,*,#10710,.F.);
#15905=ORIENTED_EDGE('',*,*,#10711,.T.);
#15906=ORIENTED_EDGE('',*,*,#10708,.T.);
#15907=ORIENTED_EDGE('',*,*,#10711,.F.);
#15908=ORIENTED_EDGE('',*,*,#10709,.F.);
#15909=ORIENTED_EDGE('',*,*,#10712,.T.);
#15910=ORIENTED_EDGE('',*,*,#10713,.F.);
#15911=ORIENTED_EDGE('',*,*,#10712,.F.);
#15912=ORIENTED_EDGE('',*,*,#10714,.F.);
#15913=ORIENTED_EDGE('',*,*,#10715,.T.);
#15914=ORIENTED_EDGE('',*,*,#10716,.T.);
#15915=ORIENTED_EDGE('',*,*,#10715,.F.);
#15916=ORIENTED_EDGE('',*,*,#10717,.F.);
#15917=ORIENTED_EDGE('',*,*,#10718,.T.);
#15918=ORIENTED_EDGE('',*,*,#10719,.T.);
#15919=ORIENTED_EDGE('',*,*,#10718,.F.);
#15920=ORIENTED_EDGE('',*,*,#10717,.T.);
#15921=ORIENTED_EDGE('',*,*,#10714,.T.);
#15922=ORIENTED_EDGE('',*,*,#10710,.T.);
#15923=ORIENTED_EDGE('',*,*,#10704,.T.);
#15924=ORIENTED_EDGE('',*,*,#10698,.T.);
#15925=ORIENTED_EDGE('',*,*,#10692,.T.);
#15926=ORIENTED_EDGE('',*,*,#10686,.T.);
#15927=ORIENTED_EDGE('',*,*,#10680,.T.);
#15928=ORIENTED_EDGE('',*,*,#10719,.F.);
#15929=ORIENTED_EDGE('',*,*,#10716,.F.);
#15930=ORIENTED_EDGE('',*,*,#10713,.T.);
#15931=ORIENTED_EDGE('',*,*,#10707,.T.);
#15932=ORIENTED_EDGE('',*,*,#10701,.T.);
#15933=ORIENTED_EDGE('',*,*,#10695,.T.);
#15934=ORIENTED_EDGE('',*,*,#10689,.T.);
#15935=ORIENTED_EDGE('',*,*,#10683,.T.);
#15936=ORIENTED_EDGE('',*,*,#10720,.F.);
#15937=ORIENTED_EDGE('',*,*,#10721,.T.);
#15938=ORIENTED_EDGE('',*,*,#10722,.T.);
#15939=ORIENTED_EDGE('',*,*,#10721,.F.);
#15940=ORIENTED_EDGE('',*,*,#10723,.F.);
#15941=ORIENTED_EDGE('',*,*,#10724,.T.);
#15942=ORIENTED_EDGE('',*,*,#10725,.T.);
#15943=ORIENTED_EDGE('',*,*,#10724,.F.);
#15944=ORIENTED_EDGE('',*,*,#10723,.T.);
#15945=ORIENTED_EDGE('',*,*,#10720,.T.);
#15946=ORIENTED_EDGE('',*,*,#10725,.F.);
#15947=ORIENTED_EDGE('',*,*,#10722,.F.);
#15948=ORIENTED_EDGE('',*,*,#10726,.F.);
#15949=ORIENTED_EDGE('',*,*,#10727,.T.);
#15950=ORIENTED_EDGE('',*,*,#10728,.T.);
#15951=ORIENTED_EDGE('',*,*,#10727,.F.);
#15952=ORIENTED_EDGE('',*,*,#10728,.F.);
#15953=ORIENTED_EDGE('',*,*,#10729,.T.);
#15954=ORIENTED_EDGE('',*,*,#10730,.F.);
#15955=ORIENTED_EDGE('',*,*,#10729,.F.);
#15956=ORIENTED_EDGE('',*,*,#10731,.F.);
#15957=ORIENTED_EDGE('',*,*,#10732,.T.);
#15958=ORIENTED_EDGE('',*,*,#10733,.T.);
#15959=ORIENTED_EDGE('',*,*,#10732,.F.);
#15960=ORIENTED_EDGE('',*,*,#10733,.F.);
#15961=ORIENTED_EDGE('',*,*,#10734,.T.);
#15962=ORIENTED_EDGE('',*,*,#10735,.F.);
#15963=ORIENTED_EDGE('',*,*,#10734,.F.);
#15964=ORIENTED_EDGE('',*,*,#10736,.F.);
#15965=ORIENTED_EDGE('',*,*,#10737,.T.);
#15966=ORIENTED_EDGE('',*,*,#10738,.T.);
#15967=ORIENTED_EDGE('',*,*,#10737,.F.);
#15968=ORIENTED_EDGE('',*,*,#10738,.F.);
#15969=ORIENTED_EDGE('',*,*,#10739,.T.);
#15970=ORIENTED_EDGE('',*,*,#10740,.F.);
#15971=ORIENTED_EDGE('',*,*,#10739,.F.);
#15972=ORIENTED_EDGE('',*,*,#10741,.F.);
#15973=ORIENTED_EDGE('',*,*,#10742,.T.);
#15974=ORIENTED_EDGE('',*,*,#10743,.T.);
#15975=ORIENTED_EDGE('',*,*,#10742,.F.);
#15976=ORIENTED_EDGE('',*,*,#10743,.F.);
#15977=ORIENTED_EDGE('',*,*,#10744,.T.);
#15978=ORIENTED_EDGE('',*,*,#10745,.F.);
#15979=ORIENTED_EDGE('',*,*,#10744,.F.);
#15980=ORIENTED_EDGE('',*,*,#10746,.F.);
#15981=ORIENTED_EDGE('',*,*,#10747,.T.);
#15982=ORIENTED_EDGE('',*,*,#10748,.T.);
#15983=ORIENTED_EDGE('',*,*,#10747,.F.);
#15984=ORIENTED_EDGE('',*,*,#10748,.F.);
#15985=ORIENTED_EDGE('',*,*,#10749,.T.);
#15986=ORIENTED_EDGE('',*,*,#10750,.F.);
#15987=ORIENTED_EDGE('',*,*,#10749,.F.);
#15988=ORIENTED_EDGE('',*,*,#10751,.F.);
#15989=ORIENTED_EDGE('',*,*,#10752,.T.);
#15990=ORIENTED_EDGE('',*,*,#10753,.T.);
#15991=ORIENTED_EDGE('',*,*,#10752,.F.);
#15992=ORIENTED_EDGE('',*,*,#10753,.F.);
#15993=ORIENTED_EDGE('',*,*,#10754,.T.);
#15994=ORIENTED_EDGE('',*,*,#10755,.F.);
#15995=ORIENTED_EDGE('',*,*,#10754,.F.);
#15996=ORIENTED_EDGE('',*,*,#10756,.F.);
#15997=ORIENTED_EDGE('',*,*,#10757,.T.);
#15998=ORIENTED_EDGE('',*,*,#10758,.T.);
#15999=ORIENTED_EDGE('',*,*,#10757,.F.);
#16000=ORIENTED_EDGE('',*,*,#10759,.F.);
#16001=ORIENTED_EDGE('',*,*,#10760,.T.);
#16002=ORIENTED_EDGE('',*,*,#10761,.T.);
#16003=ORIENTED_EDGE('',*,*,#10760,.F.);
#16004=ORIENTED_EDGE('',*,*,#10759,.T.);
#16005=ORIENTED_EDGE('',*,*,#10756,.T.);
#16006=ORIENTED_EDGE('',*,*,#10751,.T.);
#16007=ORIENTED_EDGE('',*,*,#10746,.T.);
#16008=ORIENTED_EDGE('',*,*,#10741,.T.);
#16009=ORIENTED_EDGE('',*,*,#10736,.T.);
#16010=ORIENTED_EDGE('',*,*,#10731,.T.);
#16011=ORIENTED_EDGE('',*,*,#10726,.T.);
#16012=ORIENTED_EDGE('',*,*,#10761,.F.);
#16013=ORIENTED_EDGE('',*,*,#10758,.F.);
#16014=ORIENTED_EDGE('',*,*,#10755,.T.);
#16015=ORIENTED_EDGE('',*,*,#10750,.T.);
#16016=ORIENTED_EDGE('',*,*,#10745,.T.);
#16017=ORIENTED_EDGE('',*,*,#10740,.T.);
#16018=ORIENTED_EDGE('',*,*,#10735,.T.);
#16019=ORIENTED_EDGE('',*,*,#10730,.T.);
#16020=ORIENTED_EDGE('',*,*,#10762,.F.);
#16021=ORIENTED_EDGE('',*,*,#10763,.T.);
#16022=ORIENTED_EDGE('',*,*,#10764,.T.);
#16023=ORIENTED_EDGE('',*,*,#10763,.F.);
#16024=ORIENTED_EDGE('',*,*,#10765,.F.);
#16025=ORIENTED_EDGE('',*,*,#10766,.T.);
#16026=ORIENTED_EDGE('',*,*,#10767,.T.);
#16027=ORIENTED_EDGE('',*,*,#10766,.F.);
#16028=ORIENTED_EDGE('',*,*,#10765,.T.);
#16029=ORIENTED_EDGE('',*,*,#10762,.T.);
#16030=ORIENTED_EDGE('',*,*,#10767,.F.);
#16031=ORIENTED_EDGE('',*,*,#10764,.F.);
#16032=ORIENTED_EDGE('',*,*,#10768,.F.);
#16033=ORIENTED_EDGE('',*,*,#10769,.T.);
#16034=ORIENTED_EDGE('',*,*,#10770,.T.);
#16035=ORIENTED_EDGE('',*,*,#10769,.F.);
#16036=ORIENTED_EDGE('',*,*,#10771,.F.);
#16037=ORIENTED_EDGE('',*,*,#10772,.T.);
#16038=ORIENTED_EDGE('',*,*,#10773,.T.);
#16039=ORIENTED_EDGE('',*,*,#10772,.F.);
#16040=ORIENTED_EDGE('',*,*,#10771,.T.);
#16041=ORIENTED_EDGE('',*,*,#10768,.T.);
#16042=ORIENTED_EDGE('',*,*,#10773,.F.);
#16043=ORIENTED_EDGE('',*,*,#10770,.F.);
#16044=ORIENTED_EDGE('',*,*,#10774,.F.);
#16045=ORIENTED_EDGE('',*,*,#10775,.T.);
#16046=ORIENTED_EDGE('',*,*,#10776,.T.);
#16047=ORIENTED_EDGE('',*,*,#10775,.F.);
#16048=ORIENTED_EDGE('',*,*,#10777,.F.);
#16049=ORIENTED_EDGE('',*,*,#10778,.T.);
#16050=ORIENTED_EDGE('',*,*,#10779,.T.);
#16051=ORIENTED_EDGE('',*,*,#10778,.F.);
#16052=ORIENTED_EDGE('',*,*,#10777,.T.);
#16053=ORIENTED_EDGE('',*,*,#10774,.T.);
#16054=ORIENTED_EDGE('',*,*,#10779,.F.);
#16055=ORIENTED_EDGE('',*,*,#10776,.F.);
#16056=ORIENTED_EDGE('',*,*,#10780,.F.);
#16057=ORIENTED_EDGE('',*,*,#10781,.F.);
#16058=ORIENTED_EDGE('',*,*,#10782,.F.);
#16059=ORIENTED_EDGE('',*,*,#10783,.F.);
#16060=ORIENTED_EDGE('',*,*,#10784,.F.);
#16061=ORIENTED_EDGE('',*,*,#10785,.F.);
#16062=ORIENTED_EDGE('',*,*,#10786,.F.);
#16063=ORIENTED_EDGE('',*,*,#10787,.F.);
#16064=ORIENTED_EDGE('',*,*,#10787,.T.);
#16065=ORIENTED_EDGE('',*,*,#10788,.F.);
#16066=ORIENTED_EDGE('',*,*,#10781,.T.);
#16067=ORIENTED_EDGE('',*,*,#10789,.F.);
#16068=ORIENTED_EDGE('',*,*,#10784,.T.);
#16069=ORIENTED_EDGE('',*,*,#10789,.T.);
#16070=ORIENTED_EDGE('',*,*,#10780,.T.);
#16071=ORIENTED_EDGE('',*,*,#10790,.F.);
#16072=ORIENTED_EDGE('',*,*,#10786,.T.);
#16073=ORIENTED_EDGE('',*,*,#10791,.F.);
#16074=ORIENTED_EDGE('',*,*,#10782,.T.);
#16075=ORIENTED_EDGE('',*,*,#10788,.T.);
#16076=ORIENTED_EDGE('',*,*,#10785,.T.);
#16077=ORIENTED_EDGE('',*,*,#10790,.T.);
#16078=ORIENTED_EDGE('',*,*,#10783,.T.);
#16079=ORIENTED_EDGE('',*,*,#10791,.T.);
#16080=ORIENTED_EDGE('',*,*,#10792,.F.);
#16081=ORIENTED_EDGE('',*,*,#10793,.T.);
#16082=ORIENTED_EDGE('',*,*,#10794,.F.);
#16083=ORIENTED_EDGE('',*,*,#10795,.T.);
#16084=ORIENTED_EDGE('',*,*,#10792,.T.);
#16085=ORIENTED_EDGE('',*,*,#10795,.F.);
#16086=ORIENTED_EDGE('',*,*,#10794,.T.);
#16087=ORIENTED_EDGE('',*,*,#10793,.F.);
#16088=ORIENTED_EDGE('',*,*,#10796,.T.);
#16089=ORIENTED_EDGE('',*,*,#10797,.T.);
#16090=ORIENTED_EDGE('',*,*,#10796,.F.);
#16091=ORIENTED_EDGE('',*,*,#10797,.F.);
#16092=ORIENTED_EDGE('',*,*,#10798,.T.);
#16093=ORIENTED_EDGE('',*,*,#10799,.T.);
#16094=ORIENTED_EDGE('',*,*,#10800,.F.);
#16095=ORIENTED_EDGE('',*,*,#10799,.F.);
#16096=ORIENTED_EDGE('',*,*,#10800,.T.);
#16097=ORIENTED_EDGE('',*,*,#10798,.F.);
#16098=ORIENTED_EDGE('',*,*,#10801,.F.);
#16099=ORIENTED_EDGE('',*,*,#10802,.T.);
#16100=ORIENTED_EDGE('',*,*,#10803,.T.);
#16101=ORIENTED_EDGE('',*,*,#10804,.T.);
#16102=ORIENTED_EDGE('',*,*,#10805,.F.);
#16103=ORIENTED_EDGE('',*,*,#10806,.T.);
#16104=ORIENTED_EDGE('',*,*,#10801,.T.);
#16105=ORIENTED_EDGE('',*,*,#10807,.T.);
#16106=ORIENTED_EDGE('',*,*,#10808,.F.);
#16107=ORIENTED_EDGE('',*,*,#10809,.T.);
#16108=ORIENTED_EDGE('',*,*,#10805,.T.);
#16109=ORIENTED_EDGE('',*,*,#10810,.T.);
#16110=ORIENTED_EDGE('',*,*,#10811,.F.);
#16111=ORIENTED_EDGE('',*,*,#10812,.T.);
#16112=ORIENTED_EDGE('',*,*,#10808,.T.);
#16113=ORIENTED_EDGE('',*,*,#10813,.T.);
#16114=ORIENTED_EDGE('',*,*,#10814,.F.);
#16115=ORIENTED_EDGE('',*,*,#10815,.T.);
#16116=ORIENTED_EDGE('',*,*,#10811,.T.);
#16117=ORIENTED_EDGE('',*,*,#10816,.T.);
#16118=ORIENTED_EDGE('',*,*,#10817,.F.);
#16119=ORIENTED_EDGE('',*,*,#10818,.T.);
#16120=ORIENTED_EDGE('',*,*,#10814,.T.);
#16121=ORIENTED_EDGE('',*,*,#10819,.T.);
#16122=ORIENTED_EDGE('',*,*,#10820,.F.);
#16123=ORIENTED_EDGE('',*,*,#10821,.T.);
#16124=ORIENTED_EDGE('',*,*,#10817,.T.);
#16125=ORIENTED_EDGE('',*,*,#10822,.T.);
#16126=ORIENTED_EDGE('',*,*,#10823,.F.);
#16127=ORIENTED_EDGE('',*,*,#10824,.T.);
#16128=ORIENTED_EDGE('',*,*,#10820,.T.);
#16129=ORIENTED_EDGE('',*,*,#10825,.T.);
#16130=ORIENTED_EDGE('',*,*,#10826,.F.);
#16131=ORIENTED_EDGE('',*,*,#10827,.T.);
#16132=ORIENTED_EDGE('',*,*,#10823,.T.);
#16133=ORIENTED_EDGE('',*,*,#10828,.T.);
#16134=ORIENTED_EDGE('',*,*,#10829,.F.);
#16135=ORIENTED_EDGE('',*,*,#10830,.T.);
#16136=ORIENTED_EDGE('',*,*,#10826,.T.);
#16137=ORIENTED_EDGE('',*,*,#10831,.T.);
#16138=ORIENTED_EDGE('',*,*,#10832,.F.);
#16139=ORIENTED_EDGE('',*,*,#10833,.T.);
#16140=ORIENTED_EDGE('',*,*,#10829,.T.);
#16141=ORIENTED_EDGE('',*,*,#10834,.T.);
#16142=ORIENTED_EDGE('',*,*,#10835,.F.);
#16143=ORIENTED_EDGE('',*,*,#10836,.T.);
#16144=ORIENTED_EDGE('',*,*,#10832,.T.);
#16145=ORIENTED_EDGE('',*,*,#10837,.T.);
#16146=ORIENTED_EDGE('',*,*,#10838,.F.);
#16147=ORIENTED_EDGE('',*,*,#10839,.T.);
#16148=ORIENTED_EDGE('',*,*,#10835,.T.);
#16149=ORIENTED_EDGE('',*,*,#10840,.T.);
#16150=ORIENTED_EDGE('',*,*,#10841,.F.);
#16151=ORIENTED_EDGE('',*,*,#10842,.T.);
#16152=ORIENTED_EDGE('',*,*,#10838,.T.);
#16153=ORIENTED_EDGE('',*,*,#10843,.T.);
#16154=ORIENTED_EDGE('',*,*,#10844,.F.);
#16155=ORIENTED_EDGE('',*,*,#10845,.T.);
#16156=ORIENTED_EDGE('',*,*,#10841,.T.);
#16157=ORIENTED_EDGE('',*,*,#10846,.T.);
#16158=ORIENTED_EDGE('',*,*,#10847,.F.);
#16159=ORIENTED_EDGE('',*,*,#10848,.T.);
#16160=ORIENTED_EDGE('',*,*,#10844,.T.);
#16161=ORIENTED_EDGE('',*,*,#10849,.T.);
#16162=ORIENTED_EDGE('',*,*,#10850,.F.);
#16163=ORIENTED_EDGE('',*,*,#10851,.T.);
#16164=ORIENTED_EDGE('',*,*,#10852,.T.);
#16165=ORIENTED_EDGE('',*,*,#10853,.F.);
#16166=ORIENTED_EDGE('',*,*,#10854,.F.);
#16167=ORIENTED_EDGE('',*,*,#10855,.T.);
#16168=ORIENTED_EDGE('',*,*,#10850,.T.);
#16169=ORIENTED_EDGE('',*,*,#10856,.F.);
#16170=ORIENTED_EDGE('',*,*,#10857,.F.);
#16171=ORIENTED_EDGE('',*,*,#10858,.T.);
#16172=ORIENTED_EDGE('',*,*,#10854,.T.);
#16173=ORIENTED_EDGE('',*,*,#10859,.F.);
#16174=ORIENTED_EDGE('',*,*,#10860,.F.);
#16175=ORIENTED_EDGE('',*,*,#10861,.T.);
#16176=ORIENTED_EDGE('',*,*,#10857,.T.);
#16177=ORIENTED_EDGE('',*,*,#10862,.F.);
#16178=ORIENTED_EDGE('',*,*,#10863,.F.);
#16179=ORIENTED_EDGE('',*,*,#10864,.T.);
#16180=ORIENTED_EDGE('',*,*,#10860,.T.);
#16181=ORIENTED_EDGE('',*,*,#10865,.F.);
#16182=ORIENTED_EDGE('',*,*,#10866,.F.);
#16183=ORIENTED_EDGE('',*,*,#10867,.T.);
#16184=ORIENTED_EDGE('',*,*,#10863,.T.);
#16185=ORIENTED_EDGE('',*,*,#10868,.F.);
#16186=ORIENTED_EDGE('',*,*,#10869,.F.);
#16187=ORIENTED_EDGE('',*,*,#10870,.T.);
#16188=ORIENTED_EDGE('',*,*,#10866,.T.);
#16189=ORIENTED_EDGE('',*,*,#10871,.F.);
#16190=ORIENTED_EDGE('',*,*,#10872,.F.);
#16191=ORIENTED_EDGE('',*,*,#10873,.T.);
#16192=ORIENTED_EDGE('',*,*,#10869,.T.);
#16193=ORIENTED_EDGE('',*,*,#10874,.F.);
#16194=ORIENTED_EDGE('',*,*,#10875,.F.);
#16195=ORIENTED_EDGE('',*,*,#10876,.T.);
#16196=ORIENTED_EDGE('',*,*,#10872,.T.);
#16197=ORIENTED_EDGE('',*,*,#10877,.F.);
#16198=ORIENTED_EDGE('',*,*,#10878,.F.);
#16199=ORIENTED_EDGE('',*,*,#10879,.T.);
#16200=ORIENTED_EDGE('',*,*,#10875,.T.);
#16201=ORIENTED_EDGE('',*,*,#10880,.F.);
#16202=ORIENTED_EDGE('',*,*,#10881,.F.);
#16203=ORIENTED_EDGE('',*,*,#10882,.T.);
#16204=ORIENTED_EDGE('',*,*,#10878,.T.);
#16205=ORIENTED_EDGE('',*,*,#10883,.F.);
#16206=ORIENTED_EDGE('',*,*,#10884,.F.);
#16207=ORIENTED_EDGE('',*,*,#10885,.T.);
#16208=ORIENTED_EDGE('',*,*,#10881,.T.);
#16209=ORIENTED_EDGE('',*,*,#10886,.F.);
#16210=ORIENTED_EDGE('',*,*,#10887,.F.);
#16211=ORIENTED_EDGE('',*,*,#10888,.T.);
#16212=ORIENTED_EDGE('',*,*,#10884,.T.);
#16213=ORIENTED_EDGE('',*,*,#10889,.F.);
#16214=ORIENTED_EDGE('',*,*,#10890,.F.);
#16215=ORIENTED_EDGE('',*,*,#10891,.T.);
#16216=ORIENTED_EDGE('',*,*,#10887,.T.);
#16217=ORIENTED_EDGE('',*,*,#10892,.F.);
#16218=ORIENTED_EDGE('',*,*,#10893,.F.);
#16219=ORIENTED_EDGE('',*,*,#10894,.T.);
#16220=ORIENTED_EDGE('',*,*,#10890,.T.);
#16221=ORIENTED_EDGE('',*,*,#10895,.F.);
#16222=ORIENTED_EDGE('',*,*,#10896,.F.);
#16223=ORIENTED_EDGE('',*,*,#10897,.T.);
#16224=ORIENTED_EDGE('',*,*,#10893,.T.);
#16225=ORIENTED_EDGE('',*,*,#10898,.F.);
#16226=ORIENTED_EDGE('',*,*,#10899,.F.);
#16227=ORIENTED_EDGE('',*,*,#10852,.F.);
#16228=ORIENTED_EDGE('',*,*,#10900,.F.);
#16229=ORIENTED_EDGE('',*,*,#10901,.F.);
#16230=ORIENTED_EDGE('',*,*,#10902,.F.);
#16231=ORIENTED_EDGE('',*,*,#10903,.T.);
#16232=ORIENTED_EDGE('',*,*,#10904,.F.);
#16233=ORIENTED_EDGE('',*,*,#10903,.F.);
#16234=ORIENTED_EDGE('',*,*,#10900,.T.);
#16235=ORIENTED_EDGE('',*,*,#10851,.F.);
#16236=ORIENTED_EDGE('',*,*,#10855,.F.);
#16237=ORIENTED_EDGE('',*,*,#10858,.F.);
#16238=ORIENTED_EDGE('',*,*,#10861,.F.);
#16239=ORIENTED_EDGE('',*,*,#10864,.F.);
#16240=ORIENTED_EDGE('',*,*,#10867,.F.);
#16241=ORIENTED_EDGE('',*,*,#10870,.F.);
#16242=ORIENTED_EDGE('',*,*,#10873,.F.);
#16243=ORIENTED_EDGE('',*,*,#10876,.F.);
#16244=ORIENTED_EDGE('',*,*,#10879,.F.);
#16245=ORIENTED_EDGE('',*,*,#10882,.F.);
#16246=ORIENTED_EDGE('',*,*,#10885,.F.);
#16247=ORIENTED_EDGE('',*,*,#10888,.F.);
#16248=ORIENTED_EDGE('',*,*,#10891,.F.);
#16249=ORIENTED_EDGE('',*,*,#10894,.F.);
#16250=ORIENTED_EDGE('',*,*,#10897,.F.);
#16251=ORIENTED_EDGE('',*,*,#10905,.F.);
#16252=ORIENTED_EDGE('',*,*,#10906,.F.);
#16253=ORIENTED_EDGE('',*,*,#10802,.F.);
#16254=ORIENTED_EDGE('',*,*,#10806,.F.);
#16255=ORIENTED_EDGE('',*,*,#10809,.F.);
#16256=ORIENTED_EDGE('',*,*,#10812,.F.);
#16257=ORIENTED_EDGE('',*,*,#10815,.F.);
#16258=ORIENTED_EDGE('',*,*,#10818,.F.);
#16259=ORIENTED_EDGE('',*,*,#10821,.F.);
#16260=ORIENTED_EDGE('',*,*,#10824,.F.);
#16261=ORIENTED_EDGE('',*,*,#10827,.F.);
#16262=ORIENTED_EDGE('',*,*,#10830,.F.);
#16263=ORIENTED_EDGE('',*,*,#10833,.F.);
#16264=ORIENTED_EDGE('',*,*,#10836,.F.);
#16265=ORIENTED_EDGE('',*,*,#10839,.F.);
#16266=ORIENTED_EDGE('',*,*,#10842,.F.);
#16267=ORIENTED_EDGE('',*,*,#10845,.F.);
#16268=ORIENTED_EDGE('',*,*,#10848,.F.);
#16269=ORIENTED_EDGE('',*,*,#10907,.F.);
#16270=ORIENTED_EDGE('',*,*,#10896,.T.);
#16271=ORIENTED_EDGE('',*,*,#10908,.F.);
#16272=ORIENTED_EDGE('',*,*,#10909,.F.);
#16273=ORIENTED_EDGE('',*,*,#10905,.T.);
#16274=ORIENTED_EDGE('',*,*,#10899,.T.);
#16275=ORIENTED_EDGE('',*,*,#10902,.T.);
#16276=ORIENTED_EDGE('',*,*,#10910,.F.);
#16277=ORIENTED_EDGE('',*,*,#10849,.F.);
#16278=ORIENTED_EDGE('',*,*,#10846,.F.);
#16279=ORIENTED_EDGE('',*,*,#10843,.F.);
#16280=ORIENTED_EDGE('',*,*,#10840,.F.);
#16281=ORIENTED_EDGE('',*,*,#10837,.F.);
#16282=ORIENTED_EDGE('',*,*,#10834,.F.);
#16283=ORIENTED_EDGE('',*,*,#10831,.F.);
#16284=ORIENTED_EDGE('',*,*,#10828,.F.);
#16285=ORIENTED_EDGE('',*,*,#10825,.F.);
#16286=ORIENTED_EDGE('',*,*,#10822,.F.);
#16287=ORIENTED_EDGE('',*,*,#10819,.F.);
#16288=ORIENTED_EDGE('',*,*,#10816,.F.);
#16289=ORIENTED_EDGE('',*,*,#10813,.F.);
#16290=ORIENTED_EDGE('',*,*,#10810,.F.);
#16291=ORIENTED_EDGE('',*,*,#10807,.F.);
#16292=ORIENTED_EDGE('',*,*,#10804,.F.);
#16293=ORIENTED_EDGE('',*,*,#10911,.F.);
#16294=ORIENTED_EDGE('',*,*,#10908,.T.);
#16295=ORIENTED_EDGE('',*,*,#10898,.T.);
#16296=ORIENTED_EDGE('',*,*,#10895,.T.);
#16297=ORIENTED_EDGE('',*,*,#10892,.T.);
#16298=ORIENTED_EDGE('',*,*,#10889,.T.);
#16299=ORIENTED_EDGE('',*,*,#10886,.T.);
#16300=ORIENTED_EDGE('',*,*,#10883,.T.);
#16301=ORIENTED_EDGE('',*,*,#10880,.T.);
#16302=ORIENTED_EDGE('',*,*,#10877,.T.);
#16303=ORIENTED_EDGE('',*,*,#10874,.T.);
#16304=ORIENTED_EDGE('',*,*,#10871,.T.);
#16305=ORIENTED_EDGE('',*,*,#10868,.T.);
#16306=ORIENTED_EDGE('',*,*,#10865,.T.);
#16307=ORIENTED_EDGE('',*,*,#10862,.T.);
#16308=ORIENTED_EDGE('',*,*,#10859,.T.);
#16309=ORIENTED_EDGE('',*,*,#10856,.T.);
#16310=ORIENTED_EDGE('',*,*,#10853,.T.);
#16311=ORIENTED_EDGE('',*,*,#10847,.T.);
#16312=ORIENTED_EDGE('',*,*,#10910,.T.);
#16313=ORIENTED_EDGE('',*,*,#10901,.T.);
#16314=ORIENTED_EDGE('',*,*,#10907,.T.);
#16315=ORIENTED_EDGE('',*,*,#10912,.F.);
#16316=ORIENTED_EDGE('',*,*,#10913,.T.);
#16317=ORIENTED_EDGE('',*,*,#10914,.T.);
#16318=ORIENTED_EDGE('',*,*,#10915,.F.);
#16319=ORIENTED_EDGE('',*,*,#10916,.F.);
#16320=ORIENTED_EDGE('',*,*,#10917,.T.);
#16321=ORIENTED_EDGE('',*,*,#10918,.T.);
#16322=ORIENTED_EDGE('',*,*,#10913,.F.);
#16323=ORIENTED_EDGE('',*,*,#10919,.F.);
#16324=ORIENTED_EDGE('',*,*,#10920,.T.);
#16325=ORIENTED_EDGE('',*,*,#10921,.T.);
#16326=ORIENTED_EDGE('',*,*,#10917,.F.);
#16327=ORIENTED_EDGE('',*,*,#10922,.F.);
#16328=ORIENTED_EDGE('',*,*,#10923,.T.);
#16329=ORIENTED_EDGE('',*,*,#10924,.T.);
#16330=ORIENTED_EDGE('',*,*,#10920,.F.);
#16331=ORIENTED_EDGE('',*,*,#10925,.F.);
#16332=ORIENTED_EDGE('',*,*,#10926,.T.);
#16333=ORIENTED_EDGE('',*,*,#10927,.T.);
#16334=ORIENTED_EDGE('',*,*,#10923,.F.);
#16335=ORIENTED_EDGE('',*,*,#10928,.F.);
#16336=ORIENTED_EDGE('',*,*,#10915,.T.);
#16337=ORIENTED_EDGE('',*,*,#10929,.T.);
#16338=ORIENTED_EDGE('',*,*,#10926,.F.);
#16339=ORIENTED_EDGE('',*,*,#10929,.F.);
#16340=ORIENTED_EDGE('',*,*,#10914,.F.);
#16341=ORIENTED_EDGE('',*,*,#10918,.F.);
#16342=ORIENTED_EDGE('',*,*,#10921,.F.);
#16343=ORIENTED_EDGE('',*,*,#10924,.F.);
#16344=ORIENTED_EDGE('',*,*,#10927,.F.);
#16345=ORIENTED_EDGE('',*,*,#10930,.T.);
#16346=ORIENTED_EDGE('',*,*,#10906,.T.);
#16347=ORIENTED_EDGE('',*,*,#10909,.T.);
#16348=ORIENTED_EDGE('',*,*,#10911,.T.);
#16349=ORIENTED_EDGE('',*,*,#10803,.F.);
#16350=ORIENTED_EDGE('',*,*,#10930,.F.);
#16351=ORIENTED_EDGE('',*,*,#10931,.T.);
#16352=ORIENTED_EDGE('',*,*,#10932,.T.);
#16353=ORIENTED_EDGE('',*,*,#10931,.F.);
#16354=ORIENTED_EDGE('',*,*,#10932,.F.);
#16355=ORIENTED_EDGE('',*,*,#10912,.T.);
#16356=ORIENTED_EDGE('',*,*,#10928,.T.);
#16357=ORIENTED_EDGE('',*,*,#10925,.T.);
#16358=ORIENTED_EDGE('',*,*,#10922,.T.);
#16359=ORIENTED_EDGE('',*,*,#10919,.T.);
#16360=ORIENTED_EDGE('',*,*,#10916,.T.);
#16361=ORIENTED_EDGE('',*,*,#10904,.T.);
#16362=ORIENTED_EDGE('',*,*,#10933,.F.);
#16363=ORIENTED_EDGE('',*,*,#10934,.T.);
#16364=ORIENTED_EDGE('',*,*,#10935,.T.);
#16365=ORIENTED_EDGE('',*,*,#10936,.T.);
#16366=ORIENTED_EDGE('',*,*,#10937,.F.);
#16367=ORIENTED_EDGE('',*,*,#10938,.T.);
#16368=ORIENTED_EDGE('',*,*,#10933,.T.);
#16369=ORIENTED_EDGE('',*,*,#10939,.T.);
#16370=ORIENTED_EDGE('',*,*,#10940,.F.);
#16371=ORIENTED_EDGE('',*,*,#10941,.T.);
#16372=ORIENTED_EDGE('',*,*,#10937,.T.);
#16373=ORIENTED_EDGE('',*,*,#10942,.T.);
#16374=ORIENTED_EDGE('',*,*,#10943,.F.);
#16375=ORIENTED_EDGE('',*,*,#10944,.T.);
#16376=ORIENTED_EDGE('',*,*,#10940,.T.);
#16377=ORIENTED_EDGE('',*,*,#10945,.T.);
#16378=ORIENTED_EDGE('',*,*,#10946,.F.);
#16379=ORIENTED_EDGE('',*,*,#10947,.T.);
#16380=ORIENTED_EDGE('',*,*,#10943,.T.);
#16381=ORIENTED_EDGE('',*,*,#10948,.T.);
#16382=ORIENTED_EDGE('',*,*,#10949,.F.);
#16383=ORIENTED_EDGE('',*,*,#10950,.T.);
#16384=ORIENTED_EDGE('',*,*,#10946,.T.);
#16385=ORIENTED_EDGE('',*,*,#10951,.T.);
#16386=ORIENTED_EDGE('',*,*,#10952,.F.);
#16387=ORIENTED_EDGE('',*,*,#10953,.T.);
#16388=ORIENTED_EDGE('',*,*,#10949,.T.);
#16389=ORIENTED_EDGE('',*,*,#10954,.T.);
#16390=ORIENTED_EDGE('',*,*,#10955,.F.);
#16391=ORIENTED_EDGE('',*,*,#10956,.T.);
#16392=ORIENTED_EDGE('',*,*,#10952,.T.);
#16393=ORIENTED_EDGE('',*,*,#10957,.T.);
#16394=ORIENTED_EDGE('',*,*,#10958,.F.);
#16395=ORIENTED_EDGE('',*,*,#10959,.T.);
#16396=ORIENTED_EDGE('',*,*,#10960,.T.);
#16397=ORIENTED_EDGE('',*,*,#10961,.F.);
#16398=ORIENTED_EDGE('',*,*,#10962,.F.);
#16399=ORIENTED_EDGE('',*,*,#10963,.T.);
#16400=ORIENTED_EDGE('',*,*,#10958,.T.);
#16401=ORIENTED_EDGE('',*,*,#10964,.F.);
#16402=ORIENTED_EDGE('',*,*,#10965,.F.);
#16403=ORIENTED_EDGE('',*,*,#10966,.T.);
#16404=ORIENTED_EDGE('',*,*,#10962,.T.);
#16405=ORIENTED_EDGE('',*,*,#10967,.F.);
#16406=ORIENTED_EDGE('',*,*,#10968,.F.);
#16407=ORIENTED_EDGE('',*,*,#10969,.T.);
#16408=ORIENTED_EDGE('',*,*,#10965,.T.);
#16409=ORIENTED_EDGE('',*,*,#10970,.F.);
#16410=ORIENTED_EDGE('',*,*,#10971,.F.);
#16411=ORIENTED_EDGE('',*,*,#10972,.T.);
#16412=ORIENTED_EDGE('',*,*,#10968,.T.);
#16413=ORIENTED_EDGE('',*,*,#10973,.F.);
#16414=ORIENTED_EDGE('',*,*,#10974,.F.);
#16415=ORIENTED_EDGE('',*,*,#10975,.T.);
#16416=ORIENTED_EDGE('',*,*,#10971,.T.);
#16417=ORIENTED_EDGE('',*,*,#10976,.F.);
#16418=ORIENTED_EDGE('',*,*,#10977,.F.);
#16419=ORIENTED_EDGE('',*,*,#10978,.T.);
#16420=ORIENTED_EDGE('',*,*,#10974,.T.);
#16421=ORIENTED_EDGE('',*,*,#10979,.F.);
#16422=ORIENTED_EDGE('',*,*,#10980,.F.);
#16423=ORIENTED_EDGE('',*,*,#10981,.T.);
#16424=ORIENTED_EDGE('',*,*,#10977,.T.);
#16425=ORIENTED_EDGE('',*,*,#10982,.F.);
#16426=ORIENTED_EDGE('',*,*,#10983,.F.);
#16427=ORIENTED_EDGE('',*,*,#10960,.F.);
#16428=ORIENTED_EDGE('',*,*,#10984,.F.);
#16429=ORIENTED_EDGE('',*,*,#10985,.F.);
#16430=ORIENTED_EDGE('',*,*,#10986,.F.);
#16431=ORIENTED_EDGE('',*,*,#10987,.T.);
#16432=ORIENTED_EDGE('',*,*,#10988,.F.);
#16433=ORIENTED_EDGE('',*,*,#10987,.F.);
#16434=ORIENTED_EDGE('',*,*,#10984,.T.);
#16435=ORIENTED_EDGE('',*,*,#10959,.F.);
#16436=ORIENTED_EDGE('',*,*,#10963,.F.);
#16437=ORIENTED_EDGE('',*,*,#10966,.F.);
#16438=ORIENTED_EDGE('',*,*,#10969,.F.);
#16439=ORIENTED_EDGE('',*,*,#10972,.F.);
#16440=ORIENTED_EDGE('',*,*,#10975,.F.);
#16441=ORIENTED_EDGE('',*,*,#10978,.F.);
#16442=ORIENTED_EDGE('',*,*,#10981,.F.);
#16443=ORIENTED_EDGE('',*,*,#10989,.F.);
#16444=ORIENTED_EDGE('',*,*,#10990,.F.);
#16445=ORIENTED_EDGE('',*,*,#10934,.F.);
#16446=ORIENTED_EDGE('',*,*,#10938,.F.);
#16447=ORIENTED_EDGE('',*,*,#10941,.F.);
#16448=ORIENTED_EDGE('',*,*,#10944,.F.);
#16449=ORIENTED_EDGE('',*,*,#10947,.F.);
#16450=ORIENTED_EDGE('',*,*,#10950,.F.);
#16451=ORIENTED_EDGE('',*,*,#10953,.F.);
#16452=ORIENTED_EDGE('',*,*,#10956,.F.);
#16453=ORIENTED_EDGE('',*,*,#10991,.F.);
#16454=ORIENTED_EDGE('',*,*,#10980,.T.);
#16455=ORIENTED_EDGE('',*,*,#10992,.F.);
#16456=ORIENTED_EDGE('',*,*,#10993,.F.);
#16457=ORIENTED_EDGE('',*,*,#10989,.T.);
#16458=ORIENTED_EDGE('',*,*,#10994,.F.);
#16459=ORIENTED_EDGE('',*,*,#10995,.T.);
#16460=ORIENTED_EDGE('',*,*,#10996,.T.);
#16461=ORIENTED_EDGE('',*,*,#10997,.F.);
#16462=ORIENTED_EDGE('',*,*,#10998,.F.);
#16463=ORIENTED_EDGE('',*,*,#10999,.T.);
#16464=ORIENTED_EDGE('',*,*,#11000,.T.);
#16465=ORIENTED_EDGE('',*,*,#10995,.F.);
#16466=ORIENTED_EDGE('',*,*,#11001,.F.);
#16467=ORIENTED_EDGE('',*,*,#11002,.T.);
#16468=ORIENTED_EDGE('',*,*,#11003,.T.);
#16469=ORIENTED_EDGE('',*,*,#10999,.F.);
#16470=ORIENTED_EDGE('',*,*,#11004,.F.);
#16471=ORIENTED_EDGE('',*,*,#11005,.T.);
#16472=ORIENTED_EDGE('',*,*,#11006,.T.);
#16473=ORIENTED_EDGE('',*,*,#11002,.F.);
#16474=ORIENTED_EDGE('',*,*,#11007,.F.);
#16475=ORIENTED_EDGE('',*,*,#11008,.T.);
#16476=ORIENTED_EDGE('',*,*,#11009,.T.);
#16477=ORIENTED_EDGE('',*,*,#11005,.F.);
#16478=ORIENTED_EDGE('',*,*,#11010,.F.);
#16479=ORIENTED_EDGE('',*,*,#10997,.T.);
#16480=ORIENTED_EDGE('',*,*,#11011,.T.);
#16481=ORIENTED_EDGE('',*,*,#11008,.F.);
#16482=ORIENTED_EDGE('',*,*,#11011,.F.);
#16483=ORIENTED_EDGE('',*,*,#10996,.F.);
#16484=ORIENTED_EDGE('',*,*,#11000,.F.);
#16485=ORIENTED_EDGE('',*,*,#11003,.F.);
#16486=ORIENTED_EDGE('',*,*,#11006,.F.);
#16487=ORIENTED_EDGE('',*,*,#11009,.F.);
#16488=ORIENTED_EDGE('',*,*,#10983,.T.);
#16489=ORIENTED_EDGE('',*,*,#10986,.T.);
#16490=ORIENTED_EDGE('',*,*,#11012,.F.);
#16491=ORIENTED_EDGE('',*,*,#10957,.F.);
#16492=ORIENTED_EDGE('',*,*,#10954,.F.);
#16493=ORIENTED_EDGE('',*,*,#10951,.F.);
#16494=ORIENTED_EDGE('',*,*,#10948,.F.);
#16495=ORIENTED_EDGE('',*,*,#10945,.F.);
#16496=ORIENTED_EDGE('',*,*,#10942,.F.);
#16497=ORIENTED_EDGE('',*,*,#10939,.F.);
#16498=ORIENTED_EDGE('',*,*,#10936,.F.);
#16499=ORIENTED_EDGE('',*,*,#11013,.F.);
#16500=ORIENTED_EDGE('',*,*,#10992,.T.);
#16501=ORIENTED_EDGE('',*,*,#10982,.T.);
#16502=ORIENTED_EDGE('',*,*,#10979,.T.);
#16503=ORIENTED_EDGE('',*,*,#10976,.T.);
#16504=ORIENTED_EDGE('',*,*,#10973,.T.);
#16505=ORIENTED_EDGE('',*,*,#10970,.T.);
#16506=ORIENTED_EDGE('',*,*,#10967,.T.);
#16507=ORIENTED_EDGE('',*,*,#10964,.T.);
#16508=ORIENTED_EDGE('',*,*,#10961,.T.);
#16509=ORIENTED_EDGE('',*,*,#11014,.T.);
#16510=ORIENTED_EDGE('',*,*,#11015,.T.);
#16511=ORIENTED_EDGE('',*,*,#10990,.T.);
#16512=ORIENTED_EDGE('',*,*,#10993,.T.);
#16513=ORIENTED_EDGE('',*,*,#11013,.T.);
#16514=ORIENTED_EDGE('',*,*,#10955,.T.);
#16515=ORIENTED_EDGE('',*,*,#11012,.T.);
#16516=ORIENTED_EDGE('',*,*,#10985,.T.);
#16517=ORIENTED_EDGE('',*,*,#10991,.T.);
#16518=ORIENTED_EDGE('',*,*,#11016,.F.);
#16519=ORIENTED_EDGE('',*,*,#10994,.T.);
#16520=ORIENTED_EDGE('',*,*,#11010,.T.);
#16521=ORIENTED_EDGE('',*,*,#11007,.T.);
#16522=ORIENTED_EDGE('',*,*,#11004,.T.);
#16523=ORIENTED_EDGE('',*,*,#11001,.T.);
#16524=ORIENTED_EDGE('',*,*,#10998,.T.);
#16525=ORIENTED_EDGE('',*,*,#11014,.F.);
#16526=ORIENTED_EDGE('',*,*,#10935,.F.);
#16527=ORIENTED_EDGE('',*,*,#11015,.F.);
#16528=ORIENTED_EDGE('',*,*,#11017,.T.);
#16529=ORIENTED_EDGE('',*,*,#11016,.T.);
#16530=ORIENTED_EDGE('',*,*,#11017,.F.);
#16531=ORIENTED_EDGE('',*,*,#10988,.T.);
#16532=CYLINDRICAL_SURFACE('',#18465,1.666);
#16533=CYLINDRICAL_SURFACE('',#18468,1.666);
#16534=CYLINDRICAL_SURFACE('',#18469,1.666);
#16535=CYLINDRICAL_SURFACE('',#18470,1.666);
#16536=CYLINDRICAL_SURFACE('',#18471,1.666);
#16537=CYLINDRICAL_SURFACE('',#18472,1.666);
#16538=CYLINDRICAL_SURFACE('',#18473,1.666);
#16539=CYLINDRICAL_SURFACE('',#18474,1.666);
#16540=CYLINDRICAL_SURFACE('',#18475,1.666);
#16541=CYLINDRICAL_SURFACE('',#18476,1.666);
#16542=CYLINDRICAL_SURFACE('',#18477,1.666);
#16543=CYLINDRICAL_SURFACE('',#18478,1.666);
#16544=CYLINDRICAL_SURFACE('',#18480,2.05475);
#16545=CYLINDRICAL_SURFACE('',#18482,2.05475);
#16546=CYLINDRICAL_SURFACE('',#18483,2.05475);
#16547=CYLINDRICAL_SURFACE('',#18484,2.05475);
#16548=CYLINDRICAL_SURFACE('',#18485,2.05475);
#16549=CYLINDRICAL_SURFACE('',#18486,2.05475);
#16550=CYLINDRICAL_SURFACE('',#18487,2.05475);
#16551=CYLINDRICAL_SURFACE('',#18488,2.05475);
#16552=CYLINDRICAL_SURFACE('',#18489,2.05475);
#16553=CYLINDRICAL_SURFACE('',#18490,2.05475);
#16554=CYLINDRICAL_SURFACE('',#18491,2.05475);
#16555=CYLINDRICAL_SURFACE('',#18492,2.05475);
#16556=CYLINDRICAL_SURFACE('',#18493,2.05475);
#16557=CYLINDRICAL_SURFACE('',#18495,1.666);
#16558=CYLINDRICAL_SURFACE('',#18498,1.666);
#16559=CYLINDRICAL_SURFACE('',#18499,1.666);
#16560=CYLINDRICAL_SURFACE('',#18500,1.666);
#16561=CYLINDRICAL_SURFACE('',#18501,1.666);
#16562=CYLINDRICAL_SURFACE('',#18502,1.666);
#16563=CYLINDRICAL_SURFACE('',#18503,1.666);
#16564=CYLINDRICAL_SURFACE('',#18504,1.666);
#16565=CYLINDRICAL_SURFACE('',#18505,1.666);
#16566=CYLINDRICAL_SURFACE('',#18506,1.666);
#16567=CYLINDRICAL_SURFACE('',#18507,1.666);
#16568=CYLINDRICAL_SURFACE('',#18508,1.666);
#16569=CYLINDRICAL_SURFACE('',#18510,2.05475);
#16570=CYLINDRICAL_SURFACE('',#18512,2.05475);
#16571=CYLINDRICAL_SURFACE('',#18513,2.05475);
#16572=CYLINDRICAL_SURFACE('',#18514,2.05475);
#16573=CYLINDRICAL_SURFACE('',#18515,2.05475);
#16574=CYLINDRICAL_SURFACE('',#18516,2.05475);
#16575=CYLINDRICAL_SURFACE('',#18517,2.05475);
#16576=CYLINDRICAL_SURFACE('',#18518,2.05475);
#16577=CYLINDRICAL_SURFACE('',#18519,2.05475);
#16578=CYLINDRICAL_SURFACE('',#18520,2.05475);
#16579=CYLINDRICAL_SURFACE('',#18521,2.05475);
#16580=CYLINDRICAL_SURFACE('',#18522,2.05475);
#16581=CYLINDRICAL_SURFACE('',#18523,2.05475);
#16582=CYLINDRICAL_SURFACE('',#18525,1.666);
#16583=CYLINDRICAL_SURFACE('',#18528,1.666);
#16584=CYLINDRICAL_SURFACE('',#18529,1.666);
#16585=CYLINDRICAL_SURFACE('',#18530,1.666);
#16586=CYLINDRICAL_SURFACE('',#18531,1.666);
#16587=CYLINDRICAL_SURFACE('',#18532,1.666);
#16588=CYLINDRICAL_SURFACE('',#18533,1.666);
#16589=CYLINDRICAL_SURFACE('',#18534,1.666);
#16590=CYLINDRICAL_SURFACE('',#18535,1.666);
#16591=CYLINDRICAL_SURFACE('',#18536,1.666);
#16592=CYLINDRICAL_SURFACE('',#18537,1.666);
#16593=CYLINDRICAL_SURFACE('',#18538,1.666);
#16594=CYLINDRICAL_SURFACE('',#18540,2.05475);
#16595=CYLINDRICAL_SURFACE('',#18542,2.05475);
#16596=CYLINDRICAL_SURFACE('',#18543,2.05475);
#16597=CYLINDRICAL_SURFACE('',#18544,2.05475);
#16598=CYLINDRICAL_SURFACE('',#18545,2.05475);
#16599=CYLINDRICAL_SURFACE('',#18546,2.05475);
#16600=CYLINDRICAL_SURFACE('',#18547,2.05475);
#16601=CYLINDRICAL_SURFACE('',#18548,2.05475);
#16602=CYLINDRICAL_SURFACE('',#18549,2.05475);
#16603=CYLINDRICAL_SURFACE('',#18550,2.05475);
#16604=CYLINDRICAL_SURFACE('',#18551,2.05475);
#16605=CYLINDRICAL_SURFACE('',#18552,2.05475);
#16606=CYLINDRICAL_SURFACE('',#18553,2.05475);
#16607=CYLINDRICAL_SURFACE('',#18555,1.666);
#16608=CYLINDRICAL_SURFACE('',#18558,1.666);
#16609=CYLINDRICAL_SURFACE('',#18559,1.666);
#16610=CYLINDRICAL_SURFACE('',#18560,1.666);
#16611=CYLINDRICAL_SURFACE('',#18561,1.666);
#16612=CYLINDRICAL_SURFACE('',#18562,1.666);
#16613=CYLINDRICAL_SURFACE('',#18563,1.666);
#16614=CYLINDRICAL_SURFACE('',#18564,1.666);
#16615=CYLINDRICAL_SURFACE('',#18565,1.666);
#16616=CYLINDRICAL_SURFACE('',#18566,1.666);
#16617=CYLINDRICAL_SURFACE('',#18567,1.666);
#16618=CYLINDRICAL_SURFACE('',#18568,1.666);
#16619=CYLINDRICAL_SURFACE('',#18570,2.05474999999998);
#16620=CYLINDRICAL_SURFACE('',#18572,2.05474999999998);
#16621=CYLINDRICAL_SURFACE('',#18573,2.05474999999998);
#16622=CYLINDRICAL_SURFACE('',#18574,2.05474999999998);
#16623=CYLINDRICAL_SURFACE('',#18575,2.05474999999998);
#16624=CYLINDRICAL_SURFACE('',#18576,2.05474999999998);
#16625=CYLINDRICAL_SURFACE('',#18577,2.05474999999998);
#16626=CYLINDRICAL_SURFACE('',#18578,2.05474999999998);
#16627=CYLINDRICAL_SURFACE('',#18579,2.05474999999998);
#16628=CYLINDRICAL_SURFACE('',#18580,2.05474999999998);
#16629=CYLINDRICAL_SURFACE('',#18581,2.05474999999998);
#16630=CYLINDRICAL_SURFACE('',#18582,2.05474999999998);
#16631=CYLINDRICAL_SURFACE('',#18583,2.05474999999998);
#16632=CYLINDRICAL_SURFACE('',#18585,1.666);
#16633=CYLINDRICAL_SURFACE('',#18588,1.666);
#16634=CYLINDRICAL_SURFACE('',#18589,1.666);
#16635=CYLINDRICAL_SURFACE('',#18590,1.666);
#16636=CYLINDRICAL_SURFACE('',#18591,1.666);
#16637=CYLINDRICAL_SURFACE('',#18592,1.666);
#16638=CYLINDRICAL_SURFACE('',#18593,1.666);
#16639=CYLINDRICAL_SURFACE('',#18594,1.666);
#16640=CYLINDRICAL_SURFACE('',#18595,1.666);
#16641=CYLINDRICAL_SURFACE('',#18596,1.666);
#16642=CYLINDRICAL_SURFACE('',#18597,1.666);
#16643=CYLINDRICAL_SURFACE('',#18598,1.666);
#16644=CYLINDRICAL_SURFACE('',#18600,2.05475);
#16645=CYLINDRICAL_SURFACE('',#18602,2.05475);
#16646=CYLINDRICAL_SURFACE('',#18603,2.05475);
#16647=CYLINDRICAL_SURFACE('',#18604,2.05475);
#16648=CYLINDRICAL_SURFACE('',#18605,2.05475);
#16649=CYLINDRICAL_SURFACE('',#18606,2.05475);
#16650=CYLINDRICAL_SURFACE('',#18607,2.05475);
#16651=CYLINDRICAL_SURFACE('',#18608,2.05475);
#16652=CYLINDRICAL_SURFACE('',#18609,2.05475);
#16653=CYLINDRICAL_SURFACE('',#18610,2.05475);
#16654=CYLINDRICAL_SURFACE('',#18611,2.05475);
#16655=CYLINDRICAL_SURFACE('',#18612,2.05475);
#16656=CYLINDRICAL_SURFACE('',#18613,2.05475);
#16657=CYLINDRICAL_SURFACE('',#18615,1.666);
#16658=CYLINDRICAL_SURFACE('',#18618,1.666);
#16659=CYLINDRICAL_SURFACE('',#18619,1.666);
#16660=CYLINDRICAL_SURFACE('',#18620,1.666);
#16661=CYLINDRICAL_SURFACE('',#18621,1.666);
#16662=CYLINDRICAL_SURFACE('',#18622,1.666);
#16663=CYLINDRICAL_SURFACE('',#18623,1.666);
#16664=CYLINDRICAL_SURFACE('',#18624,1.666);
#16665=CYLINDRICAL_SURFACE('',#18625,1.666);
#16666=CYLINDRICAL_SURFACE('',#18626,1.666);
#16667=CYLINDRICAL_SURFACE('',#18627,1.666);
#16668=CYLINDRICAL_SURFACE('',#18628,1.666);
#16669=CYLINDRICAL_SURFACE('',#18630,2.05474999999998);
#16670=CYLINDRICAL_SURFACE('',#18632,2.05474999999998);
#16671=CYLINDRICAL_SURFACE('',#18633,2.05474999999998);
#16672=CYLINDRICAL_SURFACE('',#18634,2.05474999999998);
#16673=CYLINDRICAL_SURFACE('',#18635,2.05474999999998);
#16674=CYLINDRICAL_SURFACE('',#18636,2.05474999999998);
#16675=CYLINDRICAL_SURFACE('',#18637,2.05474999999998);
#16676=CYLINDRICAL_SURFACE('',#18638,2.05474999999998);
#16677=CYLINDRICAL_SURFACE('',#18639,2.05474999999998);
#16678=CYLINDRICAL_SURFACE('',#18640,2.05474999999998);
#16679=CYLINDRICAL_SURFACE('',#18641,2.05474999999998);
#16680=CYLINDRICAL_SURFACE('',#18642,2.05474999999998);
#16681=CYLINDRICAL_SURFACE('',#18643,2.05474999999998);
#16682=CYLINDRICAL_SURFACE('',#18645,1.666);
#16683=CYLINDRICAL_SURFACE('',#18648,1.666);
#16684=CYLINDRICAL_SURFACE('',#18649,1.666);
#16685=CYLINDRICAL_SURFACE('',#18650,1.666);
#16686=CYLINDRICAL_SURFACE('',#18651,1.666);
#16687=CYLINDRICAL_SURFACE('',#18652,1.666);
#16688=CYLINDRICAL_SURFACE('',#18653,1.666);
#16689=CYLINDRICAL_SURFACE('',#18654,1.666);
#16690=CYLINDRICAL_SURFACE('',#18655,1.666);
#16691=CYLINDRICAL_SURFACE('',#18656,1.666);
#16692=CYLINDRICAL_SURFACE('',#18657,1.666);
#16693=CYLINDRICAL_SURFACE('',#18658,1.666);
#16694=CYLINDRICAL_SURFACE('',#18660,2.05474999999998);
#16695=CYLINDRICAL_SURFACE('',#18662,2.05474999999998);
#16696=CYLINDRICAL_SURFACE('',#18663,2.05474999999998);
#16697=CYLINDRICAL_SURFACE('',#18664,2.05474999999998);
#16698=CYLINDRICAL_SURFACE('',#18665,2.05474999999998);
#16699=CYLINDRICAL_SURFACE('',#18666,2.05474999999998);
#16700=CYLINDRICAL_SURFACE('',#18667,2.05474999999998);
#16701=CYLINDRICAL_SURFACE('',#18668,2.05474999999998);
#16702=CYLINDRICAL_SURFACE('',#18669,2.05474999999998);
#16703=CYLINDRICAL_SURFACE('',#18670,2.05474999999998);
#16704=CYLINDRICAL_SURFACE('',#18671,2.05474999999998);
#16705=CYLINDRICAL_SURFACE('',#18672,2.05474999999998);
#16706=CYLINDRICAL_SURFACE('',#18673,2.05474999999998);
#16707=CYLINDRICAL_SURFACE('',#18675,1.666);
#16708=CYLINDRICAL_SURFACE('',#18678,1.666);
#16709=CYLINDRICAL_SURFACE('',#18679,1.666);
#16710=CYLINDRICAL_SURFACE('',#18680,1.666);
#16711=CYLINDRICAL_SURFACE('',#18681,1.666);
#16712=CYLINDRICAL_SURFACE('',#18682,1.666);
#16713=CYLINDRICAL_SURFACE('',#18683,1.666);
#16714=CYLINDRICAL_SURFACE('',#18684,1.666);
#16715=CYLINDRICAL_SURFACE('',#18685,1.666);
#16716=CYLINDRICAL_SURFACE('',#18686,1.666);
#16717=CYLINDRICAL_SURFACE('',#18687,1.666);
#16718=CYLINDRICAL_SURFACE('',#18688,1.666);
#16719=CYLINDRICAL_SURFACE('',#18690,2.05475000000002);
#16720=CYLINDRICAL_SURFACE('',#18692,2.05475000000002);
#16721=CYLINDRICAL_SURFACE('',#18693,2.05475000000002);
#16722=CYLINDRICAL_SURFACE('',#18694,2.05475000000002);
#16723=CYLINDRICAL_SURFACE('',#18695,2.05475000000002);
#16724=CYLINDRICAL_SURFACE('',#18696,2.05475000000002);
#16725=CYLINDRICAL_SURFACE('',#18697,2.05475000000002);
#16726=CYLINDRICAL_SURFACE('',#18698,2.05475000000002);
#16727=CYLINDRICAL_SURFACE('',#18699,2.05475000000002);
#16728=CYLINDRICAL_SURFACE('',#18700,2.05475000000002);
#16729=CYLINDRICAL_SURFACE('',#18701,2.05475000000002);
#16730=CYLINDRICAL_SURFACE('',#18702,2.05475000000002);
#16731=CYLINDRICAL_SURFACE('',#18703,2.05475000000002);
#16732=CYLINDRICAL_SURFACE('',#18705,1.666);
#16733=CYLINDRICAL_SURFACE('',#18708,1.666);
#16734=CYLINDRICAL_SURFACE('',#18709,1.666);
#16735=CYLINDRICAL_SURFACE('',#18710,1.666);
#16736=CYLINDRICAL_SURFACE('',#18711,1.666);
#16737=CYLINDRICAL_SURFACE('',#18712,1.666);
#16738=CYLINDRICAL_SURFACE('',#18713,1.666);
#16739=CYLINDRICAL_SURFACE('',#18714,1.666);
#16740=CYLINDRICAL_SURFACE('',#18715,1.666);
#16741=CYLINDRICAL_SURFACE('',#18716,1.666);
#16742=CYLINDRICAL_SURFACE('',#18717,1.666);
#16743=CYLINDRICAL_SURFACE('',#18718,1.666);
#16744=CYLINDRICAL_SURFACE('',#18720,2.05474999999998);
#16745=CYLINDRICAL_SURFACE('',#18722,2.05474999999998);
#16746=CYLINDRICAL_SURFACE('',#18723,2.05474999999998);
#16747=CYLINDRICAL_SURFACE('',#18724,2.05474999999998);
#16748=CYLINDRICAL_SURFACE('',#18725,2.05474999999998);
#16749=CYLINDRICAL_SURFACE('',#18726,2.05474999999998);
#16750=CYLINDRICAL_SURFACE('',#18727,2.05474999999998);
#16751=CYLINDRICAL_SURFACE('',#18728,2.05474999999998);
#16752=CYLINDRICAL_SURFACE('',#18729,2.05474999999998);
#16753=CYLINDRICAL_SURFACE('',#18730,2.05474999999998);
#16754=CYLINDRICAL_SURFACE('',#18731,2.05474999999998);
#16755=CYLINDRICAL_SURFACE('',#18732,2.05474999999998);
#16756=CYLINDRICAL_SURFACE('',#18733,2.05474999999998);
#16757=CYLINDRICAL_SURFACE('',#18735,1.666);
#16758=CYLINDRICAL_SURFACE('',#18738,1.666);
#16759=CYLINDRICAL_SURFACE('',#18739,1.666);
#16760=CYLINDRICAL_SURFACE('',#18740,1.666);
#16761=CYLINDRICAL_SURFACE('',#18741,1.666);
#16762=CYLINDRICAL_SURFACE('',#18742,1.666);
#16763=CYLINDRICAL_SURFACE('',#18743,1.666);
#16764=CYLINDRICAL_SURFACE('',#18744,1.666);
#16765=CYLINDRICAL_SURFACE('',#18745,1.666);
#16766=CYLINDRICAL_SURFACE('',#18746,1.666);
#16767=CYLINDRICAL_SURFACE('',#18747,1.666);
#16768=CYLINDRICAL_SURFACE('',#18748,1.666);
#16769=CYLINDRICAL_SURFACE('',#18750,2.05475);
#16770=CYLINDRICAL_SURFACE('',#18752,2.05475);
#16771=CYLINDRICAL_SURFACE('',#18753,2.05475);
#16772=CYLINDRICAL_SURFACE('',#18754,2.05475);
#16773=CYLINDRICAL_SURFACE('',#18755,2.05475);
#16774=CYLINDRICAL_SURFACE('',#18756,2.05475);
#16775=CYLINDRICAL_SURFACE('',#18757,2.05475);
#16776=CYLINDRICAL_SURFACE('',#18758,2.05475);
#16777=CYLINDRICAL_SURFACE('',#18759,2.05475);
#16778=CYLINDRICAL_SURFACE('',#18760,2.05475);
#16779=CYLINDRICAL_SURFACE('',#18761,2.05475);
#16780=CYLINDRICAL_SURFACE('',#18762,2.05475);
#16781=CYLINDRICAL_SURFACE('',#18763,2.05475);
#16782=CYLINDRICAL_SURFACE('',#18765,1.666);
#16783=CYLINDRICAL_SURFACE('',#18768,1.666);
#16784=CYLINDRICAL_SURFACE('',#18769,1.666);
#16785=CYLINDRICAL_SURFACE('',#18770,1.666);
#16786=CYLINDRICAL_SURFACE('',#18771,1.666);
#16787=CYLINDRICAL_SURFACE('',#18772,1.666);
#16788=CYLINDRICAL_SURFACE('',#18773,1.666);
#16789=CYLINDRICAL_SURFACE('',#18774,1.666);
#16790=CYLINDRICAL_SURFACE('',#18775,1.666);
#16791=CYLINDRICAL_SURFACE('',#18776,1.666);
#16792=CYLINDRICAL_SURFACE('',#18777,1.666);
#16793=CYLINDRICAL_SURFACE('',#18778,1.666);
#16794=CYLINDRICAL_SURFACE('',#18780,2.05474999999999);
#16795=CYLINDRICAL_SURFACE('',#18782,2.05474999999999);
#16796=CYLINDRICAL_SURFACE('',#18783,2.05474999999999);
#16797=CYLINDRICAL_SURFACE('',#18784,2.05474999999999);
#16798=CYLINDRICAL_SURFACE('',#18785,2.05474999999999);
#16799=CYLINDRICAL_SURFACE('',#18786,2.05474999999999);
#16800=CYLINDRICAL_SURFACE('',#18787,2.05474999999999);
#16801=CYLINDRICAL_SURFACE('',#18788,2.05474999999999);
#16802=CYLINDRICAL_SURFACE('',#18789,2.05474999999999);
#16803=CYLINDRICAL_SURFACE('',#18790,2.05474999999999);
#16804=CYLINDRICAL_SURFACE('',#18791,2.05474999999999);
#16805=CYLINDRICAL_SURFACE('',#18792,2.05474999999999);
#16806=CYLINDRICAL_SURFACE('',#18793,2.05474999999999);
#16807=CYLINDRICAL_SURFACE('',#18795,1.666);
#16808=CYLINDRICAL_SURFACE('',#18798,1.666);
#16809=CYLINDRICAL_SURFACE('',#18799,1.666);
#16810=CYLINDRICAL_SURFACE('',#18800,1.666);
#16811=CYLINDRICAL_SURFACE('',#18801,1.666);
#16812=CYLINDRICAL_SURFACE('',#18802,1.666);
#16813=CYLINDRICAL_SURFACE('',#18803,1.666);
#16814=CYLINDRICAL_SURFACE('',#18804,1.666);
#16815=CYLINDRICAL_SURFACE('',#18805,1.666);
#16816=CYLINDRICAL_SURFACE('',#18806,1.666);
#16817=CYLINDRICAL_SURFACE('',#18807,1.666);
#16818=CYLINDRICAL_SURFACE('',#18808,1.666);
#16819=CYLINDRICAL_SURFACE('',#18810,2.05475);
#16820=CYLINDRICAL_SURFACE('',#18812,2.05475);
#16821=CYLINDRICAL_SURFACE('',#18813,2.05475);
#16822=CYLINDRICAL_SURFACE('',#18814,2.05475);
#16823=CYLINDRICAL_SURFACE('',#18815,2.05475);
#16824=CYLINDRICAL_SURFACE('',#18816,2.05475);
#16825=CYLINDRICAL_SURFACE('',#18817,2.05475);
#16826=CYLINDRICAL_SURFACE('',#18818,2.05475);
#16827=CYLINDRICAL_SURFACE('',#18819,2.05475);
#16828=CYLINDRICAL_SURFACE('',#18820,2.05475);
#16829=CYLINDRICAL_SURFACE('',#18821,2.05475);
#16830=CYLINDRICAL_SURFACE('',#18822,2.05475);
#16831=CYLINDRICAL_SURFACE('',#18823,2.05475);
#16832=CYLINDRICAL_SURFACE('',#18825,2.5175);
#16833=CYLINDRICAL_SURFACE('',#18827,2.5175);
#16834=CYLINDRICAL_SURFACE('',#18828,2.5175);
#16835=CYLINDRICAL_SURFACE('',#18829,2.5175);
#16836=CYLINDRICAL_SURFACE('',#18830,2.5175);
#16837=CYLINDRICAL_SURFACE('',#18831,2.5175);
#16838=CYLINDRICAL_SURFACE('',#18832,2.5175);
#16839=CYLINDRICAL_SURFACE('',#18833,2.5175);
#16840=CYLINDRICAL_SURFACE('',#18834,3.07350000000001);
#16841=CYLINDRICAL_SURFACE('',#18836,3.07350000000001);
#16842=CYLINDRICAL_SURFACE('',#18837,3.07350000000001);
#16843=CYLINDRICAL_SURFACE('',#18838,3.07350000000001);
#16844=CYLINDRICAL_SURFACE('',#18839,3.07350000000001);
#16845=CYLINDRICAL_SURFACE('',#18840,3.07350000000001);
#16846=CYLINDRICAL_SURFACE('',#18841,3.07350000000001);
#16847=CYLINDRICAL_SURFACE('',#18842,3.07350000000001);
#16848=CYLINDRICAL_SURFACE('',#18843,2.5175);
#16849=CYLINDRICAL_SURFACE('',#18845,2.5175);
#16850=CYLINDRICAL_SURFACE('',#18846,2.5175);
#16851=CYLINDRICAL_SURFACE('',#18847,2.5175);
#16852=CYLINDRICAL_SURFACE('',#18848,2.5175);
#16853=CYLINDRICAL_SURFACE('',#18849,2.5175);
#16854=CYLINDRICAL_SURFACE('',#18850,2.5175);
#16855=CYLINDRICAL_SURFACE('',#18851,2.5175);
#16856=CYLINDRICAL_SURFACE('',#18852,2.5175);
#16857=CYLINDRICAL_SURFACE('',#18854,2.5175);
#16858=CYLINDRICAL_SURFACE('',#18855,2.5175);
#16859=CYLINDRICAL_SURFACE('',#18856,2.5175);
#16860=CYLINDRICAL_SURFACE('',#18857,2.5175);
#16861=CYLINDRICAL_SURFACE('',#18858,2.5175);
#16862=CYLINDRICAL_SURFACE('',#18859,2.5175);
#16863=CYLINDRICAL_SURFACE('',#18860,2.5175);
#16864=CYLINDRICAL_SURFACE('',#18861,2.5175);
#16865=CYLINDRICAL_SURFACE('',#18863,2.5175);
#16866=CYLINDRICAL_SURFACE('',#18864,2.5175);
#16867=CYLINDRICAL_SURFACE('',#18865,2.5175);
#16868=CYLINDRICAL_SURFACE('',#18866,2.5175);
#16869=CYLINDRICAL_SURFACE('',#18867,2.5175);
#16870=CYLINDRICAL_SURFACE('',#18868,2.5175);
#16871=CYLINDRICAL_SURFACE('',#18869,2.5175);
#16872=CYLINDRICAL_SURFACE('',#18870,3.07350000000001);
#16873=CYLINDRICAL_SURFACE('',#18872,3.07350000000001);
#16874=CYLINDRICAL_SURFACE('',#18873,3.07350000000001);
#16875=CYLINDRICAL_SURFACE('',#18874,3.07350000000001);
#16876=CYLINDRICAL_SURFACE('',#18875,3.07350000000001);
#16877=CYLINDRICAL_SURFACE('',#18876,3.07350000000001);
#16878=CYLINDRICAL_SURFACE('',#18877,3.07350000000001);
#16879=CYLINDRICAL_SURFACE('',#18878,3.07350000000001);
#16880=CYLINDRICAL_SURFACE('',#18879,3.0735);
#16881=CYLINDRICAL_SURFACE('',#18881,3.0735);
#16882=CYLINDRICAL_SURFACE('',#18882,3.0735);
#16883=CYLINDRICAL_SURFACE('',#18883,3.0735);
#16884=CYLINDRICAL_SURFACE('',#18884,3.0735);
#16885=CYLINDRICAL_SURFACE('',#18885,3.0735);
#16886=CYLINDRICAL_SURFACE('',#18886,3.0735);
#16887=CYLINDRICAL_SURFACE('',#18887,3.0735);
#16888=CYLINDRICAL_SURFACE('',#18888,3.0735);
#16889=CYLINDRICAL_SURFACE('',#18890,3.0735);
#16890=CYLINDRICAL_SURFACE('',#18891,3.0735);
#16891=CYLINDRICAL_SURFACE('',#18892,3.0735);
#16892=CYLINDRICAL_SURFACE('',#18893,3.0735);
#16893=CYLINDRICAL_SURFACE('',#18894,3.0735);
#16894=CYLINDRICAL_SURFACE('',#18895,3.0735);
#16895=CYLINDRICAL_SURFACE('',#18896,3.0735);
#16896=CYLINDRICAL_SURFACE('',#18897,3.0735);
#16897=CYLINDRICAL_SURFACE('',#18898,3.0735);
#16898=CYLINDRICAL_SURFACE('',#18899,3.07350000000001);
#16899=CYLINDRICAL_SURFACE('',#18900,2.5175);
#16900=CYLINDRICAL_SURFACE('',#18902,2.5175);
#16901=CYLINDRICAL_SURFACE('',#18904,2.5175);
#16902=CYLINDRICAL_SURFACE('',#18906,3.07350000000001);
#16903=CYLINDRICAL_SURFACE('',#18907,2.5175);
#16904=CYLINDRICAL_SURFACE('',#18910,2.05475);
#16905=CYLINDRICAL_SURFACE('',#18911,1.666);
#16906=CYLINDRICAL_SURFACE('',#18913,2.05474999999999);
#16907=CYLINDRICAL_SURFACE('',#18914,1.666);
#16908=CYLINDRICAL_SURFACE('',#18916,2.05475);
#16909=CYLINDRICAL_SURFACE('',#18917,1.666);
#16910=CYLINDRICAL_SURFACE('',#18919,2.05474999999998);
#16911=CYLINDRICAL_SURFACE('',#18920,1.666);
#16912=CYLINDRICAL_SURFACE('',#18922,2.05475000000002);
#16913=CYLINDRICAL_SURFACE('',#18923,1.666);
#16914=CYLINDRICAL_SURFACE('',#18930,2.05474999999998);
#16915=CYLINDRICAL_SURFACE('',#18931,1.666);
#16916=CYLINDRICAL_SURFACE('',#18933,2.05474999999998);
#16917=CYLINDRICAL_SURFACE('',#18934,1.666);
#16918=CYLINDRICAL_SURFACE('',#18936,2.05475);
#16919=CYLINDRICAL_SURFACE('',#18937,1.666);
#16920=CYLINDRICAL_SURFACE('',#18939,2.05474999999998);
#16921=CYLINDRICAL_SURFACE('',#18940,1.666);
#16922=CYLINDRICAL_SURFACE('',#18942,2.05475);
#16923=CYLINDRICAL_SURFACE('',#18943,1.666);
#16924=CYLINDRICAL_SURFACE('',#18950,2.05475);
#16925=CYLINDRICAL_SURFACE('',#18951,1.666);
#16926=CYLINDRICAL_SURFACE('',#18954,2.05475);
#16927=CYLINDRICAL_SURFACE('',#18955,1.666);
#16928=CYLINDRICAL_SURFACE('',#18957,60.);
#16929=CYLINDRICAL_SURFACE('',#18960,70.);
#16930=CYLINDRICAL_SURFACE('',#18966,1.2645);
#16931=CYLINDRICAL_SURFACE('',#18972,1.2645);
#16932=CYLINDRICAL_SURFACE('',#18973,1.2645);
#16933=CYLINDRICAL_SURFACE('',#18974,1.2645);
#16934=CYLINDRICAL_SURFACE('',#18975,1.2645);
#16935=CYLINDRICAL_SURFACE('',#18976,1.2645);
#16936=CYLINDRICAL_SURFACE('',#18977,1.2645);
#16937=CYLINDRICAL_SURFACE('',#18978,1.2645);
#16938=CYLINDRICAL_SURFACE('',#18980,1.543);
#16939=CYLINDRICAL_SURFACE('',#18982,1.543);
#16940=CYLINDRICAL_SURFACE('',#18983,1.543);
#16941=CYLINDRICAL_SURFACE('',#18984,1.543);
#16942=CYLINDRICAL_SURFACE('',#18985,1.543);
#16943=CYLINDRICAL_SURFACE('',#18986,1.543);
#16944=CYLINDRICAL_SURFACE('',#18987,1.543);
#16945=CYLINDRICAL_SURFACE('',#18988,1.543);
#16946=CYLINDRICAL_SURFACE('',#18990,1.2645);
#16947=CYLINDRICAL_SURFACE('',#18996,1.2645);
#16948=CYLINDRICAL_SURFACE('',#18997,1.2645);
#16949=CYLINDRICAL_SURFACE('',#18998,1.2645);
#16950=CYLINDRICAL_SURFACE('',#18999,1.2645);
#16951=CYLINDRICAL_SURFACE('',#19000,1.2645);
#16952=CYLINDRICAL_SURFACE('',#19001,1.2645);
#16953=CYLINDRICAL_SURFACE('',#19002,1.2645);
#16954=CYLINDRICAL_SURFACE('',#19004,1.54299999999999);
#16955=CYLINDRICAL_SURFACE('',#19006,1.54299999999999);
#16956=CYLINDRICAL_SURFACE('',#19007,1.54299999999999);
#16957=CYLINDRICAL_SURFACE('',#19008,1.54299999999999);
#16958=CYLINDRICAL_SURFACE('',#19009,1.54299999999999);
#16959=CYLINDRICAL_SURFACE('',#19010,1.54299999999999);
#16960=CYLINDRICAL_SURFACE('',#19011,1.54299999999999);
#16961=CYLINDRICAL_SURFACE('',#19012,1.54299999999999);
#16962=CYLINDRICAL_SURFACE('',#19014,1.2645);
#16963=CYLINDRICAL_SURFACE('',#19020,1.2645);
#16964=CYLINDRICAL_SURFACE('',#19021,1.2645);
#16965=CYLINDRICAL_SURFACE('',#19022,1.2645);
#16966=CYLINDRICAL_SURFACE('',#19023,1.2645);
#16967=CYLINDRICAL_SURFACE('',#19024,1.2645);
#16968=CYLINDRICAL_SURFACE('',#19025,1.2645);
#16969=CYLINDRICAL_SURFACE('',#19026,1.2645);
#16970=CYLINDRICAL_SURFACE('',#19028,1.543);
#16971=CYLINDRICAL_SURFACE('',#19030,1.543);
#16972=CYLINDRICAL_SURFACE('',#19031,1.543);
#16973=CYLINDRICAL_SURFACE('',#19032,1.543);
#16974=CYLINDRICAL_SURFACE('',#19033,1.543);
#16975=CYLINDRICAL_SURFACE('',#19034,1.543);
#16976=CYLINDRICAL_SURFACE('',#19035,1.543);
#16977=CYLINDRICAL_SURFACE('',#19036,1.543);
#16978=CYLINDRICAL_SURFACE('',#19038,1.2645);
#16979=CYLINDRICAL_SURFACE('',#19044,1.2645);
#16980=CYLINDRICAL_SURFACE('',#19045,1.2645);
#16981=CYLINDRICAL_SURFACE('',#19046,1.2645);
#16982=CYLINDRICAL_SURFACE('',#19047,1.2645);
#16983=CYLINDRICAL_SURFACE('',#19048,1.2645);
#16984=CYLINDRICAL_SURFACE('',#19049,1.2645);
#16985=CYLINDRICAL_SURFACE('',#19050,1.2645);
#16986=CYLINDRICAL_SURFACE('',#19052,1.543);
#16987=CYLINDRICAL_SURFACE('',#19054,1.543);
#16988=CYLINDRICAL_SURFACE('',#19055,1.543);
#16989=CYLINDRICAL_SURFACE('',#19056,1.543);
#16990=CYLINDRICAL_SURFACE('',#19057,1.543);
#16991=CYLINDRICAL_SURFACE('',#19058,1.543);
#16992=CYLINDRICAL_SURFACE('',#19059,1.543);
#16993=CYLINDRICAL_SURFACE('',#19060,1.543);
#16994=CYLINDRICAL_SURFACE('',#19062,1.2645);
#16995=CYLINDRICAL_SURFACE('',#19068,1.2645);
#16996=CYLINDRICAL_SURFACE('',#19069,1.2645);
#16997=CYLINDRICAL_SURFACE('',#19070,1.2645);
#16998=CYLINDRICAL_SURFACE('',#19071,1.2645);
#16999=CYLINDRICAL_SURFACE('',#19072,1.2645);
#17000=CYLINDRICAL_SURFACE('',#19073,1.2645);
#17001=CYLINDRICAL_SURFACE('',#19074,1.2645);
#17002=CYLINDRICAL_SURFACE('',#19076,1.54300000000001);
#17003=CYLINDRICAL_SURFACE('',#19078,1.54300000000001);
#17004=CYLINDRICAL_SURFACE('',#19079,1.54300000000001);
#17005=CYLINDRICAL_SURFACE('',#19080,1.54300000000001);
#17006=CYLINDRICAL_SURFACE('',#19081,1.54300000000001);
#17007=CYLINDRICAL_SURFACE('',#19082,1.54300000000001);
#17008=CYLINDRICAL_SURFACE('',#19083,1.54300000000001);
#17009=CYLINDRICAL_SURFACE('',#19084,1.54300000000001);
#17010=CYLINDRICAL_SURFACE('',#19086,1.2645);
#17011=CYLINDRICAL_SURFACE('',#19092,1.2645);
#17012=CYLINDRICAL_SURFACE('',#19093,1.2645);
#17013=CYLINDRICAL_SURFACE('',#19094,1.2645);
#17014=CYLINDRICAL_SURFACE('',#19095,1.2645);
#17015=CYLINDRICAL_SURFACE('',#19096,1.2645);
#17016=CYLINDRICAL_SURFACE('',#19097,1.2645);
#17017=CYLINDRICAL_SURFACE('',#19098,1.2645);
#17018=CYLINDRICAL_SURFACE('',#19100,1.54300000000001);
#17019=CYLINDRICAL_SURFACE('',#19102,1.54300000000001);
#17020=CYLINDRICAL_SURFACE('',#19103,1.54300000000001);
#17021=CYLINDRICAL_SURFACE('',#19104,1.54300000000001);
#17022=CYLINDRICAL_SURFACE('',#19105,1.54300000000001);
#17023=CYLINDRICAL_SURFACE('',#19106,1.54300000000001);
#17024=CYLINDRICAL_SURFACE('',#19107,1.54300000000001);
#17025=CYLINDRICAL_SURFACE('',#19108,1.54300000000001);
#17026=CYLINDRICAL_SURFACE('',#19110,1.2645);
#17027=CYLINDRICAL_SURFACE('',#19116,1.2645);
#17028=CYLINDRICAL_SURFACE('',#19117,1.2645);
#17029=CYLINDRICAL_SURFACE('',#19118,1.2645);
#17030=CYLINDRICAL_SURFACE('',#19119,1.2645);
#17031=CYLINDRICAL_SURFACE('',#19120,1.2645);
#17032=CYLINDRICAL_SURFACE('',#19121,1.2645);
#17033=CYLINDRICAL_SURFACE('',#19122,1.2645);
#17034=CYLINDRICAL_SURFACE('',#19124,1.543);
#17035=CYLINDRICAL_SURFACE('',#19126,1.543);
#17036=CYLINDRICAL_SURFACE('',#19127,1.543);
#17037=CYLINDRICAL_SURFACE('',#19128,1.543);
#17038=CYLINDRICAL_SURFACE('',#19129,1.543);
#17039=CYLINDRICAL_SURFACE('',#19130,1.543);
#17040=CYLINDRICAL_SURFACE('',#19131,1.543);
#17041=CYLINDRICAL_SURFACE('',#19132,1.543);
#17042=CYLINDRICAL_SURFACE('',#19134,1.2645);
#17043=CYLINDRICAL_SURFACE('',#19140,1.2645);
#17044=CYLINDRICAL_SURFACE('',#19141,1.2645);
#17045=CYLINDRICAL_SURFACE('',#19142,1.2645);
#17046=CYLINDRICAL_SURFACE('',#19143,1.2645);
#17047=CYLINDRICAL_SURFACE('',#19144,1.2645);
#17048=CYLINDRICAL_SURFACE('',#19145,1.2645);
#17049=CYLINDRICAL_SURFACE('',#19146,1.2645);
#17050=CYLINDRICAL_SURFACE('',#19148,1.54300000000001);
#17051=CYLINDRICAL_SURFACE('',#19150,1.54300000000001);
#17052=CYLINDRICAL_SURFACE('',#19151,1.54300000000001);
#17053=CYLINDRICAL_SURFACE('',#19152,1.54300000000001);
#17054=CYLINDRICAL_SURFACE('',#19153,1.54300000000001);
#17055=CYLINDRICAL_SURFACE('',#19154,1.54300000000001);
#17056=CYLINDRICAL_SURFACE('',#19155,1.54300000000001);
#17057=CYLINDRICAL_SURFACE('',#19156,1.54300000000001);
#17058=CYLINDRICAL_SURFACE('',#19158,1.2645);
#17059=CYLINDRICAL_SURFACE('',#19164,1.2645);
#17060=CYLINDRICAL_SURFACE('',#19165,1.2645);
#17061=CYLINDRICAL_SURFACE('',#19166,1.2645);
#17062=CYLINDRICAL_SURFACE('',#19167,1.2645);
#17063=CYLINDRICAL_SURFACE('',#19168,1.2645);
#17064=CYLINDRICAL_SURFACE('',#19169,1.2645);
#17065=CYLINDRICAL_SURFACE('',#19170,1.2645);
#17066=CYLINDRICAL_SURFACE('',#19172,1.54300000000001);
#17067=CYLINDRICAL_SURFACE('',#19174,1.54300000000001);
#17068=CYLINDRICAL_SURFACE('',#19175,1.54300000000001);
#17069=CYLINDRICAL_SURFACE('',#19176,1.54300000000001);
#17070=CYLINDRICAL_SURFACE('',#19177,1.54300000000001);
#17071=CYLINDRICAL_SURFACE('',#19178,1.54300000000001);
#17072=CYLINDRICAL_SURFACE('',#19179,1.54300000000001);
#17073=CYLINDRICAL_SURFACE('',#19180,1.54300000000001);
#17074=CYLINDRICAL_SURFACE('',#19182,1.2645);
#17075=CYLINDRICAL_SURFACE('',#19188,1.2645);
#17076=CYLINDRICAL_SURFACE('',#19189,1.2645);
#17077=CYLINDRICAL_SURFACE('',#19190,1.2645);
#17078=CYLINDRICAL_SURFACE('',#19191,1.2645);
#17079=CYLINDRICAL_SURFACE('',#19192,1.2645);
#17080=CYLINDRICAL_SURFACE('',#19193,1.2645);
#17081=CYLINDRICAL_SURFACE('',#19194,1.2645);
#17082=CYLINDRICAL_SURFACE('',#19196,1.543);
#17083=CYLINDRICAL_SURFACE('',#19198,1.543);
#17084=CYLINDRICAL_SURFACE('',#19199,1.543);
#17085=CYLINDRICAL_SURFACE('',#19200,1.543);
#17086=CYLINDRICAL_SURFACE('',#19201,1.543);
#17087=CYLINDRICAL_SURFACE('',#19202,1.543);
#17088=CYLINDRICAL_SURFACE('',#19203,1.543);
#17089=CYLINDRICAL_SURFACE('',#19204,1.543);
#17090=CYLINDRICAL_SURFACE('',#19206,1.2645);
#17091=CYLINDRICAL_SURFACE('',#19212,1.2645);
#17092=CYLINDRICAL_SURFACE('',#19213,1.2645);
#17093=CYLINDRICAL_SURFACE('',#19214,1.2645);
#17094=CYLINDRICAL_SURFACE('',#19215,1.2645);
#17095=CYLINDRICAL_SURFACE('',#19216,1.2645);
#17096=CYLINDRICAL_SURFACE('',#19217,1.2645);
#17097=CYLINDRICAL_SURFACE('',#19218,1.2645);
#17098=CYLINDRICAL_SURFACE('',#19220,1.54299999999999);
#17099=CYLINDRICAL_SURFACE('',#19222,1.54299999999999);
#17100=CYLINDRICAL_SURFACE('',#19223,1.54299999999999);
#17101=CYLINDRICAL_SURFACE('',#19224,1.54299999999999);
#17102=CYLINDRICAL_SURFACE('',#19225,1.54299999999999);
#17103=CYLINDRICAL_SURFACE('',#19226,1.54299999999999);
#17104=CYLINDRICAL_SURFACE('',#19227,1.54299999999999);
#17105=CYLINDRICAL_SURFACE('',#19228,1.54299999999999);
#17106=CYLINDRICAL_SURFACE('',#19230,1.2645);
#17107=CYLINDRICAL_SURFACE('',#19236,1.2645);
#17108=CYLINDRICAL_SURFACE('',#19237,1.2645);
#17109=CYLINDRICAL_SURFACE('',#19238,1.2645);
#17110=CYLINDRICAL_SURFACE('',#19239,1.2645);
#17111=CYLINDRICAL_SURFACE('',#19240,1.2645);
#17112=CYLINDRICAL_SURFACE('',#19241,1.2645);
#17113=CYLINDRICAL_SURFACE('',#19242,1.2645);
#17114=CYLINDRICAL_SURFACE('',#19244,1.543);
#17115=CYLINDRICAL_SURFACE('',#19246,1.543);
#17116=CYLINDRICAL_SURFACE('',#19247,1.543);
#17117=CYLINDRICAL_SURFACE('',#19248,1.543);
#17118=CYLINDRICAL_SURFACE('',#19249,1.543);
#17119=CYLINDRICAL_SURFACE('',#19250,1.543);
#17120=CYLINDRICAL_SURFACE('',#19251,1.543);
#17121=CYLINDRICAL_SURFACE('',#19252,1.543);
#17122=CYLINDRICAL_SURFACE('',#19272,1.543);
#17123=CYLINDRICAL_SURFACE('',#19273,1.2645);
#17124=CYLINDRICAL_SURFACE('',#19275,1.54299999999999);
#17125=CYLINDRICAL_SURFACE('',#19276,1.2645);
#17126=CYLINDRICAL_SURFACE('',#19278,1.543);
#17127=CYLINDRICAL_SURFACE('',#19279,1.2645);
#17128=CYLINDRICAL_SURFACE('',#19281,1.54300000000001);
#17129=CYLINDRICAL_SURFACE('',#19282,1.2645);
#17130=CYLINDRICAL_SURFACE('',#19284,1.54300000000001);
#17131=CYLINDRICAL_SURFACE('',#19285,1.2645);
#17132=CYLINDRICAL_SURFACE('',#19297,1.543);
#17133=CYLINDRICAL_SURFACE('',#19298,1.2645);
#17134=CYLINDRICAL_SURFACE('',#19300,1.54300000000001);
#17135=CYLINDRICAL_SURFACE('',#19301,1.2645);
#17136=CYLINDRICAL_SURFACE('',#19303,1.54300000000001);
#17137=CYLINDRICAL_SURFACE('',#19304,1.2645);
#17138=CYLINDRICAL_SURFACE('',#19306,1.543);
#17139=CYLINDRICAL_SURFACE('',#19307,1.2645);
#17140=CYLINDRICAL_SURFACE('',#19309,1.543);
#17141=CYLINDRICAL_SURFACE('',#19310,1.2645);
#17142=CYLINDRICAL_SURFACE('',#19322,1.54299999999999);
#17143=CYLINDRICAL_SURFACE('',#19323,1.2645);
#17144=CYLINDRICAL_SURFACE('',#19327,1.543);
#17145=CYLINDRICAL_SURFACE('',#19328,1.2645);
#17146=CYLINDRICAL_SURFACE('',#19331,1.5);
#17147=CYLINDRICAL_SURFACE('',#19334,3.);
#17148=CYLINDRICAL_SURFACE('',#19338,1.5);
#17149=CYLINDRICAL_SURFACE('',#19341,3.);
#17150=CYLINDRICAL_SURFACE('',#19345,1.5);
#17151=CYLINDRICAL_SURFACE('',#19348,3.);
#17152=CYLINDRICAL_SURFACE('',#19352,1.5);
#17153=CYLINDRICAL_SURFACE('',#19355,3.);
#17154=CYLINDRICAL_SURFACE('',#19359,1.5);
#17155=CYLINDRICAL_SURFACE('',#19362,3.);
#17156=CYLINDRICAL_SURFACE('',#19366,1.5);
#17157=CYLINDRICAL_SURFACE('',#19369,3.);
#17158=CYLINDRICAL_SURFACE('',#19397,45.9999999999998);
#17159=CYLINDRICAL_SURFACE('',#19399,1.);
#17160=CYLINDRICAL_SURFACE('',#19402,45.9999999999998);
#17161=CYLINDRICAL_SURFACE('',#19404,1.);
#17162=CYLINDRICAL_SURFACE('',#19407,45.9999999999998);
#17163=CYLINDRICAL_SURFACE('',#19409,1.);
#17164=CYLINDRICAL_SURFACE('',#19421,1.);
#17165=CYLINDRICAL_SURFACE('',#19422,45.9999999999998);
#17166=CYLINDRICAL_SURFACE('',#19424,1.);
#17167=CYLINDRICAL_SURFACE('',#19425,45.9999999999998);
#17168=CYLINDRICAL_SURFACE('',#19427,1.);
#17169=CYLINDRICAL_SURFACE('',#19428,45.9999999999998);
#17170=CYLINDRICAL_SURFACE('',#19429,10.);
#17171=CYLINDRICAL_SURFACE('',#19431,3.);
#17172=CYLINDRICAL_SURFACE('',#19433,3.);
#17173=CYLINDRICAL_SURFACE('',#19436,3.);
#17174=CYLINDRICAL_SURFACE('',#19440,10.);
#17175=CYLINDRICAL_SURFACE('',#19444,3.);
#17176=CYLINDRICAL_SURFACE('',#19447,3.);
#17177=CYLINDRICAL_SURFACE('',#19451,10.);
#17178=CYLINDRICAL_SURFACE('',#19455,9.);
#17179=CYLINDRICAL_SURFACE('',#19460,9.);
#17180=CYLINDRICAL_SURFACE('',#19467,10.);
#17181=CYLINDRICAL_SURFACE('',#19473,12.);
#17182=CYLINDRICAL_SURFACE('',#19474,10.);
#17183=CYLINDRICAL_SURFACE('',#19480,3.);
#17184=CYLINDRICAL_SURFACE('',#19484,3.);
#17185=CYLINDRICAL_SURFACE('',#19490,6.);
#17186=CYLINDRICAL_SURFACE('',#19499,4.);
#17187=CYLINDRICAL_SURFACE('',#19501,2.5);
#17188=CYLINDRICAL_SURFACE('',#19506,4.);
#17189=CYLINDRICAL_SURFACE('',#19508,2.5);
#17190=CYLINDRICAL_SURFACE('',#19513,4.);
#17191=CYLINDRICAL_SURFACE('',#19515,2.5);
#17192=CYLINDRICAL_SURFACE('',#19520,4.);
#17193=CYLINDRICAL_SURFACE('',#19522,2.5);
#17194=CYLINDRICAL_SURFACE('',#19527,4.);
#17195=CYLINDRICAL_SURFACE('',#19529,2.5);
#17196=CYLINDRICAL_SURFACE('',#19534,4.);
#17197=CYLINDRICAL_SURFACE('',#19536,2.5);
#17198=CYLINDRICAL_SURFACE('',#19538,12.);
#17199=CYLINDRICAL_SURFACE('',#19541,70.);
#17200=CYLINDRICAL_SURFACE('',#19547,12.);
#17201=CYLINDRICAL_SURFACE('',#19550,60.);
#17202=CYLINDRICAL_SURFACE('',#19559,2.);
#17203=CYLINDRICAL_SURFACE('',#19564,2.);
#17204=CYLINDRICAL_SURFACE('',#19569,2.);
#17205=CYLINDRICAL_SURFACE('',#19574,2.);
#17206=CYLINDRICAL_SURFACE('',#19579,2.);
#17207=CYLINDRICAL_SURFACE('',#19584,2.);
#17208=CYLINDRICAL_SURFACE('',#19586,50.);
#17209=CYLINDRICAL_SURFACE('',#19589,59.);
#17210=CYLINDRICAL_SURFACE('',#19595,10.);
#17211=CYLINDRICAL_SURFACE('',#19598,12.);
#17212=CYLINDRICAL_SURFACE('',#19604,10.);
#17213=CYLINDRICAL_SURFACE('',#19607,12.);
#17214=CYLINDRICAL_SURFACE('',#19613,10.);
#17215=CYLINDRICAL_SURFACE('',#19616,14.);
#17216=CYLINDRICAL_SURFACE('',#19627,9.);
#17217=CYLINDRICAL_SURFACE('',#19629,14.);
#17218=CYLINDRICAL_SURFACE('',#19636,2.5);
#17219=CYLINDRICAL_SURFACE('',#19639,1.5);
#17220=CYLINDRICAL_SURFACE('',#19648,1.954);
#17221=CYLINDRICAL_SURFACE('',#19650,1.954);
#17222=CYLINDRICAL_SURFACE('',#19651,1.954);
#17223=CYLINDRICAL_SURFACE('',#19652,1.954);
#17224=CYLINDRICAL_SURFACE('',#19653,1.954);
#17225=CYLINDRICAL_SURFACE('',#19654,1.954);
#17226=CYLINDRICAL_SURFACE('',#19655,1.954);
#17227=CYLINDRICAL_SURFACE('',#19656,1.954);
#17228=CYLINDRICAL_SURFACE('',#19657,1.954);
#17229=CYLINDRICAL_SURFACE('',#19658,1.954);
#17230=CYLINDRICAL_SURFACE('',#19659,1.954);
#17231=CYLINDRICAL_SURFACE('',#19660,1.954);
#17232=CYLINDRICAL_SURFACE('',#19661,1.954);
#17233=CYLINDRICAL_SURFACE('',#19662,1.954);
#17234=CYLINDRICAL_SURFACE('',#19663,1.954);
#17235=CYLINDRICAL_SURFACE('',#19664,1.954);
#17236=CYLINDRICAL_SURFACE('',#19665,1.5555);
#17237=CYLINDRICAL_SURFACE('',#19667,1.5555);
#17238=CYLINDRICAL_SURFACE('',#19668,1.5555);
#17239=CYLINDRICAL_SURFACE('',#19669,1.5555);
#17240=CYLINDRICAL_SURFACE('',#19670,1.5555);
#17241=CYLINDRICAL_SURFACE('',#19671,1.5555);
#17242=CYLINDRICAL_SURFACE('',#19672,1.5555);
#17243=CYLINDRICAL_SURFACE('',#19673,1.5555);
#17244=CYLINDRICAL_SURFACE('',#19674,1.5555);
#17245=CYLINDRICAL_SURFACE('',#19675,1.5555);
#17246=CYLINDRICAL_SURFACE('',#19676,1.5555);
#17247=CYLINDRICAL_SURFACE('',#19677,1.5555);
#17248=CYLINDRICAL_SURFACE('',#19678,1.5555);
#17249=CYLINDRICAL_SURFACE('',#19679,1.5555);
#17250=CYLINDRICAL_SURFACE('',#19680,1.5555);
#17251=CYLINDRICAL_SURFACE('',#19681,1.5555);
#17252=CYLINDRICAL_SURFACE('',#19685,1.5555);
#17253=CYLINDRICAL_SURFACE('',#19687,1.954);
#17254=CYLINDRICAL_SURFACE('',#19697,3.5);
#17255=CYLINDRICAL_SURFACE('',#19702,1.4635);
#17256=CYLINDRICAL_SURFACE('',#19704,1.4635);
#17257=CYLINDRICAL_SURFACE('',#19705,1.4635);
#17258=CYLINDRICAL_SURFACE('',#19706,1.4635);
#17259=CYLINDRICAL_SURFACE('',#19707,1.4635);
#17260=CYLINDRICAL_SURFACE('',#19708,1.4635);
#17261=CYLINDRICAL_SURFACE('',#19709,1.4635);
#17262=CYLINDRICAL_SURFACE('',#19710,1.4635);
#17263=CYLINDRICAL_SURFACE('',#19711,1.17775);
#17264=CYLINDRICAL_SURFACE('',#19713,1.17775);
#17265=CYLINDRICAL_SURFACE('',#19714,1.17775);
#17266=CYLINDRICAL_SURFACE('',#19715,1.17775);
#17267=CYLINDRICAL_SURFACE('',#19716,1.17775);
#17268=CYLINDRICAL_SURFACE('',#19717,1.17775);
#17269=CYLINDRICAL_SURFACE('',#19718,1.17775);
#17270=CYLINDRICAL_SURFACE('',#19719,1.17775);
#17271=CYLINDRICAL_SURFACE('',#19723,1.17775);
#17272=CYLINDRICAL_SURFACE('',#19735,1.4635);
#17273=ADVANCED_FACE('',(#675),#16532,.F.);
#17274=ADVANCED_FACE('',(#676),#16533,.F.);
#17275=ADVANCED_FACE('',(#677),#16534,.F.);
#17276=ADVANCED_FACE('',(#678),#16535,.F.);
#17277=ADVANCED_FACE('',(#679),#16536,.F.);
#17278=ADVANCED_FACE('',(#680),#16537,.F.);
#17279=ADVANCED_FACE('',(#681),#16538,.F.);
#17280=ADVANCED_FACE('',(#682),#16539,.F.);
#17281=ADVANCED_FACE('',(#683),#16540,.F.);
#17282=ADVANCED_FACE('',(#684),#16541,.F.);
#17283=ADVANCED_FACE('',(#685),#16542,.F.);
#17284=ADVANCED_FACE('',(#686),#16543,.F.);
#17285=ADVANCED_FACE('',(#687),#16544,.F.);
#17286=ADVANCED_FACE('',(#688),#16545,.F.);
#17287=ADVANCED_FACE('',(#689),#16546,.F.);
#17288=ADVANCED_FACE('',(#690),#16547,.F.);
#17289=ADVANCED_FACE('',(#691),#16548,.F.);
#17290=ADVANCED_FACE('',(#692),#16549,.F.);
#17291=ADVANCED_FACE('',(#693),#16550,.F.);
#17292=ADVANCED_FACE('',(#694),#16551,.F.);
#17293=ADVANCED_FACE('',(#695),#16552,.F.);
#17294=ADVANCED_FACE('',(#696),#16553,.F.);
#17295=ADVANCED_FACE('',(#697),#16554,.F.);
#17296=ADVANCED_FACE('',(#698),#16555,.F.);
#17297=ADVANCED_FACE('',(#699),#16556,.F.);
#17298=ADVANCED_FACE('',(#700),#16557,.F.);
#17299=ADVANCED_FACE('',(#701),#16558,.F.);
#17300=ADVANCED_FACE('',(#702),#16559,.F.);
#17301=ADVANCED_FACE('',(#703),#16560,.F.);
#17302=ADVANCED_FACE('',(#704),#16561,.F.);
#17303=ADVANCED_FACE('',(#705),#16562,.F.);
#17304=ADVANCED_FACE('',(#706),#16563,.F.);
#17305=ADVANCED_FACE('',(#707),#16564,.F.);
#17306=ADVANCED_FACE('',(#708),#16565,.F.);
#17307=ADVANCED_FACE('',(#709),#16566,.F.);
#17308=ADVANCED_FACE('',(#710),#16567,.F.);
#17309=ADVANCED_FACE('',(#711),#16568,.F.);
#17310=ADVANCED_FACE('',(#712),#16569,.F.);
#17311=ADVANCED_FACE('',(#713),#16570,.F.);
#17312=ADVANCED_FACE('',(#714),#16571,.F.);
#17313=ADVANCED_FACE('',(#715),#16572,.F.);
#17314=ADVANCED_FACE('',(#716),#16573,.F.);
#17315=ADVANCED_FACE('',(#717),#16574,.F.);
#17316=ADVANCED_FACE('',(#718),#16575,.F.);
#17317=ADVANCED_FACE('',(#719),#16576,.F.);
#17318=ADVANCED_FACE('',(#720),#16577,.F.);
#17319=ADVANCED_FACE('',(#721),#16578,.F.);
#17320=ADVANCED_FACE('',(#722),#16579,.F.);
#17321=ADVANCED_FACE('',(#723),#16580,.F.);
#17322=ADVANCED_FACE('',(#724),#16581,.F.);
#17323=ADVANCED_FACE('',(#725),#16582,.F.);
#17324=ADVANCED_FACE('',(#726),#16583,.F.);
#17325=ADVANCED_FACE('',(#727),#16584,.F.);
#17326=ADVANCED_FACE('',(#728),#16585,.F.);
#17327=ADVANCED_FACE('',(#729),#16586,.F.);
#17328=ADVANCED_FACE('',(#730),#16587,.F.);
#17329=ADVANCED_FACE('',(#731),#16588,.F.);
#17330=ADVANCED_FACE('',(#732),#16589,.F.);
#17331=ADVANCED_FACE('',(#733),#16590,.F.);
#17332=ADVANCED_FACE('',(#734),#16591,.F.);
#17333=ADVANCED_FACE('',(#735),#16592,.F.);
#17334=ADVANCED_FACE('',(#736),#16593,.F.);
#17335=ADVANCED_FACE('',(#737),#16594,.F.);
#17336=ADVANCED_FACE('',(#738),#16595,.F.);
#17337=ADVANCED_FACE('',(#739),#16596,.F.);
#17338=ADVANCED_FACE('',(#740),#16597,.F.);
#17339=ADVANCED_FACE('',(#741),#16598,.F.);
#17340=ADVANCED_FACE('',(#742),#16599,.F.);
#17341=ADVANCED_FACE('',(#743),#16600,.F.);
#17342=ADVANCED_FACE('',(#744),#16601,.F.);
#17343=ADVANCED_FACE('',(#745),#16602,.F.);
#17344=ADVANCED_FACE('',(#746),#16603,.F.);
#17345=ADVANCED_FACE('',(#747),#16604,.F.);
#17346=ADVANCED_FACE('',(#748),#16605,.F.);
#17347=ADVANCED_FACE('',(#749),#16606,.F.);
#17348=ADVANCED_FACE('',(#750),#16607,.F.);
#17349=ADVANCED_FACE('',(#751),#16608,.F.);
#17350=ADVANCED_FACE('',(#752),#16609,.F.);
#17351=ADVANCED_FACE('',(#753),#16610,.F.);
#17352=ADVANCED_FACE('',(#754),#16611,.F.);
#17353=ADVANCED_FACE('',(#755),#16612,.F.);
#17354=ADVANCED_FACE('',(#756),#16613,.F.);
#17355=ADVANCED_FACE('',(#757),#16614,.F.);
#17356=ADVANCED_FACE('',(#758),#16615,.F.);
#17357=ADVANCED_FACE('',(#759),#16616,.F.);
#17358=ADVANCED_FACE('',(#760),#16617,.F.);
#17359=ADVANCED_FACE('',(#761),#16618,.F.);
#17360=ADVANCED_FACE('',(#762),#16619,.F.);
#17361=ADVANCED_FACE('',(#763),#16620,.F.);
#17362=ADVANCED_FACE('',(#764),#16621,.F.);
#17363=ADVANCED_FACE('',(#765),#16622,.F.);
#17364=ADVANCED_FACE('',(#766),#16623,.F.);
#17365=ADVANCED_FACE('',(#767),#16624,.F.);
#17366=ADVANCED_FACE('',(#768),#16625,.F.);
#17367=ADVANCED_FACE('',(#769),#16626,.F.);
#17368=ADVANCED_FACE('',(#770),#16627,.F.);
#17369=ADVANCED_FACE('',(#771),#16628,.F.);
#17370=ADVANCED_FACE('',(#772),#16629,.F.);
#17371=ADVANCED_FACE('',(#773),#16630,.F.);
#17372=ADVANCED_FACE('',(#774),#16631,.F.);
#17373=ADVANCED_FACE('',(#775),#16632,.F.);
#17374=ADVANCED_FACE('',(#776),#16633,.F.);
#17375=ADVANCED_FACE('',(#777),#16634,.F.);
#17376=ADVANCED_FACE('',(#778),#16635,.F.);
#17377=ADVANCED_FACE('',(#779),#16636,.F.);
#17378=ADVANCED_FACE('',(#780),#16637,.F.);
#17379=ADVANCED_FACE('',(#781),#16638,.F.);
#17380=ADVANCED_FACE('',(#782),#16639,.F.);
#17381=ADVANCED_FACE('',(#783),#16640,.F.);
#17382=ADVANCED_FACE('',(#784),#16641,.F.);
#17383=ADVANCED_FACE('',(#785),#16642,.F.);
#17384=ADVANCED_FACE('',(#786),#16643,.F.);
#17385=ADVANCED_FACE('',(#787),#16644,.F.);
#17386=ADVANCED_FACE('',(#788),#16645,.F.);
#17387=ADVANCED_FACE('',(#789),#16646,.F.);
#17388=ADVANCED_FACE('',(#790),#16647,.F.);
#17389=ADVANCED_FACE('',(#791),#16648,.F.);
#17390=ADVANCED_FACE('',(#792),#16649,.F.);
#17391=ADVANCED_FACE('',(#793),#16650,.F.);
#17392=ADVANCED_FACE('',(#794),#16651,.F.);
#17393=ADVANCED_FACE('',(#795),#16652,.F.);
#17394=ADVANCED_FACE('',(#796),#16653,.F.);
#17395=ADVANCED_FACE('',(#797),#16654,.F.);
#17396=ADVANCED_FACE('',(#798),#16655,.F.);
#17397=ADVANCED_FACE('',(#799),#16656,.F.);
#17398=ADVANCED_FACE('',(#800),#16657,.F.);
#17399=ADVANCED_FACE('',(#801),#16658,.F.);
#17400=ADVANCED_FACE('',(#802),#16659,.F.);
#17401=ADVANCED_FACE('',(#803),#16660,.F.);
#17402=ADVANCED_FACE('',(#804),#16661,.F.);
#17403=ADVANCED_FACE('',(#805),#16662,.F.);
#17404=ADVANCED_FACE('',(#806),#16663,.F.);
#17405=ADVANCED_FACE('',(#807),#16664,.F.);
#17406=ADVANCED_FACE('',(#808),#16665,.F.);
#17407=ADVANCED_FACE('',(#809),#16666,.F.);
#17408=ADVANCED_FACE('',(#810),#16667,.F.);
#17409=ADVANCED_FACE('',(#811),#16668,.F.);
#17410=ADVANCED_FACE('',(#812),#16669,.F.);
#17411=ADVANCED_FACE('',(#813),#16670,.F.);
#17412=ADVANCED_FACE('',(#814),#16671,.F.);
#17413=ADVANCED_FACE('',(#815),#16672,.F.);
#17414=ADVANCED_FACE('',(#816),#16673,.F.);
#17415=ADVANCED_FACE('',(#817),#16674,.F.);
#17416=ADVANCED_FACE('',(#818),#16675,.F.);
#17417=ADVANCED_FACE('',(#819),#16676,.F.);
#17418=ADVANCED_FACE('',(#820),#16677,.F.);
#17419=ADVANCED_FACE('',(#821),#16678,.F.);
#17420=ADVANCED_FACE('',(#822),#16679,.F.);
#17421=ADVANCED_FACE('',(#823),#16680,.F.);
#17422=ADVANCED_FACE('',(#824),#16681,.F.);
#17423=ADVANCED_FACE('',(#825),#16682,.F.);
#17424=ADVANCED_FACE('',(#826),#16683,.F.);
#17425=ADVANCED_FACE('',(#827),#16684,.F.);
#17426=ADVANCED_FACE('',(#828),#16685,.F.);
#17427=ADVANCED_FACE('',(#829),#16686,.F.);
#17428=ADVANCED_FACE('',(#830),#16687,.F.);
#17429=ADVANCED_FACE('',(#831),#16688,.F.);
#17430=ADVANCED_FACE('',(#832),#16689,.F.);
#17431=ADVANCED_FACE('',(#833),#16690,.F.);
#17432=ADVANCED_FACE('',(#834),#16691,.F.);
#17433=ADVANCED_FACE('',(#835),#16692,.F.);
#17434=ADVANCED_FACE('',(#836),#16693,.F.);
#17435=ADVANCED_FACE('',(#837),#16694,.F.);
#17436=ADVANCED_FACE('',(#838),#16695,.F.);
#17437=ADVANCED_FACE('',(#839),#16696,.F.);
#17438=ADVANCED_FACE('',(#840),#16697,.F.);
#17439=ADVANCED_FACE('',(#841),#16698,.F.);
#17440=ADVANCED_FACE('',(#842),#16699,.F.);
#17441=ADVANCED_FACE('',(#843),#16700,.F.);
#17442=ADVANCED_FACE('',(#844),#16701,.F.);
#17443=ADVANCED_FACE('',(#845),#16702,.F.);
#17444=ADVANCED_FACE('',(#846),#16703,.F.);
#17445=ADVANCED_FACE('',(#847),#16704,.F.);
#17446=ADVANCED_FACE('',(#848),#16705,.F.);
#17447=ADVANCED_FACE('',(#849),#16706,.F.);
#17448=ADVANCED_FACE('',(#850),#16707,.F.);
#17449=ADVANCED_FACE('',(#851),#16708,.F.);
#17450=ADVANCED_FACE('',(#852),#16709,.F.);
#17451=ADVANCED_FACE('',(#853),#16710,.F.);
#17452=ADVANCED_FACE('',(#854),#16711,.F.);
#17453=ADVANCED_FACE('',(#855),#16712,.F.);
#17454=ADVANCED_FACE('',(#856),#16713,.F.);
#17455=ADVANCED_FACE('',(#857),#16714,.F.);
#17456=ADVANCED_FACE('',(#858),#16715,.F.);
#17457=ADVANCED_FACE('',(#859),#16716,.F.);
#17458=ADVANCED_FACE('',(#860),#16717,.F.);
#17459=ADVANCED_FACE('',(#861),#16718,.F.);
#17460=ADVANCED_FACE('',(#862),#16719,.F.);
#17461=ADVANCED_FACE('',(#863),#16720,.F.);
#17462=ADVANCED_FACE('',(#864),#16721,.F.);
#17463=ADVANCED_FACE('',(#865),#16722,.F.);
#17464=ADVANCED_FACE('',(#866),#16723,.F.);
#17465=ADVANCED_FACE('',(#867),#16724,.F.);
#17466=ADVANCED_FACE('',(#868),#16725,.F.);
#17467=ADVANCED_FACE('',(#869),#16726,.F.);
#17468=ADVANCED_FACE('',(#870),#16727,.F.);
#17469=ADVANCED_FACE('',(#871),#16728,.F.);
#17470=ADVANCED_FACE('',(#872),#16729,.F.);
#17471=ADVANCED_FACE('',(#873),#16730,.F.);
#17472=ADVANCED_FACE('',(#874),#16731,.F.);
#17473=ADVANCED_FACE('',(#875),#16732,.F.);
#17474=ADVANCED_FACE('',(#876),#16733,.F.);
#17475=ADVANCED_FACE('',(#877),#16734,.F.);
#17476=ADVANCED_FACE('',(#878),#16735,.F.);
#17477=ADVANCED_FACE('',(#879),#16736,.F.);
#17478=ADVANCED_FACE('',(#880),#16737,.F.);
#17479=ADVANCED_FACE('',(#881),#16738,.F.);
#17480=ADVANCED_FACE('',(#882),#16739,.F.);
#17481=ADVANCED_FACE('',(#883),#16740,.F.);
#17482=ADVANCED_FACE('',(#884),#16741,.F.);
#17483=ADVANCED_FACE('',(#885),#16742,.F.);
#17484=ADVANCED_FACE('',(#886),#16743,.F.);
#17485=ADVANCED_FACE('',(#887),#16744,.F.);
#17486=ADVANCED_FACE('',(#888),#16745,.F.);
#17487=ADVANCED_FACE('',(#889),#16746,.F.);
#17488=ADVANCED_FACE('',(#890),#16747,.F.);
#17489=ADVANCED_FACE('',(#891),#16748,.F.);
#17490=ADVANCED_FACE('',(#892),#16749,.F.);
#17491=ADVANCED_FACE('',(#893),#16750,.F.);
#17492=ADVANCED_FACE('',(#894),#16751,.F.);
#17493=ADVANCED_FACE('',(#895),#16752,.F.);
#17494=ADVANCED_FACE('',(#896),#16753,.F.);
#17495=ADVANCED_FACE('',(#897),#16754,.F.);
#17496=ADVANCED_FACE('',(#898),#16755,.F.);
#17497=ADVANCED_FACE('',(#899),#16756,.F.);
#17498=ADVANCED_FACE('',(#900),#16757,.F.);
#17499=ADVANCED_FACE('',(#901),#16758,.F.);
#17500=ADVANCED_FACE('',(#902),#16759,.F.);
#17501=ADVANCED_FACE('',(#903),#16760,.F.);
#17502=ADVANCED_FACE('',(#904),#16761,.F.);
#17503=ADVANCED_FACE('',(#905),#16762,.F.);
#17504=ADVANCED_FACE('',(#906),#16763,.F.);
#17505=ADVANCED_FACE('',(#907),#16764,.F.);
#17506=ADVANCED_FACE('',(#908),#16765,.F.);
#17507=ADVANCED_FACE('',(#909),#16766,.F.);
#17508=ADVANCED_FACE('',(#910),#16767,.F.);
#17509=ADVANCED_FACE('',(#911),#16768,.F.);
#17510=ADVANCED_FACE('',(#912),#16769,.F.);
#17511=ADVANCED_FACE('',(#913),#16770,.F.);
#17512=ADVANCED_FACE('',(#914),#16771,.F.);
#17513=ADVANCED_FACE('',(#915),#16772,.F.);
#17514=ADVANCED_FACE('',(#916),#16773,.F.);
#17515=ADVANCED_FACE('',(#917),#16774,.F.);
#17516=ADVANCED_FACE('',(#918),#16775,.F.);
#17517=ADVANCED_FACE('',(#919),#16776,.F.);
#17518=ADVANCED_FACE('',(#920),#16777,.F.);
#17519=ADVANCED_FACE('',(#921),#16778,.F.);
#17520=ADVANCED_FACE('',(#922),#16779,.F.);
#17521=ADVANCED_FACE('',(#923),#16780,.F.);
#17522=ADVANCED_FACE('',(#924),#16781,.F.);
#17523=ADVANCED_FACE('',(#925),#16782,.F.);
#17524=ADVANCED_FACE('',(#926),#16783,.F.);
#17525=ADVANCED_FACE('',(#927),#16784,.F.);
#17526=ADVANCED_FACE('',(#928),#16785,.F.);
#17527=ADVANCED_FACE('',(#929),#16786,.F.);
#17528=ADVANCED_FACE('',(#930),#16787,.F.);
#17529=ADVANCED_FACE('',(#931),#16788,.F.);
#17530=ADVANCED_FACE('',(#932),#16789,.F.);
#17531=ADVANCED_FACE('',(#933),#16790,.F.);
#17532=ADVANCED_FACE('',(#934),#16791,.F.);
#17533=ADVANCED_FACE('',(#935),#16792,.F.);
#17534=ADVANCED_FACE('',(#936),#16793,.F.);
#17535=ADVANCED_FACE('',(#937),#16794,.F.);
#17536=ADVANCED_FACE('',(#938),#16795,.F.);
#17537=ADVANCED_FACE('',(#939),#16796,.F.);
#17538=ADVANCED_FACE('',(#940),#16797,.F.);
#17539=ADVANCED_FACE('',(#941),#16798,.F.);
#17540=ADVANCED_FACE('',(#942),#16799,.F.);
#17541=ADVANCED_FACE('',(#943),#16800,.F.);
#17542=ADVANCED_FACE('',(#944),#16801,.F.);
#17543=ADVANCED_FACE('',(#945),#16802,.F.);
#17544=ADVANCED_FACE('',(#946),#16803,.F.);
#17545=ADVANCED_FACE('',(#947),#16804,.F.);
#17546=ADVANCED_FACE('',(#948),#16805,.F.);
#17547=ADVANCED_FACE('',(#949),#16806,.F.);
#17548=ADVANCED_FACE('',(#950),#16807,.F.);
#17549=ADVANCED_FACE('',(#951),#16808,.F.);
#17550=ADVANCED_FACE('',(#952),#16809,.F.);
#17551=ADVANCED_FACE('',(#953),#16810,.F.);
#17552=ADVANCED_FACE('',(#954),#16811,.F.);
#17553=ADVANCED_FACE('',(#955),#16812,.F.);
#17554=ADVANCED_FACE('',(#956),#16813,.F.);
#17555=ADVANCED_FACE('',(#957),#16814,.F.);
#17556=ADVANCED_FACE('',(#958),#16815,.F.);
#17557=ADVANCED_FACE('',(#959),#16816,.F.);
#17558=ADVANCED_FACE('',(#960),#16817,.F.);
#17559=ADVANCED_FACE('',(#961),#16818,.F.);
#17560=ADVANCED_FACE('',(#962),#16819,.F.);
#17561=ADVANCED_FACE('',(#963),#16820,.F.);
#17562=ADVANCED_FACE('',(#964),#16821,.F.);
#17563=ADVANCED_FACE('',(#965),#16822,.F.);
#17564=ADVANCED_FACE('',(#966),#16823,.F.);
#17565=ADVANCED_FACE('',(#967),#16824,.F.);
#17566=ADVANCED_FACE('',(#968),#16825,.F.);
#17567=ADVANCED_FACE('',(#969),#16826,.F.);
#17568=ADVANCED_FACE('',(#970),#16827,.F.);
#17569=ADVANCED_FACE('',(#971),#16828,.F.);
#17570=ADVANCED_FACE('',(#972),#16829,.F.);
#17571=ADVANCED_FACE('',(#973),#16830,.F.);
#17572=ADVANCED_FACE('',(#974),#16831,.F.);
#17573=ADVANCED_FACE('',(#975),#16832,.F.);
#17574=ADVANCED_FACE('',(#976),#16833,.F.);
#17575=ADVANCED_FACE('',(#977),#16834,.F.);
#17576=ADVANCED_FACE('',(#978),#16835,.F.);
#17577=ADVANCED_FACE('',(#979),#16836,.F.);
#17578=ADVANCED_FACE('',(#980),#16837,.F.);
#17579=ADVANCED_FACE('',(#981),#16838,.F.);
#17580=ADVANCED_FACE('',(#982),#16839,.F.);
#17581=ADVANCED_FACE('',(#983),#16840,.F.);
#17582=ADVANCED_FACE('',(#984),#16841,.F.);
#17583=ADVANCED_FACE('',(#985),#16842,.F.);
#17584=ADVANCED_FACE('',(#986),#16843,.F.);
#17585=ADVANCED_FACE('',(#987),#16844,.F.);
#17586=ADVANCED_FACE('',(#988),#16845,.F.);
#17587=ADVANCED_FACE('',(#989),#16846,.F.);
#17588=ADVANCED_FACE('',(#990),#16847,.F.);
#17589=ADVANCED_FACE('',(#991),#16848,.F.);
#17590=ADVANCED_FACE('',(#992),#16849,.F.);
#17591=ADVANCED_FACE('',(#993),#16850,.F.);
#17592=ADVANCED_FACE('',(#994),#16851,.F.);
#17593=ADVANCED_FACE('',(#995),#16852,.F.);
#17594=ADVANCED_FACE('',(#996),#16853,.F.);
#17595=ADVANCED_FACE('',(#997),#16854,.F.);
#17596=ADVANCED_FACE('',(#998),#16855,.F.);
#17597=ADVANCED_FACE('',(#999),#16856,.F.);
#17598=ADVANCED_FACE('',(#1000),#16857,.F.);
#17599=ADVANCED_FACE('',(#1001),#16858,.F.);
#17600=ADVANCED_FACE('',(#1002),#16859,.F.);
#17601=ADVANCED_FACE('',(#1003),#16860,.F.);
#17602=ADVANCED_FACE('',(#1004),#16861,.F.);
#17603=ADVANCED_FACE('',(#1005),#16862,.F.);
#17604=ADVANCED_FACE('',(#1006),#16863,.F.);
#17605=ADVANCED_FACE('',(#1007),#16864,.F.);
#17606=ADVANCED_FACE('',(#1008),#16865,.F.);
#17607=ADVANCED_FACE('',(#1009),#16866,.F.);
#17608=ADVANCED_FACE('',(#1010),#16867,.F.);
#17609=ADVANCED_FACE('',(#1011),#16868,.F.);
#17610=ADVANCED_FACE('',(#1012),#16869,.F.);
#17611=ADVANCED_FACE('',(#1013),#16870,.F.);
#17612=ADVANCED_FACE('',(#1014),#16871,.F.);
#17613=ADVANCED_FACE('',(#1015),#16872,.F.);
#17614=ADVANCED_FACE('',(#1016),#16873,.F.);
#17615=ADVANCED_FACE('',(#1017),#16874,.F.);
#17616=ADVANCED_FACE('',(#1018),#16875,.F.);
#17617=ADVANCED_FACE('',(#1019),#16876,.F.);
#17618=ADVANCED_FACE('',(#1020),#16877,.F.);
#17619=ADVANCED_FACE('',(#1021),#16878,.F.);
#17620=ADVANCED_FACE('',(#1022),#16879,.F.);
#17621=ADVANCED_FACE('',(#1023),#16880,.F.);
#17622=ADVANCED_FACE('',(#1024),#16881,.F.);
#17623=ADVANCED_FACE('',(#1025),#16882,.F.);
#17624=ADVANCED_FACE('',(#1026),#16883,.F.);
#17625=ADVANCED_FACE('',(#1027),#16884,.F.);
#17626=ADVANCED_FACE('',(#1028),#16885,.F.);
#17627=ADVANCED_FACE('',(#1029),#16886,.F.);
#17628=ADVANCED_FACE('',(#1030),#16887,.F.);
#17629=ADVANCED_FACE('',(#1031),#16888,.F.);
#17630=ADVANCED_FACE('',(#1032),#16889,.F.);
#17631=ADVANCED_FACE('',(#1033),#16890,.F.);
#17632=ADVANCED_FACE('',(#1034),#16891,.F.);
#17633=ADVANCED_FACE('',(#1035),#16892,.F.);
#17634=ADVANCED_FACE('',(#1036),#16893,.F.);
#17635=ADVANCED_FACE('',(#1037),#16894,.F.);
#17636=ADVANCED_FACE('',(#1038),#16895,.F.);
#17637=ADVANCED_FACE('',(#1039),#614,.F.);
#17638=ADVANCED_FACE('',(#1040),#16896,.F.);
#17639=ADVANCED_FACE('',(#1041),#615,.F.);
#17640=ADVANCED_FACE('',(#1042),#616,.F.);
#17641=ADVANCED_FACE('',(#1043),#16897,.F.);
#17642=ADVANCED_FACE('',(#1044),#617,.F.);
#17643=ADVANCED_FACE('',(#1045),#618,.F.);
#17644=ADVANCED_FACE('',(#1046),#16898,.F.);
#17645=ADVANCED_FACE('',(#1047),#619,.F.);
#17646=ADVANCED_FACE('',(#1048),#16899,.F.);
#17647=ADVANCED_FACE('',(#1049),#440,.F.);
#17648=ADVANCED_FACE('',(#1050),#16900,.F.);
#17649=ADVANCED_FACE('',(#1051),#441,.F.);
#17650=ADVANCED_FACE('',(#1052),#16901,.F.);
#17651=ADVANCED_FACE('',(#1053),#442,.F.);
#17652=ADVANCED_FACE('',(#1054),#620,.F.);
#17653=ADVANCED_FACE('',(#1055),#16902,.F.);
#17654=ADVANCED_FACE('',(#1056),#621,.F.);
#17655=ADVANCED_FACE('',(#1057),#16903,.F.);
#17656=ADVANCED_FACE('',(#1058),#443,.F.);
#17657=ADVANCED_FACE('',(#1059),#444,.F.);
#17658=ADVANCED_FACE('',(#1060),#16904,.F.);
#17659=ADVANCED_FACE('',(#1061),#622,.F.);
#17660=ADVANCED_FACE('',(#1062),#623,.F.);
#17661=ADVANCED_FACE('',(#1063),#16905,.F.);
#17662=ADVANCED_FACE('',(#1064),#445,.F.);
#17663=ADVANCED_FACE('',(#1065),#16906,.F.);
#17664=ADVANCED_FACE('',(#1066),#624,.F.);
#17665=ADVANCED_FACE('',(#1067),#625,.F.);
#17666=ADVANCED_FACE('',(#1068),#16907,.F.);
#17667=ADVANCED_FACE('',(#1069),#446,.F.);
#17668=ADVANCED_FACE('',(#1070),#16908,.F.);
#17669=ADVANCED_FACE('',(#1071),#626,.F.);
#17670=ADVANCED_FACE('',(#1072),#627,.F.);
#17671=ADVANCED_FACE('',(#1073),#16909,.F.);
#17672=ADVANCED_FACE('',(#1074),#447,.F.);
#17673=ADVANCED_FACE('',(#1075),#16910,.F.);
#17674=ADVANCED_FACE('',(#1076),#628,.F.);
#17675=ADVANCED_FACE('',(#1077),#629,.F.);
#17676=ADVANCED_FACE('',(#1078),#16911,.F.);
#17677=ADVANCED_FACE('',(#1079),#448,.F.);
#17678=ADVANCED_FACE('',(#1080),#16912,.F.);
#17679=ADVANCED_FACE('',(#1081),#630,.F.);
#17680=ADVANCED_FACE('',(#1082),#631,.F.);
#17681=ADVANCED_FACE('',(#1083),#16913,.F.);
#17682=ADVANCED_FACE('',(#1084),#449,.F.);
#17683=ADVANCED_FACE('',(#1085),#450,.F.);
#17684=ADVANCED_FACE('',(#1086),#451,.F.);
#17685=ADVANCED_FACE('',(#1087),#452,.F.);
#17686=ADVANCED_FACE('',(#1088),#453,.F.);
#17687=ADVANCED_FACE('',(#1089),#454,.T.);
#17688=ADVANCED_FACE('',(#1090),#16914,.F.);
#17689=ADVANCED_FACE('',(#1091),#632,.F.);
#17690=ADVANCED_FACE('',(#1092),#633,.F.);
#17691=ADVANCED_FACE('',(#1093),#16915,.F.);
#17692=ADVANCED_FACE('',(#1094),#455,.T.);
#17693=ADVANCED_FACE('',(#1095),#16916,.F.);
#17694=ADVANCED_FACE('',(#1096),#634,.F.);
#17695=ADVANCED_FACE('',(#1097),#635,.F.);
#17696=ADVANCED_FACE('',(#1098),#16917,.F.);
#17697=ADVANCED_FACE('',(#1099),#456,.T.);
#17698=ADVANCED_FACE('',(#1100),#16918,.F.);
#17699=ADVANCED_FACE('',(#1101),#636,.F.);
#17700=ADVANCED_FACE('',(#1102),#637,.F.);
#17701=ADVANCED_FACE('',(#1103),#16919,.F.);
#17702=ADVANCED_FACE('',(#1104),#457,.T.);
#17703=ADVANCED_FACE('',(#1105),#16920,.F.);
#17704=ADVANCED_FACE('',(#1106),#638,.F.);
#17705=ADVANCED_FACE('',(#1107),#639,.F.);
#17706=ADVANCED_FACE('',(#1108),#16921,.F.);
#17707=ADVANCED_FACE('',(#1109),#458,.T.);
#17708=ADVANCED_FACE('',(#1110),#16922,.F.);
#17709=ADVANCED_FACE('',(#1111),#640,.F.);
#17710=ADVANCED_FACE('',(#1112),#641,.F.);
#17711=ADVANCED_FACE('',(#1113),#16923,.F.);
#17712=ADVANCED_FACE('',(#1114),#459,.F.);
#17713=ADVANCED_FACE('',(#1115),#460,.F.);
#17714=ADVANCED_FACE('',(#1116),#461,.F.);
#17715=ADVANCED_FACE('',(#1117),#462,.F.);
#17716=ADVANCED_FACE('',(#1118),#463,.F.);
#17717=ADVANCED_FACE('',(#1119),#464,.F.);
#17718=ADVANCED_FACE('',(#1120),#16924,.F.);
#17719=ADVANCED_FACE('',(#1121),#642,.F.);
#17720=ADVANCED_FACE('',(#1122),#643,.F.);
#17721=ADVANCED_FACE('',(#1123),#16925,.F.);
#17722=ADVANCED_FACE('',(#1124),#465,.F.);
#17723=ADVANCED_FACE('',(#1125),#466,.T.);
#17724=ADVANCED_FACE('',(#1126),#16926,.F.);
#17725=ADVANCED_FACE('',(#1127),#644,.F.);
#17726=ADVANCED_FACE('',(#1128),#645,.F.);
#17727=ADVANCED_FACE('',(#1129),#16927,.F.);
#17728=ADVANCED_FACE('',(#1130),#467,.F.);
#17729=ADVANCED_FACE('',(#1131),#16928,.F.);
#17730=ADVANCED_FACE('',(#1132,#332,#333,#334,#335),#16929,.T.);
#17731=ADVANCED_FACE('',(#1133,#336,#337,#338,#339,#340,#341,#342),#468,
 .T.);
#17732=ADVANCED_FACE('',(#1134,#343,#344,#345,#346,#347,#348,#349),#469,
 .F.);
#17733=ADVANCED_FACE('',(#1135),#16930,.F.);
#17734=ADVANCED_FACE('',(#1136),#16931,.F.);
#17735=ADVANCED_FACE('',(#1137),#16932,.F.);
#17736=ADVANCED_FACE('',(#1138),#16933,.F.);
#17737=ADVANCED_FACE('',(#1139),#16934,.F.);
#17738=ADVANCED_FACE('',(#1140),#16935,.F.);
#17739=ADVANCED_FACE('',(#1141),#16936,.F.);
#17740=ADVANCED_FACE('',(#1142),#16937,.F.);
#17741=ADVANCED_FACE('',(#1143),#16938,.F.);
#17742=ADVANCED_FACE('',(#1144),#16939,.F.);
#17743=ADVANCED_FACE('',(#1145),#16940,.F.);
#17744=ADVANCED_FACE('',(#1146),#16941,.F.);
#17745=ADVANCED_FACE('',(#1147),#16942,.F.);
#17746=ADVANCED_FACE('',(#1148),#16943,.F.);
#17747=ADVANCED_FACE('',(#1149),#16944,.F.);
#17748=ADVANCED_FACE('',(#1150),#16945,.F.);
#17749=ADVANCED_FACE('',(#1151),#16946,.F.);
#17750=ADVANCED_FACE('',(#1152),#16947,.F.);
#17751=ADVANCED_FACE('',(#1153),#16948,.F.);
#17752=ADVANCED_FACE('',(#1154),#16949,.F.);
#17753=ADVANCED_FACE('',(#1155),#16950,.F.);
#17754=ADVANCED_FACE('',(#1156),#16951,.F.);
#17755=ADVANCED_FACE('',(#1157),#16952,.F.);
#17756=ADVANCED_FACE('',(#1158),#16953,.F.);
#17757=ADVANCED_FACE('',(#1159),#16954,.F.);
#17758=ADVANCED_FACE('',(#1160),#16955,.F.);
#17759=ADVANCED_FACE('',(#1161),#16956,.F.);
#17760=ADVANCED_FACE('',(#1162),#16957,.F.);
#17761=ADVANCED_FACE('',(#1163),#16958,.F.);
#17762=ADVANCED_FACE('',(#1164),#16959,.F.);
#17763=ADVANCED_FACE('',(#1165),#16960,.F.);
#17764=ADVANCED_FACE('',(#1166),#16961,.F.);
#17765=ADVANCED_FACE('',(#1167),#16962,.F.);
#17766=ADVANCED_FACE('',(#1168),#16963,.F.);
#17767=ADVANCED_FACE('',(#1169),#16964,.F.);
#17768=ADVANCED_FACE('',(#1170),#16965,.F.);
#17769=ADVANCED_FACE('',(#1171),#16966,.F.);
#17770=ADVANCED_FACE('',(#1172),#16967,.F.);
#17771=ADVANCED_FACE('',(#1173),#16968,.F.);
#17772=ADVANCED_FACE('',(#1174),#16969,.F.);
#17773=ADVANCED_FACE('',(#1175),#16970,.F.);
#17774=ADVANCED_FACE('',(#1176),#16971,.F.);
#17775=ADVANCED_FACE('',(#1177),#16972,.F.);
#17776=ADVANCED_FACE('',(#1178),#16973,.F.);
#17777=ADVANCED_FACE('',(#1179),#16974,.F.);
#17778=ADVANCED_FACE('',(#1180),#16975,.F.);
#17779=ADVANCED_FACE('',(#1181),#16976,.F.);
#17780=ADVANCED_FACE('',(#1182),#16977,.F.);
#17781=ADVANCED_FACE('',(#1183),#16978,.F.);
#17782=ADVANCED_FACE('',(#1184),#16979,.F.);
#17783=ADVANCED_FACE('',(#1185),#16980,.F.);
#17784=ADVANCED_FACE('',(#1186),#16981,.F.);
#17785=ADVANCED_FACE('',(#1187),#16982,.F.);
#17786=ADVANCED_FACE('',(#1188),#16983,.F.);
#17787=ADVANCED_FACE('',(#1189),#16984,.F.);
#17788=ADVANCED_FACE('',(#1190),#16985,.F.);
#17789=ADVANCED_FACE('',(#1191),#16986,.F.);
#17790=ADVANCED_FACE('',(#1192),#16987,.F.);
#17791=ADVANCED_FACE('',(#1193),#16988,.F.);
#17792=ADVANCED_FACE('',(#1194),#16989,.F.);
#17793=ADVANCED_FACE('',(#1195),#16990,.F.);
#17794=ADVANCED_FACE('',(#1196),#16991,.F.);
#17795=ADVANCED_FACE('',(#1197),#16992,.F.);
#17796=ADVANCED_FACE('',(#1198),#16993,.F.);
#17797=ADVANCED_FACE('',(#1199),#16994,.F.);
#17798=ADVANCED_FACE('',(#1200),#16995,.F.);
#17799=ADVANCED_FACE('',(#1201),#16996,.F.);
#17800=ADVANCED_FACE('',(#1202),#16997,.F.);
#17801=ADVANCED_FACE('',(#1203),#16998,.F.);
#17802=ADVANCED_FACE('',(#1204),#16999,.F.);
#17803=ADVANCED_FACE('',(#1205),#17000,.F.);
#17804=ADVANCED_FACE('',(#1206),#17001,.F.);
#17805=ADVANCED_FACE('',(#1207),#17002,.F.);
#17806=ADVANCED_FACE('',(#1208),#17003,.F.);
#17807=ADVANCED_FACE('',(#1209),#17004,.F.);
#17808=ADVANCED_FACE('',(#1210),#17005,.F.);
#17809=ADVANCED_FACE('',(#1211),#17006,.F.);
#17810=ADVANCED_FACE('',(#1212),#17007,.F.);
#17811=ADVANCED_FACE('',(#1213),#17008,.F.);
#17812=ADVANCED_FACE('',(#1214),#17009,.F.);
#17813=ADVANCED_FACE('',(#1215),#17010,.F.);
#17814=ADVANCED_FACE('',(#1216),#17011,.F.);
#17815=ADVANCED_FACE('',(#1217),#17012,.F.);
#17816=ADVANCED_FACE('',(#1218),#17013,.F.);
#17817=ADVANCED_FACE('',(#1219),#17014,.F.);
#17818=ADVANCED_FACE('',(#1220),#17015,.F.);
#17819=ADVANCED_FACE('',(#1221),#17016,.F.);
#17820=ADVANCED_FACE('',(#1222),#17017,.F.);
#17821=ADVANCED_FACE('',(#1223),#17018,.F.);
#17822=ADVANCED_FACE('',(#1224),#17019,.F.);
#17823=ADVANCED_FACE('',(#1225),#17020,.F.);
#17824=ADVANCED_FACE('',(#1226),#17021,.F.);
#17825=ADVANCED_FACE('',(#1227),#17022,.F.);
#17826=ADVANCED_FACE('',(#1228),#17023,.F.);
#17827=ADVANCED_FACE('',(#1229),#17024,.F.);
#17828=ADVANCED_FACE('',(#1230),#17025,.F.);
#17829=ADVANCED_FACE('',(#1231),#17026,.F.);
#17830=ADVANCED_FACE('',(#1232),#17027,.F.);
#17831=ADVANCED_FACE('',(#1233),#17028,.F.);
#17832=ADVANCED_FACE('',(#1234),#17029,.F.);
#17833=ADVANCED_FACE('',(#1235),#17030,.F.);
#17834=ADVANCED_FACE('',(#1236),#17031,.F.);
#17835=ADVANCED_FACE('',(#1237),#17032,.F.);
#17836=ADVANCED_FACE('',(#1238),#17033,.F.);
#17837=ADVANCED_FACE('',(#1239),#17034,.F.);
#17838=ADVANCED_FACE('',(#1240),#17035,.F.);
#17839=ADVANCED_FACE('',(#1241),#17036,.F.);
#17840=ADVANCED_FACE('',(#1242),#17037,.F.);
#17841=ADVANCED_FACE('',(#1243),#17038,.F.);
#17842=ADVANCED_FACE('',(#1244),#17039,.F.);
#17843=ADVANCED_FACE('',(#1245),#17040,.F.);
#17844=ADVANCED_FACE('',(#1246),#17041,.F.);
#17845=ADVANCED_FACE('',(#1247),#17042,.F.);
#17846=ADVANCED_FACE('',(#1248),#17043,.F.);
#17847=ADVANCED_FACE('',(#1249),#17044,.F.);
#17848=ADVANCED_FACE('',(#1250),#17045,.F.);
#17849=ADVANCED_FACE('',(#1251),#17046,.F.);
#17850=ADVANCED_FACE('',(#1252),#17047,.F.);
#17851=ADVANCED_FACE('',(#1253),#17048,.F.);
#17852=ADVANCED_FACE('',(#1254),#17049,.F.);
#17853=ADVANCED_FACE('',(#1255),#17050,.F.);
#17854=ADVANCED_FACE('',(#1256),#17051,.F.);
#17855=ADVANCED_FACE('',(#1257),#17052,.F.);
#17856=ADVANCED_FACE('',(#1258),#17053,.F.);
#17857=ADVANCED_FACE('',(#1259),#17054,.F.);
#17858=ADVANCED_FACE('',(#1260),#17055,.F.);
#17859=ADVANCED_FACE('',(#1261),#17056,.F.);
#17860=ADVANCED_FACE('',(#1262),#17057,.F.);
#17861=ADVANCED_FACE('',(#1263),#17058,.F.);
#17862=ADVANCED_FACE('',(#1264),#17059,.F.);
#17863=ADVANCED_FACE('',(#1265),#17060,.F.);
#17864=ADVANCED_FACE('',(#1266),#17061,.F.);
#17865=ADVANCED_FACE('',(#1267),#17062,.F.);
#17866=ADVANCED_FACE('',(#1268),#17063,.F.);
#17867=ADVANCED_FACE('',(#1269),#17064,.F.);
#17868=ADVANCED_FACE('',(#1270),#17065,.F.);
#17869=ADVANCED_FACE('',(#1271),#17066,.F.);
#17870=ADVANCED_FACE('',(#1272),#17067,.F.);
#17871=ADVANCED_FACE('',(#1273),#17068,.F.);
#17872=ADVANCED_FACE('',(#1274),#17069,.F.);
#17873=ADVANCED_FACE('',(#1275),#17070,.F.);
#17874=ADVANCED_FACE('',(#1276),#17071,.F.);
#17875=ADVANCED_FACE('',(#1277),#17072,.F.);
#17876=ADVANCED_FACE('',(#1278),#17073,.F.);
#17877=ADVANCED_FACE('',(#1279),#17074,.F.);
#17878=ADVANCED_FACE('',(#1280),#17075,.F.);
#17879=ADVANCED_FACE('',(#1281),#17076,.F.);
#17880=ADVANCED_FACE('',(#1282),#17077,.F.);
#17881=ADVANCED_FACE('',(#1283),#17078,.F.);
#17882=ADVANCED_FACE('',(#1284),#17079,.F.);
#17883=ADVANCED_FACE('',(#1285),#17080,.F.);
#17884=ADVANCED_FACE('',(#1286),#17081,.F.);
#17885=ADVANCED_FACE('',(#1287),#17082,.F.);
#17886=ADVANCED_FACE('',(#1288),#17083,.F.);
#17887=ADVANCED_FACE('',(#1289),#17084,.F.);
#17888=ADVANCED_FACE('',(#1290),#17085,.F.);
#17889=ADVANCED_FACE('',(#1291),#17086,.F.);
#17890=ADVANCED_FACE('',(#1292),#17087,.F.);
#17891=ADVANCED_FACE('',(#1293),#17088,.F.);
#17892=ADVANCED_FACE('',(#1294),#17089,.F.);
#17893=ADVANCED_FACE('',(#1295),#17090,.F.);
#17894=ADVANCED_FACE('',(#1296),#17091,.F.);
#17895=ADVANCED_FACE('',(#1297),#17092,.F.);
#17896=ADVANCED_FACE('',(#1298),#17093,.F.);
#17897=ADVANCED_FACE('',(#1299),#17094,.F.);
#17898=ADVANCED_FACE('',(#1300),#17095,.F.);
#17899=ADVANCED_FACE('',(#1301),#17096,.F.);
#17900=ADVANCED_FACE('',(#1302),#17097,.F.);
#17901=ADVANCED_FACE('',(#1303),#17098,.F.);
#17902=ADVANCED_FACE('',(#1304),#17099,.F.);
#17903=ADVANCED_FACE('',(#1305),#17100,.F.);
#17904=ADVANCED_FACE('',(#1306),#17101,.F.);
#17905=ADVANCED_FACE('',(#1307),#17102,.F.);
#17906=ADVANCED_FACE('',(#1308),#17103,.F.);
#17907=ADVANCED_FACE('',(#1309),#17104,.F.);
#17908=ADVANCED_FACE('',(#1310),#17105,.F.);
#17909=ADVANCED_FACE('',(#1311),#17106,.F.);
#17910=ADVANCED_FACE('',(#1312),#17107,.F.);
#17911=ADVANCED_FACE('',(#1313),#17108,.F.);
#17912=ADVANCED_FACE('',(#1314),#17109,.F.);
#17913=ADVANCED_FACE('',(#1315),#17110,.F.);
#17914=ADVANCED_FACE('',(#1316),#17111,.F.);
#17915=ADVANCED_FACE('',(#1317),#17112,.F.);
#17916=ADVANCED_FACE('',(#1318),#17113,.F.);
#17917=ADVANCED_FACE('',(#1319),#17114,.F.);
#17918=ADVANCED_FACE('',(#1320),#17115,.F.);
#17919=ADVANCED_FACE('',(#1321),#17116,.F.);
#17920=ADVANCED_FACE('',(#1322),#17117,.F.);
#17921=ADVANCED_FACE('',(#1323),#17118,.F.);
#17922=ADVANCED_FACE('',(#1324),#17119,.F.);
#17923=ADVANCED_FACE('',(#1325),#17120,.F.);
#17924=ADVANCED_FACE('',(#1326),#17121,.F.);
#17925=ADVANCED_FACE('',(#1327),#470,.F.);
#17926=ADVANCED_FACE('',(#1328),#471,.F.);
#17927=ADVANCED_FACE('',(#1329),#472,.F.);
#17928=ADVANCED_FACE('',(#1330,#350,#351,#352,#353,#354,#355,#356),#473,
 .F.);
#17929=ADVANCED_FACE('',(#1331),#474,.F.);
#17930=ADVANCED_FACE('',(#1332),#17122,.F.);
#17931=ADVANCED_FACE('',(#1333),#646,.F.);
#17932=ADVANCED_FACE('',(#1334),#647,.F.);
#17933=ADVANCED_FACE('',(#1335),#17123,.F.);
#17934=ADVANCED_FACE('',(#1336),#475,.F.);
#17935=ADVANCED_FACE('',(#1337),#17124,.F.);
#17936=ADVANCED_FACE('',(#1338),#648,.F.);
#17937=ADVANCED_FACE('',(#1339),#649,.F.);
#17938=ADVANCED_FACE('',(#1340),#17125,.F.);
#17939=ADVANCED_FACE('',(#1341),#476,.F.);
#17940=ADVANCED_FACE('',(#1342),#17126,.F.);
#17941=ADVANCED_FACE('',(#1343),#650,.F.);
#17942=ADVANCED_FACE('',(#1344),#651,.F.);
#17943=ADVANCED_FACE('',(#1345),#17127,.F.);
#17944=ADVANCED_FACE('',(#1346),#477,.F.);
#17945=ADVANCED_FACE('',(#1347),#17128,.F.);
#17946=ADVANCED_FACE('',(#1348),#652,.F.);
#17947=ADVANCED_FACE('',(#1349),#653,.F.);
#17948=ADVANCED_FACE('',(#1350),#17129,.F.);
#17949=ADVANCED_FACE('',(#1351),#478,.F.);
#17950=ADVANCED_FACE('',(#1352),#17130,.F.);
#17951=ADVANCED_FACE('',(#1353),#654,.F.);
#17952=ADVANCED_FACE('',(#1354),#655,.F.);
#17953=ADVANCED_FACE('',(#1355),#17131,.F.);
#17954=ADVANCED_FACE('',(#1356),#479,.F.);
#17955=ADVANCED_FACE('',(#1357),#480,.F.);
#17956=ADVANCED_FACE('',(#1358),#481,.F.);
#17957=ADVANCED_FACE('',(#1359),#482,.F.);
#17958=ADVANCED_FACE('',(#1360),#483,.F.);
#17959=ADVANCED_FACE('',(#1361),#484,.F.);
#17960=ADVANCED_FACE('',(#1362),#485,.F.);
#17961=ADVANCED_FACE('',(#1363),#486,.F.);
#17962=ADVANCED_FACE('',(#1364),#487,.F.);
#17963=ADVANCED_FACE('',(#1365),#488,.F.);
#17964=ADVANCED_FACE('',(#1366),#489,.T.);
#17965=ADVANCED_FACE('',(#1367),#17132,.F.);
#17966=ADVANCED_FACE('',(#1368),#656,.F.);
#17967=ADVANCED_FACE('',(#1369),#657,.F.);
#17968=ADVANCED_FACE('',(#1370),#17133,.F.);
#17969=ADVANCED_FACE('',(#1371),#490,.T.);
#17970=ADVANCED_FACE('',(#1372),#17134,.F.);
#17971=ADVANCED_FACE('',(#1373),#658,.F.);
#17972=ADVANCED_FACE('',(#1374),#659,.F.);
#17973=ADVANCED_FACE('',(#1375),#17135,.F.);
#17974=ADVANCED_FACE('',(#1376),#491,.T.);
#17975=ADVANCED_FACE('',(#1377),#17136,.F.);
#17976=ADVANCED_FACE('',(#1378),#660,.F.);
#17977=ADVANCED_FACE('',(#1379),#661,.F.);
#17978=ADVANCED_FACE('',(#1380),#17137,.F.);
#17979=ADVANCED_FACE('',(#1381),#492,.T.);
#17980=ADVANCED_FACE('',(#1382),#17138,.F.);
#17981=ADVANCED_FACE('',(#1383),#662,.F.);
#17982=ADVANCED_FACE('',(#1384),#663,.F.);
#17983=ADVANCED_FACE('',(#1385),#17139,.F.);
#17984=ADVANCED_FACE('',(#1386),#493,.T.);
#17985=ADVANCED_FACE('',(#1387),#17140,.F.);
#17986=ADVANCED_FACE('',(#1388),#664,.F.);
#17987=ADVANCED_FACE('',(#1389),#665,.F.);
#17988=ADVANCED_FACE('',(#1390),#17141,.F.);
#17989=ADVANCED_FACE('',(#1391),#494,.F.);
#17990=ADVANCED_FACE('',(#1392),#495,.F.);
#17991=ADVANCED_FACE('',(#1393),#496,.F.);
#17992=ADVANCED_FACE('',(#1394),#497,.F.);
#17993=ADVANCED_FACE('',(#1395),#498,.F.);
#17994=ADVANCED_FACE('',(#1396),#499,.F.);
#17995=ADVANCED_FACE('',(#1397),#500,.F.);
#17996=ADVANCED_FACE('',(#1398),#501,.F.);
#17997=ADVANCED_FACE('',(#1399),#502,.F.);
#17998=ADVANCED_FACE('',(#1400),#503,.F.);
#17999=ADVANCED_FACE('',(#1401),#504,.F.);
#18000=ADVANCED_FACE('',(#1402),#17142,.F.);
#18001=ADVANCED_FACE('',(#1403),#666,.F.);
#18002=ADVANCED_FACE('',(#1404),#667,.F.);
#18003=ADVANCED_FACE('',(#1405),#17143,.F.);
#18004=ADVANCED_FACE('',(#1406),#505,.F.);
#18005=ADVANCED_FACE('',(#1407),#506,.F.);
#18006=ADVANCED_FACE('',(#1408),#507,.T.);
#18007=ADVANCED_FACE('',(#1409),#17144,.F.);
#18008=ADVANCED_FACE('',(#1410),#668,.F.);
#18009=ADVANCED_FACE('',(#1411),#669,.F.);
#18010=ADVANCED_FACE('',(#1412),#17145,.F.);
#18011=ADVANCED_FACE('',(#1413),#508,.F.);
#18012=ADVANCED_FACE('',(#1414),#509,.F.);
#18013=ADVANCED_FACE('',(#1415),#17146,.F.);
#18014=ADVANCED_FACE('',(#1416,#357),#17147,.F.);
#18015=ADVANCED_FACE('',(#1417,#358),#510,.F.);
#18016=ADVANCED_FACE('',(#1418),#17148,.F.);
#18017=ADVANCED_FACE('',(#1419,#359),#17149,.F.);
#18018=ADVANCED_FACE('',(#1420,#360),#511,.F.);
#18019=ADVANCED_FACE('',(#1421),#17150,.F.);
#18020=ADVANCED_FACE('',(#1422,#361),#17151,.F.);
#18021=ADVANCED_FACE('',(#1423,#362),#512,.F.);
#18022=ADVANCED_FACE('',(#1424),#17152,.F.);
#18023=ADVANCED_FACE('',(#1425,#363),#17153,.F.);
#18024=ADVANCED_FACE('',(#1426,#364),#513,.F.);
#18025=ADVANCED_FACE('',(#1427),#17154,.F.);
#18026=ADVANCED_FACE('',(#1428,#365),#17155,.F.);
#18027=ADVANCED_FACE('',(#1429,#366),#514,.F.);
#18028=ADVANCED_FACE('',(#1430),#17156,.F.);
#18029=ADVANCED_FACE('',(#1431,#367),#17157,.F.);
#18030=ADVANCED_FACE('',(#1432,#368),#515,.F.);
#18031=ADVANCED_FACE('',(#1433),#516,.T.);
#18032=ADVANCED_FACE('',(#1434,#369),#517,.T.);
#18033=ADVANCED_FACE('',(#1435),#518,.T.);
#18034=ADVANCED_FACE('',(#1436,#370),#519,.T.);
#18035=ADVANCED_FACE('',(#1437,#371),#520,.T.);
#18036=ADVANCED_FACE('',(#1438),#521,.T.);
#18037=ADVANCED_FACE('',(#1439,#372),#522,.T.);
#18038=ADVANCED_FACE('',(#1440),#523,.T.);
#18039=ADVANCED_FACE('',(#1441,#373),#524,.T.);
#18040=ADVANCED_FACE('',(#1442),#525,.T.);
#18041=ADVANCED_FACE('',(#1443,#374),#526,.T.);
#18042=ADVANCED_FACE('',(#1444),#527,.T.);
#18043=ADVANCED_FACE('',(#1445,#375),#528,.T.);
#18044=ADVANCED_FACE('',(#1446),#529,.T.);
#18045=ADVANCED_FACE('',(#1447,#376),#530,.T.);
#18046=ADVANCED_FACE('',(#1448),#531,.T.);
#18047=ADVANCED_FACE('',(#1449),#532,.T.);
#18048=ADVANCED_FACE('',(#1450,#377),#533,.T.);
#18049=ADVANCED_FACE('',(#1451),#534,.T.);
#18050=ADVANCED_FACE('',(#1452,#378),#535,.T.);
#18051=ADVANCED_FACE('',(#1453),#256,.F.);
#18052=ADVANCED_FACE('',(#1454),#257,.F.);
#18053=ADVANCED_FACE('',(#1455),#258,.F.);
#18054=ADVANCED_FACE('',(#1456),#259,.F.);
#18055=ADVANCED_FACE('',(#1457),#260,.F.);
#18056=ADVANCED_FACE('',(#1458),#261,.F.);
#18057=ADVANCED_FACE('',(#1459),#262,.F.);
#18058=ADVANCED_FACE('',(#1460),#263,.F.);
#18059=ADVANCED_FACE('',(#1461),#536,.T.);
#18060=ADVANCED_FACE('',(#1462,#379),#537,.T.);
#18061=ADVANCED_FACE('',(#1463),#538,.T.);
#18062=ADVANCED_FACE('',(#1464,#380),#539,.T.);
#18063=ADVANCED_FACE('',(#1465),#264,.F.);
#18064=ADVANCED_FACE('',(#1466),#17158,.T.);
#18065=ADVANCED_FACE('',(#1467),#17159,.F.);
#18066=ADVANCED_FACE('',(#1468),#540,.F.);
#18067=ADVANCED_FACE('',(#1469),#17160,.T.);
#18068=ADVANCED_FACE('',(#1470),#17161,.F.);
#18069=ADVANCED_FACE('',(#1471),#541,.F.);
#18070=ADVANCED_FACE('',(#1472),#17162,.T.);
#18071=ADVANCED_FACE('',(#1473),#17163,.F.);
#18072=ADVANCED_FACE('',(#1474),#542,.F.);
#18073=ADVANCED_FACE('',(#1475,#381,#382,#383,#384,#385,#386,#387),#543,
 .F.);
#18074=ADVANCED_FACE('',(#1476),#544,.F.);
#18075=ADVANCED_FACE('',(#1477),#17164,.F.);
#18076=ADVANCED_FACE('',(#1478),#17165,.T.);
#18077=ADVANCED_FACE('',(#1479),#265,.F.);
#18078=ADVANCED_FACE('',(#1480),#545,.F.);
#18079=ADVANCED_FACE('',(#1481),#17166,.F.);
#18080=ADVANCED_FACE('',(#1482),#17167,.T.);
#18081=ADVANCED_FACE('',(#1483),#266,.F.);
#18082=ADVANCED_FACE('',(#1484),#546,.F.);
#18083=ADVANCED_FACE('',(#1485),#267,.F.);
#18084=ADVANCED_FACE('',(#1486),#17168,.F.);
#18085=ADVANCED_FACE('',(#1487),#17169,.T.);
#18086=ADVANCED_FACE('',(#1488),#17170,.F.);
#18087=ADVANCED_FACE('',(#1489),#17171,.F.);
#18088=ADVANCED_FACE('',(#1490),#17172,.F.);
#18089=ADVANCED_FACE('',(#1491),#547,.F.);
#18090=ADVANCED_FACE('',(#1492),#17173,.F.);
#18091=ADVANCED_FACE('',(#1493),#548,.F.);
#18092=ADVANCED_FACE('',(#1494),#549,.T.);
#18093=ADVANCED_FACE('',(#1495),#17174,.T.);
#18094=ADVANCED_FACE('',(#1496),#17175,.F.);
#18095=ADVANCED_FACE('',(#1497),#550,.F.);
#18096=ADVANCED_FACE('',(#1498),#17176,.F.);
#18097=ADVANCED_FACE('',(#1499),#551,.F.);
#18098=ADVANCED_FACE('',(#1500),#552,.T.);
#18099=ADVANCED_FACE('',(#1501),#17177,.T.);
#18100=ADVANCED_FACE('',(#1502),#17178,.T.);
#18101=ADVANCED_FACE('',(#1503,#388),#553,.F.);
#18102=ADVANCED_FACE('',(#1504,#389),#554,.F.);
#18103=ADVANCED_FACE('',(#1505),#17179,.T.);
#18104=ADVANCED_FACE('',(#1506,#390),#555,.F.);
#18105=ADVANCED_FACE('',(#1507,#391),#556,.F.);
#18106=ADVANCED_FACE('',(#1508),#17180,.T.);
#18107=ADVANCED_FACE('',(#1509,#392),#557,.T.);
#18108=ADVANCED_FACE('',(#1510,#393),#558,.F.);
#18109=ADVANCED_FACE('',(#1511),#17181,.T.);
#18110=ADVANCED_FACE('',(#1512),#17182,.T.);
#18111=ADVANCED_FACE('',(#1513),#559,.T.);
#18112=ADVANCED_FACE('',(#1514),#560,.F.);
#18113=ADVANCED_FACE('',(#1515),#561,.T.);
#18114=ADVANCED_FACE('',(#1516),#17183,.T.);
#18115=ADVANCED_FACE('',(#1517),#562,.T.);
#18116=ADVANCED_FACE('',(#1518),#17184,.T.);
#18117=ADVANCED_FACE('',(#1519),#563,.T.);
#18118=ADVANCED_FACE('',(#1520),#564,.F.);
#18119=ADVANCED_FACE('',(#1521),#17185,.T.);
#18120=ADVANCED_FACE('',(#1522),#565,.T.);
#18121=ADVANCED_FACE('',(#1523),#566,.F.);
#18122=ADVANCED_FACE('',(#1524,#394),#567,.F.);
#18123=ADVANCED_FACE('',(#1525),#17186,.F.);
#18124=ADVANCED_FACE('',(#1526),#17187,.F.);
#18125=ADVANCED_FACE('',(#1527,#395),#568,.F.);
#18126=ADVANCED_FACE('',(#1528),#17188,.F.);
#18127=ADVANCED_FACE('',(#1529),#17189,.F.);
#18128=ADVANCED_FACE('',(#1530,#396),#569,.F.);
#18129=ADVANCED_FACE('',(#1531),#17190,.F.);
#18130=ADVANCED_FACE('',(#1532),#17191,.F.);
#18131=ADVANCED_FACE('',(#1533,#397),#570,.F.);
#18132=ADVANCED_FACE('',(#1534),#17192,.F.);
#18133=ADVANCED_FACE('',(#1535),#17193,.F.);
#18134=ADVANCED_FACE('',(#1536,#398),#571,.F.);
#18135=ADVANCED_FACE('',(#1537),#17194,.F.);
#18136=ADVANCED_FACE('',(#1538),#17195,.F.);
#18137=ADVANCED_FACE('',(#1539,#399),#572,.F.);
#18138=ADVANCED_FACE('',(#1540),#17196,.F.);
#18139=ADVANCED_FACE('',(#1541),#17197,.F.);
#18140=ADVANCED_FACE('',(#1542),#17198,.F.);
#18141=ADVANCED_FACE('',(#1543),#17199,.T.);
#18142=ADVANCED_FACE('',(#1544,#400,#401,#402,#403,#404,#405,#406),#573,
 .T.);
#18143=ADVANCED_FACE('',(#1545,#407,#408,#409,#410,#411,#412,#413),#574,
 .F.);
#18144=ADVANCED_FACE('',(#1546),#17200,.F.);
#18145=ADVANCED_FACE('',(#1547),#17201,.T.);
#18146=ADVANCED_FACE('',(#1548,#414),#575,.T.);
#18147=ADVANCED_FACE('',(#1549,#415),#576,.F.);
#18148=ADVANCED_FACE('',(#1550),#247,.F.);
#18149=ADVANCED_FACE('',(#1551),#17202,.F.);
#18150=ADVANCED_FACE('',(#1552),#248,.F.);
#18151=ADVANCED_FACE('',(#1553),#17203,.F.);
#18152=ADVANCED_FACE('',(#1554),#249,.F.);
#18153=ADVANCED_FACE('',(#1555),#17204,.F.);
#18154=ADVANCED_FACE('',(#1556),#250,.F.);
#18155=ADVANCED_FACE('',(#1557),#17205,.F.);
#18156=ADVANCED_FACE('',(#1558),#251,.F.);
#18157=ADVANCED_FACE('',(#1559),#17206,.F.);
#18158=ADVANCED_FACE('',(#1560),#252,.F.);
#18159=ADVANCED_FACE('',(#1561),#17207,.F.);
#18160=ADVANCED_FACE('',(#1562),#17208,.F.);
#18161=ADVANCED_FACE('',(#1563),#17209,.T.);
#18162=ADVANCED_FACE('',(#1564,#416,#417,#418,#419,#420,#421,#422),#577,
 .T.);
#18163=ADVANCED_FACE('',(#1565,#423,#424,#425,#426,#427,#428,#429),#578,
 .F.);
#18164=ADVANCED_FACE('',(#1566),#17210,.F.);
#18165=ADVANCED_FACE('',(#1567),#17211,.T.);
#18166=ADVANCED_FACE('',(#1568,#430),#579,.T.);
#18167=ADVANCED_FACE('',(#1569,#431),#580,.F.);
#18168=ADVANCED_FACE('',(#1570),#17212,.F.);
#18169=ADVANCED_FACE('',(#1571),#17213,.T.);
#18170=ADVANCED_FACE('',(#1572,#432),#581,.T.);
#18171=ADVANCED_FACE('',(#1573,#433),#582,.F.);
#18172=ADVANCED_FACE('',(#1574),#17214,.F.);
#18173=ADVANCED_FACE('',(#1575),#17215,.T.);
#18174=ADVANCED_FACE('',(#1576,#434),#583,.T.);
#18175=ADVANCED_FACE('',(#1577,#435),#584,.F.);
#18176=ADVANCED_FACE('',(#1578),#585,.F.);
#18177=ADVANCED_FACE('',(#1579),#586,.F.);
#18178=ADVANCED_FACE('',(#1580),#587,.F.);
#18179=ADVANCED_FACE('',(#1581),#17216,.F.);
#18180=ADVANCED_FACE('',(#1582),#17217,.T.);
#18181=ADVANCED_FACE('',(#1583),#588,.T.);
#18182=ADVANCED_FACE('',(#1584,#436),#589,.F.);
#18183=ADVANCED_FACE('',(#1585),#17218,.T.);
#18184=ADVANCED_FACE('',(#1586),#590,.T.);
#18185=ADVANCED_FACE('',(#1587),#17219,.T.);
#18186=ADVANCED_FACE('',(#1588),#591,.F.);
#18187=ADVANCED_FACE('',(#1589),#670,.T.);
#18188=ADVANCED_FACE('',(#1590),#592,.F.);
#18189=ADVANCED_FACE('',(#1591),#593,.T.);
#18190=ADVANCED_FACE('',(#1592),#17220,.T.);
#18191=ADVANCED_FACE('',(#1593),#17221,.T.);
#18192=ADVANCED_FACE('',(#1594),#17222,.T.);
#18193=ADVANCED_FACE('',(#1595),#17223,.T.);
#18194=ADVANCED_FACE('',(#1596),#17224,.T.);
#18195=ADVANCED_FACE('',(#1597),#17225,.T.);
#18196=ADVANCED_FACE('',(#1598),#17226,.T.);
#18197=ADVANCED_FACE('',(#1599),#17227,.T.);
#18198=ADVANCED_FACE('',(#1600),#17228,.T.);
#18199=ADVANCED_FACE('',(#1601),#17229,.T.);
#18200=ADVANCED_FACE('',(#1602),#17230,.T.);
#18201=ADVANCED_FACE('',(#1603),#17231,.T.);
#18202=ADVANCED_FACE('',(#1604),#17232,.T.);
#18203=ADVANCED_FACE('',(#1605),#17233,.T.);
#18204=ADVANCED_FACE('',(#1606),#17234,.T.);
#18205=ADVANCED_FACE('',(#1607),#17235,.T.);
#18206=ADVANCED_FACE('',(#1608),#17236,.T.);
#18207=ADVANCED_FACE('',(#1609),#17237,.T.);
#18208=ADVANCED_FACE('',(#1610),#17238,.T.);
#18209=ADVANCED_FACE('',(#1611),#17239,.T.);
#18210=ADVANCED_FACE('',(#1612),#17240,.T.);
#18211=ADVANCED_FACE('',(#1613),#17241,.T.);
#18212=ADVANCED_FACE('',(#1614),#17242,.T.);
#18213=ADVANCED_FACE('',(#1615),#17243,.T.);
#18214=ADVANCED_FACE('',(#1616),#17244,.T.);
#18215=ADVANCED_FACE('',(#1617),#17245,.T.);
#18216=ADVANCED_FACE('',(#1618),#17246,.T.);
#18217=ADVANCED_FACE('',(#1619),#17247,.T.);
#18218=ADVANCED_FACE('',(#1620),#17248,.T.);
#18219=ADVANCED_FACE('',(#1621),#17249,.T.);
#18220=ADVANCED_FACE('',(#1622),#17250,.T.);
#18221=ADVANCED_FACE('',(#1623),#17251,.T.);
#18222=ADVANCED_FACE('',(#1624),#253,.T.);
#18223=ADVANCED_FACE('',(#1625),#671,.F.);
#18224=ADVANCED_FACE('',(#1626),#17252,.T.);
#18225=ADVANCED_FACE('',(#1627),#672,.F.);
#18226=ADVANCED_FACE('',(#1628),#17253,.T.);
#18227=ADVANCED_FACE('',(#1629),#594,.F.);
#18228=ADVANCED_FACE('',(#1630),#595,.F.);
#18229=ADVANCED_FACE('',(#1631),#596,.F.);
#18230=ADVANCED_FACE('',(#1632),#597,.F.);
#18231=ADVANCED_FACE('',(#1633),#598,.F.);
#18232=ADVANCED_FACE('',(#1634),#599,.F.);
#18233=ADVANCED_FACE('',(#1635),#600,.F.);
#18234=ADVANCED_FACE('',(#1636,#437),#601,.T.);
#18235=ADVANCED_FACE('',(#1637),#17254,.T.);
#18236=ADVANCED_FACE('',(#1638,#438),#602,.F.);
#18237=ADVANCED_FACE('',(#1639),#603,.T.);
#18238=ADVANCED_FACE('',(#1640),#17255,.T.);
#18239=ADVANCED_FACE('',(#1641),#17256,.T.);
#18240=ADVANCED_FACE('',(#1642),#17257,.T.);
#18241=ADVANCED_FACE('',(#1643),#17258,.T.);
#18242=ADVANCED_FACE('',(#1644),#17259,.T.);
#18243=ADVANCED_FACE('',(#1645),#17260,.T.);
#18244=ADVANCED_FACE('',(#1646),#17261,.T.);
#18245=ADVANCED_FACE('',(#1647),#17262,.T.);
#18246=ADVANCED_FACE('',(#1648),#17263,.T.);
#18247=ADVANCED_FACE('',(#1649),#17264,.T.);
#18248=ADVANCED_FACE('',(#1650),#17265,.T.);
#18249=ADVANCED_FACE('',(#1651),#17266,.T.);
#18250=ADVANCED_FACE('',(#1652),#17267,.T.);
#18251=ADVANCED_FACE('',(#1653),#17268,.T.);
#18252=ADVANCED_FACE('',(#1654),#17269,.T.);
#18253=ADVANCED_FACE('',(#1655),#17270,.T.);
#18254=ADVANCED_FACE('',(#1656),#254,.T.);
#18255=ADVANCED_FACE('',(#1657),#673,.F.);
#18256=ADVANCED_FACE('',(#1658),#17271,.T.);
#18257=ADVANCED_FACE('',(#1659),#604,.F.);
#18258=ADVANCED_FACE('',(#1660),#605,.F.);
#18259=ADVANCED_FACE('',(#1661),#606,.F.);
#18260=ADVANCED_FACE('',(#1662),#607,.F.);
#18261=ADVANCED_FACE('',(#1663),#608,.F.);
#18262=ADVANCED_FACE('',(#1664),#609,.F.);
#18263=ADVANCED_FACE('',(#1665),#610,.F.);
#18264=ADVANCED_FACE('',(#1666),#674,.F.);
#18265=ADVANCED_FACE('',(#1667),#611,.T.);
#18266=ADVANCED_FACE('',(#1668),#17272,.T.);
#18267=ADVANCED_FACE('',(#1669,#439),#612,.T.);
#18268=ADVANCED_FACE('',(#1670),#255,.T.);
#18269=ADVANCED_FACE('',(#1671),#613,.T.);
#18270=CLOSED_SHELL('',(#17273,#17274,#17275,#17276,#17277,#17278,#17279,
#17280,#17281,#17282,#17283,#17284,#17285,#17286,#17287,#17288,#17289,#17290,
#17291,#17292,#17293,#17294,#17295,#17296,#17297,#17298,#17299,#17300,#17301,
#17302,#17303,#17304,#17305,#17306,#17307,#17308,#17309,#17310,#17311,#17312,
#17313,#17314,#17315,#17316,#17317,#17318,#17319,#17320,#17321,#17322,#17323,
#17324,#17325,#17326,#17327,#17328,#17329,#17330,#17331,#17332,#17333,#17334,
#17335,#17336,#17337,#17338,#17339,#17340,#17341,#17342,#17343,#17344,#17345,
#17346,#17347,#17348,#17349,#17350,#17351,#17352,#17353,#17354,#17355,#17356,
#17357,#17358,#17359,#17360,#17361,#17362,#17363,#17364,#17365,#17366,#17367,
#17368,#17369,#17370,#17371,#17372,#17373,#17374,#17375,#17376,#17377,#17378,
#17379,#17380,#17381,#17382,#17383,#17384,#17385,#17386,#17387,#17388,#17389,
#17390,#17391,#17392,#17393,#17394,#17395,#17396,#17397,#17398,#17399,#17400,
#17401,#17402,#17403,#17404,#17405,#17406,#17407,#17408,#17409,#17410,#17411,
#17412,#17413,#17414,#17415,#17416,#17417,#17418,#17419,#17420,#17421,#17422,
#17423,#17424,#17425,#17426,#17427,#17428,#17429,#17430,#17431,#17432,#17433,
#17434,#17435,#17436,#17437,#17438,#17439,#17440,#17441,#17442,#17443,#17444,
#17445,#17446,#17447,#17448,#17449,#17450,#17451,#17452,#17453,#17454,#17455,
#17456,#17457,#17458,#17459,#17460,#17461,#17462,#17463,#17464,#17465,#17466,
#17467,#17468,#17469,#17470,#17471,#17472,#17473,#17474,#17475,#17476,#17477,
#17478,#17479,#17480,#17481,#17482,#17483,#17484,#17485,#17486,#17487,#17488,
#17489,#17490,#17491,#17492,#17493,#17494,#17495,#17496,#17497,#17498,#17499,
#17500,#17501,#17502,#17503,#17504,#17505,#17506,#17507,#17508,#17509,#17510,
#17511,#17512,#17513,#17514,#17515,#17516,#17517,#17518,#17519,#17520,#17521,
#17522,#17523,#17524,#17525,#17526,#17527,#17528,#17529,#17530,#17531,#17532,
#17533,#17534,#17535,#17536,#17537,#17538,#17539,#17540,#17541,#17542,#17543,
#17544,#17545,#17546,#17547,#17548,#17549,#17550,#17551,#17552,#17553,#17554,
#17555,#17556,#17557,#17558,#17559,#17560,#17561,#17562,#17563,#17564,#17565,
#17566,#17567,#17568,#17569,#17570,#17571,#17572,#17573,#17574,#17575,#17576,
#17577,#17578,#17579,#17580,#17581,#17582,#17583,#17584,#17585,#17586,#17587,
#17588,#17589,#17590,#17591,#17592,#17593,#17594,#17595,#17596,#17597,#17598,
#17599,#17600,#17601,#17602,#17603,#17604,#17605,#17606,#17607,#17608,#17609,
#17610,#17611,#17612,#17613,#17614,#17615,#17616,#17617,#17618,#17619,#17620,
#17621,#17622,#17623,#17624,#17625,#17626,#17627,#17628,#17629,#17630,#17631,
#17632,#17633,#17634,#17635,#17636,#17637,#17638,#17639,#17640,#17641,#17642,
#17643,#17644,#17645,#17646,#17647,#17648,#17649,#17650,#17651,#17652,#17653,
#17654,#17655,#17656,#17657,#17658,#17659,#17660,#17661,#17662,#17663,#17664,
#17665,#17666,#17667,#17668,#17669,#17670,#17671,#17672,#17673,#17674,#17675,
#17676,#17677,#17678,#17679,#17680,#17681,#17682,#17683,#17684,#17685,#17686,
#17687,#17688,#17689,#17690,#17691,#17692,#17693,#17694,#17695,#17696,#17697,
#17698,#17699,#17700,#17701,#17702,#17703,#17704,#17705,#17706,#17707,#17708,
#17709,#17710,#17711,#17712,#17713,#17714,#17715,#17716,#17717,#17718,#17719,
#17720,#17721,#17722,#17723,#17724,#17725,#17726,#17727,#17728,#17729,#17730,
#17731,#17732));
#18271=CLOSED_SHELL('',(#17733,#17734,#17735,#17736,#17737,#17738,#17739,
#17740,#17741,#17742,#17743,#17744,#17745,#17746,#17747,#17748,#17749,#17750,
#17751,#17752,#17753,#17754,#17755,#17756,#17757,#17758,#17759,#17760,#17761,
#17762,#17763,#17764,#17765,#17766,#17767,#17768,#17769,#17770,#17771,#17772,
#17773,#17774,#17775,#17776,#17777,#17778,#17779,#17780,#17781,#17782,#17783,
#17784,#17785,#17786,#17787,#17788,#17789,#17790,#17791,#17792,#17793,#17794,
#17795,#17796,#17797,#17798,#17799,#17800,#17801,#17802,#17803,#17804,#17805,
#17806,#17807,#17808,#17809,#17810,#17811,#17812,#17813,#17814,#17815,#17816,
#17817,#17818,#17819,#17820,#17821,#17822,#17823,#17824,#17825,#17826,#17827,
#17828,#17829,#17830,#17831,#17832,#17833,#17834,#17835,#17836,#17837,#17838,
#17839,#17840,#17841,#17842,#17843,#17844,#17845,#17846,#17847,#17848,#17849,
#17850,#17851,#17852,#17853,#17854,#17855,#17856,#17857,#17858,#17859,#17860,
#17861,#17862,#17863,#17864,#17865,#17866,#17867,#17868,#17869,#17870,#17871,
#17872,#17873,#17874,#17875,#17876,#17877,#17878,#17879,#17880,#17881,#17882,
#17883,#17884,#17885,#17886,#17887,#17888,#17889,#17890,#17891,#17892,#17893,
#17894,#17895,#17896,#17897,#17898,#17899,#17900,#17901,#17902,#17903,#17904,
#17905,#17906,#17907,#17908,#17909,#17910,#17911,#17912,#17913,#17914,#17915,
#17916,#17917,#17918,#17919,#17920,#17921,#17922,#17923,#17924,#17925,#17926,
#17927,#17928,#17929,#17930,#17931,#17932,#17933,#17934,#17935,#17936,#17937,
#17938,#17939,#17940,#17941,#17942,#17943,#17944,#17945,#17946,#17947,#17948,
#17949,#17950,#17951,#17952,#17953,#17954,#17955,#17956,#17957,#17958,#17959,
#17960,#17961,#17962,#17963,#17964,#17965,#17966,#17967,#17968,#17969,#17970,
#17971,#17972,#17973,#17974,#17975,#17976,#17977,#17978,#17979,#17980,#17981,
#17982,#17983,#17984,#17985,#17986,#17987,#17988,#17989,#17990,#17991,#17992,
#17993,#17994,#17995,#17996,#17997,#17998,#17999,#18000,#18001,#18002,#18003,
#18004,#18005,#18006,#18007,#18008,#18009,#18010,#18011,#18012,#18013,#18014,
#18015,#18016,#18017,#18018,#18019,#18020,#18021,#18022,#18023,#18024,#18025,
#18026,#18027,#18028,#18029,#18030,#18031,#18032,#18033,#18034,#18035,#18036,
#18037,#18038,#18039,#18040,#18041,#18042,#18043,#18044,#18045,#18046,#18047,
#18048,#18049,#18050,#18051,#18052,#18053,#18054,#18055,#18056,#18057,#18058,
#18059,#18060,#18061,#18062,#18063,#18064,#18065,#18066,#18067,#18068,#18069,
#18070,#18071,#18072,#18073,#18074,#18075,#18076,#18077,#18078,#18079,#18080,
#18081,#18082,#18083,#18084,#18085,#18086));
#18272=CLOSED_SHELL('',(#18087,#18088,#18089,#18090,#18091,#18092,#18093,
#18094,#18095,#18096,#18097,#18098,#18099,#18100,#18101,#18102,#18103,#18104,
#18105,#18106,#18107,#18108,#18109,#18110,#18111,#18112));
#18273=CLOSED_SHELL('',(#18113,#18114,#18115,#18116,#18117,#18118));
#18274=CLOSED_SHELL('',(#18119,#18120,#18121));
#18275=CLOSED_SHELL('',(#18122,#18123,#18124,#18125,#18126,#18127,#18128,
#18129,#18130,#18131,#18132,#18133,#18134,#18135,#18136,#18137,#18138,#18139,
#18140,#18141,#18142,#18143));
#18276=CLOSED_SHELL('',(#18144,#18145,#18146,#18147));
#18277=CLOSED_SHELL('',(#18148,#18149,#18150,#18151,#18152,#18153,#18154,
#18155,#18156,#18157,#18158,#18159,#18160,#18161,#18162,#18163));
#18278=CLOSED_SHELL('',(#18164,#18165,#18166,#18167));
#18279=CLOSED_SHELL('',(#18168,#18169,#18170,#18171));
#18280=CLOSED_SHELL('',(#18172,#18173,#18174,#18175));
#18281=CLOSED_SHELL('',(#18176,#18177,#18178,#18179,#18180,#18181));
#18282=CLOSED_SHELL('',(#18182,#18183,#18184,#18185,#18186));
#18283=CLOSED_SHELL('',(#18187,#18188,#18189));
#18284=CLOSED_SHELL('',(#18190,#18191,#18192,#18193,#18194,#18195,#18196,
#18197,#18198,#18199,#18200,#18201,#18202,#18203,#18204,#18205,#18206,#18207,
#18208,#18209,#18210,#18211,#18212,#18213,#18214,#18215,#18216,#18217,#18218,
#18219,#18220,#18221,#18222,#18223,#18224,#18225,#18226,#18227,#18228,#18229,
#18230,#18231,#18232,#18233,#18234,#18235,#18236,#18237));
#18285=CLOSED_SHELL('',(#18238,#18239,#18240,#18241,#18242,#18243,#18244,
#18245,#18246,#18247,#18248,#18249,#18250,#18251,#18252,#18253,#18254,#18255,
#18256,#18257,#18258,#18259,#18260,#18261,#18262,#18263,#18264,#18265,#18266,
#18267,#18268,#18269));
#18286=DERIVED_UNIT_ELEMENT(#18318,1.);
#18287=DERIVED_UNIT_ELEMENT(#99528,-3.);
#18288=DERIVED_UNIT_ELEMENT(#18318,1.);
#18289=DERIVED_UNIT_ELEMENT(#99528,-3.);
#18290=DERIVED_UNIT_ELEMENT(#18318,1.);
#18291=DERIVED_UNIT_ELEMENT(#99528,-3.);
#18292=DERIVED_UNIT_ELEMENT(#18318,1.);
#18293=DERIVED_UNIT_ELEMENT(#99528,-3.);
#18294=DERIVED_UNIT_ELEMENT(#18318,1.);
#18295=DERIVED_UNIT_ELEMENT(#99528,-3.);
#18296=DERIVED_UNIT_ELEMENT(#18318,1.);
#18297=DERIVED_UNIT_ELEMENT(#99528,-3.);
#18298=DERIVED_UNIT_ELEMENT(#18318,1.);
#18299=DERIVED_UNIT_ELEMENT(#99528,-3.);
#18300=DERIVED_UNIT_ELEMENT(#18318,1.);
#18301=DERIVED_UNIT_ELEMENT(#99528,-3.);
#18302=DERIVED_UNIT_ELEMENT(#18318,1.);
#18303=DERIVED_UNIT_ELEMENT(#99528,-3.);
#18304=DERIVED_UNIT_ELEMENT(#18318,1.);
#18305=DERIVED_UNIT_ELEMENT(#99528,-3.);
#18306=DERIVED_UNIT_ELEMENT(#18318,1.);
#18307=DERIVED_UNIT_ELEMENT(#99528,-3.);
#18308=DERIVED_UNIT_ELEMENT(#18318,1.);
#18309=DERIVED_UNIT_ELEMENT(#99528,-3.);
#18310=DERIVED_UNIT_ELEMENT(#18318,1.);
#18311=DERIVED_UNIT_ELEMENT(#99528,-3.);
#18312=DERIVED_UNIT_ELEMENT(#18318,1.);
#18313=DERIVED_UNIT_ELEMENT(#99528,-3.);
#18314=DERIVED_UNIT_ELEMENT(#18318,1.);
#18315=DERIVED_UNIT_ELEMENT(#99528,-3.);
#18316=DERIVED_UNIT_ELEMENT(#18318,1.);
#18317=DERIVED_UNIT_ELEMENT(#99528,-3.);
#18318=(
MASS_UNIT()
NAMED_UNIT(*)
SI_UNIT(.KILO.,.GRAM.)
);
#18319=DERIVED_UNIT((#18286,#18287));
#18320=DERIVED_UNIT((#18288,#18289));
#18321=DERIVED_UNIT((#18290,#18291));
#18322=DERIVED_UNIT((#18292,#18293));
#18323=DERIVED_UNIT((#18294,#18295));
#18324=DERIVED_UNIT((#18296,#18297));
#18325=DERIVED_UNIT((#18298,#18299));
#18326=DERIVED_UNIT((#18300,#18301));
#18327=DERIVED_UNIT((#18302,#18303));
#18328=DERIVED_UNIT((#18304,#18305));
#18329=DERIVED_UNIT((#18306,#18307));
#18330=DERIVED_UNIT((#18308,#18309));
#18331=DERIVED_UNIT((#18310,#18311));
#18332=DERIVED_UNIT((#18312,#18313));
#18333=DERIVED_UNIT((#18314,#18315));
#18334=DERIVED_UNIT((#18316,#18317));
#18335=MEASURE_REPRESENTATION_ITEM('density measure',
POSITIVE_RATIO_MEASURE(7850.),#18319);
#18336=MEASURE_REPRESENTATION_ITEM('density measure',
POSITIVE_RATIO_MEASURE(7850.),#18320);
#18337=MEASURE_REPRESENTATION_ITEM('density measure',
POSITIVE_RATIO_MEASURE(7850.),#18321);
#18338=MEASURE_REPRESENTATION_ITEM('density measure',
POSITIVE_RATIO_MEASURE(7850.),#18322);
#18339=MEASURE_REPRESENTATION_ITEM('density measure',
POSITIVE_RATIO_MEASURE(7850.),#18323);
#18340=MEASURE_REPRESENTATION_ITEM('density measure',
POSITIVE_RATIO_MEASURE(7850.),#18324);
#18341=MEASURE_REPRESENTATION_ITEM('density measure',
POSITIVE_RATIO_MEASURE(8920.),#18325);
#18342=MEASURE_REPRESENTATION_ITEM('density measure',
POSITIVE_RATIO_MEASURE(7850.),#18326);
#18343=MEASURE_REPRESENTATION_ITEM('density measure',
POSITIVE_RATIO_MEASURE(8920.),#18327);
#18344=MEASURE_REPRESENTATION_ITEM('density measure',
POSITIVE_RATIO_MEASURE(8920.),#18328);
#18345=MEASURE_REPRESENTATION_ITEM('density measure',
POSITIVE_RATIO_MEASURE(7850.),#18329);
#18346=MEASURE_REPRESENTATION_ITEM('density measure',
POSITIVE_RATIO_MEASURE(7850.),#18330);
#18347=MEASURE_REPRESENTATION_ITEM('density measure',
POSITIVE_RATIO_MEASURE(7850.),#18331);
#18348=MEASURE_REPRESENTATION_ITEM('density measure',
POSITIVE_RATIO_MEASURE(7850.),#18332);
#18349=MEASURE_REPRESENTATION_ITEM('density measure',
POSITIVE_RATIO_MEASURE(7850.),#18333);
#18350=MEASURE_REPRESENTATION_ITEM('density measure',
POSITIVE_RATIO_MEASURE(7850.),#18334);
#18351=PROPERTY_DEFINITION_REPRESENTATION(#18431,#18383);
#18352=PROPERTY_DEFINITION_REPRESENTATION(#18432,#18384);
#18353=PROPERTY_DEFINITION_REPRESENTATION(#18433,#18385);
#18354=PROPERTY_DEFINITION_REPRESENTATION(#18434,#18386);
#18355=PROPERTY_DEFINITION_REPRESENTATION(#18435,#18387);
#18356=PROPERTY_DEFINITION_REPRESENTATION(#18436,#18388);
#18357=PROPERTY_DEFINITION_REPRESENTATION(#18437,#18389);
#18358=PROPERTY_DEFINITION_REPRESENTATION(#18438,#18390);
#18359=PROPERTY_DEFINITION_REPRESENTATION(#18439,#18391);
#18360=PROPERTY_DEFINITION_REPRESENTATION(#18440,#18392);
#18361=PROPERTY_DEFINITION_REPRESENTATION(#18441,#18393);
#18362=PROPERTY_DEFINITION_REPRESENTATION(#18442,#18394);
#18363=PROPERTY_DEFINITION_REPRESENTATION(#18443,#18395);
#18364=PROPERTY_DEFINITION_REPRESENTATION(#18444,#18396);
#18365=PROPERTY_DEFINITION_REPRESENTATION(#18445,#18397);
#18366=PROPERTY_DEFINITION_REPRESENTATION(#18446,#18398);
#18367=PROPERTY_DEFINITION_REPRESENTATION(#18447,#18399);
#18368=PROPERTY_DEFINITION_REPRESENTATION(#18448,#18400);
#18369=PROPERTY_DEFINITION_REPRESENTATION(#18449,#18401);
#18370=PROPERTY_DEFINITION_REPRESENTATION(#18450,#18402);
#18371=PROPERTY_DEFINITION_REPRESENTATION(#18451,#18403);
#18372=PROPERTY_DEFINITION_REPRESENTATION(#18452,#18404);
#18373=PROPERTY_DEFINITION_REPRESENTATION(#18453,#18405);
#18374=PROPERTY_DEFINITION_REPRESENTATION(#18454,#18406);
#18375=PROPERTY_DEFINITION_REPRESENTATION(#18455,#18407);
#18376=PROPERTY_DEFINITION_REPRESENTATION(#18456,#18408);
#18377=PROPERTY_DEFINITION_REPRESENTATION(#18457,#18409);
#18378=PROPERTY_DEFINITION_REPRESENTATION(#18458,#18410);
#18379=PROPERTY_DEFINITION_REPRESENTATION(#18459,#18411);
#18380=PROPERTY_DEFINITION_REPRESENTATION(#18460,#18412);
#18381=PROPERTY_DEFINITION_REPRESENTATION(#18461,#18413);
#18382=PROPERTY_DEFINITION_REPRESENTATION(#18462,#18414);
#18383=REPRESENTATION('material name',(#18415),#99510);
#18384=REPRESENTATION('density',(#18335),#99510);
#18385=REPRESENTATION('material name',(#18416),#99511);
#18386=REPRESENTATION('density',(#18336),#99511);
#18387=REPRESENTATION('material name',(#18417),#99512);
#18388=REPRESENTATION('density',(#18337),#99512);
#18389=REPRESENTATION('material name',(#18418),#99513);
#18390=REPRESENTATION('density',(#18338),#99513);
#18391=REPRESENTATION('material name',(#18419),#99514);
#18392=REPRESENTATION('density',(#18339),#99514);
#18393=REPRESENTATION('material name',(#18420),#99515);
#18394=REPRESENTATION('density',(#18340),#99515);
#18395=REPRESENTATION('material name',(#18421),#99516);
#18396=REPRESENTATION('density',(#18341),#99516);
#18397=REPRESENTATION('material name',(#18422),#99517);
#18398=REPRESENTATION('density',(#18342),#99517);
#18399=REPRESENTATION('material name',(#18423),#99518);
#18400=REPRESENTATION('density',(#18343),#99518);
#18401=REPRESENTATION('material name',(#18424),#99519);
#18402=REPRESENTATION('density',(#18344),#99519);
#18403=REPRESENTATION('material name',(#18425),#99520);
#18404=REPRESENTATION('density',(#18345),#99520);
#18405=REPRESENTATION('material name',(#18426),#99521);
#18406=REPRESENTATION('density',(#18346),#99521);
#18407=REPRESENTATION('material name',(#18427),#99522);
#18408=REPRESENTATION('density',(#18347),#99522);
#18409=REPRESENTATION('material name',(#18428),#99523);
#18410=REPRESENTATION('density',(#18348),#99523);
#18411=REPRESENTATION('material name',(#18429),#99524);
#18412=REPRESENTATION('density',(#18349),#99524);
#18413=REPRESENTATION('material name',(#18430),#99525);
#18414=REPRESENTATION('density',(#18350),#99525);
#18415=DESCRIPTIVE_REPRESENTATION_ITEM('Steel','Steel');
#18416=DESCRIPTIVE_REPRESENTATION_ITEM('Steel','Steel');
#18417=DESCRIPTIVE_REPRESENTATION_ITEM('Steel','Steel');
#18418=DESCRIPTIVE_REPRESENTATION_ITEM('Steel','Steel');
#18419=DESCRIPTIVE_REPRESENTATION_ITEM('Steel','Steel');
#18420=DESCRIPTIVE_REPRESENTATION_ITEM('Steel','Steel');
#18421=DESCRIPTIVE_REPRESENTATION_ITEM('Copper, Alloy','Copper, Alloy');
#18422=DESCRIPTIVE_REPRESENTATION_ITEM('Steel','Steel');
#18423=DESCRIPTIVE_REPRESENTATION_ITEM('Copper, Alloy','Copper, Alloy');
#18424=DESCRIPTIVE_REPRESENTATION_ITEM('Copper, Alloy','Copper, Alloy');
#18425=DESCRIPTIVE_REPRESENTATION_ITEM('Steel','Steel');
#18426=DESCRIPTIVE_REPRESENTATION_ITEM('Steel','Steel');
#18427=DESCRIPTIVE_REPRESENTATION_ITEM('Steel','Steel');
#18428=DESCRIPTIVE_REPRESENTATION_ITEM('Steel','Steel');
#18429=DESCRIPTIVE_REPRESENTATION_ITEM('Steel','Steel');
#18430=DESCRIPTIVE_REPRESENTATION_ITEM('Steel','Steel');
#18431=PROPERTY_DEFINITION('material property','material name',#99643);
#18432=PROPERTY_DEFINITION('material property','density of part',#99643);
#18433=PROPERTY_DEFINITION('material property','material name',#99644);
#18434=PROPERTY_DEFINITION('material property','density of part',#99644);
#18435=PROPERTY_DEFINITION('material property','material name',#99645);
#18436=PROPERTY_DEFINITION('material property','density of part',#99645);
#18437=PROPERTY_DEFINITION('material property','material name',#99646);
#18438=PROPERTY_DEFINITION('material property','density of part',#99646);
#18439=PROPERTY_DEFINITION('material property','material name',#99647);
#18440=PROPERTY_DEFINITION('material property','density of part',#99647);
#18441=PROPERTY_DEFINITION('material property','material name',#99648);
#18442=PROPERTY_DEFINITION('material property','density of part',#99648);
#18443=PROPERTY_DEFINITION('material property','material name',#99649);
#18444=PROPERTY_DEFINITION('material property','density of part',#99649);
#18445=PROPERTY_DEFINITION('material property','material name',#99650);
#18446=PROPERTY_DEFINITION('material property','density of part',#99650);
#18447=PROPERTY_DEFINITION('material property','material name',#99651);
#18448=PROPERTY_DEFINITION('material property','density of part',#99651);
#18449=PROPERTY_DEFINITION('material property','material name',#99652);
#18450=PROPERTY_DEFINITION('material property','density of part',#99652);
#18451=PROPERTY_DEFINITION('material property','material name',#99653);
#18452=PROPERTY_DEFINITION('material property','density of part',#99653);
#18453=PROPERTY_DEFINITION('material property','material name',#99654);
#18454=PROPERTY_DEFINITION('material property','density of part',#99654);
#18455=PROPERTY_DEFINITION('material property','material name',#99655);
#18456=PROPERTY_DEFINITION('material property','density of part',#99655);
#18457=PROPERTY_DEFINITION('material property','material name',#99656);
#18458=PROPERTY_DEFINITION('material property','density of part',#99656);
#18459=PROPERTY_DEFINITION('material property','material name',#99657);
#18460=PROPERTY_DEFINITION('material property','density of part',#99657);
#18461=PROPERTY_DEFINITION('material property','material name',#99658);
#18462=PROPERTY_DEFINITION('material property','density of part',#99658);
#18463=AXIS2_PLACEMENT_3D('',#23375,#19799,#19800);
#18464=AXIS2_PLACEMENT_3D('',#23376,#19801,#19802);
#18465=AXIS2_PLACEMENT_3D('',#23377,#19803,#19804);
#18466=AXIS2_PLACEMENT_3D('',#23405,#19806,#19807);
#18467=AXIS2_PLACEMENT_3D('',#23416,#19809,#19810);
#18468=AXIS2_PLACEMENT_3D('',#23439,#19811,#19812);
#18469=AXIS2_PLACEMENT_3D('',#23490,#19814,#19815);
#18470=AXIS2_PLACEMENT_3D('',#23538,#19817,#19818);
#18471=AXIS2_PLACEMENT_3D('',#23586,#19820,#19821);
#18472=AXIS2_PLACEMENT_3D('',#23637,#19823,#19824);
#18473=AXIS2_PLACEMENT_3D('',#23685,#19826,#19827);
#18474=AXIS2_PLACEMENT_3D('',#23733,#19829,#19830);
#18475=AXIS2_PLACEMENT_3D('',#23784,#19832,#19833);
#18476=AXIS2_PLACEMENT_3D('',#23835,#19835,#19836);
#18477=AXIS2_PLACEMENT_3D('',#23883,#19838,#19839);
#18478=AXIS2_PLACEMENT_3D('',#23934,#19841,#19842);
#18479=AXIS2_PLACEMENT_3D('',#23953,#19844,#19845);
#18480=AXIS2_PLACEMENT_3D('',#23973,#19846,#19847);
#18481=AXIS2_PLACEMENT_3D('',#23986,#19849,#19850);
#18482=AXIS2_PLACEMENT_3D('',#23995,#19851,#19852);
#18483=AXIS2_PLACEMENT_3D('',#24019,#19854,#19855);
#18484=AXIS2_PLACEMENT_3D('',#24044,#19857,#19858);
#18485=AXIS2_PLACEMENT_3D('',#24069,#19860,#19861);
#18486=AXIS2_PLACEMENT_3D('',#24093,#19863,#19864);
#18487=AXIS2_PLACEMENT_3D('',#24118,#19866,#19867);
#18488=AXIS2_PLACEMENT_3D('',#24142,#19869,#19870);
#18489=AXIS2_PLACEMENT_3D('',#24167,#19872,#19873);
#18490=AXIS2_PLACEMENT_3D('',#24191,#19875,#19876);
#18491=AXIS2_PLACEMENT_3D('',#24216,#19878,#19879);
#18492=AXIS2_PLACEMENT_3D('',#24241,#19881,#19882);
#18493=AXIS2_PLACEMENT_3D('',#24265,#19884,#19885);
#18494=AXIS2_PLACEMENT_3D('',#24276,#19887,#19888);
#18495=AXIS2_PLACEMENT_3D('',#24282,#19889,#19890);
#18496=AXIS2_PLACEMENT_3D('',#24310,#19892,#19893);
#18497=AXIS2_PLACEMENT_3D('',#24321,#19895,#19896);
#18498=AXIS2_PLACEMENT_3D('',#24344,#19897,#19898);
#18499=AXIS2_PLACEMENT_3D('',#24395,#19900,#19901);
#18500=AXIS2_PLACEMENT_3D('',#24443,#19903,#19904);
#18501=AXIS2_PLACEMENT_3D('',#24491,#19906,#19907);
#18502=AXIS2_PLACEMENT_3D('',#24542,#19909,#19910);
#18503=AXIS2_PLACEMENT_3D('',#24590,#19912,#19913);
#18504=AXIS2_PLACEMENT_3D('',#24638,#19915,#19916);
#18505=AXIS2_PLACEMENT_3D('',#24689,#19918,#19919);
#18506=AXIS2_PLACEMENT_3D('',#24740,#19921,#19922);
#18507=AXIS2_PLACEMENT_3D('',#24788,#19924,#19925);
#18508=AXIS2_PLACEMENT_3D('',#24839,#19927,#19928);
#18509=AXIS2_PLACEMENT_3D('',#24858,#19930,#19931);
#18510=AXIS2_PLACEMENT_3D('',#24878,#19932,#19933);
#18511=AXIS2_PLACEMENT_3D('',#24891,#19935,#19936);
#18512=AXIS2_PLACEMENT_3D('',#24900,#19937,#19938);
#18513=AXIS2_PLACEMENT_3D('',#24924,#19940,#19941);
#18514=AXIS2_PLACEMENT_3D('',#24949,#19943,#19944);
#18515=AXIS2_PLACEMENT_3D('',#24974,#19946,#19947);
#18516=AXIS2_PLACEMENT_3D('',#24998,#19949,#19950);
#18517=AXIS2_PLACEMENT_3D('',#25023,#19952,#19953);
#18518=AXIS2_PLACEMENT_3D('',#25047,#19955,#19956);
#18519=AXIS2_PLACEMENT_3D('',#25072,#19958,#19959);
#18520=AXIS2_PLACEMENT_3D('',#25096,#19961,#19962);
#18521=AXIS2_PLACEMENT_3D('',#25121,#19964,#19965);
#18522=AXIS2_PLACEMENT_3D('',#25146,#19967,#19968);
#18523=AXIS2_PLACEMENT_3D('',#25170,#19970,#19971);
#18524=AXIS2_PLACEMENT_3D('',#25181,#19973,#19974);
#18525=AXIS2_PLACEMENT_3D('',#25187,#19975,#19976);
#18526=AXIS2_PLACEMENT_3D('',#25215,#19978,#19979);
#18527=AXIS2_PLACEMENT_3D('',#25226,#19981,#19982);
#18528=AXIS2_PLACEMENT_3D('',#25249,#19983,#19984);
#18529=AXIS2_PLACEMENT_3D('',#25300,#19986,#19987);
#18530=AXIS2_PLACEMENT_3D('',#25348,#19989,#19990);
#18531=AXIS2_PLACEMENT_3D('',#25396,#19992,#19993);
#18532=AXIS2_PLACEMENT_3D('',#25447,#19995,#19996);
#18533=AXIS2_PLACEMENT_3D('',#25495,#19998,#19999);
#18534=AXIS2_PLACEMENT_3D('',#25543,#20001,#20002);
#18535=AXIS2_PLACEMENT_3D('',#25594,#20004,#20005);
#18536=AXIS2_PLACEMENT_3D('',#25645,#20007,#20008);
#18537=AXIS2_PLACEMENT_3D('',#25693,#20010,#20011);
#18538=AXIS2_PLACEMENT_3D('',#25744,#20013,#20014);
#18539=AXIS2_PLACEMENT_3D('',#25763,#20016,#20017);
#18540=AXIS2_PLACEMENT_3D('',#25783,#20018,#20019);
#18541=AXIS2_PLACEMENT_3D('',#25796,#20021,#20022);
#18542=AXIS2_PLACEMENT_3D('',#25805,#20023,#20024);
#18543=AXIS2_PLACEMENT_3D('',#25829,#20026,#20027);
#18544=AXIS2_PLACEMENT_3D('',#25854,#20029,#20030);
#18545=AXIS2_PLACEMENT_3D('',#25879,#20032,#20033);
#18546=AXIS2_PLACEMENT_3D('',#25903,#20035,#20036);
#18547=AXIS2_PLACEMENT_3D('',#25928,#20038,#20039);
#18548=AXIS2_PLACEMENT_3D('',#25952,#20041,#20042);
#18549=AXIS2_PLACEMENT_3D('',#25977,#20044,#20045);
#18550=AXIS2_PLACEMENT_3D('',#26001,#20047,#20048);
#18551=AXIS2_PLACEMENT_3D('',#26026,#20050,#20051);
#18552=AXIS2_PLACEMENT_3D('',#26051,#20053,#20054);
#18553=AXIS2_PLACEMENT_3D('',#26075,#20056,#20057);
#18554=AXIS2_PLACEMENT_3D('',#26086,#20059,#20060);
#18555=AXIS2_PLACEMENT_3D('',#26092,#20061,#20062);
#18556=AXIS2_PLACEMENT_3D('',#26120,#20064,#20065);
#18557=AXIS2_PLACEMENT_3D('',#26131,#20067,#20068);
#18558=AXIS2_PLACEMENT_3D('',#26154,#20069,#20070);
#18559=AXIS2_PLACEMENT_3D('',#26205,#20072,#20073);
#18560=AXIS2_PLACEMENT_3D('',#26253,#20075,#20076);
#18561=AXIS2_PLACEMENT_3D('',#26301,#20078,#20079);
#18562=AXIS2_PLACEMENT_3D('',#26352,#20081,#20082);
#18563=AXIS2_PLACEMENT_3D('',#26400,#20084,#20085);
#18564=AXIS2_PLACEMENT_3D('',#26448,#20087,#20088);
#18565=AXIS2_PLACEMENT_3D('',#26499,#20090,#20091);
#18566=AXIS2_PLACEMENT_3D('',#26550,#20093,#20094);
#18567=AXIS2_PLACEMENT_3D('',#26598,#20096,#20097);
#18568=AXIS2_PLACEMENT_3D('',#26649,#20099,#20100);
#18569=AXIS2_PLACEMENT_3D('',#26668,#20102,#20103);
#18570=AXIS2_PLACEMENT_3D('',#26688,#20104,#20105);
#18571=AXIS2_PLACEMENT_3D('',#26701,#20107,#20108);
#18572=AXIS2_PLACEMENT_3D('',#26710,#20109,#20110);
#18573=AXIS2_PLACEMENT_3D('',#26734,#20112,#20113);
#18574=AXIS2_PLACEMENT_3D('',#26759,#20115,#20116);
#18575=AXIS2_PLACEMENT_3D('',#26784,#20118,#20119);
#18576=AXIS2_PLACEMENT_3D('',#26808,#20121,#20122);
#18577=AXIS2_PLACEMENT_3D('',#26833,#20124,#20125);
#18578=AXIS2_PLACEMENT_3D('',#26857,#20127,#20128);
#18579=AXIS2_PLACEMENT_3D('',#26882,#20130,#20131);
#18580=AXIS2_PLACEMENT_3D('',#26906,#20133,#20134);
#18581=AXIS2_PLACEMENT_3D('',#26931,#20136,#20137);
#18582=AXIS2_PLACEMENT_3D('',#26956,#20139,#20140);
#18583=AXIS2_PLACEMENT_3D('',#26980,#20142,#20143);
#18584=AXIS2_PLACEMENT_3D('',#26991,#20145,#20146);
#18585=AXIS2_PLACEMENT_3D('',#26997,#20147,#20148);
#18586=AXIS2_PLACEMENT_3D('',#27025,#20150,#20151);
#18587=AXIS2_PLACEMENT_3D('',#27036,#20153,#20154);
#18588=AXIS2_PLACEMENT_3D('',#27059,#20155,#20156);
#18589=AXIS2_PLACEMENT_3D('',#27110,#20158,#20159);
#18590=AXIS2_PLACEMENT_3D('',#27158,#20161,#20162);
#18591=AXIS2_PLACEMENT_3D('',#27206,#20164,#20165);
#18592=AXIS2_PLACEMENT_3D('',#27257,#20167,#20168);
#18593=AXIS2_PLACEMENT_3D('',#27305,#20170,#20171);
#18594=AXIS2_PLACEMENT_3D('',#27353,#20173,#20174);
#18595=AXIS2_PLACEMENT_3D('',#27404,#20176,#20177);
#18596=AXIS2_PLACEMENT_3D('',#27455,#20179,#20180);
#18597=AXIS2_PLACEMENT_3D('',#27503,#20182,#20183);
#18598=AXIS2_PLACEMENT_3D('',#27554,#20185,#20186);
#18599=AXIS2_PLACEMENT_3D('',#27573,#20188,#20189);
#18600=AXIS2_PLACEMENT_3D('',#27593,#20190,#20191);
#18601=AXIS2_PLACEMENT_3D('',#27606,#20193,#20194);
#18602=AXIS2_PLACEMENT_3D('',#27615,#20195,#20196);
#18603=AXIS2_PLACEMENT_3D('',#27639,#20198,#20199);
#18604=AXIS2_PLACEMENT_3D('',#27664,#20201,#20202);
#18605=AXIS2_PLACEMENT_3D('',#27689,#20204,#20205);
#18606=AXIS2_PLACEMENT_3D('',#27713,#20207,#20208);
#18607=AXIS2_PLACEMENT_3D('',#27738,#20210,#20211);
#18608=AXIS2_PLACEMENT_3D('',#27762,#20213,#20214);
#18609=AXIS2_PLACEMENT_3D('',#27787,#20216,#20217);
#18610=AXIS2_PLACEMENT_3D('',#27811,#20219,#20220);
#18611=AXIS2_PLACEMENT_3D('',#27836,#20222,#20223);
#18612=AXIS2_PLACEMENT_3D('',#27861,#20225,#20226);
#18613=AXIS2_PLACEMENT_3D('',#27885,#20228,#20229);
#18614=AXIS2_PLACEMENT_3D('',#27896,#20231,#20232);
#18615=AXIS2_PLACEMENT_3D('',#27902,#20233,#20234);
#18616=AXIS2_PLACEMENT_3D('',#27930,#20236,#20237);
#18617=AXIS2_PLACEMENT_3D('',#27941,#20239,#20240);
#18618=AXIS2_PLACEMENT_3D('',#27964,#20241,#20242);
#18619=AXIS2_PLACEMENT_3D('',#28015,#20244,#20245);
#18620=AXIS2_PLACEMENT_3D('',#28063,#20247,#20248);
#18621=AXIS2_PLACEMENT_3D('',#28111,#20250,#20251);
#18622=AXIS2_PLACEMENT_3D('',#28162,#20253,#20254);
#18623=AXIS2_PLACEMENT_3D('',#28210,#20256,#20257);
#18624=AXIS2_PLACEMENT_3D('',#28258,#20259,#20260);
#18625=AXIS2_PLACEMENT_3D('',#28309,#20262,#20263);
#18626=AXIS2_PLACEMENT_3D('',#28360,#20265,#20266);
#18627=AXIS2_PLACEMENT_3D('',#28408,#20268,#20269);
#18628=AXIS2_PLACEMENT_3D('',#28459,#20271,#20272);
#18629=AXIS2_PLACEMENT_3D('',#28478,#20274,#20275);
#18630=AXIS2_PLACEMENT_3D('',#28498,#20276,#20277);
#18631=AXIS2_PLACEMENT_3D('',#28511,#20279,#20280);
#18632=AXIS2_PLACEMENT_3D('',#28520,#20281,#20282);
#18633=AXIS2_PLACEMENT_3D('',#28544,#20284,#20285);
#18634=AXIS2_PLACEMENT_3D('',#28569,#20287,#20288);
#18635=AXIS2_PLACEMENT_3D('',#28594,#20290,#20291);
#18636=AXIS2_PLACEMENT_3D('',#28618,#20293,#20294);
#18637=AXIS2_PLACEMENT_3D('',#28643,#20296,#20297);
#18638=AXIS2_PLACEMENT_3D('',#28667,#20299,#20300);
#18639=AXIS2_PLACEMENT_3D('',#28692,#20302,#20303);
#18640=AXIS2_PLACEMENT_3D('',#28716,#20305,#20306);
#18641=AXIS2_PLACEMENT_3D('',#28741,#20308,#20309);
#18642=AXIS2_PLACEMENT_3D('',#28766,#20311,#20312);
#18643=AXIS2_PLACEMENT_3D('',#28790,#20314,#20315);
#18644=AXIS2_PLACEMENT_3D('',#28801,#20317,#20318);
#18645=AXIS2_PLACEMENT_3D('',#28807,#20319,#20320);
#18646=AXIS2_PLACEMENT_3D('',#28835,#20322,#20323);
#18647=AXIS2_PLACEMENT_3D('',#28846,#20325,#20326);
#18648=AXIS2_PLACEMENT_3D('',#28869,#20327,#20328);
#18649=AXIS2_PLACEMENT_3D('',#28920,#20330,#20331);
#18650=AXIS2_PLACEMENT_3D('',#28968,#20333,#20334);
#18651=AXIS2_PLACEMENT_3D('',#29016,#20336,#20337);
#18652=AXIS2_PLACEMENT_3D('',#29067,#20339,#20340);
#18653=AXIS2_PLACEMENT_3D('',#29115,#20342,#20343);
#18654=AXIS2_PLACEMENT_3D('',#29163,#20345,#20346);
#18655=AXIS2_PLACEMENT_3D('',#29214,#20348,#20349);
#18656=AXIS2_PLACEMENT_3D('',#29265,#20351,#20352);
#18657=AXIS2_PLACEMENT_3D('',#29313,#20354,#20355);
#18658=AXIS2_PLACEMENT_3D('',#29364,#20357,#20358);
#18659=AXIS2_PLACEMENT_3D('',#29383,#20360,#20361);
#18660=AXIS2_PLACEMENT_3D('',#29403,#20362,#20363);
#18661=AXIS2_PLACEMENT_3D('',#29416,#20365,#20366);
#18662=AXIS2_PLACEMENT_3D('',#29425,#20367,#20368);
#18663=AXIS2_PLACEMENT_3D('',#29449,#20370,#20371);
#18664=AXIS2_PLACEMENT_3D('',#29474,#20373,#20374);
#18665=AXIS2_PLACEMENT_3D('',#29499,#20376,#20377);
#18666=AXIS2_PLACEMENT_3D('',#29523,#20379,#20380);
#18667=AXIS2_PLACEMENT_3D('',#29548,#20382,#20383);
#18668=AXIS2_PLACEMENT_3D('',#29572,#20385,#20386);
#18669=AXIS2_PLACEMENT_3D('',#29597,#20388,#20389);
#18670=AXIS2_PLACEMENT_3D('',#29621,#20391,#20392);
#18671=AXIS2_PLACEMENT_3D('',#29646,#20394,#20395);
#18672=AXIS2_PLACEMENT_3D('',#29671,#20397,#20398);
#18673=AXIS2_PLACEMENT_3D('',#29695,#20400,#20401);
#18674=AXIS2_PLACEMENT_3D('',#29706,#20403,#20404);
#18675=AXIS2_PLACEMENT_3D('',#29712,#20405,#20406);
#18676=AXIS2_PLACEMENT_3D('',#29740,#20408,#20409);
#18677=AXIS2_PLACEMENT_3D('',#29751,#20411,#20412);
#18678=AXIS2_PLACEMENT_3D('',#29774,#20413,#20414);
#18679=AXIS2_PLACEMENT_3D('',#29825,#20416,#20417);
#18680=AXIS2_PLACEMENT_3D('',#29873,#20419,#20420);
#18681=AXIS2_PLACEMENT_3D('',#29921,#20422,#20423);
#18682=AXIS2_PLACEMENT_3D('',#29972,#20425,#20426);
#18683=AXIS2_PLACEMENT_3D('',#30020,#20428,#20429);
#18684=AXIS2_PLACEMENT_3D('',#30068,#20431,#20432);
#18685=AXIS2_PLACEMENT_3D('',#30119,#20434,#20435);
#18686=AXIS2_PLACEMENT_3D('',#30170,#20437,#20438);
#18687=AXIS2_PLACEMENT_3D('',#30218,#20440,#20441);
#18688=AXIS2_PLACEMENT_3D('',#30269,#20443,#20444);
#18689=AXIS2_PLACEMENT_3D('',#30288,#20446,#20447);
#18690=AXIS2_PLACEMENT_3D('',#30308,#20448,#20449);
#18691=AXIS2_PLACEMENT_3D('',#30321,#20451,#20452);
#18692=AXIS2_PLACEMENT_3D('',#30330,#20453,#20454);
#18693=AXIS2_PLACEMENT_3D('',#30354,#20456,#20457);
#18694=AXIS2_PLACEMENT_3D('',#30379,#20459,#20460);
#18695=AXIS2_PLACEMENT_3D('',#30404,#20462,#20463);
#18696=AXIS2_PLACEMENT_3D('',#30428,#20465,#20466);
#18697=AXIS2_PLACEMENT_3D('',#30453,#20468,#20469);
#18698=AXIS2_PLACEMENT_3D('',#30477,#20471,#20472);
#18699=AXIS2_PLACEMENT_3D('',#30502,#20474,#20475);
#18700=AXIS2_PLACEMENT_3D('',#30526,#20477,#20478);
#18701=AXIS2_PLACEMENT_3D('',#30551,#20480,#20481);
#18702=AXIS2_PLACEMENT_3D('',#30576,#20483,#20484);
#18703=AXIS2_PLACEMENT_3D('',#30600,#20486,#20487);
#18704=AXIS2_PLACEMENT_3D('',#30611,#20489,#20490);
#18705=AXIS2_PLACEMENT_3D('',#30617,#20491,#20492);
#18706=AXIS2_PLACEMENT_3D('',#30645,#20494,#20495);
#18707=AXIS2_PLACEMENT_3D('',#30656,#20497,#20498);
#18708=AXIS2_PLACEMENT_3D('',#30679,#20499,#20500);
#18709=AXIS2_PLACEMENT_3D('',#30730,#20502,#20503);
#18710=AXIS2_PLACEMENT_3D('',#30778,#20505,#20506);
#18711=AXIS2_PLACEMENT_3D('',#30826,#20508,#20509);
#18712=AXIS2_PLACEMENT_3D('',#30877,#20511,#20512);
#18713=AXIS2_PLACEMENT_3D('',#30925,#20514,#20515);
#18714=AXIS2_PLACEMENT_3D('',#30973,#20517,#20518);
#18715=AXIS2_PLACEMENT_3D('',#31024,#20520,#20521);
#18716=AXIS2_PLACEMENT_3D('',#31075,#20523,#20524);
#18717=AXIS2_PLACEMENT_3D('',#31123,#20526,#20527);
#18718=AXIS2_PLACEMENT_3D('',#31174,#20529,#20530);
#18719=AXIS2_PLACEMENT_3D('',#31193,#20532,#20533);
#18720=AXIS2_PLACEMENT_3D('',#31213,#20534,#20535);
#18721=AXIS2_PLACEMENT_3D('',#31226,#20537,#20538);
#18722=AXIS2_PLACEMENT_3D('',#31235,#20539,#20540);
#18723=AXIS2_PLACEMENT_3D('',#31259,#20542,#20543);
#18724=AXIS2_PLACEMENT_3D('',#31284,#20545,#20546);
#18725=AXIS2_PLACEMENT_3D('',#31309,#20548,#20549);
#18726=AXIS2_PLACEMENT_3D('',#31333,#20551,#20552);
#18727=AXIS2_PLACEMENT_3D('',#31358,#20554,#20555);
#18728=AXIS2_PLACEMENT_3D('',#31382,#20557,#20558);
#18729=AXIS2_PLACEMENT_3D('',#31407,#20560,#20561);
#18730=AXIS2_PLACEMENT_3D('',#31431,#20563,#20564);
#18731=AXIS2_PLACEMENT_3D('',#31456,#20566,#20567);
#18732=AXIS2_PLACEMENT_3D('',#31481,#20569,#20570);
#18733=AXIS2_PLACEMENT_3D('',#31505,#20572,#20573);
#18734=AXIS2_PLACEMENT_3D('',#31516,#20575,#20576);
#18735=AXIS2_PLACEMENT_3D('',#31522,#20577,#20578);
#18736=AXIS2_PLACEMENT_3D('',#31550,#20580,#20581);
#18737=AXIS2_PLACEMENT_3D('',#31561,#20583,#20584);
#18738=AXIS2_PLACEMENT_3D('',#31584,#20585,#20586);
#18739=AXIS2_PLACEMENT_3D('',#31635,#20588,#20589);
#18740=AXIS2_PLACEMENT_3D('',#31683,#20591,#20592);
#18741=AXIS2_PLACEMENT_3D('',#31731,#20594,#20595);
#18742=AXIS2_PLACEMENT_3D('',#31782,#20597,#20598);
#18743=AXIS2_PLACEMENT_3D('',#31830,#20600,#20601);
#18744=AXIS2_PLACEMENT_3D('',#31878,#20603,#20604);
#18745=AXIS2_PLACEMENT_3D('',#31929,#20606,#20607);
#18746=AXIS2_PLACEMENT_3D('',#31980,#20609,#20610);
#18747=AXIS2_PLACEMENT_3D('',#32028,#20612,#20613);
#18748=AXIS2_PLACEMENT_3D('',#32079,#20615,#20616);
#18749=AXIS2_PLACEMENT_3D('',#32098,#20618,#20619);
#18750=AXIS2_PLACEMENT_3D('',#32118,#20620,#20621);
#18751=AXIS2_PLACEMENT_3D('',#32131,#20623,#20624);
#18752=AXIS2_PLACEMENT_3D('',#32140,#20625,#20626);
#18753=AXIS2_PLACEMENT_3D('',#32164,#20628,#20629);
#18754=AXIS2_PLACEMENT_3D('',#32189,#20631,#20632);
#18755=AXIS2_PLACEMENT_3D('',#32214,#20634,#20635);
#18756=AXIS2_PLACEMENT_3D('',#32238,#20637,#20638);
#18757=AXIS2_PLACEMENT_3D('',#32263,#20640,#20641);
#18758=AXIS2_PLACEMENT_3D('',#32287,#20643,#20644);
#18759=AXIS2_PLACEMENT_3D('',#32312,#20646,#20647);
#18760=AXIS2_PLACEMENT_3D('',#32336,#20649,#20650);
#18761=AXIS2_PLACEMENT_3D('',#32361,#20652,#20653);
#18762=AXIS2_PLACEMENT_3D('',#32386,#20655,#20656);
#18763=AXIS2_PLACEMENT_3D('',#32410,#20658,#20659);
#18764=AXIS2_PLACEMENT_3D('',#32421,#20661,#20662);
#18765=AXIS2_PLACEMENT_3D('',#32427,#20663,#20664);
#18766=AXIS2_PLACEMENT_3D('',#32455,#20666,#20667);
#18767=AXIS2_PLACEMENT_3D('',#32466,#20669,#20670);
#18768=AXIS2_PLACEMENT_3D('',#32489,#20671,#20672);
#18769=AXIS2_PLACEMENT_3D('',#32540,#20674,#20675);
#18770=AXIS2_PLACEMENT_3D('',#32588,#20677,#20678);
#18771=AXIS2_PLACEMENT_3D('',#32636,#20680,#20681);
#18772=AXIS2_PLACEMENT_3D('',#32687,#20683,#20684);
#18773=AXIS2_PLACEMENT_3D('',#32735,#20686,#20687);
#18774=AXIS2_PLACEMENT_3D('',#32783,#20689,#20690);
#18775=AXIS2_PLACEMENT_3D('',#32834,#20692,#20693);
#18776=AXIS2_PLACEMENT_3D('',#32885,#20695,#20696);
#18777=AXIS2_PLACEMENT_3D('',#32933,#20698,#20699);
#18778=AXIS2_PLACEMENT_3D('',#32984,#20701,#20702);
#18779=AXIS2_PLACEMENT_3D('',#33003,#20704,#20705);
#18780=AXIS2_PLACEMENT_3D('',#33023,#20706,#20707);
#18781=AXIS2_PLACEMENT_3D('',#33036,#20709,#20710);
#18782=AXIS2_PLACEMENT_3D('',#33045,#20711,#20712);
#18783=AXIS2_PLACEMENT_3D('',#33069,#20714,#20715);
#18784=AXIS2_PLACEMENT_3D('',#33094,#20717,#20718);
#18785=AXIS2_PLACEMENT_3D('',#33119,#20720,#20721);
#18786=AXIS2_PLACEMENT_3D('',#33143,#20723,#20724);
#18787=AXIS2_PLACEMENT_3D('',#33168,#20726,#20727);
#18788=AXIS2_PLACEMENT_3D('',#33192,#20729,#20730);
#18789=AXIS2_PLACEMENT_3D('',#33217,#20732,#20733);
#18790=AXIS2_PLACEMENT_3D('',#33241,#20735,#20736);
#18791=AXIS2_PLACEMENT_3D('',#33266,#20738,#20739);
#18792=AXIS2_PLACEMENT_3D('',#33291,#20741,#20742);
#18793=AXIS2_PLACEMENT_3D('',#33315,#20744,#20745);
#18794=AXIS2_PLACEMENT_3D('',#33326,#20747,#20748);
#18795=AXIS2_PLACEMENT_3D('',#33332,#20749,#20750);
#18796=AXIS2_PLACEMENT_3D('',#33360,#20752,#20753);
#18797=AXIS2_PLACEMENT_3D('',#33371,#20755,#20756);
#18798=AXIS2_PLACEMENT_3D('',#33394,#20757,#20758);
#18799=AXIS2_PLACEMENT_3D('',#33445,#20760,#20761);
#18800=AXIS2_PLACEMENT_3D('',#33493,#20763,#20764);
#18801=AXIS2_PLACEMENT_3D('',#33541,#20766,#20767);
#18802=AXIS2_PLACEMENT_3D('',#33592,#20769,#20770);
#18803=AXIS2_PLACEMENT_3D('',#33640,#20772,#20773);
#18804=AXIS2_PLACEMENT_3D('',#33688,#20775,#20776);
#18805=AXIS2_PLACEMENT_3D('',#33739,#20778,#20779);
#18806=AXIS2_PLACEMENT_3D('',#33790,#20781,#20782);
#18807=AXIS2_PLACEMENT_3D('',#33838,#20784,#20785);
#18808=AXIS2_PLACEMENT_3D('',#33889,#20787,#20788);
#18809=AXIS2_PLACEMENT_3D('',#33908,#20790,#20791);
#18810=AXIS2_PLACEMENT_3D('',#33928,#20792,#20793);
#18811=AXIS2_PLACEMENT_3D('',#33941,#20795,#20796);
#18812=AXIS2_PLACEMENT_3D('',#33950,#20797,#20798);
#18813=AXIS2_PLACEMENT_3D('',#33974,#20800,#20801);
#18814=AXIS2_PLACEMENT_3D('',#33999,#20803,#20804);
#18815=AXIS2_PLACEMENT_3D('',#34024,#20806,#20807);
#18816=AXIS2_PLACEMENT_3D('',#34048,#20809,#20810);
#18817=AXIS2_PLACEMENT_3D('',#34073,#20812,#20813);
#18818=AXIS2_PLACEMENT_3D('',#34097,#20815,#20816);
#18819=AXIS2_PLACEMENT_3D('',#34122,#20818,#20819);
#18820=AXIS2_PLACEMENT_3D('',#34146,#20821,#20822);
#18821=AXIS2_PLACEMENT_3D('',#34171,#20824,#20825);
#18822=AXIS2_PLACEMENT_3D('',#34196,#20827,#20828);
#18823=AXIS2_PLACEMENT_3D('',#34220,#20830,#20831);
#18824=AXIS2_PLACEMENT_3D('',#34231,#20833,#20834);
#18825=AXIS2_PLACEMENT_3D('',#34237,#20835,#20836);
#18826=AXIS2_PLACEMENT_3D('',#34247,#20838,#20839);
#18827=AXIS2_PLACEMENT_3D('',#34258,#20840,#20841);
#18828=AXIS2_PLACEMENT_3D('',#34309,#20843,#20844);
#18829=AXIS2_PLACEMENT_3D('',#34360,#20846,#20847);
#18830=AXIS2_PLACEMENT_3D('',#34408,#20849,#20850);
#18831=AXIS2_PLACEMENT_3D('',#34462,#20852,#20853);
#18832=AXIS2_PLACEMENT_3D('',#34510,#20855,#20856);
#18833=AXIS2_PLACEMENT_3D('',#34558,#20858,#20859);
#18834=AXIS2_PLACEMENT_3D('',#34608,#20861,#20862);
#18835=AXIS2_PLACEMENT_3D('',#34622,#20864,#20865);
#18836=AXIS2_PLACEMENT_3D('',#34632,#20866,#20867);
#18837=AXIS2_PLACEMENT_3D('',#34656,#20869,#20870);
#18838=AXIS2_PLACEMENT_3D('',#34681,#20872,#20873);
#18839=AXIS2_PLACEMENT_3D('',#34706,#20875,#20876);
#18840=AXIS2_PLACEMENT_3D('',#34731,#20878,#20879);
#18841=AXIS2_PLACEMENT_3D('',#34755,#20881,#20882);
#18842=AXIS2_PLACEMENT_3D('',#34780,#20884,#20885);
#18843=AXIS2_PLACEMENT_3D('',#34806,#20887,#20888);
#18844=AXIS2_PLACEMENT_3D('',#34816,#20890,#20891);
#18845=AXIS2_PLACEMENT_3D('',#34827,#20892,#20893);
#18846=AXIS2_PLACEMENT_3D('',#34878,#20895,#20896);
#18847=AXIS2_PLACEMENT_3D('',#34929,#20898,#20899);
#18848=AXIS2_PLACEMENT_3D('',#34977,#20901,#20902);
#18849=AXIS2_PLACEMENT_3D('',#35031,#20904,#20905);
#18850=AXIS2_PLACEMENT_3D('',#35079,#20907,#20908);
#18851=AXIS2_PLACEMENT_3D('',#35127,#20910,#20911);
#18852=AXIS2_PLACEMENT_3D('',#35177,#20913,#20914);
#18853=AXIS2_PLACEMENT_3D('',#35187,#20916,#20917);
#18854=AXIS2_PLACEMENT_3D('',#35198,#20918,#20919);
#18855=AXIS2_PLACEMENT_3D('',#35249,#20921,#20922);
#18856=AXIS2_PLACEMENT_3D('',#35300,#20924,#20925);
#18857=AXIS2_PLACEMENT_3D('',#35348,#20927,#20928);
#18858=AXIS2_PLACEMENT_3D('',#35402,#20930,#20931);
#18859=AXIS2_PLACEMENT_3D('',#35450,#20933,#20934);
#18860=AXIS2_PLACEMENT_3D('',#35498,#20936,#20937);
#18861=AXIS2_PLACEMENT_3D('',#35548,#20939,#20940);
#18862=AXIS2_PLACEMENT_3D('',#35558,#20942,#20943);
#18863=AXIS2_PLACEMENT_3D('',#35569,#20944,#20945);
#18864=AXIS2_PLACEMENT_3D('',#35620,#20947,#20948);
#18865=AXIS2_PLACEMENT_3D('',#35671,#20950,#20951);
#18866=AXIS2_PLACEMENT_3D('',#35719,#20953,#20954);
#18867=AXIS2_PLACEMENT_3D('',#35773,#20956,#20957);
#18868=AXIS2_PLACEMENT_3D('',#35821,#20959,#20960);
#18869=AXIS2_PLACEMENT_3D('',#35869,#20962,#20963);
#18870=AXIS2_PLACEMENT_3D('',#35919,#20965,#20966);
#18871=AXIS2_PLACEMENT_3D('',#35933,#20968,#20969);
#18872=AXIS2_PLACEMENT_3D('',#35943,#20970,#20971);
#18873=AXIS2_PLACEMENT_3D('',#35967,#20973,#20974);
#18874=AXIS2_PLACEMENT_3D('',#35992,#20976,#20977);
#18875=AXIS2_PLACEMENT_3D('',#36017,#20979,#20980);
#18876=AXIS2_PLACEMENT_3D('',#36042,#20982,#20983);
#18877=AXIS2_PLACEMENT_3D('',#36066,#20985,#20986);
#18878=AXIS2_PLACEMENT_3D('',#36091,#20988,#20989);
#18879=AXIS2_PLACEMENT_3D('',#36117,#20991,#20992);
#18880=AXIS2_PLACEMENT_3D('',#36131,#20994,#20995);
#18881=AXIS2_PLACEMENT_3D('',#36141,#20996,#20997);
#18882=AXIS2_PLACEMENT_3D('',#36165,#20999,#21000);
#18883=AXIS2_PLACEMENT_3D('',#36190,#21002,#21003);
#18884=AXIS2_PLACEMENT_3D('',#36215,#21005,#21006);
#18885=AXIS2_PLACEMENT_3D('',#36240,#21008,#21009);
#18886=AXIS2_PLACEMENT_3D('',#36264,#21011,#21012);
#18887=AXIS2_PLACEMENT_3D('',#36289,#21014,#21015);
#18888=AXIS2_PLACEMENT_3D('',#36315,#21017,#21018);
#18889=AXIS2_PLACEMENT_3D('',#36329,#21020,#21021);
#18890=AXIS2_PLACEMENT_3D('',#36339,#21022,#21023);
#18891=AXIS2_PLACEMENT_3D('',#36363,#21025,#21026);
#18892=AXIS2_PLACEMENT_3D('',#36388,#21028,#21029);
#18893=AXIS2_PLACEMENT_3D('',#36413,#21031,#21032);
#18894=AXIS2_PLACEMENT_3D('',#36438,#21034,#21035);
#18895=AXIS2_PLACEMENT_3D('',#36462,#21037,#21038);
#18896=AXIS2_PLACEMENT_3D('',#36487,#21040,#21041);
#18897=AXIS2_PLACEMENT_3D('',#36879,#21043,#21044);
#18898=AXIS2_PLACEMENT_3D('',#37613,#21045,#21046);
#18899=AXIS2_PLACEMENT_3D('',#38347,#21047,#21048);
#18900=AXIS2_PLACEMENT_3D('',#38715,#21049,#21050);
#18901=AXIS2_PLACEMENT_3D('',#38716,#21051,#21052);
#18902=AXIS2_PLACEMENT_3D('',#38717,#21053,#21054);
#18903=AXIS2_PLACEMENT_3D('',#38718,#21055,#21056);
#18904=AXIS2_PLACEMENT_3D('',#38719,#21057,#21058);
#18905=AXIS2_PLACEMENT_3D('',#38720,#21059,#21060);
#18906=AXIS2_PLACEMENT_3D('',#39087,#21061,#21062);
#18907=AXIS2_PLACEMENT_3D('',#39455,#21063,#21064);
#18908=AXIS2_PLACEMENT_3D('',#39456,#21065,#21066);
#18909=AXIS2_PLACEMENT_3D('',#39457,#21067,#21068);
#18910=AXIS2_PLACEMENT_3D('',#39631,#21069,#21070);
#18911=AXIS2_PLACEMENT_3D('',#40555,#21071,#21072);
#18912=AXIS2_PLACEMENT_3D('',#40556,#21073,#21074);
#18913=AXIS2_PLACEMENT_3D('',#40730,#21075,#21076);
#18914=AXIS2_PLACEMENT_3D('',#41654,#21077,#21078);
#18915=AXIS2_PLACEMENT_3D('',#41655,#21079,#21080);
#18916=AXIS2_PLACEMENT_3D('',#41829,#21081,#21082);
#18917=AXIS2_PLACEMENT_3D('',#42753,#21083,#21084);
#18918=AXIS2_PLACEMENT_3D('',#42754,#21085,#21086);
#18919=AXIS2_PLACEMENT_3D('',#42928,#21087,#21088);
#18920=AXIS2_PLACEMENT_3D('',#43852,#21089,#21090);
#18921=AXIS2_PLACEMENT_3D('',#43853,#21091,#21092);
#18922=AXIS2_PLACEMENT_3D('',#44027,#21093,#21094);
#18923=AXIS2_PLACEMENT_3D('',#44951,#21095,#21096);
#18924=AXIS2_PLACEMENT_3D('',#44952,#21097,#21098);
#18925=AXIS2_PLACEMENT_3D('',#44953,#21099,#21100);
#18926=AXIS2_PLACEMENT_3D('',#44954,#21101,#21102);
#18927=AXIS2_PLACEMENT_3D('',#44955,#21103,#21104);
#18928=AXIS2_PLACEMENT_3D('',#44956,#21105,#21106);
#18929=AXIS2_PLACEMENT_3D('',#44957,#21107,#21108);
#18930=AXIS2_PLACEMENT_3D('',#45131,#21109,#21110);
#18931=AXIS2_PLACEMENT_3D('',#46055,#21111,#21112);
#18932=AXIS2_PLACEMENT_3D('',#46056,#21113,#21114);
#18933=AXIS2_PLACEMENT_3D('',#46230,#21115,#21116);
#18934=AXIS2_PLACEMENT_3D('',#47154,#21117,#21118);
#18935=AXIS2_PLACEMENT_3D('',#47155,#21119,#21120);
#18936=AXIS2_PLACEMENT_3D('',#47329,#21121,#21122);
#18937=AXIS2_PLACEMENT_3D('',#48253,#21123,#21124);
#18938=AXIS2_PLACEMENT_3D('',#48254,#21125,#21126);
#18939=AXIS2_PLACEMENT_3D('',#48428,#21127,#21128);
#18940=AXIS2_PLACEMENT_3D('',#49352,#21129,#21130);
#18941=AXIS2_PLACEMENT_3D('',#49353,#21131,#21132);
#18942=AXIS2_PLACEMENT_3D('',#49527,#21133,#21134);
#18943=AXIS2_PLACEMENT_3D('',#50451,#21135,#21136);
#18944=AXIS2_PLACEMENT_3D('',#50452,#21137,#21138);
#18945=AXIS2_PLACEMENT_3D('',#50453,#21139,#21140);
#18946=AXIS2_PLACEMENT_3D('',#50454,#21141,#21142);
#18947=AXIS2_PLACEMENT_3D('',#50455,#21143,#21144);
#18948=AXIS2_PLACEMENT_3D('',#50456,#21145,#21146);
#18949=AXIS2_PLACEMENT_3D('',#50457,#21147,#21148);
#18950=AXIS2_PLACEMENT_3D('',#50631,#21149,#21150);
#18951=AXIS2_PLACEMENT_3D('',#51555,#21151,#21152);
#18952=AXIS2_PLACEMENT_3D('',#51556,#21153,#21154);
#18953=AXIS2_PLACEMENT_3D('',#51557,#21155,#21156);
#18954=AXIS2_PLACEMENT_3D('',#51731,#21157,#21158);
#18955=AXIS2_PLACEMENT_3D('',#52655,#21159,#21160);
#18956=AXIS2_PLACEMENT_3D('',#52656,#21161,#21162);
#18957=AXIS2_PLACEMENT_3D('',#52657,#21163,#21164);
#18958=AXIS2_PLACEMENT_3D('',#52659,#21165,#21166);
#18959=AXIS2_PLACEMENT_3D('',#52662,#21168,#21169);
#18960=AXIS2_PLACEMENT_3D('',#52663,#21170,#21171);
#18961=AXIS2_PLACEMENT_3D('',#52665,#21172,#21173);
#18962=AXIS2_PLACEMENT_3D('',#52668,#21175,#21176);
#18963=AXIS2_PLACEMENT_3D('',#52669,#21177,#21178);
#18964=AXIS2_PLACEMENT_3D('',#52670,#21179,#21180);
#18965=AXIS2_PLACEMENT_3D('',#52671,#21181,#21182);
#18966=AXIS2_PLACEMENT_3D('',#52672,#21183,#21184);
#18967=AXIS2_PLACEMENT_3D('',#52682,#21186,#21187);
#18968=AXIS2_PLACEMENT_3D('',#52686,#21189,#21190);
#18969=AXIS2_PLACEMENT_3D('',#52688,#21191,#21192);
#18970=AXIS2_PLACEMENT_3D('',#52689,#21193,#21194);
#18971=AXIS2_PLACEMENT_3D('',#52691,#21195,#21196);
#18972=AXIS2_PLACEMENT_3D('',#52702,#21197,#21198);
#18973=AXIS2_PLACEMENT_3D('',#52753,#21200,#21201);
#18974=AXIS2_PLACEMENT_3D('',#52804,#21203,#21204);
#18975=AXIS2_PLACEMENT_3D('',#52852,#21206,#21207);
#18976=AXIS2_PLACEMENT_3D('',#52903,#21209,#21210);
#18977=AXIS2_PLACEMENT_3D('',#52954,#21212,#21213);
#18978=AXIS2_PLACEMENT_3D('',#53002,#21215,#21216);
#18979=AXIS2_PLACEMENT_3D('',#53021,#21218,#21219);
#18980=AXIS2_PLACEMENT_3D('',#53041,#21220,#21221);
#18981=AXIS2_PLACEMENT_3D('',#53055,#21223,#21224);
#18982=AXIS2_PLACEMENT_3D('',#53065,#21225,#21226);
#18983=AXIS2_PLACEMENT_3D('',#53089,#21228,#21229);
#18984=AXIS2_PLACEMENT_3D('',#53114,#21231,#21232);
#18985=AXIS2_PLACEMENT_3D('',#53139,#21234,#21235);
#18986=AXIS2_PLACEMENT_3D('',#53163,#21237,#21238);
#18987=AXIS2_PLACEMENT_3D('',#53188,#21240,#21241);
#18988=AXIS2_PLACEMENT_3D('',#53213,#21243,#21244);
#18989=AXIS2_PLACEMENT_3D('',#53224,#21246,#21247);
#18990=AXIS2_PLACEMENT_3D('',#53230,#21248,#21249);
#18991=AXIS2_PLACEMENT_3D('',#53240,#21251,#21252);
#18992=AXIS2_PLACEMENT_3D('',#53244,#21254,#21255);
#18993=AXIS2_PLACEMENT_3D('',#53246,#21256,#21257);
#18994=AXIS2_PLACEMENT_3D('',#53247,#21258,#21259);
#18995=AXIS2_PLACEMENT_3D('',#53249,#21260,#21261);
#18996=AXIS2_PLACEMENT_3D('',#53260,#21262,#21263);
#18997=AXIS2_PLACEMENT_3D('',#53311,#21265,#21266);
#18998=AXIS2_PLACEMENT_3D('',#53362,#21268,#21269);
#18999=AXIS2_PLACEMENT_3D('',#53410,#21271,#21272);
#19000=AXIS2_PLACEMENT_3D('',#53461,#21274,#21275);
#19001=AXIS2_PLACEMENT_3D('',#53512,#21277,#21278);
#19002=AXIS2_PLACEMENT_3D('',#53560,#21280,#21281);
#19003=AXIS2_PLACEMENT_3D('',#53579,#21283,#21284);
#19004=AXIS2_PLACEMENT_3D('',#53599,#21285,#21286);
#19005=AXIS2_PLACEMENT_3D('',#53613,#21288,#21289);
#19006=AXIS2_PLACEMENT_3D('',#53623,#21290,#21291);
#19007=AXIS2_PLACEMENT_3D('',#53647,#21293,#21294);
#19008=AXIS2_PLACEMENT_3D('',#53672,#21296,#21297);
#19009=AXIS2_PLACEMENT_3D('',#53697,#21299,#21300);
#19010=AXIS2_PLACEMENT_3D('',#53721,#21302,#21303);
#19011=AXIS2_PLACEMENT_3D('',#53746,#21305,#21306);
#19012=AXIS2_PLACEMENT_3D('',#53771,#21308,#21309);
#19013=AXIS2_PLACEMENT_3D('',#53782,#21311,#21312);
#19014=AXIS2_PLACEMENT_3D('',#53788,#21313,#21314);
#19015=AXIS2_PLACEMENT_3D('',#53798,#21316,#21317);
#19016=AXIS2_PLACEMENT_3D('',#53802,#21319,#21320);
#19017=AXIS2_PLACEMENT_3D('',#53804,#21321,#21322);
#19018=AXIS2_PLACEMENT_3D('',#53805,#21323,#21324);
#19019=AXIS2_PLACEMENT_3D('',#53807,#21325,#21326);
#19020=AXIS2_PLACEMENT_3D('',#53818,#21327,#21328);
#19021=AXIS2_PLACEMENT_3D('',#53869,#21330,#21331);
#19022=AXIS2_PLACEMENT_3D('',#53920,#21333,#21334);
#19023=AXIS2_PLACEMENT_3D('',#53968,#21336,#21337);
#19024=AXIS2_PLACEMENT_3D('',#54019,#21339,#21340);
#19025=AXIS2_PLACEMENT_3D('',#54070,#21342,#21343);
#19026=AXIS2_PLACEMENT_3D('',#54118,#21345,#21346);
#19027=AXIS2_PLACEMENT_3D('',#54137,#21348,#21349);
#19028=AXIS2_PLACEMENT_3D('',#54157,#21350,#21351);
#19029=AXIS2_PLACEMENT_3D('',#54171,#21353,#21354);
#19030=AXIS2_PLACEMENT_3D('',#54181,#21355,#21356);
#19031=AXIS2_PLACEMENT_3D('',#54205,#21358,#21359);
#19032=AXIS2_PLACEMENT_3D('',#54230,#21361,#21362);
#19033=AXIS2_PLACEMENT_3D('',#54255,#21364,#21365);
#19034=AXIS2_PLACEMENT_3D('',#54279,#21367,#21368);
#19035=AXIS2_PLACEMENT_3D('',#54304,#21370,#21371);
#19036=AXIS2_PLACEMENT_3D('',#54329,#21373,#21374);
#19037=AXIS2_PLACEMENT_3D('',#54340,#21376,#21377);
#19038=AXIS2_PLACEMENT_3D('',#54346,#21378,#21379);
#19039=AXIS2_PLACEMENT_3D('',#54356,#21381,#21382);
#19040=AXIS2_PLACEMENT_3D('',#54360,#21384,#21385);
#19041=AXIS2_PLACEMENT_3D('',#54362,#21386,#21387);
#19042=AXIS2_PLACEMENT_3D('',#54363,#21388,#21389);
#19043=AXIS2_PLACEMENT_3D('',#54365,#21390,#21391);
#19044=AXIS2_PLACEMENT_3D('',#54376,#21392,#21393);
#19045=AXIS2_PLACEMENT_3D('',#54427,#21395,#21396);
#19046=AXIS2_PLACEMENT_3D('',#54478,#21398,#21399);
#19047=AXIS2_PLACEMENT_3D('',#54526,#21401,#21402);
#19048=AXIS2_PLACEMENT_3D('',#54577,#21404,#21405);
#19049=AXIS2_PLACEMENT_3D('',#54628,#21407,#21408);
#19050=AXIS2_PLACEMENT_3D('',#54676,#21410,#21411);
#19051=AXIS2_PLACEMENT_3D('',#54695,#21413,#21414);
#19052=AXIS2_PLACEMENT_3D('',#54715,#21415,#21416);
#19053=AXIS2_PLACEMENT_3D('',#54729,#21418,#21419);
#19054=AXIS2_PLACEMENT_3D('',#54739,#21420,#21421);
#19055=AXIS2_PLACEMENT_3D('',#54763,#21423,#21424);
#19056=AXIS2_PLACEMENT_3D('',#54788,#21426,#21427);
#19057=AXIS2_PLACEMENT_3D('',#54813,#21429,#21430);
#19058=AXIS2_PLACEMENT_3D('',#54837,#21432,#21433);
#19059=AXIS2_PLACEMENT_3D('',#54862,#21435,#21436);
#19060=AXIS2_PLACEMENT_3D('',#54887,#21438,#21439);
#19061=AXIS2_PLACEMENT_3D('',#54898,#21441,#21442);
#19062=AXIS2_PLACEMENT_3D('',#54904,#21443,#21444);
#19063=AXIS2_PLACEMENT_3D('',#54914,#21446,#21447);
#19064=AXIS2_PLACEMENT_3D('',#54918,#21449,#21450);
#19065=AXIS2_PLACEMENT_3D('',#54920,#21451,#21452);
#19066=AXIS2_PLACEMENT_3D('',#54921,#21453,#21454);
#19067=AXIS2_PLACEMENT_3D('',#54923,#21455,#21456);
#19068=AXIS2_PLACEMENT_3D('',#54934,#21457,#21458);
#19069=AXIS2_PLACEMENT_3D('',#54985,#21460,#21461);
#19070=AXIS2_PLACEMENT_3D('',#55036,#21463,#21464);
#19071=AXIS2_PLACEMENT_3D('',#55084,#21466,#21467);
#19072=AXIS2_PLACEMENT_3D('',#55135,#21469,#21470);
#19073=AXIS2_PLACEMENT_3D('',#55186,#21472,#21473);
#19074=AXIS2_PLACEMENT_3D('',#55234,#21475,#21476);
#19075=AXIS2_PLACEMENT_3D('',#55253,#21478,#21479);
#19076=AXIS2_PLACEMENT_3D('',#55273,#21480,#21481);
#19077=AXIS2_PLACEMENT_3D('',#55287,#21483,#21484);
#19078=AXIS2_PLACEMENT_3D('',#55297,#21485,#21486);
#19079=AXIS2_PLACEMENT_3D('',#55321,#21488,#21489);
#19080=AXIS2_PLACEMENT_3D('',#55346,#21491,#21492);
#19081=AXIS2_PLACEMENT_3D('',#55371,#21494,#21495);
#19082=AXIS2_PLACEMENT_3D('',#55395,#21497,#21498);
#19083=AXIS2_PLACEMENT_3D('',#55420,#21500,#21501);
#19084=AXIS2_PLACEMENT_3D('',#55445,#21503,#21504);
#19085=AXIS2_PLACEMENT_3D('',#55456,#21506,#21507);
#19086=AXIS2_PLACEMENT_3D('',#55462,#21508,#21509);
#19087=AXIS2_PLACEMENT_3D('',#55472,#21511,#21512);
#19088=AXIS2_PLACEMENT_3D('',#55476,#21514,#21515);
#19089=AXIS2_PLACEMENT_3D('',#55478,#21516,#21517);
#19090=AXIS2_PLACEMENT_3D('',#55479,#21518,#21519);
#19091=AXIS2_PLACEMENT_3D('',#55481,#21520,#21521);
#19092=AXIS2_PLACEMENT_3D('',#55492,#21522,#21523);
#19093=AXIS2_PLACEMENT_3D('',#55543,#21525,#21526);
#19094=AXIS2_PLACEMENT_3D('',#55594,#21528,#21529);
#19095=AXIS2_PLACEMENT_3D('',#55642,#21531,#21532);
#19096=AXIS2_PLACEMENT_3D('',#55693,#21534,#21535);
#19097=AXIS2_PLACEMENT_3D('',#55744,#21537,#21538);
#19098=AXIS2_PLACEMENT_3D('',#55792,#21540,#21541);
#19099=AXIS2_PLACEMENT_3D('',#55811,#21543,#21544);
#19100=AXIS2_PLACEMENT_3D('',#55831,#21545,#21546);
#19101=AXIS2_PLACEMENT_3D('',#55845,#21548,#21549);
#19102=AXIS2_PLACEMENT_3D('',#55855,#21550,#21551);
#19103=AXIS2_PLACEMENT_3D('',#55879,#21553,#21554);
#19104=AXIS2_PLACEMENT_3D('',#55904,#21556,#21557);
#19105=AXIS2_PLACEMENT_3D('',#55929,#21559,#21560);
#19106=AXIS2_PLACEMENT_3D('',#55953,#21562,#21563);
#19107=AXIS2_PLACEMENT_3D('',#55978,#21565,#21566);
#19108=AXIS2_PLACEMENT_3D('',#56003,#21568,#21569);
#19109=AXIS2_PLACEMENT_3D('',#56014,#21571,#21572);
#19110=AXIS2_PLACEMENT_3D('',#56020,#21573,#21574);
#19111=AXIS2_PLACEMENT_3D('',#56030,#21576,#21577);
#19112=AXIS2_PLACEMENT_3D('',#56034,#21579,#21580);
#19113=AXIS2_PLACEMENT_3D('',#56036,#21581,#21582);
#19114=AXIS2_PLACEMENT_3D('',#56037,#21583,#21584);
#19115=AXIS2_PLACEMENT_3D('',#56039,#21585,#21586);
#19116=AXIS2_PLACEMENT_3D('',#56050,#21587,#21588);
#19117=AXIS2_PLACEMENT_3D('',#56101,#21590,#21591);
#19118=AXIS2_PLACEMENT_3D('',#56152,#21593,#21594);
#19119=AXIS2_PLACEMENT_3D('',#56200,#21596,#21597);
#19120=AXIS2_PLACEMENT_3D('',#56251,#21599,#21600);
#19121=AXIS2_PLACEMENT_3D('',#56302,#21602,#21603);
#19122=AXIS2_PLACEMENT_3D('',#56350,#21605,#21606);
#19123=AXIS2_PLACEMENT_3D('',#56369,#21608,#21609);
#19124=AXIS2_PLACEMENT_3D('',#56389,#21610,#21611);
#19125=AXIS2_PLACEMENT_3D('',#56403,#21613,#21614);
#19126=AXIS2_PLACEMENT_3D('',#56413,#21615,#21616);
#19127=AXIS2_PLACEMENT_3D('',#56437,#21618,#21619);
#19128=AXIS2_PLACEMENT_3D('',#56462,#21621,#21622);
#19129=AXIS2_PLACEMENT_3D('',#56487,#21624,#21625);
#19130=AXIS2_PLACEMENT_3D('',#56511,#21627,#21628);
#19131=AXIS2_PLACEMENT_3D('',#56536,#21630,#21631);
#19132=AXIS2_PLACEMENT_3D('',#56561,#21633,#21634);
#19133=AXIS2_PLACEMENT_3D('',#56572,#21636,#21637);
#19134=AXIS2_PLACEMENT_3D('',#56578,#21638,#21639);
#19135=AXIS2_PLACEMENT_3D('',#56588,#21641,#21642);
#19136=AXIS2_PLACEMENT_3D('',#56592,#21644,#21645);
#19137=AXIS2_PLACEMENT_3D('',#56594,#21646,#21647);
#19138=AXIS2_PLACEMENT_3D('',#56595,#21648,#21649);
#19139=AXIS2_PLACEMENT_3D('',#56597,#21650,#21651);
#19140=AXIS2_PLACEMENT_3D('',#56608,#21652,#21653);
#19141=AXIS2_PLACEMENT_3D('',#56659,#21655,#21656);
#19142=AXIS2_PLACEMENT_3D('',#56710,#21658,#21659);
#19143=AXIS2_PLACEMENT_3D('',#56758,#21661,#21662);
#19144=AXIS2_PLACEMENT_3D('',#56809,#21664,#21665);
#19145=AXIS2_PLACEMENT_3D('',#56860,#21667,#21668);
#19146=AXIS2_PLACEMENT_3D('',#56908,#21670,#21671);
#19147=AXIS2_PLACEMENT_3D('',#56927,#21673,#21674);
#19148=AXIS2_PLACEMENT_3D('',#56947,#21675,#21676);
#19149=AXIS2_PLACEMENT_3D('',#56961,#21678,#21679);
#19150=AXIS2_PLACEMENT_3D('',#56971,#21680,#21681);
#19151=AXIS2_PLACEMENT_3D('',#56995,#21683,#21684);
#19152=AXIS2_PLACEMENT_3D('',#57020,#21686,#21687);
#19153=AXIS2_PLACEMENT_3D('',#57045,#21689,#21690);
#19154=AXIS2_PLACEMENT_3D('',#57069,#21692,#21693);
#19155=AXIS2_PLACEMENT_3D('',#57094,#21695,#21696);
#19156=AXIS2_PLACEMENT_3D('',#57119,#21698,#21699);
#19157=AXIS2_PLACEMENT_3D('',#57130,#21701,#21702);
#19158=AXIS2_PLACEMENT_3D('',#57136,#21703,#21704);
#19159=AXIS2_PLACEMENT_3D('',#57146,#21706,#21707);
#19160=AXIS2_PLACEMENT_3D('',#57150,#21709,#21710);
#19161=AXIS2_PLACEMENT_3D('',#57152,#21711,#21712);
#19162=AXIS2_PLACEMENT_3D('',#57153,#21713,#21714);
#19163=AXIS2_PLACEMENT_3D('',#57155,#21715,#21716);
#19164=AXIS2_PLACEMENT_3D('',#57166,#21717,#21718);
#19165=AXIS2_PLACEMENT_3D('',#57217,#21720,#21721);
#19166=AXIS2_PLACEMENT_3D('',#57268,#21723,#21724);
#19167=AXIS2_PLACEMENT_3D('',#57316,#21726,#21727);
#19168=AXIS2_PLACEMENT_3D('',#57367,#21729,#21730);
#19169=AXIS2_PLACEMENT_3D('',#57418,#21732,#21733);
#19170=AXIS2_PLACEMENT_3D('',#57466,#21735,#21736);
#19171=AXIS2_PLACEMENT_3D('',#57485,#21738,#21739);
#19172=AXIS2_PLACEMENT_3D('',#57505,#21740,#21741);
#19173=AXIS2_PLACEMENT_3D('',#57519,#21743,#21744);
#19174=AXIS2_PLACEMENT_3D('',#57529,#21745,#21746);
#19175=AXIS2_PLACEMENT_3D('',#57553,#21748,#21749);
#19176=AXIS2_PLACEMENT_3D('',#57578,#21751,#21752);
#19177=AXIS2_PLACEMENT_3D('',#57603,#21754,#21755);
#19178=AXIS2_PLACEMENT_3D('',#57627,#21757,#21758);
#19179=AXIS2_PLACEMENT_3D('',#57652,#21760,#21761);
#19180=AXIS2_PLACEMENT_3D('',#57677,#21763,#21764);
#19181=AXIS2_PLACEMENT_3D('',#57688,#21766,#21767);
#19182=AXIS2_PLACEMENT_3D('',#57694,#21768,#21769);
#19183=AXIS2_PLACEMENT_3D('',#57704,#21771,#21772);
#19184=AXIS2_PLACEMENT_3D('',#57708,#21774,#21775);
#19185=AXIS2_PLACEMENT_3D('',#57710,#21776,#21777);
#19186=AXIS2_PLACEMENT_3D('',#57711,#21778,#21779);
#19187=AXIS2_PLACEMENT_3D('',#57713,#21780,#21781);
#19188=AXIS2_PLACEMENT_3D('',#57724,#21782,#21783);
#19189=AXIS2_PLACEMENT_3D('',#57775,#21785,#21786);
#19190=AXIS2_PLACEMENT_3D('',#57826,#21788,#21789);
#19191=AXIS2_PLACEMENT_3D('',#57874,#21791,#21792);
#19192=AXIS2_PLACEMENT_3D('',#57925,#21794,#21795);
#19193=AXIS2_PLACEMENT_3D('',#57976,#21797,#21798);
#19194=AXIS2_PLACEMENT_3D('',#58024,#21800,#21801);
#19195=AXIS2_PLACEMENT_3D('',#58043,#21803,#21804);
#19196=AXIS2_PLACEMENT_3D('',#58063,#21805,#21806);
#19197=AXIS2_PLACEMENT_3D('',#58077,#21808,#21809);
#19198=AXIS2_PLACEMENT_3D('',#58087,#21810,#21811);
#19199=AXIS2_PLACEMENT_3D('',#58111,#21813,#21814);
#19200=AXIS2_PLACEMENT_3D('',#58136,#21816,#21817);
#19201=AXIS2_PLACEMENT_3D('',#58161,#21819,#21820);
#19202=AXIS2_PLACEMENT_3D('',#58185,#21822,#21823);
#19203=AXIS2_PLACEMENT_3D('',#58210,#21825,#21826);
#19204=AXIS2_PLACEMENT_3D('',#58235,#21828,#21829);
#19205=AXIS2_PLACEMENT_3D('',#58246,#21831,#21832);
#19206=AXIS2_PLACEMENT_3D('',#58252,#21833,#21834);
#19207=AXIS2_PLACEMENT_3D('',#58262,#21836,#21837);
#19208=AXIS2_PLACEMENT_3D('',#58266,#21839,#21840);
#19209=AXIS2_PLACEMENT_3D('',#58268,#21841,#21842);
#19210=AXIS2_PLACEMENT_3D('',#58269,#21843,#21844);
#19211=AXIS2_PLACEMENT_3D('',#58271,#21845,#21846);
#19212=AXIS2_PLACEMENT_3D('',#58282,#21847,#21848);
#19213=AXIS2_PLACEMENT_3D('',#58333,#21850,#21851);
#19214=AXIS2_PLACEMENT_3D('',#58384,#21853,#21854);
#19215=AXIS2_PLACEMENT_3D('',#58432,#21856,#21857);
#19216=AXIS2_PLACEMENT_3D('',#58483,#21859,#21860);
#19217=AXIS2_PLACEMENT_3D('',#58534,#21862,#21863);
#19218=AXIS2_PLACEMENT_3D('',#58582,#21865,#21866);
#19219=AXIS2_PLACEMENT_3D('',#58601,#21868,#21869);
#19220=AXIS2_PLACEMENT_3D('',#58621,#21870,#21871);
#19221=AXIS2_PLACEMENT_3D('',#58635,#21873,#21874);
#19222=AXIS2_PLACEMENT_3D('',#58645,#21875,#21876);
#19223=AXIS2_PLACEMENT_3D('',#58669,#21878,#21879);
#19224=AXIS2_PLACEMENT_3D('',#58694,#21881,#21882);
#19225=AXIS2_PLACEMENT_3D('',#58719,#21884,#21885);
#19226=AXIS2_PLACEMENT_3D('',#58743,#21887,#21888);
#19227=AXIS2_PLACEMENT_3D('',#58768,#21890,#21891);
#19228=AXIS2_PLACEMENT_3D('',#58793,#21893,#21894);
#19229=AXIS2_PLACEMENT_3D('',#58804,#21896,#21897);
#19230=AXIS2_PLACEMENT_3D('',#58810,#21898,#21899);
#19231=AXIS2_PLACEMENT_3D('',#58820,#21901,#21902);
#19232=AXIS2_PLACEMENT_3D('',#58824,#21904,#21905);
#19233=AXIS2_PLACEMENT_3D('',#58826,#21906,#21907);
#19234=AXIS2_PLACEMENT_3D('',#58827,#21908,#21909);
#19235=AXIS2_PLACEMENT_3D('',#58829,#21910,#21911);
#19236=AXIS2_PLACEMENT_3D('',#58840,#21912,#21913);
#19237=AXIS2_PLACEMENT_3D('',#58891,#21915,#21916);
#19238=AXIS2_PLACEMENT_3D('',#58942,#21918,#21919);
#19239=AXIS2_PLACEMENT_3D('',#58990,#21921,#21922);
#19240=AXIS2_PLACEMENT_3D('',#59041,#21924,#21925);
#19241=AXIS2_PLACEMENT_3D('',#59092,#21927,#21928);
#19242=AXIS2_PLACEMENT_3D('',#59140,#21930,#21931);
#19243=AXIS2_PLACEMENT_3D('',#59159,#21933,#21934);
#19244=AXIS2_PLACEMENT_3D('',#59179,#21935,#21936);
#19245=AXIS2_PLACEMENT_3D('',#59193,#21938,#21939);
#19246=AXIS2_PLACEMENT_3D('',#59203,#21940,#21941);
#19247=AXIS2_PLACEMENT_3D('',#59227,#21943,#21944);
#19248=AXIS2_PLACEMENT_3D('',#59252,#21946,#21947);
#19249=AXIS2_PLACEMENT_3D('',#59277,#21949,#21950);
#19250=AXIS2_PLACEMENT_3D('',#59301,#21952,#21953);
#19251=AXIS2_PLACEMENT_3D('',#59326,#21955,#21956);
#19252=AXIS2_PLACEMENT_3D('',#59351,#21958,#21959);
#19253=AXIS2_PLACEMENT_3D('',#59362,#21961,#21962);
#19254=AXIS2_PLACEMENT_3D('',#59368,#21963,#21964);
#19255=AXIS2_PLACEMENT_3D('',#59377,#21969,#21970);
#19256=AXIS2_PLACEMENT_3D('',#59383,#21974,#21975);
#19257=AXIS2_PLACEMENT_3D('',#59389,#21979,#21980);
#19258=AXIS2_PLACEMENT_3D('',#59423,#21982,#21983);
#19259=AXIS2_PLACEMENT_3D('',#59425,#21984,#21985);
#19260=AXIS2_PLACEMENT_3D('',#59471,#21991,#21992);
#19261=AXIS2_PLACEMENT_3D('',#59473,#21993,#21994);
#19262=AXIS2_PLACEMENT_3D('',#59519,#22000,#22001);
#19263=AXIS2_PLACEMENT_3D('',#59521,#22002,#22003);
#19264=AXIS2_PLACEMENT_3D('',#59545,#22009,#22010);
#19265=AXIS2_PLACEMENT_3D('',#59547,#22011,#22012);
#19266=AXIS2_PLACEMENT_3D('',#59593,#22018,#22019);
#19267=AXIS2_PLACEMENT_3D('',#59595,#22020,#22021);
#19268=AXIS2_PLACEMENT_3D('',#59641,#22027,#22028);
#19269=AXIS2_PLACEMENT_3D('',#59643,#22029,#22030);
#19270=AXIS2_PLACEMENT_3D('',#59817,#22035,#22036);
#19271=AXIS2_PLACEMENT_3D('',#60623,#22037,#22038);
#19272=AXIS2_PLACEMENT_3D('',#60782,#22039,#22040);
#19273=AXIS2_PLACEMENT_3D('',#61463,#22041,#22042);
#19274=AXIS2_PLACEMENT_3D('',#61464,#22043,#22044);
#19275=AXIS2_PLACEMENT_3D('',#61623,#22045,#22046);
#19276=AXIS2_PLACEMENT_3D('',#62304,#22047,#22048);
#19277=AXIS2_PLACEMENT_3D('',#62305,#22049,#22050);
#19278=AXIS2_PLACEMENT_3D('',#62464,#22051,#22052);
#19279=AXIS2_PLACEMENT_3D('',#63145,#22053,#22054);
#19280=AXIS2_PLACEMENT_3D('',#63146,#22055,#22056);
#19281=AXIS2_PLACEMENT_3D('',#63305,#22057,#22058);
#19282=AXIS2_PLACEMENT_3D('',#63986,#22059,#22060);
#19283=AXIS2_PLACEMENT_3D('',#63987,#22061,#22062);
#19284=AXIS2_PLACEMENT_3D('',#64146,#22063,#22064);
#19285=AXIS2_PLACEMENT_3D('',#64827,#22065,#22066);
#19286=AXIS2_PLACEMENT_3D('',#64828,#22067,#22068);
#19287=AXIS2_PLACEMENT_3D('',#64830,#22070,#22071);
#19288=AXIS2_PLACEMENT_3D('',#64832,#22073,#22074);
#19289=AXIS2_PLACEMENT_3D('',#64834,#22076,#22077);
#19290=AXIS2_PLACEMENT_3D('',#64836,#22079,#22080);
#19291=AXIS2_PLACEMENT_3D('',#64838,#22082,#22083);
#19292=AXIS2_PLACEMENT_3D('',#64840,#22085,#22086);
#19293=AXIS2_PLACEMENT_3D('',#64842,#22088,#22089);
#19294=AXIS2_PLACEMENT_3D('',#64844,#22091,#22092);
#19295=AXIS2_PLACEMENT_3D('',#64846,#22094,#22095);
#19296=AXIS2_PLACEMENT_3D('',#64848,#22097,#22098);
#19297=AXIS2_PLACEMENT_3D('',#65007,#22099,#22100);
#19298=AXIS2_PLACEMENT_3D('',#65527,#22101,#22102);
#19299=AXIS2_PLACEMENT_3D('',#65528,#22103,#22104);
#19300=AXIS2_PLACEMENT_3D('',#65687,#22105,#22106);
#19301=AXIS2_PLACEMENT_3D('',#66207,#22107,#22108);
#19302=AXIS2_PLACEMENT_3D('',#66208,#22109,#22110);
#19303=AXIS2_PLACEMENT_3D('',#66367,#22111,#22112);
#19304=AXIS2_PLACEMENT_3D('',#66887,#22113,#22114);
#19305=AXIS2_PLACEMENT_3D('',#66888,#22115,#22116);
#19306=AXIS2_PLACEMENT_3D('',#67047,#22117,#22118);
#19307=AXIS2_PLACEMENT_3D('',#67567,#22119,#22120);
#19308=AXIS2_PLACEMENT_3D('',#67568,#22121,#22122);
#19309=AXIS2_PLACEMENT_3D('',#67727,#22123,#22124);
#19310=AXIS2_PLACEMENT_3D('',#68247,#22125,#22126);
#19311=AXIS2_PLACEMENT_3D('',#68248,#22127,#22128);
#19312=AXIS2_PLACEMENT_3D('',#68250,#22130,#22131);
#19313=AXIS2_PLACEMENT_3D('',#68252,#22133,#22134);
#19314=AXIS2_PLACEMENT_3D('',#68254,#22136,#22137);
#19315=AXIS2_PLACEMENT_3D('',#68256,#22139,#22140);
#19316=AXIS2_PLACEMENT_3D('',#68258,#22142,#22143);
#19317=AXIS2_PLACEMENT_3D('',#68260,#22145,#22146);
#19318=AXIS2_PLACEMENT_3D('',#68262,#22148,#22149);
#19319=AXIS2_PLACEMENT_3D('',#68264,#22151,#22152);
#19320=AXIS2_PLACEMENT_3D('',#68266,#22154,#22155);
#19321=AXIS2_PLACEMENT_3D('',#68268,#22157,#22158);
#19322=AXIS2_PLACEMENT_3D('',#68427,#22159,#22160);
#19323=AXIS2_PLACEMENT_3D('',#69108,#22161,#22162);
#19324=AXIS2_PLACEMENT_3D('',#69109,#22163,#22164);
#19325=AXIS2_PLACEMENT_3D('',#69111,#22166,#22167);
#19326=AXIS2_PLACEMENT_3D('',#69113,#22169,#22170);
#19327=AXIS2_PLACEMENT_3D('',#69272,#22171,#22172);
#19328=AXIS2_PLACEMENT_3D('',#69792,#22173,#22174);
#19329=AXIS2_PLACEMENT_3D('',#69793,#22175,#22176);
#19330=AXIS2_PLACEMENT_3D('',#69795,#22178,#22179);
#19331=AXIS2_PLACEMENT_3D('',#69797,#22181,#22182);
#19332=AXIS2_PLACEMENT_3D('',#69799,#22183,#22184);
#19333=AXIS2_PLACEMENT_3D('',#69802,#22186,#22187);
#19334=AXIS2_PLACEMENT_3D('',#69803,#22188,#22189);
#19335=AXIS2_PLACEMENT_3D('',#69805,#22190,#22191);
#19336=AXIS2_PLACEMENT_3D('',#69809,#22194,#22195);
#19337=AXIS2_PLACEMENT_3D('',#69810,#22196,#22197);
#19338=AXIS2_PLACEMENT_3D('',#69811,#22198,#22199);
#19339=AXIS2_PLACEMENT_3D('',#69813,#22200,#22201);
#19340=AXIS2_PLACEMENT_3D('',#69816,#22203,#22204);
#19341=AXIS2_PLACEMENT_3D('',#69817,#22205,#22206);
#19342=AXIS2_PLACEMENT_3D('',#69819,#22207,#22208);
#19343=AXIS2_PLACEMENT_3D('',#69823,#22211,#22212);
#19344=AXIS2_PLACEMENT_3D('',#69824,#22213,#22214);
#19345=AXIS2_PLACEMENT_3D('',#69825,#22215,#22216);
#19346=AXIS2_PLACEMENT_3D('',#69827,#22217,#22218);
#19347=AXIS2_PLACEMENT_3D('',#69830,#22220,#22221);
#19348=AXIS2_PLACEMENT_3D('',#69831,#22222,#22223);
#19349=AXIS2_PLACEMENT_3D('',#69833,#22224,#22225);
#19350=AXIS2_PLACEMENT_3D('',#69837,#22228,#22229);
#19351=AXIS2_PLACEMENT_3D('',#69838,#22230,#22231);
#19352=AXIS2_PLACEMENT_3D('',#69839,#22232,#22233);
#19353=AXIS2_PLACEMENT_3D('',#69841,#22234,#22235);
#19354=AXIS2_PLACEMENT_3D('',#69844,#22237,#22238);
#19355=AXIS2_PLACEMENT_3D('',#69845,#22239,#22240);
#19356=AXIS2_PLACEMENT_3D('',#69847,#22241,#22242);
#19357=AXIS2_PLACEMENT_3D('',#69851,#22245,#22246);
#19358=AXIS2_PLACEMENT_3D('',#69852,#22247,#22248);
#19359=AXIS2_PLACEMENT_3D('',#69853,#22249,#22250);
#19360=AXIS2_PLACEMENT_3D('',#69855,#22251,#22252);
#19361=AXIS2_PLACEMENT_3D('',#69858,#22254,#22255);
#19362=AXIS2_PLACEMENT_3D('',#69859,#22256,#22257);
#19363=AXIS2_PLACEMENT_3D('',#69861,#22258,#22259);
#19364=AXIS2_PLACEMENT_3D('',#69865,#22262,#22263);
#19365=AXIS2_PLACEMENT_3D('',#69866,#22264,#22265);
#19366=AXIS2_PLACEMENT_3D('',#69867,#22266,#22267);
#19367=AXIS2_PLACEMENT_3D('',#69869,#22268,#22269);
#19368=AXIS2_PLACEMENT_3D('',#69872,#22271,#22272);
#19369=AXIS2_PLACEMENT_3D('',#69873,#22273,#22274);
#19370=AXIS2_PLACEMENT_3D('',#69875,#22275,#22276);
#19371=AXIS2_PLACEMENT_3D('',#69879,#22279,#22280);
#19372=AXIS2_PLACEMENT_3D('',#69880,#22281,#22282);
#19373=AXIS2_PLACEMENT_3D('',#69881,#22283,#22284);
#19374=AXIS2_PLACEMENT_3D('',#69892,#22287,#22288);
#19375=AXIS2_PLACEMENT_3D('',#69903,#22291,#22292);
#19376=AXIS2_PLACEMENT_3D('',#69907,#22295,#22296);
#19377=AXIS2_PLACEMENT_3D('',#69909,#22298,#22299);
#19378=AXIS2_PLACEMENT_3D('',#69920,#22302,#22303);
#19379=AXIS2_PLACEMENT_3D('',#69924,#22306,#22307);
#19380=AXIS2_PLACEMENT_3D('',#69928,#22310,#22311);
#19381=AXIS2_PLACEMENT_3D('',#69937,#22313,#22314);
#19382=AXIS2_PLACEMENT_3D('',#69948,#22317,#22318);
#19383=AXIS2_PLACEMENT_3D('',#69952,#22321,#22322);
#19384=AXIS2_PLACEMENT_3D('',#69956,#22325,#22326);
#19385=AXIS2_PLACEMENT_3D('',#69965,#22328,#22329);
#19386=AXIS2_PLACEMENT_3D('',#69976,#22332,#22333);
#19387=AXIS2_PLACEMENT_3D('',#69980,#22336,#22337);
#19388=AXIS2_PLACEMENT_3D('',#69984,#22340,#22341);
#19389=AXIS2_PLACEMENT_3D('',#69993,#22343,#22344);
#19390=AXIS2_PLACEMENT_3D('',#70004,#22347,#22348);
#19391=AXIS2_PLACEMENT_3D('',#70015,#22351,#22352);
#19392=AXIS2_PLACEMENT_3D('',#70019,#22355,#22356);
#19393=AXIS2_PLACEMENT_3D('',#86269,#22366,#22367);
#19394=AXIS2_PLACEMENT_3D('',#86280,#22370,#22371);
#19395=AXIS2_PLACEMENT_3D('',#86291,#22374,#22375);
#19396=AXIS2_PLACEMENT_3D('',#86295,#22378,#22379);
#19397=AXIS2_PLACEMENT_3D('',#88337,#22382,#22383);
#19398=AXIS2_PLACEMENT_3D('',#88340,#22385,#22386);
#19399=AXIS2_PLACEMENT_3D('',#88341,#22387,#22388);
#19400=AXIS2_PLACEMENT_3D('',#88344,#22390,#22391);
#19401=AXIS2_PLACEMENT_3D('',#88345,#22392,#22393);
#19402=AXIS2_PLACEMENT_3D('',#88347,#22395,#22396);
#19403=AXIS2_PLACEMENT_3D('',#88350,#22398,#22399);
#19404=AXIS2_PLACEMENT_3D('',#88351,#22400,#22401);
#19405=AXIS2_PLACEMENT_3D('',#88354,#22403,#22404);
#19406=AXIS2_PLACEMENT_3D('',#88355,#22405,#22406);
#19407=AXIS2_PLACEMENT_3D('',#88357,#22408,#22409);
#19408=AXIS2_PLACEMENT_3D('',#88360,#22411,#22412);
#19409=AXIS2_PLACEMENT_3D('',#88361,#22413,#22414);
#19410=AXIS2_PLACEMENT_3D('',#88364,#22416,#22417);
#19411=AXIS2_PLACEMENT_3D('',#88365,#22418,#22419);
#19412=AXIS2_PLACEMENT_3D('',#88367,#22421,#22422);
#19413=AXIS2_PLACEMENT_3D('',#88374,#22423,#22424);
#19414=AXIS2_PLACEMENT_3D('',#88376,#22425,#22426);
#19415=AXIS2_PLACEMENT_3D('',#88384,#22428,#22429);
#19416=AXIS2_PLACEMENT_3D('',#88386,#22430,#22431);
#19417=AXIS2_PLACEMENT_3D('',#88394,#22433,#22434);
#19418=AXIS2_PLACEMENT_3D('',#88396,#22435,#22436);
#19419=AXIS2_PLACEMENT_3D('',#88398,#22438,#22439);
#19420=AXIS2_PLACEMENT_3D('',#88399,#22440,#22441);
#19421=AXIS2_PLACEMENT_3D('',#88401,#22443,#22444);
#19422=AXIS2_PLACEMENT_3D('',#88403,#22446,#22447);
#19423=AXIS2_PLACEMENT_3D('',#90415,#22449,#22450);
#19424=AXIS2_PLACEMENT_3D('',#90417,#22452,#22453);
#19425=AXIS2_PLACEMENT_3D('',#90419,#22455,#22456);
#19426=AXIS2_PLACEMENT_3D('',#92431,#22458,#22459);
#19427=AXIS2_PLACEMENT_3D('',#94444,#22462,#22463);
#19428=AXIS2_PLACEMENT_3D('',#94446,#22465,#22466);
#19429=AXIS2_PLACEMENT_3D('',#94447,#22467,#22468);
#19430=AXIS2_PLACEMENT_3D('',#94448,#22469,#22470);
#19431=AXIS2_PLACEMENT_3D('',#94449,#22471,#22472);
#19432=AXIS2_PLACEMENT_3D('',#94454,#22474,#22475);
#19433=AXIS2_PLACEMENT_3D('',#94467,#22477,#22478);
#19434=AXIS2_PLACEMENT_3D('',#94481,#22480,#22481);
#19435=AXIS2_PLACEMENT_3D('',#94483,#22483,#22484);
#19436=AXIS2_PLACEMENT_3D('',#94489,#22488,#22489);
#19437=AXIS2_PLACEMENT_3D('',#94510,#22490,#22491);
#19438=AXIS2_PLACEMENT_3D('',#94512,#22493,#22494);
#19439=AXIS2_PLACEMENT_3D('',#94515,#22497,#22498);
#19440=AXIS2_PLACEMENT_3D('',#94516,#22499,#22500);
#19441=AXIS2_PLACEMENT_3D('',#94518,#22501,#22502);
#19442=AXIS2_PLACEMENT_3D('',#94519,#22503,#22504);
#19443=AXIS2_PLACEMENT_3D('',#94522,#22506,#22507);
#19444=AXIS2_PLACEMENT_3D('',#94523,#22508,#22509);
#19445=AXIS2_PLACEMENT_3D('',#94547,#22511,#22512);
#19446=AXIS2_PLACEMENT_3D('',#94549,#22514,#22515);
#19447=AXIS2_PLACEMENT_3D('',#94555,#22519,#22520);
#19448=AXIS2_PLACEMENT_3D('',#94579,#22521,#22522);
#19449=AXIS2_PLACEMENT_3D('',#94581,#22524,#22525);
#19450=AXIS2_PLACEMENT_3D('',#94584,#22528,#22529);
#19451=AXIS2_PLACEMENT_3D('',#94585,#22530,#22531);
#19452=AXIS2_PLACEMENT_3D('',#94587,#22532,#22533);
#19453=AXIS2_PLACEMENT_3D('',#94590,#22535,#22536);
#19454=AXIS2_PLACEMENT_3D('',#94591,#22537,#22538);
#19455=AXIS2_PLACEMENT_3D('',#94592,#22539,#22540);
#19456=AXIS2_PLACEMENT_3D('',#94594,#22541,#22542);
#19457=AXIS2_PLACEMENT_3D('',#94597,#22544,#22545);
#19458=AXIS2_PLACEMENT_3D('',#94598,#22546,#22547);
#19459=AXIS2_PLACEMENT_3D('',#94599,#22548,#22549);
#19460=AXIS2_PLACEMENT_3D('',#94600,#22550,#22551);
#19461=AXIS2_PLACEMENT_3D('',#94602,#22552,#22553);
#19462=AXIS2_PLACEMENT_3D('',#94605,#22555,#22556);
#19463=AXIS2_PLACEMENT_3D('',#94606,#22557,#22558);
#19464=AXIS2_PLACEMENT_3D('',#94608,#22559,#22560);
#19465=AXIS2_PLACEMENT_3D('',#94609,#22561,#22562);
#19466=AXIS2_PLACEMENT_3D('',#94611,#22563,#22564);
#19467=AXIS2_PLACEMENT_3D('',#94612,#22565,#22566);
#19468=AXIS2_PLACEMENT_3D('',#94614,#22567,#22568);
#19469=AXIS2_PLACEMENT_3D('',#94616,#22570,#22571);
#19470=AXIS2_PLACEMENT_3D('',#94618,#22572,#22573);
#19471=AXIS2_PLACEMENT_3D('',#94619,#22574,#22575);
#19472=AXIS2_PLACEMENT_3D('',#94621,#22576,#22577);
#19473=AXIS2_PLACEMENT_3D('',#94622,#22578,#22579);
#19474=AXIS2_PLACEMENT_3D('',#94624,#22581,#22582);
#19475=AXIS2_PLACEMENT_3D('',#94627,#22584,#22585);
#19476=AXIS2_PLACEMENT_3D('',#94628,#22586,#22587);
#19477=AXIS2_PLACEMENT_3D('',#94629,#22588,#22589);
#19478=AXIS2_PLACEMENT_3D('',#94630,#22590,#22591);
#19479=AXIS2_PLACEMENT_3D('',#94631,#22592,#22593);
#19480=AXIS2_PLACEMENT_3D('',#94640,#22598,#22599);
#19481=AXIS2_PLACEMENT_3D('',#94642,#22600,#22601);
#19482=AXIS2_PLACEMENT_3D('',#94644,#22602,#22603);
#19483=AXIS2_PLACEMENT_3D('',#94646,#22605,#22606);
#19484=AXIS2_PLACEMENT_3D('',#94652,#22610,#22611);
#19485=AXIS2_PLACEMENT_3D('',#94653,#22612,#22613);
#19486=AXIS2_PLACEMENT_3D('',#94654,#22614,#22615);
#19487=AXIS2_PLACEMENT_3D('',#94655,#22616,#22617);
#19488=AXIS2_PLACEMENT_3D('',#94656,#22618,#22619);
#19489=AXIS2_PLACEMENT_3D('',#94657,#22620,#22621);
#19490=AXIS2_PLACEMENT_3D('',#94658,#22622,#22623);
#19491=AXIS2_PLACEMENT_3D('',#94660,#22624,#22625);
#19492=AXIS2_PLACEMENT_3D('',#94663,#22627,#22628);
#19493=AXIS2_PLACEMENT_3D('',#94664,#22629,#22630);
#19494=AXIS2_PLACEMENT_3D('',#94665,#22631,#22632);
#19495=AXIS2_PLACEMENT_3D('',#94666,#22633,#22634);
#19496=AXIS2_PLACEMENT_3D('',#94667,#22635,#22636);
#19497=AXIS2_PLACEMENT_3D('',#94669,#22637,#22638);
#19498=AXIS2_PLACEMENT_3D('',#94671,#22639,#22640);
#19499=AXIS2_PLACEMENT_3D('',#94672,#22641,#22642);
#19500=AXIS2_PLACEMENT_3D('',#94674,#22643,#22644);
#19501=AXIS2_PLACEMENT_3D('',#94676,#22646,#22647);
#19502=AXIS2_PLACEMENT_3D('',#94679,#22649,#22650);
#19503=AXIS2_PLACEMENT_3D('',#94680,#22651,#22652);
#19504=AXIS2_PLACEMENT_3D('',#94682,#22653,#22654);
#19505=AXIS2_PLACEMENT_3D('',#94684,#22655,#22656);
#19506=AXIS2_PLACEMENT_3D('',#94685,#22657,#22658);
#19507=AXIS2_PLACEMENT_3D('',#94687,#22659,#22660);
#19508=AXIS2_PLACEMENT_3D('',#94689,#22662,#22663);
#19509=AXIS2_PLACEMENT_3D('',#94692,#22665,#22666);
#19510=AXIS2_PLACEMENT_3D('',#94693,#22667,#22668);
#19511=AXIS2_PLACEMENT_3D('',#94695,#22669,#22670);
#19512=AXIS2_PLACEMENT_3D('',#94697,#22671,#22672);
#19513=AXIS2_PLACEMENT_3D('',#94698,#22673,#22674);
#19514=AXIS2_PLACEMENT_3D('',#94700,#22675,#22676);
#19515=AXIS2_PLACEMENT_3D('',#94702,#22678,#22679);
#19516=AXIS2_PLACEMENT_3D('',#94705,#22681,#22682);
#19517=AXIS2_PLACEMENT_3D('',#94706,#22683,#22684);
#19518=AXIS2_PLACEMENT_3D('',#94708,#22685,#22686);
#19519=AXIS2_PLACEMENT_3D('',#94710,#22687,#22688);
#19520=AXIS2_PLACEMENT_3D('',#94711,#22689,#22690);
#19521=AXIS2_PLACEMENT_3D('',#94713,#22691,#22692);
#19522=AXIS2_PLACEMENT_3D('',#94715,#22694,#22695);
#19523=AXIS2_PLACEMENT_3D('',#94718,#22697,#22698);
#19524=AXIS2_PLACEMENT_3D('',#94719,#22699,#22700);
#19525=AXIS2_PLACEMENT_3D('',#94721,#22701,#22702);
#19526=AXIS2_PLACEMENT_3D('',#94723,#22703,#22704);
#19527=AXIS2_PLACEMENT_3D('',#94724,#22705,#22706);
#19528=AXIS2_PLACEMENT_3D('',#94726,#22707,#22708);
#19529=AXIS2_PLACEMENT_3D('',#94728,#22710,#22711);
#19530=AXIS2_PLACEMENT_3D('',#94731,#22713,#22714);
#19531=AXIS2_PLACEMENT_3D('',#94732,#22715,#22716);
#19532=AXIS2_PLACEMENT_3D('',#94734,#22717,#22718);
#19533=AXIS2_PLACEMENT_3D('',#94736,#22719,#22720);
#19534=AXIS2_PLACEMENT_3D('',#94737,#22721,#22722);
#19535=AXIS2_PLACEMENT_3D('',#94739,#22723,#22724);
#19536=AXIS2_PLACEMENT_3D('',#94741,#22726,#22727);
#19537=AXIS2_PLACEMENT_3D('',#94744,#22729,#22730);
#19538=AXIS2_PLACEMENT_3D('',#94745,#22731,#22732);
#19539=AXIS2_PLACEMENT_3D('',#94747,#22733,#22734);
#19540=AXIS2_PLACEMENT_3D('',#94750,#22736,#22737);
#19541=AXIS2_PLACEMENT_3D('',#94751,#22738,#22739);
#19542=AXIS2_PLACEMENT_3D('',#94753,#22740,#22741);
#19543=AXIS2_PLACEMENT_3D('',#94756,#22743,#22744);
#19544=AXIS2_PLACEMENT_3D('',#94757,#22745,#22746);
#19545=AXIS2_PLACEMENT_3D('',#94758,#22747,#22748);
#19546=AXIS2_PLACEMENT_3D('',#94759,#22749,#22750);
#19547=AXIS2_PLACEMENT_3D('',#94760,#22751,#22752);
#19548=AXIS2_PLACEMENT_3D('',#94762,#22753,#22754);
#19549=AXIS2_PLACEMENT_3D('',#94765,#22756,#22757);
#19550=AXIS2_PLACEMENT_3D('',#94766,#22758,#22759);
#19551=AXIS2_PLACEMENT_3D('',#94768,#22760,#22761);
#19552=AXIS2_PLACEMENT_3D('',#94771,#22763,#22764);
#19553=AXIS2_PLACEMENT_3D('',#94772,#22765,#22766);
#19554=AXIS2_PLACEMENT_3D('',#94773,#22767,#22768);
#19555=AXIS2_PLACEMENT_3D('',#94774,#22769,#22770);
#19556=AXIS2_PLACEMENT_3D('',#94775,#22771,#22772);
#19557=AXIS2_PLACEMENT_3D('',#94777,#22773,#22774);
#19558=AXIS2_PLACEMENT_3D('',#94780,#22776,#22777);
#19559=AXIS2_PLACEMENT_3D('',#94781,#22778,#22779);
#19560=AXIS2_PLACEMENT_3D('',#94784,#22781,#22782);
#19561=AXIS2_PLACEMENT_3D('',#94785,#22783,#22784);
#19562=AXIS2_PLACEMENT_3D('',#94787,#22785,#22786);
#19563=AXIS2_PLACEMENT_3D('',#94790,#22788,#22789);
#19564=AXIS2_PLACEMENT_3D('',#94791,#22790,#22791);
#19565=AXIS2_PLACEMENT_3D('',#94794,#22793,#22794);
#19566=AXIS2_PLACEMENT_3D('',#94795,#22795,#22796);
#19567=AXIS2_PLACEMENT_3D('',#94797,#22797,#22798);
#19568=AXIS2_PLACEMENT_3D('',#94800,#22800,#22801);
#19569=AXIS2_PLACEMENT_3D('',#94801,#22802,#22803);
#19570=AXIS2_PLACEMENT_3D('',#94804,#22805,#22806);
#19571=AXIS2_PLACEMENT_3D('',#94805,#22807,#22808);
#19572=AXIS2_PLACEMENT_3D('',#94807,#22809,#22810);
#19573=AXIS2_PLACEMENT_3D('',#94810,#22812,#22813);
#19574=AXIS2_PLACEMENT_3D('',#94811,#22814,#22815);
#19575=AXIS2_PLACEMENT_3D('',#94814,#22817,#22818);
#19576=AXIS2_PLACEMENT_3D('',#94815,#22819,#22820);
#19577=AXIS2_PLACEMENT_3D('',#94817,#22821,#22822);
#19578=AXIS2_PLACEMENT_3D('',#94820,#22824,#22825);
#19579=AXIS2_PLACEMENT_3D('',#94821,#22826,#22827);
#19580=AXIS2_PLACEMENT_3D('',#94824,#22829,#22830);
#19581=AXIS2_PLACEMENT_3D('',#94825,#22831,#22832);
#19582=AXIS2_PLACEMENT_3D('',#94827,#22833,#22834);
#19583=AXIS2_PLACEMENT_3D('',#94830,#22836,#22837);
#19584=AXIS2_PLACEMENT_3D('',#94831,#22838,#22839);
#19585=AXIS2_PLACEMENT_3D('',#94834,#22841,#22842);
#19586=AXIS2_PLACEMENT_3D('',#94835,#22843,#22844);
#19587=AXIS2_PLACEMENT_3D('',#94837,#22845,#22846);
#19588=AXIS2_PLACEMENT_3D('',#94840,#22848,#22849);
#19589=AXIS2_PLACEMENT_3D('',#94841,#22850,#22851);
#19590=AXIS2_PLACEMENT_3D('',#94843,#22852,#22853);
#19591=AXIS2_PLACEMENT_3D('',#94846,#22855,#22856);
#19592=AXIS2_PLACEMENT_3D('',#94847,#22857,#22858);
#19593=AXIS2_PLACEMENT_3D('',#94848,#22859,#22860);
#19594=AXIS2_PLACEMENT_3D('',#94849,#22861,#22862);
#19595=AXIS2_PLACEMENT_3D('',#94850,#22863,#22864);
#19596=AXIS2_PLACEMENT_3D('',#94852,#22865,#22866);
#19597=AXIS2_PLACEMENT_3D('',#94855,#22868,#22869);
#19598=AXIS2_PLACEMENT_3D('',#94856,#22870,#22871);
#19599=AXIS2_PLACEMENT_3D('',#94858,#22872,#22873);
#19600=AXIS2_PLACEMENT_3D('',#94861,#22875,#22876);
#19601=AXIS2_PLACEMENT_3D('',#94862,#22877,#22878);
#19602=AXIS2_PLACEMENT_3D('',#94863,#22879,#22880);
#19603=AXIS2_PLACEMENT_3D('',#94864,#22881,#22882);
#19604=AXIS2_PLACEMENT_3D('',#94865,#22883,#22884);
#19605=AXIS2_PLACEMENT_3D('',#94867,#22885,#22886);
#19606=AXIS2_PLACEMENT_3D('',#94870,#22888,#22889);
#19607=AXIS2_PLACEMENT_3D('',#94871,#22890,#22891);
#19608=AXIS2_PLACEMENT_3D('',#94873,#22892,#22893);
#19609=AXIS2_PLACEMENT_3D('',#94876,#22895,#22896);
#19610=AXIS2_PLACEMENT_3D('',#94877,#22897,#22898);
#19611=AXIS2_PLACEMENT_3D('',#94878,#22899,#22900);
#19612=AXIS2_PLACEMENT_3D('',#94879,#22901,#22902);
#19613=AXIS2_PLACEMENT_3D('',#94880,#22903,#22904);
#19614=AXIS2_PLACEMENT_3D('',#94882,#22905,#22906);
#19615=AXIS2_PLACEMENT_3D('',#94885,#22908,#22909);
#19616=AXIS2_PLACEMENT_3D('',#94886,#22910,#22911);
#19617=AXIS2_PLACEMENT_3D('',#94888,#22912,#22913);
#19618=AXIS2_PLACEMENT_3D('',#94891,#22915,#22916);
#19619=AXIS2_PLACEMENT_3D('',#94892,#22917,#22918);
#19620=AXIS2_PLACEMENT_3D('',#94893,#22919,#22920);
#19621=AXIS2_PLACEMENT_3D('',#94894,#22921,#22922);
#19622=AXIS2_PLACEMENT_3D('',#94895,#22923,#22924);
#19623=AXIS2_PLACEMENT_3D('',#94904,#22929,#22930);
#19624=AXIS2_PLACEMENT_3D('',#94913,#22935,#22936);
#19625=AXIS2_PLACEMENT_3D('',#94914,#22937,#22938);
#19626=AXIS2_PLACEMENT_3D('',#94915,#22939,#22940);
#19627=AXIS2_PLACEMENT_3D('',#94916,#22941,#22942);
#19628=AXIS2_PLACEMENT_3D('',#94917,#22943,#22944);
#19629=AXIS2_PLACEMENT_3D('',#94918,#22945,#22946);
#19630=AXIS2_PLACEMENT_3D('',#94919,#22947,#22948);
#19631=AXIS2_PLACEMENT_3D('',#94920,#22949,#22950);
#19632=AXIS2_PLACEMENT_3D('',#94921,#22951,#22952);
#19633=AXIS2_PLACEMENT_3D('',#94922,#22953,#22954);
#19634=AXIS2_PLACEMENT_3D('',#94924,#22955,#22956);
#19635=AXIS2_PLACEMENT_3D('',#94926,#22957,#22958);
#19636=AXIS2_PLACEMENT_3D('',#94927,#22959,#22960);
#19637=AXIS2_PLACEMENT_3D('',#94929,#22961,#22962);
#19638=AXIS2_PLACEMENT_3D('',#94931,#22964,#22965);
#19639=AXIS2_PLACEMENT_3D('',#94932,#22966,#22967);
#19640=AXIS2_PLACEMENT_3D('',#94935,#22969,#22970);
#19641=AXIS2_PLACEMENT_3D('',#94936,#22971,#22972);
#19642=AXIS2_PLACEMENT_3D('',#94937,#22973,#22974);
#19643=AXIS2_PLACEMENT_3D('',#95229,#22975,#22976);
#19644=AXIS2_PLACEMENT_3D('',#95260,#22977,#22978);
#19645=AXIS2_PLACEMENT_3D('',#95261,#22979,#22980);
#19646=AXIS2_PLACEMENT_3D('',#95262,#22981,#22982);
#19647=AXIS2_PLACEMENT_3D('',#95263,#22983,#22984);
#19648=AXIS2_PLACEMENT_3D('',#95264,#22985,#22986);
#19649=AXIS2_PLACEMENT_3D('',#95280,#22988,#22989);
#19650=AXIS2_PLACEMENT_3D('',#95288,#22990,#22991);
#19651=AXIS2_PLACEMENT_3D('',#95336,#22993,#22994);
#19652=AXIS2_PLACEMENT_3D('',#95384,#22996,#22997);
#19653=AXIS2_PLACEMENT_3D('',#95438,#22999,#23000);
#19654=AXIS2_PLACEMENT_3D('',#95486,#23002,#23003);
#19655=AXIS2_PLACEMENT_3D('',#95534,#23005,#23006);
#19656=AXIS2_PLACEMENT_3D('',#95582,#23008,#23009);
#19657=AXIS2_PLACEMENT_3D('',#95636,#23011,#23012);
#19658=AXIS2_PLACEMENT_3D('',#95684,#23014,#23015);
#19659=AXIS2_PLACEMENT_3D('',#95732,#23017,#23018);
#19660=AXIS2_PLACEMENT_3D('',#95786,#23020,#23021);
#19661=AXIS2_PLACEMENT_3D('',#95834,#23023,#23024);
#19662=AXIS2_PLACEMENT_3D('',#95882,#23026,#23027);
#19663=AXIS2_PLACEMENT_3D('',#95933,#23029,#23030);
#19664=AXIS2_PLACEMENT_3D('',#95984,#23032,#23033);
#19665=AXIS2_PLACEMENT_3D('',#96032,#23035,#23036);
#19666=AXIS2_PLACEMENT_3D('',#96046,#23038,#23039);
#19667=AXIS2_PLACEMENT_3D('',#96054,#23040,#23041);
#19668=AXIS2_PLACEMENT_3D('',#96078,#23043,#23044);
#19669=AXIS2_PLACEMENT_3D('',#96102,#23046,#23047);
#19670=AXIS2_PLACEMENT_3D('',#96128,#23049,#23050);
#19671=AXIS2_PLACEMENT_3D('',#96152,#23052,#23053);
#19672=AXIS2_PLACEMENT_3D('',#96176,#23055,#23056);
#19673=AXIS2_PLACEMENT_3D('',#96201,#23058,#23059);
#19674=AXIS2_PLACEMENT_3D('',#96226,#23061,#23062);
#19675=AXIS2_PLACEMENT_3D('',#96250,#23064,#23065);
#19676=AXIS2_PLACEMENT_3D('',#96275,#23067,#23068);
#19677=AXIS2_PLACEMENT_3D('',#96300,#23070,#23071);
#19678=AXIS2_PLACEMENT_3D('',#96324,#23073,#23074);
#19679=AXIS2_PLACEMENT_3D('',#96348,#23076,#23077);
#19680=AXIS2_PLACEMENT_3D('',#96373,#23079,#23080);
#19681=AXIS2_PLACEMENT_3D('',#96398,#23082,#23083);
#19682=AXIS2_PLACEMENT_3D('',#96422,#23085,#23086);
#19683=AXIS2_PLACEMENT_3D('',#96611,#23087,#23088);
#19684=AXIS2_PLACEMENT_3D('',#96717,#23090,#23091);
#19685=AXIS2_PLACEMENT_3D('',#97249,#23092,#23093);
#19686=AXIS2_PLACEMENT_3D('',#97260,#23094,#23095);
#19687=AXIS2_PLACEMENT_3D('',#97794,#23096,#23097);
#19688=AXIS2_PLACEMENT_3D('',#97795,#23098,#23099);
#19689=AXIS2_PLACEMENT_3D('',#97804,#23104,#23105);
#19690=AXIS2_PLACEMENT_3D('',#97810,#23109,#23110);
#19691=AXIS2_PLACEMENT_3D('',#97816,#23114,#23115);
#19692=AXIS2_PLACEMENT_3D('',#97822,#23119,#23120);
#19693=AXIS2_PLACEMENT_3D('',#97828,#23124,#23125);
#19694=AXIS2_PLACEMENT_3D('',#97831,#23128,#23129);
#19695=AXIS2_PLACEMENT_3D('',#97832,#23130,#23131);
#19696=AXIS2_PLACEMENT_3D('',#97834,#23132,#23133);
#19697=AXIS2_PLACEMENT_3D('',#97835,#23134,#23135);
#19698=AXIS2_PLACEMENT_3D('',#97838,#23137,#23138);
#19699=AXIS2_PLACEMENT_3D('',#97839,#23139,#23140);
#19700=AXIS2_PLACEMENT_3D('',#97840,#23141,#23142);
#19701=AXIS2_PLACEMENT_3D('',#97841,#23143,#23144);
#19702=AXIS2_PLACEMENT_3D('',#97842,#23145,#23146);
#19703=AXIS2_PLACEMENT_3D('',#97858,#23148,#23149);
#19704=AXIS2_PLACEMENT_3D('',#97866,#23150,#23151);
#19705=AXIS2_PLACEMENT_3D('',#97914,#23153,#23154);
#19706=AXIS2_PLACEMENT_3D('',#97962,#23156,#23157);
#19707=AXIS2_PLACEMENT_3D('',#98010,#23159,#23160);
#19708=AXIS2_PLACEMENT_3D('',#98058,#23162,#23163);
#19709=AXIS2_PLACEMENT_3D('',#98106,#23165,#23166);
#19710=AXIS2_PLACEMENT_3D('',#98154,#23168,#23169);
#19711=AXIS2_PLACEMENT_3D('',#98208,#23171,#23172);
#19712=AXIS2_PLACEMENT_3D('',#98223,#23174,#23175);
#19713=AXIS2_PLACEMENT_3D('',#98232,#23176,#23177);
#19714=AXIS2_PLACEMENT_3D('',#98257,#23179,#23180);
#19715=AXIS2_PLACEMENT_3D('',#98282,#23182,#23183);
#19716=AXIS2_PLACEMENT_3D('',#98306,#23185,#23186);
#19717=AXIS2_PLACEMENT_3D('',#98330,#23188,#23189);
#19718=AXIS2_PLACEMENT_3D('',#98356,#23191,#23192);
#19719=AXIS2_PLACEMENT_3D('',#98380,#23194,#23195);
#19720=AXIS2_PLACEMENT_3D('',#98404,#23197,#23198);
#19721=AXIS2_PLACEMENT_3D('',#98653,#23199,#23200);
#19722=AXIS2_PLACEMENT_3D('',#98696,#23202,#23203);
#19723=AXIS2_PLACEMENT_3D('',#99032,#23204,#23205);
#19724=AXIS2_PLACEMENT_3D('',#99043,#23206,#23207);
#19725=AXIS2_PLACEMENT_3D('',#99044,#23208,#23209);
#19726=AXIS2_PLACEMENT_3D('',#99053,#23214,#23215);
#19727=AXIS2_PLACEMENT_3D('',#99059,#23219,#23220);
#19728=AXIS2_PLACEMENT_3D('',#99065,#23224,#23225);
#19729=AXIS2_PLACEMENT_3D('',#99071,#23229,#23230);
#19730=AXIS2_PLACEMENT_3D('',#99077,#23234,#23235);
#19731=AXIS2_PLACEMENT_3D('',#99080,#23238,#23239);
#19732=AXIS2_PLACEMENT_3D('',#99421,#23240,#23241);
#19733=AXIS2_PLACEMENT_3D('',#99423,#23242,#23243);
#19734=AXIS2_PLACEMENT_3D('',#99424,#23244,#23245);
#19735=AXIS2_PLACEMENT_3D('',#99425,#23246,#23247);
#19736=AXIS2_PLACEMENT_3D('',#99426,#23248,#23249);
#19737=AXIS2_PLACEMENT_3D('',#99428,#23250,#23251);
#19738=AXIS2_PLACEMENT_3D('',#99429,#23252,#23253);
#19739=AXIS2_PLACEMENT_3D('',#99431,#23255,#23256);
#19740=AXIS2_PLACEMENT_3D('',#99432,#23257,#23258);
#19741=AXIS2_PLACEMENT_3D('',#99433,#23259,#23260);
#19742=AXIS2_PLACEMENT_3D('',#99434,#23261,#23262);
#19743=AXIS2_PLACEMENT_3D('',#99435,#23263,#23264);
#19744=AXIS2_PLACEMENT_3D('',#99436,#23265,#23266);
#19745=AXIS2_PLACEMENT_3D('',#99437,#23267,#23268);
#19746=AXIS2_PLACEMENT_3D('',#99438,#23269,#23270);
#19747=AXIS2_PLACEMENT_3D('',#99439,#23271,#23272);
#19748=AXIS2_PLACEMENT_3D('',#99440,#23273,#23274);
#19749=AXIS2_PLACEMENT_3D('',#99441,#23275,#23276);
#19750=AXIS2_PLACEMENT_3D('',#99442,#23277,#23278);
#19751=AXIS2_PLACEMENT_3D('',#99443,#23279,#23280);
#19752=AXIS2_PLACEMENT_3D('',#99444,#23281,#23282);
#19753=AXIS2_PLACEMENT_3D('',#99445,#23283,#23284);
#19754=AXIS2_PLACEMENT_3D('',#99446,#23285,#23286);
#19755=AXIS2_PLACEMENT_3D('',#99447,#23287,#23288);
#19756=AXIS2_PLACEMENT_3D('',#99448,#23289,#23290);
#19757=AXIS2_PLACEMENT_3D('',#99449,#23291,#23292);
#19758=AXIS2_PLACEMENT_3D('',#99450,#23293,#23294);
#19759=AXIS2_PLACEMENT_3D('',#99451,#23295,#23296);
#19760=AXIS2_PLACEMENT_3D('',#99452,#23297,#23298);
#19761=AXIS2_PLACEMENT_3D('',#99453,#23299,#23300);
#19762=AXIS2_PLACEMENT_3D('',#99454,#23301,#23302);
#19763=AXIS2_PLACEMENT_3D('',#99455,#23303,#23304);
#19764=AXIS2_PLACEMENT_3D('',#99456,#23305,#23306);
#19765=AXIS2_PLACEMENT_3D('',#99457,#23307,#23308);
#19766=AXIS2_PLACEMENT_3D('',#99458,#23309,#23310);
#19767=AXIS2_PLACEMENT_3D('',#99459,#23311,#23312);
#19768=AXIS2_PLACEMENT_3D('',#99460,#23313,#23314);
#19769=AXIS2_PLACEMENT_3D('',#99461,#23315,#23316);
#19770=AXIS2_PLACEMENT_3D('',#99462,#23317,#23318);
#19771=AXIS2_PLACEMENT_3D('',#99463,#23319,#23320);
#19772=AXIS2_PLACEMENT_3D('',#99464,#23321,#23322);
#19773=AXIS2_PLACEMENT_3D('',#99465,#23323,#23324);
#19774=AXIS2_PLACEMENT_3D('',#99466,#23325,#23326);
#19775=AXIS2_PLACEMENT_3D('',#99467,#23327,#23328);
#19776=AXIS2_PLACEMENT_3D('',#99468,#23329,#23330);
#19777=AXIS2_PLACEMENT_3D('',#99469,#23331,#23332);
#19778=AXIS2_PLACEMENT_3D('',#99470,#23333,#23334);
#19779=AXIS2_PLACEMENT_3D('',#99471,#23335,#23336);
#19780=AXIS2_PLACEMENT_3D('',#99472,#23337,#23338);
#19781=AXIS2_PLACEMENT_3D('',#99473,#23339,#23340);
#19782=AXIS2_PLACEMENT_3D('',#99474,#23341,#23342);
#19783=AXIS2_PLACEMENT_3D('',#99475,#23343,#23344);
#19784=AXIS2_PLACEMENT_3D('',#99476,#23345,#23346);
#19785=AXIS2_PLACEMENT_3D('',#99477,#23347,#23348);
#19786=AXIS2_PLACEMENT_3D('',#99478,#23349,#23350);
#19787=AXIS2_PLACEMENT_3D('',#99479,#23351,#23352);
#19788=AXIS2_PLACEMENT_3D('',#99480,#23353,#23354);
#19789=AXIS2_PLACEMENT_3D('',#99481,#23355,#23356);
#19790=AXIS2_PLACEMENT_3D('',#99482,#23357,#23358);
#19791=AXIS2_PLACEMENT_3D('',#99483,#23359,#23360);
#19792=AXIS2_PLACEMENT_3D('',#99484,#23361,#23362);
#19793=AXIS2_PLACEMENT_3D('',#99485,#23363,#23364);
#19794=AXIS2_PLACEMENT_3D('',#99486,#23365,#23366);
#19795=AXIS2_PLACEMENT_3D('',#99487,#23367,#23368);
#19796=AXIS2_PLACEMENT_3D('',#99488,#23369,#23370);
#19797=AXIS2_PLACEMENT_3D('',#99489,#23371,#23372);
#19798=AXIS2_PLACEMENT_3D('',#99490,#23373,#23374);
#19799=DIRECTION('axis',(0.,0.,1.));
#19800=DIRECTION('refdir',(1.,0.,0.));
#19801=DIRECTION('axis',(0.,0.,1.));
#19802=DIRECTION('refdir',(1.,0.,0.));
#19803=DIRECTION('center_axis',(0.,0.,-1.));
#19804=DIRECTION('ref_axis',(1.,0.,0.));
#19805=DIRECTION('',(0.,0.,-1.));
#19806=DIRECTION('center_axis',(0.,0.,1.));
#19807=DIRECTION('ref_axis',(1.,0.,0.));
#19808=DIRECTION('',(0.,0.,-1.));
#19809=DIRECTION('center_axis',(0.,0.,1.));
#19810=DIRECTION('ref_axis',(1.,0.,0.));
#19811=DIRECTION('center_axis',(0.,0.,-1.));
#19812=DIRECTION('ref_axis',(1.,0.,0.));
#19813=DIRECTION('',(0.,0.,-1.));
#19814=DIRECTION('center_axis',(0.,0.,-1.));
#19815=DIRECTION('ref_axis',(1.,0.,0.));
#19816=DIRECTION('',(0.,0.,-1.));
#19817=DIRECTION('center_axis',(0.,0.,-1.));
#19818=DIRECTION('ref_axis',(1.,0.,0.));
#19819=DIRECTION('',(0.,0.,-1.));
#19820=DIRECTION('center_axis',(0.,0.,-1.));
#19821=DIRECTION('ref_axis',(1.,0.,0.));
#19822=DIRECTION('',(0.,0.,-1.));
#19823=DIRECTION('center_axis',(0.,0.,-1.));
#19824=DIRECTION('ref_axis',(1.,0.,0.));
#19825=DIRECTION('',(0.,0.,-1.));
#19826=DIRECTION('center_axis',(0.,0.,-1.));
#19827=DIRECTION('ref_axis',(1.,0.,0.));
#19828=DIRECTION('',(0.,0.,-1.));
#19829=DIRECTION('center_axis',(0.,0.,-1.));
#19830=DIRECTION('ref_axis',(1.,0.,0.));
#19831=DIRECTION('',(0.,0.,-1.));
#19832=DIRECTION('center_axis',(0.,0.,-1.));
#19833=DIRECTION('ref_axis',(1.,0.,0.));
#19834=DIRECTION('',(0.,0.,-1.));
#19835=DIRECTION('center_axis',(0.,0.,-1.));
#19836=DIRECTION('ref_axis',(1.,0.,0.));
#19837=DIRECTION('',(0.,0.,-1.));
#19838=DIRECTION('center_axis',(0.,0.,-1.));
#19839=DIRECTION('ref_axis',(1.,0.,0.));
#19840=DIRECTION('',(0.,0.,-1.));
#19841=DIRECTION('center_axis',(0.,0.,-1.));
#19842=DIRECTION('ref_axis',(0.938437885424521,-0.345448020981382,0.));
#19843=DIRECTION('',(0.,0.,-1.));
#19844=DIRECTION('center_axis',(0.,0.,-1.));
#19845=DIRECTION('ref_axis',(1.,0.,0.));
#19846=DIRECTION('center_axis',(0.,0.,-1.));
#19847=DIRECTION('ref_axis',(0.450150052286485,0.892952927329585,0.));
#19848=DIRECTION('',(1.22464679914735E-16,-7.67327966807698E-30,-1.));
#19849=DIRECTION('center_axis',(0.,0.,1.));
#19850=DIRECTION('ref_axis',(1.,-6.25346187617716E-14,0.));
#19851=DIRECTION('center_axis',(0.,0.,-1.));
#19852=DIRECTION('ref_axis',(1.,-6.25346187617716E-14,0.));
#19853=DIRECTION('',(1.22464679914735E-16,-7.67327966807698E-30,-1.));
#19854=DIRECTION('center_axis',(0.,0.,-1.));
#19855=DIRECTION('ref_axis',(1.,-6.25346187617716E-14,0.));
#19856=DIRECTION('',(1.22464679914735E-16,-7.67327966807698E-30,-1.));
#19857=DIRECTION('center_axis',(0.,0.,-1.));
#19858=DIRECTION('ref_axis',(1.,-6.25346187617716E-14,0.));
#19859=DIRECTION('',(1.22464679914735E-16,-7.67327966807698E-30,-1.));
#19860=DIRECTION('center_axis',(0.,0.,-1.));
#19861=DIRECTION('ref_axis',(1.,-6.25346187617716E-14,0.));
#19862=DIRECTION('',(1.22464679914735E-16,-7.67327966807698E-30,-1.));
#19863=DIRECTION('center_axis',(0.,0.,-1.));
#19864=DIRECTION('ref_axis',(1.,-6.25346187617716E-14,0.));
#19865=DIRECTION('',(1.22464679914735E-16,-7.67327966807698E-30,-1.));
#19866=DIRECTION('center_axis',(0.,0.,-1.));
#19867=DIRECTION('ref_axis',(1.,-6.25346187617716E-14,0.));
#19868=DIRECTION('',(1.22464679914735E-16,-7.67327966807698E-30,-1.));
#19869=DIRECTION('center_axis',(0.,0.,-1.));
#19870=DIRECTION('ref_axis',(1.,-6.25346187617716E-14,0.));
#19871=DIRECTION('',(1.22464679914735E-16,-7.67327966807698E-30,-1.));
#19872=DIRECTION('center_axis',(0.,0.,-1.));
#19873=DIRECTION('ref_axis',(1.,-6.25346187617716E-14,0.));
#19874=DIRECTION('',(1.22464679914735E-16,-7.67327966807698E-30,-1.));
#19875=DIRECTION('center_axis',(0.,0.,-1.));
#19876=DIRECTION('ref_axis',(1.,-6.25346187617716E-14,0.));
#19877=DIRECTION('',(1.22464679914735E-16,-7.67327966807698E-30,-1.));
#19878=DIRECTION('center_axis',(0.,0.,-1.));
#19879=DIRECTION('ref_axis',(1.,-6.25346187617716E-14,0.));
#19880=DIRECTION('',(1.22464679914735E-16,-7.67327966807698E-30,-1.));
#19881=DIRECTION('center_axis',(0.,0.,-1.));
#19882=DIRECTION('ref_axis',(1.,-6.25346187617716E-14,0.));
#19883=DIRECTION('',(1.22464679914735E-16,-7.67327966807698E-30,-1.));
#19884=DIRECTION('center_axis',(0.,0.,-1.));
#19885=DIRECTION('ref_axis',(-0.609343127961874,-0.792906647976696,0.));
#19886=DIRECTION('',(1.22464679914735E-16,-7.67327966807698E-30,-1.));
#19887=DIRECTION('center_axis',(0.,0.,-1.));
#19888=DIRECTION('ref_axis',(1.,-6.25346187617716E-14,0.));
#19889=DIRECTION('center_axis',(0.,0.,1.));
#19890=DIRECTION('ref_axis',(-1.,0.,0.));
#19891=DIRECTION('',(0.,0.,1.));
#19892=DIRECTION('center_axis',(0.,0.,-1.));
#19893=DIRECTION('ref_axis',(-1.,0.,0.));
#19894=DIRECTION('',(0.,0.,1.));
#19895=DIRECTION('center_axis',(0.,0.,-1.));
#19896=DIRECTION('ref_axis',(-1.,0.,0.));
#19897=DIRECTION('center_axis',(0.,0.,1.));
#19898=DIRECTION('ref_axis',(-1.,0.,0.));
#19899=DIRECTION('',(0.,0.,1.));
#19900=DIRECTION('center_axis',(0.,0.,1.));
#19901=DIRECTION('ref_axis',(-1.,0.,0.));
#19902=DIRECTION('',(0.,0.,1.));
#19903=DIRECTION('center_axis',(0.,0.,1.));
#19904=DIRECTION('ref_axis',(-1.,0.,0.));
#19905=DIRECTION('',(0.,0.,1.));
#19906=DIRECTION('center_axis',(0.,0.,1.));
#19907=DIRECTION('ref_axis',(-1.,0.,0.));
#19908=DIRECTION('',(0.,0.,1.));
#19909=DIRECTION('center_axis',(0.,0.,1.));
#19910=DIRECTION('ref_axis',(-1.,0.,0.));
#19911=DIRECTION('',(0.,0.,1.));
#19912=DIRECTION('center_axis',(0.,0.,1.));
#19913=DIRECTION('ref_axis',(-1.,0.,0.));
#19914=DIRECTION('',(0.,0.,1.));
#19915=DIRECTION('center_axis',(0.,0.,1.));
#19916=DIRECTION('ref_axis',(-1.,0.,0.));
#19917=DIRECTION('',(0.,0.,1.));
#19918=DIRECTION('center_axis',(0.,0.,1.));
#19919=DIRECTION('ref_axis',(-1.,0.,0.));
#19920=DIRECTION('',(0.,0.,1.));
#19921=DIRECTION('center_axis',(0.,0.,1.));
#19922=DIRECTION('ref_axis',(-1.,0.,0.));
#19923=DIRECTION('',(0.,0.,1.));
#19924=DIRECTION('center_axis',(0.,0.,1.));
#19925=DIRECTION('ref_axis',(-1.,0.,0.));
#19926=DIRECTION('',(0.,0.,1.));
#19927=DIRECTION('center_axis',(0.,0.,1.));
#19928=DIRECTION('ref_axis',(-0.938437365767004,-0.345449432670379,0.));
#19929=DIRECTION('',(0.,0.,1.));
#19930=DIRECTION('center_axis',(0.,0.,-1.));
#19931=DIRECTION('ref_axis',(-1.,0.,0.));
#19932=DIRECTION('center_axis',(0.,0.,1.));
#19933=DIRECTION('ref_axis',(-0.450147885469881,0.892954019648825,0.));
#19934=DIRECTION('',(-1.22464679914735E-16,-6.15178233488065E-30,1.));
#19935=DIRECTION('center_axis',(0.,0.,-1.));
#19936=DIRECTION('ref_axis',(-1.,-5.01106501999328E-14,0.));
#19937=DIRECTION('center_axis',(0.,0.,1.));
#19938=DIRECTION('ref_axis',(-1.,-5.01106501999328E-14,0.));
#19939=DIRECTION('',(-1.22464679914735E-16,-6.15178233488065E-30,1.));
#19940=DIRECTION('center_axis',(0.,0.,1.));
#19941=DIRECTION('ref_axis',(-1.,-5.01106501999328E-14,0.));
#19942=DIRECTION('',(-1.22464679914735E-16,-6.15178233488065E-30,1.));
#19943=DIRECTION('center_axis',(0.,0.,1.));
#19944=DIRECTION('ref_axis',(-1.,-5.01106501999328E-14,0.));
#19945=DIRECTION('',(-1.22464679914735E-16,-6.15178233488065E-30,1.));
#19946=DIRECTION('center_axis',(0.,0.,1.));
#19947=DIRECTION('ref_axis',(-1.,-5.01106501999328E-14,0.));
#19948=DIRECTION('',(-1.22464679914735E-16,-6.15178233488065E-30,1.));
#19949=DIRECTION('center_axis',(0.,0.,1.));
#19950=DIRECTION('ref_axis',(-1.,-5.01106501999328E-14,0.));
#19951=DIRECTION('',(-1.22464679914735E-16,-6.15178233488065E-30,1.));
#19952=DIRECTION('center_axis',(0.,0.,1.));
#19953=DIRECTION('ref_axis',(-1.,-5.01106501999328E-14,0.));
#19954=DIRECTION('',(-1.22464679914735E-16,-6.15178233488065E-30,1.));
#19955=DIRECTION('center_axis',(0.,0.,1.));
#19956=DIRECTION('ref_axis',(-1.,-5.01106501999328E-14,0.));
#19957=DIRECTION('',(-1.22464679914735E-16,-6.15178233488065E-30,1.));
#19958=DIRECTION('center_axis',(0.,0.,1.));
#19959=DIRECTION('ref_axis',(-1.,-5.01106501999328E-14,0.));
#19960=DIRECTION('',(-1.22464679914735E-16,-6.15178233488065E-30,1.));
#19961=DIRECTION('center_axis',(0.,0.,1.));
#19962=DIRECTION('ref_axis',(-1.,-5.01106501999328E-14,0.));
#19963=DIRECTION('',(-1.22464679914735E-16,-6.15178233488065E-30,1.));
#19964=DIRECTION('center_axis',(0.,0.,1.));
#19965=DIRECTION('ref_axis',(-1.,-5.01106501999328E-14,0.));
#19966=DIRECTION('',(-1.22464679914735E-16,-6.15178233488065E-30,1.));
#19967=DIRECTION('center_axis',(0.,0.,1.));
#19968=DIRECTION('ref_axis',(-1.,-5.01106501999328E-14,0.));
#19969=DIRECTION('',(-1.22464679914735E-16,-6.15178233488065E-30,1.));
#19970=DIRECTION('center_axis',(0.,0.,1.));
#19971=DIRECTION('ref_axis',(0.609344456561462,-0.792905626955577,0.));
#19972=DIRECTION('',(-1.22464679914735E-16,-6.15178233488065E-30,1.));
#19973=DIRECTION('center_axis',(0.,0.,1.));
#19974=DIRECTION('ref_axis',(-1.,-5.01106501999328E-14,0.));
#19975=DIRECTION('center_axis',(0.,0.,-1.));
#19976=DIRECTION('ref_axis',(0.5,0.866025403784439,0.));
#19977=DIRECTION('',(0.,0.,-1.));
#19978=DIRECTION('center_axis',(0.,0.,1.));
#19979=DIRECTION('ref_axis',(0.5,0.866025403784439,0.));
#19980=DIRECTION('',(0.,0.,-1.));
#19981=DIRECTION('center_axis',(0.,0.,1.));
#19982=DIRECTION('ref_axis',(0.5,0.866025403784439,0.));
#19983=DIRECTION('center_axis',(0.,0.,-1.));
#19984=DIRECTION('ref_axis',(0.5,0.866025403784439,0.));
#19985=DIRECTION('',(0.,0.,-1.));
#19986=DIRECTION('center_axis',(0.,0.,-1.));
#19987=DIRECTION('ref_axis',(0.5,0.866025403784439,0.));
#19988=DIRECTION('',(0.,0.,-1.));
#19989=DIRECTION('center_axis',(0.,0.,-1.));
#19990=DIRECTION('ref_axis',(0.5,0.866025403784439,0.));
#19991=DIRECTION('',(0.,0.,-1.));
#19992=DIRECTION('center_axis',(0.,0.,-1.));
#19993=DIRECTION('ref_axis',(0.5,0.866025403784439,0.));
#19994=DIRECTION('',(0.,0.,-1.));
#19995=DIRECTION('center_axis',(0.,0.,-1.));
#19996=DIRECTION('ref_axis',(0.5,0.866025403784439,0.));
#19997=DIRECTION('',(0.,0.,-1.));
#19998=DIRECTION('center_axis',(0.,0.,-1.));
#19999=DIRECTION('ref_axis',(0.5,0.866025403784439,0.));
#20000=DIRECTION('',(0.,0.,-1.));
#20001=DIRECTION('center_axis',(0.,0.,-1.));
#20002=DIRECTION('ref_axis',(0.5,0.866025403784439,0.));
#20003=DIRECTION('',(0.,0.,-1.));
#20004=DIRECTION('center_axis',(0.,0.,-1.));
#20005=DIRECTION('ref_axis',(0.5,0.866025403784439,0.));
#20006=DIRECTION('',(0.,0.,-1.));
#20007=DIRECTION('center_axis',(0.,0.,-1.));
#20008=DIRECTION('ref_axis',(0.5,0.866025403784439,0.));
#20009=DIRECTION('',(0.,0.,-1.));
#20010=DIRECTION('center_axis',(0.,0.,-1.));
#20011=DIRECTION('ref_axis',(0.5,0.866025403784439,0.));
#20012=DIRECTION('',(0.,0.,-1.));
#20013=DIRECTION('center_axis',(0.,0.,-1.));
#20014=DIRECTION('ref_axis',(0.76838443895182,0.639988557692008,0.));
#20015=DIRECTION('',(0.,0.,-1.));
#20016=DIRECTION('center_axis',(0.,0.,-1.));
#20017=DIRECTION('ref_axis',(0.5,0.866025403784439,0.));
#20018=DIRECTION('center_axis',(0.,0.,-1.));
#20019=DIRECTION('ref_axis',(-0.548242225181982,0.836319593533183,0.));
#20020=DIRECTION('',(6.12323399573741E-17,1.06057523872487E-16,-1.));
#20021=DIRECTION('center_axis',(0.,0.,1.));
#20022=DIRECTION('ref_axis',(0.500000000000052,0.866025403784409,0.));
#20023=DIRECTION('center_axis',(0.,0.,-1.));
#20024=DIRECTION('ref_axis',(0.500000000000052,0.866025403784408,0.));
#20025=DIRECTION('',(6.12323399573741E-17,1.06057523872487E-16,-1.));
#20026=DIRECTION('center_axis',(0.,0.,-1.));
#20027=DIRECTION('ref_axis',(0.500000000000052,0.866025403784408,0.));
#20028=DIRECTION('',(6.12323399573741E-17,1.06057523872487E-16,-1.));
#20029=DIRECTION('center_axis',(0.,0.,-1.));
#20030=DIRECTION('ref_axis',(0.500000000000052,0.866025403784408,0.));
#20031=DIRECTION('',(6.12323399573741E-17,1.06057523872487E-16,-1.));
#20032=DIRECTION('center_axis',(0.,0.,-1.));
#20033=DIRECTION('ref_axis',(0.500000000000052,0.866025403784408,0.));
#20034=DIRECTION('',(6.12323399573741E-17,1.06057523872487E-16,-1.));
#20035=DIRECTION('center_axis',(0.,0.,-1.));
#20036=DIRECTION('ref_axis',(0.500000000000052,0.866025403784408,0.));
#20037=DIRECTION('',(6.12323399573741E-17,1.06057523872487E-16,-1.));
#20038=DIRECTION('center_axis',(0.,0.,-1.));
#20039=DIRECTION('ref_axis',(0.500000000000052,0.866025403784408,0.));
#20040=DIRECTION('',(6.12323399573741E-17,1.06057523872487E-16,-1.));
#20041=DIRECTION('center_axis',(0.,0.,-1.));
#20042=DIRECTION('ref_axis',(0.500000000000052,0.866025403784408,0.));
#20043=DIRECTION('',(6.12323399573741E-17,1.06057523872487E-16,-1.));
#20044=DIRECTION('center_axis',(0.,0.,-1.));
#20045=DIRECTION('ref_axis',(0.500000000000052,0.866025403784408,0.));
#20046=DIRECTION('',(6.12323399573741E-17,1.06057523872487E-16,-1.));
#20047=DIRECTION('center_axis',(0.,0.,-1.));
#20048=DIRECTION('ref_axis',(0.500000000000052,0.866025403784408,0.));
#20049=DIRECTION('',(6.12323399573741E-17,1.06057523872487E-16,-1.));
#20050=DIRECTION('center_axis',(0.,0.,-1.));
#20051=DIRECTION('ref_axis',(0.500000000000052,0.866025403784408,0.));
#20052=DIRECTION('',(6.12323399573741E-17,1.06057523872487E-16,-1.));
#20053=DIRECTION('center_axis',(0.,0.,-1.));
#20054=DIRECTION('ref_axis',(0.500000000000052,0.866025403784408,0.));
#20055=DIRECTION('',(6.12323399573741E-17,1.06057523872487E-16,-1.));
#20056=DIRECTION('center_axis',(0.,0.,-1.));
#20057=DIRECTION('ref_axis',(0.382007546651495,-0.924159203980194,0.));
#20058=DIRECTION('',(6.12323399573741E-17,1.06057523872487E-16,-1.));
#20059=DIRECTION('center_axis',(0.,0.,-1.));
#20060=DIRECTION('ref_axis',(0.500000000000052,0.866025403784409,0.));
#20061=DIRECTION('center_axis',(0.,0.,-1.));
#20062=DIRECTION('ref_axis',(-0.5,0.866025403784439,0.));
#20063=DIRECTION('',(0.,0.,-1.));
#20064=DIRECTION('center_axis',(0.,0.,1.));
#20065=DIRECTION('ref_axis',(-0.5,0.866025403784439,0.));
#20066=DIRECTION('',(0.,0.,-1.));
#20067=DIRECTION('center_axis',(0.,0.,1.));
#20068=DIRECTION('ref_axis',(-0.5,0.866025403784439,0.));
#20069=DIRECTION('center_axis',(0.,0.,-1.));
#20070=DIRECTION('ref_axis',(-0.5,0.866025403784439,0.));
#20071=DIRECTION('',(0.,0.,-1.));
#20072=DIRECTION('center_axis',(0.,0.,-1.));
#20073=DIRECTION('ref_axis',(-0.5,0.866025403784439,0.));
#20074=DIRECTION('',(0.,0.,-1.));
#20075=DIRECTION('center_axis',(0.,0.,-1.));
#20076=DIRECTION('ref_axis',(-0.5,0.866025403784439,0.));
#20077=DIRECTION('',(0.,0.,-1.));
#20078=DIRECTION('center_axis',(0.,0.,-1.));
#20079=DIRECTION('ref_axis',(-0.5,0.866025403784439,0.));
#20080=DIRECTION('',(0.,0.,-1.));
#20081=DIRECTION('center_axis',(0.,0.,-1.));
#20082=DIRECTION('ref_axis',(-0.5,0.866025403784439,0.));
#20083=DIRECTION('',(0.,0.,-1.));
#20084=DIRECTION('center_axis',(0.,0.,-1.));
#20085=DIRECTION('ref_axis',(-0.5,0.866025403784439,0.));
#20086=DIRECTION('',(0.,0.,-1.));
#20087=DIRECTION('center_axis',(0.,0.,-1.));
#20088=DIRECTION('ref_axis',(-0.5,0.866025403784439,0.));
#20089=DIRECTION('',(0.,0.,-1.));
#20090=DIRECTION('center_axis',(0.,0.,-1.));
#20091=DIRECTION('ref_axis',(-0.5,0.866025403784439,0.));
#20092=DIRECTION('',(0.,0.,-1.));
#20093=DIRECTION('center_axis',(0.,0.,-1.));
#20094=DIRECTION('ref_axis',(-0.5,0.866025403784439,0.));
#20095=DIRECTION('',(0.,0.,-1.));
#20096=DIRECTION('center_axis',(0.,0.,-1.));
#20097=DIRECTION('ref_axis',(-0.5,0.866025403784439,0.));
#20098=DIRECTION('',(0.,0.,-1.));
#20099=DIRECTION('center_axis',(0.,0.,-1.));
#20100=DIRECTION('ref_axis',(-0.170054135023851,0.98543472191784,0.));
#20101=DIRECTION('',(0.,0.,-1.));
#20102=DIRECTION('center_axis',(0.,0.,-1.));
#20103=DIRECTION('ref_axis',(-0.5,0.866025403784439,0.));
#20104=DIRECTION('center_axis',(0.,0.,-1.));
#20105=DIRECTION('ref_axis',(-0.998395126723898,-0.0566318897262918,0.));
#20106=DIRECTION('',(-6.12323399573607E-17,1.06057523872495E-16,-1.));
#20107=DIRECTION('center_axis',(0.,0.,1.));
#20108=DIRECTION('ref_axis',(-0.499999999999944,0.866025403784471,0.));
#20109=DIRECTION('center_axis',(0.,0.,-1.));
#20110=DIRECTION('ref_axis',(-0.499999999999944,0.866025403784471,0.));
#20111=DIRECTION('',(-6.12323399573607E-17,1.06057523872495E-16,-1.));
#20112=DIRECTION('center_axis',(0.,0.,-1.));
#20113=DIRECTION('ref_axis',(-0.499999999999944,0.866025403784471,0.));
#20114=DIRECTION('',(-6.12323399573607E-17,1.06057523872495E-16,-1.));
#20115=DIRECTION('center_axis',(0.,0.,-1.));
#20116=DIRECTION('ref_axis',(-0.499999999999944,0.866025403784471,0.));
#20117=DIRECTION('',(-6.12323399573607E-17,1.06057523872495E-16,-1.));
#20118=DIRECTION('center_axis',(0.,0.,-1.));
#20119=DIRECTION('ref_axis',(-0.499999999999944,0.866025403784471,0.));
#20120=DIRECTION('',(-6.12323399573607E-17,1.06057523872495E-16,-1.));
#20121=DIRECTION('center_axis',(0.,0.,-1.));
#20122=DIRECTION('ref_axis',(-0.499999999999944,0.866025403784471,0.));
#20123=DIRECTION('',(-6.12323399573607E-17,1.06057523872495E-16,-1.));
#20124=DIRECTION('center_axis',(0.,0.,-1.));
#20125=DIRECTION('ref_axis',(-0.499999999999944,0.866025403784471,0.));
#20126=DIRECTION('',(-6.12323399573607E-17,1.06057523872495E-16,-1.));
#20127=DIRECTION('center_axis',(0.,0.,-1.));
#20128=DIRECTION('ref_axis',(-0.499999999999944,0.866025403784471,0.));
#20129=DIRECTION('',(-6.12323399573607E-17,1.06057523872495E-16,-1.));
#20130=DIRECTION('center_axis',(0.,0.,-1.));
#20131=DIRECTION('ref_axis',(-0.499999999999944,0.866025403784471,0.));
#20132=DIRECTION('',(-6.12323399573607E-17,1.06057523872495E-16,-1.));
#20133=DIRECTION('center_axis',(0.,0.,-1.));
#20134=DIRECTION('ref_axis',(-0.499999999999944,0.866025403784471,0.));
#20135=DIRECTION('',(-6.12323399573607E-17,1.06057523872495E-16,-1.));
#20136=DIRECTION('center_axis',(0.,0.,-1.));
#20137=DIRECTION('ref_axis',(-0.499999999999944,0.866025403784471,0.));
#20138=DIRECTION('',(-6.12323399573607E-17,1.06057523872495E-16,-1.));
#20139=DIRECTION('center_axis',(0.,0.,-1.));
#20140=DIRECTION('ref_axis',(-0.499999999999944,0.866025403784471,0.));
#20141=DIRECTION('',(-6.12323399573607E-17,1.06057523872495E-16,-1.));
#20142=DIRECTION('center_axis',(0.,0.,-1.));
#20143=DIRECTION('ref_axis',(0.991349121590847,-0.131251358549376,0.));
#20144=DIRECTION('',(-6.12323399573607E-17,1.06057523872495E-16,-1.));
#20145=DIRECTION('center_axis',(0.,0.,-1.));
#20146=DIRECTION('ref_axis',(-0.499999999999944,0.866025403784471,0.));
#20147=DIRECTION('center_axis',(0.,0.,-1.));
#20148=DIRECTION('ref_axis',(-1.,1.38777878078145E-16,0.));
#20149=DIRECTION('',(0.,0.,-1.));
#20150=DIRECTION('center_axis',(0.,0.,1.));
#20151=DIRECTION('ref_axis',(-1.,1.38777878078145E-16,0.));
#20152=DIRECTION('',(0.,0.,-1.));
#20153=DIRECTION('center_axis',(0.,0.,1.));
#20154=DIRECTION('ref_axis',(-1.,1.38777878078145E-16,0.));
#20155=DIRECTION('center_axis',(0.,0.,-1.));
#20156=DIRECTION('ref_axis',(-1.,1.38777878078145E-16,0.));
#20157=DIRECTION('',(0.,0.,-1.));
#20158=DIRECTION('center_axis',(0.,0.,-1.));
#20159=DIRECTION('ref_axis',(-1.,1.38777878078145E-16,0.));
#20160=DIRECTION('',(0.,0.,-1.));
#20161=DIRECTION('center_axis',(0.,0.,-1.));
#20162=DIRECTION('ref_axis',(-1.,1.38777878078145E-16,0.));
#20163=DIRECTION('',(0.,0.,-1.));
#20164=DIRECTION('center_axis',(0.,0.,-1.));
#20165=DIRECTION('ref_axis',(-1.,1.38777878078145E-16,0.));
#20166=DIRECTION('',(0.,0.,-1.));
#20167=DIRECTION('center_axis',(0.,0.,-1.));
#20168=DIRECTION('ref_axis',(-1.,1.38777878078145E-16,0.));
#20169=DIRECTION('',(0.,0.,-1.));
#20170=DIRECTION('center_axis',(0.,0.,-1.));
#20171=DIRECTION('ref_axis',(-1.,1.38777878078145E-16,0.));
#20172=DIRECTION('',(0.,0.,-1.));
#20173=DIRECTION('center_axis',(0.,0.,-1.));
#20174=DIRECTION('ref_axis',(-1.,1.38777878078145E-16,0.));
#20175=DIRECTION('',(0.,0.,-1.));
#20176=DIRECTION('center_axis',(0.,0.,-1.));
#20177=DIRECTION('ref_axis',(-1.,1.38777878078145E-16,0.));
#20178=DIRECTION('',(0.,0.,-1.));
#20179=DIRECTION('center_axis',(0.,0.,-1.));
#20180=DIRECTION('ref_axis',(-1.,1.38777878078145E-16,0.));
#20181=DIRECTION('',(0.,0.,-1.));
#20182=DIRECTION('center_axis',(0.,0.,-1.));
#20183=DIRECTION('ref_axis',(-1.,1.38777878078145E-16,0.));
#20184=DIRECTION('',(0.,0.,-1.));
#20185=DIRECTION('center_axis',(0.,0.,-1.));
#20186=DIRECTION('ref_axis',(-0.938437885424518,0.34544802098139,0.));
#20187=DIRECTION('',(0.,0.,-1.));
#20188=DIRECTION('center_axis',(0.,0.,-1.));
#20189=DIRECTION('ref_axis',(-1.,1.38777878078145E-16,0.));
#20190=DIRECTION('center_axis',(0.,0.,-1.));
#20191=DIRECTION('ref_axis',(-0.450150052286485,-0.892952927329585,0.));
#20192=DIRECTION('',(-1.22464679914735E-16,7.70405498938443E-30,-1.));
#20193=DIRECTION('center_axis',(0.,0.,1.));
#20194=DIRECTION('ref_axis',(-1.,6.27859183309933E-14,0.));
#20195=DIRECTION('center_axis',(0.,0.,-1.));
#20196=DIRECTION('ref_axis',(-1.,6.27859183309933E-14,0.));
#20197=DIRECTION('',(-1.22464679914735E-16,7.70405498938443E-30,-1.));
#20198=DIRECTION('center_axis',(0.,0.,-1.));
#20199=DIRECTION('ref_axis',(-1.,6.27859183309933E-14,0.));
#20200=DIRECTION('',(-1.22464679914735E-16,7.70405498938443E-30,-1.));
#20201=DIRECTION('center_axis',(0.,0.,-1.));
#20202=DIRECTION('ref_axis',(-1.,6.27859183309933E-14,0.));
#20203=DIRECTION('',(-1.22464679914735E-16,7.70405498938443E-30,-1.));
#20204=DIRECTION('center_axis',(0.,0.,-1.));
#20205=DIRECTION('ref_axis',(-1.,6.27859183309933E-14,0.));
#20206=DIRECTION('',(-1.22464679914735E-16,7.70405498938443E-30,-1.));
#20207=DIRECTION('center_axis',(0.,0.,-1.));
#20208=DIRECTION('ref_axis',(-1.,6.27859183309933E-14,0.));
#20209=DIRECTION('',(-1.22464679914735E-16,7.70405498938443E-30,-1.));
#20210=DIRECTION('center_axis',(0.,0.,-1.));
#20211=DIRECTION('ref_axis',(-1.,6.27859183309933E-14,0.));
#20212=DIRECTION('',(-1.22464679914735E-16,7.70405498938443E-30,-1.));
#20213=DIRECTION('center_axis',(0.,0.,-1.));
#20214=DIRECTION('ref_axis',(-1.,6.27859183309933E-14,0.));
#20215=DIRECTION('',(-1.22464679914735E-16,7.70405498938443E-30,-1.));
#20216=DIRECTION('center_axis',(0.,0.,-1.));
#20217=DIRECTION('ref_axis',(-1.,6.27859183309933E-14,0.));
#20218=DIRECTION('',(-1.22464679914735E-16,7.70405498938443E-30,-1.));
#20219=DIRECTION('center_axis',(0.,0.,-1.));
#20220=DIRECTION('ref_axis',(-1.,6.27859183309933E-14,0.));
#20221=DIRECTION('',(-1.22464679914735E-16,7.70405498938443E-30,-1.));
#20222=DIRECTION('center_axis',(0.,0.,-1.));
#20223=DIRECTION('ref_axis',(-1.,6.27859183309933E-14,0.));
#20224=DIRECTION('',(-1.22464679914735E-16,7.70405498938443E-30,-1.));
#20225=DIRECTION('center_axis',(0.,0.,-1.));
#20226=DIRECTION('ref_axis',(-1.,6.27859183309933E-14,0.));
#20227=DIRECTION('',(-1.22464679914735E-16,7.70405498938443E-30,-1.));
#20228=DIRECTION('center_axis',(0.,0.,-1.));
#20229=DIRECTION('ref_axis',(0.609343127961874,0.792906647976696,0.));
#20230=DIRECTION('',(-1.22464679914735E-16,7.70405498938443E-30,-1.));
#20231=DIRECTION('center_axis',(0.,0.,-1.));
#20232=DIRECTION('ref_axis',(-1.,6.27859183309933E-14,0.));
#20233=DIRECTION('center_axis',(0.,0.,-1.));
#20234=DIRECTION('ref_axis',(-0.5,-0.866025403784438,0.));
#20235=DIRECTION('',(0.,0.,-1.));
#20236=DIRECTION('center_axis',(0.,0.,1.));
#20237=DIRECTION('ref_axis',(-0.5,-0.866025403784438,0.));
#20238=DIRECTION('',(0.,0.,-1.));
#20239=DIRECTION('center_axis',(0.,0.,1.));
#20240=DIRECTION('ref_axis',(-0.5,-0.866025403784438,0.));
#20241=DIRECTION('center_axis',(0.,0.,-1.));
#20242=DIRECTION('ref_axis',(-0.5,-0.866025403784438,0.));
#20243=DIRECTION('',(0.,0.,-1.));
#20244=DIRECTION('center_axis',(0.,0.,-1.));
#20245=DIRECTION('ref_axis',(-0.5,-0.866025403784438,0.));
#20246=DIRECTION('',(0.,0.,-1.));
#20247=DIRECTION('center_axis',(0.,0.,-1.));
#20248=DIRECTION('ref_axis',(-0.5,-0.866025403784438,0.));
#20249=DIRECTION('',(0.,0.,-1.));
#20250=DIRECTION('center_axis',(0.,0.,-1.));
#20251=DIRECTION('ref_axis',(-0.5,-0.866025403784438,0.));
#20252=DIRECTION('',(0.,0.,-1.));
#20253=DIRECTION('center_axis',(0.,0.,-1.));
#20254=DIRECTION('ref_axis',(-0.5,-0.866025403784438,0.));
#20255=DIRECTION('',(0.,0.,-1.));
#20256=DIRECTION('center_axis',(0.,0.,-1.));
#20257=DIRECTION('ref_axis',(-0.5,-0.866025403784438,0.));
#20258=DIRECTION('',(0.,0.,-1.));
#20259=DIRECTION('center_axis',(0.,0.,-1.));
#20260=DIRECTION('ref_axis',(-0.5,-0.866025403784438,0.));
#20261=DIRECTION('',(0.,0.,-1.));
#20262=DIRECTION('center_axis',(0.,0.,-1.));
#20263=DIRECTION('ref_axis',(-0.5,-0.866025403784438,0.));
#20264=DIRECTION('',(0.,0.,-1.));
#20265=DIRECTION('center_axis',(0.,0.,-1.));
#20266=DIRECTION('ref_axis',(-0.5,-0.866025403784438,0.));
#20267=DIRECTION('',(0.,0.,-1.));
#20268=DIRECTION('center_axis',(0.,0.,-1.));
#20269=DIRECTION('ref_axis',(-0.5,-0.866025403784438,0.));
#20270=DIRECTION('',(0.,0.,-1.));
#20271=DIRECTION('center_axis',(0.,0.,-1.));
#20272=DIRECTION('ref_axis',(-0.768384438951799,-0.639988557692033,0.));
#20273=DIRECTION('',(0.,0.,-1.));
#20274=DIRECTION('center_axis',(0.,0.,-1.));
#20275=DIRECTION('ref_axis',(-0.5,-0.866025403784438,0.));
#20276=DIRECTION('center_axis',(0.,0.,-1.));
#20277=DIRECTION('ref_axis',(0.548242225181956,-0.8363195935332,0.));
#20278=DIRECTION('',(-6.12323399573746E-17,-1.06057523872487E-16,-1.));
#20279=DIRECTION('center_axis',(0.,0.,1.));
#20280=DIRECTION('ref_axis',(-0.500000000000056,-0.866025403784406,0.));
#20281=DIRECTION('center_axis',(0.,0.,-1.));
#20282=DIRECTION('ref_axis',(-0.500000000000056,-0.866025403784406,0.));
#20283=DIRECTION('',(-6.12323399573746E-17,-1.06057523872487E-16,-1.));
#20284=DIRECTION('center_axis',(0.,0.,-1.));
#20285=DIRECTION('ref_axis',(-0.500000000000056,-0.866025403784406,0.));
#20286=DIRECTION('',(-6.12323399573746E-17,-1.06057523872487E-16,-1.));
#20287=DIRECTION('center_axis',(0.,0.,-1.));
#20288=DIRECTION('ref_axis',(-0.500000000000056,-0.866025403784406,0.));
#20289=DIRECTION('',(-6.12323399573746E-17,-1.06057523872487E-16,-1.));
#20290=DIRECTION('center_axis',(0.,0.,-1.));
#20291=DIRECTION('ref_axis',(-0.500000000000056,-0.866025403784406,0.));
#20292=DIRECTION('',(-6.12323399573746E-17,-1.06057523872487E-16,-1.));
#20293=DIRECTION('center_axis',(0.,0.,-1.));
#20294=DIRECTION('ref_axis',(-0.500000000000056,-0.866025403784406,0.));
#20295=DIRECTION('',(-6.12323399573746E-17,-1.06057523872487E-16,-1.));
#20296=DIRECTION('center_axis',(0.,0.,-1.));
#20297=DIRECTION('ref_axis',(-0.500000000000056,-0.866025403784406,0.));
#20298=DIRECTION('',(-6.12323399573746E-17,-1.06057523872487E-16,-1.));
#20299=DIRECTION('center_axis',(0.,0.,-1.));
#20300=DIRECTION('ref_axis',(-0.500000000000056,-0.866025403784406,0.));
#20301=DIRECTION('',(-6.12323399573746E-17,-1.06057523872487E-16,-1.));
#20302=DIRECTION('center_axis',(0.,0.,-1.));
#20303=DIRECTION('ref_axis',(-0.500000000000056,-0.866025403784406,0.));
#20304=DIRECTION('',(-6.12323399573746E-17,-1.06057523872487E-16,-1.));
#20305=DIRECTION('center_axis',(0.,0.,-1.));
#20306=DIRECTION('ref_axis',(-0.500000000000056,-0.866025403784406,0.));
#20307=DIRECTION('',(-6.12323399573746E-17,-1.06057523872487E-16,-1.));
#20308=DIRECTION('center_axis',(0.,0.,-1.));
#20309=DIRECTION('ref_axis',(-0.500000000000056,-0.866025403784406,0.));
#20310=DIRECTION('',(-6.12323399573746E-17,-1.06057523872487E-16,-1.));
#20311=DIRECTION('center_axis',(0.,0.,-1.));
#20312=DIRECTION('ref_axis',(-0.500000000000056,-0.866025403784406,0.));
#20313=DIRECTION('',(-6.12323399573746E-17,-1.06057523872487E-16,-1.));
#20314=DIRECTION('center_axis',(0.,0.,-1.));
#20315=DIRECTION('ref_axis',(-0.382007546651474,0.924159203980203,0.));
#20316=DIRECTION('',(-6.12323399573746E-17,-1.06057523872487E-16,-1.));
#20317=DIRECTION('center_axis',(0.,0.,-1.));
#20318=DIRECTION('ref_axis',(-0.500000000000056,-0.866025403784406,0.));
#20319=DIRECTION('center_axis',(0.,0.,-1.));
#20320=DIRECTION('ref_axis',(0.499999999999999,-0.866025403784439,0.));
#20321=DIRECTION('',(0.,0.,-1.));
#20322=DIRECTION('center_axis',(0.,0.,1.));
#20323=DIRECTION('ref_axis',(0.499999999999999,-0.866025403784439,0.));
#20324=DIRECTION('',(0.,0.,-1.));
#20325=DIRECTION('center_axis',(0.,0.,1.));
#20326=DIRECTION('ref_axis',(0.499999999999999,-0.866025403784439,0.));
#20327=DIRECTION('center_axis',(0.,0.,-1.));
#20328=DIRECTION('ref_axis',(0.499999999999999,-0.866025403784439,0.));
#20329=DIRECTION('',(0.,0.,-1.));
#20330=DIRECTION('center_axis',(0.,0.,-1.));
#20331=DIRECTION('ref_axis',(0.499999999999999,-0.866025403784439,0.));
#20332=DIRECTION('',(0.,0.,-1.));
#20333=DIRECTION('center_axis',(0.,0.,-1.));
#20334=DIRECTION('ref_axis',(0.499999999999999,-0.866025403784439,0.));
#20335=DIRECTION('',(0.,0.,-1.));
#20336=DIRECTION('center_axis',(0.,0.,-1.));
#20337=DIRECTION('ref_axis',(0.499999999999999,-0.866025403784439,0.));
#20338=DIRECTION('',(0.,0.,-1.));
#20339=DIRECTION('center_axis',(0.,0.,-1.));
#20340=DIRECTION('ref_axis',(0.499999999999999,-0.866025403784439,0.));
#20341=DIRECTION('',(0.,0.,-1.));
#20342=DIRECTION('center_axis',(0.,0.,-1.));
#20343=DIRECTION('ref_axis',(0.499999999999999,-0.866025403784439,0.));
#20344=DIRECTION('',(0.,0.,-1.));
#20345=DIRECTION('center_axis',(0.,0.,-1.));
#20346=DIRECTION('ref_axis',(0.499999999999999,-0.866025403784439,0.));
#20347=DIRECTION('',(0.,0.,-1.));
#20348=DIRECTION('center_axis',(0.,0.,-1.));
#20349=DIRECTION('ref_axis',(0.499999999999999,-0.866025403784439,0.));
#20350=DIRECTION('',(0.,0.,-1.));
#20351=DIRECTION('center_axis',(0.,0.,-1.));
#20352=DIRECTION('ref_axis',(0.499999999999999,-0.866025403784439,0.));
#20353=DIRECTION('',(0.,0.,-1.));
#20354=DIRECTION('center_axis',(0.,0.,-1.));
#20355=DIRECTION('ref_axis',(0.499999999999999,-0.866025403784439,0.));
#20356=DIRECTION('',(0.,0.,-1.));
#20357=DIRECTION('center_axis',(0.,0.,-1.));
#20358=DIRECTION('ref_axis',(0.170054135023835,-0.985434721917842,0.));
#20359=DIRECTION('',(0.,0.,-1.));
#20360=DIRECTION('center_axis',(0.,0.,-1.));
#20361=DIRECTION('ref_axis',(0.499999999999999,-0.866025403784439,0.));
#20362=DIRECTION('center_axis',(0.,0.,-1.));
#20363=DIRECTION('ref_axis',(0.998395126723898,0.0566318897262945,0.));
#20364=DIRECTION('',(6.12323399573609E-17,-1.06057523872495E-16,-1.));
#20365=DIRECTION('center_axis',(0.,0.,1.));
#20366=DIRECTION('ref_axis',(0.499999999999945,-0.86602540378447,0.));
#20367=DIRECTION('center_axis',(0.,0.,-1.));
#20368=DIRECTION('ref_axis',(0.499999999999945,-0.86602540378447,0.));
#20369=DIRECTION('',(6.12323399573609E-17,-1.06057523872495E-16,-1.));
#20370=DIRECTION('center_axis',(0.,0.,-1.));
#20371=DIRECTION('ref_axis',(0.499999999999945,-0.86602540378447,0.));
#20372=DIRECTION('',(6.12323399573609E-17,-1.06057523872495E-16,-1.));
#20373=DIRECTION('center_axis',(0.,0.,-1.));
#20374=DIRECTION('ref_axis',(0.499999999999945,-0.86602540378447,0.));
#20375=DIRECTION('',(6.12323399573609E-17,-1.06057523872495E-16,-1.));
#20376=DIRECTION('center_axis',(0.,0.,-1.));
#20377=DIRECTION('ref_axis',(0.499999999999945,-0.86602540378447,0.));
#20378=DIRECTION('',(6.12323399573609E-17,-1.06057523872495E-16,-1.));
#20379=DIRECTION('center_axis',(0.,0.,-1.));
#20380=DIRECTION('ref_axis',(0.499999999999945,-0.86602540378447,0.));
#20381=DIRECTION('',(6.12323399573609E-17,-1.06057523872495E-16,-1.));
#20382=DIRECTION('center_axis',(0.,0.,-1.));
#20383=DIRECTION('ref_axis',(0.499999999999945,-0.86602540378447,0.));
#20384=DIRECTION('',(6.12323399573609E-17,-1.06057523872495E-16,-1.));
#20385=DIRECTION('center_axis',(0.,0.,-1.));
#20386=DIRECTION('ref_axis',(0.499999999999945,-0.86602540378447,0.));
#20387=DIRECTION('',(6.12323399573609E-17,-1.06057523872495E-16,-1.));
#20388=DIRECTION('center_axis',(0.,0.,-1.));
#20389=DIRECTION('ref_axis',(0.499999999999945,-0.86602540378447,0.));
#20390=DIRECTION('',(6.12323399573609E-17,-1.06057523872495E-16,-1.));
#20391=DIRECTION('center_axis',(0.,0.,-1.));
#20392=DIRECTION('ref_axis',(0.499999999999945,-0.86602540378447,0.));
#20393=DIRECTION('',(6.12323399573609E-17,-1.06057523872495E-16,-1.));
#20394=DIRECTION('center_axis',(0.,0.,-1.));
#20395=DIRECTION('ref_axis',(0.499999999999945,-0.86602540378447,0.));
#20396=DIRECTION('',(6.12323399573609E-17,-1.06057523872495E-16,-1.));
#20397=DIRECTION('center_axis',(0.,0.,-1.));
#20398=DIRECTION('ref_axis',(0.499999999999945,-0.86602540378447,0.));
#20399=DIRECTION('',(6.12323399573609E-17,-1.06057523872495E-16,-1.));
#20400=DIRECTION('center_axis',(0.,0.,-1.));
#20401=DIRECTION('ref_axis',(-0.991349121590847,0.13125135854937,0.));
#20402=DIRECTION('',(6.12323399573609E-17,-1.06057523872495E-16,-1.));
#20403=DIRECTION('center_axis',(0.,0.,-1.));
#20404=DIRECTION('ref_axis',(0.499999999999945,-0.86602540378447,0.));
#20405=DIRECTION('center_axis',(0.,0.,1.));
#20406=DIRECTION('ref_axis',(-0.5,-0.866025403784439,0.));
#20407=DIRECTION('',(0.,0.,1.));
#20408=DIRECTION('center_axis',(0.,0.,-1.));
#20409=DIRECTION('ref_axis',(-0.5,-0.866025403784439,0.));
#20410=DIRECTION('',(0.,0.,1.));
#20411=DIRECTION('center_axis',(0.,0.,-1.));
#20412=DIRECTION('ref_axis',(-0.5,-0.866025403784439,0.));
#20413=DIRECTION('center_axis',(0.,0.,1.));
#20414=DIRECTION('ref_axis',(-0.5,-0.866025403784439,0.));
#20415=DIRECTION('',(0.,0.,1.));
#20416=DIRECTION('center_axis',(0.,0.,1.));
#20417=DIRECTION('ref_axis',(-0.5,-0.866025403784439,0.));
#20418=DIRECTION('',(0.,0.,1.));
#20419=DIRECTION('center_axis',(0.,0.,1.));
#20420=DIRECTION('ref_axis',(-0.5,-0.866025403784439,0.));
#20421=DIRECTION('',(0.,0.,1.));
#20422=DIRECTION('center_axis',(0.,0.,1.));
#20423=DIRECTION('ref_axis',(-0.5,-0.866025403784439,0.));
#20424=DIRECTION('',(0.,0.,1.));
#20425=DIRECTION('center_axis',(0.,0.,1.));
#20426=DIRECTION('ref_axis',(-0.5,-0.866025403784439,0.));
#20427=DIRECTION('',(0.,0.,1.));
#20428=DIRECTION('center_axis',(0.,0.,1.));
#20429=DIRECTION('ref_axis',(-0.5,-0.866025403784439,0.));
#20430=DIRECTION('',(0.,0.,1.));
#20431=DIRECTION('center_axis',(0.,0.,1.));
#20432=DIRECTION('ref_axis',(-0.5,-0.866025403784439,0.));
#20433=DIRECTION('',(0.,0.,1.));
#20434=DIRECTION('center_axis',(0.,0.,1.));
#20435=DIRECTION('ref_axis',(-0.5,-0.866025403784439,0.));
#20436=DIRECTION('',(0.,0.,1.));
#20437=DIRECTION('center_axis',(0.,0.,1.));
#20438=DIRECTION('ref_axis',(-0.5,-0.866025403784439,0.));
#20439=DIRECTION('',(0.,0.,1.));
#20440=DIRECTION('center_axis',(0.,0.,1.));
#20441=DIRECTION('ref_axis',(-0.5,-0.866025403784439,0.));
#20442=DIRECTION('',(0.,0.,1.));
#20443=DIRECTION('center_axis',(0.,0.,1.));
#20444=DIRECTION('ref_axis',(-0.170053080456876,-0.985434903901383,0.));
#20445=DIRECTION('',(0.,0.,1.));
#20446=DIRECTION('center_axis',(0.,0.,-1.));
#20447=DIRECTION('ref_axis',(-0.5,-0.866025403784439,0.));
#20448=DIRECTION('center_axis',(0.,0.,1.));
#20449=DIRECTION('ref_axis',(-0.998395022062647,0.0566337348276312,0.));
#20450=DIRECTION('',(-6.12323399573623E-17,-1.06057523872494E-16,1.));
#20451=DIRECTION('center_axis',(0.,0.,-1.));
#20452=DIRECTION('ref_axis',(-0.499999999999956,-0.866025403784464,0.));
#20453=DIRECTION('center_axis',(0.,0.,1.));
#20454=DIRECTION('ref_axis',(-0.499999999999956,-0.866025403784464,0.));
#20455=DIRECTION('',(-6.12323399573623E-17,-1.06057523872494E-16,1.));
#20456=DIRECTION('center_axis',(0.,0.,1.));
#20457=DIRECTION('ref_axis',(-0.499999999999956,-0.866025403784464,0.));
#20458=DIRECTION('',(-6.12323399573623E-17,-1.06057523872494E-16,1.));
#20459=DIRECTION('center_axis',(0.,0.,1.));
#20460=DIRECTION('ref_axis',(-0.499999999999956,-0.866025403784464,0.));
#20461=DIRECTION('',(-6.12323399573623E-17,-1.06057523872494E-16,1.));
#20462=DIRECTION('center_axis',(0.,0.,1.));
#20463=DIRECTION('ref_axis',(-0.499999999999956,-0.866025403784464,0.));
#20464=DIRECTION('',(-6.12323399573623E-17,-1.06057523872494E-16,1.));
#20465=DIRECTION('center_axis',(0.,0.,1.));
#20466=DIRECTION('ref_axis',(-0.499999999999956,-0.866025403784464,0.));
#20467=DIRECTION('',(-6.12323399573623E-17,-1.06057523872494E-16,1.));
#20468=DIRECTION('center_axis',(0.,0.,1.));
#20469=DIRECTION('ref_axis',(-0.499999999999956,-0.866025403784464,0.));
#20470=DIRECTION('',(-6.12323399573623E-17,-1.06057523872494E-16,1.));
#20471=DIRECTION('center_axis',(0.,0.,1.));
#20472=DIRECTION('ref_axis',(-0.499999999999956,-0.866025403784464,0.));
#20473=DIRECTION('',(-6.12323399573623E-17,-1.06057523872494E-16,1.));
#20474=DIRECTION('center_axis',(0.,0.,1.));
#20475=DIRECTION('ref_axis',(-0.499999999999956,-0.866025403784464,0.));
#20476=DIRECTION('',(-6.12323399573623E-17,-1.06057523872494E-16,1.));
#20477=DIRECTION('center_axis',(0.,0.,1.));
#20478=DIRECTION('ref_axis',(-0.499999999999956,-0.866025403784464,0.));
#20479=DIRECTION('',(-6.12323399573623E-17,-1.06057523872494E-16,1.));
#20480=DIRECTION('center_axis',(0.,0.,1.));
#20481=DIRECTION('ref_axis',(-0.499999999999956,-0.866025403784464,0.));
#20482=DIRECTION('',(-6.12323399573623E-17,-1.06057523872494E-16,1.));
#20483=DIRECTION('center_axis',(0.,0.,1.));
#20484=DIRECTION('ref_axis',(-0.499999999999956,-0.866025403784464,0.));
#20485=DIRECTION('',(-6.12323399573623E-17,-1.06057523872494E-16,1.));
#20486=DIRECTION('center_axis',(0.,0.,1.));
#20487=DIRECTION('ref_axis',(0.991348961503156,0.131252567695316,0.));
#20488=DIRECTION('',(-6.12323399573623E-17,-1.06057523872494E-16,1.));
#20489=DIRECTION('center_axis',(0.,0.,1.));
#20490=DIRECTION('ref_axis',(-0.499999999999956,-0.866025403784464,0.));
#20491=DIRECTION('center_axis',(0.,0.,1.));
#20492=DIRECTION('ref_axis',(0.5,-0.866025403784439,0.));
#20493=DIRECTION('',(0.,0.,1.));
#20494=DIRECTION('center_axis',(0.,0.,-1.));
#20495=DIRECTION('ref_axis',(0.5,-0.866025403784439,0.));
#20496=DIRECTION('',(0.,0.,1.));
#20497=DIRECTION('center_axis',(0.,0.,-1.));
#20498=DIRECTION('ref_axis',(0.5,-0.866025403784439,0.));
#20499=DIRECTION('center_axis',(0.,0.,1.));
#20500=DIRECTION('ref_axis',(0.5,-0.866025403784439,0.));
#20501=DIRECTION('',(0.,0.,1.));
#20502=DIRECTION('center_axis',(0.,0.,1.));
#20503=DIRECTION('ref_axis',(0.5,-0.866025403784439,0.));
#20504=DIRECTION('',(0.,0.,1.));
#20505=DIRECTION('center_axis',(0.,0.,1.));
#20506=DIRECTION('ref_axis',(0.5,-0.866025403784439,0.));
#20507=DIRECTION('',(0.,0.,1.));
#20508=DIRECTION('center_axis',(0.,0.,1.));
#20509=DIRECTION('ref_axis',(0.5,-0.866025403784439,0.));
#20510=DIRECTION('',(0.,0.,1.));
#20511=DIRECTION('center_axis',(0.,0.,1.));
#20512=DIRECTION('ref_axis',(0.5,-0.866025403784439,0.));
#20513=DIRECTION('',(0.,0.,1.));
#20514=DIRECTION('center_axis',(0.,0.,1.));
#20515=DIRECTION('ref_axis',(0.5,-0.866025403784439,0.));
#20516=DIRECTION('',(0.,0.,1.));
#20517=DIRECTION('center_axis',(0.,0.,1.));
#20518=DIRECTION('ref_axis',(0.5,-0.866025403784439,0.));
#20519=DIRECTION('',(0.,0.,1.));
#20520=DIRECTION('center_axis',(0.,0.,1.));
#20521=DIRECTION('ref_axis',(0.5,-0.866025403784439,0.));
#20522=DIRECTION('',(0.,0.,1.));
#20523=DIRECTION('center_axis',(0.,0.,1.));
#20524=DIRECTION('ref_axis',(0.5,-0.866025403784439,0.));
#20525=DIRECTION('',(0.,0.,1.));
#20526=DIRECTION('center_axis',(0.,0.,1.));
#20527=DIRECTION('ref_axis',(0.5,-0.866025403784439,0.));
#20528=DIRECTION('',(0.,0.,1.));
#20529=DIRECTION('center_axis',(0.,0.,1.));
#20530=DIRECTION('ref_axis',(0.768385143082245,-0.639987712296477,0.));
#20531=DIRECTION('',(0.,0.,1.));
#20532=DIRECTION('center_axis',(0.,0.,-1.));
#20533=DIRECTION('ref_axis',(0.5,-0.866025403784439,0.));
#20534=DIRECTION('center_axis',(0.,0.,1.));
#20535=DIRECTION('ref_axis',(-0.548243791989891,-0.836318566423432,0.));
#20536=DIRECTION('',(6.12323399573727E-17,-1.06057523872488E-16,1.));
#20537=DIRECTION('center_axis',(0.,0.,-1.));
#20538=DIRECTION('ref_axis',(0.500000000000041,-0.866025403784415,0.));
#20539=DIRECTION('center_axis',(0.,0.,1.));
#20540=DIRECTION('ref_axis',(0.500000000000041,-0.866025403784415,0.));
#20541=DIRECTION('',(6.12323399573727E-17,-1.06057523872488E-16,1.));
#20542=DIRECTION('center_axis',(0.,0.,1.));
#20543=DIRECTION('ref_axis',(0.500000000000041,-0.866025403784415,0.));
#20544=DIRECTION('',(6.12323399573727E-17,-1.06057523872488E-16,1.));
#20545=DIRECTION('center_axis',(0.,0.,1.));
#20546=DIRECTION('ref_axis',(0.500000000000041,-0.866025403784415,0.));
#20547=DIRECTION('',(6.12323399573727E-17,-1.06057523872488E-16,1.));
#20548=DIRECTION('center_axis',(0.,0.,1.));
#20549=DIRECTION('ref_axis',(0.500000000000041,-0.866025403784415,0.));
#20550=DIRECTION('',(6.12323399573727E-17,-1.06057523872488E-16,1.));
#20551=DIRECTION('center_axis',(0.,0.,1.));
#20552=DIRECTION('ref_axis',(0.500000000000041,-0.866025403784415,0.));
#20553=DIRECTION('',(6.12323399573727E-17,-1.06057523872488E-16,1.));
#20554=DIRECTION('center_axis',(0.,0.,1.));
#20555=DIRECTION('ref_axis',(0.500000000000041,-0.866025403784415,0.));
#20556=DIRECTION('',(6.12323399573727E-17,-1.06057523872488E-16,1.));
#20557=DIRECTION('center_axis',(0.,0.,1.));
#20558=DIRECTION('ref_axis',(0.500000000000041,-0.866025403784415,0.));
#20559=DIRECTION('',(6.12323399573727E-17,-1.06057523872488E-16,1.));
#20560=DIRECTION('center_axis',(0.,0.,1.));
#20561=DIRECTION('ref_axis',(0.500000000000041,-0.866025403784415,0.));
#20562=DIRECTION('',(6.12323399573727E-17,-1.06057523872488E-16,1.));
#20563=DIRECTION('center_axis',(0.,0.,1.));
#20564=DIRECTION('ref_axis',(0.500000000000041,-0.866025403784415,0.));
#20565=DIRECTION('',(6.12323399573727E-17,-1.06057523872488E-16,1.));
#20566=DIRECTION('center_axis',(0.,0.,1.));
#20567=DIRECTION('ref_axis',(0.500000000000041,-0.866025403784415,0.));
#20568=DIRECTION('',(6.12323399573727E-17,-1.06057523872488E-16,1.));
#20569=DIRECTION('center_axis',(0.,0.,1.));
#20570=DIRECTION('ref_axis',(0.500000000000041,-0.866025403784415,0.));
#20571=DIRECTION('',(6.12323399573727E-17,-1.06057523872488E-16,1.));
#20572=DIRECTION('center_axis',(0.,0.,1.));
#20573=DIRECTION('ref_axis',(0.382006426201404,0.92415966712513,0.));
#20574=DIRECTION('',(6.12323399573727E-17,-1.06057523872488E-16,1.));
#20575=DIRECTION('center_axis',(0.,0.,1.));
#20576=DIRECTION('ref_axis',(0.500000000000041,-0.866025403784415,0.));
#20577=DIRECTION('center_axis',(0.,0.,1.));
#20578=DIRECTION('ref_axis',(1.,-1.38777878078145E-16,0.));
#20579=DIRECTION('',(0.,0.,1.));
#20580=DIRECTION('center_axis',(0.,0.,-1.));
#20581=DIRECTION('ref_axis',(1.,-1.38777878078145E-16,0.));
#20582=DIRECTION('',(0.,0.,1.));
#20583=DIRECTION('center_axis',(0.,0.,-1.));
#20584=DIRECTION('ref_axis',(1.,-1.38777878078145E-16,0.));
#20585=DIRECTION('center_axis',(0.,0.,1.));
#20586=DIRECTION('ref_axis',(1.,-1.38777878078145E-16,0.));
#20587=DIRECTION('',(0.,0.,1.));
#20588=DIRECTION('center_axis',(0.,0.,1.));
#20589=DIRECTION('ref_axis',(1.,-1.38777878078145E-16,0.));
#20590=DIRECTION('',(0.,0.,1.));
#20591=DIRECTION('center_axis',(0.,0.,1.));
#20592=DIRECTION('ref_axis',(1.,-1.38777878078145E-16,0.));
#20593=DIRECTION('',(0.,0.,1.));
#20594=DIRECTION('center_axis',(0.,0.,1.));
#20595=DIRECTION('ref_axis',(1.,-1.38777878078145E-16,0.));
#20596=DIRECTION('',(0.,0.,1.));
#20597=DIRECTION('center_axis',(0.,0.,1.));
#20598=DIRECTION('ref_axis',(1.,-1.38777878078145E-16,0.));
#20599=DIRECTION('',(0.,0.,1.));
#20600=DIRECTION('center_axis',(0.,0.,1.));
#20601=DIRECTION('ref_axis',(1.,-1.38777878078145E-16,0.));
#20602=DIRECTION('',(0.,0.,1.));
#20603=DIRECTION('center_axis',(0.,0.,1.));
#20604=DIRECTION('ref_axis',(1.,-1.38777878078145E-16,0.));
#20605=DIRECTION('',(0.,0.,1.));
#20606=DIRECTION('center_axis',(0.,0.,1.));
#20607=DIRECTION('ref_axis',(1.,-1.38777878078145E-16,0.));
#20608=DIRECTION('',(0.,0.,1.));
#20609=DIRECTION('center_axis',(0.,0.,1.));
#20610=DIRECTION('ref_axis',(1.,-1.38777878078145E-16,0.));
#20611=DIRECTION('',(0.,0.,1.));
#20612=DIRECTION('center_axis',(0.,0.,1.));
#20613=DIRECTION('ref_axis',(1.,-1.38777878078145E-16,0.));
#20614=DIRECTION('',(0.,0.,1.));
#20615=DIRECTION('center_axis',(0.,0.,1.));
#20616=DIRECTION('ref_axis',(0.938437365767004,0.345449432670379,0.));
#20617=DIRECTION('',(0.,0.,1.));
#20618=DIRECTION('center_axis',(0.,0.,-1.));
#20619=DIRECTION('ref_axis',(1.,-1.38777878078145E-16,0.));
#20620=DIRECTION('center_axis',(0.,0.,1.));
#20621=DIRECTION('ref_axis',(0.450147885469881,-0.892954019648825,0.));
#20622=DIRECTION('',(1.22464679914735E-16,6.13548173299478E-30,1.));
#20623=DIRECTION('center_axis',(0.,0.,-1.));
#20624=DIRECTION('ref_axis',(1.,4.99775456844331E-14,0.));
#20625=DIRECTION('center_axis',(0.,0.,1.));
#20626=DIRECTION('ref_axis',(1.,4.99775456844331E-14,0.));
#20627=DIRECTION('',(1.22464679914735E-16,6.13548173299478E-30,1.));
#20628=DIRECTION('center_axis',(0.,0.,1.));
#20629=DIRECTION('ref_axis',(1.,4.99775456844331E-14,0.));
#20630=DIRECTION('',(1.22464679914735E-16,6.13548173299478E-30,1.));
#20631=DIRECTION('center_axis',(0.,0.,1.));
#20632=DIRECTION('ref_axis',(1.,4.99775456844331E-14,0.));
#20633=DIRECTION('',(1.22464679914735E-16,6.13548173299478E-30,1.));
#20634=DIRECTION('center_axis',(0.,0.,1.));
#20635=DIRECTION('ref_axis',(1.,4.99775456844331E-14,0.));
#20636=DIRECTION('',(1.22464679914735E-16,6.13548173299478E-30,1.));
#20637=DIRECTION('center_axis',(0.,0.,1.));
#20638=DIRECTION('ref_axis',(1.,4.99775456844331E-14,0.));
#20639=DIRECTION('',(1.22464679914735E-16,6.13548173299478E-30,1.));
#20640=DIRECTION('center_axis',(0.,0.,1.));
#20641=DIRECTION('ref_axis',(1.,4.99775456844331E-14,0.));
#20642=DIRECTION('',(1.22464679914735E-16,6.13548173299478E-30,1.));
#20643=DIRECTION('center_axis',(0.,0.,1.));
#20644=DIRECTION('ref_axis',(1.,4.99775456844331E-14,0.));
#20645=DIRECTION('',(1.22464679914735E-16,6.13548173299478E-30,1.));
#20646=DIRECTION('center_axis',(0.,0.,1.));
#20647=DIRECTION('ref_axis',(1.,4.99775456844331E-14,0.));
#20648=DIRECTION('',(1.22464679914735E-16,6.13548173299478E-30,1.));
#20649=DIRECTION('center_axis',(0.,0.,1.));
#20650=DIRECTION('ref_axis',(1.,4.99775456844331E-14,0.));
#20651=DIRECTION('',(1.22464679914735E-16,6.13548173299478E-30,1.));
#20652=DIRECTION('center_axis',(0.,0.,1.));
#20653=DIRECTION('ref_axis',(1.,4.99775456844331E-14,0.));
#20654=DIRECTION('',(1.22464679914735E-16,6.13548173299478E-30,1.));
#20655=DIRECTION('center_axis',(0.,0.,1.));
#20656=DIRECTION('ref_axis',(1.,4.99775456844331E-14,0.));
#20657=DIRECTION('',(1.22464679914735E-16,6.13548173299478E-30,1.));
#20658=DIRECTION('center_axis',(0.,0.,1.));
#20659=DIRECTION('ref_axis',(-0.609344456561461,0.792905626955577,0.));
#20660=DIRECTION('',(1.22464679914735E-16,6.13548173299478E-30,1.));
#20661=DIRECTION('center_axis',(0.,0.,1.));
#20662=DIRECTION('ref_axis',(1.,4.99775456844331E-14,0.));
#20663=DIRECTION('center_axis',(0.,0.,1.));
#20664=DIRECTION('ref_axis',(0.5,0.866025403784438,0.));
#20665=DIRECTION('',(0.,0.,1.));
#20666=DIRECTION('center_axis',(0.,0.,-1.));
#20667=DIRECTION('ref_axis',(0.5,0.866025403784438,0.));
#20668=DIRECTION('',(0.,0.,1.));
#20669=DIRECTION('center_axis',(0.,0.,-1.));
#20670=DIRECTION('ref_axis',(0.5,0.866025403784438,0.));
#20671=DIRECTION('center_axis',(0.,0.,1.));
#20672=DIRECTION('ref_axis',(0.5,0.866025403784438,0.));
#20673=DIRECTION('',(0.,0.,1.));
#20674=DIRECTION('center_axis',(0.,0.,1.));
#20675=DIRECTION('ref_axis',(0.5,0.866025403784438,0.));
#20676=DIRECTION('',(0.,0.,1.));
#20677=DIRECTION('center_axis',(0.,0.,1.));
#20678=DIRECTION('ref_axis',(0.5,0.866025403784438,0.));
#20679=DIRECTION('',(0.,0.,1.));
#20680=DIRECTION('center_axis',(0.,0.,1.));
#20681=DIRECTION('ref_axis',(0.5,0.866025403784438,0.));
#20682=DIRECTION('',(0.,0.,1.));
#20683=DIRECTION('center_axis',(0.,0.,1.));
#20684=DIRECTION('ref_axis',(0.5,0.866025403784438,0.));
#20685=DIRECTION('',(0.,0.,1.));
#20686=DIRECTION('center_axis',(0.,0.,1.));
#20687=DIRECTION('ref_axis',(0.5,0.866025403784438,0.));
#20688=DIRECTION('',(0.,0.,1.));
#20689=DIRECTION('center_axis',(0.,0.,1.));
#20690=DIRECTION('ref_axis',(0.5,0.866025403784438,0.));
#20691=DIRECTION('',(0.,0.,1.));
#20692=DIRECTION('center_axis',(0.,0.,1.));
#20693=DIRECTION('ref_axis',(0.5,0.866025403784438,0.));
#20694=DIRECTION('',(0.,0.,1.));
#20695=DIRECTION('center_axis',(0.,0.,1.));
#20696=DIRECTION('ref_axis',(0.5,0.866025403784438,0.));
#20697=DIRECTION('',(0.,0.,1.));
#20698=DIRECTION('center_axis',(0.,0.,1.));
#20699=DIRECTION('ref_axis',(0.5,0.866025403784438,0.));
#20700=DIRECTION('',(0.,0.,1.));
#20701=DIRECTION('center_axis',(0.,0.,1.));
#20702=DIRECTION('ref_axis',(0.170053080456934,0.985434903901373,0.));
#20703=DIRECTION('',(0.,0.,1.));
#20704=DIRECTION('center_axis',(0.,0.,-1.));
#20705=DIRECTION('ref_axis',(0.5,0.866025403784438,0.));
#20706=DIRECTION('center_axis',(0.,0.,1.));
#20707=DIRECTION('ref_axis',(0.998395022062648,-0.0566337348276226,0.));
#20708=DIRECTION('',(6.12323399573605E-17,1.06057523872495E-16,1.));
#20709=DIRECTION('center_axis',(0.,0.,-1.));
#20710=DIRECTION('ref_axis',(0.499999999999942,0.866025403784472,0.));
#20711=DIRECTION('center_axis',(0.,0.,1.));
#20712=DIRECTION('ref_axis',(0.499999999999942,0.866025403784472,0.));
#20713=DIRECTION('',(6.12323399573605E-17,1.06057523872495E-16,1.));
#20714=DIRECTION('center_axis',(0.,0.,1.));
#20715=DIRECTION('ref_axis',(0.499999999999942,0.866025403784472,0.));
#20716=DIRECTION('',(6.12323399573605E-17,1.06057523872495E-16,1.));
#20717=DIRECTION('center_axis',(0.,0.,1.));
#20718=DIRECTION('ref_axis',(0.499999999999942,0.866025403784472,0.));
#20719=DIRECTION('',(6.12323399573605E-17,1.06057523872495E-16,1.));
#20720=DIRECTION('center_axis',(0.,0.,1.));
#20721=DIRECTION('ref_axis',(0.499999999999942,0.866025403784472,0.));
#20722=DIRECTION('',(6.12323399573605E-17,1.06057523872495E-16,1.));
#20723=DIRECTION('center_axis',(0.,0.,1.));
#20724=DIRECTION('ref_axis',(0.499999999999942,0.866025403784472,0.));
#20725=DIRECTION('',(6.12323399573605E-17,1.06057523872495E-16,1.));
#20726=DIRECTION('center_axis',(0.,0.,1.));
#20727=DIRECTION('ref_axis',(0.499999999999942,0.866025403784472,0.));
#20728=DIRECTION('',(6.12323399573605E-17,1.06057523872495E-16,1.));
#20729=DIRECTION('center_axis',(0.,0.,1.));
#20730=DIRECTION('ref_axis',(0.499999999999942,0.866025403784472,0.));
#20731=DIRECTION('',(6.12323399573605E-17,1.06057523872495E-16,1.));
#20732=DIRECTION('center_axis',(0.,0.,1.));
#20733=DIRECTION('ref_axis',(0.499999999999942,0.866025403784472,0.));
#20734=DIRECTION('',(6.12323399573605E-17,1.06057523872495E-16,1.));
#20735=DIRECTION('center_axis',(0.,0.,1.));
#20736=DIRECTION('ref_axis',(0.499999999999942,0.866025403784472,0.));
#20737=DIRECTION('',(6.12323399573605E-17,1.06057523872495E-16,1.));
#20738=DIRECTION('center_axis',(0.,0.,1.));
#20739=DIRECTION('ref_axis',(0.499999999999942,0.866025403784472,0.));
#20740=DIRECTION('',(6.12323399573605E-17,1.06057523872495E-16,1.));
#20741=DIRECTION('center_axis',(0.,0.,1.));
#20742=DIRECTION('ref_axis',(0.499999999999942,0.866025403784472,0.));
#20743=DIRECTION('',(6.12323399573605E-17,1.06057523872495E-16,1.));
#20744=DIRECTION('center_axis',(0.,0.,1.));
#20745=DIRECTION('ref_axis',(-0.991348961503154,-0.131252567695333,0.));
#20746=DIRECTION('',(6.12323399573605E-17,1.06057523872495E-16,1.));
#20747=DIRECTION('center_axis',(0.,0.,1.));
#20748=DIRECTION('ref_axis',(0.499999999999942,0.866025403784472,0.));
#20749=DIRECTION('center_axis',(0.,0.,1.));
#20750=DIRECTION('ref_axis',(-0.499999999999999,0.866025403784439,0.));
#20751=DIRECTION('',(0.,0.,1.));
#20752=DIRECTION('center_axis',(0.,0.,-1.));
#20753=DIRECTION('ref_axis',(-0.499999999999999,0.866025403784439,0.));
#20754=DIRECTION('',(0.,0.,1.));
#20755=DIRECTION('center_axis',(0.,0.,-1.));
#20756=DIRECTION('ref_axis',(-0.499999999999999,0.866025403784439,0.));
#20757=DIRECTION('center_axis',(0.,0.,1.));
#20758=DIRECTION('ref_axis',(-0.499999999999999,0.866025403784439,0.));
#20759=DIRECTION('',(0.,0.,1.));
#20760=DIRECTION('center_axis',(0.,0.,1.));
#20761=DIRECTION('ref_axis',(-0.499999999999999,0.866025403784439,0.));
#20762=DIRECTION('',(0.,0.,1.));
#20763=DIRECTION('center_axis',(0.,0.,1.));
#20764=DIRECTION('ref_axis',(-0.499999999999999,0.866025403784439,0.));
#20765=DIRECTION('',(0.,0.,1.));
#20766=DIRECTION('center_axis',(0.,0.,1.));
#20767=DIRECTION('ref_axis',(-0.499999999999999,0.866025403784439,0.));
#20768=DIRECTION('',(0.,0.,1.));
#20769=DIRECTION('center_axis',(0.,0.,1.));
#20770=DIRECTION('ref_axis',(-0.499999999999999,0.866025403784439,0.));
#20771=DIRECTION('',(0.,0.,1.));
#20772=DIRECTION('center_axis',(0.,0.,1.));
#20773=DIRECTION('ref_axis',(-0.499999999999999,0.866025403784439,0.));
#20774=DIRECTION('',(0.,0.,1.));
#20775=DIRECTION('center_axis',(0.,0.,1.));
#20776=DIRECTION('ref_axis',(-0.499999999999999,0.866025403784439,0.));
#20777=DIRECTION('',(0.,0.,1.));
#20778=DIRECTION('center_axis',(0.,0.,1.));
#20779=DIRECTION('ref_axis',(-0.499999999999999,0.866025403784439,0.));
#20780=DIRECTION('',(0.,0.,1.));
#20781=DIRECTION('center_axis',(0.,0.,1.));
#20782=DIRECTION('ref_axis',(-0.499999999999999,0.866025403784439,0.));
#20783=DIRECTION('',(0.,0.,1.));
#20784=DIRECTION('center_axis',(0.,0.,1.));
#20785=DIRECTION('ref_axis',(-0.499999999999999,0.866025403784439,0.));
#20786=DIRECTION('',(0.,0.,1.));
#20787=DIRECTION('center_axis',(0.,0.,1.));
#20788=DIRECTION('ref_axis',(-0.768385143082287,0.639987712296426,0.));
#20789=DIRECTION('',(0.,0.,1.));
#20790=DIRECTION('center_axis',(0.,0.,-1.));
#20791=DIRECTION('ref_axis',(-0.499999999999999,0.866025403784439,0.));
#20792=DIRECTION('center_axis',(0.,0.,1.));
#20793=DIRECTION('ref_axis',(0.548243791989886,0.836318566423436,0.));
#20794=DIRECTION('',(-6.12323399573743E-17,1.06057523872487E-16,1.));
#20795=DIRECTION('center_axis',(0.,0.,-1.));
#20796=DIRECTION('ref_axis',(-0.500000000000054,0.866025403784408,0.));
#20797=DIRECTION('center_axis',(0.,0.,1.));
#20798=DIRECTION('ref_axis',(-0.500000000000054,0.866025403784408,0.));
#20799=DIRECTION('',(-6.12323399573743E-17,1.06057523872487E-16,1.));
#20800=DIRECTION('center_axis',(0.,0.,1.));
#20801=DIRECTION('ref_axis',(-0.500000000000054,0.866025403784408,0.));
#20802=DIRECTION('',(-6.12323399573743E-17,1.06057523872487E-16,1.));
#20803=DIRECTION('center_axis',(0.,0.,1.));
#20804=DIRECTION('ref_axis',(-0.500000000000054,0.866025403784408,0.));
#20805=DIRECTION('',(-6.12323399573743E-17,1.06057523872487E-16,1.));
#20806=DIRECTION('center_axis',(0.,0.,1.));
#20807=DIRECTION('ref_axis',(-0.500000000000054,0.866025403784408,0.));
#20808=DIRECTION('',(-6.12323399573743E-17,1.06057523872487E-16,1.));
#20809=DIRECTION('center_axis',(0.,0.,1.));
#20810=DIRECTION('ref_axis',(-0.500000000000054,0.866025403784408,0.));
#20811=DIRECTION('',(-6.12323399573743E-17,1.06057523872487E-16,1.));
#20812=DIRECTION('center_axis',(0.,0.,1.));
#20813=DIRECTION('ref_axis',(-0.500000000000054,0.866025403784408,0.));
#20814=DIRECTION('',(-6.12323399573743E-17,1.06057523872487E-16,1.));
#20815=DIRECTION('center_axis',(0.,0.,1.));
#20816=DIRECTION('ref_axis',(-0.500000000000054,0.866025403784408,0.));
#20817=DIRECTION('',(-6.12323399573743E-17,1.06057523872487E-16,1.));
#20818=DIRECTION('center_axis',(0.,0.,1.));
#20819=DIRECTION('ref_axis',(-0.500000000000054,0.866025403784408,0.));
#20820=DIRECTION('',(-6.12323399573743E-17,1.06057523872487E-16,1.));
#20821=DIRECTION('center_axis',(0.,0.,1.));
#20822=DIRECTION('ref_axis',(-0.500000000000054,0.866025403784408,0.));
#20823=DIRECTION('',(-6.12323399573743E-17,1.06057523872487E-16,1.));
#20824=DIRECTION('center_axis',(0.,0.,1.));
#20825=DIRECTION('ref_axis',(-0.500000000000054,0.866025403784408,0.));
#20826=DIRECTION('',(-6.12323399573743E-17,1.06057523872487E-16,1.));
#20827=DIRECTION('center_axis',(0.,0.,1.));
#20828=DIRECTION('ref_axis',(-0.500000000000054,0.866025403784408,0.));
#20829=DIRECTION('',(-6.12323399573743E-17,1.06057523872487E-16,1.));
#20830=DIRECTION('center_axis',(0.,0.,1.));
#20831=DIRECTION('ref_axis',(-0.382006426201385,-0.924159667125138,0.));
#20832=DIRECTION('',(-6.12323399573743E-17,1.06057523872487E-16,1.));
#20833=DIRECTION('center_axis',(0.,0.,1.));
#20834=DIRECTION('ref_axis',(-0.500000000000054,0.866025403784407,0.));
#20835=DIRECTION('center_axis',(-0.965925826289068,-0.258819045102521,3.59183578855394E-17));
#20836=DIRECTION('ref_axis',(0.0897739762313162,-0.335041040492753,0.937916912299353));
#20837=DIRECTION('',(-0.965925826289068,-0.258819045102521,3.59183578855394E-17));
#20838=DIRECTION('center_axis',(0.965925826289068,0.258819045102521,-3.59183578855394E-17));
#20839=DIRECTION('ref_axis',(-0.258819045102521,0.965925826289068,0.));
#20840=DIRECTION('center_axis',(-0.965925826289068,-0.258819045102521,3.59183578855394E-17));
#20841=DIRECTION('ref_axis',(-0.258819045102521,0.965925826289068,0.));
#20842=DIRECTION('',(-0.965925826289068,-0.258819045102521,3.59183578855394E-17));
#20843=DIRECTION('center_axis',(-0.965925826289068,-0.258819045102521,3.59183578855394E-17));
#20844=DIRECTION('ref_axis',(-0.258819045102521,0.965925826289068,0.));
#20845=DIRECTION('',(-0.965925826289068,-0.258819045102521,3.59183578855394E-17));
#20846=DIRECTION('center_axis',(-0.965925826289068,-0.258819045102521,3.59183578855394E-17));
#20847=DIRECTION('ref_axis',(-0.258819045102521,0.965925826289068,0.));
#20848=DIRECTION('',(-0.965925826289068,-0.258819045102521,3.59183578855394E-17));
#20849=DIRECTION('center_axis',(-0.965925826289068,-0.258819045102521,3.59183578855394E-17));
#20850=DIRECTION('ref_axis',(-0.258819045102521,0.965925826289068,0.));
#20851=DIRECTION('',(-0.965925826289068,-0.258819045102521,3.59183578855394E-17));
#20852=DIRECTION('center_axis',(-0.965925826289068,-0.258819045102521,3.59183578855394E-17));
#20853=DIRECTION('ref_axis',(-0.258819045102521,0.965925826289068,0.));
#20854=DIRECTION('',(-0.965925826289068,-0.258819045102521,3.59183578855394E-17));
#20855=DIRECTION('center_axis',(-0.965925826289068,-0.258819045102521,3.59183578855394E-17));
#20856=DIRECTION('ref_axis',(-0.258819045102521,0.965925826289068,0.));
#20857=DIRECTION('',(-0.965925826289068,-0.258819045102521,3.59183578855394E-17));
#20858=DIRECTION('center_axis',(-0.965925826289068,-0.258819045102521,3.59183578855394E-17));
#20859=DIRECTION('ref_axis',(-0.236559838638084,0.882853336827626,-0.405720874981618));
#20860=DIRECTION('',(-0.965925826289068,-0.258819045102521,3.59183578855394E-17));
#20861=DIRECTION('center_axis',(-0.965925826289068,-0.258819045102521,3.59183578855394E-17));
#20862=DIRECTION('ref_axis',(-0.205298336336054,0.766183821915523,0.608945764524699));
#20863=DIRECTION('',(-0.965925826289067,-0.258819045102527,3.59183578857433E-17));
#20864=DIRECTION('center_axis',(0.965925826289068,0.258819045102521,0.));
#20865=DIRECTION('ref_axis',(-0.25881904510252,0.965925826289069,-3.10652936774893E-14));
#20866=DIRECTION('center_axis',(-0.965925826289068,-0.258819045102521,3.59183578855394E-17));
#20867=DIRECTION('ref_axis',(-0.25881904510252,0.965925826289069,-3.10652936774893E-14));
#20868=DIRECTION('',(-0.965925826289067,-0.258819045102527,3.59183578857433E-17));
#20869=DIRECTION('center_axis',(-0.965925826289068,-0.258819045102521,3.59183578855394E-17));
#20870=DIRECTION('ref_axis',(-0.25881904510252,0.965925826289069,-3.10652936774893E-14));
#20871=DIRECTION('',(-0.965925826289067,-0.258819045102527,3.59183578857433E-17));
#20872=DIRECTION('center_axis',(-0.965925826289068,-0.258819045102521,3.59183578855394E-17));
#20873=DIRECTION('ref_axis',(-0.25881904510252,0.965925826289069,-3.10652936774893E-14));
#20874=DIRECTION('',(-0.965925826289067,-0.258819045102527,3.59183578857433E-17));
#20875=DIRECTION('center_axis',(-0.965925826289068,-0.258819045102521,3.59183578855394E-17));
#20876=DIRECTION('ref_axis',(-0.25881904510252,0.965925826289069,-3.10652936774893E-14));
#20877=DIRECTION('',(-0.965925826289067,-0.258819045102527,3.59183578857433E-17));
#20878=DIRECTION('center_axis',(-0.965925826289068,-0.258819045102521,3.59183578855394E-17));
#20879=DIRECTION('ref_axis',(-0.25881904510252,0.965925826289069,-3.10652936774893E-14));
#20880=DIRECTION('',(-0.965925826289067,-0.258819045102527,3.59183578857433E-17));
#20881=DIRECTION('center_axis',(-0.965925826289068,-0.258819045102521,3.59183578855394E-17));
#20882=DIRECTION('ref_axis',(-0.25881904510252,0.965925826289069,-3.10652936774893E-14));
#20883=DIRECTION('',(-0.965925826289067,-0.258819045102527,3.59183578857433E-17));
#20884=DIRECTION('center_axis',(-0.965925826289068,-0.258819045102521,3.59183578855394E-17));
#20885=DIRECTION('ref_axis',(0.16010022241081,-0.597502164340218,-0.785722013432718));
#20886=DIRECTION('',(-0.965925826289067,-0.258819045102527,3.59183578857433E-17));
#20887=DIRECTION('center_axis',(0.258819045102521,-0.965925826289068,3.59183578855394E-17));
#20888=DIRECTION('ref_axis',(0.335041040492769,0.0897739762313205,0.937916912299347));
#20889=DIRECTION('',(0.258819045102521,-0.965925826289068,3.59183578855394E-17));
#20890=DIRECTION('center_axis',(-0.258819045102521,0.965925826289068,-3.59183578855394E-17));
#20891=DIRECTION('ref_axis',(-0.965925826289068,-0.258819045102521,0.));
#20892=DIRECTION('center_axis',(0.258819045102521,-0.965925826289068,3.59183578855394E-17));
#20893=DIRECTION('ref_axis',(-0.965925826289068,-0.258819045102521,0.));
#20894=DIRECTION('',(0.258819045102521,-0.965925826289068,3.59183578855394E-17));
#20895=DIRECTION('center_axis',(0.258819045102521,-0.965925826289068,3.59183578855394E-17));
#20896=DIRECTION('ref_axis',(-0.965925826289068,-0.258819045102521,0.));
#20897=DIRECTION('',(0.258819045102521,-0.965925826289068,3.59183578855394E-17));
#20898=DIRECTION('center_axis',(0.258819045102521,-0.965925826289068,3.59183578855394E-17));
#20899=DIRECTION('ref_axis',(-0.965925826289068,-0.258819045102521,0.));
#20900=DIRECTION('',(0.258819045102521,-0.965925826289068,3.59183578855394E-17));
#20901=DIRECTION('center_axis',(0.258819045102521,-0.965925826289068,3.59183578855394E-17));
#20902=DIRECTION('ref_axis',(-0.965925826289068,-0.258819045102521,0.));
#20903=DIRECTION('',(0.258819045102521,-0.965925826289068,3.59183578855394E-17));
#20904=DIRECTION('center_axis',(0.258819045102521,-0.965925826289068,3.59183578855394E-17));
#20905=DIRECTION('ref_axis',(-0.965925826289068,-0.258819045102521,0.));
#20906=DIRECTION('',(0.258819045102521,-0.965925826289068,3.59183578855394E-17));
#20907=DIRECTION('center_axis',(0.258819045102521,-0.965925826289068,3.59183578855394E-17));
#20908=DIRECTION('ref_axis',(-0.965925826289068,-0.258819045102521,0.));
#20909=DIRECTION('',(0.258819045102521,-0.965925826289068,3.59183578855394E-17));
#20910=DIRECTION('center_axis',(0.258819045102521,-0.965925826289068,3.59183578855394E-17));
#20911=DIRECTION('ref_axis',(-0.882853336827661,-0.236559838638094,-0.405720874981536));
#20912=DIRECTION('',(0.258819045102521,-0.965925826289068,3.59183578855394E-17));
#20913=DIRECTION('center_axis',(0.965925826289068,0.258819045102521,3.59183578855394E-17));
#20914=DIRECTION('ref_axis',(-0.0897739762312974,0.335041040492683,0.93791691229938));
#20915=DIRECTION('',(0.965925826289068,0.258819045102521,3.59183578855394E-17));
#20916=DIRECTION('center_axis',(-0.965925826289068,-0.258819045102521,-3.59183578855394E-17));
#20917=DIRECTION('ref_axis',(0.258819045102521,-0.965925826289068,0.));
#20918=DIRECTION('center_axis',(0.965925826289068,0.258819045102521,3.59183578855394E-17));
#20919=DIRECTION('ref_axis',(0.258819045102521,-0.965925826289068,0.));
#20920=DIRECTION('',(0.965925826289068,0.258819045102521,3.59183578855394E-17));
#20921=DIRECTION('center_axis',(0.965925826289068,0.258819045102521,3.59183578855394E-17));
#20922=DIRECTION('ref_axis',(0.258819045102521,-0.965925826289068,0.));
#20923=DIRECTION('',(0.965925826289068,0.258819045102521,3.59183578855394E-17));
#20924=DIRECTION('center_axis',(0.965925826289068,0.258819045102521,3.59183578855394E-17));
#20925=DIRECTION('ref_axis',(0.258819045102521,-0.965925826289068,0.));
#20926=DIRECTION('',(0.965925826289068,0.258819045102521,3.59183578855394E-17));
#20927=DIRECTION('center_axis',(0.965925826289068,0.258819045102521,3.59183578855394E-17));
#20928=DIRECTION('ref_axis',(0.258819045102521,-0.965925826289068,0.));
#20929=DIRECTION('',(0.965925826289068,0.258819045102521,3.59183578855394E-17));
#20930=DIRECTION('center_axis',(0.965925826289068,0.258819045102521,3.59183578855394E-17));
#20931=DIRECTION('ref_axis',(0.258819045102521,-0.965925826289068,0.));
#20932=DIRECTION('',(0.965925826289068,0.258819045102521,3.59183578855394E-17));
#20933=DIRECTION('center_axis',(0.965925826289068,0.258819045102521,3.59183578855394E-17));
#20934=DIRECTION('ref_axis',(0.258819045102521,-0.965925826289068,0.));
#20935=DIRECTION('',(0.965925826289068,0.258819045102521,3.59183578855394E-17));
#20936=DIRECTION('center_axis',(0.965925826289068,0.258819045102521,3.59183578855394E-17));
#20937=DIRECTION('ref_axis',(0.236559838638087,-0.882853336827637,-0.405720874981593));
#20938=DIRECTION('',(0.965925826289068,0.258819045102521,3.59183578855394E-17));
#20939=DIRECTION('center_axis',(-0.258819045102521,0.965925826289068,3.59183578855394E-17));
#20940=DIRECTION('ref_axis',(-0.335041040492721,-0.0897739762313076,0.937916912299365));
#20941=DIRECTION('',(-0.258819045102521,0.965925826289068,3.59183578855394E-17));
#20942=DIRECTION('center_axis',(0.258819045102521,-0.965925826289068,-3.59183578855394E-17));
#20943=DIRECTION('ref_axis',(0.965925826289068,0.25881904510252,0.));
#20944=DIRECTION('center_axis',(-0.258819045102521,0.965925826289068,3.59183578855394E-17));
#20945=DIRECTION('ref_axis',(0.965925826289068,0.25881904510252,0.));
#20946=DIRECTION('',(-0.258819045102521,0.965925826289068,3.59183578855394E-17));
#20947=DIRECTION('center_axis',(-0.258819045102521,0.965925826289068,3.59183578855394E-17));
#20948=DIRECTION('ref_axis',(0.965925826289068,0.25881904510252,0.));
#20949=DIRECTION('',(-0.258819045102521,0.965925826289068,3.59183578855394E-17));
#20950=DIRECTION('center_axis',(-0.258819045102521,0.965925826289068,3.59183578855394E-17));
#20951=DIRECTION('ref_axis',(0.965925826289068,0.25881904510252,0.));
#20952=DIRECTION('',(-0.258819045102521,0.965925826289068,3.59183578855394E-17));
#20953=DIRECTION('center_axis',(-0.258819045102521,0.965925826289068,3.59183578855394E-17));
#20954=DIRECTION('ref_axis',(0.965925826289068,0.25881904510252,0.));
#20955=DIRECTION('',(-0.258819045102521,0.965925826289068,3.59183578855394E-17));
#20956=DIRECTION('center_axis',(-0.258819045102521,0.965925826289068,3.59183578855394E-17));
#20957=DIRECTION('ref_axis',(0.965925826289068,0.25881904510252,0.));
#20958=DIRECTION('',(-0.258819045102521,0.965925826289068,3.59183578855394E-17));
#20959=DIRECTION('center_axis',(-0.258819045102521,0.965925826289068,3.59183578855394E-17));
#20960=DIRECTION('ref_axis',(0.965925826289068,0.25881904510252,0.));
#20961=DIRECTION('',(-0.258819045102521,0.965925826289068,3.59183578855394E-17));
#20962=DIRECTION('center_axis',(-0.258819045102521,0.965925826289068,3.59183578855394E-17));
#20963=DIRECTION('ref_axis',(0.882853336827629,0.236559838638085,-0.40572087498161));
#20964=DIRECTION('',(-0.258819045102521,0.965925826289068,3.59183578855394E-17));
#20965=DIRECTION('center_axis',(0.258819045102521,-0.965925826289068,3.59183578855394E-17));
#20966=DIRECTION('ref_axis',(-0.766183821915484,-0.205298336336044,0.608945764524752));
#20967=DIRECTION('',(0.258819045102527,-0.965925826289067,3.59183578856725E-17));
#20968=DIRECTION('center_axis',(-0.258819045102521,0.965925826289068,0.));
#20969=DIRECTION('ref_axis',(-0.965925826289069,-0.25881904510252,-2.02285633248767E-14));
#20970=DIRECTION('center_axis',(0.258819045102521,-0.965925826289068,3.59183578855394E-17));
#20971=DIRECTION('ref_axis',(-0.965925826289069,-0.25881904510252,-2.02285633248767E-14));
#20972=DIRECTION('',(0.258819045102527,-0.965925826289067,3.59183578856725E-17));
#20973=DIRECTION('center_axis',(0.258819045102521,-0.965925826289068,3.59183578855394E-17));
#20974=DIRECTION('ref_axis',(-0.965925826289069,-0.25881904510252,-2.02285633248767E-14));
#20975=DIRECTION('',(0.258819045102527,-0.965925826289067,3.59183578856725E-17));
#20976=DIRECTION('center_axis',(0.258819045102521,-0.965925826289068,3.59183578855394E-17));
#20977=DIRECTION('ref_axis',(-0.965925826289069,-0.25881904510252,-2.02285633248767E-14));
#20978=DIRECTION('',(0.258819045102527,-0.965925826289067,3.59183578856725E-17));
#20979=DIRECTION('center_axis',(0.258819045102521,-0.965925826289068,3.59183578855394E-17));
#20980=DIRECTION('ref_axis',(-0.965925826289069,-0.25881904510252,-2.02285633248767E-14));
#20981=DIRECTION('',(0.258819045102527,-0.965925826289067,3.59183578856725E-17));
#20982=DIRECTION('center_axis',(0.258819045102521,-0.965925826289068,3.59183578855394E-17));
#20983=DIRECTION('ref_axis',(-0.965925826289069,-0.25881904510252,-2.02285633248767E-14));
#20984=DIRECTION('',(0.258819045102527,-0.965925826289067,3.59183578856725E-17));
#20985=DIRECTION('center_axis',(0.258819045102521,-0.965925826289068,3.59183578855394E-17));
#20986=DIRECTION('ref_axis',(-0.965925826289069,-0.25881904510252,-2.02285633248767E-14));
#20987=DIRECTION('',(0.258819045102527,-0.965925826289067,3.59183578856725E-17));
#20988=DIRECTION('center_axis',(0.258819045102521,-0.965925826289068,3.59183578855394E-17));
#20989=DIRECTION('ref_axis',(0.597502164340198,0.160100222410805,-0.785722013432735));
#20990=DIRECTION('',(0.258819045102527,-0.965925826289067,3.59183578856725E-17));
#20991=DIRECTION('center_axis',(0.965925826289068,0.258819045102521,3.59183578855394E-17));
#20992=DIRECTION('ref_axis',(0.205298336336062,-0.766183821915549,0.608945764524665));
#20993=DIRECTION('',(0.965925826289067,0.258819045102527,3.59183578857386E-17));
#20994=DIRECTION('center_axis',(-0.965925826289068,-0.258819045102521,0.));
#20995=DIRECTION('ref_axis',(0.25881904510252,-0.965925826289069,-3.03428449873152E-14));
#20996=DIRECTION('center_axis',(0.965925826289068,0.258819045102521,3.59183578855394E-17));
#20997=DIRECTION('ref_axis',(0.25881904510252,-0.965925826289069,-3.03428449873152E-14));
#20998=DIRECTION('',(0.965925826289067,0.258819045102527,3.59183578857386E-17));
#20999=DIRECTION('center_axis',(0.965925826289068,0.258819045102521,3.59183578855394E-17));
#21000=DIRECTION('ref_axis',(0.25881904510252,-0.965925826289069,-3.03428449873152E-14));
#21001=DIRECTION('',(0.965925826289067,0.258819045102527,3.59183578857386E-17));
#21002=DIRECTION('center_axis',(0.965925826289068,0.258819045102521,3.59183578855394E-17));
#21003=DIRECTION('ref_axis',(0.25881904510252,-0.965925826289069,-3.03428449873152E-14));
#21004=DIRECTION('',(0.965925826289067,0.258819045102527,3.59183578857386E-17));
#21005=DIRECTION('center_axis',(0.965925826289068,0.258819045102521,3.59183578855394E-17));
#21006=DIRECTION('ref_axis',(0.25881904510252,-0.965925826289069,-3.03428449873152E-14));
#21007=DIRECTION('',(0.965925826289067,0.258819045102527,3.59183578857386E-17));
#21008=DIRECTION('center_axis',(0.965925826289068,0.258819045102521,3.59183578855394E-17));
#21009=DIRECTION('ref_axis',(0.25881904510252,-0.965925826289069,-3.03428449873152E-14));
#21010=DIRECTION('',(0.965925826289067,0.258819045102527,3.59183578857386E-17));
#21011=DIRECTION('center_axis',(0.965925826289068,0.258819045102521,3.59183578855394E-17));
#21012=DIRECTION('ref_axis',(0.25881904510252,-0.965925826289069,-3.03428449873152E-14));
#21013=DIRECTION('',(0.965925826289067,0.258819045102527,3.59183578857386E-17));
#21014=DIRECTION('center_axis',(0.965925826289068,0.258819045102521,3.59183578855394E-17));
#21015=DIRECTION('ref_axis',(-0.16010022241082,0.597502164340256,-0.785722013432687));
#21016=DIRECTION('',(0.965925826289067,0.258819045102527,3.59183578857386E-17));
#21017=DIRECTION('center_axis',(-0.258819045102521,0.965925826289068,3.59183578855394E-17));
#21018=DIRECTION('ref_axis',(0.766183821915516,0.205298336336053,0.608945764524709));
#21019=DIRECTION('',(-0.258819045102527,0.965925826289067,3.59183578856961E-17));
#21020=DIRECTION('center_axis',(0.258819045102521,-0.965925826289068,0.));
#21021=DIRECTION('ref_axis',(0.965925826289069,0.25881904510252,-2.38408067757476E-14));
#21022=DIRECTION('center_axis',(-0.258819045102521,0.965925826289068,3.59183578855394E-17));
#21023=DIRECTION('ref_axis',(0.965925826289069,0.25881904510252,-2.38408067757476E-14));
#21024=DIRECTION('',(-0.258819045102527,0.965925826289067,3.59183578856961E-17));
#21025=DIRECTION('center_axis',(-0.258819045102521,0.965925826289068,3.59183578855394E-17));
#21026=DIRECTION('ref_axis',(0.965925826289069,0.25881904510252,-2.38408067757476E-14));
#21027=DIRECTION('',(-0.258819045102527,0.965925826289067,3.59183578856961E-17));
#21028=DIRECTION('center_axis',(-0.258819045102521,0.965925826289068,3.59183578855394E-17));
#21029=DIRECTION('ref_axis',(0.965925826289069,0.25881904510252,-2.38408067757476E-14));
#21030=DIRECTION('',(-0.258819045102527,0.965925826289067,3.59183578856961E-17));
#21031=DIRECTION('center_axis',(-0.258819045102521,0.965925826289068,3.59183578855394E-17));
#21032=DIRECTION('ref_axis',(0.965925826289069,0.25881904510252,-2.38408067757476E-14));
#21033=DIRECTION('',(-0.258819045102527,0.965925826289067,3.59183578856961E-17));
#21034=DIRECTION('center_axis',(-0.258819045102521,0.965925826289068,3.59183578855394E-17));
#21035=DIRECTION('ref_axis',(0.965925826289069,0.25881904510252,-2.38408067757476E-14));
#21036=DIRECTION('',(-0.258819045102527,0.965925826289067,3.59183578856961E-17));
#21037=DIRECTION('center_axis',(-0.258819045102521,0.965925826289068,3.59183578855394E-17));
#21038=DIRECTION('ref_axis',(0.965925826289069,0.25881904510252,-2.38408067757476E-14));
#21039=DIRECTION('',(-0.258819045102527,0.965925826289067,3.59183578856961E-17));
#21040=DIRECTION('center_axis',(-0.258819045102521,0.965925826289068,3.59183578855394E-17));
#21041=DIRECTION('ref_axis',(-0.597502164340203,-0.160100222410806,-0.78572201343273));
#21042=DIRECTION('',(-0.258819045102527,0.965925826289067,3.59183578856961E-17));
#21043=DIRECTION('center_axis',(-0.258819045102521,0.965925826289068,3.59183578855394E-17));
#21044=DIRECTION('ref_axis',(0.965925826289069,0.25881904510252,-2.38408067757476E-14));
#21045=DIRECTION('center_axis',(0.965925826289068,0.258819045102521,3.59183578855394E-17));
#21046=DIRECTION('ref_axis',(0.25881904510252,-0.965925826289069,-3.03428449873152E-14));
#21047=DIRECTION('center_axis',(0.258819045102521,-0.965925826289068,3.59183578855394E-17));
#21048=DIRECTION('ref_axis',(-0.965925826289069,-0.25881904510252,-2.02285633248767E-14));
#21049=DIRECTION('center_axis',(-0.258819045102521,0.965925826289068,3.59183578855394E-17));
#21050=DIRECTION('ref_axis',(0.965925826289068,0.25881904510252,0.));
#21051=DIRECTION('center_axis',(-0.258819045102521,0.965925826289068,3.59183578855394E-17));
#21052=DIRECTION('ref_axis',(0.965925826289068,0.25881904510252,0.));
#21053=DIRECTION('center_axis',(0.965925826289068,0.258819045102521,3.59183578855394E-17));
#21054=DIRECTION('ref_axis',(0.258819045102521,-0.965925826289068,0.));
#21055=DIRECTION('center_axis',(0.965925826289068,0.258819045102521,3.59183578855394E-17));
#21056=DIRECTION('ref_axis',(0.258819045102521,-0.965925826289068,0.));
#21057=DIRECTION('center_axis',(0.258819045102521,-0.965925826289068,3.59183578855394E-17));
#21058=DIRECTION('ref_axis',(-0.965925826289068,-0.258819045102521,0.));
#21059=DIRECTION('center_axis',(0.258819045102521,-0.965925826289068,3.59183578855394E-17));
#21060=DIRECTION('ref_axis',(-0.965925826289068,-0.258819045102521,0.));
#21061=DIRECTION('center_axis',(-0.965925826289068,-0.258819045102521,3.59183578855394E-17));
#21062=DIRECTION('ref_axis',(-0.25881904510252,0.965925826289069,-3.10652936774893E-14));
#21063=DIRECTION('center_axis',(-0.965925826289068,-0.258819045102521,3.59183578855394E-17));
#21064=DIRECTION('ref_axis',(-0.258819045102521,0.965925826289068,0.));
#21065=DIRECTION('center_axis',(-0.965925826289068,-0.258819045102521,3.59183578855394E-17));
#21066=DIRECTION('ref_axis',(-0.258819045102521,0.965925826289068,0.));
#21067=DIRECTION('center_axis',(0.,0.,1.));
#21068=DIRECTION('ref_axis',(1.,0.,0.));
#21069=DIRECTION('center_axis',(0.,0.,1.));
#21070=DIRECTION('ref_axis',(-0.500000000000054,0.866025403784408,0.));
#21071=DIRECTION('center_axis',(0.,0.,1.));
#21072=DIRECTION('ref_axis',(-0.499999999999999,0.866025403784439,0.));
#21073=DIRECTION('center_axis',(0.,0.,1.));
#21074=DIRECTION('ref_axis',(1.,0.,0.));
#21075=DIRECTION('center_axis',(0.,0.,1.));
#21076=DIRECTION('ref_axis',(0.499999999999942,0.866025403784472,0.));
#21077=DIRECTION('center_axis',(0.,0.,1.));
#21078=DIRECTION('ref_axis',(0.5,0.866025403784438,0.));
#21079=DIRECTION('center_axis',(0.,0.,1.));
#21080=DIRECTION('ref_axis',(1.,0.,0.));
#21081=DIRECTION('center_axis',(0.,0.,1.));
#21082=DIRECTION('ref_axis',(1.,4.99775456844331E-14,0.));
#21083=DIRECTION('center_axis',(0.,0.,1.));
#21084=DIRECTION('ref_axis',(1.,-1.38777878078145E-16,0.));
#21085=DIRECTION('center_axis',(0.,0.,1.));
#21086=DIRECTION('ref_axis',(1.,0.,0.));
#21087=DIRECTION('center_axis',(0.,0.,1.));
#21088=DIRECTION('ref_axis',(0.500000000000041,-0.866025403784415,0.));
#21089=DIRECTION('center_axis',(0.,0.,1.));
#21090=DIRECTION('ref_axis',(0.5,-0.866025403784439,0.));
#21091=DIRECTION('center_axis',(0.,0.,1.));
#21092=DIRECTION('ref_axis',(1.,0.,0.));
#21093=DIRECTION('center_axis',(0.,0.,1.));
#21094=DIRECTION('ref_axis',(-0.499999999999956,-0.866025403784464,0.));
#21095=DIRECTION('center_axis',(0.,0.,1.));
#21096=DIRECTION('ref_axis',(-0.5,-0.866025403784439,0.));
#21097=DIRECTION('center_axis',(0.,0.,1.));
#21098=DIRECTION('ref_axis',(-0.499999999999999,0.866025403784439,0.));
#21099=DIRECTION('center_axis',(0.,0.,1.));
#21100=DIRECTION('ref_axis',(0.5,0.866025403784438,0.));
#21101=DIRECTION('center_axis',(0.,0.,1.));
#21102=DIRECTION('ref_axis',(1.,-1.66533453693773E-16,0.));
#21103=DIRECTION('center_axis',(0.,0.,1.));
#21104=DIRECTION('ref_axis',(0.5,-0.866025403784439,0.));
#21105=DIRECTION('center_axis',(0.,0.,1.));
#21106=DIRECTION('ref_axis',(-0.5,-0.866025403784439,0.));
#21107=DIRECTION('center_axis',(0.,0.,1.));
#21108=DIRECTION('ref_axis',(1.,0.,0.));
#21109=DIRECTION('center_axis',(0.,0.,-1.));
#21110=DIRECTION('ref_axis',(0.499999999999945,-0.86602540378447,0.));
#21111=DIRECTION('center_axis',(0.,0.,-1.));
#21112=DIRECTION('ref_axis',(0.499999999999999,-0.866025403784439,0.));
#21113=DIRECTION('center_axis',(0.,0.,1.));
#21114=DIRECTION('ref_axis',(1.,0.,0.));
#21115=DIRECTION('center_axis',(0.,0.,-1.));
#21116=DIRECTION('ref_axis',(-0.500000000000056,-0.866025403784406,0.));
#21117=DIRECTION('center_axis',(0.,0.,-1.));
#21118=DIRECTION('ref_axis',(-0.5,-0.866025403784438,0.));
#21119=DIRECTION('center_axis',(0.,0.,1.));
#21120=DIRECTION('ref_axis',(1.,0.,0.));
#21121=DIRECTION('center_axis',(0.,0.,-1.));
#21122=DIRECTION('ref_axis',(-1.,6.27859183309933E-14,0.));
#21123=DIRECTION('center_axis',(0.,0.,-1.));
#21124=DIRECTION('ref_axis',(-1.,1.38777878078145E-16,0.));
#21125=DIRECTION('center_axis',(0.,0.,1.));
#21126=DIRECTION('ref_axis',(1.,0.,0.));
#21127=DIRECTION('center_axis',(0.,0.,-1.));
#21128=DIRECTION('ref_axis',(-0.499999999999944,0.866025403784471,0.));
#21129=DIRECTION('center_axis',(0.,0.,-1.));
#21130=DIRECTION('ref_axis',(-0.5,0.866025403784439,0.));
#21131=DIRECTION('center_axis',(0.,0.,1.));
#21132=DIRECTION('ref_axis',(1.,0.,0.));
#21133=DIRECTION('center_axis',(0.,0.,-1.));
#21134=DIRECTION('ref_axis',(0.500000000000052,0.866025403784408,0.));
#21135=DIRECTION('center_axis',(0.,0.,-1.));
#21136=DIRECTION('ref_axis',(0.5,0.866025403784439,0.));
#21137=DIRECTION('center_axis',(0.,0.,-1.));
#21138=DIRECTION('ref_axis',(0.499999999999999,-0.866025403784439,0.));
#21139=DIRECTION('center_axis',(0.,0.,-1.));
#21140=DIRECTION('ref_axis',(-0.5,-0.866025403784438,0.));
#21141=DIRECTION('center_axis',(0.,0.,-1.));
#21142=DIRECTION('ref_axis',(-1.,1.66533453693773E-16,0.));
#21143=DIRECTION('center_axis',(0.,0.,-1.));
#21144=DIRECTION('ref_axis',(-0.5,0.866025403784439,0.));
#21145=DIRECTION('center_axis',(0.,0.,-1.));
#21146=DIRECTION('ref_axis',(0.5,0.866025403784439,0.));
#21147=DIRECTION('center_axis',(0.,0.,1.));
#21148=DIRECTION('ref_axis',(1.,0.,0.));
#21149=DIRECTION('center_axis',(0.,0.,1.));
#21150=DIRECTION('ref_axis',(-1.,-5.01106501999328E-14,0.));
#21151=DIRECTION('center_axis',(0.,0.,1.));
#21152=DIRECTION('ref_axis',(-1.,0.,0.));
#21153=DIRECTION('center_axis',(0.,0.,1.));
#21154=DIRECTION('ref_axis',(-1.,0.,0.));
#21155=DIRECTION('center_axis',(0.,0.,1.));
#21156=DIRECTION('ref_axis',(1.,0.,0.));
#21157=DIRECTION('center_axis',(0.,0.,-1.));
#21158=DIRECTION('ref_axis',(1.,-6.25346187617716E-14,0.));
#21159=DIRECTION('center_axis',(0.,0.,-1.));
#21160=DIRECTION('ref_axis',(1.,0.,0.));
#21161=DIRECTION('center_axis',(0.,0.,-1.));
#21162=DIRECTION('ref_axis',(1.,0.,0.));
#21163=DIRECTION('center_axis',(0.,0.,1.));
#21164=DIRECTION('ref_axis',(1.,0.,0.));
#21165=DIRECTION('center_axis',(0.,0.,-1.));
#21166=DIRECTION('ref_axis',(1.,0.,0.));
#21167=DIRECTION('',(0.,0.,-1.));
#21168=DIRECTION('center_axis',(0.,0.,-1.));
#21169=DIRECTION('ref_axis',(1.,0.,0.));
#21170=DIRECTION('center_axis',(0.,0.,1.));
#21171=DIRECTION('ref_axis',(1.,0.,0.));
#21172=DIRECTION('center_axis',(0.,0.,1.));
#21173=DIRECTION('ref_axis',(1.,0.,0.));
#21174=DIRECTION('',(0.,0.,-1.));
#21175=DIRECTION('center_axis',(0.,0.,1.));
#21176=DIRECTION('ref_axis',(1.,0.,0.));
#21177=DIRECTION('center_axis',(0.,0.,1.));
#21178=DIRECTION('ref_axis',(1.,0.,0.));
#21179=DIRECTION('center_axis',(0.,0.,1.));
#21180=DIRECTION('ref_axis',(1.,0.,0.));
#21181=DIRECTION('axis',(0.,0.,1.));
#21182=DIRECTION('refdir',(1.,0.,0.));
#21183=DIRECTION('center_axis',(0.,0.,-1.));
#21184=DIRECTION('ref_axis',(1.,0.,0.));
#21185=DIRECTION('',(0.,0.,-1.));
#21186=DIRECTION('center_axis',(0.,0.,1.));
#21187=DIRECTION('ref_axis',(1.,0.,0.));
#21188=DIRECTION('',(0.,0.,-1.));
#21189=DIRECTION('center_axis',(0.,0.,1.));
#21190=DIRECTION('ref_axis',(1.,0.,0.));
#21191=DIRECTION('center_axis',(0.,0.,1.));
#21192=DIRECTION('ref_axis',(1.,0.,0.));
#21193=DIRECTION('center_axis',(0.,0.,1.));
#21194=DIRECTION('ref_axis',(1.,0.,0.));
#21195=DIRECTION('center_axis',(0.,0.,1.));
#21196=DIRECTION('ref_axis',(1.,0.,0.));
#21197=DIRECTION('center_axis',(0.,0.,-1.));
#21198=DIRECTION('ref_axis',(1.,0.,0.));
#21199=DIRECTION('',(0.,0.,-1.));
#21200=DIRECTION('center_axis',(0.,0.,-1.));
#21201=DIRECTION('ref_axis',(1.,0.,0.));
#21202=DIRECTION('',(0.,0.,-1.));
#21203=DIRECTION('center_axis',(0.,0.,-1.));
#21204=DIRECTION('ref_axis',(1.,0.,0.));
#21205=DIRECTION('',(0.,0.,-1.));
#21206=DIRECTION('center_axis',(0.,0.,-1.));
#21207=DIRECTION('ref_axis',(1.,0.,0.));
#21208=DIRECTION('',(0.,0.,-1.));
#21209=DIRECTION('center_axis',(0.,0.,-1.));
#21210=DIRECTION('ref_axis',(1.,0.,0.));
#21211=DIRECTION('',(0.,0.,-1.));
#21212=DIRECTION('center_axis',(0.,0.,-1.));
#21213=DIRECTION('ref_axis',(1.,0.,0.));
#21214=DIRECTION('',(0.,0.,-1.));
#21215=DIRECTION('center_axis',(0.,0.,-1.));
#21216=DIRECTION('ref_axis',(0.937375356024964,-0.348320889291861,0.));
#21217=DIRECTION('',(0.,0.,-1.));
#21218=DIRECTION('center_axis',(0.,0.,1.));
#21219=DIRECTION('ref_axis',(1.,0.,0.));
#21220=DIRECTION('center_axis',(0.,0.,-1.));
#21221=DIRECTION('ref_axis',(0.793245518852996,0.608901918883199,0.));
#21222=DIRECTION('',(1.22464679914735E-16,-4.24456931042874E-30,-1.));
#21223=DIRECTION('center_axis',(0.,0.,1.));
#21224=DIRECTION('ref_axis',(1.,-3.45370740000048E-14,0.));
#21225=DIRECTION('center_axis',(0.,0.,-1.));
#21226=DIRECTION('ref_axis',(1.,-3.45370740000048E-14,0.));
#21227=DIRECTION('',(1.22464679914735E-16,-4.24456931042874E-30,-1.));
#21228=DIRECTION('center_axis',(0.,0.,-1.));
#21229=DIRECTION('ref_axis',(1.,-3.45370740000048E-14,0.));
#21230=DIRECTION('',(1.22464679914735E-16,-4.24456931042874E-30,-1.));
#21231=DIRECTION('center_axis',(0.,0.,-1.));
#21232=DIRECTION('ref_axis',(1.,-3.45370740000048E-14,0.));
#21233=DIRECTION('',(1.22464679914735E-16,-4.24456931042874E-30,-1.));
#21234=DIRECTION('center_axis',(0.,0.,-1.));
#21235=DIRECTION('ref_axis',(1.,-3.45370740000048E-14,0.));
#21236=DIRECTION('',(1.22464679914735E-16,-4.24456931042874E-30,-1.));
#21237=DIRECTION('center_axis',(0.,0.,-1.));
#21238=DIRECTION('ref_axis',(1.,-3.45370740000048E-14,0.));
#21239=DIRECTION('',(1.22464679914735E-16,-4.24456931042874E-30,-1.));
#21240=DIRECTION('center_axis',(0.,0.,-1.));
#21241=DIRECTION('ref_axis',(1.,-3.45370740000048E-14,0.));
#21242=DIRECTION('',(1.22464679914735E-16,-4.24456931042874E-30,-1.));
#21243=DIRECTION('center_axis',(0.,0.,-1.));
#21244=DIRECTION('ref_axis',(-0.609079509840797,-0.793109166944939,0.));
#21245=DIRECTION('',(1.22464679914735E-16,-4.24456931042874E-30,-1.));
#21246=DIRECTION('center_axis',(0.,0.,-1.));
#21247=DIRECTION('ref_axis',(1.,-3.45370740000048E-14,0.));
#21248=DIRECTION('center_axis',(0.,0.,1.));
#21249=DIRECTION('ref_axis',(-1.,0.,0.));
#21250=DIRECTION('',(0.,0.,1.));
#21251=DIRECTION('center_axis',(0.,0.,-1.));
#21252=DIRECTION('ref_axis',(-1.,0.,0.));
#21253=DIRECTION('',(0.,0.,1.));
#21254=DIRECTION('center_axis',(0.,0.,-1.));
#21255=DIRECTION('ref_axis',(-1.,0.,0.));
#21256=DIRECTION('center_axis',(0.,0.,-1.));
#21257=DIRECTION('ref_axis',(-1.,0.,0.));
#21258=DIRECTION('center_axis',(0.,0.,-1.));
#21259=DIRECTION('ref_axis',(-1.,0.,0.));
#21260=DIRECTION('center_axis',(0.,0.,-1.));
#21261=DIRECTION('ref_axis',(-1.,0.,0.));
#21262=DIRECTION('center_axis',(0.,0.,1.));
#21263=DIRECTION('ref_axis',(-1.,0.,0.));
#21264=DIRECTION('',(0.,0.,1.));
#21265=DIRECTION('center_axis',(0.,0.,1.));
#21266=DIRECTION('ref_axis',(-1.,0.,0.));
#21267=DIRECTION('',(0.,0.,1.));
#21268=DIRECTION('center_axis',(0.,0.,1.));
#21269=DIRECTION('ref_axis',(-1.,0.,0.));
#21270=DIRECTION('',(0.,0.,1.));
#21271=DIRECTION('center_axis',(0.,0.,1.));
#21272=DIRECTION('ref_axis',(-1.,0.,0.));
#21273=DIRECTION('',(0.,0.,1.));
#21274=DIRECTION('center_axis',(0.,0.,1.));
#21275=DIRECTION('ref_axis',(-1.,0.,0.));
#21276=DIRECTION('',(0.,0.,1.));
#21277=DIRECTION('center_axis',(0.,0.,1.));
#21278=DIRECTION('ref_axis',(-1.,0.,0.));
#21279=DIRECTION('',(0.,0.,1.));
#21280=DIRECTION('center_axis',(0.,0.,1.));
#21281=DIRECTION('ref_axis',(-0.937374823573184,-0.348322322183265,0.));
#21282=DIRECTION('',(0.,0.,1.));
#21283=DIRECTION('center_axis',(0.,0.,-1.));
#21284=DIRECTION('ref_axis',(-1.,0.,0.));
#21285=DIRECTION('center_axis',(0.,0.,1.));
#21286=DIRECTION('ref_axis',(-0.793244897475727,0.608902728380094,0.));
#21287=DIRECTION('',(-1.22464679914735E-16,-2.12978345412769E-30,1.));
#21288=DIRECTION('center_axis',(0.,0.,-1.));
#21289=DIRECTION('ref_axis',(-1.,-1.72685370000025E-14,0.));
#21290=DIRECTION('center_axis',(0.,0.,1.));
#21291=DIRECTION('ref_axis',(-1.,-1.72685370000025E-14,0.));
#21292=DIRECTION('',(-1.22464679914735E-16,-2.12978345412769E-30,1.));
#21293=DIRECTION('center_axis',(0.,0.,1.));
#21294=DIRECTION('ref_axis',(-1.,-1.72685370000025E-14,0.));
#21295=DIRECTION('',(-1.22464679914735E-16,-2.12978345412769E-30,1.));
#21296=DIRECTION('center_axis',(0.,0.,1.));
#21297=DIRECTION('ref_axis',(-1.,-1.72685370000025E-14,0.));
#21298=DIRECTION('',(-1.22464679914735E-16,-2.12978345412769E-30,1.));
#21299=DIRECTION('center_axis',(0.,0.,1.));
#21300=DIRECTION('ref_axis',(-1.,-1.72685370000025E-14,0.));
#21301=DIRECTION('',(-1.22464679914735E-16,-2.12978345412769E-30,1.));
#21302=DIRECTION('center_axis',(0.,0.,1.));
#21303=DIRECTION('ref_axis',(-1.,-1.72685370000025E-14,0.));
#21304=DIRECTION('',(-1.22464679914735E-16,-2.12978345412769E-30,1.));
#21305=DIRECTION('center_axis',(0.,0.,1.));
#21306=DIRECTION('ref_axis',(-1.,-1.72685370000025E-14,0.));
#21307=DIRECTION('',(-1.22464679914735E-16,-2.12978345412769E-30,1.));
#21308=DIRECTION('center_axis',(0.,0.,1.));
#21309=DIRECTION('ref_axis',(0.609080360598175,-0.793108513592937,0.));
#21310=DIRECTION('',(-1.22464679914735E-16,-2.12978345412769E-30,1.));
#21311=DIRECTION('center_axis',(0.,0.,1.));
#21312=DIRECTION('ref_axis',(-1.,-1.72685370000025E-14,0.));
#21313=DIRECTION('center_axis',(0.,0.,-1.));
#21314=DIRECTION('ref_axis',(0.5,0.866025403784439,0.));
#21315=DIRECTION('',(0.,0.,-1.));
#21316=DIRECTION('center_axis',(0.,0.,1.));
#21317=DIRECTION('ref_axis',(0.5,0.866025403784439,0.));
#21318=DIRECTION('',(0.,0.,-1.));
#21319=DIRECTION('center_axis',(0.,0.,1.));
#21320=DIRECTION('ref_axis',(0.5,0.866025403784439,0.));
#21321=DIRECTION('center_axis',(0.,0.,1.));
#21322=DIRECTION('ref_axis',(0.5,0.866025403784439,0.));
#21323=DIRECTION('center_axis',(0.,0.,1.));
#21324=DIRECTION('ref_axis',(0.5,0.866025403784439,0.));
#21325=DIRECTION('center_axis',(0.,0.,1.));
#21326=DIRECTION('ref_axis',(0.5,0.866025403784439,0.));
#21327=DIRECTION('center_axis',(0.,0.,-1.));
#21328=DIRECTION('ref_axis',(0.5,0.866025403784439,0.));
#21329=DIRECTION('',(0.,0.,-1.));
#21330=DIRECTION('center_axis',(0.,0.,-1.));
#21331=DIRECTION('ref_axis',(0.5,0.866025403784439,0.));
#21332=DIRECTION('',(0.,0.,-1.));
#21333=DIRECTION('center_axis',(0.,0.,-1.));
#21334=DIRECTION('ref_axis',(0.5,0.866025403784439,0.));
#21335=DIRECTION('',(0.,0.,-1.));
#21336=DIRECTION('center_axis',(0.,0.,-1.));
#21337=DIRECTION('ref_axis',(0.5,0.866025403784439,0.));
#21338=DIRECTION('',(0.,0.,-1.));
#21339=DIRECTION('center_axis',(0.,0.,-1.));
#21340=DIRECTION('ref_axis',(0.5,0.866025403784439,0.));
#21341=DIRECTION('',(0.,0.,-1.));
#21342=DIRECTION('center_axis',(0.,0.,-1.));
#21343=DIRECTION('ref_axis',(0.5,0.866025403784439,0.));
#21344=DIRECTION('',(0.,0.,-1.));
#21345=DIRECTION('center_axis',(0.,0.,-1.));
#21346=DIRECTION('ref_axis',(0.77034243979566,0.637630398781041,0.));
#21347=DIRECTION('',(0.,0.,-1.));
#21348=DIRECTION('center_axis',(0.,0.,1.));
#21349=DIRECTION('ref_axis',(0.5,0.866025403784439,0.));
#21350=DIRECTION('center_axis',(0.,0.,-1.));
#21351=DIRECTION('ref_axis',(-0.130701796389753,0.991421726824912,0.));
#21352=DIRECTION('',(6.12323399573733E-17,1.06057523872487E-16,-1.));
#21353=DIRECTION('center_axis',(0.,0.,1.));
#21354=DIRECTION('ref_axis',(0.500000000000046,0.866025403784412,0.));
#21355=DIRECTION('center_axis',(0.,0.,-1.));
#21356=DIRECTION('ref_axis',(0.500000000000046,0.866025403784412,0.));
#21357=DIRECTION('',(6.12323399573733E-17,1.06057523872487E-16,-1.));
#21358=DIRECTION('center_axis',(0.,0.,-1.));
#21359=DIRECTION('ref_axis',(0.500000000000046,0.866025403784412,0.));
#21360=DIRECTION('',(6.12323399573733E-17,1.06057523872487E-16,-1.));
#21361=DIRECTION('center_axis',(0.,0.,-1.));
#21362=DIRECTION('ref_axis',(0.500000000000046,0.866025403784412,0.));
#21363=DIRECTION('',(6.12323399573733E-17,1.06057523872487E-16,-1.));
#21364=DIRECTION('center_axis',(0.,0.,-1.));
#21365=DIRECTION('ref_axis',(0.500000000000046,0.866025403784412,0.));
#21366=DIRECTION('',(6.12323399573733E-17,1.06057523872487E-16,-1.));
#21367=DIRECTION('center_axis',(0.,0.,-1.));
#21368=DIRECTION('ref_axis',(0.500000000000046,0.866025403784412,0.));
#21369=DIRECTION('',(6.12323399573733E-17,1.06057523872487E-16,-1.));
#21370=DIRECTION('center_axis',(0.,0.,-1.));
#21371=DIRECTION('ref_axis',(0.500000000000046,0.866025403784412,0.));
#21372=DIRECTION('',(6.12323399573733E-17,1.06057523872487E-16,-1.));
#21373=DIRECTION('center_axis',(0.,0.,-1.));
#21374=DIRECTION('ref_axis',(0.382312913538214,-0.924032919403807,0.));
#21375=DIRECTION('',(6.12323399573733E-17,1.06057523872487E-16,-1.));
#21376=DIRECTION('center_axis',(0.,0.,-1.));
#21377=DIRECTION('ref_axis',(0.500000000000046,0.866025403784412,0.));
#21378=DIRECTION('center_axis',(0.,0.,-1.));
#21379=DIRECTION('ref_axis',(-0.5,0.866025403784439,0.));
#21380=DIRECTION('',(0.,0.,-1.));
#21381=DIRECTION('center_axis',(0.,0.,1.));
#21382=DIRECTION('ref_axis',(-0.5,0.866025403784439,0.));
#21383=DIRECTION('',(0.,0.,-1.));
#21384=DIRECTION('center_axis',(0.,0.,1.));
#21385=DIRECTION('ref_axis',(-0.5,0.866025403784439,0.));
#21386=DIRECTION('center_axis',(0.,0.,1.));
#21387=DIRECTION('ref_axis',(-0.5,0.866025403784439,0.));
#21388=DIRECTION('center_axis',(0.,0.,1.));
#21389=DIRECTION('ref_axis',(-0.5,0.866025403784439,0.));
#21390=DIRECTION('center_axis',(0.,0.,1.));
#21391=DIRECTION('ref_axis',(-0.5,0.866025403784439,0.));
#21392=DIRECTION('center_axis',(0.,0.,-1.));
#21393=DIRECTION('ref_axis',(-0.5,0.866025403784439,0.));
#21394=DIRECTION('',(0.,0.,-1.));
#21395=DIRECTION('center_axis',(0.,0.,-1.));
#21396=DIRECTION('ref_axis',(-0.5,0.866025403784439,0.));
#21397=DIRECTION('',(0.,0.,-1.));
#21398=DIRECTION('center_axis',(0.,0.,-1.));
#21399=DIRECTION('ref_axis',(-0.5,0.866025403784439,0.));
#21400=DIRECTION('',(0.,0.,-1.));
#21401=DIRECTION('center_axis',(0.,0.,-1.));
#21402=DIRECTION('ref_axis',(-0.5,0.866025403784439,0.));
#21403=DIRECTION('',(0.,0.,-1.));
#21404=DIRECTION('center_axis',(0.,0.,-1.));
#21405=DIRECTION('ref_axis',(-0.5,0.866025403784439,0.));
#21406=DIRECTION('',(0.,0.,-1.));
#21407=DIRECTION('center_axis',(0.,0.,-1.));
#21408=DIRECTION('ref_axis',(-0.5,0.866025403784439,0.));
#21409=DIRECTION('',(0.,0.,-1.));
#21410=DIRECTION('center_axis',(0.,0.,-1.));
#21411=DIRECTION('ref_axis',(-0.167034001011808,0.985951135962623,0.));
#21412=DIRECTION('',(0.,0.,-1.));
#21413=DIRECTION('center_axis',(0.,0.,1.));
#21414=DIRECTION('ref_axis',(-0.5,0.866025403784439,0.));
#21415=DIRECTION('center_axis',(0.,0.,-1.));
#21416=DIRECTION('ref_axis',(-0.923947020235643,0.382520461933313,0.));
#21417=DIRECTION('',(-6.12323399573632E-17,1.06057523872493E-16,-1.));
#21418=DIRECTION('center_axis',(0.,0.,1.));
#21419=DIRECTION('ref_axis',(-0.499999999999964,0.86602540378446,0.));
#21420=DIRECTION('center_axis',(0.,0.,-1.));
#21421=DIRECTION('ref_axis',(-0.499999999999964,0.86602540378446,0.));
#21422=DIRECTION('',(-6.12323399573632E-17,1.06057523872493E-16,-1.));
#21423=DIRECTION('center_axis',(0.,0.,-1.));
#21424=DIRECTION('ref_axis',(-0.499999999999964,0.86602540378446,0.));
#21425=DIRECTION('',(-6.12323399573632E-17,1.06057523872493E-16,-1.));
#21426=DIRECTION('center_axis',(0.,0.,-1.));
#21427=DIRECTION('ref_axis',(-0.499999999999964,0.86602540378446,0.));
#21428=DIRECTION('',(-6.12323399573632E-17,1.06057523872493E-16,-1.));
#21429=DIRECTION('center_axis',(0.,0.,-1.));
#21430=DIRECTION('ref_axis',(-0.499999999999964,0.86602540378446,0.));
#21431=DIRECTION('',(-6.12323399573632E-17,1.06057523872493E-16,-1.));
#21432=DIRECTION('center_axis',(0.,0.,-1.));
#21433=DIRECTION('ref_axis',(-0.499999999999964,0.86602540378446,0.));
#21434=DIRECTION('',(-6.12323399573632E-17,1.06057523872493E-16,-1.));
#21435=DIRECTION('center_axis',(0.,0.,-1.));
#21436=DIRECTION('ref_axis',(-0.499999999999964,0.86602540378446,0.));
#21437=DIRECTION('',(-6.12323399573632E-17,1.06057523872493E-16,-1.));
#21438=DIRECTION('center_axis',(0.,0.,-1.));
#21439=DIRECTION('ref_axis',(0.991392525759238,-0.130923106702819,0.));
#21440=DIRECTION('',(-6.12323399573632E-17,1.06057523872493E-16,-1.));
#21441=DIRECTION('center_axis',(0.,0.,-1.));
#21442=DIRECTION('ref_axis',(-0.499999999999964,0.86602540378446,0.));
#21443=DIRECTION('center_axis',(0.,0.,-1.));
#21444=DIRECTION('ref_axis',(-1.,9.25185853854297E-17,0.));
#21445=DIRECTION('',(0.,0.,-1.));
#21446=DIRECTION('center_axis',(0.,0.,1.));
#21447=DIRECTION('ref_axis',(-1.,9.25185853854297E-17,0.));
#21448=DIRECTION('',(0.,0.,-1.));
#21449=DIRECTION('center_axis',(0.,0.,1.));
#21450=DIRECTION('ref_axis',(-1.,9.25185853854297E-17,0.));
#21451=DIRECTION('center_axis',(0.,0.,1.));
#21452=DIRECTION('ref_axis',(-1.,9.25185853854297E-17,0.));
#21453=DIRECTION('center_axis',(0.,0.,1.));
#21454=DIRECTION('ref_axis',(-1.,9.25185853854297E-17,0.));
#21455=DIRECTION('center_axis',(0.,0.,1.));
#21456=DIRECTION('ref_axis',(-1.,9.25185853854297E-17,0.));
#21457=DIRECTION('center_axis',(0.,0.,-1.));
#21458=DIRECTION('ref_axis',(-1.,9.25185853854297E-17,0.));
#21459=DIRECTION('',(0.,0.,-1.));
#21460=DIRECTION('center_axis',(0.,0.,-1.));
#21461=DIRECTION('ref_axis',(-1.,9.25185853854297E-17,0.));
#21462=DIRECTION('',(0.,0.,-1.));
#21463=DIRECTION('center_axis',(0.,0.,-1.));
#21464=DIRECTION('ref_axis',(-1.,9.25185853854297E-17,0.));
#21465=DIRECTION('',(0.,0.,-1.));
#21466=DIRECTION('center_axis',(0.,0.,-1.));
#21467=DIRECTION('ref_axis',(-1.,9.25185853854297E-17,0.));
#21468=DIRECTION('',(0.,0.,-1.));
#21469=DIRECTION('center_axis',(0.,0.,-1.));
#21470=DIRECTION('ref_axis',(-1.,9.25185853854297E-17,0.));
#21471=DIRECTION('',(0.,0.,-1.));
#21472=DIRECTION('center_axis',(0.,0.,-1.));
#21473=DIRECTION('ref_axis',(-1.,9.25185853854297E-17,0.));
#21474=DIRECTION('',(0.,0.,-1.));
#21475=DIRECTION('center_axis',(0.,0.,-1.));
#21476=DIRECTION('ref_axis',(-0.937375356024962,0.348320889291865,0.));
#21477=DIRECTION('',(0.,0.,-1.));
#21478=DIRECTION('center_axis',(0.,0.,1.));
#21479=DIRECTION('ref_axis',(-1.,9.25185853854297E-17,0.));
#21480=DIRECTION('center_axis',(0.,0.,-1.));
#21481=DIRECTION('ref_axis',(-0.793245518852988,-0.608901918883209,0.));
#21482=DIRECTION('',(-1.22464679914735E-16,2.65847991820293E-30,-1.));
#21483=DIRECTION('center_axis',(0.,0.,1.));
#21484=DIRECTION('ref_axis',(-1.,2.15856712500029E-14,0.));
#21485=DIRECTION('center_axis',(0.,0.,-1.));
#21486=DIRECTION('ref_axis',(-1.,2.15856712500029E-14,0.));
#21487=DIRECTION('',(-1.22464679914735E-16,2.65847991820293E-30,-1.));
#21488=DIRECTION('center_axis',(0.,0.,-1.));
#21489=DIRECTION('ref_axis',(-1.,2.15856712500029E-14,0.));
#21490=DIRECTION('',(-1.22464679914735E-16,2.65847991820293E-30,-1.));
#21491=DIRECTION('center_axis',(0.,0.,-1.));
#21492=DIRECTION('ref_axis',(-1.,2.15856712500029E-14,0.));
#21493=DIRECTION('',(-1.22464679914735E-16,2.65847991820293E-30,-1.));
#21494=DIRECTION('center_axis',(0.,0.,-1.));
#21495=DIRECTION('ref_axis',(-1.,2.15856712500029E-14,0.));
#21496=DIRECTION('',(-1.22464679914735E-16,2.65847991820293E-30,-1.));
#21497=DIRECTION('center_axis',(0.,0.,-1.));
#21498=DIRECTION('ref_axis',(-1.,2.15856712500029E-14,0.));
#21499=DIRECTION('',(-1.22464679914735E-16,2.65847991820293E-30,-1.));
#21500=DIRECTION('center_axis',(0.,0.,-1.));
#21501=DIRECTION('ref_axis',(-1.,2.15856712500029E-14,0.));
#21502=DIRECTION('',(-1.22464679914735E-16,2.65847991820293E-30,-1.));
#21503=DIRECTION('center_axis',(0.,0.,-1.));
#21504=DIRECTION('ref_axis',(0.609079509840783,0.793109166944949,0.));
#21505=DIRECTION('',(-1.22464679914735E-16,2.65847991820293E-30,-1.));
#21506=DIRECTION('center_axis',(0.,0.,-1.));
#21507=DIRECTION('ref_axis',(-1.,2.15856712500029E-14,0.));
#21508=DIRECTION('center_axis',(0.,0.,-1.));
#21509=DIRECTION('ref_axis',(-0.5,-0.866025403784438,0.));
#21510=DIRECTION('',(0.,0.,-1.));
#21511=DIRECTION('center_axis',(0.,0.,1.));
#21512=DIRECTION('ref_axis',(-0.5,-0.866025403784438,0.));
#21513=DIRECTION('',(0.,0.,-1.));
#21514=DIRECTION('center_axis',(0.,0.,1.));
#21515=DIRECTION('ref_axis',(-0.5,-0.866025403784438,0.));
#21516=DIRECTION('center_axis',(0.,0.,1.));
#21517=DIRECTION('ref_axis',(-0.5,-0.866025403784438,0.));
#21518=DIRECTION('center_axis',(0.,0.,1.));
#21519=DIRECTION('ref_axis',(-0.5,-0.866025403784438,0.));
#21520=DIRECTION('center_axis',(0.,0.,1.));
#21521=DIRECTION('ref_axis',(-0.5,-0.866025403784438,0.));
#21522=DIRECTION('center_axis',(0.,0.,-1.));
#21523=DIRECTION('ref_axis',(-0.5,-0.866025403784438,0.));
#21524=DIRECTION('',(0.,0.,-1.));
#21525=DIRECTION('center_axis',(0.,0.,-1.));
#21526=DIRECTION('ref_axis',(-0.5,-0.866025403784438,0.));
#21527=DIRECTION('',(0.,0.,-1.));
#21528=DIRECTION('center_axis',(0.,0.,-1.));
#21529=DIRECTION('ref_axis',(-0.5,-0.866025403784438,0.));
#21530=DIRECTION('',(0.,0.,-1.));
#21531=DIRECTION('center_axis',(0.,0.,-1.));
#21532=DIRECTION('ref_axis',(-0.5,-0.866025403784438,0.));
#21533=DIRECTION('',(0.,0.,-1.));
#21534=DIRECTION('center_axis',(0.,0.,-1.));
#21535=DIRECTION('ref_axis',(-0.5,-0.866025403784438,0.));
#21536=DIRECTION('',(0.,0.,-1.));
#21537=DIRECTION('center_axis',(0.,0.,-1.));
#21538=DIRECTION('ref_axis',(-0.5,-0.866025403784438,0.));
#21539=DIRECTION('',(0.,0.,-1.));
#21540=DIRECTION('center_axis',(0.,0.,-1.));
#21541=DIRECTION('ref_axis',(-0.770342439795701,-0.637630398780992,0.));
#21542=DIRECTION('',(0.,0.,-1.));
#21543=DIRECTION('center_axis',(0.,0.,1.));
#21544=DIRECTION('ref_axis',(-0.5,-0.866025403784438,0.));
#21545=DIRECTION('center_axis',(0.,0.,-1.));
#21546=DIRECTION('ref_axis',(0.130701796389773,-0.99142172682491,0.));
#21547=DIRECTION('',(-6.12323399573712E-17,-1.06057523872489E-16,-1.));
#21548=DIRECTION('center_axis',(0.,0.,1.));
#21549=DIRECTION('ref_axis',(-0.500000000000029,-0.866025403784422,0.));
#21550=DIRECTION('center_axis',(0.,0.,-1.));
#21551=DIRECTION('ref_axis',(-0.500000000000029,-0.866025403784422,0.));
#21552=DIRECTION('',(-6.12323399573712E-17,-1.06057523872489E-16,-1.));
#21553=DIRECTION('center_axis',(0.,0.,-1.));
#21554=DIRECTION('ref_axis',(-0.500000000000029,-0.866025403784422,0.));
#21555=DIRECTION('',(-6.12323399573712E-17,-1.06057523872489E-16,-1.));
#21556=DIRECTION('center_axis',(0.,0.,-1.));
#21557=DIRECTION('ref_axis',(-0.500000000000029,-0.866025403784422,0.));
#21558=DIRECTION('',(-6.12323399573712E-17,-1.06057523872489E-16,-1.));
#21559=DIRECTION('center_axis',(0.,0.,-1.));
#21560=DIRECTION('ref_axis',(-0.500000000000029,-0.866025403784422,0.));
#21561=DIRECTION('',(-6.12323399573712E-17,-1.06057523872489E-16,-1.));
#21562=DIRECTION('center_axis',(0.,0.,-1.));
#21563=DIRECTION('ref_axis',(-0.500000000000029,-0.866025403784422,0.));
#21564=DIRECTION('',(-6.12323399573712E-17,-1.06057523872489E-16,-1.));
#21565=DIRECTION('center_axis',(0.,0.,-1.));
#21566=DIRECTION('ref_axis',(-0.500000000000029,-0.866025403784422,0.));
#21567=DIRECTION('',(-6.12323399573712E-17,-1.06057523872489E-16,-1.));
#21568=DIRECTION('center_axis',(0.,0.,-1.));
#21569=DIRECTION('ref_axis',(-0.382312913538216,0.924032919403806,0.));
#21570=DIRECTION('',(-6.12323399573712E-17,-1.06057523872489E-16,-1.));
#21571=DIRECTION('center_axis',(0.,0.,-1.));
#21572=DIRECTION('ref_axis',(-0.500000000000029,-0.866025403784422,0.));
#21573=DIRECTION('center_axis',(0.,0.,-1.));
#21574=DIRECTION('ref_axis',(0.499999999999999,-0.866025403784439,0.));
#21575=DIRECTION('',(0.,0.,-1.));
#21576=DIRECTION('center_axis',(0.,0.,1.));
#21577=DIRECTION('ref_axis',(0.499999999999999,-0.866025403784439,0.));
#21578=DIRECTION('',(0.,0.,-1.));
#21579=DIRECTION('center_axis',(0.,0.,1.));
#21580=DIRECTION('ref_axis',(0.499999999999999,-0.866025403784439,0.));
#21581=DIRECTION('center_axis',(0.,0.,1.));
#21582=DIRECTION('ref_axis',(0.499999999999999,-0.866025403784439,0.));
#21583=DIRECTION('center_axis',(0.,0.,1.));
#21584=DIRECTION('ref_axis',(0.499999999999999,-0.866025403784439,0.));
#21585=DIRECTION('center_axis',(0.,0.,1.));
#21586=DIRECTION('ref_axis',(0.499999999999999,-0.866025403784439,0.));
#21587=DIRECTION('center_axis',(0.,0.,-1.));
#21588=DIRECTION('ref_axis',(0.499999999999999,-0.866025403784439,0.));
#21589=DIRECTION('',(0.,0.,-1.));
#21590=DIRECTION('center_axis',(0.,0.,-1.));
#21591=DIRECTION('ref_axis',(0.499999999999999,-0.866025403784439,0.));
#21592=DIRECTION('',(0.,0.,-1.));
#21593=DIRECTION('center_axis',(0.,0.,-1.));
#21594=DIRECTION('ref_axis',(0.499999999999999,-0.866025403784439,0.));
#21595=DIRECTION('',(0.,0.,-1.));
#21596=DIRECTION('center_axis',(0.,0.,-1.));
#21597=DIRECTION('ref_axis',(0.499999999999999,-0.866025403784439,0.));
#21598=DIRECTION('',(0.,0.,-1.));
#21599=DIRECTION('center_axis',(0.,0.,-1.));
#21600=DIRECTION('ref_axis',(0.499999999999999,-0.866025403784439,0.));
#21601=DIRECTION('',(0.,0.,-1.));
#21602=DIRECTION('center_axis',(0.,0.,-1.));
#21603=DIRECTION('ref_axis',(0.499999999999999,-0.866025403784439,0.));
#21604=DIRECTION('',(0.,0.,-1.));
#21605=DIRECTION('center_axis',(0.,0.,-1.));
#21606=DIRECTION('ref_axis',(0.167034001011813,-0.985951135962623,0.));
#21607=DIRECTION('',(0.,0.,-1.));
#21608=DIRECTION('center_axis',(0.,0.,1.));
#21609=DIRECTION('ref_axis',(0.499999999999999,-0.866025403784439,0.));
#21610=DIRECTION('center_axis',(0.,0.,-1.));
#21611=DIRECTION('ref_axis',(0.923947020235649,-0.382520461933299,0.));
#21612=DIRECTION('',(6.12323399573637E-17,-1.06057523872493E-16,-1.));
#21613=DIRECTION('center_axis',(0.,0.,1.));
#21614=DIRECTION('ref_axis',(0.499999999999968,-0.866025403784457,0.));
#21615=DIRECTION('center_axis',(0.,0.,-1.));
#21616=DIRECTION('ref_axis',(0.499999999999968,-0.866025403784457,0.));
#21617=DIRECTION('',(6.12323399573637E-17,-1.06057523872493E-16,-1.));
#21618=DIRECTION('center_axis',(0.,0.,-1.));
#21619=DIRECTION('ref_axis',(0.499999999999968,-0.866025403784457,0.));
#21620=DIRECTION('',(6.12323399573637E-17,-1.06057523872493E-16,-1.));
#21621=DIRECTION('center_axis',(0.,0.,-1.));
#21622=DIRECTION('ref_axis',(0.499999999999968,-0.866025403784457,0.));
#21623=DIRECTION('',(6.12323399573637E-17,-1.06057523872493E-16,-1.));
#21624=DIRECTION('center_axis',(0.,0.,-1.));
#21625=DIRECTION('ref_axis',(0.499999999999968,-0.866025403784457,0.));
#21626=DIRECTION('',(6.12323399573637E-17,-1.06057523872493E-16,-1.));
#21627=DIRECTION('center_axis',(0.,0.,-1.));
#21628=DIRECTION('ref_axis',(0.499999999999968,-0.866025403784457,0.));
#21629=DIRECTION('',(6.12323399573637E-17,-1.06057523872493E-16,-1.));
#21630=DIRECTION('center_axis',(0.,0.,-1.));
#21631=DIRECTION('ref_axis',(0.499999999999968,-0.866025403784457,0.));
#21632=DIRECTION('',(6.12323399573637E-17,-1.06057523872493E-16,-1.));
#21633=DIRECTION('center_axis',(0.,0.,-1.));
#21634=DIRECTION('ref_axis',(-0.99139252575924,0.130923106702811,0.));
#21635=DIRECTION('',(6.12323399573637E-17,-1.06057523872493E-16,-1.));
#21636=DIRECTION('center_axis',(0.,0.,-1.));
#21637=DIRECTION('ref_axis',(0.499999999999968,-0.866025403784457,0.));
#21638=DIRECTION('center_axis',(0.,0.,1.));
#21639=DIRECTION('ref_axis',(-0.5,-0.866025403784439,0.));
#21640=DIRECTION('',(0.,0.,1.));
#21641=DIRECTION('center_axis',(0.,0.,-1.));
#21642=DIRECTION('ref_axis',(-0.5,-0.866025403784439,0.));
#21643=DIRECTION('',(0.,0.,1.));
#21644=DIRECTION('center_axis',(0.,0.,-1.));
#21645=DIRECTION('ref_axis',(-0.5,-0.866025403784439,0.));
#21646=DIRECTION('center_axis',(0.,0.,-1.));
#21647=DIRECTION('ref_axis',(-0.5,-0.866025403784439,0.));
#21648=DIRECTION('center_axis',(0.,0.,-1.));
#21649=DIRECTION('ref_axis',(-0.5,-0.866025403784439,0.));
#21650=DIRECTION('center_axis',(0.,0.,-1.));
#21651=DIRECTION('ref_axis',(-0.5,-0.866025403784439,0.));
#21652=DIRECTION('center_axis',(0.,0.,1.));
#21653=DIRECTION('ref_axis',(-0.5,-0.866025403784439,0.));
#21654=DIRECTION('',(0.,0.,1.));
#21655=DIRECTION('center_axis',(0.,0.,1.));
#21656=DIRECTION('ref_axis',(-0.5,-0.866025403784439,0.));
#21657=DIRECTION('',(0.,0.,1.));
#21658=DIRECTION('center_axis',(0.,0.,1.));
#21659=DIRECTION('ref_axis',(-0.5,-0.866025403784439,0.));
#21660=DIRECTION('',(0.,0.,1.));
#21661=DIRECTION('center_axis',(0.,0.,1.));
#21662=DIRECTION('ref_axis',(-0.5,-0.866025403784439,0.));
#21663=DIRECTION('',(0.,0.,1.));
#21664=DIRECTION('center_axis',(0.,0.,1.));
#21665=DIRECTION('ref_axis',(-0.5,-0.866025403784439,0.));
#21666=DIRECTION('',(0.,0.,1.));
#21667=DIRECTION('center_axis',(0.,0.,1.));
#21668=DIRECTION('ref_axis',(-0.5,-0.866025403784439,0.));
#21669=DIRECTION('',(0.,0.,1.));
#21670=DIRECTION('center_axis',(0.,0.,1.));
#21671=DIRECTION('ref_axis',(-0.167031392512161,-0.985951577875632,0.));
#21672=DIRECTION('',(0.,0.,1.));
#21673=DIRECTION('center_axis',(0.,0.,-1.));
#21674=DIRECTION('ref_axis',(-0.5,-0.866025403784439,0.));
#21675=DIRECTION('center_axis',(0.,0.,1.));
#21676=DIRECTION('ref_axis',(-0.923947690185482,-0.382518843720034,0.));
#21677=DIRECTION('',(-6.12323399573653E-17,-1.06057523872492E-16,1.));
#21678=DIRECTION('center_axis',(0.,0.,-1.));
#21679=DIRECTION('ref_axis',(-0.499999999999981,-0.86602540378445,0.));
#21680=DIRECTION('center_axis',(0.,0.,1.));
#21681=DIRECTION('ref_axis',(-0.499999999999981,-0.86602540378445,0.));
#21682=DIRECTION('',(-6.12323399573653E-17,-1.06057523872492E-16,1.));
#21683=DIRECTION('center_axis',(0.,0.,1.));
#21684=DIRECTION('ref_axis',(-0.499999999999981,-0.86602540378445,0.));
#21685=DIRECTION('',(-6.12323399573653E-17,-1.06057523872492E-16,1.));
#21686=DIRECTION('center_axis',(0.,0.,1.));
#21687=DIRECTION('ref_axis',(-0.499999999999981,-0.86602540378445,0.));
#21688=DIRECTION('',(-6.12323399573653E-17,-1.06057523872492E-16,1.));
#21689=DIRECTION('center_axis',(0.,0.,1.));
#21690=DIRECTION('ref_axis',(-0.499999999999981,-0.86602540378445,0.));
#21691=DIRECTION('',(-6.12323399573653E-17,-1.06057523872492E-16,1.));
#21692=DIRECTION('center_axis',(0.,0.,1.));
#21693=DIRECTION('ref_axis',(-0.499999999999981,-0.86602540378445,0.));
#21694=DIRECTION('',(-6.12323399573653E-17,-1.06057523872492E-16,1.));
#21695=DIRECTION('center_axis',(0.,0.,1.));
#21696=DIRECTION('ref_axis',(-0.499999999999981,-0.86602540378445,0.));
#21697=DIRECTION('',(-6.12323399573653E-17,-1.06057523872492E-16,1.));
#21698=DIRECTION('center_axis',(0.,0.,1.));
#21699=DIRECTION('ref_axis',(0.99139229699987,0.130924838931818,0.));
#21700=DIRECTION('',(-6.12323399573653E-17,-1.06057523872492E-16,1.));
#21701=DIRECTION('center_axis',(0.,0.,1.));
#21702=DIRECTION('ref_axis',(-0.499999999999981,-0.86602540378445,0.));
#21703=DIRECTION('center_axis',(0.,0.,1.));
#21704=DIRECTION('ref_axis',(0.5,-0.866025403784439,0.));
#21705=DIRECTION('',(0.,0.,1.));
#21706=DIRECTION('center_axis',(0.,0.,-1.));
#21707=DIRECTION('ref_axis',(0.5,-0.866025403784439,0.));
#21708=DIRECTION('',(0.,0.,1.));
#21709=DIRECTION('center_axis',(0.,0.,-1.));
#21710=DIRECTION('ref_axis',(0.5,-0.866025403784439,0.));
#21711=DIRECTION('center_axis',(0.,0.,-1.));
#21712=DIRECTION('ref_axis',(0.5,-0.866025403784439,0.));
#21713=DIRECTION('center_axis',(0.,0.,-1.));
#21714=DIRECTION('ref_axis',(0.5,-0.866025403784439,0.));
#21715=DIRECTION('center_axis',(0.,0.,-1.));
#21716=DIRECTION('ref_axis',(0.5,-0.866025403784439,0.));
#21717=DIRECTION('center_axis',(0.,0.,1.));
#21718=DIRECTION('ref_axis',(0.5,-0.866025403784439,0.));
#21719=DIRECTION('',(0.,0.,1.));
#21720=DIRECTION('center_axis',(0.,0.,1.));
#21721=DIRECTION('ref_axis',(0.5,-0.866025403784439,0.));
#21722=DIRECTION('',(0.,0.,1.));
#21723=DIRECTION('center_axis',(0.,0.,1.));
#21724=DIRECTION('ref_axis',(0.5,-0.866025403784439,0.));
#21725=DIRECTION('',(0.,0.,1.));
#21726=DIRECTION('center_axis',(0.,0.,1.));
#21727=DIRECTION('ref_axis',(0.5,-0.866025403784439,0.));
#21728=DIRECTION('',(0.,0.,1.));
#21729=DIRECTION('center_axis',(0.,0.,1.));
#21730=DIRECTION('ref_axis',(0.5,-0.866025403784439,0.));
#21731=DIRECTION('',(0.,0.,1.));
#21732=DIRECTION('center_axis',(0.,0.,1.));
#21733=DIRECTION('ref_axis',(0.5,-0.866025403784439,0.));
#21734=DIRECTION('',(0.,0.,1.));
#21735=DIRECTION('center_axis',(0.,0.,1.));
#21736=DIRECTION('ref_axis',(0.770342508707589,-0.637630315526244,0.));
#21737=DIRECTION('',(0.,0.,1.));
#21738=DIRECTION('center_axis',(0.,0.,-1.));
#21739=DIRECTION('ref_axis',(0.5,-0.866025403784439,0.));
#21740=DIRECTION('center_axis',(0.,0.,1.));
#21741=DIRECTION('ref_axis',(-0.130701828608467,-0.991421722577432,0.));
#21742=DIRECTION('',(6.12323399573711E-17,-1.06057523872489E-16,1.));
#21743=DIRECTION('center_axis',(0.,0.,-1.));
#21744=DIRECTION('ref_axis',(0.500000000000028,-0.866025403784423,0.));
#21745=DIRECTION('center_axis',(0.,0.,1.));
#21746=DIRECTION('ref_axis',(0.500000000000028,-0.866025403784422,0.));
#21747=DIRECTION('',(6.12323399573711E-17,-1.06057523872489E-16,1.));
#21748=DIRECTION('center_axis',(0.,0.,1.));
#21749=DIRECTION('ref_axis',(0.500000000000028,-0.866025403784422,0.));
#21750=DIRECTION('',(6.12323399573711E-17,-1.06057523872489E-16,1.));
#21751=DIRECTION('center_axis',(0.,0.,1.));
#21752=DIRECTION('ref_axis',(0.500000000000028,-0.866025403784422,0.));
#21753=DIRECTION('',(6.12323399573711E-17,-1.06057523872489E-16,1.));
#21754=DIRECTION('center_axis',(0.,0.,1.));
#21755=DIRECTION('ref_axis',(0.500000000000028,-0.866025403784422,0.));
#21756=DIRECTION('',(6.12323399573711E-17,-1.06057523872489E-16,1.));
#21757=DIRECTION('center_axis',(0.,0.,1.));
#21758=DIRECTION('ref_axis',(0.500000000000028,-0.866025403784422,0.));
#21759=DIRECTION('',(6.12323399573711E-17,-1.06057523872489E-16,1.));
#21760=DIRECTION('center_axis',(0.,0.,1.));
#21761=DIRECTION('ref_axis',(0.500000000000028,-0.866025403784422,0.));
#21762=DIRECTION('',(6.12323399573711E-17,-1.06057523872489E-16,1.));
#21763=DIRECTION('center_axis',(0.,0.,1.));
#21764=DIRECTION('ref_axis',(0.382312780236439,0.924032974556582,0.));
#21765=DIRECTION('',(6.12323399573711E-17,-1.06057523872489E-16,1.));
#21766=DIRECTION('center_axis',(0.,0.,1.));
#21767=DIRECTION('ref_axis',(0.500000000000028,-0.866025403784422,0.));
#21768=DIRECTION('center_axis',(0.,0.,1.));
#21769=DIRECTION('ref_axis',(1.,-9.25185853854297E-17,0.));
#21770=DIRECTION('',(0.,0.,1.));
#21771=DIRECTION('center_axis',(0.,0.,-1.));
#21772=DIRECTION('ref_axis',(1.,-9.25185853854297E-17,0.));
#21773=DIRECTION('',(0.,0.,1.));
#21774=DIRECTION('center_axis',(0.,0.,-1.));
#21775=DIRECTION('ref_axis',(1.,-9.25185853854297E-17,0.));
#21776=DIRECTION('center_axis',(0.,0.,-1.));
#21777=DIRECTION('ref_axis',(1.,-9.25185853854297E-17,0.));
#21778=DIRECTION('center_axis',(0.,0.,-1.));
#21779=DIRECTION('ref_axis',(1.,-9.25185853854297E-17,0.));
#21780=DIRECTION('center_axis',(0.,0.,-1.));
#21781=DIRECTION('ref_axis',(1.,-9.25185853854297E-17,0.));
#21782=DIRECTION('center_axis',(0.,0.,1.));
#21783=DIRECTION('ref_axis',(1.,-9.25185853854297E-17,0.));
#21784=DIRECTION('',(0.,0.,1.));
#21785=DIRECTION('center_axis',(0.,0.,1.));
#21786=DIRECTION('ref_axis',(1.,-9.25185853854297E-17,0.));
#21787=DIRECTION('',(0.,0.,1.));
#21788=DIRECTION('center_axis',(0.,0.,1.));
#21789=DIRECTION('ref_axis',(1.,-9.25185853854297E-17,0.));
#21790=DIRECTION('',(0.,0.,1.));
#21791=DIRECTION('center_axis',(0.,0.,1.));
#21792=DIRECTION('ref_axis',(1.,-9.25185853854297E-17,0.));
#21793=DIRECTION('',(0.,0.,1.));
#21794=DIRECTION('center_axis',(0.,0.,1.));
#21795=DIRECTION('ref_axis',(1.,-9.25185853854297E-17,0.));
#21796=DIRECTION('',(0.,0.,1.));
#21797=DIRECTION('center_axis',(0.,0.,1.));
#21798=DIRECTION('ref_axis',(1.,-9.25185853854297E-17,0.));
#21799=DIRECTION('',(0.,0.,1.));
#21800=DIRECTION('center_axis',(0.,0.,1.));
#21801=DIRECTION('ref_axis',(0.937374823573167,0.34832232218331,0.));
#21802=DIRECTION('',(0.,0.,1.));
#21803=DIRECTION('center_axis',(0.,0.,-1.));
#21804=DIRECTION('ref_axis',(1.,-9.25185853854297E-17,0.));
#21805=DIRECTION('center_axis',(0.,0.,1.));
#21806=DIRECTION('ref_axis',(0.793244897475736,-0.608902728380083,0.));
#21807=DIRECTION('',(1.22464679914735E-16,3.89210500104523E-30,1.));
#21808=DIRECTION('center_axis',(0.,0.,-1.));
#21809=DIRECTION('ref_axis',(1.,3.16589845000044E-14,0.));
#21810=DIRECTION('center_axis',(0.,0.,1.));
#21811=DIRECTION('ref_axis',(1.,3.16589845000044E-14,0.));
#21812=DIRECTION('',(1.22464679914735E-16,3.89210500104523E-30,1.));
#21813=DIRECTION('center_axis',(0.,0.,1.));
#21814=DIRECTION('ref_axis',(1.,3.16589845000044E-14,0.));
#21815=DIRECTION('',(1.22464679914735E-16,3.89210500104523E-30,1.));
#21816=DIRECTION('center_axis',(0.,0.,1.));
#21817=DIRECTION('ref_axis',(1.,3.16589845000044E-14,0.));
#21818=DIRECTION('',(1.22464679914735E-16,3.89210500104523E-30,1.));
#21819=DIRECTION('center_axis',(0.,0.,1.));
#21820=DIRECTION('ref_axis',(1.,3.16589845000044E-14,0.));
#21821=DIRECTION('',(1.22464679914735E-16,3.89210500104523E-30,1.));
#21822=DIRECTION('center_axis',(0.,0.,1.));
#21823=DIRECTION('ref_axis',(1.,3.16589845000044E-14,0.));
#21824=DIRECTION('',(1.22464679914735E-16,3.89210500104523E-30,1.));
#21825=DIRECTION('center_axis',(0.,0.,1.));
#21826=DIRECTION('ref_axis',(1.,3.16589845000044E-14,0.));
#21827=DIRECTION('',(1.22464679914735E-16,3.89210500104523E-30,1.));
#21828=DIRECTION('center_axis',(0.,0.,1.));
#21829=DIRECTION('ref_axis',(-0.609080360598175,0.793108513592936,0.));
#21830=DIRECTION('',(1.22464679914735E-16,3.89210500104523E-30,1.));
#21831=DIRECTION('center_axis',(0.,0.,1.));
#21832=DIRECTION('ref_axis',(1.,3.16589845000044E-14,0.));
#21833=DIRECTION('center_axis',(0.,0.,1.));
#21834=DIRECTION('ref_axis',(0.5,0.866025403784438,0.));
#21835=DIRECTION('',(0.,0.,1.));
#21836=DIRECTION('center_axis',(0.,0.,-1.));
#21837=DIRECTION('ref_axis',(0.5,0.866025403784438,0.));
#21838=DIRECTION('',(0.,0.,1.));
#21839=DIRECTION('center_axis',(0.,0.,-1.));
#21840=DIRECTION('ref_axis',(0.5,0.866025403784438,0.));
#21841=DIRECTION('center_axis',(0.,0.,-1.));
#21842=DIRECTION('ref_axis',(0.5,0.866025403784438,0.));
#21843=DIRECTION('center_axis',(0.,0.,-1.));
#21844=DIRECTION('ref_axis',(0.5,0.866025403784438,0.));
#21845=DIRECTION('center_axis',(0.,0.,-1.));
#21846=DIRECTION('ref_axis',(0.5,0.866025403784438,0.));
#21847=DIRECTION('center_axis',(0.,0.,1.));
#21848=DIRECTION('ref_axis',(0.5,0.866025403784438,0.));
#21849=DIRECTION('',(0.,0.,1.));
#21850=DIRECTION('center_axis',(0.,0.,1.));
#21851=DIRECTION('ref_axis',(0.5,0.866025403784438,0.));
#21852=DIRECTION('',(0.,0.,1.));
#21853=DIRECTION('center_axis',(0.,0.,1.));
#21854=DIRECTION('ref_axis',(0.5,0.866025403784438,0.));
#21855=DIRECTION('',(0.,0.,1.));
#21856=DIRECTION('center_axis',(0.,0.,1.));
#21857=DIRECTION('ref_axis',(0.5,0.866025403784438,0.));
#21858=DIRECTION('',(0.,0.,1.));
#21859=DIRECTION('center_axis',(0.,0.,1.));
#21860=DIRECTION('ref_axis',(0.5,0.866025403784438,0.));
#21861=DIRECTION('',(0.,0.,1.));
#21862=DIRECTION('center_axis',(0.,0.,1.));
#21863=DIRECTION('ref_axis',(0.5,0.866025403784438,0.));
#21864=DIRECTION('',(0.,0.,1.));
#21865=DIRECTION('center_axis',(0.,0.,1.));
#21866=DIRECTION('ref_axis',(0.167031392512228,0.98595157787562,0.));
#21867=DIRECTION('',(0.,0.,1.));
#21868=DIRECTION('center_axis',(0.,0.,-1.));
#21869=DIRECTION('ref_axis',(0.5,0.866025403784438,0.));
#21870=DIRECTION('center_axis',(0.,0.,1.));
#21871=DIRECTION('ref_axis',(0.923947690185483,0.382518843720034,0.));
#21872=DIRECTION('',(6.12323399573657E-17,1.06057523872492E-16,1.));
#21873=DIRECTION('center_axis',(0.,0.,-1.));
#21874=DIRECTION('ref_axis',(0.499999999999984,0.866025403784448,0.));
#21875=DIRECTION('center_axis',(0.,0.,1.));
#21876=DIRECTION('ref_axis',(0.499999999999984,0.866025403784448,0.));
#21877=DIRECTION('',(6.12323399573657E-17,1.06057523872492E-16,1.));
#21878=DIRECTION('center_axis',(0.,0.,1.));
#21879=DIRECTION('ref_axis',(0.499999999999984,0.866025403784448,0.));
#21880=DIRECTION('',(6.12323399573657E-17,1.06057523872492E-16,1.));
#21881=DIRECTION('center_axis',(0.,0.,1.));
#21882=DIRECTION('ref_axis',(0.499999999999984,0.866025403784448,0.));
#21883=DIRECTION('',(6.12323399573657E-17,1.06057523872492E-16,1.));
#21884=DIRECTION('center_axis',(0.,0.,1.));
#21885=DIRECTION('ref_axis',(0.499999999999984,0.866025403784448,0.));
#21886=DIRECTION('',(6.12323399573657E-17,1.06057523872492E-16,1.));
#21887=DIRECTION('center_axis',(0.,0.,1.));
#21888=DIRECTION('ref_axis',(0.499999999999984,0.866025403784448,0.));
#21889=DIRECTION('',(6.12323399573657E-17,1.06057523872492E-16,1.));
#21890=DIRECTION('center_axis',(0.,0.,1.));
#21891=DIRECTION('ref_axis',(0.499999999999984,0.866025403784448,0.));
#21892=DIRECTION('',(6.12323399573657E-17,1.06057523872492E-16,1.));
#21893=DIRECTION('center_axis',(0.,0.,1.));
#21894=DIRECTION('ref_axis',(-0.991392296999871,-0.130924838931808,0.));
#21895=DIRECTION('',(6.12323399573657E-17,1.06057523872492E-16,1.));
#21896=DIRECTION('center_axis',(0.,0.,1.));
#21897=DIRECTION('ref_axis',(0.499999999999984,0.866025403784448,0.));
#21898=DIRECTION('center_axis',(0.,0.,1.));
#21899=DIRECTION('ref_axis',(-0.499999999999999,0.866025403784439,0.));
#21900=DIRECTION('',(0.,0.,1.));
#21901=DIRECTION('center_axis',(0.,0.,-1.));
#21902=DIRECTION('ref_axis',(-0.499999999999999,0.866025403784439,0.));
#21903=DIRECTION('',(0.,0.,1.));
#21904=DIRECTION('center_axis',(0.,0.,-1.));
#21905=DIRECTION('ref_axis',(-0.499999999999999,0.866025403784439,0.));
#21906=DIRECTION('center_axis',(0.,0.,-1.));
#21907=DIRECTION('ref_axis',(-0.499999999999999,0.866025403784439,0.));
#21908=DIRECTION('center_axis',(0.,0.,-1.));
#21909=DIRECTION('ref_axis',(-0.499999999999999,0.866025403784439,0.));
#21910=DIRECTION('center_axis',(0.,0.,-1.));
#21911=DIRECTION('ref_axis',(-0.499999999999999,0.866025403784439,0.));
#21912=DIRECTION('center_axis',(0.,0.,1.));
#21913=DIRECTION('ref_axis',(-0.499999999999999,0.866025403784439,0.));
#21914=DIRECTION('',(0.,0.,1.));
#21915=DIRECTION('center_axis',(0.,0.,1.));
#21916=DIRECTION('ref_axis',(-0.499999999999999,0.866025403784439,0.));
#21917=DIRECTION('',(0.,0.,1.));
#21918=DIRECTION('center_axis',(0.,0.,1.));
#21919=DIRECTION('ref_axis',(-0.499999999999999,0.866025403784439,0.));
#21920=DIRECTION('',(0.,0.,1.));
#21921=DIRECTION('center_axis',(0.,0.,1.));
#21922=DIRECTION('ref_axis',(-0.499999999999999,0.866025403784439,0.));
#21923=DIRECTION('',(0.,0.,1.));
#21924=DIRECTION('center_axis',(0.,0.,1.));
#21925=DIRECTION('ref_axis',(-0.499999999999999,0.866025403784439,0.));
#21926=DIRECTION('',(0.,0.,1.));
#21927=DIRECTION('center_axis',(0.,0.,1.));
#21928=DIRECTION('ref_axis',(-0.499999999999999,0.866025403784439,0.));
#21929=DIRECTION('',(0.,0.,1.));
#21930=DIRECTION('center_axis',(0.,0.,1.));
#21931=DIRECTION('ref_axis',(-0.770342508707554,0.637630315526286,0.));
#21932=DIRECTION('',(0.,0.,1.));
#21933=DIRECTION('center_axis',(0.,0.,-1.));
#21934=DIRECTION('ref_axis',(-0.499999999999999,0.866025403784439,0.));
#21935=DIRECTION('center_axis',(0.,0.,1.));
#21936=DIRECTION('ref_axis',(0.130701828608463,0.991421722577433,0.));
#21937=DIRECTION('',(-6.12323399573709E-17,1.06057523872489E-16,1.));
#21938=DIRECTION('center_axis',(0.,0.,-1.));
#21939=DIRECTION('ref_axis',(-0.500000000000026,0.866025403784424,0.));
#21940=DIRECTION('center_axis',(0.,0.,1.));
#21941=DIRECTION('ref_axis',(-0.500000000000026,0.866025403784424,0.));
#21942=DIRECTION('',(-6.12323399573709E-17,1.06057523872489E-16,1.));
#21943=DIRECTION('center_axis',(0.,0.,1.));
#21944=DIRECTION('ref_axis',(-0.500000000000026,0.866025403784424,0.));
#21945=DIRECTION('',(-6.12323399573709E-17,1.06057523872489E-16,1.));
#21946=DIRECTION('center_axis',(0.,0.,1.));
#21947=DIRECTION('ref_axis',(-0.500000000000026,0.866025403784424,0.));
#21948=DIRECTION('',(-6.12323399573709E-17,1.06057523872489E-16,1.));
#21949=DIRECTION('center_axis',(0.,0.,1.));
#21950=DIRECTION('ref_axis',(-0.500000000000026,0.866025403784424,0.));
#21951=DIRECTION('',(-6.12323399573709E-17,1.06057523872489E-16,1.));
#21952=DIRECTION('center_axis',(0.,0.,1.));
#21953=DIRECTION('ref_axis',(-0.500000000000026,0.866025403784424,0.));
#21954=DIRECTION('',(-6.12323399573709E-17,1.06057523872489E-16,1.));
#21955=DIRECTION('center_axis',(0.,0.,1.));
#21956=DIRECTION('ref_axis',(-0.500000000000026,0.866025403784424,0.));
#21957=DIRECTION('',(-6.12323399573709E-17,1.06057523872489E-16,1.));
#21958=DIRECTION('center_axis',(0.,0.,1.));
#21959=DIRECTION('ref_axis',(-0.382312780236439,-0.924032974556582,0.));
#21960=DIRECTION('',(-6.12323399573709E-17,1.06057523872489E-16,1.));
#21961=DIRECTION('center_axis',(0.,0.,1.));
#21962=DIRECTION('ref_axis',(-0.500000000000026,0.866025403784424,0.));
#21963=DIRECTION('center_axis',(0.,-1.,0.));
#21964=DIRECTION('ref_axis',(-1.,0.,0.));
#21965=DIRECTION('',(0.,0.,-1.));
#21966=DIRECTION('',(-1.,0.,0.));
#21967=DIRECTION('',(0.,0.,-1.));
#21968=DIRECTION('',(1.,0.,0.));
#21969=DIRECTION('center_axis',(1.,0.,0.));
#21970=DIRECTION('ref_axis',(0.,-1.,0.));
#21971=DIRECTION('',(0.,-1.,0.));
#21972=DIRECTION('',(0.,0.,-1.));
#21973=DIRECTION('',(0.,1.,0.));
#21974=DIRECTION('center_axis',(0.,1.,0.));
#21975=DIRECTION('ref_axis',(1.,0.,0.));
#21976=DIRECTION('',(0.,0.,1.));
#21977=DIRECTION('',(-1.,0.,0.));
#21978=DIRECTION('',(1.,0.,0.));
#21979=DIRECTION('center_axis',(0.,0.,-1.));
#21980=DIRECTION('ref_axis',(-1.,0.,0.));
#21981=DIRECTION('',(0.939692620785908,-0.342020143325669,0.));
#21982=DIRECTION('center_axis',(0.,0.,1.));
#21983=DIRECTION('ref_axis',(-0.901760301405889,-0.43223646168314,0.));
#21984=DIRECTION('center_axis',(0.,0.,-1.));
#21985=DIRECTION('ref_axis',(0.939692620785908,-0.34202014332567,0.));
#21986=DIRECTION('',(0.4486637512204,-0.893700642464152,0.));
#21987=DIRECTION('',(0.893700642464153,0.4486637512204,0.));
#21988=DIRECTION('',(-0.4486637512204,0.893700642464153,0.));
#21989=DIRECTION('',(-0.893700642464153,-0.4486637512204,0.));
#21990=DIRECTION('',(0.766044443118978,0.64278760968654,0.));
#21991=DIRECTION('center_axis',(0.,0.,1.));
#21992=DIRECTION('ref_axis',(-0.0765523944434513,-0.997065559983382,0.));
#21993=DIRECTION('center_axis',(0.,0.,-1.));
#21994=DIRECTION('ref_axis',(0.766044443118978,0.642787609686539,0.));
#21995=DIRECTION('',(0.99829933536263,-0.058296114917988,0.));
#21996=DIRECTION('',(0.0582961149179888,0.99829933536263,0.));
#21997=DIRECTION('',(-0.99829933536263,0.0582961149179891,0.));
#21998=DIRECTION('',(-0.0582961149179891,-0.99829933536263,0.));
#21999=DIRECTION('',(-0.173648177666931,0.984807753012208,0.));
#22000=DIRECTION('center_axis',(0.,0.,1.));
#22001=DIRECTION('ref_axis',(0.825207906962445,-0.564829098300239,0.));
#22002=DIRECTION('center_axis',(0.,0.,-1.));
#22003=DIRECTION('ref_axis',(-0.173648177666929,0.984807753012208,0.));
#22004=DIRECTION('',(0.54963558414223,0.835404527546164,0.));
#22005=DIRECTION('',(-0.835404527546164,0.54963558414223,0.));
#22006=DIRECTION('',(-0.54963558414223,-0.835404527546164,0.));
#22007=DIRECTION('',(0.835404527546164,-0.54963558414223,0.));
#22008=DIRECTION('',(-0.939692620785909,0.342020143325668,0.));
#22009=DIRECTION('center_axis',(0.,0.,1.));
#22010=DIRECTION('ref_axis',(0.901760301405891,0.432236461683135,0.));
#22011=DIRECTION('center_axis',(0.,0.,-1.));
#22012=DIRECTION('ref_axis',(-0.939692620785908,0.342020143325669,0.));
#22013=DIRECTION('',(-0.4486637512204,0.893700642464152,0.));
#22014=DIRECTION('',(-0.893700642464153,-0.4486637512204,0.));
#22015=DIRECTION('',(0.448663751220399,-0.893700642464153,0.));
#22016=DIRECTION('',(0.893700642464153,0.448663751220399,0.));
#22017=DIRECTION('',(-0.766044443118978,-0.64278760968654,0.));
#22018=DIRECTION('center_axis',(0.,0.,1.));
#22019=DIRECTION('ref_axis',(0.0765523944434456,0.997065559983382,0.));
#22020=DIRECTION('center_axis',(0.,0.,-1.));
#22021=DIRECTION('ref_axis',(-0.766044443118979,-0.642787609686539,0.));
#22022=DIRECTION('',(-0.99829933536263,0.0582961149179884,0.));
#22023=DIRECTION('',(-0.0582961149179891,-0.99829933536263,0.));
#22024=DIRECTION('',(0.99829933536263,-0.0582961149179895,0.));
#22025=DIRECTION('',(0.0582961149179895,0.99829933536263,0.));
#22026=DIRECTION('',(0.173648177666931,-0.984807753012208,0.));
#22027=DIRECTION('center_axis',(0.,0.,1.));
#22028=DIRECTION('ref_axis',(-0.82520790696244,0.564829098300246,0.));
#22029=DIRECTION('center_axis',(0.,0.,-1.));
#22030=DIRECTION('ref_axis',(0.173648177666929,-0.984807753012208,0.));
#22031=DIRECTION('',(-0.54963558414223,-0.835404527546164,0.));
#22032=DIRECTION('',(0.835404527546163,-0.549635584142231,0.));
#22033=DIRECTION('',(0.549635584142231,0.835404527546163,0.));
#22034=DIRECTION('',(-0.835404527546163,0.549635584142231,0.));
#22035=DIRECTION('center_axis',(0.,0.,1.));
#22036=DIRECTION('ref_axis',(1.,0.,0.));
#22037=DIRECTION('center_axis',(0.,0.,1.));
#22038=DIRECTION('ref_axis',(1.,0.,0.));
#22039=DIRECTION('center_axis',(0.,0.,1.));
#22040=DIRECTION('ref_axis',(-0.500000000000026,0.866025403784424,0.));
#22041=DIRECTION('center_axis',(0.,0.,1.));
#22042=DIRECTION('ref_axis',(-0.499999999999999,0.866025403784439,0.));
#22043=DIRECTION('center_axis',(0.,0.,1.));
#22044=DIRECTION('ref_axis',(1.,0.,0.));
#22045=DIRECTION('center_axis',(0.,0.,1.));
#22046=DIRECTION('ref_axis',(0.499999999999984,0.866025403784448,0.));
#22047=DIRECTION('center_axis',(0.,0.,1.));
#22048=DIRECTION('ref_axis',(0.5,0.866025403784438,0.));
#22049=DIRECTION('center_axis',(0.,0.,1.));
#22050=DIRECTION('ref_axis',(1.,0.,0.));
#22051=DIRECTION('center_axis',(0.,0.,1.));
#22052=DIRECTION('ref_axis',(1.,3.16589845000044E-14,0.));
#22053=DIRECTION('center_axis',(0.,0.,1.));
#22054=DIRECTION('ref_axis',(1.,-9.25185853854297E-17,0.));
#22055=DIRECTION('center_axis',(0.,0.,1.));
#22056=DIRECTION('ref_axis',(1.,0.,0.));
#22057=DIRECTION('center_axis',(0.,0.,1.));
#22058=DIRECTION('ref_axis',(0.500000000000028,-0.866025403784422,0.));
#22059=DIRECTION('center_axis',(0.,0.,1.));
#22060=DIRECTION('ref_axis',(0.5,-0.866025403784439,0.));
#22061=DIRECTION('center_axis',(0.,0.,1.));
#22062=DIRECTION('ref_axis',(1.,0.,0.));
#22063=DIRECTION('center_axis',(0.,0.,1.));
#22064=DIRECTION('ref_axis',(-0.499999999999981,-0.86602540378445,0.));
#22065=DIRECTION('center_axis',(0.,0.,1.));
#22066=DIRECTION('ref_axis',(-0.5,-0.866025403784439,0.));
#22067=DIRECTION('center_axis',(0.,0.,1.));
#22068=DIRECTION('ref_axis',(-0.499999999999999,0.866025403784439,0.));
#22069=DIRECTION('',(0.54963558414223,0.835404527546164,0.));
#22070=DIRECTION('center_axis',(0.,0.,1.));
#22071=DIRECTION('ref_axis',(-0.499999999999999,0.866025403784439,0.));
#22072=DIRECTION('',(0.54963558414223,0.835404527546164,0.));
#22073=DIRECTION('center_axis',(0.,0.,1.));
#22074=DIRECTION('ref_axis',(0.5,0.866025403784438,0.));
#22075=DIRECTION('',(0.99829933536263,-0.0582961149179893,-3.10967490252419E-18));
#22076=DIRECTION('center_axis',(0.,0.,1.));
#22077=DIRECTION('ref_axis',(0.5,0.866025403784438,0.));
#22078=DIRECTION('',(0.99829933536263,-0.0582961149179893,-3.10967490252419E-18));
#22079=DIRECTION('center_axis',(0.,0.,1.));
#22080=DIRECTION('ref_axis',(1.,-1.66533453693773E-16,0.));
#22081=DIRECTION('',(0.4486637512204,-0.893700642464152,2.01331172658311E-19));
#22082=DIRECTION('center_axis',(0.,0.,1.));
#22083=DIRECTION('ref_axis',(1.,-1.66533453693773E-16,0.));
#22084=DIRECTION('',(0.4486637512204,-0.893700642464152,2.01331172658311E-19));
#22085=DIRECTION('center_axis',(0.,0.,1.));
#22086=DIRECTION('ref_axis',(0.5,-0.866025403784439,0.));
#22087=DIRECTION('',(-0.54963558414223,-0.835404527546164,-1.46475409989076E-17));
#22088=DIRECTION('center_axis',(0.,0.,1.));
#22089=DIRECTION('ref_axis',(0.5,-0.866025403784439,0.));
#22090=DIRECTION('',(-0.54963558414223,-0.835404527546164,-1.46475409989076E-17));
#22091=DIRECTION('center_axis',(0.,0.,1.));
#22092=DIRECTION('ref_axis',(-0.5,-0.866025403784439,0.));
#22093=DIRECTION('',(-0.99829933536263,0.0582961149179884,-2.12383052760723E-18));
#22094=DIRECTION('center_axis',(0.,0.,1.));
#22095=DIRECTION('ref_axis',(-0.5,-0.866025403784439,0.));
#22096=DIRECTION('',(-0.99829933536263,0.0582961149179884,-2.12383052760723E-18));
#22097=DIRECTION('center_axis',(0.,0.,1.));
#22098=DIRECTION('ref_axis',(1.,0.,0.));
#22099=DIRECTION('center_axis',(0.,0.,-1.));
#22100=DIRECTION('ref_axis',(0.499999999999968,-0.866025403784457,0.));
#22101=DIRECTION('center_axis',(0.,0.,-1.));
#22102=DIRECTION('ref_axis',(0.499999999999999,-0.866025403784439,0.));
#22103=DIRECTION('center_axis',(0.,0.,1.));
#22104=DIRECTION('ref_axis',(1.,0.,0.));
#22105=DIRECTION('center_axis',(0.,0.,-1.));
#22106=DIRECTION('ref_axis',(-0.500000000000029,-0.866025403784422,0.));
#22107=DIRECTION('center_axis',(0.,0.,-1.));
#22108=DIRECTION('ref_axis',(-0.5,-0.866025403784438,0.));
#22109=DIRECTION('center_axis',(0.,0.,1.));
#22110=DIRECTION('ref_axis',(1.,0.,0.));
#22111=DIRECTION('center_axis',(0.,0.,-1.));
#22112=DIRECTION('ref_axis',(-1.,2.15856712500029E-14,0.));
#22113=DIRECTION('center_axis',(0.,0.,-1.));
#22114=DIRECTION('ref_axis',(-1.,9.25185853854297E-17,0.));
#22115=DIRECTION('center_axis',(0.,0.,1.));
#22116=DIRECTION('ref_axis',(1.,0.,0.));
#22117=DIRECTION('center_axis',(0.,0.,-1.));
#22118=DIRECTION('ref_axis',(-0.499999999999964,0.86602540378446,0.));
#22119=DIRECTION('center_axis',(0.,0.,-1.));
#22120=DIRECTION('ref_axis',(-0.5,0.866025403784439,0.));
#22121=DIRECTION('center_axis',(0.,0.,1.));
#22122=DIRECTION('ref_axis',(1.,0.,0.));
#22123=DIRECTION('center_axis',(0.,0.,-1.));
#22124=DIRECTION('ref_axis',(0.500000000000046,0.866025403784412,0.));
#22125=DIRECTION('center_axis',(0.,0.,-1.));
#22126=DIRECTION('ref_axis',(0.5,0.866025403784439,0.));
#22127=DIRECTION('center_axis',(0.,0.,-1.));
#22128=DIRECTION('ref_axis',(0.499999999999999,-0.866025403784439,0.));
#22129=DIRECTION('',(0.54963558414223,0.835404527546164,0.));
#22130=DIRECTION('center_axis',(0.,0.,-1.));
#22131=DIRECTION('ref_axis',(0.499999999999999,-0.866025403784439,0.));
#22132=DIRECTION('',(0.54963558414223,0.835404527546164,0.));
#22133=DIRECTION('center_axis',(0.,0.,-1.));
#22134=DIRECTION('ref_axis',(-0.5,-0.866025403784438,0.));
#22135=DIRECTION('',(0.99829933536263,-0.0582961149179893,-3.10967490252419E-18));
#22136=DIRECTION('center_axis',(0.,0.,-1.));
#22137=DIRECTION('ref_axis',(-0.5,-0.866025403784438,0.));
#22138=DIRECTION('',(0.99829933536263,-0.0582961149179893,-3.10967490252419E-18));
#22139=DIRECTION('center_axis',(0.,0.,-1.));
#22140=DIRECTION('ref_axis',(-1.,1.66533453693773E-16,0.));
#22141=DIRECTION('',(0.4486637512204,-0.893700642464152,2.01331172658311E-19));
#22142=DIRECTION('center_axis',(0.,0.,-1.));
#22143=DIRECTION('ref_axis',(-1.,1.66533453693773E-16,0.));
#22144=DIRECTION('',(0.4486637512204,-0.893700642464152,2.01331172658311E-19));
#22145=DIRECTION('center_axis',(0.,0.,-1.));
#22146=DIRECTION('ref_axis',(-0.5,0.866025403784439,0.));
#22147=DIRECTION('',(-0.54963558414223,-0.835404527546164,-1.46475409989076E-17));
#22148=DIRECTION('center_axis',(0.,0.,-1.));
#22149=DIRECTION('ref_axis',(-0.5,0.866025403784439,0.));
#22150=DIRECTION('',(-0.54963558414223,-0.835404527546164,-1.46475409989076E-17));
#22151=DIRECTION('center_axis',(0.,0.,-1.));
#22152=DIRECTION('ref_axis',(0.5,0.866025403784439,0.));
#22153=DIRECTION('',(-0.99829933536263,0.0582961149179884,-2.12383052760723E-18));
#22154=DIRECTION('center_axis',(0.,0.,-1.));
#22155=DIRECTION('ref_axis',(0.5,0.866025403784439,0.));
#22156=DIRECTION('',(-0.99829933536263,0.0582961149179884,-2.12383052760723E-18));
#22157=DIRECTION('center_axis',(0.,0.,1.));
#22158=DIRECTION('ref_axis',(1.,0.,0.));
#22159=DIRECTION('center_axis',(0.,0.,1.));
#22160=DIRECTION('ref_axis',(-1.,-1.72685370000025E-14,0.));
#22161=DIRECTION('center_axis',(0.,0.,1.));
#22162=DIRECTION('ref_axis',(-1.,0.,0.));
#22163=DIRECTION('center_axis',(0.,0.,1.));
#22164=DIRECTION('ref_axis',(-1.,0.,0.));
#22165=DIRECTION('',(-0.4486637512204,0.893700642464152,2.01331172658311E-19));
#22166=DIRECTION('center_axis',(0.,0.,1.));
#22167=DIRECTION('ref_axis',(-1.,0.,0.));
#22168=DIRECTION('',(-0.4486637512204,0.893700642464152,2.01331172658311E-19));
#22169=DIRECTION('center_axis',(0.,0.,1.));
#22170=DIRECTION('ref_axis',(1.,0.,0.));
#22171=DIRECTION('center_axis',(0.,0.,-1.));
#22172=DIRECTION('ref_axis',(1.,-3.45370740000048E-14,0.));
#22173=DIRECTION('center_axis',(0.,0.,-1.));
#22174=DIRECTION('ref_axis',(1.,0.,0.));
#22175=DIRECTION('center_axis',(0.,0.,-1.));
#22176=DIRECTION('ref_axis',(1.,0.,0.));
#22177=DIRECTION('',(-0.4486637512204,0.893700642464152,2.01331172658311E-19));
#22178=DIRECTION('center_axis',(0.,0.,-1.));
#22179=DIRECTION('ref_axis',(1.,0.,0.));
#22180=DIRECTION('',(-0.4486637512204,0.893700642464152,2.01331172658311E-19));
#22181=DIRECTION('center_axis',(-0.54963558414223,-0.835404527546164,0.));
#22182=DIRECTION('ref_axis',(0.,0.,1.));
#22183=DIRECTION('center_axis',(-0.54963558414223,-0.835404527546164,0.));
#22184=DIRECTION('ref_axis',(0.,0.,1.));
#22185=DIRECTION('',(-0.54963558414223,-0.835404527546164,0.));
#22186=DIRECTION('center_axis',(0.549635584142231,0.835404527546164,0.));
#22187=DIRECTION('ref_axis',(0.,0.,1.));
#22188=DIRECTION('center_axis',(-0.54963558414223,-0.835404527546164,0.));
#22189=DIRECTION('ref_axis',(0.,0.,1.));
#22190=DIRECTION('center_axis',(-0.549635584142231,-0.835404527546163,0.));
#22191=DIRECTION('ref_axis',(0.,0.,1.));
#22192=DIRECTION('',(-0.54963558414223,-0.835404527546164,0.));
#22193=DIRECTION('',(-0.54963558414223,-0.835404527546164,0.));
#22194=DIRECTION('center_axis',(-0.54963558414223,-0.835404527546164,0.));
#22195=DIRECTION('ref_axis',(0.,0.,1.));
#22196=DIRECTION('center_axis',(-0.54963558414223,-0.835404527546164,0.));
#22197=DIRECTION('ref_axis',(0.,0.,1.));
#22198=DIRECTION('center_axis',(-0.99829933536263,0.0582961149179893,3.10967490252419E-18));
#22199=DIRECTION('ref_axis',(0.0582961149179893,0.99829933536263,0.));
#22200=DIRECTION('center_axis',(-0.99829933536263,0.0582961149179893,3.10967490252419E-18));
#22201=DIRECTION('ref_axis',(0.0582961149179893,0.99829933536263,0.));
#22202=DIRECTION('',(-0.99829933536263,0.0582961149179893,3.10967490252419E-18));
#22203=DIRECTION('center_axis',(0.99829933536263,-0.0582961149179891,0.));
#22204=DIRECTION('ref_axis',(0.0582961149179893,0.99829933536263,0.));
#22205=DIRECTION('center_axis',(-0.99829933536263,0.0582961149179893,3.10967490252419E-18));
#22206=DIRECTION('ref_axis',(-2.31296463463574E-17,-1.84314369322536E-16,
1.));
#22207=DIRECTION('center_axis',(-0.99829933536263,0.0582961149179895,0.));
#22208=DIRECTION('ref_axis',(0.0582961149179893,0.99829933536263,0.));
#22209=DIRECTION('',(-0.99829933536263,0.0582961149179893,3.10967490252419E-18));
#22210=DIRECTION('',(-0.99829933536263,0.0582961149179893,3.10967490252419E-18));
#22211=DIRECTION('center_axis',(-0.99829933536263,0.0582961149179893,3.10967490252419E-18));
#22212=DIRECTION('ref_axis',(0.0582961149179893,0.99829933536263,0.));
#22213=DIRECTION('center_axis',(-0.99829933536263,0.0582961149179893,3.10967490252419E-18));
#22214=DIRECTION('ref_axis',(0.0582961149179893,0.99829933536263,0.));
#22215=DIRECTION('center_axis',(-0.4486637512204,0.893700642464152,-2.01331172658311E-19));
#22216=DIRECTION('ref_axis',(0.,-2.2527808876045E-19,-1.));
#22217=DIRECTION('center_axis',(-0.4486637512204,0.893700642464152,-2.01331172658311E-19));
#22218=DIRECTION('ref_axis',(0.,-2.2527808876045E-19,-1.));
#22219=DIRECTION('',(-0.4486637512204,0.893700642464152,-2.01331172658311E-19));
#22220=DIRECTION('center_axis',(0.4486637512204,-0.893700642464153,0.));
#22221=DIRECTION('ref_axis',(0.,-2.2527808876045E-19,-1.));
#22222=DIRECTION('center_axis',(-0.4486637512204,0.893700642464152,-2.01331172658311E-19));
#22223=DIRECTION('ref_axis',(-1.09446763118966E-16,-5.47201845937903E-17,
1.));
#22224=DIRECTION('center_axis',(-0.448663751220399,0.893700642464153,0.));
#22225=DIRECTION('ref_axis',(0.,-2.2527808876045E-19,-1.));
#22226=DIRECTION('',(-0.4486637512204,0.893700642464152,-2.01331172658311E-19));
#22227=DIRECTION('',(-0.4486637512204,0.893700642464152,-2.01331172658311E-19));
#22228=DIRECTION('center_axis',(-0.4486637512204,0.893700642464152,-2.01331172658311E-19));
#22229=DIRECTION('ref_axis',(0.,-2.2527808876045E-19,-1.));
#22230=DIRECTION('center_axis',(-0.4486637512204,0.893700642464152,-2.01331172658311E-19));
#22231=DIRECTION('ref_axis',(0.,-2.2527808876045E-19,-1.));
#22232=DIRECTION('center_axis',(0.54963558414223,0.835404527546164,1.46475409989076E-17));
#22233=DIRECTION('ref_axis',(0.,1.75334709304627E-17,-1.));
#22234=DIRECTION('center_axis',(0.54963558414223,0.835404527546164,1.46475409989076E-17));
#22235=DIRECTION('ref_axis',(0.,1.75334709304627E-17,-1.));
#22236=DIRECTION('',(0.54963558414223,0.835404527546164,1.46475409989076E-17));
#22237=DIRECTION('center_axis',(-0.54963558414223,-0.835404527546164,0.));
#22238=DIRECTION('ref_axis',(0.,1.75334709304627E-17,-1.));
#22239=DIRECTION('center_axis',(0.54963558414223,0.835404527546164,1.46475409989076E-17));
#22240=DIRECTION('ref_axis',(2.12365727119358E-15,-1.41474591865194E-15,
1.));
#22241=DIRECTION('center_axis',(0.549635584142231,0.835404527546164,0.));
#22242=DIRECTION('ref_axis',(0.,1.75334709304627E-17,-1.));
#22243=DIRECTION('',(0.54963558414223,0.835404527546164,1.46475409989076E-17));
#22244=DIRECTION('',(0.54963558414223,0.835404527546164,1.46475409989076E-17));
#22245=DIRECTION('center_axis',(0.54963558414223,0.835404527546164,1.46475409989076E-17));
#22246=DIRECTION('ref_axis',(0.,1.75334709304627E-17,-1.));
#22247=DIRECTION('center_axis',(0.54963558414223,0.835404527546164,1.46475409989076E-17));
#22248=DIRECTION('ref_axis',(0.,1.75334709304627E-17,-1.));
#22249=DIRECTION('center_axis',(0.99829933536263,-0.0582961149179884,2.12383052760723E-18));
#22250=DIRECTION('ref_axis',(-0.0582961149179884,-0.99829933536263,0.));
#22251=DIRECTION('center_axis',(0.99829933536263,-0.0582961149179884,2.12383052760723E-18));
#22252=DIRECTION('ref_axis',(-0.0582961149179884,-0.99829933536263,0.));
#22253=DIRECTION('',(0.99829933536263,-0.0582961149179884,2.12383052760723E-18));
#22254=DIRECTION('center_axis',(-0.99829933536263,0.0582961149179888,0.));
#22255=DIRECTION('ref_axis',(-0.0582961149179884,-0.99829933536263,0.));
#22256=DIRECTION('center_axis',(0.99829933536263,-0.0582961149179884,2.12383052760723E-18));
#22257=DIRECTION('ref_axis',(6.93889390390723E-17,1.07046894496735E-15,
1.));
#22258=DIRECTION('center_axis',(0.99829933536263,-0.0582961149179891,0.));
#22259=DIRECTION('ref_axis',(-0.0582961149179884,-0.99829933536263,0.));
#22260=DIRECTION('',(0.99829933536263,-0.0582961149179884,2.12383052760723E-18));
#22261=DIRECTION('',(0.99829933536263,-0.0582961149179884,2.12383052760723E-18));
#22262=DIRECTION('center_axis',(0.99829933536263,-0.0582961149179884,2.12383052760723E-18));
#22263=DIRECTION('ref_axis',(-0.0582961149179884,-0.99829933536263,0.));
#22264=DIRECTION('center_axis',(0.99829933536263,-0.0582961149179884,2.12383052760723E-18));
#22265=DIRECTION('ref_axis',(-0.0582961149179884,-0.99829933536263,0.));
#22266=DIRECTION('center_axis',(0.4486637512204,-0.893700642464152,-2.01331172658311E-19));
#22267=DIRECTION('ref_axis',(0.,-2.2527808876045E-19,1.));
#22268=DIRECTION('center_axis',(0.4486637512204,-0.893700642464152,-2.01331172658311E-19));
#22269=DIRECTION('ref_axis',(0.,-2.2527808876045E-19,1.));
#22270=DIRECTION('',(0.4486637512204,-0.893700642464152,-2.01331172658311E-19));
#22271=DIRECTION('center_axis',(-0.4486637512204,0.893700642464153,0.));
#22272=DIRECTION('ref_axis',(0.,-2.2527808876045E-19,1.));
#22273=DIRECTION('center_axis',(0.4486637512204,-0.893700642464152,-2.01331172658311E-19));
#22274=DIRECTION('ref_axis',(0.,-2.2527808876045E-19,1.));
#22275=DIRECTION('center_axis',(0.4486637512204,-0.893700642464153,0.));
#22276=DIRECTION('ref_axis',(0.,-2.2527808876045E-19,1.));
#22277=DIRECTION('',(0.4486637512204,-0.893700642464152,-2.01331172658311E-19));
#22278=DIRECTION('',(0.4486637512204,-0.893700642464152,-2.01331172658311E-19));
#22279=DIRECTION('center_axis',(0.4486637512204,-0.893700642464152,-2.01331172658311E-19));
#22280=DIRECTION('ref_axis',(0.,-2.2527808876045E-19,1.));
#22281=DIRECTION('center_axis',(0.4486637512204,-0.893700642464152,-2.01331172658311E-19));
#22282=DIRECTION('ref_axis',(0.,-2.2527808876045E-19,1.));
#22283=DIRECTION('center_axis',(-0.835404527546164,0.54963558414223,0.));
#22284=DIRECTION('ref_axis',(-0.54963558414223,-0.835404527546164,0.));
#22285=DIRECTION('',(-0.54963558414223,-0.835404527546164,0.));
#22286=DIRECTION('',(0.,0.,1.));
#22287=DIRECTION('center_axis',(0.549635584142231,0.835404527546163,0.));
#22288=DIRECTION('ref_axis',(-0.835404527546163,0.549635584142231,0.));
#22289=DIRECTION('',(0.,0.,1.));
#22290=DIRECTION('',(-0.835404527546163,0.549635584142231,0.));
#22291=DIRECTION('center_axis',(0.835404527546163,-0.549635584142231,0.));
#22292=DIRECTION('ref_axis',(0.549635584142231,0.835404527546163,0.));
#22293=DIRECTION('',(0.549635584142231,0.835404527546163,0.));
#22294=DIRECTION('',(0.,0.,1.));
#22295=DIRECTION('center_axis',(-0.549635584142231,-0.835404527546164,0.));
#22296=DIRECTION('ref_axis',(0.835404527546163,-0.549635584142231,0.));
#22297=DIRECTION('',(0.835404527546163,-0.549635584142231,0.));
#22298=DIRECTION('center_axis',(0.99829933536263,-0.0582961149179895,0.));
#22299=DIRECTION('ref_axis',(0.0582961149179895,0.99829933536263,0.));
#22300=DIRECTION('',(0.,0.,1.));
#22301=DIRECTION('',(0.0582961149179895,0.99829933536263,0.));
#22302=DIRECTION('center_axis',(-0.0582961149179895,-0.99829933536263,0.));
#22303=DIRECTION('ref_axis',(0.99829933536263,-0.0582961149179895,0.));
#22304=DIRECTION('',(0.99829933536263,-0.0582961149179895,0.));
#22305=DIRECTION('',(0.,0.,1.));
#22306=DIRECTION('center_axis',(-0.99829933536263,0.0582961149179891,0.));
#22307=DIRECTION('ref_axis',(-0.0582961149179891,-0.99829933536263,0.));
#22308=DIRECTION('',(-0.0582961149179891,-0.99829933536263,0.));
#22309=DIRECTION('',(0.,0.,1.));
#22310=DIRECTION('center_axis',(0.0582961149179884,0.99829933536263,0.));
#22311=DIRECTION('ref_axis',(-0.99829933536263,0.0582961149179884,0.));
#22312=DIRECTION('',(-0.99829933536263,0.0582961149179884,0.));
#22313=DIRECTION('center_axis',(0.448663751220399,-0.893700642464153,0.));
#22314=DIRECTION('ref_axis',(0.893700642464153,0.448663751220399,0.));
#22315=DIRECTION('',(0.,0.,1.));
#22316=DIRECTION('',(0.893700642464153,0.448663751220399,0.));
#22317=DIRECTION('center_axis',(-0.893700642464153,-0.448663751220399,0.));
#22318=DIRECTION('ref_axis',(0.448663751220399,-0.893700642464153,0.));
#22319=DIRECTION('',(0.448663751220399,-0.893700642464153,0.));
#22320=DIRECTION('',(0.,0.,1.));
#22321=DIRECTION('center_axis',(-0.4486637512204,0.893700642464153,0.));
#22322=DIRECTION('ref_axis',(-0.893700642464153,-0.4486637512204,0.));
#22323=DIRECTION('',(-0.893700642464153,-0.4486637512204,0.));
#22324=DIRECTION('',(0.,0.,1.));
#22325=DIRECTION('center_axis',(0.893700642464152,0.4486637512204,0.));
#22326=DIRECTION('ref_axis',(-0.448663751220401,0.893700642464152,0.));
#22327=DIRECTION('',(-0.4486637512204,0.893700642464152,0.));
#22328=DIRECTION('center_axis',(-0.549635584142231,-0.835404527546164,0.));
#22329=DIRECTION('ref_axis',(0.835404527546164,-0.54963558414223,0.));
#22330=DIRECTION('',(0.,0.,1.));
#22331=DIRECTION('',(0.835404527546164,-0.54963558414223,0.));
#22332=DIRECTION('center_axis',(-0.835404527546164,0.549635584142231,0.));
#22333=DIRECTION('ref_axis',(-0.54963558414223,-0.835404527546164,0.));
#22334=DIRECTION('',(-0.54963558414223,-0.835404527546164,0.));
#22335=DIRECTION('',(0.,0.,1.));
#22336=DIRECTION('center_axis',(0.54963558414223,0.835404527546164,0.));
#22337=DIRECTION('ref_axis',(-0.835404527546164,0.54963558414223,0.));
#22338=DIRECTION('',(-0.835404527546164,0.54963558414223,0.));
#22339=DIRECTION('',(0.,0.,1.));
#22340=DIRECTION('center_axis',(0.835404527546164,-0.54963558414223,0.));
#22341=DIRECTION('ref_axis',(0.54963558414223,0.835404527546164,0.));
#22342=DIRECTION('',(0.54963558414223,0.835404527546164,0.));
#22343=DIRECTION('center_axis',(-0.058296114917988,-0.99829933536263,0.));
#22344=DIRECTION('ref_axis',(0.99829933536263,-0.058296114917988,0.));
#22345=DIRECTION('',(0.99829933536263,-0.058296114917988,0.));
#22346=DIRECTION('',(0.,0.,1.));
#22347=DIRECTION('center_axis',(-0.99829933536263,0.0582961149179891,0.));
#22348=DIRECTION('ref_axis',(-0.0582961149179891,-0.99829933536263,0.));
#22349=DIRECTION('',(0.,0.,1.));
#22350=DIRECTION('',(-0.0582961149179891,-0.99829933536263,0.));
#22351=DIRECTION('center_axis',(0.0582961149179891,0.99829933536263,0.));
#22352=DIRECTION('ref_axis',(-0.99829933536263,0.0582961149179891,0.));
#22353=DIRECTION('',(-0.99829933536263,0.0582961149179891,0.));
#22354=DIRECTION('',(0.,0.,1.));
#22355=DIRECTION('center_axis',(0.99829933536263,-0.0582961149179888,0.));
#22356=DIRECTION('ref_axis',(0.0582961149179888,0.99829933536263,0.));
#22357=DIRECTION('',(0.0582961149179888,0.99829933536263,0.));
#22358=DIRECTION('',(0.,0.,-1.));
#22359=DIRECTION('',(0.,0.,-1.));
#22360=DIRECTION('',(0.,0.,1.));
#22361=DIRECTION('',(0.,0.,-1.));
#22362=DIRECTION('',(0.,0.,1.));
#22363=DIRECTION('',(0.,0.,-1.));
#22364=DIRECTION('',(0.,0.,1.));
#22365=DIRECTION('',(0.,0.,-1.));
#22366=DIRECTION('center_axis',(-0.893700642464152,-0.448663751220401,0.));
#22367=DIRECTION('ref_axis',(0.448663751220401,-0.893700642464152,0.));
#22368=DIRECTION('',(0.4486637512204,-0.893700642464152,0.));
#22369=DIRECTION('',(0.,0.,1.));
#22370=DIRECTION('center_axis',(-0.4486637512204,0.893700642464153,0.));
#22371=DIRECTION('ref_axis',(-0.893700642464153,-0.4486637512204,0.));
#22372=DIRECTION('',(0.,0.,1.));
#22373=DIRECTION('',(-0.893700642464153,-0.4486637512204,0.));
#22374=DIRECTION('center_axis',(0.893700642464153,0.4486637512204,0.));
#22375=DIRECTION('ref_axis',(-0.4486637512204,0.893700642464153,0.));
#22376=DIRECTION('',(-0.4486637512204,0.893700642464153,0.));
#22377=DIRECTION('',(0.,0.,1.));
#22378=DIRECTION('center_axis',(0.4486637512204,-0.893700642464153,0.));
#22379=DIRECTION('ref_axis',(0.893700642464153,0.4486637512204,0.));
#22380=DIRECTION('',(0.893700642464153,0.4486637512204,0.));
#22381=DIRECTION('',(0.,0.,-1.));
#22382=DIRECTION('center_axis',(0.,0.,1.));
#22383=DIRECTION('ref_axis',(-0.766044443118979,-0.642787609686539,0.));
#22384=DIRECTION('',(0.,0.,1.));
#22385=DIRECTION('center_axis',(0.,0.,1.));
#22386=DIRECTION('ref_axis',(-0.766044443118979,-0.642787609686539,0.));
#22387=DIRECTION('center_axis',(0.,0.,1.));
#22388=DIRECTION('ref_axis',(0.0765523944434456,0.997065559983382,0.));
#22389=DIRECTION('',(0.,0.,-1.));
#22390=DIRECTION('center_axis',(0.,0.,-1.));
#22391=DIRECTION('ref_axis',(0.0765523944434456,0.997065559983382,0.));
#22392=DIRECTION('center_axis',(-0.64278760968654,0.766044443118978,0.));
#22393=DIRECTION('ref_axis',(-0.766044443118978,-0.64278760968654,0.));
#22394=DIRECTION('',(0.766044443118978,0.64278760968654,0.));
#22395=DIRECTION('center_axis',(0.,0.,1.));
#22396=DIRECTION('ref_axis',(-0.939692620785908,0.342020143325669,0.));
#22397=DIRECTION('',(0.,0.,1.));
#22398=DIRECTION('center_axis',(0.,0.,1.));
#22399=DIRECTION('ref_axis',(-0.939692620785908,0.342020143325669,0.));
#22400=DIRECTION('center_axis',(0.,0.,1.));
#22401=DIRECTION('ref_axis',(0.901760301405891,0.432236461683135,0.));
#22402=DIRECTION('',(0.,0.,-1.));
#22403=DIRECTION('center_axis',(0.,0.,-1.));
#22404=DIRECTION('ref_axis',(0.901760301405891,0.432236461683135,0.));
#22405=DIRECTION('center_axis',(0.342020143325668,0.939692620785909,0.));
#22406=DIRECTION('ref_axis',(-0.939692620785909,0.342020143325668,0.));
#22407=DIRECTION('',(0.939692620785909,-0.342020143325668,0.));
#22408=DIRECTION('center_axis',(0.,0.,1.));
#22409=DIRECTION('ref_axis',(-0.173648177666929,0.984807753012208,0.));
#22410=DIRECTION('',(0.,0.,1.));
#22411=DIRECTION('center_axis',(0.,0.,1.));
#22412=DIRECTION('ref_axis',(-0.173648177666929,0.984807753012208,0.));
#22413=DIRECTION('center_axis',(0.,0.,1.));
#22414=DIRECTION('ref_axis',(0.825207906962445,-0.564829098300239,0.));
#22415=DIRECTION('',(0.,0.,-1.));
#22416=DIRECTION('center_axis',(0.,0.,-1.));
#22417=DIRECTION('ref_axis',(0.825207906962445,-0.564829098300239,0.));
#22418=DIRECTION('center_axis',(0.984807753012208,0.173648177666931,0.));
#22419=DIRECTION('ref_axis',(-0.173648177666931,0.984807753012208,0.));
#22420=DIRECTION('',(0.173648177666931,-0.984807753012208,0.));
#22421=DIRECTION('center_axis',(0.,0.,1.));
#22422=DIRECTION('ref_axis',(1.,0.,0.));
#22423=DIRECTION('center_axis',(0.,0.,1.));
#22424=DIRECTION('ref_axis',(0.173648177666929,-0.984807753012208,0.));
#22425=DIRECTION('center_axis',(0.,0.,-1.));
#22426=DIRECTION('ref_axis',(-0.82520790696244,0.564829098300246,0.));
#22427=DIRECTION('',(-0.173648177666931,0.984807753012208,0.));
#22428=DIRECTION('center_axis',(0.,0.,1.));
#22429=DIRECTION('ref_axis',(0.766044443118978,0.642787609686539,0.));
#22430=DIRECTION('center_axis',(0.,0.,-1.));
#22431=DIRECTION('ref_axis',(-0.0765523944434513,-0.997065559983382,0.));
#22432=DIRECTION('',(-0.766044443118978,-0.64278760968654,0.));
#22433=DIRECTION('center_axis',(0.,0.,1.));
#22434=DIRECTION('ref_axis',(0.939692620785908,-0.34202014332567,0.));
#22435=DIRECTION('center_axis',(0.,0.,-1.));
#22436=DIRECTION('ref_axis',(-0.901760301405889,-0.43223646168314,0.));
#22437=DIRECTION('',(-0.939692620785908,0.342020143325669,0.));
#22438=DIRECTION('center_axis',(0.,0.,-1.));
#22439=DIRECTION('ref_axis',(1.,0.,0.));
#22440=DIRECTION('center_axis',(-0.984807753012208,-0.173648177666931,0.));
#22441=DIRECTION('ref_axis',(0.173648177666931,-0.984807753012208,0.));
#22442=DIRECTION('',(0.,0.,-1.));
#22443=DIRECTION('center_axis',(0.,0.,1.));
#22444=DIRECTION('ref_axis',(-0.82520790696244,0.564829098300246,0.));
#22445=DIRECTION('',(0.,0.,1.));
#22446=DIRECTION('center_axis',(0.,0.,1.));
#22447=DIRECTION('ref_axis',(0.173648177666929,-0.984807753012208,0.));
#22448=DIRECTION('',(0.,0.,1.));
#22449=DIRECTION('center_axis',(-0.342020143325669,-0.939692620785908,0.));
#22450=DIRECTION('ref_axis',(0.939692620785908,-0.342020143325669,0.));
#22451=DIRECTION('',(0.,0.,-1.));
#22452=DIRECTION('center_axis',(0.,0.,1.));
#22453=DIRECTION('ref_axis',(-0.901760301405889,-0.43223646168314,0.));
#22454=DIRECTION('',(0.,0.,1.));
#22455=DIRECTION('center_axis',(0.,0.,1.));
#22456=DIRECTION('ref_axis',(0.939692620785908,-0.34202014332567,0.));
#22457=DIRECTION('',(0.,0.,1.));
#22458=DIRECTION('center_axis',(0.64278760968654,-0.766044443118978,0.));
#22459=DIRECTION('ref_axis',(0.766044443118978,0.64278760968654,0.));
#22460=DIRECTION('',(0.,0.,-1.));
#22461=DIRECTION('',(0.,0.,1.));
#22462=DIRECTION('center_axis',(0.,0.,1.));
#22463=DIRECTION('ref_axis',(-0.0765523944434513,-0.997065559983382,0.));
#22464=DIRECTION('',(0.,0.,1.));
#22465=DIRECTION('center_axis',(0.,0.,1.));
#22466=DIRECTION('ref_axis',(0.766044443118978,0.642787609686539,0.));
#22467=DIRECTION('center_axis',(0.,0.,1.));
#22468=DIRECTION('ref_axis',(-1.,1.22464679914735E-16,0.));
#22469=DIRECTION('axis',(0.,0.,1.));
#22470=DIRECTION('refdir',(1.,0.,0.));
#22471=DIRECTION('center_axis',(1.,0.,0.));
#22472=DIRECTION('ref_axis',(0.,1.,-2.96059473233375E-15));
#22473=DIRECTION('',(1.,0.,0.));
#22474=DIRECTION('center_axis',(1.,0.,0.));
#22475=DIRECTION('ref_axis',(0.,1.,-2.96059473233375E-15));
#22476=DIRECTION('',(1.,0.,0.));
#22477=DIRECTION('center_axis',(1.,0.,0.));
#22478=DIRECTION('ref_axis',(0.,1.,-2.96059473233375E-15));
#22479=DIRECTION('',(1.,0.,0.));
#22480=DIRECTION('center_axis',(1.,0.,0.));
#22481=DIRECTION('ref_axis',(0.,1.,-2.96059473233375E-15));
#22482=DIRECTION('',(1.,0.,0.));
#22483=DIRECTION('center_axis',(0.,1.,0.));
#22484=DIRECTION('ref_axis',(0.,0.,1.));
#22485=DIRECTION('',(0.,0.,-1.));
#22486=DIRECTION('',(0.,0.,-1.));
#22487=DIRECTION('',(1.,0.,0.));
#22488=DIRECTION('center_axis',(1.,0.,0.));
#22489=DIRECTION('ref_axis',(0.,-1.,-2.96059473233375E-15));
#22490=DIRECTION('center_axis',(1.,0.,0.));
#22491=DIRECTION('ref_axis',(0.,-1.,-2.96059473233375E-15));
#22492=DIRECTION('',(1.,0.,0.));
#22493=DIRECTION('center_axis',(0.,-1.,0.));
#22494=DIRECTION('ref_axis',(0.,0.,-1.));
#22495=DIRECTION('',(0.,0.,1.));
#22496=DIRECTION('',(0.,0.,1.));
#22497=DIRECTION('center_axis',(1.,0.,0.));
#22498=DIRECTION('ref_axis',(0.,0.,-1.));
#22499=DIRECTION('center_axis',(0.,0.,1.));
#22500=DIRECTION('ref_axis',(1.,0.,0.));
#22501=DIRECTION('center_axis',(0.,0.,1.));
#22502=DIRECTION('ref_axis',(1.,0.,0.));
#22503=DIRECTION('center_axis',(0.,0.,1.));
#22504=DIRECTION('ref_axis',(1.,0.,0.));
#22505=DIRECTION('',(0.,0.,-1.));
#22506=DIRECTION('center_axis',(0.,0.,1.));
#22507=DIRECTION('ref_axis',(1.,0.,0.));
#22508=DIRECTION('center_axis',(1.,0.,0.));
#22509=DIRECTION('ref_axis',(0.,1.,0.));
#22510=DIRECTION('',(1.,0.,0.));
#22511=DIRECTION('center_axis',(1.,0.,0.));
#22512=DIRECTION('ref_axis',(0.,1.,0.));
#22513=DIRECTION('',(1.,0.,0.));
#22514=DIRECTION('center_axis',(0.,1.,0.));
#22515=DIRECTION('ref_axis',(0.,0.,1.));
#22516=DIRECTION('',(0.,0.,-1.));
#22517=DIRECTION('',(0.,0.,-1.));
#22518=DIRECTION('',(1.,0.,0.));
#22519=DIRECTION('center_axis',(1.,0.,0.));
#22520=DIRECTION('ref_axis',(0.,-1.,0.));
#22521=DIRECTION('center_axis',(1.,0.,0.));
#22522=DIRECTION('ref_axis',(0.,-1.,0.));
#22523=DIRECTION('',(1.,0.,0.));
#22524=DIRECTION('center_axis',(0.,-1.,0.));
#22525=DIRECTION('ref_axis',(0.,0.,-1.));
#22526=DIRECTION('',(0.,0.,1.));
#22527=DIRECTION('',(0.,0.,1.));
#22528=DIRECTION('center_axis',(1.,0.,0.));
#22529=DIRECTION('ref_axis',(0.,0.,-1.));
#22530=DIRECTION('center_axis',(0.,0.,1.));
#22531=DIRECTION('ref_axis',(1.,0.,0.));
#22532=DIRECTION('center_axis',(0.,0.,-1.));
#22533=DIRECTION('ref_axis',(1.,0.,0.));
#22534=DIRECTION('',(0.,0.,-1.));
#22535=DIRECTION('center_axis',(0.,0.,1.));
#22536=DIRECTION('ref_axis',(1.,0.,0.));
#22537=DIRECTION('center_axis',(0.,0.,1.));
#22538=DIRECTION('ref_axis',(1.,0.,0.));
#22539=DIRECTION('center_axis',(0.,0.,1.));
#22540=DIRECTION('ref_axis',(1.,0.,0.));
#22541=DIRECTION('center_axis',(0.,0.,1.));
#22542=DIRECTION('ref_axis',(1.,0.,0.));
#22543=DIRECTION('',(0.,0.,1.));
#22544=DIRECTION('center_axis',(0.,0.,1.));
#22545=DIRECTION('ref_axis',(1.,0.,0.));
#22546=DIRECTION('center_axis',(0.,0.,-1.));
#22547=DIRECTION('ref_axis',(-1.,0.,0.));
#22548=DIRECTION('center_axis',(0.,0.,1.));
#22549=DIRECTION('ref_axis',(1.,0.,0.));
#22550=DIRECTION('center_axis',(0.,0.,1.));
#22551=DIRECTION('ref_axis',(1.,0.,0.));
#22552=DIRECTION('center_axis',(0.,0.,1.));
#22553=DIRECTION('ref_axis',(1.,0.,0.));
#22554=DIRECTION('',(0.,0.,1.));
#22555=DIRECTION('center_axis',(0.,0.,1.));
#22556=DIRECTION('ref_axis',(1.,0.,0.));
#22557=DIRECTION('center_axis',(0.,0.,-1.));
#22558=DIRECTION('ref_axis',(-1.,0.,0.));
#22559=DIRECTION('center_axis',(0.,0.,-1.));
#22560=DIRECTION('ref_axis',(1.,0.,0.));
#22561=DIRECTION('center_axis',(0.,0.,1.));
#22562=DIRECTION('ref_axis',(1.,0.,0.));
#22563=DIRECTION('center_axis',(0.,0.,1.));
#22564=DIRECTION('ref_axis',(1.,0.,0.));
#22565=DIRECTION('center_axis',(0.,0.,1.));
#22566=DIRECTION('ref_axis',(1.,0.,0.));
#22567=DIRECTION('center_axis',(0.,0.,-1.));
#22568=DIRECTION('ref_axis',(1.,0.,0.));
#22569=DIRECTION('',(0.,0.,-1.));
#22570=DIRECTION('center_axis',(0.,0.,1.));
#22571=DIRECTION('ref_axis',(1.,0.,0.));
#22572=DIRECTION('center_axis',(0.,0.,1.));
#22573=DIRECTION('ref_axis',(1.,0.,0.));
#22574=DIRECTION('center_axis',(0.,0.,1.));
#22575=DIRECTION('ref_axis',(1.,0.,0.));
#22576=DIRECTION('center_axis',(0.,0.,1.));
#22577=DIRECTION('ref_axis',(1.,0.,0.));
#22578=DIRECTION('center_axis',(0.,0.,1.));
#22579=DIRECTION('ref_axis',(1.,0.,0.));
#22580=DIRECTION('',(0.,0.,-1.));
#22581=DIRECTION('center_axis',(0.,0.,1.));
#22582=DIRECTION('ref_axis',(1.,0.,0.));
#22583=DIRECTION('',(0.,0.,-1.));
#22584=DIRECTION('center_axis',(0.,0.,1.));
#22585=DIRECTION('ref_axis',(1.,0.,0.));
#22586=DIRECTION('center_axis',(0.,0.,1.));
#22587=DIRECTION('ref_axis',(1.,0.,0.));
#22588=DIRECTION('center_axis',(0.,0.,1.));
#22589=DIRECTION('ref_axis',(1.,0.,0.));
#22590=DIRECTION('axis',(0.,0.,1.));
#22591=DIRECTION('refdir',(1.,0.,0.));
#22592=DIRECTION('center_axis',(0.,1.,0.));
#22593=DIRECTION('ref_axis',(0.,0.,1.));
#22594=DIRECTION('',(0.,0.,-1.));
#22595=DIRECTION('',(1.,0.,0.));
#22596=DIRECTION('',(0.,0.,1.));
#22597=DIRECTION('',(1.,0.,0.));
#22598=DIRECTION('center_axis',(1.,0.,0.));
#22599=DIRECTION('ref_axis',(0.,-1.,0.));
#22600=DIRECTION('center_axis',(1.,0.,0.));
#22601=DIRECTION('ref_axis',(0.,-1.,0.));
#22602=DIRECTION('center_axis',(1.,0.,0.));
#22603=DIRECTION('ref_axis',(0.,-1.,0.));
#22604=DIRECTION('',(1.,0.,0.));
#22605=DIRECTION('center_axis',(0.,-1.,0.));
#22606=DIRECTION('ref_axis',(0.,0.,-1.));
#22607=DIRECTION('',(0.,0.,1.));
#22608=DIRECTION('',(0.,0.,-1.));
#22609=DIRECTION('',(1.,0.,0.));
#22610=DIRECTION('center_axis',(1.,0.,0.));
#22611=DIRECTION('ref_axis',(0.,1.,0.));
#22612=DIRECTION('center_axis',(1.,0.,0.));
#22613=DIRECTION('ref_axis',(0.,1.,0.));
#22614=DIRECTION('center_axis',(1.,0.,0.));
#22615=DIRECTION('ref_axis',(0.,1.,0.));
#22616=DIRECTION('center_axis',(1.,0.,0.));
#22617=DIRECTION('ref_axis',(0.,0.,-1.));
#22618=DIRECTION('center_axis',(1.,0.,0.));
#22619=DIRECTION('ref_axis',(0.,0.,-1.));
#22620=DIRECTION('axis',(0.,0.,1.));
#22621=DIRECTION('refdir',(1.,0.,0.));
#22622=DIRECTION('center_axis',(0.,0.,1.));
#22623=DIRECTION('ref_axis',(1.,0.,0.));
#22624=DIRECTION('center_axis',(0.,0.,1.));
#22625=DIRECTION('ref_axis',(1.,0.,0.));
#22626=DIRECTION('',(0.,0.,-1.));
#22627=DIRECTION('center_axis',(0.,0.,1.));
#22628=DIRECTION('ref_axis',(1.,0.,0.));
#22629=DIRECTION('center_axis',(0.,0.,1.));
#22630=DIRECTION('ref_axis',(1.,0.,0.));
#22631=DIRECTION('center_axis',(0.,0.,1.));
#22632=DIRECTION('ref_axis',(1.,0.,0.));
#22633=DIRECTION('axis',(0.,0.,1.));
#22634=DIRECTION('refdir',(1.,0.,0.));
#22635=DIRECTION('center_axis',(0.,0.,-1.));
#22636=DIRECTION('ref_axis',(1.,0.,0.));
#22637=DIRECTION('center_axis',(0.,0.,-1.));
#22638=DIRECTION('ref_axis',(1.,0.,0.));
#22639=DIRECTION('center_axis',(0.,0.,-1.));
#22640=DIRECTION('ref_axis',(1.,0.,0.));
#22641=DIRECTION('center_axis',(0.,0.,-1.));
#22642=DIRECTION('ref_axis',(1.,0.,0.));
#22643=DIRECTION('center_axis',(0.,0.,-1.));
#22644=DIRECTION('ref_axis',(1.,0.,0.));
#22645=DIRECTION('',(0.,0.,-1.));
#22646=DIRECTION('center_axis',(0.,0.,-1.));
#22647=DIRECTION('ref_axis',(1.,0.,0.));
#22648=DIRECTION('',(0.,0.,-1.));
#22649=DIRECTION('center_axis',(0.,0.,1.));
#22650=DIRECTION('ref_axis',(1.,0.,0.));
#22651=DIRECTION('center_axis',(0.,0.,-1.));
#22652=DIRECTION('ref_axis',(1.,0.,0.));
#22653=DIRECTION('center_axis',(0.,0.,-1.));
#22654=DIRECTION('ref_axis',(1.,0.,0.));
#22655=DIRECTION('center_axis',(0.,0.,-1.));
#22656=DIRECTION('ref_axis',(1.,0.,0.));
#22657=DIRECTION('center_axis',(0.,0.,-1.));
#22658=DIRECTION('ref_axis',(1.,0.,0.));
#22659=DIRECTION('center_axis',(0.,0.,-1.));
#22660=DIRECTION('ref_axis',(1.,0.,0.));
#22661=DIRECTION('',(0.,0.,-1.));
#22662=DIRECTION('center_axis',(0.,0.,-1.));
#22663=DIRECTION('ref_axis',(1.,0.,0.));
#22664=DIRECTION('',(0.,0.,-1.));
#22665=DIRECTION('center_axis',(0.,0.,1.));
#22666=DIRECTION('ref_axis',(1.,0.,0.));
#22667=DIRECTION('center_axis',(0.,0.,-1.));
#22668=DIRECTION('ref_axis',(1.,0.,0.));
#22669=DIRECTION('center_axis',(0.,0.,-1.));
#22670=DIRECTION('ref_axis',(1.,0.,0.));
#22671=DIRECTION('center_axis',(0.,0.,-1.));
#22672=DIRECTION('ref_axis',(1.,0.,0.));
#22673=DIRECTION('center_axis',(0.,0.,-1.));
#22674=DIRECTION('ref_axis',(1.,0.,0.));
#22675=DIRECTION('center_axis',(0.,0.,-1.));
#22676=DIRECTION('ref_axis',(1.,0.,0.));
#22677=DIRECTION('',(0.,0.,-1.));
#22678=DIRECTION('center_axis',(0.,0.,-1.));
#22679=DIRECTION('ref_axis',(1.,0.,0.));
#22680=DIRECTION('',(0.,0.,-1.));
#22681=DIRECTION('center_axis',(0.,0.,1.));
#22682=DIRECTION('ref_axis',(1.,0.,0.));
#22683=DIRECTION('center_axis',(0.,0.,-1.));
#22684=DIRECTION('ref_axis',(1.,0.,0.));
#22685=DIRECTION('center_axis',(0.,0.,-1.));
#22686=DIRECTION('ref_axis',(1.,0.,0.));
#22687=DIRECTION('center_axis',(0.,0.,-1.));
#22688=DIRECTION('ref_axis',(1.,0.,0.));
#22689=DIRECTION('center_axis',(0.,0.,-1.));
#22690=DIRECTION('ref_axis',(1.,0.,0.));
#22691=DIRECTION('center_axis',(0.,0.,-1.));
#22692=DIRECTION('ref_axis',(1.,0.,0.));
#22693=DIRECTION('',(0.,0.,-1.));
#22694=DIRECTION('center_axis',(0.,0.,-1.));
#22695=DIRECTION('ref_axis',(1.,0.,0.));
#22696=DIRECTION('',(0.,0.,-1.));
#22697=DIRECTION('center_axis',(0.,0.,1.));
#22698=DIRECTION('ref_axis',(1.,0.,0.));
#22699=DIRECTION('center_axis',(0.,0.,-1.));
#22700=DIRECTION('ref_axis',(1.,0.,0.));
#22701=DIRECTION('center_axis',(0.,0.,-1.));
#22702=DIRECTION('ref_axis',(1.,0.,0.));
#22703=DIRECTION('center_axis',(0.,0.,-1.));
#22704=DIRECTION('ref_axis',(1.,0.,0.));
#22705=DIRECTION('center_axis',(0.,0.,-1.));
#22706=DIRECTION('ref_axis',(1.,0.,0.));
#22707=DIRECTION('center_axis',(0.,0.,-1.));
#22708=DIRECTION('ref_axis',(1.,0.,0.));
#22709=DIRECTION('',(0.,0.,-1.));
#22710=DIRECTION('center_axis',(0.,0.,-1.));
#22711=DIRECTION('ref_axis',(1.,0.,0.));
#22712=DIRECTION('',(0.,0.,-1.));
#22713=DIRECTION('center_axis',(0.,0.,1.));
#22714=DIRECTION('ref_axis',(1.,0.,0.));
#22715=DIRECTION('center_axis',(0.,0.,-1.));
#22716=DIRECTION('ref_axis',(1.,0.,0.));
#22717=DIRECTION('center_axis',(0.,0.,-1.));
#22718=DIRECTION('ref_axis',(1.,0.,0.));
#22719=DIRECTION('center_axis',(0.,0.,-1.));
#22720=DIRECTION('ref_axis',(1.,0.,0.));
#22721=DIRECTION('center_axis',(0.,0.,-1.));
#22722=DIRECTION('ref_axis',(1.,0.,0.));
#22723=DIRECTION('center_axis',(0.,0.,-1.));
#22724=DIRECTION('ref_axis',(1.,0.,0.));
#22725=DIRECTION('',(0.,0.,-1.));
#22726=DIRECTION('center_axis',(0.,0.,-1.));
#22727=DIRECTION('ref_axis',(1.,0.,0.));
#22728=DIRECTION('',(0.,0.,-1.));
#22729=DIRECTION('center_axis',(0.,0.,1.));
#22730=DIRECTION('ref_axis',(1.,0.,0.));
#22731=DIRECTION('center_axis',(0.,0.,1.));
#22732=DIRECTION('ref_axis',(1.,0.,0.));
#22733=DIRECTION('center_axis',(0.,0.,-1.));
#22734=DIRECTION('ref_axis',(1.,0.,0.));
#22735=DIRECTION('',(0.,0.,-1.));
#22736=DIRECTION('center_axis',(0.,0.,-1.));
#22737=DIRECTION('ref_axis',(1.,0.,0.));
#22738=DIRECTION('center_axis',(0.,0.,1.));
#22739=DIRECTION('ref_axis',(1.,0.,0.));
#22740=DIRECTION('center_axis',(0.,0.,1.));
#22741=DIRECTION('ref_axis',(1.,0.,0.));
#22742=DIRECTION('',(0.,0.,-1.));
#22743=DIRECTION('center_axis',(0.,0.,1.));
#22744=DIRECTION('ref_axis',(1.,0.,0.));
#22745=DIRECTION('center_axis',(0.,0.,1.));
#22746=DIRECTION('ref_axis',(1.,0.,0.));
#22747=DIRECTION('center_axis',(0.,0.,1.));
#22748=DIRECTION('ref_axis',(1.,0.,0.));
#22749=DIRECTION('axis',(0.,0.,1.));
#22750=DIRECTION('refdir',(1.,0.,0.));
#22751=DIRECTION('center_axis',(0.,0.,1.));
#22752=DIRECTION('ref_axis',(1.,0.,0.));
#22753=DIRECTION('center_axis',(0.,0.,-1.));
#22754=DIRECTION('ref_axis',(1.,0.,0.));
#22755=DIRECTION('',(0.,0.,-1.));
#22756=DIRECTION('center_axis',(0.,0.,-1.));
#22757=DIRECTION('ref_axis',(1.,0.,0.));
#22758=DIRECTION('center_axis',(0.,0.,1.));
#22759=DIRECTION('ref_axis',(1.,0.,0.));
#22760=DIRECTION('center_axis',(0.,0.,1.));
#22761=DIRECTION('ref_axis',(1.,0.,0.));
#22762=DIRECTION('',(0.,0.,-1.));
#22763=DIRECTION('center_axis',(0.,0.,1.));
#22764=DIRECTION('ref_axis',(1.,0.,0.));
#22765=DIRECTION('center_axis',(0.,0.,1.));
#22766=DIRECTION('ref_axis',(1.,0.,0.));
#22767=DIRECTION('center_axis',(0.,0.,1.));
#22768=DIRECTION('ref_axis',(1.,0.,0.));
#22769=DIRECTION('axis',(0.,0.,1.));
#22770=DIRECTION('refdir',(1.,0.,0.));
#22771=DIRECTION('center_axis',(0.,0.,1.));
#22772=DIRECTION('ref_axis',(1.,0.,0.));
#22773=DIRECTION('center_axis',(0.,0.,-1.));
#22774=DIRECTION('ref_axis',(1.,0.,0.));
#22775=DIRECTION('',(0.707106781186547,-8.65956056235493E-17,-0.707106781186548));
#22776=DIRECTION('center_axis',(0.,0.,-1.));
#22777=DIRECTION('ref_axis',(1.,0.,0.));
#22778=DIRECTION('center_axis',(0.,0.,-1.));
#22779=DIRECTION('ref_axis',(1.,0.,0.));
#22780=DIRECTION('',(0.,0.,-1.));
#22781=DIRECTION('center_axis',(0.,0.,1.));
#22782=DIRECTION('ref_axis',(1.,0.,0.));
#22783=DIRECTION('center_axis',(0.,0.,1.));
#22784=DIRECTION('ref_axis',(1.,0.,0.));
#22785=DIRECTION('center_axis',(0.,0.,-1.));
#22786=DIRECTION('ref_axis',(1.,0.,0.));
#22787=DIRECTION('',(0.707106781186547,-8.65956056235493E-17,-0.707106781186548));
#22788=DIRECTION('center_axis',(0.,0.,-1.));
#22789=DIRECTION('ref_axis',(1.,0.,0.));
#22790=DIRECTION('center_axis',(0.,0.,-1.));
#22791=DIRECTION('ref_axis',(1.,0.,0.));
#22792=DIRECTION('',(0.,0.,-1.));
#22793=DIRECTION('center_axis',(0.,0.,1.));
#22794=DIRECTION('ref_axis',(1.,0.,0.));
#22795=DIRECTION('center_axis',(0.,0.,1.));
#22796=DIRECTION('ref_axis',(1.,0.,0.));
#22797=DIRECTION('center_axis',(0.,0.,-1.));
#22798=DIRECTION('ref_axis',(1.,0.,0.));
#22799=DIRECTION('',(0.707106781186547,-8.65956056235493E-17,-0.707106781186548));
#22800=DIRECTION('center_axis',(0.,0.,-1.));
#22801=DIRECTION('ref_axis',(1.,0.,0.));
#22802=DIRECTION('center_axis',(0.,0.,-1.));
#22803=DIRECTION('ref_axis',(1.,0.,0.));
#22804=DIRECTION('',(0.,0.,-1.));
#22805=DIRECTION('center_axis',(0.,0.,1.));
#22806=DIRECTION('ref_axis',(1.,0.,0.));
#22807=DIRECTION('center_axis',(0.,0.,1.));
#22808=DIRECTION('ref_axis',(1.,0.,0.));
#22809=DIRECTION('center_axis',(0.,0.,-1.));
#22810=DIRECTION('ref_axis',(1.,0.,0.));
#22811=DIRECTION('',(0.707106781186547,-8.65956056235493E-17,-0.707106781186548));
#22812=DIRECTION('center_axis',(0.,0.,-1.));
#22813=DIRECTION('ref_axis',(1.,0.,0.));
#22814=DIRECTION('center_axis',(0.,0.,-1.));
#22815=DIRECTION('ref_axis',(1.,0.,0.));
#22816=DIRECTION('',(0.,0.,-1.));
#22817=DIRECTION('center_axis',(0.,0.,1.));
#22818=DIRECTION('ref_axis',(1.,0.,0.));
#22819=DIRECTION('center_axis',(0.,0.,1.));
#22820=DIRECTION('ref_axis',(1.,0.,0.));
#22821=DIRECTION('center_axis',(0.,0.,-1.));
#22822=DIRECTION('ref_axis',(1.,0.,0.));
#22823=DIRECTION('',(0.707106781186547,-8.65956056235493E-17,-0.707106781186548));
#22824=DIRECTION('center_axis',(0.,0.,-1.));
#22825=DIRECTION('ref_axis',(1.,0.,0.));
#22826=DIRECTION('center_axis',(0.,0.,-1.));
#22827=DIRECTION('ref_axis',(1.,0.,0.));
#22828=DIRECTION('',(0.,0.,-1.));
#22829=DIRECTION('center_axis',(0.,0.,1.));
#22830=DIRECTION('ref_axis',(1.,0.,0.));
#22831=DIRECTION('center_axis',(0.,0.,1.));
#22832=DIRECTION('ref_axis',(1.,0.,0.));
#22833=DIRECTION('center_axis',(0.,0.,-1.));
#22834=DIRECTION('ref_axis',(1.,0.,0.));
#22835=DIRECTION('',(0.707106781186547,-8.65956056235493E-17,-0.707106781186548));
#22836=DIRECTION('center_axis',(0.,0.,-1.));
#22837=DIRECTION('ref_axis',(1.,0.,0.));
#22838=DIRECTION('center_axis',(0.,0.,-1.));
#22839=DIRECTION('ref_axis',(1.,0.,0.));
#22840=DIRECTION('',(0.,0.,-1.));
#22841=DIRECTION('center_axis',(0.,0.,1.));
#22842=DIRECTION('ref_axis',(1.,0.,0.));
#22843=DIRECTION('center_axis',(0.,0.,1.));
#22844=DIRECTION('ref_axis',(1.,0.,0.));
#22845=DIRECTION('center_axis',(0.,0.,-1.));
#22846=DIRECTION('ref_axis',(1.,0.,0.));
#22847=DIRECTION('',(0.,0.,-1.));
#22848=DIRECTION('center_axis',(0.,0.,-1.));
#22849=DIRECTION('ref_axis',(1.,0.,0.));
#22850=DIRECTION('center_axis',(0.,0.,1.));
#22851=DIRECTION('ref_axis',(1.,0.,0.));
#22852=DIRECTION('center_axis',(0.,0.,1.));
#22853=DIRECTION('ref_axis',(1.,0.,0.));
#22854=DIRECTION('',(0.,0.,-1.));
#22855=DIRECTION('center_axis',(0.,0.,1.));
#22856=DIRECTION('ref_axis',(1.,0.,0.));
#22857=DIRECTION('center_axis',(0.,0.,1.));
#22858=DIRECTION('ref_axis',(1.,0.,0.));
#22859=DIRECTION('center_axis',(0.,0.,1.));
#22860=DIRECTION('ref_axis',(1.,0.,0.));
#22861=DIRECTION('axis',(0.,0.,1.));
#22862=DIRECTION('refdir',(1.,0.,0.));
#22863=DIRECTION('center_axis',(0.,0.,1.));
#22864=DIRECTION('ref_axis',(1.,0.,0.));
#22865=DIRECTION('center_axis',(0.,0.,-1.));
#22866=DIRECTION('ref_axis',(1.,0.,0.));
#22867=DIRECTION('',(0.,0.,-1.));
#22868=DIRECTION('center_axis',(0.,0.,-1.));
#22869=DIRECTION('ref_axis',(1.,0.,0.));
#22870=DIRECTION('center_axis',(0.,0.,1.));
#22871=DIRECTION('ref_axis',(1.,0.,0.));
#22872=DIRECTION('center_axis',(0.,0.,1.));
#22873=DIRECTION('ref_axis',(1.,0.,0.));
#22874=DIRECTION('',(0.,0.,-1.));
#22875=DIRECTION('center_axis',(0.,0.,1.));
#22876=DIRECTION('ref_axis',(1.,0.,0.));
#22877=DIRECTION('center_axis',(0.,0.,1.));
#22878=DIRECTION('ref_axis',(1.,0.,0.));
#22879=DIRECTION('center_axis',(0.,0.,1.));
#22880=DIRECTION('ref_axis',(1.,0.,0.));
#22881=DIRECTION('axis',(0.,0.,1.));
#22882=DIRECTION('refdir',(1.,0.,0.));
#22883=DIRECTION('center_axis',(0.,0.,1.));
#22884=DIRECTION('ref_axis',(1.,0.,0.));
#22885=DIRECTION('center_axis',(0.,0.,-1.));
#22886=DIRECTION('ref_axis',(1.,0.,0.));
#22887=DIRECTION('',(0.,0.,-1.));
#22888=DIRECTION('center_axis',(0.,0.,-1.));
#22889=DIRECTION('ref_axis',(1.,0.,0.));
#22890=DIRECTION('center_axis',(0.,0.,1.));
#22891=DIRECTION('ref_axis',(1.,0.,0.));
#22892=DIRECTION('center_axis',(0.,0.,1.));
#22893=DIRECTION('ref_axis',(1.,0.,0.));
#22894=DIRECTION('',(0.,0.,-1.));
#22895=DIRECTION('center_axis',(0.,0.,1.));
#22896=DIRECTION('ref_axis',(1.,0.,0.));
#22897=DIRECTION('center_axis',(0.,0.,1.));
#22898=DIRECTION('ref_axis',(1.,0.,0.));
#22899=DIRECTION('center_axis',(0.,0.,1.));
#22900=DIRECTION('ref_axis',(1.,0.,0.));
#22901=DIRECTION('axis',(0.,0.,1.));
#22902=DIRECTION('refdir',(1.,0.,0.));
#22903=DIRECTION('center_axis',(0.,0.,1.));
#22904=DIRECTION('ref_axis',(1.,0.,0.));
#22905=DIRECTION('center_axis',(0.,0.,-1.));
#22906=DIRECTION('ref_axis',(1.,0.,0.));
#22907=DIRECTION('',(0.,0.,-1.));
#22908=DIRECTION('center_axis',(0.,0.,-1.));
#22909=DIRECTION('ref_axis',(1.,0.,0.));
#22910=DIRECTION('center_axis',(0.,0.,1.));
#22911=DIRECTION('ref_axis',(1.,0.,0.));
#22912=DIRECTION('center_axis',(0.,0.,1.));
#22913=DIRECTION('ref_axis',(1.,0.,0.));
#22914=DIRECTION('',(0.,0.,-1.));
#22915=DIRECTION('center_axis',(0.,0.,1.));
#22916=DIRECTION('ref_axis',(1.,0.,0.));
#22917=DIRECTION('center_axis',(0.,0.,1.));
#22918=DIRECTION('ref_axis',(1.,0.,0.));
#22919=DIRECTION('center_axis',(0.,0.,1.));
#22920=DIRECTION('ref_axis',(1.,0.,0.));
#22921=DIRECTION('axis',(0.,0.,1.));
#22922=DIRECTION('refdir',(1.,0.,0.));
#22923=DIRECTION('center_axis',(-1.,0.,0.));
#22924=DIRECTION('ref_axis',(0.,1.,0.));
#22925=DIRECTION('',(0.,0.,1.));
#22926=DIRECTION('',(0.,-1.,0.));
#22927=DIRECTION('',(0.,0.,-1.));
#22928=DIRECTION('',(0.,1.,0.));
#22929=DIRECTION('center_axis',(1.,0.,0.));
#22930=DIRECTION('ref_axis',(0.,-1.,0.));
#22931=DIRECTION('',(0.,0.,-1.));
#22932=DIRECTION('',(0.,-1.,0.));
#22933=DIRECTION('',(0.,0.,1.));
#22934=DIRECTION('',(0.,1.,0.));
#22935=DIRECTION('center_axis',(0.,0.,1.));
#22936=DIRECTION('ref_axis',(1.,0.,0.));
#22937=DIRECTION('center_axis',(0.,0.,1.));
#22938=DIRECTION('ref_axis',(1.,0.,0.));
#22939=DIRECTION('center_axis',(0.,0.,-1.));
#22940=DIRECTION('ref_axis',(1.,0.,0.));
#22941=DIRECTION('center_axis',(0.,0.,1.));
#22942=DIRECTION('ref_axis',(6.12323399573677E-17,-1.,0.));
#22943=DIRECTION('center_axis',(0.,0.,-1.));
#22944=DIRECTION('ref_axis',(1.,0.,0.));
#22945=DIRECTION('center_axis',(0.,0.,1.));
#22946=DIRECTION('ref_axis',(6.12323399573677E-17,-1.,0.));
#22947=DIRECTION('center_axis',(0.,0.,1.));
#22948=DIRECTION('ref_axis',(1.,0.,0.));
#22949=DIRECTION('center_axis',(0.,0.,1.));
#22950=DIRECTION('ref_axis',(1.,0.,0.));
#22951=DIRECTION('axis',(0.,0.,1.));
#22952=DIRECTION('refdir',(1.,0.,0.));
#22953=DIRECTION('center_axis',(0.,0.,1.));
#22954=DIRECTION('ref_axis',(1.,0.,0.));
#22955=DIRECTION('center_axis',(0.,0.,1.));
#22956=DIRECTION('ref_axis',(1.,0.,0.));
#22957=DIRECTION('center_axis',(0.,0.,1.));
#22958=DIRECTION('ref_axis',(1.,0.,0.));
#22959=DIRECTION('center_axis',(0.,0.,1.));
#22960=DIRECTION('ref_axis',(1.,0.,0.));
#22961=DIRECTION('center_axis',(0.,0.,1.));
#22962=DIRECTION('ref_axis',(1.,0.,0.));
#22963=DIRECTION('',(0.,0.,-1.));
#22964=DIRECTION('center_axis',(0.,0.,1.));
#22965=DIRECTION('ref_axis',(1.,0.,0.));
#22966=DIRECTION('center_axis',(0.,0.,1.));
#22967=DIRECTION('ref_axis',(1.,0.,0.));
#22968=DIRECTION('',(0.,0.,-1.));
#22969=DIRECTION('center_axis',(0.,0.,1.));
#22970=DIRECTION('ref_axis',(1.,0.,0.));
#22971=DIRECTION('center_axis',(0.,0.,1.));
#22972=DIRECTION('ref_axis',(1.,0.,0.));
#22973=DIRECTION('axis',(0.,0.,1.));
#22974=DIRECTION('refdir',(1.,0.,0.));
#22975=DIRECTION('center_axis',(0.,0.,-1.));
#22976=DIRECTION('ref_axis',(-1.,0.,0.));
#22977=DIRECTION('center_axis',(4.89858719658941E-16,0.,-1.));
#22978=DIRECTION('ref_axis',(-1.,0.,-4.89858719658941E-16));
#22979=DIRECTION('center_axis',(-4.89858719658941E-16,0.,1.));
#22980=DIRECTION('ref_axis',(1.,0.,4.89858719658941E-16));
#22981=DIRECTION('center_axis',(0.,0.,1.));
#22982=DIRECTION('ref_axis',(1.,0.,0.));
#22983=DIRECTION('axis',(0.,0.,1.));
#22984=DIRECTION('refdir',(1.,0.,0.));
#22985=DIRECTION('center_axis',(0.,0.,1.));
#22986=DIRECTION('ref_axis',(1.,0.,0.));
#22987=DIRECTION('',(0.,0.,-1.));
#22988=DIRECTION('center_axis',(0.,0.,-1.));
#22989=DIRECTION('ref_axis',(1.,0.,0.));
#22990=DIRECTION('center_axis',(0.,0.,1.));
#22991=DIRECTION('ref_axis',(1.,0.,0.));
#22992=DIRECTION('',(0.,0.,-1.));
#22993=DIRECTION('center_axis',(0.,0.,1.));
#22994=DIRECTION('ref_axis',(1.,0.,0.));
#22995=DIRECTION('',(0.,0.,-1.));
#22996=DIRECTION('center_axis',(0.,0.,1.));
#22997=DIRECTION('ref_axis',(1.,0.,0.));
#22998=DIRECTION('',(0.,0.,-1.));
#22999=DIRECTION('center_axis',(0.,0.,1.));
#23000=DIRECTION('ref_axis',(1.,0.,0.));
#23001=DIRECTION('',(0.,0.,-1.));
#23002=DIRECTION('center_axis',(0.,0.,1.));
#23003=DIRECTION('ref_axis',(1.,0.,0.));
#23004=DIRECTION('',(0.,0.,-1.));
#23005=DIRECTION('center_axis',(0.,0.,1.));
#23006=DIRECTION('ref_axis',(1.,0.,0.));
#23007=DIRECTION('',(0.,0.,-1.));
#23008=DIRECTION('center_axis',(0.,0.,1.));
#23009=DIRECTION('ref_axis',(1.,0.,0.));
#23010=DIRECTION('',(0.,0.,-1.));
#23011=DIRECTION('center_axis',(0.,0.,1.));
#23012=DIRECTION('ref_axis',(1.,0.,0.));
#23013=DIRECTION('',(0.,0.,-1.));
#23014=DIRECTION('center_axis',(0.,0.,1.));
#23015=DIRECTION('ref_axis',(1.,0.,0.));
#23016=DIRECTION('',(0.,0.,-1.));
#23017=DIRECTION('center_axis',(0.,0.,1.));
#23018=DIRECTION('ref_axis',(1.,0.,0.));
#23019=DIRECTION('',(0.,0.,-1.));
#23020=DIRECTION('center_axis',(0.,0.,1.));
#23021=DIRECTION('ref_axis',(1.,0.,0.));
#23022=DIRECTION('',(0.,0.,-1.));
#23023=DIRECTION('center_axis',(0.,0.,1.));
#23024=DIRECTION('ref_axis',(1.,0.,0.));
#23025=DIRECTION('',(0.,0.,-1.));
#23026=DIRECTION('center_axis',(0.,0.,1.));
#23027=DIRECTION('ref_axis',(1.,0.,0.));
#23028=DIRECTION('',(0.,0.,-1.));
#23029=DIRECTION('center_axis',(0.,0.,1.));
#23030=DIRECTION('ref_axis',(1.,0.,0.));
#23031=DIRECTION('',(0.,0.,-1.));
#23032=DIRECTION('center_axis',(0.,0.,1.));
#23033=DIRECTION('ref_axis',(1.,0.,0.));
#23034=DIRECTION('',(0.,0.,-1.));
#23035=DIRECTION('center_axis',(0.,0.,1.));
#23036=DIRECTION('ref_axis',(1.,1.29731060939901E-13,0.));
#23037=DIRECTION('',(0.,0.,1.));
#23038=DIRECTION('center_axis',(0.,0.,-1.));
#23039=DIRECTION('ref_axis',(1.,1.29731060939901E-13,0.));
#23040=DIRECTION('center_axis',(0.,0.,1.));
#23041=DIRECTION('ref_axis',(1.,1.29731060939901E-13,0.));
#23042=DIRECTION('',(0.,0.,1.));
#23043=DIRECTION('center_axis',(0.,0.,1.));
#23044=DIRECTION('ref_axis',(1.,1.29731060939901E-13,0.));
#23045=DIRECTION('',(0.,0.,1.));
#23046=DIRECTION('center_axis',(0.,0.,1.));
#23047=DIRECTION('ref_axis',(1.,1.29731060939901E-13,0.));
#23048=DIRECTION('',(0.,0.,1.));
#23049=DIRECTION('center_axis',(0.,0.,1.));
#23050=DIRECTION('ref_axis',(1.,1.29731060939901E-13,0.));
#23051=DIRECTION('',(0.,0.,1.));
#23052=DIRECTION('center_axis',(0.,0.,1.));
#23053=DIRECTION('ref_axis',(1.,1.29731060939901E-13,0.));
#23054=DIRECTION('',(0.,0.,1.));
#23055=DIRECTION('center_axis',(0.,0.,1.));
#23056=DIRECTION('ref_axis',(1.,1.29731060939901E-13,0.));
#23057=DIRECTION('',(0.,0.,1.));
#23058=DIRECTION('center_axis',(0.,0.,1.));
#23059=DIRECTION('ref_axis',(1.,1.29731060939901E-13,0.));
#23060=DIRECTION('',(0.,0.,1.));
#23061=DIRECTION('center_axis',(0.,0.,1.));
#23062=DIRECTION('ref_axis',(1.,1.29731060939901E-13,0.));
#23063=DIRECTION('',(0.,0.,1.));
#23064=DIRECTION('center_axis',(0.,0.,1.));
#23065=DIRECTION('ref_axis',(1.,1.29731060939901E-13,0.));
#23066=DIRECTION('',(0.,0.,1.));
#23067=DIRECTION('center_axis',(0.,0.,1.));
#23068=DIRECTION('ref_axis',(1.,1.29731060939901E-13,0.));
#23069=DIRECTION('',(0.,0.,1.));
#23070=DIRECTION('center_axis',(0.,0.,1.));
#23071=DIRECTION('ref_axis',(1.,1.29731060939901E-13,0.));
#23072=DIRECTION('',(0.,0.,1.));
#23073=DIRECTION('center_axis',(0.,0.,1.));
#23074=DIRECTION('ref_axis',(1.,1.29731060939901E-13,0.));
#23075=DIRECTION('',(0.,0.,1.));
#23076=DIRECTION('center_axis',(0.,0.,1.));
#23077=DIRECTION('ref_axis',(1.,1.29731060939901E-13,0.));
#23078=DIRECTION('',(0.,0.,1.));
#23079=DIRECTION('center_axis',(0.,0.,1.));
#23080=DIRECTION('ref_axis',(1.,1.29731060939901E-13,0.));
#23081=DIRECTION('',(0.,0.,1.));
#23082=DIRECTION('center_axis',(0.,0.,1.));
#23083=DIRECTION('ref_axis',(1.,1.29731060939901E-13,0.));
#23084=DIRECTION('',(0.,0.,1.));
#23085=DIRECTION('center_axis',(0.,0.,-1.));
#23086=DIRECTION('ref_axis',(1.,0.,0.));
#23087=DIRECTION('center_axis',(0.,0.,-1.));
#23088=DIRECTION('ref_axis',(1.,0.,0.));
#23089=DIRECTION('',(0.707106781186548,8.65956056235494E-17,0.707106781186547));
#23090=DIRECTION('center_axis',(0.,0.,1.));
#23091=DIRECTION('ref_axis',(1.,0.,0.));
#23092=DIRECTION('center_axis',(0.,0.,1.));
#23093=DIRECTION('ref_axis',(1.,1.29731060939901E-13,0.));
#23094=DIRECTION('center_axis',(0.,0.,-1.));
#23095=DIRECTION('ref_axis',(1.,1.29731060939901E-13,0.));
#23096=DIRECTION('center_axis',(0.,0.,1.));
#23097=DIRECTION('ref_axis',(1.,0.,0.));
#23098=DIRECTION('center_axis',(-1.60246890531964E-16,-1.,0.));
#23099=DIRECTION('ref_axis',(1.,-1.60246890531964E-16,0.));
#23100=DIRECTION('',(1.,-1.60246890531964E-16,0.));
#23101=DIRECTION('',(0.,0.,1.));
#23102=DIRECTION('',(1.,-1.60246890531964E-16,0.));
#23103=DIRECTION('',(0.,0.,1.));
#23104=DIRECTION('center_axis',(-0.866025403784439,-0.5,0.));
#23105=DIRECTION('ref_axis',(0.5,-0.866025403784439,0.));
#23106=DIRECTION('',(0.5,-0.866025403784439,0.));
#23107=DIRECTION('',(0.,0.,1.));
#23108=DIRECTION('',(0.5,-0.866025403784439,0.));
#23109=DIRECTION('center_axis',(-0.866025403784439,0.5,0.));
#23110=DIRECTION('ref_axis',(-0.5,-0.866025403784439,0.));
#23111=DIRECTION('',(-0.5,-0.866025403784439,0.));
#23112=DIRECTION('',(0.,0.,1.));
#23113=DIRECTION('',(-0.5,-0.866025403784439,0.));
#23114=DIRECTION('center_axis',(1.60246890531964E-16,1.,0.));
#23115=DIRECTION('ref_axis',(-1.,1.60246890531964E-16,0.));
#23116=DIRECTION('',(-1.,1.60246890531964E-16,0.));
#23117=DIRECTION('',(0.,0.,1.));
#23118=DIRECTION('',(-1.,1.60246890531964E-16,0.));
#23119=DIRECTION('center_axis',(0.866025403784439,0.5,0.));
#23120=DIRECTION('ref_axis',(-0.5,0.866025403784439,0.));
#23121=DIRECTION('',(-0.5,0.866025403784439,0.));
#23122=DIRECTION('',(0.,0.,1.));
#23123=DIRECTION('',(-0.5,0.866025403784439,0.));
#23124=DIRECTION('center_axis',(0.866025403784439,-0.5,0.));
#23125=DIRECTION('ref_axis',(0.5,0.866025403784439,0.));
#23126=DIRECTION('',(0.5,0.866025403784439,0.));
#23127=DIRECTION('',(0.5,0.866025403784439,0.));
#23128=DIRECTION('center_axis',(0.,0.,1.));
#23129=DIRECTION('ref_axis',(1.,0.,0.));
#23130=DIRECTION('center_axis',(0.,0.,1.));
#23131=DIRECTION('ref_axis',(1.,0.,0.));
#23132=DIRECTION('center_axis',(0.,0.,1.));
#23133=DIRECTION('ref_axis',(1.,0.,0.));
#23134=DIRECTION('center_axis',(0.,0.,1.));
#23135=DIRECTION('ref_axis',(1.,0.,0.));
#23136=DIRECTION('',(0.,0.,-1.));
#23137=DIRECTION('center_axis',(0.,0.,1.));
#23138=DIRECTION('ref_axis',(1.,0.,0.));
#23139=DIRECTION('center_axis',(0.,0.,1.));
#23140=DIRECTION('ref_axis',(1.,0.,0.));
#23141=DIRECTION('center_axis',(0.,0.,1.));
#23142=DIRECTION('ref_axis',(1.,0.,0.));
#23143=DIRECTION('axis',(0.,0.,1.));
#23144=DIRECTION('refdir',(1.,0.,0.));
#23145=DIRECTION('center_axis',(0.,0.,1.));
#23146=DIRECTION('ref_axis',(1.,0.,0.));
#23147=DIRECTION('',(0.,0.,-1.));
#23148=DIRECTION('center_axis',(0.,0.,-1.));
#23149=DIRECTION('ref_axis',(1.,0.,0.));
#23150=DIRECTION('center_axis',(0.,0.,1.));
#23151=DIRECTION('ref_axis',(1.,0.,0.));
#23152=DIRECTION('',(0.,0.,-1.));
#23153=DIRECTION('center_axis',(0.,0.,1.));
#23154=DIRECTION('ref_axis',(1.,0.,0.));
#23155=DIRECTION('',(0.,0.,-1.));
#23156=DIRECTION('center_axis',(0.,0.,1.));
#23157=DIRECTION('ref_axis',(1.,0.,0.));
#23158=DIRECTION('',(0.,0.,-1.));
#23159=DIRECTION('center_axis',(0.,0.,1.));
#23160=DIRECTION('ref_axis',(1.,0.,0.));
#23161=DIRECTION('',(0.,0.,-1.));
#23162=DIRECTION('center_axis',(0.,0.,1.));
#23163=DIRECTION('ref_axis',(1.,0.,0.));
#23164=DIRECTION('',(0.,0.,-1.));
#23165=DIRECTION('center_axis',(0.,0.,1.));
#23166=DIRECTION('ref_axis',(1.,0.,0.));
#23167=DIRECTION('',(0.,0.,-1.));
#23168=DIRECTION('center_axis',(0.,0.,1.));
#23169=DIRECTION('ref_axis',(1.,0.,0.));
#23170=DIRECTION('',(0.,0.,-1.));
#23171=DIRECTION('center_axis',(0.,0.,1.));
#23172=DIRECTION('ref_axis',(0.968655785309639,-0.24840686300134,0.));
#23173=DIRECTION('',(0.,0.,1.));
#23174=DIRECTION('center_axis',(0.,0.,-1.));
#23175=DIRECTION('ref_axis',(1.,4.0036529262094E-14,0.));
#23176=DIRECTION('center_axis',(0.,0.,1.));
#23177=DIRECTION('ref_axis',(1.,4.0036529262094E-14,0.));
#23178=DIRECTION('',(0.,0.,1.));
#23179=DIRECTION('center_axis',(0.,0.,1.));
#23180=DIRECTION('ref_axis',(1.,4.0036529262094E-14,0.));
#23181=DIRECTION('',(0.,0.,1.));
#23182=DIRECTION('center_axis',(0.,0.,1.));
#23183=DIRECTION('ref_axis',(1.,4.0036529262094E-14,0.));
#23184=DIRECTION('',(0.,0.,1.));
#23185=DIRECTION('center_axis',(0.,0.,1.));
#23186=DIRECTION('ref_axis',(1.,4.0036529262094E-14,0.));
#23187=DIRECTION('',(0.,0.,1.));
#23188=DIRECTION('center_axis',(0.,0.,1.));
#23189=DIRECTION('ref_axis',(1.,4.0036529262094E-14,0.));
#23190=DIRECTION('',(0.,0.,1.));
#23191=DIRECTION('center_axis',(0.,0.,1.));
#23192=DIRECTION('ref_axis',(1.,4.0036529262094E-14,0.));
#23193=DIRECTION('',(0.,0.,1.));
#23194=DIRECTION('center_axis',(0.,0.,1.));
#23195=DIRECTION('ref_axis',(1.,4.0036529262094E-14,0.));
#23196=DIRECTION('',(0.,0.,1.));
#23197=DIRECTION('center_axis',(0.,0.,-1.));
#23198=DIRECTION('ref_axis',(1.,0.,0.));
#23199=DIRECTION('center_axis',(0.,0.,-1.));
#23200=DIRECTION('ref_axis',(1.,0.,0.));
#23201=DIRECTION('',(0.707106781186548,8.65956056235494E-17,0.707106781186547));
#23202=DIRECTION('center_axis',(0.,0.,1.));
#23203=DIRECTION('ref_axis',(1.,0.,0.));
#23204=DIRECTION('center_axis',(0.,0.,1.));
#23205=DIRECTION('ref_axis',(1.,4.0036529262094E-14,0.));
#23206=DIRECTION('center_axis',(0.,0.,-1.));
#23207=DIRECTION('ref_axis',(1.,4.0036529262094E-14,0.));
#23208=DIRECTION('center_axis',(-2.40370335797945E-16,-1.,0.));
#23209=DIRECTION('ref_axis',(1.,-2.40370335797945E-16,0.));
#23210=DIRECTION('',(1.,-2.40370335797945E-16,0.));
#23211=DIRECTION('',(0.,0.,1.));
#23212=DIRECTION('',(1.,-2.40370335797945E-16,0.));
#23213=DIRECTION('',(0.,0.,1.));
#23214=DIRECTION('center_axis',(-0.866025403784439,-0.5,0.));
#23215=DIRECTION('ref_axis',(0.5,-0.866025403784439,0.));
#23216=DIRECTION('',(0.5,-0.866025403784439,0.));
#23217=DIRECTION('',(0.,0.,1.));
#23218=DIRECTION('',(0.5,-0.866025403784439,0.));
#23219=DIRECTION('center_axis',(-0.866025403784439,0.5,0.));
#23220=DIRECTION('ref_axis',(-0.5,-0.866025403784439,0.));
#23221=DIRECTION('',(-0.5,-0.866025403784439,0.));
#23222=DIRECTION('',(0.,0.,1.));
#23223=DIRECTION('',(-0.5,-0.866025403784439,0.));
#23224=DIRECTION('center_axis',(1.20185167898973E-16,1.,0.));
#23225=DIRECTION('ref_axis',(-1.,1.20185167898973E-16,0.));
#23226=DIRECTION('',(-1.,1.20185167898973E-16,0.));
#23227=DIRECTION('',(0.,0.,1.));
#23228=DIRECTION('',(-1.,1.20185167898973E-16,0.));
#23229=DIRECTION('center_axis',(0.866025403784439,0.5,0.));
#23230=DIRECTION('ref_axis',(-0.5,0.866025403784439,0.));
#23231=DIRECTION('',(-0.5,0.866025403784439,0.));
#23232=DIRECTION('',(0.,0.,1.));
#23233=DIRECTION('',(-0.5,0.866025403784439,0.));
#23234=DIRECTION('center_axis',(0.866025403784439,-0.5,0.));
#23235=DIRECTION('ref_axis',(0.5,0.866025403784439,0.));
#23236=DIRECTION('',(0.5,0.866025403784439,0.));
#23237=DIRECTION('',(0.5,0.866025403784439,0.));
#23238=DIRECTION('center_axis',(0.,0.,1.));
#23239=DIRECTION('ref_axis',(1.,0.,0.));
#23240=DIRECTION('center_axis',(0.,0.,1.));
#23241=DIRECTION('ref_axis',(1.,0.,0.));
#23242=DIRECTION('center_axis',(0.,0.,-1.));
#23243=DIRECTION('ref_axis',(1.,0.,0.));
#23244=DIRECTION('center_axis',(0.,0.,-1.));
#23245=DIRECTION('ref_axis',(1.,0.,0.));
#23246=DIRECTION('center_axis',(0.,0.,1.));
#23247=DIRECTION('ref_axis',(0.846289845614947,-0.532722720755394,0.));
#23248=DIRECTION('center_axis',(0.,0.,-1.));
#23249=DIRECTION('ref_axis',(-1.,0.,0.));
#23250=DIRECTION('center_axis',(0.,0.,1.));
#23251=DIRECTION('ref_axis',(1.,0.,0.));
#23252=DIRECTION('center_axis',(0.,0.,-1.));
#23253=DIRECTION('ref_axis',(1.,0.,0.));
#23254=DIRECTION('',(-0.707106781186548,-8.65956056235493E-17,-0.707106781186547));
#23255=DIRECTION('center_axis',(0.,0.,1.));
#23256=DIRECTION('ref_axis',(1.,0.,0.));
#23257=DIRECTION('',(0.,0.,1.));
#23258=DIRECTION('',(1.,0.,0.));
#23259=DIRECTION('',(0.,0.,1.));
#23260=DIRECTION('',(1.,0.,0.));
#23261=DIRECTION('',(0.,0.,1.));
#23262=DIRECTION('',(1.,0.,0.));
#23263=DIRECTION('',(0.,0.,1.));
#23264=DIRECTION('',(1.,0.,0.));
#23265=DIRECTION('',(0.,0.,1.));
#23266=DIRECTION('',(1.,0.,0.));
#23267=DIRECTION('',(0.,0.,1.));
#23268=DIRECTION('',(1.,0.,0.));
#23269=DIRECTION('',(0.,0.,1.));
#23270=DIRECTION('',(1.,0.,0.));
#23271=DIRECTION('',(0.,0.,1.));
#23272=DIRECTION('',(1.,0.,0.));
#23273=DIRECTION('',(0.,0.,1.));
#23274=DIRECTION('',(1.,0.,0.));
#23275=DIRECTION('',(0.,0.,1.));
#23276=DIRECTION('',(1.,0.,0.));
#23277=DIRECTION('',(0.,0.,1.));
#23278=DIRECTION('',(1.,0.,0.));
#23279=DIRECTION('',(0.,0.,1.));
#23280=DIRECTION('',(1.,0.,0.));
#23281=DIRECTION('',(0.,0.,1.));
#23282=DIRECTION('',(1.,0.,0.));
#23283=DIRECTION('',(0.,0.,1.));
#23284=DIRECTION('',(1.,0.,0.));
#23285=DIRECTION('',(0.,-1.22464679914735E-16,-1.));
#23286=DIRECTION('',(1.,0.,0.));
#23287=DIRECTION('',(0.,0.,1.));
#23288=DIRECTION('',(1.,0.,0.));
#23289=DIRECTION('',(6.17652310995481E-17,-1.05748068794839E-16,-1.));
#23290=DIRECTION('',(0.863498511313343,0.504351386396073,0.));
#23291=DIRECTION('',(0.,0.,1.));
#23292=DIRECTION('',(1.,0.,0.));
#23293=DIRECTION('',(0.,0.,1.));
#23294=DIRECTION('',(1.,0.,0.));
#23295=DIRECTION('',(0.,0.,1.));
#23296=DIRECTION('',(1.,0.,0.));
#23297=DIRECTION('',(0.,0.,1.));
#23298=DIRECTION('',(1.,0.,0.));
#23299=DIRECTION('',(-0.4486637512204,0.893700642464153,0.));
#23300=DIRECTION('',(0.893700642464153,0.4486637512204,0.));
#23301=DIRECTION('',(0.,0.,1.));
#23302=DIRECTION('',(0.893700642464153,0.4486637512204,0.));
#23303=DIRECTION('',(0.,0.,1.));
#23304=DIRECTION('',(1.,0.,0.));
#23305=DIRECTION('',(0.,0.,1.));
#23306=DIRECTION('',(1.,0.,0.));
#23307=DIRECTION('',(-0.99829933536263,0.0582961149179891,0.));
#23308=DIRECTION('',(0.0582961149179891,0.99829933536263,0.));
#23309=DIRECTION('',(-0.54963558414223,-0.835404527546164,0.));
#23310=DIRECTION('',(-0.835404527546164,0.54963558414223,0.));
#23311=DIRECTION('',(0.4486637512204,-0.893700642464153,0.));
#23312=DIRECTION('',(-0.893700642464153,-0.4486637512204,0.));
#23313=DIRECTION('',(0.99829933536263,-0.0582961149179892,0.));
#23314=DIRECTION('',(-0.0582961149179892,-0.99829933536263,0.));
#23315=DIRECTION('',(0.54963558414223,0.835404527546164,0.));
#23316=DIRECTION('',(0.835404527546164,-0.54963558414223,0.));
#23317=DIRECTION('',(0.,-1.22464679914735E-16,-1.));
#23318=DIRECTION('',(-0.766044443118978,-0.64278760968654,7.87187788734199E-17));
#23319=DIRECTION('',(0.,-1.22464679914735E-16,-1.));
#23320=DIRECTION('',(0.984807753012208,-0.17364817766693,2.12657684957577E-17));
#23321=DIRECTION('',(0.,0.,1.));
#23322=DIRECTION('',(0.0582961149179891,0.99829933536263,0.));
#23323=DIRECTION('',(0.,0.,1.));
#23324=DIRECTION('',(-0.835404527546164,0.54963558414223,0.));
#23325=DIRECTION('',(0.,0.,1.));
#23326=DIRECTION('',(-0.893700642464153,-0.4486637512204,0.));
#23327=DIRECTION('',(0.,0.,1.));
#23328=DIRECTION('',(-0.0582961149179892,-0.99829933536263,0.));
#23329=DIRECTION('',(0.,0.,1.));
#23330=DIRECTION('',(0.835404527546164,-0.54963558414223,0.));
#23331=DIRECTION('',(1.06057523872491E-16,-6.12323399573677E-17,-1.));
#23332=DIRECTION('',(0.173648177666931,-0.984807753012208,7.87187788734199E-17));
#23333=DIRECTION('',(1.06057523872491E-16,6.12323399573676E-17,-1.));
#23334=DIRECTION('',(0.939692620785908,-0.342020143325669,7.87187788734199E-17));
#23335=DIRECTION('',(0.,1.22464679914735E-16,-1.));
#23336=DIRECTION('',(0.766044443118978,0.642787609686539,7.87187788734199E-17));
#23337=DIRECTION('',(-1.06057523872491E-16,6.12323399573677E-17,-1.));
#23338=DIRECTION('',(-0.17364817766693,0.984807753012208,7.87187788734199E-17));
#23339=DIRECTION('',(-1.06057523872491E-16,-6.12323399573677E-17,-1.));
#23340=DIRECTION('',(-0.939692620785909,0.342020143325668,7.87187788734199E-17));
#23341=DIRECTION('',(0.,-2.46519032881566E-32,1.));
#23342=DIRECTION('',(0.766044443118978,-0.64278760968654,-1.23259516440783E-32));
#23343=DIRECTION('',(0.,-2.46519032881566E-32,1.));
#23344=DIRECTION('',(0.939692620785909,0.342020143325668,0.));
#23345=DIRECTION('',(0.,-2.46519032881566E-32,1.));
#23346=DIRECTION('',(0.173648177666931,0.984807753012208,0.));
#23347=DIRECTION('',(0.,-2.46519032881566E-32,1.));
#23348=DIRECTION('',(-0.766044443118978,0.64278760968654,1.23259516440783E-32));
#23349=DIRECTION('',(0.,-2.46519032881566E-32,1.));
#23350=DIRECTION('',(-0.939692620785909,-0.342020143325668,0.));
#23351=DIRECTION('',(0.,-2.46519032881566E-32,1.));
#23352=DIRECTION('',(-0.173648177666931,-0.984807753012208,-2.46519032881566E-32));
#23353=DIRECTION('',(1.06057523872491E-16,-6.12323399573677E-17,-1.));
#23354=DIRECTION('',(0.642787609686539,0.766044443118978,2.12657684957577E-17));
#23355=DIRECTION('',(1.06057523872491E-16,6.12323399573676E-17,-1.));
#23356=DIRECTION('',(-0.342020143325668,0.939692620785909,2.12657684957577E-17));
#23357=DIRECTION('',(1.23259516440783E-32,1.22464679914735E-16,-1.));
#23358=DIRECTION('',(-0.984807753012208,0.17364817766693,2.12657684957577E-17));
#23359=DIRECTION('',(-1.06057523872491E-16,6.12323399573677E-17,-1.));
#23360=DIRECTION('',(-0.64278760968654,-0.766044443118978,2.12657684957577E-17));
#23361=DIRECTION('',(-1.06057523872491E-16,-6.12323399573677E-17,-1.));
#23362=DIRECTION('',(0.342020143325669,-0.939692620785908,2.12657684957577E-17));
#23363=DIRECTION('',(3.08148791101958E-33,0.,1.));
#23364=DIRECTION('',(-0.984807753012208,-0.17364817766693,-6.16297582203915E-33));
#23365=DIRECTION('',(3.08148791101958E-33,0.,1.));
#23366=DIRECTION('',(-0.342020143325669,-0.939692620785909,2.46519032881566E-32));
#23367=DIRECTION('',(3.08148791101958E-33,0.,1.));
#23368=DIRECTION('',(0.642787609686539,-0.766044443118978,1.23259516440783E-32));
#23369=DIRECTION('',(3.08148791101958E-33,0.,1.));
#23370=DIRECTION('',(0.984807753012208,0.17364817766693,9.24446373305873E-33));
#23371=DIRECTION('',(3.08148791101958E-33,0.,1.));
#23372=DIRECTION('',(0.342020143325669,0.939692620785908,0.));
#23373=DIRECTION('',(3.08148791101958E-33,0.,1.));
#23374=DIRECTION('',(-0.64278760968654,0.766044443118978,-1.23259516440783E-32));
#23375=CARTESIAN_POINT('',(0.,0.,0.));
#23376=CARTESIAN_POINT('',(0.,0.,0.));
#23377=CARTESIAN_POINT('Origin',(65.,0.,17.));
#23378=CARTESIAN_POINT('',(63.3324486297716,-0.00121435961605691,13.8714803633902));
#23379=CARTESIAN_POINT('',(63.3320009243657,0.000968828099764776,13.6785196366098));
#23380=CARTESIAN_POINT('',(63.334,2.04026156737949E-16,17.));
#23381=CARTESIAN_POINT('',(63.3648706727485,-0.3192304546283,13.));
#23382=CARTESIAN_POINT('Ctrl Pts',(63.3320009243657,0.000968828099764776,
13.6785196366098));
#23383=CARTESIAN_POINT('Ctrl Pts',(63.3315933114009,0.059054876303456,13.6746222055426));
#23384=CARTESIAN_POINT('Ctrl Pts',(63.3343634348107,0.117102016123704,13.6707247744754));
#23385=CARTESIAN_POINT('Ctrl Pts',(63.3404396356832,0.174801282227228,13.6668273434083));
#23386=CARTESIAN_POINT('Ctrl Pts',(63.3981952988365,0.723245852641101,13.6297813798856));
#23387=CARTESIAN_POINT('Ctrl Pts',(63.7546528235523,1.24026026815388,13.5927354163629));
#23388=CARTESIAN_POINT('Ctrl Pts',(64.2467810781753,1.48913792445445,13.5556894528402));
#23389=CARTESIAN_POINT('Ctrl Pts',(64.7389093327983,1.73801558075501,13.5186434893175));
#23390=CARTESIAN_POINT('Ctrl Pts',(65.3667083173286,1.71875647784335,13.4815975257948));
#23391=CARTESIAN_POINT('Ctrl Pts',(65.8426564295865,1.44035726535855,13.4445515622722));
#23392=CARTESIAN_POINT('Ctrl Pts',(66.3186045418444,1.16195805287375,13.4075055987495));
#23393=CARTESIAN_POINT('Ctrl Pts',(66.6427017818299,0.624418730815826,13.3704596352268));
#23394=CARTESIAN_POINT('Ctrl Pts',(66.6670336186705,0.0733842827933222,
13.3334136717041));
#23395=CARTESIAN_POINT('Ctrl Pts',(66.691365455511,-0.477650165229181,13.2963677081814));
#23396=CARTESIAN_POINT('Ctrl Pts',(66.4159318892067,-1.04217973921626,13.2593217446588));
#23397=CARTESIAN_POINT('Ctrl Pts',(65.9659478490025,-1.36111593499208,13.2222757811361));
#23398=CARTESIAN_POINT('Ctrl Pts',(65.5159638087983,-1.6800521307679,13.1852298176134));
#23399=CARTESIAN_POINT('Ctrl Pts',(64.8914292946943,-1.75339494833247,13.1481838540907));
#23400=CARTESIAN_POINT('Ctrl Pts',(64.3801939409253,-1.54911937996348,13.111137890568));
#23401=CARTESIAN_POINT('Ctrl Pts',(63.8689585871564,-1.34484381159449,13.0740919270454));
#23402=CARTESIAN_POINT('Ctrl Pts',(63.4710223937224,-0.862949857291961,
13.0370459635227));
#23403=CARTESIAN_POINT('Ctrl Pts',(63.3648706727485,-0.319230454628348,
13.));
#23404=CARTESIAN_POINT('',(64.9474239245698,1.66819769235427,13.));
#23405=CARTESIAN_POINT('Origin',(65.,0.,13.));
#23406=CARTESIAN_POINT('',(63.3365558121435,-0.000651319618122093,13.1714803633902));
#23407=CARTESIAN_POINT('Ctrl Pts',(64.9474239513002,1.66819938802347,13.));
#23408=CARTESIAN_POINT('Ctrl Pts',(64.4069183000551,1.6504713908779,13.0363229181856));
#23409=CARTESIAN_POINT('Ctrl Pts',(63.874833765777,1.34577267304803,13.0726458363711));
#23410=CARTESIAN_POINT('Ctrl Pts',(63.5871509129382,0.887831743084597,13.1089687545567));
#23411=CARTESIAN_POINT('Ctrl Pts',(63.42211720178,0.625126856723245,13.1298059575012));
#23412=CARTESIAN_POINT('Ctrl Pts',(63.3375141386089,0.311991178117364,13.1506431604457));
#23413=CARTESIAN_POINT('Ctrl Pts',(63.3365558121435,-0.000651319618122093,
13.1714803633902));
#23414=CARTESIAN_POINT('',(63.334,-2.04026156737949E-16,12.));
#23415=CARTESIAN_POINT('',(63.334,2.04026156737949E-16,17.));
#23416=CARTESIAN_POINT('Origin',(65.,0.,12.));
#23417=CARTESIAN_POINT('Ctrl Pts',(63.3365558121435,-0.000651319618122093,
13.1714803633902));
#23418=CARTESIAN_POINT('Ctrl Pts',(63.3358103529628,-0.243848422696125,
13.1876891239684));
#23419=CARTESIAN_POINT('Ctrl Pts',(63.385677580256,-0.486747106414449,13.2038978845465));
#23420=CARTESIAN_POINT('Ctrl Pts',(63.4876703201545,-0.7053781763955,13.2201066451247));
#23421=CARTESIAN_POINT('Ctrl Pts',(63.7207800205315,-1.20507083360908,13.2571526086474));
#23422=CARTESIAN_POINT('Ctrl Pts',(64.2261802362228,-1.57799560462435,13.2941985721701));
#23423=CARTESIAN_POINT('Ctrl Pts',(64.7725065735009,-1.65321436231664,13.3312445356927));
#23424=CARTESIAN_POINT('Ctrl Pts',(65.318832910779,-1.72843312000893,13.3682904992154));
#23425=CARTESIAN_POINT('Ctrl Pts',(65.906085369644,-1.50594586437824,13.4053364627381));
#23426=CARTESIAN_POINT('Ctrl Pts',(66.265537296365,-1.08770963232589,13.4423824262608));
#23427=CARTESIAN_POINT('Ctrl Pts',(66.6249892230859,-0.669473400273535,
13.4794283897835));
#23428=CARTESIAN_POINT('Ctrl Pts',(66.7566406176629,-0.0554881917995138,
13.5164743533061));
#23429=CARTESIAN_POINT('Ctrl Pts',(66.6002239654009,0.47331994937011,13.5535203168288));
#23430=CARTESIAN_POINT('Ctrl Pts',(66.4438073131388,1.00212809053973,13.5905662803515));
#23431=CARTESIAN_POINT('Ctrl Pts',(65.9993226140377,1.44575916440496,13.6276122438742));
#23432=CARTESIAN_POINT('Ctrl Pts',(65.470199129815,1.60114874218549,13.6646582073969));
#23433=CARTESIAN_POINT('Ctrl Pts',(64.9410756455923,1.75653831996602,13.7017041709195));
#23434=CARTESIAN_POINT('Ctrl Pts',(64.327313376248,1.62368640166186,13.7387501344422));
#23435=CARTESIAN_POINT('Ctrl Pts',(63.9097999122987,1.26341063241475,13.7757960979649));
#23436=CARTESIAN_POINT('Ctrl Pts',(63.550341325322,0.953230889441892,13.8076908531067));
#23437=CARTESIAN_POINT('Ctrl Pts',(63.3363495020968,0.474476303274697,13.8395856082484));
#23438=CARTESIAN_POINT('Ctrl Pts',(63.3324486297716,-0.00121435961605691,
13.8714803633902));
#23439=CARTESIAN_POINT('Origin',(65.,0.,17.));
#23440=CARTESIAN_POINT('',(63.3327604959513,0.00132477262097364,14.5714803633902));
#23441=CARTESIAN_POINT('',(63.3362968330887,0.000832304224862905,14.3785196366098));
#23442=CARTESIAN_POINT('',(63.334,2.04026156737949E-16,17.));
#23443=CARTESIAN_POINT('Ctrl Pts',(63.3362968330887,0.000832304224862905,
14.3785196366098));
#23444=CARTESIAN_POINT('Ctrl Pts',(63.3352820110227,0.225194784962812,14.3635646533454));
#23445=CARTESIAN_POINT('Ctrl Pts',(63.3774911908197,0.449191325190215,14.3486096700809));
#23446=CARTESIAN_POINT('Ctrl Pts',(63.4647380475121,0.65400242785626,14.3336546868165));
#23447=CARTESIAN_POINT('Ctrl Pts',(63.6808629212981,1.16135335592135,14.2966087232938));
#23448=CARTESIAN_POINT('Ctrl Pts',(64.1733546191173,1.55097577727799,14.2595627597711));
#23449=CARTESIAN_POINT('Ctrl Pts',(64.7168232236993,1.64455527160813,14.2225167962485));
#23450=CARTESIAN_POINT('Ctrl Pts',(65.2602918282814,1.73813476593827,14.1854708327258));
#23451=CARTESIAN_POINT('Ctrl Pts',(65.8547373396264,1.53567133324193,14.1484248692031));
#23452=CARTESIAN_POINT('Ctrl Pts',(66.2281050246363,1.12982650677502,14.1113789056804));
#23453=CARTESIAN_POINT('Ctrl Pts',(66.6014727096463,0.723981680308096,14.0743329421577));
#23454=CARTESIAN_POINT('Ctrl Pts',(66.7537625683213,0.114755460070602,14.0372869786351));
#23455=CARTESIAN_POINT('Ctrl Pts',(66.6152849767096,-0.419042261543969,
14.0002410151124));
#23456=CARTESIAN_POINT('Ctrl Pts',(66.4768073850979,-0.952839983158524,
13.9631950515897));
#23457=CARTESIAN_POINT('Ctrl Pts',(66.0475623431996,-1.41120920615016,13.926149088067));
#23458=CARTESIAN_POINT('Ctrl Pts',(65.5239830002582,-1.58436286925844,13.8891031245443));
#23459=CARTESIAN_POINT('Ctrl Pts',(65.0004036573169,-1.75751653236671,13.8520571610217));
#23460=CARTESIAN_POINT('Ctrl Pts',(64.3824900133324,-1.64545463559162,13.815011197499));
#23461=CARTESIAN_POINT('Ctrl Pts',(63.9530600921357,-1.29948632454661,13.7779652339763));
#23462=CARTESIAN_POINT('Ctrl Pts',(63.5688084672201,-0.989915707487894,
13.7448167015208));
#23463=CARTESIAN_POINT('Ctrl Pts',(63.3354677647952,-0.493066145425912,
13.7116681690653));
#23464=CARTESIAN_POINT('Ctrl Pts',(63.3320009243657,0.000968828099764776,
13.6785196366098));
#23465=CARTESIAN_POINT('Ctrl Pts',(63.3324486297716,-0.00121435961605691,
13.8714803633902));
#23466=CARTESIAN_POINT('Ctrl Pts',(63.3318186137667,-0.0780414654682614,
13.8766315717711));
#23467=CARTESIAN_POINT('Ctrl Pts',(63.3366686795385,-0.154788650933411,
13.881782780152));
#23468=CARTESIAN_POINT('Ctrl Pts',(63.3472710750459,-0.230732838385404,
13.8869339885329));
#23469=CARTESIAN_POINT('Ctrl Pts',(63.4235203602966,-0.776900919748414,
13.9239799520556));
#23470=CARTESIAN_POINT('Ctrl Pts',(63.7972835893523,-1.28153746228441,13.9610259155783));
#23471=CARTESIAN_POINT('Ctrl Pts',(64.2975048362999,-1.51368831950505,13.998071879101));
#23472=CARTESIAN_POINT('Ctrl Pts',(64.7977260832475,-1.7458391767257,14.0351178426237));
#23473=CARTESIAN_POINT('Ctrl Pts',(65.424405348087,-1.70550434863098,14.0721638061464));
#23474=CARTESIAN_POINT('Ctrl Pts',(65.8907398483472,-1.41114550098828,14.109209769669));
#23475=CARTESIAN_POINT('Ctrl Pts',(66.3570743486074,-1.1167866533456,14.1462557331917));
#23476=CARTESIAN_POINT('Ctrl Pts',(66.6630640842882,-0.568403786154937,
14.1833016967144));
#23477=CARTESIAN_POINT('Ctrl Pts',(66.6686708473517,-0.0169663179122549,
14.2203476602371));
#23478=CARTESIAN_POINT('Ctrl Pts',(66.6742776104151,0.534471150330427,14.2573936237598));
#23479=CARTESIAN_POINT('Ctrl Pts',(66.3795014008612,1.08896321962513,14.2944395872824));
#23480=CARTESIAN_POINT('Ctrl Pts',(65.9192483587705,1.39274289076842,14.3314855508051));
#23481=CARTESIAN_POINT('Ctrl Pts',(65.4589953166798,1.69652256191171,14.3685315143278));
#23482=CARTESIAN_POINT('Ctrl Pts',(64.8332654420522,1.74958983490358,14.4055774778505));
#23483=CARTESIAN_POINT('Ctrl Pts',(64.3284274914591,1.52765845331761,14.4426234413732));
#23484=CARTESIAN_POINT('Ctrl Pts',(63.823589540866,1.30572707173164,14.4796694048958));
#23485=CARTESIAN_POINT('Ctrl Pts',(63.4396435143075,0.808797035567841,14.5167153684185));
#23486=CARTESIAN_POINT('Ctrl Pts',(63.352304522573,0.264291051559231,14.5537613319412));
#23487=CARTESIAN_POINT('Ctrl Pts',(63.3383798175659,0.177478906704716,14.5596676757575));
#23488=CARTESIAN_POINT('Ctrl Pts',(63.3319945181308,0.0894574366348187,
14.5655740195739));
#23489=CARTESIAN_POINT('Ctrl Pts',(63.3327604959513,0.00132477262097364,
14.5714803633902));
#23490=CARTESIAN_POINT('Origin',(65.,0.,17.));
#23491=CARTESIAN_POINT('',(63.3366282199437,0.000380246208316198,15.2714803633902));
#23492=CARTESIAN_POINT('',(63.3350218272016,-0.00143128727516526,15.0785196366098));
#23493=CARTESIAN_POINT('',(63.334,2.04026156737949E-16,17.));
#23494=CARTESIAN_POINT('Ctrl Pts',(63.3350218272016,-0.00143128727516526,
15.0785196366098));
#23495=CARTESIAN_POINT('Ctrl Pts',(63.3382129761596,0.388071089145999,15.0525071011481));
#23496=CARTESIAN_POINT('Ctrl Pts',(63.4745702784036,0.77958633576253,15.0264945656864));
#23497=CARTESIAN_POINT('Ctrl Pts',(63.7241632245643,1.07563467970709,15.0004820302248));
#23498=CARTESIAN_POINT('Ctrl Pts',(64.0796230447962,1.49725433177356,14.9634360667021));
#23499=CARTESIAN_POINT('Ctrl Pts',(64.6647503809125,1.72524549701854,14.9263901031794));
#23500=CARTESIAN_POINT('Ctrl Pts',(65.2117584175496,1.65526670109563,14.8893441396567));
#23501=CARTESIAN_POINT('Ctrl Pts',(65.7587664541868,1.58528790517272,14.852298176134));
#23502=CARTESIAN_POINT('Ctrl Pts',(66.2676551913447,1.21733914808192,14.8152522126113));
#23503=CARTESIAN_POINT('Ctrl Pts',(66.5055287575052,0.719814314063385,14.7782062490887));
#23504=CARTESIAN_POINT('Ctrl Pts',(66.7434023236657,0.222289480044847,14.741160285566));
#23505=CARTESIAN_POINT('Ctrl Pts',(66.7102607188288,-0.40481143090143,14.7041143220433));
#23506=CARTESIAN_POINT('Ctrl Pts',(66.4212714962,-0.874492228471354,14.6670683585206));
#23507=CARTESIAN_POINT('Ctrl Pts',(66.1322822735712,-1.34417302604128,14.630022394998));
#23508=CARTESIAN_POINT('Ctrl Pts',(65.5874454331506,-1.65643371023485,14.5929764314753));
#23509=CARTESIAN_POINT('Ctrl Pts',(65.0361084265221,-1.66836621488623,14.5559304679526));
#23510=CARTESIAN_POINT('Ctrl Pts',(64.4847714198936,-1.6802987195376,14.5188845044299));
#23511=CARTESIAN_POINT('Ctrl Pts',(63.9269342470572,-1.39190304464678,14.4818385409072));
#23512=CARTESIAN_POINT('Ctrl Pts',(63.6178946855153,-0.935165489814587,
14.4447925773845));
#23513=CARTESIAN_POINT('Ctrl Pts',(63.4336104557676,-0.662807064022192,
14.4227015971263));
#23514=CARTESIAN_POINT('Ctrl Pts',(63.3377958928888,-0.330588135707226,
14.400610616868));
#23515=CARTESIAN_POINT('Ctrl Pts',(63.3362968330887,0.000832304224862905,
14.3785196366098));
#23516=CARTESIAN_POINT('Ctrl Pts',(63.3327604959513,0.00132477262097364,
14.5714803633902));
#23517=CARTESIAN_POINT('Ctrl Pts',(63.336798909355,-0.463331150982518,14.6026199830965));
#23518=CARTESIAN_POINT('Ctrl Pts',(63.5396173640042,-0.931077870254258,
14.6337596028029));
#23519=CARTESIAN_POINT('Ctrl Pts',(63.8843359278475,-1.24098501894124,14.6648992225092));
#23520=CARTESIAN_POINT('Ctrl Pts',(64.294438281767,-1.60967317357969,14.7019451860319));
#23521=CARTESIAN_POINT('Ctrl Pts',(64.9053749465165,-1.75496755100317,14.7389911495546));
#23522=CARTESIAN_POINT('Ctrl Pts',(65.4375473020178,-1.61037339159949,14.7760371130773));
#23523=CARTESIAN_POINT('Ctrl Pts',(65.9697196575191,-1.46577923219581,14.8130830766));
#23524=CARTESIAN_POINT('Ctrl Pts',(66.4231277037722,-1.03129653596498,14.8501290401226));
#23525=CARTESIAN_POINT('Ctrl Pts',(66.5902666729806,-0.505768754333085,
14.8871750036453));
#23526=CARTESIAN_POINT('Ctrl Pts',(66.757405642189,0.0197590272988233,14.924220967168));
#23527=CARTESIAN_POINT('Ctrl Pts',(66.6382755343526,0.636331894331814,14.9612669306907));
#23528=CARTESIAN_POINT('Ctrl Pts',(66.2873969210692,1.06177176879601,14.9983128942134));
#23529=CARTESIAN_POINT('Ctrl Pts',(65.9365183077858,1.4872116432602,15.0353588577361));
#23530=CARTESIAN_POINT('Ctrl Pts',(65.3538911890554,1.7215185251556,15.0724048212587));
#23531=CARTESIAN_POINT('Ctrl Pts',(64.8061581683602,1.65746054599185,15.1094507847814));
#23532=CARTESIAN_POINT('Ctrl Pts',(64.2584251476649,1.5934025668281,15.1464967483041));
#23533=CARTESIAN_POINT('Ctrl Pts',(63.7455862250048,1.23097972660522,15.1835427118268));
#23534=CARTESIAN_POINT('Ctrl Pts',(63.5023450418969,0.736056890900436,15.2205886753495));
#23535=CARTESIAN_POINT('Ctrl Pts',(63.390961297378,0.509424385728741,15.237552571363));
#23536=CARTESIAN_POINT('Ctrl Pts',(63.336108421692,0.255008487872148,15.2545164673766));
#23537=CARTESIAN_POINT('Ctrl Pts',(63.3366282199437,0.000380246208316198,
15.2714803633902));
#23538=CARTESIAN_POINT('Origin',(65.,0.,17.));
#23539=CARTESIAN_POINT('',(63.3341549687971,-0.00152342623458264,15.9714803633902));
#23540=CARTESIAN_POINT('',(63.3312431600774,6.71117920464596E-6,15.7785196366098));
#23541=CARTESIAN_POINT('',(63.334,2.04026156737949E-16,17.));
#23542=CARTESIAN_POINT('Ctrl Pts',(63.3312431738575,6.7111456588167E-6,
15.7785196366098));
#23543=CARTESIAN_POINT('Ctrl Pts',(63.3312102147262,0.551831913054104,15.7414495489509));
#23544=CARTESIAN_POINT('Ctrl Pts',(63.6320564203023,1.10362622346454,15.7043794612919));
#23545=CARTESIAN_POINT('Ctrl Pts',(64.0958701387024,1.4026042396328,15.667309373633));
#23546=CARTESIAN_POINT('Ctrl Pts',(64.5593820206073,1.70138768959276,15.6302634101103));
#23547=CARTESIAN_POINT('Ctrl Pts',(65.1856492588609,1.74768378931892,15.5932174465876));
#23548=CARTESIAN_POINT('Ctrl Pts',(65.6880571011576,1.52030486584838,15.556171483065));
#23549=CARTESIAN_POINT('Ctrl Pts',(66.1904649434542,1.29292594237784,15.5191255195423));
#23550=CARTESIAN_POINT('Ctrl Pts',(66.569013389794,0.791871995710604,15.4820795560196));
#23551=CARTESIAN_POINT('Ctrl Pts',(66.6504575962853,0.246453206514432,15.4450335924969));
#23552=CARTESIAN_POINT('Ctrl Pts',(66.7319018027767,-0.29896558268174,15.4079876289742));
#23553=CARTESIAN_POINT('Ctrl Pts',(66.5162417694196,-0.888749214406839,
15.3709416654516));
#23554=CARTESIAN_POINT('Ctrl Pts',(66.1021755351577,-1.25297986690093,15.3338957019289));
#23555=CARTESIAN_POINT('Ctrl Pts',(65.6881093008957,-1.61721051939501,15.2968497384062));
#23556=CARTESIAN_POINT('Ctrl Pts',(65.0756368657288,-1.75588819265809,15.2598037748835));
#23557=CARTESIAN_POINT('Ctrl Pts',(64.5450597089912,-1.60554625999198,15.2227578113608));
#23558=CARTESIAN_POINT('Ctrl Pts',(64.0144825522536,-1.45520432732587,15.1857118478382));
#23559=CARTESIAN_POINT('Ctrl Pts',(63.5658006739452,-1.01584278873058,15.1486658843155));
#23560=CARTESIAN_POINT('Ctrl Pts',(63.4043558869649,-0.488537949988941,
15.1116199207928));
#23561=CARTESIAN_POINT('Ctrl Pts',(63.3562726607889,-0.331490340715363,
15.1005864927318));
#23562=CARTESIAN_POINT('Ctrl Pts',(63.3336682754684,-0.166641881842641,
15.0895530646708));
#23563=CARTESIAN_POINT('Ctrl Pts',(63.3350218272016,-0.00143128727516526,
15.0785196366098));
#23564=CARTESIAN_POINT('Ctrl Pts',(63.3366282199437,0.000380246208316198,
15.2714803633902));
#23565=CARTESIAN_POINT('Ctrl Pts',(63.3372435634692,-0.301051779472626,
15.2915624308993));
#23566=CARTESIAN_POINT('Ctrl Pts',(63.4154588028067,-0.602781386183098,
15.3116444984084));
#23567=CARTESIAN_POINT('Ctrl Pts',(63.5693524834351,-0.859067985064377,
15.3317265659175));
#23568=CARTESIAN_POINT('Ctrl Pts',(63.8532445516371,-1.3318471941377,15.3687725294402));
#23569=CARTESIAN_POINT('Ctrl Pts',(64.3946721315968,-1.64998278109766,15.4058184929629));
#23570=CARTESIAN_POINT('Ctrl Pts',(64.9458478213867,-1.66787819121184,15.4428644564855));
#23571=CARTESIAN_POINT('Ctrl Pts',(65.4970235111765,-1.68577360132601,15.4799104200082));
#23572=CARTESIAN_POINT('Ctrl Pts',(66.0579473107965,-1.40342883459439,15.5169563835309));
#23573=CARTESIAN_POINT('Ctrl Pts',(66.3719092626235,-0.950060574217453,
15.5540023470536));
#23574=CARTESIAN_POINT('Ctrl Pts',(66.6858712144506,-0.496692313840509,
15.5910483105763));
#23575=CARTESIAN_POINT('Ctrl Pts',(66.7528713184848,0.127699440181754,15.6280942740989));
#23576=CARTESIAN_POINT('Ctrl Pts',(66.542246597235,0.637358260928835,15.6651402376216));
#23577=CARTESIAN_POINT('Ctrl Pts',(66.3316218759853,1.14701708167591,15.7021862011443));
#23578=CARTESIAN_POINT('Ctrl Pts',(65.8433723294516,1.54194296914781,15.739232164667));
#23579=CARTESIAN_POINT('Ctrl Pts',(65.3009481311498,1.64139585163659,15.7762781281897));
#23580=CARTESIAN_POINT('Ctrl Pts',(64.7585239328481,1.74084873412538,15.8133240917123));
#23581=CARTESIAN_POINT('Ctrl Pts',(64.1619250827784,1.54482861163106,15.850370055235));
#23582=CARTESIAN_POINT('Ctrl Pts',(63.7841884276299,1.14304520468472,15.8874160187577));
#23583=CARTESIAN_POINT('Ctrl Pts',(63.4984696309493,0.839137521926606,15.9154374669685));
#23584=CARTESIAN_POINT('Ctrl Pts',(63.3379698006251,0.417505232584558,15.9434589151794));
#23585=CARTESIAN_POINT('Ctrl Pts',(63.3341549687971,-0.00152342623458264,
15.9714803633902));
#23586=CARTESIAN_POINT('Origin',(65.,0.,17.));
#23587=CARTESIAN_POINT('',(63.3314647116295,0.000550350488423834,16.6714803633902));
#23588=CARTESIAN_POINT('',(63.3350414063796,0.00142706819227928,16.4785196366098));
#23589=CARTESIAN_POINT('',(63.334,2.04026156737949E-16,17.));
#23590=CARTESIAN_POINT('Ctrl Pts',(63.3350414063796,0.00142706819227928,
16.4785196366098));
#23591=CARTESIAN_POINT('Ctrl Pts',(63.3336871074336,0.167365053879281,16.4674379602763));
#23592=CARTESIAN_POINT('Ctrl Pts',(63.3564935743301,0.33293915311042,16.4563562839428));
#23593=CARTESIAN_POINT('Ctrl Pts',(63.4049919569221,0.490610641878083,16.4452746076093));
#23594=CARTESIAN_POINT('Ctrl Pts',(63.5671216977971,1.0177052840304,16.4082286440866));
#23595=CARTESIAN_POINT('Ctrl Pts',(64.0163740234165,1.45648350908886,16.3711826805639));
#23596=CARTESIAN_POINT('Ctrl Pts',(64.5471460595228,1.60613597431706,16.3341367170413));
#23597=CARTESIAN_POINT('Ctrl Pts',(65.0779180956292,1.75578843954526,16.2970907535186));
#23598=CARTESIAN_POINT('Ctrl Pts',(65.6902098422225,1.61631514494319,16.2600447899959));
#23599=CARTESIAN_POINT('Ctrl Pts',(66.1038025095515,1.2515468346462,16.2229988264732));
#23600=CARTESIAN_POINT('Ctrl Pts',(66.5173951768805,0.886778524349212,16.1859528629505));
#23601=CARTESIAN_POINT('Ctrl Pts',(66.7322887649452,0.296715198357295,16.1489068994279));
#23602=CARTESIAN_POINT('Ctrl Pts',(66.6501360046234,-0.248597316289489,
16.1118609359052));
#23603=CARTESIAN_POINT('Ctrl Pts',(66.5679832443015,-0.793909830936272,
16.0748149723825));
#23604=CARTESIAN_POINT('Ctrl Pts',(66.1887841355932,-1.29447153423793,16.0377690088598));
#23605=CARTESIAN_POINT('Ctrl Pts',(65.6860813008334,-1.52119752432679,16.0007230453371));
#23606=CARTESIAN_POINT('Ctrl Pts',(65.1833784660736,-1.74792351441565,15.9636770818144));
#23607=CARTESIAN_POINT('Ctrl Pts',(64.5571719052625,-1.70081379129173,15.9266311182918));
#23608=CARTESIAN_POINT('Ctrl Pts',(64.0940486017292,-1.40142838682091,15.8895851547691));
#23609=CARTESIAN_POINT('Ctrl Pts',(63.6312268816509,-1.10223794054801,15.8525633153827));
#23610=CARTESIAN_POINT('Ctrl Pts',(63.3312760900911,-0.551100267138433,
15.8155414759962));
#23611=CARTESIAN_POINT('Ctrl Pts',(63.3312431738575,6.7111456588167E-6,
15.7785196366098));
#23612=CARTESIAN_POINT('Ctrl Pts',(63.3341549687971,-0.00152342623458264,
15.9714803633902));
#23613=CARTESIAN_POINT('Ctrl Pts',(63.3329263739013,-0.136474714946136,
15.980504878702));
#23614=CARTESIAN_POINT('Ctrl Pts',(63.3479493008663,-0.271155952543882,
15.9895293940139));
#23615=CARTESIAN_POINT('Ctrl Pts',(63.3802748445461,-0.401547681148703,
15.9985539093257));
#23616=CARTESIAN_POINT('Ctrl Pts',(63.5129723768379,-0.936810468637373,
16.0355998728484));
#23617=CARTESIAN_POINT('Ctrl Pts',(63.9372419016487,-1.39978935221634,16.0726458363711));
#23618=CARTESIAN_POINT('Ctrl Pts',(64.4589140651794,-1.57859942055654,16.1096917998938));
#23619=CARTESIAN_POINT('Ctrl Pts',(64.9805862287101,-1.75740948889674,16.1467377634165));
#23620=CARTESIAN_POINT('Ctrl Pts',(65.5996610309607,-1.65205074199818,16.1837837269391));
#23621=CARTESIAN_POINT('Ctrl Pts',(66.0328153782871,-1.31074120779883,16.2208296904618));
#23622=CARTESIAN_POINT('Ctrl Pts',(66.4659697256135,-0.969431673599482,
16.2578756539845));
#23623=CARTESIAN_POINT('Ctrl Pts',(66.7132036180157,-0.392171352099344,
16.2949216175072));
#23624=CARTESIAN_POINT('Ctrl Pts',(66.661369062725,0.156853297275929,16.3319675810299));
#23625=CARTESIAN_POINT('Ctrl Pts',(66.6095345074342,0.705877946651205,16.3690135445526));
#23626=CARTESIAN_POINT('Ctrl Pts',(66.2586315044505,1.22666692390161,16.4060595080752));
#23627=CARTESIAN_POINT('Ctrl Pts',(65.7692528028443,1.48087820051541,16.4431054715979));
#23628=CARTESIAN_POINT('Ctrl Pts',(65.2798741012382,1.73508947712919,16.4801514351206));
#23629=CARTESIAN_POINT('Ctrl Pts',(64.6520197010096,1.72272305310636,16.5171973986433));
#23630=CARTESIAN_POINT('Ctrl Pts',(64.1730307286,1.44943849252272,16.5542433621659));
#23631=CARTESIAN_POINT('Ctrl Pts',(63.6940417561904,1.17615393193908,16.5912893256886));
#23632=CARTESIAN_POINT('Ctrl Pts',(63.3639182115997,0.641951234794639,16.6283352892113));
#23633=CARTESIAN_POINT('Ctrl Pts',(63.3337430069376,0.0913112945731737,
16.665381252734));
#23634=CARTESIAN_POINT('Ctrl Pts',(63.3320870288426,0.0610928523301667,
16.6674142896194));
#23635=CARTESIAN_POINT('Ctrl Pts',(63.3313343989597,0.0308249063821219,
16.6694473265048));
#23636=CARTESIAN_POINT('Ctrl Pts',(63.3314647116295,0.000550350488423834,
16.6714803633902));
#23637=CARTESIAN_POINT('Origin',(65.,0.,17.));
#23638=CARTESIAN_POINT('',(63.3357797744869,0.00117646094453,17.3714803633902));
#23639=CARTESIAN_POINT('',(63.3362856132907,-0.000842509924175838,17.1785196366098));
#23640=CARTESIAN_POINT('',(63.334,2.04026156737949E-16,17.));
#23641=CARTESIAN_POINT('Ctrl Pts',(63.3362856132907,-0.000842509924175838,
17.1785196366098));
#23642=CARTESIAN_POINT('Ctrl Pts',(63.3378066597351,0.331296382409458,17.156380408079));
#23643=CARTESIAN_POINT('Ctrl Pts',(63.4340697022003,0.664247316775266,17.1342411795483));
#23644=CARTESIAN_POINT('Ctrl Pts',(63.6191109651628,0.936960475618686,17.1121019510176));
#23645=CARTESIAN_POINT('Ctrl Pts',(63.9287437903708,1.39329623820574,17.0750559874949));
#23646=CARTESIAN_POINT('Ctrl Pts',(64.4869549413411,1.68096669861507,17.0380100239722));
#23647=CARTESIAN_POINT('Ctrl Pts',(65.0382759195595,1.66831783943796,17.0009640604495));
#23648=CARTESIAN_POINT('Ctrl Pts',(65.5895968977779,1.65566898026085,16.9639180969268));
#23649=CARTESIAN_POINT('Ctrl Pts',(66.1340277032444,1.34270080149729,16.9268721334041));
#23650=CARTESIAN_POINT('Ctrl Pts',(66.4224064907048,0.872644964808594,16.8898261698815));
#23651=CARTESIAN_POINT('Ctrl Pts',(66.7107852781652,0.402589128119899,16.8527802063588));
#23652=CARTESIAN_POINT('Ctrl Pts',(66.7431120476195,-0.224554366493935,
16.8157342428361));
#23653=CARTESIAN_POINT('Ctrl Pts',(66.5045922697214,-0.721769742577186,
16.7786882793134));
#23654=CARTESIAN_POINT('Ctrl Pts',(66.2660724918233,-1.21898511866044,16.7416423157907));
#23655=CARTESIAN_POINT('Ctrl Pts',(65.7567061665729,-1.58627237621311,16.7045963522681));
#23656=CARTESIAN_POINT('Ctrl Pts',(65.2096076810249,-1.65554041915625,16.6675503887454));
#23657=CARTESIAN_POINT('Ctrl Pts',(64.6625091954769,-1.72480846209938,16.6305044252227));
#23658=CARTESIAN_POINT('Ctrl Pts',(64.0776785496314,-1.49605729043299,16.5934584617));
#23659=CARTESIAN_POINT('Ctrl Pts',(63.7227668047739,-1.07397617497671,16.5564124981773));
#23660=CARTESIAN_POINT('Ctrl Pts',(63.4740209335901,-0.778153519638626,
16.5304482109881));
#23661=CARTESIAN_POINT('Ctrl Pts',(63.338214518977,-0.38736442745422,16.504483923799));
#23662=CARTESIAN_POINT('Ctrl Pts',(63.3350414063796,0.00142706819227928,
16.4785196366098));
#23663=CARTESIAN_POINT('Ctrl Pts',(63.3314647116295,0.000550350488423834,
16.6714803633902));
#23664=CARTESIAN_POINT('Ctrl Pts',(63.3337089542098,-0.520837535827165,
16.7064932900275));
#23665=CARTESIAN_POINT('Ctrl Pts',(63.5978310421932,-1.04418591019567,16.7415062166648));
#23666=CARTESIAN_POINT('Ctrl Pts',(64.0195992076647,-1.35039416683956,16.776519143302));
#23667=CARTESIAN_POINT('Ctrl Pts',(64.4658574777874,-1.67438250473233,16.8135651068247));
#23668=CARTESIAN_POINT('Ctrl Pts',(65.0886008827663,-1.7552819972194,16.8506110703474));
#23669=CARTESIAN_POINT('Ctrl Pts',(65.6028273721175,-1.55606853283267,16.8876570338701));
#23670=CARTESIAN_POINT('Ctrl Pts',(66.1170538614687,-1.35685506844592,16.9247029973928));
#23671=CARTESIAN_POINT('Ctrl Pts',(66.5227634351922,-0.877528647185354,
16.9617489609154));
#23672=CARTESIAN_POINT('Ctrl Pts',(66.6342808063438,-0.337455723706574,
16.9987949244381));
#23673=CARTESIAN_POINT('Ctrl Pts',(66.7457981774953,0.202617199772198,17.0358408879608));
#23674=CARTESIAN_POINT('Ctrl Pts',(66.5631233460748,0.803436625469181,17.0728868514835));
#23675=CARTESIAN_POINT('Ctrl Pts',(66.1698584845187,1.19003413633631,17.1099328150062));
#23676=CARTESIAN_POINT('Ctrl Pts',(65.7765936229625,1.57663164720344,17.1469787785288));
#23677=CARTESIAN_POINT('Ctrl Pts',(65.1727387312707,1.74900724324072,17.1840247420515));
#23678=CARTESIAN_POINT('Ctrl Pts',(64.6346514247161,1.62827225548557,17.2210707055742));
#23679=CARTESIAN_POINT('Ctrl Pts',(64.0965641181614,1.50753726773042,17.2581166690969));
#23680=CARTESIAN_POINT('Ctrl Pts',(63.624244396744,1.09369169618284,17.2951626326196));
#23681=CARTESIAN_POINT('Ctrl Pts',(63.4338520592054,0.576134313325577,17.3322085961422));
#23682=CARTESIAN_POINT('Ctrl Pts',(63.3665748819314,0.393249853550898,17.3452991852249));
#23683=CARTESIAN_POINT('Ctrl Pts',(63.334500232668,0.197415541610634,17.3583897743076));
#23684=CARTESIAN_POINT('Ctrl Pts',(63.3357797744869,0.00117646094453,17.3714803633902));
#23685=CARTESIAN_POINT('Origin',(65.,0.,17.));
#23686=CARTESIAN_POINT('',(63.3357162681914,-0.00120644382256618,18.0714803633902));
#23687=CARTESIAN_POINT('',(63.331966723543,-0.000974733628950259,17.8785196366098));
#23688=CARTESIAN_POINT('',(63.334,2.04026156737949E-16,17.));
#23689=CARTESIAN_POINT('Ctrl Pts',(63.331966723543,-0.000974733628950259,
17.8785196366098));
#23690=CARTESIAN_POINT('Ctrl Pts',(63.3354056721751,0.493761861582914,17.8453228558818));
#23691=CARTESIAN_POINT('Ctrl Pts',(63.569536843221,0.991325263991038,17.8121260751538));
#23692=CARTESIAN_POINT('Ctrl Pts',(63.9547567233169,1.30085201001267,17.7789292944258));
#23693=CARTESIAN_POINT('Ctrl Pts',(64.3846430349799,1.64626853206536,17.7418833309031));
#23694=CARTESIAN_POINT('Ctrl Pts',(65.002686987972,1.75751445347199,17.7048373673804));
#23695=CARTESIAN_POINT('Ctrl Pts',(65.5260372626587,1.58367744749354,17.6677914038578));
#23696=CARTESIAN_POINT('Ctrl Pts',(66.0493875373455,1.4098404415151,17.6307454403351));
#23697=CARTESIAN_POINT('Ctrl Pts',(66.4780441337267,0.950920508151569,17.5936994768124));
#23698=CARTESIAN_POINT('Ctrl Pts',(66.6158299298206,0.41694495715979,17.5566535132897));
#23699=CARTESIAN_POINT('Ctrl Pts',(66.7536157259145,-0.117030593831986,
17.519607549767));
#23700=CARTESIAN_POINT('Ctrl Pts',(66.6005307217209,-0.726061762452014,
17.4825615862444));
#23701=CARTESIAN_POINT('Ctrl Pts',(66.22663513746,-1.13142198093973,17.4455156227217));
#23702=CARTESIAN_POINT('Ctrl Pts',(65.8527395531992,-1.53678219942745,17.408469659199));
#23703=CARTESIAN_POINT('Ctrl Pts',(65.258033388871,-1.73847146778285,17.3714236956763));
#23704=CARTESIAN_POINT('Ctrl Pts',(64.7146872927936,-1.64418554868716,17.3343777321536));
#23705=CARTESIAN_POINT('Ctrl Pts',(64.1713411967163,-1.54989962959146,17.2973317686309));
#23706=CARTESIAN_POINT('Ctrl Pts',(63.6793551688898,-1.15963852304467,17.2602858051083));
#23707=CARTESIAN_POINT('Ctrl Pts',(63.4638894046994,-0.652007437388898,
17.2232398415856));
#23708=CARTESIAN_POINT('Ctrl Pts',(63.37718924249,-0.447744372051043,17.2083331065937));
#23709=CARTESIAN_POINT('Ctrl Pts',(63.3352614657588,-0.224477513359574,
17.1934263716017));
#23710=CARTESIAN_POINT('Ctrl Pts',(63.3362856132907,-0.000842509924175838,
17.1785196366098));
#23711=CARTESIAN_POINT('Ctrl Pts',(63.3357797744869,0.00117646094453,17.3714803633902));
#23712=CARTESIAN_POINT('Ctrl Pts',(63.3381212965673,-0.357935006648061,
17.3954357378302));
#23713=CARTESIAN_POINT('Ctrl Pts',(63.4521589055967,-0.71840195855398,17.4193911122702));
#23714=CARTESIAN_POINT('Ctrl Pts',(63.6665656652298,-1.00334589962881,17.4433464867103));
#23715=CARTESIAN_POINT('Ctrl Pts',(63.9981365624523,-1.443999535559,17.480392450233));
#23716=CARTESIAN_POINT('Ctrl Pts',(64.569743310557,-1.70403761325245,17.5174384137557));
#23717=CARTESIAN_POINT('Ctrl Pts',(65.1197868400431,-1.66445223193655,17.5544843772783));
#23718=CARTESIAN_POINT('Ctrl Pts',(65.6698303695292,-1.62486685062064,17.591530340801));
#23719=CARTESIAN_POINT('Ctrl Pts',(66.1983106803967,-1.28565801029538,17.6285763043237));
#23720=CARTESIAN_POINT('Ctrl Pts',(66.4633657616898,-0.802066560180589,
17.6656222678464));
#23721=CARTESIAN_POINT('Ctrl Pts',(66.728420842983,-0.318475110065801,17.702668231369));
#23722=CARTESIAN_POINT('Ctrl Pts',(66.7300506947019,0.309498949838513,17.7397141948917));
#23723=CARTESIAN_POINT('Ctrl Pts',(66.4675094059654,0.794459730162078,17.7767601584144));
#23724=CARTESIAN_POINT('Ctrl Pts',(66.2049681172289,1.27942051048565,17.8138061219371));
#23725=CARTESIAN_POINT('Ctrl Pts',(65.6782556880371,1.62136801122845,17.8508520854598));
#23726=CARTESIAN_POINT('Ctrl Pts',(65.1284250482722,1.66380801970131,17.8878980489824));
#23727=CARTESIAN_POINT('Ctrl Pts',(64.5785944085073,1.70624802817416,17.9249440125051));
#23728=CARTESIAN_POINT('Ctrl Pts',(64.0056455581693,1.44918054437705,17.9619899760278));
#23729=CARTESIAN_POINT('Ctrl Pts',(63.6717917874564,1.01025395994159,17.9990359395505));
#23730=CARTESIAN_POINT('Ctrl Pts',(63.4541716406064,0.724142865382969,18.0231840808304));
#23731=CARTESIAN_POINT('Ctrl Pts',(63.3381427347181,0.36076003548376,18.0473322221103));
#23732=CARTESIAN_POINT('Ctrl Pts',(63.3357162681914,-0.00120644382256618,
18.0714803633902));
#23733=CARTESIAN_POINT('Origin',(65.,0.,17.));
#23734=CARTESIAN_POINT('',(63.3314263973441,-0.000500571934790497,18.7714803633902));
#23735=CARTESIAN_POINT('',(63.3333325352018,0.00145874397800797,18.5785196366098));
#23736=CARTESIAN_POINT('',(63.334,2.04026156737949E-16,17.));
#23737=CARTESIAN_POINT('Ctrl Pts',(63.3333325352018,0.00145874397800797,
18.5785196366098));
#23738=CARTESIAN_POINT('Ctrl Pts',(63.3323458932764,0.109115274956356,18.5713112672072));
#23739=CARTESIAN_POINT('Ctrl Pts',(63.3418839056658,0.216597722493275,18.5641028978047));
#23740=CARTESIAN_POINT('Ctrl Pts',(63.3625817175621,0.321886358429003,18.5568945284021));
#23741=CARTESIAN_POINT('Ctrl Pts',(63.4689539553991,0.862996108553322,18.5198485648794));
#23742=CARTESIAN_POINT('Ctrl Pts',(63.8700831830826,1.34616204853444,18.4828026013567));
#23743=CARTESIAN_POINT('Ctrl Pts',(64.382390335006,1.55026054620228,18.445756637834));
#23744=CARTESIAN_POINT('Ctrl Pts',(64.8946974869294,1.75435904387011,18.4087106743114));
#23745=CARTESIAN_POINT('Ctrl Pts',(65.5181825630929,1.67939009922466,18.3716647107887));
#23746=CARTESIAN_POINT('Ctrl Pts',(65.9675040829891,1.359663674886,18.334618747266));
#23747=CARTESIAN_POINT('Ctrl Pts',(66.4168256028854,1.03993725054733,18.2975727837433));
#23748=CARTESIAN_POINT('Ctrl Pts',(66.6919835665143,0.475453346515458,18.2605268202206));
#23749=CARTESIAN_POINT('Ctrl Pts',(66.6670503715696,-0.0754487776881312,
18.223480856698));
#23750=CARTESIAN_POINT('Ctrl Pts',(66.6421171766249,-0.626350901891724,
18.1864348931753));
#23751=CARTESIAN_POINT('Ctrl Pts',(66.3170928231065,-1.16367124626703,18.1493889296526));
#23752=CARTESIAN_POINT('Ctrl Pts',(65.8407265494155,-1.44150210839705,18.1123429661299));
#23753=CARTESIAN_POINT('Ctrl Pts',(65.3643602757244,-1.71933297052706,18.0752970026072));
#23754=CARTESIAN_POINT('Ctrl Pts',(64.7366520818608,-1.73767435041179,18.0382510390846));
#23755=CARTESIAN_POINT('Ctrl Pts',(64.2448761820938,-1.48813221154433,18.0012050755619));
#23756=CARTESIAN_POINT('Ctrl Pts',(63.7531002823268,-1.23859007267686,17.9641591120392));
#23757=CARTESIAN_POINT('Ctrl Pts',(63.3972566766564,-0.721164415057194,
17.9271131485165));
#23758=CARTESIAN_POINT('Ctrl Pts',(63.3401992089882,-0.172658024897985,
17.8900671849938));
#23759=CARTESIAN_POINT('Ctrl Pts',(63.3342707730138,-0.115666623972996,
17.8862180021992));
#23760=CARTESIAN_POINT('Ctrl Pts',(63.3315679757844,-0.0583396813265016,
17.8823688194045));
#23761=CARTESIAN_POINT('Ctrl Pts',(63.331966723543,-0.000974733628950259,
17.8785196366098));
#23762=CARTESIAN_POINT('Ctrl Pts',(63.3357162681914,-0.00120644382256618,
18.0714803633902));
#23763=CARTESIAN_POINT('Ctrl Pts',(63.3344202622762,-0.194537237022046,
18.084378185633));
#23764=CARTESIAN_POINT('Ctrl Pts',(63.3655323149503,-0.387463979276361,
18.0972760078758));
#23765=CARTESIAN_POINT('Ctrl Pts',(63.4308825664874,-0.567997006411725,
18.1101738301185));
#23766=CARTESIAN_POINT('Ctrl Pts',(63.6185858073192,-1.08653570325577,18.1472197936412));
#23767=CARTESIAN_POINT('Ctrl Pts',(64.0887509800707,-1.50282741187005,18.1842657571639));
#23768=CARTESIAN_POINT('Ctrl Pts',(64.6262043274144,-1.62635387127239,18.2213117206866));
#23769=CARTESIAN_POINT('Ctrl Pts',(65.1636576747581,-1.74988033067472,18.2583576842093));
#23770=CARTESIAN_POINT('Ctrl Pts',(65.768399196694,-1.5806415408651,18.2954036477319));
#23771=CARTESIAN_POINT('Ctrl Pts',(66.1636655065904,-1.19609059364975,18.3324496112546));
#23772=CARTESIAN_POINT('Ctrl Pts',(66.5589318164868,-0.811539646434406,
18.3694955747773));
#23773=CARTESIAN_POINT('Ctrl Pts',(66.7447229143437,-0.21167654181333,18.4065415383));
#23774=CARTESIAN_POINT('Ctrl Pts',(66.6360104507197,0.328967968929765,18.4435875018227));
#23775=CARTESIAN_POINT('Ctrl Pts',(66.5272979870957,0.869612479672864,18.4806334653453));
#23776=CARTESIAN_POINT('Ctrl Pts',(66.1240819619909,1.35103839653798,18.517679428868));
#23777=CARTESIAN_POINT('Ctrl Pts',(65.6108964756848,1.55291841879865,18.5547253923907));
#23778=CARTESIAN_POINT('Ctrl Pts',(65.0977109893788,1.75479844105931,18.5917713559134));
#23779=CARTESIAN_POINT('Ctrl Pts',(64.4745560418716,1.67713256871553,18.6288173194361));
#23780=CARTESIAN_POINT('Ctrl Pts',(64.0266220284185,1.3554650286459,18.6658632829587));
#23781=CARTESIAN_POINT('Ctrl Pts',(63.6009392798522,1.04977642615326,18.7010689764359));
#23782=CARTESIAN_POINT('Ctrl Pts',(63.3335015355576,0.523725769548793,18.7362746699131));
#23783=CARTESIAN_POINT('Ctrl Pts',(63.3314263973441,-0.000500571934790497,
18.7714803633902));
#23784=CARTESIAN_POINT('Origin',(65.,0.,17.));
#23785=CARTESIAN_POINT('',(63.3342413915565,0.00152189757970267,19.4714803633902));
#23786=CARTESIAN_POINT('',(63.3367061905351,6.33250723265802E-5,19.2785196366098));
#23787=CARTESIAN_POINT('',(63.334,2.04026156737949E-16,17.));
#23788=CARTESIAN_POINT('Ctrl Pts',(63.3367061905351,6.33250723265801E-5,
19.2785196366098));
#23789=CARTESIAN_POINT('Ctrl Pts',(63.336613224224,0.274266937448926,19.26025371501));
#23790=CARTESIAN_POINT('Ctrl Pts',(63.4006540507369,0.548429669491752,19.2419877934101));
#23791=CARTESIAN_POINT('Ctrl Pts',(63.5290671316579,0.788102757387651,19.2237218718103));
#23792=CARTESIAN_POINT('Ctrl Pts',(63.7895076621637,1.27419487286283,19.1866759082877));
#23793=CARTESIAN_POINT('Ctrl Pts',(64.3147356017013,1.61841804812355,19.149629944765));
#23794=CARTESIAN_POINT('Ctrl Pts',(64.8643774055205,1.66323659510229,19.1125839812423));
#23795=CARTESIAN_POINT('Ctrl Pts',(65.4140192093397,1.70805514208103,19.0755380177196));
#23796=CARTESIAN_POINT('Ctrl Pts',(65.9880748774405,1.4534690607778,19.0384920541969));
#23797=CARTESIAN_POINT('Ctrl Pts',(66.3238245781873,1.01599111491805,19.0014460906742));
#23798=CARTESIAN_POINT('Ctrl Pts',(66.6595742789341,0.578513169058305,18.9644001271516));
#23799=CARTESIAN_POINT('Ctrl Pts',(66.757018012327,-0.0418566413579579,
18.9273541636289));
#23800=CARTESIAN_POINT('Ctrl Pts',(66.5715601012413,-0.561202554865601,
18.8903082001062));
#23801=CARTESIAN_POINT('Ctrl Pts',(66.3861021901555,-1.08054846837324,18.8532622365835));
#23802=CARTESIAN_POINT('Ctrl Pts',(65.9177426345912,-1.49887048497226,18.8162162730609));
#23803=CARTESIAN_POINT('Ctrl Pts',(65.3808288409285,-1.62472116171495,18.7791703095382));
#23804=CARTESIAN_POINT('Ctrl Pts',(64.8439150472658,-1.75057183845763,18.7421243460155));
#23805=CARTESIAN_POINT('Ctrl Pts',(64.2384470155047,-1.58395117534399,18.7050783824928));
#23806=CARTESIAN_POINT('Ctrl Pts',(63.8415206236195,-1.20111406365341,18.6680324189701));
#23807=CARTESIAN_POINT('Ctrl Pts',(63.5218278028516,-0.892769043939022,
18.63819482485));
#23808=CARTESIAN_POINT('Ctrl Pts',(63.3374165408442,-0.444163795089777,
18.6083572307299));
#23809=CARTESIAN_POINT('Ctrl Pts',(63.3333325352018,0.00145874397800797,
18.5785196366098));
#23810=CARTESIAN_POINT('Ctrl Pts',(63.3314263973441,-0.000500571934790497,
18.7714803633902));
#23811=CARTESIAN_POINT('Ctrl Pts',(63.3313179258352,-0.0279029020134356,
18.7733206334357));
#23812=CARTESIAN_POINT('Ctrl Pts',(63.3319345194755,-0.0553002474134368,
18.7751609034813));
#23813=CARTESIAN_POINT('Ctrl Pts',(63.3332914773975,-0.0826608742403259,
18.7770011735268));
#23814=CARTESIAN_POINT('Ctrl Pts',(63.3606080192284,-0.633450029261446,
18.8140471370495));
#23815=CARTESIAN_POINT('Ctrl Pts',(63.6879541822893,-1.16935913150821,18.8510931005721));
#23816=CARTESIAN_POINT('Ctrl Pts',(64.1655181388753,-1.44512634150632,18.8881390640948));
#23817=CARTESIAN_POINT('Ctrl Pts',(64.6430820954612,-1.72089355150444,18.9251850276175));
#23818=CARTESIAN_POINT('Ctrl Pts',(65.2708638455722,-1.73651886925392,18.9622309911402));
#23819=CARTESIAN_POINT('Ctrl Pts',(65.7615555115074,-1.48485127952433,18.9992769546629));
#23820=CARTESIAN_POINT('Ctrl Pts',(66.2522471774427,-1.23318368979475,19.0363229181856));
#23821=CARTESIAN_POINT('Ctrl Pts',(66.6058487592021,-0.714223192586113,
19.0733688817082));
#23822=CARTESIAN_POINT('Ctrl Pts',(66.6605324878321,-0.165475002074327,
19.1104148452309));
#23823=CARTESIAN_POINT('Ctrl Pts',(66.715216216462,0.383273188437468,19.1474608087536));
#23824=CARTESIAN_POINT('Ctrl Pts',(66.4709820919624,0.961809072252411,19.1845067722763));
#23825=CARTESIAN_POINT('Ctrl Pts',(66.0396052463205,1.30536242146667,19.221552735799));
#23826=CARTESIAN_POINT('Ctrl Pts',(65.6082284006786,1.64891577068093,19.2585986993216));
#23827=CARTESIAN_POINT('Ctrl Pts',(64.9897088338945,1.7574865852945,19.2956446628443));
#23828=CARTESIAN_POINT('Ctrl Pts',(64.4671155329348,1.58138681666735,19.332690626367));
#23829=CARTESIAN_POINT('Ctrl Pts',(63.9445222319752,1.4052870480402,19.3697365898897));
#23830=CARTESIAN_POINT('Ctrl Pts',(63.5178551968399,0.94451669617232,19.4067825534124));
#23831=CARTESIAN_POINT('Ctrl Pts',(63.3823810155581,0.409949924733969,19.443828516935));
#23832=CARTESIAN_POINT('Ctrl Pts',(63.34867413809,0.27694615609758,19.4530457990868));
#23833=CARTESIAN_POINT('Ctrl Pts',(63.3329934814549,0.139374038553371,19.4622630812385));
#23834=CARTESIAN_POINT('Ctrl Pts',(63.3342413915565,0.00152189757970267,
19.4714803633902));
#23835=CARTESIAN_POINT('Origin',(65.,0.,17.));
#23836=CARTESIAN_POINT('',(63.33660733148,-0.000426122236795029,20.1714803633902));
#23837=CARTESIAN_POINT('',(63.3335649842428,-0.00149162251194977,19.9785196366098));
#23838=CARTESIAN_POINT('',(63.334,2.04026156737949E-16,17.));
#23839=CARTESIAN_POINT('Ctrl Pts',(63.3335649842428,-0.00149162251194977,
19.9785196366098));
#23840=CARTESIAN_POINT('Ctrl Pts',(63.3376081205507,0.436609739463929,19.9491961628127));
#23841=CARTESIAN_POINT('Ctrl Pts',(63.5150446040949,0.877608758866625,19.9198726890157));
#23842=CARTESIAN_POINT('Ctrl Pts',(63.8250037086467,1.18496125357119,19.8905492152186));
#23843=CARTESIAN_POINT('Ctrl Pts',(64.2165921595995,1.57325663038185,19.8535032516959));
#23844=CARTESIAN_POINT('Ctrl Pts',(64.8196955128484,1.748243279982,19.8164572881732));
#23845=CARTESIAN_POINT('Ctrl Pts',(65.3583001004237,1.62983756803352,19.7794113246505));
#23846=CARTESIAN_POINT('Ctrl Pts',(65.896904687999,1.51143185608505,19.7423653611279));
#23847=CARTESIAN_POINT('Ctrl Pts',(66.3710105099008,1.09963378258794,19.7053193976052));
#23848=CARTESIAN_POINT('Ctrl Pts',(66.5636403476301,0.582905071893254,19.6682734340825));
#23849=CARTESIAN_POINT('Ctrl Pts',(66.7562701853594,0.0661763611985695,
19.6312274705598));
#23850=CARTESIAN_POINT('Ctrl Pts',(66.6674240389162,-0.55548298669369,19.5941815070372));
#23851=CARTESIAN_POINT('Ctrl Pts',(66.3377628513866,-0.997567046656913,
19.5571355435145));
#23852=CARTESIAN_POINT('Ctrl Pts',(66.008101663857,-1.43965110662013,19.5200895799918));
#23853=CARTESIAN_POINT('Ctrl Pts',(65.437625435241,-1.70215987865432,19.4830436164691));
#23854=CARTESIAN_POINT('Ctrl Pts',(64.8874158461961,-1.6649547344678,19.4459976529464));
#23855=CARTESIAN_POINT('Ctrl Pts',(64.3372062571513,-1.62774959028127,19.4089516894237));
#23856=CARTESIAN_POINT('Ctrl Pts',(63.8072633076776,-1.29083052987404,19.3719057259011));
#23857=CARTESIAN_POINT('Ctrl Pts',(63.5401183936778,-0.808390471825603,
19.3348597623784));
#23858=CARTESIAN_POINT('Ctrl Pts',(63.404692230951,-0.563822814410766,19.3160797204555));
#23859=CARTESIAN_POINT('Ctrl Pts',(63.3368017735151,-0.28185813767411,19.2972996785327));
#23860=CARTESIAN_POINT('Ctrl Pts',(63.3367061905351,6.33250723265801E-5,
19.2785196366098));
#23861=CARTESIAN_POINT('Ctrl Pts',(63.3342413915565,0.00152189757970267,
19.4714803633902));
#23862=CARTESIAN_POINT('Ctrl Pts',(63.3380090632001,-0.414679238971563,
19.4993090447612));
#23863=CARTESIAN_POINT('Ctrl Pts',(63.496088728647,-0.833432923200605,19.5271377261321));
#23864=CARTESIAN_POINT('Ctrl Pts',(63.778271499721,-1.1367187830676,19.5549664075031));
#23865=CARTESIAN_POINT('Ctrl Pts',(64.1539174925939,-1.54045752842199,19.5920123710258));
#23866=CARTESIAN_POINT('Ctrl Pts',(64.7494908057681,-1.73957182812194,19.6290583345484));
#23867=CARTESIAN_POINT('Ctrl Pts',(65.2924239354676,-1.64293589624755,19.6661042980711));
#23868=CARTESIAN_POINT('Ctrl Pts',(65.835357065167,-1.54629996437316,19.7031502615938));
#23869=CARTESIAN_POINT('Ctrl Pts',(66.3256500113918,-1.15391380092443,19.7401962251165));
#23870=CARTESIAN_POINT('Ctrl Pts',(66.5389174268969,-0.645355153836869,
19.7772421886392));
#23871=CARTESIAN_POINT('Ctrl Pts',(66.7521848424021,-0.136796506749309,
19.8142881521618));
#23872=CARTESIAN_POINT('Ctrl Pts',(66.6884267271877,0.487934623977085,19.8513341156845));
#23873=CARTESIAN_POINT('Ctrl Pts',(66.3768223447206,0.942926484478224,19.8883800792072));
#23874=CARTESIAN_POINT('Ctrl Pts',(66.0652179622535,1.39791834497936,19.9254260427299));
#23875=CARTESIAN_POINT('Ctrl Pts',(65.5057673125336,1.68317093525526,19.9624720062526));
#23876=CARTESIAN_POINT('Ctrl Pts',(64.9545061567026,1.6681368085672,19.9995179697752));
#23877=CARTESIAN_POINT('Ctrl Pts',(64.4032450008716,1.65310268187915,20.0365639332979));
#23878=CARTESIAN_POINT('Ctrl Pts',(63.8601733389293,1.33778183822715,20.0736098968206));
#23879=CARTESIAN_POINT('Ctrl Pts',(63.5738309983811,0.866482612606734,20.1106558603433));
#23880=CARTESIAN_POINT('Ctrl Pts',(63.4171190932323,0.608545908587611,20.1309306946923));
#23881=CARTESIAN_POINT('Ctrl Pts',(63.3373039960783,0.303889805224319,20.1512055290412));
#23882=CARTESIAN_POINT('Ctrl Pts',(63.33660733148,-0.000426122236795029,
20.1714803633902));
#23883=CARTESIAN_POINT('Origin',(65.,0.,17.));
#23884=CARTESIAN_POINT('',(63.3326792503596,-0.00130047270866476,20.8714803633902));
#23885=CARTESIAN_POINT('',(63.3318013787731,0.000864016794202189,20.6785196366098));
#23886=CARTESIAN_POINT('',(63.334,2.04026156737949E-16,17.));
#23887=CARTESIAN_POINT('Ctrl Pts',(63.3318013787731,0.000864016794202189,
20.6785196366098));
#23888=CARTESIAN_POINT('Ctrl Pts',(63.3314877360124,0.050553985174294,20.6751845741382));
#23889=CARTESIAN_POINT('Ctrl Pts',(63.3335154742976,0.100217999006552,20.6718495116665));
#23890=CARTESIAN_POINT('Ctrl Pts',(63.3379679807618,0.149663664483466,20.6685144491949));
#23891=CARTESIAN_POINT('Ctrl Pts',(63.3874265421712,0.698907444829377,20.6314684856722));
#23892=CARTESIAN_POINT('Ctrl Pts',(63.7360730319708,1.22120960136622,20.5944225221495));
#23893=CARTESIAN_POINT('Ctrl Pts',(64.2243472290266,1.47753582103746,20.5573765586268));
#23894=CARTESIAN_POINT('Ctrl Pts',(64.7126214260825,1.73386204070869,20.5203305951042));
#23895=CARTESIAN_POINT('Ctrl Pts',(65.3405233303947,1.72421232351432,20.4832846315815));
#23896=CARTESIAN_POINT('Ctrl Pts',(65.8206901647961,1.453002801034,20.4462386680588));
#23897=CARTESIAN_POINT('Ctrl Pts',(66.3008569991975,1.18179327855368,20.4091927045361));
#23898=CARTESIAN_POINT('Ctrl Pts',(66.6332887636883,0.649023950787429,20.3721467410134));
#23899=CARTESIAN_POINT('Ctrl Pts',(66.6658461309716,0.0985197801765333,
20.3351007774908));
#23900=CARTESIAN_POINT('Ctrl Pts',(66.698403498255,-0.451984390434366,20.2980548139681));
#23901=CARTESIAN_POINT('Ctrl Pts',(66.431086468331,-1.02022340388991,20.2610088504454));
#23902=CARTESIAN_POINT('Ctrl Pts',(65.9862342185508,-1.34613948307828,20.2239628869227));
#23903=CARTESIAN_POINT('Ctrl Pts',(65.5413819687707,-1.67205556226665,20.1869169234));
#23904=CARTESIAN_POINT('Ctrl Pts',(64.9189944991343,-1.75564870718784,20.1498709598773));
#23905=CARTESIAN_POINT('Ctrl Pts',(64.4039109527966,-1.55866202617724,20.1128249963547));
#23906=CARTESIAN_POINT('Ctrl Pts',(63.8888274064588,-1.36167534516664,20.075779032832));
#23907=CARTESIAN_POINT('Ctrl Pts',(63.4810477834196,-0.884108838224231,
20.0387330693093));
#23908=CARTESIAN_POINT('Ctrl Pts',(63.3671947462284,-0.344523532742441,
20.0016871057866));
#23909=CARTESIAN_POINT('Ctrl Pts',(63.3434612857827,-0.232043208803138,
19.993964616061));
#23910=CARTESIAN_POINT('Ctrl Pts',(63.332500203214,-0.116867900576725,19.9862421263354));
#23911=CARTESIAN_POINT('Ctrl Pts',(63.3335649842428,-0.00149162251194977,
19.9785196366098));
#23912=CARTESIAN_POINT('Ctrl Pts',(63.33660733148,-0.000426122236795029,
20.1714803633902));
#23913=CARTESIAN_POINT('Ctrl Pts',(63.3360310578707,-0.252153048396656,
20.1882514925639));
#23914=CARTESIAN_POINT('Ctrl Pts',(63.3895909699888,-0.503647211782716,
20.2050226217376));
#23915=CARTESIAN_POINT('Ctrl Pts',(63.4985445030998,-0.728272982538809,
20.2217937509113));
#23916=CARTESIAN_POINT('Ctrl Pts',(63.7392133675209,-1.2244517444751,20.258839714434));
#23917=CARTESIAN_POINT('Ctrl Pts',(64.2501641155174,-1.58953166075886,20.2958856779567));
#23918=CARTESIAN_POINT('Ctrl Pts',(64.7975572478223,-1.65643198360555,20.3329316414794));
#23919=CARTESIAN_POINT('Ctrl Pts',(65.3449503801273,-1.72333230645224,20.369977605002));
#23920=CARTESIAN_POINT('Ctrl Pts',(65.9287858967409,-1.49205303586186,20.4070235685247));
#23921=CARTESIAN_POINT('Ctrl Pts',(66.2818681473523,-1.06844015166583,20.4440695320474));
#23922=CARTESIAN_POINT('Ctrl Pts',(66.6349503979637,-0.644827267469802,
20.4811154955701));
#23923=CARTESIAN_POINT('Ctrl Pts',(66.757279382573,-0.0288807696681307,
20.5181614590928));
#23924=CARTESIAN_POINT('Ctrl Pts',(66.5928705785965,0.497507359328871,20.5552074226155));
#23925=CARTESIAN_POINT('Ctrl Pts',(66.42846177462,1.02389548832587,20.5922533861381));
#23926=CARTESIAN_POINT('Ctrl Pts',(65.9773151820577,1.4607252485182,20.6292993496608));
#23927=CARTESIAN_POINT('Ctrl Pts',(65.4459005359057,1.60808016419334,20.6663453131835));
#23928=CARTESIAN_POINT('Ctrl Pts',(64.9144858897538,1.75543507986848,20.7033912767062));
#23929=CARTESIAN_POINT('Ctrl Pts',(64.3028031900122,1.61331515102643,20.7404372402289));
#23930=CARTESIAN_POINT('Ctrl Pts',(63.8907926142615,1.24676010485229,20.7774832037515));
#23931=CARTESIAN_POINT('Ctrl Pts',(63.5423261851822,0.936738625989566,20.8088155902978));
#23932=CARTESIAN_POINT('Ctrl Pts',(63.3366907965296,0.466172446764657,20.840147976844));
#23933=CARTESIAN_POINT('Ctrl Pts',(63.3326792503596,-0.00130047270866476,
20.8714803633902));
#23934=CARTESIAN_POINT('Origin',(65.,0.,17.));
#23935=CARTESIAN_POINT('',(63.3325282901756,0.00121307831918299,21.5714803633902));
#23936=CARTESIAN_POINT('',(63.3361634080255,0.000941845566869666,21.3785196366098));
#23937=CARTESIAN_POINT('',(63.334,2.04026156737949E-16,17.));
#23938=CARTESIAN_POINT('',(66.2690708798524,1.07935865304853,22.));
#23939=CARTESIAN_POINT('Ctrl Pts',(63.3325282901756,0.00121307831918299,
21.5714803633902));
#23940=CARTESIAN_POINT('Ctrl Pts',(63.3364666394986,-0.471552579298224,
21.6031823516921));
#23941=CARTESIAN_POINT('Ctrl Pts',(63.5475594887738,-0.947301871471163,
21.634884339994));
#23942=CARTESIAN_POINT('Ctrl Pts',(63.9032471486994,-1.25758535694561,21.6665863282959));
#23943=CARTESIAN_POINT('Ctrl Pts',(64.3188927526783,-1.62017304624496,21.7036322918186));
#23944=CARTESIAN_POINT('Ctrl Pts',(64.9319903369097,-1.75680828918912,21.7406782553412));
#23945=CARTESIAN_POINT('Ctrl Pts',(65.4619049207954,-1.60385028487085,21.7777242188639));
#23946=CARTESIAN_POINT('Ctrl Pts',(65.991819504681,-1.45089228055259,21.8147701823866));
#23947=CARTESIAN_POINT('Ctrl Pts',(66.4385510882208,-1.0083410289719,21.8518161459093));
#23948=CARTESIAN_POINT('Ctrl Pts',(66.5975920398022,-0.481277360573865,
21.8888621094319));
#23949=CARTESIAN_POINT('Ctrl Pts',(66.7566329913836,0.0457863078241707,
21.9259080729546));
#23950=CARTESIAN_POINT('Ctrl Pts',(66.6279833110066,0.657362393039556,21.9629540364773));
#23951=CARTESIAN_POINT('Ctrl Pts',(66.2690708798524,1.07935865304855,22.));
#23952=CARTESIAN_POINT('',(63.7285313545748,1.08121009939331,22.));
#23953=CARTESIAN_POINT('Origin',(65.,0.,22.));
#23954=CARTESIAN_POINT('Ctrl Pts',(63.7285300176229,1.0812111317272,22.));
#23955=CARTESIAN_POINT('Ctrl Pts',(64.0793901440196,1.49274250755582,21.9636770818144));
#23956=CARTESIAN_POINT('Ctrl Pts',(64.6493623256457,1.71876565001736,21.9273541636289));
#23957=CARTESIAN_POINT('Ctrl Pts',(65.1867621807782,1.65816351020322,21.8910312454434));
#23958=CARTESIAN_POINT('Ctrl Pts',(65.7348595370708,1.59635502197871,21.8539852819207));
#23959=CARTESIAN_POINT('Ctrl Pts',(66.2490748882323,1.23639652943471,21.816939318398));
#23960=CARTESIAN_POINT('Ctrl Pts',(66.4944088007071,0.742590901212614,21.7798933548753));
#23961=CARTESIAN_POINT('Ctrl Pts',(66.7397427131819,0.248785272990521,21.7428473913526));
#23962=CARTESIAN_POINT('Ctrl Pts',(66.7161951869699,-0.378867490909659,
21.7058014278299));
#23963=CARTESIAN_POINT('Ctrl Pts',(66.4343747134738,-0.852900746623158,
21.6687554643073));
#23964=CARTESIAN_POINT('Ctrl Pts',(66.1525542399776,-1.32693400233666,21.6317095007846));
#23965=CARTESIAN_POINT('Ctrl Pts',(65.6124608191971,-1.64734774986348,21.5946635372619));
#23966=CARTESIAN_POINT('Ctrl Pts',(65.061356017574,-1.66761252399562,21.5576175737392));
#23967=CARTESIAN_POINT('Ctrl Pts',(64.5102512159508,-1.68787729812775,21.5205716102165));
#23968=CARTESIAN_POINT('Ctrl Pts',(63.9481350334849,-1.40799309886521,21.4835256466939));
#23969=CARTESIAN_POINT('Ctrl Pts',(63.6322204085561,-0.95599522362411,21.4464796831712));
#23970=CARTESIAN_POINT('Ctrl Pts',(63.4390408141815,-0.679601668824516,
21.4238263343174));
#23971=CARTESIAN_POINT('Ctrl Pts',(63.3379218264913,-0.338850724949921,
21.4011729854636));
#23972=CARTESIAN_POINT('Ctrl Pts',(63.3361634080255,0.000941845566869666,
21.3785196366098));
#23973=CARTESIAN_POINT('Origin',(65.,0.,23.5459252805377));
#23974=CARTESIAN_POINT('',(62.9427844533856,0.00119489768198394,13.4540747194623));
#23975=CARTESIAN_POINT('',(62.9484021938786,-0.000803300711486093,13.3959252805377));
#23976=CARTESIAN_POINT('',(62.94525,1.28744642201805E-13,23.5459252805377));
#23977=CARTESIAN_POINT('',(66.8826275096638,-0.823232180103057,13.));
#23978=CARTESIAN_POINT('Ctrl Pts',(62.9484021938786,-0.000803300711485905,
13.3959252805377));
#23979=CARTESIAN_POINT('Ctrl Pts',(62.9495841394398,0.384792240838318,13.3750880775932));
#23980=CARTESIAN_POINT('Ctrl Pts',(63.239440569463,1.45761852527274,13.3172049111259));
#23981=CARTESIAN_POINT('Ctrl Pts',(64.970198323091,2.42992595215152,13.2222757811361));
#23982=CARTESIAN_POINT('Ctrl Pts',(67.0251392906009,1.33877286094185,13.111137890568));
#23983=CARTESIAN_POINT('Ctrl Pts',(67.1563717950601,-0.197213743559485,
13.0370459635227));
#23984=CARTESIAN_POINT('Ctrl Pts',(66.8826275096638,-0.823232180103057,
13.));
#23985=CARTESIAN_POINT('',(66.2235927967208,-1.65534565011393,13.));
#23986=CARTESIAN_POINT('Origin',(65.,0.,13.));
#23987=CARTESIAN_POINT('Ctrl Pts',(62.9427844533856,0.00119489768198401,
13.4540747194623));
#23988=CARTESIAN_POINT('Ctrl Pts',(62.9422817266512,0.0728349382260934,
13.4501772883951));
#23989=CARTESIAN_POINT('Ctrl Pts',(62.9781729708452,0.824925643882596,13.4092338938053));
#23990=CARTESIAN_POINT('Ctrl Pts',(63.9036938704104,2.16732302296764,13.3312445356927));
#23991=CARTESIAN_POINT('Ctrl Pts',(66.2265689546786,2.09606376419022,13.2201066451247));
#23992=CARTESIAN_POINT('Ctrl Pts',(67.4179368644029,0.120091680801066,13.1096917998938));
#23993=CARTESIAN_POINT('Ctrl Pts',(66.7594496906129,-1.25819328818366,13.0363229181856));
#23994=CARTESIAN_POINT('Ctrl Pts',(66.2235939546714,-1.65534738192936,13.));
#23995=CARTESIAN_POINT('Origin',(65.,0.,23.5459252805377));
#23996=CARTESIAN_POINT('',(62.9480827837869,0.00102651687048705,14.1540747194623));
#23997=CARTESIAN_POINT('',(62.9433366278651,-0.0014977223415923,14.0959252805377));
#23998=CARTESIAN_POINT('',(62.94525,1.28744642201805E-13,23.5459252805377));
#23999=CARTESIAN_POINT('Ctrl Pts',(62.9433366278651,-0.00149772234159223,
14.0959252805377));
#24000=CARTESIAN_POINT('Ctrl Pts',(62.9481477427571,0.585192187367158,14.0640305253959));
#24001=CARTESIAN_POINT('Ctrl Pts',(63.5186241718586,1.86149425637258,13.9950898067315));
#24002=CARTESIAN_POINT('Ctrl Pts',(65.684305645688,2.3302668619962,13.8891031245443));
#24003=CARTESIAN_POINT('Ctrl Pts',(67.3289123722387,0.688818574436941,13.7779652339763));
#24004=CARTESIAN_POINT('Ctrl Pts',(66.8417982611818,-1.58294512384396,13.6668273434083));
#24005=CARTESIAN_POINT('Ctrl Pts',(64.6689465387577,-2.4061546469661,13.5556894528402));
#24006=CARTESIAN_POINT('Ctrl Pts',(63.14955544062,-1.28502616351135,13.4653887652167));
#24007=CARTESIAN_POINT('Ctrl Pts',(62.9474827867649,-0.300748827451898,
13.4121340411158));
#24008=CARTESIAN_POINT('Ctrl Pts',(62.9484021938786,-0.000803300711485905,
13.3959252805377));
#24009=CARTESIAN_POINT('Ctrl Pts',(62.9480827837869,0.00102651687048705,
14.1540747194623));
#24010=CARTESIAN_POINT('Ctrl Pts',(62.9468311597533,0.277742487636534,14.1391197361979));
#24011=CARTESIAN_POINT('Ctrl Pts',(63.1278468516848,1.23836027065323,14.0871187894108));
#24012=CARTESIAN_POINT('Ctrl Pts',(64.5878737813476,2.39342385873018,13.998071879101));
#24013=CARTESIAN_POINT('Ctrl Pts',(66.7873400138256,1.64430308142019,13.8869339885329));
#24014=CARTESIAN_POINT('Ctrl Pts',(67.3508170614469,-0.609852217558742,
13.7757960979649));
#24015=CARTESIAN_POINT('Ctrl Pts',(65.7625975239189,-2.30583209920716,13.6646582073969));
#24016=CARTESIAN_POINT('Ctrl Pts',(63.5564754082319,-1.90574022357351,13.557417747896));
#24017=CARTESIAN_POINT('Ctrl Pts',(62.9470602579309,-0.608119845326389,
13.4872232519178));
#24018=CARTESIAN_POINT('Ctrl Pts',(62.9427844533856,0.00119489768198401,
13.4540747194623));
#24019=CARTESIAN_POINT('Origin',(65.,0.,23.5459252805377));
#24020=CARTESIAN_POINT('',(62.9465102637711,-0.00176526862452037,14.8540747194623));
#24021=CARTESIAN_POINT('',(62.94372126594,0.00163389948556141,14.7959252805377));
#24022=CARTESIAN_POINT('',(62.94525,1.28744642201805E-13,23.5459252805377));
#24023=CARTESIAN_POINT('Ctrl Pts',(62.94372126594,0.00163389948556124,14.7959252805377));
#24024=CARTESIAN_POINT('Ctrl Pts',(62.9427765522985,0.110331733448615,14.7900189367213));
#24025=CARTESIAN_POINT('Ctrl Pts',(63.0000473239053,0.899810372641752,14.7470666293823));
#24026=CARTESIAN_POINT('Ctrl Pts',(64.0226192720082,2.22329513352231,14.6670683585206));
#24027=CARTESIAN_POINT('Ctrl Pts',(66.3378385875382,2.02694463079714,14.5559304679526));
#24028=CARTESIAN_POINT('Ctrl Pts',(67.4285194097127,-0.0246926670119161,
14.4447925773845));
#24029=CARTESIAN_POINT('Ctrl Pts',(66.2963482043283,-2.05372573368659,14.3336546868165));
#24030=CARTESIAN_POINT('Ctrl Pts',(63.9776161165208,-2.20296580816612,14.2225167962485));
#24031=CARTESIAN_POINT('Ctrl Pts',(62.9915607037629,-0.871642779145011,
14.1432736608222));
#24032=CARTESIAN_POINT('Ctrl Pts',(62.942559601823,-0.0962519214711344,
14.1010764889186));
#24033=CARTESIAN_POINT('Ctrl Pts',(62.9433366278651,-0.00149772234159223,
14.0959252805377));
#24034=CARTESIAN_POINT('Ctrl Pts',(62.946510263771,-0.00176526862452042,
14.8540747194623));
#24035=CARTESIAN_POINT('Ctrl Pts',(62.9504460460768,0.478624892210608,14.8280621840006));
#24036=CARTESIAN_POINT('Ctrl Pts',(63.3581297348817,1.64918471803046,14.7650036850163));
#24037=CARTESIAN_POINT('Ctrl Pts',(65.308185017446,2.40901142364104,14.6648992225093));
#24038=CARTESIAN_POINT('Ctrl Pts',(67.1910886177016,1.04758997952522,14.5537613319412));
#24039=CARTESIAN_POINT('Ctrl Pts',(67.068463685159,-1.27270221153156,14.4426234413732));
#24040=CARTESIAN_POINT('Ctrl Pts',(65.0525510239567,-2.42807611461693,14.3314855508051));
#24041=CARTESIAN_POINT('Ctrl Pts',(63.2662754947239,-1.50459133827137,14.2353026435015));
#24042=CARTESIAN_POINT('Ctrl Pts',(62.9499316392037,-0.407728674576407,
14.1761656997206));
#24043=CARTESIAN_POINT('Ctrl Pts',(62.9480827837869,0.00102651687048705,
14.1540747194623));
#24044=CARTESIAN_POINT('Origin',(65.,0.,23.5459252805377));
#24045=CARTESIAN_POINT('',(62.9418498698494,8.27718827440684E-6,15.5540747194623));
#24046=CARTESIAN_POINT('',(62.9484914975566,0.000468974127544061,15.4959252805377));
#24047=CARTESIAN_POINT('',(62.94525,1.28744642201805E-13,23.5459252805377));
#24048=CARTESIAN_POINT('Ctrl Pts',(62.9484914975566,0.000468974127544111,
15.4959252805377));
#24049=CARTESIAN_POINT('Ctrl Pts',(62.9478504078462,0.31451301948094,15.4789613845241));
#24050=CARTESIAN_POINT('Ctrl Pts',(63.1632430376845,1.31353647315873,15.4249515249878));
#24051=CARTESIAN_POINT('Ctrl Pts',(64.7178900651262,2.41220423477674,15.3338957019289));
#24052=CARTESIAN_POINT('Ctrl Pts',(66.8736278902366,1.54526173974448,15.2227578113608));
#24053=CARTESIAN_POINT('Ctrl Pts',(67.3144128645646,-0.736076372865367,
15.1116199207928));
#24054=CARTESIAN_POINT('Ctrl Pts',(65.6367894857436,-2.34367538861624,15.0004820302248));
#24055=CARTESIAN_POINT('Ctrl Pts',(63.4964372981478,-1.83465185719793,14.895250483473));
#24056=CARTESIAN_POINT('Ctrl Pts',(62.9487020162047,-0.571446388044015,
14.827064900244));
#24057=CARTESIAN_POINT('Ctrl Pts',(62.94372126594,0.00163389948556124,14.7959252805377));
#24058=CARTESIAN_POINT('Ctrl Pts',(62.9418498868449,8.27714690067514E-6,
15.5540747194623));
#24059=CARTESIAN_POINT('Ctrl Pts',(62.9418498603911,0.000451185307771551,
15.5540505953261));
#24060=CARTESIAN_POINT('Ctrl Pts',(62.9420505595996,0.681041096754115,15.5169805076671));
#24061=CARTESIAN_POINT('Ctrl Pts',(63.6841642251148,2.04129618504104,15.4428644564855));
#24062=CARTESIAN_POINT('Ctrl Pts',(66.0013718021885,2.21259314346663,15.3317265659175));
#24063=CARTESIAN_POINT('Ctrl Pts',(67.4020124146433,0.358678503164372,15.2205886753494));
#24064=CARTESIAN_POINT('Ctrl Pts',(66.6040638188323,-1.82353863480769,15.1094507847814));
#24065=CARTESIAN_POINT('Ctrl Pts',(64.3378974271891,-2.33665018787605,14.9983128942134));
#24066=CARTESIAN_POINT('Ctrl Pts',(63.0663265778663,-1.09149331437408,14.913187539107));
#24067=CARTESIAN_POINT('Ctrl Pts',(62.9448408697591,-0.205526654691508,
14.8651081475233));
#24068=CARTESIAN_POINT('Ctrl Pts',(62.946510263771,-0.00176526862452042,
14.8540747194623));
#24069=CARTESIAN_POINT('Origin',(65.,0.,23.5459252805377));
#24070=CARTESIAN_POINT('',(62.9465344116198,0.00176006504695819,16.2540747194623));
#24071=CARTESIAN_POINT('',(62.9454411297334,-0.00187890759640223,16.1959252805377));
#24072=CARTESIAN_POINT('',(62.94525,1.28744642201805E-13,23.5459252805377));
#24073=CARTESIAN_POINT('Ctrl Pts',(62.9454411297334,-0.0018789075964022,
16.1959252805377));
#24074=CARTESIAN_POINT('Ctrl Pts',(62.9501461271515,0.514927296910589,16.1679038323268));
#24075=CARTESIAN_POINT('Ctrl Pts',(63.4098006358751,1.7224375006787,16.1028364205933));
#24076=CARTESIAN_POINT('Ctrl Pts',(65.4379883182475,2.38882429960344,16.0007230453371));
#24077=CARTESIAN_POINT('Ctrl Pts',(67.24452629377,0.927586663439804,15.8895851547691));
#24078=CARTESIAN_POINT('Ctrl Pts',(66.996623898036,-1.3826815656909,15.7784472642011));
#24079=CARTESIAN_POINT('Ctrl Pts',(64.9211890049946,-2.42736567633038,15.667309373633));
#24080=CARTESIAN_POINT('Ctrl Pts',(63.223670707888,-1.42992668390708,15.5731353790785));
#24081=CARTESIAN_POINT('Ctrl Pts',(62.9492504273939,-0.37130020640541,15.5160073480468));
#24082=CARTESIAN_POINT('Ctrl Pts',(62.9484914975566,0.000468974127544111,
15.4959252805377));
#24083=CARTESIAN_POINT('Ctrl Pts',(62.9465344116198,0.00176006504695823,
16.2540747194623));
#24084=CARTESIAN_POINT('Ctrl Pts',(62.944864096038,0.206418574104773,16.2429930431288));
#24085=CARTESIAN_POINT('Ctrl Pts',(63.0670246817589,1.09329987115452,16.1948654032727));
#24086=CARTESIAN_POINT('Ctrl Pts',(64.3409338179361,2.33750843231645,16.1096917998938));
#24087=CARTESIAN_POINT('Ctrl Pts',(66.6064316564341,1.82145305641563,15.9985539093258));
#24088=CARTESIAN_POINT('Ctrl Pts',(67.401544381661,-0.361798958737837,15.8874160187577));
#24089=CARTESIAN_POINT('Ctrl Pts',(65.9984962989145,-2.2138922838142,15.7762781281897));
#24090=CARTESIAN_POINT('Ctrl Pts',(63.6820161659208,-2.03962273041628,15.6651643617579));
#24091=CARTESIAN_POINT('Ctrl Pts',(62.9418904838623,-0.679695842678602,
15.5910965588488));
#24092=CARTESIAN_POINT('Ctrl Pts',(62.9418498868449,8.27714690067514E-6,
15.5540747194623));
#24093=CARTESIAN_POINT('Origin',(65.,0.,23.5459252805377));
#24094=CARTESIAN_POINT('',(62.9480689459238,-0.00103910400150425,16.9540747194623));
#24095=CARTESIAN_POINT('',(62.9421231189799,0.000678771108096866,16.8959252805377));
#24096=CARTESIAN_POINT('',(62.94525,1.28744642201805E-13,23.5459252805377));
#24097=CARTESIAN_POINT('Ctrl Pts',(62.9421231189799,0.000678771108097069,
16.8959252805377));
#24098=CARTESIAN_POINT('Ctrl Pts',(62.9419623987169,0.0380176929103635,
16.8938922436523));
#24099=CARTESIAN_POINT('Ctrl Pts',(62.9598052246296,0.755589108274135,16.8548132432442));
#24100=CARTESIAN_POINT('Ctrl Pts',(63.7964607753782,2.1094569529468,16.7786882793134));
#24101=CARTESIAN_POINT('Ctrl Pts',(66.119540899393,2.15521309297247,16.6675503887454));
#24102=CARTESIAN_POINT('Ctrl Pts',(67.4178925417354,0.228278247224652,16.5564124981773));
#24103=CARTESIAN_POINT('Ctrl Pts',(66.5031197198625,-1.90760226706539,16.4452746076093));
#24104=CARTESIAN_POINT('Ctrl Pts',(64.2125243718594,-2.29743279261728,16.3341367170413));
#24105=CARTESIAN_POINT('Ctrl Pts',(63.0385141433925,-1.01630861777053,16.251020274684));
#24106=CARTESIAN_POINT('Ctrl Pts',(62.9439258504044,-0.168320180393539,
16.2049497958495));
#24107=CARTESIAN_POINT('Ctrl Pts',(62.9454411297334,-0.0018789075964022,
16.1959252805377));
#24108=CARTESIAN_POINT('Ctrl Pts',(62.9480689459238,-0.00103910400150412,
16.9540747194623));
#24109=CARTESIAN_POINT('Ctrl Pts',(62.9499449184218,0.408602185927949,16.9319354909316));
#24110=CARTESIAN_POINT('Ctrl Pts',(63.2673355867028,1.50638090616108,16.8727502988781));
#24111=CARTESIAN_POINT('Ctrl Pts',(65.0557052990257,2.42800552371272,16.776519143302));
#24112=CARTESIAN_POINT('Ctrl Pts',(67.0701156187118,1.27001386948508,16.665381252734));
#24113=CARTESIAN_POINT('Ctrl Pts',(67.1897256358837,-1.05043588241968,16.5542433621659));
#24114=CARTESIAN_POINT('Ctrl Pts',(65.3050549453524,-2.40940975839149,16.4431054715979));
#24115=CARTESIAN_POINT('Ctrl Pts',(63.3569278527547,-1.64741761903889,16.3430492573633));
#24116=CARTESIAN_POINT('Ctrl Pts',(62.9504479489003,-0.477753335721165,
16.2800390066515));
#24117=CARTESIAN_POINT('Ctrl Pts',(62.9465344116198,0.00176006504695823,
16.2540747194623));
#24118=CARTESIAN_POINT('Origin',(65.,0.,23.5459252805377));
#24119=CARTESIAN_POINT('',(62.9427422720288,-0.00120218122682567,17.6540747194623));
#24120=CARTESIAN_POINT('',(62.9474450730054,0.00145098026757097,17.5959252805377));
#24121=CARTESIAN_POINT('',(62.94525,1.28744642201805E-13,23.5459252805377));
#24122=CARTESIAN_POINT('Ctrl Pts',(62.9474450730054,0.00145098026757093,
17.5959252805377));
#24123=CARTESIAN_POINT('Ctrl Pts',(62.9458669586282,0.243481142931844,17.582834691455));
#24124=CARTESIAN_POINT('Ctrl Pts',(63.0973769195488,1.16853721152032,17.5326981388497));
#24125=CARTESIAN_POINT('Ctrl Pts',(64.4682857559272,2.3697247232932,17.4455156227217));
#24126=CARTESIAN_POINT('Ctrl Pts',(66.7025669780829,1.73192984461804,17.3343777321536));
#24127=CARTESIAN_POINT('Ctrl Pts',(67.3784693367765,-0.491120062256288,
17.2232398415856));
#24128=CARTESIAN_POINT('Ctrl Pts',(65.8773317378418,-2.26464220646722,17.1121019510175));
#24129=CARTESIAN_POINT('Ctrl Pts',(63.6153124412349,-1.97078728704393,17.0029970973349));
#24130=CARTESIAN_POINT('Ctrl Pts',(62.9448910406138,-0.642371504646379,
16.930938207175));
#24131=CARTESIAN_POINT('Ctrl Pts',(62.9421231189799,0.000678771108097069,
16.8959252805377));
#24132=CARTESIAN_POINT('Ctrl Pts',(62.9427422720288,-0.00120218122682566,
17.6540747194623));
#24133=CARTESIAN_POINT('Ctrl Pts',(62.9469836764117,0.60897790221346,17.6208779387343));
#24134=CARTESIAN_POINT('Ctrl Pts',(63.5579942556341,1.90746584530599,17.5506351944836));
#24135=CARTESIAN_POINT('Ctrl Pts',(65.7655743703156,2.30482315743208,17.4433464867103));
#24136=CARTESIAN_POINT('Ctrl Pts',(67.3516166417705,0.606805630879791,17.3322085961422));
#24137=CARTESIAN_POINT('Ctrl Pts',(66.7851975318663,-1.64662797126069,17.2210707055742));
#24138=CARTESIAN_POINT('Ctrl Pts',(64.5847668755277,-2.39288431727495,17.1099328150062));
#24139=CARTESIAN_POINT('Ctrl Pts',(63.1270293146865,-1.23655417501041,17.0209341529689));
#24140=CARTESIAN_POINT('Ctrl Pts',(62.9468058203889,-0.276857845483467,
16.9689814544543));
#24141=CARTESIAN_POINT('Ctrl Pts',(62.9480689459238,-0.00103910400150412,
16.9540747194623));
#24142=CARTESIAN_POINT('Origin',(65.,0.,23.5459252805377));
#24143=CARTESIAN_POINT('',(62.9444267867382,0.0017991321662697,18.3540747194623));
#24144=CARTESIAN_POINT('',(62.9473667479389,-0.00148795945043145,18.2959252805377));
#24145=CARTESIAN_POINT('',(62.94525,1.28744642201805E-13,23.5459252805377));
#24146=CARTESIAN_POINT('Ctrl Pts',(62.9473667479389,-0.00148795945043152,
18.2959252805377));
#24147=CARTESIAN_POINT('Ctrl Pts',(62.9503594142629,0.444940986140609,18.2717771392578));
#24148=CARTESIAN_POINT('Ctrl Pts',(63.3129997156342,1.58066882860309,18.2105830344552));
#24149=CARTESIAN_POINT('Ctrl Pts',(65.1869048686148,2.42144210577608,18.1123429661299));
#24150=CARTESIAN_POINT('Ctrl Pts',(67.1357566643205,1.15622609049767,18.0012050755618));
#24151=CARTESIAN_POINT('Ctrl Pts',(67.1297261640456,-1.16729677790885,17.8900671849939));
#24152=CARTESIAN_POINT('Ctrl Pts',(65.1743331530824,-2.42237966744962,17.7789292944258));
#24153=CARTESIAN_POINT('Ctrl Pts',(63.3084858902886,-1.57355950027139,17.6808819929404));
#24154=CARTESIAN_POINT('Ctrl Pts',(62.9503329736625,-0.441456755648323,
17.6198806549777));
#24155=CARTESIAN_POINT('Ctrl Pts',(62.9474450730054,0.00145098026757093,
17.5959252805377));
#24156=CARTESIAN_POINT('Ctrl Pts',(62.9444267867382,0.00179913216626967,
18.3540747194623));
#24157=CARTESIAN_POINT('Ctrl Pts',(62.9432099184932,0.134576597368968,18.3468663500598));
#24158=CARTESIAN_POINT('Ctrl Pts',(63.0154304430432,0.94841898130449,18.3026120171345));
#24159=CARTESIAN_POINT('Ctrl Pts',(64.1011546824859,2.25618948643599,18.2213117206866));
#24160=CARTESIAN_POINT('Ctrl Pts',(66.4080681763277,1.97880214127948,18.1101738301185));
#24161=CARTESIAN_POINT('Ctrl Pts',(67.4261608997972,-0.109805244932086,
17.9990359395505));
#24162=CARTESIAN_POINT('Ctrl Pts',(66.2235610371465,-2.09790664518147,17.8878980489825));
#24163=CARTESIAN_POINT('Ctrl Pts',(63.9010218810697,-2.16577030121656,17.7767601584144));
#24164=CARTESIAN_POINT('Ctrl Pts',(62.9776665752518,-0.823136293702506,
17.6988190485744));
#24165=CARTESIAN_POINT('Ctrl Pts',(62.9422504791375,-0.0719528572662064,
17.657923902257));
#24166=CARTESIAN_POINT('Ctrl Pts',(62.9427422720288,-0.00120218122682566,
17.6540747194623));
#24167=CARTESIAN_POINT('Origin',(65.,0.,23.5459252805377));
#24168=CARTESIAN_POINT('',(62.948587662066,7.8101556172383E-5,19.0540747194623));
#24169=CARTESIAN_POINT('',(62.9420758643114,-0.000617377060631522,18.9959252805377));
#24170=CARTESIAN_POINT('',(62.94525,1.28744642201805E-13,23.5459252805377));
#24171=CARTESIAN_POINT('Ctrl Pts',(62.9420758643114,-0.000617377060631477,
18.9959252805377));
#24172=CARTESIAN_POINT('Ctrl Pts',(62.9446352222011,0.645933688463614,18.9607195870605));
#24173=CARTESIAN_POINT('Ctrl Pts',(63.621561854257,1.97744992677629,18.8884679300607));
#24174=CARTESIAN_POINT('Ctrl Pts',(65.88907520037,2.26005765183973,18.7791703095382));
#24175=CARTESIAN_POINT('Ctrl Pts',(67.3809865945794,0.478767310881884,18.6680324189701));
#24176=CARTESIAN_POINT('Ctrl Pts',(66.6935539565454,-1.74074417931048,18.5568945284021));
#24177=CARTESIAN_POINT('Ctrl Pts',(64.4559921758773,-2.36693278080144,18.445756637834));
#24178=CARTESIAN_POINT('Ctrl Pts',(63.0943542721865,-1.16131696258989,18.3587668885459));
#24179=CARTESIAN_POINT('Ctrl Pts',(62.9457683276783,-0.239931205144687,
18.3088231027804));
#24180=CARTESIAN_POINT('Ctrl Pts',(62.9473667479389,-0.00148795945043152,
18.2959252805377));
#24181=CARTESIAN_POINT('Ctrl Pts',(62.948587662066,7.81015561724177E-5,
19.0540747194623));
#24182=CARTESIAN_POINT('Ctrl Pts',(62.9484730026856,0.338265299953978,19.0358087978625));
#24183=CARTESIAN_POINT('Ctrl Pts',(63.1876491089047,1.36219297688967,18.98049691274));
#24184=CARTESIAN_POINT('Ctrl Pts',(64.8026200998564,2.42061047643986,18.8881390640948));
#24185=CARTESIAN_POINT('Ctrl Pts',(66.9266433003906,1.47863433497921,18.7770011735268));
#24186=CARTESIAN_POINT('Ctrl Pts',(67.2871880384261,-0.816752582102671,
18.6658632829587));
#24187=CARTESIAN_POINT('Ctrl Pts',(65.5542436264288,-2.36455659820143,18.5547253923907));
#24188=CARTESIAN_POINT('Ctrl Pts',(63.4592956564195,-1.78804123877568,18.4507958712252));
#24189=CARTESIAN_POINT('Ctrl Pts',(62.9494637678869,-0.547806457359297,
18.3839123135824));
#24190=CARTESIAN_POINT('Ctrl Pts',(62.9444267867382,0.00179913216626967,
18.3540747194623));
#24191=CARTESIAN_POINT('Origin',(65.,0.,23.5459252805377));
#24192=CARTESIAN_POINT('',(62.9447134762142,-0.00183968268685886,19.7540747194623));
#24193=CARTESIAN_POINT('',(62.9455477186679,0.0018770222400039,19.6959252805377));
#24194=CARTESIAN_POINT('',(62.94525,1.28744642201805E-13,23.5459252805377));
#24195=CARTESIAN_POINT('Ctrl Pts',(62.9455477186679,0.00187702224000372,
19.6959252805377));
#24196=CARTESIAN_POINT('Ctrl Pts',(62.9440086170586,0.171896041847239,19.6867079983859));
#24197=CARTESIAN_POINT('Ctrl Pts',(63.0410778177033,1.02351952878433,19.6404447527115));
#24198=CARTESIAN_POINT('Ctrl Pts',(64.2244604721458,2.30148946126118,19.5571355435145));
#24199=CARTESIAN_POINT('Ctrl Pts',(66.5130014322595,1.89977418876314,19.4459976529464));
#24200=CARTESIAN_POINT('Ctrl Pts',(67.4166750228635,-0.240825944373849,
19.3348597623784));
#24201=CARTESIAN_POINT('Ctrl Pts',(66.1083385580613,-2.16099535909078,19.2237218718103));
#24202=CARTESIAN_POINT('Ctrl Pts',(63.7855272416616,-2.10318121447058,19.1125839812423));
#24203=CARTESIAN_POINT('Ctrl Pts',(62.9580113964128,-0.748427978399199,
19.0366517841514));
#24204=CARTESIAN_POINT('Ctrl Pts',(62.9419420816986,-0.0344138582905811,
18.9977655505832));
#24205=CARTESIAN_POINT('Ctrl Pts',(62.9420758643114,-0.000617377060631477,
18.9959252805377));
#24206=CARTESIAN_POINT('Ctrl Pts',(62.9447134762142,-0.00183968268685889,
19.7540747194623));
#24207=CARTESIAN_POINT('Ctrl Pts',(62.9497000514415,0.538489713183427,19.7247512456653));
#24208=CARTESIAN_POINT('Ctrl Pts',(63.44501294369,1.7695358622959,19.6583818083455));
#24209=CARTESIAN_POINT('Ctrl Pts',(65.5214561645339,2.37200281981328,19.5549664075031));
#24210=CARTESIAN_POINT('Ctrl Pts',(67.2756619344365,0.848337588988218,19.443828516935));
#24211=CARTESIAN_POINT('Ctrl Pts',(66.9469285261459,-1.45182065545646,19.332690626367));
#24212=CARTESIAN_POINT('Ctrl Pts',(64.8361493591312,-2.42311099039749,19.221552735799));
#24213=CARTESIAN_POINT('Ctrl Pts',(63.1976100342287,-1.38138540402114,19.1286807668307));
#24214=CARTESIAN_POINT('Ctrl Pts',(62.9487055486976,-0.347627856173908,
19.0728547613852));
#24215=CARTESIAN_POINT('Ctrl Pts',(62.948587662066,7.81015561724177E-5,
19.0540747194623));
#24216=CARTESIAN_POINT('Origin',(65.,0.,23.5459252805377));
#24217=CARTESIAN_POINT('',(62.9425383451584,0.00106562935659804,20.4540747194623));
#24218=CARTESIAN_POINT('',(62.9484657349091,-0.000525555021677807,20.3959252805377));
#24219=CARTESIAN_POINT('',(62.94525,1.28744642201805E-13,23.5459252805377));
#24220=CARTESIAN_POINT('Ctrl Pts',(62.9484657349091,-0.000525555021677684,
20.3959252805377));
#24221=CARTESIAN_POINT('Ctrl Pts',(62.9493249615497,0.3748004665574,20.3756504461887));
#24222=CARTESIAN_POINT('Ctrl Pts',(63.2276318468978,1.43710439466948,20.318329648317));
#24223=CARTESIAN_POINT('Ctrl Pts',(64.9337900137556,2.42774204026718,20.2239628869227));
#24224=CARTESIAN_POINT('Ctrl Pts',(67.0037742079544,1.37229889524427,20.1128249963547));
#24225=CARTESIAN_POINT('Ctrl Pts',(67.2396811477566,-0.939225037877053,
20.0016871057866));
#24226=CARTESIAN_POINT('Ctrl Pts',(65.4255825320509,-2.39106561893279,19.8905492152186));
#24227=CARTESIAN_POINT('Ctrl Pts',(63.4047034238819,-1.71543774995268,19.7886286068023));
#24228=CARTESIAN_POINT('Ctrl Pts',(62.9501945513868,-0.511441876516717,
19.7237539619086));
#24229=CARTESIAN_POINT('Ctrl Pts',(62.9455477186679,0.00187702224000372,
19.6959252805377));
#24230=CARTESIAN_POINT('Ctrl Pts',(62.9425383451584,0.00106562935659771,
20.4540747194623));
#24231=CARTESIAN_POINT('Ctrl Pts',(62.9421515159492,0.0623504207905263,
20.4507396569907));
#24232=CARTESIAN_POINT('Ctrl Pts',(62.9724324501069,0.804000733271032,20.4103586309964));
#24233=CARTESIAN_POINT('Ctrl Pts',(63.8711449203827,2.15034861017487,20.3329316414794));
#24234=CARTESIAN_POINT('Ctrl Pts',(66.1944008109328,2.11464436694832,20.2217937509113));
#24235=CARTESIAN_POINT('Ctrl Pts',(67.4244083164919,0.143381864737545,20.1106558603433));
#24236=CARTESIAN_POINT('Ctrl Pts',(66.4353272830534,-1.95911953903995,19.9995179697752));
#24237=CARTESIAN_POINT('Ctrl Pts',(64.132474966303,-2.26841668404625,19.8883800792072));
#24238=CARTESIAN_POINT('Ctrl Pts',(63.0217706588138,-0.967627859876295,
19.8065656624362));
#24239=CARTESIAN_POINT('Ctrl Pts',(62.9434002356266,-0.144138246524576,
19.7617972091879));
#24240=CARTESIAN_POINT('Ctrl Pts',(62.9447134762142,-0.00183968268685889,
19.7540747194623));
#24241=CARTESIAN_POINT('Origin',(65.,0.,23.5459252805377));
#24242=CARTESIAN_POINT('',(62.9479182248742,0.00116161895481429,21.1540747194623));
#24243=CARTESIAN_POINT('',(62.9436210622307,-0.00160392935065391,21.0959252805377));
#24244=CARTESIAN_POINT('',(62.94525,1.28744642201805E-13,23.5459252805377));
#24245=CARTESIAN_POINT('Ctrl Pts',(62.9436210622307,-0.00160392935065416,
21.0959252805377));
#24246=CARTESIAN_POINT('Ctrl Pts',(62.9485686759719,0.574950681266289,21.0645928939915));
#24247=CARTESIAN_POINT('Ctrl Pts',(63.5020551216143,1.84152256699688,20.9962145439225));
#24248=CARTESIAN_POINT('Ctrl Pts',(65.6489465241691,2.34033682721966,20.8907902303309));
#24249=CARTESIAN_POINT('Ctrl Pts',(67.3182024564633,0.724053604371175,20.7796523397629));
#24250=CARTESIAN_POINT('Ctrl Pts',(66.865581542071,-1.55496692328425,20.6685144491949));
#24251=CARTESIAN_POINT('Ctrl Pts',(64.7053726085262,-2.41070716562325,20.5573765586268));
#24252=CARTESIAN_POINT('Ctrl Pts',(63.1597285921146,-1.30632755500751,20.4665135024078));
#24253=CARTESIAN_POINT('Ctrl Pts',(62.9477549916925,-0.310991282228732,
20.4126964097114));
#24254=CARTESIAN_POINT('Ctrl Pts',(62.9484657349091,-0.000525555021677684,
20.3959252805377));
#24255=CARTESIAN_POINT('Ctrl Pts',(62.9479182248742,0.00116161895481415,
21.1540747194623));
#24256=CARTESIAN_POINT('Ctrl Pts',(62.9465403381585,0.26742114595832,21.1396821047934));
#24257=CARTESIAN_POINT('Ctrl Pts',(63.1184075387479,1.2173158745075,21.0882435266019));
#24258=CARTESIAN_POINT('Ctrl Pts',(64.5516876929394,2.3868968681091,20.9997589848876));
#24259=CARTESIAN_POINT('Ctrl Pts',(66.7622271403759,1.67118893435552,20.8886210943196));
#24260=CARTESIAN_POINT('Ctrl Pts',(67.3597936726881,-0.574194749175797,
20.7774832037516));
#24261=CARTESIAN_POINT('Ctrl Pts',(65.7974074532359,-2.2940026123021,20.6663453131835));
#24262=CARTESIAN_POINT('Ctrl Pts',(63.573935456952,-1.92548892520573,20.5585424850871));
#24263=CARTESIAN_POINT('Ctrl Pts',(62.9464484251963,-0.618402688713485,
20.4877856205134));
#24264=CARTESIAN_POINT('Ctrl Pts',(62.9425383451584,0.00106562935659771,
20.4540747194623));
#24265=CARTESIAN_POINT('Origin',(65.,0.,23.5459252805377));
#24266=CARTESIAN_POINT('',(62.9473239618077,-0.00235074752840472,21.8540747194623));
#24267=CARTESIAN_POINT('',(62.9434348764936,0.00149614206266628,21.7959252805377));
#24268=CARTESIAN_POINT('',(62.94525,1.28744642201805E-13,23.5459252805377));
#24269=CARTESIAN_POINT('',(64.4698297828114,-1.98517432567172,22.));
#24270=CARTESIAN_POINT('Ctrl Pts',(64.4698297828114,-1.98517432567172,22.));
#24271=CARTESIAN_POINT('Ctrl Pts',(63.8097120902545,-1.80888011517989,21.9629540364773));
#24272=CARTESIAN_POINT('Ctrl Pts',(63.0750422655367,-1.11280694816751,21.9143122762981));
#24273=CARTESIAN_POINT('Ctrl Pts',(62.9457054195483,-0.216594706141779,
21.8656705161189));
#24274=CARTESIAN_POINT('Ctrl Pts',(62.9473239618077,-0.00235074752840471,
21.8540747194623));
#24275=CARTESIAN_POINT('',(65.5313040526013,-1.98873440678485,22.));
#24276=CARTESIAN_POINT('Origin',(65.,0.,22.));
#24277=CARTESIAN_POINT('Ctrl Pts',(65.5313046873329,-1.98873639975131,22.));
#24278=CARTESIAN_POINT('Ctrl Pts',(64.8866967734446,-2.16006352763733,21.9636770818144));
#24279=CARTESIAN_POINT('Ctrl Pts',(63.5069411366323,-1.84063802220702,21.895652175327));
#24280=CARTESIAN_POINT('Ctrl Pts',(62.9482922133912,-0.581586231880544,
21.8276272688395));
#24281=CARTESIAN_POINT('Ctrl Pts',(62.9434348764936,0.0014961420626663,
21.7959252805377));
#24282=CARTESIAN_POINT('Origin',(65.,0.,3.));
#24283=CARTESIAN_POINT('',(66.6675465985015,-0.0012143044629161,6.12851963660979));
#24284=CARTESIAN_POINT('',(66.6679935094968,0.00096847687651065,6.32148036339021));
#24285=CARTESIAN_POINT('',(66.666,2.04026156737949E-16,3.));
#24286=CARTESIAN_POINT('',(66.6351293272515,-0.319230454628274,7.));
#24287=CARTESIAN_POINT('Ctrl Pts',(66.6679935094968,0.00096847687651065,
6.32148036339021));
#24288=CARTESIAN_POINT('Ctrl Pts',(66.6684011451999,0.0590543694261956,
6.32537779445739));
#24289=CARTESIAN_POINT('Ctrl Pts',(66.6656310767024,0.117101359876407,6.32927522552457));
#24290=CARTESIAN_POINT('Ctrl Pts',(66.6595549679121,0.174800485042606,6.33317265659175));
#24291=CARTESIAN_POINT('Ctrl Pts',(66.6018001800214,0.723243715815273,6.37021862011443));
#24292=CARTESIAN_POINT('Ctrl Pts',(66.2453468888446,1.24025755357674,6.40726458363711));
#24293=CARTESIAN_POINT('Ctrl Pts',(65.7532186868383,1.48913446656882,6.44431054715979));
#24294=CARTESIAN_POINT('Ctrl Pts',(65.261090484832,1.73801137956089,6.48135651068247));
#24295=CARTESIAN_POINT('Ctrl Pts',(64.6332873719962,1.71875136778355,6.51840247420515));
#24296=CARTESIAN_POINT('Ctrl Pts',(64.1573426907198,1.44035276658659,6.55544843772783));
#24297=CARTESIAN_POINT('Ctrl Pts',(63.6813980094435,1.16195416538963,6.59249440125051));
#24298=CARTESIAN_POINT('Ctrl Pts',(63.3573117597265,0.624416974773041,6.6295403647732));
#24299=CARTESIAN_POINT('Ctrl Pts',(63.3329761432024,0.0733847413024343,
6.66658632829588));
#24300=CARTESIAN_POINT('Ctrl Pts',(63.3086405266783,-0.477647492168164,
6.70363229181856));
#24301=CARTESIAN_POINT('Ctrl Pts',(63.5840555433469,-1.04217476849279,6.74067825534123));
#24302=CARTESIAN_POINT('Ctrl Pts',(64.0340468080883,-1.36111204342973,6.77772421886391));
#24303=CARTESIAN_POINT('Ctrl Pts',(64.4840380728297,-1.68004931836668,6.81477018238659));
#24304=CARTESIAN_POINT('Ctrl Pts',(65.1086055856438,-1.75339659191593,6.85181614590928));
#24305=CARTESIAN_POINT('Ctrl Pts',(65.6198404690058,-1.54912172664724,6.88886210943196));
#24306=CARTESIAN_POINT('Ctrl Pts',(66.1310753523678,-1.34484686137855,6.92590807295464));
#24307=CARTESIAN_POINT('Ctrl Pts',(66.5289776062776,-0.862949857291923,
6.96295403647732));
#24308=CARTESIAN_POINT('Ctrl Pts',(66.6351293272514,-0.319230454628298,
7.));
#24309=CARTESIAN_POINT('',(65.0525836066607,1.66819787866867,7.));
#24310=CARTESIAN_POINT('Origin',(65.,0.,7.));
#24311=CARTESIAN_POINT('',(66.6634369488939,-0.000652451249335551,6.82851963660979));
#24312=CARTESIAN_POINT('Ctrl Pts',(65.0525835864496,1.66819940096574,7.));
#24313=CARTESIAN_POINT('Ctrl Pts',(65.5930952523355,1.65047433913271,6.96367708181444));
#24314=CARTESIAN_POINT('Ctrl Pts',(66.1251624614536,1.34576660284025,6.92735416362889));
#24315=CARTESIAN_POINT('Ctrl Pts',(66.412840678391,0.887825324655541,6.89103124544334));
#24316=CARTESIAN_POINT('Ctrl Pts',(66.5778717300928,0.625120238531672,6.87019404249883));
#24317=CARTESIAN_POINT('Ctrl Pts',(66.6624763097416,0.311987213470675,6.84935683955431));
#24318=CARTESIAN_POINT('Ctrl Pts',(66.6634369488939,-0.000652451249335551,
6.82851963660979));
#24319=CARTESIAN_POINT('',(66.666,-2.04026156737949E-16,8.));
#24320=CARTESIAN_POINT('',(66.666,2.04026156737949E-16,3.));
#24321=CARTESIAN_POINT('Origin',(65.,0.,8.));
#24322=CARTESIAN_POINT('Ctrl Pts',(66.6634369488939,-0.000652451249335551,
6.82851963660979));
#24323=CARTESIAN_POINT('Ctrl Pts',(66.6641842070583,-0.243847350592474,
6.81231087603163));
#24324=CARTESIAN_POINT('Ctrl Pts',(66.614319260528,-0.486743721979875,6.79610211545346));
#24325=CARTESIAN_POINT('Ctrl Pts',(66.5123276923829,-0.705373629571154,
6.7798933548753));
#24326=CARTESIAN_POINT('Ctrl Pts',(66.2792206701092,-1.20506363008265,6.74284739135262));
#24327=CARTESIAN_POINT('Ctrl Pts',(65.7738173393357,-1.57799175139799,6.70580142782994));
#24328=CARTESIAN_POINT('Ctrl Pts',(65.2274915068526,-1.65321113835932,6.66875546430726));
#24329=CARTESIAN_POINT('Ctrl Pts',(64.6811656743696,-1.72843052532064,6.63170950078458));
#24330=CARTESIAN_POINT('Ctrl Pts',(64.0939173401772,-1.50594117792796,6.5946635372619));
#24331=CARTESIAN_POINT('Ctrl Pts',(63.734467017542,-1.08770559986528,6.55761757373921));
#24332=CARTESIAN_POINT('Ctrl Pts',(63.3750166949069,-0.669470021802595,
6.52057161021653));
#24333=CARTESIAN_POINT('Ctrl Pts',(63.2433643838291,-0.0554882130699084,
6.48352564669385));
#24334=CARTESIAN_POINT('Ctrl Pts',(63.3997802821251,0.473318066669373,6.44647968317117));
#24335=CARTESIAN_POINT('Ctrl Pts',(63.556196180421,1.00212434640864,6.40943371964849));
#24336=CARTESIAN_POINT('Ctrl Pts',(64.0006802880906,1.44575509715451,6.37238775612581));
#24337=CARTESIAN_POINT('Ctrl Pts',(64.5298024116317,1.6011444312508,6.33534179260313));
#24338=CARTESIAN_POINT('Ctrl Pts',(65.0589245351728,1.7565337653471,6.29829582908045));
#24339=CARTESIAN_POINT('Ctrl Pts',(65.6726846745854,1.62368168279382,6.26124986555777));
#24340=CARTESIAN_POINT('Ctrl Pts',(66.0901968514498,1.26340683134223,6.22420390203509));
#24341=CARTESIAN_POINT('Ctrl Pts',(66.4496543303097,0.953227878546208,6.19230914689332));
#24342=CARTESIAN_POINT('Ctrl Pts',(66.6636456701669,0.474474884606731,6.16041439175156));
#24343=CARTESIAN_POINT('Ctrl Pts',(66.6675465985015,-0.0012143044629161,
6.12851963660979));
#24344=CARTESIAN_POINT('Origin',(65.,0.,3.));
#24345=CARTESIAN_POINT('',(66.6672347084384,0.00132477166025269,5.42851963660979));
#24346=CARTESIAN_POINT('',(66.6636987213601,0.0008322902000487,5.62148036339021));
#24347=CARTESIAN_POINT('',(66.666,2.04026156737949E-16,3.));
#24348=CARTESIAN_POINT('Ctrl Pts',(66.6636987213601,0.0008322902000487,
5.62148036339021));
#24349=CARTESIAN_POINT('Ctrl Pts',(66.6647135334695,0.225194170777295,5.63643534665464));
#24350=CARTESIAN_POINT('Ctrl Pts',(66.6225044629126,0.449190113916435,5.65139032991907));
#24351=CARTESIAN_POINT('Ctrl Pts',(66.5352578465541,0.65400067617093,5.6663453131835));
#24352=CARTESIAN_POINT('Ctrl Pts',(66.3191335681149,1.16135026554737,5.70339127670618));
#24353=CARTESIAN_POINT('Ctrl Pts',(65.8266432700797,1.55097169600335,5.74043724022886));
#24354=CARTESIAN_POINT('Ctrl Pts',(65.2831760713863,1.64455092497836,5.77748320375154));
#24355=CARTESIAN_POINT('Ctrl Pts',(64.739708872693,1.73813015395337,5.81452916727422));
#24356=CARTESIAN_POINT('Ctrl Pts',(64.1452647733414,1.53566718144742,5.8515751307969));
#24357=CARTESIAN_POINT('Ctrl Pts',(63.771898150977,1.12982346148107,5.88862109431958));
#24358=CARTESIAN_POINT('Ctrl Pts',(63.3985315286127,0.72397974151472,5.92566705784226));
#24359=CARTESIAN_POINT('Ctrl Pts',(63.2462423832356,0.114755274087973,5.96271302136494));
#24360=CARTESIAN_POINT('Ctrl Pts',(63.3847194791661,-0.419041074004903,
5.99975898488762));
#24361=CARTESIAN_POINT('Ctrl Pts',(63.5231965750967,-0.952837422097788,
6.0368049484103));
#24362=CARTESIAN_POINT('Ctrl Pts',(63.952439912335,-1.41120565085679,6.07385091193298));
#24363=CARTESIAN_POINT('Ctrl Pts',(64.4760180935273,-1.58435878418327,6.11089687545566));
#24364=CARTESIAN_POINT('Ctrl Pts',(64.9995962747196,-1.75751191750976,6.14794283897834));
#24365=CARTESIAN_POINT('Ctrl Pts',(65.6175092998659,-1.64544995540374,6.18498880250103));
#24366=CARTESIAN_POINT('Ctrl Pts',(66.0469376701368,-1.29948266245882,6.22203476602371));
#24367=CARTESIAN_POINT('Ctrl Pts',(66.431187907292,-0.989912956390696,6.25518329847921));
#24368=CARTESIAN_POINT('Ctrl Pts',(66.6645264756734,-0.49306517277657,6.28833183093471));
#24369=CARTESIAN_POINT('Ctrl Pts',(66.6679935094968,0.00096847687651065,
6.32148036339021));
#24370=CARTESIAN_POINT('Ctrl Pts',(66.6675465985015,-0.0012143044629161,
6.12851963660979));
#24371=CARTESIAN_POINT('Ctrl Pts',(66.6681766235524,-0.0780411722834827,
6.12336842822888));
#24372=CARTESIAN_POINT('Ctrl Pts',(66.6633265808958,-0.154788122805552,
6.11821721984797));
#24373=CARTESIAN_POINT('Ctrl Pts',(66.6527242222132,-0.230732082280714,
6.11306601146705));
#24374=CARTESIAN_POINT('Ctrl Pts',(66.5764752017958,-0.776898524102169,
6.07602004794437));
#24375=CARTESIAN_POINT('Ctrl Pts',(66.202712946645,-1.2815337873952,6.03897408442169));
#24376=CARTESIAN_POINT('Ctrl Pts',(65.7024931149025,-1.51368401519416,6.00192812089901));
#24377=CARTESIAN_POINT('Ctrl Pts',(65.20227328316,-1.74583424299313,5.96488215737633));
#24378=CARTESIAN_POINT('Ctrl Pts',(64.5755958748258,-1.70549943529801,5.92783619385365));
#24379=CARTESIAN_POINT('Ctrl Pts',(64.1092627289642,-1.41114141304213,5.89079023033097));
#24380=CARTESIAN_POINT('Ctrl Pts',(63.6429295831026,-1.11678339078625,5.85374426680829));
#24381=CARTESIAN_POINT('Ctrl Pts',(63.3369406997136,-0.568402153969608,
5.81669830328561));
#24382=CARTESIAN_POINT('Ctrl Pts',(63.3313339461091,-0.0169662842418651,
5.77965233976292));
#24383=CARTESIAN_POINT('Ctrl Pts',(63.3257271925045,0.534469585485878,5.74260637624024));
#24384=CARTESIAN_POINT('Ctrl Pts',(63.6205025686844,1.08896008812472,5.70556041271756));
#24385=CARTESIAN_POINT('Ctrl Pts',(64.0807542900534,1.39273889179928,5.66851444919488));
#24386=CARTESIAN_POINT('Ctrl Pts',(64.5410060114225,1.69651769547383,5.6314684856722));
#24387=CARTESIAN_POINT('Ctrl Pts',(65.1667340779808,1.7495848001841,5.59442252214952));
#24388=CARTESIAN_POINT('Ctrl Pts',(65.6715705742232,1.52765405355124,5.55737655862684));
#24389=CARTESIAN_POINT('Ctrl Pts',(66.1764070704656,1.30572330691839,5.52033059510416));
#24390=CARTESIAN_POINT('Ctrl Pts',(66.5603519963922,0.80879470894242,5.48328463158148));
#24391=CARTESIAN_POINT('Ctrl Pts',(66.6476907378026,0.264290293520936,5.4462386680588));
#24392=CARTESIAN_POINT('Ctrl Pts',(66.6616154028998,0.177478398750718,5.44033232424247));
#24393=CARTESIAN_POINT('Ctrl Pts',(66.6680006840388,0.0894571820797134,
5.43442598042613));
#24394=CARTESIAN_POINT('Ctrl Pts',(66.6672347084384,0.00132477166025269,
5.42851963660979));
#24395=CARTESIAN_POINT('Origin',(65.,0.,3.));
#24396=CARTESIAN_POINT('',(66.663366994258,0.000380245158983772,4.72851963660979));
#24397=CARTESIAN_POINT('',(66.664973747664,-0.00143128352026757,4.92148036339021));
#24398=CARTESIAN_POINT('',(66.666,2.04026156737949E-16,3.));
#24399=CARTESIAN_POINT('Ctrl Pts',(66.664973747664,-0.00143128352026757,
4.92148036339021));
#24400=CARTESIAN_POINT('Ctrl Pts',(66.6617826067969,0.38807005747555,4.94749289885189));
#24401=CARTESIAN_POINT('Ctrl Pts',(66.5254256665028,0.779584263278044,4.97350543431357));
#24402=CARTESIAN_POINT('Ctrl Pts',(66.27583338404,1.07563182061435,4.99951796977525));
#24403=CARTESIAN_POINT('Ctrl Pts',(65.9203745090186,1.49725035242627,5.03656393329793));
#24404=CARTESIAN_POINT('Ctrl Pts',(65.3352487301258,1.72524091300359,5.07360989682061));
#24405=CARTESIAN_POINT('Ctrl Pts',(64.7882421463444,1.65526230253066,5.11065586034329));
#24406=CARTESIAN_POINT('Ctrl Pts',(64.2412355625629,1.58528369205773,5.14770182386597));
#24407=CARTESIAN_POINT('Ctrl Pts',(63.7323481738928,1.21733591053454,5.18474778738865));
#24408=CARTESIAN_POINT('Ctrl Pts',(63.4944752416899,0.71981239976822,5.22179375091133));
#24409=CARTESIAN_POINT('Ctrl Pts',(63.256602309487,0.222288889001918,5.25883971443401));
#24410=CARTESIAN_POINT('Ctrl Pts',(63.2897438337514,-0.404810351007516,
5.29588567795669));
#24411=CARTESIAN_POINT('Ctrl Pts',(63.5787322850456,-0.874489902053352,
5.33293164147937));
#24412=CARTESIAN_POINT('Ctrl Pts',(63.8677207363397,-1.34416945309919,5.36997760500205));
#24413=CARTESIAN_POINT('Ctrl Pts',(64.4125561146635,-1.65642931518145,5.40702356852474));
#24414=CARTESIAN_POINT('Ctrl Pts',(64.9638916621075,-1.66836178497851,5.44406953204742));
#24415=CARTESIAN_POINT('Ctrl Pts',(65.5152272095514,-1.68029425477557,5.4811154955701));
#24416=CARTESIAN_POINT('Ctrl Pts',(66.0730629261155,-1.39189933228743,5.51816145909277));
#24417=CARTESIAN_POINT('Ctrl Pts',(66.382101654976,-0.935162996894911,5.55520742261545));
#24418=CARTESIAN_POINT('Ctrl Pts',(66.5663853881852,-0.662805298269937,
5.5772984028737));
#24419=CARTESIAN_POINT('Ctrl Pts',(66.6621996762674,-0.330587263195562,
5.59938938313196));
#24420=CARTESIAN_POINT('Ctrl Pts',(66.6636987213601,0.0008322902000487,
5.62148036339021));
#24421=CARTESIAN_POINT('Ctrl Pts',(66.6672347084384,0.00132477166025269,
5.42851963660979));
#24422=CARTESIAN_POINT('Ctrl Pts',(66.6631963067396,-0.463329814934398,
5.39738001690345));
#24423=CARTESIAN_POINT('Ctrl Pts',(66.4603784340712,-0.931075191763351,
5.3662403971971));
#24424=CARTESIAN_POINT('Ctrl Pts',(66.1156608616196,-1.24098144967673,5.33510077749075));
#24425=CARTESIAN_POINT('Ctrl Pts',(65.705559687132,-1.60966854458595,5.29805481396807));
#24426=CARTESIAN_POINT('Ctrl Pts',(65.0946247812625,-1.75496250153736,5.2610088504454));
#24427=CARTESIAN_POINT('Ctrl Pts',(64.5624539571804,-1.61036875759037,5.22396288692272));
#24428=CARTESIAN_POINT('Ctrl Pts',(64.0302831330983,-1.46577501364339,5.18691692340004));
#24429=CARTESIAN_POINT('Ctrl Pts',(63.5768763908035,-1.031293568798,5.14987095987736));
#24430=CARTESIAN_POINT('Ctrl Pts',(63.4097379023455,-0.505767299507011,
5.11282499635467));
#24431=CARTESIAN_POINT('Ctrl Pts',(63.2425994138875,0.019758969783971,5.07577903283199));
#24432=CARTESIAN_POINT('Ctrl Pts',(63.3617291792663,0.636330063520549,5.03873306930931));
#24433=CARTESIAN_POINT('Ctrl Pts',(63.7126067830815,1.06176871408086,5.00168710578663));
#24434=CARTESIAN_POINT('Ctrl Pts',(64.0634843868967,1.48720736464117,4.96464114226395));
#24435=CARTESIAN_POINT('Ctrl Pts',(64.6461098291483,1.72151357202522,4.92759517874127));
#24436=CARTESIAN_POINT('Ctrl Pts',(65.1938412738804,1.65745577708112,4.89054921521859));
#24437=CARTESIAN_POINT('Ctrl Pts',(65.7415727186126,1.59339798213702,4.85350325169591));
#24438=CARTESIAN_POINT('Ctrl Pts',(66.2544101658253,1.23097618486478,4.81645728817322));
#24439=CARTESIAN_POINT('Ctrl Pts',(66.4976506491047,0.73605477318722,4.77941132465054));
#24440=CARTESIAN_POINT('Ctrl Pts',(66.6090340731616,0.509422920098692,4.76244742863696));
#24441=CARTESIAN_POINT('Ctrl Pts',(66.6638867910221,0.255007754231684,4.74548353262337));
#24442=CARTESIAN_POINT('Ctrl Pts',(66.663366994258,0.000380245158983772,
4.72851963660979));
#24443=CARTESIAN_POINT('Origin',(65.,0.,3.));
#24444=CARTESIAN_POINT('',(66.66584023827,-0.00152342185141638,4.02851963660979));
#24445=CARTESIAN_POINT('',(66.668752404953,6.71116607201819E-6,4.22148036339021));
#24446=CARTESIAN_POINT('',(66.666,2.04026156737949E-16,3.));
#24447=CARTESIAN_POINT('Ctrl Pts',(66.6687523910643,6.71113220718263E-6,
4.22148036339021));
#24448=CARTESIAN_POINT('Ctrl Pts',(66.6687853501023,0.551830446441275,4.25855045104914));
#24449=CARTESIAN_POINT('Ctrl Pts',(66.3679399440666,1.10362329032225,4.29562053870807));
#24450=CARTESIAN_POINT('Ctrl Pts',(65.9041274583633,1.40260051189836,4.332690626367));
#24451=CARTESIAN_POINT('Ctrl Pts',(65.440616808353,1.70138316778325,4.36973658988968));
#24452=CARTESIAN_POINT('Ctrl Pts',(64.8143512345865,1.74767914449738,4.40678255341236));
#24453=CARTESIAN_POINT('Ctrl Pts',(64.3119447275275,1.52030082532265,4.44382851693504));
#24454=CARTESIAN_POINT('Ctrl Pts',(63.8095382204685,1.29292250614791,4.48087448045772));
#24455=CARTESIAN_POINT('Ctrl Pts',(63.430990780117,0.79186989108431,4.5179204439804));
#24456=CARTESIAN_POINT('Ctrl Pts',(63.3495467901205,0.246452551482041,4.55496640750308));
#24457=CARTESIAN_POINT('Ctrl Pts',(63.2681028001239,-0.298964788120227,
4.59201237102576));
#24458=CARTESIAN_POINT('Ctrl Pts',(63.4837622604823,-0.888746852261164,
4.62905833454844));
#24459=CARTESIAN_POINT('Ctrl Pts',(63.897827394199,-1.25297653677901,4.66610429807112));
#24460=CARTESIAN_POINT('Ctrl Pts',(64.3118925279157,-1.61720622129685,4.7031502615938));
#24461=CARTESIAN_POINT('Ctrl Pts',(64.9243633349907,-1.75588352619159,4.74019622511648));
#24462=CARTESIAN_POINT('Ctrl Pts',(65.4549390817441,-1.60554199300636,4.77724218863916));
#24463=CARTESIAN_POINT('Ctrl Pts',(65.9855148284976,-1.45520045982112,4.81428815216184));
#24464=CARTESIAN_POINT('Ctrl Pts',(66.4341955149294,-1.0158400885559,4.85133411568453));
#24465=CARTESIAN_POINT('Ctrl Pts',(66.5956398725704,-0.488536651400016,
4.88838007920721));
#24466=CARTESIAN_POINT('Ctrl Pts',(66.6437229708759,-0.331489459561807,
4.89941350726821));
#24467=CARTESIAN_POINT('Ctrl Pts',(66.6663272959654,-0.166641438903674,
4.91044693532921));
#24468=CARTESIAN_POINT('Ctrl Pts',(66.664973747664,-0.00143128352026757,
4.92148036339021));
#24469=CARTESIAN_POINT('Ctrl Pts',(66.663366994258,0.000380245158983772,
4.72851963660979));
#24470=CARTESIAN_POINT('Ctrl Pts',(66.6627516524935,-0.301050913271577,
4.7084375691007));
#24471=CARTESIAN_POINT('Ctrl Pts',(66.5845366381801,-0.602779651888649,
4.6883555015916));
#24472=CARTESIAN_POINT('Ctrl Pts',(66.4306434003258,-0.859065513400935,
4.66827343408251));
#24473=CARTESIAN_POINT('Ctrl Pts',(66.1467521489217,-1.33184336222865,4.63122747055983));
#24474=CARTESIAN_POINT('Ctrl Pts',(65.6053261267676,-1.6499780338012,4.59418150703714));
#24475=CARTESIAN_POINT('Ctrl Pts',(65.0541520228137,-1.66787339241419,4.55713554351446));
#24476=CARTESIAN_POINT('Ctrl Pts',(64.5029779188599,-1.68576875102718,4.52008957999178));
#24477=CARTESIAN_POINT('Ctrl Pts',(63.9420557331062,-1.4034247966806,4.4830436164691));
#24478=CARTESIAN_POINT('Ctrl Pts',(63.6280946846009,-0.950057840731758,
4.44599765294642));
#24479=CARTESIAN_POINT('Ctrl Pts',(63.3141336360955,-0.496690884782916,
4.40895168942374));
#24480=CARTESIAN_POINT('Ctrl Pts',(63.2471337248385,0.127699072768189,4.37190572590106));
#24481=CARTESIAN_POINT('Ctrl Pts',(63.4577578400848,0.637356427139633,4.33485976237838));
#24482=CARTESIAN_POINT('Ctrl Pts',(63.6683819553311,1.14701378151106,4.2978137988557));
#24483=CARTESIAN_POINT('Ctrl Pts',(64.1566300970808,1.54193853270284,4.26076783533302));
#24484=CARTESIAN_POINT('Ctrl Pts',(64.6990527347307,1.64139112904609,4.22372187181034));
#24485=CARTESIAN_POINT('Ctrl Pts',(65.2414753723806,1.74084372538933,4.18667590828766));
#24486=CARTESIAN_POINT('Ctrl Pts',(65.8380725059307,1.54482416688403,4.14962994476498));
#24487=CARTESIAN_POINT('Ctrl Pts',(66.2158080742639,1.14304191594115,4.1125839812423));
#24488=CARTESIAN_POINT('Ctrl Pts',(66.501526048881,0.839135107580338,4.08456253303146));
#24489=CARTESIAN_POINT('Ctrl Pts',(66.6620254174182,0.417504031348421,4.05654108482063));
#24490=CARTESIAN_POINT('Ctrl Pts',(66.66584023827,-0.00152342185141638,
4.02851963660979));
#24491=CARTESIAN_POINT('Origin',(65.,0.,3.));
#24492=CARTESIAN_POINT('',(66.6685304876972,0.000550348904958531,3.32851963660979));
#24493=CARTESIAN_POINT('',(66.6649541686305,0.00142706439964306,3.52148036339021));
#24494=CARTESIAN_POINT('',(66.666,2.04026156737949E-16,3.));
#24495=CARTESIAN_POINT('Ctrl Pts',(66.6649541686305,0.00142706439964306,
3.52148036339021));
#24496=CARTESIAN_POINT('Ctrl Pts',(66.6663084639771,0.16736460907033,3.53256203972371));
#24497=CARTESIAN_POINT('Ctrl Pts',(66.6435020576938,0.332938268252247,3.5436437160572));
#24498=CARTESIAN_POINT('Ctrl Pts',(66.5950038039968,0.490609337973574,3.5547253923907));
#24499=CARTESIAN_POINT('Ctrl Pts',(66.4328744940168,1.01770257925701,3.59177135591338));
#24500=CARTESIAN_POINT('Ctrl Pts',(65.9836233623828,1.45647963816643,3.62881731943606));
#24501=CARTESIAN_POINT('Ctrl Pts',(65.4528527369189,1.60613170566075,3.66586328295875));
#24502=CARTESIAN_POINT('Ctrl Pts',(64.9220821114551,1.75578377315508,3.70290924648143));
#24503=CARTESIAN_POINT('Ctrl Pts',(64.3097919921614,1.6163108492343,3.73995521000411));
#24504=CARTESIAN_POINT('Ctrl Pts',(63.8962004240445,1.25154350838824,3.77700117352679));
#24505=CARTESIAN_POINT('Ctrl Pts',(63.4826088559276,0.886776167542176,3.81404713704947));
#24506=CARTESIAN_POINT('Ctrl Pts',(63.2677158389876,0.29671440977082,3.85109310057215));
#24507=CARTESIAN_POINT('Ctrl Pts',(63.3498683809715,-0.248596655588643,
3.88813906409483));
#24508=CARTESIAN_POINT('Ctrl Pts',(63.4320209229553,-0.793907720948105,
3.92518502761751));
#24509=CARTESIAN_POINT('Ctrl Pts',(63.8112190238629,-1.29446809389567,3.96223099114019));
#24510=CARTESIAN_POINT('Ctrl Pts',(64.3139205225789,-1.52119348141188,3.99927695466287));
#24511=CARTESIAN_POINT('Ctrl Pts',(64.8166220212948,-1.74791886892809,4.03632291818555));
#24512=CARTESIAN_POINT('Ctrl Pts',(65.4428269178191,-1.70080927101294,4.07336888170823));
#24513=CARTESIAN_POINT('Ctrl Pts',(65.9059489905043,-1.40142466222204,4.11041484523092));
#24514=CARTESIAN_POINT('Ctrl Pts',(66.368769480536,-1.10223501111091,4.14743668461735));
#24515=CARTESIAN_POINT('Ctrl Pts',(66.6687194749238,-0.551098802461342,
4.18445852400377));
#24516=CARTESIAN_POINT('Ctrl Pts',(66.6687523910643,6.71113220718263E-6,
4.22148036339021));
#24517=CARTESIAN_POINT('Ctrl Pts',(66.66584023827,-0.00152342185141638,
4.02851963660979));
#24518=CARTESIAN_POINT('Ctrl Pts',(66.6670688296308,-0.136474322284296,
4.01949512129795));
#24519=CARTESIAN_POINT('Ctrl Pts',(66.6520459458893,-0.271155172380326,
4.0104706059861));
#24520=CARTESIAN_POINT('Ctrl Pts',(66.6197204952158,-0.401546525825014,
4.00144609067426));
#24521=CARTESIAN_POINT('Ctrl Pts',(66.4870233447183,-0.936807773267794,
3.96440012715158));
#24522=CARTESIAN_POINT('Ctrl Pts',(66.0627550406069,-1.39978532477287,3.92735416362889));
#24523=CARTESIAN_POINT('Ctrl Pts',(65.5410843780201,-1.57859487864439,3.89030820010621));
#24524=CARTESIAN_POINT('Ctrl Pts',(65.0194137154332,-1.7574044325159,3.85326223658353));
#24525=CARTESIAN_POINT('Ctrl Pts',(64.400340694371,-1.65204598875385,3.81621627306085));
#24526=CARTESIAN_POINT('Ctrl Pts',(63.9671875933068,-1.310737436563,3.77917030953817));
#24527=CARTESIAN_POINT('Ctrl Pts',(63.5340344922426,-0.969428884372161,
3.74212434601549));
#24528=CARTESIAN_POINT('Ctrl Pts',(63.2868013111764,-0.392170223752528,
3.70507838249281));
#24529=CARTESIAN_POINT('Ctrl Pts',(63.3386357173299,0.156852845981076,3.66803241897013));
#24530=CARTESIAN_POINT('Ctrl Pts',(63.3904701234834,0.70587591571468,3.63098645544745));
#24531=CARTESIAN_POINT('Ctrl Pts',(63.7413721168566,1.22666339456225,3.59394049192477));
#24532=CARTESIAN_POINT('Ctrl Pts',(64.230749410433,1.48087393976488,3.55689452840209));
#24533=CARTESIAN_POINT('Ctrl Pts',(64.7201267040094,1.7350844849675,3.51984856487941));
#24534=CARTESIAN_POINT('Ctrl Pts',(65.347979297789,1.72271809652518,3.48280260135673));
#24535=CARTESIAN_POINT('Ctrl Pts',(65.826966892062,1.44943432222995,3.44575663783405));
#24536=CARTESIAN_POINT('Ctrl Pts',(66.305954486335,1.17615054793472,3.40871067431137));
#24537=CARTESIAN_POINT('Ctrl Pts',(66.6360770811014,0.641949387786594,3.37166471078869));
#24538=CARTESIAN_POINT('Ctrl Pts',(66.6662521989441,0.0913110318543479,
3.33461874726601));
#24539=CARTESIAN_POINT('Ctrl Pts',(66.6679081722746,0.0610926765551679,
3.3325857103806));
#24540=CARTESIAN_POINT('Ctrl Pts',(66.668660799992,0.0308248176933807,3.3305526734952));
#24541=CARTESIAN_POINT('Ctrl Pts',(66.6685304876972,0.000550348904958531,
3.32851963660979));
#24542=CARTESIAN_POINT('Origin',(65.,0.,3.));
#24543=CARTESIAN_POINT('',(66.664215437255,0.00117645755965692,2.62851963660979));
#24544=CARTESIAN_POINT('',(66.663709965026,-0.000842507685006553,2.82148036339021));
#24545=CARTESIAN_POINT('',(66.666,2.04026156737949E-16,3.));
#24546=CARTESIAN_POINT('Ctrl Pts',(66.663709965026,-0.000842507685006553,
2.82148036339021));
#24547=CARTESIAN_POINT('Ctrl Pts',(66.6621889226241,0.331295501917188,2.84361959192095));
#24548=CARTESIAN_POINT('Ctrl Pts',(66.565926135999,0.664245551393377,2.8657588204517));
#24549=CARTESIAN_POINT('Ctrl Pts',(66.3808853648239,0.936957985442183,2.88789804898245));
#24550=CARTESIAN_POINT('Ctrl Pts',(66.0712533625325,1.39329253521756,2.92494401250513));
#24551=CARTESIAN_POINT('Ctrl Pts',(65.5130436951299,1.68096223107998,2.96198997602781));
#24552=CARTESIAN_POINT('Ctrl Pts',(64.9617241821671,1.66831340551997,2.9990359395505));
#24553=CARTESIAN_POINT('Ctrl Pts',(64.4104046692042,1.65566457995996,3.03608190307317));
#24554=CARTESIAN_POINT('Ctrl Pts',(63.8659753106812,1.34269723297749,3.07312786659585));
#24555=CARTESIAN_POINT('Ctrl Pts',(63.5775972896502,0.872642645564547,3.11017383011853));
#24556=CARTESIAN_POINT('Ctrl Pts',(63.2892192686192,0.4025880581516,3.14721979364122));
#24557=CARTESIAN_POINT('Ctrl Pts',(63.2568925850803,-0.224553769691831,
3.1842657571639));
#24558=CARTESIAN_POINT('Ctrl Pts',(63.4954117290602,-0.721767824316922,
3.22131172068658));
#24559=CARTESIAN_POINT('Ctrl Pts',(63.73393087304,-1.21898187894202,3.25835768420926));
#24560=CARTESIAN_POINT('Ctrl Pts',(64.2432958445387,-1.58626816034877,3.29540364773194));
#24561=CARTESIAN_POINT('Ctrl Pts',(64.7903928760533,-1.65553601919701,3.33244961125462));
#24562=CARTESIAN_POINT('Ctrl Pts',(65.3374899075679,-1.72480387804526,3.3694955747773));
#24563=CARTESIAN_POINT('Ctrl Pts',(65.9223189990984,-1.49605331433501,3.40654153829998));
#24564=CARTESIAN_POINT('Ctrl Pts',(66.2772298007007,-1.07397332065116,3.44358750182266));
#24565=CARTESIAN_POINT('Ctrl Pts',(66.5259750107882,-0.778151451526181,
3.46955178901184));
#24566=CARTESIAN_POINT('Ctrl Pts',(66.6617810644663,-0.387363397948804,
3.49551607620103));
#24567=CARTESIAN_POINT('Ctrl Pts',(66.6649541686305,0.00142706439964306,
3.52148036339021));
#24568=CARTESIAN_POINT('Ctrl Pts',(66.6685304876972,0.000550348904958531,
3.32851963660979));
#24569=CARTESIAN_POINT('Ctrl Pts',(66.6662862515739,-0.520836037284763,
3.29350670997252));
#24570=CARTESIAN_POINT('Ctrl Pts',(66.4021649235169,-1.0441829058867,3.25849378333524));
#24571=CARTESIAN_POINT('Ctrl Pts',(65.9803979715476,-1.35039028151487,3.22348085669796));
#24572=CARTESIAN_POINT('Ctrl Pts',(65.5341409853895,-1.67437768723548,3.18643489317528));
#24573=CARTESIAN_POINT('Ctrl Pts',(64.9113993721543,-1.75527694696033,3.1493889296526));
#24574=CARTESIAN_POINT('Ctrl Pts',(64.3971743623243,-1.55606405574624,3.11234296612992));
#24575=CARTESIAN_POINT('Ctrl Pts',(63.8829493524943,-1.35685116453215,3.07529700260724));
#24576=CARTESIAN_POINT('Ctrl Pts',(63.4772409460695,-0.877526122379129,
3.03825103908456));
#24577=CARTESIAN_POINT('Ctrl Pts',(63.3657238957733,-0.337454752786397,
3.00120507556188));
#24578=CARTESIAN_POINT('Ctrl Pts',(63.2542068454771,0.202616616806336,2.9641591120392));
#24579=CARTESIAN_POINT('Ctrl Pts',(63.4368811513095,0.803434313838776,2.92711314851652));
#24580=CARTESIAN_POINT('Ctrl Pts',(63.8301448813726,1.190030712396,2.89006718499384));
#24581=CARTESIAN_POINT('Ctrl Pts',(64.2234086114356,1.57662711095322,2.85302122147116));
#24582=CARTESIAN_POINT('Ctrl Pts',(64.8272617657294,1.74900221103522,2.81597525794848));
#24583=CARTESIAN_POINT('Ctrl Pts',(65.3653475241109,1.62826757065616,2.7789292944258));
#24584=CARTESIAN_POINT('Ctrl Pts',(65.9034332824925,1.50753293027711,2.74188333090311));
#24585=CARTESIAN_POINT('Ctrl Pts',(66.3757516449619,1.093688549437,2.70483736738043));
#24586=CARTESIAN_POINT('Ctrl Pts',(66.5661434347078,0.576132655684555,2.66779140385775));
#24587=CARTESIAN_POINT('Ctrl Pts',(66.6334204184134,0.393248722101042,2.6547008147751));
#24588=CARTESIAN_POINT('Ctrl Pts',(66.6654949753924,0.197414973610974,2.64161022569244));
#24589=CARTESIAN_POINT('Ctrl Pts',(66.664215437255,0.00117645755965692,
2.62851963660979));
#24590=CARTESIAN_POINT('Origin',(65.,0.,3.));
#24591=CARTESIAN_POINT('',(66.6642789433678,-0.00120644035140824,1.92851963660979));
#24592=CARTESIAN_POINT('',(66.6680288432953,-0.000974731038369267,2.1214803633902));
#24593=CARTESIAN_POINT('',(66.666,2.04026156737949E-16,3.));
#24594=CARTESIAN_POINT('Ctrl Pts',(66.6680288432953,-0.000974731038369267,
2.1214803633902));
#24595=CARTESIAN_POINT('Ctrl Pts',(66.6645899038029,0.493760549303249,2.1546771441182));
#24596=CARTESIAN_POINT('Ctrl Pts',(66.4304593550116,0.991322629328269,2.1878739248462));
#24597=CARTESIAN_POINT('Ctrl Pts',(66.0452404987214,1.30084855271516,2.2210707055742));
#24598=CARTESIAN_POINT('Ctrl Pts',(65.6153553295749,1.64626415674821,2.25811666909688));
#24599=CARTESIAN_POINT('Ctrl Pts',(64.9973130191693,1.75750978249458,2.29516263261956));
#24600=CARTESIAN_POINT('Ctrl Pts',(64.4739641353999,1.58367323852582,2.33220859614224));
#24601=CARTESIAN_POINT('Ctrl Pts',(63.9506152516305,1.40983669455707,2.36925455966492));
#24602=CARTESIAN_POINT('Ctrl Pts',(63.5219597944974,0.950917980873213,2.40630052318761));
#24603=CARTESIAN_POINT('Ctrl Pts',(63.3841743645993,0.416943849037749,2.44334648671029));
#24604=CARTESIAN_POINT('Ctrl Pts',(63.2463889347012,-0.117030282797714,
2.48039245023297));
#24605=CARTESIAN_POINT('Ctrl Pts',(63.399473532038,-0.72605983278478,2.51743841375565));
#24606=CARTESIAN_POINT('Ctrl Pts',(63.77336812259,-1.13141897393943,2.55448437727833));
#24607=CARTESIAN_POINT('Ctrl Pts',(64.1472627131419,-1.53677811509408,2.59153034080101));
#24608=CARTESIAN_POINT('Ctrl Pts',(64.741967296909,-1.73846684741632,2.62857630432369));
#24609=CARTESIAN_POINT('Ctrl Pts',(65.2853119489257,-1.64418117890598,2.66562226784637));
#24610=CARTESIAN_POINT('Ctrl Pts',(65.8286566009425,-1.54989551039565,2.70266823136905));
#24611=CARTESIAN_POINT('Ctrl Pts',(66.3206413212089,-1.15963544105274,2.73971419489173));
#24612=CARTESIAN_POINT('Ctrl Pts',(66.5361065127521,-0.652005704537125,
2.77676015841441));
#24613=CARTESIAN_POINT('Ctrl Pts',(66.6228064445369,-0.447743182072849,
2.79166689340634));
#24614=CARTESIAN_POINT('Ctrl Pts',(66.664734109836,-0.22447691676168,2.80657362839827));
#24615=CARTESIAN_POINT('Ctrl Pts',(66.663709965026,-0.000842507685006553,
2.82148036339021));
#24616=CARTESIAN_POINT('Ctrl Pts',(66.664215437255,0.00117645755965692,
2.62851963660979));
#24617=CARTESIAN_POINT('Ctrl Pts',(66.6618739219115,-0.357933976805237,
2.60456426216976));
#24618=CARTESIAN_POINT('Ctrl Pts',(66.5478366409886,-0.718399891583488,
2.58060888772974));
#24619=CARTESIAN_POINT('Ctrl Pts',(66.3334304982421,-1.00334301282382,2.55665351328971));
#24620=CARTESIAN_POINT('Ctrl Pts',(66.0018605550081,-1.443995380915,2.51960754976703));
#24621=CARTESIAN_POINT('Ctrl Pts',(65.4302554515179,-1.70403271043258,2.48256158624435));
#24622=CARTESIAN_POINT('Ctrl Pts',(64.880213504605,-1.66444744301089,2.44551562272167));
#24623=CARTESIAN_POINT('Ctrl Pts',(64.3301715576922,-1.6248621755892,2.40846965919899));
#24624=CARTESIAN_POINT('Ctrl Pts',(63.8016927673567,-1.28565431122825,2.37142369567631));
#24625=CARTESIAN_POINT('Ctrl Pts',(63.5366384486743,-0.802064252492239,
2.33437773215363));
#24626=CARTESIAN_POINT('Ctrl Pts',(63.2715841299918,-0.318474193756233,
2.29733176863095));
#24627=CARTESIAN_POINT('Ctrl Pts',(63.2699542829623,0.309498059354825,2.26028580510827));
#24628=CARTESIAN_POINT('Ctrl Pts',(63.5324948163207,0.794457444359823,2.22323984158559));
#24629=CARTESIAN_POINT('Ctrl Pts',(63.795035349679,1.27941682936482,2.18619387806291));
#24630=CARTESIAN_POINT('Ctrl Pts',(64.3217462634253,1.62136334626376,2.14914791454023));
#24631=CARTESIAN_POINT('Ctrl Pts',(64.8715753212295,1.66380323262916,2.11210195101754));
#24632=CARTESIAN_POINT('Ctrl Pts',(65.4214043790337,1.70624311899456,2.07505598749486));
#24633=CARTESIAN_POINT('Ctrl Pts',(65.9943515808958,1.44917637482642,2.03801002397218));
#24634=CARTESIAN_POINT('Ctrl Pts',(66.3282043910519,1.01025105326097,2.0009640604495));
#24635=CARTESIAN_POINT('Ctrl Pts',(66.54582391177,0.724140781894946,1.9768159191696));
#24636=CARTESIAN_POINT('Ctrl Pts',(66.6618524838225,0.360758997512877,1.95266777788969));
#24637=CARTESIAN_POINT('Ctrl Pts',(66.6642789433678,-0.00120644035140824,
1.92851963660979));
#24638=CARTESIAN_POINT('Origin',(65.,0.,3.));
#24639=CARTESIAN_POINT('',(66.6685688018723,-0.000500570493866259,1.22851963660979));
#24640=CARTESIAN_POINT('',(66.6666630352664,0.00145874010108481,1.4214803633902));
#24641=CARTESIAN_POINT('',(66.666,2.04026156737949E-16,3.));
#24642=CARTESIAN_POINT('Ctrl Pts',(66.6666630352664,0.00145874010108481,
1.4214803633902));
#24643=CARTESIAN_POINT('Ctrl Pts',(66.6676496745696,0.109114984958744,1.42868873279277));
#24644=CARTESIAN_POINT('Ctrl Pts',(66.6581116875295,0.216597146837641,1.43589710219534));
#24645=CARTESIAN_POINT('Ctrl Pts',(66.6374139306422,0.321885502945882,1.44310547159791));
#24646=CARTESIAN_POINT('Ctrl Pts',(66.5310419755125,0.862993814953162,1.48015143512059));
#24647=CARTESIAN_POINT('Ctrl Pts',(66.1299138139174,1.34615847081564,1.51719739864327));
#24648=CARTESIAN_POINT('Ctrl Pts',(65.6176080235618,1.55025642604728,1.55424336216595));
#24649=CARTESIAN_POINT('Ctrl Pts',(65.1053022332063,1.75435438127892,1.59128932568863));
#24650=CARTESIAN_POINT('Ctrl Pts',(64.4818188140901,1.67938563587972,1.62833528921131));
#24651=CARTESIAN_POINT('Ctrl Pts',(64.0324984883637,1.35966006128365,1.66538125273399));
#24652=CARTESIAN_POINT('Ctrl Pts',(63.5831781626372,1.03993448668758,1.70242721625667));
#24653=CARTESIAN_POINT('Ctrl Pts',(63.3080209303004,0.475452082894629,1.73947317977936));
#24654=CARTESIAN_POINT('Ctrl Pts',(63.3329540589798,-0.0754485771665831,
1.77651914330204));
#24655=CARTESIAN_POINT('Ctrl Pts',(63.3578871876591,-0.626349237227795,
1.81356510682472));
#24656=CARTESIAN_POINT('Ctrl Pts',(63.6829106773545,-1.16366815355727,1.8506110703474));
#24657=CARTESIAN_POINT('Ctrl Pts',(64.1592756849985,-1.44149827729127,1.88765703387008));
#24658=CARTESIAN_POINT('Ctrl Pts',(64.6356406926424,-1.71932840102526,1.92470299739276));
#24659=CARTESIAN_POINT('Ctrl Pts',(65.2633472182348,-1.73766973216377,1.96174896091544));
#24660=CARTESIAN_POINT('Ctrl Pts',(65.7551218110002,-1.48812825650888,1.99879492443812));
#24661=CARTESIAN_POINT('Ctrl Pts',(66.2468964037657,-1.23858678085398,2.0358408879608));
#24662=CARTESIAN_POINT('Ctrl Pts',(66.6027390637042,-0.72116249840569,2.07288685148348));
#24663=CARTESIAN_POINT('Ctrl Pts',(66.6597963797297,-0.172657566021668,
2.10993281500616));
#24664=CARTESIAN_POINT('Ctrl Pts',(66.6657247999481,-0.115666316563739,
2.11378199780084));
#24665=CARTESIAN_POINT('Ctrl Pts',(66.6684275899941,-0.058339526276079,
2.11763118059552));
#24666=CARTESIAN_POINT('Ctrl Pts',(66.6680288432953,-0.000974731038369267,
2.1214803633902));
#24667=CARTESIAN_POINT('Ctrl Pts',(66.6642789433678,-0.00120644035140824,
1.92851963660979));
#24668=CARTESIAN_POINT('Ctrl Pts',(66.6655749455541,-0.194536677303716,
1.91562181436701));
#24669=CARTESIAN_POINT('Ctrl Pts',(66.634462982395,-0.387462864473387,1.90272399212424));
#24670=CARTESIAN_POINT('Ctrl Pts',(66.5691129188822,-0.567995372183044,
1.88982616988146));
#24671=CARTESIAN_POINT('Ctrl Pts',(66.3814102181061,-1.08653257709889,1.85278020635878));
#24672=CARTESIAN_POINT('Ctrl Pts',(65.9112463981035,-1.50282308796781,1.8157342428361));
#24673=CARTESIAN_POINT('Ctrl Pts',(65.3737945971089,-1.62634919196251,1.77868827931342));
#24674=CARTESIAN_POINT('Ctrl Pts',(64.8363427961142,-1.74987529595721,1.74164231579074));
#24675=CARTESIAN_POINT('Ctrl Pts',(64.2316030141275,-1.58063699307767,1.70459635226806));
#24676=CARTESIAN_POINT('Ctrl Pts',(63.8363378414827,-1.19608715228398,1.66755038874538));
#24677=CARTESIAN_POINT('Ctrl Pts',(63.4410726688379,-0.811537311490284,
1.6305044252227));
#24678=CARTESIAN_POINT('Ctrl Pts',(63.2552821055351,-0.211675932782416,
1.59345846170002));
#24679=CARTESIAN_POINT('Ctrl Pts',(63.3639942563739,0.328967022430173,1.55641249817734));
#24680=CARTESIAN_POINT('Ctrl Pts',(63.4727064072127,0.869609977642756,1.51936653465465));
#24681=CARTESIAN_POINT('Ctrl Pts',(63.8759212721932,1.35103450936006,1.48232057113197));
#24682=CARTESIAN_POINT('Ctrl Pts',(64.3891052819731,1.55291395077579,1.44527460760929));
#24683=CARTESIAN_POINT('Ctrl Pts',(64.9022892917531,1.75479339219152,1.40822864408661));
#24684=CARTESIAN_POINT('Ctrl Pts',(65.5254424463325,1.67712774330567,1.37118268056393));
#24685=CARTESIAN_POINT('Ctrl Pts',(65.9733751709996,1.35546112873118,1.33413671704125));
#24686=CARTESIAN_POINT('Ctrl Pts',(66.3990566948007,1.04977340575941,1.2989310235641));
#24687=CARTESIAN_POINT('Ctrl Pts',(66.6664936696292,0.523724262697509,1.26372533008694));
#24688=CARTESIAN_POINT('Ctrl Pts',(66.6685688018723,-0.000500570493866259,
1.22851963660979));
#24689=CARTESIAN_POINT('Origin',(65.,0.,3.));
#24690=CARTESIAN_POINT('',(66.6657538157597,0.00152189319961124,0.528519636609788));
#24691=CARTESIAN_POINT('',(66.6632893889008,6.33249066023143E-5,0.721480363390204));
#24692=CARTESIAN_POINT('',(66.666,2.04026156737949E-16,3.));
#24693=CARTESIAN_POINT('Ctrl Pts',(66.6632893889008,6.33249066023143E-5,
0.721480363390204));
#24694=CARTESIAN_POINT('Ctrl Pts',(66.663382354964,0.274266208525867,0.739746284990023));
#24695=CARTESIAN_POINT('Ctrl Pts',(66.5993416986523,0.548428211919456,0.758012206589841));
#24696=CARTESIAN_POINT('Ctrl Pts',(66.4709289590166,0.78810066283112,0.77627812818966));
#24697=CARTESIAN_POINT('Ctrl Pts',(66.2104891206872,1.27419148640901,0.81332409171234));
#24698=CARTESIAN_POINT('Ctrl Pts',(65.6852625770594,1.61841374682523,0.850370055235021));
#24699=CARTESIAN_POINT('Ctrl Pts',(65.1356222340335,1.66323217468977,0.887416018757702));
#24700=CARTESIAN_POINT('Ctrl Pts',(64.5859818910076,1.70805060255431,0.924461982280382));
#24701=CARTESIAN_POINT('Ctrl Pts',(64.0119277485837,1.45346519786717,0.961507945803063));
#24702=CARTESIAN_POINT('Ctrl Pts',(63.6761789401645,1.01598841469989,0.998553909325744));
#24703=CARTESIAN_POINT('Ctrl Pts',(63.3404301317454,0.578511631532615,1.03559987284842));
#24704=CARTESIAN_POINT('Ctrl Pts',(63.242986657331,-0.0418565301147992,
1.0726458363711));
#24705=CARTESIAN_POINT('Ctrl Pts',(63.4284440755221,-0.561201063347335,
1.10969179989379));
#24706=CARTESIAN_POINT('Ctrl Pts',(63.6139014937132,-1.08054559657987,1.14673776341647));
#24707=CARTESIAN_POINT('Ctrl Pts',(64.0822598045097,-1.49886650139754,1.18378372693915));
#24708=CARTESIAN_POINT('Ctrl Pts',(64.619172171207,-1.62471684366476,1.22082969046183));
#24709=CARTESIAN_POINT('Ctrl Pts',(65.1560845379043,-1.75056718593198,1.25787565398451));
#24710=CARTESIAN_POINT('Ctrl Pts',(65.7615509605024,-1.58394696564878,1.29492161750719));
#24711=CARTESIAN_POINT('Ctrl Pts',(66.1584762974693,-1.20111087143113,1.33196758102987));
#24712=CARTESIAN_POINT('Ctrl Pts',(66.4781682685839,-0.892766671210736,
1.36180517514998));
#24713=CARTESIAN_POINT('Ctrl Pts',(66.6625790404782,-0.444162614627704,
1.39164276927009));
#24714=CARTESIAN_POINT('Ctrl Pts',(66.6666630352664,0.00145874010108481,
1.4214803633902));
#24715=CARTESIAN_POINT('Ctrl Pts',(66.6685688018723,-0.000500570493866259,
1.22851963660979));
#24716=CARTESIAN_POINT('Ctrl Pts',(66.6686772730691,-0.0279028217311245,
1.22667936656426));
#24717=CARTESIAN_POINT('Ctrl Pts',(66.6680606812028,-0.0553000883040847,
1.22483909651874));
#24718=CARTESIAN_POINT('Ctrl Pts',(66.6667037271851,-0.0826606364095831,
1.22299882647321));
#24719=CARTESIAN_POINT('Ctrl Pts',(66.6393872639487,-0.633448206712713,
1.18595286295053));
#24720=CARTESIAN_POINT('Ctrl Pts',(66.3120420427213,-1.16935576705583,1.14890689942785));
#24721=CARTESIAN_POINT('Ctrl Pts',(65.8344794601719,-1.4451221836215,1.11186093590517));
#24722=CARTESIAN_POINT('Ctrl Pts',(65.3569168776225,-1.72088860018717,1.07481497238249));
#24723=CARTESIAN_POINT('Ctrl Pts',(64.729136933751,-1.73651387297538,1.03776900885981));
#24724=CARTESIAN_POINT('Ctrl Pts',(64.2384466796233,-1.48484700734034,1.00072304533713));
#24725=CARTESIAN_POINT('Ctrl Pts',(63.7477564254956,-1.2331801417053,0.963677081814447));
#24726=CARTESIAN_POINT('Ctrl Pts',(63.3941558611116,-0.714221137647012,
0.926631118291766));
#24727=CARTESIAN_POINT('Ctrl Pts',(63.3394722898162,-0.165474525977688,
0.889585154769085));
#24728=CARTESIAN_POINT('Ctrl Pts',(63.2847887185207,0.383272085691634,0.852539191246405));
#24729=CARTESIAN_POINT('Ctrl Pts',(63.5290221403138,0.961806304971985,0.815493227723724));
#24730=CARTESIAN_POINT('Ctrl Pts',(63.9603977448083,1.30535866571472,0.778447264201044));
#24731=CARTESIAN_POINT('Ctrl Pts',(64.3917733493027,1.64891102645746,0.741401300678363));
#24732=CARTESIAN_POINT('Ctrl Pts',(65.0102911364986,1.75748152866258,0.704355337155683));
#24733=CARTESIAN_POINT('Ctrl Pts',(65.5328829338629,1.58138226671976,0.667309373633002));
#24734=CARTESIAN_POINT('Ctrl Pts',(66.0554747312272,1.40528300477694,0.630263410110321));
#24735=CARTESIAN_POINT('Ctrl Pts',(66.4821405387599,0.944513978686174,0.593217446587641));
#24736=CARTESIAN_POINT('Ctrl Pts',(66.6176143302611,0.409948745265365,0.55617148306496));
#24737=CARTESIAN_POINT('Ctrl Pts',(66.6513211107492,0.276945359297953,0.546954200913236));
#24738=CARTESIAN_POINT('Ctrl Pts',(66.6670017222694,0.13937363756141,0.537736918761512));
#24739=CARTESIAN_POINT('Ctrl Pts',(66.6657538157597,0.00152189319961124,
0.528519636609788));
#24740=CARTESIAN_POINT('Origin',(65.,0.,3.));
#24741=CARTESIAN_POINT('',(66.6633878829795,-0.000426123154284863,-0.171480363390211));
#24742=CARTESIAN_POINT('',(66.6664305869533,-0.00149161834301985,0.0214803633902055));
#24743=CARTESIAN_POINT('',(66.666,2.04026156737949E-16,3.));
#24744=CARTESIAN_POINT('Ctrl Pts',(66.6664305869533,-0.00149161834301985,
0.0214803633902055));
#24745=CARTESIAN_POINT('Ctrl Pts',(66.6623874613811,0.436608579267598,0.0508038371872736));
#24746=CARTESIAN_POINT('Ctrl Pts',(66.484951449296,0.877606426402575,0.0801273109843417));
#24747=CARTESIAN_POINT('Ctrl Pts',(66.1749931684956,1.18495810418996,0.10945078478141));
#24748=CARTESIAN_POINT('Ctrl Pts',(65.7834057582335,1.57325244894404,0.146496748304091));
#24749=CARTESIAN_POINT('Ctrl Pts',(65.1803040079573,1.74823863365067,0.183542711826771));
#24750=CARTESIAN_POINT('Ctrl Pts',(64.641700851863,1.62983323643182,0.220588675349452));
#24751=CARTESIAN_POINT('Ctrl Pts',(64.1030976957686,1.51142783921297,0.257634638872132));
#24752=CARTESIAN_POINT('Ctrl Pts',(63.6289931338561,1.09963086006864,0.294680602394813));
#24753=CARTESIAN_POINT('Ctrl Pts',(63.4363638080708,0.582903522671605,0.331726565917493));
#24754=CARTESIAN_POINT('Ctrl Pts',(63.2437344822855,0.0661761852745729,
0.368772529440174));
#24755=CARTESIAN_POINT('Ctrl Pts',(63.3325803926274,-0.555481510375157,
0.405818492962855));
#24756=CARTESIAN_POINT('Ctrl Pts',(63.6622407040169,-0.997564395392433,
0.442864456485535));
#24757=CARTESIAN_POINT('Ctrl Pts',(63.9919010154063,-1.43964728040971,0.479910420008216));
#24758=CARTESIAN_POINT('Ctrl Pts',(64.5623757278433,-1.70215535479453,0.516956383530896));
#24759=CARTESIAN_POINT('Ctrl Pts',(65.1125838545831,-1.6649503094947,0.554002347053577));
#24760=CARTESIAN_POINT('Ctrl Pts',(65.6627919813228,-1.62774526419487,0.591048310576258));
#24761=CARTESIAN_POINT('Ctrl Pts',(66.1927335223652,-1.29082709921038,0.628094274098938));
#24762=CARTESIAN_POINT('Ctrl Pts',(66.4598777263709,-0.808388323348352,
0.665140237621619));
#24763=CARTESIAN_POINT('Ctrl Pts',(66.5953035291742,-0.563821315923748,
0.683920279544481));
#24764=CARTESIAN_POINT('Ctrl Pts',(66.6631938061757,-0.281857388570597,
0.702700321467342));
#24765=CARTESIAN_POINT('Ctrl Pts',(66.6632893889008,6.33249066023143E-5,
0.721480363390204));
#24766=CARTESIAN_POINT('Ctrl Pts',(66.6657538157597,0.00152189319961124,
0.528519636609788));
#24767=CARTESIAN_POINT('Ctrl Pts',(66.6619861549602,-0.414678045906902,
0.500690955238832));
#24768=CARTESIAN_POINT('Ctrl Pts',(66.5039069443419,-0.833430525360481,
0.472862273867875));
#24769=CARTESIAN_POINT('Ctrl Pts',(66.2217249851539,-1.13671551258266,0.445033592496918));
#24770=CARTESIAN_POINT('Ctrl Pts',(65.8460800730759,-1.54045309625902,0.407987628974238));
#24771=CARTESIAN_POINT('Ctrl Pts',(65.2505084734505,-1.73956682286089,0.370941665451557));
#24772=CARTESIAN_POINT('Ctrl Pts',(64.7075769058774,-1.64293116911907,0.333895701928877));
#24773=CARTESIAN_POINT('Ctrl Pts',(64.1646453383043,-1.54629551537724,0.296849738406196));
#24774=CARTESIAN_POINT('Ctrl Pts',(63.6743538027836,-1.15391048129172,0.259803774883516));
#24775=CARTESIAN_POINT('Ctrl Pts',(63.4610870008646,-0.645353297241682,
0.222757811360835));
#24776=CARTESIAN_POINT('Ctrl Pts',(63.2478201989456,-0.136796113191638,
0.185711847838155));
#24777=CARTESIAN_POINT('Ctrl Pts',(63.3115781306282,0.48793322082293,0.148665884315474));
#24778=CARTESIAN_POINT('Ctrl Pts',(63.6231816165986,0.942923771900633,0.111619920792793));
#24779=CARTESIAN_POINT('Ctrl Pts',(63.9347851025691,1.39791432297834,0.0745739572701125));
#24780=CARTESIAN_POINT('Ctrl Pts',(64.4942341428273,1.68316609111917,0.0375279937474321));
#24781=CARTESIAN_POINT('Ctrl Pts',(65.0454937124919,1.6681320083057,0.000482030224751638));
#24782=CARTESIAN_POINT('Ctrl Pts',(65.5967532821565,1.65309792549222,-0.0365639332979289));
#24783=CARTESIAN_POINT('Ctrl Pts',(66.1398233812275,1.33777799172443,-0.0736098968206095));
#24784=CARTESIAN_POINT('Ctrl Pts',(66.4261648980985,0.866480120962494,-0.11065586034329));
#24785=CARTESIAN_POINT('Ctrl Pts',(66.5828763524582,0.608544158441986,-0.130930694692264));
#24786=CARTESIAN_POINT('Ctrl Pts',(66.6626912202299,0.303888929858147,-0.151205529041237));
#24787=CARTESIAN_POINT('Ctrl Pts',(66.6633878829795,-0.000426123154284863,
-0.171480363390211));
#24788=CARTESIAN_POINT('Origin',(65.,0.,3.));
#24789=CARTESIAN_POINT('',(66.6673159824367,-0.00130059074131283,-0.871480363390211));
#24790=CARTESIAN_POINT('',(66.6681941903091,0.000864019930038266,-0.678519636609795));
#24791=CARTESIAN_POINT('',(66.666,2.04026156737949E-16,3.));
#24792=CARTESIAN_POINT('Ctrl Pts',(66.6681941903091,0.000864019930038266,
-0.678519636609795));
#24793=CARTESIAN_POINT('Ctrl Pts',(66.6685078326159,0.0505538571114843,
-0.675184574138157));
#24794=CARTESIAN_POINT('Ctrl Pts',(66.6664801000417,0.100217739688425,-0.67184951166652));
#24795=CARTESIAN_POINT('Ctrl Pts',(66.6620276056557,0.149663274321063,-0.668514449194882));
#24796=CARTESIAN_POINT('Ctrl Pts',(66.6125691784105,0.698905601245373,-0.631468485672201));
#24797=CARTESIAN_POINT('Ctrl Pts',(66.2639236084022,1.22120635507833,-0.594422522149521));
#24798=CARTESIAN_POINT('Ctrl Pts',(65.7756507075141,1.47753189011202,-0.557376558626841));
#24799=CARTESIAN_POINT('Ctrl Pts',(65.287377806626,1.7338574251457,-0.52033059510416));
#24800=CARTESIAN_POINT('Ctrl Pts',(64.659477574858,1.7242077413801,-0.483284631581479));
#24801=CARTESIAN_POINT('Ctrl Pts',(64.1793120174543,1.4529989415171,-0.446238668058799));
#24802=CARTESIAN_POINT('Ctrl Pts',(63.6991464600505,1.18179014165409,-0.409192704536118));
#24803=CARTESIAN_POINT('Ctrl Pts',(63.3667155770108,0.649022225693674,-0.372146741013438));
#24804=CARTESIAN_POINT('Ctrl Pts',(63.334158295787,0.0985195171959843,-0.335100777490757));
#24805=CARTESIAN_POINT('Ctrl Pts',(63.3016010145631,-0.451983191301702,
-0.298054813968077));
#24806=CARTESIAN_POINT('Ctrl Pts',(63.568917335155,-1.02022069233666,-0.261008850445396));
#24807=CARTESIAN_POINT('Ctrl Pts',(64.0137684029003,-1.34613590481465,-0.223962886922715));
#24808=CARTESIAN_POINT('Ctrl Pts',(64.4586194706456,-1.67205111729263,-0.186916923400034));
#24809=CARTESIAN_POINT('Ctrl Pts',(65.0810052855443,-1.75564404121364,-0.149870959877354));
#24810=CARTESIAN_POINT('Ctrl Pts',(65.5960874627955,-1.5586578840129,-0.112824996354674));
#24811=CARTESIAN_POINT('Ctrl Pts',(66.1111696400466,-1.36167172681217,-0.0757790328319931));
#24812=CARTESIAN_POINT('Ctrl Pts',(66.5189481796502,-0.884106488489677,
-0.0387330693093125));
#24813=CARTESIAN_POINT('Ctrl Pts',(66.632800914328,-0.344522616927666,-0.00168710578663189));
#24814=CARTESIAN_POINT('Ctrl Pts',(66.6565343117127,-0.232042591898955,
0.00603538393898058));
#24815=CARTESIAN_POINT('Ctrl Pts',(66.6674953651548,-0.116867589766127,
0.013757873664593));
#24816=CARTESIAN_POINT('Ctrl Pts',(66.6664305869533,-0.00149161834301985,
0.0214803633902055));
#24817=CARTESIAN_POINT('Ctrl Pts',(66.6633878829795,-0.000426123154284863,
-0.171480363390211));
#24818=CARTESIAN_POINT('Ctrl Pts',(66.6639641550595,-0.252152325979383,
-0.188251492563918));
#24819=CARTESIAN_POINT('Ctrl Pts',(66.6104043971,-0.50364576625701,-0.205022621737625));
#24820=CARTESIAN_POINT('Ctrl Pts',(66.5014511773033,-0.728270889754927,
-0.221793750911332));
#24821=CARTESIAN_POINT('Ctrl Pts',(66.2607830049661,-1.22444822195432,-0.258839714434013));
#24822=CARTESIAN_POINT('Ctrl Pts',(65.7498337256207,-1.58952707859704,-0.295885677956694));
#24823=CARTESIAN_POINT('Ctrl Pts',(65.2024421689935,-1.65642721292161,-0.332931641479375));
#24824=CARTESIAN_POINT('Ctrl Pts',(64.6550506123664,-1.72332734724617,-0.369977605002055));
#24825=CARTESIAN_POINT('Ctrl Pts',(64.0712167784575,-1.49204875925259,-0.407023568524736));
#24826=CARTESIAN_POINT('Ctrl Pts',(63.7181355422591,-1.06843708657372,-0.444069532047416));
#24827=CARTESIAN_POINT('Ctrl Pts',(63.3650543060608,-0.644825413894849,
-0.481115495570097));
#24828=CARTESIAN_POINT('Ctrl Pts',(63.242725667573,-0.028880656530687,-0.518161459092778));
#24829=CARTESIAN_POINT('Ctrl Pts',(63.4071340014642,0.497505944605294,-0.555207422615458));
#24830=CARTESIAN_POINT('Ctrl Pts',(63.5715423353554,1.02389254574128,-0.592253386138139));
#24831=CARTESIAN_POINT('Ctrl Pts',(64.0226876416257,1.46072099064907,-0.629299349660819));
#24832=CARTESIAN_POINT('Ctrl Pts',(64.5541007528815,1.60807550663331,-0.6663453131835));
#24833=CARTESIAN_POINT('Ctrl Pts',(65.0855138641373,1.75543002261754,-0.70339127670618));
#24834=CARTESIAN_POINT('Ctrl Pts',(65.6971947803788,1.61331060967821,-0.740437240228861));
#24835=CARTESIAN_POINT('Ctrl Pts',(66.1092041825925,1.24675657433954,-0.777483203751541));
#24836=CARTESIAN_POINT('Ctrl Pts',(66.4576696191289,0.936735950411711,-0.808815590297765));
#24837=CARTESIAN_POINT('Ctrl Pts',(66.6633044515624,0.466170980160881,-0.840147976843988));
#24838=CARTESIAN_POINT('Ctrl Pts',(66.6673159824367,-0.00130059074131283,
-0.871480363390211));
#24839=CARTESIAN_POINT('Origin',(65.,0.,3.));
#24840=CARTESIAN_POINT('',(66.6674675207825,0.00121113675536799,-1.57148036339021));
#24841=CARTESIAN_POINT('',(66.6638321395092,0.000941642735149761,-1.3785196366098));
#24842=CARTESIAN_POINT('',(66.666,2.04026156737949E-16,3.));
#24843=CARTESIAN_POINT('',(63.7309291201476,1.0793586530485,-2.));
#24844=CARTESIAN_POINT('Ctrl Pts',(66.6674675207825,0.00121113675536799,
-1.57148036339021));
#24845=CARTESIAN_POINT('Ctrl Pts',(66.6635269376583,-0.471550204230264,
-1.6031823516921));
#24846=CARTESIAN_POINT('Ctrl Pts',(66.452430524463,-0.947291842680174,-1.63488433999399));
#24847=CARTESIAN_POINT('Ctrl Pts',(66.0967466510819,-1.25757678610753,-1.66658632829587));
#24848=CARTESIAN_POINT('Ctrl Pts',(65.6811054719418,-1.62016617912558,-1.70363229181856));
#24849=CARTESIAN_POINT('Ctrl Pts',(65.0680223500032,-1.75681556827131,-1.74067825534124));
#24850=CARTESIAN_POINT('Ctrl Pts',(64.5381019768621,-1.60385217794778,-1.77772421886392));
#24851=CARTESIAN_POINT('Ctrl Pts',(64.008181603721,-1.45088878762425,-1.8147701823866));
#24852=CARTESIAN_POINT('Ctrl Pts',(63.5614239793774,-1.00831261783145,-1.85181614590928));
#24853=CARTESIAN_POINT('Ctrl Pts',(63.4023827506955,-0.481249822665511,
-1.88886210943196));
#24854=CARTESIAN_POINT('Ctrl Pts',(63.2433415220136,0.0458129725004276,
-1.92590807295464));
#24855=CARTESIAN_POINT('Ctrl Pts',(63.3720166889934,0.657362393039508,-1.96295403647732));
#24856=CARTESIAN_POINT('Ctrl Pts',(63.7309291201476,1.07935865304851,-2.));
#24857=CARTESIAN_POINT('',(66.2714644419457,1.08121564890977,-2.));
#24858=CARTESIAN_POINT('Origin',(65.,0.,-2.));
#24859=CARTESIAN_POINT('Ctrl Pts',(66.2714656498818,1.0812165860621,-2.));
#24860=CARTESIAN_POINT('Ctrl Pts',(65.9206041791687,1.49275399655515,-1.96367708181445));
#24861=CARTESIAN_POINT('Ctrl Pts',(65.3506354631191,1.71875942899393,-1.92735416362889));
#24862=CARTESIAN_POINT('Ctrl Pts',(64.8132380266977,1.65815373977101,-1.89103124544334));
#24863=CARTESIAN_POINT('Ctrl Pts',(64.2651431372632,1.59634163148308,-1.85398528192066));
#24864=CARTESIAN_POINT('Ctrl Pts',(63.7509291640017,1.23639424886419,-1.81693931839798));
#24865=CARTESIAN_POINT('Ctrl Pts',(63.5055956276972,0.74259208529255,-1.7798933548753));
#24866=CARTESIAN_POINT('Ctrl Pts',(63.2602620913927,0.248789921720905,-1.74284739135262));
#24867=CARTESIAN_POINT('Ctrl Pts',(63.2838089920452,-0.378867022803494,
-1.70580142782994));
#24868=CARTESIAN_POINT('Ctrl Pts',(63.5656287203753,-0.852900276652179,
-1.66875546430726));
#24869=CARTESIAN_POINT('Ctrl Pts',(63.8474484487053,-1.32693353050086,-1.63170950078458));
#24870=CARTESIAN_POINT('Ctrl Pts',(64.387541004713,-1.64734309367383,-1.5946635372619));
#24871=CARTESIAN_POINT('Ctrl Pts',(64.9386444101885,-1.66760708582442,-1.55761757373922));
#24872=CARTESIAN_POINT('Ctrl Pts',(65.4897478156641,-1.68787107797502,-1.52057161021654));
#24873=CARTESIAN_POINT('Ctrl Pts',(66.0518620706076,-1.40798949910323,-1.48352564669385));
#24874=CARTESIAN_POINT('Ctrl Pts',(66.3677757854406,-0.955993240532984,
-1.44647968317117));
#24875=CARTESIAN_POINT('Ctrl Pts',(66.5609548232979,-0.679600674316361,
-1.42382633431738));
#24876=CARTESIAN_POINT('Ctrl Pts',(66.6620736349107,-0.338850343710036,
-1.40117298546359));
#24877=CARTESIAN_POINT('Ctrl Pts',(66.6638321395092,0.000941642735149761,
-1.3785196366098));
#24878=CARTESIAN_POINT('Origin',(65.,0.,-3.54592528053767));
#24879=CARTESIAN_POINT('',(67.0572086816557,0.00119446450309507,6.54592528053768));
#24880=CARTESIAN_POINT('',(67.0515888779951,-0.000804696401304116,6.60407471946233));
#24881=CARTESIAN_POINT('',(67.05475,1.03216492799367E-13,-3.54592528053767));
#24882=CARTESIAN_POINT('',(63.1173724903363,-0.82323218010314,7.));
#24883=CARTESIAN_POINT('Ctrl Pts',(67.0515888779951,-0.000804696401304414,
6.60407471946233));
#24884=CARTESIAN_POINT('Ctrl Pts',(67.0504040800969,0.384787351067748,6.62491192240684));
#24885=CARTESIAN_POINT('Ctrl Pts',(66.7605424545076,1.45760454425864,6.68279508887404));
#24886=CARTESIAN_POINT('Ctrl Pts',(65.029841359516,2.42994159679627,6.77772421886392));
#24887=CARTESIAN_POINT('Ctrl Pts',(62.9747815436376,1.33872801408516,6.88886210943195));
#24888=CARTESIAN_POINT('Ctrl Pts',(62.8436282049399,-0.197213743559581,
6.96295403647732));
#24889=CARTESIAN_POINT('Ctrl Pts',(63.1173724903363,-0.82323218010314,7.));
#24890=CARTESIAN_POINT('',(63.7764000215903,-1.65534094402445,7.));
#24891=CARTESIAN_POINT('Origin',(65.,0.,7.));
#24892=CARTESIAN_POINT('Ctrl Pts',(67.0572086816557,0.00119446450309495,
6.54592528053768));
#24893=CARTESIAN_POINT('Ctrl Pts',(67.0577114364342,0.0728343130723821,
6.54982271160486));
#24894=CARTESIAN_POINT('Ctrl Pts',(67.0218209037147,0.824923083408356,6.59076610619472));
#24895=CARTESIAN_POINT('Ctrl Pts',(66.0963109962835,2.16731896239629,6.66875546430726));
#24896=CARTESIAN_POINT('Ctrl Pts',(63.7734206371606,2.09605634078856,6.77989335487529));
#24897=CARTESIAN_POINT('Ctrl Pts',(62.5820931272045,0.120092092488812,6.89030820010622));
#24898=CARTESIAN_POINT('Ctrl Pts',(63.2405356955179,-1.25818726815371,6.96367708181445));
#24899=CARTESIAN_POINT('Ctrl Pts',(63.7763989699203,-1.65534250909262,7.));
#24900=CARTESIAN_POINT('Origin',(65.,0.,-3.54592528053767));
#24901=CARTESIAN_POINT('',(67.0519117333221,0.00102649957301762,5.84592528053768));
#24902=CARTESIAN_POINT('',(67.0566574869574,-0.00149765431883365,5.90407471946233));
#24903=CARTESIAN_POINT('',(67.05475,1.03216492799367E-13,-3.54592528053767));
#24904=CARTESIAN_POINT('Ctrl Pts',(67.0566574869574,-0.00149765431883376,
5.90407471946233));
#24905=CARTESIAN_POINT('Ctrl Pts',(67.0518463029865,0.585190437662473,5.93596947460409));
#24906=CARTESIAN_POINT('Ctrl Pts',(66.4813711624858,1.86148826198051,6.00491019326854));
#24907=CARTESIAN_POINT('Ctrl Pts',(64.3156972041947,2.33026144716285,6.11089687545566));
#24908=CARTESIAN_POINT('Ctrl Pts',(62.6710926659578,0.688814355154883,6.22203476602371));
#24909=CARTESIAN_POINT('Ctrl Pts',(63.1582101680956,-1.58293676398101,6.33317265659174));
#24910=CARTESIAN_POINT('Ctrl Pts',(65.3310466291073,-2.4061540266853,6.4443105471598));
#24911=CARTESIAN_POINT('Ctrl Pts',(66.8504470921567,-1.28501547118086,6.53461123478332));
#24912=CARTESIAN_POINT('Ctrl Pts',(67.0525105038734,-0.300747505180004,
6.58786595888416));
#24913=CARTESIAN_POINT('Ctrl Pts',(67.0515888779951,-0.000804696401304414,
6.60407471946233));
#24914=CARTESIAN_POINT('Ctrl Pts',(67.0519117333221,0.00102649957301758,
5.84592528053768));
#24915=CARTESIAN_POINT('Ctrl Pts',(67.0531633450758,0.277741730134882,5.86088026380211));
#24916=CARTESIAN_POINT('Ctrl Pts',(66.8721481216246,1.23835695251561,5.91288121058921));
#24917=CARTESIAN_POINT('Ctrl Pts',(65.4121253417219,2.39341760299657,6.001928120899));
#24918=CARTESIAN_POINT('Ctrl Pts',(63.2126643336617,1.64429852840487,6.11306601146706));
#24919=CARTESIAN_POINT('Ctrl Pts',(62.649189925264,-0.609850285121809,6.22420390203508));
#24920=CARTESIAN_POINT('Ctrl Pts',(64.2374031554985,-2.30582648807954,6.33534179260314));
#24921=CARTESIAN_POINT('Ctrl Pts',(66.4435230617629,-1.90573437919648,6.44258225210399));
#24922=CARTESIAN_POINT('Ctrl Pts',(67.0529326385894,-0.608118645715823,
6.51277674808218));
#24923=CARTESIAN_POINT('Ctrl Pts',(67.0572086816557,0.00119446450309495,
6.54592528053768));
#24924=CARTESIAN_POINT('Origin',(65.,0.,-3.54592528053767));
#24925=CARTESIAN_POINT('',(67.0534842785189,-0.00176526399347135,5.14592528053768));
#24926=CARTESIAN_POINT('',(67.0562728194261,0.00163389830066306,5.20407471946232));
#24927=CARTESIAN_POINT('',(67.05475,1.03216492799367E-13,-3.54592528053767));
#24928=CARTESIAN_POINT('Ctrl Pts',(67.0562728194261,0.00163389830066316,
5.20407471946232));
#24929=CARTESIAN_POINT('Ctrl Pts',(67.0572175303294,0.110331419494773,5.20998106327866));
#24930=CARTESIAN_POINT('Ctrl Pts',(66.9999469228229,0.899807785912472,5.25293337061767));
#24931=CARTESIAN_POINT('Ctrl Pts',(65.9773779060574,2.22328871643559,5.33293164147938));
#24932=CARTESIAN_POINT('Ctrl Pts',(63.6621652804381,2.02693883635741,5.44406953204741));
#24933=CARTESIAN_POINT('Ctrl Pts',(62.5714875417724,-0.0246926647779473,
5.55520742261546));
#24934=CARTESIAN_POINT('Ctrl Pts',(63.7036555936518,-2.05371969901983,5.66634531318349));
#24935=CARTESIAN_POINT('Ctrl Pts',(66.0223808123334,-2.20295969802021,5.77748320375154));
#24936=CARTESIAN_POINT('Ctrl Pts',(67.0084336557534,-0.871640043874865,
5.85672633917782));
#24937=CARTESIAN_POINT('Ctrl Pts',(67.0574345241562,-0.0962515598736413,
5.89892351108141));
#24938=CARTESIAN_POINT('Ctrl Pts',(67.0566574869574,-0.00149765431883376,
5.90407471946233));
#24939=CARTESIAN_POINT('Ctrl Pts',(67.0534842785189,-0.00176526399347133,
5.14592528053768));
#24940=CARTESIAN_POINT('Ctrl Pts',(67.049548506192,0.478623619806713,5.17193781599936));
#24941=CARTESIAN_POINT('Ctrl Pts',(66.641865899552,1.64918033378071,5.23499631498372));
#24942=CARTESIAN_POINT('Ctrl Pts',(64.6918158067503,2.4090050242139,5.33510077749075));
#24943=CARTESIAN_POINT('Ctrl Pts',(62.8089171959401,1.04758718972752,5.4462386680588));
#24944=CARTESIAN_POINT('Ctrl Pts',(62.931541830362,-1.27269881881276,5.55737655862684));
#24945=CARTESIAN_POINT('Ctrl Pts',(64.9474490817621,-2.42806968006158,5.66851444919488));
#24946=CARTESIAN_POINT('Ctrl Pts',(66.7337199477999,-1.50458731301855,5.7646973564985));
#24947=CARTESIAN_POINT('Ctrl Pts',(67.0500628960447,-0.407727598469997,
5.82383430027943));
#24948=CARTESIAN_POINT('Ctrl Pts',(67.0519117333221,0.00102649957301758,
5.84592528053768));
#24949=CARTESIAN_POINT('Origin',(65.,0.,-3.54592528053767));
#24950=CARTESIAN_POINT('',(67.0581446603105,8.27717201815131E-6,4.44592528053768));
#24951=CARTESIAN_POINT('',(67.051502599911,0.000468972833328433,4.50407471946232));
#24952=CARTESIAN_POINT('',(67.05475,1.03216492799367E-13,-3.54592528053767));
#24953=CARTESIAN_POINT('Ctrl Pts',(67.051502599911,0.000468972833328023,
4.50407471946232));
#24954=CARTESIAN_POINT('Ctrl Pts',(67.0521436877867,0.314512114650352,4.52103861547591));
#24955=CARTESIAN_POINT('Ctrl Pts',(66.8367516776872,1.31353269400003,4.57504847501217));
#24956=CARTESIAN_POINT('Ctrl Pts',(65.2821091229946,2.41219729396229,4.66610429807113));
#24957=CARTESIAN_POINT('Ctrl Pts',(63.1263775009061,1.54525729464231,4.77724218863916));
#24958=CARTESIAN_POINT('Ctrl Pts',(62.6855937936814,-0.736074256717675,
4.88838007920721));
#24959=CARTESIAN_POINT('Ctrl Pts',(64.3632123478174,-2.3436686423048,4.99951796977525));
#24960=CARTESIAN_POINT('Ctrl Pts',(66.5035583733625,-1.83464658396606,5.10474951652696));
#24961=CARTESIAN_POINT('Ctrl Pts',(67.0512920835974,-0.571444740237977,
5.17293509975598));
#24962=CARTESIAN_POINT('Ctrl Pts',(67.0562728194261,0.00163389830066316,
5.20407471946232));
#24963=CARTESIAN_POINT('Ctrl Pts',(67.0581446431809,8.27713025121955E-6,
4.44592528053768));
#24964=CARTESIAN_POINT('Ctrl Pts',(67.0581446696346,0.000451184114013542,
4.44594940467392));
#24965=CARTESIAN_POINT('Ctrl Pts',(67.0579439709526,0.681039286739863,4.48301949233285));
#24966=CARTESIAN_POINT('Ctrl Pts',(66.3158322777071,2.04129075981349,4.55713554351446));
#24967=CARTESIAN_POINT('Ctrl Pts',(63.9986308592856,2.21258726309085,4.66827343408251));
#24968=CARTESIAN_POINT('Ctrl Pts',(62.5979939690176,0.358677549762036,4.77941132465055));
#24969=CARTESIAN_POINT('Ctrl Pts',(63.3959404447162,-1.82353378810157,4.89054921521859));
#24970=CARTESIAN_POINT('Ctrl Pts',(65.6621008123707,-2.33664397819607,5.00168710578663));
#24971=CARTESIAN_POINT('Ctrl Pts',(66.9336682838985,-1.09149041292419,5.08681246089299));
#24972=CARTESIAN_POINT('Ctrl Pts',(67.0551536682982,-0.205526108395694,
5.13489185247667));
#24973=CARTESIAN_POINT('Ctrl Pts',(67.0534842785189,-0.00176526399347133,
5.14592528053768));
#24974=CARTESIAN_POINT('Origin',(65.,0.,-3.54592528053767));
#24975=CARTESIAN_POINT('',(67.0534601308484,0.00176006036930576,3.74592528053768));
#24976=CARTESIAN_POINT('',(67.0545529589347,-0.00187890219045319,3.80407471946232));
#24977=CARTESIAN_POINT('',(67.05475,1.03216492799367E-13,-3.54592528053767));
#24978=CARTESIAN_POINT('Ctrl Pts',(67.0545529589347,-0.00187890219045316,
3.80407471946232));
#24979=CARTESIAN_POINT('Ctrl Pts',(67.049847975054,0.514925815374004,3.83209616767316));
#24980=CARTESIAN_POINT('Ctrl Pts',(66.5901947888396,1.72243254492319,3.89716357940667));
#24981=CARTESIAN_POINT('Ctrl Pts',(64.5620129419189,2.3888174265201,3.99927695466288));
#24982=CARTESIAN_POINT('Ctrl Pts',(62.7554801641395,0.927583994626953,4.11041484523091));
#24983=CARTESIAN_POINT('Ctrl Pts',(63.0033818465923,-1.38267758750649,4.22155273579896));
#24984=CARTESIAN_POINT('Ctrl Pts',(65.0788107682801,-2.42735869229696,4.33269062636699));
#24985=CARTESIAN_POINT('Ctrl Pts',(66.7763241812549,-1.4299225698547,4.42686462092146));
#24986=CARTESIAN_POINT('Ctrl Pts',(67.0507436722455,-0.371299138082136,
4.48399265195323));
#24987=CARTESIAN_POINT('Ctrl Pts',(67.051502599911,0.000468972833328023,
4.50407471946232));
#24988=CARTESIAN_POINT('Ctrl Pts',(67.0534601308484,0.00176006036930547,
3.74592528053768));
#24989=CARTESIAN_POINT('Ctrl Pts',(67.055130441991,0.206418025502595,3.75700695687117));
#24990=CARTESIAN_POINT('Ctrl Pts',(66.9329701809384,1.09329696547217,3.80513459672735));
#24991=CARTESIAN_POINT('Ctrl Pts',(65.6590644304509,2.33750221987791,3.89030820010621));
#24992=CARTESIAN_POINT('Ctrl Pts',(63.39357261301,1.82144821550899,4.00144609067426));
#24993=CARTESIAN_POINT('Ctrl Pts',(62.5984620009619,-0.361797997181331,
4.1125839812423));
#24994=CARTESIAN_POINT('Ctrl Pts',(64.0015063548152,-2.21388639990766,4.22372187181034));
#24995=CARTESIAN_POINT('Ctrl Pts',(66.3179803312342,-2.0396173096854,4.33483563824213));
#24996=CARTESIAN_POINT('Ctrl Pts',(67.0581040462783,-0.679694036228919,
4.40890344115124));
#24997=CARTESIAN_POINT('Ctrl Pts',(67.0581446431809,8.27713025121955E-6,
4.44592528053768));
#24998=CARTESIAN_POINT('Origin',(65.,0.,-3.54592528053767));
#24999=CARTESIAN_POINT('',(67.0519256006226,-0.00103910123988304,3.04592528053768));
#25000=CARTESIAN_POINT('',(67.0578709601416,0.000678769155110521,3.10407471946232));
#25001=CARTESIAN_POINT('',(67.05475,1.03216492799367E-13,-3.54592528053767));
#25002=CARTESIAN_POINT('Ctrl Pts',(67.0578709601415,0.000678769155110595,
3.10407471946232));
#25003=CARTESIAN_POINT('Ctrl Pts',(67.0580316799421,0.0380175835266752,
3.10610775634773));
#25004=CARTESIAN_POINT('Ctrl Pts',(67.0401889053665,0.755586934309662,3.14518675675581));
#25005=CARTESIAN_POINT('Ctrl Pts',(66.2035357618251,2.10945088366341,3.22131172068658));
#25006=CARTESIAN_POINT('Ctrl Pts',(63.8804623217255,2.15520689204012,3.33244961125462));
#25007=CARTESIAN_POINT('Ctrl Pts',(62.5821144149725,0.228277590427784,3.44358750182266));
#25008=CARTESIAN_POINT('Ctrl Pts',(63.4968846048806,-1.90759677855456,3.55472539239071));
#25009=CARTESIAN_POINT('Ctrl Pts',(65.7874733624335,-2.29742618249227,3.66586328295874));
#25010=CARTESIAN_POINT('Ctrl Pts',(66.9614802130625,-1.01630569367123,3.74897972531595));
#25011=CARTESIAN_POINT('Ctrl Pts',(67.0560682339038,-0.168319696106675,
3.79505020415048));
#25012=CARTESIAN_POINT('Ctrl Pts',(67.0545529589347,-0.00187890219045316,
3.80407471946232));
#25013=CARTESIAN_POINT('Ctrl Pts',(67.0519256006226,-0.00103910123988287,
3.04592528053768));
#25014=CARTESIAN_POINT('Ctrl Pts',(67.0500496331103,0.408601099978646,3.06806450906842));
#25015=CARTESIAN_POINT('Ctrl Pts',(66.7326598083642,1.50637690262578,3.12724970112185));
#25016=CARTESIAN_POINT('Ctrl Pts',(64.9442948490232,2.42799907075925,3.22348085669796));
#25017=CARTESIAN_POINT('Ctrl Pts',(62.9298898830713,1.27001049414665,3.334618747266));
#25018=CARTESIAN_POINT('Ctrl Pts',(62.8102801837889,-1.05043309065764,3.44575663783405));
#25019=CARTESIAN_POINT('Ctrl Pts',(64.6949458653977,-2.40940335486022,3.55689452840209));
#25020=CARTESIAN_POINT('Ctrl Pts',(66.643067780423,-1.64741324066796,3.65695074263663));
#25021=CARTESIAN_POINT('Ctrl Pts',(67.0495466039689,-0.47775206598754,3.71996099334849));
#25022=CARTESIAN_POINT('Ctrl Pts',(67.0534601308484,0.00176006036930547,
3.74592528053768));
#25023=CARTESIAN_POINT('Origin',(65.,0.,-3.54592528053767));
#25024=CARTESIAN_POINT('',(67.0572522603608,-0.00120217803179352,2.34592528053767));
#25025=CARTESIAN_POINT('',(67.0525490214284,0.00145097609281634,2.40407471946232));
#25026=CARTESIAN_POINT('',(67.05475,1.03216492799367E-13,-3.54592528053767));
#25027=CARTESIAN_POINT('Ctrl Pts',(67.0525490214284,0.00145097609281618,
2.40407471946232));
#25028=CARTESIAN_POINT('Ctrl Pts',(67.054127131265,0.243480442393218,2.41716530854498));
#25029=CARTESIAN_POINT('Ctrl Pts',(66.9026176062656,1.16853384943059,2.46730186115031));
#25030=CARTESIAN_POINT('Ctrl Pts',(65.5317127142361,2.36971790517293,2.55448437727833));
#25031=CARTESIAN_POINT('Ctrl Pts',(63.2974379205056,1.7319248615472,2.66562226784637));
#25032=CARTESIAN_POINT('Ctrl Pts',(62.6215375065036,-0.491118649216439,
2.77676015841441));
#25033=CARTESIAN_POINT('Ctrl Pts',(64.122670786398,-2.2646356906881,2.88789804898245));
#25034=CARTESIAN_POINT('Ctrl Pts',(66.3846835747723,-1.97078161673766,2.99700290266509));
#25035=CARTESIAN_POINT('Ctrl Pts',(67.0551030464715,-0.642369656429112,
3.06906179282505));
#25036=CARTESIAN_POINT('Ctrl Pts',(67.0578709601415,0.000678769155110595,
3.10407471946232));
#25037=CARTESIAN_POINT('Ctrl Pts',(67.0572522603608,-0.00120217803179366,
2.34592528053767));
#25038=CARTESIAN_POINT('Ctrl Pts',(67.0530108672503,0.608976283722048,2.37912206126567));
#25039=CARTESIAN_POINT('Ctrl Pts',(66.4420019119215,1.9074607758001,2.44936480551635));
#25040=CARTESIAN_POINT('Ctrl Pts',(64.234427664365,2.30481703186258,2.55665351328971));
#25041=CARTESIAN_POINT('Ctrl Pts',(62.6483896081628,0.606804018161656,2.66779140385776));
#25042=CARTESIAN_POINT('Ctrl Pts',(63.214807212685,-1.64662359498827,2.77892929442579));
#25043=CARTESIAN_POINT('Ctrl Pts',(65.4152320208998,-2.39287795766375,2.89006718499384));
#25044=CARTESIAN_POINT('Ctrl Pts',(66.8729657074861,-1.23655088859839,2.97906584703113));
#25045=CARTESIAN_POINT('Ctrl Pts',(67.0531887228005,-0.276857109673458,
3.03101854554574));
#25046=CARTESIAN_POINT('Ctrl Pts',(67.0519256006226,-0.00103910123988287,
3.04592528053768));
#25047=CARTESIAN_POINT('Origin',(65.,0.,-3.54592528053767));
#25048=CARTESIAN_POINT('',(67.0555677501283,0.00179912738464932,1.64592528053767));
#25049=CARTESIAN_POINT('',(67.0526273462695,-0.00148795516933082,1.70407471946232));
#25050=CARTESIAN_POINT('',(67.05475,1.03216492799367E-13,-3.54592528053767));
#25051=CARTESIAN_POINT('Ctrl Pts',(67.0526273462695,-0.00148795516933075,
1.70407471946232));
#25052=CARTESIAN_POINT('Ctrl Pts',(67.049634688556,0.444939705966117,1.72822286074222));
#25053=CARTESIAN_POINT('Ctrl Pts',(66.6869954305654,1.58066428073723,1.78941696554481));
#25054=CARTESIAN_POINT('Ctrl Pts',(64.8130956691436,2.42143513885567,1.88765703387008));
#25055=CARTESIAN_POINT('Ctrl Pts',(62.864249480632,1.15622276382909,1.99879492443812));
#25056=CARTESIAN_POINT('Ctrl Pts',(62.8702799635561,-1.16729341938809,2.10993281500616));
#25057=CARTESIAN_POINT('Ctrl Pts',(64.8256673485052,-2.42237269783168,2.2210707055742));
#25058=CARTESIAN_POINT('Ctrl Pts',(66.6915092429239,-1.57355497286027,2.31911800705959));
#25059=CARTESIAN_POINT('Ctrl Pts',(67.0496611290802,-0.441455485498565,
2.3801193450223));
#25060=CARTESIAN_POINT('Ctrl Pts',(67.0525490214284,0.00145097609281618,
2.40407471946232));
#25061=CARTESIAN_POINT('Ctrl Pts',(67.0555677501283,0.00179912738464925,
1.64592528053767));
#25062=CARTESIAN_POINT('Ctrl Pts',(67.0567846151392,0.134576239702318,1.65313364994024));
#25063=CARTESIAN_POINT('Ctrl Pts',(66.9845642825309,0.948416460674401,1.69738798286549));
#25064=CARTESIAN_POINT('Ctrl Pts',(65.898842928637,2.25618349012117,1.77868827931342));
#25065=CARTESIAN_POINT('Ctrl Pts',(63.5919355659201,1.97879688218179,1.88982616988146));
#25066=CARTESIAN_POINT('Ctrl Pts',(62.5738455482538,-0.109804953100732,
2.0009640604495));
#25067=CARTESIAN_POINT('Ctrl Pts',(63.7764422147334,-2.09790106953769,2.11210195101754));
#25068=CARTESIAN_POINT('Ctrl Pts',(66.0989751981566,-2.1657645452103,2.22323984158559));
#25069=CARTESIAN_POINT('Ctrl Pts',(67.0223280499568,-0.823134106038537,
2.30118095142563));
#25070=CARTESIAN_POINT('Ctrl Pts',(67.0577440519451,-0.0719526660358301,
2.34207609774299));
#25071=CARTESIAN_POINT('Ctrl Pts',(67.0572522603608,-0.00120217803179366,
2.34592528053767));
#25072=CARTESIAN_POINT('Origin',(65.,0.,-3.54592528053767));
#25073=CARTESIAN_POINT('',(67.0514068858608,7.8101351718568E-5,0.945925280537675));
#25074=CARTESIAN_POINT('',(67.0579182146741,-0.000617375283490038,1.00407471946232));
#25075=CARTESIAN_POINT('',(67.05475,1.03216492799367E-13,-3.54592528053767));
#25076=CARTESIAN_POINT('Ctrl Pts',(67.0579182146741,-0.000617375283489987,
1.00407471946232));
#25077=CARTESIAN_POINT('Ctrl Pts',(67.0553588641481,0.645931829998614,1.03928041293948));
#25078=CARTESIAN_POINT('Ctrl Pts',(66.378434179731,1.97744423729901,1.11153206993931));
#25079=CARTESIAN_POINT('Ctrl Pts',(64.1109273576576,2.26005114925193,1.22082969046183));
#25080=CARTESIAN_POINT('Ctrl Pts',(62.6190202559434,0.478765933382519,1.33196758102987));
#25081=CARTESIAN_POINT('Ctrl Pts',(63.3064509161112,-1.74073917087913,1.44310547159791));
#25082=CARTESIAN_POINT('Ctrl Pts',(65.5440062589152,-2.36692597071416,1.55424336216595));
#25083=CARTESIAN_POINT('Ctrl Pts',(66.9056402449312,-1.16131362127399,1.64123311145409));
#25084=CARTESIAN_POINT('Ctrl Pts',(67.0542257619312,-0.239930514819838,
1.69117689721954));
#25085=CARTESIAN_POINT('Ctrl Pts',(67.0526273462695,-0.00148795516933075,
1.70407471946232));
#25086=CARTESIAN_POINT('Ctrl Pts',(67.0514068858608,7.81013517185333E-5,
0.945925280537675));
#25087=CARTESIAN_POINT('Ctrl Pts',(67.0515215449353,0.33826440094154,0.964191202137492));
#25088=CARTESIAN_POINT('Ctrl Pts',(66.8123460743743,1.36218935655875,1.01950308725999));
#25089=CARTESIAN_POINT('Ctrl Pts',(65.1973793755662,2.42060404314488,1.11186093590517));
#25090=CARTESIAN_POINT('Ctrl Pts',(63.0733618200821,1.47863040518407,1.22299882647321));
#25091=CARTESIAN_POINT('Ctrl Pts',(62.7128180402749,-0.816750411403602,
1.33413671704125));
#25092=CARTESIAN_POINT('Ctrl Pts',(64.4457578465939,-2.36455031387796,1.4452746076093));
#25093=CARTESIAN_POINT('Ctrl Pts',(66.5407002488233,-1.7880364866664,1.54920412877477));
#25094=CARTESIAN_POINT('Ctrl Pts',(67.0505307823665,-0.547805001444293,
1.61608768641756));
#25095=CARTESIAN_POINT('Ctrl Pts',(67.0555677501283,0.00179912738464925,
1.64592528053767));
#25096=CARTESIAN_POINT('Origin',(65.,0.,-3.54592528053767));
#25097=CARTESIAN_POINT('',(67.05528106155,-0.00183967754518108,0.245925280537674));
#25098=CARTESIAN_POINT('',(67.0544463703074,0.00187701683783275,0.304074719462319));
#25099=CARTESIAN_POINT('',(67.05475,1.03216492799367E-13,-3.54592528053767));
#25100=CARTESIAN_POINT('Ctrl Pts',(67.0544463703074,0.00187701683783252,
0.304074719462319));
#25101=CARTESIAN_POINT('Ctrl Pts',(67.0559854674868,0.17189554728647,0.313292001614044));
#25102=CARTESIAN_POINT('Ctrl Pts',(66.9589165461202,1.02351658402418,0.359555247288449));
#25103=CARTESIAN_POINT('Ctrl Pts',(65.7755372964953,2.301482839391,0.442864456485536));
#25104=CARTESIAN_POINT('Ctrl Pts',(63.4870029209119,1.89976872281362,0.554002347053577));
#25105=CARTESIAN_POINT('Ctrl Pts',(62.5833319303427,-0.24082525149545,0.665140237621619));
#25106=CARTESIAN_POINT('Ctrl Pts',(63.8916646308255,-2.16098914151125,0.77627812818966));
#25107=CARTESIAN_POINT('Ctrl Pts',(66.2144692640843,-2.1031751632491,0.887416018757702));
#25108=CARTESIAN_POINT('Ctrl Pts',(67.0419827284221,-0.748425825038277,
0.963348215848589));
#25109=CARTESIAN_POINT('Ctrl Pts',(67.058051996902,-0.0344137592749356,
1.0022344494168));
#25110=CARTESIAN_POINT('Ctrl Pts',(67.0579182146741,-0.000617375283489987,
1.00407471946232));
#25111=CARTESIAN_POINT('Ctrl Pts',(67.05528106155,-0.00183967754518099,
0.245925280537674));
#25112=CARTESIAN_POINT('Ctrl Pts',(67.0502944995635,0.538488282262984,0.275248754334741));
#25113=CARTESIAN_POINT('Ctrl Pts',(66.5549829233901,1.76953115899708,0.341618191654489));
#25114=CARTESIAN_POINT('Ctrl Pts',(64.4785452214709,2.37199651591817,0.445033592496919));
#25115=CARTESIAN_POINT('Ctrl Pts',(62.7243441135659,0.848335334231218,0.55617148306496));
#25116=CARTESIAN_POINT('Ctrl Pts',(63.0530766482751,-1.45181679686653,0.667309373633002));
#25117=CARTESIAN_POINT('Ctrl Pts',(65.1638502053818,-2.42310455048396,0.778447264201043));
#25118=CARTESIAN_POINT('Ctrl Pts',(66.8023851755325,-1.38138173267994,0.871319233169269));
#25119=CARTESIAN_POINT('Ctrl Pts',(67.0512889995436,-0.347626932272121,
0.927145238614812));
#25120=CARTESIAN_POINT('Ctrl Pts',(67.0514068858608,7.81013517185333E-5,
0.945925280537675));
#25121=CARTESIAN_POINT('Origin',(65.,0.,-3.54592528053767));
#25122=CARTESIAN_POINT('',(67.0574561899986,0.00106563322408104,-0.454074719462326));
#25123=CARTESIAN_POINT('',(67.0515283628764,-0.00052555615327251,-0.39592528053768));
#25124=CARTESIAN_POINT('',(67.05475,1.03216492799367E-13,-3.54592528053767));
#25125=CARTESIAN_POINT('Ctrl Pts',(67.0515283628764,-0.000525556153272815,
-0.39592528053768));
#25126=CARTESIAN_POINT('Ctrl Pts',(67.0506691385159,0.374799386930355,-0.375650446188706));
#25127=CARTESIAN_POINT('Ctrl Pts',(66.7723630529996,1.43710026477805,-0.318329648317051));
#25128=CARTESIAN_POINT('Ctrl Pts',(65.0662097961853,2.42773505180943,-0.223962886922715));
#25129=CARTESIAN_POINT('Ctrl Pts',(62.9962315570428,1.3722949487109,-0.112824996354674));
#25130=CARTESIAN_POINT('Ctrl Pts',(62.7603252963136,-0.939222336522784,
-0.00168710578663132));
#25131=CARTESIAN_POINT('Ctrl Pts',(64.5744186923722,-2.39105873890072,0.10945078478141));
#25132=CARTESIAN_POINT('Ctrl Pts',(66.5952919861857,-1.71543281453754,0.211371393197727));
#25133=CARTESIAN_POINT('Ctrl Pts',(67.0497995509631,-0.511440405058377,
0.276246038091363));
#25134=CARTESIAN_POINT('Ctrl Pts',(67.0544463703074,0.00187701683783252,
0.304074719462319));
#25135=CARTESIAN_POINT('Ctrl Pts',(67.0574561899986,0.00106563322408115,
-0.454074719462326));
#25136=CARTESIAN_POINT('Ctrl Pts',(67.057843018648,0.0623502628450632,-0.450739656990689));
#25137=CARTESIAN_POINT('Ctrl Pts',(67.0275621697751,0.8039986152436,-0.410358630996372));
#25138=CARTESIAN_POINT('Ctrl Pts',(66.1288520704621,2.15034287637184,-0.332931641479373));
#25139=CARTESIAN_POINT('Ctrl Pts',(63.8056023683761,2.11463875683278,-0.221793750911332));
#25140=CARTESIAN_POINT('Ctrl Pts',(62.5755981242121,0.143381478345983,-0.110655860343291));
#25141=CARTESIAN_POINT('Ctrl Pts',(63.5646765331008,-1.95911432942998,0.00048203022475183));
#25142=CARTESIAN_POINT('Ctrl Pts',(65.8675227272721,-2.26841065672895,0.111619920792793));
#25143=CARTESIAN_POINT('Ctrl Pts',(66.9782240837151,-0.967625288007803,
0.193434337563767));
#25144=CARTESIAN_POINT('Ctrl Pts',(67.0565942986505,-0.144137863188426,
0.238202790812061));
#25145=CARTESIAN_POINT('Ctrl Pts',(67.05528106155,-0.00183967754518099,
0.245925280537674));
#25146=CARTESIAN_POINT('Origin',(65.,0.,-3.54592528053767));
#25147=CARTESIAN_POINT('',(67.0520762837074,0.00116136879359838,-1.15407471946233));
#25148=CARTESIAN_POINT('',(67.0563730581704,-0.00160407492545605,-1.09592528053768));
#25149=CARTESIAN_POINT('',(67.05475,1.03216492799367E-13,-3.54592528053767));
#25150=CARTESIAN_POINT('Ctrl Pts',(67.0563730581704,-0.00160407492545608,
-1.09592528053768));
#25151=CARTESIAN_POINT('Ctrl Pts',(67.051425463294,0.574948872440279,-1.06459289399146));
#25152=CARTESIAN_POINT('Ctrl Pts',(66.4979405147664,1.84151750410659,-0.99621454392255));
#25153=CARTESIAN_POINT('Ctrl Pts',(64.3510553719621,2.34032995360773,-0.890790230330967));
#25154=CARTESIAN_POINT('Ctrl Pts',(62.6818041989874,0.724051597351488,-0.779652339762924));
#25155=CARTESIAN_POINT('Ctrl Pts',(63.1344238327198,-1.55496249063293,-0.668514449194883));
#25156=CARTESIAN_POINT('Ctrl Pts',(65.2946265402067,-2.41070020734327,-0.55737655862684));
#25157=CARTESIAN_POINT('Ctrl Pts',(66.8402661138972,-1.30632380217904,-0.466513502407773));
#25158=CARTESIAN_POINT('Ctrl Pts',(67.0522391042067,-0.310990391240213,
-0.412696409711387));
#25159=CARTESIAN_POINT('Ctrl Pts',(67.0515283628764,-0.000525556153272815,
-0.39592528053768));
#25160=CARTESIAN_POINT('Ctrl Pts',(67.0520762837074,0.0011613687935982,
-1.15407471946233));
#25161=CARTESIAN_POINT('Ctrl Pts',(67.053454237916,0.267420438121936,-1.13968210479344));
#25162=CARTESIAN_POINT('Ctrl Pts',(66.8815877450925,1.2173135829094,-1.08824352660187));
#25163=CARTESIAN_POINT('Ctrl Pts',(65.4483108550045,2.38688976599863,-0.999758984887625));
#25164=CARTESIAN_POINT('Ctrl Pts',(63.2377776981899,1.67118490708906,-0.888621094319582));
#25165=CARTESIAN_POINT('Ctrl Pts',(62.6402125087857,-0.574193448178934,
-0.777483203751542));
#25166=CARTESIAN_POINT('Ctrl Pts',(64.2025947176117,-2.29399639382145,-0.666345313183498));
#25167=CARTESIAN_POINT('Ctrl Pts',(66.4260607263055,-1.92548386768538,-0.558542485087094));
#25168=CARTESIAN_POINT('Ctrl Pts',(67.0535461156186,-0.61840104923623,-0.48778562051337));
#25169=CARTESIAN_POINT('Ctrl Pts',(67.0574561899986,0.00106563322408115,
-0.454074719462326));
#25170=CARTESIAN_POINT('Origin',(65.,0.,-3.54592528053767));
#25171=CARTESIAN_POINT('',(67.052679279082,-0.00238369513522838,-1.85407471946233));
#25172=CARTESIAN_POINT('',(67.0565599569794,0.00149374744778724,-1.79592528053768));
#25173=CARTESIAN_POINT('',(67.05475,1.03216492799367E-13,-3.54592528053767));
#25174=CARTESIAN_POINT('',(65.5301702171886,-1.98517432567172,-2.));
#25175=CARTESIAN_POINT('Ctrl Pts',(65.5301702171886,-1.98517432567172,-2.));
#25176=CARTESIAN_POINT('Ctrl Pts',(66.1902879097456,-1.80888011517988,-1.96295403647732));
#25177=CARTESIAN_POINT('Ctrl Pts',(66.9249664054372,-1.11286144556363,-1.91431227629809));
#25178=CARTESIAN_POINT('Ctrl Pts',(67.0542991139265,-0.216633244974144,
-1.86567051611887));
#25179=CARTESIAN_POINT('Ctrl Pts',(67.052679279082,-0.0023836951352286,
-1.85407471946232));
#25180=CARTESIAN_POINT('',(64.468704775017,-1.98873730573667,-2.));
#25181=CARTESIAN_POINT('Origin',(65.,0.,-2.));
#25182=CARTESIAN_POINT('Ctrl Pts',(64.4687042096542,-1.98873909628092,-2.));
#25183=CARTESIAN_POINT('Ctrl Pts',(65.1133181823237,-2.16007183004145,-1.96367708181445));
#25184=CARTESIAN_POINT('Ctrl Pts',(66.4930415100228,-1.84061483765584,-1.89565217532701));
#25185=CARTESIAN_POINT('Ctrl Pts',(67.051699865038,-0.581583302606355,-1.82762726883957));
#25186=CARTESIAN_POINT('Ctrl Pts',(67.0565599569794,0.0014937474477871,
-1.79592528053768));
#25187=CARTESIAN_POINT('Origin',(32.5,56.2916512459885,17.));
#25188=CARTESIAN_POINT('',(31.6672724934037,54.8468960395935,13.8714803633902));
#25189=CARTESIAN_POINT('',(31.6651566506305,54.8475988206466,13.6785196366098));
#25190=CARTESIAN_POINT('',(31.667,54.8488529232836,17.));
#25191=CARTESIAN_POINT('',(31.9588970197441,54.7159724828016,13.));
#25192=CARTESIAN_POINT('Ctrl Pts',(31.6651566506305,54.8475988206466,13.6785196366098));
#25193=CARTESIAN_POINT('Ctrl Pts',(31.6146486514652,54.8762889946569,13.6746222055426));
#25194=CARTESIAN_POINT('Ctrl Pts',(31.5657632473174,54.9077117506004,13.6707247744754));
#25195=CARTESIAN_POINT('Ctrl Pts',(31.5188321868552,54.9418237568819,13.6668273434082));
#25196=CARTESIAN_POINT('Ctrl Pts',(31.0727418458088,55.2660660894878,13.6297813798856));
#25197=CARTESIAN_POINT('Ctrl Pts',(30.8032251342758,55.8332803703507,13.5927354163629));
#25198=CARTESIAN_POINT('Ctrl Pts',(30.8337540098497,56.3839156387153,13.5556894528402));
#25199=CARTESIAN_POINT('Ctrl Pts',(30.8642828854237,56.93455090708,13.5186434893175));
#25200=CARTESIAN_POINT('Ctrl Pts',(31.1948573481046,57.4686071629464,13.4815975257948));
#25201=CARTESIAN_POINT('Ctrl Pts',(31.6739356569701,57.7415946577538,13.4445515622722));
#25202=CARTESIAN_POINT('Ctrl Pts',(32.1530139658356,58.0145821525613,13.4075055987495));
#25203=CARTESIAN_POINT('Ctrl Pts',(32.7805961208856,58.0265008863098,13.3704596352268));
#25204=CARTESIAN_POINT('Ctrl Pts',(33.2699721109727,57.7720492096737,13.3334136717041));
#25205=CARTESIAN_POINT('Ctrl Pts',(33.7593481010598,57.5175975330377,13.2963677081814));
#25206=CARTESIAN_POINT('Ctrl Pts',(34.1105179261839,56.9967754460172,13.2593217446588));
#25207=CARTESIAN_POINT('Ctrl Pts',(34.1617369653364,56.4476202824107,13.2222757811361));
#25208=CARTESIAN_POINT('Ctrl Pts',(34.2129560044889,55.8984651188042,13.1852298176134));
#25209=CARTESIAN_POINT('Ctrl Pts',(33.9642242576698,55.3209768786118,13.1481838540907));
#25210=CARTESIAN_POINT('Ctrl Pts',(33.5316971804146,54.9803713160329,13.111137890568));
#25211=CARTESIAN_POINT('Ctrl Pts',(33.0991701031595,54.639765753454,13.0740919270454));
#25212=CARTESIAN_POINT('Ctrl Pts',(32.4828476954683,54.5360428684886,13.0370459635227));
#25213=CARTESIAN_POINT('Ctrl Pts',(31.9588970197441,54.7159724828016,13.));
#25214=CARTESIAN_POINT('',(31.0290140863628,57.0802261258961,13.));
#25215=CARTESIAN_POINT('Origin',(32.5,56.2916512459885,13.));
#25216=CARTESIAN_POINT('',(31.6688354432561,54.8507324474214,13.1714803633902));
#25217=CARTESIAN_POINT('Ctrl Pts',(31.0290124456509,57.0802271145804,13.));
#25218=CARTESIAN_POINT('Ctrl Pts',(30.774120583937,56.6032768580681,13.0363229181856));
#25219=CARTESIAN_POINT('Ctrl Pts',(30.7719333897513,55.9901147282721,13.0726458363711));
#25220=CARTESIAN_POINT('Ctrl Pts',(31.0246770579875,55.5119982833858,13.1089687545567));
#25221=CARTESIAN_POINT('Ctrl Pts',(31.1696673663398,55.2377194013227,13.1298059575012));
#25222=CARTESIAN_POINT('Ctrl Pts',(31.3985533923309,55.0078829792344,13.1506431604457));
#25223=CARTESIAN_POINT('Ctrl Pts',(31.6688354432561,54.8507324474214,13.1714803633902));
#25224=CARTESIAN_POINT('',(31.667,54.8488529232836,12.));
#25225=CARTESIAN_POINT('',(31.667,54.8488529232836,17.));
#25226=CARTESIAN_POINT('Origin',(32.5,56.2916512459885,12.));
#25227=CARTESIAN_POINT('Ctrl Pts',(31.6688354432561,54.8507324474214,13.1714803633902));
#25228=CARTESIAN_POINT('Ctrl Pts',(31.8790813703937,54.7284888165622,13.1876891239684));
#25229=CARTESIAN_POINT('Ctrl Pts',(32.1143756641562,54.6502267716398,13.2038978845465));
#25230=CARTESIAN_POINT('Ctrl Pts',(32.354714319885,54.6292400960994,13.2201066451247));
#25231=CARTESIAN_POINT('Ctrl Pts',(32.9040207909308,54.5812739599608,13.2571526086474));
#25232=CARTESIAN_POINT('Ctrl Pts',(33.4796777351052,54.8324998905166,13.2941985721701));
#25233=CARTESIAN_POINT('Ctrl Pts',(33.8179820369827,55.2680242179702,13.3312445356927));
#25234=CARTESIAN_POINT('Ctrl Pts',(34.1562863388601,55.7035485454237,13.3682904992154));
#25235=CARTESIAN_POINT('Ctrl Pts',(34.2572379984405,56.323371269775,13.4053364627381));
#25236=CARTESIAN_POINT('Ctrl Pts',(34.074760972003,56.8437863823056,13.4423824262608));
#25237=CARTESIAN_POINT('Ctrl Pts',(33.8922839455655,57.3642014948362,13.4794283897835));
#25238=CARTESIAN_POINT('Ctrl Pts',(33.4263782331101,57.7852089955461,13.5164743533061));
#25239=CARTESIAN_POINT('Ctrl Pts',(32.8902057561615,57.9141527098528,13.5535203168288));
#25240=CARTESIAN_POINT('Ctrl Pts',(32.3540332792128,58.0430964241595,13.5905662803515));
#25241=CARTESIAN_POINT('Ctrl Pts',(31.7475940377708,57.879976352063,13.6276122438742));
#25242=CARTESIAN_POINT('Ctrl Pts',(31.3484595971705,57.499435180452,13.6646582073969));
#25243=CARTESIAN_POINT('Ctrl Pts',(30.9493251565702,57.1188940088411,13.7017041709196));
#25244=CARTESIAN_POINT('Ctrl Pts',(30.7574955168115,56.5209317377157,13.7387501344422));
#25245=CARTESIAN_POINT('Ctrl Pts',(30.8607470097836,55.9792142563288,13.7757960979649));
#25246=CARTESIAN_POINT('Ctrl Pts',(30.9496414742062,55.5128221104133,13.8076908531067));
#25247=CARTESIAN_POINT('Ctrl Pts',(31.2572608237868,55.0881206516064,13.8395856082484));
#25248=CARTESIAN_POINT('Ctrl Pts',(31.6672724934037,54.8468960395935,13.8714803633902));
#25249=CARTESIAN_POINT('Origin',(32.5,56.2916512459885,17.));
#25250=CARTESIAN_POINT('',(31.6652293984911,54.8484357012869,14.5714803633902));
#25251=CARTESIAN_POINT('',(31.6674240358463,54.8512520230129,14.3785196366098));
#25252=CARTESIAN_POINT('',(31.667,54.8488529232836,17.));
#25253=CARTESIAN_POINT('Ctrl Pts',(31.6674240358463,54.8512520230129,14.3785196366098));
#25254=CARTESIAN_POINT('Ctrl Pts',(31.4726121759195,54.9625548712859,14.3635646533454));
#25255=CARTESIAN_POINT('Ctrl Pts',(31.2997293296831,55.1111079954895,14.3486096700809));
#25256=CARTESIAN_POINT('Ctrl Pts',(31.1659805795344,55.289072307877,14.3336546868165));
#25257=CARTESIAN_POINT('Ctrl Pts',(30.8346628353681,55.7299193023853,14.2966087232938));
#25258=CARTESIAN_POINT('Ctrl Pts',(30.7434854934753,56.3512435601479,14.2595627597711));
#25259=CARTESIAN_POINT('Ctrl Pts',(30.9341783443449,56.8686931008725,14.2225167962485));
#25260=CARTESIAN_POINT('Ctrl Pts',(31.1248711952145,57.386142641597,14.1854708327258));
#25261=CARTESIAN_POINT('Ctrl Pts',(31.5974342388466,57.7997174652835,14.1484248692031));
#25262=CARTESIAN_POINT('Ctrl Pts',(32.1355923903503,57.9201415291698,14.1113789056804));
#25263=CARTESIAN_POINT('Ctrl Pts',(32.6737505418539,58.0405655930561,14.0743329421577));
#25264=CARTESIAN_POINT('Ctrl Pts',(33.2775038012292,57.8678388971422,14.0372869786351));
#25265=CARTESIAN_POINT('Ctrl Pts',(33.6705489273999,57.4810131538507,14.0002410151124));
#25266=CARTESIAN_POINT('Ctrl Pts',(34.0635940535707,57.0941874105591,13.9631950515897));
#25267=CARTESIAN_POINT('Ctrl Pts',(34.2459310465369,56.4932626198898,13.926149088067));
#25268=CARTESIAN_POINT('Ctrl Pts',(34.1340966146064,55.9532506956148,13.8891031245443));
#25269=CARTESIAN_POINT('Ctrl Pts',(34.0222621826759,55.4132387713398,13.8520571610217));
#25270=CARTESIAN_POINT('Ctrl Pts',(33.6162563258486,54.934139713459,13.815011197499));
#25271=CARTESIAN_POINT('Ctrl Pts',(33.1019214121551,54.7352253766931,13.7779652339763));
#25272=CARTESIAN_POINT('Ctrl Pts',(32.6416972484852,54.5572378789698,13.7448167015208));
#25273=CARTESIAN_POINT('Ctrl Pts',(32.0947386036493,54.6035824036932,13.7116681690653));
#25274=CARTESIAN_POINT('Ctrl Pts',(31.6651566506305,54.8475988206466,13.6785196366098));
#25275=CARTESIAN_POINT('Ctrl Pts',(31.6672724934037,54.8468960395935,13.8714803633902));
#25276=CARTESIAN_POINT('Ctrl Pts',(31.7334920188215,54.8079367110906,13.8766315717711));
#25277=CARTESIAN_POINT('Ctrl Pts',(31.8023823793453,54.7737632532799,13.881782780152));
#25278=CARTESIAN_POINT('Ctrl Pts',(31.8734534906151,54.7449729811027,13.886933988533));
#25279=CARTESIAN_POINT('Ctrl Pts',(32.3845758527714,54.537921878912,13.9239799520556));
#25280=CARTESIAN_POINT('Ctrl Pts',(33.0084879513813,54.609292366179,13.9610259155783));
#25281=CARTESIAN_POINT('Ctrl Pts',(33.4596489857383,54.9264225988407,13.998071879101));
#25282=CARTESIAN_POINT('Ctrl Pts',(33.9108100200953,55.2435528315024,14.0351178426237));
#25283=CARTESIAN_POINT('Ctrl Pts',(34.1892199901994,55.8064428095589,14.0721638061464));
#25284=CARTESIAN_POINT('Ctrl Pts',(34.1674649383536,56.3574821112237,14.109209769669));
#25285=CARTESIAN_POINT('Ctrl Pts',(34.1457098865078,56.9085214128884,14.1462557331917));
#25286=CARTESIAN_POINT('Ctrl Pts',(33.8237898127121,57.4477100381615,14.1833016967144));
#25287=CARTESIAN_POINT('Ctrl Pts',(33.3490322930752,57.7282855707718,14.2203476602371));
#25288=CARTESIAN_POINT('Ctrl Pts',(32.8742747734382,58.0088611033821,14.2573936237598));
#25289=CARTESIAN_POINT('Ctrl Pts',(32.2466798079601,58.0308235433297,14.2944395872824));
#25290=CARTESIAN_POINT('Ctrl Pts',(31.7534702764192,57.7841214978257,14.3314855508051));
#25291=CARTESIAN_POINT('Ctrl Pts',(31.2602607448784,57.5374194523217,14.3685315143278));
#25292=CARTESIAN_POINT('Ctrl Pts',(30.9014366472749,57.022052921366,14.4055774778505));
#25293=CARTESIAN_POINT('Ctrl Pts',(30.8412156241946,56.4738823989159,14.4426234413732));
#25294=CARTESIAN_POINT('Ctrl Pts',(30.7809946011142,55.9257118764658,14.4796694048958));
#25295=CARTESIAN_POINT('Ctrl Pts',(31.019376652557,55.3447373625211,14.5167153684185));
#25296=CARTESIAN_POINT('Ctrl Pts',(31.4472650020351,54.9968450984029,14.5537613319412));
#25297=CARTESIAN_POINT('Ctrl Pts',(31.5154844642033,54.9413796406974,14.5596676757575));
#25298=CARTESIAN_POINT('Ctrl Pts',(31.5885209558805,54.8918388624727,14.5655740195739));
#25299=CARTESIAN_POINT('Ctrl Pts',(31.6652293984911,54.8484357012869,14.5714803633902));
#25300=CARTESIAN_POINT('Origin',(32.5,56.2916512459885,17.));
#25301=CARTESIAN_POINT('',(31.6679812524744,54.8513129979877,15.2714803633902));
#25302=CARTESIAN_POINT('',(31.6687468960361,54.8490160493388,15.0785196366098));
#25303=CARTESIAN_POINT('',(31.667,54.8488529232836,17.));
#25304=CARTESIAN_POINT('Ctrl Pts',(31.6687468960361,54.8490160493388,15.0785196366098));
#25305=CARTESIAN_POINT('Ctrl Pts',(31.3330220839914,55.0465316965332,15.0525071011481));
#25306=CARTESIAN_POINT('Ctrl Pts',(31.0621374285877,55.3603795470759,15.0264945656864));
#25307=CARTESIAN_POINT('Ctrl Pts',(30.930547953771,55.7245591059458,15.0004820302248));
#25308=CARTESIAN_POINT('Ctrl Pts',(30.7431437350931,56.2432083807723,14.9634360667021));
#25309=CARTESIAN_POINT('Ctrl Pts',(30.8382616710438,56.8639417522836,14.9263901031794));
#25310=CARTESIAN_POINT('Ctrl Pts',(31.1723705294372,57.3026770823852,14.8893441396567));
#25311=CARTESIAN_POINT('Ctrl Pts',(31.5064793878305,57.7414124124868,14.852298176134));
#25312=CARTESIAN_POINT('Ctrl Pts',(32.0795791686666,57.9981497011789,14.8152522126114));
#25313=CARTESIAN_POINT('Ctrl Pts',(32.6293874463964,57.9553916541296,14.7782062490887));
#25314=CARTESIAN_POINT('Ctrl Pts',(33.1791957241261,57.9126336070804,14.741160285566));
#25315=CARTESIAN_POINT('Ctrl Pts',(33.7057124987496,57.5703802242898,14.7041143220433));
#25316=CARTESIAN_POINT('Ctrl Pts',(33.9679745051883,57.0852657438482,14.6670683585206));
#25317=CARTESIAN_POINT('Ctrl Pts',(34.2302365116269,56.6001512634066,14.6300223949979));
#25318=CARTESIAN_POINT('Ctrl Pts',(34.2282437498807,55.972175685314,14.5929764314753));
#25319=CARTESIAN_POINT('Ctrl Pts',(33.9629079737486,55.4887355202075,14.5559304679526));
#25320=CARTESIAN_POINT('Ctrl Pts',(33.6975721976164,55.0052953551011,14.5188845044299));
#25321=CARTESIAN_POINT('Ctrl Pts',(33.1688934070983,54.6663906029808,14.4818385409072));
#25322=CARTESIAN_POINT('Ctrl Pts',(32.6188249386194,54.6271230925477,14.4447925773845));
#25323=CARTESIAN_POINT('Ctrl Pts',(32.2908120993686,54.6037073755496,14.4227015971263));
#25324=CARTESIAN_POINT('Ctrl Pts',(31.9551933282369,54.6868393332485,14.400610616868));
#25325=CARTESIAN_POINT('Ctrl Pts',(31.6674240358463,54.8512520230129,14.3785196366098));
#25326=CARTESIAN_POINT('Ctrl Pts',(31.6652293984911,54.8484357012869,14.5714803633902));
#25327=CARTESIAN_POINT('Ctrl Pts',(32.0696541670855,54.6196041304525,14.6026199830966));
#25328=CARTESIAN_POINT('Ctrl Pts',(32.5761460954187,54.5613764565911,14.6337596028029));
#25329=CARTESIAN_POINT('Ctrl Pts',(33.0168947227899,54.7049585292357,14.6648992225092));
#25330=CARTESIAN_POINT('Ctrl Pts',(33.5412414465535,54.8757742384787,14.7019451860319));
#25331=CARTESIAN_POINT('Ctrl Pts',(33.9725402465673,55.3322156712569,14.7389911495546));
#25332=CARTESIAN_POINT('Ctrl Pts',(34.1134048115911,55.8653898078431,14.7760371130773));
#25333=CARTESIAN_POINT('Ctrl Pts',(34.2542693766149,56.3985639444293,14.8130830766));
#25334=CARTESIAN_POINT('Ctrl Pts',(34.1046997066485,57.0084707848237,14.8501290401226));
#25335=CARTESIAN_POINT('Ctrl Pts',(33.7331471941746,57.415983010017,14.8871750036453));
#25336=CARTESIAN_POINT('Ctrl Pts',(33.3615946817007,57.8234952352103,14.924220967168));
#25337=CARTESIAN_POINT('Ctrl Pts',(32.7680593267191,58.0286128452026,14.9612669306907));
#25338=CARTESIAN_POINT('Ctrl Pts',(32.2241759575529,57.9374626002348,14.9983128942134));
#25339=CARTESIAN_POINT('Ctrl Pts',(31.6802925883866,57.8463123552671,15.0353588577361));
#25340=CARTESIAN_POINT('Ctrl Pts',(31.1860612050356,57.4588942553394,15.0724048212587));
#25341=CARTESIAN_POINT('Ctrl Pts',(30.9676695988056,56.9525123919175,15.1094507847814));
#25342=CARTESIAN_POINT('Ctrl Pts',(30.7492779925756,56.4461305284957,15.1464967483041));
#25343=CARTESIAN_POINT('Ctrl Pts',(30.8067261634667,55.8207849015799,15.1835427118268));
#25344=CARTESIAN_POINT('Ctrl Pts',(31.1137226321993,55.3626684826674,15.2205886753495));
#25345=CARTESIAN_POINT('Ctrl Pts',(31.2543008673673,55.1528901815095,15.237552571363));
#25346=CARTESIAN_POINT('Ctrl Pts',(31.4472058843405,54.9781775023347,15.2545164673766));
#25347=CARTESIAN_POINT('Ctrl Pts',(31.6679812524744,54.8513129979877,15.2714803633902));
#25348=CARTESIAN_POINT('Origin',(32.5,56.2916512459885,17.));
#25349=CARTESIAN_POINT('',(31.668393257303,54.8482192502339,15.9714803633902));
#25350=CARTESIAN_POINT('',(31.6656122060936,54.8464626161314,15.7785196366098));
#25351=CARTESIAN_POINT('',(31.667,54.8488529232836,17.));
#25352=CARTESIAN_POINT('Ctrl Pts',(31.6656122129471,54.8464626279357,15.7785196366098));
#25353=CARTESIAN_POINT('Ctrl Pts',(31.1876990498809,55.1223478631842,15.7414495489509));
#25354=CARTESIAN_POINT('Ctrl Pts',(30.860252864304,55.6587877650758,15.7043794612919));
#25355=CARTESIAN_POINT('Ctrl Pts',(30.8332370510141,56.2099535888295,15.667309373633));
#25356=CARTESIAN_POINT('Ctrl Pts',(30.8062388188308,56.7607607298753,15.6302634101103));
#25357=CARTESIAN_POINT('Ctrl Pts',(31.0792800051602,57.3262745318078,15.5932174465876));
#25358=CARTESIAN_POINT('Ctrl Pts',(31.5274017633055,57.6476843966343,15.556171483065));
#25359=CARTESIAN_POINT('Ctrl Pts',(31.9755235214509,57.9690942614607,15.5191255195423));
#25360=CARTESIAN_POINT('Ctrl Pts',(32.5987258514122,58.0464001891811,15.4820795560196));
#25361=CARTESIAN_POINT('Ctrl Pts',(33.1117966721331,57.8442226833339,15.4450335924969));
#25362=CARTESIAN_POINT('Ctrl Pts',(33.624867492854,57.6420451774866,15.4079876289742));
#25363=CARTESIAN_POINT('Ctrl Pts',(34.0278068043346,57.1603842380718,15.3709416654516));
#25364=CARTESIAN_POINT('Ctrl Pts',(34.1362071477595,56.6196747257879,15.3338957019289));
#25365=CARTESIAN_POINT('Ctrl Pts',(34.2446074911845,56.0789652135039,15.2968497384062));
#25366=CARTESIAN_POINT('Ctrl Pts',(34.0584688665537,55.479207128351,15.2598037748835));
#25367=CARTESIAN_POINT('Ctrl Pts',(33.6629786670948,55.094883157714,15.2227578113608));
#25368=CARTESIAN_POINT('Ctrl Pts',(33.267488467636,54.7105591870771,15.1857118478381));
#25369=CARTESIAN_POINT('Ctrl Pts',(32.662646693349,54.5416693309562,15.1486658843155));
#25370=CARTESIAN_POINT('Ctrl Pts',(32.1252626195522,54.6655069919667,15.1116199207928));
#25371=CARTESIAN_POINT('Ctrl Pts',(31.9652131038813,54.7023896586347,15.1005864927318));
#25372=CARTESIAN_POINT('Ctrl Pts',(31.8111473001584,54.7652381843378,15.0895530646708));
#25373=CARTESIAN_POINT('Ctrl Pts',(31.6687468960361,54.8490160493388,15.0785196366098));
#25374=CARTESIAN_POINT('Ctrl Pts',(31.6679812524744,54.8513129979877,15.2714803633902));
#25375=CARTESIAN_POINT('Ctrl Pts',(31.9293378325702,54.7011292466392,15.2915624308993));
#25376=CARTESIAN_POINT('Ctrl Pts',(32.2297522401559,54.6180004723649,15.3116444984084));
#25377=CARTESIAN_POINT('Ctrl Pts',(32.5286510627353,54.6231330317608,15.3317265659175));
#25378=CARTESIAN_POINT('Ctrl Pts',(33.0800382579645,54.6326012106758,15.3687725294402));
#25379=CARTESIAN_POINT('Ctrl Pts',(33.626267881849,54.942424779415,15.4058184929629));
#25380=CARTESIAN_POINT('Ctrl Pts',(33.917354850155,55.4108112247729,15.4428644564855));
#25381=CARTESIAN_POINT('Ctrl Pts',(34.2084418184611,55.8791976701309,15.4799104200082));
#25382=CARTESIAN_POINT('Ctrl Pts',(34.2443861311887,56.5061469921078,15.5169563835309));
#25383=CARTESIAN_POINT('Ctrl Pts',(34.0087376695652,57.0047322785327,15.5540023470536));
#25384=CARTESIAN_POINT('Ctrl Pts',(33.7730892079418,57.5033175649576,15.5910483105763));
#25385=CARTESIAN_POINT('Ctrl Pts',(33.2658479719673,57.8735388158304,15.6280942740989));
#25386=CARTESIAN_POINT('Ctrl Pts',(32.7191557896563,57.9459621763539,15.6651402376216));
#25387=CARTESIAN_POINT('Ctrl Pts',(32.1724636073452,58.0183855368774,15.7021862011443));
#25388=CARTESIAN_POINT('Ctrl Pts',(31.5863204786975,57.7930110070515,15.739232164667));
#25389=CARTESIAN_POINT('Ctrl Pts',(31.2289781301378,57.3729825184307,15.7762781281897));
#25390=CARTESIAN_POINT('Ctrl Pts',(30.8716357815781,56.9529540298098,15.8133240917123));
#25391=CARTESIAN_POINT('Ctrl Pts',(30.7430942131064,56.3382715823939,15.850370055235));
#25392=CARTESIAN_POINT('Ctrl Pts',(30.9021812024433,55.8102480837199,15.8874160187577));
#25393=CARTESIAN_POINT('Ctrl Pts',(31.022514091882,55.4108527997199,15.9154374669685));
#25394=CARTESIAN_POINT('Ctrl Pts',(31.3074096675184,55.0610382301548,15.9434589151794));
#25395=CARTESIAN_POINT('Ctrl Pts',(31.668393257303,54.8482192502339,15.9714803633902));
#25396=CARTESIAN_POINT('Origin',(32.5,56.2916512459885,17.));
#25397=CARTESIAN_POINT('',(31.6652521719754,54.8469263020216,16.6714803633902));
#25398=CARTESIAN_POINT('',(31.6662812667712,54.8504621893828,16.4785196366098));
#25399=CARTESIAN_POINT('',(31.667,54.8488529232836,17.));
#25400=CARTESIAN_POINT('Ctrl Pts',(31.6662812667712,54.8504621893828,16.4785196366098));
#25401=CARTESIAN_POINT('Ctrl Pts',(31.5218969898699,54.9322586741207,16.4674379602763));
#25402=CARTESIAN_POINT('Ctrl Pts',(31.3899082837209,55.0347971411717,16.4563562839428));
#25403=CARTESIAN_POINT('Ctrl Pts',(31.2776094808925,55.1556342327712,16.4452746076093));
#25404=CARTESIAN_POINT('Ctrl Pts',(30.9021953983998,55.5595917526322,16.4082286440866));
#25405=CARTESIAN_POINT('Ctrl Pts',(30.7468278084228,56.1680473893291,16.3711826805639));
#25406=CARTESIAN_POINT('Ctrl Pts',(30.882611569505,56.7025379705484,16.3341367170413));
#25407=CARTESIAN_POINT('Ctrl Pts',(31.0183953305873,57.2370285517677,16.2970907535186));
#25408=CARTESIAN_POINT('Ctrl Pts',(31.4453304427286,57.6975540775093,16.2600447899959));
#25409=CARTESIAN_POINT('Ctrl Pts',(31.9680276309783,57.8733524295625,16.2229988264732));
#25410=CARTESIAN_POINT('Ctrl Pts',(32.490724819228,58.0491507816157,16.1859528629505));
#25411=CARTESIAN_POINT('Ctrl Pts',(33.109184083586,57.9402219599804,16.1489068994279));
#25412=CARTESIAN_POINT('Ctrl Pts',(33.5403640348015,57.5964178575421,16.1118609359052));
#25413=CARTESIAN_POINT('Ctrl Pts',(33.971543986017,57.2526137551037,16.0748149723825));
#25414=CARTESIAN_POINT('Ctrl Pts',(34.2154446240901,56.6739343718623,16.0377690088598));
#25415=CARTESIAN_POINT('Ctrl Pts',(34.1604434390255,56.1252156089025,16.0007230453371));
#25416=CARTESIAN_POINT('Ctrl Pts',(34.1054422539609,55.5764968459426,15.9636770818144));
#25417=CARTESIAN_POINT('Ctrl Pts',(33.7515392457586,55.0577387032643,15.9266311182918));
#25418=CARTESIAN_POINT('Ctrl Pts',(33.2607001328297,54.8063537864051,15.8895851547691));
#25419=CARTESIAN_POINT('Ctrl Pts',(32.7701806517449,54.5551325700793,15.8525633153827));
#25420=CARTESIAN_POINT('Ctrl Pts',(32.1429033520047,54.5709364688817,15.8155414759962));
#25421=CARTESIAN_POINT('Ctrl Pts',(31.6656122129471,54.8464626279357,15.7785196366098));
#25422=CARTESIAN_POINT('Ctrl Pts',(31.668393257303,54.8482192502339,15.9714803633902));
#25423=CARTESIAN_POINT('Ctrl Pts',(31.7846507008451,54.7796793186609,15.980504878702));
#25424=CARTESIAN_POINT('Ctrl Pts',(31.9088000679097,54.7253487041335,15.9895293940139));
#25425=CARTESIAN_POINT('Ctrl Pts',(32.0378859406647,54.688147422912,15.9985539093257));
#25426=CARTESIAN_POINT('Ctrl Pts',(32.5677881424037,54.5354348107102,16.0355998728484));
#25427=CARTESIAN_POINT('Ctrl Pts',(33.180876998736,54.6713741362387,16.0726458363711));
#25428=CARTESIAN_POINT('Ctrl Pts',(33.5965689181183,55.0337519963386,16.1096917998938));
#25429=CARTESIAN_POINT('Ctrl Pts',(34.0122608375006,55.3961298564385,16.1467377634165));
#25430=CARTESIAN_POINT('Ctrl Pts',(34.2305558199328,55.9849462511098,16.1837837269391));
#25431=CARTESIAN_POINT('Ctrl Pts',(34.1515499288845,56.5307260185163,16.2208296904618));
#25432=CARTESIAN_POINT('Ctrl Pts',(34.0725440378362,57.0765057859228,16.2578756539845));
#25433=CARTESIAN_POINT('Ctrl Pts',(33.6962372733073,57.5792489260645,16.2949216175072));
#25434=CARTESIAN_POINT('Ctrl Pts',(33.1948485598908,57.8088721901076,16.3319675810299));
#25435=CARTESIAN_POINT('Ctrl Pts',(32.6934598464743,58.0384954541506,16.3690135445526));
#25436=CARTESIAN_POINT('Ctrl Pts',(32.0669891841703,57.9949988420949,16.4060595080752));
#25437=CARTESIAN_POINT('Ctrl Pts',(31.6021444239114,57.6982888250906,16.4431054715979));
#25438=CARTESIAN_POINT('Ctrl Pts',(31.1372996636525,57.4015788080863,16.4801514351206));
#25439=CARTESIAN_POINT('Ctrl Pts',(30.8340808054388,56.8516553861335,16.5171973986433));
#25440=CARTESIAN_POINT('Ctrl Pts',(30.8312576791002,56.3001941315665,16.554243362166));
#25441=CARTESIAN_POINT('Ctrl Pts',(30.8284345527615,55.7487328769996,16.5912893256886));
#25442=CARTESIAN_POINT('Ctrl Pts',(31.1260071582979,55.1957337898185,16.6283352892113));
#25443=CARTESIAN_POINT('Ctrl Pts',(31.5877897054339,54.8942800379899,16.665381252734));
#25444=CARTESIAN_POINT('Ctrl Pts',(31.6131317633018,54.8777366270907,16.6674142896194));
#25445=CARTESIAN_POINT('Ctrl Pts',(31.6389683688547,54.8619507900759,16.6694473265048));
#25446=CARTESIAN_POINT('Ctrl Pts',(31.6652521719754,54.8469263020216,16.6714803633902));
#25447=CARTESIAN_POINT('Origin',(32.5,56.2916512459885,17.));
#25448=CARTESIAN_POINT('',(31.6668674827448,54.8509763286063,17.3714803633902));
#25449=CARTESIAN_POINT('',(31.6688688935777,54.8504049148726,17.1785196366098));
#25450=CARTESIAN_POINT('',(31.667,54.8488529232836,17.));
#25451=CARTESIAN_POINT('Ctrl Pts',(31.6688688935777,54.8504049148726,17.1785196366098));
#25452=CARTESIAN_POINT('Ctrl Pts',(31.3819874737691,55.0177923404708,17.156380408079));
#25453=CARTESIAN_POINT('Ctrl Pts',(31.1417740021656,55.2676351144427,17.1342411795483));
#25454=CARTESIAN_POINT('Ctrl Pts',(30.9981174968784,55.5642433945469,17.1121019510175));
#25455=CARTESIAN_POINT('Ctrl Pts',(30.7577345202416,56.0605632870855,17.0750559874949));
#25456=CARTESIAN_POINT('Ctrl Pts',(30.7877102970592,56.6878262324661,17.0380100239722));
#25457=CARTESIAN_POINT('Ctrl Pts',(31.0743262430964,57.1589617869125,17.0009640604495));
#25458=CARTESIAN_POINT('Ctrl Pts',(31.3609421891337,57.6300973413589,16.9639180969268));
#25459=CARTESIAN_POINT('Ctrl Pts',(31.9041983043906,57.9451055048711,16.9268721334042));
#25460=CARTESIAN_POINT('Ctrl Pts',(32.4554703472483,57.9598210051999,16.8898261698815));
#25461=CARTESIAN_POINT('Ctrl Pts',(33.0067423901059,57.9745365055287,16.8527802063588));
#25462=CARTESIAN_POINT('Ctrl Pts',(33.5660303605644,57.6889593426742,16.8157342428361));
#25463=CARTESIAN_POINT('Ctrl Pts',(33.8773729475645,57.2337855245493,16.7786882793134));
#25464=CARTESIAN_POINT('Ctrl Pts',(34.1887155345647,56.7786117064244,16.7416423157907));
#25465=CARTESIAN_POINT('Ctrl Pts',(34.2521127381065,56.1538412330292,16.7045963522681));
#25466=CARTESIAN_POINT('Ctrl Pts',(34.0385504685031,55.6454038542026,16.6675503887454));
#25467=CARTESIAN_POINT('Ctrl Pts',(33.8249881988996,55.1369664753759,16.6305044252227));
#25468=CARTESIAN_POINT('Ctrl Pts',(33.3344664561508,54.7448621911179,16.5934584617));
#25469=CARTESIAN_POINT('Ctrl Pts',(32.7914752972722,54.6485397505015,16.5564124981773));
#25470=CARTESIAN_POINT('Ctrl Pts',(32.4109108025283,54.5810305464448,16.5304482109881));
#25471=CARTESIAN_POINT('Ctrl Pts',(32.0045725792269,54.658813619538,16.504483923799));
#25472=CARTESIAN_POINT('Ctrl Pts',(31.6662812667712,54.8504621893828,16.4785196366098));
#25473=CARTESIAN_POINT('Ctrl Pts',(31.6652521719754,54.8469263020216,16.6714803633902));
#25474=CARTESIAN_POINT('Ctrl Pts',(32.1179113819592,54.5881748244737,16.7064932900275));
#25475=CARTESIAN_POINT('Ctrl Pts',(32.7032079137753,54.5552369344614,16.7415062166648));
#25476=CARTESIAN_POINT('Ctrl Pts',(33.1792781595522,54.7673956583618,16.776519143302));
#25477=CARTESIAN_POINT('Ctrl Pts',(33.6829915777989,54.9918734470384,16.8135651068247));
#25478=CARTESIAN_POINT('Ctrl Pts',(34.0644259255566,55.4907374408677,16.8506110703474));
#25479=CARTESIAN_POINT('Ctrl Pts',(34.1490156106942,56.0356797043225,16.8876570338701));
#25480=CARTESIAN_POINT('Ctrl Pts',(34.2336052958317,56.5806219677773,16.9247029973928));
#25481=CARTESIAN_POINT('Ctrl Pts',(34.0213503183491,57.1716425008576,16.9617489609154));
#25482=CARTESIAN_POINT('Ctrl Pts',(33.6093903722588,57.5382574052848,16.9987949244381));
#25483=CARTESIAN_POINT('Ctrl Pts',(33.1974304261685,57.904872309712,17.0358408879608));
#25484=CARTESIAN_POINT('Ctrl Pts',(32.5857655114706,58.0470815854862,17.0728868514835));
#25485=CARTESIAN_POINT('Ctrl Pts',(32.0543275447524,57.8998023511679,17.1099328150062));
#25486=CARTESIAN_POINT('Ctrl Pts',(31.5228895780343,57.7525231168495,17.1469787785289));
#25487=CARTESIAN_POINT('Ctrl Pts',(31.071678559296,57.3157553724386,17.1840247420515));
#25488=CARTESIAN_POINT('Ctrl Pts',(30.9071937698036,56.7893883528063,17.2210707055742));
#25489=CARTESIAN_POINT('Ctrl Pts',(30.7427089803112,56.263021333174,17.2581166690969));
#25490=CARTESIAN_POINT('Ctrl Pts',(30.8649504200646,55.6470550383205,17.2951626326196));
#25491=CARTESIAN_POINT('Ctrl Pts',(31.2179736010047,55.2233899358517,17.3322085961422));
#25492=CARTESIAN_POINT('Ctrl Pts',(31.3427181334424,55.073683321751,17.3452991852249));
#25493=CARTESIAN_POINT('Ctrl Pts',(31.4962789539492,54.9479881676876,17.3583897743076));
#25494=CARTESIAN_POINT('Ctrl Pts',(31.6668674827448,54.8509763286063,17.3714803633902));
#25495=CARTESIAN_POINT('Origin',(32.5,56.2916512459885,17.));
#25496=CARTESIAN_POINT('',(31.6688993943412,54.8497298728322,18.0714803633902));
#25497=CARTESIAN_POINT('',(31.6668239490614,54.8465985185332,17.8785196366098));
#25498=CARTESIAN_POINT('',(31.667,54.8488529232836,17.));
#25499=CARTESIAN_POINT('Ctrl Pts',(31.6668239490614,54.8465985185332,17.8785196366098));
#25500=CARTESIAN_POINT('Ctrl Pts',(31.2400871420202,55.0969461017405,17.8453228558818));
#25501=CARTESIAN_POINT('Ctrl Pts',(30.9262488413014,55.5484932725246,17.8121260751538));
#25502=CARTESIAN_POINT('Ctrl Pts',(30.8508004340577,56.036868932597,17.7789292944258));
#25503=CARTESIAN_POINT('Ctrl Pts',(30.7666037474724,56.5818719868586,17.7418833309031));
#25504=CARTESIAN_POINT('Ctrl Pts',(30.9792848378897,57.1727392338966,17.7048373673804));
#25505=CARTESIAN_POINT('Ctrl Pts',(31.3915089982964,57.539056927659,17.6677914038578));
#25506=CARTESIAN_POINT('Ctrl Pts',(31.8037331587031,57.9053746214214,17.6307454403351));
#25507=CARTESIAN_POINT('Ctrl Pts',(32.4155003890991,58.0471427619081,17.5936994768124));
#25508=CARTESIAN_POINT('Ctrl Pts',(32.9468319475375,57.8994803557454,17.5566535132897));
#25509=CARTESIAN_POINT('Ctrl Pts',(33.4781635059759,57.7518179495826,17.519607549767));
#25510=CARTESIAN_POINT('Ctrl Pts',(33.9290593924568,57.3147249967705,17.4825615862444));
#25511=CARTESIAN_POINT('Ctrl Pts',(34.0931645477785,56.788239565649,17.4455156227217));
#25512=CARTESIAN_POINT('Ctrl Pts',(34.2572697031003,56.2617541345275,17.408469659199));
#25513=CARTESIAN_POINT('Ctrl Pts',(34.134584127263,55.6458762250967,17.3714236956763));
#25514=CARTESIAN_POINT('Ctrl Pts',(33.7812555697231,55.2224658548728,17.3343777321536));
#25515=CARTESIAN_POINT('Ctrl Pts',(33.4279270121832,54.799055484649,17.2973317686309));
#25516=CARTESIAN_POINT('Ctrl Pts',(32.8439554729406,54.568112653632,17.2602858051083));
#25517=CARTESIAN_POINT('Ctrl Pts',(32.2965988382737,54.6353296579719,17.2232398415856));
#25518=CARTESIAN_POINT('Ctrl Pts',(32.0763508133016,54.6623767631182,17.2083331065936));
#25519=CARTESIAN_POINT('Ctrl Pts',(31.8620312385645,54.7376999942423,17.1934263716017));
#25520=CARTESIAN_POINT('Ctrl Pts',(31.6688688935777,54.8504049148726,17.1785196366098));
#25521=CARTESIAN_POINT('Ctrl Pts',(31.6668674827448,54.8509763286063,17.3714803633902));
#25522=CARTESIAN_POINT('Ctrl Pts',(31.9790392312177,54.6734476539505,17.3954357378302));
#25523=CARTESIAN_POINT('Ctrl Pts',(32.3482331506335,54.5919732963168,17.4193911122703));
#25524=CARTESIAN_POINT('Ctrl Pts',(32.7022067343745,54.6351832109726,17.4433464867103));
#25525=CARTESIAN_POINT('Ctrl Pts',(33.2496117646775,54.702005498646,17.480392450233));
#25526=CARTESIAN_POINT('Ctrl Pts',(33.7606169031567,55.0670139840769,17.5174384137557));
#25527=CARTESIAN_POINT('Ctrl Pts',(34.001357750591,55.5631604641687,17.5544843772783));
#25528=CARTESIAN_POINT('Ctrl Pts',(34.2420985980252,56.0593069442606,17.591530340801));
#25529=CARTESIAN_POINT('Ctrl Pts',(34.2125751544145,56.6865914190135,17.6285763043237));
#25530=CARTESIAN_POINT('Ctrl Pts',(33.9262989911366,57.1579335916119,17.6656222678464));
#25531=CARTESIAN_POINT('Ctrl Pts',(33.6400228278586,57.6292757642103,17.7026682313691));
#25532=CARTESIAN_POINT('Ctrl Pts',(33.0969939449135,57.9446756346541,17.7397141948917));
#25533=CARTESIAN_POINT('Ctrl Pts',(32.5457325897642,57.959788663796,17.7767601584144));
#25534=CARTESIAN_POINT('Ctrl Pts',(31.9944712346149,57.9749016929378,17.8138061219371));
#25535=CARTESIAN_POINT('Ctrl Pts',(31.4349774072613,57.6897278807776,17.8508520854598));
#25536=CARTESIAN_POINT('Ctrl Pts',(31.1233066303378,57.2347786394959,17.8878980489825));
#25537=CARTESIAN_POINT('Ctrl Pts',(30.8116358534142,56.7798293982142,17.9249440125051));
#25538=CARTESIAN_POINT('Ctrl Pts',(30.7477881269206,56.1551047278111,17.9619899760278));
#25539=CARTESIAN_POINT('Ctrl Pts',(30.960983724928,55.6465134161264,17.9990359395505));
#25540=CARTESIAN_POINT('Ctrl Pts',(31.0999537214239,55.3149918769234,18.0231840808304));
#25541=CARTESIAN_POINT('Ctrl Pts',(31.3566391271215,55.0328152763439,18.0473322221103));
#25542=CARTESIAN_POINT('Ctrl Pts',(31.6688993943412,54.8497298728322,18.0714803633902));
#25543=CARTESIAN_POINT('Origin',(32.5,56.2916512459885,17.));
#25544=CARTESIAN_POINT('',(31.6661431441558,54.8463676572785,18.7714803633902));
#25545=CARTESIAN_POINT('',(31.6653993953823,54.8489980951737,18.5785196366098));
#25546=CARTESIAN_POINT('',(31.667,54.8488529232836,17.));
#25547=CARTESIAN_POINT('Ctrl Pts',(31.6653993953823,54.8489980951737,18.5785196366098));
#25548=CARTESIAN_POINT('Ctrl Pts',(31.5716723835922,54.901972129835,18.5713112672072));
#25549=CARTESIAN_POINT('Ctrl Pts',(31.4833584827506,54.9639737793168,18.5641028978047));
#25550=CARTESIAN_POINT('Ctrl Pts',(31.4025244101712,55.0345432294477,18.5568945284021));
#25551=CARTESIAN_POINT('Ctrl Pts',(30.9870939657909,55.3972207129895,18.5198485648794));
#25552=CARTESIAN_POINT('Ctrl Pts',(30.7692236712863,55.9861942986586,18.4828026013567));
#25553=CARTESIAN_POINT('Ctrl Pts',(30.8486231023463,56.5319168852662,18.445756637834));
#25554=CARTESIAN_POINT('Ctrl Pts',(30.9280225334064,57.0776394718738,18.4087106743114));
#25555=CARTESIAN_POINT('Ctrl Pts',(31.3046916900312,57.5801110594199,18.3716647107887));
#25556=CARTESIAN_POINT('Ctrl Pts',(31.8062457968318,57.8093726766562,18.334618747266));
#25557=CARTESIAN_POINT('Ctrl Pts',(32.3077999036324,58.0386342938926,18.2975727837433));
#25558=CARTESIAN_POINT('Ctrl Pts',(32.9342389606089,57.9946859408193,18.2605268202206));
#25559=CARTESIAN_POINT('Ctrl Pts',(33.3988695811848,57.6976408304244,18.223480856698));
#25560=CARTESIAN_POINT('Ctrl Pts',(33.8635002017608,57.4005957200295,18.1864348931753));
#25561=CARTESIAN_POINT('Ctrl Pts',(34.1663223859364,56.8504538523131,18.1493889296526));
#25562=CARTESIAN_POINT('Ctrl Pts',(34.168747844005,56.298990772552,18.1123429661299));
#25563=CARTESIAN_POINT('Ctrl Pts',(34.1711733020736,55.747527692791,18.0752970026072));
#25564=CARTESIAN_POINT('Ctrl Pts',(33.8732020340353,55.1947434009854,18.0382510390846));
#25565=CARTESIAN_POINT('Ctrl Pts',(33.4112022803197,54.8936227627802,18.0012050755619));
#25566=CARTESIAN_POINT('Ctrl Pts',(32.9492025266042,54.5925021245749,17.9641591120392));
#25567=CARTESIAN_POINT('Ctrl Pts',(32.3231742872114,54.5430451399701,17.9271131485165));
#25568=CARTESIAN_POINT('Ctrl Pts',(31.8196229357211,54.7678860784103,17.8900671849938));
#25569=CARTESIAN_POINT('Ctrl Pts',(31.7673024933817,54.791247702444,17.8862180021992));
#25570=CARTESIAN_POINT('Ctrl Pts',(31.7163042884046,54.8175705950767,17.8823688194045));
#25571=CARTESIAN_POINT('Ctrl Pts',(31.6668239490614,54.8465985185332,17.8785196366098));
#25572=CARTESIAN_POINT('Ctrl Pts',(31.6688993943412,54.8497298728322,18.0714803633902));
#25573=CARTESIAN_POINT('Ctrl Pts',(31.8356814821797,54.751941684401,18.084378185633));
#25574=CARTESIAN_POINT('Ctrl Pts',(32.0183177486645,54.6824218442404,18.0972760078758));
#25575=CARTESIAN_POINT('Ctrl Pts',(32.2073398697232,54.6487501647903,18.1101738301185));
#25576=CARTESIAN_POINT('Ctrl Pts',(32.7502614940028,54.5520361781053,18.1472197936412));
#25577=CARTESIAN_POINT('Ctrl Pts',(33.3458658200538,54.7510661577016,18.1842657571639));
#25578=CARTESIAN_POINT('Ctrl Pts',(33.7215711507525,55.1547529048404,18.2213117206866));
#25579=CARTESIAN_POINT('Ctrl Pts',(34.0972764814512,55.5584396519791,18.2583576842093));
#25580=CARTESIAN_POINT('Ctrl Pts',(34.2530828167975,56.1667831666603,18.2954036477319));
#25581=CARTESIAN_POINT('Ctrl Pts',(34.1176845039388,56.7013715898475,18.3324496112546));
#25582=CARTESIAN_POINT('Ctrl Pts',(33.98228619108,57.2359600130348,18.3694955747773));
#25583=CARTESIAN_POINT('Ctrl Pts',(33.5556832300161,57.696793344728,18.4065415383));
#25584=CARTESIAN_POINT('Ctrl Pts',(33.0331128848803,57.8729685975756,18.4435875018227));
#25585=CARTESIAN_POINT('Ctrl Pts',(32.5105425397446,58.0491438504232,18.4806334653453));
#25586=CARTESIAN_POINT('Ctrl Pts',(31.892004810537,57.940661024425,18.517679428868));
#25587=CARTESIAN_POINT('Ctrl Pts',(31.4605769963787,57.5971679000379,18.5547253923907));
#25588=CARTESIAN_POINT('Ctrl Pts',(31.0291491822204,57.2536747756508,18.5917713559134));
#25589=CARTESIAN_POINT('Ctrl Pts',(30.7848312831113,56.6751713528746,18.6288173194361));
#25590=CARTESIAN_POINT('Ctrl Pts',(30.839436770952,56.1264130034822,18.6658632829588));
#25591=CARTESIAN_POINT('Ctrl Pts',(30.89132971378,55.6049143999997,18.7010689764359));
#25592=CARTESIAN_POINT('Ctrl Pts',(31.2131854490111,55.1102790779514,18.736274669913));
#25593=CARTESIAN_POINT('Ctrl Pts',(31.6661431441558,54.8463676572785,18.7714803633902));
#25594=CARTESIAN_POINT('Origin',(32.5,56.2916512459885,17.));
#25595=CARTESIAN_POINT('',(31.6657991298123,54.8498167632728,19.4714803633902));
#25596=CARTESIAN_POINT('',(31.6682947036337,54.8512220664372,19.2785196366098));
#25597=CARTESIAN_POINT('',(31.667,54.8488529232836,17.));
#25598=CARTESIAN_POINT('Ctrl Pts',(31.6682947036337,54.8512220664372,19.2785196366098));
#25599=CARTESIAN_POINT('Ctrl Pts',(31.4307799124075,54.9882439463791,19.26025371501));
#25600=CARTESIAN_POINT('Ctrl Pts',(31.2253675580441,55.1807871169989,19.2419877934101));
#25601=CARTESIAN_POINT('Ctrl Pts',(31.0820105037967,55.4118336375308,19.2237218718103));
#25602=CARTESIAN_POINT('Ctrl Pts',(30.7912614072705,55.8804298112795,19.1866759082877));
#25603=CARTESIAN_POINT('Ctrl Pts',(30.7557692111823,56.5074048138577,19.149629944765));
#25604=CARTESIAN_POINT('Ctrl Pts',(30.9917771203569,57.0058199801505,19.1125839812423));
#25605=CARTESIAN_POINT('Ctrl Pts',(31.2277850295315,57.5042351464433,19.0755380177196));
#25606=CARTESIAN_POINT('Ctrl Pts',(31.7352930439689,57.8740904764507,19.0384920541969));
#25607=CARTESIAN_POINT('Ctrl Pts',(32.2820372430805,57.9461195811699,19.0014460906743));
#25608=CARTESIAN_POINT('Ctrl Pts',(32.828781442192,58.0181486858891,18.9644001271516));
#25609=CARTESIAN_POINT('Ctrl Pts',(33.4147618259776,57.7923515653202,18.9273541636289));
#25610=CARTESIAN_POINT('Ctrl Pts',(33.7718011490706,57.3720655520495,18.8903082001062));
#25611=CARTESIAN_POINT('Ctrl Pts',(34.1288404721637,56.9517795387787,18.8532622365835));
#25612=CARTESIAN_POINT('Ctrl Pts',(34.2569387345642,56.3370046328063,18.8162162730609));
#25613=CARTESIAN_POINT('Ctrl Pts',(34.0974710401143,55.8090960558605,18.7791703095382));
#25614=CARTESIAN_POINT('Ctrl Pts',(33.9380033456643,55.2811874789147,18.7421243460155));
#25615=CARTESIAN_POINT('Ctrl Pts',(33.4909696943638,54.8401452309957,18.7050783824928));
#25616=CARTESIAN_POINT('Ctrl Pts',(32.9609575715857,54.6878147977434,18.6680324189701));
#25617=CARTESIAN_POINT('Ctrl Pts',(32.5340747186531,54.565124679649,18.63819482485));
#25618=CARTESIAN_POINT('Ctrl Pts',(32.0533634937381,54.6297227421977,18.6083572307299));
#25619=CARTESIAN_POINT('Ctrl Pts',(31.6653993953823,54.8489980951737,18.5785196366098));
#25620=CARTESIAN_POINT('Ctrl Pts',(31.6661431441558,54.8463676572785,18.7714803633902));
#25621=CARTESIAN_POINT('Ctrl Pts',(31.6898201235287,54.832572494219,18.7733206334357));
#25622=CARTESIAN_POINT('Ctrl Pts',(31.7138553201483,54.819407751031,18.7751609034813));
#25623=CARTESIAN_POINT('Ctrl Pts',(31.7382289011373,54.8069025442232,18.7770011735268));
#25624=CARTESIAN_POINT('Ctrl Pts',(32.2288866686916,54.5551637103656,18.8140471370495));
#25625=CARTESIAN_POINT('Ctrl Pts',(32.8566733290096,54.5706993186593,18.8510931005722));
#25626=CARTESIAN_POINT('Ctrl Pts',(33.3342787571905,54.8463994098823,18.8881390640948));
#25627=CARTESIAN_POINT('Ctrl Pts',(33.8118841853713,55.1220995011053,18.9251850276175));
#25628=CARTESIAN_POINT('Ctrl Pts',(34.1393083814151,55.6579640752576,18.9622309911402));
#25629=CARTESIAN_POINT('Ctrl Pts',(34.1667038054086,56.2087516714065,18.9992769546629));
#25630=CARTESIAN_POINT('Ctrl Pts',(34.1940992294022,56.7595392675554,19.0363229181855));
#25631=CARTESIAN_POINT('Ctrl Pts',(33.9214658813456,57.325249885701,19.0733688817082));
#25632=CARTESIAN_POINT('Ctrl Pts',(33.4735759588574,57.6469828536777,19.1104148452309));
#25633=CARTESIAN_POINT('Ctrl Pts',(33.0256860363692,57.9687158216544,19.1474608087536));
#25634=CARTESIAN_POINT('Ctrl Pts',(32.4025395394495,58.0464711394622,19.1845067722763));
#25635=CARTESIAN_POINT('Ctrl Pts',(31.889322996006,57.8446636449513,19.221552735799));
#25636=CARTESIAN_POINT('Ctrl Pts',(31.3761064525625,57.6428561504404,19.2585986993216));
#25637=CARTESIAN_POINT('Ctrl Pts',(30.9728198625952,57.1614858436107,19.2956446628443));
#25638=CARTESIAN_POINT('Ctrl Pts',(30.86402962057,56.6208545750433,19.332690626367));
#25639=CARTESIAN_POINT('Ctrl Pts',(30.7552393785448,56.0802233064759,19.3697365898897));
#25640=CARTESIAN_POINT('Ctrl Pts',(30.9409454844617,55.4803310761708,19.4067825534124));
#25641=CARTESIAN_POINT('Ctrl Pts',(31.3361584863692,55.0957219647369,19.443828516935));
#25642=CARTESIAN_POINT('Ctrl Pts',(31.4344901101744,55.000028659418,19.4530457990868));
#25643=CARTESIAN_POINT('Ctrl Pts',(31.5457912060088,54.917662401762,19.4622630812385));
#25644=CARTESIAN_POINT('Ctrl Pts',(31.6657991298123,54.8498167632728,19.4714803633902));
#25645=CARTESIAN_POINT('Origin',(32.5,56.2916512459885,17.));
#25646=CARTESIAN_POINT('',(31.6686691446489,54.8508917236136,20.1714803633902));
#25647=CARTESIAN_POINT('',(31.6680707239275,54.8477242132621,19.9785196366098));
#25648=CARTESIAN_POINT('',(31.667,54.8488529232836,17.));
#25649=CARTESIAN_POINT('Ctrl Pts',(31.6680707239275,54.8477242132621,19.9785196366098));
#25650=CARTESIAN_POINT('Ctrl Pts',(31.2906837721071,55.0702773030723,19.9491961628127));
#25651=CARTESIAN_POINT('Ctrl Pts',(30.9974844080691,55.4444429123815,19.9198726890157));
#25652=CARTESIAN_POINT('Ctrl Pts',(30.8862884172365,55.8665534203839,19.8905492152186));
#25653=CARTESIAN_POINT('Ctrl Pts',(30.7458083824097,56.3998289316761,19.8535032516959));
#25654=CARTESIAN_POINT('Ctrl Pts',(30.8958178157836,57.0096276847031,19.8164572881732));
#25655=CARTESIAN_POINT('Ctrl Pts',(31.2676640515259,57.4168718226721,19.7794113246505));
#25656=CARTESIAN_POINT('Ctrl Pts',(31.6395102872682,57.8241159606411,19.7423653611279));
#25657=CARTESIAN_POINT('Ctrl Pts',(32.2331933253789,58.0288054835523,19.7053193976052));
#25658=CARTESIAN_POINT('Ctrl Pts',(32.7770107560741,57.9372630704146,19.6682734340825));
#25659=CARTESIAN_POINT('Ctrl Pts',(33.3208281867694,57.8457206572769,19.6312274705598));
#25660=CARTESIAN_POINT('Ctrl Pts',(33.8147800100492,57.4579463080904,19.5941815070371));
#25661=CARTESIAN_POINT('Ctrl Pts',(34.0328063735823,56.9514071526715,19.5571355435145));
#25662=CARTESIAN_POINT('Ctrl Pts',(34.2508327371153,56.4448679972525,19.5200895799918));
#25663=CARTESIAN_POINT('Ctrl Pts',(34.1929336409016,55.8195640356011,19.4830436164691));
#25664=CARTESIAN_POINT('Ctrl Pts',(33.8856069343887,55.3616691714411,19.4459976529464));
#25665=CARTESIAN_POINT('Ctrl Pts',(33.5782802278758,54.9037743072811,19.4089516894237));
#25666=CARTESIAN_POINT('Ctrl Pts',(33.0215259110637,54.6132885406125,19.3719057259011));
#25667=CARTESIAN_POINT('Ctrl Pts',(32.4701457541755,54.6231543297377,19.3348597623784));
#25668=CARTESIAN_POINT('Ctrl Pts',(32.1906296753062,54.6281556825372,19.3160797204555));
#25669=CARTESIAN_POINT('Ctrl Pts',(31.9124946862161,54.7103435109481,19.2972996785326));
#25670=CARTESIAN_POINT('Ctrl Pts',(31.6682947036337,54.8512220664372,19.2785196366098));
#25671=CARTESIAN_POINT('Ctrl Pts',(31.6657991298123,54.8498167632728,19.4714803633902));
#25672=CARTESIAN_POINT('Ctrl Pts',(32.0281252709183,54.6449782192373,19.4993090447612));
#25673=CARTESIAN_POINT('Ctrl Pts',(32.46981831913,54.5725020736119,19.5271377261321));
#25674=CARTESIAN_POINT('Ctrl Pts',(32.8735646889017,54.6652369881102,19.5549664075031));
#25675=CARTESIAN_POINT('Ctrl Pts',(33.4110379916282,54.7886871154801,19.5920123710258));
#25676=CARTESIAN_POINT('Ctrl Pts',(33.8812646991831,55.2049133627827,19.6290583345484));
#25677=CARTESIAN_POINT('Ctrl Pts',(34.069042894277,55.7234274269329,19.6661042980711));
#25678=CARTESIAN_POINT('Ctrl Pts',(34.2568210893708,56.2419414910831,19.7031502615938));
#25679=CARTESIAN_POINT('Ctrl Pts',(34.1621507720038,56.8627433720808,19.7401962251165));
#25680=CARTESIAN_POINT('Ctrl Pts',(33.8283583461529,57.3017195705904,19.7772421886392));
#25681=CARTESIAN_POINT('Ctrl Pts',(33.494565920302,57.7406957691,19.8142881521619));
#25682=CARTESIAN_POINT('Ctrl Pts',(32.9216513859673,57.9978462851214,19.8513341156845));
#25683=CARTESIAN_POINT('Ctrl Pts',(32.3718123356058,57.9554847234739,19.8883800792072));
#25684=CARTESIAN_POINT('Ctrl Pts',(31.8219732852442,57.9131231618264,19.9254260427299));
#25685=CARTESIAN_POINT('Ctrl Pts',(31.2952097188558,57.5712495225101,19.9624720062526));
#25686=CARTESIAN_POINT('Ctrl Pts',(31.0325979551939,57.086324221881,19.9995179697753));
#25687=CARTESIAN_POINT('Ctrl Pts',(30.769986191532,56.601398921252,20.0365639332979));
#25688=CARTESIAN_POINT('Ctrl Pts',(30.7715262305966,55.9734219593102,20.0736098968206));
#25689=CARTESIAN_POINT('Ctrl Pts',(31.0365132935154,55.489790540013,20.1106558603433));
#25690=CARTESIAN_POINT('Ctrl Pts',(31.1815376981853,55.225104566703,20.1309306946923));
#25691=CARTESIAN_POINT('Ctrl Pts',(31.4054710295806,55.0036536684416,20.1512055290412));
#25692=CARTESIAN_POINT('Ctrl Pts',(31.6686691446489,54.8508917236136,20.1714803633902));
#25693=CARTESIAN_POINT('Origin',(32.5,56.2916512459885,17.));
#25694=CARTESIAN_POINT('',(31.6674621971265,54.8470528177236,20.8714803633902));
#25695=CARTESIAN_POINT('',(31.6651488727496,54.8473747039336,20.6785196366098));
#25696=CARTESIAN_POINT('',(31.667,54.8488529232836,17.));
#25697=CARTESIAN_POINT('Ctrl Pts',(31.6651488727496,54.8473747039336,20.6785196366098));
#25698=CARTESIAN_POINT('Ctrl Pts',(31.6219590933013,54.8719481703147,20.6751845741382));
#25699=CARTESIAN_POINT('Ctrl Pts',(31.579962486587,54.8985363635017,20.6718495116665));
#25700=CARTESIAN_POINT('Ctrl Pts',(31.539367364925,54.9271153018697,20.6685144491949));
#25701=CARTESIAN_POINT('Ctrl Pts',(31.0884356630212,55.2445709169594,20.6314684856722));
#25702=CARTESIAN_POINT('Ctrl Pts',(30.8104307642169,55.8076611175674,20.5944225221495));
#25703=CARTESIAN_POINT('Ctrl Pts',(30.8325829345476,56.3586844387663,20.5573765586268));
#25704=CARTESIAN_POINT('Ctrl Pts',(30.8547351048784,56.9097077599651,20.5203305951042));
#25705=CARTESIAN_POINT('Ctrl Pts',(31.1770443443443,57.4486642017546,20.4832846315815));
#25706=CARTESIAN_POINT('Ctrl Pts',(31.6520041279563,57.7288973132865,20.4462386680588));
#25707=CARTESIAN_POINT('Ctrl Pts',(32.1269639115684,58.0091304248183,20.4091927045361));
#25708=CARTESIAN_POINT('Ctrl Pts',(32.7545742393267,58.0306402060925,20.3721467410134));
#25709=CARTESIAN_POINT('Ctrl Pts',(33.2476056229439,57.7835825733328,20.3351007774907));
#25710=CARTESIAN_POINT('Ctrl Pts',(33.7406370065611,57.5365249405731,20.2980548139681));
#25711=CARTESIAN_POINT('Ctrl Pts',(34.0990894460373,57.0208998937796,20.2610088504454));
#25712=CARTESIAN_POINT('Ctrl Pts',(34.158915181361,56.4726861646106,20.2239628869227));
#25713=CARTESIAN_POINT('Ctrl Pts',(34.2187409166848,55.9244724354416,20.1869169234));
#25714=CARTESIAN_POINT('Ctrl Pts',(33.9799399478562,55.3436700238972,20.1498709598773));
#25715=CARTESIAN_POINT('Ctrl Pts',(33.5518008766237,54.9960864443956,20.1128249963547));
#25716=CARTESIAN_POINT('Ctrl Pts',(33.1236618053912,54.648502864894,20.075779032832));
#25717=CARTESIAN_POINT('Ctrl Pts',(32.5061846317548,54.5341381174352,20.0387330693093));
#25718=CARTESIAN_POINT('Ctrl Pts',(31.9819612934228,54.7053318784847,20.0016871057866));
#25719=CARTESIAN_POINT('Ctrl Pts',(31.8726832787825,54.7410184131319,19.993964616061));
#25720=CARTESIAN_POINT('Ctrl Pts',(31.7674575454952,54.7891136966038,19.9862421263354));
#25721=CARTESIAN_POINT('Ctrl Pts',(31.6680707239275,54.8477242132621,19.9785196366098));
#25722=CARTESIAN_POINT('Ctrl Pts',(31.6686691446489,54.8508917236136,20.1714803633902));
#25723=CARTESIAN_POINT('Ctrl Pts',(31.8863838499881,54.724528653739,20.1882514925639));
#25724=CARTESIAN_POINT('Ctrl Pts',(32.1309651849205,54.6451654778256,20.2050226217376));
#25725=CARTESIAN_POINT('Ctrl Pts',(32.3799746400722,54.6272090425041,20.2217937509113));
#25726=CARTESIAN_POINT('Ctrl Pts',(32.9300148369371,54.587544840945,20.258839714434));
#25727=CARTESIAN_POINT('Ctrl Pts',(33.5016611438935,54.8475023144793,20.2958856779567));
#25728=CARTESIAN_POINT('Ctrl Pts',(33.8332965022582,55.2881103970044,20.3329316414794));
#25729=CARTESIAN_POINT('Ctrl Pts',(34.1649318606228,55.7287184795295,20.3699776050021));
#25730=CARTESIAN_POINT('Ctrl Pts',(34.2565562703956,56.3499771710453,20.4070235685247));
#25731=CARTESIAN_POINT('Ctrl Pts',(34.0662370704008,56.8675640172576,20.4440695320474));
#25732=CARTESIAN_POINT('Ctrl Pts',(33.8759178704059,57.3851508634698,20.4811154955701));
#25733=CARTESIAN_POINT('Ctrl Pts',(33.4036550606434,57.7990658643784,20.5181614590928));
#25734=CARTESIAN_POINT('Ctrl Pts',(32.8655828553033,57.9198782552653,20.5552074226155));
#25735=CARTESIAN_POINT('Ctrl Pts',(32.3275106499632,58.0406906461521,20.5922533861382));
#25736=CARTESIAN_POINT('Ctrl Pts',(31.7236290490454,57.8684004270172,20.6292993496608));
#25737=CARTESIAN_POINT('Ctrl Pts',(31.3303069678814,57.4818576289614,20.6663453131835));
#25738=CARTESIAN_POINT('Ctrl Pts',(30.9369848867174,57.0953148309056,20.7033912767062));
#25739=CARTESIAN_POINT('Ctrl Pts',(30.754222325307,56.494519453929,20.7404372402289));
#25740=CARTESIAN_POINT('Ctrl Pts',(30.8656634549365,55.954428037577,20.7774832037515));
#25741=CARTESIAN_POINT('Ctrl Pts',(30.959917085256,55.497634599958,20.8088155902978));
#25742=CARTESIAN_POINT('Ctrl Pts',(31.2646228230038,55.0842643987965,20.840147976844));
#25743=CARTESIAN_POINT('Ctrl Pts',(31.6674621971265,54.8470528177236,20.8714803633902));
#25744=CARTESIAN_POINT('Origin',(32.5,56.2916512459885,17.));
#25745=CARTESIAN_POINT('',(31.6652082225275,54.8481806306042,21.5714803633902));
#25746=CARTESIAN_POINT('',(31.667262219952,54.851191363199,21.3785196366098));
#25747=CARTESIAN_POINT('',(31.667,54.8488529232836,17.));
#25748=CARTESIAN_POINT('',(32.1997834265915,57.930378193668,22.));
#25749=CARTESIAN_POINT('Ctrl Pts',(31.6652082225275,54.8481806306042,21.5714803633902));
#25750=CARTESIAN_POINT('Ctrl Pts',(32.0766081468896,54.6152030336121,21.6031823516921));
#25751=CARTESIAN_POINT('Ctrl Pts',(32.5941722167266,54.5601311343425,21.634884339994));
#25752=CARTESIAN_POINT('Ctrl Pts',(33.0407304570643,54.7130293475826,21.6665863282959));
#25753=CARTESIAN_POINT('Ctrl Pts',(33.5625646122208,54.8917014730163,21.7036322918186));
#25754=CARTESIAN_POINT('Ctrl Pts',(33.987436493413,55.3543679573327,21.7406782553412));
#25755=CARTESIAN_POINT('Ctrl Pts',(34.119930861687,55.8897554009177,21.7777242188639));
#25756=CARTESIAN_POINT('Ctrl Pts',(34.2524252299611,56.4251428445027,21.8147701823866));
#25757=CARTESIAN_POINT('Ctrl Pts',(34.092542085317,57.0332512473564,21.8518161459093));
#25758=CARTESIAN_POINT('Ctrl Pts',(33.7156105587364,57.434517372925,21.888862109432));
#25759=CARTESIAN_POINT('Ctrl Pts',(33.3386790321557,57.8357834984935,21.9259080729546));
#25760=CARTESIAN_POINT('Ctrl Pts',(32.7446991236384,58.0302073467771,21.9629540364773));
#25761=CARTESIAN_POINT('Ctrl Pts',(32.1997834265915,57.930378193668,22.));
#25762=CARTESIAN_POINT('',(30.9279127562903,55.7311233941164,22.));
#25763=CARTESIAN_POINT('Origin',(32.5,56.2916512459885,22.));
#25764=CARTESIAN_POINT('Ctrl Pts',(30.9279109916837,55.7311226632894,22.));
#25765=CARTESIAN_POINT('Ctrl Pts',(30.7469516062031,56.2407356224363,21.9636770818144));
#25766=CARTESIAN_POINT('Ctrl Pts',(30.8361764319304,56.8473747622876,21.9273541636289));
#25767=CARTESIAN_POINT('Ctrl Pts',(31.157356786616,57.282481394961,21.8910312454433));
#25768=CARTESIAN_POINT('Ctrl Pts',(31.4849305691822,57.7262492761691,21.8539852819207));
#25769=CARTESIAN_POINT('Ctrl Pts',(32.053786423629,57.9915876156774,21.816939318398));
#25770=CARTESIAN_POINT('Ctrl Pts',(32.604106443046,57.9571481822401,21.7798933548753));
#25771=CARTESIAN_POINT('Ctrl Pts',(33.154426462463,57.9227087488028,21.7428473913526));
#25772=CARTESIAN_POINT('Ctrl Pts',(33.6862106468503,57.5884915424199,21.7058014278299));
#25773=CARTESIAN_POINT('Ctrl Pts',(33.9558248450097,57.1074100574699,21.6687554643072));
#25774=CARTESIAN_POINT('Ctrl Pts',(34.2254390431691,56.6263285725199,21.6317095007846));
#25775=CARTESIAN_POINT('Ctrl Pts',(34.2328832551006,55.9983828090028,21.5946635372619));
#25776=CARTESIAN_POINT('Ctrl Pts',(33.9748805050844,55.5109771631464,21.5576175737392));
#25777=CARTESIAN_POINT('Ctrl Pts',(33.7168777550681,55.02357151729,21.5205716102165));
#25778=CARTESIAN_POINT('Ctrl Pts',(33.1934280431042,54.6767059890943,21.4835256466938));
#25779=CARTESIAN_POINT('Ctrl Pts',(32.6440261878896,54.6291148312821,21.4464796831712));
#25780=CARTESIAN_POINT('Ctrl Pts',(32.3080707772689,54.6000131695149,21.4238263343174));
#25781=CARTESIAN_POINT('Ctrl Pts',(31.962411244236,54.6828172989956,21.4011729854636));
#25782=CARTESIAN_POINT('Ctrl Pts',(31.667262219952,54.851191363199,21.3785196366098));
#25783=CARTESIAN_POINT('Origin',(32.5,56.2916512459885,23.5459252805377));
#25784=CARTESIAN_POINT('',(31.4703515173367,54.5106388084307,13.4540747194623));
#25785=CARTESIAN_POINT('',(31.474888731711,54.5145036461351,13.3959252805377));
#25786=CARTESIAN_POINT('',(31.4726249999999,54.5121855475625,23.5459252805377));
#25787=CARTESIAN_POINT('',(34.1542537360139,57.5104384051693,13.));
#25788=CARTESIAN_POINT('Ctrl Pts',(31.474888731711,54.5145036461351,13.3959252805377));
#25789=CARTESIAN_POINT('Ctrl Pts',(31.1415381650012,54.7083242075053,13.3750880775932));
#25790=CARTESIAN_POINT('Ctrl Pts',(30.3573574995582,55.4957610011485,13.317204911126));
#25791=CARTESIAN_POINT('Ctrl Pts',(30.3807647535574,57.4808407355902,13.2222757811361));
#25792=CARTESIAN_POINT('Ctrl Pts',(32.3530480505924,58.7147951819942,13.1111378905681));
#25793=CARTESIAN_POINT('Ctrl Pts',(33.7489780094279,58.0605171287351,13.0370459635227));
#25794=CARTESIAN_POINT('Ctrl Pts',(34.1542537360139,57.5104384051693,13.));
#25795=CARTESIAN_POINT('',(34.5453697724994,56.5236298181907,13.));
#25796=CARTESIAN_POINT('Origin',(32.5,56.2916512459885,13.));
#25797=CARTESIAN_POINT('Ctrl Pts',(31.4703515173367,54.5106388084307,13.4540747194623));
#25798=CARTESIAN_POINT('Ctrl Pts',(31.4080578130841,54.5460236433933,13.4501772883951));
#25799=CARTESIAN_POINT('Ctrl Pts',(30.7746715994701,54.9531541715192,13.4092338938053));
#25800=CARTESIAN_POINT('Ctrl Pts',(30.0748873839319,56.4258925346357,13.3312445356927));
#25801=CARTESIAN_POINT('Ctrl Pts',(31.2980228170538,58.4019167094404,13.2201066451247));
#25802=CARTESIAN_POINT('Ctrl Pts',(33.60498859151,58.4457294765997,13.1096917998938));
#25803=CARTESIAN_POINT('Ctrl Pts',(34.469350039682,57.1862605871606,13.0363229181856));
#25804=CARTESIAN_POINT('Ctrl Pts',(34.5453721234943,56.5236299659801,13.));
#25805=CARTESIAN_POINT('Origin',(32.5,56.2916512459885,23.5459252805377));
#25806=CARTESIAN_POINT('',(31.4731479817858,54.5151444612292,14.1540747194623));
#25807=CARTESIAN_POINT('',(31.472961077924,54.5097720381012,14.0959252805377));
#25808=CARTESIAN_POINT('',(31.4726249999999,54.5121855475625,23.5459252805377));
#25809=CARTESIAN_POINT('Ctrl Pts',(31.472961077924,54.5097720381012,14.0959252805377));
#25810=CARTESIAN_POINT('Ctrl Pts',(30.9672759169724,54.8072848061285,14.0640305253959));
#25811=CARTESIAN_POINT('Ctrl Pts',(30.1471997784249,55.9394877473567,13.9950898067314));
#25812=CARTESIAN_POINT('Ctrl Pts',(30.8240773215828,58.0494183789814,13.8891031245444));
#25813=CARTESIAN_POINT('Ctrl Pts',(33.0679207153753,58.652967541299,13.7779652339763));
#25814=CARTESIAN_POINT('Ctrl Pts',(34.7917858342248,57.0952271533931,13.6668273434083));
#25815=CARTESIAN_POINT('Ctrl Pts',(34.4182616640155,54.8018644711708,13.5556894528402));
#25816=CARTESIAN_POINT('Ctrl Pts',(32.6876568692323,54.0466007600429,13.4653887652167));
#25817=CARTESIAN_POINT('Ctrl Pts',(31.734194145148,54.3637352784833,13.4121340411158));
#25818=CARTESIAN_POINT('Ctrl Pts',(31.474888731711,54.5145036461351,13.3959252805377));
#25819=CARTESIAN_POINT('Ctrl Pts',(31.4731479817858,54.5151444612292,14.1540747194623));
#25820=CARTESIAN_POINT('Ctrl Pts',(31.2328780723112,54.6524190875731,14.1391197361979));
#25821=CARTESIAN_POINT('Ctrl Pts',(30.4914633330274,55.2894948776179,14.0871187894108));
#25822=CARTESIAN_POINT('Ctrl Pts',(30.2211615693062,57.1314551632494,13.998071879101));
#25823=CARTESIAN_POINT('Ctrl Pts',(31.969659013309,58.6616944230992,13.886933988533));
#25824=CARTESIAN_POINT('Ctrl Pts',(34.2035641928434,58.0226004643432,13.7757960979649));
#25825=CARTESIAN_POINT('Ctrl Pts',(34.8782165391171,55.7991607039093,13.6646582073969));
#25826=CARTESIAN_POINT('Ctrl Pts',(33.428663662975,54.088644942548,13.557417747896));
#25827=CARTESIAN_POINT('Ctrl Pts',(32.0001735569317,54.2096827863809,13.4872232519178));
#25828=CARTESIAN_POINT('Ctrl Pts',(31.4703515173367,54.5106388084307,13.4540747194623));
#25829=CARTESIAN_POINT('Origin',(32.5,56.2916512459885,23.5459252805377));
#25830=CARTESIAN_POINT('',(31.4747795225871,54.5123867379958,14.8540747194623));
#25831=CARTESIAN_POINT('',(31.4704412404259,54.5116709695926,14.7959252805377));
#25832=CARTESIAN_POINT('',(31.4726249999999,54.5121855475625,23.5459252805377));
#25833=CARTESIAN_POINT('Ctrl Pts',(31.4704412404259,54.5116709695925,14.7959252805377));
#25834=CARTESIAN_POINT('Ctrl Pts',(31.3758333938148,54.5652019692603,14.7900189367213));
#25835=CARTESIAN_POINT('Ctrl Pts',(30.7207574218389,55.0095411304487,14.7470666293823));
#25836=CARTESIAN_POINT('Ctrl Pts',(30.0858692295542,56.5568634086541,14.6670683585206));
#25837=CARTESIAN_POINT('Ctrl Pts',(31.4135291597177,58.4637350403728,14.5559304679526));
#25838=CARTESIAN_POINT('Ctrl Pts',(33.73564936737,58.3824733534297,14.4447925773845));
#25839=CARTESIAN_POINT('Ctrl Pts',(34.926763301881,56.387459257788,14.3336546868165));
#25840=CARTESIAN_POINT('Ctrl Pts',(33.8966380568543,54.3047494455222,14.2225167962484));
#25841=CARTESIAN_POINT('Ctrl Pts',(32.2506444060776,54.1164611126689,14.1432736608222));
#25842=CARTESIAN_POINT('Ctrl Pts',(31.5546324883995,54.4617218098652,14.1010764889186));
#25843=CARTESIAN_POINT('Ctrl Pts',(31.472961077924,54.5097720381012,14.0959252805377));
#25844=CARTESIAN_POINT('Ctrl Pts',(31.4747795225871,54.5123867379958,14.8540747194623));
#25845=CARTESIAN_POINT('Ctrl Pts',(31.0607155624738,54.7559913454825,14.8280621840006));
#25846=CARTESIAN_POINT('Ctrl Pts',(30.250819401885,55.6943396944676,14.7650036850163));
#25847=CARTESIAN_POINT('Ctrl Pts',(30.5678191761536,57.7630592969624,14.6648992225092));
#25848=CARTESIAN_POINT('Ctrl Pts',(32.6883055651204,58.7129949703237,14.5537613319412));
#25849=CARTESIAN_POINT('Ctrl Pts',(34.6364334330514,57.4466471822884,14.4426234413732));
#25850=CARTESIAN_POINT('Ctrl Pts',(34.6290601547835,55.1231186965397,14.3314855508051));
#25851=CARTESIAN_POINT('Ctrl Pts',(32.9361539945055,54.0378965296929,14.2353026435015));
#25852=CARTESIAN_POINT('Ctrl Pts',(31.8280663212454,54.3123671657349,14.1761656997206));
#25853=CARTESIAN_POINT('Ctrl Pts',(31.4731479817858,54.5151444612292,14.1540747194623));
#25854=CARTESIAN_POINT('Origin',(32.5,56.2916512459885,23.5459252805377));
#25855=CARTESIAN_POINT('',(31.4709133736318,54.5092374781621,15.5540747194623));
#25856=CARTESIAN_POINT('',(31.4738352212016,54.515219664308,15.4959252805377));
#25857=CARTESIAN_POINT('',(31.4726249999999,54.5121855475625,23.5459252805377));
#25858=CARTESIAN_POINT('Ctrl Pts',(31.4738352212016,54.515219664308,15.4959252805377));
#25859=CARTESIAN_POINT('Ctrl Pts',(31.201543391866,54.6716871554887,15.4789613845241));
#25860=CARTESIAN_POINT('Ctrl Pts',(30.4440567807226,55.3577373025941,15.4249515249878));
#25861=CARTESIAN_POINT('Ctrl Pts',(30.269905357807,57.2534431023133,15.3338957019289));
#25862=CARTESIAN_POINT('Ctrl Pts',(32.0985763090804,58.6869016992398,15.2227578113608));
#25863=CARTESIAN_POINT('Ctrl Pts',(34.2946749356979,57.9279603862777,15.1116199207928));
#25864=CARTESIAN_POINT('Ctrl Pts',(34.848087203459,55.6712867722916,15.0004820302248));
#25865=CARTESIAN_POINT('Ctrl Pts',(33.3370773338915,54.0721923398817,14.895250483473));
#25866=CARTESIAN_POINT('Ctrl Pts',(31.9692358342251,54.2294430763321,14.827064900244));
#25867=CARTESIAN_POINT('Ctrl Pts',(31.4704412404259,54.5116709695925,14.7959252805377));
#25868=CARTESIAN_POINT('Ctrl Pts',(31.4709133820845,54.5092374927209,15.5540747194623));
#25869=CARTESIAN_POINT('Ctrl Pts',(31.4705297975013,54.5094589248369,15.5540505953261));
#25870=CARTESIAN_POINT('Ctrl Pts',(30.8812194784826,54.8499291446222,15.5169805076671));
#25871=CARTESIAN_POINT('Ctrl Pts',(30.074257404191,56.1727516226363,15.4428644564855));
#25872=CARTESIAN_POINT('Ctrl Pts',(31.0845179881232,58.2651696619898,15.3317265659175));
#25873=CARTESIAN_POINT('Ctrl Pts',(33.3903853125313,58.551203914661,15.2205886753495));
#25874=CARTESIAN_POINT('Ctrl Pts',(34.881272858026,56.7690439832157,15.1094507847814));
#25875=CARTESIAN_POINT('Ctrl Pts',(34.192554360499,54.5499210682071,14.9983128942134));
#25876=CARTESIAN_POINT('Ctrl Pts',(32.4784241363503,54.0712848045823,14.913187539107));
#25877=CARTESIAN_POINT('Ctrl Pts',(31.6504081122452,54.4090598663806,14.8651081475233));
#25878=CARTESIAN_POINT('Ctrl Pts',(31.4747795225871,54.5123867379958,14.8540747194623));
#25879=CARTESIAN_POINT('Origin',(32.5,56.2916512459885,23.5459252805377));
#25880=CARTESIAN_POINT('',(31.4717385551609,54.5141703251839,16.2540747194623));
#25881=CARTESIAN_POINT('',(31.4743433646119,54.5114040111285,16.1959252805377));
#25882=CARTESIAN_POINT('',(31.4726249999999,54.5121855475625,23.5459252805377));
#25883=CARTESIAN_POINT('Ctrl Pts',(31.4743433646119,54.5114040111285,16.1959252805377));
#25884=CARTESIAN_POINT('Ctrl Pts',(31.0291266592638,54.7738828820724,16.1679038323268));
#25885=CARTESIAN_POINT('Ctrl Pts',(30.2132159159802,55.7757147456512,16.1028364205933));
#25886=CARTESIAN_POINT('Ctrl Pts',(30.6502037274999,57.8653791294726,16.0007230453371));
#25887=CARTESIAN_POINT('Ctrl Pts',(32.8189508948268,58.6992716537698,15.8895851547691));
#25888=CARTESIAN_POINT('Ctrl Pts',(34.6957586912586,57.3294419144583,15.778447264201));
#25889=CARTESIAN_POINT('Ctrl Pts',(34.5627636554058,55.0097106071378,15.667309373633));
#25890=CARTESIAN_POINT('Ctrl Pts',(32.8501896837687,54.0383319846292,15.5731353790785));
#25891=CARTESIAN_POINT('Ctrl Pts',(31.7961776179314,54.3299915352064,15.5160073480468));
#25892=CARTESIAN_POINT('Ctrl Pts',(31.4738352212016,54.515219664308,15.4959252805377));
#25893=CARTESIAN_POINT('Ctrl Pts',(31.4717385551609,54.5141703251839,16.2540747194623));
#25894=CARTESIAN_POINT('Ctrl Pts',(31.2936631692287,54.6150534746527,16.2429930431288));
#25895=CARTESIAN_POINT('Ctrl Pts',(30.586678710615,55.1642906384242,16.1948654032726));
#25896=CARTESIAN_POINT('Ctrl Pts',(30.1461151763815,56.8896399584928,16.1096917998938));
#25897=CARTESIAN_POINT('Ctrl Pts',(31.7257879044833,58.5935982250311,15.9985539093258));
#25898=CARTESIAN_POINT('Ctrl Pts',(34.0141057438103,58.1905583158083,15.8874160187577));
#25899=CARTESIAN_POINT('Ctrl Pts',(34.9165454246276,56.0494272304867,15.7762781281897));
#25900=CARTESIAN_POINT('Ctrl Pts',(33.6073779089676,54.1304231724864,15.6651643617579));
#25901=CARTESIAN_POINT('Ctrl Pts',(32.0595772284103,54.1694191401902,15.5910965588487));
#25902=CARTESIAN_POINT('Ctrl Pts',(31.4709133820845,54.5092374927209,15.5540747194623));
#25903=CARTESIAN_POINT('Origin',(32.5,56.2916512459885,23.5459252805377));
#25904=CARTESIAN_POINT('',(31.4749299874422,54.5140996860483,16.9540747194623));
#25905=CARTESIAN_POINT('',(31.4704693279511,54.5098093620654,16.8959252805377));
#25906=CARTESIAN_POINT('',(31.4726249999999,54.5121855475625,23.5459252805377));
#25907=CARTESIAN_POINT('Ctrl Pts',(31.4704693279511,54.5098093620654,16.8959252805377));
#25908=CARTESIAN_POINT('Ctrl Pts',(31.4380523744924,54.528339714304,16.8938922436523));
#25909=CARTESIAN_POINT('Ctrl Pts',(30.8255360958299,54.9025793613845,16.8548132432442));
#25910=CARTESIAN_POINT('Ctrl Pts',(30.0713767023175,56.3040842326063,16.7786882793134));
#25911=CARTESIAN_POINT('Ctrl Pts',(31.1932955779139,58.3388173981362,16.6675503887454));
#25912=CARTESIAN_POINT('Ctrl Pts',(33.5112558300795,58.4997561681628,16.5564124981773));
#25913=CARTESIAN_POINT('Ctrl Pts',(34.9036021525568,56.6395914613089,16.4452746076093));
#25914=CARTESIAN_POINT('Ctrl Pts',(34.0959041660874,54.4609531294646,16.3341367170413));
#25915=CARTESIAN_POINT('Ctrl Pts',(32.3994057229947,54.0847909276367,16.251020274684));
#25916=CARTESIAN_POINT('Ctrl Pts',(31.6177287080201,54.4268707431815,16.2049497958495));
#25917=CARTESIAN_POINT('Ctrl Pts',(31.4743433646119,54.5114040111285,16.1959252805377));
#25918=CARTESIAN_POINT('Ctrl Pts',(31.4749299874422,54.5140996860483,16.9540747194623));
#25919=CARTESIAN_POINT('Ctrl Pts',(31.1211066997161,54.7205458521634,16.9319354909316));
#25920=CARTESIAN_POINT('Ctrl Pts',(30.3290943933324,55.5443071105387,16.8727502988782));
#25921=CARTESIAN_POINT('Ctrl Pts',(30.4251293279101,57.5539016004218,16.776519143302));
#25922=CARTESIAN_POINT('Ctrl Pts',(32.4351932585659,58.7194412594432,16.665381252734));
#25923=CARTESIAN_POINT('Ctrl Pts',(34.5045755346152,57.6627971861383,16.554243362166));
#25924=CARTESIAN_POINT('Ctrl Pts',(34.7391470903975,55.3511276839614,16.4431054715979));
#25925=CARTESIAN_POINT('Ctrl Pts',(33.1051720185616,54.0449906258011,16.3430492573634));
#25926=CARTESIAN_POINT('Ctrl Pts',(31.8889678914564,54.277801838456,16.2800390066515));
#25927=CARTESIAN_POINT('Ctrl Pts',(31.4717385551609,54.5141703251839,16.2540747194623));
#25928=CARTESIAN_POINT('Origin',(32.5,56.2916512459885,23.5459252805377));
#25929=CARTESIAN_POINT('',(31.4724078687478,54.5094050924838,17.6540747194623));
#25930=CARTESIAN_POINT('',(31.4724615607262,54.5148044353696,17.5959252805377));
#25931=CARTESIAN_POINT('',(31.4726249999999,54.5121855475625,23.5459252805377));
#25932=CARTESIAN_POINT('Ctrl Pts',(31.4724615607262,54.5148044353696,17.5959252805377));
#25933=CARTESIAN_POINT('Ctrl Pts',(31.2620673353104,54.6344533407431,17.582834691455));
#25934=CARTESIAN_POINT('Ctrl Pts',(30.5366971614125,55.228195386795,17.5326981388497));
#25935=CARTESIAN_POINT('Ctrl Pts',(30.181891163842,57.0160386595509,17.4455156227217));
#25936=CARTESIAN_POINT('Ctrl Pts',(31.8513854749211,58.6320924221469,17.3343777321536));
#25937=CARTESIAN_POINT('Ctrl Pts',(34.1145640165938,58.105913833797,17.2232398415856));
#25938=CARTESIAN_POINT('Ctrl Pts',(34.899913803477,55.9191201236888,17.1121019510176));
#25939=CARTESIAN_POINT('Ctrl Pts',(33.5144124105784,54.1070736669905,17.0029970973349));
#25940=CARTESIAN_POINT('Ctrl Pts',(32.0287535486679,54.190679951206,16.930938207175));
#25941=CARTESIAN_POINT('Ctrl Pts',(31.4704693279511,54.5098093620654,16.8959252805377));
#25942=CARTESIAN_POINT('Ctrl Pts',(31.4724078687478,54.5094050924838,17.6540747194623));
#25943=CARTESIAN_POINT('Ctrl Pts',(30.9460948709879,54.8181696162505,17.6208779387343));
#25944=CARTESIAN_POINT('Ctrl Pts',(30.1270731190026,55.9965693019247,17.5506351944836));
#25945=CARTESIAN_POINT('Ctrl Pts',(30.8867448926705,58.1070774278645,17.4433464867103));
#25946=CARTESIAN_POINT('Ctrl Pts',(33.1503020054966,58.6316238024116,17.3322085961423));
#25947=CARTESIAN_POINT('Ctrl Pts',(34.8186303177654,57.0143667589708,17.2210707055742));
#25948=CARTESIAN_POINT('Ctrl Pts',(34.3646900051272,54.7356000103461,17.1099328150062));
#25949=CARTESIAN_POINT('Ctrl Pts',(32.6344025598171,54.051324400594,17.0209341529688));
#25950=CARTESIAN_POINT('Ctrl Pts',(31.7131654786556,54.375095823104,16.9689814544542));
#25951=CARTESIAN_POINT('Ctrl Pts',(31.4749299874422,54.5140996860483,16.9540747194623));
#25952=CARTESIAN_POINT('Origin',(32.5,56.2916512459885,23.5459252805377));
#25953=CARTESIAN_POINT('',(31.470650904959,54.5123645943458,18.3540747194623));
#25954=CARTESIAN_POINT('',(31.4749676053556,54.5132671274454,18.2959252805377));
#25955=CARTESIAN_POINT('',(31.4726249999999,54.5121855475625,23.5459252805377));
#25956=CARTESIAN_POINT('Ctrl Pts',(31.4749676053556,54.5132671274454,18.2959252805377));
#25957=CARTESIAN_POINT('Ctrl Pts',(31.0898434852659,54.7390742900298,18.2717771392578));
#25958=CARTESIAN_POINT('Ctrl Pts',(30.2875910450901,55.6209976925706,18.2105830344552));
#25959=CARTESIAN_POINT('Ctrl Pts',(30.4964134968881,57.664242527379,18.1123429661299));
#25960=CARTESIAN_POINT('Ctrl Pts',(32.5665574496276,58.7193941910096,18.0012050755619));
#25961=CARTESIAN_POINT('Ctrl Pts',(34.57578061391,57.552405204585,17.8900671849938));
#25962=CARTESIAN_POINT('Ctrl Pts',(34.6850182413274,55.2314338219344,17.7789292944258));
#25963=CARTESIAN_POINT('Ctrl Pts',(33.0169876554982,54.0399676860015,17.6808819929404));
#25964=CARTESIAN_POINT('Ctrl Pts',(31.8574765068094,54.2958506272969,17.6198806549777));
#25965=CARTESIAN_POINT('Ctrl Pts',(31.4724615607262,54.5148044353696,17.5959252805377));
#25966=CARTESIAN_POINT('Ctrl Pts',(31.470650904959,54.5123645943458,18.3540747194623));
#25967=CARTESIAN_POINT('Ctrl Pts',(31.3550533194394,54.5776997670471,18.3468663500598));
#25968=CARTESIAN_POINT('Ctrl Pts',(30.6863525478933,55.0471677720896,18.3026120171345));
#25969=CARTESIAN_POINT('Ctrl Pts',(30.0966496704334,56.6413246029078,18.2213117206866));
#25970=CARTESIAN_POINT('Ctrl Pts',(31.4903368545417,58.5004845570079,18.1101738301185));
#25971=CARTESIAN_POINT('Ctrl Pts',(33.8081801660464,58.3378743316585,17.9990359395505));
#25972=CARTESIAN_POINT('Ctrl Pts',(34.9286313357969,56.3023329102471,17.8878980489824));
#25973=CARTESIAN_POINT('Ctrl Pts',(33.8261287013398,54.2570144404017,17.7767601584144));
#25974=CARTESIAN_POINT('Ctrl Pts',(32.2016889552716,54.1286817447541,17.6988190485744));
#25975=CARTESIAN_POINT('Ctrl Pts',(31.5334341156057,54.4736036964922,17.657923902257));
#25976=CARTESIAN_POINT('Ctrl Pts',(31.4724078687478,54.5094050924838,17.6540747194623));
#25977=CARTESIAN_POINT('Origin',(32.5,56.2916512459885,23.5459252805377));
#25978=CARTESIAN_POINT('',(31.4742218141003,54.5151075144861,19.0540747194623));
#25979=CARTESIAN_POINT('',(31.4715682025536,54.5091203612934,18.9959252805377));
#25980=CARTESIAN_POINT('',(31.4726249999999,54.5121855475625,23.5459252805377));
#25981=CARTESIAN_POINT('Ctrl Pts',(31.4715682025535,54.5091203612934,18.9959252805377));
#25982=CARTESIAN_POINT('Ctrl Pts',(30.9129158471523,54.834613753627,18.9607195870605));
#25983=CARTESIAN_POINT('Ctrl Pts',(30.0982487947041,56.0866128816227,18.8884679300607));
#25984=CARTESIAN_POINT('Ctrl Pts',(30.9872637967357,58.1916498987633,18.7791703095382));
#25985=CARTESIAN_POINT('Ctrl Pts',(33.275871958361,58.5930396107435,18.6680324189701));
#25986=CARTESIAN_POINT('Ctrl Pts',(34.8543157175076,56.8879424529462,18.5568945284021));
#25987=CARTESIAN_POINT('Ctrl Pts',(34.2778276006656,54.6370531910173,18.445756637834));
#25988=CARTESIAN_POINT('Ctrl Pts',(32.5529073535807,54.0606456221556,18.3587668885459));
#25989=CARTESIAN_POINT('Ctrl Pts',(31.6806671821781,54.3926607167737,18.3088231027804));
#25990=CARTESIAN_POINT('Ctrl Pts',(31.4749676053556,54.5132671274454,18.2959252805377));
#25991=CARTESIAN_POINT('Ctrl Pts',(31.4742218141003,54.5151075144861,19.0540747194623));
#25992=CARTESIAN_POINT('Ctrl Pts',(31.1812845288231,54.6841025371816,19.0358087978625));
#25993=CARTESIAN_POINT('Ctrl Pts',(30.4141219270718,55.4032020294196,18.98049691274));
#25994=CARTESIAN_POINT('Ctrl Pts',(30.3049905142645,57.3310249135316,18.8881390640948));
#25995=CARTESIAN_POINT('Ctrl Pts',(32.1827853990159,58.6995007346589,18.7770011735268));
#25996=CARTESIAN_POINT('Ctrl Pts',(34.3509304054687,57.8640446119295,18.6658632829587));
#25997=CARTESIAN_POINT('Ctrl Pts',(34.8248978208363,55.5893590092039,18.5547253923907));
#25998=CARTESIAN_POINT('Ctrl Pts',(33.2781402858533,54.0633320127348,18.4507958712252));
#25999=CARTESIAN_POINT('Ctrl Pts',(31.9491438407913,54.2419227987112,18.3839123135824));
#26000=CARTESIAN_POINT('Ctrl Pts',(31.470650904959,54.5123645943458,18.3540747194623));
#26001=CARTESIAN_POINT('Origin',(32.5,56.2916512459885,23.5459252805377));
#26002=CARTESIAN_POINT('',(31.4739455702221,54.5107934605777,19.7540747194623));
#26003=CARTESIAN_POINT('',(31.471143914755,54.5133742931913,19.6959252805377));
#26004=CARTESIAN_POINT('',(31.4726249999999,54.5121855475625,23.5459252805377));
#26005=CARTESIAN_POINT('Ctrl Pts',(31.471143914755,54.5133742931914,19.6959252805377));
#26006=CARTESIAN_POINT('Ctrl Pts',(31.3231329415045,54.5970512593892,19.686707998386));
#26007=CARTESIAN_POINT('Ctrl Pts',(30.6341370241162,55.106929574873,19.6404447527115));
#26008=CARTESIAN_POINT('Ctrl Pts',(30.1190717238489,56.77076109083,19.5571355435145));
#26009=CARTESIAN_POINT('Ctrl Pts',(31.6112442101669,58.5518456729879,19.4459976529464));
#26010=CARTESIAN_POINT('Ctrl Pts',(33.9169049506455,58.2641486635057,19.3348597623784));
#26011=CARTESIAN_POINT('Ctrl Pts',(34.9256565207284,56.1710023982575,19.2237218718104));
#26012=CARTESIAN_POINT('Ctrl Pts',(33.71417716871,54.1882873915237,19.1125839812423));
#26013=CARTESIAN_POINT('Ctrl Pts',(32.1271617475077,54.1490140977469,19.0366517841514));
#26014=CARTESIAN_POINT('Ctrl Pts',(31.5007700473113,54.4921061888466,18.9977655505832));
#26015=CARTESIAN_POINT('Ctrl Pts',(31.4715682025535,54.5091203612934,18.9959252805377));
#26016=CARTESIAN_POINT('Ctrl Pts',(31.4739455702221,54.5107934605777,19.7540747194623));
#26017=CARTESIAN_POINT('Ctrl Pts',(31.0084978875972,54.7852778310984,19.7247512456653));
#26018=CARTESIAN_POINT('Ctrl Pts',(30.190033600511,55.8297589120184,19.6583818083455));
#26019=CARTESIAN_POINT('Ctrl Pts',(30.7065057264144,57.9292539322016,19.5549664075031));
#26020=CARTESIAN_POINT('Ctrl Pts',(32.9031507850421,58.6866113101155,19.443828516935));
#26021=CARTESIAN_POINT('Ctrl Pts',(34.7307873556619,57.2518345802401,19.332690626367));
#26022=CARTESIAN_POINT('Ctrl Pts',(34.5165589620033,54.9381911555042,19.221552735799));
#26023=CARTESIAN_POINT('Ctrl Pts',(32.7951211292858,54.0400334340294,19.1286807668307));
#26024=CARTESIAN_POINT('Ctrl Pts',(31.7754042355957,54.3413558867002,19.0728547613852));
#26025=CARTESIAN_POINT('Ctrl Pts',(31.4742218141003,54.5151075144861,19.0540747194623));
#26026=CARTESIAN_POINT('Origin',(32.5,56.2916512459885,23.5459252805377));
#26027=CARTESIAN_POINT('',(31.4703419245392,54.5103623955759,20.4540747194623));
#26028=CARTESIAN_POINT('',(31.4746836284318,54.5147000883656,20.3959252805377));
#26029=CARTESIAN_POINT('',(31.4726249999999,54.5121855475625,23.5459252805377));
#26030=CARTESIAN_POINT('Ctrl Pts',(31.4746836284318,54.5147000883656,20.3959252805377));
#26031=CARTESIAN_POINT('Ctrl Pts',(31.1500699868132,54.7031080152175,20.3756504461887));
#26032=CARTESIAN_POINT('Ctrl Pts',(30.3692379110719,55.4752841065875,20.318329648317));
#26033=CARTESIAN_POINT('Ctrl Pts',(30.364399598909,57.4481876795404,20.2239628869227));
#26034=CARTESIAN_POINT('Ctrl Pts',(32.3134406037768,58.7131304053242,20.1128249963547));
#26035=CARTESIAN_POINT('Ctrl Pts',(34.4332415751289,57.7616657784424,20.0016871057866));
#26036=CARTESIAN_POINT('Ctrl Pts',(34.7835245906331,55.4646801872418,19.8905492152186));
#26037=CARTESIAN_POINT('Ctrl Pts',(33.187967321057,54.052355442598,19.7886286068023));
#26038=CARTESIAN_POINT('Ctrl Pts',(31.9180164468304,54.2607380396757,19.7237539619086));
#26039=CARTESIAN_POINT('Ctrl Pts',(31.471143914755,54.5133742931914,19.6959252805377));
#26040=CARTESIAN_POINT('Ctrl Pts',(31.4703419245392,54.5103623955759,20.4540747194623));
#26041=CARTESIAN_POINT('Ctrl Pts',(31.4170740978156,54.5406699166123,20.4507396569907));
#26042=CARTESIAN_POINT('Ctrl Pts',(30.7899238920755,54.9377208245812,20.4103586309964));
#26043=CARTESIAN_POINT('Ctrl Pts',(30.0733055503939,56.3892087930031,20.3329316414794));
#26044=CARTESIAN_POINT('Ctrl Pts',(31.2658594095642,58.3833638027877,20.2217937509113));
#26045=CARTESIAN_POINT('Ctrl Pts',(33.5880364581139,58.4629506390537,20.1106558603433));
#26046=CARTESIAN_POINT('Ctrl Pts',(34.914321242052,56.5551224909764,19.9995179697752));
#26047=CARTESIAN_POINT('Ctrl Pts',(34.0307504904903,54.406136137217,19.8883800792072));
#26048=CARTESIAN_POINT('Ctrl Pts',(32.3488749925858,54.0946310730832,19.8065656624362));
#26049=CARTESIAN_POINT('Ctrl Pts',(31.5965236444215,54.4385065703594,19.7617972091879));
#26050=CARTESIAN_POINT('Ctrl Pts',(31.4739455702221,54.5107934605777,19.7540747194623));
#26051=CARTESIAN_POINT('Origin',(32.5,56.2916512459885,23.5459252805377));
#26052=CARTESIAN_POINT('',(31.4729484072307,54.5150696468519,21.1540747194623));
#26053=CARTESIAN_POINT('',(31.4731950477465,54.5099653993635,21.0959252805377));
#26054=CARTESIAN_POINT('',(31.4726249999999,54.5121855475625,23.5459252805377));
#26055=CARTESIAN_POINT('Ctrl Pts',(31.4731950477465,54.5099653993635,21.0959252805377));
#26056=CARTESIAN_POINT('Ctrl Pts',(30.9763557896561,54.8025287224184,21.0645928939914));
#26057=CARTESIAN_POINT('Ctrl Pts',(30.1562124434263,55.91515240492,20.9962145439225));
#26058=CARTESIAN_POINT('Ctrl Pts',(30.7976747113088,58.0238313492005,20.890790230331));
#26059=CARTESIAN_POINT('Ctrl Pts',(33.0320547584019,58.6613103307746,20.7796523397629));
#26060=CARTESIAN_POINT('Ctrl Pts',(34.7794413280769,57.1298124049937,20.6685144491949));
#26061=CARTESIAN_POINT('Ctrl Pts',(34.4404282620852,54.8311366011664,20.5573765586268));
#26062=CARTESIAN_POINT('Ctrl Pts',(32.711178041167,54.0447560839335,20.4665135024078));
#26063=CARTESIAN_POINT('Ctrl Pts',(31.7432006097017,54.3588510380505,20.4126964097114));
#26064=CARTESIAN_POINT('Ctrl Pts',(31.4746836284318,54.5147000883656,20.3959252805377));
#26065=CARTESIAN_POINT('Ctrl Pts',(31.4729484072307,54.5150696468519,21.1540747194623));
#26066=CARTESIAN_POINT('Ctrl Pts',(31.2416713093181,54.6470066065867,21.1396821047934));
#26067=CARTESIAN_POINT('Ctrl Pts',(30.5049700979161,55.27079766484,21.0882435266019));
#26068=CARTESIAN_POINT('Ctrl Pts',(30.2087196709517,57.0968534624393,20.9997589848876));
#26069=CARTESIAN_POINT('Ctrl Pts',(31.9338196700205,58.6533891775714,20.8886210943196));
#26070=CARTESIAN_POINT('Ctrl Pts',(34.1771709144469,58.0482026788783,20.7774832037515));
#26071=CARTESIAN_POINT('Ctrl Pts',(34.8853786224564,55.8352230845946,20.6663453131835));
#26072=CARTESIAN_POINT('Ctrl Pts',(33.4544940412401,54.0938892869953,20.5585424850871));
#26073=CARTESIAN_POINT('Ctrl Pts',(32.0087745479626,54.2040131588077,20.4877856205134));
#26074=CARTESIAN_POINT('Ctrl Pts',(31.4703419245392,54.5103623955759,20.4540747194623));
#26075=CARTESIAN_POINT('Origin',(32.5,56.2916512459885,23.5459252805377));
#26076=CARTESIAN_POINT('',(31.4756555660462,54.5128362942924,21.8540747194623));
#26077=CARTESIAN_POINT('',(31.4704151231924,54.5113563798656,21.7959252805377));
#26078=CARTESIAN_POINT('',(31.4726249999999,54.5121855475625,23.5459252805377));
#26079=CARTESIAN_POINT('',(33.9541262883781,54.8399232067374,22.));
#26080=CARTESIAN_POINT('Ctrl Pts',(33.9541262883781,54.8399232067375,22.));
#26081=CARTESIAN_POINT('Ctrl Pts',(33.4713921772736,54.3563916207415,21.9629540364773));
#26082=CARTESIAN_POINT('Ctrl Pts',(32.5011748783928,54.0682382375652,21.9143122762981));
#26083=CARTESIAN_POINT('Ctrl Pts',(31.6603808354701,54.4043184181514,21.8656705161189));
#26084=CARTESIAN_POINT('Ctrl Pts',(31.4756555660462,54.5128362942924,21.8540747194623));
#26085=CARTESIAN_POINT('',(34.4879501863793,55.7574173922323,22.));
#26086=CARTESIAN_POINT('Origin',(32.5,56.2916512459885,22.));
#26087=CARTESIAN_POINT('Ctrl Pts',(34.4879524958972,55.7574168944053,22.));
#26088=CARTESIAN_POINT('Ctrl Pts',(34.3140194691063,55.1135181402384,21.9636770818144));
#26089=CARTESIAN_POINT('Ctrl Pts',(33.3475254337068,54.0782693974497,21.895652175327));
#26090=CARTESIAN_POINT('Ctrl Pts',(31.9778124788844,54.224015012867,21.8276272688396));
#26091=CARTESIAN_POINT('Ctrl Pts',(31.4704151231923,54.5113563798656,21.7959252805377));
#26092=CARTESIAN_POINT('Origin',(-32.5,56.2916512459885,17.));
#26093=CARTESIAN_POINT('',(-31.665169034441,54.8481104542882,13.8714803633902));
#26094=CARTESIAN_POINT('',(-31.6668355785528,54.8466294620446,13.6785196366098));
#26095=CARTESIAN_POINT('',(-31.667,54.8488529232836,17.));
#26096=CARTESIAN_POINT('',(-31.4059736530045,55.03520293743,13.));
#26097=CARTESIAN_POINT('Ctrl Pts',(-31.6668355785528,54.8466294620446,13.6785196366098));
#26098=CARTESIAN_POINT('Ctrl Pts',(-31.7169359983484,54.8172333383902,13.6746222055426));
#26099=CARTESIAN_POINT('Ctrl Pts',(-31.7685916060498,54.790608714332,13.6707247744754));
#26100=CARTESIAN_POINT('Ctrl Pts',(-31.8215990010623,54.7670212268678,13.6668273434082));
#26101=CARTESIAN_POINT('Ctrl Pts',(-32.3254462758995,54.5428168252686,13.6297813798856));
#26102=CARTESIAN_POINT('Ctrl Pts',(-32.951426619549,54.5930156597358,13.5927354163629));
#26103=CARTESIAN_POINT('Ctrl Pts',(-33.413026316092,54.8947720750737,13.5556894528402));
#26104=CARTESIAN_POINT('Ctrl Pts',(-33.8746260126349,55.1965284904116,13.5186434893175));
#26105=CARTESIAN_POINT('Ctrl Pts',(-34.1718450620713,55.74984248662,13.4815975257948));
#26106=CARTESIAN_POINT('Ctrl Pts',(-34.1687200176702,56.3012302340885,13.4445515622722));
#26107=CARTESIAN_POINT('Ctrl Pts',(-34.165594973269,56.852617981557,13.4075055987495));
#26108=CARTESIAN_POINT('Ctrl Pts',(-33.8621258350302,57.4020794802856,13.3704596352268));
#26109=CARTESIAN_POINT('Ctrl Pts',(-33.397076207884,57.6986656733007,13.3334136717041));
#26110=CARTESIAN_POINT('Ctrl Pts',(-32.9320265807378,57.9952518663159,13.2963677081814));
#26111=CARTESIAN_POINT('Ctrl Pts',(-32.3053964646841,58.0389627536176,13.2593217446587));
#26112=CARTESIAN_POINT('Ctrl Pts',(-31.8042046430419,57.8087421867188,13.2222757811361));
#26113=CARTESIAN_POINT('Ctrl Pts',(-31.3030128213997,57.5785216198199,13.1852298176134));
#26114=CARTESIAN_POINT('Ctrl Pts',(-30.927259294169,57.0743695987204,13.1481838540907));
#26115=CARTESIAN_POINT('Ctrl Pts',(-30.8485497633826,56.5294873752105,13.111137890568));
#26116=CARTESIAN_POINT('Ctrl Pts',(-30.7698402325962,55.9846051517008,13.0740919270453));
#26117=CARTESIAN_POINT('Ctrl Pts',(-30.9881746982541,55.3989927257806,13.0370459635227));
#26118=CARTESIAN_POINT('Ctrl Pts',(-31.4059736530044,55.03520293743,13.));
#26119=CARTESIAN_POINT('',(-33.9184188470959,55.4120275291384,13.));
#26120=CARTESIAN_POINT('Origin',(-32.5,56.2916512459885,13.));
#26121=CARTESIAN_POINT('',(-31.6677099856843,54.8513822049942,13.1714803633902));
#26122=CARTESIAN_POINT('Ctrl Pts',(-33.9184205240577,55.4120266023846,13.));
#26123=CARTESIAN_POINT('Ctrl Pts',(-33.6328154176796,54.9528086674659,13.0363229181856));
#26124=CARTESIAN_POINT('Ctrl Pts',(-33.1028950308971,54.6443333840239,13.0726458363711));
#26125=CARTESIAN_POINT('Ctrl Pts',(-32.5624622032656,54.6241575874771,13.1089687545567));
#26126=CARTESIAN_POINT('Ctrl Pts',(-32.2524345659017,54.6125834302173,13.1298059575012));
#26127=CARTESIAN_POINT('Ctrl Pts',(-31.9389473679306,54.6958863393048,13.1506431604457));
#26128=CARTESIAN_POINT('Ctrl Pts',(-31.6677099856843,54.8513822049942,13.1714803633902));
#26129=CARTESIAN_POINT('',(-31.667,54.8488529232836,12.));
#26130=CARTESIAN_POINT('',(-31.667,54.8488529232836,17.));
#26131=CARTESIAN_POINT('Origin',(-32.5,56.2916512459885,12.));
#26132=CARTESIAN_POINT('Ctrl Pts',(-31.6677099856843,54.8513822049942,13.1714803633902));
#26133=CARTESIAN_POINT('Ctrl Pts',(-31.456720929217,54.9723387107481,13.1876891239684));
#26134=CARTESIAN_POINT('Ctrl Pts',(-31.2712968605908,55.1369785326558,13.2038978845465));
#26135=CARTESIAN_POINT('Ctrl Pts',(-31.1329525371814,55.334624580881,13.2201066451247));
#26136=CARTESIAN_POINT('Ctrl Pts',(-30.8167594060732,55.7863548817661,13.2571526086474));
#26137=CARTESIAN_POINT('Ctrl Pts',(-30.74649897558,56.4105013743272,13.2941985721701));
#26138=CARTESIAN_POINT('Ctrl Pts',(-30.9545219587097,56.9212436588755,13.3312445356927));
#26139=CARTESIAN_POINT('Ctrl Pts',(-31.1625449418395,57.4319859434239,13.3682904992154));
#26140=CARTESIAN_POINT('Ctrl Pts',(-31.6488513385922,57.8293240199595,13.4053364627381));
#26141=CARTESIAN_POINT('Ctrl Pts',(-32.1907825642961,57.9315018386831,13.4423824262608));
#26142=CARTESIAN_POINT('Ctrl Pts',(-32.73271379,58.0336796574067,13.4794283897835));
#26143=CARTESIAN_POINT('Ctrl Pts',(-33.3302698446549,57.8406972183184,13.5164743533061));
#26144=CARTESIAN_POINT('Ctrl Pts',(-33.7100246193121,57.4408300847798,13.5535203168288));
#26145=CARTESIAN_POINT('Ctrl Pts',(-34.0897793939694,57.0409629512412,13.5905662803515));
#26146=CARTESIAN_POINT('Ctrl Pts',(-34.2517328886288,56.4342111232524,13.6276122438742));
#26147=CARTESIAN_POINT('Ctrl Pts',(-34.1217417856583,55.8982799679713,13.6646582073969));
#26148=CARTESIAN_POINT('Ctrl Pts',(-33.9917506826877,55.3623488126902,13.7017041709196));
#26149=CARTESIAN_POINT('Ctrl Pts',(-33.5698149820872,54.8972383301168,13.7387501344422));
#26150=CARTESIAN_POINT('Ctrl Pts',(-33.0490481303448,54.7157980032898,13.7757960979649));
#26151=CARTESIAN_POINT('Ctrl Pts',(-32.6006934475977,54.5595867930335,13.8076908531067));
#26152=CARTESIAN_POINT('Ctrl Pts',(-32.0790815152818,54.6136422361012,13.8395856082484));
#26153=CARTESIAN_POINT('Ctrl Pts',(-31.665169034441,54.8481104542882,13.8714803633902));
#26154=CARTESIAN_POINT('Origin',(-32.5,56.2916512459885,17.));
#26155=CARTESIAN_POINT('',(-31.6675239681331,54.8471109129233,14.5714803633902));
#26156=CARTESIAN_POINT('',(-31.6688656529171,54.8504196807178,14.3785196366098));
#26157=CARTESIAN_POINT('',(-31.667,54.8488529232836,17.));
#26158=CARTESIAN_POINT('Ctrl Pts',(-31.6688656529171,54.8504196807178,14.3785196366098));
#26159=CARTESIAN_POINT('Ctrl Pts',(-31.8626626794392,54.7373590837469,14.3635646533453));
#26160=CARTESIAN_POINT('Ctrl Pts',(-32.0777548846389,54.6619147081679,14.3486096700809));
#26161=CARTESIAN_POINT('Ctrl Pts',(-32.2987508779934,54.6350670487033,14.3336546868165));
#26162=CARTESIAN_POINT('Ctrl Pts',(-32.8461944534029,54.5685609620293,14.2966087232938));
#26163=CARTESIAN_POINT('Ctrl Pts',(-33.4298657229247,54.8002611998549,14.2595627597711));
#26164=CARTESIAN_POINT('Ctrl Pts',(-33.7826437493636,55.2241308285784,14.2225167962484));
#26165=CARTESIAN_POINT('Ctrl Pts',(-34.1354217758025,55.648000457302,14.1854708327258));
#26166=CARTESIAN_POINT('Ctrl Pts',(-34.2573065591586,56.2640394769235,14.1484248692031));
#26167=CARTESIAN_POINT('Ctrl Pts',(-34.0925177799173,56.7903101462247,14.1113789056804));
#26168=CARTESIAN_POINT('Ctrl Pts',(-33.9277290006759,57.316580815526,14.0743329421577));
#26169=CARTESIAN_POINT('Ctrl Pts',(-33.4762666588371,57.7530831345071,14.037286978635));
#26170=CARTESIAN_POINT('Ctrl Pts',(-32.9447431684491,57.9000573283161,14.0002410151124));
#26171=CARTESIAN_POINT('Ctrl Pts',(-32.4132196780611,58.0470315221252,13.9631950515897));
#26172=CARTESIAN_POINT('Ctrl Pts',(-31.8016350391239,57.9044775907622,13.926149088067));
#26173=CARTESIAN_POINT('Ctrl Pts',(-31.3898882053201,57.5376201658139,13.8891031245443));
#26174=CARTESIAN_POINT('Ctrl Pts',(-30.9781413715162,57.1707627408656,13.8520571610216));
#26175=CARTESIAN_POINT('Ctrl Pts',(-30.7662323428457,56.579601822332,13.815011197499));
#26176=CARTESIAN_POINT('Ctrl Pts',(-30.8511349315229,56.0347175442324,13.7779652339763));
#26177=CARTESIAN_POINT('Ctrl Pts',(-30.9271053193521,55.5471579706766,13.7448167015208));
#26178=CARTESIAN_POINT('Ctrl Pts',(-31.2407201802287,55.0966501403397,13.7116681690653));
#26179=CARTESIAN_POINT('Ctrl Pts',(-31.6668355785528,54.8466294620446,13.6785196366098));
#26180=CARTESIAN_POINT('Ctrl Pts',(-31.665169034441,54.8481104542882,13.8714803633902));
#26181=CARTESIAN_POINT('Ctrl Pts',(-31.5983195028865,54.885978581672,13.8766315717711));
#26182=CARTESIAN_POINT('Ctrl Pts',(-31.5342792394079,54.92855265549,13.881782780152));
#26183=CARTESIAN_POINT('Ctrl Pts',(-31.4738105761083,54.9757069077013,13.886933988533));
#26184=CARTESIAN_POINT('Ctrl Pts',(-31.0389378764983,55.3148263100205,13.9239799520556));
#26185=CARTESIAN_POINT('Ctrl Pts',(-30.7887904801626,55.8908352857396,13.9610259155783));
#26186=CARTESIAN_POINT('Ctrl Pts',(-30.83785280129,56.4401173240505,13.998071879101));
#26187=CARTESIAN_POINT('Ctrl Pts',(-30.8869151224175,56.9893993623614,14.0351178426237));
#26188=CARTESIAN_POINT('Ctrl Pts',(-31.235187161008,57.5119544632642,14.0721638061464));
#26189=CARTESIAN_POINT('Ctrl Pts',(-31.72327872518,57.7686336889847,14.109209769669));
#26190=CARTESIAN_POINT('Ctrl Pts',(-32.2113702893519,58.0253129147052,14.1462557331917));
#26191=CARTESIAN_POINT('Ctrl Pts',(-32.8392813791053,58.0161162652434,14.1833016967144));
#26192=CARTESIAN_POINT('Ctrl Pts',(-33.3196456823451,57.7452519563499,14.2203476602371));
#26193=CARTESIAN_POINT('Ctrl Pts',(-33.8000099855849,57.4743876474564,14.2573936237598));
#26194=CARTESIAN_POINT('Ctrl Pts',(-34.1328275023111,56.9418556791311,14.2944395872824));
#26195=CARTESIAN_POINT('Ctrl Pts',(-34.1657820298073,56.3913726675535,14.3314855508051));
#26196=CARTESIAN_POINT('Ctrl Pts',(-34.1987365573035,55.8408896559759,14.3685315143278));
#26197=CARTESIAN_POINT('Ctrl Pts',(-33.9318280955697,55.2724556011459,14.4055774778505));
#26198=CARTESIAN_POINT('Ctrl Pts',(-33.4872090049183,54.9462174010391,14.4426234413732));
#26199=CARTESIAN_POINT('Ctrl Pts',(-33.0425899142668,54.6199792009323,14.4796694048958));
#26200=CARTESIAN_POINT('Ctrl Pts',(-32.4202601946978,54.5359368555486,14.5167153684185));
#26201=CARTESIAN_POINT('Ctrl Pts',(-31.9050324766411,54.7325529059597,14.5537613319412));
#26202=CARTESIAN_POINT('Ctrl Pts',(-31.8228882493844,54.7638999646704,14.5596676757575));
#26203=CARTESIAN_POINT('Ctrl Pts',(-31.7434664303386,54.8023810331132,14.5655740195739));
#26204=CARTESIAN_POINT('Ctrl Pts',(-31.6675239681331,54.8471109129233,14.5714803633902));
#26205=CARTESIAN_POINT('Origin',(-32.5,56.2916512459885,17.));
#26206=CARTESIAN_POINT('',(-31.6686398531931,54.8509327367609,15.2714803633902));
#26207=CARTESIAN_POINT('',(-31.6662678127889,54.8504473245041,15.0785196366098));
#26208=CARTESIAN_POINT('',(-31.667,54.8488529232836,17.));
#26209=CARTESIAN_POINT('Ctrl Pts',(-31.6662678127889,54.8504473245041,15.0785196366098));
#26210=CARTESIAN_POINT('Ctrl Pts',(-32.0051837911953,54.6584589297703,15.0525071011481));
#26211=CARTESIAN_POINT('Ctrl Pts',(-32.4124263355195,54.5807898609867,15.0264945656864));
#26212=CARTESIAN_POINT('Ctrl Pts',(-32.7936098272491,54.6489198132192,15.0004820302247));
#26213=CARTESIAN_POINT('Ctrl Pts',(-33.3364753910795,54.745947637705,14.9634360667021));
#26214=CARTESIAN_POINT('Ctrl Pts',(-33.8264872979809,55.138688877304,14.9263901031794));
#26215=CARTESIAN_POINT('Ctrl Pts',(-34.0393888128716,55.6474033077565,14.8893441396567));
#26216=CARTESIAN_POINT('Ctrl Pts',(-34.2522903277622,56.1561177382089,14.852298176134));
#26217=CARTESIAN_POINT('Ctrl Pts',(-34.1880814506421,56.7808053595149,14.8152522126113));
#26218=CARTESIAN_POINT('Ctrl Pts',(-33.8761477528875,57.2355742774498,14.7782062490887));
#26219=CARTESIAN_POINT('Ctrl Pts',(-33.5642140551329,57.6903431953847,14.741160285566));
#26220=CARTESIAN_POINT('Ctrl Pts',(-33.0045555367438,57.9751934099486,14.7041143220433));
#26221=CARTESIAN_POINT('Ctrl Pts',(-32.4533030627753,57.959761729544,14.6670683585206));
#26222=CARTESIAN_POINT('Ctrl Pts',(-31.9020505888069,57.9443300491394,14.6300223949979));
#26223=CARTESIAN_POINT('Ctrl Pts',(-31.3592041592591,57.6286164737664,14.5929764314753));
#26224=CARTESIAN_POINT('Ctrl Pts',(-31.0732005795316,57.1571088626351,14.5559304679526));
#26225=CARTESIAN_POINT('Ctrl Pts',(-30.787196999804,56.6856012515039,14.5188845044299));
#26226=CARTESIAN_POINT('Ctrl Pts',(-30.7580362698967,56.0582996046144,14.4818385409072));
#26227=CARTESIAN_POINT('Ctrl Pts',(-30.9990638455916,55.5622925755827,14.4447925773845));
#26228=CARTESIAN_POINT('Ctrl Pts',(-31.142791661258,55.2665172617733,14.4227015971263));
#26229=CARTESIAN_POINT('Ctrl Pts',(-31.3825954370759,55.0174288556201,14.400610616868));
#26230=CARTESIAN_POINT('Ctrl Pts',(-31.6688656529171,54.8504196807178,14.3785196366098));
#26231=CARTESIAN_POINT('Ctrl Pts',(-31.6675239681331,54.8471109129233,14.5714803633902));
#26232=CARTESIAN_POINT('Ctrl Pts',(-31.2671376265686,55.0829372532297,14.6026199830965));
#26233=CARTESIAN_POINT('Ctrl Pts',(-30.9634650148059,55.4924582968624,14.6337596028029));
#26234=CARTESIAN_POINT('Ctrl Pts',(-30.8674364226636,55.9459488454016,14.6648992225092));
#26235=CARTESIAN_POINT('Ctrl Pts',(-30.7531938032872,56.4854542882262,14.7019451860319));
#26236=CARTESIAN_POINT('Ctrl Pts',(-30.9328342810788,57.0871907276693,14.7389911495546));
#26237=CARTESIAN_POINT('Ctrl Pts',(-31.3241443491424,57.4757700913935,14.7760371130773));
#26238=CARTESIAN_POINT('Ctrl Pts',(-31.715454417206,57.8643494551177,14.8130830766));
#26239=CARTESIAN_POINT('Ctrl Pts',(-32.3184340755416,58.039771743123,14.8501290401227));
#26240=CARTESIAN_POINT('Ctrl Pts',(-32.8571262761764,57.9217539399754,14.8871750036453));
#26241=CARTESIAN_POINT('Ctrl Pts',(-33.3958184768112,57.8037361368277,14.924220967168));
#26242=CARTESIAN_POINT('Ctrl Pts',(-33.8702232197452,57.3922782425271,14.9612669306907));
#26243=CARTESIAN_POINT('Ctrl Pts',(-34.063226478426,56.8756863008287,14.9983128942134));
#26244=CARTESIAN_POINT('Ctrl Pts',(-34.2562297371068,56.3590943591303,15.0353588577361));
#26245=CARTESIAN_POINT('Ctrl Pts',(-34.1678315115345,55.737368370034,15.0724048212587));
#26246=CARTESIAN_POINT('Ctrl Pts',(-33.8384877538371,55.2950447552266,15.1094507847814));
#26247=CARTESIAN_POINT('Ctrl Pts',(-33.5091439961397,54.8527211404192,15.1464967483041));
#26248=CARTESIAN_POINT('Ctrl Pts',(-32.9388547063171,54.5897998999006,15.1835427118268));
#26249=CARTESIAN_POINT('Ctrl Pts',(-32.3886160101468,54.6266084315825,15.2205886753495));
#26250=CARTESIAN_POINT('Ctrl Pts',(-32.1366535522459,54.6434636040355,15.237552571363));
#26251=CARTESIAN_POINT('Ctrl Pts',(-31.8888954229186,54.7231679104083,15.2545164673766));
#26252=CARTESIAN_POINT('Ctrl Pts',(-31.6686398531931,54.8509327367609,15.2714803633902));
#26253=CARTESIAN_POINT('Origin',(-32.5,56.2916512459885,17.));
#26254=CARTESIAN_POINT('',(-31.6657545866043,54.8497426695208,15.9714803633902));
#26255=CARTESIAN_POINT('',(-31.6656238197278,54.8464558867275,15.7785196366098));
#26256=CARTESIAN_POINT('',(-31.667,54.8488529232836,17.));
#26257=CARTESIAN_POINT('Ctrl Pts',(-31.6656238265237,54.8464558985647,15.7785196366098));
#26258=CARTESIAN_POINT('Ctrl Pts',(-32.1435040363299,54.5705135726952,15.7414495489508));
#26259=CARTESIAN_POINT('Ctrl Pts',(-32.7717977196734,54.5551568083656,15.7043794612919));
#26260=CARTESIAN_POINT('Ctrl Pts',(-33.2626292375688,54.8073433428058,15.667309373633));
#26261=CARTESIAN_POINT('Ctrl Pts',(-33.7531413365699,55.0593657615749,15.6302634101103));
#26262=CARTESIAN_POINT('Ctrl Pts',(-34.1063700665184,55.5785832727215,15.5932174465876));
#26263=CARTESIAN_POINT('Ctrl Pts',(-34.1606582960962,56.127373038589,15.5561714830649));
#26264=CARTESIAN_POINT('Ctrl Pts',(-34.2149465256739,56.6761628044566,15.5191255195423));
#26265=CARTESIAN_POINT('Ctrl Pts',(-33.9702942548808,57.254524825045,15.4820795560196));
#26266=CARTESIAN_POINT('Ctrl Pts',(-33.5386679829466,57.5977684411295,15.4450335924969));
#26267=CARTESIAN_POINT('Ctrl Pts',(-33.1070417110123,57.941012057214,15.4079876289742));
#26268=CARTESIAN_POINT('Ctrl Pts',(-32.4884414379368,58.0491372687945,15.3709416654515));
#26269=CARTESIAN_POINT('Ctrl Pts',(-31.9659730859382,57.8726599616145,15.3338957019289));
#26270=CARTESIAN_POINT('Ctrl Pts',(-31.4435047339396,57.6961826544345,15.2968497384062));
#26271=CARTESIAN_POINT('Ctrl Pts',(-31.0171683030177,57.2351028284939,15.2598037748835));
#26272=CARTESIAN_POINT('Ctrl Pts',(-30.8820790791908,56.7004362767628,15.2227578113608));
#26273=CARTESIAN_POINT('Ctrl Pts',(-30.7469898553639,56.1657697250316,15.1857118478381));
#26274=CARTESIAN_POINT('Ctrl Pts',(-30.9031478386319,55.5575164475099,15.1486658843155));
#26275=CARTESIAN_POINT('Ctrl Pts',(-31.2790864406456,55.1540470134353,15.1116199207928));
#26276=CARTESIAN_POINT('Ctrl Pts',(-31.391052526185,55.0338813988212,15.1005864927318));
#26277=CARTESIAN_POINT('Ctrl Pts',(-31.5225138495515,54.9318807605089,15.0895530646708));
#26278=CARTESIAN_POINT('Ctrl Pts',(-31.6662678127889,54.8504473245041,15.0785196366098));
#26279=CARTESIAN_POINT('Ctrl Pts',(-31.6686398531931,54.8509327367609,15.2714803633902));
#26280=CARTESIAN_POINT('Ctrl Pts',(-31.4078986168085,55.0021823003073,15.2915624308993));
#26281=CARTESIAN_POINT('Ctrl Pts',(-31.1856997806351,55.2207844238422,15.3116444984084));
#26282=CARTESIAN_POINT('Ctrl Pts',(-31.0406952948155,55.4822046794947,15.3317265659175));
#26283=CARTESIAN_POINT('Ctrl Pts',(-30.7732013781725,55.9644540918427,15.3687725294402));
#26284=CARTESIAN_POINT('Ctrl Pts',(-30.7684016474046,56.5924146126563,15.4058184929629));
#26285=CARTESIAN_POINT('Ctrl Pts',(-31.0284927261472,57.0786965491371,15.4428644564855));
#26286=CARTESIAN_POINT('Ctrl Pts',(-31.2885838048897,57.5649784856178,15.4799104200082));
#26287=CARTESIAN_POINT('Ctrl Pts',(-31.8135656931427,57.9095818377658,15.5169563835309));
#26288=CARTESIAN_POINT('Ctrl Pts',(-32.3631774530806,57.9547969272716,15.5540023470536));
#26289=CARTESIAN_POINT('Ctrl Pts',(-32.9127892130186,58.0000120167773,15.5910483105763));
#26290=CARTESIAN_POINT('Ctrl Pts',(-33.4870308446415,57.7458388436409,15.6280942740989));
#26291=CARTESIAN_POINT('Ctrl Pts',(-33.8230974089741,57.3086012018905,15.6651402376216));
#26292=CARTESIAN_POINT('Ctrl Pts',(-34.1591639733067,56.87136356014,15.7021862011443));
#26293=CARTESIAN_POINT('Ctrl Pts',(-34.257055470349,56.2510614497756,15.739232164667));
#26294=CARTESIAN_POINT('Ctrl Pts',(-34.0719713014427,55.7315796489165,15.7762781281897));
#26295=CARTESIAN_POINT('Ctrl Pts',(-33.8868871325364,55.2120978480574,15.8133240917123));
#26296=CARTESIAN_POINT('Ctrl Pts',(-33.4188272976816,54.7934363567036,15.850370055235));
#26297=CARTESIAN_POINT('Ctrl Pts',(-32.8820020343565,54.6671979803659,15.8874160187577));
#26298=CARTESIAN_POINT('Ctrl Pts',(-32.4759491237521,54.5717116766394,15.9154374669685));
#26299=CARTESIAN_POINT('Ctrl Pts',(-32.03055302792,54.6435311984541,15.9434589151794));
#26300=CARTESIAN_POINT('Ctrl Pts',(-31.6657545866043,54.8497426695208,15.9714803633902));
#26301=CARTESIAN_POINT('Origin',(-32.5,56.2916512459885,17.));
#26302=CARTESIAN_POINT('',(-31.6662054032747,54.8463759356941,16.6714803633902));
#26303=CARTESIAN_POINT('',(-31.6687530214683,54.8490350969289,16.4785196366098));
#26304=CARTESIAN_POINT('',(-31.667,54.8488529232836,17.));
#26305=CARTESIAN_POINT('Ctrl Pts',(-31.6687530214683,54.8490350969289,16.4785196366098));
#26306=CARTESIAN_POINT('Ctrl Pts',(-31.8117829954436,54.7648928865345,16.4674379602763));
#26307=CARTESIAN_POINT('Ctrl Pts',(-31.9665782677991,54.7018565467284,16.4563562839428));
#26308=CARTESIAN_POINT('Ctrl Pts',(-32.1273756622831,54.6650214760002,16.4452746076093));
#26309=CARTESIAN_POINT('Ctrl Pts',(-32.6649201845491,54.5418821020027,16.4082286440866));
#26310=CARTESIAN_POINT('Ctrl Pts',(-33.2695420256081,54.7115576426435,16.3711826805639));
#26311=CARTESIAN_POINT('Ctrl Pts',(-33.6645325714613,55.0963951246187,16.3341367170412));
#26312=CARTESIAN_POINT('Ctrl Pts',(-34.0595231173144,55.4812326065939,16.2970907535186));
#26313=CARTESIAN_POINT('Ctrl Pts',(-34.2448823679618,56.0812320299036,16.2600447899959));
#26314=CARTESIAN_POINT('Ctrl Pts',(-34.1357796112843,56.6218002562495,16.2229988264732));
#26315=CARTESIAN_POINT('Ctrl Pts',(-34.0266768546068,57.1623684825954,16.1859528629505));
#26316=CARTESIAN_POINT('Ctrl Pts',(-33.6231120906045,57.6435055119775,16.1489068994278));
#26317=CARTESIAN_POINT('Ctrl Pts',(-33.1097790218944,57.8450162546515,16.1118609359052));
#26318=CARTESIAN_POINT('Ctrl Pts',(-32.5964459531844,58.0465269973256,16.0748149723825));
#26319=CARTESIAN_POINT('Ctrl Pts',(-31.9733445797666,57.9684114532915,16.0377690088598));
#26320=CARTESIAN_POINT('Ctrl Pts',(-31.5256407784037,57.6464196442519,16.0007230453371));
#26321=CARTESIAN_POINT('Ctrl Pts',(-31.0779369770408,57.3244278352123,15.9636770818144));
#26322=CARTESIAN_POINT('Ctrl Pts',(-30.8056307477328,56.7585597611672,15.9266311182918));
#26323=CARTESIAN_POINT('Ctrl Pts',(-30.8333445804181,56.2077881548333,15.8895851547691));
#26324=CARTESIAN_POINT('Ctrl Pts',(-30.8610403660015,55.6573752080673,15.8525633153826));
#26325=CARTESIAN_POINT('Ctrl Pts',(-31.188365597836,55.1220390739338,15.8155414759962));
#26326=CARTESIAN_POINT('Ctrl Pts',(-31.6656238265237,54.8464558985647,15.7785196366098));
#26327=CARTESIAN_POINT('Ctrl Pts',(-31.6657545866043,54.8497426695208,15.9714803633902));
#26328=CARTESIAN_POINT('Ctrl Pts',(-31.5482685418209,54.9161546038405,15.9805048787021));
#26329=CARTESIAN_POINT('Ctrl Pts',(-31.4391421648863,54.9965058030685,15.9895293940139));
#26330=CARTESIAN_POINT('Ctrl Pts',(-31.3423819730147,55.0896968084029,15.9985539093258));
#26331=CARTESIAN_POINT('Ctrl Pts',(-30.9451778667933,55.4722492740994,16.0355998728484));
#26332=CARTESIAN_POINT('Ctrl Pts',(-30.7563603461461,56.0711694668139,16.0726458363711));
#26333=CARTESIAN_POINT('Ctrl Pts',(-30.8623428200595,56.6123581642473,16.1096917998938));
#26334=CARTESIAN_POINT('Ctrl Pts',(-30.968325293973,57.1535468616808,16.1467377634165));
#26335=CARTESIAN_POINT('Ctrl Pts',(-31.3691077624472,57.6370040638332,16.1837837269392));
#26336=CARTESIAN_POINT('Ctrl Pts',(-31.8812698561966,57.8414728407482,16.2208296904618));
#26337=CARTESIAN_POINT('Ctrl Pts',(-32.393431949946,58.0459416176631,16.2578756539845));
#26338=CARTESIAN_POINT('Ctrl Pts',(-33.0169736689706,57.9714219693406,16.2949216175072));
#26339=CARTESIAN_POINT('Ctrl Pts',(-33.4665276098354,57.6520182353919,16.3319675810299));
#26340=CARTESIAN_POINT('Ctrl Pts',(-33.9160815507002,57.3326145014431,16.3690135445526));
#26341=CARTESIAN_POINT('Ctrl Pts',(-34.1916477134051,56.7683266818682,16.4060595080752));
#26342=CARTESIAN_POINT('Ctrl Pts',(-34.1671116810226,56.2174042970244,16.4431054715979));
#26343=CARTESIAN_POINT('Ctrl Pts',(-34.14257564864,55.6664819121806,16.4801514351206));
#26344=CARTESIAN_POINT('Ctrl Pts',(-33.81793742117,55.128924962068,16.5171973986433));
#26345=CARTESIAN_POINT('Ctrl Pts',(-33.3417695242377,54.8507494330611,16.554243362166));
#26346=CARTESIAN_POINT('Ctrl Pts',(-32.8656016273055,54.5725739040542,16.5912893256886));
#26347=CARTESIAN_POINT('Ctrl Pts',(-32.237904060911,54.5537797961531,16.6283352892113));
#26348=CARTESIAN_POINT('Ctrl Pts',(-31.7459461756022,54.8029683394084,16.665381252734));
#26349=CARTESIAN_POINT('Ctrl Pts',(-31.7189481323125,54.8166434999842,16.6674142896194));
#26350=CARTESIAN_POINT('Ctrl Pts',(-31.692358893413,54.8311257383683,16.6694473265048));
#26351=CARTESIAN_POINT('Ctrl Pts',(-31.6662054032747,54.8463759356941,16.6714803633902));
#26352=CARTESIAN_POINT('Origin',(-32.5,56.2916512459885,17.));
#26353=CARTESIAN_POINT('',(-31.6689051738235,54.8497998491797,17.3714803633902));
#26354=CARTESIAN_POINT('',(-31.6674096068672,54.8512474102517,17.1785196366098));
#26355=CARTESIAN_POINT('',(-31.667,54.8488529232836,17.));
#26356=CARTESIAN_POINT('Ctrl Pts',(-31.6674096068672,54.8512474102517,17.1785196366098));
#26357=CARTESIAN_POINT('Ctrl Pts',(-31.955812083246,54.6864945235477,17.156380408079));
#26358=CARTESIAN_POINT('Ctrl Pts',(-32.2922890124973,54.603384940747,17.1342411795483));
#26359=CARTESIAN_POINT('Ctrl Pts',(-32.6209875748239,54.6272788981025,17.1121019510175));
#26360=CARTESIAN_POINT('Ctrl Pts',(-33.1710047054118,54.6672610804705,17.0750559874948));
#26361=CARTESIAN_POINT('Ctrl Pts',(-33.6992424692084,55.0068523416601,17.0380100239722));
#26362=CARTESIAN_POINT('Ctrl Pts',(-33.9639498583003,55.4906368153745,17.0009640604495));
#26363=CARTESIAN_POINT('Ctrl Pts',(-34.2286572473923,55.9744212890889,16.9639180969268));
#26364=CARTESIAN_POINT('Ctrl Pts',(-34.2298342617796,56.602398975328,16.9268721334041));
#26365=CARTESIAN_POINT('Ctrl Pts',(-33.9669422341539,57.087172325109,16.8898261698814));
#26366=CARTESIAN_POINT('Ctrl Pts',(-33.7040502065281,57.57194567489,16.8527802063588));
#26367=CARTESIAN_POINT('Ctrl Pts',(-33.1770891368891,57.9135146882128,16.8157342428361));
#26368=CARTESIAN_POINT('Ctrl Pts',(-32.6272257468299,57.955558369302,16.7786882793134));
#26369=CARTESIAN_POINT('Ctrl Pts',(-32.0773623567706,57.9976020503911,16.7416423157907));
#26370=CARTESIAN_POINT('Ctrl Pts',(-31.5045966462911,57.7401203992467,16.704596352268));
#26371=CARTESIAN_POINT('Ctrl Pts',(-31.1710580905945,57.3009513535357,16.6675503887454));
#26372=CARTESIAN_POINT('Ctrl Pts',(-30.8375195348979,56.8617823078246,16.6305044252227));
#26373=CARTESIAN_POINT('Ctrl Pts',(-30.7432081339843,56.2409258675469,16.5934584617));
#26374=CARTESIAN_POINT('Ctrl Pts',(-30.9312860352641,55.7225205030902,16.5564124981773));
#26375=CARTESIAN_POINT('Ctrl Pts',(-31.063103598594,55.3591873762591,16.5304482109881));
#26376=CARTESIAN_POINT('Ctrl Pts',(-31.333634830935,55.0461796849558,16.504483923799));
#26377=CARTESIAN_POINT('Ctrl Pts',(-31.6687530214683,54.8490350969289,16.4785196366098));
#26378=CARTESIAN_POINT('Ctrl Pts',(-31.6662054032747,54.8463759356941,16.6714803633902));
#26379=CARTESIAN_POINT('Ctrl Pts',(-31.2157904412561,55.1090145744741,16.7064932900275));
#26380=CARTESIAN_POINT('Ctrl Pts',(-30.8946171228531,55.5994272993444,16.7415062166648));
#26381=CARTESIAN_POINT('Ctrl Pts',(-30.8403168439901,56.1177955929608,16.776519143302));
#26382=CARTESIAN_POINT('Ctrl Pts',(-30.7828636019099,56.6662631088463,16.8135651068247));
#26383=CARTESIAN_POINT('Ctrl Pts',(-31.0241753219725,57.2460269462056,16.8506110703474));
#26384=CARTESIAN_POINT('Ctrl Pts',(-31.4538143271609,57.5917548973867,16.8876570338701));
#26385=CARTESIAN_POINT('Ctrl Pts',(-31.8834533323493,57.9374828485678,16.9247029973928));
#26386=CARTESIAN_POINT('Ctrl Pts',(-32.5014196226634,58.0491749135707,16.9617489609154));
#26387=CARTESIAN_POINT('Ctrl Pts',(-33.0248974212339,57.8757145855096,16.9987949244381));
#26388=CARTESIAN_POINT('Ctrl Pts',(-33.5483752198042,57.7022542574486,17.0358408879608));
#26389=CARTESIAN_POINT('Ctrl Pts',(-33.9773645266309,57.2436415363237,17.0728868514835));
#26390=CARTESIAN_POINT('Ctrl Pts',(-34.1155359529098,56.7097631344687,17.1099328150062));
#26391=CARTESIAN_POINT('Ctrl Pts',(-34.2537073791887,56.1758847326138,17.1469787785289));
#26392=CARTESIAN_POINT('Ctrl Pts',(-34.1010609249198,55.5667406500288,17.1840247420515));
#26393=CARTESIAN_POINT('Ctrl Pts',(-33.7274561054636,55.1611091301906,17.2210707055742));
#26394=CARTESIAN_POINT('Ctrl Pts',(-33.3538512860073,54.7554776103524,17.2581166690969));
#26395=CARTESIAN_POINT('Ctrl Pts',(-32.7592881013638,54.5533586532611,17.2951626326196));
#26396=CARTESIAN_POINT('Ctrl Pts',(-32.2158717643875,54.6472531457219,17.3322085961422));
#26397=CARTESIAN_POINT('Ctrl Pts',(-32.023849765451,54.6804317730554,17.3452991852249));
#26398=CARTESIAN_POINT('Ctrl Pts',(-31.8382141569136,54.7505717682631,17.3583897743076));
#26399=CARTESIAN_POINT('Ctrl Pts',(-31.6689051738235,54.8497998491797,17.3714803633902));
#26400=CARTESIAN_POINT('Origin',(-32.5,56.2916512459885,17.));
#26401=CARTESIAN_POINT('',(-31.6668097556407,54.850936308364,18.0714803633902));
#26402=CARTESIAN_POINT('',(-31.6651356431699,54.8475732381352,17.8785196366098));
#26403=CARTESIAN_POINT('',(-31.667,54.8488529232836,17.));
#26404=CARTESIAN_POINT('Ctrl Pts',(-31.6651356431699,54.8475732381352,17.8785196366098));
#26405=CARTESIAN_POINT('Ctrl Pts',(-32.0953114189421,54.6031821110332,17.8453228558818));
#26406=CARTESIAN_POINT('Ctrl Pts',(-32.6432818971092,54.5571637547426,17.8121260751538));
#26407=CARTESIAN_POINT('Ctrl Pts',(-33.1039518347459,54.7360113496833,17.7789292944258));
#26408=CARTESIAN_POINT('Ctrl Pts',(-33.618036674644,54.9355964098305,17.7418833309031));
#26409=CARTESIAN_POINT('Ctrl Pts',(-34.0234021807399,55.4152172665963,17.7048373673804));
#26410=CARTESIAN_POINT('Ctrl Pts',(-34.1345305305902,55.9553727152466,17.6677914038577));
#26411=CARTESIAN_POINT('Ctrl Pts',(-34.2456588804405,56.4955281638969,17.6307454403351));
#26412=CARTESIAN_POINT('Ctrl Pts',(-34.062550074045,57.0962182044316,17.5936994768124));
#26413=CARTESIAN_POINT('Ctrl Pts',(-33.6690048949483,57.4825336336559,17.5566535132897));
#26414=CARTESIAN_POINT('Ctrl Pts',(-33.2754597158516,57.8688490628802,17.519607549767));
#26415=CARTESIAN_POINT('Ctrl Pts',(-32.6714781640536,58.040789880794,17.4825615862443));
#26416=CARTESIAN_POINT('Ctrl Pts',(-32.133475821543,57.9196663971084,17.4455156227217));
#26417=CARTESIAN_POINT('Ctrl Pts',(-31.5954734790324,57.7985429134228,17.408469659199));
#26418=CARTESIAN_POINT('Ctrl Pts',(-31.1234503458092,57.3843551281376,17.3714236956763));
#26419=CARTESIAN_POINT('Ctrl Pts',(-30.9334304853463,56.8666584297933,17.3343777321536));
#26420=CARTESIAN_POINT('Ctrl Pts',(-30.7434106248833,56.3489617314489,17.2973317686309));
#26421=CARTESIAN_POINT('Ctrl Pts',(-30.8353940371805,55.7277561200453,17.2602858051083));
#26422=CARTESIAN_POINT('Ctrl Pts',(-31.1672839920187,55.2873398661167,17.2232398415856));
#26423=CARTESIAN_POINT('Ctrl Pts',(-31.3008314863423,55.1101230316987,17.2083331065936));
#26424=CARTESIAN_POINT('Ctrl Pts',(-31.4732231075307,54.9621784491468,17.1934263716017));
#26425=CARTESIAN_POINT('Ctrl Pts',(-31.6674096068672,54.8512474102517,17.1785196366098));
#26426=CARTESIAN_POINT('Ctrl Pts',(-31.6689051738235,54.8497998491797,17.3714803633902));
#26427=CARTESIAN_POINT('Ctrl Pts',(-31.3590749545435,55.0313841780677,17.3954357378302));
#26428=CARTESIAN_POINT('Ctrl Pts',(-31.1039191289866,55.3103783149913,17.4193911122703));
#26429=CARTESIAN_POINT('Ctrl Pts',(-30.9643532196009,55.6385333911701,17.4433464867103));
#26430=CARTESIAN_POINT('Ctrl Pts',(-30.7485205010994,56.1460112021445,17.480392450233));
#26431=CARTESIAN_POINT('Ctrl Pts',(-30.8091245534054,56.7710588820805,17.5174384137557));
#26432=CARTESIAN_POINT('Ctrl Pts',(-31.1184295883325,57.2276198159938,17.5544843772783));
#26433=CARTESIAN_POINT('Ctrl Pts',(-31.4277346232597,57.6841807499072,17.591530340801));
#26434=CARTESIAN_POINT('Ctrl Pts',(-31.9857406408082,57.9722549377979,17.6285763043237));
#26435=CARTESIAN_POINT('Ctrl Pts',(-32.5370730229375,57.9600035940862,17.6656222678464));
#26436=CARTESIAN_POINT('Ctrl Pts',(-33.0884054050668,57.9477522503744,17.7026682313691));
#26437=CARTESIAN_POINT('Ctrl Pts',(-33.633064151777,57.6351753750601,17.7397141948917));
#26438=CARTESIAN_POINT('Ctrl Pts',(-33.9217830992111,57.1653255475623,17.7767601584144));
#26439=CARTESIAN_POINT('Ctrl Pts',(-34.2105020466451,56.6954757200644,17.8138061219371));
#26440=CARTESIAN_POINT('Ctrl Pts',(-34.2432811948029,56.0683529403831,17.8508520854598));
#26441=CARTESIAN_POINT('Ctrl Pts',(-34.0051189806597,55.5709635046674,17.8878980489825));
#26442=CARTESIAN_POINT('Ctrl Pts',(-33.7669567665165,55.0735740689517,17.9249440125051));
#26443=CARTESIAN_POINT('Ctrl Pts',(-33.2578531900722,54.7059179772018,17.9619899760278));
#26444=CARTESIAN_POINT('Ctrl Pts',(-32.7108023899003,54.6362551245587,17.9990359395505));
#26445=CARTESIAN_POINT('Ctrl Pts',(-32.3542113134731,54.5908459018627,18.0231840808304));
#26446=CARTESIAN_POINT('Ctrl Pts',(-31.9814965026906,54.6720536844457,18.0473322221103));
#26447=CARTESIAN_POINT('Ctrl Pts',(-31.6668097556407,54.850936308364,18.0714803633902));
#26448=CARTESIAN_POINT('Origin',(-32.5,56.2916512459885,17.));
#26449=CARTESIAN_POINT('',(-31.6652761166365,54.8468682178694,18.7714803633902));
#26450=CARTESIAN_POINT('',(-31.6679260143736,54.8475393267799,18.5785196366098));
#26451=CARTESIAN_POINT('',(-31.667,54.8488529232836,17.));
#26452=CARTESIAN_POINT('Ctrl Pts',(-31.6679260143736,54.8475393267799,18.5785196366098));
#26453=CARTESIAN_POINT('Ctrl Pts',(-31.7606663811944,54.7928563701908,18.5713112672072));
#26454=CARTESIAN_POINT('Ctrl Pts',(-31.8585183363754,54.7473751127227,18.5641028978046));
#26455=CARTESIAN_POINT('Ctrl Pts',(-31.9600503104883,54.7126554770058,18.5568945284021));
#26456=CARTESIAN_POINT('Ctrl Pts',(-32.4818534533784,54.5342208981905,18.5198485648794));
#26457=CARTESIAN_POINT('Ctrl Pts',(-33.1008546957744,54.6400264825866,18.4828026013567));
#26458=CARTESIAN_POINT('Ctrl Pts',(-33.533764609118,54.9816497045372,18.445756637834));
#26459=CARTESIAN_POINT('Ctrl Pts',(-33.9666745224615,55.3232729264878,18.4087106743114));
#26460=CARTESIAN_POINT('Ctrl Pts',(-34.2134931067525,55.9007137859928,18.3716647107887));
#26461=CARTESIAN_POINT('Ctrl Pts',(-34.1612624373338,56.4497031993872,18.334618747266));
#26462=CARTESIAN_POINT('Ctrl Pts',(-34.109031767915,56.9986926127816,18.2975727837433));
#26463=CARTESIAN_POINT('Ctrl Pts',(-33.7577518447865,57.5192305800653,18.2605268202206));
#26464=CARTESIAN_POINT('Ctrl Pts',(-33.2681879166606,57.7730899488601,18.223480856698));
#26465=CARTESIAN_POINT('Ctrl Pts',(-32.7786239885347,58.0269493176549,18.1864348931753));
#26466=CARTESIAN_POINT('Ctrl Pts',(-32.1507760554113,58.0141300879608,18.1493889296526));
#26467=CARTESIAN_POINT('Ctrl Pts',(-31.6719822840244,57.7404990529372,18.1123429661299));
#26468=CARTESIAN_POINT('Ctrl Pts',(-31.1931885126375,57.4668680179136,18.0752970026072));
#26469=CARTESIAN_POINT('Ctrl Pts',(-30.863448902987,56.9324251775604,18.0382510390845));
#26470=CARTESIAN_POINT('Ctrl Pts',(-30.8336706571803,56.3817613282624,18.0012050755619));
#26471=CARTESIAN_POINT('Ctrl Pts',(-30.8038924113735,55.8310974789644,17.9641591120392));
#26472=CARTESIAN_POINT('Ctrl Pts',(-31.0740755294104,55.2642126207216,17.9271131485165));
#26473=CARTESIAN_POINT('Ctrl Pts',(-31.520569175279,54.9405448233645,17.8900671849938));
#26474=CARTESIAN_POINT('Ctrl Pts',(-31.5669611569199,54.9069148027547,17.8862180021991));
#26475=CARTESIAN_POINT('Ctrl Pts',(-31.6152565537378,54.8759105076229,17.8823688194045));
#26476=CARTESIAN_POINT('Ctrl Pts',(-31.6651356431699,54.8475732381352,17.8785196366098));
#26477=CARTESIAN_POINT('Ctrl Pts',(-31.6668097556407,54.850936308364,18.0714803633902));
#26478=CARTESIAN_POINT('Ctrl Pts',(-31.4987316547814,54.9464797400044,18.084378185633));
#26479=CARTESIAN_POINT('Ctrl Pts',(-31.3472075724788,55.0698874675039,18.0972760078758));
#26480=CARTESIAN_POINT('Ctrl Pts',(-31.2235359810035,55.2167495878635,18.1101738301185));
#26481=CARTESIAN_POINT('Ctrl Pts',(-30.8683183961782,55.6385765173477,18.1472197936412));
#26482=CARTESIAN_POINT('Ctrl Pts',(-30.7428812504272,56.2538999898523,18.1842657571639));
#26483=CARTESIAN_POINT('Ctrl Pts',(-30.9046315647806,56.7811137290641,18.2213117206866));
#26484=CARTESIAN_POINT('Ctrl Pts',(-31.066381879134,57.3083274682759,18.2583576842093));
#26485=CARTESIAN_POINT('Ctrl Pts',(-31.5153196535918,57.7474314741949,18.295403647732));
#26486=CARTESIAN_POINT('Ctrl Pts',(-32.0459859700228,57.8974673086234,18.3324496112546));
#26487=CARTESIAN_POINT('Ctrl Pts',(-32.5766522864537,58.0475031430519,18.3694955747773));
#26488=CARTESIAN_POINT('Ctrl Pts',(-33.1890471448578,57.90847080599,18.4065415383));
#26489=CARTESIAN_POINT('Ctrl Pts',(-33.602904565772,57.5439992348605,18.4435875018227));
#26490=CARTESIAN_POINT('Ctrl Pts',(-34.0167619866863,57.179527663731,18.4806334653453));
#26491=CARTESIAN_POINT('Ctrl Pts',(-34.2320819701108,56.5896168585338,18.517679428868));
#26492=CARTESIAN_POINT('Ctrl Pts',(-34.1503221046824,56.0442428442903,18.5547253923907));
#26493=CARTESIAN_POINT('Ctrl Pts',(-34.068562239254,55.4988688300469,18.5917713559134));
#26494=CARTESIAN_POINT('Ctrl Pts',(-33.6897225249727,54.9980316067572,18.6288173194361));
#26495=CARTESIAN_POINT('Ctrl Pts',(-33.1871811052498,54.7709421695977,18.6658632829587));
#26496=CARTESIAN_POINT('Ctrl Pts',(-32.709603590725,54.5551334726087,18.7010689764359));
#26497=CARTESIAN_POINT('Ctrl Pts',(-32.120308963107,54.5865510549416,18.7362746699131));
#26498=CARTESIAN_POINT('Ctrl Pts',(-31.6652761166365,54.8468682178694,18.7714803633902));
#26499=CARTESIAN_POINT('Origin',(-32.5,56.2916512459885,17.));
#26500=CARTESIAN_POINT('',(-31.6684351372492,54.8482948457192,19.4714803633902));
#26501=CARTESIAN_POINT('',(-31.6684043758654,54.8511587229547,19.2785196366098));
#26502=CARTESIAN_POINT('',(-31.667,54.8488529232836,17.));
#26503=CARTESIAN_POINT('Ctrl Pts',(-31.6684043758654,54.8511587229547,19.2785196366098));
#26504=CARTESIAN_POINT('Ctrl Pts',(-31.9058262033729,54.7139758182214,19.26025371501));
#26505=CARTESIAN_POINT('Ctrl Pts',(-32.1752796610303,54.6323550853735,19.2419877934101));
#26506=CARTESIAN_POINT('Ctrl Pts',(-32.4470503478135,54.6237274947408,19.2237218718103));
#26507=CARTESIAN_POINT('Ctrl Pts',(-32.9982410936014,54.6062294776757,19.1866759082876));
#26508=CARTESIAN_POINT('Ctrl Pts',(-33.5589634784782,54.8889798390775,19.149629944765));
#26509=CARTESIAN_POINT('Ctrl Pts',(-33.8725997234821,55.3425762727761,19.1125839812423));
#26510=CARTESIAN_POINT('Ctrl Pts',(-34.186235968486,55.7961727064748,19.0755380177196));
#26511=CARTESIAN_POINT('Ctrl Pts',(-34.252786073617,56.4206152124703,19.0384920541969));
#26512=CARTESIAN_POINT('Ctrl Pts',(-34.0417930059025,56.9301241370495,19.0014460906742));
#26513=CARTESIAN_POINT('Ctrl Pts',(-33.830799938188,57.4396330616286,18.9644001271515));
#26514=CARTESIAN_POINT('Ctrl Pts',(-33.3422636976281,57.8342084047915,18.9273541636289));
#26515=CARTESIAN_POINT('Ctrl Pts',(-32.7997656649011,57.9332705233524,18.8903082001062));
#26516=CARTESIAN_POINT('Ctrl Pts',(-32.2572676321741,58.0323326419133,18.8532622365835));
#26517=CARTESIAN_POINT('Ctrl Pts',(-31.6608078072802,57.8358815358723,18.8162162730608));
#26518=CARTESIAN_POINT('Ctrl Pts',(-31.2833594112405,57.4338241678589,18.7791703095382));
#26519=CARTESIAN_POINT('Ctrl Pts',(-30.9059110152008,57.0317667998456,18.7421243460155));
#26520=CARTESIAN_POINT('Ctrl Pts',(-30.7474740480155,56.4241031698599,18.7050783824928));
#26521=CARTESIAN_POINT('Ctrl Pts',(-30.8805580861148,55.8889339838537,18.6680324189701));
#26522=CARTESIAN_POINT('Ctrl Pts',(-30.987746754868,55.4578975242981,18.63819482485));
#26523=CARTESIAN_POINT('Ctrl Pts',(-31.2840459342598,55.0738884180752,18.6083572307299));
#26524=CARTESIAN_POINT('Ctrl Pts',(-31.6679260143736,54.8475393267799,18.5785196366098));
#26525=CARTESIAN_POINT('Ctrl Pts',(-31.6652761166365,54.8468682178694,18.7714803633902));
#26526=CARTESIAN_POINT('Ctrl Pts',(-31.6414906650693,54.8604755020885,18.7733206334357));
#26527=CARTESIAN_POINT('Ctrl Pts',(-31.6180720645058,54.8747082214848,18.7751609034813));
#26528=CARTESIAN_POINT('Ctrl Pts',(-31.5950554470214,54.8895637585373,18.7770011735268));
#26529=CARTESIAN_POINT('Ctrl Pts',(-31.1317143336805,55.1886164356654,18.8140471370495));
#26530=CARTESIAN_POINT('Ctrl Pts',(-30.8312752321632,55.7400634409509,18.8510931005722));
#26531=CARTESIAN_POINT('Ctrl Pts',(-30.8312358008972,56.2915319254989,18.8881390640948));
#26532=CARTESIAN_POINT('Ctrl Pts',(-30.8311963696312,56.8430004100469,18.9251850276175));
#26533=CARTESIAN_POINT('Ctrl Pts',(-31.1315566086164,57.3944903738573,18.9622309911402));
#26534=CARTESIAN_POINT('Ctrl Pts',(-31.5948549512976,57.6936093078491,18.9992769546629));
#26535=CARTESIAN_POINT('Ctrl Pts',(-32.0581532939788,57.9927282418409,19.0363229181856));
#26536=CARTESIAN_POINT('Ctrl Pts',(-32.684389740356,58.039476146014,19.0733688817082));
#26537=CARTESIAN_POINT('Ctrl Pts',(-33.1869636297931,57.81245857691,19.1104148452309));
#26538=CARTESIAN_POINT('Ctrl Pts',(-33.6895375192301,57.585441007806,19.1474608087536));
#26539=CARTESIAN_POINT('Ctrl Pts',(-34.068448851727,57.0846579654247,19.1845067722763));
#26540=CARTESIAN_POINT('Ctrl Pts',(-34.150286707292,56.5392956488152,19.221552735799));
#26541=CARTESIAN_POINT('Ctrl Pts',(-34.2321245628569,55.9939333322058,19.2585986993216));
#26542=CARTESIAN_POINT('Ctrl Pts',(-34.01688894149,55.4039917413681,19.2956446628443));
#26543=CARTESIAN_POINT('Ctrl Pts',(-33.6030836459812,55.0394609904048,19.332690626367));
#26544=CARTESIAN_POINT('Ctrl Pts',(-33.1892783504725,54.6749302394415,19.3697365898897));
#26545=CARTESIAN_POINT('Ctrl Pts',(-32.5769033808219,54.5358103283526,19.4067825534124));
#26546=CARTESIAN_POINT('Ctrl Pts',(-32.0462156138869,54.685770273593,19.4438285169351));
#26547=CARTESIAN_POINT('Ctrl Pts',(-31.9141769673738,54.7230813054923,19.4530457990868));
#26548=CARTESIAN_POINT('Ctrl Pts',(-31.7871951467268,54.7782877536412,19.4622630812385));
#26549=CARTESIAN_POINT('Ctrl Pts',(-31.6684351372492,54.8482948457192,19.4714803633902));
#26550=CARTESIAN_POINT('Origin',(-32.5,56.2916512459885,17.));
#26551=CARTESIAN_POINT('',(-31.667931072794,54.8513178316736,20.1714803633902));
#26552=CARTESIAN_POINT('',(-31.6654871359732,54.8492158242279,19.9785196366098));
#26553=CARTESIAN_POINT('',(-31.667,54.8488529232836,17.));
#26554=CARTESIAN_POINT('Ctrl Pts',(-31.6654871359732,54.8492158242279,19.9785196366098));
#26555=CARTESIAN_POINT('Ctrl Pts',(-32.0469172461538,54.6336656790848,19.9491961628127));
#26556=CARTESIAN_POINT('Ctrl Pts',(-32.517553856985,54.5668303852667,19.9198726890156));
#26557=CARTESIAN_POINT('Ctrl Pts',(-32.9387102808403,54.6815870878529,19.8905492152186));
#26558=CARTESIAN_POINT('Ctrl Pts',(-33.4707804449504,54.8265655664402,19.8535032516959));
#26559=CARTESIAN_POINT('Ctrl Pts',(-33.9238769452873,55.2613769285398,19.8164572881732));
#26560=CARTESIAN_POINT('Ctrl Pts',(-34.0906375985399,55.7870272905994,19.7794113246505));
#26561=CARTESIAN_POINT('Ctrl Pts',(-34.2573982517925,56.312677652659,19.7423653611279));
#26562=CARTESIAN_POINT('Ctrl Pts',(-34.1378230579607,56.9291670146787,19.7053193976052));
#26563=CARTESIAN_POINT('Ctrl Pts',(-33.786636282889,57.3543555234679,19.6682734340825));
#26564=CARTESIAN_POINT('Ctrl Pts',(-33.4354495078173,57.779544032257,19.6312274705598));
#26565=CARTESIAN_POINT('Ctrl Pts',(-32.8526511515056,58.0134316878157,19.5941815070371));
#26566=CARTESIAN_POINT('Ctrl Pts',(-32.3049621862367,57.9489784788088,19.5571355435145));
#26567=CARTESIAN_POINT('Ctrl Pts',(-31.7572732209677,57.884525269802,19.5200895799918));
#26568=CARTESIAN_POINT('Ctrl Pts',(-31.2446936467415,57.5217311962296,19.4830436164691));
#26569=CARTESIAN_POINT('Ctrl Pts',(-31.0018084123139,57.0266310228123,19.4459976529464));
#26570=CARTESIAN_POINT('Ctrl Pts',(-30.7589231778862,56.531530849395,19.4089516894237));
#26571=CARTESIAN_POINT('Ctrl Pts',(-30.7857322832571,55.9041245761326,19.3719057259011));
#26572=CARTESIAN_POINT('Ctrl Pts',(-31.069966389292,55.4315482417354,19.3348597623784));
#26573=CARTESIAN_POINT('Ctrl Pts',(-31.2140557291191,55.1919808900508,19.3160797204555));
#26574=CARTESIAN_POINT('Ctrl Pts',(-31.4242999735977,54.9922028355067,19.2972996785326));
#26575=CARTESIAN_POINT('Ctrl Pts',(-31.6684043758654,54.8511587229547,19.2785196366098));
#26576=CARTESIAN_POINT('Ctrl Pts',(-31.6684351372492,54.8482948457192,19.4714803633902));
#26577=CARTESIAN_POINT('Ctrl Pts',(-31.3098766805411,55.0596592183268,19.4993090447612));
#26578=CARTESIAN_POINT('Ctrl Pts',(-31.0262639705086,55.405938549172,19.5271377261321));
#26579=CARTESIAN_POINT('Ctrl Pts',(-30.9047015762615,55.801960623025,19.5549664075031));
#26580=CARTESIAN_POINT('Ctrl Pts',(-30.7428758697907,56.329151225647,19.5920123710258));
#26581=CARTESIAN_POINT('Ctrl Pts',(-30.8682250210687,56.9444926293215,19.6290583345484));
#26582=CARTESIAN_POINT('Ctrl Pts',(-31.2233822786099,57.3663703525617,19.6661042980711));
#26583=CARTESIAN_POINT('Ctrl Pts',(-31.5785395361512,57.7882480758019,19.7031502615938));
#26584=CARTESIAN_POINT('Ctrl Pts',(-32.1635048999558,58.0166621186078,19.7401962251165));
#26585=CARTESIAN_POINT('Ctrl Pts',(-32.7105656575522,57.9470774968357,19.7772421886392));
#26586=CARTESIAN_POINT('Ctrl Pts',(-33.2576264151486,57.8774928750636,19.8142881521619));
#26587=CARTESIAN_POINT('Ctrl Pts',(-33.7667825665369,57.5099095887134,19.8513341156845));
#26588=CARTESIAN_POINT('Ctrl Pts',(-34.005015905411,57.0125542176421,19.8883800792072));
#26589=CARTESIAN_POINT('Ctrl Pts',(-34.243249244285,56.5151988465708,19.9254260427299));
#26590=CARTESIAN_POINT('Ctrl Pts',(-34.2105597706448,55.8880713907783,19.9624720062526));
#26591=CARTESIAN_POINT('Ctrl Pts',(-33.9219080204981,55.4181802774153,19.9995179697753));
#26592=CARTESIAN_POINT('Ctrl Pts',(-33.6332562703514,54.9482891640523,20.0365639332979));
#26593=CARTESIAN_POINT('Ctrl Pts',(-33.0886422436983,54.6356343931188,20.0736098968206));
#26594=CARTESIAN_POINT('Ctrl Pts',(-32.5373116119164,54.623304211516,20.1106558603433));
#26595=CARTESIAN_POINT('Ctrl Pts',(-32.235574629855,54.6165560434103,20.1309306946923));
#26596=CARTESIAN_POINT('Ctrl Pts',(-31.9318258577411,54.6997625487969,20.1512055290412));
#26597=CARTESIAN_POINT('Ctrl Pts',(-31.667931072794,54.8513178316736,20.1714803633902));
#26598=CARTESIAN_POINT('Origin',(-32.5,56.2916512459885,17.));
#26599=CARTESIAN_POINT('',(-31.6652099567911,54.8483531313949,20.8714803633902));
#26600=CARTESIAN_POINT('',(-31.666645377609,54.8465106721999,20.6785196366098));
#26601=CARTESIAN_POINT('',(-31.667,54.8488529232836,17.));
#26602=CARTESIAN_POINT('Ctrl Pts',(-31.666645377609,54.8465106721999,20.6785196366098));
#26603=CARTESIAN_POINT('Ctrl Pts',(-31.7095215140164,54.8213939588906,20.6751845741381));
#26604=CARTESIAN_POINT('Ctrl Pts',(-31.7535458686671,54.7983179269085,20.6718495116665));
#26605=CARTESIAN_POINT('Ctrl Pts',(-31.7985935167041,54.7774509892024,20.6685144491949));
#26606=CARTESIAN_POINT('Ctrl Pts',(-32.2989840011864,54.545660484627,20.6314684856722));
#26607=CARTESIAN_POINT('Ctrl Pts',(-32.9256368768597,54.5864462806581,20.5944225221495));
#26608=CARTESIAN_POINT('Ctrl Pts',(-33.3917609918081,54.881142287214,20.5573765586268));
#26609=CARTESIAN_POINT('Ctrl Pts',(-33.8578851067565,55.1758382937699,20.5203305951041));
#26610=CARTESIAN_POINT('Ctrl Pts',(-34.16348046098,55.7244445108505,20.4832846315815));
#26611=CARTESIAN_POINT('Ctrl Pts',(-34.168689562804,56.2758883119516,20.4462386680588));
#26612=CARTESIAN_POINT('Ctrl Pts',(-34.1738986646279,56.8273321130526,20.4091927045361));
#26613=CARTESIAN_POINT('Ctrl Pts',(-33.8787215140524,57.3816134981739,20.3721467410134));
#26614=CARTESIAN_POINT('Ctrl Pts',(-33.4182476302774,57.6850623886884,20.3351007774907));
#26615=CARTESIAN_POINT('Ctrl Pts',(-32.9577737465024,57.9885112792029,20.2980548139681));
#26616=CARTESIAN_POINT('Ctrl Pts',(-32.3320031295279,58.0411276751107,20.2610088504454));
#26617=CARTESIAN_POINT('Ctrl Pts',(-31.8273232393449,57.8188314143185,20.2239628869227));
#26618=CARTESIAN_POINT('Ctrl Pts',(-31.3226433491619,57.5965351535262,20.1869169234));
#26619=CARTESIAN_POINT('Ctrl Pts',(-30.9390541857702,57.0993262360341,20.1498709598773));
#26620=CARTESIAN_POINT('Ctrl Pts',(-30.8521075105052,56.5547551273836,20.1128249963547));
#26621=CARTESIAN_POINT('Ctrl Pts',(-30.7651608352402,56.0101840187331,20.075779032832));
#26622=CARTESIAN_POINT('Ctrl Pts',(-30.9748566481018,55.4182507189243,20.0387330693093));
#26623=CARTESIAN_POINT('Ctrl Pts',(-31.3852264684743,55.0498568665574,20.0016871057866));
#26624=CARTESIAN_POINT('Ctrl Pts',(-31.4707709224493,54.9730625961603,19.993964616061));
#26625=CARTESIAN_POINT('Ctrl Pts',(-31.5650355275691,54.9059820788927,19.9862421263354));
#26626=CARTESIAN_POINT('Ctrl Pts',(-31.6654871359732,54.8492158242279,19.9785196366098));
#26627=CARTESIAN_POINT('Ctrl Pts',(-31.667931072794,54.8513178316736,20.1714803633902));
#26628=CARTESIAN_POINT('Ctrl Pts',(-31.4496400894775,54.9766827635065,20.1882514925639));
#26629=CARTESIAN_POINT('Ctrl Pts',(-31.2586188937636,55.1488148264988,20.2050226217376));
#26630=CARTESIAN_POINT('Ctrl Pts',(-31.1185634357287,55.3554851247115,20.2217937509113));
#26631=CARTESIAN_POINT('Ctrl Pts',(-30.8091931282335,55.8120018117817,20.258839714434));
#26632=CARTESIAN_POINT('Ctrl Pts',(-30.7484997501537,56.4370407781941,20.2958856779567));
#26633=CARTESIAN_POINT('Ctrl Pts',(-30.9642598655732,56.9445494693264,20.3329316414794));
#26634=CARTESIAN_POINT('Ctrl Pts',(-31.1800199809926,57.4520581604587,20.3699776050021));
#26635=CARTESIAN_POINT('Ctrl Pts',(-31.6722335899114,57.842036576311,20.4070235685247));
#26636=CARTESIAN_POINT('Ctrl Pts',(-32.215636552448,57.9360087382767,20.4440695320474));
#26637=CARTESIAN_POINT('Ctrl Pts',(-32.7590395149846,58.0299809002424,20.4811154955701));
#26638=CARTESIAN_POINT('Ctrl Pts',(-33.353631831139,57.8279468083215,20.5181614590928));
#26639=CARTESIAN_POINT('Ctrl Pts',(-33.727294536927,57.4223688010744,20.5552074226155));
#26640=CARTESIAN_POINT('Ctrl Pts',(-34.1009572427151,57.0167907938272,20.5922533861381));
#26641=CARTESIAN_POINT('Ctrl Pts',(-34.2536903381367,56.4076688712538,20.6292993496608));
#26642=CARTESIAN_POINT('Ctrl Pts',(-34.1155954946062,55.8737705531045,20.6663453131835));
#26643=CARTESIAN_POINT('Ctrl Pts',(-33.9775006510756,55.3398722349553,20.7033912767062));
#26644=CARTESIAN_POINT('Ctrl Pts',(-33.5485778685929,54.8811975212302,20.7404372402289));
#26645=CARTESIAN_POINT('Ctrl Pts',(-33.0251244120732,54.707662660689,20.7774832037515));
#26646=CARTESIAN_POINT('Ctrl Pts',(-32.5824028716121,54.5608919787389,20.8088155902978));
#26647=CARTESIAN_POINT('Ctrl Pts',(-32.0720609029457,54.6180897881501,20.840147976844));
#26648=CARTESIAN_POINT('Ctrl Pts',(-31.6652099567911,54.8483531313949,20.8714803633902));
#26649=CARTESIAN_POINT('Origin',(-32.5,56.2916512459885,17.));
#26650=CARTESIAN_POINT('',(-31.6673136634551,54.8469650373412,21.5714803633902));
#26651=CARTESIAN_POINT('',(-31.6688940285233,54.8502492137286,21.3785196366098));
#26652=CARTESIAN_POINT('',(-31.667,54.8488529232836,17.));
#26653=CARTESIAN_POINT('',(-34.0692874532608,56.8510195406194,22.));
#26654=CARTESIAN_POINT('Ctrl Pts',(-31.6673136634551,54.8469650373412,21.5714803633902));
#26655=CARTESIAN_POINT('Ctrl Pts',(-31.2598491701087,55.0867590255674,21.6031823516921));
#26656=CARTESIAN_POINT('Ctrl Pts',(-30.9533734485755,55.5074467114501,21.634884339994));
#26657=CARTESIAN_POINT('Ctrl Pts',(-30.8625080737328,55.9706266060894,21.6665863282959));
#26658=CARTESIAN_POINT('Ctrl Pts',(-30.7563256056226,56.511884312636,21.7036322918186));
#26659=CARTESIAN_POINT('Ctrl Pts',(-30.9445706465323,57.1111674125324,21.7406782553412));
#26660=CARTESIAN_POINT('Ctrl Pts',(-31.341982566131,57.4936046161573,21.7777242188639));
#26661=CARTESIAN_POINT('Ctrl Pts',(-31.7393944857298,57.8760418197822,21.8147701823866));
#26662=CARTESIAN_POINT('Ctrl Pts',(-32.3459732840176,58.0416331271358,21.8518161459093));
#26663=CARTESIAN_POINT('Ctrl Pts',(-32.8819457094272,57.9158339106246,21.888862109432));
#26664=CARTESIAN_POINT('Ctrl Pts',(-33.4179181348368,57.7900346941134,21.9259080729547));
#26665=CARTESIAN_POINT('Ctrl Pts',(-33.8832841873681,57.3728449537375,21.9629540364773));
#26666=CARTESIAN_POINT('Ctrl Pts',(-34.0692874532608,56.8510195406194,22.));
#26667=CARTESIAN_POINT('',(-32.8006122403834,54.64991982209,22.));
#26668=CARTESIAN_POINT('Origin',(-32.5,56.2916512459885,22.));
#26669=CARTESIAN_POINT('Ctrl Pts',(-32.8006124898337,54.6499179279034,22.));
#26670=CARTESIAN_POINT('Ctrl Pts',(-33.3324299245223,54.7480089912901,21.9636770818144));
#26671=CARTESIAN_POINT('Ctrl Pts',(-33.8131824856956,55.1285995043637,21.9273541636289));
#26672=CARTESIAN_POINT('Ctrl Pts',(-34.0294057231266,55.6243031692819,21.8910312454433));
#26673=CARTESIAN_POINT('Ctrl Pts',(-34.2499331082255,56.1298743294735,21.8539852819206));
#26674=CARTESIAN_POINT('Ctrl Pts',(-34.195294888985,56.7551871483463,21.816939318398));
#26675=CARTESIAN_POINT('Ctrl Pts',(-33.8903094432865,57.2145585578539,21.7798933548753));
#26676=CARTESIAN_POINT('Ctrl Pts',(-33.585323997588,57.6739299673614,21.7428473913526));
#26677=CARTESIAN_POINT('Ctrl Pts',(-33.0299913254315,57.9673599675038,21.7058014278299));
#26678=CARTESIAN_POINT('Ctrl Pts',(-32.4785554363758,57.9603119672566,21.6687554643072));
#26679=CARTESIAN_POINT('Ctrl Pts',(-31.9271195473201,57.9532639670095,21.6317095007846));
#26680=CARTESIAN_POINT('Ctrl Pts',(-31.3795804413653,57.6457379663728,21.5946635372619));
#26681=CARTESIAN_POINT('Ctrl Pts',(-31.0864761391558,57.1785982034713,21.5576175737392));
#26682=CARTESIAN_POINT('Ctrl Pts',(-30.7933718369464,56.7114584405698,21.5205716102165));
#26683=CARTESIAN_POINT('Ctrl Pts',(-30.7547023384823,56.0847049154035,21.4835256466938));
#26684=CARTESIAN_POINT('Ctrl Pts',(-30.9881881185804,55.5851133656589,21.4464796831712));
#26685=CARTESIAN_POINT('Ctrl Pts',(-31.1309630480468,55.2796166101529,21.4238263343174));
#26686=CARTESIAN_POINT('Ctrl Pts',(-31.3755032965772,55.0216687358222,21.4011729854636));
#26687=CARTESIAN_POINT('Ctrl Pts',(-31.6688940285233,54.8502492137286,21.3785196366098));
#26688=CARTESIAN_POINT('Origin',(-32.5,56.2916512459885,23.5459252805377));
#26689=CARTESIAN_POINT('',(-31.4724222119036,54.5094432564574,13.4540747194623));
#26690=CARTESIAN_POINT('',(-31.4735006561134,54.5153050203083,13.3959252805377));
#26691=CARTESIAN_POINT('',(-31.4726250000001,54.5121855475624,23.5459252805377));
#26692=CARTESIAN_POINT('',(-32.7283737736498,58.3336705852723,13.));
#26693=CARTESIAN_POINT('Ctrl Pts',(-31.4735006561133,54.5153050203083,13.3959252805377));
#26694=CARTESIAN_POINT('Ctrl Pts',(-31.808029474343,54.3235252303772,13.3750880775931));
#26695=CARTESIAN_POINT('Ctrl Pts',(-32.8820600904465,54.0381232256078,13.3172049111259));
#26696=CARTESIAN_POINT('Ctrl Pts',(-34.5894859509232,55.0509345423224,13.2222757811361));
#26697=CARTESIAN_POINT('Ctrl Pts',(-34.6719801790384,57.3759588223509,13.111137890568));
#26698=CARTESIAN_POINT('Ctrl Pts',(-33.4073937856322,58.2577308722945,13.0370459635227));
#26699=CARTESIAN_POINT('Ctrl Pts',(-32.7283737736498,58.3336705852723,13.));
#26700=CARTESIAN_POINT('',(-31.6782144221994,58.1789827080509,13.));
#26701=CARTESIAN_POINT('Origin',(-32.5,56.2916512459885,13.));
#26702=CARTESIAN_POINT('Ctrl Pts',(-31.4724222119036,54.5094432564574,13.4540747194623));
#26703=CARTESIAN_POINT('Ctrl Pts',(-31.5342132308563,54.4731877432048,13.4501772883951));
#26704=CARTESIAN_POINT('Ctrl Pts',(-32.2034917270507,54.1282244537508,13.4092338938053));
#26705=CARTESIAN_POINT('Ctrl Pts',(-33.8288126996591,54.2585627611561,13.3312445356927));
#26706=CARTESIAN_POINT('Ctrl Pts',(-34.9285321027134,56.3058411531895,13.2201066451247));
#26707=CARTESIAN_POINT('Ctrl Pts',(-33.8129922329338,58.3256386597759,13.1096917998938));
#26708=CARTESIAN_POINT('Ctrl Pts',(-32.2900793461073,58.444463046046,13.0363229181856));
#26709=CARTESIAN_POINT('Ctrl Pts',(-31.6782133743559,58.178984818602,13.));
#26710=CARTESIAN_POINT('Origin',(-32.5,56.2916512459885,23.5459252805377));
#26711=CARTESIAN_POINT('',(-31.4749259905952,54.514117897405,14.1540747194623));
#26712=CARTESIAN_POINT('',(-31.470366790827,54.5112698283738,14.0959252805377));
#26713=CARTESIAN_POINT('',(-31.4726250000001,54.5121855475624,23.5459252805377));
#26714=CARTESIAN_POINT('Ctrl Pts',(-31.470366790827,54.5112698283738,14.0959252805377));
#26715=CARTESIAN_POINT('Ctrl Pts',(-31.9808629913117,54.2220900136561,14.0640305253959));
#26716=CARTESIAN_POINT('Ctrl Pts',(-33.371417583723,54.0779847124814,13.9950898067314));
#26717=CARTESIAN_POINT('Ctrl Pts',(-34.8602323505772,55.7191431963174,13.8891031245444));
#26718=CARTESIAN_POINT('Ctrl Pts',(-34.2609995597881,57.9641431697148,13.7779652339763));
#26719=CARTESIAN_POINT('Ctrl Pts',(-32.0500242237096,58.6781839861315,13.6668273434083));
#26720=CARTESIAN_POINT('Ctrl Pts',(-30.2506759606945,57.2080211780376,13.5556894528402));
#26721=CARTESIAN_POINT('Ctrl Pts',(-30.46190078674,55.3316416370552,13.4653887652167));
#26722=CARTESIAN_POINT('Ctrl Pts',(-31.2132787090688,54.6644859207873,13.4121340411158));
#26723=CARTESIAN_POINT('Ctrl Pts',(-31.4735006561133,54.5153050203083,13.3959252805377));
#26724=CARTESIAN_POINT('Ctrl Pts',(-31.4749259905952,54.514117897405,14.1540747194623));
#26725=CARTESIAN_POINT('Ctrl Pts',(-31.7139442620515,54.3746753634158,14.1391197361979));
#26726=CARTESIAN_POINT('Ctrl Pts',(-32.6363754616289,54.0511292553545,14.0871187894108));
#26727=CARTESIAN_POINT('Ctrl Pts',(-34.3667107654438,54.7380212138031,13.998071879101));
#26728=CARTESIAN_POINT('Ctrl Pts',(-34.817688121868,57.0173840749687,13.886933988533));
#26729=CARTESIAN_POINT('Ctrl Pts',(-33.1472639077745,58.6324557555082,13.7757960979649));
#26730=CARTESIAN_POINT('Ctrl Pts',(-30.8843823888258,58.105001931136,13.6646582073969));
#26731=CARTESIAN_POINT('Ctrl Pts',(-30.1278087167359,55.9943944231075,13.557417747896));
#26732=CARTESIAN_POINT('Ctrl Pts',(-30.9468756244448,54.8178045942286,13.4872232519178));
#26733=CARTESIAN_POINT('Ctrl Pts',(-31.4724222119036,54.5094432564574,13.4540747194623));
#26734=CARTESIAN_POINT('Origin',(-32.5,56.2916512459885,23.5459252805377));
#26735=CARTESIAN_POINT('',(-31.4717219617817,54.5141519916847,14.8540747194623));
#26736=CARTESIAN_POINT('',(-31.4732712326059,54.510037050691,14.7959252805377));
#26737=CARTESIAN_POINT('',(-31.4726250000001,54.5121855475624,23.5459252805377));
#26738=CARTESIAN_POINT('Ctrl Pts',(-31.4732712326059,54.510037050691,14.7959252805377));
#26739=CARTESIAN_POINT('Ctrl Pts',(-31.5669343623879,54.4548697514474,14.7900189367213));
#26740=CARTESIAN_POINT('Ctrl Pts',(-32.279281356511,54.1097268956778,14.7470666293823));
#26741=CARTESIAN_POINT('Ctrl Pts',(-33.9367458689222,54.3335587337424,14.6670683585206));
#26742=CARTESIAN_POINT('Ctrl Pts',(-34.9243151877952,56.4367817964587,14.5559304679526));
#26743=CARTESIAN_POINT('Ctrl Pts',(-33.6928803873875,58.4071660616143,14.4447925773845));
#26744=CARTESIAN_POINT('Ctrl Pts',(-31.3695905104292,58.4411939406326,14.3336546868165));
#26745=CARTESIAN_POINT('Ctrl Pts',(-30.0809735153022,56.5077243843662,14.2225167962484));
#26746=CARTESIAN_POINT('Ctrl Pts',(-30.7409078667025,54.9881078888109,14.1432736608222));
#26747=CARTESIAN_POINT('Ctrl Pts',(-31.3879183664803,54.55797423098,14.1010764889186));
#26748=CARTESIAN_POINT('Ctrl Pts',(-31.470366790827,54.5112698283738,14.0959252805377));
#26749=CARTESIAN_POINT('Ctrl Pts',(-31.4717219617817,54.5141519916847,14.8540747194623));
#26750=CARTESIAN_POINT('Ctrl Pts',(-31.8897217256655,54.2773643841942,14.8280621840006));
#26751=CARTESIAN_POINT('Ctrl Pts',(-33.1073033291158,54.0451479062597,14.7650036850163));
#26752=CARTESIAN_POINT('Ctrl Pts',(-34.7403671916158,55.3540375815297,14.6648992225092));
#26753=CARTESIAN_POINT('Ctrl Pts',(-34.5027924192342,57.6654005284895,14.5537613319412));
#26754=CARTESIAN_POINT('Ctrl Pts',(-32.4320391047204,58.7193548713018,14.4426234413732));
#26755=CARTESIAN_POINT('Ctrl Pts',(-30.4234910234841,57.5512051672244,14.3314855508051));
#26756=CARTESIAN_POINT('Ctrl Pts',(-30.3301141372088,55.5424943178044,14.2353026435015));
#26757=CARTESIAN_POINT('Ctrl Pts',(-31.12185652721,54.7200975505445,14.1761656997206));
#26758=CARTESIAN_POINT('Ctrl Pts',(-31.4749259905952,54.514117897405,14.1540747194623));
#26759=CARTESIAN_POINT('Origin',(-32.5,56.2916512459885,23.5459252805377));
#26760=CARTESIAN_POINT('',(-31.4709276972304,54.5092291784965,15.5540747194623));
#26761=CARTESIAN_POINT('',(-31.47464750201,54.5147506716574,15.4959252805377));
#26762=CARTESIAN_POINT('',(-31.4726250000001,54.5121855475624,23.5459252805377));
#26763=CARTESIAN_POINT('Ctrl Pts',(-31.47464750201,54.5147506716575,15.4959252805377));
#26764=CARTESIAN_POINT('Ctrl Pts',(-31.7462982414418,54.3571727743297,15.4789613845241));
#26765=CARTESIAN_POINT('Ctrl Pts',(-32.7191784117559,54.0441951966849,15.4249515249878));
#26766=CARTESIAN_POINT('Ctrl Pts',(-34.4479835200066,54.8412285476315,15.3338957019289));
#26767=CARTESIAN_POINT('Ctrl Pts',(-34.7750596076319,57.1416333665308,15.2227578113608));
#26768=CARTESIAN_POINT('Ctrl Pts',(-33.0197478209391,58.6640399241194,15.1116199207928));
#26769=CARTESIAN_POINT('Ctrl Pts',(-30.7887049884687,58.0149721937252,15.0004820302248));
#26770=CARTESIAN_POINT('Ctrl Pts',(-30.1593535158744,55.9068520254157,14.895250483473));
#26771=CARTESIAN_POINT('Ctrl Pts',(-30.9794574058775,54.8008918962759,14.827064900244));
#26772=CARTESIAN_POINT('Ctrl Pts',(-31.4732712326059,54.510037050691,14.7959252805377));
#26773=CARTESIAN_POINT('Ctrl Pts',(-31.4709277056121,54.5092291930958,15.5540747194623));
#26774=CARTESIAN_POINT('Ctrl Pts',(-31.4713112637463,54.5090077151575,15.5540505953261));
#26775=CARTESIAN_POINT('Ctrl Pts',(-32.0608222902466,54.1688851137838,15.5169805076671));
#26776=CARTESIAN_POINT('Ctrl Pts',(-33.6099012175602,54.1314466960921,15.4428644564855));
#26777=CARTESIAN_POINT('Ctrl Pts',(-34.916858119472,56.052567070093,15.3317265659175));
#26778=CARTESIAN_POINT('Ctrl Pts',(-34.0116373750326,58.1925239040739,15.2205886753494));
#26779=CARTESIAN_POINT('Ctrl Pts',(-31.722797799219,58.5925904319764,15.1094507847814));
#26780=CARTESIAN_POINT('Ctrl Pts',(-30.1453402095974,56.8865812380663,14.9983128942134));
#26781=CARTESIAN_POINT('Ctrl Pts',(-30.5878941637737,55.1627827650417,14.913187539107));
#26782=CARTESIAN_POINT('Ctrl Pts',(-31.2944239690072,54.6145873774176,14.8651081475233));
#26783=CARTESIAN_POINT('Ctrl Pts',(-31.4717219617817,54.5141519916847,14.8540747194623));
#26784=CARTESIAN_POINT('Origin',(-32.5,56.2916512459885,23.5459252805377));
#26785=CARTESIAN_POINT('',(-31.4747870773482,54.5124102302141,16.2540747194623));
#26786=CARTESIAN_POINT('',(-31.4710889776862,54.513282910156,16.1959252805377));
#26787=CARTESIAN_POINT('',(-31.4726250000001,54.5121855475624,23.5459252805377));
#26788=CARTESIAN_POINT('Ctrl Pts',(-31.4710889776862,54.513282910156,16.1959252805377));
#26789=CARTESIAN_POINT('Ctrl Pts',(-31.9210107047531,54.2589533662338,16.1679038323268));
#26790=CARTESIAN_POINT('Ctrl Pts',(-33.1965779324789,54.0532698651996,16.1028364205933));
#26791=CARTESIAN_POINT('Ctrl Pts',(-34.7877864833416,55.4765446163128,16.0007230453371));
#26792=CARTESIAN_POINT('Ctrl Pts',(-34.4255850063652,57.7716810411711,15.8895851547691));
#26793=CARTESIAN_POINT('Ctrl Pts',(-32.3008737352177,58.7121294100224,15.778447264201));
#26794=CARTESIAN_POINT('Ctrl Pts',(-30.3584249929228,57.4370866648374,15.667309373633));
#26795=CARTESIAN_POINT('Ctrl Pts',(-30.3734734150964,55.4682647699114,15.5731353790785));
#26796=CARTESIAN_POINT('Ctrl Pts',(-31.1530640353465,54.7012933131322,15.5160073480468));
#26797=CARTESIAN_POINT('Ctrl Pts',(-31.47464750201,54.5147506716575,15.4959252805377));
#26798=CARTESIAN_POINT('Ctrl Pts',(-31.4747870773482,54.5124102302141,16.2540747194623));
#26799=CARTESIAN_POINT('Ctrl Pts',(-31.6511921427898,54.4086339956355,16.2429930431288));
#26800=CARTESIAN_POINT('Ctrl Pts',(-32.4803377190683,54.0709860720282,16.1948654032726));
#26801=CARTESIAN_POINT('Ctrl Pts',(-34.1948158493603,54.5521215254953,16.1096917998938));
#26802=CARTESIAN_POINT('Ctrl Pts',(-34.880650639758,56.7721373989267,15.9985539093257));
#26803=CARTESIAN_POINT('Ctrl Pts',(-33.387448901162,58.5523588475275,15.8874160187577));
#26804=CARTESIAN_POINT('Ctrl Pts',(-31.0819551189948,58.2633289901972,15.7762781281897));
#26805=CARTESIAN_POINT('Ctrl Pts',(-30.074632599944,56.1700546084616,15.6651643617579));
#26806=CARTESIAN_POINT('Ctrl Pts',(-30.8823044490718,54.8491178663189,15.5910965588487));
#26807=CARTESIAN_POINT('Ctrl Pts',(-31.4709277056121,54.5092291930958,15.5540747194623));
#26808=CARTESIAN_POINT('Origin',(-32.5,56.2916512459885,23.5459252805377));
#26809=CARTESIAN_POINT('',(-31.4731301859007,54.5151387721107,16.9540747194623));
#26810=CARTESIAN_POINT('',(-31.471644989423,54.5091305714222,16.8959252805377));
#26811=CARTESIAN_POINT('',(-31.4726250000001,54.5121855475624,23.5459252805377));
#26812=CARTESIAN_POINT('Ctrl Pts',(-31.471644989423,54.5091305714222,16.8959252805377));
#26813=CARTESIAN_POINT('Ctrl Pts',(-31.5039012222331,54.4903218421575,16.8938922436523));
#26814=CARTESIAN_POINT('Ctrl Pts',(-32.1342604089221,54.1469870049404,16.8548132432442));
#26815=CARTESIAN_POINT('Ctrl Pts',(-33.72507894253,54.1946182477114,16.7786882793134));
#26816=CARTESIAN_POINT('Ctrl Pts',(-34.9262501272131,56.1835950962899,16.6675503887454));
#26817=CARTESIAN_POINT('Ctrl Pts',(-33.9066470549119,58.2714769641261,16.5564124981773));
#26818=CARTESIAN_POINT('Ctrl Pts',(-31.5995239807838,58.5472018994032,16.4452746076093));
#26819=CARTESIAN_POINT('Ctrl Pts',(-30.1166168191438,56.7583957419196,16.3341367170413));
#26820=CARTESIAN_POINT('Ctrl Pts',(-30.6391000228397,55.1011038763401,16.251020274684));
#26821=CARTESIAN_POINT('Ctrl Pts',(-31.3261883471228,54.5951916268687,16.2049497958495));
#26822=CARTESIAN_POINT('Ctrl Pts',(-31.4710889776862,54.513282910156,16.1959252805377));
#26823=CARTESIAN_POINT('Ctrl Pts',(-31.4731301859007,54.5151387721107,16.9540747194623));
#26824=CARTESIAN_POINT('Ctrl Pts',(-31.8288294586133,54.3119418969877,16.9319354909316));
#26825=CARTESIAN_POINT('Ctrl Pts',(-32.9382338021844,54.0379197452859,16.8727502988782));
#26826=CARTESIAN_POINT('Ctrl Pts',(-34.6305762357544,55.1258856969253,16.776519143302));
#26827=CARTESIAN_POINT('Ctrl Pts',(-34.6349312243122,57.4494219828794,16.665381252734));
#26828=CARTESIAN_POINT('Ctrl Pts',(-32.6851594514901,58.7132375833447,16.554243362166));
#26829=CARTESIAN_POINT('Ctrl Pts',(-30.5659091328683,57.7605477465697,16.4431054715979));
#26830=CARTESIAN_POINT('Ctrl Pts',(-30.2517487916384,55.6924152700813,16.3430492573634));
#26831=CARTESIAN_POINT('Ctrl Pts',(-31.0614712898343,54.7555571943486,16.2800390066515));
#26832=CARTESIAN_POINT('Ctrl Pts',(-31.4747870773482,54.5124102302141,16.2540747194623));
#26833=CARTESIAN_POINT('Origin',(-32.5,56.2916512459885,23.5459252805377));
#26834=CARTESIAN_POINT('',(-31.4703256079253,54.5106072564107,17.6540747194623));
#26835=CARTESIAN_POINT('',(-31.4749747334417,54.5133534323073,17.5959252805377));
#26836=CARTESIAN_POINT('',(-31.4726250000001,54.5121855475624,23.5459252805377));
#26837=CARTESIAN_POINT('Ctrl Pts',(-31.4749747334417,54.5133534323073,17.5959252805377));
#26838=CARTESIAN_POINT('Ctrl Pts',(-31.6837908396868,54.3909711398323,17.582834691455));
#26839=CARTESIAN_POINT('Ctrl Pts',(-32.560671629995,54.0596531620232,17.5326981388497));
#26840=CARTESIAN_POINT('Ctrl Pts',(-34.2863923370768,54.6463037965648,17.4455156227217));
#26841=CARTESIAN_POINT('Ctrl Pts',(-34.8511887990978,56.9001551837646,17.3343777321536));
#26842=CARTESIAN_POINT('Ctrl Pts',(-33.26391548901,58.5970360158137,17.2232398415856));
#26843=CARTESIAN_POINT('Ctrl Pts',(-30.9774216684405,58.1837720232006,17.1121019510176));
#26844=CARTESIAN_POINT('Ctrl Pts',(-30.1008940923714,56.0778693719696,17.0029970973349));
#26845=CARTESIAN_POINT('Ctrl Pts',(-30.9161286969814,54.8330541866883,16.9309382071749));
#26846=CARTESIAN_POINT('Ctrl Pts',(-31.471644989423,54.5091305714222,16.8959252805377));
#26847=CARTESIAN_POINT('Ctrl Pts',(-31.4703256079253,54.5106072564107,17.6540747194623));
#26848=CARTESIAN_POINT('Ctrl Pts',(-32.0008800348569,54.2091890880957,17.6208779387343));
#26849=CARTESIAN_POINT('Ctrl Pts',(-33.4309149924661,54.0890952859489,17.5506351944836));
#26850=CARTESIAN_POINT('Ctrl Pts',(-34.8788327758259,55.8022444250302,17.4433464867103));
#26851=CARTESIAN_POINT('Ctrl Pts',(-34.2013246967004,58.0248156029211,17.3322085961422));
#26852=CARTESIAN_POINT('Ctrl Pts',(-31.9665748283507,58.6610017894909,17.2210707055742));
#26853=CARTESIAN_POINT('Ctrl Pts',(-30.2200750690644,57.1284945533303,17.1099328150062));
#26854=CARTESIAN_POINT('Ctrl Pts',(-30.4926187339169,55.2878838417841,17.0209341529689));
#26855=CARTESIAN_POINT('Ctrl Pts',(-31.2336315607436,54.6519548298357,16.9689814544542));
#26856=CARTESIAN_POINT('Ctrl Pts',(-31.4731301859007,54.5151387721107,16.9540747194623));
#26857=CARTESIAN_POINT('Origin',(-32.5,56.2916512459885,23.5459252805377));
#26858=CARTESIAN_POINT('',(-31.4737670936581,54.5105654320665,18.3540747194623));
#26859=CARTESIAN_POINT('',(-31.4723903633871,54.5147550766703,18.2959252805377));
#26860=CARTESIAN_POINT('',(-31.4726250000001,54.5121855475624,23.5459252805377));
#26861=CARTESIAN_POINT('Ctrl Pts',(-31.4723903633871,54.5147550766704,18.2959252805377));
#26862=CARTESIAN_POINT('Ctrl Pts',(-31.8605071662086,54.2941313842958,18.2717771392578));
#26863=CARTESIAN_POINT('Ctrl Pts',(-33.02540146796,54.0403220897572,18.2105830344552));
#26864=CARTESIAN_POINT('Ctrl Pts',(-34.6904921906955,55.242790066521,18.1123429661299));
#26865=CARTESIAN_POINT('Ctrl Pts',(-34.5692083587435,57.5631631725538,18.0012050755619));
#26866=CARTESIAN_POINT('Ctrl Pts',(-32.5539546496148,58.7197069922753,17.8900671849939));
#26867=CARTESIAN_POINT('Ctrl Pts',(-30.4893156378063,57.6538238513956,17.7789292944258));
#26868=CARTESIAN_POINT('Ctrl Pts',(-30.2914909874078,55.613533902771,17.6808819929404));
#26869=CARTESIAN_POINT('Ctrl Pts',(-31.0928476967877,54.7373092545057,17.6198806549777));
#26870=CARTESIAN_POINT('Ctrl Pts',(-31.4749747334417,54.5133534323073,17.5959252805377));
#26871=CARTESIAN_POINT('Ctrl Pts',(-31.4737670936581,54.5105654320665,18.3540747194623));
#26872=CARTESIAN_POINT('Ctrl Pts',(-31.5881478071784,54.4431225718916,18.3468663500598));
#26873=CARTESIAN_POINT('Ctrl Pts',(-32.3290694209142,54.0987447143864,18.3026120171345));
#26874=CARTESIAN_POINT('Ctrl Pts',(-34.004501193851,54.3851254608372,18.2213117206866));
#26875=CARTESIAN_POINT('Ctrl Pts',(-34.9177373632483,56.5216739711636,18.1101738301186));
#26876=CARTESIAN_POINT('Ctrl Pts',(-33.6179911050581,58.4476800725015,17.9990359395505));
#26877=CARTESIAN_POINT('Ctrl Pts',(-31.2949349095266,58.4002485379024,17.8878980489825));
#26878=CARTESIAN_POINT('Ctrl Pts',(-30.0748884576731,56.4227939888947,17.7767601584144));
#26879=CARTESIAN_POINT('Ctrl Pts',(-30.7759689649703,54.951821535532,17.6988190485744));
#26880=CARTESIAN_POINT('Ctrl Pts',(-31.4088075653018,54.5455568389317,17.657923902257));
#26881=CARTESIAN_POINT('Ctrl Pts',(-31.4703256079253,54.5106072564107,17.6540747194623));
#26882=CARTESIAN_POINT('Origin',(-32.5,56.2916512459885,23.5459252805377));
#26883=CARTESIAN_POINT('',(-31.4743570776169,54.5150293902239,19.0540747194623));
#26884=CARTESIAN_POINT('',(-31.4704988599393,54.5097377243633,18.9959252805377));
#26885=CARTESIAN_POINT('',(-31.4726250000001,54.5121855475624,23.5459252805377));
#26886=CARTESIAN_POINT('Ctrl Pts',(-31.4704988599393,54.5097377243633,18.9959252805377));
#26887=CARTESIAN_POINT('Ctrl Pts',(-32.0317105894022,54.1886772858723,18.9607195870605));
#26888=CARTESIAN_POINT('Ctrl Pts',(-33.5233071799065,54.1091544860817,18.8884679300607));
#26889=CARTESIAN_POINT('Ctrl Pts',(-34.9018152245058,55.9315825877643,18.7791703095382));
#26890=CARTESIAN_POINT('Ctrl Pts',(-34.1051248236508,58.1142702713998,18.6680324189701));
#26891=CARTESIAN_POINT('Ctrl Pts',(-31.8392454683584,58.628694091168,18.5568945284021));
#26892=CARTESIAN_POINT('Ctrl Pts',(-30.1781622293418,57.0039960908762,18.445756637834));
#26893=CARTESIAN_POINT('Ctrl Pts',(-30.5414387587065,55.2219675363373,18.3587668885459));
#26894=CARTESIAN_POINT('Ctrl Pts',(-31.2650923575404,54.6325929315102,18.3088231027804));
#26895=CARTESIAN_POINT('Ctrl Pts',(-31.4723903633871,54.5147550766704,18.2959252805377));
#26896=CARTESIAN_POINT('Ctrl Pts',(-31.4743570776169,54.5150293902239,19.0540747194623));
#26897=CARTESIAN_POINT('Ctrl Pts',(-31.767179706711,54.3458357686749,19.0358087978625));
#26898=CARTESIAN_POINT('Ctrl Pts',(-32.7735194483881,54.0410032090046,18.98049691274));
#26899=CARTESIAN_POINT('Ctrl Pts',(-34.4976287681445,54.9104040861686,18.8881390640948));
#26900=CARTESIAN_POINT('Ctrl Pts',(-34.7438661544312,57.2208600991234,18.7770011735268));
#26901=CARTESIAN_POINT('Ctrl Pts',(-32.9362674024074,58.680800710823,18.6658632829587));
#26902=CARTESIAN_POINT('Ctrl Pts',(-30.7293481493446,57.9539257225797,18.5547253923907));
#26903=CARTESIAN_POINT('Ctrl Pts',(-30.1811487641285,55.8513808790735,18.4507958712252));
#26904=CARTESIAN_POINT('Ctrl Pts',(-31.0003111545141,54.7897315757275,18.3839123135824));
#26905=CARTESIAN_POINT('Ctrl Pts',(-31.4737670936581,54.5105654320665,18.3540747194623));
#26906=CARTESIAN_POINT('Origin',(-32.5,56.2916512459885,23.5459252805377));
#26907=CARTESIAN_POINT('',(-31.4707591192323,54.5126331290241,19.7540747194623));
#26908=CARTESIAN_POINT('',(-31.4743950169646,54.5114972463166,19.6959252805377));
#26909=CARTESIAN_POINT('',(-31.4726250000001,54.5121855475624,23.5459252805377));
#26910=CARTESIAN_POINT('Ctrl Pts',(-31.4743950169646,54.5114972463166,19.6959252805377));
#26911=CARTESIAN_POINT('Ctrl Pts',(-31.6208668833956,54.425154465736,19.686707998386));
#26912=CARTESIAN_POINT('Ctrl Pts',(-32.4069324234732,54.0834056527267,19.6404447527116));
#26913=CARTESIAN_POINT('Ctrl Pts',(-34.1053854498936,54.4692617796665,19.5571355435145));
#26914=CARTESIAN_POINT('Ctrl Pts',(-34.9017637086039,56.6520633710957,19.4459976529464));
#26915=CARTESIAN_POINT('Ctrl Pts',(-33.4997804064767,58.5049756574094,19.3348597623784));
#26916=CARTESIAN_POINT('Ctrl Pts',(-31.1826867602698,58.3320070089704,19.2237218718103));
#26917=CARTESIAN_POINT('Ctrl Pts',(-30.0713448616116,56.2914775915524,19.1125839812423));
#26918=CARTESIAN_POINT('Ctrl Pts',(-30.8308409091996,54.8974452606956,19.0366517841514));
#26919=CARTESIAN_POINT('Ctrl Pts',(-31.4411632317234,54.5265201776941,18.9977655505832));
#26920=CARTESIAN_POINT('Ctrl Pts',(-31.4704988599393,54.5097377243633,18.9959252805377));
#26921=CARTESIAN_POINT('Ctrl Pts',(-31.4707591192323,54.5126331290241,19.7540747194623));
#26922=CARTESIAN_POINT('Ctrl Pts',(-31.9411934042825,54.2467857936503,19.7247512456653));
#26923=CARTESIAN_POINT('Ctrl Pts',(-33.2549727142225,54.0602154670517,19.6583818083455));
#26924=CARTESIAN_POINT('Ctrl Pts',(-34.8149526935152,55.5572409773789,19.5549664075031));
#26925=CARTESIAN_POINT('Ctrl Pts',(-34.3725208876465,57.8382701189333,19.443828516935));
#26926=CARTESIAN_POINT('Ctrl Pts',(-32.2161494783462,58.7036614639378,19.332690626367));
#26927=CARTESIAN_POINT('Ctrl Pts',(-30.3195896701686,57.3613125035425,19.221552735799));
#26928=CARTESIAN_POINT('Ctrl Pts',(-30.4024811841689,55.4214247242036,19.1286807668307));
#26929=CARTESIAN_POINT('Ctrl Pts',(-31.1732925394658,54.6889852067103,19.0728547613852));
#26930=CARTESIAN_POINT('Ctrl Pts',(-31.4743570776169,54.5150293902239,19.0540747194623));
#26931=CARTESIAN_POINT('Origin',(-32.5,56.2916512459885,23.5459252805377));
#26932=CARTESIAN_POINT('',(-31.4721876288368,54.5092967477939,20.4540747194623));
#26933=CARTESIAN_POINT('',(-31.4737733324271,54.5152256259023,20.3959252805377));
#26934=CARTESIAN_POINT('',(-31.4726250000001,54.5121855475624,23.5459252805377));
#26935=CARTESIAN_POINT('Ctrl Pts',(-31.4737733324271,54.5152256259023,20.3959252805377));
#26936=CARTESIAN_POINT('Ctrl Pts',(-31.799246207199,54.3283059275284,20.3756504461887));
#26937=CARTESIAN_POINT('Ctrl Pts',(-32.8583863662624,54.0381735568298,20.318329648317));
#26938=CARTESIAN_POINT('Ctrl Pts',(-34.5693901517228,55.0204352512209,20.2239628869227));
#26939=CARTESIAN_POINT('Ctrl Pts',(-34.6903421852682,57.3408256590054,20.1128249963547));
#26940=CARTESIAN_POINT('Ctrl Pts',(-32.8064491443347,58.7008948504121,20.0016871057866));
#26941=CARTESIAN_POINT('Ctrl Pts',(-30.6420597422744,57.8557560368672,19.8905492152186));
#26942=CARTESIAN_POINT('Ctrl Pts',(-30.2167292658396,55.767800516413,19.7886286068022));
#26943=CARTESIAN_POINT('Ctrl Pts',(-31.0321693333385,54.7721820870222,19.7237539619086));
#26944=CARTESIAN_POINT('Ctrl Pts',(-31.4743950169646,54.5114972463166,19.6959252805377));
#26945=CARTESIAN_POINT('Ctrl Pts',(-31.4721876288368,54.5092967477939,20.4540747194623));
#26946=CARTESIAN_POINT('Ctrl Pts',(-31.5250686260056,54.4783192167782,20.4507396569907));
#26947=CARTESIAN_POINT('Ctrl Pts',(-32.182499910029,54.133716656297,20.4103586309964));
#26948=CARTESIAN_POINT('Ctrl Pts',(-33.7978345552325,54.2388509530007,20.3329316414794));
#26949=CARTESIAN_POINT('Ctrl Pts',(-34.9285465373885,56.2687104209715,20.2217937509113));
#26950=CARTESIAN_POINT('Ctrl Pts',(-33.8363822214011,58.3195681810162,20.1106558603433));
#26951=CARTESIAN_POINT('Ctrl Pts',(-31.5210121579647,58.5142504249981,19.9995179697753));
#26952=CARTESIAN_POINT('Ctrl Pts',(-30.101720741136,56.674562508041,19.8883800792072));
#26953=CARTESIAN_POINT('Ctrl Pts',(-30.6728871983316,55.0622630484846,19.8065656624362));
#26954=CARTESIAN_POINT('Ctrl Pts',(-31.3468677972825,54.5826454110005,19.7617972091879));
#26955=CARTESIAN_POINT('Ctrl Pts',(-31.4707591192323,54.5126331290241,19.7540747194623));
#26956=CARTESIAN_POINT('Origin',(-32.5,56.2916512459885,23.5459252805377));
#26957=CARTESIAN_POINT('',(-31.47496098746,54.5139076530798,21.1540747194623));
#26958=CARTESIAN_POINT('',(-31.4704172621348,54.5115691325664,21.0959252805377));
#26959=CARTESIAN_POINT('',(-31.4726250000001,54.5121855475624,23.5459252805377));
#26960=CARTESIAN_POINT('Ctrl Pts',(-31.4704172621348,54.5115691325664,21.0959252805377));
#26961=CARTESIAN_POINT('Ctrl Pts',(-31.9722041658629,54.227575372343,21.0645928939915));
#26962=CARTESIAN_POINT('Ctrl Pts',(-33.3458362247711,54.0736222398741,20.9962145439225));
#26963=CARTESIAN_POINT('Ctrl Pts',(-34.8512746399183,55.6834843462922,20.8907902303309));
#26964=CARTESIAN_POINT('Ctrl Pts',(-34.2861576030319,57.9372537407841,20.7796523397629));
#26965=CARTESIAN_POINT('Ctrl Pts',(-32.0861481883531,58.6847859443394,20.6685144491949));
#26966=CARTESIAN_POINT('Ctrl Pts',(-30.2649430630365,57.2418541016518,20.5573765586268));
#26967=CARTESIAN_POINT('Ctrl Pts',(-30.4485426703035,55.3510892045502,20.4665135024078));
#26968=CARTESIAN_POINT('Ctrl Pts',(-31.2045456025534,54.6698436293139,20.4126964097114));
#26969=CARTESIAN_POINT('Ctrl Pts',(-31.4737733324271,54.5152256259023,20.3959252805377));
#26970=CARTESIAN_POINT('Ctrl Pts',(-31.47496098746,54.5139076530797,21.1540747194623));
#26971=CARTESIAN_POINT('Ctrl Pts',(-31.70486029749,54.3795842898515,21.1396821047934));
#26972=CARTESIAN_POINT('Ctrl Pts',(-32.6134298152417,54.053477853398,21.0882435266019));
#26973=CARTESIAN_POINT('Ctrl Pts',(-34.3429657642117,54.7099453599152,20.9997589848876));
#26974=CARTESIAN_POINT('Ctrl Pts',(-34.8284152391772,56.982193672835,20.8886210943196));
#26975=CARTESIAN_POINT('Ctrl Pts',(-33.18263271582,58.6223996095027,20.7774832037515));
#26976=CARTESIAN_POINT('Ctrl Pts',(-30.9120322857352,58.129235673502,20.6663453131835));
#26977=CARTESIAN_POINT('Ctrl Pts',(-30.1194352615649,56.0193863503515,20.5585424850871));
#26978=CARTESIAN_POINT('Ctrl Pts',(-30.9376650889446,54.8224184634311,20.4877856205134));
#26979=CARTESIAN_POINT('Ctrl Pts',(-31.4721876288368,54.5092967477939,20.4540747194623));
#26980=CARTESIAN_POINT('Origin',(-32.5,56.2916512459885,23.5459252805377));
#26981=CARTESIAN_POINT('',(-31.4716734168817,54.5151354051885,21.8540747194623));
#26982=CARTESIAN_POINT('',(-31.4730118547325,54.5098571360137,21.7959252805377));
#26983=CARTESIAN_POINT('',(-31.4726250000001,54.5121855475624,23.5459252805377));
#26984=CARTESIAN_POINT('',(-30.5157034944334,56.8250975324092,22.));
#26985=CARTESIAN_POINT('Ctrl Pts',(-30.5157034944334,56.8250975324092,22.));
#26986=CARTESIAN_POINT('Ctrl Pts',(-30.3383199129809,56.1652717359214,21.9629540364773));
#26987=CARTESIAN_POINT('Ctrl Pts',(-30.5738806361657,55.1809621297242,21.9143122762981));
#26988=CARTESIAN_POINT('Ctrl Pts',(-31.2853315674048,54.6208532363719,21.8656705161189));
#26989=CARTESIAN_POINT('Ctrl Pts',(-31.4716734168817,54.5151354051885,21.8540747194623));
#26990=CARTESIAN_POINT('',(-31.043364830276,57.7461496994442,22.));
#26991=CARTESIAN_POINT('Origin',(-32.5,56.2916512459885,22.));
#26992=CARTESIAN_POINT('Ctrl Pts',(-31.0433632440414,57.7461514510325,22.));
#26993=CARTESIAN_POINT('Ctrl Pts',(-30.5726971034828,57.2735716615611,21.9636770818144));
#26994=CARTESIAN_POINT('Ctrl Pts',(-30.1593922934378,55.9189388685996,21.895652175327));
#26995=CARTESIAN_POINT('Ctrl Pts',(-30.9704682366631,54.8056054537255,21.8276272688396));
#26996=CARTESIAN_POINT('Ctrl Pts',(-31.4730118547325,54.5098571360137,21.7959252805377));
#26997=CARTESIAN_POINT('Origin',(-65.,8.88178419700125E-15,17.));
#26998=CARTESIAN_POINT('',(-63.3324486297716,0.0012143596160653,13.8714803633902));
#26999=CARTESIAN_POINT('',(-63.3320009243657,-0.000968828099756215,13.6785196366098));
#27000=CARTESIAN_POINT('',(-63.334,8.44655409538511E-15,17.));
#27001=CARTESIAN_POINT('',(-63.3648706727485,0.319230454628309,13.));
#27002=CARTESIAN_POINT('Ctrl Pts',(-63.3320009243657,-0.000968828099756215,
13.6785196366098));
#27003=CARTESIAN_POINT('Ctrl Pts',(-63.3315933114009,-0.0590548763034475,
13.6746222055426));
#27004=CARTESIAN_POINT('Ctrl Pts',(-63.3343634348107,-0.117102016123696,
13.6707247744754));
#27005=CARTESIAN_POINT('Ctrl Pts',(-63.3404396356832,-0.174801282227219,
13.6668273434083));
#27006=CARTESIAN_POINT('Ctrl Pts',(-63.3981952988365,-0.723245852641092,
13.6297813798856));
#27007=CARTESIAN_POINT('Ctrl Pts',(-63.7546528235523,-1.24026026815387,
13.5927354163629));
#27008=CARTESIAN_POINT('Ctrl Pts',(-64.2467810781753,-1.48913792445444,
13.5556894528402));
#27009=CARTESIAN_POINT('Ctrl Pts',(-64.7389093327983,-1.738015580755,13.5186434893175));
#27010=CARTESIAN_POINT('Ctrl Pts',(-65.3667083173286,-1.71875647784334,
13.4815975257948));
#27011=CARTESIAN_POINT('Ctrl Pts',(-65.8426564295865,-1.44035726535854,
13.4445515622722));
#27012=CARTESIAN_POINT('Ctrl Pts',(-66.3186045418444,-1.16195805287374,
13.4075055987495));
#27013=CARTESIAN_POINT('Ctrl Pts',(-66.6427017818299,-0.624418730815817,
13.3704596352268));
#27014=CARTESIAN_POINT('Ctrl Pts',(-66.6670336186705,-0.0733842827933133,
13.3334136717041));
#27015=CARTESIAN_POINT('Ctrl Pts',(-66.691365455511,0.477650165229191,13.2963677081814));
#27016=CARTESIAN_POINT('Ctrl Pts',(-66.4159318892067,1.04217973921627,13.2593217446588));
#27017=CARTESIAN_POINT('Ctrl Pts',(-65.9659478490025,1.36111593499209,13.2222757811361));
#27018=CARTESIAN_POINT('Ctrl Pts',(-65.5159638087983,1.68005213076791,13.1852298176134));
#27019=CARTESIAN_POINT('Ctrl Pts',(-64.8914292946943,1.75339494833248,13.1481838540907));
#27020=CARTESIAN_POINT('Ctrl Pts',(-64.3801939409253,1.54911937996348,13.111137890568));
#27021=CARTESIAN_POINT('Ctrl Pts',(-63.8689585871564,1.3448438115945,13.0740919270454));
#27022=CARTESIAN_POINT('Ctrl Pts',(-63.4710223937224,0.86294985729197,13.0370459635227));
#27023=CARTESIAN_POINT('Ctrl Pts',(-63.3648706727485,0.319230454628356,
13.));
#27024=CARTESIAN_POINT('',(-64.9474239245698,-1.66819769235426,13.));
#27025=CARTESIAN_POINT('Origin',(-65.,8.88178419700125E-15,13.));
#27026=CARTESIAN_POINT('',(-63.3365558121435,0.000651319618130558,13.1714803633902));
#27027=CARTESIAN_POINT('Ctrl Pts',(-64.9474239513002,-1.66819938802346,
13.));
#27028=CARTESIAN_POINT('Ctrl Pts',(-64.4069183000551,-1.65047139087789,
13.0363229181856));
#27029=CARTESIAN_POINT('Ctrl Pts',(-63.874833765777,-1.34577267304802,13.0726458363711));
#27030=CARTESIAN_POINT('Ctrl Pts',(-63.5871509129382,-0.887831743084588,
13.1089687545567));
#27031=CARTESIAN_POINT('Ctrl Pts',(-63.42211720178,-0.625126856723237,13.1298059575012));
#27032=CARTESIAN_POINT('Ctrl Pts',(-63.3375141386089,-0.311991178117355,
13.1506431604457));
#27033=CARTESIAN_POINT('Ctrl Pts',(-63.3365558121435,0.000651319618130558,
13.1714803633902));
#27034=CARTESIAN_POINT('',(-63.334,8.85460640886101E-15,12.));
#27035=CARTESIAN_POINT('',(-63.334,8.44655409538511E-15,17.));
#27036=CARTESIAN_POINT('Origin',(-65.,8.88178419700125E-15,12.));
#27037=CARTESIAN_POINT('Ctrl Pts',(-63.3365558121435,0.000651319618130558,
13.1714803633902));
#27038=CARTESIAN_POINT('Ctrl Pts',(-63.3358103529628,0.243848422696133,
13.1876891239684));
#27039=CARTESIAN_POINT('Ctrl Pts',(-63.385677580256,0.486747106414457,13.2038978845465));
#27040=CARTESIAN_POINT('Ctrl Pts',(-63.4876703201545,0.705378176395509,
13.2201066451247));
#27041=CARTESIAN_POINT('Ctrl Pts',(-63.7207800205315,1.20507083360909,13.2571526086474));
#27042=CARTESIAN_POINT('Ctrl Pts',(-64.2261802362228,1.57799560462436,13.2941985721701));
#27043=CARTESIAN_POINT('Ctrl Pts',(-64.7725065735009,1.65321436231665,13.3312445356927));
#27044=CARTESIAN_POINT('Ctrl Pts',(-65.318832910779,1.72843312000894,13.3682904992154));
#27045=CARTESIAN_POINT('Ctrl Pts',(-65.906085369644,1.50594586437825,13.4053364627381));
#27046=CARTESIAN_POINT('Ctrl Pts',(-66.265537296365,1.0877096323259,13.4423824262608));
#27047=CARTESIAN_POINT('Ctrl Pts',(-66.6249892230859,0.669473400273544,
13.4794283897835));
#27048=CARTESIAN_POINT('Ctrl Pts',(-66.7566406176629,0.0554881917995234,
13.5164743533061));
#27049=CARTESIAN_POINT('Ctrl Pts',(-66.6002239654009,-0.4733199493701,13.5535203168288));
#27050=CARTESIAN_POINT('Ctrl Pts',(-66.4438073131388,-1.00212809053972,
13.5905662803515));
#27051=CARTESIAN_POINT('Ctrl Pts',(-65.9993226140377,-1.44575916440495,
13.6276122438742));
#27052=CARTESIAN_POINT('Ctrl Pts',(-65.470199129815,-1.60114874218548,13.6646582073969));
#27053=CARTESIAN_POINT('Ctrl Pts',(-64.9410756455923,-1.75653831996601,
13.7017041709195));
#27054=CARTESIAN_POINT('Ctrl Pts',(-64.327313376248,-1.62368640166185,13.7387501344422));
#27055=CARTESIAN_POINT('Ctrl Pts',(-63.9097999122987,-1.26341063241475,
13.7757960979649));
#27056=CARTESIAN_POINT('Ctrl Pts',(-63.550341325322,-0.953230889441883,
13.8076908531067));
#27057=CARTESIAN_POINT('Ctrl Pts',(-63.3363495020968,-0.474476303274688,
13.8395856082484));
#27058=CARTESIAN_POINT('Ctrl Pts',(-63.3324486297716,0.0012143596160653,
13.8714803633902));
#27059=CARTESIAN_POINT('Origin',(-65.,8.88178419700125E-15,17.));
#27060=CARTESIAN_POINT('',(-63.3327604959513,-0.00132477262096475,14.5714803633902));
#27061=CARTESIAN_POINT('',(-63.3362968330887,-0.00083230422485394,14.3785196366098));
#27062=CARTESIAN_POINT('',(-63.334,8.44655409538511E-15,17.));
#27063=CARTESIAN_POINT('Ctrl Pts',(-63.3362968330887,-0.00083230422485394,
14.3785196366098));
#27064=CARTESIAN_POINT('Ctrl Pts',(-63.3352820110227,-0.225194784962803,
14.3635646533454));
#27065=CARTESIAN_POINT('Ctrl Pts',(-63.3774911908197,-0.449191325190206,
14.3486096700809));
#27066=CARTESIAN_POINT('Ctrl Pts',(-63.4647380475121,-0.654002427856251,
14.3336546868165));
#27067=CARTESIAN_POINT('Ctrl Pts',(-63.6808629212981,-1.16135335592135,
14.2966087232938));
#27068=CARTESIAN_POINT('Ctrl Pts',(-64.1733546191173,-1.55097577727798,
14.2595627597711));
#27069=CARTESIAN_POINT('Ctrl Pts',(-64.7168232236993,-1.64455527160812,
14.2225167962485));
#27070=CARTESIAN_POINT('Ctrl Pts',(-65.2602918282814,-1.73813476593826,
14.1854708327258));
#27071=CARTESIAN_POINT('Ctrl Pts',(-65.8547373396264,-1.53567133324192,
14.1484248692031));
#27072=CARTESIAN_POINT('Ctrl Pts',(-66.2281050246363,-1.12982650677501,
14.1113789056804));
#27073=CARTESIAN_POINT('Ctrl Pts',(-66.6014727096463,-0.723981680308087,
14.0743329421577));
#27074=CARTESIAN_POINT('Ctrl Pts',(-66.7537625683213,-0.114755460070592,
14.0372869786351));
#27075=CARTESIAN_POINT('Ctrl Pts',(-66.6152849767096,0.419042261543978,
14.0002410151124));
#27076=CARTESIAN_POINT('Ctrl Pts',(-66.4768073850979,0.952839983158533,
13.9631950515897));
#27077=CARTESIAN_POINT('Ctrl Pts',(-66.0475623431996,1.41120920615017,13.926149088067));
#27078=CARTESIAN_POINT('Ctrl Pts',(-65.5239830002582,1.58436286925844,13.8891031245443));
#27079=CARTESIAN_POINT('Ctrl Pts',(-65.0004036573169,1.75751653236672,13.8520571610217));
#27080=CARTESIAN_POINT('Ctrl Pts',(-64.3824900133324,1.64545463559163,13.815011197499));
#27081=CARTESIAN_POINT('Ctrl Pts',(-63.9530600921357,1.29948632454661,13.7779652339763));
#27082=CARTESIAN_POINT('Ctrl Pts',(-63.5688084672201,0.989915707487903,
13.7448167015208));
#27083=CARTESIAN_POINT('Ctrl Pts',(-63.3354677647952,0.493066145425921,
13.7116681690653));
#27084=CARTESIAN_POINT('Ctrl Pts',(-63.3320009243657,-0.000968828099756215,
13.6785196366098));
#27085=CARTESIAN_POINT('Ctrl Pts',(-63.3324486297716,0.0012143596160653,
13.8714803633902));
#27086=CARTESIAN_POINT('Ctrl Pts',(-63.3318186137667,0.0780414654682698,
13.8766315717711));
#27087=CARTESIAN_POINT('Ctrl Pts',(-63.3366686795385,0.154788650933419,
13.881782780152));
#27088=CARTESIAN_POINT('Ctrl Pts',(-63.3472710750459,0.230732838385412,
13.8869339885329));
#27089=CARTESIAN_POINT('Ctrl Pts',(-63.4235203602966,0.776900919748422,
13.9239799520556));
#27090=CARTESIAN_POINT('Ctrl Pts',(-63.7972835893523,1.28153746228441,13.9610259155783));
#27091=CARTESIAN_POINT('Ctrl Pts',(-64.2975048362999,1.51368831950506,13.998071879101));
#27092=CARTESIAN_POINT('Ctrl Pts',(-64.7977260832475,1.74583917672571,14.0351178426237));
#27093=CARTESIAN_POINT('Ctrl Pts',(-65.424405348087,1.70550434863099,14.0721638061464));
#27094=CARTESIAN_POINT('Ctrl Pts',(-65.8907398483472,1.41114550098829,14.109209769669));
#27095=CARTESIAN_POINT('Ctrl Pts',(-66.3570743486074,1.1167866533456,14.1462557331917));
#27096=CARTESIAN_POINT('Ctrl Pts',(-66.6630640842882,0.568403786154946,
14.1833016967144));
#27097=CARTESIAN_POINT('Ctrl Pts',(-66.6686708473517,0.0169663179122643,
14.2203476602371));
#27098=CARTESIAN_POINT('Ctrl Pts',(-66.6742776104151,-0.534471150330418,
14.2573936237598));
#27099=CARTESIAN_POINT('Ctrl Pts',(-66.3795014008612,-1.08896321962512,
14.2944395872824));
#27100=CARTESIAN_POINT('Ctrl Pts',(-65.9192483587705,-1.39274289076841,
14.3314855508051));
#27101=CARTESIAN_POINT('Ctrl Pts',(-65.4589953166798,-1.6965225619117,14.3685315143278));
#27102=CARTESIAN_POINT('Ctrl Pts',(-64.8332654420522,-1.74958983490357,
14.4055774778505));
#27103=CARTESIAN_POINT('Ctrl Pts',(-64.3284274914591,-1.5276584533176,14.4426234413732));
#27104=CARTESIAN_POINT('Ctrl Pts',(-63.823589540866,-1.30572707173164,14.4796694048958));
#27105=CARTESIAN_POINT('Ctrl Pts',(-63.4396435143075,-0.808797035567833,
14.5167153684185));
#27106=CARTESIAN_POINT('Ctrl Pts',(-63.352304522573,-0.264291051559223,
14.5537613319412));
#27107=CARTESIAN_POINT('Ctrl Pts',(-63.3383798175659,-0.177478906704707,
14.5596676757575));
#27108=CARTESIAN_POINT('Ctrl Pts',(-63.3319945181308,-0.0894574366348098,
14.5655740195739));
#27109=CARTESIAN_POINT('Ctrl Pts',(-63.3327604959513,-0.00132477262096475,
14.5714803633902));
#27110=CARTESIAN_POINT('Origin',(-65.,8.88178419700125E-15,17.));
#27111=CARTESIAN_POINT('',(-63.3366282199437,-0.000380246208307872,15.2714803633902));
#27112=CARTESIAN_POINT('',(-63.3350218272016,0.00143128727517339,15.0785196366098));
#27113=CARTESIAN_POINT('',(-63.334,8.44655409538511E-15,17.));
#27114=CARTESIAN_POINT('Ctrl Pts',(-63.3350218272016,0.00143128727517339,
15.0785196366098));
#27115=CARTESIAN_POINT('Ctrl Pts',(-63.3382129761596,-0.388071089145991,
15.0525071011481));
#27116=CARTESIAN_POINT('Ctrl Pts',(-63.4745702784036,-0.779586335762523,
15.0264945656864));
#27117=CARTESIAN_POINT('Ctrl Pts',(-63.7241632245643,-1.07563467970708,
15.0004820302248));
#27118=CARTESIAN_POINT('Ctrl Pts',(-64.0796230447962,-1.49725433177355,
14.9634360667021));
#27119=CARTESIAN_POINT('Ctrl Pts',(-64.6647503809125,-1.72524549701853,
14.9263901031794));
#27120=CARTESIAN_POINT('Ctrl Pts',(-65.2117584175496,-1.65526670109562,
14.8893441396567));
#27121=CARTESIAN_POINT('Ctrl Pts',(-65.7587664541868,-1.58528790517271,
14.852298176134));
#27122=CARTESIAN_POINT('Ctrl Pts',(-66.2676551913447,-1.21733914808191,
14.8152522126113));
#27123=CARTESIAN_POINT('Ctrl Pts',(-66.5055287575052,-0.719814314063376,
14.7782062490887));
#27124=CARTESIAN_POINT('Ctrl Pts',(-66.7434023236657,-0.222289480044837,
14.741160285566));
#27125=CARTESIAN_POINT('Ctrl Pts',(-66.7102607188288,0.40481143090144,14.7041143220433));
#27126=CARTESIAN_POINT('Ctrl Pts',(-66.4212714962,0.874492228471364,14.6670683585206));
#27127=CARTESIAN_POINT('Ctrl Pts',(-66.1322822735712,1.34417302604129,14.630022394998));
#27128=CARTESIAN_POINT('Ctrl Pts',(-65.5874454331506,1.65643371023486,14.5929764314753));
#27129=CARTESIAN_POINT('Ctrl Pts',(-65.0361084265221,1.66836621488623,14.5559304679526));
#27130=CARTESIAN_POINT('Ctrl Pts',(-64.4847714198936,1.68029871953761,14.5188845044299));
#27131=CARTESIAN_POINT('Ctrl Pts',(-63.9269342470572,1.39190304464679,14.4818385409072));
#27132=CARTESIAN_POINT('Ctrl Pts',(-63.6178946855153,0.935165489814596,
14.4447925773845));
#27133=CARTESIAN_POINT('Ctrl Pts',(-63.4336104557676,0.662807064022201,
14.4227015971263));
#27134=CARTESIAN_POINT('Ctrl Pts',(-63.3377958928888,0.330588135707235,
14.400610616868));
#27135=CARTESIAN_POINT('Ctrl Pts',(-63.3362968330887,-0.00083230422485394,
14.3785196366098));
#27136=CARTESIAN_POINT('Ctrl Pts',(-63.3327604959513,-0.00132477262096475,
14.5714803633902));
#27137=CARTESIAN_POINT('Ctrl Pts',(-63.336798909355,0.463331150982527,14.6026199830965));
#27138=CARTESIAN_POINT('Ctrl Pts',(-63.5396173640042,0.931077870254266,
14.6337596028029));
#27139=CARTESIAN_POINT('Ctrl Pts',(-63.8843359278475,1.24098501894125,14.6648992225092));
#27140=CARTESIAN_POINT('Ctrl Pts',(-64.294438281767,1.6096731735797,14.7019451860319));
#27141=CARTESIAN_POINT('Ctrl Pts',(-64.9053749465165,1.75496755100318,14.7389911495546));
#27142=CARTESIAN_POINT('Ctrl Pts',(-65.4375473020178,1.6103733915995,14.7760371130773));
#27143=CARTESIAN_POINT('Ctrl Pts',(-65.9697196575191,1.46577923219582,14.8130830766));
#27144=CARTESIAN_POINT('Ctrl Pts',(-66.4231277037722,1.03129653596499,14.8501290401226));
#27145=CARTESIAN_POINT('Ctrl Pts',(-66.5902666729806,0.505768754333094,
14.8871750036453));
#27146=CARTESIAN_POINT('Ctrl Pts',(-66.757405642189,-0.0197590272988146,
14.924220967168));
#27147=CARTESIAN_POINT('Ctrl Pts',(-66.6382755343526,-0.636331894331805,
14.9612669306907));
#27148=CARTESIAN_POINT('Ctrl Pts',(-66.2873969210692,-1.061771768796,14.9983128942134));
#27149=CARTESIAN_POINT('Ctrl Pts',(-65.9365183077858,-1.48721164326019,
15.0353588577361));
#27150=CARTESIAN_POINT('Ctrl Pts',(-65.3538911890554,-1.72151852515559,
15.0724048212587));
#27151=CARTESIAN_POINT('Ctrl Pts',(-64.8061581683602,-1.65746054599184,
15.1094507847814));
#27152=CARTESIAN_POINT('Ctrl Pts',(-64.2584251476649,-1.59340256682809,
15.1464967483041));
#27153=CARTESIAN_POINT('Ctrl Pts',(-63.7455862250048,-1.23097972660521,
15.1835427118268));
#27154=CARTESIAN_POINT('Ctrl Pts',(-63.5023450418969,-0.736056890900427,
15.2205886753495));
#27155=CARTESIAN_POINT('Ctrl Pts',(-63.390961297378,-0.509424385728733,
15.237552571363));
#27156=CARTESIAN_POINT('Ctrl Pts',(-63.336108421692,-0.25500848787214,15.2545164673766));
#27157=CARTESIAN_POINT('Ctrl Pts',(-63.3366282199437,-0.000380246208307872,
15.2714803633902));
#27158=CARTESIAN_POINT('Origin',(-65.,8.88178419700125E-15,17.));
#27159=CARTESIAN_POINT('',(-63.3341549687971,0.00152342623459117,15.9714803633902));
#27160=CARTESIAN_POINT('',(-63.3312431600774,-6.71117919643557E-6,15.7785196366098));
#27161=CARTESIAN_POINT('',(-63.334,8.44655409538511E-15,17.));
#27162=CARTESIAN_POINT('Ctrl Pts',(-63.3312431738575,-6.71114565062814E-6,
15.7785196366098));
#27163=CARTESIAN_POINT('Ctrl Pts',(-63.3312102147262,-0.551831913054096,
15.7414495489509));
#27164=CARTESIAN_POINT('Ctrl Pts',(-63.6320564203023,-1.10362622346452,
15.7043794612919));
#27165=CARTESIAN_POINT('Ctrl Pts',(-64.0958701387024,-1.40260423963279,
15.667309373633));
#27166=CARTESIAN_POINT('Ctrl Pts',(-64.5593820206073,-1.70138768959275,
15.6302634101103));
#27167=CARTESIAN_POINT('Ctrl Pts',(-65.1856492588609,-1.74768378931891,
15.5932174465876));
#27168=CARTESIAN_POINT('Ctrl Pts',(-65.6880571011575,-1.52030486584838,
15.556171483065));
#27169=CARTESIAN_POINT('Ctrl Pts',(-66.1904649434542,-1.29292594237784,
15.5191255195423));
#27170=CARTESIAN_POINT('Ctrl Pts',(-66.569013389794,-0.791871995710595,
15.4820795560196));
#27171=CARTESIAN_POINT('Ctrl Pts',(-66.6504575962853,-0.246453206514422,
15.4450335924969));
#27172=CARTESIAN_POINT('Ctrl Pts',(-66.7319018027767,0.29896558268175,15.4079876289742));
#27173=CARTESIAN_POINT('Ctrl Pts',(-66.5162417694196,0.888749214406848,
15.3709416654516));
#27174=CARTESIAN_POINT('Ctrl Pts',(-66.1021755351577,1.25297986690094,15.3338957019289));
#27175=CARTESIAN_POINT('Ctrl Pts',(-65.6881093008957,1.61721051939502,15.2968497384062));
#27176=CARTESIAN_POINT('Ctrl Pts',(-65.0756368657288,1.75588819265809,15.2598037748835));
#27177=CARTESIAN_POINT('Ctrl Pts',(-64.5450597089912,1.60554625999199,15.2227578113608));
#27178=CARTESIAN_POINT('Ctrl Pts',(-64.0144825522536,1.45520432732588,15.1857118478382));
#27179=CARTESIAN_POINT('Ctrl Pts',(-63.5658006739452,1.01584278873058,15.1486658843155));
#27180=CARTESIAN_POINT('Ctrl Pts',(-63.4043558869649,0.488537949988949,
15.1116199207928));
#27181=CARTESIAN_POINT('Ctrl Pts',(-63.3562726607889,0.331490340715371,
15.1005864927318));
#27182=CARTESIAN_POINT('Ctrl Pts',(-63.3336682754684,0.166641881842649,
15.0895530646708));
#27183=CARTESIAN_POINT('Ctrl Pts',(-63.3350218272016,0.00143128727517339,
15.0785196366098));
#27184=CARTESIAN_POINT('Ctrl Pts',(-63.3366282199437,-0.000380246208307872,
15.2714803633902));
#27185=CARTESIAN_POINT('Ctrl Pts',(-63.3372435634692,0.301051779472634,
15.2915624308993));
#27186=CARTESIAN_POINT('Ctrl Pts',(-63.4154588028067,0.602781386183106,
15.3116444984084));
#27187=CARTESIAN_POINT('Ctrl Pts',(-63.5693524834351,0.859067985064386,
15.3317265659175));
#27188=CARTESIAN_POINT('Ctrl Pts',(-63.8532445516371,1.33184719413771,15.3687725294402));
#27189=CARTESIAN_POINT('Ctrl Pts',(-64.3946721315968,1.64998278109767,15.4058184929629));
#27190=CARTESIAN_POINT('Ctrl Pts',(-64.9458478213867,1.66787819121185,15.4428644564855));
#27191=CARTESIAN_POINT('Ctrl Pts',(-65.4970235111765,1.68577360132602,15.4799104200082));
#27192=CARTESIAN_POINT('Ctrl Pts',(-66.0579473107965,1.4034288345944,15.5169563835309));
#27193=CARTESIAN_POINT('Ctrl Pts',(-66.3719092626235,0.950060574217461,
15.5540023470536));
#27194=CARTESIAN_POINT('Ctrl Pts',(-66.6858712144506,0.496692313840518,
15.5910483105763));
#27195=CARTESIAN_POINT('Ctrl Pts',(-66.7528713184848,-0.127699440181744,
15.6280942740989));
#27196=CARTESIAN_POINT('Ctrl Pts',(-66.542246597235,-0.637358260928825,
15.6651402376216));
#27197=CARTESIAN_POINT('Ctrl Pts',(-66.3316218759853,-1.1470170816759,15.7021862011443));
#27198=CARTESIAN_POINT('Ctrl Pts',(-65.8433723294516,-1.5419429691478,15.739232164667));
#27199=CARTESIAN_POINT('Ctrl Pts',(-65.3009481311498,-1.64139585163659,
15.7762781281897));
#27200=CARTESIAN_POINT('Ctrl Pts',(-64.7585239328481,-1.74084873412537,
15.8133240917123));
#27201=CARTESIAN_POINT('Ctrl Pts',(-64.1619250827784,-1.54482861163105,
15.850370055235));
#27202=CARTESIAN_POINT('Ctrl Pts',(-63.7841884276299,-1.14304520468471,
15.8874160187577));
#27203=CARTESIAN_POINT('Ctrl Pts',(-63.4984696309493,-0.839137521926598,
15.9154374669685));
#27204=CARTESIAN_POINT('Ctrl Pts',(-63.3379698006251,-0.417505232584549,
15.9434589151794));
#27205=CARTESIAN_POINT('Ctrl Pts',(-63.3341549687971,0.00152342623459117,
15.9714803633902));
#27206=CARTESIAN_POINT('Origin',(-65.,8.88178419700125E-15,17.));
#27207=CARTESIAN_POINT('',(-63.3314647116295,-0.000550350488415785,16.6714803633902));
#27208=CARTESIAN_POINT('',(-63.3350414063796,-0.00142706819227155,16.4785196366098));
#27209=CARTESIAN_POINT('',(-63.334,8.44655409538511E-15,17.));
#27210=CARTESIAN_POINT('Ctrl Pts',(-63.3350414063796,-0.00142706819227155,
16.4785196366098));
#27211=CARTESIAN_POINT('Ctrl Pts',(-63.3336871074336,-0.167365053879273,
16.4674379602763));
#27212=CARTESIAN_POINT('Ctrl Pts',(-63.3564935743301,-0.332939153110412,
16.4563562839428));
#27213=CARTESIAN_POINT('Ctrl Pts',(-63.4049919569221,-0.490610641878076,
16.4452746076093));
#27214=CARTESIAN_POINT('Ctrl Pts',(-63.5671216977971,-1.01770528403039,
16.4082286440866));
#27215=CARTESIAN_POINT('Ctrl Pts',(-64.0163740234165,-1.45648350908885,
16.3711826805639));
#27216=CARTESIAN_POINT('Ctrl Pts',(-64.5471460595228,-1.60613597431705,
16.3341367170413));
#27217=CARTESIAN_POINT('Ctrl Pts',(-65.0779180956292,-1.75578843954525,
16.2970907535186));
#27218=CARTESIAN_POINT('Ctrl Pts',(-65.6902098422225,-1.61631514494319,
16.2600447899959));
#27219=CARTESIAN_POINT('Ctrl Pts',(-66.1038025095515,-1.25154683464619,
16.2229988264732));
#27220=CARTESIAN_POINT('Ctrl Pts',(-66.5173951768805,-0.886778524349203,
16.1859528629505));
#27221=CARTESIAN_POINT('Ctrl Pts',(-66.7322887649452,-0.296715198357285,
16.1489068994279));
#27222=CARTESIAN_POINT('Ctrl Pts',(-66.6501360046234,0.248597316289499,
16.1118609359052));
#27223=CARTESIAN_POINT('Ctrl Pts',(-66.5679832443015,0.793909830936282,
16.0748149723825));
#27224=CARTESIAN_POINT('Ctrl Pts',(-66.1887841355932,1.29447153423794,16.0377690088598));
#27225=CARTESIAN_POINT('Ctrl Pts',(-65.6860813008334,1.5211975243268,16.0007230453371));
#27226=CARTESIAN_POINT('Ctrl Pts',(-65.1833784660736,1.74792351441566,15.9636770818144));
#27227=CARTESIAN_POINT('Ctrl Pts',(-64.5571719052625,1.70081379129174,15.9266311182918));
#27228=CARTESIAN_POINT('Ctrl Pts',(-64.0940486017292,1.40142838682092,15.8895851547691));
#27229=CARTESIAN_POINT('Ctrl Pts',(-63.631226881651,1.10223794054802,15.8525633153827));
#27230=CARTESIAN_POINT('Ctrl Pts',(-63.3312760900911,0.551100267138441,
15.8155414759962));
#27231=CARTESIAN_POINT('Ctrl Pts',(-63.3312431738575,-6.71114565062814E-6,
15.7785196366098));
#27232=CARTESIAN_POINT('Ctrl Pts',(-63.3341549687971,0.00152342623459117,
15.9714803633902));
#27233=CARTESIAN_POINT('Ctrl Pts',(-63.3329263739013,0.136474714946144,
15.980504878702));
#27234=CARTESIAN_POINT('Ctrl Pts',(-63.3479493008663,0.271155952543891,
15.9895293940139));
#27235=CARTESIAN_POINT('Ctrl Pts',(-63.3802748445461,0.401547681148712,
15.9985539093257));
#27236=CARTESIAN_POINT('Ctrl Pts',(-63.5129723768379,0.936810468637382,
16.0355998728484));
#27237=CARTESIAN_POINT('Ctrl Pts',(-63.9372419016487,1.39978935221635,16.0726458363711));
#27238=CARTESIAN_POINT('Ctrl Pts',(-64.4589140651794,1.57859942055654,16.1096917998938));
#27239=CARTESIAN_POINT('Ctrl Pts',(-64.9805862287101,1.75740948889675,16.1467377634165));
#27240=CARTESIAN_POINT('Ctrl Pts',(-65.5996610309607,1.65205074199819,16.1837837269391));
#27241=CARTESIAN_POINT('Ctrl Pts',(-66.0328153782871,1.31074120779884,16.2208296904618));
#27242=CARTESIAN_POINT('Ctrl Pts',(-66.4659697256135,0.969431673599491,
16.2578756539845));
#27243=CARTESIAN_POINT('Ctrl Pts',(-66.7132036180157,0.392171352099354,
16.2949216175072));
#27244=CARTESIAN_POINT('Ctrl Pts',(-66.661369062725,-0.156853297275919,
16.3319675810299));
#27245=CARTESIAN_POINT('Ctrl Pts',(-66.6095345074342,-0.705877946651196,
16.3690135445526));
#27246=CARTESIAN_POINT('Ctrl Pts',(-66.2586315044505,-1.22666692390161,
16.4060595080752));
#27247=CARTESIAN_POINT('Ctrl Pts',(-65.7692528028443,-1.4808782005154,16.4431054715979));
#27248=CARTESIAN_POINT('Ctrl Pts',(-65.2798741012382,-1.73508947712918,
16.4801514351206));
#27249=CARTESIAN_POINT('Ctrl Pts',(-64.6520197010096,-1.72272305310635,
16.5171973986433));
#27250=CARTESIAN_POINT('Ctrl Pts',(-64.1730307286,-1.44943849252271,16.5542433621659));
#27251=CARTESIAN_POINT('Ctrl Pts',(-63.6940417561904,-1.17615393193907,
16.5912893256886));
#27252=CARTESIAN_POINT('Ctrl Pts',(-63.3639182115997,-0.641951234794631,
16.6283352892113));
#27253=CARTESIAN_POINT('Ctrl Pts',(-63.3337430069376,-0.0913112945731656,
16.665381252734));
#27254=CARTESIAN_POINT('Ctrl Pts',(-63.3320870288426,-0.0610928523301586,
16.6674142896194));
#27255=CARTESIAN_POINT('Ctrl Pts',(-63.3313343989597,-0.0308249063821139,
16.6694473265048));
#27256=CARTESIAN_POINT('Ctrl Pts',(-63.3314647116295,-0.000550350488415785,
16.6714803633902));
#27257=CARTESIAN_POINT('Origin',(-65.,8.88178419700125E-15,17.));
#27258=CARTESIAN_POINT('',(-63.3357797744869,-0.00117646094452181,17.3714803633902));
#27259=CARTESIAN_POINT('',(-63.3362856132907,0.000842509924184317,17.1785196366098));
#27260=CARTESIAN_POINT('',(-63.334,8.44655409538511E-15,17.));
#27261=CARTESIAN_POINT('Ctrl Pts',(-63.3362856132907,0.000842509924184317,
17.1785196366098));
#27262=CARTESIAN_POINT('Ctrl Pts',(-63.3378066597351,-0.331296382409449,
17.156380408079));
#27263=CARTESIAN_POINT('Ctrl Pts',(-63.4340697022003,-0.664247316775257,
17.1342411795483));
#27264=CARTESIAN_POINT('Ctrl Pts',(-63.6191109651628,-0.936960475618677,
17.1121019510176));
#27265=CARTESIAN_POINT('Ctrl Pts',(-63.9287437903708,-1.39329623820573,
17.0750559874949));
#27266=CARTESIAN_POINT('Ctrl Pts',(-64.4869549413411,-1.68096669861506,
17.0380100239722));
#27267=CARTESIAN_POINT('Ctrl Pts',(-65.0382759195595,-1.66831783943795,
17.0009640604495));
#27268=CARTESIAN_POINT('Ctrl Pts',(-65.5895968977779,-1.65566898026084,
16.9639180969268));
#27269=CARTESIAN_POINT('Ctrl Pts',(-66.1340277032444,-1.34270080149728,
16.9268721334041));
#27270=CARTESIAN_POINT('Ctrl Pts',(-66.4224064907048,-0.872644964808584,
16.8898261698815));
#27271=CARTESIAN_POINT('Ctrl Pts',(-66.7107852781652,-0.402589128119889,
16.8527802063588));
#27272=CARTESIAN_POINT('Ctrl Pts',(-66.7431120476195,0.224554366493944,
16.8157342428361));
#27273=CARTESIAN_POINT('Ctrl Pts',(-66.5045922697214,0.721769742577195,
16.7786882793134));
#27274=CARTESIAN_POINT('Ctrl Pts',(-66.2660724918233,1.21898511866045,16.7416423157907));
#27275=CARTESIAN_POINT('Ctrl Pts',(-65.7567061665729,1.58627237621312,16.7045963522681));
#27276=CARTESIAN_POINT('Ctrl Pts',(-65.2096076810249,1.65554041915625,16.6675503887454));
#27277=CARTESIAN_POINT('Ctrl Pts',(-64.6625091954769,1.72480846209939,16.6305044252227));
#27278=CARTESIAN_POINT('Ctrl Pts',(-64.0776785496314,1.496057290433,16.5934584617));
#27279=CARTESIAN_POINT('Ctrl Pts',(-63.7227668047739,1.07397617497671,16.5564124981773));
#27280=CARTESIAN_POINT('Ctrl Pts',(-63.4740209335901,0.778153519638634,
16.5304482109881));
#27281=CARTESIAN_POINT('Ctrl Pts',(-63.338214518977,0.387364427454228,16.504483923799));
#27282=CARTESIAN_POINT('Ctrl Pts',(-63.3350414063796,-0.00142706819227155,
16.4785196366098));
#27283=CARTESIAN_POINT('Ctrl Pts',(-63.3314647116295,-0.000550350488415785,
16.6714803633902));
#27284=CARTESIAN_POINT('Ctrl Pts',(-63.3337089542098,0.520837535827173,
16.7064932900275));
#27285=CARTESIAN_POINT('Ctrl Pts',(-63.5978310421932,1.04418591019568,16.7415062166648));
#27286=CARTESIAN_POINT('Ctrl Pts',(-64.0195992076647,1.35039416683957,16.776519143302));
#27287=CARTESIAN_POINT('Ctrl Pts',(-64.4658574777874,1.67438250473234,16.8135651068247));
#27288=CARTESIAN_POINT('Ctrl Pts',(-65.0886008827663,1.75528199721941,16.8506110703474));
#27289=CARTESIAN_POINT('Ctrl Pts',(-65.6028273721175,1.55606853283267,16.8876570338701));
#27290=CARTESIAN_POINT('Ctrl Pts',(-66.1170538614687,1.35685506844593,16.9247029973928));
#27291=CARTESIAN_POINT('Ctrl Pts',(-66.5227634351922,0.877528647185364,
16.9617489609154));
#27292=CARTESIAN_POINT('Ctrl Pts',(-66.6342808063438,0.337455723706583,
16.9987949244381));
#27293=CARTESIAN_POINT('Ctrl Pts',(-66.7457981774953,-0.202617199772189,
17.0358408879608));
#27294=CARTESIAN_POINT('Ctrl Pts',(-66.5631233460748,-0.803436625469172,
17.0728868514835));
#27295=CARTESIAN_POINT('Ctrl Pts',(-66.1698584845187,-1.1900341363363,17.1099328150062));
#27296=CARTESIAN_POINT('Ctrl Pts',(-65.7765936229625,-1.57663164720343,
17.1469787785288));
#27297=CARTESIAN_POINT('Ctrl Pts',(-65.1727387312707,-1.74900724324071,
17.1840247420515));
#27298=CARTESIAN_POINT('Ctrl Pts',(-64.6346514247161,-1.62827225548556,
17.2210707055742));
#27299=CARTESIAN_POINT('Ctrl Pts',(-64.0965641181614,-1.50753726773041,
17.2581166690969));
#27300=CARTESIAN_POINT('Ctrl Pts',(-63.624244396744,-1.09369169618283,17.2951626326196));
#27301=CARTESIAN_POINT('Ctrl Pts',(-63.4338520592054,-0.57613431332557,
17.3322085961422));
#27302=CARTESIAN_POINT('Ctrl Pts',(-63.3665748819314,-0.393249853550889,
17.3452991852249));
#27303=CARTESIAN_POINT('Ctrl Pts',(-63.334500232668,-0.197415541610626,
17.3583897743076));
#27304=CARTESIAN_POINT('Ctrl Pts',(-63.3357797744869,-0.00117646094452181,
17.3714803633902));
#27305=CARTESIAN_POINT('Origin',(-65.,8.88178419700125E-15,17.));
#27306=CARTESIAN_POINT('',(-63.3357162681914,0.001206443822575,18.0714803633902));
#27307=CARTESIAN_POINT('',(-63.331966723543,0.00097473362895843,17.8785196366098));
#27308=CARTESIAN_POINT('',(-63.334,8.44655409538511E-15,17.));
#27309=CARTESIAN_POINT('Ctrl Pts',(-63.331966723543,0.00097473362895843,
17.8785196366098));
#27310=CARTESIAN_POINT('Ctrl Pts',(-63.3354056721751,-0.493761861582906,
17.8453228558818));
#27311=CARTESIAN_POINT('Ctrl Pts',(-63.569536843221,-0.991325263991029,
17.8121260751538));
#27312=CARTESIAN_POINT('Ctrl Pts',(-63.9547567233169,-1.30085201001266,
17.7789292944258));
#27313=CARTESIAN_POINT('Ctrl Pts',(-64.3846430349799,-1.64626853206535,
17.7418833309031));
#27314=CARTESIAN_POINT('Ctrl Pts',(-65.002686987972,-1.75751445347198,17.7048373673804));
#27315=CARTESIAN_POINT('Ctrl Pts',(-65.5260372626587,-1.58367744749353,
17.6677914038578));
#27316=CARTESIAN_POINT('Ctrl Pts',(-66.0493875373455,-1.40984044151509,
17.6307454403351));
#27317=CARTESIAN_POINT('Ctrl Pts',(-66.4780441337267,-0.95092050815156,
17.5936994768124));
#27318=CARTESIAN_POINT('Ctrl Pts',(-66.6158299298206,-0.416944957159781,
17.5566535132897));
#27319=CARTESIAN_POINT('Ctrl Pts',(-66.7536157259145,0.117030593831996,
17.519607549767));
#27320=CARTESIAN_POINT('Ctrl Pts',(-66.6005307217209,0.726061762452023,
17.4825615862444));
#27321=CARTESIAN_POINT('Ctrl Pts',(-66.22663513746,1.13142198093974,17.4455156227217));
#27322=CARTESIAN_POINT('Ctrl Pts',(-65.8527395531992,1.53678219942746,17.408469659199));
#27323=CARTESIAN_POINT('Ctrl Pts',(-65.258033388871,1.73847146778286,17.3714236956763));
#27324=CARTESIAN_POINT('Ctrl Pts',(-64.7146872927936,1.64418554868717,17.3343777321536));
#27325=CARTESIAN_POINT('Ctrl Pts',(-64.1713411967163,1.54989962959147,17.2973317686309));
#27326=CARTESIAN_POINT('Ctrl Pts',(-63.6793551688898,1.15963852304468,17.2602858051083));
#27327=CARTESIAN_POINT('Ctrl Pts',(-63.4638894046994,0.652007437388906,
17.2232398415856));
#27328=CARTESIAN_POINT('Ctrl Pts',(-63.37718924249,0.447744372051051,17.2083331065937));
#27329=CARTESIAN_POINT('Ctrl Pts',(-63.3352614657588,0.224477513359583,
17.1934263716017));
#27330=CARTESIAN_POINT('Ctrl Pts',(-63.3362856132907,0.000842509924184317,
17.1785196366098));
#27331=CARTESIAN_POINT('Ctrl Pts',(-63.3357797744869,-0.00117646094452181,
17.3714803633902));
#27332=CARTESIAN_POINT('Ctrl Pts',(-63.3381212965673,0.35793500664807,17.3954357378302));
#27333=CARTESIAN_POINT('Ctrl Pts',(-63.4521589055967,0.718401958553989,
17.4193911122702));
#27334=CARTESIAN_POINT('Ctrl Pts',(-63.6665656652298,1.00334589962882,17.4433464867103));
#27335=CARTESIAN_POINT('Ctrl Pts',(-63.9981365624523,1.44399953555901,17.480392450233));
#27336=CARTESIAN_POINT('Ctrl Pts',(-64.569743310557,1.70403761325246,17.5174384137557));
#27337=CARTESIAN_POINT('Ctrl Pts',(-65.1197868400431,1.66445223193655,17.5544843772783));
#27338=CARTESIAN_POINT('Ctrl Pts',(-65.6698303695292,1.62486685062065,17.591530340801));
#27339=CARTESIAN_POINT('Ctrl Pts',(-66.1983106803967,1.28565801029539,17.6285763043237));
#27340=CARTESIAN_POINT('Ctrl Pts',(-66.4633657616898,0.802066560180599,
17.6656222678464));
#27341=CARTESIAN_POINT('Ctrl Pts',(-66.728420842983,0.318475110065811,17.702668231369));
#27342=CARTESIAN_POINT('Ctrl Pts',(-66.7300506947019,-0.309498949838504,
17.7397141948917));
#27343=CARTESIAN_POINT('Ctrl Pts',(-66.4675094059654,-0.794459730162069,
17.7767601584144));
#27344=CARTESIAN_POINT('Ctrl Pts',(-66.2049681172289,-1.27942051048564,
17.8138061219371));
#27345=CARTESIAN_POINT('Ctrl Pts',(-65.6782556880371,-1.62136801122844,
17.8508520854598));
#27346=CARTESIAN_POINT('Ctrl Pts',(-65.1284250482722,-1.6638080197013,17.8878980489824));
#27347=CARTESIAN_POINT('Ctrl Pts',(-64.5785944085073,-1.70624802817415,
17.9249440125051));
#27348=CARTESIAN_POINT('Ctrl Pts',(-64.0056455581693,-1.44918054437704,
17.9619899760278));
#27349=CARTESIAN_POINT('Ctrl Pts',(-63.6717917874564,-1.01025395994158,
17.9990359395505));
#27350=CARTESIAN_POINT('Ctrl Pts',(-63.4541716406064,-0.72414286538296,
18.0231840808304));
#27351=CARTESIAN_POINT('Ctrl Pts',(-63.3381427347181,-0.360760035483751,
18.0473322221103));
#27352=CARTESIAN_POINT('Ctrl Pts',(-63.3357162681914,0.001206443822575,
18.0714803633902));
#27353=CARTESIAN_POINT('Origin',(-65.,8.88178419700125E-15,17.));
#27354=CARTESIAN_POINT('',(-63.3314263973441,0.000500571934799431,18.7714803633902));
#27355=CARTESIAN_POINT('',(-63.3333325352018,-0.00145874397799977,18.5785196366098));
#27356=CARTESIAN_POINT('',(-63.334,8.44655409538511E-15,17.));
#27357=CARTESIAN_POINT('Ctrl Pts',(-63.3333325352018,-0.00145874397799977,
18.5785196366098));
#27358=CARTESIAN_POINT('Ctrl Pts',(-63.3323458932764,-0.109115274956348,
18.5713112672072));
#27359=CARTESIAN_POINT('Ctrl Pts',(-63.3418839056658,-0.216597722493267,
18.5641028978047));
#27360=CARTESIAN_POINT('Ctrl Pts',(-63.3625817175621,-0.321886358428994,
18.5568945284021));
#27361=CARTESIAN_POINT('Ctrl Pts',(-63.4689539553991,-0.862996108553313,
18.5198485648794));
#27362=CARTESIAN_POINT('Ctrl Pts',(-63.8700831830826,-1.34616204853444,
18.4828026013567));
#27363=CARTESIAN_POINT('Ctrl Pts',(-64.382390335006,-1.55026054620227,18.445756637834));
#27364=CARTESIAN_POINT('Ctrl Pts',(-64.8946974869294,-1.75435904387011,
18.4087106743114));
#27365=CARTESIAN_POINT('Ctrl Pts',(-65.5181825630929,-1.67939009922465,
18.3716647107887));
#27366=CARTESIAN_POINT('Ctrl Pts',(-65.9675040829891,-1.35966367488599,
18.334618747266));
#27367=CARTESIAN_POINT('Ctrl Pts',(-66.4168256028854,-1.03993725054732,
18.2975727837433));
#27368=CARTESIAN_POINT('Ctrl Pts',(-66.6919835665143,-0.475453346515448,
18.2605268202206));
#27369=CARTESIAN_POINT('Ctrl Pts',(-66.6670503715696,0.0754487776881411,
18.223480856698));
#27370=CARTESIAN_POINT('Ctrl Pts',(-66.6421171766249,0.626350901891734,
18.1864348931753));
#27371=CARTESIAN_POINT('Ctrl Pts',(-66.3170928231065,1.16367124626704,18.1493889296526));
#27372=CARTESIAN_POINT('Ctrl Pts',(-65.8407265494155,1.44150210839706,18.1123429661299));
#27373=CARTESIAN_POINT('Ctrl Pts',(-65.3643602757244,1.71933297052707,18.0752970026072));
#27374=CARTESIAN_POINT('Ctrl Pts',(-64.7366520818608,1.7376743504118,18.0382510390846));
#27375=CARTESIAN_POINT('Ctrl Pts',(-64.2448761820938,1.48813221154433,18.0012050755619));
#27376=CARTESIAN_POINT('Ctrl Pts',(-63.7531002823268,1.23859007267687,17.9641591120392));
#27377=CARTESIAN_POINT('Ctrl Pts',(-63.3972566766564,0.721164415057202,
17.9271131485165));
#27378=CARTESIAN_POINT('Ctrl Pts',(-63.3401992089882,0.172658024897994,
17.8900671849938));
#27379=CARTESIAN_POINT('Ctrl Pts',(-63.3342707730138,0.115666623973004,
17.8862180021992));
#27380=CARTESIAN_POINT('Ctrl Pts',(-63.3315679757844,0.0583396813265098,
17.8823688194045));
#27381=CARTESIAN_POINT('Ctrl Pts',(-63.331966723543,0.00097473362895843,
17.8785196366098));
#27382=CARTESIAN_POINT('Ctrl Pts',(-63.3357162681914,0.001206443822575,
18.0714803633902));
#27383=CARTESIAN_POINT('Ctrl Pts',(-63.3344202622762,0.194537237022054,
18.084378185633));
#27384=CARTESIAN_POINT('Ctrl Pts',(-63.3655323149503,0.38746397927637,18.0972760078758));
#27385=CARTESIAN_POINT('Ctrl Pts',(-63.4308825664874,0.567997006411733,
18.1101738301185));
#27386=CARTESIAN_POINT('Ctrl Pts',(-63.6185858073192,1.08653570325578,18.1472197936412));
#27387=CARTESIAN_POINT('Ctrl Pts',(-64.0887509800707,1.50282741187006,18.1842657571639));
#27388=CARTESIAN_POINT('Ctrl Pts',(-64.6262043274144,1.62635387127239,18.2213117206866));
#27389=CARTESIAN_POINT('Ctrl Pts',(-65.1636576747581,1.74988033067473,18.2583576842093));
#27390=CARTESIAN_POINT('Ctrl Pts',(-65.768399196694,1.58064154086511,18.2954036477319));
#27391=CARTESIAN_POINT('Ctrl Pts',(-66.1636655065904,1.19609059364976,18.3324496112546));
#27392=CARTESIAN_POINT('Ctrl Pts',(-66.5589318164868,0.811539646434416,
18.3694955747773));
#27393=CARTESIAN_POINT('Ctrl Pts',(-66.7447229143437,0.211676541813339,
18.4065415383));
#27394=CARTESIAN_POINT('Ctrl Pts',(-66.6360104507197,-0.328967968929756,
18.4435875018227));
#27395=CARTESIAN_POINT('Ctrl Pts',(-66.5272979870957,-0.869612479672855,
18.4806334653453));
#27396=CARTESIAN_POINT('Ctrl Pts',(-66.1240819619909,-1.35103839653797,
18.517679428868));
#27397=CARTESIAN_POINT('Ctrl Pts',(-65.6108964756848,-1.55291841879864,
18.5547253923907));
#27398=CARTESIAN_POINT('Ctrl Pts',(-65.0977109893788,-1.7547984410593,18.5917713559134));
#27399=CARTESIAN_POINT('Ctrl Pts',(-64.4745560418716,-1.67713256871552,
18.6288173194361));
#27400=CARTESIAN_POINT('Ctrl Pts',(-64.0266220284185,-1.35546502864589,
18.6658632829587));
#27401=CARTESIAN_POINT('Ctrl Pts',(-63.6009392798522,-1.04977642615326,
18.7010689764359));
#27402=CARTESIAN_POINT('Ctrl Pts',(-63.3335015355576,-0.523725769548784,
18.7362746699131));
#27403=CARTESIAN_POINT('Ctrl Pts',(-63.3314263973441,0.000500571934799431,
18.7714803633902));
#27404=CARTESIAN_POINT('Origin',(-65.,8.88178419700125E-15,17.));
#27405=CARTESIAN_POINT('',(-63.3342413915565,-0.00152189757969434,19.4714803633902));
#27406=CARTESIAN_POINT('',(-63.3367061905351,-6.33250723186663E-5,19.2785196366098));
#27407=CARTESIAN_POINT('',(-63.334,8.44655409538511E-15,17.));
#27408=CARTESIAN_POINT('Ctrl Pts',(-63.3367061905351,-6.33250723186663E-5,
19.2785196366098));
#27409=CARTESIAN_POINT('Ctrl Pts',(-63.336613224224,-0.274266937448918,
19.26025371501));
#27410=CARTESIAN_POINT('Ctrl Pts',(-63.4006540507369,-0.548429669491744,
19.2419877934101));
#27411=CARTESIAN_POINT('Ctrl Pts',(-63.5290671316579,-0.788102757387643,
19.2237218718103));
#27412=CARTESIAN_POINT('Ctrl Pts',(-63.7895076621637,-1.27419487286282,
19.1866759082877));
#27413=CARTESIAN_POINT('Ctrl Pts',(-64.3147356017013,-1.61841804812354,
19.149629944765));
#27414=CARTESIAN_POINT('Ctrl Pts',(-64.8643774055205,-1.66323659510228,
19.1125839812423));
#27415=CARTESIAN_POINT('Ctrl Pts',(-65.4140192093397,-1.70805514208102,
19.0755380177196));
#27416=CARTESIAN_POINT('Ctrl Pts',(-65.9880748774405,-1.45346906077779,
19.0384920541969));
#27417=CARTESIAN_POINT('Ctrl Pts',(-66.3238245781873,-1.01599111491804,
19.0014460906742));
#27418=CARTESIAN_POINT('Ctrl Pts',(-66.6595742789341,-0.578513169058296,
18.9644001271516));
#27419=CARTESIAN_POINT('Ctrl Pts',(-66.757018012327,0.0418566413579672,
18.9273541636289));
#27420=CARTESIAN_POINT('Ctrl Pts',(-66.5715601012413,0.561202554865611,
18.8903082001062));
#27421=CARTESIAN_POINT('Ctrl Pts',(-66.3861021901555,1.08054846837325,18.8532622365835));
#27422=CARTESIAN_POINT('Ctrl Pts',(-65.9177426345912,1.49887048497227,18.8162162730609));
#27423=CARTESIAN_POINT('Ctrl Pts',(-65.3808288409285,1.62472116171496,18.7791703095382));
#27424=CARTESIAN_POINT('Ctrl Pts',(-64.8439150472658,1.75057183845764,18.7421243460155));
#27425=CARTESIAN_POINT('Ctrl Pts',(-64.2384470155047,1.58395117534399,18.7050783824928));
#27426=CARTESIAN_POINT('Ctrl Pts',(-63.8415206236195,1.20111406365342,18.6680324189701));
#27427=CARTESIAN_POINT('Ctrl Pts',(-63.5218278028516,0.89276904393903,18.63819482485));
#27428=CARTESIAN_POINT('Ctrl Pts',(-63.3374165408442,0.444163795089785,
18.6083572307299));
#27429=CARTESIAN_POINT('Ctrl Pts',(-63.3333325352018,-0.00145874397799977,
18.5785196366098));
#27430=CARTESIAN_POINT('Ctrl Pts',(-63.3314263973441,0.000500571934799431,
18.7714803633902));
#27431=CARTESIAN_POINT('Ctrl Pts',(-63.3313179258352,0.0279029020134445,
18.7733206334357));
#27432=CARTESIAN_POINT('Ctrl Pts',(-63.3319345194755,0.0553002474134458,
18.7751609034813));
#27433=CARTESIAN_POINT('Ctrl Pts',(-63.3332914773975,0.0826608742403348,
18.7770011735268));
#27434=CARTESIAN_POINT('Ctrl Pts',(-63.3606080192284,0.633450029261455,
18.8140471370495));
#27435=CARTESIAN_POINT('Ctrl Pts',(-63.6879541822893,1.16935913150821,18.8510931005721));
#27436=CARTESIAN_POINT('Ctrl Pts',(-64.1655181388753,1.44512634150633,18.8881390640948));
#27437=CARTESIAN_POINT('Ctrl Pts',(-64.6430820954612,1.72089355150444,18.9251850276175));
#27438=CARTESIAN_POINT('Ctrl Pts',(-65.2708638455722,1.73651886925393,18.9622309911402));
#27439=CARTESIAN_POINT('Ctrl Pts',(-65.7615555115074,1.48485127952435,18.9992769546629));
#27440=CARTESIAN_POINT('Ctrl Pts',(-66.2522471774427,1.23318368979477,19.0363229181856));
#27441=CARTESIAN_POINT('Ctrl Pts',(-66.6058487592021,0.714223192586123,
19.0733688817082));
#27442=CARTESIAN_POINT('Ctrl Pts',(-66.6605324878321,0.165475002074336,
19.1104148452309));
#27443=CARTESIAN_POINT('Ctrl Pts',(-66.715216216462,-0.383273188437459,
19.1474608087536));
#27444=CARTESIAN_POINT('Ctrl Pts',(-66.4709820919624,-0.961809072252402,
19.1845067722763));
#27445=CARTESIAN_POINT('Ctrl Pts',(-66.0396052463205,-1.30536242146666,
19.221552735799));
#27446=CARTESIAN_POINT('Ctrl Pts',(-65.6082284006786,-1.64891577068092,
19.2585986993216));
#27447=CARTESIAN_POINT('Ctrl Pts',(-64.9897088338945,-1.75748658529449,
19.2956446628443));
#27448=CARTESIAN_POINT('Ctrl Pts',(-64.4671155329348,-1.58138681666734,
19.332690626367));
#27449=CARTESIAN_POINT('Ctrl Pts',(-63.9445222319752,-1.40528704804019,
19.3697365898897));
#27450=CARTESIAN_POINT('Ctrl Pts',(-63.5178551968399,-0.944516696172312,
19.4067825534124));
#27451=CARTESIAN_POINT('Ctrl Pts',(-63.3823810155581,-0.409949924733961,
19.443828516935));
#27452=CARTESIAN_POINT('Ctrl Pts',(-63.34867413809,-0.276946156097573,19.4530457990868));
#27453=CARTESIAN_POINT('Ctrl Pts',(-63.3329934814549,-0.139374038553363,
19.4622630812385));
#27454=CARTESIAN_POINT('Ctrl Pts',(-63.3342413915565,-0.00152189757969434,
19.4714803633902));
#27455=CARTESIAN_POINT('Origin',(-65.,8.88178419700125E-15,17.));
#27456=CARTESIAN_POINT('',(-63.33660733148,0.000426122236803078,20.1714803633902));
#27457=CARTESIAN_POINT('',(-63.3335649842428,0.0014916225119581,19.9785196366098));
#27458=CARTESIAN_POINT('',(-63.334,8.44655409538511E-15,17.));
#27459=CARTESIAN_POINT('Ctrl Pts',(-63.3335649842428,0.0014916225119581,
19.9785196366098));
#27460=CARTESIAN_POINT('Ctrl Pts',(-63.3376081205507,-0.436609739463921,
19.9491961628127));
#27461=CARTESIAN_POINT('Ctrl Pts',(-63.5150446040949,-0.877608758866617,
19.9198726890157));
#27462=CARTESIAN_POINT('Ctrl Pts',(-63.8250037086467,-1.18496125357118,
19.8905492152186));
#27463=CARTESIAN_POINT('Ctrl Pts',(-64.2165921595995,-1.57325663038184,
19.8535032516959));
#27464=CARTESIAN_POINT('Ctrl Pts',(-64.8196955128484,-1.74824327998199,
19.8164572881732));
#27465=CARTESIAN_POINT('Ctrl Pts',(-65.3583001004237,-1.62983756803352,
19.7794113246505));
#27466=CARTESIAN_POINT('Ctrl Pts',(-65.896904687999,-1.51143185608504,19.7423653611279));
#27467=CARTESIAN_POINT('Ctrl Pts',(-66.3710105099008,-1.09963378258793,
19.7053193976052));
#27468=CARTESIAN_POINT('Ctrl Pts',(-66.5636403476301,-0.582905071893245,
19.6682734340825));
#27469=CARTESIAN_POINT('Ctrl Pts',(-66.7562701853594,-0.06617636119856,
19.6312274705598));
#27470=CARTESIAN_POINT('Ctrl Pts',(-66.6674240389162,0.555482986693699,
19.5941815070372));
#27471=CARTESIAN_POINT('Ctrl Pts',(-66.3377628513866,0.997567046656923,
19.5571355435145));
#27472=CARTESIAN_POINT('Ctrl Pts',(-66.008101663857,1.43965110662014,19.5200895799918));
#27473=CARTESIAN_POINT('Ctrl Pts',(-65.437625435241,1.70215987865433,19.4830436164691));
#27474=CARTESIAN_POINT('Ctrl Pts',(-64.8874158461961,1.66495473446781,19.4459976529464));
#27475=CARTESIAN_POINT('Ctrl Pts',(-64.3372062571513,1.62774959028128,19.4089516894237));
#27476=CARTESIAN_POINT('Ctrl Pts',(-63.8072633076776,1.29083052987405,19.3719057259011));
#27477=CARTESIAN_POINT('Ctrl Pts',(-63.5401183936778,0.808390471825612,
19.3348597623784));
#27478=CARTESIAN_POINT('Ctrl Pts',(-63.404692230951,0.563822814410774,19.3160797204555));
#27479=CARTESIAN_POINT('Ctrl Pts',(-63.3368017735151,0.281858137674118,
19.2972996785327));
#27480=CARTESIAN_POINT('Ctrl Pts',(-63.3367061905351,-6.33250723186663E-5,
19.2785196366098));
#27481=CARTESIAN_POINT('Ctrl Pts',(-63.3342413915565,-0.00152189757969434,
19.4714803633902));
#27482=CARTESIAN_POINT('Ctrl Pts',(-63.3380090632001,0.414679238971572,
19.4993090447612));
#27483=CARTESIAN_POINT('Ctrl Pts',(-63.496088728647,0.833432923200615,19.5271377261321));
#27484=CARTESIAN_POINT('Ctrl Pts',(-63.778271499721,1.13671878306761,19.5549664075031));
#27485=CARTESIAN_POINT('Ctrl Pts',(-64.1539174925939,1.540457528422,19.5920123710258));
#27486=CARTESIAN_POINT('Ctrl Pts',(-64.7494908057681,1.73957182812195,19.6290583345484));
#27487=CARTESIAN_POINT('Ctrl Pts',(-65.2924239354676,1.64293589624756,19.6661042980711));
#27488=CARTESIAN_POINT('Ctrl Pts',(-65.835357065167,1.54629996437316,19.7031502615938));
#27489=CARTESIAN_POINT('Ctrl Pts',(-66.3256500113918,1.15391380092444,19.7401962251165));
#27490=CARTESIAN_POINT('Ctrl Pts',(-66.5389174268969,0.645355153836879,
19.7772421886392));
#27491=CARTESIAN_POINT('Ctrl Pts',(-66.7521848424021,0.136796506749319,
19.8142881521618));
#27492=CARTESIAN_POINT('Ctrl Pts',(-66.6884267271877,-0.487934623977076,
19.8513341156845));
#27493=CARTESIAN_POINT('Ctrl Pts',(-66.3768223447206,-0.942926484478215,
19.8883800792072));
#27494=CARTESIAN_POINT('Ctrl Pts',(-66.0652179622535,-1.39791834497936,
19.9254260427299));
#27495=CARTESIAN_POINT('Ctrl Pts',(-65.5057673125336,-1.68317093525525,
19.9624720062526));
#27496=CARTESIAN_POINT('Ctrl Pts',(-64.9545061567026,-1.66813680856719,
19.9995179697752));
#27497=CARTESIAN_POINT('Ctrl Pts',(-64.4032450008716,-1.65310268187914,
20.0365639332979));
#27498=CARTESIAN_POINT('Ctrl Pts',(-63.8601733389293,-1.33778183822714,
20.0736098968206));
#27499=CARTESIAN_POINT('Ctrl Pts',(-63.5738309983811,-0.866482612606725,
20.1106558603433));
#27500=CARTESIAN_POINT('Ctrl Pts',(-63.4171190932323,-0.608545908587603,
20.1309306946923));
#27501=CARTESIAN_POINT('Ctrl Pts',(-63.3373039960783,-0.303889805224311,
20.1512055290412));
#27502=CARTESIAN_POINT('Ctrl Pts',(-63.33660733148,0.000426122236803078,
20.1714803633902));
#27503=CARTESIAN_POINT('Origin',(-65.,8.88178419700125E-15,17.));
#27504=CARTESIAN_POINT('',(-63.3326792503596,0.00130047270867312,20.8714803633902));
#27505=CARTESIAN_POINT('',(-63.3318013787731,-0.000864016794193591,20.6785196366098));
#27506=CARTESIAN_POINT('',(-63.334,8.44655409538511E-15,17.));
#27507=CARTESIAN_POINT('Ctrl Pts',(-63.3318013787731,-0.000864016794193591,
20.6785196366098));
#27508=CARTESIAN_POINT('Ctrl Pts',(-63.3314877360124,-0.0505539851742854,
20.6751845741382));
#27509=CARTESIAN_POINT('Ctrl Pts',(-63.3335154742976,-0.100217999006543,
20.6718495116665));
#27510=CARTESIAN_POINT('Ctrl Pts',(-63.3379679807618,-0.149663664483458,
20.6685144491949));
#27511=CARTESIAN_POINT('Ctrl Pts',(-63.3874265421712,-0.698907444829369,
20.6314684856722));
#27512=CARTESIAN_POINT('Ctrl Pts',(-63.7360730319708,-1.22120960136621,
20.5944225221495));
#27513=CARTESIAN_POINT('Ctrl Pts',(-64.2243472290266,-1.47753582103745,
20.5573765586268));
#27514=CARTESIAN_POINT('Ctrl Pts',(-64.7126214260825,-1.73386204070869,
20.5203305951042));
#27515=CARTESIAN_POINT('Ctrl Pts',(-65.3405233303947,-1.72421232351431,
20.4832846315815));
#27516=CARTESIAN_POINT('Ctrl Pts',(-65.8206901647961,-1.45300280103399,
20.4462386680588));
#27517=CARTESIAN_POINT('Ctrl Pts',(-66.3008569991975,-1.18179327855367,
20.4091927045361));
#27518=CARTESIAN_POINT('Ctrl Pts',(-66.6332887636883,-0.649023950787419,
20.3721467410134));
#27519=CARTESIAN_POINT('Ctrl Pts',(-66.6658461309716,-0.098519780176524,
20.3351007774908));
#27520=CARTESIAN_POINT('Ctrl Pts',(-66.698403498255,0.451984390434375,20.2980548139681));
#27521=CARTESIAN_POINT('Ctrl Pts',(-66.431086468331,1.02022340388992,20.2610088504454));
#27522=CARTESIAN_POINT('Ctrl Pts',(-65.9862342185508,1.34613948307829,20.2239628869227));
#27523=CARTESIAN_POINT('Ctrl Pts',(-65.5413819687707,1.67205556226665,20.1869169234));
#27524=CARTESIAN_POINT('Ctrl Pts',(-64.9189944991343,1.75564870718785,20.1498709598773));
#27525=CARTESIAN_POINT('Ctrl Pts',(-64.4039109527966,1.55866202617725,20.1128249963547));
#27526=CARTESIAN_POINT('Ctrl Pts',(-63.8888274064588,1.36167534516665,20.075779032832));
#27527=CARTESIAN_POINT('Ctrl Pts',(-63.4810477834196,0.88410883822424,20.0387330693093));
#27528=CARTESIAN_POINT('Ctrl Pts',(-63.3671947462284,0.344523532742449,
20.0016871057866));
#27529=CARTESIAN_POINT('Ctrl Pts',(-63.3434612857827,0.232043208803146,
19.993964616061));
#27530=CARTESIAN_POINT('Ctrl Pts',(-63.332500203214,0.116867900576733,19.9862421263354));
#27531=CARTESIAN_POINT('Ctrl Pts',(-63.3335649842428,0.0014916225119581,
19.9785196366098));
#27532=CARTESIAN_POINT('Ctrl Pts',(-63.33660733148,0.000426122236803078,
20.1714803633902));
#27533=CARTESIAN_POINT('Ctrl Pts',(-63.3360310578706,0.252153048396664,
20.1882514925639));
#27534=CARTESIAN_POINT('Ctrl Pts',(-63.3895909699888,0.503647211782724,
20.2050226217376));
#27535=CARTESIAN_POINT('Ctrl Pts',(-63.4985445030998,0.728272982538817,
20.2217937509113));
#27536=CARTESIAN_POINT('Ctrl Pts',(-63.7392133675209,1.22445174447511,20.258839714434));
#27537=CARTESIAN_POINT('Ctrl Pts',(-64.2501641155174,1.58953166075887,20.2958856779567));
#27538=CARTESIAN_POINT('Ctrl Pts',(-64.7975572478224,1.65643198360556,20.3329316414794));
#27539=CARTESIAN_POINT('Ctrl Pts',(-65.3449503801273,1.72333230645225,20.369977605002));
#27540=CARTESIAN_POINT('Ctrl Pts',(-65.9287858967409,1.49205303586186,20.4070235685247));
#27541=CARTESIAN_POINT('Ctrl Pts',(-66.2818681473523,1.06844015166584,20.4440695320474));
#27542=CARTESIAN_POINT('Ctrl Pts',(-66.6349503979637,0.644827267469811,
20.4811154955701));
#27543=CARTESIAN_POINT('Ctrl Pts',(-66.757279382573,0.0288807696681399,
20.5181614590928));
#27544=CARTESIAN_POINT('Ctrl Pts',(-66.5928705785965,-0.497507359328862,
20.5552074226155));
#27545=CARTESIAN_POINT('Ctrl Pts',(-66.42846177462,-1.02389548832586,20.5922533861381));
#27546=CARTESIAN_POINT('Ctrl Pts',(-65.9773151820577,-1.46072524851819,
20.6292993496608));
#27547=CARTESIAN_POINT('Ctrl Pts',(-65.4459005359057,-1.60808016419333,
20.6663453131835));
#27548=CARTESIAN_POINT('Ctrl Pts',(-64.9144858897538,-1.75543507986847,
20.7033912767062));
#27549=CARTESIAN_POINT('Ctrl Pts',(-64.3028031900122,-1.61331515102642,
20.7404372402289));
#27550=CARTESIAN_POINT('Ctrl Pts',(-63.8907926142615,-1.24676010485228,
20.7774832037515));
#27551=CARTESIAN_POINT('Ctrl Pts',(-63.5423261851822,-0.936738625989558,
20.8088155902978));
#27552=CARTESIAN_POINT('Ctrl Pts',(-63.3366907965296,-0.466172446764649,
20.840147976844));
#27553=CARTESIAN_POINT('Ctrl Pts',(-63.3326792503596,0.00130047270867312,
20.8714803633902));
#27554=CARTESIAN_POINT('Origin',(-65.,8.88178419700125E-15,17.));
#27555=CARTESIAN_POINT('',(-63.3325282901756,-0.00121307831917494,21.5714803633902));
#27556=CARTESIAN_POINT('',(-63.3361634080255,-0.000941845566861395,21.3785196366098));
#27557=CARTESIAN_POINT('',(-63.334,8.44655409538511E-15,17.));
#27558=CARTESIAN_POINT('',(-66.2690708798524,-1.07935865304852,22.));
#27559=CARTESIAN_POINT('Ctrl Pts',(-63.3325282901756,-0.00121307831917494,
21.5714803633902));
#27560=CARTESIAN_POINT('Ctrl Pts',(-63.3364666394986,0.471552579298233,
21.6031823516921));
#27561=CARTESIAN_POINT('Ctrl Pts',(-63.5475594887738,0.947301871471172,
21.634884339994));
#27562=CARTESIAN_POINT('Ctrl Pts',(-63.9032471486994,1.25758535694562,21.6665863282959));
#27563=CARTESIAN_POINT('Ctrl Pts',(-64.3188927526783,1.62017304624496,21.7036322918186));
#27564=CARTESIAN_POINT('Ctrl Pts',(-64.9319903369098,1.75680828918912,21.7406782553412));
#27565=CARTESIAN_POINT('Ctrl Pts',(-65.4619049207954,1.60385028487086,21.7777242188639));
#27566=CARTESIAN_POINT('Ctrl Pts',(-65.991819504681,1.4508922805526,21.8147701823866));
#27567=CARTESIAN_POINT('Ctrl Pts',(-66.4385510882207,1.00834102897191,21.8518161459093));
#27568=CARTESIAN_POINT('Ctrl Pts',(-66.5975920398021,0.481277360573874,
21.8888621094319));
#27569=CARTESIAN_POINT('Ctrl Pts',(-66.7566329913835,-0.0457863078241613,
21.9259080729546));
#27570=CARTESIAN_POINT('Ctrl Pts',(-66.6279833110066,-0.657362393039546,
21.9629540364773));
#27571=CARTESIAN_POINT('Ctrl Pts',(-66.2690708798524,-1.07935865304854,
22.));
#27572=CARTESIAN_POINT('',(-63.7285313545748,-1.0812100993933,22.));
#27573=CARTESIAN_POINT('Origin',(-65.,8.88178419700125E-15,22.));
#27574=CARTESIAN_POINT('Ctrl Pts',(-63.7285300176229,-1.0812111317272,22.));
#27575=CARTESIAN_POINT('Ctrl Pts',(-64.0793901440197,-1.49274250755581,
21.9636770818144));
#27576=CARTESIAN_POINT('Ctrl Pts',(-64.6493623256457,-1.71876565001735,
21.9273541636289));
#27577=CARTESIAN_POINT('Ctrl Pts',(-65.1867621807782,-1.65816351020321,
21.8910312454434));
#27578=CARTESIAN_POINT('Ctrl Pts',(-65.7348595370708,-1.5963550219787,21.8539852819207));
#27579=CARTESIAN_POINT('Ctrl Pts',(-66.2490748882323,-1.2363965294347,21.816939318398));
#27580=CARTESIAN_POINT('Ctrl Pts',(-66.4944088007071,-0.742590901212604,
21.7798933548753));
#27581=CARTESIAN_POINT('Ctrl Pts',(-66.7397427131819,-0.248785272990512,
21.7428473913526));
#27582=CARTESIAN_POINT('Ctrl Pts',(-66.71619518697,0.378867490909668,21.7058014278299));
#27583=CARTESIAN_POINT('Ctrl Pts',(-66.4343747134738,0.852900746623167,
21.6687554643073));
#27584=CARTESIAN_POINT('Ctrl Pts',(-66.1525542399776,1.32693400233667,21.6317095007846));
#27585=CARTESIAN_POINT('Ctrl Pts',(-65.6124608191971,1.64734774986349,21.5946635372619));
#27586=CARTESIAN_POINT('Ctrl Pts',(-65.061356017574,1.66761252399563,21.5576175737392));
#27587=CARTESIAN_POINT('Ctrl Pts',(-64.5102512159508,1.68787729812776,21.5205716102165));
#27588=CARTESIAN_POINT('Ctrl Pts',(-63.9481350334849,1.40799309886521,21.4835256466939));
#27589=CARTESIAN_POINT('Ctrl Pts',(-63.6322204085561,0.955995223624118,
21.4464796831712));
#27590=CARTESIAN_POINT('Ctrl Pts',(-63.4390408141815,0.679601668824523,
21.4238263343174));
#27591=CARTESIAN_POINT('Ctrl Pts',(-63.3379218264913,0.338850724949929,
21.4011729854636));
#27592=CARTESIAN_POINT('Ctrl Pts',(-63.3361634080255,-0.000941845566861395,
21.3785196366098));
#27593=CARTESIAN_POINT('Origin',(-65.,8.88178419700125E-15,23.5459252805377));
#27594=CARTESIAN_POINT('',(-62.9427844533856,-0.00119489768197589,13.4540747194623));
#27595=CARTESIAN_POINT('',(-62.9484021938786,0.000803300711494623,13.3959252805377));
#27596=CARTESIAN_POINT('',(-62.94525,-1.20379215794662E-13,23.5459252805377));
#27597=CARTESIAN_POINT('',(-66.8826275096638,0.823232180103066,13.));
#27598=CARTESIAN_POINT('Ctrl Pts',(-62.9484021938786,0.000803300711494474,
13.3959252805377));
#27599=CARTESIAN_POINT('Ctrl Pts',(-62.9495841394398,-0.384792240838309,
13.3750880775932));
#27600=CARTESIAN_POINT('Ctrl Pts',(-63.239440569463,-1.45761852527273,13.3172049111259));
#27601=CARTESIAN_POINT('Ctrl Pts',(-64.970198323091,-2.42992595215151,13.2222757811361));
#27602=CARTESIAN_POINT('Ctrl Pts',(-67.0251392906009,-1.33877286094185,
13.111137890568));
#27603=CARTESIAN_POINT('Ctrl Pts',(-67.1563717950601,0.197213743559495,
13.0370459635227));
#27604=CARTESIAN_POINT('Ctrl Pts',(-66.8826275096638,0.823232180103066,
13.));
#27605=CARTESIAN_POINT('',(-66.2235927967208,1.65534565011394,13.));
#27606=CARTESIAN_POINT('Origin',(-65.,8.88178419700125E-15,13.));
#27607=CARTESIAN_POINT('Ctrl Pts',(-62.9427844533856,-0.00119489768197575,
13.4540747194623));
#27608=CARTESIAN_POINT('Ctrl Pts',(-62.9422817266512,-0.0728349382260852,
13.4501772883951));
#27609=CARTESIAN_POINT('Ctrl Pts',(-62.9781729708452,-0.824925643882587,
13.4092338938053));
#27610=CARTESIAN_POINT('Ctrl Pts',(-63.9036938704104,-2.16732302296763,
13.3312445356927));
#27611=CARTESIAN_POINT('Ctrl Pts',(-66.2265689546786,-2.09606376419021,
13.2201066451247));
#27612=CARTESIAN_POINT('Ctrl Pts',(-67.4179368644029,-0.120091680801057,
13.1096917998938));
#27613=CARTESIAN_POINT('Ctrl Pts',(-66.7594496906129,1.25819328818367,13.0363229181856));
#27614=CARTESIAN_POINT('Ctrl Pts',(-66.2235939546714,1.65534738192937,13.));
#27615=CARTESIAN_POINT('Origin',(-65.,8.88178419700125E-15,23.5459252805377));
#27616=CARTESIAN_POINT('',(-62.9480827837869,-0.00102651687047844,14.1540747194623));
#27617=CARTESIAN_POINT('',(-62.9433366278651,0.00149772234160084,14.0959252805377));
#27618=CARTESIAN_POINT('',(-62.94525,-1.20379215794662E-13,23.5459252805377));
#27619=CARTESIAN_POINT('Ctrl Pts',(-62.9433366278651,0.0014977223416008,
14.0959252805377));
#27620=CARTESIAN_POINT('Ctrl Pts',(-62.9481477427571,-0.585192187367149,
14.0640305253959));
#27621=CARTESIAN_POINT('Ctrl Pts',(-63.5186241718586,-1.86149425637257,
13.9950898067315));
#27622=CARTESIAN_POINT('Ctrl Pts',(-65.684305645688,-2.33026686199619,13.8891031245443));
#27623=CARTESIAN_POINT('Ctrl Pts',(-67.3289123722387,-0.688818574436933,
13.7779652339763));
#27624=CARTESIAN_POINT('Ctrl Pts',(-66.8417982611818,1.58294512384397,13.6668273434083));
#27625=CARTESIAN_POINT('Ctrl Pts',(-64.6689465387577,2.4061546469661,13.5556894528402));
#27626=CARTESIAN_POINT('Ctrl Pts',(-63.14955544062,1.28502616351136,13.4653887652167));
#27627=CARTESIAN_POINT('Ctrl Pts',(-62.9474827867649,0.300748827451906,
13.4121340411158));
#27628=CARTESIAN_POINT('Ctrl Pts',(-62.9484021938786,0.000803300711494474,
13.3959252805377));
#27629=CARTESIAN_POINT('Ctrl Pts',(-62.9480827837869,-0.00102651687047834,
14.1540747194623));
#27630=CARTESIAN_POINT('Ctrl Pts',(-62.9468311597533,-0.277742487636526,
14.1391197361979));
#27631=CARTESIAN_POINT('Ctrl Pts',(-63.1278468516848,-1.23836027065323,
14.0871187894108));
#27632=CARTESIAN_POINT('Ctrl Pts',(-64.5878737813476,-2.39342385873017,
13.998071879101));
#27633=CARTESIAN_POINT('Ctrl Pts',(-66.7873400138256,-1.64430308142018,
13.8869339885329));
#27634=CARTESIAN_POINT('Ctrl Pts',(-67.3508170614469,0.60985221755875,13.7757960979649));
#27635=CARTESIAN_POINT('Ctrl Pts',(-65.7625975239189,2.30583209920717,13.6646582073969));
#27636=CARTESIAN_POINT('Ctrl Pts',(-63.5564754082319,1.90574022357352,13.557417747896));
#27637=CARTESIAN_POINT('Ctrl Pts',(-62.9470602579309,0.608119845326397,
13.4872232519178));
#27638=CARTESIAN_POINT('Ctrl Pts',(-62.9427844533856,-0.00119489768197575,
13.4540747194623));
#27639=CARTESIAN_POINT('Origin',(-65.,8.88178419700125E-15,23.5459252805377));
#27640=CARTESIAN_POINT('',(-62.946510263771,0.00176526862452855,14.8540747194623));
#27641=CARTESIAN_POINT('',(-62.94372126594,-0.00163389948555286,14.7959252805377));
#27642=CARTESIAN_POINT('',(-62.94525,-1.20379215794662E-13,23.5459252805377));
#27643=CARTESIAN_POINT('Ctrl Pts',(-62.94372126594,-0.00163389948555279,
14.7959252805377));
#27644=CARTESIAN_POINT('Ctrl Pts',(-62.9427765522985,-0.110331733448607,
14.7900189367213));
#27645=CARTESIAN_POINT('Ctrl Pts',(-63.0000473239053,-0.899810372641744,
14.7470666293823));
#27646=CARTESIAN_POINT('Ctrl Pts',(-64.0226192720082,-2.2232951335223,14.6670683585206));
#27647=CARTESIAN_POINT('Ctrl Pts',(-66.3378385875382,-2.02694463079713,
14.5559304679526));
#27648=CARTESIAN_POINT('Ctrl Pts',(-67.4285194097127,0.0246926670119235,
14.4447925773845));
#27649=CARTESIAN_POINT('Ctrl Pts',(-66.2963482043283,2.05372573368661,14.3336546868165));
#27650=CARTESIAN_POINT('Ctrl Pts',(-63.9776161165208,2.20296580816612,14.2225167962485));
#27651=CARTESIAN_POINT('Ctrl Pts',(-62.9915607037629,0.87164277914502,14.1432736608222));
#27652=CARTESIAN_POINT('Ctrl Pts',(-62.942559601823,0.0962519214711429,
14.1010764889186));
#27653=CARTESIAN_POINT('Ctrl Pts',(-62.9433366278651,0.0014977223416008,
14.0959252805377));
#27654=CARTESIAN_POINT('Ctrl Pts',(-62.946510263771,0.00176526862452855,
14.8540747194623));
#27655=CARTESIAN_POINT('Ctrl Pts',(-62.9504460460768,-0.4786248922106,14.8280621840006));
#27656=CARTESIAN_POINT('Ctrl Pts',(-63.3581297348818,-1.64918471803045,
14.7650036850163));
#27657=CARTESIAN_POINT('Ctrl Pts',(-65.3081850174459,-2.40901142364103,
14.6648992225093));
#27658=CARTESIAN_POINT('Ctrl Pts',(-67.1910886177016,-1.04758997952521,
14.5537613319412));
#27659=CARTESIAN_POINT('Ctrl Pts',(-67.068463685159,1.27270221153157,14.4426234413732));
#27660=CARTESIAN_POINT('Ctrl Pts',(-65.0525510239567,2.42807611461694,14.3314855508051));
#27661=CARTESIAN_POINT('Ctrl Pts',(-63.2662754947239,1.50459133827138,14.2353026435015));
#27662=CARTESIAN_POINT('Ctrl Pts',(-62.9499316392037,0.407728674576415,
14.1761656997206));
#27663=CARTESIAN_POINT('Ctrl Pts',(-62.9480827837869,-0.00102651687047834,
14.1540747194623));
#27664=CARTESIAN_POINT('Origin',(-65.,8.88178419700125E-15,23.5459252805377));
#27665=CARTESIAN_POINT('',(-62.9418498698494,-8.27718826610594E-6,15.5540747194623));
#27666=CARTESIAN_POINT('',(-62.9484914975566,-0.00046897412753623,15.4959252805377));
#27667=CARTESIAN_POINT('',(-62.94525,-1.20379215794662E-13,23.5459252805377));
#27668=CARTESIAN_POINT('Ctrl Pts',(-62.9484914975566,-0.000468974127536166,
15.4959252805377));
#27669=CARTESIAN_POINT('Ctrl Pts',(-62.9478504078462,-0.314513019480932,
15.4789613845241));
#27670=CARTESIAN_POINT('Ctrl Pts',(-63.1632430376845,-1.31353647315872,
15.4249515249878));
#27671=CARTESIAN_POINT('Ctrl Pts',(-64.7178900651262,-2.41220423477673,
15.3338957019289));
#27672=CARTESIAN_POINT('Ctrl Pts',(-66.8736278902366,-1.54526173974447,
15.2227578113608));
#27673=CARTESIAN_POINT('Ctrl Pts',(-67.3144128645646,0.736076372865376,
15.1116199207928));
#27674=CARTESIAN_POINT('Ctrl Pts',(-65.6367894857436,2.34367538861625,15.0004820302248));
#27675=CARTESIAN_POINT('Ctrl Pts',(-63.4964372981478,1.83465185719793,14.895250483473));
#27676=CARTESIAN_POINT('Ctrl Pts',(-62.9487020162047,0.571446388044023,
14.827064900244));
#27677=CARTESIAN_POINT('Ctrl Pts',(-62.94372126594,-0.00163389948555279,
14.7959252805377));
#27678=CARTESIAN_POINT('Ctrl Pts',(-62.9418498868449,-8.27714689220955E-6,
15.5540747194623));
#27679=CARTESIAN_POINT('Ctrl Pts',(-62.9418498603911,-0.000451185307763086,
15.5540505953261));
#27680=CARTESIAN_POINT('Ctrl Pts',(-62.9420505595996,-0.681041096754107,
15.5169805076671));
#27681=CARTESIAN_POINT('Ctrl Pts',(-63.6841642251148,-2.04129618504103,
15.4428644564855));
#27682=CARTESIAN_POINT('Ctrl Pts',(-66.0013718021885,-2.21259314346662,
15.3317265659175));
#27683=CARTESIAN_POINT('Ctrl Pts',(-67.4020124146433,-0.358678503164364,
15.2205886753494));
#27684=CARTESIAN_POINT('Ctrl Pts',(-66.6040638188323,1.82353863480769,15.1094507847814));
#27685=CARTESIAN_POINT('Ctrl Pts',(-64.3378974271891,2.33665018787606,14.9983128942134));
#27686=CARTESIAN_POINT('Ctrl Pts',(-63.0663265778663,1.09149331437409,14.913187539107));
#27687=CARTESIAN_POINT('Ctrl Pts',(-62.9448408697591,0.205526654691516,
14.8651081475233));
#27688=CARTESIAN_POINT('Ctrl Pts',(-62.946510263771,0.00176526862452855,
14.8540747194623));
#27689=CARTESIAN_POINT('Origin',(-65.,8.88178419700125E-15,23.5459252805377));
#27690=CARTESIAN_POINT('',(-62.9465344116198,-0.00176006504695014,16.2540747194623));
#27691=CARTESIAN_POINT('',(-62.9454411297334,0.00187890759641046,16.1959252805377));
#27692=CARTESIAN_POINT('',(-62.94525,-1.20379215794662E-13,23.5459252805377));
#27693=CARTESIAN_POINT('Ctrl Pts',(-62.9454411297334,0.00187890759641044,
16.1959252805377));
#27694=CARTESIAN_POINT('Ctrl Pts',(-62.9501461271515,-0.514927296910581,
16.1679038323268));
#27695=CARTESIAN_POINT('Ctrl Pts',(-63.4098006358751,-1.72243750067869,
16.1028364205933));
#27696=CARTESIAN_POINT('Ctrl Pts',(-65.4379883182475,-2.38882429960344,
16.0007230453371));
#27697=CARTESIAN_POINT('Ctrl Pts',(-67.24452629377,-0.927586663439792,15.8895851547691));
#27698=CARTESIAN_POINT('Ctrl Pts',(-66.996623898036,1.38268156569091,15.7784472642011));
#27699=CARTESIAN_POINT('Ctrl Pts',(-64.9211890049946,2.42736567633039,15.667309373633));
#27700=CARTESIAN_POINT('Ctrl Pts',(-63.223670707888,1.42992668390708,15.5731353790785));
#27701=CARTESIAN_POINT('Ctrl Pts',(-62.9492504273939,0.371300206405418,
15.5160073480468));
#27702=CARTESIAN_POINT('Ctrl Pts',(-62.9484914975566,-0.000468974127536166,
15.4959252805377));
#27703=CARTESIAN_POINT('Ctrl Pts',(-62.9465344116198,-0.00176006504695018,
16.2540747194623));
#27704=CARTESIAN_POINT('Ctrl Pts',(-62.944864096038,-0.206418574104765,
16.2429930431288));
#27705=CARTESIAN_POINT('Ctrl Pts',(-63.0670246817589,-1.09329987115451,
16.1948654032727));
#27706=CARTESIAN_POINT('Ctrl Pts',(-64.3409338179361,-2.33750843231644,
16.1096917998938));
#27707=CARTESIAN_POINT('Ctrl Pts',(-66.6064316564341,-1.82145305641562,
15.9985539093258));
#27708=CARTESIAN_POINT('Ctrl Pts',(-67.401544381661,0.361798958737847,15.8874160187577));
#27709=CARTESIAN_POINT('Ctrl Pts',(-65.9984962989145,2.21389228381421,15.7762781281897));
#27710=CARTESIAN_POINT('Ctrl Pts',(-63.6820161659208,2.03962273041629,15.6651643617579));
#27711=CARTESIAN_POINT('Ctrl Pts',(-62.9418904838623,0.679695842678611,
15.5910965588488));
#27712=CARTESIAN_POINT('Ctrl Pts',(-62.9418498868449,-8.27714689220955E-6,
15.5540747194623));
#27713=CARTESIAN_POINT('Origin',(-65.,8.88178419700125E-15,23.5459252805377));
#27714=CARTESIAN_POINT('',(-62.9480689459238,0.00103910400151244,16.9540747194623));
#27715=CARTESIAN_POINT('',(-62.9421231189799,-0.000678771108088527,16.8959252805377));
#27716=CARTESIAN_POINT('',(-62.94525,-1.20379215794662E-13,23.5459252805377));
#27717=CARTESIAN_POINT('Ctrl Pts',(-62.9421231189799,-0.000678771108088587,
16.8959252805377));
#27718=CARTESIAN_POINT('Ctrl Pts',(-62.9419623987169,-0.038017692910355,
16.8938922436523));
#27719=CARTESIAN_POINT('Ctrl Pts',(-62.9598052246296,-0.755589108274127,
16.8548132432442));
#27720=CARTESIAN_POINT('Ctrl Pts',(-63.7964607753782,-2.1094569529468,16.7786882793134));
#27721=CARTESIAN_POINT('Ctrl Pts',(-66.119540899393,-2.15521309297246,16.6675503887454));
#27722=CARTESIAN_POINT('Ctrl Pts',(-67.4178925417354,-0.228278247224643,
16.5564124981773));
#27723=CARTESIAN_POINT('Ctrl Pts',(-66.5031197198625,1.9076022670654,16.4452746076093));
#27724=CARTESIAN_POINT('Ctrl Pts',(-64.2125243718594,2.29743279261729,16.3341367170413));
#27725=CARTESIAN_POINT('Ctrl Pts',(-63.0385141433925,1.01630861777054,16.251020274684));
#27726=CARTESIAN_POINT('Ctrl Pts',(-62.9439258504044,0.168320180393547,
16.2049497958495));
#27727=CARTESIAN_POINT('Ctrl Pts',(-62.9454411297334,0.00187890759641044,
16.1959252805377));
#27728=CARTESIAN_POINT('Ctrl Pts',(-62.9480689459238,0.00103910400151244,
16.9540747194623));
#27729=CARTESIAN_POINT('Ctrl Pts',(-62.9499449184218,-0.408602185927941,
16.9319354909316));
#27730=CARTESIAN_POINT('Ctrl Pts',(-63.2673355867028,-1.50638090616107,
16.8727502988781));
#27731=CARTESIAN_POINT('Ctrl Pts',(-65.0557052990257,-2.42800552371271,
16.776519143302));
#27732=CARTESIAN_POINT('Ctrl Pts',(-67.0701156187118,-1.27001386948507,
16.665381252734));
#27733=CARTESIAN_POINT('Ctrl Pts',(-67.1897256358837,1.05043588241969,16.5542433621659));
#27734=CARTESIAN_POINT('Ctrl Pts',(-65.3050549453524,2.4094097583915,16.4431054715979));
#27735=CARTESIAN_POINT('Ctrl Pts',(-63.3569278527547,1.6474176190389,16.3430492573633));
#27736=CARTESIAN_POINT('Ctrl Pts',(-62.9504479489003,0.477753335721173,
16.2800390066515));
#27737=CARTESIAN_POINT('Ctrl Pts',(-62.9465344116198,-0.00176006504695018,
16.2540747194623));
#27738=CARTESIAN_POINT('Origin',(-65.,8.88178419700125E-15,23.5459252805377));
#27739=CARTESIAN_POINT('',(-62.9427422720288,0.00120218122683403,17.6540747194623));
#27740=CARTESIAN_POINT('',(-62.9474450730054,-0.0014509802675629,17.5959252805377));
#27741=CARTESIAN_POINT('',(-62.94525,-1.20379215794662E-13,23.5459252805377));
#27742=CARTESIAN_POINT('Ctrl Pts',(-62.9474450730054,-0.00145098026756288,
17.5959252805377));
#27743=CARTESIAN_POINT('Ctrl Pts',(-62.9458669586282,-0.243481142931835,
17.582834691455));
#27744=CARTESIAN_POINT('Ctrl Pts',(-63.0973769195488,-1.16853721152032,
17.5326981388497));
#27745=CARTESIAN_POINT('Ctrl Pts',(-64.4682857559272,-2.36972472329319,
17.4455156227217));
#27746=CARTESIAN_POINT('Ctrl Pts',(-66.7025669780829,-1.73192984461803,
17.3343777321536));
#27747=CARTESIAN_POINT('Ctrl Pts',(-67.3784693367765,0.491120062256299,
17.2232398415856));
#27748=CARTESIAN_POINT('Ctrl Pts',(-65.8773317378418,2.26464220646723,17.1121019510175));
#27749=CARTESIAN_POINT('Ctrl Pts',(-63.6153124412349,1.97078728704394,17.0029970973349));
#27750=CARTESIAN_POINT('Ctrl Pts',(-62.9448910406138,0.642371504646387,
16.930938207175));
#27751=CARTESIAN_POINT('Ctrl Pts',(-62.9421231189799,-0.000678771108088587,
16.8959252805377));
#27752=CARTESIAN_POINT('Ctrl Pts',(-62.9427422720288,0.00120218122683403,
17.6540747194623));
#27753=CARTESIAN_POINT('Ctrl Pts',(-62.9469836764117,-0.608977902213451,
17.6208779387343));
#27754=CARTESIAN_POINT('Ctrl Pts',(-63.5579942556341,-1.90746584530598,
17.5506351944836));
#27755=CARTESIAN_POINT('Ctrl Pts',(-65.7655743703156,-2.30482315743207,
17.4433464867103));
#27756=CARTESIAN_POINT('Ctrl Pts',(-67.3516166417705,-0.606805630879782,
17.3322085961422));
#27757=CARTESIAN_POINT('Ctrl Pts',(-66.7851975318663,1.6466279712607,17.2210707055742));
#27758=CARTESIAN_POINT('Ctrl Pts',(-64.5847668755277,2.39288431727496,17.1099328150062));
#27759=CARTESIAN_POINT('Ctrl Pts',(-63.1270293146865,1.23655417501042,17.0209341529689));
#27760=CARTESIAN_POINT('Ctrl Pts',(-62.9468058203889,0.276857845483475,
16.9689814544543));
#27761=CARTESIAN_POINT('Ctrl Pts',(-62.9480689459238,0.00103910400151244,
16.9540747194623));
#27762=CARTESIAN_POINT('Origin',(-65.,8.88178419700125E-15,23.5459252805377));
#27763=CARTESIAN_POINT('',(-62.9444267867382,-0.0017991321662611,18.3540747194623));
#27764=CARTESIAN_POINT('',(-62.9473667479389,0.00148795945043925,18.2959252805377));
#27765=CARTESIAN_POINT('',(-62.94525,-1.20379215794662E-13,23.5459252805377));
#27766=CARTESIAN_POINT('Ctrl Pts',(-62.9473667479389,0.00148795945043927,
18.2959252805377));
#27767=CARTESIAN_POINT('Ctrl Pts',(-62.9503594142629,-0.444940986140601,
18.2717771392578));
#27768=CARTESIAN_POINT('Ctrl Pts',(-63.3129997156342,-1.58066882860308,
18.2105830344552));
#27769=CARTESIAN_POINT('Ctrl Pts',(-65.1869048686148,-2.42144210577607,
18.1123429661299));
#27770=CARTESIAN_POINT('Ctrl Pts',(-67.1357566643205,-1.15622609049766,
18.0012050755618));
#27771=CARTESIAN_POINT('Ctrl Pts',(-67.1297261640456,1.16729677790886,17.8900671849939));
#27772=CARTESIAN_POINT('Ctrl Pts',(-65.1743331530824,2.42237966744963,17.7789292944258));
#27773=CARTESIAN_POINT('Ctrl Pts',(-63.3084858902886,1.5735595002714,17.6808819929404));
#27774=CARTESIAN_POINT('Ctrl Pts',(-62.9503329736625,0.44145675564833,17.6198806549777));
#27775=CARTESIAN_POINT('Ctrl Pts',(-62.9474450730054,-0.00145098026756288,
17.5959252805377));
#27776=CARTESIAN_POINT('Ctrl Pts',(-62.9444267867382,-0.0017991321662612,
18.3540747194623));
#27777=CARTESIAN_POINT('Ctrl Pts',(-62.9432099184932,-0.13457659736896,
18.3468663500598));
#27778=CARTESIAN_POINT('Ctrl Pts',(-63.0154304430432,-0.948418981304482,
18.3026120171345));
#27779=CARTESIAN_POINT('Ctrl Pts',(-64.1011546824859,-2.25618948643599,
18.2213117206866));
#27780=CARTESIAN_POINT('Ctrl Pts',(-66.4080681763277,-1.97880214127948,
18.1101738301185));
#27781=CARTESIAN_POINT('Ctrl Pts',(-67.4261608997972,0.109805244932097,
17.9990359395505));
#27782=CARTESIAN_POINT('Ctrl Pts',(-66.2235610371465,2.09790664518148,17.8878980489825));
#27783=CARTESIAN_POINT('Ctrl Pts',(-63.9010218810697,2.16577030121657,17.7767601584144));
#27784=CARTESIAN_POINT('Ctrl Pts',(-62.9776665752518,0.823136293702514,
17.6988190485744));
#27785=CARTESIAN_POINT('Ctrl Pts',(-62.9422504791375,0.0719528572662148,
17.657923902257));
#27786=CARTESIAN_POINT('Ctrl Pts',(-62.9427422720288,0.00120218122683403,
17.6540747194623));
#27787=CARTESIAN_POINT('Origin',(-65.,8.88178419700125E-15,23.5459252805377));
#27788=CARTESIAN_POINT('',(-62.948587662066,-7.81015561640563E-5,19.0540747194623));
#27789=CARTESIAN_POINT('',(-62.9420758643114,0.000617377060639333,18.9959252805377));
#27790=CARTESIAN_POINT('',(-62.94525,-1.20379215794662E-13,23.5459252805377));
#27791=CARTESIAN_POINT('Ctrl Pts',(-62.9420758643114,0.000617377060639374,
18.9959252805377));
#27792=CARTESIAN_POINT('Ctrl Pts',(-62.9446352222011,-0.645933688463607,
18.9607195870605));
#27793=CARTESIAN_POINT('Ctrl Pts',(-63.621561854257,-1.97744992677628,18.8884679300607));
#27794=CARTESIAN_POINT('Ctrl Pts',(-65.88907520037,-2.26005765183972,18.7791703095382));
#27795=CARTESIAN_POINT('Ctrl Pts',(-67.3809865945794,-0.478767310881874,
18.6680324189701));
#27796=CARTESIAN_POINT('Ctrl Pts',(-66.6935539565454,1.74074417931049,18.5568945284021));
#27797=CARTESIAN_POINT('Ctrl Pts',(-64.4559921758773,2.36693278080145,18.445756637834));
#27798=CARTESIAN_POINT('Ctrl Pts',(-63.0943542721865,1.1613169625899,18.3587668885459));
#27799=CARTESIAN_POINT('Ctrl Pts',(-62.9457683276783,0.239931205144695,
18.3088231027804));
#27800=CARTESIAN_POINT('Ctrl Pts',(-62.9473667479389,0.00148795945043927,
18.2959252805377));
#27801=CARTESIAN_POINT('Ctrl Pts',(-62.948587662066,-7.81015561641604E-5,
19.0540747194623));
#27802=CARTESIAN_POINT('Ctrl Pts',(-62.9484730026856,-0.33826529995397,
19.0358087978625));
#27803=CARTESIAN_POINT('Ctrl Pts',(-63.1876491089047,-1.36219297688966,
18.98049691274));
#27804=CARTESIAN_POINT('Ctrl Pts',(-64.8026200998564,-2.42061047643985,
18.8881390640948));
#27805=CARTESIAN_POINT('Ctrl Pts',(-66.9266433003906,-1.4786343349792,18.7770011735268));
#27806=CARTESIAN_POINT('Ctrl Pts',(-67.2871880384261,0.816752582102682,
18.6658632829587));
#27807=CARTESIAN_POINT('Ctrl Pts',(-65.5542436264288,2.36455659820144,18.5547253923907));
#27808=CARTESIAN_POINT('Ctrl Pts',(-63.4592956564195,1.78804123877569,18.4507958712252));
#27809=CARTESIAN_POINT('Ctrl Pts',(-62.9494637678869,0.547806457359306,
18.3839123135824));
#27810=CARTESIAN_POINT('Ctrl Pts',(-62.9444267867382,-0.0017991321662612,
18.3540747194623));
#27811=CARTESIAN_POINT('Origin',(-65.,8.88178419700125E-15,23.5459252805377));
#27812=CARTESIAN_POINT('',(-62.9447134762142,0.00183968268686788,19.7540747194623));
#27813=CARTESIAN_POINT('',(-62.9455477186679,-0.00187702223999529,19.6959252805377));
#27814=CARTESIAN_POINT('',(-62.94525,-1.20379215794662E-13,23.5459252805377));
#27815=CARTESIAN_POINT('Ctrl Pts',(-62.9455477186679,-0.00187702223999513,
19.6959252805377));
#27816=CARTESIAN_POINT('Ctrl Pts',(-62.9440086170586,-0.171896041847231,
19.6867079983859));
#27817=CARTESIAN_POINT('Ctrl Pts',(-63.0410778177033,-1.02351952878432,
19.6404447527115));
#27818=CARTESIAN_POINT('Ctrl Pts',(-64.2244604721458,-2.30148946126117,
19.5571355435145));
#27819=CARTESIAN_POINT('Ctrl Pts',(-66.5130014322595,-1.89977418876313,
19.4459976529464));
#27820=CARTESIAN_POINT('Ctrl Pts',(-67.4166750228636,0.24082594437386,19.3348597623784));
#27821=CARTESIAN_POINT('Ctrl Pts',(-66.1083385580613,2.16099535909079,19.2237218718103));
#27822=CARTESIAN_POINT('Ctrl Pts',(-63.7855272416617,2.10318121447059,19.1125839812423));
#27823=CARTESIAN_POINT('Ctrl Pts',(-62.9580113964128,0.748427978399207,
19.0366517841514));
#27824=CARTESIAN_POINT('Ctrl Pts',(-62.9419420816985,0.034413858290589,
18.9977655505832));
#27825=CARTESIAN_POINT('Ctrl Pts',(-62.9420758643114,0.000617377060639374,
18.9959252805377));
#27826=CARTESIAN_POINT('Ctrl Pts',(-62.9447134762142,0.00183968268686788,
19.7540747194623));
#27827=CARTESIAN_POINT('Ctrl Pts',(-62.9497000514415,-0.538489713183419,
19.7247512456653));
#27828=CARTESIAN_POINT('Ctrl Pts',(-63.44501294369,-1.76953586229589,19.6583818083455));
#27829=CARTESIAN_POINT('Ctrl Pts',(-65.5214561645339,-2.37200281981328,
19.5549664075031));
#27830=CARTESIAN_POINT('Ctrl Pts',(-67.2756619344365,-0.848337588988209,
19.443828516935));
#27831=CARTESIAN_POINT('Ctrl Pts',(-66.9469285261459,1.45182065545647,19.332690626367));
#27832=CARTESIAN_POINT('Ctrl Pts',(-64.8361493591312,2.42311099039749,19.221552735799));
#27833=CARTESIAN_POINT('Ctrl Pts',(-63.1976100342287,1.38138540402115,19.1286807668307));
#27834=CARTESIAN_POINT('Ctrl Pts',(-62.9487055486976,0.347627856173917,
19.0728547613852));
#27835=CARTESIAN_POINT('Ctrl Pts',(-62.948587662066,-7.81015561641604E-5,
19.0540747194623));
#27836=CARTESIAN_POINT('Origin',(-65.,8.88178419700125E-15,23.5459252805377));
#27837=CARTESIAN_POINT('',(-62.9425383451584,-0.00106562935658971,20.4540747194623));
#27838=CARTESIAN_POINT('',(-62.9484657349091,0.000525555021686121,20.3959252805377));
#27839=CARTESIAN_POINT('',(-62.94525,-1.20379215794662E-13,23.5459252805377));
#27840=CARTESIAN_POINT('Ctrl Pts',(-62.9484657349091,0.000525555021685942,
20.3959252805377));
#27841=CARTESIAN_POINT('Ctrl Pts',(-62.9493249615497,-0.374800466557392,
20.3756504461887));
#27842=CARTESIAN_POINT('Ctrl Pts',(-63.2276318468978,-1.43710439466947,
20.318329648317));
#27843=CARTESIAN_POINT('Ctrl Pts',(-64.9337900137556,-2.42774204026717,
20.2239628869227));
#27844=CARTESIAN_POINT('Ctrl Pts',(-67.0037742079544,-1.37229889524426,
20.1128249963547));
#27845=CARTESIAN_POINT('Ctrl Pts',(-67.2396811477566,0.939225037877063,
20.0016871057866));
#27846=CARTESIAN_POINT('Ctrl Pts',(-65.4255825320509,2.3910656189328,19.8905492152186));
#27847=CARTESIAN_POINT('Ctrl Pts',(-63.4047034238819,1.71543774995269,19.7886286068023));
#27848=CARTESIAN_POINT('Ctrl Pts',(-62.9501945513868,0.511441876516725,
19.7237539619086));
#27849=CARTESIAN_POINT('Ctrl Pts',(-62.9455477186679,-0.00187702223999513,
19.6959252805377));
#27850=CARTESIAN_POINT('Ctrl Pts',(-62.9425383451584,-0.00106562935658957,
20.4540747194623));
#27851=CARTESIAN_POINT('Ctrl Pts',(-62.9421515159492,-0.0623504207905182,
20.4507396569907));
#27852=CARTESIAN_POINT('Ctrl Pts',(-62.9724324501069,-0.804000733271024,
20.4103586309964));
#27853=CARTESIAN_POINT('Ctrl Pts',(-63.8711449203827,-2.15034861017486,
20.3329316414794));
#27854=CARTESIAN_POINT('Ctrl Pts',(-66.1944008109328,-2.11464436694831,
20.2217937509113));
#27855=CARTESIAN_POINT('Ctrl Pts',(-67.4244083164919,-0.143381864737536,
20.1106558603433));
#27856=CARTESIAN_POINT('Ctrl Pts',(-66.4353272830534,1.95911953903996,19.9995179697752));
#27857=CARTESIAN_POINT('Ctrl Pts',(-64.132474966303,2.26841668404626,19.8883800792072));
#27858=CARTESIAN_POINT('Ctrl Pts',(-63.0217706588138,0.967627859876304,
19.8065656624362));
#27859=CARTESIAN_POINT('Ctrl Pts',(-62.9434002356266,0.144138246524585,
19.7617972091879));
#27860=CARTESIAN_POINT('Ctrl Pts',(-62.9447134762142,0.00183968268686788,
19.7540747194623));
#27861=CARTESIAN_POINT('Origin',(-65.,8.88178419700125E-15,23.5459252805377));
#27862=CARTESIAN_POINT('',(-62.9479182248742,-0.00116161895480638,21.1540747194623));
#27863=CARTESIAN_POINT('',(-62.9436210622307,0.00160392935066218,21.0959252805377));
#27864=CARTESIAN_POINT('',(-62.94525,-1.20379215794662E-13,23.5459252805377));
#27865=CARTESIAN_POINT('Ctrl Pts',(-62.9436210622307,0.00160392935066219,
21.0959252805377));
#27866=CARTESIAN_POINT('Ctrl Pts',(-62.9485686759719,-0.574950681266282,
21.0645928939915));
#27867=CARTESIAN_POINT('Ctrl Pts',(-63.5020551216143,-1.84152256699687,
20.9962145439225));
#27868=CARTESIAN_POINT('Ctrl Pts',(-65.648946524169,-2.34033682721966,20.8907902303309));
#27869=CARTESIAN_POINT('Ctrl Pts',(-67.3182024564633,-0.724053604371166,
20.7796523397629));
#27870=CARTESIAN_POINT('Ctrl Pts',(-66.865581542071,1.55496692328426,20.6685144491949));
#27871=CARTESIAN_POINT('Ctrl Pts',(-64.7053726085262,2.41070716562326,20.5573765586268));
#27872=CARTESIAN_POINT('Ctrl Pts',(-63.1597285921146,1.30632755500752,20.4665135024078));
#27873=CARTESIAN_POINT('Ctrl Pts',(-62.9477549916925,0.310991282228741,
20.4126964097114));
#27874=CARTESIAN_POINT('Ctrl Pts',(-62.9484657349091,0.000525555021685942,
20.3959252805377));
#27875=CARTESIAN_POINT('Ctrl Pts',(-62.9479182248742,-0.00116161895480603,
21.1540747194623));
#27876=CARTESIAN_POINT('Ctrl Pts',(-62.9465403381585,-0.267421145958312,
21.1396821047934));
#27877=CARTESIAN_POINT('Ctrl Pts',(-63.1184075387479,-1.21731587450749,
21.0882435266019));
#27878=CARTESIAN_POINT('Ctrl Pts',(-64.5516876929394,-2.38689686810909,
20.9997589848876));
#27879=CARTESIAN_POINT('Ctrl Pts',(-66.7622271403759,-1.67118893435551,
20.8886210943196));
#27880=CARTESIAN_POINT('Ctrl Pts',(-67.3597936726881,0.574194749175807,
20.7774832037516));
#27881=CARTESIAN_POINT('Ctrl Pts',(-65.7974074532359,2.29400261230211,20.6663453131835));
#27882=CARTESIAN_POINT('Ctrl Pts',(-63.573935456952,1.92548892520574,20.5585424850871));
#27883=CARTESIAN_POINT('Ctrl Pts',(-62.9464484251963,0.618402688713493,
20.4877856205134));
#27884=CARTESIAN_POINT('Ctrl Pts',(-62.9425383451584,-0.00106562935658957,
20.4540747194623));
#27885=CARTESIAN_POINT('Origin',(-65.,8.88178419700125E-15,23.5459252805377));
#27886=CARTESIAN_POINT('',(-62.9473239618077,0.00235074752841319,21.8540747194623));
#27887=CARTESIAN_POINT('',(-62.9434348764936,-0.00149614206265777,21.7959252805377));
#27888=CARTESIAN_POINT('',(-62.94525,-1.20379215794662E-13,23.5459252805377));
#27889=CARTESIAN_POINT('',(-64.4698297828114,1.98517432567172,22.));
#27890=CARTESIAN_POINT('Ctrl Pts',(-64.4698297828114,1.98517432567173,22.));
#27891=CARTESIAN_POINT('Ctrl Pts',(-63.8097120902545,1.8088801151799,21.9629540364773));
#27892=CARTESIAN_POINT('Ctrl Pts',(-63.0750422655367,1.11280694816752,21.9143122762981));
#27893=CARTESIAN_POINT('Ctrl Pts',(-62.9457054195483,0.216594706141787,
21.8656705161189));
#27894=CARTESIAN_POINT('Ctrl Pts',(-62.9473239618077,0.00235074752841319,
21.8540747194623));
#27895=CARTESIAN_POINT('',(-65.5313040526013,1.98873440678486,22.));
#27896=CARTESIAN_POINT('Origin',(-65.,8.88178419700125E-15,22.));
#27897=CARTESIAN_POINT('Ctrl Pts',(-65.5313046873329,1.98873639975132,22.));
#27898=CARTESIAN_POINT('Ctrl Pts',(-64.8866967734446,2.16006352763734,21.9636770818144));
#27899=CARTESIAN_POINT('Ctrl Pts',(-63.5069411366323,1.84063802220702,21.895652175327));
#27900=CARTESIAN_POINT('Ctrl Pts',(-62.9482922133912,0.581586231880553,
21.8276272688395));
#27901=CARTESIAN_POINT('Ctrl Pts',(-62.9434348764936,-0.00149614206265759,
21.7959252805377));
#27902=CARTESIAN_POINT('Origin',(-32.5,-56.2916512459885,17.));
#27903=CARTESIAN_POINT('',(-31.6672724934037,-54.8468960395934,13.8714803633902));
#27904=CARTESIAN_POINT('',(-31.6651566506306,-54.8475988206465,13.6785196366098));
#27905=CARTESIAN_POINT('',(-31.667,-54.8488529232836,17.));
#27906=CARTESIAN_POINT('',(-31.9588970197441,-54.7159724828016,13.));
#27907=CARTESIAN_POINT('Ctrl Pts',(-31.6651566506306,-54.8475988206465,
13.6785196366098));
#27908=CARTESIAN_POINT('Ctrl Pts',(-31.6146486514652,-54.8762889946568,
13.6746222055426));
#27909=CARTESIAN_POINT('Ctrl Pts',(-31.5657632473174,-54.9077117506003,
13.6707247744754));
#27910=CARTESIAN_POINT('Ctrl Pts',(-31.5188321868552,-54.9418237568819,
13.6668273434082));
#27911=CARTESIAN_POINT('Ctrl Pts',(-31.0727418458088,-55.2660660894878,
13.6297813798856));
#27912=CARTESIAN_POINT('Ctrl Pts',(-30.8032251342758,-55.8332803703507,
13.5927354163629));
#27913=CARTESIAN_POINT('Ctrl Pts',(-30.8337540098498,-56.3839156387154,
13.5556894528402));
#27914=CARTESIAN_POINT('Ctrl Pts',(-30.8642828854237,-56.93455090708,13.5186434893175));
#27915=CARTESIAN_POINT('Ctrl Pts',(-31.1948573481046,-57.4686071629464,
13.4815975257948));
#27916=CARTESIAN_POINT('Ctrl Pts',(-31.6739356569701,-57.7415946577538,
13.4445515622722));
#27917=CARTESIAN_POINT('Ctrl Pts',(-32.1530139658356,-58.0145821525613,
13.4075055987495));
#27918=CARTESIAN_POINT('Ctrl Pts',(-32.7805961208857,-58.0265008863097,
13.3704596352268));
#27919=CARTESIAN_POINT('Ctrl Pts',(-33.2699721109727,-57.7720492096737,
13.3334136717041));
#27920=CARTESIAN_POINT('Ctrl Pts',(-33.7593481010598,-57.5175975330377,
13.2963677081814));
#27921=CARTESIAN_POINT('Ctrl Pts',(-34.1105179261839,-56.9967754460171,
13.2593217446588));
#27922=CARTESIAN_POINT('Ctrl Pts',(-34.1617369653364,-56.4476202824107,
13.2222757811361));
#27923=CARTESIAN_POINT('Ctrl Pts',(-34.2129560044889,-55.8984651188042,
13.1852298176134));
#27924=CARTESIAN_POINT('Ctrl Pts',(-33.9642242576698,-55.3209768786118,
13.1481838540907));
#27925=CARTESIAN_POINT('Ctrl Pts',(-33.5316971804146,-54.9803713160329,
13.111137890568));
#27926=CARTESIAN_POINT('Ctrl Pts',(-33.0991701031595,-54.639765753454,13.0740919270454));
#27927=CARTESIAN_POINT('Ctrl Pts',(-32.4828476954683,-54.5360428684886,
13.0370459635227));
#27928=CARTESIAN_POINT('Ctrl Pts',(-31.9588970197442,-54.7159724828016,
13.));
#27929=CARTESIAN_POINT('',(-31.0290140863629,-57.0802261258962,13.));
#27930=CARTESIAN_POINT('Origin',(-32.5,-56.2916512459885,13.));
#27931=CARTESIAN_POINT('',(-31.6688354432562,-54.8507324474214,13.1714803633902));
#27932=CARTESIAN_POINT('Ctrl Pts',(-31.029012445651,-57.0802271145805,13.));
#27933=CARTESIAN_POINT('Ctrl Pts',(-30.774120583937,-56.6032768580682,13.0363229181856));
#27934=CARTESIAN_POINT('Ctrl Pts',(-30.7719333897513,-55.9901147282721,
13.0726458363711));
#27935=CARTESIAN_POINT('Ctrl Pts',(-31.0246770579875,-55.5119982833858,
13.1089687545567));
#27936=CARTESIAN_POINT('Ctrl Pts',(-31.1696673663398,-55.2377194013227,
13.1298059575012));
#27937=CARTESIAN_POINT('Ctrl Pts',(-31.3985533923309,-55.0078829792344,
13.1506431604457));
#27938=CARTESIAN_POINT('Ctrl Pts',(-31.6688354432562,-54.8507324474214,
13.1714803633902));
#27939=CARTESIAN_POINT('',(-31.667,-54.8488529232836,12.));
#27940=CARTESIAN_POINT('',(-31.667,-54.8488529232836,17.));
#27941=CARTESIAN_POINT('Origin',(-32.5,-56.2916512459885,12.));
#27942=CARTESIAN_POINT('Ctrl Pts',(-31.6688354432562,-54.8507324474214,
13.1714803633902));
#27943=CARTESIAN_POINT('Ctrl Pts',(-31.8790813703937,-54.7284888165622,
13.1876891239684));
#27944=CARTESIAN_POINT('Ctrl Pts',(-32.1143756641563,-54.6502267716398,
13.2038978845465));
#27945=CARTESIAN_POINT('Ctrl Pts',(-32.3547143198851,-54.6292400960994,
13.2201066451247));
#27946=CARTESIAN_POINT('Ctrl Pts',(-32.9040207909308,-54.5812739599609,
13.2571526086474));
#27947=CARTESIAN_POINT('Ctrl Pts',(-33.4796777351052,-54.8324998905166,
13.2941985721701));
#27948=CARTESIAN_POINT('Ctrl Pts',(-33.8179820369827,-55.2680242179701,
13.3312445356928));
#27949=CARTESIAN_POINT('Ctrl Pts',(-34.1562863388601,-55.7035485454237,
13.3682904992154));
#27950=CARTESIAN_POINT('Ctrl Pts',(-34.2572379984406,-56.323371269775,13.4053364627381));
#27951=CARTESIAN_POINT('Ctrl Pts',(-34.0747609720031,-56.8437863823056,
13.4423824262608));
#27952=CARTESIAN_POINT('Ctrl Pts',(-33.8922839455656,-57.3642014948362,
13.4794283897835));
#27953=CARTESIAN_POINT('Ctrl Pts',(-33.4263782331101,-57.7852089955461,
13.5164743533062));
#27954=CARTESIAN_POINT('Ctrl Pts',(-32.8902057561615,-57.9141527098528,
13.5535203168288));
#27955=CARTESIAN_POINT('Ctrl Pts',(-32.3540332792128,-58.0430964241595,
13.5905662803515));
#27956=CARTESIAN_POINT('Ctrl Pts',(-31.7475940377709,-57.879976352063,13.6276122438742));
#27957=CARTESIAN_POINT('Ctrl Pts',(-31.3484595971706,-57.499435180452,13.6646582073969));
#27958=CARTESIAN_POINT('Ctrl Pts',(-30.9493251565703,-57.1188940088411,
13.7017041709196));
#27959=CARTESIAN_POINT('Ctrl Pts',(-30.7574955168115,-56.5209317377157,
13.7387501344422));
#27960=CARTESIAN_POINT('Ctrl Pts',(-30.8607470097836,-55.9792142563288,
13.7757960979649));
#27961=CARTESIAN_POINT('Ctrl Pts',(-30.9496414742062,-55.5128221104134,
13.8076908531067));
#27962=CARTESIAN_POINT('Ctrl Pts',(-31.2572608237869,-55.0881206516064,
13.8395856082484));
#27963=CARTESIAN_POINT('Ctrl Pts',(-31.6672724934037,-54.8468960395934,
13.8714803633902));
#27964=CARTESIAN_POINT('Origin',(-32.5,-56.2916512459885,17.));
#27965=CARTESIAN_POINT('',(-31.6652293984911,-54.8484357012869,14.5714803633902));
#27966=CARTESIAN_POINT('',(-31.6674240358463,-54.8512520230129,14.3785196366098));
#27967=CARTESIAN_POINT('',(-31.667,-54.8488529232836,17.));
#27968=CARTESIAN_POINT('Ctrl Pts',(-31.6674240358463,-54.8512520230129,
14.3785196366098));
#27969=CARTESIAN_POINT('Ctrl Pts',(-31.4726121759195,-54.9625548712859,
14.3635646533454));
#27970=CARTESIAN_POINT('Ctrl Pts',(-31.2997293296832,-55.1111079954895,
14.3486096700809));
#27971=CARTESIAN_POINT('Ctrl Pts',(-31.1659805795344,-55.289072307877,14.3336546868165));
#27972=CARTESIAN_POINT('Ctrl Pts',(-30.8346628353681,-55.7299193023853,
14.2966087232938));
#27973=CARTESIAN_POINT('Ctrl Pts',(-30.7434854934753,-56.3512435601479,
14.2595627597711));
#27974=CARTESIAN_POINT('Ctrl Pts',(-30.9341783443449,-56.8686931008725,
14.2225167962484));
#27975=CARTESIAN_POINT('Ctrl Pts',(-31.1248711952146,-57.386142641597,14.1854708327258));
#27976=CARTESIAN_POINT('Ctrl Pts',(-31.5974342388466,-57.7997174652835,
14.1484248692031));
#27977=CARTESIAN_POINT('Ctrl Pts',(-32.1355923903503,-57.9201415291698,
14.1113789056804));
#27978=CARTESIAN_POINT('Ctrl Pts',(-32.6737505418539,-58.0405655930561,
14.0743329421577));
#27979=CARTESIAN_POINT('Ctrl Pts',(-33.2775038012292,-57.8678388971422,
14.037286978635));
#27980=CARTESIAN_POINT('Ctrl Pts',(-33.6705489274,-57.4810131538507,14.0002410151124));
#27981=CARTESIAN_POINT('Ctrl Pts',(-34.0635940535707,-57.0941874105591,
13.9631950515897));
#27982=CARTESIAN_POINT('Ctrl Pts',(-34.245931046537,-56.4932626198898,13.926149088067));
#27983=CARTESIAN_POINT('Ctrl Pts',(-34.1340966146064,-55.9532506956148,
13.8891031245443));
#27984=CARTESIAN_POINT('Ctrl Pts',(-34.0222621826759,-55.4132387713397,
13.8520571610216));
#27985=CARTESIAN_POINT('Ctrl Pts',(-33.6162563258487,-54.934139713459,13.815011197499));
#27986=CARTESIAN_POINT('Ctrl Pts',(-33.1019214121551,-54.7352253766931,
13.7779652339763));
#27987=CARTESIAN_POINT('Ctrl Pts',(-32.6416972484853,-54.5572378789698,
13.7448167015208));
#27988=CARTESIAN_POINT('Ctrl Pts',(-32.0947386036493,-54.6035824036932,
13.7116681690653));
#27989=CARTESIAN_POINT('Ctrl Pts',(-31.6651566506306,-54.8475988206465,
13.6785196366098));
#27990=CARTESIAN_POINT('Ctrl Pts',(-31.6672724934037,-54.8468960395934,
13.8714803633902));
#27991=CARTESIAN_POINT('Ctrl Pts',(-31.7334920188216,-54.8079367110906,
13.8766315717711));
#27992=CARTESIAN_POINT('Ctrl Pts',(-31.8023823793453,-54.7737632532799,
13.881782780152));
#27993=CARTESIAN_POINT('Ctrl Pts',(-31.8734534906151,-54.7449729811027,
13.886933988533));
#27994=CARTESIAN_POINT('Ctrl Pts',(-32.3845758527715,-54.537921878912,13.9239799520556));
#27995=CARTESIAN_POINT('Ctrl Pts',(-33.0084879513813,-54.609292366179,13.9610259155783));
#27996=CARTESIAN_POINT('Ctrl Pts',(-33.4596489857383,-54.9264225988407,
13.998071879101));
#27997=CARTESIAN_POINT('Ctrl Pts',(-33.9108100200953,-55.2435528315024,
14.0351178426237));
#27998=CARTESIAN_POINT('Ctrl Pts',(-34.1892199901994,-55.8064428095589,
14.0721638061464));
#27999=CARTESIAN_POINT('Ctrl Pts',(-34.1674649383537,-56.3574821112236,
14.109209769669));
#28000=CARTESIAN_POINT('Ctrl Pts',(-34.1457098865079,-56.9085214128884,
14.1462557331917));
#28001=CARTESIAN_POINT('Ctrl Pts',(-33.8237898127121,-57.4477100381614,
14.1833016967144));
#28002=CARTESIAN_POINT('Ctrl Pts',(-33.3490322930752,-57.7282855707718,
14.2203476602371));
#28003=CARTESIAN_POINT('Ctrl Pts',(-32.8742747734383,-58.0088611033821,
14.2573936237598));
#28004=CARTESIAN_POINT('Ctrl Pts',(-32.2466798079601,-58.0308235433297,
14.2944395872824));
#28005=CARTESIAN_POINT('Ctrl Pts',(-31.7534702764193,-57.7841214978257,
14.3314855508051));
#28006=CARTESIAN_POINT('Ctrl Pts',(-31.2602607448784,-57.5374194523217,
14.3685315143278));
#28007=CARTESIAN_POINT('Ctrl Pts',(-30.901436647275,-57.0220529213661,14.4055774778505));
#28008=CARTESIAN_POINT('Ctrl Pts',(-30.8412156241946,-56.4738823989159,
14.4426234413732));
#28009=CARTESIAN_POINT('Ctrl Pts',(-30.7809946011143,-55.9257118764658,
14.4796694048958));
#28010=CARTESIAN_POINT('Ctrl Pts',(-31.0193766525571,-55.3447373625211,
14.5167153684185));
#28011=CARTESIAN_POINT('Ctrl Pts',(-31.4472650020351,-54.9968450984028,
14.5537613319412));
#28012=CARTESIAN_POINT('Ctrl Pts',(-31.5154844642033,-54.9413796406974,
14.5596676757575));
#28013=CARTESIAN_POINT('Ctrl Pts',(-31.5885209558805,-54.8918388624727,
14.5655740195739));
#28014=CARTESIAN_POINT('Ctrl Pts',(-31.6652293984911,-54.8484357012869,
14.5714803633902));
#28015=CARTESIAN_POINT('Origin',(-32.5,-56.2916512459885,17.));
#28016=CARTESIAN_POINT('',(-31.6679812524744,-54.8513129979877,15.2714803633902));
#28017=CARTESIAN_POINT('',(-31.6687468960362,-54.8490160493388,15.0785196366098));
#28018=CARTESIAN_POINT('',(-31.667,-54.8488529232836,17.));
#28019=CARTESIAN_POINT('Ctrl Pts',(-31.6687468960362,-54.8490160493388,
15.0785196366098));
#28020=CARTESIAN_POINT('Ctrl Pts',(-31.3330220839915,-55.0465316965332,
15.0525071011481));
#28021=CARTESIAN_POINT('Ctrl Pts',(-31.0621374285877,-55.3603795470759,
15.0264945656864));
#28022=CARTESIAN_POINT('Ctrl Pts',(-30.930547953771,-55.7245591059458,15.0004820302247));
#28023=CARTESIAN_POINT('Ctrl Pts',(-30.7431437350931,-56.2432083807723,
14.9634360667021));
#28024=CARTESIAN_POINT('Ctrl Pts',(-30.8382616710438,-56.8639417522836,
14.9263901031794));
#28025=CARTESIAN_POINT('Ctrl Pts',(-31.1723705294372,-57.3026770823852,
14.8893441396567));
#28026=CARTESIAN_POINT('Ctrl Pts',(-31.5064793878306,-57.7414124124868,
14.852298176134));
#28027=CARTESIAN_POINT('Ctrl Pts',(-32.0795791686666,-57.9981497011789,
14.8152522126113));
#28028=CARTESIAN_POINT('Ctrl Pts',(-32.6293874463964,-57.9553916541296,
14.7782062490887));
#28029=CARTESIAN_POINT('Ctrl Pts',(-33.1791957241262,-57.9126336070803,
14.741160285566));
#28030=CARTESIAN_POINT('Ctrl Pts',(-33.7057124987497,-57.5703802242898,
14.7041143220433));
#28031=CARTESIAN_POINT('Ctrl Pts',(-33.9679745051883,-57.0852657438482,
14.6670683585206));
#28032=CARTESIAN_POINT('Ctrl Pts',(-34.230236511627,-56.6001512634066,14.6300223949979));
#28033=CARTESIAN_POINT('Ctrl Pts',(-34.2282437498808,-55.9721756853139,
14.5929764314753));
#28034=CARTESIAN_POINT('Ctrl Pts',(-33.9629079737486,-55.4887355202075,
14.5559304679526));
#28035=CARTESIAN_POINT('Ctrl Pts',(-33.6975721976164,-55.0052953551011,
14.5188845044299));
#28036=CARTESIAN_POINT('Ctrl Pts',(-33.1688934070984,-54.6663906029808,
14.4818385409072));
#28037=CARTESIAN_POINT('Ctrl Pts',(-32.6188249386194,-54.6271230925477,
14.4447925773845));
#28038=CARTESIAN_POINT('Ctrl Pts',(-32.2908120993686,-54.6037073755496,
14.4227015971263));
#28039=CARTESIAN_POINT('Ctrl Pts',(-31.955193328237,-54.6868393332485,14.400610616868));
#28040=CARTESIAN_POINT('Ctrl Pts',(-31.6674240358463,-54.8512520230129,
14.3785196366098));
#28041=CARTESIAN_POINT('Ctrl Pts',(-31.6652293984911,-54.8484357012869,
14.5714803633902));
#28042=CARTESIAN_POINT('Ctrl Pts',(-32.0696541670855,-54.6196041304525,
14.6026199830966));
#28043=CARTESIAN_POINT('Ctrl Pts',(-32.5761460954187,-54.5613764565911,
14.6337596028029));
#28044=CARTESIAN_POINT('Ctrl Pts',(-33.0168947227899,-54.7049585292357,
14.6648992225093));
#28045=CARTESIAN_POINT('Ctrl Pts',(-33.5412414465535,-54.8757742384787,
14.7019451860319));
#28046=CARTESIAN_POINT('Ctrl Pts',(-33.9725402465673,-55.3322156712569,
14.7389911495546));
#28047=CARTESIAN_POINT('Ctrl Pts',(-34.1134048115911,-55.8653898078431,
14.7760371130773));
#28048=CARTESIAN_POINT('Ctrl Pts',(-34.2542693766149,-56.3985639444293,
14.8130830766));
#28049=CARTESIAN_POINT('Ctrl Pts',(-34.1046997066486,-57.0084707848236,
14.8501290401227));
#28050=CARTESIAN_POINT('Ctrl Pts',(-33.7331471941746,-57.415983010017,14.8871750036453));
#28051=CARTESIAN_POINT('Ctrl Pts',(-33.3615946817007,-57.8234952352103,
14.924220967168));
#28052=CARTESIAN_POINT('Ctrl Pts',(-32.7680593267192,-58.0286128452026,
14.9612669306907));
#28053=CARTESIAN_POINT('Ctrl Pts',(-32.2241759575529,-57.9374626002348,
14.9983128942134));
#28054=CARTESIAN_POINT('Ctrl Pts',(-31.6802925883866,-57.8463123552671,
15.0353588577361));
#28055=CARTESIAN_POINT('Ctrl Pts',(-31.1860612050356,-57.4588942553394,
15.0724048212587));
#28056=CARTESIAN_POINT('Ctrl Pts',(-30.9676695988057,-56.9525123919175,
15.1094507847814));
#28057=CARTESIAN_POINT('Ctrl Pts',(-30.7492779925757,-56.4461305284957,
15.1464967483041));
#28058=CARTESIAN_POINT('Ctrl Pts',(-30.8067261634667,-55.8207849015799,
15.1835427118268));
#28059=CARTESIAN_POINT('Ctrl Pts',(-31.1137226321993,-55.3626684826674,
15.2205886753495));
#28060=CARTESIAN_POINT('Ctrl Pts',(-31.2543008673673,-55.1528901815095,
15.2375525713631));
#28061=CARTESIAN_POINT('Ctrl Pts',(-31.4472058843405,-54.9781775023347,
15.2545164673766));
#28062=CARTESIAN_POINT('Ctrl Pts',(-31.6679812524744,-54.8513129979877,
15.2714803633902));
#28063=CARTESIAN_POINT('Origin',(-32.5,-56.2916512459885,17.));
#28064=CARTESIAN_POINT('',(-31.668393257303,-54.8482192502339,15.9714803633902));
#28065=CARTESIAN_POINT('',(-31.6656122060936,-54.8464626161313,15.7785196366098));
#28066=CARTESIAN_POINT('',(-31.667,-54.8488529232836,17.));
#28067=CARTESIAN_POINT('Ctrl Pts',(-31.6656122129471,-54.8464626279357,
15.7785196366098));
#28068=CARTESIAN_POINT('Ctrl Pts',(-31.187699049881,-55.1223478631842,15.7414495489509));
#28069=CARTESIAN_POINT('Ctrl Pts',(-30.860252864304,-55.6587877650758,15.7043794612919));
#28070=CARTESIAN_POINT('Ctrl Pts',(-30.8332370510141,-56.2099535888295,
15.667309373633));
#28071=CARTESIAN_POINT('Ctrl Pts',(-30.8062388188308,-56.7607607298753,
15.6302634101103));
#28072=CARTESIAN_POINT('Ctrl Pts',(-31.0792800051602,-57.3262745318078,
15.5932174465876));
#28073=CARTESIAN_POINT('Ctrl Pts',(-31.5274017633056,-57.6476843966343,
15.556171483065));
#28074=CARTESIAN_POINT('Ctrl Pts',(-31.9755235214509,-57.9690942614608,
15.5191255195423));
#28075=CARTESIAN_POINT('Ctrl Pts',(-32.5987258514122,-58.0464001891811,
15.4820795560196));
#28076=CARTESIAN_POINT('Ctrl Pts',(-33.1117966721332,-57.8442226833339,
15.4450335924969));
#28077=CARTESIAN_POINT('Ctrl Pts',(-33.6248674928541,-57.6420451774866,
15.4079876289742));
#28078=CARTESIAN_POINT('Ctrl Pts',(-34.0278068043346,-57.1603842380717,
15.3709416654516));
#28079=CARTESIAN_POINT('Ctrl Pts',(-34.1362071477596,-56.6196747257878,
15.3338957019289));
#28080=CARTESIAN_POINT('Ctrl Pts',(-34.2446074911845,-56.0789652135039,
15.2968497384062));
#28081=CARTESIAN_POINT('Ctrl Pts',(-34.0584688665537,-55.479207128351,15.2598037748835));
#28082=CARTESIAN_POINT('Ctrl Pts',(-33.6629786670949,-55.0948831577141,
15.2227578113608));
#28083=CARTESIAN_POINT('Ctrl Pts',(-33.267488467636,-54.7105591870771,15.1857118478381));
#28084=CARTESIAN_POINT('Ctrl Pts',(-32.662646693349,-54.5416693309562,15.1486658843155));
#28085=CARTESIAN_POINT('Ctrl Pts',(-32.1252626195522,-54.6655069919667,
15.1116199207928));
#28086=CARTESIAN_POINT('Ctrl Pts',(-31.9652131038814,-54.7023896586347,
15.1005864927318));
#28087=CARTESIAN_POINT('Ctrl Pts',(-31.8111473001585,-54.7652381843378,
15.0895530646708));
#28088=CARTESIAN_POINT('Ctrl Pts',(-31.6687468960362,-54.8490160493388,
15.0785196366098));
#28089=CARTESIAN_POINT('Ctrl Pts',(-31.6679812524744,-54.8513129979877,
15.2714803633902));
#28090=CARTESIAN_POINT('Ctrl Pts',(-31.9293378325702,-54.7011292466392,
15.2915624308993));
#28091=CARTESIAN_POINT('Ctrl Pts',(-32.2297522401559,-54.6180004723649,
15.3116444984084));
#28092=CARTESIAN_POINT('Ctrl Pts',(-32.5286510627353,-54.6231330317608,
15.3317265659175));
#28093=CARTESIAN_POINT('Ctrl Pts',(-33.0800382579646,-54.6326012106758,
15.3687725294402));
#28094=CARTESIAN_POINT('Ctrl Pts',(-33.626267881849,-54.9424247794149,15.4058184929629));
#28095=CARTESIAN_POINT('Ctrl Pts',(-33.9173548501551,-55.4108112247729,
15.4428644564855));
#28096=CARTESIAN_POINT('Ctrl Pts',(-34.2084418184611,-55.8791976701309,
15.4799104200082));
#28097=CARTESIAN_POINT('Ctrl Pts',(-34.2443861311887,-56.5061469921078,
15.5169563835309));
#28098=CARTESIAN_POINT('Ctrl Pts',(-34.0087376695652,-57.0047322785327,
15.5540023470536));
#28099=CARTESIAN_POINT('Ctrl Pts',(-33.7730892079418,-57.5033175649576,
15.5910483105763));
#28100=CARTESIAN_POINT('Ctrl Pts',(-33.2658479719674,-57.8735388158304,
15.628094274099));
#28101=CARTESIAN_POINT('Ctrl Pts',(-32.7191557896563,-57.9459621763539,
15.6651402376216));
#28102=CARTESIAN_POINT('Ctrl Pts',(-32.1724636073452,-58.0183855368774,
15.7021862011443));
#28103=CARTESIAN_POINT('Ctrl Pts',(-31.5863204786975,-57.7930110070515,
15.739232164667));
#28104=CARTESIAN_POINT('Ctrl Pts',(-31.2289781301378,-57.3729825184307,
15.7762781281897));
#28105=CARTESIAN_POINT('Ctrl Pts',(-30.8716357815781,-56.9529540298098,
15.8133240917123));
#28106=CARTESIAN_POINT('Ctrl Pts',(-30.7430942131064,-56.3382715823939,
15.850370055235));
#28107=CARTESIAN_POINT('Ctrl Pts',(-30.9021812024434,-55.8102480837199,
15.8874160187577));
#28108=CARTESIAN_POINT('Ctrl Pts',(-31.022514091882,-55.4108527997199,15.9154374669685));
#28109=CARTESIAN_POINT('Ctrl Pts',(-31.3074096675184,-55.0610382301548,
15.9434589151794));
#28110=CARTESIAN_POINT('Ctrl Pts',(-31.668393257303,-54.8482192502339,15.9714803633902));
#28111=CARTESIAN_POINT('Origin',(-32.5,-56.2916512459885,17.));
#28112=CARTESIAN_POINT('',(-31.6652521719754,-54.8469263020217,16.6714803633902));
#28113=CARTESIAN_POINT('',(-31.6662812667712,-54.8504621893828,16.4785196366098));
#28114=CARTESIAN_POINT('',(-31.667,-54.8488529232836,17.));
#28115=CARTESIAN_POINT('Ctrl Pts',(-31.6662812667712,-54.8504621893828,
16.4785196366098));
#28116=CARTESIAN_POINT('Ctrl Pts',(-31.5218969898699,-54.9322586741207,
16.4674379602763));
#28117=CARTESIAN_POINT('Ctrl Pts',(-31.3899082837209,-55.0347971411717,
16.4563562839428));
#28118=CARTESIAN_POINT('Ctrl Pts',(-31.2776094808925,-55.1556342327712,
16.4452746076093));
#28119=CARTESIAN_POINT('Ctrl Pts',(-30.9021953983998,-55.5595917526322,
16.4082286440866));
#28120=CARTESIAN_POINT('Ctrl Pts',(-30.7468278084228,-56.1680473893291,
16.3711826805639));
#28121=CARTESIAN_POINT('Ctrl Pts',(-30.8826115695051,-56.7025379705484,
16.3341367170412));
#28122=CARTESIAN_POINT('Ctrl Pts',(-31.0183953305873,-57.2370285517677,
16.2970907535186));
#28123=CARTESIAN_POINT('Ctrl Pts',(-31.4453304427287,-57.6975540775093,
16.2600447899959));
#28124=CARTESIAN_POINT('Ctrl Pts',(-31.9680276309783,-57.8733524295625,
16.2229988264732));
#28125=CARTESIAN_POINT('Ctrl Pts',(-32.490724819228,-58.0491507816157,16.1859528629505));
#28126=CARTESIAN_POINT('Ctrl Pts',(-33.109184083586,-57.9402219599804,16.1489068994278));
#28127=CARTESIAN_POINT('Ctrl Pts',(-33.5403640348016,-57.596417857542,16.1118609359052));
#28128=CARTESIAN_POINT('Ctrl Pts',(-33.9715439860171,-57.2526137551037,
16.0748149723825));
#28129=CARTESIAN_POINT('Ctrl Pts',(-34.2154446240901,-56.6739343718623,
16.0377690088598));
#28130=CARTESIAN_POINT('Ctrl Pts',(-34.1604434390255,-56.1252156089025,
16.0007230453371));
#28131=CARTESIAN_POINT('Ctrl Pts',(-34.1054422539609,-55.5764968459426,
15.9636770818144));
#28132=CARTESIAN_POINT('Ctrl Pts',(-33.7515392457587,-55.0577387032643,
15.9266311182918));
#28133=CARTESIAN_POINT('Ctrl Pts',(-33.2607001328297,-54.8063537864051,
15.8895851547691));
#28134=CARTESIAN_POINT('Ctrl Pts',(-32.7701806517449,-54.5551325700793,
15.8525633153826));
#28135=CARTESIAN_POINT('Ctrl Pts',(-32.1429033520047,-54.5709364688817,
15.8155414759962));
#28136=CARTESIAN_POINT('Ctrl Pts',(-31.6656122129471,-54.8464626279357,
15.7785196366098));
#28137=CARTESIAN_POINT('Ctrl Pts',(-31.668393257303,-54.8482192502339,15.9714803633902));
#28138=CARTESIAN_POINT('Ctrl Pts',(-31.7846507008451,-54.7796793186608,
15.9805048787021));
#28139=CARTESIAN_POINT('Ctrl Pts',(-31.9088000679097,-54.7253487041335,
15.9895293940139));
#28140=CARTESIAN_POINT('Ctrl Pts',(-32.0378859406647,-54.688147422912,15.9985539093258));
#28141=CARTESIAN_POINT('Ctrl Pts',(-32.5677881424037,-54.5354348107102,
16.0355998728484));
#28142=CARTESIAN_POINT('Ctrl Pts',(-33.180876998736,-54.6713741362387,16.0726458363711));
#28143=CARTESIAN_POINT('Ctrl Pts',(-33.5965689181183,-55.0337519963386,
16.1096917998938));
#28144=CARTESIAN_POINT('Ctrl Pts',(-34.0122608375006,-55.3961298564385,
16.1467377634165));
#28145=CARTESIAN_POINT('Ctrl Pts',(-34.2305558199328,-55.9849462511098,
16.1837837269391));
#28146=CARTESIAN_POINT('Ctrl Pts',(-34.1515499288845,-56.5307260185163,
16.2208296904618));
#28147=CARTESIAN_POINT('Ctrl Pts',(-34.0725440378362,-57.0765057859228,
16.2578756539845));
#28148=CARTESIAN_POINT('Ctrl Pts',(-33.6962372733073,-57.5792489260645,
16.2949216175072));
#28149=CARTESIAN_POINT('Ctrl Pts',(-33.1948485598908,-57.8088721901075,
16.3319675810299));
#28150=CARTESIAN_POINT('Ctrl Pts',(-32.6934598464744,-58.0384954541505,
16.3690135445526));
#28151=CARTESIAN_POINT('Ctrl Pts',(-32.0669891841703,-57.9949988420949,
16.4060595080752));
#28152=CARTESIAN_POINT('Ctrl Pts',(-31.6021444239114,-57.6982888250906,
16.4431054715979));
#28153=CARTESIAN_POINT('Ctrl Pts',(-31.1372996636525,-57.4015788080863,
16.4801514351206));
#28154=CARTESIAN_POINT('Ctrl Pts',(-30.8340808054389,-56.8516553861334,
16.5171973986433));
#28155=CARTESIAN_POINT('Ctrl Pts',(-30.8312576791002,-56.3001941315665,
16.554243362166));
#28156=CARTESIAN_POINT('Ctrl Pts',(-30.8284345527615,-55.7487328769995,
16.5912893256886));
#28157=CARTESIAN_POINT('Ctrl Pts',(-31.1260071582979,-55.1957337898185,
16.6283352892113));
#28158=CARTESIAN_POINT('Ctrl Pts',(-31.5877897054339,-54.8942800379899,
16.665381252734));
#28159=CARTESIAN_POINT('Ctrl Pts',(-31.6131317633018,-54.8777366270908,
16.6674142896194));
#28160=CARTESIAN_POINT('Ctrl Pts',(-31.6389683688547,-54.8619507900759,
16.6694473265048));
#28161=CARTESIAN_POINT('Ctrl Pts',(-31.6652521719754,-54.8469263020217,
16.6714803633902));
#28162=CARTESIAN_POINT('Origin',(-32.5,-56.2916512459885,17.));
#28163=CARTESIAN_POINT('',(-31.6668674827448,-54.8509763286063,17.3714803633902));
#28164=CARTESIAN_POINT('',(-31.6688688935778,-54.8504049148725,17.1785196366098));
#28165=CARTESIAN_POINT('',(-31.667,-54.8488529232836,17.));
#28166=CARTESIAN_POINT('Ctrl Pts',(-31.6688688935778,-54.8504049148725,
17.1785196366098));
#28167=CARTESIAN_POINT('Ctrl Pts',(-31.3819874737692,-55.0177923404707,
17.156380408079));
#28168=CARTESIAN_POINT('Ctrl Pts',(-31.1417740021657,-55.2676351144426,
17.1342411795483));
#28169=CARTESIAN_POINT('Ctrl Pts',(-30.9981174968785,-55.5642433945469,
17.1121019510175));
#28170=CARTESIAN_POINT('Ctrl Pts',(-30.7577345202416,-56.0605632870855,
17.0750559874949));
#28171=CARTESIAN_POINT('Ctrl Pts',(-30.7877102970592,-56.6878262324662,
17.0380100239722));
#28172=CARTESIAN_POINT('Ctrl Pts',(-31.0743262430964,-57.1589617869126,
17.0009640604495));
#28173=CARTESIAN_POINT('Ctrl Pts',(-31.3609421891337,-57.630097341359,16.9639180969268));
#28174=CARTESIAN_POINT('Ctrl Pts',(-31.9041983043906,-57.9451055048711,
16.9268721334041));
#28175=CARTESIAN_POINT('Ctrl Pts',(-32.4554703472483,-57.9598210051999,
16.8898261698815));
#28176=CARTESIAN_POINT('Ctrl Pts',(-33.006742390106,-57.9745365055287,16.8527802063588));
#28177=CARTESIAN_POINT('Ctrl Pts',(-33.5660303605644,-57.6889593426742,
16.8157342428361));
#28178=CARTESIAN_POINT('Ctrl Pts',(-33.8773729475645,-57.2337855245493,
16.7786882793134));
#28179=CARTESIAN_POINT('Ctrl Pts',(-34.1887155345647,-56.7786117064244,
16.7416423157907));
#28180=CARTESIAN_POINT('Ctrl Pts',(-34.2521127381066,-56.1538412330292,
16.704596352268));
#28181=CARTESIAN_POINT('Ctrl Pts',(-34.0385504685031,-55.6454038542025,
16.6675503887454));
#28182=CARTESIAN_POINT('Ctrl Pts',(-33.8249881988997,-55.1369664753759,
16.6305044252227));
#28183=CARTESIAN_POINT('Ctrl Pts',(-33.3344664561509,-54.7448621911179,
16.5934584617));
#28184=CARTESIAN_POINT('Ctrl Pts',(-32.7914752972722,-54.6485397505015,
16.5564124981773));
#28185=CARTESIAN_POINT('Ctrl Pts',(-32.4109108025283,-54.5810305464448,
16.5304482109881));
#28186=CARTESIAN_POINT('Ctrl Pts',(-32.0045725792269,-54.658813619538,16.504483923799));
#28187=CARTESIAN_POINT('Ctrl Pts',(-31.6662812667712,-54.8504621893828,
16.4785196366098));
#28188=CARTESIAN_POINT('Ctrl Pts',(-31.6652521719754,-54.8469263020217,
16.6714803633902));
#28189=CARTESIAN_POINT('Ctrl Pts',(-32.1179113819592,-54.5881748244737,
16.7064932900275));
#28190=CARTESIAN_POINT('Ctrl Pts',(-32.7032079137753,-54.5552369344614,
16.7415062166648));
#28191=CARTESIAN_POINT('Ctrl Pts',(-33.1792781595522,-54.7673956583618,
16.776519143302));
#28192=CARTESIAN_POINT('Ctrl Pts',(-33.6829915777989,-54.9918734470383,
16.8135651068247));
#28193=CARTESIAN_POINT('Ctrl Pts',(-34.0644259255566,-55.4907374408677,
16.8506110703474));
#28194=CARTESIAN_POINT('Ctrl Pts',(-34.1490156106942,-56.0356797043225,
16.8876570338701));
#28195=CARTESIAN_POINT('Ctrl Pts',(-34.2336052958317,-56.5806219677773,
16.9247029973928));
#28196=CARTESIAN_POINT('Ctrl Pts',(-34.0213503183491,-57.1716425008576,
16.9617489609154));
#28197=CARTESIAN_POINT('Ctrl Pts',(-33.6093903722588,-57.5382574052848,
16.9987949244381));
#28198=CARTESIAN_POINT('Ctrl Pts',(-33.1974304261685,-57.904872309712,17.0358408879608));
#28199=CARTESIAN_POINT('Ctrl Pts',(-32.5857655114706,-58.0470815854862,
17.0728868514835));
#28200=CARTESIAN_POINT('Ctrl Pts',(-32.0543275447525,-57.8998023511678,
17.1099328150062));
#28201=CARTESIAN_POINT('Ctrl Pts',(-31.5228895780343,-57.7525231168495,
17.1469787785289));
#28202=CARTESIAN_POINT('Ctrl Pts',(-31.071678559296,-57.3157553724386,17.1840247420515));
#28203=CARTESIAN_POINT('Ctrl Pts',(-30.9071937698036,-56.7893883528063,
17.2210707055742));
#28204=CARTESIAN_POINT('Ctrl Pts',(-30.7427089803112,-56.2630213331741,
17.2581166690969));
#28205=CARTESIAN_POINT('Ctrl Pts',(-30.8649504200647,-55.6470550383205,
17.2951626326196));
#28206=CARTESIAN_POINT('Ctrl Pts',(-31.2179736010048,-55.2233899358517,
17.3322085961423));
#28207=CARTESIAN_POINT('Ctrl Pts',(-31.3427181334424,-55.073683321751,17.3452991852249));
#28208=CARTESIAN_POINT('Ctrl Pts',(-31.4962789539492,-54.9479881676876,
17.3583897743076));
#28209=CARTESIAN_POINT('Ctrl Pts',(-31.6668674827448,-54.8509763286063,
17.3714803633902));
#28210=CARTESIAN_POINT('Origin',(-32.5,-56.2916512459885,17.));
#28211=CARTESIAN_POINT('',(-31.6688993943412,-54.8497298728322,18.0714803633902));
#28212=CARTESIAN_POINT('',(-31.6668239490615,-54.8465985185331,17.8785196366098));
#28213=CARTESIAN_POINT('',(-31.667,-54.8488529232836,17.));
#28214=CARTESIAN_POINT('Ctrl Pts',(-31.6668239490615,-54.8465985185331,
17.8785196366098));
#28215=CARTESIAN_POINT('Ctrl Pts',(-31.2400871420202,-55.0969461017405,
17.8453228558818));
#28216=CARTESIAN_POINT('Ctrl Pts',(-30.9262488413014,-55.5484932725245,
17.8121260751538));
#28217=CARTESIAN_POINT('Ctrl Pts',(-30.8508004340577,-56.036868932597,17.7789292944258));
#28218=CARTESIAN_POINT('Ctrl Pts',(-30.7666037474724,-56.5818719868586,
17.7418833309031));
#28219=CARTESIAN_POINT('Ctrl Pts',(-30.9792848378898,-57.1727392338966,
17.7048373673804));
#28220=CARTESIAN_POINT('Ctrl Pts',(-31.3915089982965,-57.539056927659,17.6677914038577));
#28221=CARTESIAN_POINT('Ctrl Pts',(-31.8037331587031,-57.9053746214214,
17.6307454403351));
#28222=CARTESIAN_POINT('Ctrl Pts',(-32.4155003890991,-58.0471427619081,
17.5936994768124));
#28223=CARTESIAN_POINT('Ctrl Pts',(-32.9468319475375,-57.8994803557453,
17.5566535132897));
#28224=CARTESIAN_POINT('Ctrl Pts',(-33.4781635059759,-57.7518179495826,
17.519607549767));
#28225=CARTESIAN_POINT('Ctrl Pts',(-33.9290593924568,-57.3147249967705,
17.4825615862443));
#28226=CARTESIAN_POINT('Ctrl Pts',(-34.0931645477786,-56.788239565649,17.4455156227217));
#28227=CARTESIAN_POINT('Ctrl Pts',(-34.2572697031003,-56.2617541345275,
17.408469659199));
#28228=CARTESIAN_POINT('Ctrl Pts',(-34.134584127263,-55.6458762250967,17.3714236956763));
#28229=CARTESIAN_POINT('Ctrl Pts',(-33.7812555697231,-55.2224658548728,
17.3343777321536));
#28230=CARTESIAN_POINT('Ctrl Pts',(-33.4279270121832,-54.7990554846489,
17.2973317686309));
#28231=CARTESIAN_POINT('Ctrl Pts',(-32.8439554729406,-54.568112653632,17.2602858051083));
#28232=CARTESIAN_POINT('Ctrl Pts',(-32.2965988382737,-54.6353296579719,
17.2232398415856));
#28233=CARTESIAN_POINT('Ctrl Pts',(-32.0763508133016,-54.6623767631182,
17.2083331065936));
#28234=CARTESIAN_POINT('Ctrl Pts',(-31.8620312385645,-54.7376999942423,
17.1934263716017));
#28235=CARTESIAN_POINT('Ctrl Pts',(-31.6688688935778,-54.8504049148725,
17.1785196366098));
#28236=CARTESIAN_POINT('Ctrl Pts',(-31.6668674827448,-54.8509763286063,
17.3714803633902));
#28237=CARTESIAN_POINT('Ctrl Pts',(-31.9790392312177,-54.6734476539504,
17.3954357378302));
#28238=CARTESIAN_POINT('Ctrl Pts',(-32.3482331506335,-54.5919732963168,
17.4193911122703));
#28239=CARTESIAN_POINT('Ctrl Pts',(-32.7022067343745,-54.6351832109726,
17.4433464867103));
#28240=CARTESIAN_POINT('Ctrl Pts',(-33.2496117646775,-54.702005498646,17.480392450233));
#28241=CARTESIAN_POINT('Ctrl Pts',(-33.7606169031567,-55.0670139840768,
17.5174384137557));
#28242=CARTESIAN_POINT('Ctrl Pts',(-34.001357750591,-55.5631604641687,17.5544843772783));
#28243=CARTESIAN_POINT('Ctrl Pts',(-34.2420985980252,-56.0593069442606,
17.591530340801));
#28244=CARTESIAN_POINT('Ctrl Pts',(-34.2125751544145,-56.6865914190135,
17.6285763043237));
#28245=CARTESIAN_POINT('Ctrl Pts',(-33.9262989911366,-57.1579335916119,
17.6656222678464));
#28246=CARTESIAN_POINT('Ctrl Pts',(-33.6400228278587,-57.6292757642103,
17.7026682313691));
#28247=CARTESIAN_POINT('Ctrl Pts',(-33.0969939449135,-57.9446756346541,
17.7397141948917));
#28248=CARTESIAN_POINT('Ctrl Pts',(-32.5457325897642,-57.959788663796,17.7767601584144));
#28249=CARTESIAN_POINT('Ctrl Pts',(-31.9944712346149,-57.9749016929378,
17.8138061219371));
#28250=CARTESIAN_POINT('Ctrl Pts',(-31.4349774072614,-57.6897278807776,
17.8508520854598));
#28251=CARTESIAN_POINT('Ctrl Pts',(-31.1233066303378,-57.2347786394959,
17.8878980489825));
#28252=CARTESIAN_POINT('Ctrl Pts',(-30.8116358534142,-56.7798293982142,
17.9249440125051));
#28253=CARTESIAN_POINT('Ctrl Pts',(-30.7477881269207,-56.1551047278111,
17.9619899760278));
#28254=CARTESIAN_POINT('Ctrl Pts',(-30.960983724928,-55.6465134161264,17.9990359395505));
#28255=CARTESIAN_POINT('Ctrl Pts',(-31.0999537214239,-55.3149918769235,
18.0231840808304));
#28256=CARTESIAN_POINT('Ctrl Pts',(-31.3566391271215,-55.0328152763439,
18.0473322221103));
#28257=CARTESIAN_POINT('Ctrl Pts',(-31.6688993943412,-54.8497298728322,
18.0714803633902));
#28258=CARTESIAN_POINT('Origin',(-32.5,-56.2916512459885,17.));
#28259=CARTESIAN_POINT('',(-31.6661431441559,-54.8463676572785,18.7714803633902));
#28260=CARTESIAN_POINT('',(-31.6653993953823,-54.8489980951737,18.5785196366098));
#28261=CARTESIAN_POINT('',(-31.667,-54.8488529232836,17.));
#28262=CARTESIAN_POINT('Ctrl Pts',(-31.6653993953823,-54.8489980951737,
18.5785196366098));
#28263=CARTESIAN_POINT('Ctrl Pts',(-31.5716723835923,-54.901972129835,18.5713112672072));
#28264=CARTESIAN_POINT('Ctrl Pts',(-31.4833584827506,-54.9639737793168,
18.5641028978046));
#28265=CARTESIAN_POINT('Ctrl Pts',(-31.4025244101713,-55.0345432294477,
18.5568945284021));
#28266=CARTESIAN_POINT('Ctrl Pts',(-30.987093965791,-55.3972207129895,18.5198485648794));
#28267=CARTESIAN_POINT('Ctrl Pts',(-30.7692236712863,-55.9861942986586,
18.4828026013567));
#28268=CARTESIAN_POINT('Ctrl Pts',(-30.8486231023463,-56.5319168852662,
18.445756637834));
#28269=CARTESIAN_POINT('Ctrl Pts',(-30.9280225334064,-57.0776394718738,
18.4087106743114));
#28270=CARTESIAN_POINT('Ctrl Pts',(-31.3046916900312,-57.5801110594199,
18.3716647107887));
#28271=CARTESIAN_POINT('Ctrl Pts',(-31.8062457968319,-57.8093726766562,
18.334618747266));
#28272=CARTESIAN_POINT('Ctrl Pts',(-32.3077999036325,-58.0386342938926,
18.2975727837433));
#28273=CARTESIAN_POINT('Ctrl Pts',(-32.9342389606089,-57.9946859408192,
18.2605268202206));
#28274=CARTESIAN_POINT('Ctrl Pts',(-33.3988695811849,-57.6976408304243,
18.223480856698));
#28275=CARTESIAN_POINT('Ctrl Pts',(-33.8635002017609,-57.4005957200295,
18.1864348931753));
#28276=CARTESIAN_POINT('Ctrl Pts',(-34.1663223859365,-56.850453852313,18.1493889296526));
#28277=CARTESIAN_POINT('Ctrl Pts',(-34.1687478440051,-56.298990772552,18.1123429661299));
#28278=CARTESIAN_POINT('Ctrl Pts',(-34.1711733020737,-55.747527692791,18.0752970026072));
#28279=CARTESIAN_POINT('Ctrl Pts',(-33.8732020340353,-55.1947434009853,
18.0382510390845));
#28280=CARTESIAN_POINT('Ctrl Pts',(-33.4112022803197,-54.8936227627801,
18.0012050755619));
#28281=CARTESIAN_POINT('Ctrl Pts',(-32.9492025266041,-54.5925021245749,
17.9641591120392));
#28282=CARTESIAN_POINT('Ctrl Pts',(-32.3231742872114,-54.5430451399701,
17.9271131485165));
#28283=CARTESIAN_POINT('Ctrl Pts',(-31.8196229357211,-54.7678860784103,
17.8900671849938));
#28284=CARTESIAN_POINT('Ctrl Pts',(-31.7673024933817,-54.791247702444,17.8862180021991));
#28285=CARTESIAN_POINT('Ctrl Pts',(-31.7163042884046,-54.8175705950767,
17.8823688194045));
#28286=CARTESIAN_POINT('Ctrl Pts',(-31.6668239490615,-54.8465985185331,
17.8785196366098));
#28287=CARTESIAN_POINT('Ctrl Pts',(-31.6688993943412,-54.8497298728322,
18.0714803633902));
#28288=CARTESIAN_POINT('Ctrl Pts',(-31.8356814821797,-54.751941684401,18.084378185633));
#28289=CARTESIAN_POINT('Ctrl Pts',(-32.0183177486645,-54.6824218442403,
18.0972760078758));
#28290=CARTESIAN_POINT('Ctrl Pts',(-32.2073398697232,-54.6487501647903,
18.1101738301185));
#28291=CARTESIAN_POINT('Ctrl Pts',(-32.7502614940028,-54.5520361781053,
18.1472197936412));
#28292=CARTESIAN_POINT('Ctrl Pts',(-33.3458658200538,-54.7510661577016,
18.1842657571639));
#28293=CARTESIAN_POINT('Ctrl Pts',(-33.7215711507525,-55.1547529048404,
18.2213117206866));
#28294=CARTESIAN_POINT('Ctrl Pts',(-34.0972764814512,-55.5584396519791,
18.2583576842093));
#28295=CARTESIAN_POINT('Ctrl Pts',(-34.2530828167976,-56.1667831666603,
18.2954036477319));
#28296=CARTESIAN_POINT('Ctrl Pts',(-34.1176845039388,-56.7013715898475,
18.3324496112546));
#28297=CARTESIAN_POINT('Ctrl Pts',(-33.98228619108,-57.2359600130347,18.3694955747773));
#28298=CARTESIAN_POINT('Ctrl Pts',(-33.5556832300161,-57.696793344728,18.4065415383));
#28299=CARTESIAN_POINT('Ctrl Pts',(-33.0331128848803,-57.8729685975756,
18.4435875018227));
#28300=CARTESIAN_POINT('Ctrl Pts',(-32.5105425397446,-58.0491438504232,
18.4806334653454));
#28301=CARTESIAN_POINT('Ctrl Pts',(-31.892004810537,-57.9406610244251,18.517679428868));
#28302=CARTESIAN_POINT('Ctrl Pts',(-31.4605769963787,-57.5971679000379,
18.5547253923907));
#28303=CARTESIAN_POINT('Ctrl Pts',(-31.0291491822204,-57.2536747756508,
18.5917713559134));
#28304=CARTESIAN_POINT('Ctrl Pts',(-30.7848312831114,-56.6751713528747,
18.6288173194361));
#28305=CARTESIAN_POINT('Ctrl Pts',(-30.839436770952,-56.1264130034822,18.6658632829588));
#28306=CARTESIAN_POINT('Ctrl Pts',(-30.89132971378,-55.6049143999997,18.7010689764359));
#28307=CARTESIAN_POINT('Ctrl Pts',(-31.2131854490112,-55.1102790779514,
18.7362746699131));
#28308=CARTESIAN_POINT('Ctrl Pts',(-31.6661431441559,-54.8463676572785,
18.7714803633902));
#28309=CARTESIAN_POINT('Origin',(-32.5,-56.2916512459885,17.));
#28310=CARTESIAN_POINT('',(-31.6657991298123,-54.8498167632728,19.4714803633902));
#28311=CARTESIAN_POINT('',(-31.6682947036337,-54.8512220664372,19.2785196366098));
#28312=CARTESIAN_POINT('',(-31.667,-54.8488529232836,17.));
#28313=CARTESIAN_POINT('Ctrl Pts',(-31.6682947036337,-54.8512220664372,
19.2785196366098));
#28314=CARTESIAN_POINT('Ctrl Pts',(-31.4307799124075,-54.9882439463791,
19.26025371501));
#28315=CARTESIAN_POINT('Ctrl Pts',(-31.2253675580441,-55.1807871169989,
19.2419877934101));
#28316=CARTESIAN_POINT('Ctrl Pts',(-31.0820105037967,-55.4118336375308,
19.2237218718103));
#28317=CARTESIAN_POINT('Ctrl Pts',(-30.7912614072705,-55.8804298112795,
19.1866759082876));
#28318=CARTESIAN_POINT('Ctrl Pts',(-30.7557692111823,-56.5074048138577,
19.149629944765));
#28319=CARTESIAN_POINT('Ctrl Pts',(-30.9917771203569,-57.0058199801505,
19.1125839812423));
#28320=CARTESIAN_POINT('Ctrl Pts',(-31.2277850295315,-57.5042351464432,
19.0755380177196));
#28321=CARTESIAN_POINT('Ctrl Pts',(-31.735293043969,-57.8740904764506,19.0384920541969));
#28322=CARTESIAN_POINT('Ctrl Pts',(-32.2820372430805,-57.9461195811699,
19.0014460906742));
#28323=CARTESIAN_POINT('Ctrl Pts',(-32.828781442192,-58.0181486858891,18.9644001271516));
#28324=CARTESIAN_POINT('Ctrl Pts',(-33.4147618259776,-57.7923515653202,
18.9273541636289));
#28325=CARTESIAN_POINT('Ctrl Pts',(-33.7718011490707,-57.3720655520494,
18.8903082001062));
#28326=CARTESIAN_POINT('Ctrl Pts',(-34.1288404721637,-56.9517795387787,
18.8532622365835));
#28327=CARTESIAN_POINT('Ctrl Pts',(-34.2569387345642,-56.3370046328062,
18.8162162730608));
#28328=CARTESIAN_POINT('Ctrl Pts',(-34.0974710401143,-55.8090960558605,
18.7791703095382));
#28329=CARTESIAN_POINT('Ctrl Pts',(-33.9380033456643,-55.2811874789147,
18.7421243460155));
#28330=CARTESIAN_POINT('Ctrl Pts',(-33.4909696943638,-54.8401452309956,
18.7050783824928));
#28331=CARTESIAN_POINT('Ctrl Pts',(-32.9609575715857,-54.6878147977434,
18.6680324189701));
#28332=CARTESIAN_POINT('Ctrl Pts',(-32.5340747186532,-54.565124679649,18.63819482485));
#28333=CARTESIAN_POINT('Ctrl Pts',(-32.0533634937382,-54.6297227421977,
18.6083572307299));
#28334=CARTESIAN_POINT('Ctrl Pts',(-31.6653993953823,-54.8489980951737,
18.5785196366098));
#28335=CARTESIAN_POINT('Ctrl Pts',(-31.6661431441559,-54.8463676572785,
18.7714803633902));
#28336=CARTESIAN_POINT('Ctrl Pts',(-31.6898201235287,-54.832572494219,18.7733206334357));
#28337=CARTESIAN_POINT('Ctrl Pts',(-31.7138553201483,-54.819407751031,18.7751609034813));
#28338=CARTESIAN_POINT('Ctrl Pts',(-31.7382289011374,-54.8069025442232,
18.7770011735268));
#28339=CARTESIAN_POINT('Ctrl Pts',(-32.2288866686916,-54.5551637103656,
18.8140471370495));
#28340=CARTESIAN_POINT('Ctrl Pts',(-32.8566733290096,-54.5706993186593,
18.8510931005722));
#28341=CARTESIAN_POINT('Ctrl Pts',(-33.3342787571905,-54.8463994098822,
18.8881390640948));
#28342=CARTESIAN_POINT('Ctrl Pts',(-33.8118841853713,-55.1220995011052,
18.9251850276175));
#28343=CARTESIAN_POINT('Ctrl Pts',(-34.1393083814151,-55.6579640752576,
18.9622309911402));
#28344=CARTESIAN_POINT('Ctrl Pts',(-34.1667038054087,-56.2087516714065,
18.9992769546629));
#28345=CARTESIAN_POINT('Ctrl Pts',(-34.1940992294022,-56.7595392675554,
19.0363229181855));
#28346=CARTESIAN_POINT('Ctrl Pts',(-33.9214658813456,-57.3252498857009,
19.0733688817082));
#28347=CARTESIAN_POINT('Ctrl Pts',(-33.4735759588574,-57.6469828536776,
19.1104148452309));
#28348=CARTESIAN_POINT('Ctrl Pts',(-33.0256860363693,-57.9687158216544,
19.1474608087536));
#28349=CARTESIAN_POINT('Ctrl Pts',(-32.4025395394495,-58.0464711394622,
19.1845067722763));
#28350=CARTESIAN_POINT('Ctrl Pts',(-31.889322996006,-57.8446636449513,19.221552735799));
#28351=CARTESIAN_POINT('Ctrl Pts',(-31.3761064525625,-57.6428561504404,
19.2585986993216));
#28352=CARTESIAN_POINT('Ctrl Pts',(-30.9728198625952,-57.1614858436107,
19.2956446628443));
#28353=CARTESIAN_POINT('Ctrl Pts',(-30.86402962057,-56.6208545750433,19.332690626367));
#28354=CARTESIAN_POINT('Ctrl Pts',(-30.7552393785448,-56.0802233064759,
19.3697365898897));
#28355=CARTESIAN_POINT('Ctrl Pts',(-30.9409454844617,-55.4803310761708,
19.4067825534124));
#28356=CARTESIAN_POINT('Ctrl Pts',(-31.3361584863693,-55.0957219647369,
19.443828516935));
#28357=CARTESIAN_POINT('Ctrl Pts',(-31.4344901101744,-55.000028659418,19.4530457990868));
#28358=CARTESIAN_POINT('Ctrl Pts',(-31.5457912060088,-54.917662401762,19.4622630812385));
#28359=CARTESIAN_POINT('Ctrl Pts',(-31.6657991298123,-54.8498167632728,
19.4714803633902));
#28360=CARTESIAN_POINT('Origin',(-32.5,-56.2916512459885,17.));
#28361=CARTESIAN_POINT('',(-31.6686691446489,-54.8508917236136,20.1714803633902));
#28362=CARTESIAN_POINT('',(-31.6680707239276,-54.8477242132621,19.9785196366098));
#28363=CARTESIAN_POINT('',(-31.667,-54.8488529232836,17.));
#28364=CARTESIAN_POINT('Ctrl Pts',(-31.6680707239276,-54.8477242132621,
19.9785196366098));
#28365=CARTESIAN_POINT('Ctrl Pts',(-31.2906837721071,-55.0702773030723,
19.9491961628127));
#28366=CARTESIAN_POINT('Ctrl Pts',(-30.9974844080692,-55.4444429123815,
19.9198726890156));
#28367=CARTESIAN_POINT('Ctrl Pts',(-30.8862884172365,-55.8665534203839,
19.8905492152186));
#28368=CARTESIAN_POINT('Ctrl Pts',(-30.7458083824097,-56.3998289316761,
19.8535032516959));
#28369=CARTESIAN_POINT('Ctrl Pts',(-30.8958178157836,-57.0096276847031,
19.8164572881732));
#28370=CARTESIAN_POINT('Ctrl Pts',(-31.2676640515259,-57.4168718226721,
19.7794113246505));
#28371=CARTESIAN_POINT('Ctrl Pts',(-31.6395102872682,-57.8241159606411,
19.7423653611279));
#28372=CARTESIAN_POINT('Ctrl Pts',(-32.2331933253789,-58.0288054835522,
19.7053193976052));
#28373=CARTESIAN_POINT('Ctrl Pts',(-32.7770107560741,-57.9372630704145,
19.6682734340825));
#28374=CARTESIAN_POINT('Ctrl Pts',(-33.3208281867694,-57.8457206572769,
19.6312274705598));
#28375=CARTESIAN_POINT('Ctrl Pts',(-33.8147800100492,-57.4579463080904,
19.5941815070371));
#28376=CARTESIAN_POINT('Ctrl Pts',(-34.0328063735823,-56.9514071526715,
19.5571355435145));
#28377=CARTESIAN_POINT('Ctrl Pts',(-34.2508327371153,-56.4448679972525,
19.5200895799918));
#28378=CARTESIAN_POINT('Ctrl Pts',(-34.1929336409016,-55.8195640356011,
19.4830436164691));
#28379=CARTESIAN_POINT('Ctrl Pts',(-33.8856069343887,-55.3616691714411,
19.4459976529464));
#28380=CARTESIAN_POINT('Ctrl Pts',(-33.5782802278758,-54.9037743072811,
19.4089516894237));
#28381=CARTESIAN_POINT('Ctrl Pts',(-33.0215259110637,-54.6132885406125,
19.3719057259011));
#28382=CARTESIAN_POINT('Ctrl Pts',(-32.4701457541755,-54.6231543297377,
19.3348597623784));
#28383=CARTESIAN_POINT('Ctrl Pts',(-32.1906296753062,-54.6281556825373,
19.3160797204555));
#28384=CARTESIAN_POINT('Ctrl Pts',(-31.9124946862162,-54.7103435109481,
19.2972996785326));
#28385=CARTESIAN_POINT('Ctrl Pts',(-31.6682947036337,-54.8512220664372,
19.2785196366098));
#28386=CARTESIAN_POINT('Ctrl Pts',(-31.6657991298123,-54.8498167632728,
19.4714803633902));
#28387=CARTESIAN_POINT('Ctrl Pts',(-32.0281252709183,-54.6449782192373,
19.4993090447612));
#28388=CARTESIAN_POINT('Ctrl Pts',(-32.4698183191301,-54.5725020736119,
19.5271377261321));
#28389=CARTESIAN_POINT('Ctrl Pts',(-32.8735646889017,-54.6652369881101,
19.5549664075031));
#28390=CARTESIAN_POINT('Ctrl Pts',(-33.4110379916282,-54.7886871154801,
19.5920123710258));
#28391=CARTESIAN_POINT('Ctrl Pts',(-33.8812646991831,-55.2049133627827,
19.6290583345484));
#28392=CARTESIAN_POINT('Ctrl Pts',(-34.069042894277,-55.7234274269329,19.6661042980711));
#28393=CARTESIAN_POINT('Ctrl Pts',(-34.2568210893709,-56.2419414910831,
19.7031502615938));
#28394=CARTESIAN_POINT('Ctrl Pts',(-34.1621507720038,-56.8627433720808,
19.7401962251165));
#28395=CARTESIAN_POINT('Ctrl Pts',(-33.8283583461529,-57.3017195705904,
19.7772421886392));
#28396=CARTESIAN_POINT('Ctrl Pts',(-33.494565920302,-57.7406957690999,19.8142881521619));
#28397=CARTESIAN_POINT('Ctrl Pts',(-32.9216513859674,-57.9978462851214,
19.8513341156845));
#28398=CARTESIAN_POINT('Ctrl Pts',(-32.3718123356058,-57.9554847234739,
19.8883800792072));
#28399=CARTESIAN_POINT('Ctrl Pts',(-31.8219732852443,-57.9131231618264,
19.9254260427299));
#28400=CARTESIAN_POINT('Ctrl Pts',(-31.2952097188559,-57.5712495225101,
19.9624720062526));
#28401=CARTESIAN_POINT('Ctrl Pts',(-31.0325979551939,-57.086324221881,19.9995179697753));
#28402=CARTESIAN_POINT('Ctrl Pts',(-30.769986191532,-56.601398921252,20.0365639332979));
#28403=CARTESIAN_POINT('Ctrl Pts',(-30.7715262305966,-55.9734219593102,
20.0736098968206));
#28404=CARTESIAN_POINT('Ctrl Pts',(-31.0365132935154,-55.489790540013,20.1106558603433));
#28405=CARTESIAN_POINT('Ctrl Pts',(-31.1815376981853,-55.225104566703,20.1309306946923));
#28406=CARTESIAN_POINT('Ctrl Pts',(-31.4054710295806,-55.0036536684416,
20.1512055290412));
#28407=CARTESIAN_POINT('Ctrl Pts',(-31.6686691446489,-54.8508917236136,
20.1714803633902));
#28408=CARTESIAN_POINT('Origin',(-32.5,-56.2916512459885,17.));
#28409=CARTESIAN_POINT('',(-31.6674621971265,-54.8470528177236,20.8714803633902));
#28410=CARTESIAN_POINT('',(-31.6651488727497,-54.8473747039335,20.6785196366098));
#28411=CARTESIAN_POINT('',(-31.667,-54.8488529232836,17.));
#28412=CARTESIAN_POINT('Ctrl Pts',(-31.6651488727497,-54.8473747039335,
20.6785196366098));
#28413=CARTESIAN_POINT('Ctrl Pts',(-31.6219590933013,-54.8719481703147,
20.6751845741381));
#28414=CARTESIAN_POINT('Ctrl Pts',(-31.579962486587,-54.8985363635017,20.6718495116665));
#28415=CARTESIAN_POINT('Ctrl Pts',(-31.539367364925,-54.9271153018696,20.6685144491949));
#28416=CARTESIAN_POINT('Ctrl Pts',(-31.0884356630213,-55.2445709169594,
20.6314684856722));
#28417=CARTESIAN_POINT('Ctrl Pts',(-30.8104307642169,-55.8076611175675,
20.5944225221495));
#28418=CARTESIAN_POINT('Ctrl Pts',(-30.8325829345476,-56.3586844387663,
20.5573765586268));
#28419=CARTESIAN_POINT('Ctrl Pts',(-30.8547351048784,-56.9097077599651,
20.5203305951041));
#28420=CARTESIAN_POINT('Ctrl Pts',(-31.1770443443443,-57.4486642017546,
20.4832846315815));
#28421=CARTESIAN_POINT('Ctrl Pts',(-31.6520041279564,-57.7288973132864,
20.4462386680588));
#28422=CARTESIAN_POINT('Ctrl Pts',(-32.1269639115685,-58.0091304248183,
20.4091927045361));
#28423=CARTESIAN_POINT('Ctrl Pts',(-32.7545742393267,-58.0306402060925,
20.3721467410134));
#28424=CARTESIAN_POINT('Ctrl Pts',(-33.2476056229439,-57.7835825733328,
20.3351007774907));
#28425=CARTESIAN_POINT('Ctrl Pts',(-33.7406370065611,-57.5365249405731,
20.2980548139681));
#28426=CARTESIAN_POINT('Ctrl Pts',(-34.0990894460373,-57.0208998937796,
20.2610088504454));
#28427=CARTESIAN_POINT('Ctrl Pts',(-34.1589151813611,-56.4726861646106,
20.2239628869227));
#28428=CARTESIAN_POINT('Ctrl Pts',(-34.2187409166848,-55.9244724354416,
20.1869169234));
#28429=CARTESIAN_POINT('Ctrl Pts',(-33.9799399478562,-55.3436700238972,
20.1498709598773));
#28430=CARTESIAN_POINT('Ctrl Pts',(-33.5518008766237,-54.9960864443956,
20.1128249963547));
#28431=CARTESIAN_POINT('Ctrl Pts',(-33.1236618053912,-54.648502864894,20.075779032832));
#28432=CARTESIAN_POINT('Ctrl Pts',(-32.5061846317548,-54.5341381174352,
20.0387330693093));
#28433=CARTESIAN_POINT('Ctrl Pts',(-31.9819612934229,-54.7053318784846,
20.0016871057866));
#28434=CARTESIAN_POINT('Ctrl Pts',(-31.8726832787826,-54.7410184131319,
19.993964616061));
#28435=CARTESIAN_POINT('Ctrl Pts',(-31.7674575454953,-54.7891136966038,
19.9862421263354));
#28436=CARTESIAN_POINT('Ctrl Pts',(-31.6680707239276,-54.8477242132621,
19.9785196366098));
#28437=CARTESIAN_POINT('Ctrl Pts',(-31.6686691446489,-54.8508917236136,
20.1714803633902));
#28438=CARTESIAN_POINT('Ctrl Pts',(-31.8863838499881,-54.724528653739,20.1882514925639));
#28439=CARTESIAN_POINT('Ctrl Pts',(-32.1309651849206,-54.6451654778256,
20.2050226217376));
#28440=CARTESIAN_POINT('Ctrl Pts',(-32.3799746400723,-54.6272090425041,
20.2217937509113));
#28441=CARTESIAN_POINT('Ctrl Pts',(-32.9300148369371,-54.5875448409449,
20.258839714434));
#28442=CARTESIAN_POINT('Ctrl Pts',(-33.5016611438935,-54.8475023144793,
20.2958856779567));
#28443=CARTESIAN_POINT('Ctrl Pts',(-33.8332965022582,-55.2881103970044,
20.3329316414794));
#28444=CARTESIAN_POINT('Ctrl Pts',(-34.1649318606228,-55.7287184795295,
20.3699776050021));
#28445=CARTESIAN_POINT('Ctrl Pts',(-34.2565562703957,-56.3499771710453,
20.4070235685247));
#28446=CARTESIAN_POINT('Ctrl Pts',(-34.0662370704008,-56.8675640172575,
20.4440695320474));
#28447=CARTESIAN_POINT('Ctrl Pts',(-33.875917870406,-57.3851508634698,20.4811154955701));
#28448=CARTESIAN_POINT('Ctrl Pts',(-33.4036550606434,-57.7990658643784,
20.5181614590928));
#28449=CARTESIAN_POINT('Ctrl Pts',(-32.8655828553033,-57.9198782552652,
20.5552074226155));
#28450=CARTESIAN_POINT('Ctrl Pts',(-32.3275106499632,-58.0406906461521,
20.5922533861382));
#28451=CARTESIAN_POINT('Ctrl Pts',(-31.7236290490455,-57.8684004270172,
20.6292993496608));
#28452=CARTESIAN_POINT('Ctrl Pts',(-31.3303069678814,-57.4818576289614,
20.6663453131835));
#28453=CARTESIAN_POINT('Ctrl Pts',(-30.9369848867174,-57.0953148309056,
20.7033912767062));
#28454=CARTESIAN_POINT('Ctrl Pts',(-30.754222325307,-56.494519453929,20.7404372402289));
#28455=CARTESIAN_POINT('Ctrl Pts',(-30.8656634549365,-55.954428037577,20.7774832037516));
#28456=CARTESIAN_POINT('Ctrl Pts',(-30.959917085256,-55.4976345999579,20.8088155902978));
#28457=CARTESIAN_POINT('Ctrl Pts',(-31.2646228230038,-55.0842643987964,
20.840147976844));
#28458=CARTESIAN_POINT('Ctrl Pts',(-31.6674621971265,-54.8470528177236,
20.8714803633902));
#28459=CARTESIAN_POINT('Origin',(-32.5,-56.2916512459885,17.));
#28460=CARTESIAN_POINT('',(-31.6652082225275,-54.8481806306043,21.5714803633902));
#28461=CARTESIAN_POINT('',(-31.667262219952,-54.851191363199,21.3785196366098));
#28462=CARTESIAN_POINT('',(-31.667,-54.8488529232836,17.));
#28463=CARTESIAN_POINT('',(-32.1997834265916,-57.9303781936679,22.));
#28464=CARTESIAN_POINT('Ctrl Pts',(-31.6652082225275,-54.8481806306043,
21.5714803633902));
#28465=CARTESIAN_POINT('Ctrl Pts',(-32.0766081468896,-54.6152030336121,
21.6031823516921));
#28466=CARTESIAN_POINT('Ctrl Pts',(-32.5941722167266,-54.5601311343425,
21.634884339994));
#28467=CARTESIAN_POINT('Ctrl Pts',(-33.0407304570642,-54.7130293475825,
21.6665863282959));
#28468=CARTESIAN_POINT('Ctrl Pts',(-33.5625646122208,-54.8917014730163,
21.7036322918186));
#28469=CARTESIAN_POINT('Ctrl Pts',(-33.987436493413,-55.3543679573327,21.7406782553412));
#28470=CARTESIAN_POINT('Ctrl Pts',(-34.1199308616871,-55.8897554009177,
21.7777242188639));
#28471=CARTESIAN_POINT('Ctrl Pts',(-34.2524252299611,-56.4251428445027,
21.8147701823866));
#28472=CARTESIAN_POINT('Ctrl Pts',(-34.0925420853171,-57.0332512473563,
21.8518161459093));
#28473=CARTESIAN_POINT('Ctrl Pts',(-33.7156105587364,-57.4345173729249,
21.888862109432));
#28474=CARTESIAN_POINT('Ctrl Pts',(-33.3386790321557,-57.8357834984935,
21.9259080729546));
#28475=CARTESIAN_POINT('Ctrl Pts',(-32.7446991236385,-58.0302073467771,
21.9629540364773));
#28476=CARTESIAN_POINT('Ctrl Pts',(-32.1997834265916,-57.930378193668,22.));
#28477=CARTESIAN_POINT('',(-30.9279127562904,-55.7311233941162,22.));
#28478=CARTESIAN_POINT('Origin',(-32.5,-56.2916512459885,22.));
#28479=CARTESIAN_POINT('Ctrl Pts',(-30.9279109916838,-55.7311226632893,
22.));
#28480=CARTESIAN_POINT('Ctrl Pts',(-30.7469516062031,-56.2407356224362,
21.9636770818144));
#28481=CARTESIAN_POINT('Ctrl Pts',(-30.8361764319304,-56.8473747622875,
21.9273541636289));
#28482=CARTESIAN_POINT('Ctrl Pts',(-31.157356786616,-57.282481394961,21.8910312454433));
#28483=CARTESIAN_POINT('Ctrl Pts',(-31.4849305691822,-57.726249276169,21.8539852819207));
#28484=CARTESIAN_POINT('Ctrl Pts',(-32.053786423629,-57.9915876156774,21.816939318398));
#28485=CARTESIAN_POINT('Ctrl Pts',(-32.604106443046,-57.9571481822401,21.7798933548753));
#28486=CARTESIAN_POINT('Ctrl Pts',(-33.1544264624631,-57.9227087488028,
21.7428473913526));
#28487=CARTESIAN_POINT('Ctrl Pts',(-33.6862106468504,-57.5884915424199,
21.7058014278299));
#28488=CARTESIAN_POINT('Ctrl Pts',(-33.9558248450097,-57.1074100574699,
21.6687554643072));
#28489=CARTESIAN_POINT('Ctrl Pts',(-34.2254390431691,-56.6263285725199,
21.6317095007845));
#28490=CARTESIAN_POINT('Ctrl Pts',(-34.2328832551006,-55.9983828090028,
21.5946635372619));
#28491=CARTESIAN_POINT('Ctrl Pts',(-33.9748805050844,-55.5109771631464,
21.5576175737392));
#28492=CARTESIAN_POINT('Ctrl Pts',(-33.7168777550681,-55.02357151729,21.5205716102165));
#28493=CARTESIAN_POINT('Ctrl Pts',(-33.1934280431042,-54.6767059890943,
21.4835256466938));
#28494=CARTESIAN_POINT('Ctrl Pts',(-32.6440261878896,-54.6291148312821,
21.4464796831712));
#28495=CARTESIAN_POINT('Ctrl Pts',(-32.3080707772689,-54.6000131695149,
21.4238263343174));
#28496=CARTESIAN_POINT('Ctrl Pts',(-31.9624112442361,-54.6828172989955,
21.4011729854636));
#28497=CARTESIAN_POINT('Ctrl Pts',(-31.667262219952,-54.851191363199,21.3785196366098));
#28498=CARTESIAN_POINT('Origin',(-32.5,-56.2916512459885,23.5459252805377));
#28499=CARTESIAN_POINT('',(-31.4703515173367,-54.5106388084307,13.4540747194623));
#28500=CARTESIAN_POINT('',(-31.474888731711,-54.5145036461352,13.3959252805377));
#28501=CARTESIAN_POINT('',(-31.4726249999999,-54.5121855475625,23.5459252805377));
#28502=CARTESIAN_POINT('',(-34.1542537360139,-57.5104384051693,13.));
#28503=CARTESIAN_POINT('Ctrl Pts',(-31.474888731711,-54.5145036461352,13.3959252805377));
#28504=CARTESIAN_POINT('Ctrl Pts',(-31.1415381650012,-54.7083242075053,
13.3750880775932));
#28505=CARTESIAN_POINT('Ctrl Pts',(-30.3573574995583,-55.4957610011486,
13.317204911126));
#28506=CARTESIAN_POINT('Ctrl Pts',(-30.3807647535574,-57.4808407355902,
13.2222757811361));
#28507=CARTESIAN_POINT('Ctrl Pts',(-32.3530480505925,-58.7147951819942,
13.1111378905681));
#28508=CARTESIAN_POINT('Ctrl Pts',(-33.748978009428,-58.0605171287351,13.0370459635227));
#28509=CARTESIAN_POINT('Ctrl Pts',(-34.1542537360139,-57.5104384051693,
13.));
#28510=CARTESIAN_POINT('',(-34.5453697724995,-56.5236298181907,13.));
#28511=CARTESIAN_POINT('Origin',(-32.5,-56.2916512459885,13.));
#28512=CARTESIAN_POINT('Ctrl Pts',(-31.4703515173367,-54.5106388084307,
13.4540747194623));
#28513=CARTESIAN_POINT('Ctrl Pts',(-31.4080578130841,-54.5460236433933,
13.4501772883951));
#28514=CARTESIAN_POINT('Ctrl Pts',(-30.7746715994702,-54.9531541715192,
13.4092338938053));
#28515=CARTESIAN_POINT('Ctrl Pts',(-30.074887383932,-56.4258925346357,13.3312445356927));
#28516=CARTESIAN_POINT('Ctrl Pts',(-31.2980228170538,-58.4019167094403,
13.2201066451247));
#28517=CARTESIAN_POINT('Ctrl Pts',(-33.60498859151,-58.4457294765997,13.1096917998938));
#28518=CARTESIAN_POINT('Ctrl Pts',(-34.469350039682,-57.1862605871605,13.0363229181856));
#28519=CARTESIAN_POINT('Ctrl Pts',(-34.5453721234944,-56.52362996598,13.));
#28520=CARTESIAN_POINT('Origin',(-32.5,-56.2916512459885,23.5459252805377));
#28521=CARTESIAN_POINT('',(-31.4731479817858,-54.5151444612292,14.1540747194623));
#28522=CARTESIAN_POINT('',(-31.472961077924,-54.5097720381012,14.0959252805377));
#28523=CARTESIAN_POINT('',(-31.4726249999999,-54.5121855475625,23.5459252805377));
#28524=CARTESIAN_POINT('Ctrl Pts',(-31.472961077924,-54.5097720381012,14.0959252805377));
#28525=CARTESIAN_POINT('Ctrl Pts',(-30.9672759169724,-54.8072848061286,
14.0640305253959));
#28526=CARTESIAN_POINT('Ctrl Pts',(-30.1471997784249,-55.9394877473567,
13.9950898067314));
#28527=CARTESIAN_POINT('Ctrl Pts',(-30.8240773215828,-58.0494183789814,
13.8891031245444));
#28528=CARTESIAN_POINT('Ctrl Pts',(-33.0679207153753,-58.6529675412989,
13.7779652339763));
#28529=CARTESIAN_POINT('Ctrl Pts',(-34.7917858342248,-57.0952271533932,
13.6668273434083));
#28530=CARTESIAN_POINT('Ctrl Pts',(-34.4182616640155,-54.8018644711707,
13.5556894528402));
#28531=CARTESIAN_POINT('Ctrl Pts',(-32.6876568692322,-54.0466007600429,
13.4653887652167));
#28532=CARTESIAN_POINT('Ctrl Pts',(-31.7341941451479,-54.3637352784833,
13.4121340411158));
#28533=CARTESIAN_POINT('Ctrl Pts',(-31.474888731711,-54.5145036461352,13.3959252805377));
#28534=CARTESIAN_POINT('Ctrl Pts',(-31.4731479817858,-54.5151444612292,
14.1540747194623));
#28535=CARTESIAN_POINT('Ctrl Pts',(-31.2328780723112,-54.6524190875731,
14.1391197361979));
#28536=CARTESIAN_POINT('Ctrl Pts',(-30.4914633330274,-55.2894948776179,
14.0871187894108));
#28537=CARTESIAN_POINT('Ctrl Pts',(-30.2211615693062,-57.1314551632494,
13.998071879101));
#28538=CARTESIAN_POINT('Ctrl Pts',(-31.9696590133091,-58.6616944230991,
13.886933988533));
#28539=CARTESIAN_POINT('Ctrl Pts',(-34.2035641928434,-58.0226004643432,
13.7757960979649));
#28540=CARTESIAN_POINT('Ctrl Pts',(-34.8782165391171,-55.7991607039093,
13.6646582073969));
#28541=CARTESIAN_POINT('Ctrl Pts',(-33.4286636629751,-54.0886449425481,
13.557417747896));
#28542=CARTESIAN_POINT('Ctrl Pts',(-32.0001735569318,-54.2096827863809,
13.4872232519178));
#28543=CARTESIAN_POINT('Ctrl Pts',(-31.4703515173367,-54.5106388084307,
13.4540747194623));
#28544=CARTESIAN_POINT('Origin',(-32.5,-56.2916512459885,23.5459252805377));
#28545=CARTESIAN_POINT('',(-31.4747795225871,-54.5123867379958,14.8540747194623));
#28546=CARTESIAN_POINT('',(-31.4704412404259,-54.5116709695925,14.7959252805377));
#28547=CARTESIAN_POINT('',(-31.4726249999999,-54.5121855475625,23.5459252805377));
#28548=CARTESIAN_POINT('Ctrl Pts',(-31.4704412404259,-54.5116709695925,
14.7959252805377));
#28549=CARTESIAN_POINT('Ctrl Pts',(-31.3758333938148,-54.5652019692603,
14.7900189367213));
#28550=CARTESIAN_POINT('Ctrl Pts',(-30.720757421839,-55.0095411304486,14.7470666293823));
#28551=CARTESIAN_POINT('Ctrl Pts',(-30.0858692295543,-56.5568634086542,
14.6670683585206));
#28552=CARTESIAN_POINT('Ctrl Pts',(-31.4135291597177,-58.4637350403727,
14.5559304679526));
#28553=CARTESIAN_POINT('Ctrl Pts',(-33.73564936737,-58.3824733534297,14.4447925773845));
#28554=CARTESIAN_POINT('Ctrl Pts',(-34.926763301881,-56.3874592577879,14.3336546868165));
#28555=CARTESIAN_POINT('Ctrl Pts',(-33.8966380568543,-54.3047494455222,
14.2225167962484));
#28556=CARTESIAN_POINT('Ctrl Pts',(-32.2506444060776,-54.1164611126689,
14.1432736608222));
#28557=CARTESIAN_POINT('Ctrl Pts',(-31.5546324883995,-54.4617218098652,
14.1010764889186));
#28558=CARTESIAN_POINT('Ctrl Pts',(-31.472961077924,-54.5097720381012,14.0959252805377));
#28559=CARTESIAN_POINT('Ctrl Pts',(-31.4747795225871,-54.5123867379958,
14.8540747194623));
#28560=CARTESIAN_POINT('Ctrl Pts',(-31.0607155624738,-54.7559913454825,
14.8280621840006));
#28561=CARTESIAN_POINT('Ctrl Pts',(-30.2508194018851,-55.6943396944676,
14.7650036850163));
#28562=CARTESIAN_POINT('Ctrl Pts',(-30.5678191761536,-57.7630592969624,
14.6648992225092));
#28563=CARTESIAN_POINT('Ctrl Pts',(-32.6883055651204,-58.7129949703236,
14.5537613319412));
#28564=CARTESIAN_POINT('Ctrl Pts',(-34.6364334330514,-57.4466471822883,
14.4426234413732));
#28565=CARTESIAN_POINT('Ctrl Pts',(-34.6290601547835,-55.1231186965397,
14.3314855508051));
#28566=CARTESIAN_POINT('Ctrl Pts',(-32.9361539945055,-54.0378965296929,
14.2353026435015));
#28567=CARTESIAN_POINT('Ctrl Pts',(-31.8280663212454,-54.3123671657349,
14.1761656997206));
#28568=CARTESIAN_POINT('Ctrl Pts',(-31.4731479817858,-54.5151444612292,
14.1540747194623));
#28569=CARTESIAN_POINT('Origin',(-32.5,-56.2916512459885,23.5459252805377));
#28570=CARTESIAN_POINT('',(-31.4709133736318,-54.5092374781621,15.5540747194623));
#28571=CARTESIAN_POINT('',(-31.4738352212016,-54.5152196643081,15.4959252805377));
#28572=CARTESIAN_POINT('',(-31.4726249999999,-54.5121855475625,23.5459252805377));
#28573=CARTESIAN_POINT('Ctrl Pts',(-31.4738352212016,-54.515219664308,15.4959252805377));
#28574=CARTESIAN_POINT('Ctrl Pts',(-31.201543391866,-54.6716871554888,15.4789613845241));
#28575=CARTESIAN_POINT('Ctrl Pts',(-30.4440567807226,-55.3577373025941,
15.4249515249878));
#28576=CARTESIAN_POINT('Ctrl Pts',(-30.269905357807,-57.2534431023133,15.3338957019289));
#28577=CARTESIAN_POINT('Ctrl Pts',(-32.0985763090804,-58.6869016992398,
15.2227578113608));
#28578=CARTESIAN_POINT('Ctrl Pts',(-34.2946749356979,-57.9279603862777,
15.1116199207928));
#28579=CARTESIAN_POINT('Ctrl Pts',(-34.848087203459,-55.6712867722916,15.0004820302248));
#28580=CARTESIAN_POINT('Ctrl Pts',(-33.3370773338915,-54.0721923398817,
14.895250483473));
#28581=CARTESIAN_POINT('Ctrl Pts',(-31.9692358342251,-54.229443076332,14.827064900244));
#28582=CARTESIAN_POINT('Ctrl Pts',(-31.4704412404259,-54.5116709695925,
14.7959252805377));
#28583=CARTESIAN_POINT('Ctrl Pts',(-31.4709133820845,-54.5092374927209,
15.5540747194623));
#28584=CARTESIAN_POINT('Ctrl Pts',(-31.4705297975013,-54.5094589248369,
15.5540505953261));
#28585=CARTESIAN_POINT('Ctrl Pts',(-30.8812194784826,-54.8499291446222,
15.5169805076671));
#28586=CARTESIAN_POINT('Ctrl Pts',(-30.074257404191,-56.1727516226364,15.4428644564856));
#28587=CARTESIAN_POINT('Ctrl Pts',(-31.0845179881232,-58.2651696619898,
15.3317265659175));
#28588=CARTESIAN_POINT('Ctrl Pts',(-33.3903853125313,-58.551203914661,15.2205886753495));
#28589=CARTESIAN_POINT('Ctrl Pts',(-34.8812728580259,-56.7690439832156,
15.1094507847814));
#28590=CARTESIAN_POINT('Ctrl Pts',(-34.192554360499,-54.5499210682071,14.9983128942134));
#28591=CARTESIAN_POINT('Ctrl Pts',(-32.4784241363503,-54.0712848045823,
14.913187539107));
#28592=CARTESIAN_POINT('Ctrl Pts',(-31.6504081122452,-54.4090598663806,
14.8651081475233));
#28593=CARTESIAN_POINT('Ctrl Pts',(-31.4747795225871,-54.5123867379958,
14.8540747194623));
#28594=CARTESIAN_POINT('Origin',(-32.5,-56.2916512459885,23.5459252805377));
#28595=CARTESIAN_POINT('',(-31.4717385551609,-54.5141703251839,16.2540747194623));
#28596=CARTESIAN_POINT('',(-31.4743433646119,-54.5114040111285,16.1959252805377));
#28597=CARTESIAN_POINT('',(-31.4726249999999,-54.5121855475625,23.5459252805377));
#28598=CARTESIAN_POINT('Ctrl Pts',(-31.4743433646119,-54.5114040111285,
16.1959252805377));
#28599=CARTESIAN_POINT('Ctrl Pts',(-31.0291266592638,-54.7738828820724,
16.1679038323268));
#28600=CARTESIAN_POINT('Ctrl Pts',(-30.2132159159802,-55.7757147456513,
16.1028364205933));
#28601=CARTESIAN_POINT('Ctrl Pts',(-30.6502037274999,-57.8653791294726,
16.0007230453371));
#28602=CARTESIAN_POINT('Ctrl Pts',(-32.8189508948268,-58.6992716537698,
15.8895851547691));
#28603=CARTESIAN_POINT('Ctrl Pts',(-34.6957586912586,-57.3294419144583,
15.778447264201));
#28604=CARTESIAN_POINT('Ctrl Pts',(-34.5627636554057,-55.0097106071377,
15.667309373633));
#28605=CARTESIAN_POINT('Ctrl Pts',(-32.8501896837687,-54.0383319846292,
15.5731353790785));
#28606=CARTESIAN_POINT('Ctrl Pts',(-31.7961776179314,-54.3299915352064,
15.5160073480468));
#28607=CARTESIAN_POINT('Ctrl Pts',(-31.4738352212016,-54.515219664308,15.4959252805377));
#28608=CARTESIAN_POINT('Ctrl Pts',(-31.4717385551609,-54.5141703251839,
16.2540747194623));
#28609=CARTESIAN_POINT('Ctrl Pts',(-31.2936631692288,-54.6150534746527,
16.2429930431288));
#28610=CARTESIAN_POINT('Ctrl Pts',(-30.586678710615,-55.1642906384242,16.1948654032726));
#28611=CARTESIAN_POINT('Ctrl Pts',(-30.1461151763816,-56.8896399584928,
16.1096917998938));
#28612=CARTESIAN_POINT('Ctrl Pts',(-31.7257879044833,-58.5935982250311,
15.9985539093258));
#28613=CARTESIAN_POINT('Ctrl Pts',(-34.0141057438103,-58.1905583158083,
15.8874160187577));
#28614=CARTESIAN_POINT('Ctrl Pts',(-34.9165454246277,-56.0494272304867,
15.7762781281897));
#28615=CARTESIAN_POINT('Ctrl Pts',(-33.6073779089676,-54.1304231724864,
15.6651643617579));
#28616=CARTESIAN_POINT('Ctrl Pts',(-32.0595772284103,-54.1694191401902,
15.5910965588487));
#28617=CARTESIAN_POINT('Ctrl Pts',(-31.4709133820845,-54.5092374927209,
15.5540747194623));
#28618=CARTESIAN_POINT('Origin',(-32.5,-56.2916512459885,23.5459252805377));
#28619=CARTESIAN_POINT('',(-31.4749299874422,-54.5140996860483,16.9540747194623));
#28620=CARTESIAN_POINT('',(-31.4704693279511,-54.5098093620654,16.8959252805377));
#28621=CARTESIAN_POINT('',(-31.4726249999999,-54.5121855475625,23.5459252805377));
#28622=CARTESIAN_POINT('Ctrl Pts',(-31.4704693279511,-54.5098093620654,
16.8959252805377));
#28623=CARTESIAN_POINT('Ctrl Pts',(-31.4380523744923,-54.528339714304,16.8938922436523));
#28624=CARTESIAN_POINT('Ctrl Pts',(-30.8255360958299,-54.9025793613845,
16.8548132432442));
#28625=CARTESIAN_POINT('Ctrl Pts',(-30.0713767023175,-56.3040842326063,
16.7786882793134));
#28626=CARTESIAN_POINT('Ctrl Pts',(-31.1932955779139,-58.3388173981362,
16.6675503887454));
#28627=CARTESIAN_POINT('Ctrl Pts',(-33.5112558300796,-58.4997561681628,
16.5564124981773));
#28628=CARTESIAN_POINT('Ctrl Pts',(-34.9036021525567,-56.6395914613089,
16.4452746076093));
#28629=CARTESIAN_POINT('Ctrl Pts',(-34.0959041660875,-54.4609531294646,
16.3341367170413));
#28630=CARTESIAN_POINT('Ctrl Pts',(-32.3994057229947,-54.0847909276367,
16.251020274684));
#28631=CARTESIAN_POINT('Ctrl Pts',(-31.61772870802,-54.4268707431815,16.2049497958495));
#28632=CARTESIAN_POINT('Ctrl Pts',(-31.4743433646119,-54.5114040111285,
16.1959252805377));
#28633=CARTESIAN_POINT('Ctrl Pts',(-31.4749299874422,-54.5140996860483,
16.9540747194623));
#28634=CARTESIAN_POINT('Ctrl Pts',(-31.1211066997161,-54.7205458521634,
16.9319354909316));
#28635=CARTESIAN_POINT('Ctrl Pts',(-30.3290943933324,-55.5443071105387,
16.8727502988781));
#28636=CARTESIAN_POINT('Ctrl Pts',(-30.4251293279102,-57.5539016004218,
16.776519143302));
#28637=CARTESIAN_POINT('Ctrl Pts',(-32.4351932585659,-58.7194412594432,
16.665381252734));
#28638=CARTESIAN_POINT('Ctrl Pts',(-34.5045755346153,-57.6627971861383,
16.554243362166));
#28639=CARTESIAN_POINT('Ctrl Pts',(-34.7391470903974,-55.3511276839614,
16.4431054715979));
#28640=CARTESIAN_POINT('Ctrl Pts',(-33.1051720185616,-54.0449906258011,
16.3430492573634));
#28641=CARTESIAN_POINT('Ctrl Pts',(-31.8889678914565,-54.277801838456,16.2800390066515));
#28642=CARTESIAN_POINT('Ctrl Pts',(-31.4717385551609,-54.5141703251839,
16.2540747194623));
#28643=CARTESIAN_POINT('Origin',(-32.5,-56.2916512459885,23.5459252805377));
#28644=CARTESIAN_POINT('',(-31.4724078687478,-54.5094050924838,17.6540747194623));
#28645=CARTESIAN_POINT('',(-31.4724615607262,-54.5148044353696,17.5959252805377));
#28646=CARTESIAN_POINT('',(-31.4726249999999,-54.5121855475625,23.5459252805377));
#28647=CARTESIAN_POINT('Ctrl Pts',(-31.4724615607262,-54.5148044353696,
17.5959252805377));
#28648=CARTESIAN_POINT('Ctrl Pts',(-31.2620673353104,-54.6344533407431,
17.582834691455));
#28649=CARTESIAN_POINT('Ctrl Pts',(-30.5366971614125,-55.2281953867951,
17.5326981388497));
#28650=CARTESIAN_POINT('Ctrl Pts',(-30.1818911638421,-57.0160386595509,
17.4455156227217));
#28651=CARTESIAN_POINT('Ctrl Pts',(-31.8513854749211,-58.6320924221469,
17.3343777321536));
#28652=CARTESIAN_POINT('Ctrl Pts',(-34.1145640165938,-58.1059138337969,
17.2232398415856));
#28653=CARTESIAN_POINT('Ctrl Pts',(-34.899913803477,-55.9191201236888,17.1121019510176));
#28654=CARTESIAN_POINT('Ctrl Pts',(-33.5144124105785,-54.1070736669905,
17.0029970973349));
#28655=CARTESIAN_POINT('Ctrl Pts',(-32.0287535486679,-54.190679951206,16.930938207175));
#28656=CARTESIAN_POINT('Ctrl Pts',(-31.4704693279511,-54.5098093620654,
16.8959252805377));
#28657=CARTESIAN_POINT('Ctrl Pts',(-31.4724078687478,-54.5094050924838,
17.6540747194623));
#28658=CARTESIAN_POINT('Ctrl Pts',(-30.946094870988,-54.8181696162505,17.6208779387343));
#28659=CARTESIAN_POINT('Ctrl Pts',(-30.1270731190027,-55.9965693019247,
17.5506351944836));
#28660=CARTESIAN_POINT('Ctrl Pts',(-30.8867448926705,-58.1070774278645,
17.4433464867103));
#28661=CARTESIAN_POINT('Ctrl Pts',(-33.1503020054966,-58.6316238024116,
17.3322085961423));
#28662=CARTESIAN_POINT('Ctrl Pts',(-34.8186303177654,-57.0143667589707,
17.2210707055742));
#28663=CARTESIAN_POINT('Ctrl Pts',(-34.3646900051272,-54.7356000103461,
17.1099328150062));
#28664=CARTESIAN_POINT('Ctrl Pts',(-32.6344025598171,-54.051324400594,17.0209341529689));
#28665=CARTESIAN_POINT('Ctrl Pts',(-31.7131654786556,-54.375095823104,16.9689814544542));
#28666=CARTESIAN_POINT('Ctrl Pts',(-31.4749299874422,-54.5140996860483,
16.9540747194623));
#28667=CARTESIAN_POINT('Origin',(-32.5,-56.2916512459885,23.5459252805377));
#28668=CARTESIAN_POINT('',(-31.470650904959,-54.5123645943458,18.3540747194623));
#28669=CARTESIAN_POINT('',(-31.4749676053556,-54.5132671274454,18.2959252805377));
#28670=CARTESIAN_POINT('',(-31.4726249999999,-54.5121855475625,23.5459252805377));
#28671=CARTESIAN_POINT('Ctrl Pts',(-31.4749676053556,-54.5132671274454,
18.2959252805377));
#28672=CARTESIAN_POINT('Ctrl Pts',(-31.0898434852659,-54.7390742900299,
18.2717771392578));
#28673=CARTESIAN_POINT('Ctrl Pts',(-30.2875910450901,-55.6209976925707,
18.2105830344552));
#28674=CARTESIAN_POINT('Ctrl Pts',(-30.4964134968882,-57.664242527379,18.1123429661299));
#28675=CARTESIAN_POINT('Ctrl Pts',(-32.5665574496276,-58.7193941910097,
18.0012050755619));
#28676=CARTESIAN_POINT('Ctrl Pts',(-34.57578061391,-57.5524052045849,17.8900671849938));
#28677=CARTESIAN_POINT('Ctrl Pts',(-34.6850182413274,-55.2314338219344,
17.7789292944258));
#28678=CARTESIAN_POINT('Ctrl Pts',(-33.0169876554982,-54.0399676860015,
17.6808819929404));
#28679=CARTESIAN_POINT('Ctrl Pts',(-31.8574765068094,-54.295850627297,17.6198806549777));
#28680=CARTESIAN_POINT('Ctrl Pts',(-31.4724615607262,-54.5148044353696,
17.5959252805377));
#28681=CARTESIAN_POINT('Ctrl Pts',(-31.470650904959,-54.5123645943458,18.3540747194623));
#28682=CARTESIAN_POINT('Ctrl Pts',(-31.3550533194394,-54.5776997670471,
18.3468663500598));
#28683=CARTESIAN_POINT('Ctrl Pts',(-30.6863525478934,-55.0471677720896,
18.3026120171345));
#28684=CARTESIAN_POINT('Ctrl Pts',(-30.0966496704334,-56.6413246029078,
18.2213117206866));
#28685=CARTESIAN_POINT('Ctrl Pts',(-31.4903368545418,-58.5004845570078,
18.1101738301185));
#28686=CARTESIAN_POINT('Ctrl Pts',(-33.8081801660464,-58.3378743316584,
17.9990359395505));
#28687=CARTESIAN_POINT('Ctrl Pts',(-34.928631335797,-56.3023329102471,17.8878980489824));
#28688=CARTESIAN_POINT('Ctrl Pts',(-33.8261287013397,-54.2570144404017,
17.7767601584144));
#28689=CARTESIAN_POINT('Ctrl Pts',(-32.2016889552716,-54.1286817447541,
17.6988190485744));
#28690=CARTESIAN_POINT('Ctrl Pts',(-31.5334341156058,-54.4736036964922,
17.657923902257));
#28691=CARTESIAN_POINT('Ctrl Pts',(-31.4724078687478,-54.5094050924838,
17.6540747194623));
#28692=CARTESIAN_POINT('Origin',(-32.5,-56.2916512459885,23.5459252805377));
#28693=CARTESIAN_POINT('',(-31.4742218141004,-54.5151075144861,19.0540747194623));
#28694=CARTESIAN_POINT('',(-31.4715682025536,-54.5091203612935,18.9959252805377));
#28695=CARTESIAN_POINT('',(-31.4726249999999,-54.5121855475625,23.5459252805377));
#28696=CARTESIAN_POINT('Ctrl Pts',(-31.4715682025536,-54.5091203612935,
18.9959252805377));
#28697=CARTESIAN_POINT('Ctrl Pts',(-30.9129158471523,-54.834613753627,18.9607195870605));
#28698=CARTESIAN_POINT('Ctrl Pts',(-30.0982487947042,-56.0866128816227,
18.8884679300607));
#28699=CARTESIAN_POINT('Ctrl Pts',(-30.9872637967358,-58.1916498987633,
18.7791703095382));
#28700=CARTESIAN_POINT('Ctrl Pts',(-33.2758719583609,-58.5930396107435,
18.6680324189701));
#28701=CARTESIAN_POINT('Ctrl Pts',(-34.8543157175077,-56.8879424529461,
18.5568945284021));
#28702=CARTESIAN_POINT('Ctrl Pts',(-34.2778276006655,-54.6370531910174,
18.445756637834));
#28703=CARTESIAN_POINT('Ctrl Pts',(-32.5529073535807,-54.0606456221556,
18.3587668885459));
#28704=CARTESIAN_POINT('Ctrl Pts',(-31.6806671821781,-54.3926607167737,
18.3088231027804));
#28705=CARTESIAN_POINT('Ctrl Pts',(-31.4749676053556,-54.5132671274454,
18.2959252805377));
#28706=CARTESIAN_POINT('Ctrl Pts',(-31.4742218141004,-54.5151075144861,
19.0540747194623));
#28707=CARTESIAN_POINT('Ctrl Pts',(-31.1812845288231,-54.6841025371816,
19.0358087978625));
#28708=CARTESIAN_POINT('Ctrl Pts',(-30.4141219270718,-55.4032020294196,
18.98049691274));
#28709=CARTESIAN_POINT('Ctrl Pts',(-30.3049905142645,-57.3310249135316,
18.8881390640948));
#28710=CARTESIAN_POINT('Ctrl Pts',(-32.182785399016,-58.6995007346588,18.7770011735268));
#28711=CARTESIAN_POINT('Ctrl Pts',(-34.3509304054687,-57.8640446119295,
18.6658632829587));
#28712=CARTESIAN_POINT('Ctrl Pts',(-34.8248978208363,-55.5893590092039,
18.5547253923907));
#28713=CARTESIAN_POINT('Ctrl Pts',(-33.2781402858533,-54.0633320127348,
18.4507958712252));
#28714=CARTESIAN_POINT('Ctrl Pts',(-31.9491438407914,-54.2419227987111,
18.3839123135824));
#28715=CARTESIAN_POINT('Ctrl Pts',(-31.470650904959,-54.5123645943458,18.3540747194623));
#28716=CARTESIAN_POINT('Origin',(-32.5,-56.2916512459885,23.5459252805377));
#28717=CARTESIAN_POINT('',(-31.4739455702221,-54.5107934605777,19.7540747194623));
#28718=CARTESIAN_POINT('',(-31.471143914755,-54.5133742931914,19.6959252805377));
#28719=CARTESIAN_POINT('',(-31.4726249999999,-54.5121855475625,23.5459252805377));
#28720=CARTESIAN_POINT('Ctrl Pts',(-31.471143914755,-54.5133742931914,19.6959252805377));
#28721=CARTESIAN_POINT('Ctrl Pts',(-31.3231329415045,-54.5970512593892,
19.6867079983859));
#28722=CARTESIAN_POINT('Ctrl Pts',(-30.6341370241162,-55.106929574873,19.6404447527115));
#28723=CARTESIAN_POINT('Ctrl Pts',(-30.1190717238489,-56.77076109083,19.5571355435145));
#28724=CARTESIAN_POINT('Ctrl Pts',(-31.611244210167,-58.5518456729879,19.4459976529464));
#28725=CARTESIAN_POINT('Ctrl Pts',(-33.9169049506455,-58.2641486635056,
19.3348597623784));
#28726=CARTESIAN_POINT('Ctrl Pts',(-34.9256565207284,-56.1710023982575,
19.2237218718104));
#28727=CARTESIAN_POINT('Ctrl Pts',(-33.71417716871,-54.1882873915237,19.1125839812423));
#28728=CARTESIAN_POINT('Ctrl Pts',(-32.1271617475077,-54.1490140977469,
19.0366517841514));
#28729=CARTESIAN_POINT('Ctrl Pts',(-31.5007700473113,-54.4921061888467,
18.9977655505832));
#28730=CARTESIAN_POINT('Ctrl Pts',(-31.4715682025536,-54.5091203612935,
18.9959252805377));
#28731=CARTESIAN_POINT('Ctrl Pts',(-31.4739455702221,-54.5107934605777,
19.7540747194623));
#28732=CARTESIAN_POINT('Ctrl Pts',(-31.0084978875972,-54.7852778310984,
19.7247512456653));
#28733=CARTESIAN_POINT('Ctrl Pts',(-30.1900336005111,-55.8297589120183,
19.6583818083455));
#28734=CARTESIAN_POINT('Ctrl Pts',(-30.7065057264145,-57.9292539322017,
19.5549664075031));
#28735=CARTESIAN_POINT('Ctrl Pts',(-32.9031507850421,-58.6866113101154,
19.443828516935));
#28736=CARTESIAN_POINT('Ctrl Pts',(-34.730787355662,-57.2518345802401,19.332690626367));
#28737=CARTESIAN_POINT('Ctrl Pts',(-34.5165589620033,-54.9381911555042,
19.2215527357989));
#28738=CARTESIAN_POINT('Ctrl Pts',(-32.7951211292858,-54.0400334340293,
19.1286807668307));
#28739=CARTESIAN_POINT('Ctrl Pts',(-31.7754042355958,-54.3413558867002,
19.0728547613852));
#28740=CARTESIAN_POINT('Ctrl Pts',(-31.4742218141004,-54.5151075144861,
19.0540747194623));
#28741=CARTESIAN_POINT('Origin',(-32.5,-56.2916512459885,23.5459252805377));
#28742=CARTESIAN_POINT('',(-31.4703419245392,-54.5103623955759,20.4540747194623));
#28743=CARTESIAN_POINT('',(-31.4746836284317,-54.5147000883656,20.3959252805377));
#28744=CARTESIAN_POINT('',(-31.4726249999999,-54.5121855475625,23.5459252805377));
#28745=CARTESIAN_POINT('Ctrl Pts',(-31.4746836284317,-54.5147000883656,
20.3959252805377));
#28746=CARTESIAN_POINT('Ctrl Pts',(-31.1500699868132,-54.7031080152175,
20.3756504461887));
#28747=CARTESIAN_POINT('Ctrl Pts',(-30.3692379110719,-55.4752841065875,
20.318329648317));
#28748=CARTESIAN_POINT('Ctrl Pts',(-30.3643995989091,-57.4481876795404,
20.2239628869227));
#28749=CARTESIAN_POINT('Ctrl Pts',(-32.3134406037768,-58.7131304053242,
20.1128249963547));
#28750=CARTESIAN_POINT('Ctrl Pts',(-34.4332415751289,-57.7616657784424,
20.0016871057866));
#28751=CARTESIAN_POINT('Ctrl Pts',(-34.7835245906331,-55.4646801872418,
19.8905492152186));
#28752=CARTESIAN_POINT('Ctrl Pts',(-33.1879673210569,-54.052355442598,19.7886286068023));
#28753=CARTESIAN_POINT('Ctrl Pts',(-31.9180164468303,-54.2607380396757,
19.7237539619086));
#28754=CARTESIAN_POINT('Ctrl Pts',(-31.471143914755,-54.5133742931914,19.6959252805377));
#28755=CARTESIAN_POINT('Ctrl Pts',(-31.4703419245392,-54.5103623955759,
20.4540747194623));
#28756=CARTESIAN_POINT('Ctrl Pts',(-31.4170740978156,-54.5406699166123,
20.4507396569907));
#28757=CARTESIAN_POINT('Ctrl Pts',(-30.7899238920755,-54.9377208245812,
20.4103586309964));
#28758=CARTESIAN_POINT('Ctrl Pts',(-30.073305550394,-56.3892087930031,20.3329316414794));
#28759=CARTESIAN_POINT('Ctrl Pts',(-31.2658594095642,-58.3833638027876,
20.2217937509113));
#28760=CARTESIAN_POINT('Ctrl Pts',(-33.588036458114,-58.4629506390538,20.1106558603433));
#28761=CARTESIAN_POINT('Ctrl Pts',(-34.914321242052,-56.5551224909764,19.9995179697752));
#28762=CARTESIAN_POINT('Ctrl Pts',(-34.0307504904903,-54.406136137217,19.8883800792072));
#28763=CARTESIAN_POINT('Ctrl Pts',(-32.3488749925859,-54.0946310730832,
19.8065656624362));
#28764=CARTESIAN_POINT('Ctrl Pts',(-31.5965236444216,-54.4385065703594,
19.7617972091879));
#28765=CARTESIAN_POINT('Ctrl Pts',(-31.4739455702221,-54.5107934605777,
19.7540747194623));
#28766=CARTESIAN_POINT('Origin',(-32.5,-56.2916512459885,23.5459252805377));
#28767=CARTESIAN_POINT('',(-31.4729484072307,-54.5150696468519,21.1540747194623));
#28768=CARTESIAN_POINT('',(-31.4731950477465,-54.5099653993635,21.0959252805377));
#28769=CARTESIAN_POINT('',(-31.4726249999999,-54.5121855475625,23.5459252805377));
#28770=CARTESIAN_POINT('Ctrl Pts',(-31.4731950477465,-54.5099653993635,
21.0959252805377));
#28771=CARTESIAN_POINT('Ctrl Pts',(-30.9763557896561,-54.8025287224184,
21.0645928939914));
#28772=CARTESIAN_POINT('Ctrl Pts',(-30.1562124434263,-55.91515240492,20.9962145439225));
#28773=CARTESIAN_POINT('Ctrl Pts',(-30.7976747113088,-58.0238313492005,
20.890790230331));
#28774=CARTESIAN_POINT('Ctrl Pts',(-33.0320547584019,-58.6613103307746,
20.7796523397629));
#28775=CARTESIAN_POINT('Ctrl Pts',(-34.779441328077,-57.1298124049937,20.6685144491949));
#28776=CARTESIAN_POINT('Ctrl Pts',(-34.4404282620852,-54.8311366011663,
20.5573765586268));
#28777=CARTESIAN_POINT('Ctrl Pts',(-32.711178041167,-54.0447560839335,20.4665135024078));
#28778=CARTESIAN_POINT('Ctrl Pts',(-31.7432006097017,-54.3588510380505,
20.4126964097114));
#28779=CARTESIAN_POINT('Ctrl Pts',(-31.4746836284317,-54.5147000883656,
20.3959252805377));
#28780=CARTESIAN_POINT('Ctrl Pts',(-31.4729484072307,-54.5150696468519,
21.1540747194623));
#28781=CARTESIAN_POINT('Ctrl Pts',(-31.2416713093181,-54.6470066065867,
21.1396821047934));
#28782=CARTESIAN_POINT('Ctrl Pts',(-30.5049700979161,-55.27079766484,21.0882435266019));
#28783=CARTESIAN_POINT('Ctrl Pts',(-30.2087196709518,-57.0968534624393,
20.9997589848876));
#28784=CARTESIAN_POINT('Ctrl Pts',(-31.9338196700205,-58.6533891775714,
20.8886210943196));
#28785=CARTESIAN_POINT('Ctrl Pts',(-34.1771709144469,-58.0482026788782,
20.7774832037515));
#28786=CARTESIAN_POINT('Ctrl Pts',(-34.8853786224564,-55.8352230845946,
20.6663453131835));
#28787=CARTESIAN_POINT('Ctrl Pts',(-33.4544940412401,-54.0938892869953,
20.5585424850871));
#28788=CARTESIAN_POINT('Ctrl Pts',(-32.0087745479626,-54.2040131588077,
20.4877856205134));
#28789=CARTESIAN_POINT('Ctrl Pts',(-31.4703419245392,-54.5103623955759,
20.4540747194623));
#28790=CARTESIAN_POINT('Origin',(-32.5,-56.2916512459885,23.5459252805377));
#28791=CARTESIAN_POINT('',(-31.4756555660462,-54.5128362942924,21.8540747194623));
#28792=CARTESIAN_POINT('',(-31.4704151231923,-54.5113563798656,21.7959252805377));
#28793=CARTESIAN_POINT('',(-31.4726249999999,-54.5121855475625,23.5459252805377));
#28794=CARTESIAN_POINT('',(-33.9541262883781,-54.8399232067374,22.));
#28795=CARTESIAN_POINT('Ctrl Pts',(-33.9541262883781,-54.8399232067375,
22.));
#28796=CARTESIAN_POINT('Ctrl Pts',(-33.4713921772736,-54.3563916207415,
21.9629540364773));
#28797=CARTESIAN_POINT('Ctrl Pts',(-32.5011748783928,-54.0682382375653,
21.9143122762981));
#28798=CARTESIAN_POINT('Ctrl Pts',(-31.6603808354702,-54.4043184181514,
21.8656705161189));
#28799=CARTESIAN_POINT('Ctrl Pts',(-31.4756555660462,-54.5128362942924,
21.8540747194623));
#28800=CARTESIAN_POINT('',(-34.4879501863793,-55.7574173922323,22.));
#28801=CARTESIAN_POINT('Origin',(-32.5,-56.2916512459885,22.));
#28802=CARTESIAN_POINT('Ctrl Pts',(-34.4879524958972,-55.7574168944053,
22.));
#28803=CARTESIAN_POINT('Ctrl Pts',(-34.3140194691063,-55.1135181402384,
21.9636770818144));
#28804=CARTESIAN_POINT('Ctrl Pts',(-33.3475254337068,-54.0782693974496,
21.895652175327));
#28805=CARTESIAN_POINT('Ctrl Pts',(-31.9778124788844,-54.224015012867,21.8276272688396));
#28806=CARTESIAN_POINT('Ctrl Pts',(-31.4704151231923,-54.5113563798656,
21.7959252805377));
#28807=CARTESIAN_POINT('Origin',(32.5,-56.2916512459885,17.));
#28808=CARTESIAN_POINT('',(31.665169034441,-54.8481104542883,13.8714803633902));
#28809=CARTESIAN_POINT('',(31.6668355785527,-54.8466294620446,13.6785196366098));
#28810=CARTESIAN_POINT('',(31.667,-54.8488529232837,17.));
#28811=CARTESIAN_POINT('',(31.4059736530044,-55.03520293743,13.));
#28812=CARTESIAN_POINT('Ctrl Pts',(31.6668355785527,-54.8466294620446,13.6785196366098));
#28813=CARTESIAN_POINT('Ctrl Pts',(31.7169359983484,-54.8172333383902,13.6746222055426));
#28814=CARTESIAN_POINT('Ctrl Pts',(31.7685916060498,-54.790608714332,13.6707247744754));
#28815=CARTESIAN_POINT('Ctrl Pts',(31.8215990010622,-54.7670212268678,13.6668273434082));
#28816=CARTESIAN_POINT('Ctrl Pts',(32.3254462758994,-54.5428168252686,13.6297813798856));
#28817=CARTESIAN_POINT('Ctrl Pts',(32.9514266195489,-54.5930156597359,13.5927354163629));
#28818=CARTESIAN_POINT('Ctrl Pts',(33.4130263160919,-54.8947720750738,13.5556894528402));
#28819=CARTESIAN_POINT('Ctrl Pts',(33.8746260126349,-55.1965284904116,13.5186434893175));
#28820=CARTESIAN_POINT('Ctrl Pts',(34.1718450620713,-55.74984248662,13.4815975257948));
#28821=CARTESIAN_POINT('Ctrl Pts',(34.1687200176701,-56.3012302340885,13.4445515622722));
#28822=CARTESIAN_POINT('Ctrl Pts',(34.165594973269,-56.852617981557,13.4075055987495));
#28823=CARTESIAN_POINT('Ctrl Pts',(33.8621258350302,-57.4020794802856,13.3704596352268));
#28824=CARTESIAN_POINT('Ctrl Pts',(33.397076207884,-57.6986656733008,13.3334136717041));
#28825=CARTESIAN_POINT('Ctrl Pts',(32.9320265807378,-57.9952518663159,13.2963677081814));
#28826=CARTESIAN_POINT('Ctrl Pts',(32.3053964646841,-58.0389627536177,13.2593217446588));
#28827=CARTESIAN_POINT('Ctrl Pts',(31.8042046430419,-57.8087421867188,13.2222757811361));
#28828=CARTESIAN_POINT('Ctrl Pts',(31.3030128213997,-57.5785216198199,13.1852298176134));
#28829=CARTESIAN_POINT('Ctrl Pts',(30.927259294169,-57.0743695987204,13.1481838540907));
#28830=CARTESIAN_POINT('Ctrl Pts',(30.8485497633826,-56.5294873752106,13.111137890568));
#28831=CARTESIAN_POINT('Ctrl Pts',(30.7698402325962,-55.9846051517008,13.0740919270453));
#28832=CARTESIAN_POINT('Ctrl Pts',(30.9881746982541,-55.3989927257807,13.0370459635227));
#28833=CARTESIAN_POINT('Ctrl Pts',(31.4059736530044,-55.03520293743,13.));
#28834=CARTESIAN_POINT('',(33.9184188470958,-55.4120275291385,13.));
#28835=CARTESIAN_POINT('Origin',(32.5,-56.2916512459885,13.));
#28836=CARTESIAN_POINT('',(31.6677099856842,-54.8513822049942,13.1714803633902));
#28837=CARTESIAN_POINT('Ctrl Pts',(33.9184205240577,-55.4120266023846,13.));
#28838=CARTESIAN_POINT('Ctrl Pts',(33.6328154176795,-54.952808667466,13.0363229181856));
#28839=CARTESIAN_POINT('Ctrl Pts',(33.102895030897,-54.644333384024,13.0726458363711));
#28840=CARTESIAN_POINT('Ctrl Pts',(32.5624622032656,-54.6241575874771,13.1089687545567));
#28841=CARTESIAN_POINT('Ctrl Pts',(32.2524345659016,-54.6125834302173,13.1298059575012));
#28842=CARTESIAN_POINT('Ctrl Pts',(31.9389473679306,-54.6958863393048,13.1506431604457));
#28843=CARTESIAN_POINT('Ctrl Pts',(31.6677099856842,-54.8513822049942,13.1714803633902));
#28844=CARTESIAN_POINT('',(31.667,-54.8488529232837,12.));
#28845=CARTESIAN_POINT('',(31.667,-54.8488529232837,17.));
#28846=CARTESIAN_POINT('Origin',(32.5,-56.2916512459885,12.));
#28847=CARTESIAN_POINT('Ctrl Pts',(31.6677099856842,-54.8513822049942,13.1714803633902));
#28848=CARTESIAN_POINT('Ctrl Pts',(31.4567209292169,-54.9723387107482,13.1876891239684));
#28849=CARTESIAN_POINT('Ctrl Pts',(31.2712968605907,-55.1369785326559,13.2038978845465));
#28850=CARTESIAN_POINT('Ctrl Pts',(31.1329525371814,-55.334624580881,13.2201066451247));
#28851=CARTESIAN_POINT('Ctrl Pts',(30.8167594060732,-55.7863548817662,13.2571526086474));
#28852=CARTESIAN_POINT('Ctrl Pts',(30.7464989755799,-56.4105013743272,13.2941985721701));
#28853=CARTESIAN_POINT('Ctrl Pts',(30.9545219587097,-56.9212436588756,13.3312445356927));
#28854=CARTESIAN_POINT('Ctrl Pts',(31.1625449418395,-57.4319859434239,13.3682904992154));
#28855=CARTESIAN_POINT('Ctrl Pts',(31.6488513385922,-57.8293240199595,13.4053364627381));
#28856=CARTESIAN_POINT('Ctrl Pts',(32.1907825642961,-57.9315018386831,13.4423824262608));
#28857=CARTESIAN_POINT('Ctrl Pts',(32.7327137899999,-58.0336796574068,13.4794283897835));
#28858=CARTESIAN_POINT('Ctrl Pts',(33.3302698446549,-57.8406972183184,13.5164743533061));
#28859=CARTESIAN_POINT('Ctrl Pts',(33.7100246193121,-57.4408300847799,13.5535203168288));
#28860=CARTESIAN_POINT('Ctrl Pts',(34.0897793939693,-57.0409629512413,13.5905662803515));
#28861=CARTESIAN_POINT('Ctrl Pts',(34.2517328886288,-56.4342111232524,13.6276122438742));
#28862=CARTESIAN_POINT('Ctrl Pts',(34.1217417856583,-55.8982799679713,13.6646582073969));
#28863=CARTESIAN_POINT('Ctrl Pts',(33.9917506826877,-55.3623488126902,13.7017041709196));
#28864=CARTESIAN_POINT('Ctrl Pts',(33.5698149820871,-54.8972383301169,13.7387501344422));
#28865=CARTESIAN_POINT('Ctrl Pts',(33.0490481303447,-54.7157980032898,13.7757960979649));
#28866=CARTESIAN_POINT('Ctrl Pts',(32.6006934475977,-54.5595867930335,13.8076908531067));
#28867=CARTESIAN_POINT('Ctrl Pts',(32.0790815152818,-54.6136422361013,13.8395856082484));
#28868=CARTESIAN_POINT('Ctrl Pts',(31.665169034441,-54.8481104542883,13.8714803633902));
#28869=CARTESIAN_POINT('Origin',(32.5,-56.2916512459885,17.));
#28870=CARTESIAN_POINT('',(31.667523968133,-54.8471109129233,14.5714803633902));
#28871=CARTESIAN_POINT('',(31.668865652917,-54.8504196807178,14.3785196366098));
#28872=CARTESIAN_POINT('',(31.667,-54.8488529232837,17.));
#28873=CARTESIAN_POINT('Ctrl Pts',(31.668865652917,-54.8504196807178,14.3785196366098));
#28874=CARTESIAN_POINT('Ctrl Pts',(31.8626626794392,-54.7373590837469,14.3635646533453));
#28875=CARTESIAN_POINT('Ctrl Pts',(32.0777548846389,-54.6619147081679,14.3486096700809));
#28876=CARTESIAN_POINT('Ctrl Pts',(32.2987508779934,-54.6350670487033,14.3336546868165));
#28877=CARTESIAN_POINT('Ctrl Pts',(32.8461944534029,-54.5685609620293,14.2966087232938));
#28878=CARTESIAN_POINT('Ctrl Pts',(33.4298657229247,-54.8002611998549,14.2595627597711));
#28879=CARTESIAN_POINT('Ctrl Pts',(33.7826437493636,-55.2241308285784,14.2225167962484));
#28880=CARTESIAN_POINT('Ctrl Pts',(34.1354217758025,-55.648000457302,14.1854708327258));
#28881=CARTESIAN_POINT('Ctrl Pts',(34.2573065591586,-56.2640394769235,14.1484248692031));
#28882=CARTESIAN_POINT('Ctrl Pts',(34.0925177799173,-56.7903101462248,14.1113789056804));
#28883=CARTESIAN_POINT('Ctrl Pts',(33.9277290006759,-57.3165808155261,14.0743329421577));
#28884=CARTESIAN_POINT('Ctrl Pts',(33.4762666588371,-57.7530831345071,14.037286978635));
#28885=CARTESIAN_POINT('Ctrl Pts',(32.9447431684491,-57.9000573283161,14.0002410151124));
#28886=CARTESIAN_POINT('Ctrl Pts',(32.4132196780611,-58.0470315221252,13.9631950515897));
#28887=CARTESIAN_POINT('Ctrl Pts',(31.8016350391239,-57.9044775907623,13.926149088067));
#28888=CARTESIAN_POINT('Ctrl Pts',(31.38988820532,-57.537620165814,13.8891031245443));
#28889=CARTESIAN_POINT('Ctrl Pts',(30.9781413715162,-57.1707627408657,13.8520571610216));
#28890=CARTESIAN_POINT('Ctrl Pts',(30.7662323428457,-56.5796018223321,13.815011197499));
#28891=CARTESIAN_POINT('Ctrl Pts',(30.8511349315229,-56.0347175442324,13.7779652339763));
#28892=CARTESIAN_POINT('Ctrl Pts',(30.9271053193521,-55.5471579706766,13.7448167015208));
#28893=CARTESIAN_POINT('Ctrl Pts',(31.2407201802287,-55.0966501403397,13.7116681690653));
#28894=CARTESIAN_POINT('Ctrl Pts',(31.6668355785527,-54.8466294620446,13.6785196366098));
#28895=CARTESIAN_POINT('Ctrl Pts',(31.665169034441,-54.8481104542883,13.8714803633902));
#28896=CARTESIAN_POINT('Ctrl Pts',(31.5983195028865,-54.8859785816721,13.8766315717711));
#28897=CARTESIAN_POINT('Ctrl Pts',(31.5342792394079,-54.92855265549,13.881782780152));
#28898=CARTESIAN_POINT('Ctrl Pts',(31.4738105761082,-54.9757069077013,13.886933988533));
#28899=CARTESIAN_POINT('Ctrl Pts',(31.0389378764983,-55.3148263100205,13.9239799520556));
#28900=CARTESIAN_POINT('Ctrl Pts',(30.7887904801626,-55.8908352857396,13.9610259155783));
#28901=CARTESIAN_POINT('Ctrl Pts',(30.83785280129,-56.4401173240505,13.998071879101));
#28902=CARTESIAN_POINT('Ctrl Pts',(30.8869151224174,-56.9893993623615,14.0351178426237));
#28903=CARTESIAN_POINT('Ctrl Pts',(31.2351871610079,-57.5119544632642,14.0721638061464));
#28904=CARTESIAN_POINT('Ctrl Pts',(31.7232787251799,-57.7686336889847,14.109209769669));
#28905=CARTESIAN_POINT('Ctrl Pts',(32.2113702893519,-58.0253129147052,14.1462557331917));
#28906=CARTESIAN_POINT('Ctrl Pts',(32.8392813791053,-58.0161162652435,14.1833016967144));
#28907=CARTESIAN_POINT('Ctrl Pts',(33.3196456823451,-57.74525195635,14.2203476602371));
#28908=CARTESIAN_POINT('Ctrl Pts',(33.8000099855849,-57.4743876474564,14.2573936237598));
#28909=CARTESIAN_POINT('Ctrl Pts',(34.1328275023111,-56.9418556791311,14.2944395872824));
#28910=CARTESIAN_POINT('Ctrl Pts',(34.1657820298073,-56.3913726675535,14.3314855508051));
#28911=CARTESIAN_POINT('Ctrl Pts',(34.1987365573035,-55.8408896559759,14.3685315143278));
#28912=CARTESIAN_POINT('Ctrl Pts',(33.9318280955697,-55.272455601146,14.4055774778505));
#28913=CARTESIAN_POINT('Ctrl Pts',(33.4872090049183,-54.9462174010392,14.4426234413732));
#28914=CARTESIAN_POINT('Ctrl Pts',(33.0425899142668,-54.6199792009323,14.4796694048958));
#28915=CARTESIAN_POINT('Ctrl Pts',(32.4202601946977,-54.5359368555486,14.5167153684185));
#28916=CARTESIAN_POINT('Ctrl Pts',(31.905032476641,-54.7325529059598,14.5537613319412));
#28917=CARTESIAN_POINT('Ctrl Pts',(31.8228882493844,-54.7638999646704,14.5596676757575));
#28918=CARTESIAN_POINT('Ctrl Pts',(31.7434664303385,-54.8023810331132,14.5655740195739));
#28919=CARTESIAN_POINT('Ctrl Pts',(31.667523968133,-54.8471109129233,14.5714803633902));
#28920=CARTESIAN_POINT('Origin',(32.5,-56.2916512459885,17.));
#28921=CARTESIAN_POINT('',(31.6686398531931,-54.8509327367609,15.2714803633902));
#28922=CARTESIAN_POINT('',(31.6662678127889,-54.8504473245041,15.0785196366098));
#28923=CARTESIAN_POINT('',(31.667,-54.8488529232837,17.));
#28924=CARTESIAN_POINT('Ctrl Pts',(31.6662678127889,-54.8504473245041,15.0785196366098));
#28925=CARTESIAN_POINT('Ctrl Pts',(32.0051837911952,-54.6584589297703,15.0525071011481));
#28926=CARTESIAN_POINT('Ctrl Pts',(32.4124263355195,-54.5807898609867,15.0264945656864));
#28927=CARTESIAN_POINT('Ctrl Pts',(32.7936098272491,-54.6489198132192,15.0004820302247));
#28928=CARTESIAN_POINT('Ctrl Pts',(33.3364753910795,-54.745947637705,14.9634360667021));
#28929=CARTESIAN_POINT('Ctrl Pts',(33.8264872979809,-55.138688877304,14.9263901031794));
#28930=CARTESIAN_POINT('Ctrl Pts',(34.0393888128715,-55.6474033077565,14.8893441396567));
#28931=CARTESIAN_POINT('Ctrl Pts',(34.2522903277622,-56.156117738209,14.852298176134));
#28932=CARTESIAN_POINT('Ctrl Pts',(34.1880814506421,-56.7808053595149,14.8152522126113));
#28933=CARTESIAN_POINT('Ctrl Pts',(33.8761477528874,-57.2355742774498,14.7782062490887));
#28934=CARTESIAN_POINT('Ctrl Pts',(33.5642140551328,-57.6903431953847,14.741160285566));
#28935=CARTESIAN_POINT('Ctrl Pts',(33.0045555367437,-57.9751934099486,14.7041143220433));
#28936=CARTESIAN_POINT('Ctrl Pts',(32.4533030627753,-57.959761729544,14.6670683585206));
#28937=CARTESIAN_POINT('Ctrl Pts',(31.9020505888069,-57.9443300491395,14.6300223949979));
#28938=CARTESIAN_POINT('Ctrl Pts',(31.3592041592591,-57.6286164737664,14.5929764314753));
#28939=CARTESIAN_POINT('Ctrl Pts',(31.0732005795316,-57.1571088626351,14.5559304679526));
#28940=CARTESIAN_POINT('Ctrl Pts',(30.787196999804,-56.6856012515039,14.5188845044299));
#28941=CARTESIAN_POINT('Ctrl Pts',(30.7580362698966,-56.0582996046144,14.4818385409072));
#28942=CARTESIAN_POINT('Ctrl Pts',(30.9990638455916,-55.5622925755828,14.4447925773845));
#28943=CARTESIAN_POINT('Ctrl Pts',(31.142791661258,-55.2665172617734,14.4227015971263));
#28944=CARTESIAN_POINT('Ctrl Pts',(31.3825954370759,-55.0174288556201,14.400610616868));
#28945=CARTESIAN_POINT('Ctrl Pts',(31.668865652917,-54.8504196807178,14.3785196366098));
#28946=CARTESIAN_POINT('Ctrl Pts',(31.667523968133,-54.8471109129233,14.5714803633902));
#28947=CARTESIAN_POINT('Ctrl Pts',(31.2671376265686,-55.0829372532297,14.6026199830965));
#28948=CARTESIAN_POINT('Ctrl Pts',(30.9634650148059,-55.4924582968625,14.6337596028029));
#28949=CARTESIAN_POINT('Ctrl Pts',(30.8674364226636,-55.9459488454016,14.6648992225092));
#28950=CARTESIAN_POINT('Ctrl Pts',(30.7531938032872,-56.4854542882262,14.7019451860319));
#28951=CARTESIAN_POINT('Ctrl Pts',(30.9328342810787,-57.0871907276693,14.7389911495546));
#28952=CARTESIAN_POINT('Ctrl Pts',(31.3241443491424,-57.4757700913936,14.7760371130773));
#28953=CARTESIAN_POINT('Ctrl Pts',(31.715454417206,-57.8643494551178,14.8130830766));
#28954=CARTESIAN_POINT('Ctrl Pts',(32.3184340755416,-58.0397717431231,14.8501290401227));
#28955=CARTESIAN_POINT('Ctrl Pts',(32.8571262761764,-57.9217539399754,14.8871750036453));
#28956=CARTESIAN_POINT('Ctrl Pts',(33.3958184768112,-57.8037361368278,14.924220967168));
#28957=CARTESIAN_POINT('Ctrl Pts',(33.8702232197451,-57.3922782425271,14.9612669306907));
#28958=CARTESIAN_POINT('Ctrl Pts',(34.063226478426,-56.8756863008287,14.9983128942134));
#28959=CARTESIAN_POINT('Ctrl Pts',(34.2562297371068,-56.3590943591303,15.0353588577361));
#28960=CARTESIAN_POINT('Ctrl Pts',(34.1678315115345,-55.7373683700341,15.0724048212587));
#28961=CARTESIAN_POINT('Ctrl Pts',(33.8384877538371,-55.2950447552267,15.1094507847814));
#28962=CARTESIAN_POINT('Ctrl Pts',(33.5091439961397,-54.8527211404193,15.1464967483041));
#28963=CARTESIAN_POINT('Ctrl Pts',(32.9388547063171,-54.5897998999006,15.1835427118268));
#28964=CARTESIAN_POINT('Ctrl Pts',(32.3886160101468,-54.6266084315825,15.2205886753495));
#28965=CARTESIAN_POINT('Ctrl Pts',(32.1366535522459,-54.6434636040356,15.237552571363));
#28966=CARTESIAN_POINT('Ctrl Pts',(31.8888954229186,-54.7231679104083,15.2545164673766));
#28967=CARTESIAN_POINT('Ctrl Pts',(31.6686398531931,-54.8509327367609,15.2714803633902));
#28968=CARTESIAN_POINT('Origin',(32.5,-56.2916512459885,17.));
#28969=CARTESIAN_POINT('',(31.6657545866042,-54.8497426695209,15.9714803633902));
#28970=CARTESIAN_POINT('',(31.6656238197277,-54.8464558867275,15.7785196366098));
#28971=CARTESIAN_POINT('',(31.667,-54.8488529232837,17.));
#28972=CARTESIAN_POINT('Ctrl Pts',(31.6656238265237,-54.8464558985647,15.7785196366098));
#28973=CARTESIAN_POINT('Ctrl Pts',(32.1435040363299,-54.5705135726953,15.7414495489508));
#28974=CARTESIAN_POINT('Ctrl Pts',(32.7717977196734,-54.5551568083656,15.7043794612919));
#28975=CARTESIAN_POINT('Ctrl Pts',(33.2626292375688,-54.8073433428058,15.667309373633));
#28976=CARTESIAN_POINT('Ctrl Pts',(33.7531413365699,-55.0593657615749,15.6302634101103));
#28977=CARTESIAN_POINT('Ctrl Pts',(34.1063700665184,-55.5785832727215,15.5932174465876));
#28978=CARTESIAN_POINT('Ctrl Pts',(34.1606582960961,-56.1273730385891,15.5561714830649));
#28979=CARTESIAN_POINT('Ctrl Pts',(34.2149465256738,-56.6761628044566,15.5191255195423));
#28980=CARTESIAN_POINT('Ctrl Pts',(33.9702942548808,-57.254524825045,15.4820795560196));
#28981=CARTESIAN_POINT('Ctrl Pts',(33.5386679829465,-57.5977684411295,15.4450335924969));
#28982=CARTESIAN_POINT('Ctrl Pts',(33.1070417110123,-57.941012057214,15.4079876289742));
#28983=CARTESIAN_POINT('Ctrl Pts',(32.4884414379368,-58.0491372687946,15.3709416654515));
#28984=CARTESIAN_POINT('Ctrl Pts',(31.9659730859382,-57.8726599616146,15.3338957019289));
#28985=CARTESIAN_POINT('Ctrl Pts',(31.4435047339395,-57.6961826544346,15.2968497384062));
#28986=CARTESIAN_POINT('Ctrl Pts',(31.0171683030177,-57.235102828494,15.2598037748835));
#28987=CARTESIAN_POINT('Ctrl Pts',(30.8820790791908,-56.7004362767628,15.2227578113608));
#28988=CARTESIAN_POINT('Ctrl Pts',(30.7469898553639,-56.1657697250317,15.1857118478381));
#28989=CARTESIAN_POINT('Ctrl Pts',(30.9031478386319,-55.5575164475099,15.1486658843155));
#28990=CARTESIAN_POINT('Ctrl Pts',(31.2790864406456,-55.1540470134354,15.1116199207928));
#28991=CARTESIAN_POINT('Ctrl Pts',(31.391052526185,-55.0338813988213,15.1005864927318));
#28992=CARTESIAN_POINT('Ctrl Pts',(31.5225138495514,-54.931880760509,15.0895530646708));
#28993=CARTESIAN_POINT('Ctrl Pts',(31.6662678127889,-54.8504473245041,15.0785196366098));
#28994=CARTESIAN_POINT('Ctrl Pts',(31.6686398531931,-54.8509327367609,15.2714803633902));
#28995=CARTESIAN_POINT('Ctrl Pts',(31.4078986168085,-55.0021823003073,15.2915624308993));
#28996=CARTESIAN_POINT('Ctrl Pts',(31.185699780635,-55.2207844238422,15.3116444984084));
#28997=CARTESIAN_POINT('Ctrl Pts',(31.0406952948155,-55.4822046794948,15.3317265659175));
#28998=CARTESIAN_POINT('Ctrl Pts',(30.7732013781725,-55.9644540918428,15.3687725294402));
#28999=CARTESIAN_POINT('Ctrl Pts',(30.7684016474046,-56.5924146126563,15.4058184929629));
#29000=CARTESIAN_POINT('Ctrl Pts',(31.0284927261471,-57.0786965491371,15.4428644564855));
#29001=CARTESIAN_POINT('Ctrl Pts',(31.2885838048897,-57.5649784856179,15.4799104200082));
#29002=CARTESIAN_POINT('Ctrl Pts',(31.8135656931426,-57.9095818377658,15.5169563835309));
#29003=CARTESIAN_POINT('Ctrl Pts',(32.3631774530806,-57.9547969272716,15.5540023470536));
#29004=CARTESIAN_POINT('Ctrl Pts',(32.9127892130185,-58.0000120167774,15.5910483105763));
#29005=CARTESIAN_POINT('Ctrl Pts',(33.4870308446415,-57.7458388436409,15.6280942740989));
#29006=CARTESIAN_POINT('Ctrl Pts',(33.8230974089741,-57.3086012018905,15.6651402376216));
#29007=CARTESIAN_POINT('Ctrl Pts',(34.1591639733067,-56.8713635601401,15.7021862011443));
#29008=CARTESIAN_POINT('Ctrl Pts',(34.2570554703489,-56.2510614497756,15.739232164667));
#29009=CARTESIAN_POINT('Ctrl Pts',(34.0719713014427,-55.7315796489166,15.7762781281897));
#29010=CARTESIAN_POINT('Ctrl Pts',(33.8868871325364,-55.2120978480575,15.8133240917123));
#29011=CARTESIAN_POINT('Ctrl Pts',(33.4188272976816,-54.7934363567037,15.850370055235));
#29012=CARTESIAN_POINT('Ctrl Pts',(32.8820020343565,-54.667197980366,15.8874160187577));
#29013=CARTESIAN_POINT('Ctrl Pts',(32.475949123752,-54.5717116766395,15.9154374669685));
#29014=CARTESIAN_POINT('Ctrl Pts',(32.03055302792,-54.6435311984541,15.9434589151794));
#29015=CARTESIAN_POINT('Ctrl Pts',(31.6657545866042,-54.8497426695209,15.9714803633902));
#29016=CARTESIAN_POINT('Origin',(32.5,-56.2916512459885,17.));
#29017=CARTESIAN_POINT('',(31.6662054032747,-54.8463759356941,16.6714803633902));
#29018=CARTESIAN_POINT('',(31.6687530214682,-54.849035096929,16.4785196366098));
#29019=CARTESIAN_POINT('',(31.667,-54.8488529232837,17.));
#29020=CARTESIAN_POINT('Ctrl Pts',(31.6687530214682,-54.849035096929,16.4785196366098));
#29021=CARTESIAN_POINT('Ctrl Pts',(31.8117829954435,-54.7648928865345,16.4674379602763));
#29022=CARTESIAN_POINT('Ctrl Pts',(31.966578267799,-54.7018565467284,16.4563562839428));
#29023=CARTESIAN_POINT('Ctrl Pts',(32.127375662283,-54.6650214760003,16.4452746076093));
#29024=CARTESIAN_POINT('Ctrl Pts',(32.6649201845491,-54.5418821020028,16.4082286440866));
#29025=CARTESIAN_POINT('Ctrl Pts',(33.2695420256081,-54.7115576426435,16.3711826805639));
#29026=CARTESIAN_POINT('Ctrl Pts',(33.6645325714613,-55.0963951246187,16.3341367170412));
#29027=CARTESIAN_POINT('Ctrl Pts',(34.0595231173144,-55.4812326065939,16.2970907535186));
#29028=CARTESIAN_POINT('Ctrl Pts',(34.2448823679617,-56.0812320299036,16.2600447899959));
#29029=CARTESIAN_POINT('Ctrl Pts',(34.1357796112842,-56.6218002562495,16.2229988264732));
#29030=CARTESIAN_POINT('Ctrl Pts',(34.0266768546067,-57.1623684825954,16.1859528629505));
#29031=CARTESIAN_POINT('Ctrl Pts',(33.6231120906044,-57.6435055119775,16.1489068994278));
#29032=CARTESIAN_POINT('Ctrl Pts',(33.1097790218944,-57.8450162546516,16.1118609359052));
#29033=CARTESIAN_POINT('Ctrl Pts',(32.5964459531844,-58.0465269973256,16.0748149723825));
#29034=CARTESIAN_POINT('Ctrl Pts',(31.9733445797666,-57.9684114532915,16.0377690088598));
#29035=CARTESIAN_POINT('Ctrl Pts',(31.5256407784037,-57.646419644252,16.0007230453371));
#29036=CARTESIAN_POINT('Ctrl Pts',(31.0779369770408,-57.3244278352124,15.9636770818144));
#29037=CARTESIAN_POINT('Ctrl Pts',(30.8056307477328,-56.7585597611673,15.9266311182918));
#29038=CARTESIAN_POINT('Ctrl Pts',(30.833344580418,-56.2077881548333,15.8895851547691));
#29039=CARTESIAN_POINT('Ctrl Pts',(30.8610403660015,-55.6573752080674,15.8525633153826));
#29040=CARTESIAN_POINT('Ctrl Pts',(31.188365597836,-55.1220390739338,15.8155414759962));
#29041=CARTESIAN_POINT('Ctrl Pts',(31.6656238265237,-54.8464558985647,15.7785196366098));
#29042=CARTESIAN_POINT('Ctrl Pts',(31.6657545866042,-54.8497426695209,15.9714803633902));
#29043=CARTESIAN_POINT('Ctrl Pts',(31.5482685418209,-54.9161546038406,15.9805048787021));
#29044=CARTESIAN_POINT('Ctrl Pts',(31.4391421648863,-54.9965058030685,15.9895293940139));
#29045=CARTESIAN_POINT('Ctrl Pts',(31.3423819730146,-55.089696808403,15.9985539093258));
#29046=CARTESIAN_POINT('Ctrl Pts',(30.9451778667933,-55.4722492740994,16.0355998728484));
#29047=CARTESIAN_POINT('Ctrl Pts',(30.756360346146,-56.0711694668139,16.0726458363711));
#29048=CARTESIAN_POINT('Ctrl Pts',(30.8623428200595,-56.6123581642474,16.1096917998938));
#29049=CARTESIAN_POINT('Ctrl Pts',(30.9683252939729,-57.1535468616808,16.1467377634165));
#29050=CARTESIAN_POINT('Ctrl Pts',(31.3691077624471,-57.6370040638332,16.1837837269392));
#29051=CARTESIAN_POINT('Ctrl Pts',(31.8812698561966,-57.8414728407482,16.2208296904618));
#29052=CARTESIAN_POINT('Ctrl Pts',(32.393431949946,-58.0459416176631,16.2578756539845));
#29053=CARTESIAN_POINT('Ctrl Pts',(33.0169736689706,-57.9714219693406,16.2949216175072));
#29054=CARTESIAN_POINT('Ctrl Pts',(33.4665276098354,-57.6520182353919,16.3319675810299));
#29055=CARTESIAN_POINT('Ctrl Pts',(33.9160815507002,-57.3326145014432,16.3690135445526));
#29056=CARTESIAN_POINT('Ctrl Pts',(34.1916477134051,-56.7683266818682,16.4060595080752));
#29057=CARTESIAN_POINT('Ctrl Pts',(34.1671116810225,-56.2174042970244,16.4431054715979));
#29058=CARTESIAN_POINT('Ctrl Pts',(34.14257564864,-55.6664819121806,16.4801514351206));
#29059=CARTESIAN_POINT('Ctrl Pts',(33.8179374211699,-55.128924962068,16.5171973986433));
#29060=CARTESIAN_POINT('Ctrl Pts',(33.3417695242377,-54.8507494330611,16.554243362166));
#29061=CARTESIAN_POINT('Ctrl Pts',(32.8656016273054,-54.5725739040543,16.5912893256886));
#29062=CARTESIAN_POINT('Ctrl Pts',(32.237904060911,-54.5537797961531,16.6283352892113));
#29063=CARTESIAN_POINT('Ctrl Pts',(31.7459461756022,-54.8029683394084,16.665381252734));
#29064=CARTESIAN_POINT('Ctrl Pts',(31.7189481323124,-54.8166434999842,16.6674142896194));
#29065=CARTESIAN_POINT('Ctrl Pts',(31.6923588934129,-54.8311257383684,16.6694473265048));
#29066=CARTESIAN_POINT('Ctrl Pts',(31.6662054032747,-54.8463759356941,16.6714803633902));
#29067=CARTESIAN_POINT('Origin',(32.5,-56.2916512459885,17.));
#29068=CARTESIAN_POINT('',(31.6689051738235,-54.8497998491797,17.3714803633902));
#29069=CARTESIAN_POINT('',(31.6674096068672,-54.8512474102517,17.1785196366098));
#29070=CARTESIAN_POINT('',(31.667,-54.8488529232837,17.));
#29071=CARTESIAN_POINT('Ctrl Pts',(31.6674096068672,-54.8512474102517,17.1785196366098));
#29072=CARTESIAN_POINT('Ctrl Pts',(31.9558120832459,-54.6864945235477,17.156380408079));
#29073=CARTESIAN_POINT('Ctrl Pts',(32.2922890124972,-54.603384940747,17.1342411795483));
#29074=CARTESIAN_POINT('Ctrl Pts',(32.6209875748239,-54.6272788981025,17.1121019510175));
#29075=CARTESIAN_POINT('Ctrl Pts',(33.1710047054117,-54.6672610804705,17.0750559874949));
#29076=CARTESIAN_POINT('Ctrl Pts',(33.6992424692083,-55.0068523416602,17.0380100239722));
#29077=CARTESIAN_POINT('Ctrl Pts',(33.9639498583003,-55.4906368153746,17.0009640604495));
#29078=CARTESIAN_POINT('Ctrl Pts',(34.2286572473923,-55.974421289089,16.9639180969268));
#29079=CARTESIAN_POINT('Ctrl Pts',(34.2298342617796,-56.6023989753281,16.9268721334041));
#29080=CARTESIAN_POINT('Ctrl Pts',(33.9669422341538,-57.087172325109,16.8898261698815));
#29081=CARTESIAN_POINT('Ctrl Pts',(33.704050206528,-57.57194567489,16.8527802063588));
#29082=CARTESIAN_POINT('Ctrl Pts',(33.1770891368891,-57.9135146882128,16.8157342428361));
#29083=CARTESIAN_POINT('Ctrl Pts',(32.6272257468299,-57.955558369302,16.7786882793134));
#29084=CARTESIAN_POINT('Ctrl Pts',(32.0773623567706,-57.9976020503912,16.7416423157907));
#29085=CARTESIAN_POINT('Ctrl Pts',(31.504596646291,-57.7401203992468,16.704596352268));
#29086=CARTESIAN_POINT('Ctrl Pts',(31.1710580905944,-57.3009513535357,16.6675503887454));
#29087=CARTESIAN_POINT('Ctrl Pts',(30.8375195348978,-56.8617823078247,16.6305044252227));
#29088=CARTESIAN_POINT('Ctrl Pts',(30.7432081339843,-56.240925867547,16.5934584617));
#29089=CARTESIAN_POINT('Ctrl Pts',(30.9312860352641,-55.7225205030903,16.5564124981773));
#29090=CARTESIAN_POINT('Ctrl Pts',(31.0631035985939,-55.3591873762591,16.5304482109881));
#29091=CARTESIAN_POINT('Ctrl Pts',(31.333634830935,-55.0461796849558,16.504483923799));
#29092=CARTESIAN_POINT('Ctrl Pts',(31.6687530214682,-54.849035096929,16.4785196366098));
#29093=CARTESIAN_POINT('Ctrl Pts',(31.6662054032747,-54.8463759356941,16.6714803633902));
#29094=CARTESIAN_POINT('Ctrl Pts',(31.215790441256,-55.1090145744741,16.7064932900275));
#29095=CARTESIAN_POINT('Ctrl Pts',(30.894617122853,-55.5994272993444,16.7415062166648));
#29096=CARTESIAN_POINT('Ctrl Pts',(30.84031684399,-56.1177955929609,16.776519143302));
#29097=CARTESIAN_POINT('Ctrl Pts',(30.7828636019098,-56.6662631088463,16.8135651068247));
#29098=CARTESIAN_POINT('Ctrl Pts',(31.0241753219725,-57.2460269462057,16.8506110703474));
#29099=CARTESIAN_POINT('Ctrl Pts',(31.4538143271609,-57.5917548973867,16.8876570338701));
#29100=CARTESIAN_POINT('Ctrl Pts',(31.8834533323493,-57.9374828485678,16.9247029973928));
#29101=CARTESIAN_POINT('Ctrl Pts',(32.5014196226634,-58.0491749135707,16.9617489609154));
#29102=CARTESIAN_POINT('Ctrl Pts',(33.0248974212338,-57.8757145855097,16.9987949244381));
#29103=CARTESIAN_POINT('Ctrl Pts',(33.5483752198042,-57.7022542574486,17.0358408879608));
#29104=CARTESIAN_POINT('Ctrl Pts',(33.9773645266309,-57.2436415363237,17.0728868514835));
#29105=CARTESIAN_POINT('Ctrl Pts',(34.1155359529098,-56.7097631344687,17.1099328150062));
#29106=CARTESIAN_POINT('Ctrl Pts',(34.2537073791887,-56.1758847326138,17.1469787785289));
#29107=CARTESIAN_POINT('Ctrl Pts',(34.1010609249198,-55.5667406500288,17.1840247420515));
#29108=CARTESIAN_POINT('Ctrl Pts',(33.7274561054635,-55.1611091301907,17.2210707055742));
#29109=CARTESIAN_POINT('Ctrl Pts',(33.3538512860073,-54.7554776103525,17.2581166690969));
#29110=CARTESIAN_POINT('Ctrl Pts',(32.7592881013637,-54.5533586532611,17.2951626326196));
#29111=CARTESIAN_POINT('Ctrl Pts',(32.2158717643875,-54.6472531457219,17.3322085961422));
#29112=CARTESIAN_POINT('Ctrl Pts',(32.0238497654509,-54.6804317730554,17.3452991852249));
#29113=CARTESIAN_POINT('Ctrl Pts',(31.8382141569135,-54.7505717682631,17.3583897743076));
#29114=CARTESIAN_POINT('Ctrl Pts',(31.6689051738235,-54.8497998491797,17.3714803633902));
#29115=CARTESIAN_POINT('Origin',(32.5,-56.2916512459885,17.));
#29116=CARTESIAN_POINT('',(31.6668097556407,-54.850936308364,18.0714803633902));
#29117=CARTESIAN_POINT('',(31.6651356431699,-54.8475732381353,17.8785196366098));
#29118=CARTESIAN_POINT('',(31.667,-54.8488529232837,17.));
#29119=CARTESIAN_POINT('Ctrl Pts',(31.6651356431699,-54.8475732381353,17.8785196366098));
#29120=CARTESIAN_POINT('Ctrl Pts',(32.0953114189421,-54.6031821110332,17.8453228558818));
#29121=CARTESIAN_POINT('Ctrl Pts',(32.6432818971092,-54.5571637547426,17.8121260751538));
#29122=CARTESIAN_POINT('Ctrl Pts',(33.1039518347459,-54.7360113496833,17.7789292944258));
#29123=CARTESIAN_POINT('Ctrl Pts',(33.6180366746439,-54.9355964098306,17.7418833309031));
#29124=CARTESIAN_POINT('Ctrl Pts',(34.0234021807399,-55.4152172665964,17.7048373673804));
#29125=CARTESIAN_POINT('Ctrl Pts',(34.1345305305902,-55.9553727152466,17.6677914038577));
#29126=CARTESIAN_POINT('Ctrl Pts',(34.2456588804404,-56.4955281638969,17.6307454403351));
#29127=CARTESIAN_POINT('Ctrl Pts',(34.062550074045,-57.0962182044316,17.5936994768124));
#29128=CARTESIAN_POINT('Ctrl Pts',(33.6690048949483,-57.4825336336559,17.5566535132897));
#29129=CARTESIAN_POINT('Ctrl Pts',(33.2754597158515,-57.8688490628802,17.519607549767));
#29130=CARTESIAN_POINT('Ctrl Pts',(32.6714781640536,-58.0407898807941,17.4825615862443));
#29131=CARTESIAN_POINT('Ctrl Pts',(32.133475821543,-57.9196663971084,17.4455156227217));
#29132=CARTESIAN_POINT('Ctrl Pts',(31.5954734790324,-57.7985429134228,17.408469659199));
#29133=CARTESIAN_POINT('Ctrl Pts',(31.1234503458092,-57.3843551281377,17.3714236956763));
#29134=CARTESIAN_POINT('Ctrl Pts',(30.9334304853463,-56.8666584297933,17.3343777321536));
#29135=CARTESIAN_POINT('Ctrl Pts',(30.7434106248833,-56.348961731449,17.2973317686309));
#29136=CARTESIAN_POINT('Ctrl Pts',(30.8353940371805,-55.7277561200454,17.2602858051083));
#29137=CARTESIAN_POINT('Ctrl Pts',(31.1672839920187,-55.2873398661168,17.2232398415856));
#29138=CARTESIAN_POINT('Ctrl Pts',(31.3008314863423,-55.1101230316988,17.2083331065936));
#29139=CARTESIAN_POINT('Ctrl Pts',(31.4732231075307,-54.9621784491468,17.1934263716017));
#29140=CARTESIAN_POINT('Ctrl Pts',(31.6674096068672,-54.8512474102517,17.1785196366098));
#29141=CARTESIAN_POINT('Ctrl Pts',(31.6689051738235,-54.8497998491797,17.3714803633902));
#29142=CARTESIAN_POINT('Ctrl Pts',(31.3590749545435,-55.0313841780677,17.3954357378302));
#29143=CARTESIAN_POINT('Ctrl Pts',(31.1039191289866,-55.3103783149914,17.4193911122703));
#29144=CARTESIAN_POINT('Ctrl Pts',(30.9643532196009,-55.6385333911701,17.4433464867103));
#29145=CARTESIAN_POINT('Ctrl Pts',(30.7485205010994,-56.1460112021445,17.480392450233));
#29146=CARTESIAN_POINT('Ctrl Pts',(30.8091245534053,-56.7710588820805,17.5174384137557));
#29147=CARTESIAN_POINT('Ctrl Pts',(31.1184295883325,-57.2276198159938,17.5544843772783));
#29148=CARTESIAN_POINT('Ctrl Pts',(31.4277346232597,-57.6841807499072,17.591530340801));
#29149=CARTESIAN_POINT('Ctrl Pts',(31.9857406408081,-57.9722549377979,17.6285763043237));
#29150=CARTESIAN_POINT('Ctrl Pts',(32.5370730229374,-57.9600035940862,17.6656222678464));
#29151=CARTESIAN_POINT('Ctrl Pts',(33.0884054050668,-57.9477522503744,17.7026682313691));
#29152=CARTESIAN_POINT('Ctrl Pts',(33.633064151777,-57.6351753750602,17.7397141948917));
#29153=CARTESIAN_POINT('Ctrl Pts',(33.921783099211,-57.1653255475623,17.7767601584144));
#29154=CARTESIAN_POINT('Ctrl Pts',(34.2105020466451,-56.6954757200645,17.8138061219371));
#29155=CARTESIAN_POINT('Ctrl Pts',(34.2432811948029,-56.0683529403831,17.8508520854598));
#29156=CARTESIAN_POINT('Ctrl Pts',(34.0051189806597,-55.5709635046674,17.8878980489825));
#29157=CARTESIAN_POINT('Ctrl Pts',(33.7669567665165,-55.0735740689518,17.9249440125051));
#29158=CARTESIAN_POINT('Ctrl Pts',(33.2578531900722,-54.7059179772018,17.9619899760278));
#29159=CARTESIAN_POINT('Ctrl Pts',(32.7108023899003,-54.6362551245587,17.9990359395505));
#29160=CARTESIAN_POINT('Ctrl Pts',(32.3542113134731,-54.5908459018628,18.0231840808304));
#29161=CARTESIAN_POINT('Ctrl Pts',(31.9814965026905,-54.6720536844457,18.0473322221103));
#29162=CARTESIAN_POINT('Ctrl Pts',(31.6668097556407,-54.850936308364,18.0714803633902));
#29163=CARTESIAN_POINT('Origin',(32.5,-56.2916512459885,17.));
#29164=CARTESIAN_POINT('',(31.6652761166364,-54.8468682178695,18.7714803633902));
#29165=CARTESIAN_POINT('',(31.6679260143736,-54.8475393267799,18.5785196366098));
#29166=CARTESIAN_POINT('',(31.667,-54.8488529232837,17.));
#29167=CARTESIAN_POINT('Ctrl Pts',(31.6679260143736,-54.8475393267799,18.5785196366098));
#29168=CARTESIAN_POINT('Ctrl Pts',(31.7606663811943,-54.7928563701909,18.5713112672072));
#29169=CARTESIAN_POINT('Ctrl Pts',(31.8585183363754,-54.7473751127228,18.5641028978046));
#29170=CARTESIAN_POINT('Ctrl Pts',(31.9600503104883,-54.7126554770058,18.5568945284021));
#29171=CARTESIAN_POINT('Ctrl Pts',(32.4818534533783,-54.5342208981906,18.5198485648794));
#29172=CARTESIAN_POINT('Ctrl Pts',(33.1008546957744,-54.6400264825866,18.4828026013567));
#29173=CARTESIAN_POINT('Ctrl Pts',(33.533764609118,-54.9816497045372,18.445756637834));
#29174=CARTESIAN_POINT('Ctrl Pts',(33.9666745224615,-55.3232729264878,18.4087106743114));
#29175=CARTESIAN_POINT('Ctrl Pts',(34.2134931067525,-55.9007137859928,18.3716647107887));
#29176=CARTESIAN_POINT('Ctrl Pts',(34.1612624373338,-56.4497031993872,18.334618747266));
#29177=CARTESIAN_POINT('Ctrl Pts',(34.109031767915,-56.9986926127816,18.2975727837433));
#29178=CARTESIAN_POINT('Ctrl Pts',(33.7577518447865,-57.5192305800653,18.2605268202206));
#29179=CARTESIAN_POINT('Ctrl Pts',(33.2681879166606,-57.7730899488602,18.223480856698));
#29180=CARTESIAN_POINT('Ctrl Pts',(32.7786239885346,-58.026949317655,18.1864348931753));
#29181=CARTESIAN_POINT('Ctrl Pts',(32.1507760554113,-58.0141300879609,18.1493889296526));
#29182=CARTESIAN_POINT('Ctrl Pts',(31.6719822840244,-57.7404990529372,18.1123429661299));
#29183=CARTESIAN_POINT('Ctrl Pts',(31.1931885126375,-57.4668680179136,18.0752970026072));
#29184=CARTESIAN_POINT('Ctrl Pts',(30.863448902987,-56.9324251775604,18.0382510390845));
#29185=CARTESIAN_POINT('Ctrl Pts',(30.8336706571802,-56.3817613282625,18.0012050755619));
#29186=CARTESIAN_POINT('Ctrl Pts',(30.8038924113734,-55.8310974789645,17.9641591120392));
#29187=CARTESIAN_POINT('Ctrl Pts',(31.0740755294104,-55.2642126207216,17.9271131485165));
#29188=CARTESIAN_POINT('Ctrl Pts',(31.520569175279,-54.9405448233645,17.8900671849938));
#29189=CARTESIAN_POINT('Ctrl Pts',(31.5669611569199,-54.9069148027547,17.8862180021991));
#29190=CARTESIAN_POINT('Ctrl Pts',(31.6152565537377,-54.875910507623,17.8823688194045));
#29191=CARTESIAN_POINT('Ctrl Pts',(31.6651356431699,-54.8475732381353,17.8785196366098));
#29192=CARTESIAN_POINT('Ctrl Pts',(31.6668097556407,-54.850936308364,18.0714803633902));
#29193=CARTESIAN_POINT('Ctrl Pts',(31.4987316547814,-54.9464797400044,18.084378185633));
#29194=CARTESIAN_POINT('Ctrl Pts',(31.3472075724787,-55.0698874675039,18.0972760078758));
#29195=CARTESIAN_POINT('Ctrl Pts',(31.2235359810034,-55.2167495878635,18.1101738301185));
#29196=CARTESIAN_POINT('Ctrl Pts',(30.8683183961781,-55.6385765173477,18.1472197936412));
#29197=CARTESIAN_POINT('Ctrl Pts',(30.7428812504271,-56.2538999898523,18.1842657571639));
#29198=CARTESIAN_POINT('Ctrl Pts',(30.9046315647805,-56.7811137290641,18.2213117206866));
#29199=CARTESIAN_POINT('Ctrl Pts',(31.066381879134,-57.3083274682759,18.2583576842093));
#29200=CARTESIAN_POINT('Ctrl Pts',(31.5153196535918,-57.7474314741949,18.2954036477319));
#29201=CARTESIAN_POINT('Ctrl Pts',(32.0459859700228,-57.8974673086234,18.3324496112546));
#29202=CARTESIAN_POINT('Ctrl Pts',(32.5766522864537,-58.0475031430519,18.3694955747773));
#29203=CARTESIAN_POINT('Ctrl Pts',(33.1890471448577,-57.9084708059901,18.4065415383));
#29204=CARTESIAN_POINT('Ctrl Pts',(33.602904565772,-57.5439992348605,18.4435875018227));
#29205=CARTESIAN_POINT('Ctrl Pts',(34.0167619866863,-57.179527663731,18.4806334653453));
#29206=CARTESIAN_POINT('Ctrl Pts',(34.2320819701108,-56.5896168585339,18.517679428868));
#29207=CARTESIAN_POINT('Ctrl Pts',(34.1503221046824,-56.0442428442904,18.5547253923907));
#29208=CARTESIAN_POINT('Ctrl Pts',(34.068562239254,-55.4988688300469,18.5917713559134));
#29209=CARTESIAN_POINT('Ctrl Pts',(33.6897225249727,-54.9980316067572,18.6288173194361));
#29210=CARTESIAN_POINT('Ctrl Pts',(33.1871811052497,-54.7709421695978,18.6658632829587));
#29211=CARTESIAN_POINT('Ctrl Pts',(32.7096035907249,-54.5551334726087,18.7010689764359));
#29212=CARTESIAN_POINT('Ctrl Pts',(32.1203089631069,-54.5865510549417,18.7362746699131));
#29213=CARTESIAN_POINT('Ctrl Pts',(31.6652761166364,-54.8468682178695,18.7714803633902));
#29214=CARTESIAN_POINT('Origin',(32.5,-56.2916512459885,17.));
#29215=CARTESIAN_POINT('',(31.6684351372492,-54.8482948457192,19.4714803633902));
#29216=CARTESIAN_POINT('',(31.6684043758654,-54.8511587229547,19.2785196366098));
#29217=CARTESIAN_POINT('',(31.667,-54.8488529232837,17.));
#29218=CARTESIAN_POINT('Ctrl Pts',(31.6684043758654,-54.8511587229547,19.2785196366098));
#29219=CARTESIAN_POINT('Ctrl Pts',(31.9058262033729,-54.7139758182214,19.26025371501));
#29220=CARTESIAN_POINT('Ctrl Pts',(32.1752796610303,-54.6323550853735,19.2419877934101));
#29221=CARTESIAN_POINT('Ctrl Pts',(32.4470503478135,-54.6237274947409,19.2237218718103));
#29222=CARTESIAN_POINT('Ctrl Pts',(32.9982410936013,-54.6062294776757,19.1866759082876));
#29223=CARTESIAN_POINT('Ctrl Pts',(33.5589634784782,-54.8889798390775,19.149629944765));
#29224=CARTESIAN_POINT('Ctrl Pts',(33.8725997234821,-55.3425762727762,19.1125839812423));
#29225=CARTESIAN_POINT('Ctrl Pts',(34.186235968486,-55.7961727064748,19.0755380177196));
#29226=CARTESIAN_POINT('Ctrl Pts',(34.252786073617,-56.4206152124703,19.0384920541969));
#29227=CARTESIAN_POINT('Ctrl Pts',(34.0417930059025,-56.9301241370495,19.0014460906742));
#29228=CARTESIAN_POINT('Ctrl Pts',(33.830799938188,-57.4396330616287,18.9644001271515));
#29229=CARTESIAN_POINT('Ctrl Pts',(33.342263697628,-57.8342084047915,18.9273541636289));
#29230=CARTESIAN_POINT('Ctrl Pts',(32.7997656649011,-57.9332705233524,18.8903082001062));
#29231=CARTESIAN_POINT('Ctrl Pts',(32.2572676321741,-58.0323326419133,18.8532622365835));
#29232=CARTESIAN_POINT('Ctrl Pts',(31.6608078072801,-57.8358815358723,18.8162162730608));
#29233=CARTESIAN_POINT('Ctrl Pts',(31.2833594112405,-57.433824167859,18.7791703095382));
#29234=CARTESIAN_POINT('Ctrl Pts',(30.9059110152008,-57.0317667998456,18.7421243460155));
#29235=CARTESIAN_POINT('Ctrl Pts',(30.7474740480154,-56.4241031698599,18.7050783824928));
#29236=CARTESIAN_POINT('Ctrl Pts',(30.8805580861148,-55.8889339838537,18.6680324189701));
#29237=CARTESIAN_POINT('Ctrl Pts',(30.987746754868,-55.4578975242981,18.63819482485));
#29238=CARTESIAN_POINT('Ctrl Pts',(31.2840459342598,-55.0738884180753,18.6083572307299));
#29239=CARTESIAN_POINT('Ctrl Pts',(31.6679260143736,-54.8475393267799,18.5785196366098));
#29240=CARTESIAN_POINT('Ctrl Pts',(31.6652761166364,-54.8468682178695,18.7714803633902));
#29241=CARTESIAN_POINT('Ctrl Pts',(31.6414906650692,-54.8604755020886,18.7733206334357));
#29242=CARTESIAN_POINT('Ctrl Pts',(31.6180720645057,-54.8747082214849,18.7751609034813));
#29243=CARTESIAN_POINT('Ctrl Pts',(31.5950554470213,-54.8895637585373,18.7770011735268));
#29244=CARTESIAN_POINT('Ctrl Pts',(31.1317143336804,-55.1886164356655,18.8140471370495));
#29245=CARTESIAN_POINT('Ctrl Pts',(30.8312752321632,-55.740063440951,18.8510931005722));
#29246=CARTESIAN_POINT('Ctrl Pts',(30.8312358008972,-56.2915319254989,18.8881390640948));
#29247=CARTESIAN_POINT('Ctrl Pts',(30.8311963696312,-56.8430004100469,18.9251850276175));
#29248=CARTESIAN_POINT('Ctrl Pts',(31.1315566086164,-57.3944903738573,18.9622309911402));
#29249=CARTESIAN_POINT('Ctrl Pts',(31.5948549512976,-57.6936093078491,18.9992769546629));
#29250=CARTESIAN_POINT('Ctrl Pts',(32.0581532939788,-57.9927282418409,19.0363229181856));
#29251=CARTESIAN_POINT('Ctrl Pts',(32.684389740356,-58.0394761460141,19.0733688817082));
#29252=CARTESIAN_POINT('Ctrl Pts',(33.186963629793,-57.81245857691,19.1104148452309));
#29253=CARTESIAN_POINT('Ctrl Pts',(33.6895375192301,-57.585441007806,19.1474608087536));
#29254=CARTESIAN_POINT('Ctrl Pts',(34.068448851727,-57.0846579654248,19.1845067722763));
#29255=CARTESIAN_POINT('Ctrl Pts',(34.150286707292,-56.5392956488153,19.221552735799));
#29256=CARTESIAN_POINT('Ctrl Pts',(34.2321245628569,-55.9939333322058,19.2585986993216));
#29257=CARTESIAN_POINT('Ctrl Pts',(34.01688894149,-55.4039917413682,19.2956446628443));
#29258=CARTESIAN_POINT('Ctrl Pts',(33.6030836459812,-55.0394609904048,19.332690626367));
#29259=CARTESIAN_POINT('Ctrl Pts',(33.1892783504724,-54.6749302394416,19.3697365898897));
#29260=CARTESIAN_POINT('Ctrl Pts',(32.5769033808219,-54.5358103283526,19.4067825534124));
#29261=CARTESIAN_POINT('Ctrl Pts',(32.0462156138869,-54.685770273593,19.443828516935));
#29262=CARTESIAN_POINT('Ctrl Pts',(31.9141769673738,-54.7230813054923,19.4530457990868));
#29263=CARTESIAN_POINT('Ctrl Pts',(31.7871951467268,-54.7782877536412,19.4622630812385));
#29264=CARTESIAN_POINT('Ctrl Pts',(31.6684351372492,-54.8482948457192,19.4714803633902));
#29265=CARTESIAN_POINT('Origin',(32.5,-56.2916512459885,17.));
#29266=CARTESIAN_POINT('',(31.667931072794,-54.8513178316736,20.1714803633902));
#29267=CARTESIAN_POINT('',(31.6654871359731,-54.8492158242279,19.9785196366098));
#29268=CARTESIAN_POINT('',(31.667,-54.8488529232837,17.));
#29269=CARTESIAN_POINT('Ctrl Pts',(31.6654871359731,-54.8492158242279,19.9785196366098));
#29270=CARTESIAN_POINT('Ctrl Pts',(32.0469172461538,-54.6336656790849,19.9491961628127));
#29271=CARTESIAN_POINT('Ctrl Pts',(32.517553856985,-54.5668303852667,19.9198726890156));
#29272=CARTESIAN_POINT('Ctrl Pts',(32.9387102808402,-54.6815870878529,19.8905492152186));
#29273=CARTESIAN_POINT('Ctrl Pts',(33.4707804449503,-54.8265655664402,19.8535032516959));
#29274=CARTESIAN_POINT('Ctrl Pts',(33.9238769452872,-55.2613769285398,19.8164572881732));
#29275=CARTESIAN_POINT('Ctrl Pts',(34.0906375985398,-55.7870272905994,19.7794113246505));
#29276=CARTESIAN_POINT('Ctrl Pts',(34.2573982517924,-56.312677652659,19.7423653611279));
#29277=CARTESIAN_POINT('Ctrl Pts',(34.1378230579607,-56.9291670146787,19.7053193976052));
#29278=CARTESIAN_POINT('Ctrl Pts',(33.786636282889,-57.3543555234679,19.6682734340825));
#29279=CARTESIAN_POINT('Ctrl Pts',(33.4354495078173,-57.779544032257,19.6312274705598));
#29280=CARTESIAN_POINT('Ctrl Pts',(32.8526511515056,-58.0134316878157,19.5941815070371));
#29281=CARTESIAN_POINT('Ctrl Pts',(32.3049621862366,-57.9489784788088,19.5571355435145));
#29282=CARTESIAN_POINT('Ctrl Pts',(31.7572732209677,-57.884525269802,19.5200895799918));
#29283=CARTESIAN_POINT('Ctrl Pts',(31.2446936467415,-57.5217311962297,19.4830436164691));
#29284=CARTESIAN_POINT('Ctrl Pts',(31.0018084123138,-57.0266310228124,19.4459976529464));
#29285=CARTESIAN_POINT('Ctrl Pts',(30.7589231778862,-56.531530849395,19.4089516894237));
#29286=CARTESIAN_POINT('Ctrl Pts',(30.7857322832571,-55.9041245761327,19.3719057259011));
#29287=CARTESIAN_POINT('Ctrl Pts',(31.0699663892919,-55.4315482417354,19.3348597623784));
#29288=CARTESIAN_POINT('Ctrl Pts',(31.214055729119,-55.1919808900508,19.3160797204555));
#29289=CARTESIAN_POINT('Ctrl Pts',(31.4242999735977,-54.9922028355067,19.2972996785326));
#29290=CARTESIAN_POINT('Ctrl Pts',(31.6684043758654,-54.8511587229547,19.2785196366098));
#29291=CARTESIAN_POINT('Ctrl Pts',(31.6684351372492,-54.8482948457192,19.4714803633902));
#29292=CARTESIAN_POINT('Ctrl Pts',(31.3098766805411,-55.0596592183269,19.4993090447612));
#29293=CARTESIAN_POINT('Ctrl Pts',(31.0262639705086,-55.405938549172,19.5271377261321));
#29294=CARTESIAN_POINT('Ctrl Pts',(30.9047015762615,-55.801960623025,19.5549664075031));
#29295=CARTESIAN_POINT('Ctrl Pts',(30.7428758697907,-56.3291512256471,19.5920123710258));
#29296=CARTESIAN_POINT('Ctrl Pts',(30.8682250210686,-56.9444926293215,19.6290583345485));
#29297=CARTESIAN_POINT('Ctrl Pts',(31.2233822786099,-57.3663703525617,19.6661042980711));
#29298=CARTESIAN_POINT('Ctrl Pts',(31.5785395361512,-57.7882480758019,19.7031502615938));
#29299=CARTESIAN_POINT('Ctrl Pts',(32.1635048999558,-58.0166621186079,19.7401962251165));
#29300=CARTESIAN_POINT('Ctrl Pts',(32.7105656575522,-57.9470774968357,19.7772421886392));
#29301=CARTESIAN_POINT('Ctrl Pts',(33.2576264151486,-57.8774928750636,19.8142881521619));
#29302=CARTESIAN_POINT('Ctrl Pts',(33.7667825665369,-57.5099095887134,19.8513341156845));
#29303=CARTESIAN_POINT('Ctrl Pts',(34.0050159054109,-57.0125542176421,19.8883800792072));
#29304=CARTESIAN_POINT('Ctrl Pts',(34.243249244285,-56.5151988465708,19.9254260427299));
#29305=CARTESIAN_POINT('Ctrl Pts',(34.2105597706447,-55.8880713907783,19.9624720062526));
#29306=CARTESIAN_POINT('Ctrl Pts',(33.9219080204981,-55.4181802774153,19.9995179697753));
#29307=CARTESIAN_POINT('Ctrl Pts',(33.6332562703514,-54.9482891640523,20.0365639332979));
#29308=CARTESIAN_POINT('Ctrl Pts',(33.0886422436983,-54.6356343931188,20.0736098968206));
#29309=CARTESIAN_POINT('Ctrl Pts',(32.5373116119164,-54.6233042115161,20.1106558603433));
#29310=CARTESIAN_POINT('Ctrl Pts',(32.235574629855,-54.6165560434104,20.1309306946923));
#29311=CARTESIAN_POINT('Ctrl Pts',(31.9318258577411,-54.6997625487969,20.1512055290412));
#29312=CARTESIAN_POINT('Ctrl Pts',(31.667931072794,-54.8513178316736,20.1714803633902));
#29313=CARTESIAN_POINT('Origin',(32.5,-56.2916512459885,17.));
#29314=CARTESIAN_POINT('',(31.6652099567911,-54.8483531313949,20.8714803633902));
#29315=CARTESIAN_POINT('',(31.6666453776089,-54.8465106722,20.6785196366098));
#29316=CARTESIAN_POINT('',(31.667,-54.8488529232837,17.));
#29317=CARTESIAN_POINT('Ctrl Pts',(31.6666453776089,-54.8465106722,20.6785196366098));
#29318=CARTESIAN_POINT('Ctrl Pts',(31.7095215140163,-54.8213939588907,20.6751845741381));
#29319=CARTESIAN_POINT('Ctrl Pts',(31.7535458686671,-54.7983179269086,20.6718495116665));
#29320=CARTESIAN_POINT('Ctrl Pts',(31.7985935167041,-54.7774509892024,20.6685144491949));
#29321=CARTESIAN_POINT('Ctrl Pts',(32.2989840011863,-54.5456604846271,20.6314684856722));
#29322=CARTESIAN_POINT('Ctrl Pts',(32.9256368768596,-54.5864462806581,20.5944225221495));
#29323=CARTESIAN_POINT('Ctrl Pts',(33.3917609918081,-54.881142287214,20.5573765586268));
#29324=CARTESIAN_POINT('Ctrl Pts',(33.8578851067565,-55.1758382937699,20.5203305951041));
#29325=CARTESIAN_POINT('Ctrl Pts',(34.16348046098,-55.7244445108506,20.4832846315815));
#29326=CARTESIAN_POINT('Ctrl Pts',(34.1686895628039,-56.2758883119516,20.4462386680588));
#29327=CARTESIAN_POINT('Ctrl Pts',(34.1738986646279,-56.8273321130526,20.4091927045361));
#29328=CARTESIAN_POINT('Ctrl Pts',(33.8787215140524,-57.3816134981739,20.3721467410134));
#29329=CARTESIAN_POINT('Ctrl Pts',(33.4182476302774,-57.6850623886885,20.3351007774907));
#29330=CARTESIAN_POINT('Ctrl Pts',(32.9577737465024,-57.988511279203,20.2980548139681));
#29331=CARTESIAN_POINT('Ctrl Pts',(32.3320031295279,-58.0411276751107,20.2610088504454));
#29332=CARTESIAN_POINT('Ctrl Pts',(31.8273232393449,-57.8188314143185,20.2239628869227));
#29333=CARTESIAN_POINT('Ctrl Pts',(31.3226433491619,-57.5965351535263,20.1869169234));
#29334=CARTESIAN_POINT('Ctrl Pts',(30.9390541857702,-57.0993262360342,20.1498709598773));
#29335=CARTESIAN_POINT('Ctrl Pts',(30.8521075105052,-56.5547551273837,20.1128249963547));
#29336=CARTESIAN_POINT('Ctrl Pts',(30.7651608352402,-56.0101840187332,20.075779032832));
#29337=CARTESIAN_POINT('Ctrl Pts',(30.9748566481017,-55.4182507189243,20.0387330693093));
#29338=CARTESIAN_POINT('Ctrl Pts',(31.3852264684742,-55.0498568665574,20.0016871057866));
#29339=CARTESIAN_POINT('Ctrl Pts',(31.4707709224493,-54.9730625961603,19.993964616061));
#29340=CARTESIAN_POINT('Ctrl Pts',(31.565035527569,-54.9059820788928,19.9862421263354));
#29341=CARTESIAN_POINT('Ctrl Pts',(31.6654871359731,-54.8492158242279,19.9785196366098));
#29342=CARTESIAN_POINT('Ctrl Pts',(31.667931072794,-54.8513178316736,20.1714803633902));
#29343=CARTESIAN_POINT('Ctrl Pts',(31.4496400894775,-54.9766827635065,20.1882514925639));
#29344=CARTESIAN_POINT('Ctrl Pts',(31.2586188937636,-55.1488148264988,20.2050226217376));
#29345=CARTESIAN_POINT('Ctrl Pts',(31.1185634357287,-55.3554851247115,20.2217937509113));
#29346=CARTESIAN_POINT('Ctrl Pts',(30.8091931282335,-55.8120018117817,20.258839714434));
#29347=CARTESIAN_POINT('Ctrl Pts',(30.7484997501537,-56.4370407781941,20.2958856779567));
#29348=CARTESIAN_POINT('Ctrl Pts',(30.9642598655731,-56.9445494693264,20.3329316414794));
#29349=CARTESIAN_POINT('Ctrl Pts',(31.1800199809926,-57.4520581604587,20.3699776050021));
#29350=CARTESIAN_POINT('Ctrl Pts',(31.6722335899113,-57.842036576311,20.4070235685247));
#29351=CARTESIAN_POINT('Ctrl Pts',(32.2156365524479,-57.9360087382767,20.4440695320474));
#29352=CARTESIAN_POINT('Ctrl Pts',(32.7590395149845,-58.0299809002424,20.4811154955701));
#29353=CARTESIAN_POINT('Ctrl Pts',(33.353631831139,-57.8279468083216,20.5181614590928));
#29354=CARTESIAN_POINT('Ctrl Pts',(33.727294536927,-57.4223688010744,20.5552074226155));
#29355=CARTESIAN_POINT('Ctrl Pts',(34.1009572427151,-57.0167907938273,20.5922533861381));
#29356=CARTESIAN_POINT('Ctrl Pts',(34.2536903381367,-56.4076688712538,20.6292993496608));
#29357=CARTESIAN_POINT('Ctrl Pts',(34.1155954946061,-55.8737705531045,20.6663453131835));
#29358=CARTESIAN_POINT('Ctrl Pts',(33.9775006510756,-55.3398722349553,20.7033912767062));
#29359=CARTESIAN_POINT('Ctrl Pts',(33.5485778685929,-54.8811975212302,20.7404372402289));
#29360=CARTESIAN_POINT('Ctrl Pts',(33.0251244120732,-54.707662660689,20.7774832037515));
#29361=CARTESIAN_POINT('Ctrl Pts',(32.5824028716121,-54.560891978739,20.8088155902978));
#29362=CARTESIAN_POINT('Ctrl Pts',(32.0720609029457,-54.6180897881502,20.840147976844));
#29363=CARTESIAN_POINT('Ctrl Pts',(31.6652099567911,-54.8483531313949,20.8714803633902));
#29364=CARTESIAN_POINT('Origin',(32.5,-56.2916512459885,17.));
#29365=CARTESIAN_POINT('',(31.6673136634551,-54.8469650373412,21.5714803633902));
#29366=CARTESIAN_POINT('',(31.6688940285232,-54.8502492137287,21.3785196366098));
#29367=CARTESIAN_POINT('',(31.667,-54.8488529232837,17.));
#29368=CARTESIAN_POINT('',(34.0692874532607,-56.8510195406194,22.));
#29369=CARTESIAN_POINT('Ctrl Pts',(31.6673136634551,-54.8469650373412,21.5714803633902));
#29370=CARTESIAN_POINT('Ctrl Pts',(31.2598491701086,-55.0867590255674,21.6031823516921));
#29371=CARTESIAN_POINT('Ctrl Pts',(30.9533734485754,-55.5074467114501,21.634884339994));
#29372=CARTESIAN_POINT('Ctrl Pts',(30.8625080737328,-55.9706266060895,21.6665863282959));
#29373=CARTESIAN_POINT('Ctrl Pts',(30.7563256056225,-56.5118843126361,21.7036322918186));
#29374=CARTESIAN_POINT('Ctrl Pts',(30.9445706465322,-57.1111674125324,21.7406782553412));
#29375=CARTESIAN_POINT('Ctrl Pts',(31.341982566131,-57.4936046161573,21.7777242188639));
#29376=CARTESIAN_POINT('Ctrl Pts',(31.7393944857297,-57.8760418197823,21.8147701823866));
#29377=CARTESIAN_POINT('Ctrl Pts',(32.3459732840176,-58.0416331271359,21.8518161459093));
#29378=CARTESIAN_POINT('Ctrl Pts',(32.8819457094271,-57.9158339106247,21.888862109432));
#29379=CARTESIAN_POINT('Ctrl Pts',(33.4179181348367,-57.7900346941135,21.9259080729546));
#29380=CARTESIAN_POINT('Ctrl Pts',(33.8832841873681,-57.3728449537375,21.9629540364773));
#29381=CARTESIAN_POINT('Ctrl Pts',(34.0692874532607,-56.8510195406194,22.));
#29382=CARTESIAN_POINT('',(32.8006122403835,-54.6499198220901,22.));
#29383=CARTESIAN_POINT('Origin',(32.5,-56.2916512459885,22.));
#29384=CARTESIAN_POINT('Ctrl Pts',(32.8006124898337,-54.6499179279034,22.));
#29385=CARTESIAN_POINT('Ctrl Pts',(33.3324299245223,-54.7480089912901,21.9636770818144));
#29386=CARTESIAN_POINT('Ctrl Pts',(33.8131824856955,-55.1285995043638,21.9273541636289));
#29387=CARTESIAN_POINT('Ctrl Pts',(34.0294057231265,-55.6243031692819,21.8910312454433));
#29388=CARTESIAN_POINT('Ctrl Pts',(34.2499331082255,-56.1298743294735,21.8539852819206));
#29389=CARTESIAN_POINT('Ctrl Pts',(34.195294888985,-56.7551871483463,21.816939318398));
#29390=CARTESIAN_POINT('Ctrl Pts',(33.8903094432865,-57.2145585578539,21.7798933548753));
#29391=CARTESIAN_POINT('Ctrl Pts',(33.585323997588,-57.6739299673615,21.7428473913526));
#29392=CARTESIAN_POINT('Ctrl Pts',(33.0299913254315,-57.9673599675038,21.7058014278299));
#29393=CARTESIAN_POINT('Ctrl Pts',(32.4785554363758,-57.9603119672567,21.6687554643073));
#29394=CARTESIAN_POINT('Ctrl Pts',(31.9271195473201,-57.9532639670095,21.6317095007846));
#29395=CARTESIAN_POINT('Ctrl Pts',(31.3795804413652,-57.6457379663728,21.5946635372619));
#29396=CARTESIAN_POINT('Ctrl Pts',(31.0864761391558,-57.1785982034714,21.5576175737392));
#29397=CARTESIAN_POINT('Ctrl Pts',(30.7933718369463,-56.7114584405699,21.5205716102165));
#29398=CARTESIAN_POINT('Ctrl Pts',(30.7547023384823,-56.0847049154036,21.4835256466938));
#29399=CARTESIAN_POINT('Ctrl Pts',(30.9881881185804,-55.5851133656589,21.4464796831712));
#29400=CARTESIAN_POINT('Ctrl Pts',(31.1309630480468,-55.2796166101529,21.4238263343174));
#29401=CARTESIAN_POINT('Ctrl Pts',(31.3755032965772,-55.0216687358223,21.4011729854636));
#29402=CARTESIAN_POINT('Ctrl Pts',(31.6688940285232,-54.8502492137287,21.3785196366098));
#29403=CARTESIAN_POINT('Origin',(32.5,-56.2916512459885,23.5459252805377));
#29404=CARTESIAN_POINT('',(31.4724222119036,-54.5094432564574,13.4540747194623));
#29405=CARTESIAN_POINT('',(31.4735006561133,-54.5153050203084,13.3959252805377));
#29406=CARTESIAN_POINT('',(31.4726250000001,-54.5121855475624,23.5459252805377));
#29407=CARTESIAN_POINT('',(32.7283737736498,-58.3336705852723,13.));
#29408=CARTESIAN_POINT('Ctrl Pts',(31.4735006561133,-54.5153050203084,13.3959252805377));
#29409=CARTESIAN_POINT('Ctrl Pts',(31.808029474343,-54.3235252303773,13.3750880775931));
#29410=CARTESIAN_POINT('Ctrl Pts',(32.8820600904465,-54.0381232256079,13.3172049111259));
#29411=CARTESIAN_POINT('Ctrl Pts',(34.5894859509232,-55.0509345423224,13.2222757811361));
#29412=CARTESIAN_POINT('Ctrl Pts',(34.6719801790384,-57.3759588223509,13.111137890568));
#29413=CARTESIAN_POINT('Ctrl Pts',(33.4073937856322,-58.2577308722946,13.0370459635227));
#29414=CARTESIAN_POINT('Ctrl Pts',(32.7283737736498,-58.3336705852723,13.));
#29415=CARTESIAN_POINT('',(31.6782144221994,-58.178982708051,13.));
#29416=CARTESIAN_POINT('Origin',(32.5,-56.2916512459885,13.));
#29417=CARTESIAN_POINT('Ctrl Pts',(31.4724222119036,-54.5094432564574,13.4540747194623));
#29418=CARTESIAN_POINT('Ctrl Pts',(31.5342132308562,-54.4731877432048,13.4501772883951));
#29419=CARTESIAN_POINT('Ctrl Pts',(32.2034917270506,-54.1282244537509,13.4092338938053));
#29420=CARTESIAN_POINT('Ctrl Pts',(33.8288126996591,-54.2585627611561,13.3312445356927));
#29421=CARTESIAN_POINT('Ctrl Pts',(34.9285321027134,-56.3058411531895,13.2201066451247));
#29422=CARTESIAN_POINT('Ctrl Pts',(33.8129922329338,-58.325638659776,13.1096917998938));
#29423=CARTESIAN_POINT('Ctrl Pts',(32.2900793461072,-58.4444630460461,13.0363229181856));
#29424=CARTESIAN_POINT('Ctrl Pts',(31.6782133743559,-58.1789848186021,13.));
#29425=CARTESIAN_POINT('Origin',(32.5,-56.2916512459885,23.5459252805377));
#29426=CARTESIAN_POINT('',(31.4749259905951,-54.514117897405,14.1540747194623));
#29427=CARTESIAN_POINT('',(31.470366790827,-54.5112698283738,14.0959252805377));
#29428=CARTESIAN_POINT('',(31.4726250000001,-54.5121855475624,23.5459252805377));
#29429=CARTESIAN_POINT('Ctrl Pts',(31.470366790827,-54.5112698283738,14.0959252805377));
#29430=CARTESIAN_POINT('Ctrl Pts',(31.9808629913117,-54.2220900136561,14.0640305253959));
#29431=CARTESIAN_POINT('Ctrl Pts',(33.3714175837229,-54.0779847124815,13.9950898067314));
#29432=CARTESIAN_POINT('Ctrl Pts',(34.8602323505772,-55.7191431963173,13.8891031245444));
#29433=CARTESIAN_POINT('Ctrl Pts',(34.2609995597881,-57.9641431697149,13.7779652339763));
#29434=CARTESIAN_POINT('Ctrl Pts',(32.0500242237095,-58.6781839861316,13.6668273434083));
#29435=CARTESIAN_POINT('Ctrl Pts',(30.2506759606945,-57.2080211780376,13.5556894528402));
#29436=CARTESIAN_POINT('Ctrl Pts',(30.4619007867399,-55.3316416370552,13.4653887652167));
#29437=CARTESIAN_POINT('Ctrl Pts',(31.2132787090688,-54.6644859207873,13.4121340411158));
#29438=CARTESIAN_POINT('Ctrl Pts',(31.4735006561133,-54.5153050203084,13.3959252805377));
#29439=CARTESIAN_POINT('Ctrl Pts',(31.4749259905951,-54.514117897405,14.1540747194623));
#29440=CARTESIAN_POINT('Ctrl Pts',(31.7139442620515,-54.3746753634159,14.1391197361979));
#29441=CARTESIAN_POINT('Ctrl Pts',(32.6363754616288,-54.0511292553545,14.0871187894108));
#29442=CARTESIAN_POINT('Ctrl Pts',(34.3667107654437,-54.7380212138032,13.998071879101));
#29443=CARTESIAN_POINT('Ctrl Pts',(34.817688121868,-57.0173840749687,13.886933988533));
#29444=CARTESIAN_POINT('Ctrl Pts',(33.1472639077745,-58.6324557555082,13.7757960979649));
#29445=CARTESIAN_POINT('Ctrl Pts',(30.8843823888257,-58.1050019311361,13.6646582073969));
#29446=CARTESIAN_POINT('Ctrl Pts',(30.1278087167359,-55.9943944231075,13.557417747896));
#29447=CARTESIAN_POINT('Ctrl Pts',(30.9468756244448,-54.8178045942286,13.4872232519178));
#29448=CARTESIAN_POINT('Ctrl Pts',(31.4724222119036,-54.5094432564574,13.4540747194623));
#29449=CARTESIAN_POINT('Origin',(32.5,-56.2916512459885,23.5459252805377));
#29450=CARTESIAN_POINT('',(31.4717219617816,-54.5141519916847,14.8540747194623));
#29451=CARTESIAN_POINT('',(31.4732712326059,-54.510037050691,14.7959252805377));
#29452=CARTESIAN_POINT('',(31.4726250000001,-54.5121855475624,23.5459252805377));
#29453=CARTESIAN_POINT('Ctrl Pts',(31.4732712326059,-54.510037050691,14.7959252805377));
#29454=CARTESIAN_POINT('Ctrl Pts',(31.5669343623879,-54.4548697514475,14.7900189367213));
#29455=CARTESIAN_POINT('Ctrl Pts',(32.2792813565109,-54.1097268956779,14.7470666293823));
#29456=CARTESIAN_POINT('Ctrl Pts',(33.9367458689222,-54.3335587337424,14.6670683585206));
#29457=CARTESIAN_POINT('Ctrl Pts',(34.9243151877952,-56.4367817964588,14.5559304679526));
#29458=CARTESIAN_POINT('Ctrl Pts',(33.6928803873874,-58.4071660616143,14.4447925773845));
#29459=CARTESIAN_POINT('Ctrl Pts',(31.3695905104292,-58.4411939406326,14.3336546868165));
#29460=CARTESIAN_POINT('Ctrl Pts',(30.0809735153021,-56.5077243843663,14.2225167962484));
#29461=CARTESIAN_POINT('Ctrl Pts',(30.7409078667025,-54.9881078888109,14.1432736608222));
#29462=CARTESIAN_POINT('Ctrl Pts',(31.3879183664802,-54.55797423098,14.1010764889186));
#29463=CARTESIAN_POINT('Ctrl Pts',(31.470366790827,-54.5112698283738,14.0959252805377));
#29464=CARTESIAN_POINT('Ctrl Pts',(31.4717219617816,-54.5141519916847,14.8540747194623));
#29465=CARTESIAN_POINT('Ctrl Pts',(31.8897217256654,-54.2773643841942,14.8280621840006));
#29466=CARTESIAN_POINT('Ctrl Pts',(33.1073033291158,-54.0451479062597,14.7650036850163));
#29467=CARTESIAN_POINT('Ctrl Pts',(34.7403671916158,-55.3540375815297,14.6648992225092));
#29468=CARTESIAN_POINT('Ctrl Pts',(34.5027924192342,-57.6654005284896,14.5537613319412));
#29469=CARTESIAN_POINT('Ctrl Pts',(32.4320391047204,-58.7193548713018,14.4426234413732));
#29470=CARTESIAN_POINT('Ctrl Pts',(30.423491023484,-57.5512051672244,14.3314855508051));
#29471=CARTESIAN_POINT('Ctrl Pts',(30.3301141372088,-55.5424943178045,14.2353026435015));
#29472=CARTESIAN_POINT('Ctrl Pts',(31.12185652721,-54.7200975505446,14.1761656997206));
#29473=CARTESIAN_POINT('Ctrl Pts',(31.4749259905951,-54.514117897405,14.1540747194623));
#29474=CARTESIAN_POINT('Origin',(32.5,-56.2916512459885,23.5459252805377));
#29475=CARTESIAN_POINT('',(31.4709276972304,-54.5092291784965,15.5540747194623));
#29476=CARTESIAN_POINT('',(31.4746475020099,-54.5147506716575,15.4959252805377));
#29477=CARTESIAN_POINT('',(31.4726250000001,-54.5121855475624,23.5459252805377));
#29478=CARTESIAN_POINT('Ctrl Pts',(31.4746475020099,-54.5147506716575,15.4959252805377));
#29479=CARTESIAN_POINT('Ctrl Pts',(31.7462982414417,-54.3571727743297,15.4789613845241));
#29480=CARTESIAN_POINT('Ctrl Pts',(32.7191784117559,-54.0441951966849,15.4249515249878));
#29481=CARTESIAN_POINT('Ctrl Pts',(34.4479835200066,-54.8412285476316,15.3338957019289));
#29482=CARTESIAN_POINT('Ctrl Pts',(34.7750596076319,-57.1416333665308,15.2227578113608));
#29483=CARTESIAN_POINT('Ctrl Pts',(33.019747820939,-58.6640399241195,15.1116199207928));
#29484=CARTESIAN_POINT('Ctrl Pts',(30.7887049884687,-58.0149721937253,15.0004820302248));
#29485=CARTESIAN_POINT('Ctrl Pts',(30.1593535158744,-55.9068520254157,14.895250483473));
#29486=CARTESIAN_POINT('Ctrl Pts',(30.9794574058775,-54.800891896276,14.827064900244));
#29487=CARTESIAN_POINT('Ctrl Pts',(31.4732712326059,-54.510037050691,14.7959252805377));
#29488=CARTESIAN_POINT('Ctrl Pts',(31.4709277056121,-54.5092291930959,15.5540747194623));
#29489=CARTESIAN_POINT('Ctrl Pts',(31.4713112637463,-54.5090077151575,15.5540505953261));
#29490=CARTESIAN_POINT('Ctrl Pts',(32.0608222902465,-54.1688851137838,15.5169805076671));
#29491=CARTESIAN_POINT('Ctrl Pts',(33.6099012175602,-54.1314466960922,15.4428644564855));
#29492=CARTESIAN_POINT('Ctrl Pts',(34.9168581194719,-56.052567070093,15.3317265659175));
#29493=CARTESIAN_POINT('Ctrl Pts',(34.0116373750326,-58.1925239040739,15.2205886753494));
#29494=CARTESIAN_POINT('Ctrl Pts',(31.722797799219,-58.5925904319764,15.1094507847814));
#29495=CARTESIAN_POINT('Ctrl Pts',(30.1453402095973,-56.8865812380664,14.9983128942134));
#29496=CARTESIAN_POINT('Ctrl Pts',(30.5878941637736,-55.1627827650417,14.913187539107));
#29497=CARTESIAN_POINT('Ctrl Pts',(31.2944239690072,-54.6145873774176,14.8651081475233));
#29498=CARTESIAN_POINT('Ctrl Pts',(31.4717219617816,-54.5141519916847,14.8540747194623));
#29499=CARTESIAN_POINT('Origin',(32.5,-56.2916512459885,23.5459252805377));
#29500=CARTESIAN_POINT('',(31.4747870773481,-54.5124102302141,16.2540747194623));
#29501=CARTESIAN_POINT('',(31.4710889776862,-54.513282910156,16.1959252805377));
#29502=CARTESIAN_POINT('',(31.4726250000001,-54.5121855475624,23.5459252805377));
#29503=CARTESIAN_POINT('Ctrl Pts',(31.4710889776862,-54.513282910156,16.1959252805377));
#29504=CARTESIAN_POINT('Ctrl Pts',(31.9210107047531,-54.2589533662338,16.1679038323268));
#29505=CARTESIAN_POINT('Ctrl Pts',(33.1965779324789,-54.0532698651996,16.1028364205933));
#29506=CARTESIAN_POINT('Ctrl Pts',(34.7877864833415,-55.4765446163129,16.0007230453371));
#29507=CARTESIAN_POINT('Ctrl Pts',(34.4255850063652,-57.7716810411711,15.8895851547691));
#29508=CARTESIAN_POINT('Ctrl Pts',(32.3008737352177,-58.7121294100224,15.778447264201));
#29509=CARTESIAN_POINT('Ctrl Pts',(30.3584249929227,-57.4370866648374,15.667309373633));
#29510=CARTESIAN_POINT('Ctrl Pts',(30.3734734150964,-55.4682647699115,15.5731353790785));
#29511=CARTESIAN_POINT('Ctrl Pts',(31.1530640353465,-54.7012933131323,15.5160073480468));
#29512=CARTESIAN_POINT('Ctrl Pts',(31.4746475020099,-54.5147506716575,15.4959252805377));
#29513=CARTESIAN_POINT('Ctrl Pts',(31.4747870773481,-54.5124102302141,16.2540747194623));
#29514=CARTESIAN_POINT('Ctrl Pts',(31.6511921427898,-54.4086339956355,16.2429930431288));
#29515=CARTESIAN_POINT('Ctrl Pts',(32.4803377190682,-54.0709860720283,16.1948654032727));
#29516=CARTESIAN_POINT('Ctrl Pts',(34.1948158493603,-54.5521215254954,16.1096917998938));
#29517=CARTESIAN_POINT('Ctrl Pts',(34.880650639758,-56.7721373989267,15.9985539093257));
#29518=CARTESIAN_POINT('Ctrl Pts',(33.387448901162,-58.5523588475275,15.8874160187577));
#29519=CARTESIAN_POINT('Ctrl Pts',(31.0819551189947,-58.2633289901972,15.7762781281897));
#29520=CARTESIAN_POINT('Ctrl Pts',(30.074632599944,-56.1700546084616,15.6651643617579));
#29521=CARTESIAN_POINT('Ctrl Pts',(30.8823044490718,-54.849117866319,15.5910965588487));
#29522=CARTESIAN_POINT('Ctrl Pts',(31.4709277056121,-54.5092291930959,15.5540747194623));
#29523=CARTESIAN_POINT('Origin',(32.5,-56.2916512459885,23.5459252805377));
#29524=CARTESIAN_POINT('',(31.4731301859007,-54.5151387721108,16.9540747194623));
#29525=CARTESIAN_POINT('',(31.471644989423,-54.5091305714223,16.8959252805377));
#29526=CARTESIAN_POINT('',(31.4726250000001,-54.5121855475624,23.5459252805377));
#29527=CARTESIAN_POINT('Ctrl Pts',(31.471644989423,-54.5091305714223,16.8959252805377));
#29528=CARTESIAN_POINT('Ctrl Pts',(31.5039012222331,-54.4903218421575,16.8938922436523));
#29529=CARTESIAN_POINT('Ctrl Pts',(32.1342604089221,-54.1469870049404,16.8548132432442));
#29530=CARTESIAN_POINT('Ctrl Pts',(33.7250789425299,-54.1946182477115,16.7786882793134));
#29531=CARTESIAN_POINT('Ctrl Pts',(34.9262501272131,-56.1835950962899,16.6675503887454));
#29532=CARTESIAN_POINT('Ctrl Pts',(33.9066470549119,-58.2714769641261,16.5564124981774));
#29533=CARTESIAN_POINT('Ctrl Pts',(31.5995239807838,-58.5472018994033,16.4452746076093));
#29534=CARTESIAN_POINT('Ctrl Pts',(30.1166168191438,-56.7583957419196,16.3341367170413));
#29535=CARTESIAN_POINT('Ctrl Pts',(30.6391000228397,-55.1011038763401,16.251020274684));
#29536=CARTESIAN_POINT('Ctrl Pts',(31.3261883471228,-54.5951916268688,16.2049497958495));
#29537=CARTESIAN_POINT('Ctrl Pts',(31.4710889776862,-54.513282910156,16.1959252805377));
#29538=CARTESIAN_POINT('Ctrl Pts',(31.4731301859007,-54.5151387721108,16.9540747194623));
#29539=CARTESIAN_POINT('Ctrl Pts',(31.8288294586133,-54.3119418969878,16.9319354909316));
#29540=CARTESIAN_POINT('Ctrl Pts',(32.9382338021843,-54.037919745286,16.8727502988781));
#29541=CARTESIAN_POINT('Ctrl Pts',(34.6305762357544,-55.1258856969254,16.776519143302));
#29542=CARTESIAN_POINT('Ctrl Pts',(34.6349312243122,-57.4494219828794,16.665381252734));
#29543=CARTESIAN_POINT('Ctrl Pts',(32.68515945149,-58.7132375833447,16.5542433621659));
#29544=CARTESIAN_POINT('Ctrl Pts',(30.5659091328683,-57.7605477465697,16.4431054715979));
#29545=CARTESIAN_POINT('Ctrl Pts',(30.2517487916383,-55.6924152700814,16.3430492573634));
#29546=CARTESIAN_POINT('Ctrl Pts',(31.0614712898342,-54.7555571943486,16.2800390066515));
#29547=CARTESIAN_POINT('Ctrl Pts',(31.4747870773481,-54.5124102302141,16.2540747194623));
#29548=CARTESIAN_POINT('Origin',(32.5,-56.2916512459885,23.5459252805377));
#29549=CARTESIAN_POINT('',(31.4703256079253,-54.5106072564107,17.6540747194623));
#29550=CARTESIAN_POINT('',(31.4749747334417,-54.5133534323073,17.5959252805377));
#29551=CARTESIAN_POINT('',(31.4726250000001,-54.5121855475624,23.5459252805377));
#29552=CARTESIAN_POINT('Ctrl Pts',(31.4749747334417,-54.5133534323073,17.5959252805377));
#29553=CARTESIAN_POINT('Ctrl Pts',(31.6837908396868,-54.3909711398323,17.582834691455));
#29554=CARTESIAN_POINT('Ctrl Pts',(32.560671629995,-54.0596531620232,17.5326981388497));
#29555=CARTESIAN_POINT('Ctrl Pts',(34.2863923370768,-54.6463037965649,17.4455156227217));
#29556=CARTESIAN_POINT('Ctrl Pts',(34.8511887990977,-56.9001551837646,17.3343777321536));
#29557=CARTESIAN_POINT('Ctrl Pts',(33.26391548901,-58.5970360158138,17.2232398415856));
#29558=CARTESIAN_POINT('Ctrl Pts',(30.9774216684404,-58.1837720232006,17.1121019510175));
#29559=CARTESIAN_POINT('Ctrl Pts',(30.1008940923714,-56.0778693719696,17.0029970973349));
#29560=CARTESIAN_POINT('Ctrl Pts',(30.9161286969814,-54.8330541866883,16.9309382071749));
#29561=CARTESIAN_POINT('Ctrl Pts',(31.471644989423,-54.5091305714223,16.8959252805377));
#29562=CARTESIAN_POINT('Ctrl Pts',(31.4703256079253,-54.5106072564107,17.6540747194623));
#29563=CARTESIAN_POINT('Ctrl Pts',(32.0008800348568,-54.2091890880958,17.6208779387343));
#29564=CARTESIAN_POINT('Ctrl Pts',(33.430914992466,-54.089095285949,17.5506351944836));
#29565=CARTESIAN_POINT('Ctrl Pts',(34.8788327758259,-55.8022444250302,17.4433464867103));
#29566=CARTESIAN_POINT('Ctrl Pts',(34.2013246967004,-58.0248156029211,17.3322085961422));
#29567=CARTESIAN_POINT('Ctrl Pts',(31.9665748283507,-58.6610017894909,17.2210707055742));
#29568=CARTESIAN_POINT('Ctrl Pts',(30.2200750690644,-57.1284945533304,17.1099328150062));
#29569=CARTESIAN_POINT('Ctrl Pts',(30.4926187339168,-55.2878838417842,17.0209341529689));
#29570=CARTESIAN_POINT('Ctrl Pts',(31.2336315607436,-54.6519548298357,16.9689814544542));
#29571=CARTESIAN_POINT('Ctrl Pts',(31.4731301859007,-54.5151387721108,16.9540747194623));
#29572=CARTESIAN_POINT('Origin',(32.5,-56.2916512459885,23.5459252805377));
#29573=CARTESIAN_POINT('',(31.4737670936581,-54.5105654320666,18.3540747194623));
#29574=CARTESIAN_POINT('',(31.472390363387,-54.5147550766704,18.2959252805377));
#29575=CARTESIAN_POINT('',(31.4726250000001,-54.5121855475624,23.5459252805377));
#29576=CARTESIAN_POINT('Ctrl Pts',(31.472390363387,-54.5147550766704,18.2959252805377));
#29577=CARTESIAN_POINT('Ctrl Pts',(31.8605071662086,-54.2941313842958,18.2717771392578));
#29578=CARTESIAN_POINT('Ctrl Pts',(33.02540146796,-54.0403220897573,18.2105830344552));
#29579=CARTESIAN_POINT('Ctrl Pts',(34.6904921906955,-55.242790066521,18.1123429661299));
#29580=CARTESIAN_POINT('Ctrl Pts',(34.5692083587434,-57.5631631725538,18.0012050755619));
#29581=CARTESIAN_POINT('Ctrl Pts',(32.5539546496148,-58.7197069922754,17.8900671849938));
#29582=CARTESIAN_POINT('Ctrl Pts',(30.4893156378063,-57.6538238513956,17.7789292944258));
#29583=CARTESIAN_POINT('Ctrl Pts',(30.2914909874078,-55.613533902771,17.6808819929404));
#29584=CARTESIAN_POINT('Ctrl Pts',(31.0928476967877,-54.7373092545057,17.6198806549777));
#29585=CARTESIAN_POINT('Ctrl Pts',(31.4749747334417,-54.5133534323073,17.5959252805377));
#29586=CARTESIAN_POINT('Ctrl Pts',(31.4737670936581,-54.5105654320666,18.3540747194623));
#29587=CARTESIAN_POINT('Ctrl Pts',(31.5881478071784,-54.4431225718917,18.3468663500598));
#29588=CARTESIAN_POINT('Ctrl Pts',(32.3290694209141,-54.0987447143864,18.3026120171345));
#29589=CARTESIAN_POINT('Ctrl Pts',(34.004501193851,-54.3851254608373,18.2213117206866));
#29590=CARTESIAN_POINT('Ctrl Pts',(34.9177373632483,-56.5216739711635,18.1101738301186));
#29591=CARTESIAN_POINT('Ctrl Pts',(33.6179911050581,-58.4476800725016,17.9990359395505));
#29592=CARTESIAN_POINT('Ctrl Pts',(31.2949349095266,-58.4002485379024,17.8878980489825));
#29593=CARTESIAN_POINT('Ctrl Pts',(30.074888457673,-56.4227939888948,17.7767601584144));
#29594=CARTESIAN_POINT('Ctrl Pts',(30.7759689649702,-54.951821535532,17.6988190485744));
#29595=CARTESIAN_POINT('Ctrl Pts',(31.4088075653018,-54.5455568389317,17.657923902257));
#29596=CARTESIAN_POINT('Ctrl Pts',(31.4703256079253,-54.5106072564107,17.6540747194623));
#29597=CARTESIAN_POINT('Origin',(32.5,-56.2916512459885,23.5459252805377));
#29598=CARTESIAN_POINT('',(31.4743570776169,-54.515029390224,19.0540747194623));
#29599=CARTESIAN_POINT('',(31.4704988599393,-54.5097377243633,18.9959252805377));
#29600=CARTESIAN_POINT('',(31.4726250000001,-54.5121855475624,23.5459252805377));
#29601=CARTESIAN_POINT('Ctrl Pts',(31.4704988599393,-54.5097377243633,18.9959252805377));
#29602=CARTESIAN_POINT('Ctrl Pts',(32.0317105894022,-54.1886772858723,18.9607195870605));
#29603=CARTESIAN_POINT('Ctrl Pts',(33.5233071799065,-54.1091544860817,18.8884679300607));
#29604=CARTESIAN_POINT('Ctrl Pts',(34.9018152245058,-55.9315825877644,18.7791703095382));
#29605=CARTESIAN_POINT('Ctrl Pts',(34.1051248236507,-58.1142702713998,18.6680324189701));
#29606=CARTESIAN_POINT('Ctrl Pts',(31.8392454683584,-58.628694091168,18.5568945284021));
#29607=CARTESIAN_POINT('Ctrl Pts',(30.1781622293417,-57.0039960908763,18.445756637834));
#29608=CARTESIAN_POINT('Ctrl Pts',(30.5414387587065,-55.2219675363374,18.3587668885459));
#29609=CARTESIAN_POINT('Ctrl Pts',(31.2650923575403,-54.6325929315102,18.3088231027804));
#29610=CARTESIAN_POINT('Ctrl Pts',(31.472390363387,-54.5147550766704,18.2959252805377));
#29611=CARTESIAN_POINT('Ctrl Pts',(31.4743570776169,-54.515029390224,19.0540747194623));
#29612=CARTESIAN_POINT('Ctrl Pts',(31.767179706711,-54.345835768675,19.0358087978625));
#29613=CARTESIAN_POINT('Ctrl Pts',(32.773519448388,-54.0410032090046,18.98049691274));
#29614=CARTESIAN_POINT('Ctrl Pts',(34.4976287681445,-54.9104040861686,18.8881390640948));
#29615=CARTESIAN_POINT('Ctrl Pts',(34.7438661544311,-57.2208600991234,18.7770011735268));
#29616=CARTESIAN_POINT('Ctrl Pts',(32.9362674024074,-58.680800710823,18.6658632829587));
#29617=CARTESIAN_POINT('Ctrl Pts',(30.7293481493445,-57.9539257225797,18.5547253923907));
#29618=CARTESIAN_POINT('Ctrl Pts',(30.1811487641285,-55.8513808790736,18.4507958712252));
#29619=CARTESIAN_POINT('Ctrl Pts',(31.0003111545141,-54.7897315757275,18.3839123135824));
#29620=CARTESIAN_POINT('Ctrl Pts',(31.4737670936581,-54.5105654320666,18.3540747194623));
#29621=CARTESIAN_POINT('Origin',(32.5,-56.2916512459885,23.5459252805377));
#29622=CARTESIAN_POINT('',(31.4707591192322,-54.5126331290242,19.7540747194623));
#29623=CARTESIAN_POINT('',(31.4743950169645,-54.5114972463166,19.6959252805377));
#29624=CARTESIAN_POINT('',(31.4726250000001,-54.5121855475624,23.5459252805377));
#29625=CARTESIAN_POINT('Ctrl Pts',(31.4743950169645,-54.5114972463166,19.6959252805377));
#29626=CARTESIAN_POINT('Ctrl Pts',(31.6208668833956,-54.425154465736,19.686707998386));
#29627=CARTESIAN_POINT('Ctrl Pts',(32.4069324234732,-54.0834056527267,19.6404447527116));
#29628=CARTESIAN_POINT('Ctrl Pts',(34.1053854498936,-54.4692617796666,19.5571355435145));
#29629=CARTESIAN_POINT('Ctrl Pts',(34.9017637086038,-56.6520633710957,19.4459976529464));
#29630=CARTESIAN_POINT('Ctrl Pts',(33.4997804064766,-58.5049756574095,19.3348597623784));
#29631=CARTESIAN_POINT('Ctrl Pts',(31.1826867602698,-58.3320070089704,19.2237218718103));
#29632=CARTESIAN_POINT('Ctrl Pts',(30.0713448616115,-56.2914775915524,19.1125839812423));
#29633=CARTESIAN_POINT('Ctrl Pts',(30.8308409091996,-54.8974452606956,19.0366517841514));
#29634=CARTESIAN_POINT('Ctrl Pts',(31.4411632317234,-54.5265201776941,18.9977655505832));
#29635=CARTESIAN_POINT('Ctrl Pts',(31.4704988599393,-54.5097377243633,18.9959252805377));
#29636=CARTESIAN_POINT('Ctrl Pts',(31.4707591192322,-54.5126331290242,19.7540747194623));
#29637=CARTESIAN_POINT('Ctrl Pts',(31.9411934042825,-54.2467857936504,19.7247512456653));
#29638=CARTESIAN_POINT('Ctrl Pts',(33.2549727142225,-54.0602154670517,19.6583818083455));
#29639=CARTESIAN_POINT('Ctrl Pts',(34.8149526935151,-55.5572409773789,19.5549664075031));
#29640=CARTESIAN_POINT('Ctrl Pts',(34.3725208876465,-57.8382701189333,19.443828516935));
#29641=CARTESIAN_POINT('Ctrl Pts',(32.2161494783462,-58.7036614639378,19.332690626367));
#29642=CARTESIAN_POINT('Ctrl Pts',(30.3195896701685,-57.3613125035426,19.221552735799));
#29643=CARTESIAN_POINT('Ctrl Pts',(30.4024811841689,-55.4214247242036,19.1286807668307));
#29644=CARTESIAN_POINT('Ctrl Pts',(31.1732925394658,-54.6889852067103,19.0728547613852));
#29645=CARTESIAN_POINT('Ctrl Pts',(31.4743570776169,-54.515029390224,19.0540747194623));
#29646=CARTESIAN_POINT('Origin',(32.5,-56.2916512459885,23.5459252805377));
#29647=CARTESIAN_POINT('',(31.4721876288368,-54.5092967477939,20.4540747194623));
#29648=CARTESIAN_POINT('',(31.4737733324271,-54.5152256259023,20.3959252805377));
#29649=CARTESIAN_POINT('',(31.4726250000001,-54.5121855475624,23.5459252805377));
#29650=CARTESIAN_POINT('Ctrl Pts',(31.4737733324271,-54.5152256259023,20.3959252805377));
#29651=CARTESIAN_POINT('Ctrl Pts',(31.799246207199,-54.3283059275285,20.3756504461887));
#29652=CARTESIAN_POINT('Ctrl Pts',(32.8583863662623,-54.0381735568299,20.318329648317));
#29653=CARTESIAN_POINT('Ctrl Pts',(34.5693901517228,-55.0204352512209,20.2239628869227));
#29654=CARTESIAN_POINT('Ctrl Pts',(34.6903421852681,-57.3408256590054,20.1128249963547));
#29655=CARTESIAN_POINT('Ctrl Pts',(32.8064491443347,-58.7008948504122,20.0016871057866));
#29656=CARTESIAN_POINT('Ctrl Pts',(30.6420597422744,-57.8557560368671,19.8905492152186));
#29657=CARTESIAN_POINT('Ctrl Pts',(30.2167292658396,-55.7678005164131,19.7886286068023));
#29658=CARTESIAN_POINT('Ctrl Pts',(31.0321693333385,-54.7721820870222,19.7237539619086));
#29659=CARTESIAN_POINT('Ctrl Pts',(31.4743950169645,-54.5114972463166,19.6959252805377));
#29660=CARTESIAN_POINT('Ctrl Pts',(31.4721876288368,-54.5092967477939,20.4540747194623));
#29661=CARTESIAN_POINT('Ctrl Pts',(31.5250686260056,-54.4783192167782,20.4507396569907));
#29662=CARTESIAN_POINT('Ctrl Pts',(32.1824999100289,-54.133716656297,20.4103586309964));
#29663=CARTESIAN_POINT('Ctrl Pts',(33.7978345552324,-54.2388509530007,20.3329316414794));
#29664=CARTESIAN_POINT('Ctrl Pts',(34.9285465373885,-56.2687104209716,20.2217937509113));
#29665=CARTESIAN_POINT('Ctrl Pts',(33.836382221401,-58.3195681810162,20.1106558603433));
#29666=CARTESIAN_POINT('Ctrl Pts',(31.5210121579647,-58.5142504249981,19.9995179697753));
#29667=CARTESIAN_POINT('Ctrl Pts',(30.101720741136,-56.674562508041,19.8883800792072));
#29668=CARTESIAN_POINT('Ctrl Pts',(30.6728871983315,-55.0622630484847,19.8065656624362));
#29669=CARTESIAN_POINT('Ctrl Pts',(31.3468677972824,-54.5826454110005,19.7617972091879));
#29670=CARTESIAN_POINT('Ctrl Pts',(31.4707591192322,-54.5126331290242,19.7540747194623));
#29671=CARTESIAN_POINT('Origin',(32.5,-56.2916512459885,23.5459252805377));
#29672=CARTESIAN_POINT('',(31.4749609874599,-54.5139076530798,21.1540747194623));
#29673=CARTESIAN_POINT('',(31.4704172621348,-54.5115691325664,21.0959252805377));
#29674=CARTESIAN_POINT('',(31.4726250000001,-54.5121855475624,23.5459252805377));
#29675=CARTESIAN_POINT('Ctrl Pts',(31.4704172621348,-54.5115691325664,21.0959252805377));
#29676=CARTESIAN_POINT('Ctrl Pts',(31.9722041658629,-54.227575372343,21.0645928939914));
#29677=CARTESIAN_POINT('Ctrl Pts',(33.3458362247711,-54.0736222398741,20.9962145439225));
#29678=CARTESIAN_POINT('Ctrl Pts',(34.8512746399183,-55.6834843462923,20.890790230331));
#29679=CARTESIAN_POINT('Ctrl Pts',(34.2861576030319,-57.9372537407841,20.7796523397629));
#29680=CARTESIAN_POINT('Ctrl Pts',(32.086148188353,-58.6847859443394,20.6685144491949));
#29681=CARTESIAN_POINT('Ctrl Pts',(30.2649430630364,-57.2418541016519,20.5573765586268));
#29682=CARTESIAN_POINT('Ctrl Pts',(30.4485426703034,-55.3510892045502,20.4665135024078));
#29683=CARTESIAN_POINT('Ctrl Pts',(31.2045456025534,-54.6698436293139,20.4126964097114));
#29684=CARTESIAN_POINT('Ctrl Pts',(31.4737733324271,-54.5152256259023,20.3959252805377));
#29685=CARTESIAN_POINT('Ctrl Pts',(31.4749609874599,-54.5139076530798,21.1540747194623));
#29686=CARTESIAN_POINT('Ctrl Pts',(31.70486029749,-54.3795842898515,21.1396821047934));
#29687=CARTESIAN_POINT('Ctrl Pts',(32.6134298152417,-54.053477853398,21.0882435266019));
#29688=CARTESIAN_POINT('Ctrl Pts',(34.3429657642116,-54.7099453599153,20.9997589848876));
#29689=CARTESIAN_POINT('Ctrl Pts',(34.8284152391772,-56.982193672835,20.8886210943196));
#29690=CARTESIAN_POINT('Ctrl Pts',(33.18263271582,-58.6223996095028,20.7774832037515));
#29691=CARTESIAN_POINT('Ctrl Pts',(30.9120322857351,-58.1292356735021,20.6663453131835));
#29692=CARTESIAN_POINT('Ctrl Pts',(30.1194352615649,-56.0193863503516,20.5585424850871));
#29693=CARTESIAN_POINT('Ctrl Pts',(30.9376650889446,-54.8224184634311,20.4877856205134));
#29694=CARTESIAN_POINT('Ctrl Pts',(31.4721876288368,-54.5092967477939,20.4540747194623));
#29695=CARTESIAN_POINT('Origin',(32.5,-56.2916512459885,23.5459252805377));
#29696=CARTESIAN_POINT('',(31.4716734168817,-54.5151354051885,21.8540747194623));
#29697=CARTESIAN_POINT('',(31.4730118547325,-54.5098571360138,21.7959252805377));
#29698=CARTESIAN_POINT('',(31.4726250000001,-54.5121855475624,23.5459252805377));
#29699=CARTESIAN_POINT('',(30.5157034944333,-56.8250975324092,22.));
#29700=CARTESIAN_POINT('Ctrl Pts',(30.5157034944333,-56.8250975324092,22.));
#29701=CARTESIAN_POINT('Ctrl Pts',(30.3383199129809,-56.1652717359215,21.9629540364773));
#29702=CARTESIAN_POINT('Ctrl Pts',(30.5738806361657,-55.1809621297242,21.9143122762981));
#29703=CARTESIAN_POINT('Ctrl Pts',(31.2853315674047,-54.6208532363719,21.8656705161189));
#29704=CARTESIAN_POINT('Ctrl Pts',(31.4716734168817,-54.5151354051885,21.8540747194623));
#29705=CARTESIAN_POINT('',(31.043364830276,-57.7461496994443,22.));
#29706=CARTESIAN_POINT('Origin',(32.5,-56.2916512459885,22.));
#29707=CARTESIAN_POINT('Ctrl Pts',(31.0433632440414,-57.7461514510325,22.));
#29708=CARTESIAN_POINT('Ctrl Pts',(30.5726971034827,-57.2735716615612,21.9636770818144));
#29709=CARTESIAN_POINT('Ctrl Pts',(30.1593922934378,-55.9189388685996,21.895652175327));
#29710=CARTESIAN_POINT('Ctrl Pts',(30.9704682366631,-54.8056054537255,21.8276272688396));
#29711=CARTESIAN_POINT('Ctrl Pts',(31.4730118547325,-54.5098571360138,21.7959252805377));
#29712=CARTESIAN_POINT('Origin',(32.5,56.2916512459885,3.));
#29713=CARTESIAN_POINT('',(33.334828594439,57.735188017533,6.12851963660981));
#29714=CARTESIAN_POINT('',(33.3331620889267,57.736668395617,6.3214803633902));
#29715=CARTESIAN_POINT('',(33.333,57.7344495686934,3.));
#29716=CARTESIAN_POINT('',(33.5940263469955,57.5480995545471,7.));
#29717=CARTESIAN_POINT('Ctrl Pts',(33.3331620889267,57.736668395617,6.3214803633902));
#29718=CARTESIAN_POINT('Ctrl Pts',(33.2830618082469,57.7660644611829,6.32537779445737));
#29719=CARTESIAN_POINT('Ctrl Pts',(33.2314063486239,57.7926890534068,6.32927522552456));
#29720=CARTESIAN_POINT('Ctrl Pts',(33.1783991110197,57.816276539757,6.33317265659174));
#29721=CARTESIAN_POINT('Ctrl Pts',(32.6745533323838,58.0404809307674,6.37021862011442));
#29722=CARTESIAN_POINT('Ctrl Pts',(32.0485753278831,57.9902848612727,6.4072645836371));
#29723=CARTESIAN_POINT('Ctrl Pts',(31.5869763637319,57.6885282775577,6.44431054715978));
#29724=CARTESIAN_POINT('Ctrl Pts',(31.1253773995808,57.3867716938426,6.48135651068246));
#29725=CARTESIAN_POINT('Ctrl Pts',(30.8281574757791,56.8334545959073,6.51840247420514));
#29726=CARTESIAN_POINT('Ctrl Pts',(30.8312835014825,56.2820697925607,6.55544843772782));
#29727=CARTESIAN_POINT('Ctrl Pts',(30.8344095271858,55.730684989214,6.5924944012505));
#29728=CARTESIAN_POINT('Ctrl Pts',(31.1378815023941,55.181232480456,6.62954036477319));
#29729=CARTESIAN_POINT('Ctrl Pts',(31.6029277671501,54.8846445462125,6.66658632829587));
#29730=CARTESIAN_POINT('Ctrl Pts',(32.0679740319062,54.5880566119689,6.70363229181855));
#29731=CARTESIAN_POINT('Ctrl Pts',(32.6945945862099,54.5443332522399,6.74067825534123));
#29732=CARTESIAN_POINT('Ctrl Pts',(33.1957905862086,54.7745591362764,6.77772421886391));
#29733=CARTESIAN_POINT('Ctrl Pts',(33.6969865862073,55.0047850203128,6.81477018238659));
#29734=CARTESIAN_POINT('Ctrl Pts',(34.072758031901,55.5089601481147,6.85181614590928));
#29735=CARTESIAN_POINT('Ctrl Pts',(34.1514677107856,56.0538413345857,6.88886210943196));
#29736=CARTESIAN_POINT('Ctrl Pts',(34.2301773896702,56.5987225210566,6.92590807295464));
#29737=CARTESIAN_POINT('Ctrl Pts',(34.0118253017458,57.1843097661965,6.96295403647732));
#29738=CARTESIAN_POINT('Ctrl Pts',(33.5940263469955,57.5480995545471,7.));
#29739=CARTESIAN_POINT('',(31.0815846268763,57.1712794637625,6.99999999999998));
#29740=CARTESIAN_POINT('Origin',(32.5,56.2916512459885,7.));
#29741=CARTESIAN_POINT('',(33.3322874886545,57.7319139206534,6.8285196366098));
#29742=CARTESIAN_POINT('Ctrl Pts',(31.0815830733445,57.1712803260698,6.99999999999998));
#29743=CARTESIAN_POINT('Ctrl Pts',(31.3671885733958,57.6305045882043,6.96367708181444));
#29744=CARTESIAN_POINT('Ctrl Pts',(31.8971081113246,57.9389632567025,6.92735416362889));
#29745=CARTESIAN_POINT('Ctrl Pts',(32.4375390310397,57.9591354579207,6.89103124544335));
#29746=CARTESIAN_POINT('Ctrl Pts',(32.7475655738981,57.9707075526647,6.87019404249883));
#29747=CARTESIAN_POINT('Ctrl Pts',(33.0610513288344,57.8874068657131,6.84935683955432));
#29748=CARTESIAN_POINT('Ctrl Pts',(33.3322874886545,57.7319139206534,6.8285196366098));
#29749=CARTESIAN_POINT('',(33.333,57.7344495686934,8.));
#29750=CARTESIAN_POINT('',(33.333,57.7344495686934,3.));
#29751=CARTESIAN_POINT('Origin',(32.5,56.2916512459885,8.));
#29752=CARTESIAN_POINT('Ctrl Pts',(33.3322874886545,57.7319139206534,6.8285196366098));
#29753=CARTESIAN_POINT('Ctrl Pts',(33.5432755942256,57.6109596867872,6.81231087603164));
#29754=CARTESIAN_POINT('Ctrl Pts',(33.7286988454439,57.4463225594197,6.79610211545347));
#29755=CARTESIAN_POINT('Ctrl Pts',(33.8670427528185,57.2486779404332,6.77989335487531));
#29756=CARTESIAN_POINT('Ctrl Pts',(34.1832349330579,56.7969509061471,6.74284739135263));
#29757=CARTESIAN_POINT('Ctrl Pts',(34.2534965093545,56.1728010705694,6.70580142782995));
#29758=CARTESIAN_POINT('Ctrl Pts',(34.0454742915244,55.6620590905692,6.66875546430727));
#29759=CARTESIAN_POINT('Ctrl Pts',(33.8374520736943,55.1513171105689,6.63170950078459));
#29760=CARTESIAN_POINT('Ctrl Pts',(33.3511460617374,54.7539829861461,6.59466353726191));
#29761=CARTESIAN_POINT('Ctrl Pts',(32.8092161915406,54.6518060909041,6.55761757373923));
#29762=CARTESIAN_POINT('Ctrl Pts',(32.2672863213437,54.549629195662,6.52057161021655));
#29763=CARTESIAN_POINT('Ctrl Pts',(31.6697325929069,54.7426095296009,6.48352564669386));
#29764=CARTESIAN_POINT('Ctrl Pts',(31.2899790079621,55.1424751852064,6.44647968317118));
#29765=CARTESIAN_POINT('Ctrl Pts',(30.9102254230173,55.542340840812,6.4094337196485));
#29766=CARTESIAN_POINT('Ctrl Pts',(30.7482719815646,56.1490918180843,6.37238775612583));
#29767=CARTESIAN_POINT('Ctrl Pts',(30.8782626384457,56.6850216626073,6.33534179260315));
#29768=CARTESIAN_POINT('Ctrl Pts',(31.0082532953267,57.2209515071302,6.29829582908047));
#29769=CARTESIAN_POINT('Ctrl Pts',(31.4301880505415,57.6860602189039,6.26124986555778));
#29770=CARTESIAN_POINT('Ctrl Pts',(31.9509534890593,57.8674999291041,6.2242039020351));
#29771=CARTESIAN_POINT('Ctrl Pts',(32.3993069550895,58.023710608475,6.19230914689333));
#29772=CARTESIAN_POINT('Ctrl Pts',(32.9209173239095,57.9696554900369,6.16041439175157));
#29773=CARTESIAN_POINT('Ctrl Pts',(33.334828594439,57.735188017533,6.12851963660981));
#29774=CARTESIAN_POINT('Origin',(32.5,56.2916512459885,3.));
#29775=CARTESIAN_POINT('',(33.3324736911222,57.73618752158,5.4285196366098));
#29776=CARTESIAN_POINT('',(33.3311322154952,57.7328790961699,5.6214803633902));
#29777=CARTESIAN_POINT('',(33.333,57.7344495686934,3.));
#29778=CARTESIAN_POINT('Ctrl Pts',(33.3311322154952,57.7328790961699,5.6214803633902));
#29779=CARTESIAN_POINT('Ctrl Pts',(33.1373356857267,57.8459393971242,5.63643534665463));
#29780=CARTESIAN_POINT('Ctrl Pts',(32.9222440320564,57.9213835767879,5.65139032991906));
#29781=CARTESIAN_POINT('Ctrl Pts',(32.7012486057465,57.9482311745983,5.66634531318349));
#29782=CARTESIAN_POINT('Ctrl Pts',(32.1538064350001,58.0147371085448,5.70339127670617));
#29783=CARTESIAN_POINT('Ctrl Pts',(31.5701366653479,57.7830375418651,5.74043724022885));
#29784=CARTESIAN_POINT('Ctrl Pts',(31.2173595401895,57.3591689672607,5.77748320375153));
#29785=CARTESIAN_POINT('Ctrl Pts',(30.8645824150311,56.9353003926564,5.81452916727421));
#29786=CARTESIAN_POINT('Ctrl Pts',(30.7426979343665,56.3192628101275,5.85157513079689));
#29787=CARTESIAN_POINT('Ctrl Pts',(30.9074862986933,55.7929935490273,5.88862109431957));
#29788=CARTESIAN_POINT('Ctrl Pts',(31.0722746630201,55.266724287927,5.92566705784225));
#29789=CARTESIAN_POINT('Ctrl Pts',(31.5237358723383,54.8302233482555,5.96271302136494));
#29790=CARTESIAN_POINT('Ctrl Pts',(32.0552579823815,54.6832494251182,5.99975898488761));
#29791=CARTESIAN_POINT('Ctrl Pts',(32.5867800924248,54.5362755019809,6.0368049484103));
#29792=CARTESIAN_POINT('Ctrl Pts',(33.1983631031929,54.6788285953779,6.07385091193297));
#29793=CARTESIAN_POINT('Ctrl Pts',(33.6101089221164,55.0456852682332,6.11089687545565));
#29794=CARTESIAN_POINT('Ctrl Pts',(34.02185474104,55.4125419410885,6.14794283897833));
#29795=CARTESIAN_POINT('Ctrl Pts',(34.2337633681189,56.003702193402,6.18498880250102));
#29796=CARTESIAN_POINT('Ctrl Pts',(34.1488609052729,56.5485847453165,6.2220347660237));
#29797=CARTESIAN_POINT('Ctrl Pts',(34.0728906300367,57.036142774291,6.2551832984792));
#29798=CARTESIAN_POINT('Ctrl Pts',(33.7592763040381,57.4866482113774,6.2883318309347));
#29799=CARTESIAN_POINT('Ctrl Pts',(33.3331620889267,57.736668395617,6.3214803633902));
#29800=CARTESIAN_POINT('Ctrl Pts',(33.334828594439,57.735188017533,6.12851963660981));
#29801=CARTESIAN_POINT('Ctrl Pts',(33.4016779305205,57.6973200105818,6.12336842822889));
#29802=CARTESIAN_POINT('Ctrl Pts',(33.4657180077386,57.6547460681795,6.11821721984798));
#29803=CARTESIAN_POINT('Ctrl Pts',(33.5261864969391,57.6075919565364,6.11306601146706));
#29804=CARTESIAN_POINT('Ctrl Pts',(33.96105794448,57.2684735651416,6.07602004794438));
#29805=CARTESIAN_POINT('Ctrl Pts',(34.2112047177408,56.6924660737253,6.0389740844217));
#29806=CARTESIAN_POINT('Ctrl Pts',(34.1621425519641,56.1431855476953,6.00192812089902));
#29807=CARTESIAN_POINT('Ctrl Pts',(34.1130803861875,55.5939050216654,5.96488215737634));
#29808=CARTESIAN_POINT('Ctrl Pts',(33.7648092813734,55.0713514610218,5.92783619385366));
#29809=CARTESIAN_POINT('Ctrl Pts',(33.2767190788242,54.8146729733941,5.89079023033098));
#29810=CARTESIAN_POINT('Ctrl Pts',(32.7886288762749,54.5579944857664,5.8537442668083));
#29811=CARTESIAN_POINT('Ctrl Pts',(32.1607195759905,54.5671910711545,5.81669830328562));
#29812=CARTESIAN_POINT('Ctrl Pts',(31.6803566282497,54.8380546099094,5.77965233976293));
#29813=CARTESIAN_POINT('Ctrl Pts',(31.199993680509,55.1089181486644,5.74260637624025));
#29814=CARTESIAN_POINT('Ctrl Pts',(30.8671770853118,55.6414486407862,5.70556041271757));
#29815=CARTESIAN_POINT('Ctrl Pts',(30.8342226473039,56.1919301102113,5.66851444919489));
#29816=CARTESIAN_POINT('Ctrl Pts',(30.801268209296,56.7424115796364,5.63146848567221));
#29817=CARTESIAN_POINT('Ctrl Pts',(31.0681759284774,57.3108440263648,5.59442252214954));
#29818=CARTESIAN_POINT('Ctrl Pts',(31.5127937714062,57.6370813071645,5.55737655862686));
#29819=CARTESIAN_POINT('Ctrl Pts',(31.9574116143351,57.9633185879642,5.52033059510418));
#29820=CARTESIAN_POINT('Ctrl Pts',(32.5797395810114,58.0473607028353,5.48328463158149));
#29821=CARTESIAN_POINT('Ctrl Pts',(33.0949658502734,57.8507452062818,5.44623866805881));
#29822=CARTESIAN_POINT('Ctrl Pts',(33.1771098465446,57.8193982358743,5.44033232424248));
#29823=CARTESIAN_POINT('Ctrl Pts',(33.2565314423349,57.7809172756723,5.43442598042614));
#29824=CARTESIAN_POINT('Ctrl Pts',(33.3324736911222,57.73618752158,5.4285196366098));
#29825=CARTESIAN_POINT('Origin',(32.5,56.2916512459885,3.));
#29826=CARTESIAN_POINT('',(33.3313578105535,57.7323657066332,4.7285196366098));
#29827=CARTESIAN_POINT('',(33.3337300498339,57.7328514726872,4.9214803633902));
#29828=CARTESIAN_POINT('',(33.333,57.7344495686934,3.));
#29829=CARTESIAN_POINT('Ctrl Pts',(33.3337300498339,57.7328514726872,4.9214803633902));
#29830=CARTESIAN_POINT('Ctrl Pts',(32.9948149402967,57.9248393749082,4.94749289885188));
#29831=CARTESIAN_POINT('Ctrl Pts',(32.5875734400098,58.0025082442025,4.97350543431356));
#29832=CARTESIAN_POINT('Ctrl Pts',(32.2063909254829,57.9343784669252,4.99951796977524));
#29833=CARTESIAN_POINT('Ctrl Pts',(31.6635267533437,57.8373508916032,5.03656393329792));
#29834=CARTESIAN_POINT('Ctrl Pts',(31.1735161025779,57.4446106606262,5.0736098968206));
#29835=CARTESIAN_POINT('Ctrl Pts',(30.9606151335011,56.935897533533,5.11065586034328));
#29836=CARTESIAN_POINT('Ctrl Pts',(30.7477141644243,56.4271844064398,5.14770182386596));
#29837=CARTESIAN_POINT('Ctrl Pts',(30.8119228770365,55.8024983832305,5.18474778738864));
#29838=CARTESIAN_POINT('Ctrl Pts',(31.1238557751029,55.3477306326436,5.22179375091132));
#29839=CARTESIAN_POINT('Ctrl Pts',(31.4357886731693,54.8929628820567,5.258839714434));
#29840=CARTESIAN_POINT('Ctrl Pts',(31.9954457566899,54.6081134040922,5.29588567795668));
#29841=CARTESIAN_POINT('Ctrl Pts',(32.5466968174263,54.6235450421449,5.33293164147937));
#29842=CARTESIAN_POINT('Ctrl Pts',(33.0979478781627,54.6389766801977,5.36997760500205));
#29843=CARTESIAN_POINT('Ctrl Pts',(33.6407929161149,54.9546894342676,5.40702356852472));
#29844=CARTESIAN_POINT('Ctrl Pts',(33.9267957627755,55.4261958418307,5.44406953204741));
#29845=CARTESIAN_POINT('Ctrl Pts',(34.2127986094361,55.8977022493938,5.48111549557009));
#29846=CARTESIAN_POINT('Ctrl Pts',(34.2419592648052,56.52500231045,5.51816145909277));
#29847=CARTESIAN_POINT('Ctrl Pts',(34.0009323065694,57.0210080582645,5.55520742261545));
#29848=CARTESIAN_POINT('Ctrl Pts',(33.8572048591017,57.3167826080678,5.5772984028737));
#29849=CARTESIAN_POINT('Ctrl Pts',(33.6174016975492,57.565870358533,5.59938938313195));
#29850=CARTESIAN_POINT('Ctrl Pts',(33.3311322154952,57.7328790961699,5.6214803633902));
#29851=CARTESIAN_POINT('Ctrl Pts',(33.3324736911222,57.73618752158,5.4285196366098));
#29852=CARTESIAN_POINT('Ctrl Pts',(33.7328589074961,57.5003618440874,5.39738001690346));
#29853=CARTESIAN_POINT('Ctrl Pts',(34.0365306675145,57.0908419490654,5.36624039719712));
#29854=CARTESIAN_POINT('Ctrl Pts',(34.1325589902306,56.6373526743003,5.33510077749077));
#29855=CARTESIAN_POINT('Ctrl Pts',(34.246801289078,56.0978487468504,5.29805481396809));
#29856=CARTESIAN_POINT('Ctrl Pts',(34.0671613149251,55.4961139999285,5.26100885044541));
#29857=CARTESIAN_POINT('Ctrl Pts',(33.6758523462208,55.1075357285356,5.22396288692273));
#29858=CARTESIAN_POINT('Ctrl Pts',(33.2845433775165,54.7189574571428,5.18691692340005));
#29859=CARTESIAN_POINT('Ctrl Pts',(32.6815654142609,54.543535661279,5.14987095987737));
#29860=CARTESIAN_POINT('Ctrl Pts',(32.1428747275693,54.6615531325857,5.11282499635469));
#29861=CARTESIAN_POINT('Ctrl Pts',(31.6041840408777,54.7795706038924,5.07577903283201));
#29862=CARTESIAN_POINT('Ctrl Pts',(31.12978063075,55.1910273423697,5.03873306930933));
#29863=CARTESIAN_POINT('Ctrl Pts',(30.9367779143554,55.7076178324787,5.00168710578665));
#29864=CARTESIAN_POINT('Ctrl Pts',(30.7437751979608,56.2242083225877,4.96464114226396));
#29865=CARTESIAN_POINT('Ctrl Pts',(30.8321731752993,56.8459325643283,4.92759517874128));
#29866=CARTESIAN_POINT('Ctrl Pts',(31.1615160075389,57.2882549360944,4.8905492152186));
#29867=CARTESIAN_POINT('Ctrl Pts',(31.4908588397784,57.7305773078605,4.85350325169592));
#29868=CARTESIAN_POINT('Ctrl Pts',(32.0611465269191,57.9934978096521,4.81645728817324));
#29869=CARTESIAN_POINT('Ctrl Pts',(32.6113836768238,57.956689381435,4.77941132465056));
#29870=CARTESIAN_POINT('Ctrl Pts',(32.8633454266668,57.93983425636,4.76244742863697));
#29871=CARTESIAN_POINT('Ctrl Pts',(33.1111028597659,57.8601301739612,4.74548353262339));
#29872=CARTESIAN_POINT('Ctrl Pts',(33.3313578105535,57.7323657066332,4.7285196366098));
#29873=CARTESIAN_POINT('Origin',(32.5,56.2916512459885,3.));
#29874=CARTESIAN_POINT('',(33.3342430690557,57.7335557705024,4.0285196366098));
#29875=CARTESIAN_POINT('',(33.3343740412804,57.7368429003791,4.2214803633902));
#29876=CARTESIAN_POINT('',(33.333,57.7344495686934,3.));
#29877=CARTESIAN_POINT('Ctrl Pts',(33.3343740344483,57.7368428884789,4.2214803633902));
#29878=CARTESIAN_POINT('Ctrl Pts',(32.8564950497481,58.0127845069312,4.25855045104913));
#29879=CARTESIAN_POINT('Ctrl Pts',(32.2282029771155,58.0281412318725,4.29562053870805));
#29880=CARTESIAN_POINT('Ctrl Pts',(31.7373727175272,57.7759553439527,4.33269062636698));
#29881=CARTESIAN_POINT('Ctrl Pts',(31.2468618760144,57.5239335712834,4.36973658988966));
#29882=CARTESIAN_POINT('Ctrl Pts',(30.8936340516087,57.0047173912526,4.40678255341235));
#29883=CARTESIAN_POINT('Ctrl Pts',(30.8393459612069,56.4559290322592,4.44382851693503));
#29884=CARTESIAN_POINT('Ctrl Pts',(30.7850578708051,55.9071406732657,4.48087448045771));
#29885=CARTESIAN_POINT('Ctrl Pts',(31.0297095144071,55.3287801353096,4.51792044398039));
#29886=CARTESIAN_POINT('Ctrl Pts',(31.4613346798115,54.9855373992054,4.55496640750307));
#29887=CARTESIAN_POINT('Ctrl Pts',(31.8929598452158,54.6422946631012,4.59201237102575));
#29888=CARTESIAN_POINT('Ctrl Pts',(32.5115585324225,54.5341697288488,4.62905833454843));
#29889=CARTESIAN_POINT('Ctrl Pts',(33.0340255450119,54.7106465835455,4.66610429807111));
#29890=CARTESIAN_POINT('Ctrl Pts',(33.5564925576013,54.8871234382422,4.70315026159379));
#29891=CARTESIAN_POINT('Ctrl Pts',(33.9828278955733,55.348202081888,4.74019622511647));
#29892=CARTESIAN_POINT('Ctrl Pts',(34.1179167730764,55.8828672630521,4.77724218863915));
#29893=CARTESIAN_POINT('Ctrl Pts',(34.2530056505794,56.4175324442162,4.81428815216183));
#29894=CARTESIAN_POINT('Ctrl Pts',(34.0968480676134,57.0257841628987,4.85133411568452));
#29895=CARTESIAN_POINT('Ctrl Pts',(33.7209104293741,57.4292525624064,4.8883800792072));
#29896=CARTESIAN_POINT('Ctrl Pts',(33.6089446308763,57.5494178688947,4.8994135072682));
#29897=CARTESIAN_POINT('Ctrl Pts',(33.4774836445333,57.6514182455857,4.9104469353292));
#29898=CARTESIAN_POINT('Ctrl Pts',(33.3337300498339,57.7328514726872,4.9214803633902));
#29899=CARTESIAN_POINT('Ctrl Pts',(33.3313578105535,57.7323657066332,4.7285196366098));
#29900=CARTESIAN_POINT('Ctrl Pts',(33.5920983142318,57.5811165681046,4.70843756910071));
#29901=CARTESIAN_POINT('Ctrl Pts',(33.8142965260144,57.3625150588492,4.68835550159161));
#29902=CARTESIAN_POINT('Ctrl Pts',(33.9593006043585,57.1010955378143,4.66827343408252));
#29903=CARTESIAN_POINT('Ctrl Pts',(34.2267937693199,56.6188474806365,4.63122747055984));
#29904=CARTESIAN_POINT('Ctrl Pts',(34.2315934865741,55.9908887245065,4.59418150703716));
#29905=CARTESIAN_POINT('Ctrl Pts',(33.9715031387158,55.5046081545499,4.55713554351448));
#29906=CARTESIAN_POINT('Ctrl Pts',(33.7114127908575,55.0183275845932,4.5200895799918));
#29907=CARTESIAN_POINT('Ctrl Pts',(33.1864323778867,54.6737252008098,4.48304361646911));
#29908=CARTESIAN_POINT('Ctrl Pts',(32.6368221624337,54.6285102383604,4.44599765294643));
#29909=CARTESIAN_POINT('Ctrl Pts',(32.0872119469807,54.5832952759111,4.40895168942375));
#29910=CARTESIAN_POINT('Ctrl Pts',(31.5129719290456,54.8374677347958,4.37190572590108));
#29911=CARTESIAN_POINT('Ctrl Pts',(31.1769063091028,55.2747041478526,4.3348597623784));
#29912=CARTESIAN_POINT('Ctrl Pts',(30.84084068916,55.7119405609094,4.29781379885572));
#29913=CARTESIAN_POINT('Ctrl Pts',(30.7429494672094,56.3322409281384,4.26076783533303));
#29914=CARTESIAN_POINT('Ctrl Pts',(30.9280331160056,56.8517212691839,4.22372187181035));
#29915=CARTESIAN_POINT('Ctrl Pts',(31.1131167648017,57.3712016102294,4.18667590828767));
#29916=CARTESIAN_POINT('Ctrl Pts',(31.5811752843444,57.7898619250913,4.14962994476499));
#29917=CARTESIAN_POINT('Ctrl Pts',(32.117999039119,57.9160999466831,4.11258398124231));
#29918=CARTESIAN_POINT('Ctrl Pts',(32.5240508086608,58.0115859820809,4.08456253303148));
#29919=CARTESIAN_POINT('Ctrl Pts',(32.9694456528715,57.939766662088,4.05654108482064));
#29920=CARTESIAN_POINT('Ctrl Pts',(33.3342430690557,57.7335557705024,4.0285196366098));
#29921=CARTESIAN_POINT('Origin',(32.5,56.2916512459885,3.));
#29922=CARTESIAN_POINT('',(33.3337922536522,57.7369224948681,3.3285196366098));
#29923=CARTESIAN_POINT('',(33.3312448475263,57.7342636967217,3.5214803633902));
#29924=CARTESIAN_POINT('',(33.333,57.7344495686934,3.));
#29925=CARTESIAN_POINT('Ctrl Pts',(33.3312448475263,57.7342636967217,3.5214803633902));
#29926=CARTESIAN_POINT('Ctrl Pts',(33.1882152402262,57.8184056914071,3.5325620397237));
#29927=CARTESIAN_POINT('Ctrl Pts',(33.0334203647077,57.8814418696117,3.5436437160572));
#29928=CARTESIAN_POINT('Ctrl Pts',(32.8726233824478,57.9182768459085,3.5547253923907));
#29929=CARTESIAN_POINT('Ctrl Pts',(32.3350802382442,58.0414159042228,3.59177135591338));
#29930=CARTESIAN_POINT('Ctrl Pts',(31.7304599472088,57.8717407985661,3.62881731943606));
#29931=CARTESIAN_POINT('Ctrl Pts',(31.3354704139632,57.4869043031699,3.66586328295874));
#29932=CARTESIAN_POINT('Ctrl Pts',(30.9404808807176,57.1020678077737,3.70290924648142));
#29933=CARTESIAN_POINT('Ctrl Pts',(30.7551221052618,56.5020699226381,3.7399552100041));
#29934=CARTESIAN_POINT('Ctrl Pts',(30.8642245822408,55.961503082106,3.77700117352678));
#29935=CARTESIAN_POINT('Ctrl Pts',(30.9733270592199,55.4209362415738,3.81404713704946));
#29936=CARTESIAN_POINT('Ctrl Pts',(31.3768907886337,54.9398004456451,3.85109310057214));
#29937=CARTESIAN_POINT('Ctrl Pts',(31.8902225413503,54.7382902195697,3.88813906409482));
#29938=CARTESIAN_POINT('Ctrl Pts',(32.4035542940669,54.5367799934943,3.9251850276175));
#29939=CARTESIAN_POINT('Ctrl Pts',(33.0266540700863,54.6148953372722,3.96223099114018));
#29940=CARTESIAN_POINT('Ctrl Pts',(33.4743567237047,54.9368863208444,3.99927695466286));
#29941=CARTESIAN_POINT('Ctrl Pts',(33.9220593773232,55.2588773044166,4.03632291818554));
#29942=CARTESIAN_POINT('Ctrl Pts',(34.1943649085407,55.824743927783,4.07336888170822));
#29943=CARTESIAN_POINT('Ctrl Pts',(34.1666511469031,56.3755141221476,4.1104148452309));
#29944=CARTESIAN_POINT('Ctrl Pts',(34.138955432321,56.9259256578637,4.14743668461733));
#29945=CARTESIAN_POINT('Ctrl Pts',(33.8116310396246,57.4612604196062,4.18445852400377));
#29946=CARTESIAN_POINT('Ctrl Pts',(33.3343740344483,57.7368428884789,4.2214803633902));
#29947=CARTESIAN_POINT('Ctrl Pts',(33.3342430690557,57.7335557705024,4.0285196366098));
#29948=CARTESIAN_POINT('Ctrl Pts',(33.4517287836878,57.6671440228089,4.01949512129796));
#29949=CARTESIAN_POINT('Ctrl Pts',(33.560854853963,57.5867930493783,4.01047060598611));
#29950=CARTESIAN_POINT('Ctrl Pts',(33.6576147739257,57.4936023059229,4.00144609067427));
#29951=CARTESIAN_POINT('Ctrl Pts',(34.0548177639512,57.1110509152493,3.96440012715159));
#29952=CARTESIAN_POINT('Ctrl Pts',(34.2436347539958,56.5121324055803,3.92735416362891));
#29953=CARTESIAN_POINT('Ctrl Pts',(34.137652577907,55.9709452289588,3.89030820010623));
#29954=CARTESIAN_POINT('Ctrl Pts',(34.0316704018183,55.4297580523373,3.85326223658355));
#29955=CARTESIAN_POINT('Ctrl Pts',(33.6308890595961,54.9463022087633,3.81621627306086));
#29956=CARTESIAN_POINT('Ctrl Pts',(33.11872840509,54.7418340064325,3.77917030953818));
#29957=CARTESIAN_POINT('Ctrl Pts',(32.6065677505839,54.5373658041018,3.7421243460155));
#29958=CARTESIAN_POINT('Ctrl Pts',(31.9830277837939,54.6118852430143,3.70507838249282));
#29959=CARTESIAN_POINT('Ctrl Pts',(31.5334751062351,54.9312880793963,3.66803241897014));
#29960=CARTESIAN_POINT('Ctrl Pts',(31.0839224286763,55.2506909157783,3.63098645544746));
#29961=CARTESIAN_POINT('Ctrl Pts',(30.8083570403488,55.8149771496297,3.59394049192478));
#29962=CARTESIAN_POINT('Ctrl Pts',(30.8328930037818,56.3658979863088,3.5568945284021));
#29963=CARTESIAN_POINT('Ctrl Pts',(30.8574289672149,56.9168188229878,3.51984856487942));
#29964=CARTESIAN_POINT('Ctrl Pts',(31.1820662824084,57.4543742624943,3.48280260135674));
#29965=CARTESIAN_POINT('Ctrl Pts',(31.6582328412459,57.7325490097912,3.44575663783406));
#29966=CARTESIAN_POINT('Ctrl Pts',(32.1343994000833,58.010723757088,3.40871067431137));
#29967=CARTESIAN_POINT('Ctrl Pts',(32.7620952025646,58.0295178121752,3.3716647107887));
#29968=CARTESIAN_POINT('Ctrl Pts',(33.2540517054067,57.7803299691728,3.33461874726602));
#29969=CARTESIAN_POINT('Ctrl Pts',(33.2810496728284,57.7666548470259,3.33258571038061));
#29970=CARTESIAN_POINT('Ctrl Pts',(33.3076388370087,57.7521726493388,3.33055267349521));
#29971=CARTESIAN_POINT('Ctrl Pts',(33.3337922536522,57.7369224948681,3.3285196366098));
#29972=CARTESIAN_POINT('Origin',(32.5,56.2916512459885,3.));
#29973=CARTESIAN_POINT('',(33.3310924906901,57.7334985910042,2.6285196366098));
#29974=CARTESIAN_POINT('',(33.3325882586834,57.7320513890704,2.8214803633902));
#29975=CARTESIAN_POINT('',(33.333,57.7344495686934,3.));
#29976=CARTESIAN_POINT('Ctrl Pts',(33.3325882586834,57.7320513890704,2.8214803633902));
#29977=CARTESIAN_POINT('Ctrl Pts',(33.0441865216604,57.8968038534098,2.84361959192095));
#29978=CARTESIAN_POINT('Ctrl Pts',(32.7077104550097,57.9799132231487,2.8657588204517));
#29979=CARTESIAN_POINT('Ctrl Pts',(32.3790127353428,57.9560193270484,2.88789804898244));
#29980=CARTESIAN_POINT('Ctrl Pts',(31.8289970147924,57.9160372471796,2.92494401250512));
#29981=CARTESIAN_POINT('Ctrl Pts',(31.3007606051993,57.5764468565745,2.9619899760278));
#29982=CARTESIAN_POINT('Ctrl Pts',(31.0360538947178,57.092663623102,2.99903593955048));
#29983=CARTESIAN_POINT('Ctrl Pts',(30.7713471842362,56.6088803896294,3.03608190307317));
#29984=CARTESIAN_POINT('Ctrl Pts',(30.7701701728664,55.9809043132895,3.07312786659585));
#29985=CARTESIAN_POINT('Ctrl Pts',(31.0330615265356,55.4961322062855,3.11017383011853));
#29986=CARTESIAN_POINT('Ctrl Pts',(31.2959528802049,55.0113600992815,3.14721979364121));
#29987=CARTESIAN_POINT('Ctrl Pts',(31.8229125989134,54.6697919616135,3.18426575716389));
#29988=CARTESIAN_POINT('Ctrl Pts',(32.3727745793293,54.6277483883085,3.22131172068657));
#29989=CARTESIAN_POINT('Ctrl Pts',(32.9226365597451,54.5857048150036,3.25835768420925));
#29990=CARTESIAN_POINT('Ctrl Pts',(33.4954008018683,54.8431858060618,3.29540364773193));
#29991=CARTESIAN_POINT('Ctrl Pts',(33.8289385024972,55.2823537259082,3.33244961125461));
#29992=CARTESIAN_POINT('Ctrl Pts',(34.162476203126,55.7215216457546,3.3694955747773));
#29993=CARTESIAN_POINT('Ctrl Pts',(34.2567873622605,56.3423764943892,3.40654153829998));
#29994=CARTESIAN_POINT('Ctrl Pts',(34.0687099431419,56.8607805298492,3.44358750182266));
#29995=CARTESIAN_POINT('Ctrl Pts',(33.9368927177428,57.2241127252305,3.46955178901184));
#29996=CARTESIAN_POINT('Ctrl Pts',(33.6663621789423,57.5371196140996,3.49551607620102));
#29997=CARTESIAN_POINT('Ctrl Pts',(33.3312448475263,57.7342636967217,3.5214803633902));
#29998=CARTESIAN_POINT('Ctrl Pts',(33.3337922536522,57.7369224948681,3.3285196366098));
#29999=CARTESIAN_POINT('Ctrl Pts',(33.7842059499452,57.4742845941374,3.29350670997253));
#30000=CARTESIAN_POINT('Ctrl Pts',(34.1053783658086,56.9838732473919,3.25849378333525));
#30001=CARTESIAN_POINT('Ctrl Pts',(34.1596784920807,56.465506410459,3.22348085669797));
#30002=CARTESIAN_POINT('Ctrl Pts',(34.2171315727097,55.9170404358397,3.18643489317529));
#30003=CARTESIAN_POINT('Ctrl Pts',(33.975820530765,55.3372782276934,3.14938892965261));
#30004=CARTESIAN_POINT('Ctrl Pts',(33.546182732919,54.9915512480536,3.11234296612993));
#30005=CARTESIAN_POINT('Ctrl Pts',(33.1165449350731,54.6458242684137,3.07529700260725));
#30006=CARTESIAN_POINT('Ctrl Pts',(32.498580381326,54.5341325172804,3.03825103908457));
#30007=CARTESIAN_POINT('Ctrl Pts',(31.9751040537975,54.7075923578949,3.00120507556189));
#30008=CARTESIAN_POINT('Ctrl Pts',(31.4516277262689,54.8810521985095,2.96415911203921));
#30009=CARTESIAN_POINT('Ctrl Pts',(31.0226396249589,55.3396636308718,2.92711314851653));
#30010=CARTESIAN_POINT('Ctrl Pts',(30.88446858696,55.8735405324579,2.89006718499385));
#30011=CARTESIAN_POINT('Ctrl Pts',(30.746297548961,56.4074174340438,2.85302122147117));
#30012=CARTESIAN_POINT('Ctrl Pts',(30.8989435742731,57.0165598048535,2.81597525794848));
#30013=CARTESIAN_POINT('Ctrl Pts',(31.2725473438504,57.4221901848135,2.7789292944258));
#30014=CARTESIAN_POINT('Ctrl Pts',(31.6461511134276,57.8278205647734,2.74188333090312));
#30015=CARTESIAN_POINT('Ctrl Pts',(32.24071262727,58.0299389538838,2.70483736738045));
#30016=CARTESIAN_POINT('Ctrl Pts',(32.7841274371744,57.9360447252789,2.66779140385776));
#30017=CARTESIAN_POINT('Ctrl Pts',(32.9761488965038,57.9028661911818,2.65470081477511));
#30018=CARTESIAN_POINT('Ctrl Pts',(33.1617839833806,57.8327263930767,2.64161022569246));
#30019=CARTESIAN_POINT('Ctrl Pts',(33.3310924906901,57.7334985910042,2.6285196366098));
#30020=CARTESIAN_POINT('Origin',(32.5,56.2916512459885,3.));
#30021=CARTESIAN_POINT('',(33.3331879029845,57.7323621350135,1.9285196366098));
#30022=CARTESIAN_POINT('',(33.3348622165511,57.7357255517677,2.12148036339019));
#30023=CARTESIAN_POINT('',(33.333,57.7344495686934,3.));
#30024=CARTESIAN_POINT('Ctrl Pts',(33.3348622165511,57.7357255517677,2.12148036339019));
#30025=CARTESIAN_POINT('Ctrl Pts',(32.9046875435881,57.9801160523425,2.15467714411819));
#30026=CARTESIAN_POINT('Ctrl Pts',(32.3567184702118,58.0261342906593,2.18787392484619));
#30027=CARTESIAN_POINT('Ctrl Pts',(31.8960497135599,57.8472871542167,2.22107070557419));
#30028=CARTESIAN_POINT('Ctrl Pts',(31.3819661915825,57.6477026057306,2.25811666909687));
#30029=CARTESIAN_POINT('Ctrl Pts',(30.9766017246916,57.1680829785327,2.29516263261955));
#30030=CARTESIAN_POINT('Ctrl Pts',(30.8654736597327,56.6279289146384,2.33220859614223));
#30031=CARTESIAN_POINT('Ctrl Pts',(30.7543455947739,56.087774850744,2.36925455966492));
#30032=CARTESIAN_POINT('Ctrl Pts',(30.9374539317471,55.4870863501531,2.4063005231876));
#30033=CARTESIAN_POINT('Ctrl Pts',(31.3309981019417,55.1007719112967,2.44334648671028));
#30034=CARTESIAN_POINT('Ctrl Pts',(31.7245422721362,54.7144574724402,2.48039245023296));
#30035=CARTESIAN_POINT('Ctrl Pts',(32.3285222755522,54.5425170953181,2.51743841375564));
#30036=CARTESIAN_POINT('Ctrl Pts',(32.8665232388266,54.6636402684886,2.55448437727832));
#30037=CARTESIAN_POINT('Ctrl Pts',(33.404524202101,54.7847634416591,2.591530340801));
#30038=CARTESIAN_POINT('Ctrl Pts',(33.876546125234,55.1989501651222,2.62857630432368));
#30039=CARTESIAN_POINT('Ctrl Pts',(34.0665654985573,55.7166455362864,2.66562226784636));
#30040=CARTESIAN_POINT('Ctrl Pts',(34.2565848718806,56.2343409074507,2.70266823136904));
#30041=CARTESIAN_POINT('Ctrl Pts',(34.1646016953943,56.8555449263162,2.73971419489172));
#30042=CARTESIAN_POINT('Ctrl Pts',(33.8327125913974,57.2959600511828,2.7767601584144));
#30043=CARTESIAN_POINT('Ctrl Pts',(33.6991654394395,57.4731764312833,2.79166689340633));
#30044=CARTESIAN_POINT('Ctrl Pts',(33.5267742601986,57.6211206345609,2.80657362839827));
#30045=CARTESIAN_POINT('Ctrl Pts',(33.3325882586834,57.7320513890704,2.8214803633902));
#30046=CARTESIAN_POINT('Ctrl Pts',(33.3310924906901,57.7334985910042,2.6285196366098));
#30047=CARTESIAN_POINT('Ctrl Pts',(33.6409218393061,57.5519147723922,2.60456426216977));
#30048=CARTESIAN_POINT('Ctrl Pts',(33.8960769478414,57.272921419479,2.58060888772975));
#30049=CARTESIAN_POINT('Ctrl Pts',(34.0356424650284,56.9447672654595,2.55665351328972));
#30050=CARTESIAN_POINT('Ctrl Pts',(34.2514745770115,56.4372908805649,2.51960754976704));
#30051=CARTESIAN_POINT('Ctrl Pts',(34.190870695011,55.8122449570956,2.48256158624436));
#30052=CARTESIAN_POINT('Ctrl Pts',(33.8815665292719,55.3556853061788,2.44551562272168));
#30053=CARTESIAN_POINT('Ctrl Pts',(33.5722623635328,54.899125655262,2.408469659199));
#30054=CARTESIAN_POINT('Ctrl Pts',(33.0142579140551,54.6110522768978,2.37142369567632));
#30055=CARTESIAN_POINT('Ctrl Pts',(32.4629270812427,54.6233035861816,2.33437773215364));
#30056=CARTESIAN_POINT('Ctrl Pts',(31.9115962484303,54.6355548954655,2.29733176863096));
#30057=CARTESIAN_POINT('Ctrl Pts',(31.3669390322832,54.9481308923974,2.26028580510828));
#30058=CARTESIAN_POINT('Ctrl Pts',(31.0782208961876,55.417979399555,2.2232398415856));
#30059=CARTESIAN_POINT('Ctrl Pts',(30.789502760092,55.8878279067126,2.18619387806292));
#30060=CARTESIAN_POINT('Ctrl Pts',(30.7567237040478,56.514948924096,2.14914791454024));
#30061=CARTESIAN_POINT('Ctrl Pts',(30.9948852489236,57.0123369620816,2.11210195101756));
#30062=CARTESIAN_POINT('Ctrl Pts',(31.2330467937995,57.5097250000671,2.07505598749488));
#30063=CARTESIAN_POINT('Ctrl Pts',(31.7421489395953,57.8773800586549,2.0380100239722));
#30064=CARTESIAN_POINT('Ctrl Pts',(32.2891982024821,57.9470427155363,2.00096406044951));
#30065=CARTESIAN_POINT('Ctrl Pts',(32.6457882768413,57.9924518106263,1.97681591916961));
#30066=CARTESIAN_POINT('Ctrl Pts',(33.0185020402459,57.9112442562479,1.95266777788971));
#30067=CARTESIAN_POINT('Ctrl Pts',(33.3331879029845,57.7323621350135,1.9285196366098));
#30068=CARTESIAN_POINT('Origin',(32.5,56.2916512459885,3.));
#30069=CARTESIAN_POINT('',(33.3347215376785,57.7364302140763,1.2285196366098));
#30070=CARTESIAN_POINT('',(33.3320718525009,57.735759463036,1.4214803633902));
#30071=CARTESIAN_POINT('',(33.333,57.7344495686934,3.));
#30072=CARTESIAN_POINT('Ctrl Pts',(33.3320718525009,57.735759463036,1.4214803633902));
#30073=CARTESIAN_POINT('Ctrl Pts',(33.2393317234316,57.7904422794385,1.42868873279277));
#30074=CARTESIAN_POINT('Ctrl Pts',(33.1414800191062,57.8359234203097,1.43589710219533));
#30075=CARTESIAN_POINT('Ctrl Pts',(33.0399483052832,57.8706429670186,1.4431054715979));
#30076=CARTESIAN_POINT('Ctrl Pts',(32.5181465001006,58.0490770883944,1.48015143512058));
#30077=CARTESIAN_POINT('Ctrl Pts',(31.8991468445915,57.9432717752442,1.51719739864326));
#30078=CARTESIAN_POINT('Ctrl Pts',(31.4662380410665,57.6016494290874,1.55424336216595));
#30079=CARTESIAN_POINT('Ctrl Pts',(31.0333292375416,57.2600270829306,1.59128932568863));
#30080=CARTESIAN_POINT('Ctrl Pts',(30.7865112860008,56.6825877037672,1.62833528921131));
#30081=CARTESIAN_POINT('Ctrl Pts',(30.8387418215197,56.1335996977757,1.66538125273399));
#30082=CARTESIAN_POINT('Ctrl Pts',(30.8909723570387,55.5846116917841,1.70242721625667));
#30083=CARTESIAN_POINT('Ctrl Pts',(31.2422513796173,55.0640750589644,1.73947317977935));
#30084=CARTESIAN_POINT('Ctrl Pts',(31.731814052685,54.8102163409698,1.77651914330203));
#30085=CARTESIAN_POINT('Ctrl Pts',(32.2213767257528,54.5563576229752,1.81356510682471));
#30086=CARTESIAN_POINT('Ctrl Pts',(32.8492230493096,54.5691768198056,1.85061107034739));
#30087=CARTESIAN_POINT('Ctrl Pts',(33.3280155932489,54.842807153342,1.88765703387007));
#30088=CARTESIAN_POINT('Ctrl Pts',(33.8068081371882,55.1164374868783,1.92470299739275));
#30089=CARTESIAN_POINT('Ctrl Pts',(34.1365469015101,55.6508789571206,1.96174896091543));
#30090=CARTESIAN_POINT('Ctrl Pts',(34.1663250709766,56.2015413947231,1.99879492443811));
#30091=CARTESIAN_POINT('Ctrl Pts',(34.1961032404431,56.7522038323256,2.03584088796079));
#30092=CARTESIAN_POINT('Ctrl Pts',(33.9259208150542,57.3190872372884,2.07288685148347));
#30093=CARTESIAN_POINT('Ctrl Pts',(33.4794283138278,57.6427542048827,2.10993281500615));
#30094=CARTESIAN_POINT('Ctrl Pts',(33.4330364511186,57.6763841392778,2.11378199780083));
#30095=CARTESIAN_POINT('Ctrl Pts',(33.384741178112,57.7073883549261,2.11763118059551));
#30096=CARTESIAN_POINT('Ctrl Pts',(33.3348622165511,57.7357255517677,2.12148036339019));
#30097=CARTESIAN_POINT('Ctrl Pts',(33.3331879029845,57.7323621350135,1.9285196366098));
#30098=CARTESIAN_POINT('Ctrl Pts',(33.501265531522,57.6368189718628,1.91562181436702));
#30099=CARTESIAN_POINT('Ctrl Pts',(33.6527891880219,57.5134115911553,1.90272399212425));
#30100=CARTESIAN_POINT('Ctrl Pts',(33.7764604319637,57.3665498834978,1.88982616988147));
#30101=CARTESIAN_POINT('Ctrl Pts',(34.1316770185806,56.9447241394031,1.85278020635879));
#30102=CARTESIAN_POINT('Ctrl Pts',(34.2571138118367,56.3294023960388,1.81573424283611));
#30103=CARTESIAN_POINT('Ctrl Pts',(34.0953639520231,55.8021901383674,1.77868827931343));
#30104=CARTESIAN_POINT('Ctrl Pts',(33.9336140922095,55.2749778806959,1.74164231579075));
#30105=CARTESIAN_POINT('Ctrl Pts',(33.4846775793261,54.8358751087172,1.70459635226807));
#30106=CARTESIAN_POINT('Ctrl Pts',(32.9540127541378,54.6858396959092,1.66755038874539));
#30107=CARTESIAN_POINT('Ctrl Pts',(32.4233479289494,54.5358042831012,1.63050442522271));
#30108=CARTESIAN_POINT('Ctrl Pts',(31.8109547914561,54.6748362294637,1.59345846170003));
#30109=CARTESIAN_POINT('Ctrl Pts',(31.3970985335358,55.0393067763799,1.55641249817735));
#30110=CARTESIAN_POINT('Ctrl Pts',(30.9832422756156,55.4037773232961,1.51936653465467));
#30111=CARTESIAN_POINT('Ctrl Pts',(30.7679228972685,55.993686470766,1.48232057113199));
#30112=CARTESIAN_POINT('Ctrl Pts',(30.8496825329409,56.5390589524362,1.44527460760931));
#30113=CARTESIAN_POINT('Ctrl Pts',(30.9314421686133,57.0844314341065,1.40822864408663));
#30114=CARTESIAN_POINT('Ctrl Pts',(31.3102808183052,57.5852672499772,1.37118268056395));
#30115=CARTESIAN_POINT('Ctrl Pts',(31.8128208258201,57.8123560489854,1.33413671704127));
#30116=CARTESIAN_POINT('Ctrl Pts',(32.2903969982888,58.0281641395237,1.29893102356411));
#30117=CARTESIAN_POINT('Ctrl Pts',(32.8796899699103,57.9967466454787,1.26372533008696));
#30118=CARTESIAN_POINT('Ctrl Pts',(33.3347215376785,57.7364302140763,1.2285196366098));
#30119=CARTESIAN_POINT('Origin',(32.5,56.2916512459885,3.));
#30120=CARTESIAN_POINT('',(33.3315625259448,57.7350035902351,0.5285196366098));
#30121=CARTESIAN_POINT('',(33.3315934922344,57.7321400761417,0.721480363390196));
#30122=CARTESIAN_POINT('',(33.333,57.7344495686934,3.));
#30123=CARTESIAN_POINT('Ctrl Pts',(33.3315934922344,57.7321400761417,0.721480363390196));
#30124=CARTESIAN_POINT('Ctrl Pts',(33.094172273388,57.8693226291885,0.739746284990015));
#30125=CARTESIAN_POINT('Ctrl Pts',(32.8247195065089,57.9509431527901,0.758012206589833));
#30126=CARTESIAN_POINT('Ctrl Pts',(32.552949516444,57.9595707213043,0.776278128189651));
#30127=CARTESIAN_POINT('Ctrl Pts',(32.001760183703,57.97706869351,0.813324091712332));
#30128=CARTESIAN_POINT('Ctrl Pts',(31.4410392363067,57.6943190569764,0.850370055235013));
#30129=CARTESIAN_POINT('Ctrl Pts',(31.1274037953482,57.2407237861293,0.887416018757693));
#30130=CARTESIAN_POINT('Ctrl Pts',(30.8137683543896,56.7871285152823,0.924461982280374));
#30131=CARTESIAN_POINT('Ctrl Pts',(30.7472184198688,56.1626876101218,0.961507945803055));
#30132=CARTESIAN_POINT('Ctrl Pts',(30.9582109466764,55.6531799917321,0.998553909325736));
#30133=CARTESIAN_POINT('Ctrl Pts',(31.169203473484,55.1436723733423,1.03559987284842));
#30134=CARTESIAN_POINT('Ctrl Pts',(31.6577384616201,54.7490980417232,1.0726458363711));
#30135=CARTESIAN_POINT('Ctrl Pts',(32.2002351035856,54.6500361771206,1.10969179989378));
#30136=CARTESIAN_POINT('Ctrl Pts',(32.742731745551,54.550974312518,1.14673776341646));
#30137=CARTESIAN_POINT('Ctrl Pts',(33.339190041346,54.7474249149318,1.18378372693914));
#30138=CARTESIAN_POINT('Ctrl Pts',(33.7166374697496,55.1494812522208,1.22082969046182));
#30139=CARTESIAN_POINT('Ctrl Pts',(34.0940848981533,55.5515375895099,1.2578756539845));
#30140=CARTESIAN_POINT('Ctrl Pts',(34.2525214591656,56.1591996616742,1.29492161750718));
#30141=CARTESIAN_POINT('Ctrl Pts',(34.1194377622437,56.6943674757074,1.33196758102986));
#30142=CARTESIAN_POINT('Ctrl Pts',(34.0122493682821,57.1254028302473,1.36180517514997));
#30143=CARTESIAN_POINT('Ctrl Pts',(33.7159509484902,57.5094109520148,1.39164276927008));
#30144=CARTESIAN_POINT('Ctrl Pts',(33.3320718525009,57.735759463036,1.4214803633902));
#30145=CARTESIAN_POINT('Ctrl Pts',(33.3347215376785,57.7364302140763,1.2285196366098));
#30146=CARTESIAN_POINT('Ctrl Pts',(33.3585069224055,57.7228229680956,1.22667936656428));
#30147=CARTESIAN_POINT('Ctrl Pts',(33.3819254571596,57.7085902886951,1.22483909651875));
#30148=CARTESIAN_POINT('Ctrl Pts',(33.4049420099642,57.6937347933887,1.22299882647322));
#30149=CARTESIAN_POINT('Ctrl Pts',(33.8682818212557,57.394682956638,1.18595286295054));
#30150=CARTESIAN_POINT('Ctrl Pts',(34.1687200785007,56.8432375009908,1.14890689942786));
#30151=CARTESIAN_POINT('Ctrl Pts',(34.1687595096553,56.2917705661426,1.11186093590518));
#30152=CARTESIAN_POINT('Ctrl Pts',(34.1687989408099,55.7403036312943,1.0748149723825));
#30153=CARTESIAN_POINT('Ctrl Pts',(33.8684395458741,55.188815217245,1.03776900885982));
#30154=CARTESIAN_POINT('Ctrl Pts',(33.4051425051238,54.8896971238163,1.00072304533714));
#30155=CARTESIAN_POINT('Ctrl Pts',(32.9418454643735,54.5905790303876,0.963677081814459));
#30156=CARTESIAN_POINT('Ctrl Pts',(32.3156107778087,54.5438312575796,0.926631118291778));
#30157=CARTESIAN_POINT('Ctrl Pts',(31.8130383006683,54.7708481887354,0.889585154769097));
#30158=CARTESIAN_POINT('Ctrl Pts',(31.310465823528,54.9978651198912,0.852539191246416));
#30159=CARTESIAN_POINT('Ctrl Pts',(30.9315555558121,55.4986467550108,0.815493227723736));
#30160=CARTESIAN_POINT('Ctrl Pts',(30.8497179302269,56.0440075390777,0.778447264201056));
#30161=CARTESIAN_POINT('Ctrl Pts',(30.7678803046417,56.5893683231447,0.741401300678375));
#30162=CARTESIAN_POINT('Ctrl Pts',(30.9831153211871,57.179308256159,0.704355337155694));
#30163=CARTESIAN_POINT('Ctrl Pts',(31.3969194538394,57.543837982747,0.667309373633013));
#30164=CARTESIAN_POINT('Ctrl Pts',(31.8107235864917,57.9083677093349,0.630263410110333));
#30165=CARTESIAN_POINT('Ctrl Pts',(32.423096835251,58.0474872294965,0.593217446587652));
#30166=CARTESIAN_POINT('Ctrl Pts',(32.9537831109001,57.8975277056554,0.556171483064972));
#30167=CARTESIAN_POINT('Ctrl Pts',(33.0858213863713,57.860216778603,0.546954200913248));
#30168=CARTESIAN_POINT('Ctrl Pts',(33.2128028501901,57.805010485588,0.537736918761524));
#30169=CARTESIAN_POINT('Ctrl Pts',(33.3315625259448,57.7350035902351,0.5285196366098));
#30170=CARTESIAN_POINT('Origin',(32.5,56.2916512459885,3.));
#30171=CARTESIAN_POINT('',(33.332066590478,57.7319806121586,-0.171480363390199));
#30172=CARTESIAN_POINT('',(33.3345107245665,57.7340829700271,0.0214803633901963));
#30173=CARTESIAN_POINT('',(33.333,57.7344495686934,3.));
#30174=CARTESIAN_POINT('Ctrl Pts',(33.3345107245665,57.7340829700271,0.0214803633901963));
#30175=CARTESIAN_POINT('Ctrl Pts',(32.9530815922346,57.9496325625699,0.0508038371872645));
#30176=CARTESIAN_POINT('Ctrl Pts',(32.482446188026,58.016467684898,0.0801273109843327));
#30177=CARTESIAN_POINT('Ctrl Pts',(32.0612908438827,57.9017112764627,0.109450784781401));
#30178=CARTESIAN_POINT('Ctrl Pts',(31.5292220438323,57.7567331694926,0.146496748304082));
#30179=CARTESIAN_POINT('Ctrl Pts',(31.0761267049973,57.3219229222043,0.183542711826762));
#30180=CARTESIAN_POINT('Ctrl Pts',(30.9093664792402,56.796273907743,0.220588675349443));
#30181=CARTESIAN_POINT('Ctrl Pts',(30.7426062534831,56.2706248932818,0.257634638872123));
#30182=CARTESIAN_POINT('Ctrl Pts',(30.8621811408039,55.6541371116476,0.294680602394804));
#30183=CARTESIAN_POINT('Ctrl Pts',(31.2133670155729,55.2289496928674,0.331726565917484));
#30184=CARTESIAN_POINT('Ctrl Pts',(31.5645528903419,54.8037622740873,0.368772529440165));
#30185=CARTESIAN_POINT('Ctrl Pts',(32.1473497525593,54.5698752181613,0.405818492962845));
#30186=CARTESIAN_POINT('Ctrl Pts',(32.6950373137549,54.6343282619421,0.442864456485526));
#30187=CARTESIAN_POINT('Ctrl Pts',(33.2427248749505,54.6987813057228,0.479910420008206));
#30188=CARTESIAN_POINT('Ctrl Pts',(33.7553031351243,55.0615744492104,0.516956383530887));
#30189=CARTESIAN_POINT('Ctrl Pts',(33.9981877468876,55.5566733533726,0.554002347053568));
#30190=CARTESIAN_POINT('Ctrl Pts',(34.2410723586509,56.0517722575349,0.591048310576249));
#30191=CARTESIAN_POINT('Ctrl Pts',(34.2142633220036,56.6791769223718,0.628094274098929));
#30192=CARTESIAN_POINT('Ctrl Pts',(33.9300299446371,57.1517520452627,0.66514023762161));
#30193=CARTESIAN_POINT('Ctrl Pts',(33.7859409742004,57.3913187827875,0.683920279544472));
#30194=CARTESIAN_POINT('Ctrl Pts',(33.5756972687095,57.591096325175,0.702700321467334));
#30195=CARTESIAN_POINT('Ctrl Pts',(33.3315934922344,57.7321400761417,0.721480363390196));
#30196=CARTESIAN_POINT('Ctrl Pts',(33.3315625259448,57.7350035902351,0.5285196366098));
#30197=CARTESIAN_POINT('Ctrl Pts',(33.6901199750815,57.523639811577,0.500690955238843));
#30198=CARTESIAN_POINT('Ctrl Pts',(33.9737318881584,57.1773614538062,0.472862273867886));
#30199=CARTESIAN_POINT('Ctrl Pts',(34.0952939407749,56.781340492839,0.44503359249693));
#30200=CARTESIAN_POINT('Ctrl Pts',(34.2571191924618,56.2541513717075,0.407987628974249));
#30201=CARTESIAN_POINT('Ctrl Pts',(34.1317703932969,55.6388116972881,0.370941665451569));
#30202=CARTESIAN_POINT('Ctrl Pts',(33.7766141338562,55.2169351595517,0.333895701928889));
#30203=CARTESIAN_POINT('Ctrl Pts',(33.4214578744154,54.7950586218153,0.296849738406208));
#30204=CARTESIAN_POINT('Ctrl Pts',(32.8364941546988,54.566645220762,0.259803774883528));
#30205=CARTESIAN_POINT('Ctrl Pts',(32.289434934298,54.636229647045,0.222757811360847));
#30206=CARTESIAN_POINT('Ctrl Pts',(31.7423757138972,54.705814073328,0.185711847838166));
#30207=CARTESIAN_POINT('Ctrl Pts',(31.2332209928121,55.0733963269474,0.148665884315486));
#30208=CARTESIAN_POINT('Ctrl Pts',(30.9949883236289,55.5707503002861,0.111619920792805));
#30209=CARTESIAN_POINT('Ctrl Pts',(30.7567556544457,56.0681042736248,0.0745739572701246));
#30210=CARTESIAN_POINT('Ctrl Pts',(30.7894450371643,56.6952299666827,0.0375279937474443));
#30211=CARTESIAN_POINT('Ctrl Pts',(31.0780959757366,57.1651197597709,0.000482030224763866));
#30212=CARTESIAN_POINT('Ctrl Pts',(31.3667469143089,57.635009552859,-0.0365639332979165));
#30213=CARTESIAN_POINT('Ctrl Pts',(31.9113594087348,57.9476634459773,-0.073609896820597));
#30214=CARTESIAN_POINT('Ctrl Pts',(32.4626884920092,57.9599935925982,-0.110655860343278));
#30215=CARTESIAN_POINT('Ctrl Pts',(32.7644246265901,57.9667417415587,-0.130930694692251));
#30216=CARTESIAN_POINT('Ctrl Pts',(33.0681725463472,57.8835354694765,-0.151205529041225));
#30217=CARTESIAN_POINT('Ctrl Pts',(33.332066590478,57.7319806121586,-0.171480363390199));
#30218=CARTESIAN_POINT('Origin',(32.5,56.2916512459885,3.));
#30219=CARTESIAN_POINT('',(33.3347877909358,57.7349452754743,-0.871480363390197));
#30220=CARTESIAN_POINT('',(33.3333524836119,57.7367881187288,-0.678519636609802));
#30221=CARTESIAN_POINT('',(33.333,57.7344495686934,3.));
#30222=CARTESIAN_POINT('Ctrl Pts',(33.3333524836119,57.7367881187288,-0.678519636609802));
#30223=CARTESIAN_POINT('Ctrl Pts',(33.2904764567157,57.7619047682301,-0.675184574138165));
#30224=CARTESIAN_POINT('Ctrl Pts',(33.2464522145773,57.7849807415505,-0.671849511666528));
#30225=CARTESIAN_POINT('Ctrl Pts',(33.201404681754,57.8058476261432,-0.66851444919489));
#30226=CARTESIAN_POINT('Ctrl Pts',(32.701015477069,58.0376375407333,-0.631468485672209));
#30227=CARTESIAN_POINT('Ctrl Pts',(32.0743642145054,57.9968518393257,-0.594422522149529));
#30228=CARTESIAN_POINT('Ctrl Pts',(31.608241296104,57.7021565859588,-0.557376558626848));
#30229=CARTESIAN_POINT('Ctrl Pts',(31.1421183777026,57.407461332592,-0.520330595104168));
#30230=CARTESIAN_POINT('Ctrl Pts',(30.8365238034633,56.8588565272658,-0.483284631581487));
#30231=CARTESIAN_POINT('Ctrl Pts',(30.8313147141678,56.3074141411014,-0.446238668058807));
#30232=CARTESIAN_POINT('Ctrl Pts',(30.8261056248723,55.7559717549371,-0.409192704536126));
#30233=CARTESIAN_POINT('Ctrl Pts',(31.1212820205206,55.2016917879345,-0.372146741013446));
#30234=CARTESIAN_POINT('Ctrl Pts',(31.5817547242443,54.8982436746825,-0.335100777490766));
#30235=CARTESIAN_POINT('Ctrl Pts',(32.0422274279679,54.5947955614305,-0.298054813968085));
#30236=CARTESIAN_POINT('Ctrl Pts',(32.6679964397669,54.5421793019291,-0.261008850445404));
#30237=CARTESIAN_POINT('Ctrl Pts',(33.1726750359156,54.7644749931934,-0.223962886922724));
#30238=CARTESIAN_POINT('Ctrl Pts',(33.6773536320643,54.9867706844577,-0.186916923400043));
#30239=CARTESIAN_POINT('Ctrl Pts',(34.0609418125626,55.4839783264877,-0.149870959877363));
#30240=CARTESIAN_POINT('Ctrl Pts',(34.1478882650457,56.0285480388725,-0.112824996354682));
#30241=CARTESIAN_POINT('Ctrl Pts',(34.2348347175289,56.5731177512574,-0.0757790328320021));
#30242=CARTESIAN_POINT('Ctrl Pts',(34.0251394419968,57.1650495339971,-0.0387330693093216));
#30243=CARTESIAN_POINT('Ctrl Pts',(33.6147706735978,57.5334424420409,-0.00168710578664105));
#30244=CARTESIAN_POINT('Ctrl Pts',(33.529226438914,57.6102365155873,0.00603538393897141));
#30245=CARTESIAN_POINT('Ctrl Pts',(33.434962075449,57.6773168608924,0.0137578736645838));
#30246=CARTESIAN_POINT('Ctrl Pts',(33.3345107245665,57.7340829700271,0.0214803633901963));
#30247=CARTESIAN_POINT('Ctrl Pts',(33.332066590478,57.7319806121586,-0.171480363390199));
#30248=CARTESIAN_POINT('Ctrl Pts',(33.550356960999,57.6066160323434,-0.188251492563906));
#30249=CARTESIAN_POINT('Ctrl Pts',(33.7413776202381,57.4344844529175,-0.205022621737613));
#30250=CARTESIAN_POINT('Ctrl Pts',(33.8814326840108,57.2278147357495,-0.22179375091132));
#30251=CARTESIAN_POINT('Ctrl Pts',(34.1908021206151,56.7712993321564,-0.258839714434));
#30252=CARTESIAN_POINT('Ctrl Pts',(34.251495321701,56.1462621248467,-0.29588567795668));
#30253=CARTESIAN_POINT('Ctrl Pts',(34.0357358154562,55.638754858791,-0.33293164147936));
#30254=CARTESIAN_POINT('Ctrl Pts',(33.8199763092115,55.1312475927353,-0.369977605002041));
#30255=CARTESIAN_POINT('Ctrl Pts',(33.3277640956362,54.7412702679337,-0.407023568524722));
#30256=CARTESIAN_POINT('Ctrl Pts',(32.7843626547691,54.6472983719835,-0.444069532047402));
#30257=CARTESIAN_POINT('Ctrl Pts',(32.2409612139021,54.5533264760334,-0.481115495570083));
#30258=CARTESIAN_POINT('Ctrl Pts',(31.6463705457434,54.7553600089348,-0.518161459092763));
#30259=CARTESIAN_POINT('Ctrl Pts',(31.2727089000175,55.1609368730463,-0.555207422615444));
#30260=CARTESIAN_POINT('Ctrl Pts',(30.8990472542916,55.5665137371577,-0.592253386138124));
#30261=CARTESIAN_POINT('Ctrl Pts',(30.7463146309986,56.1756339324792,-0.629299349660805));
#30262=CARTESIAN_POINT('Ctrl Pts',(30.8844090678351,56.7095307561729,-0.666345313183486));
#30263=CARTESIAN_POINT('Ctrl Pts',(31.0225035046717,57.2434275798666,-0.703391276706166));
#30264=CARTESIAN_POINT('Ctrl Pts',(31.4514250016378,57.7021010319325,-0.740437240228847));
#30265=CARTESIAN_POINT('Ctrl Pts',(31.9748770216296,57.8756353949644,-0.777483203751527));
#30266=CARTESIAN_POINT('Ctrl Pts',(32.4175973471179,58.0224056561357,-0.80881559029775));
#30267=CARTESIAN_POINT('Ctrl Pts',(32.9279379927888,57.9652079725634,-0.840147976843973));
#30268=CARTESIAN_POINT('Ctrl Pts',(33.3347877909358,57.7349452754743,-0.871480363390197));
#30269=CARTESIAN_POINT('Origin',(32.5,56.2916512459885,3.));
#30270=CARTESIAN_POINT('',(33.332685602761,57.7363329907929,-1.5714803633902));
#30271=CARTESIAN_POINT('',(33.3311039683456,57.7330494773494,-1.3785196366098));
#30272=CARTESIAN_POINT('',(33.333,57.7344495686934,3.));
#30273=CARTESIAN_POINT('',(30.9307125467392,55.7322829513575,-2.));
#30274=CARTESIAN_POINT('Ctrl Pts',(33.332685602761,57.7363329907929,-1.5714803633902));
#30275=CARTESIAN_POINT('Ctrl Pts',(33.7401458440335,57.4965393115171,-1.60318235169209));
#30276=CARTESIAN_POINT('Ctrl Pts',(34.046614399938,57.0758524794489,-1.63488433999398));
#30277=CARTESIAN_POINT('Ctrl Pts',(34.1374824480444,56.6126749242948,-1.66658632829587));
#30278=CARTESIAN_POINT('Ctrl Pts',(34.2436680400479,56.0714199515982,-1.70363229181855));
#30279=CARTESIAN_POINT('Ctrl Pts',(34.0554395585675,55.472141614315,-1.74067825534123));
#30280=CARTESIAN_POINT('Ctrl Pts',(33.6580205398159,55.0897022763625,-1.77772421886391));
#30281=CARTESIAN_POINT('Ctrl Pts',(33.2606015210643,54.70726293841,-1.81477018238659));
#30282=CARTESIAN_POINT('Ctrl Pts',(32.6539919650415,54.5416625997882,-1.85181614590927));
#30283=CARTESIAN_POINT('Ctrl Pts',(32.1180205379334,54.6674612497455,-1.88886210943196));
#30284=CARTESIAN_POINT('Ctrl Pts',(31.5820491108253,54.7932598997029,-1.92590807295464));
#30285=CARTESIAN_POINT('Ctrl Pts',(31.116715812632,55.2104575382394,-1.96295403647732));
#30286=CARTESIAN_POINT('Ctrl Pts',(30.9307125467392,55.7322829513575,-2.));
#30287=CARTESIAN_POINT('',(32.1993827818326,57.933381219007,-1.99999999999999));
#30288=CARTESIAN_POINT('Origin',(32.5,56.2916512459885,-2.));
#30289=CARTESIAN_POINT('Ctrl Pts',(32.1993825459686,57.9333829869217,-1.99999999999999));
#30290=CARTESIAN_POINT('Ctrl Pts',(31.6675596070896,57.835293698039,-1.96367708181444));
#30291=CARTESIAN_POINT('Ctrl Pts',(31.1868214355218,57.4546983693859,-1.92735416362889));
#30292=CARTESIAN_POINT('Ctrl Pts',(30.9706018866112,56.9589951265537,-1.89103124544334));
#30293=CARTESIAN_POINT('Ctrl Pts',(30.7500782634565,56.4534243968501,-1.85398528192066));
#30294=CARTESIAN_POINT('Ctrl Pts',(30.8047091132838,55.8281174567283,-1.81693931839798));
#30295=CARTESIAN_POINT('Ctrl Pts',(31.1096921022323,55.3687479433185,-1.7798933548753));
#30296=CARTESIAN_POINT('Ctrl Pts',(31.4146750911809,54.9093784299087,-1.74284739135262));
#30297=CARTESIAN_POINT('Ctrl Pts',(31.9700102192507,54.6159463432109,-1.70580142782994));
#30298=CARTESIAN_POINT('Ctrl Pts',(32.521445594378,54.6229937951642,-1.66875546430726));
#30299=CARTESIAN_POINT('Ctrl Pts',(33.0728809695053,54.6300412471175,-1.63170950078458));
#30300=CARTESIAN_POINT('Ctrl Pts',(33.62041659169,54.9375682377219,-1.5946635372619));
#30301=CARTESIAN_POINT('Ctrl Pts',(33.9135196580232,55.4047071572134,-1.55761757373922));
#30302=CARTESIAN_POINT('Ctrl Pts',(34.2066227243565,55.8718460767048,-1.52057161021654));
#30303=CARTESIAN_POINT('Ctrl Pts',(34.2452932348383,56.4985969250833,-1.48352564669386));
#30304=CARTESIAN_POINT('Ctrl Pts',(34.0118083132187,56.9981869719763,-1.44647968317118));
#30305=CARTESIAN_POINT('Ctrl Pts',(33.869033908706,57.3036828084989,-1.42382633431739));
#30306=CARTESIAN_POINT('Ctrl Pts',(33.6244941277173,57.5616302028089,-1.4011729854636));
#30307=CARTESIAN_POINT('Ctrl Pts',(33.3311039683456,57.7330494773494,-1.3785196366098));
#30308=CARTESIAN_POINT('Origin',(32.5,56.2916512459885,-3.54592528053767));
#30309=CARTESIAN_POINT('',(33.5275749112977,58.0738535198176,6.54592528053768));
#30310=CARTESIAN_POINT('',(33.5264962288793,58.0679896197986,6.60407471946233));
#30311=CARTESIAN_POINT('',(33.5273749999999,58.0711169444147,-3.54592528053767));
#30312=CARTESIAN_POINT('',(32.2716262263503,54.2496319067047,7.));
#30313=CARTESIAN_POINT('Ctrl Pts',(33.5264962288793,58.0679896197986,6.60407471946233));
#30314=CARTESIAN_POINT('Ctrl Pts',(33.1919689183208,58.2597658075907,6.62491192240684));
#30315=CARTESIAN_POINT('Ctrl Pts',(32.1179432461623,58.5451601991561,6.68279508887403));
#30316=CARTESIAN_POINT('Ctrl Pts',(30.4105200538552,57.5324032730233,6.77772421886391));
#30317=CARTESIAN_POINT('Ctrl Pts',(30.3280193568976,55.2072605605051,6.88886210943196));
#30318=CARTESIAN_POINT('Ctrl Pts',(31.592606214368,54.3255716196824,6.96295403647732));
#30319=CARTESIAN_POINT('Ctrl Pts',(32.2716262263503,54.2496319067047,7.));
#30320=CARTESIAN_POINT('',(33.3217794842373,54.4043178444011,6.99999999999999));
#30321=CARTESIAN_POINT('Origin',(32.5,56.2916512459885,7.));
#30322=CARTESIAN_POINT('Ctrl Pts',(33.5275749112977,58.0738535198176,6.54592528053768));
#30323=CARTESIAN_POINT('Ctrl Pts',(33.4657840639228,58.1101089614272,6.54982271160486));
#30324=CARTESIAN_POINT('Ctrl Pts',(32.7965074863137,58.4550718384181,6.59076610619471));
#30325=CARTESIAN_POINT('Ctrl Pts',(31.1711925871668,58.3247407101007,6.66875546430726));
#30326=CARTESIAN_POINT('Ctrl Pts',(30.0714699489351,56.2774508415846,6.77989335487529));
#30327=CARTESIAN_POINT('Ctrl Pts',(31.1870202472961,54.2576863817542,6.89030820010621));
#30328=CARTESIAN_POINT('Ctrl Pts',(32.7099100739971,54.1388320417446,6.96367708181444));
#30329=CARTESIAN_POINT('Ctrl Pts',(33.3217804591137,54.4043158724519,7.));
#30330=CARTESIAN_POINT('Origin',(32.5,56.2916512459885,-3.54592528053767));
#30331=CARTESIAN_POINT('',(33.5250713804254,58.0691800125914,5.84592528053768));
#30332=CARTESIAN_POINT('',(33.5296302847681,58.0720277053709,5.90407471946232));
#30333=CARTESIAN_POINT('',(33.5273749999999,58.0711169444147,-3.54592528053767));
#30334=CARTESIAN_POINT('Ctrl Pts',(33.5296302847681,58.0720277053709,5.90407471946233));
#30335=CARTESIAN_POINT('Ctrl Pts',(33.0191355770127,58.3612066004053,5.93596947460409));
#30336=CARTESIAN_POINT('Ctrl Pts',(31.6285851526934,58.5053110361567,6.00491019326853));
#30337=CARTESIAN_POINT('Ctrl Pts',(30.1397737216656,56.8641588006487,6.11089687545567));
#30338=CARTESIAN_POINT('Ctrl Pts',(30.7390063155881,54.6191619749282,6.2220347660237));
#30339=CARTESIAN_POINT('Ctrl Pts',(32.9499730445898,53.9051289476276,6.33317265659175));
#30340=CARTESIAN_POINT('Ctrl Pts',(34.7493198838486,55.375277132786,6.44431054715978));
#30341=CARTESIAN_POINT('Ctrl Pts',(34.5380916131598,57.2516667239214,6.53461123478332));
#30342=CARTESIAN_POINT('Ctrl Pts',(33.7867170031423,57.9188115213373,6.58786595888416));
#30343=CARTESIAN_POINT('Ctrl Pts',(33.5264962288793,58.0679896197986,6.60407471946233));
#30344=CARTESIAN_POINT('Ctrl Pts',(33.5250713804254,58.0691800125914,5.84592528053768));
#30345=CARTESIAN_POINT('Ctrl Pts',(33.2860537216368,58.2086221814904,5.8608802638021));
#30346=CARTESIAN_POINT('Ctrl Pts',(32.3636248873145,58.5321674493612,5.91288121058921));
#30347=CARTESIAN_POINT('Ctrl Pts',(30.6332940299706,57.8452774805726,6.00192812089902));
#30348=CARTESIAN_POINT('Ctrl Pts',(30.1823177935136,55.5659199366929,6.11306601146704));
#30349=CARTESIAN_POINT('Ctrl Pts',(31.8527378172473,53.9508533596396,6.2242039020351));
#30350=CARTESIAN_POINT('Ctrl Pts',(34.1156133119216,54.4783040835128,6.33534179260312));
#30351=CARTESIAN_POINT('Ctrl Pts',(34.8721855502189,56.5889092129518,6.442582252104));
#30352=CARTESIAN_POINT('Ctrl Pts',(34.0531200394492,57.7654927913865,6.51277674808218));
#30353=CARTESIAN_POINT('Ctrl Pts',(33.5275749112977,58.0738535198176,6.54592528053768));
#30354=CARTESIAN_POINT('Origin',(32.5,56.2916512459885,-3.54592528053767));
#30355=CARTESIAN_POINT('',(33.5282754020985,58.069145943353,5.14592528053768));
#30356=CARTESIAN_POINT('',(33.5267258804522,58.073260437028,5.20407471946232));
#30357=CARTESIAN_POINT('',(33.5273749999999,58.0711169444147,-3.54592528053767));
#30358=CARTESIAN_POINT('Ctrl Pts',(33.5267258804522,58.073260437028,5.20407471946232));
#30359=CARTESIAN_POINT('Ctrl Pts',(33.4330630138882,58.1284275812183,5.20998106327866));
#30360=CARTESIAN_POINT('Ctrl Pts',(32.7207180221807,58.4735694661581,5.25293337061768));
#30361=CARTESIAN_POINT('Ctrl Pts',(31.0632581782873,58.2497382420229,5.33293164147937));
#30362=CARTESIAN_POINT('Ctrl Pts',(30.0756916068806,56.1465211293306,5.44406953204742));
#30363=CARTESIAN_POINT('Ctrl Pts',(31.3071229976033,54.1761423261722,5.55520742261545));
#30364=CARTESIAN_POINT('Ctrl Pts',(33.6304062534725,54.1421146842281,5.6663453131835));
#30365=CARTESIAN_POINT('Ctrl Pts',(34.9190197935988,56.0755785414894,5.77748320375153));
#30366=CARTESIAN_POINT('Ctrl Pts',(34.2590870859834,57.5951911211838,5.85672633917782));
#30367=CARTESIAN_POINT('Ctrl Pts',(33.6120784680294,58.0253234512995,5.89892351108141));
#30368=CARTESIAN_POINT('Ctrl Pts',(33.5296302847681,58.0720277053709,5.90407471946233));
#30369=CARTESIAN_POINT('Ctrl Pts',(33.5282754020985,58.069145943353,5.14592528053768));
#30370=CARTESIAN_POINT('Ctrl Pts',(33.1102767098287,58.3059329434062,5.17193781599936));
#30371=CARTESIAN_POINT('Ctrl Pts',(31.892698227861,58.5381488249037,5.23499631498371));
#30372=CARTESIAN_POINT('Ctrl Pts',(30.2596385516873,57.2292625110706,5.33510077749076));
#30373=CARTESIAN_POINT('Ctrl Pts',(30.4972127153845,54.9179054771161,5.44623866805879));
#30374=CARTESIAN_POINT('Ctrl Pts',(32.5679607208418,53.8639538597437,5.55737655862684));
#30375=CARTESIAN_POINT('Ctrl Pts',(34.5765036531329,55.0321005249752,5.66851444919487));
#30376=CARTESIAN_POINT('Ctrl Pts',(34.6698803007257,57.0408062963268,5.7646973564985));
#30377=CARTESIAN_POINT('Ctrl Pts',(33.8781399387991,57.8632008987502,5.82383430027942));
#30378=CARTESIAN_POINT('Ctrl Pts',(33.5250713804254,58.0691800125914,5.84592528053768));
#30379=CARTESIAN_POINT('Origin',(32.5,56.2916512459885,-3.54592528053767));
#30380=CARTESIAN_POINT('',(33.5290696646583,58.0740687441032,4.44592528053768));
#30381=CARTESIAN_POINT('',(33.5253496165875,58.0685468270267,4.50407471946232));
#30382=CARTESIAN_POINT('',(33.5273749999999,58.0711169444147,-3.54592528053767));
#30383=CARTESIAN_POINT('Ctrl Pts',(33.5253496165875,58.0685468270267,4.50407471946232));
#30384=CARTESIAN_POINT('Ctrl Pts',(33.2536996405186,58.2261242815538,4.52103861547591));
#30385=CARTESIAN_POINT('Ctrl Pts',(32.2808222041073,58.539100979713,4.57504847501218));
#30386=CARTESIAN_POINT('Ctrl Pts',(30.5520219543112,57.7420698681825,4.66610429807112));
#30387=CARTESIAN_POINT('Ctrl Pts',(30.2249467851584,55.4416715145514,4.77724218863916));
#30388=CARTESIAN_POINT('Ctrl Pts',(31.980253640428,53.9192692335435,4.8883800792072));
#30389=CARTESIAN_POINT('Ctrl Pts',(34.2112902010514,54.5683351429997,4.99951796977525));
#30390=CARTESIAN_POINT('Ctrl Pts',(34.8406399092008,56.6764493817393,5.10474951652695));
#30391=CARTESIAN_POINT('Ctrl Pts',(34.0205383194344,57.7824064089199,5.17293509975598));
#30392=CARTESIAN_POINT('Ctrl Pts',(33.5267258804522,58.073260437028,5.20407471946232));
#30393=CARTESIAN_POINT('Ctrl Pts',(33.529069656232,58.0740687294262,4.44592528053768));
#30394=CARTESIAN_POINT('Ctrl Pts',(33.5286860990811,58.0742902067968,4.44594940467393));
#30395=CARTESIAN_POINT('Ctrl Pts',(32.9391765838663,58.4144119362181,4.48301949233286));
#30396=CARTESIAN_POINT('Ctrl Pts',(31.390101627814,58.451850257884,4.55713554351446));
#30397=CARTESIAN_POINT('Ctrl Pts',(30.0831480764379,56.5307348090518,4.66827343408251));
#30398=CARTESIAN_POINT('Ctrl Pts',(30.9883665002516,54.3907834608547,4.77941132465054));
#30399=CARTESIAN_POINT('Ctrl Pts',(33.2772002083032,53.9907179590751,4.89054921521859));
#30400=CARTESIAN_POINT('Ctrl Pts',(34.8546537539781,55.6967227784588,5.00168710578663));
#30401=CARTESIAN_POINT('Ctrl Pts',(34.4121009342633,57.4205168337107,5.08681246089299));
#30402=CARTESIAN_POINT('Ctrl Pts',(33.705572940339,57.9687108152697,5.13489185247668));
#30403=CARTESIAN_POINT('Ctrl Pts',(33.5282754020985,58.069145943353,5.14592528053768));
#30404=CARTESIAN_POINT('Origin',(32.5,56.2916512459885,-3.54592528053767));
#30405=CARTESIAN_POINT('',(33.5252102943906,58.0708877004567,3.74592528053768));
#30406=CARTESIAN_POINT('',(33.5289081309378,58.0700145843707,3.80407471946232));
#30407=CARTESIAN_POINT('',(33.5273749999999,58.0711169444147,-3.54592528053767));
#30408=CARTESIAN_POINT('Ctrl Pts',(33.5289081309378,58.0700145843707,3.80407471946232));
#30409=CARTESIAN_POINT('Ctrl Pts',(33.0789876682099,58.3243434135939,3.83209616767316));
#30410=CARTESIAN_POINT('Ctrl Pts',(31.8034240249952,58.5300263366319,3.89716357940668));
#30411=CARTESIAN_POINT('Ctrl Pts',(30.2122199456457,57.1067555851009,3.99927695466286));
#30412=CARTESIAN_POINT('Ctrl Pts',(30.5744204047745,54.811625609896,4.11041484523092));
#30413=CARTESIAN_POINT('Ctrl Pts',(32.6991257052286,53.8711798837977,4.22155273579895));
#30414=CARTESIAN_POINT('Ctrl Pts',(34.6415689889353,55.1462190460046,4.332690626367));
#30415=CARTESIAN_POINT('Ctrl Pts',(34.6265206091308,57.1150354081819,4.42686462092145));
#30416=CARTESIAN_POINT('Ctrl Pts',(33.8469321795725,57.8820047097448,4.48399265195323));
#30417=CARTESIAN_POINT('Ctrl Pts',(33.5253496165875,58.0685468270267,4.50407471946232));
#30418=CARTESIAN_POINT('Ctrl Pts',(33.5252102943906,58.0708877004567,3.74592528053768));
#30419=CARTESIAN_POINT('Ctrl Pts',(33.3488056811853,58.174663668992,3.75700695687117));
#30420=CARTESIAN_POINT('Ctrl Pts',(32.5196622305249,58.5123107269967,3.80513459672736));
#30421=CARTESIAN_POINT('Ctrl Pts',(30.8051884955116,58.0311765069792,3.89030820010621));
#30422=CARTESIAN_POINT('Ctrl Pts',(30.1193554633367,55.8111663248381,4.00144609067426));
#30423=CARTESIAN_POINT('Ctrl Pts',(31.6125533739245,54.0309494400521,4.11258398124229));
#30424=CARTESIAN_POINT('Ctrl Pts',(33.9180412456697,54.3199785564283,4.22372187181034));
#30425=CARTESIAN_POINT('Ctrl Pts',(34.9253611823253,56.4132475717747,4.33483563824213));
#30426=CARTESIAN_POINT('Ctrl Pts',(34.1176914037627,57.7341809275558,4.40890344115124));
#30427=CARTESIAN_POINT('Ctrl Pts',(33.529069656232,58.0740687294262,4.44592528053768));
#30428=CARTESIAN_POINT('Origin',(32.5,56.2916512459885,-3.54592528053767));
#30429=CARTESIAN_POINT('',(33.5268671815904,58.0681591655549,3.04592528053767));
#30430=CARTESIAN_POINT('',(33.5283521207634,58.0741669114358,3.10407471946232));
#30431=CARTESIAN_POINT('',(33.5273749999999,58.0711169444147,-3.54592528053767));
#30432=CARTESIAN_POINT('Ctrl Pts',(33.5283521207634,58.0741669114358,3.10407471946232));
#30433=CARTESIAN_POINT('Ctrl Pts',(33.4960959785976,58.0929755878456,3.10610775634772));
#30434=CARTESIAN_POINT('Ctrl Pts',(32.8657385633012,58.4363094602464,3.14518675675581));
#30435=CARTESIAN_POINT('Ctrl Pts',(31.2749245001037,58.3886783513255,3.22131172068658));
#30436=CARTESIAN_POINT('Ctrl Pts',(30.0737566908708,56.3997070920348,3.33244961125462));
#30437=CARTESIAN_POINT('Ctrl Pts',(31.0933568979523,54.3118310914232,3.44358750182266));
#30438=CARTESIAN_POINT('Ctrl Pts',(33.40047348876,54.0361069309691,3.5547253923907));
#30439=CARTESIAN_POINT('Ctrl Pts',(34.8833764832335,55.8249080616723,3.66586328295875));
#30440=CARTESIAN_POINT('Ctrl Pts',(34.3608947477859,57.4821952700404,3.74897972531595));
#30441=CARTESIAN_POINT('Ctrl Pts',(33.6738083543113,57.9881060978322,3.79505020415047));
#30442=CARTESIAN_POINT('Ctrl Pts',(33.5289081309378,58.0700145843707,3.80407471946232));
#30443=CARTESIAN_POINT('Ctrl Pts',(33.5268671815904,58.0681591655549,3.04592528053768));
#30444=CARTESIAN_POINT('Ctrl Pts',(33.1711688207572,58.2713555197574,3.06806450906842));
#30445=CARTESIAN_POINT('Ctrl Pts',(32.0617673212826,58.5453769689693,3.12724970112185));
#30446=CARTESIAN_POINT('Ctrl Pts',(30.3694292262435,57.4574138064661,3.22348085669796));
#30447=CARTESIAN_POINT('Ctrl Pts',(30.3650742488504,55.1338834771873,3.33461874726601));
#30448=CARTESIAN_POINT('Ctrl Pts',(32.3148410231894,53.870071116671,3.44575663783404));
#30449=CARTESIAN_POINT('Ctrl Pts',(34.4340859088485,54.822758511107,3.55689452840209));
#30450=CARTESIAN_POINT('Ctrl Pts',(34.7482454446892,56.8908856856794,3.65695074263663));
#30451=CARTESIAN_POINT('Ctrl Pts',(33.9385250223179,57.8277413596598,3.71996099334849));
#30452=CARTESIAN_POINT('Ctrl Pts',(33.5252102943906,58.0708877004567,3.74592528053768));
#30453=CARTESIAN_POINT('Origin',(32.5,56.2916512459885,-3.54592528053767));
#30454=CARTESIAN_POINT('',(33.5296717523759,58.0726906696378,2.34592528053768));
#30455=CARTESIAN_POINT('',(33.5250223861017,58.0699440624176,2.40407471946232));
#30456=CARTESIAN_POINT('',(33.5273749999999,58.0711169444147,-3.54592528053767));
#30457=CARTESIAN_POINT('Ctrl Pts',(33.5250223861017,58.0699440624176,2.40407471946232));
#30458=CARTESIAN_POINT('Ctrl Pts',(33.3162068666575,58.1923260109822,2.41716530854498));
#30459=CARTESIAN_POINT('Ctrl Pts',(32.4393285405002,58.523643057744,2.46730186115031));
#30460=CARTESIAN_POINT('Ctrl Pts',(30.7136126829218,57.9369940717681,2.55448437727833));
#30461=CARTESIAN_POINT('Ctrl Pts',(30.1488178080538,55.6831490181888,2.66562226784637));
#30462=CARTESIAN_POINT('Ctrl Pts',(31.7360866576937,53.9862729545993,2.77676015841441));
#30463=CARTESIAN_POINT('Ctrl Pts',(34.0225740529132,54.3995357858862,2.88789804898245));
#30464=CARTESIAN_POINT('Ctrl Pts',(34.8990991658236,56.5054325192522,2.99700290266509));
#30465=CARTESIAN_POINT('Ctrl Pts',(34.0838668521307,57.750244206438,3.06906179282504));
#30466=CARTESIAN_POINT('Ctrl Pts',(33.5283521207634,58.0741669114358,3.10407471946232));
#30467=CARTESIAN_POINT('Ctrl Pts',(33.5296717523759,58.0726906696378,2.34592528053768));
#30468=CARTESIAN_POINT('Ctrl Pts',(32.9991186855868,58.3741080652298,2.37912206126567));
#30469=CARTESIAN_POINT('Ctrl Pts',(31.5690873940506,58.494201559501,2.44936480551635));
#30470=CARTESIAN_POINT('Ctrl Pts',(30.1211733226086,56.7810568122913,2.55665351328971));
#30471=CARTESIAN_POINT('Ctrl Pts',(30.7986796648578,54.558491332239,2.66779140385775));
#30472=CARTESIAN_POINT('Ctrl Pts',(33.0334238041474,53.9223067766118,2.7789292944258));
#30473=CARTESIAN_POINT('Ctrl Pts',(34.7799190860636,55.4548100839991,2.89006718499383));
#30474=CARTESIAN_POINT('Ctrl Pts',(34.5073761199108,57.2954160769099,2.97906584703113));
#30475=CARTESIAN_POINT('Ctrl Pts',(33.7663651927629,57.931343458575,3.03101854554574));
#30476=CARTESIAN_POINT('Ctrl Pts',(33.5268671815904,58.0681591655549,3.04592528053768));
#30477=CARTESIAN_POINT('Origin',(32.5,56.2916512459885,-3.54592528053767));
#30478=CARTESIAN_POINT('',(33.5262302754658,58.0727324938748,1.64592528053768));
#30479=CARTESIAN_POINT('',(33.527606748894,58.0685424219933,1.70407471946232));
#30480=CARTESIAN_POINT('',(33.5273749999999,58.0711169444147,-3.54592528053767));
#30481=CARTESIAN_POINT('Ctrl Pts',(33.527606748894,58.0685424219933,1.70407471946232));
#30482=CARTESIAN_POINT('Ctrl Pts',(33.1394910367319,58.2891654943862,1.72822286074223));
#30483=CARTESIAN_POINT('Ctrl Pts',(31.9746000084876,58.542974075687,1.78941696554481));
#30484=CARTESIAN_POINT('Ctrl Pts',(30.3095139648772,57.3405094780172,1.88765703387008));
#30485=CARTESIAN_POINT('Ctrl Pts',(30.4307974560058,55.0201428925398,1.99879492443812));
#30486=CARTESIAN_POINT('Ctrl Pts',(32.4460455020051,53.8636023228594,2.10993281500616));
#30487=CARTESIAN_POINT('Ctrl Pts',(34.5106787119048,54.9294824684667,2.2210707055742));
#30488=CARTESIAN_POINT('Ctrl Pts',(34.7085028063897,56.9697666836067,2.31911800705959));
#30489=CARTESIAN_POINT('Ctrl Pts',(33.9071483489282,57.8459888695647,2.3801193450223));
#30490=CARTESIAN_POINT('Ctrl Pts',(33.5250223861017,58.0699440624176,2.40407471946232));
#30491=CARTESIAN_POINT('Ctrl Pts',(33.5262302754658,58.0727324938748,1.64592528053767));
#30492=CARTESIAN_POINT('Ctrl Pts',(33.4118498551747,58.1401751811515,1.65313364994024));
#30493=CARTESIAN_POINT('Ctrl Pts',(32.670930140884,58.4845521558011,1.69738798286549));
#30494=CARTESIAN_POINT('Ctrl Pts',(30.9955026631254,58.198172143523,1.77868827931342));
#30495=CARTESIAN_POINT('Ctrl Pts',(30.082268834923,56.0616291105053,1.88982616988146));
#30496=CARTESIAN_POINT('Ctrl Pts',(31.3820117610517,54.1356279467244,2.0009640604495));
#30497=CARTESIAN_POINT('Ctrl Pts',(33.7050620011388,54.1830593597268,2.11210195101754));
#30498=CARTESIAN_POINT('Ctrl Pts',(34.9251053252509,56.1605088392832,2.22323984158559));
#30499=CARTESIAN_POINT('Ctrl Pts',(34.224026615261,57.6314775216245,2.30118095142563));
#30500=CARTESIAN_POINT('Ctrl Pts',(33.5911896372902,58.0377411767145,2.34207609774299));
#30501=CARTESIAN_POINT('Ctrl Pts',(33.5296717523759,58.0726906696378,2.34592528053768));
#30502=CARTESIAN_POINT('Origin',(32.5,56.2916512459885,-3.54592528053767));
#30503=CARTESIAN_POINT('',(33.5256402930184,58.0682685471634,0.945925280537676));
#30504=CARTESIAN_POINT('',(33.5294982470258,58.0735597602013,1.00407471946232));
#30505=CARTESIAN_POINT('',(33.5273749999999,58.0711169444147,-3.54592528053767));
#30506=CARTESIAN_POINT('Ctrl Pts',(33.5294982470258,58.0735597602013,1.00407471946232));
#30507=CARTESIAN_POINT('Ctrl Pts',(32.9682880946418,58.3946192964702,1.03928041293948));
#30508=CARTESIAN_POINT('Ctrl Pts',(31.4766956957228,58.4741418727902,1.11153206993931));
#30509=CARTESIAN_POINT('Ctrl Pts',(30.0981915249122,56.6517188923722,1.22082969046183));
#30510=CARTESIAN_POINT('Ctrl Pts',(30.8948796869627,54.4690373423775,1.33196758102987));
#30511=CARTESIAN_POINT('Ctrl Pts',(33.1607526748339,53.9546149682086,1.44310547159791));
#30512=CARTESIAN_POINT('Ctrl Pts',(34.8218312459871,55.5793084028842,1.55424336216595));
#30513=CARTESIAN_POINT('Ctrl Pts',(34.4585557374772,57.361331949687,1.64123311145409));
#30514=CARTESIAN_POINT('Ctrl Pts',(33.7349041722058,57.9507048982935,1.69117689721955));
#30515=CARTESIAN_POINT('Ctrl Pts',(33.527606748894,58.0685424219933,1.70407471946232));
#30516=CARTESIAN_POINT('Ctrl Pts',(33.5256402930184,58.0682685471634,0.945925280537675));
#30517=CARTESIAN_POINT('Ctrl Pts',(33.2328184146122,58.2374617349622,0.964191202137492));
#30518=CARTESIAN_POINT('Ctrl Pts',(32.2264812528154,58.542293513151,1.01950308725999));
#30519=CARTESIAN_POINT('Ctrl Pts',(30.5023763530244,57.672894864812,1.11186093590517));
#30520=CARTESIAN_POINT('Ctrl Pts',(30.2561395980005,55.3624447749947,1.22299882647321));
#30521=CARTESIAN_POINT('Ctrl Pts',(32.0637337160182,53.9025079060376,1.33413671704125));
#30522=CARTESIAN_POINT('Ctrl Pts',(34.2706473113688,54.6293810308449,1.44527460760929));
#30523=CARTESIAN_POINT('Ctrl Pts',(34.8188452912069,56.7319204842157,1.54920412877477));
#30524=CARTESIAN_POINT('Ctrl Pts',(33.9996850008464,57.7935670658911,1.61608768641756));
#30525=CARTESIAN_POINT('Ctrl Pts',(33.5262302754658,58.0727324938748,1.64592528053767));
#30526=CARTESIAN_POINT('Origin',(32.5,56.2916512459885,-3.54592528053767));
#30527=CARTESIAN_POINT('',(33.5292382420787,58.0706648023921,0.245925280537672));
#30528=CARTESIAN_POINT('',(33.5256021009515,58.0718002431918,0.30407471946232));
#30529=CARTESIAN_POINT('',(33.5273749999999,58.0711169444147,-3.54592528053767));
#30530=CARTESIAN_POINT('Ctrl Pts',(33.5256021009515,58.0718002431918,0.304074719462319));
#30531=CARTESIAN_POINT('Ctrl Pts',(33.3791306461153,58.1581427811428,0.313292001614043));
#30532=CARTESIAN_POINT('Ctrl Pts',(32.5930673149394,58.4998906338152,0.359555247288449));
#30533=CARTESIAN_POINT('Ctrl Pts',(30.894619061498,58.1140355911319,0.442864456485535));
#30534=CARTESIAN_POINT('Ctrl Pts',(30.0982430406458,55.931240133699,0.554002347053577));
#30535=CARTESIAN_POINT('Ctrl Pts',(31.5002224030512,54.0783330542954,0.665140237621618));
#30536=CARTESIAN_POINT('Ctrl Pts',(33.8173095378994,54.2513012166796,0.776278128189661));
#30537=CARTESIAN_POINT('Ctrl Pts',(34.9286483135496,56.2918248999351,0.887416018757702));
#30538=CARTESIAN_POINT('Ctrl Pts',(34.1691544002424,57.6858533133783,0.963348215848589));
#30539=CARTESIAN_POINT('Ctrl Pts',(33.5588337928047,58.0567773540314,1.00223444941679));
#30540=CARTESIAN_POINT('Ctrl Pts',(33.5294982470258,58.0735597602013,1.00407471946232));
#30541=CARTESIAN_POINT('Ctrl Pts',(33.5292382420787,58.0706648023921,0.245925280537674));
#30542=CARTESIAN_POINT('Ctrl Pts',(33.0588051630517,58.33651145622,0.275248754334741));
#30543=CARTESIAN_POINT('Ctrl Pts',(31.7450292213916,58.5230813041052,0.34161819165449));
#30544=CARTESIAN_POINT('Ctrl Pts',(30.1850532410697,57.0260596319961,0.445033592496918));
#30545=CARTESIAN_POINT('Ctrl Pts',(30.6274839128385,54.7450363379153,0.55617148306496));
#30546=CARTESIAN_POINT('Ctrl Pts',(32.783849793945,53.8796472115696,0.667309373633002));
#30547=CARTESIAN_POINT('Ctrl Pts',(34.6804047400893,55.2219927306231,0.778447264201043));
#30548=CARTESIAN_POINT('Ctrl Pts',(34.5975134385768,57.1618755368451,0.871319233169269));
#30549=CARTESIAN_POINT('Ctrl Pts',(33.8267040593522,57.8943131766358,0.927145238614812));
#30550=CARTESIAN_POINT('Ctrl Pts',(33.5256402930184,58.0682685471634,0.945925280537675));
#30551=CARTESIAN_POINT('Origin',(32.5,56.2916512459885,-3.54592528053767));
#30552=CARTESIAN_POINT('',(33.5278097333143,58.0740011795199,-0.454074719462328));
#30553=CARTESIAN_POINT('',(33.5262237855851,58.0680718733222,-0.395925280537679));
#30554=CARTESIAN_POINT('',(33.5273749999999,58.0711169444147,-3.54592528053767));
#30555=CARTESIAN_POINT('Ctrl Pts',(33.5262237855851,58.0680718733222,-0.395925280537681));
#30556=CARTESIAN_POINT('Ctrl Pts',(33.2007518244939,58.254991046836,-0.375650446188706));
#30557=CARTESIAN_POINT('Ctrl Pts',(32.1416146375096,58.5451226040269,-0.318329648317051));
#30558=CARTESIAN_POINT('Ctrl Pts',(30.4306156658191,57.5628636674516,-0.223962886922716));
#30559=CARTESIAN_POINT('Ctrl Pts',(30.309663968686,55.2424797818377,-0.112824996354674));
#30560=CARTESIAN_POINT('Ctrl Pts',(32.1935517174548,53.8824144115655,-0.00168710578663204));
#30561=CARTESIAN_POINT('Ctrl Pts',(34.3579350363403,54.7275508506072,0.10945078478141));
#30562=CARTESIAN_POINT('Ctrl Pts',(34.7832643179971,56.8155005034113,0.211371393197726));
#30563=CARTESIAN_POINT('Ctrl Pts',(33.9678265418961,57.8111161350299,0.276246038091363));
#30564=CARTESIAN_POINT('Ctrl Pts',(33.5256021009515,58.0718002431918,0.304074719462319));
#30565=CARTESIAN_POINT('Ctrl Pts',(33.5278097333143,58.0740011795199,-0.454074719462326));
#30566=CARTESIAN_POINT('Ctrl Pts',(33.4749288712104,58.1049786318385,-0.450739656990689));
#30567=CARTESIAN_POINT('Ctrl Pts',(32.8174992673745,58.4495803163018,-0.410358630996372));
#30568=CARTESIAN_POINT('Ctrl Pts',(31.2021687803137,58.344446263511,-0.332931641479374));
#30569=CARTESIAN_POINT('Ctrl Pts',(30.0714596841225,56.3145920190741,-0.221793750911332));
#30570=CARTESIAN_POINT('Ctrl Pts',(31.1636212068566,54.2637395061115,-0.110655860343291));
#30571=CARTESIAN_POINT('Ctrl Pts',(33.4789853310955,54.0690577668369,0.000482030224751639));
#30572=CARTESIAN_POINT('Ctrl Pts',(34.8982731111897,55.908740964546,0.111619920792793));
#30573=CARTESIAN_POINT('Ctrl Pts',(34.3271081175644,57.521036291931,0.193434337563767));
#30574=CARTESIAN_POINT('Ctrl Pts',(33.6531292464159,58.0006526999044,0.238202790812061));
#30575=CARTESIAN_POINT('Ctrl Pts',(33.5292382420787,58.0706648023921,0.245925280537674));
#30576=CARTESIAN_POINT('Origin',(32.5,56.2916512459885,-3.54592528053767));
#30577=CARTESIAN_POINT('',(33.5250365419916,58.0693901510839,-1.15407471946233));
#30578=CARTESIAN_POINT('',(33.5295799600394,58.0717283210701,-1.09592528053768));
#30579=CARTESIAN_POINT('',(33.5273749999999,58.0711169444147,-3.54592528053767));
#30580=CARTESIAN_POINT('Ctrl Pts',(33.5295799600394,58.0717283210701,-1.09592528053768));
#30581=CARTESIAN_POINT('Ctrl Pts',(33.0277944721986,58.3557212843618,-1.06459289399146));
#30582=CARTESIAN_POINT('Ctrl Pts',(31.6541659742537,58.5096740781238,-0.996214543922551));
#30583=CARTESIAN_POINT('Ctrl Pts',(30.1487320710281,56.8998163998922,-0.890790230330966));
#30584=CARTESIAN_POINT('Ctrl Pts',(30.7138473610246,54.6460533962845,-0.779652339762924));
#30585=CARTESIAN_POINT('Ctrl Pts',(32.9138506780699,53.8985232611178,-0.668514449194883));
#30586=CARTESIAN_POINT('Ctrl Pts',(34.7350506405739,55.3414510668855,-0.55737655862684));
#30587=CARTESIAN_POINT('Ctrl Pts',(34.5514515687201,57.2322106426396,-0.466513502407774));
#30588=CARTESIAN_POINT('Ctrl Pts',(33.7954507596715,57.9134543040694,-0.412696409711387));
#30589=CARTESIAN_POINT('Ctrl Pts',(33.5262237855851,58.0680718733222,-0.395925280537681));
#30590=CARTESIAN_POINT('Ctrl Pts',(33.5250365419916,58.0693901510839,-1.15407471946233));
#30591=CARTESIAN_POINT('Ctrl Pts',(33.2951376806275,58.2037133203311,-1.13968210479344));
#30592=CARTESIAN_POINT('Ctrl Pts',(32.3865699532721,58.5298194771329,-1.08824352660187));
#30593=CARTESIAN_POINT('Ctrl Pts',(30.6570393620672,57.873352597378,-0.999758984887625));
#30594=CARTESIAN_POINT('Ctrl Pts',(30.1715905180572,55.6011108576298,-0.888621094319582));
#30595=CARTESIAN_POINT('Ctrl Pts',(31.817369145763,53.960908709333,-0.777483203751541));
#30596=CARTESIAN_POINT('Ctrl Pts',(34.087963584719,54.4540716106361,-0.666345313183499));
#30597=CARTESIAN_POINT('Ctrl Pts',(34.8805586635865,56.5639154031852,-0.558542485087094));
#30598=CARTESIAN_POINT('Ctrl Pts',(34.0623309079662,57.7608802593548,-0.48778562051337));
#30599=CARTESIAN_POINT('Ctrl Pts',(33.5278097333143,58.0740011795199,-0.454074719462326));
#30600=CARTESIAN_POINT('Origin',(32.5,56.2916512459885,-3.54592528053767));
#30601=CARTESIAN_POINT('',(33.5283546803393,58.0681541983481,-1.85407471946233));
#30602=CARTESIAN_POINT('',(33.5269872402601,58.0734398505124,-1.79592528053768));
#30603=CARTESIAN_POINT('',(33.5273749999999,58.0711169444147,-3.54592528053767));
#30604=CARTESIAN_POINT('',(34.4842965055667,55.7582049595679,-2.));
#30605=CARTESIAN_POINT('Ctrl Pts',(34.4842965055667,55.7582049595679,-2.));
#30606=CARTESIAN_POINT('Ctrl Pts',(34.6616800870191,56.4180307560557,-1.96295403647732));
#30607=CARTESIAN_POINT('Ctrl Pts',(34.426165795488,57.4023224375313,-1.91431227629809));
#30608=CARTESIAN_POINT('Ctrl Pts',(33.7147012993046,57.9624349357751,-1.86567051611887));
#30609=CARTESIAN_POINT('Ctrl Pts',(33.5283546803393,58.0681541983481,-1.85407471946233));
#30610=CARTESIAN_POINT('',(33.9566395923166,54.8371582344187,-2.));
#30611=CARTESIAN_POINT('Origin',(32.5,56.2916512459885,-2.));
#30612=CARTESIAN_POINT('Ctrl Pts',(33.9566410663199,54.8371566128168,-2.));
#30613=CARTESIAN_POINT('Ctrl Pts',(34.4273146919907,55.3097386618185,-1.96367708181445));
#30614=CARTESIAN_POINT('Ctrl Pts',(34.8405825937333,56.6643607585548,-1.89565217532701));
#30615=CARTESIAN_POINT('Ctrl Pts',(34.0295256140624,57.7776919138425,-1.82762726883957));
#30616=CARTESIAN_POINT('Ctrl Pts',(33.5269872402601,58.0734398505124,-1.79592528053768));
#30617=CARTESIAN_POINT('Origin',(-32.5,56.2916512459885,3.));
#30618=CARTESIAN_POINT('',(-33.3327252244639,57.7364024133913,6.12851963660979));
#30619=CARTESIAN_POINT('',(-33.3348404573524,57.735699266238,6.32148036339022));
#30620=CARTESIAN_POINT('',(-33.333,57.7344495686934,3.));
#30621=CARTESIAN_POINT('',(-33.041102980256,57.8673300091754,7.));
#30622=CARTESIAN_POINT('Ctrl Pts',(-33.3348404573524,57.735699266238,6.32148036339022));
#30623=CARTESIAN_POINT('Ctrl Pts',(-33.3853483348094,57.7070091850913,6.3253777944574));
#30624=CARTESIAN_POINT('Ctrl Pts',(-33.4342336358034,57.6755865432426,6.32927522552458));
#30625=CARTESIAN_POINT('Ctrl Pts',(-33.4811646154108,57.6414746748817,6.33317265659176));
#30626=CARTESIAN_POINT('Ctrl Pts',(-33.9272541879144,57.3172336532427,6.37021862011444));
#30627=CARTESIAN_POINT('Ctrl Pts',(-34.196772145609,56.7500228359925,6.40726458363712));
#30628=CARTESIAN_POINT('Ctrl Pts',(-34.1662427495344,56.1993881251834,6.44431054715981));
#30629=CARTESIAN_POINT('Ctrl Pts',(-34.1357133534599,55.6487534143743,6.48135651068249));
#30630=CARTESIAN_POINT('Ctrl Pts',(-33.8051366036161,55.1146948100063,6.51840247420516));
#30631=CARTESIAN_POINT('Ctrl Pts',(-33.3260603863118,54.8417096746676,6.55544843772784));
#30632=CARTESIAN_POINT('Ctrl Pts',(-32.8469841690075,54.5687245393289,6.59249440125052));
#30633=CARTESIAN_POINT('Ctrl Pts',(-32.2194084842428,54.5568128730195,6.62954036477321));
#30634=CARTESIAN_POINT('Ctrl Pts',(-31.7300326690206,54.8112607055414,6.66658632829589));
#30635=CARTESIAN_POINT('Ctrl Pts',(-31.2406568537983,55.0657085380633,6.70363229181857));
#30636=CARTESIAN_POINT('Ctrl Pts',(-30.8894809081185,55.5865158694165,6.74067825534124));
#30637=CARTESIAN_POINT('Ctrl Pts',(-30.8382644239114,56.1356774091288,6.77772421886393));
#30638=CARTESIAN_POINT('Ctrl Pts',(-30.7870479397043,56.6848389488411,6.81477018238661));
#30639=CARTESIAN_POINT('Ctrl Pts',(-31.0357909169699,57.2623546969124,6.85181614590929));
#30640=CARTESIAN_POINT('Ctrl Pts',(-31.4683170081768,57.6029598655743,6.88886210943197));
#30641=CARTESIAN_POINT('Ctrl Pts',(-31.9008430993837,57.9435650342361,6.92590807295465));
#30642=CARTESIAN_POINT('Ctrl Pts',(-32.5171523045318,58.0472596234884,6.96295403647733));
#30643=CARTESIAN_POINT('Ctrl Pts',(-33.0411029802559,57.8673300091754,7.00000000000001));
#30644=CARTESIAN_POINT('',(-33.9709880617747,55.5030815934933,7.));
#30645=CARTESIAN_POINT('Origin',(-32.5,56.2916512459885,7.));
#30646=CARTESIAN_POINT('',(-33.3311603318024,57.7325647065031,6.82851963660978));
#30647=CARTESIAN_POINT('Ctrl Pts',(-33.9709895856634,55.5030806790319,7.));
#30648=CARTESIAN_POINT('Ctrl Pts',(-34.2258866982027,55.9800344189509,6.96367708181444));
#30649=CARTESIAN_POINT('Ctrl Pts',(-34.2280600118628,56.5931875605704,6.92735416362888));
#30650=CARTESIAN_POINT('Ctrl Pts',(-33.9753141969146,57.071300576271,6.89103124544333));
#30651=CARTESIAN_POINT('Ctrl Pts',(-33.8303226570678,57.3455774911288,6.87019404249881));
#30652=CARTESIAN_POINT('Ctrl Pts',(-33.6014392610868,57.5754137754314,6.8493568395543));
#30653=CARTESIAN_POINT('Ctrl Pts',(-33.3311603318024,57.7325647065031,6.82851963660978));
#30654=CARTESIAN_POINT('',(-33.333,57.7344495686934,8.));
#30655=CARTESIAN_POINT('',(-33.333,57.7344495686934,3.));
#30656=CARTESIAN_POINT('Origin',(-32.5,56.2916512459885,8.));
#30657=CARTESIAN_POINT('Ctrl Pts',(-33.3311603318024,57.7325647065031,6.82851963660978));
#30658=CARTESIAN_POINT('Ctrl Pts',(-33.1209168329143,57.8548086479361,6.81231087603162));
#30659=CARTESIAN_POINT('Ctrl Pts',(-32.8856252648826,57.9330713283931,6.79610211545345));
#30660=CARTESIAN_POINT('Ctrl Pts',(-32.6452880462139,57.9540583561262,6.77989335487529));
#30661=CARTESIAN_POINT('Ctrl Pts',(-32.0959848596434,58.0020252972197,6.74284739135261));
#30662=CARTESIAN_POINT('Ctrl Pts',(-31.5203244682533,57.7507986915124,6.70580142782992));
#30663=CARTESIAN_POINT('Ctrl Pts',(-31.1820200481675,57.3152751741701,6.66875546430724));
#30664=CARTESIAN_POINT('Ctrl Pts',(-30.8437156280816,56.8797516568278,6.63170950078456));
#30665=CARTESIAN_POINT('Ctrl Pts',(-30.7427671793001,56.2599312278504,6.59466353726189));
#30666=CARTESIAN_POINT('Ctrl Pts',(-30.9252443270204,55.7395177410929,6.55761757373921));
#30667=CARTESIAN_POINT('Ctrl Pts',(-31.1077214747407,55.2191042543355,6.52057161021653));
#30668=CARTESIAN_POINT('Ctrl Pts',(-31.5736242189628,54.7980977097981,6.48352564669384));
#30669=CARTESIAN_POINT('Ctrl Pts',(-32.1097948324389,54.6691542850845,6.44647968317116));
#30670=CARTESIAN_POINT('Ctrl Pts',(-32.645965445915,54.540210860371,6.40943371964848));
#30671=CARTESIAN_POINT('Ctrl Pts',(-33.2524039286451,54.7033305554813,6.37238775612581));
#30672=CARTESIAN_POINT('Ctrl Pts',(-33.6515374626529,55.0838706916793,6.33534179260313));
#30673=CARTESIAN_POINT('Ctrl Pts',(-34.0506709966607,55.4644108278773,6.29829582908045));
#30674=CARTESIAN_POINT('Ctrl Pts',(-34.2424995819463,56.0623714051628,6.26124986555776));
#30675=CARTESIAN_POINT('Ctrl Pts',(-34.1392482605268,56.604087363599,6.22420390203508));
#30676=CARTESIAN_POINT('Ctrl Pts',(-34.0503539438026,57.0704781983288,6.19230914689331));
#30677=CARTESIAN_POINT('Ctrl Pts',(-33.7427356506951,57.4951784726193,6.16041439175155));
#30678=CARTESIAN_POINT('Ctrl Pts',(-33.3327252244639,57.7364024133913,6.12851963660979));
#30679=CARTESIAN_POINT('Origin',(-32.5,56.2916512459885,3.));
#30680=CARTESIAN_POINT('',(-33.3347682721563,57.7348627592985,5.42851963660978));
#30681=CARTESIAN_POINT('',(-33.3325737793451,57.732046708219,5.62148036339022));
#30682=CARTESIAN_POINT('',(-33.333,57.7344495686934,3.));
#30683=CARTESIAN_POINT('Ctrl Pts',(-33.3325737793451,57.732046708219,5.62148036339022));
#30684=CARTESIAN_POINT('Ctrl Pts',(-33.5273851267367,57.6207441464882,5.63643534665465));
#30685=CARTESIAN_POINT('Ctrl Pts',(-33.7002675206604,57.4721914078235,5.65139032991908));
#30686=CARTESIAN_POINT('Ctrl Pts',(-33.8340159287013,57.2942275627961,5.66634531318351));
#30687=CARTESIAN_POINT('Ctrl Pts',(-34.1653328254098,56.853381726016,5.70339127670619));
#30688=CARTESIAN_POINT('Ctrl Pts',(-34.2565099960996,56.2320591280652,5.74043724022887));
#30689=CARTESIAN_POINT('Ctrl Pts',(-34.0658176145799,55.7146109150825,5.77748320375155));
#30690=CARTESIAN_POINT('Ctrl Pts',(-33.8751252330602,55.1971627020998,5.81452916727423));
#30691=CARTESIAN_POINT('Ctrl Pts',(-33.4025632993311,54.7835888740851,5.85157513079691));
#30692=CARTESIAN_POINT('Ctrl Pts',(-32.8644065969169,54.6631651603563,5.88862109431959));
#30693=CARTESIAN_POINT('Ctrl Pts',(-32.3262498945026,54.5427414466275,5.92566705784227));
#30694=CARTESIAN_POINT('Ctrl Pts',(-31.7224984234031,54.7154678471845,5.96271302136495));
#30695=CARTESIAN_POINT('Ctrl Pts',(-31.3294542359752,55.1022925139247,5.99975898488763));
#30696=CARTESIAN_POINT('Ctrl Pts',(-30.9364100485472,55.4891171806648,6.03680494841031));
#30697=CARTESIAN_POINT('Ctrl Pts',(-30.7540731447909,56.0900401135881,6.073850911933));
#30698=CARTESIAN_POINT('Ctrl Pts',(-30.8659074307874,56.6300507637272,6.11089687545568));
#30699=CARTESIAN_POINT('Ctrl Pts',(-30.9777417167839,57.1700614138663,6.14794283897836));
#30700=CARTESIAN_POINT('Ctrl Pts',(-31.3837471925331,57.6491597812212,6.18498880250104));
#30701=CARTESIAN_POINT('Ctrl Pts',(-31.898080524064,57.8480733518848,6.22203476602372));
#30702=CARTESIAN_POINT('Ctrl Pts',(-32.358303272023,58.0260601641038,6.25518329847922));
#30703=CARTESIAN_POINT('Ctrl Pts',(-32.9052595394904,57.9797148933651,6.28833183093472));
#30704=CARTESIAN_POINT('Ctrl Pts',(-33.3348404573524,57.735699266238,6.32148036339022));
#30705=CARTESIAN_POINT('Ctrl Pts',(-33.3327252244639,57.7364024133913,6.12851963660979));
#30706=CARTESIAN_POINT('Ctrl Pts',(-33.2665058998609,57.7753616334844,6.12336842822888));
#30707=CARTESIAN_POINT('Ctrl Pts',(-33.1976157450274,57.8095349962739,6.11821721984796));
#30708=CARTESIAN_POINT('Ctrl Pts',(-33.1265448412825,57.8383251884469,6.11306601146705));
#30709=CARTESIAN_POINT('Ctrl Pts',(-32.6154239715823,58.0453757152716,6.07602004794436));
#30710=CARTESIAN_POINT('Ctrl Pts',(-31.9915134603068,57.9740054293342,6.03897408442168));
#30711=CARTESIAN_POINT('Ctrl Pts',(-31.5403536505083,57.6568760819726,6.001928120899));
#30712=CARTESIAN_POINT('Ctrl Pts',(-31.0891938407098,57.3397467346111,5.96488215737631));
#30713=CARTESIAN_POINT('Ctrl Pts',(-30.8107847323884,56.7768583258254,5.92783619385363));
#30714=CARTESIAN_POINT('Ctrl Pts',(-30.8325397428817,56.2258205630586,5.89079023033096));
#30715=CARTESIAN_POINT('Ctrl Pts',(-30.854294753375,55.6747828002917,5.85374426680828));
#30716=CARTESIAN_POINT('Ctrl Pts',(-31.1762138826829,55.1355956835436,5.81669830328559));
#30717=CARTESIAN_POINT('Ctrl Pts',(-31.6509700657299,54.8550209349976,5.77965233976292));
#30718=CARTESIAN_POINT('Ctrl Pts',(-32.1257262487769,54.5744461864516,5.74260637624023));
#30719=CARTESIAN_POINT('Ctrl Pts',(-32.7533194855629,54.5524838061077,5.70556041271756));
#30720=CARTESIAN_POINT('Ctrl Pts',(-33.2465276451507,54.7991851622225,5.66851444919487));
#30721=CARTESIAN_POINT('Ctrl Pts',(-33.7397358047386,55.0458865183372,5.63146848567219));
#30722=CARTESIAN_POINT('Ctrl Pts',(-34.0985588871282,55.5612516109106,5.59442252214951));
#30723=CARTESIAN_POINT('Ctrl Pts',(-34.1587797389667,56.1094206024476,5.55737655862683));
#30724=CARTESIAN_POINT('Ctrl Pts',(-34.2190005908052,56.6575895939846,5.52033059510415));
#30725=CARTESIAN_POINT('Ctrl Pts',(-33.9806192120925,57.2385624844852,5.48328463158147));
#30726=CARTESIAN_POINT('Ctrl Pts',(-33.5527320593966,57.5864537767431,5.44623866805879));
#30727=CARTESIAN_POINT('Ctrl Pts',(-33.4845127880347,57.6419190795021,5.44033232424245));
#30728=CARTESIAN_POINT('Ctrl Pts',(-33.4114765004847,57.6914597193429,5.43442598042612));
#30729=CARTESIAN_POINT('Ctrl Pts',(-33.3347682721563,57.7348627592985,5.42851963660978));
#30730=CARTESIAN_POINT('Origin',(-32.5,56.2916512459885,3.));
#30731=CARTESIAN_POINT('',(-33.3320164235939,57.7319854708823,4.72851963660978));
#30732=CARTESIAN_POINT('',(-33.3312509399777,57.7342826871321,4.92148036339022));
#30733=CARTESIAN_POINT('',(-33.333,57.7344495686934,3.));
#30734=CARTESIAN_POINT('Ctrl Pts',(-33.3312509399777,57.7342826871321,4.92148036339022));
#30735=CARTESIAN_POINT('Ctrl Pts',(-33.6669748777684,57.5367675539577,4.9474928988519));
#30736=CARTESIAN_POINT('Ctrl Pts',(-33.937858827665,57.2229205202501,4.97350543431358));
#30737=CARTESIAN_POINT('Ctrl Pts',(-34.0694479601931,56.8587419095544,4.99951796977526));
#30738=CARTESIAN_POINT('Ctrl Pts',(-34.2568516913979,56.3400939850778,5.03656393329794));
#30739=CARTESIAN_POINT('Ctrl Pts',(-34.1617340046634,55.7193622303022,5.07360989682062));
#30740=CARTESIAN_POINT('Ctrl Pts',(-33.8276260153151,55.2806280419242,5.1106558603433));
#30741=CARTESIAN_POINT('Ctrl Pts',(-33.4935180259667,54.8418938535461,5.14770182386598));
#30742=CARTESIAN_POINT('Ctrl Pts',(-32.9204197340046,54.5851572315657,5.18474778738866));
#30743=CARTESIAN_POINT('Ctrl Pts',(-32.370612888852,54.6279151680597,5.22179375091134));
#30744=CARTESIAN_POINT('Ctrl Pts',(-31.8208060436993,54.6706731045536,5.25883971443402));
#30745=CARTESIAN_POINT('Ctrl Pts',(-31.2942906453562,55.0129255995219,5.2958856779567));
#30746=CARTESIAN_POINT('Ctrl Pts',(-31.032029319193,55.4980388156703,5.33293164147938));
#30747=CARTESIAN_POINT('Ctrl Pts',(-30.7697679930298,55.9831520318186,5.36997760500206));
#30748=CARTESIAN_POINT('Ctrl Pts',(-30.7717607390465,56.611125969147,5.40702356852474));
#30749=CARTESIAN_POINT('Ctrl Pts',(-31.0370958289673,57.0945648785311,5.44406953204742));
#30750=CARTESIAN_POINT('Ctrl Pts',(-31.3024309188881,57.5780037879153,5.48111549557011));
#30751=CARTESIAN_POINT('Ctrl Pts',(-31.831108352713,57.9169076693552,5.51816145909279));
#30752=CARTESIAN_POINT('Ctrl Pts',(-32.3811753809891,57.9561750722705,5.55520742261547));
#30753=CARTESIAN_POINT('Ctrl Pts',(-32.7091873614286,57.9795907251543,5.57729840287372));
#30754=CARTESIAN_POINT('Ctrl Pts',(-33.0448052440539,57.8964589747132,5.59938938313197));
#30755=CARTESIAN_POINT('Ctrl Pts',(-33.3325737793451,57.732046708219,5.62148036339022));
#30756=CARTESIAN_POINT('Ctrl Pts',(-33.3347682721563,57.7348627592985,5.42851963660978));
#30757=CARTESIAN_POINT('Ctrl Pts',(-32.9303446333077,57.9636936909789,5.39738001690344));
#30758=CARTESIAN_POINT('Ctrl Pts',(-32.4238541169951,58.0219212024995,5.36624039719709));
#30759=CARTESIAN_POINT('Ctrl Pts',(-31.9831067199836,57.8783395309755,5.33510077749075));
#30760=CARTESIAN_POINT('Ctrl Pts',(-31.4587614599457,57.7075242989346,5.29805481396806));
#30761=CARTESIAN_POINT('Ctrl Pts',(-31.0274638665491,57.2510841408376,5.26100885044538));
#30762=CARTESIAN_POINT('Ctrl Pts',(-30.8865996954395,56.7179114934437,5.2239628869227));
#30763=CARTESIAN_POINT('Ctrl Pts',(-30.7457355243299,56.1847388460498,5.18691692340002));
#30764=CARTESIAN_POINT('Ctrl Pts',(-30.8953047755072,55.5748337093591,5.14987095987734));
#30765=CARTESIAN_POINT('Ctrl Pts',(-31.2668562499327,55.1673226224438,5.11282499635466));
#30766=CARTESIAN_POINT('Ctrl Pts',(-31.6384077243582,54.7598115355286,5.07577903283198));
#30767=CARTESIAN_POINT('Ctrl Pts',(-32.231941422032,54.5546944983887,5.0387330693093));
#30768=CARTESIAN_POINT('Ctrl Pts',(-32.7758232721695,54.6458444887421,5.00168710578662));
#30769=CARTESIAN_POINT('Ctrl Pts',(-33.319705122307,54.7369944790955,4.96464114226394));
#30770=CARTESIAN_POINT('Ctrl Pts',(-33.8139351249082,55.1244114969421,4.92759517874126));
#30771=CARTESIAN_POINT('Ctrl Pts',(-34.0323261210678,55.6307919459654,4.89054921521858));
#30772=CARTESIAN_POINT('Ctrl Pts',(-34.2507171172273,56.1371723949886,4.8535032516959));
#30773=CARTESIAN_POINT('Ctrl Pts',(-34.1932691069452,56.7625162751885,4.81645728817321));
#30774=CARTESIAN_POINT('Ctrl Pts',(-33.8862734957393,57.2206314145012,4.77941132465053));
#30775=CARTESIAN_POINT('Ctrl Pts',(-33.7456956532455,57.4304091297115,4.76244742863695));
#30776=CARTESIAN_POINT('Ctrl Pts',(-33.5527911750803,57.6051213208863,4.74548353262336));
#30777=CARTESIAN_POINT('Ctrl Pts',(-33.3320164235939,57.7319854708823,4.72851963660978));
#30778=CARTESIAN_POINT('Origin',(-32.5,56.2916512459885,3.));
#30779=CARTESIAN_POINT('',(-33.3316044198825,57.73507921,4.02851963660978));
#30780=CARTESIAN_POINT('',(-33.3343856218719,57.7368361137997,4.22148036339022));
#30781=CARTESIAN_POINT('',(-33.333,57.7344495686934,3.));
#30782=CARTESIAN_POINT('Ctrl Pts',(-33.3343856149812,57.7368361019314,4.22148036339022));
#30783=CARTESIAN_POINT('Ctrl Pts',(-33.8122975339405,57.4609515848648,4.25855045104915));
#30784=CARTESIAN_POINT('Ctrl Pts',(-34.1397428670923,56.9245130794241,4.29562053870808));
#30785=CARTESIAN_POINT('Ctrl Pts',(-34.1667586100628,56.373348690468,4.33269062636701));
#30786=CARTESIAN_POINT('Ctrl Pts',(-34.1937567719725,55.8225429832862,4.36973658988969));
#30787=CARTESIAN_POINT('Ctrl Pts',(-33.9207162964576,55.2570306535141,4.40678255341237));
#30788=CARTESIAN_POINT('Ctrl Pts',(-33.4725957048463,54.9356216253736,4.44382851693505));
#30789=CARTESIAN_POINT('Ctrl Pts',(-33.024475113235,54.6142125972331,4.48087448045773));
#30790=CARTESIAN_POINT('Ctrl Pts',(-32.4012744055273,54.5369068707243,4.51792044398041));
#30791=CARTESIAN_POINT('Ctrl Pts',(-31.8882049204609,54.7390838502781,4.55496640750309));
#30792=CARTESIAN_POINT('Ctrl Pts',(-31.3751354353946,54.9412608298319,4.59201237102577));
#30793=CARTESIAN_POINT('Ctrl Pts',(-30.9721971729695,55.4229205154484,4.62905833454845));
#30794=CARTESIAN_POINT('Ctrl Pts',(-30.8637971116759,55.9636286201302,4.66610429807113));
#30795=CARTESIAN_POINT('Ctrl Pts',(-30.7553970503824,56.5043367248119,4.70315026159382));
#30796=CARTESIAN_POINT('Ctrl Pts',(-30.9415351902204,57.1040932485588,4.7401962251165));
#30797=CARTESIAN_POINT('Ctrl Pts',(-31.3370243602463,57.488416218779,4.77724218863918));
#30798=CARTESIAN_POINT('Ctrl Pts',(-31.7325135302723,57.8727391889992,4.81428815216186));
#30799=CARTESIAN_POINT('Ctrl Pts',(-32.3373537304862,58.0416286056926,4.85133411568454));
#30800=CARTESIAN_POINT('Ctrl Pts',(-32.8747364051652,57.9177912669505,4.88838007920722));
#30801=CARTESIAN_POINT('Ctrl Pts',(-33.0347855041357,57.880908696264,4.89941350726822));
#30802=CARTESIAN_POINT('Ctrl Pts',(-33.1888509066774,57.8180603341073,4.91044693532922));
#30803=CARTESIAN_POINT('Ctrl Pts',(-33.3312509399777,57.7342826871321,4.92148036339022));
#30804=CARTESIAN_POINT('Ctrl Pts',(-33.3320164235939,57.7319854708823,4.72851963660978));
#30805=CARTESIAN_POINT('Ctrl Pts',(-33.0706605734929,57.8821688027457,4.70843756910068));
#30806=CARTESIAN_POINT('Ctrl Pts',(-32.7702470049871,57.965297344832,4.68835550159159));
#30807=CARTESIAN_POINT('Ctrl Pts',(-32.4713490172715,57.9601647997737,4.6682734340825));
#30808=CARTESIAN_POINT('Ctrl Pts',(-31.919963362139,57.9506966473077,4.63122747055982));
#30809=CARTESIAN_POINT('Ctrl Pts',(-31.3737352640037,57.6408739439502,4.59418150703713));
#30810=CARTESIAN_POINT('Ctrl Pts',(-31.0826491087611,57.1724888068711,4.55713554351445));
#30811=CARTESIAN_POINT('Ctrl Pts',(-30.7915629535184,56.704103669792,4.52008957999177));
#30812=CARTESIAN_POINT('Ctrl Pts',(-30.7556187411683,56.0771560989914,4.48304361646909));
#30813=CARTESIAN_POINT('Ctrl Pts',(-30.9912665445818,55.5785722051981,4.44599765294641));
#30814=CARTESIAN_POINT('Ctrl Pts',(-31.2269143479953,55.0799883114048,4.40895168942373));
#30815=CARTESIAN_POINT('Ctrl Pts',(-31.7341541671722,54.7097680946189,4.37190572590105));
#30816=CARTESIAN_POINT('Ctrl Pts',(-32.2808448224847,54.6373449363853,4.33485976237837));
#30817=CARTESIAN_POINT('Ctrl Pts',(-32.8275354777971,54.5649217781517,4.29781379885569));
#30818=CARTESIAN_POINT('Ctrl Pts',(-33.413676969245,54.7902956784704,4.26076783533301));
#30819=CARTESIAN_POINT('Ctrl Pts',(-33.7710183196873,55.2103229938828,4.22372187181033));
#30820=CARTESIAN_POINT('Ctrl Pts',(-34.1283596701297,55.6303503092951,4.18667590828765));
#30821=CARTESIAN_POINT('Ctrl Pts',(-34.2569008795666,56.2450310398012,4.14962994476497));
#30822=CARTESIAN_POINT('Ctrl Pts',(-34.0978143345866,56.7730530636186,4.11258398124229));
#30823=CARTESIAN_POINT('Ctrl Pts',(-33.9774817812581,57.1724472320418,4.08456253303145));
#30824=CARTESIAN_POINT('Ctrl Pts',(-33.6925870013811,57.5222608245174,4.05654108482062));
#30825=CARTESIAN_POINT('Ctrl Pts',(-33.3316044198825,57.73507921,4.02851963660978));
#30826=CARTESIAN_POINT('Origin',(-32.5,56.2916512459885,3.));
#30827=CARTESIAN_POINT('',(-33.3347454964365,57.7363721546008,3.32851963660978));
#30828=CARTESIAN_POINT('',(-33.333716562894,57.7328365508938,3.52148036339022));
#30829=CARTESIAN_POINT('',(-33.333,57.7344495686934,3.));
#30830=CARTESIAN_POINT('Ctrl Pts',(-33.333716562894,57.7328365508938,3.52148036339022));
#30831=CARTESIAN_POINT('Ctrl Pts',(-33.4781004639345,57.6510402790884,3.53256203972372));
#30832=CARTESIAN_POINT('Ctrl Pts',(-33.6100888264908,57.5485020789653,3.54364371605722));
#30833=CARTESIAN_POINT('Ctrl Pts',(-33.7223873369832,57.4276653019286,3.55472539239072));
#30834=CARTESIAN_POINT('Ctrl Pts',(-34.0978004421986,57.0237088336489,3.5917713559134));
#30835=CARTESIAN_POINT('Ctrl Pts',(-34.2531676277225,56.4152547808823,3.62881731943608));
#30836=CARTESIAN_POINT('Ctrl Pts',(-34.1173842201124,55.8807655910479,3.66586328295876));
#30837=CARTESIAN_POINT('Ctrl Pts',(-33.9816008125024,55.3462764012135,3.70290924648144));
#30838=CARTESIAN_POINT('Ctrl Pts',(-33.5546668117583,54.8857520743114,3.73995521000412));
#30839=CARTESIAN_POINT('Ctrl Pts',(-33.0319709841926,54.709954179896,3.7770011735268));
#30840=CARTESIAN_POINT('Ctrl Pts',(-32.5092751566268,54.5341562854806,3.81404713704948));
#30841=CARTESIAN_POINT('Ctrl Pts',(-31.8908175022394,54.643084823552,3.85109310057216));
#30842=CARTESIAN_POINT('Ctrl Pts',(-31.4596386734712,54.9868880310005,3.88813906409484));
#30843=CARTESIAN_POINT('Ctrl Pts',(-31.0284598447031,55.330691238449,3.92518502761752));
#30844=CARTESIAN_POINT('Ctrl Pts',(-30.7845598415543,55.9093691152746,3.9622309911402));
#30845=CARTESIAN_POINT('Ctrl Pts',(-30.8395608834388,56.4580864498103,3.99927695466289));
#30846=CARTESIAN_POINT('Ctrl Pts',(-30.8945619253233,57.0068037843461,4.03632291818557));
#30847=CARTESIAN_POINT('Ctrl Pts',(-31.2484640122411,57.525560576592,4.07336888170825));
#30848=CARTESIAN_POINT('Ctrl Pts',(-31.7393018474209,57.7769448390475,4.11041484523093));
#30849=CARTESIAN_POINT('Ctrl Pts',(-32.2298200515887,58.0281654013957,4.14743668461736));
#30850=CARTESIAN_POINT('Ctrl Pts',(-32.8570957184112,58.0123615437382,4.18445852400379));
#30851=CARTESIAN_POINT('Ctrl Pts',(-33.3343856149812,57.7368361019314,4.22148036339022));
#30852=CARTESIAN_POINT('Ctrl Pts',(-33.3316044198825,57.73507921,4.02851963660978));
#30853=CARTESIAN_POINT('Ctrl Pts',(-33.2153473010665,57.8036189501297,4.01949512129794));
#30854=CARTESIAN_POINT('Ctrl Pts',(-33.0911982807713,57.8579494129027,4.01047060598609));
#30855=CARTESIAN_POINT('Ctrl Pts',(-32.9621127685743,57.8951505902149,4.00144609067424));
#30856=CARTESIAN_POINT('Ctrl Pts',(-32.4322120469391,58.0478627758654,3.96440012715156));
#30857=CARTESIAN_POINT('Ctrl Pts',(-31.8191249030656,57.9119238300377,3.92735416362888));
#30858=CARTESIAN_POINT('Ctrl Pts',(-31.4034341447795,57.5495469821188,3.8903082001062));
#30859=CARTESIAN_POINT('Ctrl Pts',(-30.9877433864933,57.1871701341999,3.85326223658352));
#30860=CARTESIAN_POINT('Ctrl Pts',(-30.7694490137945,56.5983553841898,3.81621627306084));
#30861=CARTESIAN_POINT('Ctrl Pts',(-30.8484546841662,56.0525771412361,3.77917030953816));
#30862=CARTESIAN_POINT('Ctrl Pts',(-30.9274603545379,55.5067988982823,3.74212434601548));
#30863=CARTESIAN_POINT('Ctrl Pts',(-31.3037660679802,55.0040571623848,3.7050783824928));
#30864=CARTESIAN_POINT('Ctrl Pts',(-31.8051533809355,54.7744345397173,3.66803241897012));
#30865=CARTESIAN_POINT('Ctrl Pts',(-32.3065406938908,54.5448119170498,3.63098645544744));
#30866=CARTESIAN_POINT('Ctrl Pts',(-32.9330096063591,54.5883084076123,3.59394049192476));
#30867=CARTESIAN_POINT('Ctrl Pts',(-33.3978530682301,54.8850175958567,3.55689452840208));
#30868=CARTESIAN_POINT('Ctrl Pts',(-33.862696530101,55.181726784101,3.5198485648794));
#30869=CARTESIAN_POINT('Ctrl Pts',(-34.1659145413746,55.7316486700272,3.48280260135672));
#30870=CARTESIAN_POINT('Ctrl Pts',(-34.1687376598278,56.2831083842721,3.44575663783404));
#30871=CARTESIAN_POINT('Ctrl Pts',(-34.1715607782811,56.834568098517,3.40871067431136));
#30872=CARTESIAN_POINT('Ctrl Pts',(-33.873989003914,57.3875656410806,3.37166471078867));
#30873=CARTESIAN_POINT('Ctrl Pts',(-33.4122077466127,57.6890185508992,3.33461874726599));
#30874=CARTESIAN_POINT('Ctrl Pts',(-33.3868657595293,57.7055619155899,3.33258571038059));
#30875=CARTESIAN_POINT('Ctrl Pts',(-33.3610292261422,57.7213477085124,3.33055267349519));
#30876=CARTESIAN_POINT('Ctrl Pts',(-33.3347454964365,57.7363721546008,3.32851963660978));
#30877=CARTESIAN_POINT('Origin',(-32.5,56.2916512459885,3.));
#30878=CARTESIAN_POINT('',(-33.333130190179,57.7323221393285,2.62851963660978));
#30879=CARTESIAN_POINT('',(-33.3311289428234,57.7328938252549,2.82148036339022));
#30880=CARTESIAN_POINT('',(-33.333,57.7344495686934,3.));
#30881=CARTESIAN_POINT('Ctrl Pts',(-33.3311289428234,57.7328938252549,2.82148036339022));
#30882=CARTESIAN_POINT('Ctrl Pts',(-33.6180096158229,57.5655068353994,2.84361959192097));
#30883=CARTESIAN_POINT('Ctrl Pts',(-33.8582224621032,57.3156647118177,2.86575882045172));
#30884=CARTESIAN_POINT('Ctrl Pts',(-34.0018785934241,57.0190572038434,2.88789804898247));
#30885=CARTESIAN_POINT('Ctrl Pts',(-34.2422609442965,56.5227386033237,2.92494401250515));
#30886=CARTESIAN_POINT('Ctrl Pts',(-34.2122852455117,55.8954772908327,2.96198997602783));
#30887=CARTESIAN_POINT('Ctrl Pts',(-33.9256700455925,55.4243429628454,2.99903593955051));
#30888=CARTESIAN_POINT('Ctrl Pts',(-33.6390548456733,54.9532086348582,3.03608190307319));
#30889=CARTESIAN_POINT('Ctrl Pts',(-33.0958001446196,54.6382012913747,3.07312786659587));
#30890=CARTESIAN_POINT('Ctrl Pts',(-32.5445295368321,54.6234858293533,3.11017383011855));
#30891=CARTESIAN_POINT('Ctrl Pts',(-31.9932589290447,54.6087703673319,3.14721979364123));
#30892=CARTESIAN_POINT('Ctrl Pts',(-31.4339724145236,54.8943467867725,3.18426575716391));
#30893=CARTESIAN_POINT('Ctrl Pts',(-31.1226306380099,55.3495194199898,3.22131172068659));
#30894=CARTESIAN_POINT('Ctrl Pts',(-30.8112888614961,55.8046920532072,3.25835768420927));
#30895=CARTESIAN_POINT('Ctrl Pts',(-30.7478918229898,56.4294609002012,3.29540364773196));
#30896=CARTESIAN_POINT('Ctrl Pts',(-30.9614535366484,56.9378969554647,3.33244961125464));
#30897=CARTESIAN_POINT('Ctrl Pts',(-31.175015250307,57.4463330107282,3.36949557477732));
#30898=CARTESIAN_POINT('Ctrl Pts',(-31.6655357161305,57.8384362742609,3.40654153829999));
#30899=CARTESIAN_POINT('Ctrl Pts',(-32.2085254614957,57.934758464131,3.44358750182267));
#30900=CARTESIAN_POINT('Ctrl Pts',(-32.5890889655549,58.0022674924478,3.46955178901185));
#30901=CARTESIAN_POINT('Ctrl Pts',(-32.9954261310775,57.9244846218395,3.49551607620104));
#30902=CARTESIAN_POINT('Ctrl Pts',(-33.333716562894,57.7328365508938,3.52148036339022));
#30903=CARTESIAN_POINT('Ctrl Pts',(-33.3347454964365,57.7363721546008,3.32851963660978));
#30904=CARTESIAN_POINT('Ctrl Pts',(-32.8820875508044,57.9951229094133,3.2935067099725));
#30905=CARTESIAN_POINT('Ctrl Pts',(-32.2967926538179,58.0280607074246,3.25849378333523));
#30906=CARTESIAN_POINT('Ctrl Pts',(-31.8207237377836,57.8159025761185,3.22348085669795));
#30907=CARTESIAN_POINT('Ctrl Pts',(-31.3170117264914,57.5914254144454,3.18643489317527));
#30908=CARTESIAN_POINT('Ctrl Pts',(-30.9355784441425,57.0925628140254,3.14938892965259));
#30909=CARTESIAN_POINT('Ctrl Pts',(-30.8509889952779,56.547622072684,3.11234296612991));
#30910=CARTESIAN_POINT('Ctrl Pts',(-30.7663995464132,56.0026813313427,3.07529700260723));
#30911=CARTESIAN_POINT('Ctrl Pts',(-30.9786539310327,55.41166244908,3.03825103908455));
#30912=CARTESIAN_POINT('Ctrl Pts',(-31.390612726451,55.0450485686685,3.00120507556187));
#30913=CARTESIAN_POINT('Ctrl Pts',(-31.8025715218694,54.678434688257,2.96415911203919));
#30914=CARTESIAN_POINT('Ctrl Pts',(-32.4142347280865,54.5362258096967,2.92711314851651));
#30915=CARTESIAN_POINT('Ctrl Pts',(-32.9456712104109,54.6835046326399,2.89006718499383));
#30916=CARTESIAN_POINT('Ctrl Pts',(-33.4771076927354,54.8307834555831,2.85302122147115));
#30917=CARTESIAN_POINT('Ctrl Pts',(-33.9283174511671,55.2675499800297,2.81597525794846));
#30918=CARTESIAN_POINT('Ctrl Pts',(-34.0928017812264,55.7939155294323,2.77892929442578));
#30919=CARTESIAN_POINT('Ctrl Pts',(-34.2572861112858,56.3202810788348,2.7418833309031));
#30920=CARTESIAN_POINT('Ctrl Pts',(-34.1350450129728,56.9362456531931,2.70483736738042));
#30921=CARTESIAN_POINT('Ctrl Pts',(-33.7820228180846,57.3599095722955,2.66779140385774));
#30922=CARTESIAN_POINT('Ctrl Pts',(-33.6572786340789,57.509615768241,2.65470081477509));
#30923=CARTESIAN_POINT('Ctrl Pts',(-33.5037182424927,57.6353105712173,2.64161022569243));
#30924=CARTESIAN_POINT('Ctrl Pts',(-33.333130190179,57.7323221393285,2.62851963660978));
#30925=CARTESIAN_POINT('Origin',(-32.5,56.2916512459885,3.));
#30926=CARTESIAN_POINT('',(-33.3310982842581,57.7335685916211,1.92851963660978));
#30927=CARTESIAN_POINT('',(-33.3331738820164,57.7367002116855,2.12148036339022));
#30928=CARTESIAN_POINT('',(-33.333,57.7344495686934,3.));
#30929=CARTESIAN_POINT('Ctrl Pts',(-33.3331738820164,57.7367002116855,2.12148036339022));
#30930=CARTESIAN_POINT('Ctrl Pts',(-33.7599095781773,57.4863532801825,2.15467714411822));
#30931=CARTESIAN_POINT('Ctrl Pts',(-34.0737470619129,57.0348072848651,2.18787392484622));
#30932=CARTESIAN_POINT('Ctrl Pts',(-34.1491952727494,56.5464328961311,2.22107070557422));
#30933=CARTESIAN_POINT('Ctrl Pts',(-34.233391740154,56.0014312606204,2.2581166690969));
#30934=CARTESIAN_POINT('Ctrl Pts',(-34.0207112033876,55.4105655517268,2.29516263261958));
#30935=CARTESIAN_POINT('Ctrl Pts',(-33.608488116082,55.0442488115619,2.33220859614226));
#30936=CARTESIAN_POINT('Ctrl Pts',(-33.1962650287764,54.6779320713971,2.36925455966494));
#30937=CARTESIAN_POINT('Ctrl Pts',(-32.5844993909317,54.5361642999609,2.40630052318762));
#30938=CARTESIAN_POINT('Ctrl Pts',(-32.0531692156545,54.6838263217292,2.4433464867103));
#30939=CARTESIAN_POINT('Ctrl Pts',(-31.5218390403773,54.8314883434974,2.48039245023298));
#30940=CARTESIAN_POINT('Ctrl Pts',(-31.0709443276677,55.2685801584701,2.51743841375566));
#30941=CARTESIAN_POINT('Ctrl Pts',(-30.9068395995442,55.7950642190458,2.55448437727834));
#30942=CARTESIAN_POINT('Ctrl Pts',(-30.7427348714206,56.3215482796215,2.59153034080102));
#30943=CARTESIAN_POINT('Ctrl Pts',(-30.8654201278831,56.9374245858002,2.6285763043237));
#30944=CARTESIAN_POINT('Ctrl Pts',(-31.2187477656388,57.360833853803,2.66562226784638));
#30945=CARTESIAN_POINT('Ctrl Pts',(-31.5720754033946,57.7842431218059,2.70266823136906));
#30946=CARTESIAN_POINT('Ctrl Pts',(-32.1560454224436,58.0151853516328,2.73971419489175));
#30947=CARTESIAN_POINT('Ctrl Pts',(-32.7034006322329,57.9479685222721,2.77676015841443));
#30948=CARTESIAN_POINT('Ctrl Pts',(-32.9236480838557,57.9209214875348,2.79166689340636));
#30949=CARTESIAN_POINT('Ctrl Pts',(-33.1379671006766,57.845598452492,2.80657362839829));
#30950=CARTESIAN_POINT('Ctrl Pts',(-33.3311289428234,57.7328938252549,2.82148036339022));
#30951=CARTESIAN_POINT('Ctrl Pts',(-33.333130190179,57.7323221393285,2.62851963660978));
#30952=CARTESIAN_POINT('Ctrl Pts',(-33.0209593136532,57.9098503181175,2.60456426216975));
#30953=CARTESIAN_POINT('Ctrl Pts',(-32.6517664254568,57.9913244481799,2.58060888772973));
#30954=CARTESIAN_POINT('Ctrl Pts',(-32.2977938304223,57.9481146542165,2.5566535132897));
#30955=CARTESIAN_POINT('Ctrl Pts',(-31.7503903291117,57.8812925531888,2.51960754976702));
#30956=CARTESIAN_POINT('Ctrl Pts',(-31.2393866179539,57.5162850872868,2.48256158624434));
#30957=CARTESIAN_POINT('Ctrl Pts',(-30.9986464429484,57.0201399930138,2.44551562272166));
#30958=CARTESIAN_POINT('Ctrl Pts',(-30.7579062679429,56.5239948987407,2.40846965919898));
#30959=CARTESIAN_POINT('Ctrl Pts',(-30.7874296290898,55.8967121760965,2.3714236956763));
#30960=CARTESIAN_POINT('Ctrl Pts',(-31.0737049927512,55.4253713200344,2.33437773215362));
#30961=CARTESIAN_POINT('Ctrl Pts',(-31.3599803564127,54.9540304639722,2.29733176863094));
#30962=CARTESIAN_POINT('Ctrl Pts',(-31.9030077225887,54.6386314744921,2.26028580510826));
#30963=CARTESIAN_POINT('Ctrl Pts',(-32.4542675379743,54.6235184875634,2.22323984158558));
#30964=CARTESIAN_POINT('Ctrl Pts',(-33.00552735336,54.6084055006347,2.1861938780629));
#30965=CARTESIAN_POINT('Ctrl Pts',(-33.5650196179551,54.8935785162575,2.14914791454022));
#30966=CARTESIAN_POINT('Ctrl Pts',(-33.8766895243309,55.3485264867911,2.11210195101753));
#30967=CARTESIAN_POINT('Ctrl Pts',(-34.1883594307067,55.8034744573246,2.07505598749485));
#30968=CARTESIAN_POINT('Ctrl Pts',(-34.2522069788632,56.4281973827689,2.03801002397217));
#30969=CARTESIAN_POINT('Ctrl Pts',(-34.0390119763463,56.9367872738744,2.00096406044949));
#30970=CARTESIAN_POINT('Ctrl Pts',(-33.9000423680165,57.2683078870831,1.97681591916959));
#30971=CARTESIAN_POINT('Ctrl Pts',(-33.6433576792834,57.550483699497,1.95266777788969));
#30972=CARTESIAN_POINT('Ctrl Pts',(-33.3310982842581,57.7335685916211,1.92851963660978));
#30973=CARTESIAN_POINT('Origin',(-32.5,56.2916512459885,3.));
#30974=CARTESIAN_POINT('',(-33.3338545267451,57.7369307977834,1.22851963660978));
#30975=CARTESIAN_POINT('',(-33.3345984319871,57.7343006412916,1.42148036339021));
#30976=CARTESIAN_POINT('',(-33.333,57.7344495686934,3.));
#30977=CARTESIAN_POINT('Ctrl Pts',(-33.3345984319871,57.7343006412916,1.42148036339021));
#30978=CARTESIAN_POINT('Ctrl Pts',(-33.4283251997872,57.6813267445322,1.42868873279278));
#30979=CARTESIAN_POINT('Ctrl Pts',(-33.5166388707303,57.6193252564529,1.43589710219535));
#30980=CARTESIAN_POINT('Ctrl Pts',(-33.5974727328826,57.5487559900283,1.44310547159792));
#30981=CARTESIAN_POINT('Ctrl Pts',(-34.0129020958151,57.1860794506077,1.4801514351206));
#30982=CARTESIAN_POINT('Ctrl Pts',(-34.2307718231603,56.5971073981534,1.51719739864329));
#30983=CARTESIAN_POINT('Ctrl Pts',(-34.1513725987927,56.0513862321698,1.55424336216597));
#30984=CARTESIAN_POINT('Ctrl Pts',(-34.071973374425,55.5056650661861,1.59128932568865));
#30985=CARTESIAN_POINT('Ctrl Pts',(-33.6953051983445,55.0031947866731,1.62833528921133));
#30986=CARTESIAN_POINT('Ctrl Pts',(-33.1937523971885,54.7739337662501,1.66538125273401));
#30987=CARTESIAN_POINT('Ctrl Pts',(-32.6921995960325,54.5446727458271,1.70242721625669));
#30988=CARTESIAN_POINT('Ctrl Pts',(-32.0657621698011,54.5886209844942,1.73947317977937));
#30989=CARTESIAN_POINT('Ctrl Pts',(-31.6011327587506,54.8856653216219,1.77651914330205));
#30990=CARTESIAN_POINT('Ctrl Pts',(-31.1365033477001,55.1827096587496,1.81356510682473));
#30991=CARTESIAN_POINT('Ctrl Pts',(-30.8336819518306,55.7328500943379,1.85061107034741));
#30992=CARTESIAN_POINT('Ctrl Pts',(-30.831256500076,56.2843117385313,1.88765703387009));
#30993=CARTESIAN_POINT('Ctrl Pts',(-30.8288310483213,56.8357733827248,1.92470299739277));
#30994=CARTESIAN_POINT('Ctrl Pts',(-31.1268015406815,57.3885562355234,1.96174896091545));
#30995=CARTESIAN_POINT('Ctrl Pts',(-31.5888000917203,57.689676089852,1.99879492443813));
#30996=CARTESIAN_POINT('Ctrl Pts',(-32.050798642759,57.9907959441805,2.03584088796081));
#30997=CARTESIAN_POINT('Ctrl Pts',(-32.6768252524764,58.040252800039,2.07288685148349));
#30998=CARTESIAN_POINT('Ctrl Pts',(-33.1803752931228,57.8154124469043,2.10993281500617));
#30999=CARTESIAN_POINT('Ctrl Pts',(-33.2326955992617,57.7920508836856,2.11378199780085));
#31000=CARTESIAN_POINT('Ctrl Pts',(-33.2836936714804,57.7657280595765,2.11763118059554));
#31001=CARTESIAN_POINT('Ctrl Pts',(-33.3331738820164,57.7367002116855,2.12148036339022));
#31002=CARTESIAN_POINT('Ctrl Pts',(-33.3310982842581,57.7335685916211,1.92851963660978));
#31003=CARTESIAN_POINT('Ctrl Pts',(-33.1643166622694,57.8313565069137,1.91562181436701));
#31004=CARTESIAN_POINT('Ctrl Pts',(-32.9816809059178,57.900876152894,1.90272399212423));
#31005=CARTESIAN_POINT('Ctrl Pts',(-32.792659312829,57.9345477382935,1.88982616988145));
#31006=CARTESIAN_POINT('Ctrl Pts',(-32.2497392050189,58.0312614548405,1.85278020635877));
#31007=CARTESIAN_POINT('Ctrl Pts',(-31.6541365425887,57.8322320311677,1.81573424283609));
#31008=CARTESIAN_POINT('Ctrl Pts',(-31.2784322612969,57.4285464115925,1.77868827931341));
#31009=CARTESIAN_POINT('Ctrl Pts',(-30.902727980005,57.0248607920173,1.74164231579073));
#31010=CARTESIAN_POINT('Ctrl Pts',(-30.7469220798514,56.4165189765397,1.70459635226805));
#31011=CARTESIAN_POINT('Ctrl Pts',(-30.8823200145203,55.8819320465459,1.66755038874537));
#31012=CARTESIAN_POINT('Ctrl Pts',(-31.0177179491892,55.3473451165522,1.63050442522269));
#31013=CARTESIAN_POINT('Ctrl Pts',(-31.4443197186808,54.8865130720423,1.59345846170001));
#31014=CARTESIAN_POINT('Ctrl Pts',(-31.9668886041916,54.7103383112811,1.55641249817733));
#31015=CARTESIAN_POINT('Ctrl Pts',(-32.4894574897024,54.53416355052,1.51936653465465));
#31016=CARTESIAN_POINT('Ctrl Pts',(-33.1079934912324,54.6426460735076,1.48232057113197));
#31017=CARTESIAN_POINT('Ctrl Pts',(-33.5394201003418,54.9861382384619,1.44527460760928));
#31018=CARTESIAN_POINT('Ctrl Pts',(-33.9708467094511,55.3296304034162,1.4082286440866));
#31019=CARTESIAN_POINT('Ctrl Pts',(-34.2151639261398,55.9081322103372,1.37118268056392));
#31020=CARTESIAN_POINT('Ctrl Pts',(-34.1605585908214,56.4568890269572,1.33413671704124));
#31021=CARTESIAN_POINT('Ctrl Pts',(-34.1086657929391,56.9783861738082,1.29893102356409));
#31022=CARTESIAN_POINT('Ctrl Pts',(-33.7868109567046,57.4730201142583,1.26372533008693));
#31023=CARTESIAN_POINT('Ctrl Pts',(-33.3338545267451,57.7369307977834,1.22851963660978));
#31024=CARTESIAN_POINT('Origin',(-32.5,56.2916512459885,3.));
#31025=CARTESIAN_POINT('',(-33.3341985401264,57.7334817014241,0.528519636609781));
#31026=CARTESIAN_POINT('',(-33.3317031312748,57.7320766758176,0.721480363390217));
#31027=CARTESIAN_POINT('',(-33.333,57.7344495686934,3.));
#31028=CARTESIAN_POINT('Ctrl Pts',(-33.3317031312748,57.7320766758176,0.721480363390217));
#31029=CARTESIAN_POINT('Ctrl Pts',(-33.5692173042018,57.5950551525707,0.739746284990036));
#31030=CARTESIAN_POINT('Ctrl Pts',(-33.7746291238346,57.4025124831788,0.758012206589854));
#31031=CARTESIAN_POINT('Ctrl Pts',(-33.9179858048945,57.1714665641067,0.776278128189673));
#31032=CARTESIAN_POINT('Ctrl Pts',(-34.208734144542,56.7028716102066,0.813324091712354));
#31033=CARTESIAN_POINT('Ctrl Pts',(-34.2442262482397,56.0758982397685,0.850370055235033));
#31034=CARTESIAN_POINT('Ctrl Pts',(-34.0082189534411,55.5774843709491,0.887416018757714));
#31035=CARTESIAN_POINT('Ctrl Pts',(-33.7722116586424,55.0790705021297,0.924461982280394));
#31036=CARTESIAN_POINT('Ctrl Pts',(-33.2647049653473,54.7092161349289,0.961507945803076));
#31037=CARTESIAN_POINT('Ctrl Pts',(-32.7179621895189,54.6371872177157,0.998553909325756));
#31038=CARTESIAN_POINT('Ctrl Pts',(-32.1712194136904,54.5651583005025,1.03559987284844));
#31039=CARTESIAN_POINT('Ctrl Pts',(-31.5852405553285,54.7909548332769,1.07264583637112));
#31040=CARTESIAN_POINT('Ctrl Pts',(-31.2282021616797,55.21123975246,1.1096917998938));
#31041=CARTESIAN_POINT('Ctrl Pts',(-30.8711637680309,55.631524671643,1.14673776341648));
#31042=CARTESIAN_POINT('Ctrl Pts',(-30.7430658390951,56.2462979772347,1.18378372693916));
#31043=CARTESIAN_POINT('Ctrl Pts',(-30.902533118419,56.7742051799299,1.22082969046184));
#31044=CARTESIAN_POINT('Ctrl Pts',(-31.0620003977429,57.3021123826251,1.25787565398452));
#31045=CARTESIAN_POINT('Ctrl Pts',(-31.5090328853265,57.7431534824239,1.2949216175072));
#31046=CARTESIAN_POINT('Ctrl Pts',(-32.0390436283783,57.8954835191298,1.33196758102988));
#31047=CARTESIAN_POINT('Ctrl Pts',(-32.4659253700502,58.0181733178376,1.36180517514999));
#31048=CARTESIAN_POINT('Ctrl Pts',(-32.9466353435787,57.9535754234504,1.3916427692701));
#31049=CARTESIAN_POINT('Ctrl Pts',(-33.3345984319871,57.7343006412916,1.42148036339021));
#31050=CARTESIAN_POINT('Ctrl Pts',(-33.3338545267451,57.7369307977834,1.22851963660978));
#31051=CARTESIAN_POINT('Ctrl Pts',(-33.3101776135059,57.7507259223106,1.22667936656425));
#31052=CARTESIAN_POINT('Ctrl Pts',(-33.2861424840206,57.7638906287274,1.22483909651873));
#31053=CARTESIAN_POINT('Ctrl Pts',(-33.261768971111,57.776395800606,1.2229988264732));
#31054=CARTESIAN_POINT('Ctrl Pts',(-32.7711125740444,58.0281339313158,1.18595286295052));
#31055=CARTESIAN_POINT('Ctrl Pts',(-32.1433276672366,58.0125983664166,1.14890689942784));
#31056=CARTESIAN_POINT('Ctrl Pts',(-31.6657235730869,57.7368990452689,1.11186093590516));
#31057=CARTESIAN_POINT('Ctrl Pts',(-31.1881194789371,57.4611997241213,1.07481497238248));
#31058=CARTESIAN_POINT('Ctrl Pts',(-30.8606961974455,56.9253366467254,1.0377690088598));
#31059=CARTESIAN_POINT('Ctrl Pts',(-30.8333008499707,56.3745505890176,1.00072304533712));
#31060=CARTESIAN_POINT('Ctrl Pts',(-30.8059055024959,55.8237645313099,0.963677081814436));
#31061=CARTESIAN_POINT('Ctrl Pts',(-31.0785380890379,55.2580554932903,0.926631118291755));
#31062=CARTESIAN_POINT('Ctrl Pts',(-31.526426760498,54.9363234239653,0.889585154769075));
#31063=CARTESIAN_POINT('Ctrl Pts',(-31.9743154319581,54.6145913546402,0.852539191246395));
#31064=CARTESIAN_POINT('Ctrl Pts',(-32.5974601883362,54.5368362540097,0.815493227723714));
#31065=CARTESIAN_POINT('Ctrl Pts',(-33.1106752982773,54.7386431848418,0.778447264201034));
#31066=CARTESIAN_POINT('Ctrl Pts',(-33.6238904082183,54.940450115674,0.741401300678353));
#31067=CARTESIAN_POINT('Ctrl Pts',(-34.0271758717221,55.4218190779688,0.704355337155672));
#31068=CARTESIAN_POINT('Ctrl Pts',(-34.1359658098863,55.9624488364586,0.667309373632992));
#31069=CARTESIAN_POINT('Ctrl Pts',(-34.2447557480506,56.5030785949484,0.630263410110312));
#31070=CARTESIAN_POINT('Ctrl Pts',(-34.0590501608752,57.1029691496333,0.593217446587631));
#31071=CARTESIAN_POINT('Ctrl Pts',(-33.6638382628473,57.4875771868012,0.556171483064951));
#31072=CARTESIAN_POINT('Ctrl Pts',(-33.5655069136947,57.5832702248356,0.546954200913227));
#31073=CARTESIAN_POINT('Ctrl Pts',(-33.4542061287358,57.6656362524338,0.537736918761504));
#31074=CARTESIAN_POINT('Ctrl Pts',(-33.3341985401264,57.7334817014241,0.528519636609781));
#31075=CARTESIAN_POINT('Origin',(-32.5,56.2916512459885,3.));
#31076=CARTESIAN_POINT('',(-33.3313285320323,57.7324067450656,-0.171480363390219));
#31077=CARTESIAN_POINT('',(-33.3319271105623,57.7355745198861,0.0214803633902191));
#31078=CARTESIAN_POINT('',(-33.333,57.7344495686934,3.));
#31079=CARTESIAN_POINT('Ctrl Pts',(-33.3319271105623,57.7355745198861,0.0214803633902191));
#31080=CARTESIAN_POINT('Ctrl Pts',(-33.7093130799579,57.5130220094248,0.0508038371872872));
#31081=CARTESIAN_POINT('Ctrl Pts',(-34.0025116805638,57.1388573741433,0.0801273109843555));
#31082=CARTESIAN_POINT('Ctrl Pts',(-34.1137073818815,56.7167479649787,0.109450784781424));
#31083=CARTESIAN_POINT('Ctrl Pts',(-34.254187050948,56.1834738419088,0.146496748304104));
#31084=CARTESIAN_POINT('Ctrl Pts',(-34.1041780082168,55.5736766763093,0.183542711826784));
#31085=CARTESIAN_POINT('Ctrl Pts',(-33.7323327404969,55.1664335984773,0.220588675349465));
#31086=CARTESIAN_POINT('Ctrl Pts',(-33.360487472777,54.7591905206453,0.257634638872145));
#31087=CARTESIAN_POINT('Ctrl Pts',(-32.7668059800683,54.5545015305809,0.294680602394826));
#31088=CARTESIAN_POINT('Ctrl Pts',(-32.2229899650202,54.6460437054155,0.331726565917507));
#31089=CARTESIAN_POINT('Ctrl Pts',(-31.6791739499721,54.7375858802501,0.368772529440187));
#31090=CARTESIAN_POINT('Ctrl Pts',(-31.1852234125845,55.1253592199837,0.405818492962867));
#31091=CARTESIAN_POINT('Ctrl Pts',(-30.9671976166263,55.6318970567811,0.442864456485548));
#31092=CARTESIAN_POINT('Ctrl Pts',(-30.7491718206681,56.1384348935784,0.479910420008228));
#31093=CARTESIAN_POINT('Ctrl Pts',(-30.8070707661393,56.7637372274395,0.516956383530909));
#31094=CARTESIAN_POINT('Ctrl Pts',(-31.1143966726152,57.2216308996084,0.55400234705359));
#31095=CARTESIAN_POINT('Ctrl Pts',(-31.4217225790911,57.6795245717774,0.59104831057627));
#31096=CARTESIAN_POINT('Ctrl Pts',(-31.9784754465718,57.9700095822542,0.62809427409895));
#31097=CARTESIAN_POINT('Ctrl Pts',(-32.5298541681108,57.9601438188116,0.665140237621631));
#31098=CARTESIAN_POINT('Ctrl Pts',(-32.8093695193456,57.9551424790316,0.683920279544493));
#31099=CARTESIAN_POINT('Ctrl Pts',(-33.0875037843945,57.8729548645719,0.702700321467355));
#31100=CARTESIAN_POINT('Ctrl Pts',(-33.3317031312748,57.7320766758176,0.721480363390217));
#31101=CARTESIAN_POINT('Ctrl Pts',(-33.3341985401264,57.7334817014241,0.528519636609781));
#31102=CARTESIAN_POINT('Ctrl Pts',(-32.9718734110338,57.9383196733276,0.500690955238824));
#31103=CARTESIAN_POINT('Ctrl Pts',(-32.5301815965127,58.010795616536,0.472862273867866));
#31104=CARTESIAN_POINT('Ctrl Pts',(-32.1264363544929,57.9180609610464,0.445033592496909));
#31105=CARTESIAN_POINT('Ctrl Pts',(-31.5889645530468,57.7946111784728,0.407987628974228));
#31106=CARTESIAN_POINT('Ctrl Pts',(-31.1187391590349,57.3783860936747,0.370941665451548));
#31107=CARTESIAN_POINT('Ctrl Pts',(-30.9309614883814,56.8598734778586,0.333895701928867));
#31108=CARTESIAN_POINT('Ctrl Pts',(-30.7431838177278,56.3413608620425,0.296849738406187));
#31109=CARTESIAN_POINT('Ctrl Pts',(-30.8378538704327,55.7205607152083,0.259803774883506));
#31110=CARTESIAN_POINT('Ctrl Pts',(-31.1716453640503,55.2815857427567,0.222757811360826));
#31111=CARTESIAN_POINT('Ctrl Pts',(-31.5054368576679,54.842610770305,0.185711847838145));
#31112=CARTESIAN_POINT('Ctrl Pts',(-32.0783497921982,54.5854609722358,0.148665884315465));
#31113=CARTESIAN_POINT('Ctrl Pts',(-32.6281873065731,54.6278224157042,0.111619920792784));
#31114=CARTESIAN_POINT('Ctrl Pts',(-33.178024820948,54.6701838591725,0.0745739572701037));
#31115=CARTESIAN_POINT('Ctrl Pts',(-33.7047869151673,55.0120565441784,0.0375279937474228));
#31116=CARTESIAN_POINT('Ctrl Pts',(-33.9673979456785,55.4969804900557,0.000482030224742209));
#31117=CARTESIAN_POINT('Ctrl Pts',(-34.2300089761898,55.981904435933,-0.0365639332979384));
#31118=CARTESIAN_POINT('Ctrl Pts',(-34.2284689429929,56.6098796426817,-0.0736098968206187));
#31119=CARTESIAN_POINT('Ctrl Pts',(-33.9634826195406,57.0935097116441,-0.110655860343299));
#31120=CARTESIAN_POINT('Ctrl Pts',(-33.8184586195722,57.3581949459313,-0.130930694692273));
#31121=CARTESIAN_POINT('Ctrl Pts',(-33.5945259126096,57.5796452264349,-0.151205529041246));
#31122=CARTESIAN_POINT('Ctrl Pts',(-33.3313285320323,57.7324067450656,-0.171480363390219));
#31123=CARTESIAN_POINT('Origin',(-32.5,56.2916512459885,3.));
#31124=CARTESIAN_POINT('',(-33.3325354057627,57.7362457052863,-0.87148036339022));
#31125=CARTESIAN_POINT('',(-33.3348489584778,57.7359240281238,-0.678519636609784));
#31126=CARTESIAN_POINT('',(-33.333,57.7344495686934,3.));
#31127=CARTESIAN_POINT('Ctrl Pts',(-33.3348489584778,57.7359240281238,-0.678519636609784));
#31128=CARTESIAN_POINT('Ctrl Pts',(-33.3780386262143,57.7113506256494,-0.675184574138146));
#31129=CARTESIAN_POINT('Ctrl Pts',(-33.4200351242183,57.6847625016212,-0.671849511666509));
#31130=CARTESIAN_POINT('Ctrl Pts',(-33.4606301406774,57.6561836376047,-0.668514449194871));
#31131=CARTESIAN_POINT('Ctrl Pts',(-33.9115606739847,57.3387288484125,-0.631468485672191));
#31132=CARTESIAN_POINT('Ctrl Pts',(-34.1895648369722,56.7756401144087,-0.59442252214951));
#31133=CARTESIAN_POINT('Ctrl Pts',(-34.1674127214773,56.2246182278545,-0.557376558626829));
#31134=CARTESIAN_POINT('Ctrl Pts',(-34.1452606059824,55.6735963413002,-0.520330595104149));
#31135=CARTESIAN_POINT('Ctrl Pts',(-33.8229522120051,55.1346413021956,-0.483284631581468));
#31136=CARTESIAN_POINT('Ctrl Pts',(-33.3479936663214,54.8544089200699,-0.446238668058787));
#31137=CARTESIAN_POINT('Ctrl Pts',(-32.8730351206376,54.5741765379441,-0.409192704536106));
#31138=CARTESIAN_POINT('Ctrl Pts',(-32.2454264232474,54.5526668127973,-0.372146741013426));
#31139=CARTESIAN_POINT('Ctrl Pts',(-31.7523963222819,54.7997238024577,-0.335100777490745));
#31140=CARTESIAN_POINT('Ctrl Pts',(-31.2593662213165,55.0467807921182,-0.298054813968064));
#31141=CARTESIAN_POINT('Ctrl Pts',(-30.9009147167759,55.562404496586,-0.261008850445383));
#31142=CARTESIAN_POINT('Ctrl Pts',(-30.8410891376185,56.1106167986295,-0.223962886922702));
#31143=CARTESIAN_POINT('Ctrl Pts',(-30.7812635584611,56.658829100673,-0.186916923400021));
#31144=CARTESIAN_POINT('Ctrl Pts',(-31.020063904687,57.2396300002921,-0.149870959877341));
#31145=CARTESIAN_POINT('Ctrl Pts',(-31.4482018611622,57.5872126749713,-0.11282499635466));
#31146=CARTESIAN_POINT('Ctrl Pts',(-31.8763398176374,57.9347953496505,-0.0757790328319798));
#31147=CARTESIAN_POINT('Ctrl Pts',(-32.4938153843619,58.0491597993896,-0.0387330693092992));
#31148=CARTESIAN_POINT('Ctrl Pts',(-33.0180373581563,57.8779664839892,-0.00168710578661843));
#31149=CARTESIAN_POINT('Ctrl Pts',(-33.1273150883492,57.8422800422405,0.00603538393899408));
#31150=CARTESIAN_POINT('Ctrl Pts',(-33.2325405477213,57.7941848839699,0.0137578736646066));
#31151=CARTESIAN_POINT('Ctrl Pts',(-33.3319271105623,57.7355745198861,0.0214803633902191));
#31152=CARTESIAN_POINT('Ctrl Pts',(-33.3313285320323,57.7324067450656,-0.171480363390219));
#31153=CARTESIAN_POINT('Ctrl Pts',(-33.1136144342564,57.8587694623943,-0.188251492563927));
#31154=CARTESIAN_POINT('Ctrl Pts',(-32.8690337821938,57.9381324168355,-0.205022621737634));
#31155=CARTESIAN_POINT('Ctrl Pts',(-32.6200250231441,57.9560888015457,-0.221793750911342));
#31156=CARTESIAN_POINT('Ctrl Pts',(-32.0699863639079,57.9957528913089,-0.258839714434022));
#31157=CARTESIAN_POINT('Ctrl Pts',(-31.4983416591433,57.7357961396592,-0.295885677956703));
#31158=CARTESIAN_POINT('Ctrl Pts',(-31.166707224731,57.2951892897454,-0.332931641479383));
#31159=CARTESIAN_POINT('Ctrl Pts',(-30.8350727903188,56.8545824398317,-0.369977605002064));
#31160=CARTESIAN_POINT('Ctrl Pts',(-30.7434486262588,56.233325491654,-0.407023568524745));
#31161=CARTESIAN_POINT('Ctrl Pts',(-30.9337672989981,55.7157400874939,-0.444069532047425));
#31162=CARTESIAN_POINT('Ctrl Pts',(-31.1240859717375,55.1981546833338,-0.481115495570106));
#31163=CARTESIAN_POINT('Ctrl Pts',(-31.5963474812763,54.7842408231913,-0.518161459092787));
#31164=CARTESIAN_POINT('Ctrl Pts',(-32.1344181757785,54.6634287766855,-0.555207422615468));
#31165=CARTESIAN_POINT('Ctrl Pts',(-32.6724888702807,54.5426167301798,-0.592253386138148));
#31166=CARTESIAN_POINT('Ctrl Pts',(-33.2763687497463,54.7149064973108,-0.629299349660829));
#31167=CARTESIAN_POINT('Ctrl Pts',(-33.6696897466081,55.1014482025695,-0.666345313183509));
#31168=CARTESIAN_POINT('Ctrl Pts',(-34.0630107434699,55.4879899078282,-0.70339127670619));
#31169=CARTESIAN_POINT('Ctrl Pts',(-34.2457728577278,56.0887835512146,-0.740437240228871));
#31170=CARTESIAN_POINT('Ctrl Pts',(-34.1343320137705,56.6288734837568,-0.777483203751551));
#31171=CARTESIAN_POINT('Ctrl Pts',(-34.040078625064,57.0856656664133,-0.808815590297774));
#31172=CARTESIAN_POINT('Ctrl Pts',(-33.7353736531391,57.4990347912871,-0.840147976843997));
#31173=CARTESIAN_POINT('Ctrl Pts',(-33.3325354057627,57.7362457052863,-0.87148036339022));
#31174=CARTESIAN_POINT('Origin',(-32.5,56.2916512459885,3.));
#31175=CARTESIAN_POINT('',(-33.3347882996638,57.7351190113229,-1.57148036339022));
#31176=CARTESIAN_POINT('',(-33.3327354544031,57.732107437543,-1.37851963660978));
#31177=CARTESIAN_POINT('',(-33.333,57.7344495686934,3.));
#31178=CARTESIAN_POINT('',(-32.8002165734084,54.652924298309,-2.));
#31179=CARTESIAN_POINT('Ctrl Pts',(-33.3347882996638,57.7351190113229,-1.57148036339022));
#31180=CARTESIAN_POINT('Ctrl Pts',(-32.9233907544682,57.9680931016245,-1.60318235169211));
#31181=CARTESIAN_POINT('Ctrl Pts',(-32.4058309808294,58.0231592569491,-1.634884339994));
#31182=CARTESIAN_POINT('Ctrl Pts',(-31.9592734257388,57.8702645075936,-1.66658632829588));
#31183=CARTESIAN_POINT('Ctrl Pts',(-31.4374400713406,57.6915964299482,-1.70363229181857));
#31184=CARTESIAN_POINT('Ctrl Pts',(-31.0125640599592,57.2289465672061,-1.74067825534125));
#31185=CARTESIAN_POINT('Ctrl Pts',(-30.880071382614,56.6935519519193,-1.77772421886393));
#31186=CARTESIAN_POINT('Ctrl Pts',(-30.7475787052689,56.1581573366325,-1.81477018238661));
#31187=CARTESIAN_POINT('Ctrl Pts',(-30.9074693619599,55.550017968801,-1.85181614590929));
#31188=CARTESIAN_POINT('Ctrl Pts',(-31.2843999047331,55.1487524209429,-1.88886210943197));
#31189=CARTESIAN_POINT('Ctrl Pts',(-31.6613304475062,54.7474868730847,-1.92590807295465));
#31190=CARTESIAN_POINT('Ctrl Pts',(-32.2553008763615,54.5530951451999,-1.96295403647733));
#31191=CARTESIAN_POINT('Ctrl Pts',(-32.8002165734084,54.652924298309,-2.00000000000001));
#31192=CARTESIAN_POINT('',(-34.0720885049226,56.8521739755918,-2.));
#31193=CARTESIAN_POINT('Origin',(-32.5,56.2916512459885,-2.));
#31194=CARTESIAN_POINT('Ctrl Pts',(-34.0720901513885,56.8521746541718,-2.));
#31195=CARTESIAN_POINT('Ctrl Pts',(-34.2530538927521,56.3425577544553,-1.96367708181444));
#31196=CARTESIAN_POINT('Ctrl Pts',(-34.16381751404,55.7359288334825,-1.92735416362889));
#31197=CARTESIAN_POINT('Ctrl Pts',(-33.8426356554965,55.3008256611299,-1.89103124544333));
#31198=CARTESIAN_POINT('Ctrl Pts',(-33.5150603391364,54.857061309124,-1.85398528192065));
#31199=CARTESIAN_POINT('Ctrl Pts',(-32.9462134040812,54.59171946851,-1.81693931839797));
#31200=CARTESIAN_POINT('Ctrl Pts',(-32.3958963008479,54.6261577029506,-1.77989335487529));
#31201=CARTESIAN_POINT('Ctrl Pts',(-31.8455791976147,54.6605959373911,-1.74284739135261));
#31202=CARTESIAN_POINT('Ctrl Pts',(-31.3137919262033,54.9948142468862,-1.70580142782993));
#31203=CARTESIAN_POINT('Ctrl Pts',(-31.0441775058384,55.4758950021693,-1.66875546430725));
#31204=CARTESIAN_POINT('Ctrl Pts',(-30.7745630854735,55.9569757574525,-1.63170950078457));
#31205=CARTESIAN_POINT('Ctrl Pts',(-30.767121516155,56.5849189585236,-1.59466353726188));
#31206=CARTESIAN_POINT('Ctrl Pts',(-31.0251241525943,57.0723230889947,-1.5576175737392));
#31207=CARTESIAN_POINT('Ctrl Pts',(-31.2831267890337,57.5597272194657,-1.52057161021652));
#31208=CARTESIAN_POINT('Ctrl Pts',(-31.8065736312309,57.9065922793366,-1.48352564669384));
#31209=CARTESIAN_POINT('Ctrl Pts',(-32.3559737285805,57.9541834292484,-1.44647968317116));
#31210=CARTESIAN_POINT('Ctrl Pts',(-32.6919280642789,57.9832850861845,-1.42382633431737));
#31211=CARTESIAN_POINT('Ctrl Pts',(-33.0375869381561,57.9004811240364,-1.40117298546358));
#31212=CARTESIAN_POINT('Ctrl Pts',(-33.3327354544031,57.732107437543,-1.37851963660978));
#31213=CARTESIAN_POINT('Origin',(-32.5,56.2916512459885,-3.54592528053767));
#31214=CARTESIAN_POINT('',(-33.5296449158133,58.0726582505548,6.54592528053768));
#31215=CARTESIAN_POINT('',(-33.5251060574855,58.0687922621904,6.60407471946233));
#31216=CARTESIAN_POINT('',(-33.5273750000001,58.0711169444145,-3.54592528053767));
#31217=CARTESIAN_POINT('',(-30.845746263986,55.0728640868079,7.));
#31218=CARTESIAN_POINT('Ctrl Pts',(-33.5251060574855,58.0687922621904,6.60407471946233));
#31219=CARTESIAN_POINT('Ctrl Pts',(-33.8584527741405,57.8749712083971,6.62491192240684));
#31220=CARTESIAN_POINT('Ctrl Pts',(-34.6426244289716,57.0875348868181,6.68279508887404));
#31221=CARTESIAN_POINT('Ctrl Pts',(-34.6192626691618,55.1024844807855,6.77772421886391));
#31222=CARTESIAN_POINT('Ctrl Pts',(-32.6468806392671,53.8684656063832,6.88886210943196));
#31223=CARTESIAN_POINT('Ctrl Pts',(-31.2510219905719,54.522785363242,6.96295403647732));
#31224=CARTESIAN_POINT('Ctrl Pts',(-30.845746263986,55.0728640868079,7.));
#31225=CARTESIAN_POINT('',(-30.4546316093048,56.0596663160167,7.));
#31226=CARTESIAN_POINT('Origin',(-32.5,56.2916512459885,7.));
#31227=CARTESIAN_POINT('Ctrl Pts',(-33.5296449158133,58.0726582505548,6.54592528053768));
#31228=CARTESIAN_POINT('Ctrl Pts',(-33.5919384699578,58.0372735301249,6.54982271160486));
#31229=CARTESIAN_POINT('Ctrl Pts',(-34.225323347054,57.6301444802746,6.59076610619471));
#31230=CARTESIAN_POINT('Ctrl Pts',(-34.9251107981772,56.1574151102239,6.66875546430726));
#31231=CARTESIAN_POINT('Ctrl Pts',(-33.7019669024841,54.1813822458926,6.77989335487529));
#31232=CARTESIAN_POINT('Ctrl Pts',(-31.3950249125263,54.1375954583441,6.89030820010622));
#31233=CARTESIAN_POINT('Ctrl Pts',(-30.5306488143205,55.3970288255657,6.96367708181445));
#31234=CARTESIAN_POINT('Ctrl Pts',(-30.4546294175093,56.0596661744468,7.));
#31235=CARTESIAN_POINT('Origin',(-32.5,56.2916512459885,-3.54592528053767));
#31236=CARTESIAN_POINT('',(-33.5268493235952,58.0681533924579,5.84592528053768));
#31237=CARTESIAN_POINT('',(-33.5270361074232,58.0735254724117,5.90407471946233));
#31238=CARTESIAN_POINT('',(-33.5273750000001,58.0711169444145,-3.54592528053767));
#31239=CARTESIAN_POINT('Ctrl Pts',(-33.5270361074232,58.0735254724117,5.90407471946232));
#31240=CARTESIAN_POINT('Ctrl Pts',(-34.0327197348533,57.7760135322548,5.93596947460409));
#31241=CARTESIAN_POINT('Ctrl Pts',(-34.8527930569705,56.6438137488048,6.00491019326854));
#31242=CARTESIAN_POINT('Ctrl Pts',(-34.1759192345577,54.5338890939528,6.11089687545567));
#31243=CARTESIAN_POINT('Ctrl Pts',(-31.9320786480218,53.9303413264953,6.2220347660237));
#31244=CARTESIAN_POINT('Ctrl Pts',(-30.2082245117245,55.4880781765344,6.33317265659175));
#31245=CARTESIAN_POINT('Ctrl Pts',(-30.5817368018815,57.7814323658043,6.44431054715979));
#31246=CARTESIAN_POINT('Ctrl Pts',(-32.3123519600732,58.5366981066488,6.53461123478332));
#31247=CARTESIAN_POINT('Ctrl Pts',(-33.265803638914,58.2195610128864,6.58786595888416));
#31248=CARTESIAN_POINT('Ctrl Pts',(-33.5251060574855,58.0687922621904,6.60407471946233));
#31249=CARTESIAN_POINT('Ctrl Pts',(-33.5268493235952,58.0681533924579,5.84592528053768));
#31250=CARTESIAN_POINT('Ctrl Pts',(-33.7671186009377,57.9308791195189,5.86088026380211));
#31251=CARTESIAN_POINT('Ctrl Pts',(-34.5085314004615,57.2938049828723,5.91288121058922));
#31252=CARTESIAN_POINT('Ctrl Pts',(-34.7788326566387,55.451849617872,6.00192812089901));
#31253=CARTESIAN_POINT('Ctrl Pts',(-33.0303393193103,53.921614042038,6.11306601146705));
#31254=CARTESIAN_POINT('Ctrl Pts',(-30.79644075645,54.5607069079647,6.22420390203509));
#31255=CARTESIAN_POINT('Ctrl Pts',(-30.1217887402557,56.7841397946825,6.33534179260313));
#31256=CARTESIAN_POINT('Ctrl Pts',(-31.5713402558441,58.4946530906761,6.442582252104));
#31257=CARTESIAN_POINT('Ctrl Pts',(-32.999824152922,58.3736132984777,6.51277674808218));
#31258=CARTESIAN_POINT('Ctrl Pts',(-33.5296449158133,58.0726582505548,6.54592528053768));
#31259=CARTESIAN_POINT('Origin',(-32.5,56.2916512459885,-3.54592528053767));
#31260=CARTESIAN_POINT('',(-33.525217808475,58.0709111221528,5.14592528053768));
#31261=CARTESIAN_POINT('',(-33.5295558866825,58.0716265502945,5.20407471946232));
#31262=CARTESIAN_POINT('',(-33.5273750000001,58.0711169444145,-3.54592528053767));
#31263=CARTESIAN_POINT('Ctrl Pts',(-33.5295558866825,58.0716265502945,5.20407471946232));
#31264=CARTESIAN_POINT('Ctrl Pts',(-33.6241634690101,58.0180957001452,5.20998106327865));
#31265=CARTESIAN_POINT('Ctrl Pts',(-34.2792376101367,57.5737577801449,5.25293337061767));
#31266=CARTESIAN_POINT('Ctrl Pts',(-34.9141240107244,56.0264398256936,5.33293164147938));
#31267=CARTESIAN_POINT('Ctrl Pts',(-33.5864678368826,54.1195735160326,5.44406953204741));
#31268=CARTESIAN_POINT('Ctrl Pts',(-31.2643540254432,54.2008349824401,5.55520742261546));
#31269=CARTESIAN_POINT('Ctrl Pts',(-30.0732435855652,56.1958434964943,5.66634531318349));
#31270=CARTESIAN_POINT('Ctrl Pts',(-31.10336564197,58.2785475024108,5.77748320375154));
#31271=CARTESIAN_POINT('Ctrl Pts',(-32.7493551050699,58.4668353041202,5.85672633917781));
#31272=CARTESIAN_POINT('Ctrl Pts',(-33.4453649446213,58.1215755669412,5.89892351108141));
#31273=CARTESIAN_POINT('Ctrl Pts',(-33.5270361074232,58.0735254724117,5.90407471946232));
#31274=CARTESIAN_POINT('Ctrl Pts',(-33.525217808475,58.0709111221528,5.14592528053768));
#31275=CARTESIAN_POINT('Ctrl Pts',(-33.9392806903329,57.8273071486293,5.17193781599936));
#31276=CARTESIAN_POINT('Ctrl Pts',(-34.7491747415829,56.8889612418332,5.23499631498372));
#31277=CARTESIAN_POINT('Ctrl Pts',(-34.4321757978777,54.8202470274371,5.33510077749076));
#31278=CARTESIAN_POINT('Ctrl Pts',(-32.3116949177892,53.8703138209288,5.44623866805879));
#31279=CARTESIAN_POINT('Ctrl Pts',(-30.3635721421369,55.1366583239951,5.55737655862684));
#31280=CARTESIAN_POINT('Ctrl Pts',(-30.3709453622051,57.4601807388668,5.66851444919488));
#31281=CARTESIAN_POINT('Ctrl Pts',(-32.0638471781548,58.5454001176689,5.76469735649849));
#31282=CARTESIAN_POINT('Ctrl Pts',(-33.1719319178991,58.2709301659147,5.82383430027943));
#31283=CARTESIAN_POINT('Ctrl Pts',(-33.5268493235952,58.0681533924579,5.84592528053768));
#31284=CARTESIAN_POINT('Origin',(-32.5,56.2916512459885,-3.54592528053767));
#31285=CARTESIAN_POINT('',(-33.5290839475038,58.0740603739206,4.44592528053768));
#31286=CARTESIAN_POINT('',(-33.5261619125926,58.0680778657968,4.50407471946232));
#31287=CARTESIAN_POINT('',(-33.5273750000001,58.0711169444145,-3.54592528053767));
#31288=CARTESIAN_POINT('Ctrl Pts',(-33.5261619125926,58.0680778657968,4.50407471946232));
#31289=CARTESIAN_POINT('Ctrl Pts',(-33.7984529813903,57.9116108116526,4.5210386154759));
#31290=CARTESIAN_POINT('Ctrl Pts',(-34.5559374767779,57.225562580793,4.57504847501217));
#31291=CARTESIAN_POINT('Ctrl Pts',(-34.7300884128152,55.3298620761609,4.66610429807112));
#31292=CARTESIAN_POINT('Ctrl Pts',(-32.9014225703573,53.8964074829672,4.77724218863916));
#31293=CARTESIAN_POINT('Ctrl Pts',(-30.7053300758283,54.6553466763578,4.88838007920721));
#31294=CARTESIAN_POINT('Ctrl Pts',(-30.1519193575992,56.9120139865896,4.99951796977524));
#31295=CARTESIAN_POINT('Ctrl Pts',(-31.6629249999102,58.5111039532885,5.10474951652696));
#31296=CARTESIAN_POINT('Ctrl Pts',(-33.0307626862479,58.3538536552586,5.17293509975597));
#31297=CARTESIAN_POINT('Ctrl Pts',(-33.5295558866825,58.0716265502945,5.20407471946232));
#31298=CARTESIAN_POINT('Ctrl Pts',(-33.5290839390052,58.0740603592829,4.44592528053768));
#31299=CARTESIAN_POINT('Ctrl Pts',(-33.5294675225899,58.0738389277433,4.44594940467393));
#31300=CARTESIAN_POINT('Ctrl Pts',(-34.118776307512,57.7333695942669,4.48301949233285));
#31301=CARTESIAN_POINT('Ctrl Pts',(-34.9257362810773,56.410550559801,4.55713554351447));
#31302=CARTESIAN_POINT('Ctrl Pts',(-33.91547832718,54.3181379674856,4.6682734340825));
#31303=CARTESIAN_POINT('Ctrl Pts',(-31.6096170051591,54.0321044593028,4.77941132465055));
#31304=CARTESIAN_POINT('Ctrl Pts',(-30.1187333412011,55.8142597516568,4.89054921521859));
#31305=CARTESIAN_POINT('Ctrl Pts',(-30.8074500449804,58.033376889416,5.00168710578664));
#31306=CARTESIAN_POINT('Ctrl Pts',(-32.5215758081835,58.5120119076972,5.08681246089299));
#31307=CARTESIAN_POINT('Ctrl Pts',(-33.3495896761677,58.1742377248673,5.13489185247668));
#31308=CARTESIAN_POINT('Ctrl Pts',(-33.525217808475,58.0709111221528,5.14592528053768));
#31309=CARTESIAN_POINT('Origin',(-32.5,56.2916512459885,-3.54592528053767));
#31310=CARTESIAN_POINT('',(-33.5282587680712,58.0691275396584,3.74592528053768));
#31311=CARTESIAN_POINT('',(-33.5256537705603,58.0718935083249,3.80407471946232));
#31312=CARTESIAN_POINT('',(-33.5273750000001,58.0711169444145,-3.54592528053767));
#31313=CARTESIAN_POINT('Ctrl Pts',(-33.5256537705603,58.0718935083249,3.80407471946232));
#31314=CARTESIAN_POINT('Ctrl Pts',(-33.9708692323456,57.8094153705276,3.83209616767316));
#31315=CARTESIAN_POINT('Ctrl Pts',(-34.7867776966583,56.8075863052296,3.89716357940667));
#31316=CARTESIAN_POINT('Ctrl Pts',(-34.3497911057075,54.7179277581866,3.99927695466287));
#31317=CARTESIAN_POINT('Ctrl Pts',(-32.1810499960691,53.8840375630848,4.11041484523091));
#31318=CARTESIAN_POINT('Ctrl Pts',(-30.3042474418304,55.2538634762437,4.22155273579896));
#31319=CARTESIAN_POINT('Ctrl Pts',(-30.4372421062834,57.5735883041595,4.332690626367));
#31320=CARTESIAN_POINT('Ctrl Pts',(-32.1498112942942,58.5449642134685,4.42686462092145));
#31321=CARTESIAN_POINT('Ctrl Pts',(-33.2038204161972,58.2533054775292,4.48399265195323));
#31322=CARTESIAN_POINT('Ctrl Pts',(-33.5261619125926,58.0680778657968,4.50407471946232));
#31323=CARTESIAN_POINT('Ctrl Pts',(-33.5282587680712,58.0691275396584,3.74592528053768));
#31324=CARTESIAN_POINT('Ctrl Pts',(-33.7063336904378,57.9682446528084,3.75700695687118));
#31325=CARTESIAN_POINT('Ctrl Pts',(-34.4133163086311,57.41900891881,3.80513459672736));
#31326=CARTESIAN_POINT('Ctrl Pts',(-34.8538786959893,55.6936640901667,3.89030820010621));
#31327=CARTESIAN_POINT('Ctrl Pts',(-33.2742100800909,53.9897102593704,4.00144609067426));
#31328=CARTESIAN_POINT('Ctrl Pts',(-30.9858981977034,54.3927491193984,4.1125839812423));
#31329=CARTESIAN_POINT('Ctrl Pts',(-30.0834608661247,56.5338746309361,4.22372187181034));
#31330=CARTESIAN_POINT('Ctrl Pts',(-31.3926249737446,58.4528736933808,4.33483563824213));
#31331=CARTESIAN_POINT('Ctrl Pts',(-32.9404216250933,58.4138778272017,4.40890344115124));
#31332=CARTESIAN_POINT('Ctrl Pts',(-33.5290839390052,58.0740603592829,4.44592528053768));
#31333=CARTESIAN_POINT('Origin',(-32.5,56.2916512459885,-3.54592528053767));
#31334=CARTESIAN_POINT('',(-33.5250673440976,58.0691981786101,3.04592528053768));
#31335=CARTESIAN_POINT('',(-33.5295277964002,58.073488152934,3.10407471946232));
#31336=CARTESIAN_POINT('',(-33.5273750000001,58.0711169444145,-3.54592528053767));
#31337=CARTESIAN_POINT('Ctrl Pts',(-33.5295277964002,58.073488152934,3.10407471946232));
#31338=CARTESIAN_POINT('Ctrl Pts',(-33.5619446593131,58.0549578524536,3.10610775634773));
#31339=CARTESIAN_POINT('Ctrl Pts',(-34.1744592271169,57.680719250686,3.14518675675581));
#31340=CARTESIAN_POINT('Ctrl Pts',(-34.9286165141379,56.2792182940979,3.22131172068658));
#31341=CARTESIAN_POINT('Ctrl Pts',(-33.8067007722453,54.2444908119128,3.33244961125462));
#31342=CARTESIAN_POINT('Ctrl Pts',(-31.4887469945246,54.0835524914147,3.44358750182266));
#31343=CARTESIAN_POINT('Ctrl Pts',(-30.0964045610992,55.9437120025227,3.5547253923907));
#31344=CARTESIAN_POINT('Ctrl Pts',(-30.9041002915367,58.1223442490711,3.66586328295875));
#31345=CARTESIAN_POINT('Ctrl Pts',(-32.6005939960278,58.4985054002163,3.74897972531595));
#31346=CARTESIAN_POINT('Ctrl Pts',(-33.3822688276508,58.1564265401566,3.79505020415048));
#31347=CARTESIAN_POINT('Ctrl Pts',(-33.5256537705603,58.0718935083249,3.80407471946232));
#31348=CARTESIAN_POINT('Ctrl Pts',(-33.5250673440976,58.0691981786101,3.04592528053768));
#31349=CARTESIAN_POINT('Ctrl Pts',(-33.8788897107517,57.8627525499152,3.06806450906843));
#31350=CARTESIAN_POINT('Ctrl Pts',(-34.6708999553705,57.0389934359535,3.12724970112185));
#31351=CARTESIAN_POINT('Ctrl Pts',(-34.5748652707907,55.0294041774427,3.22348085669796));
#31352=CARTESIAN_POINT('Ctrl Pts',(-32.5648065727292,53.8638675525518,3.334618747266));
#31353=CARTESIAN_POINT('Ctrl Pts',(-30.4954296836916,54.9205088752031,3.44575663783405));
#31354=CARTESIAN_POINT('Ctrl Pts',(-30.2608587385459,57.2321723596468,3.55689452840209));
#31355=CARTESIAN_POINT('Ctrl Pts',(-31.8948295568209,58.5383060176734,3.65695074263663));
#31356=CARTESIAN_POINT('Ctrl Pts',(-33.1110305179062,58.3054954110723,3.71996099334849));
#31357=CARTESIAN_POINT('Ctrl Pts',(-33.5282587680712,58.0691275396584,3.74592528053768));
#31358=CARTESIAN_POINT('Origin',(-32.5,56.2916512459885,-3.54592528053767));
#31359=CARTESIAN_POINT('',(-33.5275894562265,58.0738927599536,2.34592528053768));
#31360=CARTESIAN_POINT('',(-33.5275355691898,58.0684930935818,2.40407471946232));
#31361=CARTESIAN_POINT('',(-33.5273750000001,58.0711169444145,-3.54592528053767));
#31362=CARTESIAN_POINT('Ctrl Pts',(-33.5275355691898,58.0684930935818,2.40407471946232));
#31363=CARTESIAN_POINT('Ctrl Pts',(-33.7379292069399,57.9488445224074,2.41716530854498));
#31364=CARTESIAN_POINT('Ctrl Pts',(-34.4632973547596,57.3551041347746,2.46730186115031));
#31365=CARTESIAN_POINT('Ctrl Pts',(-34.8181023612983,55.5672658557593,2.55448437727833));
#31366=CARTESIAN_POINT('Ctrl Pts',(-33.1486127133916,53.9512166070675,2.66562226784637));
#31367=CARTESIAN_POINT('Ctrl Pts',(-30.8854404931491,54.4773937257141,2.77676015841441));
#31368=CARTESIAN_POINT('Ctrl Pts',(-30.1000928998773,56.6641813277477,2.88789804898245));
#31369=CARTESIAN_POINT('Ctrl Pts',(-31.4855904228425,58.4762227231016,2.99700290266509));
#31370=CARTESIAN_POINT('Ctrl Pts',(-32.9712451350632,58.3926166724123,3.06906179282505));
#31371=CARTESIAN_POINT('Ctrl Pts',(-33.5295277964002,58.073488152934,3.10407471946232));
#31372=CARTESIAN_POINT('Ctrl Pts',(-33.5275894562265,58.0738927599536,2.34592528053768));
#31373=CARTESIAN_POINT('Ctrl Pts',(-34.0539010838894,57.7651290399621,2.37912206126568));
#31374=CARTESIAN_POINT('Ctrl Pts',(-34.8729207037989,56.5867324218955,2.44936480551635));
#31375=CARTESIAN_POINT('Ctrl Pts',(-34.113250907707,54.4762297900261,2.55665351328971));
#31376=CARTESIAN_POINT('Ctrl Pts',(-31.8496996873681,53.9516847809774,2.66779140385775));
#31377=CARTESIAN_POINT('Ctrl Pts',(-30.1813757180884,55.5689376143778,2.7789292944258));
#31378=CARTESIAN_POINT('Ctrl Pts',(-30.6353148490301,57.8476984309217,2.89006718499383));
#31379=CARTESIAN_POINT('Ctrl Pts',(-32.3655977900595,58.5319722593687,2.97906584703113));
#31380=CARTESIAN_POINT('Ctrl Pts',(-33.2868324730584,58.2082016796998,3.03101854554575));
#31381=CARTESIAN_POINT('Ctrl Pts',(-33.5250673440976,58.0691981786101,3.04592528053768));
#31382=CARTESIAN_POINT('Origin',(-32.5,56.2916512459885,-3.54592528053767));
#31383=CARTESIAN_POINT('',(-33.5293464154416,58.0709332657958,1.64592528053768));
#31384=CARTESIAN_POINT('',(-33.5250295315601,58.0700303972121,1.70407471946232));
#31385=CARTESIAN_POINT('',(-33.5273750000001,58.0711169444145,-3.54592528053767));
#31386=CARTESIAN_POINT('Ctrl Pts',(-33.5250295315601,58.0700303972121,1.70407471946232));
#31387=CARTESIAN_POINT('Ctrl Pts',(-33.9101525759349,57.8442238653441,1.72822286074222));
#31388=CARTESIAN_POINT('Ctrl Pts',(-34.7124027752876,56.9623029261605,1.78941696554481));
#31389=CARTESIAN_POINT('Ctrl Pts',(-34.5035809067649,54.9190637984713,1.88765703387008));
#31390=CARTESIAN_POINT('Ctrl Pts',(-32.4334427362781,53.863915082053,1.99879492443812));
#31391=CARTESIAN_POINT('Ctrl Pts',(-30.4242251840869,55.0309008088856,2.10993281500616));
#31392=CARTESIAN_POINT('Ctrl Pts',(-30.3149878617883,57.3518657086808,2.22107070557421));
#31393=CARTESIAN_POINT('Ctrl Pts',(-31.9830137885335,58.5433285166527,2.31911800705959));
#31394=CARTESIAN_POINT('Ctrl Pts',(-33.1425216985167,58.2874462900804,2.3801193450223));
#31395=CARTESIAN_POINT('Ctrl Pts',(-33.5275355691898,58.0684930935818,2.40407471946232));
#31396=CARTESIAN_POINT('Ctrl Pts',(-33.5293464154416,58.0709332657958,1.64592528053768));
#31397=CARTESIAN_POINT('Ctrl Pts',(-33.6449437000377,58.0055982631749,1.65313364994024));
#31398=CARTESIAN_POINT('Ctrl Pts',(-34.3136427308233,57.5361314802505,1.69738798286549));
#31399=CARTESIAN_POINT('Ctrl Pts',(-34.90334407317,55.9419787993381,1.77868827931342));
#31400=CARTESIAN_POINT('Ctrl Pts',(-33.5096605171051,54.0828236849994,1.88982616988146));
#31401=CARTESIAN_POINT('Ctrl Pts',(-31.1918232394055,54.2454334870425,2.0009640604495));
#31402=CARTESIAN_POINT('Ctrl Pts',(-30.0713749864112,56.2809696095364,2.11210195101755));
#31403=CARTESIAN_POINT('Ctrl Pts',(-31.1738747508359,58.326282755013,2.22323984158559));
#31404=CARTESIAN_POINT('Ctrl Pts',(-32.7983102681658,58.4546151165851,2.30118095142563));
#31405=CARTESIAN_POINT('Ctrl Pts',(-33.4665633682319,58.1096940627471,2.342076097743));
#31406=CARTESIAN_POINT('Ctrl Pts',(-33.5275894562265,58.0738927599536,2.34592528053768));
#31407=CARTESIAN_POINT('Origin',(-32.5,56.2916512459885,-3.54592528053767));
#31408=CARTESIAN_POINT('',(-33.5257755155985,58.0681903527959,0.945925280537675));
#31409=CARTESIAN_POINT('',(-33.5284289248676,58.0741771517811,1.00407471946232));
#31410=CARTESIAN_POINT('',(-33.5273750000001,58.0711169444145,-3.54592528053767));
#31411=CARTESIAN_POINT('Ctrl Pts',(-33.5284289248676,58.0741771517811,1.00407471946232));
#31412=CARTESIAN_POINT('Ctrl Pts',(-34.0870797198612,57.7486846686039,1.03928041293948));
#31413=CARTESIAN_POINT('Ctrl Pts',(-34.9017444968086,56.4966890376489,1.11153206993931));
#31414=CARTESIAN_POINT('Ctrl Pts',(-34.0127319779434,54.3916579002222,1.22082969046183));
#31415=CARTESIAN_POINT('Ctrl Pts',(-31.7241302087768,53.9902693093903,1.33196758102987));
#31416=CARTESIAN_POINT('Ctrl Pts',(-30.1456908584837,55.6953617045703,1.44310547159791));
#31417=CARTESIAN_POINT('Ctrl Pts',(-30.7221773650996,57.9462446793952,1.55424336216595));
#31418=CARTESIAN_POINT('Ctrl Pts',(-32.4470927941984,58.5226506382554,1.64123311145409));
#31419=CARTESIAN_POINT('Ctrl Pts',(-33.3193305292905,58.1906364710101,1.69117689721954));
#31420=CARTESIAN_POINT('Ctrl Pts',(-33.5250295315601,58.0700303972121,1.70407471946232));
#31421=CARTESIAN_POINT('Ctrl Pts',(-33.5257755155985,58.0681903527959,0.945925280537676));
#31422=CARTESIAN_POINT('Ctrl Pts',(-33.8187120383006,57.8991957700279,0.964191202137494));
#31423=CARTESIAN_POINT('Ctrl Pts',(-34.5858726429697,57.180098149748,1.01950308725999));
#31424=CARTESIAN_POINT('Ctrl Pts',(-34.6950037716947,55.2522802841409,1.11186093590517));
#31425=CARTESIAN_POINT('Ctrl Pts',(-32.8172137752098,53.883808025427,1.22299882647321));
#31426=CARTESIAN_POINT('Ctrl Pts',(-30.6490744128705,54.7192619732989,1.33413671704125));
#31427=CARTESIAN_POINT('Ctrl Pts',(-30.1751082313325,56.9939416545675,1.44527460760929));
#31428=CARTESIAN_POINT('Ctrl Pts',(-31.7218617398002,58.5199646784861,1.54920412877477));
#31429=CARTESIAN_POINT('Ctrl Pts',(-33.0508547252211,58.3413743574169,1.61608768641756));
#31430=CARTESIAN_POINT('Ctrl Pts',(-33.5293464154416,58.0709332657958,1.64592528053768));
#31431=CARTESIAN_POINT('Origin',(-32.5,56.2916512459885,-3.54592528053767));
#31432=CARTESIAN_POINT('',(-33.5260517589603,58.0725043954729,0.245925280537674));
#31433=CARTESIAN_POINT('',(-33.5288532114794,58.0699232317666,0.304074719462319));
#31434=CARTESIAN_POINT('',(-33.5273750000001,58.0711169444145,-3.54592528053767));
#31435=CARTESIAN_POINT('Ctrl Pts',(-33.5288532114794,58.0699232317666,0.304074719462319));
#31436=CARTESIAN_POINT('Ctrl Pts',(-33.6768637713204,57.9862464992859,0.313292001614044));
#31437=CARTESIAN_POINT('Ctrl Pts',(-34.3658577642721,57.4763696079473,0.359555247288449));
#31438=CARTESIAN_POINT('Ctrl Pts',(-34.8809216257836,55.8125427394079,0.442864456485535));
#31439=CARTESIAN_POINT('Ctrl Pts',(-33.3887533074142,54.0314631320695,0.554002347053576));
#31440=CARTESIAN_POINT('Ctrl Pts',(-31.0830990069914,54.3191593379889,0.665140237621618));
#31441=CARTESIAN_POINT('Ctrl Pts',(-30.0743502545356,56.4122997567237,0.77627812818966));
#31442=CARTESIAN_POINT('Ctrl Pts',(-31.2858262226837,58.3950092254139,0.887416018757703));
#31443=CARTESIAN_POINT('Ctrl Pts',(-32.8728372110939,58.4342824094917,0.963348215848589));
#31444=CARTESIAN_POINT('Ctrl Pts',(-33.4992271616754,58.0911912767045,1.00223444941679));
#31445=CARTESIAN_POINT('Ctrl Pts',(-33.5284289248676,58.0741771517811,1.00407471946232));
#31446=CARTESIAN_POINT('Ctrl Pts',(-33.5260517589603,58.0725043954729,0.245925280537675));
#31447=CARTESIAN_POINT('Ctrl Pts',(-33.991498229918,57.7980207394882,0.275248754334742));
#31448=CARTESIAN_POINT('Ctrl Pts',(-34.8099603858883,56.7535423775609,0.34161819165449));
#31449=CARTESIAN_POINT('Ctrl Pts',(-34.2934896049409,54.6540528227808,0.445033592496919));
#31450=CARTESIAN_POINT('Ctrl Pts',(-32.0968502643471,53.8966974164155,0.55617148306496));
#31451=CARTESIAN_POINT('Ctrl Pts',(-30.2692184515671,55.3314704112852,0.667309373633001));
#31452=CARTESIAN_POINT('Ctrl Pts',(-30.4834462874739,57.6451078131478,0.778447264201044));
#31453=CARTESIAN_POINT('Ctrl Pts',(-32.2048796389798,58.5432631965409,0.871319233169268));
#31454=CARTESIAN_POINT('Ctrl Pts',(-33.224593878142,58.2419415282719,0.927145238614813));
#31455=CARTESIAN_POINT('Ctrl Pts',(-33.5257755155985,58.0681903527959,0.945925280537676));
#31456=CARTESIAN_POINT('Origin',(-32.5,56.2916512459885,-3.54592528053767));
#31457=CARTESIAN_POINT('',(-33.5296554006197,58.0729354591291,-0.454074719462322));
#31458=CARTESIAN_POINT('',(-33.5253135061185,58.0685974415039,-0.395925280537681));
#31459=CARTESIAN_POINT('',(-33.5273750000001,58.0711169444145,-3.54592528053767));
#31460=CARTESIAN_POINT('Ctrl Pts',(-33.5253135061185,58.0685974415039,-0.395925280537681));
#31461=CARTESIAN_POINT('Ctrl Pts',(-33.8499262418575,57.8801900402997,-0.375650446188706));
#31462=CARTESIAN_POINT('Ctrl Pts',(-34.6307561402676,57.1080161029863,-0.318329648317051));
#31463=CARTESIAN_POINT('Ctrl Pts',(-34.6355944339958,55.1351180442908,-0.223962886922716));
#31464=CARTESIAN_POINT('Ctrl Pts',(-32.6865588761979,53.8701788494842,-0.112824996354674));
#31465=CARTESIAN_POINT('Ctrl Pts',(-30.5667638241697,54.8216408199214,-0.00168710578663194));
#31466=CARTESIAN_POINT('Ctrl Pts',(-30.2164817879238,57.1186199946645,0.109450784781409));
#31467=CARTESIAN_POINT('Ctrl Pts',(-31.8120346004306,58.5309407947375,0.211371393197727));
#31468=CARTESIAN_POINT('Ctrl Pts',(-33.081981927564,58.322558779647,0.276246038091363));
#31469=CARTESIAN_POINT('Ctrl Pts',(-33.5288532114794,58.0699232317666,0.304074719462319));
#31470=CARTESIAN_POINT('Ctrl Pts',(-33.5296554006197,58.0729354591291,-0.454074719462324));
#31471=CARTESIAN_POINT('Ctrl Pts',(-33.5829230895642,58.0426280169118,-0.450739656990688));
#31472=CARTESIAN_POINT('Ctrl Pts',(-34.2100716718942,57.6455781417159,-0.410358630996371));
#31473=CARTESIAN_POINT('Ctrl Pts',(-34.926688116847,56.1940939537868,-0.332931641479374));
#31474=CARTESIAN_POINT('Ctrl Pts',(-33.7341373860101,54.1999441339785,-0.221793750911332));
#31475=CARTESIAN_POINT('Ctrl Pts',(-31.4119663698709,54.1203575053851,-0.110655860343291));
#31476=CARTESIAN_POINT('Ctrl Pts',(-30.0856850452223,56.0281806868171,0.000482030224751779));
#31477=CARTESIAN_POINT('Ctrl Pts',(-30.9692534931352,58.1771614464074,0.111619920792793));
#31478=CARTESIAN_POINT('Ctrl Pts',(-32.6511246141561,58.4886656996171,0.193434337563768));
#31479=CARTESIAN_POINT('Ctrl Pts',(-33.4034740038598,58.1447910975144,0.238202790812062));
#31480=CARTESIAN_POINT('Ctrl Pts',(-33.5260517589603,58.0725043954729,0.245925280537675));
#31481=CARTESIAN_POINT('Origin',(-32.5,56.2916512459885,-3.54592528053767));
#31482=CARTESIAN_POINT('',(-33.5270487244507,58.0682282925651,-1.15407471946232));
#31483=CARTESIAN_POINT('',(-33.5268019957928,58.0733321975144,-1.09592528053768));
#31484=CARTESIAN_POINT('',(-33.5273750000001,58.0711169444145,-3.54592528053767));
#31485=CARTESIAN_POINT('Ctrl Pts',(-33.5268019957928,58.0733321975144,-1.09592528053768));
#31486=CARTESIAN_POINT('Ctrl Pts',(-34.0236398642182,57.7807696971903,-1.06459289399146));
#31487=CARTESIAN_POINT('Ctrl Pts',(-34.8437811491657,56.6681489116154,-0.996214543922552));
#31488=CARTESIAN_POINT('Ctrl Pts',(-34.2023204507042,54.559476051911,-0.890790230330966));
#31489=CARTESIAN_POINT('Ctrl Pts',(-31.9679467730355,53.921998742765,-0.779652339762925));
#31490=CARTESIAN_POINT('Ctrl Pts',(-30.2205650142274,55.453492447677,-0.668514449194883));
#31491=CARTESIAN_POINT('Ctrl Pts',(-30.5595771710743,57.752161801101,-0.557376558626841));
#31492=CARTESIAN_POINT('Ctrl Pts',(-32.2888225453055,58.5385401346074,-0.466513502407774));
#31493=CARTESIAN_POINT('Ctrl Pts',(-33.2567972741826,58.2244460570088,-0.412696409711387));
#31494=CARTESIAN_POINT('Ctrl Pts',(-33.5253135061185,58.0685974415039,-0.395925280537681));
#31495=CARTESIAN_POINT('Ctrl Pts',(-33.5270487244507,58.0682282925651,-1.15407471946232));
#31496=CARTESIAN_POINT('Ctrl Pts',(-33.7583254242685,57.9362916288017,-1.13968210479344));
#31497=CARTESIAN_POINT('Ctrl Pts',(-34.4950254817816,57.3125020026611,-1.08824352660187));
#31498=CARTESIAN_POINT('Ctrl Pts',(-34.7912737376158,55.4864512354733,-0.999758984887624));
#31499=CARTESIAN_POINT('Ctrl Pts',(-33.0661792001092,53.929919412126,-0.888621094319583));
#31500=CARTESIAN_POINT('Ctrl Pts',(-30.822833264184,54.5351044086333,-0.77748320375154));
#31501=CARTESIAN_POINT('Ctrl Pts',(-30.114627688562,56.7480782089187,-0.666345313183499));
#31502=CARTESIAN_POINT('Ctrl Pts',(-31.5455083936009,58.4894074878942,-0.558542485087094));
#31503=CARTESIAN_POINT('Ctrl Pts',(-32.9912241698708,58.3792838991923,-0.487785620513369));
#31504=CARTESIAN_POINT('Ctrl Pts',(-33.5296554006197,58.0729354591291,-0.454074719462324));
#31505=CARTESIAN_POINT('Origin',(-32.5,56.2916512459885,-3.54592528053767));
#31506=CARTESIAN_POINT('',(-33.5243188290626,58.0704843676251,-1.85407471946232));
#31507=CARTESIAN_POINT('',(-33.5295805874755,58.0719425970214,-1.79592528053768));
#31508=CARTESIAN_POINT('',(-33.5273750000001,58.0711169444145,-3.54592528053767));
#31509=CARTESIAN_POINT('',(-31.045873711622,57.7433792852396,-2.));
#31510=CARTESIAN_POINT('Ctrl Pts',(-31.045873711622,57.7433792852396,-2.));
#31511=CARTESIAN_POINT('Ctrl Pts',(-31.5286078227265,58.2269108712356,-1.96295403647732));
#31512=CARTESIAN_POINT('Ctrl Pts',(-32.4987857659729,58.5150960016802,-1.91431227629809));
#31513=CARTESIAN_POINT('Ctrl Pts',(-33.339589876325,58.1790057138553,-1.86567051611887));
#31514=CARTESIAN_POINT('Ctrl Pts',(-33.5243188290626,58.0704843676251,-1.85407471946232));
#31515=CARTESIAN_POINT('',(-30.5120522999331,56.8258916115681,-2.));
#31516=CARTESIAN_POINT('Origin',(-32.5,56.2916512459885,-2.));
#31517=CARTESIAN_POINT('Ctrl Pts',(-30.5120501580915,56.825892077386,-2.));
#31518=CARTESIAN_POINT('Ctrl Pts',(-30.6859814099171,57.4697983977034,-1.96367708181445));
#31519=CARTESIAN_POINT('Ctrl Pts',(-31.6524845810095,58.5050100533592,-1.89565217532701));
#31520=CARTESIAN_POINT('Ctrl Pts',(-33.0221861661125,58.3592796390666,-1.82762726883957));
#31521=CARTESIAN_POINT('Ctrl Pts',(-33.5295805874755,58.0719425970214,-1.79592528053768));
#31522=CARTESIAN_POINT('Origin',(-65.,8.88178419700125E-15,3.));
#31523=CARTESIAN_POINT('',(-66.6675465985015,0.00121430446292491,6.12851963660979));
#31524=CARTESIAN_POINT('',(-66.6679935094968,-0.00096847687650235,6.32148036339021));
#31525=CARTESIAN_POINT('',(-66.666,8.90896198514149E-15,3.));
#31526=CARTESIAN_POINT('',(-66.6351293272515,0.319230454628283,7.));
#31527=CARTESIAN_POINT('Ctrl Pts',(-66.6679935094968,-0.00096847687650235,
6.32148036339021));
#31528=CARTESIAN_POINT('Ctrl Pts',(-66.6684011451999,-0.0590543694261873,
6.32537779445739));
#31529=CARTESIAN_POINT('Ctrl Pts',(-66.6656310767024,-0.117101359876398,
6.32927522552457));
#31530=CARTESIAN_POINT('Ctrl Pts',(-66.6595549679121,-0.174800485042597,
6.33317265659175));
#31531=CARTESIAN_POINT('Ctrl Pts',(-66.6018001800214,-0.723243715815264,
6.37021862011443));
#31532=CARTESIAN_POINT('Ctrl Pts',(-66.2453468888447,-1.24025755357673,
6.40726458363711));
#31533=CARTESIAN_POINT('Ctrl Pts',(-65.7532186868384,-1.48913446656881,
6.44431054715979));
#31534=CARTESIAN_POINT('Ctrl Pts',(-65.2610904848321,-1.73801137956088,
6.48135651068247));
#31535=CARTESIAN_POINT('Ctrl Pts',(-64.6332873719962,-1.71875136778354,
6.51840247420515));
#31536=CARTESIAN_POINT('Ctrl Pts',(-64.1573426907198,-1.44035276658658,
6.55544843772783));
#31537=CARTESIAN_POINT('Ctrl Pts',(-63.6813980094434,-1.16195416538962,
6.59249440125051));
#31538=CARTESIAN_POINT('Ctrl Pts',(-63.3573117597265,-0.624416974773032,
6.6295403647732));
#31539=CARTESIAN_POINT('Ctrl Pts',(-63.3329761432024,-0.0733847413024255,
6.66658632829588));
#31540=CARTESIAN_POINT('Ctrl Pts',(-63.3086405266783,0.477647492168173,
6.70363229181856));
#31541=CARTESIAN_POINT('Ctrl Pts',(-63.5840555433469,1.04217476849279,6.74067825534123));
#31542=CARTESIAN_POINT('Ctrl Pts',(-64.0340468080883,1.36111204342974,6.77772421886391));
#31543=CARTESIAN_POINT('Ctrl Pts',(-64.4840380728297,1.68004931836668,6.81477018238659));
#31544=CARTESIAN_POINT('Ctrl Pts',(-65.1086055856438,1.75339659191594,6.85181614590928));
#31545=CARTESIAN_POINT('Ctrl Pts',(-65.6198404690058,1.54912172664725,6.88886210943196));
#31546=CARTESIAN_POINT('Ctrl Pts',(-66.1310753523678,1.34484686137856,6.92590807295464));
#31547=CARTESIAN_POINT('Ctrl Pts',(-66.5289776062776,0.862949857291932,
6.96295403647732));
#31548=CARTESIAN_POINT('Ctrl Pts',(-66.6351293272514,0.319230454628307,
7.));
#31549=CARTESIAN_POINT('',(-65.0525836066607,-1.66819787866866,7.));
#31550=CARTESIAN_POINT('Origin',(-65.,8.88178419700125E-15,7.));
#31551=CARTESIAN_POINT('',(-66.6634369488939,0.000652451249345126,6.82851963660979));
#31552=CARTESIAN_POINT('Ctrl Pts',(-65.0525835864496,-1.66819940096573,
7.));
#31553=CARTESIAN_POINT('Ctrl Pts',(-65.5930952523355,-1.6504743391327,6.96367708181444));
#31554=CARTESIAN_POINT('Ctrl Pts',(-66.1251624614536,-1.34576660284024,
6.92735416362889));
#31555=CARTESIAN_POINT('Ctrl Pts',(-66.412840678391,-0.887825324655531,
6.89103124544334));
#31556=CARTESIAN_POINT('Ctrl Pts',(-66.5778717300928,-0.625120238531662,
6.87019404249883));
#31557=CARTESIAN_POINT('Ctrl Pts',(-66.6624763097416,-0.311987213470665,
6.84935683955431));
#31558=CARTESIAN_POINT('Ctrl Pts',(-66.6634369488939,0.000652451249345126,
6.82851963660979));
#31559=CARTESIAN_POINT('',(-66.666,9.31701429861739E-15,8.));
#31560=CARTESIAN_POINT('',(-66.666,8.90896198514149E-15,3.));
#31561=CARTESIAN_POINT('Origin',(-65.,8.88178419700125E-15,8.));
#31562=CARTESIAN_POINT('Ctrl Pts',(-66.6634369488939,0.000652451249345126,
6.82851963660979));
#31563=CARTESIAN_POINT('Ctrl Pts',(-66.6641842070583,0.243847350592484,
6.81231087603163));
#31564=CARTESIAN_POINT('Ctrl Pts',(-66.614319260528,0.486743721979884,6.79610211545346));
#31565=CARTESIAN_POINT('Ctrl Pts',(-66.5123276923829,0.705373629571163,
6.7798933548753));
#31566=CARTESIAN_POINT('Ctrl Pts',(-66.2792206701092,1.20506363008265,6.74284739135262));
#31567=CARTESIAN_POINT('Ctrl Pts',(-65.7738173393357,1.577991751398,6.70580142782994));
#31568=CARTESIAN_POINT('Ctrl Pts',(-65.2274915068526,1.65321113835932,6.66875546430726));
#31569=CARTESIAN_POINT('Ctrl Pts',(-64.6811656743696,1.72843052532065,6.63170950078458));
#31570=CARTESIAN_POINT('Ctrl Pts',(-64.0939173401772,1.50594117792797,6.5946635372619));
#31571=CARTESIAN_POINT('Ctrl Pts',(-63.734467017542,1.08770559986529,6.55761757373921));
#31572=CARTESIAN_POINT('Ctrl Pts',(-63.3750166949069,0.669470021802603,
6.52057161021653));
#31573=CARTESIAN_POINT('Ctrl Pts',(-63.2433643838291,0.0554882130699169,
6.48352564669385));
#31574=CARTESIAN_POINT('Ctrl Pts',(-63.3997802821251,-0.473318066669364,
6.44647968317117));
#31575=CARTESIAN_POINT('Ctrl Pts',(-63.556196180421,-1.00212434640863,6.40943371964849));
#31576=CARTESIAN_POINT('Ctrl Pts',(-64.0006802880906,-1.4457550971545,6.37238775612581));
#31577=CARTESIAN_POINT('Ctrl Pts',(-64.5298024116317,-1.60114443125079,
6.33534179260313));
#31578=CARTESIAN_POINT('Ctrl Pts',(-65.0589245351728,-1.75653376534709,
6.29829582908045));
#31579=CARTESIAN_POINT('Ctrl Pts',(-65.6726846745854,-1.62368168279381,
6.26124986555777));
#31580=CARTESIAN_POINT('Ctrl Pts',(-66.0901968514498,-1.26340683134222,
6.22420390203509));
#31581=CARTESIAN_POINT('Ctrl Pts',(-66.4496543303097,-0.9532278785462,6.19230914689332));
#31582=CARTESIAN_POINT('Ctrl Pts',(-66.6636456701669,-0.474474884606722,
6.16041439175156));
#31583=CARTESIAN_POINT('Ctrl Pts',(-66.6675465985015,0.00121430446292491,
6.12851963660979));
#31584=CARTESIAN_POINT('Origin',(-65.,8.88178419700125E-15,3.));
#31585=CARTESIAN_POINT('',(-66.6672347084384,-0.00132477166024408,5.42851963660979));
#31586=CARTESIAN_POINT('',(-66.6636987213601,-0.000832290200039209,5.62148036339021));
#31587=CARTESIAN_POINT('',(-66.666,8.90896198514149E-15,3.));
#31588=CARTESIAN_POINT('Ctrl Pts',(-66.6636987213601,-0.000832290200039209,
5.62148036339021));
#31589=CARTESIAN_POINT('Ctrl Pts',(-66.6647135334695,-0.225194170777286,
5.63643534665464));
#31590=CARTESIAN_POINT('Ctrl Pts',(-66.6225044629126,-0.449190113916426,
5.65139032991907));
#31591=CARTESIAN_POINT('Ctrl Pts',(-66.5352578465541,-0.654000676170921,
5.6663453131835));
#31592=CARTESIAN_POINT('Ctrl Pts',(-66.3191335681149,-1.16135026554736,
5.70339127670618));
#31593=CARTESIAN_POINT('Ctrl Pts',(-65.8266432700797,-1.55097169600334,
5.74043724022886));
#31594=CARTESIAN_POINT('Ctrl Pts',(-65.2831760713864,-1.64455092497835,
5.77748320375154));
#31595=CARTESIAN_POINT('Ctrl Pts',(-64.739708872693,-1.73813015395336,5.81452916727422));
#31596=CARTESIAN_POINT('Ctrl Pts',(-64.1452647733414,-1.53566718144741,
5.8515751307969));
#31597=CARTESIAN_POINT('Ctrl Pts',(-63.771898150977,-1.12982346148107,5.88862109431958));
#31598=CARTESIAN_POINT('Ctrl Pts',(-63.3985315286127,-0.723979741514712,
5.92566705784226));
#31599=CARTESIAN_POINT('Ctrl Pts',(-63.2462423832356,-0.114755274087964,
5.96271302136494));
#31600=CARTESIAN_POINT('Ctrl Pts',(-63.3847194791661,0.419041074004913,
5.99975898488762));
#31601=CARTESIAN_POINT('Ctrl Pts',(-63.5231965750967,0.952837422097797,
6.0368049484103));
#31602=CARTESIAN_POINT('Ctrl Pts',(-63.952439912335,1.4112056508568,6.07385091193298));
#31603=CARTESIAN_POINT('Ctrl Pts',(-64.4760180935273,1.58435878418328,6.11089687545566));
#31604=CARTESIAN_POINT('Ctrl Pts',(-64.9995962747196,1.75751191750977,6.14794283897834));
#31605=CARTESIAN_POINT('Ctrl Pts',(-65.617509299866,1.64544995540375,6.18498880250103));
#31606=CARTESIAN_POINT('Ctrl Pts',(-66.0469376701368,1.29948266245883,6.22203476602371));
#31607=CARTESIAN_POINT('Ctrl Pts',(-66.431187907292,0.989912956390705,6.25518329847921));
#31608=CARTESIAN_POINT('Ctrl Pts',(-66.6645264756734,0.493065172776578,
6.28833183093471));
#31609=CARTESIAN_POINT('Ctrl Pts',(-66.6679935094968,-0.00096847687650235,
6.32148036339021));
#31610=CARTESIAN_POINT('Ctrl Pts',(-66.6675465985015,0.00121430446292491,
6.12851963660979));
#31611=CARTESIAN_POINT('Ctrl Pts',(-66.6681766235524,0.0780411722834916,
6.12336842822888));
#31612=CARTESIAN_POINT('Ctrl Pts',(-66.6633265808958,0.154788122805561,
6.11821721984797));
#31613=CARTESIAN_POINT('Ctrl Pts',(-66.6527242222132,0.230732082280723,
6.11306601146705));
#31614=CARTESIAN_POINT('Ctrl Pts',(-66.5764752017958,0.776898524102178,
6.07602004794437));
#31615=CARTESIAN_POINT('Ctrl Pts',(-66.202712946645,1.28153378739521,6.03897408442169));
#31616=CARTESIAN_POINT('Ctrl Pts',(-65.7024931149025,1.51368401519417,6.00192812089901));
#31617=CARTESIAN_POINT('Ctrl Pts',(-65.20227328316,1.74583424299314,5.96488215737633));
#31618=CARTESIAN_POINT('Ctrl Pts',(-64.5755958748258,1.70549943529802,5.92783619385365));
#31619=CARTESIAN_POINT('Ctrl Pts',(-64.1092627289642,1.41114141304214,5.89079023033097));
#31620=CARTESIAN_POINT('Ctrl Pts',(-63.6429295831026,1.11678339078626,5.85374426680829));
#31621=CARTESIAN_POINT('Ctrl Pts',(-63.3369406997136,0.568402153969617,
5.81669830328561));
#31622=CARTESIAN_POINT('Ctrl Pts',(-63.3313339461091,0.0169662842418741,
5.77965233976292));
#31623=CARTESIAN_POINT('Ctrl Pts',(-63.3257271925045,-0.534469585485869,
5.74260637624024));
#31624=CARTESIAN_POINT('Ctrl Pts',(-63.6205025686844,-1.08896008812472,
5.70556041271756));
#31625=CARTESIAN_POINT('Ctrl Pts',(-64.0807542900534,-1.39273889179927,
5.66851444919488));
#31626=CARTESIAN_POINT('Ctrl Pts',(-64.5410060114225,-1.69651769547382,
5.6314684856722));
#31627=CARTESIAN_POINT('Ctrl Pts',(-65.1667340779808,-1.74958480018409,
5.59442252214952));
#31628=CARTESIAN_POINT('Ctrl Pts',(-65.6715705742232,-1.52765405355123,
5.55737655862684));
#31629=CARTESIAN_POINT('Ctrl Pts',(-66.1764070704656,-1.30572330691838,
5.52033059510416));
#31630=CARTESIAN_POINT('Ctrl Pts',(-66.5603519963922,-0.808794708942411,
5.48328463158148));
#31631=CARTESIAN_POINT('Ctrl Pts',(-66.6476907378026,-0.264290293520927,
5.4462386680588));
#31632=CARTESIAN_POINT('Ctrl Pts',(-66.6616154028998,-0.177478398750709,
5.44033232424247));
#31633=CARTESIAN_POINT('Ctrl Pts',(-66.6680006840388,-0.0894571820797048,
5.43442598042613));
#31634=CARTESIAN_POINT('Ctrl Pts',(-66.6672347084384,-0.00132477166024408,
5.42851963660979));
#31635=CARTESIAN_POINT('Origin',(-65.,8.88178419700125E-15,3.));
#31636=CARTESIAN_POINT('',(-66.663366994258,-0.000380245158974196,4.72851963660979));
#31637=CARTESIAN_POINT('',(-66.664973747664,0.00143128352027648,4.92148036339021));
#31638=CARTESIAN_POINT('',(-66.666,8.90896198514149E-15,3.));
#31639=CARTESIAN_POINT('Ctrl Pts',(-66.664973747664,0.00143128352027648,
4.92148036339021));
#31640=CARTESIAN_POINT('Ctrl Pts',(-66.6617826067969,-0.388070057475542,
4.94749289885189));
#31641=CARTESIAN_POINT('Ctrl Pts',(-66.5254256665028,-0.779584263278036,
4.97350543431356));
#31642=CARTESIAN_POINT('Ctrl Pts',(-66.27583338404,-1.07563182061434,4.99951796977524));
#31643=CARTESIAN_POINT('Ctrl Pts',(-65.9203745090186,-1.49725035242627,
5.03656393329793));
#31644=CARTESIAN_POINT('Ctrl Pts',(-65.3352487301258,-1.72524091300358,
5.07360989682061));
#31645=CARTESIAN_POINT('Ctrl Pts',(-64.7882421463444,-1.65526230253065,
5.11065586034329));
#31646=CARTESIAN_POINT('Ctrl Pts',(-64.2412355625629,-1.58528369205772,
5.14770182386597));
#31647=CARTESIAN_POINT('Ctrl Pts',(-63.7323481738928,-1.21733591053453,
5.18474778738865));
#31648=CARTESIAN_POINT('Ctrl Pts',(-63.4944752416899,-0.719812399768212,
5.22179375091133));
#31649=CARTESIAN_POINT('Ctrl Pts',(-63.256602309487,-0.22228888900191,5.25883971443401));
#31650=CARTESIAN_POINT('Ctrl Pts',(-63.2897438337514,0.404810351007526,
5.29588567795669));
#31651=CARTESIAN_POINT('Ctrl Pts',(-63.5787322850456,0.874489902053361,
5.33293164147937));
#31652=CARTESIAN_POINT('Ctrl Pts',(-63.8677207363397,1.3441694530992,5.36997760500205));
#31653=CARTESIAN_POINT('Ctrl Pts',(-64.4125561146635,1.65642931518146,5.40702356852473));
#31654=CARTESIAN_POINT('Ctrl Pts',(-64.9638916621075,1.66836178497852,5.44406953204741));
#31655=CARTESIAN_POINT('Ctrl Pts',(-65.5152272095514,1.68029425477557,5.48111549557009));
#31656=CARTESIAN_POINT('Ctrl Pts',(-66.0730629261155,1.39189933228744,5.51816145909277));
#31657=CARTESIAN_POINT('Ctrl Pts',(-66.382101654976,0.935162996894921,5.55520742261545));
#31658=CARTESIAN_POINT('Ctrl Pts',(-66.5663853881852,0.662805298269947,
5.57729840287371));
#31659=CARTESIAN_POINT('Ctrl Pts',(-66.6621996762674,0.330587263195571,
5.59938938313196));
#31660=CARTESIAN_POINT('Ctrl Pts',(-66.6636987213601,-0.000832290200039209,
5.62148036339021));
#31661=CARTESIAN_POINT('Ctrl Pts',(-66.6672347084384,-0.00132477166024408,
5.42851963660979));
#31662=CARTESIAN_POINT('Ctrl Pts',(-66.6631963067396,0.463329814934407,
5.39738001690345));
#31663=CARTESIAN_POINT('Ctrl Pts',(-66.4603784340712,0.93107519176336,5.3662403971971));
#31664=CARTESIAN_POINT('Ctrl Pts',(-66.1156608616196,1.24098144967674,5.33510077749075));
#31665=CARTESIAN_POINT('Ctrl Pts',(-65.705559687132,1.60966854458596,5.29805481396807));
#31666=CARTESIAN_POINT('Ctrl Pts',(-65.0946247812625,1.75496250153737,5.2610088504454));
#31667=CARTESIAN_POINT('Ctrl Pts',(-64.5624539571804,1.61036875759038,5.22396288692272));
#31668=CARTESIAN_POINT('Ctrl Pts',(-64.0302831330983,1.4657750136434,5.18691692340004));
#31669=CARTESIAN_POINT('Ctrl Pts',(-63.5768763908035,1.03129356879801,5.14987095987736));
#31670=CARTESIAN_POINT('Ctrl Pts',(-63.4097379023455,0.50576729950702,5.11282499635467));
#31671=CARTESIAN_POINT('Ctrl Pts',(-63.2425994138875,-0.0197589697839626,
5.07577903283199));
#31672=CARTESIAN_POINT('Ctrl Pts',(-63.3617291792663,-0.636330063520541,
5.03873306930931));
#31673=CARTESIAN_POINT('Ctrl Pts',(-63.7126067830815,-1.06176871408085,
5.00168710578663));
#31674=CARTESIAN_POINT('Ctrl Pts',(-64.0634843868967,-1.48720736464116,
4.96464114226395));
#31675=CARTESIAN_POINT('Ctrl Pts',(-64.6461098291483,-1.72151357202521,
4.92759517874127));
#31676=CARTESIAN_POINT('Ctrl Pts',(-65.1938412738805,-1.65745577708111,
4.89054921521859));
#31677=CARTESIAN_POINT('Ctrl Pts',(-65.7415727186126,-1.59339798213701,
4.85350325169591));
#31678=CARTESIAN_POINT('Ctrl Pts',(-66.2544101658253,-1.23097618486477,
4.81645728817322));
#31679=CARTESIAN_POINT('Ctrl Pts',(-66.4976506491046,-0.73605477318721,
4.77941132465054));
#31680=CARTESIAN_POINT('Ctrl Pts',(-66.6090340731616,-0.509422920098683,
4.76244742863696));
#31681=CARTESIAN_POINT('Ctrl Pts',(-66.6638867910221,-0.255007754231674,
4.74548353262337));
#31682=CARTESIAN_POINT('Ctrl Pts',(-66.663366994258,-0.000380245158974196,
4.72851963660979));
#31683=CARTESIAN_POINT('Origin',(-65.,8.88178419700125E-15,3.));
#31684=CARTESIAN_POINT('',(-66.66584023827,0.00152342185142561,4.02851963660979));
#31685=CARTESIAN_POINT('',(-66.668752404953,-6.71116606238314E-6,4.22148036339021));
#31686=CARTESIAN_POINT('',(-66.666,8.90896198514149E-15,3.));
#31687=CARTESIAN_POINT('Ctrl Pts',(-66.6687523910643,-6.71113219753621E-6,
4.22148036339021));
#31688=CARTESIAN_POINT('Ctrl Pts',(-66.6687853501023,-0.551830446441265,
4.25855045104914));
#31689=CARTESIAN_POINT('Ctrl Pts',(-66.3679399440666,-1.10362329032224,
4.29562053870807));
#31690=CARTESIAN_POINT('Ctrl Pts',(-65.9041274583633,-1.40260051189835,
4.332690626367));
#31691=CARTESIAN_POINT('Ctrl Pts',(-65.440616808353,-1.70138316778324,4.36973658988968));
#31692=CARTESIAN_POINT('Ctrl Pts',(-64.8143512345865,-1.74767914449737,
4.40678255341236));
#31693=CARTESIAN_POINT('Ctrl Pts',(-64.3119447275275,-1.52030082532264,
4.44382851693504));
#31694=CARTESIAN_POINT('Ctrl Pts',(-63.8095382204685,-1.2929225061479,4.48087448045772));
#31695=CARTESIAN_POINT('Ctrl Pts',(-63.430990780117,-0.791869891084301,
4.5179204439804));
#31696=CARTESIAN_POINT('Ctrl Pts',(-63.3495467901205,-0.246452551482032,
4.55496640750308));
#31697=CARTESIAN_POINT('Ctrl Pts',(-63.2681028001239,0.298964788120236,
4.59201237102576));
#31698=CARTESIAN_POINT('Ctrl Pts',(-63.4837622604823,0.888746852261173,
4.62905833454844));
#31699=CARTESIAN_POINT('Ctrl Pts',(-63.897827394199,1.25297653677901,4.66610429807112));
#31700=CARTESIAN_POINT('Ctrl Pts',(-64.3118925279157,1.61720622129685,4.7031502615938));
#31701=CARTESIAN_POINT('Ctrl Pts',(-64.9243633349907,1.7558835261916,4.74019622511648));
#31702=CARTESIAN_POINT('Ctrl Pts',(-65.4549390817441,1.60554199300636,4.77724218863916));
#31703=CARTESIAN_POINT('Ctrl Pts',(-65.9855148284976,1.45520045982113,4.81428815216184));
#31704=CARTESIAN_POINT('Ctrl Pts',(-66.4341955149295,1.01584008855591,4.85133411568453));
#31705=CARTESIAN_POINT('Ctrl Pts',(-66.5956398725704,0.488536651400025,
4.88838007920721));
#31706=CARTESIAN_POINT('Ctrl Pts',(-66.643722970876,0.331489459561816,4.89941350726821));
#31707=CARTESIAN_POINT('Ctrl Pts',(-66.6663272959654,0.166641438903683,
4.91044693532921));
#31708=CARTESIAN_POINT('Ctrl Pts',(-66.664973747664,0.00143128352027648,
4.92148036339021));
#31709=CARTESIAN_POINT('Ctrl Pts',(-66.663366994258,-0.000380245158974196,
4.72851963660979));
#31710=CARTESIAN_POINT('Ctrl Pts',(-66.6627516524935,0.301050913271586,
4.7084375691007));
#31711=CARTESIAN_POINT('Ctrl Pts',(-66.5845366381801,0.602779651888659,
4.6883555015916));
#31712=CARTESIAN_POINT('Ctrl Pts',(-66.4306434003258,0.859065513400944,
4.66827343408251));
#31713=CARTESIAN_POINT('Ctrl Pts',(-66.1467521489217,1.33184336222866,4.63122747055983));
#31714=CARTESIAN_POINT('Ctrl Pts',(-65.6053261267676,1.64997803380121,4.59418150703714));
#31715=CARTESIAN_POINT('Ctrl Pts',(-65.0541520228137,1.6678733924142,4.55713554351446));
#31716=CARTESIAN_POINT('Ctrl Pts',(-64.5029779188599,1.68576875102718,4.52008957999178));
#31717=CARTESIAN_POINT('Ctrl Pts',(-63.9420557331062,1.40342479668061,4.4830436164691));
#31718=CARTESIAN_POINT('Ctrl Pts',(-63.6280946846009,0.950057840731767,
4.44599765294642));
#31719=CARTESIAN_POINT('Ctrl Pts',(-63.3141336360955,0.496690884782925,
4.40895168942374));
#31720=CARTESIAN_POINT('Ctrl Pts',(-63.2471337248385,-0.12769907276818,
4.37190572590106));
#31721=CARTESIAN_POINT('Ctrl Pts',(-63.4577578400848,-0.637356427139624,
4.33485976237838));
#31722=CARTESIAN_POINT('Ctrl Pts',(-63.6683819553311,-1.14701378151105,
4.2978137988557));
#31723=CARTESIAN_POINT('Ctrl Pts',(-64.1566300970808,-1.54193853270284,
4.26076783533302));
#31724=CARTESIAN_POINT('Ctrl Pts',(-64.6990527347307,-1.64139112904608,
4.22372187181034));
#31725=CARTESIAN_POINT('Ctrl Pts',(-65.2414753723806,-1.74084372538932,
4.18667590828766));
#31726=CARTESIAN_POINT('Ctrl Pts',(-65.8380725059307,-1.54482416688402,
4.14962994476498));
#31727=CARTESIAN_POINT('Ctrl Pts',(-66.2158080742639,-1.14304191594114,
4.1125839812423));
#31728=CARTESIAN_POINT('Ctrl Pts',(-66.501526048881,-0.839135107580329,
4.08456253303146));
#31729=CARTESIAN_POINT('Ctrl Pts',(-66.6620254174182,-0.417504031348412,
4.05654108482063));
#31730=CARTESIAN_POINT('Ctrl Pts',(-66.66584023827,0.00152342185142561,
4.02851963660979));
#31731=CARTESIAN_POINT('Origin',(-65.,8.88178419700125E-15,3.));
#31732=CARTESIAN_POINT('',(-66.6685304876972,-0.000550348904949371,3.32851963660979));
#31733=CARTESIAN_POINT('',(-66.6649541686305,-0.00142706439963382,3.52148036339021));
#31734=CARTESIAN_POINT('',(-66.666,8.90896198514149E-15,3.));
#31735=CARTESIAN_POINT('Ctrl Pts',(-66.6649541686305,-0.00142706439963382,
3.52148036339021));
#31736=CARTESIAN_POINT('Ctrl Pts',(-66.6663084639771,-0.167364609070321,
3.53256203972371));
#31737=CARTESIAN_POINT('Ctrl Pts',(-66.6435020576938,-0.332938268252238,
3.5436437160572));
#31738=CARTESIAN_POINT('Ctrl Pts',(-66.5950038039968,-0.490609337973565,
3.5547253923907));
#31739=CARTESIAN_POINT('Ctrl Pts',(-66.4328744940168,-1.017702579257,3.59177135591338));
#31740=CARTESIAN_POINT('Ctrl Pts',(-65.9836233623828,-1.45647963816642,
3.62881731943606));
#31741=CARTESIAN_POINT('Ctrl Pts',(-65.4528527369189,-1.60613170566074,
3.66586328295875));
#31742=CARTESIAN_POINT('Ctrl Pts',(-64.9220821114551,-1.75578377315507,
3.70290924648143));
#31743=CARTESIAN_POINT('Ctrl Pts',(-64.3097919921614,-1.6163108492343,3.73995521000411));
#31744=CARTESIAN_POINT('Ctrl Pts',(-63.8962004240445,-1.25154350838823,
3.77700117352679));
#31745=CARTESIAN_POINT('Ctrl Pts',(-63.4826088559277,-0.886776167542167,
3.81404713704947));
#31746=CARTESIAN_POINT('Ctrl Pts',(-63.2677158389876,-0.296714409770812,
3.85109310057215));
#31747=CARTESIAN_POINT('Ctrl Pts',(-63.3498683809715,0.248596655588651,
3.88813906409483));
#31748=CARTESIAN_POINT('Ctrl Pts',(-63.4320209229553,0.793907720948114,
3.92518502761751));
#31749=CARTESIAN_POINT('Ctrl Pts',(-63.8112190238629,1.29446809389569,3.96223099114019));
#31750=CARTESIAN_POINT('Ctrl Pts',(-64.3139205225789,1.52119348141189,3.99927695466287));
#31751=CARTESIAN_POINT('Ctrl Pts',(-64.8166220212948,1.7479188689281,4.03632291818555));
#31752=CARTESIAN_POINT('Ctrl Pts',(-65.4428269178191,1.70080927101295,4.07336888170823));
#31753=CARTESIAN_POINT('Ctrl Pts',(-65.9059489905043,1.40142466222205,4.11041484523092));
#31754=CARTESIAN_POINT('Ctrl Pts',(-66.368769480536,1.10223501111092,4.14743668461735));
#31755=CARTESIAN_POINT('Ctrl Pts',(-66.6687194749238,0.551098802461351,
4.18445852400378));
#31756=CARTESIAN_POINT('Ctrl Pts',(-66.6687523910643,-6.71113219753621E-6,
4.22148036339021));
#31757=CARTESIAN_POINT('Ctrl Pts',(-66.66584023827,0.00152342185142561,
4.02851963660979));
#31758=CARTESIAN_POINT('Ctrl Pts',(-66.6670688296308,0.136474322284305,
4.01949512129795));
#31759=CARTESIAN_POINT('Ctrl Pts',(-66.6520459458893,0.271155172380335,
4.0104706059861));
#31760=CARTESIAN_POINT('Ctrl Pts',(-66.6197204952159,0.401546525825023,
4.00144609067426));
#31761=CARTESIAN_POINT('Ctrl Pts',(-66.4870233447183,0.936807773267803,
3.96440012715158));
#31762=CARTESIAN_POINT('Ctrl Pts',(-66.0627550406069,1.39978532477288,3.92735416362889));
#31763=CARTESIAN_POINT('Ctrl Pts',(-65.54108437802,1.5785948786444,3.89030820010621));
#31764=CARTESIAN_POINT('Ctrl Pts',(-65.0194137154332,1.75740443251591,3.85326223658353));
#31765=CARTESIAN_POINT('Ctrl Pts',(-64.400340694371,1.65204598875386,3.81621627306085));
#31766=CARTESIAN_POINT('Ctrl Pts',(-63.9671875933068,1.31073743656301,3.77917030953817));
#31767=CARTESIAN_POINT('Ctrl Pts',(-63.5340344922426,0.96942888437217,3.74212434601549));
#31768=CARTESIAN_POINT('Ctrl Pts',(-63.2868013111764,0.392170223752536,
3.70507838249281));
#31769=CARTESIAN_POINT('Ctrl Pts',(-63.3386357173299,-0.156852845981067,
3.66803241897013));
#31770=CARTESIAN_POINT('Ctrl Pts',(-63.3904701234834,-0.705875915714671,
3.63098645544745));
#31771=CARTESIAN_POINT('Ctrl Pts',(-63.7413721168566,-1.22666339456225,
3.59394049192477));
#31772=CARTESIAN_POINT('Ctrl Pts',(-64.230749410433,-1.48087393976487,3.55689452840209));
#31773=CARTESIAN_POINT('Ctrl Pts',(-64.7201267040094,-1.73508448496749,
3.51984856487941));
#31774=CARTESIAN_POINT('Ctrl Pts',(-65.347979297789,-1.72271809652517,3.48280260135673));
#31775=CARTESIAN_POINT('Ctrl Pts',(-65.826966892062,-1.44943432222994,3.44575663783405));
#31776=CARTESIAN_POINT('Ctrl Pts',(-66.305954486335,-1.17615054793471,3.40871067431137));
#31777=CARTESIAN_POINT('Ctrl Pts',(-66.6360770811014,-0.641949387786585,
3.37166471078869));
#31778=CARTESIAN_POINT('Ctrl Pts',(-66.6662521989441,-0.0913110318543388,
3.33461874726601));
#31779=CARTESIAN_POINT('Ctrl Pts',(-66.6679081722746,-0.0610926765551588,
3.3325857103806));
#31780=CARTESIAN_POINT('Ctrl Pts',(-66.668660799992,-0.0308248176933715,
3.3305526734952));
#31781=CARTESIAN_POINT('Ctrl Pts',(-66.6685304876972,-0.000550348904949371,
3.32851963660979));
#31782=CARTESIAN_POINT('Origin',(-65.,8.88178419700125E-15,3.));
#31783=CARTESIAN_POINT('',(-66.664215437255,-0.00117645755964804,2.62851963660979));
#31784=CARTESIAN_POINT('',(-66.663709965026,0.000842507685015625,2.82148036339021));
#31785=CARTESIAN_POINT('',(-66.666,8.90896198514149E-15,3.));
#31786=CARTESIAN_POINT('Ctrl Pts',(-66.663709965026,0.000842507685015625,
2.82148036339021));
#31787=CARTESIAN_POINT('Ctrl Pts',(-66.6621889226241,-0.331295501917179,
2.84361959192095));
#31788=CARTESIAN_POINT('Ctrl Pts',(-66.565926135999,-0.664245551393369,
2.8657588204517));
#31789=CARTESIAN_POINT('Ctrl Pts',(-66.3808853648239,-0.936957985442174,
2.88789804898245));
#31790=CARTESIAN_POINT('Ctrl Pts',(-66.0712533625325,-1.39329253521755,
2.92494401250513));
#31791=CARTESIAN_POINT('Ctrl Pts',(-65.5130436951299,-1.68096223107997,
2.96198997602781));
#31792=CARTESIAN_POINT('Ctrl Pts',(-64.9617241821671,-1.66831340551996,
2.9990359395505));
#31793=CARTESIAN_POINT('Ctrl Pts',(-64.4104046692042,-1.65566457995995,
3.03608190307317));
#31794=CARTESIAN_POINT('Ctrl Pts',(-63.8659753106812,-1.34269723297749,
3.07312786659585));
#31795=CARTESIAN_POINT('Ctrl Pts',(-63.5775972896502,-0.872642645564539,
3.11017383011853));
#31796=CARTESIAN_POINT('Ctrl Pts',(-63.2892192686192,-0.402588058151592,
3.14721979364122));
#31797=CARTESIAN_POINT('Ctrl Pts',(-63.2568925850803,0.22455376969184,3.1842657571639));
#31798=CARTESIAN_POINT('Ctrl Pts',(-63.4954117290602,0.721767824316931,
3.22131172068658));
#31799=CARTESIAN_POINT('Ctrl Pts',(-63.73393087304,1.21898187894203,3.25835768420926));
#31800=CARTESIAN_POINT('Ctrl Pts',(-64.2432958445387,1.58626816034878,3.29540364773194));
#31801=CARTESIAN_POINT('Ctrl Pts',(-64.7903928760533,1.65553601919702,3.33244961125462));
#31802=CARTESIAN_POINT('Ctrl Pts',(-65.3374899075679,1.72480387804527,3.3694955747773));
#31803=CARTESIAN_POINT('Ctrl Pts',(-65.9223189990984,1.49605331433501,3.40654153829998));
#31804=CARTESIAN_POINT('Ctrl Pts',(-66.2772298007007,1.07397332065117,3.44358750182266));
#31805=CARTESIAN_POINT('Ctrl Pts',(-66.5259750107882,0.77815145152619,3.46955178901184));
#31806=CARTESIAN_POINT('Ctrl Pts',(-66.6617810644663,0.387363397948813,
3.49551607620103));
#31807=CARTESIAN_POINT('Ctrl Pts',(-66.6649541686305,-0.00142706439963382,
3.52148036339021));
#31808=CARTESIAN_POINT('Ctrl Pts',(-66.6685304876972,-0.000550348904949371,
3.32851963660979));
#31809=CARTESIAN_POINT('Ctrl Pts',(-66.6662862515739,0.520836037284772,
3.29350670997252));
#31810=CARTESIAN_POINT('Ctrl Pts',(-66.4021649235169,1.04418290588671,3.25849378333524));
#31811=CARTESIAN_POINT('Ctrl Pts',(-65.9803979715476,1.35039028151488,3.22348085669796));
#31812=CARTESIAN_POINT('Ctrl Pts',(-65.5341409853895,1.67437768723549,3.18643489317528));
#31813=CARTESIAN_POINT('Ctrl Pts',(-64.9113993721543,1.75527694696034,3.1493889296526));
#31814=CARTESIAN_POINT('Ctrl Pts',(-64.3971743623243,1.55606405574625,3.11234296612992));
#31815=CARTESIAN_POINT('Ctrl Pts',(-63.8829493524943,1.35685116453216,3.07529700260724));
#31816=CARTESIAN_POINT('Ctrl Pts',(-63.4772409460695,0.877526122379138,
3.03825103908456));
#31817=CARTESIAN_POINT('Ctrl Pts',(-63.3657238957733,0.337454752786405,
3.00120507556188));
#31818=CARTESIAN_POINT('Ctrl Pts',(-63.2542068454771,-0.202616616806327,
2.9641591120392));
#31819=CARTESIAN_POINT('Ctrl Pts',(-63.4368811513095,-0.803434313838767,
2.92711314851652));
#31820=CARTESIAN_POINT('Ctrl Pts',(-63.8301448813726,-1.19003071239599,
2.89006718499384));
#31821=CARTESIAN_POINT('Ctrl Pts',(-64.2234086114356,-1.57662711095321,
2.85302122147116));
#31822=CARTESIAN_POINT('Ctrl Pts',(-64.8272617657294,-1.74900221103521,
2.81597525794848));
#31823=CARTESIAN_POINT('Ctrl Pts',(-65.3653475241109,-1.62826757065615,
2.7789292944258));
#31824=CARTESIAN_POINT('Ctrl Pts',(-65.9034332824925,-1.5075329302771,2.74188333090311));
#31825=CARTESIAN_POINT('Ctrl Pts',(-66.3757516449619,-1.09368854943699,
2.70483736738043));
#31826=CARTESIAN_POINT('Ctrl Pts',(-66.5661434347078,-0.576132655684546,
2.66779140385775));
#31827=CARTESIAN_POINT('Ctrl Pts',(-66.6334204184134,-0.393248722101033,
2.6547008147751));
#31828=CARTESIAN_POINT('Ctrl Pts',(-66.6654949753924,-0.197414973610965,
2.64161022569244));
#31829=CARTESIAN_POINT('Ctrl Pts',(-66.664215437255,-0.00117645755964804,
2.62851963660979));
#31830=CARTESIAN_POINT('Origin',(-65.,8.88178419700125E-15,3.));
#31831=CARTESIAN_POINT('',(-66.6642789433678,0.00120644035141754,1.92851963660979));
#31832=CARTESIAN_POINT('',(-66.6680288432953,0.000974731038378531,2.1214803633902));
#31833=CARTESIAN_POINT('',(-66.666,8.90896198514149E-15,3.));
#31834=CARTESIAN_POINT('Ctrl Pts',(-66.6680288432953,0.000974731038378531,
2.1214803633902));
#31835=CARTESIAN_POINT('Ctrl Pts',(-66.6645899038029,-0.49376054930324,
2.1546771441182));
#31836=CARTESIAN_POINT('Ctrl Pts',(-66.4304593550116,-0.99132262932826,
2.1878739248462));
#31837=CARTESIAN_POINT('Ctrl Pts',(-66.0452404987214,-1.30084855271515,
2.2210707055742));
#31838=CARTESIAN_POINT('Ctrl Pts',(-65.6153553295749,-1.64626415674821,
2.25811666909688));
#31839=CARTESIAN_POINT('Ctrl Pts',(-64.9973130191693,-1.75750978249457,
2.29516263261956));
#31840=CARTESIAN_POINT('Ctrl Pts',(-64.4739641353999,-1.58367323852582,
2.33220859614224));
#31841=CARTESIAN_POINT('Ctrl Pts',(-63.9506152516305,-1.40983669455707,
2.36925455966492));
#31842=CARTESIAN_POINT('Ctrl Pts',(-63.5219597944974,-0.950917980873204,
2.40630052318761));
#31843=CARTESIAN_POINT('Ctrl Pts',(-63.3841743645993,-0.41694384903774,
2.44334648671029));
#31844=CARTESIAN_POINT('Ctrl Pts',(-63.2463889347012,0.117030282797723,
2.48039245023297));
#31845=CARTESIAN_POINT('Ctrl Pts',(-63.399473532038,0.726059832784788,2.51743841375565));
#31846=CARTESIAN_POINT('Ctrl Pts',(-63.77336812259,1.13141897393944,2.55448437727833));
#31847=CARTESIAN_POINT('Ctrl Pts',(-64.1472627131419,1.53677811509409,2.59153034080101));
#31848=CARTESIAN_POINT('Ctrl Pts',(-64.741967296909,1.73846684741633,2.62857630432369));
#31849=CARTESIAN_POINT('Ctrl Pts',(-65.2853119489257,1.64418117890599,2.66562226784637));
#31850=CARTESIAN_POINT('Ctrl Pts',(-65.8286566009425,1.54989551039566,2.70266823136905));
#31851=CARTESIAN_POINT('Ctrl Pts',(-66.3206413212089,1.15963544105275,2.73971419489173));
#31852=CARTESIAN_POINT('Ctrl Pts',(-66.5361065127521,0.652005704537134,
2.77676015841441));
#31853=CARTESIAN_POINT('Ctrl Pts',(-66.6228064445369,0.447743182072859,
2.79166689340634));
#31854=CARTESIAN_POINT('Ctrl Pts',(-66.664734109836,0.224476916761689,2.80657362839827));
#31855=CARTESIAN_POINT('Ctrl Pts',(-66.663709965026,0.000842507685015625,
2.82148036339021));
#31856=CARTESIAN_POINT('Ctrl Pts',(-66.664215437255,-0.00117645755964804,
2.62851963660979));
#31857=CARTESIAN_POINT('Ctrl Pts',(-66.6618739219115,0.357933976805246,
2.60456426216976));
#31858=CARTESIAN_POINT('Ctrl Pts',(-66.5478366409886,0.718399891583497,
2.58060888772974));
#31859=CARTESIAN_POINT('Ctrl Pts',(-66.3334304982421,1.00334301282383,2.55665351328971));
#31860=CARTESIAN_POINT('Ctrl Pts',(-66.0018605550081,1.44399538091501,2.51960754976703));
#31861=CARTESIAN_POINT('Ctrl Pts',(-65.4302554515179,1.70403271043259,2.48256158624435));
#31862=CARTESIAN_POINT('Ctrl Pts',(-64.880213504605,1.6644474430109,2.44551562272167));
#31863=CARTESIAN_POINT('Ctrl Pts',(-64.3301715576922,1.62486217558921,2.40846965919899));
#31864=CARTESIAN_POINT('Ctrl Pts',(-63.8016927673567,1.28565431122825,2.37142369567631));
#31865=CARTESIAN_POINT('Ctrl Pts',(-63.5366384486743,0.802064252492247,
2.33437773215363));
#31866=CARTESIAN_POINT('Ctrl Pts',(-63.2715841299918,0.318474193756241,
2.29733176863095));
#31867=CARTESIAN_POINT('Ctrl Pts',(-63.2699542829623,-0.309498059354816,
2.26028580510827));
#31868=CARTESIAN_POINT('Ctrl Pts',(-63.5324948163207,-0.794457444359814,
2.22323984158559));
#31869=CARTESIAN_POINT('Ctrl Pts',(-63.795035349679,-1.27941682936481,2.18619387806291));
#31870=CARTESIAN_POINT('Ctrl Pts',(-64.3217462634253,-1.62136334626375,
2.14914791454023));
#31871=CARTESIAN_POINT('Ctrl Pts',(-64.8715753212295,-1.66380323262915,
2.11210195101754));
#31872=CARTESIAN_POINT('Ctrl Pts',(-65.4214043790337,-1.70624311899455,
2.07505598749486));
#31873=CARTESIAN_POINT('Ctrl Pts',(-65.9943515808958,-1.44917637482641,
2.03801002397218));
#31874=CARTESIAN_POINT('Ctrl Pts',(-66.3282043910519,-1.01025105326097,
2.0009640604495));
#31875=CARTESIAN_POINT('Ctrl Pts',(-66.54582391177,-0.724140781894937,1.9768159191696));
#31876=CARTESIAN_POINT('Ctrl Pts',(-66.6618524838225,-0.360758997512868,
1.95266777788969));
#31877=CARTESIAN_POINT('Ctrl Pts',(-66.6642789433678,0.00120644035141754,
1.92851963660979));
#31878=CARTESIAN_POINT('Origin',(-65.,8.88178419700125E-15,3.));
#31879=CARTESIAN_POINT('',(-66.6685688018723,0.000500570493875176,1.22851963660979));
#31880=CARTESIAN_POINT('',(-66.6666630352664,-0.00145874010107553,1.4214803633902));
#31881=CARTESIAN_POINT('',(-66.666,8.90896198514149E-15,3.));
#31882=CARTESIAN_POINT('Ctrl Pts',(-66.6666630352664,-0.00145874010107553,
1.4214803633902));
#31883=CARTESIAN_POINT('Ctrl Pts',(-66.6676496745696,-0.109114984958735,
1.42868873279277));
#31884=CARTESIAN_POINT('Ctrl Pts',(-66.6581116875295,-0.216597146837632,
1.43589710219534));
#31885=CARTESIAN_POINT('Ctrl Pts',(-66.6374139306422,-0.321885502945873,
1.44310547159791));
#31886=CARTESIAN_POINT('Ctrl Pts',(-66.5310419755125,-0.862993814953153,
1.48015143512059));
#31887=CARTESIAN_POINT('Ctrl Pts',(-66.1299138139174,-1.34615847081563,
1.51719739864327));
#31888=CARTESIAN_POINT('Ctrl Pts',(-65.6176080235618,-1.55025642604728,
1.55424336216595));
#31889=CARTESIAN_POINT('Ctrl Pts',(-65.1053022332063,-1.75435438127892,
1.59128932568863));
#31890=CARTESIAN_POINT('Ctrl Pts',(-64.4818188140901,-1.67938563587972,
1.62833528921131));
#31891=CARTESIAN_POINT('Ctrl Pts',(-64.0324984883637,-1.35966006128364,
1.66538125273399));
#31892=CARTESIAN_POINT('Ctrl Pts',(-63.5831781626372,-1.03993448668757,
1.70242721625667));
#31893=CARTESIAN_POINT('Ctrl Pts',(-63.3080209303004,-0.475452082894621,
1.73947317977936));
#31894=CARTESIAN_POINT('Ctrl Pts',(-63.3329540589798,0.0754485771665916,
1.77651914330204));
#31895=CARTESIAN_POINT('Ctrl Pts',(-63.3578871876591,0.626349237227804,
1.81356510682472));
#31896=CARTESIAN_POINT('Ctrl Pts',(-63.6829106773545,1.16366815355728,1.8506110703474));
#31897=CARTESIAN_POINT('Ctrl Pts',(-64.1592756849985,1.44149827729127,1.88765703387008));
#31898=CARTESIAN_POINT('Ctrl Pts',(-64.6356406926424,1.71932840102527,1.92470299739276));
#31899=CARTESIAN_POINT('Ctrl Pts',(-65.2633472182348,1.73766973216378,1.96174896091544));
#31900=CARTESIAN_POINT('Ctrl Pts',(-65.7551218110002,1.48812825650889,1.99879492443812));
#31901=CARTESIAN_POINT('Ctrl Pts',(-66.2468964037657,1.23858678085399,2.0358408879608));
#31902=CARTESIAN_POINT('Ctrl Pts',(-66.6027390637042,0.721162498405699,
2.07288685148348));
#31903=CARTESIAN_POINT('Ctrl Pts',(-66.6597963797297,0.172657566021677,
2.10993281500616));
#31904=CARTESIAN_POINT('Ctrl Pts',(-66.6657247999481,0.115666316563748,
2.11378199780084));
#31905=CARTESIAN_POINT('Ctrl Pts',(-66.6684275899941,0.0583395262760883,
2.11763118059552));
#31906=CARTESIAN_POINT('Ctrl Pts',(-66.6680288432953,0.000974731038378531,
2.1214803633902));
#31907=CARTESIAN_POINT('Ctrl Pts',(-66.6642789433678,0.00120644035141754,
1.92851963660979));
#31908=CARTESIAN_POINT('Ctrl Pts',(-66.6655749455541,0.194536677303725,
1.91562181436701));
#31909=CARTESIAN_POINT('Ctrl Pts',(-66.634462982395,0.387462864473397,1.90272399212424));
#31910=CARTESIAN_POINT('Ctrl Pts',(-66.5691129188822,0.567995372183053,
1.88982616988146));
#31911=CARTESIAN_POINT('Ctrl Pts',(-66.3814102181061,1.08653257709889,1.85278020635878));
#31912=CARTESIAN_POINT('Ctrl Pts',(-65.9112463981035,1.50282308796782,1.8157342428361));
#31913=CARTESIAN_POINT('Ctrl Pts',(-65.3737945971089,1.62634919196252,1.77868827931342));
#31914=CARTESIAN_POINT('Ctrl Pts',(-64.8363427961142,1.74987529595721,1.74164231579074));
#31915=CARTESIAN_POINT('Ctrl Pts',(-64.2316030141275,1.58063699307768,1.70459635226806));
#31916=CARTESIAN_POINT('Ctrl Pts',(-63.8363378414827,1.19608715228399,1.66755038874538));
#31917=CARTESIAN_POINT('Ctrl Pts',(-63.4410726688379,0.811537311490293,
1.6305044252227));
#31918=CARTESIAN_POINT('Ctrl Pts',(-63.2552821055351,0.211675932782425,
1.59345846170002));
#31919=CARTESIAN_POINT('Ctrl Pts',(-63.3639942563739,-0.328967022430164,
1.55641249817734));
#31920=CARTESIAN_POINT('Ctrl Pts',(-63.4727064072127,-0.869609977642748,
1.51936653465465));
#31921=CARTESIAN_POINT('Ctrl Pts',(-63.8759212721932,-1.35103450936006,
1.48232057113197));
#31922=CARTESIAN_POINT('Ctrl Pts',(-64.3891052819731,-1.55291395077578,
1.44527460760929));
#31923=CARTESIAN_POINT('Ctrl Pts',(-64.9022892917531,-1.75479339219151,
1.40822864408661));
#31924=CARTESIAN_POINT('Ctrl Pts',(-65.5254424463325,-1.67712774330567,
1.37118268056393));
#31925=CARTESIAN_POINT('Ctrl Pts',(-65.9733751709996,-1.35546112873117,
1.33413671704125));
#31926=CARTESIAN_POINT('Ctrl Pts',(-66.3990566948007,-1.0497734057594,1.2989310235641));
#31927=CARTESIAN_POINT('Ctrl Pts',(-66.6664936696292,-0.5237242626975,1.26372533008694));
#31928=CARTESIAN_POINT('Ctrl Pts',(-66.6685688018723,0.000500570493875176,
1.22851963660979));
#31929=CARTESIAN_POINT('Origin',(-65.,8.88178419700125E-15,3.));
#31930=CARTESIAN_POINT('',(-66.6657538157597,-0.00152189319960278,0.528519636609788));
#31931=CARTESIAN_POINT('',(-66.6632893889008,-6.33249066055908E-5,0.721480363390205));
#31932=CARTESIAN_POINT('',(-66.666,8.90896198514149E-15,3.));
#31933=CARTESIAN_POINT('Ctrl Pts',(-66.6632893889008,-6.33249066055908E-5,
0.721480363390205));
#31934=CARTESIAN_POINT('Ctrl Pts',(-66.663382354964,-0.274266208525866,
0.739746284990023));
#31935=CARTESIAN_POINT('Ctrl Pts',(-66.5993416986523,-0.548428211919451,
0.758012206589842));
#31936=CARTESIAN_POINT('Ctrl Pts',(-66.4709289590166,-0.788100662831112,
0.77627812818966));
#31937=CARTESIAN_POINT('Ctrl Pts',(-66.2104891206872,-1.274191486409,0.81332409171234));
#31938=CARTESIAN_POINT('Ctrl Pts',(-65.6852625770594,-1.61841374682522,
0.850370055235021));
#31939=CARTESIAN_POINT('Ctrl Pts',(-65.1356222340335,-1.66323217468976,
0.887416018757702));
#31940=CARTESIAN_POINT('Ctrl Pts',(-64.5859818910076,-1.7080506025543,0.924461982280382));
#31941=CARTESIAN_POINT('Ctrl Pts',(-64.0119277485837,-1.45346519786716,
0.961507945803063));
#31942=CARTESIAN_POINT('Ctrl Pts',(-63.6761789401645,-1.01598841469988,
0.998553909325744));
#31943=CARTESIAN_POINT('Ctrl Pts',(-63.3404301317454,-0.578511631532607,
1.03559987284842));
#31944=CARTESIAN_POINT('Ctrl Pts',(-63.242986657331,0.0418565301148077,
1.0726458363711));
#31945=CARTESIAN_POINT('Ctrl Pts',(-63.4284440755221,0.561201063347344,
1.10969179989379));
#31946=CARTESIAN_POINT('Ctrl Pts',(-63.6139014937132,1.08054559657989,1.14673776341647));
#31947=CARTESIAN_POINT('Ctrl Pts',(-64.0822598045097,1.49886650139754,1.18378372693915));
#31948=CARTESIAN_POINT('Ctrl Pts',(-64.619172171207,1.62471684366477,1.22082969046183));
#31949=CARTESIAN_POINT('Ctrl Pts',(-65.1560845379043,1.75056718593199,1.25787565398451));
#31950=CARTESIAN_POINT('Ctrl Pts',(-65.7615509605024,1.58394696564878,1.29492161750719));
#31951=CARTESIAN_POINT('Ctrl Pts',(-66.1584762974693,1.20111087143114,1.33196758102987));
#31952=CARTESIAN_POINT('Ctrl Pts',(-66.4781682685839,0.892766671210744,
1.36180517514998));
#31953=CARTESIAN_POINT('Ctrl Pts',(-66.6625790404782,0.444162614627713,
1.39164276927009));
#31954=CARTESIAN_POINT('Ctrl Pts',(-66.6666630352664,-0.00145874010107553,
1.4214803633902));
#31955=CARTESIAN_POINT('Ctrl Pts',(-66.6685688018723,0.000500570493875176,
1.22851963660979));
#31956=CARTESIAN_POINT('Ctrl Pts',(-66.6686772730691,0.0279028217311334,
1.22667936656426));
#31957=CARTESIAN_POINT('Ctrl Pts',(-66.6680606812028,0.0553000883040936,
1.22483909651874));
#31958=CARTESIAN_POINT('Ctrl Pts',(-66.6667037271851,0.082660636409592,
1.22299882647321));
#31959=CARTESIAN_POINT('Ctrl Pts',(-66.6393872639487,0.633448206712722,
1.18595286295053));
#31960=CARTESIAN_POINT('Ctrl Pts',(-66.3120420427213,1.16935576705584,1.14890689942785));
#31961=CARTESIAN_POINT('Ctrl Pts',(-65.8344794601719,1.44512218362151,1.11186093590517));
#31962=CARTESIAN_POINT('Ctrl Pts',(-65.3569168776225,1.72088860018718,1.07481497238249));
#31963=CARTESIAN_POINT('Ctrl Pts',(-64.729136933751,1.73651387297539,1.03776900885981));
#31964=CARTESIAN_POINT('Ctrl Pts',(-64.2384466796233,1.48484700734035,1.00072304533713));
#31965=CARTESIAN_POINT('Ctrl Pts',(-63.7477564254956,1.23318014170531,0.963677081814447));
#31966=CARTESIAN_POINT('Ctrl Pts',(-63.3941558611116,0.714221137647021,
0.926631118291766));
#31967=CARTESIAN_POINT('Ctrl Pts',(-63.3394722898162,0.165474525977697,
0.889585154769085));
#31968=CARTESIAN_POINT('Ctrl Pts',(-63.2847887185207,-0.383272085691625,
0.852539191246405));
#31969=CARTESIAN_POINT('Ctrl Pts',(-63.5290221403138,-0.961806304971977,
0.815493227723724));
#31970=CARTESIAN_POINT('Ctrl Pts',(-63.9603977448083,-1.30535866571471,
0.778447264201044));
#31971=CARTESIAN_POINT('Ctrl Pts',(-64.3917733493027,-1.64891102645745,
0.741401300678363));
#31972=CARTESIAN_POINT('Ctrl Pts',(-65.0102911364986,-1.75748152866257,
0.704355337155683));
#31973=CARTESIAN_POINT('Ctrl Pts',(-65.5328829338629,-1.58138226671975,
0.667309373633002));
#31974=CARTESIAN_POINT('Ctrl Pts',(-66.0554747312272,-1.40528300477693,
0.630263410110321));
#31975=CARTESIAN_POINT('Ctrl Pts',(-66.4821405387599,-0.944513978686166,
0.593217446587641));
#31976=CARTESIAN_POINT('Ctrl Pts',(-66.6176143302611,-0.409948745265357,
0.55617148306496));
#31977=CARTESIAN_POINT('Ctrl Pts',(-66.6513211107492,-0.276945359297945,
0.546954200913236));
#31978=CARTESIAN_POINT('Ctrl Pts',(-66.6670017222694,-0.139373637561401,
0.537736918761512));
#31979=CARTESIAN_POINT('Ctrl Pts',(-66.6657538157597,-0.00152189319960278,
0.528519636609788));
#31980=CARTESIAN_POINT('Origin',(-65.,8.88178419700125E-15,3.));
#31981=CARTESIAN_POINT('',(-66.6633878829795,0.000426123154294022,-0.171480363390211));
#31982=CARTESIAN_POINT('',(-66.6664305869533,0.00149161834302873,0.0214803633902054));
#31983=CARTESIAN_POINT('',(-66.666,8.90896198514149E-15,3.));
#31984=CARTESIAN_POINT('Ctrl Pts',(-66.6664305869533,0.00149161834302873,
0.0214803633902054));
#31985=CARTESIAN_POINT('Ctrl Pts',(-66.6623874613811,-0.43660857926759,
0.0508038371872736));
#31986=CARTESIAN_POINT('Ctrl Pts',(-66.484951449296,-0.877606426402566,
0.0801273109843417));
#31987=CARTESIAN_POINT('Ctrl Pts',(-66.1749931684956,-1.18495810418995,
0.10945078478141));
#31988=CARTESIAN_POINT('Ctrl Pts',(-65.7834057582335,-1.57325244894403,
0.146496748304091));
#31989=CARTESIAN_POINT('Ctrl Pts',(-65.1803040079573,-1.74823863365067,
0.183542711826771));
#31990=CARTESIAN_POINT('Ctrl Pts',(-64.641700851863,-1.62983323643182,0.220588675349452));
#31991=CARTESIAN_POINT('Ctrl Pts',(-64.1030976957686,-1.51142783921296,
0.257634638872132));
#31992=CARTESIAN_POINT('Ctrl Pts',(-63.6289931338561,-1.09963086006863,
0.294680602394813));
#31993=CARTESIAN_POINT('Ctrl Pts',(-63.4363638080708,-0.582903522671596,
0.331726565917493));
#31994=CARTESIAN_POINT('Ctrl Pts',(-63.2437344822855,-0.0661761852745638,
0.368772529440174));
#31995=CARTESIAN_POINT('Ctrl Pts',(-63.3325803926274,0.555481510375165,
0.405818492962854));
#31996=CARTESIAN_POINT('Ctrl Pts',(-63.6622407040169,0.997564395392442,
0.442864456485535));
#31997=CARTESIAN_POINT('Ctrl Pts',(-63.9919010154063,1.43964728040972,0.479910420008216));
#31998=CARTESIAN_POINT('Ctrl Pts',(-64.5623757278433,1.70215535479454,0.516956383530896));
#31999=CARTESIAN_POINT('Ctrl Pts',(-65.1125838545831,1.66495030949471,0.554002347053577));
#32000=CARTESIAN_POINT('Ctrl Pts',(-65.6627919813228,1.62774526419488,0.591048310576258));
#32001=CARTESIAN_POINT('Ctrl Pts',(-66.1927335223652,1.29082709921039,0.628094274098938));
#32002=CARTESIAN_POINT('Ctrl Pts',(-66.4598777263709,0.808388323348361,
0.665140237621619));
#32003=CARTESIAN_POINT('Ctrl Pts',(-66.5953035291742,0.563821315923753,
0.683920279544481));
#32004=CARTESIAN_POINT('Ctrl Pts',(-66.6631938061757,0.281857388570598,
0.702700321467343));
#32005=CARTESIAN_POINT('Ctrl Pts',(-66.6632893889008,-6.33249066055908E-5,
0.721480363390205));
#32006=CARTESIAN_POINT('Ctrl Pts',(-66.6657538157597,-0.00152189319960278,
0.528519636609788));
#32007=CARTESIAN_POINT('Ctrl Pts',(-66.6619861549602,0.414678045906911,
0.500690955238832));
#32008=CARTESIAN_POINT('Ctrl Pts',(-66.5039069443419,0.833430525360491,
0.472862273867875));
#32009=CARTESIAN_POINT('Ctrl Pts',(-66.2217249851539,1.13671551258267,0.445033592496918));
#32010=CARTESIAN_POINT('Ctrl Pts',(-65.8460800730759,1.54045309625903,0.407987628974238));
#32011=CARTESIAN_POINT('Ctrl Pts',(-65.2505084734505,1.7395668228609,0.370941665451557));
#32012=CARTESIAN_POINT('Ctrl Pts',(-64.7075769058774,1.64293116911908,0.333895701928877));
#32013=CARTESIAN_POINT('Ctrl Pts',(-64.1646453383043,1.54629551537725,0.296849738406196));
#32014=CARTESIAN_POINT('Ctrl Pts',(-63.6743538027836,1.15391048129173,0.259803774883516));
#32015=CARTESIAN_POINT('Ctrl Pts',(-63.4610870008646,0.645353297241691,
0.222757811360835));
#32016=CARTESIAN_POINT('Ctrl Pts',(-63.2478201989456,0.136796113191647,
0.185711847838155));
#32017=CARTESIAN_POINT('Ctrl Pts',(-63.3115781306282,-0.487933220822921,
0.148665884315474));
#32018=CARTESIAN_POINT('Ctrl Pts',(-63.6231816165986,-0.942923771900624,
0.111619920792793));
#32019=CARTESIAN_POINT('Ctrl Pts',(-63.9347851025691,-1.39791432297833,
0.0745739572701125));
#32020=CARTESIAN_POINT('Ctrl Pts',(-64.4942341428273,-1.68316609111917,
0.0375279937474321));
#32021=CARTESIAN_POINT('Ctrl Pts',(-65.0454937124919,-1.66813200830569,
0.000482030224751638));
#32022=CARTESIAN_POINT('Ctrl Pts',(-65.5967532821565,-1.65309792549221,
-0.0365639332979289));
#32023=CARTESIAN_POINT('Ctrl Pts',(-66.1398233812275,-1.33777799172442,
-0.0736098968206095));
#32024=CARTESIAN_POINT('Ctrl Pts',(-66.4261648980985,-0.866480120962484,
-0.11065586034329));
#32025=CARTESIAN_POINT('Ctrl Pts',(-66.5828763524582,-0.608544158441976,
-0.130930694692264));
#32026=CARTESIAN_POINT('Ctrl Pts',(-66.6626912202299,-0.303888929858138,
-0.151205529041237));
#32027=CARTESIAN_POINT('Ctrl Pts',(-66.6633878829795,0.000426123154294022,
-0.171480363390211));
#32028=CARTESIAN_POINT('Origin',(-65.,8.88178419700125E-15,3.));
#32029=CARTESIAN_POINT('',(-66.6673159824367,0.00130059074132209,-0.871480363390211));
#32030=CARTESIAN_POINT('',(-66.6681941903091,-0.000864019930029195,-0.678519636609795));
#32031=CARTESIAN_POINT('',(-66.666,8.90896198514149E-15,3.));
#32032=CARTESIAN_POINT('Ctrl Pts',(-66.6681941903091,-0.000864019930029195,
-0.678519636609795));
#32033=CARTESIAN_POINT('Ctrl Pts',(-66.6685078326159,-0.0505538571114753,
-0.675184574138157));
#32034=CARTESIAN_POINT('Ctrl Pts',(-66.6664801000417,-0.100217739688416,
-0.67184951166652));
#32035=CARTESIAN_POINT('Ctrl Pts',(-66.6620276056557,-0.149663274321054,
-0.668514449194882));
#32036=CARTESIAN_POINT('Ctrl Pts',(-66.6125691784105,-0.698905601245364,
-0.631468485672201));
#32037=CARTESIAN_POINT('Ctrl Pts',(-66.2639236084022,-1.22120635507833,
-0.594422522149521));
#32038=CARTESIAN_POINT('Ctrl Pts',(-65.7756507075141,-1.47753189011201,
-0.557376558626841));
#32039=CARTESIAN_POINT('Ctrl Pts',(-65.287377806626,-1.73385742514569,-0.52033059510416));
#32040=CARTESIAN_POINT('Ctrl Pts',(-64.659477574858,-1.72420774138009,-0.483284631581479));
#32041=CARTESIAN_POINT('Ctrl Pts',(-64.1793120174543,-1.45299894151709,
-0.446238668058799));
#32042=CARTESIAN_POINT('Ctrl Pts',(-63.6991464600505,-1.18179014165408,
-0.409192704536118));
#32043=CARTESIAN_POINT('Ctrl Pts',(-63.3667155770108,-0.649022225693665,
-0.372146741013438));
#32044=CARTESIAN_POINT('Ctrl Pts',(-63.334158295787,-0.098519517195975,
-0.335100777490757));
#32045=CARTESIAN_POINT('Ctrl Pts',(-63.3016010145631,0.451983191301712,
-0.298054813968077));
#32046=CARTESIAN_POINT('Ctrl Pts',(-63.568917335155,1.02022069233667,-0.261008850445396));
#32047=CARTESIAN_POINT('Ctrl Pts',(-64.0137684029003,1.34613590481466,-0.223962886922715));
#32048=CARTESIAN_POINT('Ctrl Pts',(-64.4586194706456,1.67205111729264,-0.186916923400034));
#32049=CARTESIAN_POINT('Ctrl Pts',(-65.0810052855443,1.75564404121365,-0.149870959877354));
#32050=CARTESIAN_POINT('Ctrl Pts',(-65.5960874627954,1.55865788401291,-0.112824996354674));
#32051=CARTESIAN_POINT('Ctrl Pts',(-66.1111696400466,1.36167172681217,-0.0757790328319931));
#32052=CARTESIAN_POINT('Ctrl Pts',(-66.5189481796502,0.884106488489685,
-0.0387330693093125));
#32053=CARTESIAN_POINT('Ctrl Pts',(-66.632800914328,0.344522616927675,-0.00168710578663189));
#32054=CARTESIAN_POINT('Ctrl Pts',(-66.6565343117127,0.232042591898964,
0.00603538393898058));
#32055=CARTESIAN_POINT('Ctrl Pts',(-66.6674953651548,0.116867589766136,
0.013757873664593));
#32056=CARTESIAN_POINT('Ctrl Pts',(-66.6664305869533,0.00149161834302873,
0.0214803633902054));
#32057=CARTESIAN_POINT('Ctrl Pts',(-66.6633878829795,0.000426123154294022,
-0.171480363390211));
#32058=CARTESIAN_POINT('Ctrl Pts',(-66.6639641550595,0.252152325979392,
-0.188251492563918));
#32059=CARTESIAN_POINT('Ctrl Pts',(-66.6104043971,0.503645766257019,-0.205022621737625));
#32060=CARTESIAN_POINT('Ctrl Pts',(-66.5014511773033,0.728270889754936,
-0.221793750911332));
#32061=CARTESIAN_POINT('Ctrl Pts',(-66.2607830049661,1.22444822195433,-0.258839714434013));
#32062=CARTESIAN_POINT('Ctrl Pts',(-65.7498337256207,1.58952707859705,-0.295885677956694));
#32063=CARTESIAN_POINT('Ctrl Pts',(-65.2024421689935,1.65642721292162,-0.332931641479375));
#32064=CARTESIAN_POINT('Ctrl Pts',(-64.6550506123664,1.72332734724618,-0.369977605002055));
#32065=CARTESIAN_POINT('Ctrl Pts',(-64.0712167784575,1.4920487592526,-0.407023568524736));
#32066=CARTESIAN_POINT('Ctrl Pts',(-63.7181355422591,1.06843708657373,-0.444069532047416));
#32067=CARTESIAN_POINT('Ctrl Pts',(-63.3650543060608,0.644825413894857,
-0.481115495570097));
#32068=CARTESIAN_POINT('Ctrl Pts',(-63.242725667573,0.0288806565306957,
-0.518161459092778));
#32069=CARTESIAN_POINT('Ctrl Pts',(-63.4071340014642,-0.497505944605285,
-0.555207422615458));
#32070=CARTESIAN_POINT('Ctrl Pts',(-63.5715423353554,-1.02389254574127,
-0.592253386138139));
#32071=CARTESIAN_POINT('Ctrl Pts',(-64.0226876416257,-1.46072099064906,
-0.629299349660819));
#32072=CARTESIAN_POINT('Ctrl Pts',(-64.5541007528815,-1.6080755066333,-0.6663453131835));
#32073=CARTESIAN_POINT('Ctrl Pts',(-65.0855138641373,-1.75543002261753,
-0.70339127670618));
#32074=CARTESIAN_POINT('Ctrl Pts',(-65.6971947803788,-1.6133106096782,-0.740437240228861));
#32075=CARTESIAN_POINT('Ctrl Pts',(-66.1092041825925,-1.24675657433953,
-0.777483203751541));
#32076=CARTESIAN_POINT('Ctrl Pts',(-66.4576696191289,-0.936735950411702,
-0.808815590297765));
#32077=CARTESIAN_POINT('Ctrl Pts',(-66.6633044515624,-0.466170980160872,
-0.840147976843988));
#32078=CARTESIAN_POINT('Ctrl Pts',(-66.6673159824367,0.00130059074132209,
-0.871480363390211));
#32079=CARTESIAN_POINT('Origin',(-65.,8.88178419700125E-15,3.));
#32080=CARTESIAN_POINT('',(-66.6674675207825,-0.00121113675535883,-1.57148036339021));
#32081=CARTESIAN_POINT('',(-66.6638321395092,-0.000941642735140673,-1.3785196366098));
#32082=CARTESIAN_POINT('',(-66.666,8.90896198514149E-15,3.));
#32083=CARTESIAN_POINT('',(-63.7309291201476,-1.0793586530485,-2.));
#32084=CARTESIAN_POINT('Ctrl Pts',(-66.6674675207825,-0.00121113675535883,
-1.57148036339021));
#32085=CARTESIAN_POINT('Ctrl Pts',(-66.6635269376583,0.471550204230273,
-1.6031823516921));
#32086=CARTESIAN_POINT('Ctrl Pts',(-66.452430524463,0.947291842680182,-1.63488433999399));
#32087=CARTESIAN_POINT('Ctrl Pts',(-66.0967466510819,1.25757678610754,-1.66658632829587));
#32088=CARTESIAN_POINT('Ctrl Pts',(-65.6811054719418,1.62016617912559,-1.70363229181856));
#32089=CARTESIAN_POINT('Ctrl Pts',(-65.0680223500032,1.75681556827132,-1.74067825534124));
#32090=CARTESIAN_POINT('Ctrl Pts',(-64.5381019768621,1.60385217794779,-1.77772421886392));
#32091=CARTESIAN_POINT('Ctrl Pts',(-64.008181603721,1.45088878762426,-1.8147701823866));
#32092=CARTESIAN_POINT('Ctrl Pts',(-63.5614239793774,1.00831261783146,-1.85181614590928));
#32093=CARTESIAN_POINT('Ctrl Pts',(-63.4023827506955,0.481249822665519,
-1.88886210943196));
#32094=CARTESIAN_POINT('Ctrl Pts',(-63.2433415220136,-0.0458129725004199,
-1.92590807295464));
#32095=CARTESIAN_POINT('Ctrl Pts',(-63.3720166889934,-0.6573623930395,-1.96295403647732));
#32096=CARTESIAN_POINT('Ctrl Pts',(-63.7309291201476,-1.0793586530485,-2.));
#32097=CARTESIAN_POINT('',(-66.2714644419457,-1.08121564890976,-2.));
#32098=CARTESIAN_POINT('Origin',(-65.,8.88178419700125E-15,-2.));
#32099=CARTESIAN_POINT('Ctrl Pts',(-66.2714656498818,-1.08121658606209,
-2.));
#32100=CARTESIAN_POINT('Ctrl Pts',(-65.9206041791687,-1.49275399655514,
-1.96367708181445));
#32101=CARTESIAN_POINT('Ctrl Pts',(-65.350635463119,-1.71875942899392,-1.92735416362889));
#32102=CARTESIAN_POINT('Ctrl Pts',(-64.8132380266976,-1.65815373977101,
-1.89103124544334));
#32103=CARTESIAN_POINT('Ctrl Pts',(-64.2651431372632,-1.59634163148307,
-1.85398528192066));
#32104=CARTESIAN_POINT('Ctrl Pts',(-63.7509291640016,-1.23639424886418,
-1.81693931839798));
#32105=CARTESIAN_POINT('Ctrl Pts',(-63.5055956276972,-0.742592085292541,
-1.7798933548753));
#32106=CARTESIAN_POINT('Ctrl Pts',(-63.2602620913927,-0.248789921720896,
-1.74284739135262));
#32107=CARTESIAN_POINT('Ctrl Pts',(-63.2838089920452,0.378867022803503,
-1.70580142782994));
#32108=CARTESIAN_POINT('Ctrl Pts',(-63.5656287203753,0.852900276652188,
-1.66875546430726));
#32109=CARTESIAN_POINT('Ctrl Pts',(-63.8474484487053,1.32693353050087,-1.63170950078458));
#32110=CARTESIAN_POINT('Ctrl Pts',(-64.387541004713,1.64734309367384,-1.5946635372619));
#32111=CARTESIAN_POINT('Ctrl Pts',(-64.9386444101885,1.66760708582443,-1.55761757373922));
#32112=CARTESIAN_POINT('Ctrl Pts',(-65.4897478156641,1.68787107797503,-1.52057161021654));
#32113=CARTESIAN_POINT('Ctrl Pts',(-66.0518620706076,1.40798949910324,-1.48352564669385));
#32114=CARTESIAN_POINT('Ctrl Pts',(-66.3677757854406,0.955993240532992,
-1.44647968317117));
#32115=CARTESIAN_POINT('Ctrl Pts',(-66.5609548232979,0.67960067431637,-1.42382633431738));
#32116=CARTESIAN_POINT('Ctrl Pts',(-66.6620736349107,0.338850343710045,
-1.40117298546359));
#32117=CARTESIAN_POINT('Ctrl Pts',(-66.6638321395092,-0.000941642735140673,
-1.3785196366098));
#32118=CARTESIAN_POINT('Origin',(-65.,8.88178419700125E-15,-3.54592528053767));
#32119=CARTESIAN_POINT('',(-67.0572086816557,-0.00119446450308647,6.54592528053768));
#32120=CARTESIAN_POINT('',(-67.0515888779951,0.000804696401313844,6.60407471946233));
#32121=CARTESIAN_POINT('',(-67.05475,-9.40612120991423E-14,-3.54592528053767));
#32122=CARTESIAN_POINT('',(-63.1173724903363,0.823232180103149,7.));
#32123=CARTESIAN_POINT('Ctrl Pts',(-67.0515888779951,0.000804696401313851,
6.60407471946233));
#32124=CARTESIAN_POINT('Ctrl Pts',(-67.0504040800969,-0.384787351067738,
6.62491192240684));
#32125=CARTESIAN_POINT('Ctrl Pts',(-66.7605424545076,-1.45760454425863,
6.68279508887404));
#32126=CARTESIAN_POINT('Ctrl Pts',(-65.029841359516,-2.42994159679626,6.77772421886392));
#32127=CARTESIAN_POINT('Ctrl Pts',(-62.9747815436376,-1.33872801408515,
6.88886210943195));
#32128=CARTESIAN_POINT('Ctrl Pts',(-62.8436282049399,0.19721374355959,6.96295403647732));
#32129=CARTESIAN_POINT('Ctrl Pts',(-63.1173724903363,0.823232180103149,
7.));
#32130=CARTESIAN_POINT('',(-63.7764000215903,1.65534094402446,7.));
#32131=CARTESIAN_POINT('Origin',(-65.,8.88178419700125E-15,7.));
#32132=CARTESIAN_POINT('Ctrl Pts',(-67.0572086816557,-0.00119446450308609,
6.54592528053768));
#32133=CARTESIAN_POINT('Ctrl Pts',(-67.0577114364342,-0.0728343130723733,
6.54982271160486));
#32134=CARTESIAN_POINT('Ctrl Pts',(-67.0218209037147,-0.824923083408348,
6.59076610619472));
#32135=CARTESIAN_POINT('Ctrl Pts',(-66.0963109962835,-2.16731896239628,
6.66875546430726));
#32136=CARTESIAN_POINT('Ctrl Pts',(-63.7734206371606,-2.09605634078855,
6.77989335487529));
#32137=CARTESIAN_POINT('Ctrl Pts',(-62.5820931272045,-0.120092092488803,
6.89030820010622));
#32138=CARTESIAN_POINT('Ctrl Pts',(-63.2405356955179,1.25818726815372,6.96367708181444));
#32139=CARTESIAN_POINT('Ctrl Pts',(-63.7763989699203,1.65534250909263,7.));
#32140=CARTESIAN_POINT('Origin',(-65.,8.88178419700125E-15,-3.54592528053767));
#32141=CARTESIAN_POINT('',(-67.0519117333221,-0.00102649957300818,5.84592528053768));
#32142=CARTESIAN_POINT('',(-67.0566574869574,0.00149765431884231,5.90407471946233));
#32143=CARTESIAN_POINT('',(-67.05475,-9.40612120991423E-14,-3.54592528053767));
#32144=CARTESIAN_POINT('Ctrl Pts',(-67.0566574869574,0.00149765431884247,
5.90407471946233));
#32145=CARTESIAN_POINT('Ctrl Pts',(-67.0518463029865,-0.585190437662465,
5.93596947460409));
#32146=CARTESIAN_POINT('Ctrl Pts',(-66.4813711624858,-1.8614882619805,6.00491019326854));
#32147=CARTESIAN_POINT('Ctrl Pts',(-64.3156972041947,-2.33026144716284,
6.11089687545566));
#32148=CARTESIAN_POINT('Ctrl Pts',(-62.6710926659578,-0.688814355154873,
6.22203476602371));
#32149=CARTESIAN_POINT('Ctrl Pts',(-63.1582101680956,1.58293676398102,6.33317265659174));
#32150=CARTESIAN_POINT('Ctrl Pts',(-65.3310466291073,2.40615402668531,6.4443105471598));
#32151=CARTESIAN_POINT('Ctrl Pts',(-66.8504470921567,1.28501547118087,6.53461123478332));
#32152=CARTESIAN_POINT('Ctrl Pts',(-67.0525105038734,0.300747505180014,
6.58786595888416));
#32153=CARTESIAN_POINT('Ctrl Pts',(-67.0515888779951,0.000804696401313851,
6.60407471946233));
#32154=CARTESIAN_POINT('Ctrl Pts',(-67.0519117333221,-0.00102649957300794,
5.84592528053768));
#32155=CARTESIAN_POINT('Ctrl Pts',(-67.0531633450758,-0.277741730134872,
5.86088026380211));
#32156=CARTESIAN_POINT('Ctrl Pts',(-66.8721481216246,-1.2383569525156,5.91288121058921));
#32157=CARTESIAN_POINT('Ctrl Pts',(-65.4121253417219,-2.39341760299656,
6.00192812089901));
#32158=CARTESIAN_POINT('Ctrl Pts',(-63.2126643336617,-1.64429852840487,
6.11306601146705));
#32159=CARTESIAN_POINT('Ctrl Pts',(-62.649189925264,0.60985028512182,6.22420390203509));
#32160=CARTESIAN_POINT('Ctrl Pts',(-64.2374031554986,2.30582648807955,6.33534179260313));
#32161=CARTESIAN_POINT('Ctrl Pts',(-66.4435230617628,1.90573437919649,6.44258225210399));
#32162=CARTESIAN_POINT('Ctrl Pts',(-67.0529326385893,0.608118645715832,
6.51277674808218));
#32163=CARTESIAN_POINT('Ctrl Pts',(-67.0572086816557,-0.00119446450308609,
6.54592528053768));
#32164=CARTESIAN_POINT('Origin',(-65.,8.88178419700125E-15,-3.54592528053767));
#32165=CARTESIAN_POINT('',(-67.0534842785189,0.00176526399348016,5.14592528053768));
#32166=CARTESIAN_POINT('',(-67.0562728194261,-0.00163389830065408,5.20407471946232));
#32167=CARTESIAN_POINT('',(-67.05475,-9.40612120991423E-14,-3.54592528053767));
#32168=CARTESIAN_POINT('Ctrl Pts',(-67.0562728194261,-0.00163389830065397,
5.20407471946232));
#32169=CARTESIAN_POINT('Ctrl Pts',(-67.0572175303294,-0.110331419494764,
5.20998106327866));
#32170=CARTESIAN_POINT('Ctrl Pts',(-66.9999469228229,-0.899807785912462,
5.25293337061767));
#32171=CARTESIAN_POINT('Ctrl Pts',(-65.9773779060574,-2.22328871643558,
5.33293164147938));
#32172=CARTESIAN_POINT('Ctrl Pts',(-63.6621652804381,-2.0269388363574,5.44406953204741));
#32173=CARTESIAN_POINT('Ctrl Pts',(-62.5714875417724,0.0246926647779575,
5.55520742261546));
#32174=CARTESIAN_POINT('Ctrl Pts',(-63.7036555936518,2.05371969901984,5.66634531318349));
#32175=CARTESIAN_POINT('Ctrl Pts',(-66.0223808123334,2.20295969802022,5.77748320375154));
#32176=CARTESIAN_POINT('Ctrl Pts',(-67.0084336557534,0.871640043874873,
5.85672633917782));
#32177=CARTESIAN_POINT('Ctrl Pts',(-67.0574345241562,0.0962515598736501,
5.89892351108141));
#32178=CARTESIAN_POINT('Ctrl Pts',(-67.0566574869574,0.00149765431884247,
5.90407471946233));
#32179=CARTESIAN_POINT('Ctrl Pts',(-67.0534842785189,0.00176526399348016,
5.14592528053768));
#32180=CARTESIAN_POINT('Ctrl Pts',(-67.049548506192,-0.478623619806704,
5.17193781599936));
#32181=CARTESIAN_POINT('Ctrl Pts',(-66.6418658995519,-1.6491803337807,5.23499631498372));
#32182=CARTESIAN_POINT('Ctrl Pts',(-64.6918158067504,-2.40900502421389,
5.33510077749075));
#32183=CARTESIAN_POINT('Ctrl Pts',(-62.80891719594,-1.04758718972751,5.4462386680588));
#32184=CARTESIAN_POINT('Ctrl Pts',(-62.9315418303621,1.27269881881277,5.55737655862684));
#32185=CARTESIAN_POINT('Ctrl Pts',(-64.947449081762,2.42806968006159,5.66851444919488));
#32186=CARTESIAN_POINT('Ctrl Pts',(-66.7337199477999,1.50458731301856,5.7646973564985));
#32187=CARTESIAN_POINT('Ctrl Pts',(-67.0500628960447,0.407727598470006,
5.82383430027943));
#32188=CARTESIAN_POINT('Ctrl Pts',(-67.0519117333221,-0.00102649957300794,
5.84592528053768));
#32189=CARTESIAN_POINT('Origin',(-65.,8.88178419700125E-15,-3.54592528053767));
#32190=CARTESIAN_POINT('',(-67.0581446603105,-8.27717200928135E-6,4.44592528053768));
#32191=CARTESIAN_POINT('',(-67.051502599911,-0.00046897283331893,4.50407471946232));
#32192=CARTESIAN_POINT('',(-67.05475,-9.40612120991423E-14,-3.54592528053767));
#32193=CARTESIAN_POINT('Ctrl Pts',(-67.051502599911,-0.00046897283331862,
4.50407471946232));
#32194=CARTESIAN_POINT('Ctrl Pts',(-67.0521436877867,-0.314512114650342,
4.52103861547591));
#32195=CARTESIAN_POINT('Ctrl Pts',(-66.8367516776872,-1.31353269400002,
4.57504847501217));
#32196=CARTESIAN_POINT('Ctrl Pts',(-65.2821091229946,-2.41219729396228,
4.66610429807113));
#32197=CARTESIAN_POINT('Ctrl Pts',(-63.1263775009061,-1.5452572946423,4.77724218863916));
#32198=CARTESIAN_POINT('Ctrl Pts',(-62.6855937936814,0.736074256717683,
4.88838007920721));
#32199=CARTESIAN_POINT('Ctrl Pts',(-64.3632123478174,2.34366864230481,4.99951796977525));
#32200=CARTESIAN_POINT('Ctrl Pts',(-66.5035583733625,1.83464658396607,5.10474951652696));
#32201=CARTESIAN_POINT('Ctrl Pts',(-67.0512920835974,0.571444740237986,
5.17293509975598));
#32202=CARTESIAN_POINT('Ctrl Pts',(-67.0562728194261,-0.00163389830065397,
5.20407471946232));
#32203=CARTESIAN_POINT('Ctrl Pts',(-67.0581446431809,-8.27713024233776E-6,
4.44592528053768));
#32204=CARTESIAN_POINT('Ctrl Pts',(-67.0581446696346,-0.00045118411400466,
4.44594940467392));
#32205=CARTESIAN_POINT('Ctrl Pts',(-67.0579439709526,-0.681039286739854,
4.48301949233285));
#32206=CARTESIAN_POINT('Ctrl Pts',(-66.315832277707,-2.04129075981347,4.55713554351446));
#32207=CARTESIAN_POINT('Ctrl Pts',(-63.9986308592856,-2.21258726309084,
4.66827343408251));
#32208=CARTESIAN_POINT('Ctrl Pts',(-62.5979939690176,-0.358677549762027,
4.77941132465054));
#32209=CARTESIAN_POINT('Ctrl Pts',(-63.3959404447163,1.82353378810158,4.89054921521859));
#32210=CARTESIAN_POINT('Ctrl Pts',(-65.6621008123707,2.33664397819608,5.00168710578663));
#32211=CARTESIAN_POINT('Ctrl Pts',(-66.9336682838985,1.0914904129242,5.08681246089299));
#32212=CARTESIAN_POINT('Ctrl Pts',(-67.0551536682982,0.205526108395703,
5.13489185247667));
#32213=CARTESIAN_POINT('Ctrl Pts',(-67.0534842785189,0.00176526399348016,
5.14592528053768));
#32214=CARTESIAN_POINT('Origin',(-65.,8.88178419700125E-15,-3.54592528053767));
#32215=CARTESIAN_POINT('',(-67.0534601308484,-0.00176006036929743,3.74592528053768));
#32216=CARTESIAN_POINT('',(-67.0545529589347,0.00187890219046263,3.80407471946232));
#32217=CARTESIAN_POINT('',(-67.05475,-9.40612120991423E-14,-3.54592528053767));
#32218=CARTESIAN_POINT('Ctrl Pts',(-67.0545529589347,0.00187890219046255,
3.80407471946232));
#32219=CARTESIAN_POINT('Ctrl Pts',(-67.049847975054,-0.514925815373994,
3.83209616767316));
#32220=CARTESIAN_POINT('Ctrl Pts',(-66.5901947888396,-1.72243254492318,
3.89716357940667));
#32221=CARTESIAN_POINT('Ctrl Pts',(-64.5620129419189,-2.3888174265201,3.99927695466288));
#32222=CARTESIAN_POINT('Ctrl Pts',(-62.7554801641395,-0.927583994626942,
4.11041484523091));
#32223=CARTESIAN_POINT('Ctrl Pts',(-63.0033818465923,1.3826775875065,4.22155273579896));
#32224=CARTESIAN_POINT('Ctrl Pts',(-65.0788107682801,2.42735869229697,4.33269062636699));
#32225=CARTESIAN_POINT('Ctrl Pts',(-66.7763241812549,1.4299225698547,4.42686462092146));
#32226=CARTESIAN_POINT('Ctrl Pts',(-67.0507436722455,0.371299138082145,
4.48399265195323));
#32227=CARTESIAN_POINT('Ctrl Pts',(-67.051502599911,-0.00046897283331862,
4.50407471946232));
#32228=CARTESIAN_POINT('Ctrl Pts',(-67.0534601308484,-0.0017600603692971,
3.74592528053768));
#32229=CARTESIAN_POINT('Ctrl Pts',(-67.055130441991,-0.206418025502587,
3.75700695687117));
#32230=CARTESIAN_POINT('Ctrl Pts',(-66.9329701809384,-1.09329696547216,
3.80513459672735));
#32231=CARTESIAN_POINT('Ctrl Pts',(-65.6590644304509,-2.3375022198779,3.89030820010621));
#32232=CARTESIAN_POINT('Ctrl Pts',(-63.39357261301,-1.82144821550898,4.00144609067426));
#32233=CARTESIAN_POINT('Ctrl Pts',(-62.5984620009619,0.361797997181342,
4.1125839812423));
#32234=CARTESIAN_POINT('Ctrl Pts',(-64.0015063548152,2.21388639990767,4.22372187181034));
#32235=CARTESIAN_POINT('Ctrl Pts',(-66.3179803312342,2.03961730968541,4.33483563824213));
#32236=CARTESIAN_POINT('Ctrl Pts',(-67.0581040462783,0.679694036228928,
4.40890344115124));
#32237=CARTESIAN_POINT('Ctrl Pts',(-67.0581446431809,-8.27713024233776E-6,
4.44592528053768));
#32238=CARTESIAN_POINT('Origin',(-65.,8.88178419700125E-15,-3.54592528053767));
#32239=CARTESIAN_POINT('',(-67.0519256006226,0.00103910123989234,3.04592528053768));
#32240=CARTESIAN_POINT('',(-67.0578709601416,-0.000678769155100989,3.10407471946232));
#32241=CARTESIAN_POINT('',(-67.05475,-9.40612120991423E-14,-3.54592528053767));
#32242=CARTESIAN_POINT('Ctrl Pts',(-67.0578709601415,-0.000678769155101162,
3.10407471946232));
#32243=CARTESIAN_POINT('Ctrl Pts',(-67.0580316799421,-0.0380175835266657,
3.10610775634773));
#32244=CARTESIAN_POINT('Ctrl Pts',(-67.0401889053665,-0.755586934309652,
3.14518675675581));
#32245=CARTESIAN_POINT('Ctrl Pts',(-66.2035357618251,-2.1094508836634,3.22131172068658));
#32246=CARTESIAN_POINT('Ctrl Pts',(-63.8804623217255,-2.15520689204011,
3.33244961125462));
#32247=CARTESIAN_POINT('Ctrl Pts',(-62.5821144149725,-0.228277590427775,
3.44358750182266));
#32248=CARTESIAN_POINT('Ctrl Pts',(-63.4968846048806,1.90759677855457,3.55472539239071));
#32249=CARTESIAN_POINT('Ctrl Pts',(-65.7874733624335,2.29742618249228,3.66586328295874));
#32250=CARTESIAN_POINT('Ctrl Pts',(-66.9614802130625,1.01630569367124,3.74897972531595));
#32251=CARTESIAN_POINT('Ctrl Pts',(-67.0560682339038,0.168319696106685,
3.79505020415048));
#32252=CARTESIAN_POINT('Ctrl Pts',(-67.0545529589347,0.00187890219046255,
3.80407471946232));
#32253=CARTESIAN_POINT('Ctrl Pts',(-67.0519256006226,0.00103910123989245,
3.04592528053768));
#32254=CARTESIAN_POINT('Ctrl Pts',(-67.0500496331103,-0.408601099978636,
3.06806450906842));
#32255=CARTESIAN_POINT('Ctrl Pts',(-66.7326598083642,-1.50637690262577,
3.12724970112185));
#32256=CARTESIAN_POINT('Ctrl Pts',(-64.9442948490232,-2.42799907075925,
3.22348085669796));
#32257=CARTESIAN_POINT('Ctrl Pts',(-62.9298898830714,-1.27001049414664,
3.334618747266));
#32258=CARTESIAN_POINT('Ctrl Pts',(-62.8102801837888,1.05043309065765,3.44575663783405));
#32259=CARTESIAN_POINT('Ctrl Pts',(-64.6949458653977,2.40940335486023,3.55689452840209));
#32260=CARTESIAN_POINT('Ctrl Pts',(-66.643067780423,1.64741324066797,3.65695074263663));
#32261=CARTESIAN_POINT('Ctrl Pts',(-67.0495466039689,0.477752065987548,
3.71996099334849));
#32262=CARTESIAN_POINT('Ctrl Pts',(-67.0534601308484,-0.0017600603692971,
3.74592528053768));
#32263=CARTESIAN_POINT('Origin',(-65.,8.88178419700125E-15,-3.54592528053767));
#32264=CARTESIAN_POINT('',(-67.0572522603608,0.00120217803180264,2.34592528053767));
#32265=CARTESIAN_POINT('',(-67.0525490214284,-0.00145097609280704,2.40407471946232));
#32266=CARTESIAN_POINT('',(-67.05475,-9.40612120991423E-14,-3.54592528053767));
#32267=CARTESIAN_POINT('Ctrl Pts',(-67.0525490214284,-0.00145097609280675,
2.40407471946232));
#32268=CARTESIAN_POINT('Ctrl Pts',(-67.054127131265,-0.243480442393208,
2.41716530854498));
#32269=CARTESIAN_POINT('Ctrl Pts',(-66.9026176062656,-1.16853384943058,
2.46730186115031));
#32270=CARTESIAN_POINT('Ctrl Pts',(-65.5317127142361,-2.36971790517293,
2.55448437727833));
#32271=CARTESIAN_POINT('Ctrl Pts',(-63.2974379205056,-1.73192486154719,
2.66562226784637));
#32272=CARTESIAN_POINT('Ctrl Pts',(-62.6215375065036,0.491118649216447,
2.77676015841441));
#32273=CARTESIAN_POINT('Ctrl Pts',(-64.122670786398,2.26463569068811,2.88789804898245));
#32274=CARTESIAN_POINT('Ctrl Pts',(-66.3846835747723,1.97078161673767,2.99700290266509));
#32275=CARTESIAN_POINT('Ctrl Pts',(-67.0551030464715,0.642369656429121,
3.06906179282505));
#32276=CARTESIAN_POINT('Ctrl Pts',(-67.0578709601415,-0.000678769155101162,
3.10407471946232));
#32277=CARTESIAN_POINT('Ctrl Pts',(-67.0572522603608,0.00120217803180282,
2.34592528053767));
#32278=CARTESIAN_POINT('Ctrl Pts',(-67.0530108672503,-0.608976283722039,
2.37912206126567));
#32279=CARTESIAN_POINT('Ctrl Pts',(-66.4420019119215,-1.9074607758001,2.44936480551635));
#32280=CARTESIAN_POINT('Ctrl Pts',(-64.234427664365,-2.30481703186257,2.55665351328971));
#32281=CARTESIAN_POINT('Ctrl Pts',(-62.6483896081628,-0.606804018161647,
2.66779140385776));
#32282=CARTESIAN_POINT('Ctrl Pts',(-63.214807212685,1.64662359498827,2.77892929442579));
#32283=CARTESIAN_POINT('Ctrl Pts',(-65.4152320208998,2.39287795766376,2.89006718499384));
#32284=CARTESIAN_POINT('Ctrl Pts',(-66.8729657074861,1.23655088859839,2.97906584703113));
#32285=CARTESIAN_POINT('Ctrl Pts',(-67.0531887228005,0.276857109673468,
3.03101854554574));
#32286=CARTESIAN_POINT('Ctrl Pts',(-67.0519256006226,0.00103910123989245,
3.04592528053768));
#32287=CARTESIAN_POINT('Origin',(-65.,8.88178419700125E-15,-3.54592528053767));
#32288=CARTESIAN_POINT('',(-67.0555677501283,-0.00179912738464016,1.64592528053767));
#32289=CARTESIAN_POINT('',(-67.0526273462695,0.00148795516933967,1.70407471946232));
#32290=CARTESIAN_POINT('',(-67.05475,-9.40612120991423E-14,-3.54592528053767));
#32291=CARTESIAN_POINT('Ctrl Pts',(-67.0526273462695,0.00148795516933968,
1.70407471946232));
#32292=CARTESIAN_POINT('Ctrl Pts',(-67.049634688556,-0.444939705966109,
1.72822286074222));
#32293=CARTESIAN_POINT('Ctrl Pts',(-66.6869954305654,-1.58066428073723,
1.78941696554481));
#32294=CARTESIAN_POINT('Ctrl Pts',(-64.8130956691436,-2.42143513885566,
1.88765703387008));
#32295=CARTESIAN_POINT('Ctrl Pts',(-62.864249480632,-1.15622276382909,1.99879492443812));
#32296=CARTESIAN_POINT('Ctrl Pts',(-62.8702799635561,1.1672934193881,2.10993281500616));
#32297=CARTESIAN_POINT('Ctrl Pts',(-64.8256673485052,2.42237269783169,2.2210707055742));
#32298=CARTESIAN_POINT('Ctrl Pts',(-66.6915092429239,1.57355497286028,2.31911800705959));
#32299=CARTESIAN_POINT('Ctrl Pts',(-67.0496611290802,0.441455485498574,
2.3801193450223));
#32300=CARTESIAN_POINT('Ctrl Pts',(-67.0525490214284,-0.00145097609280675,
2.40407471946232));
#32301=CARTESIAN_POINT('Ctrl Pts',(-67.0555677501283,-0.00179912738464004,
1.64592528053767));
#32302=CARTESIAN_POINT('Ctrl Pts',(-67.0567846151392,-0.134576239702309,
1.65313364994024));
#32303=CARTESIAN_POINT('Ctrl Pts',(-66.9845642825309,-0.948416460674393,
1.69738798286549));
#32304=CARTESIAN_POINT('Ctrl Pts',(-65.898842928637,-2.25618349012117,1.77868827931342));
#32305=CARTESIAN_POINT('Ctrl Pts',(-63.5919355659201,-1.97879688218178,
1.88982616988146));
#32306=CARTESIAN_POINT('Ctrl Pts',(-62.5738455482538,0.109804953100741,
2.0009640604495));
#32307=CARTESIAN_POINT('Ctrl Pts',(-63.7764422147334,2.0979010695377,2.11210195101754));
#32308=CARTESIAN_POINT('Ctrl Pts',(-66.0989751981566,2.16576454521031,2.22323984158559));
#32309=CARTESIAN_POINT('Ctrl Pts',(-67.0223280499568,0.823134106038546,
2.30118095142563));
#32310=CARTESIAN_POINT('Ctrl Pts',(-67.0577440519451,0.0719526660358392,
2.34207609774299));
#32311=CARTESIAN_POINT('Ctrl Pts',(-67.0572522603608,0.00120217803180282,
2.34592528053767));
#32312=CARTESIAN_POINT('Origin',(-65.,8.88178419700125E-15,-3.54592528053767));
#32313=CARTESIAN_POINT('',(-67.0514068858608,-7.81013517094087E-5,0.945925280537675));
#32314=CARTESIAN_POINT('',(-67.0579182146741,0.000617375283499791,1.00407471946232));
#32315=CARTESIAN_POINT('',(-67.05475,-9.40612120991423E-14,-3.54592528053767));
#32316=CARTESIAN_POINT('Ctrl Pts',(-67.0579182146741,0.000617375283499685,
1.00407471946232));
#32317=CARTESIAN_POINT('Ctrl Pts',(-67.0553588641481,-0.645931829998605,
1.03928041293948));
#32318=CARTESIAN_POINT('Ctrl Pts',(-66.378434179731,-1.977444237299,1.11153206993931));
#32319=CARTESIAN_POINT('Ctrl Pts',(-64.1109273576576,-2.26005114925192,
1.22082969046183));
#32320=CARTESIAN_POINT('Ctrl Pts',(-62.6190202559434,-0.47876593338251,
1.33196758102987));
#32321=CARTESIAN_POINT('Ctrl Pts',(-63.3064509161112,1.74073917087914,1.44310547159791));
#32322=CARTESIAN_POINT('Ctrl Pts',(-65.5440062589152,2.36692597071417,1.55424336216595));
#32323=CARTESIAN_POINT('Ctrl Pts',(-66.9056402449312,1.161313621274,1.64123311145409));
#32324=CARTESIAN_POINT('Ctrl Pts',(-67.0542257619312,0.239930514819847,
1.69117689721954));
#32325=CARTESIAN_POINT('Ctrl Pts',(-67.0526273462695,0.00148795516933968,
1.70407471946232));
#32326=CARTESIAN_POINT('Ctrl Pts',(-67.0514068858608,-7.81013517092005E-5,
0.945925280537675));
#32327=CARTESIAN_POINT('Ctrl Pts',(-67.0515215449353,-0.338264400941531,
0.964191202137492));
#32328=CARTESIAN_POINT('Ctrl Pts',(-66.8123460743743,-1.36218935655874,
1.01950308725999));
#32329=CARTESIAN_POINT('Ctrl Pts',(-65.1973793755662,-2.42060404314487,
1.11186093590517));
#32330=CARTESIAN_POINT('Ctrl Pts',(-63.0733618200821,-1.47863040518406,
1.22299882647321));
#32331=CARTESIAN_POINT('Ctrl Pts',(-62.7128180402749,0.816750411403611,
1.33413671704125));
#32332=CARTESIAN_POINT('Ctrl Pts',(-64.4457578465939,2.36455031387797,1.4452746076093));
#32333=CARTESIAN_POINT('Ctrl Pts',(-66.5407002488233,1.78803648666642,1.54920412877477));
#32334=CARTESIAN_POINT('Ctrl Pts',(-67.0505307823665,0.547805001444303,
1.61608768641756));
#32335=CARTESIAN_POINT('Ctrl Pts',(-67.0555677501283,-0.00179912738464004,
1.64592528053767));
#32336=CARTESIAN_POINT('Origin',(-65.,8.88178419700125E-15,-3.54592528053767));
#32337=CARTESIAN_POINT('',(-67.05528106155,0.00183967754518982,0.245925280537674));
#32338=CARTESIAN_POINT('',(-67.0544463703074,-0.0018770168378236,0.304074719462319));
#32339=CARTESIAN_POINT('',(-67.05475,-9.40612120991423E-14,-3.54592528053767));
#32340=CARTESIAN_POINT('Ctrl Pts',(-67.0544463703074,-0.00187701683782321,
0.304074719462319));
#32341=CARTESIAN_POINT('Ctrl Pts',(-67.0559854674868,-0.171895547286461,
0.313292001614044));
#32342=CARTESIAN_POINT('Ctrl Pts',(-66.9589165461202,-1.02351658402418,
0.359555247288449));
#32343=CARTESIAN_POINT('Ctrl Pts',(-65.7755372964953,-2.30148283939099,
0.442864456485536));
#32344=CARTESIAN_POINT('Ctrl Pts',(-63.4870029209119,-1.89976872281361,
0.554002347053577));
#32345=CARTESIAN_POINT('Ctrl Pts',(-62.5833319303427,0.240825251495458,
0.665140237621619));
#32346=CARTESIAN_POINT('Ctrl Pts',(-63.8916646308255,2.16098914151126,0.77627812818966));
#32347=CARTESIAN_POINT('Ctrl Pts',(-66.2144692640843,2.10317516324911,0.887416018757702));
#32348=CARTESIAN_POINT('Ctrl Pts',(-67.0419827284221,0.748425825038287,
0.963348215848589));
#32349=CARTESIAN_POINT('Ctrl Pts',(-67.058051996902,0.0344137592749453,
1.0022344494168));
#32350=CARTESIAN_POINT('Ctrl Pts',(-67.0579182146741,0.000617375283499685,
1.00407471946232));
#32351=CARTESIAN_POINT('Ctrl Pts',(-67.05528106155,0.00183967754518984,
0.245925280537674));
#32352=CARTESIAN_POINT('Ctrl Pts',(-67.0502944995635,-0.538488282262975,
0.275248754334741));
#32353=CARTESIAN_POINT('Ctrl Pts',(-66.5549829233901,-1.76953115899707,
0.341618191654489));
#32354=CARTESIAN_POINT('Ctrl Pts',(-64.4785452214709,-2.37199651591817,
0.445033592496919));
#32355=CARTESIAN_POINT('Ctrl Pts',(-62.7243441135659,-0.848335334231208,
0.55617148306496));
#32356=CARTESIAN_POINT('Ctrl Pts',(-63.0530766482751,1.45181679686654,0.667309373633002));
#32357=CARTESIAN_POINT('Ctrl Pts',(-65.1638502053818,2.42310455048397,0.778447264201043));
#32358=CARTESIAN_POINT('Ctrl Pts',(-66.8023851755325,1.38138173267995,0.871319233169269));
#32359=CARTESIAN_POINT('Ctrl Pts',(-67.0512889995436,0.34762693227213,0.927145238614812));
#32360=CARTESIAN_POINT('Ctrl Pts',(-67.0514068858608,-7.81013517092005E-5,
0.945925280537675));
#32361=CARTESIAN_POINT('Origin',(-65.,8.88178419700125E-15,-3.54592528053767));
#32362=CARTESIAN_POINT('',(-67.0574561899986,-0.00106563322407216,-0.454074719462326));
#32363=CARTESIAN_POINT('',(-67.0515283628764,0.0005255561532822,-0.39592528053768));
#32364=CARTESIAN_POINT('',(-67.05475,-9.40612120991423E-14,-3.54592528053767));
#32365=CARTESIAN_POINT('Ctrl Pts',(-67.0515283628764,0.000525556153282321,
-0.39592528053768));
#32366=CARTESIAN_POINT('Ctrl Pts',(-67.0506691385159,-0.374799386930345,
-0.375650446188706));
#32367=CARTESIAN_POINT('Ctrl Pts',(-66.7723630529996,-1.43710026477804,
-0.318329648317051));
#32368=CARTESIAN_POINT('Ctrl Pts',(-65.0662097961853,-2.42773505180942,
-0.223962886922715));
#32369=CARTESIAN_POINT('Ctrl Pts',(-62.9962315570428,-1.37229494871089,
-0.112824996354674));
#32370=CARTESIAN_POINT('Ctrl Pts',(-62.7603252963136,0.939222336522791,
-0.00168710578663132));
#32371=CARTESIAN_POINT('Ctrl Pts',(-64.5744186923722,2.39105873890073,0.10945078478141));
#32372=CARTESIAN_POINT('Ctrl Pts',(-66.5952919861857,1.71543281453755,0.211371393197727));
#32373=CARTESIAN_POINT('Ctrl Pts',(-67.0497995509631,0.511440405058386,
0.276246038091363));
#32374=CARTESIAN_POINT('Ctrl Pts',(-67.0544463703074,-0.00187701683782321,
0.304074719462319));
#32375=CARTESIAN_POINT('Ctrl Pts',(-67.0574561899986,-0.00106563322407194,
-0.454074719462326));
#32376=CARTESIAN_POINT('Ctrl Pts',(-67.057843018648,-0.062350262845054,
-0.450739656990689));
#32377=CARTESIAN_POINT('Ctrl Pts',(-67.0275621697751,-0.803998615243591,
-0.410358630996372));
#32378=CARTESIAN_POINT('Ctrl Pts',(-66.1288520704621,-2.15034287637184,
-0.332931641479373));
#32379=CARTESIAN_POINT('Ctrl Pts',(-63.8056023683761,-2.11463875683277,
-0.221793750911332));
#32380=CARTESIAN_POINT('Ctrl Pts',(-62.5755981242121,-0.143381478345974,
-0.110655860343291));
#32381=CARTESIAN_POINT('Ctrl Pts',(-63.5646765331008,1.95911432942999,0.00048203022475183));
#32382=CARTESIAN_POINT('Ctrl Pts',(-65.8675227272721,2.26841065672896,0.111619920792793));
#32383=CARTESIAN_POINT('Ctrl Pts',(-66.9782240837151,0.967625288007812,
0.193434337563767));
#32384=CARTESIAN_POINT('Ctrl Pts',(-67.0565942986505,0.144137863188435,
0.238202790812061));
#32385=CARTESIAN_POINT('Ctrl Pts',(-67.05528106155,0.00183967754518984,
0.245925280537674));
#32386=CARTESIAN_POINT('Origin',(-65.,8.88178419700125E-15,-3.54592528053767));
#32387=CARTESIAN_POINT('',(-67.0520762837074,-0.00116136879358866,-1.15407471946233));
#32388=CARTESIAN_POINT('',(-67.0563730581704,0.00160407492546517,-1.09592528053768));
#32389=CARTESIAN_POINT('',(-67.05475,-9.40612120991423E-14,-3.54592528053767));
#32390=CARTESIAN_POINT('Ctrl Pts',(-67.0563730581704,0.00160407492546514,
-1.09592528053768));
#32391=CARTESIAN_POINT('Ctrl Pts',(-67.051425463294,-0.57494887244027,-1.06459289399146));
#32392=CARTESIAN_POINT('Ctrl Pts',(-66.4979405147664,-1.84151750410658,
-0.99621454392255));
#32393=CARTESIAN_POINT('Ctrl Pts',(-64.3510553719621,-2.34032995360773,
-0.890790230330967));
#32394=CARTESIAN_POINT('Ctrl Pts',(-62.6818041989874,-0.724051597351479,
-0.779652339762924));
#32395=CARTESIAN_POINT('Ctrl Pts',(-63.1344238327198,1.55496249063294,-0.668514449194883));
#32396=CARTESIAN_POINT('Ctrl Pts',(-65.2946265402067,2.41070020734328,-0.55737655862684));
#32397=CARTESIAN_POINT('Ctrl Pts',(-66.8402661138972,1.30632380217905,-0.466513502407773));
#32398=CARTESIAN_POINT('Ctrl Pts',(-67.0522391042067,0.310990391240222,
-0.412696409711387));
#32399=CARTESIAN_POINT('Ctrl Pts',(-67.0515283628764,0.000525556153282321,
-0.39592528053768));
#32400=CARTESIAN_POINT('Ctrl Pts',(-67.0520762837074,-0.0011613687935888,
-1.15407471946233));
#32401=CARTESIAN_POINT('Ctrl Pts',(-67.053454237916,-0.267420438121926,
-1.13968210479344));
#32402=CARTESIAN_POINT('Ctrl Pts',(-66.8815877450925,-1.21731358290939,
-1.08824352660187));
#32403=CARTESIAN_POINT('Ctrl Pts',(-65.4483108550045,-2.38688976599862,
-0.999758984887625));
#32404=CARTESIAN_POINT('Ctrl Pts',(-63.2377776981899,-1.67118490708905,
-0.888621094319582));
#32405=CARTESIAN_POINT('Ctrl Pts',(-62.6402125087857,0.574193448178942,
-0.777483203751542));
#32406=CARTESIAN_POINT('Ctrl Pts',(-64.2025947176117,2.29399639382146,-0.666345313183498));
#32407=CARTESIAN_POINT('Ctrl Pts',(-66.4260607263055,1.92548386768539,-0.558542485087094));
#32408=CARTESIAN_POINT('Ctrl Pts',(-67.0535461156186,0.618401049236239,
-0.48778562051337));
#32409=CARTESIAN_POINT('Ctrl Pts',(-67.0574561899986,-0.00106563322407194,
-0.454074719462326));
#32410=CARTESIAN_POINT('Origin',(-65.,8.88178419700125E-15,-3.54592528053767));
#32411=CARTESIAN_POINT('',(-67.052679279082,0.0023836951352374,-1.85407471946233));
#32412=CARTESIAN_POINT('',(-67.0565599569794,-0.0014937474477788,-1.79592528053768));
#32413=CARTESIAN_POINT('',(-67.05475,-9.40612120991423E-14,-3.54592528053767));
#32414=CARTESIAN_POINT('',(-65.5301702171886,1.98517432567173,-2.));
#32415=CARTESIAN_POINT('Ctrl Pts',(-65.5301702171886,1.98517432567173,-2.));
#32416=CARTESIAN_POINT('Ctrl Pts',(-66.1902879097456,1.80888011517989,-1.96295403647732));
#32417=CARTESIAN_POINT('Ctrl Pts',(-66.9249664054372,1.11286144556364,-1.91431227629809));
#32418=CARTESIAN_POINT('Ctrl Pts',(-67.0542991139265,0.216633244974153,
-1.86567051611887));
#32419=CARTESIAN_POINT('Ctrl Pts',(-67.052679279082,0.0023836951352375,
-1.85407471946232));
#32420=CARTESIAN_POINT('',(-64.468704775017,1.98873730573667,-2.));
#32421=CARTESIAN_POINT('Origin',(-65.,8.88178419700125E-15,-2.));
#32422=CARTESIAN_POINT('Ctrl Pts',(-64.4687042096542,1.98873909628093,-2.));
#32423=CARTESIAN_POINT('Ctrl Pts',(-65.1133181823237,2.16007183004146,-1.96367708181445));
#32424=CARTESIAN_POINT('Ctrl Pts',(-66.4930415100228,1.84061483765585,-1.89565217532701));
#32425=CARTESIAN_POINT('Ctrl Pts',(-67.051699865038,0.581583302606364,-1.82762726883957));
#32426=CARTESIAN_POINT('Ctrl Pts',(-67.0565599569794,-0.00149374744777858,
-1.79592528053768));
#32427=CARTESIAN_POINT('Origin',(-32.5,-56.2916512459885,3.));
#32428=CARTESIAN_POINT('',(-33.334828594439,-57.735188017533,6.12851963660979));
#32429=CARTESIAN_POINT('',(-33.3331620889267,-57.736668395617,6.32148036339022));
#32430=CARTESIAN_POINT('',(-33.333,-57.7344495686934,3.));
#32431=CARTESIAN_POINT('',(-33.5940263469955,-57.5480995545471,7.));
#32432=CARTESIAN_POINT('Ctrl Pts',(-33.3331620889267,-57.736668395617,6.32148036339022));
#32433=CARTESIAN_POINT('Ctrl Pts',(-33.2830618082469,-57.7660644611829,
6.3253777944574));
#32434=CARTESIAN_POINT('Ctrl Pts',(-33.2314063486239,-57.7926890534068,
6.32927522552458));
#32435=CARTESIAN_POINT('Ctrl Pts',(-33.1783991110197,-57.816276539757,6.33317265659176));
#32436=CARTESIAN_POINT('Ctrl Pts',(-32.6745533323838,-58.0404809307675,
6.37021862011444));
#32437=CARTESIAN_POINT('Ctrl Pts',(-32.0485753278831,-57.9902848612727,
6.40726458363712));
#32438=CARTESIAN_POINT('Ctrl Pts',(-31.5869763637319,-57.6885282775577,
6.4443105471598));
#32439=CARTESIAN_POINT('Ctrl Pts',(-31.1253773995808,-57.3867716938426,
6.48135651068248));
#32440=CARTESIAN_POINT('Ctrl Pts',(-30.8281574757792,-56.8334545959073,
6.51840247420516));
#32441=CARTESIAN_POINT('Ctrl Pts',(-30.8312835014825,-56.2820697925606,
6.55544843772784));
#32442=CARTESIAN_POINT('Ctrl Pts',(-30.8344095271858,-55.730684989214,6.59249440125052));
#32443=CARTESIAN_POINT('Ctrl Pts',(-31.1378815023941,-55.181232480456,6.6295403647732));
#32444=CARTESIAN_POINT('Ctrl Pts',(-31.6029277671502,-54.8846445462124,
6.66658632829588));
#32445=CARTESIAN_POINT('Ctrl Pts',(-32.0679740319062,-54.5880566119689,
6.70363229181856));
#32446=CARTESIAN_POINT('Ctrl Pts',(-32.69459458621,-54.5443332522399,6.74067825534124));
#32447=CARTESIAN_POINT('Ctrl Pts',(-33.1957905862087,-54.7745591362764,
6.77772421886393));
#32448=CARTESIAN_POINT('Ctrl Pts',(-33.6969865862074,-55.0047850203128,
6.81477018238661));
#32449=CARTESIAN_POINT('Ctrl Pts',(-34.072758031901,-55.5089601481148,6.85181614590929));
#32450=CARTESIAN_POINT('Ctrl Pts',(-34.1514677107856,-56.0538413345857,
6.88886210943197));
#32451=CARTESIAN_POINT('Ctrl Pts',(-34.2301773896702,-56.5987225210566,
6.92590807295465));
#32452=CARTESIAN_POINT('Ctrl Pts',(-34.0118253017458,-57.1843097661965,
6.96295403647733));
#32453=CARTESIAN_POINT('Ctrl Pts',(-33.5940263469955,-57.5480995545471,
7.00000000000001));
#32454=CARTESIAN_POINT('',(-31.0815846268762,-57.1712794637622,7.));
#32455=CARTESIAN_POINT('Origin',(-32.5,-56.2916512459885,7.));
#32456=CARTESIAN_POINT('',(-33.3322874886545,-57.7319139206533,6.82851963660979));
#32457=CARTESIAN_POINT('Ctrl Pts',(-31.0815830733444,-57.1712803260695,
7.));
#32458=CARTESIAN_POINT('Ctrl Pts',(-31.3671885733957,-57.6305045882042,
6.96367708181444));
#32459=CARTESIAN_POINT('Ctrl Pts',(-31.8971081113245,-57.9389632567025,
6.92735416362889));
#32460=CARTESIAN_POINT('Ctrl Pts',(-32.4375390310396,-57.9591354579208,
6.89103124544334));
#32461=CARTESIAN_POINT('Ctrl Pts',(-32.747565573898,-57.9707075526648,6.87019404249882));
#32462=CARTESIAN_POINT('Ctrl Pts',(-33.0610513288344,-57.8874068657131,
6.8493568395543));
#32463=CARTESIAN_POINT('Ctrl Pts',(-33.3322874886545,-57.7319139206533,
6.82851963660979));
#32464=CARTESIAN_POINT('',(-33.333,-57.7344495686934,8.));
#32465=CARTESIAN_POINT('',(-33.333,-57.7344495686934,3.));
#32466=CARTESIAN_POINT('Origin',(-32.5,-56.2916512459885,8.));
#32467=CARTESIAN_POINT('Ctrl Pts',(-33.3322874886545,-57.7319139206533,
6.82851963660979));
#32468=CARTESIAN_POINT('Ctrl Pts',(-33.5432755942256,-57.6109596867872,
6.81231087603162));
#32469=CARTESIAN_POINT('Ctrl Pts',(-33.7286988454439,-57.4463225594196,
6.79610211545346));
#32470=CARTESIAN_POINT('Ctrl Pts',(-33.8670427528186,-57.2486779404331,
6.77989335487529));
#32471=CARTESIAN_POINT('Ctrl Pts',(-34.1832349330579,-56.796950906147,6.74284739135261));
#32472=CARTESIAN_POINT('Ctrl Pts',(-34.2534965093546,-56.1728010705694,
6.70580142782993));
#32473=CARTESIAN_POINT('Ctrl Pts',(-34.0454742915244,-55.6620590905692,
6.66875546430725));
#32474=CARTESIAN_POINT('Ctrl Pts',(-33.8374520736943,-55.151317110569,6.63170950078457));
#32475=CARTESIAN_POINT('Ctrl Pts',(-33.3511460617375,-54.7539829861461,
6.59466353726189));
#32476=CARTESIAN_POINT('Ctrl Pts',(-32.8092161915406,-54.651806090904,6.55761757373921));
#32477=CARTESIAN_POINT('Ctrl Pts',(-32.2672863213437,-54.549629195662,6.52057161021653));
#32478=CARTESIAN_POINT('Ctrl Pts',(-31.6697325929069,-54.7426095296008,
6.48352564669385));
#32479=CARTESIAN_POINT('Ctrl Pts',(-31.2899790079621,-55.1424751852064,
6.44647968317117));
#32480=CARTESIAN_POINT('Ctrl Pts',(-30.9102254230173,-55.542340840812,6.40943371964849));
#32481=CARTESIAN_POINT('Ctrl Pts',(-30.7482719815646,-56.1490918180843,
6.37238775612581));
#32482=CARTESIAN_POINT('Ctrl Pts',(-30.8782626384457,-56.6850216626072,
6.33534179260313));
#32483=CARTESIAN_POINT('Ctrl Pts',(-31.0082532953267,-57.2209515071302,
6.29829582908045));
#32484=CARTESIAN_POINT('Ctrl Pts',(-31.4301880505415,-57.6860602189039,
6.26124986555777));
#32485=CARTESIAN_POINT('Ctrl Pts',(-31.9509534890594,-57.8674999291041,
6.22420390203509));
#32486=CARTESIAN_POINT('Ctrl Pts',(-32.3993069550896,-58.023710608475,6.19230914689332));
#32487=CARTESIAN_POINT('Ctrl Pts',(-32.9209173239095,-57.9696554900369,
6.16041439175155));
#32488=CARTESIAN_POINT('Ctrl Pts',(-33.334828594439,-57.735188017533,6.12851963660979));
#32489=CARTESIAN_POINT('Origin',(-32.5,-56.2916512459885,3.));
#32490=CARTESIAN_POINT('',(-33.3324736911222,-57.7361875215801,5.42851963660979));
#32491=CARTESIAN_POINT('',(-33.3311322154953,-57.7328790961699,5.62148036339021));
#32492=CARTESIAN_POINT('',(-33.333,-57.7344495686934,3.));
#32493=CARTESIAN_POINT('Ctrl Pts',(-33.3311322154953,-57.7328790961699,
5.62148036339021));
#32494=CARTESIAN_POINT('Ctrl Pts',(-33.1373356857267,-57.8459393971242,
5.63643534665465));
#32495=CARTESIAN_POINT('Ctrl Pts',(-32.9222440320564,-57.9213835767879,
5.65139032991907));
#32496=CARTESIAN_POINT('Ctrl Pts',(-32.7012486057465,-57.9482311745983,
5.6663453131835));
#32497=CARTESIAN_POINT('Ctrl Pts',(-32.1538064350001,-58.0147371085448,
5.70339127670618));
#32498=CARTESIAN_POINT('Ctrl Pts',(-31.5701366653479,-57.7830375418651,
5.74043724022886));
#32499=CARTESIAN_POINT('Ctrl Pts',(-31.2173595401895,-57.3591689672607,
5.77748320375154));
#32500=CARTESIAN_POINT('Ctrl Pts',(-30.8645824150311,-56.9353003926564,
5.81452916727423));
#32501=CARTESIAN_POINT('Ctrl Pts',(-30.7426979343665,-56.3192628101275,
5.85157513079691));
#32502=CARTESIAN_POINT('Ctrl Pts',(-30.9074862986933,-55.7929935490272,
5.88862109431959));
#32503=CARTESIAN_POINT('Ctrl Pts',(-31.0722746630201,-55.266724287927,5.92566705784227));
#32504=CARTESIAN_POINT('Ctrl Pts',(-31.5237358723384,-54.8302233482555,
5.96271302136495));
#32505=CARTESIAN_POINT('Ctrl Pts',(-32.0552579823816,-54.6832494251182,
5.99975898488763));
#32506=CARTESIAN_POINT('Ctrl Pts',(-32.5867800924248,-54.5362755019809,
6.03680494841031));
#32507=CARTESIAN_POINT('Ctrl Pts',(-33.1983631031929,-54.6788285953779,
6.07385091193299));
#32508=CARTESIAN_POINT('Ctrl Pts',(-33.6101089221165,-55.0456852682332,
6.11089687545567));
#32509=CARTESIAN_POINT('Ctrl Pts',(-34.02185474104,-55.4125419410885,6.14794283897835));
#32510=CARTESIAN_POINT('Ctrl Pts',(-34.233763368119,-56.003702193402,6.18498880250103));
#32511=CARTESIAN_POINT('Ctrl Pts',(-34.1488609052729,-56.5485847453165,
6.22203476602372));
#32512=CARTESIAN_POINT('Ctrl Pts',(-34.0728906300368,-57.0361427742909,
6.25518329847922));
#32513=CARTESIAN_POINT('Ctrl Pts',(-33.7592763040381,-57.4866482113774,
6.28833183093472));
#32514=CARTESIAN_POINT('Ctrl Pts',(-33.3331620889267,-57.736668395617,6.32148036339022));
#32515=CARTESIAN_POINT('Ctrl Pts',(-33.334828594439,-57.735188017533,6.12851963660979));
#32516=CARTESIAN_POINT('Ctrl Pts',(-33.4016779305205,-57.6973200105818,
6.12336842822887));
#32517=CARTESIAN_POINT('Ctrl Pts',(-33.4657180077386,-57.6547460681795,
6.11821721984796));
#32518=CARTESIAN_POINT('Ctrl Pts',(-33.5261864969391,-57.6075919565364,
6.11306601146705));
#32519=CARTESIAN_POINT('Ctrl Pts',(-33.96105794448,-57.2684735651416,6.07602004794436));
#32520=CARTESIAN_POINT('Ctrl Pts',(-34.2112047177408,-56.6924660737253,
6.03897408442168));
#32521=CARTESIAN_POINT('Ctrl Pts',(-34.1621425519641,-56.1431855476954,
6.001928120899));
#32522=CARTESIAN_POINT('Ctrl Pts',(-34.1130803861875,-55.5939050216654,
5.96488215737632));
#32523=CARTESIAN_POINT('Ctrl Pts',(-33.7648092813734,-55.0713514610218,
5.92783619385364));
#32524=CARTESIAN_POINT('Ctrl Pts',(-33.2767190788242,-54.8146729733941,
5.89079023033096));
#32525=CARTESIAN_POINT('Ctrl Pts',(-32.788628876275,-54.5579944857664,5.85374426680828));
#32526=CARTESIAN_POINT('Ctrl Pts',(-32.1607195759906,-54.5671910711545,
5.8166983032856));
#32527=CARTESIAN_POINT('Ctrl Pts',(-31.6803566282498,-54.8380546099095,
5.77965233976292));
#32528=CARTESIAN_POINT('Ctrl Pts',(-31.199993680509,-55.1089181486644,5.74260637624024));
#32529=CARTESIAN_POINT('Ctrl Pts',(-30.8671770853119,-55.6414486407862,
5.70556041271756));
#32530=CARTESIAN_POINT('Ctrl Pts',(-30.834222647304,-56.1919301102113,5.66851444919488));
#32531=CARTESIAN_POINT('Ctrl Pts',(-30.8012682092961,-56.7424115796364,
5.63146848567219));
#32532=CARTESIAN_POINT('Ctrl Pts',(-31.0681759284774,-57.3108440263648,
5.59442252214951));
#32533=CARTESIAN_POINT('Ctrl Pts',(-31.5127937714062,-57.6370813071645,
5.55737655862683));
#32534=CARTESIAN_POINT('Ctrl Pts',(-31.9574116143351,-57.9633185879642,
5.52033059510415));
#32535=CARTESIAN_POINT('Ctrl Pts',(-32.5797395810114,-58.0473607028353,
5.48328463158148));
#32536=CARTESIAN_POINT('Ctrl Pts',(-33.0949658502735,-57.8507452062819,
5.4462386680588));
#32537=CARTESIAN_POINT('Ctrl Pts',(-33.1771098465446,-57.8193982358743,
5.44033232424246));
#32538=CARTESIAN_POINT('Ctrl Pts',(-33.2565314423349,-57.7809172756724,
5.43442598042612));
#32539=CARTESIAN_POINT('Ctrl Pts',(-33.3324736911222,-57.7361875215801,
5.42851963660979));
#32540=CARTESIAN_POINT('Origin',(-32.5,-56.2916512459885,3.));
#32541=CARTESIAN_POINT('',(-33.3313578105535,-57.7323657066332,4.72851963660978));
#32542=CARTESIAN_POINT('',(-33.3337300498339,-57.7328514726872,4.92148036339021));
#32543=CARTESIAN_POINT('',(-33.333,-57.7344495686934,3.));
#32544=CARTESIAN_POINT('Ctrl Pts',(-33.3337300498339,-57.7328514726872,
4.92148036339021));
#32545=CARTESIAN_POINT('Ctrl Pts',(-32.9948149402968,-57.9248393749082,
4.94749289885189));
#32546=CARTESIAN_POINT('Ctrl Pts',(-32.5875734400098,-58.0025082442025,
4.97350543431357));
#32547=CARTESIAN_POINT('Ctrl Pts',(-32.2063909254829,-57.9343784669252,
4.99951796977525));
#32548=CARTESIAN_POINT('Ctrl Pts',(-31.6635267533437,-57.8373508916032,
5.03656393329793));
#32549=CARTESIAN_POINT('Ctrl Pts',(-31.1735161025779,-57.4446106606261,
5.07360989682062));
#32550=CARTESIAN_POINT('Ctrl Pts',(-30.9606151335011,-56.9358975335329,
5.1106558603433));
#32551=CARTESIAN_POINT('Ctrl Pts',(-30.7477141644243,-56.4271844064398,
5.14770182386598));
#32552=CARTESIAN_POINT('Ctrl Pts',(-30.8119228770365,-55.8024983832305,
5.18474778738865));
#32553=CARTESIAN_POINT('Ctrl Pts',(-31.1238557751029,-55.3477306326436,
5.22179375091133));
#32554=CARTESIAN_POINT('Ctrl Pts',(-31.4357886731693,-54.8929628820567,
5.25883971443402));
#32555=CARTESIAN_POINT('Ctrl Pts',(-31.9954457566899,-54.6081134040922,
5.2958856779567));
#32556=CARTESIAN_POINT('Ctrl Pts',(-32.5466968174263,-54.6235450421449,
5.33293164147938));
#32557=CARTESIAN_POINT('Ctrl Pts',(-33.0979478781627,-54.6389766801977,
5.36997760500206));
#32558=CARTESIAN_POINT('Ctrl Pts',(-33.6407929161149,-54.9546894342676,
5.40702356852474));
#32559=CARTESIAN_POINT('Ctrl Pts',(-33.9267957627755,-55.4261958418307,
5.44406953204742));
#32560=CARTESIAN_POINT('Ctrl Pts',(-34.2127986094362,-55.8977022493938,
5.4811154955701));
#32561=CARTESIAN_POINT('Ctrl Pts',(-34.2419592648052,-56.5250023104501,
5.51816145909278));
#32562=CARTESIAN_POINT('Ctrl Pts',(-34.0009323065694,-57.0210080582645,
5.55520742261547));
#32563=CARTESIAN_POINT('Ctrl Pts',(-33.8572048591017,-57.3167826080678,
5.57729840287372));
#32564=CARTESIAN_POINT('Ctrl Pts',(-33.6174016975492,-57.565870358533,5.59938938313197));
#32565=CARTESIAN_POINT('Ctrl Pts',(-33.3311322154953,-57.7328790961699,
5.62148036339021));
#32566=CARTESIAN_POINT('Ctrl Pts',(-33.3324736911222,-57.7361875215801,
5.42851963660979));
#32567=CARTESIAN_POINT('Ctrl Pts',(-33.7328589074961,-57.5003618440874,
5.39738001690344));
#32568=CARTESIAN_POINT('Ctrl Pts',(-34.0365306675145,-57.0908419490654,
5.36624039719709));
#32569=CARTESIAN_POINT('Ctrl Pts',(-34.1325589902306,-56.6373526743003,
5.33510077749075));
#32570=CARTESIAN_POINT('Ctrl Pts',(-34.246801289078,-56.0978487468504,5.29805481396807));
#32571=CARTESIAN_POINT('Ctrl Pts',(-34.0671613149251,-55.4961139999285,
5.26100885044539));
#32572=CARTESIAN_POINT('Ctrl Pts',(-33.6758523462209,-55.1075357285357,
5.22396288692271));
#32573=CARTESIAN_POINT('Ctrl Pts',(-33.2845433775166,-54.7189574571428,
5.18691692340003));
#32574=CARTESIAN_POINT('Ctrl Pts',(-32.681565414261,-54.5435356612789,5.14987095987735));
#32575=CARTESIAN_POINT('Ctrl Pts',(-32.1428747275693,-54.6615531325857,
5.11282499635467));
#32576=CARTESIAN_POINT('Ctrl Pts',(-31.6041840408777,-54.7795706038924,
5.07577903283198));
#32577=CARTESIAN_POINT('Ctrl Pts',(-31.12978063075,-55.1910273423697,5.03873306930931));
#32578=CARTESIAN_POINT('Ctrl Pts',(-30.9367779143555,-55.7076178324787,
5.00168710578663));
#32579=CARTESIAN_POINT('Ctrl Pts',(-30.7437751979609,-56.2242083225877,
4.96464114226394));
#32580=CARTESIAN_POINT('Ctrl Pts',(-30.8321731752993,-56.8459325643283,
4.92759517874126));
#32581=CARTESIAN_POINT('Ctrl Pts',(-31.1615160075389,-57.2882549360944,
4.89054921521858));
#32582=CARTESIAN_POINT('Ctrl Pts',(-31.4908588397784,-57.7305773078605,
4.8535032516959));
#32583=CARTESIAN_POINT('Ctrl Pts',(-32.0611465269192,-57.9934978096521,
4.81645728817322));
#32584=CARTESIAN_POINT('Ctrl Pts',(-32.6113836768238,-57.956689381435,4.77941132465054));
#32585=CARTESIAN_POINT('Ctrl Pts',(-32.8633454266668,-57.93983425636,4.76244742863696));
#32586=CARTESIAN_POINT('Ctrl Pts',(-33.1111028597659,-57.8601301739612,
4.74548353262337));
#32587=CARTESIAN_POINT('Ctrl Pts',(-33.3313578105535,-57.7323657066332,
4.72851963660978));
#32588=CARTESIAN_POINT('Origin',(-32.5,-56.2916512459885,3.));
#32589=CARTESIAN_POINT('',(-33.3342430690557,-57.7335557705023,4.02851963660978));
#32590=CARTESIAN_POINT('',(-33.3343740412804,-57.7368429003791,4.22148036339021));
#32591=CARTESIAN_POINT('',(-33.333,-57.7344495686934,3.));
#32592=CARTESIAN_POINT('Ctrl Pts',(-33.3343740344483,-57.7368428884788,
4.22148036339021));
#32593=CARTESIAN_POINT('Ctrl Pts',(-32.8564950497481,-58.0127845069312,
4.25855045104914));
#32594=CARTESIAN_POINT('Ctrl Pts',(-32.2282029771155,-58.0281412318725,
4.29562053870807));
#32595=CARTESIAN_POINT('Ctrl Pts',(-31.7373727175272,-57.7759553439527,
4.332690626367));
#32596=CARTESIAN_POINT('Ctrl Pts',(-31.2468618760144,-57.5239335712834,
4.36973658988968));
#32597=CARTESIAN_POINT('Ctrl Pts',(-30.8936340516087,-57.0047173912526,
4.40678255341236));
#32598=CARTESIAN_POINT('Ctrl Pts',(-30.8393459612069,-56.4559290322592,
4.44382851693504));
#32599=CARTESIAN_POINT('Ctrl Pts',(-30.7850578708051,-55.9071406732657,
4.48087448045772));
#32600=CARTESIAN_POINT('Ctrl Pts',(-31.0297095144072,-55.3287801353096,
4.51792044398041));
#32601=CARTESIAN_POINT('Ctrl Pts',(-31.4613346798115,-54.9855373992054,
4.55496640750309));
#32602=CARTESIAN_POINT('Ctrl Pts',(-31.8929598452159,-54.6422946631012,
4.59201237102577));
#32603=CARTESIAN_POINT('Ctrl Pts',(-32.5115585324226,-54.5341697288488,
4.62905833454844));
#32604=CARTESIAN_POINT('Ctrl Pts',(-33.0340255450119,-54.7106465835455,
4.66610429807112));
#32605=CARTESIAN_POINT('Ctrl Pts',(-33.5564925576013,-54.8871234382422,
4.70315026159381));
#32606=CARTESIAN_POINT('Ctrl Pts',(-33.9828278955734,-55.348202081888,4.74019622511649));
#32607=CARTESIAN_POINT('Ctrl Pts',(-34.1179167730764,-55.8828672630521,
4.77724218863917));
#32608=CARTESIAN_POINT('Ctrl Pts',(-34.2530056505794,-56.4175324442162,
4.81428815216185));
#32609=CARTESIAN_POINT('Ctrl Pts',(-34.0968480676134,-57.0257841628987,
4.85133411568453));
#32610=CARTESIAN_POINT('Ctrl Pts',(-33.7209104293741,-57.4292525624064,
4.88838007920721));
#32611=CARTESIAN_POINT('Ctrl Pts',(-33.6089446308763,-57.5494178688947,
4.89941350726821));
#32612=CARTESIAN_POINT('Ctrl Pts',(-33.4774836445334,-57.6514182455857,
4.91044693532921));
#32613=CARTESIAN_POINT('Ctrl Pts',(-33.3337300498339,-57.7328514726872,
4.92148036339021));
#32614=CARTESIAN_POINT('Ctrl Pts',(-33.3313578105535,-57.7323657066332,
4.72851963660978));
#32615=CARTESIAN_POINT('Ctrl Pts',(-33.5920983142318,-57.5811165681046,
4.70843756910069));
#32616=CARTESIAN_POINT('Ctrl Pts',(-33.8142965260144,-57.3625150588492,
4.68835550159159));
#32617=CARTESIAN_POINT('Ctrl Pts',(-33.9593006043585,-57.1010955378143,
4.6682734340825));
#32618=CARTESIAN_POINT('Ctrl Pts',(-34.22679376932,-56.6188474806364,4.63122747055982));
#32619=CARTESIAN_POINT('Ctrl Pts',(-34.2315934865741,-55.9908887245065,
4.59418150703714));
#32620=CARTESIAN_POINT('Ctrl Pts',(-33.9715031387158,-55.5046081545498,
4.55713554351446));
#32621=CARTESIAN_POINT('Ctrl Pts',(-33.7114127908575,-55.0183275845932,
4.52008957999178));
#32622=CARTESIAN_POINT('Ctrl Pts',(-33.1864323778867,-54.6737252008098,
4.4830436164691));
#32623=CARTESIAN_POINT('Ctrl Pts',(-32.6368221624337,-54.6285102383604,
4.44599765294642));
#32624=CARTESIAN_POINT('Ctrl Pts',(-32.0872119469808,-54.5832952759111,
4.40895168942373));
#32625=CARTESIAN_POINT('Ctrl Pts',(-31.5129719290456,-54.8374677347958,
4.37190572590106));
#32626=CARTESIAN_POINT('Ctrl Pts',(-31.1769063091028,-55.2747041478526,
4.33485976237838));
#32627=CARTESIAN_POINT('Ctrl Pts',(-30.84084068916,-55.7119405609094,4.2978137988557));
#32628=CARTESIAN_POINT('Ctrl Pts',(-30.7429494672094,-56.3322409281384,
4.26076783533301));
#32629=CARTESIAN_POINT('Ctrl Pts',(-30.9280331160056,-56.8517212691839,
4.22372187181033));
#32630=CARTESIAN_POINT('Ctrl Pts',(-31.1131167648017,-57.3712016102293,
4.18667590828765));
#32631=CARTESIAN_POINT('Ctrl Pts',(-31.5811752843445,-57.7898619250913,
4.14962994476497));
#32632=CARTESIAN_POINT('Ctrl Pts',(-32.1179990391191,-57.9160999466831,
4.11258398124229));
#32633=CARTESIAN_POINT('Ctrl Pts',(-32.5240508086608,-58.0115859820809,
4.08456253303146));
#32634=CARTESIAN_POINT('Ctrl Pts',(-32.9694456528715,-57.939766662088,4.05654108482062));
#32635=CARTESIAN_POINT('Ctrl Pts',(-33.3342430690557,-57.7335557705023,
4.02851963660978));
#32636=CARTESIAN_POINT('Origin',(-32.5,-56.2916512459885,3.));
#32637=CARTESIAN_POINT('',(-33.3337922536522,-57.7369224948681,3.32851963660979));
#32638=CARTESIAN_POINT('',(-33.3312448475264,-57.7342636967217,3.52148036339021));
#32639=CARTESIAN_POINT('',(-33.333,-57.7344495686934,3.));
#32640=CARTESIAN_POINT('Ctrl Pts',(-33.3312448475264,-57.7342636967217,
3.52148036339021));
#32641=CARTESIAN_POINT('Ctrl Pts',(-33.1882152402262,-57.8184056914071,
3.53256203972371));
#32642=CARTESIAN_POINT('Ctrl Pts',(-33.0334203647077,-57.8814418696117,
3.54364371605721));
#32643=CARTESIAN_POINT('Ctrl Pts',(-32.8726233824478,-57.9182768459085,
3.55472539239071));
#32644=CARTESIAN_POINT('Ctrl Pts',(-32.3350802382442,-58.0414159042227,
3.59177135591339));
#32645=CARTESIAN_POINT('Ctrl Pts',(-31.7304599472088,-57.871740798566,3.62881731943607));
#32646=CARTESIAN_POINT('Ctrl Pts',(-31.3354704139632,-57.4869043031699,
3.66586328295875));
#32647=CARTESIAN_POINT('Ctrl Pts',(-30.9404808807176,-57.1020678077737,
3.70290924648143));
#32648=CARTESIAN_POINT('Ctrl Pts',(-30.7551221052618,-56.5020699226381,
3.73995521000411));
#32649=CARTESIAN_POINT('Ctrl Pts',(-30.8642245822409,-55.961503082106,3.77700117352679));
#32650=CARTESIAN_POINT('Ctrl Pts',(-30.9733270592199,-55.4209362415738,
3.81404713704947));
#32651=CARTESIAN_POINT('Ctrl Pts',(-31.3768907886338,-54.9398004456451,
3.85109310057215));
#32652=CARTESIAN_POINT('Ctrl Pts',(-31.8902225413504,-54.7382902195697,
3.88813906409484));
#32653=CARTESIAN_POINT('Ctrl Pts',(-32.403554294067,-54.5367799934943,3.92518502761751));
#32654=CARTESIAN_POINT('Ctrl Pts',(-33.0266540700863,-54.6148953372722,
3.96223099114019));
#32655=CARTESIAN_POINT('Ctrl Pts',(-33.4743567237048,-54.9368863208444,
3.99927695466287));
#32656=CARTESIAN_POINT('Ctrl Pts',(-33.9220593773232,-55.2588773044166,
4.03632291818555));
#32657=CARTESIAN_POINT('Ctrl Pts',(-34.1943649085407,-55.8247439277831,
4.07336888170824));
#32658=CARTESIAN_POINT('Ctrl Pts',(-34.1666511469031,-56.3755141221477,
4.11041484523092));
#32659=CARTESIAN_POINT('Ctrl Pts',(-34.138955432321,-56.9259256578638,4.14743668461735));
#32660=CARTESIAN_POINT('Ctrl Pts',(-33.8116310396246,-57.4612604196062,
4.18445852400378));
#32661=CARTESIAN_POINT('Ctrl Pts',(-33.3343740344483,-57.7368428884788,
4.22148036339021));
#32662=CARTESIAN_POINT('Ctrl Pts',(-33.3342430690557,-57.7335557705023,
4.02851963660978));
#32663=CARTESIAN_POINT('Ctrl Pts',(-33.4517287836878,-57.6671440228088,
4.01949512129794));
#32664=CARTESIAN_POINT('Ctrl Pts',(-33.560854853963,-57.5867930493783,4.01047060598609));
#32665=CARTESIAN_POINT('Ctrl Pts',(-33.6576147739257,-57.4936023059229,
4.00144609067425));
#32666=CARTESIAN_POINT('Ctrl Pts',(-34.0548177639512,-57.1110509152492,
3.96440012715157));
#32667=CARTESIAN_POINT('Ctrl Pts',(-34.2436347539959,-56.5121324055803,
3.92735416362889));
#32668=CARTESIAN_POINT('Ctrl Pts',(-34.1376525779071,-55.9709452289588,
3.89030820010621));
#32669=CARTESIAN_POINT('Ctrl Pts',(-34.0316704018183,-55.4297580523374,
3.85326223658353));
#32670=CARTESIAN_POINT('Ctrl Pts',(-33.6308890595962,-54.9463022087633,
3.81621627306085));
#32671=CARTESIAN_POINT('Ctrl Pts',(-33.1187284050901,-54.7418340064325,
3.77917030953817));
#32672=CARTESIAN_POINT('Ctrl Pts',(-32.6065677505839,-54.5373658041018,
3.74212434601549));
#32673=CARTESIAN_POINT('Ctrl Pts',(-31.9830277837939,-54.6118852430143,
3.70507838249281));
#32674=CARTESIAN_POINT('Ctrl Pts',(-31.5334751062351,-54.9312880793963,
3.66803241897012));
#32675=CARTESIAN_POINT('Ctrl Pts',(-31.0839224286763,-55.2506909157783,
3.63098645544744));
#32676=CARTESIAN_POINT('Ctrl Pts',(-30.8083570403488,-55.8149771496297,
3.59394049192477));
#32677=CARTESIAN_POINT('Ctrl Pts',(-30.8328930037818,-56.3658979863087,
3.55689452840208));
#32678=CARTESIAN_POINT('Ctrl Pts',(-30.8574289672149,-56.9168188229877,
3.5198485648794));
#32679=CARTESIAN_POINT('Ctrl Pts',(-31.1820662824085,-57.4543742624943,
3.48280260135672));
#32680=CARTESIAN_POINT('Ctrl Pts',(-31.6582328412459,-57.7325490097911,
3.44575663783404));
#32681=CARTESIAN_POINT('Ctrl Pts',(-32.1343994000833,-58.010723757088,3.40871067431136));
#32682=CARTESIAN_POINT('Ctrl Pts',(-32.7620952025646,-58.0295178121752,
3.37166471078868));
#32683=CARTESIAN_POINT('Ctrl Pts',(-33.2540517054067,-57.7803299691728,
3.334618747266));
#32684=CARTESIAN_POINT('Ctrl Pts',(-33.2810496728284,-57.766654847026,3.3325857103806));
#32685=CARTESIAN_POINT('Ctrl Pts',(-33.3076388370087,-57.7521726493388,
3.33055267349519));
#32686=CARTESIAN_POINT('Ctrl Pts',(-33.3337922536522,-57.7369224948681,
3.32851963660979));
#32687=CARTESIAN_POINT('Origin',(-32.5,-56.2916512459885,3.));
#32688=CARTESIAN_POINT('',(-33.3310924906901,-57.7334985910042,2.62851963660979));
#32689=CARTESIAN_POINT('',(-33.3325882586835,-57.7320513890704,2.82148036339021));
#32690=CARTESIAN_POINT('',(-33.333,-57.7344495686934,3.));
#32691=CARTESIAN_POINT('Ctrl Pts',(-33.3325882586835,-57.7320513890704,
2.82148036339021));
#32692=CARTESIAN_POINT('Ctrl Pts',(-33.0441865216604,-57.8968038534098,
2.84361959192096));
#32693=CARTESIAN_POINT('Ctrl Pts',(-32.7077104550096,-57.9799132231487,
2.86575882045171));
#32694=CARTESIAN_POINT('Ctrl Pts',(-32.3790127353427,-57.9560193270483,
2.88789804898246));
#32695=CARTESIAN_POINT('Ctrl Pts',(-31.8289970147924,-57.9160372471796,
2.92494401250514));
#32696=CARTESIAN_POINT('Ctrl Pts',(-31.3007606051993,-57.5764468565745,
2.96198997602782));
#32697=CARTESIAN_POINT('Ctrl Pts',(-31.0360538947178,-57.0926636231019,
2.9990359395505));
#32698=CARTESIAN_POINT('Ctrl Pts',(-30.7713471842363,-56.6088803896294,
3.03608190307318));
#32699=CARTESIAN_POINT('Ctrl Pts',(-30.7701701728664,-55.9809043132894,
3.07312786659586));
#32700=CARTESIAN_POINT('Ctrl Pts',(-31.0330615265357,-55.4961322062854,
3.11017383011854));
#32701=CARTESIAN_POINT('Ctrl Pts',(-31.2959528802049,-55.0113600992815,
3.14721979364122));
#32702=CARTESIAN_POINT('Ctrl Pts',(-31.8229125989134,-54.6697919616135,
3.1842657571639));
#32703=CARTESIAN_POINT('Ctrl Pts',(-32.3727745793293,-54.6277483883086,
3.22131172068658));
#32704=CARTESIAN_POINT('Ctrl Pts',(-32.9226365597451,-54.5857048150036,
3.25835768420926));
#32705=CARTESIAN_POINT('Ctrl Pts',(-33.4954008018683,-54.8431858060618,
3.29540364773194));
#32706=CARTESIAN_POINT('Ctrl Pts',(-33.8289385024972,-55.2823537259082,
3.33244961125463));
#32707=CARTESIAN_POINT('Ctrl Pts',(-34.162476203126,-55.7215216457546,3.36949557477731));
#32708=CARTESIAN_POINT('Ctrl Pts',(-34.2567873622605,-56.3423764943892,
3.40654153829999));
#32709=CARTESIAN_POINT('Ctrl Pts',(-34.0687099431419,-56.8607805298492,
3.44358750182267));
#32710=CARTESIAN_POINT('Ctrl Pts',(-33.9368927177428,-57.2241127252305,
3.46955178901185));
#32711=CARTESIAN_POINT('Ctrl Pts',(-33.6663621789423,-57.5371196140996,
3.49551607620103));
#32712=CARTESIAN_POINT('Ctrl Pts',(-33.3312448475264,-57.7342636967217,
3.52148036339021));
#32713=CARTESIAN_POINT('Ctrl Pts',(-33.3337922536522,-57.7369224948681,
3.32851963660979));
#32714=CARTESIAN_POINT('Ctrl Pts',(-33.7842059499452,-57.4742845941374,
3.29350670997251));
#32715=CARTESIAN_POINT('Ctrl Pts',(-34.1053783658087,-56.9838732473919,
3.25849378333524));
#32716=CARTESIAN_POINT('Ctrl Pts',(-34.1596784920807,-56.465506410459,3.22348085669796));
#32717=CARTESIAN_POINT('Ctrl Pts',(-34.2171315727097,-55.9170404358397,
3.18643489317528));
#32718=CARTESIAN_POINT('Ctrl Pts',(-33.975820530765,-55.3372782276934,3.1493889296526));
#32719=CARTESIAN_POINT('Ctrl Pts',(-33.5461827329191,-54.9915512480536,
3.11234296612992));
#32720=CARTESIAN_POINT('Ctrl Pts',(-33.1165449350731,-54.6458242684137,
3.07529700260724));
#32721=CARTESIAN_POINT('Ctrl Pts',(-32.498580381326,-54.5341325172804,3.03825103908455));
#32722=CARTESIAN_POINT('Ctrl Pts',(-31.9751040537975,-54.7075923578949,
3.00120507556188));
#32723=CARTESIAN_POINT('Ctrl Pts',(-31.4516277262689,-54.8810521985094,
2.96415911203919));
#32724=CARTESIAN_POINT('Ctrl Pts',(-31.0226396249589,-55.3396636308718,
2.92711314851652));
#32725=CARTESIAN_POINT('Ctrl Pts',(-30.88446858696,-55.8735405324578,2.89006718499383));
#32726=CARTESIAN_POINT('Ctrl Pts',(-30.746297548961,-56.4074174340438,2.85302122147115));
#32727=CARTESIAN_POINT('Ctrl Pts',(-30.8989435742731,-57.0165598048535,
2.81597525794847));
#32728=CARTESIAN_POINT('Ctrl Pts',(-31.2725473438504,-57.4221901848134,
2.77892929442579));
#32729=CARTESIAN_POINT('Ctrl Pts',(-31.6461511134276,-57.8278205647734,
2.74188333090311));
#32730=CARTESIAN_POINT('Ctrl Pts',(-32.24071262727,-58.0299389538838,2.70483736738043));
#32731=CARTESIAN_POINT('Ctrl Pts',(-32.7841274371744,-57.9360447252789,
2.66779140385775));
#32732=CARTESIAN_POINT('Ctrl Pts',(-32.9761488965038,-57.9028661911818,
2.6547008147751));
#32733=CARTESIAN_POINT('Ctrl Pts',(-33.1617839833806,-57.8327263930767,
2.64161022569244));
#32734=CARTESIAN_POINT('Ctrl Pts',(-33.3310924906901,-57.7334985910042,
2.62851963660979));
#32735=CARTESIAN_POINT('Origin',(-32.5,-56.2916512459885,3.));
#32736=CARTESIAN_POINT('',(-33.3331879029845,-57.7323621350135,1.92851963660978));
#32737=CARTESIAN_POINT('',(-33.3348622165511,-57.7357255517676,2.12148036339021));
#32738=CARTESIAN_POINT('',(-33.333,-57.7344495686934,3.));
#32739=CARTESIAN_POINT('Ctrl Pts',(-33.3348622165511,-57.7357255517676,
2.12148036339021));
#32740=CARTESIAN_POINT('Ctrl Pts',(-32.9046875435881,-57.9801160523425,
2.15467714411821));
#32741=CARTESIAN_POINT('Ctrl Pts',(-32.3567184702117,-58.0261342906593,
2.18787392484621));
#32742=CARTESIAN_POINT('Ctrl Pts',(-31.8960497135599,-57.8472871542167,
2.22107070557421));
#32743=CARTESIAN_POINT('Ctrl Pts',(-31.3819661915825,-57.6477026057306,
2.25811666909689));
#32744=CARTESIAN_POINT('Ctrl Pts',(-30.9766017246916,-57.1680829785327,
2.29516263261957));
#32745=CARTESIAN_POINT('Ctrl Pts',(-30.8654736597328,-56.6279289146383,
2.33220859614225));
#32746=CARTESIAN_POINT('Ctrl Pts',(-30.7543455947739,-56.0877748507439,
2.36925455966493));
#32747=CARTESIAN_POINT('Ctrl Pts',(-30.9374539317471,-55.4870863501531,
2.40630052318761));
#32748=CARTESIAN_POINT('Ctrl Pts',(-31.3309981019417,-55.1007719112966,
2.44334648671029));
#32749=CARTESIAN_POINT('Ctrl Pts',(-31.7245422721363,-54.7144574724402,
2.48039245023297));
#32750=CARTESIAN_POINT('Ctrl Pts',(-32.3285222755522,-54.5425170953181,
2.51743841375565));
#32751=CARTESIAN_POINT('Ctrl Pts',(-32.8665232388267,-54.6636402684886,
2.55448437727833));
#32752=CARTESIAN_POINT('Ctrl Pts',(-33.4045242021011,-54.7847634416591,
2.59153034080102));
#32753=CARTESIAN_POINT('Ctrl Pts',(-33.876546125234,-55.1989501651221,2.62857630432369));
#32754=CARTESIAN_POINT('Ctrl Pts',(-34.0665654985573,-55.7166455362864,
2.66562226784638));
#32755=CARTESIAN_POINT('Ctrl Pts',(-34.2565848718806,-56.2343409074507,
2.70266823136906));
#32756=CARTESIAN_POINT('Ctrl Pts',(-34.1646016953943,-56.8555449263162,
2.73971419489174));
#32757=CARTESIAN_POINT('Ctrl Pts',(-33.8327125913974,-57.2959600511828,
2.77676015841442));
#32758=CARTESIAN_POINT('Ctrl Pts',(-33.6991654394395,-57.4731764312833,
2.79166689340635));
#32759=CARTESIAN_POINT('Ctrl Pts',(-33.5267742601986,-57.6211206345609,
2.80657362839828));
#32760=CARTESIAN_POINT('Ctrl Pts',(-33.3325882586835,-57.7320513890704,
2.82148036339021));
#32761=CARTESIAN_POINT('Ctrl Pts',(-33.3310924906901,-57.7334985910042,
2.62851963660979));
#32762=CARTESIAN_POINT('Ctrl Pts',(-33.6409218393061,-57.5519147723922,
2.60456426216976));
#32763=CARTESIAN_POINT('Ctrl Pts',(-33.8960769478414,-57.272921419479,2.58060888772973));
#32764=CARTESIAN_POINT('Ctrl Pts',(-34.0356424650284,-56.9447672654595,
2.55665351328971));
#32765=CARTESIAN_POINT('Ctrl Pts',(-34.2514745770115,-56.4372908805649,
2.51960754976703));
#32766=CARTESIAN_POINT('Ctrl Pts',(-34.190870695011,-55.8122449570956,2.48256158624435));
#32767=CARTESIAN_POINT('Ctrl Pts',(-33.8815665292719,-55.3556853061788,
2.44551562272167));
#32768=CARTESIAN_POINT('Ctrl Pts',(-33.5722623635329,-54.899125655262,2.40846965919899));
#32769=CARTESIAN_POINT('Ctrl Pts',(-33.0142579140552,-54.6110522768978,
2.37142369567631));
#32770=CARTESIAN_POINT('Ctrl Pts',(-32.4629270812427,-54.6233035861816,
2.33437773215363));
#32771=CARTESIAN_POINT('Ctrl Pts',(-31.9115962484303,-54.6355548954655,
2.29733176863094));
#32772=CARTESIAN_POINT('Ctrl Pts',(-31.3669390322832,-54.9481308923973,
2.26028580510826));
#32773=CARTESIAN_POINT('Ctrl Pts',(-31.0782208961876,-55.417979399555,2.22323984158558));
#32774=CARTESIAN_POINT('Ctrl Pts',(-30.789502760092,-55.8878279067126,2.1861938780629));
#32775=CARTESIAN_POINT('Ctrl Pts',(-30.7567237040478,-56.514948924096,2.14914791454022));
#32776=CARTESIAN_POINT('Ctrl Pts',(-30.9948852489237,-57.0123369620816,
2.11210195101754));
#32777=CARTESIAN_POINT('Ctrl Pts',(-31.2330467937995,-57.5097250000671,
2.07505598749486));
#32778=CARTESIAN_POINT('Ctrl Pts',(-31.7421489395953,-57.8773800586549,
2.03801002397218));
#32779=CARTESIAN_POINT('Ctrl Pts',(-32.2891982024822,-57.9470427155362,
2.0009640604495));
#32780=CARTESIAN_POINT('Ctrl Pts',(-32.6457882768413,-57.9924518106263,
1.9768159191696));
#32781=CARTESIAN_POINT('Ctrl Pts',(-33.018502040246,-57.9112442562479,1.95266777788969));
#32782=CARTESIAN_POINT('Ctrl Pts',(-33.3331879029845,-57.7323621350135,
1.92851963660978));
#32783=CARTESIAN_POINT('Origin',(-32.5,-56.2916512459885,3.));
#32784=CARTESIAN_POINT('',(-33.3347215376786,-57.7364302140763,1.22851963660979));
#32785=CARTESIAN_POINT('',(-33.3320718525009,-57.735759463036,1.42148036339021));
#32786=CARTESIAN_POINT('',(-33.333,-57.7344495686934,3.));
#32787=CARTESIAN_POINT('Ctrl Pts',(-33.3320718525009,-57.735759463036,1.42148036339021));
#32788=CARTESIAN_POINT('Ctrl Pts',(-33.2393317234316,-57.7904422794385,
1.42868873279278));
#32789=CARTESIAN_POINT('Ctrl Pts',(-33.1414800191062,-57.8359234203097,
1.43589710219535));
#32790=CARTESIAN_POINT('Ctrl Pts',(-33.0399483052832,-57.8706429670186,
1.44310547159792));
#32791=CARTESIAN_POINT('Ctrl Pts',(-32.5181465001006,-58.0490770883944,
1.4801514351206));
#32792=CARTESIAN_POINT('Ctrl Pts',(-31.8991468445914,-57.9432717752442,
1.51719739864328));
#32793=CARTESIAN_POINT('Ctrl Pts',(-31.4662380410665,-57.6016494290873,
1.55424336216596));
#32794=CARTESIAN_POINT('Ctrl Pts',(-31.0333292375416,-57.2600270829305,
1.59128932568864));
#32795=CARTESIAN_POINT('Ctrl Pts',(-30.7865112860008,-56.6825877037672,
1.62833528921132));
#32796=CARTESIAN_POINT('Ctrl Pts',(-30.8387418215198,-56.1335996977756,
1.665381252734));
#32797=CARTESIAN_POINT('Ctrl Pts',(-30.8909723570387,-55.5846116917841,
1.70242721625668));
#32798=CARTESIAN_POINT('Ctrl Pts',(-31.2422513796173,-55.0640750589644,
1.73947317977936));
#32799=CARTESIAN_POINT('Ctrl Pts',(-31.7318140526851,-54.8102163409698,
1.77651914330204));
#32800=CARTESIAN_POINT('Ctrl Pts',(-32.2213767257528,-54.5563576229751,
1.81356510682472));
#32801=CARTESIAN_POINT('Ctrl Pts',(-32.8492230493096,-54.5691768198056,
1.8506110703474));
#32802=CARTESIAN_POINT('Ctrl Pts',(-33.3280155932489,-54.842807153342,1.88765703387008));
#32803=CARTESIAN_POINT('Ctrl Pts',(-33.8068081371883,-55.1164374868783,
1.92470299739276));
#32804=CARTESIAN_POINT('Ctrl Pts',(-34.1365469015101,-55.6508789571206,
1.96174896091544));
#32805=CARTESIAN_POINT('Ctrl Pts',(-34.1663250709766,-56.2015413947231,
1.99879492443812));
#32806=CARTESIAN_POINT('Ctrl Pts',(-34.1961032404431,-56.7522038323256,
2.03584088796081));
#32807=CARTESIAN_POINT('Ctrl Pts',(-33.9259208150542,-57.3190872372884,
2.07288685148349));
#32808=CARTESIAN_POINT('Ctrl Pts',(-33.4794283138278,-57.6427542048827,
2.10993281500617));
#32809=CARTESIAN_POINT('Ctrl Pts',(-33.4330364511186,-57.6763841392777,
2.11378199780085));
#32810=CARTESIAN_POINT('Ctrl Pts',(-33.384741178112,-57.707388354926,2.11763118059553));
#32811=CARTESIAN_POINT('Ctrl Pts',(-33.3348622165511,-57.7357255517676,
2.12148036339021));
#32812=CARTESIAN_POINT('Ctrl Pts',(-33.3331879029845,-57.7323621350135,
1.92851963660978));
#32813=CARTESIAN_POINT('Ctrl Pts',(-33.501265531522,-57.6368189718627,1.91562181436701));
#32814=CARTESIAN_POINT('Ctrl Pts',(-33.6527891880219,-57.5134115911553,
1.90272399212423));
#32815=CARTESIAN_POINT('Ctrl Pts',(-33.7764604319637,-57.3665498834978,
1.88982616988146));
#32816=CARTESIAN_POINT('Ctrl Pts',(-34.1316770185806,-56.9447241394031,
1.85278020635878));
#32817=CARTESIAN_POINT('Ctrl Pts',(-34.2571138118367,-56.3294023960388,
1.8157342428361));
#32818=CARTESIAN_POINT('Ctrl Pts',(-34.0953639520231,-55.8021901383674,
1.77868827931342));
#32819=CARTESIAN_POINT('Ctrl Pts',(-33.9336140922095,-55.2749778806959,
1.74164231579074));
#32820=CARTESIAN_POINT('Ctrl Pts',(-33.4846775793262,-54.8358751087172,
1.70459635226806));
#32821=CARTESIAN_POINT('Ctrl Pts',(-32.9540127541378,-54.6858396959092,
1.66755038874538));
#32822=CARTESIAN_POINT('Ctrl Pts',(-32.4233479289495,-54.5358042831011,
1.63050442522269));
#32823=CARTESIAN_POINT('Ctrl Pts',(-31.8109547914561,-54.6748362294637,
1.59345846170001));
#32824=CARTESIAN_POINT('Ctrl Pts',(-31.3970985335358,-55.0393067763799,
1.55641249817733));
#32825=CARTESIAN_POINT('Ctrl Pts',(-30.9832422756156,-55.4037773232961,
1.51936653465465));
#32826=CARTESIAN_POINT('Ctrl Pts',(-30.7679228972685,-55.993686470766,1.48232057113197));
#32827=CARTESIAN_POINT('Ctrl Pts',(-30.8496825329409,-56.5390589524362,
1.44527460760929));
#32828=CARTESIAN_POINT('Ctrl Pts',(-30.9314421686133,-57.0844314341065,
1.40822864408661));
#32829=CARTESIAN_POINT('Ctrl Pts',(-31.3102808183052,-57.5852672499772,
1.37118268056393));
#32830=CARTESIAN_POINT('Ctrl Pts',(-31.8128208258201,-57.8123560489854,
1.33413671704125));
#32831=CARTESIAN_POINT('Ctrl Pts',(-32.2903969982888,-58.0281641395237,
1.29893102356409));
#32832=CARTESIAN_POINT('Ctrl Pts',(-32.8796899699103,-57.9967466454786,
1.26372533008694));
#32833=CARTESIAN_POINT('Ctrl Pts',(-33.3347215376786,-57.7364302140763,
1.22851963660979));
#32834=CARTESIAN_POINT('Origin',(-32.5,-56.2916512459885,3.));
#32835=CARTESIAN_POINT('',(-33.3315625259448,-57.7350035902351,0.528519636609785));
#32836=CARTESIAN_POINT('',(-33.3315934922345,-57.7321400761417,0.721480363390208));
#32837=CARTESIAN_POINT('',(-33.333,-57.7344495686934,3.));
#32838=CARTESIAN_POINT('Ctrl Pts',(-33.3315934922345,-57.7321400761417,
0.721480363390208));
#32839=CARTESIAN_POINT('Ctrl Pts',(-33.094172273388,-57.8693226291885,0.739746284990028));
#32840=CARTESIAN_POINT('Ctrl Pts',(-32.8247195065089,-57.9509431527902,
0.758012206589848));
#32841=CARTESIAN_POINT('Ctrl Pts',(-32.552949516444,-57.9595707213043,0.776278128189667));
#32842=CARTESIAN_POINT('Ctrl Pts',(-32.001760183703,-57.97706869351,0.813324091712348));
#32843=CARTESIAN_POINT('Ctrl Pts',(-31.4410392363067,-57.6943190569763,
0.850370055235028));
#32844=CARTESIAN_POINT('Ctrl Pts',(-31.1274037953482,-57.2407237861293,
0.887416018757709));
#32845=CARTESIAN_POINT('Ctrl Pts',(-30.8137683543896,-56.7871285152822,
0.92446198228039));
#32846=CARTESIAN_POINT('Ctrl Pts',(-30.7472184198688,-56.1626876101218,
0.96150794580307));
#32847=CARTESIAN_POINT('Ctrl Pts',(-30.9582109466765,-55.653179991732,0.998553909325751));
#32848=CARTESIAN_POINT('Ctrl Pts',(-31.1692034734841,-55.1436723733423,
1.03559987284843));
#32849=CARTESIAN_POINT('Ctrl Pts',(-31.6577384616201,-54.7490980417232,
1.07264583637111));
#32850=CARTESIAN_POINT('Ctrl Pts',(-32.2002351035856,-54.6500361771206,
1.10969179989379));
#32851=CARTESIAN_POINT('Ctrl Pts',(-32.7427317455511,-54.550974312518,1.14673776341647));
#32852=CARTESIAN_POINT('Ctrl Pts',(-33.3391900413461,-54.7474249149318,
1.18378372693915));
#32853=CARTESIAN_POINT('Ctrl Pts',(-33.7166374697497,-55.1494812522209,
1.22082969046183));
#32854=CARTESIAN_POINT('Ctrl Pts',(-34.0940848981533,-55.5515375895099,
1.25787565398451));
#32855=CARTESIAN_POINT('Ctrl Pts',(-34.2525214591656,-56.1591996616743,
1.2949216175072));
#32856=CARTESIAN_POINT('Ctrl Pts',(-34.1194377622437,-56.6943674757075,
1.33196758102988));
#32857=CARTESIAN_POINT('Ctrl Pts',(-34.0122493682821,-57.1254028302473,
1.36180517514999));
#32858=CARTESIAN_POINT('Ctrl Pts',(-33.7159509484902,-57.5094109520148,
1.3916427692701));
#32859=CARTESIAN_POINT('Ctrl Pts',(-33.3320718525009,-57.735759463036,1.42148036339021));
#32860=CARTESIAN_POINT('Ctrl Pts',(-33.3347215376786,-57.7364302140763,
1.22851963660979));
#32861=CARTESIAN_POINT('Ctrl Pts',(-33.3585069224055,-57.7228229680956,
1.22667936656426));
#32862=CARTESIAN_POINT('Ctrl Pts',(-33.3819254571596,-57.7085902886951,
1.22483909651873));
#32863=CARTESIAN_POINT('Ctrl Pts',(-33.4049420099643,-57.6937347933887,
1.22299882647321));
#32864=CARTESIAN_POINT('Ctrl Pts',(-33.8682818212557,-57.394682956638,1.18595286295053));
#32865=CARTESIAN_POINT('Ctrl Pts',(-34.1687200785007,-56.8432375009908,
1.14890689942785));
#32866=CARTESIAN_POINT('Ctrl Pts',(-34.1687595096553,-56.2917705661426,
1.11186093590517));
#32867=CARTESIAN_POINT('Ctrl Pts',(-34.1687989408099,-55.7403036312943,
1.07481497238249));
#32868=CARTESIAN_POINT('Ctrl Pts',(-33.8684395458741,-55.188815217245,1.03776900885981));
#32869=CARTESIAN_POINT('Ctrl Pts',(-33.4051425051238,-54.8896971238163,
1.00072304533712));
#32870=CARTESIAN_POINT('Ctrl Pts',(-32.9418454643735,-54.5905790303876,
0.963677081814444));
#32871=CARTESIAN_POINT('Ctrl Pts',(-32.3156107778087,-54.5438312575796,
0.926631118291762));
#32872=CARTESIAN_POINT('Ctrl Pts',(-31.8130383006683,-54.7708481887354,
0.889585154769081));
#32873=CARTESIAN_POINT('Ctrl Pts',(-31.310465823528,-54.9978651198912,0.8525391912464));
#32874=CARTESIAN_POINT('Ctrl Pts',(-30.9315555558122,-55.4986467550108,
0.815493227723721));
#32875=CARTESIAN_POINT('Ctrl Pts',(-30.8497179302269,-56.0440075390777,
0.778447264201041));
#32876=CARTESIAN_POINT('Ctrl Pts',(-30.7678803046417,-56.5893683231447,
0.74140130067836));
#32877=CARTESIAN_POINT('Ctrl Pts',(-30.9831153211871,-57.179308256159,0.704355337155679));
#32878=CARTESIAN_POINT('Ctrl Pts',(-31.3969194538394,-57.5438379827469,
0.667309373632999));
#32879=CARTESIAN_POINT('Ctrl Pts',(-31.8107235864918,-57.9083677093349,
0.630263410110318));
#32880=CARTESIAN_POINT('Ctrl Pts',(-32.4230968352511,-58.0474872294965,
0.593217446587637));
#32881=CARTESIAN_POINT('Ctrl Pts',(-32.9537831109001,-57.8975277056554,
0.556171483064956));
#32882=CARTESIAN_POINT('Ctrl Pts',(-33.0858213863713,-57.860216778603,0.546954200913232));
#32883=CARTESIAN_POINT('Ctrl Pts',(-33.2128028501901,-57.805010485588,0.537736918761509));
#32884=CARTESIAN_POINT('Ctrl Pts',(-33.3315625259448,-57.7350035902351,
0.528519636609785));
#32885=CARTESIAN_POINT('Origin',(-32.5,-56.2916512459885,3.));
#32886=CARTESIAN_POINT('',(-33.332066590478,-57.7319806121586,-0.171480363390217));
#32887=CARTESIAN_POINT('',(-33.3345107245666,-57.7340829700271,0.0214803633902086));
#32888=CARTESIAN_POINT('',(-33.333,-57.7344495686934,3.));
#32889=CARTESIAN_POINT('Ctrl Pts',(-33.3345107245666,-57.7340829700271,
0.0214803633902086));
#32890=CARTESIAN_POINT('Ctrl Pts',(-32.9530815922347,-57.9496325625699,
0.0508038371872777));
#32891=CARTESIAN_POINT('Ctrl Pts',(-32.4824461880261,-58.016467684898,0.0801273109843468));
#32892=CARTESIAN_POINT('Ctrl Pts',(-32.0612908438827,-57.9017112764627,
0.109450784781416));
#32893=CARTESIAN_POINT('Ctrl Pts',(-31.5292220438324,-57.7567331694926,
0.146496748304096));
#32894=CARTESIAN_POINT('Ctrl Pts',(-31.0761267049974,-57.3219229222043,
0.183542711826777));
#32895=CARTESIAN_POINT('Ctrl Pts',(-30.9093664792402,-56.796273907743,0.220588675349458));
#32896=CARTESIAN_POINT('Ctrl Pts',(-30.7426062534831,-56.2706248932817,
0.257634638872138));
#32897=CARTESIAN_POINT('Ctrl Pts',(-30.8621811408039,-55.6541371116475,
0.294680602394819));
#32898=CARTESIAN_POINT('Ctrl Pts',(-31.2133670155729,-55.2289496928674,
0.3317265659175));
#32899=CARTESIAN_POINT('Ctrl Pts',(-31.564552890342,-54.8037622740873,0.36877252944018));
#32900=CARTESIAN_POINT('Ctrl Pts',(-32.1473497525593,-54.5698752181613,
0.405818492962861));
#32901=CARTESIAN_POINT('Ctrl Pts',(-32.6950373137549,-54.6343282619421,
0.442864456485541));
#32902=CARTESIAN_POINT('Ctrl Pts',(-33.2427248749505,-54.6987813057228,
0.479910420008222));
#32903=CARTESIAN_POINT('Ctrl Pts',(-33.7553031351243,-55.0615744492104,
0.516956383530902));
#32904=CARTESIAN_POINT('Ctrl Pts',(-33.9981877468876,-55.5566733533727,
0.554002347053583));
#32905=CARTESIAN_POINT('Ctrl Pts',(-34.2410723586509,-56.0517722575349,
0.591048310576264));
#32906=CARTESIAN_POINT('Ctrl Pts',(-34.2142633220036,-56.6791769223718,
0.628094274098944));
#32907=CARTESIAN_POINT('Ctrl Pts',(-33.9300299446371,-57.1517520452627,
0.665140237621625));
#32908=CARTESIAN_POINT('Ctrl Pts',(-33.7859409742004,-57.3913187827875,
0.683920279544486));
#32909=CARTESIAN_POINT('Ctrl Pts',(-33.5756972687095,-57.5910963251749,
0.702700321467347));
#32910=CARTESIAN_POINT('Ctrl Pts',(-33.3315934922345,-57.7321400761417,
0.721480363390208));
#32911=CARTESIAN_POINT('Ctrl Pts',(-33.3315625259448,-57.7350035902351,
0.528519636609785));
#32912=CARTESIAN_POINT('Ctrl Pts',(-33.6901199750816,-57.523639811577,0.500690955238828));
#32913=CARTESIAN_POINT('Ctrl Pts',(-33.9737318881584,-57.1773614538061,
0.472862273867871));
#32914=CARTESIAN_POINT('Ctrl Pts',(-34.0952939407749,-56.781340492839,0.445033592496915));
#32915=CARTESIAN_POINT('Ctrl Pts',(-34.2571191924618,-56.2541513717075,
0.407987628974234));
#32916=CARTESIAN_POINT('Ctrl Pts',(-34.131770393297,-55.6388116972881,0.370941665451553));
#32917=CARTESIAN_POINT('Ctrl Pts',(-33.7766141338562,-55.2169351595517,
0.333895701928873));
#32918=CARTESIAN_POINT('Ctrl Pts',(-33.4214578744155,-54.7950586218153,
0.296849738406192));
#32919=CARTESIAN_POINT('Ctrl Pts',(-32.8364941546989,-54.566645220762,0.259803774883511));
#32920=CARTESIAN_POINT('Ctrl Pts',(-32.289434934298,-54.636229647045,0.222757811360831));
#32921=CARTESIAN_POINT('Ctrl Pts',(-31.7423757138972,-54.705814073328,0.18571184783815));
#32922=CARTESIAN_POINT('Ctrl Pts',(-31.2332209928121,-55.0733963269474,
0.148665884315469));
#32923=CARTESIAN_POINT('Ctrl Pts',(-30.9949883236289,-55.5707503002861,
0.111619920792788));
#32924=CARTESIAN_POINT('Ctrl Pts',(-30.7567556544457,-56.0681042736247,
0.0745739572701072));
#32925=CARTESIAN_POINT('Ctrl Pts',(-30.7894450371644,-56.6952299666827,
0.0375279937474265));
#32926=CARTESIAN_POINT('Ctrl Pts',(-31.0780959757366,-57.1651197597709,
0.000482030224745822));
#32927=CARTESIAN_POINT('Ctrl Pts',(-31.3667469143089,-57.635009552859,-0.0365639332979349));
#32928=CARTESIAN_POINT('Ctrl Pts',(-31.9113594087348,-57.9476634459773,
-0.0736098968206155));
#32929=CARTESIAN_POINT('Ctrl Pts',(-32.4626884920092,-57.9599935925982,
-0.110655860343296));
#32930=CARTESIAN_POINT('Ctrl Pts',(-32.7644246265901,-57.9667417415587,
-0.13093069469227));
#32931=CARTESIAN_POINT('Ctrl Pts',(-33.0681725463472,-57.8835354694765,
-0.151205529041244));
#32932=CARTESIAN_POINT('Ctrl Pts',(-33.332066590478,-57.7319806121586,-0.171480363390217));
#32933=CARTESIAN_POINT('Origin',(-32.5,-56.2916512459885,3.));
#32934=CARTESIAN_POINT('',(-33.3347877909359,-57.7349452754743,-0.871480363390215));
#32935=CARTESIAN_POINT('',(-33.333352483612,-57.7367881187288,-0.678519636609791));
#32936=CARTESIAN_POINT('',(-33.333,-57.7344495686934,3.));
#32937=CARTESIAN_POINT('Ctrl Pts',(-33.333352483612,-57.7367881187288,-0.678519636609791));
#32938=CARTESIAN_POINT('Ctrl Pts',(-33.2904764567157,-57.7619047682302,
-0.675184574138153));
#32939=CARTESIAN_POINT('Ctrl Pts',(-33.2464522145773,-57.7849807415505,
-0.671849511666514));
#32940=CARTESIAN_POINT('Ctrl Pts',(-33.2014046817541,-57.8058476261432,
-0.668514449194876));
#32941=CARTESIAN_POINT('Ctrl Pts',(-32.701015477069,-58.0376375407332,-0.631468485672195));
#32942=CARTESIAN_POINT('Ctrl Pts',(-32.0743642145055,-57.9968518393257,
-0.594422522149515));
#32943=CARTESIAN_POINT('Ctrl Pts',(-31.608241296104,-57.7021565859588,-0.557376558626834));
#32944=CARTESIAN_POINT('Ctrl Pts',(-31.1421183777026,-57.407461332592,-0.520330595104154));
#32945=CARTESIAN_POINT('Ctrl Pts',(-30.8365238034633,-56.8588565272658,
-0.483284631581473));
#32946=CARTESIAN_POINT('Ctrl Pts',(-30.8313147141679,-56.3074141411014,
-0.446238668058792));
#32947=CARTESIAN_POINT('Ctrl Pts',(-30.8261056248724,-55.755971754937,-0.409192704536112));
#32948=CARTESIAN_POINT('Ctrl Pts',(-31.1212820205207,-55.2016917879344,
-0.372146741013431));
#32949=CARTESIAN_POINT('Ctrl Pts',(-31.5817547242443,-54.8982436746824,
-0.335100777490751));
#32950=CARTESIAN_POINT('Ctrl Pts',(-32.042227427968,-54.5947955614304,-0.29805481396807));
#32951=CARTESIAN_POINT('Ctrl Pts',(-32.667996439767,-54.5421793019291,-0.26100885044539));
#32952=CARTESIAN_POINT('Ctrl Pts',(-33.1726750359156,-54.7644749931934,
-0.223962886922709));
#32953=CARTESIAN_POINT('Ctrl Pts',(-33.6773536320643,-54.9867706844577,
-0.186916923400029));
#32954=CARTESIAN_POINT('Ctrl Pts',(-34.0609418125626,-55.4839783264877,
-0.149870959877348));
#32955=CARTESIAN_POINT('Ctrl Pts',(-34.1478882650458,-56.0285480388725,
-0.112824996354667));
#32956=CARTESIAN_POINT('Ctrl Pts',(-34.2348347175289,-56.5731177512574,
-0.0757790328319867));
#32957=CARTESIAN_POINT('Ctrl Pts',(-34.0251394419968,-57.1650495339971,
-0.038733069309306));
#32958=CARTESIAN_POINT('Ctrl Pts',(-33.6147706735979,-57.533442442041,-0.00168710578662554));
#32959=CARTESIAN_POINT('Ctrl Pts',(-33.529226438914,-57.6102365155873,0.00603538393898582));
#32960=CARTESIAN_POINT('Ctrl Pts',(-33.4349620754491,-57.6773168608924,
0.0137578736645972));
#32961=CARTESIAN_POINT('Ctrl Pts',(-33.3345107245666,-57.7340829700271,
0.0214803633902086));
#32962=CARTESIAN_POINT('Ctrl Pts',(-33.332066590478,-57.7319806121586,-0.171480363390217));
#32963=CARTESIAN_POINT('Ctrl Pts',(-33.550356960999,-57.6066160323434,-0.188251492563924));
#32964=CARTESIAN_POINT('Ctrl Pts',(-33.7413776202382,-57.4344844529175,
-0.205022621737631));
#32965=CARTESIAN_POINT('Ctrl Pts',(-33.8814326840108,-57.2278147357495,
-0.221793750911338));
#32966=CARTESIAN_POINT('Ctrl Pts',(-34.1908021206152,-56.7712993321565,
-0.258839714434018));
#32967=CARTESIAN_POINT('Ctrl Pts',(-34.251495321701,-56.1462621248468,-0.295885677956699));
#32968=CARTESIAN_POINT('Ctrl Pts',(-34.0357358154562,-55.6387548587911,
-0.332931641479379));
#32969=CARTESIAN_POINT('Ctrl Pts',(-33.8199763092115,-55.1312475927354,
-0.36997760500206));
#32970=CARTESIAN_POINT('Ctrl Pts',(-33.3277640956362,-54.7412702679336,
-0.40702356852474));
#32971=CARTESIAN_POINT('Ctrl Pts',(-32.7843626547692,-54.6472983719835,
-0.444069532047421));
#32972=CARTESIAN_POINT('Ctrl Pts',(-32.2409612139021,-54.5533264760334,
-0.481115495570101));
#32973=CARTESIAN_POINT('Ctrl Pts',(-31.6463705457434,-54.7553600089348,
-0.518161459092782));
#32974=CARTESIAN_POINT('Ctrl Pts',(-31.2727089000175,-55.1609368730463,
-0.555207422615462));
#32975=CARTESIAN_POINT('Ctrl Pts',(-30.8990472542916,-55.5665137371577,
-0.592253386138142));
#32976=CARTESIAN_POINT('Ctrl Pts',(-30.7463146309986,-56.1756339324792,
-0.629299349660823));
#32977=CARTESIAN_POINT('Ctrl Pts',(-30.8844090678351,-56.7095307561729,
-0.666345313183503));
#32978=CARTESIAN_POINT('Ctrl Pts',(-31.0225035046717,-57.2434275798666,
-0.703391276706184));
#32979=CARTESIAN_POINT('Ctrl Pts',(-31.4514250016378,-57.7021010319326,
-0.740437240228864));
#32980=CARTESIAN_POINT('Ctrl Pts',(-31.9748770216297,-57.8756353949644,
-0.777483203751545));
#32981=CARTESIAN_POINT('Ctrl Pts',(-32.4175973471179,-58.0224056561358,
-0.808815590297768));
#32982=CARTESIAN_POINT('Ctrl Pts',(-32.9279379927888,-57.9652079725634,
-0.840147976843991));
#32983=CARTESIAN_POINT('Ctrl Pts',(-33.3347877909359,-57.7349452754743,
-0.871480363390215));
#32984=CARTESIAN_POINT('Origin',(-32.5,-56.2916512459885,3.));
#32985=CARTESIAN_POINT('',(-33.3326856027611,-57.7363329907929,-1.57148036339021));
#32986=CARTESIAN_POINT('',(-33.3311039683456,-57.7330494773494,-1.37851963660979));
#32987=CARTESIAN_POINT('',(-33.333,-57.7344495686934,3.));
#32988=CARTESIAN_POINT('',(-30.9307125467393,-55.7322829513575,-2.));
#32989=CARTESIAN_POINT('Ctrl Pts',(-33.3326856027611,-57.7363329907929,
-1.57148036339021));
#32990=CARTESIAN_POINT('Ctrl Pts',(-33.7401458440335,-57.496539311517,-1.6031823516921));
#32991=CARTESIAN_POINT('Ctrl Pts',(-34.0466143999381,-57.0758524794489,
-1.63488433999399));
#32992=CARTESIAN_POINT('Ctrl Pts',(-34.1374824480444,-56.6126749242947,
-1.66658632829588));
#32993=CARTESIAN_POINT('Ctrl Pts',(-34.243668040048,-56.0714199515982,-1.70363229181856));
#32994=CARTESIAN_POINT('Ctrl Pts',(-34.0554395585675,-55.472141614315,-1.74067825534124));
#32995=CARTESIAN_POINT('Ctrl Pts',(-33.6580205398159,-55.0897022763625,
-1.77772421886392));
#32996=CARTESIAN_POINT('Ctrl Pts',(-33.2606015210643,-54.70726293841,-1.8147701823866));
#32997=CARTESIAN_POINT('Ctrl Pts',(-32.6539919650415,-54.5416625997882,
-1.85181614590928));
#32998=CARTESIAN_POINT('Ctrl Pts',(-32.1180205379334,-54.6674612497455,
-1.88886210943196));
#32999=CARTESIAN_POINT('Ctrl Pts',(-31.5820491108253,-54.7932598997029,
-1.92590807295464));
#33000=CARTESIAN_POINT('Ctrl Pts',(-31.116715812632,-55.2104575382394,-1.96295403647732));
#33001=CARTESIAN_POINT('Ctrl Pts',(-30.9307125467393,-55.7322829513575,
-2.));
#33002=CARTESIAN_POINT('',(-32.1993827818329,-57.933381219007,-2.));
#33003=CARTESIAN_POINT('Origin',(-32.5,-56.2916512459885,-2.));
#33004=CARTESIAN_POINT('Ctrl Pts',(-32.1993825459688,-57.9333829869217,
-2.));
#33005=CARTESIAN_POINT('Ctrl Pts',(-31.6675596070897,-57.835293698039,-1.96367708181444));
#33006=CARTESIAN_POINT('Ctrl Pts',(-31.1868214355218,-57.454698369386,-1.92735416362889));
#33007=CARTESIAN_POINT('Ctrl Pts',(-30.9706018866113,-56.9589951265537,
-1.89103124544334));
#33008=CARTESIAN_POINT('Ctrl Pts',(-30.7500782634566,-56.4534243968501,
-1.85398528192066));
#33009=CARTESIAN_POINT('Ctrl Pts',(-30.8047091132838,-55.8281174567283,
-1.81693931839798));
#33010=CARTESIAN_POINT('Ctrl Pts',(-31.1096921022324,-55.3687479433185,
-1.77989335487529));
#33011=CARTESIAN_POINT('Ctrl Pts',(-31.4146750911809,-54.9093784299087,
-1.74284739135261));
#33012=CARTESIAN_POINT('Ctrl Pts',(-31.9700102192507,-54.6159463432109,
-1.70580142782993));
#33013=CARTESIAN_POINT('Ctrl Pts',(-32.521445594378,-54.6229937951642,-1.66875546430725));
#33014=CARTESIAN_POINT('Ctrl Pts',(-33.0728809695053,-54.6300412471175,
-1.63170950078457));
#33015=CARTESIAN_POINT('Ctrl Pts',(-33.62041659169,-54.9375682377219,-1.59466353726189));
#33016=CARTESIAN_POINT('Ctrl Pts',(-33.9135196580233,-55.4047071572134,
-1.55761757373921));
#33017=CARTESIAN_POINT('Ctrl Pts',(-34.2066227243565,-55.8718460767048,
-1.52057161021653));
#33018=CARTESIAN_POINT('Ctrl Pts',(-34.2452932348383,-56.4985969250833,
-1.48352564669385));
#33019=CARTESIAN_POINT('Ctrl Pts',(-34.0118083132187,-56.9981869719763,
-1.44647968317117));
#33020=CARTESIAN_POINT('Ctrl Pts',(-33.869033908706,-57.3036828084989,-1.42382633431738));
#33021=CARTESIAN_POINT('Ctrl Pts',(-33.6244941277174,-57.5616302028088,
-1.40117298546358));
#33022=CARTESIAN_POINT('Ctrl Pts',(-33.3311039683456,-57.7330494773494,
-1.37851963660979));
#33023=CARTESIAN_POINT('Origin',(-32.5,-56.2916512459885,-3.54592528053767));
#33024=CARTESIAN_POINT('',(-33.5275749112977,-58.0738535198176,6.54592528053768));
#33025=CARTESIAN_POINT('',(-33.5264962288792,-58.0679896197986,6.60407471946233));
#33026=CARTESIAN_POINT('',(-33.5273749999999,-58.0711169444146,-3.54592528053767));
#33027=CARTESIAN_POINT('',(-32.2716262263503,-54.2496319067047,7.));
#33028=CARTESIAN_POINT('Ctrl Pts',(-33.5264962288792,-58.0679896197986,
6.60407471946233));
#33029=CARTESIAN_POINT('Ctrl Pts',(-33.1919689183208,-58.2597658075907,
6.62491192240684));
#33030=CARTESIAN_POINT('Ctrl Pts',(-32.1179432461624,-58.5451601991561,
6.68279508887404));
#33031=CARTESIAN_POINT('Ctrl Pts',(-30.4105200538552,-57.5324032730232,
6.77772421886391));
#33032=CARTESIAN_POINT('Ctrl Pts',(-30.3280193568976,-55.2072605605051,
6.88886210943196));
#33033=CARTESIAN_POINT('Ctrl Pts',(-31.592606214368,-54.3255716196824,6.96295403647732));
#33034=CARTESIAN_POINT('Ctrl Pts',(-32.2716262263503,-54.2496319067047,
7.));
#33035=CARTESIAN_POINT('',(-33.3217794842373,-54.4043178444011,6.99999999999999));
#33036=CARTESIAN_POINT('Origin',(-32.5,-56.2916512459885,7.));
#33037=CARTESIAN_POINT('Ctrl Pts',(-33.5275749112977,-58.0738535198176,
6.54592528053768));
#33038=CARTESIAN_POINT('Ctrl Pts',(-33.4657840639227,-58.1101089614272,
6.54982271160486));
#33039=CARTESIAN_POINT('Ctrl Pts',(-32.7965074863137,-58.455071838418,6.59076610619472));
#33040=CARTESIAN_POINT('Ctrl Pts',(-31.1711925871668,-58.3247407101007,
6.66875546430726));
#33041=CARTESIAN_POINT('Ctrl Pts',(-30.0714699489351,-56.2774508415845,
6.7798933548753));
#33042=CARTESIAN_POINT('Ctrl Pts',(-31.1870202472961,-54.2576863817542,
6.89030820010621));
#33043=CARTESIAN_POINT('Ctrl Pts',(-32.7099100739971,-54.1388320417446,
6.96367708181444));
#33044=CARTESIAN_POINT('Ctrl Pts',(-33.3217804591137,-54.4043158724519,
6.99999999999999));
#33045=CARTESIAN_POINT('Origin',(-32.5,-56.2916512459885,-3.54592528053767));
#33046=CARTESIAN_POINT('',(-33.5250713804254,-58.0691800125914,5.84592528053768));
#33047=CARTESIAN_POINT('',(-33.5296302847681,-58.0720277053709,5.90407471946233));
#33048=CARTESIAN_POINT('',(-33.5273749999999,-58.0711169444146,-3.54592528053767));
#33049=CARTESIAN_POINT('Ctrl Pts',(-33.5296302847681,-58.0720277053709,
5.90407471946233));
#33050=CARTESIAN_POINT('Ctrl Pts',(-33.0191355770127,-58.3612066004053,
5.93596947460409));
#33051=CARTESIAN_POINT('Ctrl Pts',(-31.6285851526934,-58.5053110361567,
6.00491019326854));
#33052=CARTESIAN_POINT('Ctrl Pts',(-30.1397737216657,-56.8641588006487,
6.11089687545567));
#33053=CARTESIAN_POINT('Ctrl Pts',(-30.7390063155881,-54.6191619749281,
6.2220347660237));
#33054=CARTESIAN_POINT('Ctrl Pts',(-32.9499730445898,-53.9051289476276,
6.33317265659175));
#33055=CARTESIAN_POINT('Ctrl Pts',(-34.7493198838486,-55.3752771327861,
6.44431054715979));
#33056=CARTESIAN_POINT('Ctrl Pts',(-34.5380916131597,-57.2516667239215,
6.53461123478332));
#33057=CARTESIAN_POINT('Ctrl Pts',(-33.7867170031423,-57.9188115213373,
6.58786595888416));
#33058=CARTESIAN_POINT('Ctrl Pts',(-33.5264962288792,-58.0679896197986,
6.60407471946233));
#33059=CARTESIAN_POINT('Ctrl Pts',(-33.5250713804254,-58.0691800125914,
5.84592528053768));
#33060=CARTESIAN_POINT('Ctrl Pts',(-33.2860537216367,-58.2086221814904,
5.86088026380211));
#33061=CARTESIAN_POINT('Ctrl Pts',(-32.3636248873145,-58.5321674493612,
5.91288121058921));
#33062=CARTESIAN_POINT('Ctrl Pts',(-30.6332940299706,-57.8452774805725,
6.00192812089901));
#33063=CARTESIAN_POINT('Ctrl Pts',(-30.1823177935136,-55.5659199366928,
6.11306601146705));
#33064=CARTESIAN_POINT('Ctrl Pts',(-31.8527378172474,-53.9508533596396,
6.22420390203509));
#33065=CARTESIAN_POINT('Ctrl Pts',(-34.1156133119216,-54.4783040835128,
6.33534179260312));
#33066=CARTESIAN_POINT('Ctrl Pts',(-34.8721855502189,-56.5889092129518,
6.442582252104));
#33067=CARTESIAN_POINT('Ctrl Pts',(-34.0531200394491,-57.7654927913865,
6.51277674808218));
#33068=CARTESIAN_POINT('Ctrl Pts',(-33.5275749112977,-58.0738535198176,
6.54592528053768));
#33069=CARTESIAN_POINT('Origin',(-32.5,-56.2916512459885,-3.54592528053767));
#33070=CARTESIAN_POINT('',(-33.5282754020984,-58.069145943353,5.14592528053768));
#33071=CARTESIAN_POINT('',(-33.5267258804522,-58.0732604370279,5.20407471946232));
#33072=CARTESIAN_POINT('',(-33.5273749999999,-58.0711169444146,-3.54592528053767));
#33073=CARTESIAN_POINT('Ctrl Pts',(-33.5267258804522,-58.0732604370279,
5.20407471946232));
#33074=CARTESIAN_POINT('Ctrl Pts',(-33.4330630138881,-58.1284275812183,
5.20998106327866));
#33075=CARTESIAN_POINT('Ctrl Pts',(-32.7207180221807,-58.473569466158,5.25293337061767));
#33076=CARTESIAN_POINT('Ctrl Pts',(-31.0632581782874,-58.2497382420229,
5.33293164147938));
#33077=CARTESIAN_POINT('Ctrl Pts',(-30.0756916068807,-56.1465211293305,
5.44406953204741));
#33078=CARTESIAN_POINT('Ctrl Pts',(-31.3071229976034,-54.1761423261723,
5.55520742261546));
#33079=CARTESIAN_POINT('Ctrl Pts',(-33.6304062534726,-54.1421146842281,
5.66634531318349));
#33080=CARTESIAN_POINT('Ctrl Pts',(-34.9190197935987,-56.0755785414895,
5.77748320375154));
#33081=CARTESIAN_POINT('Ctrl Pts',(-34.2590870859834,-57.5951911211838,
5.85672633917782));
#33082=CARTESIAN_POINT('Ctrl Pts',(-33.6120784680294,-58.0253234512995,
5.89892351108141));
#33083=CARTESIAN_POINT('Ctrl Pts',(-33.5296302847681,-58.0720277053709,
5.90407471946233));
#33084=CARTESIAN_POINT('Ctrl Pts',(-33.5282754020984,-58.069145943353,5.14592528053768));
#33085=CARTESIAN_POINT('Ctrl Pts',(-33.1102767098287,-58.3059329434062,
5.17193781599936));
#33086=CARTESIAN_POINT('Ctrl Pts',(-31.8926982278611,-58.5381488249037,
5.23499631498372));
#33087=CARTESIAN_POINT('Ctrl Pts',(-30.2596385516872,-57.2292625110704,
5.33510077749076));
#33088=CARTESIAN_POINT('Ctrl Pts',(-30.4972127153845,-54.9179054771162,
5.44623866805879));
#33089=CARTESIAN_POINT('Ctrl Pts',(-32.5679607208419,-53.8639538597436,
5.55737655862685));
#33090=CARTESIAN_POINT('Ctrl Pts',(-34.5765036531329,-55.0321005249753,
5.66851444919488));
#33091=CARTESIAN_POINT('Ctrl Pts',(-34.6698803007257,-57.0408062963268,
5.7646973564985));
#33092=CARTESIAN_POINT('Ctrl Pts',(-33.878139938799,-57.8632008987502,5.82383430027943));
#33093=CARTESIAN_POINT('Ctrl Pts',(-33.5250713804254,-58.0691800125914,
5.84592528053768));
#33094=CARTESIAN_POINT('Origin',(-32.5,-56.2916512459885,-3.54592528053767));
#33095=CARTESIAN_POINT('',(-33.5290696646583,-58.0740687441032,4.44592528053768));
#33096=CARTESIAN_POINT('',(-33.5253496165875,-58.0685468270268,4.50407471946233));
#33097=CARTESIAN_POINT('',(-33.5273749999999,-58.0711169444146,-3.54592528053767));
#33098=CARTESIAN_POINT('Ctrl Pts',(-33.5253496165874,-58.0685468270268,
4.50407471946233));
#33099=CARTESIAN_POINT('Ctrl Pts',(-33.2536996405186,-58.2261242815538,
4.52103861547591));
#33100=CARTESIAN_POINT('Ctrl Pts',(-32.2808222041073,-58.5391009797129,
4.57504847501218));
#33101=CARTESIAN_POINT('Ctrl Pts',(-30.5520219543112,-57.7420698681824,
4.66610429807112));
#33102=CARTESIAN_POINT('Ctrl Pts',(-30.2249467851584,-55.4416715145514,
4.77724218863917));
#33103=CARTESIAN_POINT('Ctrl Pts',(-31.9802536404281,-53.9192692335435,
4.8883800792072));
#33104=CARTESIAN_POINT('Ctrl Pts',(-34.2112902010514,-54.5683351429997,
4.99951796977525));
#33105=CARTESIAN_POINT('Ctrl Pts',(-34.8406399092008,-56.6764493817394,
5.10474951652696));
#33106=CARTESIAN_POINT('Ctrl Pts',(-34.0205383194344,-57.7824064089199,
5.17293509975598));
#33107=CARTESIAN_POINT('Ctrl Pts',(-33.5267258804522,-58.0732604370279,
5.20407471946232));
#33108=CARTESIAN_POINT('Ctrl Pts',(-33.529069656232,-58.0740687294261,4.44592528053768));
#33109=CARTESIAN_POINT('Ctrl Pts',(-33.5286860990811,-58.0742902067967,
4.44594940467393));
#33110=CARTESIAN_POINT('Ctrl Pts',(-32.9391765838663,-58.414411936218,4.48301949233286));
#33111=CARTESIAN_POINT('Ctrl Pts',(-31.3901016278141,-58.451850257884,4.55713554351447));
#33112=CARTESIAN_POINT('Ctrl Pts',(-30.0831480764379,-56.5307348090517,
4.6682734340825));
#33113=CARTESIAN_POINT('Ctrl Pts',(-30.9883665002518,-54.3907834608548,
4.77941132465055));
#33114=CARTESIAN_POINT('Ctrl Pts',(-33.2772002083032,-53.990717959075,4.89054921521859));
#33115=CARTESIAN_POINT('Ctrl Pts',(-34.8546537539781,-55.6967227784588,
5.00168710578663));
#33116=CARTESIAN_POINT('Ctrl Pts',(-34.4121009342633,-57.4205168337107,
5.08681246089299));
#33117=CARTESIAN_POINT('Ctrl Pts',(-33.705572940339,-57.9687108152697,5.13489185247668));
#33118=CARTESIAN_POINT('Ctrl Pts',(-33.5282754020984,-58.069145943353,5.14592528053768));
#33119=CARTESIAN_POINT('Origin',(-32.5,-56.2916512459885,-3.54592528053767));
#33120=CARTESIAN_POINT('',(-33.5252102943906,-58.0708877004567,3.74592528053768));
#33121=CARTESIAN_POINT('',(-33.5289081309377,-58.0700145843707,3.80407471946232));
#33122=CARTESIAN_POINT('',(-33.5273749999999,-58.0711169444146,-3.54592528053767));
#33123=CARTESIAN_POINT('Ctrl Pts',(-33.5289081309377,-58.0700145843707,
3.80407471946232));
#33124=CARTESIAN_POINT('Ctrl Pts',(-33.0789876682099,-58.3243434135938,
3.83209616767316));
#33125=CARTESIAN_POINT('Ctrl Pts',(-31.8034240249953,-58.5300263366319,
3.89716357940668));
#33126=CARTESIAN_POINT('Ctrl Pts',(-30.2122199456457,-57.106755585101,3.99927695466286));
#33127=CARTESIAN_POINT('Ctrl Pts',(-30.5744204047746,-54.811625609896,4.11041484523092));
#33128=CARTESIAN_POINT('Ctrl Pts',(-32.6991257052286,-53.8711798837978,
4.22155273579895));
#33129=CARTESIAN_POINT('Ctrl Pts',(-34.6415689889353,-55.1462190460047,
4.332690626367));
#33130=CARTESIAN_POINT('Ctrl Pts',(-34.6265206091307,-57.1150354081818,
4.42686462092145));
#33131=CARTESIAN_POINT('Ctrl Pts',(-33.8469321795724,-57.8820047097448,
4.48399265195323));
#33132=CARTESIAN_POINT('Ctrl Pts',(-33.5253496165874,-58.0685468270268,
4.50407471946233));
#33133=CARTESIAN_POINT('Ctrl Pts',(-33.5252102943906,-58.0708877004567,
3.74592528053768));
#33134=CARTESIAN_POINT('Ctrl Pts',(-33.3488056811853,-58.174663668992,3.75700695687117));
#33135=CARTESIAN_POINT('Ctrl Pts',(-32.5196622305249,-58.5123107269966,
3.80513459672735));
#33136=CARTESIAN_POINT('Ctrl Pts',(-30.8051884955116,-58.0311765069792,
3.89030820010621));
#33137=CARTESIAN_POINT('Ctrl Pts',(-30.1193554633367,-55.8111663248381,
4.00144609067426));
#33138=CARTESIAN_POINT('Ctrl Pts',(-31.6125533739246,-54.0309494400522,
4.11258398124229));
#33139=CARTESIAN_POINT('Ctrl Pts',(-33.9180412456697,-54.3199785564283,
4.22372187181034));
#33140=CARTESIAN_POINT('Ctrl Pts',(-34.9253611823253,-56.4132475717748,
4.33483563824213));
#33141=CARTESIAN_POINT('Ctrl Pts',(-34.1176914037626,-57.7341809275558,
4.40890344115124));
#33142=CARTESIAN_POINT('Ctrl Pts',(-33.529069656232,-58.0740687294261,4.44592528053768));
#33143=CARTESIAN_POINT('Origin',(-32.5,-56.2916512459885,-3.54592528053767));
#33144=CARTESIAN_POINT('',(-33.5268671815904,-58.0681591655549,3.04592528053768));
#33145=CARTESIAN_POINT('',(-33.5283521207634,-58.0741669114358,3.10407471946233));
#33146=CARTESIAN_POINT('',(-33.5273749999999,-58.0711169444146,-3.54592528053767));
#33147=CARTESIAN_POINT('Ctrl Pts',(-33.5283521207634,-58.0741669114359,
3.10407471946232));
#33148=CARTESIAN_POINT('Ctrl Pts',(-33.4960959785975,-58.0929755878456,
3.10610775634773));
#33149=CARTESIAN_POINT('Ctrl Pts',(-32.8657385633012,-58.4363094602464,
3.14518675675581));
#33150=CARTESIAN_POINT('Ctrl Pts',(-31.2749245001037,-58.3886783513254,
3.22131172068658));
#33151=CARTESIAN_POINT('Ctrl Pts',(-30.0737566908708,-56.3997070920348,
3.33244961125462));
#33152=CARTESIAN_POINT('Ctrl Pts',(-31.0933568979523,-54.3118310914232,
3.44358750182266));
#33153=CARTESIAN_POINT('Ctrl Pts',(-33.4004734887601,-54.0361069309691,
3.5547253923907));
#33154=CARTESIAN_POINT('Ctrl Pts',(-34.8833764832336,-55.8249080616723,
3.66586328295875));
#33155=CARTESIAN_POINT('Ctrl Pts',(-34.3608947477859,-57.4821952700404,
3.74897972531595));
#33156=CARTESIAN_POINT('Ctrl Pts',(-33.6738083543112,-57.9881060978322,
3.79505020415048));
#33157=CARTESIAN_POINT('Ctrl Pts',(-33.5289081309377,-58.0700145843707,
3.80407471946232));
#33158=CARTESIAN_POINT('Ctrl Pts',(-33.5268671815904,-58.0681591655549,
3.04592528053768));
#33159=CARTESIAN_POINT('Ctrl Pts',(-33.1711688207572,-58.2713555197574,
3.06806450906843));
#33160=CARTESIAN_POINT('Ctrl Pts',(-32.0617673212825,-58.5453769689692,
3.12724970112185));
#33161=CARTESIAN_POINT('Ctrl Pts',(-30.3694292262435,-57.4574138064661,
3.22348085669796));
#33162=CARTESIAN_POINT('Ctrl Pts',(-30.3650742488504,-55.1338834771873,
3.334618747266));
#33163=CARTESIAN_POINT('Ctrl Pts',(-32.3148410231895,-53.870071116671,3.44575663783405));
#33164=CARTESIAN_POINT('Ctrl Pts',(-34.4340859088485,-54.822758511107,3.55689452840208));
#33165=CARTESIAN_POINT('Ctrl Pts',(-34.7482454446892,-56.8908856856794,
3.65695074263663));
#33166=CARTESIAN_POINT('Ctrl Pts',(-33.9385250223179,-57.8277413596598,
3.71996099334849));
#33167=CARTESIAN_POINT('Ctrl Pts',(-33.5252102943906,-58.0708877004567,
3.74592528053768));
#33168=CARTESIAN_POINT('Origin',(-32.5,-56.2916512459885,-3.54592528053767));
#33169=CARTESIAN_POINT('',(-33.5296717523759,-58.0726906696378,2.34592528053768));
#33170=CARTESIAN_POINT('',(-33.5250223861017,-58.0699440624176,2.40407471946232));
#33171=CARTESIAN_POINT('',(-33.5273749999999,-58.0711169444146,-3.54592528053767));
#33172=CARTESIAN_POINT('Ctrl Pts',(-33.5250223861017,-58.0699440624176,
2.40407471946232));
#33173=CARTESIAN_POINT('Ctrl Pts',(-33.3162068666574,-58.1923260109822,
2.41716530854498));
#33174=CARTESIAN_POINT('Ctrl Pts',(-32.4393285405002,-58.523643057744,2.46730186115031));
#33175=CARTESIAN_POINT('Ctrl Pts',(-30.7136126829218,-57.9369940717681,
2.55448437727833));
#33176=CARTESIAN_POINT('Ctrl Pts',(-30.1488178080539,-55.6831490181888,
2.66562226784637));
#33177=CARTESIAN_POINT('Ctrl Pts',(-31.7360866576937,-53.9862729545993,
2.77676015841441));
#33178=CARTESIAN_POINT('Ctrl Pts',(-34.0225740529132,-54.3995357858862,
2.88789804898245));
#33179=CARTESIAN_POINT('Ctrl Pts',(-34.8990991658235,-56.5054325192522,
2.99700290266509));
#33180=CARTESIAN_POINT('Ctrl Pts',(-34.0838668521307,-57.7502442064381,
3.06906179282505));
#33181=CARTESIAN_POINT('Ctrl Pts',(-33.5283521207634,-58.0741669114359,
3.10407471946232));
#33182=CARTESIAN_POINT('Ctrl Pts',(-33.5296717523759,-58.0726906696378,
2.34592528053768));
#33183=CARTESIAN_POINT('Ctrl Pts',(-32.9991186855868,-58.3741080652297,
2.37912206126567));
#33184=CARTESIAN_POINT('Ctrl Pts',(-31.5690873940506,-58.494201559501,2.44936480551635));
#33185=CARTESIAN_POINT('Ctrl Pts',(-30.1211733226087,-56.7810568122912,
2.55665351328971));
#33186=CARTESIAN_POINT('Ctrl Pts',(-30.7986796648578,-54.5584913322389,
2.66779140385775));
#33187=CARTESIAN_POINT('Ctrl Pts',(-33.0334238041475,-53.9223067766118,
2.7789292944258));
#33188=CARTESIAN_POINT('Ctrl Pts',(-34.7799190860636,-55.4548100839991,
2.89006718499384));
#33189=CARTESIAN_POINT('Ctrl Pts',(-34.5073761199108,-57.29541607691,2.97906584703113));
#33190=CARTESIAN_POINT('Ctrl Pts',(-33.7663651927628,-57.931343458575,3.03101854554575));
#33191=CARTESIAN_POINT('Ctrl Pts',(-33.5268671815904,-58.0681591655549,
3.04592528053768));
#33192=CARTESIAN_POINT('Origin',(-32.5,-56.2916512459885,-3.54592528053767));
#33193=CARTESIAN_POINT('',(-33.5262302754658,-58.0727324938748,1.64592528053768));
#33194=CARTESIAN_POINT('',(-33.5276067488939,-58.0685424219934,1.70407471946232));
#33195=CARTESIAN_POINT('',(-33.5273749999999,-58.0711169444146,-3.54592528053767));
#33196=CARTESIAN_POINT('Ctrl Pts',(-33.5276067488939,-58.0685424219934,
1.70407471946232));
#33197=CARTESIAN_POINT('Ctrl Pts',(-33.1394910367319,-58.2891654943862,
1.72822286074223));
#33198=CARTESIAN_POINT('Ctrl Pts',(-31.9746000084876,-58.542974075687,1.78941696554481));
#33199=CARTESIAN_POINT('Ctrl Pts',(-30.3095139648772,-57.3405094780172,
1.88765703387008));
#33200=CARTESIAN_POINT('Ctrl Pts',(-30.4307974560059,-55.0201428925398,
1.99879492443812));
#33201=CARTESIAN_POINT('Ctrl Pts',(-32.4460455020051,-53.8636023228594,
2.10993281500616));
#33202=CARTESIAN_POINT('Ctrl Pts',(-34.5106787119048,-54.9294824684668,
2.2210707055742));
#33203=CARTESIAN_POINT('Ctrl Pts',(-34.7085028063896,-56.9697666836067,
2.31911800705959));
#33204=CARTESIAN_POINT('Ctrl Pts',(-33.9071483489281,-57.8459888695647,
2.3801193450223));
#33205=CARTESIAN_POINT('Ctrl Pts',(-33.5250223861017,-58.0699440624176,
2.40407471946232));
#33206=CARTESIAN_POINT('Ctrl Pts',(-33.5262302754658,-58.0727324938748,
1.64592528053768));
#33207=CARTESIAN_POINT('Ctrl Pts',(-33.4118498551747,-58.1401751811515,
1.65313364994024));
#33208=CARTESIAN_POINT('Ctrl Pts',(-32.670930140884,-58.4845521558011,1.69738798286549));
#33209=CARTESIAN_POINT('Ctrl Pts',(-30.9955026631254,-58.198172143523,1.77868827931342));
#33210=CARTESIAN_POINT('Ctrl Pts',(-30.0822688349231,-56.0616291105052,
1.88982616988146));
#33211=CARTESIAN_POINT('Ctrl Pts',(-31.3820117610517,-54.1356279467243,
2.0009640604495));
#33212=CARTESIAN_POINT('Ctrl Pts',(-33.7050620011389,-54.1830593597269,
2.11210195101755));
#33213=CARTESIAN_POINT('Ctrl Pts',(-34.9251053252509,-56.1605088392832,
2.22323984158559));
#33214=CARTESIAN_POINT('Ctrl Pts',(-34.224026615261,-57.6314775216245,2.30118095142563));
#33215=CARTESIAN_POINT('Ctrl Pts',(-33.5911896372902,-58.0377411767145,
2.34207609774299));
#33216=CARTESIAN_POINT('Ctrl Pts',(-33.5296717523759,-58.0726906696378,
2.34592528053768));
#33217=CARTESIAN_POINT('Origin',(-32.5,-56.2916512459885,-3.54592528053767));
#33218=CARTESIAN_POINT('',(-33.5256402930183,-58.0682685471634,0.945925280537677));
#33219=CARTESIAN_POINT('',(-33.5294982470258,-58.0735597602013,1.00407471946232));
#33220=CARTESIAN_POINT('',(-33.5273749999999,-58.0711169444146,-3.54592528053767));
#33221=CARTESIAN_POINT('Ctrl Pts',(-33.5294982470258,-58.0735597602013,
1.00407471946232));
#33222=CARTESIAN_POINT('Ctrl Pts',(-32.9682880946418,-58.3946192964701,
1.03928041293948));
#33223=CARTESIAN_POINT('Ctrl Pts',(-31.4766956957228,-58.4741418727902,
1.11153206993931));
#33224=CARTESIAN_POINT('Ctrl Pts',(-30.0981915249122,-56.6517188923722,
1.22082969046183));
#33225=CARTESIAN_POINT('Ctrl Pts',(-30.8948796869627,-54.4690373423775,
1.33196758102987));
#33226=CARTESIAN_POINT('Ctrl Pts',(-33.1607526748339,-53.9546149682087,
1.44310547159791));
#33227=CARTESIAN_POINT('Ctrl Pts',(-34.8218312459871,-55.5793084028841,
1.55424336216595));
#33228=CARTESIAN_POINT('Ctrl Pts',(-34.4585557374772,-57.3613319496871,
1.64123311145409));
#33229=CARTESIAN_POINT('Ctrl Pts',(-33.7349041722058,-57.9507048982935,
1.69117689721955));
#33230=CARTESIAN_POINT('Ctrl Pts',(-33.5276067488939,-58.0685424219934,
1.70407471946232));
#33231=CARTESIAN_POINT('Ctrl Pts',(-33.5256402930184,-58.0682685471634,
0.945925280537676));
#33232=CARTESIAN_POINT('Ctrl Pts',(-33.2328184146122,-58.2374617349622,
0.964191202137493));
#33233=CARTESIAN_POINT('Ctrl Pts',(-32.2264812528154,-58.542293513151,1.01950308725999));
#33234=CARTESIAN_POINT('Ctrl Pts',(-30.5023763530244,-57.6728948648119,
1.11186093590517));
#33235=CARTESIAN_POINT('Ctrl Pts',(-30.2561395980006,-55.3624447749947,
1.22299882647321));
#33236=CARTESIAN_POINT('Ctrl Pts',(-32.0637337160182,-53.9025079060376,
1.33413671704125));
#33237=CARTESIAN_POINT('Ctrl Pts',(-34.2706473113688,-54.629381030845,1.4452746076093));
#33238=CARTESIAN_POINT('Ctrl Pts',(-34.8188452912069,-56.7319204842157,
1.54920412877477));
#33239=CARTESIAN_POINT('Ctrl Pts',(-33.9996850008464,-57.7935670658911,
1.61608768641756));
#33240=CARTESIAN_POINT('Ctrl Pts',(-33.5262302754658,-58.0727324938748,
1.64592528053768));
#33241=CARTESIAN_POINT('Origin',(-32.5,-56.2916512459885,-3.54592528053767));
#33242=CARTESIAN_POINT('',(-33.5292382420786,-58.0706648023921,0.245925280537673));
#33243=CARTESIAN_POINT('',(-33.5256021009514,-58.0718002431918,0.304074719462323));
#33244=CARTESIAN_POINT('',(-33.5273749999999,-58.0711169444146,-3.54592528053767));
#33245=CARTESIAN_POINT('Ctrl Pts',(-33.5256021009514,-58.0718002431918,
0.304074719462322));
#33246=CARTESIAN_POINT('Ctrl Pts',(-33.3791306461153,-58.1581427811428,
0.313292001614045));
#33247=CARTESIAN_POINT('Ctrl Pts',(-32.5930673149393,-58.4998906338152,
0.35955524728845));
#33248=CARTESIAN_POINT('Ctrl Pts',(-30.8946190614981,-58.1140355911318,
0.442864456485535));
#33249=CARTESIAN_POINT('Ctrl Pts',(-30.0982430406458,-55.931240133699,0.554002347053576));
#33250=CARTESIAN_POINT('Ctrl Pts',(-31.5002224030512,-54.0783330542954,
0.665140237621618));
#33251=CARTESIAN_POINT('Ctrl Pts',(-33.8173095378994,-54.2513012166797,
0.776278128189661));
#33252=CARTESIAN_POINT('Ctrl Pts',(-34.9286483135496,-56.291824899935,0.887416018757701));
#33253=CARTESIAN_POINT('Ctrl Pts',(-34.1691544002423,-57.6858533133783,
0.96334821584859));
#33254=CARTESIAN_POINT('Ctrl Pts',(-33.5588337928047,-58.0567773540314,
1.0022344494168));
#33255=CARTESIAN_POINT('Ctrl Pts',(-33.5294982470258,-58.0735597602013,
1.00407471946232));
#33256=CARTESIAN_POINT('Ctrl Pts',(-33.5292382420786,-58.0706648023921,
0.245925280537675));
#33257=CARTESIAN_POINT('Ctrl Pts',(-33.0588051630516,-58.33651145622,0.275248754334742));
#33258=CARTESIAN_POINT('Ctrl Pts',(-31.7450292213916,-58.5230813041051,
0.34161819165449));
#33259=CARTESIAN_POINT('Ctrl Pts',(-30.1850532410697,-57.0260596319961,
0.445033592496918));
#33260=CARTESIAN_POINT('Ctrl Pts',(-30.6274839128386,-54.7450363379152,
0.556171483064961));
#33261=CARTESIAN_POINT('Ctrl Pts',(-32.783849793945,-53.8796472115696,0.667309373633002));
#33262=CARTESIAN_POINT('Ctrl Pts',(-34.6804047400893,-55.2219927306232,
0.778447264201044));
#33263=CARTESIAN_POINT('Ctrl Pts',(-34.5975134385767,-57.1618755368451,
0.871319233169269));
#33264=CARTESIAN_POINT('Ctrl Pts',(-33.8267040593522,-57.8943131766358,
0.927145238614813));
#33265=CARTESIAN_POINT('Ctrl Pts',(-33.5256402930184,-58.0682685471634,
0.945925280537676));
#33266=CARTESIAN_POINT('Origin',(-32.5,-56.2916512459885,-3.54592528053767));
#33267=CARTESIAN_POINT('',(-33.5278097333142,-58.0740011795199,-0.454074719462327));
#33268=CARTESIAN_POINT('',(-33.526223785585,-58.0680718733222,-0.395925280537678));
#33269=CARTESIAN_POINT('',(-33.5273749999999,-58.0711169444146,-3.54592528053767));
#33270=CARTESIAN_POINT('Ctrl Pts',(-33.526223785585,-58.0680718733222,-0.395925280537677));
#33271=CARTESIAN_POINT('Ctrl Pts',(-33.2007518244939,-58.254991046836,-0.375650446188704));
#33272=CARTESIAN_POINT('Ctrl Pts',(-32.1416146375096,-58.5451226040268,
-0.31832964831705));
#33273=CARTESIAN_POINT('Ctrl Pts',(-30.4306156658192,-57.5628636674515,
-0.223962886922716));
#33274=CARTESIAN_POINT('Ctrl Pts',(-30.3096639686861,-55.2424797818376,
-0.112824996354674));
#33275=CARTESIAN_POINT('Ctrl Pts',(-32.1935517174549,-53.8824144115655,
-0.00168710578663172));
#33276=CARTESIAN_POINT('Ctrl Pts',(-34.3579350363402,-54.7275508506072,
0.10945078478141));
#33277=CARTESIAN_POINT('Ctrl Pts',(-34.7832643179972,-56.8155005034113,
0.211371393197728));
#33278=CARTESIAN_POINT('Ctrl Pts',(-33.967826541896,-57.8111161350299,0.276246038091365));
#33279=CARTESIAN_POINT('Ctrl Pts',(-33.5256021009514,-58.0718002431918,
0.304074719462322));
#33280=CARTESIAN_POINT('Ctrl Pts',(-33.5278097333142,-58.0740011795199,
-0.454074719462325));
#33281=CARTESIAN_POINT('Ctrl Pts',(-33.4749288712104,-58.1049786318385,
-0.450739656990689));
#33282=CARTESIAN_POINT('Ctrl Pts',(-32.8174992673745,-58.4495803163018,
-0.410358630996371));
#33283=CARTESIAN_POINT('Ctrl Pts',(-31.2021687803137,-58.3444462635109,
-0.332931641479373));
#33284=CARTESIAN_POINT('Ctrl Pts',(-30.0714596841225,-56.3145920190741,
-0.221793750911332));
#33285=CARTESIAN_POINT('Ctrl Pts',(-31.1636212068567,-54.2637395061114,
-0.11065586034329));
#33286=CARTESIAN_POINT('Ctrl Pts',(-33.4789853310955,-54.069057766837,0.000482030224751219));
#33287=CARTESIAN_POINT('Ctrl Pts',(-34.8982731111897,-55.908740964546,0.111619920792794));
#33288=CARTESIAN_POINT('Ctrl Pts',(-34.3271081175644,-57.521036291931,0.193434337563768));
#33289=CARTESIAN_POINT('Ctrl Pts',(-33.6531292464159,-58.0006526999044,
0.238202790812062));
#33290=CARTESIAN_POINT('Ctrl Pts',(-33.5292382420786,-58.0706648023921,
0.245925280537675));
#33291=CARTESIAN_POINT('Origin',(-32.5,-56.2916512459885,-3.54592528053767));
#33292=CARTESIAN_POINT('',(-33.5250365419916,-58.0693901510839,-1.15407471946233));
#33293=CARTESIAN_POINT('',(-33.5295799600393,-58.0717283210701,-1.09592528053768));
#33294=CARTESIAN_POINT('',(-33.5273749999999,-58.0711169444146,-3.54592528053767));
#33295=CARTESIAN_POINT('Ctrl Pts',(-33.5295799600393,-58.0717283210701,
-1.09592528053768));
#33296=CARTESIAN_POINT('Ctrl Pts',(-33.0277944721986,-58.3557212843617,
-1.06459289399145));
#33297=CARTESIAN_POINT('Ctrl Pts',(-31.6541659742537,-58.5096740781238,
-0.99621454392255));
#33298=CARTESIAN_POINT('Ctrl Pts',(-30.1487320710282,-56.8998163998922,
-0.890790230330965));
#33299=CARTESIAN_POINT('Ctrl Pts',(-30.7138473610247,-54.6460533962845,
-0.779652339762925));
#33300=CARTESIAN_POINT('Ctrl Pts',(-32.91385067807,-53.8985232611178,-0.668514449194883));
#33301=CARTESIAN_POINT('Ctrl Pts',(-34.7350506405739,-55.3414510668855,
-0.557376558626841));
#33302=CARTESIAN_POINT('Ctrl Pts',(-34.5514515687201,-57.2322106426396,
-0.466513502407772));
#33303=CARTESIAN_POINT('Ctrl Pts',(-33.7954507596715,-57.9134543040693,
-0.412696409711384));
#33304=CARTESIAN_POINT('Ctrl Pts',(-33.526223785585,-58.0680718733222,-0.395925280537677));
#33305=CARTESIAN_POINT('Ctrl Pts',(-33.5250365419916,-58.0693901510839,
-1.15407471946233));
#33306=CARTESIAN_POINT('Ctrl Pts',(-33.2951376806275,-58.203713320331,-1.13968210479344));
#33307=CARTESIAN_POINT('Ctrl Pts',(-32.3865699532721,-58.5298194771329,
-1.08824352660187));
#33308=CARTESIAN_POINT('Ctrl Pts',(-30.6570393620673,-57.873352597378,-0.999758984887624));
#33309=CARTESIAN_POINT('Ctrl Pts',(-30.1715905180573,-55.6011108576298,
-0.888621094319583));
#33310=CARTESIAN_POINT('Ctrl Pts',(-31.817369145763,-53.960908709333,-0.77748320375154));
#33311=CARTESIAN_POINT('Ctrl Pts',(-34.087963584719,-54.4540716106361,-0.666345313183499));
#33312=CARTESIAN_POINT('Ctrl Pts',(-34.8805586635865,-56.5639154031852,
-0.558542485087094));
#33313=CARTESIAN_POINT('Ctrl Pts',(-34.0623309079662,-57.7608802593549,
-0.487785620513369));
#33314=CARTESIAN_POINT('Ctrl Pts',(-33.5278097333142,-58.0740011795199,
-0.454074719462325));
#33315=CARTESIAN_POINT('Origin',(-32.5,-56.2916512459885,-3.54592528053767));
#33316=CARTESIAN_POINT('',(-33.5283546803393,-58.0681541983481,-1.85407471946233));
#33317=CARTESIAN_POINT('',(-33.5269872402601,-58.0734398505124,-1.79592528053768));
#33318=CARTESIAN_POINT('',(-33.5273749999999,-58.0711169444146,-3.54592528053767));
#33319=CARTESIAN_POINT('',(-34.4842965055667,-55.7582049595679,-2.));
#33320=CARTESIAN_POINT('Ctrl Pts',(-34.4842965055667,-55.7582049595679,
-2.));
#33321=CARTESIAN_POINT('Ctrl Pts',(-34.6616800870191,-56.4180307560557,
-1.96295403647732));
#33322=CARTESIAN_POINT('Ctrl Pts',(-34.426165795488,-57.4023224375314,-1.91431227629809));
#33323=CARTESIAN_POINT('Ctrl Pts',(-33.7147012993046,-57.9624349357751,
-1.86567051611887));
#33324=CARTESIAN_POINT('Ctrl Pts',(-33.5283546803393,-58.0681541983481,
-1.85407471946233));
#33325=CARTESIAN_POINT('',(-33.9566395923166,-54.8371582344187,-2.));
#33326=CARTESIAN_POINT('Origin',(-32.5,-56.2916512459885,-2.));
#33327=CARTESIAN_POINT('Ctrl Pts',(-33.9566410663199,-54.8371566128168,
-2.));
#33328=CARTESIAN_POINT('Ctrl Pts',(-34.4273146919907,-55.3097386618185,
-1.96367708181445));
#33329=CARTESIAN_POINT('Ctrl Pts',(-34.8405825937333,-56.6643607585548,
-1.89565217532701));
#33330=CARTESIAN_POINT('Ctrl Pts',(-34.0295256140623,-57.7776919138425,
-1.82762726883957));
#33331=CARTESIAN_POINT('Ctrl Pts',(-33.5269872402601,-58.0734398505124,
-1.79592528053768));
#33332=CARTESIAN_POINT('Origin',(32.5,-56.2916512459885,3.));
#33333=CARTESIAN_POINT('',(33.3327252244638,-57.7364024133914,6.12851963660979));
#33334=CARTESIAN_POINT('',(33.3348404573523,-57.735699266238,6.32148036339021));
#33335=CARTESIAN_POINT('',(33.333,-57.7344495686934,3.));
#33336=CARTESIAN_POINT('',(33.0411029802559,-57.8673300091754,7.));
#33337=CARTESIAN_POINT('Ctrl Pts',(33.3348404573523,-57.735699266238,6.32148036339021));
#33338=CARTESIAN_POINT('Ctrl Pts',(33.3853483348093,-57.7070091850913,6.32537779445739));
#33339=CARTESIAN_POINT('Ctrl Pts',(33.4342336358034,-57.6755865432426,6.32927522552457));
#33340=CARTESIAN_POINT('Ctrl Pts',(33.4811646154108,-57.6414746748817,6.33317265659175));
#33341=CARTESIAN_POINT('Ctrl Pts',(33.9272541879144,-57.3172336532427,6.37021862011443));
#33342=CARTESIAN_POINT('Ctrl Pts',(34.196772145609,-56.7500228359926,6.40726458363711));
#33343=CARTESIAN_POINT('Ctrl Pts',(34.1662427495344,-56.1993881251835,6.44431054715979));
#33344=CARTESIAN_POINT('Ctrl Pts',(34.1357133534598,-55.6487534143744,6.48135651068247));
#33345=CARTESIAN_POINT('Ctrl Pts',(33.805136603616,-55.1146948100064,6.51840247420515));
#33346=CARTESIAN_POINT('Ctrl Pts',(33.3260603863118,-54.8417096746677,6.55544843772783));
#33347=CARTESIAN_POINT('Ctrl Pts',(32.8469841690075,-54.5687245393289,6.59249440125051));
#33348=CARTESIAN_POINT('Ctrl Pts',(32.2194084842428,-54.5568128730195,6.62954036477319));
#33349=CARTESIAN_POINT('Ctrl Pts',(31.7300326690205,-54.8112607055414,6.66658632829587));
#33350=CARTESIAN_POINT('Ctrl Pts',(31.2406568537983,-55.0657085380633,6.70363229181855));
#33351=CARTESIAN_POINT('Ctrl Pts',(30.8894809081185,-55.5865158694165,6.74067825534124));
#33352=CARTESIAN_POINT('Ctrl Pts',(30.8382644239114,-56.1356774091288,6.77772421886392));
#33353=CARTESIAN_POINT('Ctrl Pts',(30.7870479397043,-56.6848389488411,6.8147701823866));
#33354=CARTESIAN_POINT('Ctrl Pts',(31.0357909169699,-57.2623546969125,6.85181614590928));
#33355=CARTESIAN_POINT('Ctrl Pts',(31.4683170081768,-57.6029598655743,6.88886210943196));
#33356=CARTESIAN_POINT('Ctrl Pts',(31.9008430993836,-57.9435650342362,6.92590807295464));
#33357=CARTESIAN_POINT('Ctrl Pts',(32.5171523045318,-58.0472596234885,6.96295403647732));
#33358=CARTESIAN_POINT('Ctrl Pts',(33.0411029802559,-57.8673300091754,7.));
#33359=CARTESIAN_POINT('',(33.9709880617748,-55.5030815934935,7.));
#33360=CARTESIAN_POINT('Origin',(32.5,-56.2916512459885,7.));
#33361=CARTESIAN_POINT('',(33.3311603318023,-57.7325647065031,6.82851963660979));
#33362=CARTESIAN_POINT('Ctrl Pts',(33.9709895856635,-55.503080679032,7.));
#33363=CARTESIAN_POINT('Ctrl Pts',(34.2258866982027,-55.980034418951,6.96367708181445));
#33364=CARTESIAN_POINT('Ctrl Pts',(34.2280600118627,-56.5931875605705,6.92735416362889));
#33365=CARTESIAN_POINT('Ctrl Pts',(33.9753141969146,-57.071300576271,6.89103124544334));
#33366=CARTESIAN_POINT('Ctrl Pts',(33.8303226570678,-57.3455774911288,6.87019404249882));
#33367=CARTESIAN_POINT('Ctrl Pts',(33.6014392610868,-57.5754137754314,6.84935683955431));
#33368=CARTESIAN_POINT('Ctrl Pts',(33.3311603318023,-57.7325647065031,6.82851963660979));
#33369=CARTESIAN_POINT('',(33.333,-57.7344495686934,8.));
#33370=CARTESIAN_POINT('',(33.333,-57.7344495686934,3.));
#33371=CARTESIAN_POINT('Origin',(32.5,-56.2916512459885,8.));
#33372=CARTESIAN_POINT('Ctrl Pts',(33.3311603318023,-57.7325647065031,6.82851963660979));
#33373=CARTESIAN_POINT('Ctrl Pts',(33.1209168329143,-57.8548086479361,6.81231087603163));
#33374=CARTESIAN_POINT('Ctrl Pts',(32.8856252648826,-57.9330713283932,6.79610211545346));
#33375=CARTESIAN_POINT('Ctrl Pts',(32.6452880462139,-57.9540583561263,6.7798933548753));
#33376=CARTESIAN_POINT('Ctrl Pts',(32.0959848596434,-58.0020252972197,6.74284739135262));
#33377=CARTESIAN_POINT('Ctrl Pts',(31.5203244682533,-57.7507986915125,6.70580142782993));
#33378=CARTESIAN_POINT('Ctrl Pts',(31.1820200481674,-57.3152751741702,6.66875546430725));
#33379=CARTESIAN_POINT('Ctrl Pts',(30.8437156280816,-56.8797516568278,6.63170950078457));
#33380=CARTESIAN_POINT('Ctrl Pts',(30.7427671793,-56.2599312278504,6.59466353726189));
#33381=CARTESIAN_POINT('Ctrl Pts',(30.9252443270203,-55.739517741093,6.55761757373921));
#33382=CARTESIAN_POINT('Ctrl Pts',(31.1077214747406,-55.2191042543355,6.52057161021653));
#33383=CARTESIAN_POINT('Ctrl Pts',(31.5736242189628,-54.7980977097981,6.48352564669386));
#33384=CARTESIAN_POINT('Ctrl Pts',(32.1097948324389,-54.6691542850846,6.44647968317117));
#33385=CARTESIAN_POINT('Ctrl Pts',(32.645965445915,-54.540210860371,6.40943371964849));
#33386=CARTESIAN_POINT('Ctrl Pts',(33.2524039286451,-54.7033305554813,6.37238775612581));
#33387=CARTESIAN_POINT('Ctrl Pts',(33.6515374626529,-55.0838706916793,6.33534179260313));
#33388=CARTESIAN_POINT('Ctrl Pts',(34.0506709966607,-55.4644108278772,6.29829582908045));
#33389=CARTESIAN_POINT('Ctrl Pts',(34.2424995819463,-56.0623714051629,6.26124986555777));
#33390=CARTESIAN_POINT('Ctrl Pts',(34.1392482605268,-56.6040873635991,6.22420390203509));
#33391=CARTESIAN_POINT('Ctrl Pts',(34.0503539438025,-57.0704781983289,6.19230914689333));
#33392=CARTESIAN_POINT('Ctrl Pts',(33.7427356506951,-57.4951784726194,6.16041439175156));
#33393=CARTESIAN_POINT('Ctrl Pts',(33.3327252244638,-57.7364024133914,6.12851963660979));
#33394=CARTESIAN_POINT('Origin',(32.5,-56.2916512459885,3.));
#33395=CARTESIAN_POINT('',(33.3347682721563,-57.7348627592986,5.4285196366098));
#33396=CARTESIAN_POINT('',(33.3325737793451,-57.732046708219,5.62148036339021));
#33397=CARTESIAN_POINT('',(33.333,-57.7344495686934,3.));
#33398=CARTESIAN_POINT('Ctrl Pts',(33.3325737793451,-57.732046708219,5.62148036339021));
#33399=CARTESIAN_POINT('Ctrl Pts',(33.5273851267366,-57.6207441464882,5.63643534665464));
#33400=CARTESIAN_POINT('Ctrl Pts',(33.7002675206604,-57.4721914078235,5.65139032991906));
#33401=CARTESIAN_POINT('Ctrl Pts',(33.8340159287012,-57.2942275627961,5.66634531318349));
#33402=CARTESIAN_POINT('Ctrl Pts',(34.1653328254098,-56.853381726016,5.70339127670617));
#33403=CARTESIAN_POINT('Ctrl Pts',(34.2565099960995,-56.2320591280653,5.74043724022885));
#33404=CARTESIAN_POINT('Ctrl Pts',(34.0658176145798,-55.7146109150825,5.77748320375153));
#33405=CARTESIAN_POINT('Ctrl Pts',(33.8751252330602,-55.1971627020998,5.81452916727421));
#33406=CARTESIAN_POINT('Ctrl Pts',(33.4025632993312,-54.7835888740851,5.8515751307969));
#33407=CARTESIAN_POINT('Ctrl Pts',(32.8644065969169,-54.6631651603563,5.88862109431958));
#33408=CARTESIAN_POINT('Ctrl Pts',(32.3262498945026,-54.5427414466275,5.92566705784226));
#33409=CARTESIAN_POINT('Ctrl Pts',(31.722498423403,-54.7154678471846,5.96271302136494));
#33410=CARTESIAN_POINT('Ctrl Pts',(31.3294542359751,-55.1022925139248,5.99975898488762));
#33411=CARTESIAN_POINT('Ctrl Pts',(30.9364100485472,-55.4891171806649,6.0368049484103));
#33412=CARTESIAN_POINT('Ctrl Pts',(30.7540731447909,-56.0900401135881,6.07385091193298));
#33413=CARTESIAN_POINT('Ctrl Pts',(30.8659074307874,-56.6300507637272,6.11089687545566));
#33414=CARTESIAN_POINT('Ctrl Pts',(30.9777417167839,-57.1700614138663,6.14794283897834));
#33415=CARTESIAN_POINT('Ctrl Pts',(31.3837471925331,-57.6491597812213,6.18498880250102));
#33416=CARTESIAN_POINT('Ctrl Pts',(31.8980805240639,-57.8480733518849,6.2220347660237));
#33417=CARTESIAN_POINT('Ctrl Pts',(32.3583032720229,-58.0260601641038,6.25518329847921));
#33418=CARTESIAN_POINT('Ctrl Pts',(32.9052595394904,-57.9797148933652,6.28833183093471));
#33419=CARTESIAN_POINT('Ctrl Pts',(33.3348404573523,-57.735699266238,6.32148036339021));
#33420=CARTESIAN_POINT('Ctrl Pts',(33.3327252244638,-57.7364024133914,6.12851963660979));
#33421=CARTESIAN_POINT('Ctrl Pts',(33.2665058998609,-57.7753616334844,6.12336842822888));
#33422=CARTESIAN_POINT('Ctrl Pts',(33.1976157450274,-57.8095349962739,6.11821721984796));
#33423=CARTESIAN_POINT('Ctrl Pts',(33.1265448412824,-57.8383251884469,6.11306601146705));
#33424=CARTESIAN_POINT('Ctrl Pts',(32.6154239715823,-58.0453757152716,6.07602004794436));
#33425=CARTESIAN_POINT('Ctrl Pts',(31.9915134603068,-57.9740054293342,6.03897408442169));
#33426=CARTESIAN_POINT('Ctrl Pts',(31.5403536505083,-57.6568760819726,6.00192812089901));
#33427=CARTESIAN_POINT('Ctrl Pts',(31.0891938407098,-57.3397467346111,5.96488215737633));
#33428=CARTESIAN_POINT('Ctrl Pts',(30.8107847323884,-56.7768583258254,5.92783619385365));
#33429=CARTESIAN_POINT('Ctrl Pts',(30.8325397428816,-56.2258205630586,5.89079023033097));
#33430=CARTESIAN_POINT('Ctrl Pts',(30.8542947533749,-55.6747828002917,5.85374426680828));
#33431=CARTESIAN_POINT('Ctrl Pts',(31.1762138826829,-55.1355956835437,5.8166983032856));
#33432=CARTESIAN_POINT('Ctrl Pts',(31.6509700657299,-54.8550209349977,5.77965233976292));
#33433=CARTESIAN_POINT('Ctrl Pts',(32.1257262487769,-54.5744461864517,5.74260637624024));
#33434=CARTESIAN_POINT('Ctrl Pts',(32.7533194855629,-54.5524838061078,5.70556041271756));
#33435=CARTESIAN_POINT('Ctrl Pts',(33.2465276451507,-54.7991851622225,5.66851444919488));
#33436=CARTESIAN_POINT('Ctrl Pts',(33.7397358047385,-55.0458865183372,5.6314684856722));
#33437=CARTESIAN_POINT('Ctrl Pts',(34.0985588871282,-55.5612516109106,5.59442252214952));
#33438=CARTESIAN_POINT('Ctrl Pts',(34.1587797389667,-56.1094206024476,5.55737655862684));
#33439=CARTESIAN_POINT('Ctrl Pts',(34.2190005908051,-56.6575895939847,5.52033059510416));
#33440=CARTESIAN_POINT('Ctrl Pts',(33.9806192120925,-57.2385624844853,5.48328463158148));
#33441=CARTESIAN_POINT('Ctrl Pts',(33.5527320593965,-57.5864537767432,5.4462386680588));
#33442=CARTESIAN_POINT('Ctrl Pts',(33.4845127880347,-57.6419190795022,5.44033232424247));
#33443=CARTESIAN_POINT('Ctrl Pts',(33.4114765004846,-57.691459719343,5.43442598042613));
#33444=CARTESIAN_POINT('Ctrl Pts',(33.3347682721563,-57.7348627592986,5.4285196366098));
#33445=CARTESIAN_POINT('Origin',(32.5,-56.2916512459885,3.));
#33446=CARTESIAN_POINT('',(33.3320164235938,-57.7319854708824,4.72851963660979));
#33447=CARTESIAN_POINT('',(33.3312509399777,-57.7342826871321,4.9214803633902));
#33448=CARTESIAN_POINT('',(33.333,-57.7344495686934,3.));
#33449=CARTESIAN_POINT('Ctrl Pts',(33.3312509399777,-57.7342826871321,4.9214803633902));
#33450=CARTESIAN_POINT('Ctrl Pts',(33.6669748777683,-57.5367675539577,4.94749289885188));
#33451=CARTESIAN_POINT('Ctrl Pts',(33.937858827665,-57.2229205202501,4.97350543431356));
#33452=CARTESIAN_POINT('Ctrl Pts',(34.0694479601931,-56.8587419095544,4.99951796977524));
#33453=CARTESIAN_POINT('Ctrl Pts',(34.2568516913978,-56.3400939850778,5.03656393329793));
#33454=CARTESIAN_POINT('Ctrl Pts',(34.1617340046633,-55.7193622303022,5.07360989682061));
#33455=CARTESIAN_POINT('Ctrl Pts',(33.827626015315,-55.2806280419242,5.11065586034329));
#33456=CARTESIAN_POINT('Ctrl Pts',(33.4935180259667,-54.8418938535462,5.14770182386597));
#33457=CARTESIAN_POINT('Ctrl Pts',(32.9204197340046,-54.5851572315658,5.18474778738864));
#33458=CARTESIAN_POINT('Ctrl Pts',(32.370612888852,-54.6279151680597,5.22179375091132));
#33459=CARTESIAN_POINT('Ctrl Pts',(31.8208060436993,-54.6706731045537,5.25883971443401));
#33460=CARTESIAN_POINT('Ctrl Pts',(31.2942906453562,-55.0129255995219,5.29588567795669));
#33461=CARTESIAN_POINT('Ctrl Pts',(31.032029319193,-55.4980388156703,5.33293164147937));
#33462=CARTESIAN_POINT('Ctrl Pts',(30.7697679930298,-55.9831520318186,5.36997760500205));
#33463=CARTESIAN_POINT('Ctrl Pts',(30.7717607390465,-56.611125969147,5.40702356852473));
#33464=CARTESIAN_POINT('Ctrl Pts',(31.0370958289673,-57.0945648785311,5.44406953204741));
#33465=CARTESIAN_POINT('Ctrl Pts',(31.3024309188881,-57.5780037879153,5.48111549557009));
#33466=CARTESIAN_POINT('Ctrl Pts',(31.831108352713,-57.9169076693553,5.51816145909277));
#33467=CARTESIAN_POINT('Ctrl Pts',(32.3811753809891,-57.9561750722705,5.55520742261545));
#33468=CARTESIAN_POINT('Ctrl Pts',(32.7091873614286,-57.9795907251543,5.57729840287371));
#33469=CARTESIAN_POINT('Ctrl Pts',(33.0448052440539,-57.8964589747132,5.59938938313196));
#33470=CARTESIAN_POINT('Ctrl Pts',(33.3325737793451,-57.732046708219,5.62148036339021));
#33471=CARTESIAN_POINT('Ctrl Pts',(33.3347682721563,-57.7348627592986,5.4285196366098));
#33472=CARTESIAN_POINT('Ctrl Pts',(32.9303446333077,-57.9636936909789,5.39738001690345));
#33473=CARTESIAN_POINT('Ctrl Pts',(32.423854116995,-58.0219212024995,5.3662403971971));
#33474=CARTESIAN_POINT('Ctrl Pts',(31.9831067199835,-57.8783395309755,5.33510077749076));
#33475=CARTESIAN_POINT('Ctrl Pts',(31.4587614599457,-57.7075242989346,5.29805481396807));
#33476=CARTESIAN_POINT('Ctrl Pts',(31.0274638665491,-57.2510841408376,5.2610088504454));
#33477=CARTESIAN_POINT('Ctrl Pts',(30.8865996954395,-56.7179114934438,5.22396288692272));
#33478=CARTESIAN_POINT('Ctrl Pts',(30.7457355243298,-56.1847388460499,5.18691692340004));
#33479=CARTESIAN_POINT('Ctrl Pts',(30.8953047755071,-55.5748337093591,5.14987095987736));
#33480=CARTESIAN_POINT('Ctrl Pts',(31.2668562499327,-55.1673226224439,5.11282499635467));
#33481=CARTESIAN_POINT('Ctrl Pts',(31.6384077243582,-54.7598115355286,5.07577903283199));
#33482=CARTESIAN_POINT('Ctrl Pts',(32.2319414220319,-54.5546944983888,5.03873306930931));
#33483=CARTESIAN_POINT('Ctrl Pts',(32.7758232721694,-54.6458444887422,5.00168710578663));
#33484=CARTESIAN_POINT('Ctrl Pts',(33.3197051223069,-54.7369944790956,4.96464114226395));
#33485=CARTESIAN_POINT('Ctrl Pts',(33.8139351249082,-55.1244114969421,4.92759517874127));
#33486=CARTESIAN_POINT('Ctrl Pts',(34.0323261210678,-55.6307919459654,4.89054921521859));
#33487=CARTESIAN_POINT('Ctrl Pts',(34.2507171172273,-56.1371723949886,4.85350325169591));
#33488=CARTESIAN_POINT('Ctrl Pts',(34.1932691069451,-56.7625162751886,4.81645728817323));
#33489=CARTESIAN_POINT('Ctrl Pts',(33.8862734957393,-57.2206314145013,4.77941132465055));
#33490=CARTESIAN_POINT('Ctrl Pts',(33.7456956532454,-57.4304091297116,4.76244742863696));
#33491=CARTESIAN_POINT('Ctrl Pts',(33.5527911750803,-57.6051213208864,4.74548353262338));
#33492=CARTESIAN_POINT('Ctrl Pts',(33.3320164235938,-57.7319854708824,4.72851963660979));
#33493=CARTESIAN_POINT('Origin',(32.5,-56.2916512459885,3.));
#33494=CARTESIAN_POINT('',(33.3316044198824,-57.73507921,4.02851963660979));
#33495=CARTESIAN_POINT('',(33.3343856218718,-57.7368361137997,4.2214803633902));
#33496=CARTESIAN_POINT('',(33.333,-57.7344495686934,3.));
#33497=CARTESIAN_POINT('Ctrl Pts',(33.3343856149812,-57.7368361019314,4.2214803633902));
#33498=CARTESIAN_POINT('Ctrl Pts',(33.8122975339405,-57.4609515848648,4.25855045104913));
#33499=CARTESIAN_POINT('Ctrl Pts',(34.1397428670922,-56.9245130794241,4.29562053870806));
#33500=CARTESIAN_POINT('Ctrl Pts',(34.1667586100627,-56.373348690468,4.33269062636699));
#33501=CARTESIAN_POINT('Ctrl Pts',(34.1937567719725,-55.8225429832862,4.36973658988968));
#33502=CARTESIAN_POINT('Ctrl Pts',(33.9207162964575,-55.2570306535141,4.40678255341236));
#33503=CARTESIAN_POINT('Ctrl Pts',(33.4725957048462,-54.9356216253737,4.44382851693504));
#33504=CARTESIAN_POINT('Ctrl Pts',(33.0244751132349,-54.6142125972332,4.48087448045772));
#33505=CARTESIAN_POINT('Ctrl Pts',(32.4012744055273,-54.5369068707243,4.5179204439804));
#33506=CARTESIAN_POINT('Ctrl Pts',(31.8882049204609,-54.7390838502781,4.55496640750308));
#33507=CARTESIAN_POINT('Ctrl Pts',(31.3751354353946,-54.9412608298319,4.59201237102576));
#33508=CARTESIAN_POINT('Ctrl Pts',(30.9721971729695,-55.4229205154485,4.62905833454844));
#33509=CARTESIAN_POINT('Ctrl Pts',(30.8637971116759,-55.9636286201302,4.66610429807112));
#33510=CARTESIAN_POINT('Ctrl Pts',(30.7553970503824,-56.5043367248119,4.7031502615938));
#33511=CARTESIAN_POINT('Ctrl Pts',(30.9415351902203,-57.1040932485588,4.74019622511648));
#33512=CARTESIAN_POINT('Ctrl Pts',(31.3370243602463,-57.488416218779,4.77724218863916));
#33513=CARTESIAN_POINT('Ctrl Pts',(31.7325135302722,-57.8727391889992,4.81428815216184));
#33514=CARTESIAN_POINT('Ctrl Pts',(32.3373537304862,-58.0416286056927,4.85133411568452));
#33515=CARTESIAN_POINT('Ctrl Pts',(32.8747364051652,-57.9177912669506,4.8883800792072));
#33516=CARTESIAN_POINT('Ctrl Pts',(33.0347855041357,-57.8809086962641,4.8994135072682));
#33517=CARTESIAN_POINT('Ctrl Pts',(33.1888509066773,-57.8180603341074,4.9104469353292));
#33518=CARTESIAN_POINT('Ctrl Pts',(33.3312509399777,-57.7342826871321,4.9214803633902));
#33519=CARTESIAN_POINT('Ctrl Pts',(33.3320164235938,-57.7319854708824,4.72851963660979));
#33520=CARTESIAN_POINT('Ctrl Pts',(33.0706605734929,-57.8821688027457,4.70843756910069));
#33521=CARTESIAN_POINT('Ctrl Pts',(32.770247004987,-57.965297344832,4.6883555015916));
#33522=CARTESIAN_POINT('Ctrl Pts',(32.4713490172714,-57.9601647997737,4.66827343408251));
#33523=CARTESIAN_POINT('Ctrl Pts',(31.919963362139,-57.9506966473078,4.63122747055982));
#33524=CARTESIAN_POINT('Ctrl Pts',(31.3737352640037,-57.6408739439503,4.59418150703715));
#33525=CARTESIAN_POINT('Ctrl Pts',(31.082649108761,-57.1724888068712,4.55713554351447));
#33526=CARTESIAN_POINT('Ctrl Pts',(30.7915629535184,-56.7041036697921,4.52008957999179));
#33527=CARTESIAN_POINT('Ctrl Pts',(30.7556187411683,-56.0771560989914,4.4830436164691));
#33528=CARTESIAN_POINT('Ctrl Pts',(30.9912665445818,-55.5785722051981,4.44599765294642));
#33529=CARTESIAN_POINT('Ctrl Pts',(31.2269143479953,-55.0799883114048,4.40895168942374));
#33530=CARTESIAN_POINT('Ctrl Pts',(31.7341541671722,-54.709768094619,4.37190572590106));
#33531=CARTESIAN_POINT('Ctrl Pts',(32.2808448224847,-54.6373449363854,4.33485976237838));
#33532=CARTESIAN_POINT('Ctrl Pts',(32.8275354777971,-54.5649217781518,4.2978137988557));
#33533=CARTESIAN_POINT('Ctrl Pts',(33.4136769692449,-54.7902956784704,4.26076783533302));
#33534=CARTESIAN_POINT('Ctrl Pts',(33.7710183196873,-55.2103229938828,4.22372187181034));
#33535=CARTESIAN_POINT('Ctrl Pts',(34.1283596701297,-55.6303503092952,4.18667590828766));
#33536=CARTESIAN_POINT('Ctrl Pts',(34.2569008795666,-56.2450310398012,4.14962994476498));
#33537=CARTESIAN_POINT('Ctrl Pts',(34.0978143345865,-56.7730530636186,4.1125839812423));
#33538=CARTESIAN_POINT('Ctrl Pts',(33.977481781258,-57.1724472320418,4.08456253303146));
#33539=CARTESIAN_POINT('Ctrl Pts',(33.692587001381,-57.5222608245174,4.05654108482063));
#33540=CARTESIAN_POINT('Ctrl Pts',(33.3316044198824,-57.73507921,4.02851963660979));
#33541=CARTESIAN_POINT('Origin',(32.5,-56.2916512459885,3.));
#33542=CARTESIAN_POINT('',(33.3347454964364,-57.7363721546008,3.32851963660979));
#33543=CARTESIAN_POINT('',(33.333716562894,-57.7328365508938,3.5214803633902));
#33544=CARTESIAN_POINT('',(33.333,-57.7344495686934,3.));
#33545=CARTESIAN_POINT('Ctrl Pts',(33.333716562894,-57.7328365508938,3.5214803633902));
#33546=CARTESIAN_POINT('Ctrl Pts',(33.4781004639345,-57.6510402790884,3.5325620397237));
#33547=CARTESIAN_POINT('Ctrl Pts',(33.6100888264908,-57.5485020789653,3.5436437160572));
#33548=CARTESIAN_POINT('Ctrl Pts',(33.7223873369831,-57.4276653019287,3.5547253923907));
#33549=CARTESIAN_POINT('Ctrl Pts',(34.0978004421985,-57.023708833649,3.59177135591338));
#33550=CARTESIAN_POINT('Ctrl Pts',(34.2531676277225,-56.4152547808823,3.62881731943606));
#33551=CARTESIAN_POINT('Ctrl Pts',(34.1173842201124,-55.880765591048,3.66586328295874));
#33552=CARTESIAN_POINT('Ctrl Pts',(33.9816008125024,-55.3462764012136,3.70290924648142));
#33553=CARTESIAN_POINT('Ctrl Pts',(33.5546668117583,-54.8857520743114,3.7399552100041));
#33554=CARTESIAN_POINT('Ctrl Pts',(33.0319709841925,-54.709954179896,3.77700117352679));
#33555=CARTESIAN_POINT('Ctrl Pts',(32.5092751566268,-54.5341562854806,3.81404713704947));
#33556=CARTESIAN_POINT('Ctrl Pts',(31.8908175022394,-54.643084823552,3.85109310057215));
#33557=CARTESIAN_POINT('Ctrl Pts',(31.4596386734713,-54.9868880310005,3.88813906409483));
#33558=CARTESIAN_POINT('Ctrl Pts',(31.0284598447031,-55.330691238449,3.92518502761751));
#33559=CARTESIAN_POINT('Ctrl Pts',(30.7845598415543,-55.9093691152746,3.96223099114019));
#33560=CARTESIAN_POINT('Ctrl Pts',(30.8395608834388,-56.4580864498104,3.99927695466287));
#33561=CARTESIAN_POINT('Ctrl Pts',(30.8945619253233,-57.0068037843461,4.03632291818555));
#33562=CARTESIAN_POINT('Ctrl Pts',(31.248464012241,-57.525560576592,4.07336888170823));
#33563=CARTESIAN_POINT('Ctrl Pts',(31.7393018474208,-57.7769448390475,4.11041484523091));
#33564=CARTESIAN_POINT('Ctrl Pts',(32.2298200515886,-58.0281654013958,4.14743668461734));
#33565=CARTESIAN_POINT('Ctrl Pts',(32.8570957184111,-58.0123615437382,4.18445852400377));
#33566=CARTESIAN_POINT('Ctrl Pts',(33.3343856149812,-57.7368361019314,4.2214803633902));
#33567=CARTESIAN_POINT('Ctrl Pts',(33.3316044198824,-57.73507921,4.02851963660979));
#33568=CARTESIAN_POINT('Ctrl Pts',(33.2153473010664,-57.8036189501297,4.01949512129795));
#33569=CARTESIAN_POINT('Ctrl Pts',(33.0911982807713,-57.8579494129027,4.0104706059861));
#33570=CARTESIAN_POINT('Ctrl Pts',(32.9621127685743,-57.8951505902149,4.00144609067425));
#33571=CARTESIAN_POINT('Ctrl Pts',(32.4322120469391,-58.0478627758654,3.96440012715157));
#33572=CARTESIAN_POINT('Ctrl Pts',(31.8191249030656,-57.9119238300377,3.9273541636289));
#33573=CARTESIAN_POINT('Ctrl Pts',(31.4034341447794,-57.5495469821188,3.89030820010621));
#33574=CARTESIAN_POINT('Ctrl Pts',(30.9877433864933,-57.1871701341999,3.85326223658353));
#33575=CARTESIAN_POINT('Ctrl Pts',(30.7694490137944,-56.5983553841899,3.81621627306085));
#33576=CARTESIAN_POINT('Ctrl Pts',(30.8484546841662,-56.0525771412361,3.77917030953817));
#33577=CARTESIAN_POINT('Ctrl Pts',(30.9274603545379,-55.5067988982823,3.74212434601549));
#33578=CARTESIAN_POINT('Ctrl Pts',(31.3037660679802,-55.0040571623848,3.70507838249281));
#33579=CARTESIAN_POINT('Ctrl Pts',(31.8051533809355,-54.7744345397173,3.66803241897013));
#33580=CARTESIAN_POINT('Ctrl Pts',(32.3065406938908,-54.5448119170498,3.63098645544745));
#33581=CARTESIAN_POINT('Ctrl Pts',(32.9330096063591,-54.5883084076123,3.59394049192477));
#33582=CARTESIAN_POINT('Ctrl Pts',(33.39785306823,-54.8850175958567,3.55689452840209));
#33583=CARTESIAN_POINT('Ctrl Pts',(33.862696530101,-55.181726784101,3.5198485648794));
#33584=CARTESIAN_POINT('Ctrl Pts',(34.1659145413745,-55.7316486700272,3.48280260135672));
#33585=CARTESIAN_POINT('Ctrl Pts',(34.1687376598278,-56.2831083842721,3.44575663783404));
#33586=CARTESIAN_POINT('Ctrl Pts',(34.1715607782811,-56.834568098517,3.40871067431136));
#33587=CARTESIAN_POINT('Ctrl Pts',(33.873989003914,-57.3875656410806,3.37166471078868));
#33588=CARTESIAN_POINT('Ctrl Pts',(33.4122077466127,-57.6890185508993,3.334618747266));
#33589=CARTESIAN_POINT('Ctrl Pts',(33.3868657595293,-57.70556191559,3.3325857103806));
#33590=CARTESIAN_POINT('Ctrl Pts',(33.3610292261422,-57.7213477085124,3.33055267349519));
#33591=CARTESIAN_POINT('Ctrl Pts',(33.3347454964364,-57.7363721546008,3.32851963660979));
#33592=CARTESIAN_POINT('Origin',(32.5,-56.2916512459885,3.));
#33593=CARTESIAN_POINT('',(33.3331301901789,-57.7323221393285,2.62851963660979));
#33594=CARTESIAN_POINT('',(33.3311289428234,-57.732893825255,2.82148036339021));
#33595=CARTESIAN_POINT('',(33.333,-57.7344495686934,3.));
#33596=CARTESIAN_POINT('Ctrl Pts',(33.3311289428234,-57.732893825255,2.82148036339021));
#33597=CARTESIAN_POINT('Ctrl Pts',(33.6180096158229,-57.5655068353994,2.84361959192095));
#33598=CARTESIAN_POINT('Ctrl Pts',(33.8582224621032,-57.3156647118177,2.8657588204517));
#33599=CARTESIAN_POINT('Ctrl Pts',(34.0018785934241,-57.0190572038434,2.88789804898245));
#33600=CARTESIAN_POINT('Ctrl Pts',(34.2422609442965,-56.5227386033238,2.92494401250513));
#33601=CARTESIAN_POINT('Ctrl Pts',(34.2122852455117,-55.8954772908328,2.96198997602781));
#33602=CARTESIAN_POINT('Ctrl Pts',(33.9256700455925,-55.4243429628455,2.99903593955049));
#33603=CARTESIAN_POINT('Ctrl Pts',(33.6390548456733,-54.9532086348582,3.03608190307317));
#33604=CARTESIAN_POINT('Ctrl Pts',(33.0958001446195,-54.6382012913747,3.07312786659585));
#33605=CARTESIAN_POINT('Ctrl Pts',(32.5445295368321,-54.6234858293533,3.11017383011853));
#33606=CARTESIAN_POINT('Ctrl Pts',(31.9932589290447,-54.6087703673318,3.14721979364121));
#33607=CARTESIAN_POINT('Ctrl Pts',(31.4339724145236,-54.8943467867725,3.1842657571639));
#33608=CARTESIAN_POINT('Ctrl Pts',(31.1226306380098,-55.3495194199899,3.22131172068658));
#33609=CARTESIAN_POINT('Ctrl Pts',(30.8112888614961,-55.8046920532072,3.25835768420926));
#33610=CARTESIAN_POINT('Ctrl Pts',(30.7478918229898,-56.4294609002013,3.29540364773194));
#33611=CARTESIAN_POINT('Ctrl Pts',(30.9614535366484,-56.9378969554647,3.33244961125462));
#33612=CARTESIAN_POINT('Ctrl Pts',(31.175015250307,-57.4463330107281,3.3694955747773));
#33613=CARTESIAN_POINT('Ctrl Pts',(31.6655357161305,-57.838436274261,3.40654153829998));
#33614=CARTESIAN_POINT('Ctrl Pts',(32.2085254614957,-57.9347584641311,3.44358750182266));
#33615=CARTESIAN_POINT('Ctrl Pts',(32.5890889655549,-58.0022674924479,3.46955178901184));
#33616=CARTESIAN_POINT('Ctrl Pts',(32.9954261310775,-57.9244846218395,3.49551607620102));
#33617=CARTESIAN_POINT('Ctrl Pts',(33.333716562894,-57.7328365508938,3.5214803633902));
#33618=CARTESIAN_POINT('Ctrl Pts',(33.3347454964364,-57.7363721546008,3.32851963660979));
#33619=CARTESIAN_POINT('Ctrl Pts',(32.8820875508043,-57.9951229094133,3.29350670997251));
#33620=CARTESIAN_POINT('Ctrl Pts',(32.2967926538178,-58.0280607074246,3.25849378333523));
#33621=CARTESIAN_POINT('Ctrl Pts',(31.8207237377836,-57.8159025761185,3.22348085669796));
#33622=CARTESIAN_POINT('Ctrl Pts',(31.3170117264913,-57.5914254144454,3.18643489317528));
#33623=CARTESIAN_POINT('Ctrl Pts',(30.9355784441425,-57.0925628140254,3.1493889296526));
#33624=CARTESIAN_POINT('Ctrl Pts',(30.8509889952778,-56.547622072684,3.11234296612992));
#33625=CARTESIAN_POINT('Ctrl Pts',(30.7663995464132,-56.0026813313427,3.07529700260724));
#33626=CARTESIAN_POINT('Ctrl Pts',(30.9786539310327,-55.41166244908,3.03825103908456));
#33627=CARTESIAN_POINT('Ctrl Pts',(31.390612726451,-55.0450485686685,3.00120507556188));
#33628=CARTESIAN_POINT('Ctrl Pts',(31.8025715218693,-54.678434688257,2.96415911203919));
#33629=CARTESIAN_POINT('Ctrl Pts',(32.4142347280865,-54.5362258096967,2.92711314851652));
#33630=CARTESIAN_POINT('Ctrl Pts',(32.9456712104109,-54.6835046326399,2.89006718499383));
#33631=CARTESIAN_POINT('Ctrl Pts',(33.4771076927353,-54.8307834555831,2.85302122147115));
#33632=CARTESIAN_POINT('Ctrl Pts',(33.928317451167,-55.2675499800298,2.81597525794847));
#33633=CARTESIAN_POINT('Ctrl Pts',(34.0928017812263,-55.7939155294323,2.77892929442579));
#33634=CARTESIAN_POINT('Ctrl Pts',(34.2572861112857,-56.3202810788348,2.74188333090311));
#33635=CARTESIAN_POINT('Ctrl Pts',(34.1350450129727,-56.9362456531932,2.70483736738043));
#33636=CARTESIAN_POINT('Ctrl Pts',(33.7820228180845,-57.3599095722955,2.66779140385775));
#33637=CARTESIAN_POINT('Ctrl Pts',(33.6572786340789,-57.509615768241,2.6547008147751));
#33638=CARTESIAN_POINT('Ctrl Pts',(33.5037182424927,-57.6353105712173,2.64161022569244));
#33639=CARTESIAN_POINT('Ctrl Pts',(33.3331301901789,-57.7323221393285,2.62851963660979));
#33640=CARTESIAN_POINT('Origin',(32.5,-56.2916512459885,3.));
#33641=CARTESIAN_POINT('',(33.331098284258,-57.7335685916211,1.92851963660978));
#33642=CARTESIAN_POINT('',(33.3331738820163,-57.7367002116856,2.12148036339021));
#33643=CARTESIAN_POINT('',(33.333,-57.7344495686934,3.));
#33644=CARTESIAN_POINT('Ctrl Pts',(33.3331738820163,-57.7367002116856,2.12148036339021));
#33645=CARTESIAN_POINT('Ctrl Pts',(33.7599095781772,-57.4863532801825,2.1546771441182));
#33646=CARTESIAN_POINT('Ctrl Pts',(34.0737470619128,-57.0348072848651,2.1878739248462));
#33647=CARTESIAN_POINT('Ctrl Pts',(34.1491952727494,-56.5464328961311,2.2210707055742));
#33648=CARTESIAN_POINT('Ctrl Pts',(34.2333917401539,-56.0014312606204,2.25811666909688));
#33649=CARTESIAN_POINT('Ctrl Pts',(34.0207112033875,-55.4105655517268,2.29516263261956));
#33650=CARTESIAN_POINT('Ctrl Pts',(33.608488116082,-55.044248811562,2.33220859614224));
#33651=CARTESIAN_POINT('Ctrl Pts',(33.1962650287764,-54.6779320713971,2.36925455966492));
#33652=CARTESIAN_POINT('Ctrl Pts',(32.5844993909316,-54.5361642999609,2.40630052318761));
#33653=CARTESIAN_POINT('Ctrl Pts',(32.0531692156544,-54.6838263217292,2.44334648671029));
#33654=CARTESIAN_POINT('Ctrl Pts',(31.5218390403773,-54.8314883434974,2.48039245023297));
#33655=CARTESIAN_POINT('Ctrl Pts',(31.0709443276677,-55.2685801584701,2.51743841375565));
#33656=CARTESIAN_POINT('Ctrl Pts',(30.9068395995441,-55.7950642190458,2.55448437727833));
#33657=CARTESIAN_POINT('Ctrl Pts',(30.7427348714206,-56.3215482796215,2.59153034080101));
#33658=CARTESIAN_POINT('Ctrl Pts',(30.8654201278831,-56.9374245858002,2.62857630432369));
#33659=CARTESIAN_POINT('Ctrl Pts',(31.2187477656388,-57.360833853803,2.66562226784637));
#33660=CARTESIAN_POINT('Ctrl Pts',(31.5720754033946,-57.7842431218059,2.70266823136905));
#33661=CARTESIAN_POINT('Ctrl Pts',(32.1560454224436,-58.0151853516329,2.73971419489173));
#33662=CARTESIAN_POINT('Ctrl Pts',(32.7034006322329,-57.9479685222722,2.77676015841441));
#33663=CARTESIAN_POINT('Ctrl Pts',(32.9236480838557,-57.9209214875348,2.79166689340634));
#33664=CARTESIAN_POINT('Ctrl Pts',(33.1379671006765,-57.845598452492,2.80657362839827));
#33665=CARTESIAN_POINT('Ctrl Pts',(33.3311289428234,-57.732893825255,2.82148036339021));
#33666=CARTESIAN_POINT('Ctrl Pts',(33.3331301901789,-57.7323221393285,2.62851963660979));
#33667=CARTESIAN_POINT('Ctrl Pts',(33.0209593136532,-57.9098503181175,2.60456426216976));
#33668=CARTESIAN_POINT('Ctrl Pts',(32.6517664254568,-57.9913244481799,2.58060888772973));
#33669=CARTESIAN_POINT('Ctrl Pts',(32.2977938304223,-57.9481146542166,2.55665351328971));
#33670=CARTESIAN_POINT('Ctrl Pts',(31.7503903291116,-57.8812925531888,2.51960754976703));
#33671=CARTESIAN_POINT('Ctrl Pts',(31.2393866179539,-57.5162850872868,2.48256158624435));
#33672=CARTESIAN_POINT('Ctrl Pts',(30.9986464429484,-57.0201399930138,2.44551562272167));
#33673=CARTESIAN_POINT('Ctrl Pts',(30.7579062679429,-56.5239948987407,2.40846965919899));
#33674=CARTESIAN_POINT('Ctrl Pts',(30.7874296290897,-55.8967121760966,2.37142369567631));
#33675=CARTESIAN_POINT('Ctrl Pts',(31.0737049927512,-55.4253713200344,2.33437773215363));
#33676=CARTESIAN_POINT('Ctrl Pts',(31.3599803564126,-54.9540304639723,2.29733176863094));
#33677=CARTESIAN_POINT('Ctrl Pts',(31.9030077225887,-54.6386314744921,2.26028580510827));
#33678=CARTESIAN_POINT('Ctrl Pts',(32.4542675379743,-54.6235184875634,2.22323984158558));
#33679=CARTESIAN_POINT('Ctrl Pts',(33.0055273533599,-54.6084055006347,2.1861938780629));
#33680=CARTESIAN_POINT('Ctrl Pts',(33.5650196179551,-54.8935785162575,2.14914791454022));
#33681=CARTESIAN_POINT('Ctrl Pts',(33.8766895243309,-55.3485264867911,2.11210195101754));
#33682=CARTESIAN_POINT('Ctrl Pts',(34.1883594307067,-55.8034744573246,2.07505598749486));
#33683=CARTESIAN_POINT('Ctrl Pts',(34.2522069788631,-56.4281973827689,2.03801002397218));
#33684=CARTESIAN_POINT('Ctrl Pts',(34.0390119763463,-56.9367872738744,2.0009640604495));
#33685=CARTESIAN_POINT('Ctrl Pts',(33.9000423680164,-57.2683078870831,1.97681591916959));
#33686=CARTESIAN_POINT('Ctrl Pts',(33.6433576792833,-57.550483699497,1.95266777788969));
#33687=CARTESIAN_POINT('Ctrl Pts',(33.331098284258,-57.7335685916211,1.92851963660978));
#33688=CARTESIAN_POINT('Origin',(32.5,-56.2916512459885,3.));
#33689=CARTESIAN_POINT('',(33.333854526745,-57.7369307977834,1.22851963660979));
#33690=CARTESIAN_POINT('',(33.3345984319871,-57.7343006412916,1.4214803633902));
#33691=CARTESIAN_POINT('',(33.333,-57.7344495686934,3.));
#33692=CARTESIAN_POINT('Ctrl Pts',(33.3345984319871,-57.7343006412916,1.4214803633902));
#33693=CARTESIAN_POINT('Ctrl Pts',(33.4283251997872,-57.6813267445322,1.42868873279277));
#33694=CARTESIAN_POINT('Ctrl Pts',(33.5166388707302,-57.6193252564529,1.43589710219534));
#33695=CARTESIAN_POINT('Ctrl Pts',(33.5974727328825,-57.5487559900283,1.44310547159791));
#33696=CARTESIAN_POINT('Ctrl Pts',(34.0129020958151,-57.1860794506077,1.48015143512059));
#33697=CARTESIAN_POINT('Ctrl Pts',(34.2307718231603,-56.5971073981535,1.51719739864327));
#33698=CARTESIAN_POINT('Ctrl Pts',(34.1513725987927,-56.0513862321698,1.55424336216595));
#33699=CARTESIAN_POINT('Ctrl Pts',(34.071973374425,-55.5056650661862,1.59128932568863));
#33700=CARTESIAN_POINT('Ctrl Pts',(33.6953051983445,-55.0031947866731,1.62833528921131));
#33701=CARTESIAN_POINT('Ctrl Pts',(33.1937523971885,-54.7739337662501,1.66538125273399));
#33702=CARTESIAN_POINT('Ctrl Pts',(32.6921995960325,-54.5446727458272,1.70242721625667));
#33703=CARTESIAN_POINT('Ctrl Pts',(32.065762169801,-54.5886209844943,1.73947317977935));
#33704=CARTESIAN_POINT('Ctrl Pts',(31.6011327587505,-54.8856653216219,1.77651914330203));
#33705=CARTESIAN_POINT('Ctrl Pts',(31.1365033477,-55.1827096587496,1.81356510682471));
#33706=CARTESIAN_POINT('Ctrl Pts',(30.8336819518306,-55.7328500943379,1.8506110703474));
#33707=CARTESIAN_POINT('Ctrl Pts',(30.8312565000759,-56.2843117385314,1.88765703387008));
#33708=CARTESIAN_POINT('Ctrl Pts',(30.8288310483213,-56.8357733827248,1.92470299739276));
#33709=CARTESIAN_POINT('Ctrl Pts',(31.1268015406815,-57.3885562355235,1.96174896091544));
#33710=CARTESIAN_POINT('Ctrl Pts',(31.5888000917202,-57.689676089852,1.99879492443812));
#33711=CARTESIAN_POINT('Ctrl Pts',(32.050798642759,-57.9907959441805,2.0358408879608));
#33712=CARTESIAN_POINT('Ctrl Pts',(32.6768252524763,-58.040252800039,2.07288685148348));
#33713=CARTESIAN_POINT('Ctrl Pts',(33.1803752931228,-57.8154124469044,2.10993281500616));
#33714=CARTESIAN_POINT('Ctrl Pts',(33.2326955992617,-57.7920508836856,2.11378199780084));
#33715=CARTESIAN_POINT('Ctrl Pts',(33.2836936714803,-57.7657280595765,2.11763118059552));
#33716=CARTESIAN_POINT('Ctrl Pts',(33.3331738820163,-57.7367002116856,2.12148036339021));
#33717=CARTESIAN_POINT('Ctrl Pts',(33.331098284258,-57.7335685916211,1.92851963660978));
#33718=CARTESIAN_POINT('Ctrl Pts',(33.1643166622693,-57.8313565069137,1.91562181436701));
#33719=CARTESIAN_POINT('Ctrl Pts',(32.9816809059177,-57.9008761528941,1.90272399212423));
#33720=CARTESIAN_POINT('Ctrl Pts',(32.792659312829,-57.9345477382936,1.88982616988146));
#33721=CARTESIAN_POINT('Ctrl Pts',(32.2497392050189,-58.0312614548405,1.85278020635878));
#33722=CARTESIAN_POINT('Ctrl Pts',(31.6541365425887,-57.8322320311678,1.8157342428361));
#33723=CARTESIAN_POINT('Ctrl Pts',(31.2784322612968,-57.4285464115926,1.77868827931342));
#33724=CARTESIAN_POINT('Ctrl Pts',(30.902727980005,-57.0248607920174,1.74164231579074));
#33725=CARTESIAN_POINT('Ctrl Pts',(30.7469220798513,-56.4165189765397,1.70459635226806));
#33726=CARTESIAN_POINT('Ctrl Pts',(30.8823200145202,-55.881932046546,1.66755038874538));
#33727=CARTESIAN_POINT('Ctrl Pts',(31.0177179491892,-55.3473451165522,1.6305044252227));
#33728=CARTESIAN_POINT('Ctrl Pts',(31.4443197186807,-54.8865130720423,1.59345846170001));
#33729=CARTESIAN_POINT('Ctrl Pts',(31.9668886041915,-54.7103383112812,1.55641249817733));
#33730=CARTESIAN_POINT('Ctrl Pts',(32.4894574897023,-54.53416355052,1.51936653465465));
#33731=CARTESIAN_POINT('Ctrl Pts',(33.1079934912324,-54.6426460735076,1.48232057113197));
#33732=CARTESIAN_POINT('Ctrl Pts',(33.5394201003417,-54.9861382384619,1.44527460760929));
#33733=CARTESIAN_POINT('Ctrl Pts',(33.9708467094511,-55.3296304034162,1.40822864408661));
#33734=CARTESIAN_POINT('Ctrl Pts',(34.2151639261397,-55.9081322103373,1.37118268056393));
#33735=CARTESIAN_POINT('Ctrl Pts',(34.1605585908213,-56.4568890269573,1.33413671704125));
#33736=CARTESIAN_POINT('Ctrl Pts',(34.1086657929391,-56.9783861738082,1.29893102356409));
#33737=CARTESIAN_POINT('Ctrl Pts',(33.7868109567046,-57.4730201142583,1.26372533008694));
#33738=CARTESIAN_POINT('Ctrl Pts',(33.333854526745,-57.7369307977834,1.22851963660979));
#33739=CARTESIAN_POINT('Origin',(32.5,-56.2916512459885,3.));
#33740=CARTESIAN_POINT('',(33.3341985401264,-57.7334817014242,0.528519636609787));
#33741=CARTESIAN_POINT('',(33.3317031312748,-57.7320766758176,0.721480363390202));
#33742=CARTESIAN_POINT('',(33.333,-57.7344495686934,3.));
#33743=CARTESIAN_POINT('Ctrl Pts',(33.3317031312748,-57.7320766758176,0.721480363390202));
#33744=CARTESIAN_POINT('Ctrl Pts',(33.5692173042018,-57.5950551525707,0.739746284990021));
#33745=CARTESIAN_POINT('Ctrl Pts',(33.7746291238346,-57.4025124831788,0.75801220658984));
#33746=CARTESIAN_POINT('Ctrl Pts',(33.9179858048945,-57.1714665641067,0.776278128189658));
#33747=CARTESIAN_POINT('Ctrl Pts',(34.208734144542,-56.7028716102066,0.813324091712339));
#33748=CARTESIAN_POINT('Ctrl Pts',(34.2442262482397,-56.0758982397686,0.850370055235019));
#33749=CARTESIAN_POINT('Ctrl Pts',(34.008218953441,-55.5774843709492,0.887416018757699));
#33750=CARTESIAN_POINT('Ctrl Pts',(33.7722116586424,-55.0790705021297,0.92446198228038));
#33751=CARTESIAN_POINT('Ctrl Pts',(33.2647049653473,-54.7092161349289,0.961507945803061));
#33752=CARTESIAN_POINT('Ctrl Pts',(32.7179621895189,-54.6371872177157,0.998553909325741));
#33753=CARTESIAN_POINT('Ctrl Pts',(32.1712194136904,-54.5651583005025,1.03559987284842));
#33754=CARTESIAN_POINT('Ctrl Pts',(31.5852405553285,-54.790954833277,1.0726458363711));
#33755=CARTESIAN_POINT('Ctrl Pts',(31.2282021616797,-55.21123975246,1.10969179989378));
#33756=CARTESIAN_POINT('Ctrl Pts',(30.8711637680308,-55.6315246716431,1.14673776341646));
#33757=CARTESIAN_POINT('Ctrl Pts',(30.7430658390951,-56.2462979772347,1.18378372693914));
#33758=CARTESIAN_POINT('Ctrl Pts',(30.902533118419,-56.77420517993,1.22082969046182));
#33759=CARTESIAN_POINT('Ctrl Pts',(31.0620003977429,-57.3021123826252,1.2578756539845));
#33760=CARTESIAN_POINT('Ctrl Pts',(31.5090328853265,-57.7431534824239,1.29492161750718));
#33761=CARTESIAN_POINT('Ctrl Pts',(32.0390436283783,-57.8954835191299,1.33196758102987));
#33762=CARTESIAN_POINT('Ctrl Pts',(32.4659253700502,-58.0181733178376,1.36180517514998));
#33763=CARTESIAN_POINT('Ctrl Pts',(32.9466353435786,-57.9535754234504,1.39164276927009));
#33764=CARTESIAN_POINT('Ctrl Pts',(33.3345984319871,-57.7343006412916,1.4214803633902));
#33765=CARTESIAN_POINT('Ctrl Pts',(33.333854526745,-57.7369307977834,1.22851963660979));
#33766=CARTESIAN_POINT('Ctrl Pts',(33.3101776135059,-57.7507259223106,1.22667936656426));
#33767=CARTESIAN_POINT('Ctrl Pts',(33.2861424840206,-57.7638906287274,1.22483909651873));
#33768=CARTESIAN_POINT('Ctrl Pts',(33.261768971111,-57.776395800606,1.22299882647321));
#33769=CARTESIAN_POINT('Ctrl Pts',(32.7711125740444,-58.0281339313159,1.18595286295053));
#33770=CARTESIAN_POINT('Ctrl Pts',(32.1433276672365,-58.0125983664166,1.14890689942785));
#33771=CARTESIAN_POINT('Ctrl Pts',(31.6657235730868,-57.7368990452689,1.11186093590517));
#33772=CARTESIAN_POINT('Ctrl Pts',(31.1881194789371,-57.4611997241213,1.07481497238249));
#33773=CARTESIAN_POINT('Ctrl Pts',(30.8606961974455,-56.9253366467254,1.03776900885981));
#33774=CARTESIAN_POINT('Ctrl Pts',(30.8333008499707,-56.3745505890177,1.00072304533712));
#33775=CARTESIAN_POINT('Ctrl Pts',(30.8059055024959,-55.8237645313099,0.963677081814445));
#33776=CARTESIAN_POINT('Ctrl Pts',(31.0785380890378,-55.2580554932903,0.926631118291764));
#33777=CARTESIAN_POINT('Ctrl Pts',(31.5264267604979,-54.9363234239653,0.889585154769083));
#33778=CARTESIAN_POINT('Ctrl Pts',(31.974315431958,-54.6145913546402,0.852539191246403));
#33779=CARTESIAN_POINT('Ctrl Pts',(32.5974601883362,-54.5368362540097,0.815493227723723));
#33780=CARTESIAN_POINT('Ctrl Pts',(33.1106752982772,-54.7386431848419,0.778447264201043));
#33781=CARTESIAN_POINT('Ctrl Pts',(33.6238904082182,-54.940450115674,0.741401300678362));
#33782=CARTESIAN_POINT('Ctrl Pts',(34.0271758717221,-55.4218190779688,0.704355337155682));
#33783=CARTESIAN_POINT('Ctrl Pts',(34.1359658098863,-55.9624488364586,0.667309373633001));
#33784=CARTESIAN_POINT('Ctrl Pts',(34.2447557480505,-56.5030785949484,0.630263410110321));
#33785=CARTESIAN_POINT('Ctrl Pts',(34.0590501608751,-57.1029691496333,0.59321744658764));
#33786=CARTESIAN_POINT('Ctrl Pts',(33.6638382628472,-57.4875771868012,0.55617148306496));
#33787=CARTESIAN_POINT('Ctrl Pts',(33.5655069136947,-57.5832702248356,0.546954200913235));
#33788=CARTESIAN_POINT('Ctrl Pts',(33.4542061287357,-57.6656362524338,0.537736918761511));
#33789=CARTESIAN_POINT('Ctrl Pts',(33.3341985401264,-57.7334817014242,0.528519636609787));
#33790=CARTESIAN_POINT('Origin',(32.5,-56.2916512459885,3.));
#33791=CARTESIAN_POINT('',(33.3313285320323,-57.7324067450656,-0.171480363390211));
#33792=CARTESIAN_POINT('',(33.3319271105622,-57.7355745198861,0.0214803633902046));
#33793=CARTESIAN_POINT('',(33.333,-57.7344495686934,3.));
#33794=CARTESIAN_POINT('Ctrl Pts',(33.3319271105622,-57.7355745198861,0.0214803633902046));
#33795=CARTESIAN_POINT('Ctrl Pts',(33.7093130799578,-57.5130220094248,0.0508038371872728));
#33796=CARTESIAN_POINT('Ctrl Pts',(34.0025116805637,-57.1388573741434,0.080127310984341));
#33797=CARTESIAN_POINT('Ctrl Pts',(34.1137073818814,-56.7167479649788,0.109450784781409));
#33798=CARTESIAN_POINT('Ctrl Pts',(34.2541870509479,-56.1834738419089,0.14649674830409));
#33799=CARTESIAN_POINT('Ctrl Pts',(34.1041780082168,-55.5736766763093,0.18354271182677));
#33800=CARTESIAN_POINT('Ctrl Pts',(33.7323327404969,-55.1664335984773,0.22058867534945));
#33801=CARTESIAN_POINT('Ctrl Pts',(33.3604874727769,-54.7591905206453,0.257634638872131));
#33802=CARTESIAN_POINT('Ctrl Pts',(32.7668059800683,-54.5545015305809,0.294680602394811));
#33803=CARTESIAN_POINT('Ctrl Pts',(32.2229899650201,-54.6460437054155,0.331726565917492));
#33804=CARTESIAN_POINT('Ctrl Pts',(31.679173949972,-54.7375858802501,0.368772529440172));
#33805=CARTESIAN_POINT('Ctrl Pts',(31.1852234125845,-55.1253592199838,0.405818492962853));
#33806=CARTESIAN_POINT('Ctrl Pts',(30.9671976166263,-55.6318970567811,0.442864456485533));
#33807=CARTESIAN_POINT('Ctrl Pts',(30.7491718206681,-56.1384348935784,0.479910420008214));
#33808=CARTESIAN_POINT('Ctrl Pts',(30.8070707661392,-56.7637372274395,0.516956383530895));
#33809=CARTESIAN_POINT('Ctrl Pts',(31.1143966726152,-57.2216308996084,0.554002347053575));
#33810=CARTESIAN_POINT('Ctrl Pts',(31.4217225790911,-57.6795245717774,0.591048310576256));
#33811=CARTESIAN_POINT('Ctrl Pts',(31.9784754465718,-57.9700095822543,0.628094274098936));
#33812=CARTESIAN_POINT('Ctrl Pts',(32.5298541681108,-57.9601438188116,0.665140237621616));
#33813=CARTESIAN_POINT('Ctrl Pts',(32.8093695193456,-57.9551424790316,0.683920279544479));
#33814=CARTESIAN_POINT('Ctrl Pts',(33.0875037843944,-57.872954864572,0.702700321467341));
#33815=CARTESIAN_POINT('Ctrl Pts',(33.3317031312748,-57.7320766758176,0.721480363390202));
#33816=CARTESIAN_POINT('Ctrl Pts',(33.3341985401264,-57.7334817014242,0.528519636609787));
#33817=CARTESIAN_POINT('Ctrl Pts',(32.9718734110338,-57.9383196733276,0.500690955238831));
#33818=CARTESIAN_POINT('Ctrl Pts',(32.5301815965126,-58.010795616536,0.472862273867874));
#33819=CARTESIAN_POINT('Ctrl Pts',(32.1264363544929,-57.9180609610465,0.445033592496918));
#33820=CARTESIAN_POINT('Ctrl Pts',(31.5889645530468,-57.7946111784729,0.407987628974237));
#33821=CARTESIAN_POINT('Ctrl Pts',(31.1187391590349,-57.3783860936747,0.370941665451557));
#33822=CARTESIAN_POINT('Ctrl Pts',(30.9309614883813,-56.8598734778586,0.333895701928876));
#33823=CARTESIAN_POINT('Ctrl Pts',(30.7431838177278,-56.3413608620425,0.296849738406196));
#33824=CARTESIAN_POINT('Ctrl Pts',(30.8378538704326,-55.7205607152084,0.259803774883515));
#33825=CARTESIAN_POINT('Ctrl Pts',(31.1716453640502,-55.2815857427568,0.222757811360835));
#33826=CARTESIAN_POINT('Ctrl Pts',(31.5054368576678,-54.8426107703051,0.185711847838154));
#33827=CARTESIAN_POINT('Ctrl Pts',(32.0783497921982,-54.5854609722359,0.148665884315473));
#33828=CARTESIAN_POINT('Ctrl Pts',(32.6281873065731,-54.6278224157042,0.111619920792793));
#33829=CARTESIAN_POINT('Ctrl Pts',(33.1780248209479,-54.6701838591725,0.0745739572701122));
#33830=CARTESIAN_POINT('Ctrl Pts',(33.7047869151672,-55.0120565441784,0.0375279937474315));
#33831=CARTESIAN_POINT('Ctrl Pts',(33.9673979456785,-55.4969804900557,0.00048203022475119));
#33832=CARTESIAN_POINT('Ctrl Pts',(34.2300089761898,-55.981904435933,-0.0365639332979294));
#33833=CARTESIAN_POINT('Ctrl Pts',(34.2284689429929,-56.6098796426817,-0.0736098968206097));
#33834=CARTESIAN_POINT('Ctrl Pts',(33.9634826195406,-57.0935097116441,-0.11065586034329));
#33835=CARTESIAN_POINT('Ctrl Pts',(33.8184586195722,-57.3581949459313,-0.130930694692264));
#33836=CARTESIAN_POINT('Ctrl Pts',(33.5945259126096,-57.579645226435,-0.151205529041238));
#33837=CARTESIAN_POINT('Ctrl Pts',(33.3313285320323,-57.7324067450656,-0.171480363390211));
#33838=CARTESIAN_POINT('Origin',(32.5,-56.2916512459885,3.));
#33839=CARTESIAN_POINT('',(33.3325354057626,-57.7362457052863,-0.871480363390211));
#33840=CARTESIAN_POINT('',(33.3348489584778,-57.7359240281238,-0.678519636609799));
#33841=CARTESIAN_POINT('',(33.333,-57.7344495686934,3.));
#33842=CARTESIAN_POINT('Ctrl Pts',(33.3348489584778,-57.7359240281238,-0.678519636609799));
#33843=CARTESIAN_POINT('Ctrl Pts',(33.3780386262143,-57.7113506256495,-0.675184574138161));
#33844=CARTESIAN_POINT('Ctrl Pts',(33.4200351242182,-57.6847625016212,-0.671849511666524));
#33845=CARTESIAN_POINT('Ctrl Pts',(33.4606301406774,-57.6561836376047,-0.668514449194886));
#33846=CARTESIAN_POINT('Ctrl Pts',(33.9115606739847,-57.3387288484125,-0.631468485672205));
#33847=CARTESIAN_POINT('Ctrl Pts',(34.1895648369722,-56.7756401144087,-0.594422522149525));
#33848=CARTESIAN_POINT('Ctrl Pts',(34.1674127214773,-56.2246182278545,-0.557376558626844));
#33849=CARTESIAN_POINT('Ctrl Pts',(34.1452606059824,-55.6735963413003,-0.520330595104164));
#33850=CARTESIAN_POINT('Ctrl Pts',(33.8229522120051,-55.1346413021957,-0.483284631581482));
#33851=CARTESIAN_POINT('Ctrl Pts',(33.3479936663214,-54.8544089200699,-0.446238668058801));
#33852=CARTESIAN_POINT('Ctrl Pts',(32.8730351206376,-54.5741765379442,-0.40919270453612));
#33853=CARTESIAN_POINT('Ctrl Pts',(32.2454264232473,-54.5526668127973,-0.37214674101344));
#33854=CARTESIAN_POINT('Ctrl Pts',(31.7523963222819,-54.7997238024578,-0.33510077749076));
#33855=CARTESIAN_POINT('Ctrl Pts',(31.2593662213165,-55.0467807921182,-0.298054813968079));
#33856=CARTESIAN_POINT('Ctrl Pts',(30.9009147167759,-55.562404496586,-0.261008850445398));
#33857=CARTESIAN_POINT('Ctrl Pts',(30.8410891376185,-56.1106167986295,-0.223962886922717));
#33858=CARTESIAN_POINT('Ctrl Pts',(30.7812635584611,-56.658829100673,-0.186916923400036));
#33859=CARTESIAN_POINT('Ctrl Pts',(31.020063904687,-57.2396300002922,-0.149870959877356));
#33860=CARTESIAN_POINT('Ctrl Pts',(31.4482018611622,-57.5872126749714,-0.112824996354675));
#33861=CARTESIAN_POINT('Ctrl Pts',(31.8763398176374,-57.9347953496505,-0.0757790328319943));
#33862=CARTESIAN_POINT('Ctrl Pts',(32.4938153843619,-58.0491597993897,-0.0387330693093137));
#33863=CARTESIAN_POINT('Ctrl Pts',(33.0180373581563,-57.8779664839892,-0.00168710578663283));
#33864=CARTESIAN_POINT('Ctrl Pts',(33.1273150883492,-57.8422800422406,0.00603538393897965));
#33865=CARTESIAN_POINT('Ctrl Pts',(33.2325405477213,-57.7941848839699,0.0137578736645921));
#33866=CARTESIAN_POINT('Ctrl Pts',(33.3319271105622,-57.7355745198861,0.0214803633902046));
#33867=CARTESIAN_POINT('Ctrl Pts',(33.3313285320323,-57.7324067450656,-0.171480363390211));
#33868=CARTESIAN_POINT('Ctrl Pts',(33.1136144342564,-57.8587694623943,-0.188251492563918));
#33869=CARTESIAN_POINT('Ctrl Pts',(32.8690337821938,-57.9381324168355,-0.205022621737625));
#33870=CARTESIAN_POINT('Ctrl Pts',(32.6200250231441,-57.9560888015458,-0.221793750911332));
#33871=CARTESIAN_POINT('Ctrl Pts',(32.0699863639079,-57.995752891309,-0.258839714434013));
#33872=CARTESIAN_POINT('Ctrl Pts',(31.4983416591433,-57.7357961396592,-0.295885677956694));
#33873=CARTESIAN_POINT('Ctrl Pts',(31.166707224731,-57.2951892897455,-0.332931641479374));
#33874=CARTESIAN_POINT('Ctrl Pts',(30.8350727903187,-56.8545824398317,-0.369977605002055));
#33875=CARTESIAN_POINT('Ctrl Pts',(30.7434486262587,-56.233325491654,-0.407023568524736));
#33876=CARTESIAN_POINT('Ctrl Pts',(30.9337672989981,-55.7157400874939,-0.444069532047416));
#33877=CARTESIAN_POINT('Ctrl Pts',(31.1240859717375,-55.1981546833338,-0.481115495570097));
#33878=CARTESIAN_POINT('Ctrl Pts',(31.5963474812762,-54.7842408231913,-0.518161459092778));
#33879=CARTESIAN_POINT('Ctrl Pts',(32.1344181757784,-54.6634287766856,-0.555207422615458));
#33880=CARTESIAN_POINT('Ctrl Pts',(32.6724888702806,-54.5426167301798,-0.592253386138139));
#33881=CARTESIAN_POINT('Ctrl Pts',(33.2763687497463,-54.7149064973108,-0.629299349660819));
#33882=CARTESIAN_POINT('Ctrl Pts',(33.6696897466081,-55.1014482025695,-0.6663453131835));
#33883=CARTESIAN_POINT('Ctrl Pts',(34.0630107434698,-55.4879899078282,-0.70339127670618));
#33884=CARTESIAN_POINT('Ctrl Pts',(34.2457728577278,-56.0887835512146,-0.74043724022886));
#33885=CARTESIAN_POINT('Ctrl Pts',(34.1343320137704,-56.6288734837568,-0.777483203751541));
#33886=CARTESIAN_POINT('Ctrl Pts',(34.040078625064,-57.0856656664133,-0.808815590297764));
#33887=CARTESIAN_POINT('Ctrl Pts',(33.7353736531391,-57.4990347912871,-0.840147976843988));
#33888=CARTESIAN_POINT('Ctrl Pts',(33.3325354057626,-57.7362457052863,-0.871480363390211));
#33889=CARTESIAN_POINT('Origin',(32.5,-56.2916512459885,3.));
#33890=CARTESIAN_POINT('',(33.3347882996638,-57.7351190113229,-1.57148036339021));
#33891=CARTESIAN_POINT('',(33.3327354544031,-57.732107437543,-1.3785196366098));
#33892=CARTESIAN_POINT('',(33.333,-57.7344495686934,3.));
#33893=CARTESIAN_POINT('',(32.8002165734083,-54.6529242983091,-2.));
#33894=CARTESIAN_POINT('Ctrl Pts',(33.3347882996638,-57.7351190113229,-1.57148036339021));
#33895=CARTESIAN_POINT('Ctrl Pts',(32.9233907544682,-57.9680931016246,-1.6031823516921));
#33896=CARTESIAN_POINT('Ctrl Pts',(32.4058309808294,-58.0231592569492,-1.63488433999399));
#33897=CARTESIAN_POINT('Ctrl Pts',(31.9592734257387,-57.8702645075936,-1.66658632829588));
#33898=CARTESIAN_POINT('Ctrl Pts',(31.4374400713406,-57.6915964299483,-1.70363229181856));
#33899=CARTESIAN_POINT('Ctrl Pts',(31.0125640599592,-57.2289465672062,-1.74067825534124));
#33900=CARTESIAN_POINT('Ctrl Pts',(30.880071382614,-56.6935519519194,-1.77772421886392));
#33901=CARTESIAN_POINT('Ctrl Pts',(30.7475787052688,-56.1581573366326,-1.8147701823866));
#33902=CARTESIAN_POINT('Ctrl Pts',(30.9074693619599,-55.5500179688011,-1.85181614590928));
#33903=CARTESIAN_POINT('Ctrl Pts',(31.2843999047331,-55.1487524209429,-1.88886210943196));
#33904=CARTESIAN_POINT('Ctrl Pts',(31.6613304475062,-54.7474868730848,-1.92590807295464));
#33905=CARTESIAN_POINT('Ctrl Pts',(32.2553008763614,-54.5530951452,-1.96295403647732));
#33906=CARTESIAN_POINT('Ctrl Pts',(32.8002165734083,-54.6529242983091,-2.));
#33907=CARTESIAN_POINT('',(34.0720885049227,-56.8521739755916,-2.));
#33908=CARTESIAN_POINT('Origin',(32.5,-56.2916512459885,-2.));
#33909=CARTESIAN_POINT('Ctrl Pts',(34.0720901513885,-56.8521746541717,-2.));
#33910=CARTESIAN_POINT('Ctrl Pts',(34.2530538927521,-56.3425577544552,-1.96367708181445));
#33911=CARTESIAN_POINT('Ctrl Pts',(34.16381751404,-55.7359288334824,-1.92735416362889));
#33912=CARTESIAN_POINT('Ctrl Pts',(33.8426356554964,-55.3008256611299,-1.89103124544334));
#33913=CARTESIAN_POINT('Ctrl Pts',(33.5150603391364,-54.8570613091241,-1.85398528192066));
#33914=CARTESIAN_POINT('Ctrl Pts',(32.9462134040812,-54.5917194685101,-1.81693931839798));
#33915=CARTESIAN_POINT('Ctrl Pts',(32.3958963008479,-54.6261577029506,-1.7798933548753));
#33916=CARTESIAN_POINT('Ctrl Pts',(31.8455791976147,-54.6605959373912,-1.74284739135262));
#33917=CARTESIAN_POINT('Ctrl Pts',(31.3137919262033,-54.9948142468862,-1.70580142782994));
#33918=CARTESIAN_POINT('Ctrl Pts',(31.0441775058384,-55.4758950021694,-1.66875546430726));
#33919=CARTESIAN_POINT('Ctrl Pts',(30.7745630854734,-55.9569757574525,-1.63170950078458));
#33920=CARTESIAN_POINT('Ctrl Pts',(30.7671215161549,-56.5849189585237,-1.5946635372619));
#33921=CARTESIAN_POINT('Ctrl Pts',(31.0251241525943,-57.0723230889947,-1.55761757373922));
#33922=CARTESIAN_POINT('Ctrl Pts',(31.2831267890336,-57.5597272194658,-1.52057161021654));
#33923=CARTESIAN_POINT('Ctrl Pts',(31.8065736312308,-57.9065922793366,-1.48352564669386));
#33924=CARTESIAN_POINT('Ctrl Pts',(32.3559737285805,-57.9541834292484,-1.44647968317118));
#33925=CARTESIAN_POINT('Ctrl Pts',(32.6919280642789,-57.9832850861845,-1.42382633431738));
#33926=CARTESIAN_POINT('Ctrl Pts',(33.0375869381561,-57.9004811240364,-1.40117298546359));
#33927=CARTESIAN_POINT('Ctrl Pts',(33.3327354544031,-57.732107437543,-1.3785196366098));
#33928=CARTESIAN_POINT('Origin',(32.5,-56.2916512459885,-3.54592528053767));
#33929=CARTESIAN_POINT('',(33.5296449158132,-58.0726582505549,6.54592528053768));
#33930=CARTESIAN_POINT('',(33.5251060574855,-58.0687922621904,6.60407471946232));
#33931=CARTESIAN_POINT('',(33.5273750000001,-58.0711169444146,-3.54592528053767));
#33932=CARTESIAN_POINT('',(30.8457462639859,-55.0728640868079,7.));
#33933=CARTESIAN_POINT('Ctrl Pts',(33.5251060574855,-58.0687922621904,6.60407471946233));
#33934=CARTESIAN_POINT('Ctrl Pts',(33.8584527741405,-57.8749712083972,6.62491192240684));
#33935=CARTESIAN_POINT('Ctrl Pts',(34.6426244289716,-57.0875348868182,6.68279508887404));
#33936=CARTESIAN_POINT('Ctrl Pts',(34.6192626691618,-55.1024844807854,6.77772421886392));
#33937=CARTESIAN_POINT('Ctrl Pts',(32.6468806392671,-53.8684656063833,6.88886210943196));
#33938=CARTESIAN_POINT('Ctrl Pts',(31.2510219905719,-54.522785363242,6.96295403647732));
#33939=CARTESIAN_POINT('Ctrl Pts',(30.8457462639859,-55.0728640868079,7.));
#33940=CARTESIAN_POINT('',(30.4546316093048,-56.0596663160167,7.));
#33941=CARTESIAN_POINT('Origin',(32.5,-56.2916512459885,7.));
#33942=CARTESIAN_POINT('Ctrl Pts',(33.5296449158132,-58.0726582505549,6.54592528053768));
#33943=CARTESIAN_POINT('Ctrl Pts',(33.5919384699578,-58.037273530125,6.54982271160486));
#33944=CARTESIAN_POINT('Ctrl Pts',(34.225323347054,-57.6301444802746,6.59076610619471));
#33945=CARTESIAN_POINT('Ctrl Pts',(34.9251107981772,-56.157415110224,6.66875546430726));
#33946=CARTESIAN_POINT('Ctrl Pts',(33.7019669024841,-54.1813822458926,6.7798933548753));
#33947=CARTESIAN_POINT('Ctrl Pts',(31.3950249125263,-54.1375954583441,6.8903082001062));
#33948=CARTESIAN_POINT('Ctrl Pts',(30.5306488143205,-55.3970288255657,6.96367708181445));
#33949=CARTESIAN_POINT('Ctrl Pts',(30.4546294175093,-56.0596661744469,7.));
#33950=CARTESIAN_POINT('Origin',(32.5,-56.2916512459885,-3.54592528053767));
#33951=CARTESIAN_POINT('',(33.5268493235952,-58.068153392458,5.84592528053768));
#33952=CARTESIAN_POINT('',(33.5270361074232,-58.0735254724117,5.90407471946233));
#33953=CARTESIAN_POINT('',(33.5273750000001,-58.0711169444146,-3.54592528053767));
#33954=CARTESIAN_POINT('Ctrl Pts',(33.5270361074232,-58.0735254724117,5.90407471946233));
#33955=CARTESIAN_POINT('Ctrl Pts',(34.0327197348534,-57.7760135322548,5.93596947460409));
#33956=CARTESIAN_POINT('Ctrl Pts',(34.8527930569705,-56.6438137488049,6.00491019326854));
#33957=CARTESIAN_POINT('Ctrl Pts',(34.1759192345576,-54.5338890939528,6.11089687545566));
#33958=CARTESIAN_POINT('Ctrl Pts',(31.9320786480218,-53.9303413264954,6.22203476602372));
#33959=CARTESIAN_POINT('Ctrl Pts',(30.2082245117244,-55.4880781765343,6.33317265659174));
#33960=CARTESIAN_POINT('Ctrl Pts',(30.5817368018815,-57.7814323658044,6.44431054715979));
#33961=CARTESIAN_POINT('Ctrl Pts',(32.3123519600731,-58.5366981066488,6.53461123478331));
#33962=CARTESIAN_POINT('Ctrl Pts',(33.265803638914,-58.2195610128864,6.58786595888416));
#33963=CARTESIAN_POINT('Ctrl Pts',(33.5251060574855,-58.0687922621904,6.60407471946233));
#33964=CARTESIAN_POINT('Ctrl Pts',(33.5268493235952,-58.068153392458,5.84592528053768));
#33965=CARTESIAN_POINT('Ctrl Pts',(33.7671186009377,-57.930879119519,5.86088026380211));
#33966=CARTESIAN_POINT('Ctrl Pts',(34.5085314004614,-57.2938049828724,5.91288121058922));
#33967=CARTESIAN_POINT('Ctrl Pts',(34.7788326566388,-55.451849617872,6.00192812089901));
#33968=CARTESIAN_POINT('Ctrl Pts',(33.0303393193103,-53.921614042038,6.11306601146705));
#33969=CARTESIAN_POINT('Ctrl Pts',(30.7964407564499,-54.5607069079647,6.22420390203509));
#33970=CARTESIAN_POINT('Ctrl Pts',(30.1217887402557,-56.7841397946826,6.33534179260313));
#33971=CARTESIAN_POINT('Ctrl Pts',(31.571340255844,-58.4946530906763,6.442582252104));
#33972=CARTESIAN_POINT('Ctrl Pts',(32.999824152922,-58.3736132984778,6.51277674808218));
#33973=CARTESIAN_POINT('Ctrl Pts',(33.5296449158132,-58.0726582505549,6.54592528053768));
#33974=CARTESIAN_POINT('Origin',(32.5,-56.2916512459885,-3.54592528053767));
#33975=CARTESIAN_POINT('',(33.525217808475,-58.0709111221528,5.14592528053768));
#33976=CARTESIAN_POINT('',(33.5295558866825,-58.0716265502945,5.20407471946233));
#33977=CARTESIAN_POINT('',(33.5273750000001,-58.0711169444146,-3.54592528053767));
#33978=CARTESIAN_POINT('Ctrl Pts',(33.5295558866825,-58.0716265502945,5.20407471946233));
#33979=CARTESIAN_POINT('Ctrl Pts',(33.6241634690101,-58.0180957001452,5.20998106327866));
#33980=CARTESIAN_POINT('Ctrl Pts',(34.2792376101367,-57.5737577801449,5.25293337061768));
#33981=CARTESIAN_POINT('Ctrl Pts',(34.9141240107243,-56.0264398256937,5.33293164147937));
#33982=CARTESIAN_POINT('Ctrl Pts',(33.5864678368826,-54.1195735160326,5.44406953204741));
#33983=CARTESIAN_POINT('Ctrl Pts',(31.2643540254432,-54.2008349824401,5.55520742261546));
#33984=CARTESIAN_POINT('Ctrl Pts',(30.0732435855651,-56.1958434964943,5.6663453131835));
#33985=CARTESIAN_POINT('Ctrl Pts',(31.10336564197,-58.2785475024108,5.77748320375154));
#33986=CARTESIAN_POINT('Ctrl Pts',(32.7493551050699,-58.4668353041202,5.85672633917782));
#33987=CARTESIAN_POINT('Ctrl Pts',(33.4453649446213,-58.1215755669412,5.89892351108141));
#33988=CARTESIAN_POINT('Ctrl Pts',(33.5270361074232,-58.0735254724117,5.90407471946233));
#33989=CARTESIAN_POINT('Ctrl Pts',(33.525217808475,-58.0709111221528,5.14592528053768));
#33990=CARTESIAN_POINT('Ctrl Pts',(33.9392806903329,-57.8273071486294,5.17193781599936));
#33991=CARTESIAN_POINT('Ctrl Pts',(34.7491747415829,-56.8889612418333,5.23499631498371));
#33992=CARTESIAN_POINT('Ctrl Pts',(34.4321757978777,-54.8202470274371,5.33510077749076));
#33993=CARTESIAN_POINT('Ctrl Pts',(32.3116949177892,-53.8703138209288,5.44623866805879));
#33994=CARTESIAN_POINT('Ctrl Pts',(30.3635721421369,-55.1366583239951,5.55737655862685));
#33995=CARTESIAN_POINT('Ctrl Pts',(30.370945362205,-57.4601807388668,5.66851444919488));
#33996=CARTESIAN_POINT('Ctrl Pts',(32.0638471781547,-58.5454001176689,5.7646973564985));
#33997=CARTESIAN_POINT('Ctrl Pts',(33.1719319178991,-58.2709301659147,5.82383430027943));
#33998=CARTESIAN_POINT('Ctrl Pts',(33.5268493235952,-58.068153392458,5.84592528053768));
#33999=CARTESIAN_POINT('Origin',(32.5,-56.2916512459885,-3.54592528053767));
#34000=CARTESIAN_POINT('',(33.5290839475038,-58.0740603739207,4.44592528053768));
#34001=CARTESIAN_POINT('',(33.5261619125927,-58.0680778657968,4.50407471946233));
#34002=CARTESIAN_POINT('',(33.5273750000001,-58.0711169444146,-3.54592528053767));
#34003=CARTESIAN_POINT('Ctrl Pts',(33.5261619125927,-58.0680778657968,4.50407471946233));
#34004=CARTESIAN_POINT('Ctrl Pts',(33.7984529813903,-57.9116108116526,4.52103861547591));
#34005=CARTESIAN_POINT('Ctrl Pts',(34.5559374767779,-57.225562580793,4.57504847501218));
#34006=CARTESIAN_POINT('Ctrl Pts',(34.7300884128151,-55.3298620761609,4.66610429807112));
#34007=CARTESIAN_POINT('Ctrl Pts',(32.9014225703573,-53.8964074829672,4.77724218863916));
#34008=CARTESIAN_POINT('Ctrl Pts',(30.7053300758282,-54.6553466763579,4.8883800792072));
#34009=CARTESIAN_POINT('Ctrl Pts',(30.1519193575992,-56.9120139865897,4.99951796977525));
#34010=CARTESIAN_POINT('Ctrl Pts',(31.6629249999102,-58.5111039532885,5.10474951652695));
#34011=CARTESIAN_POINT('Ctrl Pts',(33.0307626862479,-58.3538536552587,5.17293509975598));
#34012=CARTESIAN_POINT('Ctrl Pts',(33.5295558866825,-58.0716265502945,5.20407471946233));
#34013=CARTESIAN_POINT('Ctrl Pts',(33.5290839390052,-58.0740603592831,4.44592528053768));
#34014=CARTESIAN_POINT('Ctrl Pts',(33.5294675225899,-58.0738389277434,4.44594940467393));
#34015=CARTESIAN_POINT('Ctrl Pts',(34.1187763075119,-57.733369594267,4.48301949233286));
#34016=CARTESIAN_POINT('Ctrl Pts',(34.9257362810773,-56.410550559801,4.55713554351446));
#34017=CARTESIAN_POINT('Ctrl Pts',(33.91547832718,-54.3181379674856,4.66827343408251));
#34018=CARTESIAN_POINT('Ctrl Pts',(31.609617005159,-54.0321044593028,4.77941132465054));
#34019=CARTESIAN_POINT('Ctrl Pts',(30.1187333412011,-55.8142597516569,4.89054921521859));
#34020=CARTESIAN_POINT('Ctrl Pts',(30.8074500449804,-58.0333768894161,5.00168710578662));
#34021=CARTESIAN_POINT('Ctrl Pts',(32.5215758081834,-58.5120119076972,5.086812460893));
#34022=CARTESIAN_POINT('Ctrl Pts',(33.3495896761677,-58.1742377248673,5.13489185247668));
#34023=CARTESIAN_POINT('Ctrl Pts',(33.525217808475,-58.0709111221528,5.14592528053768));
#34024=CARTESIAN_POINT('Origin',(32.5,-56.2916512459885,-3.54592528053767));
#34025=CARTESIAN_POINT('',(33.5282587680711,-58.0691275396584,3.74592528053768));
#34026=CARTESIAN_POINT('',(33.5256537705603,-58.071893508325,3.80407471946232));
#34027=CARTESIAN_POINT('',(33.5273750000001,-58.0711169444146,-3.54592528053767));
#34028=CARTESIAN_POINT('Ctrl Pts',(33.5256537705603,-58.071893508325,3.80407471946232));
#34029=CARTESIAN_POINT('Ctrl Pts',(33.9708692323456,-57.8094153705276,3.83209616767316));
#34030=CARTESIAN_POINT('Ctrl Pts',(34.7867776966583,-56.8075863052296,3.89716357940668));
#34031=CARTESIAN_POINT('Ctrl Pts',(34.3497911057074,-54.7179277581866,3.99927695466287));
#34032=CARTESIAN_POINT('Ctrl Pts',(32.181049996069,-53.8840375630849,4.11041484523092));
#34033=CARTESIAN_POINT('Ctrl Pts',(30.3042474418304,-55.2538634762437,4.22155273579895));
#34034=CARTESIAN_POINT('Ctrl Pts',(30.4372421062834,-57.5735883041596,4.332690626367));
#34035=CARTESIAN_POINT('Ctrl Pts',(32.1498112942942,-58.5449642134686,4.42686462092145));
#34036=CARTESIAN_POINT('Ctrl Pts',(33.2038204161972,-58.2533054775293,4.48399265195323));
#34037=CARTESIAN_POINT('Ctrl Pts',(33.5261619125927,-58.0680778657968,4.50407471946233));
#34038=CARTESIAN_POINT('Ctrl Pts',(33.5282587680711,-58.0691275396585,3.74592528053768));
#34039=CARTESIAN_POINT('Ctrl Pts',(33.7063336904378,-57.9682446528084,3.75700695687118));
#34040=CARTESIAN_POINT('Ctrl Pts',(34.4133163086311,-57.41900891881,3.80513459672736));
#34041=CARTESIAN_POINT('Ctrl Pts',(34.8538786959893,-55.6936640901668,3.89030820010621));
#34042=CARTESIAN_POINT('Ctrl Pts',(33.2742100800909,-53.9897102593703,4.00144609067426));
#34043=CARTESIAN_POINT('Ctrl Pts',(30.9858981977034,-54.3927491193985,4.11258398124229));
#34044=CARTESIAN_POINT('Ctrl Pts',(30.0834608661246,-56.5338746309362,4.22372187181035));
#34045=CARTESIAN_POINT('Ctrl Pts',(31.3926249737445,-58.4528736933808,4.33483563824212));
#34046=CARTESIAN_POINT('Ctrl Pts',(32.9404216250933,-58.4138778272018,4.40890344115125));
#34047=CARTESIAN_POINT('Ctrl Pts',(33.5290839390052,-58.0740603592831,4.44592528053768));
#34048=CARTESIAN_POINT('Origin',(32.5,-56.2916512459885,-3.54592528053767));
#34049=CARTESIAN_POINT('',(33.5250673440976,-58.0691981786102,3.04592528053768));
#34050=CARTESIAN_POINT('',(33.5295277964003,-58.073488152934,3.10407471946232));
#34051=CARTESIAN_POINT('',(33.5273750000001,-58.0711169444146,-3.54592528053767));
#34052=CARTESIAN_POINT('Ctrl Pts',(33.5295277964003,-58.073488152934,3.10407471946232));
#34053=CARTESIAN_POINT('Ctrl Pts',(33.5619446593132,-58.0549578524537,3.10610775634773));
#34054=CARTESIAN_POINT('Ctrl Pts',(34.1744592271169,-57.6807192506861,3.14518675675581));
#34055=CARTESIAN_POINT('Ctrl Pts',(34.9286165141379,-56.2792182940979,3.22131172068658));
#34056=CARTESIAN_POINT('Ctrl Pts',(33.8067007722452,-54.2444908119128,3.33244961125462));
#34057=CARTESIAN_POINT('Ctrl Pts',(31.4887469945245,-54.0835524914147,3.44358750182266));
#34058=CARTESIAN_POINT('Ctrl Pts',(30.0964045610991,-55.9437120025227,3.5547253923907));
#34059=CARTESIAN_POINT('Ctrl Pts',(30.9041002915367,-58.1223442490711,3.66586328295875));
#34060=CARTESIAN_POINT('Ctrl Pts',(32.6005939960278,-58.4985054002164,3.74897972531595));
#34061=CARTESIAN_POINT('Ctrl Pts',(33.3822688276508,-58.1564265401567,3.79505020415048));
#34062=CARTESIAN_POINT('Ctrl Pts',(33.5256537705603,-58.071893508325,3.80407471946232));
#34063=CARTESIAN_POINT('Ctrl Pts',(33.5250673440976,-58.0691981786102,3.04592528053768));
#34064=CARTESIAN_POINT('Ctrl Pts',(33.8788897107516,-57.8627525499152,3.06806450906843));
#34065=CARTESIAN_POINT('Ctrl Pts',(34.6708999553705,-57.0389934359536,3.12724970112185));
#34066=CARTESIAN_POINT('Ctrl Pts',(34.5748652707907,-55.0294041774428,3.22348085669796));
#34067=CARTESIAN_POINT('Ctrl Pts',(32.5648065727292,-53.8638675525518,3.33461874726601));
#34068=CARTESIAN_POINT('Ctrl Pts',(30.4954296836915,-54.9205088752032,3.44575663783404));
#34069=CARTESIAN_POINT('Ctrl Pts',(30.2608587385459,-57.2321723596467,3.55689452840209));
#34070=CARTESIAN_POINT('Ctrl Pts',(31.8948295568209,-58.5383060176735,3.65695074263663));
#34071=CARTESIAN_POINT('Ctrl Pts',(33.1110305179061,-58.3054954110724,3.7199609933485));
#34072=CARTESIAN_POINT('Ctrl Pts',(33.5282587680711,-58.0691275396585,3.74592528053768));
#34073=CARTESIAN_POINT('Origin',(32.5,-56.2916512459885,-3.54592528053767));
#34074=CARTESIAN_POINT('',(33.5275894562264,-58.0738927599537,2.34592528053768));
#34075=CARTESIAN_POINT('',(33.5275355691898,-58.0684930935818,2.40407471946232));
#34076=CARTESIAN_POINT('',(33.5273750000001,-58.0711169444146,-3.54592528053767));
#34077=CARTESIAN_POINT('Ctrl Pts',(33.5275355691898,-58.0684930935818,2.40407471946232));
#34078=CARTESIAN_POINT('Ctrl Pts',(33.7379292069399,-57.9488445224074,2.41716530854498));
#34079=CARTESIAN_POINT('Ctrl Pts',(34.4632973547596,-57.3551041347746,2.46730186115031));
#34080=CARTESIAN_POINT('Ctrl Pts',(34.8181023612983,-55.5672658557593,2.55448437727833));
#34081=CARTESIAN_POINT('Ctrl Pts',(33.1486127133916,-53.9512166070675,2.66562226784637));
#34082=CARTESIAN_POINT('Ctrl Pts',(30.8854404931491,-54.4773937257142,2.77676015841441));
#34083=CARTESIAN_POINT('Ctrl Pts',(30.1000928998772,-56.6641813277477,2.88789804898245));
#34084=CARTESIAN_POINT('Ctrl Pts',(31.4855904228425,-58.4762227231017,2.99700290266509));
#34085=CARTESIAN_POINT('Ctrl Pts',(32.9712451350632,-58.3926166724123,3.06906179282505));
#34086=CARTESIAN_POINT('Ctrl Pts',(33.5295277964003,-58.073488152934,3.10407471946232));
#34087=CARTESIAN_POINT('Ctrl Pts',(33.5275894562264,-58.0738927599537,2.34592528053768));
#34088=CARTESIAN_POINT('Ctrl Pts',(34.0539010838894,-57.7651290399622,2.37912206126567));
#34089=CARTESIAN_POINT('Ctrl Pts',(34.8729207037989,-56.5867324218956,2.44936480551635));
#34090=CARTESIAN_POINT('Ctrl Pts',(34.113250907707,-54.4762297900261,2.55665351328972));
#34091=CARTESIAN_POINT('Ctrl Pts',(31.8496996873681,-53.9516847809773,2.66779140385775));
#34092=CARTESIAN_POINT('Ctrl Pts',(30.1813757180883,-55.5689376143779,2.7789292944258));
#34093=CARTESIAN_POINT('Ctrl Pts',(30.63531484903,-57.8476984309217,2.89006718499383));
#34094=CARTESIAN_POINT('Ctrl Pts',(32.3655977900595,-58.5319722593688,2.97906584703113));
#34095=CARTESIAN_POINT('Ctrl Pts',(33.2868324730584,-58.2082016796998,3.03101854554575));
#34096=CARTESIAN_POINT('Ctrl Pts',(33.5250673440976,-58.0691981786102,3.04592528053768));
#34097=CARTESIAN_POINT('Origin',(32.5,-56.2916512459885,-3.54592528053767));
#34098=CARTESIAN_POINT('',(33.5293464154415,-58.0709332657958,1.64592528053768));
#34099=CARTESIAN_POINT('',(33.5250295315601,-58.0700303972121,1.70407471946232));
#34100=CARTESIAN_POINT('',(33.5273750000001,-58.0711169444146,-3.54592528053767));
#34101=CARTESIAN_POINT('Ctrl Pts',(33.5250295315601,-58.0700303972121,1.70407471946232));
#34102=CARTESIAN_POINT('Ctrl Pts',(33.9101525759349,-57.8442238653441,1.72822286074223));
#34103=CARTESIAN_POINT('Ctrl Pts',(34.7124027752875,-56.9623029261605,1.78941696554481));
#34104=CARTESIAN_POINT('Ctrl Pts',(34.5035809067649,-54.9190637984713,1.88765703387008));
#34105=CARTESIAN_POINT('Ctrl Pts',(32.4334427362781,-53.863915082053,1.99879492443812));
#34106=CARTESIAN_POINT('Ctrl Pts',(30.4242251840868,-55.0309008088856,2.10993281500616));
#34107=CARTESIAN_POINT('Ctrl Pts',(30.3149878617883,-57.3518657086808,2.2210707055742));
#34108=CARTESIAN_POINT('Ctrl Pts',(31.9830137885335,-58.5433285166528,2.31911800705959));
#34109=CARTESIAN_POINT('Ctrl Pts',(33.1425216985167,-58.2874462900805,2.3801193450223));
#34110=CARTESIAN_POINT('Ctrl Pts',(33.5275355691898,-58.0684930935818,2.40407471946232));
#34111=CARTESIAN_POINT('Ctrl Pts',(33.5293464154415,-58.0709332657958,1.64592528053768));
#34112=CARTESIAN_POINT('Ctrl Pts',(33.6449437000377,-58.0055982631749,1.65313364994024));
#34113=CARTESIAN_POINT('Ctrl Pts',(34.3136427308233,-57.5361314802505,1.69738798286549));
#34114=CARTESIAN_POINT('Ctrl Pts',(34.90334407317,-55.9419787993381,1.77868827931342));
#34115=CARTESIAN_POINT('Ctrl Pts',(33.5096605171051,-54.0828236849995,1.88982616988146));
#34116=CARTESIAN_POINT('Ctrl Pts',(31.1918232394055,-54.2454334870425,2.0009640604495));
#34117=CARTESIAN_POINT('Ctrl Pts',(30.0713749864112,-56.2809696095364,2.11210195101754));
#34118=CARTESIAN_POINT('Ctrl Pts',(31.1738747508358,-58.326282755013,2.22323984158559));
#34119=CARTESIAN_POINT('Ctrl Pts',(32.7983102681658,-58.4546151165852,2.30118095142563));
#34120=CARTESIAN_POINT('Ctrl Pts',(33.4665633682319,-58.1096940627472,2.342076097743));
#34121=CARTESIAN_POINT('Ctrl Pts',(33.5275894562264,-58.0738927599537,2.34592528053768));
#34122=CARTESIAN_POINT('Origin',(32.5,-56.2916512459885,-3.54592528053767));
#34123=CARTESIAN_POINT('',(33.5257755155984,-58.068190352796,0.945925280537676));
#34124=CARTESIAN_POINT('',(33.5284289248676,-58.0741771517811,1.00407471946232));
#34125=CARTESIAN_POINT('',(33.5273750000001,-58.0711169444146,-3.54592528053767));
#34126=CARTESIAN_POINT('Ctrl Pts',(33.5284289248676,-58.0741771517811,1.00407471946232));
#34127=CARTESIAN_POINT('Ctrl Pts',(34.0870797198612,-57.748684668604,1.03928041293948));
#34128=CARTESIAN_POINT('Ctrl Pts',(34.9017444968086,-56.4966890376489,1.11153206993931));
#34129=CARTESIAN_POINT('Ctrl Pts',(34.0127319779433,-54.3916579002223,1.22082969046183));
#34130=CARTESIAN_POINT('Ctrl Pts',(31.7241302087767,-53.9902693093903,1.33196758102987));
#34131=CARTESIAN_POINT('Ctrl Pts',(30.1456908584837,-55.6953617045704,1.44310547159791));
#34132=CARTESIAN_POINT('Ctrl Pts',(30.7221773650996,-57.9462446793952,1.55424336216595));
#34133=CARTESIAN_POINT('Ctrl Pts',(32.4470927941984,-58.5226506382555,1.64123311145409));
#34134=CARTESIAN_POINT('Ctrl Pts',(33.3193305292905,-58.1906364710101,1.69117689721955));
#34135=CARTESIAN_POINT('Ctrl Pts',(33.5250295315601,-58.0700303972121,1.70407471946232));
#34136=CARTESIAN_POINT('Ctrl Pts',(33.5257755155984,-58.068190352796,0.945925280537677));
#34137=CARTESIAN_POINT('Ctrl Pts',(33.8187120383005,-57.8991957700279,0.964191202137494));
#34138=CARTESIAN_POINT('Ctrl Pts',(34.5858726429697,-57.180098149748,1.01950308725999));
#34139=CARTESIAN_POINT('Ctrl Pts',(34.6950037716947,-55.2522802841409,1.11186093590517));
#34140=CARTESIAN_POINT('Ctrl Pts',(32.8172137752097,-53.883808025427,1.22299882647321));
#34141=CARTESIAN_POINT('Ctrl Pts',(30.6490744128704,-54.7192619732989,1.33413671704125));
#34142=CARTESIAN_POINT('Ctrl Pts',(30.1751082313325,-56.9939416545676,1.44527460760929));
#34143=CARTESIAN_POINT('Ctrl Pts',(31.7218617398001,-58.5199646784861,1.54920412877477));
#34144=CARTESIAN_POINT('Ctrl Pts',(33.0508547252211,-58.341374357417,1.61608768641756));
#34145=CARTESIAN_POINT('Ctrl Pts',(33.5293464154415,-58.0709332657958,1.64592528053768));
#34146=CARTESIAN_POINT('Origin',(32.5,-56.2916512459885,-3.54592528053767));
#34147=CARTESIAN_POINT('',(33.5260517589603,-58.0725043954729,0.245925280537677));
#34148=CARTESIAN_POINT('',(33.5288532114794,-58.0699232317666,0.304074719462321));
#34149=CARTESIAN_POINT('',(33.5273750000001,-58.0711169444146,-3.54592528053767));
#34150=CARTESIAN_POINT('Ctrl Pts',(33.5288532114794,-58.0699232317667,0.304074719462322));
#34151=CARTESIAN_POINT('Ctrl Pts',(33.6768637713204,-57.9862464992859,0.313292001614045));
#34152=CARTESIAN_POINT('Ctrl Pts',(34.365857764272,-57.4763696079473,0.35955524728845));
#34153=CARTESIAN_POINT('Ctrl Pts',(34.8809216257836,-55.8125427394079,0.442864456485535));
#34154=CARTESIAN_POINT('Ctrl Pts',(33.388753307414,-54.0314631320695,0.554002347053576));
#34155=CARTESIAN_POINT('Ctrl Pts',(31.0830990069914,-54.3191593379889,0.665140237621618));
#34156=CARTESIAN_POINT('Ctrl Pts',(30.0743502545355,-56.4122997567237,0.77627812818966));
#34157=CARTESIAN_POINT('Ctrl Pts',(31.2858262226837,-58.3950092254139,0.887416018757702));
#34158=CARTESIAN_POINT('Ctrl Pts',(32.8728372110939,-58.4342824094917,0.963348215848589));
#34159=CARTESIAN_POINT('Ctrl Pts',(33.4992271616754,-58.0911912767045,1.0022344494168));
#34160=CARTESIAN_POINT('Ctrl Pts',(33.5284289248676,-58.0741771517811,1.00407471946232));
#34161=CARTESIAN_POINT('Ctrl Pts',(33.5260517589603,-58.0725043954729,0.245925280537675));
#34162=CARTESIAN_POINT('Ctrl Pts',(33.991498229918,-57.7980207394883,0.275248754334743));
#34163=CARTESIAN_POINT('Ctrl Pts',(34.8099603858882,-56.753542377561,0.34161819165449));
#34164=CARTESIAN_POINT('Ctrl Pts',(34.2934896049409,-54.6540528227808,0.445033592496919));
#34165=CARTESIAN_POINT('Ctrl Pts',(32.096850264347,-53.8966974164154,0.55617148306496));
#34166=CARTESIAN_POINT('Ctrl Pts',(30.2692184515671,-55.3314704112853,0.667309373633002));
#34167=CARTESIAN_POINT('Ctrl Pts',(30.4834462874739,-57.6451078131478,0.778447264201044));
#34168=CARTESIAN_POINT('Ctrl Pts',(32.2048796389797,-58.543263196541,0.871319233169268));
#34169=CARTESIAN_POINT('Ctrl Pts',(33.224593878142,-58.241941528272,0.927145238614813));
#34170=CARTESIAN_POINT('Ctrl Pts',(33.5257755155984,-58.068190352796,0.945925280537677));
#34171=CARTESIAN_POINT('Origin',(32.5,-56.2916512459885,-3.54592528053767));
#34172=CARTESIAN_POINT('',(33.5296554006196,-58.0729354591292,-0.454074719462323));
#34173=CARTESIAN_POINT('',(33.5253135061185,-58.0685974415039,-0.395925280537675));
#34174=CARTESIAN_POINT('',(33.5273750000001,-58.0711169444146,-3.54592528053767));
#34175=CARTESIAN_POINT('Ctrl Pts',(33.5253135061185,-58.0685974415039,-0.395925280537677));
#34176=CARTESIAN_POINT('Ctrl Pts',(33.8499262418575,-57.8801900402997,-0.375650446188704));
#34177=CARTESIAN_POINT('Ctrl Pts',(34.6307561402675,-57.1080161029863,-0.31832964831705));
#34178=CARTESIAN_POINT('Ctrl Pts',(34.6355944339958,-55.1351180442909,-0.223962886922716));
#34179=CARTESIAN_POINT('Ctrl Pts',(32.6865588761979,-53.8701788494842,-0.112824996354674));
#34180=CARTESIAN_POINT('Ctrl Pts',(30.5667638241697,-54.8216408199215,-0.00168710578663165));
#34181=CARTESIAN_POINT('Ctrl Pts',(30.2164817879238,-57.1186199946645,0.109450784781409));
#34182=CARTESIAN_POINT('Ctrl Pts',(31.8120346004307,-58.5309407947376,0.211371393197728));
#34183=CARTESIAN_POINT('Ctrl Pts',(33.081981927564,-58.322558779647,0.276246038091365));
#34184=CARTESIAN_POINT('Ctrl Pts',(33.5288532114794,-58.0699232317667,0.304074719462322));
#34185=CARTESIAN_POINT('Ctrl Pts',(33.5296554006196,-58.0729354591292,-0.454074719462325));
#34186=CARTESIAN_POINT('Ctrl Pts',(33.5829230895642,-58.0426280169118,-0.450739656990688));
#34187=CARTESIAN_POINT('Ctrl Pts',(34.2100716718942,-57.645578141716,-0.410358630996372));
#34188=CARTESIAN_POINT('Ctrl Pts',(34.926688116847,-56.1940939537869,-0.332931641479374));
#34189=CARTESIAN_POINT('Ctrl Pts',(33.7341373860101,-54.1999441339785,-0.221793750911332));
#34190=CARTESIAN_POINT('Ctrl Pts',(31.4119663698708,-54.1203575053852,-0.11065586034329));
#34191=CARTESIAN_POINT('Ctrl Pts',(30.0856850452223,-56.0281806868171,0.000482030224751475));
#34192=CARTESIAN_POINT('Ctrl Pts',(30.9692534931351,-58.1771614464075,0.111619920792793));
#34193=CARTESIAN_POINT('Ctrl Pts',(32.6511246141561,-58.4886656996171,0.193434337563768));
#34194=CARTESIAN_POINT('Ctrl Pts',(33.4034740038597,-58.1447910975144,0.238202790812062));
#34195=CARTESIAN_POINT('Ctrl Pts',(33.5260517589603,-58.0725043954729,0.245925280537675));
#34196=CARTESIAN_POINT('Origin',(32.5,-56.2916512459885,-3.54592528053767));
#34197=CARTESIAN_POINT('',(33.5270487244507,-58.0682282925652,-1.15407471946232));
#34198=CARTESIAN_POINT('',(33.5268019957928,-58.0733321975144,-1.09592528053768));
#34199=CARTESIAN_POINT('',(33.5273750000001,-58.0711169444146,-3.54592528053767));
#34200=CARTESIAN_POINT('Ctrl Pts',(33.5268019957928,-58.0733321975144,-1.09592528053768));
#34201=CARTESIAN_POINT('Ctrl Pts',(34.0236398642182,-57.7807696971903,-1.06459289399145));
#34202=CARTESIAN_POINT('Ctrl Pts',(34.8437811491657,-56.6681489116154,-0.996214543922551));
#34203=CARTESIAN_POINT('Ctrl Pts',(34.2023204507043,-54.559476051911,-0.890790230330967));
#34204=CARTESIAN_POINT('Ctrl Pts',(31.9679467730355,-53.921998742765,-0.779652339762925));
#34205=CARTESIAN_POINT('Ctrl Pts',(30.2205650142273,-55.453492447677,-0.668514449194883));
#34206=CARTESIAN_POINT('Ctrl Pts',(30.5595771710743,-57.7521618011011,-0.557376558626841));
#34207=CARTESIAN_POINT('Ctrl Pts',(32.2888225453055,-58.5385401346075,-0.466513502407773));
#34208=CARTESIAN_POINT('Ctrl Pts',(33.2567972741827,-58.2244460570089,-0.412696409711385));
#34209=CARTESIAN_POINT('Ctrl Pts',(33.5253135061185,-58.0685974415039,-0.395925280537677));
#34210=CARTESIAN_POINT('Ctrl Pts',(33.5270487244507,-58.0682282925651,-1.15407471946232));
#34211=CARTESIAN_POINT('Ctrl Pts',(33.7583254242685,-57.9362916288018,-1.13968210479344));
#34212=CARTESIAN_POINT('Ctrl Pts',(34.4950254817816,-57.3125020026611,-1.08824352660187));
#34213=CARTESIAN_POINT('Ctrl Pts',(34.7912737376158,-55.4864512354733,-0.999758984887625));
#34214=CARTESIAN_POINT('Ctrl Pts',(33.0661792001092,-53.929919412126,-0.888621094319583));
#34215=CARTESIAN_POINT('Ctrl Pts',(30.822833264184,-54.5351044086332,-0.777483203751541));
#34216=CARTESIAN_POINT('Ctrl Pts',(30.1146276885619,-56.7480782089188,-0.6663453131835));
#34217=CARTESIAN_POINT('Ctrl Pts',(31.5455083936008,-58.4894074878943,-0.558542485087093));
#34218=CARTESIAN_POINT('Ctrl Pts',(32.9912241698707,-58.3792838991923,-0.487785620513369));
#34219=CARTESIAN_POINT('Ctrl Pts',(33.5296554006196,-58.0729354591292,-0.454074719462325));
#34220=CARTESIAN_POINT('Origin',(32.5,-56.2916512459885,-3.54592528053767));
#34221=CARTESIAN_POINT('',(33.5243188290626,-58.0704843676252,-1.85407471946232));
#34222=CARTESIAN_POINT('',(33.5295805874755,-58.0719425970214,-1.79592528053768));
#34223=CARTESIAN_POINT('',(33.5273750000001,-58.0711169444146,-3.54592528053767));
#34224=CARTESIAN_POINT('',(31.0458737116219,-57.7433792852397,-2.));
#34225=CARTESIAN_POINT('Ctrl Pts',(31.0458737116219,-57.7433792852397,-2.));
#34226=CARTESIAN_POINT('Ctrl Pts',(31.5286078227264,-58.2269108712356,-1.96295403647732));
#34227=CARTESIAN_POINT('Ctrl Pts',(32.4987857659728,-58.5150960016803,-1.91431227629809));
#34228=CARTESIAN_POINT('Ctrl Pts',(33.339589876325,-58.1790057138554,-1.86567051611887));
#34229=CARTESIAN_POINT('Ctrl Pts',(33.5243188290626,-58.0704843676252,-1.85407471946232));
#34230=CARTESIAN_POINT('',(30.5120522999331,-56.8258916115682,-2.));
#34231=CARTESIAN_POINT('Origin',(32.5,-56.2916512459885,-2.));
#34232=CARTESIAN_POINT('Ctrl Pts',(30.5120501580915,-56.825892077386,-2.));
#34233=CARTESIAN_POINT('Ctrl Pts',(30.6859814099171,-57.4697983977034,-1.96367708181445));
#34234=CARTESIAN_POINT('Ctrl Pts',(31.6524845810096,-58.5050100533593,-1.89565217532701));
#34235=CARTESIAN_POINT('Ctrl Pts',(33.0221861661125,-58.3592796390667,-1.82762726883957));
#34236=CARTESIAN_POINT('Ctrl Pts',(33.5295805874755,-58.0719425970214,-1.79592528053768));
#34237=CARTESIAN_POINT('Origin',(63.7511045350785,17.0820569767664,10.));
#34238=CARTESIAN_POINT('',(60.9122168113323,13.7189801527801,9.99965378812963));
#34239=CARTESIAN_POINT('',(60.6472937215209,13.6458118873637,9.99664393251001));
#34240=CARTESIAN_POINT('',(64.4026814811241,14.6503387090836,10.));
#34241=CARTESIAN_POINT('',(60.3826426720153,14.1985145724513,11.6359872033747));
#34242=CARTESIAN_POINT('Ctrl Pts',(60.6472937215209,13.6458118873637,9.99664393251001));
#34243=CARTESIAN_POINT('Ctrl Pts',(60.6097205320263,13.6410407802455,10.5892058593235));
#34244=CARTESIAN_POINT('Ctrl Pts',(60.5187326677745,13.8356159531908,11.1848035603042));
#34245=CARTESIAN_POINT('Ctrl Pts',(60.3826426720153,14.1985145724514,11.6359872033748));
#34246=CARTESIAN_POINT('',(59.3912531651588,17.8984305821304,11.6380816927071));
#34247=CARTESIAN_POINT('Origin',(59.8874012299222,16.0467807963563,10.));
#34248=CARTESIAN_POINT('Ctrl Pts',(59.3912467107623,17.8984546702662,11.6380966037225));
#34249=CARTESIAN_POINT('Ctrl Pts',(59.5701794123024,17.4212611177616,12.2270179049202));
#34250=CARTESIAN_POINT('Ctrl Pts',(59.8253574740883,16.659516006978,12.567422198156));
#34251=CARTESIAN_POINT('Ctrl Pts',(60.0736878712827,15.9233267283634,12.5157167035403));
#34252=CARTESIAN_POINT('Ctrl Pts',(60.3360206084697,15.1456267338052,12.4610957466079));
#34253=CARTESIAN_POINT('Ctrl Pts',(60.5907116859352,14.3964458015818,11.9688993897472));
#34254=CARTESIAN_POINT('Ctrl Pts',(60.7469740189126,14.014605944713,11.2575578209417));
#34255=CARTESIAN_POINT('Ctrl Pts',(60.8300361143405,13.8116368860468,10.8794403300265));
#34256=CARTESIAN_POINT('Ctrl Pts',(60.8852870497793,13.7124604894775,10.4394030962359));
#34257=CARTESIAN_POINT('Ctrl Pts',(60.9122168113323,13.7189801527801,9.99965378812962));
#34258=CARTESIAN_POINT('Origin',(63.7511045350785,17.0820569767664,10.));
#34259=CARTESIAN_POINT('',(61.8799991994799,13.9708704146993,9.99901528063939));
#34260=CARTESIAN_POINT('',(61.614467077582,13.8999750879731,10.0012573013837));
#34261=CARTESIAN_POINT('',(64.4026814811241,14.6503387090836,10.));
#34262=CARTESIAN_POINT('Ctrl Pts',(61.614467077582,13.8999750879731,10.0012573013837));
#34263=CARTESIAN_POINT('Ctrl Pts',(61.6099667912196,13.8982899610888,10.0766544396887));
#34264=CARTESIAN_POINT('Ctrl Pts',(61.6045451170745,13.900043500223,10.1520128061815));
#34265=CARTESIAN_POINT('Ctrl Pts',(61.5981695663354,13.9053569552699,10.2270376921985));
#34266=CARTESIAN_POINT('Ctrl Pts',(61.5284611611194,13.9634527171371,11.047337830936));
#34267=CARTESIAN_POINT('Ctrl Pts',(61.3447206686645,14.4471220222725,11.8277717281245));
#34268=CARTESIAN_POINT('Ctrl Pts',(61.1066011161457,15.1337367424348,12.2189611289229));
#34269=CARTESIAN_POINT('Ctrl Pts',(60.8684815636268,15.8203514625971,12.6101505297212));
#34270=CARTESIAN_POINT('Ctrl Pts',(60.5759829510439,16.7099115977863,12.6120954341293));
#34271=CARTESIAN_POINT('Ctrl Pts',(60.3374667150895,17.3980067606845,12.2237523563129));
#34272=CARTESIAN_POINT('Ctrl Pts',(60.0989504791351,18.0861019235826,11.8354092784964));
#34273=CARTESIAN_POINT('Ctrl Pts',(59.9144166198093,18.5727321141896,11.0567782184554));
#34274=CARTESIAN_POINT('Ctrl Pts',(59.8438645695582,18.6339764021913,10.2368654679638));
#34275=CARTESIAN_POINT('Ctrl Pts',(59.7733125193071,18.6952206901929,9.41695271747214));
#34276=CARTESIAN_POINT('Ctrl Pts',(59.8167422781307,18.3310790755891,8.55575827652985));
#34277=CARTESIAN_POINT('Ctrl Pts',(59.932110753931,17.6984585141966,8.03819621078674));
#34278=CARTESIAN_POINT('Ctrl Pts',(60.0474792297314,17.0658379528042,7.52063414504363));
#34279=CARTESIAN_POINT('Ctrl Pts',(60.2347864225085,16.1647384446231,7.34670445449967));
#34280=CARTESIAN_POINT('Ctrl Pts',(60.3874931590402,15.392769597115,7.59575134544314));
#34281=CARTESIAN_POINT('Ctrl Pts',(60.540199895572,14.6208007496069,7.84479823638661));
#34282=CARTESIAN_POINT('Ctrl Pts',(60.6583061758583,13.9779625627717,8.51682170881751));
#34283=CARTESIAN_POINT('Ctrl Pts',(60.6663289586339,13.7459615817213,9.30743209219171));
#34284=CARTESIAN_POINT('Ctrl Pts',(60.6685946628634,13.6804424696227,9.5307073994776));
#34285=CARTESIAN_POINT('Ctrl Pts',(60.6620806891943,13.6476895615158,9.76344057197144));
#34286=CARTESIAN_POINT('Ctrl Pts',(60.6472937215209,13.6458118873637,9.99664393251001));
#34287=CARTESIAN_POINT('Ctrl Pts',(60.9122168113323,13.7189801527801,9.99965378812962));
#34288=CARTESIAN_POINT('Ctrl Pts',(60.9359492362449,13.7247257446778,9.61211536100745));
#34289=CARTESIAN_POINT('Ctrl Pts',(60.9376863320054,13.8125590225005,9.22480054821085));
#34290=CARTESIAN_POINT('Ctrl Pts',(60.9170790299751,13.9837827281427,8.88028612326221));
#34291=CARTESIAN_POINT('Ctrl Pts',(60.8730881195708,14.3492981499552,8.14484277513855));
#34292=CARTESIAN_POINT('Ctrl Pts',(60.7272727102727,15.0948277750946,7.60444285964154));
#34293=CARTESIAN_POINT('Ctrl Pts',(60.5669204894781,15.8946095193188,7.49935843056474));
#34294=CARTESIAN_POINT('Ctrl Pts',(60.4065682686835,16.694391263543,7.39427400148793));
#34295=CARTESIAN_POINT('Ctrl Pts',(60.2316792363924,17.5484251268522,7.72450505883134));
#34296=CARTESIAN_POINT('Ctrl Pts',(60.1424305723414,18.0828447847106,8.34320956294502));
#34297=CARTESIAN_POINT('Ctrl Pts',(60.0531819082903,18.617264442569,8.96191406705869));
#34298=CARTESIAN_POINT('Ctrl Pts',(60.0495736124794,18.8320698949766,9.86909201794265));
#34299=CARTESIAN_POINT('Ctrl Pts',(60.1556096340356,18.6376771842086,10.6611508664113));
#34300=CARTESIAN_POINT('Ctrl Pts',(60.2616456555918,18.4432844734405,11.4532097148801));
#34301=CARTESIAN_POINT('Ctrl Pts',(60.4773259945153,17.8396935994968,12.1301494609335));
#34302=CARTESIAN_POINT('Ctrl Pts',(60.7290924921509,17.1014273477893,12.3908459426517));
#34303=CARTESIAN_POINT('Ctrl Pts',(60.9808589897866,16.3631610960817,12.6515424243699));
#34304=CARTESIAN_POINT('Ctrl Pts',(61.2687116461343,15.4902194666104,12.4959956417528));
#34305=CARTESIAN_POINT('Ctrl Pts',(61.4869914228006,14.8769273589395,11.9933937214366));
#34306=CARTESIAN_POINT('Ctrl Pts',(61.6896056365773,14.3076501674883,11.5268626736099));
#34307=CARTESIAN_POINT('Ctrl Pts',(61.8322748736988,13.9620906745726,10.7613040129743));
#34308=CARTESIAN_POINT('Ctrl Pts',(61.8799991994799,13.9708704146993,9.99901528063939));
#34309=CARTESIAN_POINT('Origin',(63.7511045350785,17.0820569767664,10.));
#34310=CARTESIAN_POINT('',(62.8445369550162,14.2348698103755,10.0018466754434));
#34311=CARTESIAN_POINT('',(62.5785998445538,14.1654859215485,10.0004462653845));
#34312=CARTESIAN_POINT('',(64.4026814811241,14.6503387090836,10.));
#34313=CARTESIAN_POINT('Ctrl Pts',(62.5785998445538,14.1654859215485,10.0004462653845));
#34314=CARTESIAN_POINT('Ctrl Pts',(62.5552558244195,14.1585827534688,10.3867702486341));
#34315=CARTESIAN_POINT('Ctrl Pts',(62.5100553152291,14.2332491130213,10.7728367424032));
#34316=CARTESIAN_POINT('Ctrl Pts',(62.4426252563818,14.3908772813227,11.1164878478952));
#34317=CARTESIAN_POINT('Ctrl Pts',(62.2977170112848,14.7296226663468,11.8549994178656));
#34318=CARTESIAN_POINT('Ctrl Pts',(62.0501467519025,15.4515079046906,12.397625364221));
#34319=CARTESIAN_POINT('Ctrl Pts',(61.7881520526304,16.2272258855741,12.501389418797));
#34320=CARTESIAN_POINT('Ctrl Pts',(61.5261573533583,17.0029438664577,12.605153473373));
#34321=CARTESIAN_POINT('Ctrl Pts',(61.2497382141963,17.832494589881,12.2700556361696));
#34322=CARTESIAN_POINT('Ctrl Pts',(61.0600503079339,18.3383599455201,11.646143814324));
#34323=CARTESIAN_POINT('Ctrl Pts',(60.8703624016714,18.8442253011592,11.0222319924783));
#34324=CARTESIAN_POINT('Ctrl Pts',(60.7674057283085,19.0264052890141,10.1095061859904));
#34325=CARTESIAN_POINT('Ctrl Pts',(60.7746625458238,18.7972629292321,9.31667252204681));
#34326=CARTESIAN_POINT('Ctrl Pts',(60.7819193633391,18.5681205694502,8.52383885810325));
#34327=CARTESIAN_POINT('Ctrl Pts',(60.8993896717325,17.9276558620313,7.85089733670406));
#34328=CARTESIAN_POINT('Ctrl Pts',(61.0518532638259,17.1565944419206,7.59916807226838));
#34329=CARTESIAN_POINT('Ctrl Pts',(61.2043168559193,16.3855330218099,7.3474388078327));
#34330=CARTESIAN_POINT('Ctrl Pts',(61.3917737317127,15.4838748890073,7.51692180036051));
#34331=CARTESIAN_POINT('Ctrl Pts',(61.5076640106207,14.8493069319055,8.03174648676759));
#34332=CARTESIAN_POINT('Ctrl Pts',(61.6129549313732,14.2727767422054,8.49948515966272));
#34333=CARTESIAN_POINT('Ctrl Pts',(61.6591716047613,13.9167146450877,9.25228420341931));
#34334=CARTESIAN_POINT('Ctrl Pts',(61.614467077582,13.8999750879731,10.0012573013837));
#34335=CARTESIAN_POINT('Ctrl Pts',(61.8799991994799,13.9708704146993,9.99901528063939));
#34336=CARTESIAN_POINT('Ctrl Pts',(61.8836891105328,13.971549239588,9.94007725327275));
#34337=CARTESIAN_POINT('Ctrl Pts',(61.8868114457663,13.9743462862715,9.88115877337008));
#34338=CARTESIAN_POINT('Ctrl Pts',(61.8893500282724,13.9793219277933,9.82239956232278));
#34339=CARTESIAN_POINT('Ctrl Pts',(61.9247219600932,14.0486511901886,9.00366438154032));
#34340=CARTESIAN_POINT('Ctrl Pts',(61.84675892675,14.5409523008496,8.21585107799066));
#34341=CARTESIAN_POINT('Ctrl Pts',(61.712535142454,15.243221392539,7.80941972573588));
#34342=CARTESIAN_POINT('Ctrl Pts',(61.5783113581579,15.9454904842284,7.4029883734811));
#34343=CARTESIAN_POINT('Ctrl Pts',(61.3878268229089,16.8577275569461,7.37793897252118));
#34344=CARTESIAN_POINT('Ctrl Pts',(61.2482107604141,17.5801209048418,7.74541574302332));
#34345=CARTESIAN_POINT('Ctrl Pts',(61.1085946979193,18.3025142527376,8.11289251352547));
#34346=CARTESIAN_POINT('Ctrl Pts',(61.0198471081785,18.8350638758114,8.8728954554897));
#34347=CARTESIAN_POINT('Ctrl Pts',(61.0438394390411,18.9468623871525,9.6873337892666));
#34348=CARTESIAN_POINT('Ctrl Pts',(61.0678317699037,19.0586608984936,10.5017721230435));
#34349=CARTESIAN_POINT('Ctrl Pts',(61.2045640213697,18.749708298102,11.370645848633));
#34350=CARTESIAN_POINT('Ctrl Pts',(61.4156018821482,18.1634433884681,11.9074332417686));
#34351=CARTESIAN_POINT('Ctrl Pts',(61.6266397429268,17.5771784788342,12.4442206349041));
#34352=CARTESIAN_POINT('Ctrl Pts',(61.9119832130179,16.7136012599581,12.6489216955856));
#34353=CARTESIAN_POINT('Ctrl Pts',(62.1670877632026,15.9628772265393,12.4304742338454));
#34354=CARTESIAN_POINT('Ctrl Pts',(62.4221923133873,15.2121531931204,12.2120267721052));
#34355=CARTESIAN_POINT('Ctrl Pts',(62.6470579436654,14.5742823451588,11.5704307879433));
#34356=CARTESIAN_POINT('Ctrl Pts',(62.7640438959386,14.3390239366156,10.7911028658272));
#34357=CARTESIAN_POINT('Ctrl Pts',(62.8020535673526,14.2625865983512,10.537892991755));
#34358=CARTESIAN_POINT('Ctrl Pts',(62.8286748982889,14.2286511253629,10.2701434172214));
#34359=CARTESIAN_POINT('Ctrl Pts',(62.8445369550162,14.2348698103755,10.0018466754434));
#34360=CARTESIAN_POINT('Origin',(63.7511045350785,17.0820569767664,10.));
#34361=CARTESIAN_POINT('',(63.8107147438123,14.4927485186002,9.99793352624083));
#34362=CARTESIAN_POINT('',(63.5459612763502,14.4189472139579,9.9981100037851));
#34363=CARTESIAN_POINT('',(64.4026814811241,14.6503387090836,10.));
#34364=CARTESIAN_POINT('Ctrl Pts',(63.5459612763502,14.4189472139579,9.9981100037851));
#34365=CARTESIAN_POINT('Ctrl Pts',(63.5020657997403,14.4131993125783,10.6909216248416));
#34366=CARTESIAN_POINT('Ctrl Pts',(63.3825723034678,14.6895870615306,11.3881278716997));
#34367=CARTESIAN_POINT('Ctrl Pts',(63.2084966963919,15.1696780211856,11.8560065223221));
#34368=CARTESIAN_POINT('Ctrl Pts',(63.0010658835769,15.7417608055527,12.4135369565263));
#34369=CARTESIAN_POINT('Ctrl Pts',(62.7161316220184,16.6030903983924,12.6454354329572));
#34370=CARTESIAN_POINT('Ctrl Pts',(62.4586624096387,17.3619190322645,12.4478622804133));
#34371=CARTESIAN_POINT('Ctrl Pts',(62.201193197259,18.1207476661366,12.2502891278695));
#34372=CARTESIAN_POINT('Ctrl Pts',(61.9711890340581,18.7770753410411,11.6232443463508));
#34373=CARTESIAN_POINT('Ctrl Pts',(61.8490217755359,19.0309502087539,10.8475065234706));
#34374=CARTESIAN_POINT('Ctrl Pts',(61.7268545170136,19.2848250764668,10.0717687005904));
#34375=CARTESIAN_POINT('Ctrl Pts',(61.7125241631699,19.136247136988,9.14733783634869));
#34376=CARTESIAN_POINT('Ctrl Pts',(61.7898279718489,18.6456858472656,8.48815640829364));
#34377=CARTESIAN_POINT('Ctrl Pts',(61.867131780528,18.1551245575431,7.82897498023858));
#34378=CARTESIAN_POINT('Ctrl Pts',(62.0360697517297,17.3225799175771,7.43504298837021));
#34379=CARTESIAN_POINT('Ctrl Pts',(62.1983751106924,16.5147885234738,7.48275547481141));
#34380=CARTESIAN_POINT('Ctrl Pts',(62.3606804696551,15.7069971293706,7.53046796125261));
#34381=CARTESIAN_POINT('Ctrl Pts',(62.5163532163788,14.9239589811301,8.01982492600339));
#34382=CARTESIAN_POINT('Ctrl Pts',(62.5730664743348,14.5102426728621,8.73170200517146));
#34383=CARTESIAN_POINT('Ctrl Pts',(62.6033893890854,14.2890407035395,9.11232178902007));
#34384=CARTESIAN_POINT('Ctrl Pts',(62.6054224867212,14.1734177690261,9.55655400073804));
#34385=CARTESIAN_POINT('Ctrl Pts',(62.5785998445538,14.1654859215485,10.0004462653845));
#34386=CARTESIAN_POINT('Ctrl Pts',(62.8445369550162,14.2348698103755,10.0018466754434));
#34387=CARTESIAN_POINT('Ctrl Pts',(62.8774950470096,14.2477909590166,9.44438121878217));
#34388=CARTESIAN_POINT('Ctrl Pts',(62.8640028840737,14.4340668190784,8.88455351560662));
#34389=CARTESIAN_POINT('Ctrl Pts',(62.8097033887246,14.7726377170274,8.44788099502234));
#34390=CARTESIAN_POINT('Ctrl Pts',(62.729270654969,15.2741558751071,7.80104690640396));
#34391=CARTESIAN_POINT('Ctrl Pts',(62.5592989131896,16.1098381603915,7.42443858923753));
#34392=CARTESIAN_POINT('Ctrl Pts',(62.3977923938505,16.913927805431,7.48559176785146));
#34393=CARTESIAN_POINT('Ctrl Pts',(62.2362858745114,17.7180174504704,7.5467449464654));
#34394=CARTESIAN_POINT('Ctrl Pts',(62.0832445776126,18.490514455265,8.04565962085973));
#34395=CARTESIAN_POINT('Ctrl Pts',(62.0291411621378,18.8937702597925,8.76039160250516));
#34396=CARTESIAN_POINT('Ctrl Pts',(61.9750377466629,19.2970260643199,9.47512358415059));
#34397=CARTESIAN_POINT('Ctrl Pts',(62.0198722126119,19.3310406685804,10.4056728730471));
#34398=CARTESIAN_POINT('Ctrl Pts',(62.1660913946905,18.9866823611344,11.138080910744));
#34399=CARTESIAN_POINT('Ctrl Pts',(62.312310576769,18.6423240536885,11.8704889484409));
#34400=CARTESIAN_POINT('Ctrl Pts',(62.5599144749771,17.9195928345362,12.4047557349382));
#34401=CARTESIAN_POINT('Ctrl Pts',(62.8211471346509,17.1459983851495,12.5032105584454));
#34402=CARTESIAN_POINT('Ctrl Pts',(63.0823797943247,16.3724039357629,12.6016653819527));
#34403=CARTESIAN_POINT('Ctrl Pts',(63.3572412154642,15.5479462561419,12.2643082424698));
#34404=CARTESIAN_POINT('Ctrl Pts',(63.5458498251155,15.0453884512907,11.6412138093996));
#34405=CARTESIAN_POINT('Ctrl Pts',(63.6819468306564,14.6827506455303,11.1915986689941));
#34406=CARTESIAN_POINT('Ctrl Pts',(63.7731333897311,14.4877209077723,10.5932047327949));
#34407=CARTESIAN_POINT('Ctrl Pts',(63.8107147438123,14.4927485186002,9.99793352624083));
#34408=CARTESIAN_POINT('Origin',(63.7511045350785,17.0820569767664,10.));
#34409=CARTESIAN_POINT('',(64.7775781358098,14.7480685208434,10.0015051238181));
#34410=CARTESIAN_POINT('',(64.511567991272,14.6789571988966,10.0021294030496));
#34411=CARTESIAN_POINT('',(64.4026814811241,14.6503387090836,10.));
#34412=CARTESIAN_POINT('Ctrl Pts',(64.511567991272,14.6789571988966,10.0021294030496));
#34413=CARTESIAN_POINT('Ctrl Pts',(64.5012097288919,14.6745624451438,10.1782532036584));
#34414=CARTESIAN_POINT('Ctrl Pts',(64.4860602506939,14.6880487522533,10.354078307347));
#34415=CARTESIAN_POINT('Ctrl Pts',(64.4658270415774,14.7205078014429,10.5257161206906));
#34416=CARTESIAN_POINT('Ctrl Pts',(64.3708655262953,14.8728494531259,11.3312723100704));
#34417=CARTESIAN_POINT('Ctrl Pts',(64.163921993672,15.4431136830602,12.0445928505661));
#34418=CARTESIAN_POINT('Ctrl Pts',(63.9150421900725,16.1698862069573,12.3462664892695));
#34419=CARTESIAN_POINT('Ctrl Pts',(63.6661623864731,16.8966587308544,12.6479401279729));
#34420=CARTESIAN_POINT('Ctrl Pts',(63.3753463118975,17.7799395487143,12.5379668648842));
#34421=CARTESIAN_POINT('Ctrl Pts',(63.1501962278718,18.4181515535133,12.0655906176062));
#34422=CARTESIAN_POINT('Ctrl Pts',(62.925046143846,19.0563635583122,11.5932143703281));
#34423=CARTESIAN_POINT('Ctrl Pts',(62.76556205037,19.4495067500502,10.7584351388608));
#34424=CARTESIAN_POINT('Ctrl Pts',(62.7205382674991,19.4154782471595,9.93505104704534));
#34425=CARTESIAN_POINT('Ctrl Pts',(62.6755144846283,19.3814497442687,9.11166695522985));
#34426=CARTESIAN_POINT('Ctrl Pts',(62.7449510123626,18.9202495467492,8.2996780030662));
#34427=CARTESIAN_POINT('Ctrl Pts',(62.8751359084421,18.2323333520888,7.8626772661126));
#34428=CARTESIAN_POINT('Ctrl Pts',(63.0053208045215,17.5444171574285,7.425676529159));
#34429=CARTESIAN_POINT('Ctrl Pts',(63.1962540689461,16.6297849656272,7.36366400741544));
#34430=CARTESIAN_POINT('Ctrl Pts',(63.3398198518216,15.8919306215938,7.70440771629217));
#34431=CARTESIAN_POINT('Ctrl Pts',(63.4833856346971,15.1540762775605,8.04515142516891));
#34432=CARTESIAN_POINT('Ctrl Pts',(63.5795839360234,14.592999781295,8.78865136466594));
#34433=CARTESIAN_POINT('Ctrl Pts',(63.5627194046509,14.4538795211095,9.60198253040318));
#34434=CARTESIAN_POINT('Ctrl Pts',(63.5600075610921,14.4315087612499,9.73276747984737));
#34435=CARTESIAN_POINT('Ctrl Pts',(63.5543722345421,14.4200485884486,9.86535806600962));
#34436=CARTESIAN_POINT('Ctrl Pts',(63.5459612763502,14.4189472139579,9.9981100037851));
#34437=CARTESIAN_POINT('Ctrl Pts',(63.8107147438123,14.4927485186002,9.99793352624083));
#34438=CARTESIAN_POINT('Ctrl Pts',(63.8252151156581,14.494688369579,9.7682543660517));
#34439=CARTESIAN_POINT('Ctrl Pts',(63.8317351659301,14.5264111861321,9.53904009330699));
#34440=CARTESIAN_POINT('Ctrl Pts',(63.8297754611263,14.5897808794637,9.3190160464461));
#34441=CARTESIAN_POINT('Ctrl Pts',(63.8227366893229,14.8173890425695,8.52874444322035));
#34442=CARTESIAN_POINT('Ctrl Pts',(63.7063033475529,15.4532632988625,7.85703296342644));
#34443=CARTESIAN_POINT('Ctrl Pts',(63.5546628984882,16.2205322683665,7.60269513736945));
#34444=CARTESIAN_POINT('Ctrl Pts',(63.4030224494236,16.9878012378706,7.34835731131246));
#34445=CARTESIAN_POINT('Ctrl Pts',(63.2161748930644,17.8864649205859,7.51139313899242));
#34446=CARTESIAN_POINT('Ctrl Pts',(63.0996317362701,18.522749012129,8.01927548227232));
#34447=CARTESIAN_POINT('Ctrl Pts',(62.9830885794757,19.1590331036721,8.52715782555223));
#34448=CARTESIAN_POINT('Ctrl Pts',(62.9368498222464,19.5329376040432,9.37988668443209));
#34449=CARTESIAN_POINT('Ctrl Pts',(63.0038765864645,19.4841294236266,10.1981222260488));
#34450=CARTESIAN_POINT('Ctrl Pts',(63.0709033506826,19.43532124321,11.0163577676655));
#34451=CARTESIAN_POINT('Ctrl Pts',(63.2511956363482,18.9638003820057,11.8000999920191));
#34452=CARTESIAN_POINT('Ctrl Pts',(63.4869413276822,18.2853245933941,12.2006980454406));
#34453=CARTESIAN_POINT('Ctrl Pts',(63.7226870190161,17.6068488047825,12.6012960988622));
#34454=CARTESIAN_POINT('Ctrl Pts',(64.0138861160186,16.7214180887636,12.6187499813517));
#34455=CARTESIAN_POINT('Ctrl Pts',(64.253389165651,16.02891964808,12.2452952639449));
#34456=CARTESIAN_POINT('Ctrl Pts',(64.4928922152834,15.3364212073964,11.871840546538));
#34457=CARTESIAN_POINT('Ctrl Pts',(64.6806992175459,14.8368550420482,11.1074772292348));
#34458=CARTESIAN_POINT('Ctrl Pts',(64.755655105023,14.7584549707696,10.2922353809894));
#34459=CARTESIAN_POINT('Ctrl Pts',(64.7645194286933,14.7491833360657,10.195824440425));
#34460=CARTESIAN_POINT('Ctrl Pts',(64.7718054668758,14.7458019429916,10.0987019353608));
#34461=CARTESIAN_POINT('Ctrl Pts',(64.7775781358098,14.7480685208434,10.0015051238181));
#34462=CARTESIAN_POINT('Origin',(63.7511045350785,17.0820569767664,10.));
#34463=CARTESIAN_POINT('',(65.7418454548454,15.0130771992805,9.99981028982562));
#34464=CARTESIAN_POINT('',(65.4764820235065,14.9415523108175,9.99892236192922));
#34465=CARTESIAN_POINT('',(64.4026814811241,14.6503387090836,10.));
#34466=CARTESIAN_POINT('Ctrl Pts',(65.4764820235065,14.9415523108175,9.99892236192922));
#34467=CARTESIAN_POINT('Ctrl Pts',(65.4463344353996,14.9354685130878,10.4860098738008));
#34468=CARTESIAN_POINT('Ctrl Pts',(65.3812875674044,15.0596306010493,10.9740976137645));
#34469=CARTESIAN_POINT('Ctrl Pts',(65.2832167053678,15.3070399126418,11.3788468299413));
#34470=CARTESIAN_POINT('Ctrl Pts',(65.1161273209563,15.7285664365572,12.0684430664547));
#34471=CARTESIAN_POINT('Ctrl Pts',(64.8531757502037,16.5078555104223,12.5161238918082));
#34472=CARTESIAN_POINT('Ctrl Pts',(64.5894870640691,17.2898955363443,12.5214264196761));
#34473=CARTESIAN_POINT('Ctrl Pts',(64.3257983779344,18.0719355622663,12.526728947544));
#34474=CARTESIAN_POINT('Ctrl Pts',(64.0613725764177,18.8567265402451,12.0896531779262));
#34475=CARTESIAN_POINT('Ctrl Pts',(63.8919948632527,19.2867932233327,11.4059132558295));
#34476=CARTESIAN_POINT('Ctrl Pts',(63.7226171500878,19.7168599064204,10.7221733337328));
#34477=CARTESIAN_POINT('Ctrl Pts',(63.6482875252747,19.7922022946169,9.7917692591572));
#34478=CARTESIAN_POINT('Ctrl Pts',(63.6796697714155,19.4730226094499,9.03131812620868));
#34479=CARTESIAN_POINT('Ctrl Pts',(63.7110520175564,19.153842924283,8.27086699326015));
#34480=CARTESIAN_POINT('Ctrl Pts',(63.8481461346512,18.4401411657526,7.68036880193875));
#34481=CARTESIAN_POINT('Ctrl Pts',(64.0069444100312,17.6454383857665,7.524237313639));
#34482=CARTESIAN_POINT('Ctrl Pts',(64.1657426854112,16.8507356057803,7.36810582533925));
#34483=CARTESIAN_POINT('Ctrl Pts',(64.3462451190763,15.9750318043384,7.64634104006116));
#34484=CARTESIAN_POINT('Ctrl Pts',(64.4450065869384,15.4043894403333,8.23435456655407));
#34485=CARTESIAN_POINT('Ctrl Pts',(64.5227251994293,14.9553323969431,8.6970815429164));
#34486=CARTESIAN_POINT('Ctrl Pts',(64.5498246710713,14.6951885590369,9.35164270965612));
#34487=CARTESIAN_POINT('Ctrl Pts',(64.511567991272,14.6789571988966,10.0021294030496));
#34488=CARTESIAN_POINT('Ctrl Pts',(64.7775781358098,14.7480685208434,10.0015051238181));
#34489=CARTESIAN_POINT('Ctrl Pts',(64.8206186125989,14.7649679121881,9.27681483601603));
#34490=CARTESIAN_POINT('Ctrl Pts',(64.7795300848962,15.0958410226864,8.54799381140139));
#34491=CARTESIAN_POINT('Ctrl Pts',(64.6812188924136,15.6402720254874,8.07917134860806));
#34492=CARTESIAN_POINT('Ctrl Pts',(64.5697220196355,16.2577231286926,7.54746954365975));
#34493=CARTESIAN_POINT('Ctrl Pts',(64.3846235013876,17.1498593123119,7.35018631295075));
#34494=CARTESIAN_POINT('Ctrl Pts',(64.23065677798,17.9258100558562,7.57508388624565));
#34495=CARTESIAN_POINT('Ctrl Pts',(64.0766900545725,18.7017607994006,7.79998145954056));
#34496=CARTESIAN_POINT('Ctrl Pts',(63.9538551260052,19.3615261028699,8.44705983683936));
#34497=CARTESIAN_POINT('Ctrl Pts',(63.9391872263039,19.6176065589079,9.22846362604928));
#34498=CARTESIAN_POINT('Ctrl Pts',(63.9245193266025,19.873687014946,10.0098674152592));
#34499=CARTESIAN_POINT('Ctrl Pts',(64.0180184557671,19.7260826235527,10.9255966163803));
#34500=CARTESIAN_POINT('Ctrl Pts',(64.200482779956,19.2464556042235,11.5682854345738));
#34501=CARTESIAN_POINT('Ctrl Pts',(64.3829471041448,18.7668285848942,12.2109742527672));
#34502=CARTESIAN_POINT('Ctrl Pts',(64.654376623358,17.9551789376289,12.5806226880332));
#34503=CARTESIAN_POINT('Ctrl Pts',(64.916416459657,17.1785720640666,12.5127911771402));
#34504=CARTESIAN_POINT('Ctrl Pts',(65.1784562959559,16.4019651905042,12.4449596662473));
#34505=CARTESIAN_POINT('Ctrl Pts',(65.4311064493406,15.6604010906447,11.9396482091956));
#34506=CARTESIAN_POINT('Ctrl Pts',(65.5843661188994,15.2897673262124,11.2216465877776));
#34507=CARTESIAN_POINT('Ctrl Pts',(65.6632851643038,15.0989143577318,10.8519211229877));
#34508=CARTESIAN_POINT('Ctrl Pts',(65.7158498370977,15.0064172468355,10.4257987515067));
#34509=CARTESIAN_POINT('Ctrl Pts',(65.7418454548454,15.0130771992805,9.99981028982562));
#34510=CARTESIAN_POINT('Origin',(63.7511045350785,17.0820569767664,10.));
#34511=CARTESIAN_POINT('',(66.709565290414,15.2652009106025,9.99881345470567));
#34512=CARTESIAN_POINT('',(66.4442667934687,15.1934336836835,9.99943462192776));
#34513=CARTESIAN_POINT('',(64.4026814811241,14.6503387090836,10.));
#34514=CARTESIAN_POINT('Ctrl Pts',(66.4442667934687,15.1934336836835,9.99943462192776));
#34515=CARTESIAN_POINT('Ctrl Pts',(66.3950965524831,15.1827995799555,10.7909504295074));
#34516=CARTESIAN_POINT('Ctrl Pts',(66.242026625676,15.5599243826036,11.5846294221379));
#34517=CARTESIAN_POINT('Ctrl Pts',(66.0272275066145,16.1674256670555,12.0468004663334));
#34518=CARTESIAN_POINT('Ctrl Pts',(65.8036660249293,16.7997089272065,12.5278249876806));
#34519=CARTESIAN_POINT('Ctrl Pts',(65.5132363543,17.6815476659072,12.6497433013673));
#34520=CARTESIAN_POINT('Ctrl Pts',(65.2633677075892,18.4120106025366,12.3579626123137));
#34521=CARTESIAN_POINT('Ctrl Pts',(65.0134990608784,19.1424735391661,12.06618192326));
#34522=CARTESIAN_POINT('Ctrl Pts',(64.8041914380861,19.7215606737244,11.3607022314659));
#34523=CARTESIAN_POINT('Ctrl Pts',(64.7065491918251,19.8839069496221,10.5574238638963));
#34524=CARTESIAN_POINT('Ctrl Pts',(64.608906945564,20.0462532255198,9.75414549632672));
#34525=CARTESIAN_POINT('Ctrl Pts',(64.6229300758342,19.7918586427569,8.85306845298168));
#34526=CARTESIAN_POINT('Ctrl Pts',(64.7197196907436,19.2285753341563,8.2576777189159));
#34527=CARTESIAN_POINT('Ctrl Pts',(64.816509305653,18.6652920255557,7.66228698485014));
#34528=CARTESIAN_POINT('Ctrl Pts',(64.9960654052016,17.7931199911174,7.37258256006362));
#34529=CARTESIAN_POINT('Ctrl Pts',(65.1553666185042,16.9965402212509,7.51828854147109));
#34530=CARTESIAN_POINT('Ctrl Pts',(65.3146678318069,16.1999604513844,7.66399452287857));
#34531=CARTESIAN_POINT('Ctrl Pts',(65.4537141588635,15.4789729460896,8.24511091048004));
#34532=CARTESIAN_POINT('Ctrl Pts',(65.4876237233566,15.1503611804251,9.00142492811739));
#34533=CARTESIAN_POINT('Ctrl Pts',(65.5016305260266,15.0146236613656,9.31383062721454));
#34534=CARTESIAN_POINT('Ctrl Pts',(65.4976987431426,14.9458338550092,9.65612879778036));
#34535=CARTESIAN_POINT('Ctrl Pts',(65.4764820235065,14.9415523108175,9.99892236192922));
#34536=CARTESIAN_POINT('Ctrl Pts',(65.7418454548454,15.0130771992805,9.99981028982562));
#34537=CARTESIAN_POINT('Ctrl Pts',(65.7663329589547,15.0193507802528,9.59853518618479));
#34538=CARTESIAN_POINT('Ctrl Pts',(65.7672447483348,15.1136101264191,9.19737890571013));
#34539=CARTESIAN_POINT('Ctrl Pts',(65.744401378692,15.2965249330007,8.84359325274525));
#34540=CARTESIAN_POINT('Ctrl Pts',(65.6973077831931,15.6736197332262,8.11423332491524));
#34541=CARTESIAN_POINT('Ctrl Pts',(65.5492514064624,16.4275127626822,7.58620525503953));
#34542=CARTESIAN_POINT('Ctrl Pts',(65.3884873478827,17.2288315064447,7.49440429239112));
#34543=CARTESIAN_POINT('Ctrl Pts',(65.2277232893031,18.0301502502071,7.40260332974272));
#34544=CARTESIAN_POINT('Ctrl Pts',(65.0542515488746,18.8788947082761,7.74702947432164));
#34545=CARTESIAN_POINT('Ctrl Pts',(64.9676333413308,19.4034973688025,8.37446367269953));
#34546=CARTESIAN_POINT('Ctrl Pts',(64.8810151337869,19.9281000293289,9.00189787107742));
#34547=CARTESIAN_POINT('Ctrl Pts',(64.8812504591278,20.1285608923127,9.91234012325428));
#34548=CARTESIAN_POINT('Ctrl Pts',(64.9906262726288,19.9217039083204,10.7007759738115));
#34549=CARTESIAN_POINT('Ctrl Pts',(65.1000020861297,19.7148469243281,11.4892118243687));
#34550=CARTESIAN_POINT('Ctrl Pts',(65.3185183877907,19.1006720933596,12.1556412733063));
#34551=CARTESIAN_POINT('Ctrl Pts',(65.5713589268319,18.3583974645568,12.4036017192683));
#34552=CARTESIAN_POINT('Ctrl Pts',(65.8241994658732,17.616122835754,12.6515621652302));
#34553=CARTESIAN_POINT('Ctrl Pts',(66.1113642422948,16.7457484091169,12.4810536082165));
#34554=CARTESIAN_POINT('Ctrl Pts',(66.3274985456645,16.1404633167949,11.9679250313905));
#34555=CARTESIAN_POINT('Ctrl Pts',(66.5245294039924,15.5886775085546,11.5001503082284));
#34556=CARTESIAN_POINT('Ctrl Pts',(66.662531210899,15.2571911193414,10.7476451883995));
#34557=CARTESIAN_POINT('Ctrl Pts',(66.709565290414,15.2652009106025,9.99881345470567));
#34558=CARTESIAN_POINT('Origin',(63.7511045350785,17.0820569767664,10.));
#34559=CARTESIAN_POINT('',(67.6742507328171,15.5286491313886,10.0019962882659));
#34560=CARTESIAN_POINT('',(67.4086397233445,15.458048217099,10.0018117506529));
#34561=CARTESIAN_POINT('',(64.4026814811241,14.6503387090836,10.));
#34562=CARTESIAN_POINT('',(67.0040126136404,20.25986904378,11.1728309286208));
#34563=CARTESIAN_POINT('Ctrl Pts',(67.6742507328171,15.5286491313886,10.0019962882659));
#34564=CARTESIAN_POINT('Ctrl Pts',(67.7079511930089,15.5421457071954,9.43113200366987));
#34565=CARTESIAN_POINT('Ctrl Pts',(67.6927226550025,15.7382477902416,8.8576382151147));
#34566=CARTESIAN_POINT('Ctrl Pts',(67.635211832767,16.0921495062908,8.41584216487544));
#34567=CARTESIAN_POINT('Ctrl Pts',(67.5520689427972,16.6037821050588,7.77714150008993));
#34568=CARTESIAN_POINT('Ctrl Pts',(67.3805551035975,17.4452195762655,7.41369214583754));
#34569=CARTESIAN_POINT('Ctrl Pts',(67.2193238791372,18.2482818068304,7.48861537411896));
#34570=CARTESIAN_POINT('Ctrl Pts',(67.0580926546768,19.0513440373952,7.56353860240038));
#34571=CARTESIAN_POINT('Ctrl Pts',(66.9071440449558,19.8160310273183,8.07683441321561));
#34572=CARTESIAN_POINT('Ctrl Pts',(66.8561932299011,20.2075211669018,8.79681637620264));
#34573=CARTESIAN_POINT('Ctrl Pts',(66.8052424148463,20.5990113064853,9.51679833918967));
#34574=CARTESIAN_POINT('Ctrl Pts',(66.854289394458,20.6173045957293,10.4434664543485));
#34575=CARTESIAN_POINT('Ctrl Pts',(67.0040126136404,20.25986904378,11.1728309286208));
#34576=CARTESIAN_POINT('',(68.0323660008166,16.4802525979518,11.8670505687058));
#34577=CARTESIAN_POINT('Ctrl Pts',(68.0322473001841,16.4806955947433,11.8669181223571));
#34578=CARTESIAN_POINT('Ctrl Pts',(67.9835336336721,16.6817854205938,12.0540417240897));
#34579=CARTESIAN_POINT('Ctrl Pts',(67.9238765324049,16.9239334961962,12.2143044024353));
#34580=CARTESIAN_POINT('Ctrl Pts',(67.7816176378542,17.4856657502708,12.4543153408643));
#34581=CARTESIAN_POINT('Ctrl Pts',(67.6966288605656,17.8119729521746,12.5175));
#34582=CARTESIAN_POINT('Ctrl Pts',(67.5329868199039,18.4226933621783,12.5175));
#34583=CARTESIAN_POINT('Ctrl Pts',(67.4434356591205,18.7477780771091,12.4543153408643));
#34584=CARTESIAN_POINT('Ctrl Pts',(67.274655929957,19.3446857260753,12.1973867613172));
#34585=CARTESIAN_POINT('Ctrl Pts',(67.1955448337828,19.6165425195547,12.003644350162));
#34586=CARTESIAN_POINT('Ctrl Pts',(67.0834304248293,19.9960747381914,11.6080270340044));
#34587=CARTESIAN_POINT('Ctrl Pts',(67.0387983068925,20.1448248140073,11.4009948671634));
#34588=CARTESIAN_POINT('Ctrl Pts',(67.0040126136404,20.25986904378,11.1728309286208));
#34589=CARTESIAN_POINT('Ctrl Pts',(68.0330516124712,16.4776938604227,11.8678155752478));
#34590=CARTESIAN_POINT('Ctrl Pts',(67.8522271893252,16.9785524830602,12.3404055365588));
#34591=CARTESIAN_POINT('Ctrl Pts',(67.6166367512168,17.6838006560656,12.5855412104357));
#34592=CARTESIAN_POINT('Ctrl Pts',(67.3907294446844,18.3529108900531,12.5051234941037));
#34593=CARTESIAN_POINT('Ctrl Pts',(67.1283727946319,19.129979689639,12.4117306641613));
#34594=CARTESIAN_POINT('Ctrl Pts',(66.8790760319582,19.8583083259861,11.879255644893));
#34595=CARTESIAN_POINT('Ctrl Pts',(66.7317311985187,20.2061471825013,11.1455779206959));
#34596=CARTESIAN_POINT('Ctrl Pts',(66.5843863650793,20.5539860390166,10.4119001964987));
#34597=CARTESIAN_POINT('Ctrl Pts',(66.5389934608741,20.5213351156999,9.47701976737268));
#34598=CARTESIAN_POINT('Ctrl Pts',(66.5933174195301,20.1165357938135,8.75982961781548));
#34599=CARTESIAN_POINT('Ctrl Pts',(66.6476413781862,19.7117364719271,8.04263946825828));
#34600=CARTESIAN_POINT('Ctrl Pts',(66.8016821997035,18.934788751471,7.54313959826992));
#34601=CARTESIAN_POINT('Ctrl Pts',(66.9638149498406,18.1276415422747,7.48486270274577));
#34602=CARTESIAN_POINT('Ctrl Pts',(67.1259476999777,17.3204943330785,7.42658580722162));
#34603=CARTESIAN_POINT('Ctrl Pts',(67.2961723787346,16.483147635142,7.80953188616167));
#34604=CARTESIAN_POINT('Ctrl Pts',(67.3756602454435,15.9844353298855,8.46229096311828));
#34605=CARTESIAN_POINT('Ctrl Pts',(67.4285455390929,15.6526293851286,8.89658813193756));
#34606=CARTESIAN_POINT('Ctrl Pts',(67.4412654718215,15.4707226080322,9.45032013874419));
#34607=CARTESIAN_POINT('Ctrl Pts',(67.4086397233445,15.458048217099,10.0018117506529));
#34608=CARTESIAN_POINT('Origin',(69.7479810832458,18.6889152049569,10.));
#34609=CARTESIAN_POINT('',(61.4484819638689,13.2791651259751,10.0015349814512));
#34610=CARTESIAN_POINT('',(61.3659731009889,13.2658134652031,9.99957732584559));
#34611=CARTESIAN_POINT('',(70.5434614183684,15.7201421778575,10.0000000000001));
#34612=CARTESIAN_POINT('',(59.681950857614,16.8135320242448,7.03077704625437));
#34613=CARTESIAN_POINT('Ctrl Pts',(61.3659731009889,13.2658134652031,9.99957732584559));
#34614=CARTESIAN_POINT('Ctrl Pts',(61.3390049028546,13.2594372491749,10.5364470372516));
#34615=CARTESIAN_POINT('Ctrl Pts',(61.1616793186458,13.6128633281576,12.0843271181651));
#34616=CARTESIAN_POINT('Ctrl Pts',(60.4026582657957,15.9358673415302,13.6055385422089));
#34617=CARTESIAN_POINT('Ctrl Pts',(59.447210195013,18.8976307583478,12.2029441264611));
#34618=CARTESIAN_POINT('Ctrl Pts',(59.1533281063616,19.3903963172923,8.83503768583792));
#34619=CARTESIAN_POINT('Ctrl Pts',(59.4806667221929,17.7660737535059,7.2906822312505));
#34620=CARTESIAN_POINT('Ctrl Pts',(59.6819508576139,16.8135320242448,7.03077704625438));
#34621=CARTESIAN_POINT('',(60.0933746109221,15.2780776734582,7.02605498021599));
#34622=CARTESIAN_POINT('Origin',(59.8874012299222,16.0467807963563,10.));
#34623=CARTESIAN_POINT('Ctrl Pts',(61.4484819638689,13.2791651259751,10.0015349814512));
#34624=CARTESIAN_POINT('Ctrl Pts',(61.4440081401684,13.277381239092,10.0935838809865));
#34625=CARTESIAN_POINT('Ctrl Pts',(61.3771948495716,13.3061918618692,11.1915036202383));
#34626=CARTESIAN_POINT('Ctrl Pts',(60.9313710113775,14.5474295567701,13.1842383274677));
#34627=CARTESIAN_POINT('Ctrl Pts',(59.8935459365979,17.8144668208753,13.1913616605739));
#34628=CARTESIAN_POINT('Ctrl Pts',(59.2511484715134,19.6057481548832,10.3395770770156));
#34629=CARTESIAN_POINT('Ctrl Pts',(59.4407261981541,18.3013616530663,7.23382086599183));
#34630=CARTESIAN_POINT('Ctrl Pts',(59.9014396609592,16.1871423562507,6.78116218790437));
#34631=CARTESIAN_POINT('Ctrl Pts',(60.0933772939441,15.2780676602836,7.02603075613026));
#34632=CARTESIAN_POINT('Origin',(69.7479810832458,18.6889152049569,10.));
#34633=CARTESIAN_POINT('',(62.4122187264791,13.5461538679481,10.0005448248896));
#34634=CARTESIAN_POINT('',(62.3341655182897,13.5161734774897,9.99879780140841));
#34635=CARTESIAN_POINT('',(70.5434614183684,15.7201421778575,10.0000000000001));
#34636=CARTESIAN_POINT('Ctrl Pts',(62.3341655182897,13.5161734774897,9.99879780140841));
#34637=CARTESIAN_POINT('Ctrl Pts',(62.286219899295,13.5082196148795,10.9294410660881));
#34638=CARTESIAN_POINT('Ctrl Pts',(61.9458317508115,14.3903370215027,12.870975191806));
#34639=CARTESIAN_POINT('Ctrl Pts',(60.949326866107,17.5197763142875,13.4270461480336));
#34640=CARTESIAN_POINT('Ctrl Pts',(60.1927341524847,19.7394014348252,10.947712313481));
#34641=CARTESIAN_POINT('Ctrl Pts',(60.2392996738452,18.96159921589,7.62511676387808));
#34642=CARTESIAN_POINT('Ctrl Pts',(60.9131915231956,15.8425832679708,6.41562502038855));
#34643=CARTESIAN_POINT('Ctrl Pts',(61.3800631690209,13.6032001394547,8.04417985348944));
#34644=CARTESIAN_POINT('Ctrl Pts',(61.389739398956,13.2714326411404,9.52644947847322));
#34645=CARTESIAN_POINT('Ctrl Pts',(61.3659731009889,13.2658134652031,9.99957732584559));
#34646=CARTESIAN_POINT('Ctrl Pts',(62.4122187264791,13.5461538679481,10.0005448248896));
#34647=CARTESIAN_POINT('Ctrl Pts',(62.3889104933502,13.5391171409457,10.4721900135758));
#34648=CARTESIAN_POINT('Ctrl Pts',(62.231485488278,13.8305514728694,11.9564181322135));
#34649=CARTESIAN_POINT('Ctrl Pts',(61.5138509672066,16.0106566332716,13.5896176377583));
#34650=CARTESIAN_POINT('Ctrl Pts',(60.5349179618126,19.0579057022675,12.3623010109723));
#34651=CARTESIAN_POINT('Ctrl Pts',(60.1913020034494,19.734119272829,9.01938609588907));
#34652=CARTESIAN_POINT('Ctrl Pts',(60.6550135466888,17.3973455890623,6.55469600728483));
#34653=CARTESIAN_POINT('Ctrl Pts',(61.3531034969372,14.2043402063785,7.15651357330655));
#34654=CARTESIAN_POINT('Ctrl Pts',(61.4929236187117,13.2968857360054,9.087148162546));
#34655=CARTESIAN_POINT('Ctrl Pts',(61.4484819638689,13.2791651259751,10.0015349814512));
#34656=CARTESIAN_POINT('Origin',(69.7479810832458,18.6889152049569,10.));
#34657=CARTESIAN_POINT('',(63.3798972175256,13.7984318791273,9.99769259051996));
#34658=CARTESIAN_POINT('',(63.2983967128177,13.7813169744248,10.0022545211423));
#34659=CARTESIAN_POINT('',(70.5434614183684,15.7201421778575,10.0000000000001));
#34660=CARTESIAN_POINT('Ctrl Pts',(63.2983967128177,13.7813169744248,10.0022545211423));
#34661=CARTESIAN_POINT('Ctrl Pts',(63.282643341652,13.7746926693741,10.3298056773904));
#34662=CARTESIAN_POINT('Ctrl Pts',(63.1648404527592,13.9475832402569,11.6627679218546));
#34663=CARTESIAN_POINT('Ctrl Pts',(62.552433017135,15.7650240000834,13.4838568188229));
#34664=CARTESIAN_POINT('Ctrl Pts',(61.540694761931,18.936865245129,12.7341264791949));
#34665=CARTESIAN_POINT('Ctrl Pts',(61.0732543185778,20.0773594018982,9.55182253210507));
#34666=CARTESIAN_POINT('Ctrl Pts',(61.4316477881723,18.1357994369342,6.76826458716723));
#34667=CARTESIAN_POINT('Ctrl Pts',(62.1626591350493,14.8036106221425,6.86000957288757));
#34668=CARTESIAN_POINT('Ctrl Pts',(62.3828842093693,13.5645914770419,8.8526467410516));
#34669=CARTESIAN_POINT('Ctrl Pts',(62.3378725391134,13.5167884478446,9.92684307365804));
#34670=CARTESIAN_POINT('Ctrl Pts',(62.3341655182897,13.5161734774897,9.99879780140841));
#34671=CARTESIAN_POINT('Ctrl Pts',(63.3798972175256,13.7984318791273,9.99769259051996));
#34672=CARTESIAN_POINT('Ctrl Pts',(63.3356696948373,13.7939231905821,10.8435144444691));
#34673=CARTESIAN_POINT('Ctrl Pts',(63.0364669859301,14.5389353035617,12.70898732583));
#34674=CARTESIAN_POINT('Ctrl Pts',(62.080489794707,17.5330036055456,13.5128046754735));
#34675=CARTESIAN_POINT('Ctrl Pts',(61.2715545195409,19.9458125081592,11.2162142452876));
#34676=CARTESIAN_POINT('Ctrl Pts',(61.2525379570576,19.4106046411913,7.83042882970038));
#34677=CARTESIAN_POINT('Ctrl Pts',(61.9047530097005,16.3703262829254,6.38762845988019));
#34678=CARTESIAN_POINT('Ctrl Pts',(62.4147543833102,13.9548208376169,7.90192541386342));
#34679=CARTESIAN_POINT('Ctrl Pts',(62.4390002488206,13.5542391767051,9.45861716832917));
#34680=CARTESIAN_POINT('Ctrl Pts',(62.4122187264791,13.5461538679481,10.0005448248896));
#34681=CARTESIAN_POINT('Origin',(69.7479810832458,18.6889152049569,10.));
#34682=CARTESIAN_POINT('',(64.3454334554184,14.0587048879185,10.0025996902775));
#34683=CARTESIAN_POINT('',(64.2646301485468,14.038988005468,9.99747713720023));
#34684=CARTESIAN_POINT('',(70.5434614183684,15.7201421778575,10.0000000000001));
#34685=CARTESIAN_POINT('Ctrl Pts',(64.2646301485468,14.038988005468,9.99747713720024));
#34686=CARTESIAN_POINT('Ctrl Pts',(64.226770392365,14.0349994054245,10.7242163838114));
#34687=CARTESIAN_POINT('Ctrl Pts',(63.980303897263,14.6082026447201,12.4671953710476));
#34688=CARTESIAN_POINT('Ctrl Pts',(63.0972885120504,17.3556995742977,13.5881174655937));
#34689=CARTESIAN_POINT('Ctrl Pts',(62.2237737811953,20.0116836036718,11.6313322004901));
#34690=CARTESIAN_POINT('Ctrl Pts',(62.0929146809836,19.8960390869576,8.22313767486128));
#34691=CARTESIAN_POINT('Ctrl Pts',(62.686787843468,17.0756569439774,6.3958317144828));
#34692=CARTESIAN_POINT('Ctrl Pts',(63.271636045696,14.3543730978417,7.6257956239861));
#34693=CARTESIAN_POINT('Ctrl Pts',(63.3311289785642,13.7950809180928,9.32167057633655));
#34694=CARTESIAN_POINT('Ctrl Pts',(63.2983967128177,13.7813169744248,10.0022545211423));
#34695=CARTESIAN_POINT('Ctrl Pts',(64.3454334554184,14.0587048879185,10.0025996902775));
#34696=CARTESIAN_POINT('Ctrl Pts',(64.3351645983746,14.0539764689082,10.2176211405936));
#34697=CARTESIAN_POINT('Ctrl Pts',(64.2433978747176,14.1513426806932,11.4397371699227));
#34698=CARTESIAN_POINT('Ctrl Pts',(63.708961052588,15.6987166428558,13.3670096553836));
#34699=CARTESIAN_POINT('Ctrl Pts',(62.6772983776882,18.9427555175133,12.9642257537709));
#34700=CARTESIAN_POINT('Ctrl Pts',(62.1266472347557,20.3916349158421,9.9067950074971));
#34701=CARTESIAN_POINT('Ctrl Pts',(62.4144320750886,18.7114286257305,6.93283507366395));
#34702=CARTESIAN_POINT('Ctrl Pts',(63.1472062543101,15.3704995140598,6.70571036393744));
#34703=CARTESIAN_POINT('Ctrl Pts',(63.425086417853,13.8968260312721,8.66708054183157));
#34704=CARTESIAN_POINT('Ctrl Pts',(63.3883718001703,13.7992958039273,9.83562185337871));
#34705=CARTESIAN_POINT('Ctrl Pts',(63.3798972175256,13.7984318791273,9.99769259051996));
#34706=CARTESIAN_POINT('Origin',(69.7479810832458,18.6889152049569,10.));
#34707=CARTESIAN_POINT('',(65.3101240288667,14.3221339593831,9.99868436122737));
#34708=CARTESIAN_POINT('',(65.2317006057018,14.2935352300231,10.0018375364667));
#34709=CARTESIAN_POINT('',(70.5434614183684,15.7201421778575,10.0000000000001));
#34710=CARTESIAN_POINT('Ctrl Pts',(65.2317006057018,14.2935352300231,10.0018375364667));
#34711=CARTESIAN_POINT('Ctrl Pts',(65.2259676792212,14.2911203313162,10.1205006547493));
#34712=CARTESIAN_POINT('Ctrl Pts',(65.1542869058501,14.333487038742,11.241710128915));
#34713=CARTESIAN_POINT('Ctrl Pts',(64.6921496134354,15.6317182042723,13.2184200895793));
#34714=CARTESIAN_POINT('Ctrl Pts',(63.6589647612363,18.8835992389528,13.1544941616769));
#34715=CARTESIAN_POINT('Ctrl Pts',(63.0319829890499,20.6195097408352,10.2839896215965));
#34716=CARTESIAN_POINT('Ctrl Pts',(63.2346852212378,19.2589973841656,7.16081725087092));
#34717=CARTESIAN_POINT('Ctrl Pts',(63.9523759072002,15.9765219526977,6.56368841308618));
#34718=CARTESIAN_POINT('Ctrl Pts',(64.30157672835,14.2145525524613,8.43212980411671));
#34719=CARTESIAN_POINT('Ctrl Pts',(64.2792379389272,14.0405269650183,9.71707241074883));
#34720=CARTESIAN_POINT('Ctrl Pts',(64.2646301485468,14.038988005468,9.99747713720024));
#34721=CARTESIAN_POINT('Ctrl Pts',(65.3101240288667,14.3221339593831,9.99868436122737));
#34722=CARTESIAN_POINT('Ctrl Pts',(65.2798663326535,14.3164610907008,10.5933471090872));
#34723=CARTESIAN_POINT('Ctrl Pts',(65.0828577529568,14.7310514432719,12.2044751575878));
#34724=CARTESIAN_POINT('Ctrl Pts',(64.2812461473764,17.199991458738,13.6183729089162));
#34725=CARTESIAN_POINT('Ctrl Pts',(63.346239485481,20.0833051820057,12.017555775347));
#34726=CARTESIAN_POINT('Ctrl Pts',(63.1074718691846,20.3682194128848,8.60989310618131));
#34727=CARTESIAN_POINT('Ctrl Pts',(63.6430568297551,17.7632104839249,6.4471568308768));
#34728=CARTESIAN_POINT('Ctrl Pts',(64.2882973111131,14.7920138952888,7.39383484183733));
#34729=CARTESIAN_POINT('Ctrl Pts',(64.3833599300929,14.0761685903618,9.20845039448992));
#34730=CARTESIAN_POINT('Ctrl Pts',(64.3454334554184,14.0587048879185,10.0025996902775));
#34731=CARTESIAN_POINT('Origin',(69.7479810832458,18.6889152049569,10.));
#34732=CARTESIAN_POINT('',(66.2783193540156,14.5724831194333,9.99930975590662));
#34733=CARTESIAN_POINT('',(66.1956016367402,14.559910913876,9.99976839157063));
#34734=CARTESIAN_POINT('',(70.5434614183684,15.7201421778575,10.0000000000001));
#34735=CARTESIAN_POINT('Ctrl Pts',(66.1956016367402,14.559910913876,9.99976839157063));
#34736=CARTESIAN_POINT('Ctrl Pts',(66.1695891483769,14.5533139234257,10.5198381182744));
#34737=CARTESIAN_POINT('Ctrl Pts',(65.9976317638641,14.890051591398,12.0503568643789));
#34738=CARTESIAN_POINT('Ctrl Pts',(65.2498597727098,17.1744195179844,13.6018503664189));
#34739=CARTESIAN_POINT('Ctrl Pts',(64.2890822261735,20.1560728090925,12.2479900298274));
#34740=CARTESIAN_POINT('Ctrl Pts',(63.9799857765362,20.7056191362412,8.89407499549297));
#34741=CARTESIAN_POINT('Ctrl Pts',(64.4632262402319,18.2981238461185,6.52411027736645));
#34742=CARTESIAN_POINT('Ctrl Pts',(65.146471993839,15.1680091238728,7.21818882738257));
#34743=CARTESIAN_POINT('Ctrl Pts',(65.2744447664955,14.3115404877175,9.11709648401003));
#34744=CARTESIAN_POINT('Ctrl Pts',(65.2317006057018,14.2935352300231,10.0018375364667));
#34745=CARTESIAN_POINT('Ctrl Pts',(66.2783193540156,14.5724831194333,9.99930975590662));
#34746=CARTESIAN_POINT('Ctrl Pts',(66.2290088142628,14.5623726178326,10.9656350129457));
#34747=CARTESIAN_POINT('Ctrl Pts',(65.869509017197,15.5078446363722,12.9430947115651));
#34748=CARTESIAN_POINT('Ctrl Pts',(64.852721554462,18.704288070265,13.3837942299379));
#34749=CARTESIAN_POINT('Ctrl Pts',(64.1195886430847,20.8341986998846,10.7999310727631));
#34750=CARTESIAN_POINT('Ctrl Pts',(64.2044184759422,19.9114308093214,7.49968047567758));
#34751=CARTESIAN_POINT('Ctrl Pts',(64.8955230826759,16.7260146593053,6.43862003923501));
#34752=CARTESIAN_POINT('Ctrl Pts',(65.3320744591731,14.6092002260328,8.15058790184904));
#34753=CARTESIAN_POINT('Ctrl Pts',(65.3314182383775,14.3261263074255,9.58018345977288));
#34754=CARTESIAN_POINT('Ctrl Pts',(65.3101240288667,14.3221339593831,9.99868436122737));
#34755=CARTESIAN_POINT('Origin',(69.7479810832458,18.6889152049569,10.));
#34756=CARTESIAN_POINT('',(67.242349320473,14.8383776097513,10.0022118830713));
#34757=CARTESIAN_POINT('',(67.1637176864735,14.810555933805,9.99855140140545));
#34758=CARTESIAN_POINT('',(70.5434614183684,15.7201421778575,10.0000000000001));
#34759=CARTESIAN_POINT('Ctrl Pts',(67.1637176864735,14.810555933805,9.99855140140544));
#34760=CARTESIAN_POINT('Ctrl Pts',(67.1164300139581,14.8034925645055,10.9127656351722));
#34761=CARTESIAN_POINT('Ctrl Pts',(66.7843853462346,15.6578176600211,12.8392373747717));
#34762=CARTESIAN_POINT('Ctrl Pts',(65.795981118425,18.7603708726991,13.4453363911884));
#34763=CARTESIAN_POINT('Ctrl Pts',(65.0290015152611,21.0187603927389,11.00449717215));
#34764=CARTESIAN_POINT('Ctrl Pts',(65.0614895355965,20.2934961228732,7.66994591646111));
#34765=CARTESIAN_POINT('Ctrl Pts',(65.7301904655353,17.1938529499358,6.40846378494576));
#34766=CARTESIAN_POINT('Ctrl Pts',(66.2070041644091,14.9140195913108,8.0104478238207));
#34767=CARTESIAN_POINT('Ctrl Pts',(66.2201050327307,14.5661251855401,9.50987006742361));
#34768=CARTESIAN_POINT('Ctrl Pts',(66.1956016367402,14.559910913876,9.99976839157063));
#34769=CARTESIAN_POINT('Ctrl Pts',(67.242349320473,14.8383776097513,10.0022118830713));
#34770=CARTESIAN_POINT('Ctrl Pts',(67.2260470012181,14.8315944872623,10.3408933046043));
#34771=CARTESIAN_POINT('Ctrl Pts',(67.1051700296205,15.0130297323863,11.6887868410754));
#34772=CARTESIAN_POINT('Ctrl Pts',(66.4816292855382,16.868372167434,13.5013274912989));
#34773=CARTESIAN_POINT('Ctrl Pts',(65.468753391891,20.0422978199459,12.6947822329673));
#34774=CARTESIAN_POINT('Ctrl Pts',(65.0155990043222,21.1273143736846,9.47487431060687));
#34775=CARTESIAN_POINT('Ctrl Pts',(65.3922823621304,19.1153342996381,6.72525821930946));
#34776=CARTESIAN_POINT('Ctrl Pts',(66.1257396929251,15.7718556315866,6.9083705731136));
#34777=CARTESIAN_POINT('Ctrl Pts',(66.3280678631807,14.604717917356,8.91484226317838));
#34778=CARTESIAN_POINT('Ctrl Pts',(66.2803308931335,14.572895560051,9.95989017005526));
#34779=CARTESIAN_POINT('Ctrl Pts',(66.2783193540156,14.5724831194333,9.99930975590662));
#34780=CARTESIAN_POINT('Origin',(69.7479810832458,18.6889152049569,10.));
#34781=CARTESIAN_POINT('',(68.2083503098983,15.0969161422106,9.99673640007591));
#34782=CARTESIAN_POINT('',(68.1281291851066,15.0750265266586,10.0024371765582));
#34783=CARTESIAN_POINT('',(70.5434614183684,15.7201421778575,10.0000000000001));
#34784=CARTESIAN_POINT('',(67.8425423025985,17.2449834421531,7.06170475438605));
#34785=CARTESIAN_POINT('Ctrl Pts',(67.8425423025985,17.244983442153,7.06170475438608));
#34786=CARTESIAN_POINT('Ctrl Pts',(68.0419164156808,16.2988495743024,7.35795147289591));
#34787=CARTESIAN_POINT('Ctrl Pts',(68.2441585752431,15.2831204824219,8.39983158504209));
#34788=CARTESIAN_POINT('Ctrl Pts',(68.2236687995603,15.0986382893443,9.7020767480265));
#34789=CARTESIAN_POINT('Ctrl Pts',(68.2083503098983,15.0969161422106,9.99673640007591));
#34790=CARTESIAN_POINT('',(67.6148078402348,18.1173331571764,6.92649999999998));
#34791=CARTESIAN_POINT('Ctrl Pts',(67.6148078402348,18.1173331571765,6.92649999999999));
#34792=CARTESIAN_POINT('Ctrl Pts',(67.6909584745889,17.8331351207384,6.92649999999999));
#34793=CARTESIAN_POINT('Ctrl Pts',(67.7691522152652,17.5337033543061,6.97030621012384));
#34794=CARTESIAN_POINT('Ctrl Pts',(67.8425423025985,17.2449834421531,7.06170475438605));
#34795=CARTESIAN_POINT('',(67.4240381925641,18.8148375643561,7.01163591529246));
#34796=CARTESIAN_POINT('Ctrl Pts',(67.4238662472344,18.8154792730625,7.01293629783556));
#34797=CARTESIAN_POINT('Ctrl Pts',(67.4888593221927,18.5825814377542,6.95435125823854));
#34798=CARTESIAN_POINT('Ctrl Pts',(67.5537087055993,18.3453582319347,6.92649999999999));
#34799=CARTESIAN_POINT('Ctrl Pts',(67.6148078402348,18.1173331571765,6.92649999999999));
#34800=CARTESIAN_POINT('Ctrl Pts',(67.4242662328515,18.8139865064172,7.00991129962864));
#34801=CARTESIAN_POINT('Ctrl Pts',(67.4544236505276,18.6713424458928,6.97326843816114));
#34802=CARTESIAN_POINT('Ctrl Pts',(67.6913073253836,17.5558463812024,6.77617107551512));
#34803=CARTESIAN_POINT('Ctrl Pts',(68.0973070404756,15.6699322564948,7.59313914445674));
#34804=CARTESIAN_POINT('Ctrl Pts',(68.1615830306033,15.0894434810379,9.30549521878025));
#34805=CARTESIAN_POINT('Ctrl Pts',(68.1281291851066,15.0750265266586,10.0024371765582));
#34806=CARTESIAN_POINT('Origin',(-17.0820569767664,63.7511045350785,10.));
#34807=CARTESIAN_POINT('',(-13.7189801527801,60.9122168113323,9.99965378812947));
#34808=CARTESIAN_POINT('',(-13.6458118873637,60.6472937215209,9.99664393250999));
#34809=CARTESIAN_POINT('',(-14.6503387090836,64.4026814811241,10.));
#34810=CARTESIAN_POINT('',(-14.1985145724512,60.3826426720153,11.6359872033746));
#34811=CARTESIAN_POINT('Ctrl Pts',(-13.6458118873637,60.6472937215209,9.99664393250999));
#34812=CARTESIAN_POINT('Ctrl Pts',(-13.6410407802454,60.6097205320263,10.5892058593234));
#34813=CARTESIAN_POINT('Ctrl Pts',(-13.8356159531907,60.5187326677745,11.184803560304));
#34814=CARTESIAN_POINT('Ctrl Pts',(-14.1985145724512,60.3826426720153,11.6359872033745));
#34815=CARTESIAN_POINT('',(-17.8984305821303,59.3912531651588,11.6380816927072));
#34816=CARTESIAN_POINT('Origin',(-16.0467807963563,59.8874012299222,10.));
#34817=CARTESIAN_POINT('Ctrl Pts',(-17.8984546702661,59.3912467107623,11.6380966037226));
#34818=CARTESIAN_POINT('Ctrl Pts',(-17.4212611177615,59.5701794123024,12.2270179049202));
#34819=CARTESIAN_POINT('Ctrl Pts',(-16.6595160069779,59.8253574740883,12.567422198156));
#34820=CARTESIAN_POINT('Ctrl Pts',(-15.9233267283634,60.0736878712827,12.5157167035403));
#34821=CARTESIAN_POINT('Ctrl Pts',(-15.1456267338051,60.3360206084697,12.4610957466079));
#34822=CARTESIAN_POINT('Ctrl Pts',(-14.3964458015818,60.5907116859352,11.9688993897472));
#34823=CARTESIAN_POINT('Ctrl Pts',(-14.014605944713,60.7469740189126,11.2575578209417));
#34824=CARTESIAN_POINT('Ctrl Pts',(-13.8116368860468,60.8300361143406,10.8794403300265));
#34825=CARTESIAN_POINT('Ctrl Pts',(-13.7124604894775,60.8852870497794,10.4394030962358));
#34826=CARTESIAN_POINT('Ctrl Pts',(-13.7189801527801,60.9122168113323,9.99965378812947));
#34827=CARTESIAN_POINT('Origin',(-17.0820569767664,63.7511045350785,10.));
#34828=CARTESIAN_POINT('',(-13.9708704146993,61.8799991994798,9.9990152806394));
#34829=CARTESIAN_POINT('',(-13.899975087973,61.614467077582,10.0012573013837));
#34830=CARTESIAN_POINT('',(-14.6503387090836,64.4026814811241,10.));
#34831=CARTESIAN_POINT('Ctrl Pts',(-13.899975087973,61.614467077582,10.0012573013837));
#34832=CARTESIAN_POINT('Ctrl Pts',(-13.8982899610888,61.6099667912195,10.0766544396886));
#34833=CARTESIAN_POINT('Ctrl Pts',(-13.900043500223,61.6045451170745,10.1520128061813));
#34834=CARTESIAN_POINT('Ctrl Pts',(-13.9053569552699,61.5981695663354,10.2270376921982));
#34835=CARTESIAN_POINT('Ctrl Pts',(-13.963452717137,61.5284611611194,11.0473378309357));
#34836=CARTESIAN_POINT('Ctrl Pts',(-14.4471220222723,61.3447206686646,11.8277717281243));
#34837=CARTESIAN_POINT('Ctrl Pts',(-15.1337367424346,61.1066011161458,12.2189611289227));
#34838=CARTESIAN_POINT('Ctrl Pts',(-15.8203514625968,60.8684815636269,12.6101505297211));
#34839=CARTESIAN_POINT('Ctrl Pts',(-16.709911597786,60.575982951044,12.6120954341294));
#34840=CARTESIAN_POINT('Ctrl Pts',(-17.3980067606842,60.3374667150896,12.223752356313));
#34841=CARTESIAN_POINT('Ctrl Pts',(-18.0861019235824,60.0989504791352,11.8354092784967));
#34842=CARTESIAN_POINT('Ctrl Pts',(-18.5727321141895,59.9144166198093,11.0567782184557));
#34843=CARTESIAN_POINT('Ctrl Pts',(-18.6339764021912,59.8438645695582,10.2368654679641));
#34844=CARTESIAN_POINT('Ctrl Pts',(-18.695220690193,59.773312519307,9.41695271747245));
#34845=CARTESIAN_POINT('Ctrl Pts',(-18.3310790755893,59.8167422781306,8.55575827653014));
#34846=CARTESIAN_POINT('Ctrl Pts',(-17.6984585141969,59.932110753931,8.03819621078695));
#34847=CARTESIAN_POINT('Ctrl Pts',(-17.0658379528045,60.0474792297313,7.52063414504374));
#34848=CARTESIAN_POINT('Ctrl Pts',(-16.1647384446234,60.2347864225084,7.34670445449967));
#34849=CARTESIAN_POINT('Ctrl Pts',(-15.3927695971153,60.3874931590402,7.59575134544305));
#34850=CARTESIAN_POINT('Ctrl Pts',(-14.6208007496071,60.5401998955719,7.84479823638644));
#34851=CARTESIAN_POINT('Ctrl Pts',(-13.9779625627719,60.6583061758582,8.51682170881728));
#34852=CARTESIAN_POINT('Ctrl Pts',(-13.7459615817214,60.6663289586339,9.30743209219145));
#34853=CARTESIAN_POINT('Ctrl Pts',(-13.6804424696227,60.6685946628634,9.53070739947741));
#34854=CARTESIAN_POINT('Ctrl Pts',(-13.6476895615158,60.6620806891943,9.76344057197133));
#34855=CARTESIAN_POINT('Ctrl Pts',(-13.6458118873637,60.6472937215209,9.99664393250999));
#34856=CARTESIAN_POINT('Ctrl Pts',(-13.7189801527801,60.9122168113323,9.99965378812947));
#34857=CARTESIAN_POINT('Ctrl Pts',(-13.7247257446778,60.9359492362449,9.61211536100735));
#34858=CARTESIAN_POINT('Ctrl Pts',(-13.8125590225005,60.9376863320054,9.2248005482108));
#34859=CARTESIAN_POINT('Ctrl Pts',(-13.9837827281427,60.9170790299751,8.8802861232622));
#34860=CARTESIAN_POINT('Ctrl Pts',(-14.3492981499552,60.8730881195708,8.14484277513853));
#34861=CARTESIAN_POINT('Ctrl Pts',(-15.0948277750946,60.7272727102727,7.60444285964153));
#34862=CARTESIAN_POINT('Ctrl Pts',(-15.8946095193188,60.5669204894781,7.49935843056473));
#34863=CARTESIAN_POINT('Ctrl Pts',(-16.6943912635431,60.4065682686835,7.39427400148794));
#34864=CARTESIAN_POINT('Ctrl Pts',(-17.5484251268522,60.2316792363924,7.72450505883135));
#34865=CARTESIAN_POINT('Ctrl Pts',(-18.0828447847106,60.1424305723414,8.34320956294503));
#34866=CARTESIAN_POINT('Ctrl Pts',(-18.617264442569,60.0531819082903,8.96191406705872));
#34867=CARTESIAN_POINT('Ctrl Pts',(-18.8320698949766,60.0495736124794,9.86909201794267));
#34868=CARTESIAN_POINT('Ctrl Pts',(-18.6376771842086,60.1556096340356,10.6611508664114));
#34869=CARTESIAN_POINT('Ctrl Pts',(-18.4432844734405,60.2616456555919,11.4532097148801));
#34870=CARTESIAN_POINT('Ctrl Pts',(-17.8396935994968,60.4773259945153,12.1301494609335));
#34871=CARTESIAN_POINT('Ctrl Pts',(-17.1014273477892,60.7290924921509,12.3908459426517));
#34872=CARTESIAN_POINT('Ctrl Pts',(-16.3631610960817,60.9808589897866,12.6515424243699));
#34873=CARTESIAN_POINT('Ctrl Pts',(-15.4902194666104,61.2687116461344,12.4959956417528));
#34874=CARTESIAN_POINT('Ctrl Pts',(-14.8769273589395,61.4869914228006,11.9933937214366));
#34875=CARTESIAN_POINT('Ctrl Pts',(-14.3076501674883,61.6896056365773,11.5268626736099));
#34876=CARTESIAN_POINT('Ctrl Pts',(-13.9620906745726,61.8322748736987,10.7613040129743));
#34877=CARTESIAN_POINT('Ctrl Pts',(-13.9708704146993,61.8799991994798,9.9990152806394));
#34878=CARTESIAN_POINT('Origin',(-17.0820569767664,63.7511045350785,10.));
#34879=CARTESIAN_POINT('',(-14.2348698103755,62.8445369550162,10.0018466754434));
#34880=CARTESIAN_POINT('',(-14.1654859215485,62.5785998445538,10.0004462653844));
#34881=CARTESIAN_POINT('',(-14.6503387090836,64.4026814811241,10.));
#34882=CARTESIAN_POINT('Ctrl Pts',(-14.1654859215485,62.5785998445538,10.0004462653844));
#34883=CARTESIAN_POINT('Ctrl Pts',(-14.1585827534688,62.5552558244194,10.3867702486339));
#34884=CARTESIAN_POINT('Ctrl Pts',(-14.2332491130212,62.5100553152291,10.772836742403));
#34885=CARTESIAN_POINT('Ctrl Pts',(-14.3908772813225,62.4426252563818,11.1164878478949));
#34886=CARTESIAN_POINT('Ctrl Pts',(-14.7296226663466,62.2977170112848,11.8549994178653));
#34887=CARTESIAN_POINT('Ctrl Pts',(-15.4515079046903,62.0501467519026,12.3976253642208));
#34888=CARTESIAN_POINT('Ctrl Pts',(-16.2272258855738,61.7881520526305,12.5013894187969));
#34889=CARTESIAN_POINT('Ctrl Pts',(-17.0029438664574,61.5261573533584,12.6051534733731));
#34890=CARTESIAN_POINT('Ctrl Pts',(-17.8324945898807,61.2497382141964,12.2700556361698));
#34891=CARTESIAN_POINT('Ctrl Pts',(-18.3383599455199,61.0600503079339,11.6461438143242));
#34892=CARTESIAN_POINT('Ctrl Pts',(-18.8442253011591,60.8703624016714,11.0222319924786));
#34893=CARTESIAN_POINT('Ctrl Pts',(-19.0264052890141,60.7674057283085,10.1095061859907));
#34894=CARTESIAN_POINT('Ctrl Pts',(-18.7972629292322,60.7746625458238,9.31667252204711));
#34895=CARTESIAN_POINT('Ctrl Pts',(-18.5681205694503,60.781919363339,8.52383885810353));
#34896=CARTESIAN_POINT('Ctrl Pts',(-17.9276558620316,60.8993896717325,7.85089733670426));
#34897=CARTESIAN_POINT('Ctrl Pts',(-17.1565944419209,61.0518532638259,7.59916807226848));
#34898=CARTESIAN_POINT('Ctrl Pts',(-16.3855330218102,61.2043168559192,7.34743880783269));
#34899=CARTESIAN_POINT('Ctrl Pts',(-15.4838748890076,61.3917737317126,7.5169218003604));
#34900=CARTESIAN_POINT('Ctrl Pts',(-14.8493069319057,61.5076640106206,8.03174648676741));
#34901=CARTESIAN_POINT('Ctrl Pts',(-14.2727767422055,61.6129549313731,8.49948515966252));
#34902=CARTESIAN_POINT('Ctrl Pts',(-13.9167146450877,61.6591716047613,9.2522842034192));
#34903=CARTESIAN_POINT('Ctrl Pts',(-13.899975087973,61.614467077582,10.0012573013837));
#34904=CARTESIAN_POINT('Ctrl Pts',(-13.9708704146993,61.8799991994798,9.9990152806394));
#34905=CARTESIAN_POINT('Ctrl Pts',(-13.971549239588,61.8836891105327,9.94007725327275));
#34906=CARTESIAN_POINT('Ctrl Pts',(-13.9743462862715,61.8868114457663,9.88115877337007));
#34907=CARTESIAN_POINT('Ctrl Pts',(-13.9793219277933,61.8893500282724,9.82239956232277));
#34908=CARTESIAN_POINT('Ctrl Pts',(-14.0486511901886,61.9247219600931,9.00366438154032));
#34909=CARTESIAN_POINT('Ctrl Pts',(-14.5409523008496,61.84675892675,8.21585107799066));
#34910=CARTESIAN_POINT('Ctrl Pts',(-15.243221392539,61.712535142454,7.80941972573588));
#34911=CARTESIAN_POINT('Ctrl Pts',(-15.9454904842284,61.5783113581579,7.4029883734811));
#34912=CARTESIAN_POINT('Ctrl Pts',(-16.8577275569461,61.3878268229089,7.37793897252118));
#34913=CARTESIAN_POINT('Ctrl Pts',(-17.5801209048419,61.2482107604141,7.74541574302333));
#34914=CARTESIAN_POINT('Ctrl Pts',(-18.3025142527376,61.1085946979192,8.11289251352548));
#34915=CARTESIAN_POINT('Ctrl Pts',(-18.8350638758114,61.0198471081786,8.8728954554897));
#34916=CARTESIAN_POINT('Ctrl Pts',(-18.9468623871525,61.0438394390412,9.68733378926659));
#34917=CARTESIAN_POINT('Ctrl Pts',(-19.0586608984936,61.0678317699038,10.5017721230435));
#34918=CARTESIAN_POINT('Ctrl Pts',(-18.749708298102,61.2045640213696,11.3706458486331));
#34919=CARTESIAN_POINT('Ctrl Pts',(-18.1634433884681,61.4156018821482,11.9074332417686));
#34920=CARTESIAN_POINT('Ctrl Pts',(-17.5771784788342,61.6266397429268,12.4442206349041));
#34921=CARTESIAN_POINT('Ctrl Pts',(-16.7136012599581,61.911983213018,12.6489216955856));
#34922=CARTESIAN_POINT('Ctrl Pts',(-15.9628772265393,62.1670877632026,12.4304742338454));
#34923=CARTESIAN_POINT('Ctrl Pts',(-15.2121531931204,62.4221923133873,12.2120267721052));
#34924=CARTESIAN_POINT('Ctrl Pts',(-14.5742823451588,62.6470579436654,11.5704307879433));
#34925=CARTESIAN_POINT('Ctrl Pts',(-14.3390239366156,62.7640438959386,10.7911028658272));
#34926=CARTESIAN_POINT('Ctrl Pts',(-14.2625865983512,62.8020535673525,10.5378929917549));
#34927=CARTESIAN_POINT('Ctrl Pts',(-14.2286511253629,62.8286748982889,10.2701434172214));
#34928=CARTESIAN_POINT('Ctrl Pts',(-14.2348698103755,62.8445369550162,10.0018466754434));
#34929=CARTESIAN_POINT('Origin',(-17.0820569767664,63.7511045350785,10.));
#34930=CARTESIAN_POINT('',(-14.4927485186002,63.8107147438123,9.9979335262408));
#34931=CARTESIAN_POINT('',(-14.4189472139579,63.5459612763502,9.99811000378505));
#34932=CARTESIAN_POINT('',(-14.6503387090836,64.4026814811241,10.));
#34933=CARTESIAN_POINT('Ctrl Pts',(-14.4189472139579,63.5459612763502,9.99811000378505));
#34934=CARTESIAN_POINT('Ctrl Pts',(-14.4131993125783,63.5020657997402,10.6909216248415));
#34935=CARTESIAN_POINT('Ctrl Pts',(-14.6895870615305,63.3825723034678,11.3881278716994));
#34936=CARTESIAN_POINT('Ctrl Pts',(-15.1696780211854,63.208496696392,11.8560065223218));
#34937=CARTESIAN_POINT('Ctrl Pts',(-15.7417608055524,63.001065883577,12.4135369565261));
#34938=CARTESIAN_POINT('Ctrl Pts',(-16.6030903983921,62.7161316220186,12.6454354329572));
#34939=CARTESIAN_POINT('Ctrl Pts',(-17.3619190322642,62.4586624096389,12.4478622804134));
#34940=CARTESIAN_POINT('Ctrl Pts',(-18.1207476661363,62.2011931972591,12.2502891278697));
#34941=CARTESIAN_POINT('Ctrl Pts',(-18.7770753410409,61.9711890340582,11.6232443463511));
#34942=CARTESIAN_POINT('Ctrl Pts',(-19.0309502087538,61.8490217755359,10.847506523471));
#34943=CARTESIAN_POINT('Ctrl Pts',(-19.2848250764668,61.7268545170135,10.0717687005908));
#34944=CARTESIAN_POINT('Ctrl Pts',(-19.1362471369881,61.7125241631699,9.14733783634905));
#34945=CARTESIAN_POINT('Ctrl Pts',(-18.6456858472658,61.7898279718489,8.48815640829392));
#34946=CARTESIAN_POINT('Ctrl Pts',(-18.1551245575434,61.8671317805279,7.8289749802388));
#34947=CARTESIAN_POINT('Ctrl Pts',(-17.3225799175774,62.0360697517296,7.4350429883703));
#34948=CARTESIAN_POINT('Ctrl Pts',(-16.5147885234742,62.1983751106923,7.48275547481138));
#34949=CARTESIAN_POINT('Ctrl Pts',(-15.7069971293709,62.360680469655,7.53046796125247));
#34950=CARTESIAN_POINT('Ctrl Pts',(-14.9239589811304,62.5163532163788,8.01982492600314));
#34951=CARTESIAN_POINT('Ctrl Pts',(-14.5102426728623,62.5730664743347,8.73170200517114));
#34952=CARTESIAN_POINT('Ctrl Pts',(-14.2890407035395,62.6033893890854,9.11232178901981));
#34953=CARTESIAN_POINT('Ctrl Pts',(-14.1734177690261,62.6054224867212,9.5565540007379));
#34954=CARTESIAN_POINT('Ctrl Pts',(-14.1654859215485,62.5785998445538,10.0004462653844));
#34955=CARTESIAN_POINT('Ctrl Pts',(-14.2348698103755,62.8445369550162,10.0018466754434));
#34956=CARTESIAN_POINT('Ctrl Pts',(-14.2477909590166,62.8774950470096,9.44438121878215));
#34957=CARTESIAN_POINT('Ctrl Pts',(-14.4340668190784,62.8640028840736,8.88455351560663));
#34958=CARTESIAN_POINT('Ctrl Pts',(-14.7726377170273,62.8097033887246,8.44788099502235));
#34959=CARTESIAN_POINT('Ctrl Pts',(-15.2741558751071,62.7292706549691,7.80104690640396));
#34960=CARTESIAN_POINT('Ctrl Pts',(-16.1098381603915,62.5592989131896,7.42443858923752));
#34961=CARTESIAN_POINT('Ctrl Pts',(-16.913927805431,62.3977923938505,7.48559176785147));
#34962=CARTESIAN_POINT('Ctrl Pts',(-17.7180174504704,62.2362858745114,7.54674494646541));
#34963=CARTESIAN_POINT('Ctrl Pts',(-18.490514455265,62.0832445776126,8.04565962085972));
#34964=CARTESIAN_POINT('Ctrl Pts',(-18.8937702597925,62.0291411621378,8.76039160250515));
#34965=CARTESIAN_POINT('Ctrl Pts',(-19.2970260643199,61.9750377466629,9.47512358415058));
#34966=CARTESIAN_POINT('Ctrl Pts',(-19.3310406685804,62.0198722126119,10.4056728730471));
#34967=CARTESIAN_POINT('Ctrl Pts',(-18.9866823611344,62.1660913946905,11.138080910744));
#34968=CARTESIAN_POINT('Ctrl Pts',(-18.6423240536885,62.312310576769,11.8704889484409));
#34969=CARTESIAN_POINT('Ctrl Pts',(-17.9195928345362,62.5599144749771,12.4047557349382));
#34970=CARTESIAN_POINT('Ctrl Pts',(-17.1459983851495,62.8211471346509,12.5032105584454));
#34971=CARTESIAN_POINT('Ctrl Pts',(-16.3724039357629,63.0823797943247,12.6016653819527));
#34972=CARTESIAN_POINT('Ctrl Pts',(-15.5479462561419,63.3572412154642,12.2643082424698));
#34973=CARTESIAN_POINT('Ctrl Pts',(-15.0453884512907,63.5458498251155,11.6412138093996));
#34974=CARTESIAN_POINT('Ctrl Pts',(-14.6827506455303,63.6819468306564,11.1915986689941));
#34975=CARTESIAN_POINT('Ctrl Pts',(-14.4877209077723,63.7731333897311,10.5932047327948));
#34976=CARTESIAN_POINT('Ctrl Pts',(-14.4927485186002,63.8107147438123,9.9979335262408));
#34977=CARTESIAN_POINT('Origin',(-17.0820569767664,63.7511045350785,10.));
#34978=CARTESIAN_POINT('',(-14.7480685208434,64.7775781358098,10.0015051238181));
#34979=CARTESIAN_POINT('',(-14.6789571988966,64.5115679912719,10.0021294030496));
#34980=CARTESIAN_POINT('',(-14.6503387090836,64.4026814811241,10.));
#34981=CARTESIAN_POINT('Ctrl Pts',(-14.6789571988966,64.5115679912719,10.0021294030496));
#34982=CARTESIAN_POINT('Ctrl Pts',(-14.6745624451438,64.5012097288919,10.1782532036582));
#34983=CARTESIAN_POINT('Ctrl Pts',(-14.6880487522533,64.4860602506939,10.3540783073467));
#34984=CARTESIAN_POINT('Ctrl Pts',(-14.7205078014428,64.4658270415774,10.5257161206902));
#34985=CARTESIAN_POINT('Ctrl Pts',(-14.8728494531256,64.3708655262953,11.33127231007));
#34986=CARTESIAN_POINT('Ctrl Pts',(-15.4431136830598,64.163921993672,12.0445928505658));
#34987=CARTESIAN_POINT('Ctrl Pts',(-16.1698862069569,63.9150421900726,12.3462664892694));
#34988=CARTESIAN_POINT('Ctrl Pts',(-16.896658730854,63.6661623864732,12.6479401279729));
#34989=CARTESIAN_POINT('Ctrl Pts',(-17.7799395487139,63.3753463118977,12.5379668648843));
#34990=CARTESIAN_POINT('Ctrl Pts',(-18.418151553513,63.1501962278719,12.0655906176064));
#34991=CARTESIAN_POINT('Ctrl Pts',(-19.056363558312,62.9250461438461,11.5932143703284));
#34992=CARTESIAN_POINT('Ctrl Pts',(-19.4495067500501,62.76556205037,10.7584351388612));
#34993=CARTESIAN_POINT('Ctrl Pts',(-19.4154782471595,62.7205382674991,9.93505104704572));
#34994=CARTESIAN_POINT('Ctrl Pts',(-19.3814497442688,62.6755144846282,9.11166695523024));
#34995=CARTESIAN_POINT('Ctrl Pts',(-18.9202495467495,62.7449510123625,8.29967800306651));
#34996=CARTESIAN_POINT('Ctrl Pts',(-18.2323333520892,62.875135908442,7.8626772661128));
#34997=CARTESIAN_POINT('Ctrl Pts',(-17.5444171574288,63.0053208045214,7.42567652915909));
#34998=CARTESIAN_POINT('Ctrl Pts',(-16.6297849656276,63.196254068946,7.36366400741539));
#34999=CARTESIAN_POINT('Ctrl Pts',(-15.8919306215942,63.3398198518215,7.70440771629202));
#35000=CARTESIAN_POINT('Ctrl Pts',(-15.1540762775607,63.483385634697,8.04515142516864));
#35001=CARTESIAN_POINT('Ctrl Pts',(-14.5929997812951,63.5795839360234,8.78865136466559));
#35002=CARTESIAN_POINT('Ctrl Pts',(-14.4538795211095,63.5627194046509,9.60198253040281));
#35003=CARTESIAN_POINT('Ctrl Pts',(-14.4315087612499,63.5600075610921,9.73276747984711));
#35004=CARTESIAN_POINT('Ctrl Pts',(-14.4200485884486,63.5543722345421,9.86535806600947));
#35005=CARTESIAN_POINT('Ctrl Pts',(-14.4189472139579,63.5459612763502,9.99811000378505));
#35006=CARTESIAN_POINT('Ctrl Pts',(-14.4927485186002,63.8107147438123,9.9979335262408));
#35007=CARTESIAN_POINT('Ctrl Pts',(-14.494688369579,63.8252151156581,9.76825436605168));
#35008=CARTESIAN_POINT('Ctrl Pts',(-14.5264111861321,63.8317351659301,9.53904009330699));
#35009=CARTESIAN_POINT('Ctrl Pts',(-14.5897808794637,63.8297754611264,9.3190160464461));
#35010=CARTESIAN_POINT('Ctrl Pts',(-14.8173890425695,63.8227366893229,8.52874444322036));
#35011=CARTESIAN_POINT('Ctrl Pts',(-15.4532632988625,63.7063033475529,7.85703296342643));
#35012=CARTESIAN_POINT('Ctrl Pts',(-16.2205322683666,63.5546628984882,7.60269513736945));
#35013=CARTESIAN_POINT('Ctrl Pts',(-16.9878012378706,63.4030224494236,7.34835731131247));
#35014=CARTESIAN_POINT('Ctrl Pts',(-17.8864649205859,63.2161748930643,7.51139313899242));
#35015=CARTESIAN_POINT('Ctrl Pts',(-18.522749012129,63.09963173627,8.01927548227232));
#35016=CARTESIAN_POINT('Ctrl Pts',(-19.1590331036721,62.9830885794757,8.52715782555222));
#35017=CARTESIAN_POINT('Ctrl Pts',(-19.5329376040432,62.9368498222464,9.37988668443207));
#35018=CARTESIAN_POINT('Ctrl Pts',(-19.4841294236266,63.0038765864645,10.1981222260488));
#35019=CARTESIAN_POINT('Ctrl Pts',(-19.43532124321,63.0709033506826,11.0163577676655));
#35020=CARTESIAN_POINT('Ctrl Pts',(-18.9638003820057,63.2511956363482,11.8000999920191));
#35021=CARTESIAN_POINT('Ctrl Pts',(-18.2853245933941,63.4869413276821,12.2006980454407));
#35022=CARTESIAN_POINT('Ctrl Pts',(-17.6068488047825,63.7226870190161,12.6012960988622));
#35023=CARTESIAN_POINT('Ctrl Pts',(-16.7214180887636,64.0138861160186,12.6187499813517));
#35024=CARTESIAN_POINT('Ctrl Pts',(-16.02891964808,64.253389165651,12.2452952639449));
#35025=CARTESIAN_POINT('Ctrl Pts',(-15.3364212073964,64.4928922152834,11.871840546538));
#35026=CARTESIAN_POINT('Ctrl Pts',(-14.8368550420482,64.6806992175459,11.1074772292348));
#35027=CARTESIAN_POINT('Ctrl Pts',(-14.7584549707696,64.755655105023,10.2922353809894));
#35028=CARTESIAN_POINT('Ctrl Pts',(-14.7491833360657,64.7645194286933,10.195824440425));
#35029=CARTESIAN_POINT('Ctrl Pts',(-14.7458019429916,64.7718054668758,10.0987019353608));
#35030=CARTESIAN_POINT('Ctrl Pts',(-14.7480685208434,64.7775781358098,10.0015051238181));
#35031=CARTESIAN_POINT('Origin',(-17.0820569767664,63.7511045350785,10.));
#35032=CARTESIAN_POINT('',(-15.0130771992805,65.7418454548454,9.99981028982561));
#35033=CARTESIAN_POINT('',(-14.9415523108175,65.4764820235065,9.9989223619292));
#35034=CARTESIAN_POINT('',(-14.6503387090836,64.4026814811241,10.));
#35035=CARTESIAN_POINT('Ctrl Pts',(-14.9415523108175,65.4764820235065,9.9989223619292));
#35036=CARTESIAN_POINT('Ctrl Pts',(-14.9354685130878,65.4463344353997,10.4860098738006));
#35037=CARTESIAN_POINT('Ctrl Pts',(-15.0596306010492,65.3812875674045,10.9740976137642));
#35038=CARTESIAN_POINT('Ctrl Pts',(-15.3070399126416,65.283216705368,11.378846829941));
#35039=CARTESIAN_POINT('Ctrl Pts',(-15.7285664365569,65.1161273209565,12.0684430664544));
#35040=CARTESIAN_POINT('Ctrl Pts',(-16.5078555104219,64.8531757502039,12.5161238918081));
#35041=CARTESIAN_POINT('Ctrl Pts',(-17.2898955363439,64.5894870640692,12.5214264196761));
#35042=CARTESIAN_POINT('Ctrl Pts',(-18.0719355622658,64.3257983779345,12.5267289475441));
#35043=CARTESIAN_POINT('Ctrl Pts',(-18.8567265402447,64.0613725764178,12.0896531779265));
#35044=CARTESIAN_POINT('Ctrl Pts',(-19.2867932233325,63.8919948632528,11.4059132558299));
#35045=CARTESIAN_POINT('Ctrl Pts',(-19.7168599064203,63.7226171500879,10.7221733337333));
#35046=CARTESIAN_POINT('Ctrl Pts',(-19.7922022946169,63.6482875252747,9.79176925915765));
#35047=CARTESIAN_POINT('Ctrl Pts',(-19.4730226094501,63.6796697714155,9.03131812620907));
#35048=CARTESIAN_POINT('Ctrl Pts',(-19.1538429242832,63.7110520175563,8.27086699326049));
#35049=CARTESIAN_POINT('Ctrl Pts',(-18.440141165753,63.8481461346511,7.68036880193896));
#35050=CARTESIAN_POINT('Ctrl Pts',(-17.6454383857669,64.0069444100311,7.52423731363907));
#35051=CARTESIAN_POINT('Ctrl Pts',(-16.8507356057808,64.165742685411,7.36810582533919));
#35052=CARTESIAN_POINT('Ctrl Pts',(-15.9750318043388,64.3462451190762,7.64634104006095));
#35053=CARTESIAN_POINT('Ctrl Pts',(-15.4043894403336,64.4450065869383,8.23435456655376));
#35054=CARTESIAN_POINT('Ctrl Pts',(-14.9553323969433,64.5227251994293,8.69708154291612));
#35055=CARTESIAN_POINT('Ctrl Pts',(-14.6951885590369,64.5498246710713,9.35164270965597));
#35056=CARTESIAN_POINT('Ctrl Pts',(-14.6789571988966,64.5115679912719,10.0021294030496));
#35057=CARTESIAN_POINT('Ctrl Pts',(-14.7480685208434,64.7775781358098,10.0015051238181));
#35058=CARTESIAN_POINT('Ctrl Pts',(-14.7649679121881,64.8206186125989,9.27681483601603));
#35059=CARTESIAN_POINT('Ctrl Pts',(-15.0958410226864,64.7795300848962,8.54799381140138));
#35060=CARTESIAN_POINT('Ctrl Pts',(-15.6402720254874,64.6812188924136,8.07917134860805));
#35061=CARTESIAN_POINT('Ctrl Pts',(-16.2577231286926,64.5697220196355,7.54746954365975));
#35062=CARTESIAN_POINT('Ctrl Pts',(-17.1498593123119,64.3846235013876,7.35018631295075));
#35063=CARTESIAN_POINT('Ctrl Pts',(-17.9258100558562,64.23065677798,7.57508388624565));
#35064=CARTESIAN_POINT('Ctrl Pts',(-18.7017607994005,64.0766900545725,7.79998145954055));
#35065=CARTESIAN_POINT('Ctrl Pts',(-19.3615261028699,63.9538551260052,8.44705983683934));
#35066=CARTESIAN_POINT('Ctrl Pts',(-19.6176065589079,63.9391872263039,9.22846362604928));
#35067=CARTESIAN_POINT('Ctrl Pts',(-19.873687014946,63.9245193266025,10.0098674152592));
#35068=CARTESIAN_POINT('Ctrl Pts',(-19.7260826235527,64.0180184557671,10.9255966163803));
#35069=CARTESIAN_POINT('Ctrl Pts',(-19.2464556042234,64.200482779956,11.5682854345738));
#35070=CARTESIAN_POINT('Ctrl Pts',(-18.7668285848942,64.3829471041448,12.2109742527673));
#35071=CARTESIAN_POINT('Ctrl Pts',(-17.9551789376289,64.654376623358,12.5806226880331));
#35072=CARTESIAN_POINT('Ctrl Pts',(-17.1785720640665,64.9164164596569,12.5127911771402));
#35073=CARTESIAN_POINT('Ctrl Pts',(-16.4019651905042,65.1784562959559,12.4449596662473));
#35074=CARTESIAN_POINT('Ctrl Pts',(-15.6604010906447,65.4311064493406,11.9396482091956));
#35075=CARTESIAN_POINT('Ctrl Pts',(-15.2897673262124,65.5843661188994,11.2216465877776));
#35076=CARTESIAN_POINT('Ctrl Pts',(-15.0989143577318,65.6632851643039,10.8519211229877));
#35077=CARTESIAN_POINT('Ctrl Pts',(-15.0064172468355,65.7158498370977,10.4257987515067));
#35078=CARTESIAN_POINT('Ctrl Pts',(-15.0130771992805,65.7418454548454,9.99981028982561));
#35079=CARTESIAN_POINT('Origin',(-17.0820569767664,63.7511045350785,10.));
#35080=CARTESIAN_POINT('',(-15.2652009106025,66.709565290414,9.99881345470565));
#35081=CARTESIAN_POINT('',(-15.1934336836835,66.4442667934687,9.99943462192771));
#35082=CARTESIAN_POINT('',(-14.6503387090836,64.4026814811241,10.));
#35083=CARTESIAN_POINT('Ctrl Pts',(-15.1934336836835,66.4442667934687,9.99943462192771));
#35084=CARTESIAN_POINT('Ctrl Pts',(-15.1827995799555,66.3950965524831,10.7909504295072));
#35085=CARTESIAN_POINT('Ctrl Pts',(-15.5599243826034,66.242026625676,11.5846294221375));
#35086=CARTESIAN_POINT('Ctrl Pts',(-16.1674256670552,66.0272275066146,12.0468004663331));
#35087=CARTESIAN_POINT('Ctrl Pts',(-16.799708927206,65.8036660249294,12.5278249876805));
#35088=CARTESIAN_POINT('Ctrl Pts',(-17.6815476659067,65.5132363543001,12.6497433013674));
#35089=CARTESIAN_POINT('Ctrl Pts',(-18.4120106025362,65.2633677075893,12.3579626123138));
#35090=CARTESIAN_POINT('Ctrl Pts',(-19.1424735391658,65.0134990608785,12.0661819232603));
#35091=CARTESIAN_POINT('Ctrl Pts',(-19.7215606737242,64.8041914380862,11.3607022314663));
#35092=CARTESIAN_POINT('Ctrl Pts',(-19.883906949622,64.7065491918251,10.5574238638967));
#35093=CARTESIAN_POINT('Ctrl Pts',(-20.0462532255198,64.608906945564,9.75414549632719));
#35094=CARTESIAN_POINT('Ctrl Pts',(-19.7918586427571,64.6229300758341,8.85306845298211));
#35095=CARTESIAN_POINT('Ctrl Pts',(-19.2285753341566,64.7197196907435,8.25767771891623));
#35096=CARTESIAN_POINT('Ctrl Pts',(-18.6652920255561,64.8165093056529,7.66228698485035));
#35097=CARTESIAN_POINT('Ctrl Pts',(-17.7931199911179,64.9960654052015,7.37258256006368));
#35098=CARTESIAN_POINT('Ctrl Pts',(-16.9965402212513,65.1553666185042,7.51828854147102));
#35099=CARTESIAN_POINT('Ctrl Pts',(-16.1999604513847,65.3146678318068,7.66399452287836));
#35100=CARTESIAN_POINT('Ctrl Pts',(-15.4789729460898,65.4537141588634,8.2451109104797));
#35101=CARTESIAN_POINT('Ctrl Pts',(-15.1503611804252,65.4876237233566,9.001424928117));
#35102=CARTESIAN_POINT('Ctrl Pts',(-15.0146236613657,65.5016305260265,9.31383062721425));
#35103=CARTESIAN_POINT('Ctrl Pts',(-14.9458338550092,65.4976987431426,9.6561287977802));
#35104=CARTESIAN_POINT('Ctrl Pts',(-14.9415523108175,65.4764820235065,9.9989223619292));
#35105=CARTESIAN_POINT('Ctrl Pts',(-15.0130771992805,65.7418454548454,9.99981028982561));
#35106=CARTESIAN_POINT('Ctrl Pts',(-15.0193507802528,65.7663329589547,9.59853518618478));
#35107=CARTESIAN_POINT('Ctrl Pts',(-15.1136101264191,65.7672447483348,9.19737890571013));
#35108=CARTESIAN_POINT('Ctrl Pts',(-15.2965249330007,65.744401378692,8.84359325274526));
#35109=CARTESIAN_POINT('Ctrl Pts',(-15.6736197332262,65.6973077831931,8.11423332491525));
#35110=CARTESIAN_POINT('Ctrl Pts',(-16.4275127626822,65.5492514064624,7.58620525503953));
#35111=CARTESIAN_POINT('Ctrl Pts',(-17.2288315064447,65.3884873478827,7.49440429239113));
#35112=CARTESIAN_POINT('Ctrl Pts',(-18.0301502502071,65.2277232893031,7.40260332974273));
#35113=CARTESIAN_POINT('Ctrl Pts',(-18.8788947082761,65.0542515488746,7.74702947432164));
#35114=CARTESIAN_POINT('Ctrl Pts',(-19.4034973688025,64.9676333413308,8.37446367269952));
#35115=CARTESIAN_POINT('Ctrl Pts',(-19.9281000293289,64.8810151337869,9.00189787107741));
#35116=CARTESIAN_POINT('Ctrl Pts',(-20.1285608923127,64.8812504591278,9.91234012325427));
#35117=CARTESIAN_POINT('Ctrl Pts',(-19.9217039083204,64.9906262726287,10.7007759738115));
#35118=CARTESIAN_POINT('Ctrl Pts',(-19.7148469243281,65.1000020861297,11.4892118243687));
#35119=CARTESIAN_POINT('Ctrl Pts',(-19.1006720933596,65.3185183877906,12.1556412733063));
#35120=CARTESIAN_POINT('Ctrl Pts',(-18.3583974645568,65.5713589268319,12.4036017192683));
#35121=CARTESIAN_POINT('Ctrl Pts',(-17.616122835754,65.8241994658732,12.6515621652302));
#35122=CARTESIAN_POINT('Ctrl Pts',(-16.745748409117,66.1113642422947,12.4810536082165));
#35123=CARTESIAN_POINT('Ctrl Pts',(-16.1404633167949,66.3274985456644,11.9679250313905));
#35124=CARTESIAN_POINT('Ctrl Pts',(-15.5886775085546,66.5245294039924,11.5001503082284));
#35125=CARTESIAN_POINT('Ctrl Pts',(-15.2571911193414,66.662531210899,10.7476451883995));
#35126=CARTESIAN_POINT('Ctrl Pts',(-15.2652009106025,66.709565290414,9.99881345470565));
#35127=CARTESIAN_POINT('Origin',(-17.0820569767664,63.7511045350785,10.));
#35128=CARTESIAN_POINT('',(-15.5286491313886,67.6742507328171,10.0019962882658));
#35129=CARTESIAN_POINT('',(-15.458048217099,67.4086397233445,10.0018117506529));
#35130=CARTESIAN_POINT('',(-14.6503387090836,64.4026814811241,10.));
#35131=CARTESIAN_POINT('',(-20.2598690437799,67.0040126136404,11.1728309286209));
#35132=CARTESIAN_POINT('Ctrl Pts',(-15.5286491313886,67.6742507328171,10.0019962882658));
#35133=CARTESIAN_POINT('Ctrl Pts',(-15.5421457071955,67.7079511930089,9.43113200366978));
#35134=CARTESIAN_POINT('Ctrl Pts',(-15.7382477902416,67.6927226550025,8.85763821511467));
#35135=CARTESIAN_POINT('Ctrl Pts',(-16.0921495062908,67.635211832767,8.41584216487545));
#35136=CARTESIAN_POINT('Ctrl Pts',(-16.6037821050588,67.5520689427971,7.77714150008994));
#35137=CARTESIAN_POINT('Ctrl Pts',(-17.4452195762655,67.3805551035975,7.41369214583754));
#35138=CARTESIAN_POINT('Ctrl Pts',(-18.2482818068303,67.2193238791371,7.48861537411896));
#35139=CARTESIAN_POINT('Ctrl Pts',(-19.0513440373952,67.0580926546768,7.56353860240037));
#35140=CARTESIAN_POINT('Ctrl Pts',(-19.8160310273183,66.9071440449558,8.07683441321559));
#35141=CARTESIAN_POINT('Ctrl Pts',(-20.2075211669018,66.8561932299011,8.79681637620262));
#35142=CARTESIAN_POINT('Ctrl Pts',(-20.5990113064853,66.8052424148464,9.51679833918964));
#35143=CARTESIAN_POINT('Ctrl Pts',(-20.6173045957293,66.854289394458,10.4434664543485));
#35144=CARTESIAN_POINT('Ctrl Pts',(-20.25986904378,67.0040126136404,11.1728309286208));
#35145=CARTESIAN_POINT('',(-16.4802525979517,68.0323660008167,11.867050568706));
#35146=CARTESIAN_POINT('Ctrl Pts',(-16.4806955947431,68.0322473001842,11.8669181223568));
#35147=CARTESIAN_POINT('Ctrl Pts',(-16.6817854205936,67.9835336336722,12.0540417240895));
#35148=CARTESIAN_POINT('Ctrl Pts',(-16.9239334961961,67.923876532405,12.2143044024353));
#35149=CARTESIAN_POINT('Ctrl Pts',(-17.4856657502708,67.7816176378542,12.4543153408643));
#35150=CARTESIAN_POINT('Ctrl Pts',(-17.8119729521746,67.6966288605656,12.5175));
#35151=CARTESIAN_POINT('Ctrl Pts',(-18.4226933621783,67.5329868199039,12.5175));
#35152=CARTESIAN_POINT('Ctrl Pts',(-18.7477780771091,67.4434356591205,12.4543153408643));
#35153=CARTESIAN_POINT('Ctrl Pts',(-19.3446857260753,67.274655929957,12.1973867613172));
#35154=CARTESIAN_POINT('Ctrl Pts',(-19.6165425195547,67.1955448337828,12.0036443501621));
#35155=CARTESIAN_POINT('Ctrl Pts',(-19.9960747381914,67.0834304248293,11.6080270340045));
#35156=CARTESIAN_POINT('Ctrl Pts',(-20.1448248140072,67.0387983068925,11.4009948671635));
#35157=CARTESIAN_POINT('Ctrl Pts',(-20.2598690437799,67.0040126136404,11.1728309286209));
#35158=CARTESIAN_POINT('Ctrl Pts',(-16.4776938604224,68.0330516124713,11.8678155752476));
#35159=CARTESIAN_POINT('Ctrl Pts',(-16.9785524830599,67.8522271893254,12.3404055365586));
#35160=CARTESIAN_POINT('Ctrl Pts',(-17.6838006560652,67.616636751217,12.5855412104356));
#35161=CARTESIAN_POINT('Ctrl Pts',(-18.3529108900526,67.3907294446846,12.5051234941038));
#35162=CARTESIAN_POINT('Ctrl Pts',(-19.1299796896385,67.1283727946321,12.4117306641615));
#35163=CARTESIAN_POINT('Ctrl Pts',(-19.8583083259858,66.8790760319583,11.8792556448934));
#35164=CARTESIAN_POINT('Ctrl Pts',(-20.2061471825011,66.7317311985188,11.1455779206963));
#35165=CARTESIAN_POINT('Ctrl Pts',(-20.5539860390165,66.5843863650793,10.4119001964992));
#35166=CARTESIAN_POINT('Ctrl Pts',(-20.5213351157,66.538993460874,9.4770197673732));
#35167=CARTESIAN_POINT('Ctrl Pts',(-20.1165357938137,66.5933174195301,8.75982961781592));
#35168=CARTESIAN_POINT('Ctrl Pts',(-19.7117364719275,66.6476413781861,8.04263946825864));
#35169=CARTESIAN_POINT('Ctrl Pts',(-18.9347887514715,66.8016821997034,7.54313959827013));
#35170=CARTESIAN_POINT('Ctrl Pts',(-18.1276415422752,66.9638149498405,7.48486270274581));
#35171=CARTESIAN_POINT('Ctrl Pts',(-17.320494333079,67.1259476999776,7.42658580722149));
#35172=CARTESIAN_POINT('Ctrl Pts',(-16.4831476351424,67.2961723787345,7.80953188616136));
#35173=CARTESIAN_POINT('Ctrl Pts',(-15.9844353298858,67.3756602454434,8.46229096311787));
#35174=CARTESIAN_POINT('Ctrl Pts',(-15.6526293851287,67.4285455390928,8.89658813193721));
#35175=CARTESIAN_POINT('Ctrl Pts',(-15.4707226080323,67.4412654718215,9.450320138744));
#35176=CARTESIAN_POINT('Ctrl Pts',(-15.458048217099,67.4086397233445,10.0018117506529));
#35177=CARTESIAN_POINT('Origin',(-63.7511045350785,-17.0820569767664,10.));
#35178=CARTESIAN_POINT('',(-60.9122168113323,-13.7189801527801,9.99965378812949));
#35179=CARTESIAN_POINT('',(-60.6472937215209,-13.6458118873637,9.99664393251001));
#35180=CARTESIAN_POINT('',(-64.4026814811241,-14.6503387090836,10.));
#35181=CARTESIAN_POINT('',(-60.3826426720153,-14.1985145724515,11.6359872033749));
#35182=CARTESIAN_POINT('Ctrl Pts',(-60.6472937215209,-13.6458118873637,
9.99664393251001));
#35183=CARTESIAN_POINT('Ctrl Pts',(-60.6097205320263,-13.6410407802455,
10.5892058593235));
#35184=CARTESIAN_POINT('Ctrl Pts',(-60.5187326677745,-13.8356159531908,
11.1848035603043));
#35185=CARTESIAN_POINT('Ctrl Pts',(-60.3826426720153,-14.1985145724514,
11.6359872033748));
#35186=CARTESIAN_POINT('',(-59.3912531651587,-17.8984305821306,11.6380816927068));
#35187=CARTESIAN_POINT('Origin',(-59.8874012299222,-16.0467807963563,10.));
#35188=CARTESIAN_POINT('Ctrl Pts',(-59.3912467107622,-17.8984546702664,
11.6380966037222));
#35189=CARTESIAN_POINT('Ctrl Pts',(-59.5701794123022,-17.4212611177619,
12.2270179049199));
#35190=CARTESIAN_POINT('Ctrl Pts',(-59.8253574740882,-16.6595160069785,
12.5674221981558));
#35191=CARTESIAN_POINT('Ctrl Pts',(-60.0736878712825,-15.9233267283639,
12.5157167035403));
#35192=CARTESIAN_POINT('Ctrl Pts',(-60.3360206084695,-15.1456267338057,
12.4610957466082));
#35193=CARTESIAN_POINT('Ctrl Pts',(-60.590711685935,-14.3964458015822,11.9688993897476));
#35194=CARTESIAN_POINT('Ctrl Pts',(-60.7469740189125,-14.0146059447133,
11.2575578209422));
#35195=CARTESIAN_POINT('Ctrl Pts',(-60.8300361143405,-13.8116368860469,
10.8794403300268));
#35196=CARTESIAN_POINT('Ctrl Pts',(-60.8852870497794,-13.7124604894775,
10.439403096236));
#35197=CARTESIAN_POINT('Ctrl Pts',(-60.9122168113323,-13.7189801527801,
9.99965378812949));
#35198=CARTESIAN_POINT('Origin',(-63.7511045350785,-17.0820569767664,10.));
#35199=CARTESIAN_POINT('',(-61.8799991994799,-13.9708704146993,9.99901528063941));
#35200=CARTESIAN_POINT('',(-61.614467077582,-13.8999750879731,10.0012573013837));
#35201=CARTESIAN_POINT('',(-64.4026814811241,-14.6503387090836,10.));
#35202=CARTESIAN_POINT('Ctrl Pts',(-61.614467077582,-13.8999750879731,10.0012573013837));
#35203=CARTESIAN_POINT('Ctrl Pts',(-61.6099667912196,-13.8982899610888,
10.0766544396887));
#35204=CARTESIAN_POINT('Ctrl Pts',(-61.6045451170745,-13.900043500223,10.1520128061816));
#35205=CARTESIAN_POINT('Ctrl Pts',(-61.5981695663354,-13.90535695527,10.2270376921987));
#35206=CARTESIAN_POINT('Ctrl Pts',(-61.5284611611193,-13.9634527171372,
11.0473378309362));
#35207=CARTESIAN_POINT('Ctrl Pts',(-61.3447206686645,-14.4471220222726,
11.8277717281247));
#35208=CARTESIAN_POINT('Ctrl Pts',(-61.1066011161456,-15.1337367424349,
12.218961128923));
#35209=CARTESIAN_POINT('Ctrl Pts',(-60.8684815636268,-15.8203514625973,
12.6101505297213));
#35210=CARTESIAN_POINT('Ctrl Pts',(-60.5759829510438,-16.7099115977865,
12.6120954341293));
#35211=CARTESIAN_POINT('Ctrl Pts',(-60.3374667150895,-17.3980067606846,
12.2237523563128));
#35212=CARTESIAN_POINT('Ctrl Pts',(-60.0989504791351,-18.0861019235828,
11.8354092784963));
#35213=CARTESIAN_POINT('Ctrl Pts',(-59.9144166198093,-18.5727321141897,
11.0567782184552));
#35214=CARTESIAN_POINT('Ctrl Pts',(-59.8438645695582,-18.6339764021913,
10.2368654679636));
#35215=CARTESIAN_POINT('Ctrl Pts',(-59.7733125193071,-18.6952206901928,
9.41695271747191));
#35216=CARTESIAN_POINT('Ctrl Pts',(-59.8167422781307,-18.3310790755889,
8.55575827652964));
#35217=CARTESIAN_POINT('Ctrl Pts',(-59.9321107539311,-17.6984585141965,
8.03819621078659));
#35218=CARTESIAN_POINT('Ctrl Pts',(-60.0474792297314,-17.065837952804,7.52063414504355));
#35219=CARTESIAN_POINT('Ctrl Pts',(-60.2347864225086,-16.1647384446229,
7.34670445449967));
#35220=CARTESIAN_POINT('Ctrl Pts',(-60.3874931590403,-15.3927695971148,
7.5957513454432));
#35221=CARTESIAN_POINT('Ctrl Pts',(-60.540199895572,-14.6208007496067,7.84479823638674));
#35222=CARTESIAN_POINT('Ctrl Pts',(-60.6583061758583,-13.9779625627716,
8.5168217088177));
#35223=CARTESIAN_POINT('Ctrl Pts',(-60.6663289586339,-13.7459615817213,
9.30743209219192));
#35224=CARTESIAN_POINT('Ctrl Pts',(-60.6685946628634,-13.6804424696226,
9.53070739947774));
#35225=CARTESIAN_POINT('Ctrl Pts',(-60.6620806891943,-13.6476895615158,
9.76344057197151));
#35226=CARTESIAN_POINT('Ctrl Pts',(-60.6472937215209,-13.6458118873637,
9.99664393251001));
#35227=CARTESIAN_POINT('Ctrl Pts',(-60.9122168113323,-13.7189801527801,
9.99965378812949));
#35228=CARTESIAN_POINT('Ctrl Pts',(-60.9359492362449,-13.7247257446778,
9.61211536100754));
#35229=CARTESIAN_POINT('Ctrl Pts',(-60.9376863320054,-13.8125590225004,
9.22480054821117));
#35230=CARTESIAN_POINT('Ctrl Pts',(-60.9170790299752,-13.9837827281424,
8.88028612326268));
#35231=CARTESIAN_POINT('Ctrl Pts',(-60.8730881195709,-14.3492981499548,
8.14484277513894));
#35232=CARTESIAN_POINT('Ctrl Pts',(-60.7272727102728,-15.0948277750941,
7.60444285964178));
#35233=CARTESIAN_POINT('Ctrl Pts',(-60.5669204894782,-15.8946095193183,
7.4993584305648));
#35234=CARTESIAN_POINT('Ctrl Pts',(-60.4065682686836,-16.6943912635425,
7.39427400148783));
#35235=CARTESIAN_POINT('Ctrl Pts',(-60.2316792363925,-17.5484251268517,
7.72450505883104));
#35236=CARTESIAN_POINT('Ctrl Pts',(-60.1424305723415,-18.0828447847102,
8.34320956294461));
#35237=CARTESIAN_POINT('Ctrl Pts',(-60.0531819082904,-18.6172644425688,
8.96191406705817));
#35238=CARTESIAN_POINT('Ctrl Pts',(-60.0495736124794,-18.8320698949766,
9.86909201794208));
#35239=CARTESIAN_POINT('Ctrl Pts',(-60.1556096340356,-18.6376771842087,
10.6611508664108));
#35240=CARTESIAN_POINT('Ctrl Pts',(-60.2616456555918,-18.4432844734408,
11.4532097148796));
#35241=CARTESIAN_POINT('Ctrl Pts',(-60.4773259945152,-17.8396935994972,
12.1301494609332));
#35242=CARTESIAN_POINT('Ctrl Pts',(-60.7290924921508,-17.1014273477897,
12.3908459426515));
#35243=CARTESIAN_POINT('Ctrl Pts',(-60.9808589897864,-16.3631610960823,
12.6515424243699));
#35244=CARTESIAN_POINT('Ctrl Pts',(-61.2687116461342,-15.4902194666109,
12.495995641753));
#35245=CARTESIAN_POINT('Ctrl Pts',(-61.4869914228005,-14.8769273589399,
11.993393721437));
#35246=CARTESIAN_POINT('Ctrl Pts',(-61.6896056365772,-14.3076501674885,
11.5268626736103));
#35247=CARTESIAN_POINT('Ctrl Pts',(-61.8322748736988,-13.9620906745725,
10.7613040129745));
#35248=CARTESIAN_POINT('Ctrl Pts',(-61.8799991994799,-13.9708704146993,
9.99901528063941));
#35249=CARTESIAN_POINT('Origin',(-63.7511045350785,-17.0820569767664,10.));
#35250=CARTESIAN_POINT('',(-62.8445369550162,-14.2348698103756,10.0018466754434));
#35251=CARTESIAN_POINT('',(-62.5785998445538,-14.1654859215485,10.0004462653844));
#35252=CARTESIAN_POINT('',(-64.4026814811241,-14.6503387090836,10.));
#35253=CARTESIAN_POINT('Ctrl Pts',(-62.5785998445538,-14.1654859215485,
10.0004462653844));
#35254=CARTESIAN_POINT('Ctrl Pts',(-62.5552558244195,-14.1585827534688,
10.3867702486341));
#35255=CARTESIAN_POINT('Ctrl Pts',(-62.5100553152291,-14.2332491130213,
10.7728367424034));
#35256=CARTESIAN_POINT('Ctrl Pts',(-62.4426252563818,-14.3908772813228,
11.1164878478954));
#35257=CARTESIAN_POINT('Ctrl Pts',(-62.2977170112847,-14.729622666347,11.8549994178658));
#35258=CARTESIAN_POINT('Ctrl Pts',(-62.0501467519025,-15.4515079046908,
12.3976253642211));
#35259=CARTESIAN_POINT('Ctrl Pts',(-61.7881520526304,-16.2272258855744,
12.501389418797));
#35260=CARTESIAN_POINT('Ctrl Pts',(-61.5261573533583,-17.0029438664579,
12.6051534733729));
#35261=CARTESIAN_POINT('Ctrl Pts',(-61.2497382141963,-17.8324945898812,
12.2700556361695));
#35262=CARTESIAN_POINT('Ctrl Pts',(-61.0600503079338,-18.3383599455202,
11.6461438143238));
#35263=CARTESIAN_POINT('Ctrl Pts',(-60.8703624016714,-18.8442253011593,
11.0222319924781));
#35264=CARTESIAN_POINT('Ctrl Pts',(-60.7674057283085,-19.0264052890141,
10.1095061859902));
#35265=CARTESIAN_POINT('Ctrl Pts',(-60.7746625458238,-18.7972629292321,
9.31667252204661));
#35266=CARTESIAN_POINT('Ctrl Pts',(-60.7819193633391,-18.56812056945,8.52383885810307));
#35267=CARTESIAN_POINT('Ctrl Pts',(-60.8993896717326,-17.9276558620312,
7.85089733670394));
#35268=CARTESIAN_POINT('Ctrl Pts',(-61.051853263826,-17.1565944419204,7.59916807226832));
#35269=CARTESIAN_POINT('Ctrl Pts',(-61.2043168559194,-16.3855330218097,
7.3474388078327));
#35270=CARTESIAN_POINT('Ctrl Pts',(-61.3917737317128,-15.4838748890071,
7.51692180036059));
#35271=CARTESIAN_POINT('Ctrl Pts',(-61.5076640106208,-14.8493069319054,
8.03174648676773));
#35272=CARTESIAN_POINT('Ctrl Pts',(-61.6129549313732,-14.2727767422054,
8.49948515966285));
#35273=CARTESIAN_POINT('Ctrl Pts',(-61.6591716047613,-13.9167146450877,
9.25228420341937));
#35274=CARTESIAN_POINT('Ctrl Pts',(-61.614467077582,-13.8999750879731,10.0012573013837));
#35275=CARTESIAN_POINT('Ctrl Pts',(-61.8799991994799,-13.9708704146993,
9.99901528063941));
#35276=CARTESIAN_POINT('Ctrl Pts',(-61.8836891105327,-13.971549239588,9.94007725327294));
#35277=CARTESIAN_POINT('Ctrl Pts',(-61.8868114457663,-13.9743462862715,
9.88115877337042));
#35278=CARTESIAN_POINT('Ctrl Pts',(-61.8893500282723,-13.9793219277933,
9.82239956232329));
#35279=CARTESIAN_POINT('Ctrl Pts',(-61.9247219600932,-14.0486511901884,
9.00366438154083));
#35280=CARTESIAN_POINT('Ctrl Pts',(-61.8467589267501,-14.5409523008493,
8.21585107799109));
#35281=CARTESIAN_POINT('Ctrl Pts',(-61.7125351424541,-15.2432213925386,
7.80941972573615));
#35282=CARTESIAN_POINT('Ctrl Pts',(-61.5783113581581,-15.9454904842279,
7.40298837348122));
#35283=CARTESIAN_POINT('Ctrl Pts',(-61.3878268229091,-16.8577275569455,
7.3779389725211));
#35284=CARTESIAN_POINT('Ctrl Pts',(-61.2482107604142,-17.5801209048414,
7.74541574302308));
#35285=CARTESIAN_POINT('Ctrl Pts',(-61.1085946979193,-18.3025142527372,
8.11289251352506));
#35286=CARTESIAN_POINT('Ctrl Pts',(-61.0198471081786,-18.8350638758112,
8.87289545548915));
#35287=CARTESIAN_POINT('Ctrl Pts',(-61.0438394390412,-18.9468623871524,
9.68733378926602));
#35288=CARTESIAN_POINT('Ctrl Pts',(-61.0678317699037,-19.0586608984937,
10.5017721230429));
#35289=CARTESIAN_POINT('Ctrl Pts',(-61.2045640213696,-18.7497082981023,
11.3706458486326));
#35290=CARTESIAN_POINT('Ctrl Pts',(-61.4156018821481,-18.1634433884685,
11.9074332417682));
#35291=CARTESIAN_POINT('Ctrl Pts',(-61.6266397429266,-17.5771784788347,
12.4442206349039));
#35292=CARTESIAN_POINT('Ctrl Pts',(-61.9119832130178,-16.7136012599587,
12.6489216955855));
#35293=CARTESIAN_POINT('Ctrl Pts',(-62.1670877632025,-15.9628772265398,
12.4304742338455));
#35294=CARTESIAN_POINT('Ctrl Pts',(-62.4221923133871,-15.2121531931209,
12.2120267721055));
#35295=CARTESIAN_POINT('Ctrl Pts',(-62.6470579436653,-14.5742823451591,
11.5704307879438));
#35296=CARTESIAN_POINT('Ctrl Pts',(-62.7640438959386,-14.3390239366158,
10.7911028658277));
#35297=CARTESIAN_POINT('Ctrl Pts',(-62.8020535673525,-14.2625865983513,
10.5378929917554));
#35298=CARTESIAN_POINT('Ctrl Pts',(-62.828674898289,-14.2286511253629,10.2701434172216));
#35299=CARTESIAN_POINT('Ctrl Pts',(-62.8445369550162,-14.2348698103756,
10.0018466754434));
#35300=CARTESIAN_POINT('Origin',(-63.7511045350785,-17.0820569767664,10.));
#35301=CARTESIAN_POINT('',(-63.8107147438124,-14.4927485186002,9.99793352624079));
#35302=CARTESIAN_POINT('',(-63.5459612763503,-14.4189472139579,9.99811000378506));
#35303=CARTESIAN_POINT('',(-64.4026814811241,-14.6503387090836,10.));
#35304=CARTESIAN_POINT('Ctrl Pts',(-63.5459612763503,-14.4189472139579,
9.99811000378506));
#35305=CARTESIAN_POINT('Ctrl Pts',(-63.5020657997403,-14.4131993125783,
10.6909216248416));
#35306=CARTESIAN_POINT('Ctrl Pts',(-63.3825723034678,-14.6895870615306,
11.3881278716998));
#35307=CARTESIAN_POINT('Ctrl Pts',(-63.2084966963919,-15.1696780211858,
11.8560065223222));
#35308=CARTESIAN_POINT('Ctrl Pts',(-63.0010658835769,-15.7417608055529,
12.4135369565264));
#35309=CARTESIAN_POINT('Ctrl Pts',(-62.7161316220184,-16.6030903983926,
12.6454354329572));
#35310=CARTESIAN_POINT('Ctrl Pts',(-62.4586624096387,-17.3619190322647,
12.4478622804133));
#35311=CARTESIAN_POINT('Ctrl Pts',(-62.201193197259,-18.1207476661368,12.2502891278694));
#35312=CARTESIAN_POINT('Ctrl Pts',(-61.9711890340581,-18.7770753410412,
11.6232443463506));
#35313=CARTESIAN_POINT('Ctrl Pts',(-61.8490217755358,-19.030950208754,10.8475065234704));
#35314=CARTESIAN_POINT('Ctrl Pts',(-61.7268545170136,-19.2848250764668,
10.0717687005902));
#35315=CARTESIAN_POINT('Ctrl Pts',(-61.71252416317,-19.1362471369879,9.14733783634849));
#35316=CARTESIAN_POINT('Ctrl Pts',(-61.789827971849,-18.6456858472655,8.48815640829349));
#35317=CARTESIAN_POINT('Ctrl Pts',(-61.867131780528,-18.155124557543,7.82897498023847));
#35318=CARTESIAN_POINT('Ctrl Pts',(-62.0360697517297,-17.3225799175769,
7.43504298837015));
#35319=CARTESIAN_POINT('Ctrl Pts',(-62.1983751106924,-16.5147885234736,
7.48275547481142));
#35320=CARTESIAN_POINT('Ctrl Pts',(-62.3606804696551,-15.7069971293704,
7.53046796125269));
#35321=CARTESIAN_POINT('Ctrl Pts',(-62.5163532163789,-14.9239589811299,
8.01982492600353));
#35322=CARTESIAN_POINT('Ctrl Pts',(-62.5730664743348,-14.510242672862,8.73170200517163));
#35323=CARTESIAN_POINT('Ctrl Pts',(-62.6033893890854,-14.2890407035394,
9.11232178902019));
#35324=CARTESIAN_POINT('Ctrl Pts',(-62.6054224867212,-14.1734177690262,
9.55655400073809));
#35325=CARTESIAN_POINT('Ctrl Pts',(-62.5785998445538,-14.1654859215485,
10.0004462653844));
#35326=CARTESIAN_POINT('Ctrl Pts',(-62.8445369550162,-14.2348698103756,
10.0018466754434));
#35327=CARTESIAN_POINT('Ctrl Pts',(-62.8774950470096,-14.2477909590166,
9.44438121878235));
#35328=CARTESIAN_POINT('Ctrl Pts',(-62.8640028840737,-14.4340668190783,
8.884553515607));
#35329=CARTESIAN_POINT('Ctrl Pts',(-62.8097033887247,-14.772637717027,8.44788099502279));
#35330=CARTESIAN_POINT('Ctrl Pts',(-62.7292706549692,-15.2741558751066,
7.80104690640428));
#35331=CARTESIAN_POINT('Ctrl Pts',(-62.5592989131897,-16.109838160391,7.42443858923766));
#35332=CARTESIAN_POINT('Ctrl Pts',(-62.3977923938506,-16.9139278054305,
7.48559176785143));
#35333=CARTESIAN_POINT('Ctrl Pts',(-62.2362858745115,-17.7180174504699,
7.54674494646519));
#35334=CARTESIAN_POINT('Ctrl Pts',(-62.0832445776127,-18.4905144552645,
8.04565962085933));
#35335=CARTESIAN_POINT('Ctrl Pts',(-62.0291411621378,-18.8937702597922,
8.76039160250466));
#35336=CARTESIAN_POINT('Ctrl Pts',(-61.9750377466629,-19.2970260643198,
9.47512358415));
#35337=CARTESIAN_POINT('Ctrl Pts',(-62.0198722126119,-19.3310406685804,
10.4056728730465));
#35338=CARTESIAN_POINT('Ctrl Pts',(-62.1660913946904,-18.9866823611347,
11.1380809107435));
#35339=CARTESIAN_POINT('Ctrl Pts',(-62.3123105767689,-18.6423240536889,
11.8704889484405));
#35340=CARTESIAN_POINT('Ctrl Pts',(-62.5599144749769,-17.9195928345367,
12.404755734938));
#35341=CARTESIAN_POINT('Ctrl Pts',(-62.8211471346507,-17.1459983851501,
12.5032105584454));
#35342=CARTESIAN_POINT('Ctrl Pts',(-63.0823797943245,-16.3724039357634,
12.6016653819528));
#35343=CARTESIAN_POINT('Ctrl Pts',(-63.3572412154641,-15.5479462561424,
12.2643082424701));
#35344=CARTESIAN_POINT('Ctrl Pts',(-63.5458498251154,-15.045388451291,11.6412138094001));
#35345=CARTESIAN_POINT('Ctrl Pts',(-63.6819468306564,-14.6827506455304,
11.1915986689945));
#35346=CARTESIAN_POINT('Ctrl Pts',(-63.7731333897311,-14.4877209077723,
10.593204732795));
#35347=CARTESIAN_POINT('Ctrl Pts',(-63.8107147438124,-14.4927485186002,
9.99793352624079));
#35348=CARTESIAN_POINT('Origin',(-63.7511045350785,-17.0820569767664,10.));
#35349=CARTESIAN_POINT('',(-64.7775781358098,-14.7480685208434,10.001505123818));
#35350=CARTESIAN_POINT('',(-64.511567991272,-14.6789571988966,10.0021294030496));
#35351=CARTESIAN_POINT('',(-64.4026814811241,-14.6503387090836,10.));
#35352=CARTESIAN_POINT('Ctrl Pts',(-64.511567991272,-14.6789571988966,10.0021294030496));
#35353=CARTESIAN_POINT('Ctrl Pts',(-64.5012097288919,-14.6745624451438,
10.1782532036584));
#35354=CARTESIAN_POINT('Ctrl Pts',(-64.4860602506939,-14.6880487522533,
10.3540783073471));
#35355=CARTESIAN_POINT('Ctrl Pts',(-64.4658270415774,-14.7205078014429,
10.5257161206908));
#35356=CARTESIAN_POINT('Ctrl Pts',(-64.3708655262952,-14.872849453126,11.3312723100706));
#35357=CARTESIAN_POINT('Ctrl Pts',(-64.1639219936719,-15.4431136830603,
12.0445928505662));
#35358=CARTESIAN_POINT('Ctrl Pts',(-63.9150421900725,-16.1698862069574,
12.3462664892696));
#35359=CARTESIAN_POINT('Ctrl Pts',(-63.666162386473,-16.8966587308546,12.6479401279729));
#35360=CARTESIAN_POINT('Ctrl Pts',(-63.3753463118975,-17.7799395487145,
12.5379668648841));
#35361=CARTESIAN_POINT('Ctrl Pts',(-63.1501962278717,-18.4181515535134,
12.065590617606));
#35362=CARTESIAN_POINT('Ctrl Pts',(-62.9250461438459,-19.0563635583123,
11.5932143703279));
#35363=CARTESIAN_POINT('Ctrl Pts',(-62.7655620503699,-19.4495067500503,
10.7584351388606));
#35364=CARTESIAN_POINT('Ctrl Pts',(-62.7205382674991,-19.4154782471594,
9.93505104704512));
#35365=CARTESIAN_POINT('Ctrl Pts',(-62.6755144846283,-19.3814497442686,
9.11166695522964));
#35366=CARTESIAN_POINT('Ctrl Pts',(-62.7449510123627,-18.9202495467491,
8.29967800306603));
#35367=CARTESIAN_POINT('Ctrl Pts',(-62.8751359084421,-18.2323333520887,
7.86267726611249));
#35368=CARTESIAN_POINT('Ctrl Pts',(-63.0053208045216,-17.5444171574283,
7.42567652915895));
#35369=CARTESIAN_POINT('Ctrl Pts',(-63.1962540689462,-16.629784965627,7.36366400741547));
#35370=CARTESIAN_POINT('Ctrl Pts',(-63.3398198518216,-15.8919306215937,
7.70440771629226));
#35371=CARTESIAN_POINT('Ctrl Pts',(-63.4833856346971,-15.1540762775603,
8.04515142516905));
#35372=CARTESIAN_POINT('Ctrl Pts',(-63.5795839360235,-14.5929997812949,
8.78865136466612));
#35373=CARTESIAN_POINT('Ctrl Pts',(-63.5627194046509,-14.4538795211094,
9.60198253040337));
#35374=CARTESIAN_POINT('Ctrl Pts',(-63.5600075610921,-14.4315087612499,
9.73276747984748));
#35375=CARTESIAN_POINT('Ctrl Pts',(-63.5543722345421,-14.4200485884486,
9.86535806600966));
#35376=CARTESIAN_POINT('Ctrl Pts',(-63.5459612763503,-14.4189472139579,
9.99811000378506));
#35377=CARTESIAN_POINT('Ctrl Pts',(-63.8107147438124,-14.4927485186002,
9.99793352624079));
#35378=CARTESIAN_POINT('Ctrl Pts',(-63.8252151156582,-14.494688369579,9.76825436605187));
#35379=CARTESIAN_POINT('Ctrl Pts',(-63.8317351659301,-14.526411186132,9.53904009330736));
#35380=CARTESIAN_POINT('Ctrl Pts',(-63.8297754611264,-14.5897808794636,
9.31901604644665));
#35381=CARTESIAN_POINT('Ctrl Pts',(-63.822736689323,-14.8173890425691,8.52874444322085));
#35382=CARTESIAN_POINT('Ctrl Pts',(-63.706303347553,-15.453263298862,7.85703296342678));
#35383=CARTESIAN_POINT('Ctrl Pts',(-63.5546628984884,-16.220532268366,7.60269513736962));
#35384=CARTESIAN_POINT('Ctrl Pts',(-63.4030224494238,-16.9878012378701,
7.34835731131246));
#35385=CARTESIAN_POINT('Ctrl Pts',(-63.2161748930645,-17.8864649205853,
7.51139313899221));
#35386=CARTESIAN_POINT('Ctrl Pts',(-63.0996317362701,-18.5227490121286,
8.01927548227196));
#35387=CARTESIAN_POINT('Ctrl Pts',(-62.9830885794758,-19.1590331036718,
8.52715782555172));
#35388=CARTESIAN_POINT('Ctrl Pts',(-62.9368498222464,-19.532937604043,9.37988668443149));
#35389=CARTESIAN_POINT('Ctrl Pts',(-63.0038765864645,-19.4841294236266,
10.1981222260482));
#35390=CARTESIAN_POINT('Ctrl Pts',(-63.0709033506825,-19.4353212432102,
11.016357767665));
#35391=CARTESIAN_POINT('Ctrl Pts',(-63.2511956363481,-18.9638003820061,
11.8000999920187));
#35392=CARTESIAN_POINT('Ctrl Pts',(-63.486941327682,-18.2853245933946,12.2006980454404));
#35393=CARTESIAN_POINT('Ctrl Pts',(-63.722687019016,-17.6068488047831,12.6012960988621));
#35394=CARTESIAN_POINT('Ctrl Pts',(-64.0138861160184,-16.7214180887641,
12.6187499813518));
#35395=CARTESIAN_POINT('Ctrl Pts',(-64.2533891656508,-16.0289196480805,
12.2452952639451));
#35396=CARTESIAN_POINT('Ctrl Pts',(-64.4928922152833,-15.3364212073968,
11.8718405465384));
#35397=CARTESIAN_POINT('Ctrl Pts',(-64.6806992175458,-14.8368550420484,
11.1074772292354));
#35398=CARTESIAN_POINT('Ctrl Pts',(-64.7556551050229,-14.7584549707697,
10.29223538099));
#35399=CARTESIAN_POINT('Ctrl Pts',(-64.7645194286933,-14.7491833360657,
10.1958244404253));
#35400=CARTESIAN_POINT('Ctrl Pts',(-64.7718054668758,-14.7458019429916,
10.0987019353609));
#35401=CARTESIAN_POINT('Ctrl Pts',(-64.7775781358098,-14.7480685208434,
10.001505123818));
#35402=CARTESIAN_POINT('Origin',(-63.7511045350785,-17.0820569767664,10.));
#35403=CARTESIAN_POINT('',(-65.7418454548455,-15.0130771992805,9.99981028982562));
#35404=CARTESIAN_POINT('',(-65.4764820235065,-14.9415523108175,9.99892236192921));
#35405=CARTESIAN_POINT('',(-64.4026814811241,-14.6503387090836,10.));
#35406=CARTESIAN_POINT('Ctrl Pts',(-65.4764820235065,-14.9415523108175,
9.99892236192921));
#35407=CARTESIAN_POINT('Ctrl Pts',(-65.4463344353997,-14.9354685130878,
10.4860098738008));
#35408=CARTESIAN_POINT('Ctrl Pts',(-65.3812875674044,-15.0596306010494,
10.9740976137646));
#35409=CARTESIAN_POINT('Ctrl Pts',(-65.2832167053678,-15.3070399126419,
11.3788468299415));
#35410=CARTESIAN_POINT('Ctrl Pts',(-65.1161273209563,-15.7285664365574,
12.0684430664548));
#35411=CARTESIAN_POINT('Ctrl Pts',(-64.8531757502037,-16.5078555104225,
12.5161238918083));
#35412=CARTESIAN_POINT('Ctrl Pts',(-64.589487064069,-17.2898955363445,12.5214264196761));
#35413=CARTESIAN_POINT('Ctrl Pts',(-64.3257983779344,-18.0719355622664,
12.5267289475439));
#35414=CARTESIAN_POINT('Ctrl Pts',(-64.0613725764176,-18.8567265402452,
12.0896531779261));
#35415=CARTESIAN_POINT('Ctrl Pts',(-63.8919948632527,-19.2867932233328,
11.4059132558293));
#35416=CARTESIAN_POINT('Ctrl Pts',(-63.7226171500878,-19.7168599064204,
10.7221733337326));
#35417=CARTESIAN_POINT('Ctrl Pts',(-63.6482875252747,-19.7922022946168,
9.79176925915698));
#35418=CARTESIAN_POINT('Ctrl Pts',(-63.6796697714156,-19.4730226094498,
9.03131812620849));
#35419=CARTESIAN_POINT('Ctrl Pts',(-63.7110520175564,-19.1538429242828,
8.27086699325998));
#35420=CARTESIAN_POINT('Ctrl Pts',(-63.8481461346512,-18.4401411657524,
7.68036880193864));
#35421=CARTESIAN_POINT('Ctrl Pts',(-64.0069444100312,-17.6454383857663,
7.52423731363896));
#35422=CARTESIAN_POINT('Ctrl Pts',(-64.1657426854112,-16.8507356057801,
7.36810582533927));
#35423=CARTESIAN_POINT('Ctrl Pts',(-64.3462451190763,-15.9750318043382,
7.64634104006127));
#35424=CARTESIAN_POINT('Ctrl Pts',(-64.4450065869384,-15.4043894403332,
8.23435456655423));
#35425=CARTESIAN_POINT('Ctrl Pts',(-64.5227251994293,-14.9553323969431,
8.69708154291655));
#35426=CARTESIAN_POINT('Ctrl Pts',(-64.5498246710713,-14.6951885590369,
9.35164270965619));
#35427=CARTESIAN_POINT('Ctrl Pts',(-64.511567991272,-14.6789571988966,10.0021294030496));
#35428=CARTESIAN_POINT('Ctrl Pts',(-64.7775781358098,-14.7480685208434,
10.001505123818));
#35429=CARTESIAN_POINT('Ctrl Pts',(-64.8206186125989,-14.7649679121881,
9.27681483601613));
#35430=CARTESIAN_POINT('Ctrl Pts',(-64.7795300848962,-15.0958410226862,
8.54799381140172));
#35431=CARTESIAN_POINT('Ctrl Pts',(-64.6812188924137,-15.640272025487,8.07917134860842));
#35432=CARTESIAN_POINT('Ctrl Pts',(-64.5697220196357,-16.2577231286921,
7.54746954365997));
#35433=CARTESIAN_POINT('Ctrl Pts',(-64.3846235013878,-17.1498593123113,
7.35018631295078));
#35434=CARTESIAN_POINT('Ctrl Pts',(-64.2306567779802,-17.9258100558557,
7.5750838862455));
#35435=CARTESIAN_POINT('Ctrl Pts',(-64.0766900545726,-18.7017607994001,
7.79998145954022));
#35436=CARTESIAN_POINT('Ctrl Pts',(-63.9538551260053,-19.3615261028695,
8.44705983683885));
#35437=CARTESIAN_POINT('Ctrl Pts',(-63.9391872263039,-19.6176065589078,
9.22846362604872));
#35438=CARTESIAN_POINT('Ctrl Pts',(-63.9245193266025,-19.873687014946,10.0098674152586));
#35439=CARTESIAN_POINT('Ctrl Pts',(-64.018018455767,-19.7260826235529,10.9255966163797));
#35440=CARTESIAN_POINT('Ctrl Pts',(-64.2004827799559,-19.2464556042238,
11.5682854345733));
#35441=CARTESIAN_POINT('Ctrl Pts',(-64.3829471041447,-18.7668285848947,
12.2109742527669));
#35442=CARTESIAN_POINT('Ctrl Pts',(-64.6543766233579,-17.9551789376295,
12.580622688033));
#35443=CARTESIAN_POINT('Ctrl Pts',(-64.9164164596568,-17.1785720640671,
12.5127911771403));
#35444=CARTESIAN_POINT('Ctrl Pts',(-65.1784562959558,-16.4019651905047,
12.4449596662476));
#35445=CARTESIAN_POINT('Ctrl Pts',(-65.4311064493405,-15.6604010906451,
11.939648209196));
#35446=CARTESIAN_POINT('Ctrl Pts',(-65.5843661188993,-15.2897673262127,
11.2216465877781));
#35447=CARTESIAN_POINT('Ctrl Pts',(-65.6632851643038,-15.0989143577319,
10.8519211229881));
#35448=CARTESIAN_POINT('Ctrl Pts',(-65.7158498370977,-15.0064172468355,
10.4257987515069));
#35449=CARTESIAN_POINT('Ctrl Pts',(-65.7418454548455,-15.0130771992805,
9.99981028982562));
#35450=CARTESIAN_POINT('Origin',(-63.7511045350785,-17.0820569767664,10.));
#35451=CARTESIAN_POINT('',(-66.7095652904141,-15.2652009106025,9.99881345470568));
#35452=CARTESIAN_POINT('',(-66.4442667934687,-15.1934336836835,9.99943462192771));
#35453=CARTESIAN_POINT('',(-64.4026814811241,-14.6503387090836,10.));
#35454=CARTESIAN_POINT('Ctrl Pts',(-66.4442667934687,-15.1934336836835,
9.99943462192771));
#35455=CARTESIAN_POINT('Ctrl Pts',(-66.3950965524831,-15.1827995799555,
10.7909504295074));
#35456=CARTESIAN_POINT('Ctrl Pts',(-66.242026625676,-15.5599243826037,11.584629422138));
#35457=CARTESIAN_POINT('Ctrl Pts',(-66.0272275066145,-16.1674256670557,
12.0468004663335));
#35458=CARTESIAN_POINT('Ctrl Pts',(-65.8036660249293,-16.7997089272067,
12.5278249876807));
#35459=CARTESIAN_POINT('Ctrl Pts',(-65.5132363542999,-17.6815476659074,
12.6497433013673));
#35460=CARTESIAN_POINT('Ctrl Pts',(-65.2633677075891,-18.4120106025368,
12.3579626123136));
#35461=CARTESIAN_POINT('Ctrl Pts',(-65.0134990608783,-19.1424735391663,
12.0661819232598));
#35462=CARTESIAN_POINT('Ctrl Pts',(-64.8041914380861,-19.7215606737245,
11.3607022314657));
#35463=CARTESIAN_POINT('Ctrl Pts',(-64.7065491918251,-19.8839069496222,
10.5574238638961));
#35464=CARTESIAN_POINT('Ctrl Pts',(-64.608906945564,-20.0462532255198,9.75414549632649));
#35465=CARTESIAN_POINT('Ctrl Pts',(-64.6229300758342,-19.7918586427568,
8.8530684529815));
#35466=CARTESIAN_POINT('Ctrl Pts',(-64.7197196907436,-19.2285753341561,
8.25767771891577));
#35467=CARTESIAN_POINT('Ctrl Pts',(-64.816509305653,-18.6652920255555,7.66228698485004));
#35468=CARTESIAN_POINT('Ctrl Pts',(-64.9960654052017,-17.7931199911172,
7.37258256006359));
#35469=CARTESIAN_POINT('Ctrl Pts',(-65.1553666185043,-16.9965402212507,
7.51828854147113));
#35470=CARTESIAN_POINT('Ctrl Pts',(-65.314667831807,-16.1999604513842,7.66399452287867));
#35471=CARTESIAN_POINT('Ctrl Pts',(-65.4537141588636,-15.4789729460894,
8.24511091048021));
#35472=CARTESIAN_POINT('Ctrl Pts',(-65.4876237233567,-15.150361180425,9.00142492811759));
#35473=CARTESIAN_POINT('Ctrl Pts',(-65.5016305260266,-15.0146236613656,
9.31383062721468));
#35474=CARTESIAN_POINT('Ctrl Pts',(-65.4976987431426,-14.9458338550092,
9.65612879778042));
#35475=CARTESIAN_POINT('Ctrl Pts',(-65.4764820235065,-14.9415523108175,
9.99892236192921));
#35476=CARTESIAN_POINT('Ctrl Pts',(-65.7418454548455,-15.0130771992805,
9.99981028982562));
#35477=CARTESIAN_POINT('Ctrl Pts',(-65.7663329589547,-15.0193507802528,
9.59853518618498));
#35478=CARTESIAN_POINT('Ctrl Pts',(-65.7672447483349,-15.113610126419,9.19737890571051));
#35479=CARTESIAN_POINT('Ctrl Pts',(-65.7444013786921,-15.2965249330005,
8.84359325274577));
#35480=CARTESIAN_POINT('Ctrl Pts',(-65.6973077831932,-15.6736197332258,
8.11423332491567));
#35481=CARTESIAN_POINT('Ctrl Pts',(-65.5492514064625,-16.4275127626816,
7.58620525503978));
#35482=CARTESIAN_POINT('Ctrl Pts',(-65.3884873478829,-17.2288315064441,
7.49440429239119));
#35483=CARTESIAN_POINT('Ctrl Pts',(-65.2277232893032,-18.0301502502066,
7.4026033297426));
#35484=CARTESIAN_POINT('Ctrl Pts',(-65.0542515488747,-18.8788947082756,
7.74702947432132));
#35485=CARTESIAN_POINT('Ctrl Pts',(-64.9676333413309,-19.4034973688022,
8.3744636726991));
#35486=CARTESIAN_POINT('Ctrl Pts',(-64.881015133787,-19.9281000293287,9.00189787107686));
#35487=CARTESIAN_POINT('Ctrl Pts',(-64.8812504591278,-20.1285608923127,
9.91234012325367));
#35488=CARTESIAN_POINT('Ctrl Pts',(-64.9906262726287,-19.9217039083206,
10.7007759738109));
#35489=CARTESIAN_POINT('Ctrl Pts',(-65.1000020861296,-19.7148469243284,
11.4892118243682));
#35490=CARTESIAN_POINT('Ctrl Pts',(-65.3185183877905,-19.1006720933601,
12.155641273306));
#35491=CARTESIAN_POINT('Ctrl Pts',(-65.5713589268317,-18.3583974645574,
12.4036017192681));
#35492=CARTESIAN_POINT('Ctrl Pts',(-65.824199465873,-17.6161228357546,12.6515621652302));
#35493=CARTESIAN_POINT('Ctrl Pts',(-66.1113642422946,-16.7457484091175,
12.4810536082167));
#35494=CARTESIAN_POINT('Ctrl Pts',(-66.3274985456644,-16.1404633167953,
11.9679250313909));
#35495=CARTESIAN_POINT('Ctrl Pts',(-66.5245294039924,-15.5886775085548,
11.5001503082288));
#35496=CARTESIAN_POINT('Ctrl Pts',(-66.662531210899,-15.2571911193414,10.7476451883997));
#35497=CARTESIAN_POINT('Ctrl Pts',(-66.7095652904141,-15.2652009106025,
9.99881345470568));
#35498=CARTESIAN_POINT('Origin',(-63.7511045350785,-17.0820569767664,10.));
#35499=CARTESIAN_POINT('',(-67.6742507328171,-15.5286491313886,10.0019962882658));
#35500=CARTESIAN_POINT('',(-67.4086397233445,-15.458048217099,10.0018117506529));
#35501=CARTESIAN_POINT('',(-64.4026814811241,-14.6503387090836,10.));
#35502=CARTESIAN_POINT('',(-67.0040126136404,-20.2598690437802,11.1728309286204));
#35503=CARTESIAN_POINT('Ctrl Pts',(-67.6742507328171,-15.5286491313886,
10.0019962882658));
#35504=CARTESIAN_POINT('Ctrl Pts',(-67.707951193009,-15.5421457071955,9.43113200366998));
#35505=CARTESIAN_POINT('Ctrl Pts',(-67.6927226550026,-15.7382477902415,
8.85763821511506));
#35506=CARTESIAN_POINT('Ctrl Pts',(-67.6352118327672,-16.0921495062904,
8.4158421648759));
#35507=CARTESIAN_POINT('Ctrl Pts',(-67.5520689427973,-16.6037821050583,
7.77714150009027));
#35508=CARTESIAN_POINT('Ctrl Pts',(-67.3805551035977,-17.4452195762649,
7.41369214583768));
#35509=CARTESIAN_POINT('Ctrl Pts',(-67.2193238791373,-18.2482818068298,
7.4886153741189));
#35510=CARTESIAN_POINT('Ctrl Pts',(-67.0580926546769,-19.0513440373947,
7.56353860240013));
#35511=CARTESIAN_POINT('Ctrl Pts',(-66.9071440449559,-19.8160310273179,
8.07683441321518));
#35512=CARTESIAN_POINT('Ctrl Pts',(-66.8561932299011,-20.2075211669015,
8.79681637620211));
#35513=CARTESIAN_POINT('Ctrl Pts',(-66.8052424148464,-20.5990113064852,
9.51679833918905));
#35514=CARTESIAN_POINT('Ctrl Pts',(-66.854289394458,-20.6173045957294,10.4434664543479));
#35515=CARTESIAN_POINT('Ctrl Pts',(-67.0040126136403,-20.2598690437802,
11.1728309286203));
#35516=CARTESIAN_POINT('',(-68.0323660008166,-16.4802525979519,11.8670505687061));
#35517=CARTESIAN_POINT('Ctrl Pts',(-68.0322473001841,-16.4806955947434,
11.8669181223572));
#35518=CARTESIAN_POINT('Ctrl Pts',(-67.9835336336721,-16.6817854205938,
12.0540417240897));
#35519=CARTESIAN_POINT('Ctrl Pts',(-67.9238765324049,-16.9239334961962,
12.2143044024353));
#35520=CARTESIAN_POINT('Ctrl Pts',(-67.7816176378542,-17.4856657502708,
12.4543153408643));
#35521=CARTESIAN_POINT('Ctrl Pts',(-67.6966288605656,-17.8119729521746,
12.5175));
#35522=CARTESIAN_POINT('Ctrl Pts',(-67.5329868199039,-18.4226933621783,
12.5175));
#35523=CARTESIAN_POINT('Ctrl Pts',(-67.4434356591205,-18.747778077109,12.4543153408643));
#35524=CARTESIAN_POINT('Ctrl Pts',(-67.2746559299571,-19.3446857260753,
12.1973867613172));
#35525=CARTESIAN_POINT('Ctrl Pts',(-67.1955448337828,-19.6165425195547,
12.0036443501621));
#35526=CARTESIAN_POINT('Ctrl Pts',(-67.0834304248293,-19.9960747381915,
11.6080270340043));
#35527=CARTESIAN_POINT('Ctrl Pts',(-67.0387983068925,-20.1448248140074,
11.4009948671632));
#35528=CARTESIAN_POINT('Ctrl Pts',(-67.0040126136404,-20.2598690437802,
11.1728309286204));
#35529=CARTESIAN_POINT('Ctrl Pts',(-68.0330516124712,-16.4776938604227,
11.8678155752478));
#35530=CARTESIAN_POINT('Ctrl Pts',(-67.8522271893252,-16.9785524830602,
12.3404055365588));
#35531=CARTESIAN_POINT('Ctrl Pts',(-67.6166367512168,-17.6838006560658,
12.5855412104358));
#35532=CARTESIAN_POINT('Ctrl Pts',(-67.3907294446844,-18.3529108900533,
12.5051234941037));
#35533=CARTESIAN_POINT('Ctrl Pts',(-67.1283727946319,-19.1299796896392,
12.4117306641612));
#35534=CARTESIAN_POINT('Ctrl Pts',(-66.8790760319581,-19.8583083259863,
11.8792556448929));
#35535=CARTESIAN_POINT('Ctrl Pts',(-66.7317311985187,-20.2061471825014,
11.1455779206957));
#35536=CARTESIAN_POINT('Ctrl Pts',(-66.5843863650792,-20.5539860390166,
10.4119001964985));
#35537=CARTESIAN_POINT('Ctrl Pts',(-66.5389934608741,-20.5213351156998,
9.47701976737246));
#35538=CARTESIAN_POINT('Ctrl Pts',(-66.5933174195301,-20.1165357938134,
8.7598296178153));
#35539=CARTESIAN_POINT('Ctrl Pts',(-66.6476413781862,-19.7117364719269,
8.04263946825813));
#35540=CARTESIAN_POINT('Ctrl Pts',(-66.8016821997036,-18.9347887514708,
7.54313959826985));
#35541=CARTESIAN_POINT('Ctrl Pts',(-66.9638149498407,-18.1276415422745,
7.48486270274577));
#35542=CARTESIAN_POINT('Ctrl Pts',(-67.1259476999778,-17.3204943330783,
7.42658580722168));
#35543=CARTESIAN_POINT('Ctrl Pts',(-67.2961723787346,-16.4831476351418,
7.80953188616179));
#35544=CARTESIAN_POINT('Ctrl Pts',(-67.3756602454435,-15.9844353298854,
8.46229096311843));
#35545=CARTESIAN_POINT('Ctrl Pts',(-67.4285455390928,-15.6526293851286,
8.89658813193769));
#35546=CARTESIAN_POINT('Ctrl Pts',(-67.4412654718215,-15.4707226080323,
9.45032013874425));
#35547=CARTESIAN_POINT('Ctrl Pts',(-67.4086397233445,-15.458048217099,10.0018117506529));
#35548=CARTESIAN_POINT('Origin',(17.0820569767664,-63.7511045350785,10.));
#35549=CARTESIAN_POINT('',(13.7189801527801,-60.9122168113323,9.99965378812953));
#35550=CARTESIAN_POINT('',(13.6458118873637,-60.6472937215209,9.99664393250996));
#35551=CARTESIAN_POINT('',(14.6503387090836,-64.4026814811241,10.));
#35552=CARTESIAN_POINT('',(14.1985145724514,-60.3826426720153,11.6359872033748));
#35553=CARTESIAN_POINT('Ctrl Pts',(13.6458118873637,-60.6472937215209,9.99664393250996));
#35554=CARTESIAN_POINT('Ctrl Pts',(13.6410407802454,-60.6097205320263,10.5892058593235));
#35555=CARTESIAN_POINT('Ctrl Pts',(13.8356159531907,-60.5187326677745,11.1848035603042));
#35556=CARTESIAN_POINT('Ctrl Pts',(14.1985145724514,-60.3826426720153,11.6359872033748));
#35557=CARTESIAN_POINT('',(17.8984305821305,-59.3912531651587,11.6380816927068));
#35558=CARTESIAN_POINT('Origin',(16.0467807963563,-59.8874012299222,10.));
#35559=CARTESIAN_POINT('Ctrl Pts',(17.8984546702663,-59.3912467107622,11.6380966037224));
#35560=CARTESIAN_POINT('Ctrl Pts',(17.4212611177617,-59.5701794123023,12.2270179049201));
#35561=CARTESIAN_POINT('Ctrl Pts',(16.6595160069781,-59.8253574740882,12.5674221981559));
#35562=CARTESIAN_POINT('Ctrl Pts',(15.9233267283635,-60.0736878712826,12.5157167035403));
#35563=CARTESIAN_POINT('Ctrl Pts',(15.1456267338053,-60.3360206084696,12.461095746608));
#35564=CARTESIAN_POINT('Ctrl Pts',(14.3964458015819,-60.5907116859351,11.9688993897473));
#35565=CARTESIAN_POINT('Ctrl Pts',(14.0146059447131,-60.7469740189126,11.2575578209418));
#35566=CARTESIAN_POINT('Ctrl Pts',(13.8116368860468,-60.8300361143405,10.8794403300266));
#35567=CARTESIAN_POINT('Ctrl Pts',(13.7124604894775,-60.8852870497794,10.4394030962359));
#35568=CARTESIAN_POINT('Ctrl Pts',(13.7189801527801,-60.9122168113323,9.99965378812953));
#35569=CARTESIAN_POINT('Origin',(17.0820569767664,-63.7511045350785,10.));
#35570=CARTESIAN_POINT('',(13.9708704146993,-61.8799991994799,9.99901528063934));
#35571=CARTESIAN_POINT('',(13.899975087973,-61.614467077582,10.0012573013838));
#35572=CARTESIAN_POINT('',(14.6503387090836,-64.4026814811241,10.));
#35573=CARTESIAN_POINT('Ctrl Pts',(13.899975087973,-61.614467077582,10.0012573013838));
#35574=CARTESIAN_POINT('Ctrl Pts',(13.8982899610888,-61.6099667912195,10.0766544396888));
#35575=CARTESIAN_POINT('Ctrl Pts',(13.900043500223,-61.6045451170744,10.1520128061815));
#35576=CARTESIAN_POINT('Ctrl Pts',(13.9053569552699,-61.5981695663354,10.2270376921985));
#35577=CARTESIAN_POINT('Ctrl Pts',(13.9634527171371,-61.5284611611193,11.047337830936));
#35578=CARTESIAN_POINT('Ctrl Pts',(14.4471220222725,-61.3447206686646,11.8277717281245));
#35579=CARTESIAN_POINT('Ctrl Pts',(15.1337367424348,-61.1066011161457,12.2189611289229));
#35580=CARTESIAN_POINT('Ctrl Pts',(15.8203514625971,-60.8684815636268,12.6101505297212));
#35581=CARTESIAN_POINT('Ctrl Pts',(16.7099115977863,-60.5759829510439,12.6120954341293));
#35582=CARTESIAN_POINT('Ctrl Pts',(17.3980067606845,-60.3374667150895,12.2237523563129));
#35583=CARTESIAN_POINT('Ctrl Pts',(18.0861019235826,-60.0989504791351,11.8354092784964));
#35584=CARTESIAN_POINT('Ctrl Pts',(18.5727321141896,-59.9144166198093,11.0567782184554));
#35585=CARTESIAN_POINT('Ctrl Pts',(18.6339764021913,-59.8438645695582,10.2368654679638));
#35586=CARTESIAN_POINT('Ctrl Pts',(18.6952206901929,-59.7733125193071,9.41695271747212));
#35587=CARTESIAN_POINT('Ctrl Pts',(18.3310790755891,-59.8167422781306,8.55575827652985));
#35588=CARTESIAN_POINT('Ctrl Pts',(17.6984585141966,-59.932110753931,8.03819621078674));
#35589=CARTESIAN_POINT('Ctrl Pts',(17.0658379528042,-60.0474792297314,7.52063414504363));
#35590=CARTESIAN_POINT('Ctrl Pts',(16.1647384446231,-60.2347864225085,7.34670445449967));
#35591=CARTESIAN_POINT('Ctrl Pts',(15.392769597115,-60.3874931590403,7.59575134544315));
#35592=CARTESIAN_POINT('Ctrl Pts',(14.6208007496069,-60.540199895572,7.84479823638662));
#35593=CARTESIAN_POINT('Ctrl Pts',(13.9779625627717,-60.6583061758583,8.51682170881753));
#35594=CARTESIAN_POINT('Ctrl Pts',(13.7459615817213,-60.6663289586339,9.30743209219173));
#35595=CARTESIAN_POINT('Ctrl Pts',(13.6804424696227,-60.6685946628634,9.5307073994776));
#35596=CARTESIAN_POINT('Ctrl Pts',(13.6476895615158,-60.6620806891943,9.76344057197141));
#35597=CARTESIAN_POINT('Ctrl Pts',(13.6458118873637,-60.6472937215209,9.99664393250996));
#35598=CARTESIAN_POINT('Ctrl Pts',(13.7189801527801,-60.9122168113323,9.99965378812953));
#35599=CARTESIAN_POINT('Ctrl Pts',(13.7247257446778,-60.9359492362449,9.61211536100744));
#35600=CARTESIAN_POINT('Ctrl Pts',(13.8125590225005,-60.9376863320054,9.22480054821092));
#35601=CARTESIAN_POINT('Ctrl Pts',(13.9837827281426,-60.9170790299751,8.88028612326233));
#35602=CARTESIAN_POINT('Ctrl Pts',(14.3492981499551,-60.8730881195708,8.14484277513865));
#35603=CARTESIAN_POINT('Ctrl Pts',(15.0948277750944,-60.7272727102727,7.60444285964159));
#35604=CARTESIAN_POINT('Ctrl Pts',(15.8946095193187,-60.5669204894781,7.49935843056475));
#35605=CARTESIAN_POINT('Ctrl Pts',(16.6943912635429,-60.4065682686835,7.3942740014879));
#35606=CARTESIAN_POINT('Ctrl Pts',(17.548425126852,-60.2316792363924,7.72450505883126));
#35607=CARTESIAN_POINT('Ctrl Pts',(18.0828447847105,-60.1424305723414,8.3432095629449));
#35608=CARTESIAN_POINT('Ctrl Pts',(18.6172644425689,-60.0531819082903,8.96191406705854));
#35609=CARTESIAN_POINT('Ctrl Pts',(18.8320698949766,-60.0495736124793,9.86909201794247));
#35610=CARTESIAN_POINT('Ctrl Pts',(18.6376771842086,-60.1556096340356,10.6611508664112));
#35611=CARTESIAN_POINT('Ctrl Pts',(18.4432844734406,-60.2616456555918,11.4532097148799));
#35612=CARTESIAN_POINT('Ctrl Pts',(17.8396935994969,-60.4773259945153,12.1301494609334));
#35613=CARTESIAN_POINT('Ctrl Pts',(17.1014273477894,-60.7290924921509,12.3908459426517));
#35614=CARTESIAN_POINT('Ctrl Pts',(16.3631610960819,-60.9808589897865,12.6515424243699));
#35615=CARTESIAN_POINT('Ctrl Pts',(15.4902194666106,-61.2687116461343,12.4959956417529));
#35616=CARTESIAN_POINT('Ctrl Pts',(14.8769273589396,-61.4869914228006,11.9933937214367));
#35617=CARTESIAN_POINT('Ctrl Pts',(14.3076501674883,-61.6896056365772,11.52686267361));
#35618=CARTESIAN_POINT('Ctrl Pts',(13.9620906745725,-61.8322748736988,10.7613040129743));
#35619=CARTESIAN_POINT('Ctrl Pts',(13.9708704146993,-61.8799991994799,9.99901528063934));
#35620=CARTESIAN_POINT('Origin',(17.0820569767664,-63.7511045350785,10.));
#35621=CARTESIAN_POINT('',(14.2348698103755,-62.8445369550162,10.0018466754434));
#35622=CARTESIAN_POINT('',(14.1654859215485,-62.5785998445538,10.0004462653844));
#35623=CARTESIAN_POINT('',(14.6503387090836,-64.4026814811241,10.));
#35624=CARTESIAN_POINT('Ctrl Pts',(14.1654859215485,-62.5785998445538,10.0004462653844));
#35625=CARTESIAN_POINT('Ctrl Pts',(14.1585827534688,-62.5552558244195,10.386770248634));
#35626=CARTESIAN_POINT('Ctrl Pts',(14.2332491130212,-62.5100553152291,10.7728367424032));
#35627=CARTESIAN_POINT('Ctrl Pts',(14.3908772813227,-62.4426252563818,11.1164878478952));
#35628=CARTESIAN_POINT('Ctrl Pts',(14.7296226663468,-62.2977170112848,11.8549994178656));
#35629=CARTESIAN_POINT('Ctrl Pts',(15.4515079046906,-62.0501467519025,12.397625364221));
#35630=CARTESIAN_POINT('Ctrl Pts',(16.2272258855742,-61.7881520526304,12.501389418797));
#35631=CARTESIAN_POINT('Ctrl Pts',(17.0029438664577,-61.5261573533583,12.605153473373));
#35632=CARTESIAN_POINT('Ctrl Pts',(17.832494589881,-61.2497382141963,12.2700556361696));
#35633=CARTESIAN_POINT('Ctrl Pts',(18.3383599455201,-61.0600503079339,11.6461438143239));
#35634=CARTESIAN_POINT('Ctrl Pts',(18.8442253011592,-60.8703624016714,11.0222319924783));
#35635=CARTESIAN_POINT('Ctrl Pts',(19.0264052890141,-60.7674057283086,10.1095061859904));
#35636=CARTESIAN_POINT('Ctrl Pts',(18.7972629292321,-60.7746625458238,9.3166725220468));
#35637=CARTESIAN_POINT('Ctrl Pts',(18.5681205694502,-60.7819193633391,8.52383885810324));
#35638=CARTESIAN_POINT('Ctrl Pts',(17.9276558620313,-60.8993896717325,7.85089733670406));
#35639=CARTESIAN_POINT('Ctrl Pts',(17.1565944419206,-61.0518532638259,7.59916807226838));
#35640=CARTESIAN_POINT('Ctrl Pts',(16.3855330218099,-61.2043168559193,7.3474388078327));
#35641=CARTESIAN_POINT('Ctrl Pts',(15.4838748890073,-61.3917737317127,7.51692180036052));
#35642=CARTESIAN_POINT('Ctrl Pts',(14.8493069319055,-61.5076640106208,8.0317464867676));
#35643=CARTESIAN_POINT('Ctrl Pts',(14.2727767422054,-61.6129549313732,8.49948515966275));
#35644=CARTESIAN_POINT('Ctrl Pts',(13.9167146450877,-61.6591716047613,9.25228420341938));
#35645=CARTESIAN_POINT('Ctrl Pts',(13.899975087973,-61.614467077582,10.0012573013838));
#35646=CARTESIAN_POINT('Ctrl Pts',(13.9708704146993,-61.8799991994799,9.99901528063934));
#35647=CARTESIAN_POINT('Ctrl Pts',(13.971549239588,-61.8836891105328,9.94007725327275));
#35648=CARTESIAN_POINT('Ctrl Pts',(13.9743462862715,-61.8868114457664,9.88115877337014));
#35649=CARTESIAN_POINT('Ctrl Pts',(13.9793219277933,-61.8893500282724,9.8223995623229));
#35650=CARTESIAN_POINT('Ctrl Pts',(14.0486511901885,-61.9247219600932,9.00366438154045));
#35651=CARTESIAN_POINT('Ctrl Pts',(14.5409523008495,-61.8467589267501,8.21585107799077));
#35652=CARTESIAN_POINT('Ctrl Pts',(15.2432213925389,-61.712535142454,7.80941972573595));
#35653=CARTESIAN_POINT('Ctrl Pts',(15.9454904842283,-61.578311358158,7.40298837348113));
#35654=CARTESIAN_POINT('Ctrl Pts',(16.8577275569459,-61.387826822909,7.37793897252116));
#35655=CARTESIAN_POINT('Ctrl Pts',(17.5801209048417,-61.2482107604141,7.74541574302326));
#35656=CARTESIAN_POINT('Ctrl Pts',(18.3025142527375,-61.1085946979193,8.11289251352536));
#35657=CARTESIAN_POINT('Ctrl Pts',(18.8350638758114,-61.0198471081786,8.87289545548955));
#35658=CARTESIAN_POINT('Ctrl Pts',(18.9468623871525,-61.0438394390412,9.68733378926645));
#35659=CARTESIAN_POINT('Ctrl Pts',(19.0586608984936,-61.0678317699038,10.5017721230433));
#35660=CARTESIAN_POINT('Ctrl Pts',(18.749708298102,-61.2045640213696,11.3706458486329));
#35661=CARTESIAN_POINT('Ctrl Pts',(18.1634433884682,-61.4156018821482,11.9074332417685));
#35662=CARTESIAN_POINT('Ctrl Pts',(17.5771784788343,-61.6266397429267,12.444220634904));
#35663=CARTESIAN_POINT('Ctrl Pts',(16.7136012599583,-61.9119832130179,12.6489216955856));
#35664=CARTESIAN_POINT('Ctrl Pts',(15.9628772265394,-62.1670877632026,12.4304742338454));
#35665=CARTESIAN_POINT('Ctrl Pts',(15.2121531931205,-62.4221923133873,12.2120267721052));
#35666=CARTESIAN_POINT('Ctrl Pts',(14.5742823451589,-62.6470579436654,11.5704307879434));
#35667=CARTESIAN_POINT('Ctrl Pts',(14.3390239366156,-62.7640438959386,10.7911028658273));
#35668=CARTESIAN_POINT('Ctrl Pts',(14.2625865983512,-62.8020535673526,10.5378929917551));
#35669=CARTESIAN_POINT('Ctrl Pts',(14.2286511253629,-62.828674898289,10.2701434172215));
#35670=CARTESIAN_POINT('Ctrl Pts',(14.2348698103755,-62.8445369550162,10.0018466754434));
#35671=CARTESIAN_POINT('Origin',(17.0820569767664,-63.7511045350785,10.));
#35672=CARTESIAN_POINT('',(14.4927485186002,-63.8107147438123,9.99793352624086));
#35673=CARTESIAN_POINT('',(14.4189472139579,-63.5459612763503,9.99811000378502));
#35674=CARTESIAN_POINT('',(14.6503387090836,-64.4026814811241,10.));
#35675=CARTESIAN_POINT('Ctrl Pts',(14.4189472139579,-63.5459612763503,9.99811000378502));
#35676=CARTESIAN_POINT('Ctrl Pts',(14.4131993125783,-63.5020657997403,10.6909216248416));
#35677=CARTESIAN_POINT('Ctrl Pts',(14.6895870615306,-63.3825723034678,11.3881278716996));
#35678=CARTESIAN_POINT('Ctrl Pts',(15.1696780211856,-63.2084966963919,11.8560065223221));
#35679=CARTESIAN_POINT('Ctrl Pts',(15.7417608055527,-63.0010658835769,12.4135369565263));
#35680=CARTESIAN_POINT('Ctrl Pts',(16.6030903983924,-62.7161316220184,12.6454354329572));
#35681=CARTESIAN_POINT('Ctrl Pts',(17.3619190322645,-62.4586624096387,12.4478622804133));
#35682=CARTESIAN_POINT('Ctrl Pts',(18.1207476661366,-62.201193197259,12.2502891278695));
#35683=CARTESIAN_POINT('Ctrl Pts',(18.7770753410411,-61.9711890340581,11.6232443463508));
#35684=CARTESIAN_POINT('Ctrl Pts',(19.0309502087539,-61.8490217755358,10.8475065234706));
#35685=CARTESIAN_POINT('Ctrl Pts',(19.2848250764668,-61.7268545170136,10.0717687005904));
#35686=CARTESIAN_POINT('Ctrl Pts',(19.136247136988,-61.7125241631699,9.14733783634868));
#35687=CARTESIAN_POINT('Ctrl Pts',(18.6456858472655,-61.789827971849,8.48815640829363));
#35688=CARTESIAN_POINT('Ctrl Pts',(18.1551245575431,-61.867131780528,7.82897498023858));
#35689=CARTESIAN_POINT('Ctrl Pts',(17.3225799175771,-62.0360697517297,7.43504298837021));
#35690=CARTESIAN_POINT('Ctrl Pts',(16.5147885234738,-62.1983751106924,7.48275547481141));
#35691=CARTESIAN_POINT('Ctrl Pts',(15.7069971293705,-62.3606804696551,7.53046796125262));
#35692=CARTESIAN_POINT('Ctrl Pts',(14.9239589811301,-62.5163532163788,8.0198249260034));
#35693=CARTESIAN_POINT('Ctrl Pts',(14.5102426728621,-62.5730664743348,8.73170200517146));
#35694=CARTESIAN_POINT('Ctrl Pts',(14.2890407035395,-62.6033893890854,9.11232178902005));
#35695=CARTESIAN_POINT('Ctrl Pts',(14.1734177690262,-62.6054224867212,9.55655400073801));
#35696=CARTESIAN_POINT('Ctrl Pts',(14.1654859215485,-62.5785998445538,10.0004462653844));
#35697=CARTESIAN_POINT('Ctrl Pts',(14.2348698103755,-62.8445369550162,10.0018466754434));
#35698=CARTESIAN_POINT('Ctrl Pts',(14.2477909590166,-62.8774950470096,9.44438121878225));
#35699=CARTESIAN_POINT('Ctrl Pts',(14.4340668190784,-62.8640028840737,8.88455351560674));
#35700=CARTESIAN_POINT('Ctrl Pts',(14.7726377170273,-62.8097033887247,8.44788099502246));
#35701=CARTESIAN_POINT('Ctrl Pts',(15.274155875107,-62.7292706549691,7.80104690640403));
#35702=CARTESIAN_POINT('Ctrl Pts',(16.1098381603914,-62.5592989131896,7.42443858923755));
#35703=CARTESIAN_POINT('Ctrl Pts',(16.9139278054309,-62.3977923938505,7.48559176785145));
#35704=CARTESIAN_POINT('Ctrl Pts',(17.7180174504703,-62.2362858745114,7.54674494646536));
#35705=CARTESIAN_POINT('Ctrl Pts',(18.4905144552649,-62.0832445776126,8.04565962085964));
#35706=CARTESIAN_POINT('Ctrl Pts',(18.8937702597924,-62.0291411621378,8.76039160250505));
#35707=CARTESIAN_POINT('Ctrl Pts',(19.2970260643199,-61.9750377466629,9.47512358415046));
#35708=CARTESIAN_POINT('Ctrl Pts',(19.3310406685804,-62.0198722126119,10.405672873047));
#35709=CARTESIAN_POINT('Ctrl Pts',(18.9866823611345,-62.1660913946905,11.1380809107439));
#35710=CARTESIAN_POINT('Ctrl Pts',(18.6423240536885,-62.312310576769,11.8704889484408));
#35711=CARTESIAN_POINT('Ctrl Pts',(17.9195928345363,-62.5599144749771,12.4047557349382));
#35712=CARTESIAN_POINT('Ctrl Pts',(17.1459983851496,-62.8211471346509,12.5032105584454));
#35713=CARTESIAN_POINT('Ctrl Pts',(16.372403935763,-63.0823797943246,12.6016653819527));
#35714=CARTESIAN_POINT('Ctrl Pts',(15.547946256142,-63.3572412154642,12.2643082424699));
#35715=CARTESIAN_POINT('Ctrl Pts',(15.0453884512907,-63.5458498251155,11.6412138093997));
#35716=CARTESIAN_POINT('Ctrl Pts',(14.6827506455303,-63.6819468306564,11.1915986689942));
#35717=CARTESIAN_POINT('Ctrl Pts',(14.4877209077723,-63.7731333897311,10.5932047327949));
#35718=CARTESIAN_POINT('Ctrl Pts',(14.4927485186002,-63.8107147438123,9.99793352624086));
#35719=CARTESIAN_POINT('Origin',(17.0820569767664,-63.7511045350785,10.));
#35720=CARTESIAN_POINT('',(14.7480685208434,-64.7775781358098,10.001505123818));
#35721=CARTESIAN_POINT('',(14.6789571988966,-64.511567991272,10.0021294030496));
#35722=CARTESIAN_POINT('',(14.6503387090836,-64.4026814811241,10.));
#35723=CARTESIAN_POINT('Ctrl Pts',(14.6789571988966,-64.511567991272,10.0021294030496));
#35724=CARTESIAN_POINT('Ctrl Pts',(14.6745624451438,-64.5012097288919,10.1782532036583));
#35725=CARTESIAN_POINT('Ctrl Pts',(14.6880487522533,-64.4860602506939,10.354078307347));
#35726=CARTESIAN_POINT('Ctrl Pts',(14.7205078014429,-64.4658270415774,10.5257161206906));
#35727=CARTESIAN_POINT('Ctrl Pts',(14.8728494531258,-64.3708655262953,11.3312723100704));
#35728=CARTESIAN_POINT('Ctrl Pts',(15.4431136830601,-64.1639219936719,12.0445928505661));
#35729=CARTESIAN_POINT('Ctrl Pts',(16.1698862069573,-63.9150421900725,12.3462664892695));
#35730=CARTESIAN_POINT('Ctrl Pts',(16.8966587308544,-63.6661623864731,12.6479401279729));
#35731=CARTESIAN_POINT('Ctrl Pts',(17.7799395487143,-63.3753463118976,12.5379668648842));
#35732=CARTESIAN_POINT('Ctrl Pts',(18.4181515535132,-63.1501962278718,12.0655906176062));
#35733=CARTESIAN_POINT('Ctrl Pts',(19.0563635583122,-62.925046143846,11.5932143703281));
#35734=CARTESIAN_POINT('Ctrl Pts',(19.4495067500502,-62.7655620503699,10.7584351388608));
#35735=CARTESIAN_POINT('Ctrl Pts',(19.4154782471595,-62.7205382674991,9.93505104704534));
#35736=CARTESIAN_POINT('Ctrl Pts',(19.3814497442687,-62.6755144846282,9.11166695522986));
#35737=CARTESIAN_POINT('Ctrl Pts',(18.9202495467492,-62.7449510123626,8.29967800306621));
#35738=CARTESIAN_POINT('Ctrl Pts',(18.2323333520888,-62.8751359084421,7.8626772661126));
#35739=CARTESIAN_POINT('Ctrl Pts',(17.5444171574285,-63.0053208045216,7.425676529159));
#35740=CARTESIAN_POINT('Ctrl Pts',(16.6297849656272,-63.1962540689461,7.36366400741544));
#35741=CARTESIAN_POINT('Ctrl Pts',(15.8919306215938,-63.3398198518216,7.70440771629217));
#35742=CARTESIAN_POINT('Ctrl Pts',(15.1540762775605,-63.4833856346971,8.04515142516891));
#35743=CARTESIAN_POINT('Ctrl Pts',(14.592999781295,-63.5795839360235,8.78865136466594));
#35744=CARTESIAN_POINT('Ctrl Pts',(14.4538795211095,-63.5627194046509,9.60198253040318));
#35745=CARTESIAN_POINT('Ctrl Pts',(14.4315087612499,-63.5600075610921,9.73276747984734));
#35746=CARTESIAN_POINT('Ctrl Pts',(14.4200485884486,-63.5543722345421,9.86535806600957));
#35747=CARTESIAN_POINT('Ctrl Pts',(14.4189472139579,-63.5459612763503,9.99811000378502));
#35748=CARTESIAN_POINT('Ctrl Pts',(14.4927485186002,-63.8107147438123,9.99793352624086));
#35749=CARTESIAN_POINT('Ctrl Pts',(14.494688369579,-63.8252151156581,9.76825436605176));
#35750=CARTESIAN_POINT('Ctrl Pts',(14.5264111861321,-63.8317351659301,9.53904009330709));
#35751=CARTESIAN_POINT('Ctrl Pts',(14.5897808794637,-63.8297754611264,9.31901604644622));
#35752=CARTESIAN_POINT('Ctrl Pts',(14.8173890425694,-63.8227366893229,8.52874444322046));
#35753=CARTESIAN_POINT('Ctrl Pts',(15.4532632988624,-63.7063033475529,7.85703296342649));
#35754=CARTESIAN_POINT('Ctrl Pts',(16.2205322683665,-63.5546628984883,7.60269513736947));
#35755=CARTESIAN_POINT('Ctrl Pts',(16.9878012378705,-63.4030224494237,7.34835731131246));
#35756=CARTESIAN_POINT('Ctrl Pts',(17.8864649205858,-63.2161748930643,7.51139313899238));
#35757=CARTESIAN_POINT('Ctrl Pts',(18.5227490121289,-63.09963173627,8.01927548227225));
#35758=CARTESIAN_POINT('Ctrl Pts',(19.1590331036721,-62.9830885794757,8.52715782555213));
#35759=CARTESIAN_POINT('Ctrl Pts',(19.5329376040431,-62.9368498222464,9.37988668443198));
#35760=CARTESIAN_POINT('Ctrl Pts',(19.4841294236266,-63.0038765864645,10.1981222260487));
#35761=CARTESIAN_POINT('Ctrl Pts',(19.43532124321,-63.0709033506826,11.0163577676654));
#35762=CARTESIAN_POINT('Ctrl Pts',(18.9638003820058,-63.2511956363481,11.800099992019));
#35763=CARTESIAN_POINT('Ctrl Pts',(18.2853245933942,-63.4869413276821,12.2006980454406));
#35764=CARTESIAN_POINT('Ctrl Pts',(17.6068488047826,-63.7226870190161,12.6012960988622));
#35765=CARTESIAN_POINT('Ctrl Pts',(16.7214180887637,-64.0138861160185,12.6187499813517));
#35766=CARTESIAN_POINT('Ctrl Pts',(16.0289196480801,-64.253389165651,12.2452952639449));
#35767=CARTESIAN_POINT('Ctrl Pts',(15.3364212073965,-64.4928922152834,11.8718405465381));
#35768=CARTESIAN_POINT('Ctrl Pts',(14.8368550420482,-64.6806992175459,11.1074772292349));
#35769=CARTESIAN_POINT('Ctrl Pts',(14.7584549707696,-64.7556551050229,10.2922353809895));
#35770=CARTESIAN_POINT('Ctrl Pts',(14.7491833360657,-64.7645194286933,10.195824440425));
#35771=CARTESIAN_POINT('Ctrl Pts',(14.7458019429916,-64.7718054668758,10.0987019353608));
#35772=CARTESIAN_POINT('Ctrl Pts',(14.7480685208434,-64.7775781358098,10.001505123818));
#35773=CARTESIAN_POINT('Origin',(17.0820569767664,-63.7511045350785,10.));
#35774=CARTESIAN_POINT('',(15.0130771992805,-65.7418454548454,9.99981028982554));
#35775=CARTESIAN_POINT('',(14.9415523108175,-65.4764820235065,9.9989223619293));
#35776=CARTESIAN_POINT('',(14.6503387090836,-64.4026814811241,10.));
#35777=CARTESIAN_POINT('Ctrl Pts',(14.9415523108175,-65.4764820235065,9.9989223619293));
#35778=CARTESIAN_POINT('Ctrl Pts',(14.9354685130879,-65.4463344353997,10.4860098738008));
#35779=CARTESIAN_POINT('Ctrl Pts',(15.0596306010493,-65.3812875674044,10.9740976137645));
#35780=CARTESIAN_POINT('Ctrl Pts',(15.3070399126418,-65.2832167053679,11.3788468299413));
#35781=CARTESIAN_POINT('Ctrl Pts',(15.7285664365572,-65.1161273209564,12.0684430664547));
#35782=CARTESIAN_POINT('Ctrl Pts',(16.5078555104223,-64.8531757502037,12.5161238918082));
#35783=CARTESIAN_POINT('Ctrl Pts',(17.2898955363443,-64.5894870640691,12.5214264196761));
#35784=CARTESIAN_POINT('Ctrl Pts',(18.0719355622662,-64.3257983779344,12.526728947544));
#35785=CARTESIAN_POINT('Ctrl Pts',(18.856726540245,-64.0613725764177,12.0896531779262));
#35786=CARTESIAN_POINT('Ctrl Pts',(19.2867932233327,-63.8919948632527,11.4059132558295));
#35787=CARTESIAN_POINT('Ctrl Pts',(19.7168599064204,-63.7226171500878,10.7221733337328));
#35788=CARTESIAN_POINT('Ctrl Pts',(19.7922022946168,-63.6482875252747,9.7917692591572));
#35789=CARTESIAN_POINT('Ctrl Pts',(19.4730226094499,-63.6796697714155,9.03131812620868));
#35790=CARTESIAN_POINT('Ctrl Pts',(19.153842924283,-63.7110520175564,8.27086699326015));
#35791=CARTESIAN_POINT('Ctrl Pts',(18.4401411657526,-63.8481461346512,7.68036880193875));
#35792=CARTESIAN_POINT('Ctrl Pts',(17.6454383857665,-64.0069444100312,7.524237313639));
#35793=CARTESIAN_POINT('Ctrl Pts',(16.8507356057803,-64.1657426854112,7.36810582533925));
#35794=CARTESIAN_POINT('Ctrl Pts',(15.9750318043384,-64.3462451190763,7.64634104006116));
#35795=CARTESIAN_POINT('Ctrl Pts',(15.4043894403333,-64.4450065869384,8.23435456655407));
#35796=CARTESIAN_POINT('Ctrl Pts',(14.9553323969432,-64.5227251994293,8.69708154291638));
#35797=CARTESIAN_POINT('Ctrl Pts',(14.6951885590369,-64.5498246710713,9.35164270965608));
#35798=CARTESIAN_POINT('Ctrl Pts',(14.6789571988966,-64.511567991272,10.0021294030496));
#35799=CARTESIAN_POINT('Ctrl Pts',(14.7480685208434,-64.7775781358098,10.001505123818));
#35800=CARTESIAN_POINT('Ctrl Pts',(14.7649679121881,-64.8206186125989,9.276814836016));
#35801=CARTESIAN_POINT('Ctrl Pts',(15.0958410226864,-64.7795300848962,8.54799381140143));
#35802=CARTESIAN_POINT('Ctrl Pts',(15.6402720254873,-64.6812188924137,8.07917134860812));
#35803=CARTESIAN_POINT('Ctrl Pts',(16.2577231286925,-64.5697220196356,7.54746954365978));
#35804=CARTESIAN_POINT('Ctrl Pts',(17.1498593123118,-64.3846235013877,7.35018631295075));
#35805=CARTESIAN_POINT('Ctrl Pts',(17.9258100558561,-64.2306567779801,7.57508388624563));
#35806=CARTESIAN_POINT('Ctrl Pts',(18.7017607994005,-64.0766900545725,7.7999814595405));
#35807=CARTESIAN_POINT('Ctrl Pts',(19.3615261028698,-63.9538551260052,8.44705983683928));
#35808=CARTESIAN_POINT('Ctrl Pts',(19.6176065589079,-63.9391872263039,9.22846362604921));
#35809=CARTESIAN_POINT('Ctrl Pts',(19.873687014946,-63.9245193266025,10.0098674152591));
#35810=CARTESIAN_POINT('Ctrl Pts',(19.7260826235527,-64.0180184557671,10.9255966163802));
#35811=CARTESIAN_POINT('Ctrl Pts',(19.2464556042235,-64.200482779956,11.5682854345737));
#35812=CARTESIAN_POINT('Ctrl Pts',(18.7668285848942,-64.3829471041448,12.2109742527672));
#35813=CARTESIAN_POINT('Ctrl Pts',(17.955178937629,-64.654376623358,12.5806226880331));
#35814=CARTESIAN_POINT('Ctrl Pts',(17.1785720640666,-64.9164164596569,12.5127911771402));
#35815=CARTESIAN_POINT('Ctrl Pts',(16.4019651905042,-65.1784562959559,12.4449596662474));
#35816=CARTESIAN_POINT('Ctrl Pts',(15.6604010906447,-65.4311064493406,11.9396482091957));
#35817=CARTESIAN_POINT('Ctrl Pts',(15.2897673262125,-65.5843661188994,11.2216465877777));
#35818=CARTESIAN_POINT('Ctrl Pts',(15.0989143577318,-65.6632851643039,10.8519211229878));
#35819=CARTESIAN_POINT('Ctrl Pts',(15.0064172468355,-65.7158498370977,10.4257987515067));
#35820=CARTESIAN_POINT('Ctrl Pts',(15.0130771992805,-65.7418454548454,9.99981028982554));
#35821=CARTESIAN_POINT('Origin',(17.0820569767664,-63.7511045350785,10.));
#35822=CARTESIAN_POINT('',(15.2652009106025,-66.709565290414,9.99881345470574));
#35823=CARTESIAN_POINT('',(15.1934336836835,-66.4442667934687,9.99943462192768));
#35824=CARTESIAN_POINT('',(14.6503387090836,-64.4026814811241,10.));
#35825=CARTESIAN_POINT('Ctrl Pts',(15.1934336836835,-66.4442667934687,9.99943462192768));
#35826=CARTESIAN_POINT('Ctrl Pts',(15.1827995799554,-66.3950965524831,10.7909504295073));
#35827=CARTESIAN_POINT('Ctrl Pts',(15.5599243826036,-66.2420266256761,11.5846294221378));
#35828=CARTESIAN_POINT('Ctrl Pts',(16.1674256670555,-66.0272275066146,12.0468004663334));
#35829=CARTESIAN_POINT('Ctrl Pts',(16.7997089272064,-65.8036660249294,12.5278249876806));
#35830=CARTESIAN_POINT('Ctrl Pts',(17.6815476659071,-65.5132363543,12.6497433013673));
#35831=CARTESIAN_POINT('Ctrl Pts',(18.4120106025366,-65.2633677075892,12.3579626123137));
#35832=CARTESIAN_POINT('Ctrl Pts',(19.1424735391661,-65.0134990608784,12.06618192326));
#35833=CARTESIAN_POINT('Ctrl Pts',(19.7215606737244,-64.8041914380861,11.3607022314659));
#35834=CARTESIAN_POINT('Ctrl Pts',(19.8839069496221,-64.7065491918251,10.5574238638963));
#35835=CARTESIAN_POINT('Ctrl Pts',(20.0462532255198,-64.608906945564,9.75414549632673));
#35836=CARTESIAN_POINT('Ctrl Pts',(19.7918586427569,-64.6229300758342,8.8530684529817));
#35837=CARTESIAN_POINT('Ctrl Pts',(19.2285753341563,-64.7197196907436,8.25767771891592));
#35838=CARTESIAN_POINT('Ctrl Pts',(18.6652920255557,-64.816509305653,7.66228698485014));
#35839=CARTESIAN_POINT('Ctrl Pts',(17.7931199911174,-64.9960654052016,7.37258256006362));
#35840=CARTESIAN_POINT('Ctrl Pts',(16.9965402212509,-65.1553666185043,7.51828854147109));
#35841=CARTESIAN_POINT('Ctrl Pts',(16.1999604513844,-65.3146678318069,7.66399452287857));
#35842=CARTESIAN_POINT('Ctrl Pts',(15.4789729460896,-65.4537141588635,8.24511091048004));
#35843=CARTESIAN_POINT('Ctrl Pts',(15.1503611804251,-65.4876237233566,9.00142492811739));
#35844=CARTESIAN_POINT('Ctrl Pts',(15.0146236613656,-65.5016305260266,9.31383062721456));
#35845=CARTESIAN_POINT('Ctrl Pts',(14.9458338550092,-65.4976987431426,9.65612879778041));
#35846=CARTESIAN_POINT('Ctrl Pts',(14.9415523108175,-65.4764820235065,9.9989223619293));
#35847=CARTESIAN_POINT('Ctrl Pts',(15.0130771992805,-65.7418454548454,9.99981028982554));
#35848=CARTESIAN_POINT('Ctrl Pts',(15.0193507802528,-65.7663329589547,9.59853518618477));
#35849=CARTESIAN_POINT('Ctrl Pts',(15.1136101264191,-65.7672447483348,9.19737890571016));
#35850=CARTESIAN_POINT('Ctrl Pts',(15.2965249330007,-65.744401378692,8.84359325274533));
#35851=CARTESIAN_POINT('Ctrl Pts',(15.6736197332262,-65.6973077831931,8.1142333249153));
#35852=CARTESIAN_POINT('Ctrl Pts',(16.4275127626821,-65.5492514064624,7.58620525503956));
#35853=CARTESIAN_POINT('Ctrl Pts',(17.2288315064446,-65.3884873478828,7.49440429239113));
#35854=CARTESIAN_POINT('Ctrl Pts',(18.030150250207,-65.2277232893031,7.4026033297427));
#35855=CARTESIAN_POINT('Ctrl Pts',(18.878894708276,-65.0542515488746,7.74702947432161));
#35856=CARTESIAN_POINT('Ctrl Pts',(19.4034973688025,-64.9676333413308,8.37446367269948));
#35857=CARTESIAN_POINT('Ctrl Pts',(19.9281000293289,-64.8810151337869,9.00189787107735));
#35858=CARTESIAN_POINT('Ctrl Pts',(20.1285608923127,-64.8812504591278,9.91234012325419));
#35859=CARTESIAN_POINT('Ctrl Pts',(19.9217039083204,-64.9906262726287,10.7007759738114));
#35860=CARTESIAN_POINT('Ctrl Pts',(19.7148469243281,-65.1000020861296,11.4892118243687));
#35861=CARTESIAN_POINT('Ctrl Pts',(19.1006720933597,-65.3185183877906,12.1556412733063));
#35862=CARTESIAN_POINT('Ctrl Pts',(18.3583974645569,-65.5713589268319,12.4036017192683));
#35863=CARTESIAN_POINT('Ctrl Pts',(17.6161228357541,-65.8241994658732,12.6515621652302));
#35864=CARTESIAN_POINT('Ctrl Pts',(16.745748409117,-66.1113642422947,12.4810536082165));
#35865=CARTESIAN_POINT('Ctrl Pts',(16.1404633167949,-66.3274985456645,11.9679250313906));
#35866=CARTESIAN_POINT('Ctrl Pts',(15.5886775085547,-66.5245294039924,11.5001503082285));
#35867=CARTESIAN_POINT('Ctrl Pts',(15.2571911193414,-66.662531210899,10.7476451883996));
#35868=CARTESIAN_POINT('Ctrl Pts',(15.2652009106025,-66.709565290414,9.99881345470574));
#35869=CARTESIAN_POINT('Origin',(17.0820569767664,-63.7511045350785,10.));
#35870=CARTESIAN_POINT('',(15.5286491313886,-67.6742507328171,10.0019962882658));
#35871=CARTESIAN_POINT('',(15.458048217099,-67.4086397233445,10.0018117506528));
#35872=CARTESIAN_POINT('',(14.6503387090836,-64.4026814811241,10.));
#35873=CARTESIAN_POINT('',(20.2598690437801,-67.0040126136404,11.1728309286207));
#35874=CARTESIAN_POINT('Ctrl Pts',(15.5286491313886,-67.6742507328171,10.0019962882658));
#35875=CARTESIAN_POINT('Ctrl Pts',(15.5421457071955,-67.7079511930089,9.43113200366982));
#35876=CARTESIAN_POINT('Ctrl Pts',(15.7382477902416,-67.6927226550026,8.85763821511471));
#35877=CARTESIAN_POINT('Ctrl Pts',(16.0921495062908,-67.6352118327671,8.41584216487548));
#35878=CARTESIAN_POINT('Ctrl Pts',(16.6037821050588,-67.5520689427972,7.77714150008996));
#35879=CARTESIAN_POINT('Ctrl Pts',(17.4452195762654,-67.3805551035975,7.41369214583755));
#35880=CARTESIAN_POINT('Ctrl Pts',(18.2482818068303,-67.2193238791372,7.48861537411895));
#35881=CARTESIAN_POINT('Ctrl Pts',(19.0513440373952,-67.0580926546768,7.56353860240036));
#35882=CARTESIAN_POINT('Ctrl Pts',(19.8160310273183,-66.9071440449558,8.07683441321558));
#35883=CARTESIAN_POINT('Ctrl Pts',(20.2075211669018,-66.8561932299011,8.7968163762026));
#35884=CARTESIAN_POINT('Ctrl Pts',(20.5990113064853,-66.8052424148464,9.51679833918955));
#35885=CARTESIAN_POINT('Ctrl Pts',(20.6173045957293,-66.854289394458,10.4434664543483));
#35886=CARTESIAN_POINT('Ctrl Pts',(20.2598690437801,-67.0040126136404,11.1728309286206));
#35887=CARTESIAN_POINT('',(16.4802525979518,-68.0323660008166,11.8670505687059));
#35888=CARTESIAN_POINT('Ctrl Pts',(16.4806955947433,-68.0322473001841,11.8669181223571));
#35889=CARTESIAN_POINT('Ctrl Pts',(16.6817854205938,-67.9835336336721,12.0540417240897));
#35890=CARTESIAN_POINT('Ctrl Pts',(16.9239334961962,-67.923876532405,12.2143044024353));
#35891=CARTESIAN_POINT('Ctrl Pts',(17.4856657502708,-67.7816176378542,12.4543153408643));
#35892=CARTESIAN_POINT('Ctrl Pts',(17.8119729521746,-67.6966288605656,12.5175));
#35893=CARTESIAN_POINT('Ctrl Pts',(18.4226933621783,-67.5329868199039,12.5175));
#35894=CARTESIAN_POINT('Ctrl Pts',(18.747778077109,-67.4434356591205,12.4543153408643));
#35895=CARTESIAN_POINT('Ctrl Pts',(19.3446857260753,-67.2746559299571,12.1973867613172));
#35896=CARTESIAN_POINT('Ctrl Pts',(19.6165425195547,-67.1955448337828,12.0036443501621));
#35897=CARTESIAN_POINT('Ctrl Pts',(19.9960747381915,-67.0834304248293,11.6080270340044));
#35898=CARTESIAN_POINT('Ctrl Pts',(20.1448248140073,-67.0387983068925,11.4009948671633));
#35899=CARTESIAN_POINT('Ctrl Pts',(20.2598690437801,-67.0040126136404,11.1728309286206));
#35900=CARTESIAN_POINT('Ctrl Pts',(16.4776938604227,-68.0330516124712,11.8678155752478));
#35901=CARTESIAN_POINT('Ctrl Pts',(16.9785524830602,-67.8522271893252,12.3404055365588));
#35902=CARTESIAN_POINT('Ctrl Pts',(17.6838006560656,-67.6166367512168,12.5855412104357));
#35903=CARTESIAN_POINT('Ctrl Pts',(18.3529108900531,-67.3907294446845,12.5051234941037));
#35904=CARTESIAN_POINT('Ctrl Pts',(19.129979689639,-67.1283727946319,12.4117306641613));
#35905=CARTESIAN_POINT('Ctrl Pts',(19.8583083259861,-66.8790760319582,11.879255644893));
#35906=CARTESIAN_POINT('Ctrl Pts',(20.2061471825013,-66.7317311985187,11.1455779206959));
#35907=CARTESIAN_POINT('Ctrl Pts',(20.5539860390166,-66.5843863650793,10.4119001964987));
#35908=CARTESIAN_POINT('Ctrl Pts',(20.5213351156999,-66.5389934608741,9.47701976737269));
#35909=CARTESIAN_POINT('Ctrl Pts',(20.1165357938135,-66.5933174195301,8.75982961781549));
#35910=CARTESIAN_POINT('Ctrl Pts',(19.7117364719271,-66.6476413781862,8.04263946825829));
#35911=CARTESIAN_POINT('Ctrl Pts',(18.934788751471,-66.8016821997035,7.54313959826994));
#35912=CARTESIAN_POINT('Ctrl Pts',(18.1276415422747,-66.9638149498406,7.48486270274578));
#35913=CARTESIAN_POINT('Ctrl Pts',(17.3204943330785,-67.1259476999777,7.42658580722162));
#35914=CARTESIAN_POINT('Ctrl Pts',(16.483147635142,-67.2961723787346,7.80953188616166));
#35915=CARTESIAN_POINT('Ctrl Pts',(15.9844353298855,-67.3756602454435,8.46229096311826));
#35916=CARTESIAN_POINT('Ctrl Pts',(15.6526293851286,-67.4285455390929,8.89658813193753));
#35917=CARTESIAN_POINT('Ctrl Pts',(15.4707226080323,-67.4412654718215,9.45032013874414));
#35918=CARTESIAN_POINT('Ctrl Pts',(15.458048217099,-67.4086397233445,10.0018117506528));
#35919=CARTESIAN_POINT('Origin',(-18.6889152049569,69.7479810832458,10.));
#35920=CARTESIAN_POINT('',(-13.2791651259751,61.4484819638688,10.0015349814512));
#35921=CARTESIAN_POINT('',(-13.2658134652031,61.3659731009889,9.99957732584554));
#35922=CARTESIAN_POINT('',(-15.7201421778575,70.5434614183684,10.0000000000001));
#35923=CARTESIAN_POINT('',(-16.8135320242448,59.6819508576139,7.03077704625437));
#35924=CARTESIAN_POINT('Ctrl Pts',(-13.2658134652031,61.3659731009889,9.99957732584554));
#35925=CARTESIAN_POINT('Ctrl Pts',(-13.2594372491749,61.3390049028546,10.5364470372516));
#35926=CARTESIAN_POINT('Ctrl Pts',(-13.6128633281576,61.1616793186458,12.0843271181651));
#35927=CARTESIAN_POINT('Ctrl Pts',(-15.9358673415301,60.4026582657957,13.6055385422089));
#35928=CARTESIAN_POINT('Ctrl Pts',(-18.8976307583477,59.447210195013,12.2029441264611));
#35929=CARTESIAN_POINT('Ctrl Pts',(-19.3903963172923,59.1533281063616,8.83503768583798));
#35930=CARTESIAN_POINT('Ctrl Pts',(-17.7660737535059,59.4806667221929,7.29068223125052));
#35931=CARTESIAN_POINT('Ctrl Pts',(-16.8135320242448,59.6819508576139,7.03077704625438));
#35932=CARTESIAN_POINT('',(-15.2780776734586,60.093374610922,7.02605498021586));
#35933=CARTESIAN_POINT('Origin',(-16.0467807963563,59.8874012299222,10.));
#35934=CARTESIAN_POINT('Ctrl Pts',(-13.2791651259751,61.4484819638689,10.0015349814512));
#35935=CARTESIAN_POINT('Ctrl Pts',(-13.2773812390919,61.4440081401684,10.0935838809863));
#35936=CARTESIAN_POINT('Ctrl Pts',(-13.3061918618691,61.3771948495716,11.1915036202381));
#35937=CARTESIAN_POINT('Ctrl Pts',(-14.5474295567697,60.9313710113776,13.1842383274674));
#35938=CARTESIAN_POINT('Ctrl Pts',(-17.8144668208749,59.893545936598,13.1913616605741));
#35939=CARTESIAN_POINT('Ctrl Pts',(-19.6057481548832,59.2511484715134,10.339577077016));
#35940=CARTESIAN_POINT('Ctrl Pts',(-18.3013616530666,59.440726198154,7.2338208659921));
#35941=CARTESIAN_POINT('Ctrl Pts',(-16.187142356251,59.9014396609591,6.78116218790437));
#35942=CARTESIAN_POINT('Ctrl Pts',(-15.2780676602839,60.0933772939441,7.02603075613017));
#35943=CARTESIAN_POINT('Origin',(-18.6889152049569,69.7479810832458,10.));
#35944=CARTESIAN_POINT('',(-13.5461538679481,62.4122187264791,10.0005448248896));
#35945=CARTESIAN_POINT('',(-13.5161734774897,62.3341655182897,9.99879780140835));
#35946=CARTESIAN_POINT('',(-15.7201421778575,70.5434614183684,10.0000000000001));
#35947=CARTESIAN_POINT('Ctrl Pts',(-13.5161734774897,62.3341655182897,9.99879780140835));
#35948=CARTESIAN_POINT('Ctrl Pts',(-13.5082196148794,62.286219899295,10.9294410660881));
#35949=CARTESIAN_POINT('Ctrl Pts',(-14.3903370215027,61.9458317508116,12.870975191806));
#35950=CARTESIAN_POINT('Ctrl Pts',(-17.5197763142875,60.9493268661069,13.4270461480336));
#35951=CARTESIAN_POINT('Ctrl Pts',(-19.7394014348252,60.1927341524848,10.9477123134811));
#35952=CARTESIAN_POINT('Ctrl Pts',(-18.96159921589,60.2392996738452,7.62511676387811));
#35953=CARTESIAN_POINT('Ctrl Pts',(-15.8425832679708,60.9131915231956,6.41562502038854));
#35954=CARTESIAN_POINT('Ctrl Pts',(-13.6032001394547,61.3800631690208,8.04417985348941));
#35955=CARTESIAN_POINT('Ctrl Pts',(-13.2714326411404,61.389739398956,9.52644947847317));
#35956=CARTESIAN_POINT('Ctrl Pts',(-13.2658134652031,61.3659731009889,9.99957732584554));
#35957=CARTESIAN_POINT('Ctrl Pts',(-13.5461538679481,62.4122187264791,10.0005448248896));
#35958=CARTESIAN_POINT('Ctrl Pts',(-13.5391171409456,62.3889104933502,10.4721900135757));
#35959=CARTESIAN_POINT('Ctrl Pts',(-13.8305514728693,62.231485488278,11.9564181322133));
#35960=CARTESIAN_POINT('Ctrl Pts',(-16.0106566332711,61.5138509672068,13.5896176377582));
#35961=CARTESIAN_POINT('Ctrl Pts',(-19.0579057022672,60.5349179618126,12.3623010109727));
#35962=CARTESIAN_POINT('Ctrl Pts',(-19.7341192728292,60.1913020034494,9.0193860958895));
#35963=CARTESIAN_POINT('Ctrl Pts',(-17.3973455890627,60.6550135466887,6.55469600728496));
#35964=CARTESIAN_POINT('Ctrl Pts',(-14.2043402063787,61.3531034969371,7.15651357330629));
#35965=CARTESIAN_POINT('Ctrl Pts',(-13.2968857360054,61.4929236187117,9.08714816254585));
#35966=CARTESIAN_POINT('Ctrl Pts',(-13.2791651259751,61.4484819638689,10.0015349814512));
#35967=CARTESIAN_POINT('Origin',(-18.6889152049569,69.7479810832458,10.));
#35968=CARTESIAN_POINT('',(-13.7984318791272,63.3798972175256,9.9976925905199));
#35969=CARTESIAN_POINT('',(-13.7813169744248,63.2983967128177,10.0022545211422));
#35970=CARTESIAN_POINT('',(-15.7201421778575,70.5434614183684,10.0000000000001));
#35971=CARTESIAN_POINT('Ctrl Pts',(-13.7813169744248,63.2983967128177,10.0022545211422));
#35972=CARTESIAN_POINT('Ctrl Pts',(-13.7746926693741,63.282643341652,10.3298056773904));
#35973=CARTESIAN_POINT('Ctrl Pts',(-13.9475832402569,63.1648404527592,11.6627679218545));
#35974=CARTESIAN_POINT('Ctrl Pts',(-15.7650240000833,62.5524330171351,13.4838568188229));
#35975=CARTESIAN_POINT('Ctrl Pts',(-18.936865245129,61.5406947619309,12.7341264791949));
#35976=CARTESIAN_POINT('Ctrl Pts',(-20.0773594018982,61.0732543185779,9.55182253210509));
#35977=CARTESIAN_POINT('Ctrl Pts',(-18.1357994369342,61.4316477881722,6.76826458716724));
#35978=CARTESIAN_POINT('Ctrl Pts',(-14.8036106221425,62.1626591350494,6.86000957288756));
#35979=CARTESIAN_POINT('Ctrl Pts',(-13.5645914770419,62.3828842093692,8.85264674105157));
#35980=CARTESIAN_POINT('Ctrl Pts',(-13.5167884478445,62.3378725391134,9.926843073658));
#35981=CARTESIAN_POINT('Ctrl Pts',(-13.5161734774897,62.3341655182897,9.99879780140835));
#35982=CARTESIAN_POINT('Ctrl Pts',(-13.7984318791272,63.3798972175256,9.9976925905199));
#35983=CARTESIAN_POINT('Ctrl Pts',(-13.7939231905821,63.3356696948373,10.8435144444689));
#35984=CARTESIAN_POINT('Ctrl Pts',(-14.5389353035615,63.0364669859302,12.7089873258297));
#35985=CARTESIAN_POINT('Ctrl Pts',(-17.5330036055452,62.0804897947072,13.5128046754736));
#35986=CARTESIAN_POINT('Ctrl Pts',(-19.945812508159,61.2715545195409,11.2162142452881));
#35987=CARTESIAN_POINT('Ctrl Pts',(-19.4106046411916,61.2525379570574,7.83042882970079));
#35988=CARTESIAN_POINT('Ctrl Pts',(-16.3703262829259,61.9047530097004,6.38762845988016));
#35989=CARTESIAN_POINT('Ctrl Pts',(-13.9548208376171,62.4147543833102,7.90192541386312));
#35990=CARTESIAN_POINT('Ctrl Pts',(-13.5542391767051,62.4390002488206,9.45861716832901));
#35991=CARTESIAN_POINT('Ctrl Pts',(-13.5461538679481,62.4122187264791,10.0005448248896));
#35992=CARTESIAN_POINT('Origin',(-18.6889152049569,69.7479810832458,10.));
#35993=CARTESIAN_POINT('',(-14.0587048879185,64.3454334554184,10.0025996902774));
#35994=CARTESIAN_POINT('',(-14.038988005468,64.2646301485468,9.99747713720018));
#35995=CARTESIAN_POINT('',(-15.7201421778575,70.5434614183684,10.0000000000001));
#35996=CARTESIAN_POINT('Ctrl Pts',(-14.038988005468,64.2646301485468,9.99747713720018));
#35997=CARTESIAN_POINT('Ctrl Pts',(-14.0349994054244,64.226770392365,10.7242163838114));
#35998=CARTESIAN_POINT('Ctrl Pts',(-14.6082026447201,63.980303897263,12.4671953710476));
#35999=CARTESIAN_POINT('Ctrl Pts',(-17.3556995742977,63.0972885120503,13.5881174655937));
#36000=CARTESIAN_POINT('Ctrl Pts',(-20.0116836036718,62.2237737811954,11.6313322004901));
#36001=CARTESIAN_POINT('Ctrl Pts',(-19.8960390869576,62.0929146809836,8.2231376748613));
#36002=CARTESIAN_POINT('Ctrl Pts',(-17.0756569439774,62.686787843468,6.39583171448279));
#36003=CARTESIAN_POINT('Ctrl Pts',(-14.3543730978417,63.271636045696,7.6257956239861));
#36004=CARTESIAN_POINT('Ctrl Pts',(-13.7950809180928,63.3311289785642,9.32167057633652));
#36005=CARTESIAN_POINT('Ctrl Pts',(-13.7813169744248,63.2983967128177,10.0022545211422));
#36006=CARTESIAN_POINT('Ctrl Pts',(-14.0587048879185,64.3454334554184,10.0025996902774));
#36007=CARTESIAN_POINT('Ctrl Pts',(-14.0539764689082,64.3351645983746,10.2176211405934));
#36008=CARTESIAN_POINT('Ctrl Pts',(-14.1513426806931,64.2433978747177,11.4397371699224));
#36009=CARTESIAN_POINT('Ctrl Pts',(-15.6987166428553,63.7089610525881,13.3670096553834));
#36010=CARTESIAN_POINT('Ctrl Pts',(-18.9427555175128,62.6772983776883,12.9642257537712));
#36011=CARTESIAN_POINT('Ctrl Pts',(-20.3916349158421,62.1266472347557,9.90679500749766));
#36012=CARTESIAN_POINT('Ctrl Pts',(-18.7114286257309,62.4144320750885,6.93283507366423));
#36013=CARTESIAN_POINT('Ctrl Pts',(-15.3704995140603,63.14720625431,6.70571036393722));
#36014=CARTESIAN_POINT('Ctrl Pts',(-13.8968260312722,63.425086417853,8.66708054183125));
#36015=CARTESIAN_POINT('Ctrl Pts',(-13.7992958039273,63.3883718001703,9.83562185337852));
#36016=CARTESIAN_POINT('Ctrl Pts',(-13.7984318791272,63.3798972175256,9.9976925905199));
#36017=CARTESIAN_POINT('Origin',(-18.6889152049569,69.7479810832458,10.));
#36018=CARTESIAN_POINT('',(-14.322133959383,65.3101240288667,9.99868436122735));
#36019=CARTESIAN_POINT('',(-14.2935352300231,65.2317006057018,10.0018375364667));
#36020=CARTESIAN_POINT('',(-15.7201421778575,70.5434614183684,10.0000000000001));
#36021=CARTESIAN_POINT('Ctrl Pts',(-14.2935352300231,65.2317006057018,10.0018375364667));
#36022=CARTESIAN_POINT('Ctrl Pts',(-14.2911203313162,65.2259676792212,10.1205006547493));
#36023=CARTESIAN_POINT('Ctrl Pts',(-14.333487038742,65.1542869058501,11.241710128915));
#36024=CARTESIAN_POINT('Ctrl Pts',(-15.6317182042723,64.6921496134353,13.2184200895793));
#36025=CARTESIAN_POINT('Ctrl Pts',(-18.8835992389528,63.6589647612364,13.1544941616769));
#36026=CARTESIAN_POINT('Ctrl Pts',(-20.6195097408352,63.0319829890498,10.2839896215965));
#36027=CARTESIAN_POINT('Ctrl Pts',(-19.2589973841656,63.2346852212378,7.16081725087092));
#36028=CARTESIAN_POINT('Ctrl Pts',(-15.9765219526977,63.9523759072002,6.56368841308618));
#36029=CARTESIAN_POINT('Ctrl Pts',(-14.2145525524614,64.3015767283499,8.4321298041167));
#36030=CARTESIAN_POINT('Ctrl Pts',(-14.0405269650183,64.2792379389272,9.71707241074879));
#36031=CARTESIAN_POINT('Ctrl Pts',(-14.038988005468,64.2646301485468,9.99747713720018));
#36032=CARTESIAN_POINT('Ctrl Pts',(-14.322133959383,65.3101240288667,9.99868436122735));
#36033=CARTESIAN_POINT('Ctrl Pts',(-14.3164610907008,65.2798663326535,10.593347109087));
#36034=CARTESIAN_POINT('Ctrl Pts',(-14.7310514432717,65.082857752957,12.2044751575874));
#36035=CARTESIAN_POINT('Ctrl Pts',(-17.1999914587374,64.2812461473765,13.6183729089162));
#36036=CARTESIAN_POINT('Ctrl Pts',(-20.0833051820053,63.3462394854811,12.0175557753475));
#36037=CARTESIAN_POINT('Ctrl Pts',(-20.368219412885,63.1074718691845,8.60989310618186));
#36038=CARTESIAN_POINT('Ctrl Pts',(-17.7632104839254,63.6430568297549,6.44715683087691));
#36039=CARTESIAN_POINT('Ctrl Pts',(-14.7920138952891,64.288297311113,7.39383484183699));
#36040=CARTESIAN_POINT('Ctrl Pts',(-14.0761685903618,64.3833599300929,9.20845039448972));
#36041=CARTESIAN_POINT('Ctrl Pts',(-14.0587048879185,64.3454334554184,10.0025996902774));
#36042=CARTESIAN_POINT('Origin',(-18.6889152049569,69.7479810832458,10.));
#36043=CARTESIAN_POINT('',(-14.5724831194333,66.2783193540155,9.99930975590676));
#36044=CARTESIAN_POINT('',(-14.559910913876,66.1956016367402,9.99976839157055));
#36045=CARTESIAN_POINT('',(-15.7201421778575,70.5434614183684,10.0000000000001));
#36046=CARTESIAN_POINT('Ctrl Pts',(-14.559910913876,66.1956016367402,9.99976839157055));
#36047=CARTESIAN_POINT('Ctrl Pts',(-14.5533139234257,66.1695891483769,10.5198381182744));
#36048=CARTESIAN_POINT('Ctrl Pts',(-14.890051591398,65.9976317638641,12.0503568643789));
#36049=CARTESIAN_POINT('Ctrl Pts',(-17.1744195179844,65.2498597727098,13.6018503664189));
#36050=CARTESIAN_POINT('Ctrl Pts',(-20.1560728090925,64.2890822261736,12.2479900298274));
#36051=CARTESIAN_POINT('Ctrl Pts',(-20.7056191362412,63.9799857765361,8.89407499549296));
#36052=CARTESIAN_POINT('Ctrl Pts',(-18.2981238461185,64.4632262402319,6.52411027736645));
#36053=CARTESIAN_POINT('Ctrl Pts',(-15.1680091238728,65.146471993839,7.21818882738257));
#36054=CARTESIAN_POINT('Ctrl Pts',(-14.3115404877175,65.2744447664955,9.11709648401));
#36055=CARTESIAN_POINT('Ctrl Pts',(-14.2935352300231,65.2317006057018,10.0018375364667));
#36056=CARTESIAN_POINT('Ctrl Pts',(-14.5724831194333,66.2783193540155,9.99930975590676));
#36057=CARTESIAN_POINT('Ctrl Pts',(-14.5623726178327,66.2290088142627,10.9656350129456));
#36058=CARTESIAN_POINT('Ctrl Pts',(-15.5078446363719,65.8695090171971,12.9430947115647));
#36059=CARTESIAN_POINT('Ctrl Pts',(-18.7042880702644,64.8527215544621,13.3837942299381));
#36060=CARTESIAN_POINT('Ctrl Pts',(-20.8341986998844,64.1195886430847,10.7999310727637));
#36061=CARTESIAN_POINT('Ctrl Pts',(-19.9114308093218,64.2044184759421,7.49968047567802));
#36062=CARTESIAN_POINT('Ctrl Pts',(-16.7260146593058,64.8955230826759,6.4386200392349));
#36063=CARTESIAN_POINT('Ctrl Pts',(-14.609200226033,65.332074459173,8.15058790184868));
#36064=CARTESIAN_POINT('Ctrl Pts',(-14.3261263074255,65.3314182383775,9.58018345977269));
#36065=CARTESIAN_POINT('Ctrl Pts',(-14.322133959383,65.3101240288667,9.99868436122735));
#36066=CARTESIAN_POINT('Origin',(-18.6889152049569,69.7479810832458,10.));
#36067=CARTESIAN_POINT('',(-14.8383776097513,67.242349320473,10.0022118830713));
#36068=CARTESIAN_POINT('',(-14.810555933805,67.1637176864734,9.9985514014054));
#36069=CARTESIAN_POINT('',(-15.7201421778575,70.5434614183684,10.0000000000001));
#36070=CARTESIAN_POINT('Ctrl Pts',(-14.810555933805,67.1637176864734,9.9985514014054));
#36071=CARTESIAN_POINT('Ctrl Pts',(-14.8034925645054,67.1164300139581,10.9127656351722));
#36072=CARTESIAN_POINT('Ctrl Pts',(-15.6578176600211,66.7843853462346,12.8392373747718));
#36073=CARTESIAN_POINT('Ctrl Pts',(-18.7603708726991,65.795981118425,13.4453363911884));
#36074=CARTESIAN_POINT('Ctrl Pts',(-21.0187603927389,65.0290015152611,11.00449717215));
#36075=CARTESIAN_POINT('Ctrl Pts',(-20.2934961228732,65.0614895355965,7.6699459164611));
#36076=CARTESIAN_POINT('Ctrl Pts',(-17.1938529499358,65.7301904655353,6.40846378494576));
#36077=CARTESIAN_POINT('Ctrl Pts',(-14.9140195913108,66.207004164409,8.01044782382069));
#36078=CARTESIAN_POINT('Ctrl Pts',(-14.5661251855401,66.2201050327307,9.50987006742356));
#36079=CARTESIAN_POINT('Ctrl Pts',(-14.559910913876,66.1956016367402,9.99976839157055));
#36080=CARTESIAN_POINT('Ctrl Pts',(-14.8383776097513,67.242349320473,10.0022118830713));
#36081=CARTESIAN_POINT('Ctrl Pts',(-14.8315944872623,67.2260470012181,10.3408933046041));
#36082=CARTESIAN_POINT('Ctrl Pts',(-15.0130297323862,67.1051700296206,11.688786841075));
#36083=CARTESIAN_POINT('Ctrl Pts',(-16.8683721674333,66.4816292855384,13.5013274912987));
#36084=CARTESIAN_POINT('Ctrl Pts',(-20.0422978199454,65.4687533918912,12.6947822329677));
#36085=CARTESIAN_POINT('Ctrl Pts',(-21.1273143736847,65.0155990043222,9.47487431060756));
#36086=CARTESIAN_POINT('Ctrl Pts',(-19.1153342996386,65.3922823621301,6.72525821930975));
#36087=CARTESIAN_POINT('Ctrl Pts',(-15.7718556315871,66.125739692925,6.90837057311325));
#36088=CARTESIAN_POINT('Ctrl Pts',(-14.6047179173561,66.3280678631807,8.91484226317803));
#36089=CARTESIAN_POINT('Ctrl Pts',(-14.5728955600509,66.2803308931335,9.95989017005515));
#36090=CARTESIAN_POINT('Ctrl Pts',(-14.5724831194333,66.2783193540155,9.99930975590676));
#36091=CARTESIAN_POINT('Origin',(-18.6889152049569,69.7479810832458,10.));
#36092=CARTESIAN_POINT('',(-15.0969161422106,68.2083503098983,9.99673640007589));
#36093=CARTESIAN_POINT('',(-15.0750265266586,68.1281291851066,10.0024371765581));
#36094=CARTESIAN_POINT('',(-15.7201421778575,70.5434614183684,10.0000000000001));
#36095=CARTESIAN_POINT('',(-17.2449834421536,67.8425423025984,7.0617047543859));
#36096=CARTESIAN_POINT('Ctrl Pts',(-17.2449834421536,67.8425423025984,7.06170475438588));
#36097=CARTESIAN_POINT('Ctrl Pts',(-16.2988495743029,68.0419164156806,7.35795147289551));
#36098=CARTESIAN_POINT('Ctrl Pts',(-15.283120482422,68.2441585752431,8.39983158504164));
#36099=CARTESIAN_POINT('Ctrl Pts',(-15.0986382893443,68.2236687995603,9.70207674802626));
#36100=CARTESIAN_POINT('Ctrl Pts',(-15.0969161422106,68.2083503098983,9.99673640007589));
#36101=CARTESIAN_POINT('',(-18.1173331571764,67.6148078402348,6.92649999999998));
#36102=CARTESIAN_POINT('Ctrl Pts',(-18.1173331571765,67.6148078402348,6.92649999999999));
#36103=CARTESIAN_POINT('Ctrl Pts',(-17.8331351207385,67.6909584745888,6.92649999999999));
#36104=CARTESIAN_POINT('Ctrl Pts',(-17.5337033543064,67.7691522152651,6.97030621012379));
#36105=CARTESIAN_POINT('Ctrl Pts',(-17.2449834421535,67.8425423025984,7.06170475438591));
#36106=CARTESIAN_POINT('',(-18.8148375643562,67.424038192564,7.01163591529244));
#36107=CARTESIAN_POINT('Ctrl Pts',(-18.8154792730626,67.4238662472344,7.01293629783559));
#36108=CARTESIAN_POINT('Ctrl Pts',(-18.5825814377542,67.4888593221927,6.95435125823855));
#36109=CARTESIAN_POINT('Ctrl Pts',(-18.3453582319348,67.5537087055992,6.92649999999999));
#36110=CARTESIAN_POINT('Ctrl Pts',(-18.1173331571764,67.6148078402348,6.92649999999999));
#36111=CARTESIAN_POINT('Ctrl Pts',(-18.8139865064172,67.4242662328515,7.00991129962864));
#36112=CARTESIAN_POINT('Ctrl Pts',(-18.6713424458927,67.4544236505276,6.97326843816113));
#36113=CARTESIAN_POINT('Ctrl Pts',(-17.5558463812024,67.6913073253836,6.77617107551512));
#36114=CARTESIAN_POINT('Ctrl Pts',(-15.6699322564948,68.0973070404755,7.59313914445675));
#36115=CARTESIAN_POINT('Ctrl Pts',(-15.0894434810379,68.1615830306032,9.30549521878024));
#36116=CARTESIAN_POINT('Ctrl Pts',(-15.0750265266586,68.1281291851066,10.0024371765581));
#36117=CARTESIAN_POINT('Origin',(-69.7479810832458,-18.6889152049569,10.));
#36118=CARTESIAN_POINT('',(-61.4484819638689,-13.2791651259751,10.0015349814514));
#36119=CARTESIAN_POINT('',(-61.3659731009889,-13.2658134652031,9.99957732584557));
#36120=CARTESIAN_POINT('',(-70.5434614183684,-15.7201421778575,10.0000000000001));
#36121=CARTESIAN_POINT('',(-59.6819508576141,-16.8135320242443,7.03077704625423));
#36122=CARTESIAN_POINT('Ctrl Pts',(-61.3659731009889,-13.2658134652031,
9.99957732584557));
#36123=CARTESIAN_POINT('Ctrl Pts',(-61.3390049028546,-13.2594372491749,
10.5364470372518));
#36124=CARTESIAN_POINT('Ctrl Pts',(-61.1616793186457,-13.6128633281578,
12.0843271181655));
#36125=CARTESIAN_POINT('Ctrl Pts',(-60.4026582657955,-15.9358673415309,
13.605538542209));
#36126=CARTESIAN_POINT('Ctrl Pts',(-59.4472101950129,-18.8976307583482,
12.2029441264605));
#36127=CARTESIAN_POINT('Ctrl Pts',(-59.1533281063617,-19.3903963172921,
8.83503768583721));
#36128=CARTESIAN_POINT('Ctrl Pts',(-59.4806667221931,-17.7660737535053,
7.29068223125013));
#36129=CARTESIAN_POINT('Ctrl Pts',(-59.6819508576141,-16.8135320242442,
7.03077704625421));
#36130=CARTESIAN_POINT('',(-60.0933746109222,-15.2780776734579,7.02605498021606));
#36131=CARTESIAN_POINT('Origin',(-59.8874012299222,-16.0467807963563,10.));
#36132=CARTESIAN_POINT('Ctrl Pts',(-61.4484819638689,-13.2791651259751,
10.0015349814514));
#36133=CARTESIAN_POINT('Ctrl Pts',(-61.4440081401684,-13.2773812390919,
10.0935838809867));
#36134=CARTESIAN_POINT('Ctrl Pts',(-61.3771948495715,-13.3061918618692,
11.1915036202386));
#36135=CARTESIAN_POINT('Ctrl Pts',(-60.9313710113774,-14.5474295567703,
13.1842383274678));
#36136=CARTESIAN_POINT('Ctrl Pts',(-59.8935459365978,-17.8144668208756,
13.1913616605738));
#36137=CARTESIAN_POINT('Ctrl Pts',(-59.2511484715134,-19.6057481548832,
10.3395770770153));
#36138=CARTESIAN_POINT('Ctrl Pts',(-59.4407261981542,-18.301361653066,7.23382086599162));
#36139=CARTESIAN_POINT('Ctrl Pts',(-59.9014396609593,-16.1871423562504,
6.78116218790435));
#36140=CARTESIAN_POINT('Ctrl Pts',(-60.0933772939442,-15.2780676602833,
7.02603075613034));
#36141=CARTESIAN_POINT('Origin',(-69.7479810832458,-18.6889152049569,10.));
#36142=CARTESIAN_POINT('',(-62.4122187264791,-13.5461538679481,10.0005448248896));
#36143=CARTESIAN_POINT('',(-62.3341655182897,-13.5161734774897,9.99879780140837));
#36144=CARTESIAN_POINT('',(-70.5434614183684,-15.7201421778575,10.0000000000001));
#36145=CARTESIAN_POINT('Ctrl Pts',(-62.3341655182897,-13.5161734774897,
9.99879780140837));
#36146=CARTESIAN_POINT('Ctrl Pts',(-62.286219899295,-13.5082196148794,10.9294410660883));
#36147=CARTESIAN_POINT('Ctrl Pts',(-61.9458317508115,-14.3903370215031,
12.8709751918064));
#36148=CARTESIAN_POINT('Ctrl Pts',(-60.9493268661068,-17.5197763142882,
13.4270461480333));
#36149=CARTESIAN_POINT('Ctrl Pts',(-60.1927341524846,-19.7394014348254,
10.9477123134803));
#36150=CARTESIAN_POINT('Ctrl Pts',(-60.2392996738453,-18.9615992158895,
7.62511676387751));
#36151=CARTESIAN_POINT('Ctrl Pts',(-60.9131915231958,-15.84258326797,6.41562502038865));
#36152=CARTESIAN_POINT('Ctrl Pts',(-61.3800631690209,-13.6032001394545,
8.04417985348988));
#36153=CARTESIAN_POINT('Ctrl Pts',(-61.389739398956,-13.2714326411404,9.52644947847341));
#36154=CARTESIAN_POINT('Ctrl Pts',(-61.3659731009889,-13.2658134652031,
9.99957732584557));
#36155=CARTESIAN_POINT('Ctrl Pts',(-62.4122187264791,-13.5461538679481,
10.0005448248896));
#36156=CARTESIAN_POINT('Ctrl Pts',(-62.3889104933502,-13.5391171409457,
10.4721900135759));
#36157=CARTESIAN_POINT('Ctrl Pts',(-62.231485488278,-13.8305514728695,11.9564181322137));
#36158=CARTESIAN_POINT('Ctrl Pts',(-61.5138509672066,-16.0106566332719,
13.5896176377583));
#36159=CARTESIAN_POINT('Ctrl Pts',(-60.5349179618125,-19.0579057022677,
12.362301010972));
#36160=CARTESIAN_POINT('Ctrl Pts',(-60.1913020034495,-19.7341192728289,
9.01938609588879));
#36161=CARTESIAN_POINT('Ctrl Pts',(-60.6550135466889,-17.397345589062,6.55469600728472));
#36162=CARTESIAN_POINT('Ctrl Pts',(-61.3531034969373,-14.2043402063782,
7.15651357330673));
#36163=CARTESIAN_POINT('Ctrl Pts',(-61.4929236187118,-13.2968857360053,
9.08714816254619));
#36164=CARTESIAN_POINT('Ctrl Pts',(-61.4484819638689,-13.2791651259751,
10.0015349814514));
#36165=CARTESIAN_POINT('Origin',(-69.7479810832458,-18.6889152049569,10.));
#36166=CARTESIAN_POINT('',(-63.3798972175256,-13.7984318791272,9.99769259051991));
#36167=CARTESIAN_POINT('',(-63.2983967128177,-13.7813169744248,10.0022545211422));
#36168=CARTESIAN_POINT('',(-70.5434614183684,-15.7201421778575,10.0000000000001));
#36169=CARTESIAN_POINT('Ctrl Pts',(-63.2983967128177,-13.7813169744248,
10.0022545211422));
#36170=CARTESIAN_POINT('Ctrl Pts',(-63.2826433416521,-13.7746926693741,
10.3298056773906));
#36171=CARTESIAN_POINT('Ctrl Pts',(-63.1648404527592,-13.9475832402571,
11.662767921855));
#36172=CARTESIAN_POINT('Ctrl Pts',(-62.5524330171347,-15.7650240000841,
13.4838568188231));
#36173=CARTESIAN_POINT('Ctrl Pts',(-61.5406947619308,-18.9368652451296,
12.7341264791944));
#36174=CARTESIAN_POINT('Ctrl Pts',(-61.0732543185779,-20.0773594018981,
9.5518225321043));
#36175=CARTESIAN_POINT('Ctrl Pts',(-61.4316477881724,-18.1357994369335,
6.76826458716688));
#36176=CARTESIAN_POINT('Ctrl Pts',(-62.1626591350496,-14.8036106221418,
6.86000957288797));
#36177=CARTESIAN_POINT('Ctrl Pts',(-62.3828842093693,-13.5645914770418,
8.85264674105202));
#36178=CARTESIAN_POINT('Ctrl Pts',(-62.3378725391134,-13.5167884478445,
9.92684307365823));
#36179=CARTESIAN_POINT('Ctrl Pts',(-62.3341655182897,-13.5161734774897,
9.99879780140837));
#36180=CARTESIAN_POINT('Ctrl Pts',(-63.3798972175256,-13.7984318791272,
9.99769259051991));
#36181=CARTESIAN_POINT('Ctrl Pts',(-63.3356696948373,-13.7939231905821,
10.8435144444692));
#36182=CARTESIAN_POINT('Ctrl Pts',(-63.0364669859302,-14.5389353035618,
12.7089873258301));
#36183=CARTESIAN_POINT('Ctrl Pts',(-62.0804897947069,-17.5330036055459,
13.5128046754734));
#36184=CARTESIAN_POINT('Ctrl Pts',(-61.271554519541,-19.9458125081593,11.2162142452873));
#36185=CARTESIAN_POINT('Ctrl Pts',(-61.2525379570575,-19.4106046411911,
7.83042882970014));
#36186=CARTESIAN_POINT('Ctrl Pts',(-61.9047530097006,-16.3703262829251,
6.3876284598802));
#36187=CARTESIAN_POINT('Ctrl Pts',(-62.4147543833102,-13.9548208376168,
7.9019254138636));
#36188=CARTESIAN_POINT('Ctrl Pts',(-62.4390002488206,-13.5542391767051,
9.45861716832925));
#36189=CARTESIAN_POINT('Ctrl Pts',(-62.4122187264791,-13.5461538679481,
10.0005448248896));
#36190=CARTESIAN_POINT('Origin',(-69.7479810832458,-18.6889152049569,10.));
#36191=CARTESIAN_POINT('',(-64.3454334554185,-14.0587048879185,10.0025996902775));
#36192=CARTESIAN_POINT('',(-64.2646301485469,-14.038988005468,9.99747713720016));
#36193=CARTESIAN_POINT('',(-70.5434614183684,-15.7201421778575,10.0000000000001));
#36194=CARTESIAN_POINT('Ctrl Pts',(-64.2646301485469,-14.038988005468,9.99747713720016));
#36195=CARTESIAN_POINT('Ctrl Pts',(-64.2267703923651,-14.0349994054244,
10.7242163838116));
#36196=CARTESIAN_POINT('Ctrl Pts',(-63.9803038972629,-14.6082026447204,
12.4671953710481));
#36197=CARTESIAN_POINT('Ctrl Pts',(-63.0972885120501,-17.3556995742985,
13.5881174655936));
#36198=CARTESIAN_POINT('Ctrl Pts',(-62.2237737811953,-20.0116836036721,
11.6313322004894));
#36199=CARTESIAN_POINT('Ctrl Pts',(-62.0929146809836,-19.8960390869572,
8.2231376748606));
#36200=CARTESIAN_POINT('Ctrl Pts',(-62.6867878434683,-17.0756569439767,
6.39583171448275));
#36201=CARTESIAN_POINT('Ctrl Pts',(-63.271636045696,-14.3543730978414,7.62579562398654));
#36202=CARTESIAN_POINT('Ctrl Pts',(-63.3311289785642,-13.7950809180928,
9.32167057633674));
#36203=CARTESIAN_POINT('Ctrl Pts',(-63.2983967128177,-13.7813169744248,
10.0022545211422));
#36204=CARTESIAN_POINT('Ctrl Pts',(-64.3454334554185,-14.0587048879185,
10.0025996902775));
#36205=CARTESIAN_POINT('Ctrl Pts',(-64.3351645983747,-14.0539764689082,
10.2176211405936));
#36206=CARTESIAN_POINT('Ctrl Pts',(-64.2433978747177,-14.1513426806932,
11.4397371699229));
#36207=CARTESIAN_POINT('Ctrl Pts',(-63.7089610525879,-15.6987166428561,
13.3670096553837));
#36208=CARTESIAN_POINT('Ctrl Pts',(-62.6772983776881,-18.9427555175135,
12.9642257537707));
#36209=CARTESIAN_POINT('Ctrl Pts',(-62.1266472347557,-20.391634915842,9.90679500749681));
#36210=CARTESIAN_POINT('Ctrl Pts',(-62.4144320750887,-18.7114286257302,
6.93283507366378));
#36211=CARTESIAN_POINT('Ctrl Pts',(-63.1472062543103,-15.3704995140596,
6.70571036393757));
#36212=CARTESIAN_POINT('Ctrl Pts',(-63.4250864178529,-13.8968260312721,
8.66708054183172));
#36213=CARTESIAN_POINT('Ctrl Pts',(-63.3883718001703,-13.7992958039273,
9.83562185337876));
#36214=CARTESIAN_POINT('Ctrl Pts',(-63.3798972175256,-13.7984318791272,
9.99769259051991));
#36215=CARTESIAN_POINT('Origin',(-69.7479810832458,-18.6889152049569,10.));
#36216=CARTESIAN_POINT('',(-65.3101240288668,-14.322133959383,9.99868436122753));
#36217=CARTESIAN_POINT('',(-65.2317006057018,-14.2935352300231,10.0018375364667));
#36218=CARTESIAN_POINT('',(-70.5434614183684,-15.7201421778575,10.0000000000001));
#36219=CARTESIAN_POINT('Ctrl Pts',(-65.2317006057018,-14.2935352300231,
10.0018375364667));
#36220=CARTESIAN_POINT('Ctrl Pts',(-65.2259676792212,-14.2911203313162,
10.1205006547495));
#36221=CARTESIAN_POINT('Ctrl Pts',(-65.15428690585,-14.3334870387421,11.2417101289155));
#36222=CARTESIAN_POINT('Ctrl Pts',(-64.6921496134352,-15.631718204273,13.2184200895797));
#36223=CARTESIAN_POINT('Ctrl Pts',(-63.6589647612361,-18.8835992389535,
13.1544941616765));
#36224=CARTESIAN_POINT('Ctrl Pts',(-63.0319829890499,-20.6195097408353,
10.2839896215957));
#36225=CARTESIAN_POINT('Ctrl Pts',(-63.2346852212379,-19.2589973841649,
7.16081725087042));
#36226=CARTESIAN_POINT('Ctrl Pts',(-63.9523759072004,-15.9765219526969,
6.56368841308645));
#36227=CARTESIAN_POINT('Ctrl Pts',(-64.30157672835,-14.2145525524612,8.43212980411715));
#36228=CARTESIAN_POINT('Ctrl Pts',(-64.2792379389272,-14.0405269650183,
9.71707241074901));
#36229=CARTESIAN_POINT('Ctrl Pts',(-64.2646301485469,-14.038988005468,9.99747713720016));
#36230=CARTESIAN_POINT('Ctrl Pts',(-65.3101240288668,-14.322133959383,9.99868436122753));
#36231=CARTESIAN_POINT('Ctrl Pts',(-65.2798663326535,-14.3164610907008,
10.5933471090874));
#36232=CARTESIAN_POINT('Ctrl Pts',(-65.0828577529568,-14.7310514432721,
12.204475157588));
#36233=CARTESIAN_POINT('Ctrl Pts',(-64.2812461473762,-17.1999914587382,
13.6183729089162));
#36234=CARTESIAN_POINT('Ctrl Pts',(-63.346239485481,-20.0833051820058,12.0175557753468));
#36235=CARTESIAN_POINT('Ctrl Pts',(-63.1074718691846,-20.3682194128847,
8.60989310618102));
#36236=CARTESIAN_POINT('Ctrl Pts',(-63.6430568297552,-17.7632104839245,
6.44715683087674));
#36237=CARTESIAN_POINT('Ctrl Pts',(-64.2882973111131,-14.7920138952887,
7.3938348418375));
#36238=CARTESIAN_POINT('Ctrl Pts',(-64.3833599300929,-14.0761685903618,
9.20845039449));
#36239=CARTESIAN_POINT('Ctrl Pts',(-64.3454334554185,-14.0587048879185,
10.0025996902775));
#36240=CARTESIAN_POINT('Origin',(-69.7479810832458,-18.6889152049569,10.));
#36241=CARTESIAN_POINT('',(-66.2783193540156,-14.5724831194333,9.99930975590678));
#36242=CARTESIAN_POINT('',(-66.1956016367402,-14.559910913876,9.99976839157072));
#36243=CARTESIAN_POINT('',(-70.5434614183684,-15.7201421778575,10.0000000000001));
#36244=CARTESIAN_POINT('Ctrl Pts',(-66.1956016367402,-14.559910913876,9.99976839157072));
#36245=CARTESIAN_POINT('Ctrl Pts',(-66.1695891483769,-14.5533139234258,
10.5198381182747));
#36246=CARTESIAN_POINT('Ctrl Pts',(-65.9976317638641,-14.8900515913983,
12.0503568643794));
#36247=CARTESIAN_POINT('Ctrl Pts',(-65.2498597727096,-17.1744195179851,
13.601850366419));
#36248=CARTESIAN_POINT('Ctrl Pts',(-64.2890822261733,-20.156072809093,12.2479900298267));
#36249=CARTESIAN_POINT('Ctrl Pts',(-63.9799857765362,-20.705619136241,8.89407499549219));
#36250=CARTESIAN_POINT('Ctrl Pts',(-64.4632262402321,-18.2981238461178,
6.52411027736622));
#36251=CARTESIAN_POINT('Ctrl Pts',(-65.1464719938391,-15.1680091238725,
7.21818882738302));
#36252=CARTESIAN_POINT('Ctrl Pts',(-65.2744447664955,-14.3115404877176,
9.11709648401023));
#36253=CARTESIAN_POINT('Ctrl Pts',(-65.2317006057018,-14.2935352300231,
10.0018375364667));
#36254=CARTESIAN_POINT('Ctrl Pts',(-66.2783193540156,-14.5724831194333,
9.99930975590678));
#36255=CARTESIAN_POINT('Ctrl Pts',(-66.2290088142628,-14.5623726178327,
10.9656350129459));
#36256=CARTESIAN_POINT('Ctrl Pts',(-65.869509017197,-15.5078446363724,12.9430947115652));
#36257=CARTESIAN_POINT('Ctrl Pts',(-64.8527215544619,-18.7042880702652,
13.3837942299378));
#36258=CARTESIAN_POINT('Ctrl Pts',(-64.1195886430846,-20.8341986998846,
10.7999310727628));
#36259=CARTESIAN_POINT('Ctrl Pts',(-64.2044184759423,-19.9114308093211,
7.49968047567736));
#36260=CARTESIAN_POINT('Ctrl Pts',(-64.895523082676,-16.726014659305,6.43862003923507));
#36261=CARTESIAN_POINT('Ctrl Pts',(-65.3320744591731,-14.6092002260327,
8.15058790184925));
#36262=CARTESIAN_POINT('Ctrl Pts',(-65.3314182383775,-14.3261263074255,
9.58018345977307));
#36263=CARTESIAN_POINT('Ctrl Pts',(-65.3101240288668,-14.322133959383,9.99868436122753));
#36264=CARTESIAN_POINT('Origin',(-69.7479810832458,-18.6889152049569,10.));
#36265=CARTESIAN_POINT('',(-67.242349320473,-14.8383776097513,10.0022118830713));
#36266=CARTESIAN_POINT('',(-67.1637176864735,-14.810555933805,9.9985514014054));
#36267=CARTESIAN_POINT('',(-70.5434614183684,-15.7201421778575,10.0000000000001));
#36268=CARTESIAN_POINT('Ctrl Pts',(-67.1637176864735,-14.810555933805,9.9985514014054));
#36269=CARTESIAN_POINT('Ctrl Pts',(-67.1164300139581,-14.8034925645054,
10.9127656351724));
#36270=CARTESIAN_POINT('Ctrl Pts',(-66.7843853462345,-15.6578176600215,
12.8392373747722));
#36271=CARTESIAN_POINT('Ctrl Pts',(-65.7959811184248,-18.7603708726999,
13.4453363911881));
#36272=CARTESIAN_POINT('Ctrl Pts',(-65.0290015152611,-21.0187603927391,
11.0044971721492));
#36273=CARTESIAN_POINT('Ctrl Pts',(-65.0614895355965,-20.2934961228726,
7.66994591646049));
#36274=CARTESIAN_POINT('Ctrl Pts',(-65.7301904655356,-17.193852949935,6.40846378494586));
#36275=CARTESIAN_POINT('Ctrl Pts',(-66.2070041644091,-14.9140195913105,
8.01044782382119));
#36276=CARTESIAN_POINT('Ctrl Pts',(-66.2201050327307,-14.5661251855401,
9.50987006742391));
#36277=CARTESIAN_POINT('Ctrl Pts',(-66.1956016367402,-14.559910913876,9.99976839157072));
#36278=CARTESIAN_POINT('Ctrl Pts',(-67.242349320473,-14.8383776097513,10.0022118830713));
#36279=CARTESIAN_POINT('Ctrl Pts',(-67.2260470012181,-14.8315944872623,
10.3408933046044));
#36280=CARTESIAN_POINT('Ctrl Pts',(-67.1051700296205,-15.0130297323864,
11.6887868410756));
#36281=CARTESIAN_POINT('Ctrl Pts',(-66.4816292855381,-16.8683721674343,
13.501327491299));
#36282=CARTESIAN_POINT('Ctrl Pts',(-65.468753391891,-20.0422978199461,12.6947822329671));
#36283=CARTESIAN_POINT('Ctrl Pts',(-65.0155990043222,-21.1273143736846,
9.47487431060658));
#36284=CARTESIAN_POINT('Ctrl Pts',(-65.3922823621304,-19.1153342996378,
6.72525821930933));
#36285=CARTESIAN_POINT('Ctrl Pts',(-66.1257396929252,-15.7718556315863,
6.90837057311376));
#36286=CARTESIAN_POINT('Ctrl Pts',(-66.3280678631807,-14.604717917356,8.9148422631786));
#36287=CARTESIAN_POINT('Ctrl Pts',(-66.2803308931335,-14.5728955600509,
9.95989017005544));
#36288=CARTESIAN_POINT('Ctrl Pts',(-66.2783193540156,-14.5724831194333,
9.99930975590678));
#36289=CARTESIAN_POINT('Origin',(-69.7479810832458,-18.6889152049569,10.));
#36290=CARTESIAN_POINT('',(-68.2083503098983,-15.0969161422106,9.99673640007589));
#36291=CARTESIAN_POINT('',(-68.1281291851066,-15.0750265266586,10.0024371765581));
#36292=CARTESIAN_POINT('',(-70.5434614183684,-15.7201421778575,10.0000000000001));
#36293=CARTESIAN_POINT('',(-67.8425423025986,-17.2449834421528,7.06170475438615));
#36294=CARTESIAN_POINT('Ctrl Pts',(-67.8425423025986,-17.2449834421528,
7.06170475438615));
#36295=CARTESIAN_POINT('Ctrl Pts',(-68.0419164156808,-16.2988495743022,
7.35795147289606));
#36296=CARTESIAN_POINT('Ctrl Pts',(-68.2441585752431,-15.2831204824218,
8.39983158504225));
#36297=CARTESIAN_POINT('Ctrl Pts',(-68.2236687995604,-15.0986382893443,
9.70207674802657));
#36298=CARTESIAN_POINT('Ctrl Pts',(-68.2083503098983,-15.0969161422106,
9.99673640007589));
#36299=CARTESIAN_POINT('',(-67.6148078402348,-18.1173331571764,6.92649999999999));
#36300=CARTESIAN_POINT('Ctrl Pts',(-67.6148078402348,-18.1173331571764,
6.9265));
#36301=CARTESIAN_POINT('Ctrl Pts',(-67.6909584745889,-17.8331351207383,
6.9265));
#36302=CARTESIAN_POINT('Ctrl Pts',(-67.7691522152653,-17.5337033543059,
6.97030621012388));
#36303=CARTESIAN_POINT('Ctrl Pts',(-67.8425423025986,-17.2449834421528,
7.06170475438616));
#36304=CARTESIAN_POINT('',(-67.4240381925642,-18.8148375643558,7.01163591529236));
#36305=CARTESIAN_POINT('Ctrl Pts',(-67.4238662472345,-18.8154792730621,
7.01293629783548));
#36306=CARTESIAN_POINT('Ctrl Pts',(-67.4888593221928,-18.5825814377539,
6.95435125823852));
#36307=CARTESIAN_POINT('Ctrl Pts',(-67.5537087055993,-18.3453582319346,
6.9265));
#36308=CARTESIAN_POINT('Ctrl Pts',(-67.6148078402348,-18.1173331571764,
6.9265));
#36309=CARTESIAN_POINT('Ctrl Pts',(-67.4242662328516,-18.8139865064169,
7.00991129962856));
#36310=CARTESIAN_POINT('Ctrl Pts',(-67.4544236505277,-18.6713424458923,
6.97326843816105));
#36311=CARTESIAN_POINT('Ctrl Pts',(-67.6913073253837,-17.5558463812018,
6.7761710755152));
#36312=CARTESIAN_POINT('Ctrl Pts',(-68.0973070404756,-15.6699322564945,
7.59313914445722));
#36313=CARTESIAN_POINT('Ctrl Pts',(-68.1615830306033,-15.0894434810379,
9.30549521878046));
#36314=CARTESIAN_POINT('Ctrl Pts',(-68.1281291851067,-15.0750265266586,
10.0024371765581));
#36315=CARTESIAN_POINT('Origin',(18.6889152049569,-69.7479810832458,10.));
#36316=CARTESIAN_POINT('',(13.2791651259751,-61.4484819638689,10.0015349814511));
#36317=CARTESIAN_POINT('',(13.2658134652031,-61.3659731009889,9.99957732584551));
#36318=CARTESIAN_POINT('',(15.7201421778575,-70.5434614183684,10.0000000000001));
#36319=CARTESIAN_POINT('',(16.8135320242446,-59.681950857614,7.03077704625433));
#36320=CARTESIAN_POINT('Ctrl Pts',(13.2658134652031,-61.3659731009889,9.99957732584551));
#36321=CARTESIAN_POINT('Ctrl Pts',(13.2594372491749,-61.3390049028546,10.5364470372516));
#36322=CARTESIAN_POINT('Ctrl Pts',(13.6128633281576,-61.1616793186458,12.0843271181652));
#36323=CARTESIAN_POINT('Ctrl Pts',(15.9358673415304,-60.4026582657957,13.6055385422089));
#36324=CARTESIAN_POINT('Ctrl Pts',(18.8976307583479,-59.4472101950129,12.2029441264609));
#36325=CARTESIAN_POINT('Ctrl Pts',(19.3903963172922,-59.1533281063617,8.83503768583773));
#36326=CARTESIAN_POINT('Ctrl Pts',(17.7660737535057,-59.480666722193,7.29068223125039));
#36327=CARTESIAN_POINT('Ctrl Pts',(16.8135320242446,-59.681950857614,7.03077704625433));
#36328=CARTESIAN_POINT('',(15.2780776734582,-60.0933746109221,7.02605498021597));
#36329=CARTESIAN_POINT('Origin',(16.0467807963563,-59.8874012299222,10.));
#36330=CARTESIAN_POINT('Ctrl Pts',(13.2791651259751,-61.4484819638689,10.0015349814511));
#36331=CARTESIAN_POINT('Ctrl Pts',(13.277381239092,-61.4440081401684,10.0935838809864));
#36332=CARTESIAN_POINT('Ctrl Pts',(13.3061918618692,-61.3771948495716,11.1915036202383));
#36333=CARTESIAN_POINT('Ctrl Pts',(14.5474295567701,-60.9313710113775,13.1842383274677));
#36334=CARTESIAN_POINT('Ctrl Pts',(17.8144668208753,-59.8935459365978,13.1913616605739));
#36335=CARTESIAN_POINT('Ctrl Pts',(19.6057481548832,-59.2511484715134,10.3395770770155));
#36336=CARTESIAN_POINT('Ctrl Pts',(18.3013616530662,-59.4407261981541,7.23382086599181));
#36337=CARTESIAN_POINT('Ctrl Pts',(16.1871423562507,-59.9014396609592,6.78116218790437));
#36338=CARTESIAN_POINT('Ctrl Pts',(15.2780676602835,-60.0933772939442,7.02603075613028));
#36339=CARTESIAN_POINT('Origin',(18.6889152049569,-69.7479810832458,10.));
#36340=CARTESIAN_POINT('',(13.5461538679481,-62.4122187264791,10.0005448248895));
#36341=CARTESIAN_POINT('',(13.5161734774897,-62.3341655182897,9.99879780140832));
#36342=CARTESIAN_POINT('',(15.7201421778575,-70.5434614183684,10.0000000000001));
#36343=CARTESIAN_POINT('Ctrl Pts',(13.5161734774897,-62.3341655182897,9.99879780140832));
#36344=CARTESIAN_POINT('Ctrl Pts',(13.5082196148794,-62.286219899295,10.9294410660881));
#36345=CARTESIAN_POINT('Ctrl Pts',(14.3903370215028,-61.9458317508116,12.8709751918061));
#36346=CARTESIAN_POINT('Ctrl Pts',(17.5197763142877,-60.9493268661069,13.4270461480335));
#36347=CARTESIAN_POINT('Ctrl Pts',(19.7394014348253,-60.1927341524847,10.9477123134808));
#36348=CARTESIAN_POINT('Ctrl Pts',(18.9615992158899,-60.2392996738452,7.62511676387795));
#36349=CARTESIAN_POINT('Ctrl Pts',(15.8425832679706,-60.9131915231956,6.41562502038857));
#36350=CARTESIAN_POINT('Ctrl Pts',(13.6032001394546,-61.3800631690209,8.04417985348955));
#36351=CARTESIAN_POINT('Ctrl Pts',(13.2714326411404,-61.389739398956,9.52644947847322));
#36352=CARTESIAN_POINT('Ctrl Pts',(13.2658134652031,-61.3659731009889,9.99957732584551));
#36353=CARTESIAN_POINT('Ctrl Pts',(13.5461538679481,-62.4122187264791,10.0005448248895));
#36354=CARTESIAN_POINT('Ctrl Pts',(13.5391171409456,-62.3889104933503,10.4721900135758));
#36355=CARTESIAN_POINT('Ctrl Pts',(13.8305514728694,-62.231485488278,11.9564181322135));
#36356=CARTESIAN_POINT('Ctrl Pts',(16.0106566332716,-61.5138509672066,13.5896176377583));
#36357=CARTESIAN_POINT('Ctrl Pts',(19.0579057022675,-60.5349179618126,12.3623010109723));
#36358=CARTESIAN_POINT('Ctrl Pts',(19.734119272829,-60.1913020034494,9.01938609588904));
#36359=CARTESIAN_POINT('Ctrl Pts',(17.3973455890623,-60.6550135466889,6.55469600728483));
#36360=CARTESIAN_POINT('Ctrl Pts',(14.2043402063785,-61.3531034969372,7.15651357330655));
#36361=CARTESIAN_POINT('Ctrl Pts',(13.2968857360054,-61.4929236187117,9.08714816254594));
#36362=CARTESIAN_POINT('Ctrl Pts',(13.2791651259751,-61.4484819638689,10.0015349814511));
#36363=CARTESIAN_POINT('Origin',(18.6889152049569,-69.7479810832458,10.));
#36364=CARTESIAN_POINT('',(13.7984318791273,-63.3798972175256,9.99769259051987));
#36365=CARTESIAN_POINT('',(13.7813169744248,-63.2983967128177,10.0022545211422));
#36366=CARTESIAN_POINT('',(15.7201421778575,-70.5434614183684,10.0000000000001));
#36367=CARTESIAN_POINT('Ctrl Pts',(13.7813169744248,-63.2983967128177,10.0022545211422));
#36368=CARTESIAN_POINT('Ctrl Pts',(13.7746926693741,-63.2826433416521,10.3298056773904));
#36369=CARTESIAN_POINT('Ctrl Pts',(13.9475832402569,-63.1648404527592,11.6627679218547));
#36370=CARTESIAN_POINT('Ctrl Pts',(15.7650240000835,-62.5524330171349,13.483856818823));
#36371=CARTESIAN_POINT('Ctrl Pts',(18.9368652451291,-61.5406947619309,12.7341264791948));
#36372=CARTESIAN_POINT('Ctrl Pts',(20.0773594018982,-61.0732543185779,9.5518225321049));
#36373=CARTESIAN_POINT('Ctrl Pts',(18.135799436934,-61.4316477881723,6.76826458716716));
#36374=CARTESIAN_POINT('Ctrl Pts',(14.8036106221423,-62.1626591350494,6.86000957288767));
#36375=CARTESIAN_POINT('Ctrl Pts',(13.5645914770419,-62.3828842093692,8.85264674105167));
#36376=CARTESIAN_POINT('Ctrl Pts',(13.5167884478445,-62.3378725391134,9.92684307365803));
#36377=CARTESIAN_POINT('Ctrl Pts',(13.5161734774897,-62.3341655182897,9.99879780140832));
#36378=CARTESIAN_POINT('Ctrl Pts',(13.7984318791273,-63.3798972175256,9.99769259051987));
#36379=CARTESIAN_POINT('Ctrl Pts',(13.7939231905821,-63.3356696948374,10.8435144444691));
#36380=CARTESIAN_POINT('Ctrl Pts',(14.5389353035617,-63.0364669859302,12.70898732583));
#36381=CARTESIAN_POINT('Ctrl Pts',(17.5330036055456,-62.080489794707,13.5128046754735));
#36382=CARTESIAN_POINT('Ctrl Pts',(19.9458125081592,-61.2715545195409,11.2162142452876));
#36383=CARTESIAN_POINT('Ctrl Pts',(19.4106046411912,-61.2525379570576,7.83042882970036));
#36384=CARTESIAN_POINT('Ctrl Pts',(16.3703262829254,-61.9047530097005,6.3876284598802));
#36385=CARTESIAN_POINT('Ctrl Pts',(13.9548208376169,-62.4147543833103,7.90192541386342));
#36386=CARTESIAN_POINT('Ctrl Pts',(13.5542391767051,-62.4390002488207,9.45861716832912));
#36387=CARTESIAN_POINT('Ctrl Pts',(13.5461538679481,-62.4122187264791,10.0005448248895));
#36388=CARTESIAN_POINT('Origin',(18.6889152049569,-69.7479810832458,10.));
#36389=CARTESIAN_POINT('',(14.0587048879185,-64.3454334554184,10.0025996902774));
#36390=CARTESIAN_POINT('',(14.038988005468,-64.2646301485468,9.99747713720016));
#36391=CARTESIAN_POINT('',(15.7201421778575,-70.5434614183684,10.0000000000001));
#36392=CARTESIAN_POINT('Ctrl Pts',(14.038988005468,-64.2646301485468,9.99747713720016));
#36393=CARTESIAN_POINT('Ctrl Pts',(14.0349994054244,-64.226770392365,10.7242163838114));
#36394=CARTESIAN_POINT('Ctrl Pts',(14.6082026447201,-63.9803038972629,12.4671953710477));
#36395=CARTESIAN_POINT('Ctrl Pts',(17.3556995742979,-63.0972885120504,13.5881174655936));
#36396=CARTESIAN_POINT('Ctrl Pts',(20.0116836036718,-62.2237737811953,11.6313322004899));
#36397=CARTESIAN_POINT('Ctrl Pts',(19.8960390869576,-62.0929146809836,8.22313767486115));
#36398=CARTESIAN_POINT('Ctrl Pts',(17.0756569439772,-62.6867878434681,6.39583171448279));
#36399=CARTESIAN_POINT('Ctrl Pts',(14.3543730978416,-63.271636045696,7.62579562398619));
#36400=CARTESIAN_POINT('Ctrl Pts',(13.7950809180928,-63.3311289785642,9.32167057633656));
#36401=CARTESIAN_POINT('Ctrl Pts',(13.7813169744248,-63.2983967128177,10.0022545211422));
#36402=CARTESIAN_POINT('Ctrl Pts',(14.0587048879185,-64.3454334554185,10.0025996902774));
#36403=CARTESIAN_POINT('Ctrl Pts',(14.0539764689082,-64.3351645983746,10.2176211405935));
#36404=CARTESIAN_POINT('Ctrl Pts',(14.1513426806932,-64.2433978747176,11.4397371699227));
#36405=CARTESIAN_POINT('Ctrl Pts',(15.6987166428558,-63.708961052588,13.3670096553836));
#36406=CARTESIAN_POINT('Ctrl Pts',(18.9427555175132,-62.6772983776882,12.9642257537709));
#36407=CARTESIAN_POINT('Ctrl Pts',(20.3916349158421,-62.1266472347557,9.9067950074971));
#36408=CARTESIAN_POINT('Ctrl Pts',(18.7114286257305,-62.4144320750886,6.93283507366396));
#36409=CARTESIAN_POINT('Ctrl Pts',(15.3704995140598,-63.1472062543102,6.70571036393745));
#36410=CARTESIAN_POINT('Ctrl Pts',(13.8968260312721,-63.425086417853,8.66708054183155));
#36411=CARTESIAN_POINT('Ctrl Pts',(13.7992958039273,-63.3883718001703,9.83562185337865));
#36412=CARTESIAN_POINT('Ctrl Pts',(13.7984318791273,-63.3798972175256,9.99769259051987));
#36413=CARTESIAN_POINT('Origin',(18.6889152049569,-69.7479810832458,10.));
#36414=CARTESIAN_POINT('',(14.3221339593831,-65.3101240288668,9.99868436122731));
#36415=CARTESIAN_POINT('',(14.2935352300231,-65.2317006057018,10.0018375364666));
#36416=CARTESIAN_POINT('',(15.7201421778575,-70.5434614183684,10.0000000000001));
#36417=CARTESIAN_POINT('Ctrl Pts',(14.2935352300231,-65.2317006057018,10.0018375364666));
#36418=CARTESIAN_POINT('Ctrl Pts',(14.2911203313162,-65.2259676792212,10.1205006547493));
#36419=CARTESIAN_POINT('Ctrl Pts',(14.333487038742,-65.1542869058501,11.2417101289151));
#36420=CARTESIAN_POINT('Ctrl Pts',(15.6317182042724,-64.6921496134353,13.2184200895794));
#36421=CARTESIAN_POINT('Ctrl Pts',(18.8835992389529,-63.6589647612363,13.1544941616768));
#36422=CARTESIAN_POINT('Ctrl Pts',(20.6195097408352,-63.0319829890498,10.2839896215964));
#36423=CARTESIAN_POINT('Ctrl Pts',(19.2589973841654,-63.2346852212378,7.16081725087081));
#36424=CARTESIAN_POINT('Ctrl Pts',(15.9765219526975,-63.9523759072003,6.56368841308624));
#36425=CARTESIAN_POINT('Ctrl Pts',(14.2145525524613,-64.30157672835,8.43212980411679));
#36426=CARTESIAN_POINT('Ctrl Pts',(14.0405269650183,-64.2792379389272,9.71707241074883));
#36427=CARTESIAN_POINT('Ctrl Pts',(14.038988005468,-64.2646301485468,9.99747713720016));
#36428=CARTESIAN_POINT('Ctrl Pts',(14.3221339593831,-65.3101240288668,9.99868436122731));
#36429=CARTESIAN_POINT('Ctrl Pts',(14.3164610907008,-65.2798663326535,10.5933471090872));
#36430=CARTESIAN_POINT('Ctrl Pts',(14.7310514432719,-65.0828577529568,12.2044751575878));
#36431=CARTESIAN_POINT('Ctrl Pts',(17.1999914587379,-64.2812461473763,13.6183729089162));
#36432=CARTESIAN_POINT('Ctrl Pts',(20.0833051820056,-63.346239485481,12.017555775347));
#36433=CARTESIAN_POINT('Ctrl Pts',(20.3682194128848,-63.1074718691846,8.60989310618131));
#36434=CARTESIAN_POINT('Ctrl Pts',(17.7632104839249,-63.6430568297551,6.44715683087681));
#36435=CARTESIAN_POINT('Ctrl Pts',(14.7920138952889,-64.2882973111131,7.39383484183733));
#36436=CARTESIAN_POINT('Ctrl Pts',(14.0761685903618,-64.3833599300929,9.20845039448988));
#36437=CARTESIAN_POINT('Ctrl Pts',(14.0587048879185,-64.3454334554185,10.0025996902774));
#36438=CARTESIAN_POINT('Origin',(18.6889152049569,-69.7479810832458,10.));
#36439=CARTESIAN_POINT('',(14.5724831194333,-66.2783193540155,9.99930975590673));
#36440=CARTESIAN_POINT('',(14.559910913876,-66.1956016367402,9.99976839157072));
#36441=CARTESIAN_POINT('',(15.7201421778575,-70.5434614183684,10.0000000000001));
#36442=CARTESIAN_POINT('Ctrl Pts',(14.559910913876,-66.1956016367402,9.99976839157072));
#36443=CARTESIAN_POINT('Ctrl Pts',(14.5533139234257,-66.1695891483769,10.5198381182745));
#36444=CARTESIAN_POINT('Ctrl Pts',(14.8900515913981,-65.9976317638641,12.050356864379));
#36445=CARTESIAN_POINT('Ctrl Pts',(17.1744195179845,-65.2498597727098,13.6018503664189));
#36446=CARTESIAN_POINT('Ctrl Pts',(20.1560728090925,-64.2890822261735,12.2479900298273));
#36447=CARTESIAN_POINT('Ctrl Pts',(20.7056191362412,-63.9799857765361,8.89407499549286));
#36448=CARTESIAN_POINT('Ctrl Pts',(18.2981238461184,-64.463226240232,6.52411027736642));
#36449=CARTESIAN_POINT('Ctrl Pts',(15.1680091238728,-65.146471993839,7.21818882738264));
#36450=CARTESIAN_POINT('Ctrl Pts',(14.3115404877176,-65.2744447664955,9.11709648401002));
#36451=CARTESIAN_POINT('Ctrl Pts',(14.2935352300231,-65.2317006057018,10.0018375364666));
#36452=CARTESIAN_POINT('Ctrl Pts',(14.5724831194333,-66.2783193540155,9.99930975590673));
#36453=CARTESIAN_POINT('Ctrl Pts',(14.5623726178327,-66.2290088142627,10.9656350129458));
#36454=CARTESIAN_POINT('Ctrl Pts',(15.5078446363722,-65.8695090171971,12.9430947115651));
#36455=CARTESIAN_POINT('Ctrl Pts',(18.7042880702649,-64.8527215544619,13.3837942299379));
#36456=CARTESIAN_POINT('Ctrl Pts',(20.8341986998846,-64.1195886430847,10.7999310727631));
#36457=CARTESIAN_POINT('Ctrl Pts',(19.9114308093213,-64.2044184759422,7.49968047567758));
#36458=CARTESIAN_POINT('Ctrl Pts',(16.7260146593053,-64.895523082676,6.43862003923502));
#36459=CARTESIAN_POINT('Ctrl Pts',(14.6092002260328,-65.3320744591731,8.15058790184903));
#36460=CARTESIAN_POINT('Ctrl Pts',(14.3261263074255,-65.3314182383775,9.58018345977284));
#36461=CARTESIAN_POINT('Ctrl Pts',(14.3221339593831,-65.3101240288668,9.99868436122731));
#36462=CARTESIAN_POINT('Origin',(18.6889152049569,-69.7479810832458,10.));
#36463=CARTESIAN_POINT('',(14.8383776097513,-67.242349320473,10.0022118830713));
#36464=CARTESIAN_POINT('',(14.810555933805,-67.1637176864735,9.99855140140539));
#36465=CARTESIAN_POINT('',(15.7201421778575,-70.5434614183684,10.0000000000001));
#36466=CARTESIAN_POINT('Ctrl Pts',(14.810555933805,-67.1637176864735,9.99855140140538));
#36467=CARTESIAN_POINT('Ctrl Pts',(14.8034925645054,-67.1164300139582,10.9127656351722));
#36468=CARTESIAN_POINT('Ctrl Pts',(15.6578176600211,-66.7843853462345,12.8392373747718));
#36469=CARTESIAN_POINT('Ctrl Pts',(18.7603708726992,-65.795981118425,13.4453363911883));
#36470=CARTESIAN_POINT('Ctrl Pts',(21.0187603927389,-65.0290015152611,11.0044971721499));
#36471=CARTESIAN_POINT('Ctrl Pts',(20.2934961228731,-65.0614895355965,7.66994591646104));
#36472=CARTESIAN_POINT('Ctrl Pts',(17.1938529499357,-65.7301904655353,6.40846378494577));
#36473=CARTESIAN_POINT('Ctrl Pts',(14.9140195913107,-66.2070041644091,8.01044782382078));
#36474=CARTESIAN_POINT('Ctrl Pts',(14.5661251855401,-66.2201050327307,9.50987006742371));
#36475=CARTESIAN_POINT('Ctrl Pts',(14.559910913876,-66.1956016367402,9.99976839157072));
#36476=CARTESIAN_POINT('Ctrl Pts',(14.8383776097513,-67.242349320473,10.0022118830713));
#36477=CARTESIAN_POINT('Ctrl Pts',(14.8315944872623,-67.2260470012181,10.3408933046043));
#36478=CARTESIAN_POINT('Ctrl Pts',(15.0130297323863,-67.1051700296206,11.6887868410754));
#36479=CARTESIAN_POINT('Ctrl Pts',(16.868372167434,-66.4816292855382,13.5013274912989));
#36480=CARTESIAN_POINT('Ctrl Pts',(20.0422978199459,-65.468753391891,12.6947822329673));
#36481=CARTESIAN_POINT('Ctrl Pts',(21.1273143736846,-65.0155990043222,9.47487431060689));
#36482=CARTESIAN_POINT('Ctrl Pts',(19.1153342996381,-65.3922823621302,6.72525821930947));
#36483=CARTESIAN_POINT('Ctrl Pts',(15.7718556315866,-66.1257396929252,6.90837057311361));
#36484=CARTESIAN_POINT('Ctrl Pts',(14.604717917356,-66.3280678631807,8.9148422631784));
#36485=CARTESIAN_POINT('Ctrl Pts',(14.5728955600509,-66.2803308931334,9.95989017005532));
#36486=CARTESIAN_POINT('Ctrl Pts',(14.5724831194333,-66.2783193540155,9.99930975590673));
#36487=CARTESIAN_POINT('Origin',(18.6889152049569,-69.7479810832458,10.));
#36488=CARTESIAN_POINT('',(15.0969161422106,-68.2083503098983,9.99673640007585));
#36489=CARTESIAN_POINT('',(15.0750265266586,-68.1281291851066,10.0024371765581));
#36490=CARTESIAN_POINT('',(15.7201421778575,-70.5434614183684,10.0000000000001));
#36491=CARTESIAN_POINT('',(17.2449834421531,-67.8425423025985,7.06170475438607));
#36492=CARTESIAN_POINT('Ctrl Pts',(17.244983442153,-67.8425423025985,7.06170475438608));
#36493=CARTESIAN_POINT('Ctrl Pts',(16.2988495743024,-68.0419164156808,7.35795147289589));
#36494=CARTESIAN_POINT('Ctrl Pts',(15.2831204824219,-68.2441585752431,8.39983158504204));
#36495=CARTESIAN_POINT('Ctrl Pts',(15.0986382893443,-68.2236687995604,9.70207674802644));
#36496=CARTESIAN_POINT('Ctrl Pts',(15.0969161422106,-68.2083503098983,9.99673640007585));
#36497=CARTESIAN_POINT('',(18.1173331571764,-67.6148078402348,6.92649999999999));
#36498=CARTESIAN_POINT('Ctrl Pts',(18.1173331571764,-67.6148078402348,6.9265));
#36499=CARTESIAN_POINT('Ctrl Pts',(17.8331351207384,-67.6909584745889,6.9265));
#36500=CARTESIAN_POINT('Ctrl Pts',(17.5337033543061,-67.7691522152652,6.97030621012385));
#36501=CARTESIAN_POINT('Ctrl Pts',(17.2449834421531,-67.8425423025985,7.06170475438607));
#36502=CARTESIAN_POINT('',(18.814837564356,-67.4240381925641,7.01163591529248));
#36503=CARTESIAN_POINT('Ctrl Pts',(18.8154792730625,-67.4238662472344,7.01293629783558));
#36504=CARTESIAN_POINT('Ctrl Pts',(18.5825814377542,-67.4888593221927,6.95435125823855));
#36505=CARTESIAN_POINT('Ctrl Pts',(18.3453582319347,-67.5537087055993,6.9265));
#36506=CARTESIAN_POINT('Ctrl Pts',(18.1173331571764,-67.6148078402348,6.9265));
#36507=CARTESIAN_POINT('Ctrl Pts',(18.8139865064172,-67.4242662328515,7.00991129962864));
#36508=CARTESIAN_POINT('Ctrl Pts',(18.6713424458927,-67.4544236505276,6.97326843816114));
#36509=CARTESIAN_POINT('Ctrl Pts',(17.5558463812023,-67.6913073253836,6.77617107551513));
#36510=CARTESIAN_POINT('Ctrl Pts',(15.6699322564948,-68.0973070404755,7.59313914445677));
#36511=CARTESIAN_POINT('Ctrl Pts',(15.0894434810379,-68.1615830306033,9.30549521878023));
#36512=CARTESIAN_POINT('Ctrl Pts',(15.0750265266586,-68.1281291851066,10.0024371765581));
#36513=CARTESIAN_POINT('Ctrl Pts',(20.25986904378,-67.0040126136404,11.1728309286208));
#36514=CARTESIAN_POINT('Ctrl Pts',(20.6173045957293,-66.854289394458,10.4434664543484));
#36515=CARTESIAN_POINT('Ctrl Pts',(20.5807180172414,-66.7561954352348,8.5901302240308));
#36516=CARTESIAN_POINT('Ctrl Pts',(18.2866570474721,-67.2090412643978,7.05024279158514));
#36517=CARTESIAN_POINT('Ctrl Pts',(15.7623446338521,-67.7235827819969,8.14059085434237));
#36518=CARTESIAN_POINT('Ctrl Pts',(15.216861454864,-67.7078986042171,10.8824467802982));
#36519=CARTESIAN_POINT('Ctrl Pts',(17.0999173665986,-67.0414893382909,12.8405694561119));
#36520=CARTESIAN_POINT('Ctrl Pts',(19.6999556621849,-66.1829652216241,12.2707319173769));
#36521=CARTESIAN_POINT('Ctrl Pts',(20.6677950818131,-65.7617874756575,9.68094249642519));
#36522=CARTESIAN_POINT('Ctrl Pts',(19.1062967313386,-66.0183437425752,7.37485535276709));
#36523=CARTESIAN_POINT('Ctrl Pts',(16.3687616678974,-66.5900180970019,7.40446197973339));
#36524=CARTESIAN_POINT('Ctrl Pts',(14.8547867084588,-66.83384050967,9.74329926128826));
#36525=CARTESIAN_POINT('Ctrl Pts',(15.8753739824799,-66.3985290187163,12.3105450512028));
#36526=CARTESIAN_POINT('Ctrl Pts',(18.4864972623912,-65.5370346894516,12.8220707222439));
#36527=CARTESIAN_POINT('Ctrl Pts',(20.3290217552966,-64.8814857844687,10.822782375431));
#36528=CARTESIAN_POINT('Ctrl Pts',(19.727639166345,-64.8807798084461,8.09145561890051));
#36529=CARTESIAN_POINT('Ctrl Pts',(17.1814057921381,-65.4011950297317,7.0581771851638));
#36530=CARTESIAN_POINT('Ctrl Pts',(14.9197267037702,-65.8453641599238,8.64226139479105));
#36531=CARTESIAN_POINT('Ctrl Pts',(14.9188369907852,-65.6837566027253,11.434336752144));
#36532=CARTESIAN_POINT('Ctrl Pts',(17.1435292903638,-64.9258061425711,12.950271123299));
#36533=CARTESIAN_POINT('Ctrl Pts',(19.5784782321595,-64.1115175849317,11.8413258175013));
#36534=CARTESIAN_POINT('Ctrl Pts',(20.0212914063392,-63.831020197438,9.09413821413805));
#36535=CARTESIAN_POINT('Ctrl Pts',(18.0419954959311,-64.1995249831398,7.15290308224172));
#36536=CARTESIAN_POINT('Ctrl Pts',(15.3655869450732,-64.7548205378835,7.74475277436881));
#36537=CARTESIAN_POINT('Ctrl Pts',(14.3372888766999,-64.8685062198083,10.3431139119317));
#36538=CARTESIAN_POINT('Ctrl Pts',(15.8359873727447,-64.305085213021,12.6362038638413));
#36539=CARTESIAN_POINT('Ctrl Pts',(18.4922795208016,-63.4314879220136,12.5838422163726));
#36540=CARTESIAN_POINT('Ctrl Pts',(19.9068421044142,-62.8906110650171,10.2326155433118));
#36541=CARTESIAN_POINT('Ctrl Pts',(18.785128603301,-63.0293273367051,7.67442896667229));
#36542=CARTESIAN_POINT('Ctrl Pts',(16.0891375551553,-63.589870005783,7.18532148363254));
#36543=CARTESIAN_POINT('Ctrl Pts',(14.1815147862765,-63.9391700310929,9.20045592301443));
#36544=CARTESIAN_POINT('Ctrl Pts',(14.723488576521,-63.6321026366037,11.9269511029871));
#36545=CARTESIAN_POINT('Ctrl Pts',(17.196861615384,-62.8075183731851,12.9390225214355));
#36546=CARTESIAN_POINT('Ctrl Pts',(19.3650552728408,-62.064706678561,11.3362221619435));
#36547=CARTESIAN_POINT('Ctrl Pts',(19.2630114600594,-61.9302032807139,8.54457429525393));
#36548=CARTESIAN_POINT('Ctrl Pts',(16.9455204456758,-62.3893271714101,7.04783027207107));
#36549=CARTESIAN_POINT('Ctrl Pts',(14.4384735898226,-62.8992423967486,8.17765522357052));
#36550=CARTESIAN_POINT('Ctrl Pts',(13.9364114971972,-62.8719235739435,10.9288348037816));
#36551=CARTESIAN_POINT('Ctrl Pts',(15.8500240410822,-62.1973266831091,12.8536227562671));
#36552=CARTESIAN_POINT('Ctrl Pts',(18.4407556977104,-61.3412962728355,12.2395195742225));
#36553=CARTESIAN_POINT('Ctrl Pts',(19.3676134988852,-60.9310995184379,9.63289839745374));
#36554=CARTESIAN_POINT('Ctrl Pts',(17.7699646296637,-61.19734228766,7.35288957156119));
#36555=CARTESIAN_POINT('Ctrl Pts',(15.0332534115106,-61.768795893407,7.4280377744411));
#36556=CARTESIAN_POINT('Ctrl Pts',(13.5563500795275,-62.0026849934363,9.79147768509013));
#36557=CARTESIAN_POINT('Ctrl Pts',(14.6172778371392,-61.5565643024821,12.3404488591358));
#36558=CARTESIAN_POINT('Ctrl Pts',(17.2361027255532,-60.6930063334387,12.8070892069869));
#36559=CARTESIAN_POINT('Ctrl Pts',(19.0468753473843,-60.0459653166684,10.7762699688264));
#36560=CARTESIAN_POINT('Ctrl Pts',(18.4024589901612,-60.0567902041013,8.05473611617462));
#36561=CARTESIAN_POINT('Ctrl Pts',(15.8403574002337,-60.5814573009746,7.06404294414454));
#36562=CARTESIAN_POINT('Ctrl Pts',(13.6037685248158,-61.0189035288689,8.6852426906357));
#36563=CARTESIAN_POINT('Ctrl Pts',(13.6472648693585,-60.8454027634006,11.4767030328866));
#36564=CARTESIAN_POINT('Ctrl Pts',(15.8948076660286,-60.0813295310042,12.9532921034687));
#36565=CARTESIAN_POINT('Ctrl Pts',(18.3134648367079,-59.2714063402785,11.8044287744804));
#36566=CARTESIAN_POINT('Ctrl Pts',(18.7097689547776,-59.0033710168103,9.04578082775224));
#36567=CARTESIAN_POINT('Ctrl Pts',(17.3744086881426,-59.2532824184769,7.78080120942667));
#36568=CARTESIAN_POINT('Ctrl Pts',(16.5917431062327,-59.4090483774018,7.56791319796495));
#36569=CARTESIAN_POINT('Ctrl Pts',(20.4459680138347,-67.0649244254632,11.259172404465));
#36570=CARTESIAN_POINT('Ctrl Pts',(20.8307101569087,-66.9078844272409,10.4761135710142));
#36571=CARTESIAN_POINT('Ctrl Pts',(20.7934159435358,-66.8099800782137,8.48633842059632));
#36572=CARTESIAN_POINT('Ctrl Pts',(18.3334494707627,-67.3072801529265,6.83308754393487));
#36573=CARTESIAN_POINT('Ctrl Pts',(15.6262809016687,-67.8708178297157,8.00370485831645));
#36574=CARTESIAN_POINT('Ctrl Pts',(15.0436190322123,-67.8650956520227,10.9474107537966));
#36575=CARTESIAN_POINT('Ctrl Pts',(17.0682804619448,-67.160743301905,13.049686519018));
#36576=CARTESIAN_POINT('Ctrl Pts',(19.8627070898848,-66.2501329885662,12.4378986762067));
#36577=CARTESIAN_POINT('Ctrl Pts',(20.9047756131301,-65.8090656142303,9.65745411880352));
#36578=CARTESIAN_POINT('Ctrl Pts',(19.2313015598939,-66.0956256802751,7.18159743500985));
#36579=CARTESIAN_POINT('Ctrl Pts',(16.2952133143914,-66.7205021994896,7.21338364285578));
#36580=CARTESIAN_POINT('Ctrl Pts',(14.6727612295383,-66.9933909703099,9.72440146443637));
#36581=CARTESIAN_POINT('Ctrl Pts',(15.7714607991054,-66.5371493528456,12.4806427736085));
#36582=CARTESIAN_POINT('Ctrl Pts',(18.5777884658272,-65.6233501657762,13.0298259452254));
#36583=CARTESIAN_POINT('Ctrl Pts',(20.558934634444,-64.9306576947328,10.8833539743373));
#36584=CARTESIAN_POINT('Ctrl Pts',(19.9162581518544,-64.9410163841629,7.95095238475401));
#36585=CARTESIAN_POINT('Ctrl Pts',(17.1855548447373,-65.5108601749996,6.8416060517578));
#36586=CARTESIAN_POINT('Ctrl Pts',(14.7603541429464,-65.9988447894534,8.54230738426523));
#36587=CARTESIAN_POINT('Ctrl Pts',(14.7623776252392,-65.836456643933,11.5399297656087));
#36588=CARTESIAN_POINT('Ctrl Pts',(17.153826032904,-65.033824019284,13.167464204339));
#36589=CARTESIAN_POINT('Ctrl Pts',(19.7710097578038,-64.170705798679,11.9768805549433));
#36590=CARTESIAN_POINT('Ctrl Pts',(20.2494006496399,-63.8806753904707,9.02745047458965));
#36591=CARTESIAN_POINT('Ctrl Pts',(18.1273716126602,-64.2874254021705,6.94330548061662));
#36592=CARTESIAN_POINT('Ctrl Pts',(15.2569098917896,-64.8947173471079,7.57872596768878));
#36593=CARTESIAN_POINT('Ctrl Pts',(14.1558892629051,-65.0278889803931,10.368373274399));
#36594=CARTESIAN_POINT('Ctrl Pts',(15.7678976499206,-64.4341066798257,12.8302759390873));
#36595=CARTESIAN_POINT('Ctrl Pts',(18.622719426852,-63.5073135350879,12.774059531474));
#36596=CARTESIAN_POINT('Ctrl Pts',(20.1443979832212,-62.9377350396947,10.2497402360733));
#36597=CARTESIAN_POINT('Ctrl Pts',(18.9430848635891,-63.0977799648827,7.50322506140514));
#36598=CARTESIAN_POINT('Ctrl Pts',(16.0515990210027,-63.7107053062554,6.97811046011711));
#36599=CARTESIAN_POINT('Ctrl Pts',(14.0065195594074,-64.096836741373,9.14159508133232));
#36600=CARTESIAN_POINT('Ctrl Pts',(14.5913710742638,-63.7782802952007,12.0688094033195));
#36601=CARTESIAN_POINT('Ctrl Pts',(17.2498076016886,-62.9041084194736,13.1553875028215));
#36602=CARTESIAN_POINT('Ctrl Pts',(19.5805980497845,-62.1177290461057,11.4345921747923));
#36603=CARTESIAN_POINT('Ctrl Pts',(19.4740206690255,-61.9844404141372,8.43742875512301));
#36604=CARTESIAN_POINT('Ctrl Pts',(16.9888992784429,-62.4884807287627,6.83049741954164));
#36605=CARTESIAN_POINT('Ctrl Pts',(14.3002673230732,-63.0470515348742,8.04349783254836));
#36606=CARTESIAN_POINT('Ctrl Pts',(13.7642231138315,-63.0288381927736,10.9972137711305));
#36607=CARTESIAN_POINT('Ctrl Pts',(15.8216906940826,-62.3156954611178,13.063700777119));
#36608=CARTESIAN_POINT('Ctrl Pts',(18.60612554685,-61.4077624358673,12.4043885425466));
#36609=CARTESIAN_POINT('Ctrl Pts',(19.6041954665562,-60.9784844518179,9.60587310900414));
#36610=CARTESIAN_POINT('Ctrl Pts',(17.8919095654204,-61.275444121164,7.15801457676317));
#36611=CARTESIAN_POINT('Ctrl Pts',(14.9567058150545,-61.9000836406211,7.23869504058996));
#36612=CARTESIAN_POINT('Ctrl Pts',(13.374054496997,-62.1623078281203,9.77612668779255));
#36613=CARTESIAN_POINT('Ctrl Pts',(14.5160643361694,-61.6944612588913,12.5127480402917));
#36614=CARTESIAN_POINT('Ctrl Pts',(17.3306605884647,-60.7784465109949,13.0137415206691));
#36615=CARTESIAN_POINT('Ctrl Pts',(19.2777173765313,-60.0948882619405,10.8334174170446));
#36616=CARTESIAN_POINT('Ctrl Pts',(18.5888390654041,-60.117626694016,7.91152966540906));
#36617=CARTESIAN_POINT('Ctrl Pts',(15.841099356146,-60.6920353750482,6.84790363622589));
#36618=CARTESIAN_POINT('Ctrl Pts',(13.4428359587848,-61.172802160534,8.58845287746038));
#36619=CARTESIAN_POINT('Ctrl Pts',(13.4925131117116,-60.9976452524506,11.5854149675156));
#36620=CARTESIAN_POINT('Ctrl Pts',(15.9084942245292,-60.188439109268,13.1707075830488));
#36621=CARTESIAN_POINT('Ctrl Pts',(18.5081868105879,-59.33000762519,11.9372672251406));
#36622=CARTESIAN_POINT('Ctrl Pts',(18.9366447422825,-59.0533567133274,8.97553311378072));
#36623=CARTESIAN_POINT('Ctrl Pts',(17.5049637099303,-59.3290771863823,7.61742821670124));
#36624=CARTESIAN_POINT('Ctrl Pts',(16.66567274557,-59.5000158708059,7.38886781406141));
#36625=CARTESIAN_POINT('Ctrl Pts',(20.6320669838895,-67.125836237286,11.3455138803092));
#36626=CARTESIAN_POINT('Ctrl Pts',(21.0441157180881,-66.9614794600238,10.5087606876799));
#36627=CARTESIAN_POINT('Ctrl Pts',(21.0061138698302,-66.8637647211925,8.38254661716184));
#36628=CARTESIAN_POINT('Ctrl Pts',(18.3802418940532,-67.4055190414551,6.6159322962846));
#36629=CARTESIAN_POINT('Ctrl Pts',(15.4902171694852,-68.0180528774347,7.86681886229056));
#36630=CARTESIAN_POINT('Ctrl Pts',(14.8703766095605,-68.0222926998283,11.0123747272948));
#36631=CARTESIAN_POINT('Ctrl Pts',(17.036643557291,-67.2799972655193,13.2588035819241));
#36632=CARTESIAN_POINT('Ctrl Pts',(20.0254585175847,-66.3173007555082,12.6050654350364));
#36633=CARTESIAN_POINT('Ctrl Pts',(21.1417561444472,-65.8563437528032,9.63396574118186));
#36634=CARTESIAN_POINT('Ctrl Pts',(19.3563063884492,-66.1729076179749,6.98833951725262));
#36635=CARTESIAN_POINT('Ctrl Pts',(16.2216649608854,-66.8509863019774,7.02230530597816));
#36636=CARTESIAN_POINT('Ctrl Pts',(14.4907357506179,-67.1529414309498,9.70550366758451));
#36637=CARTESIAN_POINT('Ctrl Pts',(15.667547615731,-66.675769686975,12.6507404960141));
#36638=CARTESIAN_POINT('Ctrl Pts',(18.6690796692632,-65.7096656421006,13.2375811682069));
#36639=CARTESIAN_POINT('Ctrl Pts',(20.7888475135915,-64.979829604997,10.9439255732436));
#36640=CARTESIAN_POINT('Ctrl Pts',(20.1048771373637,-65.0012529598797,7.81044915060753));
#36641=CARTESIAN_POINT('Ctrl Pts',(17.1897038973365,-65.6205253202675,6.62503491835177));
#36642=CARTESIAN_POINT('Ctrl Pts',(14.6009815821227,-66.152325418983,8.44235337373943));
#36643=CARTESIAN_POINT('Ctrl Pts',(14.6059182596933,-65.9891566851404,11.6455227790734));
#36644=CARTESIAN_POINT('Ctrl Pts',(17.1641227754442,-65.1418418959969,13.384657285379));
#36645=CARTESIAN_POINT('Ctrl Pts',(19.9635412834482,-64.2298940124262,12.1124352923853));
#36646=CARTESIAN_POINT('Ctrl Pts',(20.4775098929405,-63.9303305835035,8.96076273504126));
#36647=CARTESIAN_POINT('Ctrl Pts',(18.2127477293893,-64.3753258212012,6.73370787899151));
#36648=CARTESIAN_POINT('Ctrl Pts',(15.1482328385059,-65.0346141563323,7.41269916100874));
#36649=CARTESIAN_POINT('Ctrl Pts',(13.9744896491103,-65.1872717409779,10.3936326368663));
#36650=CARTESIAN_POINT('Ctrl Pts',(15.6998079270965,-64.5631281466306,13.0243480143334));
#36651=CARTESIAN_POINT('Ctrl Pts',(18.7531593329025,-63.5831391481621,12.9642768465754));
#36652=CARTESIAN_POINT('Ctrl Pts',(20.3819538620282,-62.9848590143723,10.2668649288348));
#36653=CARTESIAN_POINT('Ctrl Pts',(19.1010411238773,-63.1662325930602,7.33202115613798));
#36654=CARTESIAN_POINT('Ctrl Pts',(16.0140604868501,-63.8315406067279,6.77089943660167));
#36655=CARTESIAN_POINT('Ctrl Pts',(13.8315243325383,-64.254503451653,9.08273423965024));
#36656=CARTESIAN_POINT('Ctrl Pts',(14.4592535720066,-63.9244579537978,12.210667703652));
#36657=CARTESIAN_POINT('Ctrl Pts',(17.3027535879932,-63.000698465762,13.3717524842076));
#36658=CARTESIAN_POINT('Ctrl Pts',(19.7961408267282,-62.1707514136505,11.5329621876411));
#36659=CARTESIAN_POINT('Ctrl Pts',(19.6850298779915,-62.0386775475604,8.33028321499209));
#36660=CARTESIAN_POINT('Ctrl Pts',(17.0322781112101,-62.5876342861154,6.61316456701221));
#36661=CARTESIAN_POINT('Ctrl Pts',(14.1620610563238,-63.1948606729999,7.90934044152622));
#36662=CARTESIAN_POINT('Ctrl Pts',(13.5920347304658,-63.1857528116036,11.0655927384794));
#36663=CARTESIAN_POINT('Ctrl Pts',(15.7933573470831,-62.4340642391264,13.273778797971));
#36664=CARTESIAN_POINT('Ctrl Pts',(18.7714953959895,-61.4742285988991,12.5692575108707));
#36665=CARTESIAN_POINT('Ctrl Pts',(19.8407774342272,-61.0258693851979,9.57884782055452));
#36666=CARTESIAN_POINT('Ctrl Pts',(18.0138545011772,-61.3535459546681,6.96313958196516));
#36667=CARTESIAN_POINT('Ctrl Pts',(14.8801582185984,-62.0313713878353,7.04935230673882));
#36668=CARTESIAN_POINT('Ctrl Pts',(13.1917589144664,-62.3219306628043,9.76077569049498));
#36669=CARTESIAN_POINT('Ctrl Pts',(14.4148508351996,-61.8323582153005,12.6850472214475));
#36670=CARTESIAN_POINT('Ctrl Pts',(17.4252184513762,-60.8638866885509,13.2203938343513));
#36671=CARTESIAN_POINT('Ctrl Pts',(19.5085594056783,-60.1438112072126,10.8905648652627));
#36672=CARTESIAN_POINT('Ctrl Pts',(18.775219140647,-60.1784631839306,7.7683232146435));
#36673=CARTESIAN_POINT('Ctrl Pts',(15.8418413120583,-60.8026134491219,6.63176432830724));
#36674=CARTESIAN_POINT('Ctrl Pts',(13.2819033927537,-61.3267007921991,8.49166306428506));
#36675=CARTESIAN_POINT('Ctrl Pts',(13.3377613540647,-61.1498877415006,11.6941269021445));
#36676=CARTESIAN_POINT('Ctrl Pts',(15.9221807830298,-60.2955486875318,13.3881230626288));
#36677=CARTESIAN_POINT('Ctrl Pts',(18.7029087844679,-59.3886089101015,12.0701056758008));
#36678=CARTESIAN_POINT('Ctrl Pts',(19.1635205297874,-59.1033424098446,8.90528539980922));
#36679=CARTESIAN_POINT('Ctrl Pts',(17.635518731718,-59.4048719542876,7.45405522397582));
#36680=CARTESIAN_POINT('Ctrl Pts',(16.7396023849073,-59.5909833642099,7.20982243015787));
#36681=CARTESIAN_POINT('Ctrl Pts',(20.8181659539443,-67.1867480491087,11.4318553561533));
#36682=CARTESIAN_POINT('Ctrl Pts',(21.2575212792675,-67.0150744928066,10.5414078043456));
#36683=CARTESIAN_POINT('Ctrl Pts',(21.2188117961245,-66.9175493641713,8.27875481372736));
#36684=CARTESIAN_POINT('Ctrl Pts',(18.4270343173438,-67.5037579299837,6.39877704863433));
#36685=CARTESIAN_POINT('Ctrl Pts',(15.3541534373018,-68.1652879251536,7.72993286626466));
#36686=CARTESIAN_POINT('Ctrl Pts',(14.6971341869088,-68.1794897476338,11.0773387007931));
#36687=CARTESIAN_POINT('Ctrl Pts',(17.0050066526373,-67.3992512291335,13.4679206448302));
#36688=CARTESIAN_POINT('Ctrl Pts',(20.1882099452846,-66.3844685224502,12.7722321938661));
#36689=CARTESIAN_POINT('Ctrl Pts',(21.3787366757643,-65.9036218913761,9.6104773635602));
#36690=CARTESIAN_POINT('Ctrl Pts',(19.4813112170045,-66.2501895556748,6.79508159949539));
#36691=CARTESIAN_POINT('Ctrl Pts',(16.1481166073794,-66.9814704044651,6.83122696910054));
#36692=CARTESIAN_POINT('Ctrl Pts',(14.3087102716975,-67.3124918915897,9.68660587073265));
#36693=CARTESIAN_POINT('Ctrl Pts',(15.5636344323565,-66.8143900211043,12.8208382184198));
#36694=CARTESIAN_POINT('Ctrl Pts',(18.7603708726992,-65.795981118425,13.4453363911883));
#36695=CARTESIAN_POINT('Ctrl Pts',(21.0187603927389,-65.0290015152611,11.0044971721499));
#36696=CARTESIAN_POINT('Ctrl Pts',(20.2934961228731,-65.0614895355965,7.66994591646104));
#36697=CARTESIAN_POINT('Ctrl Pts',(17.1938529499357,-65.7301904655353,6.40846378494577));
#36698=CARTESIAN_POINT('Ctrl Pts',(14.4416090212989,-66.3058060485126,8.34239936321361));
#36699=CARTESIAN_POINT('Ctrl Pts',(14.4494588941473,-66.141856726348,11.7511157925381));
#36700=CARTESIAN_POINT('Ctrl Pts',(17.1744195179845,-65.2498597727098,13.6018503664189));
#36701=CARTESIAN_POINT('Ctrl Pts',(20.1560728090925,-64.2890822261735,12.2479900298273));
#36702=CARTESIAN_POINT('Ctrl Pts',(20.7056191362412,-63.9799857765361,8.89407499549286));
#36703=CARTESIAN_POINT('Ctrl Pts',(18.2981238461184,-64.463226240232,6.52411027736642));
#36704=CARTESIAN_POINT('Ctrl Pts',(15.0395557852222,-65.1745109655565,7.24667235432871));
#36705=CARTESIAN_POINT('Ctrl Pts',(13.7930900353155,-65.3466545015629,10.4188919993335));
#36706=CARTESIAN_POINT('Ctrl Pts',(15.6317182042724,-64.6921496134353,13.2184200895794));
#36707=CARTESIAN_POINT('Ctrl Pts',(18.8835992389529,-63.6589647612363,13.1544941616768));
#36708=CARTESIAN_POINT('Ctrl Pts',(20.6195097408352,-63.0319829890498,10.2839896215964));
#36709=CARTESIAN_POINT('Ctrl Pts',(19.2589973841654,-63.2346852212378,7.16081725087081));
#36710=CARTESIAN_POINT('Ctrl Pts',(15.9765219526975,-63.9523759072003,6.56368841308624));
#36711=CARTESIAN_POINT('Ctrl Pts',(13.6565291056692,-64.4121701619331,9.02387339796815));
#36712=CARTESIAN_POINT('Ctrl Pts',(14.3271360697494,-64.0706356123948,12.3525260039844));
#36713=CARTESIAN_POINT('Ctrl Pts',(17.3556995742979,-63.0972885120504,13.5881174655936));
#36714=CARTESIAN_POINT('Ctrl Pts',(20.0116836036718,-62.2237737811953,11.6313322004899));
#36715=CARTESIAN_POINT('Ctrl Pts',(19.8960390869576,-62.0929146809836,8.22313767486115));
#36716=CARTESIAN_POINT('Ctrl Pts',(17.0756569439772,-62.6867878434681,6.39583171448279));
#36717=CARTESIAN_POINT('Ctrl Pts',(14.0238547895744,-63.3426698111255,7.77518305050405));
#36718=CARTESIAN_POINT('Ctrl Pts',(13.4198463471001,-63.3426674304337,11.1339717058283));
#36719=CARTESIAN_POINT('Ctrl Pts',(15.7650240000835,-62.5524330171349,13.483856818823));
#36720=CARTESIAN_POINT('Ctrl Pts',(18.9368652451291,-61.5406947619309,12.7341264791948));
#36721=CARTESIAN_POINT('Ctrl Pts',(20.0773594018982,-61.0732543185779,9.5518225321049));
#36722=CARTESIAN_POINT('Ctrl Pts',(18.135799436934,-61.4316477881723,6.76826458716716));
#36723=CARTESIAN_POINT('Ctrl Pts',(14.8036106221423,-62.1626591350494,6.86000957288767));
#36724=CARTESIAN_POINT('Ctrl Pts',(13.0094633319359,-62.4815534974883,9.74542469319742));
#36725=CARTESIAN_POINT('Ctrl Pts',(14.3136373342298,-61.9702551717097,12.8573464026033));
#36726=CARTESIAN_POINT('Ctrl Pts',(17.5197763142877,-60.9493268661069,13.4270461480335));
#36727=CARTESIAN_POINT('Ctrl Pts',(19.7394014348253,-60.1927341524847,10.9477123134808));
#36728=CARTESIAN_POINT('Ctrl Pts',(18.9615992158899,-60.2392996738452,7.62511676387795));
#36729=CARTESIAN_POINT('Ctrl Pts',(15.8425832679706,-60.9131915231956,6.41562502038857));
#36730=CARTESIAN_POINT('Ctrl Pts',(13.1209708267227,-61.4805994238643,8.39487325110976));
#36731=CARTESIAN_POINT('Ctrl Pts',(13.1830095964177,-61.3021302305506,11.8028388367734));
#36732=CARTESIAN_POINT('Ctrl Pts',(15.9358673415304,-60.4026582657957,13.6055385422089));
#36733=CARTESIAN_POINT('Ctrl Pts',(18.8976307583479,-59.4472101950129,12.2029441264609));
#36734=CARTESIAN_POINT('Ctrl Pts',(19.3903963172922,-59.1533281063617,8.83503768583773));
#36735=CARTESIAN_POINT('Ctrl Pts',(17.7660737535057,-59.480666722193,7.29068223125039));
#36736=CARTESIAN_POINT('Ctrl Pts',(16.8135320242446,-59.681950857614,7.03077704625433));
#36737=CARTESIAN_POINT('Ctrl Pts',(20.25986904378,-67.0040126136404,11.1728309286208));
#36738=CARTESIAN_POINT('Ctrl Pts',(20.4203000043805,-66.9555034255254,10.9082027524038));
#36739=CARTESIAN_POINT('Ctrl Pts',(20.5332184525385,-66.9207835851305,10.6149904639443));
#36740=CARTESIAN_POINT('Ctrl Pts',(20.6611539455099,-66.8813975908017,9.99178401342259));
#36741=CARTESIAN_POINT('Ctrl Pts',(20.6720025707686,-66.8780249511107,9.66515229429175));
#36742=CARTESIAN_POINT('Ctrl Pts',(20.5855924444283,-66.904675210205,9.0009848649648));
#36743=CARTESIAN_POINT('Ctrl Pts',(20.4815398383751,-66.9367881932439,8.66883374311742));
#36744=CARTESIAN_POINT('Ctrl Pts',(20.1690707048657,-67.0315956493191,8.06423785428596));
#36745=CARTESIAN_POINT('Ctrl Pts',(19.9644265611133,-67.09312085238,7.79496359360541));
#36746=CARTESIAN_POINT('Ctrl Pts',(19.4553169386786,-67.2425937581436,7.32570054462934));
#36747=CARTESIAN_POINT('Ctrl Pts',(19.148781829213,-67.33085397004,7.13688275745718));
#36748=CARTESIAN_POINT('Ctrl Pts',(18.8154792730625,-67.4238662472344,7.01293629783558));
#36749=CARTESIAN_POINT('Ctrl Pts',(15.2652009106025,-66.709565290414,9.99881345470574));
#36750=CARTESIAN_POINT('Ctrl Pts',(15.2659775128488,-66.7141255555458,9.92620926472465));
#36751=CARTESIAN_POINT('Ctrl Pts',(15.2699455778512,-66.7178306708093,9.85363960672275));
#36752=CARTESIAN_POINT('Ctrl Pts',(15.2772137473688,-66.7206515257331,9.78136734601486));
#36753=CARTESIAN_POINT('Ctrl Pts',(15.3594450282717,-66.752566372114,8.9636868341033));
#36754=CARTESIAN_POINT('Ctrl Pts',(15.8641033480846,-66.6712922345579,8.18407440691835));
#36755=CARTESIAN_POINT('Ctrl Pts',(16.5726883518979,-66.5353761067088,7.78933375549815));
#36756=CARTESIAN_POINT('Ctrl Pts',(17.2812733557112,-66.3994599788597,7.39459310407796));
#36757=CARTESIAN_POINT('Ctrl Pts',(18.1937850435249,-66.2089018607175,7.38472422842252));
#36758=CARTESIAN_POINT('Ctrl Pts',(18.9102906125108,-66.0708634238267,7.76413764787115));
#36759=CARTESIAN_POINT('Ctrl Pts',(19.6267961814968,-65.932824986936,8.14355106731979));
#36760=CARTESIAN_POINT('Ctrl Pts',(20.1472956316549,-65.8473062312967,8.91224678187249));
#36761=CARTESIAN_POINT('Ctrl Pts',(20.246238786796,-65.8747431444716,9.72822620930746));
#36762=CARTESIAN_POINT('Ctrl Pts',(20.345181941937,-65.9021800576464,10.5442056367424));
#36763=CARTESIAN_POINT('Ctrl Pts',(20.0225688020609,-66.0425726396352,11.4074687770597));
#36764=CARTESIAN_POINT('Ctrl Pts',(19.4279225161919,-66.2558562834075,11.9340732703408));
#36765=CARTESIAN_POINT('Ctrl Pts',(18.8332762303228,-66.4691399271797,12.4606777636219));
#36766=CARTESIAN_POINT('Ctrl Pts',(17.9665967984607,-66.7553146327353,12.6506236098669));
#36767=CARTESIAN_POINT('Ctrl Pts',(17.2194144305739,-67.0094701965008,12.4192427536872));
#36768=CARTESIAN_POINT('Ctrl Pts',(16.4722320626871,-67.2636257602663,12.1878618975074));
#36769=CARTESIAN_POINT('Ctrl Pts',(15.8445467587756,-67.4857621822417,11.5351543389028));
#36770=CARTESIAN_POINT('Ctrl Pts',(15.6216179699845,-67.5994444228593,10.7518245719412));
#36771=CARTESIAN_POINT('Ctrl Pts',(15.5528913979792,-67.6344914472383,10.5103323450966));
#36772=CARTESIAN_POINT('Ctrl Pts',(15.5226338262371,-67.6592307340631,10.2564254798708));
#36773=CARTESIAN_POINT('Ctrl Pts',(15.5286491313886,-67.6742507328171,10.0019962882658));
#36774=CARTESIAN_POINT('Ctrl Pts',(16.8135320242446,-59.681950857614,7.03077704625433));
#36775=CARTESIAN_POINT('Ctrl Pts',(16.9051481187087,-59.6574023990886,7.06547285383011));
#36776=CARTESIAN_POINT('Ctrl Pts',(16.9947948727223,-59.6333816237466,7.10515219318068));
#36777=CARTESIAN_POINT('Ctrl Pts',(17.082237786682,-59.6099513655673,7.14949694326817));
#36778=CARTESIAN_POINT('Ctrl Pts',(17.1708871306384,-59.5861978454446,7.19445350778722));
#36779=CARTESIAN_POINT('Ctrl Pts',(17.257272050493,-59.5630510759314,7.2442058054096));
#36780=CARTESIAN_POINT('Ctrl Pts',(17.3411153578246,-59.5405853294411,7.29846300340358));
#36781=CARTESIAN_POINT('Ctrl Pts',(17.3650399830487,-59.5341747454331,7.31394525439086));
#36782=CARTESIAN_POINT('Ctrl Pts',(17.3887574233665,-59.5278196764534,7.32979452698956));
#36783=CARTESIAN_POINT('Ctrl Pts',(17.4122606427146,-59.5215220078096,7.34600453500901));
#36784=CARTESIAN_POINT('Ctrl Pts',(17.4307316092674,-59.5165727272383,7.35874383303933));
#36785=CARTESIAN_POINT('Ctrl Pts',(17.4490721037676,-59.5116584065482,7.37170741304488));
#36786=CARTESIAN_POINT('Ctrl Pts',(17.4672605740137,-59.5067848206342,7.38487881928224));
#36787=CARTESIAN_POINT('Ctrl Pts',(17.5471418516652,-59.4853806967971,7.4427258368968));
#36788=CARTESIAN_POINT('Ctrl Pts',(17.6241706060797,-59.4647409042578,7.50463022536142));
#36789=CARTESIAN_POINT('Ctrl Pts',(17.6980879988856,-59.4449347985488,7.57029723839113));
#36790=CARTESIAN_POINT('Ctrl Pts',(17.7541980617666,-59.4299001525126,7.62014450830199));
#36791=CARTESIAN_POINT('Ctrl Pts',(17.808514662402,-59.4153460632368,7.67216077851682));
#36792=CARTESIAN_POINT('Ctrl Pts',(17.8609084969736,-59.4013071775749,7.72622830914027));
#36793=CARTESIAN_POINT('Ctrl Pts',(17.887929214397,-59.3940669981624,7.75411219049193));
#36794=CARTESIAN_POINT('Ctrl Pts',(17.9144382908043,-59.386963912547,7.78254178039818));
#36795=CARTESIAN_POINT('Ctrl Pts',(17.9404163406947,-59.3800031150579,7.81150163987195));
#36796=CARTESIAN_POINT('Ctrl Pts',(17.9513656352696,-59.3770692604189,7.82370771513786));
#36797=CARTESIAN_POINT('Ctrl Pts',(17.9622216783077,-59.3741603924538,7.83600935553802));
#36798=CARTESIAN_POINT('Ctrl Pts',(17.9729722066068,-59.3712797970779,7.84839276276143));
#36799=CARTESIAN_POINT('Ctrl Pts',(18.0365635528686,-59.3542405472014,7.9216428872886));
#36800=CARTESIAN_POINT('Ctrl Pts',(18.0965497610003,-59.3381672911755,7.99784282323338));
#36801=CARTESIAN_POINT('Ctrl Pts',(18.1526942045728,-59.3231234328608,8.07671631116857));
#36802=CARTESIAN_POINT('Ctrl Pts',(18.2078226719183,-59.3083518045556,8.15416252360535));
#36803=CARTESIAN_POINT('Ctrl Pts',(18.2592474979931,-59.2945725639379,8.23418719299189));
#36804=CARTESIAN_POINT('Ctrl Pts',(18.306701932207,-59.281857186613,8.3165506094164));
#36805=CARTESIAN_POINT('Ctrl Pts',(18.3532560644286,-59.2693830444799,8.39735143323749));
#36806=CARTESIAN_POINT('Ctrl Pts',(18.3959893039731,-59.257932707454,8.48040377572554));
#36807=CARTESIAN_POINT('Ctrl Pts',(18.4346037832467,-59.2475859889165,8.56549184002203));
#36808=CARTESIAN_POINT('Ctrl Pts',(18.4539341349641,-59.2424064367844,8.60808680027398));
#36809=CARTESIAN_POINT('Ctrl Pts',(18.4722315774893,-59.2375036518362,8.65119201445444));
#36810=CARTESIAN_POINT('Ctrl Pts',(18.4894539567762,-59.2328889292146,8.69478065000367));
#36811=CARTESIAN_POINT('Ctrl Pts',(18.4977385366612,-59.2306690827247,8.71574834135866));
#36812=CARTESIAN_POINT('Ctrl Pts',(18.5057743024797,-59.2285159057631,8.73682789347791));
#36813=CARTESIAN_POINT('Ctrl Pts',(18.5135562806062,-59.2264307310086,8.75801630574046));
#36814=CARTESIAN_POINT('Ctrl Pts',(18.5185237400553,-59.2250997042608,8.77154147594721));
#36815=CARTESIAN_POINT('Ctrl Pts',(18.5233877588239,-59.2237963943598,8.78511114924033));
#36816=CARTESIAN_POINT('Ctrl Pts',(18.5281423789793,-59.2225223977288,8.79871063662932));
#36817=CARTESIAN_POINT('Ctrl Pts',(18.5587083682319,-59.2143322655927,8.88613755440161));
#36818=CARTESIAN_POINT('Ctrl Pts',(18.5848098578286,-59.207338392534,8.97493705334007));
#36819=CARTESIAN_POINT('Ctrl Pts',(18.6062022975288,-59.2016063055922,9.06488740567675));
#36820=CARTESIAN_POINT('Ctrl Pts',(18.6087806599844,-59.2009154354544,9.07572883445171));
#36821=CARTESIAN_POINT('Ctrl Pts',(18.6112905562915,-59.2002429107659,9.08658699313079));
#36822=CARTESIAN_POINT('Ctrl Pts',(18.6137315088206,-59.199588859507,9.09746150181113));
#36823=CARTESIAN_POINT('Ctrl Pts',(18.6343037125501,-59.1940765541311,9.18911121861902));
#36824=CARTESIAN_POINT('Ctrl Pts',(18.6499830153446,-59.1898752976094,9.28192246232578));
#36825=CARTESIAN_POINT('Ctrl Pts',(18.6608728938762,-59.1869573634512,9.37550443036849));
#36826=CARTESIAN_POINT('Ctrl Pts',(18.672143984606,-59.1839372837923,9.47236233832657));
#36827=CARTESIAN_POINT('Ctrl Pts',(18.678284396888,-59.1822919652802,9.57004704527406));
#36828=CARTESIAN_POINT('Ctrl Pts',(18.6793547107854,-59.1820051755357,9.66811274307749));
#36829=CARTESIAN_POINT('Ctrl Pts',(18.679876498809,-59.1818653628562,9.71592068686325));
#36830=CARTESIAN_POINT('Ctrl Pts',(18.6791925043488,-59.1820486386194,9.76381888086314));
#36831=CARTESIAN_POINT('Ctrl Pts',(18.6773054175282,-59.182554282009,9.81175333277687));
#36832=CARTESIAN_POINT('Ctrl Pts',(18.6767477018728,-59.1827037214685,9.82592003352112));
#36833=CARTESIAN_POINT('Ctrl Pts',(18.6760848075141,-59.1828813434766,9.84008999100378));
#36834=CARTESIAN_POINT('Ctrl Pts',(18.6753177565931,-59.1830868741514,9.85424725645943));
#36835=CARTESIAN_POINT('Ctrl Pts',(18.6702850237357,-59.1844353908563,9.94713513791762));
#36836=CARTESIAN_POINT('Ctrl Pts',(18.660767260643,-59.1869856677907,10.039633649145));
#36837=CARTESIAN_POINT('Ctrl Pts',(18.6468763518991,-59.1907077255708,10.1313703607271));
#36838=CARTESIAN_POINT('Ctrl Pts',(18.633025285787,-59.1944191075498,10.2228439482696));
#36839=CARTESIAN_POINT('Ctrl Pts',(18.6148257395458,-59.1992956612678,10.3135610431858));
#36840=CARTESIAN_POINT('Ctrl Pts',(18.5923417342414,-59.2053202323317,10.4031353906328));
#36841=CARTESIAN_POINT('Ctrl Pts',(18.5702449117701,-59.2112410580682,10.4911672349027));
#36842=CARTESIAN_POINT('Ctrl Pts',(18.544009480218,-59.2182708207657,10.5780961319276));
#36843=CARTESIAN_POINT('Ctrl Pts',(18.5136570926348,-59.2264037185069,10.6635263253263));
#36844=CARTESIAN_POINT('Ctrl Pts',(18.499101256118,-59.2303039431468,10.7044953570147));
#36845=CARTESIAN_POINT('Ctrl Pts',(18.4835980629778,-59.2344580112288,10.7451192119765));
#36846=CARTESIAN_POINT('Ctrl Pts',(18.4671470633348,-59.2388660432978,10.7853510160082));
#36847=CARTESIAN_POINT('Ctrl Pts',(18.4616118760651,-59.2403491922567,10.7988876140478));
#36848=CARTESIAN_POINT('Ctrl Pts',(18.455969374247,-59.2418610960621,10.8123798087171));
#36849=CARTESIAN_POINT('Ctrl Pts',(18.4502194972982,-59.2434017709471,10.8258257522335));
#36850=CARTESIAN_POINT('Ctrl Pts',(18.4447502513563,-59.2448672509805,10.8386154471551));
#36851=CARTESIAN_POINT('Ctrl Pts',(18.4391855696994,-59.2463583029366,10.8513591677142));
#36852=CARTESIAN_POINT('Ctrl Pts',(18.4335294175004,-59.2478738643506,10.864047091407));
#36853=CARTESIAN_POINT('Ctrl Pts',(18.3974943892325,-59.2575294210742,10.9448811412784));
#36854=CARTESIAN_POINT('Ctrl Pts',(18.3577058350311,-59.2681907320404,11.0235565035315));
#36855=CARTESIAN_POINT('Ctrl Pts',(18.3142251103267,-59.2798413571113,11.0997253732369));
#36856=CARTESIAN_POINT('Ctrl Pts',(18.2714642927549,-59.2912990836474,11.1746331206183));
#36857=CARTESIAN_POINT('Ctrl Pts',(18.2251321272566,-59.3037137499762,11.2471173606622));
#36858=CARTESIAN_POINT('Ctrl Pts',(18.1752516289959,-59.3170791892032,11.3168132015522));
#36859=CARTESIAN_POINT('Ctrl Pts',(18.1268143228897,-59.330057926258,11.3844925330993));
#36860=CARTESIAN_POINT('Ctrl Pts',(18.0750306258251,-59.3439333260675,11.4495429414388));
#36861=CARTESIAN_POINT('Ctrl Pts',(18.0198942246886,-59.3587070802256,11.5115898438695));
#36862=CARTESIAN_POINT('Ctrl Pts',(18.0099245352413,-59.3613784504618,11.52280908081));
#36863=CARTESIAN_POINT('Ctrl Pts',(17.9998451629738,-59.364079210121,11.5339299972363));
#36864=CARTESIAN_POINT('Ctrl Pts',(17.9896559870012,-59.3668093915945,11.5449502145346));
#36865=CARTESIAN_POINT('Ctrl Pts',(17.9601614990779,-59.3747124158147,11.576850308015));
#36866=CARTESIAN_POINT('Ctrl Pts',(17.9297469672236,-59.3828619650632,11.6079068412472));
#36867=CARTESIAN_POINT('Ctrl Pts',(17.8984546702662,-59.3912467107622,11.6380966037224));
#36868=CARTESIAN_POINT('Ctrl Pts',(15.0750265266586,-68.1281291851066,10.0024371765581));
#36869=CARTESIAN_POINT('Ctrl Pts',(15.0686010168709,-68.1132191003537,10.3130580784043));
#36870=CARTESIAN_POINT('Ctrl Pts',(15.229260839257,-67.9995899840862,11.6285356953996));
#36871=CARTESIAN_POINT('Ctrl Pts',(17.0050066526373,-67.3992512291335,13.4679206448302));
#36872=CARTESIAN_POINT('Ctrl Pts',(20.1882099452846,-66.3844685224502,12.7722321938661));
#36873=CARTESIAN_POINT('Ctrl Pts',(21.3787366757643,-65.9036218913761,9.6104773635602));
#36874=CARTESIAN_POINT('Ctrl Pts',(19.4813112170045,-66.2501895556748,6.79508159949539));
#36875=CARTESIAN_POINT('Ctrl Pts',(16.1481166073794,-66.9814704044651,6.83122696910054));
#36876=CARTESIAN_POINT('Ctrl Pts',(14.8676525643411,-67.2119040522751,8.81893895087676));
#36877=CARTESIAN_POINT('Ctrl Pts',(14.8112407741816,-67.1683025391241,9.90991228406403));
#36878=CARTESIAN_POINT('Ctrl Pts',(14.810555933805,-67.1637176864735,9.99855140140538));
#36879=CARTESIAN_POINT('Origin',(18.6889152049569,-69.7479810832458,10.));
#36880=CARTESIAN_POINT('Ctrl Pts',(15.0969161422106,-68.2083503098983,9.99673640007585));
#36881=CARTESIAN_POINT('Ctrl Pts',(15.0927295232038,-68.1711103559359,10.7130675867));
#36882=CARTESIAN_POINT('Ctrl Pts',(15.6514186592595,-67.9289066052254,12.4513417391716));
#36883=CARTESIAN_POINT('Ctrl Pts',(18.3902480628713,-67.0483943376965,13.5944453497599));
#36884=CARTESIAN_POINT('Ctrl Pts',(21.0667649555471,-66.1687987195556,11.6442225433397));
#36885=CARTESIAN_POINT('Ctrl Pts',(20.9561469803459,-66.036013638459,8.22016494780579));
#36886=CARTESIAN_POINT('Ctrl Pts',(18.1194957904382,-66.6336669557833,6.39071567224368));
#36887=CARTESIAN_POINT('Ctrl Pts',(15.4027596845032,-67.2173089746449,7.63681194520568));
#36888=CARTESIAN_POINT('Ctrl Pts',(14.8518622987657,-67.2747579502335,9.32892113065756));
#36889=CARTESIAN_POINT('Ctrl Pts',(14.8383776097513,-67.242349320473,10.0022118830713));
#36890=CARTESIAN_POINT('Ctrl Pts',(17.244983442153,-67.8425423025985,7.06170475438608));
#36891=CARTESIAN_POINT('Ctrl Pts',(16.2988495743024,-68.0419164156808,7.35795147289589));
#36892=CARTESIAN_POINT('Ctrl Pts',(14.725851572522,-68.3551165744735,8.97144797270218));
#36893=CARTESIAN_POINT('Ctrl Pts',(15.3567034243025,-68.0236552520251,12.3283366156213));
#36894=CARTESIAN_POINT('Ctrl Pts',(18.3902480628713,-67.0483943376965,13.5944453497599));
#36895=CARTESIAN_POINT('Ctrl Pts',(21.0667649555471,-66.1687987195556,11.6442225433397));
#36896=CARTESIAN_POINT('Ctrl Pts',(20.9561469803459,-66.036013638459,8.22016494780579));
#36897=CARTESIAN_POINT('Ctrl Pts',(18.1194957904382,-66.6336669557833,6.39071567224368));
#36898=CARTESIAN_POINT('Ctrl Pts',(15.0616295968133,-67.2905946547074,7.79327945411719));
#36899=CARTESIAN_POINT('Ctrl Pts',(14.4843023646232,-67.282863942121,11.1722569386416));
#36900=CARTESIAN_POINT('Ctrl Pts',(16.868372167434,-66.4816292855382,13.5013274912989));
#36901=CARTESIAN_POINT('Ctrl Pts',(20.0422978199459,-65.468753391891,12.6947822329673));
#36902=CARTESIAN_POINT('Ctrl Pts',(21.1273143736846,-65.0155990043222,9.47487431060689));
#36903=CARTESIAN_POINT('Ctrl Pts',(19.1153342996381,-65.3922823621302,6.72525821930947));
#36904=CARTESIAN_POINT('Ctrl Pts',(15.7718556315866,-66.1257396929252,6.90837057311361));
#36905=CARTESIAN_POINT('Ctrl Pts',(14.0547985877671,-66.4233986629546,9.86022990097492));
#36906=CARTESIAN_POINT('Ctrl Pts',(15.4655309000317,-65.8829690009266,12.9372608391342));
#36907=CARTESIAN_POINT('Ctrl Pts',(18.7042880702649,-64.8527215544619,13.3837942299379));
#36908=CARTESIAN_POINT('Ctrl Pts',(20.8341986998846,-64.1195886430847,10.7999310727631));
#36909=CARTESIAN_POINT('Ctrl Pts',(19.9114308093213,-64.2044184759422,7.49968047567758));
#36910=CARTESIAN_POINT('Ctrl Pts',(16.7260146593053,-64.895523082676,6.43862003923502));
#36911=CARTESIAN_POINT('Ctrl Pts',(14.0943212306268,-65.4382581333965,8.56699487612852));
#36912=CARTESIAN_POINT('Ctrl Pts',(14.3368288007655,-65.2108533475991,11.9787141005062));
#36913=CARTESIAN_POINT('Ctrl Pts',(17.1999914587379,-64.2812461473763,13.6183729089162));
#36914=CARTESIAN_POINT('Ctrl Pts',(20.0833051820056,-63.346239485481,12.017555775347));
#36915=CARTESIAN_POINT('Ctrl Pts',(20.3682194128848,-63.1074718691846,8.60989310618131));
#36916=CARTESIAN_POINT('Ctrl Pts',(17.7632104839249,-63.6430568297551,6.44715683087681));
#36917=CARTESIAN_POINT('Ctrl Pts',(14.564859018057,-64.3376274439251,7.46621057361502));
#36918=CARTESIAN_POINT('Ctrl Pts',(13.60112044902,-64.4334353369931,10.7544289031929));
#36919=CARTESIAN_POINT('Ctrl Pts',(15.6987166428558,-63.708961052588,13.3670096553836));
#36920=CARTESIAN_POINT('Ctrl Pts',(18.9427555175132,-62.6772983776882,12.9642257537709));
#36921=CARTESIAN_POINT('Ctrl Pts',(20.3916349158421,-62.1266472347557,9.9067950074971));
#36922=CARTESIAN_POINT('Ctrl Pts',(18.7114286257305,-62.4144320750886,6.93283507366396));
#36923=CARTESIAN_POINT('Ctrl Pts',(15.3704995140598,-63.1472062543102,6.70571036393745));
#36924=CARTESIAN_POINT('Ctrl Pts',(13.3244900809145,-63.5330077514078,9.42882503807144));
#36925=CARTESIAN_POINT('Ctrl Pts',(14.3693624549396,-63.090609964374,12.6634621126407));
#36926=CARTESIAN_POINT('Ctrl Pts',(17.5330036055456,-62.080489794707,13.5128046754735));
#36927=CARTESIAN_POINT('Ctrl Pts',(19.9458125081592,-61.2715545195409,11.2162142452876));
#36928=CARTESIAN_POINT('Ctrl Pts',(19.4106046411912,-61.2525379570576,7.83042882970036));
#36929=CARTESIAN_POINT('Ctrl Pts',(16.3703262829254,-61.9047530097005,6.3876284598802));
#36930=CARTESIAN_POINT('Ctrl Pts',(13.5113685232516,-62.5083833543796,8.17992871548479));
#36931=CARTESIAN_POINT('Ctrl Pts',(13.357739085696,-62.3871231598861,11.6022164308586));
#36932=CARTESIAN_POINT('Ctrl Pts',(16.0106566332716,-61.5138509672066,13.5896176377583));
#36933=CARTESIAN_POINT('Ctrl Pts',(19.0579057022675,-60.5349179618126,12.3623010109723));
#36934=CARTESIAN_POINT('Ctrl Pts',(19.734119272829,-60.1913020034494,9.01938609588904));
#36935=CARTESIAN_POINT('Ctrl Pts',(17.3973455890623,-60.6550135466889,6.55469600728483));
#36936=CARTESIAN_POINT('Ctrl Pts',(14.1039347737162,-61.3750552367845,7.17543798647161));
#36937=CARTESIAN_POINT('Ctrl Pts',(12.7669926495712,-61.5708627210562,10.3258507409624));
#36938=CARTESIAN_POINT('Ctrl Pts',(14.5474295567701,-60.9313710113775,13.1842383274677));
#36939=CARTESIAN_POINT('Ctrl Pts',(17.8144668208753,-59.8935459365978,13.1913616605739));
#36940=CARTESIAN_POINT('Ctrl Pts',(19.6057481548832,-59.2511484715134,10.3395770770155));
#36941=CARTESIAN_POINT('Ctrl Pts',(18.2810249486938,-59.4436819065863,7.18539898656541));
#36942=CARTESIAN_POINT('Ctrl Pts',(14.9896601306954,-60.1631753733452,6.54837069990781));
#36943=CARTESIAN_POINT('Ctrl Pts',(12.6441934312551,-60.629216203114,9.00969837718652));
#36944=CARTESIAN_POINT('Ctrl Pts',(13.0868379849885,-60.402326566927,11.2296927240265));
#36945=CARTESIAN_POINT('Ctrl Pts',(13.707234883037,-60.181950026368,11.9973015569304));
#36946=CARTESIAN_POINT('Ctrl Pts',(17.3251900988197,-67.9318278742783,7.23888518457547));
#36947=CARTESIAN_POINT('Ctrl Pts',(16.4352923065869,-68.1161335763132,7.51726810226197));
#36948=CARTESIAN_POINT('Ctrl Pts',(14.9555143577762,-68.4043554971943,9.03347008941793));
#36949=CARTESIAN_POINT('Ctrl Pts',(15.5458770044743,-68.0837432245499,12.1879369455073));
#36950=CARTESIAN_POINT('Ctrl Pts',(18.3940490596781,-67.1581527442329,13.3776987943165));
#36951=CARTESIAN_POINT('Ctrl Pts',(20.9067222911425,-66.3224589027986,11.5450752374347));
#36952=CARTESIAN_POINT('Ctrl Pts',(20.800326051025,-66.1885426111956,8.32748974461941));
#36953=CARTESIAN_POINT('Ctrl Pts',(18.1322775372971,-66.7410189775958,6.60835702425632));
#36954=CARTESIAN_POINT('Ctrl Pts',(15.256353376944,-67.3491954556355,7.92634562444536));
#36955=CARTESIAN_POINT('Ctrl Pts',(14.7113906429075,-67.3327927019053,11.1015693557681));
#36956=CARTESIAN_POINT('Ctrl Pts',(16.9492514661363,-66.5707346233278,13.2901959816018));
#36957=CARTESIAN_POINT('Ctrl Pts',(19.9293395015267,-65.609797362651,12.5322857391188));
#36958=CARTESIAN_POINT('Ctrl Pts',(20.9464805290194,-65.1748301675257,9.5065396089424));
#36959=CARTESIAN_POINT('Ctrl Pts',(19.0533751185266,-65.5196611552341,6.92272651604652));
#36960=CARTESIAN_POINT('Ctrl Pts',(15.9090610352118,-66.1997524963877,7.09479711845809));
#36961=CARTESIAN_POINT('Ctrl Pts',(14.2930946730788,-66.4703242998971,9.86865809630684));
#36962=CARTESIAN_POINT('Ctrl Pts',(15.6163106628564,-65.9533445658039,12.7601427840874));
#36963=CARTESIAN_POINT('Ctrl Pts',(18.6573208483792,-64.9760832641982,13.1797500249766));
#36964=CARTESIAN_POINT('Ctrl Pts',(20.6563484026839,-64.2780203671544,10.751694895066));
#36965=CARTESIAN_POINT('Ctrl Pts',(19.7867752262122,-64.3485967193296,7.65045078699729));
#36966=CARTESIAN_POINT('Ctrl Pts',(16.7909924250965,-64.9888892233674,6.65337273791571));
#36967=CARTESIAN_POINT('Ctrl Pts',(14.3155426340162,-65.489758917571,8.65340568344619));
#36968=CARTESIAN_POINT('Ctrl Pts',(14.5409783214077,-65.2669285289691,11.8593968140379));
#36969=CARTESIAN_POINT('Ctrl Pts',(17.2290425005878,-64.3842388247346,13.4001835116647));
#36970=CARTESIAN_POINT('Ctrl Pts',(19.9360426274117,-63.496475248621,11.8958963196675));
#36971=CARTESIAN_POINT('Ctrl Pts',(20.2013278361943,-63.2629672129436,8.69371713231473));
#36972=CARTESIAN_POINT('Ctrl Pts',(17.7509534583573,-63.7571179704187,6.66139475745698));
#36973=CARTESIAN_POINT('Ctrl Pts',(14.7430153463368,-64.4006674801972,7.61899913400437));
#36974=CARTESIAN_POINT('Ctrl Pts',(13.8349420404105,-64.4815599109683,10.7089365253202));
#36975=CARTESIAN_POINT('Ctrl Pts',(15.803603732902,-63.7916335220748,13.1639775672763));
#36976=CARTESIAN_POINT('Ctrl Pts',(18.8495771338669,-62.8130423308995,12.7854817031124));
#36977=CARTESIAN_POINT('Ctrl Pts',(20.2086399244908,-62.2864574754684,9.91241530746257));
#36978=CARTESIAN_POINT('Ctrl Pts',(18.6273022002302,-62.5477505634248,7.11778639941016));
#36979=CARTESIAN_POINT('Ctrl Pts',(15.4853839339819,-63.2271999473303,6.90435740451559));
#36980=CARTESIAN_POINT('Ctrl Pts',(13.5603011489528,-63.5805992467218,9.46326712676862));
#36981=CARTESIAN_POINT('Ctrl Pts',(14.5397187075307,-63.1557400246277,12.5028542351256));
#36982=CARTESIAN_POINT('Ctrl Pts',(17.5101424007745,-62.1973923166247,13.3009810867784));
#36983=CARTESIAN_POINT('Ctrl Pts',(19.775009344088,-61.4280979699796,11.1428760184691));
#36984=CARTESIAN_POINT('Ctrl Pts',(19.2696261599639,-61.4010899078139,7.96125487716922));
#36985=CARTESIAN_POINT('Ctrl Pts',(16.4102292811539,-62.0048379141108,6.60545597208742));
#36986=CARTESIAN_POINT('Ctrl Pts',(13.721219293131,-62.5629308906206,8.28967977390791));
#36987=CARTESIAN_POINT('Ctrl Pts',(13.5744051997984,-62.4398445301463,11.5056021110758));
#36988=CARTESIAN_POINT('Ctrl Pts',(16.0649021365259,-61.6100928089779,13.3731621953643));
#36989=CARTESIAN_POINT('Ctrl Pts',(18.9259522392798,-60.6810516662198,12.2198532736369));
#36990=CARTESIAN_POINT('Ctrl Pts',(19.5589412741757,-60.3490176872814,9.07851752376016));
#36991=CARTESIAN_POINT('Ctrl Pts',(17.3606274442457,-60.7756290245013,6.76244927662485));
#36992=CARTESIAN_POINT('Ctrl Pts',(14.2633621012124,-61.4431136936917,7.34576025527719));
#36993=CARTESIAN_POINT('Ctrl Pts',(13.0045895703814,-61.6179756985622,10.306201805224));
#36994=CARTESIAN_POINT('Ctrl Pts',(14.6752168136493,-61.0079073996549,12.9922274267495));
#36995=CARTESIAN_POINT('Ctrl Pts',(17.7428017915754,-60.0235254038855,12.9989212198951));
#36996=CARTESIAN_POINT('Ctrl Pts',(19.4236195381877,-59.4107265678368,10.3191004374818));
#36997=CARTESIAN_POINT('Ctrl Pts',(18.1763291194576,-59.5825119500423,7.35512060290615));
#36998=CARTESIAN_POINT('Ctrl Pts',(15.0809863992776,-60.249481453992,6.75650538792377));
#36999=CARTESIAN_POINT('Ctrl Pts',(12.8745037461489,-60.6782816207909,9.06941397854051));
#37000=CARTESIAN_POINT('Ctrl Pts',(13.2888242651274,-60.4589813868428,11.1555417393121));
#37001=CARTESIAN_POINT('Ctrl Pts',(13.8709947795085,-60.2488475749171,11.8768634390786));
#37002=CARTESIAN_POINT('Ctrl Pts',(17.4053967554863,-68.0211134459581,7.41606561476487));
#37003=CARTESIAN_POINT('Ctrl Pts',(16.5717350388713,-68.1903507369457,7.67658473162804));
#37004=CARTESIAN_POINT('Ctrl Pts',(15.1851771430305,-68.4535944199151,9.09549220613369));
#37005=CARTESIAN_POINT('Ctrl Pts',(15.7350505846462,-68.1438311970748,12.0475372753934));
#37006=CARTESIAN_POINT('Ctrl Pts',(18.397850056485,-67.2679111507693,13.160952238873));
#37007=CARTESIAN_POINT('Ctrl Pts',(20.7466796267378,-66.4761190860415,11.4459279315297));
#37008=CARTESIAN_POINT('Ctrl Pts',(20.6445051217041,-66.3410715839322,8.43481454143305));
#37009=CARTESIAN_POINT('Ctrl Pts',(18.145059284156,-66.8483709994082,6.82599837626894));
#37010=CARTESIAN_POINT('Ctrl Pts',(15.4510771570748,-67.4077962565635,8.05941179477353));
#37011=CARTESIAN_POINT('Ctrl Pts',(14.9384789211918,-67.3827214616897,11.0308817728946));
#37012=CARTESIAN_POINT('Ctrl Pts',(17.0301307648387,-66.6598399611173,13.0790644719047));
#37013=CARTESIAN_POINT('Ctrl Pts',(19.8163811831075,-65.7508413334111,12.3697892452703));
#37014=CARTESIAN_POINT('Ctrl Pts',(20.7656466843542,-65.3340613307291,9.53820490727791));
#37015=CARTESIAN_POINT('Ctrl Pts',(18.9914159374152,-65.6470399483378,7.12019481278356));
#37016=CARTESIAN_POINT('Ctrl Pts',(16.0462664388369,-66.2737652998505,7.28122366380257));
#37017=CARTESIAN_POINT('Ctrl Pts',(14.5313907583906,-66.5172499368395,9.87708629163875));
#37018=CARTESIAN_POINT('Ctrl Pts',(15.7670904256811,-66.0237201306814,12.5830247290407));
#37019=CARTESIAN_POINT('Ctrl Pts',(18.6103536264935,-65.0994449739343,12.9757058200154));
#37020=CARTESIAN_POINT('Ctrl Pts',(20.4784981054833,-64.4364520912242,10.7034587173689));
#37021=CARTESIAN_POINT('Ctrl Pts',(19.6621196431031,-64.492774962717,7.80122109831697));
#37022=CARTESIAN_POINT('Ctrl Pts',(16.8559701908879,-65.0822553640589,6.86812543659641));
#37023=CARTESIAN_POINT('Ctrl Pts',(14.5367640374054,-65.5412597017456,8.73981649076384));
#37024=CARTESIAN_POINT('Ctrl Pts',(14.7451278420499,-65.323003710339,11.7400795275695));
#37025=CARTESIAN_POINT('Ctrl Pts',(17.2580935424376,-64.4872315020928,13.1819941144132));
#37026=CARTESIAN_POINT('Ctrl Pts',(19.7887800728178,-63.6467110117609,11.774236863988));
#37027=CARTESIAN_POINT('Ctrl Pts',(20.0344362595038,-63.4184625567026,8.77754115844814));
#37028=CARTESIAN_POINT('Ctrl Pts',(17.7386964327898,-63.8711791110824,6.87563268403716));
#37029=CARTESIAN_POINT('Ctrl Pts',(14.9211716746167,-64.4637075164694,7.77178769439372));
#37030=CARTESIAN_POINT('Ctrl Pts',(14.068763631801,-64.5296844849434,10.6634441474475));
#37031=CARTESIAN_POINT('Ctrl Pts',(15.9084908229482,-63.8743059915618,12.960945479169));
#37032=CARTESIAN_POINT('Ctrl Pts',(18.7563987502206,-62.9487862841108,12.6067376524539));
#37033=CARTESIAN_POINT('Ctrl Pts',(20.0256449331395,-62.4462677161812,9.91803560742804));
#37034=CARTESIAN_POINT('Ctrl Pts',(18.5431757747299,-62.6810690517609,7.30273772515637));
#37035=CARTESIAN_POINT('Ctrl Pts',(15.6002683539039,-63.3071936403505,7.10300444509373));
#37036=CARTESIAN_POINT('Ctrl Pts',(13.7961122169911,-63.6281907420358,9.49770921546579));
#37037=CARTESIAN_POINT('Ctrl Pts',(14.7100749601219,-63.2208700848816,12.3422463576105));
#37038=CARTESIAN_POINT('Ctrl Pts',(17.4872811960032,-62.3142948385424,13.0891574980833));
#37039=CARTESIAN_POINT('Ctrl Pts',(19.6042061800168,-61.5846414204184,11.0695377916506));
#37040=CARTESIAN_POINT('Ctrl Pts',(19.1286476787365,-61.5496418585701,8.09208092463809));
#37041=CARTESIAN_POINT('Ctrl Pts',(16.4501322793825,-62.104922818521,6.82328348429462));
#37042=CARTESIAN_POINT('Ctrl Pts',(13.9310700630103,-62.6174784268616,8.39943083233104));
#37043=CARTESIAN_POINT('Ctrl Pts',(13.7910713139007,-62.4925659004067,11.408987791293));
#37044=CARTESIAN_POINT('Ctrl Pts',(16.1191476397801,-61.7063346507491,13.1567067529703));
#37045=CARTESIAN_POINT('Ctrl Pts',(18.7939987762921,-60.8271853706271,12.0774055363016));
#37046=CARTESIAN_POINT('Ctrl Pts',(19.3837632755223,-60.5067333711136,9.13764895163129));
#37047=CARTESIAN_POINT('Ctrl Pts',(17.3239092994291,-60.8962445023136,6.97020254596486));
#37048=CARTESIAN_POINT('Ctrl Pts',(14.4227894287085,-61.5111721505989,7.51608252408276));
#37049=CARTESIAN_POINT('Ctrl Pts',(13.2421864911916,-61.6650886760682,10.2865528694857));
#37050=CARTESIAN_POINT('Ctrl Pts',(14.8030040705286,-61.0844437879324,12.8002165260313));
#37051=CARTESIAN_POINT('Ctrl Pts',(17.6711367622755,-60.1535048711732,12.8064807792163));
#37052=CARTESIAN_POINT('Ctrl Pts',(19.2414909214922,-59.5703046641601,10.2986237979481));
#37053=CARTESIAN_POINT('Ctrl Pts',(18.0716332902214,-59.7213419934982,7.52484221924687));
#37054=CARTESIAN_POINT('Ctrl Pts',(15.1723126678598,-60.3357875346388,6.96464007593975));
#37055=CARTESIAN_POINT('Ctrl Pts',(13.1048140610427,-60.7273470384677,9.12912957989447));
#37056=CARTESIAN_POINT('Ctrl Pts',(13.4908105452663,-60.5156362067586,11.0813907545978));
#37057=CARTESIAN_POINT('Ctrl Pts',(14.0347546759799,-60.3157451234662,11.7564253212267));
#37058=CARTESIAN_POINT('Ctrl Pts',(17.485603412153,-68.1103990176379,7.59324604495427));
#37059=CARTESIAN_POINT('Ctrl Pts',(16.7081777711558,-68.2645678975782,7.83590136099411));
#37060=CARTESIAN_POINT('Ctrl Pts',(15.4148399282848,-68.502833342636,9.15751432284945));
#37061=CARTESIAN_POINT('Ctrl Pts',(15.924224164818,-68.2039191695996,11.9071376052795));
#37062=CARTESIAN_POINT('Ctrl Pts',(18.4016510532918,-67.3776695573057,12.9442056834295));
#37063=CARTESIAN_POINT('Ctrl Pts',(20.5866369623332,-66.6297792692845,11.3467806256248));
#37064=CARTESIAN_POINT('Ctrl Pts',(20.4886841923832,-66.4936005566688,8.54213933824665));
#37065=CARTESIAN_POINT('Ctrl Pts',(18.1578410310149,-66.9557230212208,7.04363972828159));
#37066=CARTESIAN_POINT('Ctrl Pts',(15.6458009372055,-67.4663970574915,8.19247796510169));
#37067=CARTESIAN_POINT('Ctrl Pts',(15.1655671994761,-67.432650221474,10.9601941900212));
#37068=CARTESIAN_POINT('Ctrl Pts',(17.111010063541,-66.7489452989068,12.8679329622076));
#37069=CARTESIAN_POINT('Ctrl Pts',(19.7034228646883,-65.8918853041711,12.2072927514219));
#37070=CARTESIAN_POINT('Ctrl Pts',(20.584812839689,-65.4932924939326,9.56987020561342));
#37071=CARTESIAN_POINT('Ctrl Pts',(18.9294567563037,-65.7744187414415,7.3176631095206));
#37072=CARTESIAN_POINT('Ctrl Pts',(16.1834718424621,-66.3477781033132,7.46765020914706));
#37073=CARTESIAN_POINT('Ctrl Pts',(14.7696868437023,-66.5641755737819,9.88551448697067));
#37074=CARTESIAN_POINT('Ctrl Pts',(15.9178701885058,-66.0940956955587,12.4059066739939));
#37075=CARTESIAN_POINT('Ctrl Pts',(18.5633864046078,-65.2228066836706,12.7716616150541));
#37076=CARTESIAN_POINT('Ctrl Pts',(20.3006478082827,-64.5948838152939,10.6552225396718));
#37077=CARTESIAN_POINT('Ctrl Pts',(19.5374640599939,-64.6369532061044,7.95199140963667));
#37078=CARTESIAN_POINT('Ctrl Pts',(16.9209479566792,-65.1756215047503,7.08287813527709));
#37079=CARTESIAN_POINT('Ctrl Pts',(14.7579854407948,-65.5927604859202,8.82622729808152));
#37080=CARTESIAN_POINT('Ctrl Pts',(14.9492773626922,-65.379078891709,11.6207622411012));
#37081=CARTESIAN_POINT('Ctrl Pts',(17.2871445842874,-64.5902241794511,12.9638047171617));
#37082=CARTESIAN_POINT('Ctrl Pts',(19.6415175182239,-63.796946774901,11.6525774083085));
#37083=CARTESIAN_POINT('Ctrl Pts',(19.8675446828133,-63.5739579004615,8.86136518458156));
#37084=CARTESIAN_POINT('Ctrl Pts',(17.7264394072222,-63.9852402517461,7.08987061061734));
#37085=CARTESIAN_POINT('Ctrl Pts',(15.0993280028965,-64.5267475527414,7.92457625478306));
#37086=CARTESIAN_POINT('Ctrl Pts',(14.3025852231916,-64.5778090589186,10.6179517695748));
#37087=CARTESIAN_POINT('Ctrl Pts',(16.0133779129944,-63.9569784610486,12.7579133910617));
#37088=CARTESIAN_POINT('Ctrl Pts',(18.6632203665742,-63.0845302373221,12.4279936017954));
#37089=CARTESIAN_POINT('Ctrl Pts',(19.8426499417882,-62.6060779568939,9.92365590739352));
#37090=CARTESIAN_POINT('Ctrl Pts',(18.4590493492297,-62.814387540097,7.48768905090255));
#37091=CARTESIAN_POINT('Ctrl Pts',(15.715152773826,-63.3871873333707,7.30165148567188));
#37092=CARTESIAN_POINT('Ctrl Pts',(14.0319232850294,-63.6757822373498,9.53215130416297));
#37093=CARTESIAN_POINT('Ctrl Pts',(14.8804312127131,-63.2860001451354,12.1816384800953));
#37094=CARTESIAN_POINT('Ctrl Pts',(17.4644199912321,-62.4311973604599,12.8773339093881));
#37095=CARTESIAN_POINT('Ctrl Pts',(19.4334030159456,-61.7411848708572,10.9961995648321));
#37096=CARTESIAN_POINT('Ctrl Pts',(18.9876691975092,-61.6981938093263,8.22290697210694));
#37097=CARTESIAN_POINT('Ctrl Pts',(16.490035277611,-62.2050077229313,7.04111099650184));
#37098=CARTESIAN_POINT('Ctrl Pts',(14.1409208328896,-62.6720259631026,8.50918189075418));
#37099=CARTESIAN_POINT('Ctrl Pts',(14.007737428003,-62.545287270667,11.3123734715102));
#37100=CARTESIAN_POINT('Ctrl Pts',(16.1733931430344,-61.8025764925203,12.9402513105764));
#37101=CARTESIAN_POINT('Ctrl Pts',(18.6620453133043,-60.9733190750343,11.9349577989662));
#37102=CARTESIAN_POINT('Ctrl Pts',(19.208585276869,-60.6644490549457,9.19678037950242));
#37103=CARTESIAN_POINT('Ctrl Pts',(17.2871911546125,-61.016859980126,7.17795581530488));
#37104=CARTESIAN_POINT('Ctrl Pts',(14.5822167562047,-61.5792306075061,7.68640479288833));
#37105=CARTESIAN_POINT('Ctrl Pts',(13.4797834120018,-61.7122016535741,10.2669039337474));
#37106=CARTESIAN_POINT('Ctrl Pts',(14.9307913274079,-61.1609801762098,12.6082056253131));
#37107=CARTESIAN_POINT('Ctrl Pts',(17.5994717329756,-60.2834843384609,12.6140403385374));
#37108=CARTESIAN_POINT('Ctrl Pts',(19.0593623047967,-59.7298827604835,10.2781471584144));
#37109=CARTESIAN_POINT('Ctrl Pts',(17.9669374609853,-59.8601720369542,7.69456383558757));
#37110=CARTESIAN_POINT('Ctrl Pts',(15.263638936442,-60.4220936152857,7.17277476395572));
#37111=CARTESIAN_POINT('Ctrl Pts',(13.3351243759366,-60.7764124561445,9.18884518124844));
#37112=CARTESIAN_POINT('Ctrl Pts',(13.6927968254053,-60.5722910266744,11.0072397698834));
#37113=CARTESIAN_POINT('Ctrl Pts',(14.1985145724514,-60.3826426720153,11.6359872033748));
#37114=CARTESIAN_POINT('Ctrl Pts',(17.244983442153,-67.8425423025985,7.06170475438607));
#37115=CARTESIAN_POINT('Ctrl Pts',(16.875980626074,-67.9363396049609,7.20780006417485));
#37116=CARTESIAN_POINT('Ctrl Pts',(16.5358040823886,-68.0195197262117,7.42431456480016));
#37117=CARTESIAN_POINT('Ctrl Pts',(15.9848167458476,-68.150998080649,7.95780764621775));
#37118=CARTESIAN_POINT('Ctrl Pts',(15.769941108176,-68.2006822338607,8.25968161903173));
#37119=CARTESIAN_POINT('Ctrl Pts',(15.4905619320039,-68.2646302810789,8.88066242679774));
#37120=CARTESIAN_POINT('Ctrl Pts',(15.410358466988,-68.2826595052327,9.184978201574));
#37121=CARTESIAN_POINT('Ctrl Pts',(15.358433741901,-68.2943569622715,9.79677072277292));
#37122=CARTESIAN_POINT('Ctrl Pts',(15.3830449856443,-68.288855628865,10.0982078060305));
#37123=CARTESIAN_POINT('Ctrl Pts',(15.5341550196633,-68.2546420063796,10.6858944634119));
#37124=CARTESIAN_POINT('Ctrl Pts',(15.6614146465391,-68.2257386849337,10.9661810334235));
#37125=CARTESIAN_POINT('Ctrl Pts',(16.0093499903205,-68.1449424659488,11.4722931322537));
#37126=CARTESIAN_POINT('Ctrl Pts',(16.2286900565758,-68.093295210955,11.6926718707977));
#37127=CARTESIAN_POINT('Ctrl Pts',(16.4806955947432,-68.0322473001841,11.8669181223571));
#37128=CARTESIAN_POINT('Ctrl Pts',(14.1985145724514,-60.3826426720153,11.6359872033748));
#37129=CARTESIAN_POINT('Ctrl Pts',(14.1384791309758,-60.3987291200759,11.5775783984678));
#37130=CARTESIAN_POINT('Ctrl Pts',(14.081700362681,-60.4139429451877,11.5159169743213));
#37131=CARTESIAN_POINT('Ctrl Pts',(14.0281914535651,-60.4282806141732,11.451379059159));
#37132=CARTESIAN_POINT('Ctrl Pts',(13.9733764666698,-60.4429682456449,11.3852658635748));
#37133=CARTESIAN_POINT('Ctrl Pts',(13.9219924575766,-60.4567365493853,11.3161335496706));
#37134=CARTESIAN_POINT('Ctrl Pts',(13.8740814492324,-60.4695742653797,11.2443401959101));
#37135=CARTESIAN_POINT('Ctrl Pts',(13.8615442020184,-60.472933610646,11.2255534691112));
#37136=CARTESIAN_POINT('Ctrl Pts',(13.849244935159,-60.4762291892685,11.2065843091216));
#37137=CARTESIAN_POINT('Ctrl Pts',(13.8371847673053,-60.4794607015055,11.1874386951811));
#37138=CARTESIAN_POINT('Ctrl Pts',(13.8274131410429,-60.4820790008712,11.1719261595134));
#37139=CARTESIAN_POINT('Ctrl Pts',(13.8177980990068,-60.48465534362,11.1562969507259));
#37140=CARTESIAN_POINT('Ctrl Pts',(13.8083486578088,-60.4871873137579,11.1405686299001));
#37141=CARTESIAN_POINT('Ctrl Pts',(13.7625022245992,-60.4994718285123,11.0642585714397));
#37142=CARTESIAN_POINT('Ctrl Pts',(13.7205023350773,-60.5107256649919,10.9855425559687));
#37143=CARTESIAN_POINT('Ctrl Pts',(13.6823842420087,-60.5209393772466,10.9048124950817));
#37144=CARTESIAN_POINT('Ctrl Pts',(13.6519560246515,-60.5290925935146,10.8403687718475));
#37145=CARTESIAN_POINT('Ctrl Pts',(13.6240018720623,-60.536582886126,10.7746405673723));
#37146=CARTESIAN_POINT('Ctrl Pts',(13.5985556604601,-60.5434011779752,10.7078100770375));
#37147=CARTESIAN_POINT('Ctrl Pts',(13.5903398047872,-60.5456026098679,10.686232418574));
#37148=CARTESIAN_POINT('Ctrl Pts',(13.5823855107333,-60.547733956536,10.6645397510572));
#37149=CARTESIAN_POINT('Ctrl Pts',(13.5746942691753,-60.5497948185002,10.6427379426545));
#37150=CARTESIAN_POINT('Ctrl Pts',(13.5673646518884,-60.5517587835331,10.6219612045232));
#37151=CARTESIAN_POINT('Ctrl Pts',(13.5602723818286,-60.5536591515681,10.6010802045182));
#37152=CARTESIAN_POINT('Ctrl Pts',(13.5534284149517,-60.5554929869658,10.5801302249954));
#37153=CARTESIAN_POINT('Ctrl Pts',(13.5248766271769,-60.5631434154425,10.4927307124063));
#37154=CARTESIAN_POINT('Ctrl Pts',(13.5006117004043,-60.5696451829756,10.4040498989134));
#37155=CARTESIAN_POINT('Ctrl Pts',(13.4806668323773,-60.5749893942566,10.3144849192065));
#37156=CARTESIAN_POINT('Ctrl Pts',(13.460414058401,-60.5804161086881,10.2235372484701));
#37157=CARTESIAN_POINT('Ctrl Pts',(13.4446152716799,-60.5846493808314,10.1316770970802));
#37158=CARTESIAN_POINT('Ctrl Pts',(13.4333455934662,-60.5876690820077,10.0392871197263));
#37159=CARTESIAN_POINT('Ctrl Pts',(13.4221628859679,-60.5906654794511,9.94761013721475));
#37160=CARTESIAN_POINT('Ctrl Pts',(13.4154393160804,-60.5924670545727,9.85541054684674));
#37161=CARTESIAN_POINT('Ctrl Pts',(13.4132936428739,-60.5930419859756,9.76304299851744));
#37162=CARTESIAN_POINT('Ctrl Pts',(13.4122613686528,-60.5933185830195,9.71860536527655));
#37163=CARTESIAN_POINT('Ctrl Pts',(13.4122893693042,-60.5933110802676,9.67412865780575));
#37164=CARTESIAN_POINT('Ctrl Pts',(13.4133950120097,-60.5930148241975,9.62965173460712));
#37165=CARTESIAN_POINT('Ctrl Pts',(13.4137601235609,-60.5929169928522,9.61496431493879));
#37166=CARTESIAN_POINT('Ctrl Pts',(13.4142427737567,-60.592787667122,9.60027687089771));
#37167=CARTESIAN_POINT('Ctrl Pts',(13.4148436567719,-60.5926266610034,9.585590801596));
#37168=CARTESIAN_POINT('Ctrl Pts',(13.4154511643855,-60.5924638798289,9.57074282172334));
#37169=CARTESIAN_POINT('Ctrl Pts',(13.4161791917241,-60.5922688054914,9.55590504967698));
#37170=CARTESIAN_POINT('Ctrl Pts',(13.4170277181603,-60.5920414435181,9.54108357191584));
#37171=CARTESIAN_POINT('Ctrl Pts',(13.4224967665285,-60.5905760164245,9.44555398638134));
#37172=CARTESIAN_POINT('Ctrl Pts',(13.4329703612531,-60.5877696251762,9.3506422021473));
#37173=CARTESIAN_POINT('Ctrl Pts',(13.4485182643158,-60.5836035771065,9.25674298405853));
#37174=CARTESIAN_POINT('Ctrl Pts',(13.4498478809535,-60.5832473074022,9.24871296469604));
#37175=CARTESIAN_POINT('Ctrl Pts',(13.4512146356353,-60.582881086589,9.24069033920175));
#37176=CARTESIAN_POINT('Ctrl Pts',(13.4526185882087,-60.5825048986307,9.23267534878075));
#37177=CARTESIAN_POINT('Ctrl Pts',(13.4683901533207,-60.5782789204956,9.14263744743655));
#37178=CARTESIAN_POINT('Ctrl Pts',(13.4888516530664,-60.5727962781628,9.05356331283828));
#37179=CARTESIAN_POINT('Ctrl Pts',(13.5137114619786,-60.5661351124408,8.96568771725755));
#37180=CARTESIAN_POINT('Ctrl Pts',(13.5391401674861,-60.5593215113355,8.87580115983445));
#37181=CARTESIAN_POINT('Ctrl Pts',(13.5691709812857,-60.5512747790298,8.78716792582602));
#37182=CARTESIAN_POINT('Ctrl Pts',(13.6035442475271,-60.5420644900992,8.70004212727832));
#37183=CARTESIAN_POINT('Ctrl Pts',(13.6224082878578,-60.5370098857266,8.65222750977575));
#37184=CARTESIAN_POINT('Ctrl Pts',(13.6425810893193,-60.5316045998659,8.60486701428382));
#37185=CARTESIAN_POINT('Ctrl Pts',(13.6640258581899,-60.5258584913652,8.55800419893538));
#37186=CARTESIAN_POINT('Ctrl Pts',(13.6704060167659,-60.5241489330272,8.54406176873024));
#37187=CARTESIAN_POINT('Ctrl Pts',(13.676899765887,-60.5224089381943,8.53016150103107));
#37188=CARTESIAN_POINT('Ctrl Pts',(13.6834982307757,-60.5206408848561,8.51632087094479));
#37189=CARTESIAN_POINT('Ctrl Pts',(13.7247150405699,-60.5095968739572,8.4298664262631));
#37190=CARTESIAN_POINT('Ctrl Pts',(13.7700718775146,-60.4974435461266,8.34560744644018));
#37191=CARTESIAN_POINT('Ctrl Pts',(13.8192407167051,-60.4842687953727,8.26379708587707));
#37192=CARTESIAN_POINT('Ctrl Pts',(13.8693790787445,-60.4708342617545,8.18037356919415));
#37193=CARTESIAN_POINT('Ctrl Pts',(13.9234815558615,-60.4563375467024,8.09949541140026));
#37194=CARTESIAN_POINT('Ctrl Pts',(13.9812533713892,-60.4408576353865,8.02143790704939));
#37195=CARTESIAN_POINT('Ctrl Pts',(14.0394826344362,-60.4252551513772,7.94276232948411));
#37196=CARTESIAN_POINT('Ctrl Pts',(14.1014400133005,-60.4086537217454,7.86695140890492));
#37197=CARTESIAN_POINT('Ctrl Pts',(14.1668712742987,-60.3911214682012,7.79430622909373));
#37198=CARTESIAN_POINT('Ctrl Pts',(14.2014931149696,-60.3818445739529,7.75586726578238));
#37199=CARTESIAN_POINT('Ctrl Pts',(14.2370883363508,-60.3723068631294,7.71831505011915));
#37200=CARTESIAN_POINT('Ctrl Pts',(14.2736239455356,-60.3625171761534,7.68169758973408));
#37201=CARTESIAN_POINT('Ctrl Pts',(14.2866331259749,-60.3590313767605,7.66865926465863));
#37202=CARTESIAN_POINT('Ctrl Pts',(14.2997615607819,-60.3555136232561,7.65573947794386));
#37203=CARTESIAN_POINT('Ctrl Pts',(14.3130078489039,-60.3519642910511,7.64294048656779));
#37204=CARTESIAN_POINT('Ctrl Pts',(14.3231851533472,-60.3492372905443,7.6331068463357));
#37205=CARTESIAN_POINT('Ctrl Pts',(14.3334310228843,-60.3464919180761,7.62334556303852));
#37206=CARTESIAN_POINT('Ctrl Pts',(14.3437359537465,-60.3437307201735,7.61366571160746));
#37207=CARTESIAN_POINT('Ctrl Pts',(14.4166886968569,-60.3241830915715,7.54513815676625));
#37208=CARTESIAN_POINT('Ctrl Pts',(14.4927140802975,-60.3038121514743,7.48057696460985));
#37209=CARTESIAN_POINT('Ctrl Pts',(14.5714997184595,-60.2827016033536,7.42026730037134));
#37210=CARTESIAN_POINT('Ctrl Pts',(14.6503851322383,-60.261564320437,7.35988125883753));
#37211=CARTESIAN_POINT('Ctrl Pts',(14.7320383430701,-60.2396854085352,7.30375667601981));
#37212=CARTESIAN_POINT('Ctrl Pts',(14.8161894528123,-60.2171371866376,7.25220561228357));
#37213=CARTESIAN_POINT('Ctrl Pts',(14.8987454238434,-60.1950163808695,7.20163173230178));
#37214=CARTESIAN_POINT('Ctrl Pts',(14.9837061241246,-60.1722512298408,7.15545893550819));
#37215=CARTESIAN_POINT('Ctrl Pts',(15.0708497996908,-60.1489011523473,7.11401788929066));
#37216=CARTESIAN_POINT('Ctrl Pts',(15.0979686081559,-60.1416346895194,7.10112157997545));
#37217=CARTESIAN_POINT('Ctrl Pts',(15.125299031229,-60.1343115247281,7.08868381627438));
#37218=CARTESIAN_POINT('Ctrl Pts',(15.1528349118068,-60.1269333077644,7.0767154567206));
#37219=CARTESIAN_POINT('Ctrl Pts',(15.1941283917648,-60.115868753157,7.05876741202422));
#37220=CARTESIAN_POINT('Ctrl Pts',(15.2358838838841,-60.1046804027641,7.04187489341864));
#37221=CARTESIAN_POINT('Ctrl Pts',(15.2780676602835,-60.0933772939442,7.02603075613029));
#37222=CARTESIAN_POINT('Ctrl Pts',(15.458048217099,-67.4086397233445,10.0018117506528));
#37223=CARTESIAN_POINT('Ctrl Pts',(15.4516726940089,-67.3922281881599,10.2792252787835));
#37224=CARTESIAN_POINT('Ctrl Pts',(15.488118577317,-67.364342691712,10.5560719127008));
#37225=CARTESIAN_POINT('Ctrl Pts',(15.5698466331085,-67.3243238737158,10.8168646145657));
#37226=CARTESIAN_POINT('Ctrl Pts',(15.8140481541644,-67.2047485806183,11.5961071140833));
#37227=CARTESIAN_POINT('Ctrl Pts',(16.4625291088527,-66.9768469397626,12.2320200381454));
#37228=CARTESIAN_POINT('Ctrl Pts',(17.2188383863881,-66.7200527868787,12.4398697983789));
#37229=CARTESIAN_POINT('Ctrl Pts',(17.9751476639235,-66.4632586339949,12.6477195586123));
#37230=CARTESIAN_POINT('Ctrl Pts',(18.8392852643059,-66.177571969083,12.4275061550171));
#37231=CARTESIAN_POINT('Ctrl Pts',(19.4182523936639,-65.9682965015873,11.8778290289181));
#37232=CARTESIAN_POINT('Ctrl Pts',(19.9972195230219,-65.7590210340916,11.328151902819));
#37233=CARTESIAN_POINT('Ctrl Pts',(20.2910161813555,-65.6261567640121,10.4490110542162));
#37234=CARTESIAN_POINT('Ctrl Pts',(20.162021829958,-65.6065790035572,9.63407278056603));
#37235=CARTESIAN_POINT('Ctrl Pts',(20.0330274785606,-65.5870012431022,8.81913450691582));
#37236=CARTESIAN_POINT('Ctrl Pts',(19.4812421174321,-65.6807099922718,8.06839880821821));
#37237=CARTESIAN_POINT('Ctrl Pts',(18.747685284561,-65.8231242605019,7.71802880880715));
#37238=CARTESIAN_POINT('Ctrl Pts',(18.0141284516898,-65.965538528732,7.36765880939609));
#37239=CARTESIAN_POINT('Ctrl Pts',(17.0988001470759,-66.1566583160226,7.41765450927158));
#37240=CARTESIAN_POINT('Ctrl Pts',(16.4055051616424,-66.288284454746,7.84562973884659));
#37241=CARTESIAN_POINT('Ctrl Pts',(15.7122101762088,-66.4199105934694,8.2736049684216));
#37242=CARTESIAN_POINT('Ctrl Pts',(15.2409485099556,-66.4920430836256,9.07955972769613));
#37243=CARTESIAN_POINT('Ctrl Pts',(15.1966815676295,-66.4497626823332,9.90260247183727));
#37244=CARTESIAN_POINT('Ctrl Pts',(15.1949465504969,-66.4481055265244,9.93486115488332));
#37245=CARTESIAN_POINT('Ctrl Pts',(15.1938674837542,-66.4462726093384,9.96714608853553));
#37246=CARTESIAN_POINT('Ctrl Pts',(15.1934336836835,-66.4442667934687,9.99943462192768));
#37247=CARTESIAN_POINT('Ctrl Pts',(-67.0040126136403,-20.2598690437802,
11.1728309286203));
#37248=CARTESIAN_POINT('Ctrl Pts',(-66.854289394458,-20.6173045957294,10.4434664543479));
#37249=CARTESIAN_POINT('Ctrl Pts',(-66.7561954352348,-20.580718017241,8.59013022403023));
#37250=CARTESIAN_POINT('Ctrl Pts',(-67.209041264398,-18.2866570474715,7.05024279158508));
#37251=CARTESIAN_POINT('Ctrl Pts',(-67.723582781997,-15.7623446338517,8.14059085434287));
#37252=CARTESIAN_POINT('Ctrl Pts',(-67.707898604217,-15.2168614548643,10.8824467802989));
#37253=CARTESIAN_POINT('Ctrl Pts',(-67.0414893382907,-17.0999173665992,
12.8405694561121));
#37254=CARTESIAN_POINT('Ctrl Pts',(-66.182965221624,-19.6999556621853,12.2707319173765));
#37255=CARTESIAN_POINT('Ctrl Pts',(-65.7617874756575,-20.667795081813,9.68094249642456));
#37256=CARTESIAN_POINT('Ctrl Pts',(-66.0183437425753,-19.1062967313381,
7.37485535276681));
#37257=CARTESIAN_POINT('Ctrl Pts',(-66.5900180970021,-16.3687616678969,
7.4044619797337));
#37258=CARTESIAN_POINT('Ctrl Pts',(-66.83384050967,-14.8547867084588,9.74329926128886));
#37259=CARTESIAN_POINT('Ctrl Pts',(-66.3985290187163,-15.8753739824804,
12.3105450512032));
#37260=CARTESIAN_POINT('Ctrl Pts',(-65.5370346894514,-18.4864972623917,
12.8220707222437));
#37261=CARTESIAN_POINT('Ctrl Pts',(-64.8814857844687,-20.3290217552967,
10.8227823754305));
#37262=CARTESIAN_POINT('Ctrl Pts',(-64.8807798084461,-19.7276391663447,
8.09145561890004));
#37263=CARTESIAN_POINT('Ctrl Pts',(-65.4011950297318,-17.1814057921375,
7.05817718516389));
#37264=CARTESIAN_POINT('Ctrl Pts',(-65.8453641599239,-14.91972670377,8.64226139479156));
#37265=CARTESIAN_POINT('Ctrl Pts',(-65.6837566027253,-14.9188369907855,
11.4343367521445));
#37266=CARTESIAN_POINT('Ctrl Pts',(-64.925806142571,-17.1435292903643,12.9502711232991));
#37267=CARTESIAN_POINT('Ctrl Pts',(-64.1115175849316,-19.5784782321599,
11.8413258175008));
#37268=CARTESIAN_POINT('Ctrl Pts',(-63.831020197438,-20.021291406339,9.09413821413749));
#37269=CARTESIAN_POINT('Ctrl Pts',(-64.1995249831399,-18.0419954959306,
7.15290308224158));
#37270=CARTESIAN_POINT('Ctrl Pts',(-64.7548205378836,-15.3655869450728,
7.74475277436916));
#37271=CARTESIAN_POINT('Ctrl Pts',(-64.8685062198083,-14.3372888767,10.3431139119323));
#37272=CARTESIAN_POINT('Ctrl Pts',(-64.3050852130208,-15.8359873727452,
12.6362038638415));
#37273=CARTESIAN_POINT('Ctrl Pts',(-63.4314879220136,-18.4922795208021,
12.5838422163724));
#37274=CARTESIAN_POINT('Ctrl Pts',(-62.890611065017,-19.9068421044143,10.2326155433113));
#37275=CARTESIAN_POINT('Ctrl Pts',(-63.0293273367052,-18.7851286033006,
7.67442896667196));
#37276=CARTESIAN_POINT('Ctrl Pts',(-63.589870005783,-16.0891375551548,7.18532148363271));
#37277=CARTESIAN_POINT('Ctrl Pts',(-63.9391700310929,-14.1815147862763,
9.20045592301492));
#37278=CARTESIAN_POINT('Ctrl Pts',(-63.6321026366036,-14.7234885765213,
11.9269511029875));
#37279=CARTESIAN_POINT('Ctrl Pts',(-62.8075183731849,-17.1968616153845,
12.9390225214354));
#37280=CARTESIAN_POINT('Ctrl Pts',(-62.0647066785609,-19.3650552728411,
11.3362221619431));
#37281=CARTESIAN_POINT('Ctrl Pts',(-61.930203280714,-19.2630114600592,8.54457429525347));
#37282=CARTESIAN_POINT('Ctrl Pts',(-62.3893271714103,-16.9455204456753,
7.04783027207105));
#37283=CARTESIAN_POINT('Ctrl Pts',(-62.8992423967486,-14.4384735898223,
8.1776552235709));
#37284=CARTESIAN_POINT('Ctrl Pts',(-62.8719235739435,-13.9364114971974,
10.9288348037821));
#37285=CARTESIAN_POINT('Ctrl Pts',(-62.197326683109,-15.8500240410826,12.8536227562672));
#37286=CARTESIAN_POINT('Ctrl Pts',(-61.3412962728354,-18.4407556977108,
12.2395195742222));
#37287=CARTESIAN_POINT('Ctrl Pts',(-60.9310995184379,-19.3676134988852,
9.63289839745324));
#37288=CARTESIAN_POINT('Ctrl Pts',(-61.19734228766,-17.7699646296632,7.35288957156097));
#37289=CARTESIAN_POINT('Ctrl Pts',(-61.7687958934071,-15.0332534115102,
7.42803777444134));
#37290=CARTESIAN_POINT('Ctrl Pts',(-62.0026849934362,-13.5563500795274,
9.79147768509061));
#37291=CARTESIAN_POINT('Ctrl Pts',(-61.5565643024821,-14.6172778371396,
12.3404488591361));
#37292=CARTESIAN_POINT('Ctrl Pts',(-60.6930063334386,-17.2361027255536,
12.8070892069868));
#37293=CARTESIAN_POINT('Ctrl Pts',(-60.0459653166684,-19.0468753473845,
10.776269968826));
#37294=CARTESIAN_POINT('Ctrl Pts',(-60.0567902041014,-18.4024589901609,
8.05473611617426));
#37295=CARTESIAN_POINT('Ctrl Pts',(-60.5814573009747,-15.8403574002333,
7.06404294414461));
#37296=CARTESIAN_POINT('Ctrl Pts',(-61.0189035288689,-13.6037685248156,
8.6852426906361));
#37297=CARTESIAN_POINT('Ctrl Pts',(-60.8454027634005,-13.6472648693588,
11.476703032887));
#37298=CARTESIAN_POINT('Ctrl Pts',(-60.081329531004,-15.8948076660291,12.9532921034687));
#37299=CARTESIAN_POINT('Ctrl Pts',(-59.2714063402784,-18.3134648367082,
11.80442877448));
#37300=CARTESIAN_POINT('Ctrl Pts',(-59.0033710168104,-18.7097689547775,
9.0457808277518));
#37301=CARTESIAN_POINT('Ctrl Pts',(-59.253282418477,-17.3744086881423,7.78080120942645));
#37302=CARTESIAN_POINT('Ctrl Pts',(-59.4090483774019,-16.5917431062324,
7.56791319796486));
#37303=CARTESIAN_POINT('Ctrl Pts',(-67.0649244254631,-20.445968013835,11.2591724044644));
#37304=CARTESIAN_POINT('Ctrl Pts',(-66.9078844272408,-20.8307101569088,
10.4761135710135));
#37305=CARTESIAN_POINT('Ctrl Pts',(-66.8099800782137,-20.7934159435354,
8.4863384205957));
#37306=CARTESIAN_POINT('Ctrl Pts',(-67.3072801529266,-18.333449470762,6.83308754393481));
#37307=CARTESIAN_POINT('Ctrl Pts',(-67.8708178297159,-15.6262809016683,
8.003704858317));
#37308=CARTESIAN_POINT('Ctrl Pts',(-67.8650956520226,-15.0436190322125,
10.9474107537972));
#37309=CARTESIAN_POINT('Ctrl Pts',(-67.1607433019049,-17.0682804619454,
13.0496865190182));
#37310=CARTESIAN_POINT('Ctrl Pts',(-66.2501329885661,-19.8627070898853,
12.4378986762062));
#37311=CARTESIAN_POINT('Ctrl Pts',(-65.8090656142303,-20.9047756131301,
9.65745411880286));
#37312=CARTESIAN_POINT('Ctrl Pts',(-66.0956256802753,-19.2313015598933,
7.18159743500955));
#37313=CARTESIAN_POINT('Ctrl Pts',(-66.7205021994898,-16.2952133143909,
7.2133836428561));
#37314=CARTESIAN_POINT('Ctrl Pts',(-66.9933909703099,-14.6727612295383,
9.72440146443704));
#37315=CARTESIAN_POINT('Ctrl Pts',(-66.5371493528455,-15.7714607991059,
12.4806427736089));
#37316=CARTESIAN_POINT('Ctrl Pts',(-65.6233501657759,-18.5777884658278,
13.0298259452252));
#37317=CARTESIAN_POINT('Ctrl Pts',(-64.9306576947329,-20.5589346344442,
10.8833539743367));
#37318=CARTESIAN_POINT('Ctrl Pts',(-64.9410163841629,-19.916258151854,7.95095238475352));
#37319=CARTESIAN_POINT('Ctrl Pts',(-65.5108601749997,-17.1855548447367,
6.84160605175788));
#37320=CARTESIAN_POINT('Ctrl Pts',(-65.9988447894535,-14.7603541429462,
8.54230738426578));
#37321=CARTESIAN_POINT('Ctrl Pts',(-65.8364566439328,-14.7623776252395,
11.5399297656092));
#37322=CARTESIAN_POINT('Ctrl Pts',(-65.0338240192839,-17.1538260329046,
13.167464204339));
#37323=CARTESIAN_POINT('Ctrl Pts',(-64.1707057986788,-19.7710097578042,
11.9768805549428));
#37324=CARTESIAN_POINT('Ctrl Pts',(-63.8806753904707,-20.2494006496397,
9.02745047458906));
#37325=CARTESIAN_POINT('Ctrl Pts',(-64.2874254021706,-18.1273716126596,
6.94330548061646));
#37326=CARTESIAN_POINT('Ctrl Pts',(-64.894717347108,-15.2569098917891,7.57872596768916));
#37327=CARTESIAN_POINT('Ctrl Pts',(-65.0278889803931,-14.1558892629052,
10.3683732743996));
#37328=CARTESIAN_POINT('Ctrl Pts',(-64.4341066798256,-15.7678976499211,
12.8302759390876));
#37329=CARTESIAN_POINT('Ctrl Pts',(-63.5073135350877,-18.6227194268525,
12.7740595314737));
#37330=CARTESIAN_POINT('Ctrl Pts',(-62.9377350396947,-20.1443979832212,
10.2497402360727));
#37331=CARTESIAN_POINT('Ctrl Pts',(-63.0977799648827,-18.9430848635887,
7.50322506140479));
#37332=CARTESIAN_POINT('Ctrl Pts',(-63.7107053062555,-16.0515990210022,
6.97811046011729));
#37333=CARTESIAN_POINT('Ctrl Pts',(-64.096836741373,-14.0065195594072,9.14159508133287));
#37334=CARTESIAN_POINT('Ctrl Pts',(-63.7782802952007,-14.5913710742642,
12.06880940332));
#37335=CARTESIAN_POINT('Ctrl Pts',(-62.9041084194733,-17.2498076016892,
13.1553875028215));
#37336=CARTESIAN_POINT('Ctrl Pts',(-62.1177290461057,-19.5805980497848,
11.4345921747918));
#37337=CARTESIAN_POINT('Ctrl Pts',(-61.9844404141372,-19.4740206690252,
8.43742875512251));
#37338=CARTESIAN_POINT('Ctrl Pts',(-62.4884807287629,-16.9888992784424,
6.83049741954161));
#37339=CARTESIAN_POINT('Ctrl Pts',(-63.0470515348743,-14.3002673230729,
8.04349783254878));
#37340=CARTESIAN_POINT('Ctrl Pts',(-63.0288381927735,-13.7642231138317,
10.997213771131));
#37341=CARTESIAN_POINT('Ctrl Pts',(-62.3156954611176,-15.8216906940831,
13.0637007771192));
#37342=CARTESIAN_POINT('Ctrl Pts',(-61.4077624358672,-18.6061255468504,
12.4043885425463));
#37343=CARTESIAN_POINT('Ctrl Pts',(-60.9784844518179,-19.6041954665562,
9.6058731090036));
#37344=CARTESIAN_POINT('Ctrl Pts',(-61.2754441211642,-17.89190956542,7.15801457676294));
#37345=CARTESIAN_POINT('Ctrl Pts',(-61.9000836406212,-14.9567058150541,
7.23869504059023));
#37346=CARTESIAN_POINT('Ctrl Pts',(-62.1623078281202,-13.3740544969969,
9.77612668779305));
#37347=CARTESIAN_POINT('Ctrl Pts',(-61.6944612588913,-14.5160643361698,
12.512748040292));
#37348=CARTESIAN_POINT('Ctrl Pts',(-60.7784465109946,-17.3306605884652,
13.013741520669));
#37349=CARTESIAN_POINT('Ctrl Pts',(-60.0948882619405,-19.2777173765314,
10.8334174170441));
#37350=CARTESIAN_POINT('Ctrl Pts',(-60.117626694016,-18.5888390654038,7.91152966540869));
#37351=CARTESIAN_POINT('Ctrl Pts',(-60.6920353750484,-15.8410993561455,
6.84790363622595));
#37352=CARTESIAN_POINT('Ctrl Pts',(-61.1728021605341,-13.4428359587846,
8.58845287746082));
#37353=CARTESIAN_POINT('Ctrl Pts',(-60.9976452524506,-13.4925131117118,
11.585414967516));
#37354=CARTESIAN_POINT('Ctrl Pts',(-60.1884391092678,-15.9084942245297,
13.1707075830488));
#37355=CARTESIAN_POINT('Ctrl Pts',(-59.33000762519,-18.5081868105882,11.9372672251402));
#37356=CARTESIAN_POINT('Ctrl Pts',(-59.0533567133275,-18.9366447422823,
8.97553311378027));
#37357=CARTESIAN_POINT('Ctrl Pts',(-59.3290771863823,-17.5049637099299,
7.61742821670101));
#37358=CARTESIAN_POINT('Ctrl Pts',(-59.500015870806,-16.6656727455696,7.38886781406131));
#37359=CARTESIAN_POINT('Ctrl Pts',(-67.1258362372859,-20.6320669838898,
11.3455138803086));
#37360=CARTESIAN_POINT('Ctrl Pts',(-66.9614794600237,-21.0441157180882,
10.5087606876792));
#37361=CARTESIAN_POINT('Ctrl Pts',(-66.8637647211926,-21.0061138698298,
8.38254661716119));
#37362=CARTESIAN_POINT('Ctrl Pts',(-67.4055190414552,-18.3802418940525,
6.61593229628453));
#37363=CARTESIAN_POINT('Ctrl Pts',(-68.0180528774348,-15.4902171694848,
7.86681886229114));
#37364=CARTESIAN_POINT('Ctrl Pts',(-68.0222926998282,-14.8703766095608,
11.0123747272955));
#37365=CARTESIAN_POINT('Ctrl Pts',(-67.2799972655191,-17.0366435572917,
13.2588035819243));
#37366=CARTESIAN_POINT('Ctrl Pts',(-66.317300755508,-20.0254585175853,12.6050654350359));
#37367=CARTESIAN_POINT('Ctrl Pts',(-65.8563437528033,-21.1417561444472,
9.63396574118116));
#37368=CARTESIAN_POINT('Ctrl Pts',(-66.172907617975,-19.3563063884486,6.98833951725229));
#37369=CARTESIAN_POINT('Ctrl Pts',(-66.8509863019776,-16.2216649608848,
7.0223053059785));
#37370=CARTESIAN_POINT('Ctrl Pts',(-67.1529414309497,-14.4907357506179,
9.70550366758521));
#37371=CARTESIAN_POINT('Ctrl Pts',(-66.6757696869749,-15.6675476157315,
12.6507404960146));
#37372=CARTESIAN_POINT('Ctrl Pts',(-65.7096656421003,-18.6690796692638,
13.2375811682066));
#37373=CARTESIAN_POINT('Ctrl Pts',(-64.9798296049969,-20.7888475135917,
10.943925573243));
#37374=CARTESIAN_POINT('Ctrl Pts',(-65.0012529598798,-20.1048771373633,
7.810449150607));
#37375=CARTESIAN_POINT('Ctrl Pts',(-65.6205253202676,-17.1897038973359,
6.62503491835186));
#37376=CARTESIAN_POINT('Ctrl Pts',(-66.1523254189831,-14.6009815821224,
8.44235337374002));
#37377=CARTESIAN_POINT('Ctrl Pts',(-65.9891566851404,-14.6059182596936,
11.6455227790739));
#37378=CARTESIAN_POINT('Ctrl Pts',(-65.1418418959967,-17.1641227754448,
13.384657285379));
#37379=CARTESIAN_POINT('Ctrl Pts',(-64.2298940124261,-19.9635412834486,
12.1124352923848));
#37380=CARTESIAN_POINT('Ctrl Pts',(-63.9303305835035,-20.4775098929403,
8.96076273504062));
#37381=CARTESIAN_POINT('Ctrl Pts',(-64.3753258212014,-18.2127477293887,
6.73370787899134));
#37382=CARTESIAN_POINT('Ctrl Pts',(-65.0346141563324,-15.1482328385054,
7.41269916100916));
#37383=CARTESIAN_POINT('Ctrl Pts',(-65.1872717409779,-13.9744896491104,
10.3936326368669));
#37384=CARTESIAN_POINT('Ctrl Pts',(-64.5631281466304,-15.6998079270971,
13.0243480143336));
#37385=CARTESIAN_POINT('Ctrl Pts',(-63.5831391481619,-18.753159332903,12.9642768465751));
#37386=CARTESIAN_POINT('Ctrl Pts',(-62.9848590143722,-20.3819538620283,
10.2668649288342));
#37387=CARTESIAN_POINT('Ctrl Pts',(-63.1662325930603,-19.1010411238768,
7.33202115613761));
#37388=CARTESIAN_POINT('Ctrl Pts',(-63.831540606728,-16.0140604868496,6.77089943660186));
#37389=CARTESIAN_POINT('Ctrl Pts',(-64.2545034516531,-13.8315243325381,
9.08273423965082));
#37390=CARTESIAN_POINT('Ctrl Pts',(-63.9244579537977,-14.459253572007,12.2106677036524));
#37391=CARTESIAN_POINT('Ctrl Pts',(-63.0006984657617,-17.3027535879938,
13.3717524842075));
#37392=CARTESIAN_POINT('Ctrl Pts',(-62.1707514136505,-19.7961408267284,
11.5329621876406));
#37393=CARTESIAN_POINT('Ctrl Pts',(-62.0386775475603,-19.6850298779912,
8.33028321499155));
#37394=CARTESIAN_POINT('Ctrl Pts',(-62.5876342861156,-17.0322781112095,
6.61316456701218));
#37395=CARTESIAN_POINT('Ctrl Pts',(-63.1948606729999,-14.1620610563234,
7.90934044152666));
#37396=CARTESIAN_POINT('Ctrl Pts',(-63.1857528116036,-13.592034730466,11.06559273848));
#37397=CARTESIAN_POINT('Ctrl Pts',(-62.4340642391261,-15.7933573470836,
13.2737787979711));
#37398=CARTESIAN_POINT('Ctrl Pts',(-61.474228598899,-18.77149539599,12.5692575108704));
#37399=CARTESIAN_POINT('Ctrl Pts',(-61.0258693851979,-19.8407774342271,
9.57884782055393));
#37400=CARTESIAN_POINT('Ctrl Pts',(-61.3535459546682,-18.0138545011767,
6.96313958196492));
#37401=CARTESIAN_POINT('Ctrl Pts',(-62.0313713878355,-14.8801582185979,
7.04935230673909));
#37402=CARTESIAN_POINT('Ctrl Pts',(-62.3219306628042,-13.1917589144664,
9.76077569049554));
#37403=CARTESIAN_POINT('Ctrl Pts',(-61.8323582153005,-14.4148508352001,
12.6850472214478));
#37404=CARTESIAN_POINT('Ctrl Pts',(-60.8638866885507,-17.4252184513767,
13.2203938343511));
#37405=CARTESIAN_POINT('Ctrl Pts',(-60.1438112072126,-19.5085594056784,
10.8905648652622));
#37406=CARTESIAN_POINT('Ctrl Pts',(-60.1784631839307,-18.7752191406467,
7.76832321464309));
#37407=CARTESIAN_POINT('Ctrl Pts',(-60.8026134491221,-15.8418413120578,
6.63176432830731));
#37408=CARTESIAN_POINT('Ctrl Pts',(-61.3267007921992,-13.2819033927535,
8.49166306428554));
#37409=CARTESIAN_POINT('Ctrl Pts',(-61.1498877415005,-13.3377613540649,
11.6941269021449));
#37410=CARTESIAN_POINT('Ctrl Pts',(-60.2955486875317,-15.9221807830303,
13.3881230626289));
#37411=CARTESIAN_POINT('Ctrl Pts',(-59.3886089101014,-18.7029087844682,
12.0701056758003));
#37412=CARTESIAN_POINT('Ctrl Pts',(-59.1033424098446,-19.1635205297872,
8.90528539980874));
#37413=CARTESIAN_POINT('Ctrl Pts',(-59.4048719542877,-17.6355187317176,
7.45405522397557));
#37414=CARTESIAN_POINT('Ctrl Pts',(-59.59098336421,-16.7396023849069,7.20982243015776));
#37415=CARTESIAN_POINT('Ctrl Pts',(-67.1867480491086,-20.8181659539446,
11.4318553561527));
#37416=CARTESIAN_POINT('Ctrl Pts',(-67.0150744928066,-21.2575212792676,
10.5414078043449));
#37417=CARTESIAN_POINT('Ctrl Pts',(-66.9175493641714,-21.2188117961242,
8.27875481372668));
#37418=CARTESIAN_POINT('Ctrl Pts',(-67.5037579299839,-18.4270343173431,
6.39877704863426));
#37419=CARTESIAN_POINT('Ctrl Pts',(-68.1652879251537,-15.3541534373013,
7.72993286626527));
#37420=CARTESIAN_POINT('Ctrl Pts',(-68.1794897476338,-14.697134186909,11.0773387007938));
#37421=CARTESIAN_POINT('Ctrl Pts',(-67.3992512291332,-17.005006652638,13.4679206448304));
#37422=CARTESIAN_POINT('Ctrl Pts',(-66.3844685224501,-20.1882099452852,
12.7722321938656));
#37423=CARTESIAN_POINT('Ctrl Pts',(-65.9036218913761,-21.3787366757643,
9.61047736355945));
#37424=CARTESIAN_POINT('Ctrl Pts',(-66.2501895556749,-19.4813112170038,
6.79508159949504));
#37425=CARTESIAN_POINT('Ctrl Pts',(-66.9814704044654,-16.1481166073788,
6.8312269691009));
#37426=CARTESIAN_POINT('Ctrl Pts',(-67.3124918915896,-14.3087102716974,
9.68660587073339));
#37427=CARTESIAN_POINT('Ctrl Pts',(-66.8143900211042,-15.5636344323571,
12.8208382184203));
#37428=CARTESIAN_POINT('Ctrl Pts',(-65.7959811184248,-18.7603708726999,
13.4453363911881));
#37429=CARTESIAN_POINT('Ctrl Pts',(-65.0290015152611,-21.0187603927391,
11.0044971721492));
#37430=CARTESIAN_POINT('Ctrl Pts',(-65.0614895355965,-20.2934961228726,
7.66994591646049));
#37431=CARTESIAN_POINT('Ctrl Pts',(-65.7301904655356,-17.193852949935,6.40846378494586));
#37432=CARTESIAN_POINT('Ctrl Pts',(-66.3058060485127,-14.4416090212986,
8.34239936321424));
#37433=CARTESIAN_POINT('Ctrl Pts',(-66.1418567263479,-14.4494588941477,
11.7511157925387));
#37434=CARTESIAN_POINT('Ctrl Pts',(-65.2498597727096,-17.1744195179851,
13.601850366419));
#37435=CARTESIAN_POINT('Ctrl Pts',(-64.2890822261733,-20.156072809093,12.2479900298267));
#37436=CARTESIAN_POINT('Ctrl Pts',(-63.9799857765362,-20.705619136241,8.89407499549219));
#37437=CARTESIAN_POINT('Ctrl Pts',(-64.4632262402321,-18.2981238461178,
6.52411027736622));
#37438=CARTESIAN_POINT('Ctrl Pts',(-65.1745109655567,-15.0395557852216,
7.24667235432916));
#37439=CARTESIAN_POINT('Ctrl Pts',(-65.3466545015628,-13.7930900353156,
10.4188919993342));
#37440=CARTESIAN_POINT('Ctrl Pts',(-64.6921496134352,-15.631718204273,13.2184200895797));
#37441=CARTESIAN_POINT('Ctrl Pts',(-63.6589647612361,-18.8835992389535,
13.1544941616765));
#37442=CARTESIAN_POINT('Ctrl Pts',(-63.0319829890499,-20.6195097408353,
10.2839896215957));
#37443=CARTESIAN_POINT('Ctrl Pts',(-63.2346852212379,-19.2589973841649,
7.16081725087042));
#37444=CARTESIAN_POINT('Ctrl Pts',(-63.9523759072004,-15.9765219526969,
6.56368841308645));
#37445=CARTESIAN_POINT('Ctrl Pts',(-64.4121701619332,-13.656529105669,9.02387339796877));
#37446=CARTESIAN_POINT('Ctrl Pts',(-64.0706356123947,-14.3271360697498,
12.3525260039849));
#37447=CARTESIAN_POINT('Ctrl Pts',(-63.0972885120501,-17.3556995742985,
13.5881174655936));
#37448=CARTESIAN_POINT('Ctrl Pts',(-62.2237737811953,-20.0116836036721,
11.6313322004894));
#37449=CARTESIAN_POINT('Ctrl Pts',(-62.0929146809836,-19.8960390869572,
8.2231376748606));
#37450=CARTESIAN_POINT('Ctrl Pts',(-62.6867878434683,-17.0756569439767,
6.39583171448275));
#37451=CARTESIAN_POINT('Ctrl Pts',(-63.3426698111255,-14.023854789574,7.77518305050454));
#37452=CARTESIAN_POINT('Ctrl Pts',(-63.3426674304337,-13.4198463471003,
11.1339717058289));
#37453=CARTESIAN_POINT('Ctrl Pts',(-62.5524330171347,-15.7650240000841,
13.4838568188231));
#37454=CARTESIAN_POINT('Ctrl Pts',(-61.5406947619308,-18.9368652451296,
12.7341264791944));
#37455=CARTESIAN_POINT('Ctrl Pts',(-61.0732543185779,-20.0773594018981,
9.5518225321043));
#37456=CARTESIAN_POINT('Ctrl Pts',(-61.4316477881724,-18.1357994369335,
6.76826458716688));
#37457=CARTESIAN_POINT('Ctrl Pts',(-62.1626591350496,-14.8036106221418,
6.86000957288797));
#37458=CARTESIAN_POINT('Ctrl Pts',(-62.4815534974884,-13.0094633319358,
9.74542469319801));
#37459=CARTESIAN_POINT('Ctrl Pts',(-61.9702551717096,-14.3136373342303,
12.8573464026037));
#37460=CARTESIAN_POINT('Ctrl Pts',(-60.9493268661068,-17.5197763142882,
13.4270461480333));
#37461=CARTESIAN_POINT('Ctrl Pts',(-60.1927341524846,-19.7394014348254,
10.9477123134803));
#37462=CARTESIAN_POINT('Ctrl Pts',(-60.2392996738453,-18.9615992158895,
7.62511676387751));
#37463=CARTESIAN_POINT('Ctrl Pts',(-60.9131915231958,-15.84258326797,6.41562502038865));
#37464=CARTESIAN_POINT('Ctrl Pts',(-61.4805994238643,-13.1209708267224,
8.39487325111026));
#37465=CARTESIAN_POINT('Ctrl Pts',(-61.3021302305505,-13.183009596418,11.8028388367739));
#37466=CARTESIAN_POINT('Ctrl Pts',(-60.4026582657955,-15.9358673415309,
13.605538542209));
#37467=CARTESIAN_POINT('Ctrl Pts',(-59.4472101950129,-18.8976307583482,
12.2029441264605));
#37468=CARTESIAN_POINT('Ctrl Pts',(-59.1533281063617,-19.3903963172921,
8.83503768583721));
#37469=CARTESIAN_POINT('Ctrl Pts',(-59.4806667221931,-17.7660737535053,
7.29068223125013));
#37470=CARTESIAN_POINT('Ctrl Pts',(-59.6819508576141,-16.8135320242442,
7.03077704625421));
#37471=CARTESIAN_POINT('Ctrl Pts',(-67.0040126136403,-20.2598690437802,
11.1728309286203));
#37472=CARTESIAN_POINT('Ctrl Pts',(-66.9555034255254,-20.4203000043806,
10.9082027524034));
#37473=CARTESIAN_POINT('Ctrl Pts',(-66.9207835851305,-20.5332184525386,
10.6149904639439));
#37474=CARTESIAN_POINT('Ctrl Pts',(-66.8813975908017,-20.6611539455099,
9.99178401342212));
#37475=CARTESIAN_POINT('Ctrl Pts',(-66.8780249511107,-20.6720025707685,
9.66515229429124));
#37476=CARTESIAN_POINT('Ctrl Pts',(-66.904675210205,-20.5855924444281,9.00098486496444));
#37477=CARTESIAN_POINT('Ctrl Pts',(-66.9367881932439,-20.4815398383751,
8.66883374311719));
#37478=CARTESIAN_POINT('Ctrl Pts',(-67.0315956493192,-20.1690707048654,
8.06423785428561));
#37479=CARTESIAN_POINT('Ctrl Pts',(-67.0931208523801,-19.964426561113,7.79496359360514));
#37480=CARTESIAN_POINT('Ctrl Pts',(-67.2425937581437,-19.4553169386783,
7.32570054462912));
#37481=CARTESIAN_POINT('Ctrl Pts',(-67.3308539700401,-19.1487818292127,
7.13688275745703));
#37482=CARTESIAN_POINT('Ctrl Pts',(-67.4238662472345,-18.8154792730622,
7.01293629783549));
#37483=CARTESIAN_POINT('Ctrl Pts',(-66.7095652904141,-15.2652009106025,
9.99881345470568));
#37484=CARTESIAN_POINT('Ctrl Pts',(-66.7141255555458,-15.2659775128488,
9.92620926472478));
#37485=CARTESIAN_POINT('Ctrl Pts',(-66.7178306708093,-15.2699455778512,
9.85363960672308));
#37486=CARTESIAN_POINT('Ctrl Pts',(-66.7206515257331,-15.2772137473687,
9.78136734601538));
#37487=CARTESIAN_POINT('Ctrl Pts',(-66.752566372114,-15.3594450282715,8.9636868341038));
#37488=CARTESIAN_POINT('Ctrl Pts',(-66.6712922345581,-15.8641033480842,
8.18407440691875));
#37489=CARTESIAN_POINT('Ctrl Pts',(-66.5353761067089,-16.5726883518974,
7.78933375549841));
#37490=CARTESIAN_POINT('Ctrl Pts',(-66.3994599788598,-17.2812733557106,
7.39459310407807));
#37491=CARTESIAN_POINT('Ctrl Pts',(-66.2089018607176,-18.1937850435244,
7.38472422842244));
#37492=CARTESIAN_POINT('Ctrl Pts',(-66.0708634238268,-18.9102906125104,
7.76413764787091));
#37493=CARTESIAN_POINT('Ctrl Pts',(-65.9328249869361,-19.6267961814964,
8.14355106731939));
#37494=CARTESIAN_POINT('Ctrl Pts',(-65.8473062312968,-20.1472956316547,
8.91224678187198));
#37495=CARTESIAN_POINT('Ctrl Pts',(-65.8747431444716,-20.2462387867959,
9.72822620930693));
#37496=CARTESIAN_POINT('Ctrl Pts',(-65.9021800576463,-20.3451819419371,
10.5442056367419));
#37497=CARTESIAN_POINT('Ctrl Pts',(-66.0425726396352,-20.0225688020612,
11.4074687770592));
#37498=CARTESIAN_POINT('Ctrl Pts',(-66.2558562834074,-19.4279225161922,
11.9340732703405));
#37499=CARTESIAN_POINT('Ctrl Pts',(-66.4691399271796,-18.8332762303233,
12.4606777636217));
#37500=CARTESIAN_POINT('Ctrl Pts',(-66.7553146327352,-17.9665967984612,
12.6506236098669));
#37501=CARTESIAN_POINT('Ctrl Pts',(-67.0094701965007,-17.2194144305744,
12.4192427536873));
#37502=CARTESIAN_POINT('Ctrl Pts',(-67.2636257602662,-16.4722320626875,
12.1878618975077));
#37503=CARTESIAN_POINT('Ctrl Pts',(-67.4857621822416,-15.8445467587759,
11.5351543389033));
#37504=CARTESIAN_POINT('Ctrl Pts',(-67.5994444228593,-15.6216179699846,
10.7518245719417));
#37505=CARTESIAN_POINT('Ctrl Pts',(-67.6344914472383,-15.5528913979793,
10.5103323450969));
#37506=CARTESIAN_POINT('Ctrl Pts',(-67.6592307340631,-15.5226338262371,
10.2564254798709));
#37507=CARTESIAN_POINT('Ctrl Pts',(-67.6742507328171,-15.5286491313886,
10.0019962882658));
#37508=CARTESIAN_POINT('Ctrl Pts',(-59.6819508576141,-16.8135320242443,
7.03077704625424));
#37509=CARTESIAN_POINT('Ctrl Pts',(-59.6574023990845,-16.905148118724,7.06547285383592));
#37510=CARTESIAN_POINT('Ctrl Pts',(-59.6333816237385,-16.9947948727525,
7.10515219319408));
#37511=CARTESIAN_POINT('Ctrl Pts',(-59.6099513655554,-17.0822377867264,
7.1494969432907));
#37512=CARTESIAN_POINT('Ctrl Pts',(-59.5861978454359,-17.1708871306712,
7.19445350780586));
#37513=CARTESIAN_POINT('Ctrl Pts',(-59.5630510759256,-17.2572720505146,
7.24420580542308));
#37514=CARTESIAN_POINT('Ctrl Pts',(-59.5405853294381,-17.3411153578357,
7.29846300341081));
#37515=CARTESIAN_POINT('Ctrl Pts',(-59.5341747454285,-17.3650399830657,
7.31394525440213));
#37516=CARTESIAN_POINT('Ctrl Pts',(-59.5278196764473,-17.3887574233895,
7.32979452700506));
#37517=CARTESIAN_POINT('Ctrl Pts',(-59.5215220078018,-17.4122606427434,
7.3460045350289));
#37518=CARTESIAN_POINT('Ctrl Pts',(-59.5165727272691,-17.4307316091526,
7.35874383296051));
#37519=CARTESIAN_POINT('Ctrl Pts',(-59.5116584066169,-17.4490721035113,
7.37170741286395));
#37520=CARTESIAN_POINT('Ctrl Pts',(-59.5067848207402,-17.4672605736183,
7.38487881899596));
#37521=CARTESIAN_POINT('Ctrl Pts',(-59.4853806969008,-17.5471418512783,
7.44272583659645));
#37522=CARTESIAN_POINT('Ctrl Pts',(-59.464740904359,-17.6241706057018,7.50463022504743));
#37523=CARTESIAN_POINT('Ctrl Pts',(-59.4449347986475,-17.6980879985172,
7.57029723806388));
#37524=CARTESIAN_POINT('Ctrl Pts',(-59.4299001526051,-17.7541980614214,
7.62014450797887));
#37525=CARTESIAN_POINT('Ctrl Pts',(-59.4153460633232,-17.8085146620793,
7.67216077819929));
#37526=CARTESIAN_POINT('Ctrl Pts',(-59.4013071776556,-17.8609084966726,
7.72622830882967));
#37527=CARTESIAN_POINT('Ctrl Pts',(-59.3940669982599,-17.8879292140331,
7.75411219010849));
#37528=CARTESIAN_POINT('Ctrl Pts',(-59.3869639126606,-17.9144382903802,
7.78254177993925));
#37529=CARTESIAN_POINT('Ctrl Pts',(-59.380003115187,-17.940416340213,7.81150163933501));
#37530=CARTESIAN_POINT('Ctrl Pts',(-59.3770692604963,-17.9513656349807,
7.82370771481001));
#37531=CARTESIAN_POINT('Ctrl Pts',(-59.3741603924804,-17.9622216782085,
7.83600935542272));
#37532=CARTESIAN_POINT('Ctrl Pts',(-59.3712797970546,-17.9729722066936,
7.84839276286152));
#37533=CARTESIAN_POINT('Ctrl Pts',(-59.3542405471804,-18.036563552947,7.92164288738543));
#37534=CARTESIAN_POINT('Ctrl Pts',(-59.3381672911566,-18.0965497610707,
7.99784282332634));
#37535=CARTESIAN_POINT('Ctrl Pts',(-59.3231234328439,-18.1526942046358,
8.07671631125713));
#37536=CARTESIAN_POINT('Ctrl Pts',(-59.3083518045395,-18.2078226719783,
8.15416252369557));
#37537=CARTESIAN_POINT('Ctrl Pts',(-59.2945725639227,-18.25924749805,8.23418719308367));
#37538=CARTESIAN_POINT('Ctrl Pts',(-59.2818571865986,-18.3067019322607,
8.31655060950961));
#37539=CARTESIAN_POINT('Ctrl Pts',(-59.2693830444672,-18.3532560644759,
8.39735143332656));
#37540=CARTESIAN_POINT('Ctrl Pts',(-59.2579327074429,-18.3959893040146,
8.48040377581006));
#37541=CARTESIAN_POINT('Ctrl Pts',(-59.2475859889068,-18.4346037832828,
8.56549184010165));
#37542=CARTESIAN_POINT('Ctrl Pts',(-59.2424064367759,-18.4539341349959,
8.60808680034756));
#37543=CARTESIAN_POINT('Ctrl Pts',(-59.2375036518288,-18.4722315775171,
8.65119201452183));
#37544=CARTESIAN_POINT('Ctrl Pts',(-59.2328889292081,-18.4894539568003,
8.6947806500647));
#37545=CARTESIAN_POINT('Ctrl Pts',(-59.2306690827174,-18.4977385366888,
8.71574834142993));
#37546=CARTESIAN_POINT('Ctrl Pts',(-59.2285159057548,-18.5057743025105,
8.73682789355957));
#37547=CARTESIAN_POINT('Ctrl Pts',(-59.2264307309995,-18.51355628064,8.75801630583257));
#37548=CARTESIAN_POINT('Ctrl Pts',(-59.225099704237,-18.5185237401439,8.77154147619001));
#37549=CARTESIAN_POINT('Ctrl Pts',(-59.223796394322,-18.5233877589649,8.78511114963466));
#37550=CARTESIAN_POINT('Ctrl Pts',(-59.2225223976776,-18.5281423791704,
8.79871063717586));
#37551=CARTESIAN_POINT('Ctrl Pts',(-59.2143322655469,-18.5587083684028,
8.88613755494957));
#37552=CARTESIAN_POINT('Ctrl Pts',(-59.2073383924936,-18.5848098579794,
8.9749370538889));
#37553=CARTESIAN_POINT('Ctrl Pts',(-59.2016063055572,-18.6062022976594,
9.06488740622582));
#37554=CARTESIAN_POINT('Ctrl Pts',(-59.2009154354318,-18.6087806600691,
9.07572883481821));
#37555=CARTESIAN_POINT('Ctrl Pts',(-59.2002429107549,-18.6112905563326,
9.08658699331409));
#37556=CARTESIAN_POINT('Ctrl Pts',(-59.199588859507,-18.6137315088204,9.09746150181073));
#37557=CARTESIAN_POINT('Ctrl Pts',(-59.1940765541309,-18.6343037125509,
9.18911121862253));
#37558=CARTESIAN_POINT('Ctrl Pts',(-59.1898752976091,-18.6499830153458,
9.28192246233326));
#37559=CARTESIAN_POINT('Ctrl Pts',(-59.1869573634509,-18.6608728938775,
9.37550443038003));
#37560=CARTESIAN_POINT('Ctrl Pts',(-59.1839372837921,-18.6721439846069,
9.47236233833766));
#37561=CARTESIAN_POINT('Ctrl Pts',(-59.1822919652801,-18.6782843968884,
9.57004704528476));
#37562=CARTESIAN_POINT('Ctrl Pts',(-59.1820051755357,-18.6793547107854,
9.66811274308771));
#37563=CARTESIAN_POINT('Ctrl Pts',(-59.1818653628562,-18.6798764988089,
9.71592068687496));
#37564=CARTESIAN_POINT('Ctrl Pts',(-59.1820486386195,-18.6791925043485,
9.76381888087633));
#37565=CARTESIAN_POINT('Ctrl Pts',(-59.1825542820092,-18.6773054175276,
9.81175333279155));
#37566=CARTESIAN_POINT('Ctrl Pts',(-59.1827037214691,-18.6767477018707,
9.82592003357218));
#37567=CARTESIAN_POINT('Ctrl Pts',(-59.1828813434777,-18.67608480751,9.8400899910912));
#37568=CARTESIAN_POINT('Ctrl Pts',(-59.1830868741532,-18.6753177565863,
9.85424725658315));
#37569=CARTESIAN_POINT('Ctrl Pts',(-59.1844353908592,-18.670285023725,9.94713513804004));
#37570=CARTESIAN_POINT('Ctrl Pts',(-59.1869856677946,-18.6607672606286,
10.039633649266));
#37571=CARTESIAN_POINT('Ctrl Pts',(-59.1907077255756,-18.646876351881,10.1313703608465));
#37572=CARTESIAN_POINT('Ctrl Pts',(-59.1944191075557,-18.6330252857651,
10.2228439483884));
#37573=CARTESIAN_POINT('Ctrl Pts',(-59.1992956612747,-18.6148257395202,
10.3135610433039));
#37574=CARTESIAN_POINT('Ctrl Pts',(-59.2053202323396,-18.592341734212,10.40313539075));
#37575=CARTESIAN_POINT('Ctrl Pts',(-59.2112410580764,-18.5702449117395,
10.4911672350087));
#37576=CARTESIAN_POINT('Ctrl Pts',(-59.2182708207739,-18.5440094801873,
10.5780961320225));
#37577=CARTESIAN_POINT('Ctrl Pts',(-59.2264037185149,-18.513657092605,10.6635263254103));
#37578=CARTESIAN_POINT('Ctrl Pts',(-59.2303039431548,-18.499101256088,10.7044953570947));
#37579=CARTESIAN_POINT('Ctrl Pts',(-59.2344580112368,-18.483598062948,10.7451192120525));
#37580=CARTESIAN_POINT('Ctrl Pts',(-59.2388660433057,-18.4671470633053,
10.7853510160803));
#37581=CARTESIAN_POINT('Ctrl Pts',(-59.2403491922556,-18.4616118760692,
10.7988876140365));
#37582=CARTESIAN_POINT('Ctrl Pts',(-59.2418610960516,-18.4559693742862,
10.8123798086229));
#37583=CARTESIAN_POINT('Ctrl Pts',(-59.2434017709269,-18.4502194973737,
10.8258257520569));
#37584=CARTESIAN_POINT('Ctrl Pts',(-59.2448672509574,-18.4447502514423,
10.8386154469564));
#37585=CARTESIAN_POINT('Ctrl Pts',(-59.2463583029107,-18.4391855697962,
10.8513591674937));
#37586=CARTESIAN_POINT('Ctrl Pts',(-59.2478738643216,-18.4335294176084,
10.8640470911647));
#37587=CARTESIAN_POINT('Ctrl Pts',(-59.2575294210436,-18.3974943893469,
10.9448811410429));
#37588=CARTESIAN_POINT('Ctrl Pts',(-59.2681907320082,-18.3577058351517,
11.0235565033029));
#37589=CARTESIAN_POINT('Ctrl Pts',(-59.2798413570774,-18.3142251104531,
11.0997253730153));
#37590=CARTESIAN_POINT('Ctrl Pts',(-59.2912990836117,-18.271464292888,11.1746331204022));
#37591=CARTESIAN_POINT('Ctrl Pts',(-59.3037137499388,-18.2251321273963,
11.2471173604519));
#37592=CARTESIAN_POINT('Ctrl Pts',(-59.3170791891641,-18.1752516291421,
11.3168132013479));
#37593=CARTESIAN_POINT('Ctrl Pts',(-59.3300579262154,-18.1268143230484,
11.3844925328921));
#37594=CARTESIAN_POINT('Ctrl Pts',(-59.3439333260214,-18.0750306259972,
11.4495429412298));
#37595=CARTESIAN_POINT('Ctrl Pts',(-59.3587070801757,-18.0198942248749,
11.5115898436597));
#37596=CARTESIAN_POINT('Ctrl Pts',(-59.3613784504281,-18.009924535367,11.5228090806713));
#37597=CARTESIAN_POINT('Ctrl Pts',(-59.364079210104,-17.9998451630374,11.5339299971675));
#37598=CARTESIAN_POINT('Ctrl Pts',(-59.3668093915944,-17.9896559870014,
11.5449502145343));
#37599=CARTESIAN_POINT('Ctrl Pts',(-59.3747124158146,-17.9601614990781,
11.5768503080147));
#37600=CARTESIAN_POINT('Ctrl Pts',(-59.3828619650632,-17.9297469672238,
11.6079068412469));
#37601=CARTESIAN_POINT('Ctrl Pts',(-59.3912467107622,-17.8984546702664,
11.6380966037222));
#37602=CARTESIAN_POINT('Ctrl Pts',(-68.1281291851067,-15.0750265266586,
10.0024371765581));
#37603=CARTESIAN_POINT('Ctrl Pts',(-68.1132191003537,-15.0686010168709,
10.3130580784045));
#37604=CARTESIAN_POINT('Ctrl Pts',(-67.9995899840861,-15.2292608392572,
11.6285356954));
#37605=CARTESIAN_POINT('Ctrl Pts',(-67.3992512291332,-17.005006652638,13.4679206448304));
#37606=CARTESIAN_POINT('Ctrl Pts',(-66.3844685224501,-20.1882099452852,
12.7722321938656));
#37607=CARTESIAN_POINT('Ctrl Pts',(-65.9036218913761,-21.3787366757643,
9.61047736355945));
#37608=CARTESIAN_POINT('Ctrl Pts',(-66.2501895556749,-19.4813112170038,
6.79508159949504));
#37609=CARTESIAN_POINT('Ctrl Pts',(-66.9814704044654,-16.1481166073788,
6.8312269691009));
#37610=CARTESIAN_POINT('Ctrl Pts',(-67.2119040522751,-14.867652564341,8.81893895087719));
#37611=CARTESIAN_POINT('Ctrl Pts',(-67.1683025391241,-14.8112407741816,
9.90991228406425));
#37612=CARTESIAN_POINT('Ctrl Pts',(-67.1637176864735,-14.810555933805,9.9985514014054));
#37613=CARTESIAN_POINT('Origin',(-69.7479810832458,-18.6889152049569,10.));
#37614=CARTESIAN_POINT('Ctrl Pts',(-68.2083503098983,-15.0969161422106,
9.99673640007589));
#37615=CARTESIAN_POINT('Ctrl Pts',(-68.1711103559359,-15.0927295232038,
10.7130675867001));
#37616=CARTESIAN_POINT('Ctrl Pts',(-67.9289066052254,-15.6514186592596,
12.4513417391718));
#37617=CARTESIAN_POINT('Ctrl Pts',(-67.0483943376964,-18.3902480628716,
13.5944453497599));
#37618=CARTESIAN_POINT('Ctrl Pts',(-66.1687987195556,-21.0667649555472,
11.6442225433394));
#37619=CARTESIAN_POINT('Ctrl Pts',(-66.0360136384589,-20.9561469803458,
8.22016494780551));
#37620=CARTESIAN_POINT('Ctrl Pts',(-66.6336669557834,-18.1194957904379,
6.39071567224365));
#37621=CARTESIAN_POINT('Ctrl Pts',(-67.2173089746449,-15.4027596845031,
7.63681194520586));
#37622=CARTESIAN_POINT('Ctrl Pts',(-67.2747579502335,-14.8518622987657,
9.32892113065768));
#37623=CARTESIAN_POINT('Ctrl Pts',(-67.242349320473,-14.8383776097513,10.0022118830713));
#37624=CARTESIAN_POINT('Ctrl Pts',(-67.8425423025986,-17.2449834421528,
7.06170475438615));
#37625=CARTESIAN_POINT('Ctrl Pts',(-68.0419164156808,-16.2988495743022,
7.35795147289606));
#37626=CARTESIAN_POINT('Ctrl Pts',(-68.3551165744735,-14.7258515725219,
8.9714479727025));
#37627=CARTESIAN_POINT('Ctrl Pts',(-68.023655252025,-15.3567034243027,12.3283366156215));
#37628=CARTESIAN_POINT('Ctrl Pts',(-67.0483943376964,-18.3902480628716,
13.5944453497599));
#37629=CARTESIAN_POINT('Ctrl Pts',(-66.1687987195556,-21.0667649555472,
11.6442225433394));
#37630=CARTESIAN_POINT('Ctrl Pts',(-66.0360136384589,-20.9561469803458,
8.22016494780551));
#37631=CARTESIAN_POINT('Ctrl Pts',(-66.6336669557834,-18.1194957904379,
6.39071567224365));
#37632=CARTESIAN_POINT('Ctrl Pts',(-67.2905946547074,-15.0616295968131,
7.79327945411745));
#37633=CARTESIAN_POINT('Ctrl Pts',(-67.282863942121,-14.4843023646232,11.1722569386419));
#37634=CARTESIAN_POINT('Ctrl Pts',(-66.4816292855381,-16.8683721674343,
13.501327491299));
#37635=CARTESIAN_POINT('Ctrl Pts',(-65.468753391891,-20.0422978199461,12.6947822329671));
#37636=CARTESIAN_POINT('Ctrl Pts',(-65.0155990043222,-21.1273143736846,
9.47487431060658));
#37637=CARTESIAN_POINT('Ctrl Pts',(-65.3922823621304,-19.1153342996378,
6.72525821930933));
#37638=CARTESIAN_POINT('Ctrl Pts',(-66.1257396929252,-15.7718556315863,
6.90837057311376));
#37639=CARTESIAN_POINT('Ctrl Pts',(-66.4233986629546,-14.054798587767,9.86022990097523));
#37640=CARTESIAN_POINT('Ctrl Pts',(-65.8829690009265,-15.4655309000319,
12.9372608391343));
#37641=CARTESIAN_POINT('Ctrl Pts',(-64.8527215544619,-18.7042880702652,
13.3837942299378));
#37642=CARTESIAN_POINT('Ctrl Pts',(-64.1195886430846,-20.8341986998846,
10.7999310727628));
#37643=CARTESIAN_POINT('Ctrl Pts',(-64.2044184759423,-19.9114308093211,
7.49968047567736));
#37644=CARTESIAN_POINT('Ctrl Pts',(-64.895523082676,-16.726014659305,6.43862003923507));
#37645=CARTESIAN_POINT('Ctrl Pts',(-65.4382581333965,-14.0943212306267,
8.5669948761288));
#37646=CARTESIAN_POINT('Ctrl Pts',(-65.2108533475991,-14.3368288007657,
11.9787141005065));
#37647=CARTESIAN_POINT('Ctrl Pts',(-64.2812461473762,-17.1999914587382,
13.6183729089162));
#37648=CARTESIAN_POINT('Ctrl Pts',(-63.346239485481,-20.0833051820058,12.0175557753468));
#37649=CARTESIAN_POINT('Ctrl Pts',(-63.1074718691846,-20.3682194128847,
8.60989310618102));
#37650=CARTESIAN_POINT('Ctrl Pts',(-63.6430568297552,-17.7632104839245,
6.44715683087674));
#37651=CARTESIAN_POINT('Ctrl Pts',(-64.3376274439251,-14.5648590180568,
7.46621057361522));
#37652=CARTESIAN_POINT('Ctrl Pts',(-64.4334353369931,-13.60112044902,10.7544289031931));
#37653=CARTESIAN_POINT('Ctrl Pts',(-63.7089610525879,-15.6987166428561,
13.3670096553837));
#37654=CARTESIAN_POINT('Ctrl Pts',(-62.6772983776881,-18.9427555175135,
12.9642257537707));
#37655=CARTESIAN_POINT('Ctrl Pts',(-62.1266472347557,-20.391634915842,9.90679500749681));
#37656=CARTESIAN_POINT('Ctrl Pts',(-62.4144320750887,-18.7114286257302,
6.93283507366378));
#37657=CARTESIAN_POINT('Ctrl Pts',(-63.1472062543103,-15.3704995140596,
6.70571036393757));
#37658=CARTESIAN_POINT('Ctrl Pts',(-63.5330077514077,-13.3244900809144,
9.42882503807173));
#37659=CARTESIAN_POINT('Ctrl Pts',(-63.0906099643739,-14.3693624549398,
12.6634621126409));
#37660=CARTESIAN_POINT('Ctrl Pts',(-62.0804897947069,-17.5330036055459,
13.5128046754734));
#37661=CARTESIAN_POINT('Ctrl Pts',(-61.271554519541,-19.9458125081593,11.2162142452873));
#37662=CARTESIAN_POINT('Ctrl Pts',(-61.2525379570575,-19.4106046411911,
7.83042882970014));
#37663=CARTESIAN_POINT('Ctrl Pts',(-61.9047530097006,-16.3703262829251,
6.3876284598802));
#37664=CARTESIAN_POINT('Ctrl Pts',(-62.5083833543796,-13.5113685232515,
8.17992871548504));
#37665=CARTESIAN_POINT('Ctrl Pts',(-62.387123159886,-13.3577390856961,11.6022164308589));
#37666=CARTESIAN_POINT('Ctrl Pts',(-61.5138509672066,-16.0106566332719,
13.5896176377583));
#37667=CARTESIAN_POINT('Ctrl Pts',(-60.5349179618125,-19.0579057022677,
12.362301010972));
#37668=CARTESIAN_POINT('Ctrl Pts',(-60.1913020034495,-19.7341192728289,
9.01938609588879));
#37669=CARTESIAN_POINT('Ctrl Pts',(-60.6550135466889,-17.397345589062,6.55469600728472));
#37670=CARTESIAN_POINT('Ctrl Pts',(-61.3750552367846,-14.103934773716,7.1754379864718));
#37671=CARTESIAN_POINT('Ctrl Pts',(-61.5708627210562,-12.7669926495712,
10.3258507409626));
#37672=CARTESIAN_POINT('Ctrl Pts',(-60.9313710113774,-14.5474295567703,
13.1842383274678));
#37673=CARTESIAN_POINT('Ctrl Pts',(-59.8935459365978,-17.8144668208756,
13.1913616605738));
#37674=CARTESIAN_POINT('Ctrl Pts',(-59.2511484715134,-19.6057481548832,
10.3395770770153));
#37675=CARTESIAN_POINT('Ctrl Pts',(-59.4436819065864,-18.2810249486936,
7.18539898656524));
#37676=CARTESIAN_POINT('Ctrl Pts',(-60.1631753733452,-14.9896601306951,
6.54837069990788));
#37677=CARTESIAN_POINT('Ctrl Pts',(-60.629216203114,-12.644193431255,9.0096983771868));
#37678=CARTESIAN_POINT('Ctrl Pts',(-60.402326566927,-13.0868379849886,11.2296927240267));
#37679=CARTESIAN_POINT('Ctrl Pts',(-60.181950026368,-13.7072348830372,11.9973015569306));
#37680=CARTESIAN_POINT('Ctrl Pts',(-67.9318278742784,-17.3251900988194,
7.23888518457554));
#37681=CARTESIAN_POINT('Ctrl Pts',(-68.1161335763133,-16.4352923065867,
7.51726810226212));
#37682=CARTESIAN_POINT('Ctrl Pts',(-68.4043554971943,-14.9555143577762,
9.03347008941824));
#37683=CARTESIAN_POINT('Ctrl Pts',(-68.0837432245498,-15.5458770044745,
12.1879369455076));
#37684=CARTESIAN_POINT('Ctrl Pts',(-67.1581527442328,-18.3940490596784,
13.3776987943164));
#37685=CARTESIAN_POINT('Ctrl Pts',(-66.3224589027986,-20.9067222911426,
11.5450752374345));
#37686=CARTESIAN_POINT('Ctrl Pts',(-66.1885426111956,-20.8003260510249,
8.32748974461914));
#37687=CARTESIAN_POINT('Ctrl Pts',(-66.7410189775959,-18.1322775372969,
6.60835702425629));
#37688=CARTESIAN_POINT('Ctrl Pts',(-67.3491954556354,-15.2563533769438,
7.92634562444559));
#37689=CARTESIAN_POINT('Ctrl Pts',(-67.3327927019053,-14.7113906429076,
11.1015693557684));
#37690=CARTESIAN_POINT('Ctrl Pts',(-66.5707346233277,-16.9492514661366,
13.2901959816019));
#37691=CARTESIAN_POINT('Ctrl Pts',(-65.609797362651,-19.9293395015269,12.5322857391186));
#37692=CARTESIAN_POINT('Ctrl Pts',(-65.1748301675257,-20.9464805290194,
9.50653960894211));
#37693=CARTESIAN_POINT('Ctrl Pts',(-65.519661155234,-19.0533751185263,6.92272651604638));
#37694=CARTESIAN_POINT('Ctrl Pts',(-66.1997524963879,-15.9090610352115,
7.09479711845824));
#37695=CARTESIAN_POINT('Ctrl Pts',(-66.4703242998971,-14.2930946730788,
9.86865809630714));
#37696=CARTESIAN_POINT('Ctrl Pts',(-65.9533445658038,-15.6163106628566,
12.7601427840876));
#37697=CARTESIAN_POINT('Ctrl Pts',(-64.9760832641981,-18.6573208483795,
13.1797500249765));
#37698=CARTESIAN_POINT('Ctrl Pts',(-64.2780203671544,-20.656348402684,10.7516948950657));
#37699=CARTESIAN_POINT('Ctrl Pts',(-64.3485967193297,-19.786775226212,7.65045078699707));
#37700=CARTESIAN_POINT('Ctrl Pts',(-64.9888892233674,-16.7909924250963,
6.65337273791576));
#37701=CARTESIAN_POINT('Ctrl Pts',(-65.489758917571,-14.315542634016,8.65340568344645));
#37702=CARTESIAN_POINT('Ctrl Pts',(-65.266928528969,-14.5409783214079,11.8593968140381));
#37703=CARTESIAN_POINT('Ctrl Pts',(-64.3842388247345,-17.229042500588,13.4001835116647));
#37704=CARTESIAN_POINT('Ctrl Pts',(-63.496475248621,-19.9360426274119,11.8958963196673));
#37705=CARTESIAN_POINT('Ctrl Pts',(-63.2629672129436,-20.2013278361942,
8.69371713231446));
#37706=CARTESIAN_POINT('Ctrl Pts',(-63.7571179704187,-17.750953458357,6.66139475745692));
#37707=CARTESIAN_POINT('Ctrl Pts',(-64.4006674801973,-14.7430153463366,
7.61899913400456));
#37708=CARTESIAN_POINT('Ctrl Pts',(-64.4815599109683,-13.8349420404106,
10.7089365253204));
#37709=CARTESIAN_POINT('Ctrl Pts',(-63.7916335220747,-15.8036037329023,
13.1639775672764));
#37710=CARTESIAN_POINT('Ctrl Pts',(-62.8130423308995,-18.8495771338671,
12.7854817031123));
#37711=CARTESIAN_POINT('Ctrl Pts',(-62.2864574754684,-20.2086399244908,
9.91241530746228));
#37712=CARTESIAN_POINT('Ctrl Pts',(-62.5477505634248,-18.6273022002299,
7.11778639941));
#37713=CARTESIAN_POINT('Ctrl Pts',(-63.2271999473304,-15.4853839339817,
6.90435740451571));
#37714=CARTESIAN_POINT('Ctrl Pts',(-63.5805992467218,-13.5603011489527,
9.46326712676888));
#37715=CARTESIAN_POINT('Ctrl Pts',(-63.1557400246277,-14.5397187075309,
12.5028542351258));
#37716=CARTESIAN_POINT('Ctrl Pts',(-62.1973923166246,-17.5101424007747,
13.3009810867783));
#37717=CARTESIAN_POINT('Ctrl Pts',(-61.4280979699796,-19.7750093440881,
11.1428760184689));
#37718=CARTESIAN_POINT('Ctrl Pts',(-61.4010899078139,-19.2696261599638,
7.961254877169));
#37719=CARTESIAN_POINT('Ctrl Pts',(-62.0048379141108,-16.4102292811537,
6.60545597208742));
#37720=CARTESIAN_POINT('Ctrl Pts',(-62.5629308906206,-13.7212192931308,
8.28967977390814));
#37721=CARTESIAN_POINT('Ctrl Pts',(-62.4398445301463,-13.5744051997985,
11.5056021110761));
#37722=CARTESIAN_POINT('Ctrl Pts',(-61.6100928089778,-16.0649021365261,
13.3731621953643));
#37723=CARTESIAN_POINT('Ctrl Pts',(-60.6810516662197,-18.9259522392799,
12.2198532736367));
#37724=CARTESIAN_POINT('Ctrl Pts',(-60.3490176872815,-19.5589412741756,
9.07851752375991));
#37725=CARTESIAN_POINT('Ctrl Pts',(-60.7756290245013,-17.3606274442454,
6.76244927662476));
#37726=CARTESIAN_POINT('Ctrl Pts',(-61.4431136936918,-14.2633621012121,
7.34576025527735));
#37727=CARTESIAN_POINT('Ctrl Pts',(-61.6179756985622,-13.0045895703814,
10.3062018052243));
#37728=CARTESIAN_POINT('Ctrl Pts',(-61.0079073996548,-14.6752168136496,
12.9922274267496));
#37729=CARTESIAN_POINT('Ctrl Pts',(-60.0235254038855,-17.7428017915757,
12.9989212198949));
#37730=CARTESIAN_POINT('Ctrl Pts',(-59.4107265678367,-19.4236195381877,
10.3191004374816));
#37731=CARTESIAN_POINT('Ctrl Pts',(-59.5825119500424,-18.1763291194575,
7.35512060290596));
#37732=CARTESIAN_POINT('Ctrl Pts',(-60.249481453992,-15.0809863992773,6.75650538792386));
#37733=CARTESIAN_POINT('Ctrl Pts',(-60.6782816207909,-12.8745037461489,
9.06941397854074));
#37734=CARTESIAN_POINT('Ctrl Pts',(-60.4589813868428,-13.2888242651275,
11.1555417393123));
#37735=CARTESIAN_POINT('Ctrl Pts',(-60.2488475749171,-13.8709947795086,
11.8768634390787));
#37736=CARTESIAN_POINT('Ctrl Pts',(-68.0211134459581,-17.4053967554861,
7.41606561476494));
#37737=CARTESIAN_POINT('Ctrl Pts',(-68.1903507369458,-16.5717350388711,
7.67658473162818));
#37738=CARTESIAN_POINT('Ctrl Pts',(-68.4535944199152,-15.1851771430304,
9.09549220613397));
#37739=CARTESIAN_POINT('Ctrl Pts',(-68.1438311970747,-15.7350505846463,
12.0475372753936));
#37740=CARTESIAN_POINT('Ctrl Pts',(-67.2679111507692,-18.3978500564853,
13.160952238873));
#37741=CARTESIAN_POINT('Ctrl Pts',(-66.4761190860415,-20.746679626738,11.4459279315295));
#37742=CARTESIAN_POINT('Ctrl Pts',(-66.3410715839323,-20.644505121704,8.43481454143279));
#37743=CARTESIAN_POINT('Ctrl Pts',(-66.8483709994084,-18.1450592841558,
6.82599837626892));
#37744=CARTESIAN_POINT('Ctrl Pts',(-67.4077962565635,-15.4510771570746,
8.05941179477375));
#37745=CARTESIAN_POINT('Ctrl Pts',(-67.3827214616897,-14.9384789211918,
11.0308817728949));
#37746=CARTESIAN_POINT('Ctrl Pts',(-66.6598399611172,-17.030130764839,13.0790644719047));
#37747=CARTESIAN_POINT('Ctrl Pts',(-65.750841333411,-19.8163811831077,12.3697892452702));
#37748=CARTESIAN_POINT('Ctrl Pts',(-65.3340613307292,-20.7656466843542,
9.53820490727763));
#37749=CARTESIAN_POINT('Ctrl Pts',(-65.6470399483378,-18.9914159374149,
7.12019481278344));
#37750=CARTESIAN_POINT('Ctrl Pts',(-66.2737652998505,-16.0462664388367,
7.28122366380271));
#37751=CARTESIAN_POINT('Ctrl Pts',(-66.5172499368395,-14.5313907583905,
9.87708629163903));
#37752=CARTESIAN_POINT('Ctrl Pts',(-66.0237201306813,-15.7670904256813,
12.5830247290408));
#37753=CARTESIAN_POINT('Ctrl Pts',(-65.0994449739343,-18.6103536264938,
12.9757058200153));
#37754=CARTESIAN_POINT('Ctrl Pts',(-64.4364520912242,-20.4784981054834,
10.7034587173686));
#37755=CARTESIAN_POINT('Ctrl Pts',(-64.492774962717,-19.6621196431029,7.80122109831677));
#37756=CARTESIAN_POINT('Ctrl Pts',(-65.0822553640589,-16.8559701908876,
6.86812543659645));
#37757=CARTESIAN_POINT('Ctrl Pts',(-65.5412597017456,-14.5367640374053,
8.73981649076409));
#37758=CARTESIAN_POINT('Ctrl Pts',(-65.323003710339,-14.7451278420501,11.7400795275698));
#37759=CARTESIAN_POINT('Ctrl Pts',(-64.4872315020927,-17.2580935424379,
13.1819941144132));
#37760=CARTESIAN_POINT('Ctrl Pts',(-63.6467110117609,-19.7887800728179,
11.7742368639878));
#37761=CARTESIAN_POINT('Ctrl Pts',(-63.4184625567026,-20.0344362595037,
8.7775411584479));
#37762=CARTESIAN_POINT('Ctrl Pts',(-63.8711791110824,-17.7386964327895,
6.87563268403709));
#37763=CARTESIAN_POINT('Ctrl Pts',(-64.4637075164694,-14.9211716746165,
7.7717876943939));
#37764=CARTESIAN_POINT('Ctrl Pts',(-64.5296844849434,-14.0687636318011,
10.6634441474477));
#37765=CARTESIAN_POINT('Ctrl Pts',(-63.8743059915617,-15.9084908229485,
12.9609454791691));
#37766=CARTESIAN_POINT('Ctrl Pts',(-62.9487862841107,-18.7563987502208,
12.6067376524538));
#37767=CARTESIAN_POINT('Ctrl Pts',(-62.4462677161811,-20.0256449331395,
9.91803560742777));
#37768=CARTESIAN_POINT('Ctrl Pts',(-62.6810690517609,-18.5431757747297,
7.30273772515621));
#37769=CARTESIAN_POINT('Ctrl Pts',(-63.3071936403506,-15.6002683539037,
7.10300444509384));
#37770=CARTESIAN_POINT('Ctrl Pts',(-63.6281907420358,-13.7961122169911,
9.49770921546603));
#37771=CARTESIAN_POINT('Ctrl Pts',(-63.2208700848815,-14.7100749601221,
12.3422463576107));
#37772=CARTESIAN_POINT('Ctrl Pts',(-62.3142948385422,-17.4872811960035,
13.0891574980832));
#37773=CARTESIAN_POINT('Ctrl Pts',(-61.5846414204184,-19.6042061800169,
11.0695377916504));
#37774=CARTESIAN_POINT('Ctrl Pts',(-61.5496418585701,-19.1286476787364,
8.09208092463788));
#37775=CARTESIAN_POINT('Ctrl Pts',(-62.1049228185211,-16.4501322793822,
6.82328348429463));
#37776=CARTESIAN_POINT('Ctrl Pts',(-62.6174784268616,-13.9310700630102,
8.39943083233125));
#37777=CARTESIAN_POINT('Ctrl Pts',(-62.4925659004067,-13.7910713139008,
11.4089877912933));
#37778=CARTESIAN_POINT('Ctrl Pts',(-61.706334650749,-16.1191476397804,13.1567067529704));
#37779=CARTESIAN_POINT('Ctrl Pts',(-60.827185370627,-18.7939987762922,12.0774055363014));
#37780=CARTESIAN_POINT('Ctrl Pts',(-60.5067333711136,-19.3837632755223,
9.13764895163106));
#37781=CARTESIAN_POINT('Ctrl Pts',(-60.8962445023137,-17.3239092994289,
6.97020254596478));
#37782=CARTESIAN_POINT('Ctrl Pts',(-61.5111721505989,-14.4227894287083,
7.51608252408292));
#37783=CARTESIAN_POINT('Ctrl Pts',(-61.6650886760682,-13.2421864911916,
10.286552869486));
#37784=CARTESIAN_POINT('Ctrl Pts',(-61.0844437879323,-14.8030040705288,
12.8002165260314));
#37785=CARTESIAN_POINT('Ctrl Pts',(-60.1535048711732,-17.6711367622757,
12.8064807792161));
#37786=CARTESIAN_POINT('Ctrl Pts',(-59.5703046641601,-19.2414909214922,
10.2986237979478));
#37787=CARTESIAN_POINT('Ctrl Pts',(-59.7213419934984,-18.0716332902213,
7.5248422192467));
#37788=CARTESIAN_POINT('Ctrl Pts',(-60.3357875346389,-15.1723126678596,
6.96464007593981));
#37789=CARTESIAN_POINT('Ctrl Pts',(-60.7273470384677,-13.1048140610427,
9.12912957989471));
#37790=CARTESIAN_POINT('Ctrl Pts',(-60.5156362067586,-13.4908105452664,
11.081390754598));
#37791=CARTESIAN_POINT('Ctrl Pts',(-60.3157451234662,-14.0347546759801,
11.7564253212268));
#37792=CARTESIAN_POINT('Ctrl Pts',(-68.1103990176379,-17.4856034121527,
7.59324604495433));
#37793=CARTESIAN_POINT('Ctrl Pts',(-68.2645678975783,-16.7081777711556,
7.83590136099424));
#37794=CARTESIAN_POINT('Ctrl Pts',(-68.5028333426361,-15.4148399282847,
9.1575143228497));
#37795=CARTESIAN_POINT('Ctrl Pts',(-68.2039191695995,-15.9242241648182,
11.9071376052797));
#37796=CARTESIAN_POINT('Ctrl Pts',(-67.3776695573056,-18.4016510532921,
12.9442056834295));
#37797=CARTESIAN_POINT('Ctrl Pts',(-66.6297792692844,-20.5866369623334,
11.3467806256245));
#37798=CARTESIAN_POINT('Ctrl Pts',(-66.4936005566689,-20.4886841923831,
8.54213933824642));
#37799=CARTESIAN_POINT('Ctrl Pts',(-66.9557230212209,-18.1578410310147,
7.04363972828156));
#37800=CARTESIAN_POINT('Ctrl Pts',(-67.4663970574915,-15.6458009372053,
8.19247796510189));
#37801=CARTESIAN_POINT('Ctrl Pts',(-67.4326502214741,-15.1655671994762,
10.9601941900214));
#37802=CARTESIAN_POINT('Ctrl Pts',(-66.7489452989067,-17.1110100635413,
12.8679329622076));
#37803=CARTESIAN_POINT('Ctrl Pts',(-65.891885304171,-19.7034228646885,12.2072927514217));
#37804=CARTESIAN_POINT('Ctrl Pts',(-65.4932924939327,-20.584812839689,9.56987020561317));
#37805=CARTESIAN_POINT('Ctrl Pts',(-65.7744187414414,-18.9294567563035,
7.31766310952049));
#37806=CARTESIAN_POINT('Ctrl Pts',(-66.3477781033132,-16.1834718424619,
7.46765020914719));
#37807=CARTESIAN_POINT('Ctrl Pts',(-66.5641755737819,-14.7696868437023,
9.88551448697093));
#37808=CARTESIAN_POINT('Ctrl Pts',(-66.0940956955586,-15.917870188506,12.4059066739941));
#37809=CARTESIAN_POINT('Ctrl Pts',(-65.2228066836706,-18.5633864046081,
12.771661615054));
#37810=CARTESIAN_POINT('Ctrl Pts',(-64.5948838152939,-20.3006478082828,
10.6552225396715));
#37811=CARTESIAN_POINT('Ctrl Pts',(-64.6369532061044,-19.5374640599938,
7.95199140963649));
#37812=CARTESIAN_POINT('Ctrl Pts',(-65.1756215047503,-16.9209479566789,
7.08287813527712));
#37813=CARTESIAN_POINT('Ctrl Pts',(-65.5927604859202,-14.7579854407947,
8.82622729808175));
#37814=CARTESIAN_POINT('Ctrl Pts',(-65.3790788917089,-14.9492773626923,
11.6207622411014));
#37815=CARTESIAN_POINT('Ctrl Pts',(-64.5902241794511,-17.2871445842876,
12.9638047171617));
#37816=CARTESIAN_POINT('Ctrl Pts',(-63.7969467749009,-19.641517518224,11.6525774083083));
#37817=CARTESIAN_POINT('Ctrl Pts',(-63.5739579004616,-19.8675446828132,
8.86136518458133));
#37818=CARTESIAN_POINT('Ctrl Pts',(-63.985240251746,-17.726439407222,7.08987061061728));
#37819=CARTESIAN_POINT('Ctrl Pts',(-64.5267475527415,-15.0993280028964,
7.92457625478324));
#37820=CARTESIAN_POINT('Ctrl Pts',(-64.5778090589186,-14.3025852231916,
10.617951769575));
#37821=CARTESIAN_POINT('Ctrl Pts',(-63.9569784610485,-16.0133779129947,
12.7579133910618));
#37822=CARTESIAN_POINT('Ctrl Pts',(-63.084530237322,-18.6632203665744,12.4279936017953));
#37823=CARTESIAN_POINT('Ctrl Pts',(-62.6060779568938,-19.8426499417882,
9.92365590739326));
#37824=CARTESIAN_POINT('Ctrl Pts',(-62.8143875400971,-18.4590493492295,
7.48768905090242));
#37825=CARTESIAN_POINT('Ctrl Pts',(-63.3871873333707,-15.7151527738257,
7.30165148567198));
#37826=CARTESIAN_POINT('Ctrl Pts',(-63.6757822373498,-14.0319232850294,
9.53215130416319));
#37827=CARTESIAN_POINT('Ctrl Pts',(-63.2860001451353,-14.8804312127132,
12.1816384800955));
#37828=CARTESIAN_POINT('Ctrl Pts',(-62.4311973604599,-17.4644199912323,
12.8773339093881));
#37829=CARTESIAN_POINT('Ctrl Pts',(-61.7411848708572,-19.4334030159457,
10.9961995648319));
#37830=CARTESIAN_POINT('Ctrl Pts',(-61.6981938093263,-18.987669197509,8.22290697210676));
#37831=CARTESIAN_POINT('Ctrl Pts',(-62.2050077229314,-16.4900352776108,
7.04111099650183));
#37832=CARTESIAN_POINT('Ctrl Pts',(-62.6720259631026,-14.1409208328895,
8.50918189075437));
#37833=CARTESIAN_POINT('Ctrl Pts',(-62.545287270667,-14.0077374280031,11.3123734715104));
#37834=CARTESIAN_POINT('Ctrl Pts',(-61.8025764925202,-16.1733931430346,
12.9402513105764));
#37835=CARTESIAN_POINT('Ctrl Pts',(-60.9733190750343,-18.6620453133045,
11.934957798966));
#37836=CARTESIAN_POINT('Ctrl Pts',(-60.6644490549456,-19.2085852768689,
9.1967803795022));
#37837=CARTESIAN_POINT('Ctrl Pts',(-61.016859980126,-17.2871911546123,7.17795581530479));
#37838=CARTESIAN_POINT('Ctrl Pts',(-61.5792306075061,-14.5822167562045,
7.68640479288848));
#37839=CARTESIAN_POINT('Ctrl Pts',(-61.7122016535742,-13.4797834120018,
10.2669039337477));
#37840=CARTESIAN_POINT('Ctrl Pts',(-61.1609801762097,-14.930791327408,12.6082056253132));
#37841=CARTESIAN_POINT('Ctrl Pts',(-60.2834843384609,-17.5994717329758,
12.6140403385373));
#37842=CARTESIAN_POINT('Ctrl Pts',(-59.7298827604835,-19.0593623047967,
10.2781471584142));
#37843=CARTESIAN_POINT('Ctrl Pts',(-59.8601720369543,-17.9669374609851,
7.69456383558743));
#37844=CARTESIAN_POINT('Ctrl Pts',(-60.4220936152857,-15.2636389364418,
7.17277476395578));
#37845=CARTESIAN_POINT('Ctrl Pts',(-60.7764124561446,-13.3351243759365,
9.18884518124866));
#37846=CARTESIAN_POINT('Ctrl Pts',(-60.5722910266744,-13.6927968254053,
11.0072397698836));
#37847=CARTESIAN_POINT('Ctrl Pts',(-60.3826426720152,-14.1985145724515,
11.6359872033749));
#37848=CARTESIAN_POINT('Ctrl Pts',(-67.8425423025986,-17.2449834421528,
7.06170475438614));
#37849=CARTESIAN_POINT('Ctrl Pts',(-67.936339604961,-16.8759806260738,7.20780006417493));
#37850=CARTESIAN_POINT('Ctrl Pts',(-68.0195197262117,-16.5358040823885,
7.42431456480024));
#37851=CARTESIAN_POINT('Ctrl Pts',(-68.1509980806491,-15.9848167458475,
7.95780764621782));
#37852=CARTESIAN_POINT('Ctrl Pts',(-68.2006822338607,-15.769941108176,8.25968161903171));
#37853=CARTESIAN_POINT('Ctrl Pts',(-68.2646302810789,-15.490561932004,8.88066242679753));
#37854=CARTESIAN_POINT('Ctrl Pts',(-68.2826595052327,-15.410358466988,9.1849782015739));
#37855=CARTESIAN_POINT('Ctrl Pts',(-68.2943569622715,-15.358433741901,9.79677072277298));
#37856=CARTESIAN_POINT('Ctrl Pts',(-68.288855628865,-15.3830449856443,10.0982078060305));
#37857=CARTESIAN_POINT('Ctrl Pts',(-68.2546420063796,-15.5341550196633,
10.6858944634119));
#37858=CARTESIAN_POINT('Ctrl Pts',(-68.2257386849337,-15.661414646539,10.9661810334236));
#37859=CARTESIAN_POINT('Ctrl Pts',(-68.1449424659488,-16.0093499903206,
11.4722931322538));
#37860=CARTESIAN_POINT('Ctrl Pts',(-68.093295210955,-16.2286900565759,11.6926718707978));
#37861=CARTESIAN_POINT('Ctrl Pts',(-68.0322473001841,-16.4806955947434,
11.8669181223572));
#37862=CARTESIAN_POINT('Ctrl Pts',(-60.3826426720152,-14.1985145724515,
11.6359872033749));
#37863=CARTESIAN_POINT('Ctrl Pts',(-60.3987291200758,-14.1384791309761,
11.5775783984681));
#37864=CARTESIAN_POINT('Ctrl Pts',(-60.4139429451876,-14.0817003626815,
11.5159169743219));
#37865=CARTESIAN_POINT('Ctrl Pts',(-60.428280614173,-14.0281914535657,11.4513790591597));
#37866=CARTESIAN_POINT('Ctrl Pts',(-60.4429682456437,-13.9733764666745,
11.3852658635805));
#37867=CARTESIAN_POINT('Ctrl Pts',(-60.4567365493831,-13.9219924575848,
11.3161335496817));
#37868=CARTESIAN_POINT('Ctrl Pts',(-60.4695742653767,-13.8740814492437,
11.244340195927));
#37869=CARTESIAN_POINT('Ctrl Pts',(-60.4729336106422,-13.8615442020328,
11.2255534691331));
#37870=CARTESIAN_POINT('Ctrl Pts',(-60.4762291892638,-13.8492449351765,
11.2065843091488));
#37871=CARTESIAN_POINT('Ctrl Pts',(-60.4794607015,-13.8371847673257,11.1874386952136));
#37872=CARTESIAN_POINT('Ctrl Pts',(-60.4820790008577,-13.8274131410933,
11.1719261595939));
#37873=CARTESIAN_POINT('Ctrl Pts',(-60.4846553435987,-13.8177980990861,
11.156296950855));
#37874=CARTESIAN_POINT('Ctrl Pts',(-60.4871873137292,-13.808348657916,11.1405686300786));
#37875=CARTESIAN_POINT('Ctrl Pts',(-60.4994718284845,-13.7625022247027,
11.0642585716257));
#37876=CARTESIAN_POINT('Ctrl Pts',(-60.5107256649652,-13.7205023351767,
10.9855425561623));
#37877=CARTESIAN_POINT('Ctrl Pts',(-60.5209393772212,-13.6823842421036,
10.9048124952827));
#37878=CARTESIAN_POINT('Ctrl Pts',(-60.5290925934916,-13.6519560247373,
10.8403687720428));
#37879=CARTESIAN_POINT('Ctrl Pts',(-60.5365828861053,-13.6240018721396,
10.7746405675613));
#37880=CARTESIAN_POINT('Ctrl Pts',(-60.5434011779566,-13.5985556605296,
10.7078100772199));
#37881=CARTESIAN_POINT('Ctrl Pts',(-60.5456026098314,-13.5903398049234,
10.6862324189363));
#37882=CARTESIAN_POINT('Ctrl Pts',(-60.5477339564827,-13.582385510932,10.6645397516012));
#37883=CARTESIAN_POINT('Ctrl Pts',(-60.5497948184315,-13.574694269432,10.6427379433821));
#37884=CARTESIAN_POINT('Ctrl Pts',(-60.5517587834915,-13.5673646520437,
10.6219612049815));
#37885=CARTESIAN_POINT('Ctrl Pts',(-60.553659151552,-13.5602723818886,10.6010802047041));
#37886=CARTESIAN_POINT('Ctrl Pts',(-60.5554929869735,-13.5534284149229,
10.5801302249072));
#37887=CARTESIAN_POINT('Ctrl Pts',(-60.5631434154496,-13.5248766271506,
10.4927307123161));
#37888=CARTESIAN_POINT('Ctrl Pts',(-60.569645182982,-13.5006117003807,10.4040498988215));
#37889=CARTESIAN_POINT('Ctrl Pts',(-60.5749893942622,-13.4806668323564,
10.3144849191128));
#37890=CARTESIAN_POINT('Ctrl Pts',(-60.5804161086929,-13.4604140583831,
10.2235372483755));
#37891=CARTESIAN_POINT('Ctrl Pts',(-60.5846493808354,-13.4446152716651,
10.1316770969848));
#37892=CARTESIAN_POINT('Ctrl Pts',(-60.5876690820109,-13.4333455934544,
10.0392871196303));
#37893=CARTESIAN_POINT('Ctrl Pts',(-60.5906654794535,-13.4221628859587,
9.94761013711361));
#37894=CARTESIAN_POINT('Ctrl Pts',(-60.5924670545743,-13.4154393160742,
9.85541054674054));
#37895=CARTESIAN_POINT('Ctrl Pts',(-60.5930419859763,-13.4132936428713,
9.76304299840633));
#37896=CARTESIAN_POINT('Ctrl Pts',(-60.5933185830197,-13.4122613686522,
9.71860536517465));
#37897=CARTESIAN_POINT('Ctrl Pts',(-60.5933110802673,-13.4122893693051,
9.67412865771307));
#37898=CARTESIAN_POINT('Ctrl Pts',(-60.593014824197,-13.4133950120118,9.62965173452372));
#37899=CARTESIAN_POINT('Ctrl Pts',(-60.5929169928494,-13.4137601235713,
9.61496431453743));
#37900=CARTESIAN_POINT('Ctrl Pts',(-60.5927876671156,-13.4142427737806,
9.60027687017834));
#37901=CARTESIAN_POINT('Ctrl Pts',(-60.592626660992,-13.4148436568143,9.58559080055877));
#37902=CARTESIAN_POINT('Ctrl Pts',(-60.5924638798191,-13.4154511644222,
9.57074282096179));
#37903=CARTESIAN_POINT('Ctrl Pts',(-60.5922688054843,-13.4161791917507,
9.55590504919177));
#37904=CARTESIAN_POINT('Ctrl Pts',(-60.5920414435149,-13.4170277181723,
9.5410835717059));
#37905=CARTESIAN_POINT('Ctrl Pts',(-60.5905760164193,-13.4224967665479,
9.44555398617054));
#37906=CARTESIAN_POINT('Ctrl Pts',(-60.5877696251689,-13.4329703612802,
9.35064220193598));
#37907=CARTESIAN_POINT('Ctrl Pts',(-60.5836035770972,-13.4485182643508,
9.256742983847));
#37908=CARTESIAN_POINT('Ctrl Pts',(-60.5832473073958,-13.4498478809775,
9.24871296455522));
#37909=CARTESIAN_POINT('Ctrl Pts',(-60.5828810865857,-13.4512146356476,
9.24069033913143));
#37910=CARTESIAN_POINT('Ctrl Pts',(-60.5825048986307,-13.4526185882087,
9.23267534878088));
#37911=CARTESIAN_POINT('Ctrl Pts',(-60.5782789204955,-13.4683901533212,
9.14263744743344));
#37912=CARTESIAN_POINT('Ctrl Pts',(-60.5727962781624,-13.4888516530677,
9.05356331283212));
#37913=CARTESIAN_POINT('Ctrl Pts',(-60.5661351124401,-13.5137114619812,
8.9656877172483));
#37914=CARTESIAN_POINT('Ctrl Pts',(-60.559321511335,-13.5391401674879,8.87580115982938));
#37915=CARTESIAN_POINT('Ctrl Pts',(-60.5512747790297,-13.5691709812862,
8.78716792582501));
#37916=CARTESIAN_POINT('Ctrl Pts',(-60.5420644900995,-13.6035442475259,
8.70004212728124));
#37917=CARTESIAN_POINT('Ctrl Pts',(-60.5370098857273,-13.6224082878551,
8.65222750978226));
#37918=CARTESIAN_POINT('Ctrl Pts',(-60.5316045998671,-13.642581089315,8.60486701429381));
#37919=CARTESIAN_POINT('Ctrl Pts',(-60.5258584913669,-13.6640258581837,
8.5580041989488));
#37920=CARTESIAN_POINT('Ctrl Pts',(-60.5241489330315,-13.6704060167496,
8.54406176876562));
#37921=CARTESIAN_POINT('Ctrl Pts',(-60.5224089382015,-13.6768997658602,
8.53016150108827));
#37922=CARTESIAN_POINT('Ctrl Pts',(-60.5206408848662,-13.6834982307381,
8.51632087102361));
#37923=CARTESIAN_POINT('Ctrl Pts',(-60.5095968739651,-13.7247150405403,
8.42986642631845));
#37924=CARTESIAN_POINT('Ctrl Pts',(-60.4974435461318,-13.7700718774953,
8.34560744647309));
#37925=CARTESIAN_POINT('Ctrl Pts',(-60.4842687953746,-13.819240716698,8.2637970858888));
#37926=CARTESIAN_POINT('Ctrl Pts',(-60.470834261757,-13.8693790787351,8.18037356920902));
#37927=CARTESIAN_POINT('Ctrl Pts',(-60.4563375467057,-13.9234815558493,
8.09949541141806));
#37928=CARTESIAN_POINT('Ctrl Pts',(-60.4408576353906,-13.981253371374,8.02143790706986));
#37929=CARTESIAN_POINT('Ctrl Pts',(-60.4252551513805,-14.0394826344241,
7.9427623294991));
#37930=CARTESIAN_POINT('Ctrl Pts',(-60.4086537217477,-14.1014400132919,
7.86695140891473));
#37931=CARTESIAN_POINT('Ctrl Pts',(-60.3911214682024,-14.1668712742941,
7.79430622909878));
#37932=CARTESIAN_POINT('Ctrl Pts',(-60.3818445739541,-14.2014931149651,
7.75586726578716));
#37933=CARTESIAN_POINT('Ctrl Pts',(-60.3723068631306,-14.2370883363464,
7.71831505012366));
#37934=CARTESIAN_POINT('Ctrl Pts',(-60.3625171761545,-14.2736239455313,
7.68169758973832));
#37935=CARTESIAN_POINT('Ctrl Pts',(-60.3590313767661,-14.2866331259538,
7.66865926467973));
#37936=CARTESIAN_POINT('Ctrl Pts',(-60.3555136232663,-14.2997615607436,
7.65573947798149));
#37937=CARTESIAN_POINT('Ctrl Pts',(-60.351964291066,-14.3130078488481,7.64294048662165));
#37938=CARTESIAN_POINT('Ctrl Pts',(-60.34923729056,-14.3231851532886,7.63310684639187));
#37939=CARTESIAN_POINT('Ctrl Pts',(-60.3464919180926,-14.3334310228227,
7.6233455630969));
#37940=CARTESIAN_POINT('Ctrl Pts',(-60.3437307201908,-14.343735953682,7.61366571166803));
#37941=CARTESIAN_POINT('Ctrl Pts',(-60.3241830915898,-14.4166886967885,
7.54513815682638));
#37942=CARTESIAN_POINT('Ctrl Pts',(-60.3038121514937,-14.4927140802252,
7.48057696466926));
#37943=CARTESIAN_POINT('Ctrl Pts',(-60.2827016033741,-14.5714997183832,
7.42026730042969));
#37944=CARTESIAN_POINT('Ctrl Pts',(-60.261564320459,-14.650385132156,7.35988125889639));
#37945=CARTESIAN_POINT('Ctrl Pts',(-60.2396854085589,-14.7320383429816,
7.30375667607862));
#37946=CARTESIAN_POINT('Ctrl Pts',(-60.2171371866631,-14.8161894527173,
7.25220561234172));
#37947=CARTESIAN_POINT('Ctrl Pts',(-60.1950163808933,-14.8987454237543,
7.20163173235182));
#37948=CARTESIAN_POINT('Ctrl Pts',(-60.1722512298629,-14.9837061240419,
7.15545893555081));
#37949=CARTESIAN_POINT('Ctrl Pts',(-60.1489011523676,-15.0708497996151,
7.11401788932665));
#37950=CARTESIAN_POINT('Ctrl Pts',(-60.141634689533,-15.0979686081049,7.10112157999862));
#37951=CARTESIAN_POINT('Ctrl Pts',(-60.134311524735,-15.1252990312032,7.08868381628556));
#37952=CARTESIAN_POINT('Ctrl Pts',(-60.1269333077645,-15.1528349118066,
7.07671545672067));
#37953=CARTESIAN_POINT('Ctrl Pts',(-60.1158687531571,-15.1941283917646,
7.05876741202428));
#37954=CARTESIAN_POINT('Ctrl Pts',(-60.1046804027641,-15.2358838838839,
7.04187489341869));
#37955=CARTESIAN_POINT('Ctrl Pts',(-60.0933772939442,-15.2780676602833,
7.02603075613033));
#37956=CARTESIAN_POINT('Ctrl Pts',(-67.4086397233445,-15.458048217099,10.0018117506529));
#37957=CARTESIAN_POINT('Ctrl Pts',(-67.3922281881599,-15.4516726940089,
10.2792252787836));
#37958=CARTESIAN_POINT('Ctrl Pts',(-67.3643426917121,-15.488118577317,10.556071912701));
#37959=CARTESIAN_POINT('Ctrl Pts',(-67.3243238737158,-15.5698466331086,
10.8168646145659));
#37960=CARTESIAN_POINT('Ctrl Pts',(-67.2047485806183,-15.8140481541645,
11.5961071140835));
#37961=CARTESIAN_POINT('Ctrl Pts',(-66.9768469397625,-16.4625291088529,
12.2320200381456));
#37962=CARTESIAN_POINT('Ctrl Pts',(-66.7200527868787,-17.2188383863883,
12.4398697983789));
#37963=CARTESIAN_POINT('Ctrl Pts',(-66.4632586339948,-17.9751476639237,
12.6477195586123));
#37964=CARTESIAN_POINT('Ctrl Pts',(-66.1775719690829,-18.8392852643061,
12.427506155017));
#37965=CARTESIAN_POINT('Ctrl Pts',(-65.9682965015872,-19.4182523936641,
11.8778290289179));
#37966=CARTESIAN_POINT('Ctrl Pts',(-65.7590210340915,-19.997219523022,11.3281519028188));
#37967=CARTESIAN_POINT('Ctrl Pts',(-65.6261567640121,-20.2910161813555,
10.449011054216));
#37968=CARTESIAN_POINT('Ctrl Pts',(-65.6065790035572,-20.162021829958,9.63407278056581));
#37969=CARTESIAN_POINT('Ctrl Pts',(-65.5870012431023,-20.0330274785605,
8.81913450691562));
#37970=CARTESIAN_POINT('Ctrl Pts',(-65.6807099922718,-19.481242117432,8.06839880821806));
#37971=CARTESIAN_POINT('Ctrl Pts',(-65.8231242605019,-18.7476852845608,
7.71802880880706));
#37972=CARTESIAN_POINT('Ctrl Pts',(-65.965538528732,-18.0141284516896,7.36765880939607));
#37973=CARTESIAN_POINT('Ctrl Pts',(-66.1566583160226,-17.0988001470757,
7.41765450927163));
#37974=CARTESIAN_POINT('Ctrl Pts',(-66.288284454746,-16.4055051616422,7.8456297388467));
#37975=CARTESIAN_POINT('Ctrl Pts',(-66.4199105934695,-15.7122101762087,
8.27360496842178));
#37976=CARTESIAN_POINT('Ctrl Pts',(-66.4920430836257,-15.2409485099555,
9.07955972769635));
#37977=CARTESIAN_POINT('Ctrl Pts',(-66.4497626823332,-15.1966815676295,
9.90260247183749));
#37978=CARTESIAN_POINT('Ctrl Pts',(-66.4481055265244,-15.1949465504969,
9.93486115488347));
#37979=CARTESIAN_POINT('Ctrl Pts',(-66.4462726093384,-15.1938674837542,
9.96714608853563));
#37980=CARTESIAN_POINT('Ctrl Pts',(-66.4442667934687,-15.1934336836835,
9.99943462192771));
#37981=CARTESIAN_POINT('Ctrl Pts',(-20.25986904378,67.0040126136404,11.1728309286208));
#37982=CARTESIAN_POINT('Ctrl Pts',(-20.6173045957293,66.854289394458,10.4434664543485));
#37983=CARTESIAN_POINT('Ctrl Pts',(-20.5807180172414,66.7561954352347,8.59013022403081));
#37984=CARTESIAN_POINT('Ctrl Pts',(-18.2866570474721,67.2090412643978,7.05024279158514));
#37985=CARTESIAN_POINT('Ctrl Pts',(-15.7623446338521,67.7235827819969,8.14059085434233));
#37986=CARTESIAN_POINT('Ctrl Pts',(-15.216861454864,67.7078986042171,10.8824467802982));
#37987=CARTESIAN_POINT('Ctrl Pts',(-17.0999173665985,67.0414893382909,12.8405694561119));
#37988=CARTESIAN_POINT('Ctrl Pts',(-19.6999556621849,66.1829652216242,12.270731917377));
#37989=CARTESIAN_POINT('Ctrl Pts',(-20.6677950818131,65.7617874756574,9.68094249642523));
#37990=CARTESIAN_POINT('Ctrl Pts',(-19.1062967313387,66.0183437425753,7.37485535276711));
#37991=CARTESIAN_POINT('Ctrl Pts',(-16.3687616678975,66.5900180970018,7.40446197973337));
#37992=CARTESIAN_POINT('Ctrl Pts',(-14.8547867084588,66.83384050967,9.74329926128818));
#37993=CARTESIAN_POINT('Ctrl Pts',(-15.8753739824799,66.3985290187163,12.3105450512028));
#37994=CARTESIAN_POINT('Ctrl Pts',(-18.4864972623911,65.5370346894516,12.8220707222439));
#37995=CARTESIAN_POINT('Ctrl Pts',(-20.3290217552966,64.8814857844687,10.8227823754311));
#37996=CARTESIAN_POINT('Ctrl Pts',(-19.7276391663451,64.8807798084461,8.09145561890055));
#37997=CARTESIAN_POINT('Ctrl Pts',(-17.1814057921381,65.4011950297316,7.0581771851638));
#37998=CARTESIAN_POINT('Ctrl Pts',(-14.9197267037703,65.8453641599238,8.64226139479096));
#37999=CARTESIAN_POINT('Ctrl Pts',(-14.9188369907852,65.6837566027254,11.4343367521439));
#38000=CARTESIAN_POINT('Ctrl Pts',(-17.1435292903637,64.9258061425711,12.950271123299));
#38001=CARTESIAN_POINT('Ctrl Pts',(-19.5784782321595,64.1115175849317,11.8413258175014));
#38002=CARTESIAN_POINT('Ctrl Pts',(-20.0212914063393,63.8310201974379,9.09413821413813));
#38003=CARTESIAN_POINT('Ctrl Pts',(-18.0419954959312,64.1995249831397,7.15290308224175));
#38004=CARTESIAN_POINT('Ctrl Pts',(-15.3655869450733,64.7548205378834,7.74475277436873));
#38005=CARTESIAN_POINT('Ctrl Pts',(-14.3372888766999,64.8685062198083,10.3431139119316));
#38006=CARTESIAN_POINT('Ctrl Pts',(-15.8359873727446,64.305085213021,12.6362038638412));
#38007=CARTESIAN_POINT('Ctrl Pts',(-18.4922795208015,63.4314879220137,12.5838422163727));
#38008=CARTESIAN_POINT('Ctrl Pts',(-19.9068421044142,62.8906110650171,10.2326155433119));
#38009=CARTESIAN_POINT('Ctrl Pts',(-18.7851286033011,63.029327336705,7.67442896667237));
#38010=CARTESIAN_POINT('Ctrl Pts',(-16.0891375551554,63.5898700057829,7.1853214836325));
#38011=CARTESIAN_POINT('Ctrl Pts',(-14.1815147862765,63.9391700310929,9.20045592301428));
#38012=CARTESIAN_POINT('Ctrl Pts',(-14.7234885765209,63.6321026366037,11.926951102987));
#38013=CARTESIAN_POINT('Ctrl Pts',(-17.1968616153839,62.8075183731852,12.9390225214355));
#38014=CARTESIAN_POINT('Ctrl Pts',(-19.3650552728408,62.0647066785609,11.3362221619437));
#38015=CARTESIAN_POINT('Ctrl Pts',(-19.2630114600595,61.9302032807139,8.54457429525404));
#38016=CARTESIAN_POINT('Ctrl Pts',(-16.9455204456759,62.3893271714101,7.04783027207108));
#38017=CARTESIAN_POINT('Ctrl Pts',(-14.4384735898227,62.8992423967485,8.17765522357039));
#38018=CARTESIAN_POINT('Ctrl Pts',(-13.9364114971972,62.8719235739435,10.9288348037814));
#38019=CARTESIAN_POINT('Ctrl Pts',(-15.850024041082,62.1973266831092,12.853622756267));
#38020=CARTESIAN_POINT('Ctrl Pts',(-18.4407556977103,61.3412962728355,12.2395195742226));
#38021=CARTESIAN_POINT('Ctrl Pts',(-19.3676134988853,60.9310995184379,9.63289839745391));
#38022=CARTESIAN_POINT('Ctrl Pts',(-17.7699646296638,61.1973422876599,7.35288957156125));
#38023=CARTESIAN_POINT('Ctrl Pts',(-15.0332534115107,61.7687958934069,7.42803777444102));
#38024=CARTESIAN_POINT('Ctrl Pts',(-13.5563500795275,62.0026849934362,9.79147768508997));
#38025=CARTESIAN_POINT('Ctrl Pts',(-14.6172778371391,61.5565643024822,12.3404488591357));
#38026=CARTESIAN_POINT('Ctrl Pts',(-17.236102725553,60.6930063334387,12.807089206987));
#38027=CARTESIAN_POINT('Ctrl Pts',(-19.0468753473843,60.0459653166684,10.7762699688266));
#38028=CARTESIAN_POINT('Ctrl Pts',(-18.4024589901613,60.0567902041013,8.05473611617475));
#38029=CARTESIAN_POINT('Ctrl Pts',(-15.8403574002339,60.5814573009745,7.06404294414452));
#38030=CARTESIAN_POINT('Ctrl Pts',(-13.6037685248159,61.0189035288689,8.68524269063552));
#38031=CARTESIAN_POINT('Ctrl Pts',(-13.6472648693584,60.8454027634006,11.4767030328865));
#38032=CARTESIAN_POINT('Ctrl Pts',(-15.8948076660285,60.0813295310042,12.9532921034687));
#38033=CARTESIAN_POINT('Ctrl Pts',(-18.3134648367078,59.2714063402786,11.8044287744805));
#38034=CARTESIAN_POINT('Ctrl Pts',(-18.7097689547777,59.0033710168103,9.04578082775244));
#38035=CARTESIAN_POINT('Ctrl Pts',(-17.3744086881427,59.2532824184768,7.78080120942677));
#38036=CARTESIAN_POINT('Ctrl Pts',(-16.5917431062329,59.4090483774018,7.56791319796499));
#38037=CARTESIAN_POINT('Ctrl Pts',(-20.4459680138347,67.0649244254632,11.259172404465));
#38038=CARTESIAN_POINT('Ctrl Pts',(-20.8307101569087,66.9078844272409,10.4761135710142));
#38039=CARTESIAN_POINT('Ctrl Pts',(-20.7934159435358,66.8099800782136,8.48633842059633));
#38040=CARTESIAN_POINT('Ctrl Pts',(-18.3334494707627,67.3072801529265,6.83308754393487));
#38041=CARTESIAN_POINT('Ctrl Pts',(-15.6262809016687,67.8708178297157,8.00370485831642));
#38042=CARTESIAN_POINT('Ctrl Pts',(-15.0436190322123,67.8650956520227,10.9474107537965));
#38043=CARTESIAN_POINT('Ctrl Pts',(-17.0682804619448,67.1607433019051,13.049686519018));
#38044=CARTESIAN_POINT('Ctrl Pts',(-19.8627070898848,66.2501329885662,12.4378986762067));
#38045=CARTESIAN_POINT('Ctrl Pts',(-20.9047756131302,65.8090656142303,9.65745411880357));
#38046=CARTESIAN_POINT('Ctrl Pts',(-19.231301559894,66.0956256802751,7.18159743500988));
#38047=CARTESIAN_POINT('Ctrl Pts',(-16.2952133143915,66.7205021994896,7.21338364285574));
#38048=CARTESIAN_POINT('Ctrl Pts',(-14.6727612295383,66.9933909703099,9.72440146443631));
#38049=CARTESIAN_POINT('Ctrl Pts',(-15.7714607991054,66.5371493528457,12.4806427736084));
#38050=CARTESIAN_POINT('Ctrl Pts',(-18.5777884658271,65.6233501657761,13.0298259452254));
#38051=CARTESIAN_POINT('Ctrl Pts',(-20.558934634444,64.9306576947329,10.8833539743374));
#38052=CARTESIAN_POINT('Ctrl Pts',(-19.9162581518544,64.9410163841629,7.95095238475407));
#38053=CARTESIAN_POINT('Ctrl Pts',(-17.1855548447374,65.5108601749995,6.84160605175779));
#38054=CARTESIAN_POINT('Ctrl Pts',(-14.7603541429465,65.9988447894534,8.54230738426514));
#38055=CARTESIAN_POINT('Ctrl Pts',(-14.7623776252392,65.8364566439329,11.5399297656086));
#38056=CARTESIAN_POINT('Ctrl Pts',(-17.1538260329039,65.033824019284,13.167464204339));
#38057=CARTESIAN_POINT('Ctrl Pts',(-19.7710097578038,64.170705798679,11.9768805549434));
#38058=CARTESIAN_POINT('Ctrl Pts',(-20.2494006496399,63.8806753904707,9.02745047458974));
#38059=CARTESIAN_POINT('Ctrl Pts',(-18.1273716126603,64.2874254021705,6.94330548061665));
#38060=CARTESIAN_POINT('Ctrl Pts',(-15.2569098917896,64.8947173471078,7.57872596768869));
#38061=CARTESIAN_POINT('Ctrl Pts',(-14.1558892629051,65.0278889803931,10.3683732743989));
#38062=CARTESIAN_POINT('Ctrl Pts',(-15.7678976499205,64.4341066798258,12.8302759390873));
#38063=CARTESIAN_POINT('Ctrl Pts',(-18.6227194268519,63.5073135350879,12.7740595314741));
#38064=CARTESIAN_POINT('Ctrl Pts',(-20.1443979832212,62.9377350396947,10.2497402360734));
#38065=CARTESIAN_POINT('Ctrl Pts',(-18.9430848635892,63.0977799648826,7.50322506140522));
#38066=CARTESIAN_POINT('Ctrl Pts',(-16.0515990210029,63.7107053062553,6.97811046011705));
#38067=CARTESIAN_POINT('Ctrl Pts',(-14.0065195594074,64.096836741373,9.14159508133219));
#38068=CARTESIAN_POINT('Ctrl Pts',(-14.5913710742637,63.7782802952008,12.0688094033194));
#38069=CARTESIAN_POINT('Ctrl Pts',(-17.2498076016885,62.9041084194735,13.1553875028216));
#38070=CARTESIAN_POINT('Ctrl Pts',(-19.5805980497844,62.1177290461058,11.4345921747925));
#38071=CARTESIAN_POINT('Ctrl Pts',(-19.4740206690256,61.9844404141371,8.43742875512314));
#38072=CARTESIAN_POINT('Ctrl Pts',(-16.9888992784431,62.4884807287627,6.83049741954164));
#38073=CARTESIAN_POINT('Ctrl Pts',(-14.3002673230733,63.0470515348742,8.04349783254823));
#38074=CARTESIAN_POINT('Ctrl Pts',(-13.7642231138315,63.0288381927735,10.9972137711303));
#38075=CARTESIAN_POINT('Ctrl Pts',(-15.8216906940824,62.3156954611179,13.063700777119));
#38076=CARTESIAN_POINT('Ctrl Pts',(-18.6061255468499,61.4077624358672,12.4043885425467));
#38077=CARTESIAN_POINT('Ctrl Pts',(-19.6041954665562,60.9784844518179,9.6058731090043));
#38078=CARTESIAN_POINT('Ctrl Pts',(-17.8919095654206,61.275444121164,7.15801457676324));
#38079=CARTESIAN_POINT('Ctrl Pts',(-14.9567058150546,61.900083640621,7.23869504058987));
#38080=CARTESIAN_POINT('Ctrl Pts',(-13.374054496997,62.1623078281203,9.77612668779238));
#38081=CARTESIAN_POINT('Ctrl Pts',(-14.5160643361693,61.6944612588913,12.5127480402915));
#38082=CARTESIAN_POINT('Ctrl Pts',(-17.3306605884645,60.7784465109948,13.0137415206692));
#38083=CARTESIAN_POINT('Ctrl Pts',(-19.2777173765313,60.0948882619406,10.8334174170448));
#38084=CARTESIAN_POINT('Ctrl Pts',(-18.5888390654042,60.1176266940159,7.91152966540921));
#38085=CARTESIAN_POINT('Ctrl Pts',(-15.8410993561462,60.6920353750482,6.84790363622586));
#38086=CARTESIAN_POINT('Ctrl Pts',(-13.4428359587848,61.172802160534,8.58845287746019));
#38087=CARTESIAN_POINT('Ctrl Pts',(-13.4925131117115,60.9976452524507,11.5854149675154));
#38088=CARTESIAN_POINT('Ctrl Pts',(-15.908494224529,60.188439109268,13.1707075830487));
#38089=CARTESIAN_POINT('Ctrl Pts',(-18.5081868105878,59.3300076251901,11.9372672251408));
#38090=CARTESIAN_POINT('Ctrl Pts',(-18.9366447422826,59.0533567133274,8.97553311378094));
#38091=CARTESIAN_POINT('Ctrl Pts',(-17.5049637099305,59.3290771863822,7.61742821670135));
#38092=CARTESIAN_POINT('Ctrl Pts',(-16.6656727455702,59.5000158708058,7.38886781406146));
#38093=CARTESIAN_POINT('Ctrl Pts',(-20.6320669838895,67.125836237286,11.3455138803092));
#38094=CARTESIAN_POINT('Ctrl Pts',(-21.0441157180881,66.9614794600237,10.5087606876799));
#38095=CARTESIAN_POINT('Ctrl Pts',(-21.0061138698302,66.8637647211924,8.38254661716187));
#38096=CARTESIAN_POINT('Ctrl Pts',(-18.3802418940533,67.405519041455,6.61593229628459));
#38097=CARTESIAN_POINT('Ctrl Pts',(-15.4902171694853,68.0180528774347,7.86681886229054));
#38098=CARTESIAN_POINT('Ctrl Pts',(-14.8703766095605,68.0222926998282,11.0123747272948));
#38099=CARTESIAN_POINT('Ctrl Pts',(-17.036643557291,67.2799972655193,13.2588035819241));
#38100=CARTESIAN_POINT('Ctrl Pts',(-20.0254585175847,66.3173007555082,12.6050654350364));
#38101=CARTESIAN_POINT('Ctrl Pts',(-21.1417561444473,65.8563437528032,9.63396574118191));
#38102=CARTESIAN_POINT('Ctrl Pts',(-19.3563063884493,66.172907617975,6.98833951725265));
#38103=CARTESIAN_POINT('Ctrl Pts',(-16.2216649608855,66.8509863019774,7.02230530597812));
#38104=CARTESIAN_POINT('Ctrl Pts',(-14.4907357506179,67.1529414309497,9.70550366758444));
#38105=CARTESIAN_POINT('Ctrl Pts',(-15.6675476157309,66.675769686975,12.6507404960141));
#38106=CARTESIAN_POINT('Ctrl Pts',(-18.6690796692631,65.7096656421006,13.2375811682069));
#38107=CARTESIAN_POINT('Ctrl Pts',(-20.7888475135915,64.9798296049969,10.9439255732437));
#38108=CARTESIAN_POINT('Ctrl Pts',(-20.1048771373638,65.0012529598797,7.81044915060758));
#38109=CARTESIAN_POINT('Ctrl Pts',(-17.1897038973366,65.6205253202674,6.62503491835178));
#38110=CARTESIAN_POINT('Ctrl Pts',(-14.6009815821227,66.1523254189831,8.44235337373933));
#38111=CARTESIAN_POINT('Ctrl Pts',(-14.6059182596932,65.9891566851404,11.6455227790733));
#38112=CARTESIAN_POINT('Ctrl Pts',(-17.1641227754441,65.141841895997,13.3846572853789));
#38113=CARTESIAN_POINT('Ctrl Pts',(-19.9635412834481,64.2298940124263,12.1124352923854));
#38114=CARTESIAN_POINT('Ctrl Pts',(-20.4775098929406,63.9303305835034,8.96076273504135));
#38115=CARTESIAN_POINT('Ctrl Pts',(-18.2127477293894,64.3753258212012,6.73370787899156));
#38116=CARTESIAN_POINT('Ctrl Pts',(-15.1482328385059,65.0346141563322,7.41269916100865));
#38117=CARTESIAN_POINT('Ctrl Pts',(-13.9744896491103,65.1872717409779,10.3936326368661));
#38118=CARTESIAN_POINT('Ctrl Pts',(-15.6998079270964,64.5631281466306,13.0243480143333));
#38119=CARTESIAN_POINT('Ctrl Pts',(-18.7531593329024,63.5831391481621,12.9642768465755));
#38120=CARTESIAN_POINT('Ctrl Pts',(-20.3819538620282,62.9848590143722,10.266864928835));
#38121=CARTESIAN_POINT('Ctrl Pts',(-19.1010411238774,63.1662325930602,7.33202115613807));
#38122=CARTESIAN_POINT('Ctrl Pts',(-16.0140604868503,63.8315406067278,6.77089943660162));
#38123=CARTESIAN_POINT('Ctrl Pts',(-13.8315243325383,64.2545034516531,9.08273423965009));
#38124=CARTESIAN_POINT('Ctrl Pts',(-14.4592535720065,63.9244579537978,12.2106677036518));
#38125=CARTESIAN_POINT('Ctrl Pts',(-17.3027535879931,63.000698465762,13.3717524842076));
#38126=CARTESIAN_POINT('Ctrl Pts',(-19.7961408267281,62.1707514136505,11.5329621876413));
#38127=CARTESIAN_POINT('Ctrl Pts',(-19.6850298779916,62.0386775475604,8.33028321499222));
#38128=CARTESIAN_POINT('Ctrl Pts',(-17.0322781112102,62.5876342861153,6.61316456701222));
#38129=CARTESIAN_POINT('Ctrl Pts',(-14.1620610563239,63.1948606729998,7.90934044152608));
#38130=CARTESIAN_POINT('Ctrl Pts',(-13.5920347304658,63.1857528116036,11.0655927384792));
#38131=CARTESIAN_POINT('Ctrl Pts',(-15.7933573470829,62.4340642391264,13.273778797971));
#38132=CARTESIAN_POINT('Ctrl Pts',(-18.7714953959894,61.4742285988991,12.5692575108708));
#38133=CARTESIAN_POINT('Ctrl Pts',(-19.8407774342272,61.0258693851979,9.5788478205547));
#38134=CARTESIAN_POINT('Ctrl Pts',(-18.0138545011774,61.3535459546681,6.96313958196524));
#38135=CARTESIAN_POINT('Ctrl Pts',(-14.8801582185986,62.0313713878352,7.04935230673872));
#38136=CARTESIAN_POINT('Ctrl Pts',(-13.1917589144664,62.3219306628044,9.7607756904948));
#38137=CARTESIAN_POINT('Ctrl Pts',(-14.4148508351995,61.8323582153006,12.6850472214474));
#38138=CARTESIAN_POINT('Ctrl Pts',(-17.425218451376,60.8638866885509,13.2203938343514));
#38139=CARTESIAN_POINT('Ctrl Pts',(-19.5085594056783,60.1438112072127,10.8905648652629));
#38140=CARTESIAN_POINT('Ctrl Pts',(-18.7752191406471,60.1784631839305,7.76832321464366));
#38141=CARTESIAN_POINT('Ctrl Pts',(-15.8418413120585,60.8026134491219,6.6317643283072));
#38142=CARTESIAN_POINT('Ctrl Pts',(-13.2819033927538,61.326700792199,8.49166306428486));
#38143=CARTESIAN_POINT('Ctrl Pts',(-13.3377613540646,61.1498877415007,11.6941269021443));
#38144=CARTESIAN_POINT('Ctrl Pts',(-15.9221807830296,60.2955486875318,13.3881230626288));
#38145=CARTESIAN_POINT('Ctrl Pts',(-18.7029087844678,59.3886089101016,12.070105675801));
#38146=CARTESIAN_POINT('Ctrl Pts',(-19.1635205297874,59.1033424098445,8.90528539980945));
#38147=CARTESIAN_POINT('Ctrl Pts',(-17.6355187317182,59.4048719542876,7.45405522397594));
#38148=CARTESIAN_POINT('Ctrl Pts',(-16.7396023849075,59.5909833642099,7.20982243015792));
#38149=CARTESIAN_POINT('Ctrl Pts',(-20.8181659539443,67.1867480491087,11.4318553561534));
#38150=CARTESIAN_POINT('Ctrl Pts',(-21.2575212792675,67.0150744928066,10.5414078043456));
#38151=CARTESIAN_POINT('Ctrl Pts',(-21.2188117961246,66.9175493641713,8.2787548137274));
#38152=CARTESIAN_POINT('Ctrl Pts',(-18.4270343173439,67.5037579299837,6.39877704863432));
#38153=CARTESIAN_POINT('Ctrl Pts',(-15.3541534373018,68.1652879251536,7.72993286626462));
#38154=CARTESIAN_POINT('Ctrl Pts',(-14.6971341869088,68.1794897476338,11.0773387007931));
#38155=CARTESIAN_POINT('Ctrl Pts',(-17.0050066526372,67.3992512291335,13.4679206448302));
#38156=CARTESIAN_POINT('Ctrl Pts',(-20.1882099452846,66.3844685224502,12.7722321938662));
#38157=CARTESIAN_POINT('Ctrl Pts',(-21.3787366757643,65.9036218913761,9.61047736356026));
#38158=CARTESIAN_POINT('Ctrl Pts',(-19.4813112170046,66.2501895556747,6.79508159949542));
#38159=CARTESIAN_POINT('Ctrl Pts',(-16.1481166073795,66.9814704044652,6.8312269691005));
#38160=CARTESIAN_POINT('Ctrl Pts',(-14.3087102716975,67.3124918915896,9.68660587073256));
#38161=CARTESIAN_POINT('Ctrl Pts',(-15.5636344323564,66.8143900211043,12.8208382184197));
#38162=CARTESIAN_POINT('Ctrl Pts',(-18.7603708726991,65.795981118425,13.4453363911884));
#38163=CARTESIAN_POINT('Ctrl Pts',(-21.0187603927389,65.0290015152611,11.00449717215));
#38164=CARTESIAN_POINT('Ctrl Pts',(-20.2934961228732,65.0614895355965,7.6699459164611));
#38165=CARTESIAN_POINT('Ctrl Pts',(-17.1938529499358,65.7301904655353,6.40846378494576));
#38166=CARTESIAN_POINT('Ctrl Pts',(-14.441609021299,66.3058060485126,8.34239936321352));
#38167=CARTESIAN_POINT('Ctrl Pts',(-14.4494588941473,66.141856726348,11.7511157925379));
#38168=CARTESIAN_POINT('Ctrl Pts',(-17.1744195179844,65.2498597727098,13.6018503664189));
#38169=CARTESIAN_POINT('Ctrl Pts',(-20.1560728090925,64.2890822261736,12.2479900298274));
#38170=CARTESIAN_POINT('Ctrl Pts',(-20.7056191362412,63.9799857765361,8.89407499549296));
#38171=CARTESIAN_POINT('Ctrl Pts',(-18.2981238461185,64.4632262402319,6.52411027736645));
#38172=CARTESIAN_POINT('Ctrl Pts',(-15.0395557852223,65.1745109655565,7.24667235432862));
#38173=CARTESIAN_POINT('Ctrl Pts',(-13.7930900353155,65.3466545015629,10.4188919993334));
#38174=CARTESIAN_POINT('Ctrl Pts',(-15.6317182042723,64.6921496134353,13.2184200895793));
#38175=CARTESIAN_POINT('Ctrl Pts',(-18.8835992389528,63.6589647612364,13.1544941616769));
#38176=CARTESIAN_POINT('Ctrl Pts',(-20.6195097408352,63.0319829890498,10.2839896215965));
#38177=CARTESIAN_POINT('Ctrl Pts',(-19.2589973841656,63.2346852212378,7.16081725087092));
#38178=CARTESIAN_POINT('Ctrl Pts',(-15.9765219526977,63.9523759072002,6.56368841308618));
#38179=CARTESIAN_POINT('Ctrl Pts',(-13.6565291056693,64.4121701619331,9.023873397968));
#38180=CARTESIAN_POINT('Ctrl Pts',(-14.3271360697493,64.0706356123949,12.3525260039843));
#38181=CARTESIAN_POINT('Ctrl Pts',(-17.3556995742977,63.0972885120503,13.5881174655937));
#38182=CARTESIAN_POINT('Ctrl Pts',(-20.0116836036718,62.2237737811954,11.6313322004901));
#38183=CARTESIAN_POINT('Ctrl Pts',(-19.8960390869576,62.0929146809836,8.2231376748613));
#38184=CARTESIAN_POINT('Ctrl Pts',(-17.0756569439774,62.686787843468,6.39583171448279));
#38185=CARTESIAN_POINT('Ctrl Pts',(-14.0238547895745,63.3426698111255,7.77518305050392));
#38186=CARTESIAN_POINT('Ctrl Pts',(-13.4198463471001,63.3426674304337,11.1339717058281));
#38187=CARTESIAN_POINT('Ctrl Pts',(-15.7650240000833,62.5524330171351,13.4838568188229));
#38188=CARTESIAN_POINT('Ctrl Pts',(-18.936865245129,61.5406947619309,12.7341264791949));
#38189=CARTESIAN_POINT('Ctrl Pts',(-20.0773594018982,61.0732543185779,9.55182253210509));
#38190=CARTESIAN_POINT('Ctrl Pts',(-18.1357994369342,61.4316477881722,6.76826458716724));
#38191=CARTESIAN_POINT('Ctrl Pts',(-14.8036106221425,62.1626591350494,6.86000957288756));
#38192=CARTESIAN_POINT('Ctrl Pts',(-13.0094633319359,62.4815534974883,9.74542469319723));
#38193=CARTESIAN_POINT('Ctrl Pts',(-14.3136373342297,61.9702551717098,12.8573464026032));
#38194=CARTESIAN_POINT('Ctrl Pts',(-17.5197763142875,60.9493268661069,13.4270461480336));
#38195=CARTESIAN_POINT('Ctrl Pts',(-19.7394014348252,60.1927341524848,10.9477123134811));
#38196=CARTESIAN_POINT('Ctrl Pts',(-18.96159921589,60.2392996738452,7.62511676387811));
#38197=CARTESIAN_POINT('Ctrl Pts',(-15.8425832679708,60.9131915231956,6.41562502038854));
#38198=CARTESIAN_POINT('Ctrl Pts',(-13.1209708267228,61.4805994238641,8.39487325110954));
#38199=CARTESIAN_POINT('Ctrl Pts',(-13.1830095964176,61.3021302305506,11.8028388367732));
#38200=CARTESIAN_POINT('Ctrl Pts',(-15.9358673415301,60.4026582657957,13.6055385422089));
#38201=CARTESIAN_POINT('Ctrl Pts',(-18.8976307583477,59.447210195013,12.2029441264611));
#38202=CARTESIAN_POINT('Ctrl Pts',(-19.3903963172923,59.1533281063616,8.83503768583798));
#38203=CARTESIAN_POINT('Ctrl Pts',(-17.7660737535059,59.4806667221929,7.29068223125052));
#38204=CARTESIAN_POINT('Ctrl Pts',(-16.8135320242448,59.6819508576139,7.03077704625438));
#38205=CARTESIAN_POINT('Ctrl Pts',(-20.25986904378,67.0040126136404,11.1728309286207));
#38206=CARTESIAN_POINT('Ctrl Pts',(-20.4203000043805,66.9555034255254,10.9082027524038));
#38207=CARTESIAN_POINT('Ctrl Pts',(-20.5332184525385,66.9207835851305,10.6149904639444));
#38208=CARTESIAN_POINT('Ctrl Pts',(-20.6611539455099,66.8813975908017,9.99178401342257));
#38209=CARTESIAN_POINT('Ctrl Pts',(-20.6720025707686,66.8780249511107,9.66515229429171));
#38210=CARTESIAN_POINT('Ctrl Pts',(-20.5855924444283,66.904675210205,9.00098486496486));
#38211=CARTESIAN_POINT('Ctrl Pts',(-20.4815398383752,66.9367881932439,8.66883374311755));
#38212=CARTESIAN_POINT('Ctrl Pts',(-20.1690707048658,67.0315956493191,8.06423785428621));
#38213=CARTESIAN_POINT('Ctrl Pts',(-19.9644265611135,67.0931208523799,7.79496359360561));
#38214=CARTESIAN_POINT('Ctrl Pts',(-19.4553169386788,67.2425937581436,7.32570054462936));
#38215=CARTESIAN_POINT('Ctrl Pts',(-19.1487818292132,67.3308539700399,7.13688275745722));
#38216=CARTESIAN_POINT('Ctrl Pts',(-18.8154792730627,67.4238662472344,7.01293629783561));
#38217=CARTESIAN_POINT('Ctrl Pts',(-15.2652009106025,66.709565290414,9.99881345470565));
#38218=CARTESIAN_POINT('Ctrl Pts',(-15.2659775128488,66.7141255555457,9.92620926472458));
#38219=CARTESIAN_POINT('Ctrl Pts',(-15.2699455778512,66.7178306708093,9.85363960672269));
#38220=CARTESIAN_POINT('Ctrl Pts',(-15.2772137473688,66.720651525733,9.78136734601481));
#38221=CARTESIAN_POINT('Ctrl Pts',(-15.3594450282717,66.752566372114,8.96368683410325));
#38222=CARTESIAN_POINT('Ctrl Pts',(-15.8641033480846,66.6712922345579,8.18407440691831));
#38223=CARTESIAN_POINT('Ctrl Pts',(-16.5726883518979,66.5353761067088,7.78933375549813));
#38224=CARTESIAN_POINT('Ctrl Pts',(-17.2812733557112,66.3994599788597,7.39459310407796));
#38225=CARTESIAN_POINT('Ctrl Pts',(-18.193785043525,66.2089018607175,7.38472422842254));
#38226=CARTESIAN_POINT('Ctrl Pts',(-18.9102906125109,66.0708634238267,7.76413764787118));
#38227=CARTESIAN_POINT('Ctrl Pts',(-19.6267961814968,65.932824986936,8.14355106731982));
#38228=CARTESIAN_POINT('Ctrl Pts',(-20.1472956316549,65.8473062312967,8.91224678187253));
#38229=CARTESIAN_POINT('Ctrl Pts',(-20.246238786796,65.8747431444715,9.7282262093075));
#38230=CARTESIAN_POINT('Ctrl Pts',(-20.345181941937,65.9021800576463,10.5442056367425));
#38231=CARTESIAN_POINT('Ctrl Pts',(-20.0225688020609,66.0425726396353,11.4074687770597));
#38232=CARTESIAN_POINT('Ctrl Pts',(-19.4279225161918,66.2558562834075,11.9340732703408));
#38233=CARTESIAN_POINT('Ctrl Pts',(-18.8332762303227,66.4691399271797,12.4606777636219));
#38234=CARTESIAN_POINT('Ctrl Pts',(-17.9665967984606,66.7553146327353,12.6506236098669));
#38235=CARTESIAN_POINT('Ctrl Pts',(-17.2194144305738,67.0094701965008,12.4192427536871));
#38236=CARTESIAN_POINT('Ctrl Pts',(-16.472232062687,67.2636257602663,12.1878618975073));
#38237=CARTESIAN_POINT('Ctrl Pts',(-15.8445467587755,67.4857621822417,11.5351543389028));
#38238=CARTESIAN_POINT('Ctrl Pts',(-15.6216179699845,67.5994444228593,10.7518245719412));
#38239=CARTESIAN_POINT('Ctrl Pts',(-15.5528913979792,67.6344914472383,10.5103323450965));
#38240=CARTESIAN_POINT('Ctrl Pts',(-15.5226338262371,67.6592307340631,10.2564254798707));
#38241=CARTESIAN_POINT('Ctrl Pts',(-15.5286491313886,67.6742507328171,10.0019962882658));
#38242=CARTESIAN_POINT('Ctrl Pts',(-16.8135320242449,59.6819508576139,7.0307770462544));
#38243=CARTESIAN_POINT('Ctrl Pts',(-16.9051481187289,59.6574023990832,7.06547285383772));
#38244=CARTESIAN_POINT('Ctrl Pts',(-16.9947948727615,59.6333816237361,7.105152193198));
#38245=CARTESIAN_POINT('Ctrl Pts',(-17.0822377867392,59.609951365552,7.14949694329713));
#38246=CARTESIAN_POINT('Ctrl Pts',(-17.170887130687,59.5861978454316,7.1944535078144));
#38247=CARTESIAN_POINT('Ctrl Pts',(-17.2572720505333,59.5630510759206,7.24420580543408));
#38248=CARTESIAN_POINT('Ctrl Pts',(-17.3411153578571,59.5405853294324,7.29846300342455));
#38249=CARTESIAN_POINT('Ctrl Pts',(-17.3650399830872,59.5341747454228,7.31394525441622));
#38250=CARTESIAN_POINT('Ctrl Pts',(-17.388757423411,59.5278196764415,7.32979452701951));
#38251=CARTESIAN_POINT('Ctrl Pts',(-17.412260642765,59.5215220077961,7.34600453504371));
#38252=CARTESIAN_POINT('Ctrl Pts',(-17.430731609272,59.5165727272371,7.35874383304306));
#38253=CARTESIAN_POINT('Ctrl Pts',(-17.4490721037271,59.5116584065591,7.37170741301654));
#38254=CARTESIAN_POINT('Ctrl Pts',(-17.4672605739288,59.5067848206569,7.38487881922079));
#38255=CARTESIAN_POINT('Ctrl Pts',(-17.5471418515796,59.48538069682,7.44272583683044));
#38256=CARTESIAN_POINT('Ctrl Pts',(-17.6241706059935,59.4647409042809,7.50463022528993));
#38257=CARTESIAN_POINT('Ctrl Pts',(-17.6980879987993,59.4449347985719,7.57029723831441));
#38258=CARTESIAN_POINT('Ctrl Pts',(-17.7541980616857,59.4299001525343,7.62014450822626));
#38259=CARTESIAN_POINT('Ctrl Pts',(-17.8085146623264,59.415346063257,7.67216077844244));
#38260=CARTESIAN_POINT('Ctrl Pts',(-17.8609084969032,59.4013071775938,7.72622830906753));
#38261=CARTESIAN_POINT('Ctrl Pts',(-17.8879292143121,59.3940669981851,7.75411219040241));
#38262=CARTESIAN_POINT('Ctrl Pts',(-17.9144382907055,59.3869639125734,7.78254178029124));
#38263=CARTESIAN_POINT('Ctrl Pts',(-17.9404163405827,59.3800031150879,7.81150163974704));
#38264=CARTESIAN_POINT('Ctrl Pts',(-17.9513656352239,59.3770692604311,7.82370771508563));
#38265=CARTESIAN_POINT('Ctrl Pts',(-17.9622216783274,59.3741603924485,7.83600935555966));
#38266=CARTESIAN_POINT('Ctrl Pts',(-17.9729722066906,59.3712797970554,7.8483927628579));
#38267=CARTESIAN_POINT('Ctrl Pts',(-18.0365635529481,59.3542405471801,7.92164288738644));
#38268=CARTESIAN_POINT('Ctrl Pts',(-18.0965497610756,59.3381672911553,7.99784282333236));
#38269=CARTESIAN_POINT('Ctrl Pts',(-18.152694204644,59.3231234328417,8.0767163112685));
#38270=CARTESIAN_POINT('Ctrl Pts',(-18.2078226719857,59.3083518045375,8.1541625237066));
#38271=CARTESIAN_POINT('Ctrl Pts',(-18.2592474980566,59.2945725639209,8.23418719309428));
#38272=CARTESIAN_POINT('Ctrl Pts',(-18.3067019322666,59.281857186597,8.3165506095198));
#38273=CARTESIAN_POINT('Ctrl Pts',(-18.3532560644872,59.2693830444642,8.3973514333468));
#38274=CARTESIAN_POINT('Ctrl Pts',(-18.3959893040302,59.2579327074387,8.48040377584086));
#38275=CARTESIAN_POINT('Ctrl Pts',(-18.4346037833018,59.2475859889017,8.56549184014349));
#38276=CARTESIAN_POINT('Ctrl Pts',(-18.4539341350127,59.2424064367714,8.60808680038629));
#38277=CARTESIAN_POINT('Ctrl Pts',(-18.4722315775318,59.2375036518248,8.65119201455741));
#38278=CARTESIAN_POINT('Ctrl Pts',(-18.4894539568131,59.2328889292046,8.69478065009698));
#38279=CARTESIAN_POINT('Ctrl Pts',(-18.4977385367033,59.2306690827134,8.71574834146746));
#38280=CARTESIAN_POINT('Ctrl Pts',(-18.5057743025267,59.2285159057505,8.73682789360235));
#38281=CARTESIAN_POINT('Ctrl Pts',(-18.5135562806577,59.2264307309948,8.7580163058807));
#38282=CARTESIAN_POINT('Ctrl Pts',(-18.5185237400942,59.2250997042503,8.77154147605531));
#38283=CARTESIAN_POINT('Ctrl Pts',(-18.5233877588506,59.2237963943526,8.78511114931605));
#38284=CARTESIAN_POINT('Ctrl Pts',(-18.5281423789944,59.2225223977247,8.79871063667249));
#38285=CARTESIAN_POINT('Ctrl Pts',(-18.5587083682407,59.2143322655903,8.88613755443148));
#38286=CARTESIAN_POINT('Ctrl Pts',(-18.5848098578326,59.2073383925329,8.97493705335627));
#38287=CARTESIAN_POINT('Ctrl Pts',(-18.6062022975293,59.2016063055921,9.06488740567881));
#38288=CARTESIAN_POINT('Ctrl Pts',(-18.6087806599848,59.2009154354543,9.07572883445317));
#38289=CARTESIAN_POINT('Ctrl Pts',(-18.6112905562917,59.2002429107658,9.08658699313155));
#38290=CARTESIAN_POINT('Ctrl Pts',(-18.6137315088206,59.1995888595069,9.09746150181129));
#38291=CARTESIAN_POINT('Ctrl Pts',(-18.634303712552,59.1940765541306,9.18911121862735));
#38292=CARTESIAN_POINT('Ctrl Pts',(-18.6499830153474,59.1898752976086,9.28192246234248));
#38293=CARTESIAN_POINT('Ctrl Pts',(-18.6608728938791,59.1869573634504,9.37550443039365));
#38294=CARTESIAN_POINT('Ctrl Pts',(-18.6721439846079,59.1839372837918,9.47236233835083));
#38295=CARTESIAN_POINT('Ctrl Pts',(-18.678284396889,59.1822919652799,9.57004704529739));
#38296=CARTESIAN_POINT('Ctrl Pts',(-18.6793547107856,59.1820051755357,9.66811274309982));
#38297=CARTESIAN_POINT('Ctrl Pts',(-18.6798764988089,59.1818653628562,9.71592068689136));
#38298=CARTESIAN_POINT('Ctrl Pts',(-18.6791925043481,59.1820486386196,9.76381888089709));
#38299=CARTESIAN_POINT('Ctrl Pts',(-18.6773054175267,59.1825542820094,9.81175333281661));
#38300=CARTESIAN_POINT('Ctrl Pts',(-18.6767477018626,59.1827037214712,9.82592003377692));
#38301=CARTESIAN_POINT('Ctrl Pts',(-18.676084807492,59.1828813434825,9.84008999147557));
#38302=CARTESIAN_POINT('Ctrl Pts',(-18.6753177565558,59.1830868741614,9.85424725714683));
#38303=CARTESIAN_POINT('Ctrl Pts',(-18.6702850236762,59.1844353908722,9.94713513860433));
#38304=CARTESIAN_POINT('Ctrl Pts',(-18.6607672605616,59.1869856678125,10.0396336498301));
#38305=CARTESIAN_POINT('Ctrl Pts',(-18.6468763517958,59.1907077255985,10.1313703614097));
#38306=CARTESIAN_POINT('Ctrl Pts',(-18.6330252856618,59.1944191075834,10.2228439489501));
#38307=CARTESIAN_POINT('Ctrl Pts',(-18.6148257393987,59.1992956613072,10.3135610438633));
#38308=CARTESIAN_POINT('Ctrl Pts',(-18.5923417340723,59.205320232377,10.4031353913064));
#38309=CARTESIAN_POINT('Ctrl Pts',(-18.5702449115824,59.2112410581185,10.4911672355606));
#38310=CARTESIAN_POINT('Ctrl Pts',(-18.5440094800128,59.2182708208206,10.5780961325691));
#38311=CARTESIAN_POINT('Ctrl Pts',(-18.513657092413,59.2264037185664,10.6635263259507));
#38312=CARTESIAN_POINT('Ctrl Pts',(-18.4991012558957,59.2303039432063,10.7044953576096));
#38313=CARTESIAN_POINT('Ctrl Pts',(-18.4835980627564,59.2344580112881,10.745119212542));
#38314=CARTESIAN_POINT('Ctrl Pts',(-18.4671470631154,59.2388660433566,10.7853510165448));
#38315=CARTESIAN_POINT('Ctrl Pts',(-18.4616118759027,59.2403491923002,10.7988876144369));
#38316=CARTESIAN_POINT('Ctrl Pts',(-18.4559693741439,59.2418610960897,10.8123798089597));
#38317=CARTESIAN_POINT('Ctrl Pts',(-18.4502194972567,59.2434017709582,10.8258257523306));
#38318=CARTESIAN_POINT('Ctrl Pts',(-18.4447502513313,59.2448672509872,10.8386154472123));
#38319=CARTESIAN_POINT('Ctrl Pts',(-18.4391855696915,59.2463583029387,10.8513591677317));
#38320=CARTESIAN_POINT('Ctrl Pts',(-18.4335294175102,59.2478738643479,10.8640470913851));
#38321=CARTESIAN_POINT('Ctrl Pts',(-18.3974943892406,59.257529421072,10.9448811412621));
#38322=CARTESIAN_POINT('Ctrl Pts',(-18.3577058350372,59.2681907320388,11.0235565035205));
#38323=CARTESIAN_POINT('Ctrl Pts',(-18.3142251103301,59.2798413571104,11.0997253732309));
#38324=CARTESIAN_POINT('Ctrl Pts',(-18.2714642927579,59.2912990836466,11.1746331206135));
#38325=CARTESIAN_POINT('Ctrl Pts',(-18.2251321272591,59.3037137499756,11.2471173606586));
#38326=CARTESIAN_POINT('Ctrl Pts',(-18.1752516289978,59.3170791892027,11.3168132015496));
#38327=CARTESIAN_POINT('Ctrl Pts',(-18.126814322891,59.3300579262576,11.3844925330976));
#38328=CARTESIAN_POINT('Ctrl Pts',(-18.0750306258258,59.3439333260673,11.449542941438));
#38329=CARTESIAN_POINT('Ctrl Pts',(-18.0198942246886,59.3587070802256,11.5115898438694));
#38330=CARTESIAN_POINT('Ctrl Pts',(-18.0099245352413,59.3613784504618,11.5228090808101));
#38331=CARTESIAN_POINT('Ctrl Pts',(-17.9998451629737,59.3640792101211,11.5339299972364));
#38332=CARTESIAN_POINT('Ctrl Pts',(-17.9896559870011,59.3668093915945,11.5449502145347));
#38333=CARTESIAN_POINT('Ctrl Pts',(-17.9601614990778,59.3747124158147,11.5768503080151));
#38334=CARTESIAN_POINT('Ctrl Pts',(-17.9297469672235,59.3828619650632,11.6079068412473));
#38335=CARTESIAN_POINT('Ctrl Pts',(-17.8984546702662,59.3912467107622,11.6380966037225));
#38336=CARTESIAN_POINT('Ctrl Pts',(-15.0750265266586,68.1281291851066,10.0024371765581));
#38337=CARTESIAN_POINT('Ctrl Pts',(-15.0686010168709,68.1132191003536,10.3130580784043));
#38338=CARTESIAN_POINT('Ctrl Pts',(-15.229260839257,67.9995899840861,11.6285356953996));
#38339=CARTESIAN_POINT('Ctrl Pts',(-17.0050066526372,67.3992512291335,13.4679206448302));
#38340=CARTESIAN_POINT('Ctrl Pts',(-20.1882099452846,66.3844685224502,12.7722321938662));
#38341=CARTESIAN_POINT('Ctrl Pts',(-21.3787366757643,65.9036218913761,9.61047736356026));
#38342=CARTESIAN_POINT('Ctrl Pts',(-19.4813112170046,66.2501895556747,6.79508159949542));
#38343=CARTESIAN_POINT('Ctrl Pts',(-16.1481166073795,66.9814704044652,6.8312269691005));
#38344=CARTESIAN_POINT('Ctrl Pts',(-14.8676525643411,67.2119040522751,8.81893895087672));
#38345=CARTESIAN_POINT('Ctrl Pts',(-14.8112407741816,67.168302539124,9.90991228406402));
#38346=CARTESIAN_POINT('Ctrl Pts',(-14.810555933805,67.1637176864734,9.9985514014054));
#38347=CARTESIAN_POINT('Origin',(-18.6889152049569,69.7479810832458,10.));
#38348=CARTESIAN_POINT('Ctrl Pts',(-15.0969161422106,68.2083503098983,9.99673640007589));
#38349=CARTESIAN_POINT('Ctrl Pts',(-15.0927295232038,68.1711103559359,10.7130675866998));
#38350=CARTESIAN_POINT('Ctrl Pts',(-15.6514186592592,67.9289066052255,12.4513417391712));
#38351=CARTESIAN_POINT('Ctrl Pts',(-18.3902480628706,67.0483943376967,13.59444534976));
#38352=CARTESIAN_POINT('Ctrl Pts',(-21.0667649555468,66.1687987195558,11.6442225433404));
#38353=CARTESIAN_POINT('Ctrl Pts',(-20.9561469803463,66.0360136384589,8.2201649478064));
#38354=CARTESIAN_POINT('Ctrl Pts',(-18.1194957904389,66.6336669557831,6.39071567224372));
#38355=CARTESIAN_POINT('Ctrl Pts',(-15.4027596845035,67.2173089746448,7.63681194520529));
#38356=CARTESIAN_POINT('Ctrl Pts',(-14.8518622987657,67.2747579502335,9.32892113065739));
#38357=CARTESIAN_POINT('Ctrl Pts',(-14.8383776097513,67.242349320473,10.0022118830713));
#38358=CARTESIAN_POINT('Ctrl Pts',(-17.2449834421536,67.8425423025984,7.06170475438588));
#38359=CARTESIAN_POINT('Ctrl Pts',(-16.2988495743029,68.0419164156806,7.35795147289551));
#38360=CARTESIAN_POINT('Ctrl Pts',(-14.7258515725222,68.3551165744734,8.97144797270149));
#38361=CARTESIAN_POINT('Ctrl Pts',(-15.356703424302,68.0236552520252,12.3283366156207));
#38362=CARTESIAN_POINT('Ctrl Pts',(-18.3902480628706,67.0483943376967,13.59444534976));
#38363=CARTESIAN_POINT('Ctrl Pts',(-21.0667649555468,66.1687987195558,11.6442225433404));
#38364=CARTESIAN_POINT('Ctrl Pts',(-20.9561469803463,66.0360136384589,8.2201649478064));
#38365=CARTESIAN_POINT('Ctrl Pts',(-18.1194957904389,66.6336669557831,6.39071567224372));
#38366=CARTESIAN_POINT('Ctrl Pts',(-15.0616295968137,67.2905946547072,7.79327945411664));
#38367=CARTESIAN_POINT('Ctrl Pts',(-14.4843023646229,67.2828639421211,11.1722569386409));
#38368=CARTESIAN_POINT('Ctrl Pts',(-16.8683721674333,66.4816292855384,13.5013274912987));
#38369=CARTESIAN_POINT('Ctrl Pts',(-20.0422978199454,65.4687533918912,12.6947822329677));
#38370=CARTESIAN_POINT('Ctrl Pts',(-21.1273143736847,65.0155990043222,9.47487431060756));
#38371=CARTESIAN_POINT('Ctrl Pts',(-19.1153342996386,65.3922823621301,6.72525821930975));
#38372=CARTESIAN_POINT('Ctrl Pts',(-15.7718556315871,66.125739692925,6.90837057311325));
#38373=CARTESIAN_POINT('Ctrl Pts',(-14.0547985877671,66.4233986629546,9.86022990097426));
#38374=CARTESIAN_POINT('Ctrl Pts',(-15.4655309000311,65.8829690009267,12.9372608391338));
#38375=CARTESIAN_POINT('Ctrl Pts',(-18.7042880702644,64.8527215544621,13.3837942299381));
#38376=CARTESIAN_POINT('Ctrl Pts',(-20.8341986998844,64.1195886430847,10.7999310727637));
#38377=CARTESIAN_POINT('Ctrl Pts',(-19.9114308093218,64.2044184759421,7.49968047567802));
#38378=CARTESIAN_POINT('Ctrl Pts',(-16.7260146593058,64.8955230826759,6.4386200392349));
#38379=CARTESIAN_POINT('Ctrl Pts',(-14.0943212306271,65.4382581333963,8.56699487612795));
#38380=CARTESIAN_POINT('Ctrl Pts',(-14.3368288007652,65.2108533475993,11.9787141005057));
#38381=CARTESIAN_POINT('Ctrl Pts',(-17.1999914587374,64.2812461473765,13.6183729089162));
#38382=CARTESIAN_POINT('Ctrl Pts',(-20.0833051820053,63.3462394854811,12.0175557753475));
#38383=CARTESIAN_POINT('Ctrl Pts',(-20.368219412885,63.1074718691845,8.60989310618186));
#38384=CARTESIAN_POINT('Ctrl Pts',(-17.7632104839254,63.6430568297549,6.44715683087691));
#38385=CARTESIAN_POINT('Ctrl Pts',(-14.5648590180574,64.337627443925,7.46621057361457));
#38386=CARTESIAN_POINT('Ctrl Pts',(-13.6011204490198,64.4334353369931,10.7544289031923));
#38387=CARTESIAN_POINT('Ctrl Pts',(-15.6987166428553,63.7089610525881,13.3670096553834));
#38388=CARTESIAN_POINT('Ctrl Pts',(-18.9427555175128,62.6772983776883,12.9642257537712));
#38389=CARTESIAN_POINT('Ctrl Pts',(-20.3916349158421,62.1266472347557,9.90679500749766));
#38390=CARTESIAN_POINT('Ctrl Pts',(-18.7114286257309,62.4144320750885,6.93283507366423));
#38391=CARTESIAN_POINT('Ctrl Pts',(-15.3704995140603,63.14720625431,6.70571036393722));
#38392=CARTESIAN_POINT('Ctrl Pts',(-13.3244900809145,63.5330077514078,9.42882503807092));
#38393=CARTESIAN_POINT('Ctrl Pts',(-14.3693624549392,63.090609964374,12.6634621126404));
#38394=CARTESIAN_POINT('Ctrl Pts',(-17.5330036055452,62.0804897947072,13.5128046754736));
#38395=CARTESIAN_POINT('Ctrl Pts',(-19.945812508159,61.2715545195409,11.2162142452881));
#38396=CARTESIAN_POINT('Ctrl Pts',(-19.4106046411916,61.2525379570574,7.83042882970079));
#38397=CARTESIAN_POINT('Ctrl Pts',(-16.3703262829259,61.9047530097004,6.38762845988016));
#38398=CARTESIAN_POINT('Ctrl Pts',(-13.5113685232519,62.5083833543795,8.17992871548433));
#38399=CARTESIAN_POINT('Ctrl Pts',(-13.3577390856958,62.3871231598862,11.6022164308582));
#38400=CARTESIAN_POINT('Ctrl Pts',(-16.0106566332711,61.5138509672068,13.5896176377582));
#38401=CARTESIAN_POINT('Ctrl Pts',(-19.0579057022672,60.5349179618126,12.3623010109727));
#38402=CARTESIAN_POINT('Ctrl Pts',(-19.7341192728292,60.1913020034494,9.0193860958895));
#38403=CARTESIAN_POINT('Ctrl Pts',(-17.3973455890627,60.6550135466887,6.55469600728496));
#38404=CARTESIAN_POINT('Ctrl Pts',(-14.1039347737165,61.3750552367845,7.17543798647131));
#38405=CARTESIAN_POINT('Ctrl Pts',(-12.7669926495711,61.5708627210561,10.3258507409619));
#38406=CARTESIAN_POINT('Ctrl Pts',(-14.5474295567697,60.9313710113776,13.1842383274674));
#38407=CARTESIAN_POINT('Ctrl Pts',(-17.8144668208749,59.893545936598,13.1913616605741));
#38408=CARTESIAN_POINT('Ctrl Pts',(-19.6057481548832,59.2511484715134,10.339577077016));
#38409=CARTESIAN_POINT('Ctrl Pts',(-18.2810249486942,59.4436819065862,7.1853989865657));
#38410=CARTESIAN_POINT('Ctrl Pts',(-14.9896601306958,60.163175373345,6.54837069990765));
#38411=CARTESIAN_POINT('Ctrl Pts',(-12.6441934312552,60.6292162031139,9.00969837718612));
#38412=CARTESIAN_POINT('Ctrl Pts',(-13.0868379849883,60.402326566927,11.2296927240261));
#38413=CARTESIAN_POINT('Ctrl Pts',(-13.7072348830368,60.1819500263681,11.9973015569302));
#38414=CARTESIAN_POINT('Ctrl Pts',(-17.3251900988202,67.9318278742782,7.23888518457529));
#38415=CARTESIAN_POINT('Ctrl Pts',(-16.4352923065874,68.1161335763131,7.5172681022616));
#38416=CARTESIAN_POINT('Ctrl Pts',(-14.9555143577764,68.4043554971942,9.03347008941727));
#38417=CARTESIAN_POINT('Ctrl Pts',(-15.5458770044739,68.0837432245501,12.1879369455068));
#38418=CARTESIAN_POINT('Ctrl Pts',(-18.3940490596775,67.158152744233,13.3776987943165));
#38419=CARTESIAN_POINT('Ctrl Pts',(-20.9067222911422,66.3224589027987,11.5450752374354));
#38420=CARTESIAN_POINT('Ctrl Pts',(-20.8003260510253,66.1885426111955,8.32748974461997));
#38421=CARTESIAN_POINT('Ctrl Pts',(-18.1322775372978,66.7410189775957,6.60835702425636));
#38422=CARTESIAN_POINT('Ctrl Pts',(-15.2563533769444,67.3491954556353,7.92634562444483));
#38423=CARTESIAN_POINT('Ctrl Pts',(-14.7113906429073,67.3327927019054,11.1015693557675));
#38424=CARTESIAN_POINT('Ctrl Pts',(-16.9492514661357,66.5707346233279,13.2901959816016));
#38425=CARTESIAN_POINT('Ctrl Pts',(-19.9293395015263,65.6097973626512,12.5322857391193));
#38426=CARTESIAN_POINT('Ctrl Pts',(-20.9464805290196,65.1748301675256,9.50653960894302));
#38427=CARTESIAN_POINT('Ctrl Pts',(-19.0533751185271,65.5196611552339,6.92272651604678));
#38428=CARTESIAN_POINT('Ctrl Pts',(-15.9090610352123,66.1997524963876,7.09479711845775));
#38429=CARTESIAN_POINT('Ctrl Pts',(-14.2930946730788,66.4703242998971,9.86865809630622));
#38430=CARTESIAN_POINT('Ctrl Pts',(-15.6163106628559,65.9533445658041,12.7601427840871));
#38431=CARTESIAN_POINT('Ctrl Pts',(-18.6573208483787,64.9760832641984,13.1797500249769));
#38432=CARTESIAN_POINT('Ctrl Pts',(-20.6563484026838,64.2780203671544,10.7516948950666));
#38433=CARTESIAN_POINT('Ctrl Pts',(-19.7867752262126,64.3485967193295,7.65045078699769));
#38434=CARTESIAN_POINT('Ctrl Pts',(-16.7909924250971,64.9888892233673,6.65337273791561));
#38435=CARTESIAN_POINT('Ctrl Pts',(-14.3155426340163,65.4897589175709,8.65340568344564));
#38436=CARTESIAN_POINT('Ctrl Pts',(-14.5409783214074,65.2669285289692,11.8593968140374));
#38437=CARTESIAN_POINT('Ctrl Pts',(-17.2290425005872,64.3842388247347,13.4001835116647));
#38438=CARTESIAN_POINT('Ctrl Pts',(-19.9360426274114,63.4964752486211,11.895896319668));
#38439=CARTESIAN_POINT('Ctrl Pts',(-20.2013278361945,63.2629672129435,8.69371713231524));
#38440=CARTESIAN_POINT('Ctrl Pts',(-17.7509534583579,63.7571179704186,6.66139475745709));
#38441=CARTESIAN_POINT('Ctrl Pts',(-14.7430153463372,64.4006674801971,7.61899913400395));
#38442=CARTESIAN_POINT('Ctrl Pts',(-13.8349420404104,64.4815599109683,10.7089365253196));
#38443=CARTESIAN_POINT('Ctrl Pts',(-15.8036037329016,63.791633522075,13.1639775672761));
#38444=CARTESIAN_POINT('Ctrl Pts',(-18.8495771338665,62.8130423308996,12.7854817031127));
#38445=CARTESIAN_POINT('Ctrl Pts',(-20.2086399244908,62.2864574754684,9.9124153074631));
#38446=CARTESIAN_POINT('Ctrl Pts',(-18.6273022002306,62.5477505634246,7.11778639941041));
#38447=CARTESIAN_POINT('Ctrl Pts',(-15.4853839339823,63.2271999473302,6.90435740451538));
#38448=CARTESIAN_POINT('Ctrl Pts',(-13.5603011489528,63.5805992467218,9.46326712676812));
#38449=CARTESIAN_POINT('Ctrl Pts',(-14.5397187075304,63.1557400246278,12.5028542351253));
#38450=CARTESIAN_POINT('Ctrl Pts',(-17.510142400774,62.1973923166248,13.3009810867785));
#38451=CARTESIAN_POINT('Ctrl Pts',(-19.7750093440878,61.4280979699797,11.1428760184696));
#38452=CARTESIAN_POINT('Ctrl Pts',(-19.2696261599642,61.4010899078137,7.96125487716962));
#38453=CARTESIAN_POINT('Ctrl Pts',(-16.4102292811544,62.0048379141107,6.60545597208737));
#38454=CARTESIAN_POINT('Ctrl Pts',(-13.7212192931312,62.5629308906205,8.28967977390748));
#38455=CARTESIAN_POINT('Ctrl Pts',(-13.5744051997982,62.4398445301464,11.5056021110754));
#38456=CARTESIAN_POINT('Ctrl Pts',(-16.0649021365254,61.610092808978,13.3731621953642));
#38457=CARTESIAN_POINT('Ctrl Pts',(-18.9259522392795,60.6810516662199,12.2198532736373));
#38458=CARTESIAN_POINT('Ctrl Pts',(-19.5589412741758,60.3490176872815,9.0785175237606));
#38459=CARTESIAN_POINT('Ctrl Pts',(-17.3606274442461,60.7756290245011,6.76244927662497));
#38460=CARTESIAN_POINT('Ctrl Pts',(-14.2633621012127,61.4431136936916,7.34576025527691));
#38461=CARTESIAN_POINT('Ctrl Pts',(-13.0045895703813,61.6179756985622,10.3062018052236));
#38462=CARTESIAN_POINT('Ctrl Pts',(-14.675216813649,61.007907399655,12.9922274267493));
#38463=CARTESIAN_POINT('Ctrl Pts',(-17.7428017915751,60.0235254038857,12.9989212198953));
#38464=CARTESIAN_POINT('Ctrl Pts',(-19.4236195381877,59.4107265678367,10.3191004374823));
#38465=CARTESIAN_POINT('Ctrl Pts',(-18.176329119458,59.5825119500423,7.3551206029064));
#38466=CARTESIAN_POINT('Ctrl Pts',(-15.080986399278,60.2494814539918,6.75650538792364));
#38467=CARTESIAN_POINT('Ctrl Pts',(-12.874503746149,60.6782816207908,9.06941397854012));
#38468=CARTESIAN_POINT('Ctrl Pts',(-13.2888242651273,60.4589813868428,11.1555417393118));
#38469=CARTESIAN_POINT('Ctrl Pts',(-13.8709947795083,60.2488475749172,11.8768634390783));
#38470=CARTESIAN_POINT('Ctrl Pts',(-17.4053967554868,68.021113445958,7.4160656147647));
#38471=CARTESIAN_POINT('Ctrl Pts',(-16.5717350388718,68.1903507369456,7.6765847316277));
#38472=CARTESIAN_POINT('Ctrl Pts',(-15.1851771430307,68.4535944199151,9.09549220613307));
#38473=CARTESIAN_POINT('Ctrl Pts',(-15.7350505846458,68.1438311970748,12.0475372753929));
#38474=CARTESIAN_POINT('Ctrl Pts',(-18.3978500564844,67.2679111507695,13.1609522388731));
#38475=CARTESIAN_POINT('Ctrl Pts',(-20.7466796267376,66.4761190860416,11.4459279315303));
#38476=CARTESIAN_POINT('Ctrl Pts',(-20.6445051217044,66.3410715839321,8.43481454143356));
#38477=CARTESIAN_POINT('Ctrl Pts',(-18.1450592841567,66.8483709994082,6.82599837626898));
#38478=CARTESIAN_POINT('Ctrl Pts',(-15.4510771570751,67.4077962565634,8.05941179477303));
#38479=CARTESIAN_POINT('Ctrl Pts',(-14.9384789211916,67.3827214616898,11.0308817728941));
#38480=CARTESIAN_POINT('Ctrl Pts',(-17.0301307648381,66.6598399611174,13.0790644719045));
#38481=CARTESIAN_POINT('Ctrl Pts',(-19.8163811831071,65.7508413334112,12.3697892452708));
#38482=CARTESIAN_POINT('Ctrl Pts',(-20.7656466843543,65.3340613307291,9.53820490727848));
#38483=CARTESIAN_POINT('Ctrl Pts',(-18.9914159374157,65.6470399483376,7.12019481278381));
#38484=CARTESIAN_POINT('Ctrl Pts',(-16.0462664388374,66.2737652998504,7.28122366380225));
#38485=CARTESIAN_POINT('Ctrl Pts',(-14.5313907583906,66.5172499368395,9.87708629163818));
#38486=CARTESIAN_POINT('Ctrl Pts',(-15.7670904256806,66.0237201306815,12.5830247290403));
#38487=CARTESIAN_POINT('Ctrl Pts',(-18.610353626493,65.0994449739345,12.9757058200156));
#38488=CARTESIAN_POINT('Ctrl Pts',(-20.4784981054832,64.4364520912243,10.7034587173694));
#38489=CARTESIAN_POINT('Ctrl Pts',(-19.6621196431034,64.4927749627168,7.80122109831736));
#38490=CARTESIAN_POINT('Ctrl Pts',(-16.8559701908884,65.0822553640587,6.86812543659629));
#38491=CARTESIAN_POINT('Ctrl Pts',(-14.5367640374057,65.5412597017455,8.73981649076335));
#38492=CARTESIAN_POINT('Ctrl Pts',(-14.7451278420497,65.3230037103391,11.7400795275691));
#38493=CARTESIAN_POINT('Ctrl Pts',(-17.2580935424371,64.487231502093,13.1819941144132));
#38494=CARTESIAN_POINT('Ctrl Pts',(-19.7887800728175,63.6467110117611,11.7742368639884));
#38495=CARTESIAN_POINT('Ctrl Pts',(-20.034436259504,63.4184625567025,8.77754115844864));
#38496=CARTESIAN_POINT('Ctrl Pts',(-17.7386964327903,63.8711791110823,6.87563268403724));
#38497=CARTESIAN_POINT('Ctrl Pts',(-14.921171674617,64.4637075164693,7.77178769439333));
#38498=CARTESIAN_POINT('Ctrl Pts',(-14.0687636318009,64.5296844849434,10.663444147447));
#38499=CARTESIAN_POINT('Ctrl Pts',(-15.9084908229478,63.8743059915619,12.9609454791688));
#38500=CARTESIAN_POINT('Ctrl Pts',(-18.7563987502202,62.9487862841109,12.6067376524542));
#38501=CARTESIAN_POINT('Ctrl Pts',(-20.0256449331395,62.4462677161811,9.91803560742851));
#38502=CARTESIAN_POINT('Ctrl Pts',(-18.5431757747304,62.6810690517608,7.3027377251566));
#38503=CARTESIAN_POINT('Ctrl Pts',(-15.6002683539043,63.3071936403504,7.10300444509352));
#38504=CARTESIAN_POINT('Ctrl Pts',(-13.7961122169912,63.6281907420357,9.49770921546533));
#38505=CARTESIAN_POINT('Ctrl Pts',(-14.7100749601216,63.2208700848817,12.3422463576102));
#38506=CARTESIAN_POINT('Ctrl Pts',(-17.4872811960028,62.3142948385424,13.0891574980834));
#38507=CARTESIAN_POINT('Ctrl Pts',(-19.6042061800167,61.5846414204185,11.0695377916511));
#38508=CARTESIAN_POINT('Ctrl Pts',(-19.1286476787368,61.54964185857,8.09208092463846));
#38509=CARTESIAN_POINT('Ctrl Pts',(-16.4501322793829,62.104922818521,6.82328348429458));
#38510=CARTESIAN_POINT('Ctrl Pts',(-13.9310700630105,62.6174784268615,8.39943083233065));
#38511=CARTESIAN_POINT('Ctrl Pts',(-13.7910713139005,62.4925659004067,11.4089877912926));
#38512=CARTESIAN_POINT('Ctrl Pts',(-16.1191476397797,61.7063346507492,13.1567067529703));
#38513=CARTESIAN_POINT('Ctrl Pts',(-18.7939987762918,60.8271853706271,12.0774055363019));
#38514=CARTESIAN_POINT('Ctrl Pts',(-19.3837632755225,60.5067333711136,9.13764895163169));
#38515=CARTESIAN_POINT('Ctrl Pts',(-17.3239092994295,60.8962445023135,6.97020254596497));
#38516=CARTESIAN_POINT('Ctrl Pts',(-14.4227894287088,61.5111721505988,7.5160825240825));
#38517=CARTESIAN_POINT('Ctrl Pts',(-13.2421864911915,61.6650886760681,10.2865528694853));
#38518=CARTESIAN_POINT('Ctrl Pts',(-14.8030040705283,61.0844437879325,12.8002165260311));
#38519=CARTESIAN_POINT('Ctrl Pts',(-17.6711367622752,60.1535048711733,12.8064807792164));
#38520=CARTESIAN_POINT('Ctrl Pts',(-19.2414909214921,59.5703046641601,10.2986237979485));
#38521=CARTESIAN_POINT('Ctrl Pts',(-18.0716332902218,59.7213419934982,7.5248422192471));
#38522=CARTESIAN_POINT('Ctrl Pts',(-15.1723126678601,60.3357875346387,6.96464007593962));
#38523=CARTESIAN_POINT('Ctrl Pts',(-13.1048140610428,60.7273470384677,9.12912957989411));
#38524=CARTESIAN_POINT('Ctrl Pts',(-13.4908105452662,60.5156362067586,11.0813907545975));
#38525=CARTESIAN_POINT('Ctrl Pts',(-14.0347546759797,60.3157451234663,11.7564253212264));
#38526=CARTESIAN_POINT('Ctrl Pts',(-17.4856034121534,68.1103990176377,7.59324604495411));
#38527=CARTESIAN_POINT('Ctrl Pts',(-16.7081777711562,68.2645678975781,7.83590136099379));
#38528=CARTESIAN_POINT('Ctrl Pts',(-15.414839928285,68.5028333426359,9.15751432284886));
#38529=CARTESIAN_POINT('Ctrl Pts',(-15.9242241648176,68.2039191695997,11.907137605279));
#38530=CARTESIAN_POINT('Ctrl Pts',(-18.4016510532913,67.3776695573058,12.9442056834296));
#38531=CARTESIAN_POINT('Ctrl Pts',(-20.586636962333,66.6297792692846,11.3467806256253));
#38532=CARTESIAN_POINT('Ctrl Pts',(-20.4886841923835,66.4936005566688,8.54213933824715));
#38533=CARTESIAN_POINT('Ctrl Pts',(-18.1578410310155,66.9557230212207,7.04363972828162));
#38534=CARTESIAN_POINT('Ctrl Pts',(-15.6458009372058,67.4663970574914,8.19247796510122));
#38535=CARTESIAN_POINT('Ctrl Pts',(-15.1655671994759,67.4326502214742,10.9601941900207));
#38536=CARTESIAN_POINT('Ctrl Pts',(-17.1110100635405,66.7489452989069,12.8679329622074));
#38537=CARTESIAN_POINT('Ctrl Pts',(-19.703422864688,65.8918853041712,12.2072927514223));
#38538=CARTESIAN_POINT('Ctrl Pts',(-20.5848128396891,65.4932924939326,9.56987020561395));
#38539=CARTESIAN_POINT('Ctrl Pts',(-18.9294567563042,65.7744187414414,7.31766310952083));
#38540=CARTESIAN_POINT('Ctrl Pts',(-16.1834718424625,66.3477781033129,7.46765020914676));
#38541=CARTESIAN_POINT('Ctrl Pts',(-14.7696868437023,66.564175573782,9.88551448697013));
#38542=CARTESIAN_POINT('Ctrl Pts',(-15.9178701885053,66.0940956955587,12.4059066739936));
#38543=CARTESIAN_POINT('Ctrl Pts',(-18.5633864046074,65.2228066836708,12.7716616150543));
#38544=CARTESIAN_POINT('Ctrl Pts',(-20.3006478082826,64.5948838152939,10.6552225396723));
#38545=CARTESIAN_POINT('Ctrl Pts',(-19.5374640599943,64.6369532061042,7.95199140963702));
#38546=CARTESIAN_POINT('Ctrl Pts',(-16.9209479566796,65.1756215047502,7.082878135277));
#38547=CARTESIAN_POINT('Ctrl Pts',(-14.757985440795,65.5927604859201,8.82622729808104));
#38548=CARTESIAN_POINT('Ctrl Pts',(-14.9492773626919,65.3790788917091,11.6207622411008));
#38549=CARTESIAN_POINT('Ctrl Pts',(-17.2871445842869,64.5902241794512,12.9638047171617));
#38550=CARTESIAN_POINT('Ctrl Pts',(-19.6415175182236,63.796946774901,11.6525774083089));
#38551=CARTESIAN_POINT('Ctrl Pts',(-19.8675446828135,63.5739579004615,8.86136518458202));
#38552=CARTESIAN_POINT('Ctrl Pts',(-17.7264394072227,63.9852402517459,7.08987061061742));
#38553=CARTESIAN_POINT('Ctrl Pts',(-15.0993280028969,64.5267475527414,7.92457625478271));
#38554=CARTESIAN_POINT('Ctrl Pts',(-14.3025852231914,64.5778090589186,10.6179517695743));
#38555=CARTESIAN_POINT('Ctrl Pts',(-16.013377912994,63.9569784610488,12.7579133910615));
#38556=CARTESIAN_POINT('Ctrl Pts',(-18.6632203665739,63.0845302373222,12.4279936017957));
#38557=CARTESIAN_POINT('Ctrl Pts',(-19.8426499417882,62.6060779568938,9.92365590739396));
#38558=CARTESIAN_POINT('Ctrl Pts',(-18.4590493492301,62.8143875400969,7.48768905090278));
#38559=CARTESIAN_POINT('Ctrl Pts',(-15.7151527738263,63.3871873333706,7.30165148567168));
#38560=CARTESIAN_POINT('Ctrl Pts',(-14.0319232850295,63.6757822373498,9.53215130416253));
#38561=CARTESIAN_POINT('Ctrl Pts',(-14.8804312127128,63.2860001451355,12.1816384800951));
#38562=CARTESIAN_POINT('Ctrl Pts',(-17.4644199912317,62.4311973604601,12.8773339093883));
#38563=CARTESIAN_POINT('Ctrl Pts',(-19.4334030159455,61.7411848708572,10.9961995648325));
#38564=CARTESIAN_POINT('Ctrl Pts',(-18.9876691975094,61.6981938093263,8.22290697210729));
#38565=CARTESIAN_POINT('Ctrl Pts',(-16.4900352776115,62.2050077229312,7.04111099650179));
#38566=CARTESIAN_POINT('Ctrl Pts',(-14.1409208328898,62.6720259631026,8.50918189075381));
#38567=CARTESIAN_POINT('Ctrl Pts',(-14.0077374280029,62.545287270667,11.3123734715098));
#38568=CARTESIAN_POINT('Ctrl Pts',(-16.173393143034,61.8025764925204,12.9402513105763));
#38569=CARTESIAN_POINT('Ctrl Pts',(-18.6620453133041,60.9733190750344,11.9349577989665));
#38570=CARTESIAN_POINT('Ctrl Pts',(-19.2085852768691,60.6644490549456,9.19678037950279));
#38571=CARTESIAN_POINT('Ctrl Pts',(-17.2871911546129,61.0168599801259,7.17795581530498));
#38572=CARTESIAN_POINT('Ctrl Pts',(-14.582216756205,61.5792306075059,7.68640479288809));
#38573=CARTESIAN_POINT('Ctrl Pts',(-13.4797834120017,61.7122016535742,10.2669039337471));
#38574=CARTESIAN_POINT('Ctrl Pts',(-14.9307913274076,61.1609801762098,12.6082056253129));
#38575=CARTESIAN_POINT('Ctrl Pts',(-17.5994717329753,60.2834843384611,12.6140403385376));
#38576=CARTESIAN_POINT('Ctrl Pts',(-19.0593623047967,59.7298827604834,10.2781471584148));
#38577=CARTESIAN_POINT('Ctrl Pts',(-17.9669374609856,59.8601720369542,7.6945638355878));
#38578=CARTESIAN_POINT('Ctrl Pts',(-15.2636389364423,60.4220936152855,7.17277476395559));
#38579=CARTESIAN_POINT('Ctrl Pts',(-13.3351243759366,60.7764124561446,9.18884518124811));
#38580=CARTESIAN_POINT('Ctrl Pts',(-13.6927968254052,60.5722910266745,11.0072397698831));
#38581=CARTESIAN_POINT('Ctrl Pts',(-14.1985145724512,60.3826426720153,11.6359872033746));
#38582=CARTESIAN_POINT('Ctrl Pts',(-17.2449834421534,67.8425423025984,7.06170475438596));
#38583=CARTESIAN_POINT('Ctrl Pts',(-16.8759806260743,67.9363396049608,7.20780006417468));
#38584=CARTESIAN_POINT('Ctrl Pts',(-16.535804082389,68.0195197262116,7.42431456479993));
#38585=CARTESIAN_POINT('Ctrl Pts',(-15.9848167458479,68.150998080649,7.95780764621744));
#38586=CARTESIAN_POINT('Ctrl Pts',(-15.7699411081763,68.2006822338607,8.25968161903134));
#38587=CARTESIAN_POINT('Ctrl Pts',(-15.4905619320041,68.2646302810789,8.88066242679718));
#38588=CARTESIAN_POINT('Ctrl Pts',(-15.4103584669881,68.2826595052327,9.18497820157355));
#38589=CARTESIAN_POINT('Ctrl Pts',(-15.3584337419011,68.2943569622715,9.79677072277262));
#38590=CARTESIAN_POINT('Ctrl Pts',(-15.3830449856443,68.288855628865,10.0982078060301));
#38591=CARTESIAN_POINT('Ctrl Pts',(-15.5341550196632,68.2546420063796,10.6858944634116));
#38592=CARTESIAN_POINT('Ctrl Pts',(-15.6614146465389,68.2257386849337,10.9661810334232));
#38593=CARTESIAN_POINT('Ctrl Pts',(-16.0093499903202,68.1449424659489,11.4722931322534));
#38594=CARTESIAN_POINT('Ctrl Pts',(-16.2286900565756,68.0932952109551,11.6926718707975));
#38595=CARTESIAN_POINT('Ctrl Pts',(-16.4806955947431,68.0322473001842,11.8669181223569));
#38596=CARTESIAN_POINT('Ctrl Pts',(-14.1985145724512,60.3826426720153,11.6359872033746));
#38597=CARTESIAN_POINT('Ctrl Pts',(-14.1384791309752,60.3987291200761,11.5775783984672));
#38598=CARTESIAN_POINT('Ctrl Pts',(-14.0817003626801,60.413942945188,11.5159169743203));
#38599=CARTESIAN_POINT('Ctrl Pts',(-14.0281914535639,60.4282806141735,11.4513790591575));
#38600=CARTESIAN_POINT('Ctrl Pts',(-13.973376466664,60.4429682456465,11.3852658635676));
#38601=CARTESIAN_POINT('Ctrl Pts',(-13.9219924575667,60.456736549388,11.3161335496572));
#38602=CARTESIAN_POINT('Ctrl Pts',(-13.8740814492191,60.4695742653833,11.24434019589));
#38603=CARTESIAN_POINT('Ctrl Pts',(-13.8615442019958,60.4729336106521,11.225553469077));
#38604=CARTESIAN_POINT('Ctrl Pts',(-13.8492449351277,60.4762291892769,11.2065843090731));
#38605=CARTESIAN_POINT('Ctrl Pts',(-13.8371847672655,60.4794607015161,11.1874386951179));
#38606=CARTESIAN_POINT('Ctrl Pts',(-13.8274131410566,60.4820790008676,11.1719261595341));
#38607=CARTESIAN_POINT('Ctrl Pts',(-13.8177980990722,60.4846553436025,11.1562969508317));
#38608=CARTESIAN_POINT('Ctrl Pts',(-13.8083486579241,60.487187313727,11.140568630092));
#38609=CARTESIAN_POINT('Ctrl Pts',(-13.7625022247112,60.4994718284823,11.0642585716409));
#38610=CARTESIAN_POINT('Ctrl Pts',(-13.7205023351854,60.5107256649629,10.9855425561791));
#38611=CARTESIAN_POINT('Ctrl Pts',(-13.6823842421124,60.5209393772188,10.9048124953012));
#38612=CARTESIAN_POINT('Ctrl Pts',(-13.6519560247452,60.5290925934895,10.8403687720607));
#38613=CARTESIAN_POINT('Ctrl Pts',(-13.6240018721467,60.5365828861033,10.7746405675787));
#38614=CARTESIAN_POINT('Ctrl Pts',(-13.598555660536,60.5434011779549,10.7078100772367));
#38615=CARTESIAN_POINT('Ctrl Pts',(-13.5903398049439,60.5456026098259,10.6862324189903));
#38616=CARTESIAN_POINT('Ctrl Pts',(-13.5823855109655,60.5477339564738,10.6645397516926));
#38617=CARTESIAN_POINT('Ctrl Pts',(-13.5746942694777,60.5497948184192,10.6427379435114));
#38618=CARTESIAN_POINT('Ctrl Pts',(-13.5673646520995,60.5517587834765,10.6219612051427));
#38619=CARTESIAN_POINT('Ctrl Pts',(-13.5602723819539,60.5536591515346,10.6010802048978));
#38620=CARTESIAN_POINT('Ctrl Pts',(-13.5534284149968,60.5554929869537,10.5801302251332));
#38621=CARTESIAN_POINT('Ctrl Pts',(-13.5248766272142,60.5631434154325,10.4927307125355));
#38622=CARTESIAN_POINT('Ctrl Pts',(-13.5006117004349,60.5696451829675,10.4040498990336));
#38623=CARTESIAN_POINT('Ctrl Pts',(-13.480666832402,60.57498939425,10.3144849193173));
#38624=CARTESIAN_POINT('Ctrl Pts',(-13.460414058422,60.5804161086824,10.2235372485817));
#38625=CARTESIAN_POINT('Ctrl Pts',(-13.4446152716974,60.5846493808267,10.1316770971923));
#38626=CARTESIAN_POINT('Ctrl Pts',(-13.4333455934799,60.587669082004,10.0392871198388));
#38627=CARTESIAN_POINT('Ctrl Pts',(-13.4221628859774,60.5906654794485,9.94761013732271));
#38628=CARTESIAN_POINT('Ctrl Pts',(-13.4154393160861,60.5924670545712,9.85541054694995));
#38629=CARTESIAN_POINT('Ctrl Pts',(-13.4132936428762,60.593041985975,9.76304299861578));
#38630=CARTESIAN_POINT('Ctrl Pts',(-13.4122613686534,60.5933185830193,9.71860536536672));
#38631=CARTESIAN_POINT('Ctrl Pts',(-13.4122893693034,60.5933110802678,9.67412865788773));
#38632=CARTESIAN_POINT('Ctrl Pts',(-13.4133950120079,60.593014824198,9.62965173468087));
#38633=CARTESIAN_POINT('Ctrl Pts',(-13.4137601235553,60.5929169928537,9.61496431514677));
#38634=CARTESIAN_POINT('Ctrl Pts',(-13.4142427737453,60.5927876671251,9.60027687123983));
#38635=CARTESIAN_POINT('Ctrl Pts',(-13.4148436567524,60.5926266610086,9.58559080207231));
#38636=CARTESIAN_POINT('Ctrl Pts',(-13.4154511643685,60.5924638798335,9.57074282207608));
#38637=CARTESIAN_POINT('Ctrl Pts',(-13.4161791917116,60.5922688054948,9.55590504990595));
#38638=CARTESIAN_POINT('Ctrl Pts',(-13.4170277181543,60.5920414435197,9.54108357202142));
#38639=CARTESIAN_POINT('Ctrl Pts',(-13.4224967665196,60.5905760164269,9.44555398647223));
#38640=CARTESIAN_POINT('Ctrl Pts',(-13.4329703612428,60.5877696251789,9.35064220222354));
#38641=CARTESIAN_POINT('Ctrl Pts',(-13.4485182643056,60.5836035771093,9.25674298412033));
#38642=CARTESIAN_POINT('Ctrl Pts',(-13.4498478809465,60.5832473074041,9.24871296473712));
#38643=CARTESIAN_POINT('Ctrl Pts',(-13.4512146356318,60.5828810865899,9.24069033922208));
#38644=CARTESIAN_POINT('Ctrl Pts',(-13.4526185882088,60.5825048986307,9.23267534878043));
#38645=CARTESIAN_POINT('Ctrl Pts',(-13.4683901533204,60.5782789204957,9.14263744743809));
#38646=CARTESIAN_POINT('Ctrl Pts',(-13.4888516530656,60.572796278163,9.05356331284174));
#38647=CARTESIAN_POINT('Ctrl Pts',(-13.5137114619772,60.5661351124412,8.96568771726277));
#38648=CARTESIAN_POINT('Ctrl Pts',(-13.5391401674804,60.559321511337,8.8758011598541));
#38649=CARTESIAN_POINT('Ctrl Pts',(-13.5691709812742,60.5512747790329,8.78716792585963));
#38650=CARTESIAN_POINT('Ctrl Pts',(-13.6035442475085,60.5420644901042,8.70004212732541));
#38651=CARTESIAN_POINT('Ctrl Pts',(-13.6224082878329,60.5370098857333,8.65222750983641));
#38652=CARTESIAN_POINT('Ctrl Pts',(-13.6425810892874,60.5316045998745,8.60486701435782));
#38653=CARTESIAN_POINT('Ctrl Pts',(-13.6640258581501,60.5258584913759,8.55800419902235));
#38654=CARTESIAN_POINT('Ctrl Pts',(-13.6704060167119,60.5241489330416,8.54406176884704));
#38655=CARTESIAN_POINT('Ctrl Pts',(-13.6768997658184,60.5224089382127,8.53016150117742));
#38656=CARTESIAN_POINT('Ctrl Pts',(-13.6834982306919,60.5206408848786,8.51632087112045));
#38657=CARTESIAN_POINT('Ctrl Pts',(-13.7247150404844,60.5095968739801,8.42986642642761));
#38658=CARTESIAN_POINT('Ctrl Pts',(-13.7700718774285,60.4974435461497,8.3456074465938));
#38659=CARTESIAN_POINT('Ctrl Pts',(-13.8192407166192,60.4842687953957,8.2637970860201));
#38660=CARTESIAN_POINT('Ctrl Pts',(-13.869379078653,60.470834261779,8.18037356933611));
#38661=CARTESIAN_POINT('Ctrl Pts',(-13.9234815557643,60.4563375467285,8.09949541154091));
#38662=CARTESIAN_POINT('Ctrl Pts',(-13.9812533712864,60.4408576354141,8.02143790718841));
#38663=CARTESIAN_POINT('Ctrl Pts',(-14.039482634331,60.4252551514054,7.94276232961702));
#38664=CARTESIAN_POINT('Ctrl Pts',(-14.1014400131933,60.4086537217741,7.86695140903171));
#38665=CARTESIAN_POINT('Ctrl Pts',(-14.16687127419,60.3911214682303,7.79430622921448));
#38666=CARTESIAN_POINT('Ctrl Pts',(-14.2014931148633,60.3818445739814,7.75586726589624));
#38667=CARTESIAN_POINT('Ctrl Pts',(-14.2370883362474,60.3723068631571,7.71831505022628));
#38668=CARTESIAN_POINT('Ctrl Pts',(-14.2736239454352,60.3625171761803,7.68169758983469));
#38669=CARTESIAN_POINT('Ctrl Pts',(-14.2866331258705,60.3590313767884,7.66865926476215));
#38670=CARTESIAN_POINT('Ctrl Pts',(-14.2997615606732,60.3555136232852,7.65573947805022));
#38671=CARTESIAN_POINT('Ctrl Pts',(-14.313007848791,60.3519642910813,7.64294048667691));
#38672=CARTESIAN_POINT('Ctrl Pts',(-14.323185153228,60.3492372905763,7.63310684644997));
#38673=CARTESIAN_POINT('Ctrl Pts',(-14.3334310227586,60.3464919181098,7.62334556315778));
#38674=CARTESIAN_POINT('Ctrl Pts',(-14.3437359536144,60.3437307202089,7.61366571173162));
#38675=CARTESIAN_POINT('Ctrl Pts',(-14.4166886967228,60.3241830916074,7.545138156884));
#38676=CARTESIAN_POINT('Ctrl Pts',(-14.4927140801617,60.3038121515107,7.48057696472124));
#38677=CARTESIAN_POINT('Ctrl Pts',(-14.5714997183224,60.2827016033904,7.42026730047636));
#38678=CARTESIAN_POINT('Ctrl Pts',(-14.6503851320848,60.2615643204781,7.35988125894772));
#38679=CARTESIAN_POINT('Ctrl Pts',(-14.7320383428994,60.239685408581,7.30375667613358));
#38680=CARTESIAN_POINT('Ctrl Pts',(-14.8161894526237,60.2171371866881,7.25220561239913));
#38681=CARTESIAN_POINT('Ctrl Pts',(-14.8987454236577,60.1950163809192,7.20163173240665));
#38682=CARTESIAN_POINT('Ctrl Pts',(-14.9837061239422,60.1722512298896,7.15545893560281));
#38683=CARTESIAN_POINT('Ctrl Pts',(-15.0708497995124,60.1489011523951,7.11401788937555));
#38684=CARTESIAN_POINT('Ctrl Pts',(-15.0979686080361,60.1416346895515,7.10112158002999));
#38685=CARTESIAN_POINT('Ctrl Pts',(-15.1252990311688,60.1343115247443,7.08868381630056));
#38686=CARTESIAN_POINT('Ctrl Pts',(-15.1528349118071,60.1269333077643,7.07671545672048));
#38687=CARTESIAN_POINT('Ctrl Pts',(-15.1941283917652,60.1158687531569,7.05876741202411));
#38688=CARTESIAN_POINT('Ctrl Pts',(-15.2358838838844,60.104680402764,7.04187489341853));
#38689=CARTESIAN_POINT('Ctrl Pts',(-15.2780676602838,60.0933772939441,7.02603075613018));
#38690=CARTESIAN_POINT('Ctrl Pts',(-15.458048217099,67.4086397233445,10.0018117506529));
#38691=CARTESIAN_POINT('Ctrl Pts',(-15.4516726940089,67.3922281881599,10.2792252787833));
#38692=CARTESIAN_POINT('Ctrl Pts',(-15.4881185773169,67.3643426917121,10.5560719127005));
#38693=CARTESIAN_POINT('Ctrl Pts',(-15.5698466331083,67.3243238737159,10.8168646145652));
#38694=CARTESIAN_POINT('Ctrl Pts',(-15.8140481541641,67.2047485806184,11.5961071140829));
#38695=CARTESIAN_POINT('Ctrl Pts',(-16.4625291088523,66.9768469397627,12.2320200381452));
#38696=CARTESIAN_POINT('Ctrl Pts',(-17.2188383863877,66.7200527868788,12.4398697983788));
#38697=CARTESIAN_POINT('Ctrl Pts',(-17.975147663923,66.463258633995,12.6477195586124));
#38698=CARTESIAN_POINT('Ctrl Pts',(-18.8392852643055,66.1775719690831,12.4275061550173));
#38699=CARTESIAN_POINT('Ctrl Pts',(-19.4182523936636,65.9682965015874,11.8778290289184));
#38700=CARTESIAN_POINT('Ctrl Pts',(-19.9972195230217,65.7590210340917,11.3281519028195));
#38701=CARTESIAN_POINT('Ctrl Pts',(-20.2910161813554,65.6261567640121,10.4490110542167));
#38702=CARTESIAN_POINT('Ctrl Pts',(-20.1620218299581,65.6065790035572,9.63407278056648));
#38703=CARTESIAN_POINT('Ctrl Pts',(-20.0330274785608,65.5870012431022,8.81913450691625));
#38704=CARTESIAN_POINT('Ctrl Pts',(-19.4812421174325,65.6807099922718,8.06839880821855));
#38705=CARTESIAN_POINT('Ctrl Pts',(-18.7476852845614,65.8231242605018,7.71802880880736));
#38706=CARTESIAN_POINT('Ctrl Pts',(-18.0141284516903,65.9655385287319,7.36765880939615));
#38707=CARTESIAN_POINT('Ctrl Pts',(-17.0988001470764,66.1566583160224,7.41765450927146));
#38708=CARTESIAN_POINT('Ctrl Pts',(-16.4055051616428,66.2882844547459,7.84562973884635));
#38709=CARTESIAN_POINT('Ctrl Pts',(-15.7122101762091,66.4199105934693,8.27360496842124));
#38710=CARTESIAN_POINT('Ctrl Pts',(-15.2409485099557,66.4920430836257,9.07955972769568));
#38711=CARTESIAN_POINT('Ctrl Pts',(-15.1966815676295,66.4497626823333,9.90260247183681));
#38712=CARTESIAN_POINT('Ctrl Pts',(-15.194946550497,66.4481055265245,9.93486115488302));
#38713=CARTESIAN_POINT('Ctrl Pts',(-15.1938674837542,66.4462726093384,9.9671460885354));
#38714=CARTESIAN_POINT('Ctrl Pts',(-15.1934336836835,66.4442667934687,9.99943462192771));
#38715=CARTESIAN_POINT('Origin',(17.0820569767664,-63.7511045350785,10.));
#38716=CARTESIAN_POINT('Origin',(16.0467807963563,-59.8874012299222,10.));
#38717=CARTESIAN_POINT('Origin',(-63.7511045350785,-17.0820569767664,10.));
#38718=CARTESIAN_POINT('Origin',(-59.8874012299222,-16.0467807963563,10.));
#38719=CARTESIAN_POINT('Origin',(-17.0820569767664,63.7511045350785,10.));
#38720=CARTESIAN_POINT('Origin',(-16.0467807963563,59.8874012299222,10.));
#38721=CARTESIAN_POINT('Ctrl Pts',(67.0040126136404,20.25986904378,11.1728309286208));
#38722=CARTESIAN_POINT('Ctrl Pts',(66.854289394458,20.6173045957293,10.4434664543485));
#38723=CARTESIAN_POINT('Ctrl Pts',(66.7561954352347,20.5807180172414,8.59013022403084));
#38724=CARTESIAN_POINT('Ctrl Pts',(67.2090412643979,18.2866570474722,7.05024279158514));
#38725=CARTESIAN_POINT('Ctrl Pts',(67.7235827819968,15.7623446338521,8.14059085434232));
#38726=CARTESIAN_POINT('Ctrl Pts',(67.7078986042172,15.216861454864,10.8824467802982));
#38727=CARTESIAN_POINT('Ctrl Pts',(67.0414893382908,17.0999173665985,12.8405694561119));
#38728=CARTESIAN_POINT('Ctrl Pts',(66.1829652216242,19.6999556621848,12.270731917377));
#38729=CARTESIAN_POINT('Ctrl Pts',(65.7617874756575,20.6677950818131,9.68094249642526));
#38730=CARTESIAN_POINT('Ctrl Pts',(66.0183437425752,19.1062967313387,7.37485535276711));
#38731=CARTESIAN_POINT('Ctrl Pts',(66.5900180970019,16.3687616678975,7.40446197973336));
#38732=CARTESIAN_POINT('Ctrl Pts',(66.8338405096701,14.8547867084588,9.74329926128817));
#38733=CARTESIAN_POINT('Ctrl Pts',(66.3985290187163,15.8753739824799,12.3105450512028));
#38734=CARTESIAN_POINT('Ctrl Pts',(65.5370346894516,18.4864972623911,12.8220707222439));
#38735=CARTESIAN_POINT('Ctrl Pts',(64.8814857844687,20.3290217552966,10.8227823754311));
#38736=CARTESIAN_POINT('Ctrl Pts',(64.8807798084461,19.7276391663451,8.09145561890055));
#38737=CARTESIAN_POINT('Ctrl Pts',(65.4011950297316,17.1814057921382,7.0581771851638));
#38738=CARTESIAN_POINT('Ctrl Pts',(65.8453641599238,14.9197267037703,8.64226139479096));
#38739=CARTESIAN_POINT('Ctrl Pts',(65.6837566027253,14.9188369907852,11.4343367521439));
#38740=CARTESIAN_POINT('Ctrl Pts',(64.9258061425712,17.1435292903637,12.9502711232991));
#38741=CARTESIAN_POINT('Ctrl Pts',(64.1115175849317,19.5784782321595,11.8413258175013));
#38742=CARTESIAN_POINT('Ctrl Pts',(63.831020197438,20.0212914063393,9.09413821413814));
#38743=CARTESIAN_POINT('Ctrl Pts',(64.1995249831397,18.0419954959312,7.15290308224174));
#38744=CARTESIAN_POINT('Ctrl Pts',(64.7548205378835,15.3655869450733,7.74475277436874));
#38745=CARTESIAN_POINT('Ctrl Pts',(64.8685062198083,14.3372888766999,10.3431139119316));
#38746=CARTESIAN_POINT('Ctrl Pts',(64.305085213021,15.8359873727446,12.6362038638412));
#38747=CARTESIAN_POINT('Ctrl Pts',(63.4314879220137,18.4922795208015,12.5838422163727));
#38748=CARTESIAN_POINT('Ctrl Pts',(62.8906110650171,19.9068421044142,10.2326155433119));
#38749=CARTESIAN_POINT('Ctrl Pts',(63.0293273367051,18.7851286033011,7.67442896667236));
#38750=CARTESIAN_POINT('Ctrl Pts',(63.5898700057829,16.0891375551554,7.18532148363251));
#38751=CARTESIAN_POINT('Ctrl Pts',(63.9391700310929,14.1815147862765,9.20045592301428));
#38752=CARTESIAN_POINT('Ctrl Pts',(63.6321026366037,14.7234885765209,11.926951102987));
#38753=CARTESIAN_POINT('Ctrl Pts',(62.8075183731852,17.1968616153839,12.9390225214355));
#38754=CARTESIAN_POINT('Ctrl Pts',(62.0647066785609,19.3650552728408,11.3362221619436));
#38755=CARTESIAN_POINT('Ctrl Pts',(61.9302032807139,19.2630114600595,8.54457429525403));
#38756=CARTESIAN_POINT('Ctrl Pts',(62.3893271714101,16.9455204456759,7.04783027207108));
#38757=CARTESIAN_POINT('Ctrl Pts',(62.8992423967485,14.4384735898227,8.1776552235704));
#38758=CARTESIAN_POINT('Ctrl Pts',(62.8719235739435,13.9364114971972,10.9288348037815));
#38759=CARTESIAN_POINT('Ctrl Pts',(62.1973266831092,15.850024041082,12.853622756267));
#38760=CARTESIAN_POINT('Ctrl Pts',(61.3412962728356,18.4407556977103,12.2395195742226));
#38761=CARTESIAN_POINT('Ctrl Pts',(60.9310995184378,19.3676134988853,9.63289839745389));
#38762=CARTESIAN_POINT('Ctrl Pts',(61.19734228766,17.7699646296638,7.35288957156125));
#38763=CARTESIAN_POINT('Ctrl Pts',(61.7687958934069,15.0332534115107,7.42803777444101));
#38764=CARTESIAN_POINT('Ctrl Pts',(62.0026849934363,13.5563500795275,9.79147768508998));
#38765=CARTESIAN_POINT('Ctrl Pts',(61.5565643024821,14.6172778371391,12.3404488591357));
#38766=CARTESIAN_POINT('Ctrl Pts',(60.6930063334388,17.236102725553,12.807089206987));
#38767=CARTESIAN_POINT('Ctrl Pts',(60.0459653166684,19.0468753473843,10.7762699688266));
#38768=CARTESIAN_POINT('Ctrl Pts',(60.0567902041013,18.4024589901613,8.05473611617474));
#38769=CARTESIAN_POINT('Ctrl Pts',(60.5814573009746,15.8403574002339,7.06404294414452));
#38770=CARTESIAN_POINT('Ctrl Pts',(61.0189035288689,13.6037685248159,8.68524269063554));
#38771=CARTESIAN_POINT('Ctrl Pts',(60.8454027634006,13.6472648693585,11.4767030328865));
#38772=CARTESIAN_POINT('Ctrl Pts',(60.0813295310042,15.8948076660285,12.9532921034687));
#38773=CARTESIAN_POINT('Ctrl Pts',(59.2714063402786,18.3134648367079,11.8044287744805));
#38774=CARTESIAN_POINT('Ctrl Pts',(59.0033710168103,18.7097689547777,9.04578082775238));
#38775=CARTESIAN_POINT('Ctrl Pts',(59.2532824184769,17.3744086881427,7.78080120942675));
#38776=CARTESIAN_POINT('Ctrl Pts',(59.4090483774018,16.5917431062329,7.56791319796499));
#38777=CARTESIAN_POINT('Ctrl Pts',(67.0649244254632,20.4459680138347,11.259172404465));
#38778=CARTESIAN_POINT('Ctrl Pts',(66.9078844272409,20.8307101569087,10.4761135710142));
#38779=CARTESIAN_POINT('Ctrl Pts',(66.8099800782135,20.7934159435358,8.48633842059636));
#38780=CARTESIAN_POINT('Ctrl Pts',(67.3072801529265,18.3334494707627,6.83308754393488));
#38781=CARTESIAN_POINT('Ctrl Pts',(67.8708178297157,15.6262809016687,8.0037048583164));
#38782=CARTESIAN_POINT('Ctrl Pts',(67.8650956520228,15.0436190322123,10.9474107537965));
#38783=CARTESIAN_POINT('Ctrl Pts',(67.160743301905,17.0682804619447,13.049686519018));
#38784=CARTESIAN_POINT('Ctrl Pts',(66.2501329885663,19.8627070898848,12.4378986762067));
#38785=CARTESIAN_POINT('Ctrl Pts',(65.8090656142303,20.9047756131302,9.65745411880361));
#38786=CARTESIAN_POINT('Ctrl Pts',(66.0956256802751,19.231301559894,7.18159743500988));
#38787=CARTESIAN_POINT('Ctrl Pts',(66.7205021994896,16.2952133143915,7.21338364285575));
#38788=CARTESIAN_POINT('Ctrl Pts',(66.9933909703099,14.6727612295384,9.72440146443628));
#38789=CARTESIAN_POINT('Ctrl Pts',(66.5371493528457,15.7714607991054,12.4806427736084));
#38790=CARTESIAN_POINT('Ctrl Pts',(65.6233501657761,18.5777884658271,13.0298259452254));
#38791=CARTESIAN_POINT('Ctrl Pts',(64.9306576947328,20.558934634444,10.8833539743374));
#38792=CARTESIAN_POINT('Ctrl Pts',(64.9410163841629,19.9162581518544,7.95095238475408));
#38793=CARTESIAN_POINT('Ctrl Pts',(65.5108601749995,17.1855548447374,6.84160605175778));
#38794=CARTESIAN_POINT('Ctrl Pts',(65.9988447894534,14.7603541429465,8.54230738426514));
#38795=CARTESIAN_POINT('Ctrl Pts',(65.8364566439329,14.7623776252392,11.5399297656086));
#38796=CARTESIAN_POINT('Ctrl Pts',(65.0338240192841,17.1538260329039,13.167464204339));
#38797=CARTESIAN_POINT('Ctrl Pts',(64.1707057986789,19.7710097578038,11.9768805549434));
#38798=CARTESIAN_POINT('Ctrl Pts',(63.8806753904707,20.2494006496399,9.02745047458975));
#38799=CARTESIAN_POINT('Ctrl Pts',(64.2874254021705,18.1273716126603,6.94330548061664));
#38800=CARTESIAN_POINT('Ctrl Pts',(64.8947173471079,15.2569098917896,7.5787259676887));
#38801=CARTESIAN_POINT('Ctrl Pts',(65.0278889803931,14.1558892629051,10.3683732743989));
#38802=CARTESIAN_POINT('Ctrl Pts',(64.4341066798258,15.7678976499205,12.8302759390873));
#38803=CARTESIAN_POINT('Ctrl Pts',(63.5073135350879,18.6227194268519,12.7740595314741));
#38804=CARTESIAN_POINT('Ctrl Pts',(62.9377350396946,20.1443979832212,10.2497402360735));
#38805=CARTESIAN_POINT('Ctrl Pts',(63.0977799648827,18.9430848635892,7.50322506140521));
#38806=CARTESIAN_POINT('Ctrl Pts',(63.7107053062553,16.0515990210029,6.97811046011707));
#38807=CARTESIAN_POINT('Ctrl Pts',(64.096836741373,14.0065195594074,9.14159508133219));
#38808=CARTESIAN_POINT('Ctrl Pts',(63.7782802952008,14.5913710742637,12.0688094033194));
#38809=CARTESIAN_POINT('Ctrl Pts',(62.9041084194735,17.2498076016885,13.1553875028215));
#38810=CARTESIAN_POINT('Ctrl Pts',(62.1177290461058,19.5805980497845,11.4345921747925));
#38811=CARTESIAN_POINT('Ctrl Pts',(61.9844404141371,19.4740206690255,8.43742875512311));
#38812=CARTESIAN_POINT('Ctrl Pts',(62.4884807287628,16.9888992784431,6.83049741954166));
#38813=CARTESIAN_POINT('Ctrl Pts',(63.0470515348742,14.3002673230733,8.04349783254823));
#38814=CARTESIAN_POINT('Ctrl Pts',(63.0288381927736,13.7642231138315,10.9972137711304));
#38815=CARTESIAN_POINT('Ctrl Pts',(62.3156954611178,15.8216906940825,13.063700777119));
#38816=CARTESIAN_POINT('Ctrl Pts',(61.4077624358673,18.6061255468499,12.4043885425467));
#38817=CARTESIAN_POINT('Ctrl Pts',(60.9784844518179,19.6041954665562,9.60587310900428));
#38818=CARTESIAN_POINT('Ctrl Pts',(61.275444121164,17.8919095654206,7.15801457676324));
#38819=CARTESIAN_POINT('Ctrl Pts',(61.9000836406211,14.9567058150546,7.23869504058986));
#38820=CARTESIAN_POINT('Ctrl Pts',(62.1623078281203,13.374054496997,9.77612668779241));
#38821=CARTESIAN_POINT('Ctrl Pts',(61.6944612588913,14.5160643361693,12.5127480402915));
#38822=CARTESIAN_POINT('Ctrl Pts',(60.7784465109949,17.3306605884645,13.0137415206692));
#38823=CARTESIAN_POINT('Ctrl Pts',(60.0948882619405,19.2777173765313,10.8334174170447));
#38824=CARTESIAN_POINT('Ctrl Pts',(60.117626694016,18.5888390654042,7.91152966540919));
#38825=CARTESIAN_POINT('Ctrl Pts',(60.6920353750482,15.8410993561462,6.84790363622586));
#38826=CARTESIAN_POINT('Ctrl Pts',(61.172802160534,13.4428359587848,8.58845287746021));
#38827=CARTESIAN_POINT('Ctrl Pts',(60.9976452524506,13.4925131117115,11.5854149675154));
#38828=CARTESIAN_POINT('Ctrl Pts',(60.1884391092681,15.908494224529,13.1707075830487));
#38829=CARTESIAN_POINT('Ctrl Pts',(59.3300076251901,18.5081868105878,11.9372672251407));
#38830=CARTESIAN_POINT('Ctrl Pts',(59.0533567133274,18.9366447422826,8.97553311378089));
#38831=CARTESIAN_POINT('Ctrl Pts',(59.3290771863822,17.5049637099304,7.61742821670134));
#38832=CARTESIAN_POINT('Ctrl Pts',(59.5000158708058,16.6656727455702,7.38886781406145));
#38833=CARTESIAN_POINT('Ctrl Pts',(67.125836237286,20.6320669838895,11.3455138803092));
#38834=CARTESIAN_POINT('Ctrl Pts',(66.9614794600237,21.0441157180881,10.5087606876799));
#38835=CARTESIAN_POINT('Ctrl Pts',(66.8637647211924,21.0061138698302,8.38254661716189));
#38836=CARTESIAN_POINT('Ctrl Pts',(67.4055190414551,18.3802418940533,6.6159322962846));
#38837=CARTESIAN_POINT('Ctrl Pts',(68.0180528774347,15.4902171694853,7.8668188622905));
#38838=CARTESIAN_POINT('Ctrl Pts',(68.0222926998282,14.8703766095605,11.0123747272948));
#38839=CARTESIAN_POINT('Ctrl Pts',(67.2799972655193,17.036643557291,13.2588035819241));
#38840=CARTESIAN_POINT('Ctrl Pts',(66.3173007555082,20.0254585175847,12.6050654350364));
#38841=CARTESIAN_POINT('Ctrl Pts',(65.8563437528032,21.1417561444473,9.63396574118195));
#38842=CARTESIAN_POINT('Ctrl Pts',(66.1729076179749,19.3563063884493,6.98833951725265));
#38843=CARTESIAN_POINT('Ctrl Pts',(66.8509863019774,16.2216649608855,7.02230530597812));
#38844=CARTESIAN_POINT('Ctrl Pts',(67.1529414309498,14.4907357506179,9.70550366758441));
#38845=CARTESIAN_POINT('Ctrl Pts',(66.675769686975,15.6675476157309,12.6507404960141));
#38846=CARTESIAN_POINT('Ctrl Pts',(65.7096656421006,18.6690796692631,13.2375811682069));
#38847=CARTESIAN_POINT('Ctrl Pts',(64.979829604997,20.7888475135915,10.9439255732437));
#38848=CARTESIAN_POINT('Ctrl Pts',(65.0012529598797,20.1048771373638,7.81044915060759));
#38849=CARTESIAN_POINT('Ctrl Pts',(65.6205253202674,17.1897038973366,6.62503491835178));
#38850=CARTESIAN_POINT('Ctrl Pts',(66.1523254189831,14.6009815821227,8.44235337373932));
#38851=CARTESIAN_POINT('Ctrl Pts',(65.9891566851404,14.6059182596932,11.6455227790733));
#38852=CARTESIAN_POINT('Ctrl Pts',(65.141841895997,17.1641227754441,13.384657285379));
#38853=CARTESIAN_POINT('Ctrl Pts',(64.2298940124262,19.9635412834481,12.1124352923854));
#38854=CARTESIAN_POINT('Ctrl Pts',(63.9303305835034,20.4775098929406,8.96076273504136));
#38855=CARTESIAN_POINT('Ctrl Pts',(64.3753258212011,18.2127477293894,6.73370787899155));
#38856=CARTESIAN_POINT('Ctrl Pts',(65.0346141563323,15.148232838506,7.41269916100866));
#38857=CARTESIAN_POINT('Ctrl Pts',(65.1872717409779,13.9744896491103,10.3936326368662));
#38858=CARTESIAN_POINT('Ctrl Pts',(64.5631281466306,15.6998079270964,13.0243480143333));
#38859=CARTESIAN_POINT('Ctrl Pts',(63.5831391481621,18.7531593329024,12.9642768465755));
#38860=CARTESIAN_POINT('Ctrl Pts',(62.9848590143723,20.3819538620282,10.266864928835));
#38861=CARTESIAN_POINT('Ctrl Pts',(63.1662325930602,19.1010411238774,7.33202115613807));
#38862=CARTESIAN_POINT('Ctrl Pts',(63.8315406067278,16.0140604868503,6.77089943660162));
#38863=CARTESIAN_POINT('Ctrl Pts',(64.254503451653,13.8315243325383,9.08273423965009));
#38864=CARTESIAN_POINT('Ctrl Pts',(63.9244579537979,14.4592535720065,12.2106677036519));
#38865=CARTESIAN_POINT('Ctrl Pts',(63.000698465762,17.3027535879931,13.3717524842076));
#38866=CARTESIAN_POINT('Ctrl Pts',(62.1707514136505,19.7961408267281,11.5329621876413));
#38867=CARTESIAN_POINT('Ctrl Pts',(62.0386775475604,19.6850298779916,8.3302832149922));
#38868=CARTESIAN_POINT('Ctrl Pts',(62.5876342861153,17.0322781112102,6.61316456701223));
#38869=CARTESIAN_POINT('Ctrl Pts',(63.1948606729998,14.1620610563239,7.90934044152608));
#38870=CARTESIAN_POINT('Ctrl Pts',(63.1857528116037,13.5920347304658,11.0655927384792));
#38871=CARTESIAN_POINT('Ctrl Pts',(62.4340642391263,15.7933573470829,13.273778797971));
#38872=CARTESIAN_POINT('Ctrl Pts',(61.4742285988992,18.7714953959895,12.5692575108708));
#38873=CARTESIAN_POINT('Ctrl Pts',(61.0258693851979,19.8407774342272,9.57884782055468));
#38874=CARTESIAN_POINT('Ctrl Pts',(61.3535459546682,18.0138545011774,6.96313958196523));
#38875=CARTESIAN_POINT('Ctrl Pts',(62.0313713878352,14.8801582185986,7.04935230673873));
#38876=CARTESIAN_POINT('Ctrl Pts',(62.3219306628043,13.1917589144664,9.76077569049482));
#38877=CARTESIAN_POINT('Ctrl Pts',(61.8323582153006,14.4148508351995,12.6850472214474));
#38878=CARTESIAN_POINT('Ctrl Pts',(60.8638866885509,17.425218451376,13.2203938343514));
#38879=CARTESIAN_POINT('Ctrl Pts',(60.1438112072126,19.5085594056783,10.8905648652629));
#38880=CARTESIAN_POINT('Ctrl Pts',(60.1784631839306,18.7752191406471,7.76832321464364));
#38881=CARTESIAN_POINT('Ctrl Pts',(60.8026134491219,15.8418413120585,6.6317643283072));
#38882=CARTESIAN_POINT('Ctrl Pts',(61.3267007921991,13.2819033927538,8.49166306428489));
#38883=CARTESIAN_POINT('Ctrl Pts',(61.1498877415007,13.3377613540646,11.6941269021443));
#38884=CARTESIAN_POINT('Ctrl Pts',(60.2955486875319,15.9221807830296,13.3881230626288));
#38885=CARTESIAN_POINT('Ctrl Pts',(59.3886089101015,18.7029087844678,12.0701056758009));
#38886=CARTESIAN_POINT('Ctrl Pts',(59.1033424098445,19.1635205297874,8.9052853998094));
#38887=CARTESIAN_POINT('Ctrl Pts',(59.4048719542876,17.6355187317182,7.45405522397592));
#38888=CARTESIAN_POINT('Ctrl Pts',(59.5909833642099,16.7396023849075,7.20982243015791));
#38889=CARTESIAN_POINT('Ctrl Pts',(67.1867480491087,20.8181659539443,11.4318553561534));
#38890=CARTESIAN_POINT('Ctrl Pts',(67.0150744928066,21.2575212792675,10.5414078043456));
#38891=CARTESIAN_POINT('Ctrl Pts',(66.9175493641713,21.2188117961246,8.27875481372742));
#38892=CARTESIAN_POINT('Ctrl Pts',(67.5037579299836,18.4270343173439,6.39877704863433));
#38893=CARTESIAN_POINT('Ctrl Pts',(68.1652879251536,15.3541534373019,7.72993286626459));
#38894=CARTESIAN_POINT('Ctrl Pts',(68.1794897476338,14.6971341869088,11.0773387007931));
#38895=CARTESIAN_POINT('Ctrl Pts',(67.3992512291335,17.0050066526372,13.4679206448302));
#38896=CARTESIAN_POINT('Ctrl Pts',(66.3844685224502,20.1882099452846,12.7722321938662));
#38897=CARTESIAN_POINT('Ctrl Pts',(65.9036218913761,21.3787366757644,9.61047736356028));
#38898=CARTESIAN_POINT('Ctrl Pts',(66.2501895556748,19.4813112170046,6.79508159949543));
#38899=CARTESIAN_POINT('Ctrl Pts',(66.9814704044652,16.1481166073795,6.83122696910049));
#38900=CARTESIAN_POINT('Ctrl Pts',(67.3124918915896,14.3087102716975,9.68660587073254));
#38901=CARTESIAN_POINT('Ctrl Pts',(66.8143900211043,15.5636344323564,12.8208382184197));
#38902=CARTESIAN_POINT('Ctrl Pts',(65.795981118425,18.7603708726991,13.4453363911884));
#38903=CARTESIAN_POINT('Ctrl Pts',(65.0290015152611,21.0187603927389,11.00449717215));
#38904=CARTESIAN_POINT('Ctrl Pts',(65.0614895355965,20.2934961228732,7.66994591646111));
#38905=CARTESIAN_POINT('Ctrl Pts',(65.7301904655353,17.1938529499358,6.40846378494576));
#38906=CARTESIAN_POINT('Ctrl Pts',(66.3058060485126,14.441609021299,8.34239936321351));
#38907=CARTESIAN_POINT('Ctrl Pts',(66.141856726348,14.4494588941473,11.7511157925379));
#38908=CARTESIAN_POINT('Ctrl Pts',(65.2498597727098,17.1744195179844,13.6018503664189));
#38909=CARTESIAN_POINT('Ctrl Pts',(64.2890822261735,20.1560728090925,12.2479900298274));
#38910=CARTESIAN_POINT('Ctrl Pts',(63.9799857765362,20.7056191362412,8.89407499549297));
#38911=CARTESIAN_POINT('Ctrl Pts',(64.4632262402319,18.2981238461185,6.52411027736645));
#38912=CARTESIAN_POINT('Ctrl Pts',(65.1745109655566,15.0395557852223,7.24667235432862));
#38913=CARTESIAN_POINT('Ctrl Pts',(65.3466545015629,13.7930900353155,10.4188919993334));
#38914=CARTESIAN_POINT('Ctrl Pts',(64.6921496134354,15.6317182042723,13.2184200895793));
#38915=CARTESIAN_POINT('Ctrl Pts',(63.6589647612363,18.8835992389528,13.1544941616769));
#38916=CARTESIAN_POINT('Ctrl Pts',(63.0319829890499,20.6195097408352,10.2839896215965));
#38917=CARTESIAN_POINT('Ctrl Pts',(63.2346852212378,19.2589973841656,7.16081725087092));
#38918=CARTESIAN_POINT('Ctrl Pts',(63.9523759072002,15.9765219526977,6.56368841308618));
#38919=CARTESIAN_POINT('Ctrl Pts',(64.4121701619331,13.6565291056693,9.023873397968));
#38920=CARTESIAN_POINT('Ctrl Pts',(64.0706356123949,14.3271360697493,12.3525260039843));
#38921=CARTESIAN_POINT('Ctrl Pts',(63.0972885120504,17.3556995742977,13.5881174655937));
#38922=CARTESIAN_POINT('Ctrl Pts',(62.2237737811953,20.0116836036718,11.6313322004901));
#38923=CARTESIAN_POINT('Ctrl Pts',(62.0929146809836,19.8960390869576,8.22313767486128));
#38924=CARTESIAN_POINT('Ctrl Pts',(62.686787843468,17.0756569439774,6.3958317144828));
#38925=CARTESIAN_POINT('Ctrl Pts',(63.3426698111255,14.0238547895745,7.77518305050392));
#38926=CARTESIAN_POINT('Ctrl Pts',(63.3426674304337,13.4198463471001,11.1339717058281));
#38927=CARTESIAN_POINT('Ctrl Pts',(62.552433017135,15.7650240000834,13.4838568188229));
#38928=CARTESIAN_POINT('Ctrl Pts',(61.540694761931,18.936865245129,12.7341264791949));
#38929=CARTESIAN_POINT('Ctrl Pts',(61.0732543185778,20.0773594018982,9.55182253210507));
#38930=CARTESIAN_POINT('Ctrl Pts',(61.4316477881723,18.1357994369342,6.76826458716723));
#38931=CARTESIAN_POINT('Ctrl Pts',(62.1626591350493,14.8036106221425,6.86000957288757));
#38932=CARTESIAN_POINT('Ctrl Pts',(62.4815534974884,13.0094633319359,9.74542469319725));
#38933=CARTESIAN_POINT('Ctrl Pts',(61.9702551717097,14.3136373342297,12.8573464026032));
#38934=CARTESIAN_POINT('Ctrl Pts',(60.949326866107,17.5197763142875,13.4270461480336));
#38935=CARTESIAN_POINT('Ctrl Pts',(60.1927341524847,19.7394014348252,10.947712313481));
#38936=CARTESIAN_POINT('Ctrl Pts',(60.2392996738452,18.96159921589,7.62511676387808));
#38937=CARTESIAN_POINT('Ctrl Pts',(60.9131915231956,15.8425832679708,6.41562502038855));
#38938=CARTESIAN_POINT('Ctrl Pts',(61.4805994238642,13.1209708267227,8.39487325110957));
#38939=CARTESIAN_POINT('Ctrl Pts',(61.3021302305506,13.1830095964177,11.8028388367732));
#38940=CARTESIAN_POINT('Ctrl Pts',(60.4026582657957,15.9358673415302,13.6055385422089));
#38941=CARTESIAN_POINT('Ctrl Pts',(59.447210195013,18.8976307583478,12.2029441264611));
#38942=CARTESIAN_POINT('Ctrl Pts',(59.1533281063616,19.3903963172923,8.83503768583792));
#38943=CARTESIAN_POINT('Ctrl Pts',(59.4806667221929,17.7660737535059,7.2906822312505));
#38944=CARTESIAN_POINT('Ctrl Pts',(59.6819508576139,16.8135320242448,7.03077704625438));
#38945=CARTESIAN_POINT('Ctrl Pts',(67.0040126136404,20.2598690437801,11.1728309286207));
#38946=CARTESIAN_POINT('Ctrl Pts',(66.9555034255254,20.4203000043805,10.9082027524038));
#38947=CARTESIAN_POINT('Ctrl Pts',(66.9207835851305,20.5332184525385,10.6149904639444));
#38948=CARTESIAN_POINT('Ctrl Pts',(66.8813975908017,20.6611539455099,9.99178401342255));
#38949=CARTESIAN_POINT('Ctrl Pts',(66.8780249511107,20.6720025707686,9.66515229429171));
#38950=CARTESIAN_POINT('Ctrl Pts',(66.904675210205,20.5855924444283,9.00098486496477));
#38951=CARTESIAN_POINT('Ctrl Pts',(66.9367881932439,20.4815398383751,8.66883374311739));
#38952=CARTESIAN_POINT('Ctrl Pts',(67.0315956493191,20.1690707048657,8.06423785428611));
#38953=CARTESIAN_POINT('Ctrl Pts',(67.09312085238,19.9644265611134,7.79496359360553));
#38954=CARTESIAN_POINT('Ctrl Pts',(67.2425937581436,19.4553169386786,7.32570054462924));
#38955=CARTESIAN_POINT('Ctrl Pts',(67.33085397004,19.148781829213,7.13688275745713));
#38956=CARTESIAN_POINT('Ctrl Pts',(67.4238662472344,18.8154792730625,7.01293629783555));
#38957=CARTESIAN_POINT('Ctrl Pts',(66.709565290414,15.2652009106025,9.99881345470567));
#38958=CARTESIAN_POINT('Ctrl Pts',(66.7141255555458,15.2659775128488,9.92620926472459));
#38959=CARTESIAN_POINT('Ctrl Pts',(66.7178306708093,15.2699455778512,9.85363960672269));
#38960=CARTESIAN_POINT('Ctrl Pts',(66.7206515257331,15.2772137473688,9.78136734601481));
#38961=CARTESIAN_POINT('Ctrl Pts',(66.752566372114,15.3594450282717,8.96368683410324));
#38962=CARTESIAN_POINT('Ctrl Pts',(66.6712922345579,15.8641033480846,8.1840744069183));
#38963=CARTESIAN_POINT('Ctrl Pts',(66.5353761067088,16.5726883518979,7.78933375549813));
#38964=CARTESIAN_POINT('Ctrl Pts',(66.3994599788597,17.2812733557112,7.39459310407795));
#38965=CARTESIAN_POINT('Ctrl Pts',(66.2089018607174,18.193785043525,7.38472422842254));
#38966=CARTESIAN_POINT('Ctrl Pts',(66.0708634238267,18.9102906125109,7.76413764787119));
#38967=CARTESIAN_POINT('Ctrl Pts',(65.932824986936,19.6267961814968,8.14355106731984));
#38968=CARTESIAN_POINT('Ctrl Pts',(65.8473062312967,20.147295631655,8.91224678187255));
#38969=CARTESIAN_POINT('Ctrl Pts',(65.8747431444716,20.246238786796,9.72822620930753));
#38970=CARTESIAN_POINT('Ctrl Pts',(65.9021800576464,20.345181941937,10.5442056367425));
#38971=CARTESIAN_POINT('Ctrl Pts',(66.0425726396353,20.0225688020609,11.4074687770597));
#38972=CARTESIAN_POINT('Ctrl Pts',(66.2558562834075,19.4279225161918,11.9340732703408));
#38973=CARTESIAN_POINT('Ctrl Pts',(66.4691399271798,18.8332762303227,12.4606777636219));
#38974=CARTESIAN_POINT('Ctrl Pts',(66.7553146327353,17.9665967984606,12.6506236098669));
#38975=CARTESIAN_POINT('Ctrl Pts',(67.0094701965008,17.2194144305738,12.4192427536871));
#38976=CARTESIAN_POINT('Ctrl Pts',(67.2636257602663,16.472232062687,12.1878618975073));
#38977=CARTESIAN_POINT('Ctrl Pts',(67.4857621822417,15.8445467587755,11.5351543389028));
#38978=CARTESIAN_POINT('Ctrl Pts',(67.5994444228594,15.6216179699845,10.7518245719412));
#38979=CARTESIAN_POINT('Ctrl Pts',(67.6344914472383,15.5528913979793,10.5103323450966));
#38980=CARTESIAN_POINT('Ctrl Pts',(67.6592307340631,15.5226338262371,10.2564254798708));
#38981=CARTESIAN_POINT('Ctrl Pts',(67.6742507328171,15.5286491313886,10.0019962882659));
#38982=CARTESIAN_POINT('Ctrl Pts',(59.6819508576139,16.8135320242449,7.0307770462544));
#38983=CARTESIAN_POINT('Ctrl Pts',(59.6574023990872,16.905148118714,7.06547285383208));
#38984=CARTESIAN_POINT('Ctrl Pts',(59.633381623744,16.9947948727323,7.10515219318508));
#38985=CARTESIAN_POINT('Ctrl Pts',(59.6099513655634,17.0822377866965,7.14949694327549));
#38986=CARTESIAN_POINT('Ctrl Pts',(59.5861978454406,17.1708871306533,7.1944535077954));
#38987=CARTESIAN_POINT('Ctrl Pts',(59.5630510759273,17.2572720505083,7.24420580541868));
#38988=CARTESIAN_POINT('Ctrl Pts',(59.540585329437,17.3411153578402,7.2984630034136));
#38989=CARTESIAN_POINT('Ctrl Pts',(59.5341747454294,17.3650399830626,7.31394525440008));
#38990=CARTESIAN_POINT('Ctrl Pts',(59.5278196764501,17.3887574233789,7.32979452699793));
#38991=CARTESIAN_POINT('Ctrl Pts',(59.5215220078066,17.4122606427255,7.34600453501649));
#38992=CARTESIAN_POINT('Ctrl Pts',(59.5165727272894,17.4307316090769,7.358743832908));
#38993=CARTESIAN_POINT('Ctrl Pts',(59.5116584066524,17.4490721033785,7.37170741276992));
#38994=CARTESIAN_POINT('Ctrl Pts',(59.5067848207907,17.4672605734295,7.38487881885917));
#38995=CARTESIAN_POINT('Ctrl Pts',(59.4853806969507,17.547141851092,7.44272583645177));
#38996=CARTESIAN_POINT('Ctrl Pts',(59.4647409044082,17.6241706055182,7.50463022489488));
#38997=CARTESIAN_POINT('Ctrl Pts',(59.4449347986959,17.6980879983368,7.57029723790349));
#38998=CARTESIAN_POINT('Ctrl Pts',(59.4299001526504,17.7541980612524,7.62014450782053));
#38999=CARTESIAN_POINT('Ctrl Pts',(59.4153460633656,17.8085146619212,7.6721607780437));
#39000=CARTESIAN_POINT('Ctrl Pts',(59.401307177695,17.8609084965252,7.7262283086775));
#39001=CARTESIAN_POINT('Ctrl Pts',(59.3940669983074,17.8879292138559,7.75411218992159));
#39002=CARTESIAN_POINT('Ctrl Pts',(59.3869639127158,17.9144382901743,7.78254177971635));
#39003=CARTESIAN_POINT('Ctrl Pts',(59.3800031152495,17.9404163399798,7.81150163907493));
#39004=CARTESIAN_POINT('Ctrl Pts',(59.377069260484,17.9513656350265,7.82370771485813));
#39005=CARTESIAN_POINT('Ctrl Pts',(59.3741603923946,17.9622216785285,7.83600935578381));
#39006=CARTESIAN_POINT('Ctrl Pts',(59.3712797968968,17.9729722072825,7.84839276353972));
#39007=CARTESIAN_POINT('Ctrl Pts',(59.3542405470275,18.0365635535174,7.92164288808634));
#39008=CARTESIAN_POINT('Ctrl Pts',(59.338167291009,18.0965497616217,7.99784282404939));
#39009=CARTESIAN_POINT('Ctrl Pts',(59.3231234327018,18.152694205166,8.07671631200185));
#39010=CARTESIAN_POINT('Ctrl Pts',(59.3083518044045,18.2078226724821,8.15416252445319));
#39011=CARTESIAN_POINT('Ctrl Pts',(59.2945725637949,18.259247498527,8.23418719385315));
#39012=CARTESIAN_POINT('Ctrl Pts',(59.2818571864781,18.3067019327104,8.31655061029));
#39013=CARTESIAN_POINT('Ctrl Pts',(59.2693830443537,18.3532560648998,8.39735143411931));
#39014=CARTESIAN_POINT('Ctrl Pts',(59.2579327073364,18.3959893044119,8.48040377661436));
#39015=CARTESIAN_POINT('Ctrl Pts',(59.2475859888077,18.4346037836527,8.56549184091671));
#39016=CARTESIAN_POINT('Ctrl Pts',(59.2424064366885,18.4539341353218,8.60808680110125));
#39017=CARTESIAN_POINT('Ctrl Pts',(59.2375036517524,18.4722315778021,8.6511920152124));
#39018=CARTESIAN_POINT('Ctrl Pts',(59.2328889291418,18.4894539570476,8.69478065069042));
#39019=CARTESIAN_POINT('Ctrl Pts',(59.2306690826426,18.4977385369678,8.71574834215067));
#39020=CARTESIAN_POINT('Ctrl Pts',(59.2285159056722,18.505774302819,8.73682789437621));
#39021=CARTESIAN_POINT('Ctrl Pts',(59.2264307309096,18.5135562809755,8.75801630674609));
#39022=CARTESIAN_POINT('Ctrl Pts',(59.2250997041795,18.5185237403585,8.77154147678875));
#39023=CARTESIAN_POINT('Ctrl Pts',(59.2237963942956,18.5233877590632,8.78511114991627));
#39024=CARTESIAN_POINT('Ctrl Pts',(59.222522397681,18.5281423791575,8.79871063713888));
#39025=CARTESIAN_POINT('Ctrl Pts',(59.2143322655506,18.5587083683889,8.88613755490554));
#39026=CARTESIAN_POINT('Ctrl Pts',(59.2073383924974,18.5848098579651,8.97493705383762));
#39027=CARTESIAN_POINT('Ctrl Pts',(59.2016063055609,18.6062022976455,9.06488740616719));
#39028=CARTESIAN_POINT('Ctrl Pts',(59.2009154354341,18.6087806600602,9.07572883477923));
#39029=CARTESIAN_POINT('Ctrl Pts',(59.200242910756,18.6112905563283,9.08658699329483));
#39030=CARTESIAN_POINT('Ctrl Pts',(59.1995888595069,18.6137315088206,9.09746150181125));
#39031=CARTESIAN_POINT('Ctrl Pts',(59.1940765541311,18.63430371255,9.18911121861839));
#39032=CARTESIAN_POINT('Ctrl Pts',(59.1898752976095,18.6499830153444,9.28192246232436));
#39033=CARTESIAN_POINT('Ctrl Pts',(59.1869573634513,18.660872893876,9.37550443036629));
#39034=CARTESIAN_POINT('Ctrl Pts',(59.1839372837924,18.6721439846059,9.47236233832445));
#39035=CARTESIAN_POINT('Ctrl Pts',(59.1822919652802,18.6782843968879,9.57004704527203));
#39036=CARTESIAN_POINT('Ctrl Pts',(59.1820051755357,18.6793547107854,9.66811274307554));
#39037=CARTESIAN_POINT('Ctrl Pts',(59.1818653628562,18.679876498809,9.7159206868577));
#39038=CARTESIAN_POINT('Ctrl Pts',(59.1820486386194,18.6791925043489,9.76381888085402));
#39039=CARTESIAN_POINT('Ctrl Pts',(59.1825542820089,18.6773054175288,9.81175333276414));
#39040=CARTESIAN_POINT('Ctrl Pts',(59.1827037214712,18.6767477018626,9.82592003378259));
#39041=CARTESIAN_POINT('Ctrl Pts',(59.1828813434833,18.6760848074891,9.84008999153942));
#39042=CARTESIAN_POINT('Ctrl Pts',(59.1830868741632,18.6753177565492,9.85424725726874));
#39043=CARTESIAN_POINT('Ctrl Pts',(59.1844353908751,18.6702850236656,9.94713513872897));
#39044=CARTESIAN_POINT('Ctrl Pts',(59.1869856678166,18.6607672605466,10.0396336499573));
#39045=CARTESIAN_POINT('Ctrl Pts',(59.1907077256037,18.6468763517762,10.1313703615392));
#39046=CARTESIAN_POINT('Ctrl Pts',(59.1944191075896,18.6330252856387,10.2228439490746));
#39047=CARTESIAN_POINT('Ctrl Pts',(59.1992956613142,18.6148257393727,10.3135610439828));
#39048=CARTESIAN_POINT('Ctrl Pts',(59.2053202323847,18.5923417340437,10.4031353914207));
#39049=CARTESIAN_POINT('Ctrl Pts',(59.2112410581269,18.570244911551,10.4911672356704));
#39050=CARTESIAN_POINT('Ctrl Pts',(59.2182708208297,18.544009479979,10.5780961326744));
#39051=CARTESIAN_POINT('Ctrl Pts',(59.2264037185759,18.5136570923772,10.6635263260514));
#39052=CARTESIAN_POINT('Ctrl Pts',(59.2303039432159,18.4991012558599,10.7044953577056));
#39053=CARTESIAN_POINT('Ctrl Pts',(59.2344580112977,18.4835980627207,10.7451192126333));
#39054=CARTESIAN_POINT('Ctrl Pts',(59.2388660433661,18.4671470630801,10.7853510166313));
#39055=CARTESIAN_POINT('Ctrl Pts',(59.2403491923144,18.4616118758496,10.7988876145655));
#39056=CARTESIAN_POINT('Ctrl Pts',(59.2418610961089,18.4559693740725,10.81237980913));
#39057=CARTESIAN_POINT('Ctrl Pts',(59.2434017709825,18.4502194971662,10.8258257525424));
#39058=CARTESIAN_POINT('Ctrl Pts',(59.2448672510403,18.4447502511329,10.8386154476733));
#39059=CARTESIAN_POINT('Ctrl Pts',(59.2463583030217,18.4391855693816,10.8513591684399));
#39060=CARTESIAN_POINT('Ctrl Pts',(59.2478738644618,18.4335294170853,10.8640470923383));
#39061=CARTESIAN_POINT('Ctrl Pts',(59.2575294211935,18.3974943887873,10.9448811421958));
#39062=CARTESIAN_POINT('Ctrl Pts',(59.2681907321678,18.357705834556,11.0235565044334));
#39063=CARTESIAN_POINT('Ctrl Pts',(59.2798413572467,18.3142251098216,11.0997253741218));
#39064=CARTESIAN_POINT('Ctrl Pts',(59.2912990837899,18.271464292223,11.1746331214818));
#39065=CARTESIAN_POINT('Ctrl Pts',(59.3037137501258,18.2251321266983,11.247117361503));
#39066=CARTESIAN_POINT('Ctrl Pts',(59.3170791893599,18.1752516284115,11.3168132023689));
#39067=CARTESIAN_POINT('Ctrl Pts',(59.3300579264205,18.1268143222831,11.384492533888));
#39068=CARTESIAN_POINT('Ctrl Pts',(59.3439333262358,18.0750306251971,11.4495429421988));
#39069=CARTESIAN_POINT('Ctrl Pts',(59.3587070803994,18.0198942240399,11.5115898445996));
#39070=CARTESIAN_POINT('Ctrl Pts',(59.361378450579,18.009924534804,11.5228090812926));
#39071=CARTESIAN_POINT('Ctrl Pts',(59.3640792101803,17.9998451627528,11.5339299974755));
#39072=CARTESIAN_POINT('Ctrl Pts',(59.3668093915945,17.9896559870011,11.5449502145347));
#39073=CARTESIAN_POINT('Ctrl Pts',(59.3747124158147,17.9601614990778,11.5768503080151));
#39074=CARTESIAN_POINT('Ctrl Pts',(59.3828619650632,17.9297469672235,11.6079068412473));
#39075=CARTESIAN_POINT('Ctrl Pts',(59.3912467107623,17.8984546702662,11.6380966037226));
#39076=CARTESIAN_POINT('Ctrl Pts',(68.1281291851066,15.0750265266586,10.0024371765582));
#39077=CARTESIAN_POINT('Ctrl Pts',(68.1132191003536,15.0686010168709,10.3130580784043));
#39078=CARTESIAN_POINT('Ctrl Pts',(67.9995899840861,15.229260839257,11.6285356953996));
#39079=CARTESIAN_POINT('Ctrl Pts',(67.3992512291335,17.0050066526372,13.4679206448302));
#39080=CARTESIAN_POINT('Ctrl Pts',(66.3844685224502,20.1882099452846,12.7722321938662));
#39081=CARTESIAN_POINT('Ctrl Pts',(65.9036218913761,21.3787366757644,9.61047736356028));
#39082=CARTESIAN_POINT('Ctrl Pts',(66.2501895556748,19.4813112170046,6.79508159949543));
#39083=CARTESIAN_POINT('Ctrl Pts',(66.9814704044652,16.1481166073795,6.83122696910049));
#39084=CARTESIAN_POINT('Ctrl Pts',(67.2119040522751,14.8676525643411,8.81893895087672));
#39085=CARTESIAN_POINT('Ctrl Pts',(67.1683025391241,14.8112407741816,9.90991228406404));
#39086=CARTESIAN_POINT('Ctrl Pts',(67.1637176864735,14.810555933805,9.99855140140544));
#39087=CARTESIAN_POINT('Origin',(69.7479810832458,18.6889152049569,10.));
#39088=CARTESIAN_POINT('Ctrl Pts',(68.2083503098983,15.0969161422106,9.99673640007591));
#39089=CARTESIAN_POINT('Ctrl Pts',(68.1711103559359,15.0927295232038,10.7130675867));
#39090=CARTESIAN_POINT('Ctrl Pts',(67.9289066052253,15.6514186592595,12.4513417391717));
#39091=CARTESIAN_POINT('Ctrl Pts',(67.0483943376965,18.3902480628713,13.5944453497599));
#39092=CARTESIAN_POINT('Ctrl Pts',(66.1687987195556,21.0667649555471,11.6442225433397));
#39093=CARTESIAN_POINT('Ctrl Pts',(66.036013638459,20.9561469803459,8.22016494780576));
#39094=CARTESIAN_POINT('Ctrl Pts',(66.6336669557833,18.1194957904382,6.39071567224367));
#39095=CARTESIAN_POINT('Ctrl Pts',(67.2173089746449,15.4027596845032,7.6368119452057));
#39096=CARTESIAN_POINT('Ctrl Pts',(67.2747579502335,14.8518622987657,9.32892113065761));
#39097=CARTESIAN_POINT('Ctrl Pts',(67.242349320473,14.8383776097513,10.0022118830713));
#39098=CARTESIAN_POINT('Ctrl Pts',(67.8425423025985,17.244983442153,7.06170475438608));
#39099=CARTESIAN_POINT('Ctrl Pts',(68.0419164156808,16.2988495743024,7.35795147289591));
#39100=CARTESIAN_POINT('Ctrl Pts',(68.3551165744735,14.725851572522,8.97144797270223));
#39101=CARTESIAN_POINT('Ctrl Pts',(68.023655252025,15.3567034243025,12.3283366156213));
#39102=CARTESIAN_POINT('Ctrl Pts',(67.0483943376965,18.3902480628713,13.5944453497599));
#39103=CARTESIAN_POINT('Ctrl Pts',(66.1687987195556,21.0667649555471,11.6442225433397));
#39104=CARTESIAN_POINT('Ctrl Pts',(66.036013638459,20.9561469803459,8.22016494780576));
#39105=CARTESIAN_POINT('Ctrl Pts',(66.6336669557833,18.1194957904382,6.39071567224367));
#39106=CARTESIAN_POINT('Ctrl Pts',(67.2905946547074,15.0616295968133,7.79327945411721));
#39107=CARTESIAN_POINT('Ctrl Pts',(67.282863942121,14.4843023646231,11.1722569386416));
#39108=CARTESIAN_POINT('Ctrl Pts',(66.4816292855382,16.868372167434,13.5013274912989));
#39109=CARTESIAN_POINT('Ctrl Pts',(65.468753391891,20.0422978199459,12.6947822329673));
#39110=CARTESIAN_POINT('Ctrl Pts',(65.0155990043222,21.1273143736846,9.47487431060687));
#39111=CARTESIAN_POINT('Ctrl Pts',(65.3922823621304,19.1153342996381,6.72525821930946));
#39112=CARTESIAN_POINT('Ctrl Pts',(66.1257396929251,15.7718556315866,6.9083705731136));
#39113=CARTESIAN_POINT('Ctrl Pts',(66.4233986629547,14.0547985877671,9.86022990097494));
#39114=CARTESIAN_POINT('Ctrl Pts',(65.8829690009265,15.4655309000317,12.9372608391342));
#39115=CARTESIAN_POINT('Ctrl Pts',(64.852721554462,18.704288070265,13.3837942299379));
#39116=CARTESIAN_POINT('Ctrl Pts',(64.1195886430847,20.8341986998846,10.7999310727631));
#39117=CARTESIAN_POINT('Ctrl Pts',(64.2044184759422,19.9114308093214,7.49968047567758));
#39118=CARTESIAN_POINT('Ctrl Pts',(64.8955230826759,16.7260146593053,6.43862003923501));
#39119=CARTESIAN_POINT('Ctrl Pts',(65.4382581333965,14.0943212306268,8.56699487612852));
#39120=CARTESIAN_POINT('Ctrl Pts',(65.2108533475991,14.3368288007655,11.9787141005062));
#39121=CARTESIAN_POINT('Ctrl Pts',(64.2812461473764,17.199991458738,13.6183729089162));
#39122=CARTESIAN_POINT('Ctrl Pts',(63.346239485481,20.0833051820057,12.017555775347));
#39123=CARTESIAN_POINT('Ctrl Pts',(63.1074718691846,20.3682194128848,8.60989310618131));
#39124=CARTESIAN_POINT('Ctrl Pts',(63.6430568297551,17.7632104839249,6.4471568308768));
#39125=CARTESIAN_POINT('Ctrl Pts',(64.3376274439251,14.564859018057,7.46621057361501));
#39126=CARTESIAN_POINT('Ctrl Pts',(64.4334353369931,13.60112044902,10.7544289031929));
#39127=CARTESIAN_POINT('Ctrl Pts',(63.708961052588,15.6987166428558,13.3670096553836));
#39128=CARTESIAN_POINT('Ctrl Pts',(62.6772983776882,18.9427555175133,12.9642257537709));
#39129=CARTESIAN_POINT('Ctrl Pts',(62.1266472347557,20.3916349158421,9.9067950074971));
#39130=CARTESIAN_POINT('Ctrl Pts',(62.4144320750886,18.7114286257305,6.93283507366395));
#39131=CARTESIAN_POINT('Ctrl Pts',(63.1472062543101,15.3704995140598,6.70571036393744));
#39132=CARTESIAN_POINT('Ctrl Pts',(63.5330077514078,13.3244900809145,9.42882503807144));
#39133=CARTESIAN_POINT('Ctrl Pts',(63.0906099643739,14.3693624549396,12.6634621126407));
#39134=CARTESIAN_POINT('Ctrl Pts',(62.080489794707,17.5330036055456,13.5128046754735));
#39135=CARTESIAN_POINT('Ctrl Pts',(61.2715545195409,19.9458125081592,11.2162142452876));
#39136=CARTESIAN_POINT('Ctrl Pts',(61.2525379570576,19.4106046411913,7.83042882970038));
#39137=CARTESIAN_POINT('Ctrl Pts',(61.9047530097005,16.3703262829254,6.38762845988019));
#39138=CARTESIAN_POINT('Ctrl Pts',(62.5083833543796,13.5113685232517,8.17992871548476));
#39139=CARTESIAN_POINT('Ctrl Pts',(62.3871231598861,13.357739085696,11.6022164308586));
#39140=CARTESIAN_POINT('Ctrl Pts',(61.5138509672066,16.0106566332716,13.5896176377583));
#39141=CARTESIAN_POINT('Ctrl Pts',(60.5349179618126,19.0579057022675,12.3623010109723));
#39142=CARTESIAN_POINT('Ctrl Pts',(60.1913020034494,19.734119272829,9.01938609588907));
#39143=CARTESIAN_POINT('Ctrl Pts',(60.6550135466888,17.3973455890623,6.55469600728483));
#39144=CARTESIAN_POINT('Ctrl Pts',(61.3750552367845,14.1039347737162,7.1754379864716));
#39145=CARTESIAN_POINT('Ctrl Pts',(61.5708627210562,12.7669926495712,10.3258507409623));
#39146=CARTESIAN_POINT('Ctrl Pts',(60.9313710113775,14.5474295567701,13.1842383274677));
#39147=CARTESIAN_POINT('Ctrl Pts',(59.8935459365979,17.8144668208753,13.1913616605739));
#39148=CARTESIAN_POINT('Ctrl Pts',(59.2511484715134,19.6057481548832,10.3395770770156));
#39149=CARTESIAN_POINT('Ctrl Pts',(59.4436819065863,18.2810249486939,7.18539898656543));
#39150=CARTESIAN_POINT('Ctrl Pts',(60.1631753733451,14.9896601306954,6.54837069990779));
#39151=CARTESIAN_POINT('Ctrl Pts',(60.629216203114,12.6441934312551,9.0096983771865));
#39152=CARTESIAN_POINT('Ctrl Pts',(60.402326566927,13.0868379849885,11.2296927240265));
#39153=CARTESIAN_POINT('Ctrl Pts',(60.181950026368,13.707234883037,11.9973015569304));
#39154=CARTESIAN_POINT('Ctrl Pts',(67.9318278742783,17.3251900988197,7.23888518457547));
#39155=CARTESIAN_POINT('Ctrl Pts',(68.1161335763132,16.4352923065869,7.51726810226198));
#39156=CARTESIAN_POINT('Ctrl Pts',(68.4043554971943,14.9555143577762,9.03347008941797));
#39157=CARTESIAN_POINT('Ctrl Pts',(68.0837432245498,15.5458770044744,12.1879369455074));
#39158=CARTESIAN_POINT('Ctrl Pts',(67.1581527442329,18.3940490596782,13.3776987943165));
#39159=CARTESIAN_POINT('Ctrl Pts',(66.3224589027986,20.9067222911425,11.5450752374347));
#39160=CARTESIAN_POINT('Ctrl Pts',(66.1885426111956,20.800326051025,8.32748974461938));
#39161=CARTESIAN_POINT('Ctrl Pts',(66.7410189775958,18.1322775372971,6.60835702425631));
#39162=CARTESIAN_POINT('Ctrl Pts',(67.3491954556354,15.256353376944,7.92634562444538));
#39163=CARTESIAN_POINT('Ctrl Pts',(67.3327927019053,14.7113906429075,11.1015693557681));
#39164=CARTESIAN_POINT('Ctrl Pts',(66.5707346233278,16.9492514661364,13.2901959816018));
#39165=CARTESIAN_POINT('Ctrl Pts',(65.609797362651,19.9293395015267,12.5322857391188));
#39166=CARTESIAN_POINT('Ctrl Pts',(65.1748301675256,20.9464805290195,9.50653960894237));
#39167=CARTESIAN_POINT('Ctrl Pts',(65.5196611552341,19.0533751185266,6.92272651604651));
#39168=CARTESIAN_POINT('Ctrl Pts',(66.1997524963878,15.9090610352117,7.09479711845808));
#39169=CARTESIAN_POINT('Ctrl Pts',(66.470324299897,14.2930946730788,9.86865809630686));
#39170=CARTESIAN_POINT('Ctrl Pts',(65.953344565804,15.6163106628564,12.7601427840874));
#39171=CARTESIAN_POINT('Ctrl Pts',(64.9760832641982,18.6573208483792,13.1797500249766));
#39172=CARTESIAN_POINT('Ctrl Pts',(64.2780203671544,20.656348402684,10.751694895066));
#39173=CARTESIAN_POINT('Ctrl Pts',(64.3485967193296,19.7867752262122,7.65045078699728));
#39174=CARTESIAN_POINT('Ctrl Pts',(64.9888892233674,16.7909924250966,6.6533727379157));
#39175=CARTESIAN_POINT('Ctrl Pts',(65.489758917571,14.3155426340161,8.65340568344619));
#39176=CARTESIAN_POINT('Ctrl Pts',(65.2669285289691,14.5409783214077,11.8593968140379));
#39177=CARTESIAN_POINT('Ctrl Pts',(64.3842388247346,17.2290425005878,13.4001835116647));
#39178=CARTESIAN_POINT('Ctrl Pts',(63.4964752486209,19.9360426274117,11.8958963196675));
#39179=CARTESIAN_POINT('Ctrl Pts',(63.2629672129437,20.2013278361943,8.69371713231472));
#39180=CARTESIAN_POINT('Ctrl Pts',(63.7571179704186,17.7509534583573,6.66139475745697));
#39181=CARTESIAN_POINT('Ctrl Pts',(64.4006674801973,14.7430153463369,7.61899913400436));
#39182=CARTESIAN_POINT('Ctrl Pts',(64.4815599109682,13.8349420404105,10.7089365253202));
#39183=CARTESIAN_POINT('Ctrl Pts',(63.7916335220749,15.8036037329021,13.1639775672763));
#39184=CARTESIAN_POINT('Ctrl Pts',(62.8130423308994,18.8495771338669,12.7854817031124));
#39185=CARTESIAN_POINT('Ctrl Pts',(62.2864574754684,20.2086399244908,9.91241530746257));
#39186=CARTESIAN_POINT('Ctrl Pts',(62.5477505634247,18.6273022002302,7.11778639941015));
#39187=CARTESIAN_POINT('Ctrl Pts',(63.2271999473304,15.4853839339819,6.90435740451559));
#39188=CARTESIAN_POINT('Ctrl Pts',(63.5805992467218,13.5603011489528,9.46326712676861));
#39189=CARTESIAN_POINT('Ctrl Pts',(63.1557400246278,14.5397187075307,12.5028542351256));
#39190=CARTESIAN_POINT('Ctrl Pts',(62.1973923166246,17.5101424007745,13.3009810867784));
#39191=CARTESIAN_POINT('Ctrl Pts',(61.4280979699796,19.775009344088,11.1428760184691));
#39192=CARTESIAN_POINT('Ctrl Pts',(61.4010899078139,19.2696261599639,7.96125487716923));
#39193=CARTESIAN_POINT('Ctrl Pts',(62.0048379141107,16.4102292811539,6.60545597208741));
#39194=CARTESIAN_POINT('Ctrl Pts',(62.5629308906206,13.721219293131,8.28967977390788));
#39195=CARTESIAN_POINT('Ctrl Pts',(62.4398445301463,13.5744051997983,11.5056021110758));
#39196=CARTESIAN_POINT('Ctrl Pts',(61.6100928089779,16.0649021365259,13.3731621953643));
#39197=CARTESIAN_POINT('Ctrl Pts',(60.6810516662198,18.9259522392798,12.219853273637));
#39198=CARTESIAN_POINT('Ctrl Pts',(60.3490176872815,19.5589412741757,9.07851752376018));
#39199=CARTESIAN_POINT('Ctrl Pts',(60.7756290245012,17.3606274442457,6.76244927662485));
#39200=CARTESIAN_POINT('Ctrl Pts',(61.4431136936917,14.2633621012124,7.34576025527717));
#39201=CARTESIAN_POINT('Ctrl Pts',(61.6179756985622,13.0045895703814,10.306201805224));
#39202=CARTESIAN_POINT('Ctrl Pts',(61.007907399655,14.6752168136493,12.9922274267495));
#39203=CARTESIAN_POINT('Ctrl Pts',(60.0235254038855,17.7428017915754,12.9989212198951));
#39204=CARTESIAN_POINT('Ctrl Pts',(59.4107265678368,19.4236195381877,10.3191004374818));
#39205=CARTESIAN_POINT('Ctrl Pts',(59.5825119500423,18.1763291194577,7.35512060290615));
#39206=CARTESIAN_POINT('Ctrl Pts',(60.249481453992,15.0809863992776,6.75650538792376));
#39207=CARTESIAN_POINT('Ctrl Pts',(60.6782816207908,12.8745037461489,9.06941397854048));
#39208=CARTESIAN_POINT('Ctrl Pts',(60.4589813868428,13.2888242651274,11.1555417393121));
#39209=CARTESIAN_POINT('Ctrl Pts',(60.2488475749171,13.8709947795085,11.8768634390785));
#39210=CARTESIAN_POINT('Ctrl Pts',(68.0211134459581,17.4053967554863,7.41606561476487));
#39211=CARTESIAN_POINT('Ctrl Pts',(68.1903507369457,16.5717350388713,7.67658473162805));
#39212=CARTESIAN_POINT('Ctrl Pts',(68.4535944199152,15.1851771430305,9.09549220613371));
#39213=CARTESIAN_POINT('Ctrl Pts',(68.1438311970747,15.7350505846462,12.0475372753934));
#39214=CARTESIAN_POINT('Ctrl Pts',(67.2679111507693,18.397850056485,13.160952238873));
#39215=CARTESIAN_POINT('Ctrl Pts',(66.4761190860415,20.7466796267379,11.4459279315297));
#39216=CARTESIAN_POINT('Ctrl Pts',(66.3410715839322,20.6445051217041,8.43481454143301));
#39217=CARTESIAN_POINT('Ctrl Pts',(66.8483709994082,18.145059284156,6.82599837626894));
#39218=CARTESIAN_POINT('Ctrl Pts',(67.4077962565635,15.4510771570748,8.05941179477355));
#39219=CARTESIAN_POINT('Ctrl Pts',(67.3827214616896,14.9384789211918,11.0308817728947));
#39220=CARTESIAN_POINT('Ctrl Pts',(66.6598399611173,17.0301307648387,13.0790644719047));
#39221=CARTESIAN_POINT('Ctrl Pts',(65.7508413334111,19.8163811831076,12.3697892452703));
#39222=CARTESIAN_POINT('Ctrl Pts',(65.3340613307291,20.7656466843542,9.53820490727789));
#39223=CARTESIAN_POINT('Ctrl Pts',(65.6470399483378,18.9914159374152,7.12019481278355));
#39224=CARTESIAN_POINT('Ctrl Pts',(66.2737652998504,16.0462664388369,7.28122366380258));
#39225=CARTESIAN_POINT('Ctrl Pts',(66.5172499368395,14.5313907583906,9.87708629163876));
#39226=CARTESIAN_POINT('Ctrl Pts',(66.0237201306813,15.767090425681,12.5830247290407));
#39227=CARTESIAN_POINT('Ctrl Pts',(65.0994449739345,18.6103536264936,12.9757058200153));
#39228=CARTESIAN_POINT('Ctrl Pts',(64.4364520912241,20.4784981054833,10.7034587173689));
#39229=CARTESIAN_POINT('Ctrl Pts',(64.492774962717,19.6621196431031,7.80122109831696));
#39230=CARTESIAN_POINT('Ctrl Pts',(65.0822553640588,16.8559701908878,6.8681254365964));
#39231=CARTESIAN_POINT('Ctrl Pts',(65.5412597017456,14.5367640374055,8.73981649076384));
#39232=CARTESIAN_POINT('Ctrl Pts',(65.323003710339,14.7451278420499,11.7400795275695));
#39233=CARTESIAN_POINT('Ctrl Pts',(64.4872315020929,17.2580935424376,13.1819941144132));
#39234=CARTESIAN_POINT('Ctrl Pts',(63.6467110117609,19.7887800728178,11.774236863988));
#39235=CARTESIAN_POINT('Ctrl Pts',(63.4184625567026,20.0344362595038,8.77754115844814));
#39236=CARTESIAN_POINT('Ctrl Pts',(63.8711791110823,17.7386964327898,6.87563268403714));
#39237=CARTESIAN_POINT('Ctrl Pts',(64.4637075164693,14.9211716746167,7.77178769439372));
#39238=CARTESIAN_POINT('Ctrl Pts',(64.5296844849434,14.068763631801,10.6634441474475));
#39239=CARTESIAN_POINT('Ctrl Pts',(63.8743059915617,15.9084908229483,12.960945479169));
#39240=CARTESIAN_POINT('Ctrl Pts',(62.9487862841108,18.7563987502206,12.6067376524539));
#39241=CARTESIAN_POINT('Ctrl Pts',(62.4462677161811,20.0256449331395,9.91803560742804));
#39242=CARTESIAN_POINT('Ctrl Pts',(62.6810690517609,18.5431757747299,7.30273772515635));
#39243=CARTESIAN_POINT('Ctrl Pts',(63.3071936403504,15.6002683539039,7.10300444509373));
#39244=CARTESIAN_POINT('Ctrl Pts',(63.6281907420359,13.7961122169911,9.49770921546578));
#39245=CARTESIAN_POINT('Ctrl Pts',(63.2208700848815,14.7100749601219,12.3422463576105));
#39246=CARTESIAN_POINT('Ctrl Pts',(62.3142948385424,17.4872811960033,13.0891574980833));
#39247=CARTESIAN_POINT('Ctrl Pts',(61.5846414204184,19.6042061800168,11.0695377916506));
#39248=CARTESIAN_POINT('Ctrl Pts',(61.5496418585701,19.1286476787366,8.0920809246381));
#39249=CARTESIAN_POINT('Ctrl Pts',(62.1049228185211,16.4501322793825,6.82328348429461));
#39250=CARTESIAN_POINT('Ctrl Pts',(62.6174784268616,13.9310700630103,8.39943083233102));
#39251=CARTESIAN_POINT('Ctrl Pts',(62.4925659004067,13.7910713139007,11.408987791293));
#39252=CARTESIAN_POINT('Ctrl Pts',(61.7063346507491,16.1191476397801,13.1567067529703));
#39253=CARTESIAN_POINT('Ctrl Pts',(60.8271853706271,18.7939987762921,12.0774055363016));
#39254=CARTESIAN_POINT('Ctrl Pts',(60.5067333711135,19.3837632755223,9.13764895163131));
#39255=CARTESIAN_POINT('Ctrl Pts',(60.8962445023137,17.3239092994291,6.97020254596486));
#39256=CARTESIAN_POINT('Ctrl Pts',(61.5111721505988,14.4227894287085,7.51608252408274));
#39257=CARTESIAN_POINT('Ctrl Pts',(61.6650886760682,13.2421864911916,10.2865528694857));
#39258=CARTESIAN_POINT('Ctrl Pts',(61.0844437879323,14.8030040705286,12.8002165260313));
#39259=CARTESIAN_POINT('Ctrl Pts',(60.1535048711732,17.6711367622755,12.8064807792163));
#39260=CARTESIAN_POINT('Ctrl Pts',(59.5703046641601,19.2414909214922,10.2986237979481));
#39261=CARTESIAN_POINT('Ctrl Pts',(59.7213419934983,18.0716332902215,7.52484221924688));
#39262=CARTESIAN_POINT('Ctrl Pts',(60.3357875346389,15.1723126678598,6.96464007593973));
#39263=CARTESIAN_POINT('Ctrl Pts',(60.7273470384677,13.1048140610428,9.12912957989445));
#39264=CARTESIAN_POINT('Ctrl Pts',(60.5156362067586,13.4908105452663,11.0813907545978));
#39265=CARTESIAN_POINT('Ctrl Pts',(60.3157451234662,14.0347546759799,11.7564253212267));
#39266=CARTESIAN_POINT('Ctrl Pts',(68.1103990176379,17.4856034121529,7.59324604495427));
#39267=CARTESIAN_POINT('Ctrl Pts',(68.2645678975782,16.7081777711558,7.83590136099412));
#39268=CARTESIAN_POINT('Ctrl Pts',(68.502833342636,15.4148399282848,9.15751432284947));
#39269=CARTESIAN_POINT('Ctrl Pts',(68.2039191695996,15.924224164818,11.9071376052795));
#39270=CARTESIAN_POINT('Ctrl Pts',(67.3776695573056,18.4016510532919,12.9442056834295));
#39271=CARTESIAN_POINT('Ctrl Pts',(66.6297792692845,20.5866369623332,11.3467806256248));
#39272=CARTESIAN_POINT('Ctrl Pts',(66.4936005566688,20.4886841923832,8.54213933824664));
#39273=CARTESIAN_POINT('Ctrl Pts',(66.9557230212208,18.1578410310149,7.04363972828156));
#39274=CARTESIAN_POINT('Ctrl Pts',(67.4663970574915,15.6458009372055,8.19247796510172));
#39275=CARTESIAN_POINT('Ctrl Pts',(67.432650221474,15.1655671994761,10.9601941900212));
#39276=CARTESIAN_POINT('Ctrl Pts',(66.7489452989068,17.1110100635411,12.8679329622076));
#39277=CARTESIAN_POINT('Ctrl Pts',(65.8918853041711,19.7034228646884,12.2072927514219));
#39278=CARTESIAN_POINT('Ctrl Pts',(65.4932924939326,20.5848128396891,9.5698702056134));
#39279=CARTESIAN_POINT('Ctrl Pts',(65.7744187414415,18.9294567563037,7.3176631095206));
#39280=CARTESIAN_POINT('Ctrl Pts',(66.3477781033131,16.1834718424621,7.46765020914705));
#39281=CARTESIAN_POINT('Ctrl Pts',(66.564175573782,14.7696868437023,9.8855144869707));
#39282=CARTESIAN_POINT('Ctrl Pts',(66.0940956955586,15.9178701885058,12.4059066739939));
#39283=CARTESIAN_POINT('Ctrl Pts',(65.2228066836707,18.5633864046078,12.7716616150541));
#39284=CARTESIAN_POINT('Ctrl Pts',(64.5948838152938,20.3006478082827,10.6552225396717));
#39285=CARTESIAN_POINT('Ctrl Pts',(64.6369532061044,19.537464059994,7.95199140963666));
#39286=CARTESIAN_POINT('Ctrl Pts',(65.1756215047502,16.9209479566792,7.08287813527709));
#39287=CARTESIAN_POINT('Ctrl Pts',(65.5927604859202,14.7579854407948,8.82622729808151));
#39288=CARTESIAN_POINT('Ctrl Pts',(65.3790788917089,14.9492773626922,11.6207622411012));
#39289=CARTESIAN_POINT('Ctrl Pts',(64.5902241794512,17.2871445842874,12.9638047171617));
#39290=CARTESIAN_POINT('Ctrl Pts',(63.7969467749009,19.6415175182239,11.6525774083085));
#39291=CARTESIAN_POINT('Ctrl Pts',(63.5739579004615,19.8675446828134,8.86136518458155));
#39292=CARTESIAN_POINT('Ctrl Pts',(63.985240251746,17.7264394072222,7.08987061061733));
#39293=CARTESIAN_POINT('Ctrl Pts',(64.5267475527414,15.0993280028965,7.92457625478306));
#39294=CARTESIAN_POINT('Ctrl Pts',(64.5778090589186,14.3025852231916,10.6179517695748));
#39295=CARTESIAN_POINT('Ctrl Pts',(63.9569784610487,16.0133779129945,12.7579133910617));
#39296=CARTESIAN_POINT('Ctrl Pts',(63.084530237322,18.6632203665742,12.4279936017954));
#39297=CARTESIAN_POINT('Ctrl Pts',(62.6060779568939,19.8426499417882,9.92365590739351));
#39298=CARTESIAN_POINT('Ctrl Pts',(62.8143875400969,18.4590493492297,7.48768905090255));
#39299=CARTESIAN_POINT('Ctrl Pts',(63.3871873333707,15.715152773826,7.30165148567187));
#39300=CARTESIAN_POINT('Ctrl Pts',(63.6757822373498,14.0319232850294,9.53215130416296));
#39301=CARTESIAN_POINT('Ctrl Pts',(63.2860001451354,14.8804312127131,12.1816384800953));
#39302=CARTESIAN_POINT('Ctrl Pts',(62.4311973604599,17.4644199912321,12.8773339093882));
#39303=CARTESIAN_POINT('Ctrl Pts',(61.7411848708572,19.4334030159456,10.9961995648321));
#39304=CARTESIAN_POINT('Ctrl Pts',(61.6981938093262,18.9876691975092,8.22290697210695));
#39305=CARTESIAN_POINT('Ctrl Pts',(62.2050077229314,16.490035277611,7.04111099650182));
#39306=CARTESIAN_POINT('Ctrl Pts',(62.6720259631025,14.1409208328896,8.50918189075416));
#39307=CARTESIAN_POINT('Ctrl Pts',(62.545287270667,14.007737428003,11.3123734715102));
#39308=CARTESIAN_POINT('Ctrl Pts',(61.8025764925203,16.1733931430344,12.9402513105764));
#39309=CARTESIAN_POINT('Ctrl Pts',(60.9733190750344,18.6620453133043,11.9349577989662));
#39310=CARTESIAN_POINT('Ctrl Pts',(60.6644490549456,19.208585276869,9.19678037950243));
#39311=CARTESIAN_POINT('Ctrl Pts',(61.016859980126,17.2871911546125,7.17795581530488));
#39312=CARTESIAN_POINT('Ctrl Pts',(61.579230607506,14.5822167562047,7.68640479288831));
#39313=CARTESIAN_POINT('Ctrl Pts',(61.7122016535742,13.4797834120018,10.2669039337474));
#39314=CARTESIAN_POINT('Ctrl Pts',(61.1609801762097,14.9307913274078,12.6082056253131));
#39315=CARTESIAN_POINT('Ctrl Pts',(60.283484338461,17.5994717329756,12.6140403385374));
#39316=CARTESIAN_POINT('Ctrl Pts',(59.7298827604835,19.0593623047967,10.2781471584144));
#39317=CARTESIAN_POINT('Ctrl Pts',(59.8601720369542,17.9669374609853,7.69456383558759));
#39318=CARTESIAN_POINT('Ctrl Pts',(60.4220936152857,15.263638936442,7.1727747639557));
#39319=CARTESIAN_POINT('Ctrl Pts',(60.7764124561445,13.3351243759366,9.18884518124842));
#39320=CARTESIAN_POINT('Ctrl Pts',(60.5722910266744,13.6927968254053,11.0072397698834));
#39321=CARTESIAN_POINT('Ctrl Pts',(60.3826426720153,14.1985145724514,11.6359872033748));
#39322=CARTESIAN_POINT('Ctrl Pts',(67.8425423025985,17.244983442153,7.06170475438608));
#39323=CARTESIAN_POINT('Ctrl Pts',(67.9363396049609,16.875980626074,7.20780006417486));
#39324=CARTESIAN_POINT('Ctrl Pts',(68.0195197262116,16.5358040823887,7.42431456480013));
#39325=CARTESIAN_POINT('Ctrl Pts',(68.150998080649,15.9848167458477,7.95780764621763));
#39326=CARTESIAN_POINT('Ctrl Pts',(68.2006822338607,15.7699411081761,8.25968161903159));
#39327=CARTESIAN_POINT('Ctrl Pts',(68.2646302810789,15.490561932004,8.88066242679754));
#39328=CARTESIAN_POINT('Ctrl Pts',(68.2826595052327,15.4103584669881,9.1849782015738));
#39329=CARTESIAN_POINT('Ctrl Pts',(68.2943569622715,15.3584337419011,9.79677072277276));
#39330=CARTESIAN_POINT('Ctrl Pts',(68.288855628865,15.3830449856443,10.0982078060303));
#39331=CARTESIAN_POINT('Ctrl Pts',(68.2546420063796,15.5341550196633,10.6858944634116));
#39332=CARTESIAN_POINT('Ctrl Pts',(68.2257386849337,15.661414646539,10.9661810334233));
#39333=CARTESIAN_POINT('Ctrl Pts',(68.1449424659489,16.0093499903205,11.4722931322537));
#39334=CARTESIAN_POINT('Ctrl Pts',(68.093295210955,16.2286900565758,11.6926718707977));
#39335=CARTESIAN_POINT('Ctrl Pts',(68.0322473001841,16.4806955947432,11.866918122357));
#39336=CARTESIAN_POINT('Ctrl Pts',(60.3826426720153,14.1985145724513,11.6359872033747));
#39337=CARTESIAN_POINT('Ctrl Pts',(60.3987291200773,14.1384791309705,11.5775783984626));
#39338=CARTESIAN_POINT('Ctrl Pts',(60.4139429451904,14.0817003626712,11.5159169743106));
#39339=CARTESIAN_POINT('Ctrl Pts',(60.4282806141769,14.0281914535512,11.4513790591422));
#39340=CARTESIAN_POINT('Ctrl Pts',(60.4429682456479,13.9733764666589,11.3852658635604));
#39341=CARTESIAN_POINT('Ctrl Pts',(60.4567365493875,13.9219924575684,11.3161335496589));
#39342=CARTESIAN_POINT('Ctrl Pts',(60.4695742653813,13.8740814492266,11.2443401959014));
#39343=CARTESIAN_POINT('Ctrl Pts',(60.4729336106476,13.8615442020125,11.2255534691022));
#39344=CARTESIAN_POINT('Ctrl Pts',(60.47622918927,13.8492449351532,11.2065843091125));
#39345=CARTESIAN_POINT('Ctrl Pts',(60.4794607015071,13.8371847672994,11.1874386951717));
#39346=CARTESIAN_POINT('Ctrl Pts',(60.482079000826,13.8274131412115,11.1719261597808));
#39347=CARTESIAN_POINT('Ctrl Pts',(60.4846553435296,13.8177980993441,11.1562969512741));
#39348=CARTESIAN_POINT('Ctrl Pts',(60.4871873136239,13.808348658309,11.1405686307327));
#39349=CARTESIAN_POINT('Ctrl Pts',(60.4994718283844,13.7625022250763,11.0642585722979));
#39350=CARTESIAN_POINT('Ctrl Pts',(60.5107256648705,13.7205023355303,10.9855425568516));
#39351=CARTESIAN_POINT('Ctrl Pts',(60.5209393771319,13.6823842424367,10.9048124959882));
#39352=CARTESIAN_POINT('Ctrl Pts',(60.5290925934109,13.6519560250385,10.8403687727283));
#39353=CARTESIAN_POINT('Ctrl Pts',(60.5365828860325,13.624001872411,10.774640568225));
#39354=CARTESIAN_POINT('Ctrl Pts',(60.5434011778913,13.5985556607734,10.7078100778602));
#39355=CARTESIAN_POINT('Ctrl Pts',(60.5456026096946,13.5903398054339,10.6862324202928));
#39356=CARTESIAN_POINT('Ctrl Pts',(60.5477339562792,13.5823855116918,10.6645397536815));
#39357=CARTESIAN_POINT('Ctrl Pts',(60.5497948181657,13.5746942704238,10.6427379461932));
#39358=CARTESIAN_POINT('Ctrl Pts',(60.5517587833252,13.5673646526643,10.6219612068108));
#39359=CARTESIAN_POINT('Ctrl Pts',(60.5536591514791,13.5602723821607,10.6010802055411));
#39360=CARTESIAN_POINT('Ctrl Pts',(60.5554929869877,13.5534284148699,10.5801302247449));
#39361=CARTESIAN_POINT('Ctrl Pts',(60.5631434154612,13.5248766271072,10.4927307121652));
#39362=CARTESIAN_POINT('Ctrl Pts',(60.5696451829914,13.5006117003455,10.4040498986825));
#39363=CARTESIAN_POINT('Ctrl Pts',(60.5749893942698,13.4806668323283,10.3144849189863));
#39364=CARTESIAN_POINT('Ctrl Pts',(60.5804161086993,13.4604140583591,10.2235372482481));
#39365=CARTESIAN_POINT('Ctrl Pts',(60.5846493808407,13.4446152716452,10.1316770968566));
#39366=CARTESIAN_POINT('Ctrl Pts',(60.5876690820151,13.4333455934388,10.0392871195015));
#39367=CARTESIAN_POINT('Ctrl Pts',(60.5906654794564,13.4221628859479,9.94761013698967));
#39368=CARTESIAN_POINT('Ctrl Pts',(60.5924670545761,13.4154393160677,9.85541054662176));
#39369=CARTESIAN_POINT('Ctrl Pts',(60.593041985977,13.4132936428687,9.76304299829284));
#39370=CARTESIAN_POINT('Ctrl Pts',(60.5933185830198,13.4122613686516,9.71860536507053));
#39371=CARTESIAN_POINT('Ctrl Pts',(60.593311080267,13.4122893693062,9.67412865761842));
#39372=CARTESIAN_POINT('Ctrl Pts',(60.5930148241964,13.4133950120139,9.62965173443852));
#39373=CARTESIAN_POINT('Ctrl Pts',(60.5929169928498,13.4137601235697,9.61496431461915));
#39374=CARTESIAN_POINT('Ctrl Pts',(60.5927876671177,13.4142427737727,9.60027687042694));
#39375=CARTESIAN_POINT('Ctrl Pts',(60.5926266609965,13.4148436567973,9.58559080097424));
#39376=CARTESIAN_POINT('Ctrl Pts',(60.592463879823,13.4154511644075,9.57074282126799));
#39377=CARTESIAN_POINT('Ctrl Pts',(60.5922688054872,13.41617919174,9.55590504938851));
#39378=CARTESIAN_POINT('Ctrl Pts',(60.5920414435162,13.4170277181673,9.54108357179352));
#39379=CARTESIAN_POINT('Ctrl Pts',(60.5905760164217,13.4224967665389,9.44555398627452));
#39380=CARTESIAN_POINT('Ctrl Pts',(60.5877696251729,13.4329703612654,9.35064220205595));
#39381=CARTESIAN_POINT('Ctrl Pts',(60.5836035771031,13.4485182643284,9.25674298398244));
#39382=CARTESIAN_POINT('Ctrl Pts',(60.5832473073999,13.4498478809622,9.24871296464536));
#39383=CARTESIAN_POINT('Ctrl Pts',(60.5828810865878,13.4512146356398,9.24069033917638));
#39384=CARTESIAN_POINT('Ctrl Pts',(60.5825048986307,13.4526185882087,9.2326753487807));
#39385=CARTESIAN_POINT('Ctrl Pts',(60.5782789204955,13.4683901533211,9.14263744743419));
#39386=CARTESIAN_POINT('Ctrl Pts',(60.5727962781625,13.4888516530674,9.05356331283375));
#39387=CARTESIAN_POINT('Ctrl Pts',(60.5661351124403,13.5137114619805,8.96568771725081));
#39388=CARTESIAN_POINT('Ctrl Pts',(60.559321511336,13.5391401674843,8.8758011598418));
#39389=CARTESIAN_POINT('Ctrl Pts',(60.5512747790317,13.5691709812787,8.78716792584701));
#39390=CARTESIAN_POINT('Ctrl Pts',(60.5420644901028,13.6035442475136,8.7000421273125));
#39391=CARTESIAN_POINT('Ctrl Pts',(60.5370098857317,13.6224082878388,8.65222750982204));
#39392=CARTESIAN_POINT('Ctrl Pts',(60.5316045998727,13.6425810892942,8.60486701434196));
#39393=CARTESIAN_POINT('Ctrl Pts',(60.5258584913738,13.664025858158,8.55800419900509));
#39394=CARTESIAN_POINT('Ctrl Pts',(60.524148933004,13.6704060168522,8.54406176854061));
#39395=CARTESIAN_POINT('Ctrl Pts',(60.5224089381384,13.6768997660958,8.53016150058375));
#39396=CARTESIAN_POINT('Ctrl Pts',(60.5206408847664,13.6834982311107,8.51632087024207));
#39397=CARTESIAN_POINT('Ctrl Pts',(60.5095968738589,13.7247150409368,8.42986642555251));
#39398=CARTESIAN_POINT('Ctrl Pts',(60.4974435460195,13.7700718779143,8.34560744572339));
#39399=CARTESIAN_POINT('Ctrl Pts',(60.4842687952566,13.8192407171385,8.26379708515597));
#39400=CARTESIAN_POINT('Ctrl Pts',(60.4708342616313,13.869379079204,8.1803735684824));
#39401=CARTESIAN_POINT('Ctrl Pts',(60.4563375465724,13.9234815563466,8.09949541069896));
#39402=CARTESIAN_POINT('Ctrl Pts',(60.4408576352497,13.9812533718997,8.02143790635972));
#39403=CARTESIAN_POINT('Ctrl Pts',(60.4252551512339,14.0394826349709,7.94276232880787));
#39404=CARTESIAN_POINT('Ctrl Pts',(60.4086537215957,14.101440013859,7.86695140824316));
#39405=CARTESIAN_POINT('Ctrl Pts',(60.3911214680452,14.1668712748806,7.79430622844769));
#39406=CARTESIAN_POINT('Ctrl Pts',(60.3818445738006,14.2014931155381,7.7558672651732));
#39407=CARTESIAN_POINT('Ctrl Pts',(60.3723068629811,14.2370883369045,7.71831504954584));
#39408=CARTESIAN_POINT('Ctrl Pts',(60.3625171760094,14.2736239460729,7.68169758919558));
#39409=CARTESIAN_POINT('Ctrl Pts',(60.3590313766341,14.2866331264466,7.66865926419253));
#39410=CARTESIAN_POINT('Ctrl Pts',(60.3555136231476,14.2997615611866,7.65573947754891));
#39411=CARTESIAN_POINT('Ctrl Pts',(60.3519642909609,14.3130078492403,7.64294048624275));
#39412=CARTESIAN_POINT('Ctrl Pts',(60.3492372904052,14.3231851538666,7.63310684583699));
#39413=CARTESIAN_POINT('Ctrl Pts',(60.3464919178874,14.3334310235887,7.62334556236901));
#39414=CARTESIAN_POINT('Ctrl Pts',(60.3437307199346,14.3437359546381,7.61366571077001));
#39415=CARTESIAN_POINT('Ctrl Pts',(60.3241830913251,14.4166886977762,7.54513815595856));
#39416=CARTESIAN_POINT('Ctrl Pts',(60.3038121512208,14.4927140812436,7.48057696383332));
#39417=CARTESIAN_POINT('Ctrl Pts',(60.2827016030933,14.5714997194312,7.42026729962752));
#39418=CARTESIAN_POINT('Ctrl Pts',(60.261564320174,14.6503851332198,7.35988125813867));
#39419=CARTESIAN_POINT('Ctrl Pts',(60.2396854082702,14.7320383440592,7.30375667536574));
#39420=CARTESIAN_POINT('Ctrl Pts',(60.217137186371,14.8161894538073,7.25220561167405));
#39421=CARTESIAN_POINT('Ctrl Pts',(60.1950163805995,14.8987454248511,7.20163173173175));
#39422=CARTESIAN_POINT('Ctrl Pts',(60.1722512295677,14.9837061251435,7.15545893497819));
#39423=CARTESIAN_POINT('Ctrl Pts',(60.1489011520715,15.0708498007199,7.11401788880129));
#39424=CARTESIAN_POINT('Ctrl Pts',(60.1416346893341,15.0979686088474,7.1011215796608));
#39425=CARTESIAN_POINT('Ctrl Pts',(60.1343115246348,15.1252990315773,7.088683816123));
#39426=CARTESIAN_POINT('Ctrl Pts',(60.1269333077644,15.1528349118068,7.0767154567206));
#39427=CARTESIAN_POINT('Ctrl Pts',(60.115868753157,15.1941283917649,7.05876741202421));
#39428=CARTESIAN_POINT('Ctrl Pts',(60.1046804027641,15.2358838838842,7.04187489341861));
#39429=CARTESIAN_POINT('Ctrl Pts',(60.0933772939441,15.2780676602837,7.02603075613024));
#39430=CARTESIAN_POINT('Ctrl Pts',(67.4086397233445,15.458048217099,10.0018117506529));
#39431=CARTESIAN_POINT('Ctrl Pts',(67.3922281881599,15.4516726940089,10.2792252787835));
#39432=CARTESIAN_POINT('Ctrl Pts',(67.364342691712,15.488118577317,10.5560719127008));
#39433=CARTESIAN_POINT('Ctrl Pts',(67.3243238737158,15.5698466331085,10.8168646145657));
#39434=CARTESIAN_POINT('Ctrl Pts',(67.2047485806183,15.8140481541644,11.5961071140833));
#39435=CARTESIAN_POINT('Ctrl Pts',(66.9768469397625,16.4625291088528,12.2320200381455));
#39436=CARTESIAN_POINT('Ctrl Pts',(66.7200527868787,17.2188383863881,12.4398697983789));
#39437=CARTESIAN_POINT('Ctrl Pts',(66.4632586339949,17.9751476639235,12.6477195586123));
#39438=CARTESIAN_POINT('Ctrl Pts',(66.177571969083,18.8392852643059,12.4275061550171));
#39439=CARTESIAN_POINT('Ctrl Pts',(65.9682965015873,19.4182523936639,11.8778290289181));
#39440=CARTESIAN_POINT('Ctrl Pts',(65.7590210340916,19.9972195230219,11.328151902819));
#39441=CARTESIAN_POINT('Ctrl Pts',(65.6261567640121,20.2910161813555,10.4490110542162));
#39442=CARTESIAN_POINT('Ctrl Pts',(65.6065790035572,20.162021829958,9.63407278056602));
#39443=CARTESIAN_POINT('Ctrl Pts',(65.5870012431022,20.0330274785606,8.81913450691581));
#39444=CARTESIAN_POINT('Ctrl Pts',(65.6807099922719,19.4812421174321,8.0683988082182));
#39445=CARTESIAN_POINT('Ctrl Pts',(65.8231242605019,18.747685284561,7.71802880880715));
#39446=CARTESIAN_POINT('Ctrl Pts',(65.965538528732,18.0141284516898,7.36765880939609));
#39447=CARTESIAN_POINT('Ctrl Pts',(66.1566583160225,17.0988001470759,7.41765450927157));
#39448=CARTESIAN_POINT('Ctrl Pts',(66.288284454746,16.4055051616424,7.84562973884659));
#39449=CARTESIAN_POINT('Ctrl Pts',(66.4199105934694,15.7122101762088,8.2736049684216));
#39450=CARTESIAN_POINT('Ctrl Pts',(66.4920430836257,15.2409485099556,9.07955972769615));
#39451=CARTESIAN_POINT('Ctrl Pts',(66.4497626823333,15.1966815676295,9.90260247183729));
#39452=CARTESIAN_POINT('Ctrl Pts',(66.4481055265245,15.194946550497,9.93486115488336));
#39453=CARTESIAN_POINT('Ctrl Pts',(66.4462726093384,15.1938674837542,9.96714608853559));
#39454=CARTESIAN_POINT('Ctrl Pts',(66.4442667934687,15.1934336836835,9.99943462192776));
#39455=CARTESIAN_POINT('Origin',(63.7511045350785,17.0820569767664,10.));
#39456=CARTESIAN_POINT('Origin',(59.8874012299222,16.0467807963563,10.));
#39457=CARTESIAN_POINT('Origin',(32.5,-56.2916512459885,7.));
#39458=CARTESIAN_POINT('Ctrl Pts',(33.0411029802559,-57.8673300091754,7.));
#39459=CARTESIAN_POINT('Ctrl Pts',(32.9847118979684,-57.8942994847502,7.));
#39460=CARTESIAN_POINT('Ctrl Pts',(32.926851576823,-57.9177556703938,7.));
#39461=CARTESIAN_POINT('Ctrl Pts',(32.8678400671121,-57.9378112590822,7.));
#39462=CARTESIAN_POINT('Ctrl Pts',(32.8304073365834,-57.9505331069156,7.));
#39463=CARTESIAN_POINT('Ctrl Pts',(32.7925106111617,-57.9618858706107,7.));
#39464=CARTESIAN_POINT('Ctrl Pts',(32.7542246213985,-57.9718900412709,7.));
#39465=CARTESIAN_POINT('Ctrl Pts',(32.7280436563274,-57.9787311558468,7.));
#39466=CARTESIAN_POINT('Ctrl Pts',(32.701680564454,-57.9849415097954,7.));
#39467=CARTESIAN_POINT('Ctrl Pts',(32.6751582392643,-57.9905258833636,7.));
#39468=CARTESIAN_POINT('Ctrl Pts',(32.6611164412593,-57.9934824358178,7.));
#39469=CARTESIAN_POINT('Ctrl Pts',(32.6470302109915,-57.9962633359852,7.));
#39470=CARTESIAN_POINT('Ctrl Pts',(32.6329169442101,-57.9988669117463,7.));
#39471=CARTESIAN_POINT('Ctrl Pts',(32.5680410961479,-58.010835025728,7.));
#39472=CARTESIAN_POINT('Ctrl Pts',(32.5025225397611,-58.0190759833501,7.));
#39473=CARTESIAN_POINT('Ctrl Pts',(32.4367003115489,-58.0236879112333,7.));
#39474=CARTESIAN_POINT('Ctrl Pts',(32.3892242862367,-58.0270143863598,7.));
#39475=CARTESIAN_POINT('Ctrl Pts',(32.3415895125008,-58.028451944497,7.));
#39476=CARTESIAN_POINT('Ctrl Pts',(32.2939162953792,-58.0280221779963,7.));
#39477=CARTESIAN_POINT('Ctrl Pts',(32.2808248417186,-58.0279041606153,7.));
#39478=CARTESIAN_POINT('Ctrl Pts',(32.2677304665503,-58.0276452537954,7.));
#39479=CARTESIAN_POINT('Ctrl Pts',(32.2546356186087,-58.0272457331356,7.));
#39480=CARTESIAN_POINT('Ctrl Pts',(32.2413147456947,-58.0268393165083,7.));
#39481=CARTESIAN_POINT('Ctrl Pts',(32.2280015696053,-58.0262876036841,7.));
#39482=CARTESIAN_POINT('Ctrl Pts',(32.2147036648802,-58.0255917126622,7.));
#39483=CARTESIAN_POINT('Ctrl Pts',(32.1469436447844,-58.0220457713574,7.));
#39484=CARTESIAN_POINT('Ctrl Pts',(32.079541568506,-58.014758960148,7.));
#39485=CARTESIAN_POINT('Ctrl Pts',(32.0128409971697,-58.0038315324587,7.));
#39486=CARTESIAN_POINT('Ctrl Pts',(31.9451753892729,-57.992746004666,7.));
#39487=CARTESIAN_POINT('Ctrl Pts',(31.8782306837704,-57.9779139314693,7.));
#39488=CARTESIAN_POINT('Ctrl Pts',(31.8123515210902,-57.9593890229558,7.));
#39489=CARTESIAN_POINT('Ctrl Pts',(31.7715359667913,-57.9479118824071,7.));
#39490=CARTESIAN_POINT('Ctrl Pts',(31.7311291966112,-57.9350162530871,7.));
#39491=CARTESIAN_POINT('Ctrl Pts',(31.6912132914401,-57.9207048672865,7.));
#39492=CARTESIAN_POINT('Ctrl Pts',(31.6585126282316,-57.9089804229803,7.));
#39493=CARTESIAN_POINT('Ctrl Pts',(31.6261413907848,-57.8963056503894,7.));
#39494=CARTESIAN_POINT('Ctrl Pts',(31.5941456454821,-57.8826781573685,7.));
#39495=CARTESIAN_POINT('Ctrl Pts',(31.5810720086376,-57.8771098890512,7.));
#39496=CARTESIAN_POINT('Ctrl Pts',(31.5680588096177,-57.871381337824,7.));
#39497=CARTESIAN_POINT('Ctrl Pts',(31.5551310605861,-57.8655025242476,7.));
#39498=CARTESIAN_POINT('Ctrl Pts',(31.490968379375,-57.8363249434884,7.));
#39499=CARTESIAN_POINT('Ctrl Pts',(31.4287956226581,-57.803402900412,7.));
#39500=CARTESIAN_POINT('Ctrl Pts',(31.3689686687732,-57.7668089348842,7.));
#39501=CARTESIAN_POINT('Ctrl Pts',(31.3623206919839,-57.7627426099644,7.));
#39502=CARTESIAN_POINT('Ctrl Pts',(31.3557016803175,-57.7586308923568,7.));
#39503=CARTESIAN_POINT('Ctrl Pts',(31.3491121238469,-57.7544738418221,7.));
#39504=CARTESIAN_POINT('Ctrl Pts',(31.2920857291914,-57.7184984912118,7.));
#39505=CARTESIAN_POINT('Ctrl Pts',(31.2372638568357,-57.6791321880063,7.));
#39506=CARTESIAN_POINT('Ctrl Pts',(31.1847406170453,-57.6367028360903,7.));
#39507=CARTESIAN_POINT('Ctrl Pts',(31.1282350066813,-57.591056443428,7.));
#39508=CARTESIAN_POINT('Ctrl Pts',(31.0743888197088,-57.5418647466871,7.));
#39509=CARTESIAN_POINT('Ctrl Pts',(31.0233480125428,-57.4894785917789,7.));
#39510=CARTESIAN_POINT('Ctrl Pts',(31.0140057592583,-57.4798900927929,7.));
#39511=CARTESIAN_POINT('Ctrl Pts',(31.0047575885043,-57.4701944343076,7.));
#39512=CARTESIAN_POINT('Ctrl Pts',(30.9956045330475,-57.4603935892201,7.));
#39513=CARTESIAN_POINT('Ctrl Pts',(30.9877334105821,-57.4519654034288,7.));
#39514=CARTESIAN_POINT('Ctrl Pts',(30.9799390127843,-57.4434662551244,7.));
#39515=CARTESIAN_POINT('Ctrl Pts',(30.972222708447,-57.4348989264989,7.));
#39516=CARTESIAN_POINT('Ctrl Pts',(30.9246610658009,-57.3820917529218,7.));
#39517=CARTESIAN_POINT('Ctrl Pts',(30.8800520830315,-57.326684922902,7.));
#39518=CARTESIAN_POINT('Ctrl Pts',(30.8384919344894,-57.2690469053851,7.));
#39519=CARTESIAN_POINT('Ctrl Pts',(30.7960555285534,-57.2101936434387,7.));
#39520=CARTESIAN_POINT('Ctrl Pts',(30.7567972003304,-57.1490134679121,7.));
#39521=CARTESIAN_POINT('Ctrl Pts',(30.7208469686892,-57.0858509476833,7.));
#39522=CARTESIAN_POINT('Ctrl Pts',(30.6846788710275,-57.0223056491995,7.));
#39523=CARTESIAN_POINT('Ctrl Pts',(30.6518584168246,-56.9567530680472,7.));
#39524=CARTESIAN_POINT('Ctrl Pts',(30.6225557950443,-56.8895077659752,7.));
#39525=CARTESIAN_POINT('Ctrl Pts',(30.61531398285,-56.8728888486576,7.));
#39526=CARTESIAN_POINT('Ctrl Pts',(30.6082872384635,-56.8561664060562,7.));
#39527=CARTESIAN_POINT('Ctrl Pts',(30.601478558356,-56.8393449408623,7.));
#39528=CARTESIAN_POINT('Ctrl Pts',(30.5961524552616,-56.8261863173984,7.));
#39529=CARTESIAN_POINT('Ctrl Pts',(30.5909593217401,-56.8129655378888,7.));
#39530=CARTESIAN_POINT('Ctrl Pts',(30.5859080296146,-56.7997050116615,7.));
#39531=CARTESIAN_POINT('Ctrl Pts',(30.5590883753464,-56.7292987235297,7.));
#39532=CARTESIAN_POINT('Ctrl Pts',(30.5362121102666,-56.6576494456512,7.));
#39533=CARTESIAN_POINT('Ctrl Pts',(30.5174063251175,-56.5851265992832,7.));
#39534=CARTESIAN_POINT('Ctrl Pts',(30.4985800832282,-56.512524863307,7.));
#39535=CARTESIAN_POINT('Ctrl Pts',(30.4838325489478,-56.4390467231888,7.));
#39536=CARTESIAN_POINT('Ctrl Pts',(30.4733321890522,-56.3650308463661,7.));
#39537=CARTESIAN_POINT('Ctrl Pts',(30.463070824065,-56.2926996182489,7.));
#39538=CARTESIAN_POINT('Ctrl Pts',(30.456865076811,-56.219853902728,7.));
#39539=CARTESIAN_POINT('Ctrl Pts',(30.4549187470152,-56.1467933164485,7.));
#39540=CARTESIAN_POINT('Ctrl Pts',(30.4545002099162,-56.1310824302986,7.));
#39541=CARTESIAN_POINT('Ctrl Pts',(30.4542788241661,-56.1153615760887,7.));
#39542=CARTESIAN_POINT('Ctrl Pts',(30.4542569357502,-56.0996336954518,7.));
#39543=CARTESIAN_POINT('Ctrl Pts',(30.4542384011808,-56.0863157149705,7.));
#39544=CARTESIAN_POINT('Ctrl Pts',(30.454362914285,-56.0729926961468,7.));
#39545=CARTESIAN_POINT('Ctrl Pts',(30.4546294175093,-56.0596661744469,7.));
#39546=CARTESIAN_POINT('Ctrl Pts',(30.8457462639859,-55.0728640868079,7.));
#39547=CARTESIAN_POINT('Ctrl Pts',(30.8954489009101,-55.0171697369459,7.));
#39548=CARTESIAN_POINT('Ctrl Pts',(30.9483278083151,-54.9645336576406,7.));
#39549=CARTESIAN_POINT('Ctrl Pts',(31.0040355064375,-54.9150549466841,7.));
#39550=CARTESIAN_POINT('Ctrl Pts',(31.0582842091666,-54.8668720927416,7.));
#39551=CARTESIAN_POINT('Ctrl Pts',(31.1152164855574,-54.8216833321804,7.));
#39552=CARTESIAN_POINT('Ctrl Pts',(31.1745316088326,-54.7796213191208,7.));
#39553=CARTESIAN_POINT('Ctrl Pts',(31.1877704598448,-54.7702332795547,7.));
#39554=CARTESIAN_POINT('Ctrl Pts',(31.2011298591295,-54.7609999648588,7.));
#39555=CARTESIAN_POINT('Ctrl Pts',(31.2146007862069,-54.751926999635,7.));
#39556=CARTESIAN_POINT('Ctrl Pts',(31.2764177227105,-54.710291935328,7.));
#39557=CARTESIAN_POINT('Ctrl Pts',(31.3404582876332,-54.6721113383667,7.));
#39558=CARTESIAN_POINT('Ctrl Pts',(31.4063841811862,-54.6375086613779,7.));
#39559=CARTESIAN_POINT('Ctrl Pts',(31.4526685058674,-54.6132153002982,7.));
#39560=CARTESIAN_POINT('Ctrl Pts',(31.4998826441907,-54.5906864700306,7.));
#39561=CARTESIAN_POINT('Ctrl Pts',(31.5479126485799,-54.5699799289933,7.));
#39562=CARTESIAN_POINT('Ctrl Pts',(31.5661734302878,-54.5621073995064,7.));
#39563=CARTESIAN_POINT('Ctrl Pts',(31.5845521531086,-54.5544984112208,7.));
#39564=CARTESIAN_POINT('Ctrl Pts',(31.6030425567498,-54.5471566321368,7.));
#39565=CARTESIAN_POINT('Ctrl Pts',(31.6206506674855,-54.5401651752915,7.));
#39566=CARTESIAN_POINT('Ctrl Pts',(31.6383657020183,-54.533414128645,7.));
#39567=CARTESIAN_POINT('Ctrl Pts',(31.6561506796624,-54.526917958604,7.));
#39568=CARTESIAN_POINT('Ctrl Pts',(31.7243409101195,-54.502010683428,7.));
#39569=CARTESIAN_POINT('Ctrl Pts',(31.7936290797769,-54.4808156487355,7.));
#39570=CARTESIAN_POINT('Ctrl Pts',(31.8637026768779,-54.4634492156365,7.));
#39571=CARTESIAN_POINT('Ctrl Pts',(31.9322713952984,-54.4464557386294,7.));
#39572=CARTESIAN_POINT('Ctrl Pts',(32.0015931052551,-54.433128170902,7.));
#39573=CARTESIAN_POINT('Ctrl Pts',(32.0713763152269,-54.4236245382735,7.));
#39574=CARTESIAN_POINT('Ctrl Pts',(32.139629084154,-54.4143293332804,7.));
#39575=CARTESIAN_POINT('Ctrl Pts',(32.2083241022735,-54.4086921780743,7.));
#39576=CARTESIAN_POINT('Ctrl Pts',(32.277177509568,-54.4069083838669,7.));
#39577=CARTESIAN_POINT('Ctrl Pts',(32.2995513062292,-54.4063287429972,7.));
#39578=CARTESIAN_POINT('Ctrl Pts',(32.321941690546,-54.4061563640029,7.));
#39579=CARTESIAN_POINT('Ctrl Pts',(32.3443384586624,-54.406399061125,7.));
#39580=CARTESIAN_POINT('Ctrl Pts',(32.3569726508651,-54.4065359684712,7.));
#39581=CARTESIAN_POINT('Ctrl Pts',(32.3696101792394,-54.4068051101149,7.));
#39582=CARTESIAN_POINT('Ctrl Pts',(32.3822313254191,-54.4072071047832,7.));
#39583=CARTESIAN_POINT('Ctrl Pts',(32.4504997772513,-54.4093815153527,7.));
#39584=CARTESIAN_POINT('Ctrl Pts',(32.5184090639295,-54.4154389583228,7.));
#39585=CARTESIAN_POINT('Ctrl Pts',(32.5856896940916,-54.4255188703989,7.));
#39586=CARTESIAN_POINT('Ctrl Pts',(32.5954003979292,-54.4269737176655,7.));
#39587=CARTESIAN_POINT('Ctrl Pts',(32.6050979865285,-54.428512445765,7.));
#39588=CARTESIAN_POINT('Ctrl Pts',(32.6147816267371,-54.4301355621263,7.));
#39589=CARTESIAN_POINT('Ctrl Pts',(32.6832009663072,-54.4416036203246,7.));
#39590=CARTESIAN_POINT('Ctrl Pts',(32.7509260353084,-54.4572806254719,7.));
#39591=CARTESIAN_POINT('Ctrl Pts',(32.8176612516359,-54.4769468185459,7.));
#39592=CARTESIAN_POINT('Ctrl Pts',(32.8799198172925,-54.4952937879587,7.));
#39593=CARTESIAN_POINT('Ctrl Pts',(32.9413172465801,-54.5171136895536,7.));
#39594=CARTESIAN_POINT('Ctrl Pts',(33.0015881176757,-54.5422590913504,7.));
#39595=CARTESIAN_POINT('Ctrl Pts',(33.0148899910938,-54.5478087199798,7.));
#39596=CARTESIAN_POINT('Ctrl Pts',(33.0281368751359,-54.553520427398,7.));
#39597=CARTESIAN_POINT('Ctrl Pts',(33.0413257086146,-54.5593927822714,7.));
#39598=CARTESIAN_POINT('Ctrl Pts',(33.0516354979594,-54.563983236901,7.));
#39599=CARTESIAN_POINT('Ctrl Pts',(33.0619091366608,-54.5686716446485,7.));
#39600=CARTESIAN_POINT('Ctrl Pts',(33.0721334452454,-54.5734515734014,7.));
#39601=CARTESIAN_POINT('Ctrl Pts',(33.13407312627,-54.6024087649643,7.));
#39602=CARTESIAN_POINT('Ctrl Pts',(33.1943201438224,-54.6347718932536,7.));
#39603=CARTESIAN_POINT('Ctrl Pts',(33.2526025547429,-54.6703158299708,7.));
#39604=CARTESIAN_POINT('Ctrl Pts',(33.3106158338357,-54.7056956347569,7.));
#39605=CARTESIAN_POINT('Ctrl Pts',(33.36668338626,-54.7442277671426,7.));
#39606=CARTESIAN_POINT('Ctrl Pts',(33.420501371871,-54.7857268573679,7.));
#39607=CARTESIAN_POINT('Ctrl Pts',(33.4731665001685,-54.8263369784294,7.));
#39608=CARTESIAN_POINT('Ctrl Pts',(33.5236779674717,-54.8697891009245,7.));
#39609=CARTESIAN_POINT('Ctrl Pts',(33.5717071750085,-54.9159326392378,7.));
#39610=CARTESIAN_POINT('Ctrl Pts',(33.5818268624642,-54.9256550188018,7.));
#39611=CARTESIAN_POINT('Ctrl Pts',(33.5918361778029,-54.935496940484,7.));
#39612=CARTESIAN_POINT('Ctrl Pts',(33.6017317564147,-54.9454570805868,7.));
#39613=CARTESIAN_POINT('Ctrl Pts',(33.6111117333405,-54.9548982550757,7.));
#39614=CARTESIAN_POINT('Ctrl Pts',(33.6203906592327,-54.9644470263966,7.));
#39615=CARTESIAN_POINT('Ctrl Pts',(33.6295510505887,-54.9740864762536,7.));
#39616=CARTESIAN_POINT('Ctrl Pts',(33.6745642996402,-55.0214537709762,7.));
#39617=CARTESIAN_POINT('Ctrl Pts',(33.716801866203,-55.0710902388509,7.));
#39618=CARTESIAN_POINT('Ctrl Pts',(33.7559956009587,-55.1228219103356,7.));
#39619=CARTESIAN_POINT('Ctrl Pts',(33.794443925836,-55.1735697179659,7.));
#39620=CARTESIAN_POINT('Ctrl Pts',(33.8299635740397,-55.2263345331734,7.));
#39621=CARTESIAN_POINT('Ctrl Pts',(33.8622555275508,-55.2809712643406,7.));
#39622=CARTESIAN_POINT('Ctrl Pts',(33.8934985744639,-55.3338332862821,7.));
#39623=CARTESIAN_POINT('Ctrl Pts',(33.921720456862,-55.3884482094617,7.));
#39624=CARTESIAN_POINT('Ctrl Pts',(33.9466019284157,-55.4446928633988,7.));
#39625=CARTESIAN_POINT('Ctrl Pts',(33.9507443558517,-55.4540568351838,7.));
#39626=CARTESIAN_POINT('Ctrl Pts',(33.9547940777726,-55.4634659867188,7.));
#39627=CARTESIAN_POINT('Ctrl Pts',(33.9587494776695,-55.4729197548336,7.));
#39628=CARTESIAN_POINT('Ctrl Pts',(33.9629351903496,-55.4829239915992,7.));
#39629=CARTESIAN_POINT('Ctrl Pts',(33.9670152760995,-55.4929781929138,7.));
#39630=CARTESIAN_POINT('Ctrl Pts',(33.9709895856635,-55.5030806790321,7.));
#39631=CARTESIAN_POINT('Origin',(32.5,-56.2916512459885,-3.54592528053767));
#39632=CARTESIAN_POINT('Ctrl Pts',(33.5295805874755,-58.0719425970214,-1.79592528053768));
#39633=CARTESIAN_POINT('Ctrl Pts',(33.6151116017801,-58.0235064542129,-1.79058130531689));
#39634=CARTESIAN_POINT('Ctrl Pts',(34.2640553995263,-57.5898394701863,-1.74819136657341));
#39635=CARTESIAN_POINT('Ctrl Pts',(34.9180311095446,-56.062943931961,-1.66875546430726));
#39636=CARTESIAN_POINT('Ctrl Pts',(33.6191501107478,-54.1363165628765,-1.55761757373922));
#39637=CARTESIAN_POINT('Ctrl Pts',(31.2961996587745,-54.182342369509,-1.44647968317117));
#39638=CARTESIAN_POINT('Ctrl Pts',(30.0749499288325,-56.1591174155133,-1.33534179260313));
#39639=CARTESIAN_POINT('Ctrl Pts',(31.0734520820822,-58.2571645498346,-1.22420390203509));
#39640=CARTESIAN_POINT('Ctrl Pts',(32.7280434754779,-58.4718761792197,-1.14439839801327));
#39641=CARTESIAN_POINT('Ctrl Pts',(33.436201766478,-58.1266820552905,-1.10163885751414));
#39642=CARTESIAN_POINT('Ctrl Pts',(33.5268019957928,-58.0733321975144,-1.09592528053768));
#39643=CARTESIAN_POINT('Ctrl Pts',(33.5243188290626,-58.0704843676252,-1.85407471946232));
#39644=CARTESIAN_POINT('Ctrl Pts',(33.9297573522988,-57.832304408809,-1.82862455259619));
#39645=CARTESIAN_POINT('Ctrl Pts',(34.7395102025176,-56.9114816531044,-1.76612842220737));
#39646=CARTESIAN_POINT('Ctrl Pts',(34.4535014835806,-54.8495668967865,-1.66658632829587));
#39647=CARTESIAN_POINT('Ctrl Pts',(32.3487507516394,-53.8677941230741,-1.55544843772784));
#39648=CARTESIAN_POINT('Ctrl Pts',(30.3811218874152,-55.1044118987674,-1.44431054715979));
#39649=CARTESIAN_POINT('Ctrl Pts',(30.3535878576004,-57.4278205885651,-1.33317265659175));
#39650=CARTESIAN_POINT('Ctrl Pts',(32.0395408012641,-58.5450270011375,-1.2364273806926));
#39651=CARTESIAN_POINT('Ctrl Pts',(33.1630292684131,-58.2758908569843,-1.17672806831612));
#39652=CARTESIAN_POINT('Ctrl Pts',(33.5270487244507,-58.0682282925651,-1.15407471946232));
#39653=CARTESIAN_POINT('Ctrl Pts',(32.8002165734083,-54.6529242983091,-2.));
#39654=CARTESIAN_POINT('Ctrl Pts',(32.2553008763614,-54.5530951452,-1.96295403647732));
#39655=CARTESIAN_POINT('Ctrl Pts',(31.067360018651,-54.9418786009696,-1.88886210943196));
#39656=CARTESIAN_POINT('Ctrl Pts',(30.5876880485777,-56.7662967044641,-1.77772421886392));
#39657=CARTESIAN_POINT('Ctrl Pts',(31.862316082722,-58.1542462926904,-1.66658632829588));
#39658=CARTESIAN_POINT('Ctrl Pts',(33.7186881749666,-57.8383051703362,-1.55544843772784));
#39659=CARTESIAN_POINT('Ctrl Pts',(34.4605498617843,-56.1062143874073,-1.44431054715979));
#39660=CARTESIAN_POINT('Ctrl Pts',(33.4074116483785,-54.5440967590365,-1.33317265659175));
#39661=CARTESIAN_POINT('Ctrl Pts',(31.5239535863333,-54.5814146779316,-1.22203476602371));
#39662=CARTESIAN_POINT('Ctrl Pts',(30.5337591344129,-56.1841922550787,-1.11089687545567));
#39663=CARTESIAN_POINT('Ctrl Pts',(31.3433489080176,-57.8852977549106,-0.999758984887625));
#39664=CARTESIAN_POINT('Ctrl Pts',(33.2116035654679,-58.127735859695,-0.888621094319584));
#39665=CARTESIAN_POINT('Ctrl Pts',(34.4285349719857,-56.6895771946011,-0.777483203751541));
#39666=CARTESIAN_POINT('Ctrl Pts',(33.8802486292119,-54.8871962644418,-0.6663453131835));
#39667=CARTESIAN_POINT('Ctrl Pts',(32.068608990815,-54.3703269630488,-0.555207422615458));
#39668=CARTESIAN_POINT('Ctrl Pts',(30.6518244621987,-55.6120685434763,-0.444069532047416));
#39669=CARTESIAN_POINT('Ctrl Pts',(30.9266969543788,-57.4758393880095,-0.332931641479375));
#39670=CARTESIAN_POINT('Ctrl Pts',(32.6416310686724,-58.2557096429587,-0.221793750911333));
#39671=CARTESIAN_POINT('Ctrl Pts',(34.2269289097961,-57.2378548494304,-0.110655860343291));
#39672=CARTESIAN_POINT('Ctrl Pts',(34.2315490093866,-55.3539292291843,0.000482030224750882));
#39673=CARTESIAN_POINT('Ctrl Pts',(32.6512627267286,-54.3283111741666,0.111619920792793));
#39674=CARTESIAN_POINT('Ctrl Pts',(30.9325239231375,-55.0997605683743,0.222757811360835));
#39675=CARTESIAN_POINT('Ctrl Pts',(30.648513765023,-56.9621610088766,0.333895701928876));
#39676=CARTESIAN_POINT('Ctrl Pts',(32.0591899470587,-58.210836263271,0.445033592496918));
#39677=CARTESIAN_POINT('Ctrl Pts',(33.8733445736997,-57.7028597043182,0.556171483064959));
#39678=CARTESIAN_POINT('Ctrl Pts',(34.4304613352259,-55.9031880402636,0.667309373633002));
#39679=CARTESIAN_POINT('Ctrl Pts',(33.2206049447144,-54.4590811533792,0.778447264201043));
#39680=CARTESIAN_POINT('Ctrl Pts',(31.3511706755798,-54.6923464552708,0.889585154769084));
#39681=CARTESIAN_POINT('Ctrl Pts',(30.5332729159539,-56.3894735693295,1.00072304533713));
#39682=CARTESIAN_POINT('Ctrl Pts',(31.5155427604287,-57.9970628015172,1.11186093590517));
#39683=CARTESIAN_POINT('Ctrl Pts',(33.3988974808522,-58.0436694962152,1.22299882647321));
#39684=CARTESIAN_POINT('Ctrl Pts',(34.4594811428283,-56.4866340172583,1.33413671704125));
#39685=CARTESIAN_POINT('Ctrl Pts',(33.7265294927624,-54.7511285964952,1.44527460760929));
#39686=CARTESIAN_POINT('Ctrl Pts',(31.8709214881723,-54.4256810275324,1.55641249817733));
#39687=CARTESIAN_POINT('Ctrl Pts',(30.5911161796977,-55.8081771610621,1.66755038874538));
#39688=CARTESIAN_POINT('Ctrl Pts',(31.0585338801586,-57.633202607495,1.77868827931342));
#39689=CARTESIAN_POINT('Ctrl Pts',(32.845341867449,-58.2302908785133,1.88982616988146));
#39690=CARTESIAN_POINT('Ctrl Pts',(34.3160545270196,-57.0529203082132,2.0009640604495));
#39691=CARTESIAN_POINT('Ctrl Pts',(34.1245118825503,-55.1787515318803,2.11210195101754));
#39692=CARTESIAN_POINT('Ctrl Pts',(32.4460350887647,-54.323232485012,2.22323984158559));
#39693=CARTESIAN_POINT('Ctrl Pts',(30.8169529902366,-55.2694294534524,2.33437773215363));
#39694=CARTESIAN_POINT('Ctrl Pts',(30.7283829067961,-57.1512776213849,2.44551562272167));
#39695=CARTESIAN_POINT('Ctrl Pts',(32.2613940402694,-58.2463000190907,2.55665351328971));
#39696=CARTESIAN_POINT('Ctrl Pts',(34.0128039146598,-57.5522102275515,2.66779140385775));
#39697=CARTESIAN_POINT('Ctrl Pts',(34.3795272095987,-55.7043165044765,2.77892929442579));
#39698=CARTESIAN_POINT('Ctrl Pts',(33.0258979343036,-54.3940169311364,2.89006718499384));
#39699=CARTESIAN_POINT('Ctrl Pts',(31.1909083156521,-54.8206435668173,3.00120507556187));
#39700=CARTESIAN_POINT('Ctrl Pts',(30.5541451617937,-56.5937002136054,3.11234296612992));
#39701=CARTESIAN_POINT('Ctrl Pts',(31.6984450088402,-58.0902880148654,3.22348085669796));
#39702=CARTESIAN_POINT('Ctrl Pts',(33.5764172295469,-57.9405631836442,3.334618747266));
#39703=CARTESIAN_POINT('Ctrl Pts',(34.4691325526481,-56.2815705559534,3.44575663783404));
#39704=CARTESIAN_POINT('Ctrl Pts',(33.5594785188274,-54.6318048981748,3.55689452840209));
#39705=CARTESIAN_POINT('Ctrl Pts',(31.6800717814225,-54.5013154264873,3.66803241897013));
#39706=CARTESIAN_POINT('Ctrl Pts',(30.5511546410956,-56.0095406341798,3.77917030953817));
#39707=CARTESIAN_POINT('Ctrl Pts',(31.2060377591921,-57.77598488421,3.89030820010622));
#39708=CARTESIAN_POINT('Ctrl Pts',(33.0452991908126,-58.1838017216931,4.00144609067425));
#39709=CARTESIAN_POINT('Ctrl Pts',(34.3854420890035,-56.8597117703073,4.1125839812423));
#39710=CARTESIAN_POINT('Ctrl Pts',(33.9998184606928,-55.0156695787891,4.22372187181033));
#39711=CARTESIAN_POINT('Ctrl Pts',(32.2413939863492,-54.3395478778331,4.33485976237838));
#39712=CARTESIAN_POINT('Ctrl Pts',(30.7196745288183,-55.4502085281907,4.44599765294642));
#39713=CARTESIAN_POINT('Ctrl Pts',(30.8275071658684,-57.3310512405928,4.55713554351447));
#39714=CARTESIAN_POINT('Ctrl Pts',(32.4661914602743,-58.2605193506652,4.6682734340825));
#39715=CARTESIAN_POINT('Ctrl Pts',(34.135821096663,-57.3878601553885,4.77941132465055));
#39716=CARTESIAN_POINT('Ctrl Pts',(34.3081651275095,-55.5118285147887,4.89054921521859));
#39717=CARTESIAN_POINT('Ctrl Pts',(32.8254751197057,-54.349577461249,5.00168710578663));
#39718=CARTESIAN_POINT('Ctrl Pts',(31.0448740266844,-54.9649285726684,5.11282499635467));
#39719=CARTESIAN_POINT('Ctrl Pts',(30.5961662731525,-56.7946439827407,5.22396288692271));
#39720=CARTESIAN_POINT('Ctrl Pts',(31.8900590533422,-58.1639644570316,5.33510077749075));
#39721=CARTESIAN_POINT('Ctrl Pts',(33.7422378333798,-57.819535374986,5.4462386680588));
#39722=CARTESIAN_POINT('Ctrl Pts',(34.4573819695178,-56.076616703484,5.55737655862683));
#39723=CARTESIAN_POINT('Ctrl Pts',(33.3809127223489,-54.5305214257638,5.66851444919488));
#39724=CARTESIAN_POINT('Ctrl Pts',(31.4981330119909,-54.5964085667957,5.77965233976292));
#39725=CARTESIAN_POINT('Ctrl Pts',(30.5323756240669,-56.2139699170398,5.89079023033097));
#39726=CARTESIAN_POINT('Ctrl Pts',(31.3676029490312,-57.9026351433968,6.00192812089901));
#39727=CARTESIAN_POINT('Ctrl Pts',(33.2393344828578,-58.1167460012091,6.11306601146704));
#39728=CARTESIAN_POINT('Ctrl Pts',(34.4343281672319,-56.6603319824485,6.22420390203509));
#39729=CARTESIAN_POINT('Ctrl Pts',(33.8588424113751,-54.8664502505916,6.33534179260313));
#39730=CARTESIAN_POINT('Ctrl Pts',(32.0395269631849,-54.3770911652607,6.44647968317118));
#39731=CARTESIAN_POINT('Ctrl Pts',(30.6418187305185,-55.6401107988729,6.55761757373921));
#39732=CARTESIAN_POINT('Ctrl Pts',(30.9446640768632,-57.4995720858053,6.66875546430725));
#39733=CARTESIAN_POINT('Ctrl Pts',(32.6716452510335,-58.2532519029269,6.7798933548753));
#39734=CARTESIAN_POINT('Ctrl Pts',(34.2404831962862,-57.2117704392446,6.89103124544334));
#39735=CARTESIAN_POINT('Ctrl Pts',(34.2183071453089,-55.3274697977207,7.00216913601138));
#39736=CARTESIAN_POINT('Ctrl Pts',(32.6190914442238,-54.3269220694063,7.11330702657943));
#39737=CARTESIAN_POINT('Ctrl Pts',(31.4873233416682,-54.8574472987172,7.18739895362479));
#39738=CARTESIAN_POINT('Ctrl Pts',(31.1587240665777,-55.3034534568682,7.22444491714747));
#39739=CARTESIAN_POINT('Ctrl Pts',(32.8235677524625,-54.525462293325,-2.07481497238249));
#39740=CARTESIAN_POINT('Ctrl Pts',(32.2362679063105,-54.4178683176327,-2.03776900885981));
#39741=CARTESIAN_POINT('Ctrl Pts',(30.9559276871685,-54.8368917830923,-1.96367708181445));
#39742=CARTESIAN_POINT('Ctrl Pts',(30.4389462976543,-56.8032151562412,-1.85253919124641));
#39743=CARTESIAN_POINT('Ctrl Pts',(31.8127163182479,-58.2991210074574,-1.74140130067837));
#39744=CARTESIAN_POINT('Ctrl Pts',(33.8134790969391,-57.9586056331394,-1.63026341011032));
#39745=CARTESIAN_POINT('Ctrl Pts',(34.6130436110377,-56.0917909022585,-1.51912551954228));
#39746=CARTESIAN_POINT('Ctrl Pts',(33.477991135835,-54.4081700269832,-1.40798762897424));
#39747=CARTESIAN_POINT('Ctrl Pts',(31.4480356104804,-54.448390575124,-1.29684973840619));
#39748=CARTESIAN_POINT('Ctrl Pts',(30.3808227325527,-56.1758339752237,-1.18571184783816));
#39749=CARTESIAN_POINT('Ctrl Pts',(31.2533832993724,-58.0092533532185,-1.07457395727011));
#39750=CARTESIAN_POINT('Ctrl Pts',(33.2669528824098,-58.2705485634922,-0.963436066702072));
#39751=CARTESIAN_POINT('Ctrl Pts',(34.5785385674957,-56.7205283175549,-0.85229817613403));
#39752=CARTESIAN_POINT('Ctrl Pts',(33.9876059030427,-54.7779561935982,-0.741160285565989));
#39753=CARTESIAN_POINT('Ctrl Pts',(32.0350549182218,-54.2208842229542,-0.630022394997947));
#39754=CARTESIAN_POINT('Ctrl Pts',(30.5080713128749,-55.5592098448766,-0.518884504429905));
#39755=CARTESIAN_POINT('Ctrl Pts',(30.8043236932773,-57.56794685904,-0.407746613861863));
#39756=CARTESIAN_POINT('Ctrl Pts',(32.6526472907505,-58.4084762899819,-0.296608723293821));
#39757=CARTESIAN_POINT('Ctrl Pts',(34.3612513615134,-57.3114516183056,-0.185470832725779));
#39758=CARTESIAN_POINT('Ctrl Pts',(34.3662308175897,-55.2809921675532,-0.0743329421577379));
#39759=CARTESIAN_POINT('Ctrl Pts',(32.663028109885,-54.1756003992725,0.0368049484103038));
#39760=CARTESIAN_POINT('Ctrl Pts',(30.8106038901482,-55.0070539855567,0.147942838978346));
#39761=CARTESIAN_POINT('Ctrl Pts',(30.5045031059899,-57.0143140041392,0.259080729546387));
#39762=CARTESIAN_POINT('Ctrl Pts',(32.024903250764,-58.3601126089029,0.370218620114429));
#39763=CARTESIAN_POINT('Ctrl Pts',(33.9801648424124,-57.8126250680989,0.48135651068247));
#39764=CARTESIAN_POINT('Ctrl Pts',(34.5806147654118,-55.8729729399784,0.592494401250513));
#39765=CARTESIAN_POINT('Ctrl Pts',(33.2766543989476,-54.3165418129426,0.703632291818553));
#39766=CARTESIAN_POINT('Ctrl Pts',(31.261813452717,-54.5679507495102,0.814770182386596));
#39767=CARTESIAN_POINT('Ctrl Pts',(30.3802986954811,-56.3970822984609,0.925908072954637));
#39768=CARTESIAN_POINT('Ctrl Pts',(31.4389705811804,-58.1297116094828,1.03704596352268));
#39769=CARTESIAN_POINT('Ctrl Pts',(33.4688147268869,-58.1799434247417,1.14818385409072));
#39770=CARTESIAN_POINT('Ctrl Pts',(34.6118917659325,-56.5017999941152,1.25932174465876));
#39771=CARTESIAN_POINT('Ctrl Pts',(33.8219303211561,-54.6313050310709,1.3704596352268));
#39772=CARTESIAN_POINT('Ctrl Pts',(31.8219910617071,-54.2805437881517,1.48159752579485));
#39773=CARTESIAN_POINT('Ctrl Pts',(30.4426410726264,-55.7705720088982,1.59273541636289));
#39774=CARTESIAN_POINT('Ctrl Pts',(30.9464150418056,-57.7375499647951,1.70387330693093));
#39775=CARTESIAN_POINT('Ctrl Pts',(32.872202942073,-58.381080425761,1.81501119749897));
#39776=CARTESIAN_POINT('Ctrl Pts',(34.4573092683919,-57.1121326627429,1.92614908806701));
#39777=CARTESIAN_POINT('Ctrl Pts',(34.2508682239551,-55.0921889540774,2.03728697863506));
#39778=CARTESIAN_POINT('Ctrl Pts',(32.4418376379359,-54.1701266840256,2.1484248692031));
#39779=CARTESIAN_POINT('Ctrl Pts',(30.68604372152,-55.1899199052636,2.25956275977114));
#39780=CARTESIAN_POINT('Ctrl Pts',(30.5905845584601,-57.2181403171501,2.37070065033918));
#39781=CARTESIAN_POINT('Ctrl Pts',(32.2428350032855,-58.3983347751019,2.48183854090722));
#39782=CARTESIAN_POINT('Ctrl Pts',(34.1304714860531,-57.65025790744,2.59297643147526));
#39783=CARTESIAN_POINT('Ctrl Pts',(34.5257189268319,-55.6586329549041,2.70411432204331));
#39784=CARTESIAN_POINT('Ctrl Pts',(33.0668028606663,-54.2464168231134,2.81525221261135));
#39785=CARTESIAN_POINT('Ctrl Pts',(31.0890857081511,-54.7062269531163,2.92639010317939));
#39786=CARTESIAN_POINT('Ctrl Pts',(30.4027944078215,-56.6171939183195,3.03752799374743));
#39787=CARTESIAN_POINT('Ctrl Pts',(31.636099169942,-58.2301879836331,3.14866588431548));
#39788=CARTESIAN_POINT('Ctrl Pts',(33.660142159116,-58.0688173884789,3.25980377488351));
#39789=CARTESIAN_POINT('Ctrl Pts',(34.6222938731447,-56.2807864686682,3.37094166545156));
#39790=CARTESIAN_POINT('Ctrl Pts',(33.6418859366333,-54.5027002027541,3.4820795560196));
#39791=CARTESIAN_POINT('Ctrl Pts',(31.6162968524565,-54.3620611147965,3.59321744658764));
#39792=CARTESIAN_POINT('Ctrl Pts',(30.3995712810967,-55.9875977569607,3.70435533715568));
#39793=CARTESIAN_POINT('Ctrl Pts',(31.1053919366403,-57.8914380058304,3.81549322772373));
#39794=CARTESIAN_POINT('Ctrl Pts',(33.0877131684893,-58.3309752906067,3.92663111829176));
#39795=CARTESIAN_POINT('Ctrl Pts',(34.5320938721367,-56.9038961498249,4.03776900885981));
#39796=CARTESIAN_POINT('Ctrl Pts',(34.116476009031,-54.916422305255,4.14890689942785));
#39797=CARTESIAN_POINT('Ctrl Pts',(32.2212793229225,-54.1877111062503,4.26004478999589));
#39798=CARTESIAN_POINT('Ctrl Pts',(30.5811988331557,-55.3847601775417,4.37118268056393));
#39799=CARTESIAN_POINT('Ctrl Pts',(30.6974188126734,-57.4118969284484,4.48232057113197));
#39800=CARTESIAN_POINT('Ctrl Pts',(32.4635617944443,-58.4136601021044,4.59345846170002));
#39801=CARTESIAN_POINT('Ctrl Pts',(34.2630570813224,-57.4731245038337,4.70459635226806));
#39802=CARTESIAN_POINT('Ctrl Pts',(34.4488062226114,-55.4511730352461,4.8157342428361));
#39803=CARTESIAN_POINT('Ctrl Pts',(32.8507909365895,-54.1985208018218,4.92687213340414));
#39804=CARTESIAN_POINT('Ctrl Pts',(30.9316927097324,-54.8617346072315,5.03801002397219));
#39805=CARTESIAN_POINT('Ctrl Pts',(30.4480839679681,-56.833767317357,5.14914791454023));
#39806=CARTESIAN_POINT('Ctrl Pts',(31.8426171679855,-58.309595061432,5.26028580510826));
#39807=CARTESIAN_POINT('Ctrl Pts',(33.8388604739813,-57.9383759022264,5.37142369567631));
#39808=CARTESIAN_POINT('Ctrl Pts',(34.6096293165867,-56.0598910775539,5.48256158624434));
#39809=CARTESIAN_POINT('Ctrl Pts',(33.4494310938601,-54.3935387891867,5.5936994768124));
#39810=CARTESIAN_POINT('Ctrl Pts',(31.4202066831417,-54.4645507053438,5.70483736738043));
#39811=CARTESIAN_POINT('Ctrl Pts',(30.379331611233,-56.2079277768579,5.81597525794847));
#39812=CARTESIAN_POINT('Ctrl Pts',(31.2795238466775,-58.0279392630681,5.92711314851652));
#39813=CARTESIAN_POINT('Ctrl Pts',(33.2968407414035,-58.2587039015876,6.03825103908455));
#39814=CARTESIAN_POINT('Ctrl Pts',(34.5847823639129,-56.6890083802674,6.1493889296526));
#39815=CARTESIAN_POINT('Ctrl Pts',(33.9645346857693,-54.755596531712,6.26052682022064));
#39816=CARTESIAN_POINT('Ctrl Pts',(32.0037108581305,-54.2281745523389,6.37166471078869));
#39817=CARTESIAN_POINT('Ctrl Pts',(30.4972873242538,-55.5894332580934,6.48280260135673));
#39818=CARTESIAN_POINT('Ctrl Pts',(30.8236883185359,-57.5935255124717,6.59394049192477));
#39819=CARTESIAN_POINT('Ctrl Pts',(32.6849960096048,-58.4058273841964,6.70507838249281));
#39820=CARTESIAN_POINT('Ctrl Pts',(34.3758599154851,-57.2833383336781,6.81621627306086));
#39821=CARTESIAN_POINT('Ctrl Pts',(34.3519589865933,-55.2524746920757,6.92735416362889));
#39822=CARTESIAN_POINT('Ctrl Pts',(32.6283545092382,-54.1741032483986,7.03849205419694));
#39823=CARTESIAN_POINT('Ctrl Pts',(31.4085562246361,-54.7458933202255,7.1125839812423));
#39824=CARTESIAN_POINT('Ctrl Pts',(31.0543981323804,-55.2265903335148,7.14962994476498));
#39825=CARTESIAN_POINT('Ctrl Pts',(32.8469189315166,-54.3980002883409,-2.14962994476498));
#39826=CARTESIAN_POINT('Ctrl Pts',(32.2172349362596,-54.2826414900653,-2.1125839812423));
#39827=CARTESIAN_POINT('Ctrl Pts',(30.8444953556861,-54.7319049652148,-2.03849205419694));
#39828=CARTESIAN_POINT('Ctrl Pts',(30.2902045467308,-56.8401336080184,-1.92735416362889));
#39829=CARTESIAN_POINT('Ctrl Pts',(31.7631165537738,-58.4439957222243,-1.81621627306085));
#39830=CARTESIAN_POINT('Ctrl Pts',(33.9082700189114,-58.0789060959426,-1.70507838249281));
#39831=CARTESIAN_POINT('Ctrl Pts',(34.7655373602912,-56.0773674171097,-1.59394049192477));
#39832=CARTESIAN_POINT('Ctrl Pts',(33.5485706232913,-54.2722432949299,-1.48280260135673));
#39833=CARTESIAN_POINT('Ctrl Pts',(31.3721176346275,-54.3153664723165,-1.37166471078869));
#39834=CARTESIAN_POINT('Ctrl Pts',(30.2278863306926,-56.1674756953684,-1.26052682022065));
#39835=CARTESIAN_POINT('Ctrl Pts',(31.1634176907273,-58.1332089515266,-1.1493889296526));
#39836=CARTESIAN_POINT('Ctrl Pts',(33.3223021993517,-58.4133612672894,-1.03825103908456));
#39837=CARTESIAN_POINT('Ctrl Pts',(34.7285421630059,-56.7514794405087,-0.927113148516519));
#39838=CARTESIAN_POINT('Ctrl Pts',(34.0949631768734,-54.6687161227546,-0.815975257948478));
#39839=CARTESIAN_POINT('Ctrl Pts',(32.0015008456287,-54.0714414828596,-0.704837367380436));
#39840=CARTESIAN_POINT('Ctrl Pts',(30.3643181635511,-55.5063511462768,-0.593699476812395));
#39841=CARTESIAN_POINT('Ctrl Pts',(30.6819504321758,-57.6600543300705,-0.482561586244352));
#39842=CARTESIAN_POINT('Ctrl Pts',(32.6636635128286,-58.5612429370053,-0.371423695676311));
#39843=CARTESIAN_POINT('Ctrl Pts',(34.4955738132308,-57.3850483871807,-0.260285805108268));
#39844=CARTESIAN_POINT('Ctrl Pts',(34.5009126257928,-55.208055105922,-0.149147914540227));
#39845=CARTESIAN_POINT('Ctrl Pts',(32.6747934930414,-54.0228896243784,-0.038010023972185));
#39846=CARTESIAN_POINT('Ctrl Pts',(30.6886838571589,-54.9143474027391,0.0731278665958571));
#39847=CARTESIAN_POINT('Ctrl Pts',(30.3604924469568,-57.0664669994019,0.184265757163899));
#39848=CARTESIAN_POINT('Ctrl Pts',(31.9906165544693,-58.5093889545349,0.29540364773194));
#39849=CARTESIAN_POINT('Ctrl Pts',(34.086985111125,-57.9223904318795,0.406541538299982));
#39850=CARTESIAN_POINT('Ctrl Pts',(34.7307681955977,-55.8427578396932,0.517679428868024));
#39851=CARTESIAN_POINT('Ctrl Pts',(33.3327038531808,-54.1740024725061,0.628817319436065));
#39852=CARTESIAN_POINT('Ctrl Pts',(31.1724562298542,-54.4435550437495,0.739955210004107));
#39853=CARTESIAN_POINT('Ctrl Pts',(30.2273244750083,-56.4046910275923,0.851093100572148));
#39854=CARTESIAN_POINT('Ctrl Pts',(31.362398401932,-58.2623604174484,0.962230991140191));
#39855=CARTESIAN_POINT('Ctrl Pts',(33.5387319729216,-58.3162173532682,1.07336888170823));
#39856=CARTESIAN_POINT('Ctrl Pts',(34.7643023890366,-56.5169659709723,1.18450677227627));
#39857=CARTESIAN_POINT('Ctrl Pts',(33.9173311495497,-54.5114814656466,1.29564466284432));
#39858=CARTESIAN_POINT('Ctrl Pts',(31.7730606352419,-54.135406548771,1.40678255341236));
#39859=CARTESIAN_POINT('Ctrl Pts',(30.2941659655551,-55.7329668567343,1.5179204439804));
#39860=CARTESIAN_POINT('Ctrl Pts',(30.8342962034526,-57.8418973220951,1.62905833454844));
#39861=CARTESIAN_POINT('Ctrl Pts',(32.899064016697,-58.5318699730087,1.74019622511648));
#39862=CARTESIAN_POINT('Ctrl Pts',(34.5985640097642,-57.1713450172728,1.85133411568452));
#39863=CARTESIAN_POINT('Ctrl Pts',(34.37722456536,-55.0056263762742,1.96247200625257));
#39864=CARTESIAN_POINT('Ctrl Pts',(32.437640187107,-54.0170208830394,2.07360989682061));
#39865=CARTESIAN_POINT('Ctrl Pts',(30.5551344528034,-55.1104103570745,2.18474778738865));
#39866=CARTESIAN_POINT('Ctrl Pts',(30.4527862101241,-57.2850030129155,2.29588567795669));
#39867=CARTESIAN_POINT('Ctrl Pts',(32.2242759663018,-58.550369531113,2.40702356852473));
#39868=CARTESIAN_POINT('Ctrl Pts',(34.2481390574464,-57.7483055873284,2.51816145909278));
#39869=CARTESIAN_POINT('Ctrl Pts',(34.6719106440652,-55.6129494053317,2.62929934966082));
#39870=CARTESIAN_POINT('Ctrl Pts',(33.1077077870289,-54.0988167150904,2.74043724022886));
#39871=CARTESIAN_POINT('Ctrl Pts',(30.9872631006501,-54.5918103394153,2.8515751307969));
#39872=CARTESIAN_POINT('Ctrl Pts',(30.2514436538494,-56.6406876230335,2.96271302136494));
#39873=CARTESIAN_POINT('Ctrl Pts',(31.5737533310438,-58.3700879524008,3.07385091193298));
#39874=CARTESIAN_POINT('Ctrl Pts',(33.7438670886851,-58.1970715933135,3.18498880250103));
#39875=CARTESIAN_POINT('Ctrl Pts',(34.7754551936414,-56.2800023813831,3.29612669306906));
#39876=CARTESIAN_POINT('Ctrl Pts',(33.7242933544393,-54.3735955073335,3.40726458363711));
#39877=CARTESIAN_POINT('Ctrl Pts',(31.5525219234905,-54.2228068031056,3.51840247420514));
#39878=CARTESIAN_POINT('Ctrl Pts',(30.2479879210979,-55.9656548797418,3.6295403647732));
#39879=CARTESIAN_POINT('Ctrl Pts',(31.0047461140885,-58.0068911274507,3.74067825534123));
#39880=CARTESIAN_POINT('Ctrl Pts',(33.1301271461661,-58.4781488595202,3.85181614590928));
#39881=CARTESIAN_POINT('Ctrl Pts',(34.67874565527,-56.9480805293426,3.96295403647732));
#39882=CARTESIAN_POINT('Ctrl Pts',(34.2331335573692,-54.8171750317208,4.07409192704536));
#39883=CARTESIAN_POINT('Ctrl Pts',(32.2011646594958,-54.0358743346676,4.1852298176134));
#39884=CARTESIAN_POINT('Ctrl Pts',(30.442723137493,-55.3193118268927,4.29636770818144));
#39885=CARTESIAN_POINT('Ctrl Pts',(30.5673304594784,-57.492742616304,4.40750559874949));
#39886=CARTESIAN_POINT('Ctrl Pts',(32.4609321286143,-58.5668008535436,4.51864348931753));
#39887=CARTESIAN_POINT('Ctrl Pts',(34.3902930659818,-57.5583888522789,4.62978137988557));
#39888=CARTESIAN_POINT('Ctrl Pts',(34.5894473177133,-55.3905175557034,4.74091927045361));
#39889=CARTESIAN_POINT('Ctrl Pts',(32.8761067534734,-54.0474641423945,4.85205716102165));
#39890=CARTESIAN_POINT('Ctrl Pts',(30.8185113927803,-54.7585406417947,4.96319505158969));
#39891=CARTESIAN_POINT('Ctrl Pts',(30.3000016627836,-56.8728906519733,5.07433294215774));
#39892=CARTESIAN_POINT('Ctrl Pts',(31.7951752826287,-58.4552256658322,5.18547083272577));
#39893=CARTESIAN_POINT('Ctrl Pts',(33.9354831145828,-58.0572164294669,5.29660872329383));
#39894=CARTESIAN_POINT('Ctrl Pts',(34.7618766636556,-56.0431654516238,5.40774661386186));
#39895=CARTESIAN_POINT('Ctrl Pts',(33.5179494653713,-54.2565561526097,5.5188845044299));
#39896=CARTESIAN_POINT('Ctrl Pts',(31.3422803542925,-54.3326928438919,5.63002239499794));
#39897=CARTESIAN_POINT('Ctrl Pts',(30.226287598399,-56.2018856366762,5.74116028556598));
#39898=CARTESIAN_POINT('Ctrl Pts',(31.1914447443238,-58.1532433827394,5.85229817613403));
#39899=CARTESIAN_POINT('Ctrl Pts',(33.354346999949,-58.4006618019662,5.96343606670207));
#39900=CARTESIAN_POINT('Ctrl Pts',(34.7352365605938,-56.7176847780862,6.07457395727011));
#39901=CARTESIAN_POINT('Ctrl Pts',(34.0702269601635,-54.6447428128324,6.18571184783815));
#39902=CARTESIAN_POINT('Ctrl Pts',(31.9678947530762,-54.0792579394171,6.2968497384062));
#39903=CARTESIAN_POINT('Ctrl Pts',(30.3527559179891,-55.5387557173139,6.40798762897423));
#39904=CARTESIAN_POINT('Ctrl Pts',(30.7027125602088,-57.6874789391381,6.51912551954228));
#39905=CARTESIAN_POINT('Ctrl Pts',(32.6983467681761,-58.5584028654658,6.63026341011033));
#39906=CARTESIAN_POINT('Ctrl Pts',(34.5112366346842,-57.3549062281116,6.74140130067836));
#39907=CARTESIAN_POINT('Ctrl Pts',(34.4856108278775,-55.1774795864305,6.85253919124641));
#39908=CARTESIAN_POINT('Ctrl Pts',(32.6376175742527,-54.021284427391,6.96367708181444));
#39909=CARTESIAN_POINT('Ctrl Pts',(31.329789107604,-54.6343393417337,7.03776900885981));
#39910=CARTESIAN_POINT('Ctrl Pts',(30.9500721981832,-55.1497272101613,7.07481497238249));
#39911=CARTESIAN_POINT('Ctrl Pts',(32.8702701105707,-54.2705382833568,-2.22444491714747));
#39912=CARTESIAN_POINT('Ctrl Pts',(32.1982019662087,-54.147414662498,-2.18739895362479));
#39913=CARTESIAN_POINT('Ctrl Pts',(30.7330630242036,-54.6269181473375,-2.11330702657943));
#39914=CARTESIAN_POINT('Ctrl Pts',(30.1414627958074,-56.8770520597956,-2.00216913601138));
#39915=CARTESIAN_POINT('Ctrl Pts',(31.7135167892996,-58.5888704369913,-1.89103124544334));
#39916=CARTESIAN_POINT('Ctrl Pts',(34.0030609408839,-58.1992065587458,-1.7798933548753));
#39917=CARTESIAN_POINT('Ctrl Pts',(34.9180311095446,-56.062943931961,-1.66875546430726));
#39918=CARTESIAN_POINT('Ctrl Pts',(33.6191501107478,-54.1363165628765,-1.55761757373922));
#39919=CARTESIAN_POINT('Ctrl Pts',(31.2961996587745,-54.182342369509,-1.44647968317117));
#39920=CARTESIAN_POINT('Ctrl Pts',(30.0749499288325,-56.1591174155133,-1.33534179260313));
#39921=CARTESIAN_POINT('Ctrl Pts',(31.0734520820822,-58.2571645498346,-1.22420390203509));
#39922=CARTESIAN_POINT('Ctrl Pts',(33.3776515162936,-58.5561739710866,-1.11306601146705));
#39923=CARTESIAN_POINT('Ctrl Pts',(34.8785457585159,-56.7824305634625,-1.00192812089901));
#39924=CARTESIAN_POINT('Ctrl Pts',(34.2023204507043,-54.559476051911,-0.890790230330967));
#39925=CARTESIAN_POINT('Ctrl Pts',(31.9679467730355,-53.921998742765,-0.779652339762925));
#39926=CARTESIAN_POINT('Ctrl Pts',(30.2205650142273,-55.453492447677,-0.668514449194883));
#39927=CARTESIAN_POINT('Ctrl Pts',(30.5595771710743,-57.7521618011011,-0.557376558626841));
#39928=CARTESIAN_POINT('Ctrl Pts',(32.6746797349067,-58.7140095840285,-0.446238668058799));
#39929=CARTESIAN_POINT('Ctrl Pts',(34.6298962649481,-57.4586451560558,-0.335100777490757));
#39930=CARTESIAN_POINT('Ctrl Pts',(34.6355944339958,-55.1351180442909,-0.223962886922716));
#39931=CARTESIAN_POINT('Ctrl Pts',(32.6865588761979,-53.8701788494842,-0.112824996354674));
#39932=CARTESIAN_POINT('Ctrl Pts',(30.5667638241697,-54.8216408199215,-0.00168710578663165));
#39933=CARTESIAN_POINT('Ctrl Pts',(30.2164817879238,-57.1186199946645,0.109450784781409));
#39934=CARTESIAN_POINT('Ctrl Pts',(31.9563298581746,-58.6586653001669,0.220588675349451));
#39935=CARTESIAN_POINT('Ctrl Pts',(34.1938053798376,-58.0321557956601,0.331726565917493));
#39936=CARTESIAN_POINT('Ctrl Pts',(34.8809216257836,-55.8125427394079,0.442864456485535));
#39937=CARTESIAN_POINT('Ctrl Pts',(33.388753307414,-54.0314631320695,0.554002347053576));
#39938=CARTESIAN_POINT('Ctrl Pts',(31.0830990069914,-54.3191593379889,0.665140237621618));
#39939=CARTESIAN_POINT('Ctrl Pts',(30.0743502545355,-56.4122997567237,0.77627812818966));
#39940=CARTESIAN_POINT('Ctrl Pts',(31.2858262226837,-58.3950092254139,0.887416018757702));
#39941=CARTESIAN_POINT('Ctrl Pts',(33.6086492189562,-58.4524912817948,0.998553909325743));
#39942=CARTESIAN_POINT('Ctrl Pts',(34.9167130121408,-56.5321319478292,1.10969179989378));
#39943=CARTESIAN_POINT('Ctrl Pts',(34.0127319779433,-54.3916579002223,1.22082969046183));
#39944=CARTESIAN_POINT('Ctrl Pts',(31.7241302087767,-53.9902693093903,1.33196758102987));
#39945=CARTESIAN_POINT('Ctrl Pts',(30.1456908584837,-55.6953617045704,1.44310547159791));
#39946=CARTESIAN_POINT('Ctrl Pts',(30.7221773650996,-57.9462446793952,1.55424336216595));
#39947=CARTESIAN_POINT('Ctrl Pts',(32.925925091321,-58.6826595202564,1.66538125273399));
#39948=CARTESIAN_POINT('Ctrl Pts',(34.7398187511365,-57.2305573718025,1.77651914330204));
#39949=CARTESIAN_POINT('Ctrl Pts',(34.5035809067649,-54.9190637984713,1.88765703387008));
#39950=CARTESIAN_POINT('Ctrl Pts',(32.4334427362781,-53.863915082053,1.99879492443812));
#39951=CARTESIAN_POINT('Ctrl Pts',(30.4242251840868,-55.0309008088856,2.10993281500616));
#39952=CARTESIAN_POINT('Ctrl Pts',(30.3149878617883,-57.3518657086808,2.2210707055742));
#39953=CARTESIAN_POINT('Ctrl Pts',(32.2057169293179,-58.7024042871242,2.33220859614224));
#39954=CARTESIAN_POINT('Ctrl Pts',(34.3658066288398,-57.8463532672169,2.44334648671029));
#39955=CARTESIAN_POINT('Ctrl Pts',(34.8181023612983,-55.5672658557593,2.55448437727833));
#39956=CARTESIAN_POINT('Ctrl Pts',(33.1486127133916,-53.9512166070675,2.66562226784637));
#39957=CARTESIAN_POINT('Ctrl Pts',(30.8854404931491,-54.4773937257142,2.77676015841441));
#39958=CARTESIAN_POINT('Ctrl Pts',(30.1000928998772,-56.6641813277477,2.88789804898245));
#39959=CARTESIAN_POINT('Ctrl Pts',(31.5114074921456,-58.5099879211684,2.99903593955049));
#39960=CARTESIAN_POINT('Ctrl Pts',(33.8275920182542,-58.3253257981483,3.11017383011854));
#39961=CARTESIAN_POINT('Ctrl Pts',(34.9286165141379,-56.2792182940979,3.22131172068658));
#39962=CARTESIAN_POINT('Ctrl Pts',(33.8067007722452,-54.2444908119128,3.33244961125462));
#39963=CARTESIAN_POINT('Ctrl Pts',(31.4887469945245,-54.0835524914147,3.44358750182266));
#39964=CARTESIAN_POINT('Ctrl Pts',(30.0964045610991,-55.9437120025227,3.5547253923907));
#39965=CARTESIAN_POINT('Ctrl Pts',(30.9041002915367,-58.1223442490711,3.66586328295875));
#39966=CARTESIAN_POINT('Ctrl Pts',(33.1725411238428,-58.6253224284338,3.77700117352679));
#39967=CARTESIAN_POINT('Ctrl Pts',(34.8253974384033,-56.9922649088601,3.88813906409483));
#39968=CARTESIAN_POINT('Ctrl Pts',(34.3497911057074,-54.7179277581866,3.99927695466287));
#39969=CARTESIAN_POINT('Ctrl Pts',(32.181049996069,-53.8840375630849,4.11041484523092));
#39970=CARTESIAN_POINT('Ctrl Pts',(30.3042474418304,-55.2538634762437,4.22155273579895));
#39971=CARTESIAN_POINT('Ctrl Pts',(30.4372421062834,-57.5735883041596,4.332690626367));
#39972=CARTESIAN_POINT('Ctrl Pts',(32.4583024627843,-58.7199416049829,4.44382851693503));
#39973=CARTESIAN_POINT('Ctrl Pts',(34.5175290506412,-57.6436532007241,4.55496640750308));
#39974=CARTESIAN_POINT('Ctrl Pts',(34.7300884128151,-55.3298620761609,4.66610429807112));
#39975=CARTESIAN_POINT('Ctrl Pts',(32.9014225703573,-53.8964074829672,4.77724218863916));
#39976=CARTESIAN_POINT('Ctrl Pts',(30.7053300758282,-54.6553466763579,4.8883800792072));
#39977=CARTESIAN_POINT('Ctrl Pts',(30.1519193575992,-56.9120139865897,4.99951796977525));
#39978=CARTESIAN_POINT('Ctrl Pts',(31.7477333972719,-58.6008562702326,5.11065586034329));
#39979=CARTESIAN_POINT('Ctrl Pts',(34.0321057551844,-58.1760569567073,5.22179375091133));
#39980=CARTESIAN_POINT('Ctrl Pts',(34.9141240107243,-56.0264398256937,5.33293164147937));
#39981=CARTESIAN_POINT('Ctrl Pts',(33.5864678368826,-54.1195735160326,5.44406953204741));
#39982=CARTESIAN_POINT('Ctrl Pts',(31.2643540254432,-54.2008349824401,5.55520742261546));
#39983=CARTESIAN_POINT('Ctrl Pts',(30.0732435855651,-56.1958434964943,5.6663453131835));
#39984=CARTESIAN_POINT('Ctrl Pts',(31.10336564197,-58.2785475024108,5.77748320375154));
#39985=CARTESIAN_POINT('Ctrl Pts',(33.4118532584947,-58.5426197023447,5.88862109431958));
#39986=CARTESIAN_POINT('Ctrl Pts',(34.8856907572748,-56.7463611759051,5.99975898488763));
#39987=CARTESIAN_POINT('Ctrl Pts',(34.1759192345576,-54.5338890939528,6.11089687545566));
#39988=CARTESIAN_POINT('Ctrl Pts',(31.9320786480218,-53.9303413264954,6.22203476602372));
#39989=CARTESIAN_POINT('Ctrl Pts',(30.2082245117244,-55.4880781765343,6.33317265659174));
#39990=CARTESIAN_POINT('Ctrl Pts',(30.5817368018815,-57.7814323658044,6.44431054715979));
#39991=CARTESIAN_POINT('Ctrl Pts',(32.7116975267474,-58.7109783467354,6.55544843772783));
#39992=CARTESIAN_POINT('Ctrl Pts',(34.646613353883,-57.4264741225449,6.66658632829588));
#39993=CARTESIAN_POINT('Ctrl Pts',(34.6192626691618,-55.1024844807854,6.77772421886392));
#39994=CARTESIAN_POINT('Ctrl Pts',(32.6468806392671,-53.8684656063833,6.88886210943196));
#39995=CARTESIAN_POINT('Ctrl Pts',(31.2510219905719,-54.522785363242,6.96295403647732));
#39996=CARTESIAN_POINT('Ctrl Pts',(30.8457462639859,-55.0728640868079,7.));
#39997=CARTESIAN_POINT('Ctrl Pts',(32.8002165734083,-54.6529242983091,-2.));
#39998=CARTESIAN_POINT('Ctrl Pts',(32.7409294910778,-54.634811549331,-2.));
#39999=CARTESIAN_POINT('Ctrl Pts',(32.6807825146647,-54.6203475870769,-2.));
#40000=CARTESIAN_POINT('Ctrl Pts',(32.6200737029452,-54.6093586318095,-2.));
#40001=CARTESIAN_POINT('Ctrl Pts',(32.5553553259164,-54.5976439016079,-2.));
#40002=CARTESIAN_POINT('Ctrl Pts',(32.4899978846714,-54.5898778448639,-2.));
#40003=CARTESIAN_POINT('Ctrl Pts',(32.4243295074656,-54.5859022602815,-2.));
#40004=CARTESIAN_POINT('Ctrl Pts',(32.3668696774105,-54.5824236237718,-2.));
#40005=CARTESIAN_POINT('Ctrl Pts',(32.3091708471311,-54.5818478912346,-2.));
#40006=CARTESIAN_POINT('Ctrl Pts',(32.2514404192184,-54.5841026889815,-2.));
#40007=CARTESIAN_POINT('Ctrl Pts',(32.2224739676352,-54.5852340419287,-2.));
#40008=CARTESIAN_POINT('Ctrl Pts',(32.1934994333242,-54.5870784902626,-2.));
#40009=CARTESIAN_POINT('Ctrl Pts',(32.164542591354,-54.5896298423987,-2.));
#40010=CARTESIAN_POINT('Ctrl Pts',(32.1513153330264,-54.5907952800464,-2.));
#40011=CARTESIAN_POINT('Ctrl Pts',(32.1380900392148,-54.5921085587762,-2.));
#40012=CARTESIAN_POINT('Ctrl Pts',(32.1248906604594,-54.5935664859838,-2.));
#40013=CARTESIAN_POINT('Ctrl Pts',(32.0583157457256,-54.6009199668811,-2.));
#40014=CARTESIAN_POINT('Ctrl Pts',(31.9922802588125,-54.6119586521805,-2.));
#40015=CARTESIAN_POINT('Ctrl Pts',(31.9271057840968,-54.6265240331787,-2.));
#40016=CARTESIAN_POINT('Ctrl Pts',(31.8607754217499,-54.6413477353035,-2.));
#40017=CARTESIAN_POINT('Ctrl Pts',(31.7953358755732,-54.6598242742458,-2.));
#40018=CARTESIAN_POINT('Ctrl Pts',(31.7311141838614,-54.6818388621525,-2.));
#40019=CARTESIAN_POINT('Ctrl Pts',(31.6773947912155,-54.7002533613687,-2.));
#40020=CARTESIAN_POINT('Ctrl Pts',(31.624526967767,-54.7211443093805,-2.));
#40021=CARTESIAN_POINT('Ctrl Pts',(31.5727038894024,-54.7444721761566,-2.));
#40022=CARTESIAN_POINT('Ctrl Pts',(31.5488262835572,-54.7552205459113,-2.));
#40023=CARTESIAN_POINT('Ctrl Pts',(31.5251705391755,-54.7664866028724,-2.));
#40024=CARTESIAN_POINT('Ctrl Pts',(31.501756105982,-54.7782682438544,-2.));
#40025=CARTESIAN_POINT('Ctrl Pts',(31.4915364297278,-54.783410565925,-2.));
#40026=CARTESIAN_POINT('Ctrl Pts',(31.4813629900533,-54.7886510930647,-2.));
#40027=CARTESIAN_POINT('Ctrl Pts',(31.4712497594726,-54.7939828998507,-2.));
#40028=CARTESIAN_POINT('Ctrl Pts',(31.4091712444434,-54.8267113781603,-2.));
#40029=CARTESIAN_POINT('Ctrl Pts',(31.3492415725846,-54.8629343648032,-2.));
#40030=CARTESIAN_POINT('Ctrl Pts',(31.2918005106807,-54.9025187988006,-2.));
#40031=CARTESIAN_POINT('Ctrl Pts',(31.2404435140524,-54.93791051295,-2.));
#40032=CARTESIAN_POINT('Ctrl Pts',(31.1910752071398,-54.9759900914448,-2.));
#40033=CARTESIAN_POINT('Ctrl Pts',(31.1439444839342,-55.0166972030902,-2.));
#40034=CARTESIAN_POINT('Ctrl Pts',(31.0925988211616,-55.0610447854066,-2.));
#40035=CARTESIAN_POINT('Ctrl Pts',(31.043907590921,-55.1085103565108,-2.));
#40036=CARTESIAN_POINT('Ctrl Pts',(30.9979331337654,-55.1587747363377,-2.));
#40037=CARTESIAN_POINT('Ctrl Pts',(30.9801952413147,-55.1781677693093,-2.));
#40038=CARTESIAN_POINT('Ctrl Pts',(30.9628620787153,-55.1979778819377,-2.));
#40039=CARTESIAN_POINT('Ctrl Pts',(30.9459385065297,-55.218188320324,-2.));
#40040=CARTESIAN_POINT('Ctrl Pts',(30.9385143505167,-55.2270543827619,-2.));
#40041=CARTESIAN_POINT('Ctrl Pts',(30.9311694717035,-55.2359970996828,-2.));
#40042=CARTESIAN_POINT('Ctrl Pts',(30.923912574634,-55.2450044081391,-2.));
#40043=CARTESIAN_POINT('Ctrl Pts',(30.8800390053164,-55.2994605714461,-2.));
#40044=CARTESIAN_POINT('Ctrl Pts',(30.8392972474282,-55.3563704442589,-2.));
#40045=CARTESIAN_POINT('Ctrl Pts',(30.8017204449644,-55.4153538312338,-2.));
#40046=CARTESIAN_POINT('Ctrl Pts',(30.763273103291,-55.4757036822959,-2.));
#40047=CARTESIAN_POINT('Ctrl Pts',(30.7281385018843,-55.5382249057113,-2.));
#40048=CARTESIAN_POINT('Ctrl Pts',(30.6963834281664,-55.6025570259941,-2.));
#40049=CARTESIAN_POINT('Ctrl Pts',(30.6720872116783,-55.6517783609976,-2.));
#40050=CARTESIAN_POINT('Ctrl Pts',(30.6497699435205,-55.7020608595655,-2.));
#40051=CARTESIAN_POINT('Ctrl Pts',(30.629476572352,-55.7532569215707,-2.));
#40052=CARTESIAN_POINT('Ctrl Pts',(30.6168451594843,-55.7851234158567,-2.));
#40053=CARTESIAN_POINT('Ctrl Pts',(30.6049981367155,-55.8173440722639,-2.));
#40054=CARTESIAN_POINT('Ctrl Pts',(30.5939492528939,-55.8498849658379,-2.));
#40055=CARTESIAN_POINT('Ctrl Pts',(30.5877508307706,-55.868140402124,-2.));
#40056=CARTESIAN_POINT('Ctrl Pts',(30.581801893405,-55.8865028064696,-2.));
#40057=CARTESIAN_POINT('Ctrl Pts',(30.5761150803988,-55.9049328084338,-2.));
#40058=CARTESIAN_POINT('Ctrl Pts',(30.5540602837186,-55.9764086852896,-2.));
#40059=CARTESIAN_POINT('Ctrl Pts',(30.5359175198192,-56.0489705581569,-2.));
#40060=CARTESIAN_POINT('Ctrl Pts',(30.5217728584343,-56.1222396610388,-2.));
#40061=CARTESIAN_POINT('Ctrl Pts',(30.5111932477205,-56.1770418627137,-2.));
#40062=CARTESIAN_POINT('Ctrl Pts',(30.5028510892916,-56.2322406204203,-2.));
#40063=CARTESIAN_POINT('Ctrl Pts',(30.4967990447144,-56.2876867713494,-2.));
#40064=CARTESIAN_POINT('Ctrl Pts',(30.494911121078,-56.3049830912216,-2.));
#40065=CARTESIAN_POINT('Ctrl Pts',(30.4932461646271,-56.3223035268967,-2.));
#40066=CARTESIAN_POINT('Ctrl Pts',(30.4918060890607,-56.339643645384,-2.));
#40067=CARTESIAN_POINT('Ctrl Pts',(30.4904160490508,-56.3563812798787,-2.));
#40068=CARTESIAN_POINT('Ctrl Pts',(30.4892362965385,-56.3731287079821,-2.));
#40069=CARTESIAN_POINT('Ctrl Pts',(30.4882682431309,-56.3898758527173,-2.));
#40070=CARTESIAN_POINT('Ctrl Pts',(30.4839212193137,-56.465078559989,-2.));
#40071=CARTESIAN_POINT('Ctrl Pts',(30.4838360419498,-56.5403117892334,-2.));
#40072=CARTESIAN_POINT('Ctrl Pts',(30.4881238107187,-56.6152096419488,-2.));
#40073=CARTESIAN_POINT('Ctrl Pts',(30.4914053519372,-56.6725309211765,-2.));
#40074=CARTESIAN_POINT('Ctrl Pts',(30.4972490710536,-56.7296564032881,-2.));
#40075=CARTESIAN_POINT('Ctrl Pts',(30.5057249894128,-56.7864264638426,-2.));
#40076=CARTESIAN_POINT('Ctrl Pts',(30.5076920210892,-56.799601261268,-2.));
#40077=CARTESIAN_POINT('Ctrl Pts',(30.5098008972608,-56.8127569211082,-2.));
#40078=CARTESIAN_POINT('Ctrl Pts',(30.5120501580915,-56.8258920773861,-2.));
#40079=CARTESIAN_POINT('Ctrl Pts',(33.3325354057626,-57.7362457052863,-0.871480363390211));
#40080=CARTESIAN_POINT('Ctrl Pts',(33.2590763562245,-57.7795019958594,-0.877193940366669));
#40081=CARTESIAN_POINT('Ctrl Pts',(33.1823540930372,-57.8169005192734,-0.882907517343126));
#40082=CARTESIAN_POINT('Ctrl Pts',(33.1030496903124,-57.8476363980486,-0.888621094319584));
#40083=CARTESIAN_POINT('Ctrl Pts',(32.5888520129844,-58.0469231581002,-0.925667057842264));
#40084=CARTESIAN_POINT('Ctrl Pts',(31.966100460501,-57.9661104565054,-0.962713021364944));
#40085=CARTESIAN_POINT('Ctrl Pts',(31.5197930553252,-57.6421865224027,-0.999758984887625));
#40086=CARTESIAN_POINT('Ctrl Pts',(31.0734856501493,-57.3182625883,-1.03680494841031));
#40087=CARTESIAN_POINT('Ctrl Pts',(30.8036223922811,-56.7512274216894,-1.07385091193299));
#40088=CARTESIAN_POINT('Ctrl Pts',(30.8337231720004,-56.2005802421929,-1.11089687545567));
#40089=CARTESIAN_POINT('Ctrl Pts',(30.8638239517197,-55.6499330626964,-1.14794283897835));
#40090=CARTESIAN_POINT('Ctrl Pts',(31.1938887690265,-55.115673870314,-1.18498880250103));
#40091=CARTESIAN_POINT('Ctrl Pts',(31.6728308546874,-54.8423246209736,-1.22203476602371));
#40092=CARTESIAN_POINT('Ctrl Pts',(32.1517729403484,-54.5689753716333,-1.25908072954639));
#40093=CARTESIAN_POINT('Ctrl Pts',(32.7795922943635,-54.5565360653349,-1.29612669306907));
#40094=CARTESIAN_POINT('Ctrl Pts',(33.2690250069386,-54.8106693502475,-1.33317265659175));
#40095=CARTESIAN_POINT('Ctrl Pts',(33.7584577195138,-55.0648026351601,-1.37021862011443));
#40096=CARTESIAN_POINT('Ctrl Pts',(34.1095037906491,-55.5855085112837,-1.40726458363711));
#40097=CARTESIAN_POINT('Ctrl Pts',(34.1613832117471,-56.1345432465003,-1.44431054715979));
#40098=CARTESIAN_POINT('Ctrl Pts',(34.2132626328451,-56.6835779817169,-1.48135651068247));
#40099=CARTESIAN_POINT('Ctrl Pts',(33.9659754039058,-57.2609415760266,-1.51840247420515));
#40100=CARTESIAN_POINT('Ctrl Pts',(33.5329364407288,-57.6022802269071,-1.55544843772784));
#40101=CARTESIAN_POINT('Ctrl Pts',(33.470469460016,-57.6515192024594,-1.56079241294863));
#40102=CARTESIAN_POINT('Ctrl Pts',(33.4041372082081,-57.6958467816506,-1.56613638816942));
#40103=CARTESIAN_POINT('Ctrl Pts',(33.3347882996638,-57.7351190113229,-1.57148036339021));
#40104=CARTESIAN_POINT('Ctrl Pts',(31.0458737116219,-57.7433792852397,-2.));
#40105=CARTESIAN_POINT('Ctrl Pts',(31.5286078227264,-58.2269108712356,-1.96295403647732));
#40106=CARTESIAN_POINT('Ctrl Pts',(33.0063987810958,-58.6658791894418,-1.88886210943196));
#40107=CARTESIAN_POINT('Ctrl Pts',(34.7728277550873,-57.1516769644332,-1.77772421886392));
#40108=CARTESIAN_POINT('Ctrl Pts',(34.4535014835806,-54.8495668967865,-1.66658632829587));
#40109=CARTESIAN_POINT('Ctrl Pts',(32.3487507516394,-53.8677941230741,-1.55544843772784));
#40110=CARTESIAN_POINT('Ctrl Pts',(30.3811218874152,-55.1044118987674,-1.44431054715979));
#40111=CARTESIAN_POINT('Ctrl Pts',(30.3535878576004,-57.4278205885651,-1.33317265659175));
#40112=CARTESIAN_POINT('Ctrl Pts',(32.2903568834191,-58.7112317202033,-1.22203476602371));
#40113=CARTESIAN_POINT('Ctrl Pts',(34.4191815551847,-57.7799979545239,-1.11089687545567));
#40114=CARTESIAN_POINT('Ctrl Pts',(34.7912737376158,-55.4864512354733,-0.999758984887625));
#40115=CARTESIAN_POINT('Ctrl Pts',(33.0661792001092,-53.929919412126,-0.888621094319583));
#40116=CARTESIAN_POINT('Ctrl Pts',(30.822833264184,-54.5351044086332,-0.777483203751541));
#40117=CARTESIAN_POINT('Ctrl Pts',(30.1146276885619,-56.7480782089188,-0.6663453131835));
#40118=CARTESIAN_POINT('Ctrl Pts',(31.5897751037144,-58.543278448718,-0.555207422615457));
#40119=CARTESIAN_POINT('Ctrl Pts',(33.8980643703311,-58.2775391690228,-0.444069532047416));
#40120=CARTESIAN_POINT('Ctrl Pts',(34.926688116847,-56.1940939537869,-0.332931641479374));
#40121=CARTESIAN_POINT('Ctrl Pts',(33.7341373860101,-54.1999441339785,-0.221793750911332));
#40122=CARTESIAN_POINT('Ctrl Pts',(31.4119663698708,-54.1203575053852,-0.11065586034329));
#40123=CARTESIAN_POINT('Ctrl Pts',(30.0856850452223,-56.0281806868171,0.000482030224751475));
#40124=CARTESIAN_POINT('Ctrl Pts',(30.9692534931351,-58.1771614464075,0.111619920792793));
#40125=CARTESIAN_POINT('Ctrl Pts',(33.2539316216956,-58.6003133427487,0.222757811360835));
#40126=CARTESIAN_POINT('Ctrl Pts',(34.8485275651184,-56.9103206367347,0.333895701928877));
#40127=CARTESIAN_POINT('Ctrl Pts',(34.2934896049409,-54.6540528227808,0.445033592496919));
#40128=CARTESIAN_POINT('Ctrl Pts',(32.096850264347,-53.8966974164154,0.55617148306496));
#40129=CARTESIAN_POINT('Ctrl Pts',(30.2692184515671,-55.3314704112853,0.667309373633002));
#40130=CARTESIAN_POINT('Ctrl Pts',(30.4834462874739,-57.6451078131478,0.778447264201044));
#40131=CARTESIAN_POINT('Ctrl Pts',(32.5434486064222,-58.7199110699497,0.889585154769085));
#40132=CARTESIAN_POINT('Ctrl Pts',(34.563681922824,-57.5721005714895,1.00072304533713));
#40133=CARTESIAN_POINT('Ctrl Pts',(34.6950037716947,-55.2522802841409,1.11186093590517));
#40134=CARTESIAN_POINT('Ctrl Pts',(32.8172137752097,-53.883808025427,1.22299882647321));
#40135=CARTESIAN_POINT('Ctrl Pts',(30.6490744128704,-54.7192619732989,1.33413671704125));
#40136=CARTESIAN_POINT('Ctrl Pts',(30.1751082313325,-56.9939416545676,1.44527460760929));
#40137=CARTESIAN_POINT('Ctrl Pts',(31.8291418517329,-58.6258069603505,1.55641249817733));
#40138=CARTESIAN_POINT('Ctrl Pts',(34.0972195432855,-58.121193069651,1.66755038874538));
#40139=CARTESIAN_POINT('Ctrl Pts',(34.90334407317,-55.9419787993381,1.77868827931342));
#40140=CARTESIAN_POINT('Ctrl Pts',(33.5096605171051,-54.0828236849995,1.88982616988146));
#40141=CARTESIAN_POINT('Ctrl Pts',(31.1918232394055,-54.2454334870425,2.0009640604495));
#40142=CARTESIAN_POINT('Ctrl Pts',(30.0713749864112,-56.2809696095364,2.11210195101754));
#40143=CARTESIAN_POINT('Ctrl Pts',(31.1738747508358,-58.326282755013,2.22323984158559));
#40144=CARTESIAN_POINT('Ctrl Pts',(33.4901919951035,-58.5092746059889,2.33437773215363));
#40145=CARTESIAN_POINT('Ctrl Pts',(34.9001752767119,-56.6624506459969,2.44551562272167));
#40146=CARTESIAN_POINT('Ctrl Pts',(34.113250907707,-54.4762297900261,2.55665351328972));
#40147=CARTESIAN_POINT('Ctrl Pts',(31.8496996873681,-53.9516847809773,2.66779140385775));
#40148=CARTESIAN_POINT('Ctrl Pts',(30.1813757180883,-55.5689376143779,2.7789292944258));
#40149=CARTESIAN_POINT('Ctrl Pts',(30.63531484903,-57.8476984309217,2.89006718499383));
#40150=CARTESIAN_POINT('Ctrl Pts',(32.7960214456224,-58.7021916123209,3.00120507556188));
#40151=CARTESIAN_POINT('Ctrl Pts',(34.6857762559251,-57.350289859029,3.11234296612992));
#40152=CARTESIAN_POINT('Ctrl Pts',(34.5748652707907,-55.0294041774428,3.22348085669796));
#40153=CARTESIAN_POINT('Ctrl Pts',(32.5648065727292,-53.8638675525518,3.33461874726601));
#40154=CARTESIAN_POINT('Ctrl Pts',(30.4954296836915,-54.9205088752032,3.44575663783404));
#40155=CARTESIAN_POINT('Ctrl Pts',(30.2608587385459,-57.2321723596467,3.55689452840209));
#40156=CARTESIAN_POINT('Ctrl Pts',(32.0757991835954,-58.6829662025234,3.66803241897013));
#40157=CARTESIAN_POINT('Ctrl Pts',(34.2790154466699,-57.9449623463291,3.77917030953818));
#40158=CARTESIAN_POINT('Ctrl Pts',(34.8538786959893,-55.6936640901668,3.89030820010621));
#40159=CARTESIAN_POINT('Ctrl Pts',(33.2742100800909,-53.9897102593703,4.00144609067426));
#40160=CARTESIAN_POINT('Ctrl Pts',(30.9858981977034,-54.3927491193985,4.11258398124229));
#40161=CARTESIAN_POINT('Ctrl Pts',(30.0834608661246,-56.5338746309362,4.22372187181035));
#40162=CARTESIAN_POINT('Ctrl Pts',(31.3929092090316,-58.4532903311776,4.33485976237837));
#40163=CARTESIAN_POINT('Ctrl Pts',(33.71569030851,-58.394133262198,4.44599765294643));
#40164=CARTESIAN_POINT('Ctrl Pts',(34.9257362810773,-56.410550559801,4.55713554351446));
#40165=CARTESIAN_POINT('Ctrl Pts',(33.91547832718,-54.3181379674856,4.66827343408251));
#40166=CARTESIAN_POINT('Ctrl Pts',(31.609617005159,-54.0321044593028,4.77941132465054));
#40167=CARTESIAN_POINT('Ctrl Pts',(30.1187333412011,-55.8142597516569,4.89054921521859));
#40168=CARTESIAN_POINT('Ctrl Pts',(30.8074500449804,-58.0333768894161,5.00168710578662));
#40169=CARTESIAN_POINT('Ctrl Pts',(33.045376938239,-58.6582727998918,5.11282499635468));
#40170=CARTESIAN_POINT('Ctrl Pts',(34.7841140934679,-57.1169731495113,5.22396288692271));
#40171=CARTESIAN_POINT('Ctrl Pts',(34.4321757978777,-54.8202470274371,5.33510077749076));
#40172=CARTESIAN_POINT('Ctrl Pts',(32.3116949177892,-53.8703138209288,5.44623866805879));
#40173=CARTESIAN_POINT('Ctrl Pts',(30.3635721421369,-55.1366583239951,5.55737655862685));
#40174=CARTESIAN_POINT('Ctrl Pts',(30.370945362205,-57.4601807388668,5.66851444919488));
#40175=CARTESIAN_POINT('Ctrl Pts',(32.3270677340268,-58.7141352713797,5.77965233976293));
#40176=CARTESIAN_POINT('Ctrl Pts',(34.4414743886772,-57.7507618774265,5.89079023033096));
#40177=CARTESIAN_POINT('Ctrl Pts',(34.7788326566388,-55.451849617872,6.00192812089901));
#40178=CARTESIAN_POINT('Ctrl Pts',(33.0303393193103,-53.921614042038,6.11306601146705));
#40179=CARTESIAN_POINT('Ctrl Pts',(30.7964407564499,-54.5607069079647,6.22420390203509));
#40180=CARTESIAN_POINT('Ctrl Pts',(30.1217887402557,-56.7841397946826,6.33534179260313));
#40181=CARTESIAN_POINT('Ctrl Pts',(31.6240211855661,-58.5568181325984,6.44647968317118));
#40182=CARTESIAN_POINT('Ctrl Pts',(33.9278862659327,-58.2561121571832,6.55761757373921));
#40183=CARTESIAN_POINT('Ctrl Pts',(34.9251107981772,-56.157415110224,6.66875546430726));
#40184=CARTESIAN_POINT('Ctrl Pts',(33.7019669024841,-54.1813822458926,6.7798933548753));
#40185=CARTESIAN_POINT('Ctrl Pts',(31.3799180340502,-54.1373087230551,6.89103124544333));
#40186=CARTESIAN_POINT('Ctrl Pts',(30.0805564955408,-56.0643114795338,7.00216913601139));
#40187=CARTESIAN_POINT('Ctrl Pts',(31.0009129766989,-58.2011370798035,7.11330702657942));
#40188=CARTESIAN_POINT('Ctrl Pts',(32.5211546805143,-58.4569191413475,7.18739895362479));
#40189=CARTESIAN_POINT('Ctrl Pts',(33.1673657555108,-58.2350041503452,7.22444491714747));
#40190=CARTESIAN_POINT('Ctrl Pts',(31.1375785572409,-57.6518256858141,-2.07481497238249));
#40191=CARTESIAN_POINT('Ctrl Pts',(31.5898689183853,-58.1048632288923,-2.03776900885981));
#40192=CARTESIAN_POINT('Ctrl Pts',(32.974462612681,-58.516147898041,-1.96367708181445));
#40193=CARTESIAN_POINT('Ctrl Pts',(34.6294912924535,-57.0974392229326,-1.85253919124641));
#40194=CARTESIAN_POINT('Ctrl Pts',(34.3303034137843,-54.940512314437,-1.74140130067836));
#40195=CARTESIAN_POINT('Ctrl Pts',(32.3582893241016,-54.0206552913481,-1.63026341011032));
#40196=CARTESIAN_POINT('Ctrl Pts',(30.5147494765408,-55.1792854513053,-1.51912551954228));
#40197=CARTESIAN_POINT('Ctrl Pts',(30.4889518873457,-57.3561677789084,-1.40798762897424));
#40198=CARTESIAN_POINT('Ctrl Pts',(32.3035780800887,-58.5586402598713,-1.2968497384062));
#40199=CARTESIAN_POINT('Ctrl Pts',(34.2981478804346,-57.6861349893711,-1.18571184783816));
#40200=CARTESIAN_POINT('Ctrl Pts',(34.6467739743846,-55.5372313797063,-1.07457395727011));
#40201=CARTESIAN_POINT('Ctrl Pts',(33.0304729643073,-54.0788626331851,-0.963436066702072));
#40202=CARTESIAN_POINT('Ctrl Pts',(30.9286042125635,-54.6458814833823,-0.852298176134029));
#40203=CARTESIAN_POINT('Ctrl Pts',(30.2650618023749,-56.7192935259745,-0.741160285565989));
#40204=CARTESIAN_POINT('Ctrl Pts',(31.6471786691815,-58.4012790043313,-0.630022394997946));
#40205=CARTESIAN_POINT('Ctrl Pts',(33.8098950838865,-58.152298640154,-0.518884504429905));
#40206=CARTESIAN_POINT('Ctrl Pts',(34.7736484112179,-56.2002464293262,-0.407746613861864));
#40207=CARTESIAN_POINT('Ctrl Pts',(33.6563061966827,-54.3318581770161,-0.296608723293821));
#40208=CARTESIAN_POINT('Ctrl Pts',(31.4805834885329,-54.2572906994736,-0.185470832725779));
#40209=CARTESIAN_POINT('Ctrl Pts',(30.2379444342266,-56.044796524896,-0.0743329421577373));
#40210=CARTESIAN_POINT('Ctrl Pts',(31.0657904123944,-58.0582512642421,0.0368049484103042));
#40211=CARTESIAN_POINT('Ctrl Pts',(33.2063847314925,-58.4547169782088,0.147942838978346));
#40212=CARTESIAN_POINT('Ctrl Pts',(34.7004170746387,-56.8713040936593,0.259080729546388));
#40213=CARTESIAN_POINT('Ctrl Pts',(34.1803827251225,-54.7573283854238,0.370218620114429));
#40214=CARTESIAN_POINT('Ctrl Pts',(32.1222750053512,-54.0477357911158,0.481356510682471));
#40215=CARTESIAN_POINT('Ctrl Pts',(30.4099032594437,-55.3920244607626,0.592494401250513));
#40216=CARTESIAN_POINT('Ctrl Pts',(30.6106207621861,-57.5597517291987,0.703632291818554));
#40217=CARTESIAN_POINT('Ctrl Pts',(32.5407085089656,-58.5667722442102,0.814770182386597));
#40218=CARTESIAN_POINT('Ctrl Pts',(34.4335352954974,-57.4913487078745,0.925908072954637));
#40219=CARTESIAN_POINT('Ctrl Pts',(34.5565752984423,-55.3178284792041,1.03704596352268));
#40220=CARTESIAN_POINT('Ctrl Pts',(32.7972086074906,-54.0356592728607,1.14818385409072));
#40221=CARTESIAN_POINT('Ctrl Pts',(30.7658035075691,-54.8184251042163,1.25932174465876));
#40222=CARTESIAN_POINT('Ctrl Pts',(30.3217281242748,-56.9496515306538,1.37045963522681));
#40223=CARTESIAN_POINT('Ctrl Pts',(31.8714496921253,-58.4786028343079,1.48159752579484));
#40224=CARTESIAN_POINT('Ctrl Pts',(33.9964904850136,-58.0058125474547,1.59273541636289));
#40225=CARTESIAN_POINT('Ctrl Pts',(34.7517765656152,-55.9640309814584,1.70387330693093));
#40226=CARTESIAN_POINT('Ctrl Pts',(33.4459860188247,-54.2221239590531,1.81501119749897));
#40227=CARTESIAN_POINT('Ctrl Pts',(31.2743237407935,-54.3744787324154,1.92614908806701));
#40228=CARTESIAN_POINT('Ctrl Pts',(30.2245368429278,-56.2816432496664,2.03728697863506));
#40229=CARTESIAN_POINT('Ctrl Pts',(31.2575071782378,-58.1979681994494,2.1484248692031));
#40230=CARTESIAN_POINT('Ctrl Pts',(33.4277452841336,-58.3694196226251,2.25956275977114));
#40231=CARTESIAN_POINT('Ctrl Pts',(34.7488076101148,-56.6390660871692,2.37070065033918));
#40232=CARTESIAN_POINT('Ctrl Pts',(34.011510827345,-54.5907198076285,2.48183854090722));
#40233=CARTESIAN_POINT('Ctrl Pts',(31.8907110426077,-54.0992553634931,2.59297643147526));
#40234=CARTESIAN_POINT('Ctrl Pts',(30.3276003503782,-55.6145157340663,2.70411432204331));
#40235=CARTESIAN_POINT('Ctrl Pts',(30.7529116941352,-57.7495659179407,2.81525221261135));
#40236=CARTESIAN_POINT('Ctrl Pts',(32.7773527775791,-58.5501702687006,2.92639010317939));
#40237=CARTESIAN_POINT('Ctrl Pts',(34.5479297183105,-57.2835265446242,3.03752799374743));
#40238=CARTESIAN_POINT('Ctrl Pts',(34.4440133627694,-55.1090081110757,3.14866588431547));
#40239=CARTESIAN_POINT('Ctrl Pts',(32.5607195296748,-54.0169763509983,3.25980377488351));
#40240=CARTESIAN_POINT('Ctrl Pts',(30.6218484224618,-55.0069803188731,3.37094166545156));
#40241=CARTESIAN_POINT('Ctrl Pts',(30.4020707538584,-57.1728581554963,3.4820795560196));
#40242=CARTESIAN_POINT('Ctrl Pts',(32.1025515163817,-58.5321573142802,3.59321744658764));
#40243=CARTESIAN_POINT('Ctrl Pts',(34.1668213833381,-57.8406958596913,3.70435533715568));
#40244=CARTESIAN_POINT('Ctrl Pts',(34.705430735075,-55.7313763028164,3.81549322772372));
#40245=CARTESIAN_POINT('Ctrl Pts',(33.225384323732,-54.1348827553833,3.92663111829177));
#40246=CARTESIAN_POINT('Ctrl Pts',(31.0813854144196,-54.5125038668067,4.0377690088598));
#40247=CARTESIAN_POINT('Ctrl Pts',(30.2358605235516,-56.5185987513242,4.14890689942785));
#40248=CARTESIAN_POINT('Ctrl Pts',(31.4627281724074,-58.3169660103977,4.26004478999589));
#40249=CARTESIAN_POINT('Ctrl Pts',(33.6390224888347,-58.2615396970763,4.37118268056394));
#40250=CARTESIAN_POINT('Ctrl Pts',(34.772756603214,-56.4030521442201,4.48232057113197));
#40251=CARTESIAN_POINT('Ctrl Pts',(33.8262108251008,-54.4425980862378,4.59345846170002));
#40252=CARTESIAN_POINT('Ctrl Pts',(31.6657692360459,-54.1746033542736,4.70459635226805));
#40253=CARTESIAN_POINT('Ctrl Pts',(30.2689085309822,-55.8443665681263,4.81573424283611));
#40254=CARTESIAN_POINT('Ctrl Pts',(30.9141911400063,-57.923534517046,4.92687213340413));
#40255=CARTESIAN_POINT('Ctrl Pts',(33.0109826023927,-58.5090212073899,5.03801002397219));
#40256=CARTESIAN_POINT('Ctrl Pts',(34.6400658550227,-57.0649240129586,5.14914791454022));
#40257=CARTESIAN_POINT('Ctrl Pts',(34.3103226378947,-54.9130415101336,5.26028580510828));
#40258=CARTESIAN_POINT('Ctrl Pts',(32.3235704258736,-54.0230160838143,5.3714236956763));
#40259=CARTESIAN_POINT('Ctrl Pts',(30.498306510429,-55.2094982474935,5.48256158624436));
#40260=CARTESIAN_POINT('Ctrl Pts',(30.505214736491,-57.3864871280696,5.59369947681239));
#40261=CARTESIAN_POINT('Ctrl Pts',(32.3379737515305,-58.5613606978516,5.70483736738043));
#40262=CARTESIAN_POINT('Ctrl Pts',(34.3190348106915,-57.6587426929399,5.81597525794847));
#40263=CARTESIAN_POINT('Ctrl Pts',(34.6351174933556,-55.5048119219529,5.92711314851652));
#40264=CARTESIAN_POINT('Ctrl Pts',(32.9968933347409,-54.0710810433821,6.03825103908455));
#40265=CARTESIAN_POINT('Ctrl Pts',(30.9038761550678,-54.669869354557,6.1493889296526));
#40266=CARTESIAN_POINT('Ctrl Pts',(30.2717712405153,-56.7530808786254,6.26052682022064));
#40267=CARTESIAN_POINT('Ctrl Pts',(31.6792650131381,-58.4139648045911,6.37166471078869));
#40268=CARTESIAN_POINT('Ctrl Pts',(33.8378362540284,-58.1322229282863,6.48280260135672));
#40269=CARTESIAN_POINT('Ctrl Pts',(34.7721705665526,-56.1658807463968,6.59394049192477));
#40270=CARTESIAN_POINT('Ctrl Pts',(33.6261645529135,-54.3144668991412,6.70507838249281));
#40271=CARTESIAN_POINT('Ctrl Pts',(31.4505562891928,-54.2731728842735,6.81621627306085));
#40272=CARTESIAN_POINT('Ctrl Pts',(30.2331393178401,-56.0786487199456,6.9273541636289));
#40273=CARTESIAN_POINT('Ctrl Pts',(31.0954532825444,-58.080714868197,7.03849205419693));
#40274=CARTESIAN_POINT('Ctrl Pts',(32.5198205551868,-58.3203659687278,7.1125839812423));
#40275=CARTESIAN_POINT('Ctrl Pts',(33.1252781637591,-58.1124461032886,7.14962994476498));
#40276=CARTESIAN_POINT('Ctrl Pts',(31.2292834028599,-57.5602720863886,-2.14962994476498));
#40277=CARTESIAN_POINT('Ctrl Pts',(31.6511300140441,-57.982815586549,-2.1125839812423));
#40278=CARTESIAN_POINT('Ctrl Pts',(32.9425264442662,-58.3664166066402,-2.03849205419693));
#40279=CARTESIAN_POINT('Ctrl Pts',(34.4861548298198,-57.0432014814319,-1.9273541636289));
#40280=CARTESIAN_POINT('Ctrl Pts',(34.2071053439879,-55.0314577320876,-1.81621627306085));
#40281=CARTESIAN_POINT('Ctrl Pts',(32.3678278965638,-54.1735164596221,-1.70507838249281));
#40282=CARTESIAN_POINT('Ctrl Pts',(30.6483770656663,-55.2541590038433,-1.59394049192477));
#40283=CARTESIAN_POINT('Ctrl Pts',(30.6243159170911,-57.2845149692516,-1.48280260135673));
#40284=CARTESIAN_POINT('Ctrl Pts',(32.3167992767584,-58.4060487995394,-1.37166471078869));
#40285=CARTESIAN_POINT('Ctrl Pts',(34.1771142056845,-57.5922720242183,-1.26052682022064));
#40286=CARTESIAN_POINT('Ctrl Pts',(34.5022742111534,-55.5880115239392,-1.1493889296526));
#40287=CARTESIAN_POINT('Ctrl Pts',(32.9947667285052,-54.2278058542443,-1.03825103908456));
#40288=CARTESIAN_POINT('Ctrl Pts',(31.034375160943,-54.7566585581314,-0.927113148516519));
#40289=CARTESIAN_POINT('Ctrl Pts',(30.4154959161878,-56.6905088430302,-0.815975257948477));
#40290=CARTESIAN_POINT('Ctrl Pts',(31.7045822346487,-58.2592795599446,-0.704837367380435));
#40291=CARTESIAN_POINT('Ctrl Pts',(33.7217257974419,-58.0270581112851,-0.593699476812394));
#40292=CARTESIAN_POINT('Ctrl Pts',(34.6206087055887,-56.2063989048656,-0.482561586244352));
#40293=CARTESIAN_POINT('Ctrl Pts',(33.5784750073553,-54.4637722200536,-0.37142369567631));
#40294=CARTESIAN_POINT('Ctrl Pts',(31.549200607195,-54.394223893562,-0.260285805108268));
#40295=CARTESIAN_POINT('Ctrl Pts',(30.3902038232309,-56.061412362975,-0.149147914540226));
#40296=CARTESIAN_POINT('Ctrl Pts',(31.1623273316536,-57.9393410820767,-0.0380100239721848));
#40297=CARTESIAN_POINT('Ctrl Pts',(33.1588378412894,-58.3091206136688,0.0731278665958572));
#40298=CARTESIAN_POINT('Ctrl Pts',(34.5523065841589,-56.8322875505839,0.184265757163899));
#40299=CARTESIAN_POINT('Ctrl Pts',(34.067275845304,-54.8606039480667,0.295403647731941));
#40300=CARTESIAN_POINT('Ctrl Pts',(32.1476997463554,-54.1987741658161,0.406541538299982));
#40301=CARTESIAN_POINT('Ctrl Pts',(30.5505880673203,-55.45257851024,0.517679428868024));
#40302=CARTESIAN_POINT('Ctrl Pts',(30.7377952368983,-57.4743956452496,0.628817319436067));
#40303=CARTESIAN_POINT('Ctrl Pts',(32.537968411509,-58.4136334184707,0.739955210004107));
#40304=CARTESIAN_POINT('Ctrl Pts',(34.3033886681708,-57.4105968442596,0.85109310057215));
#40305=CARTESIAN_POINT('Ctrl Pts',(34.4181468251899,-55.3833766742673,0.96223099114019));
#40306=CARTESIAN_POINT('Ctrl Pts',(32.7772034397714,-54.1875105202945,1.07336888170823));
#40307=CARTESIAN_POINT('Ctrl Pts',(30.8825326022678,-54.9175882351338,1.18450677227627));
#40308=CARTESIAN_POINT('Ctrl Pts',(30.4683480172171,-56.9053614067402,1.29564466284432));
#40309=CARTESIAN_POINT('Ctrl Pts',(31.9137575325176,-58.3313987082653,1.40678255341236));
#40310=CARTESIAN_POINT('Ctrl Pts',(33.8957614267418,-57.8904320252583,1.5179204439804));
#40311=CARTESIAN_POINT('Ctrl Pts',(34.6002090580603,-55.9860831635788,1.62905833454844));
#40312=CARTESIAN_POINT('Ctrl Pts',(33.3823115205444,-54.3614242331065,1.74019622511649));
#40313=CARTESIAN_POINT('Ctrl Pts',(31.3568242421815,-54.5035239777884,1.85133411568452));
#40314=CARTESIAN_POINT('Ctrl Pts',(30.3776986994444,-56.2823168897962,1.96247200625257));
#40315=CARTESIAN_POINT('Ctrl Pts',(31.3411396056397,-58.0696536438858,2.07360989682061));
#40316=CARTESIAN_POINT('Ctrl Pts',(33.3652985731636,-58.2295646392613,2.18474778738865));
#40317=CARTESIAN_POINT('Ctrl Pts',(34.5974399435176,-56.6156815283417,2.29588567795669));
#40318=CARTESIAN_POINT('Ctrl Pts',(33.9097707469831,-54.7052098252309,2.40702356852473));
#40319=CARTESIAN_POINT('Ctrl Pts',(31.9317223978473,-54.246825946009,2.51816145909278));
#40320=CARTESIAN_POINT('Ctrl Pts',(30.4738249826682,-55.6600938537545,2.62929934966082));
#40321=CARTESIAN_POINT('Ctrl Pts',(30.8705085392404,-57.6514334049599,2.74043724022886));
#40322=CARTESIAN_POINT('Ctrl Pts',(32.7586841095359,-58.3981489250802,2.8515751307969));
#40323=CARTESIAN_POINT('Ctrl Pts',(34.4100831806958,-57.2167632302196,2.96271302136494));
#40324=CARTESIAN_POINT('Ctrl Pts',(34.3131614547482,-55.1886120447087,3.07385091193298));
#40325=CARTESIAN_POINT('Ctrl Pts',(32.5566324866203,-54.1700851494448,3.18498880250103));
#40326=CARTESIAN_POINT('Ctrl Pts',(30.7482671612322,-55.0934517625431,3.29612669306907));
#40327=CARTESIAN_POINT('Ctrl Pts',(30.5432827691709,-57.1135439513458,3.40726458363711));
#40328=CARTESIAN_POINT('Ctrl Pts',(32.1293038491678,-58.381348426037,3.51840247420515));
#40329=CARTESIAN_POINT('Ctrl Pts',(34.0546273200064,-57.7364293730534,3.6295403647732));
#40330=CARTESIAN_POINT('Ctrl Pts',(34.5569827741607,-55.769088515466,3.74067825534123));
#40331=CARTESIAN_POINT('Ctrl Pts',(33.1765585673731,-54.2800552513963,3.85181614590928));
#40332=CARTESIAN_POINT('Ctrl Pts',(31.1768726311357,-54.6322586142151,3.96295403647731));
#40333=CARTESIAN_POINT('Ctrl Pts',(30.3882601809785,-56.5033228717122,4.07409192704536));
#40334=CARTESIAN_POINT('Ctrl Pts',(31.5325471357831,-58.1806416896178,4.1852298176134));
#40335=CARTESIAN_POINT('Ctrl Pts',(33.5623546691594,-58.1289461319546,4.29636770818144));
#40336=CARTESIAN_POINT('Ctrl Pts',(34.6197769253507,-56.3955537286392,4.40750559874948));
#40337=CARTESIAN_POINT('Ctrl Pts',(33.7369433230217,-54.5670582049899,4.51864348931753));
#40338=CARTESIAN_POINT('Ctrl Pts',(31.7219214669328,-54.3171022492445,4.62978137988556));
#40339=CARTESIAN_POINT('Ctrl Pts',(30.4190837207633,-55.8744733845957,4.74091927045362));
#40340=CARTESIAN_POINT('Ctrl Pts',(31.0209322350323,-57.8136921446758,4.85205716102165));
#40341=CARTESIAN_POINT('Ctrl Pts',(32.9765882665465,-58.3597696148881,4.9631950515897));
#40342=CARTESIAN_POINT('Ctrl Pts',(34.4960176165775,-57.012874876406,5.07433294215773));
#40343=CARTESIAN_POINT('Ctrl Pts',(34.1884694779118,-55.0058359928302,5.18547083272578));
#40344=CARTESIAN_POINT('Ctrl Pts',(32.335445933958,-54.1757183466998,5.29660872329381));
#40345=CARTESIAN_POINT('Ctrl Pts',(30.633040878721,-55.2823381709919,5.40774661386187));
#40346=CARTESIAN_POINT('Ctrl Pts',(30.6394841107771,-57.3127935172724,5.5188845044299));
#40347=CARTESIAN_POINT('Ctrl Pts',(32.3488797690342,-58.4085861243234,5.63002239499795));
#40348=CARTESIAN_POINT('Ctrl Pts',(34.1965952327058,-57.5667235084533,5.74116028556598));
#40349=CARTESIAN_POINT('Ctrl Pts',(34.4914023300724,-55.5577742260338,5.85229817613403));
#40350=CARTESIAN_POINT('Ctrl Pts',(32.9634473501715,-54.2205480447262,5.96343606670206));
#40351=CARTESIAN_POINT('Ctrl Pts',(31.0113115536856,-54.7790318011494,6.07457395727011));
#40352=CARTESIAN_POINT('Ctrl Pts',(30.421753740775,-56.7220219625684,6.18571184783815));
#40353=CARTESIAN_POINT('Ctrl Pts',(31.7345088407102,-58.2711114765836,6.2968497384062));
#40354=CARTESIAN_POINT('Ctrl Pts',(33.747786242124,-58.0083336993896,6.40798762897423));
#40355=CARTESIAN_POINT('Ctrl Pts',(34.6192303349282,-56.1743463825696,6.51912551954228));
#40356=CARTESIAN_POINT('Ctrl Pts',(33.5503622033428,-54.4475515523897,6.63026341011032));
#40357=CARTESIAN_POINT('Ctrl Pts',(31.5211945443355,-54.4090370454918,6.74140130067836));
#40358=CARTESIAN_POINT('Ctrl Pts',(30.3857221401394,-56.0929859603577,6.85253919124641));
#40359=CARTESIAN_POINT('Ctrl Pts',(31.18999358839,-57.9602926565904,6.96367708181444));
#40360=CARTESIAN_POINT('Ctrl Pts',(32.5184864298593,-58.1838127961081,7.03776900885981));
#40361=CARTESIAN_POINT('Ctrl Pts',(33.0831905720075,-57.989888056232,7.07481497238249));
#40362=CARTESIAN_POINT('Ctrl Pts',(31.3209882484789,-57.468718486963,-2.22444491714747));
#40363=CARTESIAN_POINT('Ctrl Pts',(31.712391109703,-57.8607679442057,-2.18739895362479));
#40364=CARTESIAN_POINT('Ctrl Pts',(32.9105902758514,-58.2166853152393,-2.11330702657942));
#40365=CARTESIAN_POINT('Ctrl Pts',(34.342818367186,-56.9889637399312,-2.00216913601138));
#40366=CARTESIAN_POINT('Ctrl Pts',(34.0839072741917,-55.1224031497381,-1.89103124544334));
#40367=CARTESIAN_POINT('Ctrl Pts',(32.377366469026,-54.3263776278961,-1.7798933548753));
#40368=CARTESIAN_POINT('Ctrl Pts',(30.7820046547919,-55.3290325563813,-1.66875546430726));
#40369=CARTESIAN_POINT('Ctrl Pts',(30.7596799468364,-57.2128621595949,-1.55761757373921));
#40370=CARTESIAN_POINT('Ctrl Pts',(32.330020473428,-58.2534573392076,-1.44647968317118));
#40371=CARTESIAN_POINT('Ctrl Pts',(34.0560805309345,-57.4984090590655,-1.33534179260313));
#40372=CARTESIAN_POINT('Ctrl Pts',(34.3577744479221,-55.6387916681722,-1.22420390203509));
#40373=CARTESIAN_POINT('Ctrl Pts',(32.9590604927032,-54.3767490753035,-1.11306601146705));
#40374=CARTESIAN_POINT('Ctrl Pts',(31.1401461093225,-54.8674356328804,-1.00192812089901));
#40375=CARTESIAN_POINT('Ctrl Pts',(30.5659300300008,-56.6617241600859,-0.890790230330966));
#40376=CARTESIAN_POINT('Ctrl Pts',(31.7619858001159,-58.1172801155578,-0.779652339762924));
#40377=CARTESIAN_POINT('Ctrl Pts',(33.6335565109972,-57.9018175824163,-0.668514449194882));
#40378=CARTESIAN_POINT('Ctrl Pts',(34.4675689999596,-56.2125513804049,-0.557376558626841));
#40379=CARTESIAN_POINT('Ctrl Pts',(33.5006438180279,-54.595686263091,-0.446238668058798));
#40380=CARTESIAN_POINT('Ctrl Pts',(31.617817725857,-54.5311570876504,-0.335100777490757));
#40381=CARTESIAN_POINT('Ctrl Pts',(30.5424632122353,-56.0780282010539,-0.223962886922715));
#40382=CARTESIAN_POINT('Ctrl Pts',(31.2588642509128,-57.8204308999114,-0.112824996354674));
#40383=CARTESIAN_POINT('Ctrl Pts',(33.1112909510864,-58.1635242491288,-0.00168710578663179));
#40384=CARTESIAN_POINT('Ctrl Pts',(34.4041960936791,-56.7932710075085,0.10945078478141));
#40385=CARTESIAN_POINT('Ctrl Pts',(33.9541689654856,-54.9638795107098,0.220588675349452));
#40386=CARTESIAN_POINT('Ctrl Pts',(32.1731244873596,-54.3498125405165,0.331726565917493));
#40387=CARTESIAN_POINT('Ctrl Pts',(30.6912728751969,-55.5131325597174,0.442864456485535));
#40388=CARTESIAN_POINT('Ctrl Pts',(30.8649697116104,-57.3890395613005,0.554002347053577));
#40389=CARTESIAN_POINT('Ctrl Pts',(32.5352283140525,-58.2604945927311,0.665140237621618));
#40390=CARTESIAN_POINT('Ctrl Pts',(34.1732420408443,-57.3298449806446,0.776278128189661));
#40391=CARTESIAN_POINT('Ctrl Pts',(34.2797183519374,-55.4489248693306,0.887416018757702));
#40392=CARTESIAN_POINT('Ctrl Pts',(32.7571982720523,-54.3393617677281,0.998553909325745));
#40393=CARTESIAN_POINT('Ctrl Pts',(30.9992616969666,-55.0167513660514,1.10969179989379));
#40394=CARTESIAN_POINT('Ctrl Pts',(30.6149679101593,-56.8610712828264,1.22082969046183));
#40395=CARTESIAN_POINT('Ctrl Pts',(31.9560653729101,-58.1841945822227,1.33196758102987));
#40396=CARTESIAN_POINT('Ctrl Pts',(33.7950323684699,-57.775051503062,1.44310547159791));
#40397=CARTESIAN_POINT('Ctrl Pts',(34.4486415505055,-56.0081353456992,1.55424336216595));
#40398=CARTESIAN_POINT('Ctrl Pts',(33.318637022264,-54.5007245071601,1.665381252734));
#40399=CARTESIAN_POINT('Ctrl Pts',(31.4393247435695,-54.6325692231613,1.77651914330203));
#40400=CARTESIAN_POINT('Ctrl Pts',(30.5308605559611,-56.2829905299262,1.88765703387008));
#40401=CARTESIAN_POINT('Ctrl Pts',(31.4247720330417,-57.9413390883221,1.99879492443811));
#40402=CARTESIAN_POINT('Ctrl Pts',(33.3028518621937,-58.0897096558975,2.10993281500617));
#40403=CARTESIAN_POINT('Ctrl Pts',(34.4460722769204,-56.592296969514,2.2210707055742));
#40404=CARTESIAN_POINT('Ctrl Pts',(33.8080306666211,-54.8196998428333,2.33220859614224));
#40405=CARTESIAN_POINT('Ctrl Pts',(31.9727337530869,-54.3943965285248,2.44334648671029));
#40406=CARTESIAN_POINT('Ctrl Pts',(30.6200496149581,-55.7056719734428,2.55448437727833));
#40407=CARTESIAN_POINT('Ctrl Pts',(30.9881053843455,-57.5533008919789,2.66562226784637));
#40408=CARTESIAN_POINT('Ctrl Pts',(32.7400154414926,-58.2461275814599,2.77676015841441));
#40409=CARTESIAN_POINT('Ctrl Pts',(34.2722366430812,-57.1499999158147,2.88789804898245));
#40410=CARTESIAN_POINT('Ctrl Pts',(34.182309546727,-55.2682159783418,2.9990359395505));
#40411=CARTESIAN_POINT('Ctrl Pts',(32.5525454435658,-54.3231939478911,3.11017383011853));
#40412=CARTESIAN_POINT('Ctrl Pts',(30.8746859000024,-55.1799232062132,3.22131172068658));
#40413=CARTESIAN_POINT('Ctrl Pts',(30.6844947844835,-57.0542297471953,3.33244961125462));
#40414=CARTESIAN_POINT('Ctrl Pts',(32.156056181954,-58.2305395377939,3.44358750182266));
#40415=CARTESIAN_POINT('Ctrl Pts',(33.9424332566746,-57.6321628864156,3.55472539239071));
#40416=CARTESIAN_POINT('Ctrl Pts',(34.4085348132464,-55.8068007281157,3.66586328295874));
#40417=CARTESIAN_POINT('Ctrl Pts',(33.1277328110142,-54.4252277474093,3.77700117352679));
#40418=CARTESIAN_POINT('Ctrl Pts',(31.2723598478519,-54.7520133616234,3.88813906409483));
#40419=CARTESIAN_POINT('Ctrl Pts',(30.5406598384055,-56.4880469921002,3.99927695466287));
#40420=CARTESIAN_POINT('Ctrl Pts',(31.6023660991588,-58.044317368838,4.11041484523091));
#40421=CARTESIAN_POINT('Ctrl Pts',(33.4856868494842,-57.9963525668329,4.22155273579896));
#40422=CARTESIAN_POINT('Ctrl Pts',(34.4667972474874,-56.3880553130583,4.332690626367));
#40423=CARTESIAN_POINT('Ctrl Pts',(33.6476758209426,-54.6915183237421,4.44382851693504));
#40424=CARTESIAN_POINT('Ctrl Pts',(31.7780736978196,-54.4596011442154,4.55496640750308));
#40425=CARTESIAN_POINT('Ctrl Pts',(30.5692589105444,-55.904580201065,4.66610429807113));
#40426=CARTESIAN_POINT('Ctrl Pts',(31.1276733300582,-57.7038497723057,4.77724218863916));
#40427=CARTESIAN_POINT('Ctrl Pts',(32.9421939307002,-58.2105180223861,4.8883800792072));
#40428=CARTESIAN_POINT('Ctrl Pts',(34.3519693781324,-56.9608257398534,4.99951796977525));
#40429=CARTESIAN_POINT('Ctrl Pts',(34.0666163179288,-55.0986304755266,5.11065586034329));
#40430=CARTESIAN_POINT('Ctrl Pts',(32.3473214420424,-54.3284206095853,5.22179375091132));
#40431=CARTESIAN_POINT('Ctrl Pts',(30.7677752470131,-55.3551780944903,5.33293164147938));
#40432=CARTESIAN_POINT('Ctrl Pts',(30.7737534850632,-57.2390999064753,5.44406953204741));
#40433=CARTESIAN_POINT('Ctrl Pts',(32.3597857865378,-58.2558115507953,5.55520742261546));
#40434=CARTESIAN_POINT('Ctrl Pts',(34.0741556547201,-57.4747043239667,5.6663453131835));
#40435=CARTESIAN_POINT('Ctrl Pts',(34.3476871667892,-55.6107365301146,5.77748320375153));
#40436=CARTESIAN_POINT('Ctrl Pts',(32.9300013656021,-54.3700150460704,5.88862109431958));
#40437=CARTESIAN_POINT('Ctrl Pts',(31.1187469523034,-54.8881942477417,5.99975898488762));
#40438=CARTESIAN_POINT('Ctrl Pts',(30.5717362410347,-56.6909630465113,6.11089687545566));
#40439=CARTESIAN_POINT('Ctrl Pts',(31.7897526682823,-58.1282581485763,6.2220347660237));
#40440=CARTESIAN_POINT('Ctrl Pts',(33.6577362302197,-57.8844444704929,6.33317265659175));
#40441=CARTESIAN_POINT('Ctrl Pts',(34.4662901033037,-56.1828120187425,6.44431054715979));
#40442=CARTESIAN_POINT('Ctrl Pts',(33.4745598537722,-54.5806362056383,6.55544843772783));
#40443=CARTESIAN_POINT('Ctrl Pts',(31.5918327994781,-54.5449012067101,6.66658632829587));
#40444=CARTESIAN_POINT('Ctrl Pts',(30.5383049624387,-56.1073232007697,6.77772421886392));
#40445=CARTESIAN_POINT('Ctrl Pts',(31.2845338942354,-57.8398704449839,6.88886210943196));
#40446=CARTESIAN_POINT('Ctrl Pts',(32.5171523045318,-58.0472596234885,6.96295403647732));
#40447=CARTESIAN_POINT('Ctrl Pts',(33.0411029802559,-57.8673300091754,7.));
#40448=CARTESIAN_POINT('Ctrl Pts',(33.3327354544031,-57.732107437543,-1.3785196366098));
#40449=CARTESIAN_POINT('Ctrl Pts',(33.5202555818621,-57.6251326319318,-1.36412702194091));
#40450=CARTESIAN_POINT('Ctrl Pts',(33.6873867521344,-57.4836168424902,-1.34973440727202));
#40451=CARTESIAN_POINT('Ctrl Pts',(33.8186861741813,-57.3143142072736,-1.33534179260314));
#40452=CARTESIAN_POINT('Ctrl Pts',(34.1566451699303,-56.8785365954344,-1.29829582908045));
#40453=CARTESIAN_POINT('Ctrl Pts',(34.2572098089262,-56.2586641318033,-1.26124986555777));
#40454=CARTESIAN_POINT('Ctrl Pts',(34.0743731358877,-55.7383874678429,-1.22420390203509));
#40455=CARTESIAN_POINT('Ctrl Pts',(33.8915364628492,-55.2181108038826,-1.18715793851241));
#40456=CARTESIAN_POINT('Ctrl Pts',(33.4252984777762,-54.7974299395931,-1.15011197498973));
#40457=CARTESIAN_POINT('Ctrl Pts',(32.8890270880096,-54.6688706003778,-1.11306601146705));
#40458=CARTESIAN_POINT('Ctrl Pts',(32.352755698243,-54.5403112611625,-1.07602004794437));
#40459=CARTESIAN_POINT('Ctrl Pts',(31.7464509037828,-54.7038734470215,-1.03897408442169));
#40460=CARTESIAN_POINT('Ctrl Pts',(31.3475958266657,-55.0847026278185,-1.00192812089901));
#40461=CARTESIAN_POINT('Ctrl Pts',(30.9487407495486,-55.4655318086156,-0.96488215737633));
#40462=CARTESIAN_POINT('Ctrl Pts',(30.7573353897747,-56.0636279843508,-0.92783619385365));
#40463=CARTESIAN_POINT('Ctrl Pts',(30.8609753382403,-56.6052687314637,-0.890790230330969));
#40464=CARTESIAN_POINT('Ctrl Pts',(30.9646152867058,-57.1469094785766,-0.853744266808289));
#40465=CARTESIAN_POINT('Ctrl Pts',(31.3633005434108,-57.6320947970672,-0.816698303285608));
#40466=CARTESIAN_POINT('Ctrl Pts',(31.8745716235769,-57.8387770341222,-0.779652339762927));
#40467=CARTESIAN_POINT('Ctrl Pts',(32.3398155301954,-58.0268527049873,-0.745941438711884));
#40468=CARTESIAN_POINT('Ctrl Pts',(32.8982866368193,-57.9843126404343,-0.712230537660842));
#40469=CARTESIAN_POINT('Ctrl Pts',(33.3348489584778,-57.7359240281238,-0.678519636609799));
#40470=CARTESIAN_POINT('Ctrl Pts',(31.0458737116219,-57.7433792852397,-2.));
#40471=CARTESIAN_POINT('Ctrl Pts',(31.1022242475563,-57.7901329641036,-2.));
#40472=CARTESIAN_POINT('Ctrl Pts',(31.1610916221591,-57.8334666739877,-2.));
#40473=CARTESIAN_POINT('Ctrl Pts',(31.2221267441933,-57.8733637960044,-2.));
#40474=CARTESIAN_POINT('Ctrl Pts',(31.2848602944917,-57.9143711378001,-2.));
#40475=CARTESIAN_POINT('Ctrl Pts',(31.3498848969714,-57.9517482942034,-2.));
#40476=CARTESIAN_POINT('Ctrl Pts',(31.4168445551513,-57.9854278643729,-2.));
#40477=CARTESIAN_POINT('Ctrl Pts',(31.473423951905,-58.0138863394445,-2.));
#40478=CARTESIAN_POINT('Ctrl Pts',(31.5313856959209,-58.0397039720774,-2.));
#40479=CARTESIAN_POINT('Ctrl Pts',(31.5905192436884,-58.0628113946307,-2.));
#40480=CARTESIAN_POINT('Ctrl Pts',(31.6167907197732,-58.0730774131922,-2.));
#40481=CARTESIAN_POINT('Ctrl Pts',(31.6432934887176,-58.0828081409933,-2.));
#40482=CARTESIAN_POINT('Ctrl Pts',(31.6700089381818,-58.0919957886044,-2.));
#40483=CARTESIAN_POINT('Ctrl Pts',(31.6846879641888,-58.0970440180347,-2.));
#40484=CARTESIAN_POINT('Ctrl Pts',(31.6994311962746,-58.1019282705386,-2.));
#40485=CARTESIAN_POINT('Ctrl Pts',(31.7142355159248,-58.1066471169474,-2.));
#40486=CARTESIAN_POINT('Ctrl Pts',(31.7278877153664,-58.1109987274118,-2.));
#40487=CARTESIAN_POINT('Ctrl Pts',(31.7415938959754,-58.1152101596109,-2.));
#40488=CARTESIAN_POINT('Ctrl Pts',(31.7553302775603,-58.1192742594955,-2.));
#40489=CARTESIAN_POINT('Ctrl Pts',(31.8255274332676,-58.1400430660875,-2.));
#40490=CARTESIAN_POINT('Ctrl Pts',(31.8966328017476,-58.1570081793249,-2.));
#40491=CARTESIAN_POINT('Ctrl Pts',(31.9683123621892,-58.17010995281,-2.));
#40492=CARTESIAN_POINT('Ctrl Pts',(32.0394355875868,-58.1831100379521,-2.));
#40493=CARTESIAN_POINT('Ctrl Pts',(32.111125145623,-58.1923065191828,-2.));
#40494=CARTESIAN_POINT('Ctrl Pts',(32.1830533294046,-58.197590217694,-2.));
#40495=CARTESIAN_POINT('Ctrl Pts',(32.2428321680026,-58.2019814499467,-2.));
#40496=CARTESIAN_POINT('Ctrl Pts',(32.3027760709051,-58.203669194572,-2.));
#40497=CARTESIAN_POINT('Ctrl Pts',(32.3626887230984,-58.202563625202,-2.));
#40498=CARTESIAN_POINT('Ctrl Pts',(32.3876963771293,-58.2021021584617,-2.));
#40499=CARTESIAN_POINT('Ctrl Pts',(32.4126984595008,-58.2011537302573,-2.));
#40500=CARTESIAN_POINT('Ctrl Pts',(32.4376800452417,-58.1997105189462,-2.));
#40501=CARTESIAN_POINT('Ctrl Pts',(32.4492432419533,-58.1990425014528,-2.));
#40502=CARTESIAN_POINT('Ctrl Pts',(32.4608020410722,-58.1982684671836,-2.));
#40503=CARTESIAN_POINT('Ctrl Pts',(32.4723549281396,-58.1973875849089,-2.));
#40504=CARTESIAN_POINT('Ctrl Pts',(32.4844044306918,-58.1964688367937,-2.));
#40505=CARTESIAN_POINT('Ctrl Pts',(32.4964392274972,-58.1954344592285,-2.));
#40506=CARTESIAN_POINT('Ctrl Pts',(32.5084532356254,-58.1942844547156,-2.));
#40507=CARTESIAN_POINT('Ctrl Pts',(32.5768783070893,-58.1877346721503,-2.));
#40508=CARTESIAN_POINT('Ctrl Pts',(32.6446774036362,-58.1774344901189,-2.));
#40509=CARTESIAN_POINT('Ctrl Pts',(32.7115617527762,-58.1632926068254,-2.));
#40510=CARTESIAN_POINT('Ctrl Pts',(32.7721836417612,-58.150474844672,-2.));
#40511=CARTESIAN_POINT('Ctrl Pts',(32.832054420019,-58.1345005317109,-2.));
#40512=CARTESIAN_POINT('Ctrl Pts',(32.8909448795168,-58.115267443086,-2.));
#40513=CARTESIAN_POINT('Ctrl Pts',(32.9606152109761,-58.0925137462918,-2.));
#40514=CARTESIAN_POINT('Ctrl Pts',(33.0289150978522,-58.0651988064951,-2.));
#40515=CARTESIAN_POINT('Ctrl Pts',(33.0955156401826,-58.0335993051752,-2.));
#40516=CARTESIAN_POINT('Ctrl Pts',(33.1101787046012,-58.0266422218357,-2.));
#40517=CARTESIAN_POINT('Ctrl Pts',(33.1247592149198,-58.0194773027427,-2.));
#40518=CARTESIAN_POINT('Ctrl Pts',(33.1392533337009,-58.0121072627471,-2.));
#40519=CARTESIAN_POINT('Ctrl Pts',(33.1542086549699,-58.0045027082679,-2.));
#40520=CARTESIAN_POINT('Ctrl Pts',(33.1690773275608,-57.9966767059944,-2.));
#40521=CARTESIAN_POINT('Ctrl Pts',(33.1838253280879,-57.9886488037404,-2.));
#40522=CARTESIAN_POINT('Ctrl Pts',(33.244061954076,-57.9558596982169,-2.));
#40523=CARTESIAN_POINT('Ctrl Pts',(33.3023667325498,-57.9196691076173,-2.));
#40524=CARTESIAN_POINT('Ctrl Pts',(33.3585069616667,-57.8803506668589,-2.));
#40525=CARTESIAN_POINT('Ctrl Pts',(33.414635850494,-57.8410401683998,-2.));
#40526=CARTESIAN_POINT('Ctrl Pts',(33.4686017655928,-57.7986021545391,-2.));
#40527=CARTESIAN_POINT('Ctrl Pts',(33.5201343260522,-57.7532746488578,-2.));
#40528=CARTESIAN_POINT('Ctrl Pts',(33.5574338655248,-57.7204663608107,-2.));
#40529=CARTESIAN_POINT('Ctrl Pts',(33.5934578302879,-57.6861435081566,-2.));
#40530=CARTESIAN_POINT('Ctrl Pts',(33.6280882155819,-57.6503888642621,-2.));
#40531=CARTESIAN_POINT('Ctrl Pts',(33.6540651537304,-57.6235685974622,-2.));
#40532=CARTESIAN_POINT('Ctrl Pts',(33.6792576937978,-57.5959425522059,-2.));
#40533=CARTESIAN_POINT('Ctrl Pts',(33.7036104502874,-57.5675443623166,-2.));
#40534=CARTESIAN_POINT('Ctrl Pts',(33.7117026688617,-57.5581078798471,-2.));
#40535=CARTESIAN_POINT('Ctrl Pts',(33.7196957778872,-57.5485935241117,-2.));
#40536=CARTESIAN_POINT('Ctrl Pts',(33.7275879316751,-57.5390030774457,-2.));
#40537=CARTESIAN_POINT('Ctrl Pts',(33.7694510935145,-57.4881314862826,-2.));
#40538=CARTESIAN_POINT('Ctrl Pts',(33.80847982562,-57.4351175563013,-2.));
#40539=CARTESIAN_POINT('Ctrl Pts',(33.8444097934509,-57.380171662872,-2.));
#40540=CARTESIAN_POINT('Ctrl Pts',(33.8696919535248,-57.3415089265284,-2.));
#40541=CARTESIAN_POINT('Ctrl Pts',(33.8934389529984,-57.3018891510446,-2.));
#40542=CARTESIAN_POINT('Ctrl Pts',(33.9155436487628,-57.2613822920818,-2.));
#40543=CARTESIAN_POINT('Ctrl Pts',(33.9226388854396,-57.2483802695959,-2.));
#40544=CARTESIAN_POINT('Ctrl Pts',(33.9295657377069,-57.2352850255039,-2.));
#40545=CARTESIAN_POINT('Ctrl Pts',(33.9363174100524,-57.2221046384035,-2.));
#40546=CARTESIAN_POINT('Ctrl Pts',(33.965080442193,-57.1659544168891,-2.));
#40547=CARTESIAN_POINT('Ctrl Pts',(33.9906110255055,-57.1083731117427,-2.));
#40548=CARTESIAN_POINT('Ctrl Pts',(34.0126532831744,-57.0495480070032,-2.));
#40549=CARTESIAN_POINT('Ctrl Pts',(34.0329745304529,-56.9953158354375,-2.));
#40550=CARTESIAN_POINT('Ctrl Pts',(34.0503306992963,-56.9400259525623,-2.));
#40551=CARTESIAN_POINT('Ctrl Pts',(34.064482015077,-56.8838229928238,-2.));
#40552=CARTESIAN_POINT('Ctrl Pts',(34.0671303463503,-56.8733049563224,-2.));
#40553=CARTESIAN_POINT('Ctrl Pts',(34.0696663195691,-56.8627549469952,-2.));
#40554=CARTESIAN_POINT('Ctrl Pts',(34.0720901513885,-56.8521746541717,-2.));
#40555=CARTESIAN_POINT('Origin',(32.5,-56.2916512459885,3.));
#40556=CARTESIAN_POINT('Origin',(-32.5,-56.2916512459885,7.));
#40557=CARTESIAN_POINT('Ctrl Pts',(-33.5940263469955,-57.5480995545471,
7.));
#40558=CARTESIAN_POINT('Ctrl Pts',(-33.6455781063537,-57.5127482049916,
7.));
#40559=CARTESIAN_POINT('Ctrl Pts',(-33.6948218851486,-57.4743678095888,
7.));
#40560=CARTESIAN_POINT('Ctrl Pts',(-33.7416962543705,-57.4332901552822,
7.));
#40561=CARTESIAN_POINT('Ctrl Pts',(-33.7714300137986,-57.4072334187053,
7.));
#40562=CARTESIAN_POINT('Ctrl Pts',(-33.8002101105626,-57.3800903099151,
7.));
#40563=CARTESIAN_POINT('Ctrl Pts',(-33.8280169255491,-57.3519357930303,
7.));
#40564=CARTESIAN_POINT('Ctrl Pts',(-33.8470314135077,-57.3326835441645,
7.));
#40565=CARTESIAN_POINT('Ctrl Pts',(-33.865590736976,-57.3129582161004,7.));
#40566=CARTESIAN_POINT('Ctrl Pts',(-33.88368758978,-57.2927820234305,7.));
#40567=CARTESIAN_POINT('Ctrl Pts',(-33.8932692324261,-57.2820994439668,
7.));
#40568=CARTESIAN_POINT('Ctrl Pts',(-33.9027209649851,-57.2712905501713,
7.));
#40569=CARTESIAN_POINT('Ctrl Pts',(-33.9120326400169,-57.2603695730079,
7.));
#40570=CARTESIAN_POINT('Ctrl Pts',(-33.954835257131,-57.2101695389172,7.));
#40571=CARTESIAN_POINT('Ctrl Pts',(-33.9947314176855,-57.1575493212694,
7.));
#40572=CARTESIAN_POINT('Ctrl Pts',(-34.0316365850473,-57.1028515989214,
7.));
#40573=CARTESIAN_POINT('Ctrl Pts',(-34.0582554670344,-57.0633993400583,
7.));
#40574=CARTESIAN_POINT('Ctrl Pts',(-34.0833178684594,-57.0228651370504,
7.));
#40575=CARTESIAN_POINT('Ctrl Pts',(-34.1067823366534,-56.981363974441,7.));
#40576=CARTESIAN_POINT('Ctrl Pts',(-34.1132255641423,-56.9699679594307,
7.));
#40577=CARTESIAN_POINT('Ctrl Pts',(-34.1195482496941,-56.9584989762171,
7.));
#40578=CARTESIAN_POINT('Ctrl Pts',(-34.1257494077654,-56.9469592829674,
7.));
#40579=CARTESIAN_POINT('Ctrl Pts',(-34.1320583289994,-56.9352190539746,
7.));
#40580=CARTESIAN_POINT('Ctrl Pts',(-34.1382375551786,-56.9234128304559,
7.));
#40581=CARTESIAN_POINT('Ctrl Pts',(-34.1442842647394,-56.9115477362169,
7.));
#40582=CARTESIAN_POINT('Ctrl Pts',(-34.1750933788667,-56.851092865867,7.));
#40583=CARTESIAN_POINT('Ctrl Pts',(-34.2024838356472,-56.7890775491619,
7.));
#40584=CARTESIAN_POINT('Ctrl Pts',(-34.2263706778433,-56.7258494467084,
7.));
#40585=CARTESIAN_POINT('Ctrl Pts',(-34.2506031310785,-56.6617065171708,
7.));
#40586=CARTESIAN_POINT('Ctrl Pts',(-34.2712305305178,-56.5963146349483,
7.));
#40587=CARTESIAN_POINT('Ctrl Pts',(-34.2881270714822,-56.5299991241842,
7.));
#40588=CARTESIAN_POINT('Ctrl Pts',(-34.2985953641524,-56.4889131896894,
7.));
#40589=CARTESIAN_POINT('Ctrl Pts',(-34.3076308154854,-56.4474720283024,
7.));
#40590=CARTESIAN_POINT('Ctrl Pts',(-34.3151947514507,-56.4057480909205,
7.));
#40591=CARTESIAN_POINT('Ctrl Pts',(-34.3213914047069,-56.3715663139163,
7.));
#40592=CARTESIAN_POINT('Ctrl Pts',(-34.3266003410262,-56.3371946653748,
7.));
#40593=CARTESIAN_POINT('Ctrl Pts',(-34.3307964558649,-56.3026718438894,
7.));
#40594=CARTESIAN_POINT('Ctrl Pts',(-34.3325110301801,-56.2885654751929,
7.));
#40595=CARTESIAN_POINT('Ctrl Pts',(-34.334056573613,-56.274431305155,7.));
#40596=CARTESIAN_POINT('Ctrl Pts',(-34.3354292580426,-56.2602960059048,
7.));
#40597=CARTESIAN_POINT('Ctrl Pts',(-34.3422420688138,-56.1901406833092,
7.));
#40598=CARTESIAN_POINT('Ctrl Pts',(-34.344817121763,-56.1198364598138,7.));
#40599=CARTESIAN_POINT('Ctrl Pts',(-34.3430393002911,-56.0497278067116,
7.));
#40600=CARTESIAN_POINT('Ctrl Pts',(-34.3428417470506,-56.0419372654097,
7.));
#40601=CARTESIAN_POINT('Ctrl Pts',(-34.3425903992471,-56.0341491124172,
7.));
#40602=CARTESIAN_POINT('Ctrl Pts',(-34.3422850635953,-56.0263638020432,
7.));
#40603=CARTESIAN_POINT('Ctrl Pts',(-34.3396426913258,-55.9589897888101,
7.));
#40604=CARTESIAN_POINT('Ctrl Pts',(-34.3329614085342,-55.8918294784485,
7.));
#40605=CARTESIAN_POINT('Ctrl Pts',(-34.3224781325168,-55.8251283238202,
7.));
#40606=CARTESIAN_POINT('Ctrl Pts',(-34.311200007843,-55.7533698452166,7.));
#40607=CARTESIAN_POINT('Ctrl Pts',(-34.2955218532054,-55.682141849139,7.));
#40608=CARTESIAN_POINT('Ctrl Pts',(-34.275674530723,-55.6117461590084,7.));
#40609=CARTESIAN_POINT('Ctrl Pts',(-34.2720417381032,-55.5988611492648,
7.));
#40610=CARTESIAN_POINT('Ctrl Pts',(-34.2682690985559,-55.5860040383836,
7.));
#40611=CARTESIAN_POINT('Ctrl Pts',(-34.2643578043072,-55.5731767072662,
7.));
#40612=CARTESIAN_POINT('Ctrl Pts',(-34.260994380672,-55.5621461516716,7.));
#40613=CARTESIAN_POINT('Ctrl Pts',(-34.2575311418944,-55.5511465602876,
7.));
#40614=CARTESIAN_POINT('Ctrl Pts',(-34.2539698127282,-55.5401805087525,
7.));
#40615=CARTESIAN_POINT('Ctrl Pts',(-34.2320182882534,-55.4725873328828,
7.));
#40616=CARTESIAN_POINT('Ctrl Pts',(-34.2063390660098,-55.4062514121211,
7.));
#40617=CARTESIAN_POINT('Ctrl Pts',(-34.1772031614855,-55.3414402692491,
7.));
#40618=CARTESIAN_POINT('Ctrl Pts',(-34.1474529585405,-55.2752626548922,
7.));
#40619=CARTESIAN_POINT('Ctrl Pts',(-34.1140985516191,-55.2106738831258,
7.));
#40620=CARTESIAN_POINT('Ctrl Pts',(-34.0773733357091,-55.1479588367781,
7.));
#40621=CARTESIAN_POINT('Ctrl Pts',(-34.0404255621234,-55.0848637323531,
7.));
#40622=CARTESIAN_POINT('Ctrl Pts',(-34.0000656101091,-55.023664132488,7.));
#40623=CARTESIAN_POINT('Ctrl Pts',(-33.9564808025865,-54.9646647046815,
7.));
#40624=CARTESIAN_POINT('Ctrl Pts',(-33.9457092805123,-54.9500836229904,
7.));
#40625=CARTESIAN_POINT('Ctrl Pts',(-33.9347405679519,-54.9356370335807,
7.));
#40626=CARTESIAN_POINT('Ctrl Pts',(-33.9235770661179,-54.9213297828376,
7.));
#40627=CARTESIAN_POINT('Ctrl Pts',(-33.9148444639817,-54.9101379964017,
7.));
#40628=CARTESIAN_POINT('Ctrl Pts',(-33.9059915496783,-54.8990302862249,
7.));
#40629=CARTESIAN_POINT('Ctrl Pts',(-33.8970332940984,-54.8880255398733,
7.));
#40630=CARTESIAN_POINT('Ctrl Pts',(-33.8494695086148,-54.8295959282035,
7.));
#40631=CARTESIAN_POINT('Ctrl Pts',(-33.7988575668702,-54.7739598965231,
7.));
#40632=CARTESIAN_POINT('Ctrl Pts',(-33.7454538506294,-54.7214122178979,
7.));
#40633=CARTESIAN_POINT('Ctrl Pts',(-33.6919920462483,-54.6688073822592,
7.));
#40634=CARTESIAN_POINT('Ctrl Pts',(-33.635731898188,-54.6192966067788,7.));
#40635=CARTESIAN_POINT('Ctrl Pts',(-33.576882466568,-54.5731951202712,7.));
#40636=CARTESIAN_POINT('Ctrl Pts',(-33.5193724814535,-54.5281429297942,
7.));
#40637=CARTESIAN_POINT('Ctrl Pts',(-33.4593891253538,-54.4863457606538,
7.));
#40638=CARTESIAN_POINT('Ctrl Pts',(-33.3970899730292,-54.4481299156499,
7.));
#40639=CARTESIAN_POINT('Ctrl Pts',(-33.3836932591,-54.4399120390982,7.));
#40640=CARTESIAN_POINT('Ctrl Pts',(-33.3701893374023,-54.4318599153431,
7.));
#40641=CARTESIAN_POINT('Ctrl Pts',(-33.356579582449,-54.4239770468377,7.));
#40642=CARTESIAN_POINT('Ctrl Pts',(-33.3450551424613,-54.417302007843,7.));
#40643=CARTESIAN_POINT('Ctrl Pts',(-33.3334548151719,-54.4107483324245,
7.));
#40644=CARTESIAN_POINT('Ctrl Pts',(-33.3217804591138,-54.404315872452,7.));
#40645=CARTESIAN_POINT('Ctrl Pts',(-32.2716262263503,-54.2496319067047,
7.));
#40646=CARTESIAN_POINT('Ctrl Pts',(-32.1985421824115,-54.2648284787439,
7.));
#40647=CARTESIAN_POINT('Ctrl Pts',(-32.1265185433228,-54.2843049160509,
7.));
#40648=CARTESIAN_POINT('Ctrl Pts',(-32.0558148702163,-54.307809841484,7.));
#40649=CARTESIAN_POINT('Ctrl Pts',(-31.9869629438687,-54.3306991670822,
7.));
#40650=CARTESIAN_POINT('Ctrl Pts',(-31.9193621916132,-54.3574095812673,
7.));
#40651=CARTESIAN_POINT('Ctrl Pts',(-31.8532778586781,-54.3877469743477,
7.));
#40652=CARTESIAN_POINT('Ctrl Pts',(-31.8385281517267,-54.3945181353435,
7.));
#40653=CARTESIAN_POINT('Ctrl Pts',(-31.8238521663117,-54.4014710566228,
7.));
#40654=CARTESIAN_POINT('Ctrl Pts',(-31.8092592837343,-54.4086007385189,
7.));
#40655=CARTESIAN_POINT('Ctrl Pts',(-31.74229379234,-54.4413182396107,7.));
#40656=CARTESIAN_POINT('Ctrl Pts',(-31.6772081432285,-54.4776886923633,
7.));
#40657=CARTESIAN_POINT('Ctrl Pts',(-31.6142783994125,-54.5174808471838,
7.));
#40658=CARTESIAN_POINT('Ctrl Pts',(-31.5700975698183,-54.5454175636663,
7.));
#40659=CARTESIAN_POINT('Ctrl Pts',(-31.5269799619039,-54.5750417875592,
7.));
#40660=CARTESIAN_POINT('Ctrl Pts',(-31.4850325697142,-54.606283716683,7.));
#40661=CARTESIAN_POINT('Ctrl Pts',(-31.4690843649994,-54.6181617537992,
7.));
#40662=CARTESIAN_POINT('Ctrl Pts',(-31.4533054231774,-54.6302737016023,
7.));
#40663=CARTESIAN_POINT('Ctrl Pts',(-31.4377020509801,-54.6426159725235,
7.));
#40664=CARTESIAN_POINT('Ctrl Pts',(-31.422843222849,-54.6543693089207,7.));
#40665=CARTESIAN_POINT('Ctrl Pts',(-31.4081391340328,-54.6663354489501,
7.));
#40666=CARTESIAN_POINT('Ctrl Pts',(-31.3936208031221,-54.6784895996313,
7.));
#40667=CARTESIAN_POINT('Ctrl Pts',(-31.3379553553305,-54.7250904275332,
7.));
#40668=CARTESIAN_POINT('Ctrl Pts',(-31.2849558324703,-54.7744982188797,
7.));
#40669=CARTESIAN_POINT('Ctrl Pts',(-31.2348792620953,-54.8265005113965,
7.));
#40670=CARTESIAN_POINT('Ctrl Pts',(-31.1858781211836,-54.8773860182167,
7.));
#40671=CARTESIAN_POINT('Ctrl Pts',(-31.1396752549576,-54.9307565896498,
7.));
#40672=CARTESIAN_POINT('Ctrl Pts',(-31.096553263537,-54.9864387998288,7.));
#40673=CARTESIAN_POINT('Ctrl Pts',(-31.0543769959251,-55.0408998235516,
7.));
#40674=CARTESIAN_POINT('Ctrl Pts',(-31.0151475676859,-55.0975728716759,
7.));
#40675=CARTESIAN_POINT('Ctrl Pts',(-30.9791760532886,-55.1563097700977,
7.));
#40676=CARTESIAN_POINT('Ctrl Pts',(-30.9674871681193,-55.1753962298242,
7.));
#40677=CARTESIAN_POINT('Ctrl Pts',(-30.9561426884338,-55.1947006860194,
7.));
#40678=CARTESIAN_POINT('Ctrl Pts',(-30.9451544835008,-55.2142182090111,
7.));
#40679=CARTESIAN_POINT('Ctrl Pts',(-30.9389559540756,-55.2252281911972,
7.));
#40680=CARTESIAN_POINT('Ctrl Pts',(-30.9328702747781,-55.2363071797393,
7.));
#40681=CARTESIAN_POINT('Ctrl Pts',(-30.9269078406191,-55.2474384074061,
7.));
#40682=CARTESIAN_POINT('Ctrl Pts',(-30.8946567103501,-55.3076478225486,
7.));
#40683=CARTESIAN_POINT('Ctrl Pts',(-30.8659479672295,-55.3694877086145,
7.));
#40684=CARTESIAN_POINT('Ctrl Pts',(-30.8410371126545,-55.4327943978594,
7.));
#40685=CARTESIAN_POINT('Ctrl Pts',(-30.8374416946983,-55.4419315395249,
7.));
#40686=CARTESIAN_POINT('Ctrl Pts',(-30.8339254773263,-55.4510992635148,
7.));
#40687=CARTESIAN_POINT('Ctrl Pts',(-30.8304893165615,-55.4602971020131,
7.));
#40688=CARTESIAN_POINT('Ctrl Pts',(-30.8062112767693,-55.5252840174526,
7.));
#40689=CARTESIAN_POINT('Ctrl Pts',(-30.7859254272784,-55.5917741517056,
7.));
#40690=CARTESIAN_POINT('Ctrl Pts',(-30.7695892422356,-55.6594016433948,
7.));
#40691=CARTESIAN_POINT('Ctrl Pts',(-30.7543489013014,-55.722492629887,7.));
#40692=CARTESIAN_POINT('Ctrl Pts',(-30.7425467760704,-55.7865743173994,
7.));
#40693=CARTESIAN_POINT('Ctrl Pts',(-30.7341878976062,-55.8513431276971,
7.));
#40694=CARTESIAN_POINT('Ctrl Pts',(-30.7323430806796,-55.8656377005953,
7.));
#40695=CARTESIAN_POINT('Ctrl Pts',(-30.7306661227298,-55.8799656907132,
7.));
#40696=CARTESIAN_POINT('Ctrl Pts',(-30.7291573147787,-55.8943237313175,
7.));
#40697=CARTESIAN_POINT('Ctrl Pts',(-30.7279778703852,-55.9055474993793,
7.));
#40698=CARTESIAN_POINT('Ctrl Pts',(-30.7269013312117,-55.9167889366509,
7.));
#40699=CARTESIAN_POINT('Ctrl Pts',(-30.725928716623,-55.9280334133084,7.));
#40700=CARTESIAN_POINT('Ctrl Pts',(-30.7200365397427,-55.9961533512166,
7.));
#40701=CARTESIAN_POINT('Ctrl Pts',(-30.717940322368,-56.064510368579,7.));
#40702=CARTESIAN_POINT('Ctrl Pts',(-30.7195810692414,-56.1327563913084,
7.));
#40703=CARTESIAN_POINT('Ctrl Pts',(-30.7212142395892,-56.20068727235,7.));
#40704=CARTESIAN_POINT('Ctrl Pts',(-30.7265502690067,-56.2685092688714,
7.));
#40705=CARTESIAN_POINT('Ctrl Pts',(-30.7355805426345,-56.3358665624723,
7.));
#40706=CARTESIAN_POINT('Ctrl Pts',(-30.7444173748262,-56.4017809660634,
7.));
#40707=CARTESIAN_POINT('Ctrl Pts',(-30.7567922827294,-56.4672512454211,
7.));
#40708=CARTESIAN_POINT('Ctrl Pts',(-30.7727391547474,-56.5319175326533,
7.));
#40709=CARTESIAN_POINT('Ctrl Pts',(-30.7760991368497,-56.5455426227323,
7.));
#40710=CARTESIAN_POINT('Ctrl Pts',(-30.7796178313477,-56.559131898849,7.));
#40711=CARTESIAN_POINT('Ctrl Pts',(-30.7832957741898,-56.5726817853209,
7.));
#40712=CARTESIAN_POINT('Ctrl Pts',(-30.7867820846143,-56.5855256799889,
7.));
#40713=CARTESIAN_POINT('Ctrl Pts',(-30.7904121023242,-56.5983358602818,
7.));
#40714=CARTESIAN_POINT('Ctrl Pts',(-30.7941799173868,-56.6110887258481,
7.));
#40715=CARTESIAN_POINT('Ctrl Pts',(-30.81269457301,-56.6737549953548,7.));
#40716=CARTESIAN_POINT('Ctrl Pts',(-30.8345622313403,-56.7351520397333,
7.));
#40717=CARTESIAN_POINT('Ctrl Pts',(-30.8597663049837,-56.7949606498833,
7.));
#40718=CARTESIAN_POINT('Ctrl Pts',(-30.8844910319696,-56.8536317829029,
7.));
#40719=CARTESIAN_POINT('Ctrl Pts',(-30.9124268768218,-56.9107751110263,
7.));
#40720=CARTESIAN_POINT('Ctrl Pts',(-30.9435976955084,-56.9660591310642,
7.));
#40721=CARTESIAN_POINT('Ctrl Pts',(-30.9737560234748,-57.0195474152303,
7.));
#40722=CARTESIAN_POINT('Ctrl Pts',(-31.0069429902717,-57.0712957444527,
7.));
#40723=CARTESIAN_POINT('Ctrl Pts',(-31.0432115502758,-57.1209660579171,
7.));
#40724=CARTESIAN_POINT('Ctrl Pts',(-31.0492497804945,-57.1292355008643,
7.));
#40725=CARTESIAN_POINT('Ctrl Pts',(-31.0553734904689,-57.1374472482072,
7.));
#40726=CARTESIAN_POINT('Ctrl Pts',(-31.0615830007349,-57.1455996184163,
7.));
#40727=CARTESIAN_POINT('Ctrl Pts',(-31.0681540675972,-57.1542266707015,
7.));
#40728=CARTESIAN_POINT('Ctrl Pts',(-31.0748212184917,-57.1627872296296,
7.));
#40729=CARTESIAN_POINT('Ctrl Pts',(-31.0815830733445,-57.1712803260695,
7.));
#40730=CARTESIAN_POINT('Origin',(-32.5,-56.2916512459885,-3.54592528053767));
#40731=CARTESIAN_POINT('Ctrl Pts',(-33.5269872402601,-58.0734398505124,
-1.79592528053768));
#40732=CARTESIAN_POINT('Ctrl Pts',(-33.4422748054587,-58.1232938101479,
-1.79058130531689));
#40733=CARTESIAN_POINT('Ctrl Pts',(-32.7422362990183,-58.4684621317491,
-1.74819136657341));
#40734=CARTESIAN_POINT('Ctrl Pts',(-31.092918091713,-58.2713739433871,-1.66875546430726));
#40735=CARTESIAN_POINT('Ctrl Pts',(-30.0738503853478,-56.1831963302234,
-1.55761757373922));
#40736=CARTESIAN_POINT('Ctrl Pts',(-31.2751851021384,-54.1944751483927,
-1.44647968317117));
#40737=CARTESIAN_POINT('Ctrl Pts',(-33.5977473666623,-54.1252293793916,
-1.33534179260314));
#40738=CARTESIAN_POINT('Ctrl Pts',(-34.9154583912003,-56.0389811637256,
-1.22420390203509));
#40739=CARTESIAN_POINT('Ctrl Pts',(-34.2741084270659,-57.5792551456252,
-1.14439839801327));
#40740=CARTESIAN_POINT('Ctrl Pts',(-33.6210824061175,-58.0199411501776,
-1.10163885751414));
#40741=CARTESIAN_POINT('Ctrl Pts',(-33.5295799600393,-58.0717283210701,
-1.09592528053768));
#40742=CARTESIAN_POINT('Ctrl Pts',(-33.5283546803393,-58.0681541983481,
-1.85407471946233));
#40743=CARTESIAN_POINT('Ctrl Pts',(-33.1193657433931,-58.3001842134597,
-1.82862455259619));
#40744=CARTESIAN_POINT('Ctrl Pts',(-31.9170343357855,-58.5410390719136,
-1.76612842220737));
#40745=CARTESIAN_POINT('Ctrl Pts',(-30.2743670907292,-57.2623912321518,
-1.66658632829588));
#40746=CARTESIAN_POINT('Ctrl Pts',(-30.4765028746714,-54.9487367869862,
-1.55544843772783));
#40747=CARTESIAN_POINT('Ctrl Pts',(-32.5312595152503,-53.8630292597193,
-1.44431054715979));
#40748=CARTESIAN_POINT('Ctrl Pts',(-34.5571577499755,-55.0008883544571,
-1.33317265659175));
#40749=CARTESIAN_POINT('Ctrl Pts',(-34.6817103419943,-57.0195698185232,
-1.23642738069259));
#40750=CARTESIAN_POINT('Ctrl Pts',(-33.8868873402924,-57.8579713309385,
-1.17672806831612));
#40751=CARTESIAN_POINT('Ctrl Pts',(-33.5250365419916,-58.0693901510839,
-1.15407471946233));
#40752=CARTESIAN_POINT('Ctrl Pts',(-30.9307125467393,-55.7322829513575,
-2.));
#40753=CARTESIAN_POINT('Ctrl Pts',(-31.116715812632,-55.2104575382394,-1.96295403647732));
#40754=CARTESIAN_POINT('Ctrl Pts',(-32.0473824090187,-54.3760622611663,
-1.88886210943196));
#40755=CARTESIAN_POINT('Ctrl Pts',(-33.8672110770871,-54.8728632770319,
-1.77772421886392));
#40756=CARTESIAN_POINT('Ctrl Pts',(-34.4318965215284,-56.6706982888813,
-1.66658632829587));
#40757=CARTESIAN_POINT('Ctrl Pts',(-33.2300975250658,-58.1203931132112,
-1.55544843772783));
#40758=CARTESIAN_POINT('Ctrl Pts',(-31.359132031047,-57.8968187913668,-1.44431054715979));
#40759=CARTESIAN_POINT('Ctrl Pts',(-30.5328676198999,-56.2037155410781,
-1.33317265659175));
#40760=CARTESIAN_POINT('Ctrl Pts',(-31.5069148948352,-54.5912519864218,
-1.22203476602371));
#40761=CARTESIAN_POINT('Ctrl Pts',(-33.3900582128529,-54.5351072237228,
-1.11089687545567));
#40762=CARTESIAN_POINT('Ctrl Pts',(-34.4584638908576,-56.0867852734615,
-0.999758984887624));
#40763=CARTESIAN_POINT('Ctrl Pts',(-33.7342941276566,-57.8259603059919,
-0.888621094319583));
#40764=CARTESIAN_POINT('Ctrl Pts',(-31.8803464986039,-58.1607744839985,
-0.777483203751541));
#40765=CARTESIAN_POINT('Ctrl Pts',(-30.5935820077056,-56.7847541278006,
-0.6663453131835));
#40766=CARTESIAN_POINT('Ctrl Pts',(-31.0517798775847,-54.9573935418363,
-0.555207422615458));
#40767=CARTESIAN_POINT('Ctrl Pts',(-32.8355518820609,-54.3512929431319,
-0.444069532047416));
#40768=CARTESIAN_POINT('Ctrl Pts',(-34.3121885227868,-55.5212249175371,
-0.332931641479374));
#40769=CARTESIAN_POINT('Ctrl Pts',(-34.1301089195294,-57.3963365394661,
-0.221793750911332));
#40770=CARTESIAN_POINT('Ctrl Pts',(-32.4559719031607,-58.2603173390955,
-0.110655860343291));
#40771=CARTESIAN_POINT('Ctrl Pts',(-30.8221344198831,-57.3223556597407,
0.000482030224751014));
#40772=CARTESIAN_POINT('Ctrl Pts',(-30.724066271727,-55.4409785805667,0.111619920792793));
#40773=CARTESIAN_POINT('Ctrl Pts',(-32.2515304349823,-54.3382318197086,
0.222757811360835));
#40774=CARTESIAN_POINT('Ctrl Pts',(-34.0064215941321,-55.0234720228687,
0.333895701928876));
#40775=CARTESIAN_POINT('Ctrl Pts',(-34.3824679916267,-56.8694910461268,
0.445033592496918));
#40776=CARTESIAN_POINT('Ctrl Pts',(-33.0354700840103,-58.1866067496581,
0.55617148306496));
#40777=CARTESIAN_POINT('Ctrl Pts',(-31.1983503377325,-57.7692481891733,
0.667309373633001));
#40778=CARTESIAN_POINT('Ctrl Pts',(-30.5526452880963,-55.9994283901304,
0.778447264201044));
#40779=CARTESIAN_POINT('Ctrl Pts',(-31.6893760912439,-54.4970834847716,
0.889585154769084));
#40780=CARTESIAN_POINT('Ctrl Pts',(-33.5680801509383,-54.6373268031956,
1.00072304533713));
#40781=CARTESIAN_POINT('Ctrl Pts',(-34.4691583357458,-56.2917920453437,
1.11186093590517));
#40782=CARTESIAN_POINT('Ctrl Pts',(-33.5678435640106,-57.9461284122851,
1.22299882647321));
#40783=CARTESIAN_POINT('Ctrl Pts',(-31.6891194679972,-58.0861030658479,
1.33413671704125));
#40784=CARTESIAN_POINT('Ctrl Pts',(-30.5526035189214,-56.5835956182358,
1.44527460760929));
#40785=CARTESIAN_POINT('Ctrl Pts',(-31.1985616539627,-54.8138681758263,
1.55641249817734));
#40786=CARTESIAN_POINT('Ctrl Pts',(-33.0357410664429,-54.3967723367386,
1.66755038874538));
#40787=CARTESIAN_POINT('Ctrl Pts',(-34.3825506050928,-55.7140806526746,
1.77868827931342));
#40788=CARTESIAN_POINT('Ctrl Pts',(-34.0062402253245,-57.5600458827673,
1.88982616988146));
#40789=CARTESIAN_POINT('Ctrl Pts',(-32.2512510853912,-58.2450351172427,
2.0009640604495));
#40790=CARTESIAN_POINT('Ctrl Pts',(-30.7239446480037,-57.1420699414794,
2.11210195101754));
#40791=CARTESIAN_POINT('Ctrl Pts',(-30.8222818161361,-55.2607068893292,
2.22323984158559));
#40792=CARTESIAN_POINT('Ctrl Pts',(-32.4562534645774,-54.3229788985336,
2.33437773215363));
#40793=CARTESIAN_POINT('Ctrl Pts',(-34.1302668130106,-55.1871990336263,
2.44551562272167));
#40794=CARTESIAN_POINT('Ctrl Pts',(-34.3120784590119,-57.0623368040342,
2.55665351328971));
#40795=CARTESIAN_POINT('Ctrl Pts',(-32.8352741411123,-58.2320573429941,
2.66779140385776));
#40796=CARTESIAN_POINT('Ctrl Pts',(-31.0515895995852,-57.6257021756631,
2.77892929442579));
#40797=CARTESIAN_POINT('Ctrl Pts',(-30.593651523649,-55.7982750632342,2.89006718499384));
#40798=CARTESIAN_POINT('Ctrl Pts',(-31.8806158275789,-54.4224407661471,
3.00120507556188));
#40799=CARTESIAN_POINT('Ctrl Pts',(-33.7345094888202,-54.7575160195471,
3.11234296612992));
#40800=CARTESIAN_POINT('Ctrl Pts',(-34.4584426146545,-56.4968026439861,
3.22348085669796));
#40801=CARTESIAN_POINT('Ctrl Pts',(-33.3897910050459,-58.0483118672624,
3.334618747266));
#40802=CARTESIAN_POINT('Ctrl Pts',(-31.506703597602,-57.9919297020008,3.44575663783404));
#40803=CARTESIAN_POINT('Ctrl Pts',(-30.5327916520213,-56.3792633834812,
3.55689452840209));
#40804=CARTESIAN_POINT('Ctrl Pts',(-31.3594878170038,-54.6864046819268,
3.66803241897013));
#40805=CARTESIAN_POINT('Ctrl Pts',(-33.230107717374,-54.4628463651893,3.77917030953817));
#40806=CARTESIAN_POINT('Ctrl Pts',(-34.4324517440405,-55.9132138959114,
3.89030820010621));
#40807=CARTESIAN_POINT('Ctrl Pts',(-33.8660007739066,-57.7099694249181,
4.00144609067425));
#40808=CARTESIAN_POINT('Ctrl Pts',(-32.0492338038872,-58.2085222399532,
4.1125839812423));
#40809=CARTESIAN_POINT('Ctrl Pts',(-30.6450582452589,-56.9525412953674,
4.22372187181033));
#40810=CARTESIAN_POINT('Ctrl Pts',(-30.9387319111105,-55.0916401936805,
4.33485976237839));
#40811=CARTESIAN_POINT('Ctrl Pts',(-32.6614519649159,-54.3291228170264,
4.44599765294642));
#40812=CARTESIAN_POINT('Ctrl Pts',(-34.2363932038283,-55.3629299683766,
4.55713554351447));
#40813=CARTESIAN_POINT('Ctrl Pts',(-34.2219940520658,-57.2468062367663,
4.6682734340825));
#40814=CARTESIAN_POINT('Ctrl Pts',(-32.6314342140599,-58.2564183114437,
4.77941132465055));
#40815=CARTESIAN_POINT('Ctrl Pts',(-30.9205711526377,-57.4676568060689,
4.89054921521858));
#40816=CARTESIAN_POINT('Ctrl Pts',(-30.6553772206224,-55.602484080847,5.00168710578664));
#40817=CARTESIAN_POINT('Ctrl Pts',(-32.0785874510053,-54.3681138654151,
5.11282499635467));
#40818=CARTESIAN_POINT('Ctrl Pts',(-33.8875213407722,-54.8943792530067,
5.22396288692272));
#40819=CARTESIAN_POINT('Ctrl Pts',(-34.4264412632309,-56.6995834937722,
5.33510077749075));
#40820=CARTESIAN_POINT('Ctrl Pts',(-33.2020675476878,-58.1314028177064,
5.4462386680588));
#40821=CARTESIAN_POINT('Ctrl Pts',(-31.3350836476587,-57.8792764730931,
5.55737655862684));
#40822=CARTESIAN_POINT('Ctrl Pts',(-30.5343604901147,-56.173979132908,5.66851444919488));
#40823=CARTESIAN_POINT('Ctrl Pts',(-31.5328102757062,-54.5763876565427,
5.77965233976292));
#40824=CARTESIAN_POINT('Ctrl Pts',(-33.4165381765594,-54.5487979003782,
5.89079023033096));
#40825=CARTESIAN_POINT('Ctrl Pts',(-34.4613514910016,-56.1164585823091,
6.00192812089901));
#40826=CARTESIAN_POINT('Ctrl Pts',(-33.7109111712192,-57.8444810565579,
6.11306601146705));
#40827=CARTESIAN_POINT('Ctrl Pts',(-31.8521228057563,-58.1511689306775,
6.22420390203509));
#40828=CARTESIAN_POINT('Ctrl Pts',(-30.5863185401119,-56.7558427953566,
6.33534179260313));
#40829=CARTESIAN_POINT('Ctrl Pts',(-31.0721788644701,-54.9355898635397,
6.44647968317117));
#40830=CARTESIAN_POINT('Ctrl Pts',(-32.8648400497806,-54.3566488617232,
6.55761757373922));
#40831=CARTESIAN_POINT('Ctrl Pts',(-34.3237580856512,-55.5486512349919,
6.66875546430725));
#40832=CARTESIAN_POINT('Ctrl Pts',(-34.1129733567613,-57.4211007417246,
6.7798933548753));
#40833=CARTESIAN_POINT('Ctrl Pts',(-32.4266050042152,-58.2590134407085,
6.89103124544334));
#40834=CARTESIAN_POINT('Ctrl Pts',(-30.805840812616,-57.2976582429661,7.00216913601138));
#40835=CARTESIAN_POINT('Ctrl Pts',(-30.7389488982073,-55.4124226867889,
7.11330702657942));
#40836=CARTESIAN_POINT('Ctrl Pts',(-31.7642812766211,-54.697545560418,7.18739895362479));
#40837=CARTESIAN_POINT('Ctrl Pts',(-32.3148335773694,-54.6359733196,7.22444491714747));
#40838=CARTESIAN_POINT('Ctrl Pts',(-30.8086516228787,-55.6887746631347,
-2.07481497238249));
#40839=CARTESIAN_POINT('Ctrl Pts',(-31.009122429711,-55.1263610888822,-2.03776900885981));
#40840=CARTESIAN_POINT('Ctrl Pts',(-32.01217730928,-54.2270656189395,-1.96367708181445));
#40841=CARTESIAN_POINT('Ctrl Pts',(-33.97355427561,-54.7625083704828,-1.85253919124641));
#40842=CARTESIAN_POINT('Ctrl Pts',(-34.5821615821014,-56.7001809895466,
-1.74140130067836));
#40843=CARTESIAN_POINT('Ctrl Pts',(-33.2868853227587,-58.2626346900185,
-1.63026341011032));
#40844=CARTESIAN_POINT('Ctrl Pts',(-31.270394051269,-58.0216705087069,-1.51912551954228));
#40845=CARTESIAN_POINT('Ctrl Pts',(-30.3798618750492,-56.1968758041266,
-1.40798762897424));
#40846=CARTESIAN_POINT('Ctrl Pts',(-31.429671630603,-54.4589930404121,-1.2968497384062));
#40847=CARTESIAN_POINT('Ctrl Pts',(-33.4592879307893,-54.3984812756124,
-1.18571184783816));
#40848=CARTESIAN_POINT('Ctrl Pts',(-34.6107953909719,-56.0708505702162,
-1.07457395727011));
#40849=CARTESIAN_POINT('Ctrl Pts',(-33.83029889799,-57.9453005715134,-0.963436066702071));
#40850=CARTESIAN_POINT('Ctrl Pts',(-31.832149159935,-58.3061569687477,-0.852298176134031));
#40851=CARTESIAN_POINT('Ctrl Pts',(-30.4452986954798,-56.8231082184978,
-0.741160285565987));
#40852=CARTESIAN_POINT('Ctrl Pts',(-30.939135705398,-54.8536134933191,-0.630022394997947));
#40853=CARTESIAN_POINT('Ctrl Pts',(-32.8616514807306,-54.2003697157939,
-0.518884504429905));
#40854=CARTESIAN_POINT('Ctrl Pts',(-34.4531425620492,-55.4613003006531,
-0.407746613861863));
#40855=CARTESIAN_POINT('Ctrl Pts',(-34.2569006046968,-57.4822601904945,
-0.296608723293821));
#40856=CARTESIAN_POINT('Ctrl Pts',(-32.4525473488097,-58.41344237785,-0.185470832725779));
#40857=CARTESIAN_POINT('Ctrl Pts',(-30.6916281685284,-57.4025249956444,
-0.0743329421577378));
#40858=CARTESIAN_POINT('Ctrl Pts',(-30.5859321707133,-55.3748123143236,
0.0368049484103037));
#40859=CARTESIAN_POINT('Ctrl Pts',(-32.2322041958065,-54.186292683661,0.147942838978346));
#40860=CARTESIAN_POINT('Ctrl Pts',(-34.1235927415348,-54.9248316321148,
0.259080729546387));
#40861=CARTESIAN_POINT('Ctrl Pts',(-34.5288884461575,-56.9144360685966,
0.370218620114429));
#40862=CARTESIAN_POINT('Ctrl Pts',(-33.0771195428256,-58.3339984967673,
0.48135651068247));
#40863=CARTESIAN_POINT('Ctrl Pts',(-31.0971065789877,-57.8841773231594,
0.592494401250513));
#40864=CARTESIAN_POINT('Ctrl Pts',(-30.4011778722795,-55.97669897132,0.703632291818555));
#40865=CARTESIAN_POINT('Ctrl Pts',(-31.6263248618463,-54.3575000079462,
0.814770182386596));
#40866=CARTESIAN_POINT('Ctrl Pts',(-33.6511566132587,-54.5086516076903,
0.925908072954639));
#40867=CARTESIAN_POINT('Ctrl Pts',(-34.6223216616804,-56.2918029968741,
1.03704596352268));
#40868=CARTESIAN_POINT('Ctrl Pts',(-33.6509016243366,-58.0748154867945,
1.14818385409072));
#40869=CARTESIAN_POINT('Ctrl Pts',(-31.626048278158,-58.2256775246255,1.25932174465876));
#40870=CARTESIAN_POINT('Ctrl Pts',(-30.4011328542517,-56.6063033762813,
1.3704596352268));
#40871=CARTESIAN_POINT('Ctrl Pts',(-31.0973343316294,-54.6989245646767,
1.48159752579485));
#40872=CARTESIAN_POINT('Ctrl Pts',(-33.0774116025732,-54.2493865472287,
1.59273541636289));
#40873=CARTESIAN_POINT('Ctrl Pts',(-34.5289774853909,-55.669156569411,1.70387330693093));
#40874=CARTESIAN_POINT('Ctrl Pts',(-34.1233972656596,-57.6587030286353,
1.81501119749897));
#40875=CARTESIAN_POINT('Ctrl Pts',(-32.2319031180934,-58.3969714877809,
1.92614908806701));
#40876=CARTESIAN_POINT('Ctrl Pts',(-30.5858010869615,-57.2082164536586,
2.03728697863506));
#40877=CARTESIAN_POINT('Ctrl Pts',(-30.691787029426,-55.1805188903994,2.1484248692031));
#40878=CARTESIAN_POINT('Ctrl Pts',(-32.4528508103867,-54.1698533733089,
2.25956275977114));
#40879=CARTESIAN_POINT('Ctrl Pts',(-34.2570707793086,-55.1012935119064,
2.37070065033918));
#40880=CARTESIAN_POINT('Ctrl Pts',(-34.4530239373915,-57.1222815840843,
2.48183854090722));
#40881=CARTESIAN_POINT('Ctrl Pts',(-32.8613521367821,-58.3829842878142,
2.59297643147526));
#40882=CARTESIAN_POINT('Ctrl Pts',(-30.9389306273641,-57.7294661410314,
2.70411432204331));
#40883=CARTESIAN_POINT('Ctrl Pts',(-30.4453736184506,-55.7598997148858,
2.81525221261135));
#40884=CARTESIAN_POINT('Ctrl Pts',(-31.8324394376172,-54.2770514956311,
2.92639010317939));
#40885=CARTESIAN_POINT('Ctrl Pts',(-33.8305310101846,-54.6381892749935,
3.03752799374743));
#40886=CARTESIAN_POINT('Ctrl Pts',(-34.6107724598819,-56.5127595479419,
3.14866588431547));
#40887=CARTESIAN_POINT('Ctrl Pts',(-33.4589999392619,-58.1849468845733,
3.25980377488351));
#40888=CARTESIAN_POINT('Ctrl Pts',(-31.4294438984359,-58.1241792517757,
3.37094166545156));
#40889=CARTESIAN_POINT('Ctrl Pts',(-30.3797799983045,-56.386077952999,3.4820795560196));
#40890=CARTESIAN_POINT('Ctrl Pts',(-31.2707775106533,-54.5615468184256,
3.59321744658764));
#40891=CARTESIAN_POINT('Ctrl Pts',(-33.286896307836,-54.3205998871159,3.70435533715568));
#40892=CARTESIAN_POINT('Ctrl Pts',(-34.5827599904381,-55.8837786178316,
3.81549322772373));
#40893=CARTESIAN_POINT('Ctrl Pts',(-33.9722498337018,-57.8202877906762,
3.92663111829176));
#40894=CARTESIAN_POINT('Ctrl Pts',(-32.014172707701,-58.3576185982774,4.03776900885981));
#40895=CARTESIAN_POINT('Ctrl Pts',(-30.5007788120545,-57.0039460586119,
4.14890689942784));
#40896=CARTESIAN_POINT('Ctrl Pts',(-30.8172947423318,-54.9983019990856,
4.2600447899959));
#40897=CARTESIAN_POINT('Ctrl Pts',(-32.6740098783535,-54.1764751726168,
4.37118268056393));
#40898=CARTESIAN_POINT('Ctrl Pts',(-34.371451798864,-55.2906929942526,4.48232057113198));
#40899=CARTESIAN_POINT('Ctrl Pts',(-34.3559326650591,-57.3210992545064,
4.59345846170001));
#40900=CARTESIAN_POINT('Ctrl Pts',(-32.6416573134427,-58.4092400794901,
4.70459635226807));
#40901=CARTESIAN_POINT('Ctrl Pts',(-30.7977214198623,-57.5591278267734,
4.81573424283609));
#40902=CARTESIAN_POINT('Ctrl Pts',(-30.5119004088011,-55.5488798920819,
4.92687213340414));
#40903=CARTESIAN_POINT('Ctrl Pts',(-32.0458095141463,-54.2184989881245,
5.03801002397219));
#40904=CARTESIAN_POINT('Ctrl Pts',(-33.9954442941986,-54.7856978830043,
5.14914791454022));
#40905=CARTESIAN_POINT('Ctrl Pts',(-34.576282007745,-56.731312917807,5.26028580510827));
#40906=CARTESIAN_POINT('Ctrl Pts',(-33.2566751425585,-58.274500741577,5.37142369567631));
#40907=CARTESIAN_POINT('Ctrl Pts',(-31.2444751578683,-58.002763729403,5.48256158624435));
#40908=CARTESIAN_POINT('Ctrl Pts',(-30.38147086237,-56.1648264650488,5.59369947681239));
#40909=CARTESIAN_POINT('Ctrl Pts',(-31.4575811830053,-54.4429725464192,
5.70483736738043));
#40910=CARTESIAN_POINT('Ctrl Pts',(-33.4878275355304,-54.4132368283281,
5.81597525794848));
#40911=CARTESIAN_POINT('Ctrl Pts',(-34.6139075918674,-56.1028319020359,
5.92711314851651));
#40912=CARTESIAN_POINT('Ctrl Pts',(-33.8050971891886,-57.9652618866616,
6.03825103908456));
#40913=CARTESIAN_POINT('Ctrl Pts',(-31.8017301968603,-58.2958042848038,
6.1493889296526));
#40914=CARTESIAN_POINT('Ctrl Pts',(-30.4374702672965,-56.7919481304539,
6.26052682022065));
#40915=CARTESIAN_POINT('Ctrl Pts',(-30.9611213481761,-54.8301139006692,
6.37166471078868));
#40916=CARTESIAN_POINT('Ctrl Pts',(-32.893217714717,-54.2061422236913,6.48280260135673));
#40917=CARTESIAN_POINT('Ctrl Pts',(-34.4656120183837,-55.4908598675899,
6.59394049192477));
#40918=CARTESIAN_POINT('Ctrl Pts',(-34.2384322187942,-57.5089505799534,
6.70507838249281));
#40919=CARTESIAN_POINT('Ctrl Pts',(-32.4208962597951,-58.4120370607959,
6.81621627306085));
#40920=CARTESIAN_POINT('Ctrl Pts',(-30.6740672263624,-57.3759065863185,
6.92735416362889));
#40921=CARTESIAN_POINT('Ctrl Pts',(-30.6019723844374,-55.344035311361,7.03849205419694));
#40922=CARTESIAN_POINT('Ctrl Pts',(-31.70705625587,-54.5735542468395,7.1125839812423));
#40923=CARTESIAN_POINT('Ctrl Pts',(-32.3004311270297,-54.5071928486349,
7.14962994476498));
#40924=CARTESIAN_POINT('Ctrl Pts',(-30.6865906990182,-55.6452663749118,
-2.14962994476498));
#40925=CARTESIAN_POINT('Ctrl Pts',(-30.9015290467899,-55.042264639525,-2.1125839812423));
#40926=CARTESIAN_POINT('Ctrl Pts',(-31.9769722095413,-54.0780689767127,
-2.03849205419694));
#40927=CARTESIAN_POINT('Ctrl Pts',(-34.0798974741329,-54.6521534639338,
-1.92735416362889));
#40928=CARTESIAN_POINT('Ctrl Pts',(-34.7324266426746,-56.7296636902117,
-1.81621627306085));
#40929=CARTESIAN_POINT('Ctrl Pts',(-33.3436731204516,-58.4048762668258,
-1.70507838249281));
#40930=CARTESIAN_POINT('Ctrl Pts',(-31.181656071491,-58.146522226047,-1.59394049192477));
#40931=CARTESIAN_POINT('Ctrl Pts',(-30.2268561301985,-56.190036067175,-1.48280260135673));
#40932=CARTESIAN_POINT('Ctrl Pts',(-31.3524283663707,-54.3267340944024,
-1.37166471078868));
#40933=CARTESIAN_POINT('Ctrl Pts',(-33.5285176487258,-54.2618553275021,
-1.26052682022064));
#40934=CARTESIAN_POINT('Ctrl Pts',(-34.7631268910861,-56.0549158669708,
-1.1493889296526));
#40935=CARTESIAN_POINT('Ctrl Pts',(-33.9263036683235,-58.0646408370349,
-1.03825103908456));
#40936=CARTESIAN_POINT('Ctrl Pts',(-31.7839518212659,-58.4515394534968,
-0.92711314851652));
#40937=CARTESIAN_POINT('Ctrl Pts',(-30.2970153832539,-56.861462309195,-0.815975257948476));
#40938=CARTESIAN_POINT('Ctrl Pts',(-30.8264915332113,-54.7498334448018,
-0.704837367380436));
#40939=CARTESIAN_POINT('Ctrl Pts',(-32.8877510794003,-54.0494464884559,
-0.593699476812393));
#40940=CARTESIAN_POINT('Ctrl Pts',(-34.5940966013115,-55.4013756837693,
-0.482561586244352));
#40941=CARTESIAN_POINT('Ctrl Pts',(-34.3836922898643,-57.5681838415228,
-0.37142369567631));
#40942=CARTESIAN_POINT('Ctrl Pts',(-32.4491227944587,-58.5665674166046,
-0.260285805108268));
#40943=CARTESIAN_POINT('Ctrl Pts',(-30.5611219171738,-57.482694331548,-0.149147914540227));
#40944=CARTESIAN_POINT('Ctrl Pts',(-30.4477980696998,-55.3086460480806,
-0.0380100239721851));
#40945=CARTESIAN_POINT('Ctrl Pts',(-32.2128779566306,-54.0343535476132,
0.0731278665958571));
#40946=CARTESIAN_POINT('Ctrl Pts',(-34.2407638889375,-54.826191241361,0.184265757163899));
#40947=CARTESIAN_POINT('Ctrl Pts',(-34.6753089006883,-56.9593810910663,
0.29540364773194));
#40948=CARTESIAN_POINT('Ctrl Pts',(-33.1187690016409,-58.4813902438765,
0.406541538299982));
#40949=CARTESIAN_POINT('Ctrl Pts',(-30.9958628202429,-57.9991064571456,
0.517679428868024));
#40950=CARTESIAN_POINT('Ctrl Pts',(-30.2497104564626,-55.9539695525095,
0.628817319436065));
#40951=CARTESIAN_POINT('Ctrl Pts',(-31.5632736324488,-54.2179165311209,
0.739955210004108));
#40952=CARTESIAN_POINT('Ctrl Pts',(-33.734233075579,-54.379976412185,0.851093100572149));
#40953=CARTESIAN_POINT('Ctrl Pts',(-34.775484987615,-56.2918139484046,0.962230991140192));
#40954=CARTESIAN_POINT('Ctrl Pts',(-33.7339596846625,-58.2035025613039,
1.07336888170823));
#40955=CARTESIAN_POINT('Ctrl Pts',(-31.5629770883189,-58.365251983403,1.18450677227627));
#40956=CARTESIAN_POINT('Ctrl Pts',(-30.2496621895819,-56.6290111343268,
1.29564466284432));
#40957=CARTESIAN_POINT('Ctrl Pts',(-30.9961070092961,-54.583980953527,1.40678255341236));
#40958=CARTESIAN_POINT('Ctrl Pts',(-33.1190821387036,-54.1020007577187,
1.5179204439804));
#40959=CARTESIAN_POINT('Ctrl Pts',(-34.675404365689,-55.6242324861476,1.62905833454844));
#40960=CARTESIAN_POINT('Ctrl Pts',(-34.2405543059947,-57.7573601745032,
1.74019622511648));
#40961=CARTESIAN_POINT('Ctrl Pts',(-32.2125551507957,-58.5489078583191,
1.85133411568453));
#40962=CARTESIAN_POINT('Ctrl Pts',(-30.4476575259194,-57.274362965838,1.96247200625257));
#40963=CARTESIAN_POINT('Ctrl Pts',(-30.5612922427159,-55.1003308914696,
2.07360989682061));
#40964=CARTESIAN_POINT('Ctrl Pts',(-32.4494481561959,-54.0167278480842,
2.18474778738865));
#40965=CARTESIAN_POINT('Ctrl Pts',(-34.3838747456067,-55.0153879901866,
2.29588567795669));
#40966=CARTESIAN_POINT('Ctrl Pts',(-34.593969415771,-57.1822263641342,2.40702356852473));
#40967=CARTESIAN_POINT('Ctrl Pts',(-32.8874301324518,-58.5339112326344,
2.51816145909277));
#40968=CARTESIAN_POINT('Ctrl Pts',(-30.826271655143,-57.8332301063997,2.62929934966082));
#40969=CARTESIAN_POINT('Ctrl Pts',(-30.2970957132522,-55.7215243665374,
2.74043724022885));
#40970=CARTESIAN_POINT('Ctrl Pts',(-31.7842630476555,-54.1316622251152,
2.85157513079691));
#40971=CARTESIAN_POINT('Ctrl Pts',(-33.9265525315489,-54.51886253044,2.96271302136494));
#40972=CARTESIAN_POINT('Ctrl Pts',(-34.7631023051095,-56.5287164518977,
3.07385091193299));
#40973=CARTESIAN_POINT('Ctrl Pts',(-33.5282088734779,-58.3215819018844,
3.18498880250102));
#40974=CARTESIAN_POINT('Ctrl Pts',(-31.3521841992698,-58.2564288015505,
3.29612669306907));
#40975=CARTESIAN_POINT('Ctrl Pts',(-30.2267683445876,-56.3928925225169,
3.40726458363711));
#40976=CARTESIAN_POINT('Ctrl Pts',(-31.1820672043028,-54.4366889549245,
3.51840247420515));
#40977=CARTESIAN_POINT('Ctrl Pts',(-33.343684898298,-54.1783534090425,3.6295403647732));
#40978=CARTESIAN_POINT('Ctrl Pts',(-34.7330682368358,-55.854343339752,3.74067825534123));
#40979=CARTESIAN_POINT('Ctrl Pts',(-34.0784988934969,-57.9306061564343,
3.85181614590928));
#40980=CARTESIAN_POINT('Ctrl Pts',(-31.9791116115147,-58.5067149566014,
3.96295403647732));
#40981=CARTESIAN_POINT('Ctrl Pts',(-30.3564993788501,-57.0553508218565,
4.07409192704536));
#40982=CARTESIAN_POINT('Ctrl Pts',(-30.6958575735532,-54.9049638044908,
4.1852298176134));
#40983=CARTESIAN_POINT('Ctrl Pts',(-32.686567791791,-54.0238275282073,4.29636770818144));
#40984=CARTESIAN_POINT('Ctrl Pts',(-34.5065103938996,-55.2184560201286,
4.40750559874949));
#40985=CARTESIAN_POINT('Ctrl Pts',(-34.4898712780524,-57.3953922722465,
4.51864348931752));
#40986=CARTESIAN_POINT('Ctrl Pts',(-32.6518804128256,-58.5620618475364,
4.62978137988557));
#40987=CARTESIAN_POINT('Ctrl Pts',(-30.6748716870867,-57.650598847478,4.7409192704536));
#40988=CARTESIAN_POINT('Ctrl Pts',(-30.3684235969797,-55.4952757033166,
4.85205716102166));
#40989=CARTESIAN_POINT('Ctrl Pts',(-32.0130315772872,-54.0688841108341,
4.96319505158969));
#40990=CARTESIAN_POINT('Ctrl Pts',(-34.103367247625,-54.6770165130019,5.07433294215774));
#40991=CARTESIAN_POINT('Ctrl Pts',(-34.7261227522589,-56.7630423418419,
5.18547083272578));
#40992=CARTESIAN_POINT('Ctrl Pts',(-33.3112827374291,-58.4175986654476,
5.29660872329382));
#40993=CARTESIAN_POINT('Ctrl Pts',(-31.1538666680779,-58.126250985713,5.40774661386187));
#40994=CARTESIAN_POINT('Ctrl Pts',(-30.2285812346253,-56.1556737971897,
5.5188845044299));
#40995=CARTESIAN_POINT('Ctrl Pts',(-31.3823520903043,-54.3095574362958,
5.63002239499795));
#40996=CARTESIAN_POINT('Ctrl Pts',(-33.5591168945015,-54.2776757562781,
5.74116028556598));
#40997=CARTESIAN_POINT('Ctrl Pts',(-34.7664636927331,-56.0892052217628,
5.85229817613404));
#40998=CARTESIAN_POINT('Ctrl Pts',(-33.8992832071581,-58.0860427167654,
5.96343606670206));
#40999=CARTESIAN_POINT('Ctrl Pts',(-31.7513375879643,-58.4404396389301,
6.07457395727012));
#41000=CARTESIAN_POINT('Ctrl Pts',(-30.288621994481,-56.8280534655513,6.18571184783815));
#41001=CARTESIAN_POINT('Ctrl Pts',(-30.8500638318821,-54.7246379377986,
6.29684973840619));
#41002=CARTESIAN_POINT('Ctrl Pts',(-32.9215953796534,-54.0556355856595,
6.40798762897424));
#41003=CARTESIAN_POINT('Ctrl Pts',(-34.6074659511161,-55.4330685001879,
6.51912551954228));
#41004=CARTESIAN_POINT('Ctrl Pts',(-34.3638910808272,-57.5968004181822,
6.63026341011032));
#41005=CARTESIAN_POINT('Ctrl Pts',(-32.4151875153751,-58.5650606808834,
6.74140130067836));
#41006=CARTESIAN_POINT('Ctrl Pts',(-30.5422936401088,-57.4541549296709,
6.85253919124641));
#41007=CARTESIAN_POINT('Ctrl Pts',(-30.4649958706675,-55.275647935933,6.96367708181445));
#41008=CARTESIAN_POINT('Ctrl Pts',(-31.649831235119,-54.4495629332609,7.03776900885981));
#41009=CARTESIAN_POINT('Ctrl Pts',(-32.28602867669,-54.3784123776698,7.07481497238249));
#41010=CARTESIAN_POINT('Ctrl Pts',(-30.5645297751576,-55.601758086689,-2.22444491714747));
#41011=CARTESIAN_POINT('Ctrl Pts',(-30.7939356638689,-54.9581681901677,
-2.18739895362479));
#41012=CARTESIAN_POINT('Ctrl Pts',(-31.9417671098026,-53.9290723344859,
-2.11330702657942));
#41013=CARTESIAN_POINT('Ctrl Pts',(-34.1862406726558,-54.5417985573849,
-2.00216913601139));
#41014=CARTESIAN_POINT('Ctrl Pts',(-34.8826917032476,-56.7591463908769,
-1.89103124544334));
#41015=CARTESIAN_POINT('Ctrl Pts',(-33.4004609181446,-58.5471178436331,
-1.7798933548753));
#41016=CARTESIAN_POINT('Ctrl Pts',(-31.092918091713,-58.2713739433871,-1.66875546430726));
#41017=CARTESIAN_POINT('Ctrl Pts',(-30.0738503853478,-56.1831963302234,
-1.55761757373922));
#41018=CARTESIAN_POINT('Ctrl Pts',(-31.2751851021384,-54.1944751483927,
-1.44647968317117));
#41019=CARTESIAN_POINT('Ctrl Pts',(-33.5977473666623,-54.1252293793916,
-1.33534179260314));
#41020=CARTESIAN_POINT('Ctrl Pts',(-34.9154583912003,-56.0389811637256,
-1.22420390203509));
#41021=CARTESIAN_POINT('Ctrl Pts',(-34.0223084386569,-58.1839811025563,
-1.11306601146705));
#41022=CARTESIAN_POINT('Ctrl Pts',(-31.7357544825969,-58.596921938246,-1.00192812089901));
#41023=CARTESIAN_POINT('Ctrl Pts',(-30.1487320710282,-56.8998163998922,
-0.890790230330965));
#41024=CARTESIAN_POINT('Ctrl Pts',(-30.7138473610247,-54.6460533962845,
-0.779652339762925));
#41025=CARTESIAN_POINT('Ctrl Pts',(-32.91385067807,-53.8985232611178,-0.668514449194883));
#41026=CARTESIAN_POINT('Ctrl Pts',(-34.7350506405739,-55.3414510668855,
-0.557376558626841));
#41027=CARTESIAN_POINT('Ctrl Pts',(-34.5104839750318,-57.654107492551,-0.446238668058799));
#41028=CARTESIAN_POINT('Ctrl Pts',(-32.4456982401077,-58.7196924553593,
-0.335100777490757));
#41029=CARTESIAN_POINT('Ctrl Pts',(-30.4306156658192,-57.5628636674515,
-0.223962886922716));
#41030=CARTESIAN_POINT('Ctrl Pts',(-30.3096639686861,-55.2424797818376,
-0.112824996354674));
#41031=CARTESIAN_POINT('Ctrl Pts',(-32.1935517174549,-53.8824144115655,
-0.00168710578663172));
#41032=CARTESIAN_POINT('Ctrl Pts',(-34.3579350363402,-54.7275508506072,
0.10945078478141));
#41033=CARTESIAN_POINT('Ctrl Pts',(-34.8217293552191,-57.004326113536,0.220588675349451));
#41034=CARTESIAN_POINT('Ctrl Pts',(-33.1604184604562,-58.6287819909857,
0.331726565917493));
#41035=CARTESIAN_POINT('Ctrl Pts',(-30.8946190614981,-58.1140355911318,
0.442864456485535));
#41036=CARTESIAN_POINT('Ctrl Pts',(-30.0982430406458,-55.931240133699,0.554002347053576));
#41037=CARTESIAN_POINT('Ctrl Pts',(-31.5002224030512,-54.0783330542954,
0.665140237621618));
#41038=CARTESIAN_POINT('Ctrl Pts',(-33.8173095378994,-54.2513012166797,
0.776278128189661));
#41039=CARTESIAN_POINT('Ctrl Pts',(-34.9286483135496,-56.291824899935,0.887416018757701));
#41040=CARTESIAN_POINT('Ctrl Pts',(-33.8170177449885,-58.3321896358132,
0.998553909325746));
#41041=CARTESIAN_POINT('Ctrl Pts',(-31.4999058984797,-58.5048264421807,
1.10969179989378));
#41042=CARTESIAN_POINT('Ctrl Pts',(-30.0981915249122,-56.6517188923722,
1.22082969046183));
#41043=CARTESIAN_POINT('Ctrl Pts',(-30.8948796869627,-54.4690373423775,
1.33196758102987));
#41044=CARTESIAN_POINT('Ctrl Pts',(-33.1607526748339,-53.9546149682087,
1.44310547159791));
#41045=CARTESIAN_POINT('Ctrl Pts',(-34.8218312459871,-55.5793084028841,
1.55424336216595));
#41046=CARTESIAN_POINT('Ctrl Pts',(-34.3577113463298,-57.8560173203711,
1.665381252734));
#41047=CARTESIAN_POINT('Ctrl Pts',(-32.193207183498,-58.7008442288573,1.77651914330204));
#41048=CARTESIAN_POINT('Ctrl Pts',(-30.3095139648772,-57.3405094780172,
1.88765703387008));
#41049=CARTESIAN_POINT('Ctrl Pts',(-30.4307974560059,-55.0201428925398,
1.99879492443812));
#41050=CARTESIAN_POINT('Ctrl Pts',(-32.4460455020051,-53.8636023228594,
2.10993281500616));
#41051=CARTESIAN_POINT('Ctrl Pts',(-34.5106787119048,-54.9294824684668,
2.2210707055742));
#41052=CARTESIAN_POINT('Ctrl Pts',(-34.7349148941505,-57.2421711441843,
2.33220859614225));
#41053=CARTESIAN_POINT('Ctrl Pts',(-32.9135081281216,-58.6848381774545,
2.44334648671029));
#41054=CARTESIAN_POINT('Ctrl Pts',(-30.7136126829218,-57.9369940717681,
2.55448437727833));
#41055=CARTESIAN_POINT('Ctrl Pts',(-30.1488178080539,-55.6831490181888,
2.66562226784637));
#41056=CARTESIAN_POINT('Ctrl Pts',(-31.7360866576937,-53.9862729545993,
2.77676015841441));
#41057=CARTESIAN_POINT('Ctrl Pts',(-34.0225740529132,-54.3995357858862,
2.88789804898245));
#41058=CARTESIAN_POINT('Ctrl Pts',(-34.9154321503369,-56.5446733558537,
2.9990359395505));
#41059=CARTESIAN_POINT('Ctrl Pts',(-33.5974178076939,-58.4582169191953,
3.11017383011854));
#41060=CARTESIAN_POINT('Ctrl Pts',(-31.2749245001037,-58.3886783513254,
3.22131172068658));
#41061=CARTESIAN_POINT('Ctrl Pts',(-30.0737566908708,-56.3997070920348,
3.33244961125462));
#41062=CARTESIAN_POINT('Ctrl Pts',(-31.0933568979523,-54.3118310914232,
3.44358750182266));
#41063=CARTESIAN_POINT('Ctrl Pts',(-33.4004734887601,-54.0361069309691,
3.5547253923907));
#41064=CARTESIAN_POINT('Ctrl Pts',(-34.8833764832336,-55.8249080616723,
3.66586328295875));
#41065=CARTESIAN_POINT('Ctrl Pts',(-34.184747953292,-58.0409245221923,3.77700117352678));
#41066=CARTESIAN_POINT('Ctrl Pts',(-31.9440505153285,-58.6558113149255,
3.88813906409484));
#41067=CARTESIAN_POINT('Ctrl Pts',(-30.2122199456457,-57.106755585101,3.99927695466286));
#41068=CARTESIAN_POINT('Ctrl Pts',(-30.5744204047746,-54.811625609896,4.11041484523092));
#41069=CARTESIAN_POINT('Ctrl Pts',(-32.6991257052286,-53.8711798837978,
4.22155273579895));
#41070=CARTESIAN_POINT('Ctrl Pts',(-34.6415689889353,-55.1462190460047,
4.332690626367));
#41071=CARTESIAN_POINT('Ctrl Pts',(-34.6238098910457,-57.4696852899865,
4.44382851693503));
#41072=CARTESIAN_POINT('Ctrl Pts',(-32.6621035122086,-58.7148836155829,
4.55496640750309));
#41073=CARTESIAN_POINT('Ctrl Pts',(-30.5520219543112,-57.7420698681824,
4.66610429807112));
#41074=CARTESIAN_POINT('Ctrl Pts',(-30.2249467851584,-55.4416715145514,
4.77724218863917));
#41075=CARTESIAN_POINT('Ctrl Pts',(-31.9802536404281,-53.9192692335435,
4.8883800792072));
#41076=CARTESIAN_POINT('Ctrl Pts',(-34.2112902010514,-54.5683351429997,
4.99951796977525));
#41077=CARTESIAN_POINT('Ctrl Pts',(-34.8759634967729,-56.7947717658766,
5.1106558603433));
#41078=CARTESIAN_POINT('Ctrl Pts',(-33.3658903322998,-58.5606965893182,
5.22179375091132));
#41079=CARTESIAN_POINT('Ctrl Pts',(-31.0632581782874,-58.2497382420229,
5.33293164147938));
#41080=CARTESIAN_POINT('Ctrl Pts',(-30.0756916068807,-56.1465211293305,
5.44406953204741));
#41081=CARTESIAN_POINT('Ctrl Pts',(-31.3071229976034,-54.1761423261723,
5.55520742261546));
#41082=CARTESIAN_POINT('Ctrl Pts',(-33.6304062534726,-54.1421146842281,
5.66634531318349));
#41083=CARTESIAN_POINT('Ctrl Pts',(-34.9190197935987,-56.0755785414895,
5.77748320375154));
#41084=CARTESIAN_POINT('Ctrl Pts',(-33.9934692251276,-58.2068235468692,
5.88862109431958));
#41085=CARTESIAN_POINT('Ctrl Pts',(-31.7009449790683,-58.5850749930563,
5.99975898488762));
#41086=CARTESIAN_POINT('Ctrl Pts',(-30.1397737216657,-56.8641588006487,
6.11089687545567));
#41087=CARTESIAN_POINT('Ctrl Pts',(-30.7390063155881,-54.6191619749281,
6.2220347660237));
#41088=CARTESIAN_POINT('Ctrl Pts',(-32.9499730445898,-53.9051289476276,
6.33317265659175));
#41089=CARTESIAN_POINT('Ctrl Pts',(-34.7493198838486,-55.3752771327861,
6.44431054715979));
#41090=CARTESIAN_POINT('Ctrl Pts',(-34.4893499428602,-57.684650256411,6.55544843772784));
#41091=CARTESIAN_POINT('Ctrl Pts',(-32.4094787709551,-58.7180843009709,
6.66658632829587));
#41092=CARTESIAN_POINT('Ctrl Pts',(-30.4105200538552,-57.5324032730232,
6.77772421886391));
#41093=CARTESIAN_POINT('Ctrl Pts',(-30.3280193568976,-55.2072605605051,
6.88886210943196));
#41094=CARTESIAN_POINT('Ctrl Pts',(-31.592606214368,-54.3255716196824,6.96295403647732));
#41095=CARTESIAN_POINT('Ctrl Pts',(-32.2716262263503,-54.2496319067047,
7.));
#41096=CARTESIAN_POINT('Ctrl Pts',(-30.9307125467393,-55.7322829513575,
-2.));
#41097=CARTESIAN_POINT('Ctrl Pts',(-30.9446699885302,-55.6718824515124,
-2.));
#41098=CARTESIAN_POINT('Ctrl Pts',(-30.9622173189428,-55.6125616548506,
-2.));
#41099=CARTESIAN_POINT('Ctrl Pts',(-30.9830550110868,-55.5544917980889,
-2.));
#41100=CARTESIAN_POINT('Ctrl Pts',(-31.0052689439603,-55.4925866748552,
-2.));
#41101=CARTESIAN_POINT('Ctrl Pts',(-31.0312220593616,-55.4321024422544,
-2.));
#41102=CARTESIAN_POINT('Ctrl Pts',(-31.0606132871179,-55.3732441671078,
-2.));
#41103=CARTESIAN_POINT('Ctrl Pts',(-31.0863306114047,-55.3217431763545,
-2.));
#41104=CARTESIAN_POINT('Ctrl Pts',(-31.1146814237679,-55.2714866571797,
-2.));
#41105=CARTESIAN_POINT('Ctrl Pts',(-31.1454993456463,-55.222618038693,-2.));
#41106=CARTESIAN_POINT('Ctrl Pts',(-31.1609623517179,-55.1980980289612,
-2.));
#41107=CARTESIAN_POINT('Ctrl Pts',(-31.1770469579248,-55.17392756714,-2.));
#41108=CARTESIAN_POINT('Ctrl Pts',(-31.1937349146793,-55.1501258793141,
-2.));
#41109=CARTESIAN_POINT('Ctrl Pts',(-31.2013578381332,-55.1392534611361,
-2.));
#41110=CARTESIAN_POINT('Ctrl Pts',(-31.2091078133261,-55.1284566647586,
-2.));
#41111=CARTESIAN_POINT('Ctrl Pts',(-31.2169701001334,-55.1177546356319,
-2.));
#41112=CARTESIAN_POINT('Ctrl Pts',(-31.2566258561146,-55.063775804033,-2.));
#41113=CARTESIAN_POINT('Ctrl Pts',(-31.2992033789008,-55.0121067330815,
-2.));
#41114=CARTESIAN_POINT('Ctrl Pts',(-31.3444046039572,-54.9629466687741,
-2.));
#41115=CARTESIAN_POINT('Ctrl Pts',(-31.3904074837192,-54.9129147387853,
-2.));
#41116=CARTESIAN_POINT('Ctrl Pts',(-31.4391284049847,-54.865480696815,-2.));
#41117=CARTESIAN_POINT('Ctrl Pts',(-31.4903044396693,-54.8208703724992,
-2.));
#41118=CARTESIAN_POINT('Ctrl Pts',(-31.5331115543923,-54.7835552643125,
-2.));
#41119=CARTESIAN_POINT('Ctrl Pts',(-31.577637552122,-54.7482158610154,-2.));
#41120=CARTESIAN_POINT('Ctrl Pts',(-31.6237516110813,-54.7149996928445,
-2.));
#41121=CARTESIAN_POINT('Ctrl Pts',(-31.6449987764397,-54.6996952621866,
-2.));
#41122=CARTESIAN_POINT('Ctrl Pts',(-31.6665833415013,-54.684841812944,-2.));
#41123=CARTESIAN_POINT('Ctrl Pts',(-31.6884937600032,-54.6704551374906,
-2.));
#41124=CARTESIAN_POINT('Ctrl Pts',(-31.6980569751773,-54.6641758017952,
-2.));
#41125=CARTESIAN_POINT('Ctrl Pts',(-31.7076821200989,-54.6579856106301,
-2.));
#41126=CARTESIAN_POINT('Ctrl Pts',(-31.7173562109458,-54.6518932018194,
-2.));
#41127=CARTESIAN_POINT('Ctrl Pts',(-31.7767391574745,-54.6144958698777,
-2.));
#41128=CARTESIAN_POINT('Ctrl Pts',(-31.838074016068,-54.5807067450326,-2.));
#41129=CARTESIAN_POINT('Ctrl Pts',(-31.9010756694416,-54.5507535435306,
-2.));
#41130=CARTESIAN_POINT('Ctrl Pts',(-31.9574042848586,-54.5239729389342,
-2.));
#41131=CARTESIAN_POINT('Ctrl Pts',(-32.015066314809,-54.5002585220973,-2.));
#41132=CARTESIAN_POINT('Ctrl Pts',(-32.073885064195,-54.4797956759538,-2.));
#41133=CARTESIAN_POINT('Ctrl Pts',(-32.1379640249069,-54.457502819887,-2.));
#41134=CARTESIAN_POINT('Ctrl Pts',(-32.2034160279195,-54.4390677641938,
-2.));
#41135=CARTESIAN_POINT('Ctrl Pts',(-32.2699334847344,-54.4243849072971,
-2.));
#41136=CARTESIAN_POINT('Ctrl Pts',(-32.2955972920838,-54.4187199581427,
-2.));
#41137=CARTESIAN_POINT('Ctrl Pts',(-32.3214199362499,-54.413614055249,-2.));
#41138=CARTESIAN_POINT('Ctrl Pts',(-32.3473844776344,-54.4090630310329,
-2.));
#41139=CARTESIAN_POINT('Ctrl Pts',(-32.3587747917672,-54.4070665545815,
-2.));
#41140=CARTESIAN_POINT('Ctrl Pts',(-32.3701918520604,-54.4051770614555,
-2.));
#41141=CARTESIAN_POINT('Ctrl Pts',(-32.3816208594173,-54.4033960585375,
-2.));
#41142=CARTESIAN_POINT('Ctrl Pts',(-32.4507180638674,-54.3926285160109,
-2.));
#41143=CARTESIAN_POINT('Ctrl Pts',(-32.5203743381977,-54.3858000563254,
-2.));
#41144=CARTESIAN_POINT('Ctrl Pts',(-32.590243851397,-54.3827492853075,-2.));
#41145=CARTESIAN_POINT('Ctrl Pts',(-32.6617320286106,-54.3796278372085,
-2.));
#41146=CARTESIAN_POINT('Ctrl Pts',(-32.7334442999928,-54.380460992488,-2.));
#41147=CARTESIAN_POINT('Ctrl Pts',(-32.8050350906898,-54.3851263529469,
-2.));
#41148=CARTESIAN_POINT('Ctrl Pts',(-32.8598101377312,-54.38869588104,-2.));
#41149=CARTESIAN_POINT('Ctrl Pts',(-32.9145147054614,-54.3945098111846,
-2.));
#41150=CARTESIAN_POINT('Ctrl Pts',(-32.9689984939196,-54.4025332699526,
-2.));
#41151=CARTESIAN_POINT('Ctrl Pts',(-33.002911398737,-54.4075273939151,-2.));
#41152=CARTESIAN_POINT('Ctrl Pts',(-33.0367388219446,-54.4133779008071,
-2.));
#41153=CARTESIAN_POINT('Ctrl Pts',(-33.0704445092145,-54.4200797349956,
-2.));
#41154=CARTESIAN_POINT('Ctrl Pts',(-33.0893533889089,-54.4238394618153,
-2.));
#41155=CARTESIAN_POINT('Ctrl Pts',(-33.1082301633052,-54.4278687326753,
-2.));
#41156=CARTESIAN_POINT('Ctrl Pts',(-33.1270344168137,-54.4321588085735,
-2.));
#41157=CARTESIAN_POINT('Ctrl Pts',(-33.1999617463234,-54.4487967345891,
-2.));
#41158=CARTESIAN_POINT('Ctrl Pts',(-33.2718735596469,-54.4693655783604,
-2.));
#41159=CARTESIAN_POINT('Ctrl Pts',(-33.3423988006913,-54.493750495395,-2.));
#41160=CARTESIAN_POINT('Ctrl Pts',(-33.3951487097682,-54.5119893860017,
-2.));
#41161=CARTESIAN_POINT('Ctrl Pts',(-33.4471233201863,-54.532364245129,-2.));
#41162=CARTESIAN_POINT('Ctrl Pts',(-33.4981671222724,-54.5548460975971,
-2.));
#41163=CARTESIAN_POINT('Ctrl Pts',(-33.5140901369522,-54.5618592677029,
-2.));
#41164=CARTESIAN_POINT('Ctrl Pts',(-33.5299225529266,-54.5690775909281,
-2.));
#41165=CARTESIAN_POINT('Ctrl Pts',(-33.5456595742609,-54.5765005080885,
-2.));
#41166=CARTESIAN_POINT('Ctrl Pts',(-33.5608498130208,-54.5836655161015,
-2.));
#41167=CARTESIAN_POINT('Ctrl Pts',(-33.5759433895169,-54.5910175352492,
-2.));
#41168=CARTESIAN_POINT('Ctrl Pts',(-33.5909308710173,-54.5985527495268,
-2.));
#41169=CARTESIAN_POINT('Ctrl Pts',(-33.658231843262,-54.6323894716568,-2.));
#41170=CARTESIAN_POINT('Ctrl Pts',(-33.7234283245604,-54.6699323219136,
-2.));
#41171=CARTESIAN_POINT('Ctrl Pts',(-33.7861478874234,-54.7110945661211,
-2.));
#41172=CARTESIAN_POINT('Ctrl Pts',(-33.8341488046827,-54.742597105173,-2.));
#41173=CARTESIAN_POINT('Ctrl Pts',(-33.8806990672183,-54.7762206567485,
-2.));
#41174=CARTESIAN_POINT('Ctrl Pts',(-33.9256254254142,-54.8119460488582,
-2.));
#41175=CARTESIAN_POINT('Ctrl Pts',(-33.9360516193134,-54.8202369471242,
-2.));
#41176=CARTESIAN_POINT('Ctrl Pts',(-33.9463903172992,-54.8286411175249,
-2.));
#41177=CARTESIAN_POINT('Ctrl Pts',(-33.9566410663199,-54.8371566128168,
-2.));
#41178=CARTESIAN_POINT('Ctrl Pts',(-33.3347877909359,-57.7349452754743,
-0.871480363390215));
#41179=CARTESIAN_POINT('Ctrl Pts',(-33.4089783616458,-57.692956018043,-0.877193940366672));
#41180=CARTESIAN_POINT('Ctrl Pts',(-33.4797275640263,-57.6452118511612,
-0.882907517343129));
#41181=CARTESIAN_POINT('Ctrl Pts',(-33.5459978166813,-57.5919001635712,
-0.888621094319586));
#41182=CARTESIAN_POINT('Ctrl Pts',(-33.9756840487236,-57.2462352951484,
-0.925667057842266));
#41183=CARTESIAN_POINT('Ctrl Pts',(-34.2170739697906,-56.6665102843049,
-0.962713021364947));
#41184=CARTESIAN_POINT('Ctrl Pts',(-34.1597013173233,-56.1180347705934,
-0.999758984887627));
#41185=CARTESIAN_POINT('Ctrl Pts',(-34.102328664856,-55.5695592568819,-1.03680494841031));
#41186=CARTESIAN_POINT('Ctrl Pts',(-33.7461934388544,-55.0523332403023,
-1.07385091193299));
#41187=CARTESIAN_POINT('Ctrl Pts',(-33.254268606184,-54.8030776924624,-1.11089687545567));
#41188=CARTESIAN_POINT('Ctrl Pts',(-32.7623437735136,-54.5538221446225,
-1.14794283897835));
#41189=CARTESIAN_POINT('Ctrl Pts',(-32.1346293341744,-54.5725370655222,
-1.18498880250103));
#41190=CARTESIAN_POINT('Ctrl Pts',(-31.6584309020156,-54.850638451748,-1.22203476602371));
#41191=CARTESIAN_POINT('Ctrl Pts',(-31.1822324698568,-55.1287398379739,
-1.25908072954639));
#41192=CARTESIAN_POINT('Ctrl Pts',(-30.8575500448784,-55.666227689526,-1.29612669306907));
#41193=CARTESIAN_POINT('Ctrl Pts',(-30.8329195675803,-56.2171554903502,
-1.33317265659175));
#41194=CARTESIAN_POINT('Ctrl Pts',(-30.8082890902823,-56.7680832911743,
-1.37021862011443));
#41195=CARTESIAN_POINT('Ctrl Pts',(-31.0837105606646,-57.3324510412706,
-1.40726458363711));
#41196=CARTESIAN_POINT('Ctrl Pts',(-31.5332488781923,-57.6518973032928,
-1.44431054715979));
#41197=CARTESIAN_POINT('Ctrl Pts',(-31.9827871957199,-57.971343565315,-1.48135651068247));
#41198=CARTESIAN_POINT('Ctrl Pts',(-32.6064423603928,-58.0458683392631,
-1.51840247420516));
#41199=CARTESIAN_POINT('Ctrl Pts',(-33.1185697754731,-57.8415149221822,
-1.55544843772784));
#41200=CARTESIAN_POINT('Ctrl Pts',(-33.1924454681488,-57.8120364178238,
-1.56079241294863));
#41201=CARTESIAN_POINT('Ctrl Pts',(-33.2640004019439,-57.7767547923516,
-1.56613638816942));
#41202=CARTESIAN_POINT('Ctrl Pts',(-33.3326856027611,-57.7363329907929,
-1.57148036339021));
#41203=CARTESIAN_POINT('Ctrl Pts',(-34.4842965055667,-55.7582049595679,
-2.));
#41204=CARTESIAN_POINT('Ctrl Pts',(-34.6616800870191,-56.4180307560557,
-1.96295403647732));
#41205=CARTESIAN_POINT('Ctrl Pts',(-34.3029408546812,-57.9173199920238,
-1.88886210943196));
#41206=CARTESIAN_POINT('Ctrl Pts',(-32.1083909227282,-58.6899905331757,
-1.77772421886392));
#41207=CARTESIAN_POINT('Ctrl Pts',(-30.2743670907292,-57.2623912321518,
-1.66658632829588));
#41208=CARTESIAN_POINT('Ctrl Pts',(-30.4765028746714,-54.9487367869862,
-1.55544843772783));
#41209=CARTESIAN_POINT('Ctrl Pts',(-32.5312595152503,-53.8630292597193,
-1.44431054715979));
#41210=CARTESIAN_POINT('Ctrl Pts',(-34.5571577499755,-55.0008883544571,
-1.33317265659175));
#41211=CARTESIAN_POINT('Ctrl Pts',(-34.7002397993375,-57.3198853035068,
-1.22203476602371));
#41212=CARTESIAN_POINT('Ctrl Pts',(-32.8293553152893,-58.697884688863,-1.11089687545567));
#41213=CARTESIAN_POINT('Ctrl Pts',(-30.6570393620673,-57.873352597378,-0.999758984887624));
#41214=CARTESIAN_POINT('Ctrl Pts',(-30.1715905180573,-55.6011108576298,
-0.888621094319583));
#41215=CARTESIAN_POINT('Ctrl Pts',(-31.817369145763,-53.960908709333,-0.77748320375154));
#41216=CARTESIAN_POINT('Ctrl Pts',(-34.087963584719,-54.4540716106361,-0.666345313183499));
#41217=CARTESIAN_POINT('Ctrl Pts',(-34.9050789303496,-56.6291869825843,
-0.555207422615457));
#41218=CARTESIAN_POINT('Ctrl Pts',(-33.5207972588595,-58.4953545827796,
-0.444069532047416));
#41219=CARTESIAN_POINT('Ctrl Pts',(-31.2021687803137,-58.3444462635109,
-0.332931641479373));
#41220=CARTESIAN_POINT('Ctrl Pts',(-30.0714596841225,-56.3145920190741,
-0.221793750911332));
#41221=CARTESIAN_POINT('Ctrl Pts',(-31.1636212068567,-54.2637395061114,
-0.11065586034329));
#41222=CARTESIAN_POINT('Ctrl Pts',(-33.4789853310955,-54.069057766837,0.000482030224751219));
#41223=CARTESIAN_POINT('Ctrl Pts',(-34.8982731111897,-55.908740964546,0.111619920792794));
#41224=CARTESIAN_POINT('Ctrl Pts',(-34.1223942983453,-58.0989063257425,
0.222757811360835));
#41225=CARTESIAN_POINT('Ctrl Pts',(-31.8615195930587,-58.6348705964901,
0.333895701928877));
#41226=CARTESIAN_POINT('Ctrl Pts',(-30.1850532410697,-57.0260596319961,
0.445033592496918));
#41227=CARTESIAN_POINT('Ctrl Pts',(-30.6274839128386,-54.7450363379152,
0.556171483064961));
#41228=CARTESIAN_POINT('Ctrl Pts',(-32.783849793945,-53.8796472115696,0.667309373633002));
#41229=CARTESIAN_POINT('Ctrl Pts',(-34.6804047400893,-55.2219927306232,
0.778447264201044));
#41230=CARTESIAN_POINT('Ctrl Pts',(-34.5812104999015,-57.5434088201914,
0.889585154769086));
#41231=CARTESIAN_POINT('Ctrl Pts',(-32.5770606867505,-58.7190770058698,
1.00072304533713));
#41232=CARTESIAN_POINT('Ctrl Pts',(-30.5023763530244,-57.6728948648119,
1.11186093590517));
#41233=CARTESIAN_POINT('Ctrl Pts',(-30.2561395980006,-55.3624447749947,
1.22299882647321));
#41234=CARTESIAN_POINT('Ctrl Pts',(-32.0637337160182,-53.9025079060376,
1.33413671704125));
#41235=CARTESIAN_POINT('Ctrl Pts',(-34.2706473113688,-54.629381030845,1.4452746076093));
#41236=CARTESIAN_POINT('Ctrl Pts',(-34.8568673421131,-56.8777489350102,
1.55641249817734));
#41237=CARTESIAN_POINT('Ctrl Pts',(-33.2858199659299,-58.5896549776086,
1.66755038874538));
#41238=CARTESIAN_POINT('Ctrl Pts',(-30.9955026631254,-58.198172143523,1.77868827931342));
#41239=CARTESIAN_POINT('Ctrl Pts',(-30.0822688349231,-56.0616291105052,
1.88982616988146));
#41240=CARTESIAN_POINT('Ctrl Pts',(-31.3820117610517,-54.1356279467243,
2.0009640604495));
#41241=CARTESIAN_POINT('Ctrl Pts',(-33.7050620011389,-54.1830593597269,
2.11210195101755));
#41242=CARTESIAN_POINT('Ctrl Pts',(-34.9251053252509,-56.1605088392832,
2.22323984158559));
#41243=CARTESIAN_POINT('Ctrl Pts',(-33.925422242596,-58.2579944509529,2.33437773215363));
#41244=CARTESIAN_POINT('Ctrl Pts',(-31.6210340159052,-58.55566382727,2.44551562272167));
#41245=CARTESIAN_POINT('Ctrl Pts',(-30.1211733226087,-56.7810568122912,
2.55665351328971));
#41246=CARTESIAN_POINT('Ctrl Pts',(-30.7986796648578,-54.5584913322389,
2.66779140385775));
#41247=CARTESIAN_POINT('Ctrl Pts',(-33.0334238041475,-53.9223067766118,
2.7789292944258));
#41248=CARTESIAN_POINT('Ctrl Pts',(-34.7799190860636,-55.4548100839991,
2.89006718499384));
#41249=CARTESIAN_POINT('Ctrl Pts',(-34.4395785724647,-57.7532835973795,
3.00120507556188));
#41250=CARTESIAN_POINT('Ctrl Pts',(-32.3239197951718,-58.7139084434935,
3.11234296612992));
#41251=CARTESIAN_POINT('Ctrl Pts',(-30.3694292262435,-57.4574138064661,
3.22348085669796));
#41252=CARTESIAN_POINT('Ctrl Pts',(-30.3650742488504,-55.1338834771873,
3.334618747266));
#41253=CARTESIAN_POINT('Ctrl Pts',(-32.3148410231895,-53.870071116671,3.44575663783405));
#41254=CARTESIAN_POINT('Ctrl Pts',(-34.4340859088485,-54.822758511107,3.55689452840208));
#41255=CARTESIAN_POINT('Ctrl Pts',(-34.7830400281131,-57.1199400841539,
3.66803241897013));
#41256=CARTESIAN_POINT('Ctrl Pts',(-33.0423017182097,-58.6589794901991,
3.77917030953817));
#41257=CARTESIAN_POINT('Ctrl Pts',(-30.8051884955116,-58.0311765069792,
3.89030820010621));
#41258=CARTESIAN_POINT('Ctrl Pts',(-30.1193554633367,-55.8111663248381,
4.00144609067426));
#41259=CARTESIAN_POINT('Ctrl Pts',(-31.6125533739246,-54.0309494400522,
4.11258398124229));
#41260=CARTESIAN_POINT('Ctrl Pts',(-33.9180412456697,-54.3199785564283,
4.22372187181034));
#41261=CARTESIAN_POINT('Ctrl Pts',(-34.9255798836094,-56.4137020456762,
4.33485976237838));
#41262=CARTESIAN_POINT('Ctrl Pts',(-33.71295774606,-58.3957110541618,4.44599765294642));
#41263=CARTESIAN_POINT('Ctrl Pts',(-31.3901016278141,-58.451850257884,4.55713554351447));
#41264=CARTESIAN_POINT('Ctrl Pts',(-30.0831480764379,-56.5307348090517,
4.6682734340825));
#41265=CARTESIAN_POINT('Ctrl Pts',(-30.9883665002518,-54.3907834608548,
4.77941132465055));
#41266=CARTESIAN_POINT('Ctrl Pts',(-33.2772002083032,-53.990717959075,4.89054921521859));
#41267=CARTESIAN_POINT('Ctrl Pts',(-34.8546537539781,-55.6967227784588,
5.00168710578663));
#41268=CARTESIAN_POINT('Ctrl Pts',(-34.2768660104017,-57.9472723924375,
5.11282499635467));
#41269=CARTESIAN_POINT('Ctrl Pts',(-32.0726926657226,-58.6824131526073,
5.22396288692272));
#41270=CARTESIAN_POINT('Ctrl Pts',(-30.2596385516872,-57.2292625110704,
5.33510077749076));
#41271=CARTESIAN_POINT('Ctrl Pts',(-30.4972127153845,-54.9179054771162,
5.44623866805879));
#41272=CARTESIAN_POINT('Ctrl Pts',(-32.5679607208419,-53.8639538597436,
5.55737655862685));
#41273=CARTESIAN_POINT('Ctrl Pts',(-34.5765036531329,-55.0321005249753,
5.66851444919488));
#41274=CARTESIAN_POINT('Ctrl Pts',(-34.6843989531681,-57.3531295774156,
5.77965233976293));
#41275=CARTESIAN_POINT('Ctrl Pts',(-32.7928896947834,-58.7025728310562,
5.89079023033096));
#41276=CARTESIAN_POINT('Ctrl Pts',(-30.6332940299706,-57.8452774805725,
6.00192812089901));
#41277=CARTESIAN_POINT('Ctrl Pts',(-30.1823177935136,-55.5659199366928,
6.11306601146705));
#41278=CARTESIAN_POINT('Ctrl Pts',(-31.8527378172474,-53.9508533596396,
6.22420390203509));
#41279=CARTESIAN_POINT('Ctrl Pts',(-34.1156133119216,-54.4783040835128,
6.33534179260312));
#41280=CARTESIAN_POINT('Ctrl Pts',(-34.8996815919165,-56.6656147589772,
6.44647968317118));
#41281=CARTESIAN_POINT('Ctrl Pts',(-33.4873299906743,-58.510467673716,6.55761757373921));
#41282=CARTESIAN_POINT('Ctrl Pts',(-31.1711925871668,-58.3247407101007,
6.66875546430726));
#41283=CARTESIAN_POINT('Ctrl Pts',(-30.0714699489351,-56.2774508415845,
6.7798933548753));
#41284=CARTESIAN_POINT('Ctrl Pts',(-31.1943253650081,-54.2444600690086,
6.89103124544334));
#41285=CARTESIAN_POINT('Ctrl Pts',(-33.5128402220712,-54.0826823257856,
7.00216913601138));
#41286=CARTESIAN_POINT('Ctrl Pts',(-34.903205848792,-55.9481454299591,7.11330702657942));
#41287=CARTESIAN_POINT('Ctrl Pts',(-34.3645996631225,-57.3926056844023,
7.18739895362479));
#41288=CARTESIAN_POINT('Ctrl Pts',(-33.8493101059357,-57.841283396055,7.22444491714747));
#41289=CARTESIAN_POINT('Ctrl Pts',(-34.3591563398468,-55.7918468858113,
-2.07481497238249));
#41290=CARTESIAN_POINT('Ctrl Pts',(-34.5253531804484,-56.4100605999883,
-2.03776900885981));
#41291=CARTESIAN_POINT('Ctrl Pts',(-34.189237929385,-57.8147967775173,-1.96367708181445));
#41292=CARTESIAN_POINT('Ctrl Pts',(-32.1330878491652,-58.5387386537266,
-1.85253919124641));
#41293=CARTESIAN_POINT('Ctrl Pts',(-30.4147271983626,-57.2011712670918,
-1.74140130067836));
#41294=CARTESIAN_POINT('Ctrl Pts',(-30.6041152374846,-55.033428030193,-1.63026341011032));
#41295=CARTESIAN_POINT('Ctrl Pts',(-32.5292881259404,-54.0161909253172,
-1.51912551954228));
#41296=CARTESIAN_POINT('Ctrl Pts',(-34.4274225712752,-55.0822906457469,
-1.40798762897424));
#41297=CARTESIAN_POINT('Ctrl Pts',(-34.561481114665,-57.2550394601585,-1.2968497384062));
#41298=CARTESIAN_POINT('Ctrl Pts',(-32.8085844382453,-58.5461349624701,
-1.18571184783815));
#41299=CARTESIAN_POINT('Ctrl Pts',(-30.7732661452114,-57.7736021978399,
-1.07457395727011));
#41300=CARTESIAN_POINT('Ctrl Pts',(-30.3184322564854,-55.6446599635185,
-0.96343606670207));
#41301=CARTESIAN_POINT('Ctrl Pts',(-31.860419434863,-54.1078975824522,-0.85229817613403));
#41302=CARTESIAN_POINT('Ctrl Pts',(-33.9878182558372,-54.5699590394787,
-0.741160285565987));
#41303=CARTESIAN_POINT('Ctrl Pts',(-34.7534020135839,-56.6079002051822,
-0.630022394997947));
#41304=CARTESIAN_POINT('Ctrl Pts',(-33.4564204191172,-58.3563774692333,
-0.518884504429904));
#41305=CARTESIAN_POINT('Ctrl Pts',(-31.2840168375231,-58.2149862216467,
-0.407746613861863));
#41306=CARTESIAN_POINT('Ctrl Pts',(-30.2246161991564,-56.3131452533626,
-0.29660872329382));
#41307=CARTESIAN_POINT('Ctrl Pts',(-31.2479002766274,-54.3916302777182,
-0.185470832725779));
#41308=CARTESIAN_POINT('Ctrl Pts',(-33.4172453712524,-54.209226192034,-0.0743329421577374));
#41309=CARTESIAN_POINT('Ctrl Pts',(-34.7470254051468,-55.9328892992031,
0.0368049484103048));
#41310=CARTESIAN_POINT('Ctrl Pts',(-34.0200775877185,-57.9849313227407,
0.147942838978346));
#41311=CARTESIAN_POINT('Ctrl Pts',(-31.9017855229282,-58.4870948699203,
0.259080729546388));
#41312=CARTESIAN_POINT('Ctrl Pts',(-30.3310459494339,-56.9797439796361,
0.370218620114429));
#41313=CARTESIAN_POINT('Ctrl Pts',(-30.7455746179339,-54.8425740019479,
0.481356510682472));
#41314=CARTESIAN_POINT('Ctrl Pts',(-32.7659487342222,-54.0317608617915,
0.592494401250513));
#41315=CARTESIAN_POINT('Ctrl Pts',(-34.5428969584923,-55.2894510179814,
0.703632291818555));
#41316=CARTESIAN_POINT('Ctrl Pts',(-34.4499584283865,-57.4644664091971,
0.814770182386597));
#41317=CARTESIAN_POINT('Ctrl Pts',(-32.5722008348668,-58.5659907805945,
0.92590807295464));
#41318=CARTESIAN_POINT('Ctrl Pts',(-30.6283569983197,-57.5857863833555,
1.03704596352268));
#41319=CARTESIAN_POINT('Ctrl Pts',(-30.3976492271164,-55.4210454183169,
1.14818385409072));
#41320=CARTESIAN_POINT('Ctrl Pts',(-32.0912469605976,-54.0531798407264,
1.25932174465876));
#41321=CARTESIAN_POINT('Ctrl Pts',(-34.1589809866262,-54.7342125263452,
1.37045963522681));
#41322=CARTESIAN_POINT('Ctrl Pts',(-34.7082309014681,-56.8407865346196,
1.48159752579485));
#41323=CARTESIAN_POINT('Ctrl Pts',(-33.2362620291564,-58.4447307855874,
1.59273541636289));
#41324=CARTESIAN_POINT('Ctrl Pts',(-31.0903841717777,-58.0779369163799,
1.70387330693093));
#41325=CARTESIAN_POINT('Ctrl Pts',(-30.2347436681021,-56.0761355152048,
1.81501119749897));
#41326=CARTESIAN_POINT('Ctrl Pts',(-31.4525179747665,-54.2715981065311,
1.92614908806701));
#41327=CARTESIAN_POINT('Ctrl Pts',(-33.6290644583814,-54.3160382453633,
2.03728697863506));
#41328=CARTESIAN_POINT('Ctrl Pts',(-34.772165438778,-56.1687793686431,2.1484248692031));
#41329=CARTESIAN_POINT('Ctrl Pts',(-33.8355276249524,-58.133986514719,2.25956275977114));
#41330=CARTESIAN_POINT('Ctrl Pts',(-31.6764662300946,-58.4128832958229,
2.37070065033918));
#41331=CARTESIAN_POINT('Ctrl Pts',(-30.2711946343393,-56.7501923253057,
2.48183854090722));
#41332=CARTESIAN_POINT('Ctrl Pts',(-30.9059738661454,-54.66779350468,2.59297643147526));
#41333=CARTESIAN_POINT('Ctrl Pts',(-32.9997832957543,-54.0717300904733,
2.70411432204331));
#41334=CARTESIAN_POINT('Ctrl Pts',(-34.6361354068315,-55.5075856855278,
2.81525221261135));
#41335=CARTESIAN_POINT('Ctrl Pts',(-34.3172585546124,-57.6611053799802,
2.92639010317939));
#41336=CARTESIAN_POINT('Ctrl Pts',(-32.3350243382431,-58.5611481749239,
3.03752799374743));
#41337=CARTESIAN_POINT('Ctrl Pts',(-30.503794216031,-57.3838946929672,3.14866588431548));
#41338=CARTESIAN_POINT('Ctrl Pts',(-30.4997138863991,-55.206898397108,3.25980377488351));
#41339=CARTESIAN_POINT('Ctrl Pts',(-32.3265181213336,-54.0227886857625,
3.37094166545156));
#41340=CARTESIAN_POINT('Ctrl Pts',(-34.3121122872295,-54.9153946064446,
3.48207955601959));
#41341=CARTESIAN_POINT('Ctrl Pts',(-34.6390595258738,-57.0677038371105,
3.59321744658764));
#41342=CARTESIAN_POINT('Ctrl Pts',(-33.0081013218997,-58.5096833300925,
3.70435533715568));
#41343=CARTESIAN_POINT('Ctrl Pts',(-30.9120722157322,-57.9214729022893,
3.81549322772372));
#41344=CARTESIAN_POINT('Ctrl Pts',(-30.2694914188265,-55.8414682290595,
3.92663111829176));
#41345=CARTESIAN_POINT('Ctrl Pts',(-31.6685204219656,-54.173521176607,4.03776900885981));
#41346=CARTESIAN_POINT('Ctrl Pts',(-33.8286121124817,-54.4443225979688,
4.14890689942785));
#41347=CARTESIAN_POINT('Ctrl Pts',(-34.7726100689923,-56.406004880834,4.26004478999589));
#41348=CARTESIAN_POINT('Ctrl Pts',(-33.6364622561333,-58.2630179851871,
4.37118268056393));
#41349=CARTESIAN_POINT('Ctrl Pts',(-31.460097652016,-58.3156167556941,4.48232057113198));
#41350=CARTESIAN_POINT('Ctrl Pts',(-30.2355674600263,-56.5156569431084,
4.59345846170002));
#41351=CARTESIAN_POINT('Ctrl Pts',(-31.0836980528375,-54.5106621730211,
4.70459635226806));
#41352=CARTESIAN_POINT('Ctrl Pts',(-33.2281858787453,-54.1358269042488,
4.8157342428361));
#41353=CARTESIAN_POINT('Ctrl Pts',(-34.7061569138339,-55.7342420941505,
4.92687213340414));
#41354=CARTESIAN_POINT('Ctrl Pts',(-34.1648075018169,-57.842860222152,5.03801002397218));
#41355=CARTESIAN_POINT('Ctrl Pts',(-32.0996409118516,-58.5316391425983,
5.14914791454023));
#41356=CARTESIAN_POINT('Ctrl Pts',(-30.4009275183955,-57.1701318172633,
5.26028580510827));
#41357=CARTESIAN_POINT('Ctrl Pts',(-30.6235190068059,-55.0045411047512,
5.37142369567631));
#41358=CARTESIAN_POINT('Ctrl Pts',(-32.5636747606314,-54.017057215205,5.48256158624435));
#41359=CARTESIAN_POINT('Ctrl Pts',(-34.445548420111,-55.1115344127627,5.59369947681239));
#41360=CARTESIAN_POINT('Ctrl Pts',(-34.5466392755034,-57.2861871754458,
5.70483736738044));
#41361=CARTESIAN_POINT('Ctrl Pts',(-32.7744185314064,-58.550527445779,5.81597525794847));
#41362=CARTESIAN_POINT('Ctrl Pts',(-30.7510183185456,-57.7472976454435,
5.92711314851652));
#41363=CARTESIAN_POINT('Ctrl Pts',(-30.3284830135764,-55.6116883669947,
6.03825103908455));
#41364=CARTESIAN_POINT('Ctrl Pts',(-31.8935575720505,-54.0984763759544,
6.1493889296526));
#41365=CARTESIAN_POINT('Ctrl Pts',(-34.0137242459347,-54.5926632852668,
6.26052682022064));
#41366=CARTESIAN_POINT('Ctrl Pts',(-34.748345059677,-56.6420306545566,6.37166471078869));
#41367=CARTESIAN_POINT('Ctrl Pts',(-33.4250637727444,-58.3705374492314,
6.48280260135672));
#41368=CARTESIAN_POINT('Ctrl Pts',(-31.2549941659053,-58.1965234039931,
6.59394049192477));
#41369=CARTESIAN_POINT('Ctrl Pts',(-30.2246258166159,-56.2783463937137,
6.70507838249281));
#41370=CARTESIAN_POINT('Ctrl Pts',(-31.2766680692063,-54.3735667032384,
6.81621627306085));
#41371=CARTESIAN_POINT('Ctrl Pts',(-33.4489651948854,-54.221991514694,6.9273541636289));
#41372=CARTESIAN_POINT('Ctrl Pts',(-34.7516470583929,-55.9698087119449,
7.03849205419693));
#41373=CARTESIAN_POINT('Ctrl Pts',(-34.2470082093303,-57.3231737116671,
7.1125839812423));
#41374=CARTESIAN_POINT('Ctrl Pts',(-33.7642155196223,-57.7435554488857,
7.14962994476498));
#41375=CARTESIAN_POINT('Ctrl Pts',(-34.2340161741268,-55.8254888120548,
-2.14962994476498));
#41376=CARTESIAN_POINT('Ctrl Pts',(-34.3890262738776,-56.4020904439209,
-2.1125839812423));
#41377=CARTESIAN_POINT('Ctrl Pts',(-34.0755350040887,-57.7122735630108,
-2.03849205419694));
#41378=CARTESIAN_POINT('Ctrl Pts',(-32.1577847756022,-58.3874867742776,
-1.92735416362889));
#41379=CARTESIAN_POINT('Ctrl Pts',(-30.555087305996,-57.1399513020318,-1.81621627306086));
#41380=CARTESIAN_POINT('Ctrl Pts',(-30.7317276002978,-55.1181192733998,
-1.70507838249281));
#41381=CARTESIAN_POINT('Ctrl Pts',(-32.5273167366305,-54.1693525909151,
-1.59394049192477));
#41382=CARTESIAN_POINT('Ctrl Pts',(-34.297687392575,-55.1636929370367,-1.48280260135673));
#41383=CARTESIAN_POINT('Ctrl Pts',(-34.4227224299925,-57.1901936168101,
-1.37166471078869));
#41384=CARTESIAN_POINT('Ctrl Pts',(-32.7878135612013,-58.3943852360772,
-1.26052682022064));
#41385=CARTESIAN_POINT('Ctrl Pts',(-30.8894929283555,-57.6738517983019,
-1.1493889296526));
#41386=CARTESIAN_POINT('Ctrl Pts',(-30.4652739949134,-55.6882090694072,
-1.03825103908456));
#41387=CARTESIAN_POINT('Ctrl Pts',(-31.9034697239631,-54.2548864555713,
-0.927113148516517));
#41388=CARTESIAN_POINT('Ctrl Pts',(-33.8876729269555,-54.6858464683214,
-0.815975257948478));
#41389=CARTESIAN_POINT('Ctrl Pts',(-34.6017250968181,-56.5866134277799,
-0.704837367380434));
#41390=CARTESIAN_POINT('Ctrl Pts',(-33.3920435793749,-58.217400355687,-0.593699476812393));
#41391=CARTESIAN_POINT('Ctrl Pts',(-31.3658648947325,-58.0855261797824,
-0.482561586244351));
#41392=CARTESIAN_POINT('Ctrl Pts',(-30.3777727141903,-56.3116984876511,
-0.371423695676309));
#41393=CARTESIAN_POINT('Ctrl Pts',(-31.3321793463982,-54.519521049325,-0.260285805108268));
#41394=CARTESIAN_POINT('Ctrl Pts',(-33.3555054114092,-54.3493946172309,
-0.149147914540226));
#41395=CARTESIAN_POINT('Ctrl Pts',(-34.5957776991039,-55.9570376338604,
-0.0380100239721841));
#41396=CARTESIAN_POINT('Ctrl Pts',(-33.9177608770916,-57.8709563197388,
0.0731278665958575));
#41397=CARTESIAN_POINT('Ctrl Pts',(-31.9420514527978,-58.3393191433505,
0.184265757163899));
#41398=CARTESIAN_POINT('Ctrl Pts',(-30.4770386577982,-56.933428327276,0.295403647731941));
#41399=CARTESIAN_POINT('Ctrl Pts',(-30.8636653230293,-54.9401116659806,
0.406541538299983));
#41400=CARTESIAN_POINT('Ctrl Pts',(-32.7480476744994,-54.1838745120134,
0.517679428868024));
#41401=CARTESIAN_POINT('Ctrl Pts',(-34.4053891768952,-55.3569093053397,
0.628817319436066));
#41402=CARTESIAN_POINT('Ctrl Pts',(-34.3187063568714,-57.3855239982029,
0.739955210004108));
#41403=CARTESIAN_POINT('Ctrl Pts',(-32.5673409829831,-58.412904555319,0.85109310057215));
#41404=CARTESIAN_POINT('Ctrl Pts',(-30.7543376436151,-57.4986779018991,
0.962230991140191));
#41405=CARTESIAN_POINT('Ctrl Pts',(-30.5391588562322,-55.4796460616391,
1.07336888170823));
#41406=CARTESIAN_POINT('Ctrl Pts',(-32.1187602051768,-54.2038517754153,
1.18450677227628));
#41407=CARTESIAN_POINT('Ctrl Pts',(-34.0473146618836,-54.8390440218455,
1.29564466284432));
#41408=CARTESIAN_POINT('Ctrl Pts',(-34.559594460823,-56.8038241342291,1.40678255341236));
#41409=CARTESIAN_POINT('Ctrl Pts',(-33.1867040923831,-58.299806593566,1.5179204439804));
#41410=CARTESIAN_POINT('Ctrl Pts',(-31.18526568043,-57.9577016892369,1.62905833454844));
#41411=CARTESIAN_POINT('Ctrl Pts',(-30.3872185012811,-56.0906419199043,
1.74019622511648));
#41412=CARTESIAN_POINT('Ctrl Pts',(-31.5230241884812,-54.4075682663379,
1.85133411568453));
#41413=CARTESIAN_POINT('Ctrl Pts',(-33.5530669156239,-54.4490171309997,
1.96247200625257));
#41414=CARTESIAN_POINT('Ctrl Pts',(-34.6192255523049,-56.1770498980029,
2.07360989682061));
#41415=CARTESIAN_POINT('Ctrl Pts',(-33.7456330073089,-58.0099785784851,
2.18474778738865));
#41416=CARTESIAN_POINT('Ctrl Pts',(-31.731898444284,-58.2701027643757,2.29588567795669));
#41417=CARTESIAN_POINT('Ctrl Pts',(-30.42121594607,-56.7193278383203,2.40702356852474));
#41418=CARTESIAN_POINT('Ctrl Pts',(-31.0132680674328,-54.7770956771211,
2.51816145909277));
#41419=CARTESIAN_POINT('Ctrl Pts',(-32.9661427873613,-54.2211534043347,
2.62929934966082));
#41420=CARTESIAN_POINT('Ctrl Pts',(-34.4923517275992,-55.5603612870565,
2.74043724022886));
#41421=CARTESIAN_POINT('Ctrl Pts',(-34.1949385367603,-57.568927162581,2.8515751307969));
#41422=CARTESIAN_POINT('Ctrl Pts',(-32.3461288813143,-58.4083879063543,
2.96271302136494));
#41423=CARTESIAN_POINT('Ctrl Pts',(-30.6381592058186,-57.3103755794683,
3.07385091193299));
#41424=CARTESIAN_POINT('Ctrl Pts',(-30.6343535239478,-55.2799133170287,
3.18498880250102));
#41425=CARTESIAN_POINT('Ctrl Pts',(-32.3381952194778,-54.175506254854,3.29612669306907));
#41426=CARTESIAN_POINT('Ctrl Pts',(-34.1901386656105,-55.0080307017823,
3.4072645836371));
#41427=CARTESIAN_POINT('Ctrl Pts',(-34.4950790236344,-57.0154675900672,
3.51840247420515));
#41428=CARTESIAN_POINT('Ctrl Pts',(-32.9739009255896,-58.360387169986,3.62954036477319));
#41429=CARTESIAN_POINT('Ctrl Pts',(-31.0189559359529,-57.8117692975993,
3.74067825534124));
#41430=CARTESIAN_POINT('Ctrl Pts',(-30.4196273743162,-55.871770133281,3.85181614590928));
#41431=CARTESIAN_POINT('Ctrl Pts',(-31.7244874700066,-54.3160929131617,
3.96295403647732));
#41432=CARTESIAN_POINT('Ctrl Pts',(-33.7391829792937,-54.5686666395095,
4.07409192704536));
#41433=CARTESIAN_POINT('Ctrl Pts',(-34.6196402543753,-56.3983077159918,
4.1852298176134));
#41434=CARTESIAN_POINT('Ctrl Pts',(-33.5599667662066,-58.1303249162125,
4.29636770818144));
#41435=CARTESIAN_POINT('Ctrl Pts',(-31.5300936762181,-58.1793832535041,
4.40750559874949));
#41436=CARTESIAN_POINT('Ctrl Pts',(-30.3879868436147,-56.5005790771652,
4.51864348931753));
#41437=CARTESIAN_POINT('Ctrl Pts',(-31.1790296054234,-54.6305408851872,
4.62978137988557));
#41438=CARTESIAN_POINT('Ctrl Pts',(-33.1791715491872,-54.2809358494227,
4.74091927045361));
#41439=CARTESIAN_POINT('Ctrl Pts',(-34.5576600736897,-55.7717614098421,
4.85205716102165));
#41440=CARTESIAN_POINT('Ctrl Pts',(-34.0527489932321,-57.7384480518666,
4.96319505158969));
#41441=CARTESIAN_POINT('Ctrl Pts',(-32.1265891579805,-58.3808651325893,
5.07433294215774));
#41442=CARTESIAN_POINT('Ctrl Pts',(-30.5422164851038,-57.1110011234561,
5.18547083272577));
#41443=CARTESIAN_POINT('Ctrl Pts',(-30.7498252982273,-55.0911767323862,
5.29660872329383));
#41444=CARTESIAN_POINT('Ctrl Pts',(-32.559388800421,-54.1701605706663,5.40774661386186));
#41445=CARTESIAN_POINT('Ctrl Pts',(-34.314593187089,-55.1909683005502,5.51888450442991));
#41446=CARTESIAN_POINT('Ctrl Pts',(-34.4088795978388,-57.2192447734761,
5.63002239499795));
#41447=CARTESIAN_POINT('Ctrl Pts',(-32.7559473680293,-58.3984820605017,
5.74116028556599));
#41448=CARTESIAN_POINT('Ctrl Pts',(-30.8687426071208,-57.6493178103144,
5.85229817613403));
#41449=CARTESIAN_POINT('Ctrl Pts',(-30.474648233639,-55.6574567972966,5.96343606670207));
#41450=CARTESIAN_POINT('Ctrl Pts',(-31.9343773268536,-54.2460993922691,
6.07457395727011));
#41451=CARTESIAN_POINT('Ctrl Pts',(-33.9118351799479,-54.7070224870209,
6.18571184783815));
#41452=CARTESIAN_POINT('Ctrl Pts',(-34.5970085274374,-56.618446550136,6.29684973840619));
#41453=CARTESIAN_POINT('Ctrl Pts',(-33.3627975548144,-58.2306072247468,
6.40798762897424));
#41454=CARTESIAN_POINT('Ctrl Pts',(-31.3387957446438,-58.0683060978855,
6.51912551954228));
#41455=CARTESIAN_POINT('Ctrl Pts',(-30.3777816842967,-56.2792419458429,
6.63026341011032));
#41456=CARTESIAN_POINT('Ctrl Pts',(-31.3590107734043,-54.5026733374681,
6.74140130067836));
#41457=CARTESIAN_POINT('Ctrl Pts',(-33.3850901676996,-54.3613007036025,
6.8525391912464));
#41458=CARTESIAN_POINT('Ctrl Pts',(-34.6000882679937,-55.9914719939308,
6.96367708181445));
#41459=CARTESIAN_POINT('Ctrl Pts',(-34.129416755538,-57.2537417389318,7.03776900885981));
#41460=CARTESIAN_POINT('Ctrl Pts',(-33.6791209333089,-57.6458275017164,
7.07481497238249));
#41461=CARTESIAN_POINT('Ctrl Pts',(-34.1088760084069,-55.8591307382982,
-2.22444491714747));
#41462=CARTESIAN_POINT('Ctrl Pts',(-34.2526993673069,-56.3941202878534,
-2.18739895362479));
#41463=CARTESIAN_POINT('Ctrl Pts',(-33.9618320787925,-57.6097503485045,
-2.11330702657943));
#41464=CARTESIAN_POINT('Ctrl Pts',(-32.1824817020393,-58.2362348948284,
-2.00216913601138));
#41465=CARTESIAN_POINT('Ctrl Pts',(-30.6954474136293,-57.0787313369718,
-1.89103124544334));
#41466=CARTESIAN_POINT('Ctrl Pts',(-30.8593399631111,-55.2028105166065,
-1.7798933548753));
#41467=CARTESIAN_POINT('Ctrl Pts',(-32.5253453473206,-54.3225142565131,
-1.66875546430726));
#41468=CARTESIAN_POINT('Ctrl Pts',(-34.1679522138747,-55.2450952283264,
-1.55761757373922));
#41469=CARTESIAN_POINT('Ctrl Pts',(-34.28396374532,-57.1253477734617,-1.44647968317117));
#41470=CARTESIAN_POINT('Ctrl Pts',(-32.7670426841572,-58.2426355096843,
-1.33534179260313));
#41471=CARTESIAN_POINT('Ctrl Pts',(-31.0057197114997,-57.5741013987637,
-1.22420390203509));
#41472=CARTESIAN_POINT('Ctrl Pts',(-30.6121157333415,-55.7317581752959,
-1.11306601146705));
#41473=CARTESIAN_POINT('Ctrl Pts',(-31.946520013063,-54.4018753286905,-1.00192812089901));
#41474=CARTESIAN_POINT('Ctrl Pts',(-33.7875275980737,-54.8017338971639,
-0.890790230330965));
#41475=CARTESIAN_POINT('Ctrl Pts',(-34.4500481800523,-56.5653266503777,
-0.779652339762924));
#41476=CARTESIAN_POINT('Ctrl Pts',(-33.3276667396325,-58.0784232421408,
-0.668514449194882));
#41477=CARTESIAN_POINT('Ctrl Pts',(-31.4477129519419,-57.9560661379181,
-0.557376558626841));
#41478=CARTESIAN_POINT('Ctrl Pts',(-30.5309292292241,-56.3102517219397,
-0.446238668058798));
#41479=CARTESIAN_POINT('Ctrl Pts',(-31.416458416169,-54.6474118209318,-0.335100777490757));
#41480=CARTESIAN_POINT('Ctrl Pts',(-33.293765451566,-54.4895630424278,-0.223962886922715));
#41481=CARTESIAN_POINT('Ctrl Pts',(-34.444529993061,-55.9811859685177,-0.112824996354673));
#41482=CARTESIAN_POINT('Ctrl Pts',(-33.8154441664647,-57.7569813167368,
-0.00168710578663119));
#41483=CARTESIAN_POINT('Ctrl Pts',(-31.9823173826674,-58.1915434167808,
0.10945078478141));
#41484=CARTESIAN_POINT('Ctrl Pts',(-30.6230313661624,-56.887112674916,0.220588675349452));
#41485=CARTESIAN_POINT('Ctrl Pts',(-30.9817560281246,-55.0376493300133,
0.331726565917494));
#41486=CARTESIAN_POINT('Ctrl Pts',(-32.7301466147767,-54.3359881622352,
0.442864456485535));
#41487=CARTESIAN_POINT('Ctrl Pts',(-34.2678813952981,-55.424367592698,0.554002347053577));
#41488=CARTESIAN_POINT('Ctrl Pts',(-34.1874542853563,-57.3065815872086,
0.66514023762162));
#41489=CARTESIAN_POINT('Ctrl Pts',(-32.5624811310993,-58.2598183300436,
0.776278128189661));
#41490=CARTESIAN_POINT('Ctrl Pts',(-30.8803182889104,-57.4115694204427,
0.887416018757703));
#41491=CARTESIAN_POINT('Ctrl Pts',(-30.6806684853481,-55.5382467049613,
0.998553909325745));
#41492=CARTESIAN_POINT('Ctrl Pts',(-32.1462734497562,-54.3545237101042,
1.10969179989379));
#41493=CARTESIAN_POINT('Ctrl Pts',(-33.935648337141,-54.9438755173456,1.22082969046183));
#41494=CARTESIAN_POINT('Ctrl Pts',(-34.4109580201779,-56.7668617338386,
1.33196758102987));
#41495=CARTESIAN_POINT('Ctrl Pts',(-33.1371461556097,-58.1548824015447,
1.44310547159791));
#41496=CARTESIAN_POINT('Ctrl Pts',(-31.2801471890823,-57.8374664620939,
1.55424336216595));
#41497=CARTESIAN_POINT('Ctrl Pts',(-30.5396933344601,-56.1051483246038,
1.66538125273399));
#41498=CARTESIAN_POINT('Ctrl Pts',(-31.593530402196,-54.5435384261447,1.77651914330204));
#41499=CARTESIAN_POINT('Ctrl Pts',(-33.4770693728664,-54.5819960166361,
1.88765703387008));
#41500=CARTESIAN_POINT('Ctrl Pts',(-34.4662856658319,-56.1853204273629,
1.99879492443812));
#41501=CARTESIAN_POINT('Ctrl Pts',(-33.6557383896654,-57.8859706422512,
2.10993281500616));
#41502=CARTESIAN_POINT('Ctrl Pts',(-31.7873306584733,-58.1273222329285,
2.2210707055742));
#41503=CARTESIAN_POINT('Ctrl Pts',(-30.5712372578007,-56.6884633513348,
2.33220859614225));
#41504=CARTESIAN_POINT('Ctrl Pts',(-31.1205622687204,-54.8863978495622,
2.44334648671028));
#41505=CARTESIAN_POINT('Ctrl Pts',(-32.9325022789682,-54.3705767181961,
2.55448437727833));
#41506=CARTESIAN_POINT('Ctrl Pts',(-34.3485680483669,-55.6131368885852,
2.66562226784637));
#41507=CARTESIAN_POINT('Ctrl Pts',(-34.072618518908,-57.4767489451818,2.77676015841441));
#41508=CARTESIAN_POINT('Ctrl Pts',(-32.3572334243856,-58.2556276377847,
2.88789804898246));
#41509=CARTESIAN_POINT('Ctrl Pts',(-30.7725241956062,-57.2368564659694,
2.99903593955049));
#41510=CARTESIAN_POINT('Ctrl Pts',(-30.7689931614965,-55.3529282369495,
3.11017383011854));
#41511=CARTESIAN_POINT('Ctrl Pts',(-32.3498723176219,-54.3282238239455,
3.22131172068658));
#41512=CARTESIAN_POINT('Ctrl Pts',(-34.0681650439915,-55.1006667971199,
3.33244961125462));
#41513=CARTESIAN_POINT('Ctrl Pts',(-34.351098521395,-56.9632313430239,3.44358750182266));
#41514=CARTESIAN_POINT('Ctrl Pts',(-32.9397005292796,-58.2110910098794,
3.5547253923907));
#41515=CARTESIAN_POINT('Ctrl Pts',(-31.1258396561734,-57.7020656929093,
3.66586328295875));
#41516=CARTESIAN_POINT('Ctrl Pts',(-30.569763329806,-55.9020720375025,3.77700117352679));
#41517=CARTESIAN_POINT('Ctrl Pts',(-31.7804545180476,-54.4586646497165,
3.88813906409483));
#41518=CARTESIAN_POINT('Ctrl Pts',(-33.6497538461057,-54.69301068105,3.99927695466287));
#41519=CARTESIAN_POINT('Ctrl Pts',(-34.4666704397583,-56.3906105511496,
4.11041484523092));
#41520=CARTESIAN_POINT('Ctrl Pts',(-33.4834712762798,-57.9976318472376,
4.22155273579895));
#41521=CARTESIAN_POINT('Ctrl Pts',(-31.6000897004201,-58.0431497513143,
4.332690626367));
#41522=CARTESIAN_POINT('Ctrl Pts',(-30.540406227203,-56.4855012112218,4.44382851693504));
#41523=CARTESIAN_POINT('Ctrl Pts',(-31.2743611580092,-54.7504195973536,
4.55496640750308));
#41524=CARTESIAN_POINT('Ctrl Pts',(-33.1301572196292,-54.4260447945964,
4.66610429807112));
#41525=CARTESIAN_POINT('Ctrl Pts',(-34.4091632335455,-55.8092807255337,
4.77724218863916));
#41526=CARTESIAN_POINT('Ctrl Pts',(-33.9406904846474,-57.6340358815812,
4.88838007920721));
#41527=CARTESIAN_POINT('Ctrl Pts',(-32.1535374041094,-58.2300911225802,
4.99951796977525));
#41528=CARTESIAN_POINT('Ctrl Pts',(-30.6835054518121,-57.051870429649,5.11065586034329));
#41529=CARTESIAN_POINT('Ctrl Pts',(-30.8761315896487,-55.1778123600212,
5.22179375091132));
#41530=CARTESIAN_POINT('Ctrl Pts',(-32.5551028402105,-54.3232639261277,
5.33293164147938));
#41531=CARTESIAN_POINT('Ctrl Pts',(-34.1836379540671,-55.2704021883376,
5.44406953204741));
#41532=CARTESIAN_POINT('Ctrl Pts',(-34.2711199201742,-57.1523023715063,
5.55520742261546));
#41533=CARTESIAN_POINT('Ctrl Pts',(-32.7374762046522,-58.2464366752245,
5.6663453131835));
#41534=CARTESIAN_POINT('Ctrl Pts',(-30.9864668956958,-57.5513379751853,
5.77748320375154));
#41535=CARTESIAN_POINT('Ctrl Pts',(-30.6208134537018,-55.7032252275985,
5.88862109431958));
#41536=CARTESIAN_POINT('Ctrl Pts',(-31.9751970816568,-54.3937224085839,
5.99975898488763));
#41537=CARTESIAN_POINT('Ctrl Pts',(-33.809946113961,-54.8213816887749,6.11089687545566));
#41538=CARTESIAN_POINT('Ctrl Pts',(-34.4456719951979,-56.5948624457155,
6.22203476602371));
#41539=CARTESIAN_POINT('Ctrl Pts',(-33.3005313368845,-58.0906770002622,
6.33317265659175));
#41540=CARTESIAN_POINT('Ctrl Pts',(-31.4225973233824,-57.940088791778,6.44431054715979));
#41541=CARTESIAN_POINT('Ctrl Pts',(-30.5309375519776,-56.2801374979719,
6.55544843772783));
#41542=CARTESIAN_POINT('Ctrl Pts',(-31.4413534776024,-54.631779971698,6.66658632829587));
#41543=CARTESIAN_POINT('Ctrl Pts',(-33.3212151405137,-54.5006098925109,
6.77772421886392));
#41544=CARTESIAN_POINT('Ctrl Pts',(-34.4485294775946,-56.0131352759167,
6.88886210943196));
#41545=CARTESIAN_POINT('Ctrl Pts',(-34.0118253017458,-57.1843097661965,
6.96295403647732));
#41546=CARTESIAN_POINT('Ctrl Pts',(-33.5940263469955,-57.5480995545471,
7.));
#41547=CARTESIAN_POINT('Ctrl Pts',(-33.3311039683456,-57.7330494773494,
-1.37851963660979));
#41548=CARTESIAN_POINT('Ctrl Pts',(-33.1447009981387,-57.8419592717116,
-1.3641270219409));
#41549=CARTESIAN_POINT('Ctrl Pts',(-32.9385791362006,-57.9159412173671,
-1.34973440727202));
#41550=CARTESIAN_POINT('Ctrl Pts',(-32.7263090322414,-57.9449985351604,
-1.33534179260313));
#41551=CARTESIAN_POINT('Ctrl Pts',(-32.1799350266047,-58.0197908060441,
-1.29829582908045));
#41552=CARTESIAN_POINT('Ctrl Pts',(-31.5928273690522,-57.7969461024039,
-1.26124986555777));
#41553=CARTESIAN_POINT('Ctrl Pts',(-31.2336728772496,-57.3784665466725,
-1.22420390203509));
#41554=CARTESIAN_POINT('Ctrl Pts',(-30.874518385447,-56.9599869909411,-1.18715793851241));
#41555=CARTESIAN_POINT('Ctrl Pts',(-30.7433170593942,-56.3458725831185,
-1.15011197498972));
#41556=CARTESIAN_POINT('Ctrl Pts',(-30.9001171096548,-55.8171682381063,
-1.11306601146704));
#41557=CARTESIAN_POINT('Ctrl Pts',(-31.0569171599153,-55.2884638930941,
-1.07602004794436));
#41558=CARTESIAN_POINT('Ctrl Pts',(-31.5017185864892,-54.8451696108923,
-1.03897408442168));
#41559=CARTESIAN_POINT('Ctrl Pts',(-32.0309538972779,-54.690165564537,-1.001928120899));
#41560=CARTESIAN_POINT('Ctrl Pts',(-32.5601892080666,-54.5351615181817,
-0.964882157376321));
#41561=CARTESIAN_POINT('Ctrl Pts',(-33.1738584030701,-54.6684477076728,
-0.92783619385364));
#41562=CARTESIAN_POINT('Ctrl Pts',(-33.5911130975683,-55.029022927954,-0.89079023033096));
#41563=CARTESIAN_POINT('Ctrl Pts',(-34.0083677920666,-55.3895981482352,
-0.85374426680828));
#41564=CARTESIAN_POINT('Ctrl Pts',(-34.2292079860594,-55.9774623993065,
-0.816698303285599));
#41565=CARTESIAN_POINT('Ctrl Pts',(-34.1525645096526,-56.5235772901359,
-0.779652339762918));
#41566=CARTESIAN_POINT('Ctrl Pts',(-34.0828208613931,-57.0205281937339,
-0.745941438711876));
#41567=CARTESIAN_POINT('Ctrl Pts',(-33.7667445152314,-57.4829083508763,
-0.712230537660833));
#41568=CARTESIAN_POINT('Ctrl Pts',(-33.333352483612,-57.7367881187288,-0.678519636609791));
#41569=CARTESIAN_POINT('Ctrl Pts',(-34.4842965055667,-55.7582049595679,
-2.));
#41570=CARTESIAN_POINT('Ctrl Pts',(-34.4966111053925,-55.8303827605032,
-2.));
#41571=CARTESIAN_POINT('Ctrl Pts',(-34.5047055015069,-55.9030302259436,
-2.));
#41572=CARTESIAN_POINT('Ctrl Pts',(-34.5087398487957,-55.9758367243127,
-2.));
#41573=CARTESIAN_POINT('Ctrl Pts',(-34.5128864619035,-56.0506692458712,
-2.));
#41574=CARTESIAN_POINT('Ctrl Pts',(-34.5127437096053,-56.1256707869288,
-2.));
#41575=CARTESIAN_POINT('Ctrl Pts',(-34.5084312212538,-56.2004993443971,
-2.));
#41576=CARTESIAN_POINT('Ctrl Pts',(-34.5047872656981,-56.2637277905937,
-2.));
#41577=CARTESIAN_POINT('Ctrl Pts',(-34.4981650958835,-56.3268329649123,
-2.));
#41578=CARTESIAN_POINT('Ctrl Pts',(-34.4886099106142,-56.3895978470298,
-2.));
#41579=CARTESIAN_POINT('Ctrl Pts',(-34.4843647905612,-56.4174826501178,
-2.));
#41580=CARTESIAN_POINT('Ctrl Pts',(-34.4795404472607,-56.4453001134184,
-2.));
#41581=CARTESIAN_POINT('Ctrl Pts',(-34.4741394411489,-56.4730302233706,
-2.));
#41582=CARTESIAN_POINT('Ctrl Pts',(-34.4711718179615,-56.4882667396012,
-2.));
#41583=CARTESIAN_POINT('Ctrl Pts',(-34.4680300836906,-56.5034768715492,
-2.));
#41584=CARTESIAN_POINT('Ctrl Pts',(-34.4647145599135,-56.5186572039182,
-2.));
#41585=CARTESIAN_POINT('Ctrl Pts',(-34.4616570554945,-56.5326561785661,
-2.));
#41586=CARTESIAN_POINT('Ctrl Pts',(-34.4584511621501,-56.5466318131544,
-2.));
#41587=CARTESIAN_POINT('Ctrl Pts',(-34.455102574428,-56.5605599363278,-2.));
#41588=CARTESIAN_POINT('Ctrl Pts',(-34.4379902743587,-56.6317368750642,
-2.));
#41589=CARTESIAN_POINT('Ctrl Pts',(-34.4171297712858,-56.7017985031099,
-2.));
#41590=CARTESIAN_POINT('Ctrl Pts',(-34.3926364221818,-56.7704257260604,
-2.));
#41591=CARTESIAN_POINT('Ctrl Pts',(-34.3683331729296,-56.8385203136065,
-2.));
#41592=CARTESIAN_POINT('Ctrl Pts',(-34.3404527390919,-56.9052035572272,
-2.));
#41593=CARTESIAN_POINT('Ctrl Pts',(-34.3090644243598,-56.9701370641959,
-2.));
#41594=CARTESIAN_POINT('Ctrl Pts',(-34.2829778948812,-57.0241026835084,
-2.));
#41595=CARTESIAN_POINT('Ctrl Pts',(-34.2544675459326,-57.0768595084288,
-2.));
#41596=CARTESIAN_POINT('Ctrl Pts',(-34.2235537441983,-57.1281926115905,
-2.));
#41597=CARTESIAN_POINT('Ctrl Pts',(-34.2106502677957,-57.1496191411066,
-2.));
#41598=CARTESIAN_POINT('Ctrl Pts',(-34.1973278568808,-57.1707973646492,
-2.));
#41599=CARTESIAN_POINT('Ctrl Pts',(-34.1835872002804,-57.1917104459739,
-2.));
#41600=CARTESIAN_POINT('Ctrl Pts',(-34.1772270825361,-57.201390453523,-2.));
#41601=CARTESIAN_POINT('Ctrl Pts',(-34.1707773506251,-57.2110136443072,
-2.));
#41602=CARTESIAN_POINT('Ctrl Pts',(-34.1642380419192,-57.2205782911529,
-2.));
#41603=CARTESIAN_POINT('Ctrl Pts',(-34.157417623102,-57.2305541005635,-2.));
#41604=CARTESIAN_POINT('Ctrl Pts',(-34.1505044191199,-57.2404593595929,
-2.));
#41605=CARTESIAN_POINT('Ctrl Pts',(-34.1435014736481,-57.2502888014669,
-2.));
#41606=CARTESIAN_POINT('Ctrl Pts',(-34.1036166314025,-57.306271778928,-2.));
#41607=CARTESIAN_POINT('Ctrl Pts',(-34.060796839317,-57.3598374440704,-2.));
#41608=CARTESIAN_POINT('Ctrl Pts',(-34.0151074156417,-57.4106900609363,
-2.));
#41609=CARTESIAN_POINT('Ctrl Pts',(-33.9736959571746,-57.4567812755301,
-2.));
#41610=CARTESIAN_POINT('Ctrl Pts',(-33.9299264067076,-57.5006437323222,
-2.));
#41611=CARTESIAN_POINT('Ctrl Pts',(-33.8838248402233,-57.5420278185054,
-2.));
#41612=CARTESIAN_POINT('Ctrl Pts',(-33.8292843968241,-57.5909872483519,
-2.));
#41613=CARTESIAN_POINT('Ctrl Pts',(-33.7714790326439,-57.6364792135475,
-2.));
#41614=CARTESIAN_POINT('Ctrl Pts',(-33.7108128089775,-57.6783572197639,
-2.));
#41615=CARTESIAN_POINT('Ctrl Pts',(-33.6974562676305,-57.6875772649185,
-2.));
#41616=CARTESIAN_POINT('Ctrl Pts',(-33.6839610126009,-57.6966218980591,
-2.));
#41617=CARTESIAN_POINT('Ctrl Pts',(-33.6703313137196,-57.7054891532988,
-2.));
#41618=CARTESIAN_POINT('Ctrl Pts',(-33.6562679227736,-57.7146385613776,
-2.));
#41619=CARTESIAN_POINT('Ctrl Pts',(-33.6420560771609,-57.7236022055286,
-2.));
#41620=CARTESIAN_POINT('Ctrl Pts',(-33.6277297174331,-57.7323603945599,
-2.));
#41621=CARTESIAN_POINT('Ctrl Pts',(-33.569215230036,-57.7681322829829,-2.));
#41622=CARTESIAN_POINT('Ctrl Pts',(-33.5087208994633,-57.8005303979709,
-2.));
#41623=CARTESIAN_POINT('Ctrl Pts',(-33.4466000497741,-57.8294900318504,
-2.));
#41624=CARTESIAN_POINT('Ctrl Pts',(-33.3844917460994,-57.8584438170014,
-2.));
#41625=CARTESIAN_POINT('Ctrl Pts',(-33.3207564252812,-57.8839606526953,
-2.));
#41626=CARTESIAN_POINT('Ctrl Pts',(-33.2557354106634,-57.9059253945374,
-2.));
#41627=CARTESIAN_POINT('Ctrl Pts',(-33.208672827818,-57.921823600505,-2.));
#41628=CARTESIAN_POINT('Ctrl Pts',(-33.1609363812249,-57.9358598412448,
-2.));
#41629=CARTESIAN_POINT('Ctrl Pts',(-33.1126567567386,-57.9479733084138,
-2.));
#41630=CARTESIAN_POINT('Ctrl Pts',(-33.0764412555869,-57.9570598597049,
-2.));
#41631=CARTESIAN_POINT('Ctrl Pts',(-33.0399201288692,-57.9650642116716,
-2.));
#41632=CARTESIAN_POINT('Ctrl Pts',(-33.0031501969155,-57.971955216011,-2.));
#41633=CARTESIAN_POINT('Ctrl Pts',(-32.9909318988865,-57.9742450310926,
-2.));
#41634=CARTESIAN_POINT('Ctrl Pts',(-32.9786957156912,-57.9764100788847,
-2.));
#41635=CARTESIAN_POINT('Ctrl Pts',(-32.9664441134404,-57.978449652198,-2.));
#41636=CARTESIAN_POINT('Ctrl Pts',(-32.9014564692778,-57.9892684056978,
-2.));
#41637=CARTESIAN_POINT('Ctrl Pts',(-32.8360307197657,-57.9965613002934,
-2.));
#41638=CARTESIAN_POINT('Ctrl Pts',(-32.7704812212859,-58.0002046036746,
-2.));
#41639=CARTESIAN_POINT('Ctrl Pts',(-32.7243572374865,-58.0027682185004,
-2.));
#41640=CARTESIAN_POINT('Ctrl Pts',(-32.6781720129221,-58.0035238244839,
-2.));
#41641=CARTESIAN_POINT('Ctrl Pts',(-32.6320397021299,-58.0024136109099,
-2.));
#41642=CARTESIAN_POINT('Ctrl Pts',(-32.617232011996,-58.0020572511633,-2.));
#41643=CARTESIAN_POINT('Ctrl Pts',(-32.602427781608,-58.0015084555319,-2.));
#41644=CARTESIAN_POINT('Ctrl Pts',(-32.5876374051278,-58.0007653782452,
-2.));
#41645=CARTESIAN_POINT('Ctrl Pts',(-32.5246283833583,-57.9975997676203,
-2.));
#41646=CARTESIAN_POINT('Ctrl Pts',(-32.4619962285786,-57.9909192311159,
-2.));
#41647=CARTESIAN_POINT('Ctrl Pts',(-32.400031070834,-57.9805958152526,-2.));
#41648=CARTESIAN_POINT('Ctrl Pts',(-32.3429040942487,-57.9710784419776,
-2.));
#41649=CARTESIAN_POINT('Ctrl Pts',(-32.286343647263,-57.9584643876265,-2.));
#41650=CARTESIAN_POINT('Ctrl Pts',(-32.2305948723589,-57.942618319326,-2.));
#41651=CARTESIAN_POINT('Ctrl Pts',(-32.2201618224275,-57.9396528223787,
-2.));
#41652=CARTESIAN_POINT('Ctrl Pts',(-32.2097572620708,-57.9365740341467,
-2.));
#41653=CARTESIAN_POINT('Ctrl Pts',(-32.1993825459687,-57.9333829869217,
-2.));
#41654=CARTESIAN_POINT('Origin',(-32.5,-56.2916512459885,3.));
#41655=CARTESIAN_POINT('Origin',(-65.,8.89946740503873E-15,7.));
#41656=CARTESIAN_POINT('Ctrl Pts',(-66.6351293272515,0.319230454628283,
7.));
#41657=CARTESIAN_POINT('Ctrl Pts',(-66.6302897730465,0.381554702501259,
7.));
#41658=CARTESIAN_POINT('Ctrl Pts',(-66.6216732730338,0.443394711745685,
7.));
#41659=CARTESIAN_POINT('Ctrl Pts',(-66.6095363361235,0.504531338378675,
7.));
#41660=CARTESIAN_POINT('Ctrl Pts',(-66.6018369189666,0.543315126700851,
7.));
#41661=CARTESIAN_POINT('Ctrl Pts',(-66.5927196857307,0.581816142993964,
7.));
#41662=CARTESIAN_POINT('Ctrl Pts',(-66.5822397317333,0.619979888911372,
7.));
#41663=CARTESIAN_POINT('Ctrl Pts',(-66.5750556337901,0.646141462580533,
7.));
#41664=CARTESIAN_POINT('Ctrl Pts',(-66.5672309975512,0.672144565072526,
7.));
#41665=CARTESIAN_POINT('Ctrl Pts',(-66.5587815171007,0.697971622792422,
7.));
#41666=CARTESIAN_POINT('Ctrl Pts',(-66.5543304403759,0.711576981862657,
7.));
#41667=CARTESIAN_POINT('Ctrl Pts',(-66.5497059363263,0.725133119483741,
7.));
#41668=CARTESIAN_POINT('Ctrl Pts',(-66.5449151802375,0.738624322294838,
7.));
#41669=CARTESIAN_POINT('Ctrl Pts',(-66.5228385613039,0.800794079613728,
7.));
#41670=CARTESIAN_POINT('Ctrl Pts',(-66.4972129904487,0.861656595066855,
7.));
#41671=CARTESIAN_POINT('Ctrl Pts',(-66.4682928028772,0.92096726482602,7.));
#41672=CARTESIAN_POINT('Ctrl Pts',(-66.4474370013299,0.963739171303899,
7.));
#41673=CARTESIAN_POINT('Ctrl Pts',(-66.4248666019437,1.00570421605069,7.));
#41674=CARTESIAN_POINT('Ctrl Pts',(-66.4006603556943,1.04676903427261,7.));
#41675=CARTESIAN_POINT('Ctrl Pts',(-66.3939846935385,1.05809399767726,7.));
#41676=CARTESIAN_POINT('Ctrl Pts',(-66.3871845384137,1.06935047516562,7.));
#41677=CARTESIAN_POINT('Ctrl Pts',(-66.3802613700562,1.08053645880643,7.));
#41678=CARTESIAN_POINT('Ctrl Pts',(-66.3732910155434,1.09179868262147,7.));
#41679=CARTESIAN_POINT('Ctrl Pts',(-66.3662003390708,1.10298231941115,7.));
#41680=CARTESIAN_POINT('Ctrl Pts',(-66.3589938160321,1.11408178978621,7.));
#41681=CARTESIAN_POINT('Ctrl Pts',(-66.3220437714873,1.17099216425959,7.));
#41682=CARTESIAN_POINT('Ctrl Pts',(-66.282032873356,1.22572189959788,7.));
#41683=CARTESIAN_POINT('Ctrl Pts',(-66.2392195751637,1.27802354476839,7.));
#41684=CARTESIAN_POINT('Ctrl Pts',(-66.1957886597093,1.3310796844594,7.));
#41685=CARTESIAN_POINT('Ctrl Pts',(-66.1494735383167,1.38163817192085,7.));
#41686=CARTESIAN_POINT('Ctrl Pts',(-66.1004928622018,1.42942737710376,7.));
#41687=CARTESIAN_POINT('Ctrl Pts',(-66.0701495067946,1.45903262048774,7.));
#41688=CARTESIAN_POINT('Ctrl Pts',(-66.0387821881987,1.48757476215782,7.));
#41689=CARTESIAN_POINT('Ctrl Pts',(-66.0064342584863,1.5149840981904,7.));
#41690=CARTESIAN_POINT('Ctrl Pts',(-65.9799267072476,1.53744471269536,7.));
#41691=CARTESIAN_POINT('Ctrl Pts',(-65.9527605445103,1.55914459484554,7.));
#41692=CARTESIAN_POINT('Ctrl Pts',(-65.9249567185444,1.58004263011316,7.));
#41693=CARTESIAN_POINT('Ctrl Pts',(-65.9136073279895,1.58857310949302,7.));
#41694=CARTESIAN_POINT('Ctrl Pts',(-65.9021495270296,1.59697131003777,7.));
#41695=CARTESIAN_POINT('Ctrl Pts',(-65.8906044505102,1.60522061990068,7.));
#41696=CARTESIAN_POINT('Ctrl Pts',(-65.8332561981007,1.64619769817525,7.));
#41697=CARTESIAN_POINT('Ctrl Pts',(-65.7736595595608,1.68357914695984,7.));
#41698=CARTESIAN_POINT('Ctrl Pts',(-65.7120551180979,1.71709301893351,7.));
#41699=CARTESIAN_POINT('Ctrl Pts',(-65.705214574854,1.72081439169597,7.));
#41700=CARTESIAN_POINT('Ctrl Pts',(-65.6983492298774,1.72448805151161,7.));
#41701=CARTESIAN_POINT('Ctrl Pts',(-65.6914593790744,1.72811360467695,7.));
#41702=CARTESIAN_POINT('Ctrl Pts',(-65.6317930119903,1.75951103144772,7.));
#41703=CARTESIAN_POINT('Ctrl Pts',(-65.5702916682012,1.78730397727325,7.));
#41704=CARTESIAN_POINT('Ctrl Pts',(-65.5072864773022,1.81157490046172,7.));
#41705=CARTESIAN_POINT('Ctrl Pts',(-65.4395015551833,1.8376870765318,7.));
#41706=CARTESIAN_POINT('Ctrl Pts',(-65.3699753257167,1.85972336261184,7.));
#41707=CARTESIAN_POINT('Ctrl Pts',(-65.2990847711306,1.87773280074162,7.));
#41708=CARTESIAN_POINT('Ctrl Pts',(-65.2861211425289,1.88102615439927,7.));
#41709=CARTESIAN_POINT('Ctrl Pts',(-65.273111817844,1.88418469347464,7.));
#41710=CARTESIAN_POINT('Ctrl Pts',(-65.2600590169346,1.88720850991533,7.));
#41711=CARTESIAN_POINT('Ctrl Pts',(-65.2488130849145,1.88981374647487,7.));
#41712=CARTESIAN_POINT('Ctrl Pts',(-65.2375439537466,1.89231686461784,7.));
#41713=CARTESIAN_POINT('Ctrl Pts',(-65.2262547951615,1.89471805492211,7.));
#41714=CARTESIAN_POINT('Ctrl Pts',(-65.1567411013575,1.90950353307062,7.));
#41715=CARTESIAN_POINT('Ctrl Pts',(-65.0864519774285,1.92043226303262,7.));
#41716=CARTESIAN_POINT('Ctrl Pts',(-65.0157547334709,1.92760520158801,7.));
#41717=CARTESIAN_POINT('Ctrl Pts',(-64.943565800346,1.93492948684578,7.));
#41718=CARTESIAN_POINT('Ctrl Pts',(-64.8709504429878,1.93833807717024,7.));
#41719=CARTESIAN_POINT('Ctrl Pts',(-64.7982722132928,1.93789067648522,7.));
#41720=CARTESIAN_POINT('Ctrl Pts',(-64.7251526999809,1.93744055929771,7.));
#41721=CARTESIAN_POINT('Ctrl Pts',(-64.6519684871743,1.93308764503056,7.));
#41722=CARTESIAN_POINT('Ctrl Pts',(-64.5790772350549,1.92484184820749,7.));
#41723=CARTESIAN_POINT('Ctrl Pts',(-64.5610671587083,1.92280446476293,7.));
#41724=CARTESIAN_POINT('Ctrl Pts',(-64.5430749514564,1.9205291753851,7.));
#41725=CARTESIAN_POINT('Ctrl Pts',(-64.5251060094349,1.91801563698977,7.));
#41726=CARTESIAN_POINT('Ctrl Pts',(-64.5110402166547,1.91604808040399,7.));
#41727=CARTESIAN_POINT('Ctrl Pts',(-64.4969870784137,1.9139341585107,7.));
#41728=CARTESIAN_POINT('Ctrl Pts',(-64.4829704723558,1.9116773971743,7.));
#41729=CARTESIAN_POINT('Ctrl Pts',(-64.408583493524,1.89970062782901,7.));
#41730=CARTESIAN_POINT('Ctrl Pts',(-64.3350918229631,1.88368734539382,6.99999999999999));
#41731=CARTESIAN_POINT('Ctrl Pts',(-64.262879083689,1.86371221647072,7.));
#41732=CARTESIAN_POINT('Ctrl Pts',(-64.1905873442587,1.8437152349172,7.));
#41733=CARTESIAN_POINT('Ctrl Pts',(-64.1195762102382,1.81974781464992,6.99999999999999));
#41734=CARTESIAN_POINT('Ctrl Pts',(-64.0502233635423,1.79183341393623,7.));
#41735=CARTESIAN_POINT('Ctrl Pts',(-63.9824494700609,1.76455453915751,7.));
#41736=CARTESIAN_POINT('Ctrl Pts',(-63.916258181573,1.73350624794761,7.));
#41737=CARTESIAN_POINT('Ctrl Pts',(-63.8520110121349,1.69866187350007,7.));
#41738=CARTESIAN_POINT('Ctrl Pts',(-63.8381915579471,1.6911669092769,7.));
#41739=CARTESIAN_POINT('Ctrl Pts',(-63.8244621191575,1.68349613170073,7.));
#41740=CARTESIAN_POINT('Ctrl Pts',(-63.8108264207747,1.67564897964535,7.));
#41741=CARTESIAN_POINT('Ctrl Pts',(-63.7992831576295,1.66900599455043,7.));
#41742=CARTESIAN_POINT('Ctrl Pts',(-63.7878070738684,1.66223660984748,7.));
#41743=CARTESIAN_POINT('Ctrl Pts',(-63.7763989699203,1.65534250909263,7.));
#41744=CARTESIAN_POINT('Ctrl Pts',(-63.1173724903363,0.823232180103149,
7.));
#41745=CARTESIAN_POINT('Ctrl Pts',(-63.0939903977405,0.752339169258933,
7.));
#41746=CARTESIAN_POINT('Ctrl Pts',(-63.0748445296608,0.680224887836885,
7.));
#41747=CARTESIAN_POINT('Ctrl Pts',(-63.0598471165381,0.607239755688797,
7.));
#41748=CARTESIAN_POINT('Ctrl Pts',(-63.045242974325,0.536168482221851,7.));
#41749=CARTESIAN_POINT('Ctrl Pts',(-63.0345730321077,0.4642705233706,7.));
#41750=CARTESIAN_POINT('Ctrl Pts',(-63.0278019508403,0.391872562027519,
7.));
#41751=CARTESIAN_POINT('Ctrl Pts',(-63.0262906434537,0.375713315160443,
7.));
#41752=CARTESIAN_POINT('Ctrl Pts',(-63.0249735943537,0.359527040989821,
7.));
#41753=CARTESIAN_POINT('Ctrl Pts',(-63.0238511666264,0.34332437073834,7.));
#41754=CARTESIAN_POINT('Ctrl Pts',(-63.0187005423181,0.268973153977023,
7.));
#41755=CARTESIAN_POINT('Ctrl Pts',(-63.0176530289114,0.194423667889717,
7.));
#41756=CARTESIAN_POINT('Ctrl Pts',(-63.0206465481662,0.120030528064432,
7.));
#41757=CARTESIAN_POINT('Ctrl Pts',(-63.0227481861611,0.0678018848184103,
7.));
#41758=CARTESIAN_POINT('Ctrl Pts',(-63.0268427413746,0.0156503275540584,
7.));
#41759=CARTESIAN_POINT('Ctrl Pts',(-63.0329233152999,-0.036296614856767,
7.));
#41760=CARTESIAN_POINT('Ctrl Pts',(-63.0352354057117,-0.056049031149148,
7.));
#41761=CARTESIAN_POINT('Ctrl Pts',(-63.0378347617044,-0.0757718050677318,
7.));
#41762=CARTESIAN_POINT('Ctrl Pts',(-63.0407214327969,-0.0954576801195959,
7.));
#41763=CARTESIAN_POINT('Ctrl Pts',(-63.0434693778843,-0.114197502533115,
7.));
#41764=CARTESIAN_POINT('Ctrl Pts',(-63.0464788571282,-0.1329097260904,7.));
#41765=CARTESIAN_POINT('Ctrl Pts',(-63.0497439151797,-0.151555113564703,
7.));
#41766=CARTESIAN_POINT('Ctrl Pts',(-63.0622655750455,-0.223061101005544,
7.));
#41767=CARTESIAN_POINT('Ctrl Pts',(-63.0785510722461,-0.293661819118036,
6.99999999999999));
#41768=CARTESIAN_POINT('Ctrl Pts',(-63.0985450713842,-0.363028531313167,
7.));
#41769=CARTESIAN_POINT('Ctrl Pts',(-63.118109525179,-0.430904988957711,
7.));
#41770=CARTESIAN_POINT('Ctrl Pts',(-63.1412253035865,-0.497600711633542,
7.));
#41771=CARTESIAN_POINT('Ctrl Pts',(-63.1678836571873,-0.562784339590762,
7.));
#41772=CARTESIAN_POINT('Ctrl Pts',(-63.1939574718371,-0.626538683126413,
7.));
#41773=CARTESIAN_POINT('Ctrl Pts',(-63.2234205963263,-0.688847181210932,
7.));
#41774=CARTESIAN_POINT('Ctrl Pts',(-63.2563003837665,-0.749366435838956,
7.));
#41775=CARTESIAN_POINT('Ctrl Pts',(-63.2669864355877,-0.7690354161301,7.));
#41776=CARTESIAN_POINT('Ctrl Pts',(-63.2780336415132,-0.788515094659207,
7.));
#41777=CARTESIAN_POINT('Ctrl Pts',(-63.2894436727967,-0.80779272412078,
7.));
#41778=CARTESIAN_POINT('Ctrl Pts',(-63.2958782979571,-0.818664238535167,
7.));
#41779=CARTESIAN_POINT('Ctrl Pts',(-63.3024290949197,-0.829472548274647,
7.));
#41780=CARTESIAN_POINT('Ctrl Pts',(-63.3090867443711,-0.840200273664074,
7.));
#41781=CARTESIAN_POINT('Ctrl Pts',(-63.3451024516394,-0.898233761323215,
7.));
#41782=CARTESIAN_POINT('Ctrl Pts',(-63.3843017903685,-0.954015012532752,
7.));
#41783=CARTESIAN_POINT('Ctrl Pts',(-63.426670904758,-1.00724100895717,7.));
#41784=CARTESIAN_POINT('Ctrl Pts',(-63.4327868741032,-1.01492416606788,
7.));
#41785=CARTESIAN_POINT('Ctrl Pts',(-63.4389689569132,-1.02255401966981,
6.99999999999999));
#41786=CARTESIAN_POINT('Ctrl Pts',(-63.4452171764819,-1.03012959441513,
6.99999999999999));
#41787=CARTESIAN_POINT('Ctrl Pts',(-63.489358667261,-1.08364838630305,7.));
#41788=CARTESIAN_POINT('Ctrl Pts',(-63.5367987510362,-1.13446181351563,
7.));
#41789=CARTESIAN_POINT('Ctrl Pts',(-63.5871991852739,-1.18242370278709,
7.));
#41790=CARTESIAN_POINT('Ctrl Pts',(-63.6342187269495,-1.2271682786137,7.));
#41791=CARTESIAN_POINT('Ctrl Pts',(-63.6838158179714,-1.26943087719056,
7.));
#41792=CARTESIAN_POINT('Ctrl Pts',(-63.7357299598937,-1.30905529562496,
7.));
#41793=CARTESIAN_POINT('Ctrl Pts',(-63.7471862226625,-1.31779949774095,
7.));
#41794=CARTESIAN_POINT('Ctrl Pts',(-63.7587553477597,-1.326415076375,6.99999999999999));
#41795=CARTESIAN_POINT('Ctrl Pts',(-63.7704345647747,-1.33490009616143,
6.99999999999999));
#41796=CARTESIAN_POINT('Ctrl Pts',(-63.7795655910355,-1.34153384039215,
6.99999999999999));
#41797=CARTESIAN_POINT('Ctrl Pts',(-63.7887633889776,-1.3480873027534,7.));
#41798=CARTESIAN_POINT('Ctrl Pts',(-63.7980157939557,-1.35455228245181,
7.));
#41799=CARTESIAN_POINT('Ctrl Pts',(-63.8540658571293,-1.39371642640913,
7.));
#41800=CARTESIAN_POINT('Ctrl Pts',(-63.912219564704,-1.42971188598758,7.));
#41801=CARTESIAN_POINT('Ctrl Pts',(-63.9721458438494,-1.46241564585894,
7.));
#41802=CARTESIAN_POINT('Ctrl Pts',(-64.0317950323718,-1.49496818817889,
7.));
#41803=CARTESIAN_POINT('Ctrl Pts',(-64.0932015440209,-1.52425966112384,
7.));
#41804=CARTESIAN_POINT('Ctrl Pts',(-64.1560527983748,-1.55011955109708,
7.));
#41805=CARTESIAN_POINT('Ctrl Pts',(-64.2175568101543,-1.57542512365694,
7.));
#41806=CARTESIAN_POINT('Ctrl Pts',(-64.2804452599811,-1.59744473905974,
7.));
#41807=CARTESIAN_POINT('Ctrl Pts',(-64.344423329557,-1.61596906267658,7.));
#41808=CARTESIAN_POINT('Ctrl Pts',(-64.3578992522694,-1.6198709052144,7.));
#41809=CARTESIAN_POINT('Ctrl Pts',(-64.3714234817642,-1.62361749283973,
7.));
#41810=CARTESIAN_POINT('Ctrl Pts',(-64.3849931909711,-1.62720657518054,
7.));
#41811=CARTESIAN_POINT('Ctrl Pts',(-64.3978648608679,-1.63061103156344,
7.));
#41812=CARTESIAN_POINT('Ctrl Pts',(-64.4107792257301,-1.63387407363082,
6.99999999999999));
#41813=CARTESIAN_POINT('Ctrl Pts',(-64.4237128649824,-1.63698901055556,
6.99999999999999));
#41814=CARTESIAN_POINT('Ctrl Pts',(-64.487243192052,-1.65228965082931,6.99999999999999));
#41815=CARTESIAN_POINT('Ctrl Pts',(-64.5513507147979,-1.6640519139839,6.99999999999999));
#41816=CARTESIAN_POINT('Ctrl Pts',(-64.6157505860683,-1.67213050417994,
7.));
#41817=CARTESIAN_POINT('Ctrl Pts',(-64.6789248748248,-1.68005535216058,
7.));
#41818=CARTESIAN_POINT('Ctrl Pts',(-64.7423813719211,-1.68443544217815,
7.));
#41819=CARTESIAN_POINT('Ctrl Pts',(-64.8058448176641,-1.68508431664668,
7.));
#41820=CARTESIAN_POINT('Ctrl Pts',(-64.8672458810559,-1.68571210453165,
7.));
#41821=CARTESIAN_POINT('Ctrl Pts',(-64.9286541093687,-1.68284715374126,
7.));
#41822=CARTESIAN_POINT('Ctrl Pts',(-64.9898031298831,-1.67627454330083,
7.));
#41823=CARTESIAN_POINT('Ctrl Pts',(-64.9999907154541,-1.67517952933783,
7.));
#41824=CARTESIAN_POINT('Ctrl Pts',(-65.0101710541419,-1.67398149896703,
7.));
#41825=CARTESIAN_POINT('Ctrl Pts',(-65.0203428468639,-1.6726793313447,7.));
#41826=CARTESIAN_POINT('Ctrl Pts',(-65.0310998269282,-1.6713022494933,7.));
#41827=CARTESIAN_POINT('Ctrl Pts',(-65.0418472497685,-1.66980870242006,
7.));
#41828=CARTESIAN_POINT('Ctrl Pts',(-65.0525835864496,-1.66819940096573,
7.));
#41829=CARTESIAN_POINT('Origin',(-65.,8.88178419700125E-15,-3.54592528053767));
#41830=CARTESIAN_POINT('Ctrl Pts',(-67.0565599569794,-0.00149374744777858,
-1.79592528053768));
#41831=CARTESIAN_POINT('Ctrl Pts',(-67.0573792182402,-0.099782513364621,
-1.79058130531689));
#41832=CARTESIAN_POINT('Ctrl Pts',(-67.0062893847297,-0.878608585113931,
-1.74819136657341));
#41833=CARTESIAN_POINT('Ctrl Pts',(-66.0109392265833,-2.20843178543787,
-1.66875546430726));
#41834=CARTESIAN_POINT('Ctrl Pts',(-63.6930089313552,-2.04686416993215,
-1.55761757373922));
#41835=CARTESIAN_POINT('Ctrl Pts',(-62.5713939614548,-0.0121365548742068,
-1.44647968317118));
#41836=CARTESIAN_POINT('Ctrl Pts',(-63.67270376601,2.03388137208554,-1.33534179260313));
#41837=CARTESIAN_POINT('Ctrl Pts',(-65.9889058463299,2.21817250383823,-1.22420390203509));
#41838=CARTESIAN_POINT('Ctrl Pts',(-67.0021432190354,0.892617277286203,
-1.14439839801327));
#41839=CARTESIAN_POINT('Ctrl Pts',(-67.057275270459,0.106740644746507,-1.10163885751414));
#41840=CARTESIAN_POINT('Ctrl Pts',(-67.0563730581704,0.00160407492546514,
-1.09592528053768));
#41841=CARTESIAN_POINT('Ctrl Pts',(-67.052679279082,0.0023836951352375,
-1.85407471946232));
#41842=CARTESIAN_POINT('Ctrl Pts',(-67.0491241057456,-0.467845902355823,
-1.82862455259619));
#41843=CARTESIAN_POINT('Ctrl Pts',(-66.6565276815742,-1.62960580042266,
-1.76612842220737));
#41844=CARTESIAN_POINT('Ctrl Pts',(-64.7278715623352,-2.41277602144419,
-1.66658632829587));
#41845=CARTESIAN_POINT('Ctrl Pts',(-62.8252644286755,-1.08095990301172,
-1.55544843772783));
#41846=CARTESIAN_POINT('Ctrl Pts',(-62.9123886677794,1.24138962897178,-1.44431054715979));
#41847=CARTESIAN_POINT('Ctrl Pts',(-64.9107473342681,2.42691462884513,-1.33317265659175));
#41848=CARTESIAN_POINT('Ctrl Pts',(-66.7212428925551,1.52545313603056,-1.23642738069259));
#41849=CARTESIAN_POINT('Ctrl Pts',(-67.0499074437772,0.4179188137684,-1.17672806831612));
#41850=CARTESIAN_POINT('Ctrl Pts',(-67.0520762837074,-0.0011613687935888,
-1.15407471946233));
#41851=CARTESIAN_POINT('Ctrl Pts',(-63.7309291201476,-1.0793586530485,-2.));
#41852=CARTESIAN_POINT('Ctrl Pts',(-63.3720166889934,-0.657362393039501,
-1.96295403647732));
#41853=CARTESIAN_POINT('Ctrl Pts',(-63.1146663550338,0.565736448038662,
-1.88886210943196));
#41854=CARTESIAN_POINT('Ctrl Pts',(-64.4549392280646,1.89346495741706,-1.77772421886392));
#41855=CARTESIAN_POINT('Ctrl Pts',(-66.2941885938804,1.48351678997985,-1.66658632829587));
#41856=CARTESIAN_POINT('Ctrl Pts',(-66.9487863029052,-0.282071400691224,
-1.55544843772784));
#41857=CARTESIAN_POINT('Ctrl Pts',(-65.8196738053231,-1.79060584233581,
-1.44431054715979));
#41858=CARTESIAN_POINT('Ctrl Pts',(-63.9402861076227,-1.65960613559165,
-1.33317265659175));
#41859=CARTESIAN_POINT('Ctrl Pts',(-63.0308759410067,-0.0098403700792925,
-1.22203476602371));
#41860=CARTESIAN_POINT('Ctrl Pts',(-63.9238225935869,1.64907962812727,-1.11089687545567));
#41861=CARTESIAN_POINT('Ctrl Pts',(-65.8018090473224,1.79850365805791,-0.999758984887623));
#41862=CARTESIAN_POINT('Ctrl Pts',(-66.9458893611786,0.301774776475135,
-0.888621094319584));
#41863=CARTESIAN_POINT('Ctrl Pts',(-66.3088756966202,-1.47119119673886,
-0.777483203751541));
#41864=CARTESIAN_POINT('Ctrl Pts',(-64.4738329478959,-1.89754943555686,
-0.666345313183499));
#41865=CARTESIAN_POINT('Ctrl Pts',(-63.1203970290852,-0.587064100833463,
-0.555207422615458));
#41866=CARTESIAN_POINT('Ctrl Pts',(-63.4873829445486,1.26077017125902,-0.444069532047416));
#41867=CARTESIAN_POINT('Ctrl Pts',(-65.2388844462753,1.95460593523977,-0.332931641479374));
#41868=CARTESIAN_POINT('Ctrl Pts',(-66.7717322843115,0.859369365311616,
-0.221793750911332));
#41869=CARTESIAN_POINT('Ctrl Pts',(-66.6828934802986,-1.02245805795663,
-0.11065586034329));
#41870=CARTESIAN_POINT('Ctrl Pts',(-65.0536831830854,-1.96841785926,0.000482030224751804));
#41871=CARTESIAN_POINT('Ctrl Pts',(-63.3753360623109,-1.11266255483749,
0.111619920792793));
#41872=CARTESIAN_POINT('Ctrl Pts',(-63.1840622672629,0.761525447206216,
0.222757811360836));
#41873=CARTESIAN_POINT('Ctrl Pts',(-64.654936873825,1.93868054946277,0.333895701928877));
#41874=CARTESIAN_POINT('Ctrl Pts',(-66.4416516727014,1.34133936965716,0.445033592496918));
#41875=CARTESIAN_POINT('Ctrl Pts',(-66.9088063462926,-0.483744952595402,
0.55617148306496));
#41876=CARTESIAN_POINT('Ctrl Pts',(-65.6288089236944,-1.86605203086769,
0.667309373633002));
#41877=CARTESIAN_POINT('Ctrl Pts',(-63.7732555621069,-1.54034052425233,
0.778447264201044));
#41878=CARTESIAN_POINT('Ctrl Pts',(-63.0405552967276,0.195262133588727,
0.889585154769085));
#41879=CARTESIAN_POINT('Ctrl Pts',(-64.1013569898796,1.75213914576361,1.00072304533713));
#41880=CARTESIAN_POINT('Ctrl Pts',(-65.9846968214939,1.70526332739896,1.11186093590517));
#41881=CARTESIAN_POINT('Ctrl Pts',(-66.9667324851762,0.0975406463696029,
1.22299882647321));
#41882=CARTESIAN_POINT('Ctrl Pts',(-66.148595600912,-1.59946209441982,1.33413671704125));
#41883=CARTESIAN_POINT('Ctrl Pts',(-64.2791361371736,-1.83245904107736,
1.4452746076093));
#41884=CARTESIAN_POINT('Ctrl Pts',(-63.0694915422322,-0.388185445925422,
1.55641249817734));
#41885=CARTESIAN_POINT('Ctrl Pts',(-63.6268632321408,1.41139869019815,1.66755038874538));
#41886=CARTESIAN_POINT('Ctrl Pts',(-65.441082578101,1.91911359883674,1.77868827931342));
#41887=CARTESIAN_POINT('Ctrl Pts',(-66.8515740381086,0.670242066229977,
1.88982616988146));
#41888=CARTESIAN_POINT('Ctrl Pts',(-66.5672987827578,-1.19210963065827,
2.0009640604495));
#41889=CARTESIAN_POINT('Ctrl Pts',(-64.8484571771716,-1.96330986316269,
2.11210195101754));
#41890=CARTESIAN_POINT('Ctrl Pts',(-63.2683244359328,-0.937470312465873,
2.22323984158559));
#41891=CARTESIAN_POINT('Ctrl Pts',(-63.2732139770213,0.946446446867298,
2.33437773215363));
#41892=CARTESIAN_POINT('Ctrl Pts',(-64.8586503480276,1.96407003995017,2.44551562272167));
#41893=CARTESIAN_POINT('Ctrl Pts',(-66.5734656584984,1.18395805139743,2.55665351328971));
#41894=CARTESIAN_POINT('Ctrl Pts',(-66.8480700074313,-0.679844168596873,
2.66779140385775));
#41895=CARTESIAN_POINT('Ctrl Pts',(-65.4311149200231,-1.92137731111721,
2.7789292944258));
#41896=CARTESIAN_POINT('Ctrl Pts',(-63.6195554571419,-1.40425201087121,
2.89006718499384));
#41897=CARTESIAN_POINT('Ctrl Pts',(-63.0715325396448,0.398201080226113,
3.00120507556188));
#41898=CARTESIAN_POINT('Ctrl Pts',(-64.2886577589191,1.83617620668519,3.11234296612993));
#41899=CARTESIAN_POINT('Ctrl Pts',(-66.1568825986246,1.59347842751064,3.22348085669796));
#41900=CARTESIAN_POINT('Ctrl Pts',(-66.9661996758679,-0.107748227638456,
3.33461874726601));
#41901=CARTESIAN_POINT('Ctrl Pts',(-65.9758318915686,-1.71035170808284,
3.44575663783405));
#41902=CARTESIAN_POINT('Ctrl Pts',(-64.0922741102298,-1.74745087340982,
3.55689452840209));
#41903=CARTESIAN_POINT('Ctrl Pts',(-63.0395681301102,-0.185088436867097,
3.66803241897013));
#41904=CARTESIAN_POINT('Ctrl Pts',(-63.7812676733088,1.5466875449918,3.77917030953817));
#41905=CARTESIAN_POINT('Ctrl Pts',(-65.6384867364954,1.86276287627796,3.89030820010621));
#41906=CARTESIAN_POINT('Ctrl Pts',(-66.9112916488297,0.473830221762723,
4.00144609067426));
#41907=CARTESIAN_POINT('Ctrl Pts',(-66.4346696394808,-1.34880460837871,
4.11258398124229));
#41908=CARTESIAN_POINT('Ctrl Pts',(-64.6448782388305,-1.93686328389462,
4.22372187181034));
#41909=CARTESIAN_POINT('Ctrl Pts',(-63.1801338135814,-0.752089030319253,
4.33485976237838));
#41910=CARTESIAN_POINT('Ctrl Pts',(-63.3811335473526,1.12108084233402,4.44599765294643));
#41911=CARTESIAN_POINT('Ctrl Pts',(-65.0639001046135,1.96811270537377,4.55713554351446));
#41912=CARTESIAN_POINT('Ctrl Pts',(-66.6881781710758,1.01370869065611,4.66827343408251));
#41913=CARTESIAN_POINT('Ctrl Pts',(-66.767247613038,-0.868554387592529,
4.77941132465054));
#41914=CARTESIAN_POINT('Ctrl Pts',(-65.2287352713999,-1.95581977940925,
4.8905492152186));
#41915=CARTESIAN_POINT('Ctrl Pts',(-63.4808589446451,-1.25290115725712,
5.00168710578663));
#41916=CARTESIAN_POINT('Ctrl Pts',(-63.1234696485087,0.596812123952627,
5.11282499635468));
#41917=CARTESIAN_POINT('Ctrl Pts',(-64.483689875393,1.90025645848878,5.22396288692272));
#41918=CARTESIAN_POINT('Ctrl Pts',(-66.3164945930014,1.46437458763455,5.33510077749075));
#41919=CARTESIAN_POINT('Ctrl Pts',(-66.9442969223188,-0.311866110966441,
5.44623866805881));
#41920=CARTESIAN_POINT('Ctrl Pts',(-65.7924621445391,-1.80265190489435,
5.55737655862683));
#41921=CARTESIAN_POINT('Ctrl Pts',(-63.9152779448642,-1.64345059076356,
5.66851444919488));
#41922=CARTESIAN_POINT('Ctrl Pts',(-63.0309518163246,0.0200209171529774,
5.77965233976292));
#41923=CARTESIAN_POINT('Ctrl Pts',(-63.9489184664916,1.6651646276029,5.89079023033097));
#41924=CARTESIAN_POINT('Ctrl Pts',(-65.8289506914941,1.78616905068825,6.001928120899));
#41925=CARTESIAN_POINT('Ctrl Pts',(-66.9502374569467,0.272263260809152,
6.11306601146705));
#41926=CARTESIAN_POINT('Ctrl Pts',(-66.2864448139981,-1.49082960024053,
6.22420390203509));
#41927=CARTESIAN_POINT('Ctrl Pts',(-64.4451643957601,-1.88938584790037,
6.33534179260314));
#41928=CARTESIAN_POINT('Ctrl Pts',(-63.1117120727514,-0.558493595662741,
6.44647968317117));
#41929=CARTESIAN_POINT('Ctrl Pts',(-63.5066690059847,1.28345183053528,6.55761757373921));
#41930=CARTESIAN_POINT('Ctrl Pts',(-65.2684140085621,1.95091987271334,6.66875546430726));
#41931=CARTESIAN_POINT('Ctrl Pts',(-66.7846240008828,0.832135508767313,
6.77989335487529));
#41932=CARTESIAN_POINT('Ctrl Pts',(-66.6670561422041,-1.04722013035561,
6.89103124544334));
#41933=CARTESIAN_POINT('Ctrl Pts',(-65.0241955006465,-1.97020693527805,
7.00216913601138));
#41934=CARTESIAN_POINT('Ctrl Pts',(-63.3579443006206,-1.08544634211746,
7.11330702657943));
#41935=CARTESIAN_POINT('Ctrl Pts',(-63.2516046182892,0.1599017382992,7.18739895362479));
#41936=CARTESIAN_POINT('Ctrl Pts',(-63.4735576439471,0.667480137268208,
7.22444491714747));
#41937=CARTESIAN_POINT('Ctrl Pts',(-63.6322193753412,-1.16331236980973,
-2.07481497238249));
#41938=CARTESIAN_POINT('Ctrl Pts',(-63.2453903360215,-0.708492771249607,
-2.03776900885981));
#41939=CARTESIAN_POINT('Ctrl Pts',(-62.9680230067985,0.609740058317781,
-1.96367708181445));
#41940=CARTESIAN_POINT('Ctrl Pts',(-64.4125437948732,2.04074076818054,-1.85253919124641));
#41941=CARTESIAN_POINT('Ctrl Pts',(-66.3948520224261,1.59890637623529,-1.74140130067836));
#41942=CARTESIAN_POINT('Ctrl Pts',(-67.1003650694627,-0.304011228025904,
-1.63026341011032));
#41943=CARTESIAN_POINT('Ctrl Pts',(-65.8834289457431,-1.92988115670316,
-1.51912551954228));
#41944=CARTESIAN_POINT('Ctrl Pts',(-63.8578603822002,-1.78869214703848,
-1.40798762897424));
#41945=CARTESIAN_POINT('Ctrl Pts',(-62.8777152811561,-0.010605765010931,
-1.2968497384062));
#41946=CARTESIAN_POINT('Ctrl Pts',(-63.8401163177279,1.77734687611336,-1.18571184783815));
#41947=CARTESIAN_POINT('Ctrl Pts',(-65.8641746469915,1.93839327331802,-1.07457395727011));
#41948=CARTESIAN_POINT('Ctrl Pts',(-67.0972428003859,0.325247154297205,
-0.963436066702072));
#41949=CARTESIAN_POINT('Ctrl Pts',(-66.4106815043556,-1.58562208464047,
-0.852298176134029));
#41950=CARTESIAN_POINT('Ctrl Pts',(-64.4329070892513,-2.04514294157382,
-0.741160285565989));
#41951=CARTESIAN_POINT('Ctrl Pts',(-62.9741994190526,-0.632726599672803,
-0.630022394997946));
#41952=CARTESIAN_POINT('Ctrl Pts',(-63.3697299072724,1.358834277717,-0.518884504429905));
#41953=CARTESIAN_POINT('Ctrl Pts',(-65.2574651442524,2.10663735927427,-0.407746613861863));
#41954=CARTESIAN_POINT('Ctrl Pts',(-66.9095395923399,0.926212070546691,
-0.296608723293821));
#41955=CARTESIAN_POINT('Ctrl Pts',(-66.8137908073226,-1.10198598313283,
-0.185470832725779));
#41956=CARTESIAN_POINT('Ctrl Pts',(-65.0578587207854,-2.12152359010981,
-0.0743329421577371));
#41957=CARTESIAN_POINT('Ctrl Pts',(-63.2489678938882,-1.19920668612862,
0.036804948410304));
#41958=CARTESIAN_POINT('Ctrl Pts',(-63.0428166102798,0.820757743645075,
0.147942838978346));
#41959=CARTESIAN_POINT('Ctrl Pts',(-64.6280974800075,2.08947327927542,0.259080729546388));
#41960=CARTESIAN_POINT('Ctrl Pts',(-66.5537849435622,1.44567023799534,0.370218620114429));
#41961=CARTESIAN_POINT('Ctrl Pts',(-67.0572754273494,-0.521371173147915,
0.481356510682472));
#41962=CARTESIAN_POINT('Ctrl Pts',(-65.6777183812947,-2.01119563370879,
0.592494401250513));
#41963=CARTESIAN_POINT('Ctrl Pts',(-63.6778380150419,-1.66014992377275,
0.703632291818555));
#41964=CARTESIAN_POINT('Ctrl Pts',(-62.8881475079326,0.210449839557635,
0.814770182386596));
#41965=CARTESIAN_POINT('Ctrl Pts',(-64.0314595368616,1.88842247767949,0.925908072954638));
#41966=CARTESIAN_POINT('Ctrl Pts',(-66.0612876356907,1.83790060601568,1.03704596352268));
#41967=CARTESIAN_POINT('Ctrl Pts',(-67.1197071257548,0.105127466352834,
1.14818385409072));
#41968=CARTESIAN_POINT('Ctrl Pts',(-66.2379346445003,-1.72387003543737,
1.25932174465876));
#41969=CARTESIAN_POINT('Ctrl Pts',(-64.2230665440017,-1.97498974380221,
1.37045963522681));
#41970=CARTESIAN_POINT('Ctrl Pts',(-62.9193344468026,-0.418378941744453,
1.48159752579485));
#41971=CARTESIAN_POINT('Ctrl Pts',(-63.5200591267976,1.52117885042515,1.59273541636289));
#41972=CARTESIAN_POINT('Ctrl Pts',(-65.4753904717057,2.06838438946255,1.70387330693093));
#41973=CARTESIAN_POINT('Ctrl Pts',(-66.995591526567,0.722374239748765,1.81501119749897));
#41974=CARTESIAN_POINT('Ctrl Pts',(-66.6892050256144,-1.28483324388724,
1.92614908806702));
#41975=CARTESIAN_POINT('Ctrl Pts',(-64.8366700078289,-2.11601828839368,
2.03728697863506));
#41976=CARTESIAN_POINT('Ctrl Pts',(-63.1336327841659,-1.01038779625361,
2.1484248692031));
#41977=CARTESIAN_POINT('Ctrl Pts',(-63.1389026391995,1.02006210437423,2.25956275977114));
#41978=CARTESIAN_POINT('Ctrl Pts',(-64.8476560148535,2.11683759257734,2.37070065033918));
#41979=CARTESIAN_POINT('Ctrl Pts',(-66.6958515678104,1.27604762572331,2.48183854090722));
#41980=CARTESIAN_POINT('Ctrl Pts',(-66.9918149484855,-0.732723204319568,
2.59297643147526));
#41981=CARTESIAN_POINT('Ctrl Pts',(-65.4646475180941,-2.07082417580245,
2.70411432204331));
#41982=CARTESIAN_POINT('Ctrl Pts',(-63.5121829449299,-1.51347629442987,
2.81525221261135));
#41983=CARTESIAN_POINT('Ctrl Pts',(-62.9215341952643,0.429173603222892,
2.92639010317939));
#41984=CARTESIAN_POINT('Ctrl Pts',(-64.2333287680788,1.97899603468616,3.03752799374743));
#41985=CARTESIAN_POINT('Ctrl Pts',(-66.2468662141138,1.71742095225949,3.14866588431547));
#41986=CARTESIAN_POINT('Ctrl Pts',(-67.1191328739459,-0.116129004648151,
3.25980377488352));
#41987=CARTESIAN_POINT('Ctrl Pts',(-66.051733181654,-1.8433847666097,3.37094166545155));
#41988=CARTESIAN_POINT('Ctrl Pts',(-64.0216701807284,-1.88336954628658,
3.4820795560196));
#41989=CARTESIAN_POINT('Ctrl Pts',(-62.8870835583976,-0.199484821387324,
3.59321744658764));
#41990=CARTESIAN_POINT('Ctrl Pts',(-63.686473317166,1.66699062284606,3.70435533715568));
#41991=CARTESIAN_POINT('Ctrl Pts',(-65.6881489451415,2.00765064501607,3.81549322772372));
#41992=CARTESIAN_POINT('Ctrl Pts',(-67.0599540394824,0.510685263521478,
3.92663111829177));
#41993=CARTESIAN_POINT('Ctrl Pts',(-66.5462598400307,-1.45371613128932,
4.03776900885981));
#41994=CARTESIAN_POINT('Ctrl Pts',(-64.6172564731933,-2.08751466476978,
4.14890689942785));
#41995=CARTESIAN_POINT('Ctrl Pts',(-63.0385825971008,-0.81058735175515,
4.26004478999589));
#41996=CARTESIAN_POINT('Ctrl Pts',(-63.2552163137658,1.20827975739151,4.37118268056393));
#41997=CARTESIAN_POINT('Ctrl Pts',(-65.0688703258357,2.12119470101483,4.48232057113198));
#41998=CARTESIAN_POINT('Ctrl Pts',(-66.8194865472274,1.09255608031048,4.59345846170002));
#41999=CARTESIAN_POINT('Ctrl Pts',(-66.9047060983459,-0.936111514078443,
4.70459635226806));
#42000=CARTESIAN_POINT('Ctrl Pts',(-65.2465265552648,-2.1079456175936,4.8157342428361));
#42001=CARTESIAN_POINT('Ctrl Pts',(-63.3626984633988,-1.35035320305218,
4.92687213340414));
#42002=CARTESIAN_POINT('Ctrl Pts',(-62.9775110302329,0.643232834874313,
5.03801002397219));
#42003=CARTESIAN_POINT('Ctrl Pts',(-64.4435306995345,2.04806051976079,5.14914791454023));
#42004=CARTESIAN_POINT('Ctrl Pts',(-66.4188930069729,1.57827527209693,5.26028580510827));
#42005=CARTESIAN_POINT('Ctrl Pts',(-67.0955264998601,-0.336123404011301,
5.37142369567631));
#42006=CARTESIAN_POINT('Ctrl Pts',(-65.8541007317118,-1.94286417540809,
5.48256158624435));
#42007=CARTESIAN_POINT('Ctrl Pts',(-63.8309070567223,-1.77128000596151,
5.5936994768124));
#42008=CARTESIAN_POINT('Ctrl Pts',(-62.8777970581406,0.0215781663613025,
5.70483736738043));
#42009=CARTESIAN_POINT('Ctrl Pts',(-63.867164175545,1.79468298474188,5.81597525794848));
#42010=CARTESIAN_POINT('Ctrl Pts',(-65.8934273984406,1.92509926646557,5.92711314851651));
#42011=CARTESIAN_POINT('Ctrl Pts',(-67.1019290958798,0.293440200112785,
6.03825103908457));
#42012=CARTESIAN_POINT('Ctrl Pts',(-66.3865059227299,-1.60678798501314,
6.14938892965259));
#42013=CARTESIAN_POINT('Ctrl Pts',(-64.4020086652382,-2.03634438098786,
6.26052682022066));
#42014=CARTESIAN_POINT('Ctrl Pts',(-62.9648389371536,-0.601933848826785,
6.37166471078868));
#42015=CARTESIAN_POINT('Ctrl Pts',(-63.3905160600216,1.38328014168386,6.48280260135673));
#42016=CARTESIAN_POINT('Ctrl Pts',(-65.2892915487438,2.10266459070399,6.59394049192477));
#42017=CARTESIAN_POINT('Ctrl Pts',(-66.9234340409675,0.896859934344202,
6.70507838249281));
#42018=CARTESIAN_POINT('Ctrl Pts',(-66.796721623453,-1.12867407706945,6.81621627306086));
#42019=CARTESIAN_POINT('Ctrl Pts',(-65.026077453603,-2.12345182245078,6.92735416362889));
#42020=CARTESIAN_POINT('Ctrl Pts',(-63.2302233816263,-1.16987356610669,
7.03849205419693));
#42021=CARTESIAN_POINT('Ctrl Pts',(-63.1156124805061,0.172339073385996,
7.1125839812423));
#42022=CARTESIAN_POINT('Ctrl Pts',(-63.3548292594101,0.719397484879855,
7.14962994476498));
#42023=CARTESIAN_POINT('Ctrl Pts',(-63.5335096305347,-1.24726608657095,
-2.14962994476498));
#42024=CARTESIAN_POINT('Ctrl Pts',(-63.1187639830495,-0.759623149459712,
-2.1125839812423));
#42025=CARTESIAN_POINT('Ctrl Pts',(-62.8213796585631,0.653743668596897,
-2.03849205419694));
#42026=CARTESIAN_POINT('Ctrl Pts',(-64.370148361682,2.18801657894402,-1.9273541636289));
#42027=CARTESIAN_POINT('Ctrl Pts',(-66.4955154509718,1.71429596249072,-1.81621627306085));
#42028=CARTESIAN_POINT('Ctrl Pts',(-67.2519438360201,-0.325951055360581,
-1.70507838249281));
#42029=CARTESIAN_POINT('Ctrl Pts',(-65.9471840861633,-2.06915647107052,
-1.59394049192477));
#42030=CARTESIAN_POINT('Ctrl Pts',(-63.7754346567777,-1.91777815848532,
-1.48280260135673));
#42031=CARTESIAN_POINT('Ctrl Pts',(-62.7245546213054,-0.0113711599425682,
-1.37166471078869));
#42032=CARTESIAN_POINT('Ctrl Pts',(-63.756410041869,1.90561412409945,-1.26052682022064));
#42033=CARTESIAN_POINT('Ctrl Pts',(-65.9265402466607,2.07828288857813,-1.1493889296526));
#42034=CARTESIAN_POINT('Ctrl Pts',(-67.2485962395932,0.348719532119274,
-1.03825103908456));
#42035=CARTESIAN_POINT('Ctrl Pts',(-66.5124873120909,-1.70005297254208,
-0.927113148516519));
#42036=CARTESIAN_POINT('Ctrl Pts',(-64.3919812306068,-2.19273644759077,
-0.815975257948477));
#42037=CARTESIAN_POINT('Ctrl Pts',(-62.8280018090199,-0.67838909851214,
-0.704837367380436));
#42038=CARTESIAN_POINT('Ctrl Pts',(-63.2520768699961,1.45689838417497,-0.593699476812394));
#42039=CARTESIAN_POINT('Ctrl Pts',(-65.2760458422295,2.25866878330877,-0.482561586244352));
#42040=CARTESIAN_POINT('Ctrl Pts',(-67.0473469003682,0.993054775781761,
-0.37142369567631));
#42041=CARTESIAN_POINT('Ctrl Pts',(-66.9446881343466,-1.18151390830903,
-0.260285805108268));
#42042=CARTESIAN_POINT('Ctrl Pts',(-65.0620342584853,-2.27462932095962,
-0.149147914540226));
#42043=CARTESIAN_POINT('Ctrl Pts',(-63.1225997254656,-1.28575081741975,
-0.0380100239721848));
#42044=CARTESIAN_POINT('Ctrl Pts',(-62.9015709532967,0.879990040083932,
0.0731278665958575));
#42045=CARTESIAN_POINT('Ctrl Pts',(-64.6012580861897,2.24026600908808,0.184265757163899));
#42046=CARTESIAN_POINT('Ctrl Pts',(-66.6659182144232,1.55000110633352,0.295403647731941));
#42047=CARTESIAN_POINT('Ctrl Pts',(-67.2057445084059,-0.55899739370043,
0.406541538299982));
#42048=CARTESIAN_POINT('Ctrl Pts',(-65.7266278388951,-2.15633923654989,
0.517679428868024));
#42049=CARTESIAN_POINT('Ctrl Pts',(-63.5824204679769,-1.77995932329318,
0.628817319436066));
#42050=CARTESIAN_POINT('Ctrl Pts',(-62.7357397191377,0.225637545526547,
0.739955210004107));
#42051=CARTESIAN_POINT('Ctrl Pts',(-63.9615620838435,2.02470580959538,0.85109310057215));
#42052=CARTESIAN_POINT('Ctrl Pts',(-66.1378784498875,1.97053788463239,0.96223099114019));
#42053=CARTESIAN_POINT('Ctrl Pts',(-67.2726817663336,0.11271428633606,1.07336888170823));
#42054=CARTESIAN_POINT('Ctrl Pts',(-66.3272736880886,-1.84827797645492,
1.18450677227627));
#42055=CARTESIAN_POINT('Ctrl Pts',(-64.1669969508297,-2.11752044652707,
1.29564466284432));
#42056=CARTESIAN_POINT('Ctrl Pts',(-62.7691773513729,-0.44857243756348,
1.40678255341236));
#42057=CARTESIAN_POINT('Ctrl Pts',(-63.4132550214545,1.63095901065214,1.5179204439804));
#42058=CARTESIAN_POINT('Ctrl Pts',(-65.5096983653104,2.21765518008836,1.62905833454844));
#42059=CARTESIAN_POINT('Ctrl Pts',(-67.1396090150254,0.774506413267552,
1.74019622511649));
#42060=CARTESIAN_POINT('Ctrl Pts',(-66.8111112684709,-1.37755685711622,
1.85133411568452));
#42061=CARTESIAN_POINT('Ctrl Pts',(-64.8248828384863,-2.26872671362467,
1.96247200625257));
#42062=CARTESIAN_POINT('Ctrl Pts',(-62.9989411323989,-1.08330528004135,
2.07360989682061));
#42063=CARTESIAN_POINT('Ctrl Pts',(-63.0045913013778,1.09367776188117,2.18474778738865));
#42064=CARTESIAN_POINT('Ctrl Pts',(-64.8366616816794,2.26960514520452,2.29588567795669));
#42065=CARTESIAN_POINT('Ctrl Pts',(-66.8182374771223,1.36813720004919,2.40702356852474));
#42066=CARTESIAN_POINT('Ctrl Pts',(-67.1355598895398,-0.785602240042267,
2.51816145909277));
#42067=CARTESIAN_POINT('Ctrl Pts',(-65.4981801161651,-2.22027104048769,
2.62929934966082));
#42068=CARTESIAN_POINT('Ctrl Pts',(-63.4048104327177,-1.62270057798853,
2.74043724022886));
#42069=CARTESIAN_POINT('Ctrl Pts',(-62.771535850884,0.460146126219668,2.8515751307969));
#42070=CARTESIAN_POINT('Ctrl Pts',(-64.1779997772384,2.12181586268714,2.96271302136494));
#42071=CARTESIAN_POINT('Ctrl Pts',(-66.3368498296032,1.84136347700834,3.07385091193299));
#42072=CARTESIAN_POINT('Ctrl Pts',(-67.2720660720238,-0.124509781657844,
3.18498880250102));
#42073=CARTESIAN_POINT('Ctrl Pts',(-66.1276344717396,-1.97641782513655,
3.29612669306907));
#42074=CARTESIAN_POINT('Ctrl Pts',(-63.9510662512269,-2.01928821916335,
3.40726458363711));
#42075=CARTESIAN_POINT('Ctrl Pts',(-62.734598986685,-0.213881205907549,
3.51840247420515));
#42076=CARTESIAN_POINT('Ctrl Pts',(-63.5916789610234,1.78729370070031,3.62954036477319));
#42077=CARTESIAN_POINT('Ctrl Pts',(-65.7378111537875,2.15253841375417,3.74067825534123));
#42078=CARTESIAN_POINT('Ctrl Pts',(-67.2086164301352,0.547540305280233,
3.85181614590928));
#42079=CARTESIAN_POINT('Ctrl Pts',(-66.6578500405806,-1.55862765419993,
3.96295403647732));
#42080=CARTESIAN_POINT('Ctrl Pts',(-64.589634707556,-2.23816604564494,4.07409192704536));
#42081=CARTESIAN_POINT('Ctrl Pts',(-62.8970313806202,-0.869085673191047,
4.1852298176134));
#42082=CARTESIAN_POINT('Ctrl Pts',(-63.1292990801791,1.29547867244901,4.29636770818144));
#42083=CARTESIAN_POINT('Ctrl Pts',(-65.0738405470579,2.2742766966559,4.40750559874948));
#42084=CARTESIAN_POINT('Ctrl Pts',(-66.9507949233791,1.17140346996485,4.51864348931753));
#42085=CARTESIAN_POINT('Ctrl Pts',(-67.0421645836536,-1.00366864056436,
4.62978137988557));
#42086=CARTESIAN_POINT('Ctrl Pts',(-65.2643178391297,-2.26007145577794,
4.74091927045361));
#42087=CARTESIAN_POINT('Ctrl Pts',(-63.2445379821525,-1.44780524884724,
4.85205716102165));
#42088=CARTESIAN_POINT('Ctrl Pts',(-62.8315524119571,0.689653545795996,
4.96319505158969));
#42089=CARTESIAN_POINT('Ctrl Pts',(-64.4033715236759,2.1958645810328,5.07433294215774));
#42090=CARTESIAN_POINT('Ctrl Pts',(-66.5212914209443,1.6921759565593,5.18547083272578));
#42091=CARTESIAN_POINT('Ctrl Pts',(-67.2467560774014,-0.360380697056161,
5.29660872329382));
#42092=CARTESIAN_POINT('Ctrl Pts',(-65.9157393188846,-2.08307644592183,
5.40774661386186));
#42093=CARTESIAN_POINT('Ctrl Pts',(-63.7465361685802,-1.89910942115946,
5.5188845044299));
#42094=CARTESIAN_POINT('Ctrl Pts',(-62.7246422999565,0.0231354155696304,
5.63002239499795));
#42095=CARTESIAN_POINT('Ctrl Pts',(-63.7854098845984,1.92420134188086,5.74116028556599));
#42096=CARTESIAN_POINT('Ctrl Pts',(-65.957904105387,2.0640294822429,5.85229817613403));
#42097=CARTESIAN_POINT('Ctrl Pts',(-67.2536207348131,0.314617139416418,
5.96343606670207));
#42098=CARTESIAN_POINT('Ctrl Pts',(-66.4865670314617,-1.72274636978575,
6.07457395727011));
#42099=CARTESIAN_POINT('Ctrl Pts',(-64.3588529347165,-2.18330291407535,
6.18571184783816));
#42100=CARTESIAN_POINT('Ctrl Pts',(-62.8179658015557,-0.645374101990828,
6.29684973840619));
#42101=CARTESIAN_POINT('Ctrl Pts',(-63.2743631140587,1.48310845283244,6.40798762897424));
#42102=CARTESIAN_POINT('Ctrl Pts',(-65.3101690889255,2.25440930869465,6.51912551954228));
#42103=CARTESIAN_POINT('Ctrl Pts',(-67.0622440810523,0.96158435992109,6.63026341011032));
#42104=CARTESIAN_POINT('Ctrl Pts',(-66.9263871047018,-1.21012802378328,
6.74140130067837));
#42105=CARTESIAN_POINT('Ctrl Pts',(-65.0279594065595,-2.27669670962352,
6.8525391912464));
#42106=CARTESIAN_POINT('Ctrl Pts',(-63.1025024626319,-1.25430079009592,
6.96367708181444));
#42107=CARTESIAN_POINT('Ctrl Pts',(-62.979620342723,0.184776408472793,7.03776900885981));
#42108=CARTESIAN_POINT('Ctrl Pts',(-63.2361008748732,0.771314832491502,
7.07481497238249));
#42109=CARTESIAN_POINT('Ctrl Pts',(-63.4347998857283,-1.33121980333218,
-2.22444491714747));
#42110=CARTESIAN_POINT('Ctrl Pts',(-62.9921376300776,-0.810753527669818,
-2.18739895362479));
#42111=CARTESIAN_POINT('Ctrl Pts',(-62.6747363103277,0.697747278876015,
-2.11330702657943));
#42112=CARTESIAN_POINT('Ctrl Pts',(-64.3277529284907,2.3352923897075,-2.00216913601138));
#42113=CARTESIAN_POINT('Ctrl Pts',(-66.5961788795174,1.82968554874616,-1.89103124544334));
#42114=CARTESIAN_POINT('Ctrl Pts',(-67.4035226025776,-0.347890882695259,
-1.7798933548753));
#42115=CARTESIAN_POINT('Ctrl Pts',(-66.0109392265833,-2.20843178543787,
-1.66875546430726));
#42116=CARTESIAN_POINT('Ctrl Pts',(-63.6930089313552,-2.04686416993215,
-1.55761757373922));
#42117=CARTESIAN_POINT('Ctrl Pts',(-62.5713939614548,-0.0121365548742068,
-1.44647968317118));
#42118=CARTESIAN_POINT('Ctrl Pts',(-63.67270376601,2.03388137208554,-1.33534179260313));
#42119=CARTESIAN_POINT('Ctrl Pts',(-65.9889058463299,2.21817250383823,-1.22420390203509));
#42120=CARTESIAN_POINT('Ctrl Pts',(-67.3999496788005,0.372191909941345,
-1.11306601146705));
#42121=CARTESIAN_POINT('Ctrl Pts',(-66.6142931198262,-1.81448386044369,
-1.00192812089901));
#42122=CARTESIAN_POINT('Ctrl Pts',(-64.3510553719621,-2.34032995360773,
-0.890790230330967));
#42123=CARTESIAN_POINT('Ctrl Pts',(-62.6818041989874,-0.724051597351479,
-0.779652339762924));
#42124=CARTESIAN_POINT('Ctrl Pts',(-63.1344238327198,1.55496249063294,-0.668514449194883));
#42125=CARTESIAN_POINT('Ctrl Pts',(-65.2946265402067,2.41070020734328,-0.55737655862684));
#42126=CARTESIAN_POINT('Ctrl Pts',(-67.1851542083967,1.05989748101683,-0.446238668058799));
#42127=CARTESIAN_POINT('Ctrl Pts',(-67.0755854613707,-1.26104183348523,
-0.335100777490757));
#42128=CARTESIAN_POINT('Ctrl Pts',(-65.0662097961853,-2.42773505180942,
-0.223962886922715));
#42129=CARTESIAN_POINT('Ctrl Pts',(-62.9962315570428,-1.37229494871089,
-0.112824996354674));
#42130=CARTESIAN_POINT('Ctrl Pts',(-62.7603252963136,0.939222336522791,
-0.00168710578663132));
#42131=CARTESIAN_POINT('Ctrl Pts',(-64.5744186923722,2.39105873890073,0.10945078478141));
#42132=CARTESIAN_POINT('Ctrl Pts',(-66.778051485284,1.6543319746717,0.220588675349452));
#42133=CARTESIAN_POINT('Ctrl Pts',(-67.3542135894627,-0.596623614252945,
0.331726565917493));
#42134=CARTESIAN_POINT('Ctrl Pts',(-65.7755372964953,-2.30148283939099,
0.442864456485536));
#42135=CARTESIAN_POINT('Ctrl Pts',(-63.4870029209119,-1.89976872281361,
0.554002347053577));
#42136=CARTESIAN_POINT('Ctrl Pts',(-62.5833319303427,0.240825251495458,
0.665140237621619));
#42137=CARTESIAN_POINT('Ctrl Pts',(-63.8916646308255,2.16098914151126,0.77627812818966));
#42138=CARTESIAN_POINT('Ctrl Pts',(-66.2144692640843,2.10317516324911,0.887416018757702));
#42139=CARTESIAN_POINT('Ctrl Pts',(-67.4256564069122,0.12030110631929,0.998553909325744));
#42140=CARTESIAN_POINT('Ctrl Pts',(-66.416612731677,-1.97268591747247,1.10969179989378));
#42141=CARTESIAN_POINT('Ctrl Pts',(-64.1109273576576,-2.26005114925192,
1.22082969046183));
#42142=CARTESIAN_POINT('Ctrl Pts',(-62.6190202559434,-0.47876593338251,
1.33196758102987));
#42143=CARTESIAN_POINT('Ctrl Pts',(-63.3064509161112,1.74073917087914,1.44310547159791));
#42144=CARTESIAN_POINT('Ctrl Pts',(-65.5440062589152,2.36692597071417,1.55424336216595));
#42145=CARTESIAN_POINT('Ctrl Pts',(-67.2836265034836,0.82663858678634,1.665381252734));
#42146=CARTESIAN_POINT('Ctrl Pts',(-66.9330175113275,-1.47028047034519,
1.77651914330204));
#42147=CARTESIAN_POINT('Ctrl Pts',(-64.8130956691436,-2.42143513885566,
1.88765703387008));
#42148=CARTESIAN_POINT('Ctrl Pts',(-62.864249480632,-1.15622276382909,1.99879492443812));
#42149=CARTESIAN_POINT('Ctrl Pts',(-62.8702799635561,1.1672934193881,2.10993281500616));
#42150=CARTESIAN_POINT('Ctrl Pts',(-64.8256673485052,2.42237269783169,2.2210707055742));
#42151=CARTESIAN_POINT('Ctrl Pts',(-66.9406233864343,1.46022677437507,2.33220859614225));
#42152=CARTESIAN_POINT('Ctrl Pts',(-67.279304830594,-0.838481275764962,
2.44334648671029));
#42153=CARTESIAN_POINT('Ctrl Pts',(-65.5317127142361,-2.36971790517293,
2.55448437727833));
#42154=CARTESIAN_POINT('Ctrl Pts',(-63.2974379205056,-1.73192486154719,
2.66562226784637));
#42155=CARTESIAN_POINT('Ctrl Pts',(-62.6215375065036,0.491118649216447,
2.77676015841441));
#42156=CARTESIAN_POINT('Ctrl Pts',(-64.122670786398,2.26463569068811,2.88789804898245));
#42157=CARTESIAN_POINT('Ctrl Pts',(-66.4268334450924,1.96530600175719,2.9990359395505));
#42158=CARTESIAN_POINT('Ctrl Pts',(-67.4249992701018,-0.132890558667537,
3.11017383011854));
#42159=CARTESIAN_POINT('Ctrl Pts',(-66.2035357618251,-2.1094508836634,3.22131172068658));
#42160=CARTESIAN_POINT('Ctrl Pts',(-63.8804623217255,-2.15520689204011,
3.33244961125462));
#42161=CARTESIAN_POINT('Ctrl Pts',(-62.5821144149725,-0.228277590427775,
3.44358750182266));
#42162=CARTESIAN_POINT('Ctrl Pts',(-63.4968846048806,1.90759677855457,3.55472539239071));
#42163=CARTESIAN_POINT('Ctrl Pts',(-65.7874733624335,2.29742618249228,3.66586328295874));
#42164=CARTESIAN_POINT('Ctrl Pts',(-67.3572788207879,0.584395347038986,
3.77700117352679));
#42165=CARTESIAN_POINT('Ctrl Pts',(-66.7694402411304,-1.66353917711054,
3.88813906409483));
#42166=CARTESIAN_POINT('Ctrl Pts',(-64.5620129419189,-2.3888174265201,3.99927695466288));
#42167=CARTESIAN_POINT('Ctrl Pts',(-62.7554801641395,-0.927583994626942,
4.11041484523091));
#42168=CARTESIAN_POINT('Ctrl Pts',(-63.0033818465923,1.3826775875065,4.22155273579896));
#42169=CARTESIAN_POINT('Ctrl Pts',(-65.0788107682801,2.42735869229697,4.33269062636699));
#42170=CARTESIAN_POINT('Ctrl Pts',(-67.0821032995307,1.25025085961923,4.44382851693504));
#42171=CARTESIAN_POINT('Ctrl Pts',(-67.1796230689615,-1.07122576705027,
4.55496640750307));
#42172=CARTESIAN_POINT('Ctrl Pts',(-65.2821091229946,-2.41219729396228,
4.66610429807113));
#42173=CARTESIAN_POINT('Ctrl Pts',(-63.1263775009061,-1.5452572946423,4.77724218863916));
#42174=CARTESIAN_POINT('Ctrl Pts',(-62.6855937936814,0.736074256717683,
4.88838007920721));
#42175=CARTESIAN_POINT('Ctrl Pts',(-64.3632123478174,2.34366864230481,4.99951796977525));
#42176=CARTESIAN_POINT('Ctrl Pts',(-66.6236898349158,1.80607664102167,5.11065586034329));
#42177=CARTESIAN_POINT('Ctrl Pts',(-67.3979856549427,-0.384637990101019,
5.22179375091133));
#42178=CARTESIAN_POINT('Ctrl Pts',(-65.9773779060574,-2.22328871643558,
5.33293164147938));
#42179=CARTESIAN_POINT('Ctrl Pts',(-63.6621652804381,-2.0269388363574,5.44406953204741));
#42180=CARTESIAN_POINT('Ctrl Pts',(-62.5714875417724,0.0246926647779575,
5.55520742261546));
#42181=CARTESIAN_POINT('Ctrl Pts',(-63.7036555936518,2.05371969901984,5.66634531318349));
#42182=CARTESIAN_POINT('Ctrl Pts',(-66.0223808123334,2.20295969802022,5.77748320375154));
#42183=CARTESIAN_POINT('Ctrl Pts',(-67.4053123737463,0.335794078720048,
5.88862109431958));
#42184=CARTESIAN_POINT('Ctrl Pts',(-66.5866281401934,-1.83870475455836,
5.99975898488763));
#42185=CARTESIAN_POINT('Ctrl Pts',(-64.3156972041947,-2.33026144716284,
6.11089687545566));
#42186=CARTESIAN_POINT('Ctrl Pts',(-62.6710926659578,-0.688814355154873,
6.22203476602371));
#42187=CARTESIAN_POINT('Ctrl Pts',(-63.1582101680956,1.58293676398102,6.33317265659174));
#42188=CARTESIAN_POINT('Ctrl Pts',(-65.3310466291073,2.40615402668531,6.4443105471598));
#42189=CARTESIAN_POINT('Ctrl Pts',(-67.2010541211369,1.02630878549798,6.55544843772783));
#42190=CARTESIAN_POINT('Ctrl Pts',(-67.0560525859507,-1.29158197049712,
6.66658632829588));
#42191=CARTESIAN_POINT('Ctrl Pts',(-65.029841359516,-2.42994159679626,6.77772421886392));
#42192=CARTESIAN_POINT('Ctrl Pts',(-62.9747815436376,-1.33872801408515,
6.88886210943195));
#42193=CARTESIAN_POINT('Ctrl Pts',(-62.8436282049399,0.19721374355959,6.96295403647732));
#42194=CARTESIAN_POINT('Ctrl Pts',(-63.1173724903363,0.823232180103149,
7.));
#42195=CARTESIAN_POINT('Ctrl Pts',(-63.7309291201476,-1.0793586530485,-2.));
#42196=CARTESIAN_POINT('Ctrl Pts',(-63.6855968419863,-1.03706844878282,
-2.));
#42197=CARTESIAN_POINT('Ctrl Pts',(-63.6429944057487,-0.992209355217755,
-2.));
#42198=CARTESIAN_POINT('Ctrl Pts',(-63.6031204505543,-0.945126337779186,
-2.));
#42199=CARTESIAN_POINT('Ctrl Pts',(-63.5606157477688,-0.89493694340586,
-2.));
#42200=CARTESIAN_POINT('Ctrl Pts',(-63.5212107097549,-0.84222025720975,
-2.));
#42201=CARTESIAN_POINT('Ctrl Pts',(-63.4849325153247,-0.787339414503396,
-2.));
#42202=CARTESIAN_POINT('Ctrl Pts',(-63.4531890951982,-0.739318677135336,
-2.));
#42203=CARTESIAN_POINT('Ctrl Pts',(-63.423839907855,-0.689639781933985,
-2.));
#42204=CARTESIAN_POINT('Ctrl Pts',(-63.396926053755,-0.638518448146663,
-2.));
#42205=CARTESIAN_POINT('Ctrl Pts',(-63.383420898641,-0.61286617479071,-2.));
#42206=CARTESIAN_POINT('Ctrl Pts',(-63.3705293094229,-0.586850346515661,
-2.));
#42207=CARTESIAN_POINT('Ctrl Pts',(-63.3582588228031,-0.560496376493833,
-2.));
#42208=CARTESIAN_POINT('Ctrl Pts',(-63.352655640319,-0.548462126525787,
-2.));
#42209=CARTESIAN_POINT('Ctrl Pts',(-63.3471814025998,-0.536355708766487,
-2.));
#42210=CARTESIAN_POINT('Ctrl Pts',(-63.3418453144502,-0.524199442886152,
-2.));
#42211=CARTESIAN_POINT('Ctrl Pts',(-63.3149230085341,-0.462867114849718,
-2.));
#42212=CARTESIAN_POINT('Ctrl Pts',(-63.2914620509818,-0.400159371493074,
-2.));
#42213=CARTESIAN_POINT('Ctrl Pts',(-63.2714860817235,-0.33643388798648,
-2.));
#42214=CARTESIAN_POINT('Ctrl Pts',(-63.2511562856272,-0.271579658934033,
-2.));
#42215=CARTESIAN_POINT('Ctrl Pts',(-63.234435470142,-0.205670475316589,
-2.));
#42216=CARTESIAN_POINT('Ctrl Pts',(-63.2213878692165,-0.139046848337481,
-2.));
#42217=CARTESIAN_POINT('Ctrl Pts',(-63.2104743799197,-0.0833204167814306,
-2.));
#42218=CARTESIAN_POINT('Ctrl Pts',(-63.2021313216452,-0.0270932010480611,
-2.));
#42219=CARTESIAN_POINT('Ctrl Pts',(-63.196421114974,0.0294478216546492,
-2.));
#42220=CARTESIAN_POINT('Ctrl Pts',(-63.1937898541988,0.0555019005692096,
-2.));
#42221=CARTESIAN_POINT('Ctrl Pts',(-63.1917179786548,0.0816227252779034,
-2.));
#42222=CARTESIAN_POINT('Ctrl Pts',(-63.190213400761,0.10779240289025,-2.));
#42223=CARTESIAN_POINT('Ctrl Pts',(-63.1895569069957,0.119211040809892,
-2.));
#42224=CARTESIAN_POINT('Ctrl Pts',(-63.1890085369661,0.13063873197943,-2.));
#42225=CARTESIAN_POINT('Ctrl Pts',(-63.1885692788766,0.142059931628667,
-2.));
#42226=CARTESIAN_POINT('Ctrl Pts',(-63.185872337845,0.212183402760181,-2.));
#42227=CARTESIAN_POINT('Ctrl Pts',(-63.1872764272328,0.282193469675666,
-2.));
#42228=CARTESIAN_POINT('Ctrl Pts',(-63.1928363192171,0.351729486410014,
-2.));
#42229=CARTESIAN_POINT('Ctrl Pts',(-63.1978071231096,0.413897942851084,
-2.));
#42230=CARTESIAN_POINT('Ctrl Pts',(-63.2061000911937,0.475688445045345,
-2.));
#42231=CARTESIAN_POINT('Ctrl Pts',(-63.2177875010733,0.536855401025581,
-2.));
#42232=CARTESIAN_POINT('Ctrl Pts',(-63.2305203455448,0.603493719122557,
-2.));
#42233=CARTESIAN_POINT('Ctrl Pts',(-63.2472809681188,0.669392782961828,
-2.));
#42234=CARTESIAN_POINT('Ctrl Pts',(-63.2678240437403,0.734338936172986,
-2.));
#42235=CARTESIAN_POINT('Ctrl Pts',(-63.2757504472631,0.759397959811583,
-2.));
#42236=CARTESIAN_POINT('Ctrl Pts',(-63.2842405167728,0.784315071866599,
-2.));
#42237=CARTESIAN_POINT('Ctrl Pts',(-63.2932821667435,0.809077679605451,
-2.));
#42238=CARTESIAN_POINT('Ctrl Pts',(-63.2972485928261,0.81994063642485,-2.));
#42239=CARTESIAN_POINT('Ctrl Pts',(-63.3013210590997,0.830773275850983,
-2.));
#42240=CARTESIAN_POINT('Ctrl Pts',(-63.3054934693646,0.841562024914705,
-2.));
#42241=CARTESIAN_POINT('Ctrl Pts',(-63.3307175500364,0.906784824076589,
-2.));
#42242=CARTESIAN_POINT('Ctrl Pts',(-63.3596326694542,0.970522726119043,
-2.));
#42243=CARTESIAN_POINT('Ctrl Pts',(-63.3919260622227,1.03255684529061,-2.));
#42244=CARTESIAN_POINT('Ctrl Pts',(-63.4249680867552,1.09602905157818,-2.));
#42245=CARTESIAN_POINT('Ctrl Pts',(-63.4615471340117,1.157718383915,-2.));
#42246=CARTESIAN_POINT('Ctrl Pts',(-63.5013843211633,1.2173866717758,-2.));
#42247=CARTESIAN_POINT('Ctrl Pts',(-63.5318674685087,1.26304444384141,-2.));
#42248=CARTESIAN_POINT('Ctrl Pts',(-63.5642595400752,1.30751888441973,-2.));
#42249=CARTESIAN_POINT('Ctrl Pts',(-63.598455110112,1.35069719141984,-2.));
#42250=CARTESIAN_POINT('Ctrl Pts',(-63.6197386626115,1.37757165974682,-2.));
#42251=CARTESIAN_POINT('Ctrl Pts',(-63.6417211957385,1.40394389610583,-2.));
#42252=CARTESIAN_POINT('Ctrl Pts',(-63.6643801907862,1.42978501722721,-2.));
#42253=CARTESIAN_POINT('Ctrl Pts',(-63.6770896559072,1.44427934174985,-2.));
#42254=CARTESIAN_POINT('Ctrl Pts',(-63.6900164428917,1.45861113921278,-2.));
#42255=CARTESIAN_POINT('Ctrl Pts',(-63.7031327805923,1.47274978412593,-2.));
#42256=CARTESIAN_POINT('Ctrl Pts',(-63.7540080482568,1.52759034715398,-2.));
#42257=CARTESIAN_POINT('Ctrl Pts',(-63.8077798406737,1.57958602565017,-2.));
#42258=CARTESIAN_POINT('Ctrl Pts',(-63.8641630605125,1.62847278876025,-2.));
#42259=CARTESIAN_POINT('Ctrl Pts',(-63.9063355382102,1.66503820543689,-2.));
#42260=CARTESIAN_POINT('Ctrl Pts',(-63.9499701263561,1.69986415252965,-2.));
#42261=CARTESIAN_POINT('Ctrl Pts',(-63.9949639294371,1.73283039559633,-2.));
#42262=CARTESIAN_POINT('Ctrl Pts',(-64.0089991299055,1.74311376349253,-2.));
#42263=CARTESIAN_POINT('Ctrl Pts',(-64.0231666800404,1.75321609759807,-2.));
#42264=CARTESIAN_POINT('Ctrl Pts',(-64.0374636964878,1.76313352311854,-2.));
#42265=CARTESIAN_POINT('Ctrl Pts',(-64.051264901766,1.77270701881548,-2.));
#42266=CARTESIAN_POINT('Ctrl Pts',(-64.0651797317384,1.78210327688949,-2.));
#42267=CARTESIAN_POINT('Ctrl Pts',(-64.0792001599332,1.79131603215157,-2.));
#42268=CARTESIAN_POINT('Ctrl Pts',(-64.1421565047628,1.83268434052647,-2.));
#42269=CARTESIAN_POINT('Ctrl Pts',(-64.207269965244,1.87037681374959,-2.));
#42270=CARTESIAN_POINT('Ctrl Pts',(-64.2742791023089,1.90411417795052,-2.));
#42271=CARTESIAN_POINT('Ctrl Pts',(-64.3255634212839,1.92993450369772,-2.));
#42272=CARTESIAN_POINT('Ctrl Pts',(-64.3779590786546,1.95343777834416,-2.));
#42273=CARTESIAN_POINT('Ctrl Pts',(-64.4313627927198,1.97448349564832,-2.));
#42274=CARTESIAN_POINT('Ctrl Pts',(-64.4437562344803,1.97936759175068,-2.));
#42275=CARTESIAN_POINT('Ctrl Pts',(-64.4562040109557,1.98411926473273,-2.));
#42276=CARTESIAN_POINT('Ctrl Pts',(-64.4687042096542,1.98873909628093,-2.));
#42277=CARTESIAN_POINT('Ctrl Pts',(-66.6673159824367,0.00130059074132209,
-0.871480363390211));
#42278=CARTESIAN_POINT('Ctrl Pts',(-66.6680474999804,0.0865457667101201,
-0.877193940366669));
#42279=CARTESIAN_POINT('Ctrl Pts',(-66.6620744628598,0.171688078253671,
-0.882907517343126));
#42280=CARTESIAN_POINT('Ctrl Pts',(-66.6490403647761,0.255735261203265,
-0.888621094319584));
#42281=CARTESIAN_POINT('Ctrl Pts',(-66.5645292565598,0.800684403669395,
-0.925667057842264));
#42282=CARTESIAN_POINT('Ctrl Pts',(-66.1831691519411,1.29959403086365,-0.962713021364943));
#42283=CARTESIAN_POINT('Ctrl Pts',(-65.6794913573425,1.52414483947234,-0.999758984887624));
#42284=CARTESIAN_POINT('Ctrl Pts',(-65.1758135627439,1.74869564808103,-1.0368049484103));
#42285=CARTESIAN_POINT('Ctrl Pts',(-64.5498180781654,1.69888763810415,-1.07385091193299));
#42286=CARTESIAN_POINT('Ctrl Pts',(-64.0879958937795,1.39749696674795,-1.11089687545567));
#42287=CARTESIAN_POINT('Ctrl Pts',(-63.6261737093935,1.09610629539175,-1.14794283897835));
#42288=CARTESIAN_POINT('Ctrl Pts',(-63.3285248252001,0.543132962656229,
-1.18498880250103));
#42289=CARTESIAN_POINT('Ctrl Pts',(-63.3312687442061,-0.00831466463025846,
-1.22203476602371));
#42290=CARTESIAN_POINT('Ctrl Pts',(-63.3340126632121,-0.559762291916746,
-1.25908072954639));
#42291=CARTESIAN_POINT('Ctrl Pts',(-63.6371493854174,-1.1096842137542,-1.29612669306907));
#42292=CARTESIAN_POINT('Ctrl Pts',(-64.1019490294701,-1.40647845913029,
-1.33317265659175));
#42293=CARTESIAN_POINT('Ctrl Pts',(-64.5667486735228,-1.70327270450637,
-1.37021862011443));
#42294=CARTESIAN_POINT('Ctrl Pts',(-65.193211239423,-1.74693927342109,-1.40726458363711));
#42295=CARTESIAN_POINT('Ctrl Pts',(-65.6946279386367,-1.51735015093768,
-1.44431054715979));
#42296=CARTESIAN_POINT('Ctrl Pts',(-66.1960446378505,-1.28776102845428,
-1.48135651068247));
#42297=CARTESIAN_POINT('Ctrl Pts',(-66.5724154703778,-0.784916214572752,
-1.51840247420515));
#42298=CARTESIAN_POINT('Ctrl Pts',(-66.6515012684707,-0.23922910918681,
-1.55544843772783));
#42299=CARTESIAN_POINT('Ctrl Pts',(-66.6629095976148,-0.160512345140353,
-1.56079241294863));
#42300=CARTESIAN_POINT('Ctrl Pts',(-66.6681317812815,-0.0809040843243736,
-1.56613638816942));
#42301=CARTESIAN_POINT('Ctrl Pts',(-66.6674675207825,-0.00121113675535883,
-1.57148036339021));
#42302=CARTESIAN_POINT('Ctrl Pts',(-65.5301702171886,1.98517432567173,-2.));
#42303=CARTESIAN_POINT('Ctrl Pts',(-66.1902879097456,1.80888011517989,-1.96295403647732));
#42304=CARTESIAN_POINT('Ctrl Pts',(-67.3093622463653,0.748693059830641,
-1.88886210943196));
#42305=CARTESIAN_POINT('Ctrl Pts',(-66.8811995093437,-1.538373214553,-1.77772421886392));
#42306=CARTESIAN_POINT('Ctrl Pts',(-64.7278715623352,-2.41277602144419,
-1.66658632829587));
#42307=CARTESIAN_POINT('Ctrl Pts',(-62.8252644286755,-1.08095990301172,
-1.55544843772783));
#42308=CARTESIAN_POINT('Ctrl Pts',(-62.9123886677794,1.24138962897178,-1.44431054715979));
#42309=CARTESIAN_POINT('Ctrl Pts',(-64.9107473342681,2.42691462884513,-1.33317265659175));
#42310=CARTESIAN_POINT('Ctrl Pts',(-66.9905869477348,1.39134438721223,-1.22203476602371));
#42311=CARTESIAN_POINT('Ctrl Pts',(-67.24852778644,-0.917884815202466,-1.11089687545567));
#42312=CARTESIAN_POINT('Ctrl Pts',(-65.4483108550045,-2.38688976599862,
-0.999758984887625));
#42313=CARTESIAN_POINT('Ctrl Pts',(-63.2377776981899,-1.67118490708905,
-0.888621094319582));
#42314=CARTESIAN_POINT('Ctrl Pts',(-62.6402125087857,0.574193448178942,
-0.777483203751542));
#42315=CARTESIAN_POINT('Ctrl Pts',(-64.2025947176117,2.29399639382146,-0.666345313183498));
#42316=CARTESIAN_POINT('Ctrl Pts',(-66.4948474007694,1.91408331059476,-0.555207422615458));
#42317=CARTESIAN_POINT('Ctrl Pts',(-67.4188511430454,-0.217814411897149,
-0.444069532047416));
#42318=CARTESIAN_POINT('Ctrl Pts',(-66.1288520704621,-2.15034287637184,
-0.332931641479373));
#42319=CARTESIAN_POINT('Ctrl Pts',(-63.8056023683761,-2.11463875683277,
-0.221793750911332));
#42320=CARTESIAN_POINT('Ctrl Pts',(-62.5755981242121,-0.143381478345974,
-0.110655860343291));
#42321=CARTESIAN_POINT('Ctrl Pts',(-63.5646765331008,1.95911432942999,0.00048203022475183));
#42322=CARTESIAN_POINT('Ctrl Pts',(-65.8675227272721,2.26841065672896,0.111619920792793));
#42323=CARTESIAN_POINT('Ctrl Pts',(-67.3763155620569,0.501404942245523,
0.222757811360835));
#42324=CARTESIAN_POINT('Ctrl Pts',(-66.7100397977853,-1.7245423808174,0.333895701928876));
#42325=CARTESIAN_POINT('Ctrl Pts',(-64.4785452214709,-2.37199651591817,
0.445033592496919));
#42326=CARTESIAN_POINT('Ctrl Pts',(-62.7243441135659,-0.848335334231208,
0.55617148306496));
#42327=CARTESIAN_POINT('Ctrl Pts',(-63.0530766482751,1.45181679686654,0.667309373633002));
#42328=CARTESIAN_POINT('Ctrl Pts',(-65.1638502053818,2.42310455048397,0.778447264201043));
#42329=CARTESIAN_POINT('Ctrl Pts',(-67.1246498118468,1.17649722845177,0.889585154769086));
#42330=CARTESIAN_POINT('Ctrl Pts',(-67.1407333500909,-1.14697134880472,
1.00072304533713));
#42331=CARTESIAN_POINT('Ctrl Pts',(-65.1973793755662,-2.42060404314487,
1.11186093590517));
#42332=CARTESIAN_POINT('Ctrl Pts',(-63.0733618200821,-1.47863040518406,
1.22299882647321));
#42333=CARTESIAN_POINT('Ctrl Pts',(-62.7128180402749,0.816750411403611,
1.33413671704125));
#42334=CARTESIAN_POINT('Ctrl Pts',(-64.4457578465939,2.36455031387797,1.4452746076093));
#42335=CARTESIAN_POINT('Ctrl Pts',(-66.686001781468,1.74805049822323,1.55641249817733));
#42336=CARTESIAN_POINT('Ctrl Pts',(-67.3830291651992,-0.468459762690014,
1.66755038874538));
#42337=CARTESIAN_POINT('Ctrl Pts',(-65.898842928637,-2.25618349012117,1.77868827931342));
#42338=CARTESIAN_POINT('Ctrl Pts',(-63.5919355659201,-1.97879688218178,
1.88982616988146));
#42339=CARTESIAN_POINT('Ctrl Pts',(-62.5738455482538,0.109804953100741,
2.0009640604495));
#42340=CARTESIAN_POINT('Ctrl Pts',(-63.7764422147334,2.0979010695377,2.11210195101754));
#42341=CARTESIAN_POINT('Ctrl Pts',(-66.0989751981566,2.16576454521031,2.22323984158559));
#42342=CARTESIAN_POINT('Ctrl Pts',(-67.4156037194807,0.25127917121157,2.33437773215363));
#42343=CARTESIAN_POINT('Ctrl Pts',(-66.5212027615546,-1.89320487789678,
2.44551562272167));
#42344=CARTESIAN_POINT('Ctrl Pts',(-64.234427664365,-2.30481703186257,2.55665351328971));
#42345=CARTESIAN_POINT('Ctrl Pts',(-62.6483896081628,-0.606804018161647,
2.66779140385776));
#42346=CARTESIAN_POINT('Ctrl Pts',(-63.214807212685,1.64662359498827,2.77892929442579));
#42347=CARTESIAN_POINT('Ctrl Pts',(-65.4152320208998,2.39287795766376,2.89006718499384));
#42348=CARTESIAN_POINT('Ctrl Pts',(-67.2355902513335,0.948903988607916,
3.00120507556188));
#42349=CARTESIAN_POINT('Ctrl Pts',(-67.009687371404,-1.36361256252397,3.11234296612992));
#42350=CARTESIAN_POINT('Ctrl Pts',(-64.9442948490232,-2.42799907075925,
3.22348085669796));
#42351=CARTESIAN_POINT('Ctrl Pts',(-62.9298898830714,-1.27001049414664,
3.334618747266));
#42352=CARTESIAN_POINT('Ctrl Pts',(-62.8102801837888,1.05043309065765,3.44575663783405));
#42353=CARTESIAN_POINT('Ctrl Pts',(-64.6949458653977,2.40940335486023,3.55689452840209));
#42354=CARTESIAN_POINT('Ctrl Pts',(-66.8588310559542,1.56301940386929,3.66803241897013));
#42355=CARTESIAN_POINT('Ctrl Pts',(-67.3213071004237,-0.71401393333385,
3.77917030953817));
#42356=CARTESIAN_POINT('Ctrl Pts',(-65.6590644304509,-2.3375022198779,3.89030820010621));
#42357=CARTESIAN_POINT('Ctrl Pts',(-63.39357261301,-1.82144821550898,4.00144609067426));
#42358=CARTESIAN_POINT('Ctrl Pts',(-62.5984620009619,0.361797997181342,
4.1125839812423));
#42359=CARTESIAN_POINT('Ctrl Pts',(-64.0015063548152,2.21388639990767,4.22372187181034));
#42360=CARTESIAN_POINT('Ctrl Pts',(-66.3184832656195,2.03957947376812,4.33485976237838));
#42361=CARTESIAN_POINT('Ctrl Pts',(-67.4286374911296,-0.00157767540964147,
4.44599765294642));
#42362=CARTESIAN_POINT('Ctrl Pts',(-66.315832277707,-2.04129075981347,4.55713554351446));
#42363=CARTESIAN_POINT('Ctrl Pts',(-63.9986308592856,-2.21258726309084,
4.66827343408251));
#42364=CARTESIAN_POINT('Ctrl Pts',(-62.5979939690176,-0.358677549762027,
4.77941132465054));
#42365=CARTESIAN_POINT('Ctrl Pts',(-63.3959404447163,1.82353378810158,4.89054921521859));
#42366=CARTESIAN_POINT('Ctrl Pts',(-65.6621008123707,2.33664397819608,5.00168710578663));
#42367=CARTESIAN_POINT('Ctrl Pts',(-67.3222328179755,0.710997418429197,
5.11282499635467));
#42368=CARTESIAN_POINT('Ctrl Pts',(-66.8567987494513,-1.56543310762404,
5.22396288692272));
#42369=CARTESIAN_POINT('Ctrl Pts',(-64.6918158067504,-2.40900502421389,
5.33510077749075));
#42370=CARTESIAN_POINT('Ctrl Pts',(-62.80891719594,-1.04758718972751,5.4462386680588));
#42371=CARTESIAN_POINT('Ctrl Pts',(-62.9315418303621,1.27269881881277,5.55737655862684));
#42372=CARTESIAN_POINT('Ctrl Pts',(-64.947449081762,2.42806968006159,5.66851444919488));
#42373=CARTESIAN_POINT('Ctrl Pts',(-67.0114579748176,1.36099981154568,5.77965233976293));
#42374=CARTESIAN_POINT('Ctrl Pts',(-67.234354225073,-0.951806616989204,
5.89079023033096));
#42375=CARTESIAN_POINT('Ctrl Pts',(-65.4121253417219,-2.39341760299656,
6.00192812089901));
#42376=CARTESIAN_POINT('Ctrl Pts',(-63.2126643336617,-1.64429852840487,
6.11306601146705));
#42377=CARTESIAN_POINT('Ctrl Pts',(-62.649189925264,0.60985028512182,6.22420390203509));
#42378=CARTESIAN_POINT('Ctrl Pts',(-64.2374031554986,2.30582648807955,6.33534179260313));
#42379=CARTESIAN_POINT('Ctrl Pts',(-66.5236998933487,1.89119386508315,6.44647968317117));
#42380=CARTESIAN_POINT('Ctrl Pts',(-67.4151988715152,-0.254352246057023,
6.55761757373922));
#42381=CARTESIAN_POINT('Ctrl Pts',(-66.0963109962835,-2.16731896239628,
6.66875546430726));
#42382=CARTESIAN_POINT('Ctrl Pts',(-63.7734206371606,-2.09605634078855,
6.77989335487529));
#42383=CARTESIAN_POINT('Ctrl Pts',(-62.5742917867301,-0.107152602938497,
6.89103124544335));
#42384=CARTESIAN_POINT('Ctrl Pts',(-63.5933356141608,1.98161526205799,7.00216913601138));
#42385=CARTESIAN_POINT('Ctrl Pts',(-65.9042541560964,2.25300237548896,7.11330702657943));
#42386=CARTESIAN_POINT('Ctrl Pts',(-66.8857543436368,1.06431345694512,7.18739895362479));
#42387=CARTESIAN_POINT('Ctrl Pts',(-67.0166758614465,0.393720754290193,
7.22444491714747));
#42388=CARTESIAN_POINT('Ctrl Pts',(-65.4967348970877,1.85997880000277,-2.07481497238249));
#42389=CARTESIAN_POINT('Ctrl Pts',(-66.1152220988337,1.69480262890399,-2.03776900885981));
#42390=CARTESIAN_POINT('Ctrl Pts',(-67.1637217267118,0.701476540869023,
-1.96367708181445));
#42391=CARTESIAN_POINT('Ctrl Pts',(-66.7625611820115,-1.44135531502629,
-1.8525391912464));
#42392=CARTESIAN_POINT('Ctrl Pts',(-64.7450334117317,-2.26061368566345,
-1.74140130067836));
#42393=CARTESIAN_POINT('Ctrl Pts',(-62.962414682697,-1.01278889075624,-1.63026341011032));
#42394=CARTESIAN_POINT('Ctrl Pts',(-63.0440444094189,1.16310107509049,-1.51912551954228));
#42395=CARTESIAN_POINT('Ctrl Pts',(-64.9163760764189,2.27386063817903,-1.40798762897424));
#42396=CARTESIAN_POINT('Ctrl Pts',(-66.8650500736736,1.30359889821864,-1.2968497384062));
#42397=CARTESIAN_POINT('Ctrl Pts',(-67.1067238075329,-0.859998174993202,
-1.18571184783815));
#42398=CARTESIAN_POINT('Ctrl Pts',(-65.4200380164786,-2.23635995352639,
-1.07457395727011));
#42399=CARTESIAN_POINT('Ctrl Pts',(-63.3489126975537,-1.56579120426537,
-0.963436066702071));
#42400=CARTESIAN_POINT('Ctrl Pts',(-62.7890331093795,0.537981791776368,
-0.85229817613403));
#42401=CARTESIAN_POINT('Ctrl Pts',(-64.2528832853252,2.14932492558151,-0.741160285565987));
#42402=CARTESIAN_POINT('Ctrl Pts',(-66.4005744678012,1.79337115794137,-0.630022394997947));
#42403=CARTESIAN_POINT('Ctrl Pts',(-67.2663056781698,-0.204077890402237,
-0.518884504429904));
#42404=CARTESIAN_POINT('Ctrl Pts',(-66.0576607264394,-2.01473095388499,
-0.407746613861862));
#42405=CARTESIAN_POINT('Ctrl Pts',(-63.8809273599474,-1.98127852376001,
-0.296608723293821));
#42406=CARTESIAN_POINT('Ctrl Pts',(-62.7284936474651,-0.134339088808397,
-0.185470832725779));
#42407=CARTESIAN_POINT('Ctrl Pts',(-63.6551955739828,1.8355622840772,-0.0743329421577371));
#42408=CARTESIAN_POINT('Ctrl Pts',(-65.8128121849957,2.12535275953086,0.0368049484103043));
#42409=CARTESIAN_POINT('Ctrl Pts',(-67.2264526144558,0.469783711552746,
0.147942838978346));
#42410=CARTESIAN_POINT('Ctrl Pts',(-66.6021957013601,-1.61578367529074,
0.259080729546388));
#42411=CARTESIAN_POINT('Ctrl Pts',(-64.5114309002076,-2.22240595006454,
0.37021862011443));
#42412=CARTESIAN_POINT('Ctrl Pts',(-62.8678589330251,-0.794834849795569,
0.481356510682471));
#42413=CARTESIAN_POINT('Ctrl Pts',(-63.1758598665065,1.36025759991932,0.592494401250513));
#42414=CARTESIAN_POINT('Ctrl Pts',(-65.153516950348,2.27029084338244,0.703632291818555));
#42415=CARTESIAN_POINT('Ctrl Pts',(-66.9906582290337,1.10230113037648,0.814770182386596));
#42416=CARTESIAN_POINT('Ctrl Pts',(-67.0057274548323,-1.07463730786741,
0.925908072954638));
#42417=CARTESIAN_POINT('Ctrl Pts',(-65.1849315948547,-2.26794803117706,
1.03704596352268));
#42418=CARTESIAN_POINT('Ctrl Pts',(-63.1948657487746,-1.38538020118271,
1.14818385409072));
#42419=CARTESIAN_POINT('Ctrl Pts',(-62.8570597544889,0.765241838189812,
1.25932174465876));
#42420=CARTESIAN_POINT('Ctrl Pts',(-64.480711269498,2.21542934465705,1.37045963522681));
#42421=CARTESIAN_POINT('Ctrl Pts',(-66.5796736486789,1.63780924727067,1.48159752579485));
#42422=CARTESIAN_POINT('Ctrl Pts',(-67.232742822502,-0.438916228156898,
1.59273541636289));
#42423=CARTESIAN_POINT('Ctrl Pts',(-65.8421571698655,-2.11389670230682,
1.70387330693093));
#42424=CARTESIAN_POINT('Ctrl Pts',(-63.680735508938,-1.85400355161469,1.81501119749897));
#42425=CARTESIAN_POINT('Ctrl Pts',(-62.7268515981571,0.102880075699936,
1.92614908806701));
#42426=CARTESIAN_POINT('Ctrl Pts',(-63.8536061988389,1.96559640298739,2.03728697863505));
#42427=CARTESIAN_POINT('Ctrl Pts',(-66.0296680467136,2.02918005124097,2.1484248692031));
#42428=CARTESIAN_POINT('Ctrl Pts',(-67.2632630542012,0.235432186126848,
2.25956275977114));
#42429=CARTESIAN_POINT('Ctrl Pts',(-66.42526772103,-1.7738094289318,2.37070065033918));
#42430=CARTESIAN_POINT('Ctrl Pts',(-64.2827086791644,-2.15946315732203,
2.48183854090722));
#42431=CARTESIAN_POINT('Ctrl Pts',(-62.7966945178967,-0.568535767837546,
2.59297643147526));
#42432=CARTESIAN_POINT('Ctrl Pts',(-63.3273908515816,1.5427788575828,2.7041143220433));
#42433=CARTESIAN_POINT('Ctrl Pts',(-65.3890453074919,2.24197049835536,2.81525221261135));
#42434=CARTESIAN_POINT('Ctrl Pts',(-67.0946021813807,0.889061116308559,
2.92639010317939));
#42435=CARTESIAN_POINT('Ctrl Pts',(-66.8829459242478,-1.27761598813436,
3.03752799374744));
#42436=CARTESIAN_POINT('Ctrl Pts',(-64.9478079085913,-2.27487668948696,
3.14866588431547));
#42437=CARTESIAN_POINT('Ctrl Pts',(-63.0604419061002,-1.18991695809611,
3.25980377488352));
#42438=CARTESIAN_POINT('Ctrl Pts',(-62.9483754230397,0.984187259616866,
3.37094166545155));
#42439=CARTESIAN_POINT('Ctrl Pts',(-64.7141841822776,2.25745371715866,3.4820795560196));
#42440=CARTESIAN_POINT('Ctrl Pts',(-66.7416034008459,1.46444718612111,3.59321744658764));
#42441=CARTESIAN_POINT('Ctrl Pts',(-67.1749132754993,-0.668984462338426,
3.70435533715568));
#42442=CARTESIAN_POINT('Ctrl Pts',(-65.6175003638835,-2.19008704561055,
3.81549322772372));
#42443=CARTESIAN_POINT('Ctrl Pts',(-63.4948823662959,-1.70657811877716,
3.92663111829177));
#42444=CARTESIAN_POINT('Ctrl Pts',(-62.7499156079905,0.338981114121075,
4.0377690088598));
#42445=CARTESIAN_POINT('Ctrl Pts',(-64.0644766114669,2.0742670888862,4.14890689942785));
#42446=CARTESIAN_POINT('Ctrl Pts',(-66.2353327818609,1.91095287354468,4.26004478999589));
#42447=CARTESIAN_POINT('Ctrl Pts',(-67.2754748477136,-0.00147817890714668,
4.37118268056393));
#42448=CARTESIAN_POINT('Ctrl Pts',(-66.2328489791779,-1.91255623689868,
4.48232057113198));
#42449=CARTESIAN_POINT('Ctrl Pts',(-64.061782459797,-2.0730498824644,4.59345846170001));
#42450=CARTESIAN_POINT('Ctrl Pts',(-62.7494770926002,-0.336057458514918,
4.70459635226806));
#42451=CARTESIAN_POINT('Ctrl Pts',(-63.4971008700911,1.70853216420176,4.8157342428361));
#42452=CARTESIAN_POINT('Ctrl Pts',(-65.6203452556023,2.1892829291595,4.92687213340414));
#42453=CARTESIAN_POINT('Ctrl Pts',(-67.1757806124374,0.666158184716363,
5.03801002397219));
#42454=CARTESIAN_POINT('Ctrl Pts',(-66.7396992622713,-1.46670866903235,
5.14914791454022));
#42455=CARTESIAN_POINT('Ctrl Pts',(-64.7112515215779,-2.25708050733623,
5.26028580510827));
#42456=CARTESIAN_POINT('Ctrl Pts',(-62.9470983923676,-0.98152083615545,
5.3714236956763));
#42457=CARTESIAN_POINT('Ctrl Pts',(-63.0619896729133,1.19243574288083,5.48256158624435));
#42458=CARTESIAN_POINT('Ctrl Pts',(-64.9507632188372,2.27494284579563,5.59369947681239));
#42459=CARTESIAN_POINT('Ctrl Pts',(-66.8846048641049,1.27516801096355,5.70483736738043));
#42460=CARTESIAN_POINT('Ctrl Pts',(-67.093444105432,-0.89178068968993,5.81597525794848));
#42461=CARTESIAN_POINT('Ctrl Pts',(-65.3861345518295,-2.24247611081747,
5.92711314851652));
#42462=CARTESIAN_POINT('Ctrl Pts',(-63.3253831137711,-1.54060042191707,
6.03825103908456));
#42463=CARTESIAN_POINT('Ctrl Pts',(-62.7974443627954,0.571389921194157,
6.1493889296526));
#42464=CARTESIAN_POINT('Ctrl Pts',(-64.2854965201901,2.16040895192496,6.26052682022064));
#42465=CARTESIAN_POINT('Ctrl Pts',(-66.4276073705699,1.77192524115468,6.37166471078869));
#42466=CARTESIAN_POINT('Ctrl Pts',(-67.2628837380762,-0.238311456722607,
6.48280260135673));
#42467=CARTESIAN_POINT('Ctrl Pts',(-66.0271718634116,-2.03063643871026,
6.59394049192477));
#42468=CARTESIAN_POINT('Ctrl Pts',(-63.8507751778273,-1.96386801252777,
6.70507838249281));
#42469=CARTESIAN_POINT('Ctrl Pts',(-62.7272696944899,-0.100394996677825,
6.81621627306085));
#42470=CARTESIAN_POINT('Ctrl Pts',(-63.6820472627791,1.85664418964447,6.92735416362889));
#42471=CARTESIAN_POINT('Ctrl Pts',(-65.8472271368835,2.11091620548104,7.03849205419694));
#42472=CARTESIAN_POINT('Ctrl Pts',(-66.7668287645171,0.997192257060716,
7.1125839812423));
#42473=CARTESIAN_POINT('Ctrl Pts',(-66.8894936833815,0.36889065440289,7.14962994476498));
#42474=CARTESIAN_POINT('Ctrl Pts',(-65.4632995769868,1.73478327433381,-2.14962994476498));
#42475=CARTESIAN_POINT('Ctrl Pts',(-66.0401562879218,1.5807251426281,-2.1125839812423));
#42476=CARTESIAN_POINT('Ctrl Pts',(-67.0180812070583,0.654260021907404,
-2.03849205419694));
#42477=CARTESIAN_POINT('Ctrl Pts',(-66.6439228546792,-1.34433741549959,
-1.92735416362889));
#42478=CARTESIAN_POINT('Ctrl Pts',(-64.7621952611282,-2.1084513498827,-1.81621627306085));
#42479=CARTESIAN_POINT('Ctrl Pts',(-63.0995649367186,-0.944617878500769,
-1.70507838249281));
#42480=CARTESIAN_POINT('Ctrl Pts',(-63.1757001510583,1.08481252120919,-1.59394049192477));
#42481=CARTESIAN_POINT('Ctrl Pts',(-64.9220048185698,2.12080664751292,-1.48280260135673));
#42482=CARTESIAN_POINT('Ctrl Pts',(-66.7395131996123,1.21585340922505,-1.37166471078869));
#42483=CARTESIAN_POINT('Ctrl Pts',(-66.9649198286257,-0.802111534783937,
-1.26052682022064));
#42484=CARTESIAN_POINT('Ctrl Pts',(-65.3917651779528,-2.08583014105415,
-1.1493889296526));
#42485=CARTESIAN_POINT('Ctrl Pts',(-63.4600476969176,-1.46039750144169,
-1.03825103908456));
#42486=CARTESIAN_POINT('Ctrl Pts',(-62.9378537099731,0.501770135373796,
-0.927113148516519));
#42487=CARTESIAN_POINT('Ctrl Pts',(-64.3031718530388,2.00465345734157,-0.815975257948477));
#42488=CARTESIAN_POINT('Ctrl Pts',(-66.306301534833,1.67265900528797,-0.704837367380435));
#42489=CARTESIAN_POINT('Ctrl Pts',(-67.1137602132943,-0.190341368907323,
-0.593699476812392));
#42490=CARTESIAN_POINT('Ctrl Pts',(-65.9864693824166,-1.87911903139814,
-0.482561586244352));
#42491=CARTESIAN_POINT('Ctrl Pts',(-63.9562523515188,-1.84791829068725,
-0.371423695676309));
#42492=CARTESIAN_POINT('Ctrl Pts',(-62.8813891707182,-0.125296699270823,
-0.260285805108269));
#42493=CARTESIAN_POINT('Ctrl Pts',(-63.7457146148648,1.71201023872442,-0.149147914540226));
#42494=CARTESIAN_POINT('Ctrl Pts',(-65.7581016427195,1.98229486233276,-0.0380100239721847));
#42495=CARTESIAN_POINT('Ctrl Pts',(-67.0765896668548,0.438162480859971,
0.0731278665958568));
#42496=CARTESIAN_POINT('Ctrl Pts',(-66.4943516049349,-1.50702496976407,
0.184265757163899));
#42497=CARTESIAN_POINT('Ctrl Pts',(-64.5443165789444,-2.07281538421092,
0.295403647731941));
#42498=CARTESIAN_POINT('Ctrl Pts',(-63.0113737524843,-0.741334365359929,
0.406541538299983));
#42499=CARTESIAN_POINT('Ctrl Pts',(-63.298643084738,1.26869840297211,0.517679428868024));
#42500=CARTESIAN_POINT('Ctrl Pts',(-65.1431836953141,2.1174771362809,0.628817319436066));
#42501=CARTESIAN_POINT('Ctrl Pts',(-66.8566666462206,1.02810503230119,0.739955210004107));
#42502=CARTESIAN_POINT('Ctrl Pts',(-66.8707215595737,-1.0023032669301,0.851093100572149));
#42503=CARTESIAN_POINT('Ctrl Pts',(-65.1724838141431,-2.11529201920925,
0.96223099114019));
#42504=CARTESIAN_POINT('Ctrl Pts',(-63.3163696774672,-1.29212999718137,
1.07336888170823));
#42505=CARTESIAN_POINT('Ctrl Pts',(-63.0013014687027,0.713733264976017,
1.18450677227627));
#42506=CARTESIAN_POINT('Ctrl Pts',(-64.5156646924022,2.06630837543613,1.29564466284432));
#42507=CARTESIAN_POINT('Ctrl Pts',(-66.4733455158896,1.52756799631812,1.40678255341236));
#42508=CARTESIAN_POINT('Ctrl Pts',(-67.0824564798048,-0.409372693623786,
1.5179204439804));
#42509=CARTESIAN_POINT('Ctrl Pts',(-65.7854714110939,-1.97160991449247,
1.62905833454844));
#42510=CARTESIAN_POINT('Ctrl Pts',(-63.7695354519561,-1.7292102210476,1.74019622511648));
#42511=CARTESIAN_POINT('Ctrl Pts',(-62.8798576480604,0.0959551982991319,
1.85133411568453));
#42512=CARTESIAN_POINT('Ctrl Pts',(-63.9307701829444,1.83329173643707,1.96247200625256));
#42513=CARTESIAN_POINT('Ctrl Pts',(-65.9603608952703,1.89259555727163,2.07360989682061));
#42514=CARTESIAN_POINT('Ctrl Pts',(-67.110922388922,0.219585201042126,2.18474778738865));
#42515=CARTESIAN_POINT('Ctrl Pts',(-66.3293326805052,-1.65441397996682,
2.29588567795669));
#42516=CARTESIAN_POINT('Ctrl Pts',(-64.330989693964,-2.01410928278148,2.40702356852474));
#42517=CARTESIAN_POINT('Ctrl Pts',(-62.9449994276305,-0.530267517513444,
2.51816145909277));
#42518=CARTESIAN_POINT('Ctrl Pts',(-63.4399744904782,1.43893412017733,2.62929934966082));
#42519=CARTESIAN_POINT('Ctrl Pts',(-65.362858594084,2.09106303904696,2.74043724022886));
#42520=CARTESIAN_POINT('Ctrl Pts',(-66.953614111428,0.829218244009199,2.8515751307969));
#42521=CARTESIAN_POINT('Ctrl Pts',(-66.7562044770915,-1.19161941374474,
2.96271302136494));
#42522=CARTESIAN_POINT('Ctrl Pts',(-64.9513209681592,-2.12175430821468,
3.07385091193298));
#42523=CARTESIAN_POINT('Ctrl Pts',(-63.1909939291292,-1.10982342204557,
3.18498880250103));
#42524=CARTESIAN_POINT('Ctrl Pts',(-63.0864706622905,0.917941428576082,
3.29612669306907));
#42525=CARTESIAN_POINT('Ctrl Pts',(-64.7334224991575,2.10550407945709,3.40726458363711));
#42526=CARTESIAN_POINT('Ctrl Pts',(-66.6243757457373,1.36587496837294,3.51840247420515));
#42527=CARTESIAN_POINT('Ctrl Pts',(-67.0285194505751,-0.623954991343003,
3.6295403647732));
#42528=CARTESIAN_POINT('Ctrl Pts',(-65.5759362973161,-2.04267187134319,
3.74067825534123));
#42529=CARTESIAN_POINT('Ctrl Pts',(-63.5961921195818,-1.59170802204534,
3.85181614590928));
#42530=CARTESIAN_POINT('Ctrl Pts',(-62.9013692150191,0.316164231060809,
3.96295403647732));
#42531=CARTESIAN_POINT('Ctrl Pts',(-64.1274468681188,1.93464777786473,4.07409192704536));
#42532=CARTESIAN_POINT('Ctrl Pts',(-66.1521822981021,1.78232627332124,4.1852298176134));
#42533=CARTESIAN_POINT('Ctrl Pts',(-67.1223122042977,-0.00137868240465238,
4.29636770818144));
#42534=CARTESIAN_POINT('Ctrl Pts',(-66.1498656806486,-1.78382171398389,
4.40750559874949));
#42535=CARTESIAN_POINT('Ctrl Pts',(-64.1249340603086,-1.93351250183795,
4.51864348931752));
#42536=CARTESIAN_POINT('Ctrl Pts',(-62.9009602161829,-0.313437367267809,
4.62978137988557));
#42537=CARTESIAN_POINT('Ctrl Pts',(-63.5982612954659,1.59353054030193,4.74091927045361));
#42538=CARTESIAN_POINT('Ctrl Pts',(-65.578589698834,2.04192188012293,4.85205716102165));
#42539=CARTESIAN_POINT('Ctrl Pts',(-67.0293284068994,0.621318951003525,
4.96319505158969));
#42540=CARTESIAN_POINT('Ctrl Pts',(-66.6225997750913,-1.36798423044065,
5.07433294215773));
#42541=CARTESIAN_POINT('Ctrl Pts',(-64.7306872364055,-2.10515599045856,
5.18547083272578));
#42542=CARTESIAN_POINT('Ctrl Pts',(-63.0852795887951,-0.915454482583389,
5.29660872329381));
#42543=CARTESIAN_POINT('Ctrl Pts',(-63.1924375154646,1.11217266694889,5.40774661386187));
#42544=CARTESIAN_POINT('Ctrl Pts',(-64.9540773559123,2.12181601152967,5.5188845044299));
#42545=CARTESIAN_POINT('Ctrl Pts',(-66.7577517533922,1.18933621038143,5.63002239499795));
#42546=CARTESIAN_POINT('Ctrl Pts',(-66.9525339857911,-0.831754762390655,
5.74116028556598));
#42547=CARTESIAN_POINT('Ctrl Pts',(-65.360143761937,-2.09153461863839,5.85229817613403));
#42548=CARTESIAN_POINT('Ctrl Pts',(-63.4381018938804,-1.43690231542927,
5.96343606670207));
#42549=CARTESIAN_POINT('Ctrl Pts',(-62.945698800327,0.532929557266492,6.0745739572701));
#42550=CARTESIAN_POINT('Ctrl Pts',(-64.3335898848817,2.01499141577037,6.18571184783816));
#42551=CARTESIAN_POINT('Ctrl Pts',(-66.3315148477911,1.65265661722621,6.29684973840619));
#42552=CARTESIAN_POINT('Ctrl Pts',(-67.1105686046371,-0.222270667388193,
6.40798762897424));
#42553=CARTESIAN_POINT('Ctrl Pts',(-65.9580327305397,-1.89395391502424,
6.51912551954227));
#42554=CARTESIAN_POINT('Ctrl Pts',(-63.9281297184939,-1.83167968426698,
6.63026341011033));
#42555=CARTESIAN_POINT('Ctrl Pts',(-62.8802476022497,-0.0936373904171547,
6.74140130067836));
#42556=CARTESIAN_POINT('Ctrl Pts',(-63.7707589113974,1.73167311723095,6.85253919124641));
#42557=CARTESIAN_POINT('Ctrl Pts',(-65.7902001176707,1.96883003547312,6.96367708181445));
#42558=CARTESIAN_POINT('Ctrl Pts',(-66.6479031853974,0.930071057176316,
7.03776900885981));
#42559=CARTESIAN_POINT('Ctrl Pts',(-66.7623115053165,0.344060554515587,
7.07481497238249));
#42560=CARTESIAN_POINT('Ctrl Pts',(-65.4298642568859,1.60958774866485,-2.22444491714747));
#42561=CARTESIAN_POINT('Ctrl Pts',(-65.9650904770099,1.46664765635221,-2.18739895362479));
#42562=CARTESIAN_POINT('Ctrl Pts',(-66.8724406874047,0.607043502945785,
-2.11330702657942));
#42563=CARTESIAN_POINT('Ctrl Pts',(-66.5252845273472,-1.24731951597289,
-2.00216913601139));
#42564=CARTESIAN_POINT('Ctrl Pts',(-64.7793571105247,-1.95628901410196,
-1.89103124544334));
#42565=CARTESIAN_POINT('Ctrl Pts',(-63.2367151907402,-0.876446866245294,
-1.7798933548753));
#42566=CARTESIAN_POINT('Ctrl Pts',(-63.3073558926977,1.00652396732789,-1.66875546430726));
#42567=CARTESIAN_POINT('Ctrl Pts',(-64.9276335607206,1.96775265684681,-1.55761757373922));
#42568=CARTESIAN_POINT('Ctrl Pts',(-66.6139763255511,1.12810792023145,-1.44647968317117));
#42569=CARTESIAN_POINT('Ctrl Pts',(-66.8231158497185,-0.744224894574671,
-1.33534179260313));
#42570=CARTESIAN_POINT('Ctrl Pts',(-65.363492339427,-1.93530032858192,-1.22420390203509));
#42571=CARTESIAN_POINT('Ctrl Pts',(-63.5711826962814,-1.35500379861801,
-1.11306601146705));
#42572=CARTESIAN_POINT('Ctrl Pts',(-63.0866743105668,0.465558478971223,
-1.00192812089901));
#42573=CARTESIAN_POINT('Ctrl Pts',(-64.3534604207524,1.85998198910162,-0.890790230330965));
#42574=CARTESIAN_POINT('Ctrl Pts',(-66.2120286018649,1.55194685263457,-0.779652339762925));
#42575=CARTESIAN_POINT('Ctrl Pts',(-66.9612147484188,-0.176604847412408,
-0.668514449194881));
#42576=CARTESIAN_POINT('Ctrl Pts',(-65.915278038394,-1.74350710891129,-0.55737655862684));
#42577=CARTESIAN_POINT('Ctrl Pts',(-64.0315773430901,-1.7145580576145,-0.446238668058799));
#42578=CARTESIAN_POINT('Ctrl Pts',(-63.0342846939712,-0.116254309733247,
-0.335100777490757));
#42579=CARTESIAN_POINT('Ctrl Pts',(-63.8362336557469,1.58845819337163,-0.223962886922715));
#42580=CARTESIAN_POINT('Ctrl Pts',(-65.703391100443,1.83923696513466,-0.112824996354674));
#42581=CARTESIAN_POINT('Ctrl Pts',(-66.9267267192538,0.406541250167196,
-0.00168710578663183));
#42582=CARTESIAN_POINT('Ctrl Pts',(-66.3865075085097,-1.3982662642374,0.10945078478141));
#42583=CARTESIAN_POINT('Ctrl Pts',(-64.5772022576811,-1.9232248183573,0.220588675349452));
#42584=CARTESIAN_POINT('Ctrl Pts',(-63.1548885719436,-0.687833880924293,
0.331726565917493));
#42585=CARTESIAN_POINT('Ctrl Pts',(-63.4214263029693,1.17713920602489,0.442864456485535));
#42586=CARTESIAN_POINT('Ctrl Pts',(-65.1328504402804,1.96466342917937,0.554002347053577));
#42587=CARTESIAN_POINT('Ctrl Pts',(-66.7226750634076,0.953908934225895,
0.665140237621619));
#42588=CARTESIAN_POINT('Ctrl Pts',(-66.7357156643151,-0.929969225992781,
0.77627812818966));
#42589=CARTESIAN_POINT('Ctrl Pts',(-65.1600360334315,-1.96263600724144,
0.887416018757702));
#42590=CARTESIAN_POINT('Ctrl Pts',(-63.4378736061597,-1.19887979318002,
0.998553909325744));
#42591=CARTESIAN_POINT('Ctrl Pts',(-63.1455431829167,0.662224691762218,
1.10969179989378));
#42592=CARTESIAN_POINT('Ctrl Pts',(-64.5506181153062,1.91718740621521,1.22082969046183));
#42593=CARTESIAN_POINT('Ctrl Pts',(-66.3670173831005,1.41732674536556,1.33196758102987));
#42594=CARTESIAN_POINT('Ctrl Pts',(-66.9321701371076,-0.379829159090671,
1.44310547159791));
#42595=CARTESIAN_POINT('Ctrl Pts',(-65.7287856523224,-1.82932312667812,
1.55424336216595));
#42596=CARTESIAN_POINT('Ctrl Pts',(-63.858335394974,-1.60441689048052,1.66538125273399));
#42597=CARTESIAN_POINT('Ctrl Pts',(-63.0328636979636,0.0890303208983267,
1.77651914330204));
#42598=CARTESIAN_POINT('Ctrl Pts',(-64.00793416705,1.70098706988676,1.88765703387008));
#42599=CARTESIAN_POINT('Ctrl Pts',(-65.8910537438272,1.75601106330229,1.99879492443812));
#42600=CARTESIAN_POINT('Ctrl Pts',(-66.9585817236427,0.203738215957406,
2.10993281500616));
#42601=CARTESIAN_POINT('Ctrl Pts',(-66.2333976399805,-1.53501853100184,
2.2210707055742));
#42602=CARTESIAN_POINT('Ctrl Pts',(-64.3792707087636,-1.86875540824093,
2.33220859614224));
#42603=CARTESIAN_POINT('Ctrl Pts',(-63.0933043373643,-0.491999267189342,
2.44334648671029));
#42604=CARTESIAN_POINT('Ctrl Pts',(-63.5525581293749,1.33508938277185,2.55448437727833));
#42605=CARTESIAN_POINT('Ctrl Pts',(-65.336671880676,1.94015557973857,2.66562226784637));
#42606=CARTESIAN_POINT('Ctrl Pts',(-66.8126260414754,0.76937537170984,2.77676015841441));
#42607=CARTESIAN_POINT('Ctrl Pts',(-66.6294630299351,-1.10562283935512,
2.88789804898245));
#42608=CARTESIAN_POINT('Ctrl Pts',(-64.9548340277273,-1.9686319269424,2.9990359395505));
#42609=CARTESIAN_POINT('Ctrl Pts',(-63.3215459521581,-1.02972988599504,
3.11017383011853));
#42610=CARTESIAN_POINT('Ctrl Pts',(-63.2245659015414,0.851695597535297,
3.22131172068658));
#42611=CARTESIAN_POINT('Ctrl Pts',(-64.7526608160373,1.95355444175552,3.33244961125462));
#42612=CARTESIAN_POINT('Ctrl Pts',(-66.507148090629,1.26730275062476,3.44358750182267));
#42613=CARTESIAN_POINT('Ctrl Pts',(-66.8821256256507,-0.578925520347578,
3.5547253923907));
#42614=CARTESIAN_POINT('Ctrl Pts',(-65.5343722307488,-1.89525669707584,
3.66586328295875));
#42615=CARTESIAN_POINT('Ctrl Pts',(-63.6975018728677,-1.47683792531352,
3.77700117352679));
#42616=CARTESIAN_POINT('Ctrl Pts',(-63.0528228220476,0.293347348000542,
3.88813906409483));
#42617=CARTESIAN_POINT('Ctrl Pts',(-64.1904171247705,1.79502846684326,3.99927695466287));
#42618=CARTESIAN_POINT('Ctrl Pts',(-66.0690318143434,1.65369967309779,4.11041484523092));
#42619=CARTESIAN_POINT('Ctrl Pts',(-66.9691495608818,-0.0012791859021568,
4.22155273579895));
#42620=CARTESIAN_POINT('Ctrl Pts',(-66.0668823821194,-1.65508719106911,
4.332690626367));
#42621=CARTESIAN_POINT('Ctrl Pts',(-64.18808566082,-1.7939751212115,4.44382851693504));
#42622=CARTESIAN_POINT('Ctrl Pts',(-63.0524433397656,-0.2908172760207,4.55496640750308));
#42623=CARTESIAN_POINT('Ctrl Pts',(-63.6994217208407,1.47852891640211,4.66610429807113));
#42624=CARTESIAN_POINT('Ctrl Pts',(-65.5368341420657,1.89456083108635,4.77724218863916));
#42625=CARTESIAN_POINT('Ctrl Pts',(-66.8828762013613,0.576479717290691,
4.88838007920721));
#42626=CARTESIAN_POINT('Ctrl Pts',(-66.5055002879113,-1.26925979184896,
4.99951796977524));
#42627=CARTESIAN_POINT('Ctrl Pts',(-64.7501229512331,-1.95323147358089,
5.11065586034329));
#42628=CARTESIAN_POINT('Ctrl Pts',(-63.2234607852226,-0.849388129011331,
5.22179375091133));
#42629=CARTESIAN_POINT('Ctrl Pts',(-63.3228853580159,1.03190959101695,5.33293164147937));
#42630=CARTESIAN_POINT('Ctrl Pts',(-64.9573914929873,1.96868917726371,5.44406953204741));
#42631=CARTESIAN_POINT('Ctrl Pts',(-66.6308986426797,1.1035044097993,5.55520742261545));
#42632=CARTESIAN_POINT('Ctrl Pts',(-66.81162386615,-0.77172883509138,5.6663453131835));
#42633=CARTESIAN_POINT('Ctrl Pts',(-65.3341529720446,-1.94059312645931,
5.77748320375154));
#42634=CARTESIAN_POINT('Ctrl Pts',(-63.5508206739898,-1.33320420894148,
5.88862109431958));
#42635=CARTESIAN_POINT('Ctrl Pts',(-63.0939532378585,0.494469193338827,
5.99975898488762));
#42636=CARTESIAN_POINT('Ctrl Pts',(-64.3816832495733,1.86957387961578,6.11089687545566));
#42637=CARTESIAN_POINT('Ctrl Pts',(-66.2354223250123,1.53338799329774,6.22203476602371));
#42638=CARTESIAN_POINT('Ctrl Pts',(-66.9582534711981,-0.206229878053776,
6.33317265659175));
#42639=CARTESIAN_POINT('Ctrl Pts',(-65.8888935976679,-1.75727139133822,
6.44431054715979));
#42640=CARTESIAN_POINT('Ctrl Pts',(-64.0054842591603,-1.6994913560062,6.55544843772783));
#42641=CARTESIAN_POINT('Ctrl Pts',(-63.0332255100097,-0.0868797841564816,
6.66658632829588));
#42642=CARTESIAN_POINT('Ctrl Pts',(-63.8594705600155,1.60670204481743,6.77772421886391));
#42643=CARTESIAN_POINT('Ctrl Pts',(-65.733173098458,1.8267438654652,6.88886210943197));
#42644=CARTESIAN_POINT('Ctrl Pts',(-66.5289776062776,0.862949857291917,
6.96295403647732));
#42645=CARTESIAN_POINT('Ctrl Pts',(-66.6351293272515,0.319230454628283,
7.));
#42646=CARTESIAN_POINT('Ctrl Pts',(-66.6638321395092,-0.000941642735140673,
-1.3785196366098));
#42647=CARTESIAN_POINT('Ctrl Pts',(-66.664949390616,-0.216825623511897,
-1.36412702194091));
#42648=CARTESIAN_POINT('Ctrl Pts',(-66.625958965974,-0.432322760104835,
-1.34973440727202));
#42649=CARTESIAN_POINT('Ctrl Pts',(-66.5449886773087,-0.630681997774858,
-1.33534179260313));
#42650=CARTESIAN_POINT('Ctrl Pts',(-66.3365746796213,-1.14125003924375,
-1.29829582908045));
#42651=CARTESIAN_POINT('Ctrl Pts',(-65.8500335095242,-1.53827518391284,
-1.26124986555777));
#42652=CARTESIAN_POINT('Ctrl Pts',(-65.308044650618,-1.64007166792006,-1.22420390203509));
#42653=CARTESIAN_POINT('Ctrl Pts',(-64.7660557917118,-1.74186815192728,
-1.18715793851241));
#42654=CARTESIAN_POINT('Ctrl Pts',(-64.1686192439966,-1.54843597527264,
-1.15011197498973));
#42655=CARTESIAN_POINT('Ctrl Pts',(-63.7891495725199,-1.14829284068045,
-1.11306601146705));
#42656=CARTESIAN_POINT('Ctrl Pts',(-63.4096799010432,-0.748149706088263,
-1.07602004794437));
#42657=CARTESIAN_POINT('Ctrl Pts',(-63.248177105805,-0.141295613558517,
-1.03897408442169));
#42658=CARTESIAN_POINT('Ctrl Pts',(-63.3785567265502,0.394535351061421,
-1.00192812089901));
#42659=CARTESIAN_POINT('Ctrl Pts',(-63.5089363472953,0.930366315681358,
-0.964882157376327));
#42660=CARTESIAN_POINT('Ctrl Pts',(-63.9311983840238,1.39517415239149,-0.927836193853646));
#42661=CARTESIAN_POINT('Ctrl Pts',(-64.4520907659069,1.57623888133538,-0.890790230330965));
#42662=CARTESIAN_POINT('Ctrl Pts',(-64.9729831477899,1.75730361027927,-0.853744266808285));
#42663=CARTESIAN_POINT('Ctrl Pts',(-65.5925058748274,1.65462523145692,-0.816698303285605));
#42664=CARTESIAN_POINT('Ctrl Pts',(-66.0271315961051,1.31519409203792,-0.779652339762925));
#42665=CARTESIAN_POINT('Ctrl Pts',(-66.422630141453,1.00632023733061,-0.745941438711882));
#42666=CARTESIAN_POINT('Ctrl Pts',(-66.6650238854461,0.501402189087542,
-0.712230537660838));
#42667=CARTESIAN_POINT('Ctrl Pts',(-66.6681941903091,-0.000864019930029195,
-0.678519636609795));
#42668=CARTESIAN_POINT('Ctrl Pts',(-65.5301702171886,1.98517432567173,-2.));
#42669=CARTESIAN_POINT('Ctrl Pts',(-65.5988381452818,1.9597491377265,-2.));
#42670=CARTESIAN_POINT('Ctrl Pts',(-65.6658026948317,1.93043476164841,-2.));
#42671=CARTESIAN_POINT('Ctrl Pts',(-65.7308748757751,1.89752507621341,-2.));
#42672=CARTESIAN_POINT('Ctrl Pts',(-65.7977553584739,1.86370085800765,-2.));
#42673=CARTESIAN_POINT('Ctrl Pts',(-65.8626376079658,1.8260780441936,-2.));
#42674=CARTESIAN_POINT('Ctrl Pts',(-65.9252852210993,1.78493106183313,-2.));
#42675=CARTESIAN_POINT('Ctrl Pts',(-65.9782205027365,1.75016314345881,-2.));
#42676=CARTESIAN_POINT('Ctrl Pts',(-66.0295599817195,1.71287801549812,-2.));
#42677=CARTESIAN_POINT('Ctrl Pts',(-66.0791382962128,1.67322322119406,-2.));
#42678=CARTESIAN_POINT('Ctrl Pts',(-66.101163220464,1.65560677235613,-2.));
#42679=CARTESIAN_POINT('Ctrl Pts',(-66.1228402691632,1.63752248214409,-2.));
#42680=CARTESIAN_POINT('Ctrl Pts',(-66.1441533920284,1.61898256263349,-2.));
#42681=CARTESIAN_POINT('Ctrl Pts',(-66.155865605901,1.60879430895232,-2.));
#42682=CARTESIAN_POINT('Ctrl Pts',(-66.1674679023596,1.59846845594816,-2.));
#42683=CARTESIAN_POINT('Ctrl Pts',(-66.1789574836616,1.58800698854217,-2.));
#42684=CARTESIAN_POINT('Ctrl Pts',(-66.189551288702,1.57836114129823,-2.));
#42685=CARTESIAN_POINT('Ctrl Pts',(-66.200050702827,1.56859848611553,-2.));
#42686=CARTESIAN_POINT('Ctrl Pts',(-66.2104376446146,1.55873603375639,-2.));
#42687=CARTESIAN_POINT('Ctrl Pts',(-66.2635229555616,1.50833126968935,-2.));
#42688=CARTESIAN_POINT('Ctrl Pts',(-66.313768296129,1.45523826476751,-2.));
#42689=CARTESIAN_POINT('Ctrl Pts',(-66.3609549723782,1.39971629736103,-2.));
#42690=CARTESIAN_POINT('Ctrl Pts',(-66.4077748713716,1.34462589658441,-2.));
#42691=CARTESIAN_POINT('Ctrl Pts',(-66.4515839789323,1.28714326375225,-2.));
#42692=CARTESIAN_POINT('Ctrl Pts',(-66.4921238713298,1.22749743717261,-2.));
#42693=CARTESIAN_POINT('Ctrl Pts',(-66.5258166843552,1.1779256311354,-2.));
#42694=CARTESIAN_POINT('Ctrl Pts',(-66.557250703582,1.12685898698918,-2.));
#42695=CARTESIAN_POINT('Ctrl Pts',(-66.5862499617227,1.07442250688702,-2.));
#42696=CARTESIAN_POINT('Ctrl Pts',(-66.5983545270548,1.05253502286566,-2.));
#42697=CARTESIAN_POINT('Ctrl Pts',(-66.6100345605411,1.03040883225302,-2.));
#42698=CARTESIAN_POINT('Ctrl Pts',(-66.6212758238105,1.00805294268584,-2.));
#42699=CARTESIAN_POINT('Ctrl Pts',(-66.626479288449,0.99770463235463,-2.));
#42700=CARTESIAN_POINT('Ctrl Pts',(-66.6315887267729,0.987307105195716,
-2.));
#42701=CARTESIAN_POINT('Ctrl Pts',(-66.6366026612658,0.976861256572228,
-2.));
#42702=CARTESIAN_POINT('Ctrl Pts',(-66.6418315208287,0.965967640880585,
-2.));
#42703=CARTESIAN_POINT('Ctrl Pts',(-66.6469528966416,0.95502894077258,-2.));
#42704=CARTESIAN_POINT('Ctrl Pts',(-66.6519637514146,0.944050420215775,
-2.));
#42705=CARTESIAN_POINT('Ctrl Pts',(-66.6805038460108,0.88152056664477,-2.));
#42706=CARTESIAN_POINT('Ctrl Pts',(-66.7054830227983,0.817657226303972,
-2.));
#42707=CARTESIAN_POINT('Ctrl Pts',(-66.7266778091886,0.752664675159687,
-2.));
#42708=CARTESIAN_POINT('Ctrl Pts',(-66.745888539861,0.693756112801375,-2.));
#42709=CARTESIAN_POINT('Ctrl Pts',(-66.761989915918,0.633919258266641,-2.));
#42710=CARTESIAN_POINT('Ctrl Pts',(-66.7747787781587,0.573301385906269,
-2.));
#42711=CARTESIAN_POINT('Ctrl Pts',(-66.7899084885612,0.501588137552653,
-2.));
#42712=CARTESIAN_POINT('Ctrl Pts',(-66.8004026737972,0.428780273118141,
-2.));
#42713=CARTESIAN_POINT('Ctrl Pts',(-66.8063365292405,0.355301138761098,
-2.));
#42714=CARTESIAN_POINT('Ctrl Pts',(-66.8076429326892,0.339123900294253,
-2.));
#42715=CARTESIAN_POINT('Ctrl Pts',(-66.8087280690516,0.322914206659548,
-2.));
#42716=CARTESIAN_POINT('Ctrl Pts',(-66.809592371063,0.306676740191003,-2.));
#42717=CARTESIAN_POINT('Ctrl Pts',(-66.8104842013183,0.289922106189788,
-2.));
#42718=CARTESIAN_POINT('Ctrl Pts',(-66.8111409153919,0.273131754426448,
-2.));
#42719=CARTESIAN_POINT('Ctrl Pts',(-66.8115624311287,0.256344928107124,
-2.));
#42720=CARTESIAN_POINT('Ctrl Pts',(-66.8132840454943,0.187781790785841,
-2.));
#42721=CARTESIAN_POINT('Ctrl Pts',(-66.8110938642221,0.119190445572534,
-2.));
#42722=CARTESIAN_POINT('Ctrl Pts',(-66.8051125395792,0.0509093848503468,
-2.));
#42723=CARTESIAN_POINT('Ctrl Pts',(-66.7991324434424,-0.0173576516048459,
-2.));
#42724=CARTESIAN_POINT('Ctrl Pts',(-66.7893623072956,-0.0853156030450349,
-2.));
#42725=CARTESIAN_POINT('Ctrl Pts',(-66.7758731021339,-0.152611158192487,
-2.));
#42726=CARTESIAN_POINT('Ctrl Pts',(-66.7661100688796,-0.201317418857648,
-2.));
#42727=CARTESIAN_POINT('Ctrl Pts',(-66.7543977966376,-0.249676426291085,
-2.));
#42728=CARTESIAN_POINT('Ctrl Pts',(-66.7407489756121,-0.297544567370963,
-2.));
#42729=CARTESIAN_POINT('Ctrl Pts',(-66.7305106871662,-0.33345153947013,
-2.));
#42730=CARTESIAN_POINT('Ctrl Pts',(-66.7191824845106,-0.369082153865889,
-2.));
#42731=CARTESIAN_POINT('Ctrl Pts',(-66.7067658073163,-0.404371614833105,
-2.));
#42732=CARTESIAN_POINT('Ctrl Pts',(-66.7026385143847,-0.416101801623694,
-2.));
#42733=CARTESIAN_POINT('Ctrl Pts',(-66.6983941579974,-0.427785083074775,
-2.));
#42734=CARTESIAN_POINT('Ctrl Pts',(-66.6940333669371,-0.439418945656692,
-2.));
#42735=CARTESIAN_POINT('Ctrl Pts',(-66.6709086373701,-0.501111863824717,
-2.));
#42736=CARTESIAN_POINT('Ctrl Pts',(-66.6445114917904,-0.561421289136837,
-2.));
#42737=CARTESIAN_POINT('Ctrl Pts',(-66.6148919773948,-0.620012996760754,
-2.));
#42738=CARTESIAN_POINT('Ctrl Pts',(-66.5940505455908,-0.661240380249061,
-2.));
#42739=CARTESIAN_POINT('Ctrl Pts',(-66.5716128408251,-0.701616780535153,
-2.));
#42740=CARTESIAN_POINT('Ctrl Pts',(-66.5475858839724,-0.741014396591259,
-2.));
#42741=CARTESIAN_POINT('Ctrl Pts',(-66.5398732602616,-0.753660983073549,
-2.));
#42742=CARTESIAN_POINT('Ctrl Pts',(-66.5319957124564,-0.766208337095444,
-2.));
#42743=CARTESIAN_POINT('Ctrl Pts',(-66.5239568318932,-0.778646543728548,
-2.));
#42744=CARTESIAN_POINT('Ctrl Pts',(-66.489711530036,-0.831632794408527,
-2.));
#42745=CARTESIAN_POINT('Ctrl Pts',(-66.4526108600326,-0.88253505652559,
-2.));
#42746=CARTESIAN_POINT('Ctrl Pts',(-66.4126890994474,-0.931037995737605,
-2.));
#42747=CARTESIAN_POINT('Ctrl Pts',(-66.3758798548211,-0.975759383982511,
-2.));
#42748=CARTESIAN_POINT('Ctrl Pts',(-66.3366716809453,-1.01844109086248,
-2.));
#42749=CARTESIAN_POINT('Ctrl Pts',(-66.295069969863,-1.05880296618531,-2.));
#42750=CARTESIAN_POINT('Ctrl Pts',(-66.2872852045854,-1.06635572585249,
-2.));
#42751=CARTESIAN_POINT('Ctrl Pts',(-66.279416574172,-1.07382715133633,-2.));
#42752=CARTESIAN_POINT('Ctrl Pts',(-66.2714656498818,-1.08121658606209,
-2.));
#42753=CARTESIAN_POINT('Origin',(-65.,8.88178419700125E-15,3.));
#42754=CARTESIAN_POINT('Origin',(-32.5,56.2916512459885,7.));
#42755=CARTESIAN_POINT('Ctrl Pts',(-33.041102980256,57.8673300091754,7.));
#42756=CARTESIAN_POINT('Ctrl Pts',(-32.9847118979873,57.8942994847411,7.));
#42757=CARTESIAN_POINT('Ctrl Pts',(-32.9268515768618,57.917755670378,7.));
#42758=CARTESIAN_POINT('Ctrl Pts',(-32.8678400671714,57.9378112590619,7.));
#42759=CARTESIAN_POINT('Ctrl Pts',(-32.8304073366668,57.9505331068888,7.));
#42760=CARTESIAN_POINT('Ctrl Pts',(-32.7925106112697,57.9618858705791,7.));
#42761=CARTESIAN_POINT('Ctrl Pts',(-32.7542246215315,57.9718900412361,7.));
#42762=CARTESIAN_POINT('Ctrl Pts',(-32.7280436567717,57.9787311557329,7.));
#42763=CARTESIAN_POINT('Ctrl Pts',(-32.7016805652138,57.9849415096174,7.));
#42764=CARTESIAN_POINT('Ctrl Pts',(-32.6751582403431,57.9905258831364,7.));
#42765=CARTESIAN_POINT('Ctrl Pts',(-32.661116442106,57.9934824356489,7.));
#42766=CARTESIAN_POINT('Ctrl Pts',(-32.647030211604,57.9962633358689,7.));
#42767=CARTESIAN_POINT('Ctrl Pts',(-32.6329169445875,57.9988669116766,7.));
#42768=CARTESIAN_POINT('Ctrl Pts',(-32.5680410965272,58.0108350256729,7.));
#42769=CARTESIAN_POINT('Ctrl Pts',(-32.5025225401415,58.0190759833092,7.));
#42770=CARTESIAN_POINT('Ctrl Pts',(-32.4367003119297,58.0236879112065,7.));
#42771=CARTESIAN_POINT('Ctrl Pts',(-32.3892242866025,58.0270143863442,7.));
#42772=CARTESIAN_POINT('Ctrl Pts',(-32.3415895128512,58.0284519444914,7.));
#42773=CARTESIAN_POINT('Ctrl Pts',(-32.2939162957138,58.0280221779993,7.));
#42774=CARTESIAN_POINT('Ctrl Pts',(-32.2808248420334,58.0279041606205,7.));
#42775=CARTESIAN_POINT('Ctrl Pts',(-32.2677304668452,58.0276452538024,7.));
#42776=CARTESIAN_POINT('Ctrl Pts',(-32.2546356188837,58.0272457331439,7.));
#42777=CARTESIAN_POINT('Ctrl Pts',(-32.2413147458909,58.0268393165162,7.));
#42778=CARTESIAN_POINT('Ctrl Pts',(-32.2280015697223,58.0262876036899,7.));
#42779=CARTESIAN_POINT('Ctrl Pts',(-32.2147036649184,58.0255917126641,7.));
#42780=CARTESIAN_POINT('Ctrl Pts',(-32.1469436448299,58.0220457713611,7.));
#42781=CARTESIAN_POINT('Ctrl Pts',(-32.0795415685586,58.0147589601543,7.));
#42782=CARTESIAN_POINT('Ctrl Pts',(-32.0128409972292,58.0038315324684,7.));
#42783=CARTESIAN_POINT('Ctrl Pts',(-31.9451753893333,57.992746004678,7.));
#42784=CARTESIAN_POINT('Ctrl Pts',(-31.8782306838316,57.9779139314839,7.));
#42785=CARTESIAN_POINT('Ctrl Pts',(-31.8123515211519,57.9593890229731,7.));
#42786=CARTESIAN_POINT('Ctrl Pts',(-31.7715359668474,57.9479118824244,7.));
#42787=CARTESIAN_POINT('Ctrl Pts',(-31.7311291966618,57.9350162531039,7.));
#42788=CARTESIAN_POINT('Ctrl Pts',(-31.6912132914853,57.9207048673026,7.));
#42789=CARTESIAN_POINT('Ctrl Pts',(-31.6585126282827,57.9089804229995,7.));
#42790=CARTESIAN_POINT('Ctrl Pts',(-31.6261413908417,57.8963056504121,7.));
#42791=CARTESIAN_POINT('Ctrl Pts',(-31.5941456455447,57.882678157395,7.));
#42792=CARTESIAN_POINT('Ctrl Pts',(-31.5810720086146,57.8771098890419,7.));
#42793=CARTESIAN_POINT('Ctrl Pts',(-31.5680588095099,57.8713813377768,7.));
#42794=CARTESIAN_POINT('Ctrl Pts',(-31.5551310603946,57.8655025241604,7.));
#42795=CARTESIAN_POINT('Ctrl Pts',(-31.4909683792072,57.8363249434027,7.));
#42796=CARTESIAN_POINT('Ctrl Pts',(-31.4287956225132,57.8034029003303,7.));
#42797=CARTESIAN_POINT('Ctrl Pts',(-31.3689686686499,57.7668089348087,7.));
#42798=CARTESIAN_POINT('Ctrl Pts',(-31.3623206919021,57.7627426099135,7.));
#42799=CARTESIAN_POINT('Ctrl Pts',(-31.3557016802768,57.758630892331,7.));
#42800=CARTESIAN_POINT('Ctrl Pts',(-31.349112123847,57.754473841822,7.));
#42801=CARTESIAN_POINT('Ctrl Pts',(-31.292085729188,57.7184984912095,7.));
#42802=CARTESIAN_POINT('Ctrl Pts',(-31.2372638568291,57.6791321880014,7.));
#42803=CARTESIAN_POINT('Ctrl Pts',(-31.1847406170358,57.6367028360825,7.));
#42804=CARTESIAN_POINT('Ctrl Pts',(-31.1282350066725,57.5910564434202,7.));
#42805=CARTESIAN_POINT('Ctrl Pts',(-31.0743888197007,57.5418647466793,7.));
#42806=CARTESIAN_POINT('Ctrl Pts',(-31.0233480125353,57.4894785917711,7.));
#42807=CARTESIAN_POINT('Ctrl Pts',(-31.0140057588989,57.4798900924238,7.));
#42808=CARTESIAN_POINT('Ctrl Pts',(-31.0047575878001,57.4701944335691,7.));
#42809=CARTESIAN_POINT('Ctrl Pts',(-30.9956045320055,57.4603935881043,7.));
#42810=CARTESIAN_POINT('Ctrl Pts',(-30.9877334098267,57.4519654026063,7.));
#42811=CARTESIAN_POINT('Ctrl Pts',(-30.9799390123112,57.4434662546016,7.));
#42812=CARTESIAN_POINT('Ctrl Pts',(-30.97222270825,57.4348989262801,7.));
#42813=CARTESIAN_POINT('Ctrl Pts',(-30.9246610656086,57.382091752692,7.));
#42814=CARTESIAN_POINT('Ctrl Pts',(-30.8800520828446,57.3266849226614,6.99999999999999));
#42815=CARTESIAN_POINT('Ctrl Pts',(-30.8384919343084,57.269046905134,7.));
#42816=CARTESIAN_POINT('Ctrl Pts',(-30.7960555283788,57.2101936431771,7.));
#42817=CARTESIAN_POINT('Ctrl Pts',(-30.7567972001627,57.1490134676405,7.));
#42818=CARTESIAN_POINT('Ctrl Pts',(-30.7208469685291,57.0858509474018,7.));
#42819=CARTESIAN_POINT('Ctrl Pts',(-30.6846788708758,57.0223056489095,7.));
#42820=CARTESIAN_POINT('Ctrl Pts',(-30.6518584166819,56.9567530677491,7.));
#42821=CARTESIAN_POINT('Ctrl Pts',(-30.6225557949111,56.8895077656693,7.));
#42822=CARTESIAN_POINT('Ctrl Pts',(-30.615313982694,56.8728888482922,7.));
#42823=CARTESIAN_POINT('Ctrl Pts',(-30.6082872382863,56.8561664056305,7.));
#42824=CARTESIAN_POINT('Ctrl Pts',(-30.6014785581591,56.8393449403756,7.));
#42825=CARTESIAN_POINT('Ctrl Pts',(-30.5961524551096,56.8261863170131,7.));
#42826=CARTESIAN_POINT('Ctrl Pts',(-30.5909593216311,56.8129655376061,7.));
#42827=CARTESIAN_POINT('Ctrl Pts',(-30.5859080295463,56.7997050114821,7.));
#42828=CARTESIAN_POINT('Ctrl Pts',(-30.5590883752802,56.7292987233359,7.));
#42829=CARTESIAN_POINT('Ctrl Pts',(-30.5362121102038,56.657649445443,7.));
#42830=CARTESIAN_POINT('Ctrl Pts',(-30.5174063250598,56.5851265990605,7.));
#42831=CARTESIAN_POINT('Ctrl Pts',(-30.4985800831807,56.5125248630894,7.));
#42832=CARTESIAN_POINT('Ctrl Pts',(-30.4838325489097,56.4390467229768,7.));
#42833=CARTESIAN_POINT('Ctrl Pts',(-30.473332189023,56.3650308461601,7.));
#42834=CARTESIAN_POINT('Ctrl Pts',(-30.4630708240431,56.2926996180384,7.));
#42835=CARTESIAN_POINT('Ctrl Pts',(-30.4568650767968,56.2198539025132,7.));
#42836=CARTESIAN_POINT('Ctrl Pts',(-30.4549187470094,56.1467933162297,7.));
#42837=CARTESIAN_POINT('Ctrl Pts',(-30.4545002099142,56.1310824301527,7.));
#42838=CARTESIAN_POINT('Ctrl Pts',(-30.454278824166,56.1153615760157,7.));
#42839=CARTESIAN_POINT('Ctrl Pts',(-30.4542569357503,56.0996336954517,7.));
#42840=CARTESIAN_POINT('Ctrl Pts',(-30.4542384011809,56.0863157149704,7.));
#42841=CARTESIAN_POINT('Ctrl Pts',(-30.4543629142851,56.0729926961468,7.));
#42842=CARTESIAN_POINT('Ctrl Pts',(-30.4546294175093,56.0596661744468,7.));
#42843=CARTESIAN_POINT('Ctrl Pts',(-30.845746263986,55.0728640868079,7.));
#42844=CARTESIAN_POINT('Ctrl Pts',(-30.8954489009033,55.0171697369536,7.));
#42845=CARTESIAN_POINT('Ctrl Pts',(-30.9483278083006,54.9645336576551,7.));
#42846=CARTESIAN_POINT('Ctrl Pts',(-31.0040355064145,54.9150549467046,7.));
#42847=CARTESIAN_POINT('Ctrl Pts',(-31.0582842091438,54.8668720927604,7.));
#42848=CARTESIAN_POINT('Ctrl Pts',(-31.1152164855349,54.8216833321975,7.));
#42849=CARTESIAN_POINT('Ctrl Pts',(-31.1745316088105,54.7796213191364,7.));
#42850=CARTESIAN_POINT('Ctrl Pts',(-31.1877704600013,54.7702332794435,7.));
#42851=CARTESIAN_POINT('Ctrl Pts',(-31.2011298594679,54.7609999646249,7.));
#42852=CARTESIAN_POINT('Ctrl Pts',(-31.2146007867298,54.7519269992828,7.));
#42853=CARTESIAN_POINT('Ctrl Pts',(-31.2764177232488,54.7102919349934,7.));
#42854=CARTESIAN_POINT('Ctrl Pts',(-31.3404582881863,54.6721113380502,7.));
#42855=CARTESIAN_POINT('Ctrl Pts',(-31.4063841817531,54.6375086610803,7.));
#42856=CARTESIAN_POINT('Ctrl Pts',(-31.4526685064183,54.6132153000274,7.));
#42857=CARTESIAN_POINT('Ctrl Pts',(-31.4998826447241,54.5906864697851,7.));
#42858=CARTESIAN_POINT('Ctrl Pts',(-31.5479126490946,54.5699799287714,7.));
#42859=CARTESIAN_POINT('Ctrl Pts',(-31.5661734309803,54.5621073992138,7.));
#42860=CARTESIAN_POINT('Ctrl Pts',(-31.5845521539812,54.5544984108625,7.));
#42861=CARTESIAN_POINT('Ctrl Pts',(-31.6030425578044,54.547156631718,7.));
#42862=CARTESIAN_POINT('Ctrl Pts',(-31.620650668295,54.5401651749813,7.));
#42863=CARTESIAN_POINT('Ctrl Pts',(-31.6383657025794,54.5334141284368,7.));
#42864=CARTESIAN_POINT('Ctrl Pts',(-31.6561506799727,54.5269179584906,7.));
#42865=CARTESIAN_POINT('Ctrl Pts',(-31.7243409104461,54.5020106833212,7.));
#42866=CARTESIAN_POINT('Ctrl Pts',(-31.7936290801199,54.4808156486368,6.99999999999999));
#42867=CARTESIAN_POINT('Ctrl Pts',(-31.8637026772369,54.4634492155475,7.));
#42868=CARTESIAN_POINT('Ctrl Pts',(-31.9322713956587,54.4464557385536,7.));
#42869=CARTESIAN_POINT('Ctrl Pts',(-32.0015931056162,54.4331281708393,7.));
#42870=CARTESIAN_POINT('Ctrl Pts',(-32.0713763155884,54.4236245382242,7.));
#42871=CARTESIAN_POINT('Ctrl Pts',(-32.1396290845225,54.4143293332434,7.));
#42872=CARTESIAN_POINT('Ctrl Pts',(-32.2083241026487,54.4086921780503,7.));
#42873=CARTESIAN_POINT('Ctrl Pts',(-32.2771775099492,54.406908383857,7.));
#42874=CARTESIAN_POINT('Ctrl Pts',(-32.2995513064291,54.4063287429966,7.));
#42875=CARTESIAN_POINT('Ctrl Pts',(-32.3219416905641,54.4061563640051,7.));
#42876=CARTESIAN_POINT('Ctrl Pts',(-32.3443384584988,54.4063990611232,7.));
#42877=CARTESIAN_POINT('Ctrl Pts',(-32.3569726506304,54.4065359684675,7.));
#42878=CARTESIAN_POINT('Ctrl Pts',(-32.3696101789338,54.4068051101078,7.));
#42879=CARTESIAN_POINT('Ctrl Pts',(-32.3822313250428,54.4072071047712,7.));
#42880=CARTESIAN_POINT('Ctrl Pts',(-32.4504997768709,54.4093815153262,7.));
#42881=CARTESIAN_POINT('Ctrl Pts',(-32.5184090635457,54.415438958281,7.));
#42882=CARTESIAN_POINT('Ctrl Pts',(-32.585689693705,54.425518870341,7.));
#42883=CARTESIAN_POINT('Ctrl Pts',(-32.5954003976719,54.4269737176246,7.));
#42884=CARTESIAN_POINT('Ctrl Pts',(-32.6050979864,54.4285124457434,7.));
#42885=CARTESIAN_POINT('Ctrl Pts',(-32.6147816267372,54.4301355621262,7.));
#42886=CARTESIAN_POINT('Ctrl Pts',(-32.6832009663017,54.4416036203236,7.));
#42887=CARTESIAN_POINT('Ctrl Pts',(-32.7509260352975,54.4572806254693,7.));
#42888=CARTESIAN_POINT('Ctrl Pts',(-32.8176612516198,54.4769468185411,7.));
#42889=CARTESIAN_POINT('Ctrl Pts',(-32.8799198172771,54.4952937879535,7.));
#42890=CARTESIAN_POINT('Ctrl Pts',(-32.9413172465657,54.5171136895481,7.));
#42891=CARTESIAN_POINT('Ctrl Pts',(-33.001588117662,54.5422590913447,7.));
#42892=CARTESIAN_POINT('Ctrl Pts',(-33.0148899910673,54.5478087199686,7.));
#42893=CARTESIAN_POINT('Ctrl Pts',(-33.0281368750967,54.553520427381,7.));
#42894=CARTESIAN_POINT('Ctrl Pts',(-33.0413257085627,54.5593927822482,7.));
#42895=CARTESIAN_POINT('Ctrl Pts',(-33.0516354979444,54.5639832368939,7.));
#42896=CARTESIAN_POINT('Ctrl Pts',(-33.0619091366824,54.5686716446581,7.));
#42897=CARTESIAN_POINT('Ctrl Pts',(-33.0721334453033,54.5734515734285,7.));
#42898=CARTESIAN_POINT('Ctrl Pts',(-33.1340731263268,54.6024087649934,7.));
#42899=CARTESIAN_POINT('Ctrl Pts',(-33.1943201438779,54.6347718932848,7.));
#42900=CARTESIAN_POINT('Ctrl Pts',(-33.2526025547971,54.6703158300039,7.));
#42901=CARTESIAN_POINT('Ctrl Pts',(-33.3106158338828,54.7056956347883,7.));
#42902=CARTESIAN_POINT('Ctrl Pts',(-33.3666833863001,54.7442277671715,7.));
#42903=CARTESIAN_POINT('Ctrl Pts',(-33.4205013719045,54.7857268573937,7.));
#42904=CARTESIAN_POINT('Ctrl Pts',(-33.4731665002094,54.8263369784627,7.));
#42905=CARTESIAN_POINT('Ctrl Pts',(-33.5236779675191,54.8697891009662,7.));
#42906=CARTESIAN_POINT('Ctrl Pts',(-33.5717071750615,54.9159326392887,7.));
#42907=CARTESIAN_POINT('Ctrl Pts',(-33.5818268625425,54.9256550188778,7.));
#42908=CARTESIAN_POINT('Ctrl Pts',(-33.5918361779058,54.9354969405856,7.));
#42909=CARTESIAN_POINT('Ctrl Pts',(-33.6017317565417,54.9454570807147,7.));
#42910=CARTESIAN_POINT('Ctrl Pts',(-33.6111117333518,54.9548982550889,7.));
#42911=CARTESIAN_POINT('Ctrl Pts',(-33.6203906591309,54.9644470262927,7.));
#42912=CARTESIAN_POINT('Ctrl Pts',(-33.6295510503765,54.9740864760303,7.));
#42913=CARTESIAN_POINT('Ctrl Pts',(-33.6745642994388,55.021453770748,7.));
#42914=CARTESIAN_POINT('Ctrl Pts',(-33.7168018660127,55.0710902386183,7.));
#42915=CARTESIAN_POINT('Ctrl Pts',(-33.7559956007795,55.1228219100991,7.));
#42916=CARTESIAN_POINT('Ctrl Pts',(-33.7944439256698,55.1735697177282,7.));
#42917=CARTESIAN_POINT('Ctrl Pts',(-33.8299635738862,55.226334532935,7.));
#42918=CARTESIAN_POINT('Ctrl Pts',(-33.8622555274099,55.2809712641021,7.));
#42919=CARTESIAN_POINT('Ctrl Pts',(-33.8934985743347,55.3338332860427,7.));
#42920=CARTESIAN_POINT('Ctrl Pts',(-33.9217204567444,55.3884482092219,7.));
#42921=CARTESIAN_POINT('Ctrl Pts',(-33.9466019283097,55.4446928631591,7.));
#42922=CARTESIAN_POINT('Ctrl Pts',(-33.9507443557826,55.4540568350232,7.));
#42923=CARTESIAN_POINT('Ctrl Pts',(-33.9547940777389,55.4634659866381,7.));
#42924=CARTESIAN_POINT('Ctrl Pts',(-33.9587494776696,55.4729197548336,7.));
#42925=CARTESIAN_POINT('Ctrl Pts',(-33.9629351903496,55.4829239915992,7.));
#42926=CARTESIAN_POINT('Ctrl Pts',(-33.9670152760995,55.4929781929138,7.));
#42927=CARTESIAN_POINT('Ctrl Pts',(-33.9709895856635,55.5030806790321,7.));
#42928=CARTESIAN_POINT('Origin',(-32.5,56.2916512459885,-3.54592528053767));
#42929=CARTESIAN_POINT('Ctrl Pts',(-33.5295805874755,58.0719425970214,-1.79592528053768));
#42930=CARTESIAN_POINT('Ctrl Pts',(-33.61511160178,58.0235064542128,-1.79058130531689));
#42931=CARTESIAN_POINT('Ctrl Pts',(-34.2640553995263,57.5898394701862,-1.74819136657341));
#42932=CARTESIAN_POINT('Ctrl Pts',(-34.9180311095446,56.062943931961,-1.66875546430726));
#42933=CARTESIAN_POINT('Ctrl Pts',(-33.6191501107478,54.1363165628764,-1.55761757373921));
#42934=CARTESIAN_POINT('Ctrl Pts',(-31.2961996587746,54.182342369509,-1.44647968317118));
#42935=CARTESIAN_POINT('Ctrl Pts',(-30.0749499288325,56.1591174155132,-1.33534179260313));
#42936=CARTESIAN_POINT('Ctrl Pts',(-31.0734520820823,58.2571645498346,-1.22420390203509));
#42937=CARTESIAN_POINT('Ctrl Pts',(-32.7280434754779,58.4718761792196,-1.14439839801327));
#42938=CARTESIAN_POINT('Ctrl Pts',(-33.436201766478,58.1266820552905,-1.10163885751414));
#42939=CARTESIAN_POINT('Ctrl Pts',(-33.5268019957928,58.0733321975144,-1.09592528053768));
#42940=CARTESIAN_POINT('Ctrl Pts',(-33.5243188290626,58.0704843676251,-1.85407471946232));
#42941=CARTESIAN_POINT('Ctrl Pts',(-33.9297573522988,57.832304408809,-1.82862455259619));
#42942=CARTESIAN_POINT('Ctrl Pts',(-34.7395102025176,56.9114816531043,-1.76612842220737));
#42943=CARTESIAN_POINT('Ctrl Pts',(-34.4535014835806,54.8495668967864,-1.66658632829587));
#42944=CARTESIAN_POINT('Ctrl Pts',(-32.3487507516394,53.8677941230741,-1.55544843772783));
#42945=CARTESIAN_POINT('Ctrl Pts',(-30.3811218874153,55.1044118987673,-1.44431054715979));
#42946=CARTESIAN_POINT('Ctrl Pts',(-30.3535878576005,57.4278205885651,-1.33317265659175));
#42947=CARTESIAN_POINT('Ctrl Pts',(-32.0395408012642,58.5450270011374,-1.23642738069259));
#42948=CARTESIAN_POINT('Ctrl Pts',(-33.1630292684131,58.2758908569842,-1.17672806831612));
#42949=CARTESIAN_POINT('Ctrl Pts',(-33.5270487244507,58.0682282925651,-1.15407471946232));
#42950=CARTESIAN_POINT('Ctrl Pts',(-32.8002165734084,54.652924298309,-2.));
#42951=CARTESIAN_POINT('Ctrl Pts',(-32.2553008763615,54.5530951452,-1.96295403647732));
#42952=CARTESIAN_POINT('Ctrl Pts',(-31.067360018651,54.9418786009695,-1.88886210943196));
#42953=CARTESIAN_POINT('Ctrl Pts',(-30.5876880485778,56.766296704464,-1.77772421886392));
#42954=CARTESIAN_POINT('Ctrl Pts',(-31.862316082722,58.1542462926903,-1.66658632829587));
#42955=CARTESIAN_POINT('Ctrl Pts',(-33.7186881749666,57.8383051703362,-1.55544843772783));
#42956=CARTESIAN_POINT('Ctrl Pts',(-34.4605498617843,56.1062143874073,-1.44431054715979));
#42957=CARTESIAN_POINT('Ctrl Pts',(-33.4074116483786,54.5440967590365,-1.33317265659175));
#42958=CARTESIAN_POINT('Ctrl Pts',(-31.5239535863334,54.5814146779316,-1.22203476602371));
#42959=CARTESIAN_POINT('Ctrl Pts',(-30.5337591344129,56.1841922550788,-1.11089687545567));
#42960=CARTESIAN_POINT('Ctrl Pts',(-31.3433489080176,57.8852977549105,-0.999758984887625));
#42961=CARTESIAN_POINT('Ctrl Pts',(-33.2116035654679,58.127735859695,-0.888621094319583));
#42962=CARTESIAN_POINT('Ctrl Pts',(-34.4285349719857,56.689577194601,-0.777483203751541));
#42963=CARTESIAN_POINT('Ctrl Pts',(-33.880248629212,54.8871962644417,-0.6663453131835));
#42964=CARTESIAN_POINT('Ctrl Pts',(-32.068608990815,54.3703269630488,-0.555207422615458));
#42965=CARTESIAN_POINT('Ctrl Pts',(-30.6518244621988,55.6120685434762,-0.444069532047416));
#42966=CARTESIAN_POINT('Ctrl Pts',(-30.9266969543788,57.4758393880094,-0.332931641479374));
#42967=CARTESIAN_POINT('Ctrl Pts',(-32.6416310686724,58.2557096429586,-0.221793750911333));
#42968=CARTESIAN_POINT('Ctrl Pts',(-34.2269289097961,57.2378548494304,-0.11065586034329));
#42969=CARTESIAN_POINT('Ctrl Pts',(-34.2315490093866,55.3539292291843,0.000482030224750697));
#42970=CARTESIAN_POINT('Ctrl Pts',(-32.6512627267286,54.3283111741666,0.111619920792793));
#42971=CARTESIAN_POINT('Ctrl Pts',(-30.9325239231375,55.0997605683742,0.222757811360834));
#42972=CARTESIAN_POINT('Ctrl Pts',(-30.648513765023,56.9621610088766,0.333895701928876));
#42973=CARTESIAN_POINT('Ctrl Pts',(-32.0591899470587,58.2108362632709,0.445033592496918));
#42974=CARTESIAN_POINT('Ctrl Pts',(-33.8733445736998,57.7028597043182,0.55617148306496));
#42975=CARTESIAN_POINT('Ctrl Pts',(-34.4304613352259,55.9031880402636,0.667309373633001));
#42976=CARTESIAN_POINT('Ctrl Pts',(-33.2206049447144,54.4590811533792,0.778447264201042));
#42977=CARTESIAN_POINT('Ctrl Pts',(-31.3511706755799,54.6923464552708,0.889585154769085));
#42978=CARTESIAN_POINT('Ctrl Pts',(-30.5332729159539,56.3894735693294,1.00072304533713));
#42979=CARTESIAN_POINT('Ctrl Pts',(-31.5155427604288,57.9970628015172,1.11186093590517));
#42980=CARTESIAN_POINT('Ctrl Pts',(-33.3988974808522,58.0436694962151,1.22299882647321));
#42981=CARTESIAN_POINT('Ctrl Pts',(-34.4594811428284,56.4866340172583,1.33413671704125));
#42982=CARTESIAN_POINT('Ctrl Pts',(-33.7265294927624,54.7511285964951,1.44527460760929));
#42983=CARTESIAN_POINT('Ctrl Pts',(-31.8709214881723,54.4256810275324,1.55641249817734));
#42984=CARTESIAN_POINT('Ctrl Pts',(-30.5911161796977,55.808177161062,1.66755038874538));
#42985=CARTESIAN_POINT('Ctrl Pts',(-31.0585338801586,57.633202607495,1.77868827931342));
#42986=CARTESIAN_POINT('Ctrl Pts',(-32.845341867449,58.2302908785132,1.88982616988146));
#42987=CARTESIAN_POINT('Ctrl Pts',(-34.3160545270196,57.0529203082132,2.0009640604495));
#42988=CARTESIAN_POINT('Ctrl Pts',(-34.1245118825503,55.1787515318803,2.11210195101754));
#42989=CARTESIAN_POINT('Ctrl Pts',(-32.4460350887648,54.323232485012,2.22323984158559));
#42990=CARTESIAN_POINT('Ctrl Pts',(-30.8169529902366,55.2694294534524,2.33437773215363));
#42991=CARTESIAN_POINT('Ctrl Pts',(-30.7283829067961,57.1512776213849,2.44551562272167));
#42992=CARTESIAN_POINT('Ctrl Pts',(-32.2613940402695,58.2463000190907,2.55665351328971));
#42993=CARTESIAN_POINT('Ctrl Pts',(-34.0128039146597,57.5522102275515,2.66779140385775));
#42994=CARTESIAN_POINT('Ctrl Pts',(-34.3795272095987,55.7043165044764,2.77892929442579));
#42995=CARTESIAN_POINT('Ctrl Pts',(-33.0258979343037,54.3940169311364,2.89006718499384));
#42996=CARTESIAN_POINT('Ctrl Pts',(-31.1909083156522,54.8206435668173,3.00120507556188));
#42997=CARTESIAN_POINT('Ctrl Pts',(-30.5541451617937,56.5937002136053,3.11234296612992));
#42998=CARTESIAN_POINT('Ctrl Pts',(-31.6984450088403,58.0902880148654,3.22348085669796));
#42999=CARTESIAN_POINT('Ctrl Pts',(-33.5764172295469,57.9405631836441,3.334618747266));
#43000=CARTESIAN_POINT('Ctrl Pts',(-34.4691325526482,56.2815705559534,3.44575663783405));
#43001=CARTESIAN_POINT('Ctrl Pts',(-33.5594785188274,54.6318048981748,3.55689452840209));
#43002=CARTESIAN_POINT('Ctrl Pts',(-31.6800717814225,54.5013154264873,3.66803241897013));
#43003=CARTESIAN_POINT('Ctrl Pts',(-30.5511546410956,56.0095406341798,3.77917030953817));
#43004=CARTESIAN_POINT('Ctrl Pts',(-31.2060377591922,57.7759848842099,3.89030820010622));
#43005=CARTESIAN_POINT('Ctrl Pts',(-33.0452991908126,58.183801721693,4.00144609067425));
#43006=CARTESIAN_POINT('Ctrl Pts',(-34.3854420890035,56.8597117703073,4.1125839812423));
#43007=CARTESIAN_POINT('Ctrl Pts',(-33.9998184606928,55.0156695787891,4.22372187181034));
#43008=CARTESIAN_POINT('Ctrl Pts',(-32.2413939863492,54.3395478778331,4.33485976237838));
#43009=CARTESIAN_POINT('Ctrl Pts',(-30.7196745288183,55.4502085281907,4.44599765294642));
#43010=CARTESIAN_POINT('Ctrl Pts',(-30.8275071658684,57.3310512405927,4.55713554351446));
#43011=CARTESIAN_POINT('Ctrl Pts',(-32.4661914602743,58.2605193506652,4.66827343408251));
#43012=CARTESIAN_POINT('Ctrl Pts',(-34.135821096663,57.3878601553884,4.77941132465054));
#43013=CARTESIAN_POINT('Ctrl Pts',(-34.3081651275095,55.5118285147887,4.89054921521859));
#43014=CARTESIAN_POINT('Ctrl Pts',(-32.8254751197057,54.3495774612489,5.00168710578663));
#43015=CARTESIAN_POINT('Ctrl Pts',(-31.0448740266845,54.9649285726684,5.11282499635467));
#43016=CARTESIAN_POINT('Ctrl Pts',(-30.5961662731526,56.7946439827405,5.22396288692271));
#43017=CARTESIAN_POINT('Ctrl Pts',(-31.8900590533423,58.1639644570316,5.33510077749076));
#43018=CARTESIAN_POINT('Ctrl Pts',(-33.7422378333798,57.8195353749858,5.4462386680588));
#43019=CARTESIAN_POINT('Ctrl Pts',(-34.4573819695178,56.076616703484,5.55737655862684));
#43020=CARTESIAN_POINT('Ctrl Pts',(-33.3809127223489,54.5305214257639,5.66851444919489));
#43021=CARTESIAN_POINT('Ctrl Pts',(-31.4981330119909,54.5964085667956,5.77965233976292));
#43022=CARTESIAN_POINT('Ctrl Pts',(-30.532375624067,56.2139699170398,5.89079023033097));
#43023=CARTESIAN_POINT('Ctrl Pts',(-31.3676029490313,57.9026351433967,6.001928120899));
#43024=CARTESIAN_POINT('Ctrl Pts',(-33.2393344828578,58.116746001209,6.11306601146706));
#43025=CARTESIAN_POINT('Ctrl Pts',(-34.4343281672319,56.6603319824484,6.22420390203508));
#43026=CARTESIAN_POINT('Ctrl Pts',(-33.8588424113751,54.8664502505917,6.33534179260314));
#43027=CARTESIAN_POINT('Ctrl Pts',(-32.039526963185,54.3770911652606,6.44647968317117));
#43028=CARTESIAN_POINT('Ctrl Pts',(-30.6418187305185,55.640110798873,6.55761757373922));
#43029=CARTESIAN_POINT('Ctrl Pts',(-30.9446640768632,57.4995720858052,6.66875546430725));
#43030=CARTESIAN_POINT('Ctrl Pts',(-32.6716452510335,58.2532519029269,6.7798933548753));
#43031=CARTESIAN_POINT('Ctrl Pts',(-34.2404831962863,57.2117704392446,6.89103124544334));
#43032=CARTESIAN_POINT('Ctrl Pts',(-34.2183071453089,55.3274697977207,7.00216913601138));
#43033=CARTESIAN_POINT('Ctrl Pts',(-32.6190914442239,54.3269220694063,7.11330702657942));
#43034=CARTESIAN_POINT('Ctrl Pts',(-31.4873233416682,54.8574472987172,7.18739895362479));
#43035=CARTESIAN_POINT('Ctrl Pts',(-31.1587240665778,55.3034534568682,7.22444491714747));
#43036=CARTESIAN_POINT('Ctrl Pts',(-32.8235677524625,54.525462293325,-2.07481497238249));
#43037=CARTESIAN_POINT('Ctrl Pts',(-32.2362679063105,54.4178683176326,-2.03776900885981));
#43038=CARTESIAN_POINT('Ctrl Pts',(-30.9559276871686,54.8368917830921,-1.96367708181445));
#43039=CARTESIAN_POINT('Ctrl Pts',(-30.4389462976543,56.8032151562412,-1.85253919124641));
#43040=CARTESIAN_POINT('Ctrl Pts',(-31.8127163182479,58.2991210074573,-1.74140130067836));
#43041=CARTESIAN_POINT('Ctrl Pts',(-33.813479096939,57.9586056331394,-1.63026341011032));
#43042=CARTESIAN_POINT('Ctrl Pts',(-34.6130436110377,56.0917909022585,-1.51912551954228));
#43043=CARTESIAN_POINT('Ctrl Pts',(-33.477991135835,54.4081700269832,-1.40798762897424));
#43044=CARTESIAN_POINT('Ctrl Pts',(-31.4480356104804,54.448390575124,-1.29684973840619));
#43045=CARTESIAN_POINT('Ctrl Pts',(-30.3808227325528,56.1758339752236,-1.18571184783816));
#43046=CARTESIAN_POINT('Ctrl Pts',(-31.2533832993725,58.0092533532185,-1.07457395727011));
#43047=CARTESIAN_POINT('Ctrl Pts',(-33.2669528824098,58.2705485634922,-0.963436066702072));
#43048=CARTESIAN_POINT('Ctrl Pts',(-34.5785385674958,56.7205283175548,-0.85229817613403));
#43049=CARTESIAN_POINT('Ctrl Pts',(-33.9876059030427,54.7779561935981,-0.741160285565988));
#43050=CARTESIAN_POINT('Ctrl Pts',(-32.0350549182219,54.2208842229542,-0.630022394997947));
#43051=CARTESIAN_POINT('Ctrl Pts',(-30.5080713128749,55.5592098448765,-0.518884504429905));
#43052=CARTESIAN_POINT('Ctrl Pts',(-30.8043236932773,57.5679468590399,-0.407746613861863));
#43053=CARTESIAN_POINT('Ctrl Pts',(-32.6526472907505,58.4084762899819,-0.296608723293822));
#43054=CARTESIAN_POINT('Ctrl Pts',(-34.3612513615134,57.3114516183055,-0.185470832725779));
#43055=CARTESIAN_POINT('Ctrl Pts',(-34.3662308175897,55.2809921675532,-0.0743329421577381));
#43056=CARTESIAN_POINT('Ctrl Pts',(-32.6630281098851,54.1756003992724,0.0368049484103043));
#43057=CARTESIAN_POINT('Ctrl Pts',(-30.8106038901482,55.0070539855567,0.147942838978346));
#43058=CARTESIAN_POINT('Ctrl Pts',(-30.5045031059899,57.0143140041392,0.259080729546387));
#43059=CARTESIAN_POINT('Ctrl Pts',(-32.024903250764,58.3601126089029,0.370218620114429));
#43060=CARTESIAN_POINT('Ctrl Pts',(-33.9801648424124,57.8126250680988,0.48135651068247));
#43061=CARTESIAN_POINT('Ctrl Pts',(-34.5806147654118,55.8729729399783,0.592494401250512));
#43062=CARTESIAN_POINT('Ctrl Pts',(-33.2766543989477,54.3165418129426,0.703632291818553));
#43063=CARTESIAN_POINT('Ctrl Pts',(-31.2618134527171,54.5679507495101,0.814770182386596));
#43064=CARTESIAN_POINT('Ctrl Pts',(-30.3802986954812,56.3970822984609,0.925908072954637));
#43065=CARTESIAN_POINT('Ctrl Pts',(-31.4389705811804,58.1297116094828,1.03704596352268));
#43066=CARTESIAN_POINT('Ctrl Pts',(-33.4688147268869,58.1799434247416,1.14818385409072));
#43067=CARTESIAN_POINT('Ctrl Pts',(-34.6118917659325,56.5017999941153,1.25932174465876));
#43068=CARTESIAN_POINT('Ctrl Pts',(-33.8219303211561,54.6313050310708,1.3704596352268));
#43069=CARTESIAN_POINT('Ctrl Pts',(-31.8219910617071,54.2805437881517,1.48159752579485));
#43070=CARTESIAN_POINT('Ctrl Pts',(-30.4426410726264,55.7705720088982,1.59273541636289));
#43071=CARTESIAN_POINT('Ctrl Pts',(-30.9464150418056,57.737549964795,1.70387330693093));
#43072=CARTESIAN_POINT('Ctrl Pts',(-32.872202942073,58.381080425761,1.81501119749897));
#43073=CARTESIAN_POINT('Ctrl Pts',(-34.4573092683919,57.1121326627429,1.92614908806701));
#43074=CARTESIAN_POINT('Ctrl Pts',(-34.2508682239552,55.0921889540773,2.03728697863506));
#43075=CARTESIAN_POINT('Ctrl Pts',(-32.4418376379359,54.1701266840256,2.1484248692031));
#43076=CARTESIAN_POINT('Ctrl Pts',(-30.6860437215201,55.1899199052635,2.25956275977114));
#43077=CARTESIAN_POINT('Ctrl Pts',(-30.5905845584602,57.2181403171501,2.37070065033918));
#43078=CARTESIAN_POINT('Ctrl Pts',(-32.2428350032856,58.3983347751019,2.48183854090722));
#43079=CARTESIAN_POINT('Ctrl Pts',(-34.1304714860531,57.6502579074399,2.59297643147527));
#43080=CARTESIAN_POINT('Ctrl Pts',(-34.5257189268319,55.6586329549041,2.70411432204331));
#43081=CARTESIAN_POINT('Ctrl Pts',(-33.0668028606663,54.2464168231134,2.81525221261135));
#43082=CARTESIAN_POINT('Ctrl Pts',(-31.0890857081512,54.7062269531163,2.92639010317939));
#43083=CARTESIAN_POINT('Ctrl Pts',(-30.4027944078216,56.6171939183194,3.03752799374743));
#43084=CARTESIAN_POINT('Ctrl Pts',(-31.636099169942,58.2301879836331,3.14866588431547));
#43085=CARTESIAN_POINT('Ctrl Pts',(-33.660142159116,58.0688173884788,3.25980377488351));
#43086=CARTESIAN_POINT('Ctrl Pts',(-34.6222938731447,56.2807864686682,3.37094166545156));
#43087=CARTESIAN_POINT('Ctrl Pts',(-33.6418859366334,54.5027002027542,3.4820795560196));
#43088=CARTESIAN_POINT('Ctrl Pts',(-31.6162968524566,54.3620611147965,3.59321744658764));
#43089=CARTESIAN_POINT('Ctrl Pts',(-30.3995712810968,55.9875977569607,3.70435533715568));
#43090=CARTESIAN_POINT('Ctrl Pts',(-31.1053919366404,57.8914380058304,3.81549322772372));
#43091=CARTESIAN_POINT('Ctrl Pts',(-33.0877131684893,58.3309752906065,3.92663111829177));
#43092=CARTESIAN_POINT('Ctrl Pts',(-34.5320938721368,56.903896149825,4.0377690088598));
#43093=CARTESIAN_POINT('Ctrl Pts',(-34.116476009031,54.9164223052549,4.14890689942785));
#43094=CARTESIAN_POINT('Ctrl Pts',(-32.2212793229225,54.1877111062503,4.26004478999589));
#43095=CARTESIAN_POINT('Ctrl Pts',(-30.5811988331557,55.3847601775417,4.37118268056394));
#43096=CARTESIAN_POINT('Ctrl Pts',(-30.6974188126734,57.4118969284483,4.48232057113197));
#43097=CARTESIAN_POINT('Ctrl Pts',(-32.4635617944443,58.4136601021044,4.59345846170002));
#43098=CARTESIAN_POINT('Ctrl Pts',(-34.2630570813224,57.4731245038336,4.70459635226806));
#43099=CARTESIAN_POINT('Ctrl Pts',(-34.4488062226114,55.4511730352461,4.8157342428361));
#43100=CARTESIAN_POINT('Ctrl Pts',(-32.8507909365896,54.1985208018218,4.92687213340414));
#43101=CARTESIAN_POINT('Ctrl Pts',(-30.9316927097324,54.8617346072315,5.03801002397219));
#43102=CARTESIAN_POINT('Ctrl Pts',(-30.4480839679681,56.8337673173569,5.14914791454022));
#43103=CARTESIAN_POINT('Ctrl Pts',(-31.8426171679856,58.3095950614319,5.26028580510827));
#43104=CARTESIAN_POINT('Ctrl Pts',(-33.8388604739813,57.9383759022263,5.37142369567631));
#43105=CARTESIAN_POINT('Ctrl Pts',(-34.6096293165867,56.0598910775539,5.48256158624435));
#43106=CARTESIAN_POINT('Ctrl Pts',(-33.4494310938601,54.3935387891867,5.59369947681239));
#43107=CARTESIAN_POINT('Ctrl Pts',(-31.4202066831417,54.4645507053438,5.70483736738043));
#43108=CARTESIAN_POINT('Ctrl Pts',(-30.3793316112331,56.2079277768579,5.81597525794847));
#43109=CARTESIAN_POINT('Ctrl Pts',(-31.2795238466775,58.027939263068,5.92711314851652));
#43110=CARTESIAN_POINT('Ctrl Pts',(-33.2968407414035,58.2587039015876,6.03825103908456));
#43111=CARTESIAN_POINT('Ctrl Pts',(-34.5847823639128,56.6890083802673,6.1493889296526));
#43112=CARTESIAN_POINT('Ctrl Pts',(-33.9645346857694,54.7555965317121,6.26052682022065));
#43113=CARTESIAN_POINT('Ctrl Pts',(-32.0037108581305,54.2281745523389,6.37166471078868));
#43114=CARTESIAN_POINT('Ctrl Pts',(-30.4972873242539,55.5894332580934,6.48280260135673));
#43115=CARTESIAN_POINT('Ctrl Pts',(-30.823688318536,57.5935255124715,6.59394049192477));
#43116=CARTESIAN_POINT('Ctrl Pts',(-32.6849960096048,58.4058273841964,6.70507838249281));
#43117=CARTESIAN_POINT('Ctrl Pts',(-34.3758599154852,57.283338333678,6.81621627306086));
#43118=CARTESIAN_POINT('Ctrl Pts',(-34.3519589865932,55.2524746920756,6.92735416362889));
#43119=CARTESIAN_POINT('Ctrl Pts',(-32.6283545092383,54.1741032483986,7.03849205419694));
#43120=CARTESIAN_POINT('Ctrl Pts',(-31.4085562246361,54.7458933202255,7.1125839812423));
#43121=CARTESIAN_POINT('Ctrl Pts',(-31.0543981323805,55.2265903335147,7.14962994476498));
#43122=CARTESIAN_POINT('Ctrl Pts',(-32.8469189315166,54.3980002883409,-2.14962994476498));
#43123=CARTESIAN_POINT('Ctrl Pts',(-32.2172349362596,54.2826414900653,-2.1125839812423));
#43124=CARTESIAN_POINT('Ctrl Pts',(-30.8444953556861,54.7319049652148,-2.03849205419694));
#43125=CARTESIAN_POINT('Ctrl Pts',(-30.2902045467309,56.8401336080183,-1.9273541636289));
#43126=CARTESIAN_POINT('Ctrl Pts',(-31.7631165537738,58.4439957222243,-1.81621627306085));
#43127=CARTESIAN_POINT('Ctrl Pts',(-33.9082700189115,58.0789060959425,-1.70507838249281));
#43128=CARTESIAN_POINT('Ctrl Pts',(-34.7655373602912,56.0773674171098,-1.59394049192477));
#43129=CARTESIAN_POINT('Ctrl Pts',(-33.5485706232914,54.2722432949298,-1.48280260135673));
#43130=CARTESIAN_POINT('Ctrl Pts',(-31.3721176346275,54.3153664723165,-1.37166471078869));
#43131=CARTESIAN_POINT('Ctrl Pts',(-30.2278863306926,56.1674756953684,-1.26052682022064));
#43132=CARTESIAN_POINT('Ctrl Pts',(-31.1634176907274,58.1332089515266,-1.1493889296526));
#43133=CARTESIAN_POINT('Ctrl Pts',(-33.3223021993517,58.4133612672893,-1.03825103908456));
#43134=CARTESIAN_POINT('Ctrl Pts',(-34.7285421630059,56.7514794405087,-0.927113148516519));
#43135=CARTESIAN_POINT('Ctrl Pts',(-34.0949631768735,54.6687161227545,-0.815975257948477));
#43136=CARTESIAN_POINT('Ctrl Pts',(-32.0015008456287,54.0714414828596,-0.704837367380436));
#43137=CARTESIAN_POINT('Ctrl Pts',(-30.3643181635512,55.5063511462768,-0.593699476812394));
#43138=CARTESIAN_POINT('Ctrl Pts',(-30.6819504321758,57.6600543300704,-0.482561586244352));
#43139=CARTESIAN_POINT('Ctrl Pts',(-32.6636635128287,58.5612429370052,-0.371423695676311));
#43140=CARTESIAN_POINT('Ctrl Pts',(-34.4955738132308,57.3850483871807,-0.260285805108268));
#43141=CARTESIAN_POINT('Ctrl Pts',(-34.5009126257928,55.208055105922,-0.149147914540227));
#43142=CARTESIAN_POINT('Ctrl Pts',(-32.6747934930415,54.0228896243784,-0.0380100239721848));
#43143=CARTESIAN_POINT('Ctrl Pts',(-30.688683857159,54.914347402739,0.0731278665958571));
#43144=CARTESIAN_POINT('Ctrl Pts',(-30.3604924469569,57.0664669994018,0.184265757163898));
#43145=CARTESIAN_POINT('Ctrl Pts',(-31.9906165544693,58.5093889545349,0.295403647731941));
#43146=CARTESIAN_POINT('Ctrl Pts',(-34.086985111125,57.9223904318795,0.406541538299981));
#43147=CARTESIAN_POINT('Ctrl Pts',(-34.7307681955977,55.8427578396932,0.517679428868024));
#43148=CARTESIAN_POINT('Ctrl Pts',(-33.3327038531809,54.1740024725061,0.628817319436064));
#43149=CARTESIAN_POINT('Ctrl Pts',(-31.1724562298543,54.4435550437496,0.739955210004108));
#43150=CARTESIAN_POINT('Ctrl Pts',(-30.2273244750084,56.4046910275922,0.851093100572148));
#43151=CARTESIAN_POINT('Ctrl Pts',(-31.3623984019321,58.2623604174483,0.962230991140192));
#43152=CARTESIAN_POINT('Ctrl Pts',(-33.5387319729216,58.3162173532682,1.07336888170823));
#43153=CARTESIAN_POINT('Ctrl Pts',(-34.7643023890367,56.5169659709722,1.18450677227627));
#43154=CARTESIAN_POINT('Ctrl Pts',(-33.9173311495497,54.5114814656466,1.29564466284432));
#43155=CARTESIAN_POINT('Ctrl Pts',(-31.773060635242,54.135406548771,1.40678255341236));
#43156=CARTESIAN_POINT('Ctrl Pts',(-30.2941659655551,55.7329668567342,1.5179204439804));
#43157=CARTESIAN_POINT('Ctrl Pts',(-30.8342962034526,57.8418973220951,1.62905833454844));
#43158=CARTESIAN_POINT('Ctrl Pts',(-32.899064016697,58.5318699730086,1.74019622511648));
#43159=CARTESIAN_POINT('Ctrl Pts',(-34.5985640097643,57.1713450172728,1.85133411568453));
#43160=CARTESIAN_POINT('Ctrl Pts',(-34.37722456536,55.0056263762742,1.96247200625257));
#43161=CARTESIAN_POINT('Ctrl Pts',(-32.4376401871071,54.0170208830394,2.07360989682061));
#43162=CARTESIAN_POINT('Ctrl Pts',(-30.5551344528034,55.1104103570745,2.18474778738865));
#43163=CARTESIAN_POINT('Ctrl Pts',(-30.4527862101242,57.2850030129155,2.29588567795669));
#43164=CARTESIAN_POINT('Ctrl Pts',(-32.2242759663018,58.550369531113,2.40702356852473));
#43165=CARTESIAN_POINT('Ctrl Pts',(-34.2481390574465,57.7483055873284,2.51816145909278));
#43166=CARTESIAN_POINT('Ctrl Pts',(-34.6719106440651,55.6129494053317,2.62929934966082));
#43167=CARTESIAN_POINT('Ctrl Pts',(-33.107707787029,54.0988167150905,2.74043724022886));
#43168=CARTESIAN_POINT('Ctrl Pts',(-30.9872631006501,54.5918103394153,2.8515751307969));
#43169=CARTESIAN_POINT('Ctrl Pts',(-30.2514436538494,56.6406876230335,2.96271302136494));
#43170=CARTESIAN_POINT('Ctrl Pts',(-31.5737533310438,58.3700879524007,3.07385091193298));
#43171=CARTESIAN_POINT('Ctrl Pts',(-33.7438670886851,58.1970715933135,3.18498880250103));
#43172=CARTESIAN_POINT('Ctrl Pts',(-34.7754551936414,56.2800023813831,3.29612669306907));
#43173=CARTESIAN_POINT('Ctrl Pts',(-33.7242933544393,54.3735955073335,3.40726458363711));
#43174=CARTESIAN_POINT('Ctrl Pts',(-31.5525219234906,54.2228068031056,3.51840247420515));
#43175=CARTESIAN_POINT('Ctrl Pts',(-30.247987921098,55.9656548797417,3.62954036477319));
#43176=CARTESIAN_POINT('Ctrl Pts',(-31.0047461140886,58.0068911274507,3.74067825534123));
#43177=CARTESIAN_POINT('Ctrl Pts',(-33.1301271461661,58.4781488595201,3.85181614590928));
#43178=CARTESIAN_POINT('Ctrl Pts',(-34.67874565527,56.9480805293425,3.96295403647731));
#43179=CARTESIAN_POINT('Ctrl Pts',(-34.2331335573692,54.8171750317208,4.07409192704536));
#43180=CARTESIAN_POINT('Ctrl Pts',(-32.2011646594958,54.0358743346675,4.1852298176134));
#43181=CARTESIAN_POINT('Ctrl Pts',(-30.4427231374931,55.3193118268927,4.29636770818145));
#43182=CARTESIAN_POINT('Ctrl Pts',(-30.5673304594784,57.4927426163039,4.40750559874948));
#43183=CARTESIAN_POINT('Ctrl Pts',(-32.4609321286144,58.5668008535436,4.51864348931753));
#43184=CARTESIAN_POINT('Ctrl Pts',(-34.3902930659818,57.5583888522789,4.62978137988556));
#43185=CARTESIAN_POINT('Ctrl Pts',(-34.5894473177133,55.3905175557035,4.74091927045361));
#43186=CARTESIAN_POINT('Ctrl Pts',(-32.8761067534734,54.0474641423945,4.85205716102165));
#43187=CARTESIAN_POINT('Ctrl Pts',(-30.8185113927804,54.7585406417947,4.96319505158969));
#43188=CARTESIAN_POINT('Ctrl Pts',(-30.3000016627836,56.8728906519732,5.07433294215774));
#43189=CARTESIAN_POINT('Ctrl Pts',(-31.7951752826288,58.4552256658323,5.18547083272577));
#43190=CARTESIAN_POINT('Ctrl Pts',(-33.9354831145828,58.0572164294668,5.29660872329382));
#43191=CARTESIAN_POINT('Ctrl Pts',(-34.7618766636555,56.0431654516238,5.40774661386186));
#43192=CARTESIAN_POINT('Ctrl Pts',(-33.5179494653714,54.2565561526097,5.5188845044299));
#43193=CARTESIAN_POINT('Ctrl Pts',(-31.3422803542924,54.3326928438919,5.63002239499794));
#43194=CARTESIAN_POINT('Ctrl Pts',(-30.2262875983991,56.2018856366761,5.74116028556598));
#43195=CARTESIAN_POINT('Ctrl Pts',(-31.1914447443237,58.1532433827394,5.85229817613403));
#43196=CARTESIAN_POINT('Ctrl Pts',(-33.3543469999491,58.4006618019661,5.96343606670207));
#43197=CARTESIAN_POINT('Ctrl Pts',(-34.7352365605938,56.7176847780862,6.07457395727012));
#43198=CARTESIAN_POINT('Ctrl Pts',(-34.0702269601635,54.6447428128324,6.18571184783815));
#43199=CARTESIAN_POINT('Ctrl Pts',(-31.9678947530761,54.0792579394171,6.2968497384062));
#43200=CARTESIAN_POINT('Ctrl Pts',(-30.3527559179892,55.5387557173139,6.40798762897423));
#43201=CARTESIAN_POINT('Ctrl Pts',(-30.7027125602087,57.687478939138,6.51912551954228));
#43202=CARTESIAN_POINT('Ctrl Pts',(-32.6983467681761,58.5584028654659,6.63026341011033));
#43203=CARTESIAN_POINT('Ctrl Pts',(-34.5112366346841,57.3549062281114,6.74140130067836));
#43204=CARTESIAN_POINT('Ctrl Pts',(-34.4856108278775,55.1774795864306,6.85253919124641));
#43205=CARTESIAN_POINT('Ctrl Pts',(-32.6376175742527,54.0212844273909,6.96367708181445));
#43206=CARTESIAN_POINT('Ctrl Pts',(-31.329789107604,54.6343393417337,7.03776900885981));
#43207=CARTESIAN_POINT('Ctrl Pts',(-30.9500721981832,55.1497272101613,7.07481497238249));
#43208=CARTESIAN_POINT('Ctrl Pts',(-32.8702701105707,54.2705382833568,-2.22444491714747));
#43209=CARTESIAN_POINT('Ctrl Pts',(-32.1982019662087,54.147414662498,-2.18739895362479));
#43210=CARTESIAN_POINT('Ctrl Pts',(-30.7330630242036,54.6269181473375,-2.11330702657943));
#43211=CARTESIAN_POINT('Ctrl Pts',(-30.1414627958074,56.8770520597955,-2.00216913601138));
#43212=CARTESIAN_POINT('Ctrl Pts',(-31.7135167892996,58.5888704369912,-1.89103124544334));
#43213=CARTESIAN_POINT('Ctrl Pts',(-34.003060940884,58.1992065587457,-1.7798933548753));
#43214=CARTESIAN_POINT('Ctrl Pts',(-34.9180311095446,56.062943931961,-1.66875546430726));
#43215=CARTESIAN_POINT('Ctrl Pts',(-33.6191501107478,54.1363165628764,-1.55761757373921));
#43216=CARTESIAN_POINT('Ctrl Pts',(-31.2961996587746,54.182342369509,-1.44647968317118));
#43217=CARTESIAN_POINT('Ctrl Pts',(-30.0749499288325,56.1591174155132,-1.33534179260313));
#43218=CARTESIAN_POINT('Ctrl Pts',(-31.0734520820823,58.2571645498346,-1.22420390203509));
#43219=CARTESIAN_POINT('Ctrl Pts',(-33.3776515162936,58.5561739710865,-1.11306601146705));
#43220=CARTESIAN_POINT('Ctrl Pts',(-34.878545758516,56.7824305634625,-1.00192812089901));
#43221=CARTESIAN_POINT('Ctrl Pts',(-34.2023204507042,54.559476051911,-0.890790230330966));
#43222=CARTESIAN_POINT('Ctrl Pts',(-31.9679467730355,53.921998742765,-0.779652339762925));
#43223=CARTESIAN_POINT('Ctrl Pts',(-30.2205650142274,55.453492447677,-0.668514449194883));
#43224=CARTESIAN_POINT('Ctrl Pts',(-30.5595771710743,57.752161801101,-0.557376558626841));
#43225=CARTESIAN_POINT('Ctrl Pts',(-32.6746797349068,58.7140095840284,-0.4462386680588));
#43226=CARTESIAN_POINT('Ctrl Pts',(-34.6298962649481,57.4586451560558,-0.335100777490757));
#43227=CARTESIAN_POINT('Ctrl Pts',(-34.6355944339958,55.1351180442908,-0.223962886922716));
#43228=CARTESIAN_POINT('Ctrl Pts',(-32.6865588761979,53.8701788494842,-0.112824996354674));
#43229=CARTESIAN_POINT('Ctrl Pts',(-30.5667638241697,54.8216408199214,-0.00168710578663194));
#43230=CARTESIAN_POINT('Ctrl Pts',(-30.2164817879238,57.1186199946645,0.109450784781409));
#43231=CARTESIAN_POINT('Ctrl Pts',(-31.9563298581746,58.6586653001668,0.220588675349452));
#43232=CARTESIAN_POINT('Ctrl Pts',(-34.1938053798377,58.0321557956601,0.331726565917493));
#43233=CARTESIAN_POINT('Ctrl Pts',(-34.8809216257836,55.8125427394079,0.442864456485535));
#43234=CARTESIAN_POINT('Ctrl Pts',(-33.3887533074142,54.0314631320695,0.554002347053576));
#43235=CARTESIAN_POINT('Ctrl Pts',(-31.0830990069914,54.3191593379889,0.665140237621618));
#43236=CARTESIAN_POINT('Ctrl Pts',(-30.0743502545356,56.4122997567237,0.77627812818966));
#43237=CARTESIAN_POINT('Ctrl Pts',(-31.2858262226837,58.3950092254139,0.887416018757703));
#43238=CARTESIAN_POINT('Ctrl Pts',(-33.6086492189563,58.4524912817947,0.998553909325743));
#43239=CARTESIAN_POINT('Ctrl Pts',(-34.9167130121408,56.5321319478293,1.10969179989379));
#43240=CARTESIAN_POINT('Ctrl Pts',(-34.0127319779434,54.3916579002222,1.22082969046183));
#43241=CARTESIAN_POINT('Ctrl Pts',(-31.7241302087768,53.9902693093903,1.33196758102987));
#43242=CARTESIAN_POINT('Ctrl Pts',(-30.1456908584837,55.6953617045703,1.44310547159791));
#43243=CARTESIAN_POINT('Ctrl Pts',(-30.7221773650996,57.9462446793952,1.55424336216595));
#43244=CARTESIAN_POINT('Ctrl Pts',(-32.9259250913211,58.6826595202563,1.66538125273399));
#43245=CARTESIAN_POINT('Ctrl Pts',(-34.7398187511365,57.2305573718025,1.77651914330204));
#43246=CARTESIAN_POINT('Ctrl Pts',(-34.5035809067649,54.9190637984713,1.88765703387008));
#43247=CARTESIAN_POINT('Ctrl Pts',(-32.4334427362781,53.863915082053,1.99879492443812));
#43248=CARTESIAN_POINT('Ctrl Pts',(-30.4242251840869,55.0309008088856,2.10993281500616));
#43249=CARTESIAN_POINT('Ctrl Pts',(-30.3149878617883,57.3518657086808,2.22107070557421));
#43250=CARTESIAN_POINT('Ctrl Pts',(-32.2057169293179,58.7024042871241,2.33220859614224));
#43251=CARTESIAN_POINT('Ctrl Pts',(-34.3658066288398,57.8463532672169,2.44334648671029));
#43252=CARTESIAN_POINT('Ctrl Pts',(-34.8181023612983,55.5672658557593,2.55448437727833));
#43253=CARTESIAN_POINT('Ctrl Pts',(-33.1486127133916,53.9512166070675,2.66562226784637));
#43254=CARTESIAN_POINT('Ctrl Pts',(-30.8854404931491,54.4773937257141,2.77676015841441));
#43255=CARTESIAN_POINT('Ctrl Pts',(-30.1000928998773,56.6641813277477,2.88789804898245));
#43256=CARTESIAN_POINT('Ctrl Pts',(-31.5114074921456,58.5099879211684,2.99903593955049));
#43257=CARTESIAN_POINT('Ctrl Pts',(-33.8275920182542,58.3253257981482,3.11017383011854));
#43258=CARTESIAN_POINT('Ctrl Pts',(-34.9286165141379,56.2792182940979,3.22131172068658));
#43259=CARTESIAN_POINT('Ctrl Pts',(-33.8067007722453,54.2444908119128,3.33244961125462));
#43260=CARTESIAN_POINT('Ctrl Pts',(-31.4887469945246,54.0835524914147,3.44358750182266));
#43261=CARTESIAN_POINT('Ctrl Pts',(-30.0964045610992,55.9437120025227,3.5547253923907));
#43262=CARTESIAN_POINT('Ctrl Pts',(-30.9041002915367,58.1223442490711,3.66586328295875));
#43263=CARTESIAN_POINT('Ctrl Pts',(-33.1725411238429,58.6253224284337,3.77700117352679));
#43264=CARTESIAN_POINT('Ctrl Pts',(-34.8253974384033,56.9922649088601,3.88813906409483));
#43265=CARTESIAN_POINT('Ctrl Pts',(-34.3497911057075,54.7179277581866,3.99927695466287));
#43266=CARTESIAN_POINT('Ctrl Pts',(-32.1810499960691,53.8840375630848,4.11041484523091));
#43267=CARTESIAN_POINT('Ctrl Pts',(-30.3042474418304,55.2538634762437,4.22155273579896));
#43268=CARTESIAN_POINT('Ctrl Pts',(-30.4372421062834,57.5735883041595,4.332690626367));
#43269=CARTESIAN_POINT('Ctrl Pts',(-32.4583024627843,58.7199416049828,4.44382851693504));
#43270=CARTESIAN_POINT('Ctrl Pts',(-34.5175290506412,57.6436532007241,4.55496640750308));
#43271=CARTESIAN_POINT('Ctrl Pts',(-34.7300884128152,55.3298620761609,4.66610429807112));
#43272=CARTESIAN_POINT('Ctrl Pts',(-32.9014225703573,53.8964074829672,4.77724218863916));
#43273=CARTESIAN_POINT('Ctrl Pts',(-30.7053300758283,54.6553466763578,4.88838007920721));
#43274=CARTESIAN_POINT('Ctrl Pts',(-30.1519193575992,56.9120139865896,4.99951796977524));
#43275=CARTESIAN_POINT('Ctrl Pts',(-31.747733397272,58.6008562702326,5.11065586034329));
#43276=CARTESIAN_POINT('Ctrl Pts',(-34.0321057551843,58.1760569567072,5.22179375091132));
#43277=CARTESIAN_POINT('Ctrl Pts',(-34.9141240107244,56.0264398256936,5.33293164147938));
#43278=CARTESIAN_POINT('Ctrl Pts',(-33.5864678368826,54.1195735160326,5.44406953204741));
#43279=CARTESIAN_POINT('Ctrl Pts',(-31.2643540254432,54.2008349824401,5.55520742261546));
#43280=CARTESIAN_POINT('Ctrl Pts',(-30.0732435855652,56.1958434964943,5.66634531318349));
#43281=CARTESIAN_POINT('Ctrl Pts',(-31.10336564197,58.2785475024108,5.77748320375154));
#43282=CARTESIAN_POINT('Ctrl Pts',(-33.4118532584947,58.5426197023447,5.88862109431958));
#43283=CARTESIAN_POINT('Ctrl Pts',(-34.8856907572748,56.746361175905,5.99975898488762));
#43284=CARTESIAN_POINT('Ctrl Pts',(-34.1759192345577,54.5338890939528,6.11089687545567));
#43285=CARTESIAN_POINT('Ctrl Pts',(-31.9320786480218,53.9303413264953,6.2220347660237));
#43286=CARTESIAN_POINT('Ctrl Pts',(-30.2082245117245,55.4880781765344,6.33317265659175));
#43287=CARTESIAN_POINT('Ctrl Pts',(-30.5817368018815,57.7814323658043,6.44431054715979));
#43288=CARTESIAN_POINT('Ctrl Pts',(-32.7116975267474,58.7109783467354,6.55544843772783));
#43289=CARTESIAN_POINT('Ctrl Pts',(-34.646613353883,57.4264741225448,6.66658632829587));
#43290=CARTESIAN_POINT('Ctrl Pts',(-34.6192626691618,55.1024844807855,6.77772421886391));
#43291=CARTESIAN_POINT('Ctrl Pts',(-32.6468806392671,53.8684656063832,6.88886210943196));
#43292=CARTESIAN_POINT('Ctrl Pts',(-31.2510219905719,54.522785363242,6.96295403647732));
#43293=CARTESIAN_POINT('Ctrl Pts',(-30.845746263986,55.0728640868079,7.));
#43294=CARTESIAN_POINT('Ctrl Pts',(-32.8002165734084,54.652924298309,-2.));
#43295=CARTESIAN_POINT('Ctrl Pts',(-32.7409294910782,54.6348115493311,-2.));
#43296=CARTESIAN_POINT('Ctrl Pts',(-32.6807825146657,54.6203475870771,-2.));
#43297=CARTESIAN_POINT('Ctrl Pts',(-32.6200737029466,54.6093586318097,-2.));
#43298=CARTESIAN_POINT('Ctrl Pts',(-32.5553553259177,54.5976439016081,-2.));
#43299=CARTESIAN_POINT('Ctrl Pts',(-32.4899978846727,54.589877844864,-2.));
#43300=CARTESIAN_POINT('Ctrl Pts',(-32.4243295074668,54.5859022602815,-2.));
#43301=CARTESIAN_POINT('Ctrl Pts',(-32.3668696774116,54.5824236237718,-2.));
#43302=CARTESIAN_POINT('Ctrl Pts',(-32.3091708471323,54.5818478912345,-2.));
#43303=CARTESIAN_POINT('Ctrl Pts',(-32.2514404192194,54.5841026889814,-2.));
#43304=CARTESIAN_POINT('Ctrl Pts',(-32.2224739676372,54.5852340419286,-2.));
#43305=CARTESIAN_POINT('Ctrl Pts',(-32.193499433327,54.5870784902624,-2.));
#43306=CARTESIAN_POINT('Ctrl Pts',(-32.1645425913577,54.5896298423984,-2.));
#43307=CARTESIAN_POINT('Ctrl Pts',(-32.1513153330279,54.5907952800462,-2.));
#43308=CARTESIAN_POINT('Ctrl Pts',(-32.138090039214,54.5921085587763,-2.));
#43309=CARTESIAN_POINT('Ctrl Pts',(-32.1248906604564,54.5935664859841,-2.));
#43310=CARTESIAN_POINT('Ctrl Pts',(-32.058315745723,54.6009199668814,-2.));
#43311=CARTESIAN_POINT('Ctrl Pts',(-31.9922802588103,54.6119586521809,-2.));
#43312=CARTESIAN_POINT('Ctrl Pts',(-31.9271057840949,54.6265240331791,-2.));
#43313=CARTESIAN_POINT('Ctrl Pts',(-31.8607754217491,54.6413477353037,-2.));
#43314=CARTESIAN_POINT('Ctrl Pts',(-31.7953358755736,54.6598242742457,-2.));
#43315=CARTESIAN_POINT('Ctrl Pts',(-31.7311141838629,54.6818388621519,-2.));
#43316=CARTESIAN_POINT('Ctrl Pts',(-31.6773947912169,54.7002533613681,-2.));
#43317=CARTESIAN_POINT('Ctrl Pts',(-31.6245269677682,54.7211443093799,-2.));
#43318=CARTESIAN_POINT('Ctrl Pts',(-31.5727038894035,54.744472176156,-2.));
#43319=CARTESIAN_POINT('Ctrl Pts',(-31.5488262835586,54.7552205459106,-2.));
#43320=CARTESIAN_POINT('Ctrl Pts',(-31.5251705391772,54.7664866028715,-2.));
#43321=CARTESIAN_POINT('Ctrl Pts',(-31.5017561059839,54.7782682438534,-2.));
#43322=CARTESIAN_POINT('Ctrl Pts',(-31.4915364297196,54.783410565929,-2.));
#43323=CARTESIAN_POINT('Ctrl Pts',(-31.4813629900352,54.788651093074,-2.));
#43324=CARTESIAN_POINT('Ctrl Pts',(-31.4712497594445,54.7939828998655,-2.));
#43325=CARTESIAN_POINT('Ctrl Pts',(-31.4091712444154,54.8267113781765,-2.));
#43326=CARTESIAN_POINT('Ctrl Pts',(-31.3492415725568,54.8629343648207,-2.));
#43327=CARTESIAN_POINT('Ctrl Pts',(-31.2918005106532,54.9025187988196,-2.));
#43328=CARTESIAN_POINT('Ctrl Pts',(-31.2404435140348,54.9379105129636,-2.));
#43329=CARTESIAN_POINT('Ctrl Pts',(-31.1910752071313,54.9759900914521,-2.));
#43330=CARTESIAN_POINT('Ctrl Pts',(-31.1439444839342,55.0166972030901,-2.));
#43331=CARTESIAN_POINT('Ctrl Pts',(-31.0925988211627,55.0610447854056,-2.));
#43332=CARTESIAN_POINT('Ctrl Pts',(-31.043907590923,55.1085103565088,-2.));
#43333=CARTESIAN_POINT('Ctrl Pts',(-30.9979331337683,55.1587747363345,-2.));
#43334=CARTESIAN_POINT('Ctrl Pts',(-30.9801952413171,55.1781677693066,-2.));
#43335=CARTESIAN_POINT('Ctrl Pts',(-30.9628620787172,55.1979778819355,-2.));
#43336=CARTESIAN_POINT('Ctrl Pts',(-30.9459385065311,55.2181883203223,-2.));
#43337=CARTESIAN_POINT('Ctrl Pts',(-30.9385143505228,55.2270543827546,-2.));
#43338=CARTESIAN_POINT('Ctrl Pts',(-30.9311694717142,55.2359970996698,-2.));
#43339=CARTESIAN_POINT('Ctrl Pts',(-30.9239125746492,55.2450044081202,-2.));
#43340=CARTESIAN_POINT('Ctrl Pts',(-30.8800390053309,55.2994605714266,-2.));
#43341=CARTESIAN_POINT('Ctrl Pts',(-30.839297247442,55.3563704442389,-2.));
#43342=CARTESIAN_POINT('Ctrl Pts',(-30.8017204449776,55.4153538312132,-2.));
#43343=CARTESIAN_POINT('Ctrl Pts',(-30.7632731033033,55.4757036822749,-2.));
#43344=CARTESIAN_POINT('Ctrl Pts',(-30.7281385018958,55.5382249056899,-2.));
#43345=CARTESIAN_POINT('Ctrl Pts',(-30.6963834281772,55.6025570259723,-2.));
#43346=CARTESIAN_POINT('Ctrl Pts',(-30.6720872116827,55.6517783609874,-2.));
#43347=CARTESIAN_POINT('Ctrl Pts',(-30.6497699435193,55.7020608595674,-2.));
#43348=CARTESIAN_POINT('Ctrl Pts',(-30.6294765723463,55.7532569215852,-2.));
#43349=CARTESIAN_POINT('Ctrl Pts',(-30.6168451594751,55.7851234158808,-2.));
#43350=CARTESIAN_POINT('Ctrl Pts',(-30.6049981367031,55.817344072298,-2.));
#43351=CARTESIAN_POINT('Ctrl Pts',(-30.5939492528789,55.8498849658821,-2.));
#43352=CARTESIAN_POINT('Ctrl Pts',(-30.5877508307633,55.868140402147,-2.));
#43353=CARTESIAN_POINT('Ctrl Pts',(-30.5818018934048,55.8865028064712,-2.));
#43354=CARTESIAN_POINT('Ctrl Pts',(-30.576115080405,55.9049328084138,-2.));
#43355=CARTESIAN_POINT('Ctrl Pts',(-30.5540602837242,55.9764086852689,-2.));
#43356=CARTESIAN_POINT('Ctrl Pts',(-30.5359175198242,56.0489705581354,-2.));
#43357=CARTESIAN_POINT('Ctrl Pts',(-30.5217728584387,56.1222396610165,-2.));
#43358=CARTESIAN_POINT('Ctrl Pts',(-30.5111932477239,56.1770418626931,-2.));
#43359=CARTESIAN_POINT('Ctrl Pts',(-30.5028510892941,56.2322406204016,-2.));
#43360=CARTESIAN_POINT('Ctrl Pts',(-30.4967990447163,56.2876867713324,-2.));
#43361=CARTESIAN_POINT('Ctrl Pts',(-30.4949111210757,56.3049830912424,-2.));
#43362=CARTESIAN_POINT('Ctrl Pts',(-30.4932461646214,56.3223035269554,-2.));
#43363=CARTESIAN_POINT('Ctrl Pts',(-30.4918060890528,56.3396436454805,-2.));
#43364=CARTESIAN_POINT('Ctrl Pts',(-30.4904160490458,56.3563812799502,-2.));
#43365=CARTESIAN_POINT('Ctrl Pts',(-30.4892362965357,56.3731287080283,-2.));
#43366=CARTESIAN_POINT('Ctrl Pts',(-30.4882682431297,56.3898758527382,-2.));
#43367=CARTESIAN_POINT('Ctrl Pts',(-30.4839212193133,56.4650785600099,-2.));
#43368=CARTESIAN_POINT('Ctrl Pts',(-30.4838360419502,56.5403117892544,-2.));
#43369=CARTESIAN_POINT('Ctrl Pts',(-30.4881238107199,56.6152096419697,-2.));
#43370=CARTESIAN_POINT('Ctrl Pts',(-30.4914053519387,56.6725309211904,-2.));
#43371=CARTESIAN_POINT('Ctrl Pts',(-30.4972490710547,56.729656403295,-2.));
#43372=CARTESIAN_POINT('Ctrl Pts',(-30.5057249894129,56.7864264638425,-2.));
#43373=CARTESIAN_POINT('Ctrl Pts',(-30.5076920210892,56.799601261268,-2.));
#43374=CARTESIAN_POINT('Ctrl Pts',(-30.5098008972608,56.8127569211081,-2.));
#43375=CARTESIAN_POINT('Ctrl Pts',(-30.5120501580915,56.825892077386,-2.));
#43376=CARTESIAN_POINT('Ctrl Pts',(-33.3325354057627,57.7362457052863,-0.87148036339022));
#43377=CARTESIAN_POINT('Ctrl Pts',(-33.2590763562246,57.7795019958594,-0.877193940366678));
#43378=CARTESIAN_POINT('Ctrl Pts',(-33.1823540930372,57.8169005192734,-0.882907517343135));
#43379=CARTESIAN_POINT('Ctrl Pts',(-33.1030496903125,57.8476363980486,-0.888621094319593));
#43380=CARTESIAN_POINT('Ctrl Pts',(-32.5888520129845,58.0469231581002,-0.925667057842273));
#43381=CARTESIAN_POINT('Ctrl Pts',(-31.966100460501,57.9661104565053,-0.962713021364954));
#43382=CARTESIAN_POINT('Ctrl Pts',(-31.5197930553252,57.6421865224026,-0.999758984887635));
#43383=CARTESIAN_POINT('Ctrl Pts',(-31.0734856501493,57.3182625882999,-1.03680494841032));
#43384=CARTESIAN_POINT('Ctrl Pts',(-30.8036223922811,56.7512274216893,-1.073850911933));
#43385=CARTESIAN_POINT('Ctrl Pts',(-30.8337231720004,56.2005802421929,-1.11089687545568));
#43386=CARTESIAN_POINT('Ctrl Pts',(-30.8638239517197,55.6499330626964,-1.14794283897836));
#43387=CARTESIAN_POINT('Ctrl Pts',(-31.1938887690265,55.115673870314,-1.18498880250104));
#43388=CARTESIAN_POINT('Ctrl Pts',(-31.6728308546875,54.8423246209736,-1.22203476602372));
#43389=CARTESIAN_POINT('Ctrl Pts',(-32.1517729403484,54.5689753716332,-1.2590807295464));
#43390=CARTESIAN_POINT('Ctrl Pts',(-32.7795922943635,54.5565360653349,-1.29612669306908));
#43391=CARTESIAN_POINT('Ctrl Pts',(-33.2690250069387,54.8106693502475,-1.33317265659176));
#43392=CARTESIAN_POINT('Ctrl Pts',(-33.7584577195138,55.0648026351601,-1.37021862011444));
#43393=CARTESIAN_POINT('Ctrl Pts',(-34.1095037906491,55.5855085112837,-1.40726458363712));
#43394=CARTESIAN_POINT('Ctrl Pts',(-34.1613832117471,56.1345432465003,-1.4443105471598));
#43395=CARTESIAN_POINT('Ctrl Pts',(-34.2132626328451,56.6835779817169,-1.48135651068248));
#43396=CARTESIAN_POINT('Ctrl Pts',(-33.9659754039059,57.2609415760266,-1.51840247420516));
#43397=CARTESIAN_POINT('Ctrl Pts',(-33.5329364407288,57.6022802269071,-1.55544843772784));
#43398=CARTESIAN_POINT('Ctrl Pts',(-33.4704694600161,57.6515192024594,-1.56079241294864));
#43399=CARTESIAN_POINT('Ctrl Pts',(-33.4041372082081,57.6958467816506,-1.56613638816943));
#43400=CARTESIAN_POINT('Ctrl Pts',(-33.3347882996638,57.7351190113229,-1.57148036339022));
#43401=CARTESIAN_POINT('Ctrl Pts',(-31.045873711622,57.7433792852396,-2.));
#43402=CARTESIAN_POINT('Ctrl Pts',(-31.5286078227265,58.2269108712356,-1.96295403647732));
#43403=CARTESIAN_POINT('Ctrl Pts',(-33.0063987810959,58.6658791894418,-1.88886210943196));
#43404=CARTESIAN_POINT('Ctrl Pts',(-34.7728277550873,57.1516769644331,-1.77772421886392));
#43405=CARTESIAN_POINT('Ctrl Pts',(-34.4535014835806,54.8495668967864,-1.66658632829587));
#43406=CARTESIAN_POINT('Ctrl Pts',(-32.3487507516394,53.8677941230741,-1.55544843772783));
#43407=CARTESIAN_POINT('Ctrl Pts',(-30.3811218874153,55.1044118987673,-1.44431054715979));
#43408=CARTESIAN_POINT('Ctrl Pts',(-30.3535878576005,57.4278205885651,-1.33317265659175));
#43409=CARTESIAN_POINT('Ctrl Pts',(-32.2903568834191,58.7112317202032,-1.22203476602371));
#43410=CARTESIAN_POINT('Ctrl Pts',(-34.4191815551847,57.7799979545239,-1.11089687545567));
#43411=CARTESIAN_POINT('Ctrl Pts',(-34.7912737376158,55.4864512354733,-0.999758984887624));
#43412=CARTESIAN_POINT('Ctrl Pts',(-33.0661792001092,53.929919412126,-0.888621094319583));
#43413=CARTESIAN_POINT('Ctrl Pts',(-30.822833264184,54.5351044086333,-0.77748320375154));
#43414=CARTESIAN_POINT('Ctrl Pts',(-30.114627688562,56.7480782089187,-0.666345313183499));
#43415=CARTESIAN_POINT('Ctrl Pts',(-31.5897751037144,58.543278448718,-0.555207422615458));
#43416=CARTESIAN_POINT('Ctrl Pts',(-33.8980643703311,58.2775391690227,-0.444069532047415));
#43417=CARTESIAN_POINT('Ctrl Pts',(-34.926688116847,56.1940939537868,-0.332931641479374));
#43418=CARTESIAN_POINT('Ctrl Pts',(-33.7341373860101,54.1999441339785,-0.221793750911332));
#43419=CARTESIAN_POINT('Ctrl Pts',(-31.4119663698709,54.1203575053851,-0.110655860343291));
#43420=CARTESIAN_POINT('Ctrl Pts',(-30.0856850452223,56.0281806868171,0.000482030224751779));
#43421=CARTESIAN_POINT('Ctrl Pts',(-30.9692534931352,58.1771614464074,0.111619920792793));
#43422=CARTESIAN_POINT('Ctrl Pts',(-33.2539316216956,58.6003133427487,0.222757811360835));
#43423=CARTESIAN_POINT('Ctrl Pts',(-34.8485275651184,56.9103206367346,0.333895701928877));
#43424=CARTESIAN_POINT('Ctrl Pts',(-34.2934896049409,54.6540528227808,0.445033592496919));
#43425=CARTESIAN_POINT('Ctrl Pts',(-32.0968502643471,53.8966974164155,0.55617148306496));
#43426=CARTESIAN_POINT('Ctrl Pts',(-30.2692184515671,55.3314704112852,0.667309373633001));
#43427=CARTESIAN_POINT('Ctrl Pts',(-30.4834462874739,57.6451078131478,0.778447264201044));
#43428=CARTESIAN_POINT('Ctrl Pts',(-32.5434486064222,58.7199110699496,0.889585154769085));
#43429=CARTESIAN_POINT('Ctrl Pts',(-34.563681922824,57.5721005714895,1.00072304533713));
#43430=CARTESIAN_POINT('Ctrl Pts',(-34.6950037716947,55.2522802841409,1.11186093590517));
#43431=CARTESIAN_POINT('Ctrl Pts',(-32.8172137752098,53.883808025427,1.22299882647321));
#43432=CARTESIAN_POINT('Ctrl Pts',(-30.6490744128705,54.7192619732989,1.33413671704125));
#43433=CARTESIAN_POINT('Ctrl Pts',(-30.1751082313325,56.9939416545675,1.44527460760929));
#43434=CARTESIAN_POINT('Ctrl Pts',(-31.8291418517329,58.6258069603505,1.55641249817734));
#43435=CARTESIAN_POINT('Ctrl Pts',(-34.0972195432855,58.1211930696509,1.66755038874538));
#43436=CARTESIAN_POINT('Ctrl Pts',(-34.90334407317,55.9419787993381,1.77868827931342));
#43437=CARTESIAN_POINT('Ctrl Pts',(-33.5096605171051,54.0828236849994,1.88982616988146));
#43438=CARTESIAN_POINT('Ctrl Pts',(-31.1918232394055,54.2454334870425,2.0009640604495));
#43439=CARTESIAN_POINT('Ctrl Pts',(-30.0713749864112,56.2809696095364,2.11210195101755));
#43440=CARTESIAN_POINT('Ctrl Pts',(-31.1738747508359,58.326282755013,2.22323984158559));
#43441=CARTESIAN_POINT('Ctrl Pts',(-33.4901919951035,58.5092746059888,2.33437773215363));
#43442=CARTESIAN_POINT('Ctrl Pts',(-34.900175276712,56.6624506459969,2.44551562272167));
#43443=CARTESIAN_POINT('Ctrl Pts',(-34.113250907707,54.4762297900261,2.55665351328971));
#43444=CARTESIAN_POINT('Ctrl Pts',(-31.8496996873681,53.9516847809774,2.66779140385775));
#43445=CARTESIAN_POINT('Ctrl Pts',(-30.1813757180884,55.5689376143778,2.7789292944258));
#43446=CARTESIAN_POINT('Ctrl Pts',(-30.6353148490301,57.8476984309217,2.89006718499383));
#43447=CARTESIAN_POINT('Ctrl Pts',(-32.7960214456225,58.7021916123208,3.00120507556188));
#43448=CARTESIAN_POINT('Ctrl Pts',(-34.6857762559251,57.350289859029,3.11234296612992));
#43449=CARTESIAN_POINT('Ctrl Pts',(-34.5748652707907,55.0294041774427,3.22348085669796));
#43450=CARTESIAN_POINT('Ctrl Pts',(-32.5648065727292,53.8638675525518,3.334618747266));
#43451=CARTESIAN_POINT('Ctrl Pts',(-30.4954296836916,54.9205088752031,3.44575663783405));
#43452=CARTESIAN_POINT('Ctrl Pts',(-30.2608587385459,57.2321723596468,3.55689452840209));
#43453=CARTESIAN_POINT('Ctrl Pts',(-32.0757991835955,58.6829662025232,3.66803241897013));
#43454=CARTESIAN_POINT('Ctrl Pts',(-34.2790154466699,57.9449623463291,3.77917030953817));
#43455=CARTESIAN_POINT('Ctrl Pts',(-34.8538786959893,55.6936640901667,3.89030820010621));
#43456=CARTESIAN_POINT('Ctrl Pts',(-33.2742100800909,53.9897102593704,4.00144609067426));
#43457=CARTESIAN_POINT('Ctrl Pts',(-30.9858981977034,54.3927491193984,4.1125839812423));
#43458=CARTESIAN_POINT('Ctrl Pts',(-30.0834608661247,56.5338746309361,4.22372187181034));
#43459=CARTESIAN_POINT('Ctrl Pts',(-31.3929092090317,58.4532903311776,4.33485976237838));
#43460=CARTESIAN_POINT('Ctrl Pts',(-33.7156903085101,58.3941332621978,4.44599765294642));
#43461=CARTESIAN_POINT('Ctrl Pts',(-34.9257362810773,56.410550559801,4.55713554351447));
#43462=CARTESIAN_POINT('Ctrl Pts',(-33.91547832718,54.3181379674856,4.6682734340825));
#43463=CARTESIAN_POINT('Ctrl Pts',(-31.6096170051591,54.0321044593028,4.77941132465055));
#43464=CARTESIAN_POINT('Ctrl Pts',(-30.1187333412011,55.8142597516568,4.89054921521859));
#43465=CARTESIAN_POINT('Ctrl Pts',(-30.8074500449804,58.033376889416,5.00168710578664));
#43466=CARTESIAN_POINT('Ctrl Pts',(-33.045376938239,58.6582727998918,5.11282499635467));
#43467=CARTESIAN_POINT('Ctrl Pts',(-34.7841140934679,57.1169731495112,5.22396288692271));
#43468=CARTESIAN_POINT('Ctrl Pts',(-34.4321757978777,54.8202470274371,5.33510077749076));
#43469=CARTESIAN_POINT('Ctrl Pts',(-32.3116949177892,53.8703138209288,5.44623866805879));
#43470=CARTESIAN_POINT('Ctrl Pts',(-30.3635721421369,55.1366583239951,5.55737655862684));
#43471=CARTESIAN_POINT('Ctrl Pts',(-30.3709453622051,57.4601807388668,5.66851444919488));
#43472=CARTESIAN_POINT('Ctrl Pts',(-32.3270677340268,58.7141352713796,5.77965233976292));
#43473=CARTESIAN_POINT('Ctrl Pts',(-34.4414743886772,57.7507618774264,5.89079023033096));
#43474=CARTESIAN_POINT('Ctrl Pts',(-34.7788326566387,55.451849617872,6.00192812089901));
#43475=CARTESIAN_POINT('Ctrl Pts',(-33.0303393193103,53.921614042038,6.11306601146705));
#43476=CARTESIAN_POINT('Ctrl Pts',(-30.79644075645,54.5607069079647,6.22420390203509));
#43477=CARTESIAN_POINT('Ctrl Pts',(-30.1217887402557,56.7841397946825,6.33534179260313));
#43478=CARTESIAN_POINT('Ctrl Pts',(-31.6240211855661,58.5568181325983,6.44647968317118));
#43479=CARTESIAN_POINT('Ctrl Pts',(-33.9278862659328,58.2561121571831,6.55761757373921));
#43480=CARTESIAN_POINT('Ctrl Pts',(-34.9251107981772,56.1574151102239,6.66875546430726));
#43481=CARTESIAN_POINT('Ctrl Pts',(-33.7019669024841,54.1813822458926,6.77989335487529));
#43482=CARTESIAN_POINT('Ctrl Pts',(-31.3799180340502,54.137308723055,6.89103124544334));
#43483=CARTESIAN_POINT('Ctrl Pts',(-30.0805564955409,56.0643114795338,7.00216913601138));
#43484=CARTESIAN_POINT('Ctrl Pts',(-31.0009129766989,58.2011370798035,7.11330702657943));
#43485=CARTESIAN_POINT('Ctrl Pts',(-32.5211546805143,58.4569191413474,7.18739895362479));
#43486=CARTESIAN_POINT('Ctrl Pts',(-33.1673657555108,58.2350041503452,7.22444491714747));
#43487=CARTESIAN_POINT('Ctrl Pts',(-31.137578557241,57.6518256858141,-2.07481497238249));
#43488=CARTESIAN_POINT('Ctrl Pts',(-31.5898689183853,58.1048632288922,-2.03776900885981));
#43489=CARTESIAN_POINT('Ctrl Pts',(-32.9744626126811,58.5161478980409,-1.96367708181445));
#43490=CARTESIAN_POINT('Ctrl Pts',(-34.6294912924535,57.0974392229325,-1.85253919124641));
#43491=CARTESIAN_POINT('Ctrl Pts',(-34.3303034137843,54.9405123144369,-1.74140130067836));
#43492=CARTESIAN_POINT('Ctrl Pts',(-32.3582893241016,54.0206552913481,-1.63026341011032));
#43493=CARTESIAN_POINT('Ctrl Pts',(-30.5147494765409,55.1792854513053,-1.51912551954228));
#43494=CARTESIAN_POINT('Ctrl Pts',(-30.4889518873458,57.3561677789083,-1.40798762897424));
#43495=CARTESIAN_POINT('Ctrl Pts',(-32.3035780800888,58.5586402598713,-1.2968497384062));
#43496=CARTESIAN_POINT('Ctrl Pts',(-34.2981478804346,57.686134989371,-1.18571184783815));
#43497=CARTESIAN_POINT('Ctrl Pts',(-34.6467739743846,55.5372313797062,-1.07457395727011));
#43498=CARTESIAN_POINT('Ctrl Pts',(-33.0304729643072,54.0788626331852,-0.963436066702071));
#43499=CARTESIAN_POINT('Ctrl Pts',(-30.9286042125635,54.6458814833823,-0.852298176134029));
#43500=CARTESIAN_POINT('Ctrl Pts',(-30.2650618023749,56.7192935259745,-0.741160285565988));
#43501=CARTESIAN_POINT('Ctrl Pts',(-31.6471786691816,58.4012790043313,-0.630022394997946));
#43502=CARTESIAN_POINT('Ctrl Pts',(-33.8098950838865,58.1522986401539,-0.518884504429904));
#43503=CARTESIAN_POINT('Ctrl Pts',(-34.7736484112179,56.2002464293262,-0.407746613861863));
#43504=CARTESIAN_POINT('Ctrl Pts',(-33.6563061966827,54.331858177016,-0.296608723293821));
#43505=CARTESIAN_POINT('Ctrl Pts',(-31.480583488533,54.2572906994736,-0.185470832725779));
#43506=CARTESIAN_POINT('Ctrl Pts',(-30.2379444342266,56.044796524896,-0.0743329421577371));
#43507=CARTESIAN_POINT('Ctrl Pts',(-31.0657904123945,58.0582512642421,0.0368049484103043));
#43508=CARTESIAN_POINT('Ctrl Pts',(-33.2063847314925,58.4547169782087,0.147942838978346));
#43509=CARTESIAN_POINT('Ctrl Pts',(-34.7004170746387,56.8713040936592,0.259080729546388));
#43510=CARTESIAN_POINT('Ctrl Pts',(-34.1803827251225,54.7573283854237,0.37021862011443));
#43511=CARTESIAN_POINT('Ctrl Pts',(-32.1222750053513,54.0477357911158,0.481356510682471));
#43512=CARTESIAN_POINT('Ctrl Pts',(-30.4099032594437,55.3920244607626,0.592494401250513));
#43513=CARTESIAN_POINT('Ctrl Pts',(-30.6106207621861,57.5597517291987,0.703632291818555));
#43514=CARTESIAN_POINT('Ctrl Pts',(-32.5407085089656,58.5667722442101,0.814770182386597));
#43515=CARTESIAN_POINT('Ctrl Pts',(-34.4335352954974,57.4913487078745,0.925908072954637));
#43516=CARTESIAN_POINT('Ctrl Pts',(-34.5565752984423,55.3178284792041,1.03704596352268));
#43517=CARTESIAN_POINT('Ctrl Pts',(-32.7972086074906,54.0356592728607,1.14818385409072));
#43518=CARTESIAN_POINT('Ctrl Pts',(-30.7658035075692,54.8184251042164,1.25932174465876));
#43519=CARTESIAN_POINT('Ctrl Pts',(-30.3217281242748,56.9496515306538,1.3704596352268));
#43520=CARTESIAN_POINT('Ctrl Pts',(-31.8714496921254,58.4786028343079,1.48159752579485));
#43521=CARTESIAN_POINT('Ctrl Pts',(-33.9964904850136,58.0058125474546,1.59273541636289));
#43522=CARTESIAN_POINT('Ctrl Pts',(-34.7517765656152,55.9640309814584,1.70387330693093));
#43523=CARTESIAN_POINT('Ctrl Pts',(-33.4459860188247,54.222123959053,1.81501119749897));
#43524=CARTESIAN_POINT('Ctrl Pts',(-31.2743237407936,54.3744787324154,1.92614908806701));
#43525=CARTESIAN_POINT('Ctrl Pts',(-30.2245368429279,56.2816432496664,2.03728697863506));
#43526=CARTESIAN_POINT('Ctrl Pts',(-31.2575071782378,58.1979681994493,2.1484248692031));
#43527=CARTESIAN_POINT('Ctrl Pts',(-33.4277452841336,58.3694196226251,2.25956275977114));
#43528=CARTESIAN_POINT('Ctrl Pts',(-34.7488076101148,56.6390660871692,2.37070065033918));
#43529=CARTESIAN_POINT('Ctrl Pts',(-34.0115108273451,54.5907198076286,2.48183854090722));
#43530=CARTESIAN_POINT('Ctrl Pts',(-31.8907110426077,54.0992553634931,2.59297643147526));
#43531=CARTESIAN_POINT('Ctrl Pts',(-30.3276003503783,55.6145157340662,2.70411432204331));
#43532=CARTESIAN_POINT('Ctrl Pts',(-30.7529116941353,57.7495659179407,2.81525221261135));
#43533=CARTESIAN_POINT('Ctrl Pts',(-32.7773527775792,58.5501702687005,2.92639010317939));
#43534=CARTESIAN_POINT('Ctrl Pts',(-34.5479297183105,57.2835265446242,3.03752799374743));
#43535=CARTESIAN_POINT('Ctrl Pts',(-34.4440133627694,55.1090081110757,3.14866588431548));
#43536=CARTESIAN_POINT('Ctrl Pts',(-32.5607195296748,54.0169763509983,3.25980377488351));
#43537=CARTESIAN_POINT('Ctrl Pts',(-30.6218484224619,55.0069803188732,3.37094166545156));
#43538=CARTESIAN_POINT('Ctrl Pts',(-30.4020707538584,57.1728581554962,3.4820795560196));
#43539=CARTESIAN_POINT('Ctrl Pts',(-32.1025515163817,58.5321573142801,3.59321744658764));
#43540=CARTESIAN_POINT('Ctrl Pts',(-34.1668213833381,57.8406958596912,3.70435533715568));
#43541=CARTESIAN_POINT('Ctrl Pts',(-34.705430735075,55.7313763028164,3.81549322772372));
#43542=CARTESIAN_POINT('Ctrl Pts',(-33.225384323732,54.1348827553833,3.92663111829177));
#43543=CARTESIAN_POINT('Ctrl Pts',(-31.0813854144196,54.5125038668068,4.0377690088598));
#43544=CARTESIAN_POINT('Ctrl Pts',(-30.2358605235516,56.5185987513241,4.14890689942785));
#43545=CARTESIAN_POINT('Ctrl Pts',(-31.4627281724074,58.3169660103977,4.26004478999589));
#43546=CARTESIAN_POINT('Ctrl Pts',(-33.6390224888348,58.2615396970761,4.37118268056393));
#43547=CARTESIAN_POINT('Ctrl Pts',(-34.772756603214,56.4030521442201,4.48232057113198));
#43548=CARTESIAN_POINT('Ctrl Pts',(-33.8262108251009,54.4425980862377,4.59345846170001));
#43549=CARTESIAN_POINT('Ctrl Pts',(-31.6657692360459,54.1746033542736,4.70459635226806));
#43550=CARTESIAN_POINT('Ctrl Pts',(-30.2689085309823,55.8443665681263,4.8157342428361));
#43551=CARTESIAN_POINT('Ctrl Pts',(-30.9141911400064,57.9235345170459,4.92687213340414));
#43552=CARTESIAN_POINT('Ctrl Pts',(-33.0109826023927,58.5090212073898,5.03801002397218));
#43553=CARTESIAN_POINT('Ctrl Pts',(-34.6400658550227,57.0649240129586,5.14914791454022));
#43554=CARTESIAN_POINT('Ctrl Pts',(-34.3103226378947,54.9130415101336,5.26028580510827));
#43555=CARTESIAN_POINT('Ctrl Pts',(-32.3235704258736,54.0230160838143,5.3714236956763));
#43556=CARTESIAN_POINT('Ctrl Pts',(-30.498306510429,55.2094982474935,5.48256158624435));
#43557=CARTESIAN_POINT('Ctrl Pts',(-30.5052147364911,57.3864871280696,5.59369947681239));
#43558=CARTESIAN_POINT('Ctrl Pts',(-32.3379737515306,58.5613606978515,5.70483736738044));
#43559=CARTESIAN_POINT('Ctrl Pts',(-34.3190348106915,57.6587426929398,5.81597525794847));
#43560=CARTESIAN_POINT('Ctrl Pts',(-34.6351174933556,55.5048119219529,5.92711314851652));
#43561=CARTESIAN_POINT('Ctrl Pts',(-32.9968933347409,54.0710810433821,6.03825103908456));
#43562=CARTESIAN_POINT('Ctrl Pts',(-30.9038761550678,54.669869354557,6.1493889296526));
#43563=CARTESIAN_POINT('Ctrl Pts',(-30.2717712405154,56.7530808786254,6.26052682022064));
#43564=CARTESIAN_POINT('Ctrl Pts',(-31.6792650131382,58.413964804591,6.37166471078869));
#43565=CARTESIAN_POINT('Ctrl Pts',(-33.8378362540284,58.1322229282863,6.48280260135671));
#43566=CARTESIAN_POINT('Ctrl Pts',(-34.7721705665527,56.1658807463967,6.59394049192478));
#43567=CARTESIAN_POINT('Ctrl Pts',(-33.6261645529135,54.3144668991412,6.70507838249281));
#43568=CARTESIAN_POINT('Ctrl Pts',(-31.4505562891928,54.2731728842734,6.81621627306085));
#43569=CARTESIAN_POINT('Ctrl Pts',(-30.2331393178402,56.0786487199457,6.92735416362889));
#43570=CARTESIAN_POINT('Ctrl Pts',(-31.0954532825444,58.0807148681969,7.03849205419693));
#43571=CARTESIAN_POINT('Ctrl Pts',(-32.5198205551868,58.3203659687277,7.1125839812423));
#43572=CARTESIAN_POINT('Ctrl Pts',(-33.1252781637592,58.1124461032886,7.14962994476498));
#43573=CARTESIAN_POINT('Ctrl Pts',(-31.22928340286,57.5602720863885,-2.14962994476498));
#43574=CARTESIAN_POINT('Ctrl Pts',(-31.6511300140442,57.9828155865489,-2.1125839812423));
#43575=CARTESIAN_POINT('Ctrl Pts',(-32.9425264442663,58.3664166066401,-2.03849205419693));
#43576=CARTESIAN_POINT('Ctrl Pts',(-34.4861548298197,57.0432014814318,-1.9273541636289));
#43577=CARTESIAN_POINT('Ctrl Pts',(-34.207105343988,55.0314577320876,-1.81621627306085));
#43578=CARTESIAN_POINT('Ctrl Pts',(-32.3678278965638,54.1735164596221,-1.70507838249281));
#43579=CARTESIAN_POINT('Ctrl Pts',(-30.6483770656664,55.2541590038433,-1.59394049192477));
#43580=CARTESIAN_POINT('Ctrl Pts',(-30.6243159170911,57.2845149692516,-1.48280260135673));
#43581=CARTESIAN_POINT('Ctrl Pts',(-32.3167992767584,58.4060487995394,-1.37166471078869));
#43582=CARTESIAN_POINT('Ctrl Pts',(-34.1771142056845,57.5922720242182,-1.26052682022064));
#43583=CARTESIAN_POINT('Ctrl Pts',(-34.5022742111534,55.5880115239391,-1.1493889296526));
#43584=CARTESIAN_POINT('Ctrl Pts',(-32.9947667285052,54.2278058542443,-1.03825103908456));
#43585=CARTESIAN_POINT('Ctrl Pts',(-31.034375160943,54.7566585581314,-0.927113148516518));
#43586=CARTESIAN_POINT('Ctrl Pts',(-30.4154959161879,56.6905088430302,-0.815975257948476));
#43587=CARTESIAN_POINT('Ctrl Pts',(-31.7045822346488,58.2592795599445,-0.704837367380436));
#43588=CARTESIAN_POINT('Ctrl Pts',(-33.7217257974419,58.0270581112851,-0.593699476812393));
#43589=CARTESIAN_POINT('Ctrl Pts',(-34.6206087055888,56.2063989048655,-0.482561586244352));
#43590=CARTESIAN_POINT('Ctrl Pts',(-33.5784750073553,54.4637722200535,-0.37142369567631));
#43591=CARTESIAN_POINT('Ctrl Pts',(-31.5492006071951,54.394223893562,-0.260285805108268));
#43592=CARTESIAN_POINT('Ctrl Pts',(-30.3902038232309,56.0614123629749,-0.149147914540226));
#43593=CARTESIAN_POINT('Ctrl Pts',(-31.1623273316537,57.9393410820767,-0.0380100239721846));
#43594=CARTESIAN_POINT('Ctrl Pts',(-33.1588378412895,58.3091206136687,0.0731278665958569));
#43595=CARTESIAN_POINT('Ctrl Pts',(-34.5523065841589,56.8322875505838,0.184265757163899));
#43596=CARTESIAN_POINT('Ctrl Pts',(-34.067275845304,54.8606039480668,0.295403647731941));
#43597=CARTESIAN_POINT('Ctrl Pts',(-32.1476997463555,54.1987741658161,0.406541538299982));
#43598=CARTESIAN_POINT('Ctrl Pts',(-30.5505880673203,55.45257851024,0.517679428868024));
#43599=CARTESIAN_POINT('Ctrl Pts',(-30.7377952368983,57.4743956452495,0.628817319436066));
#43600=CARTESIAN_POINT('Ctrl Pts',(-32.5379684115091,58.4136334184706,0.739955210004107));
#43601=CARTESIAN_POINT('Ctrl Pts',(-34.3033886681708,57.4105968442595,0.85109310057215));
#43602=CARTESIAN_POINT('Ctrl Pts',(-34.4181468251899,55.3833766742673,0.962230991140191));
#43603=CARTESIAN_POINT('Ctrl Pts',(-32.7772034397714,54.1875105202944,1.07336888170823));
#43604=CARTESIAN_POINT('Ctrl Pts',(-30.8825326022679,54.9175882351338,1.18450677227627));
#43605=CARTESIAN_POINT('Ctrl Pts',(-30.4683480172171,56.9053614067402,1.29564466284432));
#43606=CARTESIAN_POINT('Ctrl Pts',(-31.9137575325177,58.3313987082652,1.40678255341236));
#43607=CARTESIAN_POINT('Ctrl Pts',(-33.8957614267418,57.8904320252583,1.5179204439804));
#43608=CARTESIAN_POINT('Ctrl Pts',(-34.6002090580604,55.9860831635788,1.62905833454844));
#43609=CARTESIAN_POINT('Ctrl Pts',(-33.3823115205443,54.3614242331065,1.74019622511648));
#43610=CARTESIAN_POINT('Ctrl Pts',(-31.3568242421816,54.5035239777884,1.85133411568453));
#43611=CARTESIAN_POINT('Ctrl Pts',(-30.3776986994445,56.2823168897962,1.96247200625257));
#43612=CARTESIAN_POINT('Ctrl Pts',(-31.3411396056398,58.0696536438857,2.07360989682061));
#43613=CARTESIAN_POINT('Ctrl Pts',(-33.3652985731636,58.2295646392612,2.18474778738865));
#43614=CARTESIAN_POINT('Ctrl Pts',(-34.5974399435175,56.6156815283416,2.29588567795669));
#43615=CARTESIAN_POINT('Ctrl Pts',(-33.9097707469831,54.7052098252308,2.40702356852473));
#43616=CARTESIAN_POINT('Ctrl Pts',(-31.9317223978473,54.246825946009,2.51816145909278));
#43617=CARTESIAN_POINT('Ctrl Pts',(-30.4738249826682,55.6600938537544,2.62929934966082));
#43618=CARTESIAN_POINT('Ctrl Pts',(-30.8705085392404,57.6514334049598,2.74043724022886));
#43619=CARTESIAN_POINT('Ctrl Pts',(-32.7586841095359,58.3981489250801,2.8515751307969));
#43620=CARTESIAN_POINT('Ctrl Pts',(-34.4100831806959,57.2167632302195,2.96271302136494));
#43621=CARTESIAN_POINT('Ctrl Pts',(-34.3131614547482,55.1886120447087,3.07385091193299));
#43622=CARTESIAN_POINT('Ctrl Pts',(-32.5566324866203,54.1700851494448,3.18498880250102));
#43623=CARTESIAN_POINT('Ctrl Pts',(-30.7482671612322,55.0934517625431,3.29612669306907));
#43624=CARTESIAN_POINT('Ctrl Pts',(-30.543282769171,57.1135439513457,3.40726458363711));
#43625=CARTESIAN_POINT('Ctrl Pts',(-32.1293038491678,58.381348426037,3.51840247420515));
#43626=CARTESIAN_POINT('Ctrl Pts',(-34.0546273200064,57.7364293730534,3.6295403647732));
#43627=CARTESIAN_POINT('Ctrl Pts',(-34.5569827741607,55.769088515466,3.74067825534123));
#43628=CARTESIAN_POINT('Ctrl Pts',(-33.1765585673731,54.2800552513962,3.85181614590928));
#43629=CARTESIAN_POINT('Ctrl Pts',(-31.1768726311358,54.6322586142151,3.96295403647732));
#43630=CARTESIAN_POINT('Ctrl Pts',(-30.3882601809786,56.5033228717121,4.07409192704536));
#43631=CARTESIAN_POINT('Ctrl Pts',(-31.5325471357832,58.1806416896178,4.1852298176134));
#43632=CARTESIAN_POINT('Ctrl Pts',(-33.5623546691595,58.1289461319544,4.29636770818144));
#43633=CARTESIAN_POINT('Ctrl Pts',(-34.6197769253507,56.3955537286392,4.40750559874949));
#43634=CARTESIAN_POINT('Ctrl Pts',(-33.7369433230218,54.5670582049899,4.51864348931753));
#43635=CARTESIAN_POINT('Ctrl Pts',(-31.7219214669328,54.3171022492445,4.62978137988557));
#43636=CARTESIAN_POINT('Ctrl Pts',(-30.4190837207633,55.8744733845956,4.74091927045361));
#43637=CARTESIAN_POINT('Ctrl Pts',(-31.0209322350324,57.8136921446758,4.85205716102165));
#43638=CARTESIAN_POINT('Ctrl Pts',(-32.9765882665465,58.359769614888,4.9631950515897));
#43639=CARTESIAN_POINT('Ctrl Pts',(-34.4960176165775,57.0128748764059,5.07433294215773));
#43640=CARTESIAN_POINT('Ctrl Pts',(-34.1884694779118,55.0058359928301,5.18547083272579));
#43641=CARTESIAN_POINT('Ctrl Pts',(-32.335445933958,54.1757183466999,5.29660872329381));
#43642=CARTESIAN_POINT('Ctrl Pts',(-30.6330408787211,55.2823381709918,5.40774661386187));
#43643=CARTESIAN_POINT('Ctrl Pts',(-30.6394841107772,57.3127935172725,5.51888450442989));
#43644=CARTESIAN_POINT('Ctrl Pts',(-32.3488797690342,58.4085861243233,5.63002239499795));
#43645=CARTESIAN_POINT('Ctrl Pts',(-34.1965952327058,57.5667235084533,5.74116028556598));
#43646=CARTESIAN_POINT('Ctrl Pts',(-34.4914023300724,55.5577742260337,5.85229817613403));
#43647=CARTESIAN_POINT('Ctrl Pts',(-32.9634473501715,54.2205480447262,5.96343606670206));
#43648=CARTESIAN_POINT('Ctrl Pts',(-31.0113115536856,54.7790318011494,6.07457395727011));
#43649=CARTESIAN_POINT('Ctrl Pts',(-30.4217537407751,56.7220219625683,6.18571184783815));
#43650=CARTESIAN_POINT('Ctrl Pts',(-31.7345088407103,58.2711114765837,6.29684973840619));
#43651=CARTESIAN_POINT('Ctrl Pts',(-33.7477862421241,58.0083336993895,6.40798762897424));
#43652=CARTESIAN_POINT('Ctrl Pts',(-34.6192303349282,56.1743463825696,6.51912551954228));
#43653=CARTESIAN_POINT('Ctrl Pts',(-33.5503622033428,54.4475515523897,6.63026341011032));
#43654=CARTESIAN_POINT('Ctrl Pts',(-31.5211945443355,54.4090370454918,6.74140130067836));
#43655=CARTESIAN_POINT('Ctrl Pts',(-30.3857221401394,56.0929859603577,6.8525391912464));
#43656=CARTESIAN_POINT('Ctrl Pts',(-31.18999358839,57.9602926565904,6.96367708181445));
#43657=CARTESIAN_POINT('Ctrl Pts',(-32.5184864298593,58.1838127961081,7.03776900885981));
#43658=CARTESIAN_POINT('Ctrl Pts',(-33.0831905720076,57.989888056232,7.07481497238249));
#43659=CARTESIAN_POINT('Ctrl Pts',(-31.320988248479,57.468718486963,-2.22444491714747));
#43660=CARTESIAN_POINT('Ctrl Pts',(-31.712391109703,57.8607679442056,-2.18739895362479));
#43661=CARTESIAN_POINT('Ctrl Pts',(-32.9105902758514,58.2166853152393,-2.11330702657943));
#43662=CARTESIAN_POINT('Ctrl Pts',(-34.342818367186,56.9889637399312,-2.00216913601138));
#43663=CARTESIAN_POINT('Ctrl Pts',(-34.0839072741916,55.122403149738,-1.89103124544334));
#43664=CARTESIAN_POINT('Ctrl Pts',(-32.377366469026,54.3263776278961,-1.7798933548753));
#43665=CARTESIAN_POINT('Ctrl Pts',(-30.782004654792,55.3290325563813,-1.66875546430726));
#43666=CARTESIAN_POINT('Ctrl Pts',(-30.7596799468365,57.2128621595948,-1.55761757373922));
#43667=CARTESIAN_POINT('Ctrl Pts',(-32.330020473428,58.2534573392075,-1.44647968317117));
#43668=CARTESIAN_POINT('Ctrl Pts',(-34.0560805309345,57.4984090590654,-1.33534179260313));
#43669=CARTESIAN_POINT('Ctrl Pts',(-34.3577744479221,55.6387916681721,-1.22420390203509));
#43670=CARTESIAN_POINT('Ctrl Pts',(-32.9590604927032,54.3767490753035,-1.11306601146705));
#43671=CARTESIAN_POINT('Ctrl Pts',(-31.1401461093226,54.8674356328804,-1.00192812089901));
#43672=CARTESIAN_POINT('Ctrl Pts',(-30.5659300300008,56.6617241600859,-0.890790230330966));
#43673=CARTESIAN_POINT('Ctrl Pts',(-31.761985800116,58.1172801155577,-0.779652339762924));
#43674=CARTESIAN_POINT('Ctrl Pts',(-33.6335565109972,57.9018175824163,-0.668514449194882));
#43675=CARTESIAN_POINT('Ctrl Pts',(-34.4675689999597,56.2125513804048,-0.557376558626841));
#43676=CARTESIAN_POINT('Ctrl Pts',(-33.5006438180279,54.595686263091,-0.446238668058798));
#43677=CARTESIAN_POINT('Ctrl Pts',(-31.6178177258571,54.5311570876504,-0.335100777490758));
#43678=CARTESIAN_POINT('Ctrl Pts',(-30.5424632122353,56.0780282010538,-0.223962886922715));
#43679=CARTESIAN_POINT('Ctrl Pts',(-31.2588642509129,57.8204308999113,-0.112824996354674));
#43680=CARTESIAN_POINT('Ctrl Pts',(-33.1112909510864,58.1635242491288,-0.00168710578663204));
#43681=CARTESIAN_POINT('Ctrl Pts',(-34.4041960936792,56.7932710075084,0.10945078478141));
#43682=CARTESIAN_POINT('Ctrl Pts',(-33.9541689654856,54.9638795107097,0.220588675349452));
#43683=CARTESIAN_POINT('Ctrl Pts',(-32.1731244873597,54.3498125405165,0.331726565917494));
#43684=CARTESIAN_POINT('Ctrl Pts',(-30.6912728751969,55.5131325597174,0.442864456485535));
#43685=CARTESIAN_POINT('Ctrl Pts',(-30.8649697116105,57.3890395613005,0.554002347053577));
#43686=CARTESIAN_POINT('Ctrl Pts',(-32.5352283140525,58.260494592731,0.665140237621618));
#43687=CARTESIAN_POINT('Ctrl Pts',(-34.1732420408443,57.3298449806446,0.776278128189661));
#43688=CARTESIAN_POINT('Ctrl Pts',(-34.2797183519374,55.4489248693305,0.887416018757701));
#43689=CARTESIAN_POINT('Ctrl Pts',(-32.7571982720523,54.3393617677281,0.998553909325745));
#43690=CARTESIAN_POINT('Ctrl Pts',(-30.9992616969666,55.0167513660514,1.10969179989379));
#43691=CARTESIAN_POINT('Ctrl Pts',(-30.6149679101594,56.8610712828264,1.22082969046183));
#43692=CARTESIAN_POINT('Ctrl Pts',(-31.9560653729101,58.1841945822227,1.33196758102987));
#43693=CARTESIAN_POINT('Ctrl Pts',(-33.7950323684699,57.7750515030619,1.44310547159791));
#43694=CARTESIAN_POINT('Ctrl Pts',(-34.4486415505055,56.0081353456992,1.55424336216596));
#43695=CARTESIAN_POINT('Ctrl Pts',(-33.318637022264,54.5007245071601,1.66538125273399));
#43696=CARTESIAN_POINT('Ctrl Pts',(-31.4393247435696,54.6325692231613,1.77651914330204));
#43697=CARTESIAN_POINT('Ctrl Pts',(-30.5308605559611,56.2829905299262,1.88765703387008));
#43698=CARTESIAN_POINT('Ctrl Pts',(-31.4247720330417,57.941339088322,1.99879492443812));
#43699=CARTESIAN_POINT('Ctrl Pts',(-33.3028518621937,58.0897096558975,2.10993281500616));
#43700=CARTESIAN_POINT('Ctrl Pts',(-34.4460722769204,56.592296969514,2.2210707055742));
#43701=CARTESIAN_POINT('Ctrl Pts',(-33.8080306666211,54.8196998428332,2.33220859614224));
#43702=CARTESIAN_POINT('Ctrl Pts',(-31.9727337530869,54.3943965285248,2.44334648671029));
#43703=CARTESIAN_POINT('Ctrl Pts',(-30.6200496149581,55.7056719734427,2.55448437727833));
#43704=CARTESIAN_POINT('Ctrl Pts',(-30.9881053843456,57.5533008919789,2.66562226784637));
#43705=CARTESIAN_POINT('Ctrl Pts',(-32.7400154414926,58.2461275814598,2.77676015841441));
#43706=CARTESIAN_POINT('Ctrl Pts',(-34.2722366430812,57.1499999158148,2.88789804898245));
#43707=CARTESIAN_POINT('Ctrl Pts',(-34.182309546727,55.2682159783416,2.99903593955049));
#43708=CARTESIAN_POINT('Ctrl Pts',(-32.5525454435658,54.3231939478913,3.11017383011854));
#43709=CARTESIAN_POINT('Ctrl Pts',(-30.8746859000025,55.1799232062131,3.22131172068657));
#43710=CARTESIAN_POINT('Ctrl Pts',(-30.6844947844836,57.0542297471953,3.33244961125463));
#43711=CARTESIAN_POINT('Ctrl Pts',(-32.156056181954,58.2305395377937,3.44358750182265));
#43712=CARTESIAN_POINT('Ctrl Pts',(-33.9424332566746,57.6321628864156,3.55472539239071));
#43713=CARTESIAN_POINT('Ctrl Pts',(-34.4085348132464,55.8068007281157,3.66586328295874));
#43714=CARTESIAN_POINT('Ctrl Pts',(-33.1277328110143,54.4252277474092,3.77700117352679));
#43715=CARTESIAN_POINT('Ctrl Pts',(-31.2723598478519,54.7520133616234,3.88813906409483));
#43716=CARTESIAN_POINT('Ctrl Pts',(-30.5406598384056,56.4880469921002,3.99927695466287));
#43717=CARTESIAN_POINT('Ctrl Pts',(-31.6023660991589,58.0443173688379,4.11041484523092));
#43718=CARTESIAN_POINT('Ctrl Pts',(-33.4856868494843,57.9963525668328,4.22155273579895));
#43719=CARTESIAN_POINT('Ctrl Pts',(-34.4667972474874,56.3880553130583,4.332690626367));
#43720=CARTESIAN_POINT('Ctrl Pts',(-33.6476758209426,54.691518323742,4.44382851693504));
#43721=CARTESIAN_POINT('Ctrl Pts',(-31.7780736978197,54.4596011442154,4.55496640750308));
#43722=CARTESIAN_POINT('Ctrl Pts',(-30.5692589105444,55.904580201065,4.66610429807112));
#43723=CARTESIAN_POINT('Ctrl Pts',(-31.1276733300584,57.7038497723057,4.77724218863916));
#43724=CARTESIAN_POINT('Ctrl Pts',(-32.9421939307002,58.210518022386,4.8883800792072));
#43725=CARTESIAN_POINT('Ctrl Pts',(-34.3519693781323,56.9608257398534,4.99951796977525));
#43726=CARTESIAN_POINT('Ctrl Pts',(-34.0666163179288,55.0986304755265,5.11065586034328));
#43727=CARTESIAN_POINT('Ctrl Pts',(-32.3473214420425,54.3284206095854,5.22179375091133));
#43728=CARTESIAN_POINT('Ctrl Pts',(-30.7677752470131,55.3551780944902,5.33293164147937));
#43729=CARTESIAN_POINT('Ctrl Pts',(-30.7737534850632,57.2390999064754,5.44406953204741));
#43730=CARTESIAN_POINT('Ctrl Pts',(-32.3597857865379,58.2558115507951,5.55520742261546));
#43731=CARTESIAN_POINT('Ctrl Pts',(-34.0741556547201,57.4747043239667,5.66634531318349));
#43732=CARTESIAN_POINT('Ctrl Pts',(-34.3476871667892,55.6107365301145,5.77748320375154));
#43733=CARTESIAN_POINT('Ctrl Pts',(-32.9300013656021,54.3700150460704,5.88862109431958));
#43734=CARTESIAN_POINT('Ctrl Pts',(-31.1187469523035,54.8881942477416,5.99975898488762));
#43735=CARTESIAN_POINT('Ctrl Pts',(-30.5717362410347,56.6909630465113,6.11089687545566));
#43736=CARTESIAN_POINT('Ctrl Pts',(-31.7897526682824,58.1282581485762,6.2220347660237));
#43737=CARTESIAN_POINT('Ctrl Pts',(-33.6577362302198,57.8844444704929,6.33317265659175));
#43738=CARTESIAN_POINT('Ctrl Pts',(-34.4662901033036,56.1828120187424,6.44431054715979));
#43739=CARTESIAN_POINT('Ctrl Pts',(-33.4745598537722,54.5806362056383,6.55544843772783));
#43740=CARTESIAN_POINT('Ctrl Pts',(-31.5918327994781,54.5449012067101,6.66658632829588));
#43741=CARTESIAN_POINT('Ctrl Pts',(-30.5383049624388,56.1073232007697,6.77772421886391));
#43742=CARTESIAN_POINT('Ctrl Pts',(-31.2845338942355,57.8398704449838,6.88886210943196));
#43743=CARTESIAN_POINT('Ctrl Pts',(-32.5171523045318,58.0472596234884,6.96295403647732));
#43744=CARTESIAN_POINT('Ctrl Pts',(-33.041102980256,57.8673300091754,7.));
#43745=CARTESIAN_POINT('Ctrl Pts',(-33.3327354544031,57.732107437543,-1.37851963660978));
#43746=CARTESIAN_POINT('Ctrl Pts',(-33.5202555818622,57.6251326319317,-1.36412702194089));
#43747=CARTESIAN_POINT('Ctrl Pts',(-33.6873867521344,57.4836168424902,-1.34973440727201));
#43748=CARTESIAN_POINT('Ctrl Pts',(-33.8186861741814,57.3143142072735,-1.33534179260312));
#43749=CARTESIAN_POINT('Ctrl Pts',(-34.1566451699304,56.8785365954343,-1.29829582908044));
#43750=CARTESIAN_POINT('Ctrl Pts',(-34.2572098089263,56.2586641318032,-1.26124986555776));
#43751=CARTESIAN_POINT('Ctrl Pts',(-34.0743731358877,55.7383874678429,-1.22420390203508));
#43752=CARTESIAN_POINT('Ctrl Pts',(-33.8915364628492,55.2181108038826,-1.1871579385124));
#43753=CARTESIAN_POINT('Ctrl Pts',(-33.4252984777762,54.797429939593,-1.15011197498972));
#43754=CARTESIAN_POINT('Ctrl Pts',(-32.8890270880096,54.6688706003777,-1.11306601146704));
#43755=CARTESIAN_POINT('Ctrl Pts',(-32.352755698243,54.5403112611624,-1.07602004794436));
#43756=CARTESIAN_POINT('Ctrl Pts',(-31.7464509037828,54.7038734470214,-1.03897408442168));
#43757=CARTESIAN_POINT('Ctrl Pts',(-31.3475958266657,55.0847026278185,-1.001928120899));
#43758=CARTESIAN_POINT('Ctrl Pts',(-30.9487407495486,55.4655318086156,-0.964882157376315));
#43759=CARTESIAN_POINT('Ctrl Pts',(-30.7573353897747,56.0636279843508,-0.927836193853635));
#43760=CARTESIAN_POINT('Ctrl Pts',(-30.8609753382403,56.6052687314637,-0.890790230330955));
#43761=CARTESIAN_POINT('Ctrl Pts',(-30.9646152867058,57.1469094785765,-0.853744266808274));
#43762=CARTESIAN_POINT('Ctrl Pts',(-31.3633005434109,57.6320947970672,-0.816698303285594));
#43763=CARTESIAN_POINT('Ctrl Pts',(-31.874571623577,57.8387770341222,-0.779652339762913));
#43764=CARTESIAN_POINT('Ctrl Pts',(-32.3398155301955,58.0268527049873,-0.74594143871187));
#43765=CARTESIAN_POINT('Ctrl Pts',(-32.8982866368194,57.9843126404343,-0.712230537660827));
#43766=CARTESIAN_POINT('Ctrl Pts',(-33.3348489584778,57.7359240281238,-0.678519636609784));
#43767=CARTESIAN_POINT('Ctrl Pts',(-31.045873711622,57.7433792852396,-2.));
#43768=CARTESIAN_POINT('Ctrl Pts',(-31.1022242475567,57.7901329641039,-2.));
#43769=CARTESIAN_POINT('Ctrl Pts',(-31.16109162216,57.8334666739882,-2.));
#43770=CARTESIAN_POINT('Ctrl Pts',(-31.2221267441946,57.8733637960052,-2.));
#43771=CARTESIAN_POINT('Ctrl Pts',(-31.2848602944931,57.9143711378008,-2.));
#43772=CARTESIAN_POINT('Ctrl Pts',(-31.3498848969729,57.9517482942041,-2.));
#43773=CARTESIAN_POINT('Ctrl Pts',(-31.4168445551528,57.9854278643736,-2.));
#43774=CARTESIAN_POINT('Ctrl Pts',(-31.4734239519064,58.0138863394451,-2.));
#43775=CARTESIAN_POINT('Ctrl Pts',(-31.5313856959223,58.039703972078,-2.));
#43776=CARTESIAN_POINT('Ctrl Pts',(-31.5905192436898,58.0628113946312,-2.));
#43777=CARTESIAN_POINT('Ctrl Pts',(-31.616790719774,58.0730774131924,-2.));
#43778=CARTESIAN_POINT('Ctrl Pts',(-31.6432934887177,58.0828081409933,-2.));
#43779=CARTESIAN_POINT('Ctrl Pts',(-31.6700089381812,58.0919957886042,-2.));
#43780=CARTESIAN_POINT('Ctrl Pts',(-31.684687964188,58.0970440180343,-2.));
#43781=CARTESIAN_POINT('Ctrl Pts',(-31.6994311962734,58.1019282705382,-2.));
#43782=CARTESIAN_POINT('Ctrl Pts',(-31.7142355159233,58.1066471169469,-2.));
#43783=CARTESIAN_POINT('Ctrl Pts',(-31.7278877153671,58.110998727412,-2.));
#43784=CARTESIAN_POINT('Ctrl Pts',(-31.7415938959784,58.1152101596117,-2.));
#43785=CARTESIAN_POINT('Ctrl Pts',(-31.7553302775655,58.119274259497,-2.));
#43786=CARTESIAN_POINT('Ctrl Pts',(-31.8255274332731,58.1400430660888,-2.));
#43787=CARTESIAN_POINT('Ctrl Pts',(-31.8966328017533,58.1570081793261,-2.));
#43788=CARTESIAN_POINT('Ctrl Pts',(-31.9683123621953,58.170109952811,-2.));
#43789=CARTESIAN_POINT('Ctrl Pts',(-32.0394355875927,58.1831100379529,-2.));
#43790=CARTESIAN_POINT('Ctrl Pts',(-32.1111251456288,58.1923065191834,-2.));
#43791=CARTESIAN_POINT('Ctrl Pts',(-32.1830533294103,58.1975902176944,-2.));
#43792=CARTESIAN_POINT('Ctrl Pts',(-32.2428321680078,58.2019814499469,-2.));
#43793=CARTESIAN_POINT('Ctrl Pts',(-32.3027760709099,58.203669194572,-2.));
#43794=CARTESIAN_POINT('Ctrl Pts',(-32.3626887231027,58.2025636252019,-2.));
#43795=CARTESIAN_POINT('Ctrl Pts',(-32.3876963771335,58.2021021584615,-2.));
#43796=CARTESIAN_POINT('Ctrl Pts',(-32.412698459505,58.201153730257,-2.));
#43797=CARTESIAN_POINT('Ctrl Pts',(-32.4376800452459,58.1997105189459,-2.));
#43798=CARTESIAN_POINT('Ctrl Pts',(-32.4492432419443,58.1990425014532,-2.));
#43799=CARTESIAN_POINT('Ctrl Pts',(-32.46080204105,58.198268467185,-2.));
#43800=CARTESIAN_POINT('Ctrl Pts',(-32.4723549281043,58.1973875849115,-2.));
#43801=CARTESIAN_POINT('Ctrl Pts',(-32.4844044306665,58.1964688367959,-2.));
#43802=CARTESIAN_POINT('Ctrl Pts',(-32.4964392274819,58.1954344592299,-2.));
#43803=CARTESIAN_POINT('Ctrl Pts',(-32.5084532356201,58.1942844547161,-2.));
#43804=CARTESIAN_POINT('Ctrl Pts',(-32.576878307084,58.187734672151,-2.));
#43805=CARTESIAN_POINT('Ctrl Pts',(-32.644677403631,58.1774344901198,-2.));
#43806=CARTESIAN_POINT('Ctrl Pts',(-32.7115617527711,58.1632926068264,-2.));
#43807=CARTESIAN_POINT('Ctrl Pts',(-32.7721836417578,58.1504748446728,-2.));
#43808=CARTESIAN_POINT('Ctrl Pts',(-32.8320544200173,58.1345005317114,-2.));
#43809=CARTESIAN_POINT('Ctrl Pts',(-32.8909448795169,58.1152674430859,-2.));
#43810=CARTESIAN_POINT('Ctrl Pts',(-32.9606152109761,58.0925137462918,-2.));
#43811=CARTESIAN_POINT('Ctrl Pts',(-33.0289150978522,58.0651988064951,-2.));
#43812=CARTESIAN_POINT('Ctrl Pts',(-33.0955156401827,58.0335993051752,-2.));
#43813=CARTESIAN_POINT('Ctrl Pts',(-33.1101787046012,58.0266422218357,-2.));
#43814=CARTESIAN_POINT('Ctrl Pts',(-33.1247592149198,58.0194773027427,-2.));
#43815=CARTESIAN_POINT('Ctrl Pts',(-33.1392533337008,58.0121072627471,-2.));
#43816=CARTESIAN_POINT('Ctrl Pts',(-33.1542086549745,58.0045027082655,-2.));
#43817=CARTESIAN_POINT('Ctrl Pts',(-33.1690773275701,57.9966767059895,-2.));
#43818=CARTESIAN_POINT('Ctrl Pts',(-33.1838253281019,57.9886488037328,-2.));
#43819=CARTESIAN_POINT('Ctrl Pts',(-33.2440619540896,57.9558596982087,-2.));
#43820=CARTESIAN_POINT('Ctrl Pts',(-33.3023667325631,57.9196691076086,-2.));
#43821=CARTESIAN_POINT('Ctrl Pts',(-33.3585069616797,57.8803506668497,-2.));
#43822=CARTESIAN_POINT('Ctrl Pts',(-33.4146358505063,57.8410401683904,-2.));
#43823=CARTESIAN_POINT('Ctrl Pts',(-33.4686017656045,57.7986021545295,-2.));
#43824=CARTESIAN_POINT('Ctrl Pts',(-33.5201343260632,57.753274648848,-2.));
#43825=CARTESIAN_POINT('Ctrl Pts',(-33.5574338655409,57.720466360796,-2.));
#43826=CARTESIAN_POINT('Ctrl Pts',(-33.5934578303088,57.6861435081364,-2.));
#43827=CARTESIAN_POINT('Ctrl Pts',(-33.6280882156071,57.650388864236,-2.));
#43828=CARTESIAN_POINT('Ctrl Pts',(-33.6540651537613,57.6235685974292,-2.));
#43829=CARTESIAN_POINT('Ctrl Pts',(-33.679257693834,57.5959425521655,-2.));
#43830=CARTESIAN_POINT('Ctrl Pts',(-33.7036104503286,57.5675443622685,-2.));
#43831=CARTESIAN_POINT('Ctrl Pts',(-33.7117026688921,57.558107879811,-2.));
#43832=CARTESIAN_POINT('Ctrl Pts',(-33.719695777907,57.5485935240877,-2.));
#43833=CARTESIAN_POINT('Ctrl Pts',(-33.7275879316845,57.5390030774341,-2.));
#43834=CARTESIAN_POINT('Ctrl Pts',(-33.769451093524,57.4881314862703,-2.));
#43835=CARTESIAN_POINT('Ctrl Pts',(-33.8084798256294,57.4351175562881,-2.));
#43836=CARTESIAN_POINT('Ctrl Pts',(-33.8444097934601,57.3801716628579,-2.));
#43837=CARTESIAN_POINT('Ctrl Pts',(-33.8696919535345,57.3415089265126,-2.));
#43838=CARTESIAN_POINT('Ctrl Pts',(-33.8934389530086,57.3018891510271,-2.));
#43839=CARTESIAN_POINT('Ctrl Pts',(-33.9155436487734,57.2613822920624,-2.));
#43840=CARTESIAN_POINT('Ctrl Pts',(-33.9226388854327,57.2483802696082,-2.));
#43841=CARTESIAN_POINT('Ctrl Pts',(-33.9295657376833,57.2352850255484,-2.));
#43842=CARTESIAN_POINT('Ctrl Pts',(-33.936317410013,57.2221046384805,-2.));
#43843=CARTESIAN_POINT('Ctrl Pts',(-33.9650804421564,57.1659544169675,-2.));
#43844=CARTESIAN_POINT('Ctrl Pts',(-33.9906110254719,57.1083731118225,-2.));
#43845=CARTESIAN_POINT('Ctrl Pts',(-34.012653283144,57.0495480070843,-2.));
#43846=CARTESIAN_POINT('Ctrl Pts',(-34.0329745304356,56.9953158354927,-2.));
#43847=CARTESIAN_POINT('Ctrl Pts',(-34.0503306992892,56.9400259525903,-2.));
#43848=CARTESIAN_POINT('Ctrl Pts',(-34.0644820150771,56.8838229928237,-2.));
#43849=CARTESIAN_POINT('Ctrl Pts',(-34.0671303463503,56.8733049563223,-2.));
#43850=CARTESIAN_POINT('Ctrl Pts',(-34.0696663195691,56.8627549469952,-2.));
#43851=CARTESIAN_POINT('Ctrl Pts',(-34.0720901513885,56.8521746541717,-2.));
#43852=CARTESIAN_POINT('Origin',(-32.5,56.2916512459885,3.));
#43853=CARTESIAN_POINT('Origin',(32.5,56.2916512459885,7.));
#43854=CARTESIAN_POINT('Ctrl Pts',(33.5940263469955,57.5480995545471,7.));
#43855=CARTESIAN_POINT('Ctrl Pts',(33.6455781063593,57.5127482049878,7.));
#43856=CARTESIAN_POINT('Ctrl Pts',(33.6948218851594,57.4743678095804,7.));
#43857=CARTESIAN_POINT('Ctrl Pts',(33.7416962543858,57.4332901552688,7.));
#43858=CARTESIAN_POINT('Ctrl Pts',(33.7714300138311,57.4072334186761,7.));
#43859=CARTESIAN_POINT('Ctrl Pts',(33.8002101106111,57.3800903098691,7.));
#43860=CARTESIAN_POINT('Ctrl Pts',(33.8280169256125,57.3519357929662,7.));
#43861=CARTESIAN_POINT('Ctrl Pts',(33.8470314137092,57.3326835439585,7.));
#43862=CARTESIAN_POINT('Ctrl Pts',(33.8655907373089,57.3129582157456,7.));
#43863=CARTESIAN_POINT('Ctrl Pts',(33.8836875902375,57.2927820229205,7.));
#43864=CARTESIAN_POINT('Ctrl Pts',(33.8932692328479,57.2820994434879,7.));
#43865=CARTESIAN_POINT('Ctrl Pts',(33.9027209653718,57.2712905497247,7.));
#43866=CARTESIAN_POINT('Ctrl Pts',(33.9120326403695,57.2603695725943,7.));
#43867=CARTESIAN_POINT('Ctrl Pts',(33.9548352574687,57.2101695384892,7.));
#43868=CARTESIAN_POINT('Ctrl Pts',(33.9947314180079,57.1575493208277,7.));
#43869=CARTESIAN_POINT('Ctrl Pts',(34.031636585354,57.1028515984669,7.));
#43870=CARTESIAN_POINT('Ctrl Pts',(34.0582554673164,57.0633993396144,7.));
#43871=CARTESIAN_POINT('Ctrl Pts',(34.0833178687179,57.0228651366186,7.));
#43872=CARTESIAN_POINT('Ctrl Pts',(34.1067823368899,56.9813639740226,7.));
#43873=CARTESIAN_POINT('Ctrl Pts',(34.1132255644837,56.96996795882,7.));
#43874=CARTESIAN_POINT('Ctrl Pts',(34.1195482501362,56.9584989754116,7.));
#43875=CARTESIAN_POINT('Ctrl Pts',(34.1257494083041,56.9469592819649,7.));
#43876=CARTESIAN_POINT('Ctrl Pts',(34.132058329377,56.9352190532546,7.));
#43877=CARTESIAN_POINT('Ctrl Pts',(34.1382375554008,56.9234128300226,7.));
#43878=CARTESIAN_POINT('Ctrl Pts',(34.1442842648129,56.9115477360727,7.));
#43879=CARTESIAN_POINT('Ctrl Pts',(34.1750933789438,56.8510928657025,7.));
#43880=CARTESIAN_POINT('Ctrl Pts',(34.2024838357259,56.7890775489765,7.));
#43881=CARTESIAN_POINT('Ctrl Pts',(34.2263706779214,56.7258494465016,7.));
#43882=CARTESIAN_POINT('Ctrl Pts',(34.2506031311489,56.6617065169613,7.));
#43883=CARTESIAN_POINT('Ctrl Pts',(34.2712305305803,56.5963146347364,7.));
#43884=CARTESIAN_POINT('Ctrl Pts',(34.2881270715367,56.5299991239702,7.));
#43885=CARTESIAN_POINT('Ctrl Pts',(34.2985953641974,56.4889131894921,7.));
#43886=CARTESIAN_POINT('Ctrl Pts',(34.3076308155221,56.447472028122,7.));
#43887=CARTESIAN_POINT('Ctrl Pts',(34.3151947514802,56.4057480907575,7.));
#43888=CARTESIAN_POINT('Ctrl Pts',(34.3213914047376,56.3715663137289,7.));
#43889=CARTESIAN_POINT('Ctrl Pts',(34.3266003410567,56.337194665163,7.));
#43890=CARTESIAN_POINT('Ctrl Pts',(34.3307964558936,56.3026718436529,7.));
#43891=CARTESIAN_POINT('Ctrl Pts',(34.3325110302053,56.2885654749698,7.));
#43892=CARTESIAN_POINT('Ctrl Pts',(34.3340565736349,56.2744313049453,7.));
#43893=CARTESIAN_POINT('Ctrl Pts',(34.3354292580617,56.2602960057088,7.));
#43894=CARTESIAN_POINT('Ctrl Pts',(34.3422420688248,56.1901406831141,7.));
#43895=CARTESIAN_POINT('Ctrl Pts',(34.3448171217661,56.11983645962,7.));
#43896=CARTESIAN_POINT('Ctrl Pts',(34.3430393002862,56.0497278065194,7.));
#43897=CARTESIAN_POINT('Ctrl Pts',(34.3428417470465,56.0419372652815,7.));
#43898=CARTESIAN_POINT('Ctrl Pts',(34.3425903992446,56.0341491123532,7.));
#43899=CARTESIAN_POINT('Ctrl Pts',(34.3422850635953,56.0263638020432,7.));
#43900=CARTESIAN_POINT('Ctrl Pts',(34.3396426913258,55.958989788811,7.));
#43901=CARTESIAN_POINT('Ctrl Pts',(34.3329614085344,55.8918294784504,7.));
#43902=CARTESIAN_POINT('Ctrl Pts',(34.3224781325172,55.825128323823,7.));
#43903=CARTESIAN_POINT('Ctrl Pts',(34.3112000078435,55.7533698452192,7.));
#43904=CARTESIAN_POINT('Ctrl Pts',(34.295521853206,55.6821418491415,7.));
#43905=CARTESIAN_POINT('Ctrl Pts',(34.2756745307237,55.6117461590107,7.));
#43906=CARTESIAN_POINT('Ctrl Pts',(34.2720417379785,55.5988611488225,7.));
#43907=CARTESIAN_POINT('Ctrl Pts',(34.2682690982962,55.5860040374986,7.));
#43908=CARTESIAN_POINT('Ctrl Pts',(34.2643578039031,55.5731767059407,7.));
#43909=CARTESIAN_POINT('Ctrl Pts',(34.2609943803684,55.5621461507044,7.));
#43910=CARTESIAN_POINT('Ctrl Pts',(34.2575311416983,55.5511465596784,7.));
#43911=CARTESIAN_POINT('Ctrl Pts',(34.2539698126456,55.5401805084982,7.));
#43912=CARTESIAN_POINT('Ctrl Pts',(34.2320182881598,55.4725873326265,7.));
#43913=CARTESIAN_POINT('Ctrl Pts',(34.2063390659048,55.4062514118632,7.));
#43914=CARTESIAN_POINT('Ctrl Pts',(34.1772031613691,55.3414402689902,7.));
#43915=CARTESIAN_POINT('Ctrl Pts',(34.1474529584126,55.2752626546329,7.));
#43916=CARTESIAN_POINT('Ctrl Pts',(34.1140985514797,55.2106738828667,7.));
#43917=CARTESIAN_POINT('Ctrl Pts',(34.077373335558,55.1479588365199,7.));
#43918=CARTESIAN_POINT('Ctrl Pts',(34.0404255619581,55.0848637320919,7.));
#43919=CARTESIAN_POINT('Ctrl Pts',(34.0000656099289,55.0236641322245,7.));
#43920=CARTESIAN_POINT('Ctrl Pts',(33.956480802391,54.9646647044169,7.));
#43921=CARTESIAN_POINT('Ctrl Pts',(33.9457092802779,54.9500836226779,7.));
#43922=CARTESIAN_POINT('Ctrl Pts',(33.9347405676772,54.9356370332213,7.));
#43923=CARTESIAN_POINT('Ctrl Pts',(33.9235770658016,54.9213297824322,7.));
#43924=CARTESIAN_POINT('Ctrl Pts',(33.9148444637425,54.9101379961009,7.));
#43925=CARTESIAN_POINT('Ctrl Pts',(33.9059915495185,54.8990302860272,7.));
#43926=CARTESIAN_POINT('Ctrl Pts',(33.89703329402,54.888025539777,7.));
#43927=CARTESIAN_POINT('Ctrl Pts',(33.8494695085346,54.8295959281122,7.));
#43928=CARTESIAN_POINT('Ctrl Pts',(33.7988575667886,54.7739598964368,6.99999999999999));
#43929=CARTESIAN_POINT('Ctrl Pts',(33.7454538505468,54.7214122178166,6.99999999999999));
#43930=CARTESIAN_POINT('Ctrl Pts',(33.691992046168,54.6688073821863,6.99999999999999));
#43931=CARTESIAN_POINT('Ctrl Pts',(33.6357318981107,54.6192966067137,7.));
#43932=CARTESIAN_POINT('Ctrl Pts',(33.5768824664943,54.5731951202135,7.));
#43933=CARTESIAN_POINT('Ctrl Pts',(33.5193724813759,54.5281429297379,7.));
#43934=CARTESIAN_POINT('Ctrl Pts',(33.4593891252722,54.4863457605992,7.));
#43935=CARTESIAN_POINT('Ctrl Pts',(33.3970899729434,54.4481299155973,7.));
#43936=CARTESIAN_POINT('Ctrl Pts',(33.3836932590424,54.4399120390638,7.));
#43937=CARTESIAN_POINT('Ctrl Pts',(33.3701893373732,54.4318599153263,6.99999999999999));
#43938=CARTESIAN_POINT('Ctrl Pts',(33.356579582449,54.4239770468377,6.99999999999999));
#43939=CARTESIAN_POINT('Ctrl Pts',(33.3450551424613,54.417302007843,6.99999999999999));
#43940=CARTESIAN_POINT('Ctrl Pts',(33.3334548151719,54.4107483324245,7.));
#43941=CARTESIAN_POINT('Ctrl Pts',(33.3217804591137,54.4043158724519,7.));
#43942=CARTESIAN_POINT('Ctrl Pts',(32.2716262263503,54.2496319067047,7.));
#43943=CARTESIAN_POINT('Ctrl Pts',(32.1985421824179,54.2648284787425,7.));
#43944=CARTESIAN_POINT('Ctrl Pts',(32.1265185433355,54.2843049160475,7.));
#43945=CARTESIAN_POINT('Ctrl Pts',(32.055814870235,54.3078098414778,7.));
#43946=CARTESIAN_POINT('Ctrl Pts',(31.9869629438864,54.3306991670755,7.));
#43947=CARTESIAN_POINT('Ctrl Pts',(31.9193621916298,54.3574095812603,7.));
#43948=CARTESIAN_POINT('Ctrl Pts',(31.8532778586936,54.3877469743405,7.));
#43949=CARTESIAN_POINT('Ctrl Pts',(31.8385281518176,54.3945181353016,7.));
#43950=CARTESIAN_POINT('Ctrl Pts',(31.8238521664773,54.4014710565443,7.));
#43951=CARTESIAN_POINT('Ctrl Pts',(31.8092592839734,54.4086007384021,7.));
#43952=CARTESIAN_POINT('Ctrl Pts',(31.7422937925777,54.4413182394836,7.));
#43953=CARTESIAN_POINT('Ctrl Pts',(31.6772081434645,54.4776886922259,7.));
#43954=CARTESIAN_POINT('Ctrl Pts',(31.6142783996461,54.517480847036,7.));
#43955=CARTESIAN_POINT('Ctrl Pts',(31.5700975700385,54.5454175635187,7.));
#43956=CARTESIAN_POINT('Ctrl Pts',(31.5269799621108,54.5750417874127,7.));
#43957=CARTESIAN_POINT('Ctrl Pts',(31.4850325699083,54.6062837165385,7.));
#43958=CARTESIAN_POINT('Ctrl Pts',(31.469084365258,54.6181617536036,7.));
#43959=CARTESIAN_POINT('Ctrl Pts',(31.4533054234991,54.6302737013537,7.));
#43960=CARTESIAN_POINT('Ctrl Pts',(31.4377020513635,54.6426159722202,7.));
#43961=CARTESIAN_POINT('Ctrl Pts',(31.422843223124,54.6543693086974,7.));
#43962=CARTESIAN_POINT('Ctrl Pts',(31.4081391342014,54.6663354488099,7.));
#43963=CARTESIAN_POINT('Ctrl Pts',(31.393620803187,54.6784895995769,7.));
#43964=CARTESIAN_POINT('Ctrl Pts',(31.3379553553849,54.7250904274836,7.));
#43965=CARTESIAN_POINT('Ctrl Pts',(31.284955832515,54.7744982188359,7.));
#43966=CARTESIAN_POINT('Ctrl Pts',(31.2348792621311,54.8265005113593,7.));
#43967=CARTESIAN_POINT('Ctrl Pts',(31.1858781212174,54.8773860181788,7.));
#43968=CARTESIAN_POINT('Ctrl Pts',(31.1396752549895,54.9307565896115,7.));
#43969=CARTESIAN_POINT('Ctrl Pts',(31.096553263567,54.98643879979,7.));
#43970=CARTESIAN_POINT('Ctrl Pts',(31.0543769959643,55.0408998234981,7.));
#43971=CARTESIAN_POINT('Ctrl Pts',(31.0151475677328,55.0975728716066,7.));
#43972=CARTESIAN_POINT('Ctrl Pts',(30.9791760533412,55.1563097700117,7.));
#43973=CARTESIAN_POINT('Ctrl Pts',(30.9674871681413,55.175396229786,7.));
#43974=CARTESIAN_POINT('Ctrl Pts',(30.9561426884268,55.19470068603,7.));
#43975=CARTESIAN_POINT('Ctrl Pts',(30.9451544834666,55.2142182090717,7.));
#43976=CARTESIAN_POINT('Ctrl Pts',(30.9389559539872,55.2252281913552,7.));
#43977=CARTESIAN_POINT('Ctrl Pts',(30.9328702746375,55.2363071799956,7.));
#43978=CARTESIAN_POINT('Ctrl Pts',(30.9269078404286,55.2474384077617,7.));
#43979=CARTESIAN_POINT('Ctrl Pts',(30.8946567101692,55.3076478229186,7.));
#43980=CARTESIAN_POINT('Ctrl Pts',(30.8659479670597,55.369487708999,6.99999999999999));
#43981=CARTESIAN_POINT('Ctrl Pts',(30.8410371124974,55.4327943982586,7.));
#43982=CARTESIAN_POINT('Ctrl Pts',(30.8374416945958,55.4419315397919,7.));
#43983=CARTESIAN_POINT('Ctrl Pts',(30.8339254772762,55.4510992636488,7.));
#43984=CARTESIAN_POINT('Ctrl Pts',(30.8304893165614,55.4602971020132,7.));
#43985=CARTESIAN_POINT('Ctrl Pts',(30.8062112767742,55.5252840174394,7.));
#43986=CARTESIAN_POINT('Ctrl Pts',(30.7859254272867,55.5917741516785,7.));
#43987=CARTESIAN_POINT('Ctrl Pts',(30.7695892422456,55.6594016433533,7.));
#43988=CARTESIAN_POINT('Ctrl Pts',(30.7543489013094,55.7224926298468,7.));
#43989=CARTESIAN_POINT('Ctrl Pts',(30.7425467760767,55.7865743173607,7.));
#43990=CARTESIAN_POINT('Ctrl Pts',(30.734187897611,55.8513431276599,7.));
#43991=CARTESIAN_POINT('Ctrl Pts',(30.7323430806899,55.8656377005129,7.));
#43992=CARTESIAN_POINT('Ctrl Pts',(30.7306661227445,55.8799656905854,7.));
#43993=CARTESIAN_POINT('Ctrl Pts',(30.7291573147969,55.8943237311442,7.));
#43994=CARTESIAN_POINT('Ctrl Pts',(30.7279778703883,55.905547499339,7.));
#43995=CARTESIAN_POINT('Ctrl Pts',(30.7269013312022,55.9167889367441,7.));
#43996=CARTESIAN_POINT('Ctrl Pts',(30.7259287166033,55.9280334135351,7.));
#43997=CARTESIAN_POINT('Ctrl Pts',(30.7200365397314,55.9961533514445,7.));
#43998=CARTESIAN_POINT('Ctrl Pts',(30.7179403223651,56.0645103688077,7.));
#43999=CARTESIAN_POINT('Ctrl Pts',(30.7195810692469,56.1327563915374,7.));
#44000=CARTESIAN_POINT('Ctrl Pts',(30.7212142396031,56.200687272582,7.));
#44001=CARTESIAN_POINT('Ctrl Pts',(30.7265502690293,56.2685092691059,7.));
#44002=CARTESIAN_POINT('Ctrl Pts',(30.7355805426662,56.3358665627088,7.));
#44003=CARTESIAN_POINT('Ctrl Pts',(30.7444173748676,56.4017809663077,7.));
#44004=CARTESIAN_POINT('Ctrl Pts',(30.7567922827814,56.4672512456727,7.));
#44005=CARTESIAN_POINT('Ctrl Pts',(30.7727391548109,56.5319175329114,7.));
#44006=CARTESIAN_POINT('Ctrl Pts',(30.7760991369442,56.5455426231072,7.));
#44007=CARTESIAN_POINT('Ctrl Pts',(30.7796178314759,56.5591318993402,7.));
#44008=CARTESIAN_POINT('Ctrl Pts',(30.7832957743544,56.5726817859276,7.));
#44009=CARTESIAN_POINT('Ctrl Pts',(30.786782084737,56.5855256804234,7.));
#44010=CARTESIAN_POINT('Ctrl Pts',(30.790412102401,56.5983358605448,7.));
#44011=CARTESIAN_POINT('Ctrl Pts',(30.7941799174142,56.6110887259411,7.));
#44012=CARTESIAN_POINT('Ctrl Pts',(30.8126945730391,56.6737549954412,7.));
#44013=CARTESIAN_POINT('Ctrl Pts',(30.8345622313707,56.7351520398133,7.));
#44014=CARTESIAN_POINT('Ctrl Pts',(30.8597663050147,56.794960649957,7.));
#44015=CARTESIAN_POINT('Ctrl Pts',(30.8844910320025,56.8536317829735,7.));
#44016=CARTESIAN_POINT('Ctrl Pts',(30.9124268768565,56.9107751110938,7.));
#44017=CARTESIAN_POINT('Ctrl Pts',(30.9435976955446,56.9660591311284,7.));
#44018=CARTESIAN_POINT('Ctrl Pts',(30.97375602352,57.019547415305,7.));
#44019=CARTESIAN_POINT('Ctrl Pts',(31.0069429903275,57.0712957445369,7.));
#44020=CARTESIAN_POINT('Ctrl Pts',(31.0432115503434,57.1209660580098,7.));
#44021=CARTESIAN_POINT('Ctrl Pts',(31.0492497805401,57.1292355009257,7.));
#44022=CARTESIAN_POINT('Ctrl Pts',(31.055373490492,57.1374472482377,7.));
#44023=CARTESIAN_POINT('Ctrl Pts',(31.0615830007349,57.1455996184164,7.));
#44024=CARTESIAN_POINT('Ctrl Pts',(31.0681540675971,57.1542266707015,7.));
#44025=CARTESIAN_POINT('Ctrl Pts',(31.0748212184917,57.1627872296297,7.));
#44026=CARTESIAN_POINT('Ctrl Pts',(31.0815830733444,57.1712803260696,7.));
#44027=CARTESIAN_POINT('Origin',(32.5,56.2916512459885,-3.54592528053767));
#44028=CARTESIAN_POINT('Ctrl Pts',(33.5269872402601,58.0734398505124,-1.79592528053768));
#44029=CARTESIAN_POINT('Ctrl Pts',(33.4422748054587,58.1232938101479,-1.79058130531689));
#44030=CARTESIAN_POINT('Ctrl Pts',(32.7422362990183,58.4684621317491,-1.74819136657341));
#44031=CARTESIAN_POINT('Ctrl Pts',(31.0929180917129,58.2713739433872,-1.66875546430726));
#44032=CARTESIAN_POINT('Ctrl Pts',(30.0738503853477,56.1831963302234,-1.55761757373922));
#44033=CARTESIAN_POINT('Ctrl Pts',(31.2751851021384,54.1944751483927,-1.44647968317118));
#44034=CARTESIAN_POINT('Ctrl Pts',(33.5977473666623,54.1252293793916,-1.33534179260313));
#44035=CARTESIAN_POINT('Ctrl Pts',(34.9154583912003,56.0389811637256,-1.22420390203509));
#44036=CARTESIAN_POINT('Ctrl Pts',(34.2741084270659,57.5792551456252,-1.14439839801327));
#44037=CARTESIAN_POINT('Ctrl Pts',(33.6210824061175,58.0199411501776,-1.10163885751414));
#44038=CARTESIAN_POINT('Ctrl Pts',(33.5295799600394,58.0717283210701,-1.09592528053768));
#44039=CARTESIAN_POINT('Ctrl Pts',(33.5283546803393,58.0681541983481,-1.85407471946233));
#44040=CARTESIAN_POINT('Ctrl Pts',(33.1193657433931,58.3001842134597,-1.82862455259619));
#44041=CARTESIAN_POINT('Ctrl Pts',(31.9170343357855,58.5410390719137,-1.76612842220737));
#44042=CARTESIAN_POINT('Ctrl Pts',(30.2743670907292,57.2623912321518,-1.66658632829588));
#44043=CARTESIAN_POINT('Ctrl Pts',(30.4765028746713,54.9487367869863,-1.55544843772783));
#44044=CARTESIAN_POINT('Ctrl Pts',(32.5312595152502,53.8630292597192,-1.44431054715979));
#44045=CARTESIAN_POINT('Ctrl Pts',(34.5571577499754,55.0008883544572,-1.33317265659175));
#44046=CARTESIAN_POINT('Ctrl Pts',(34.6817103419942,57.0195698185232,-1.23642738069259));
#44047=CARTESIAN_POINT('Ctrl Pts',(33.8868873402924,57.8579713309385,-1.17672806831612));
#44048=CARTESIAN_POINT('Ctrl Pts',(33.5250365419916,58.0693901510839,-1.15407471946233));
#44049=CARTESIAN_POINT('Ctrl Pts',(30.9307125467392,55.7322829513575,-2.));
#44050=CARTESIAN_POINT('Ctrl Pts',(31.116715812632,55.2104575382394,-1.96295403647732));
#44051=CARTESIAN_POINT('Ctrl Pts',(32.0473824090187,54.3760622611663,-1.88886210943196));
#44052=CARTESIAN_POINT('Ctrl Pts',(33.8672110770871,54.8728632770318,-1.77772421886392));
#44053=CARTESIAN_POINT('Ctrl Pts',(34.4318965215284,56.6706982888814,-1.66658632829588));
#44054=CARTESIAN_POINT('Ctrl Pts',(33.2300975250658,58.1203931132112,-1.55544843772783));
#44055=CARTESIAN_POINT('Ctrl Pts',(31.3591320310469,57.8968187913669,-1.44431054715979));
#44056=CARTESIAN_POINT('Ctrl Pts',(30.5328676198999,56.2037155410781,-1.33317265659175));
#44057=CARTESIAN_POINT('Ctrl Pts',(31.5069148948352,54.5912519864218,-1.22203476602371));
#44058=CARTESIAN_POINT('Ctrl Pts',(33.3900582128528,54.5351072237228,-1.11089687545567));
#44059=CARTESIAN_POINT('Ctrl Pts',(34.4584638908577,56.0867852734614,-0.999758984887625));
#44060=CARTESIAN_POINT('Ctrl Pts',(33.7342941276566,57.825960305992,-0.888621094319583));
#44061=CARTESIAN_POINT('Ctrl Pts',(31.8803464986039,58.1607744839985,-0.777483203751541));
#44062=CARTESIAN_POINT('Ctrl Pts',(30.5935820077055,56.7847541278007,-0.6663453131835));
#44063=CARTESIAN_POINT('Ctrl Pts',(31.0517798775846,54.9573935418363,-0.555207422615458));
#44064=CARTESIAN_POINT('Ctrl Pts',(32.8355518820609,54.3512929431319,-0.444069532047416));
#44065=CARTESIAN_POINT('Ctrl Pts',(34.3121885227868,55.521224917537,-0.332931641479374));
#44066=CARTESIAN_POINT('Ctrl Pts',(34.1301089195293,57.3963365394661,-0.221793750911333));
#44067=CARTESIAN_POINT('Ctrl Pts',(32.4559719031607,58.2603173390956,-0.110655860343291));
#44068=CARTESIAN_POINT('Ctrl Pts',(30.822134419883,57.3223556597407,0.000482030224751112));
#44069=CARTESIAN_POINT('Ctrl Pts',(30.724066271727,55.4409785805668,0.111619920792792));
#44070=CARTESIAN_POINT('Ctrl Pts',(32.2515304349822,54.3382318197086,0.222757811360835));
#44071=CARTESIAN_POINT('Ctrl Pts',(34.0064215941321,55.0234720228687,0.333895701928877));
#44072=CARTESIAN_POINT('Ctrl Pts',(34.3824679916267,56.8694910461269,0.445033592496917));
#44073=CARTESIAN_POINT('Ctrl Pts',(33.0354700840103,58.1866067496581,0.55617148306496));
#44074=CARTESIAN_POINT('Ctrl Pts',(31.1983503377324,57.7692481891733,0.667309373633001));
#44075=CARTESIAN_POINT('Ctrl Pts',(30.5526452880963,55.9994283901304,0.778447264201044));
#44076=CARTESIAN_POINT('Ctrl Pts',(31.6893760912438,54.4970834847716,0.889585154769084));
#44077=CARTESIAN_POINT('Ctrl Pts',(33.5680801509383,54.6373268031956,1.00072304533713));
#44078=CARTESIAN_POINT('Ctrl Pts',(34.4691583357458,56.2917920453437,1.11186093590517));
#44079=CARTESIAN_POINT('Ctrl Pts',(33.5678435640106,57.9461284122851,1.22299882647321));
#44080=CARTESIAN_POINT('Ctrl Pts',(31.6891194679972,58.086103065848,1.33413671704125));
#44081=CARTESIAN_POINT('Ctrl Pts',(30.5526035189213,56.5835956182358,1.44527460760929));
#44082=CARTESIAN_POINT('Ctrl Pts',(31.1985616539627,54.8138681758263,1.55641249817734));
#44083=CARTESIAN_POINT('Ctrl Pts',(33.0357410664428,54.3967723367386,1.66755038874538));
#44084=CARTESIAN_POINT('Ctrl Pts',(34.3825506050928,55.7140806526746,1.77868827931342));
#44085=CARTESIAN_POINT('Ctrl Pts',(34.0062402253245,57.5600458827673,1.88982616988146));
#44086=CARTESIAN_POINT('Ctrl Pts',(32.2512510853912,58.2450351172428,2.0009640604495));
#44087=CARTESIAN_POINT('Ctrl Pts',(30.7239446480036,57.1420699414794,2.11210195101754));
#44088=CARTESIAN_POINT('Ctrl Pts',(30.8222818161361,55.2607068893292,2.22323984158559));
#44089=CARTESIAN_POINT('Ctrl Pts',(32.4562534645774,54.3229788985336,2.33437773215363));
#44090=CARTESIAN_POINT('Ctrl Pts',(34.1302668130106,55.1871990336262,2.44551562272167));
#44091=CARTESIAN_POINT('Ctrl Pts',(34.3120784590119,57.0623368040342,2.55665351328971));
#44092=CARTESIAN_POINT('Ctrl Pts',(32.8352741411123,58.2320573429941,2.66779140385776));
#44093=CARTESIAN_POINT('Ctrl Pts',(31.0515895995852,57.6257021756631,2.77892929442579));
#44094=CARTESIAN_POINT('Ctrl Pts',(30.5936515236489,55.7982750632342,2.89006718499384));
#44095=CARTESIAN_POINT('Ctrl Pts',(31.8806158275789,54.4224407661471,3.00120507556188));
#44096=CARTESIAN_POINT('Ctrl Pts',(33.7345094888202,54.757516019547,3.11234296612992));
#44097=CARTESIAN_POINT('Ctrl Pts',(34.4584426146545,56.4968026439861,3.22348085669796));
#44098=CARTESIAN_POINT('Ctrl Pts',(33.3897910050459,58.0483118672624,3.33461874726601));
#44099=CARTESIAN_POINT('Ctrl Pts',(31.506703597602,57.9919297020009,3.44575663783404));
#44100=CARTESIAN_POINT('Ctrl Pts',(30.5327916520213,56.3792633834812,3.55689452840209));
#44101=CARTESIAN_POINT('Ctrl Pts',(31.3594878170038,54.6864046819268,3.66803241897013));
#44102=CARTESIAN_POINT('Ctrl Pts',(33.230107717374,54.4628463651893,3.77917030953817));
#44103=CARTESIAN_POINT('Ctrl Pts',(34.4324517440404,55.9132138959114,3.89030820010621));
#44104=CARTESIAN_POINT('Ctrl Pts',(33.8660007739066,57.7099694249182,4.00144609067425));
#44105=CARTESIAN_POINT('Ctrl Pts',(32.0492338038872,58.2085222399532,4.1125839812423));
#44106=CARTESIAN_POINT('Ctrl Pts',(30.6450582452589,56.9525412953675,4.22372187181034));
#44107=CARTESIAN_POINT('Ctrl Pts',(30.9387319111105,55.0916401936804,4.33485976237839));
#44108=CARTESIAN_POINT('Ctrl Pts',(32.6614519649159,54.3291228170264,4.44599765294642));
#44109=CARTESIAN_POINT('Ctrl Pts',(34.2363932038283,55.3629299683766,4.55713554351447));
#44110=CARTESIAN_POINT('Ctrl Pts',(34.2219940520658,57.2468062367664,4.6682734340825));
#44111=CARTESIAN_POINT('Ctrl Pts',(32.6314342140598,58.2564183114437,4.77941132465055));
#44112=CARTESIAN_POINT('Ctrl Pts',(30.9205711526377,57.4676568060689,4.89054921521858));
#44113=CARTESIAN_POINT('Ctrl Pts',(30.6553772206223,55.602484080847,5.00168710578663));
#44114=CARTESIAN_POINT('Ctrl Pts',(32.0785874510053,54.3681138654151,5.11282499635467));
#44115=CARTESIAN_POINT('Ctrl Pts',(33.8875213407722,54.8943792530066,5.22396288692271));
#44116=CARTESIAN_POINT('Ctrl Pts',(34.426441263231,56.6995834937723,5.33510077749076));
#44117=CARTESIAN_POINT('Ctrl Pts',(33.2020675476878,58.1314028177064,5.44623866805879));
#44118=CARTESIAN_POINT('Ctrl Pts',(31.3350836476587,57.8792764730932,5.55737655862684));
#44119=CARTESIAN_POINT('Ctrl Pts',(30.5343604901146,56.173979132908,5.66851444919488));
#44120=CARTESIAN_POINT('Ctrl Pts',(31.5328102757061,54.5763876565426,5.77965233976292));
#44121=CARTESIAN_POINT('Ctrl Pts',(33.4165381765593,54.5487979003783,5.89079023033096));
#44122=CARTESIAN_POINT('Ctrl Pts',(34.4613514910016,56.116458582309,6.001928120899));
#44123=CARTESIAN_POINT('Ctrl Pts',(33.7109111712192,57.8444810565579,6.11306601146705));
#44124=CARTESIAN_POINT('Ctrl Pts',(31.8521228057562,58.1511689306776,6.22420390203508));
#44125=CARTESIAN_POINT('Ctrl Pts',(30.5863185401119,56.7558427953566,6.33534179260314));
#44126=CARTESIAN_POINT('Ctrl Pts',(31.07217886447,54.9355898635396,6.44647968317117));
#44127=CARTESIAN_POINT('Ctrl Pts',(32.8648400497806,54.3566488617232,6.55761757373922));
#44128=CARTESIAN_POINT('Ctrl Pts',(34.3237580856512,55.5486512349918,6.66875546430725));
#44129=CARTESIAN_POINT('Ctrl Pts',(34.1129733567612,57.4211007417247,6.7798933548753));
#44130=CARTESIAN_POINT('Ctrl Pts',(32.4266050042152,58.2590134407084,6.89103124544334));
#44131=CARTESIAN_POINT('Ctrl Pts',(30.805840812616,57.2976582429663,7.00216913601138));
#44132=CARTESIAN_POINT('Ctrl Pts',(30.7389488982073,55.4124226867889,7.11330702657943));
#44133=CARTESIAN_POINT('Ctrl Pts',(31.764281276621,54.697545560418,7.18739895362479));
#44134=CARTESIAN_POINT('Ctrl Pts',(32.3148335773693,54.6359733196,7.22444491714747));
#44135=CARTESIAN_POINT('Ctrl Pts',(30.8086516228787,55.6887746631347,-2.07481497238249));
#44136=CARTESIAN_POINT('Ctrl Pts',(31.0091224297109,55.1263610888822,-2.03776900885981));
#44137=CARTESIAN_POINT('Ctrl Pts',(32.01217730928,54.2270656189395,-1.96367708181445));
#44138=CARTESIAN_POINT('Ctrl Pts',(33.97355427561,54.7625083704828,-1.85253919124641));
#44139=CARTESIAN_POINT('Ctrl Pts',(34.5821615821015,56.7001809895466,-1.74140130067836));
#44140=CARTESIAN_POINT('Ctrl Pts',(33.2868853227587,58.2626346900185,-1.63026341011032));
#44141=CARTESIAN_POINT('Ctrl Pts',(31.2703940512689,58.021670508707,-1.51912551954228));
#44142=CARTESIAN_POINT('Ctrl Pts',(30.3798618750492,56.1968758041265,-1.40798762897424));
#44143=CARTESIAN_POINT('Ctrl Pts',(31.4296716306029,54.4589930404121,-1.2968497384062));
#44144=CARTESIAN_POINT('Ctrl Pts',(33.4592879307893,54.3984812756124,-1.18571184783816));
#44145=CARTESIAN_POINT('Ctrl Pts',(34.6107953909719,56.0708505702161,-1.07457395727011));
#44146=CARTESIAN_POINT('Ctrl Pts',(33.83029889799,57.9453005715135,-0.963436066702072));
#44147=CARTESIAN_POINT('Ctrl Pts',(31.8321491599349,58.3061569687477,-0.85229817613403));
#44148=CARTESIAN_POINT('Ctrl Pts',(30.4452986954797,56.8231082184979,-0.741160285565988));
#44149=CARTESIAN_POINT('Ctrl Pts',(30.939135705398,54.853613493319,-0.630022394997946));
#44150=CARTESIAN_POINT('Ctrl Pts',(32.8616514807306,54.2003697157939,-0.518884504429905));
#44151=CARTESIAN_POINT('Ctrl Pts',(34.4531425620492,55.4613003006532,-0.407746613861863));
#44152=CARTESIAN_POINT('Ctrl Pts',(34.2569006046969,57.4822601904945,-0.296608723293822));
#44153=CARTESIAN_POINT('Ctrl Pts',(32.4525473488096,58.4134423778501,-0.185470832725779));
#44154=CARTESIAN_POINT('Ctrl Pts',(30.6916281685284,57.4025249956444,-0.0743329421577379));
#44155=CARTESIAN_POINT('Ctrl Pts',(30.5859321707133,55.3748123143236,0.0368049484103036));
#44156=CARTESIAN_POINT('Ctrl Pts',(32.2322041958065,54.1862926836609,0.147942838978346));
#44157=CARTESIAN_POINT('Ctrl Pts',(34.1235927415348,54.9248316321149,0.259080729546388));
#44158=CARTESIAN_POINT('Ctrl Pts',(34.5288884461575,56.9144360685965,0.370218620114429));
#44159=CARTESIAN_POINT('Ctrl Pts',(33.0771195428256,58.3339984967674,0.48135651068247));
#44160=CARTESIAN_POINT('Ctrl Pts',(31.0971065789877,57.8841773231595,0.592494401250512));
#44161=CARTESIAN_POINT('Ctrl Pts',(30.4011778722794,55.97669897132,0.703632291818555));
#44162=CARTESIAN_POINT('Ctrl Pts',(31.6263248618463,54.3575000079461,0.814770182386596));
#44163=CARTESIAN_POINT('Ctrl Pts',(33.6511566132586,54.5086516076904,0.925908072954639));
#44164=CARTESIAN_POINT('Ctrl Pts',(34.6223216616804,56.2918029968741,1.03704596352268));
#44165=CARTESIAN_POINT('Ctrl Pts',(33.6509016243366,58.0748154867945,1.14818385409072));
#44166=CARTESIAN_POINT('Ctrl Pts',(31.626048278158,58.2256775246255,1.25932174465876));
#44167=CARTESIAN_POINT('Ctrl Pts',(30.4011328542516,56.6063033762813,1.3704596352268));
#44168=CARTESIAN_POINT('Ctrl Pts',(31.0973343316293,54.6989245646766,1.48159752579485));
#44169=CARTESIAN_POINT('Ctrl Pts',(33.0774116025732,54.2493865472286,1.59273541636289));
#44170=CARTESIAN_POINT('Ctrl Pts',(34.5289774853909,55.6691565694111,1.70387330693093));
#44171=CARTESIAN_POINT('Ctrl Pts',(34.1233972656597,57.6587030286353,1.81501119749897));
#44172=CARTESIAN_POINT('Ctrl Pts',(32.2319031180934,58.396971487781,1.92614908806701));
#44173=CARTESIAN_POINT('Ctrl Pts',(30.5858010869615,57.2082164536586,2.03728697863506));
#44174=CARTESIAN_POINT('Ctrl Pts',(30.691787029426,55.1805188903994,2.1484248692031));
#44175=CARTESIAN_POINT('Ctrl Pts',(32.4528508103866,54.1698533733088,2.25956275977114));
#44176=CARTESIAN_POINT('Ctrl Pts',(34.2570707793086,55.1012935119064,2.37070065033918));
#44177=CARTESIAN_POINT('Ctrl Pts',(34.4530239373915,57.1222815840842,2.48183854090722));
#44178=CARTESIAN_POINT('Ctrl Pts',(32.8613521367821,58.3829842878143,2.59297643147526));
#44179=CARTESIAN_POINT('Ctrl Pts',(30.938930627364,57.7294661410314,2.7041143220433));
#44180=CARTESIAN_POINT('Ctrl Pts',(30.4453736184505,55.7598997148858,2.81525221261135));
#44181=CARTESIAN_POINT('Ctrl Pts',(31.8324394376172,54.2770514956311,2.92639010317939));
#44182=CARTESIAN_POINT('Ctrl Pts',(33.8305310101845,54.6381892749935,3.03752799374743));
#44183=CARTESIAN_POINT('Ctrl Pts',(34.610772459882,56.5127595479419,3.14866588431547));
#44184=CARTESIAN_POINT('Ctrl Pts',(33.4589999392618,58.1849468845734,3.25980377488351));
#44185=CARTESIAN_POINT('Ctrl Pts',(31.4294438984359,58.1241792517757,3.37094166545156));
#44186=CARTESIAN_POINT('Ctrl Pts',(30.3797799983044,56.3860779529991,3.4820795560196));
#44187=CARTESIAN_POINT('Ctrl Pts',(31.2707775106533,54.5615468184256,3.59321744658764));
#44188=CARTESIAN_POINT('Ctrl Pts',(33.2868963078361,54.3205998871158,3.70435533715568));
#44189=CARTESIAN_POINT('Ctrl Pts',(34.5827599904381,55.8837786178317,3.81549322772373));
#44190=CARTESIAN_POINT('Ctrl Pts',(33.9722498337018,57.8202877906762,3.92663111829177));
#44191=CARTESIAN_POINT('Ctrl Pts',(32.0141727077009,58.3576185982774,4.03776900885981));
#44192=CARTESIAN_POINT('Ctrl Pts',(30.5007788120545,57.0039460586119,4.14890689942785));
#44193=CARTESIAN_POINT('Ctrl Pts',(30.8172947423318,54.9983019990856,4.2600447899959));
#44194=CARTESIAN_POINT('Ctrl Pts',(32.6740098783534,54.1764751726168,4.37118268056393));
#44195=CARTESIAN_POINT('Ctrl Pts',(34.371451798864,55.2906929942526,4.48232057113198));
#44196=CARTESIAN_POINT('Ctrl Pts',(34.3559326650591,57.3210992545065,4.59345846170002));
#44197=CARTESIAN_POINT('Ctrl Pts',(32.6416573134427,58.4092400794901,4.70459635226806));
#44198=CARTESIAN_POINT('Ctrl Pts',(30.7977214198622,57.5591278267734,4.8157342428361));
#44199=CARTESIAN_POINT('Ctrl Pts',(30.511900408801,55.5488798920818,4.92687213340414));
#44200=CARTESIAN_POINT('Ctrl Pts',(32.0458095141462,54.2184989881246,5.03801002397218));
#44201=CARTESIAN_POINT('Ctrl Pts',(33.9954442941986,54.7856978830043,5.14914791454023));
#44202=CARTESIAN_POINT('Ctrl Pts',(34.576282007745,56.731312917807,5.26028580510826));
#44203=CARTESIAN_POINT('Ctrl Pts',(33.2566751425584,58.274500741577,5.37142369567632));
#44204=CARTESIAN_POINT('Ctrl Pts',(31.2444751578682,58.0027637294031,5.48256158624434));
#44205=CARTESIAN_POINT('Ctrl Pts',(30.38147086237,56.1648264650488,5.5936994768124));
#44206=CARTESIAN_POINT('Ctrl Pts',(31.4575811830052,54.4429725464192,5.70483736738043));
#44207=CARTESIAN_POINT('Ctrl Pts',(33.4878275355304,54.4132368283282,5.81597525794848));
#44208=CARTESIAN_POINT('Ctrl Pts',(34.6139075918673,56.1028319020359,5.92711314851651));
#44209=CARTESIAN_POINT('Ctrl Pts',(33.8050971891886,57.9652618866617,6.03825103908456));
#44210=CARTESIAN_POINT('Ctrl Pts',(31.8017301968603,58.2958042848038,6.1493889296526));
#44211=CARTESIAN_POINT('Ctrl Pts',(30.4374702672965,56.7919481304539,6.26052682022064));
#44212=CARTESIAN_POINT('Ctrl Pts',(30.961121348176,54.8301139006692,6.37166471078869));
#44213=CARTESIAN_POINT('Ctrl Pts',(32.893217714717,54.2061422236913,6.48280260135672));
#44214=CARTESIAN_POINT('Ctrl Pts',(34.4656120183837,55.4908598675899,6.59394049192477));
#44215=CARTESIAN_POINT('Ctrl Pts',(34.2384322187942,57.5089505799534,6.70507838249281));
#44216=CARTESIAN_POINT('Ctrl Pts',(32.4208962597951,58.4120370607959,6.81621627306085));
#44217=CARTESIAN_POINT('Ctrl Pts',(30.6740672263624,57.3759065863185,6.92735416362889));
#44218=CARTESIAN_POINT('Ctrl Pts',(30.6019723844373,55.344035311361,7.03849205419694));
#44219=CARTESIAN_POINT('Ctrl Pts',(31.70705625587,54.5735542468394,7.1125839812423));
#44220=CARTESIAN_POINT('Ctrl Pts',(32.3004311270297,54.5071928486349,7.14962994476498));
#44221=CARTESIAN_POINT('Ctrl Pts',(30.6865906990181,55.6452663749118,-2.14962994476498));
#44222=CARTESIAN_POINT('Ctrl Pts',(30.9015290467899,55.042264639525,-2.1125839812423));
#44223=CARTESIAN_POINT('Ctrl Pts',(31.9769722095413,54.0780689767127,-2.03849205419694));
#44224=CARTESIAN_POINT('Ctrl Pts',(34.0798974741329,54.6521534639338,-1.9273541636289));
#44225=CARTESIAN_POINT('Ctrl Pts',(34.7324266426746,56.7296636902118,-1.81621627306085));
#44226=CARTESIAN_POINT('Ctrl Pts',(33.3436731204516,58.4048762668258,-1.70507838249281));
#44227=CARTESIAN_POINT('Ctrl Pts',(31.1816560714909,58.1465222260471,-1.59394049192477));
#44228=CARTESIAN_POINT('Ctrl Pts',(30.2268561301985,56.1900360671749,-1.48280260135673));
#44229=CARTESIAN_POINT('Ctrl Pts',(31.3524283663706,54.3267340944024,-1.37166471078869));
#44230=CARTESIAN_POINT('Ctrl Pts',(33.5285176487258,54.261855327502,-1.26052682022064));
#44231=CARTESIAN_POINT('Ctrl Pts',(34.7631268910861,56.0549158669708,-1.1493889296526));
#44232=CARTESIAN_POINT('Ctrl Pts',(33.9263036683235,58.064640837035,-1.03825103908456));
#44233=CARTESIAN_POINT('Ctrl Pts',(31.7839518212659,58.4515394534968,-0.927113148516518));
#44234=CARTESIAN_POINT('Ctrl Pts',(30.2970153832539,56.8614623091951,-0.815975257948478));
#44235=CARTESIAN_POINT('Ctrl Pts',(30.8264915332113,54.7498334448017,-0.704837367380435));
#44236=CARTESIAN_POINT('Ctrl Pts',(32.8877510794003,54.0494464884559,-0.593699476812394));
#44237=CARTESIAN_POINT('Ctrl Pts',(34.5940966013115,55.4013756837693,-0.482561586244352));
#44238=CARTESIAN_POINT('Ctrl Pts',(34.3836922898643,57.5681838415229,-0.371423695676311));
#44239=CARTESIAN_POINT('Ctrl Pts',(32.4491227944586,58.5665674166047,-0.260285805108268));
#44240=CARTESIAN_POINT('Ctrl Pts',(30.5611219171738,57.4826943315479,-0.149147914540227));
#44241=CARTESIAN_POINT('Ctrl Pts',(30.4477980696997,55.3086460480807,-0.0380100239721852));
#44242=CARTESIAN_POINT('Ctrl Pts',(32.2128779566306,54.0343535476132,0.0731278665958569));
#44243=CARTESIAN_POINT('Ctrl Pts',(34.2407638889375,54.826191241361,0.184265757163899));
#44244=CARTESIAN_POINT('Ctrl Pts',(34.6753089006883,56.9593810910663,0.29540364773194));
#44245=CARTESIAN_POINT('Ctrl Pts',(33.1187690016409,58.4813902438765,0.406541538299981));
#44246=CARTESIAN_POINT('Ctrl Pts',(30.9958628202428,57.9991064571457,0.517679428868024));
#44247=CARTESIAN_POINT('Ctrl Pts',(30.2497104564626,55.9539695525095,0.628817319436065));
#44248=CARTESIAN_POINT('Ctrl Pts',(31.5632736324487,54.2179165311208,0.739955210004108));
#44249=CARTESIAN_POINT('Ctrl Pts',(33.7342330755791,54.379976412185,0.851093100572149));
#44250=CARTESIAN_POINT('Ctrl Pts',(34.7754849876149,56.2918139484046,0.962230991140192));
#44251=CARTESIAN_POINT('Ctrl Pts',(33.7339596846626,58.2035025613039,1.07336888170823));
#44252=CARTESIAN_POINT('Ctrl Pts',(31.5629770883188,58.3652519834031,1.18450677227628));
#44253=CARTESIAN_POINT('Ctrl Pts',(30.2496621895819,56.6290111343267,1.29564466284432));
#44254=CARTESIAN_POINT('Ctrl Pts',(30.996107009296,54.5839809535271,1.40678255341236));
#44255=CARTESIAN_POINT('Ctrl Pts',(33.1190821387036,54.1020007577187,1.5179204439804));
#44256=CARTESIAN_POINT('Ctrl Pts',(34.675404365689,55.6242324861475,1.62905833454844));
#44257=CARTESIAN_POINT('Ctrl Pts',(34.2405543059947,57.7573601745033,1.74019622511648));
#44258=CARTESIAN_POINT('Ctrl Pts',(32.2125551507957,58.5489078583191,1.85133411568452));
#44259=CARTESIAN_POINT('Ctrl Pts',(30.4476575259193,57.274362965838,1.96247200625257));
#44260=CARTESIAN_POINT('Ctrl Pts',(30.5612922427159,55.1003308914695,2.07360989682061));
#44261=CARTESIAN_POINT('Ctrl Pts',(32.4494481561958,54.0167278480842,2.18474778738865));
#44262=CARTESIAN_POINT('Ctrl Pts',(34.3838747456067,55.0153879901866,2.29588567795669));
#44263=CARTESIAN_POINT('Ctrl Pts',(34.593969415771,57.1822263641343,2.40702356852473));
#44264=CARTESIAN_POINT('Ctrl Pts',(32.8874301324519,58.5339112326344,2.51816145909278));
#44265=CARTESIAN_POINT('Ctrl Pts',(30.8262716551429,57.8332301063997,2.62929934966082));
#44266=CARTESIAN_POINT('Ctrl Pts',(30.2970957132522,55.7215243665374,2.74043724022886));
#44267=CARTESIAN_POINT('Ctrl Pts',(31.7842630476554,54.1316622251152,2.8515751307969));
#44268=CARTESIAN_POINT('Ctrl Pts',(33.9265525315489,54.5188625304399,2.96271302136494));
#44269=CARTESIAN_POINT('Ctrl Pts',(34.7631023051095,56.5287164518977,3.07385091193299));
#44270=CARTESIAN_POINT('Ctrl Pts',(33.5282088734779,58.3215819018844,3.18498880250102));
#44271=CARTESIAN_POINT('Ctrl Pts',(31.3521841992698,58.2564288015506,3.29612669306907));
#44272=CARTESIAN_POINT('Ctrl Pts',(30.2267683445876,56.3928925225169,3.40726458363711));
#44273=CARTESIAN_POINT('Ctrl Pts',(31.1820672043028,54.4366889549244,3.51840247420515));
#44274=CARTESIAN_POINT('Ctrl Pts',(33.343684898298,54.1783534090425,3.62954036477319));
#44275=CARTESIAN_POINT('Ctrl Pts',(34.7330682368358,55.8543433397519,3.74067825534124));
#44276=CARTESIAN_POINT('Ctrl Pts',(34.0784988934969,57.9306061564344,3.85181614590927));
#44277=CARTESIAN_POINT('Ctrl Pts',(31.9791116115147,58.5067149566014,3.96295403647732));
#44278=CARTESIAN_POINT('Ctrl Pts',(30.3564993788501,57.0553508218565,4.07409192704536));
#44279=CARTESIAN_POINT('Ctrl Pts',(30.6958575735531,54.9049638044908,4.18522981761341));
#44280=CARTESIAN_POINT('Ctrl Pts',(32.686567791791,54.0238275282073,4.29636770818144));
#44281=CARTESIAN_POINT('Ctrl Pts',(34.5065103938996,55.2184560201287,4.40750559874949));
#44282=CARTESIAN_POINT('Ctrl Pts',(34.4898712780524,57.3953922722465,4.51864348931753));
#44283=CARTESIAN_POINT('Ctrl Pts',(32.6518804128256,58.5620618475365,4.62978137988557));
#44284=CARTESIAN_POINT('Ctrl Pts',(30.6748716870867,57.650598847478,4.74091927045361));
#44285=CARTESIAN_POINT('Ctrl Pts',(30.3684235969797,55.4952757033166,4.85205716102166));
#44286=CARTESIAN_POINT('Ctrl Pts',(32.0130315772872,54.068884110834,4.96319505158969));
#44287=CARTESIAN_POINT('Ctrl Pts',(34.103367247625,54.677016513002,5.07433294215774));
#44288=CARTESIAN_POINT('Ctrl Pts',(34.726122752259,56.7630423418418,5.18547083272577));
#44289=CARTESIAN_POINT('Ctrl Pts',(33.3112827374291,58.4175986654477,5.29660872329383));
#44290=CARTESIAN_POINT('Ctrl Pts',(31.1538666680778,58.126250985713,5.40774661386186));
#44291=CARTESIAN_POINT('Ctrl Pts',(30.2285812346253,56.1556737971897,5.51888450442991));
#44292=CARTESIAN_POINT('Ctrl Pts',(31.3823520903042,54.3095574362957,5.63002239499793));
#44293=CARTESIAN_POINT('Ctrl Pts',(33.5591168945015,54.2776757562781,5.741160285566));
#44294=CARTESIAN_POINT('Ctrl Pts',(34.766463692733,56.0892052217627,5.85229817613402));
#44295=CARTESIAN_POINT('Ctrl Pts',(33.8992832071581,58.0860427167655,5.96343606670208));
#44296=CARTESIAN_POINT('Ctrl Pts',(31.7513375879643,58.4404396389301,6.0745739572701));
#44297=CARTESIAN_POINT('Ctrl Pts',(30.288621994481,56.8280534655513,6.18571184783816));
#44298=CARTESIAN_POINT('Ctrl Pts',(30.850063831882,54.7246379377987,6.29684973840619));
#44299=CARTESIAN_POINT('Ctrl Pts',(32.9215953796534,54.0556355856594,6.40798762897423));
#44300=CARTESIAN_POINT('Ctrl Pts',(34.6074659511161,55.433068500188,6.51912551954228));
#44301=CARTESIAN_POINT('Ctrl Pts',(34.3638910808273,57.5968004181821,6.63026341011032));
#44302=CARTESIAN_POINT('Ctrl Pts',(32.4151875153751,58.5650606808835,6.74140130067835));
#44303=CARTESIAN_POINT('Ctrl Pts',(30.5422936401087,57.4541549296709,6.85253919124641));
#44304=CARTESIAN_POINT('Ctrl Pts',(30.4649958706675,55.2756479359331,6.96367708181444));
#44305=CARTESIAN_POINT('Ctrl Pts',(31.649831235119,54.4495629332609,7.03776900885981));
#44306=CARTESIAN_POINT('Ctrl Pts',(32.28602867669,54.3784123776698,7.07481497238249));
#44307=CARTESIAN_POINT('Ctrl Pts',(30.5645297751575,55.601758086689,-2.22444491714747));
#44308=CARTESIAN_POINT('Ctrl Pts',(30.7939356638689,54.9581681901677,-2.18739895362479));
#44309=CARTESIAN_POINT('Ctrl Pts',(31.9417671098026,53.9290723344859,-2.11330702657942));
#44310=CARTESIAN_POINT('Ctrl Pts',(34.1862406726559,54.5417985573848,-2.00216913601139));
#44311=CARTESIAN_POINT('Ctrl Pts',(34.8826917032476,56.7591463908769,-1.89103124544334));
#44312=CARTESIAN_POINT('Ctrl Pts',(33.4004609181445,58.5471178436331,-1.7798933548753));
#44313=CARTESIAN_POINT('Ctrl Pts',(31.0929180917129,58.2713739433872,-1.66875546430726));
#44314=CARTESIAN_POINT('Ctrl Pts',(30.0738503853477,56.1831963302234,-1.55761757373922));
#44315=CARTESIAN_POINT('Ctrl Pts',(31.2751851021384,54.1944751483927,-1.44647968317118));
#44316=CARTESIAN_POINT('Ctrl Pts',(33.5977473666623,54.1252293793916,-1.33534179260313));
#44317=CARTESIAN_POINT('Ctrl Pts',(34.9154583912003,56.0389811637256,-1.22420390203509));
#44318=CARTESIAN_POINT('Ctrl Pts',(34.0223084386569,58.1839811025564,-1.11306601146705));
#44319=CARTESIAN_POINT('Ctrl Pts',(31.7357544825969,58.596921938246,-1.00192812089901));
#44320=CARTESIAN_POINT('Ctrl Pts',(30.1487320710281,56.8998163998922,-0.890790230330966));
#44321=CARTESIAN_POINT('Ctrl Pts',(30.7138473610246,54.6460533962845,-0.779652339762924));
#44322=CARTESIAN_POINT('Ctrl Pts',(32.9138506780699,53.8985232611178,-0.668514449194883));
#44323=CARTESIAN_POINT('Ctrl Pts',(34.7350506405739,55.3414510668855,-0.55737655862684));
#44324=CARTESIAN_POINT('Ctrl Pts',(34.5104839750318,57.654107492551,-0.4462386680588));
#44325=CARTESIAN_POINT('Ctrl Pts',(32.4456982401076,58.7196924553593,-0.335100777490757));
#44326=CARTESIAN_POINT('Ctrl Pts',(30.4306156658191,57.5628636674516,-0.223962886922716));
#44327=CARTESIAN_POINT('Ctrl Pts',(30.309663968686,55.2424797818377,-0.112824996354674));
#44328=CARTESIAN_POINT('Ctrl Pts',(32.1935517174548,53.8824144115655,-0.00168710578663204));
#44329=CARTESIAN_POINT('Ctrl Pts',(34.3579350363403,54.7275508506072,0.10945078478141));
#44330=CARTESIAN_POINT('Ctrl Pts',(34.8217293552191,57.004326113536,0.220588675349451));
#44331=CARTESIAN_POINT('Ctrl Pts',(33.1604184604563,58.6287819909857,0.331726565917493));
#44332=CARTESIAN_POINT('Ctrl Pts',(30.894619061498,58.1140355911319,0.442864456485535));
#44333=CARTESIAN_POINT('Ctrl Pts',(30.0982430406458,55.931240133699,0.554002347053577));
#44334=CARTESIAN_POINT('Ctrl Pts',(31.5002224030512,54.0783330542954,0.665140237621618));
#44335=CARTESIAN_POINT('Ctrl Pts',(33.8173095378994,54.2513012166796,0.776278128189661));
#44336=CARTESIAN_POINT('Ctrl Pts',(34.9286483135496,56.2918248999351,0.887416018757702));
#44337=CARTESIAN_POINT('Ctrl Pts',(33.8170177449885,58.3321896358132,0.998553909325745));
#44338=CARTESIAN_POINT('Ctrl Pts',(31.4999058984797,58.5048264421807,1.10969179989378));
#44339=CARTESIAN_POINT('Ctrl Pts',(30.0981915249122,56.6517188923722,1.22082969046183));
#44340=CARTESIAN_POINT('Ctrl Pts',(30.8948796869627,54.4690373423775,1.33196758102987));
#44341=CARTESIAN_POINT('Ctrl Pts',(33.1607526748339,53.9546149682086,1.44310547159791));
#44342=CARTESIAN_POINT('Ctrl Pts',(34.8218312459871,55.5793084028842,1.55424336216595));
#44343=CARTESIAN_POINT('Ctrl Pts',(34.3577113463298,57.8560173203711,1.665381252734));
#44344=CARTESIAN_POINT('Ctrl Pts',(32.1932071834979,58.7008442288574,1.77651914330203));
#44345=CARTESIAN_POINT('Ctrl Pts',(30.3095139648772,57.3405094780172,1.88765703387008));
#44346=CARTESIAN_POINT('Ctrl Pts',(30.4307974560058,55.0201428925398,1.99879492443812));
#44347=CARTESIAN_POINT('Ctrl Pts',(32.4460455020051,53.8636023228594,2.10993281500616));
#44348=CARTESIAN_POINT('Ctrl Pts',(34.5106787119048,54.9294824684667,2.2210707055742));
#44349=CARTESIAN_POINT('Ctrl Pts',(34.7349148941506,57.2421711441843,2.33220859614224));
#44350=CARTESIAN_POINT('Ctrl Pts',(32.9135081281216,58.6848381774545,2.44334648671029));
#44351=CARTESIAN_POINT('Ctrl Pts',(30.7136126829218,57.9369940717681,2.55448437727833));
#44352=CARTESIAN_POINT('Ctrl Pts',(30.1488178080538,55.6831490181888,2.66562226784637));
#44353=CARTESIAN_POINT('Ctrl Pts',(31.7360866576937,53.9862729545993,2.77676015841441));
#44354=CARTESIAN_POINT('Ctrl Pts',(34.0225740529132,54.3995357858862,2.88789804898245));
#44355=CARTESIAN_POINT('Ctrl Pts',(34.9154321503369,56.5446733558537,2.9990359395505));
#44356=CARTESIAN_POINT('Ctrl Pts',(33.5974178076939,58.4582169191954,3.11017383011853));
#44357=CARTESIAN_POINT('Ctrl Pts',(31.2749245001037,58.3886783513255,3.22131172068658));
#44358=CARTESIAN_POINT('Ctrl Pts',(30.0737566908708,56.3997070920348,3.33244961125462));
#44359=CARTESIAN_POINT('Ctrl Pts',(31.0933568979523,54.3118310914232,3.44358750182266));
#44360=CARTESIAN_POINT('Ctrl Pts',(33.40047348876,54.0361069309691,3.5547253923907));
#44361=CARTESIAN_POINT('Ctrl Pts',(34.8833764832335,55.8249080616723,3.66586328295875));
#44362=CARTESIAN_POINT('Ctrl Pts',(34.1847479532921,58.0409245221924,3.77700117352678));
#44363=CARTESIAN_POINT('Ctrl Pts',(31.9440505153284,58.6558113149256,3.88813906409484));
#44364=CARTESIAN_POINT('Ctrl Pts',(30.2122199456457,57.1067555851009,3.99927695466286));
#44365=CARTESIAN_POINT('Ctrl Pts',(30.5744204047745,54.811625609896,4.11041484523092));
#44366=CARTESIAN_POINT('Ctrl Pts',(32.6991257052286,53.8711798837977,4.22155273579895));
#44367=CARTESIAN_POINT('Ctrl Pts',(34.6415689889353,55.1462190460046,4.332690626367));
#44368=CARTESIAN_POINT('Ctrl Pts',(34.6238098910458,57.4696852899866,4.44382851693504));
#44369=CARTESIAN_POINT('Ctrl Pts',(32.6621035122085,58.7148836155828,4.55496640750308));
#44370=CARTESIAN_POINT('Ctrl Pts',(30.5520219543112,57.7420698681825,4.66610429807112));
#44371=CARTESIAN_POINT('Ctrl Pts',(30.2249467851584,55.4416715145514,4.77724218863916));
#44372=CARTESIAN_POINT('Ctrl Pts',(31.980253640428,53.9192692335435,4.8883800792072));
#44373=CARTESIAN_POINT('Ctrl Pts',(34.2112902010514,54.5683351429997,4.99951796977525));
#44374=CARTESIAN_POINT('Ctrl Pts',(34.8759634967729,56.7947717658766,5.11065586034329));
#44375=CARTESIAN_POINT('Ctrl Pts',(33.3658903322998,58.5606965893184,5.22179375091133));
#44376=CARTESIAN_POINT('Ctrl Pts',(31.0632581782873,58.2497382420229,5.33293164147937));
#44377=CARTESIAN_POINT('Ctrl Pts',(30.0756916068806,56.1465211293306,5.44406953204742));
#44378=CARTESIAN_POINT('Ctrl Pts',(31.3071229976033,54.1761423261722,5.55520742261545));
#44379=CARTESIAN_POINT('Ctrl Pts',(33.6304062534725,54.1421146842281,5.6663453131835));
#44380=CARTESIAN_POINT('Ctrl Pts',(34.9190197935988,56.0755785414894,5.77748320375153));
#44381=CARTESIAN_POINT('Ctrl Pts',(33.9934692251276,58.2068235468693,5.88862109431959));
#44382=CARTESIAN_POINT('Ctrl Pts',(31.7009449790683,58.5850749930563,5.99975898488761));
#44383=CARTESIAN_POINT('Ctrl Pts',(30.1397737216656,56.8641588006487,6.11089687545567));
#44384=CARTESIAN_POINT('Ctrl Pts',(30.7390063155881,54.6191619749282,6.2220347660237));
#44385=CARTESIAN_POINT('Ctrl Pts',(32.9499730445898,53.9051289476276,6.33317265659175));
#44386=CARTESIAN_POINT('Ctrl Pts',(34.7493198838486,55.375277132786,6.44431054715978));
#44387=CARTESIAN_POINT('Ctrl Pts',(34.4893499428603,57.684650256411,6.55544843772784));
#44388=CARTESIAN_POINT('Ctrl Pts',(32.409478770955,58.718084300971,6.66658632829587));
#44389=CARTESIAN_POINT('Ctrl Pts',(30.4105200538552,57.5324032730233,6.77772421886391));
#44390=CARTESIAN_POINT('Ctrl Pts',(30.3280193568976,55.2072605605051,6.88886210943196));
#44391=CARTESIAN_POINT('Ctrl Pts',(31.592606214368,54.3255716196824,6.96295403647732));
#44392=CARTESIAN_POINT('Ctrl Pts',(32.2716262263503,54.2496319067047,7.));
#44393=CARTESIAN_POINT('Ctrl Pts',(30.9307125467392,55.7322829513575,-2.));
#44394=CARTESIAN_POINT('Ctrl Pts',(30.9446699885302,55.6718824515121,-2.));
#44395=CARTESIAN_POINT('Ctrl Pts',(30.9622173189429,55.6125616548499,-2.));
#44396=CARTESIAN_POINT('Ctrl Pts',(30.9830550110871,55.5544917980879,-2.));
#44397=CARTESIAN_POINT('Ctrl Pts',(31.0052689439607,55.4925866748543,-2.));
#44398=CARTESIAN_POINT('Ctrl Pts',(31.031222059362,55.4321024422535,-2.));
#44399=CARTESIAN_POINT('Ctrl Pts',(31.0606132871183,55.373244167107,-2.));
#44400=CARTESIAN_POINT('Ctrl Pts',(31.0863306114051,55.3217431763537,-2.));
#44401=CARTESIAN_POINT('Ctrl Pts',(31.1146814237683,55.271486657179,-2.));
#44402=CARTESIAN_POINT('Ctrl Pts',(31.1454993456467,55.2226180386923,-2.));
#44403=CARTESIAN_POINT('Ctrl Pts',(31.1609623517183,55.1980980289605,-2.));
#44404=CARTESIAN_POINT('Ctrl Pts',(31.1770469579252,55.1739275671393,-2.));
#44405=CARTESIAN_POINT('Ctrl Pts',(31.1937349146798,55.1501258793134,-2.));
#44406=CARTESIAN_POINT('Ctrl Pts',(31.201357838137,55.1392534611306,-2.));
#44407=CARTESIAN_POINT('Ctrl Pts',(31.2091078133333,55.1284566647485,-2.));
#44408=CARTESIAN_POINT('Ctrl Pts',(31.2169701001442,55.1177546356172,-2.));
#44409=CARTESIAN_POINT('Ctrl Pts',(31.2566258561271,55.0637758040171,-2.));
#44410=CARTESIAN_POINT('Ctrl Pts',(31.2992033789151,55.0121067330646,-2.));
#44411=CARTESIAN_POINT('Ctrl Pts',(31.3444046039735,54.9629466687563,-2.));
#44412=CARTESIAN_POINT('Ctrl Pts',(31.3904074837357,54.9129147387687,-2.));
#44413=CARTESIAN_POINT('Ctrl Pts',(31.4391284050012,54.8654806967995,-2.));
#44414=CARTESIAN_POINT('Ctrl Pts',(31.4903044396858,54.8208703724848,-2.));
#44415=CARTESIAN_POINT('Ctrl Pts',(31.5331115544079,54.7835552642998,-2.));
#44416=CARTESIAN_POINT('Ctrl Pts',(31.5776375521365,54.7482158610042,-2.));
#44417=CARTESIAN_POINT('Ctrl Pts',(31.6237516110946,54.7149996928349,-2.));
#44418=CARTESIAN_POINT('Ctrl Pts',(31.6449987764552,54.6996952621757,-2.));
#44419=CARTESIAN_POINT('Ctrl Pts',(31.666583341519,54.684841812932,-2.));
#44420=CARTESIAN_POINT('Ctrl Pts',(31.6884937600232,54.6704551374775,-2.));
#44421=CARTESIAN_POINT('Ctrl Pts',(31.6980569752198,54.6641758017675,-2.));
#44422=CARTESIAN_POINT('Ctrl Pts',(31.7076821201642,54.6579856105882,-2.));
#44423=CARTESIAN_POINT('Ctrl Pts',(31.7173562110341,54.6518932017638,-2.));
#44424=CARTESIAN_POINT('Ctrl Pts',(31.7767391575644,54.6144958698259,-2.));
#44425=CARTESIAN_POINT('Ctrl Pts',(31.8380740161593,54.5807067449847,-2.));
#44426=CARTESIAN_POINT('Ctrl Pts',(31.9010756695341,54.5507535434866,-2.));
#44427=CARTESIAN_POINT('Ctrl Pts',(31.9574042849217,54.5239729389083,-2.));
#44428=CARTESIAN_POINT('Ctrl Pts',(32.0150663148412,54.5002585220861,-2.));
#44429=CARTESIAN_POINT('Ctrl Pts',(32.073885064195,54.4797956759537,-2.));
#44430=CARTESIAN_POINT('Ctrl Pts',(32.1379640249064,54.4575028198872,-2.));
#44431=CARTESIAN_POINT('Ctrl Pts',(32.2034160279184,54.4390677641941,-2.));
#44432=CARTESIAN_POINT('Ctrl Pts',(32.2699334847327,54.4243849072974,-2.));
#44433=CARTESIAN_POINT('Ctrl Pts',(32.2955972920822,54.418719958143,-2.));
#44434=CARTESIAN_POINT('Ctrl Pts',(32.3214199362483,54.4136140552492,-2.));
#44435=CARTESIAN_POINT('Ctrl Pts',(32.3473844776328,54.4090630310332,-2.));
#44436=CARTESIAN_POINT('Ctrl Pts',(32.3587747917572,54.4070665545832,-2.));
#44437=CARTESIAN_POINT('Ctrl Pts',(32.370191852042,54.4051770614586,-2.));
#44438=CARTESIAN_POINT('Ctrl Pts',(32.3816208593905,54.4033960585417,-2.));
#44439=CARTESIAN_POINT('Ctrl Pts',(32.4507180638397,54.3926285160141,-2.));
#44440=CARTESIAN_POINT('Ctrl Pts',(32.5203743381692,54.3858000563277,-2.));
#44441=CARTESIAN_POINT('Ctrl Pts',(32.5902438513676,54.3827492853088,-2.));
#44442=CARTESIAN_POINT('Ctrl Pts',(32.6617320285806,54.3796278372087,-2.));
#44443=CARTESIAN_POINT('Ctrl Pts',(32.7334442999622,54.3804609924871,-2.));
#44444=CARTESIAN_POINT('Ctrl Pts',(32.8050350906587,54.3851263529449,-2.));
#44445=CARTESIAN_POINT('Ctrl Pts',(32.8598101377162,54.3886958810382,-2.));
#44446=CARTESIAN_POINT('Ctrl Pts',(32.9145147054626,54.3945098111843,-2.));
#44447=CARTESIAN_POINT('Ctrl Pts',(32.9689984939366,54.4025332699551,-2.));
#44448=CARTESIAN_POINT('Ctrl Pts',(33.0029113987617,54.4075273939191,-2.));
#44449=CARTESIAN_POINT('Ctrl Pts',(33.036738821977,54.4133779008128,-2.));
#44450=CARTESIAN_POINT('Ctrl Pts',(33.0704445092544,54.4200797350036,-2.));
#44451=CARTESIAN_POINT('Ctrl Pts',(33.089353388944,54.4238394618227,-2.));
#44452=CARTESIAN_POINT('Ctrl Pts',(33.1082301633356,54.427868732682,-2.));
#44453=CARTESIAN_POINT('Ctrl Pts',(33.1270344168394,54.4321588085794,-2.));
#44454=CARTESIAN_POINT('Ctrl Pts',(33.1999617463517,54.4487967345966,-2.));
#44455=CARTESIAN_POINT('Ctrl Pts',(33.2718735596778,54.4693655783697,-2.));
#44456=CARTESIAN_POINT('Ctrl Pts',(33.3423988007245,54.4937504954065,-2.));
#44457=CARTESIAN_POINT('Ctrl Pts',(33.3951487097983,54.5119893860131,-2.));
#44458=CARTESIAN_POINT('Ctrl Pts',(33.4471233202134,54.5323642451401,-2.));
#44459=CARTESIAN_POINT('Ctrl Pts',(33.4981671222966,54.5548460976078,-2.));
#44460=CARTESIAN_POINT('Ctrl Pts',(33.5140901369429,54.5618592676991,-2.));
#44461=CARTESIAN_POINT('Ctrl Pts',(33.5299225528842,54.5690775909089,-2.));
#44462=CARTESIAN_POINT('Ctrl Pts',(33.5456595741859,54.5765005080531,-2.));
#44463=CARTESIAN_POINT('Ctrl Pts',(33.5608498129668,54.5836655160752,-2.));
#44464=CARTESIAN_POINT('Ctrl Pts',(33.5759433894836,54.5910175352326,-2.));
#44465=CARTESIAN_POINT('Ctrl Pts',(33.5909308710043,54.5985527495203,-2.));
#44466=CARTESIAN_POINT('Ctrl Pts',(33.6582318432482,54.6323894716492,-2.));
#44467=CARTESIAN_POINT('Ctrl Pts',(33.7234283245458,54.6699323219049,-2.));
#44468=CARTESIAN_POINT('Ctrl Pts',(33.7861478874081,54.7110945661111,-2.));
#44469=CARTESIAN_POINT('Ctrl Pts',(33.8341488046729,54.7425971051658,-2.));
#44470=CARTESIAN_POINT('Ctrl Pts',(33.8806990672136,54.7762206567448,-2.));
#44471=CARTESIAN_POINT('Ctrl Pts',(33.9256254254142,54.8119460488582,-2.));
#44472=CARTESIAN_POINT('Ctrl Pts',(33.9360516193134,54.8202369471242,-2.));
#44473=CARTESIAN_POINT('Ctrl Pts',(33.9463903172992,54.8286411175249,-2.));
#44474=CARTESIAN_POINT('Ctrl Pts',(33.9566410663199,54.8371566128168,-2.));
#44475=CARTESIAN_POINT('Ctrl Pts',(33.3347877909358,57.7349452754743,-0.871480363390197));
#44476=CARTESIAN_POINT('Ctrl Pts',(33.4089783616458,57.6929560180431,-0.877193940366654));
#44477=CARTESIAN_POINT('Ctrl Pts',(33.4797275640263,57.6452118511612,-0.882907517343111));
#44478=CARTESIAN_POINT('Ctrl Pts',(33.5459978166813,57.5919001635713,-0.888621094319568));
#44479=CARTESIAN_POINT('Ctrl Pts',(33.9756840487236,57.2462352951484,-0.925667057842249));
#44480=CARTESIAN_POINT('Ctrl Pts',(34.2170739697906,56.6665102843049,-0.96271302136493));
#44481=CARTESIAN_POINT('Ctrl Pts',(34.1597013173233,56.1180347705934,-0.99975898488761));
#44482=CARTESIAN_POINT('Ctrl Pts',(34.102328664856,55.5695592568819,-1.03680494841029));
#44483=CARTESIAN_POINT('Ctrl Pts',(33.7461934388544,55.0523332403023,-1.07385091193297));
#44484=CARTESIAN_POINT('Ctrl Pts',(33.254268606184,54.8030776924624,-1.11089687545565));
#44485=CARTESIAN_POINT('Ctrl Pts',(32.7623437735136,54.5538221446225,-1.14794283897833));
#44486=CARTESIAN_POINT('Ctrl Pts',(32.1346293341744,54.5725370655222,-1.18498880250101));
#44487=CARTESIAN_POINT('Ctrl Pts',(31.6584309020156,54.8506384517481,-1.22203476602369));
#44488=CARTESIAN_POINT('Ctrl Pts',(31.1822324698568,55.1287398379739,-1.25908072954638));
#44489=CARTESIAN_POINT('Ctrl Pts',(30.8575500448783,55.666227689526,-1.29612669306906));
#44490=CARTESIAN_POINT('Ctrl Pts',(30.8329195675803,56.2171554903502,-1.33317265659174));
#44491=CARTESIAN_POINT('Ctrl Pts',(30.8082890902823,56.7680832911743,-1.37021862011442));
#44492=CARTESIAN_POINT('Ctrl Pts',(31.0837105606646,57.3324510412706,-1.4072645836371));
#44493=CARTESIAN_POINT('Ctrl Pts',(31.5332488781922,57.6518973032928,-1.44431054715978));
#44494=CARTESIAN_POINT('Ctrl Pts',(31.9827871957199,57.971343565315,-1.48135651068246));
#44495=CARTESIAN_POINT('Ctrl Pts',(32.6064423603928,58.0458683392631,-1.51840247420514));
#44496=CARTESIAN_POINT('Ctrl Pts',(33.1185697754731,57.8415149221822,-1.55544843772782));
#44497=CARTESIAN_POINT('Ctrl Pts',(33.1924454681488,57.8120364178238,-1.56079241294861));
#44498=CARTESIAN_POINT('Ctrl Pts',(33.2640004019439,57.7767547923516,-1.56613638816941));
#44499=CARTESIAN_POINT('Ctrl Pts',(33.332685602761,57.7363329907929,-1.5714803633902));
#44500=CARTESIAN_POINT('Ctrl Pts',(34.4842965055667,55.7582049595679,-2.));
#44501=CARTESIAN_POINT('Ctrl Pts',(34.6616800870191,56.4180307560557,-1.96295403647732));
#44502=CARTESIAN_POINT('Ctrl Pts',(34.3029408546812,57.9173199920237,-1.88886210943196));
#44503=CARTESIAN_POINT('Ctrl Pts',(32.1083909227282,58.6899905331758,-1.77772421886392));
#44504=CARTESIAN_POINT('Ctrl Pts',(30.2743670907292,57.2623912321518,-1.66658632829588));
#44505=CARTESIAN_POINT('Ctrl Pts',(30.4765028746713,54.9487367869863,-1.55544843772783));
#44506=CARTESIAN_POINT('Ctrl Pts',(32.5312595152502,53.8630292597192,-1.44431054715979));
#44507=CARTESIAN_POINT('Ctrl Pts',(34.5571577499754,55.0008883544572,-1.33317265659175));
#44508=CARTESIAN_POINT('Ctrl Pts',(34.7002397993375,57.3198853035068,-1.22203476602371));
#44509=CARTESIAN_POINT('Ctrl Pts',(32.8293553152893,58.6978846888631,-1.11089687545567));
#44510=CARTESIAN_POINT('Ctrl Pts',(30.6570393620672,57.873352597378,-0.999758984887625));
#44511=CARTESIAN_POINT('Ctrl Pts',(30.1715905180572,55.6011108576298,-0.888621094319582));
#44512=CARTESIAN_POINT('Ctrl Pts',(31.817369145763,53.960908709333,-0.777483203751541));
#44513=CARTESIAN_POINT('Ctrl Pts',(34.087963584719,54.4540716106361,-0.666345313183499));
#44514=CARTESIAN_POINT('Ctrl Pts',(34.9050789303496,56.6291869825843,-0.555207422615458));
#44515=CARTESIAN_POINT('Ctrl Pts',(33.5207972588595,58.4953545827796,-0.444069532047415));
#44516=CARTESIAN_POINT('Ctrl Pts',(31.2021687803137,58.344446263511,-0.332931641479374));
#44517=CARTESIAN_POINT('Ctrl Pts',(30.0714596841225,56.3145920190741,-0.221793750911332));
#44518=CARTESIAN_POINT('Ctrl Pts',(31.1636212068566,54.2637395061115,-0.110655860343291));
#44519=CARTESIAN_POINT('Ctrl Pts',(33.4789853310955,54.0690577668369,0.000482030224751639));
#44520=CARTESIAN_POINT('Ctrl Pts',(34.8982731111897,55.908740964546,0.111619920792793));
#44521=CARTESIAN_POINT('Ctrl Pts',(34.1223942983453,58.0989063257425,0.222757811360834));
#44522=CARTESIAN_POINT('Ctrl Pts',(31.8615195930587,58.6348705964901,0.333895701928877));
#44523=CARTESIAN_POINT('Ctrl Pts',(30.1850532410697,57.0260596319961,0.445033592496918));
#44524=CARTESIAN_POINT('Ctrl Pts',(30.6274839128385,54.7450363379153,0.55617148306496));
#44525=CARTESIAN_POINT('Ctrl Pts',(32.783849793945,53.8796472115696,0.667309373633002));
#44526=CARTESIAN_POINT('Ctrl Pts',(34.6804047400893,55.2219927306231,0.778447264201043));
#44527=CARTESIAN_POINT('Ctrl Pts',(34.5812104999016,57.5434088201914,0.889585154769087));
#44528=CARTESIAN_POINT('Ctrl Pts',(32.5770606867505,58.7190770058698,1.00072304533713));
#44529=CARTESIAN_POINT('Ctrl Pts',(30.5023763530244,57.672894864812,1.11186093590517));
#44530=CARTESIAN_POINT('Ctrl Pts',(30.2561395980005,55.3624447749947,1.22299882647321));
#44531=CARTESIAN_POINT('Ctrl Pts',(32.0637337160182,53.9025079060376,1.33413671704125));
#44532=CARTESIAN_POINT('Ctrl Pts',(34.2706473113688,54.6293810308449,1.44527460760929));
#44533=CARTESIAN_POINT('Ctrl Pts',(34.8568673421132,56.8777489350101,1.55641249817734));
#44534=CARTESIAN_POINT('Ctrl Pts',(33.2858199659299,58.5896549776087,1.66755038874538));
#44535=CARTESIAN_POINT('Ctrl Pts',(30.9955026631254,58.198172143523,1.77868827931342));
#44536=CARTESIAN_POINT('Ctrl Pts',(30.082268834923,56.0616291105053,1.88982616988146));
#44537=CARTESIAN_POINT('Ctrl Pts',(31.3820117610517,54.1356279467244,2.0009640604495));
#44538=CARTESIAN_POINT('Ctrl Pts',(33.7050620011388,54.1830593597268,2.11210195101754));
#44539=CARTESIAN_POINT('Ctrl Pts',(34.9251053252509,56.1605088392832,2.22323984158559));
#44540=CARTESIAN_POINT('Ctrl Pts',(33.925422242596,58.2579944509529,2.33437773215363));
#44541=CARTESIAN_POINT('Ctrl Pts',(31.6210340159052,58.5556638272701,2.44551562272167));
#44542=CARTESIAN_POINT('Ctrl Pts',(30.1211733226086,56.7810568122913,2.55665351328971));
#44543=CARTESIAN_POINT('Ctrl Pts',(30.7986796648578,54.558491332239,2.66779140385775));
#44544=CARTESIAN_POINT('Ctrl Pts',(33.0334238041474,53.9223067766118,2.7789292944258));
#44545=CARTESIAN_POINT('Ctrl Pts',(34.7799190860636,55.4548100839991,2.89006718499383));
#44546=CARTESIAN_POINT('Ctrl Pts',(34.4395785724648,57.7532835973794,3.00120507556188));
#44547=CARTESIAN_POINT('Ctrl Pts',(32.3239197951718,58.7139084434936,3.11234296612992));
#44548=CARTESIAN_POINT('Ctrl Pts',(30.3694292262435,57.4574138064661,3.22348085669796));
#44549=CARTESIAN_POINT('Ctrl Pts',(30.3650742488504,55.1338834771873,3.33461874726601));
#44550=CARTESIAN_POINT('Ctrl Pts',(32.3148410231894,53.870071116671,3.44575663783404));
#44551=CARTESIAN_POINT('Ctrl Pts',(34.4340859088485,54.822758511107,3.55689452840209));
#44552=CARTESIAN_POINT('Ctrl Pts',(34.7830400281131,57.1199400841538,3.66803241897013));
#44553=CARTESIAN_POINT('Ctrl Pts',(33.0423017182097,58.6589794901992,3.77917030953818));
#44554=CARTESIAN_POINT('Ctrl Pts',(30.8051884955116,58.0311765069792,3.89030820010621));
#44555=CARTESIAN_POINT('Ctrl Pts',(30.1193554633367,55.8111663248381,4.00144609067426));
#44556=CARTESIAN_POINT('Ctrl Pts',(31.6125533739245,54.0309494400521,4.11258398124229));
#44557=CARTESIAN_POINT('Ctrl Pts',(33.9180412456697,54.3199785564283,4.22372187181034));
#44558=CARTESIAN_POINT('Ctrl Pts',(34.9255798836093,56.4137020456761,4.33485976237838));
#44559=CARTESIAN_POINT('Ctrl Pts',(33.7129577460601,58.3957110541619,4.44599765294642));
#44560=CARTESIAN_POINT('Ctrl Pts',(31.390101627814,58.451850257884,4.55713554351446));
#44561=CARTESIAN_POINT('Ctrl Pts',(30.0831480764379,56.5307348090518,4.66827343408251));
#44562=CARTESIAN_POINT('Ctrl Pts',(30.9883665002516,54.3907834608547,4.77941132465054));
#44563=CARTESIAN_POINT('Ctrl Pts',(33.2772002083032,53.9907179590751,4.89054921521859));
#44564=CARTESIAN_POINT('Ctrl Pts',(34.8546537539781,55.6967227784588,5.00168710578663));
#44565=CARTESIAN_POINT('Ctrl Pts',(34.2768660104017,57.9472723924375,5.11282499635467));
#44566=CARTESIAN_POINT('Ctrl Pts',(32.0726926657226,58.6824131526073,5.22396288692271));
#44567=CARTESIAN_POINT('Ctrl Pts',(30.2596385516873,57.2292625110706,5.33510077749076));
#44568=CARTESIAN_POINT('Ctrl Pts',(30.4972127153845,54.9179054771161,5.44623866805879));
#44569=CARTESIAN_POINT('Ctrl Pts',(32.5679607208418,53.8639538597437,5.55737655862684));
#44570=CARTESIAN_POINT('Ctrl Pts',(34.5765036531329,55.0321005249752,5.66851444919487));
#44571=CARTESIAN_POINT('Ctrl Pts',(34.684398953168,57.3531295774156,5.77965233976293));
#44572=CARTESIAN_POINT('Ctrl Pts',(32.7928896947834,58.7025728310562,5.89079023033095));
#44573=CARTESIAN_POINT('Ctrl Pts',(30.6332940299706,57.8452774805726,6.00192812089902));
#44574=CARTESIAN_POINT('Ctrl Pts',(30.1823177935136,55.5659199366929,6.11306601146704));
#44575=CARTESIAN_POINT('Ctrl Pts',(31.8527378172473,53.9508533596396,6.2242039020351));
#44576=CARTESIAN_POINT('Ctrl Pts',(34.1156133119216,54.4783040835128,6.33534179260312));
#44577=CARTESIAN_POINT('Ctrl Pts',(34.8996815919165,56.6656147589771,6.44647968317118));
#44578=CARTESIAN_POINT('Ctrl Pts',(33.4873299906744,58.5104676737159,6.55761757373921));
#44579=CARTESIAN_POINT('Ctrl Pts',(31.1711925871668,58.3247407101007,6.66875546430726));
#44580=CARTESIAN_POINT('Ctrl Pts',(30.0714699489351,56.2774508415846,6.77989335487529));
#44581=CARTESIAN_POINT('Ctrl Pts',(31.1943253650081,54.2444600690086,6.89103124544334));
#44582=CARTESIAN_POINT('Ctrl Pts',(33.5128402220711,54.0826823257856,7.00216913601138));
#44583=CARTESIAN_POINT('Ctrl Pts',(34.903205848792,55.948145429959,7.11330702657943));
#44584=CARTESIAN_POINT('Ctrl Pts',(34.3645996631225,57.3926056844023,7.18739895362479));
#44585=CARTESIAN_POINT('Ctrl Pts',(33.8493101059358,57.841283396055,7.22444491714747));
#44586=CARTESIAN_POINT('Ctrl Pts',(34.3591563398468,55.7918468858113,-2.07481497238249));
#44587=CARTESIAN_POINT('Ctrl Pts',(34.5253531804484,56.4100605999883,-2.03776900885981));
#44588=CARTESIAN_POINT('Ctrl Pts',(34.189237929385,57.8147967775173,-1.96367708181445));
#44589=CARTESIAN_POINT('Ctrl Pts',(32.1330878491652,58.5387386537266,-1.8525391912464));
#44590=CARTESIAN_POINT('Ctrl Pts',(30.4147271983626,57.2011712670919,-1.74140130067837));
#44591=CARTESIAN_POINT('Ctrl Pts',(30.6041152374845,55.033428030193,-1.63026341011032));
#44592=CARTESIAN_POINT('Ctrl Pts',(32.5292881259403,54.0161909253172,-1.51912551954228));
#44593=CARTESIAN_POINT('Ctrl Pts',(34.4274225712752,55.0822906457469,-1.40798762897424));
#44594=CARTESIAN_POINT('Ctrl Pts',(34.561481114665,57.2550394601585,-1.2968497384062));
#44595=CARTESIAN_POINT('Ctrl Pts',(32.8085844382453,58.5461349624701,-1.18571184783816));
#44596=CARTESIAN_POINT('Ctrl Pts',(30.7732661452114,57.77360219784,-1.07457395727011));
#44597=CARTESIAN_POINT('Ctrl Pts',(30.3184322564853,55.6446599635185,-0.963436066702072));
#44598=CARTESIAN_POINT('Ctrl Pts',(31.860419434863,54.1078975824522,-0.852298176134029));
#44599=CARTESIAN_POINT('Ctrl Pts',(33.9878182558372,54.5699590394786,-0.741160285565988));
#44600=CARTESIAN_POINT('Ctrl Pts',(34.7534020135838,56.6079002051822,-0.630022394997946));
#44601=CARTESIAN_POINT('Ctrl Pts',(33.4564204191172,58.3563774692333,-0.518884504429904));
#44602=CARTESIAN_POINT('Ctrl Pts',(31.2840168375231,58.2149862216468,-0.407746613861862));
#44603=CARTESIAN_POINT('Ctrl Pts',(30.2246161991563,56.3131452533626,-0.296608723293821));
#44604=CARTESIAN_POINT('Ctrl Pts',(31.2479002766274,54.3916302777182,-0.185470832725779));
#44605=CARTESIAN_POINT('Ctrl Pts',(33.4172453712523,54.2092261920339,-0.0743329421577372));
#44606=CARTESIAN_POINT('Ctrl Pts',(34.7470254051468,55.9328892992031,0.0368049484103043));
#44607=CARTESIAN_POINT('Ctrl Pts',(34.0200775877185,57.9849313227406,0.147942838978346));
#44608=CARTESIAN_POINT('Ctrl Pts',(31.9017855229282,58.4870948699203,0.259080729546388));
#44609=CARTESIAN_POINT('Ctrl Pts',(30.3310459494339,56.9797439796362,0.37021862011443));
#44610=CARTESIAN_POINT('Ctrl Pts',(30.7455746179339,54.8425740019479,0.481356510682471));
#44611=CARTESIAN_POINT('Ctrl Pts',(32.7659487342222,54.0317608617915,0.592494401250513));
#44612=CARTESIAN_POINT('Ctrl Pts',(34.5428969584923,55.2894510179814,0.703632291818555));
#44613=CARTESIAN_POINT('Ctrl Pts',(34.4499584283865,57.4644664091972,0.814770182386596));
#44614=CARTESIAN_POINT('Ctrl Pts',(32.5722008348668,58.5659907805944,0.925908072954638));
#44615=CARTESIAN_POINT('Ctrl Pts',(30.6283569983197,57.5857863833556,1.03704596352268));
#44616=CARTESIAN_POINT('Ctrl Pts',(30.3976492271163,55.4210454183169,1.14818385409072));
#44617=CARTESIAN_POINT('Ctrl Pts',(32.0912469605975,54.0531798407264,1.25932174465876));
#44618=CARTESIAN_POINT('Ctrl Pts',(34.1589809866262,54.7342125263452,1.3704596352268));
#44619=CARTESIAN_POINT('Ctrl Pts',(34.7082309014681,56.8407865346196,1.48159752579485));
#44620=CARTESIAN_POINT('Ctrl Pts',(33.2362620291565,58.4447307855874,1.59273541636289));
#44621=CARTESIAN_POINT('Ctrl Pts',(31.0903841717777,58.07793691638,1.70387330693093));
#44622=CARTESIAN_POINT('Ctrl Pts',(30.234743668102,56.0761355152048,1.81501119749897));
#44623=CARTESIAN_POINT('Ctrl Pts',(31.4525179747664,54.2715981065311,1.92614908806701));
#44624=CARTESIAN_POINT('Ctrl Pts',(33.6290644583814,54.3160382453632,2.03728697863505));
#44625=CARTESIAN_POINT('Ctrl Pts',(34.7721654387779,56.1687793686431,2.1484248692031));
#44626=CARTESIAN_POINT('Ctrl Pts',(33.8355276249525,58.133986514719,2.25956275977114));
#44627=CARTESIAN_POINT('Ctrl Pts',(31.6764662300946,58.4128832958229,2.37070065033918));
#44628=CARTESIAN_POINT('Ctrl Pts',(30.2711946343393,56.7501923253058,2.48183854090722));
#44629=CARTESIAN_POINT('Ctrl Pts',(30.9059738661453,54.6677935046801,2.59297643147527));
#44630=CARTESIAN_POINT('Ctrl Pts',(32.9997832957543,54.0717300904732,2.7041143220433));
#44631=CARTESIAN_POINT('Ctrl Pts',(34.6361354068314,55.5075856855278,2.81525221261135));
#44632=CARTESIAN_POINT('Ctrl Pts',(34.3172585546125,57.6611053799801,2.92639010317939));
#44633=CARTESIAN_POINT('Ctrl Pts',(32.3350243382431,58.561148174924,3.03752799374743));
#44634=CARTESIAN_POINT('Ctrl Pts',(30.503794216031,57.3838946929671,3.14866588431547));
#44635=CARTESIAN_POINT('Ctrl Pts',(30.4997138863991,55.206898397108,3.25980377488352));
#44636=CARTESIAN_POINT('Ctrl Pts',(32.3265181213336,54.0227886857625,3.37094166545156));
#44637=CARTESIAN_POINT('Ctrl Pts',(34.3121122872296,54.9153946064446,3.4820795560196));
#44638=CARTESIAN_POINT('Ctrl Pts',(34.6390595258737,57.0677038371105,3.59321744658764));
#44639=CARTESIAN_POINT('Ctrl Pts',(33.0081013218997,58.5096833300926,3.70435533715569));
#44640=CARTESIAN_POINT('Ctrl Pts',(30.9120722157322,57.9214729022892,3.81549322772372));
#44641=CARTESIAN_POINT('Ctrl Pts',(30.2694914188265,55.8414682290596,3.92663111829177));
#44642=CARTESIAN_POINT('Ctrl Pts',(31.6685204219654,54.1735211766069,4.0377690088598));
#44643=CARTESIAN_POINT('Ctrl Pts',(33.8286121124817,54.4443225979689,4.14890689942785));
#44644=CARTESIAN_POINT('Ctrl Pts',(34.7726100689922,56.4060048808339,4.26004478999589));
#44645=CARTESIAN_POINT('Ctrl Pts',(33.6364622561334,58.2630179851872,4.37118268056393));
#44646=CARTESIAN_POINT('Ctrl Pts',(31.460097652016,58.315616755694,4.48232057113198));
#44647=CARTESIAN_POINT('Ctrl Pts',(30.2355674600263,56.5156569431085,4.59345846170002));
#44648=CARTESIAN_POINT('Ctrl Pts',(31.0836980528375,54.5106621730209,4.70459635226806));
#44649=CARTESIAN_POINT('Ctrl Pts',(33.2281858787452,54.1358269042489,4.8157342428361));
#44650=CARTESIAN_POINT('Ctrl Pts',(34.7061569138339,55.7342420941504,4.92687213340414));
#44651=CARTESIAN_POINT('Ctrl Pts',(34.164807501817,57.8428602221521,5.03801002397219));
#44652=CARTESIAN_POINT('Ctrl Pts',(32.0996409118515,58.5316391425983,5.14914791454022));
#44653=CARTESIAN_POINT('Ctrl Pts',(30.4009275183955,57.1701318172634,5.26028580510827));
#44654=CARTESIAN_POINT('Ctrl Pts',(30.6235190068059,55.0045411047512,5.37142369567631));
#44655=CARTESIAN_POINT('Ctrl Pts',(32.5636747606314,54.017057215205,5.48256158624435));
#44656=CARTESIAN_POINT('Ctrl Pts',(34.4455484201109,55.1115344127627,5.59369947681239));
#44657=CARTESIAN_POINT('Ctrl Pts',(34.5466392755035,57.2861871754458,5.70483736738044));
#44658=CARTESIAN_POINT('Ctrl Pts',(32.7744185314064,58.550527445779,5.81597525794847));
#44659=CARTESIAN_POINT('Ctrl Pts',(30.7510183185457,57.7472976454435,5.92711314851652));
#44660=CARTESIAN_POINT('Ctrl Pts',(30.3284830135763,55.6116883669947,6.03825103908455));
#44661=CARTESIAN_POINT('Ctrl Pts',(31.8935575720505,54.0984763759544,6.1493889296526));
#44662=CARTESIAN_POINT('Ctrl Pts',(34.0137242459347,54.5926632852668,6.26052682022064));
#44663=CARTESIAN_POINT('Ctrl Pts',(34.748345059677,56.6420306545566,6.37166471078869));
#44664=CARTESIAN_POINT('Ctrl Pts',(33.4250637727444,58.3705374492314,6.48280260135672));
#44665=CARTESIAN_POINT('Ctrl Pts',(31.2549941659053,58.1965234039931,6.59394049192477));
#44666=CARTESIAN_POINT('Ctrl Pts',(30.2246258166159,56.2783463937137,6.70507838249281));
#44667=CARTESIAN_POINT('Ctrl Pts',(31.2766680692062,54.3735667032384,6.81621627306085));
#44668=CARTESIAN_POINT('Ctrl Pts',(33.4489651948853,54.221991514694,6.92735416362889));
#44669=CARTESIAN_POINT('Ctrl Pts',(34.7516470583929,55.9698087119448,7.03849205419693));
#44670=CARTESIAN_POINT('Ctrl Pts',(34.2470082093303,57.323173711667,7.1125839812423));
#44671=CARTESIAN_POINT('Ctrl Pts',(33.7642155196223,57.7435554488857,7.14962994476498));
#44672=CARTESIAN_POINT('Ctrl Pts',(34.2340161741268,55.8254888120548,-2.14962994476498));
#44673=CARTESIAN_POINT('Ctrl Pts',(34.3890262738776,56.4020904439209,-2.1125839812423));
#44674=CARTESIAN_POINT('Ctrl Pts',(34.0755350040887,57.7122735630109,-2.03849205419694));
#44675=CARTESIAN_POINT('Ctrl Pts',(32.1577847756023,58.3874867742776,-1.92735416362889));
#44676=CARTESIAN_POINT('Ctrl Pts',(30.5550873059959,57.1399513020318,-1.81621627306085));
#44677=CARTESIAN_POINT('Ctrl Pts',(30.7317276002978,55.1181192733998,-1.70507838249281));
#44678=CARTESIAN_POINT('Ctrl Pts',(32.5273167366304,54.169352590915,-1.59394049192477));
#44679=CARTESIAN_POINT('Ctrl Pts',(34.297687392575,55.1636929370367,-1.48280260135673));
#44680=CARTESIAN_POINT('Ctrl Pts',(34.4227224299926,57.19019361681,-1.37166471078869));
#44681=CARTESIAN_POINT('Ctrl Pts',(32.7878135612012,58.3943852360772,-1.26052682022064));
#44682=CARTESIAN_POINT('Ctrl Pts',(30.8894929283555,57.6738517983019,-1.1493889296526));
#44683=CARTESIAN_POINT('Ctrl Pts',(30.4652739949134,55.6882090694071,-1.03825103908456));
#44684=CARTESIAN_POINT('Ctrl Pts',(31.903469723963,54.2548864555714,-0.927113148516518));
#44685=CARTESIAN_POINT('Ctrl Pts',(33.8876729269554,54.6858464683213,-0.815975257948477));
#44686=CARTESIAN_POINT('Ctrl Pts',(34.6017250968181,56.5866134277799,-0.704837367380434));
#44687=CARTESIAN_POINT('Ctrl Pts',(33.3920435793748,58.2174003556871,-0.593699476812394));
#44688=CARTESIAN_POINT('Ctrl Pts',(31.3658648947325,58.0855261797825,-0.482561586244351));
#44689=CARTESIAN_POINT('Ctrl Pts',(30.3777727141902,56.3116984876511,-0.37142369567631));
#44690=CARTESIAN_POINT('Ctrl Pts',(31.3321793463981,54.519521049325,-0.260285805108268));
#44691=CARTESIAN_POINT('Ctrl Pts',(33.3555054114091,54.3493946172309,-0.149147914540226));
#44692=CARTESIAN_POINT('Ctrl Pts',(34.5957776991039,55.9570376338603,-0.0380100239721845));
#44693=CARTESIAN_POINT('Ctrl Pts',(33.9177608770916,57.8709563197388,0.0731278665958568));
#44694=CARTESIAN_POINT('Ctrl Pts',(31.9420514527978,58.3393191433506,0.184265757163899));
#44695=CARTESIAN_POINT('Ctrl Pts',(30.4770386577981,56.9334283272761,0.295403647731941));
#44696=CARTESIAN_POINT('Ctrl Pts',(30.8636653230292,54.9401116659806,0.406541538299983));
#44697=CARTESIAN_POINT('Ctrl Pts',(32.7480476744994,54.1838745120134,0.517679428868023));
#44698=CARTESIAN_POINT('Ctrl Pts',(34.4053891768952,55.3569093053397,0.628817319436067));
#44699=CARTESIAN_POINT('Ctrl Pts',(34.3187063568714,57.3855239982029,0.739955210004107));
#44700=CARTESIAN_POINT('Ctrl Pts',(32.5673409829831,58.4129045553191,0.85109310057215));
#44701=CARTESIAN_POINT('Ctrl Pts',(30.754337643615,57.4986779018991,0.962230991140189));
#44702=CARTESIAN_POINT('Ctrl Pts',(30.5391588562322,55.4796460616392,1.07336888170823));
#44703=CARTESIAN_POINT('Ctrl Pts',(32.1187602051768,54.2038517754153,1.18450677227627));
#44704=CARTESIAN_POINT('Ctrl Pts',(34.0473146618836,54.8390440218454,1.29564466284432));
#44705=CARTESIAN_POINT('Ctrl Pts',(34.559594460823,56.8038241342291,1.40678255341236));
#44706=CARTESIAN_POINT('Ctrl Pts',(33.1867040923831,58.299806593566,1.5179204439804));
#44707=CARTESIAN_POINT('Ctrl Pts',(31.18526568043,57.957701689237,1.62905833454844));
#44708=CARTESIAN_POINT('Ctrl Pts',(30.387218501281,56.0906419199043,1.74019622511648));
#44709=CARTESIAN_POINT('Ctrl Pts',(31.5230241884812,54.4075682663379,1.85133411568453));
#44710=CARTESIAN_POINT('Ctrl Pts',(33.5530669156239,54.4490171309996,1.96247200625256));
#44711=CARTESIAN_POINT('Ctrl Pts',(34.6192255523049,56.177049898003,2.07360989682061));
#44712=CARTESIAN_POINT('Ctrl Pts',(33.7456330073089,58.009978578485,2.18474778738865));
#44713=CARTESIAN_POINT('Ctrl Pts',(31.731898444284,58.2701027643758,2.29588567795669));
#44714=CARTESIAN_POINT('Ctrl Pts',(30.42121594607,56.7193278383203,2.40702356852473));
#44715=CARTESIAN_POINT('Ctrl Pts',(31.0132680674328,54.7770956771211,2.51816145909278));
#44716=CARTESIAN_POINT('Ctrl Pts',(32.9661427873612,54.2211534043346,2.62929934966082));
#44717=CARTESIAN_POINT('Ctrl Pts',(34.4923517275991,55.5603612870565,2.74043724022886));
#44718=CARTESIAN_POINT('Ctrl Pts',(34.1949385367603,57.568927162581,2.8515751307969));
#44719=CARTESIAN_POINT('Ctrl Pts',(32.3461288813143,58.4083879063544,2.96271302136494));
#44720=CARTESIAN_POINT('Ctrl Pts',(30.6381592058186,57.3103755794683,3.07385091193298));
#44721=CARTESIAN_POINT('Ctrl Pts',(30.6343535239477,55.2799133170288,3.18498880250103));
#44722=CARTESIAN_POINT('Ctrl Pts',(32.3381952194777,54.175506254854,3.29612669306906));
#44723=CARTESIAN_POINT('Ctrl Pts',(34.1901386656106,55.0080307017823,3.40726458363711));
#44724=CARTESIAN_POINT('Ctrl Pts',(34.4950790236344,57.0154675900672,3.51840247420515));
#44725=CARTESIAN_POINT('Ctrl Pts',(32.9739009255897,58.360387169986,3.6295403647732));
#44726=CARTESIAN_POINT('Ctrl Pts',(31.0189559359528,57.8117692975994,3.74067825534123));
#44727=CARTESIAN_POINT('Ctrl Pts',(30.4196273743162,55.8717701332809,3.85181614590928));
#44728=CARTESIAN_POINT('Ctrl Pts',(31.7244874700065,54.3160929131618,3.96295403647732));
#44729=CARTESIAN_POINT('Ctrl Pts',(33.7391829792937,54.5686666395094,4.07409192704536));
#44730=CARTESIAN_POINT('Ctrl Pts',(34.6196402543752,56.3983077159918,4.1852298176134));
#44731=CARTESIAN_POINT('Ctrl Pts',(33.5599667662066,58.1303249162124,4.29636770818144));
#44732=CARTESIAN_POINT('Ctrl Pts',(31.530093676218,58.1793832535041,4.40750559874948));
#44733=CARTESIAN_POINT('Ctrl Pts',(30.3879868436147,56.5005790771652,4.51864348931753));
#44734=CARTESIAN_POINT('Ctrl Pts',(31.1790296054233,54.6305408851872,4.62978137988557));
#44735=CARTESIAN_POINT('Ctrl Pts',(33.1791715491872,54.2809358494227,4.74091927045361));
#44736=CARTESIAN_POINT('Ctrl Pts',(34.5576600736896,55.771761409842,4.85205716102165));
#44737=CARTESIAN_POINT('Ctrl Pts',(34.0527489932322,57.7384480518666,4.9631950515897));
#44738=CARTESIAN_POINT('Ctrl Pts',(32.1265891579804,58.3808651325893,5.07433294215774));
#44739=CARTESIAN_POINT('Ctrl Pts',(30.5422164851039,57.1110011234562,5.18547083272578));
#44740=CARTESIAN_POINT('Ctrl Pts',(30.7498252982272,55.0911767323862,5.29660872329382));
#44741=CARTESIAN_POINT('Ctrl Pts',(32.5593888004209,54.1701605706663,5.40774661386186));
#44742=CARTESIAN_POINT('Ctrl Pts',(34.314593187089,55.1909683005501,5.5188845044299));
#44743=CARTESIAN_POINT('Ctrl Pts',(34.4088795978388,57.219244773476,5.63002239499794));
#44744=CARTESIAN_POINT('Ctrl Pts',(32.7559473680293,58.3984820605018,5.74116028556599));
#44745=CARTESIAN_POINT('Ctrl Pts',(30.8687426071207,57.6493178103144,5.85229817613403));
#44746=CARTESIAN_POINT('Ctrl Pts',(30.474648233639,55.6574567972967,5.96343606670207));
#44747=CARTESIAN_POINT('Ctrl Pts',(31.9343773268536,54.2460993922691,6.0745739572701));
#44748=CARTESIAN_POINT('Ctrl Pts',(33.9118351799479,54.7070224870208,6.18571184783815));
#44749=CARTESIAN_POINT('Ctrl Pts',(34.5970085274374,56.6184465501361,6.29684973840619));
#44750=CARTESIAN_POINT('Ctrl Pts',(33.3627975548145,58.2306072247468,6.40798762897424));
#44751=CARTESIAN_POINT('Ctrl Pts',(31.3387957446438,58.0683060978856,6.51912551954227));
#44752=CARTESIAN_POINT('Ctrl Pts',(30.3777816842967,56.2792419458429,6.63026341011033));
#44753=CARTESIAN_POINT('Ctrl Pts',(31.3590107734043,54.5026733374682,6.74140130067836));
#44754=CARTESIAN_POINT('Ctrl Pts',(33.3850901676995,54.3613007036024,6.8525391912464));
#44755=CARTESIAN_POINT('Ctrl Pts',(34.6000882679938,55.9914719939308,6.96367708181444));
#44756=CARTESIAN_POINT('Ctrl Pts',(34.129416755538,57.2537417389318,7.03776900885981));
#44757=CARTESIAN_POINT('Ctrl Pts',(33.6791209333089,57.6458275017164,7.07481497238249));
#44758=CARTESIAN_POINT('Ctrl Pts',(34.1088760084069,55.8591307382982,-2.22444491714747));
#44759=CARTESIAN_POINT('Ctrl Pts',(34.2526993673069,56.3941202878534,-2.18739895362479));
#44760=CARTESIAN_POINT('Ctrl Pts',(33.9618320787925,57.6097503485044,-2.11330702657943));
#44761=CARTESIAN_POINT('Ctrl Pts',(32.1824817020393,58.2362348948285,-2.00216913601138));
#44762=CARTESIAN_POINT('Ctrl Pts',(30.6954474136293,57.0787313369719,-1.89103124544334));
#44763=CARTESIAN_POINT('Ctrl Pts',(30.859339963111,55.2028105166065,-1.7798933548753));
#44764=CARTESIAN_POINT('Ctrl Pts',(32.5253453473205,54.3225142565131,-1.66875546430726));
#44765=CARTESIAN_POINT('Ctrl Pts',(34.1679522138747,55.2450952283263,-1.55761757373922));
#44766=CARTESIAN_POINT('Ctrl Pts',(34.28396374532,57.1253477734617,-1.44647968317117));
#44767=CARTESIAN_POINT('Ctrl Pts',(32.7670426841572,58.2426355096843,-1.33534179260313));
#44768=CARTESIAN_POINT('Ctrl Pts',(31.0057197114997,57.5741013987638,-1.22420390203509));
#44769=CARTESIAN_POINT('Ctrl Pts',(30.6121157333414,55.7317581752959,-1.11306601146705));
#44770=CARTESIAN_POINT('Ctrl Pts',(31.946520013063,54.4018753286905,-1.00192812089901));
#44771=CARTESIAN_POINT('Ctrl Pts',(33.7875275980737,54.801733897164,-0.890790230330966));
#44772=CARTESIAN_POINT('Ctrl Pts',(34.4500481800523,56.5653266503777,-0.779652339762923));
#44773=CARTESIAN_POINT('Ctrl Pts',(33.3276667396325,58.0784232421408,-0.668514449194882));
#44774=CARTESIAN_POINT('Ctrl Pts',(31.4477129519419,57.9560661379182,-0.55737655862684));
#44775=CARTESIAN_POINT('Ctrl Pts',(30.530929229224,56.3102517219396,-0.446238668058799));
#44776=CARTESIAN_POINT('Ctrl Pts',(31.4164584161689,54.6474118209319,-0.335100777490757));
#44777=CARTESIAN_POINT('Ctrl Pts',(33.2937654515659,54.4895630424277,-0.223962886922715));
#44778=CARTESIAN_POINT('Ctrl Pts',(34.444529993061,55.9811859685177,-0.112824996354674));
#44779=CARTESIAN_POINT('Ctrl Pts',(33.8154441664647,57.7569813167368,-0.00168710578663197));
#44780=CARTESIAN_POINT('Ctrl Pts',(31.9823173826673,58.1915434167809,0.10945078478141));
#44781=CARTESIAN_POINT('Ctrl Pts',(30.6230313661623,56.887112674916,0.220588675349452));
#44782=CARTESIAN_POINT('Ctrl Pts',(30.9817560281246,55.0376493300133,0.331726565917493));
#44783=CARTESIAN_POINT('Ctrl Pts',(32.7301466147766,54.3359881622353,0.442864456485535));
#44784=CARTESIAN_POINT('Ctrl Pts',(34.2678813952981,55.424367592698,0.554002347053577));
#44785=CARTESIAN_POINT('Ctrl Pts',(34.1874542853563,57.3065815872086,0.665140237621619));
#44786=CARTESIAN_POINT('Ctrl Pts',(32.5624811310993,58.2598183300436,0.776278128189661));
#44787=CARTESIAN_POINT('Ctrl Pts',(30.8803182889104,57.4115694204428,0.887416018757702));
#44788=CARTESIAN_POINT('Ctrl Pts',(30.680668485348,55.5382467049613,0.998553909325744));
#44789=CARTESIAN_POINT('Ctrl Pts',(32.1462734497561,54.3545237101042,1.10969179989378));
#44790=CARTESIAN_POINT('Ctrl Pts',(33.935648337141,54.9438755173456,1.22082969046183));
#44791=CARTESIAN_POINT('Ctrl Pts',(34.4109580201779,56.7668617338386,1.33196758102987));
#44792=CARTESIAN_POINT('Ctrl Pts',(33.1371461556097,58.1548824015447,1.44310547159791));
#44793=CARTESIAN_POINT('Ctrl Pts',(31.2801471890823,57.8374664620939,1.55424336216595));
#44794=CARTESIAN_POINT('Ctrl Pts',(30.53969333446,56.1051483246038,1.66538125273399));
#44795=CARTESIAN_POINT('Ctrl Pts',(31.593530402196,54.5435384261447,1.77651914330204));
#44796=CARTESIAN_POINT('Ctrl Pts',(33.4770693728664,54.581996016636,1.88765703387008));
#44797=CARTESIAN_POINT('Ctrl Pts',(34.4662856658319,56.1853204273628,1.99879492443812));
#44798=CARTESIAN_POINT('Ctrl Pts',(33.6557383896653,57.8859706422512,2.10993281500616));
#44799=CARTESIAN_POINT('Ctrl Pts',(31.7873306584734,58.1273222329285,2.2210707055742));
#44800=CARTESIAN_POINT('Ctrl Pts',(30.5712372578007,56.6884633513348,2.33220859614224));
#44801=CARTESIAN_POINT('Ctrl Pts',(31.1205622687203,54.8863978495623,2.44334648671029));
#44802=CARTESIAN_POINT('Ctrl Pts',(32.9325022789681,54.370576718196,2.55448437727833));
#44803=CARTESIAN_POINT('Ctrl Pts',(34.3485680483669,55.6131368885852,2.66562226784637));
#44804=CARTESIAN_POINT('Ctrl Pts',(34.0726185189081,57.4767489451818,2.77676015841441));
#44805=CARTESIAN_POINT('Ctrl Pts',(32.3572334243856,58.2556276377848,2.88789804898245));
#44806=CARTESIAN_POINT('Ctrl Pts',(30.7725241956061,57.2368564659694,2.99903593955049));
#44807=CARTESIAN_POINT('Ctrl Pts',(30.7689931614964,55.3529282369496,3.11017383011854));
#44808=CARTESIAN_POINT('Ctrl Pts',(32.3498723176219,54.3282238239454,3.22131172068658));
#44809=CARTESIAN_POINT('Ctrl Pts',(34.0681650439915,55.10066679712,3.33244961125462));
#44810=CARTESIAN_POINT('Ctrl Pts',(34.351098521395,56.9632313430239,3.44358750182266));
#44811=CARTESIAN_POINT('Ctrl Pts',(32.9397005292797,58.2110910098795,3.5547253923907));
#44812=CARTESIAN_POINT('Ctrl Pts',(31.1258396561734,57.7020656929093,3.66586328295875));
#44813=CARTESIAN_POINT('Ctrl Pts',(30.569763329806,55.9020720375025,3.77700117352679));
#44814=CARTESIAN_POINT('Ctrl Pts',(31.7804545180475,54.4586646497164,3.88813906409483));
#44815=CARTESIAN_POINT('Ctrl Pts',(33.6497538461057,54.6930106810501,3.99927695466287));
#44816=CARTESIAN_POINT('Ctrl Pts',(34.4666704397582,56.3906105511495,4.11041484523091));
#44817=CARTESIAN_POINT('Ctrl Pts',(33.4834712762799,57.9976318472377,4.22155273579896));
#44818=CARTESIAN_POINT('Ctrl Pts',(31.60008970042,58.0431497513142,4.33269062636699));
#44819=CARTESIAN_POINT('Ctrl Pts',(30.5404062272031,56.4855012112219,4.44382851693505));
#44820=CARTESIAN_POINT('Ctrl Pts',(31.2743611580091,54.7504195973535,4.55496640750307));
#44821=CARTESIAN_POINT('Ctrl Pts',(33.1301572196292,54.4260447945964,4.66610429807113));
#44822=CARTESIAN_POINT('Ctrl Pts',(34.4091632335454,55.8092807255337,4.77724218863916));
#44823=CARTESIAN_POINT('Ctrl Pts',(33.9406904846474,57.6340358815812,4.88838007920721));
#44824=CARTESIAN_POINT('Ctrl Pts',(32.1535374041094,58.2300911225802,4.99951796977524));
#44825=CARTESIAN_POINT('Ctrl Pts',(30.6835054518121,57.0518704296491,5.11065586034329));
#44826=CARTESIAN_POINT('Ctrl Pts',(30.8761315896486,55.1778123600212,5.22179375091132));
#44827=CARTESIAN_POINT('Ctrl Pts',(32.5551028402105,54.3232639261277,5.33293164147937));
#44828=CARTESIAN_POINT('Ctrl Pts',(34.1836379540671,55.2704021883376,5.44406953204741));
#44829=CARTESIAN_POINT('Ctrl Pts',(34.2711199201742,57.1523023715063,5.55520742261546));
#44830=CARTESIAN_POINT('Ctrl Pts',(32.7374762046522,58.2464366752245,5.66634531318349));
#44831=CARTESIAN_POINT('Ctrl Pts',(30.9864668956958,57.5513379751854,5.77748320375154));
#44832=CARTESIAN_POINT('Ctrl Pts',(30.6208134537018,55.7032252275986,5.88862109431957));
#44833=CARTESIAN_POINT('Ctrl Pts',(31.9751970816566,54.3937224085839,5.99975898488763));
#44834=CARTESIAN_POINT('Ctrl Pts',(33.809946113961,54.8213816887749,6.11089687545565));
#44835=CARTESIAN_POINT('Ctrl Pts',(34.4456719951979,56.5948624457155,6.22203476602371));
#44836=CARTESIAN_POINT('Ctrl Pts',(33.3005313368845,58.0906770002622,6.33317265659174));
#44837=CARTESIAN_POINT('Ctrl Pts',(31.4225973233824,57.940088791778,6.4443105471598));
#44838=CARTESIAN_POINT('Ctrl Pts',(30.5309375519775,56.280137497972,6.55544843772783));
#44839=CARTESIAN_POINT('Ctrl Pts',(31.4413534776024,54.631779971698,6.66658632829587));
#44840=CARTESIAN_POINT('Ctrl Pts',(33.3212151405137,54.5006098925109,6.77772421886391));
#44841=CARTESIAN_POINT('Ctrl Pts',(34.4485294775946,56.0131352759167,6.88886210943196));
#44842=CARTESIAN_POINT('Ctrl Pts',(34.0118253017458,57.1843097661965,6.96295403647732));
#44843=CARTESIAN_POINT('Ctrl Pts',(33.5940263469955,57.5480995545471,7.));
#44844=CARTESIAN_POINT('Ctrl Pts',(33.3311039683456,57.7330494773494,-1.3785196366098));
#44845=CARTESIAN_POINT('Ctrl Pts',(33.1447009981387,57.8419592717116,-1.36412702194092));
#44846=CARTESIAN_POINT('Ctrl Pts',(32.9385791362006,57.9159412173671,-1.34973440727203));
#44847=CARTESIAN_POINT('Ctrl Pts',(32.7263090322414,57.9449985351604,-1.33534179260314));
#44848=CARTESIAN_POINT('Ctrl Pts',(32.1799350266047,58.0197908060441,-1.29829582908046));
#44849=CARTESIAN_POINT('Ctrl Pts',(31.5928273690522,57.796946102404,-1.26124986555778));
#44850=CARTESIAN_POINT('Ctrl Pts',(31.2336728772496,57.3784665466726,-1.2242039020351));
#44851=CARTESIAN_POINT('Ctrl Pts',(30.874518385447,56.9599869909412,-1.18715793851242));
#44852=CARTESIAN_POINT('Ctrl Pts',(30.7433170593942,56.3458725831185,-1.15011197498974));
#44853=CARTESIAN_POINT('Ctrl Pts',(30.9001171096548,55.8171682381063,-1.11306601146706));
#44854=CARTESIAN_POINT('Ctrl Pts',(31.0569171599153,55.2884638930941,-1.07602004794438));
#44855=CARTESIAN_POINT('Ctrl Pts',(31.5017185864892,54.8451696108923,-1.0389740844217));
#44856=CARTESIAN_POINT('Ctrl Pts',(32.0309538972778,54.690165564537,-1.00192812089902));
#44857=CARTESIAN_POINT('Ctrl Pts',(32.5601892080665,54.5351615181817,-0.964882157376335));
#44858=CARTESIAN_POINT('Ctrl Pts',(33.1738584030701,54.6684477076728,-0.927836193853654));
#44859=CARTESIAN_POINT('Ctrl Pts',(33.5911130975683,55.029022927954,-0.890790230330973));
#44860=CARTESIAN_POINT('Ctrl Pts',(34.0083677920665,55.3895981482352,-0.853744266808293));
#44861=CARTESIAN_POINT('Ctrl Pts',(34.2292079860594,55.9774623993064,-0.816698303285612));
#44862=CARTESIAN_POINT('Ctrl Pts',(34.1525645096526,56.5235772901359,-0.779652339762931));
#44863=CARTESIAN_POINT('Ctrl Pts',(34.0828208613931,57.0205281937339,-0.745941438711888));
#44864=CARTESIAN_POINT('Ctrl Pts',(33.7667445152314,57.4829083508763,-0.712230537660845));
#44865=CARTESIAN_POINT('Ctrl Pts',(33.3333524836119,57.7367881187288,-0.678519636609802));
#44866=CARTESIAN_POINT('Ctrl Pts',(34.4842965055667,55.7582049595679,-2.));
#44867=CARTESIAN_POINT('Ctrl Pts',(34.4966111053925,55.830382760503,-2.));
#44868=CARTESIAN_POINT('Ctrl Pts',(34.5047055015068,55.9030302259432,-2.));
#44869=CARTESIAN_POINT('Ctrl Pts',(34.5087398487957,55.975836724312,-2.));
#44870=CARTESIAN_POINT('Ctrl Pts',(34.5128864619034,56.0506692458705,-2.));
#44871=CARTESIAN_POINT('Ctrl Pts',(34.5127437096053,56.1256707869282,-2.));
#44872=CARTESIAN_POINT('Ctrl Pts',(34.5084312212538,56.2004993443966,-2.));
#44873=CARTESIAN_POINT('Ctrl Pts',(34.5047872656982,56.2637277905931,-2.));
#44874=CARTESIAN_POINT('Ctrl Pts',(34.4981650958835,56.3268329649118,-2.));
#44875=CARTESIAN_POINT('Ctrl Pts',(34.4886099106143,56.3895978470293,-2.));
#44876=CARTESIAN_POINT('Ctrl Pts',(34.4843647905613,56.4174826501174,-2.));
#44877=CARTESIAN_POINT('Ctrl Pts',(34.4795404472607,56.4453001134182,-2.));
#44878=CARTESIAN_POINT('Ctrl Pts',(34.4741394411489,56.4730302233705,-2.));
#44879=CARTESIAN_POINT('Ctrl Pts',(34.4711718179616,56.4882667396007,-2.));
#44880=CARTESIAN_POINT('Ctrl Pts',(34.4680300836907,56.5034768715482,-2.));
#44881=CARTESIAN_POINT('Ctrl Pts',(34.4647145599138,56.5186572039168,-2.));
#44882=CARTESIAN_POINT('Ctrl Pts',(34.4616570554946,56.5326561785654,-2.));
#44883=CARTESIAN_POINT('Ctrl Pts',(34.45845116215,56.5466318131546,-2.));
#44884=CARTESIAN_POINT('Ctrl Pts',(34.4551025744278,56.5605599363288,-2.));
#44885=CARTESIAN_POINT('Ctrl Pts',(34.4379902743583,56.631736875066,-2.));
#44886=CARTESIAN_POINT('Ctrl Pts',(34.417129771285,56.7017985031124,-2.));
#44887=CARTESIAN_POINT('Ctrl Pts',(34.3926364221807,56.7704257260637,-2.));
#44888=CARTESIAN_POINT('Ctrl Pts',(34.3683331729278,56.8385203136112,-2.));
#44889=CARTESIAN_POINT('Ctrl Pts',(34.3404527390893,56.9052035572333,-2.));
#44890=CARTESIAN_POINT('Ctrl Pts',(34.3090644243563,56.9701370642033,-2.));
#44891=CARTESIAN_POINT('Ctrl Pts',(34.2829778948777,57.0241026835151,-2.));
#44892=CARTESIAN_POINT('Ctrl Pts',(34.2544675459293,57.0768595084347,-2.));
#44893=CARTESIAN_POINT('Ctrl Pts',(34.2235537441951,57.1281926115957,-2.));
#44894=CARTESIAN_POINT('Ctrl Pts',(34.2106502677927,57.1496191411115,-2.));
#44895=CARTESIAN_POINT('Ctrl Pts',(34.197327856878,57.1707973646537,-2.));
#44896=CARTESIAN_POINT('Ctrl Pts',(34.1835872002777,57.191710445978,-2.));
#44897=CARTESIAN_POINT('Ctrl Pts',(34.1772270825051,57.2013904535701,-2.));
#44898=CARTESIAN_POINT('Ctrl Pts',(34.1707773505651,57.2110136443968,-2.));
#44899=CARTESIAN_POINT('Ctrl Pts',(34.1642380418293,57.2205782912845,-2.));
#44900=CARTESIAN_POINT('Ctrl Pts',(34.1574176230365,57.2305541006574,-2.));
#44901=CARTESIAN_POINT('Ctrl Pts',(34.1505044190796,57.2404593596496,-2.));
#44902=CARTESIAN_POINT('Ctrl Pts',(34.1435014736337,57.2502888014871,-2.));
#44903=CARTESIAN_POINT('Ctrl Pts',(34.1036166313874,57.3062717789476,-2.));
#44904=CARTESIAN_POINT('Ctrl Pts',(34.0607968393012,57.3598374440895,-2.));
#44905=CARTESIAN_POINT('Ctrl Pts',(34.0151074156251,57.4106900609547,-2.));
#44906=CARTESIAN_POINT('Ctrl Pts',(33.9736959571629,57.4567812755417,-2.));
#44907=CARTESIAN_POINT('Ctrl Pts',(33.9299264067014,57.5006437323277,-2.));
#44908=CARTESIAN_POINT('Ctrl Pts',(33.8838248402233,57.5420278185054,-2.));
#44909=CARTESIAN_POINT('Ctrl Pts',(33.8292843968241,57.5909872483519,-2.));
#44910=CARTESIAN_POINT('Ctrl Pts',(33.7714790326439,57.6364792135475,-2.));
#44911=CARTESIAN_POINT('Ctrl Pts',(33.7108128089775,57.6783572197639,-2.));
#44912=CARTESIAN_POINT('Ctrl Pts',(33.6974562676307,57.6875772649183,-2.));
#44913=CARTESIAN_POINT('Ctrl Pts',(33.6839610126013,57.6966218980588,-2.));
#44914=CARTESIAN_POINT('Ctrl Pts',(33.6703313137203,57.7054891532984,-2.));
#44915=CARTESIAN_POINT('Ctrl Pts',(33.6562679227742,57.7146385613772,-2.));
#44916=CARTESIAN_POINT('Ctrl Pts',(33.6420560771616,57.7236022055282,-2.));
#44917=CARTESIAN_POINT('Ctrl Pts',(33.6277297174338,57.7323603945594,-2.));
#44918=CARTESIAN_POINT('Ctrl Pts',(33.569215230037,57.7681322829823,-2.));
#44919=CARTESIAN_POINT('Ctrl Pts',(33.5087208994645,57.8005303979702,-2.));
#44920=CARTESIAN_POINT('Ctrl Pts',(33.4466000497757,57.8294900318497,-2.));
#44921=CARTESIAN_POINT('Ctrl Pts',(33.3844917461018,57.8584438170004,-2.));
#44922=CARTESIAN_POINT('Ctrl Pts',(33.3207564252846,57.8839606526941,-2.));
#44923=CARTESIAN_POINT('Ctrl Pts',(33.2557354106676,57.905925394536,-2.));
#44924=CARTESIAN_POINT('Ctrl Pts',(33.2086728278312,57.9218236005007,-2.));
#44925=CARTESIAN_POINT('Ctrl Pts',(33.1609363812474,57.9358598412383,-2.));
#44926=CARTESIAN_POINT('Ctrl Pts',(33.1126567567704,57.9479733084058,-2.));
#44927=CARTESIAN_POINT('Ctrl Pts',(33.0764412556209,57.9570598596971,-2.));
#44928=CARTESIAN_POINT('Ctrl Pts',(33.0399201289053,57.9650642116641,-2.));
#44929=CARTESIAN_POINT('Ctrl Pts',(33.0031501969537,57.9719552160039,-2.));
#44930=CARTESIAN_POINT('Ctrl Pts',(32.9909318989143,57.9742450310877,-2.));
#44931=CARTESIAN_POINT('Ctrl Pts',(32.9786957157085,57.9764100788818,-2.));
#44932=CARTESIAN_POINT('Ctrl Pts',(32.9664441134471,57.9784496521969,-2.));
#44933=CARTESIAN_POINT('Ctrl Pts',(32.9014564692835,57.9892684056971,-2.));
#44934=CARTESIAN_POINT('Ctrl Pts',(32.8360307197705,57.996561300293,-2.));
#44935=CARTESIAN_POINT('Ctrl Pts',(32.7704812212897,58.0002046036744,-2.));
#44936=CARTESIAN_POINT('Ctrl Pts',(32.7243572374919,58.0027682185003,-2.));
#44937=CARTESIAN_POINT('Ctrl Pts',(32.678172012929,58.0035238244839,-2.));
#44938=CARTESIAN_POINT('Ctrl Pts',(32.6320397021384,58.0024136109102,-2.));
#44939=CARTESIAN_POINT('Ctrl Pts',(32.6172320120056,58.0020572511636,-2.));
#44940=CARTESIAN_POINT('Ctrl Pts',(32.6024277816188,58.0015084555323,-2.));
#44941=CARTESIAN_POINT('Ctrl Pts',(32.5876374051397,58.0007653782458,-2.));
#44942=CARTESIAN_POINT('Ctrl Pts',(32.5246283833708,57.9975997676214,-2.));
#44943=CARTESIAN_POINT('Ctrl Pts',(32.4619962285916,57.9909192311175,-2.));
#44944=CARTESIAN_POINT('Ctrl Pts',(32.4000310708476,57.9805958152549,-2.));
#44945=CARTESIAN_POINT('Ctrl Pts',(32.3429040942577,57.9710784419796,-2.));
#44946=CARTESIAN_POINT('Ctrl Pts',(32.2863436472675,57.9584643876278,-2.));
#44947=CARTESIAN_POINT('Ctrl Pts',(32.2305948723589,57.942618319326,-2.));
#44948=CARTESIAN_POINT('Ctrl Pts',(32.2201618224275,57.9396528223787,-2.));
#44949=CARTESIAN_POINT('Ctrl Pts',(32.2097572620709,57.9365740341467,-2.));
#44950=CARTESIAN_POINT('Ctrl Pts',(32.1993825459687,57.9333829869217,-2.));
#44951=CARTESIAN_POINT('Origin',(32.5,56.2916512459885,3.));
#44952=CARTESIAN_POINT('Origin',(32.5,-56.2916512459885,8.));
#44953=CARTESIAN_POINT('Origin',(-32.5,-56.2916512459885,8.));
#44954=CARTESIAN_POINT('Origin',(-65.,8.88178419700125E-15,8.));
#44955=CARTESIAN_POINT('Origin',(-32.5,56.2916512459885,8.));
#44956=CARTESIAN_POINT('Origin',(32.5,56.2916512459885,8.));
#44957=CARTESIAN_POINT('Origin',(32.5,-56.2916512459885,13.));
#44958=CARTESIAN_POINT('Ctrl Pts',(31.4059736530044,-55.03520293743,13.));
#44959=CARTESIAN_POINT('Ctrl Pts',(31.3544234714672,-55.070553205003,13.));
#44960=CARTESIAN_POINT('Ctrl Pts',(31.3051813503374,-55.1089326491051,13.));
#44961=CARTESIAN_POINT('Ctrl Pts',(31.2583086630398,-55.1500094432322,13.));
#44962=CARTESIAN_POINT('Ctrl Pts',(31.2285772761546,-55.1760644899685,13.));
#44963=CARTESIAN_POINT('Ctrl Pts',(31.1997994780201,-55.2032058502151,13.));
#44964=CARTESIAN_POINT('Ctrl Pts',(31.1719948710937,-55.2313585593622,13.));
#44965=CARTESIAN_POINT('Ctrl Pts',(31.1530079463075,-55.2505831926225,13.));
#44966=CARTESIAN_POINT('Ctrl Pts',(31.1344748974185,-55.2702795821264,13.));
#44967=CARTESIAN_POINT('Ctrl Pts',(31.1164029944547,-55.2904256030864,13.));
#44968=CARTESIAN_POINT('Ctrl Pts',(31.10680688574,-55.3011230602213,13.));
#44969=CARTESIAN_POINT('Ctrl Pts',(31.097341027084,-55.311947259576,13.));
#44970=CARTESIAN_POINT('Ctrl Pts',(31.0880156367974,-55.3228838799501,13.));
#44971=CARTESIAN_POINT('Ctrl Pts',(31.0452129481991,-55.373081967301,13.));
#44972=CARTESIAN_POINT('Ctrl Pts',(31.0053166517631,-55.4257004118496,13.));
#44973=CARTESIAN_POINT('Ctrl Pts',(30.9684112137071,-55.4803964712117,13.));
#44974=CARTESIAN_POINT('Ctrl Pts',(30.9417896431645,-55.5198512258336,13.));
#44975=CARTESIAN_POINT('Ctrl Pts',(30.916724774461,-55.5603881845169,13.));
#44976=CARTESIAN_POINT('Ctrl Pts',(30.8932580445526,-55.6018923080322,13.));
#44977=CARTESIAN_POINT('Ctrl Pts',(30.8868285874191,-55.6132636829126,13.));
#44978=CARTESIAN_POINT('Ctrl Pts',(30.8805191498619,-55.6247077158807,13.));
#44979=CARTESIAN_POINT('Ctrl Pts',(30.8743307104748,-55.636222162741,13.));
#44980=CARTESIAN_POINT('Ctrl Pts',(30.8680004795506,-55.648000432355,13.));
#44981=CARTESIAN_POINT('Ctrl Pts',(30.8618007209708,-55.6598452663792,13.));
#44982=CARTESIAN_POINT('Ctrl Pts',(30.8557343742871,-55.6717493028589,13.));
#44983=CARTESIAN_POINT('Ctrl Pts',(30.824926284678,-55.732204242495,13.));
#44984=CARTESIAN_POINT('Ctrl Pts',(30.7975367125457,-55.794219620245,13.));
#44985=CARTESIAN_POINT('Ctrl Pts',(30.7736505522206,-55.8574477163192,13.));
#44986=CARTESIAN_POINT('Ctrl Pts',(30.7494182331566,-55.9215921152943,13.));
#44987=CARTESIAN_POINT('Ctrl Pts',(30.72879092513,-55.9869854550098,13.));
#44988=CARTESIAN_POINT('Ctrl Pts',(30.7118943736091,-56.0533023281135,13.));
#44989=CARTESIAN_POINT('Ctrl Pts',(30.7014256021216,-56.094390960278,13.));
#44990=CARTESIAN_POINT('Ctrl Pts',(30.6923897620677,-56.1358348149116,13.));
#44991=CARTESIAN_POINT('Ctrl Pts',(30.6848255186051,-56.1775614118862,13.));
#44992=CARTESIAN_POINT('Ctrl Pts',(30.6786294263779,-56.2117408832985,13.));
#44993=CARTESIAN_POINT('Ctrl Pts',(30.6734208465555,-56.2461101538938,13.));
#44994=CARTESIAN_POINT('Ctrl Pts',(30.66922486922,-56.2806305243324,13.));
#44995=CARTESIAN_POINT('Ctrl Pts',(30.6675094773901,-56.2947430794491,13.));
#44996=CARTESIAN_POINT('Ctrl Pts',(30.6659632509475,-56.3088834624587,13.));
#44997=CARTESIAN_POINT('Ctrl Pts',(30.6645900225892,-56.3230249696056,13.));
#44998=CARTESIAN_POINT('Ctrl Pts',(30.657777408341,-56.3931812786421,13.));
#44999=CARTESIAN_POINT('Ctrl Pts',(30.6552023639046,-56.4634862436646,13.));
#45000=CARTESIAN_POINT('Ctrl Pts',(30.6569799481117,-56.5335953127025,13.));
#45001=CARTESIAN_POINT('Ctrl Pts',(30.6571775468159,-56.5413887331989,13.));
#45002=CARTESIAN_POINT('Ctrl Pts',(30.6574289761761,-56.5491797596255,13.));
#45003=CARTESIAN_POINT('Ctrl Pts',(30.6577344296099,-56.5569679370674,13.));
#45004=CARTESIAN_POINT('Ctrl Pts',(30.6603769077943,-56.6243434735914,13.));
#45005=CARTESIAN_POINT('Ctrl Pts',(30.6670582139719,-56.6915049782437,13.));
#45006=CARTESIAN_POINT('Ctrl Pts',(30.677541462644,-56.7582070441068,13.));
#45007=CARTESIAN_POINT('Ctrl Pts',(30.6888193174907,-56.8299649733815,13.));
#45008=CARTESIAN_POINT('Ctrl Pts',(30.7044969561434,-56.9011921151434,13.));
#45009=CARTESIAN_POINT('Ctrl Pts',(30.7243435713018,-56.9715867176043,13.));
#45010=CARTESIAN_POINT('Ctrl Pts',(30.72797807261,-56.9844780480751,13.));
#45011=CARTESIAN_POINT('Ctrl Pts',(30.731752555977,-56.9973414436069,13.));
#45012=CARTESIAN_POINT('Ctrl Pts',(30.7356658277082,-57.0101750208647,13.));
#45013=CARTESIAN_POINT('Ctrl Pts',(30.7390274224034,-57.0211993729146,13.));
#45014=CARTESIAN_POINT('Ctrl Pts',(30.7424887108225,-57.0321927628317,13.));
#45015=CARTESIAN_POINT('Ctrl Pts',(30.7460479825644,-57.0431526566225,13.));
#45016=CARTESIAN_POINT('Ctrl Pts',(30.7679991292784,-57.1107457638707,13.));
#45017=CARTESIAN_POINT('Ctrl Pts',(30.7936779402928,-57.177081381741,13.));
#45018=CARTESIAN_POINT('Ctrl Pts',(30.8228134385709,-57.2418920410565,13.));
#45019=CARTESIAN_POINT('Ctrl Pts',(30.8525629753419,-57.3080686025165,13.));
#45020=CARTESIAN_POINT('Ctrl Pts',(30.8859166603802,-57.3726561598101,13.));
#45021=CARTESIAN_POINT('Ctrl Pts',(30.9226411455397,-57.4353698900493,13.));
#45022=CARTESIAN_POINT('Ctrl Pts',(30.9595879478473,-57.4984632672077,13.));
#45023=CARTESIAN_POINT('Ctrl Pts',(30.9999468759528,-57.5596610610251,13.));
#45024=CARTESIAN_POINT('Ctrl Pts',(31.0435306577909,-57.618658668117,13.));
#45025=CARTESIAN_POINT('Ctrl Pts',(31.0543033138896,-57.6332411780565,13.));
#45026=CARTESIAN_POINT('Ctrl Pts',(31.0652732111657,-57.6476891601633,13.));
#45027=CARTESIAN_POINT('Ctrl Pts',(31.0764379482539,-57.6619977671329,13.));
#45028=CARTESIAN_POINT('Ctrl Pts',(31.0851682203193,-57.6731863899133,13.));
#45029=CARTESIAN_POINT('Ctrl Pts',(31.0940187404437,-57.6842909722259,13.));
#45030=CARTESIAN_POINT('Ctrl Pts',(31.1029745495045,-57.6952926419673,13.));
#45031=CARTESIAN_POINT('Ctrl Pts',(31.1505373075081,-57.7537206133534,13.));
#45032=CARTESIAN_POINT('Ctrl Pts',(31.2011482674294,-57.8093550198619,13.));
#45033=CARTESIAN_POINT('Ctrl Pts',(31.2545510980919,-57.8619011541248,13.));
#45034=CARTESIAN_POINT('Ctrl Pts',(31.3080118293392,-57.9145042601225,13.));
#45035=CARTESIAN_POINT('Ctrl Pts',(31.3642709811015,-57.9640134083886,13.));
#45036=CARTESIAN_POINT('Ctrl Pts',(31.4231195457109,-58.010113437602,13.));
#45037=CARTESIAN_POINT('Ctrl Pts',(31.4806288821152,-58.0551643595042,13.));
#45038=CARTESIAN_POINT('Ctrl Pts',(31.5406117299258,-58.0969603997432,13.));
#45039=CARTESIAN_POINT('Ctrl Pts',(31.6029105624086,-58.1351753158739,13.));
#45040=CARTESIAN_POINT('Ctrl Pts',(31.6163051637375,-58.1433917389751,13.));
#45041=CARTESIAN_POINT('Ctrl Pts',(31.6298069488463,-58.1514424691007,13.));
#45042=CARTESIAN_POINT('Ctrl Pts',(31.6434145443376,-58.1593240060195,13.));
#45043=CARTESIAN_POINT('Ctrl Pts',(31.6549388802987,-58.1659989163223,13.));
#45044=CARTESIAN_POINT('Ctrl Pts',(31.666539109872,-58.1725524712207,13.));
#45045=CARTESIAN_POINT('Ctrl Pts',(31.6782133743559,-58.1789848186021,13.));
#45046=CARTESIAN_POINT('Ctrl Pts',(32.7283737736498,-58.3336705852723,13.));
#45047=CARTESIAN_POINT('Ctrl Pts',(32.801456501431,-58.3184742869055,13.));
#45048=CARTESIAN_POINT('Ctrl Pts',(32.8734788597396,-58.298997786029,13.));
#45049=CARTESIAN_POINT('Ctrl Pts',(32.9441813035354,-58.2754925548906,13.));
#45050=CARTESIAN_POINT('Ctrl Pts',(33.0130334318726,-58.2526024664573,13.));
#45051=CARTESIAN_POINT('Ctrl Pts',(33.0806343841287,-58.2258909044602,13.));
#45052=CARTESIAN_POINT('Ctrl Pts',(33.1467189154918,-58.1955520781492,13.));
#45053=CARTESIAN_POINT('Ctrl Pts',(33.1614684625166,-58.1887806910164,13.));
#45054=CARTESIAN_POINT('Ctrl Pts',(33.1761442888062,-58.1818275349416,13.));
#45055=CARTESIAN_POINT('Ctrl Pts',(33.1907370174276,-58.1746976086672,13.));
#45056=CARTESIAN_POINT('Ctrl Pts',(33.2577025900794,-58.1419786012548,13.));
#45057=CARTESIAN_POINT('Ctrl Pts',(33.3227883256884,-58.1056063855858,13.));
#45058=CARTESIAN_POINT('Ctrl Pts',(33.3857181635784,-58.0658123209271,13.));
#45059=CARTESIAN_POINT('Ctrl Pts',(33.4298991913055,-58.0378741800863,13.));
#45060=CARTESIAN_POINT('Ctrl Pts',(33.4730169947395,-58.0082484492559,13.));
#45061=CARTESIAN_POINT('Ctrl Pts',(33.5149645797389,-57.9770049692026,13.));
#45062=CARTESIAN_POINT('Ctrl Pts',(33.5309116525527,-57.9651272400944,13.));
#45063=CARTESIAN_POINT('Ctrl Pts',(33.5466894876595,-57.9530156292951,13.));
#45064=CARTESIAN_POINT('Ctrl Pts',(33.5622917797584,-57.9406737257053,13.));
#45065=CARTESIAN_POINT('Ctrl Pts',(33.5771528445811,-57.9289181561955,13.));
#45066=CARTESIAN_POINT('Ctrl Pts',(33.5918591265304,-57.916949716641,13.));
#45067=CARTESIAN_POINT('Ctrl Pts',(33.6063795972843,-57.9047932103788,13.));
#45068=CARTESIAN_POINT('Ctrl Pts',(33.6620452141432,-57.8581900780557,13.));
#45069=CARTESIAN_POINT('Ctrl Pts',(33.7150448946165,-57.8087799685606,13.));
#45070=CARTESIAN_POINT('Ctrl Pts',(33.7651216104469,-57.7567754487711,13.));
#45071=CARTESIAN_POINT('Ctrl Pts',(33.8141231388454,-57.7058875079175,13.));
#45072=CARTESIAN_POINT('Ctrl Pts',(33.8603263529607,-57.6525145643954,13.));
#45073=CARTESIAN_POINT('Ctrl Pts',(33.9034486471934,-57.5968301466407,13.));
#45074=CARTESIAN_POINT('Ctrl Pts',(33.9456250981648,-57.5423671094322,13.));
#45075=CARTESIAN_POINT('Ctrl Pts',(33.9848546823971,-57.485692216831,13.));
#45076=CARTESIAN_POINT('Ctrl Pts',(34.0208263213787,-57.4269537423419,13.));
#45077=CARTESIAN_POINT('Ctrl Pts',(34.0325140425975,-57.4078687372078,13.));
#45078=CARTESIAN_POINT('Ctrl Pts',(34.0438574259696,-57.3885658089128,13.));
#45079=CARTESIAN_POINT('Ctrl Pts',(34.0548446057631,-57.3690498891776,13.));
#45080=CARTESIAN_POINT('Ctrl Pts',(34.0610436454207,-57.3580388779202,13.));
#45081=CARTESIAN_POINT('Ctrl Pts',(34.0671298182374,-57.3469588596036,13.));
#45082=CARTESIAN_POINT('Ctrl Pts',(34.0730927271078,-57.3358266055139,13.));
#45083=CARTESIAN_POINT('Ctrl Pts',(34.1053441709564,-57.2756158467244,13.));
#45084=CARTESIAN_POINT('Ctrl Pts',(34.1340531807434,-57.2137749292232,13.));
#45085=CARTESIAN_POINT('Ctrl Pts',(34.1589642502906,-57.1504676174455,13.));
#45086=CARTESIAN_POINT('Ctrl Pts',(34.1625594233608,-57.1413310871163,13.));
#45087=CARTESIAN_POINT('Ctrl Pts',(34.1660754069223,-57.132163987681,13.));
#45088=CARTESIAN_POINT('Ctrl Pts',(34.1695113451333,-57.1229667871477,13.));
#45089=CARTESIAN_POINT('Ctrl Pts',(34.1937894815815,-57.05797991143,13.));
#45090=CARTESIAN_POINT('Ctrl Pts',(34.2140754401812,-56.9914902794374,13.));
#45091=CARTESIAN_POINT('Ctrl Pts',(34.2304117433295,-56.9238636615664,13.));
#45092=CARTESIAN_POINT('Ctrl Pts',(34.2456521934161,-56.8607734945421,13.));
#45093=CARTESIAN_POINT('Ctrl Pts',(34.2574544361006,-56.7966929502049,13.));
#45094=CARTESIAN_POINT('Ctrl Pts',(34.2658134374973,-56.7319255341013,13.));
#45095=CARTESIAN_POINT('Ctrl Pts',(34.2676584011698,-56.7176303421036,13.));
#45096=CARTESIAN_POINT('Ctrl Pts',(34.2693354843654,-56.7033017407798,13.));
#45097=CARTESIAN_POINT('Ctrl Pts',(34.270844395972,-56.6889430967336,13.));
#45098=CARTESIAN_POINT('Ctrl Pts',(34.2720238222348,-56.6777198005427,13.));
#45099=CARTESIAN_POINT('Ctrl Pts',(34.2731003471964,-56.6664788446859,13.));
#45100=CARTESIAN_POINT('Ctrl Pts',(34.2740729517289,-56.655234855777,13.));
#45101=CARTESIAN_POINT('Ctrl Pts',(34.2799651735089,-56.5871166493205,13.));
#45102=CARTESIAN_POINT('Ctrl Pts',(34.2820614503553,-56.5187616004217,13.));
#45103=CARTESIAN_POINT('Ctrl Pts',(34.2804207734115,-56.4505176925959,13.));
#45104=CARTESIAN_POINT('Ctrl Pts',(34.2787876667758,-56.3825886715075,13.));
#45105=CARTESIAN_POINT('Ctrl Pts',(34.2734516847404,-56.3147686810319,13.));
#45106=CARTESIAN_POINT('Ctrl Pts',(34.2644214383682,-56.2474134550015,13.));
#45107=CARTESIAN_POINT('Ctrl Pts',(34.2555845575225,-56.1815005128466,13.));
#45108=CARTESIAN_POINT('Ctrl Pts',(34.2432095214319,-56.1160317615425,13.));
#45109=CARTESIAN_POINT('Ctrl Pts',(34.2272624366034,-56.0513669972495,13.));
#45110=CARTESIAN_POINT('Ctrl Pts',(34.2239018011631,-56.037739760613,13.));
#45111=CARTESIAN_POINT('Ctrl Pts',(34.2203823920739,-56.0241483506747,13.));
#45112=CARTESIAN_POINT('Ctrl Pts',(34.2167036730317,-56.0105963443819,13.));
#45113=CARTESIAN_POINT('Ctrl Pts',(34.2132180506299,-55.9977556853967,13.));
#45114=CARTESIAN_POINT('Ctrl Pts',(34.2095887842124,-55.9849487305413,13.));
#45115=CARTESIAN_POINT('Ctrl Pts',(34.2058217802463,-55.972199063853,13.));
#45116=CARTESIAN_POINT('Ctrl Pts',(34.1873069910902,-55.9095345716819,13.));
#45117=CARTESIAN_POINT('Ctrl Pts',(34.165439151763,-55.8481392502423,13.));
#45118=CARTESIAN_POINT('Ctrl Pts',(34.1402348458363,-55.7883322343982,13.));
#45119=CARTESIAN_POINT('Ctrl Pts',(34.1155097070053,-55.7296622287999,13.));
#45120=CARTESIAN_POINT('Ctrl Pts',(34.0875733532055,-55.6725199271447,13.));
#45121=CARTESIAN_POINT('Ctrl Pts',(34.0564019231628,-55.6172367681066,13.));
#45122=CARTESIAN_POINT('Ctrl Pts',(34.0262427202374,-55.5637488142492,13.));
#45123=CARTESIAN_POINT('Ctrl Pts',(33.9930547257087,-55.512000693163,13.));
#45124=CARTESIAN_POINT('Ctrl Pts',(33.9567849769708,-55.4623304145165,13.));
#45125=CARTESIAN_POINT('Ctrl Pts',(33.9507490318898,-55.4540643778192,13.));
#45126=CARTESIAN_POINT('Ctrl Pts',(33.9446276728718,-55.4458559844853,13.));
#45127=CARTESIAN_POINT('Ctrl Pts',(33.9384205797355,-55.4377069137228,13.));
#45128=CARTESIAN_POINT('Ctrl Pts',(33.931849519021,-55.4290800029336,13.));
#45129=CARTESIAN_POINT('Ctrl Pts',(33.9251823737702,-55.4205195760218,13.));
#45130=CARTESIAN_POINT('Ctrl Pts',(33.9184205240576,-55.4120266023845,13.));
#45131=CARTESIAN_POINT('Origin',(32.5,-56.2916512459885,23.5459252805377));
#45132=CARTESIAN_POINT('Ctrl Pts',(31.4730118547325,-54.5098571360138,21.7959252805377));
#45133=CARTESIAN_POINT('Ctrl Pts',(31.5577251735551,-54.4600031121465,21.7905813053169));
#45134=CARTESIAN_POINT('Ctrl Pts',(32.2577698823492,-54.1148344325097,21.7481913665734));
#45135=CARTESIAN_POINT('Ctrl Pts',(33.9070787897524,-54.3119235461293,21.6687554643073));
#45136=CARTESIAN_POINT('Ctrl Pts',(34.9261604045136,-56.4001058936205,21.5576175737392));
#45137=CARTESIAN_POINT('Ctrl Pts',(33.7248161346881,-58.3888336702692,21.4464796831712));
#45138=CARTESIAN_POINT('Ctrl Pts',(31.4022507610405,-58.458078910143,21.3353417926031));
#45139=CARTESIAN_POINT('Ctrl Pts',(30.0845341595457,-56.5443222204949,21.2242039020351));
#45140=CARTESIAN_POINT('Ctrl Pts',(30.7258866583526,-55.0040437006141,21.1443983980133));
#45141=CARTESIAN_POINT('Ctrl Pts',(31.3789145578642,-54.5633564487824,21.1016388575141));
#45142=CARTESIAN_POINT('Ctrl Pts',(31.4704172621348,-54.5115691325664,21.0959252805377));
#45143=CARTESIAN_POINT('Ctrl Pts',(31.4716734168817,-54.5151354051885,21.8540747194623));
#45144=CARTESIAN_POINT('Ctrl Pts',(31.8806518858733,-54.2831085316556,21.8286245525962));
#45145=CARTESIAN_POINT('Ctrl Pts',(33.082939422317,-54.0422681540074,21.7661284222074));
#45146=CARTESIAN_POINT('Ctrl Pts',(34.7256560234758,-55.3208993649632,21.6665863282959));
#45147=CARTESIAN_POINT('Ctrl Pts',(34.5234929724835,-57.6345755616839,21.5554484377278));
#45148=CARTESIAN_POINT('Ctrl Pts',(32.4687454188576,-58.7202753686332,21.4443105471598));
#45149=CARTESIAN_POINT('Ctrl Pts',(30.4428342940784,-57.5824199368056,21.3331726565917));
#45150=CARTESIAN_POINT('Ctrl Pts',(30.3182849616345,-55.5637298511605,21.2364273806926));
#45151=CARTESIAN_POINT('Ctrl Pts',(31.1131094829785,-54.725326778543,21.1767280683161));
#45152=CARTESIAN_POINT('Ctrl Pts',(31.4749609874599,-54.5139076530798,21.1540747194623));
#45153=CARTESIAN_POINT('Ctrl Pts',(34.0692874532607,-56.8510195406194,22.));
#45154=CARTESIAN_POINT('Ctrl Pts',(33.8832841873681,-57.3728449537375,21.9629540364773));
#45155=CARTESIAN_POINT('Ctrl Pts',(32.9525520823054,-58.2072244344894,21.888862109432));
#45156=CARTESIAN_POINT('Ctrl Pts',(31.1328156874419,-57.7104505124287,21.7777242188639));
#45157=CARTESIAN_POINT('Ctrl Pts',(30.5680805647129,-55.9126012127397,21.6665863282959));
#45158=CARTESIAN_POINT('Ctrl Pts',(31.7699104961033,-54.4629042731491,21.5554484377278));
#45159=CARTESIAN_POINT('Ctrl Pts',(33.6408654404319,-54.686479644594,21.4443105471598));
#45160=CARTESIAN_POINT('Ctrl Pts',(34.4671411285654,-56.3795867334955,21.3331726565917));
#45161=CARTESIAN_POINT('Ctrl Pts',(33.493086107989,-57.992055635258,21.2220347660237));
#45162=CARTESIAN_POINT('Ctrl Pts',(31.6099402690807,-58.0481999689384,21.1108968754557));
#45163=CARTESIAN_POINT('Ctrl Pts',(30.5415300692557,-56.4965179419503,20.9997589848876));
#45164=CARTESIAN_POINT('Ctrl Pts',(31.2657026944405,-54.7573377854331,20.8886210943196));
#45165=CARTESIAN_POINT('Ctrl Pts',(33.1196550861101,-54.4225228075052,20.7774832037515));
#45166=CARTESIAN_POINT('Ctrl Pts',(34.4064234335583,-55.7985469486803,20.6663453131835));
#45167=CARTESIAN_POINT('Ctrl Pts',(33.9482241472934,-57.6259127164007,20.5552074226154));
#45168=CARTESIAN_POINT('Ctrl Pts',(32.1644471988301,-58.2320149921633,20.4440695320474));
#45169=CARTESIAN_POINT('Ctrl Pts',(30.6878063720739,-57.0620797446065,20.3329316414794));
#45170=CARTESIAN_POINT('Ctrl Pts',(30.8698865063133,-55.1869628453693,20.2217937509113));
#45171=CARTESIAN_POINT('Ctrl Pts',(32.5440282170451,-54.3229796221854,20.1106558603433));
#45172=CARTESIAN_POINT('Ctrl Pts',(34.1778702970045,-55.2609439349858,19.9995179697752));
#45173=CARTESIAN_POINT('Ctrl Pts',(34.2759387179252,-57.1423263023633,19.8883800792072));
#45174=CARTESIAN_POINT('Ctrl Pts',(32.7484702637603,-58.2450761614138,19.7772421886392));
#45175=CARTESIAN_POINT('Ctrl Pts',(30.9935741723466,-57.559834032996,19.6661042980711));
#45176=CARTESIAN_POINT('Ctrl Pts',(30.6175267185128,-55.7138098219726,19.5549664075031));
#45177=CARTESIAN_POINT('Ctrl Pts',(31.9645284111714,-54.3966904172637,19.443828516935));
#45178=CARTESIAN_POINT('Ctrl Pts',(33.801653320123,-54.8140501505305,19.332690626367));
#45179=CARTESIAN_POINT('Ctrl Pts',(34.4473601842239,-56.5838749230435,19.221552735799));
#45180=CARTESIAN_POINT('Ctrl Pts',(33.3106261867332,-58.0862240501872,19.1104148452309));
#45181=CARTESIAN_POINT('Ctrl Pts',(31.4319168476016,-57.9459803376678,18.9992769546629));
#45182=CARTESIAN_POINT('Ctrl Pts',(30.530836130646,-56.2915104462365,18.8881390640948));
#45183=CARTESIAN_POINT('Ctrl Pts',(31.4321534351977,-54.63716943038,18.7770011735268));
#45184=CARTESIAN_POINT('Ctrl Pts',(33.3108828106914,-54.4971943834675,18.6658632829587));
#45185=CARTESIAN_POINT('Ctrl Pts',(34.4474019535353,-55.9997060533367,18.5547253923907));
#45186=CARTESIAN_POINT('Ctrl Pts',(33.8014420032617,-57.7694384689282,18.4435875018227));
#45187=CARTESIAN_POINT('Ctrl Pts',(31.9642574280497,-58.1865354801138,18.3324496112546));
#45188=CARTESIAN_POINT('Ctrl Pts',(30.6174441046761,-56.869223462357,18.2213117206866));
#45189=CARTESIAN_POINT('Ctrl Pts',(30.9937555419292,-55.023253044843,18.1101738301185));
#45190=CARTESIAN_POINT('Ctrl Pts',(32.748749613628,-54.3382618854519,17.9990359395505));
#45191=CARTESIAN_POINT('Ctrl Pts',(34.2760603429607,-55.4412301607017,17.8878980489824));
#45192=CARTESIAN_POINT('Ctrl Pts',(34.1777228984872,-57.3225984997459,17.7767601584144));
#45193=CARTESIAN_POINT('Ctrl Pts',(32.5437466583565,-58.2603291256887,17.6656222678464));
#45194=CARTESIAN_POINT('Ctrl Pts',(30.8697286057113,-57.3961065620164,17.5544843772783));
#45195=CARTESIAN_POINT('Ctrl Pts',(30.6879164487935,-55.5209635222086,17.4433464867103));
#45196=CARTESIAN_POINT('Ctrl Pts',(32.1647249167202,-54.3512396961697,17.3322085961422));
#45197=CARTESIAN_POINT('Ctrl Pts',(33.9484144706509,-54.9575965674439,17.2210707055742));
#45198=CARTESIAN_POINT('Ctrl Pts',(34.4063538334575,-56.7850288151988,17.1099328150062));
#45199=CARTESIAN_POINT('Ctrl Pts',(33.1193859129775,-58.1608669785735,16.9987949244381));
#45200=CARTESIAN_POINT('Ctrl Pts',(31.2654870420352,-57.825790783565,16.8876570338701));
#45201=CARTESIAN_POINT('Ctrl Pts',(30.5415518818472,-56.086499271487,16.776519143302));
#45202=CARTESIAN_POINT('Ctrl Pts',(31.6102064945166,-54.534985688252,16.665381252734));
#45203=CARTESIAN_POINT('Ctrl Pts',(33.4932991936999,-54.5913680119554,16.5542433621659));
#45204=CARTESIAN_POINT('Ctrl Pts',(34.46721387611,-56.2040388622933,16.4431054715979));
#45205=CARTESIAN_POINT('Ctrl Pts',(33.6405153879952,-57.8969023210181,16.3319675810299));
#45206=CARTESIAN_POINT('Ctrl Pts',(31.7698902309213,-58.1204612659856,16.2208296904618));
#45207=CARTESIAN_POINT('Ctrl Pts',(30.5675428254988,-56.6700896595285,16.1096917998938));
#45208=CARTESIAN_POINT('Ctrl Pts',(31.1339953874406,-54.8733290813849,15.9985539093257));
#45209=CARTESIAN_POINT('Ctrl Pts',(32.9507674628268,-54.3747748653499,15.8874160187577));
#45210=CARTESIAN_POINT('Ctrl Pts',(34.3549469673911,-55.6307593394112,15.7762781281896));
#45211=CARTESIAN_POINT('Ctrl Pts',(34.0612724762645,-57.4916656705044,15.6651402376216));
#45212=CARTESIAN_POINT('Ctrl Pts',(32.3385475813956,-58.2541851899138,15.5540023470536));
#45213=CARTESIAN_POINT('Ctrl Pts',(30.7636019166367,-57.2203751334699,15.4428644564855));
#45214=CARTESIAN_POINT('Ctrl Pts',(30.7780011089404,-55.3364935710292,15.3317265659175));
#45215=CARTESIAN_POINT('Ctrl Pts',(32.3685654164946,-54.326878659382,15.2205886753495));
#45216=CARTESIAN_POINT('Ctrl Pts',(34.0794332859622,-55.1156423809379,15.1094507847814));
#45217=CARTESIAN_POINT('Ctrl Pts',(34.344627962679,-56.9808203482265,14.9983128942134));
#45218=CARTESIAN_POINT('Ctrl Pts',(32.9214137338773,-58.2151940311284,14.8871750036453));
#45219=CARTESIAN_POINT('Ctrl Pts',(31.1124747588703,-57.6889271671124,14.7760371130773));
#45220=CARTESIAN_POINT('Ctrl Pts',(30.5735533254956,-55.8837178487831,14.6648992225092));
#45221=CARTESIAN_POINT('Ctrl Pts',(31.7979304751287,-54.4518945101648,14.5537613319412));
#45222=CARTESIAN_POINT('Ctrl Pts',(33.6649196338359,-54.7040215463161,14.4426234413732));
#45223=CARTESIAN_POINT('Ctrl Pts',(34.4656450190372,-56.4093237108058,14.3314855508051));
#45224=CARTESIAN_POINT('Ctrl Pts',(33.4671924688587,-58.0069196157817,14.2203476602371));
#45225=CARTESIAN_POINT('Ctrl Pts',(31.5834591995985,-58.0345095641669,14.109209769669));
#45226=CARTESIAN_POINT('Ctrl Pts',(30.5386430838269,-56.4668442614587,13.998071879101));
#45227=CARTESIAN_POINT('Ctrl Pts',(31.289085272834,-54.7388173343014,13.886933988533));
#45228=CARTESIAN_POINT('Ctrl Pts',(33.1478792814865,-54.4321278475435,13.7757960979649));
#45229=CARTESIAN_POINT('Ctrl Pts',(34.4136863832883,-55.8274592952636,13.6646582073969));
#45230=CARTESIAN_POINT('Ctrl Pts',(33.9278258993098,-57.6477147792301,13.5535203168288));
#45231=CARTESIAN_POINT('Ctrl Pts',(32.135157735345,-58.2266620964951,13.4423824262608));
#45232=CARTESIAN_POINT('Ctrl Pts',(30.6762385450867,-57.0346478668883,13.3312445356927));
#45233=CARTESIAN_POINT('Ctrl Pts',(30.8870198365664,-55.1622083892051,13.2201066451247));
#45234=CARTESIAN_POINT('Ctrl Pts',(32.5733973317359,-54.3242660615775,13.1089687545567));
#45235=CARTESIAN_POINT('Ctrl Pts',(34.1941640560837,-55.2856728893477,12.9978308639886));
#45236=CARTESIAN_POINT('Ctrl Pts',(34.2610507255277,-57.170812419961,12.8866929734206));
#45237=CARTESIAN_POINT('Ctrl Pts',(33.2357187233791,-57.885756931559,12.8126010463752));
#45238=CARTESIAN_POINT('Ctrl Pts',(32.6851664226308,-57.947329172377,12.7755550828525));
#45239=CARTESIAN_POINT('Ctrl Pts',(34.1913483771213,-56.8945278288423,22.0748149723825));
#45240=CARTESIAN_POINT('Ctrl Pts',(33.9908775702891,-57.4569414030947,22.0377690088598));
#45241=CARTESIAN_POINT('Ctrl Pts',(32.9877520867064,-58.3562198480608,21.9636770818145));
#45242=CARTESIAN_POINT('Ctrl Pts',(31.0264745706938,-57.8208062977085,21.8525391912464));
#45243=CARTESIAN_POINT('Ctrl Pts',(30.4178137218822,-55.8831182794814,21.7414013006784));
#45244=CARTESIAN_POINT('Ctrl Pts',(31.7131233223058,-54.3206622992213,21.6302634101103));
#45245=CARTESIAN_POINT('Ctrl Pts',(33.7296032235388,-54.5616276117725,21.5191255195423));
#45246=CARTESIAN_POINT('Ctrl Pts',(34.6201475538814,-56.386426453537,21.4079876289742));
#45247=CARTESIAN_POINT('Ctrl Pts',(33.570329450222,-58.1243149802618,21.2968497384062));
#45248=CARTESIAN_POINT('Ctrl Pts',(31.5407104330672,-58.1848262826732,21.1857118478381));
#45249=CARTESIAN_POINT('Ctrl Pts',(30.3891980993524,-56.5124527014652,21.0745739572701));
#45250=CARTESIAN_POINT('Ctrl Pts',(31.1696976769262,-54.6379971776318,20.9634360667021));
#45251=CARTESIAN_POINT('Ctrl Pts',(33.16785254804,-54.2771399182574,20.852298176134));
#45252=CARTESIAN_POINT('Ctrl Pts',(34.5547071690116,-55.7601927478843,20.741160285566));
#45253=CARTESIAN_POINT('Ctrl Pts',(34.0608686325396,-57.7296930578618,20.6300223949979));
#45254=CARTESIAN_POINT('Ctrl Pts',(32.1383475286711,-58.3829386428887,20.5188845044299));
#45255=CARTESIAN_POINT('Ctrl Pts',(30.546851935728,-57.1220045302883,20.4077466138619));
#45256=CARTESIAN_POINT('Ctrl Pts',(30.7430944653628,-55.1010389526641,20.2966087232938));
#45257=CARTESIAN_POINT('Ctrl Pts',(32.5474527807459,-54.1698541532471,20.1854708327258));
#45258=CARTESIAN_POINT('Ctrl Pts',(34.3083769152439,-55.1807743737309,20.0743329421578));
#45259=CARTESIAN_POINT('Ctrl Pts',(34.4140732070395,-57.2084927545773,19.9631950515897));
#45260=CARTESIAN_POINT('Ctrl Pts',(32.7677965572851,-58.3970157244133,19.8520571610217));
#45261=CARTESIAN_POINT('Ctrl Pts',(30.8764026956559,-57.6584747009531,19.7409192704536));
#45262=CARTESIAN_POINT('Ctrl Pts',(30.4711058525308,-55.6688646731958,19.6297813798856));
#45263=CARTESIAN_POINT('Ctrl Pts',(31.9228788353096,-54.2492982559659,19.5186434893175));
#45264=CARTESIAN_POINT('Ctrl Pts',(33.9028973633798,-54.6991206935759,19.4075055987495));
#45265=CARTESIAN_POINT('Ctrl Pts',(34.5988280256839,-56.6066044057275,19.2963677081814));
#45266=CARTESIAN_POINT('Ctrl Pts',(33.3736775933143,-58.2258079192614,19.1852298176134));
#45267=CARTESIAN_POINT('Ctrl Pts',(31.3488401518243,-58.0746558947686,19.0740919270453));
#45268=CARTESIAN_POINT('Ctrl Pts',(30.3776723743012,-56.2914994946751,18.9629540364773));
#45269=CARTESIAN_POINT('Ctrl Pts',(31.3490951414668,-54.5084819942419,18.8518161459093));
#45270=CARTESIAN_POINT('Ctrl Pts',(33.3739541777695,-54.357619532466,18.7406782553412));
#45271=CARTESIAN_POINT('Ctrl Pts',(34.5988730438588,-55.9769982314793,18.6295403647732));
#45272=CARTESIAN_POINT('Ctrl Pts',(33.9026696100581,-57.8843824030853,18.5184024742052));
#45273=CARTESIAN_POINT('Ctrl Pts',(31.9225867748193,-58.3339216837986,18.4072645836371));
#45274=CARTESIAN_POINT('Ctrl Pts',(30.471016812898,-56.9141476718634,18.2961266930691));
#45275=CARTESIAN_POINT('Ctrl Pts',(30.8765981723663,-54.9245956217347,18.184988802501));
#45276=CARTESIAN_POINT('Ctrl Pts',(32.7680976352963,-54.1863250879512,18.073850911933));
#45277=CARTESIAN_POINT('Ctrl Pts',(34.4142042922056,-55.3750834626415,17.9627130213649));
#45278=CARTESIAN_POINT('Ctrl Pts',(34.308218051906,-57.4027867240152,17.8515751307969));
#45279=CARTESIAN_POINT('Ctrl Pts',(32.5471493221093,-58.4134550812175,17.7404372402289));
#45280=CARTESIAN_POINT('Ctrl Pts',(30.7429242830762,-57.4820123251428,17.6292993496608));
#45281=CARTESIAN_POINT('Ctrl Pts',(30.5469705743374,-55.4610185737053,17.5181614590928));
#45282=CARTESIAN_POINT('Ctrl Pts',(32.1386468477676,-54.2003123272238,17.4070235685247));
#45283=CARTESIAN_POINT('Ctrl Pts',(34.0610737594595,-54.8538323104842,17.2958856779567));
#45284=CARTESIAN_POINT('Ctrl Pts',(34.5546321553376,-56.8234042713874,17.1847477873886));
#45285=CARTESIAN_POINT('Ctrl Pts',(33.1675624383217,-58.3062566576536,17.0736098968206));
#45286=CARTESIAN_POINT('Ctrl Pts',(31.1694652508369,-57.9451178634435,16.9624720062526));
#45287=CARTESIAN_POINT('Ctrl Pts',(30.3892216085515,-56.07054232269,16.8513341156845));
#45288=CARTESIAN_POINT('Ctrl Pts',(31.5409973658137,-54.3983502869775,16.7401962251165));
#45289=CARTESIAN_POINT('Ctrl Pts',(33.5705591099766,-54.4591180905408,16.6290583345485));
#45290=CARTESIAN_POINT('Ctrl Pts',(34.620225959811,-56.1972242736255,16.5179204439804));
#45291=CARTESIAN_POINT('Ctrl Pts',(33.7292259436341,-58.0217605353874,16.4067825534124));
#45292=CARTESIAN_POINT('Ctrl Pts',(31.7131014808755,-58.2627081437915,16.2956446628443));
#45293=CARTESIAN_POINT('Ctrl Pts',(30.4172341567137,-56.6995250203255,16.1845067722763));
#45294=CARTESIAN_POINT('Ctrl Pts',(31.0277460290708,-54.7630104056167,16.0733688817082));
#45295=CARTESIAN_POINT('Ctrl Pts',(32.9858286575395,-54.2256780880444,15.9622309911402));
#45296=CARTESIAN_POINT('Ctrl Pts',(34.4992268060413,-55.5793544317117,15.8510931005721));
#45297=CARTESIAN_POINT('Ctrl Pts',(34.182709986298,-57.5850041273934,15.7399552100041));
#45298=CARTESIAN_POINT('Ctrl Pts',(32.3259896326697,-58.4068332632833,15.628817319436));
#45299=CARTESIAN_POINT('Ctrl Pts',(30.6285429420654,-57.2926123105924,15.517679428868));
#45300=CARTESIAN_POINT('Ctrl Pts',(30.6440621195648,-55.2622003445105,15.4065415382999));
#45301=CARTESIAN_POINT('Ctrl Pts',(32.3583422883757,-54.1740564618944,15.295403647732));
#45302=CARTESIAN_POINT('Ctrl Pts',(34.202283363977,-55.0241711031691,15.1842657571639));
#45303=CARTESIAN_POINT('Ctrl Pts',(34.4881051776633,-57.0344246876612,15.0731278665959));
#45304=CARTESIAN_POINT('Ctrl Pts',(32.9541917628979,-58.3648093287921,14.9619899760278));
#45305=CARTESIAN_POINT('Ctrl Pts',(31.0045515020698,-57.7976088426501,14.8508520854598));
#45306=CARTESIAN_POINT('Ctrl Pts',(30.4237121600868,-55.8519883353451,14.7397141948917));
#45307=CARTESIAN_POINT('Ctrl Pts',(31.7433227264704,-54.3087961846243,14.6285763043237));
#45308=CARTESIAN_POINT('Ctrl Pts',(33.7555283788647,-54.5805339421248,14.5174384137556));
#45309=CARTESIAN_POINT('Ctrl Pts',(34.6185350752899,-56.4184764060235,14.4063005231876));
#45310=CARTESIAN_POINT('Ctrl Pts',(33.542421775035,-58.1403350977259,14.2951626326195));
#45311=CARTESIAN_POINT('Ctrl Pts',(31.5121696365421,-58.1700710229889,14.1840247420515));
#45312=CARTESIAN_POINT('Ctrl Pts',(30.3860865609853,-56.4804709690946,14.0728868514835));
#45313=CARTESIAN_POINT('Ctrl Pts',(31.194898978279,-54.6180361852081,13.9617489609154));
#45314=CARTESIAN_POINT('Ctrl Pts',(33.1982720527306,-54.2874920489951,13.8506110703474));
#45315=CARTESIAN_POINT('Ctrl Pts',(34.5625350390512,-55.7913539289481,13.7394731797794));
#45316=CARTESIAN_POINT('Ctrl Pts',(34.0388837861359,-57.7531909093917,13.6283352892113));
#45317=CARTESIAN_POINT('Ctrl Pts',(32.1067798981332,-58.3771693930406,13.5171973986433));
#45318=CARTESIAN_POINT('Ctrl Pts',(30.5343843502893,-57.0924389706047,13.4060595080752));
#45319=CARTESIAN_POINT('Ctrl Pts',(30.7615604451028,-55.0743590673614,13.2949216175072));
#45320=CARTESIAN_POINT('Ctrl Pts',(32.5791062578488,-54.1712406533262,13.1837837269391));
#45321=CARTESIAN_POINT('Ctrl Pts',(34.3259380210302,-55.2074267736726,13.0726458363711));
#45322=CARTESIAN_POINT('Ctrl Pts',(34.3980272100312,-57.239194554091,12.9615079458031));
#45323=CARTESIAN_POINT('Ctrl Pts',(33.2929437441301,-58.0097482451375,12.8874160187577));
#45324=CARTESIAN_POINT('Ctrl Pts',(32.6995688729705,-58.0761096433421,12.850370055235));
#45325=CARTESIAN_POINT('Ctrl Pts',(34.3134093009819,-56.9380361170651,22.149629944765));
#45326=CARTESIAN_POINT('Ctrl Pts',(34.0984709532101,-57.541037852452,22.1125839812423));
#45327=CARTESIAN_POINT('Ctrl Pts',(33.0229520911074,-58.5052152616321,22.0384920541969));
#45328=CARTESIAN_POINT('Ctrl Pts',(30.9201334539457,-57.9311620829884,21.9273541636289));
#45329=CARTESIAN_POINT('Ctrl Pts',(30.2675468790515,-55.8536353462229,21.8162162730609));
#45330=CARTESIAN_POINT('Ctrl Pts',(31.6563361485083,-54.1784203252935,21.7050783824928));
#45331=CARTESIAN_POINT('Ctrl Pts',(33.8183410066456,-54.4367755789509,21.5939404919248));
#45332=CARTESIAN_POINT('Ctrl Pts',(34.7731539791975,-56.3932661735788,21.4828026013567));
#45333=CARTESIAN_POINT('Ctrl Pts',(33.6475727924551,-58.2565743252654,21.3716647107887));
#45334=CARTESIAN_POINT('Ctrl Pts',(31.4714805970539,-58.3214525964081,21.2605268202207));
#45335=CARTESIAN_POINT('Ctrl Pts',(30.236866129449,-56.52838746098,21.1493889296526));
#45336=CARTESIAN_POINT('Ctrl Pts',(31.0736926594119,-54.5186565698304,21.0382510390846));
#45337=CARTESIAN_POINT('Ctrl Pts',(33.2160500099698,-54.1317570290097,20.9271131485165));
#45338=CARTESIAN_POINT('Ctrl Pts',(34.702990904465,-55.7218385470882,20.8159752579485));
#45339=CARTESIAN_POINT('Ctrl Pts',(34.1735131177857,-57.8334733993231,20.7048373673804));
#45340=CARTESIAN_POINT('Ctrl Pts',(32.112247858512,-58.5338622936139,20.5936994768124));
#45341=CARTESIAN_POINT('Ctrl Pts',(30.4058974993822,-57.1819293159701,20.4825615862443));
#45342=CARTESIAN_POINT('Ctrl Pts',(30.6163024244123,-55.0151150599589,20.3714236956763));
#45343=CARTESIAN_POINT('Ctrl Pts',(32.5508773444466,-54.0167286843088,20.2602858051082));
#45344=CARTESIAN_POINT('Ctrl Pts',(34.4388835334834,-55.1006048124759,20.1491479145403));
#45345=CARTESIAN_POINT('Ctrl Pts',(34.5522076961538,-57.2746592067913,20.0380100239721));
#45346=CARTESIAN_POINT('Ctrl Pts',(32.7871228508099,-58.5489552874128,19.9268721334042));
#45347=CARTESIAN_POINT('Ctrl Pts',(30.7592312189651,-57.75711536891,19.8157342428361));
#45348=CARTESIAN_POINT('Ctrl Pts',(30.3246849865488,-55.6239195244191,19.7045963522681));
#45349=CARTESIAN_POINT('Ctrl Pts',(31.8812292594478,-54.1019060946679,19.5934584617));
#45350=CARTESIAN_POINT('Ctrl Pts',(34.0041414066367,-54.5841912366213,19.482320571132));
#45351=CARTESIAN_POINT('Ctrl Pts',(34.7502958671438,-56.6293338884116,19.3711826805639));
#45352=CARTESIAN_POINT('Ctrl Pts',(33.4367289998955,-58.3653917883354,19.2600447899959));
#45353=CARTESIAN_POINT('Ctrl Pts',(31.265763456047,-58.2033314518695,19.1489068994278));
#45354=CARTESIAN_POINT('Ctrl Pts',(30.2245086179564,-56.2914885431138,19.0377690088598));
#45355=CARTESIAN_POINT('Ctrl Pts',(31.2660368477359,-54.379794558104,18.9266311182918));
#45356=CARTESIAN_POINT('Ctrl Pts',(33.4370255448476,-54.2180446814646,18.8154932277237));
#45357=CARTESIAN_POINT('Ctrl Pts',(34.7503441341823,-55.9542904096218,18.7043553371557));
#45358=CARTESIAN_POINT('Ctrl Pts',(34.0038972168544,-57.9993263372426,18.5932174465876));
#45359=CARTESIAN_POINT('Ctrl Pts',(31.8809161215888,-58.4813078874833,18.4820795560196));
#45360=CARTESIAN_POINT('Ctrl Pts',(30.3245895211199,-56.9590718813699,18.3709416654516));
#45361=CARTESIAN_POINT('Ctrl Pts',(30.7594408028035,-54.8259381986264,18.2598037748835));
#45362=CARTESIAN_POINT('Ctrl Pts',(32.7874456569645,-54.0343882904504,18.1486658843155));
#45363=CARTESIAN_POINT('Ctrl Pts',(34.5523482414506,-55.3089367645812,18.0375279937474));
#45364=CARTESIAN_POINT('Ctrl Pts',(34.4387132053247,-57.4829749482845,17.9263901031794));
#45365=CARTESIAN_POINT('Ctrl Pts',(32.550551985862,-58.5665810367465,17.8152522126113));
#45366=CARTESIAN_POINT('Ctrl Pts',(30.6161199604412,-57.5679180882693,17.7041143220433));
#45367=CARTESIAN_POINT('Ctrl Pts',(30.4060246998813,-55.4010736252019,17.5929764314753));
#45368=CARTESIAN_POINT('Ctrl Pts',(32.112568778815,-54.0493849582779,17.4818385409072));
#45369=CARTESIAN_POINT('Ctrl Pts',(34.1737330482682,-54.7500680535245,17.3707006503392));
#45370=CARTESIAN_POINT('Ctrl Pts',(34.7029104772176,-56.861779727576,17.2595627597711));
#45371=CARTESIAN_POINT('Ctrl Pts',(33.2157389636658,-58.4516463367337,17.1484248692031));
#45372=CARTESIAN_POINT('Ctrl Pts',(31.0734434596386,-58.0644449433221,17.037286978635));
#45373=CARTESIAN_POINT('Ctrl Pts',(30.2368913352558,-56.054585373893,16.926149088067));
#45374=CARTESIAN_POINT('Ctrl Pts',(31.4717882371109,-54.261714885703,16.815011197499));
#45375=CARTESIAN_POINT('Ctrl Pts',(33.6478190262533,-54.3268681691261,16.7038733069309));
#45376=CARTESIAN_POINT('Ctrl Pts',(34.773238043512,-56.1904096849576,16.5927354163629));
#45377=CARTESIAN_POINT('Ctrl Pts',(33.8179364992731,-58.1466187497568,16.4815975257948));
#45378=CARTESIAN_POINT('Ctrl Pts',(31.6563127308296,-58.4049550215973,16.3704596352268));
#45379=CARTESIAN_POINT('Ctrl Pts',(30.2669254879288,-56.7289603811226,16.2593217446588));
#45380=CARTESIAN_POINT('Ctrl Pts',(30.9214966707009,-54.6526917298483,16.1481838540907));
#45381=CARTESIAN_POINT('Ctrl Pts',(33.0208898522522,-54.0765813107389,16.0370459635227));
#45382=CARTESIAN_POINT('Ctrl Pts',(34.6435066446914,-55.5279495240122,15.9259080729546));
#45383=CARTESIAN_POINT('Ctrl Pts',(34.3041474963316,-57.6783425842823,15.8147701823866));
#45384=CARTESIAN_POINT('Ctrl Pts',(32.3134316839437,-58.5594813366529,15.7036322918185));
#45385=CARTESIAN_POINT('Ctrl Pts',(30.4934839674941,-57.364849487715,15.5924944012505));
#45386=CARTESIAN_POINT('Ctrl Pts',(30.5101231301891,-55.1879071179918,15.4813565106825));
#45387=CARTESIAN_POINT('Ctrl Pts',(32.3481191602569,-54.0212342644067,15.3702186201144));
#45388=CARTESIAN_POINT('Ctrl Pts',(34.3251334419918,-54.9326998254003,15.2590807295464));
#45389=CARTESIAN_POINT('Ctrl Pts',(34.6315823926476,-57.0880290270961,15.1479428389784));
#45390=CARTESIAN_POINT('Ctrl Pts',(32.9869697919185,-58.5144246264557,15.0368049484103));
#45391=CARTESIAN_POINT('Ctrl Pts',(30.8966282452692,-57.9062905181877,14.9256670578423));
#45392=CARTESIAN_POINT('Ctrl Pts',(30.2738709946779,-55.8202588219069,14.8145291672742));
#45393=CARTESIAN_POINT('Ctrl Pts',(31.6887149778122,-54.1656978590839,14.7033912767062));
#45394=CARTESIAN_POINT('Ctrl Pts',(33.8461371238934,-54.4570463379336,14.5922533861381));
#45395=CARTESIAN_POINT('Ctrl Pts',(34.7714251315425,-56.4276291012412,14.4811154955701));
#45396=CARTESIAN_POINT('Ctrl Pts',(33.6176510812112,-58.2737505796701,14.369977605002));
#45397=CARTESIAN_POINT('Ctrl Pts',(31.4408800734857,-58.3056324818108,14.258839714434));
#45398=CARTESIAN_POINT('Ctrl Pts',(30.2335300381437,-56.4940976767304,14.147701823866));
#45399=CARTESIAN_POINT('Ctrl Pts',(31.1007126837241,-54.4972550361148,14.0365639332979));
#45400=CARTESIAN_POINT('Ctrl Pts',(33.2486648239746,-54.1428562504465,13.9254260427299));
#45401=CARTESIAN_POINT('Ctrl Pts',(34.7113836948142,-55.7552485626328,13.8142881521619));
#45402=CARTESIAN_POINT('Ctrl Pts',(34.149941672962,-57.8586670395533,13.7031502615938));
#45403=CARTESIAN_POINT('Ctrl Pts',(32.0784020609214,-58.5276766895861,13.5920123710258));
#45404=CARTESIAN_POINT('Ctrl Pts',(30.3925301554919,-57.1502300743212,13.4808744804577));
#45405=CARTESIAN_POINT('Ctrl Pts',(30.6361010536393,-54.9865097455178,13.3697365898897));
#45406=CARTESIAN_POINT('Ctrl Pts',(32.5848151839618,-54.0182152450749,13.2585986993216));
#45407=CARTESIAN_POINT('Ctrl Pts',(34.4577119859767,-55.1291806579975,13.1474608087536));
#45408=CARTESIAN_POINT('Ctrl Pts',(34.5350036945349,-57.3075766882209,13.0363229181856));
#45409=CARTESIAN_POINT('Ctrl Pts',(33.3501687648811,-58.133739558716,12.9622309911402));
#45410=CARTESIAN_POINT('Ctrl Pts',(32.7139713233101,-58.2048901143072,12.9251850276175));
#45411=CARTESIAN_POINT('Ctrl Pts',(34.4354702248424,-56.9815444052879,22.2244449171475));
#45412=CARTESIAN_POINT('Ctrl Pts',(34.2060643361312,-57.6251343018092,22.1873989536248));
#45413=CARTESIAN_POINT('Ctrl Pts',(33.0581520955084,-58.6542106752035,22.1133070265794));
#45414=CARTESIAN_POINT('Ctrl Pts',(30.8137923371976,-58.0415178682682,22.0021691360114));
#45415=CARTESIAN_POINT('Ctrl Pts',(30.1172800362208,-55.8241524129646,21.8910312454434));
#45416=CARTESIAN_POINT('Ctrl Pts',(31.5995489747108,-54.0361783513656,21.7798933548753));
#45417=CARTESIAN_POINT('Ctrl Pts',(33.9070787897524,-54.3119235461293,21.6687554643073));
#45418=CARTESIAN_POINT('Ctrl Pts',(34.9261604045136,-56.4001058936205,21.5576175737392));
#45419=CARTESIAN_POINT('Ctrl Pts',(33.7248161346881,-58.3888336702692,21.4464796831712));
#45420=CARTESIAN_POINT('Ctrl Pts',(31.4022507610405,-58.458078910143,21.3353417926031));
#45421=CARTESIAN_POINT('Ctrl Pts',(30.0845341595457,-56.5443222204949,21.2242039020351));
#45422=CARTESIAN_POINT('Ctrl Pts',(30.9776876418977,-54.3993159620292,21.113066011467));
#45423=CARTESIAN_POINT('Ctrl Pts',(33.2642474718997,-53.9863741397619,21.001928120899));
#45424=CARTESIAN_POINT('Ctrl Pts',(34.8512746399183,-55.6834843462923,20.890790230331));
#45425=CARTESIAN_POINT('Ctrl Pts',(34.2861576030319,-57.9372537407841,20.7796523397629));
#45426=CARTESIAN_POINT('Ctrl Pts',(32.086148188353,-58.6847859443394,20.6685144491949));
#45427=CARTESIAN_POINT('Ctrl Pts',(30.2649430630364,-57.2418541016519,20.5573765586268));
#45428=CARTESIAN_POINT('Ctrl Pts',(30.4895103834618,-54.9291911672537,20.4462386680588));
#45429=CARTESIAN_POINT('Ctrl Pts',(32.5543019081473,-53.8636032153705,20.3351007774907));
#45430=CARTESIAN_POINT('Ctrl Pts',(34.5693901517228,-55.0204352512209,20.2239628869227));
#45431=CARTESIAN_POINT('Ctrl Pts',(34.6903421852681,-57.3408256590054,20.1128249963547));
#45432=CARTESIAN_POINT('Ctrl Pts',(32.8064491443347,-58.7008948504122,20.0016871057866));
#45433=CARTESIAN_POINT('Ctrl Pts',(30.6420597422744,-57.8557560368671,19.8905492152186));
#45434=CARTESIAN_POINT('Ctrl Pts',(30.1782641205668,-55.5789743756423,19.7794113246505));
#45435=CARTESIAN_POINT('Ctrl Pts',(31.8395796835861,-53.9545139333701,19.6682734340825));
#45436=CARTESIAN_POINT('Ctrl Pts',(34.1053854498936,-54.4692617796666,19.5571355435145));
#45437=CARTESIAN_POINT('Ctrl Pts',(34.9017637086038,-56.6520633710957,19.4459976529464));
#45438=CARTESIAN_POINT('Ctrl Pts',(33.4997804064766,-58.5049756574095,19.3348597623784));
#45439=CARTESIAN_POINT('Ctrl Pts',(31.1826867602698,-58.3320070089704,19.2237218718103));
#45440=CARTESIAN_POINT('Ctrl Pts',(30.0713448616115,-56.2914775915524,19.1125839812423));
#45441=CARTESIAN_POINT('Ctrl Pts',(31.1829785540051,-54.2511071219659,19.0014460906742));
#45442=CARTESIAN_POINT('Ctrl Pts',(33.5000969119256,-54.0784698304632,18.8903082001062));
#45443=CARTESIAN_POINT('Ctrl Pts',(34.9018152245058,-55.9315825877644,18.7791703095382));
#45444=CARTESIAN_POINT('Ctrl Pts',(34.1051248236507,-58.1142702713998,18.6680324189701));
#45445=CARTESIAN_POINT('Ctrl Pts',(31.8392454683584,-58.628694091168,18.5568945284021));
#45446=CARTESIAN_POINT('Ctrl Pts',(30.1781622293417,-57.0039960908763,18.445756637834));
#45447=CARTESIAN_POINT('Ctrl Pts',(30.6422834332407,-54.7272807755182,18.334618747266));
#45448=CARTESIAN_POINT('Ctrl Pts',(32.8067936786327,-53.8824514929497,18.2234808566979));
#45449=CARTESIAN_POINT('Ctrl Pts',(34.6904921906955,-55.242790066521,18.1123429661299));
#45450=CARTESIAN_POINT('Ctrl Pts',(34.5692083587434,-57.5631631725538,18.0012050755619));
#45451=CARTESIAN_POINT('Ctrl Pts',(32.5539546496148,-58.7197069922754,17.8900671849938));
#45452=CARTESIAN_POINT('Ctrl Pts',(30.4893156378063,-57.6538238513956,17.7789292944258));
#45453=CARTESIAN_POINT('Ctrl Pts',(30.2650788254252,-55.3411286766987,17.6677914038578));
#45454=CARTESIAN_POINT('Ctrl Pts',(32.0864907098624,-53.8984575893318,17.5566535132897));
#45455=CARTESIAN_POINT('Ctrl Pts',(34.2863923370768,-54.6463037965649,17.4455156227217));
#45456=CARTESIAN_POINT('Ctrl Pts',(34.8511887990977,-56.9001551837646,17.3343777321536));
#45457=CARTESIAN_POINT('Ctrl Pts',(33.26391548901,-58.5970360158138,17.2232398415856));
#45458=CARTESIAN_POINT('Ctrl Pts',(30.9774216684404,-58.1837720232006,17.1121019510175));
#45459=CARTESIAN_POINT('Ctrl Pts',(30.0845610619601,-56.038628425096,17.0009640604495));
#45460=CARTESIAN_POINT('Ctrl Pts',(31.4025791084081,-54.1250794844285,16.8898261698814));
#45461=CARTESIAN_POINT('Ctrl Pts',(33.7250789425299,-54.1946182477115,16.7786882793134));
#45462=CARTESIAN_POINT('Ctrl Pts',(34.9262501272131,-56.1835950962899,16.6675503887454));
#45463=CARTESIAN_POINT('Ctrl Pts',(33.9066470549119,-58.2714769641261,16.5564124981774));
#45464=CARTESIAN_POINT('Ctrl Pts',(31.5995239807838,-58.5472018994033,16.4452746076093));
#45465=CARTESIAN_POINT('Ctrl Pts',(30.1166168191438,-56.7583957419196,16.3341367170413));
#45466=CARTESIAN_POINT('Ctrl Pts',(30.8152473123311,-54.5423730540802,16.2229988264732));
#45467=CARTESIAN_POINT('Ctrl Pts',(33.0559510469649,-53.9274845334332,16.1118609359052));
#45468=CARTESIAN_POINT('Ctrl Pts',(34.7877864833415,-55.4765446163129,16.0007230453371));
#45469=CARTESIAN_POINT('Ctrl Pts',(34.4255850063652,-57.7716810411711,15.8895851547691));
#45470=CARTESIAN_POINT('Ctrl Pts',(32.3008737352177,-58.7121294100224,15.778447264201));
#45471=CARTESIAN_POINT('Ctrl Pts',(30.3584249929227,-57.4370866648374,15.667309373633));
#45472=CARTESIAN_POINT('Ctrl Pts',(30.3761841408135,-55.1136138914732,15.5561714830649));
#45473=CARTESIAN_POINT('Ctrl Pts',(32.3378960321381,-53.8684120669189,15.4450335924969));
#45474=CARTESIAN_POINT('Ctrl Pts',(34.4479835200066,-54.8412285476316,15.3338957019289));
#45475=CARTESIAN_POINT('Ctrl Pts',(34.7750596076319,-57.1416333665308,15.2227578113608));
#45476=CARTESIAN_POINT('Ctrl Pts',(33.019747820939,-58.6640399241195,15.1116199207928));
#45477=CARTESIAN_POINT('Ctrl Pts',(30.7887049884687,-58.0149721937253,15.0004820302248));
#45478=CARTESIAN_POINT('Ctrl Pts',(30.124029829269,-55.7885293084688,14.8893441396567));
#45479=CARTESIAN_POINT('Ctrl Pts',(31.634107229154,-54.0225995335434,14.7782062490887));
#45480=CARTESIAN_POINT('Ctrl Pts',(33.9367458689222,-54.3335587337424,14.6670683585206));
#45481=CARTESIAN_POINT('Ctrl Pts',(34.9243151877952,-56.4367817964588,14.5559304679526));
#45482=CARTESIAN_POINT('Ctrl Pts',(33.6928803873874,-58.4071660616143,14.4447925773845));
#45483=CARTESIAN_POINT('Ctrl Pts',(31.3695905104292,-58.4411939406326,14.3336546868165));
#45484=CARTESIAN_POINT('Ctrl Pts',(30.0809735153021,-56.5077243843663,14.2225167962484));
#45485=CARTESIAN_POINT('Ctrl Pts',(31.0065263891691,-54.3764738870214,14.1113789056804));
#45486=CARTESIAN_POINT('Ctrl Pts',(33.2990575952187,-53.9982204518981,14.0002410151124));
#45487=CARTESIAN_POINT('Ctrl Pts',(34.8602323505772,-55.7191431963173,13.8891031245444));
#45488=CARTESIAN_POINT('Ctrl Pts',(34.2609995597881,-57.9641431697149,13.7779652339763));
#45489=CARTESIAN_POINT('Ctrl Pts',(32.0500242237095,-58.6781839861316,13.6668273434083));
#45490=CARTESIAN_POINT('Ctrl Pts',(30.2506759606945,-57.2080211780376,13.5556894528402));
#45491=CARTESIAN_POINT('Ctrl Pts',(30.5106416621758,-54.8986604236742,13.4445515622722));
#45492=CARTESIAN_POINT('Ctrl Pts',(32.5905241100746,-53.8651898368237,13.3334136717041));
#45493=CARTESIAN_POINT('Ctrl Pts',(34.5894859509232,-55.0509345423224,13.2222757811361));
#45494=CARTESIAN_POINT('Ctrl Pts',(34.6719801790384,-57.3759588223509,13.111137890568));
#45495=CARTESIAN_POINT('Ctrl Pts',(33.4073937856322,-58.2577308722946,13.0370459635227));
#45496=CARTESIAN_POINT('Ctrl Pts',(32.7283737736498,-58.3336705852723,13.));
#45497=CARTESIAN_POINT('Ctrl Pts',(34.0692874532607,-56.8510195406194,22.));
#45498=CARTESIAN_POINT('Ctrl Pts',(34.0553305059908,-56.9114179004368,22.));
#45499=CARTESIAN_POINT('Ctrl Pts',(34.0377835201511,-56.9707365361936,22.));
#45500=CARTESIAN_POINT('Ctrl Pts',(34.0169460819157,-57.0288042521055,22.));
#45501=CARTESIAN_POINT('Ctrl Pts',(33.9947315403597,-57.0907095436108,22.));
#45502=CARTESIAN_POINT('Ctrl Pts',(33.9687774174651,-57.1511938546456,22.));
#45503=CARTESIAN_POINT('Ctrl Pts',(33.9393848899745,-57.2100521415653,22.));
#45504=CARTESIAN_POINT('Ctrl Pts',(33.9136664284202,-57.2615531426201,22.));
#45505=CARTESIAN_POINT('Ctrl Pts',(33.8853142547964,-57.311809621018,22.));
#45506=CARTESIAN_POINT('Ctrl Pts',(33.8544948148302,-57.3606781624786,22.));
#45507=CARTESIAN_POINT('Ctrl Pts',(33.8390317669678,-57.3851969920354,22.));
#45508=CARTESIAN_POINT('Ctrl Pts',(33.8229471373042,-57.4093662970867,22.));
#45509=CARTESIAN_POINT('Ctrl Pts',(33.8062591811805,-57.433166856092,22.));
#45510=CARTESIAN_POINT('Ctrl Pts',(33.7986346988524,-57.4440409823294,22.));
#45511=CARTESIAN_POINT('Ctrl Pts',(33.7908831156841,-57.4548394646073,22.));
#45512=CARTESIAN_POINT('Ctrl Pts',(33.7830191798169,-57.4655431489118,22.));
#45513=CARTESIAN_POINT('Ctrl Pts',(33.7433624663838,-57.5195203110236,22.));
#45514=CARTESIAN_POINT('Ctrl Pts',(33.7007840160683,-57.5711878026522,22.));
#45515=CARTESIAN_POINT('Ctrl Pts',(33.6555819715537,-57.6203464168852,22.));
#45516=CARTESIAN_POINT('Ctrl Pts',(33.6095776366613,-57.6703775465898,22.));
#45517=CARTESIAN_POINT('Ctrl Pts',(33.5608552987539,-57.7178108518911,22.));
#45518=CARTESIAN_POINT('Ctrl Pts',(33.5096779792476,-57.7624205360752,22.));
#45519=CARTESIAN_POINT('Ctrl Pts',(33.4668687974159,-57.7997359738536,22.));
#45520=CARTESIAN_POINT('Ctrl Pts',(33.4223407450877,-57.8350756827256,22.));
#45521=CARTESIAN_POINT('Ctrl Pts',(33.3762247079518,-57.868292142162,22.));
#45522=CARTESIAN_POINT('Ctrl Pts',(33.3549779646033,-57.883595746557,22.));
#45523=CARTESIAN_POINT('Ctrl Pts',(33.3333938801028,-57.8984484230851,22.));
#45524=CARTESIAN_POINT('Ctrl Pts',(33.3114840048116,-57.9128343832935,22.));
#45525=CARTESIAN_POINT('Ctrl Pts',(33.3019191647095,-57.9191146294054,22.));
#45526=CARTESIAN_POINT('Ctrl Pts',(33.2922923777588,-57.9253057104171,22.));
#45527=CARTESIAN_POINT('Ctrl Pts',(33.2826166374558,-57.9313989825921,22.));
#45528=CARTESIAN_POINT('Ctrl Pts',(33.2232320152038,-57.9687962932948,22.));
#45529=CARTESIAN_POINT('Ctrl Pts',(33.1618957172908,-58.0025854530623,22.));
#45530=CARTESIAN_POINT('Ctrl Pts',(33.098892967176,-58.0325387704389,22.));
#45531=CARTESIAN_POINT('Ctrl Pts',(33.042562016297,-58.0593201227882,22.));
#45532=CARTESIAN_POINT('Ctrl Pts',(32.9848978605095,-58.0830352046633,22.));
#45533=CARTESIAN_POINT('Ctrl Pts',(32.9260772832472,-58.1034986372925,22.));
#45534=CARTESIAN_POINT('Ctrl Pts',(32.8619970286521,-58.1257918896507,22.));
#45535=CARTESIAN_POINT('Ctrl Pts',(32.7965441149125,-58.1442273323774,22.));
#45536=CARTESIAN_POINT('Ctrl Pts',(32.730026067277,-58.1589105502836,22.));
#45537=CARTESIAN_POINT('Ctrl Pts',(32.7043629429453,-58.1645754376355,22.));
#45538=CARTESIAN_POINT('Ctrl Pts',(32.6785410407308,-58.1696813145168,22.));
#45539=CARTESIAN_POINT('Ctrl Pts',(32.6525772949454,-58.1742323470501,22.));
#45540=CARTESIAN_POINT('Ctrl Pts',(32.6411872717866,-58.1762288373247,22.));
#45541=CARTESIAN_POINT('Ctrl Pts',(32.6297705135365,-58.1781183496249,22.));
#45542=CARTESIAN_POINT('Ctrl Pts',(32.6183418171879,-58.1798993771494,22.));
#45543=CARTESIAN_POINT('Ctrl Pts',(32.5492442274453,-58.1906674215051,22.));
#45544=CARTESIAN_POINT('Ctrl Pts',(32.479587866051,-58.1974963222448,22.));
#45545=CARTESIAN_POINT('Ctrl Pts',(32.4097184968816,-58.2005474581315,22.));
#45546=CARTESIAN_POINT('Ctrl Pts',(32.3382311065792,-58.2036692516239,22.));
#45547=CARTESIAN_POINT('Ctrl Pts',(32.2665198680808,-58.2028364327161,22.));
#45548=CARTESIAN_POINT('Ctrl Pts',(32.1949302795595,-58.1981713779293,22.));
#45549=CARTESIAN_POINT('Ctrl Pts',(32.1401596273564,-58.1946023101568,22.));
#45550=CARTESIAN_POINT('Ctrl Pts',(32.0854595447263,-58.1887891069564,22.));
#45551=CARTESIAN_POINT('Ctrl Pts',(32.0309802701291,-58.1807666255705,22.));
#45552=CARTESIAN_POINT('Ctrl Pts',(31.9970690900463,-58.1757729502141,22.));
#45553=CARTESIAN_POINT('Ctrl Pts',(31.9632434082193,-58.1699229342579,22.));
#45554=CARTESIAN_POINT('Ctrl Pts',(31.9295394677181,-58.1632216306219,22.));
#45555=CARTESIAN_POINT('Ctrl Pts',(31.9106295175814,-58.1594617937684,22.));
#45556=CARTESIAN_POINT('Ctrl Pts',(31.891751681419,-58.155432366917,22.));
#45557=CARTESIAN_POINT('Ctrl Pts',(31.8729463795953,-58.1511420898522,22.));
#45558=CARTESIAN_POINT('Ctrl Pts',(31.8000212116739,-58.1345048043509,22.));
#45559=CARTESIAN_POINT('Ctrl Pts',(31.7281115869712,-58.1139365946325,22.));
#45560=CARTESIAN_POINT('Ctrl Pts',(31.6575884718452,-58.0895522802127,22.));
#45561=CARTESIAN_POINT('Ctrl Pts',(31.6048403101262,-58.0713138947113,22.));
#45562=CARTESIAN_POINT('Ctrl Pts',(31.5528674074715,-58.0509395358532,22.));
#45563=CARTESIAN_POINT('Ctrl Pts',(31.5018252351578,-58.0284581681729,22.));
#45564=CARTESIAN_POINT('Ctrl Pts',(31.485902371771,-58.0214449920071,22.));
#45565=CARTESIAN_POINT('Ctrl Pts',(31.4700701035634,-58.0142266520142,22.));
#45566=CARTESIAN_POINT('Ctrl Pts',(31.454333225623,-58.006803707092,22.));
#45567=CARTESIAN_POINT('Ctrl Pts',(31.4391437429471,-57.9996389636323,22.));
#45568=CARTESIAN_POINT('Ctrl Pts',(31.4240509122119,-57.9922872148314,22.));
#45569=CARTESIAN_POINT('Ctrl Pts',(31.4090641623495,-57.9847522751711,22.));
#45570=CARTESIAN_POINT('Ctrl Pts',(31.3417651306224,-57.9509161100309,22.));
#45571=CARTESIAN_POINT('Ctrl Pts',(31.2765704047207,-57.9133737616735,22.));
#45572=CARTESIAN_POINT('Ctrl Pts',(31.2138523221447,-57.8722119391925,22.));
#45573=CARTESIAN_POINT('Ctrl Pts',(31.1658528011688,-57.8407098957555,22.));
#45574=CARTESIAN_POINT('Ctrl Pts',(31.119303757925,-57.8070868161123,22.));
#45575=CARTESIAN_POINT('Ctrl Pts',(31.0743783982804,-57.7713618605751,22.));
#45576=CARTESIAN_POINT('Ctrl Pts',(31.0639523774024,-57.7630710169349,22.));
#45577=CARTESIAN_POINT('Ctrl Pts',(31.0536138415293,-57.75466689798,22.));
#45578=CARTESIAN_POINT('Ctrl Pts',(31.0433632440414,-57.7461514510325,22.));
#45579=CARTESIAN_POINT('Ctrl Pts',(31.6652099567911,-54.8483531313949,20.8714803633902));
#45580=CARTESIAN_POINT('Ctrl Pts',(31.5910191767377,-54.8903425066551,20.8771939403667));
#45581=CARTESIAN_POINT('Ctrl Pts',(31.5202697708326,-54.9380868086678,20.8829075173431));
#45582=CARTESIAN_POINT('Ctrl Pts',(31.453999322188,-54.9913986485313,20.8886210943196));
#45583=CARTESIAN_POINT('Ctrl Pts',(31.0243118193789,-55.3370645042722,20.9256670578423));
#45584=CARTESIAN_POINT('Ctrl Pts',(30.7829209443173,-55.9167912231112,20.9627130213649));
#45585=CARTESIAN_POINT('Ctrl Pts',(30.840293873424,-56.4652682536955,20.9997589848876));
#45586=CARTESIAN_POINT('Ctrl Pts',(30.8976668025307,-57.0137452842797,21.0368049484103));
#45587=CARTESIAN_POINT('Ctrl Pts',(31.2538035358057,-57.5309726266091,21.073850911933));
#45588=CARTESIAN_POINT('Ctrl Pts',(31.7457295422612,-57.780228908827,21.1108968754557));
#45589=CARTESIAN_POINT('Ctrl Pts',(32.2376555487168,-58.029485191045,21.1479428389784));
#45590=CARTESIAN_POINT('Ctrl Pts',(32.8653708283529,-58.0107704131515,21.184988802501));
#45591=CARTESIAN_POINT('Ctrl Pts',(33.3415709716003,-57.7326682072443,21.2220347660237));
#45592=CARTESIAN_POINT('Ctrl Pts',(33.8177711148478,-57.4545660013372,21.2590807295464));
#45593=CARTESIAN_POINT('Ctrl Pts',(34.1424561217066,-56.9170763674163,21.2961266930691));
#45594=CARTESIAN_POINT('Ctrl Pts',(34.1670860104471,-56.366147035639,21.3331726565918));
#45595=CARTESIAN_POINT('Ctrl Pts',(34.1917158991876,-55.8152177038616,21.3702186201144));
#45596=CARTESIAN_POINT('Ctrl Pts',(33.9162906698097,-55.2508486742278,21.4072645836371));
#45597=CARTESIAN_POINT('Ctrl Pts',(33.4667522310661,-54.9314015975034,21.4443105471598));
#45598=CARTESIAN_POINT('Ctrl Pts',(33.0172137923224,-54.611954520779,21.4813565106825));
#45599=CARTESIAN_POINT('Ctrl Pts',(32.3935621442128,-54.5374293969641,21.5184024742052));
#45600=CARTESIAN_POINT('Ctrl Pts',(31.881431331593,-54.741782991655,21.5554484377278));
#45601=CARTESIAN_POINT('Ctrl Pts',(31.8075551488135,-54.7712615216341,21.5607924129486));
#45602=CARTESIAN_POINT('Ctrl Pts',(31.7359995810404,-54.8065431837032,21.5661363881694));
#45603=CARTESIAN_POINT('Ctrl Pts',(31.6673136634551,-54.8469650373412,21.5714803633902));
#45604=CARTESIAN_POINT('Ctrl Pts',(30.5157034944333,-56.8250975324092,22.));
#45605=CARTESIAN_POINT('Ctrl Pts',(30.3383199129809,-56.1652717359215,21.9629540364773));
#45606=CARTESIAN_POINT('Ctrl Pts',(30.6971298707754,-54.6659551967235,21.888862109432));
#45607=CARTESIAN_POINT('Ctrl Pts',(32.8915770858133,-53.893318629858,21.7777242188639));
#45608=CARTESIAN_POINT('Ctrl Pts',(34.7256560234758,-55.3208993649632,21.6665863282959));
#45609=CARTESIAN_POINT('Ctrl Pts',(34.5234929724835,-57.6345755616839,21.5554484377278));
#45610=CARTESIAN_POINT('Ctrl Pts',(32.4687454188576,-58.7202753686332,21.4443105471598));
#45611=CARTESIAN_POINT('Ctrl Pts',(30.4428342940784,-57.5824199368056,21.3331726565917));
#45612=CARTESIAN_POINT('Ctrl Pts',(30.2997559892121,-55.2634130835607,21.2220347660237));
#45613=CARTESIAN_POINT('Ctrl Pts',(32.1706430815574,-53.8854124812074,21.1108968754557));
#45614=CARTESIAN_POINT('Ctrl Pts',(34.3429657642116,-54.7099453599153,20.9997589848876));
#45615=CARTESIAN_POINT('Ctrl Pts',(34.8284152391772,-56.982193672835,20.8886210943196));
#45616=CARTESIAN_POINT('Ctrl Pts',(33.18263271582,-58.6223996095028,20.7774832037515));
#45617=CARTESIAN_POINT('Ctrl Pts',(30.9120322857351,-58.1292356735021,20.6663453131835));
#45618=CARTESIAN_POINT('Ctrl Pts',(30.0949149346206,-55.954114599854,20.5552074226154));
#45619=CARTESIAN_POINT('Ctrl Pts',(31.479200108132,-54.0879422836221,20.4440695320474));
#45620=CARTESIAN_POINT('Ctrl Pts',(33.7978345552324,-54.2388509530007,20.3329316414794));
#45621=CARTESIAN_POINT('Ctrl Pts',(34.9285465373885,-56.2687104209716,20.2217937509113));
#45622=CARTESIAN_POINT('Ctrl Pts',(33.836382221401,-58.3195681810162,20.1106558603433));
#45623=CARTESIAN_POINT('Ctrl Pts',(31.5210121579647,-58.5142504249981,19.9995179697753));
#45624=CARTESIAN_POINT('Ctrl Pts',(30.101720741136,-56.674562508041,19.8883800792072));
#45625=CARTESIAN_POINT('Ctrl Pts',(30.8776015421154,-54.4843915336431,19.7772421886392));
#45626=CARTESIAN_POINT('Ctrl Pts',(33.1384820439343,-53.9484258880498,19.6661042980711));
#45627=CARTESIAN_POINT('Ctrl Pts',(34.8149526935151,-55.5572409773789,19.5549664075031));
#45628=CARTESIAN_POINT('Ctrl Pts',(34.3725208876465,-57.8382701189333,19.443828516935));
#45629=CARTESIAN_POINT('Ctrl Pts',(32.2161494783462,-58.7036614639378,19.332690626367));
#45630=CARTESIAN_POINT('Ctrl Pts',(30.3195896701685,-57.3613125035426,19.221552735799));
#45631=CARTESIAN_POINT('Ctrl Pts',(30.4187841646359,-55.039890462752,19.1104148452309));
#45632=CARTESIAN_POINT('Ctrl Pts',(32.4229391156972,-53.8642192630766,18.9992769546629));
#45633=CARTESIAN_POINT('Ctrl Pts',(34.4976287681445,-54.9104040861686,18.8881390640948));
#45634=CARTESIAN_POINT('Ctrl Pts',(34.7438661544311,-57.2208600991234,18.7770011735268));
#45635=CARTESIAN_POINT('Ctrl Pts',(32.9362674024074,-58.680800710823,18.6658632829587));
#45636=CARTESIAN_POINT('Ctrl Pts',(30.7293481493445,-57.9539257225797,18.5547253923907));
#45637=CARTESIAN_POINT('Ctrl Pts',(30.1431266157477,-55.7055520544289,18.4435875018226));
#45638=CARTESIAN_POINT('Ctrl Pts',(31.7141780195173,-53.993641623134,18.3324496112546));
#45639=CARTESIAN_POINT('Ctrl Pts',(34.004501193851,-54.3851254608373,18.2213117206866));
#45640=CARTESIAN_POINT('Ctrl Pts',(34.9177373632483,-56.5216739711635,18.1101738301186));
#45641=CARTESIAN_POINT('Ctrl Pts',(33.6179911050581,-58.4476800725016,17.9990359395505));
#45642=CARTESIAN_POINT('Ctrl Pts',(31.2949349095266,-58.4002485379024,17.8878980489825));
#45643=CARTESIAN_POINT('Ctrl Pts',(30.074888457673,-56.4227939888948,17.7767601584144));
#45644=CARTESIAN_POINT('Ctrl Pts',(31.0745741031467,-54.3253030000451,17.6656222678464));
#45645=CARTESIAN_POINT('Ctrl Pts',(33.3789682374394,-54.0276328606134,17.5544843772783));
#45646=CARTESIAN_POINT('Ctrl Pts',(34.8788327758259,-55.8022444250302,17.4433464867103));
#45647=CARTESIAN_POINT('Ctrl Pts',(34.2013246967004,-58.0248156029211,17.3322085961422));
#45648=CARTESIAN_POINT('Ctrl Pts',(31.9665748283507,-58.6610017894909,17.2210707055742));
#45649=CARTESIAN_POINT('Ctrl Pts',(30.2200750690644,-57.1284945533304,17.1099328150062));
#45650=CARTESIAN_POINT('Ctrl Pts',(30.5604164551708,-54.8300151475112,16.9987949244381));
#45651=CARTESIAN_POINT('Ctrl Pts',(32.6760806562327,-53.8693878387091,16.8876570338701));
#45652=CARTESIAN_POINT('Ctrl Pts',(34.6305762357544,-55.1258856969254,16.776519143302));
#45653=CARTESIAN_POINT('Ctrl Pts',(34.6349312243122,-57.4494219828794,16.665381252734));
#45654=CARTESIAN_POINT('Ctrl Pts',(32.68515945149,-58.7132375833447,16.5542433621659));
#45655=CARTESIAN_POINT('Ctrl Pts',(30.5659091328683,-57.7605477465697,16.4431054715979));
#45656=CARTESIAN_POINT('Ctrl Pts',(30.2169541190139,-55.4633602843959,16.3319675810299));
#45657=CARTESIAN_POINT('Ctrl Pts',(31.9576968915284,-53.9243169328214,16.2208296904618));
#45658=CARTESIAN_POINT('Ctrl Pts',(34.1948158493603,-54.5521215254954,16.1096917998938));
#45659=CARTESIAN_POINT('Ctrl Pts',(34.880650639758,-56.7721373989267,15.9985539093257));
#45660=CARTESIAN_POINT('Ctrl Pts',(33.387448901162,-58.5523588475275,15.8874160187577));
#45661=CARTESIAN_POINT('Ctrl Pts',(31.0819551189947,-58.2633289901972,15.7762781281897));
#45662=CARTESIAN_POINT('Ctrl Pts',(30.0744138980993,-56.1696001333952,15.6651402376216));
#45663=CARTESIAN_POINT('Ctrl Pts',(31.287039144361,-54.1875860438059,15.5540023470536));
#45664=CARTESIAN_POINT('Ctrl Pts',(33.6099012175602,-54.1314466960922,15.4428644564855));
#45665=CARTESIAN_POINT('Ctrl Pts',(34.9168581194719,-56.052567070093,15.3317265659175));
#45666=CARTESIAN_POINT('Ctrl Pts',(34.0116373750326,-58.1925239040739,15.2205886753494));
#45667=CARTESIAN_POINT('Ctrl Pts',(31.722797799219,-58.5925904319764,15.1094507847814));
#45668=CARTESIAN_POINT('Ctrl Pts',(30.1453402095973,-56.8865812380664,14.9983128942134));
#45669=CARTESIAN_POINT('Ctrl Pts',(30.7231294343029,-54.6360258563356,14.8871750036453));
#45670=CARTESIAN_POINT('Ctrl Pts',(32.9273084298409,-53.9008832080614,14.7760371130773));
#45671=CARTESIAN_POINT('Ctrl Pts',(34.7403671916158,-55.3540375815297,14.6648992225092));
#45672=CARTESIAN_POINT('Ctrl Pts',(34.5027924192342,-57.6654005284896,14.5537613319412));
#45673=CARTESIAN_POINT('Ctrl Pts',(32.4320391047204,-58.7193548713018,14.4426234413732));
#45674=CARTESIAN_POINT('Ctrl Pts',(30.423491023484,-57.5512051672244,14.3314855508051));
#45675=CARTESIAN_POINT('Ctrl Pts',(30.3155954476549,-55.2301702471532,14.2203476602371));
#45676=CARTESIAN_POINT('Ctrl Pts',(32.2071095510683,-53.8807233800597,14.109209769669));
#45677=CARTESIAN_POINT('Ctrl Pts',(34.3667107654437,-54.7380212138032,13.998071879101));
#45678=CARTESIAN_POINT('Ctrl Pts',(34.817688121868,-57.0173840749687,13.886933988533));
#45679=CARTESIAN_POINT('Ctrl Pts',(33.1472639077745,-58.6324557555082,13.7757960979649));
#45680=CARTESIAN_POINT('Ctrl Pts',(30.8843823888257,-58.1050019311361,13.6646582073969));
#45681=CARTESIAN_POINT('Ctrl Pts',(30.1003126229301,-55.9176887906373,13.5535203168288));
#45682=CARTESIAN_POINT('Ctrl Pts',(31.5126666412308,-54.0728255670594,13.4423824262608));
#45683=CARTESIAN_POINT('Ctrl Pts',(33.8288126996591,-54.2585627611561,13.3312445356927));
#45684=CARTESIAN_POINT('Ctrl Pts',(34.9285321027134,-56.3058411531895,13.2201066451247));
#45685=CARTESIAN_POINT('Ctrl Pts',(33.8056871835127,-58.3388651889264,13.1089687545567));
#45686=CARTESIAN_POINT('Ctrl Pts',(31.4871369476881,-58.5005967837941,12.9978308639886));
#45687=CARTESIAN_POINT('Ctrl Pts',(30.0968376198178,-56.6352191751132,12.8866929734206));
#45688=CARTESIAN_POINT('Ctrl Pts',(30.6354003368774,-55.1906968075749,12.8126010463752));
#45689=CARTESIAN_POINT('Ctrl Pts',(31.1506898940641,-54.7420190959222,12.7755550828525));
#45690=CARTESIAN_POINT('Ctrl Pts',(30.6408436601533,-56.7914556061658,22.0748149723825));
#45691=CARTESIAN_POINT('Ctrl Pts',(30.4746468195516,-56.1732418919889,22.0377690088598));
#45692=CARTESIAN_POINT('Ctrl Pts',(30.8108283357527,-54.7684801331151,21.9636770818145));
#45693=CARTESIAN_POINT('Ctrl Pts',(32.8668821769258,-54.0445700885952,21.8525391912464));
#45694=CARTESIAN_POINT('Ctrl Pts',(34.5852944581392,-55.3821200801757,21.7414013006784));
#45695=CARTESIAN_POINT('Ctrl Pts',(34.3958808715705,-57.5498836968623,21.6302634101103));
#45696=CARTESIAN_POINT('Ctrl Pts',(32.4707164969967,-58.5671135683042,21.5191255195423));
#45697=CARTESIAN_POINT('Ctrl Pts',(30.5725699745224,-57.5010172797825,21.4079876289742));
#45698=CARTESIAN_POINT('Ctrl Pts',(30.4385149394808,-55.3282591857862,21.2968497384062));
#45699=CARTESIAN_POINT('Ctrl Pts',(32.1914140597047,-54.0371625432278,21.1857118478382));
#45700=CARTESIAN_POINT('Ctrl Pts',(34.2267386577773,-54.8096960454343,21.0745739572701));
#45701=CARTESIAN_POINT('Ctrl Pts',(34.6815731376677,-56.9386444383886,20.9634360667021));
#45702=CARTESIAN_POINT('Ctrl Pts',(33.1395823093187,-58.4754103689113,20.852298176134));
#45703=CARTESIAN_POINT('Ctrl Pts',(31.0121778750478,-58.0133479424405,20.741160285566));
#45704=CARTESIAN_POINT('Ctrl Pts',(30.2465922382936,-55.9754014346165,20.6300223949979));
#45705=CARTESIAN_POINT('Ctrl Pts',(31.5435771139257,-54.2269197519468,20.5188845044299));
#45706=CARTESIAN_POINT('Ctrl Pts',(33.7159862876659,-54.3683113275636,20.4077466138618));
#45707=CARTESIAN_POINT('Ctrl Pts',(34.7753896299934,-56.2701571899581,20.2966087232938));
#45708=CARTESIAN_POINT('Ctrl Pts',(33.7521029354263,-58.1916770817759,20.1854708327258));
#45709=CARTESIAN_POINT('Ctrl Pts',(31.5827522761609,-58.3740816403382,20.0743329421578));
#45710=CARTESIAN_POINT('Ctrl Pts',(30.2529688348836,-56.6504141115414,19.9631950515897));
#45711=CARTESIAN_POINT('Ctrl Pts',(30.9799185150647,-54.5983668288006,19.8520571610217));
#45712=CARTESIAN_POINT('Ctrl Pts',(33.0982160108274,-54.0962019934801,19.7409192704536));
#45713=CARTESIAN_POINT('Ctrl Pts',(34.6689596108847,-55.6035567484657,19.6297813798856));
#45714=CARTESIAN_POINT('Ctrl Pts',(34.2544298798073,-57.7407322048549,19.5186434893175));
#45715=CARTESIAN_POINT('Ctrl Pts',(32.2340505839621,-58.5515474237501,19.4075055987495));
#45716=CARTESIAN_POINT('Ctrl Pts',(30.4570978042841,-57.2938540432475,19.2963677081814));
#45717=CARTESIAN_POINT('Ctrl Pts',(30.5500365726333,-55.1188330761249,19.1852298176134));
#45718=CARTESIAN_POINT('Ctrl Pts',(32.4277989800396,-54.017305880809,19.0740919270454));
#45719=CARTESIAN_POINT('Ctrl Pts',(34.3716477998814,-54.9975127909389,18.9629540364773));
#45720=CARTESIAN_POINT('Ctrl Pts',(34.6023561625367,-57.1622593055708,18.8518161459093));
#45721=CARTESIAN_POINT('Ctrl Pts',(32.9087540872943,-58.5301283898668,18.7406782553412));
#45722=CARTESIAN_POINT('Ctrl Pts',(30.8410147603584,-57.8490939583302,18.6295403647732));
#45723=CARTESIAN_POINT('Ctrl Pts',(30.2917634374419,-55.7425145495774,18.5184024742052));
#45724=CARTESIAN_POINT('Ctrl Pts',(31.763736083339,-54.1385661866874,18.4072645836371));
#45725=CARTESIAN_POINT('Ctrl Pts',(33.9096194419575,-54.5053609962191,18.2961266930691));
#45726=CARTESIAN_POINT('Ctrl Pts',(34.76526213918,-56.507167529275,18.184988802501));
#45727=CARTESIAN_POINT('Ctrl Pts',(33.5474847105914,-58.3117095641174,18.073850911933));
#45728=CARTESIAN_POINT('Ctrl Pts',(31.3709326471137,-58.2672693113572,17.9627130213649));
#45729=CARTESIAN_POINT('Ctrl Pts',(30.2278287362275,-56.4145234383323,17.8515751307969));
#45730=CARTESIAN_POINT('Ctrl Pts',(31.1644689512469,-54.4493112541897,17.7404372402289));
#45731=CARTESIAN_POINT('Ctrl Pts',(33.3235358811423,-54.1704137580971,17.6292993496608));
#45732=CARTESIAN_POINT('Ctrl Pts',(34.7288110794959,-55.8331089911409,17.5181614590928));
#45733=CARTESIAN_POINT('Ctrl Pts',(34.0940302203501,-57.9155131502695,17.4070235685247));
#45734=CARTESIAN_POINT('Ctrl Pts',(32.0002154229856,-58.5115780925633,17.2958856779567));
#45735=CARTESIAN_POINT('Ctrl Pts',(30.3638591169049,-57.0757188165044,17.1847477873887));
#45736=CARTESIAN_POINT('Ctrl Pts',(30.6827367866064,-54.9221936012214,17.0736098968206));
#45737=CARTESIAN_POINT('Ctrl Pts',(32.6649760846935,-54.0221484988997,16.9624720062526));
#45738=CARTESIAN_POINT('Ctrl Pts',(34.4962109015046,-55.1994049989002,16.8513341156845));
#45739=CARTESIAN_POINT('Ctrl Pts',(34.5002912415971,-57.3764068757753,16.7401962251165));
#45740=CARTESIAN_POINT('Ctrl Pts',(32.6734823234101,-58.5605196227416,16.6290583345484));
#45741=CARTESIAN_POINT('Ctrl Pts',(30.6878830671827,-57.6679114137473,16.5179204439804));
#45742=CARTESIAN_POINT('Ctrl Pts',(30.3609349903662,-55.5155966653537,16.4067825534124));
#45743=CARTESIAN_POINT('Ctrl Pts',(31.9918973755156,-54.0736134756683,16.2956446628443));
#45744=CARTESIAN_POINT('Ctrl Pts',(34.0879318551292,-54.661825411425,16.1845067722763));
#45745=CARTESIAN_POINT('Ctrl Pts',(34.730514299375,-56.7418354170223,16.0733688817082));
#45746=CARTESIAN_POINT('Ctrl Pts',(33.331481709642,-58.4097867454715,15.9622309911402));
#45747=CARTESIAN_POINT('Ctrl Pts',(31.1713844814461,-58.138984629884,15.8510931005721));
#45748=CARTESIAN_POINT('Ctrl Pts',(30.2273841048744,-56.1772973179708,15.7399552100041));
#45749=CARTESIAN_POINT('Ctrl Pts',(31.3635348303941,-54.3202794529553,15.6288173194361));
#45750=CARTESIAN_POINT('Ctrl Pts',(33.5399050139139,-54.2676805475375,15.517679428868));
#45751=CARTESIAN_POINT('Ctrl Pts',(34.7644383451369,-56.0676449746849,15.4065415383));
#45752=CARTESIAN_POINT('Ctrl Pts',(33.916305578051,-58.0726448845937,15.2954036477319));
#45753=CARTESIAN_POINT('Ctrl Pts',(31.7718122544331,-58.4474811147761,15.1842657571639));
#45754=CARTESIAN_POINT('Ctrl Pts',(30.2938374304302,-56.8490618262287,15.0731278665959));
#45755=CARTESIAN_POINT('Ctrl Pts',(30.8351882301686,-54.7404382942198,14.9619899760278));
#45756=CARTESIAN_POINT('Ctrl Pts',(32.9003601146199,-54.0516576047429,14.8508520854598));
#45757=CARTESIAN_POINT('Ctrl Pts',(34.5990778627046,-55.4131684266541,14.7397141948917));
#45758=CARTESIAN_POINT('Ctrl Pts',(34.3764858039968,-57.5787646792667,14.6285763043237));
#45759=CARTESIAN_POINT('Ctrl Pts',(32.4363250759318,-58.566251122372,14.5174384137557));
#45760=CARTESIAN_POINT('Ctrl Pts',(30.5544465922265,-57.4717710776141,14.4063005231876));
#45761=CARTESIAN_POINT('Ctrl Pts',(30.453355478433,-55.2971128173437,14.2951626326196));
#45762=CARTESIAN_POINT('Ctrl Pts',(32.2255807620059,-54.032769161441,14.1840247420515));
#45763=CARTESIAN_POINT('Ctrl Pts',(34.2489861744446,-54.8360012884289,14.0728868514835));
#45764=CARTESIAN_POINT('Ctrl Pts',(34.6715225287503,-56.9716155488275,13.9617489609154));
#45765=CARTESIAN_POINT('Ctrl Pts',(33.1064440441824,-58.4848323215015,13.8506110703474));
#45766=CARTESIAN_POINT('Ctrl Pts',(30.9862717259461,-57.9906425072238,13.7394731797794));
#45767=CARTESIAN_POINT('Ctrl Pts',(30.2516495200117,-55.9412728283577,13.6283352892113));
#45768=CARTESIAN_POINT('Ctrl Pts',(31.5749330715706,-54.2127563749734,13.5171973986433));
#45769=CARTESIAN_POINT('Ctrl Pts',(33.7450107875055,-54.386780005505,13.4060595080752));
#45770=CARTESIAN_POINT('Ctrl Pts',(34.7753761056448,-56.3049462630692,13.2949216175072));
#45771=CARTESIAN_POINT('Ctrl Pts',(33.7233436879389,-58.2097571189556,13.1837837269391));
#45772=CARTESIAN_POINT('Ctrl Pts',(31.5510134146689,-58.3612890695026,13.0726458363711));
#45773=CARTESIAN_POINT('Ctrl Pts',(30.248393668858,-56.6135519759491,12.9615079458031));
#45774=CARTESIAN_POINT('Ctrl Pts',(30.7529917906697,-55.2601287803101,12.8874160187577));
#45775=CARTESIAN_POINT('Ctrl Pts',(31.2357844803776,-54.8397470430914,12.850370055235));
#45776=CARTESIAN_POINT('Ctrl Pts',(30.7659838258732,-56.7578136799224,22.149629944765));
#45777=CARTESIAN_POINT('Ctrl Pts',(30.6109737261224,-56.1812120480563,22.1125839812423));
#45778=CARTESIAN_POINT('Ctrl Pts',(30.92452680073,-54.8710050695067,22.0384920541969));
#45779=CARTESIAN_POINT('Ctrl Pts',(32.8421872680382,-54.1958215473323,21.9273541636289));
#45780=CARTESIAN_POINT('Ctrl Pts',(34.4449328928026,-55.4433407953882,21.8162162730609));
#45781=CARTESIAN_POINT('Ctrl Pts',(34.2682687706575,-57.4651918320407,21.7050783824928));
#45782=CARTESIAN_POINT('Ctrl Pts',(32.4726875751358,-58.4139517679752,21.5939404919248));
#45783=CARTESIAN_POINT('Ctrl Pts',(30.7023056549664,-57.4196146227593,21.4828026013567));
#45784=CARTESIAN_POINT('Ctrl Pts',(30.5772738897495,-55.3931052880118,21.3716647107887));
#45785=CARTESIAN_POINT('Ctrl Pts',(32.2121850378521,-54.188912605248,21.2605268202206));
#45786=CARTESIAN_POINT('Ctrl Pts',(34.1105115513431,-54.9094467309535,21.1493889296526));
#45787=CARTESIAN_POINT('Ctrl Pts',(34.5347310361582,-56.8950952039421,21.0382510390846));
#45788=CARTESIAN_POINT('Ctrl Pts',(33.0965319028176,-58.3284211283198,20.9271131485165));
#45789=CARTESIAN_POINT('Ctrl Pts',(31.1123234643604,-57.897460211379,20.8159752579485));
#45790=CARTESIAN_POINT('Ctrl Pts',(30.3982695419666,-55.996688269379,20.7048373673804));
#45791=CARTESIAN_POINT('Ctrl Pts',(31.6079541197193,-54.3658972202713,20.5936994768124));
#45792=CARTESIAN_POINT('Ctrl Pts',(33.6341380200995,-54.4977717021264,20.4825615862443));
#45793=CARTESIAN_POINT('Ctrl Pts',(34.6222327225984,-56.2716039589447,20.3714236956763));
#45794=CARTESIAN_POINT('Ctrl Pts',(33.6678236494516,-58.0637859825356,20.2602858051083));
#45795=CARTESIAN_POINT('Ctrl Pts',(31.6444923943572,-58.2339128556783,20.1491479145402));
#45796=CARTESIAN_POINT('Ctrl Pts',(30.4042169286311,-56.6262657150416,20.0380100239722));
#45797=CARTESIAN_POINT('Ctrl Pts',(31.082235488014,-54.712342123958,19.9268721334041));
#45798=CARTESIAN_POINT('Ctrl Pts',(33.0579499777204,-54.2439780989105,19.8157342428361));
#45799=CARTESIAN_POINT('Ctrl Pts',(34.5229665282544,-55.6498725195525,19.7045963522681));
#45800=CARTESIAN_POINT('Ctrl Pts',(34.1363388719681,-57.6431942907767,19.5934584617));
#45801=CARTESIAN_POINT('Ctrl Pts',(32.251951689578,-58.3994333835621,19.482320571132));
#45802=CARTESIAN_POINT('Ctrl Pts',(30.5946059383997,-57.2263955829524,19.371182680564));
#45803=CARTESIAN_POINT('Ctrl Pts',(30.6812889806306,-55.1977756894976,19.2600447899959));
#45804=CARTESIAN_POINT('Ctrl Pts',(32.4326588443821,-54.1703924985415,19.1489068994279));
#45805=CARTESIAN_POINT('Ctrl Pts',(34.2456668316182,-55.0846214957091,19.0377690088598));
#45806=CARTESIAN_POINT('Ctrl Pts',(34.4608461706423,-57.1036585120183,18.9266311182918));
#45807=CARTESIAN_POINT('Ctrl Pts',(32.8812407721812,-58.3794560689106,18.8154932277237));
#45808=CARTESIAN_POINT('Ctrl Pts',(30.9526813713723,-57.7442621940807,18.7043553371557));
#45809=CARTESIAN_POINT('Ctrl Pts',(30.440400259136,-55.7794770447258,18.5932174465876));
#45810=CARTESIAN_POINT('Ctrl Pts',(31.8132941471606,-54.283490750241,18.4820795560196));
#45811=CARTESIAN_POINT('Ctrl Pts',(33.8147376900639,-54.625596531601,18.3709416654515));
#45812=CARTESIAN_POINT('Ctrl Pts',(34.6127869151118,-56.4926610873864,18.2598037748835));
#45813=CARTESIAN_POINT('Ctrl Pts',(33.4769783161247,-58.1757390557333,18.1486658843155));
#45814=CARTESIAN_POINT('Ctrl Pts',(31.4469303847008,-58.134290084812,18.0375279937474));
#45815=CARTESIAN_POINT('Ctrl Pts',(30.380769014782,-56.4062528877698,17.9263901031794));
#45816=CARTESIAN_POINT('Ctrl Pts',(31.2543637993471,-54.5733195083342,17.8152522126114));
#45817=CARTESIAN_POINT('Ctrl Pts',(33.2681035248451,-54.313194655581,17.7041143220433));
#45818=CARTESIAN_POINT('Ctrl Pts',(34.5787893831658,-55.8639735572515,17.5929764314753));
#45819=CARTESIAN_POINT('Ctrl Pts',(33.9867357439999,-57.8062106976179,17.4818385409072));
#45820=CARTESIAN_POINT('Ctrl Pts',(32.0338560176206,-58.3621543956356,17.3707006503392));
#45821=CARTESIAN_POINT('Ctrl Pts',(30.5076431647456,-57.0229430796785,17.2595627597712));
#45822=CARTESIAN_POINT('Ctrl Pts',(30.8050571180421,-55.0143720549317,17.1484248692031));
#45823=CARTESIAN_POINT('Ctrl Pts',(32.6538715131543,-54.1749091590902,17.0372869786351));
#45824=CARTESIAN_POINT('Ctrl Pts',(34.3618455672548,-55.2729243008751,16.926149088067));
#45825=CARTESIAN_POINT('Ctrl Pts',(34.365651258882,-57.3033917686712,16.815011197499));
#45826=CARTESIAN_POINT('Ctrl Pts',(32.6618051953302,-58.4078016621386,16.7038733069309));
#45827=CARTESIAN_POINT('Ctrl Pts',(30.809857001497,-57.5752750809248,16.5927354163629));
#45828=CARTESIAN_POINT('Ctrl Pts',(30.5049158617185,-55.5678330463115,16.4815975257948));
#45829=CARTESIAN_POINT('Ctrl Pts',(32.0260978595028,-54.2229100185152,16.3704596352268));
#45830=CARTESIAN_POINT('Ctrl Pts',(33.9810478608982,-54.7715292973546,16.2593217446587));
#45831=CARTESIAN_POINT('Ctrl Pts',(34.580377958992,-56.7115334351178,16.1481838540907));
#45832=CARTESIAN_POINT('Ctrl Pts',(33.2755145181221,-58.2672146434156,16.0370459635227));
#45833=CARTESIAN_POINT('Ctrl Pts',(31.2608138438975,-58.0146402695707,15.9259080729546));
#45834=CARTESIAN_POINT('Ctrl Pts',(30.3803543116496,-56.1849945025465,15.8147701823866));
#45835=CARTESIAN_POINT('Ctrl Pts',(31.4400305164272,-54.4529728621045,15.7036322918186));
#45836=CARTESIAN_POINT('Ctrl Pts',(33.4699088102677,-54.4039143989829,15.5924944012505));
#45837=CARTESIAN_POINT('Ctrl Pts',(34.6120185708019,-56.0827228792766,15.4813565106825));
#45838=CARTESIAN_POINT('Ctrl Pts',(33.8209737810693,-57.9527658651135,15.3702186201144));
#45839=CARTESIAN_POINT('Ctrl Pts',(31.8208267096472,-58.3023717975756,15.2590807295464));
#45840=CARTESIAN_POINT('Ctrl Pts',(30.4423346512631,-56.811542414391,15.1479428389783));
#45841=CARTESIAN_POINT('Ctrl Pts',(30.9472470260342,-54.844850732104,15.0368049484103));
#45842=CARTESIAN_POINT('Ctrl Pts',(32.873411799399,-54.2024320014244,14.9256670578423));
#45843=CARTESIAN_POINT('Ctrl Pts',(34.4577885337935,-55.4722992717786,14.8145291672742));
#45844=CARTESIAN_POINT('Ctrl Pts',(34.2501791887593,-57.4921288300438,14.7033912767062));
#45845=CARTESIAN_POINT('Ctrl Pts',(32.4406110471432,-58.4131473734422,14.5922533861381));
#45846=CARTESIAN_POINT('Ctrl Pts',(30.6854021609689,-57.3923369880037,14.4811154955701));
#45847=CARTESIAN_POINT('Ctrl Pts',(30.5911155092111,-55.3640553875343,14.3699776050021));
#45848=CARTESIAN_POINT('Ctrl Pts',(32.2440519729435,-54.1848149428223,14.258839714434));
#45849=CARTESIAN_POINT('Ctrl Pts',(34.1312615834455,-54.9339813630547,14.147701823866));
#45850=CARTESIAN_POINT('Ctrl Pts',(34.5253569356325,-56.9258470226863,14.0365639332979));
#45851=CARTESIAN_POINT('Ctrl Pts',(33.0656241805903,-58.3372088874948,13.9254260427299));
#45852=CARTESIAN_POINT('Ctrl Pts',(31.0881610630664,-57.8762830833116,13.8142881521618));
#45853=CARTESIAN_POINT('Ctrl Pts',(30.4029864170935,-55.9648568660781,13.7031502615938));
#45854=CARTESIAN_POINT('Ctrl Pts',(31.6371995019102,-54.3526871828874,13.5920123710258));
#45855=CARTESIAN_POINT('Ctrl Pts',(33.661208875352,-54.5149972498541,13.4808744804577));
#45856=CARTESIAN_POINT('Ctrl Pts',(34.6222201085763,-56.3040513729489,13.3697365898897));
#45857=CARTESIAN_POINT('Ctrl Pts',(33.6410001923651,-58.0806490489848,13.2585986993216));
#45858=CARTESIAN_POINT('Ctrl Pts',(31.6148898816497,-58.221981355211,13.1474608087536));
#45859=CARTESIAN_POINT('Ctrl Pts',(30.3999497178981,-56.591884776785,13.0363229181856));
#45860=CARTESIAN_POINT('Ctrl Pts',(30.8705832444619,-55.3295607530454,12.9622309911402));
#45861=CARTESIAN_POINT('Ctrl Pts',(31.320879066691,-54.9374749902607,12.9251850276175));
#45862=CARTESIAN_POINT('Ctrl Pts',(30.8911239915931,-56.724171753679,22.2244449171475));
#45863=CARTESIAN_POINT('Ctrl Pts',(30.7473006326931,-56.1891822041237,22.1873989536248));
#45864=CARTESIAN_POINT('Ctrl Pts',(31.0382252657072,-54.9735300058983,22.1133070265794));
#45865=CARTESIAN_POINT('Ctrl Pts',(32.8174923591507,-54.3470730060696,22.0021691360114));
#45866=CARTESIAN_POINT('Ctrl Pts',(34.3045713274659,-55.5045615106007,21.8910312454433));
#45867=CARTESIAN_POINT('Ctrl Pts',(34.1406566697445,-57.3804999672191,21.7798933548753));
#45868=CARTESIAN_POINT('Ctrl Pts',(32.474658653275,-58.2607899676461,21.6687554643073));
#45869=CARTESIAN_POINT('Ctrl Pts',(30.8320413354104,-57.3382119657362,21.5576175737392));
#45870=CARTESIAN_POINT('Ctrl Pts',(30.7160328400182,-55.4579513902373,21.4464796831712));
#45871=CARTESIAN_POINT('Ctrl Pts',(32.2329560159993,-54.3406626672684,21.3353417926031));
#45872=CARTESIAN_POINT('Ctrl Pts',(33.9942844449089,-55.0091974164724,21.2242039020351));
#45873=CARTESIAN_POINT('Ctrl Pts',(34.3878889346486,-56.8515459694957,21.1130660114671));
#45874=CARTESIAN_POINT('Ctrl Pts',(33.0534814963164,-58.1814318877282,21.001928120899));
#45875=CARTESIAN_POINT('Ctrl Pts',(31.212469053673,-57.7815724803176,20.890790230331));
#45876=CARTESIAN_POINT('Ctrl Pts',(30.5499468456396,-56.0179751041415,20.7796523397629));
#45877=CARTESIAN_POINT('Ctrl Pts',(31.672331125513,-54.504874688596,20.6685144491949));
#45878=CARTESIAN_POINT('Ctrl Pts',(33.5522897525329,-54.6272320766892,20.5573765586268));
#45879=CARTESIAN_POINT('Ctrl Pts',(34.4690758152034,-56.2730507279312,20.4462386680588));
#45880=CARTESIAN_POINT('Ctrl Pts',(33.5835443634768,-57.9358948832953,20.3351007774908));
#45881=CARTESIAN_POINT('Ctrl Pts',(31.7062325125535,-58.0937440710183,20.2239628869227));
#45882=CARTESIAN_POINT('Ctrl Pts',(30.5554650223786,-56.6021173185421,20.1128249963547));
#45883=CARTESIAN_POINT('Ctrl Pts',(31.1845524609633,-54.8263174191155,20.0016871057866));
#45884=CARTESIAN_POINT('Ctrl Pts',(33.0176839446135,-54.3917542043407,19.8905492152186));
#45885=CARTESIAN_POINT('Ctrl Pts',(34.3769734456241,-55.6961882906394,19.7794113246506));
#45886=CARTESIAN_POINT('Ctrl Pts',(34.018247864129,-57.5456563766984,19.6682734340825));
#45887=CARTESIAN_POINT('Ctrl Pts',(32.2698527951939,-58.2473193433743,19.5571355435145));
#45888=CARTESIAN_POINT('Ctrl Pts',(30.7321140725153,-57.1589371226574,19.4459976529464));
#45889=CARTESIAN_POINT('Ctrl Pts',(30.812541388628,-55.2767183028703,19.3348597623784));
#45890=CARTESIAN_POINT('Ctrl Pts',(32.4375187087245,-54.3234791162739,19.2237218718103));
#45891=CARTESIAN_POINT('Ctrl Pts',(34.119685863355,-55.1717302004793,19.1125839812423));
#45892=CARTESIAN_POINT('Ctrl Pts',(34.3193361787479,-57.0450577184658,19.0014460906742));
#45893=CARTESIAN_POINT('Ctrl Pts',(32.8537274570681,-58.2287837479543,18.8903082001062));
#45894=CARTESIAN_POINT('Ctrl Pts',(31.0643479823862,-57.6394304298313,18.7791703095382));
#45895=CARTESIAN_POINT('Ctrl Pts',(30.5890370808301,-55.8164395398742,18.6680324189701));
#45896=CARTESIAN_POINT('Ctrl Pts',(31.8628522109823,-54.4284153137945,18.5568945284021));
#45897=CARTESIAN_POINT('Ctrl Pts',(33.7198559381704,-54.7458320669827,18.4457566378341));
#45898=CARTESIAN_POINT('Ctrl Pts',(34.4603116910435,-56.4781546454979,18.334618747266));
#45899=CARTESIAN_POINT('Ctrl Pts',(33.406471921658,-58.039768547349,18.223480856698));
#45900=CARTESIAN_POINT('Ctrl Pts',(31.522928122288,-58.0013108582667,18.1123429661299));
#45901=CARTESIAN_POINT('Ctrl Pts',(30.5337092933365,-56.3979823372073,18.0012050755619));
#45902=CARTESIAN_POINT('Ctrl Pts',(31.3442586474474,-54.6973277624788,17.8900671849938));
#45903=CARTESIAN_POINT('Ctrl Pts',(33.212671168548,-54.4559755530648,17.7789292944258));
#45904=CARTESIAN_POINT('Ctrl Pts',(34.4287676868358,-55.8948381233622,17.6677914038578));
#45905=CARTESIAN_POINT('Ctrl Pts',(33.8794412676495,-57.6969082449663,17.5566535132897));
#45906=CARTESIAN_POINT('Ctrl Pts',(32.0674966122556,-58.2127306987079,17.4455156227217));
#45907=CARTESIAN_POINT('Ctrl Pts',(30.6514272125861,-56.9701673428525,17.3343777321536));
#45908=CARTESIAN_POINT('Ctrl Pts',(30.9273774494778,-55.1065505086419,17.2232398415856));
#45909=CARTESIAN_POINT('Ctrl Pts',(32.6427669416151,-54.3276698192808,17.1121019510176));
#45910=CARTESIAN_POINT('Ctrl Pts',(34.2274802330049,-55.3464436028499,17.0009640604495));
#45911=CARTESIAN_POINT('Ctrl Pts',(34.2310112761669,-57.2303766615672,16.8898261698815));
#45912=CARTESIAN_POINT('Ctrl Pts',(32.6501280672502,-58.2550837015356,16.7786882793134));
#45913=CARTESIAN_POINT('Ctrl Pts',(30.9318309358114,-57.4826387481023,16.6675503887454));
#45914=CARTESIAN_POINT('Ctrl Pts',(30.6488967330708,-55.6200694272693,16.5564124981773));
#45915=CARTESIAN_POINT('Ctrl Pts',(32.0602983434901,-54.3722065613621,16.4452746076093));
#45916=CARTESIAN_POINT('Ctrl Pts',(33.8741638666671,-54.8812331832842,16.3341367170413));
#45917=CARTESIAN_POINT('Ctrl Pts',(34.430241618609,-56.6812314532133,16.2229988264732));
#45918=CARTESIAN_POINT('Ctrl Pts',(33.2195473266021,-58.1246425413596,16.1118609359052));
#45919=CARTESIAN_POINT('Ctrl Pts',(31.3502432063489,-57.8902959092575,16.0007230453371));
#45920=CARTESIAN_POINT('Ctrl Pts',(30.5333245184248,-56.1926916871221,15.8895851547691));
#45921=CARTESIAN_POINT('Ctrl Pts',(31.5165262024604,-54.5856662712539,15.778447264201));
#45922=CARTESIAN_POINT('Ctrl Pts',(33.3999126066214,-54.5401482504283,15.667309373633));
#45923=CARTESIAN_POINT('Ctrl Pts',(34.4595987964668,-56.0978007838682,15.556171483065));
#45924=CARTESIAN_POINT('Ctrl Pts',(33.7256419840878,-57.8328868456334,15.4450335924969));
#45925=CARTESIAN_POINT('Ctrl Pts',(31.8698411648613,-58.1572624803752,15.3338957019289));
#45926=CARTESIAN_POINT('Ctrl Pts',(30.5908318720959,-56.7740230025534,15.2227578113608));
#45927=CARTESIAN_POINT('Ctrl Pts',(31.0593058218999,-54.9492631699882,15.1116199207928));
#45928=CARTESIAN_POINT('Ctrl Pts',(32.846463484178,-54.3532063981059,15.0004820302248));
#45929=CARTESIAN_POINT('Ctrl Pts',(34.3164992048823,-55.5314301169031,14.8893441396567));
#45930=CARTESIAN_POINT('Ctrl Pts',(34.1238725735219,-57.4054929808208,14.7782062490887));
#45931=CARTESIAN_POINT('Ctrl Pts',(32.4448970183546,-58.2600436245124,14.6670683585206));
#45932=CARTESIAN_POINT('Ctrl Pts',(30.8163577297114,-57.3129028983934,14.5559304679526));
#45933=CARTESIAN_POINT('Ctrl Pts',(30.7288755399893,-55.4309979577249,14.4447925773845));
#45934=CARTESIAN_POINT('Ctrl Pts',(32.2625231838811,-54.3368607242037,14.3336546868165));
#45935=CARTESIAN_POINT('Ctrl Pts',(34.0135369924464,-55.0319614376805,14.2225167962484));
#45936=CARTESIAN_POINT('Ctrl Pts',(34.3791913425147,-56.8800784965451,14.1113789056804));
#45937=CARTESIAN_POINT('Ctrl Pts',(33.0248043169983,-58.1895854534881,14.0002410151124));
#45938=CARTESIAN_POINT('Ctrl Pts',(31.1900504001867,-57.7619236593993,13.8891031245443));
#45939=CARTESIAN_POINT('Ctrl Pts',(30.5543233141752,-55.9884409037984,13.7779652339763));
#45940=CARTESIAN_POINT('Ctrl Pts',(31.69946593225,-54.4926179908013,13.6668273434083));
#45941=CARTESIAN_POINT('Ctrl Pts',(33.5774069631984,-54.6432144942032,13.5556894528402));
#45942=CARTESIAN_POINT('Ctrl Pts',(34.4690641115077,-56.3031564828284,13.4445515622722));
#45943=CARTESIAN_POINT('Ctrl Pts',(33.5586566967914,-57.9515409790141,13.3334136717041));
#45944=CARTESIAN_POINT('Ctrl Pts',(31.6787663486304,-58.0826736409194,13.2222757811361));
#45945=CARTESIAN_POINT('Ctrl Pts',(30.5515057669383,-56.5702175776209,13.111137890568));
#45946=CARTESIAN_POINT('Ctrl Pts',(30.9881746982542,-55.3989927257807,13.0370459635227));
#45947=CARTESIAN_POINT('Ctrl Pts',(31.4059736530044,-55.03520293743,13.));
#45948=CARTESIAN_POINT('Ctrl Pts',(31.6688940285232,-54.8502492137287,21.3785196366098));
#45949=CARTESIAN_POINT('Ctrl Pts',(31.8552973625104,-54.7413392620857,21.3641270219409));
#45950=CARTESIAN_POINT('Ctrl Pts',(32.061419630626,-54.6673572529873,21.349734407272));
#45951=CARTESIAN_POINT('Ctrl Pts',(32.2736902248207,-54.6382999126305,21.3353417926031));
#45952=CARTESIAN_POINT('Ctrl Pts',(32.8200654923025,-54.5635075836697,21.2982958290804));
#45953=CARTESIAN_POINT('Ctrl Pts',(33.4071749686057,-54.7863525000711,21.2612498655578));
#45954=CARTESIAN_POINT('Ctrl Pts',(33.7663304550473,-55.2048330504423,21.2242039020351));
#45955=CARTESIAN_POINT('Ctrl Pts',(34.1254859414888,-55.6233136008135,21.1871579385124));
#45956=CARTESIAN_POINT('Ctrl Pts',(34.2566874380687,-56.2374297851546,21.1501119749897));
#45957=CARTESIAN_POINT('Ctrl Pts',(34.0998869466366,-56.7661355303639,21.113066011467));
#45958=CARTESIAN_POINT('Ctrl Pts',(33.9430864552045,-57.2948412755732,21.0760200479444));
#45959=CARTESIAN_POINT('Ctrl Pts',(33.4982839757605,-57.7381365816507,21.0389740844217));
#45960=CARTESIAN_POINT('Ctrl Pts',(32.9690473289312,-57.8931410001211,21.001928120899));
#45961=CARTESIAN_POINT('Ctrl Pts',(32.4398106821019,-58.0481454185914,20.9648821573763));
#45962=CARTESIAN_POINT('Ctrl Pts',(31.8261398678875,-57.9148589494545,20.9278361938536));
#45963=CARTESIAN_POINT('Ctrl Pts',(31.4088840927747,-57.5542828188567,20.8907902303309));
#45964=CARTESIAN_POINT('Ctrl Pts',(30.9916283176618,-57.1937066882589,20.8537442668083));
#45965=CARTESIAN_POINT('Ctrl Pts',(30.7707875816507,-56.6058408962002,20.8166983032856));
#45966=CARTESIAN_POINT('Ctrl Pts',(30.8474312602907,-56.0597245975799,20.7796523397629));
#45967=CARTESIAN_POINT('Ctrl Pts',(30.9171750925773,-55.5627724129275,20.7459414387119));
#45968=CARTESIAN_POINT('Ctrl Pts',(31.2332522390469,-55.1003910850247,20.7122305376608));
#45969=CARTESIAN_POINT('Ctrl Pts',(31.6666453776089,-54.8465106722,20.6785196366098));
#45970=CARTESIAN_POINT('Ctrl Pts',(30.5157034944333,-56.8250975324092,22.));
#45971=CARTESIAN_POINT('Ctrl Pts',(30.5033891751539,-56.7529213758001,22.));
#45972=CARTESIAN_POINT('Ctrl Pts',(30.495295269616,-56.6802754208446,22.));
#45973=CARTESIAN_POINT('Ctrl Pts',(30.4912615438002,-56.6074703113041,22.));
#45974=CARTESIAN_POINT('Ctrl Pts',(30.4871154839524,-56.5326376738967,22.));
#45975=CARTESIAN_POINT('Ctrl Pts',(30.487259104724,-56.4576358814856,22.));
#45976=CARTESIAN_POINT('Ctrl Pts',(30.4915726828733,-56.3828069694724,22.));
#45977=CARTESIAN_POINT('Ctrl Pts',(30.4952175802639,-56.3195778597416,22.));
#45978=CARTESIAN_POINT('Ctrl Pts',(30.5018408843277,-56.2564719495625,22.));
#45979=CARTESIAN_POINT('Ctrl Pts',(30.5113973391132,-56.193706282076,22.));
#45980=CARTESIAN_POINT('Ctrl Pts',(30.5156431766695,-56.1658201219636,22.));
#45981=CARTESIAN_POINT('Ctrl Pts',(30.5204683060505,-56.1380012967322,22.));
#45982=CARTESIAN_POINT('Ctrl Pts',(30.5258701615124,-56.1102698241508,22.));
#45983=CARTESIAN_POINT('Ctrl Pts',(30.5288380312312,-56.0950336893986,22.));
#45984=CARTESIAN_POINT('Ctrl Pts',(30.5319800053068,-56.0798239348075,22.));
#45985=CARTESIAN_POINT('Ctrl Pts',(30.5352957613587,-56.0646439756266,22.));
#45986=CARTESIAN_POINT('Ctrl Pts',(30.5383537435175,-56.0506441386005,22.));
#45987=CARTESIAN_POINT('Ctrl Pts',(30.5415601340457,-56.0366676410971,22.));
#45988=CARTESIAN_POINT('Ctrl Pts',(30.5449092364487,-56.0227386583732,22.));
#45989=CARTESIAN_POINT('Ctrl Pts',(30.5620232882029,-55.9515609807346,22.));
#45990=CARTESIAN_POINT('Ctrl Pts',(30.5828856177102,-55.8814985818636,22.));
#45991=CARTESIAN_POINT('Ctrl Pts',(30.6073807784331,-55.8128705897493,22.));
#45992=CARTESIAN_POINT('Ctrl Pts',(30.631685982855,-55.7447747974306,22.));
#45993=CARTESIAN_POINT('Ctrl Pts',(30.6595684038277,-55.6780903688633,22.));
#45994=CARTESIAN_POINT('Ctrl Pts',(30.690958647943,-55.6131557366251,22.));
#45995=CARTESIAN_POINT('Ctrl Pts',(30.7170465723104,-55.5591896136339,22.));
#45996=CARTESIAN_POINT('Ctrl Pts',(30.7455582375761,-55.5064323069427,22.));
#45997=CARTESIAN_POINT('Ctrl Pts',(30.7764732244728,-55.4550987628706,22.));
#45998=CARTESIAN_POINT('Ctrl Pts',(30.7893770627374,-55.4336722698731,22.));
#45999=CARTESIAN_POINT('Ctrl Pts',(30.8026998040103,-55.4124940848672,22.));
#46000=CARTESIAN_POINT('Ctrl Pts',(30.816440755509,-55.3915810450006,22.));
#46001=CARTESIAN_POINT('Ctrl Pts',(30.8228008343777,-55.3819013235527,22.));
#46002=CARTESIAN_POINT('Ctrl Pts',(30.8292505148729,-55.3722784163625,22.));
#46003=CARTESIAN_POINT('Ctrl Pts',(30.8357897592244,-55.36271405055,22.));
#46004=CARTESIAN_POINT('Ctrl Pts',(30.8426105864645,-55.3527378387185,22.));
#46005=CARTESIAN_POINT('Ctrl Pts',(30.8495241989438,-55.3428321824372,22.));
#46006=CARTESIAN_POINT('Ctrl Pts',(30.8565275508842,-55.3330023511027,22.));
#46007=CARTESIAN_POINT('Ctrl Pts',(30.8964137687876,-55.2770184739693,22.));
#46008=CARTESIAN_POINT('Ctrl Pts',(30.9392347488792,-55.2234520245275,22.));
#46009=CARTESIAN_POINT('Ctrl Pts',(30.9849250921271,-55.1725987747119,22.));
#46010=CARTESIAN_POINT('Ctrl Pts',(31.0263368675565,-55.1265075613062,22.));
#46011=CARTESIAN_POINT('Ctrl Pts',(31.0701064557712,-55.0826451744781,22.));
#46012=CARTESIAN_POINT('Ctrl Pts',(31.1162077188352,-55.0412612463575,22.));
#46013=CARTESIAN_POINT('Ctrl Pts',(31.1707480896715,-54.9923017464143,22.));
#46014=CARTESIAN_POINT('Ctrl Pts',(31.2285529377194,-54.9468098709298,22.));
#46015=CARTESIAN_POINT('Ctrl Pts',(31.2892182914167,-54.9049320829474,22.));
#46016=CARTESIAN_POINT('Ctrl Pts',(31.3025747483257,-54.8957120119094,22.));
#46017=CARTESIAN_POINT('Ctrl Pts',(31.3160699039855,-54.8866673619302,22.));
#46018=CARTESIAN_POINT('Ctrl Pts',(31.3296994894169,-54.8778000986123,22.));
#46019=CARTESIAN_POINT('Ctrl Pts',(31.3437625465108,-54.8686508232411,22.));
#46020=CARTESIAN_POINT('Ctrl Pts',(31.3579740386175,-54.8596873154203,22.));
#46021=CARTESIAN_POINT('Ctrl Pts',(31.372300027318,-54.8509292655156,22.));
#46022=CARTESIAN_POINT('Ctrl Pts',(31.4308133755382,-54.8151577153271,22.));
#46023=CARTESIAN_POINT('Ctrl Pts',(31.4913062997832,-54.7827600287193,22.));
#46024=CARTESIAN_POINT('Ctrl Pts',(31.5534255550514,-54.7538008858643,22.));
#46025=CARTESIAN_POINT('Ctrl Pts',(31.6155323755402,-54.7248475399326,22.));
#46026=CARTESIAN_POINT('Ctrl Pts',(31.6792660307646,-54.6993312184063,22.));
#46027=CARTESIAN_POINT('Ctrl Pts',(31.7442852729951,-54.6773670392688,22.));
#46028=CARTESIAN_POINT('Ctrl Pts',(31.7913479559042,-54.6614687734225,22.));
#46029=CARTESIAN_POINT('Ctrl Pts',(31.8390844861912,-54.6474326076125,22.));
#46030=CARTESIAN_POINT('Ctrl Pts',(31.8873641954598,-54.6353193456966,22.));
#46031=CARTESIAN_POINT('Ctrl Pts',(31.9235796701969,-54.6262329709536,22.));
#46032=CARTESIAN_POINT('Ctrl Pts',(31.960100769596,-54.6182288635217,22.));
#46033=CARTESIAN_POINT('Ctrl Pts',(31.9968706812112,-54.6113381701337,22.));
#46034=CARTESIAN_POINT('Ctrl Pts',(32.0090868551873,-54.6090488551599,22.));
#46035=CARTESIAN_POINT('Ctrl Pts',(32.0213209007479,-54.6068842729393,22.));
#46036=CARTESIAN_POINT('Ctrl Pts',(32.033570365114,-54.6048451279827,22.));
#46037=CARTESIAN_POINT('Ctrl Pts',(32.0985567096685,-54.5940269752226,22.));
#46038=CARTESIAN_POINT('Ctrl Pts',(32.1639811762245,-54.5867347457051,22.));
#46039=CARTESIAN_POINT('Ctrl Pts',(32.2295294708195,-54.5830921510723,22.));
#46040=CARTESIAN_POINT('Ctrl Pts',(32.275653061784,-54.5805290097133,22.));
#46041=CARTESIAN_POINT('Ctrl Pts',(32.3218379338893,-54.5797739344474,22.));
#46042=CARTESIAN_POINT('Ctrl Pts',(32.3679699515865,-54.5808847307989,22.));
#46043=CARTESIAN_POINT('Ctrl Pts',(32.3827771688226,-54.5812412684858,22.));
#46044=CARTESIAN_POINT('Ctrl Pts',(32.397580934837,-54.5817902377274,22.));
#46045=CARTESIAN_POINT('Ctrl Pts',(32.4123708490296,-54.5825334834844,22.));
#46046=CARTESIAN_POINT('Ctrl Pts',(32.4753792588787,-54.5856998800343,22.));
#46047=CARTESIAN_POINT('Ctrl Pts',(32.5380109270838,-54.5923812630408,22.));
#46048=CARTESIAN_POINT('Ctrl Pts',(32.5999757761394,-54.6027055704867,22.));
#46049=CARTESIAN_POINT('Ctrl Pts',(32.6570986727354,-54.6122231333574,22.));
#46050=CARTESIAN_POINT('Ctrl Pts',(32.7136552658997,-54.6248370045754,22.));
#46051=CARTESIAN_POINT('Ctrl Pts',(32.7694005056338,-54.6406824777883,22.));
#46052=CARTESIAN_POINT('Ctrl Pts',(32.7798334333405,-54.6436480166809,22.));
#46053=CARTESIAN_POINT('Ctrl Pts',(32.7902378797118,-54.6467268441195,22.));
#46054=CARTESIAN_POINT('Ctrl Pts',(32.8006124898339,-54.6499179279035,22.));
#46055=CARTESIAN_POINT('Origin',(32.5,-56.2916512459885,17.));
#46056=CARTESIAN_POINT('Origin',(-32.5,-56.2916512459885,13.));
#46057=CARTESIAN_POINT('Ctrl Pts',(-31.9588970197441,-54.7159724828016,
13.));
#46058=CARTESIAN_POINT('Ctrl Pts',(-32.0152863485872,-54.6890038458254,
13.));
#46059=CARTESIAN_POINT('Ctrl Pts',(-32.0731449906992,-54.665548635413,13.));
#46060=CARTESIAN_POINT('Ctrl Pts',(-32.1321548892164,-54.6454940895841,
13.));
#46061=CARTESIAN_POINT('Ctrl Pts',(-32.1695849278231,-54.6327734707815,
13.));
#46062=CARTESIAN_POINT('Ctrl Pts',(-32.2074789472177,-54.6214218412685,
13.));
#46063=CARTESIAN_POINT('Ctrl Pts',(-32.2457622248769,-54.611418695037,13.));
#46064=CARTESIAN_POINT('Ctrl Pts',(-32.271904889536,-54.6045878040198,13.));
#46065=CARTESIAN_POINT('Ctrl Pts',(-32.2982291715498,-54.5983858677327,
13.));
#46066=CARTESIAN_POINT('Ctrl Pts',(-32.3247122748156,-54.592808119745,13.));
#46067=CARTESIAN_POINT('Ctrl Pts',(-32.338774499773,-54.5898463993541,13.));
#46068=CARTESIAN_POINT('Ctrl Pts',(-32.3528813607046,-54.5870608474282,
13.));
#46069=CARTESIAN_POINT('Ctrl Pts',(-32.367015346482,-54.5844531526057,13.));
#46070=CARTESIAN_POINT('Ctrl Pts',(-32.4318895175076,-54.5724839853404,
13.));
#46071=CARTESIAN_POINT('Ctrl Pts',(-32.4974065824013,-54.5642420059679,
13.));
#46072=CARTESIAN_POINT('Ctrl Pts',(-32.5632274845374,-54.5596289936312,
13.));
#46073=CARTESIAN_POINT('Ctrl Pts',(-32.6107070729831,-54.5563014195608,
13.));
#46074=CARTESIAN_POINT('Ctrl Pts',(-32.6583455261738,-54.5548630893332,
13.));
#46075=CARTESIAN_POINT('Ctrl Pts',(-32.7060224989242,-54.5552923689863,
13.));
#46076=CARTESIAN_POINT('Ctrl Pts',(-32.7190852595527,-54.5554099850392,
13.));
#46077=CARTESIAN_POINT('Ctrl Pts',(-32.7321509341772,-54.5556678729876,
13.));
#46078=CARTESIAN_POINT('Ctrl Pts',(-32.7452170898975,-54.5560657582162,
13.));
#46079=CARTESIAN_POINT('Ctrl Pts',(-32.7585822800833,-54.55647274952,13.));
#46080=CARTESIAN_POINT('Ctrl Pts',(-32.7719398800736,-54.5570260108604,
13.));
#46081=CARTESIAN_POINT('Ctrl Pts',(-32.7852820457025,-54.5577244070661,
13.));
#46082=CARTESIAN_POINT('Ctrl Pts',(-32.8530416061927,-54.5612712840324,
13.));
#46083=CARTESIAN_POINT('Ctrl Pts',(-32.9204432866946,-54.5685589036366,
13.));
#46084=CARTESIAN_POINT('Ctrl Pts',(-32.9871435059666,-54.5794869270338,
13.));
#46085=CARTESIAN_POINT('Ctrl Pts',(-33.0548103387428,-54.590573318351,13.));
#46086=CARTESIAN_POINT('Ctrl Pts',(-33.1217562803605,-54.6054062113849,
13.));
#46087=CARTESIAN_POINT('Ctrl Pts',(-33.1876366472556,-54.6239318016751,
13.));
#46088=CARTESIAN_POINT('Ctrl Pts',(-33.2284548201806,-54.6354098911825,
13.));
#46089=CARTESIAN_POINT('Ctrl Pts',(-33.2688641593019,-54.6483065466031,
13.));
#46090=CARTESIAN_POINT('Ctrl Pts',(-33.308782562507,-54.6626190129889,13.));
#46091=CARTESIAN_POINT('Ctrl Pts',(-33.3414809096879,-54.6743427784034,
13.));
#46092=CARTESIAN_POINT('Ctrl Pts',(-33.3738498713991,-54.6870166552392,
13.));
#46093=CARTESIAN_POINT('Ctrl Pts',(-33.4058433879587,-54.7006430225369,
13.));
#46094=CARTESIAN_POINT('Ctrl Pts',(-33.4189228881451,-54.7062137160015,
13.));
#46095=CARTESIAN_POINT('Ctrl Pts',(-33.431941905508,-54.7119448243305,13.));
#46096=CARTESIAN_POINT('Ctrl Pts',(-33.4448753977064,-54.7178263149142,
13.));
#46097=CARTESIAN_POINT('Ctrl Pts',(-33.5090388470795,-54.7470045691335,
13.));
#46098=CARTESIAN_POINT('Ctrl Pts',(-33.5712122519748,-54.7799269958261,
13.));
#46099=CARTESIAN_POINT('Ctrl Pts',(-33.6310396924137,-54.8165209633119,
13.));
#46100=CARTESIAN_POINT('Ctrl Pts',(-33.6376901817643,-54.8205887922091,
13.));
#46101=CARTESIAN_POINT('Ctrl Pts',(-33.6443116825685,-54.8247020426567,
13.));
#46102=CARTESIAN_POINT('Ctrl Pts',(-33.6509037041524,-54.8288606547026,
13.));
#46103=CARTESIAN_POINT('Ctrl Pts',(-33.7079313851615,-54.8648368720402,
13.));
#46104=CARTESIAN_POINT('Ctrl Pts',(-33.7627542963063,-54.9042038022182,
13.));
#46105=CARTESIAN_POINT('Ctrl Pts',(-33.8152783515972,-54.9466335926766,
13.));
#46106=CARTESIAN_POINT('Ctrl Pts',(-33.8717836154426,-54.9922794684851,
13.));
#46107=CARTESIAN_POINT('Ctrl Pts',(-33.9256293125932,-55.0414702768411,
13.));
#46108=CARTESIAN_POINT('Ctrl Pts',(-33.9766695218193,-55.0938552564662,
13.));
#46109=CARTESIAN_POINT('Ctrl Pts',(-33.98601646824,-55.1034484694492,13.));
#46110=CARTESIAN_POINT('Ctrl Pts',(-33.9952692317474,-55.113148942497,13.));
#46111=CARTESIAN_POINT('Ctrl Pts',(-34.0044267781796,-55.1229547001842,
13.));
#46112=CARTESIAN_POINT('Ctrl Pts',(-34.0122933714936,-55.1313781254359,
13.));
#46113=CARTESIAN_POINT('Ctrl Pts',(-34.0200833036472,-55.1398724074257,
13.));
#46114=CARTESIAN_POINT('Ctrl Pts',(-34.0277952351974,-55.1484347977441,
13.));
#46115=CARTESIAN_POINT('Ctrl Pts',(-34.0753570091897,-55.2012416037311,
13.));
#46116=CARTESIAN_POINT('Ctrl Pts',(-34.1199659341815,-55.2566479177152,
13.));
#46117=CARTESIAN_POINT('Ctrl Pts',(-34.1615258634594,-55.3142853318227,
13.));
#46118=CARTESIAN_POINT('Ctrl Pts',(-34.2039616811858,-55.373137472377,13.));
#46119=CARTESIAN_POINT('Ctrl Pts',(-34.2432193073455,-55.4343163954304,
13.));
#46120=CARTESIAN_POINT('Ctrl Pts',(-34.2791687520186,-55.497477603779,13.));
#46121=CARTESIAN_POINT('Ctrl Pts',(-34.3153358231374,-55.5610211698915,
13.));
#46122=CARTESIAN_POINT('Ctrl Pts',(-34.3481552082325,-55.6265719323703,
13.));
#46123=CARTESIAN_POINT('Ctrl Pts',(-34.3774567489235,-55.6938154067926,
13.));
#46124=CARTESIAN_POINT('Ctrl Pts',(-34.3846992416887,-55.7104360473981,
13.));
#46125=CARTESIAN_POINT('Ctrl Pts',(-34.3917266096161,-55.7271602398318,
13.));
#46126=CARTESIAN_POINT('Ctrl Pts',(-34.3985358555028,-55.743983480801,13.));
#46127=CARTESIAN_POINT('Ctrl Pts',(-34.4038603586072,-55.7571384468955,
13.));
#46128=CARTESIAN_POINT('Ctrl Pts',(-34.4090519561989,-55.7703555308113,
13.));
#46129=CARTESIAN_POINT('Ctrl Pts',(-34.414101784082,-55.7836123414303,13.));
#46130=CARTESIAN_POINT('Ctrl Pts',(-34.4409205169415,-55.8540168919997,
13.));
#46131=CARTESIAN_POINT('Ctrl Pts',(-34.4637958507435,-55.9256644802089,
13.));
#46132=CARTESIAN_POINT('Ctrl Pts',(-34.4826007268578,-55.9981857626967,
13.));
#46133=CARTESIAN_POINT('Ctrl Pts',(-34.5014259919704,-56.0707856756575,
13.));
#46134=CARTESIAN_POINT('Ctrl Pts',(-34.5161726005963,-56.1442621124532,
13.));
#46135=CARTESIAN_POINT('Ctrl Pts',(-34.5266721187049,-56.2182764860945,
13.));
#46136=CARTESIAN_POINT('Ctrl Pts',(-34.5369326970758,-56.290606499097,13.));
#46137=CARTESIAN_POINT('Ctrl Pts',(-34.5431377092968,-56.3634511940737,
13.));
#46138=CARTESIAN_POINT('Ctrl Pts',(-34.5450833843548,-56.4365110273052,
13.));
#46139=CARTESIAN_POINT('Ctrl Pts',(-34.5455017158062,-56.4522193162868,
13.));
#46140=CARTESIAN_POINT('Ctrl Pts',(-34.5457229607324,-56.4679375826136,
13.));
#46141=CARTESIAN_POINT('Ctrl Pts',(-34.5457447745363,-56.4836628867631,
13.));
#46142=CARTESIAN_POINT('Ctrl Pts',(-34.545763248735,-56.4969807103663,13.));
#46143=CARTESIAN_POINT('Ctrl Pts',(-34.5456386792458,-56.5103035820178,
13.));
#46144=CARTESIAN_POINT('Ctrl Pts',(-34.5453721234944,-56.52362996598,13.));
#46145=CARTESIAN_POINT('Ctrl Pts',(-34.1542537360139,-57.5104384051693,
13.));
#46146=CARTESIAN_POINT('Ctrl Pts',(-34.1045519887786,-57.5661317580893,
13.));
#46147=CARTESIAN_POINT('Ctrl Pts',(-34.0516736631806,-57.6187667033008,
13.));
#46148=CARTESIAN_POINT('Ctrl Pts',(-33.9959663128535,-57.6682442041301,
13.));
#46149=CARTESIAN_POINT('Ctrl Pts',(-33.941716853086,-57.7164268528268,13.));
#46150=CARTESIAN_POINT('Ctrl Pts',(-33.8847834892553,-57.7616152151019,
13.));
#46151=CARTESIAN_POINT('Ctrl Pts',(-33.8254670336322,-57.8036766866724,
13.));
#46152=CARTESIAN_POINT('Ctrl Pts',(-33.812228067015,-57.8130644764879,13.));
#46153=CARTESIAN_POINT('Ctrl Pts',(-33.7988685442659,-57.8222975378101,
13.));
#46154=CARTESIAN_POINT('Ctrl Pts',(-33.7853974828999,-57.8313702493365,
13.));
#46155=CARTESIAN_POINT('Ctrl Pts',(-33.7235792093242,-57.8730046349261,
13.));
#46156=CARTESIAN_POINT('Ctrl Pts',(-33.6595370838482,-57.9111844301544,
13.));
#46157=CARTESIAN_POINT('Ctrl Pts',(-33.5936094995078,-57.945786238912,13.));
#46158=CARTESIAN_POINT('Ctrl Pts',(-33.547323850303,-57.9700790625916,13.));
#46159=CARTESIAN_POINT('Ctrl Pts',(-33.5001083176739,-57.9926073121725,
13.));
#46160=CARTESIAN_POINT('Ctrl Pts',(-33.4520768824606,-58.0133132483315,
13.));
#46161=CARTESIAN_POINT('Ctrl Pts',(-33.4338169279728,-58.0211849567285,
13.));
#46162=CARTESIAN_POINT('Ctrl Pts',(-33.4154390448092,-58.0287931600018,
13.));
#46163=CARTESIAN_POINT('Ctrl Pts',(-33.3969494936981,-58.0361341920447,
13.));
#46164=CARTESIAN_POINT('Ctrl Pts',(-33.3793383498013,-58.043126464106,13.));
#46165=CARTESIAN_POINT('Ctrl Pts',(-33.3616202465966,-58.0498782554867,
13.));
#46166=CARTESIAN_POINT('Ctrl Pts',(-33.3438321785184,-58.0563750965513,
13.));
#46167=CARTESIAN_POINT('Ctrl Pts',(-33.2756398803729,-58.0812813719788,
13.));
#46168=CARTESIAN_POINT('Ctrl Pts',(-33.2063496369042,-58.1024753902403,
13.));
#46169=CARTESIAN_POINT('Ctrl Pts',(-33.1362740502616,-58.1198408416066,
13.));
#46170=CARTESIAN_POINT('Ctrl Pts',(-33.0677030440348,-58.1368334424655,
13.));
#46171=CARTESIAN_POINT('Ctrl Pts',(-32.9983791192747,-58.1501601307445,
13.));
#46172=CARTESIAN_POINT('Ctrl Pts',(-32.9285938585171,-58.1596629268823,
13.));
#46173=CARTESIAN_POINT('Ctrl Pts',(-32.860339265238,-58.1689572890207,13.));
#46174=CARTESIAN_POINT('Ctrl Pts',(-32.791642581852,-58.1745936618092,13.));
#46175=CARTESIAN_POINT('Ctrl Pts',(-32.7227877559508,-58.1763767799569,
13.));
#46176=CARTESIAN_POINT('Ctrl Pts',(-32.7004157901354,-58.1769561417914,
13.));
#46177=CARTESIAN_POINT('Ctrl Pts',(-32.6780272661539,-58.1771283364151,
13.));
#46178=CARTESIAN_POINT('Ctrl Pts',(-32.6556323878678,-58.1768855536499,
13.));
#46179=CARTESIAN_POINT('Ctrl Pts',(-32.642997056445,-58.1767485740841,13.));
#46180=CARTESIAN_POINT('Ctrl Pts',(-32.6303583965514,-58.1764793454886,
13.));
#46181=CARTESIAN_POINT('Ctrl Pts',(-32.617736131084,-58.1760772493482,13.));
#46182=CARTESIAN_POINT('Ctrl Pts',(-32.5494663667858,-58.1739024409672,
13.));
#46183=CARTESIAN_POINT('Ctrl Pts',(-32.4815560597098,-58.1678447149676,
13.));
#46184=CARTESIAN_POINT('Ctrl Pts',(-32.4142747868267,-58.1577646785827,
13.));
#46185=CARTESIAN_POINT('Ctrl Pts',(-32.4045647306857,-58.15630992431,13.));
#46186=CARTESIAN_POINT('Ctrl Pts',(-32.3948677956577,-58.1547713053032,
13.));
#46187=CARTESIAN_POINT('Ctrl Pts',(-32.3851848149705,-58.1531483143848,
13.));
#46188=CARTESIAN_POINT('Ctrl Pts',(-32.3167654615685,-58.1416803591339,
13.));
#46189=CARTESIAN_POINT('Ctrl Pts',(-32.2490407707029,-58.1260036975298,
13.));
#46190=CARTESIAN_POINT('Ctrl Pts',(-32.1823062478791,-58.1063380404035,
13.));
#46191=CARTESIAN_POINT('Ctrl Pts',(-32.1200483333854,-58.0879915722183,
13.));
#46192=CARTESIAN_POINT('Ctrl Pts',(-32.0586518297846,-58.0661723398752,
13.));
#46193=CARTESIAN_POINT('Ctrl Pts',(-31.9983820977313,-58.0410277367995,
13.));
#46194=CARTESIAN_POINT('Ctrl Pts',(-31.9850796184709,-58.0354779268115,
13.));
#46195=CARTESIAN_POINT('Ctrl Pts',(-31.9718321460664,-58.0297660234503,
13.));
#46196=CARTESIAN_POINT('Ctrl Pts',(-31.9586427416388,-58.023893457908,13.));
#46197=CARTESIAN_POINT('Ctrl Pts',(-31.9483333677394,-58.0193032222945,
13.));
#46198=CARTESIAN_POINT('Ctrl Pts',(-31.9380601507492,-58.0146150416842,
13.));
#46199=CARTESIAN_POINT('Ctrl Pts',(-31.9278362672604,-58.0098353467978,
13.));
#46200=CARTESIAN_POINT('Ctrl Pts',(-31.8658980543593,-57.9808790544257,
13.));
#46201=CARTESIAN_POINT('Ctrl Pts',(-31.8056527017084,-57.9485169556613,
13.));
#46202=CARTESIAN_POINT('Ctrl Pts',(-31.7473720765467,-57.9129741302491,
13.));
#46203=CARTESIAN_POINT('Ctrl Pts',(-31.6893603668348,-57.8775953047057,
13.));
#46204=CARTESIAN_POINT('Ctrl Pts',(-31.6332945176634,-57.8390642101102,
13.));
#46205=CARTESIAN_POINT('Ctrl Pts',(-31.5794782982672,-57.7975661709256,
13.));
#46206=CARTESIAN_POINT('Ctrl Pts',(-31.5268144521557,-57.7569567343271,
13.));
#46207=CARTESIAN_POINT('Ctrl Pts',(-31.4763043639082,-57.7135052609396,
13.));
#46208=CARTESIAN_POINT('Ctrl Pts',(-31.4282765730784,-57.6673622963473,
13.));
#46209=CARTESIAN_POINT('Ctrl Pts',(-31.4181553628237,-57.6576382878443,
13.));
#46210=CARTESIAN_POINT('Ctrl Pts',(-31.4081445660852,-57.647794690832,13.));
#46211=CARTESIAN_POINT('Ctrl Pts',(-31.3982475487379,-57.6378328293302,
13.));
#46212=CARTESIAN_POINT('Ctrl Pts',(-31.3888700148449,-57.6283938548803,
13.));
#46213=CARTESIAN_POINT('Ctrl Pts',(-31.3795934917281,-57.6188473329616,
13.));
#46214=CARTESIAN_POINT('Ctrl Pts',(-31.370435450571,-57.6092101707806,13.));
#46215=CARTESIAN_POINT('Ctrl Pts',(-31.3254237977993,-57.5618436444295,
13.));
#46216=CARTESIAN_POINT('Ctrl Pts',(-31.28318780428,-57.5122078770326,13.));
#46217=CARTESIAN_POINT('Ctrl Pts',(-31.2439955573278,-57.4604767979467,
13.));
#46218=CARTESIAN_POINT('Ctrl Pts',(-31.2055484075955,-57.4097291961098,
13.));
#46219=CARTESIAN_POINT('Ctrl Pts',(-31.1700298958942,-57.3569644529347,
13.));
#46220=CARTESIAN_POINT('Ctrl Pts',(-31.1377389873445,-57.3023276234082,
13.));
#46221=CARTESIAN_POINT('Ctrl Pts',(-31.1064966595925,-57.2494650124732,
13.));
#46222=CARTESIAN_POINT('Ctrl Pts',(-31.0782754671115,-57.1948493080738,
13.));
#46223=CARTESIAN_POINT('Ctrl Pts',(-31.0533946162939,-57.1386036481878,
13.));
#46224=CARTESIAN_POINT('Ctrl Pts',(-31.049253985217,-57.129243336156,13.));
#46225=CARTESIAN_POINT('Ctrl Pts',(-31.045205981978,-57.1198378750668,13.));
#46226=CARTESIAN_POINT('Ctrl Pts',(-31.0412522209115,-57.1103878272416,
13.));
#46227=CARTESIAN_POINT('Ctrl Pts',(-31.0370666269761,-57.1003836660893,
13.));
#46228=CARTESIAN_POINT('Ctrl Pts',(-31.032986652061,-57.0903295352429,13.));
#46229=CARTESIAN_POINT('Ctrl Pts',(-31.0290124456509,-57.0802271145803,
13.));
#46230=CARTESIAN_POINT('Origin',(-32.5,-56.2916512459885,23.5459252805377));
#46231=CARTESIAN_POINT('Ctrl Pts',(-31.4704151231923,-54.5113563798656,
21.7959252805377));
#46232=CARTESIAN_POINT('Ctrl Pts',(-31.3848836142506,-54.5597932517276,
21.7905813053169));
#46233=CARTESIAN_POINT('Ctrl Pts',(-30.7359364258277,-54.993465396867,21.7481913665734));
#46234=CARTESIAN_POINT('Ctrl Pts',(-30.0819661342964,-56.5203533893187,
21.6687554643073));
#46235=CARTESIAN_POINT('Ctrl Pts',(-31.380844296031,-58.4469950837991,21.5576175737392));
#46236=CARTESIAN_POINT('Ctrl Pts',(-33.7038051725687,-58.4009643313194,
21.4464796831712));
#46237=CARTESIAN_POINT('Ctrl Pts',(-34.9250559921582,-56.4241863460987,
21.3353417926031));
#46238=CARTESIAN_POINT('Ctrl Pts',(-33.9265523881077,-54.3261319732661,
21.2242039020351));
#46239=CARTESIAN_POINT('Ctrl Pts',(-32.2719558287363,-54.111420270443,21.1443983980133));
#46240=CARTESIAN_POINT('Ctrl Pts',(-31.5637955304719,-54.4566153915593,
21.1016388575141));
#46241=CARTESIAN_POINT('Ctrl Pts',(-31.4731950477465,-54.5099653993635,
21.0959252805377));
#46242=CARTESIAN_POINT('Ctrl Pts',(-31.4756555660462,-54.5128362942924,
21.8540747194623));
#46243=CARTESIAN_POINT('Ctrl Pts',(-31.0702251268552,-54.7510086370429,
21.8286245525962));
#46244=CARTESIAN_POINT('Ctrl Pts',(-30.2605073082537,-55.6718001447715,
21.7661284222074));
#46245=CARTESIAN_POINT('Ctrl Pts',(-30.5464763025826,-57.7337498950934,
21.6665863282958));
#46246=CARTESIAN_POINT('Ctrl Pts',(-32.6512600365403,-58.7155097146097,
21.5554484377279));
#46247=CARTESIAN_POINT('Ctrl Pts',(-34.6188774786828,-57.4788960204646,
21.4443105471598));
#46248=CARTESIAN_POINT('Ctrl Pts',(-34.6464212862449,-55.1554778495401,
21.3331726565917));
#46249=CARTESIAN_POINT('Ctrl Pts',(-32.9604590994426,-54.0382699285555,
21.2364273806926));
#46250=CARTESIAN_POINT('Ctrl Pts',(-31.8369684898523,-54.3074066165865,
21.1767280683161));
#46251=CARTESIAN_POINT('Ctrl Pts',(-31.4729484072307,-54.5150696468519,
21.1540747194623));
#46252=CARTESIAN_POINT('Ctrl Pts',(-32.1997834265916,-57.9303781936679,
22.));
#46253=CARTESIAN_POINT('Ctrl Pts',(-32.7446991236385,-58.0302073467771,
21.9629540364773));
#46254=CARTESIAN_POINT('Ctrl Pts',(-33.932658940673,-57.64135965021,21.888862109432));
#46255=CARTESIAN_POINT('Ctrl Pts',(-34.4123083746051,-55.8170344416491,
21.7777242188639));
#46256=CARTESIAN_POINT('Ctrl Pts',(-33.1376927310287,-54.4290349886999,
21.6665863282959));
#46257=CARTESIAN_POINT('Ctrl Pts',(-31.2813034436656,-54.7450016890465,
21.5554484377278));
#46258=CARTESIAN_POINT('Ctrl Pts',(-30.5394479035103,-56.4770839121465,
21.4443105471598));
#46259=CARTESIAN_POINT('Ctrl Pts',(-31.592583816614,-58.0392131556089,21.3331726565918));
#46260=CARTESIAN_POINT('Ctrl Pts',(-33.4760503309402,-58.0018912265998,
21.2220347660237));
#46261=CARTESIAN_POINT('Ctrl Pts',(-34.4662456663514,-56.3991112663237,
21.1108968754557));
#46262=CARTESIAN_POINT('Ctrl Pts',(-33.6566547164314,-54.6979998974762,
20.9997589848876));
#46263=CARTESIAN_POINT('Ctrl Pts',(-31.7883942259045,-54.4555617097706,
20.8886210943196));
#46264=CARTESIAN_POINT('Ctrl Pts',(-30.5714597638967,-55.8937240769523,
20.7774832037515));
#46265=CARTESIAN_POINT('Ctrl Pts',(-31.1197474481278,-57.6961102078823,
20.6663453131835));
#46266=CARTESIAN_POINT('Ctrl Pts',(-32.9313922508809,-58.212980865287,20.5552074226155));
#46267=CARTESIAN_POINT('Ctrl Pts',(-34.3481806801685,-56.9712358625611,
20.4440695320474));
#46268=CARTESIAN_POINT('Ctrl Pts',(-34.0733074508499,-55.1074597880137,
20.3329316414794));
#46269=CARTESIAN_POINT('Ctrl Pts',(-32.3583685299806,-54.3275873674106,
20.2217937509113));
#46270=CARTESIAN_POINT('Ctrl Pts',(-30.7730662696612,-55.3454449973685,
20.1106558603433));
#46271=CARTESIAN_POINT('Ctrl Pts',(-30.7684461524675,-57.2293758831937,
19.9995179697752));
#46272=CARTESIAN_POINT('Ctrl Pts',(-32.3487368516327,-58.2549968011428,
19.8883800792072));
#46273=CARTESIAN_POINT('Ctrl Pts',(-34.0674804546367,-57.4835452530785,
19.7772421886392));
#46274=CARTESIAN_POINT('Ctrl Pts',(-34.3514914067379,-55.6211396100853,
19.6661042980711));
#46275=CARTESIAN_POINT('Ctrl Pts',(-32.9408112840734,-54.3724608681775,
19.5549664075031));
#46276=CARTESIAN_POINT('Ctrl Pts',(-31.1266515903786,-54.8804388458658,
19.443828516935));
#46277=CARTESIAN_POINT('Ctrl Pts',(-30.569533272628,-56.680115536781,19.332690626367));
#46278=CARTESIAN_POINT('Ctrl Pts',(-31.7793930425298,-58.1242264572701,
19.2215527357989));
#46279=CARTESIAN_POINT('Ctrl Pts',(-33.6488325332889,-57.8909605038464,
19.1104148452309));
#46280=CARTESIAN_POINT('Ctrl Pts',(-34.4667325774588,-56.1938286494099,
18.9992769546628));
#46281=CARTESIAN_POINT('Ctrl Pts',(-33.4844599893276,-54.5862349269529,
18.8881390640949));
#46282=CARTESIAN_POINT('Ctrl Pts',(-31.6011000083736,-54.539628102072,18.7770011735268));
#46283=CARTESIAN_POINT('Ctrl Pts',(-30.5405133840023,-56.0966679300985,
18.6658632829588));
#46284=CARTESIAN_POINT('Ctrl Pts',(-31.2734670813295,-57.8321781984269,
18.5547253923907));
#46285=CARTESIAN_POINT('Ctrl Pts',(-33.1290802689522,-58.1576266764213,
18.4435875018227));
#46286=CARTESIAN_POINT('Ctrl Pts',(-34.4088891521439,-56.7751266813415,
18.3324496112546));
#46287=CARTESIAN_POINT('Ctrl Pts',(-33.9414701461048,-54.9500961372979,
18.2213117206866));
#46288=CARTESIAN_POINT('Ctrl Pts',(-32.1546571679518,-54.353006198509,18.1101738301185));
#46289=CARTESIAN_POINT('Ctrl Pts',(-30.6839404004271,-55.530380057408,17.9990359395505));
#46290=CARTESIAN_POINT('Ctrl Pts',(-30.8754835799079,-57.4045540686174,
17.8878980489824));
#46291=CARTESIAN_POINT('Ctrl Pts',(-32.5539650619684,-58.2600755050979,
17.7767601584144));
#46292=CARTESIAN_POINT('Ctrl Pts',(-34.1830517108038,-57.3138758937664,
17.6656222678464));
#46293=CARTESIAN_POINT('Ctrl Pts',(-34.271622041636,-55.4320224695076,17.5544843772783));
#46294=CARTESIAN_POINT('Ctrl Pts',(-32.7386066261983,-54.3369970132153,
17.4433464867103));
#46295=CARTESIAN_POINT('Ctrl Pts',(-30.9871918598182,-55.0310887434669,
17.3322085961423));
#46296=CARTESIAN_POINT('Ctrl Pts',(-30.6204675405577,-56.8789876280276,
17.2210707055742));
#46297=CARTESIAN_POINT('Ctrl Pts',(-31.9741005967727,-58.1892908612603,
17.1099328150062));
#46298=CARTESIAN_POINT('Ctrl Pts',(-33.8090953408665,-57.7626630339378,
16.9987949244381));
#46299=CARTESIAN_POINT('Ctrl Pts',(-34.4458602733144,-55.989601434697,16.8876570338701));
#46300=CARTESIAN_POINT('Ctrl Pts',(-33.3015572300412,-54.493009453209,16.776519143302));
#46301=CARTESIAN_POINT('Ctrl Pts',(-31.4235797638343,-54.6427347026375,
16.665381252734));
#46302=CARTESIAN_POINT('Ctrl Pts',(-30.5308619472252,-56.3017319641806,
16.554243362166));
#46303=CARTESIAN_POINT('Ctrl Pts',(-31.4405185218662,-57.9515022300392,
16.4431054715979));
#46304=CARTESIAN_POINT('Ctrl Pts',(-33.3199305087784,-58.0819920662062,
16.3319675810299));
#46305=CARTESIAN_POINT('Ctrl Pts',(-34.4488508023651,-56.5737626457811,
16.2208296904618));
#46306=CARTESIAN_POINT('Ctrl Pts',(-33.7939658550683,-54.8073134617672,
16.1096917998938));
#46307=CARTESIAN_POINT('Ctrl Pts',(-31.9546992860713,-54.3994954851817,
15.9985539093257));
#46308=CARTESIAN_POINT('Ctrl Pts',(-30.6145526446348,-55.7235891349781,
15.8874160187577));
#46309=CARTESIAN_POINT('Ctrl Pts',(-31.0001773500498,-57.5676364772256,
15.7762781281896));
#46310=CARTESIAN_POINT('Ctrl Pts',(-32.758606735993,-58.2437600667033,15.6651402376216));
#46311=CARTESIAN_POINT('Ctrl Pts',(-34.2803304439162,-57.1330963140847,
15.5540023470536));
#46312=CARTESIAN_POINT('Ctrl Pts',(-34.1724975057335,-55.2522483481541,
15.4428644564855));
#46313=CARTESIAN_POINT('Ctrl Pts',(-32.5338086340801,-54.3227776419367,
15.3317265659175));
#46314=CARTESIAN_POINT('Ctrl Pts',(-30.8641743343578,-55.195439274664,15.2205886753495));
#46315=CARTESIAN_POINT('Ctrl Pts',(-30.6918298216846,-57.0714761554116,
15.1094507847814));
#46316=CARTESIAN_POINT('Ctrl Pts',(-32.1745239717376,-58.2337304551948,
14.9983128942134));
#46317=CARTESIAN_POINT('Ctrl Pts',(-33.9551300366822,-57.618377625218,14.8871750036453));
#46318=CARTESIAN_POINT('Ctrl Pts',(-34.4038390465812,-55.788657104035,14.7760371130773));
#46319=CARTESIAN_POINT('Ctrl Pts',(-33.1099426465396,-54.4193328057006,
14.6648992225092));
#46320=CARTESIAN_POINT('Ctrl Pts',(-31.2577587039999,-54.7637628485765,
14.5537613319412));
#46321=CARTESIAN_POINT('Ctrl Pts',(-30.5426125496715,-56.5066863904105,
14.4426234413731));
#46322=CARTESIAN_POINT('Ctrl Pts',(-31.6190848424819,-58.0527859832772,
14.3314855508051));
#46323=CARTESIAN_POINT('Ctrl Pts',(-33.5018697389164,-57.9868986634345,
14.2203476602371));
#46324=CARTESIAN_POINT('Ctrl Pts',(-34.4676299603036,-56.3693327876153,
14.109209769669));
#46325=CARTESIAN_POINT('Ctrl Pts',(-33.6324000499911,-54.680662853446,13.998071879101));
#46326=CARTESIAN_POINT('Ctrl Pts',(-31.7606637541616,-54.466551391645,13.886933988533));
#46327=CARTESIAN_POINT('Ctrl Pts',(-30.5656658770528,-55.9229694665903,
13.7757960979649));
#46328=CARTESIAN_POINT('Ctrl Pts',(-31.141154796329,-57.7168562799665,13.6646582073969));
#46329=CARTESIAN_POINT('Ctrl Pts',(-32.9604725206547,-58.206216496256,13.5535203168288));
#46330=CARTESIAN_POINT('Ctrl Pts',(-34.358189658021,-56.9431939941263,13.4423824262608));
#46331=CARTESIAN_POINT('Ctrl Pts',(-34.0553346792797,-55.0837258210724,
13.3312445356927));
#46332=CARTESIAN_POINT('Ctrl Pts',(-32.3283638467564,-54.3300480294051,
13.2201066451247));
#46333=CARTESIAN_POINT('Ctrl Pts',(-30.7594958530052,-55.3715226379037,
13.1089687545567));
#46334=CARTESIAN_POINT('Ctrl Pts',(-30.7817150891479,-57.2558511192949,
12.9978308639886));
#46335=CARTESIAN_POINT('Ctrl Pts',(-32.3808507372123,-58.2563466091156,
12.8866929734206));
#46336=CARTESIAN_POINT('Ctrl Pts',(-33.5126766583317,-57.7258551932599,
12.8126010463752));
#46337=CARTESIAN_POINT('Ctrl Pts',(-33.8412759334222,-57.2798490351089,
12.7755550828525));
#46338=CARTESIAN_POINT('Ctrl Pts',(-32.1764322475374,-58.057840198652,22.0748149723825));
#46339=CARTESIAN_POINT('Ctrl Pts',(-32.7637320936894,-58.1654341743444,
22.0377690088598));
#46340=CARTESIAN_POINT('Ctrl Pts',(-34.0440927468328,-57.7463414713666,
21.9636770818144));
#46341=CARTESIAN_POINT('Ctrl Pts',(-34.5610498473198,-55.7801182186225,
21.8525391912464));
#46342=CARTESIAN_POINT('Ctrl Pts',(-33.1872931810462,-54.2841586241499,
21.7414013006783));
#46343=CARTESIAN_POINT('Ctrl Pts',(-31.1865118697811,-54.624701565945,21.6302634101103));
#46344=CARTESIAN_POINT('Ctrl Pts',(-30.386953980439,-56.4915070712039,21.5191255195423));
#46345=CARTESIAN_POINT('Ctrl Pts',(-31.5220039764197,-58.1751404650056,
21.4079876289743));
#46346=CARTESIAN_POINT('Ctrl Pts',(-33.551968611483,-58.1349155948397,21.2968497384062));
#46347=CARTESIAN_POINT('Ctrl Pts',(-34.6191824416203,-56.4074696262487,
21.1857118478381));
#46348=CARTESIAN_POINT('Ctrl Pts',(-33.7466206069902,-54.5740439227395,
21.0745739572701));
#46349=CARTESIAN_POINT('Ctrl Pts',(-31.7330447371731,-54.312748623095,20.963436066702));
#46350=CARTESIAN_POINT('Ctrl Pts',(-30.4214557589377,-55.8627728590726,
20.852298176134));
#46351=CARTESIAN_POINT('Ctrl Pts',(-31.0123898691881,-57.8053505883217,
20.741160285566));
#46352=CARTESIAN_POINT('Ctrl Pts',(-32.9649464200546,-58.3624240204495,
20.6300223949979));
#46353=CARTESIAN_POINT('Ctrl Pts',(-34.4919342294713,-57.0240947100386,
20.5188845044299));
#46354=CARTESIAN_POINT('Ctrl Pts',(-34.195681054595,-55.0153520590646,20.4077466138619));
#46355=CARTESIAN_POINT('Ctrl Pts',(-32.3473522766853,-54.1748202940219,
20.2966087232938));
#46356=CARTESIAN_POINT('Ctrl Pts',(-30.6387434429966,-55.2718480227484,
20.1854708327258));
#46357=CARTESIAN_POINT('Ctrl Pts',(-30.6337639679481,-57.3023131486427,
20.0743329421578));
#46358=CARTESIAN_POINT('Ctrl Pts',(-32.3369714356807,-58.4077080025365,
19.9631950515897));
#46359=CARTESIAN_POINT('Ctrl Pts',(-34.1894008281341,-57.5762520948665,
19.8520571610217));
#46360=CARTESIAN_POINT('Ctrl Pts',(-34.4955024680362,-55.5689864691375,
19.7409192704536));
#46361=CARTESIAN_POINT('Ctrl Pts',(-32.975098076127,-54.2231841055976,19.6297813798856));
#46362=CARTESIAN_POINT('Ctrl Pts',(-31.0198310233036,-54.770673175488,19.5186434893175));
#46363=CARTESIAN_POINT('Ctrl Pts',(-30.419379423035,-56.710330721464,19.4075055987495));
#46364=CARTESIAN_POINT('Ctrl Pts',(-31.7233434317422,-58.2667661958427,
19.2963677081814));
#46365=CARTESIAN_POINT('Ctrl Pts',(-33.7381900057412,-58.0153565570662,
19.1852298176134));
#46366=CARTESIAN_POINT('Ctrl Pts',(-34.6197072252153,-56.1862198990257,
19.0740919270454));
#46367=CARTESIAN_POINT('Ctrl Pts',(-33.5610323824551,-54.4535857484765,
18.9629540364773));
#46368=CARTESIAN_POINT('Ctrl Pts',(-31.5311825670481,-54.4033537929088,
18.8518161459093));
#46369=CARTESIAN_POINT('Ctrl Pts',(-30.388102335189,-56.0815019108804,18.7406782553412));
#46370=CARTESIAN_POINT('Ctrl Pts',(-31.1780659864649,-57.9520020985391,
18.6295403647732));
#46371=CARTESIAN_POINT('Ctrl Pts',(-33.1780108320884,-58.3027643211954,
18.5184024742051));
#46372=CARTESIAN_POINT('Ctrl Pts',(-34.5573646739318,-56.812731938543,18.4072645836371));
#46373=CARTESIAN_POINT('Ctrl Pts',(-34.0535892976251,-54.8457484885378,
18.296126693069));
#46374=CARTESIAN_POINT('Ctrl Pts',(-32.1277960183002,-54.20221623008,18.1849888025011));
#46375=CARTESIAN_POINT('Ctrl Pts',(-30.5426852645059,-55.4711675374879,
18.073850911933));
#46376=CARTESIAN_POINT('Ctrl Pts',(-30.749126885568,-57.4911168882046,17.962713021365));
#46377=CARTESIAN_POINT('Ctrl Pts',(-32.5581625245214,-58.4131817337352,
17.8515751307969));
#46378=CARTESIAN_POINT('Ctrl Pts',(-34.3139613451725,-57.3933856640392,
17.7404372402289));
#46379=CARTESIAN_POINT('Ctrl Pts',(-34.4094207748664,-55.3651595869832,
17.6292993496608));
#46380=CARTESIAN_POINT('Ctrl Pts',(-32.7571657150207,-54.1849618325449,
17.5181614590928));
#46381=CARTESIAN_POINT('Ctrl Pts',(-30.869523959759,-54.9330407897143,17.4070235685247));
#46382=CARTESIAN_POINT('Ctrl Pts',(-30.4742754149858,-56.9246713052021,
17.2958856779567));
#46383=CARTESIAN_POINT('Ctrl Pts',(-31.9331955561555,-58.3368913815558,
17.1847477873886));
#46384=CARTESIAN_POINT('Ctrl Pts',(-33.9109182327756,-57.8770799672243,
17.0736098968206));
#46385=CARTESIAN_POINT('Ctrl Pts',(-34.5972114500352,-55.9661076643608,
16.9624720062525));
#46386=CARTESIAN_POINT('Ctrl Pts',(-33.3639032430821,-54.3531090936767,
16.8513341156845));
#46387=CARTESIAN_POINT('Ctrl Pts',(-31.339854600407,-54.5144801395667,16.7401962251165));
#46388=CARTESIAN_POINT('Ctrl Pts',(-30.3777001989227,-56.3025160536558,
16.6290583345484));
#46389=CARTESIAN_POINT('Ctrl Pts',(-31.3581108738821,-58.0806072860715,
16.5179204439804));
#46390=CARTESIAN_POINT('Ctrl Pts',(-33.3837056158788,-58.2212467668584,
16.4067825534123));
#46391=CARTESIAN_POINT('Ctrl Pts',(-34.6004345857623,-56.5957055842903,
16.2956446628443));
#46392=CARTESIAN_POINT('Ctrl Pts',(-33.8946119587414,-54.6918600176663,
16.1845067722763));
#46393=CARTESIAN_POINT('Ctrl Pts',(-31.9122851899249,-54.252321505187,16.0733688817082));
#46394=CARTESIAN_POINT('Ctrl Pts',(-30.467900451878,-55.6794046320458,15.9622309911402));
#46395=CARTESIAN_POINT('Ctrl Pts',(-30.8835194758665,-57.6668840279746,
15.8510931005722));
#46396=CARTESIAN_POINT('Ctrl Pts',(-32.7787214556042,-58.3955972623921,
15.7399552100041));
#46397=CARTESIAN_POINT('Ctrl Pts',(-34.4188065263637,-57.1985448475426,
15.6288173194361));
#46398=CARTESIAN_POINT('Ctrl Pts',(-34.3025862222909,-55.1714024344819,
15.517679428868));
#46399=CARTESIAN_POINT('Ctrl Pts',(-32.5364383072491,-54.1696364627501,
15.4065415383));
#46400=CARTESIAN_POINT('Ctrl Pts',(-30.7369379943181,-55.1101746880588,
15.2954036477319));
#46401=CARTESIAN_POINT('Ctrl Pts',(-30.5511883337254,-57.1321318043788,
15.1842657571639));
#46402=CARTESIAN_POINT('Ctrl Pts',(-32.1492080841852,-58.3847875365432,
15.0731278665959));
#46403=CARTESIAN_POINT('Ctrl Pts',(-34.0683116696875,-57.7215718789046,
14.9619899760278));
#46404=CARTESIAN_POINT('Ctrl Pts',(-34.5519217655404,-55.7495336601205,
14.8508520854598));
#46405=CARTESIAN_POINT('Ctrl Pts',(-33.1573846641151,-54.2737017945639,
14.7397141948917));
#46406=CARTESIAN_POINT('Ctrl Pts',(-31.1611357940719,-54.644921989334,14.6285763043237));
#46407=CARTESIAN_POINT('Ctrl Pts',(-30.3903647762991,-56.5234120631583,
14.5174384137557));
#46408=CARTESIAN_POINT('Ctrl Pts',(-31.5505662815605,-58.1897690023091,
14.4063005231876));
#46409=CARTESIAN_POINT('Ctrl Pts',(-33.5797962817343,-58.1187568934328,
14.2951626326196));
#46410=CARTESIAN_POINT('Ctrl Pts',(-34.620674407496,-56.3753749443396,14.1840247420515));
#46411=CARTESIAN_POINT('Ctrl Pts',(-33.7204793856122,-54.555358384138,14.0728868514835));
#46412=CARTESIAN_POINT('Ctrl Pts',(-31.7031573584894,-54.3245930946511,
13.9617489609154));
#46413=CARTESIAN_POINT('Ctrl Pts',(-30.4152112171298,-55.8942929876505,
13.8506110703474));
#46414=CARTESIAN_POINT('Ctrl Pts',(-31.0354623047469,-57.8277103129715,
13.7394731797794));
#46415=CARTESIAN_POINT('Ctrl Pts',(-32.9962885855616,-58.3551335112703,
13.6283352892113));
#46416=CARTESIAN_POINT('Ctrl Pts',(-34.5027217167555,-56.9938717138819,
13.5171973986433));
#46417=CARTESIAN_POINT('Ctrl Pts',(-34.1763103408583,-54.9897720377718,
13.4060595080752));
#46418=CARTESIAN_POINT('Ctrl Pts',(-32.3150137958213,-54.1774723490436,
13.2949216175072));
#46419=CARTESIAN_POINT('Ctrl Pts',(-30.6241175042368,-55.2999540111744,
13.1837837269392));
#46420=CARTESIAN_POINT('Ctrl Pts',(-30.6480649772844,-57.3308476580601,
13.0726458363711));
#46421=CARTESIAN_POINT('Ctrl Pts',(-32.3715831750057,-58.4091628000751,
12.9615079458031));
#46422=CARTESIAN_POINT('Ctrl Pts',(-33.5914437753638,-57.8374091717516,
12.8874160187577));
#46423=CARTESIAN_POINT('Ctrl Pts',(-33.9456018676194,-57.3567121584624,
12.850370055235));
#46424=CARTESIAN_POINT('Ctrl Pts',(-32.1530810684833,-58.1853022036361,
22.149629944765));
#46425=CARTESIAN_POINT('Ctrl Pts',(-32.7827650637403,-58.3006610019117,
22.1125839812423));
#46426=CARTESIAN_POINT('Ctrl Pts',(-34.1555265529926,-57.8513232925233,
22.038492054197));
#46427=CARTESIAN_POINT('Ctrl Pts',(-34.7097913200344,-55.7432019955959,
21.9273541636289));
#46428=CARTESIAN_POINT('Ctrl Pts',(-33.2368936310637,-54.1392822596,21.8162162730608));
#46429=CARTESIAN_POINT('Ctrl Pts',(-31.0917202958965,-54.5044014428434,
21.7050783824928));
#46430=CARTESIAN_POINT('Ctrl Pts',(-30.2344600573677,-56.5059302302613,
21.5939404919248));
#46431=CARTESIAN_POINT('Ctrl Pts',(-31.4514241362253,-58.3110677744024,
21.4828026013567));
#46432=CARTESIAN_POINT('Ctrl Pts',(-33.6278868920259,-58.2679399630795,
21.3716647107887));
#46433=CARTESIAN_POINT('Ctrl Pts',(-34.7721192168892,-56.4158279861738,
21.2605268202206));
#46434=CARTESIAN_POINT('Ctrl Pts',(-33.836586497549,-54.4500879480027,21.1493889296526));
#46435=CARTESIAN_POINT('Ctrl Pts',(-31.6776952484417,-54.1699355364194,
21.0382510390845));
#46436=CARTESIAN_POINT('Ctrl Pts',(-30.2714517539787,-55.8318216411929,
20.9271131485165));
#46437=CARTESIAN_POINT('Ctrl Pts',(-30.9050322902485,-57.9145909687611,
20.8159752579484));
#46438=CARTESIAN_POINT('Ctrl Pts',(-32.9985005892282,-58.511867175612,20.7048373673804));
#46439=CARTESIAN_POINT('Ctrl Pts',(-34.6356877787742,-57.0769535575162,
20.5936994768124));
#46440=CARTESIAN_POINT('Ctrl Pts',(-34.3180546583401,-54.9232443301155,
20.4825615862444));
#46441=CARTESIAN_POINT('Ctrl Pts',(-32.3363360233899,-54.022053220633,20.3714236956763));
#46442=CARTESIAN_POINT('Ctrl Pts',(-30.5044206163321,-55.1982510481283,
20.2602858051083));
#46443=CARTESIAN_POINT('Ctrl Pts',(-30.4990817834286,-57.3752504140916,
20.1491479145402));
#46444=CARTESIAN_POINT('Ctrl Pts',(-32.3252060197288,-58.5604192039303,
20.0380100239722));
#46445=CARTESIAN_POINT('Ctrl Pts',(-34.3113212016315,-57.6689589366545,
19.9268721334042));
#46446=CARTESIAN_POINT('Ctrl Pts',(-34.6395135293347,-55.5168333281896,
19.8157342428361));
#46447=CARTESIAN_POINT('Ctrl Pts',(-33.0093848681805,-54.0739073430178,
19.7045963522681));
#46448=CARTESIAN_POINT('Ctrl Pts',(-30.9130104562287,-54.6609075051103,
19.5934584617));
#46449=CARTESIAN_POINT('Ctrl Pts',(-30.269225573442,-56.740545906147,19.482320571132));
#46450=CARTESIAN_POINT('Ctrl Pts',(-31.6672938209546,-58.4093059344153,
19.3711826805639));
#46451=CARTESIAN_POINT('Ctrl Pts',(-33.8275474781934,-58.1397526102859,
19.2600447899959));
#46452=CARTESIAN_POINT('Ctrl Pts',(-34.7726818729719,-56.1786111486416,
19.1489068994278));
#46453=CARTESIAN_POINT('Ctrl Pts',(-33.6376047755825,-54.3209365700001,
19.0377690088598));
#46454=CARTESIAN_POINT('Ctrl Pts',(-31.4612651257226,-54.2670794837456,
18.9266311182918));
#46455=CARTESIAN_POINT('Ctrl Pts',(-30.2356912863756,-56.0663358916622,
18.8154932277237));
#46456=CARTESIAN_POINT('Ctrl Pts',(-31.0826648916004,-58.0718259986512,
18.7043553371557));
#46457=CARTESIAN_POINT('Ctrl Pts',(-33.2269413952247,-58.4479019659694,
18.5932174465876));
#46458=CARTESIAN_POINT('Ctrl Pts',(-34.7058401957198,-56.8503371957446,
18.4820795560196));
#46459=CARTESIAN_POINT('Ctrl Pts',(-34.1657084491453,-54.7414008397775,
18.3709416654516));
#46460=CARTESIAN_POINT('Ctrl Pts',(-32.1009348686486,-54.0514262616512,
18.2598037748835));
#46461=CARTESIAN_POINT('Ctrl Pts',(-30.4014301285847,-55.4119550175678,
18.1486658843155));
#46462=CARTESIAN_POINT('Ctrl Pts',(-30.6227701912281,-57.5776797077918,
18.0375279937474));
#46463=CARTESIAN_POINT('Ctrl Pts',(-32.5623599870745,-58.5662879623725,
17.9263901031794));
#46464=CARTESIAN_POINT('Ctrl Pts',(-34.4448709795413,-57.472895434312,17.8152522126114));
#46465=CARTESIAN_POINT('Ctrl Pts',(-34.5472195080969,-55.2982967044589,
17.7041143220433));
#46466=CARTESIAN_POINT('Ctrl Pts',(-32.7757248038432,-54.0329266518745,
17.5929764314753));
#46467=CARTESIAN_POINT('Ctrl Pts',(-30.7518560596998,-54.8349928359617,
17.4818385409072));
#46468=CARTESIAN_POINT('Ctrl Pts',(-30.328083289414,-56.9703549823765,17.3707006503392));
#46469=CARTESIAN_POINT('Ctrl Pts',(-31.8922905155383,-58.4844919018513,
17.2595627597711));
#46470=CARTESIAN_POINT('Ctrl Pts',(-34.0127411246847,-57.9914969005106,
17.1484248692031));
#46471=CARTESIAN_POINT('Ctrl Pts',(-34.7485626267561,-55.9426138940248,
17.037286978635));
#46472=CARTESIAN_POINT('Ctrl Pts',(-33.426249256123,-54.2132087341443,16.926149088067));
#46473=CARTESIAN_POINT('Ctrl Pts',(-31.2561294369797,-54.3862255764959,
16.815011197499));
#46474=CARTESIAN_POINT('Ctrl Pts',(-30.2245384506201,-56.3033001431311,
16.7038733069309));
#46475=CARTESIAN_POINT('Ctrl Pts',(-31.275703225898,-58.2097123421037,16.5927354163629));
#46476=CARTESIAN_POINT('Ctrl Pts',(-33.4474807229792,-58.3605014675107,
16.4815975257949));
#46477=CARTESIAN_POINT('Ctrl Pts',(-34.7520183691595,-56.6176485227995,
16.3704596352268));
#46478=CARTESIAN_POINT('Ctrl Pts',(-33.9952580624144,-54.5764065735656,
16.2593217446588));
#46479=CARTESIAN_POINT('Ctrl Pts',(-31.8698710937785,-54.1051475251923,
16.1481838540907));
#46480=CARTESIAN_POINT('Ctrl Pts',(-30.3212482591213,-55.6352201291135,
16.0370459635227));
#46481=CARTESIAN_POINT('Ctrl Pts',(-30.7668616016832,-57.7661315787237,
15.9259080729546));
#46482=CARTESIAN_POINT('Ctrl Pts',(-32.7988361752155,-58.547434458081,15.8147701823866));
#46483=CARTESIAN_POINT('Ctrl Pts',(-34.5572826088111,-57.2639933810004,
15.7036322918185));
#46484=CARTESIAN_POINT('Ctrl Pts',(-34.4326749388483,-55.0905565208099,
15.5924944012505));
#46485=CARTESIAN_POINT('Ctrl Pts',(-32.5390679804181,-54.0164952835633,
15.4813565106825));
#46486=CARTESIAN_POINT('Ctrl Pts',(-30.6097016542784,-55.0249101014538,
15.3702186201144));
#46487=CARTESIAN_POINT('Ctrl Pts',(-30.4105468457662,-57.192787453346,15.2590807295464));
#46488=CARTESIAN_POINT('Ctrl Pts',(-32.1238921966328,-58.5358446178915,
15.1479428389784));
#46489=CARTESIAN_POINT('Ctrl Pts',(-34.1814933026927,-57.8247661325911,
15.0368049484103));
#46490=CARTESIAN_POINT('Ctrl Pts',(-34.7000044844997,-55.7104102162061,
14.9256670578423));
#46491=CARTESIAN_POINT('Ctrl Pts',(-33.2048266816906,-54.128070783427,14.8145291672742));
#46492=CARTESIAN_POINT('Ctrl Pts',(-31.064512884144,-54.5260811300915,14.7033912767062));
#46493=CARTESIAN_POINT('Ctrl Pts',(-30.2381170029267,-56.5401377359062,
14.5922533861381));
#46494=CARTESIAN_POINT('Ctrl Pts',(-31.4820477206391,-58.3267520213409,
14.4811154955701));
#46495=CARTESIAN_POINT('Ctrl Pts',(-33.6577228245522,-58.2506151234313,
14.369977605002));
#46496=CARTESIAN_POINT('Ctrl Pts',(-34.7737188546885,-56.3814171010637,
14.258839714434));
#46497=CARTESIAN_POINT('Ctrl Pts',(-33.8085587212332,-54.4300539148301,
14.147701823866));
#46498=CARTESIAN_POINT('Ctrl Pts',(-31.6456509628172,-54.182634797657,14.0365639332979));
#46499=CARTESIAN_POINT('Ctrl Pts',(-30.2647565572066,-55.8656165087107,
13.9254260427299));
#46500=CARTESIAN_POINT('Ctrl Pts',(-30.9297698131649,-57.9385643459764,
13.8142881521619));
#46501=CARTESIAN_POINT('Ctrl Pts',(-33.0321046504685,-58.5040505262846,
13.7031502615938));
#46502=CARTESIAN_POINT('Ctrl Pts',(-34.6472537754902,-57.0445494336376,
13.5920123710258));
#46503=CARTESIAN_POINT('Ctrl Pts',(-34.2972860024369,-54.8958182544712,
13.4808744804577));
#46504=CARTESIAN_POINT('Ctrl Pts',(-32.3016637448863,-54.0248966686821,
13.3697365898897));
#46505=CARTESIAN_POINT('Ctrl Pts',(-30.4887391554684,-55.2283853844451,
13.2585986993216));
#46506=CARTESIAN_POINT('Ctrl Pts',(-30.5144148654209,-57.4058441968251,
13.1474608087536));
#46507=CARTESIAN_POINT('Ctrl Pts',(-32.3623156127991,-58.5619789910346,
13.0363229181856));
#46508=CARTESIAN_POINT('Ctrl Pts',(-33.6702108923959,-57.9489631502434,
12.9622309911402));
#46509=CARTESIAN_POINT('Ctrl Pts',(-34.0499278018167,-57.4335752818158,
12.9251850276175));
#46510=CARTESIAN_POINT('Ctrl Pts',(-32.1297298894292,-58.3127642086202,
22.2244449171475));
#46511=CARTESIAN_POINT('Ctrl Pts',(-32.8017980337912,-58.4358878294791,
22.1873989536248));
#46512=CARTESIAN_POINT('Ctrl Pts',(-34.2669603591524,-57.95630511368,22.1133070265794));
#46513=CARTESIAN_POINT('Ctrl Pts',(-34.858532792749,-55.7062857725693,22.0021691360114));
#46514=CARTESIAN_POINT('Ctrl Pts',(-33.2864940810812,-53.9944058950499,
21.8910312454434));
#46515=CARTESIAN_POINT('Ctrl Pts',(-30.9969287220119,-54.384101319742,21.7798933548753));
#46516=CARTESIAN_POINT('Ctrl Pts',(-30.0819661342964,-56.5203533893187,
21.6687554643073));
#46517=CARTESIAN_POINT('Ctrl Pts',(-31.380844296031,-58.4469950837991,21.5576175737392));
#46518=CARTESIAN_POINT('Ctrl Pts',(-33.7038051725687,-58.4009643313194,
21.4464796831712));
#46519=CARTESIAN_POINT('Ctrl Pts',(-34.9250559921582,-56.4241863460987,
21.3353417926031));
#46520=CARTESIAN_POINT('Ctrl Pts',(-33.9265523881077,-54.3261319732661,
21.2242039020351));
#46521=CARTESIAN_POINT('Ctrl Pts',(-31.6223457597103,-54.0271224497437,
21.113066011467));
#46522=CARTESIAN_POINT('Ctrl Pts',(-30.1214477490197,-55.8008704233132,
21.001928120899));
#46523=CARTESIAN_POINT('Ctrl Pts',(-30.7976747113088,-58.0238313492005,
20.890790230331));
#46524=CARTESIAN_POINT('Ctrl Pts',(-33.0320547584019,-58.6613103307746,
20.7796523397629));
#46525=CARTESIAN_POINT('Ctrl Pts',(-34.779441328077,-57.1298124049937,20.6685144491949));
#46526=CARTESIAN_POINT('Ctrl Pts',(-34.4404282620852,-54.8311366011663,
20.5573765586268));
#46527=CARTESIAN_POINT('Ctrl Pts',(-32.3253197700946,-53.8692861472442,
20.4462386680588));
#46528=CARTESIAN_POINT('Ctrl Pts',(-30.3700977896676,-55.1246540735083,
20.3351007774907));
#46529=CARTESIAN_POINT('Ctrl Pts',(-30.3643995989091,-57.4481876795404,
20.2239628869227));
#46530=CARTESIAN_POINT('Ctrl Pts',(-32.3134406037768,-58.7131304053242,
20.1128249963547));
#46531=CARTESIAN_POINT('Ctrl Pts',(-34.4332415751289,-57.7616657784424,
20.0016871057866));
#46532=CARTESIAN_POINT('Ctrl Pts',(-34.7835245906331,-55.4646801872418,
19.8905492152186));
#46533=CARTESIAN_POINT('Ctrl Pts',(-33.043671660234,-53.924630580438,19.7794113246506));
#46534=CARTESIAN_POINT('Ctrl Pts',(-30.8061898891539,-54.5511418347326,
19.6682734340825));
#46535=CARTESIAN_POINT('Ctrl Pts',(-30.1190717238489,-56.77076109083,19.5571355435145));
#46536=CARTESIAN_POINT('Ctrl Pts',(-31.611244210167,-58.5518456729879,19.4459976529464));
#46537=CARTESIAN_POINT('Ctrl Pts',(-33.9169049506455,-58.2641486635056,
19.3348597623784));
#46538=CARTESIAN_POINT('Ctrl Pts',(-34.9256565207284,-56.1710023982575,
19.2237218718104));
#46539=CARTESIAN_POINT('Ctrl Pts',(-33.71417716871,-54.1882873915237,19.1125839812423));
#46540=CARTESIAN_POINT('Ctrl Pts',(-31.3913476843971,-54.1308051745824,
19.0014460906743));
#46541=CARTESIAN_POINT('Ctrl Pts',(-30.0832802375623,-56.0511698724442,
18.8903082001062));
#46542=CARTESIAN_POINT('Ctrl Pts',(-30.9872637967358,-58.1916498987633,
18.7791703095382));
#46543=CARTESIAN_POINT('Ctrl Pts',(-33.2758719583609,-58.5930396107435,
18.6680324189701));
#46544=CARTESIAN_POINT('Ctrl Pts',(-34.8543157175077,-56.8879424529461,
18.5568945284021));
#46545=CARTESIAN_POINT('Ctrl Pts',(-34.2778276006655,-54.6370531910174,
18.445756637834));
#46546=CARTESIAN_POINT('Ctrl Pts',(-32.074073718997,-53.9006362932222,18.334618747266));
#46547=CARTESIAN_POINT('Ctrl Pts',(-30.2601749926636,-55.3527424976477,
18.223480856698));
#46548=CARTESIAN_POINT('Ctrl Pts',(-30.4964134968882,-57.664242527379,18.1123429661299));
#46549=CARTESIAN_POINT('Ctrl Pts',(-32.5665574496276,-58.7193941910097,
18.0012050755619));
#46550=CARTESIAN_POINT('Ctrl Pts',(-34.57578061391,-57.5524052045849,17.8900671849938));
#46551=CARTESIAN_POINT('Ctrl Pts',(-34.6850182413274,-55.2314338219344,
17.7789292944258));
#46552=CARTESIAN_POINT('Ctrl Pts',(-32.7942838926656,-53.8808914712041,
17.6677914038577));
#46553=CARTESIAN_POINT('Ctrl Pts',(-30.6341881596407,-54.7369448822092,
17.5566535132897));
#46554=CARTESIAN_POINT('Ctrl Pts',(-30.1818911638421,-57.0160386595509,
17.4455156227217));
#46555=CARTESIAN_POINT('Ctrl Pts',(-31.8513854749211,-58.6320924221469,
17.3343777321536));
#46556=CARTESIAN_POINT('Ctrl Pts',(-34.1145640165938,-58.1059138337969,
17.2232398415856));
#46557=CARTESIAN_POINT('Ctrl Pts',(-34.899913803477,-55.9191201236888,17.1121019510176));
#46558=CARTESIAN_POINT('Ctrl Pts',(-33.4885952691639,-54.0733083746118,
17.0009640604495));
#46559=CARTESIAN_POINT('Ctrl Pts',(-31.1724042735525,-54.2579710134251,
16.8898261698815));
#46560=CARTESIAN_POINT('Ctrl Pts',(-30.0713767023175,-56.3040842326063,
16.7786882793134));
#46561=CARTESIAN_POINT('Ctrl Pts',(-31.1932955779139,-58.3388173981362,
16.6675503887454));
#46562=CARTESIAN_POINT('Ctrl Pts',(-33.5112558300796,-58.4997561681628,
16.5564124981773));
#46563=CARTESIAN_POINT('Ctrl Pts',(-34.9036021525567,-56.6395914613089,
16.4452746076093));
#46564=CARTESIAN_POINT('Ctrl Pts',(-34.0959041660875,-54.4609531294646,
16.3341367170413));
#46565=CARTESIAN_POINT('Ctrl Pts',(-31.8274569976321,-53.9579735451976,
16.2229988264732));
#46566=CARTESIAN_POINT('Ctrl Pts',(-30.1745960663645,-55.5910356261813,
16.1118609359052));
#46567=CARTESIAN_POINT('Ctrl Pts',(-30.6502037274999,-57.8653791294726,
16.0007230453371));
#46568=CARTESIAN_POINT('Ctrl Pts',(-32.8189508948268,-58.6992716537698,
15.8895851547691));
#46569=CARTESIAN_POINT('Ctrl Pts',(-34.6957586912586,-57.3294419144583,
15.778447264201));
#46570=CARTESIAN_POINT('Ctrl Pts',(-34.5627636554057,-55.0097106071377,
15.667309373633));
#46571=CARTESIAN_POINT('Ctrl Pts',(-32.5416976535871,-53.8633541043767,
15.556171483065));
#46572=CARTESIAN_POINT('Ctrl Pts',(-30.4824653142387,-54.9396455148486,
15.4450335924969));
#46573=CARTESIAN_POINT('Ctrl Pts',(-30.269905357807,-57.2534431023133,15.3338957019289));
#46574=CARTESIAN_POINT('Ctrl Pts',(-32.0985763090804,-58.6869016992398,
15.2227578113608));
#46575=CARTESIAN_POINT('Ctrl Pts',(-34.2946749356979,-57.9279603862777,
15.1116199207928));
#46576=CARTESIAN_POINT('Ctrl Pts',(-34.848087203459,-55.6712867722916,15.0004820302248));
#46577=CARTESIAN_POINT('Ctrl Pts',(-33.2522686992661,-53.9824397722902,
14.8893441396567));
#46578=CARTESIAN_POINT('Ctrl Pts',(-30.967889974216,-54.407240270849,14.7782062490887));
#46579=CARTESIAN_POINT('Ctrl Pts',(-30.0858692295543,-56.5568634086542,
14.6670683585206));
#46580=CARTESIAN_POINT('Ctrl Pts',(-31.4135291597177,-58.4637350403727,
14.5559304679526));
#46581=CARTESIAN_POINT('Ctrl Pts',(-33.73564936737,-58.3824733534297,14.4447925773845));
#46582=CARTESIAN_POINT('Ctrl Pts',(-34.926763301881,-56.3874592577879,14.3336546868165));
#46583=CARTESIAN_POINT('Ctrl Pts',(-33.8966380568543,-54.3047494455222,
14.2225167962484));
#46584=CARTESIAN_POINT('Ctrl Pts',(-31.5881445671451,-54.0406765006631,
14.1113789056804));
#46585=CARTESIAN_POINT('Ctrl Pts',(-30.1143018972835,-55.8369400297709,
14.0002410151124));
#46586=CARTESIAN_POINT('Ctrl Pts',(-30.8240773215828,-58.0494183789814,
13.8891031245444));
#46587=CARTESIAN_POINT('Ctrl Pts',(-33.0679207153753,-58.6529675412989,
13.7779652339763));
#46588=CARTESIAN_POINT('Ctrl Pts',(-34.7917858342248,-57.0952271533932,
13.6668273434083));
#46589=CARTESIAN_POINT('Ctrl Pts',(-34.4182616640155,-54.8018644711707,
13.5556894528402));
#46590=CARTESIAN_POINT('Ctrl Pts',(-32.2883136939512,-53.8723209883206,
13.4445515622722));
#46591=CARTESIAN_POINT('Ctrl Pts',(-30.3533608067001,-55.1568167577159,
13.3334136717041));
#46592=CARTESIAN_POINT('Ctrl Pts',(-30.3807647535574,-57.4808407355902,
13.2222757811361));
#46593=CARTESIAN_POINT('Ctrl Pts',(-32.3530480505925,-58.7147951819942,
13.1111378905681));
#46594=CARTESIAN_POINT('Ctrl Pts',(-33.748978009428,-58.0605171287351,13.0370459635227));
#46595=CARTESIAN_POINT('Ctrl Pts',(-34.1542537360139,-57.5104384051693,
13.));
#46596=CARTESIAN_POINT('Ctrl Pts',(-32.1997834265916,-57.9303781936679,
22.));
#46597=CARTESIAN_POINT('Ctrl Pts',(-32.2590684210029,-57.9484903047675,
22.));
#46598=CARTESIAN_POINT('Ctrl Pts',(-32.3192133660472,-57.9629534896913,
22.));
#46599=CARTESIAN_POINT('Ctrl Pts',(-32.3799202087205,-57.9739415995515,
22.));
#46600=CARTESIAN_POINT('Ctrl Pts',(-32.4446390331051,-57.9856558894247,
22.));
#46601=CARTESIAN_POINT('Ctrl Pts',(-32.5099970425764,-57.9934211178936,
22.));
#46602=CARTESIAN_POINT('Ctrl Pts',(-32.5756660758662,-57.997395589509,22.));
#46603=CARTESIAN_POINT('Ctrl Pts',(-32.6331264799947,-58.0008732521725,
22.));
#46604=CARTESIAN_POINT('Ctrl Pts',(-32.6908259517003,-58.0014477926638,
22.));
#46605=CARTESIAN_POINT('Ctrl Pts',(-32.7485570677765,-57.9991916498581,
22.));
#46606=CARTESIAN_POINT('Ctrl Pts',(-32.7775225242267,-57.9980596744067,
22.));
#46607=CARTESIAN_POINT('Ctrl Pts',(-32.8064960744402,-57.9962146309827,
22.));
#46608=CARTESIAN_POINT('Ctrl Pts',(-32.8354519444006,-57.9936627183816,
22.));
#46609=CARTESIAN_POINT('Ctrl Pts',(-32.8486814477492,-57.992496787731,22.));
#46610=CARTESIAN_POINT('Ctrl Pts',(-32.8619089919099,-57.9911829627194,
22.));
#46611=CARTESIAN_POINT('Ctrl Pts',(-32.8751106149865,-57.9897244385961,
22.));
#46612=CARTESIAN_POINT('Ctrl Pts',(-32.941684568455,-57.9823693038107,22.));
#46613=CARTESIAN_POINT('Ctrl Pts',(-33.0077191568455,-57.9713290351914,
22.));
#46614=CARTESIAN_POINT('Ctrl Pts',(-33.0728927905865,-57.9567622281368,
22.));
#46615=CARTESIAN_POINT('Ctrl Pts',(-33.1392231872252,-57.9419368757016,
22.));
#46616=CARTESIAN_POINT('Ctrl Pts',(-33.2046628033255,-57.9234587511961,
22.));
#46617=CARTESIAN_POINT('Ctrl Pts',(-33.268884582548,-57.9014427391759,22.));
#46618=CARTESIAN_POINT('Ctrl Pts',(-33.3226052862378,-57.8830266243862,
22.));
#46619=CARTESIAN_POINT('Ctrl Pts',(-33.3754743938389,-57.8621340596335,
22.));
#46620=CARTESIAN_POINT('Ctrl Pts',(-33.4272987060576,-57.8388046347892,
22.));
#46621=CARTESIAN_POINT('Ctrl Pts',(-33.4511753909088,-57.8280562176677,
22.));
#46622=CARTESIAN_POINT('Ctrl Pts',(-33.4748302312922,-57.8167901903543,
22.));
#46623=CARTESIAN_POINT('Ctrl Pts',(-33.4982437788218,-57.805008661511,22.));
#46624=CARTESIAN_POINT('Ctrl Pts',(-33.5084650463385,-57.7998653931571,
22.));
#46625=CARTESIAN_POINT('Ctrl Pts',(-33.5186400680679,-57.7946238947902,
22.));
#46626=CARTESIAN_POINT('Ctrl Pts',(-33.5287548615985,-57.7892910972224,
22.));
#46627=CARTESIAN_POINT('Ctrl Pts',(-33.5908341911573,-57.7565611658915,
22.));
#46628=CARTESIAN_POINT('Ctrl Pts',(-33.6507646084003,-57.7203369576369,
22.));
#46629=CARTESIAN_POINT('Ctrl Pts',(-33.7082063151154,-57.6807516371536,
22.));
#46630=CARTESIAN_POINT('Ctrl Pts',(-33.759565116122,-57.6453582842443,22.));
#46631=CARTESIAN_POINT('Ctrl Pts',(-33.8089350520295,-57.6072772063265,
22.));
#46632=CARTESIAN_POINT('Ctrl Pts',(-33.8560671885274,-57.566568812704,22.));
#46633=CARTESIAN_POINT('Ctrl Pts',(-33.90741383547,-57.5222203135642,22.));
#46634=CARTESIAN_POINT('Ctrl Pts',(-33.9561058514875,-57.4747541508591,
22.));
#46635=CARTESIAN_POINT('Ctrl Pts',(-34.002080913029,-57.4244894418756,22.));
#46636=CARTESIAN_POINT('Ctrl Pts',(-34.0198184128286,-57.4050969661371,
22.));
#46637=CARTESIAN_POINT('Ctrl Pts',(-34.0371511842958,-57.3852874792597,
22.));
#46638=CARTESIAN_POINT('Ctrl Pts',(-34.0540743682384,-57.365077729866,22.));
#46639=CARTESIAN_POINT('Ctrl Pts',(-34.0614983915393,-57.3562119247721,
22.));
#46640=CARTESIAN_POINT('Ctrl Pts',(-34.0688431367454,-57.3472694773831,
22.));
#46641=CARTESIAN_POINT('Ctrl Pts',(-34.0760999004284,-57.3382624488758,
22.));
#46642=CARTESIAN_POINT('Ctrl Pts',(-34.1199740932065,-57.2838062033164,
22.));
#46643=CARTESIAN_POINT('Ctrl Pts',(-34.160716274024,-57.2268964747641,22.));
#46644=CARTESIAN_POINT('Ctrl Pts',(-34.1982933189855,-57.1679133931134,
22.));
#46645=CARTESIAN_POINT('Ctrl Pts',(-34.2367405668874,-57.1075643910945,
22.));
#46646=CARTESIAN_POINT('Ctrl Pts',(-34.2718749445117,-57.0450442239734,
22.));
#46647=CARTESIAN_POINT('Ctrl Pts',(-34.303629683885,-56.9807132904548,22.));
#46648=CARTESIAN_POINT('Ctrl Pts',(-34.327924112439,-56.9314959673392,22.));
#46649=CARTESIAN_POINT('Ctrl Pts',(-34.3502397773156,-56.8812176908655,
22.));
#46650=CARTESIAN_POINT('Ctrl Pts',(-34.370531746488,-56.830026000176,22.));
#46651=CARTESIAN_POINT('Ctrl Pts',(-34.3831626883497,-56.7981612135006,
22.));
#46652=CARTESIAN_POINT('Ctrl Pts',(-34.3950092682771,-56.7659423000698,
22.));
#46653=CARTESIAN_POINT('Ctrl Pts',(-34.4060577406816,-56.7334031737991,
22.));
#46654=CARTESIAN_POINT('Ctrl Pts',(-34.4122566000728,-56.715146761412,22.));
#46655=CARTESIAN_POINT('Ctrl Pts',(-34.4182059308347,-56.6967833655941,
22.));
#46656=CARTESIAN_POINT('Ctrl Pts',(-34.423893091666,-56.6783523612847,22.));
#46657=CARTESIAN_POINT('Ctrl Pts',(-34.4459473654228,-56.6068786634752,
22.));
#46658=CARTESIAN_POINT('Ctrl Pts',(-34.4640895874025,-56.5343189897119,
22.));
#46659=CARTESIAN_POINT('Ctrl Pts',(-34.4782337109683,-56.4610520163338,
22.));
#46660=CARTESIAN_POINT('Ctrl Pts',(-34.4888128880671,-56.4062515698269,
22.));
#46661=CARTESIAN_POINT('Ctrl Pts',(-34.4971546283959,-56.3510545308008,
22.));
#46662=CARTESIAN_POINT('Ctrl Pts',(-34.5032062803068,-56.2956100237224,
22.));
#46663=CARTESIAN_POINT('Ctrl Pts',(-34.5050941235358,-56.2783138310772,
22.));
#46664=CARTESIAN_POINT('Ctrl Pts',(-34.5067589921147,-56.2609935142719,
22.));
#46665=CARTESIAN_POINT('Ctrl Pts',(-34.5081989725185,-56.2436535054264,
22.));
#46666=CARTESIAN_POINT('Ctrl Pts',(-34.509588864495,-56.2269166532411,22.));
#46667=CARTESIAN_POINT('Ctrl Pts',(-34.5107684790914,-56.2101700014401,
22.));
#46668=CARTESIAN_POINT('Ctrl Pts',(-34.5117364052776,-56.1934236229725,
22.));
#46669=CARTESIAN_POINT('Ctrl Pts',(-34.5160829441432,-56.1182228629321,
22.));
#46670=CARTESIAN_POINT('Ctrl Pts',(-34.5161676811367,-56.0429913941852,
22.));
#46671=CARTESIAN_POINT('Ctrl Pts',(-34.5118795397106,-55.9680950253044,
22.));
#46672=CARTESIAN_POINT('Ctrl Pts',(-34.5085977311867,-55.9107751943145,
22.));
#46673=CARTESIAN_POINT('Ctrl Pts',(-34.5027538123411,-55.8536509963143,
22.));
#46674=CARTESIAN_POINT('Ctrl Pts',(-34.4942777735197,-55.7968820122819,
22.));
#46675=CARTESIAN_POINT('Ctrl Pts',(-34.4923107028765,-55.783707390942,22.));
#46676=CARTESIAN_POINT('Ctrl Pts',(-34.4902017904221,-55.7705518962168,
22.));
#46677=CARTESIAN_POINT('Ctrl Pts',(-34.4879524958972,-55.7574168944054,
22.));
#46678=CARTESIAN_POINT('Ctrl Pts',(-31.6674621971265,-54.8470528177236,
20.8714803633902));
#46679=CARTESIAN_POINT('Ctrl Pts',(-31.7409214521311,-54.8037964055072,
20.8771939403667));
#46680=CARTESIAN_POINT('Ctrl Pts',(-31.8176439327865,-54.7663977740573,
20.8829075173431));
#46681=CARTESIAN_POINT('Ctrl Pts',(-31.896948563991,-54.7356618022518,20.8886210943196));
#46682=CARTESIAN_POINT('Ctrl Pts',(-32.4111477227468,-54.5363744390058,
20.9256670578423));
#46683=CARTESIAN_POINT('Ctrl Pts',(-33.0339012195891,-54.617187168241,20.962713021365));
#46684=CARTESIAN_POINT('Ctrl Pts',(-33.4802097929969,-54.9411120943331,
20.9997589848876));
#46685=CARTESIAN_POINT('Ctrl Pts',(-33.9265183664048,-55.2650370204253,
21.0368049484103));
#46686=CARTESIAN_POINT('Ctrl Pts',(-34.1963820163781,-55.8320741433745,
21.073850911933));
#46687=CARTESIAN_POINT('Ctrl Pts',(-34.1662812854629,-56.3827226982285,
21.1108968754557));
#46688=CARTESIAN_POINT('Ctrl Pts',(-34.1361805545477,-56.9333712530824,
21.1479428389784));
#46689=CARTESIAN_POINT('Ctrl Pts',(-33.806115442744,-57.4676312398412,21.184988802501));
#46690=CARTESIAN_POINT('Ctrl Pts',(-33.3271718011211,-57.740981554722,21.2220347660237));
#46691=CARTESIAN_POINT('Ctrl Pts',(-32.8482281594982,-58.0143318696029,
21.2590807295464));
#46692=CARTESIAN_POINT('Ctrl Pts',(-32.2204059880561,-58.0267725126059,
21.2961266930691));
#46693=CARTESIAN_POINT('Ctrl Pts',(-31.7309722501511,-57.772637960197,21.3331726565918));
#46694=CARTESIAN_POINT('Ctrl Pts',(-31.2415385122461,-57.5185034077881,
21.3702186201144));
#46695=CARTESIAN_POINT('Ctrl Pts',(-30.8904932078782,-56.9977936599673,
21.4072645836371));
#46696=CARTESIAN_POINT('Ctrl Pts',(-30.8386131457201,-56.4487584155402,
21.4443105471598));
#46697=CARTESIAN_POINT('Ctrl Pts',(-30.786733083562,-55.8997231711131,21.4813565106825));
#46698=CARTESIAN_POINT('Ctrl Pts',(-31.0340182636138,-55.3223624300798,
21.5184024742052));
#46699=CARTESIAN_POINT('Ctrl Pts',(-31.4670590682002,-54.9810209428387,
21.5554484377278));
#46700=CARTESIAN_POINT('Ctrl Pts',(-31.5295263145409,-54.9317815581341,
21.5607924129486));
#46701=CARTESIAN_POINT('Ctrl Pts',(-31.5958589129293,-54.8874534513961,
21.5661363881694));
#46702=CARTESIAN_POINT('Ctrl Pts',(-31.6652082225275,-54.8481806306043,
21.5714803633902));
#46703=CARTESIAN_POINT('Ctrl Pts',(-33.9541262883781,-54.8399232067375,
22.));
#46704=CARTESIAN_POINT('Ctrl Pts',(-33.4713921772736,-54.3563916207415,
21.9629540364773));
#46705=CARTESIAN_POINT('Ctrl Pts',(-31.9935412717563,-53.9174716604954,
21.888862109432));
#46706=CARTESIAN_POINT('Ctrl Pts',(-30.2271943832587,-55.4316007569426,
21.7777242188639));
#46707=CARTESIAN_POINT('Ctrl Pts',(-30.5464763025826,-57.7337498950934,
21.6665863282958));
#46708=CARTESIAN_POINT('Ctrl Pts',(-32.6512600365403,-58.7155097146097,
21.5554484377279));
#46709=CARTESIAN_POINT('Ctrl Pts',(-34.6188774786828,-57.4788960204646,
21.4443105471598));
#46710=CARTESIAN_POINT('Ctrl Pts',(-34.6464212862449,-55.1554778495401,
21.3331726565917));
#46711=CARTESIAN_POINT('Ctrl Pts',(-32.7096416422032,-53.872064985086,21.2220347660237));
#46712=CARTESIAN_POINT('Ctrl Pts',(-30.5808145803544,-54.8033004251176,
21.1108968754557));
#46713=CARTESIAN_POINT('Ctrl Pts',(-30.2087196709518,-57.0968534624393,
20.9997589848876));
#46714=CARTESIAN_POINT('Ctrl Pts',(-31.9338196700205,-58.6533891775714,
20.8886210943196));
#46715=CARTESIAN_POINT('Ctrl Pts',(-34.1771709144469,-58.0482026788782,
20.7774832037515));
#46716=CARTESIAN_POINT('Ctrl Pts',(-34.8853786224564,-55.8352230845946,
20.6663453131835));
#46717=CARTESIAN_POINT('Ctrl Pts',(-33.4102272112105,-54.0400181863803,
20.5552074226154));
#46718=CARTESIAN_POINT('Ctrl Pts',(-31.1019320194545,-54.3057581512874,
20.4440695320474));
#46719=CARTESIAN_POINT('Ctrl Pts',(-30.073305550394,-56.3892087930031,20.3329316414794));
#46720=CARTESIAN_POINT('Ctrl Pts',(-31.2658594095642,-58.3833638027876,
20.2217937509113));
#46721=CARTESIAN_POINT('Ctrl Pts',(-33.588036458114,-58.4629506390538,20.1106558603433));
#46722=CARTESIAN_POINT('Ctrl Pts',(-34.914321242052,-56.5551224909764,19.9995179697752));
#46723=CARTESIAN_POINT('Ctrl Pts',(-34.0307504904903,-54.406136137217,19.8883800792072));
#46724=CARTESIAN_POINT('Ctrl Pts',(-31.7460664163079,-53.9829831393046,
19.7772421886392));
#46725=CARTESIAN_POINT('Ctrl Pts',(-30.151466320847,-55.6729802447186,19.6661042980711));
#46726=CARTESIAN_POINT('Ctrl Pts',(-30.7065057264145,-57.9292539322017,
19.5549664075031));
#46727=CARTESIAN_POINT('Ctrl Pts',(-32.9031507850421,-58.6866113101154,
19.443828516935));
#46728=CARTESIAN_POINT('Ctrl Pts',(-34.730787355662,-57.2518345802401,19.332690626367));
#46729=CARTESIAN_POINT('Ctrl Pts',(-34.5165589620033,-54.9381911555042,
19.2215527357989));
#46730=CARTESIAN_POINT('Ctrl Pts',(-32.4565512804853,-53.8633851007702,
19.1104148452309));
#46731=CARTESIAN_POINT('Ctrl Pts',(-30.4363127049828,-55.0111985872155,
18.9992769546629));
#46732=CARTESIAN_POINT('Ctrl Pts',(-30.3049905142645,-57.3310249135316,
18.8881390640948));
#46733=CARTESIAN_POINT('Ctrl Pts',(-32.182785399016,-58.6995007346588,18.7770011735268));
#46734=CARTESIAN_POINT('Ctrl Pts',(-34.3509304054687,-57.8640446119295,
18.6658632829587));
#46735=CARTESIAN_POINT('Ctrl Pts',(-34.8248978208363,-55.5893590092039,
18.5547253923907));
#46736=CARTESIAN_POINT('Ctrl Pts',(-33.1708598946485,-53.9574894553413,
18.4435875018226));
#46737=CARTESIAN_POINT('Ctrl Pts',(-30.902776298825,-54.462104659654,18.3324496112546));
#46738=CARTESIAN_POINT('Ctrl Pts',(-30.0966496704334,-56.6413246029078,
18.2213117206866));
#46739=CARTESIAN_POINT('Ctrl Pts',(-31.4903368545418,-58.5004845570078,
18.1101738301185));
#46740=CARTESIAN_POINT('Ctrl Pts',(-33.8081801660464,-58.3378743316584,
17.9990359395505));
#46741=CARTESIAN_POINT('Ctrl Pts',(-34.928631335797,-56.3023329102471,17.8878980489824));
#46742=CARTESIAN_POINT('Ctrl Pts',(-33.8261287013397,-54.2570144404017,
17.7767601584144));
#46743=CARTESIAN_POINT('Ctrl Pts',(-31.5098054272241,-54.0740221130605,
17.6656222678464));
#46744=CARTESIAN_POINT('Ctrl Pts',(-30.0998184751404,-55.9208508807133,
17.5544843772783));
#46745=CARTESIAN_POINT('Ctrl Pts',(-30.8867448926705,-58.1070774278645,
17.4433464867103));
#46746=CARTESIAN_POINT('Ctrl Pts',(-33.1503020054966,-58.6316238024116,
17.3322085961423));
#46747=CARTESIAN_POINT('Ctrl Pts',(-34.8186303177654,-57.0143667589707,
17.2210707055742));
#46748=CARTESIAN_POINT('Ctrl Pts',(-34.3646900051272,-54.7356000103461,
17.1099328150062));
#46749=CARTESIAN_POINT('Ctrl Pts',(-32.2039777837733,-53.881104604526,16.9987949244381));
#46750=CARTESIAN_POINT('Ctrl Pts',(-30.3142180540518,-55.2330098770949,
16.8876570338701));
#46751=CARTESIAN_POINT('Ctrl Pts',(-30.4251293279102,-57.5539016004218,
16.776519143302));
#46752=CARTESIAN_POINT('Ctrl Pts',(-32.4351932585659,-58.7194412594432,
16.665381252734));
#46753=CARTESIAN_POINT('Ctrl Pts',(-34.5045755346153,-57.6627971861383,
16.554243362166));
#46754=CARTESIAN_POINT('Ctrl Pts',(-34.7391470903974,-55.3511276839614,
16.4431054715979));
#46755=CARTESIAN_POINT('Ctrl Pts',(-32.924201920686,-53.9003300643712,16.3319675810299));
#46756=CARTESIAN_POINT('Ctrl Pts',(-30.7209799221891,-54.6383358417407,
16.2208296904618));
#46757=CARTESIAN_POINT('Ctrl Pts',(-30.1461151763816,-56.8896399584928,
16.1096917998938));
#46758=CARTESIAN_POINT('Ctrl Pts',(-31.7257879044833,-58.5935982250311,
15.9985539093258));
#46759=CARTESIAN_POINT('Ctrl Pts',(-34.0141057438103,-58.1905583158083,
15.8874160187577));
#46760=CARTESIAN_POINT('Ctrl Pts',(-34.9165454246277,-56.0494272304867,
15.7762781281897));
#46761=CARTESIAN_POINT('Ctrl Pts',(-33.6070936729406,-54.130006533605,15.6651402376216));
#46762=CARTESIAN_POINT('Ctrl Pts',(-31.284306526822,-54.1891637565984,15.5540023470536));
#46763=CARTESIAN_POINT('Ctrl Pts',(-30.074257404191,-56.1727516226364,15.4428644564856));
#46764=CARTESIAN_POINT('Ctrl Pts',(-31.0845179881232,-58.2651696619898,
15.3317265659175));
#46765=CARTESIAN_POINT('Ctrl Pts',(-33.3903853125313,-58.551203914661,15.2205886753495));
#46766=CARTESIAN_POINT('Ctrl Pts',(-34.8812728580259,-56.7690439832156,
15.1094507847814));
#46767=CARTESIAN_POINT('Ctrl Pts',(-34.192554360499,-54.5499210682071,14.9983128942134));
#46768=CARTESIAN_POINT('Ctrl Pts',(-31.9546216431227,-53.9250235318367,
14.8871750036453));
#46769=CARTESIAN_POINT('Ctrl Pts',(-30.2158799584562,-55.4663271929179,
14.7760371130773));
#46770=CARTESIAN_POINT('Ctrl Pts',(-30.5678191761536,-57.7630592969624,
14.6648992225092));
#46771=CARTESIAN_POINT('Ctrl Pts',(-32.6883055651204,-58.7129949703236,
14.5537613319412));
#46772=CARTESIAN_POINT('Ctrl Pts',(-34.6364334330514,-57.4466471822883,
14.4426234413732));
#46773=CARTESIAN_POINT('Ctrl Pts',(-34.6290601547835,-55.1231186965397,
14.3314855508051));
#46774=CARTESIAN_POINT('Ctrl Pts',(-32.6729327631563,-53.8691609424836,
14.2203476602371));
#46775=CARTESIAN_POINT('Ctrl Pts',(-30.5585204707244,-54.8325367623412,
14.109209769669));
#46776=CARTESIAN_POINT('Ctrl Pts',(-30.2211615693062,-57.1314551632494,
13.998071879101));
#46777=CARTESIAN_POINT('Ctrl Pts',(-31.9696590133091,-58.6616944230991,
13.886933988533));
#46778=CARTESIAN_POINT('Ctrl Pts',(-34.2035641928434,-58.0226004643432,
13.7757960979649));
#46779=CARTESIAN_POINT('Ctrl Pts',(-34.8782165391171,-55.7991607039093,
13.6646582073969));
#46780=CARTESIAN_POINT('Ctrl Pts',(-33.3759826838065,-54.0264798110273,
13.5535203168288));
#46781=CARTESIAN_POINT('Ctrl Pts',(-31.072107305341,-54.3271826722053,13.4423824262608));
#46782=CARTESIAN_POINT('Ctrl Pts',(-30.074887383932,-56.4258925346357,13.3312445356927));
#46783=CARTESIAN_POINT('Ctrl Pts',(-31.2980228170538,-58.4019167094403,
13.2201066451247));
#46784=CARTESIAN_POINT('Ctrl Pts',(-33.6200956257376,-58.4460163820148,
13.1089687545567));
#46785=CARTESIAN_POINT('Ctrl Pts',(-34.9194345180072,-56.5189590291237,
12.9978308639886));
#46786=CARTESIAN_POINT('Ctrl Pts',(-33.9991195898381,-54.3822352088321,
12.8866929734206));
#46787=CARTESIAN_POINT('Ctrl Pts',(-32.4788453194858,-54.1263833506296,
12.8126010463752));
#46788=CARTESIAN_POINT('Ctrl Pts',(-31.8326342444893,-54.3482983416318,
12.7755550828525));
#46789=CARTESIAN_POINT('Ctrl Pts',(-33.8624214427591,-54.931476806163,22.0748149723825));
#46790=CARTESIAN_POINT('Ctrl Pts',(-33.4101310816148,-54.4784392630848,
22.0377690088598));
#46791=CARTESIAN_POINT('Ctrl Pts',(-32.0254812207533,-54.0671999021891,
21.9636770818144));
#46792=CARTESIAN_POINT('Ctrl Pts',(-30.3705294497321,-55.4858400606076,
21.8525391912464));
#46793=CARTESIAN_POINT('Ctrl Pts',(-30.6696757733002,-57.6428035756158,
21.7414013006784));
#46794=CARTESIAN_POINT('Ctrl Pts',(-32.6417207837188,-58.5626484614684,
21.6302634101103));
#46795=CARTESIAN_POINT('Ctrl Pts',(-34.4852499295344,-57.4040221256554,
21.5191255195423));
#46796=CARTESIAN_POINT('Ctrl Pts',(-34.5110566798406,-55.2271309148553,
21.4079876289742));
#46797=CARTESIAN_POINT('Ctrl Pts',(-32.6964205385156,-54.0246568103569,
21.2968497384062));
#46798=CARTESIAN_POINT('Ctrl Pts',(-30.7018484988176,-54.8971636496159,
21.1857118478381));
#46799=CARTESIAN_POINT('Ctrl Pts',(-30.3532198498734,-57.0460731790885,
21.0745739572701));
#46800=CARTESIAN_POINT('Ctrl Pts',(-31.969525977078,-58.5044455719578,20.9634360667021));
#46801=CARTESIAN_POINT('Ctrl Pts',(-34.071399702541,-57.9374253143107,20.852298176134));
#46802=CARTESIAN_POINT('Ctrl Pts',(-34.7349441106375,-55.8640078431203,
20.741160285566));
#46803=CARTESIAN_POINT('Ctrl Pts',(-33.352823499752,-54.1820180001326,20.6300223949979));
#46804=CARTESIAN_POINT('Ctrl Pts',(-31.1901015335783,-54.4309990063087,
20.5188845044299));
#46805=CARTESIAN_POINT('Ctrl Pts',(-30.2263456554001,-56.3830563013939,
20.4077466138619));
#46806=CARTESIAN_POINT('Ctrl Pts',(-31.3436908009795,-58.2514494163732,
20.2966087232938));
#46807=CARTESIAN_POINT('Ctrl Pts',(-33.5194191611043,-58.3260170884913,
20.1854708327258));
#46808=CARTESIAN_POINT('Ctrl Pts',(-34.7620614565392,-56.5385066096463,
20.0743329421577));
#46809=CARTESIAN_POINT('Ctrl Pts',(-33.9342133200027,-54.5250466289289,
19.9631950515897));
#46810=CARTESIAN_POINT('Ctrl Pts',(-31.7936134302447,-54.1285798828619,
19.8520571610216));
#46811=CARTESIAN_POINT('Ctrl Pts',(-30.2995771969099,-55.7119968893621,
19.7409192704536));
#46812=CARTESIAN_POINT('Ctrl Pts',(-30.8196129006622,-57.8259781007111,
19.6297813798856));
#46813=CARTESIAN_POINT('Ctrl Pts',(-32.8777259778579,-58.5355725422314,
19.5186434893175));
#46814=CARTESIAN_POINT('Ctrl Pts',(-34.590102181551,-57.1912803731281,19.4075055987495));
#46815=CARTESIAN_POINT('Ctrl Pts',(-34.3893841562315,-55.0235474616527,
19.2963677081814));
#46816=CARTESIAN_POINT('Ctrl Pts',(-32.4592913850741,-54.0165243251615,
19.1852298176134));
#46817=CARTESIAN_POINT('Ctrl Pts',(-30.5664596711081,-55.0919506610441,
19.0740919270453));
#46818=CARTESIAN_POINT('Ctrl Pts',(-30.4434193478744,-57.265476547833,18.9629540364773));
#46819=CARTESIAN_POINT('Ctrl Pts',(-32.2027906188128,-58.5476490919252,
18.8518161459092));
#46820=CARTESIAN_POINT('Ctrl Pts',(-34.2342010069002,-57.76488122287,18.7406782553412));
#46821=CARTESIAN_POINT('Ctrl Pts',(-34.6782775462125,-55.6336492484138,
18.6295403647732));
#46822=CARTESIAN_POINT('Ctrl Pts',(-33.1285519441201,-54.1046939645864,
18.5184024742052));
#46823=CARTESIAN_POINT('Ctrl Pts',(-31.0035056193152,-54.5774854822095,
18.4072645836371));
#46824=CARTESIAN_POINT('Ctrl Pts',(-30.2482175725494,-56.6192723633811,
18.2961266930691));
#46825=CARTESIAN_POINT('Ctrl Pts',(-31.5540115185799,-58.3611839203272,
18.184988802501));
#46826=CARTESIAN_POINT('Ctrl Pts',(-33.7256794498927,-58.2088287503542,
18.073850911933));
#46827=CARTESIAN_POINT('Ctrl Pts',(-34.7754690805687,-56.3016592683636,
17.9627130213649));
#46828=CARTESIAN_POINT('Ctrl Pts',(-33.7424960562255,-54.3853293299944,
17.8515751307969));
#46829=CARTESIAN_POINT('Ctrl Pts',(-31.5722523007556,-54.2138774604954,
17.7404372402288));
#46830=CARTESIAN_POINT('Ctrl Pts',(-30.2511865357786,-55.9442355004157,
17.6292993496608));
#46831=CARTESIAN_POINT('Ctrl Pts',(-30.9884852378828,-57.9925871122213,
17.5181614590928));
#46832=CARTESIAN_POINT('Ctrl Pts',(-33.1092905434961,-58.4840528357392,
17.4070235685247));
#46833=CARTESIAN_POINT('Ctrl Pts',(-34.6724053048228,-56.9687885206333,
17.2958856779567));
#46834=CARTESIAN_POINT('Ctrl Pts',(-34.2470928538933,-54.833732778786,17.1847477873887));
#46835=CARTESIAN_POINT('Ctrl Pts',(-32.2226465004149,-54.0331263438891,
17.0736098968206));
#46836=CARTESIAN_POINT('Ctrl Pts',(-30.4520649505092,-55.2997733652982,
16.9624720062526));
#46837=CARTESIAN_POINT('Ctrl Pts',(-30.5559815765657,-57.4742974595634,
16.8513341156845));
#46838=CARTESIAN_POINT('Ctrl Pts',(-32.4392803122598,-58.5663320624232,
16.7401962251165));
#46839=CARTESIAN_POINT('Ctrl Pts',(-34.3781564667511,-57.5763255173654,
16.6290583345484));
#46840=CARTESIAN_POINT('Ctrl Pts',(-34.5979347074811,-55.4104420425189,
16.5179204439804));
#46841=CARTESIAN_POINT('Ctrl Pts',(-32.897449518258,-54.0511393452008,16.4067825534124));
#46842=CARTESIAN_POINT('Ctrl Pts',(-30.833174277585,-54.7426025998055,16.2956446628443));
#46843=CARTESIAN_POINT('Ctrl Pts',(-30.2945635237364,-56.8519276476706,
16.1845067722763));
#46844=CARTESIAN_POINT('Ctrl Pts',(-31.7746137879455,-58.4484253511043,
16.0733688817082));
#46845=CARTESIAN_POINT('Ctrl Pts',(-33.9186182785215,-58.0708032566539,
15.9622309911402));
#46846=CARTESIAN_POINT('Ctrl Pts',(-34.7641453704728,-56.0647031498647,
15.8510931005721));
#46847=CARTESIAN_POINT('Ctrl Pts',(-33.5372745278125,-54.2663312092653,
15.7399552100041));
#46848=CARTESIAN_POINT('Ctrl Pts',(-31.3609745460779,-54.3217576668876,
15.6288173194361));
#46849=CARTESIAN_POINT('Ctrl Pts',(-30.2272374802945,-56.1802500577385,
15.517679428868));
#46850=CARTESIAN_POINT('Ctrl Pts',(-31.1737857225787,-58.14070921924,15.4065415383));
#46851=CARTESIAN_POINT('Ctrl Pts',(-33.3342329354787,-58.4087046487411,
15.2954036477319));
#46852=CARTESIAN_POINT('Ctrl Pts',(-34.731097277289,-56.7389370883627,15.1842657571639));
#46853=CARTESIAN_POINT('Ctrl Pts',(-34.0858129876404,-54.6597637265374,
15.0731278665959));
#46854=CARTESIAN_POINT('Ctrl Pts',(-31.9890160684358,-54.0742755128362,
14.9619899760278));
#46855=CARTESIAN_POINT('Ctrl Pts',(-30.3599285720183,-55.5183764650323,
14.8508520854598));
#46856=CARTESIAN_POINT('Ctrl Pts',(-30.6896726531006,-57.6702645725732,
14.7397141948917));
#46857=CARTESIAN_POINT('Ctrl Pts',(-32.6764300265812,-58.5602923101727,
14.6285763043237));
#46858=CARTESIAN_POINT('Ctrl Pts',(-34.5016987131586,-57.373807068692,14.5174384137556));
#46859=CARTESIAN_POINT('Ctrl Pts',(-34.4947904325672,-55.1968125001003,
14.4063005231876));
#46860=CARTESIAN_POINT('Ctrl Pts',(-32.6620267142976,-54.0219359119425,
14.2951626326196));
#46861=CARTESIAN_POINT('Ctrl Pts',(-30.6809603729033,-54.9245561897684,
14.1840247420515));
#46862=CARTESIAN_POINT('Ctrl Pts',(-30.3648770967317,-57.0784927148031,
14.0728868514835));
#46863=CARTESIAN_POINT('Ctrl Pts',(-32.0031051030323,-58.5122270450561,
13.9617489609154));
#46864=CARTESIAN_POINT('Ctrl Pts',(-34.0961284820971,-57.9134377099716,
13.8506110703474));
#46865=CARTESIAN_POINT('Ctrl Pts',(-34.7282337059125,-55.8302197456797,
13.7394731797794));
#46866=CARTESIAN_POINT('Ctrl Pts',(-33.3207386122115,-54.1693334258776,
13.6283352892113));
#46867=CARTESIAN_POINT('Ctrl Pts',(-31.1621577226746,-54.4510723843451,
13.5171973986433));
#46868=CARTESIAN_POINT('Ctrl Pts',(-30.2278277302023,-56.417426573495,13.4060595080752));
#46869=CARTESIAN_POINT('Ctrl Pts',(-31.3738258149644,-58.2688322792311,
13.2949216175072));
#46870=CARTESIAN_POINT('Ctrl Pts',(-33.549456509137,-58.3101507946959,13.1837837269392));
#46871=CARTESIAN_POINT('Ctrl Pts',(-34.7668522624408,-56.5046238057481,
13.0726458363711));
#46872=CARTESIAN_POINT('Ctrl Pts',(-33.9045772301756,-54.5026530186945,
12.9615079458031));
#46873=CARTESIAN_POINT('Ctrl Pts',(-32.4801794448133,-54.2629365232493,
12.8874160187577));
#46874=CARTESIAN_POINT('Ctrl Pts',(-31.8747218362409,-54.4708563886884,
12.850370055235));
#46875=CARTESIAN_POINT('Ctrl Pts',(-33.7707165971401,-55.0230304055885,
22.149629944765));
#46876=CARTESIAN_POINT('Ctrl Pts',(-33.3488699859559,-54.6004869054281,
22.1125839812423));
#46877=CARTESIAN_POINT('Ctrl Pts',(-32.0574211697503,-54.2169281438828,
22.0384920541969));
#46878=CARTESIAN_POINT('Ctrl Pts',(-30.5138645162054,-55.5400793642724,
21.9273541636289));
#46879=CARTESIAN_POINT('Ctrl Pts',(-30.7928752440178,-57.5518572561383,
21.8162162730608));
#46880=CARTESIAN_POINT('Ctrl Pts',(-32.6321815308973,-58.409787208327,21.7050783824928));
#46881=CARTESIAN_POINT('Ctrl Pts',(-34.351622380386,-57.3291482308462,21.5939404919248));
#46882=CARTESIAN_POINT('Ctrl Pts',(-34.3756920734364,-55.2987839801705,
21.4828026013567));
#46883=CARTESIAN_POINT('Ctrl Pts',(-32.6831994348279,-54.1772486356277,
21.3716647107887));
#46884=CARTESIAN_POINT('Ctrl Pts',(-30.822882417281,-54.9910268741142,21.2605268202207));
#46885=CARTESIAN_POINT('Ctrl Pts',(-30.497720028795,-56.9952928957376,21.1493889296526));
#46886=CARTESIAN_POINT('Ctrl Pts',(-32.0052322841356,-58.3555019663444,
21.0382510390845));
#46887=CARTESIAN_POINT('Ctrl Pts',(-33.965628490635,-57.8266479497429,20.9271131485165));
#46888=CARTESIAN_POINT('Ctrl Pts',(-34.5845095988185,-55.8927926016459,
20.8159752579485));
#46889=CARTESIAN_POINT('Ctrl Pts',(-33.2954197882935,-54.3240178138849,
20.7048373673804));
#46890=CARTESIAN_POINT('Ctrl Pts',(-31.278271047702,-54.55623986133,20.5936994768124));
#46891=CARTESIAN_POINT('Ctrl Pts',(-30.3793857604063,-56.3769038097847,
20.4825615862443));
#46892=CARTESIAN_POINT('Ctrl Pts',(-31.4215221923948,-58.1195350299587,
20.3714236956763));
#46893=CARTESIAN_POINT('Ctrl Pts',(-33.4508018640946,-58.1890835379289,
20.2602858051083));
#46894=CARTESIAN_POINT('Ctrl Pts',(-34.6098016710263,-56.5218907283162,
20.1491479145402));
#46895=CARTESIAN_POINT('Ctrl Pts',(-33.8376761495152,-54.6439571206407,
20.0380100239722));
#46896=CARTESIAN_POINT('Ctrl Pts',(-31.8411604441816,-54.2741766264193,
19.9268721334041));
#46897=CARTESIAN_POINT('Ctrl Pts',(-30.4476880729728,-55.7510135340056,
19.8157342428361));
#46898=CARTESIAN_POINT('Ctrl Pts',(-30.9327200749099,-57.7227022692206,
19.7045963522681));
#46899=CARTESIAN_POINT('Ctrl Pts',(-32.8523011706738,-58.3845337743473,
19.5934584617));
#46900=CARTESIAN_POINT('Ctrl Pts',(-34.44941700744,-57.1307261660161,19.482320571132));
#46901=CARTESIAN_POINT('Ctrl Pts',(-34.2622093504597,-55.1089037678011,
19.3711826805639));
#46902=CARTESIAN_POINT('Ctrl Pts',(-32.4620314896628,-54.1696635495527,
19.2600447899959));
#46903=CARTESIAN_POINT('Ctrl Pts',(-30.6966066372334,-55.1727027348726,
19.1489068994278));
#46904=CARTESIAN_POINT('Ctrl Pts',(-30.5818481814842,-57.1999281821345,
19.0377690088598));
#46905=CARTESIAN_POINT('Ctrl Pts',(-32.2227958386096,-58.3957974491916,
18.9266311182917));
#46906=CARTESIAN_POINT('Ctrl Pts',(-34.1174716083317,-57.6657178338107,
18.8154932277237));
#46907=CARTESIAN_POINT('Ctrl Pts',(-34.5316572715886,-55.6779394876238,
18.7043553371557));
#46908=CARTESIAN_POINT('Ctrl Pts',(-33.0862439935917,-54.2518984738315,
18.5932174465876));
#46909=CARTESIAN_POINT('Ctrl Pts',(-31.1042349398055,-54.692866304765,18.4820795560196));
#46910=CARTESIAN_POINT('Ctrl Pts',(-30.3997854746655,-56.5972201238544,
18.3709416654515));
#46911=CARTESIAN_POINT('Ctrl Pts',(-31.617686182618,-58.2218832836465,18.2598037748835));
#46912=CARTESIAN_POINT('Ctrl Pts',(-33.643178733739,-58.0797831690501,18.1486658843155));
#46913=CARTESIAN_POINT('Ctrl Pts',(-34.6223068253403,-56.3009856264801,
18.0375279937474));
#46914=CARTESIAN_POINT('Ctrl Pts',(-33.6588634111112,-54.5136442195871,
17.9263901031794));
#46915=CARTESIAN_POINT('Ctrl Pts',(-31.6346991742871,-54.3537328079304,
17.8152522126114));
#46916=CARTESIAN_POINT('Ctrl Pts',(-30.4025545964168,-55.9676201201181,
17.7041143220433));
#46917=CARTESIAN_POINT('Ctrl Pts',(-31.090225583095,-57.878096796578,17.5929764314753));
#46918=CARTESIAN_POINT('Ctrl Pts',(-33.0682790814956,-58.336481869067,17.4818385409072));
#46919=CARTESIAN_POINT('Ctrl Pts',(-34.5261802918802,-56.9232102822958,
17.3707006503392));
#46920=CARTESIAN_POINT('Ctrl Pts',(-34.1294957026595,-54.9318655472259,
17.2595627597711));
#46921=CARTESIAN_POINT('Ctrl Pts',(-32.2413152170565,-54.1851480832521,
17.1484248692031));
#46922=CARTESIAN_POINT('Ctrl Pts',(-30.5899118469666,-55.3665368535016,
17.037286978635));
#46923=CARTESIAN_POINT('Ctrl Pts',(-30.6868338252212,-57.3946933187052,
16.926149088067));
#46924=CARTESIAN_POINT('Ctrl Pts',(-32.4433673659537,-58.4132228654032,
16.815011197499));
#46925=CARTESIAN_POINT('Ctrl Pts',(-34.251737398887,-57.4898538485925,16.7038733069309));
#46926=CARTESIAN_POINT('Ctrl Pts',(-34.4567223245648,-55.4697564010764,
16.5927354163629));
#46927=CARTESIAN_POINT('Ctrl Pts',(-32.87069711583,-54.2019486260304,16.4815975257949));
#46928=CARTESIAN_POINT('Ctrl Pts',(-30.9453686329809,-54.8468693578704,
16.3704596352268));
#46929=CARTESIAN_POINT('Ctrl Pts',(-30.4430118710911,-56.8142153368483,
16.2593217446588));
#46930=CARTESIAN_POINT('Ctrl Pts',(-31.8234396714078,-58.3032524771776,
16.1481838540907));
#46931=CARTESIAN_POINT('Ctrl Pts',(-33.8231308132328,-57.9510481974995,
16.0370459635227));
#46932=CARTESIAN_POINT('Ctrl Pts',(-34.611745316318,-56.0799790692429,15.9259080729546));
#46933=CARTESIAN_POINT('Ctrl Pts',(-33.4674553826844,-54.4026558849256,
15.8147701823866));
#46934=CARTESIAN_POINT('Ctrl Pts',(-31.4376425653338,-54.4543515771769,
15.7036322918186));
#46935=CARTESIAN_POINT('Ctrl Pts',(-30.3802175563979,-56.1877484928405,
15.5924944012505));
#46936=CARTESIAN_POINT('Ctrl Pts',(-31.2630534570342,-58.0162487764902,
15.4813565106825));
#46937=CARTESIAN_POINT('Ctrl Pts',(-33.278080558426,-58.2662053828213,15.3702186201144));
#46938=CARTESIAN_POINT('Ctrl Pts',(-34.5809216965521,-56.7088301935098,
15.2590807295464));
#46939=CARTESIAN_POINT('Ctrl Pts',(-33.9790716147817,-54.7696063848677,
15.1479428389783));
#46940=CARTESIAN_POINT('Ctrl Pts',(-32.0234104937488,-54.2235274938358,
15.0368049484103));
#46941=CARTESIAN_POINT('Ctrl Pts',(-30.5039771855804,-55.5704257371467,
14.9256670578423));
#46942=CARTESIAN_POINT('Ctrl Pts',(-30.8115261300475,-57.577469848184,14.8145291672742));
#46943=CARTESIAN_POINT('Ctrl Pts',(-32.664554488042,-58.4075896500218,14.7033912767062));
#46944=CARTESIAN_POINT('Ctrl Pts',(-34.3669639932659,-57.3009669550956,
14.5922533861381));
#46945=CARTESIAN_POINT('Ctrl Pts',(-34.3605207103509,-55.2705063036608,
14.4811154955701));
#46946=CARTESIAN_POINT('Ctrl Pts',(-32.6511206654389,-54.1747108814015,
14.3699776050021));
#46947=CARTESIAN_POINT('Ctrl Pts',(-30.8034002750821,-55.0165756171955,
14.258839714434));
#46948=CARTESIAN_POINT('Ctrl Pts',(-30.5085926241571,-57.0255302663568,
14.147701823866));
#46949=CARTESIAN_POINT('Ctrl Pts',(-32.0365511927555,-58.3627596670131,
14.0365639332979));
#46950=CARTESIAN_POINT('Ctrl Pts',(-33.9886927713508,-57.8042749555999,
13.9254260427299));
#46951=CARTESIAN_POINT('Ctrl Pts',(-34.5782508727078,-55.8612787874501,
13.8142881521619));
#46952=CARTESIAN_POINT('Ctrl Pts',(-33.2654945406164,-54.3121870407279,
13.7031502615938));
#46953=CARTESIAN_POINT('Ctrl Pts',(-31.2522081400082,-54.574962096485,13.5920123710258));
#46954=CARTESIAN_POINT('Ctrl Pts',(-30.3807680764726,-56.4089606123543,
13.4808744804577));
#46955=CARTESIAN_POINT('Ctrl Pts',(-31.449628812875,-58.135747849022,13.3697365898897));
#46956=CARTESIAN_POINT('Ctrl Pts',(-33.4788173925363,-58.174285207377,13.2585986993216));
#46957=CARTESIAN_POINT('Ctrl Pts',(-34.6142700068744,-56.4902885823724,
13.1474608087536));
#46958=CARTESIAN_POINT('Ctrl Pts',(-33.8100348705132,-54.6230708285569,
13.0363229181856));
#46959=CARTESIAN_POINT('Ctrl Pts',(-32.4815135701408,-54.3994896958689,
12.9622309911402));
#46960=CARTESIAN_POINT('Ctrl Pts',(-31.9168094279925,-54.593414435745,12.9251850276175));
#46961=CARTESIAN_POINT('Ctrl Pts',(-33.6790117515211,-55.1145840050141,
22.2244449171475));
#46962=CARTESIAN_POINT('Ctrl Pts',(-33.2876088902971,-54.7225345477714,
22.1873989536248));
#46963=CARTESIAN_POINT('Ctrl Pts',(-32.0893611187473,-54.3666563855765,
22.1133070265794));
#46964=CARTESIAN_POINT('Ctrl Pts',(-30.6571995826787,-55.5943186679374,
22.0021691360114));
#46965=CARTESIAN_POINT('Ctrl Pts',(-30.9160747147354,-57.4609109366607,
21.8910312454433));
#46966=CARTESIAN_POINT('Ctrl Pts',(-32.6226422780758,-58.2569259551857,
21.7798933548753));
#46967=CARTESIAN_POINT('Ctrl Pts',(-34.2179948312376,-57.254274336037,21.6687554643072));
#46968=CARTESIAN_POINT('Ctrl Pts',(-34.2403274670321,-55.3704370454857,
21.5576175737392));
#46969=CARTESIAN_POINT('Ctrl Pts',(-32.6699783311403,-54.3298404608986,
21.4464796831712));
#46970=CARTESIAN_POINT('Ctrl Pts',(-30.9439163357442,-55.0848900986124,
21.3353417926032));
#46971=CARTESIAN_POINT('Ctrl Pts',(-30.6422202077166,-56.9445126123869,
21.2242039020351));
#46972=CARTESIAN_POINT('Ctrl Pts',(-32.0409385911932,-58.206558360731,21.1130660114671));
#46973=CARTESIAN_POINT('Ctrl Pts',(-33.8598572787291,-57.7158705851754,
21.001928120899));
#46974=CARTESIAN_POINT('Ctrl Pts',(-34.4340750869996,-55.9215773601716,
20.890790230331));
#46975=CARTESIAN_POINT('Ctrl Pts',(-33.238016076835,-54.4660176276372,20.7796523397629));
#46976=CARTESIAN_POINT('Ctrl Pts',(-31.3664405618257,-54.6814807163513,
20.6685144491949));
#46977=CARTESIAN_POINT('Ctrl Pts',(-30.5324258654125,-56.3707513181756,
20.5573765586268));
#46978=CARTESIAN_POINT('Ctrl Pts',(-31.4993535838102,-57.9876206435441,
20.4462386680588));
#46979=CARTESIAN_POINT('Ctrl Pts',(-33.3821845670849,-58.0521499873666,
20.3351007774907));
#46980=CARTESIAN_POINT('Ctrl Pts',(-34.4575418855134,-56.5052748469861,
20.2239628869227));
#46981=CARTESIAN_POINT('Ctrl Pts',(-33.7411389790275,-54.7628676123527,
20.1128249963547));
#46982=CARTESIAN_POINT('Ctrl Pts',(-31.8887074581185,-54.4197733699765,
20.0016871057866));
#46983=CARTESIAN_POINT('Ctrl Pts',(-30.5957989490357,-55.7900301786492,
19.8905492152186));
#46984=CARTESIAN_POINT('Ctrl Pts',(-31.0458272491576,-57.61942643773,19.7794113246506));
#46985=CARTESIAN_POINT('Ctrl Pts',(-32.8268763634896,-58.2334950064633,
19.6682734340825));
#46986=CARTESIAN_POINT('Ctrl Pts',(-34.308731833329,-57.070171958904,19.5571355435145));
#46987=CARTESIAN_POINT('Ctrl Pts',(-34.1350345446879,-55.1942600739497,
19.4459976529464));
#46988=CARTESIAN_POINT('Ctrl Pts',(-32.4647715942516,-54.3228027739439,
19.3348597623784));
#46989=CARTESIAN_POINT('Ctrl Pts',(-30.8267536033587,-55.2534548087013,
19.2237218718103));
#46990=CARTESIAN_POINT('Ctrl Pts',(-30.7202770150941,-57.1343798164359,
19.1125839812423));
#46991=CARTESIAN_POINT('Ctrl Pts',(-32.2428010584064,-58.243945806458,19.0014460906742));
#46992=CARTESIAN_POINT('Ctrl Pts',(-34.0007422097632,-57.5665544447512,
18.8903082001062));
#46993=CARTESIAN_POINT('Ctrl Pts',(-34.3850369969647,-55.7222297268337,
18.7791703095382));
#46994=CARTESIAN_POINT('Ctrl Pts',(-33.0439360430634,-54.3991029830766,
18.6680324189701));
#46995=CARTESIAN_POINT('Ctrl Pts',(-31.2049642602956,-54.8082471273205,
18.5568945284021));
#46996=CARTESIAN_POINT('Ctrl Pts',(-30.5513533767816,-56.5751678843276,
18.4457566378341));
#46997=CARTESIAN_POINT('Ctrl Pts',(-31.6813608466561,-58.082582646966,18.334618747266));
#46998=CARTESIAN_POINT('Ctrl Pts',(-33.5606780175853,-57.9507375877458,
18.223480856698));
#46999=CARTESIAN_POINT('Ctrl Pts',(-34.469144570112,-56.3003119845966,18.1123429661299));
#47000=CARTESIAN_POINT('Ctrl Pts',(-33.5752307659969,-54.6419591091798,
18.0012050755619));
#47001=CARTESIAN_POINT('Ctrl Pts',(-31.6971460478186,-54.4935881553653,
17.8900671849938));
#47002=CARTESIAN_POINT('Ctrl Pts',(-30.5539226570551,-55.9910047398205,
17.7789292944258));
#47003=CARTESIAN_POINT('Ctrl Pts',(-31.1919659283072,-57.7636064809347,
17.6677914038578));
#47004=CARTESIAN_POINT('Ctrl Pts',(-33.027267619495,-58.1889109023947,17.5566535132897));
#47005=CARTESIAN_POINT('Ctrl Pts',(-34.3799552789376,-56.8776320439583,
17.4455156227217));
#47006=CARTESIAN_POINT('Ctrl Pts',(-34.0118985514257,-55.0299983156659,
17.3343777321536));
#47007=CARTESIAN_POINT('Ctrl Pts',(-32.2599839336981,-54.3371698226151,
17.2232398415856));
#47008=CARTESIAN_POINT('Ctrl Pts',(-30.727758743424,-55.4333003417049,17.1121019510175));
#47009=CARTESIAN_POINT('Ctrl Pts',(-30.8176860738768,-57.3150891778468,
17.0009640604495));
#47010=CARTESIAN_POINT('Ctrl Pts',(-32.4474544196476,-58.2601136683832,
16.8898261698815));
#47011=CARTESIAN_POINT('Ctrl Pts',(-34.1253183310228,-57.4033821798196,
16.7786882793134));
#47012=CARTESIAN_POINT('Ctrl Pts',(-34.3155099416485,-55.5290707596339,
16.6675503887454));
#47013=CARTESIAN_POINT('Ctrl Pts',(-32.8439447134021,-54.3527579068599,
16.5564124981773));
#47014=CARTESIAN_POINT('Ctrl Pts',(-31.0575629883768,-54.9511361159353,
16.4452746076093));
#47015=CARTESIAN_POINT('Ctrl Pts',(-30.5914602184459,-56.776503026026,16.3341367170413));
#47016=CARTESIAN_POINT('Ctrl Pts',(-31.87226555487,-58.1580796032509,16.2229988264732));
#47017=CARTESIAN_POINT('Ctrl Pts',(-33.727643347944,-57.8312931383451,16.1118609359052));
#47018=CARTESIAN_POINT('Ctrl Pts',(-34.4593452621631,-56.0952549886209,
16.0007230453371));
#47019=CARTESIAN_POINT('Ctrl Pts',(-33.3976362375564,-54.5389805605859,
15.8895851547691));
#47020=CARTESIAN_POINT('Ctrl Pts',(-31.5143105845896,-54.5869454874661,
15.7784472642011));
#47021=CARTESIAN_POINT('Ctrl Pts',(-30.5331976325014,-56.1952469279427,
15.667309373633));
#47022=CARTESIAN_POINT('Ctrl Pts',(-31.3523211914896,-57.8917883337404,
15.556171483065));
#47023=CARTESIAN_POINT('Ctrl Pts',(-33.2219281813735,-58.1237061169015,
15.4450335924969));
#47024=CARTESIAN_POINT('Ctrl Pts',(-34.4307461158152,-56.6787232986569,
15.3338957019289));
#47025=CARTESIAN_POINT('Ctrl Pts',(-33.872330241923,-54.879449043198,15.2227578113608));
#47026=CARTESIAN_POINT('Ctrl Pts',(-32.057804919062,-54.3727794748353,15.1116199207928));
#47027=CARTESIAN_POINT('Ctrl Pts',(-30.6480257991425,-55.6224750092611,
15.0004820302248));
#47028=CARTESIAN_POINT('Ctrl Pts',(-30.9333796069945,-57.4846751237948,
14.8893441396567));
#47029=CARTESIAN_POINT('Ctrl Pts',(-32.6526789495027,-58.2548869898709,
14.7782062490887));
#47030=CARTESIAN_POINT('Ctrl Pts',(-34.2322292733731,-57.2281268414992,
14.6670683585206));
#47031=CARTESIAN_POINT('Ctrl Pts',(-34.2262509881345,-55.3442001072214,
14.5559304679526));
#47032=CARTESIAN_POINT('Ctrl Pts',(-32.6402146165803,-54.3274858508605,
14.4447925773845));
#47033=CARTESIAN_POINT('Ctrl Pts',(-30.9258401772609,-55.1085950446227,
14.3336546868165));
#47034=CARTESIAN_POINT('Ctrl Pts',(-30.6523081515825,-56.9725678179105,
14.2225167962485));
#47035=CARTESIAN_POINT('Ctrl Pts',(-32.0699972824786,-58.2132922889699,
14.1113789056804));
#47036=CARTESIAN_POINT('Ctrl Pts',(-33.8812570606045,-57.6951122012284,
14.0002410151124));
#47037=CARTESIAN_POINT('Ctrl Pts',(-34.4282680395032,-55.8923378292204,
13.8891031245443));
#47038=CARTESIAN_POINT('Ctrl Pts',(-33.2102504690214,-54.4550406555783,
13.7779652339763));
#47039=CARTESIAN_POINT('Ctrl Pts',(-31.3422585573418,-54.6988518086249,
13.6668273434082));
#47040=CARTESIAN_POINT('Ctrl Pts',(-30.5337084227428,-56.4004946512136,
13.5556894528402));
#47041=CARTESIAN_POINT('Ctrl Pts',(-31.5254318107855,-58.0026634188128,
13.4445515622722));
#47042=CARTESIAN_POINT('Ctrl Pts',(-33.4081782759357,-58.0384196200582,
13.3334136717041));
#47043=CARTESIAN_POINT('Ctrl Pts',(-34.4616877513079,-56.4759533589966,
13.2222757811361));
#47044=CARTESIAN_POINT('Ctrl Pts',(-33.7154925108507,-54.7434886384194,
13.111137890568));
#47045=CARTESIAN_POINT('Ctrl Pts',(-32.4828476954683,-54.5360428684886,
13.0370459635227));
#47046=CARTESIAN_POINT('Ctrl Pts',(-31.9588970197441,-54.7159724828016,
13.));
#47047=CARTESIAN_POINT('Ctrl Pts',(-31.667262219952,-54.851191363199,21.3785196366098));
#47048=CARTESIAN_POINT('Ctrl Pts',(-31.479741769716,-54.9581664087852,21.3641270219409));
#47049=CARTESIAN_POINT('Ctrl Pts',(-31.3126103376672,-55.0996825231223,
21.349734407272));
#47050=CARTESIAN_POINT('Ctrl Pts',(-31.1813106469723,-55.2689855779558,
21.3353417926031));
#47051=CARTESIAN_POINT('Ctrl Pts',(-30.843350959735,-55.7047642698706,21.2982958290804));
#47052=CARTESIAN_POINT('Ctrl Pts',(-30.7427855837258,-56.3246384411287,
21.2612498655577));
#47053=CARTESIAN_POINT('Ctrl Pts',(-30.9256226263006,-56.8449164848151,
21.2242039020351));
#47054=CARTESIAN_POINT('Ctrl Pts',(-31.1084596688754,-57.3651945285016,
21.1871579385124));
#47055=CARTESIAN_POINT('Ctrl Pts',(-31.5746991300343,-57.7858764446163,
21.1501119749897));
#47056=CARTESIAN_POINT('Ctrl Pts',(-32.1109719752031,-57.9144361067477,
21.113066011467));
#47057=CARTESIAN_POINT('Ctrl Pts',(-32.6472448203718,-58.0429957688791,
21.0760200479444));
#47058=CARTESIAN_POINT('Ctrl Pts',(-33.2535510495505,-57.8794331770273,
21.0389740844217));
#47059=CARTESIAN_POINT('Ctrl Pts',(-33.6524071321849,-57.4986030102674,
21.001928120899));
#47060=CARTESIAN_POINT('Ctrl Pts',(-34.0512632148193,-57.1177728435075,
20.9648821573763));
#47061=CARTESIAN_POINT('Ctrl Pts',(-34.2426691509094,-56.5196751018395,
20.9278361938536));
#47062=CARTESIAN_POINT('Ctrl Pts',(-34.1390289505938,-55.9780329422498,
20.890790230331));
#47063=CARTESIAN_POINT('Ctrl Pts',(-34.0353887502781,-55.4363907826601,
20.8537442668083));
#47064=CARTESIAN_POINT('Ctrl Pts',(-33.6367024135565,-54.9512042051487,
20.8166983032856));
#47065=CARTESIAN_POINT('Ctrl Pts',(-33.1254299926942,-54.7445214311786,
20.7796523397629));
#47066=CARTESIAN_POINT('Ctrl Pts',(-32.6601848660756,-54.5564452717343,
20.7459414387119));
#47067=CARTESIAN_POINT('Ctrl Pts',(-32.1017123235945,-54.5989854456511,
20.7122305376608));
#47068=CARTESIAN_POINT('Ctrl Pts',(-31.6651488727497,-54.8473747039335,
20.6785196366098));
#47069=CARTESIAN_POINT('Ctrl Pts',(-33.9541262883781,-54.8399232067375,
22.));
#47070=CARTESIAN_POINT('Ctrl Pts',(-33.8977770566593,-54.7931706099728,
22.));
#47071=CARTESIAN_POINT('Ctrl Pts',(-33.8389107618331,-54.7498380989966,
22.));
#47072=CARTESIAN_POINT('Ctrl Pts',(-33.777876546057,-54.7099422292584,22.));
#47073=CARTESIAN_POINT('Ctrl Pts',(-33.7151426127656,-54.668935315367,22.));
#47074=CARTESIAN_POINT('Ctrl Pts',(-33.6501173479606,-54.6315587953762,
22.));
#47075=CARTESIAN_POINT('Ctrl Pts',(-33.583156824249,-54.5978800039319,22.));
#47076=CARTESIAN_POINT('Ctrl Pts',(-33.5265763653144,-54.5694220204714,
22.));
#47077=CARTESIAN_POINT('Ctrl Pts',(-33.4686133977519,-54.5436050119993,
22.));
#47078=CARTESIAN_POINT('Ctrl Pts',(-33.4094785141786,-54.5204983074657,
22.));
#47079=CARTESIAN_POINT('Ctrl Pts',(-33.3832054797332,-54.5102322308718,
22.));
#47080=CARTESIAN_POINT('Ctrl Pts',(-33.3567011132793,-54.5005015028802,
22.));
#47081=CARTESIAN_POINT('Ctrl Pts',(-33.3299840335547,-54.4913139103878,
22.));
#47082=CARTESIAN_POINT('Ctrl Pts',(-33.3153052179459,-54.4862660916338,
22.));
#47083=CARTESIAN_POINT('Ctrl Pts',(-33.3005621960494,-54.4813822417943,
22.));
#47084=CARTESIAN_POINT('Ctrl Pts',(-33.2857580867463,-54.4766637893077,
22.));
#47085=CARTESIAN_POINT('Ctrl Pts',(-33.2721048859179,-54.4723121611158,
22.));
#47086=CARTESIAN_POINT('Ctrl Pts',(-33.2583976935737,-54.4681007280233,
22.));
#47087=CARTESIAN_POINT('Ctrl Pts',(-33.2446602943265,-54.4640366443481,
22.));
#47088=CARTESIAN_POINT('Ctrl Pts',(-33.1744615987436,-54.4432690035735,
22.));
#47089=CARTESIAN_POINT('Ctrl Pts',(-33.1033546243453,-54.426305105702,22.));
#47090=CARTESIAN_POINT('Ctrl Pts',(-33.0316734669904,-54.4132045353859,
22.));
#47091=CARTESIAN_POINT('Ctrl Pts',(-32.9605481884919,-54.4002055584357,
22.));
#47092=CARTESIAN_POINT('Ctrl Pts',(-32.8888565785783,-54.3910102235869,
22.));
#47093=CARTESIAN_POINT('Ctrl Pts',(-32.8169264247812,-54.3857276509517,
22.));
#47094=CARTESIAN_POINT('Ctrl Pts',(-32.7571464346349,-54.3813373900748,
22.));
#47095=CARTESIAN_POINT('Ctrl Pts',(-32.6972014393858,-54.3796505588111,
22.));
#47096=CARTESIAN_POINT('Ctrl Pts',(-32.6372877974345,-54.3807569468889,
22.));
#47097=CARTESIAN_POINT('Ctrl Pts',(-32.6122799917819,-54.3812187505304,
22.));
#47098=CARTESIAN_POINT('Ctrl Pts',(-32.58727777557,-54.3821674889407,22.));
#47099=CARTESIAN_POINT('Ctrl Pts',(-32.5622960765744,-54.3836109807411,
22.));
#47100=CARTESIAN_POINT('Ctrl Pts',(-32.5507331511287,-54.3842791093608,
22.));
#47101=CARTESIAN_POINT('Ctrl Pts',(-32.5391746274407,-54.3850532424534,
22.));
#47102=CARTESIAN_POINT('Ctrl Pts',(-32.5276220201243,-54.3859342108708,
22.));
#47103=CARTESIAN_POINT('Ctrl Pts',(-32.5155719563499,-54.3868531138787,
22.));
#47104=CARTESIAN_POINT('Ctrl Pts',(-32.5035366028335,-54.387887649022,22.));
#47105=CARTESIAN_POINT('Ctrl Pts',(-32.4915220458793,-54.3890378132804,
22.));
#47106=CARTESIAN_POINT('Ctrl Pts',(-32.4230954842274,-54.3955883490877,
22.));
#47107=CARTESIAN_POINT('Ctrl Pts',(-32.3552950943445,-54.4058891778527,
22.));
#47108=CARTESIAN_POINT('Ctrl Pts',(-32.2884097214115,-54.4200315485695,
22.));
#47109=CARTESIAN_POINT('Ctrl Pts',(-32.2277876728223,-54.4328495900511,
22.));
#47110=CARTESIAN_POINT('Ctrl Pts',(-32.1679169373206,-54.4488239715848,
22.));
#47111=CARTESIAN_POINT('Ctrl Pts',(-32.1090267714104,-54.4680568733301,
22.));
#47112=CARTESIAN_POINT('Ctrl Pts',(-32.0393564154629,-54.4908104704681,
22.));
#47113=CARTESIAN_POINT('Ctrl Pts',(-31.9710568700512,-54.5181250014914,
22.));
#47114=CARTESIAN_POINT('Ctrl Pts',(-31.904456962017,-54.5497238479896,22.));
#47115=CARTESIAN_POINT('Ctrl Pts',(-31.8897939177247,-54.5566808438693,
22.));
#47116=CARTESIAN_POINT('Ctrl Pts',(-31.8752134430768,-54.5638456669609,
22.));
#47117=CARTESIAN_POINT('Ctrl Pts',(-31.8607193748279,-54.5712156030182,
22.));
#47118=CARTESIAN_POINT('Ctrl Pts',(-31.8457643400408,-54.5788199310938,
22.));
#47119=CARTESIAN_POINT('Ctrl Pts',(-31.8308959671029,-54.5866456915096,
22.));
#47120=CARTESIAN_POINT('Ctrl Pts',(-31.816148277589,-54.5946733379087,22.));
#47121=CARTESIAN_POINT('Ctrl Pts',(-31.7559125281882,-54.6274616127308,
22.));
#47122=CARTESIAN_POINT('Ctrl Pts',(-31.6976088413262,-54.6636511833659,
22.));
#47123=CARTESIAN_POINT('Ctrl Pts',(-31.6414698544792,-54.7029684704927,
22.));
#47124=CARTESIAN_POINT('Ctrl Pts',(-31.5853421057777,-54.7422778869148,
22.));
#47125=CARTESIAN_POINT('Ctrl Pts',(-31.5313774894047,-54.7847146963307,
22.));
#47126=CARTESIAN_POINT('Ctrl Pts',(-31.4798463246137,-54.8300409282788,
22.));
#47127=CARTESIAN_POINT('Ctrl Pts',(-31.4425466815154,-54.8628492740926,
22.));
#47128=CARTESIAN_POINT('Ctrl Pts',(-31.4065227400659,-54.897172238623,22.));
#47129=CARTESIAN_POINT('Ctrl Pts',(-31.3718924922097,-54.9329270615862,
22.));
#47130=CARTESIAN_POINT('Ctrl Pts',(-31.3459157226426,-54.959747395096,22.));
#47131=CARTESIAN_POINT('Ctrl Pts',(-31.3207234114472,-54.9873735408281,
22.));
#47132=CARTESIAN_POINT('Ctrl Pts',(-31.296370938734,-55.0157718710984,22.));
#47133=CARTESIAN_POINT('Ctrl Pts',(-31.2882802397597,-55.0252067381156,
22.));
#47134=CARTESIAN_POINT('Ctrl Pts',(-31.2802886268347,-55.0347194488924,
22.));
#47135=CARTESIAN_POINT('Ctrl Pts',(-31.2723979365151,-55.0443082314672,
22.));
#47136=CARTESIAN_POINT('Ctrl Pts',(-31.2305359635119,-55.0951789843448,
22.));
#47137=CARTESIAN_POINT('Ctrl Pts',(-31.1915084683768,-55.1481921234089,
22.));
#47138=CARTESIAN_POINT('Ctrl Pts',(-31.1555797357512,-55.2031373177153,
22.));
#47139=CARTESIAN_POINT('Ctrl Pts',(-31.1302981918184,-55.2417999490479,
22.));
#47140=CARTESIAN_POINT('Ctrl Pts',(-31.1065518383412,-55.2814196841498,
22.));
#47141=CARTESIAN_POINT('Ctrl Pts',(-31.0844478042135,-55.3219265814321,
22.));
#47142=CARTESIAN_POINT('Ctrl Pts',(-31.0773529644147,-55.3349282781045,
22.));
#47143=CARTESIAN_POINT('Ctrl Pts',(-31.0704265008799,-55.3480232016838,
22.));
#47144=CARTESIAN_POINT('Ctrl Pts',(-31.0636752116797,-55.3612032674949,
22.));
#47145=CARTESIAN_POINT('Ctrl Pts',(-31.0349131818561,-55.4173533500487,
22.));
#47146=CARTESIAN_POINT('Ctrl Pts',(-31.0093835904652,-55.474934657336,22.));
#47147=CARTESIAN_POINT('Ctrl Pts',(-30.9873422739933,-55.5337599436784,
22.));
#47148=CARTESIAN_POINT('Ctrl Pts',(-30.967023266383,-55.5879886210984,22.));
#47149=CARTESIAN_POINT('Ctrl Pts',(-30.9496688942467,-55.6432750194878,
22.));
#47150=CARTESIAN_POINT('Ctrl Pts',(-30.9355188507018,-55.6994745658575,
22.));
#47151=CARTESIAN_POINT('Ctrl Pts',(-30.9328706183904,-55.7099925161458,
22.));
#47152=CARTESIAN_POINT('Ctrl Pts',(-30.9303347375364,-55.7205424451195,
22.));
#47153=CARTESIAN_POINT('Ctrl Pts',(-30.9279109916838,-55.7311226632894,
22.));
#47154=CARTESIAN_POINT('Origin',(-32.5,-56.2916512459885,17.));
#47155=CARTESIAN_POINT('Origin',(-65.,8.89946740503873E-15,13.));
#47156=CARTESIAN_POINT('Ctrl Pts',(-63.3648706727485,0.319230454628309,
13.));
#47157=CARTESIAN_POINT('Ctrl Pts',(-63.3697100624564,0.381552584091251,
13.));
#47158=CARTESIAN_POINT('Ctrl Pts',(-63.378326567255,0.443390469645943,13.));
#47159=CARTESIAN_POINT('Ctrl Pts',(-63.3904636088592,0.504524999022397,
13.));
#47160=CARTESIAN_POINT('Ctrl Pts',(-63.3981627172652,0.543305567168445,
13.));
#47161=CARTESIAN_POINT('Ctrl Pts',(-63.407279543875,0.581803401425318,13.));
#47162=CARTESIAN_POINT('Ctrl Pts',(-63.4177589835186,0.619964019244192,
13.));
#47163=CARTESIAN_POINT('Ctrl Pts',(-63.4249317270596,0.646083385764472,
13.));
#47164=CARTESIAN_POINT('Ctrl Pts',(-63.4327429983568,0.672044791355041,
13.));
#47165=CARTESIAN_POINT('Ctrl Pts',(-63.44117717048,0.697830748236588,13.));
#47166=CARTESIAN_POINT('Ctrl Pts',(-63.445633981288,0.711456641761924,13.));
#47167=CARTESIAN_POINT('Ctrl Pts',(-63.4502647769169,0.725033238553723,
13.));
#47168=CARTESIAN_POINT('Ctrl Pts',(-63.4550623359166,0.738544708502568,
13.));
#47169=CARTESIAN_POINT('Ctrl Pts',(-63.4771367982024,0.800713497636903,
13.));
#47170=CARTESIAN_POINT('Ctrl Pts',(-63.5027603464941,0.861575211953918,
13.));
#47171=CARTESIAN_POINT('Ctrl Pts',(-63.5316785435678,0.920885280715688,
13.));
#47172=CARTESIAN_POINT('Ctrl Pts',(-63.5525352082166,0.963661468017855,
13.));
#47173=CARTESIAN_POINT('Ctrl Pts',(-63.5751068651926,1.00563071995468,13.));
#47174=CARTESIAN_POINT('Ctrl Pts',(-63.5993147001603,1.04669965511365,13.));
#47175=CARTESIAN_POINT('Ctrl Pts',(-63.605972789105,1.05799519738412,13.));
#47176=CARTESIAN_POINT('Ctrl Pts',(-63.6127547253029,1.06922261593755,13.));
#47177=CARTESIAN_POINT('Ctrl Pts',(-63.6196590396186,1.08037991874502,13.));
#47178=CARTESIAN_POINT('Ctrl Pts',(-63.626655937187,1.09168683516212,13.));
#47179=CARTESIAN_POINT('Ctrl Pts',(-63.6337742037898,1.10291470667948,13.));
#47180=CARTESIAN_POINT('Ctrl Pts',(-63.6410091868788,1.11405768733435,13.));
#47181=CARTESIAN_POINT('Ctrl Pts',(-63.677959727572,1.17096717213473,13.));
#47182=CARTESIAN_POINT('Ctrl Pts',(-63.7179710364896,1.22569615332497,13.));
#47183=CARTESIAN_POINT('Ctrl Pts',(-63.7607845670049,1.27799720806722,13.));
#47184=CARTESIAN_POINT('Ctrl Pts',(-63.8042168530072,1.3310541351752,13.));
#47185=CARTESIAN_POINT('Ctrl Pts',(-63.8505333120092,1.38161344795932,13.));
#47186=CARTESIAN_POINT('Ctrl Pts',(-63.8995151782878,1.42940352748706,13.));
#47187=CARTESIAN_POINT('Ctrl Pts',(-63.9298610020025,1.4590110014124,13.));
#47188=CARTESIAN_POINT('Ctrl Pts',(-63.9612308491613,1.48755527123026,13.));
#47189=CARTESIAN_POINT('Ctrl Pts',(-63.9935813334301,1.51496662398692,13.));
#47190=CARTESIAN_POINT('Ctrl Pts',(-64.0200865946909,1.53742517701162,13.));
#47191=CARTESIAN_POINT('Ctrl Pts',(-64.047250267223,1.55912317435164,13.));
#47192=CARTESIAN_POINT('Ctrl Pts',(-64.075051394616,1.58001951663649,13.));
#47193=CARTESIAN_POINT('Ctrl Pts',(-64.0864069560373,1.58855477115841,13.));
#47194=CARTESIAN_POINT('Ctrl Pts',(-64.0978710427711,1.59695761719764,13.));
#47195=CARTESIAN_POINT('Ctrl Pts',(-64.1094224885555,1.60521141799748,13.));
#47196=CARTESIAN_POINT('Ctrl Pts',(-64.1667717340698,1.64618890751108,13.));
#47197=CARTESIAN_POINT('Ctrl Pts',(-64.226369023308,1.68357081331289,13.));
#47198=CARTESIAN_POINT('Ctrl Pts',(-64.2879736623947,1.71708519907432,13.));
#47199=CARTESIAN_POINT('Ctrl Pts',(-64.2948173902461,1.7208083494516,13.));
#47200=CARTESIAN_POINT('Ctrl Pts',(-64.3016859371774,1.72448374345449,13.));
#47201=CARTESIAN_POINT('Ctrl Pts',(-64.3085790067212,1.7281109868477,13.));
#47202=CARTESIAN_POINT('Ctrl Pts',(-64.3682468605388,1.75950916543472,13.));
#47203=CARTESIAN_POINT('Ctrl Pts',(-64.4297493247303,1.78730275834661,13.));
#47204=CARTESIAN_POINT('Ctrl Pts',(-64.492755333163,1.81157421873888,13.));
#47205=CARTESIAN_POINT('Ctrl Pts',(-64.56053950575,1.83768634520258,13.));
#47206=CARTESIAN_POINT('Ctrl Pts',(-64.6300645515071,1.85972265026168,13.));
#47207=CARTESIAN_POINT('Ctrl Pts',(-64.7009535899316,1.87773216280558,13.));
#47208=CARTESIAN_POINT('Ctrl Pts',(-64.7139243241626,1.88102740570952,13.));
#47209=CARTESIAN_POINT('Ctrl Pts',(-64.7269407953937,1.88418768229335,13.));
#47210=CARTESIAN_POINT('Ctrl Pts',(-64.7400007805811,1.88721308456642,13.));
#47211=CARTESIAN_POINT('Ctrl Pts',(-64.7512396222652,1.88981661103981,13.));
#47212=CARTESIAN_POINT('Ctrl Pts',(-64.7625015968045,1.89231813883989,13.));
#47213=CARTESIAN_POINT('Ctrl Pts',(-64.7737835811084,1.89471786797902,13.));
#47214=CARTESIAN_POINT('Ctrl Pts',(-64.8432969406401,1.90950367426388,13.));
#47215=CARTESIAN_POINT('Ctrl Pts',(-64.9135854863648,1.92043263341767,13.));
#47216=CARTESIAN_POINT('Ctrl Pts',(-64.9842819829643,1.92760569488594,13.));
#47217=CARTESIAN_POINT('Ctrl Pts',(-65.0564694634963,1.93493003569491,13.));
#47218=CARTESIAN_POINT('Ctrl Pts',(-65.1290831836877,1.93833864552109,13.));
#47219=CARTESIAN_POINT('Ctrl Pts',(-65.2017596774405,1.93789121633711,13.));
#47220=CARTESIAN_POINT('Ctrl Pts',(-65.2748769213569,1.93744107369689,13.));
#47221=CARTESIAN_POINT('Ctrl Pts',(-65.3480587637033,1.93308814118439,13.));
#47222=CARTESIAN_POINT('Ctrl Pts',(-65.4209476364575,1.92484231982115,13.));
#47223=CARTESIAN_POINT('Ctrl Pts',(-65.4389597304286,1.92280463555397,13.));
#47224=CARTESIAN_POINT('Ctrl Pts',(-65.456953949584,1.9205289761305,13.));
#47225=CARTESIAN_POINT('Ctrl Pts',(-65.4749248968271,1.91801499809801,13.));
#47226=CARTESIAN_POINT('Ctrl Pts',(-65.488986293,1.91604793199924,13.));
#47227=CARTESIAN_POINT('Ctrl Pts',(-65.5030350337315,1.91393458318872,13.));
#47228=CARTESIAN_POINT('Ctrl Pts',(-65.517047263033,1.91167847476885,13.));
#47229=CARTESIAN_POINT('Ctrl Pts',(-65.591432040293,1.89970178507336,13.));
#47230=CARTESIAN_POINT('Ctrl Pts',(-65.6649215571519,1.8836885467828,13.));
#47231=CARTESIAN_POINT('Ctrl Pts',(-65.7371322841359,1.86371341413835,13.));
#47232=CARTESIAN_POINT('Ctrl Pts',(-65.8094217303428,1.84371650596295,13.));
#47233=CARTESIAN_POINT('Ctrl Pts',(-65.8804307225326,1.81974914171634,13.));
#47234=CARTESIAN_POINT('Ctrl Pts',(-65.9497816751238,1.7918347665136,13.));
#47235=CARTESIAN_POINT('Ctrl Pts',(-66.0175539936567,1.76455580555915,13.));
#47236=CARTESIAN_POINT('Ctrl Pts',(-66.0837439306865,1.7335073683895,13.));
#47237=CARTESIAN_POINT('Ctrl Pts',(-66.1479900588654,1.69866277532066,13.));
#47238=CARTESIAN_POINT('Ctrl Pts',(-66.1618069173365,1.69116905041364,13.));
#47239=CARTESIAN_POINT('Ctrl Pts',(-66.1755338056604,1.68349956912868,13.));
#47240=CARTESIAN_POINT('Ctrl Pts',(-66.1891670016328,1.67565377050186,13.));
#47241=CARTESIAN_POINT('Ctrl Pts',(-66.2007100870974,1.66901081427424,13.));
#47242=CARTESIAN_POINT('Ctrl Pts',(-66.2121860050345,1.6622414568886,13.));
#47243=CARTESIAN_POINT('Ctrl Pts',(-66.2235939546713,1.65534738192939,13.));
#47244=CARTESIAN_POINT('Ctrl Pts',(-66.8826275096638,0.823232180103066,
13.));
#47245=CARTESIAN_POINT('Ctrl Pts',(-66.9060091418342,0.752340565238968,
13.));
#47246=CARTESIAN_POINT('Ctrl Pts',(-66.9251542481801,0.68022746278438,13.));
#47247=CARTESIAN_POINT('Ctrl Pts',(-66.9401506980285,0.607243329609344,
13.));
#47248=CARTESIAN_POINT('Ctrl Pts',(-66.9547542267029,0.536171449772777,
13.));
#47249=CARTESIAN_POINT('Ctrl Pts',(-66.9654231894066,0.464272677051844,
13.));
#47250=CARTESIAN_POINT('Ctrl Pts',(-66.9721930205228,0.391873748623409,
13.));
#47251=CARTESIAN_POINT('Ctrl Pts',(-66.9737040257789,0.375714532903923,
13.));
#47252=CARTESIAN_POINT('Ctrl Pts',(-66.9750207650679,0.359528284463992,
13.));
#47253=CARTESIAN_POINT('Ctrl Pts',(-66.9761428768271,0.343325629877727,
13.));
#47254=CARTESIAN_POINT('Ctrl Pts',(-66.9812921188236,0.268973508740579,
13.));
#47255=CARTESIAN_POINT('Ctrl Pts',(-66.9823380095277,0.194422974417003,
13.));
#47256=CARTESIAN_POINT('Ctrl Pts',(-66.9793427332487,0.120028700639496,
13.));
#47257=CARTESIAN_POINT('Ctrl Pts',(-66.977239855127,0.0677990977152428,
13.));
#47258=CARTESIAN_POINT('Ctrl Pts',(-66.9731439810344,0.0156465389589379,
13.));
#47259=CARTESIAN_POINT('Ctrl Pts',(-66.9670620462898,-0.0363014254759868,
13.));
#47260=CARTESIAN_POINT('Ctrl Pts',(-66.9647496285849,-0.0560526062653882,
13.));
#47261=CARTESIAN_POINT('Ctrl Pts',(-66.9621499864736,-0.0757741525187293,
13.));
#47262=CARTESIAN_POINT('Ctrl Pts',(-66.9592630725001,-0.0954588083553777,
13.));
#47263=CARTESIAN_POINT('Ctrl Pts',(-66.9565142387798,-0.114201952846506,
13.));
#47264=CARTESIAN_POINT('Ctrl Pts',(-66.9535037847693,-0.132917493441565,
13.));
#47265=CARTESIAN_POINT('Ctrl Pts',(-66.9502376703059,-0.151566178101122,
13.));
#47266=CARTESIAN_POINT('Ctrl Pts',(-66.9377139254706,-0.223073582635083,
13.));
#47267=CARTESIAN_POINT('Ctrl Pts',(-66.9214263256518,-0.293675712348754,
13.));
#47268=CARTESIAN_POINT('Ctrl Pts',(-66.901430305801,-0.363043772410292,
13.));
#47269=CARTESIAN_POINT('Ctrl Pts',(-66.8818637674749,-0.430921920958888,
13.));
#47270=CARTESIAN_POINT('Ctrl Pts',(-66.858745943864,-0.497619260724826,
13.));
#47271=CARTESIAN_POINT('Ctrl Pts',(-66.8320856793692,-0.562804370280902,
13.));
#47272=CARTESIAN_POINT('Ctrl Pts',(-66.8060100727734,-0.626559974544455,
13.));
#47273=CARTESIAN_POINT('Ctrl Pts',(-66.776545304655,-0.688869612388516,
13.));
#47274=CARTESIAN_POINT('Ctrl Pts',(-66.743664114667,-0.749389827227639,
13.));
#47275=CARTESIAN_POINT('Ctrl Pts',(-66.7329788263415,-0.769056875327405,
13.));
#47276=CARTESIAN_POINT('Ctrl Pts',(-66.7219324918179,-0.788534645854941,
13.));
#47277=CARTESIAN_POINT('Ctrl Pts',(-66.7105234437577,-0.807810393773745,
13.));
#47278=CARTESIAN_POINT('Ctrl Pts',(-66.7040881270254,-0.818682952330261,
13.));
#47279=CARTESIAN_POINT('Ctrl Pts',(-66.6975366287906,-0.829492290648959,
13.));
#47280=CARTESIAN_POINT('Ctrl Pts',(-66.6908782710633,-0.840221024848607,
13.));
#47281=CARTESIAN_POINT('Ctrl Pts',(-66.6548614907131,-0.898255525086147,
13.));
#47282=CARTESIAN_POINT('Ctrl Pts',(-66.615661353053,-0.954037570632601,
13.));
#47283=CARTESIAN_POINT('Ctrl Pts',(-66.5732918036362,-1.00726408538098,
13.));
#47284=CARTESIAN_POINT('Ctrl Pts',(-66.567176292694,-1.01494666255824,13.));
#47285=CARTESIAN_POINT('Ctrl Pts',(-66.5609946871419,-1.0225759395538,13.));
#47286=CARTESIAN_POINT('Ctrl Pts',(-66.5547469639699,-1.03015094108865,
13.));
#47287=CARTESIAN_POINT('Ctrl Pts',(-66.5106056086058,-1.08366977113728,
13.));
#47288=CARTESIAN_POINT('Ctrl Pts',(-66.4631661110425,-1.13448299231823,
13.));
#47289=CARTESIAN_POINT('Ctrl Pts',(-66.4127666235244,-1.18244447912767,
13.));
#47290=CARTESIAN_POINT('Ctrl Pts',(-66.3657479708622,-1.22718867396982,
13.));
#47291=CARTESIAN_POINT('Ctrl Pts',(-66.3161520834424,-1.26945072111176,
13.));
#47292=CARTESIAN_POINT('Ctrl Pts',(-66.2642393874467,-1.30907445581882,
13.));
#47293=CARTESIAN_POINT('Ctrl Pts',(-66.2527825898775,-1.31781915880077,
13.));
#47294=CARTESIAN_POINT('Ctrl Pts',(-66.2412129249561,-1.32643521268399,
13.));
#47295=CARTESIAN_POINT('Ctrl Pts',(-66.2295331629306,-1.33492068207895,
13.));
#47296=CARTESIAN_POINT('Ctrl Pts',(-66.2204025954476,-1.34155413494954,
13.));
#47297=CARTESIAN_POINT('Ctrl Pts',(-66.211205267767,-1.3481073045967,13.));
#47298=CARTESIAN_POINT('Ctrl Pts',(-66.20195334148,-1.35457199230889,13.));
#47299=CARTESIAN_POINT('Ctrl Pts',(-66.1459049971557,-1.39373519266308,
13.));
#47300=CARTESIAN_POINT('Ctrl Pts',(-66.0877532412386,-1.42972959266972,
13.));
#47301=CARTESIAN_POINT('Ctrl Pts',(-66.0278290563933,-1.46243222383127,
13.));
#47302=CARTESIAN_POINT('Ctrl Pts',(-65.9681817046083,-1.4949837779363,13.));
#47303=CARTESIAN_POINT('Ctrl Pts',(-65.906777156648,-1.52427416697934,13.));
#47304=CARTESIAN_POINT('Ctrl Pts',(-65.8439279088097,-1.55013292110232,
13.));
#47305=CARTESIAN_POINT('Ctrl Pts',(-65.7824252697681,-1.57543762522515,
13.));
#47306=CARTESIAN_POINT('Ctrl Pts',(-65.7195382072492,-1.59745625930267,
13.));
#47307=CARTESIAN_POINT('Ctrl Pts',(-65.6555614671547,-1.61597952395889,
13.));
#47308=CARTESIAN_POINT('Ctrl Pts',(-65.6420830167795,-1.6198819563599,13.));
#47309=CARTESIAN_POINT('Ctrl Pts',(-65.6285562369111,-1.6236290657015,13.));
#47310=CARTESIAN_POINT('Ctrl Pts',(-65.6149839556941,-1.62721860052123,
13.));
#47311=CARTESIAN_POINT('Ctrl Pts',(-65.6021159150352,-1.63062188102127,
13.));
#47312=CARTESIAN_POINT('Ctrl Pts',(-65.5892052056162,-1.63388381680147,
13.));
#47313=CARTESIAN_POINT('Ctrl Pts',(-65.5762752297125,-1.63699772297707,
13.));
#47314=CARTESIAN_POINT('Ctrl Pts',(-65.5127465220931,-1.65229724375406,
13.));
#47315=CARTESIAN_POINT('Ctrl Pts',(-65.4486405343066,-1.66405837362243,
13.));
#47316=CARTESIAN_POINT('Ctrl Pts',(-65.3842420394353,-1.67213585463769,
13.));
#47317=CARTESIAN_POINT('Ctrl Pts',(-65.3210685725296,-1.68005968081747,
13.));
#47318=CARTESIAN_POINT('Ctrl Pts',(-65.2576127400953,-1.68443871292178,
13.));
#47319=CARTESIAN_POINT('Ctrl Pts',(-65.1941497363329,-1.68508652435015,
13.));
#47320=CARTESIAN_POINT('Ctrl Pts',(-65.1327484539533,-1.6857132903411,13.));
#47321=CARTESIAN_POINT('Ctrl Pts',(-65.0713397980825,-1.68284723930874,
13.));
#47322=CARTESIAN_POINT('Ctrl Pts',(-65.0101900872574,-1.67627347092458,
13.));
#47323=CARTESIAN_POINT('Ctrl Pts',(-65.000007166314,-1.67517877786957,13.));
#47324=CARTESIAN_POINT('Ctrl Pts',(-64.989831478164,-1.67398116343886,13.));
#47325=CARTESIAN_POINT('Ctrl Pts',(-64.9796643197989,-1.67267950846502,
13.));
#47326=CARTESIAN_POINT('Ctrl Pts',(-64.9689074729785,-1.67130235836429,
13.));
#47327=CARTESIAN_POINT('Ctrl Pts',(-64.9581601737451,-1.66980874798798,
13.));
#47328=CARTESIAN_POINT('Ctrl Pts',(-64.9474239513002,-1.66819938802346,
13.));
#47329=CARTESIAN_POINT('Origin',(-65.,8.88178419700125E-15,23.5459252805377));
#47330=CARTESIAN_POINT('Ctrl Pts',(-62.9434348764936,-0.00149614206265766,
21.7959252805377));
#47331=CARTESIAN_POINT('Ctrl Pts',(-62.9426160796481,-0.0997858054225679,
21.7905813053169));
#47332=CARTESIAN_POINT('Ctrl Pts',(-62.9937092272654,-0.878618068249771,
21.7481913665734));
#47333=CARTESIAN_POINT('Ctrl Pts',(-63.9890540527047,-2.20843040890227,
21.6687554643073));
#47334=CARTESIAN_POINT('Ctrl Pts',(-66.3069967286646,-2.04687460564973,
21.5576175737392));
#47335=CARTESIAN_POINT('Ctrl Pts',(-67.428612079538,-0.0121339679509515,
21.4464796831712));
#47336=CARTESIAN_POINT('Ctrl Pts',(-66.3273005244664,2.03388573489001,21.3353417926031));
#47337=CARTESIAN_POINT('Ctrl Pts',(-64.0110910734901,2.21817972145312,21.2242039020351));
#47338=CARTESIAN_POINT('Ctrl Pts',(-62.9978510382059,0.892619747709234,
21.1443983980133));
#47339=CARTESIAN_POINT('Ctrl Pts',(-62.942718846502,0.106740802471778,21.1016388575141));
#47340=CARTESIAN_POINT('Ctrl Pts',(-62.9436210622307,0.00160392935066219,
21.0959252805377));
#47341=CARTESIAN_POINT('Ctrl Pts',(-62.9473239618077,0.00235074752841319,
21.8540747194623));
#47342=CARTESIAN_POINT('Ctrl Pts',(-62.9508762982105,-0.467866578479425,
21.8286245525962));
#47343=CARTESIAN_POINT('Ctrl Pts',(-63.3434621334709,-1.62957520615004,
21.7661284222074));
#47344=CARTESIAN_POINT('Ctrl Pts',(-65.2721300366129,-2.41280623887488,
21.6665863282959));
#47345=CARTESIAN_POINT('Ctrl Pts',(-67.1747422685441,-1.08094901338604,
21.5554484377278));
#47346=CARTESIAN_POINT('Ctrl Pts',(-67.0876157148515,1.24138505016238,21.4443105471598));
#47347=CARTESIAN_POINT('Ctrl Pts',(-65.0892538486774,2.42692553227055,21.3331726565917));
#47348=CARTESIAN_POINT('Ctrl Pts',(-63.2787520820962,1.52545559952442,21.2364273806926));
#47349=CARTESIAN_POINT('Ctrl Pts',(-62.9500869585733,0.417919283968027,
21.1767280683161));
#47350=CARTESIAN_POINT('Ctrl Pts',(-62.9479182248742,-0.00116161895480603,
21.1540747194623));
#47351=CARTESIAN_POINT('Ctrl Pts',(-66.2690708798524,-1.07935865304854,
22.));
#47352=CARTESIAN_POINT('Ctrl Pts',(-66.6279833110066,-0.657362393039546,
21.9629540364773));
#47353=CARTESIAN_POINT('Ctrl Pts',(-66.8852826717605,0.565789777391224,
21.8888621094319));
#47354=CARTESIAN_POINT('Ctrl Pts',(-65.5450879211412,1.89344353213328,21.7777242188639));
#47355=CARTESIAN_POINT('Ctrl Pts',(-63.7057951684468,1.4835378033008,21.6665863282959));
#47356=CARTESIAN_POINT('Ctrl Pts',(-63.0512142972679,-0.282082603662771,
21.5554484377278));
#47357=CARTESIAN_POINT('Ctrl Pts',(-64.180320745495,-1.79060472623491,21.4443105471598));
#47358=CARTESIAN_POINT('Ctrl Pts',(-66.0597184815454,-1.65961459691566,
21.3331726565917));
#47359=CARTESIAN_POINT('Ctrl Pts',(-66.9691289570557,-0.00983827259096255,
21.2220347660237));
#47360=CARTESIAN_POINT('Ctrl Pts',(-66.0761808851497,1.64908316550761,21.1108968754557));
#47361=CARTESIAN_POINT('Ctrl Pts',(-64.1981884552545,1.79850951013062,20.9997589848876));
#47362=CARTESIAN_POINT('Ctrl Pts',(-63.0541051349916,0.30177526833428,20.8886210943196));
#47363=CARTESIAN_POINT('Ctrl Pts',(-63.6911204902705,-1.47119522218438,
20.7774832037516));
#47364=CARTESIAN_POINT('Ctrl Pts',(-65.5261685894954,-1.89755500871052,
20.6663453131835));
#47365=CARTESIAN_POINT('Ctrl Pts',(-66.8796083671824,-0.587065728133525,
20.5552074226155));
#47366=CARTESIAN_POINT('Ctrl Pts',(-66.5126214133544,1.26077376527148,20.4440695320474));
#47367=CARTESIAN_POINT('Ctrl Pts',(-64.7611148635138,1.95461157704263,20.3329316414794));
#47368=CARTESIAN_POINT('Ctrl Pts',(-63.2282626195245,0.859371828191353,
20.2217937509113));
#47369=CARTESIAN_POINT('Ctrl Pts',(-63.3171016769871,-1.02246099457514,
20.1106558603433));
#47370=CARTESIAN_POINT('Ctrl Pts',(-64.9463166628138,-1.96842352553114,
19.9995179697752));
#47371=CARTESIAN_POINT('Ctrl Pts',(-66.6246686119733,-1.11266575470346,
19.8883800792072));
#47372=CARTESIAN_POINT('Ctrl Pts',(-66.8159429576165,0.761527637475698,
19.7772421886392));
#47373=CARTESIAN_POINT('Ctrl Pts',(-65.3450641189423,1.9386861278219,19.6661042980711));
#47374=CARTESIAN_POINT('Ctrl Pts',(-63.5583441794198,1.34134322872205,19.5549664075031));
#47375=CARTESIAN_POINT('Ctrl Pts',(-63.0911881617047,-0.483746344304426,
19.443828516935));
#47376=CARTESIAN_POINT('Ctrl Pts',(-64.3711892671104,-1.86605739990807,
19.332690626367));
#47377=CARTESIAN_POINT('Ctrl Pts',(-66.2267479674628,-1.54034495606734,
19.221552735799));
#47378=CARTESIAN_POINT('Ctrl Pts',(-66.9594503409616,0.195262695377469,
19.1104148452309));
#47379=CARTESIAN_POINT('Ctrl Pts',(-65.8986455956832,1.75214418700341,18.9992769546629));
#47380=CARTESIAN_POINT('Ctrl Pts',(-64.0153003453502,1.70526823375496,18.8881390640948));
#47381=CARTESIAN_POINT('Ctrl Pts',(-63.0332618561676,0.0975409270146975,
18.7770011735268));
#47382=CARTESIAN_POINT('Ctrl Pts',(-63.8514010943644,-1.59946669637174,
18.6658632829587));
#47383=CARTESIAN_POINT('Ctrl Pts',(-65.720865936886,-1.83246431340308,18.5547253923907));
#47384=CARTESIAN_POINT('Ctrl Pts',(-66.9305140122006,-0.388186562807738,
18.4435875018227));
#47385=CARTESIAN_POINT('Ctrl Pts',(-66.3731407186298,1.41140275105549,18.3324496112546));
#47386=CARTESIAN_POINT('Ctrl Pts',(-64.5589161528223,1.91911912048435,18.2213117206866));
#47387=CARTESIAN_POINT('Ctrl Pts',(-63.1484206345677,0.670243994641496,
18.1101738301185));
#47388=CARTESIAN_POINT('Ctrl Pts',(-63.4326967078313,-1.19211306057993,
17.9990359395505));
#47389=CARTESIAN_POINT('Ctrl Pts',(-65.1515432588453,-1.96331551197125,
17.8878980489824));
#47390=CARTESIAN_POINT('Ctrl Pts',(-66.7316805464207,-0.937473009742842,
17.7767601584144));
#47391=CARTESIAN_POINT('Ctrl Pts',(-66.7267909912641,0.946449169970149,
17.6656222678463));
#47392=CARTESIAN_POINT('Ctrl Pts',(-65.1413500586618,1.9640756909459,17.5544843772784));
#47393=CARTESIAN_POINT('Ctrl Pts',(-63.4265298143476,1.18396145786557,17.4433464867103));
#47394=CARTESIAN_POINT('Ctrl Pts',(-63.1519246753265,-0.679846124635249,
17.3322085961423));
#47395=CARTESIAN_POINT('Ctrl Pts',(-64.5688838395789,-1.92138283927799,
17.2210707055742));
#47396=CARTESIAN_POINT('Ctrl Pts',(-66.3804485146544,-1.40425605116614,
17.1099328150062));
#47397=CARTESIAN_POINT('Ctrl Pts',(-66.9284730089157,0.398202225924807,
16.9987949244381));
#47398=CARTESIAN_POINT('Ctrl Pts',(-65.7113442877452,1.83618148970649,16.8876570338701));
#47399=CARTESIAN_POINT('Ctrl Pts',(-63.8431140728085,1.59348301224527,16.776519143302));
#47400=CARTESIAN_POINT('Ctrl Pts',(-63.033794667009,-0.107748537650181,
16.665381252734));
#47401=CARTESIAN_POINT('Ctrl Pts',(-64.024165300781,-1.71035662908352,16.5542433621659));
#47402=CARTESIAN_POINT('Ctrl Pts',(-65.9077285014668,-1.74745590115202,
16.4431054715979));
#47403=CARTESIAN_POINT('Ctrl Pts',(-66.9604375104179,-0.18508896940078,
16.3319675810299));
#47404=CARTESIAN_POINT('Ctrl Pts',(-66.2187358332113,1.54669199509962,16.2208296904618));
#47405=CARTESIAN_POINT('Ctrl Pts',(-64.3615114264595,1.86276823579531,16.1096917998938));
#47406=CARTESIAN_POINT('Ctrl Pts',(-63.0887028520271,0.473831585058423,
15.9985539093257));
#47407=CARTESIAN_POINT('Ctrl Pts',(-63.5653262327086,-1.34880848913672,
15.8874160187577));
#47408=CARTESIAN_POINT('Ctrl Pts',(-65.3551227829179,-1.9368688566197,15.7762781281897));
#47409=CARTESIAN_POINT('Ctrl Pts',(-66.819871422519,-0.75209119420401,15.6651402376216));
#47410=CARTESIAN_POINT('Ctrl Pts',(-66.6188711104164,1.12108406786279,15.5540023470536));
#47411=CARTESIAN_POINT('Ctrl Pts',(-64.9360997115566,1.96811836805764,15.4428644564855));
#47412=CARTESIAN_POINT('Ctrl Pts',(-63.3118169716773,1.01371160717774,15.3317265659175));
#47413=CARTESIAN_POINT('Ctrl Pts',(-63.2327473023447,-0.868556886382297,
15.2205886753495));
#47414=CARTESIAN_POINT('Ctrl Pts',(-64.771264070325,-1.95582540705099,15.1094507847814));
#47415=CARTESIAN_POINT('Ctrl Pts',(-66.5191454265163,-1.25290476136478,
14.9983128942134));
#47416=CARTESIAN_POINT('Ctrl Pts',(-66.8765357500253,0.596813839734138,
14.8871750036453));
#47417=CARTESIAN_POINT('Ctrl Pts',(-65.516311611266,1.90026192842666,14.7760371130773));
#47418=CARTESIAN_POINT('Ctrl Pts',(-63.6835016170176,1.46437879615622,14.6648992225092));
#47419=CARTESIAN_POINT('Ctrl Pts',(-63.0556974877489,-0.311866999404029,
14.5537613319412));
#47420=CARTESIAN_POINT('Ctrl Pts',(-64.2075355674246,-1.80265710789544,
14.4426234413732));
#47421=CARTESIAN_POINT('Ctrl Pts',(-66.0847251913073,-1.64345528891983,
14.3314855508051));
#47422=CARTESIAN_POINT('Ctrl Pts',(-66.969053819969,0.0200209189642882,
14.2203476602371));
#47423=CARTESIAN_POINT('Ctrl Pts',(-66.0510846129266,1.66516952053626,14.109209769669));
#47424=CARTESIAN_POINT('Ctrl Pts',(-64.1710468184079,1.78617400482043,13.998071879101));
#47425=CARTESIAN_POINT('Ctrl Pts',(-63.049757131241,0.272264377212432,13.8869339885329));
#47426=CARTESIAN_POINT('Ctrl Pts',(-63.7135511069036,-1.49083448335768,
13.7757960979649));
#47427=CARTESIAN_POINT('Ctrl Pts',(-65.5548379149366,-1.88939023827018,
13.6646582073969));
#47428=CARTESIAN_POINT('Ctrl Pts',(-66.8882920122399,-0.558497016674497,
13.5535203168288));
#47429=CARTESIAN_POINT('Ctrl Pts',(-66.4933378285089,1.28345860874756,13.4423824262608));
#47430=CARTESIAN_POINT('Ctrl Pts',(-64.7315804519141,1.95092037563963,13.3312445356927));
#47431=CARTESIAN_POINT('Ctrl Pts',(-63.2153798048402,0.832146062593817,
13.2201066451247));
#47432=CARTESIAN_POINT('Ctrl Pts',(-63.3329222496525,-1.04723556764185,
13.1089687545567));
#47433=CARTESIAN_POINT('Ctrl Pts',(-64.9758366741791,-1.97019425053384,
12.9978308639886));
#47434=CARTESIAN_POINT('Ctrl Pts',(-66.6419915114447,-1.08548270413876,
12.8866929734206));
#47435=CARTESIAN_POINT('Ctrl Pts',(-66.7483953817108,0.159901738299123,
12.8126010463752));
#47436=CARTESIAN_POINT('Ctrl Pts',(-66.526442356053,0.66748013726814,12.7755550828525));
#47437=CARTESIAN_POINT('Ctrl Pts',(-66.3677806246588,-1.16331236980977,
22.0748149723825));
#47438=CARTESIAN_POINT('Ctrl Pts',(-66.7546096639785,-0.708492771249656,
22.0377690088598));
#47439=CARTESIAN_POINT('Ctrl Pts',(-67.0319220552433,0.60979753568671,21.9636770818144));
#47440=CARTESIAN_POINT('Ctrl Pts',(-65.5874854660279,2.04071767641436,21.8525391912464));
#47441=CARTESIAN_POINT('Ctrl Pts',(-63.605130476917,1.59892902399572,21.7414013006783));
#47442=CARTESIAN_POINT('Ctrl Pts',(-62.8996355773925,-0.304023302377036,
21.6302634101103));
#47443=CARTESIAN_POINT('Ctrl Pts',(-64.1165651812316,-1.9298799537907,21.5191255195423));
#47444=CARTESIAN_POINT('Ctrl Pts',(-66.1421445639184,-1.78870126649369,
21.4079876289742));
#47445=CARTESIAN_POINT('Ctrl Pts',(-67.1222899978831,-0.0106035043776257,
21.2968497384062));
#47446=CARTESIAN_POINT('Ctrl Pts',(-66.1598874315886,1.77735068863507,21.1857118478382));
#47447=CARTESIAN_POINT('Ctrl Pts',(-64.135822661333,1.93839958057146,21.0745739572701));
#47448=CARTESIAN_POINT('Ctrl Pts',(-62.9027512676903,0.325247684413701,
20.9634360667021));
#47449=CARTESIAN_POINT('Ctrl Pts',(-63.5893143859473,-1.58562642318961,
20.852298176134));
#47450=CARTESIAN_POINT('Ctrl Pts',(-65.5670945677199,-2.04514894821357,
20.741160285566));
#47451=CARTESIAN_POINT('Ctrl Pts',(-67.0258063969427,-0.632728353546071,
20.630022394998));
#47452=CARTESIAN_POINT('Ctrl Pts',(-66.6302747895932,1.35883815127574,20.5188845044299));
#47453=CARTESIAN_POINT('Ctrl Pts',(-64.7425341118513,2.10664343990284,20.4077466138619));
#47454=CARTESIAN_POINT('Ctrl Pts',(-63.0904549151108,0.92621472499195,20.2966087232938));
#47455=CARTESIAN_POINT('Ctrl Pts',(-63.1862039732914,-1.10198914816479,
20.1854708327258));
#47456=CARTESIAN_POINT('Ctrl Pts',(-64.9421411131276,-2.12152969710982,
20.0743329421577));
#47457=CARTESIAN_POINT('Ctrl Pts',(-66.7510371439672,-1.19921013488373,
19.9631950515897));
#47458=CARTESIAN_POINT('Ctrl Pts',(-66.9571890209963,0.820760104276152,
19.8520571610216));
#47459=CARTESIAN_POINT('Ctrl Pts',(-65.3719035899786,2.08947929152553,19.7409192704536));
#47460=CARTESIAN_POINT('Ctrl Pts',(-63.4462105859322,1.44567439722259,19.6297813798856));
#47461=CARTESIAN_POINT('Ctrl Pts',(-62.9427186534739,-0.521372673105617,
19.5186434893175));
#47462=CARTESIAN_POINT('Ctrl Pts',(-64.3222796687889,-2.0112014203591,19.4075055987495));
#47463=CARTESIAN_POINT('Ctrl Pts',(-66.3221657890617,-1.66015470029927,
19.2963677081814));
#47464=CARTESIAN_POINT('Ctrl Pts',(-67.1118585682623,0.210450445042934,
19.1852298176134));
#47465=CARTESIAN_POINT('Ctrl Pts',(-65.9685432498092,1.88842791103254,19.0740919270454));
#47466=CARTESIAN_POINT('Ctrl Pts',(-63.9387093107874,1.8379058939935,18.9629540364773));
#47467=CARTESIAN_POINT('Ctrl Pts',(-62.8802867754522,0.105127768826814,
18.8518161459093));
#47468=CARTESIAN_POINT('Ctrl Pts',(-63.762061793731,-1.72387499533423,18.7406782553413));
#47469=CARTESIAN_POINT('Ctrl Pts',(-65.7769356913806,-1.97499542621529,
18.6295403647732));
#47470=CARTESIAN_POINT('Ctrl Pts',(-67.0806715396602,-0.418380145499115,
18.5184024742052));
#47471=CARTESIAN_POINT('Ctrl Pts',(-66.4799451312683,1.52118322714049,18.4072645836371));
#47472=CARTESIAN_POINT('Ctrl Pts',(-64.5246081605074,2.06839034059005,18.296126693069));
#47473=CARTESIAN_POINT('Ctrl Pts',(-63.0044027317441,0.722376318154277,
18.184988802501));
#47474=CARTESIAN_POINT('Ctrl Pts',(-63.3107901142278,-1.28483694059203,
18.073850911933));
#47475=CARTESIAN_POINT('Ctrl Pts',(-65.1633304621018,-2.11602437657286,
17.962713021365));
#47476=CARTESIAN_POINT('Ctrl Pts',(-66.8663725857206,-1.01039070332778,
17.8515751307969));
#47477=CARTESIAN_POINT('Ctrl Pts',(-66.8611027155246,1.02006503928305,17.7404372402289));
#47478=CARTESIAN_POINT('Ctrl Pts',(-65.1523444234686,2.11684368311381,17.6292993496608));
#47479=CARTESIAN_POINT('Ctrl Pts',(-63.3041435529085,1.27605129715033,17.5181614590928));
#47480=CARTESIAN_POINT('Ctrl Pts',(-63.0081793206914,-0.732725312500785,
17.4070235685247));
#47481=CARTESIAN_POINT('Ctrl Pts',(-64.5353511450282,-2.07083013394973,
17.2958856779567));
#47482=CARTESIAN_POINT('Ctrl Pts',(-66.4878213357972,-1.51348064898344,
17.1847477873886));
#47483=CARTESIAN_POINT('Ctrl Pts',(-67.0784717848694,0.429174838035305,
17.0736098968206));
#47484=CARTESIAN_POINT('Ctrl Pts',(-65.7666734377774,1.97900172862673,16.9624720062526));
#47485=CARTESIAN_POINT('Ctrl Pts',(-63.7531301984196,1.71742589359988,16.8513341156845));
#47486=CARTESIAN_POINT('Ctrl Pts',(-62.8808610289137,-0.116129338772932,
16.7401962251165));
#47487=CARTESIAN_POINT('Ctrl Pts',(-63.9482637923134,-1.84339007037128,
16.6290583345485));
#47488=CARTESIAN_POINT('Ctrl Pts',(-65.9783326341088,-1.88337496509217,
16.5179204439804));
#47489=CARTESIAN_POINT('Ctrl Pts',(-67.1129225208572,-0.199485395342068,
16.4067825534124));
#47490=CARTESIAN_POINT('Ctrl Pts',(-66.3135304620949,1.66699541908822,16.2956446628443));
#47491=CARTESIAN_POINT('Ctrl Pts',(-64.3118490749262,2.00765642140263,16.1845067722763));
#47492=CARTESIAN_POINT('Ctrl Pts',(-62.9400400336448,0.510686732855833,
16.0733688817082));
#47493=CARTESIAN_POINT('Ctrl Pts',(-63.4537357110932,-1.45372031389701,
15.9622309911402));
#47494=CARTESIAN_POINT('Ctrl Pts',(-65.3827446280278,-2.08752067094761,
15.8510931005722));
#47495=CARTESIAN_POINT('Ctrl Pts',(-66.9614230462693,-0.810589683949272,
15.7399552100041));
#47496=CARTESIAN_POINT('Ctrl Pts',(-66.7447887062896,1.20828323380549,15.6288173194361));
#47497=CARTESIAN_POINT('Ctrl Pts',(-64.931129476036,2.12120080414855,15.517679428868));
#47498=CARTESIAN_POINT('Ctrl Pts',(-63.1805082177236,1.09255922368242,15.4065415383));
#47499=CARTESIAN_POINT('Ctrl Pts',(-63.0952884215498,-0.93611420722686,
15.2954036477319));
#47500=CARTESIAN_POINT('Ctrl Pts',(-64.7534727352587,-2.10795168295957,
15.1842657571639));
#47501=CARTESIAN_POINT('Ctrl Pts',(-66.6373062477565,-1.35035708749135,
15.0731278665959));
#47502=CARTESIAN_POINT('Ctrl Pts',(-67.022494788205,0.643234684111219,14.9619899760278));
#47503=CARTESIAN_POINT('Ctrl Pts',(-65.5564709027586,2.04806641515652,14.8508520854598));
#47504=CARTESIAN_POINT('Ctrl Pts',(-63.5811029082571,1.57827980796209,14.7397141948917));
#47505=CARTESIAN_POINT('Ctrl Pts',(-62.9044674754165,-0.336124361552553,
14.6285763043237));
#47506=CARTESIAN_POINT('Ctrl Pts',(-64.1458968022858,-1.94286978310439,
14.5174384137556));
#47507=CARTESIAN_POINT('Ctrl Pts',(-66.1690963233843,-1.7712850695456,14.4063005231876));
#47508=CARTESIAN_POINT('Ctrl Pts',(-67.1222090165502,0.0215781683135005,
14.2951626326196));
#47509=CARTESIAN_POINT('Ctrl Pts',(-66.1328391433939,1.79468825825304,14.1840247420515));
#47510=CARTESIAN_POINT('Ctrl Pts',(-64.1065699177788,1.92510460593566,14.0728868514835));
#47511=CARTESIAN_POINT('Ctrl Pts',(-62.8980650713711,0.293441403351154,
13.9617489609155));
#47512=CARTESIAN_POINT('Ctrl Pts',(-63.613489680895,-1.60679324794458,13.8506110703474));
#47513=CARTESIAN_POINT('Ctrl Pts',(-65.5979938251871,-2.03634911284551,
13.7394731797794));
#47514=CARTESIAN_POINT('Ctrl Pts',(-67.0351654655728,-0.601937535928643,
13.6283352892113));
#47515=CARTESIAN_POINT('Ctrl Pts',(-66.6094913060666,1.38328744711303,13.5171973986433));
#47516=CARTESIAN_POINT('Ctrl Pts',(-64.7107024808619,2.10266513274846,13.4060595080752));
#47517=CARTESIAN_POINT('Ctrl Pts',(-63.0765700607689,0.89687130905907,13.2949216175072));
#47518=CARTESIAN_POINT('Ctrl Pts',(-63.2032550876981,-1.12869071508498,
13.1837837269391));
#47519=CARTESIAN_POINT('Ctrl Pts',(-64.9739572238164,-2.12343815107306,
13.0726458363711));
#47520=CARTESIAN_POINT('Ctrl Pts',(-66.7697074378301,-1.16991275640645,
12.9615079458031));
#47521=CARTESIAN_POINT('Ctrl Pts',(-66.8843875194939,0.172339073385913,
12.8874160187577));
#47522=CARTESIAN_POINT('Ctrl Pts',(-66.6451707405899,0.719397484879782,
12.850370055235));
#47523=CARTESIAN_POINT('Ctrl Pts',(-66.4664903694652,-1.24726608657099,
22.149629944765));
#47524=CARTESIAN_POINT('Ctrl Pts',(-66.8812360169505,-0.759623149459765,
22.1125839812423));
#47525=CARTESIAN_POINT('Ctrl Pts',(-67.1785614387261,0.653805293982196,
22.0384920541969));
#47526=CARTESIAN_POINT('Ctrl Pts',(-65.6298830109146,2.18799182069543,21.9273541636289));
#47527=CARTESIAN_POINT('Ctrl Pts',(-63.5044657853871,1.71432024469064,21.8162162730608));
#47528=CARTESIAN_POINT('Ctrl Pts',(-62.7480568575172,-0.325964001091306,
21.7050783824928));
#47529=CARTESIAN_POINT('Ctrl Pts',(-64.0528096169681,-2.06915518134648,
21.5939404919247));
#47530=CARTESIAN_POINT('Ctrl Pts',(-66.2245706462915,-1.91778793607171,
21.4828026013567));
#47531=CARTESIAN_POINT('Ctrl Pts',(-67.2754510387106,-0.0113687361642878,
21.3716647107886));
#47532=CARTESIAN_POINT('Ctrl Pts',(-66.2435939780275,1.90561821176254,21.2605268202207));
#47533=CARTESIAN_POINT('Ctrl Pts',(-64.0734568674116,2.07828965101229,21.1493889296526));
#47534=CARTESIAN_POINT('Ctrl Pts',(-62.751397400389,0.348720100493122,21.0382510390846));
#47535=CARTESIAN_POINT('Ctrl Pts',(-63.4875082816241,-1.70005762419485,
20.9271131485165));
#47536=CARTESIAN_POINT('Ctrl Pts',(-65.6080205459445,-2.19274288771661,
20.8159752579485));
#47537=CARTESIAN_POINT('Ctrl Pts',(-67.172004426703,-0.678390978958618,
20.7048373673804));
#47538=CARTESIAN_POINT('Ctrl Pts',(-66.7479281658321,1.45690253728,20.5936994768124));
#47539=CARTESIAN_POINT('Ctrl Pts',(-64.7239533601888,2.25867530276305,20.4825615862443));
#47540=CARTESIAN_POINT('Ctrl Pts',(-62.9526472106971,0.993057621792547,
20.3714236956763));
#47541=CARTESIAN_POINT('Ctrl Pts',(-63.0553062695956,-1.18151730175445,
20.2602858051083));
#47542=CARTESIAN_POINT('Ctrl Pts',(-64.9379655634416,-2.27463586868849,
20.1491479145402));
#47543=CARTESIAN_POINT('Ctrl Pts',(-66.8774056759608,-1.285754515064,20.0380100239722));
#47544=CARTESIAN_POINT('Ctrl Pts',(-67.0984350843764,0.879992571076608,
19.9268721334041));
#47545=CARTESIAN_POINT('Ctrl Pts',(-65.3987430610147,2.24027245522917,19.8157342428361));
#47546=CARTESIAN_POINT('Ctrl Pts',(-63.3340769924447,1.55000556572313,19.7045963522681));
#47547=CARTESIAN_POINT('Ctrl Pts',(-62.7942491452433,-0.558999001906807,
19.5934584617));
#47548=CARTESIAN_POINT('Ctrl Pts',(-64.2733700704672,-2.15634544081014,
19.482320571132));
#47549=CARTESIAN_POINT('Ctrl Pts',(-66.4175836106607,-1.7799644445312,19.3711826805639));
#47550=CARTESIAN_POINT('Ctrl Pts',(-67.2642667955629,0.225638194708396,
19.2600447899959));
#47551=CARTESIAN_POINT('Ctrl Pts',(-66.0384409039352,2.02471163506166,19.1489068994278));
#47552=CARTESIAN_POINT('Ctrl Pts',(-63.8621182762245,1.97054355423204,19.0377690088598));
#47553=CARTESIAN_POINT('Ctrl Pts',(-62.727311694737,0.112714610638931,18.9266311182918));
#47554=CARTESIAN_POINT('Ctrl Pts',(-63.6727224930976,-1.84828329429672,
18.8154932277237));
#47555=CARTESIAN_POINT('Ctrl Pts',(-65.8330054458753,-2.11752653902751,
18.7043553371557));
#47556=CARTESIAN_POINT('Ctrl Pts',(-67.2308290671198,-0.448573728190495,
18.5932174465877));
#47557=CARTESIAN_POINT('Ctrl Pts',(-66.5867495439068,1.63096370322549,18.4820795560196));
#47558=CARTESIAN_POINT('Ctrl Pts',(-64.4903001681923,2.21766156069575,18.3709416654516));
#47559=CARTESIAN_POINT('Ctrl Pts',(-62.8603848289206,0.774508641667059,
18.2598037748835));
#47560=CARTESIAN_POINT('Ctrl Pts',(-63.1888835206242,-1.37756082060413,
18.1486658843155));
#47561=CARTESIAN_POINT('Ctrl Pts',(-65.1751176653583,-2.26873324117447,
18.0375279937474));
#47562=CARTESIAN_POINT('Ctrl Pts',(-67.0010646250206,-1.08330839691272,
17.9263901031794));
#47563=CARTESIAN_POINT('Ctrl Pts',(-66.9954144397851,1.09368090859596,17.8152522126113));
#47564=CARTESIAN_POINT('Ctrl Pts',(-65.1633387882755,2.26961167528172,17.7041143220433));
#47565=CARTESIAN_POINT('Ctrl Pts',(-63.1817572914694,1.36814113643509,17.5929764314753));
#47566=CARTESIAN_POINT('Ctrl Pts',(-62.8644339660562,-0.785604500366324,
17.4818385409072));
#47567=CARTESIAN_POINT('Ctrl Pts',(-64.5018184504777,-2.22027742862146,
17.3707006503392));
#47568=CARTESIAN_POINT('Ctrl Pts',(-66.5951941569401,-1.62270524680074,
17.2595627597711));
#47569=CARTESIAN_POINT('Ctrl Pts',(-67.2284705608229,0.460147450145801,
17.1484248692031));
#47570=CARTESIAN_POINT('Ctrl Pts',(-65.8220025878096,2.12182196754698,17.0372869786351));
#47571=CARTESIAN_POINT('Ctrl Pts',(-63.6631463240307,1.84136877495449,16.926149088067));
#47572=CARTESIAN_POINT('Ctrl Pts',(-62.7279273908184,-0.124510139895683,
16.815011197499));
#47573=CARTESIAN_POINT('Ctrl Pts',(-63.8723622838458,-1.97642351165904,
16.7038733069309));
#47574=CARTESIAN_POINT('Ctrl Pts',(-66.0489367667509,-2.01929402903231,
16.5927354163629));
#47575=CARTESIAN_POINT('Ctrl Pts',(-67.2654075312964,-0.213881821283357,
16.4815975257949));
#47576=CARTESIAN_POINT('Ctrl Pts',(-66.4083250909786,1.78729884307681,16.3704596352268));
#47577=CARTESIAN_POINT('Ctrl Pts',(-64.2621867233928,2.15254460700996,16.2593217446588));
#47578=CARTESIAN_POINT('Ctrl Pts',(-62.7913772152625,0.547541880653244,
16.1481838540907));
#47579=CARTESIAN_POINT('Ctrl Pts',(-63.3421451894777,-1.55863213865729,
16.0370459635227));
#47580=CARTESIAN_POINT('Ctrl Pts',(-65.4103664731376,-2.23817248527552,
15.9259080729546));
#47581=CARTESIAN_POINT('Ctrl Pts',(-67.1029746700197,-0.869088173694531,
15.8147701823866));
#47582=CARTESIAN_POINT('Ctrl Pts',(-66.8707063021627,1.2954823997482,15.7036322918186));
#47583=CARTESIAN_POINT('Ctrl Pts',(-64.9261592405154,2.27428324023947,15.5924944012505));
#47584=CARTESIAN_POINT('Ctrl Pts',(-63.0491994637699,1.17140684018709,15.4813565106825));
#47585=CARTESIAN_POINT('Ctrl Pts',(-62.9578295407548,-1.00367152807142,
15.3702186201144));
#47586=CARTESIAN_POINT('Ctrl Pts',(-64.7356814001924,-2.26007795886815,
15.2590807295464));
#47587=CARTESIAN_POINT('Ctrl Pts',(-66.7554670689966,-1.44780941361791,
15.1479428389783));
#47588=CARTESIAN_POINT('Ctrl Pts',(-67.1684538263848,0.689655528488298,
15.0368049484103));
#47589=CARTESIAN_POINT('Ctrl Pts',(-65.5966301942511,2.19587090188638,14.9256670578423));
#47590=CARTESIAN_POINT('Ctrl Pts',(-63.4787041994968,1.69218081976796,14.8145291672742));
#47591=CARTESIAN_POINT('Ctrl Pts',(-62.753237463084,-0.360381723701076,
14.7033912767062));
#47592=CARTESIAN_POINT('Ctrl Pts',(-64.084258037147,-2.08308245831335,14.5922533861381));
#47593=CARTESIAN_POINT('Ctrl Pts',(-66.2534674554613,-1.89911485017137,
14.4811154955701));
#47594=CARTESIAN_POINT('Ctrl Pts',(-67.2753642131315,0.0231354176627139,
14.3699776050021));
#47595=CARTESIAN_POINT('Ctrl Pts',(-66.214593673861,1.92420699596982,14.258839714434));
#47596=CARTESIAN_POINT('Ctrl Pts',(-64.0420930171499,2.06403520705089,14.147701823866));
#47597=CARTESIAN_POINT('Ctrl Pts',(-62.746373011501,0.314618429489875,14.0365639332979));
#47598=CARTESIAN_POINT('Ctrl Pts',(-63.5134282548864,-1.72275201253147,
13.9254260427299));
#47599=CARTESIAN_POINT('Ctrl Pts',(-65.6411497354375,-2.18330798742085,
13.8142881521618));
#47600=CARTESIAN_POINT('Ctrl Pts',(-67.1820389189058,-0.645378055182786,
13.7031502615938));
#47601=CARTESIAN_POINT('Ctrl Pts',(-66.7256447836243,1.4831162854785,13.5920123710258));
#47602=CARTESIAN_POINT('Ctrl Pts',(-64.6898245098097,2.25440988985728,13.4808744804577));
#47603=CARTESIAN_POINT('Ctrl Pts',(-62.9377603166977,0.961596555524325,
13.3697365898897));
#47604=CARTESIAN_POINT('Ctrl Pts',(-63.0735879257438,-1.21014586252811,
13.2585986993216));
#47605=CARTESIAN_POINT('Ctrl Pts',(-64.9720777734537,-2.27668205161229,
13.1474608087536));
#47606=CARTESIAN_POINT('Ctrl Pts',(-66.8974233642155,-1.25434280867415,
13.0363229181856));
#47607=CARTESIAN_POINT('Ctrl Pts',(-67.020379657277,0.184776408472704,12.9622309911402));
#47608=CARTESIAN_POINT('Ctrl Pts',(-66.7638991251268,0.771314832491424,
12.9251850276175));
#47609=CARTESIAN_POINT('Ctrl Pts',(-66.5652001142717,-1.33121980333222,
22.2244449171475));
#47610=CARTESIAN_POINT('Ctrl Pts',(-67.0078623699224,-0.810753527669875,
22.1873989536248));
#47611=CARTESIAN_POINT('Ctrl Pts',(-67.3252008222088,0.697813052277679,
22.1133070265794));
#47612=CARTESIAN_POINT('Ctrl Pts',(-65.6722805558013,2.33526596497651,22.0021691360114));
#47613=CARTESIAN_POINT('Ctrl Pts',(-63.4038010938572,1.82971146538555,21.8910312454434));
#47614=CARTESIAN_POINT('Ctrl Pts',(-62.5964781376417,-0.34790469980557,
21.7798933548753));
#47615=CARTESIAN_POINT('Ctrl Pts',(-63.9890540527047,-2.20843040890227,
21.6687554643073));
#47616=CARTESIAN_POINT('Ctrl Pts',(-66.3069967286646,-2.04687460564973,
21.5576175737392));
#47617=CARTESIAN_POINT('Ctrl Pts',(-67.428612079538,-0.0121339679509515,
21.4464796831712));
#47618=CARTESIAN_POINT('Ctrl Pts',(-66.3273005244664,2.03388573489001,21.3353417926031));
#47619=CARTESIAN_POINT('Ctrl Pts',(-64.0110910734901,2.21817972145312,21.2242039020351));
#47620=CARTESIAN_POINT('Ctrl Pts',(-62.6000435330876,0.372192516572544,
21.1130660114671));
#47621=CARTESIAN_POINT('Ctrl Pts',(-63.385702177301,-1.81448882520009,21.001928120899));
#47622=CARTESIAN_POINT('Ctrl Pts',(-65.648946524169,-2.34033682721966,20.8907902303309));
#47623=CARTESIAN_POINT('Ctrl Pts',(-67.3182024564633,-0.724053604371166,
20.7796523397629));
#47624=CARTESIAN_POINT('Ctrl Pts',(-66.865581542071,1.55496692328426,20.6685144491949));
#47625=CARTESIAN_POINT('Ctrl Pts',(-64.7053726085262,2.41070716562326,20.5573765586268));
#47626=CARTESIAN_POINT('Ctrl Pts',(-62.8148395062834,1.05990051859314,20.4462386680588));
#47627=CARTESIAN_POINT('Ctrl Pts',(-62.9244085658998,-1.2610454553441,20.3351007774907));
#47628=CARTESIAN_POINT('Ctrl Pts',(-64.9337900137556,-2.42774204026717,
20.2239628869227));
#47629=CARTESIAN_POINT('Ctrl Pts',(-67.0037742079544,-1.37229889524426,
20.1128249963547));
#47630=CARTESIAN_POINT('Ctrl Pts',(-67.2396811477566,0.939225037877063,
20.0016871057866));
#47631=CARTESIAN_POINT('Ctrl Pts',(-65.4255825320509,2.3910656189328,19.8905492152186));
#47632=CARTESIAN_POINT('Ctrl Pts',(-63.2219433989572,1.65433673422367,19.7794113246505));
#47633=CARTESIAN_POINT('Ctrl Pts',(-62.6457796370125,-0.596625330707996,
19.6682734340825));
#47634=CARTESIAN_POINT('Ctrl Pts',(-64.2244604721458,-2.30148946126117,
19.5571355435145));
#47635=CARTESIAN_POINT('Ctrl Pts',(-66.5130014322595,-1.89977418876313,
19.4459976529464));
#47636=CARTESIAN_POINT('Ctrl Pts',(-67.4166750228636,0.24082594437386,19.3348597623784));
#47637=CARTESIAN_POINT('Ctrl Pts',(-66.1083385580613,2.16099535909079,19.2237218718103));
#47638=CARTESIAN_POINT('Ctrl Pts',(-63.7855272416617,2.10318121447059,19.1125839812423));
#47639=CARTESIAN_POINT('Ctrl Pts',(-62.5743366140217,0.120301452451048,
19.0014460906743));
#47640=CARTESIAN_POINT('Ctrl Pts',(-63.5833831924642,-1.97269159325921,
18.8903082001062));
#47641=CARTESIAN_POINT('Ctrl Pts',(-65.88907520037,-2.26005765183972,18.7791703095382));
#47642=CARTESIAN_POINT('Ctrl Pts',(-67.3809865945794,-0.478767310881874,
18.6680324189701));
#47643=CARTESIAN_POINT('Ctrl Pts',(-66.6935539565454,1.74074417931049,18.5568945284021));
#47644=CARTESIAN_POINT('Ctrl Pts',(-64.4559921758773,2.36693278080145,18.445756637834));
#47645=CARTESIAN_POINT('Ctrl Pts',(-62.7163669260972,0.826640965179838,
18.334618747266));
#47646=CARTESIAN_POINT('Ctrl Pts',(-63.0669769270206,-1.47028470061622,
18.2234808566979));
#47647=CARTESIAN_POINT('Ctrl Pts',(-65.1869048686148,-2.42144210577607,
18.1123429661299));
#47648=CARTESIAN_POINT('Ctrl Pts',(-67.1357566643205,-1.15622609049766,
18.0012050755618));
#47649=CARTESIAN_POINT('Ctrl Pts',(-67.1297261640456,1.16729677790886,17.8900671849939));
#47650=CARTESIAN_POINT('Ctrl Pts',(-65.1743331530824,2.42237966744963,17.7789292944258));
#47651=CARTESIAN_POINT('Ctrl Pts',(-63.0593710300304,1.46023097571985,17.6677914038578));
#47652=CARTESIAN_POINT('Ctrl Pts',(-62.720688611421,-0.83848368823186,17.5566535132897));
#47653=CARTESIAN_POINT('Ctrl Pts',(-64.4682857559272,-2.36972472329319,
17.4455156227217));
#47654=CARTESIAN_POINT('Ctrl Pts',(-66.7025669780829,-1.73192984461803,
17.3343777321536));
#47655=CARTESIAN_POINT('Ctrl Pts',(-67.3784693367765,0.491120062256299,
17.2232398415856));
#47656=CARTESIAN_POINT('Ctrl Pts',(-65.8773317378418,2.26464220646723,17.1121019510175));
#47657=CARTESIAN_POINT('Ctrl Pts',(-63.5731624496418,1.9653116563091,17.0009640604495));
#47658=CARTESIAN_POINT('Ctrl Pts',(-62.5749937527231,-0.132890941018434,
16.8898261698815));
#47659=CARTESIAN_POINT('Ctrl Pts',(-63.7964607753782,-2.1094569529468,16.7786882793134));
#47660=CARTESIAN_POINT('Ctrl Pts',(-66.119540899393,-2.15521309297246,16.6675503887454));
#47661=CARTESIAN_POINT('Ctrl Pts',(-67.4178925417354,-0.228278247224643,
16.5564124981773));
#47662=CARTESIAN_POINT('Ctrl Pts',(-66.5031197198625,1.9076022670654,16.4452746076093));
#47663=CARTESIAN_POINT('Ctrl Pts',(-64.2125243718594,2.29743279261729,16.3341367170413));
#47664=CARTESIAN_POINT('Ctrl Pts',(-62.6427143968803,0.584397028450654,
16.2229988264732));
#47665=CARTESIAN_POINT('Ctrl Pts',(-63.2305546678621,-1.66354396341758,
16.1118609359052));
#47666=CARTESIAN_POINT('Ctrl Pts',(-65.4379883182475,-2.38882429960344,
16.0007230453371));
#47667=CARTESIAN_POINT('Ctrl Pts',(-67.24452629377,-0.927586663439792,15.8895851547691));
#47668=CARTESIAN_POINT('Ctrl Pts',(-66.996623898036,1.38268156569091,15.7784472642011));
#47669=CARTESIAN_POINT('Ctrl Pts',(-64.9211890049946,2.42736567633039,15.667309373633));
#47670=CARTESIAN_POINT('Ctrl Pts',(-62.9178907098163,1.25025445669176,15.556171483065));
#47671=CARTESIAN_POINT('Ctrl Pts',(-62.8203706599597,-1.07122884891598,
15.4450335924969));
#47672=CARTESIAN_POINT('Ctrl Pts',(-64.7178900651262,-2.41220423477673,
15.3338957019289));
#47673=CARTESIAN_POINT('Ctrl Pts',(-66.8736278902366,-1.54526173974447,
15.2227578113608));
#47674=CARTESIAN_POINT('Ctrl Pts',(-67.3144128645646,0.736076372865376,
15.1116199207928));
#47675=CARTESIAN_POINT('Ctrl Pts',(-65.6367894857436,2.34367538861625,15.0004820302248));
#47676=CARTESIAN_POINT('Ctrl Pts',(-63.3763054907363,1.80608183157382,14.8893441396567));
#47677=CARTESIAN_POINT('Ctrl Pts',(-62.6020074507516,-0.384639085849599,
14.7782062490887));
#47678=CARTESIAN_POINT('Ctrl Pts',(-64.0226192720082,-2.2232951335223,14.6670683585206));
#47679=CARTESIAN_POINT('Ctrl Pts',(-66.3378385875382,-2.02694463079713,
14.5559304679526));
#47680=CARTESIAN_POINT('Ctrl Pts',(-67.4285194097127,0.0246926670119235,
14.4447925773845));
#47681=CARTESIAN_POINT('Ctrl Pts',(-66.2963482043283,2.05372573368661,14.3336546868165));
#47682=CARTESIAN_POINT('Ctrl Pts',(-63.9776161165208,2.20296580816612,14.2225167962485));
#47683=CARTESIAN_POINT('Ctrl Pts',(-62.5946809516312,0.335795455628598,
14.1113789056804));
#47684=CARTESIAN_POINT('Ctrl Pts',(-63.4133668288776,-1.83871077711837,
14.0002410151124));
#47685=CARTESIAN_POINT('Ctrl Pts',(-65.684305645688,-2.33026686199619,13.8891031245443));
#47686=CARTESIAN_POINT('Ctrl Pts',(-67.3289123722387,-0.688818574436933,
13.7779652339763));
#47687=CARTESIAN_POINT('Ctrl Pts',(-66.8417982611818,1.58294512384397,13.6668273434083));
#47688=CARTESIAN_POINT('Ctrl Pts',(-64.6689465387577,2.4061546469661,13.5556894528402));
#47689=CARTESIAN_POINT('Ctrl Pts',(-62.7989505726263,1.02632180198958,13.4445515622722));
#47690=CARTESIAN_POINT('Ctrl Pts',(-62.9439207637896,-1.29160100997124,
13.3334136717041));
#47691=CARTESIAN_POINT('Ctrl Pts',(-64.970198323091,-2.42992595215151,13.2222757811361));
#47692=CARTESIAN_POINT('Ctrl Pts',(-67.0251392906009,-1.33877286094185,
13.111137890568));
#47693=CARTESIAN_POINT('Ctrl Pts',(-67.1563717950601,0.197213743559495,
13.0370459635227));
#47694=CARTESIAN_POINT('Ctrl Pts',(-66.8826275096638,0.823232180103066,
13.));
#47695=CARTESIAN_POINT('Ctrl Pts',(-66.2690708798524,-1.07935865304854,
22.));
#47696=CARTESIAN_POINT('Ctrl Pts',(-66.3144013959117,-1.03707009263694,
22.));
#47697=CARTESIAN_POINT('Ctrl Pts',(-66.3570019677261,-0.992212513379911,
22.));
#47698=CARTESIAN_POINT('Ctrl Pts',(-66.3968740280373,-0.945130914767996,
22.));
#47699=CARTESIAN_POINT('Ctrl Pts',(-66.4393785568392,-0.894940853140404,
22.));
#47700=CARTESIAN_POINT('Ctrl Pts',(-66.4787831170347,-0.842223171995407,
22.));
#47701=CARTESIAN_POINT('Ctrl Pts',(-66.5150606107891,-0.787341095408292,
22.));
#47702=CARTESIAN_POINT('Ctrl Pts',(-66.5468034178243,-0.739319278394567,
22.));
#47703=CARTESIAN_POINT('Ctrl Pts',(-66.5761518212759,-0.689639120404083,
22.));
#47704=CARTESIAN_POINT('Ctrl Pts',(-66.6030647719515,-0.638516396530674,
22.));
#47705=CARTESIAN_POINT('Ctrl Pts',(-66.6165687845846,-0.612864734721154,
22.));
#47706=CARTESIAN_POINT('Ctrl Pts',(-66.6294592637971,-0.586849522995566,
22.));
#47707=CARTESIAN_POINT('Ctrl Pts',(-66.6417286804056,-0.560496177528319,
22.));
#47708=CARTESIAN_POINT('Ctrl Pts',(-66.6473326302021,-0.548459515176508,
22.));
#47709=CARTESIAN_POINT('Ctrl Pts',(-66.6528075873815,-0.536350650682513,
22.));
#47710=CARTESIAN_POINT('Ctrl Pts',(-66.6581443434041,-0.524191916018695,
22.));
#47711=CARTESIAN_POINT('Ctrl Pts',(-66.6850645452328,-0.462859602953103,
22.));
#47712=CARTESIAN_POINT('Ctrl Pts',(-66.708523501665,-0.40015185577214,22.));
#47713=CARTESIAN_POINT('Ctrl Pts',(-66.7284976532658,-0.336426402788346,
22.));
#47714=CARTESIAN_POINT('Ctrl Pts',(-66.7488259022754,-0.271571238854653,
22.));
#47715=CARTESIAN_POINT('Ctrl Pts',(-66.7655452530591,-0.205661124512927,
22.));
#47716=CARTESIAN_POINT('Ctrl Pts',(-66.7785915546302,-0.139036642022517,
22.));
#47717=CARTESIAN_POINT('Ctrl Pts',(-66.7895042319157,-0.0833080914624547,
22.));
#47718=CARTESIAN_POINT('Ctrl Pts',(-66.7978464644169,-0.0270787840751074,
22.));
#47719=CARTESIAN_POINT('Ctrl Pts',(-66.803555876155,0.0294642474108197,
22.));
#47720=CARTESIAN_POINT('Ctrl Pts',(-66.8061865906771,0.055517469857954,
22.));
#47721=CARTESIAN_POINT('Ctrl Pts',(-66.8082580030099,0.0816374113820257,
22.));
#47722=CARTESIAN_POINT('Ctrl Pts',(-66.8097622067333,0.107806177309204,
22.));
#47723=CARTESIAN_POINT('Ctrl Pts',(-66.8104186759519,0.119226830677735,
22.));
#47724=CARTESIAN_POINT('Ctrl Pts',(-66.8109669930214,0.130656542103401,
22.));
#47725=CARTESIAN_POINT('Ctrl Pts',(-66.8114061694303,0.142079754470107,
22.));
#47726=CARTESIAN_POINT('Ctrl Pts',(-66.8141021938362,0.212204785583915,
22.));
#47727=CARTESIAN_POINT('Ctrl Pts',(-66.8126973724676,0.282216215101275,
22.));
#47728=CARTESIAN_POINT('Ctrl Pts',(-66.8071370154229,0.351753309284076,
22.));
#47729=CARTESIAN_POINT('Ctrl Pts',(-66.8021656669832,0.413924339289,22.));
#47730=CARTESIAN_POINT('Ctrl Pts',(-66.7938721956328,0.475717167657645,
22.));
#47731=CARTESIAN_POINT('Ctrl Pts',(-66.7821843766151,0.536886120776816,
22.));
#47732=CARTESIAN_POINT('Ctrl Pts',(-66.7694512323358,0.603525850935252,
22.));
#47733=CARTESIAN_POINT('Ctrl Pts',(-66.7526905137875,0.669425953598385,
22.));
#47734=CARTESIAN_POINT('Ctrl Pts',(-66.7321474941547,0.734372824653822,
22.));
#47735=CARTESIAN_POINT('Ctrl Pts',(-66.7242214209375,0.759431149301981,
22.));
#47736=CARTESIAN_POINT('Ctrl Pts',(-66.71573174826,0.7843475255859,22.));
#47737=CARTESIAN_POINT('Ctrl Pts',(-66.7066905572877,0.809109365072399,
22.));
#47738=CARTESIAN_POINT('Ctrl Pts',(-66.7027243122882,0.819972040392798,
22.));
#47739=CARTESIAN_POINT('Ctrl Pts',(-66.698652038392,0.830804390665135,22.));
#47740=CARTESIAN_POINT('Ctrl Pts',(-66.6944798306887,0.841592845029703,
22.));
#47741=CARTESIAN_POINT('Ctrl Pts',(-66.6692560535916,0.906816244118129,
22.));
#47742=CARTESIAN_POINT('Ctrl Pts',(-66.6403413435161,0.970554427317731,
22.));
#47743=CARTESIAN_POINT('Ctrl Pts',(-66.6080484131291,1.03258856562458,22.));
#47744=CARTESIAN_POINT('Ctrl Pts',(-66.5750071922411,1.09606015652187,22.));
#47745=CARTESIAN_POINT('Ctrl Pts',(-66.5384290749239,1.15774863477848,22.));
#47746=CARTESIAN_POINT('Ctrl Pts',(-66.4985928798434,1.21741589242134,22.));
#47747=CARTESIAN_POINT('Ctrl Pts',(-66.468112635167,1.26306966554027,22.));
#47748=CARTESIAN_POINT('Ctrl Pts',(-66.4357237709971,1.30754017026325,22.));
#47749=CARTESIAN_POINT('Ctrl Pts',(-66.4015316630533,1.350714655026,22.));
#47750=CARTESIAN_POINT('Ctrl Pts',(-66.3802494925467,1.37758772023045,22.));
#47751=CARTESIAN_POINT('Ctrl Pts',(-66.3582683894257,1.40395856102689,22.));
#47752=CARTESIAN_POINT('Ctrl Pts',(-66.335610863513,1.4297983034856,22.));
#47753=CARTESIAN_POINT('Ctrl Pts',(-66.3229007386857,1.44429354685069,22.));
#47754=CARTESIAN_POINT('Ctrl Pts',(-66.3099732536082,1.45862623051551,22.));
#47755=CARTESIAN_POINT('Ctrl Pts',(-66.296856182647,1.47276572504358,22.));
#47756=CARTESIAN_POINT('Ctrl Pts',(-66.2459827546405,1.52760453464138,22.));
#47757=CARTESIAN_POINT('Ctrl Pts',(-66.1922128067209,1.57959843571923,22.));
#47758=CARTESIAN_POINT('Ctrl Pts',(-66.1358313615937,1.62848347077225,22.));
#47759=CARTESIAN_POINT('Ctrl Pts',(-66.093660348142,1.66504747629138,22.));
#47760=CARTESIAN_POINT('Ctrl Pts',(-66.0500271947631,1.69987205103595,22.));
#47761=CARTESIAN_POINT('Ctrl Pts',(-66.0050347650922,1.73283699196269,22.));
#47762=CARTESIAN_POINT('Ctrl Pts',(-65.9909996372478,1.7431202143553,22.));
#47763=CARTESIAN_POINT('Ctrl Pts',(-65.9768321470569,1.75322240061157,22.));
#47764=CARTESIAN_POINT('Ctrl Pts',(-65.9625351771215,1.76313967659916,22.));
#47765=CARTESIAN_POINT('Ctrl Pts',(-65.9487346476095,1.77271259033996,22.));
#47766=CARTESIAN_POINT('Ctrl Pts',(-65.9348204929772,1.7821082799947,22.));
#47767=CARTESIAN_POINT('Ctrl Pts',(-65.9208007361055,1.79132048319868,22.));
#47768=CARTESIAN_POINT('Ctrl Pts',(-65.8578459989061,1.83268723706198,22.));
#47769=CARTESIAN_POINT('Ctrl Pts',(-65.7927339839887,1.87037831023573,22.));
#47770=CARTESIAN_POINT('Ctrl Pts',(-65.7257260556133,1.90411450231801,22.));
#47771=CARTESIAN_POINT('Ctrl Pts',(-65.6744429845673,1.92993376844555,22.));
#47772=CARTESIAN_POINT('Ctrl Pts',(-65.6220484504102,1.95343614609126,22.));
#47773=CARTESIAN_POINT('Ctrl Pts',(-65.5686456989049,1.97448116510365,22.));
#47774=CARTESIAN_POINT('Ctrl Pts',(-65.5562524015237,1.97936513028633,22.));
#47775=CARTESIAN_POINT('Ctrl Pts',(-65.54380476008,1.98411668136774,22.));
#47776=CARTESIAN_POINT('Ctrl Pts',(-65.531304687333,1.98873639975131,22.));
#47777=CARTESIAN_POINT('Ctrl Pts',(-63.3326792503596,0.00130047270867312,
20.8714803633902));
#47778=CARTESIAN_POINT('Ctrl Pts',(-63.3319477300267,0.0865458945944494,
20.8771939403667));
#47779=CARTESIAN_POINT('Ctrl Pts',(-63.3379207823453,0.171688456696982,
20.8829075173431));
#47780=CARTESIAN_POINT('Ctrl Pts',(-63.3509549142486,0.255735893547228,
20.8886210943196));
#47781=CARTESIAN_POINT('Ctrl Pts',(-63.4354662417459,0.800686682266395,
20.9256670578423));
#47782=CARTESIAN_POINT('Ctrl Pts',(-63.8168273485002,1.29959809619851,20.9627130213649));
#47783=CARTESIAN_POINT('Ctrl Pts',(-64.3205066401932,1.52414941239406,20.9997589848876));
#47784=CARTESIAN_POINT('Ctrl Pts',(-64.8241859318862,1.74870072858962,21.0368049484103));
#47785=CARTESIAN_POINT('Ctrl Pts',(-65.4501834085179,1.69889194704861,21.073850911933));
#47786=CARTESIAN_POINT('Ctrl Pts',(-65.9120068254848,1.39750064992835,21.1108968754557));
#47787=CARTESIAN_POINT('Ctrl Pts',(-66.3738302424517,1.09610935280808,21.1479428389783));
#47788=CARTESIAN_POINT('Ctrl Pts',(-66.6714795997537,0.543135540108559,
21.184988802501));
#47789=CARTESIAN_POINT('Ctrl Pts',(-66.6687358658196,-0.0083140869619841,
21.2220347660237));
#47790=CARTESIAN_POINT('Ctrl Pts',(-66.6659921318856,-0.55976371403253,
21.2590807295464));
#47791=CARTESIAN_POINT('Ctrl Pts',(-66.3628553067155,-1.1096891554741,21.2961266930691));
#47792=CARTESIAN_POINT('Ctrl Pts',(-65.898053938122,-1.40648356441475,21.3331726565917));
#47793=CARTESIAN_POINT('Ctrl Pts',(-65.4332525695286,-1.70327797335541,
21.3702186201144));
#47794=CARTESIAN_POINT('Ctrl Pts',(-64.8067866575118,-1.74694134979516,
21.4072645836371));
#47795=CARTESIAN_POINT('Ctrl Pts',(-64.3053692934656,-1.51735268425301,
21.4443105471598));
#47796=CARTESIAN_POINT('Ctrl Pts',(-63.8039519294193,-1.28776401871086,
21.4813565106825));
#47797=CARTESIAN_POINT('Ctrl Pts',(-63.4275831133436,-0.784923311186817,
21.5184024742051));
#47798=CARTESIAN_POINT('Ctrl Pts',(-63.3484955171689,-0.239232889597532,
21.5554484377278));
#47799=CARTESIAN_POINT('Ctrl Pts',(-63.337086928647,-0.160515647180253,
21.5607924129486));
#47800=CARTESIAN_POINT('Ctrl Pts',(-63.3318644062264,-0.0809067535388516,
21.5661363881694));
#47801=CARTESIAN_POINT('Ctrl Pts',(-63.3325282901756,-0.00121307831917494,
21.5714803633902));
#47802=CARTESIAN_POINT('Ctrl Pts',(-64.4698297828114,1.98517432567173,22.));
#47803=CARTESIAN_POINT('Ctrl Pts',(-63.8097120902545,1.8088801151799,21.9629540364773));
#47804=CARTESIAN_POINT('Ctrl Pts',(-62.6906509614045,0.748610048502907,
21.888862109432));
#47805=CARTESIAN_POINT('Ctrl Pts',(-63.1187889329782,-1.53833553624065,
21.7777242188639));
#47806=CARTESIAN_POINT('Ctrl Pts',(-65.2721300366129,-2.41280623887488,
21.6665863282959));
#47807=CARTESIAN_POINT('Ctrl Pts',(-67.1747422685441,-1.08094901338604,
21.5554484377278));
#47808=CARTESIAN_POINT('Ctrl Pts',(-67.0876157148515,1.24138505016238,21.4443105471598));
#47809=CARTESIAN_POINT('Ctrl Pts',(-65.0892538486774,2.42692553227055,21.3331726565917));
#47810=CARTESIAN_POINT('Ctrl Pts',(-63.0094071033202,1.39134559511319,21.2220347660237));
#47811=CARTESIAN_POINT('Ctrl Pts',(-62.7514666617416,-0.917885875238364,
21.1108968754557));
#47812=CARTESIAN_POINT('Ctrl Pts',(-64.5516876929394,-2.38689686810909,
20.9997589848876));
#47813=CARTESIAN_POINT('Ctrl Pts',(-66.7622271403759,-1.67118893435551,
20.8886210943196));
#47814=CARTESIAN_POINT('Ctrl Pts',(-67.3597936726881,0.574194749175807,
20.7774832037516));
#47815=CARTESIAN_POINT('Ctrl Pts',(-65.7974074532359,2.29400261230211,20.6663453131835));
#47816=CARTESIAN_POINT('Ctrl Pts',(-63.5051485972519,1.91408833219885,20.5552074226155));
#47817=CARTESIAN_POINT('Ctrl Pts',(-62.5811424445442,-0.217814955653705,
20.4440695320474));
#47818=CARTESIAN_POINT('Ctrl Pts',(-63.8711449203827,-2.15034861017486,
20.3329316414794));
#47819=CARTESIAN_POINT('Ctrl Pts',(-66.1944008109328,-2.11464436694831,
20.2217937509113));
#47820=CARTESIAN_POINT('Ctrl Pts',(-67.4244083164919,-0.143381864737536,
20.1106558603433));
#47821=CARTESIAN_POINT('Ctrl Pts',(-66.4353272830534,1.95911953903996,19.9995179697752));
#47822=CARTESIAN_POINT('Ctrl Pts',(-64.132474966303,2.26841668404626,19.8883800792072));
#47823=CARTESIAN_POINT('Ctrl Pts',(-62.6236781227743,0.50140627563106,19.7772421886392));
#47824=CARTESIAN_POINT('Ctrl Pts',(-63.2899556571721,-1.72454696459255,
19.6661042980711));
#47825=CARTESIAN_POINT('Ctrl Pts',(-65.5214561645339,-2.37200281981328,
19.5549664075031));
#47826=CARTESIAN_POINT('Ctrl Pts',(-67.2756619344365,-0.848337588988209,
19.443828516935));
#47827=CARTESIAN_POINT('Ctrl Pts',(-66.9469285261459,1.45182065545647,19.332690626367));
#47828=CARTESIAN_POINT('Ctrl Pts',(-64.8361493591312,2.42311099039749,19.221552735799));
#47829=CARTESIAN_POINT('Ctrl Pts',(-62.8753445414284,1.17650035527427,19.1104148452309));
#47830=CARTESIAN_POINT('Ctrl Pts',(-62.8592609604237,-1.14697439714762,
18.9992769546629));
#47831=CARTESIAN_POINT('Ctrl Pts',(-64.8026200998564,-2.42061047643985,
18.8881390640948));
#47832=CARTESIAN_POINT('Ctrl Pts',(-66.9266433003906,-1.4786343349792,18.7770011735268));
#47833=CARTESIAN_POINT('Ctrl Pts',(-67.2871880384261,0.816752582102682,
18.6658632829587));
#47834=CARTESIAN_POINT('Ctrl Pts',(-65.5542436264288,2.36455659820144,18.5547253923907));
#47835=CARTESIAN_POINT('Ctrl Pts',(-63.3139937376034,1.74805514406081,18.4435875018227));
#47836=CARTESIAN_POINT('Ctrl Pts',(-62.6169645013648,-0.468461007727317,
18.3324496112546));
#47837=CARTESIAN_POINT('Ctrl Pts',(-64.1011546824859,-2.25618948643599,
18.2213117206866));
#47838=CARTESIAN_POINT('Ctrl Pts',(-66.4080681763277,-1.97880214127948,
18.1101738301185));
#47839=CARTESIAN_POINT('Ctrl Pts',(-67.4261608997972,0.109805244932097,
17.9990359395505));
#47840=CARTESIAN_POINT('Ctrl Pts',(-66.2235610371465,2.09790664518148,17.8878980489825));
#47841=CARTESIAN_POINT('Ctrl Pts',(-63.9010218810697,2.16577030121657,17.7767601584144));
#47842=CARTESIAN_POINT('Ctrl Pts',(-62.5843898605093,0.251279839042483,
17.6656222678464));
#47843=CARTESIAN_POINT('Ctrl Pts',(-63.478793195507,-1.89320990951441,17.5544843772783));
#47844=CARTESIAN_POINT('Ctrl Pts',(-65.7655743703156,-2.30482315743207,
17.4433464867103));
#47845=CARTESIAN_POINT('Ctrl Pts',(-67.3516166417705,-0.606805630879782,
17.3322085961422));
#47846=CARTESIAN_POINT('Ctrl Pts',(-66.7851975318663,1.6466279712607,17.2210707055742));
#47847=CARTESIAN_POINT('Ctrl Pts',(-64.5847668755277,2.39288431727496,17.1099328150062));
#47848=CARTESIAN_POINT('Ctrl Pts',(-62.7644038070828,0.948906510533639,
16.9987949244381));
#47849=CARTESIAN_POINT('Ctrl Pts',(-62.9903072873999,-1.36361618663093,
16.8876570338701));
#47850=CARTESIAN_POINT('Ctrl Pts',(-65.0557052990257,-2.42800552371271,
16.776519143302));
#47851=CARTESIAN_POINT('Ctrl Pts',(-67.0701156187118,-1.27001386948507,
16.665381252734));
#47852=CARTESIAN_POINT('Ctrl Pts',(-67.1897256358837,1.05043588241969,16.5542433621659));
#47853=CARTESIAN_POINT('Ctrl Pts',(-65.3050549453524,2.4094097583915,16.4431054715979));
#47854=CARTESIAN_POINT('Ctrl Pts',(-63.141164003784,1.56302355794459,16.3319675810298));
#47855=CARTESIAN_POINT('Ctrl Pts',(-62.6786867301813,-0.714015830985951,
16.2208296904619));
#47856=CARTESIAN_POINT('Ctrl Pts',(-64.3409338179361,-2.33750843231644,
16.1096917998938));
#47857=CARTESIAN_POINT('Ctrl Pts',(-66.6064316564341,-1.82145305641562,
15.9985539093258));
#47858=CARTESIAN_POINT('Ctrl Pts',(-67.401544381661,0.361798958737847,15.8874160187577));
#47859=CARTESIAN_POINT('Ctrl Pts',(-65.9984962989145,2.21389228381421,15.7762781281897));
#47860=CARTESIAN_POINT('Ctrl Pts',(-63.6815132301988,2.03958489439844,15.6651402376216));
#47861=CARTESIAN_POINT('Ctrl Pts',(-62.5713560542506,-0.00157767958229344,
15.5540023470536));
#47862=CARTESIAN_POINT('Ctrl Pts',(-63.6841642251148,-2.04129618504103,
15.4428644564855));
#47863=CARTESIAN_POINT('Ctrl Pts',(-66.0013718021885,-2.21259314346662,
15.3317265659175));
#47864=CARTESIAN_POINT('Ctrl Pts',(-67.4020124146433,-0.358678503164364,
15.2205886753494));
#47865=CARTESIAN_POINT('Ctrl Pts',(-66.6040638188323,1.82353863480769,15.1094507847814));
#47866=CARTESIAN_POINT('Ctrl Pts',(-64.3378974271891,2.33665018787606,14.9983128942134));
#47867=CARTESIAN_POINT('Ctrl Pts',(-62.6777610116056,0.710999308952895,
14.8871750036453));
#47868=CARTESIAN_POINT('Ctrl Pts',(-63.1431963129713,-1.56543726976266,
14.7760371130773));
#47869=CARTESIAN_POINT('Ctrl Pts',(-65.3081850174459,-2.40901142364103,
14.6648992225093));
#47870=CARTESIAN_POINT('Ctrl Pts',(-67.1910886177016,-1.04758997952521,
14.5537613319412));
#47871=CARTESIAN_POINT('Ctrl Pts',(-67.068463685159,1.27270221153157,14.4426234413732));
#47872=CARTESIAN_POINT('Ctrl Pts',(-65.0525510239567,2.42807611461694,14.3314855508051));
#47873=CARTESIAN_POINT('Ctrl Pts',(-62.9885367426501,1.36100346218852,14.2203476602371));
#47874=CARTESIAN_POINT('Ctrl Pts',(-62.7656397187534,-0.951809206360656,
14.109209769669));
#47875=CARTESIAN_POINT('Ctrl Pts',(-64.5878737813476,-2.39342385873017,
13.998071879101));
#47876=CARTESIAN_POINT('Ctrl Pts',(-66.7873400138256,-1.64430308142018,
13.8869339885329));
#47877=CARTESIAN_POINT('Ctrl Pts',(-67.3508170614469,0.60985221755875,13.7757960979649));
#47878=CARTESIAN_POINT('Ctrl Pts',(-65.7625975239189,2.30583209920717,13.6646582073969));
#47879=CARTESIAN_POINT('Ctrl Pts',(-63.4762984963492,1.89119971793715,13.5535203168288));
#47880=CARTESIAN_POINT('Ctrl Pts',(-62.5847903309572,-0.254354168931198,
13.4423824262608));
#47881=CARTESIAN_POINT('Ctrl Pts',(-63.9036938704104,-2.16732302296763,
13.3312445356927));
#47882=CARTESIAN_POINT('Ctrl Pts',(-66.2265689546786,-2.09606376419021,
13.2201066451247));
#47883=CARTESIAN_POINT('Ctrl Pts',(-67.4257384694328,-0.107152139943094,
13.1089687545567));
#47884=CARTESIAN_POINT('Ctrl Pts',(-66.4066260077932,1.98162422647334,12.9978308639886));
#47885=CARTESIAN_POINT('Ctrl Pts',(-64.0958295620755,2.25299485262721,12.8866929734206));
#47886=CARTESIAN_POINT('Ctrl Pts',(-63.1142456563632,1.06431345694515,12.8126010463752));
#47887=CARTESIAN_POINT('Ctrl Pts',(-62.9833241385535,0.393720754290225,
12.7755550828525));
#47888=CARTESIAN_POINT('Ctrl Pts',(-64.5032651029123,1.85997880000277,22.0748149723825));
#47889=CARTESIAN_POINT('Ctrl Pts',(-63.8847779011663,1.69480262890401,22.0377690088598));
#47890=CARTESIAN_POINT('Ctrl Pts',(-62.8362906481067,0.701398764671866,
21.9636770818144));
#47891=CARTESIAN_POINT('Ctrl Pts',(-63.2374279891983,-1.44132001290634,
21.8525391912464));
#47892=CARTESIAN_POINT('Ctrl Pts',(-65.2549680863783,-2.26064199742415,
21.7414013006783));
#47893=CARTESIAN_POINT('Ctrl Pts',(-67.0375915921608,-1.01277868788759,
21.6302634101104));
#47894=CARTESIAN_POINT('Ctrl Pts',(-66.9559596968202,1.16309678504487,21.5191255195423));
#47895=CARTESIAN_POINT('Ctrl Pts',(-65.0836250319239,2.27387085397713,21.4079876289743));
#47896=CARTESIAN_POINT('Ctrl Pts',(-63.1349443525531,1.30360002994302,21.2968497384062));
#47897=CARTESIAN_POINT('Ctrl Pts',(-62.8932709907757,-0.859999168177664,
21.1857118478382));
#47898=CARTESIAN_POINT('Ctrl Pts',(-64.5799606230396,-2.23636660774045,
21.0745739572701));
#47899=CARTESIAN_POINT('Ctrl Pts',(-66.6510918358667,-1.56579497755124,
20.9634360667021));
#47900=CARTESIAN_POINT('Ctrl Pts',(-67.2109726822582,0.537983010725535,
20.8522981761341));
#47901=CARTESIAN_POINT('Ctrl Pts',(-65.7471187486173,2.14933075189209,20.741160285566));
#47902=CARTESIAN_POINT('Ctrl Pts',(-63.5994217826059,1.79337586285671,20.630022394998));
#47903=CARTESIAN_POINT('Ctrl Pts',(-62.73368831382,-0.204078399866647,20.5188845044299));
#47904=CARTESIAN_POINT('Ctrl Pts',(-63.9423364541786,-2.01473632608426,
20.4077466138619));
#47905=CARTESIAN_POINT('Ctrl Pts',(-66.1190756188575,-1.98128378007219,
20.2966087232938));
#47906=CARTESIAN_POINT('Ctrl Pts',(-67.2715123870543,-0.134339450832078,
20.1854708327258));
#47907=CARTESIAN_POINT('Ctrl Pts',(-66.3448080015046,1.83556716514179,20.0743329421578));
#47908=CARTESIAN_POINT('Ctrl Pts',(-64.1871856540346,2.12535840673386,19.9631950515897));
#47909=CARTESIAN_POINT('Ctrl Pts',(-62.7735414686431,0.469784960847985,
19.8520571610217));
#47910=CARTESIAN_POINT('Ctrl Pts',(-63.3978000402315,-1.61578796998893,
19.7409192704536));
#47911=CARTESIAN_POINT('Ctrl Pts',(-65.4885703983884,-2.2224118564029,19.6297813798856));
#47912=CARTESIAN_POINT('Ctrl Pts',(-67.1321467335585,-0.794836962355745,
19.5186434893175));
#47913=CARTESIAN_POINT('Ctrl Pts',(-66.8241449815883,1.3602612151663,19.4075055987495));
#47914=CARTESIAN_POINT('Ctrl Pts',(-64.8464826416291,2.27029687716117,19.2963677081814));
#47915=CARTESIAN_POINT('Ctrl Pts',(-63.0093364803535,1.10230406000512,19.1852298176134));
#47916=CARTESIAN_POINT('Ctrl Pts',(-62.9942672144912,-1.07464016396578,
19.0740919270454));
#47917=CARTESIAN_POINT('Ctrl Pts',(-64.8150679136506,-2.26795405875465,
18.9629540364773));
#47918=CARTESIAN_POINT('Ctrl Pts',(-66.8051390487741,-1.38538388314432,
18.8518161459093));
#47919=CARTESIAN_POINT('Ctrl Pts',(-67.1429459408574,0.765243871993194,
18.7406782553413));
#47920=CARTESIAN_POINT('Ctrl Pts',(-65.5192901106281,2.21543523265805,18.6295403647732));
#47921=CARTESIAN_POINT('Ctrl Pts',(-63.4203221529835,1.63781360011733,18.5184024742052));
#47922=CARTESIAN_POINT('Ctrl Pts',(-62.7672512434818,-0.438917394675609,
18.4072645836371));
#47923=CARTESIAN_POINT('Ctrl Pts',(-64.1578405919126,-2.11390232046251,
18.2961266930691));
#47924=CARTESIAN_POINT('Ctrl Pts',(-66.3192679973039,-1.85400847904605,
18.184988802501));
#47925=CARTESIAN_POINT('Ctrl Pts',(-67.2731544432459,0.102880349126872,
18.073850911933));
#47926=CARTESIAN_POINT('Ctrl Pts',(-66.1463968479604,1.96560162700177,17.9627130213649));
#47927=CARTESIAN_POINT('Ctrl Pts',(-63.9703292167121,2.02918544424322,17.8515751307969));
#47928=CARTESIAN_POINT('Ctrl Pts',(-62.7367309306682,0.235432811840836,
17.7404372402289));
#47929=CARTESIAN_POINT('Ctrl Pts',(-63.5747284910006,-1.77381414322918,
17.6292993496608));
#47930=CARTESIAN_POINT('Ctrl Pts',(-65.7172932271985,-2.15946889658092,
17.5181614590928));
#47931=CARTESIAN_POINT('Ctrl Pts',(-67.2033113378831,-0.568537278849199,
17.4070235685247));
#47932=CARTESIAN_POINT('Ctrl Pts',(-66.6726135937532,1.54278295786449,17.2958856779567));
#47933=CARTESIAN_POINT('Ctrl Pts',(-64.6109536585329,2.24197645689606,17.1847477873887));
#47934=CARTESIAN_POINT('Ctrl Pts',(-62.9053922517429,0.889063479188389,
17.0736098968206));
#47935=CARTESIAN_POINT('Ctrl Pts',(-63.1170490714002,-1.27761938368608,
16.9624720062526));
#47936=CARTESIAN_POINT('Ctrl Pts',(-65.0521922301209,-2.27488273548328,
16.8513341156845));
#47937=CARTESIAN_POINT('Ctrl Pts',(-66.9395632487115,-1.18992012056796,
16.7401962251165));
#47938=CARTESIAN_POINT('Ctrl Pts',(-67.0516300296139,0.984189875315718,
16.6290583345485));
#47939=CARTESIAN_POINT('Ctrl Pts',(-65.2858165773424,2.2574597168496,16.5179204439804));
#47940=CARTESIAN_POINT('Ctrl Pts',(-63.2583919704513,1.4644510782186,16.4067825534124));
#47941=CARTESIAN_POINT('Ctrl Pts',(-62.8250809441801,-0.668986240314613,
16.2956446628443));
#47942=CARTESIAN_POINT('Ctrl Pts',(-64.3824979949693,-2.19009286626007,
16.1845067722763));
#47943=CARTESIAN_POINT('Ctrl Pts',(-66.5051216338947,-1.70658265439078,
16.0733688817082));
#47944=CARTESIAN_POINT('Ctrl Pts',(-67.2500903721106,0.338982015036773,
15.9622309911402));
#47945=CARTESIAN_POINT('Ctrl Pts',(-65.9355258749046,2.07427260172267,15.8510931005721));
#47946=CARTESIAN_POINT('Ctrl Pts',(-63.7646639349497,1.91095795232156,15.7399552100041));
#47947=CARTESIAN_POINT('Ctrl Pts',(-62.7245191047287,-0.00147818281664962,
15.6288173194361));
#47948=CARTESIAN_POINT('Ctrl Pts',(-63.7671477441945,-1.91256131998288,
15.517679428868));
#47949=CARTESIAN_POINT('Ctrl Pts',(-65.9382200338304,-2.07305539199277,
15.4065415383));
#47950=CARTESIAN_POINT('Ctrl Pts',(-67.2505288884734,-0.336058351790693,
15.2954036477319));
#47951=CARTESIAN_POINT('Ctrl Pts',(-66.5029031245757,1.70853670524911,15.1842657571639));
#47952=CARTESIAN_POINT('Ctrl Pts',(-64.3796530949801,2.18928874722443,15.0731278665959));
#47953=CARTESIAN_POINT('Ctrl Pts',(-62.8242136062828,0.666159956013699,
14.9619899760278));
#47954=CARTESIAN_POINT('Ctrl Pts',(-63.2602961115408,-1.46671256868463,
14.8508520854598));
#47955=CARTESIAN_POINT('Ctrl Pts',(-65.2887492506402,-2.25708650318186,
14.7397141948917));
#47956=CARTESIAN_POINT('Ctrl Pts',(-67.0529070546353,-0.981523450013844,
14.6285763043237));
#47957=CARTESIAN_POINT('Ctrl Pts',(-66.93801549477,1.19243892163695,14.5174384137556));
#47958=CARTESIAN_POINT('Ctrl Pts',(-65.0492368802144,2.2749488745541,14.4063005231876));
#47959=CARTESIAN_POINT('Ctrl Pts',(-63.115390186507,1.27517143137767,14.2951626326196));
#47960=CARTESIAN_POINT('Ctrl Pts',(-62.9065502203286,-0.89178311576201,
14.1840247420515));
#47961=CARTESIAN_POINT('Ctrl Pts',(-64.6138646265439,-2.24248197203165,
14.0728868514835));
#47962=CARTESIAN_POINT('Ctrl Pts',(-66.6746209595408,-1.54060468779531,
13.9617489609154));
#47963=CARTESIAN_POINT('Ctrl Pts',(-67.2025621832966,0.571391731761459,
13.8506110703474));
#47964=CARTESIAN_POINT('Ctrl Pts',(-65.7145041163797,2.16041420918538,13.7394731797794));
#47965=CARTESIAN_POINT('Ctrl Pts',(-63.5723911206821,1.77193072489695,13.6283352892113));
#47966=CARTESIAN_POINT('Ctrl Pts',(-62.7371061453451,-0.238313258330233,
13.5171973986433));
#47967=CARTESIAN_POINT('Ctrl Pts',(-63.9728326963629,-2.03064024320064,
13.4060595080752));
#47968=CARTESIAN_POINT('Ctrl Pts',(-66.1492150704054,-1.9638749677707,13.2949216175072));
#47969=CARTESIAN_POINT('Ctrl Pts',(-67.2727586535603,-0.100394562881346,
13.1837837269391));
#47970=CARTESIAN_POINT('Ctrl Pts',(-66.3179167794963,1.85665258871667,13.0726458363711));
#47971=CARTESIAN_POINT('Ctrl Pts',(-64.1528513015804,2.11090915705048,12.9615079458031));
#47972=CARTESIAN_POINT('Ctrl Pts',(-63.2331712354829,0.997192257060744,
12.8874160187577));
#47973=CARTESIAN_POINT('Ctrl Pts',(-63.1105063166185,0.368890654402919,
12.850370055235));
#47974=CARTESIAN_POINT('Ctrl Pts',(-64.5367004230132,1.73478327433381,22.149629944765));
#47975=CARTESIAN_POINT('Ctrl Pts',(-63.9598437120782,1.58072514262811,22.1125839812423));
#47976=CARTESIAN_POINT('Ctrl Pts',(-62.9819303348089,0.654187480840823,
22.0384920541969));
#47977=CARTESIAN_POINT('Ctrl Pts',(-63.3560670454183,-1.34430448957202,
21.9273541636289));
#47978=CARTESIAN_POINT('Ctrl Pts',(-65.2378061361438,-2.10847775597343,
21.8162162730608));
#47979=CARTESIAN_POINT('Ctrl Pts',(-66.9004409157773,-0.944608362389142,
21.7050783824928));
#47980=CARTESIAN_POINT('Ctrl Pts',(-66.8243036787891,1.08480851992736,21.5939404919248));
#47981=CARTESIAN_POINT('Ctrl Pts',(-65.0779962151703,2.12081617568372,21.4828026013567));
#47982=CARTESIAN_POINT('Ctrl Pts',(-63.260481601786,1.21585446477284,21.3716647107887));
#47983=CARTESIAN_POINT('Ctrl Pts',(-63.0350753198097,-0.802112461116964,
21.2605268202206));
#47984=CARTESIAN_POINT('Ctrl Pts',(-64.6082335531397,-2.08583634737181,
21.1493889296526));
#47985=CARTESIAN_POINT('Ctrl Pts',(-66.5399565313575,-1.46040102074697,
21.0382510390845));
#47986=CARTESIAN_POINT('Ctrl Pts',(-67.0621516918281,0.501771272275262,
20.9271131485165));
#47987=CARTESIAN_POINT('Ctrl Pts',(-65.6968300439987,2.00465889148208,20.8159752579485));
#47988=CARTESIAN_POINT('Ctrl Pts',(-63.6936949679598,1.67266339351457,20.7048373673804));
#47989=CARTESIAN_POINT('Ctrl Pts',(-62.8862341830959,-0.190341844079587,
20.5936994768124));
#47990=CARTESIAN_POINT('Ctrl Pts',(-64.0135279879744,-1.87912404199366,
20.4825615862443));
#47991=CARTESIAN_POINT('Ctrl Pts',(-66.0437504267822,-1.84792319319606,
20.3714236956763));
#47992=CARTESIAN_POINT('Ctrl Pts',(-67.1186164576166,-0.125297036926618,
20.2602858051083));
#47993=CARTESIAN_POINT('Ctrl Pts',(-66.2542887199558,1.71201479124362,20.1491479145402));
#47994=CARTESIAN_POINT('Ctrl Pts',(-64.2418963417663,1.98230012942146,20.0380100239722));
#47995=CARTESIAN_POINT('Ctrl Pts',(-62.9234048145118,0.438163646064908,
19.9268721334041));
#47996=CARTESIAN_POINT('Ctrl Pts',(-63.505644423291,-1.50702897538531,19.8157342428361));
#47997=CARTESIAN_POINT('Ctrl Pts',(-65.4556846322429,-2.07282089299252,
19.7045963522681));
#47998=CARTESIAN_POINT('Ctrl Pts',(-66.9886315326805,-0.741336335723279,
19.5934584617));
#47999=CARTESIAN_POINT('Ctrl Pts',(-66.7013614370307,1.26870177487613,19.482320571132));
#48000=CARTESIAN_POINT('Ctrl Pts',(-64.856815924127,2.11748276392484,19.3711826805639));
#48001=CARTESIAN_POINT('Ctrl Pts',(-63.1433284192787,1.02810776473597,19.2600447899959));
#48002=CARTESIAN_POINT('Ctrl Pts',(-63.1292734685587,-1.00230593078394,
19.1489068994279));
#48003=CARTESIAN_POINT('Ctrl Pts',(-64.8275157274446,-2.11529764106946,
19.0377690088598));
#48004=CARTESIAN_POINT('Ctrl Pts',(-66.6836347971578,-1.29213343130944,
18.9266311182918));
#48005=CARTESIAN_POINT('Ctrl Pts',(-66.9987038432886,0.713735161883704,
18.8154932277237));
#48006=CARTESIAN_POINT('Ctrl Pts',(-65.4843365948275,2.06631386711467,18.7043553371557));
#48007=CARTESIAN_POINT('Ctrl Pts',(-63.5266505683636,1.52757205617384,18.5932174465876));
#48008=CARTESIAN_POINT('Ctrl Pts',(-62.9175379855987,-0.409373781623898,
18.4820795560196));
#48009=CARTESIAN_POINT('Ctrl Pts',(-64.2145265013393,-1.97161515448904,
18.3709416654516));
#48010=CARTESIAN_POINT('Ctrl Pts',(-66.2304678182801,-1.72921481681262,
18.2598037748835));
#48011=CARTESIAN_POINT('Ctrl Pts',(-67.1201479866946,0.0959554533216485,
18.1486658843155));
#48012=CARTESIAN_POINT('Ctrl Pts',(-66.0692326587742,1.83329660882205,18.0375279937474));
#48013=CARTESIAN_POINT('Ctrl Pts',(-64.0396365523547,1.89260058726988,17.9263901031794));
#48014=CARTESIAN_POINT('Ctrl Pts',(-62.8890720008271,0.219585784639187,
17.8152522126113));
#48015=CARTESIAN_POINT('Ctrl Pts',(-63.6706637864943,-1.65441837694395,
17.7041143220433));
#48016=CARTESIAN_POINT('Ctrl Pts',(-65.6690120840812,-2.01411463572976,
17.5929764314753));
#48017=CARTESIAN_POINT('Ctrl Pts',(-67.0550060339956,-0.530268926818617,
17.4818385409072));
#48018=CARTESIAN_POINT('Ctrl Pts',(-66.5600296556403,1.43893794446827,17.3707006503392));
#48019=CARTESIAN_POINT('Ctrl Pts',(-64.6371404415378,2.09106859651716,17.2595627597711));
#48020=CARTESIAN_POINT('Ctrl Pts',(-63.0463806964032,0.82922044784314,17.1484248692031));
#48021=CARTESIAN_POINT('Ctrl Pts',(-63.2437908554003,-1.19162258074124,
17.0372869786351));
#48022=CARTESIAN_POINT('Ctrl Pts',(-65.0486791612162,-2.12175994725384,
16.926149088067));
#48023=CARTESIAN_POINT('Ctrl Pts',(-66.8090108787112,-1.10982637165084,
16.815011197499));
#48024=CARTESIAN_POINT('Ctrl Pts',(-66.9135344233438,0.917943868211746,
16.7038733069309));
#48025=CARTESIAN_POINT('Ctrl Pts',(-65.2665782093324,2.10550967530769,16.5927354163629));
#48026=CARTESIAN_POINT('Ctrl Pts',(-63.3756199371186,1.3658785984926,16.4815975257949));
#48027=CARTESIAN_POINT('Ctrl Pts',(-62.9714751581789,-0.623956649643275,
16.3704596352268));
#48028=CARTESIAN_POINT('Ctrl Pts',(-64.4240621720026,-2.04267730020369,
16.2593217446588));
#48029=CARTESIAN_POINT('Ctrl Pts',(-66.4038116113553,-1.59171225236595,
16.1481838540907));
#48030=CARTESIAN_POINT('Ctrl Pts',(-67.0986363625603,0.316165071335702,
16.0370459635227));
#48031=CARTESIAN_POINT('Ctrl Pts',(-65.8725554508947,1.93465291963113,15.9259080729547));
#48032=CARTESIAN_POINT('Ctrl Pts',(-63.8478146397005,1.78233101024468,15.8147701823866));
#48033=CARTESIAN_POINT('Ctrl Pts',(-62.8776821552069,-0.00137868605100532,
15.7036322918186));
#48034=CARTESIAN_POINT('Ctrl Pts',(-63.8501312632741,-1.78382645492473,
15.5924944012505));
#48035=CARTESIAN_POINT('Ctrl Pts',(-65.8750682654724,-1.93351764051893,
15.4813565106825));
#48036=CARTESIAN_POINT('Ctrl Pts',(-67.0990453623036,-0.313438200417021,
15.3702186201144));
#48037=CARTESIAN_POINT('Ctrl Pts',(-66.401742430319,1.59353477569053,15.2590807295464));
#48038=CARTESIAN_POINT('Ctrl Pts',(-64.4214087627711,2.0419273065728,15.1479428389783));
#48039=CARTESIAN_POINT('Ctrl Pts',(-62.9706662009597,0.621320603074505,
15.0368049484103));
#48040=CARTESIAN_POINT('Ctrl Pts',(-63.3773959101104,-1.3679878676066,14.9256670578422));
#48041=CARTESIAN_POINT('Ctrl Pts',(-65.2693134838344,-2.10516158272268,
14.8145291672742));
#48042=CARTESIAN_POINT('Ctrl Pts',(-66.914725491569,-0.915456920502479,
14.7033912767062));
#48043=CARTESIAN_POINT('Ctrl Pts',(-66.8075673043809,1.11217563174233,14.5922533861381));
#48044=CARTESIAN_POINT('Ctrl Pts',(-65.0459227364722,2.12182163449127,14.4811154955701));
#48045=CARTESIAN_POINT('Ctrl Pts',(-63.2422436303638,1.18933940056681,14.3699776050021));
#48046=CARTESIAN_POINT('Ctrl Pts',(-63.0474607219038,-0.831757025163361,
14.258839714434));
#48047=CARTESIAN_POINT('Ctrl Pts',(-64.6398554717402,-2.09154008533313,
14.147701823866));
#48048=CARTESIAN_POINT('Ctrl Pts',(-66.5619019052561,-1.43690629417044,
14.0365639332979));
#48049=CARTESIAN_POINT('Ctrl Pts',(-67.0543073051464,0.532931245964165,
13.9254260427299));
#48050=CARTESIAN_POINT('Ctrl Pts',(-65.6664107088406,2.0149963191636,13.8142881521618));
#48051=CARTESIAN_POINT('Ctrl Pts',(-63.668483745015,1.65266173185674,13.7031502615938));
#48052=CARTESIAN_POINT('Ctrl Pts',(-62.889421959733,-0.222272347729264,
13.5920123710258));
#48053=CARTESIAN_POINT('Ctrl Pts',(-64.0419715223154,-1.89395746343365,
13.4808744804577));
#48054=CARTESIAN_POINT('Ctrl Pts',(-66.0718611861322,-1.83168617135119,
13.3697365898897));
#48055=CARTESIAN_POINT('Ctrl Pts',(-67.1197788376878,-0.0936369858196002,
13.2585986993216));
#48056=CARTESIAN_POINT('Ctrl Pts',(-66.2292075511993,1.73168095096001,13.1474608087536));
#48057=CARTESIAN_POINT('Ctrl Pts',(-64.2098730410853,1.96882346147376,13.0363229181856));
#48058=CARTESIAN_POINT('Ctrl Pts',(-63.3520968146026,0.930071057176342,
12.9622309911402));
#48059=CARTESIAN_POINT('Ctrl Pts',(-63.2376884946835,0.344060554515614,
12.9251850276175));
#48060=CARTESIAN_POINT('Ctrl Pts',(-64.5701357431142,1.60958774866485,22.2244449171475));
#48061=CARTESIAN_POINT('Ctrl Pts',(-64.0349095229901,1.46664765635222,22.1873989536248));
#48062=CARTESIAN_POINT('Ctrl Pts',(-63.1275700215111,0.606976197009781,
22.1133070265794));
#48063=CARTESIAN_POINT('Ctrl Pts',(-63.4747061016385,-1.24728896623771,
22.0021691360114));
#48064=CARTESIAN_POINT('Ctrl Pts',(-65.2206441859093,-1.95631351452271,
21.8910312454434));
#48065=CARTESIAN_POINT('Ctrl Pts',(-66.7632902393938,-0.87643803689069,
21.7798933548753));
#48066=CARTESIAN_POINT('Ctrl Pts',(-66.692647660758,1.00652025480985,21.6687554643073));
#48067=CARTESIAN_POINT('Ctrl Pts',(-65.0723673984167,1.96776149739031,21.5576175737392));
#48068=CARTESIAN_POINT('Ctrl Pts',(-63.3860188510191,1.12810889960267,21.4464796831712));
#48069=CARTESIAN_POINT('Ctrl Pts',(-63.1768796488437,-0.744225754056264,
21.3353417926031));
#48070=CARTESIAN_POINT('Ctrl Pts',(-64.6365064832399,-1.93530608700316,
21.2242039020351));
#48071=CARTESIAN_POINT('Ctrl Pts',(-66.4288212268481,-1.35500706394271,
21.113066011467));
#48072=CARTESIAN_POINT('Ctrl Pts',(-66.9133307013985,0.465559533824989,
21.001928120899));
#48073=CARTESIAN_POINT('Ctrl Pts',(-65.6465413393799,1.85998703107206,20.890790230331));
#48074=CARTESIAN_POINT('Ctrl Pts',(-63.7879681533139,1.55195092417242,20.7796523397629));
#48075=CARTESIAN_POINT('Ctrl Pts',(-63.0387800523716,-0.176605288292527,
20.6685144491949));
#48076=CARTESIAN_POINT('Ctrl Pts',(-64.0847195217704,-1.74351175790306,
20.5573765586268));
#48077=CARTESIAN_POINT('Ctrl Pts',(-65.9684252347068,-1.71456260631994,
20.4462386680588));
#48078=CARTESIAN_POINT('Ctrl Pts',(-66.965720528179,-0.116254623021161,
20.3351007774908));
#48079=CARTESIAN_POINT('Ctrl Pts',(-66.163769438407,1.58846241734546,20.2239628869227));
#48080=CARTESIAN_POINT('Ctrl Pts',(-64.296607029498,1.83924185210905,20.1128249963547));
#48081=CARTESIAN_POINT('Ctrl Pts',(-63.0732681603805,0.406542331281834,
20.0016871057866));
#48082=CARTESIAN_POINT('Ctrl Pts',(-63.6134888063506,-1.39826998078169,
19.8905492152186));
#48083=CARTESIAN_POINT('Ctrl Pts',(-65.4227988660973,-1.92322992958215,
19.7794113246506));
#48084=CARTESIAN_POINT('Ctrl Pts',(-66.8451163318026,-0.687835709090815,
19.6682734340825));
#48085=CARTESIAN_POINT('Ctrl Pts',(-66.5785778924731,1.17714233458595,19.5571355435145));
#48086=CARTESIAN_POINT('Ctrl Pts',(-64.8671492066249,1.96466865068852,19.4459976529464));
#48087=CARTESIAN_POINT('Ctrl Pts',(-63.277320358204,0.953911469466815,19.3348597623784));
#48088=CARTESIAN_POINT('Ctrl Pts',(-63.2642797226261,-0.929971697602105,
19.2237218718103));
#48089=CARTESIAN_POINT('Ctrl Pts',(-64.8399635412389,-1.96264122338425,
19.1125839812423));
#48090=CARTESIAN_POINT('Ctrl Pts',(-66.5621305455413,-1.19888297947456,
19.0014460906742));
#48091=CARTESIAN_POINT('Ctrl Pts',(-66.8544617457199,0.662226451774217,
18.8903082001062));
#48092=CARTESIAN_POINT('Ctrl Pts',(-65.4493830790269,1.91719250157129,18.7791703095382));
#48093=CARTESIAN_POINT('Ctrl Pts',(-63.6329789837436,1.41733051223035,18.6680324189701));
#48094=CARTESIAN_POINT('Ctrl Pts',(-63.0678247277157,-0.379830168572191,
18.5568945284021));
#48095=CARTESIAN_POINT('Ctrl Pts',(-64.271212410766,-1.82932798851556,18.445756637834));
#48096=CARTESIAN_POINT('Ctrl Pts',(-66.1416676392564,-1.6044211545792,18.334618747266));
#48097=CARTESIAN_POINT('Ctrl Pts',(-66.9671415301433,0.0890305575164271,
18.223480856698));
#48098=CARTESIAN_POINT('Ctrl Pts',(-65.9920684695881,1.70099159064234,18.1123429661299));
#48099=CARTESIAN_POINT('Ctrl Pts',(-64.1089438879971,1.75601573029653,18.0012050755619));
#48100=CARTESIAN_POINT('Ctrl Pts',(-63.0414130709861,0.203738757437537,
17.8900671849938));
#48101=CARTESIAN_POINT('Ctrl Pts',(-63.7665990819878,-1.53502261065872,
17.7789292944258));
#48102=CARTESIAN_POINT('Ctrl Pts',(-65.6207309409642,-1.86876037487861,
17.6677914038578));
#48103=CARTESIAN_POINT('Ctrl Pts',(-66.906700730108,-0.492000574788033,
17.5566535132897));
#48104=CARTESIAN_POINT('Ctrl Pts',(-66.4474457175273,1.33509293107206,17.4455156227217));
#48105=CARTESIAN_POINT('Ctrl Pts',(-64.6633272245428,1.94016073613826,17.3343777321536));
#48106=CARTESIAN_POINT('Ctrl Pts',(-63.1873691410633,0.769377416497892,
17.2232398415856));
#48107=CARTESIAN_POINT('Ctrl Pts',(-63.3705326394006,-1.10562577779639,
17.1121019510176));
#48108=CARTESIAN_POINT('Ctrl Pts',(-65.0451660923113,-1.9686371590244,17.0009640604495));
#48109=CARTESIAN_POINT('Ctrl Pts',(-66.6784585087109,-1.02973262273373,
16.8898261698815));
#48110=CARTESIAN_POINT('Ctrl Pts',(-66.7754388170738,0.851697861107777,
16.7786882793134));
#48111=CARTESIAN_POINT('Ctrl Pts',(-65.2473398413224,1.95355963376579,16.6675503887454));
#48112=CARTESIAN_POINT('Ctrl Pts',(-63.4928479037859,1.26730611876661,16.5564124981773));
#48113=CARTESIAN_POINT('Ctrl Pts',(-63.1178693721777,-0.578927058971938,
16.4452746076093));
#48114=CARTESIAN_POINT('Ctrl Pts',(-64.4656263490359,-1.89526173414731,
16.3341367170413));
#48115=CARTESIAN_POINT('Ctrl Pts',(-66.3025015888158,-1.47684185034112,
16.2229988264732));
#48116=CARTESIAN_POINT('Ctrl Pts',(-66.9471823530099,0.29334812763463,16.1118609359052));
#48117=CARTESIAN_POINT('Ctrl Pts',(-65.8095850268848,1.79503323753959,16.0007230453371));
#48118=CARTESIAN_POINT('Ctrl Pts',(-63.9309653444513,1.65370406816781,15.8895851547691));
#48119=CARTESIAN_POINT('Ctrl Pts',(-63.0308452056851,-0.00127918928536197,
15.778447264201));
#48120=CARTESIAN_POINT('Ctrl Pts',(-63.9331147823537,-1.65509158986658,
15.667309373633));
#48121=CARTESIAN_POINT('Ctrl Pts',(-65.8119164971145,-1.79397988904508,
15.556171483065));
#48122=CARTESIAN_POINT('Ctrl Pts',(-66.9475618361337,-0.29081804904335,
15.4450335924969));
#48123=CARTESIAN_POINT('Ctrl Pts',(-66.3005817360626,1.47853284613195,15.3338957019289));
#48124=CARTESIAN_POINT('Ctrl Pts',(-64.4631644305619,1.89456586592117,15.2227578113608));
#48125=CARTESIAN_POINT('Ctrl Pts',(-63.1171187956369,0.576481250135308,
15.1116199207928));
#48126=CARTESIAN_POINT('Ctrl Pts',(-63.4944957086799,-1.26926316652857,
15.0004820302248));
#48127=CARTESIAN_POINT('Ctrl Pts',(-65.2498777170288,-1.95323666226351,
14.8893441396567));
#48128=CARTESIAN_POINT('Ctrl Pts',(-66.7765439285027,-0.849390390991115,
14.7782062490887));
#48129=CARTESIAN_POINT('Ctrl Pts',(-66.6771191139918,1.03191234184772,14.6670683585206));
#48130=CARTESIAN_POINT('Ctrl Pts',(-65.0426085927299,1.96869439442843,14.5559304679526));
#48131=CARTESIAN_POINT('Ctrl Pts',(-63.3690970742208,1.10350736975597,14.4447925773845));
#48132=CARTESIAN_POINT('Ctrl Pts',(-63.1883712234789,-0.771730934564716,
14.3336546868165));
#48133=CARTESIAN_POINT('Ctrl Pts',(-64.6658463169365,-1.94059819863461,
14.2225167962484));
#48134=CARTESIAN_POINT('Ctrl Pts',(-66.4491828509713,-1.33320790054558,
14.1113789056804));
#48135=CARTESIAN_POINT('Ctrl Pts',(-66.9060524269962,0.494470760166873,
14.0002410151124));
#48136=CARTESIAN_POINT('Ctrl Pts',(-65.6183173013013,1.86957842914181,13.8891031245443));
#48137=CARTESIAN_POINT('Ctrl Pts',(-63.764576369348,1.53339273881654,13.7779652339763));
#48138=CARTESIAN_POINT('Ctrl Pts',(-63.0417377741208,-0.206231437128299,
13.6668273434082));
#48139=CARTESIAN_POINT('Ctrl Pts',(-64.111110348268,-1.75727468366666,13.5556894528402));
#48140=CARTESIAN_POINT('Ctrl Pts',(-65.9945073018589,-1.69949737493168,
13.4445515622722));
#48141=CARTESIAN_POINT('Ctrl Pts',(-66.9667990218154,-0.0868794087578511,
13.3334136717041));
#48142=CARTESIAN_POINT('Ctrl Pts',(-66.1404983229023,1.60670931320335,13.2222757811361));
#48143=CARTESIAN_POINT('Ctrl Pts',(-64.2668947805903,1.82673776589703,13.111137890568));
#48144=CARTESIAN_POINT('Ctrl Pts',(-63.4710223937224,0.862949857291941,
13.0370459635227));
#48145=CARTESIAN_POINT('Ctrl Pts',(-63.3648706727485,0.319230454628309,
13.));
#48146=CARTESIAN_POINT('Ctrl Pts',(-63.3361634080255,-0.000941845566861395,
21.3785196366098));
#48147=CARTESIAN_POINT('Ctrl Pts',(-63.3350462116423,-0.216826197428599,
21.3641270219409));
#48148=CARTESIAN_POINT('Ctrl Pts',(-63.3740367968513,-0.432323693321025,
21.349734407272));
#48149=CARTESIAN_POINT('Ctrl Pts',(-63.4550073216056,-0.630683367270925,
21.3353417926031));
#48150=CARTESIAN_POINT('Ctrl Pts',(-63.6634219269757,-1.14125253170523,
21.2982958290804));
#48151=CARTESIAN_POINT('Ctrl Pts',(-64.1499642051078,-1.5382793093542,21.2612498655578));
#48152=CARTESIAN_POINT('Ctrl Pts',(-64.6919544681085,-1.64007619433527,
21.2242039020351));
#48153=CARTESIAN_POINT('Ctrl Pts',(-65.2339447311093,-1.74187307931634,
21.1871579385124));
#48154=CARTESIAN_POINT('Ctrl Pts',(-65.8313829789787,-1.54844007162952,
21.1501119749897));
#48155=CARTESIAN_POINT('Ctrl Pts',(-66.2108536820051,-1.1482958014915,21.113066011467));
#48156=CARTESIAN_POINT('Ctrl Pts',(-66.5903243850316,-0.748151531353475,
21.0760200479444));
#48157=CARTESIAN_POINT('Ctrl Pts',(-66.751827543215,-0.141295998764244,
21.0389740844217));
#48158=CARTESIAN_POINT('Ctrl Pts',(-66.6214475619703,0.394536350404884,
21.001928120899));
#48159=CARTESIAN_POINT('Ctrl Pts',(-66.4910675807256,0.930368699574014,
20.9648821573763));
#48160=CARTESIAN_POINT('Ctrl Pts',(-66.0688044600528,1.39517786532304,20.9278361938536));
#48161=CARTESIAN_POINT('Ctrl Pts',(-65.5479107020387,1.57624309704761,20.890790230331));
#48162=CARTESIAN_POINT('Ctrl Pts',(-65.0270169440246,1.75730832877218,20.8537442668083));
#48163=CARTESIAN_POINT('Ctrl Pts',(-64.4074925486692,1.6546296264723,20.8166983032856));
#48164=CARTESIAN_POINT('Ctrl Pts',(-63.9728656675012,1.31519757324487,20.7796523397629));
#48165=CARTESIAN_POINT('Ctrl Pts',(-63.5773660666821,1.00632288699473,20.7459414387119));
#48166=CARTESIAN_POINT('Ctrl Pts',(-63.3349716882235,0.501403518382684,
20.7122305376608));
#48167=CARTESIAN_POINT('Ctrl Pts',(-63.3318013787731,-0.000864016794193591,
20.6785196366098));
#48168=CARTESIAN_POINT('Ctrl Pts',(-64.4698297828114,1.98517432567173,22.));
#48169=CARTESIAN_POINT('Ctrl Pts',(-64.4011635904059,1.95974978038732,22.));
#48170=CARTESIAN_POINT('Ctrl Pts',(-64.3342007656382,1.9304357713801,22.));
#48171=CARTESIAN_POINT('Ctrl Pts',(-64.2691302660859,1.89752626078927,22.));
#48172=CARTESIAN_POINT('Ctrl Pts',(-64.2022499741923,1.86370144478923,22.));
#48173=CARTESIAN_POINT('Ctrl Pts',(-64.137367961524,1.82607765547919,22.));
#48174=CARTESIAN_POINT('Ctrl Pts',(-64.0747206099689,1.78492942875572,22.));
#48175=CARTESIAN_POINT('Ctrl Pts',(-64.0217852175796,1.7501602410142,22.));
#48176=CARTESIAN_POINT('Ctrl Pts',(-63.9704456655167,1.71287362002867,22.));
#48177=CARTESIAN_POINT('Ctrl Pts',(-63.9208673056515,1.67321717698682,22.));
#48178=CARTESIAN_POINT('Ctrl Pts',(-63.8988414814125,1.65559929195073,22.));
#48179=CARTESIAN_POINT('Ctrl Pts',(-63.8771635659829,1.63751349743234,22.));
#48180=CARTESIAN_POINT('Ctrl Pts',(-63.8558496107188,1.61897201296729,22.));
#48181=CARTESIAN_POINT('Ctrl Pts',(-63.8441378985455,1.60878373366256,22.));
#48182=CARTESIAN_POINT('Ctrl Pts',(-63.8325360961551,1.59845785925715,22.));
#48183=CARTESIAN_POINT('Ctrl Pts',(-63.8210470007987,1.5879963754255,22.));
#48184=CARTESIAN_POINT('Ctrl Pts',(-63.8104526359383,1.57834959530439,22.));
#48185=CARTESIAN_POINT('Ctrl Pts',(-63.7999526722261,1.56858598842988,22.));
#48186=CARTESIAN_POINT('Ctrl Pts',(-63.7895651937358,1.55872256958795,22.));
#48187=CARTESIAN_POINT('Ctrl Pts',(-63.7364801435462,1.50831571822785,22.));
#48188=CARTESIAN_POINT('Ctrl Pts',(-63.6862350752816,1.45522053846771,22.));
#48189=CARTESIAN_POINT('Ctrl Pts',(-63.639048665253,1.39969641403416,22.));
#48190=CARTESIAN_POINT('Ctrl Pts',(-63.5922286928517,1.34460347579176,22.));
#48191=CARTESIAN_POINT('Ctrl Pts',(-63.5484195492875,1.28711828831824,22.));
#48192=CARTESIAN_POINT('Ctrl Pts',(-63.5078796466337,1.22746999892216,22.));
#48193=CARTESIAN_POINT('Ctrl Pts',(-63.4741871309004,1.17789659599364,22.));
#48194=CARTESIAN_POINT('Ctrl Pts',(-63.4427533858106,1.12682844545201,22.));
#48195=CARTESIAN_POINT('Ctrl Pts',(-63.413754367486,1.07439061084202,22.));
#48196=CARTESIAN_POINT('Ctrl Pts',(-63.4016500392281,1.0525028091188,22.));
#48197=CARTESIAN_POINT('Ctrl Pts',(-63.3899702272225,1.03037633270466,22.));
#48198=CARTESIAN_POINT('Ctrl Pts',(-63.3787291685026,1.00802019356891,22.));
#48199=CARTESIAN_POINT('Ctrl Pts',(-63.3735259415793,0.997672052174805,
22.));
#48200=CARTESIAN_POINT('Ctrl Pts',(-63.3684167321731,0.987274704423447,
22.));
#48201=CARTESIAN_POINT('Ctrl Pts',(-63.3634030175405,0.976829046042575,
22.));
#48202=CARTESIAN_POINT('Ctrl Pts',(-63.3581740167297,0.965934856774388,
22.));
#48203=CARTESIAN_POINT('Ctrl Pts',(-63.3530525040039,0.954995586464713,
22.));
#48204=CARTESIAN_POINT('Ctrl Pts',(-63.3480415178798,0.944016502307831,
22.));
#48205=CARTESIAN_POINT('Ctrl Pts',(-63.3195013216555,0.881484855154736,
22.));
#48206=CARTESIAN_POINT('Ctrl Pts',(-63.2945220500091,0.817619969386109,
22.));
#48207=CARTESIAN_POINT('Ctrl Pts',(-63.273327165115,0.752626219156414,22.));
#48208=CARTESIAN_POINT('Ctrl Pts',(-63.2541166188611,0.693717409259875,
22.));
#48209=CARTESIAN_POINT('Ctrl Pts',(-63.2380153357379,0.633880618070606,
22.));
#48210=CARTESIAN_POINT('Ctrl Pts',(-63.2252264587662,0.573263190512467,
22.));
#48211=CARTESIAN_POINT('Ctrl Pts',(-63.2100966383573,0.501550029564721,
22.));
#48212=CARTESIAN_POINT('Ctrl Pts',(-63.199602249042,0.428742773422576,22.));
#48213=CARTESIAN_POINT('Ctrl Pts',(-63.1936681155555,0.35526466203955,22.));
#48214=CARTESIAN_POINT('Ctrl Pts',(-63.1923616383022,0.339087492894985,
22.));
#48215=CARTESIAN_POINT('Ctrl Pts',(-63.1912764288138,0.32287788806267,22.));
#48216=CARTESIAN_POINT('Ctrl Pts',(-63.1904120545575,0.306640528882653,
22.));
#48217=CARTESIAN_POINT('Ctrl Pts',(-63.18952016631,0.289886316551054,22.));
#48218=CARTESIAN_POINT('Ctrl Pts',(-63.1888633864288,0.273096407564662,
22.));
#48219=CARTESIAN_POINT('Ctrl Pts',(-63.1884417974656,0.256310042500943,
22.));
#48220=CARTESIAN_POINT('Ctrl Pts',(-63.1867198704081,0.187748247191763,
22.));
#48221=CARTESIAN_POINT('Ctrl Pts',(-63.1889096770048,0.119158552219121,
22.));
#48222=CARTESIAN_POINT('Ctrl Pts',(-63.1948905827374,0.0508793566118494,
22.));
#48223=CARTESIAN_POINT('Ctrl Pts',(-63.2008702728702,-0.0173859614684271,
22.));
#48224=CARTESIAN_POINT('Ctrl Pts',(-63.2106399749853,-0.0853419781943991,
22.));
#48225=CARTESIAN_POINT('Ctrl Pts',(-63.2241287349498,-0.152635471586587,
22.));
#48226=CARTESIAN_POINT('Ctrl Pts',(-63.2338917748016,-0.201341880440236,
22.));
#48227=CARTESIAN_POINT('Ctrl Pts',(-63.2456041790335,-0.249700946127146,
22.));
#48228=CARTESIAN_POINT('Ctrl Pts',(-63.2592532629054,-0.29756907509214,
22.));
#48229=CARTESIAN_POINT('Ctrl Pts',(-63.2694917264426,-0.333475960682568,
22.));
#48230=CARTESIAN_POINT('Ctrl Pts',(-63.2808201731573,-0.369106450149086,
22.));
#48231=CARTESIAN_POINT('Ctrl Pts',(-63.2932371663006,-0.40439575621736,
22.));
#48232=CARTESIAN_POINT('Ctrl Pts',(-63.2973637241401,-0.416123503903528,
22.));
#48233=CARTESIAN_POINT('Ctrl Pts',(-63.3016073023407,-0.427804352958856,
22.));
#48234=CARTESIAN_POINT('Ctrl Pts',(-63.3059672772019,-0.439435804918062,
22.));
#48235=CARTESIAN_POINT('Ctrl Pts',(-63.3290918712168,-0.501127124918587,
22.));
#48236=CARTESIAN_POINT('Ctrl Pts',(-63.3554889558621,-0.561434936785673,
22.));
#48237=CARTESIAN_POINT('Ctrl Pts',(-63.3851084989722,-0.620025088688961,
22.));
#48238=CARTESIAN_POINT('Ctrl Pts',(-63.4059501828406,-0.661251836151812,
22.));
#48239=CARTESIAN_POINT('Ctrl Pts',(-63.4283882195983,-0.701627610070203,
22.));
#48240=CARTESIAN_POINT('Ctrl Pts',(-63.4524155940285,-0.74102463102569,
22.));
#48241=CARTESIAN_POINT('Ctrl Pts',(-63.4601281158564,-0.753670639642036,
22.));
#48242=CARTESIAN_POINT('Ctrl Pts',(-63.4680055619416,-0.76621742722543,
22.));
#48243=CARTESIAN_POINT('Ctrl Pts',(-63.476044336448,-0.778655072921202,
22.));
#48244=CARTESIAN_POINT('Ctrl Pts',(-63.5102900794466,-0.831640315592426,
22.));
#48245=CARTESIAN_POINT('Ctrl Pts',(-63.5473913229322,-0.882541662833814,
22.));
#48246=CARTESIAN_POINT('Ctrl Pts',(-63.5873138038648,-0.931043840655609,
22.));
#48247=CARTESIAN_POINT('Ctrl Pts',(-63.624120899027,-0.975761108544703,
22.));
#48248=CARTESIAN_POINT('Ctrl Pts',(-63.6633266818169,-1.01843913681673,
22.));
#48249=CARTESIAN_POINT('Ctrl Pts',(-63.7049257741094,-1.05879788933142,
22.));
#48250=CARTESIAN_POINT('Ctrl Pts',(-63.7127105119292,-1.06635051343315,
22.));
#48251=CARTESIAN_POINT('Ctrl Pts',(-63.7205791168682,-1.07382181318668,
22.));
#48252=CARTESIAN_POINT('Ctrl Pts',(-63.7285300176229,-1.08121113172717,
22.));
#48253=CARTESIAN_POINT('Origin',(-65.,8.88178419700125E-15,17.));
#48254=CARTESIAN_POINT('Origin',(-32.5,56.2916512459885,13.));
#48255=CARTESIAN_POINT('Ctrl Pts',(-31.4059736530045,55.03520293743,13.));
#48256=CARTESIAN_POINT('Ctrl Pts',(-31.3544234714595,55.0705532050083,13.));
#48257=CARTESIAN_POINT('Ctrl Pts',(-31.3051813503225,55.1089326491167,13.));
#48258=CARTESIAN_POINT('Ctrl Pts',(-31.2583086630186,55.1500094432508,13.));
#48259=CARTESIAN_POINT('Ctrl Pts',(-31.2285772760959,55.1760644900209,13.));
#48260=CARTESIAN_POINT('Ctrl Pts',(-31.1997994779263,55.203205850304,13.));
#48261=CARTESIAN_POINT('Ctrl Pts',(-31.1719948709674,55.2313585594901,13.));
#48262=CARTESIAN_POINT('Ctrl Pts',(-31.1530079458905,55.2505831930488,13.));
#48263=CARTESIAN_POINT('Ctrl Pts',(-31.1344748967249,55.2702795828656,13.));
#48264=CARTESIAN_POINT('Ctrl Pts',(-31.1164029934988,55.2904256041521,13.));
#48265=CARTESIAN_POINT('Ctrl Pts',(-31.1068068849154,55.3011230611586,13.));
#48266=CARTESIAN_POINT('Ctrl Pts',(-31.0973410263878,55.3119472603811,13.));
#48267=CARTESIAN_POINT('Ctrl Pts',(-31.088015636226,55.3228838806201,13.));
#48268=CARTESIAN_POINT('Ctrl Pts',(-31.0452129476489,55.3730819679982,13.));
#48269=CARTESIAN_POINT('Ctrl Pts',(-31.0053166512349,55.4257004125729,13.));
#48270=CARTESIAN_POINT('Ctrl Pts',(-30.9684112132021,55.4803964719602,13.));
#48271=CARTESIAN_POINT('Ctrl Pts',(-30.9417896427002,55.5198512265645,13.));
#48272=CARTESIAN_POINT('Ctrl Pts',(-30.9167247740352,55.5603881852279,13.));
#48273=CARTESIAN_POINT('Ctrl Pts',(-30.8932580441631,55.6018923087211,13.));
#48274=CARTESIAN_POINT('Ctrl Pts',(-30.8868285869199,55.6132636838069,13.));
#48275=CARTESIAN_POINT('Ctrl Pts',(-30.8805191492575,55.624707716983,13.));
#48276=CARTESIAN_POINT('Ctrl Pts',(-30.8743307097694,55.6362221640537,13.));
#48277=CARTESIAN_POINT('Ctrl Pts',(-30.8680004790577,55.6480004332951,13.));
#48278=CARTESIAN_POINT('Ctrl Pts',(-30.8618007206828,55.6598452669412,13.));
#48279=CARTESIAN_POINT('Ctrl Pts',(-30.8557343741951,55.6717493030395,13.));
#48280=CARTESIAN_POINT('Ctrl Pts',(-30.8249262845843,55.7322042426952,13.));
#48281=CARTESIAN_POINT('Ctrl Pts',(-30.7975367124524,55.7942196204653,13.));
#48282=CARTESIAN_POINT('Ctrl Pts',(-30.7736505521297,55.8574477165599,13.));
#48283=CARTESIAN_POINT('Ctrl Pts',(-30.7494182330752,55.9215921155367,13.));
#48284=CARTESIAN_POINT('Ctrl Pts',(-30.7287909250581,55.9869854552535,13.));
#48285=CARTESIAN_POINT('Ctrl Pts',(-30.7118943735469,56.0533023283581,13.));
#48286=CARTESIAN_POINT('Ctrl Pts',(-30.7014256020703,56.0943909605036,13.));
#48287=CARTESIAN_POINT('Ctrl Pts',(-30.6923897620258,56.1358348151177,13.));
#48288=CARTESIAN_POINT('Ctrl Pts',(-30.6848255185714,56.1775614120725,13.));
#48289=CARTESIAN_POINT('Ctrl Pts',(-30.6786294263425,56.2117408835145,13.));
#48290=CARTESIAN_POINT('Ctrl Pts',(-30.6734208465201,56.2461101541398,13.));
#48291=CARTESIAN_POINT('Ctrl Pts',(-30.6692248691864,56.2806305246086,13.));
#48292=CARTESIAN_POINT('Ctrl Pts',(-30.6675094773726,56.2947430796119,13.));
#48293=CARTESIAN_POINT('Ctrl Pts',(-30.6659632509433,56.3088834625076,13.));
#48294=CARTESIAN_POINT('Ctrl Pts',(-30.6645900225956,56.3230249695405,13.));
#48295=CARTESIAN_POINT('Ctrl Pts',(-30.6577774083435,56.3931812785896,13.));
#48296=CARTESIAN_POINT('Ctrl Pts',(-30.6552023639047,56.4634862436249,13.));
#48297=CARTESIAN_POINT('Ctrl Pts',(-30.656979948111,56.5335953126756,13.));
#48298=CARTESIAN_POINT('Ctrl Pts',(-30.6571775468153,56.541388733181,13.));
#48299=CARTESIAN_POINT('Ctrl Pts',(-30.6574289761758,56.5491797596165,13.));
#48300=CARTESIAN_POINT('Ctrl Pts',(-30.6577344296099,56.5569679370673,13.));
#48301=CARTESIAN_POINT('Ctrl Pts',(-30.6603769077943,56.6243434735906,13.));
#48302=CARTESIAN_POINT('Ctrl Pts',(-30.6670582139718,56.6915049782423,13.));
#48303=CARTESIAN_POINT('Ctrl Pts',(-30.6775414626437,56.7582070441046,13.));
#48304=CARTESIAN_POINT('Ctrl Pts',(-30.6888193174903,56.8299649733794,13.));
#48305=CARTESIAN_POINT('Ctrl Pts',(-30.704496956143,56.9011921151415,13.));
#48306=CARTESIAN_POINT('Ctrl Pts',(-30.7243435713014,56.9715867176024,13.));
#48307=CARTESIAN_POINT('Ctrl Pts',(-30.7279780724868,56.9844780476379,13.));
#48308=CARTESIAN_POINT('Ctrl Pts',(-30.7317525557216,56.9973414427362,13.));
#48309=CARTESIAN_POINT('Ctrl Pts',(-30.7356658273112,57.0101750195627,13.));
#48310=CARTESIAN_POINT('Ctrl Pts',(-30.7390274221048,57.0211993719635,13.));
#48311=CARTESIAN_POINT('Ctrl Pts',(-30.7424887106291,57.032192762231,13.));
#48312=CARTESIAN_POINT('Ctrl Pts',(-30.7460479824822,57.0431526563695,13.));
#48313=CARTESIAN_POINT('Ctrl Pts',(-30.767999129186,57.1107457636177,13.));
#48314=CARTESIAN_POINT('Ctrl Pts',(-30.7936779401901,57.1770813814884,13.));
#48315=CARTESIAN_POINT('Ctrl Pts',(-30.8228134384578,57.241892040805,13.));
#48316=CARTESIAN_POINT('Ctrl Pts',(-30.8525629752182,57.3080686022655,13.));
#48317=CARTESIAN_POINT('Ctrl Pts',(-30.8859166602457,57.3726561595602,13.));
#48318=CARTESIAN_POINT('Ctrl Pts',(-30.9226411453944,57.435369889801,13.));
#48319=CARTESIAN_POINT('Ctrl Pts',(-30.9595879477009,57.4984632669779,13.));
#48320=CARTESIAN_POINT('Ctrl Pts',(-30.9999468758072,57.5596610608135,13.));
#48321=CARTESIAN_POINT('Ctrl Pts',(-31.0435306576476,57.6186586679229,13.));
#48322=CARTESIAN_POINT('Ctrl Pts',(-31.0543033137161,57.633241177825,13.));
#48323=CARTESIAN_POINT('Ctrl Pts',(-31.0652732109609,57.6476891598953,13.));
#48324=CARTESIAN_POINT('Ctrl Pts',(-31.0764379480169,57.6619977668291,13.));
#48325=CARTESIAN_POINT('Ctrl Pts',(-31.0851682201236,57.6731863896666,13.));
#48326=CARTESIAN_POINT('Ctrl Pts',(-31.0940187402904,57.6842909720356,13.));
#48327=CARTESIAN_POINT('Ctrl Pts',(-31.1029745493948,57.6952926418324,13.));
#48328=CARTESIAN_POINT('Ctrl Pts',(-31.1505373073925,57.7537206132213,13.));
#48329=CARTESIAN_POINT('Ctrl Pts',(-31.2011482673078,57.8093550197329,13.));
#48330=CARTESIAN_POINT('Ctrl Pts',(-31.2545510979645,57.8619011539994,13.));
#48331=CARTESIAN_POINT('Ctrl Pts',(-31.3080118292081,57.9145042600028,13.));
#48332=CARTESIAN_POINT('Ctrl Pts',(-31.364270980967,57.9640134082748,13.));
#48333=CARTESIAN_POINT('Ctrl Pts',(-31.4231195455734,58.0101134374941,13.));
#48334=CARTESIAN_POINT('Ctrl Pts',(-31.4806288819684,58.0551643593974,13.));
#48335=CARTESIAN_POINT('Ctrl Pts',(-31.5406117297693,58.0969603996382,13.));
#48336=CARTESIAN_POINT('Ctrl Pts',(-31.6029105622421,58.1351753157717,13.));
#48337=CARTESIAN_POINT('Ctrl Pts',(-31.6163051636256,58.1433917389083,13.));
#48338=CARTESIAN_POINT('Ctrl Pts',(-31.62980694879,58.151442469068,13.));
#48339=CARTESIAN_POINT('Ctrl Pts',(-31.6434145443377,58.1593240060195,13.));
#48340=CARTESIAN_POINT('Ctrl Pts',(-31.6549388802988,58.1659989163223,13.));
#48341=CARTESIAN_POINT('Ctrl Pts',(-31.666539109872,58.1725524712207,13.));
#48342=CARTESIAN_POINT('Ctrl Pts',(-31.6782133743559,58.178984818602,13.));
#48343=CARTESIAN_POINT('Ctrl Pts',(-32.7283737736498,58.3336705852723,13.));
#48344=CARTESIAN_POINT('Ctrl Pts',(-32.8014565014342,58.3184742869048,13.));
#48345=CARTESIAN_POINT('Ctrl Pts',(-32.873478859746,58.2989977860273,13.));
#48346=CARTESIAN_POINT('Ctrl Pts',(-32.9441813035447,58.2754925548875,13.));
#48347=CARTESIAN_POINT('Ctrl Pts',(-33.0130334318814,58.252602466454,13.));
#48348=CARTESIAN_POINT('Ctrl Pts',(-33.0806343841369,58.2258909044567,13.));
#48349=CARTESIAN_POINT('Ctrl Pts',(-33.1467189154995,58.1955520781456,13.));
#48350=CARTESIAN_POINT('Ctrl Pts',(-33.1614684627314,58.1887806909176,13.));
#48351=CARTESIAN_POINT('Ctrl Pts',(-33.1761442892263,58.1818275347425,13.));
#48352=CARTESIAN_POINT('Ctrl Pts',(-33.19073701805,58.174697608363,13.));
#48353=CARTESIAN_POINT('Ctrl Pts',(-33.257702590687,58.1419786009295,13.));
#48354=CARTESIAN_POINT('Ctrl Pts',(-33.3227883262805,58.1056063852406,13.));
#48355=CARTESIAN_POINT('Ctrl Pts',(-33.3857181641543,58.0658123205629,13.));
#48356=CARTESIAN_POINT('Ctrl Pts',(-33.4298991918482,58.0378741797226,13.));
#48357=CARTESIAN_POINT('Ctrl Pts',(-33.4730169952496,58.0082484488949,13.));
#48358=CARTESIAN_POINT('Ctrl Pts',(-33.5149645802173,57.9770049688462,13.));
#48359=CARTESIAN_POINT('Ctrl Pts',(-33.5309116531909,57.9651272396118,13.));
#48360=CARTESIAN_POINT('Ctrl Pts',(-33.5466894884539,57.9530156286815,13.));
#48361=CARTESIAN_POINT('Ctrl Pts',(-33.5622917807054,57.9406737249562,13.));
#48362=CARTESIAN_POINT('Ctrl Pts',(-33.5771528452482,57.9289181556535,13.));
#48363=CARTESIAN_POINT('Ctrl Pts',(-33.5918591269232,57.9169497163141,13.));
#48364=CARTESIAN_POINT('Ctrl Pts',(-33.6063795974092,57.9047932102742,13.));
#48365=CARTESIAN_POINT('Ctrl Pts',(-33.6620452142588,57.8581900779513,13.));
#48366=CARTESIAN_POINT('Ctrl Pts',(-33.7150448947231,57.8087799684573,13.));
#48367=CARTESIAN_POINT('Ctrl Pts',(-33.7651216105449,57.7567754486693,13.));
#48368=CARTESIAN_POINT('Ctrl Pts',(-33.8141231389414,57.7058875078106,13.));
#48369=CARTESIAN_POINT('Ctrl Pts',(-33.8603263530544,57.6525145642833,13.));
#48370=CARTESIAN_POINT('Ctrl Pts',(-33.9034486472843,57.5968301465233,13.));
#48371=CARTESIAN_POINT('Ctrl Pts',(-33.9456250982487,57.5423671093153,13.));
#48372=CARTESIAN_POINT('Ctrl Pts',(-33.9848546824741,57.4856922167148,13.));
#48373=CARTESIAN_POINT('Ctrl Pts',(-34.0208263214491,57.4269537422269,13.));
#48374=CARTESIAN_POINT('Ctrl Pts',(-34.0325140426356,57.4078687371424,13.));
#48375=CARTESIAN_POINT('Ctrl Pts',(-34.0438574259773,57.388565808898,13.));
#48376=CARTESIAN_POINT('Ctrl Pts',(-34.0548446057422,57.3690498892147,13.));
#48377=CARTESIAN_POINT('Ctrl Pts',(-34.0610436453445,57.3580388780562,13.));
#48378=CARTESIAN_POINT('Ctrl Pts',(-34.067129818108,57.3469588598396,13.));
#48379=CARTESIAN_POINT('Ctrl Pts',(-34.0730927269274,57.3358266058508,13.));
#48380=CARTESIAN_POINT('Ctrl Pts',(-34.1053441707905,57.275615847065,13.));
#48381=CARTESIAN_POINT('Ctrl Pts',(-34.1340531805922,57.213774929567,13.));
#48382=CARTESIAN_POINT('Ctrl Pts',(-34.1589642501542,57.1504676177922,13.));
#48383=CARTESIAN_POINT('Ctrl Pts',(-34.1625594232719,57.1413310873482,13.));
#48384=CARTESIAN_POINT('Ctrl Pts',(-34.1660754068789,57.1321639877973,13.));
#48385=CARTESIAN_POINT('Ctrl Pts',(-34.1695113451333,57.1229667871477,13.));
#48386=CARTESIAN_POINT('Ctrl Pts',(-34.1937894815808,57.0579799114317,13.));
#48387=CARTESIAN_POINT('Ctrl Pts',(-34.2140754401802,56.9914902794409,13.));
#48388=CARTESIAN_POINT('Ctrl Pts',(-34.2304117433282,56.9238636615718,13.));
#48389=CARTESIAN_POINT('Ctrl Pts',(-34.245652193415,56.8607734945473,13.));
#48390=CARTESIAN_POINT('Ctrl Pts',(-34.2574544360998,56.7966929502099,13.));
#48391=CARTESIAN_POINT('Ctrl Pts',(-34.2658134374967,56.7319255341061,13.));
#48392=CARTESIAN_POINT('Ctrl Pts',(-34.2676584011686,56.7176303421134,13.));
#48393=CARTESIAN_POINT('Ctrl Pts',(-34.2693354843638,56.7033017407945,13.));
#48394=CARTESIAN_POINT('Ctrl Pts',(-34.27084439597,56.6889430967533,13.));
#48395=CARTESIAN_POINT('Ctrl Pts',(-34.2720238222203,56.6777198006816,13.));
#48396=CARTESIAN_POINT('Ctrl Pts',(-34.2731003471717,56.6664788449441,13.));
#48397=CARTESIAN_POINT('Ctrl Pts',(-34.2740729516962,56.6552348561548,13.));
#48398=CARTESIAN_POINT('Ctrl Pts',(-34.2799651734903,56.5871166496992,13.));
#48399=CARTESIAN_POINT('Ctrl Pts',(-34.2820614503506,56.5187616008007,13.));
#48400=CARTESIAN_POINT('Ctrl Pts',(-34.2804207734206,56.4505176929745,13.));
#48401=CARTESIAN_POINT('Ctrl Pts',(-34.2787876667987,56.3825886718839,13.));
#48402=CARTESIAN_POINT('Ctrl Pts',(-34.2734516847768,56.3147686814055,13.));
#48403=CARTESIAN_POINT('Ctrl Pts',(-34.2644214384179,56.2474134553717,13.));
#48404=CARTESIAN_POINT('Ctrl Pts',(-34.2555845575853,56.1815005132143,13.));
#48405=CARTESIAN_POINT('Ctrl Pts',(-34.2432095215078,56.1160317619071,13.));
#48406=CARTESIAN_POINT('Ctrl Pts',(-34.2272624366924,56.0513669976104,13.));
#48407=CARTESIAN_POINT('Ctrl Pts',(-34.2239018012959,56.0377397611393,13.));
#48408=CARTESIAN_POINT('Ctrl Pts',(-34.2203823922543,56.0241483513653,13.));
#48409=CARTESIAN_POINT('Ctrl Pts',(-34.2167036732636,56.010596345236,13.));
#48410=CARTESIAN_POINT('Ctrl Pts',(-34.2132180508017,55.9977556860044,13.));
#48411=CARTESIAN_POINT('Ctrl Pts',(-34.2095887843185,55.9849487309035,13.));
#48412=CARTESIAN_POINT('Ctrl Pts',(-34.2058217802814,55.9721990639717,13.));
#48413=CARTESIAN_POINT('Ctrl Pts',(-34.1873069911305,55.9095345718023,13.));
#48414=CARTESIAN_POINT('Ctrl Pts',(-34.1654391518089,55.8481392503641,13.));
#48415=CARTESIAN_POINT('Ctrl Pts',(-34.1402348458881,55.7883322345209,13.));
#48416=CARTESIAN_POINT('Ctrl Pts',(-34.1155097070604,55.7296622289178,13.));
#48417=CARTESIAN_POINT('Ctrl Pts',(-34.0875733532636,55.6725199272576,13.));
#48418=CARTESIAN_POINT('Ctrl Pts',(-34.0564019232237,55.6172367682145,13.));
#48419=CARTESIAN_POINT('Ctrl Pts',(-34.0262427202972,55.5637488143458,13.));
#48420=CARTESIAN_POINT('Ctrl Pts',(-33.9930547257666,55.5120006932486,13.));
#48421=CARTESIAN_POINT('Ctrl Pts',(-33.9567849770258,55.4623304145917,13.));
#48422=CARTESIAN_POINT('Ctrl Pts',(-33.950749031927,55.454064377869,13.));
#48423=CARTESIAN_POINT('Ctrl Pts',(-33.9446276728907,55.44585598451,13.));
#48424=CARTESIAN_POINT('Ctrl Pts',(-33.9384205797355,55.4377069137227,13.));
#48425=CARTESIAN_POINT('Ctrl Pts',(-33.931849519021,55.4290800029336,13.));
#48426=CARTESIAN_POINT('Ctrl Pts',(-33.9251823737702,55.4205195760217,13.));
#48427=CARTESIAN_POINT('Ctrl Pts',(-33.9184205240576,55.4120266023845,13.));
#48428=CARTESIAN_POINT('Origin',(-32.5,56.2916512459885,23.5459252805377));
#48429=CARTESIAN_POINT('Ctrl Pts',(-31.4730118547325,54.5098571360137,21.7959252805377));
#48430=CARTESIAN_POINT('Ctrl Pts',(-31.5577251735552,54.4600031121465,21.7905813053169));
#48431=CARTESIAN_POINT('Ctrl Pts',(-32.2577698823492,54.1148344325097,21.7481913665734));
#48432=CARTESIAN_POINT('Ctrl Pts',(-33.9070787897524,54.3119235461293,21.6687554643073));
#48433=CARTESIAN_POINT('Ctrl Pts',(-34.9261604045136,56.4001058936205,21.5576175737392));
#48434=CARTESIAN_POINT('Ctrl Pts',(-33.7248161346881,58.3888336702691,21.4464796831712));
#48435=CARTESIAN_POINT('Ctrl Pts',(-31.4022507610406,58.4580789101429,21.3353417926031));
#48436=CARTESIAN_POINT('Ctrl Pts',(-30.0845341595457,56.5443222204948,21.2242039020351));
#48437=CARTESIAN_POINT('Ctrl Pts',(-30.7258866583527,55.004043700614,21.1443983980133));
#48438=CARTESIAN_POINT('Ctrl Pts',(-31.3789145578643,54.5633564487824,21.1016388575141));
#48439=CARTESIAN_POINT('Ctrl Pts',(-31.4704172621348,54.5115691325664,21.0959252805377));
#48440=CARTESIAN_POINT('Ctrl Pts',(-31.4716734168817,54.5151354051885,21.8540747194623));
#48441=CARTESIAN_POINT('Ctrl Pts',(-31.8806518858733,54.2831085316556,21.8286245525962));
#48442=CARTESIAN_POINT('Ctrl Pts',(-33.082939422317,54.0422681540074,21.7661284222074));
#48443=CARTESIAN_POINT('Ctrl Pts',(-34.7256560234758,55.3208993649632,21.6665863282959));
#48444=CARTESIAN_POINT('Ctrl Pts',(-34.5234929724835,57.6345755616839,21.5554484377278));
#48445=CARTESIAN_POINT('Ctrl Pts',(-32.4687454188576,58.7202753686331,21.4443105471598));
#48446=CARTESIAN_POINT('Ctrl Pts',(-30.4428342940784,57.5824199368057,21.3331726565918));
#48447=CARTESIAN_POINT('Ctrl Pts',(-30.3182849616345,55.5637298511604,21.2364273806926));
#48448=CARTESIAN_POINT('Ctrl Pts',(-31.1131094829785,54.725326778543,21.1767280683161));
#48449=CARTESIAN_POINT('Ctrl Pts',(-31.47496098746,54.5139076530797,21.1540747194623));
#48450=CARTESIAN_POINT('Ctrl Pts',(-34.0692874532608,56.8510195406194,22.));
#48451=CARTESIAN_POINT('Ctrl Pts',(-33.8832841873681,57.3728449537375,21.9629540364773));
#48452=CARTESIAN_POINT('Ctrl Pts',(-32.9525520823054,58.2072244344894,21.888862109432));
#48453=CARTESIAN_POINT('Ctrl Pts',(-31.1328156874419,57.7104505124287,21.7777242188639));
#48454=CARTESIAN_POINT('Ctrl Pts',(-30.5680805647129,55.9126012127397,21.6665863282959));
#48455=CARTESIAN_POINT('Ctrl Pts',(-31.7699104961033,54.4629042731491,21.5554484377278));
#48456=CARTESIAN_POINT('Ctrl Pts',(-33.640865440432,54.686479644594,21.4443105471598));
#48457=CARTESIAN_POINT('Ctrl Pts',(-34.4671411285653,56.3795867334953,21.3331726565917));
#48458=CARTESIAN_POINT('Ctrl Pts',(-33.493086107989,57.992055635258,21.2220347660237));
#48459=CARTESIAN_POINT('Ctrl Pts',(-31.6099402690806,58.0481999689383,21.1108968754557));
#48460=CARTESIAN_POINT('Ctrl Pts',(-30.5415300692557,56.4965179419503,20.9997589848876));
#48461=CARTESIAN_POINT('Ctrl Pts',(-31.2657026944405,54.7573377854331,20.8886210943196));
#48462=CARTESIAN_POINT('Ctrl Pts',(-33.1196550861102,54.4225228075051,20.7774832037515));
#48463=CARTESIAN_POINT('Ctrl Pts',(-34.4064234335583,55.7985469486803,20.6663453131835));
#48464=CARTESIAN_POINT('Ctrl Pts',(-33.9482241472934,57.6259127164006,20.5552074226154));
#48465=CARTESIAN_POINT('Ctrl Pts',(-32.1644471988302,58.2320149921632,20.4440695320474));
#48466=CARTESIAN_POINT('Ctrl Pts',(-30.6878063720739,57.0620797446064,20.3329316414794));
#48467=CARTESIAN_POINT('Ctrl Pts',(-30.8698865063134,55.1869628453693,20.2217937509113));
#48468=CARTESIAN_POINT('Ctrl Pts',(-32.5440282170451,54.3229796221853,20.1106558603433));
#48469=CARTESIAN_POINT('Ctrl Pts',(-34.1778702970046,55.2609439349858,19.9995179697752));
#48470=CARTESIAN_POINT('Ctrl Pts',(-34.2759387179252,57.1423263023632,19.8883800792072));
#48471=CARTESIAN_POINT('Ctrl Pts',(-32.7484702637604,58.2450761614137,19.7772421886392));
#48472=CARTESIAN_POINT('Ctrl Pts',(-30.9935741723466,57.559834032996,19.6661042980711));
#48473=CARTESIAN_POINT('Ctrl Pts',(-30.6175267185128,55.7138098219725,19.5549664075031));
#48474=CARTESIAN_POINT('Ctrl Pts',(-31.9645284111714,54.3966904172638,19.443828516935));
#48475=CARTESIAN_POINT('Ctrl Pts',(-33.801653320123,54.8140501505304,19.332690626367));
#48476=CARTESIAN_POINT('Ctrl Pts',(-34.4473601842239,56.5838749230434,19.221552735799));
#48477=CARTESIAN_POINT('Ctrl Pts',(-33.3106261867332,58.0862240501872,19.1104148452309));
#48478=CARTESIAN_POINT('Ctrl Pts',(-31.4319168476017,57.9459803376677,18.9992769546629));
#48479=CARTESIAN_POINT('Ctrl Pts',(-30.530836130646,56.2915104462365,18.8881390640948));
#48480=CARTESIAN_POINT('Ctrl Pts',(-31.4321534351977,54.6371694303799,18.7770011735268));
#48481=CARTESIAN_POINT('Ctrl Pts',(-33.3108828106914,54.4971943834675,18.6658632829587));
#48482=CARTESIAN_POINT('Ctrl Pts',(-34.4474019535353,55.9997060533366,18.5547253923907));
#48483=CARTESIAN_POINT('Ctrl Pts',(-33.8014420032618,57.7694384689281,18.4435875018226));
#48484=CARTESIAN_POINT('Ctrl Pts',(-31.9642574280497,58.1865354801138,18.3324496112546));
#48485=CARTESIAN_POINT('Ctrl Pts',(-30.6174441046762,56.8692234623569,18.2213117206866));
#48486=CARTESIAN_POINT('Ctrl Pts',(-30.9937555419292,55.023253044843,18.1101738301185));
#48487=CARTESIAN_POINT('Ctrl Pts',(-32.748749613628,54.3382618854518,17.9990359395505));
#48488=CARTESIAN_POINT('Ctrl Pts',(-34.2760603429608,55.4412301607017,17.8878980489825));
#48489=CARTESIAN_POINT('Ctrl Pts',(-34.1777228984872,57.3225984997458,17.7767601584144));
#48490=CARTESIAN_POINT('Ctrl Pts',(-32.5437466583566,58.2603291256887,17.6656222678464));
#48491=CARTESIAN_POINT('Ctrl Pts',(-30.8697286057113,57.3961065620164,17.5544843772783));
#48492=CARTESIAN_POINT('Ctrl Pts',(-30.6879164487935,55.5209635222085,17.4433464867103));
#48493=CARTESIAN_POINT('Ctrl Pts',(-32.1647249167202,54.3512396961698,17.3322085961422));
#48494=CARTESIAN_POINT('Ctrl Pts',(-33.9484144706509,54.9575965674438,17.2210707055742));
#48495=CARTESIAN_POINT('Ctrl Pts',(-34.4063538334575,56.7850288151987,17.1099328150062));
#48496=CARTESIAN_POINT('Ctrl Pts',(-33.1193859129776,58.1608669785734,16.9987949244381));
#48497=CARTESIAN_POINT('Ctrl Pts',(-31.2654870420352,57.825790783565,16.8876570338701));
#48498=CARTESIAN_POINT('Ctrl Pts',(-30.5415518818472,56.086499271487,16.776519143302));
#48499=CARTESIAN_POINT('Ctrl Pts',(-31.6102064945166,54.534985688252,16.665381252734));
#48500=CARTESIAN_POINT('Ctrl Pts',(-33.4932991936999,54.5913680119553,16.5542433621659));
#48501=CARTESIAN_POINT('Ctrl Pts',(-34.46721387611,56.2040388622933,16.4431054715979));
#48502=CARTESIAN_POINT('Ctrl Pts',(-33.6405153879953,57.896902321018,16.3319675810299));
#48503=CARTESIAN_POINT('Ctrl Pts',(-31.7698902309214,58.1204612659856,16.2208296904618));
#48504=CARTESIAN_POINT('Ctrl Pts',(-30.5675428254988,56.6700896595284,16.1096917998938));
#48505=CARTESIAN_POINT('Ctrl Pts',(-31.1339953874406,54.8733290813849,15.9985539093257));
#48506=CARTESIAN_POINT('Ctrl Pts',(-32.9507674628268,54.3747748653499,15.8874160187577));
#48507=CARTESIAN_POINT('Ctrl Pts',(-34.3549469673912,55.6307593394112,15.7762781281896));
#48508=CARTESIAN_POINT('Ctrl Pts',(-34.0612724762645,57.4916656705044,15.6651402376216));
#48509=CARTESIAN_POINT('Ctrl Pts',(-32.3385475813956,58.2541851899138,15.5540023470536));
#48510=CARTESIAN_POINT('Ctrl Pts',(-30.7636019166367,57.2203751334698,15.4428644564855));
#48511=CARTESIAN_POINT('Ctrl Pts',(-30.7780011089404,55.3364935710292,15.3317265659175));
#48512=CARTESIAN_POINT('Ctrl Pts',(-32.3685654164946,54.326878659382,15.2205886753495));
#48513=CARTESIAN_POINT('Ctrl Pts',(-34.0794332859622,55.1156423809378,15.1094507847814));
#48514=CARTESIAN_POINT('Ctrl Pts',(-34.3446279626791,56.9808203482265,14.9983128942134));
#48515=CARTESIAN_POINT('Ctrl Pts',(-32.9214137338773,58.2151940311283,14.8871750036453));
#48516=CARTESIAN_POINT('Ctrl Pts',(-31.1124747588704,57.6889271671125,14.7760371130773));
#48517=CARTESIAN_POINT('Ctrl Pts',(-30.5735533254956,55.8837178487831,14.6648992225092));
#48518=CARTESIAN_POINT('Ctrl Pts',(-31.7979304751287,54.4518945101648,14.5537613319412));
#48519=CARTESIAN_POINT('Ctrl Pts',(-33.6649196338359,54.704021546316,14.4426234413732));
#48520=CARTESIAN_POINT('Ctrl Pts',(-34.4656450190373,56.4093237108058,14.3314855508051));
#48521=CARTESIAN_POINT('Ctrl Pts',(-33.4671924688587,58.0069196157817,14.2203476602371));
#48522=CARTESIAN_POINT('Ctrl Pts',(-31.5834591995985,58.0345095641669,14.109209769669));
#48523=CARTESIAN_POINT('Ctrl Pts',(-30.5386430838269,56.4668442614587,13.998071879101));
#48524=CARTESIAN_POINT('Ctrl Pts',(-31.289085272834,54.7388173343014,13.886933988533));
#48525=CARTESIAN_POINT('Ctrl Pts',(-33.1478792814866,54.4321278475435,13.7757960979649));
#48526=CARTESIAN_POINT('Ctrl Pts',(-34.4136863832883,55.8274592952635,13.6646582073969));
#48527=CARTESIAN_POINT('Ctrl Pts',(-33.9278258993099,57.6477147792301,13.5535203168288));
#48528=CARTESIAN_POINT('Ctrl Pts',(-32.135157735345,58.2266620964951,13.4423824262608));
#48529=CARTESIAN_POINT('Ctrl Pts',(-30.6762385450867,57.0346478668883,13.3312445356927));
#48530=CARTESIAN_POINT('Ctrl Pts',(-30.8870198365664,55.1622083892051,13.2201066451247));
#48531=CARTESIAN_POINT('Ctrl Pts',(-32.5733973317359,54.3242660615774,13.1089687545567));
#48532=CARTESIAN_POINT('Ctrl Pts',(-34.1941640560837,55.2856728893476,12.9978308639886));
#48533=CARTESIAN_POINT('Ctrl Pts',(-34.2610507255277,57.1708124199609,12.8866929734206));
#48534=CARTESIAN_POINT('Ctrl Pts',(-33.2357187233791,57.8857569315589,12.8126010463752));
#48535=CARTESIAN_POINT('Ctrl Pts',(-32.6851664226308,57.947329172377,12.7755550828525));
#48536=CARTESIAN_POINT('Ctrl Pts',(-34.1913483771213,56.8945278288422,22.0748149723825));
#48537=CARTESIAN_POINT('Ctrl Pts',(-33.9908775702891,57.4569414030947,22.0377690088598));
#48538=CARTESIAN_POINT('Ctrl Pts',(-32.9877520867064,58.3562198480607,21.9636770818145));
#48539=CARTESIAN_POINT('Ctrl Pts',(-31.0264745706939,57.8208062977086,21.8525391912464));
#48540=CARTESIAN_POINT('Ctrl Pts',(-30.4178137218822,55.8831182794813,21.7414013006784));
#48541=CARTESIAN_POINT('Ctrl Pts',(-31.7131233223058,54.3206622992212,21.6302634101103));
#48542=CARTESIAN_POINT('Ctrl Pts',(-33.7296032235388,54.5616276117724,21.5191255195423));
#48543=CARTESIAN_POINT('Ctrl Pts',(-34.6201475538814,56.386426453537,21.4079876289742));
#48544=CARTESIAN_POINT('Ctrl Pts',(-33.5703294502221,58.1243149802617,21.2968497384062));
#48545=CARTESIAN_POINT('Ctrl Pts',(-31.5407104330673,58.1848262826732,21.1857118478381));
#48546=CARTESIAN_POINT('Ctrl Pts',(-30.3891980993524,56.5124527014652,21.0745739572701));
#48547=CARTESIAN_POINT('Ctrl Pts',(-31.1696976769262,54.6379971776317,20.9634360667021));
#48548=CARTESIAN_POINT('Ctrl Pts',(-33.16785254804,54.2771399182574,20.852298176134));
#48549=CARTESIAN_POINT('Ctrl Pts',(-34.5547071690116,55.7601927478842,20.741160285566));
#48550=CARTESIAN_POINT('Ctrl Pts',(-34.0608686325396,57.7296930578618,20.6300223949979));
#48551=CARTESIAN_POINT('Ctrl Pts',(-32.1383475286711,58.3829386428886,20.5188845044299));
#48552=CARTESIAN_POINT('Ctrl Pts',(-30.5468519357281,57.1220045302883,20.4077466138619));
#48553=CARTESIAN_POINT('Ctrl Pts',(-30.7430944653628,55.1010389526641,20.2966087232938));
#48554=CARTESIAN_POINT('Ctrl Pts',(-32.5474527807459,54.1698541532471,20.1854708327258));
#48555=CARTESIAN_POINT('Ctrl Pts',(-34.3083769152439,55.1807743737308,20.0743329421577));
#48556=CARTESIAN_POINT('Ctrl Pts',(-34.4140732070396,57.2084927545773,19.9631950515897));
#48557=CARTESIAN_POINT('Ctrl Pts',(-32.7677965572851,58.3970157244132,19.8520571610217));
#48558=CARTESIAN_POINT('Ctrl Pts',(-30.8764026956559,57.658474700953,19.7409192704536));
#48559=CARTESIAN_POINT('Ctrl Pts',(-30.4711058525308,55.6688646731958,19.6297813798856));
#48560=CARTESIAN_POINT('Ctrl Pts',(-31.9228788353097,54.2492982559658,19.5186434893175));
#48561=CARTESIAN_POINT('Ctrl Pts',(-33.9028973633798,54.6991206935758,19.4075055987495));
#48562=CARTESIAN_POINT('Ctrl Pts',(-34.5988280256839,56.6066044057275,19.2963677081814));
#48563=CARTESIAN_POINT('Ctrl Pts',(-33.3736775933143,58.2258079192613,19.1852298176134));
#48564=CARTESIAN_POINT('Ctrl Pts',(-31.3488401518244,58.0746558947685,19.0740919270453));
#48565=CARTESIAN_POINT('Ctrl Pts',(-30.3776723743012,56.2914994946751,18.9629540364773));
#48566=CARTESIAN_POINT('Ctrl Pts',(-31.3490951414668,54.5084819942419,18.8518161459093));
#48567=CARTESIAN_POINT('Ctrl Pts',(-33.3739541777695,54.3576195324661,18.7406782553412));
#48568=CARTESIAN_POINT('Ctrl Pts',(-34.5988730438588,55.9769982314792,18.6295403647732));
#48569=CARTESIAN_POINT('Ctrl Pts',(-33.9026696100581,57.8843824030853,18.5184024742052));
#48570=CARTESIAN_POINT('Ctrl Pts',(-31.9225867748193,58.3339216837985,18.4072645836371));
#48571=CARTESIAN_POINT('Ctrl Pts',(-30.471016812898,56.9141476718634,18.2961266930691));
#48572=CARTESIAN_POINT('Ctrl Pts',(-30.8765981723664,54.9245956217347,18.184988802501));
#48573=CARTESIAN_POINT('Ctrl Pts',(-32.7680976352962,54.1863250879512,18.073850911933));
#48574=CARTESIAN_POINT('Ctrl Pts',(-34.4142042922057,55.3750834626414,17.9627130213649));
#48575=CARTESIAN_POINT('Ctrl Pts',(-34.308218051906,57.4027867240152,17.8515751307969));
#48576=CARTESIAN_POINT('Ctrl Pts',(-32.5471493221094,58.4134550812175,17.7404372402288));
#48577=CARTESIAN_POINT('Ctrl Pts',(-30.7429242830763,57.4820123251428,17.6292993496608));
#48578=CARTESIAN_POINT('Ctrl Pts',(-30.5469705743374,55.4610185737053,17.5181614590928));
#48579=CARTESIAN_POINT('Ctrl Pts',(-32.1386468477677,54.2003123272238,17.4070235685247));
#48580=CARTESIAN_POINT('Ctrl Pts',(-34.0610737594595,54.8538323104841,17.2958856779567));
#48581=CARTESIAN_POINT('Ctrl Pts',(-34.5546321553377,56.8234042713873,17.1847477873886));
#48582=CARTESIAN_POINT('Ctrl Pts',(-33.1675624383217,58.3062566576535,17.0736098968206));
#48583=CARTESIAN_POINT('Ctrl Pts',(-31.169465250837,57.9451178634435,16.9624720062526));
#48584=CARTESIAN_POINT('Ctrl Pts',(-30.3892216085515,56.07054232269,16.8513341156845));
#48585=CARTESIAN_POINT('Ctrl Pts',(-31.5409973658138,54.3983502869775,16.7401962251165));
#48586=CARTESIAN_POINT('Ctrl Pts',(-33.5705591099766,54.4591180905408,16.6290583345485));
#48587=CARTESIAN_POINT('Ctrl Pts',(-34.620225959811,56.1972242736254,16.5179204439804));
#48588=CARTESIAN_POINT('Ctrl Pts',(-33.7292259436341,58.0217605353874,16.4067825534124));
#48589=CARTESIAN_POINT('Ctrl Pts',(-31.7131014808755,58.2627081437914,16.2956446628443));
#48590=CARTESIAN_POINT('Ctrl Pts',(-30.4172341567138,56.6995250203254,16.1845067722763));
#48591=CARTESIAN_POINT('Ctrl Pts',(-31.0277460290708,54.7630104056166,16.0733688817082));
#48592=CARTESIAN_POINT('Ctrl Pts',(-32.9858286575395,54.2256780880443,15.9622309911402));
#48593=CARTESIAN_POINT('Ctrl Pts',(-34.4992268060413,55.5793544317117,15.8510931005721));
#48594=CARTESIAN_POINT('Ctrl Pts',(-34.182709986298,57.5850041273933,15.7399552100041));
#48595=CARTESIAN_POINT('Ctrl Pts',(-32.3259896326697,58.4068332632833,15.628817319436));
#48596=CARTESIAN_POINT('Ctrl Pts',(-30.6285429420654,57.2926123105923,15.517679428868));
#48597=CARTESIAN_POINT('Ctrl Pts',(-30.6440621195648,55.2622003445105,15.4065415382999));
#48598=CARTESIAN_POINT('Ctrl Pts',(-32.3583422883758,54.1740564618943,15.295403647732));
#48599=CARTESIAN_POINT('Ctrl Pts',(-34.202283363977,55.0241711031691,15.1842657571639));
#48600=CARTESIAN_POINT('Ctrl Pts',(-34.4881051776634,57.0344246876612,15.0731278665959));
#48601=CARTESIAN_POINT('Ctrl Pts',(-32.9541917628979,58.364809328792,14.9619899760278));
#48602=CARTESIAN_POINT('Ctrl Pts',(-31.0045515020698,57.79760884265,14.8508520854598));
#48603=CARTESIAN_POINT('Ctrl Pts',(-30.4237121600868,55.851988335345,14.7397141948917));
#48604=CARTESIAN_POINT('Ctrl Pts',(-31.7433227264704,54.3087961846243,14.6285763043237));
#48605=CARTESIAN_POINT('Ctrl Pts',(-33.7555283788647,54.5805339421248,14.5174384137556));
#48606=CARTESIAN_POINT('Ctrl Pts',(-34.6185350752899,56.4184764060234,14.4063005231876));
#48607=CARTESIAN_POINT('Ctrl Pts',(-33.542421775035,58.1403350977259,14.2951626326195));
#48608=CARTESIAN_POINT('Ctrl Pts',(-31.5121696365421,58.1700710229888,14.1840247420515));
#48609=CARTESIAN_POINT('Ctrl Pts',(-30.3860865609853,56.4804709690945,14.0728868514835));
#48610=CARTESIAN_POINT('Ctrl Pts',(-31.1948989782791,54.618036185208,13.9617489609154));
#48611=CARTESIAN_POINT('Ctrl Pts',(-33.1982720527306,54.287492048995,13.8506110703474));
#48612=CARTESIAN_POINT('Ctrl Pts',(-34.5625350390513,55.7913539289481,13.7394731797794));
#48613=CARTESIAN_POINT('Ctrl Pts',(-34.0388837861359,57.7531909093916,13.6283352892113));
#48614=CARTESIAN_POINT('Ctrl Pts',(-32.1067798981332,58.3771693930405,13.5171973986433));
#48615=CARTESIAN_POINT('Ctrl Pts',(-30.5343843502893,57.0924389706047,13.4060595080752));
#48616=CARTESIAN_POINT('Ctrl Pts',(-30.7615604451029,55.0743590673614,13.2949216175072));
#48617=CARTESIAN_POINT('Ctrl Pts',(-32.5791062578488,54.1712406533262,13.1837837269391));
#48618=CARTESIAN_POINT('Ctrl Pts',(-34.3259380210302,55.2074267736725,13.0726458363711));
#48619=CARTESIAN_POINT('Ctrl Pts',(-34.3980272100313,57.2391945540909,12.9615079458031));
#48620=CARTESIAN_POINT('Ctrl Pts',(-33.2929437441301,58.0097482451375,12.8874160187577));
#48621=CARTESIAN_POINT('Ctrl Pts',(-32.6995688729705,58.0761096433421,12.850370055235));
#48622=CARTESIAN_POINT('Ctrl Pts',(-34.3134093009819,56.9380361170651,22.149629944765));
#48623=CARTESIAN_POINT('Ctrl Pts',(-34.0984709532102,57.5410378524519,22.1125839812423));
#48624=CARTESIAN_POINT('Ctrl Pts',(-33.0229520911074,58.5052152616321,22.0384920541969));
#48625=CARTESIAN_POINT('Ctrl Pts',(-30.9201334539457,57.9311620829883,21.9273541636289));
#48626=CARTESIAN_POINT('Ctrl Pts',(-30.2675468790515,55.8536353462229,21.8162162730609));
#48627=CARTESIAN_POINT('Ctrl Pts',(-31.6563361485083,54.1784203252934,21.7050783824928));
#48628=CARTESIAN_POINT('Ctrl Pts',(-33.8183410066456,54.4367755789509,21.5939404919248));
#48629=CARTESIAN_POINT('Ctrl Pts',(-34.7731539791975,56.3932661735786,21.4828026013567));
#48630=CARTESIAN_POINT('Ctrl Pts',(-33.6475727924551,58.2565743252655,21.3716647107887));
#48631=CARTESIAN_POINT('Ctrl Pts',(-31.4714805970539,58.321452596408,21.2605268202206));
#48632=CARTESIAN_POINT('Ctrl Pts',(-30.2368661294491,56.52838746098,21.1493889296526));
#48633=CARTESIAN_POINT('Ctrl Pts',(-31.0736926594119,54.5186565698305,21.0382510390845));
#48634=CARTESIAN_POINT('Ctrl Pts',(-33.2160500099699,54.1317570290096,20.9271131485165));
#48635=CARTESIAN_POINT('Ctrl Pts',(-34.702990904465,55.7218385470883,20.8159752579485));
#48636=CARTESIAN_POINT('Ctrl Pts',(-34.1735131177858,57.8334733993229,20.7048373673804));
#48637=CARTESIAN_POINT('Ctrl Pts',(-32.112247858512,58.533862293614,20.5936994768124));
#48638=CARTESIAN_POINT('Ctrl Pts',(-30.4058974993823,57.18192931597,20.4825615862443));
#48639=CARTESIAN_POINT('Ctrl Pts',(-30.6163024244123,55.0151150599589,20.3714236956763));
#48640=CARTESIAN_POINT('Ctrl Pts',(-32.5508773444466,54.0167286843088,20.2602858051082));
#48641=CARTESIAN_POINT('Ctrl Pts',(-34.4388835334834,55.1006048124758,20.1491479145402));
#48642=CARTESIAN_POINT('Ctrl Pts',(-34.5522076961539,57.2746592067913,20.0380100239722));
#48643=CARTESIAN_POINT('Ctrl Pts',(-32.7871228508099,58.5489552874127,19.9268721334041));
#48644=CARTESIAN_POINT('Ctrl Pts',(-30.7592312189652,57.7571153689101,19.8157342428361));
#48645=CARTESIAN_POINT('Ctrl Pts',(-30.3246849865488,55.623919524419,19.7045963522681));
#48646=CARTESIAN_POINT('Ctrl Pts',(-31.8812292594479,54.101906094668,19.5934584617));
#48647=CARTESIAN_POINT('Ctrl Pts',(-34.0041414066367,54.5841912366211,19.482320571132));
#48648=CARTESIAN_POINT('Ctrl Pts',(-34.7502958671439,56.6293338884117,19.3711826805639));
#48649=CARTESIAN_POINT('Ctrl Pts',(-33.4367289998955,58.3653917883353,19.2600447899959));
#48650=CARTESIAN_POINT('Ctrl Pts',(-31.2657634560471,58.2033314518695,19.1489068994278));
#48651=CARTESIAN_POINT('Ctrl Pts',(-30.2245086179564,56.2914885431137,19.0377690088598));
#48652=CARTESIAN_POINT('Ctrl Pts',(-31.266036847736,54.379794558104,18.9266311182918));
#48653=CARTESIAN_POINT('Ctrl Pts',(-33.4370255448476,54.2180446814646,18.8154932277237));
#48654=CARTESIAN_POINT('Ctrl Pts',(-34.7503441341823,55.9542904096218,18.7043553371557));
#48655=CARTESIAN_POINT('Ctrl Pts',(-34.0038972168544,57.9993263372425,18.5932174465876));
#48656=CARTESIAN_POINT('Ctrl Pts',(-31.8809161215889,58.4813078874833,18.4820795560196));
#48657=CARTESIAN_POINT('Ctrl Pts',(-30.3245895211199,56.9590718813698,18.3709416654516));
#48658=CARTESIAN_POINT('Ctrl Pts',(-30.7594408028035,54.8259381986264,18.2598037748835));
#48659=CARTESIAN_POINT('Ctrl Pts',(-32.7874456569645,54.0343882904504,18.1486658843155));
#48660=CARTESIAN_POINT('Ctrl Pts',(-34.5523482414506,55.3089367645812,18.0375279937474));
#48661=CARTESIAN_POINT('Ctrl Pts',(-34.4387132053247,57.4829749482845,17.9263901031794));
#48662=CARTESIAN_POINT('Ctrl Pts',(-32.5505519858621,58.5665810367465,17.8152522126113));
#48663=CARTESIAN_POINT('Ctrl Pts',(-30.6161199604413,57.5679180882692,17.7041143220433));
#48664=CARTESIAN_POINT('Ctrl Pts',(-30.4060246998813,55.4010736252019,17.5929764314752));
#48665=CARTESIAN_POINT('Ctrl Pts',(-32.112568778815,54.0493849582778,17.4818385409072));
#48666=CARTESIAN_POINT('Ctrl Pts',(-34.1737330482682,54.7500680535245,17.3707006503392));
#48667=CARTESIAN_POINT('Ctrl Pts',(-34.7029104772177,56.8617797275759,17.2595627597711));
#48668=CARTESIAN_POINT('Ctrl Pts',(-33.2157389636659,58.4516463367336,17.1484248692031));
#48669=CARTESIAN_POINT('Ctrl Pts',(-31.0734434596387,58.064444943322,17.0372869786351));
#48670=CARTESIAN_POINT('Ctrl Pts',(-30.2368913352558,56.054585373893,16.926149088067));
#48671=CARTESIAN_POINT('Ctrl Pts',(-31.471788237111,54.2617148857029,16.815011197499));
#48672=CARTESIAN_POINT('Ctrl Pts',(-33.6478190262533,54.3268681691262,16.7038733069309));
#48673=CARTESIAN_POINT('Ctrl Pts',(-34.7732380435121,56.1904096849576,16.5927354163629));
#48674=CARTESIAN_POINT('Ctrl Pts',(-33.8179364992731,58.1466187497567,16.4815975257948));
#48675=CARTESIAN_POINT('Ctrl Pts',(-31.6563127308296,58.4049550215973,16.3704596352268));
#48676=CARTESIAN_POINT('Ctrl Pts',(-30.2669254879289,56.7289603811225,16.2593217446588));
#48677=CARTESIAN_POINT('Ctrl Pts',(-30.9214966707009,54.6526917298483,16.1481838540907));
#48678=CARTESIAN_POINT('Ctrl Pts',(-33.0208898522522,54.0765813107388,16.0370459635227));
#48679=CARTESIAN_POINT('Ctrl Pts',(-34.6435066446915,55.5279495240122,15.9259080729546));
#48680=CARTESIAN_POINT('Ctrl Pts',(-34.3041474963316,57.6783425842823,15.8147701823866));
#48681=CARTESIAN_POINT('Ctrl Pts',(-32.3134316839437,58.5594813366528,15.7036322918185));
#48682=CARTESIAN_POINT('Ctrl Pts',(-30.4934839674941,57.364849487715,15.5924944012505));
#48683=CARTESIAN_POINT('Ctrl Pts',(-30.5101231301892,55.1879071179917,15.4813565106825));
#48684=CARTESIAN_POINT('Ctrl Pts',(-32.348119160257,54.0212342644067,15.3702186201144));
#48685=CARTESIAN_POINT('Ctrl Pts',(-34.3251334419918,54.9326998254003,15.2590807295464));
#48686=CARTESIAN_POINT('Ctrl Pts',(-34.6315823926477,57.088029027096,15.1479428389784));
#48687=CARTESIAN_POINT('Ctrl Pts',(-32.9869697919185,58.5144246264557,15.0368049484103));
#48688=CARTESIAN_POINT('Ctrl Pts',(-30.8966282452692,57.9062905181876,14.9256670578423));
#48689=CARTESIAN_POINT('Ctrl Pts',(-30.2738709946779,55.8202588219069,14.8145291672742));
#48690=CARTESIAN_POINT('Ctrl Pts',(-31.6887149778123,54.1656978590838,14.7033912767062));
#48691=CARTESIAN_POINT('Ctrl Pts',(-33.8461371238934,54.4570463379336,14.5922533861381));
#48692=CARTESIAN_POINT('Ctrl Pts',(-34.7714251315426,56.4276291012411,14.4811154955701));
#48693=CARTESIAN_POINT('Ctrl Pts',(-33.6176510812113,58.2737505796701,14.369977605002));
#48694=CARTESIAN_POINT('Ctrl Pts',(-31.4408800734857,58.3056324818107,14.258839714434));
#48695=CARTESIAN_POINT('Ctrl Pts',(-30.2335300381437,56.4940976767304,14.147701823866));
#48696=CARTESIAN_POINT('Ctrl Pts',(-31.1007126837241,54.4972550361147,14.0365639332979));
#48697=CARTESIAN_POINT('Ctrl Pts',(-33.2486648239747,54.1428562504465,13.9254260427299));
#48698=CARTESIAN_POINT('Ctrl Pts',(-34.7113836948143,55.7552485626327,13.8142881521619));
#48699=CARTESIAN_POINT('Ctrl Pts',(-34.149941672962,57.8586670395532,13.7031502615938));
#48700=CARTESIAN_POINT('Ctrl Pts',(-32.0784020609214,58.5276766895861,13.5920123710258));
#48701=CARTESIAN_POINT('Ctrl Pts',(-30.3925301554919,57.1502300743211,13.4808744804577));
#48702=CARTESIAN_POINT('Ctrl Pts',(-30.6361010536393,54.9865097455178,13.3697365898897));
#48703=CARTESIAN_POINT('Ctrl Pts',(-32.5848151839618,54.0182152450749,13.2585986993216));
#48704=CARTESIAN_POINT('Ctrl Pts',(-34.4577119859767,55.1291806579975,13.1474608087536));
#48705=CARTESIAN_POINT('Ctrl Pts',(-34.5350036945349,57.3075766882209,13.0363229181856));
#48706=CARTESIAN_POINT('Ctrl Pts',(-33.3501687648812,58.133739558716,12.9622309911402));
#48707=CARTESIAN_POINT('Ctrl Pts',(-32.7139713233102,58.2048901143072,12.9251850276175));
#48708=CARTESIAN_POINT('Ctrl Pts',(-34.4354702248425,56.9815444052879,22.2244449171475));
#48709=CARTESIAN_POINT('Ctrl Pts',(-34.2060643361312,57.6251343018091,22.1873989536248));
#48710=CARTESIAN_POINT('Ctrl Pts',(-33.0581520955084,58.6542106752035,22.1133070265794));
#48711=CARTESIAN_POINT('Ctrl Pts',(-30.8137923371977,58.0415178682682,22.0021691360114));
#48712=CARTESIAN_POINT('Ctrl Pts',(-30.1172800362208,55.8241524129645,21.8910312454434));
#48713=CARTESIAN_POINT('Ctrl Pts',(-31.5995489747108,54.0361783513656,21.7798933548753));
#48714=CARTESIAN_POINT('Ctrl Pts',(-33.9070787897524,54.3119235461293,21.6687554643073));
#48715=CARTESIAN_POINT('Ctrl Pts',(-34.9261604045136,56.4001058936205,21.5576175737392));
#48716=CARTESIAN_POINT('Ctrl Pts',(-33.7248161346881,58.3888336702691,21.4464796831712));
#48717=CARTESIAN_POINT('Ctrl Pts',(-31.4022507610406,58.4580789101429,21.3353417926031));
#48718=CARTESIAN_POINT('Ctrl Pts',(-30.0845341595457,56.5443222204948,21.2242039020351));
#48719=CARTESIAN_POINT('Ctrl Pts',(-30.9776876418977,54.3993159620291,21.113066011467));
#48720=CARTESIAN_POINT('Ctrl Pts',(-33.2642474718997,53.9863741397618,21.001928120899));
#48721=CARTESIAN_POINT('Ctrl Pts',(-34.8512746399183,55.6834843462922,20.8907902303309));
#48722=CARTESIAN_POINT('Ctrl Pts',(-34.2861576030319,57.9372537407841,20.7796523397629));
#48723=CARTESIAN_POINT('Ctrl Pts',(-32.0861481883531,58.6847859443394,20.6685144491949));
#48724=CARTESIAN_POINT('Ctrl Pts',(-30.2649430630365,57.2418541016518,20.5573765586268));
#48725=CARTESIAN_POINT('Ctrl Pts',(-30.4895103834619,54.9291911672537,20.4462386680588));
#48726=CARTESIAN_POINT('Ctrl Pts',(-32.5543019081473,53.8636032153705,20.3351007774908));
#48727=CARTESIAN_POINT('Ctrl Pts',(-34.5693901517228,55.0204352512209,20.2239628869227));
#48728=CARTESIAN_POINT('Ctrl Pts',(-34.6903421852682,57.3408256590054,20.1128249963547));
#48729=CARTESIAN_POINT('Ctrl Pts',(-32.8064491443347,58.7008948504121,20.0016871057866));
#48730=CARTESIAN_POINT('Ctrl Pts',(-30.6420597422744,57.8557560368672,19.8905492152186));
#48731=CARTESIAN_POINT('Ctrl Pts',(-30.1782641205668,55.5789743756422,19.7794113246505));
#48732=CARTESIAN_POINT('Ctrl Pts',(-31.8395796835861,53.9545139333702,19.6682734340825));
#48733=CARTESIAN_POINT('Ctrl Pts',(-34.1053854498936,54.4692617796665,19.5571355435145));
#48734=CARTESIAN_POINT('Ctrl Pts',(-34.9017637086039,56.6520633710957,19.4459976529464));
#48735=CARTESIAN_POINT('Ctrl Pts',(-33.4997804064767,58.5049756574094,19.3348597623784));
#48736=CARTESIAN_POINT('Ctrl Pts',(-31.1826867602698,58.3320070089704,19.2237218718103));
#48737=CARTESIAN_POINT('Ctrl Pts',(-30.0713448616116,56.2914775915524,19.1125839812423));
#48738=CARTESIAN_POINT('Ctrl Pts',(-31.1829785540051,54.2511071219659,19.0014460906742));
#48739=CARTESIAN_POINT('Ctrl Pts',(-33.5000969119257,54.0784698304632,18.8903082001062));
#48740=CARTESIAN_POINT('Ctrl Pts',(-34.9018152245058,55.9315825877643,18.7791703095382));
#48741=CARTESIAN_POINT('Ctrl Pts',(-34.1051248236508,58.1142702713998,18.6680324189701));
#48742=CARTESIAN_POINT('Ctrl Pts',(-31.8392454683584,58.628694091168,18.5568945284021));
#48743=CARTESIAN_POINT('Ctrl Pts',(-30.1781622293418,57.0039960908762,18.445756637834));
#48744=CARTESIAN_POINT('Ctrl Pts',(-30.6422834332407,54.7272807755181,18.334618747266));
#48745=CARTESIAN_POINT('Ctrl Pts',(-32.8067936786327,53.8824514929496,18.223480856698));
#48746=CARTESIAN_POINT('Ctrl Pts',(-34.6904921906955,55.242790066521,18.1123429661299));
#48747=CARTESIAN_POINT('Ctrl Pts',(-34.5692083587435,57.5631631725538,18.0012050755619));
#48748=CARTESIAN_POINT('Ctrl Pts',(-32.5539546496148,58.7197069922753,17.8900671849939));
#48749=CARTESIAN_POINT('Ctrl Pts',(-30.4893156378063,57.6538238513956,17.7789292944258));
#48750=CARTESIAN_POINT('Ctrl Pts',(-30.2650788254252,55.3411286766987,17.6677914038578));
#48751=CARTESIAN_POINT('Ctrl Pts',(-32.0864907098624,53.8984575893318,17.5566535132897));
#48752=CARTESIAN_POINT('Ctrl Pts',(-34.2863923370768,54.6463037965648,17.4455156227217));
#48753=CARTESIAN_POINT('Ctrl Pts',(-34.8511887990978,56.9001551837646,17.3343777321536));
#48754=CARTESIAN_POINT('Ctrl Pts',(-33.26391548901,58.5970360158137,17.2232398415856));
#48755=CARTESIAN_POINT('Ctrl Pts',(-30.9774216684405,58.1837720232006,17.1121019510176));
#48756=CARTESIAN_POINT('Ctrl Pts',(-30.0845610619601,56.0386284250959,17.0009640604495));
#48757=CARTESIAN_POINT('Ctrl Pts',(-31.4025791084081,54.1250794844285,16.8898261698815));
#48758=CARTESIAN_POINT('Ctrl Pts',(-33.72507894253,54.1946182477114,16.7786882793134));
#48759=CARTESIAN_POINT('Ctrl Pts',(-34.9262501272131,56.1835950962899,16.6675503887454));
#48760=CARTESIAN_POINT('Ctrl Pts',(-33.9066470549119,58.2714769641261,16.5564124981773));
#48761=CARTESIAN_POINT('Ctrl Pts',(-31.5995239807838,58.5472018994032,16.4452746076093));
#48762=CARTESIAN_POINT('Ctrl Pts',(-30.1166168191438,56.7583957419196,16.3341367170413));
#48763=CARTESIAN_POINT('Ctrl Pts',(-30.8152473123311,54.5423730540801,16.2229988264732));
#48764=CARTESIAN_POINT('Ctrl Pts',(-33.0559510469649,53.9274845334332,16.1118609359052));
#48765=CARTESIAN_POINT('Ctrl Pts',(-34.7877864833416,55.4765446163128,16.0007230453371));
#48766=CARTESIAN_POINT('Ctrl Pts',(-34.4255850063652,57.7716810411711,15.8895851547691));
#48767=CARTESIAN_POINT('Ctrl Pts',(-32.3008737352177,58.7121294100224,15.778447264201));
#48768=CARTESIAN_POINT('Ctrl Pts',(-30.3584249929228,57.4370866648374,15.667309373633));
#48769=CARTESIAN_POINT('Ctrl Pts',(-30.3761841408135,55.1136138914731,15.5561714830649));
#48770=CARTESIAN_POINT('Ctrl Pts',(-32.3378960321382,53.868412066919,15.4450335924969));
#48771=CARTESIAN_POINT('Ctrl Pts',(-34.4479835200066,54.8412285476315,15.3338957019289));
#48772=CARTESIAN_POINT('Ctrl Pts',(-34.7750596076319,57.1416333665308,15.2227578113608));
#48773=CARTESIAN_POINT('Ctrl Pts',(-33.0197478209391,58.6640399241194,15.1116199207928));
#48774=CARTESIAN_POINT('Ctrl Pts',(-30.7887049884687,58.0149721937252,15.0004820302248));
#48775=CARTESIAN_POINT('Ctrl Pts',(-30.1240298292691,55.7885293084689,14.8893441396567));
#48776=CARTESIAN_POINT('Ctrl Pts',(-31.6341072291541,54.0225995335433,14.7782062490887));
#48777=CARTESIAN_POINT('Ctrl Pts',(-33.9367458689222,54.3335587337424,14.6670683585206));
#48778=CARTESIAN_POINT('Ctrl Pts',(-34.9243151877952,56.4367817964587,14.5559304679526));
#48779=CARTESIAN_POINT('Ctrl Pts',(-33.6928803873875,58.4071660616143,14.4447925773845));
#48780=CARTESIAN_POINT('Ctrl Pts',(-31.3695905104292,58.4411939406326,14.3336546868165));
#48781=CARTESIAN_POINT('Ctrl Pts',(-30.0809735153022,56.5077243843662,14.2225167962484));
#48782=CARTESIAN_POINT('Ctrl Pts',(-31.0065263891691,54.3764738870215,14.1113789056804));
#48783=CARTESIAN_POINT('Ctrl Pts',(-33.2990575952188,53.998220451898,14.0002410151124));
#48784=CARTESIAN_POINT('Ctrl Pts',(-34.8602323505772,55.7191431963174,13.8891031245444));
#48785=CARTESIAN_POINT('Ctrl Pts',(-34.2609995597881,57.9641431697148,13.7779652339763));
#48786=CARTESIAN_POINT('Ctrl Pts',(-32.0500242237096,58.6781839861315,13.6668273434083));
#48787=CARTESIAN_POINT('Ctrl Pts',(-30.2506759606945,57.2080211780376,13.5556894528402));
#48788=CARTESIAN_POINT('Ctrl Pts',(-30.5106416621758,54.8986604236741,13.4445515622722));
#48789=CARTESIAN_POINT('Ctrl Pts',(-32.5905241100747,53.8651898368236,13.3334136717041));
#48790=CARTESIAN_POINT('Ctrl Pts',(-34.5894859509232,55.0509345423224,13.2222757811361));
#48791=CARTESIAN_POINT('Ctrl Pts',(-34.6719801790384,57.3759588223509,13.111137890568));
#48792=CARTESIAN_POINT('Ctrl Pts',(-33.4073937856322,58.2577308722945,13.0370459635227));
#48793=CARTESIAN_POINT('Ctrl Pts',(-32.7283737736498,58.3336705852723,13.));
#48794=CARTESIAN_POINT('Ctrl Pts',(-34.0692874532608,56.8510195406194,22.));
#48795=CARTESIAN_POINT('Ctrl Pts',(-34.0553305059911,56.9114179004355,22.));
#48796=CARTESIAN_POINT('Ctrl Pts',(-34.0377835201519,56.9707365361911,22.));
#48797=CARTESIAN_POINT('Ctrl Pts',(-34.016946081917,57.0288042521019,22.));
#48798=CARTESIAN_POINT('Ctrl Pts',(-33.9947315403611,57.0907095436074,22.));
#48799=CARTESIAN_POINT('Ctrl Pts',(-33.9687774174665,57.1511938546424,22.));
#48800=CARTESIAN_POINT('Ctrl Pts',(-33.939384889976,57.2100521415623,22.));
#48801=CARTESIAN_POINT('Ctrl Pts',(-33.9136664284218,57.2615531426173,22.));
#48802=CARTESIAN_POINT('Ctrl Pts',(-33.885314254798,57.3118096210154,22.));
#48803=CARTESIAN_POINT('Ctrl Pts',(-33.8544948148318,57.3606781624761,22.));
#48804=CARTESIAN_POINT('Ctrl Pts',(-33.8390317669697,57.3851969920325,22.));
#48805=CARTESIAN_POINT('Ctrl Pts',(-33.8229471373064,57.4093662970835,22.));
#48806=CARTESIAN_POINT('Ctrl Pts',(-33.806259181183,57.4331668560883,22.));
#48807=CARTESIAN_POINT('Ctrl Pts',(-33.7986346988757,57.4440409822962,22.));
#48808=CARTESIAN_POINT('Ctrl Pts',(-33.7908831157288,57.4548394645451,22.));
#48809=CARTESIAN_POINT('Ctrl Pts',(-33.7830191798836,57.4655431488209,22.));
#48810=CARTESIAN_POINT('Ctrl Pts',(-33.7433624664543,57.5195203109348,22.));
#48811=CARTESIAN_POINT('Ctrl Pts',(-33.7007840161423,57.5711878025655,22.));
#48812=CARTESIAN_POINT('Ctrl Pts',(-33.6555819716312,57.6203464168009,22.));
#48813=CARTESIAN_POINT('Ctrl Pts',(-33.6095776367408,57.6703775465096,22.));
#48814=CARTESIAN_POINT('Ctrl Pts',(-33.5608552988351,57.7178108518149,22.));
#48815=CARTESIAN_POINT('Ctrl Pts',(-33.5096779793303,57.7624205360032,22.));
#48816=CARTESIAN_POINT('Ctrl Pts',(-33.4668687974939,57.7997359737901,22.));
#48817=CARTESIAN_POINT('Ctrl Pts',(-33.4223407451604,57.8350756826701,22.));
#48818=CARTESIAN_POINT('Ctrl Pts',(-33.3762247080186,57.8682921421139,22.));
#48819=CARTESIAN_POINT('Ctrl Pts',(-33.3549779646827,57.8835957465012,22.));
#48820=CARTESIAN_POINT('Ctrl Pts',(-33.3333938801953,57.8984484230221,22.));
#48821=CARTESIAN_POINT('Ctrl Pts',(-33.3114840049174,57.912834383224,22.));
#48822=CARTESIAN_POINT('Ctrl Pts',(-33.3019191647998,57.919114629347,22.));
#48823=CARTESIAN_POINT('Ctrl Pts',(-33.2922923778332,57.9253057103697,22.));
#48824=CARTESIAN_POINT('Ctrl Pts',(-33.2826166375141,57.9313989825554,22.));
#48825=CARTESIAN_POINT('Ctrl Pts',(-33.2232320152636,57.9687962932603,22.));
#48826=CARTESIAN_POINT('Ctrl Pts',(-33.1618957173518,58.0025854530302,22.));
#48827=CARTESIAN_POINT('Ctrl Pts',(-33.0988929672382,58.0325387704092,22.));
#48828=CARTESIAN_POINT('Ctrl Pts',(-33.0425620163395,58.0593201227707,22.));
#48829=CARTESIAN_POINT('Ctrl Pts',(-32.9848978605312,58.0830352046557,22.));
#48830=CARTESIAN_POINT('Ctrl Pts',(-32.9260772832472,58.1034986372925,22.));
#48831=CARTESIAN_POINT('Ctrl Pts',(-32.8619970286523,58.1257918896507,22.));
#48832=CARTESIAN_POINT('Ctrl Pts',(-32.7965441149127,58.1442273323773,22.));
#48833=CARTESIAN_POINT('Ctrl Pts',(-32.7300260672774,58.1589105502835,22.));
#48834=CARTESIAN_POINT('Ctrl Pts',(-32.7043629429456,58.1645754376354,22.));
#48835=CARTESIAN_POINT('Ctrl Pts',(-32.6785410407311,58.1696813145167,22.));
#48836=CARTESIAN_POINT('Ctrl Pts',(-32.6525772949456,58.1742323470501,22.));
#48837=CARTESIAN_POINT('Ctrl Pts',(-32.6411872717747,58.1762288373267,22.));
#48838=CARTESIAN_POINT('Ctrl Pts',(-32.6297705135126,58.1781183496289,22.));
#48839=CARTESIAN_POINT('Ctrl Pts',(-32.6183418171519,58.179899377155,22.));
#48840=CARTESIAN_POINT('Ctrl Pts',(-32.5492442274088,58.1906674215093,22.));
#48841=CARTESIAN_POINT('Ctrl Pts',(-32.4795878660141,58.1974963222478,22.));
#48842=CARTESIAN_POINT('Ctrl Pts',(-32.4097184968443,58.2005474581331,22.));
#48843=CARTESIAN_POINT('Ctrl Pts',(-32.3382311065414,58.2036692516242,22.));
#48844=CARTESIAN_POINT('Ctrl Pts',(-32.2665198680424,58.2028364327149,22.));
#48845=CARTESIAN_POINT('Ctrl Pts',(-32.1949302795206,58.1981713779267,22.));
#48846=CARTESIAN_POINT('Ctrl Pts',(-32.1401596273381,58.1946023101545,22.));
#48847=CARTESIAN_POINT('Ctrl Pts',(-32.0854595447284,58.188789106956,22.));
#48848=CARTESIAN_POINT('Ctrl Pts',(-32.0309802701514,58.1807666255737,22.));
#48849=CARTESIAN_POINT('Ctrl Pts',(-31.9970690900808,58.1757729502195,22.));
#48850=CARTESIAN_POINT('Ctrl Pts',(-31.9632434082658,58.169922934266,22.));
#48851=CARTESIAN_POINT('Ctrl Pts',(-31.9295394677765,58.1632216306335,22.));
#48852=CARTESIAN_POINT('Ctrl Pts',(-31.9106295176357,58.1594617937797,22.));
#48853=CARTESIAN_POINT('Ctrl Pts',(-31.8917516814693,58.155432366928,22.));
#48854=CARTESIAN_POINT('Ctrl Pts',(-31.8729463796414,58.1511420898627,22.));
#48855=CARTESIAN_POINT('Ctrl Pts',(-31.800021211719,58.1345048043629,22.));
#48856=CARTESIAN_POINT('Ctrl Pts',(-31.7281115870151,58.1139365946459,22.));
#48857=CARTESIAN_POINT('Ctrl Pts',(-31.657588471888,58.0895522802274,22.));
#48858=CARTESIAN_POINT('Ctrl Pts',(-31.604840310165,58.071313894726,22.));
#48859=CARTESIAN_POINT('Ctrl Pts',(-31.5528674075064,58.0509395358675,22.));
#48860=CARTESIAN_POINT('Ctrl Pts',(-31.5018252351889,58.0284581681865,22.));
#48861=CARTESIAN_POINT('Ctrl Pts',(-31.4859023718045,58.0214449920221,22.));
#48862=CARTESIAN_POINT('Ctrl Pts',(-31.4700701035993,58.0142266520307,22.));
#48863=CARTESIAN_POINT('Ctrl Pts',(-31.4543332256613,58.00680370711,22.));
#48864=CARTESIAN_POINT('Ctrl Pts',(-31.4391437429754,57.999638963646,22.));
#48865=CARTESIAN_POINT('Ctrl Pts',(-31.4240509122303,57.9922872148405,22.));
#48866=CARTESIAN_POINT('Ctrl Pts',(-31.4090641623582,57.9847522751755,22.));
#48867=CARTESIAN_POINT('Ctrl Pts',(-31.341765130632,57.9509161100361,22.));
#48868=CARTESIAN_POINT('Ctrl Pts',(-31.2765704047312,57.9133737616798,22.));
#48869=CARTESIAN_POINT('Ctrl Pts',(-31.213852322156,57.8722119391998,22.));
#48870=CARTESIAN_POINT('Ctrl Pts',(-31.1658528011761,57.8407098957608,22.));
#48871=CARTESIAN_POINT('Ctrl Pts',(-31.1193037579286,57.807086816115,22.));
#48872=CARTESIAN_POINT('Ctrl Pts',(-31.0743783982804,57.7713618605751,22.));
#48873=CARTESIAN_POINT('Ctrl Pts',(-31.0639523774024,57.7630710169348,22.));
#48874=CARTESIAN_POINT('Ctrl Pts',(-31.0536138415293,57.7546668979799,22.));
#48875=CARTESIAN_POINT('Ctrl Pts',(-31.0433632440414,57.7461514510325,22.));
#48876=CARTESIAN_POINT('Ctrl Pts',(-31.6652099567911,54.8483531313949,20.8714803633902));
#48877=CARTESIAN_POINT('Ctrl Pts',(-31.5910191767377,54.8903425066551,20.8771939403667));
#48878=CARTESIAN_POINT('Ctrl Pts',(-31.5202697708326,54.9380868086678,20.8829075173431));
#48879=CARTESIAN_POINT('Ctrl Pts',(-31.453999322188,54.9913986485313,20.8886210943196));
#48880=CARTESIAN_POINT('Ctrl Pts',(-31.0243118193789,55.3370645042722,20.9256670578423));
#48881=CARTESIAN_POINT('Ctrl Pts',(-30.7829209443173,55.9167912231112,20.9627130213649));
#48882=CARTESIAN_POINT('Ctrl Pts',(-30.840293873424,56.4652682536955,20.9997589848876));
#48883=CARTESIAN_POINT('Ctrl Pts',(-30.8976668025307,57.0137452842797,21.0368049484103));
#48884=CARTESIAN_POINT('Ctrl Pts',(-31.2538035358057,57.530972626609,21.073850911933));
#48885=CARTESIAN_POINT('Ctrl Pts',(-31.7457295422612,57.780228908827,21.1108968754557));
#48886=CARTESIAN_POINT('Ctrl Pts',(-32.2376555487168,58.0294851910449,21.1479428389784));
#48887=CARTESIAN_POINT('Ctrl Pts',(-32.8653708283529,58.0107704131515,21.184988802501));
#48888=CARTESIAN_POINT('Ctrl Pts',(-33.3415709716004,57.7326682072443,21.2220347660237));
#48889=CARTESIAN_POINT('Ctrl Pts',(-33.8177711148478,57.4545660013371,21.2590807295464));
#48890=CARTESIAN_POINT('Ctrl Pts',(-34.1424561217066,56.9170763674162,21.2961266930691));
#48891=CARTESIAN_POINT('Ctrl Pts',(-34.1670860104471,56.3661470356389,21.3331726565918));
#48892=CARTESIAN_POINT('Ctrl Pts',(-34.1917158991876,55.8152177038615,21.3702186201144));
#48893=CARTESIAN_POINT('Ctrl Pts',(-33.9162906698098,55.2508486742278,21.4072645836371));
#48894=CARTESIAN_POINT('Ctrl Pts',(-33.4667522310661,54.9314015975034,21.4443105471598));
#48895=CARTESIAN_POINT('Ctrl Pts',(-33.0172137923224,54.611954520779,21.4813565106825));
#48896=CARTESIAN_POINT('Ctrl Pts',(-32.3935621442129,54.537429396964,21.5184024742052));
#48897=CARTESIAN_POINT('Ctrl Pts',(-31.881431331593,54.741782991655,21.5554484377278));
#48898=CARTESIAN_POINT('Ctrl Pts',(-31.8075551488135,54.7712615216341,21.5607924129486));
#48899=CARTESIAN_POINT('Ctrl Pts',(-31.7359995810404,54.8065431837031,21.5661363881694));
#48900=CARTESIAN_POINT('Ctrl Pts',(-31.6673136634551,54.8469650373412,21.5714803633902));
#48901=CARTESIAN_POINT('Ctrl Pts',(-30.5157034944334,56.8250975324092,22.));
#48902=CARTESIAN_POINT('Ctrl Pts',(-30.3383199129809,56.1652717359214,21.9629540364773));
#48903=CARTESIAN_POINT('Ctrl Pts',(-30.6971298707754,54.6659551967235,21.8888621094319));
#48904=CARTESIAN_POINT('Ctrl Pts',(-32.8915770858134,53.8933186298579,21.7777242188639));
#48905=CARTESIAN_POINT('Ctrl Pts',(-34.7256560234758,55.3208993649632,21.6665863282959));
#48906=CARTESIAN_POINT('Ctrl Pts',(-34.5234929724835,57.6345755616839,21.5554484377278));
#48907=CARTESIAN_POINT('Ctrl Pts',(-32.4687454188576,58.7202753686331,21.4443105471598));
#48908=CARTESIAN_POINT('Ctrl Pts',(-30.4428342940784,57.5824199368057,21.3331726565918));
#48909=CARTESIAN_POINT('Ctrl Pts',(-30.2997559892122,55.2634130835606,21.2220347660237));
#48910=CARTESIAN_POINT('Ctrl Pts',(-32.1706430815575,53.8854124812075,21.1108968754557));
#48911=CARTESIAN_POINT('Ctrl Pts',(-34.3429657642117,54.7099453599152,20.9997589848876));
#48912=CARTESIAN_POINT('Ctrl Pts',(-34.8284152391772,56.982193672835,20.8886210943196));
#48913=CARTESIAN_POINT('Ctrl Pts',(-33.18263271582,58.6223996095027,20.7774832037515));
#48914=CARTESIAN_POINT('Ctrl Pts',(-30.9120322857352,58.129235673502,20.6663453131835));
#48915=CARTESIAN_POINT('Ctrl Pts',(-30.0949149346207,55.954114599854,20.5552074226154));
#48916=CARTESIAN_POINT('Ctrl Pts',(-31.479200108132,54.0879422836221,20.4440695320474));
#48917=CARTESIAN_POINT('Ctrl Pts',(-33.7978345552325,54.2388509530007,20.3329316414794));
#48918=CARTESIAN_POINT('Ctrl Pts',(-34.9285465373885,56.2687104209715,20.2217937509113));
#48919=CARTESIAN_POINT('Ctrl Pts',(-33.8363822214011,58.3195681810162,20.1106558603433));
#48920=CARTESIAN_POINT('Ctrl Pts',(-31.5210121579647,58.5142504249981,19.9995179697753));
#48921=CARTESIAN_POINT('Ctrl Pts',(-30.101720741136,56.674562508041,19.8883800792072));
#48922=CARTESIAN_POINT('Ctrl Pts',(-30.8776015421155,54.484391533643,19.7772421886392));
#48923=CARTESIAN_POINT('Ctrl Pts',(-33.1384820439344,53.9484258880499,19.6661042980711));
#48924=CARTESIAN_POINT('Ctrl Pts',(-34.8149526935152,55.5572409773789,19.5549664075031));
#48925=CARTESIAN_POINT('Ctrl Pts',(-34.3725208876465,57.8382701189333,19.443828516935));
#48926=CARTESIAN_POINT('Ctrl Pts',(-32.2161494783462,58.7036614639378,19.332690626367));
#48927=CARTESIAN_POINT('Ctrl Pts',(-30.3195896701686,57.3613125035425,19.221552735799));
#48928=CARTESIAN_POINT('Ctrl Pts',(-30.4187841646359,55.039890462752,19.1104148452309));
#48929=CARTESIAN_POINT('Ctrl Pts',(-32.4229391156973,53.8642192630766,18.9992769546629));
#48930=CARTESIAN_POINT('Ctrl Pts',(-34.4976287681445,54.9104040861686,18.8881390640948));
#48931=CARTESIAN_POINT('Ctrl Pts',(-34.7438661544312,57.2208600991234,18.7770011735268));
#48932=CARTESIAN_POINT('Ctrl Pts',(-32.9362674024074,58.680800710823,18.6658632829587));
#48933=CARTESIAN_POINT('Ctrl Pts',(-30.7293481493446,57.9539257225797,18.5547253923907));
#48934=CARTESIAN_POINT('Ctrl Pts',(-30.1431266157477,55.7055520544288,18.4435875018226));
#48935=CARTESIAN_POINT('Ctrl Pts',(-31.7141780195174,53.9936416231339,18.3324496112546));
#48936=CARTESIAN_POINT('Ctrl Pts',(-34.004501193851,54.3851254608372,18.2213117206866));
#48937=CARTESIAN_POINT('Ctrl Pts',(-34.9177373632483,56.5216739711636,18.1101738301186));
#48938=CARTESIAN_POINT('Ctrl Pts',(-33.6179911050581,58.4476800725015,17.9990359395505));
#48939=CARTESIAN_POINT('Ctrl Pts',(-31.2949349095266,58.4002485379024,17.8878980489825));
#48940=CARTESIAN_POINT('Ctrl Pts',(-30.0748884576731,56.4227939888947,17.7767601584144));
#48941=CARTESIAN_POINT('Ctrl Pts',(-31.0745741031468,54.3253030000451,17.6656222678464));
#48942=CARTESIAN_POINT('Ctrl Pts',(-33.3789682374394,54.0276328606133,17.5544843772783));
#48943=CARTESIAN_POINT('Ctrl Pts',(-34.8788327758259,55.8022444250302,17.4433464867103));
#48944=CARTESIAN_POINT('Ctrl Pts',(-34.2013246967004,58.0248156029211,17.3322085961422));
#48945=CARTESIAN_POINT('Ctrl Pts',(-31.9665748283507,58.6610017894909,17.2210707055742));
#48946=CARTESIAN_POINT('Ctrl Pts',(-30.2200750690644,57.1284945533303,17.1099328150062));
#48947=CARTESIAN_POINT('Ctrl Pts',(-30.5604164551708,54.8300151475111,16.9987949244381));
#48948=CARTESIAN_POINT('Ctrl Pts',(-32.6760806562328,53.8693878387091,16.8876570338701));
#48949=CARTESIAN_POINT('Ctrl Pts',(-34.6305762357544,55.1258856969253,16.776519143302));
#48950=CARTESIAN_POINT('Ctrl Pts',(-34.6349312243122,57.4494219828794,16.665381252734));
#48951=CARTESIAN_POINT('Ctrl Pts',(-32.6851594514901,58.7132375833447,16.554243362166));
#48952=CARTESIAN_POINT('Ctrl Pts',(-30.5659091328683,57.7605477465697,16.4431054715979));
#48953=CARTESIAN_POINT('Ctrl Pts',(-30.2169541190139,55.4633602843958,16.3319675810299));
#48954=CARTESIAN_POINT('Ctrl Pts',(-31.9576968915284,53.9243169328215,16.2208296904618));
#48955=CARTESIAN_POINT('Ctrl Pts',(-34.1948158493603,54.5521215254953,16.1096917998938));
#48956=CARTESIAN_POINT('Ctrl Pts',(-34.880650639758,56.7721373989267,15.9985539093257));
#48957=CARTESIAN_POINT('Ctrl Pts',(-33.387448901162,58.5523588475275,15.8874160187577));
#48958=CARTESIAN_POINT('Ctrl Pts',(-31.0819551189948,58.2633289901972,15.7762781281897));
#48959=CARTESIAN_POINT('Ctrl Pts',(-30.0744138980993,56.1696001333951,15.6651402376216));
#48960=CARTESIAN_POINT('Ctrl Pts',(-31.2870391443611,54.1875860438059,15.5540023470536));
#48961=CARTESIAN_POINT('Ctrl Pts',(-33.6099012175602,54.1314466960921,15.4428644564855));
#48962=CARTESIAN_POINT('Ctrl Pts',(-34.916858119472,56.052567070093,15.3317265659175));
#48963=CARTESIAN_POINT('Ctrl Pts',(-34.0116373750326,58.1925239040739,15.2205886753494));
#48964=CARTESIAN_POINT('Ctrl Pts',(-31.722797799219,58.5925904319764,15.1094507847814));
#48965=CARTESIAN_POINT('Ctrl Pts',(-30.1453402095974,56.8865812380663,14.9983128942134));
#48966=CARTESIAN_POINT('Ctrl Pts',(-30.723129434303,54.6360258563356,14.8871750036453));
#48967=CARTESIAN_POINT('Ctrl Pts',(-32.9273084298409,53.9008832080614,14.7760371130773));
#48968=CARTESIAN_POINT('Ctrl Pts',(-34.7403671916158,55.3540375815297,14.6648992225092));
#48969=CARTESIAN_POINT('Ctrl Pts',(-34.5027924192342,57.6654005284895,14.5537613319412));
#48970=CARTESIAN_POINT('Ctrl Pts',(-32.4320391047204,58.7193548713018,14.4426234413732));
#48971=CARTESIAN_POINT('Ctrl Pts',(-30.4234910234841,57.5512051672244,14.3314855508051));
#48972=CARTESIAN_POINT('Ctrl Pts',(-30.3155954476549,55.2301702471531,14.2203476602371));
#48973=CARTESIAN_POINT('Ctrl Pts',(-32.2071095510683,53.8807233800597,14.109209769669));
#48974=CARTESIAN_POINT('Ctrl Pts',(-34.3667107654438,54.7380212138031,13.998071879101));
#48975=CARTESIAN_POINT('Ctrl Pts',(-34.817688121868,57.0173840749687,13.886933988533));
#48976=CARTESIAN_POINT('Ctrl Pts',(-33.1472639077745,58.6324557555082,13.7757960979649));
#48977=CARTESIAN_POINT('Ctrl Pts',(-30.8843823888258,58.105001931136,13.6646582073969));
#48978=CARTESIAN_POINT('Ctrl Pts',(-30.1003126229301,55.9176887906373,13.5535203168288));
#48979=CARTESIAN_POINT('Ctrl Pts',(-31.5126666412309,54.0728255670593,13.4423824262608));
#48980=CARTESIAN_POINT('Ctrl Pts',(-33.8288126996591,54.2585627611561,13.3312445356927));
#48981=CARTESIAN_POINT('Ctrl Pts',(-34.9285321027134,56.3058411531895,13.2201066451247));
#48982=CARTESIAN_POINT('Ctrl Pts',(-33.8056871835127,58.3388651889263,13.1089687545567));
#48983=CARTESIAN_POINT('Ctrl Pts',(-31.4871369476881,58.5005967837941,12.9978308639886));
#48984=CARTESIAN_POINT('Ctrl Pts',(-30.0968376198179,56.6352191751131,12.8866929734206));
#48985=CARTESIAN_POINT('Ctrl Pts',(-30.6354003368774,55.1906968075748,12.8126010463752));
#48986=CARTESIAN_POINT('Ctrl Pts',(-31.1506898940642,54.7420190959221,12.7755550828525));
#48987=CARTESIAN_POINT('Ctrl Pts',(-30.6408436601533,56.7914556061658,22.0748149723825));
#48988=CARTESIAN_POINT('Ctrl Pts',(-30.4746468195517,56.1732418919888,22.0377690088598));
#48989=CARTESIAN_POINT('Ctrl Pts',(-30.8108283357527,54.7684801331151,21.9636770818145));
#48990=CARTESIAN_POINT('Ctrl Pts',(-32.8668821769258,54.0445700885951,21.8525391912464));
#48991=CARTESIAN_POINT('Ctrl Pts',(-34.5852944581392,55.3821200801757,21.7414013006784));
#48992=CARTESIAN_POINT('Ctrl Pts',(-34.3958808715705,57.5498836968622,21.6302634101103));
#48993=CARTESIAN_POINT('Ctrl Pts',(-32.4707164969967,58.5671135683041,21.5191255195423));
#48994=CARTESIAN_POINT('Ctrl Pts',(-30.5725699745224,57.5010172797825,21.4079876289743));
#48995=CARTESIAN_POINT('Ctrl Pts',(-30.4385149394808,55.3282591857861,21.2968497384062));
#48996=CARTESIAN_POINT('Ctrl Pts',(-32.1914140597048,54.0371625432278,21.1857118478382));
#48997=CARTESIAN_POINT('Ctrl Pts',(-34.2267386577774,54.8096960454343,21.0745739572701));
#48998=CARTESIAN_POINT('Ctrl Pts',(-34.6815731376677,56.9386444383885,20.9634360667021));
#48999=CARTESIAN_POINT('Ctrl Pts',(-33.1395823093187,58.4754103689113,20.852298176134));
#49000=CARTESIAN_POINT('Ctrl Pts',(-31.0121778750478,58.0133479424405,20.741160285566));
#49001=CARTESIAN_POINT('Ctrl Pts',(-30.2465922382936,55.9754014346164,20.6300223949979));
#49002=CARTESIAN_POINT('Ctrl Pts',(-31.5435771139257,54.2269197519467,20.5188845044299));
#49003=CARTESIAN_POINT('Ctrl Pts',(-33.715986287666,54.3683113275635,20.4077466138618));
#49004=CARTESIAN_POINT('Ctrl Pts',(-34.7753896299934,56.2701571899581,20.2966087232938));
#49005=CARTESIAN_POINT('Ctrl Pts',(-33.7521029354263,58.1916770817759,20.1854708327258));
#49006=CARTESIAN_POINT('Ctrl Pts',(-31.5827522761609,58.3740816403381,20.0743329421577));
#49007=CARTESIAN_POINT('Ctrl Pts',(-30.2529688348836,56.6504141115413,19.9631950515897));
#49008=CARTESIAN_POINT('Ctrl Pts',(-30.9799185150648,54.5983668288005,19.8520571610217));
#49009=CARTESIAN_POINT('Ctrl Pts',(-33.0982160108274,54.0962019934802,19.7409192704536));
#49010=CARTESIAN_POINT('Ctrl Pts',(-34.6689596108848,55.6035567484657,19.6297813798856));
#49011=CARTESIAN_POINT('Ctrl Pts',(-34.2544298798073,57.7407322048549,19.5186434893175));
#49012=CARTESIAN_POINT('Ctrl Pts',(-32.2340505839621,58.55154742375,19.4075055987495));
#49013=CARTESIAN_POINT('Ctrl Pts',(-30.4570978042841,57.2938540432474,19.2963677081815));
#49014=CARTESIAN_POINT('Ctrl Pts',(-30.5500365726333,55.1188330761248,19.1852298176134));
#49015=CARTESIAN_POINT('Ctrl Pts',(-32.4277989800397,54.017305880809,19.0740919270454));
#49016=CARTESIAN_POINT('Ctrl Pts',(-34.3716477998814,54.9975127909389,18.9629540364773));
#49017=CARTESIAN_POINT('Ctrl Pts',(-34.6023561625368,57.1622593055708,18.8518161459093));
#49018=CARTESIAN_POINT('Ctrl Pts',(-32.9087540872943,58.5301283898668,18.7406782553412));
#49019=CARTESIAN_POINT('Ctrl Pts',(-30.8410147603585,57.8490939583302,18.6295403647732));
#49020=CARTESIAN_POINT('Ctrl Pts',(-30.2917634374419,55.7425145495773,18.5184024742052));
#49021=CARTESIAN_POINT('Ctrl Pts',(-31.7637360833391,54.1385661866875,18.4072645836371));
#49022=CARTESIAN_POINT('Ctrl Pts',(-33.9096194419575,54.505360996219,18.2961266930691));
#49023=CARTESIAN_POINT('Ctrl Pts',(-34.7652621391801,56.507167529275,18.184988802501));
#49024=CARTESIAN_POINT('Ctrl Pts',(-33.5474847105914,58.3117095641174,18.073850911933));
#49025=CARTESIAN_POINT('Ctrl Pts',(-31.3709326471137,58.2672693113572,17.9627130213649));
#49026=CARTESIAN_POINT('Ctrl Pts',(-30.2278287362276,56.4145234383322,17.8515751307969));
#49027=CARTESIAN_POINT('Ctrl Pts',(-31.164468951247,54.4493112541897,17.7404372402288));
#49028=CARTESIAN_POINT('Ctrl Pts',(-33.3235358811423,54.1704137580971,17.6292993496608));
#49029=CARTESIAN_POINT('Ctrl Pts',(-34.7288110794959,55.8331089911408,17.5181614590927));
#49030=CARTESIAN_POINT('Ctrl Pts',(-34.0940302203501,57.9155131502695,17.4070235685248));
#49031=CARTESIAN_POINT('Ctrl Pts',(-32.0002154229856,58.5115780925632,17.2958856779567));
#49032=CARTESIAN_POINT('Ctrl Pts',(-30.363859116905,57.0757188165044,17.1847477873887));
#49033=CARTESIAN_POINT('Ctrl Pts',(-30.6827367866064,54.9221936012213,17.0736098968206));
#49034=CARTESIAN_POINT('Ctrl Pts',(-32.6649760846936,54.0221484988997,16.9624720062526));
#49035=CARTESIAN_POINT('Ctrl Pts',(-34.4962109015046,55.1994049989002,16.8513341156845));
#49036=CARTESIAN_POINT('Ctrl Pts',(-34.5002912415971,57.3764068757753,16.7401962251165));
#49037=CARTESIAN_POINT('Ctrl Pts',(-32.6734823234101,58.5605196227415,16.6290583345484));
#49038=CARTESIAN_POINT('Ctrl Pts',(-30.6878830671828,57.6679114137473,16.5179204439804));
#49039=CARTESIAN_POINT('Ctrl Pts',(-30.3609349903662,55.5155966653536,16.4067825534124));
#49040=CARTESIAN_POINT('Ctrl Pts',(-31.9918973755157,54.0736134756683,16.2956446628443));
#49041=CARTESIAN_POINT('Ctrl Pts',(-34.0879318551292,54.6618254114249,16.1845067722763));
#49042=CARTESIAN_POINT('Ctrl Pts',(-34.7305142993751,56.7418354170222,16.0733688817082));
#49043=CARTESIAN_POINT('Ctrl Pts',(-33.331481709642,58.4097867454715,15.9622309911402));
#49044=CARTESIAN_POINT('Ctrl Pts',(-31.1713844814461,58.1389846298839,15.8510931005721));
#49045=CARTESIAN_POINT('Ctrl Pts',(-30.2273841048745,56.1772973179708,15.7399552100041));
#49046=CARTESIAN_POINT('Ctrl Pts',(-31.3635348303942,54.3202794529552,15.6288173194361));
#49047=CARTESIAN_POINT('Ctrl Pts',(-33.539905013914,54.2676805475375,15.517679428868));
#49048=CARTESIAN_POINT('Ctrl Pts',(-34.764438345137,56.0676449746847,15.4065415383));
#49049=CARTESIAN_POINT('Ctrl Pts',(-33.916305578051,58.0726448845937,15.2954036477319));
#49050=CARTESIAN_POINT('Ctrl Pts',(-31.7718122544331,58.447481114776,15.1842657571639));
#49051=CARTESIAN_POINT('Ctrl Pts',(-30.2938374304302,56.8490618262286,15.0731278665959));
#49052=CARTESIAN_POINT('Ctrl Pts',(-30.8351882301687,54.7404382942198,14.9619899760278));
#49053=CARTESIAN_POINT('Ctrl Pts',(-32.90036011462,54.0516576047428,14.8508520854598));
#49054=CARTESIAN_POINT('Ctrl Pts',(-34.5990778627046,55.4131684266542,14.7397141948917));
#49055=CARTESIAN_POINT('Ctrl Pts',(-34.3764858039968,57.5787646792666,14.6285763043237));
#49056=CARTESIAN_POINT('Ctrl Pts',(-32.4363250759318,58.566251122372,14.5174384137557));
#49057=CARTESIAN_POINT('Ctrl Pts',(-30.5544465922265,57.4717710776139,14.4063005231876));
#49058=CARTESIAN_POINT('Ctrl Pts',(-30.453355478433,55.2971128173438,14.2951626326196));
#49059=CARTESIAN_POINT('Ctrl Pts',(-32.2255807620059,54.0327691614409,14.1840247420515));
#49060=CARTESIAN_POINT('Ctrl Pts',(-34.2489861744447,54.8360012884289,14.0728868514835));
#49061=CARTESIAN_POINT('Ctrl Pts',(-34.6715225287502,56.9716155488274,13.9617489609154));
#49062=CARTESIAN_POINT('Ctrl Pts',(-33.1064440441824,58.4848323215015,13.8506110703474));
#49063=CARTESIAN_POINT('Ctrl Pts',(-30.9862717259461,57.9906425072237,13.7394731797794));
#49064=CARTESIAN_POINT('Ctrl Pts',(-30.2516495200118,55.9412728283577,13.6283352892113));
#49065=CARTESIAN_POINT('Ctrl Pts',(-31.5749330715706,54.2127563749733,13.5171973986433));
#49066=CARTESIAN_POINT('Ctrl Pts',(-33.7450107875056,54.386780005505,13.4060595080752));
#49067=CARTESIAN_POINT('Ctrl Pts',(-34.7753761056448,56.3049462630692,13.2949216175072));
#49068=CARTESIAN_POINT('Ctrl Pts',(-33.723343687939,58.2097571189556,13.1837837269391));
#49069=CARTESIAN_POINT('Ctrl Pts',(-31.5510134146689,58.3612890695025,13.0726458363711));
#49070=CARTESIAN_POINT('Ctrl Pts',(-30.248393668858,56.613551975949,12.9615079458031));
#49071=CARTESIAN_POINT('Ctrl Pts',(-30.7529917906697,55.2601287803101,12.8874160187577));
#49072=CARTESIAN_POINT('Ctrl Pts',(-31.2357844803776,54.8397470430914,12.850370055235));
#49073=CARTESIAN_POINT('Ctrl Pts',(-30.7659838258732,56.7578136799223,22.149629944765));
#49074=CARTESIAN_POINT('Ctrl Pts',(-30.6109737261224,56.1812120480563,22.1125839812423));
#49075=CARTESIAN_POINT('Ctrl Pts',(-30.92452680073,54.8710050695066,22.0384920541969));
#49076=CARTESIAN_POINT('Ctrl Pts',(-32.8421872680382,54.1958215473324,21.9273541636289));
#49077=CARTESIAN_POINT('Ctrl Pts',(-34.4449328928026,55.4433407953881,21.8162162730609));
#49078=CARTESIAN_POINT('Ctrl Pts',(-34.2682687706575,57.4651918320407,21.7050783824928));
#49079=CARTESIAN_POINT('Ctrl Pts',(-32.4726875751359,58.4139517679751,21.5939404919248));
#49080=CARTESIAN_POINT('Ctrl Pts',(-30.7023056549664,57.4196146227593,21.4828026013567));
#49081=CARTESIAN_POINT('Ctrl Pts',(-30.5772738897496,55.3931052880117,21.3716647107887));
#49082=CARTESIAN_POINT('Ctrl Pts',(-32.2121850378521,54.1889126052481,21.2605268202207));
#49083=CARTESIAN_POINT('Ctrl Pts',(-34.1105115513431,54.9094467309533,21.1493889296526));
#49084=CARTESIAN_POINT('Ctrl Pts',(-34.5347310361582,56.8950952039422,21.0382510390846));
#49085=CARTESIAN_POINT('Ctrl Pts',(-33.0965319028176,58.3284211283196,20.9271131485165));
#49086=CARTESIAN_POINT('Ctrl Pts',(-31.1123234643604,57.8974602113791,20.8159752579485));
#49087=CARTESIAN_POINT('Ctrl Pts',(-30.3982695419667,55.9966882693789,20.7048373673804));
#49088=CARTESIAN_POINT('Ctrl Pts',(-31.6079541197193,54.3658972202714,20.5936994768124));
#49089=CARTESIAN_POINT('Ctrl Pts',(-33.6341380200995,54.4977717021263,20.4825615862443));
#49090=CARTESIAN_POINT('Ctrl Pts',(-34.6222327225984,56.2716039589447,20.3714236956763));
#49091=CARTESIAN_POINT('Ctrl Pts',(-33.6678236494516,58.0637859825355,20.2602858051082));
#49092=CARTESIAN_POINT('Ctrl Pts',(-31.6444923943572,58.2339128556783,20.1491479145402));
#49093=CARTESIAN_POINT('Ctrl Pts',(-30.4042169286311,56.6262657150416,20.0380100239722));
#49094=CARTESIAN_POINT('Ctrl Pts',(-31.0822354880141,54.712342123958,19.9268721334041));
#49095=CARTESIAN_POINT('Ctrl Pts',(-33.0579499777205,54.2439780989104,19.8157342428361));
#49096=CARTESIAN_POINT('Ctrl Pts',(-34.5229665282545,55.6498725195525,19.7045963522681));
#49097=CARTESIAN_POINT('Ctrl Pts',(-34.1363388719682,57.6431942907766,19.5934584617));
#49098=CARTESIAN_POINT('Ctrl Pts',(-32.251951689578,58.3994333835622,19.482320571132));
#49099=CARTESIAN_POINT('Ctrl Pts',(-30.5946059383997,57.2263955829523,19.371182680564));
#49100=CARTESIAN_POINT('Ctrl Pts',(-30.6812889806306,55.1977756894976,19.2600447899959));
#49101=CARTESIAN_POINT('Ctrl Pts',(-32.4326588443821,54.1703924985414,19.1489068994279));
#49102=CARTESIAN_POINT('Ctrl Pts',(-34.2456668316182,55.0846214957092,19.0377690088598));
#49103=CARTESIAN_POINT('Ctrl Pts',(-34.4608461706423,57.1036585120183,18.9266311182918));
#49104=CARTESIAN_POINT('Ctrl Pts',(-32.8812407721812,58.3794560689105,18.8154932277237));
#49105=CARTESIAN_POINT('Ctrl Pts',(-30.9526813713723,57.7442621940807,18.7043553371557));
#49106=CARTESIAN_POINT('Ctrl Pts',(-30.440400259136,55.7794770447257,18.5932174465876));
#49107=CARTESIAN_POINT('Ctrl Pts',(-31.8132941471607,54.2834907502409,18.4820795560196));
#49108=CARTESIAN_POINT('Ctrl Pts',(-33.814737690064,54.625596531601,18.3709416654516));
#49109=CARTESIAN_POINT('Ctrl Pts',(-34.6127869151118,56.4926610873864,18.2598037748835));
#49110=CARTESIAN_POINT('Ctrl Pts',(-33.4769783161247,58.1757390557332,18.1486658843155));
#49111=CARTESIAN_POINT('Ctrl Pts',(-31.4469303847008,58.1342900848119,18.0375279937474));
#49112=CARTESIAN_POINT('Ctrl Pts',(-30.3807690147821,56.4062528877698,17.9263901031794));
#49113=CARTESIAN_POINT('Ctrl Pts',(-31.2543637993472,54.5733195083342,17.8152522126114));
#49114=CARTESIAN_POINT('Ctrl Pts',(-33.2681035248452,54.3131946555809,17.7041143220433));
#49115=CARTESIAN_POINT('Ctrl Pts',(-34.5787893831659,55.8639735572515,17.5929764314753));
#49116=CARTESIAN_POINT('Ctrl Pts',(-33.9867357439999,57.8062106976179,17.4818385409072));
#49117=CARTESIAN_POINT('Ctrl Pts',(-32.0338560176206,58.3621543956355,17.3707006503392));
#49118=CARTESIAN_POINT('Ctrl Pts',(-30.5076431647456,57.0229430796784,17.2595627597712));
#49119=CARTESIAN_POINT('Ctrl Pts',(-30.8050571180421,55.0143720549316,17.1484248692031));
#49120=CARTESIAN_POINT('Ctrl Pts',(-32.6538715131544,54.1749091590902,17.0372869786351));
#49121=CARTESIAN_POINT('Ctrl Pts',(-34.3618455672547,55.2729243008751,16.926149088067));
#49122=CARTESIAN_POINT('Ctrl Pts',(-34.3656512588821,57.3033917686711,16.815011197499));
#49123=CARTESIAN_POINT('Ctrl Pts',(-32.6618051953302,58.4078016621386,16.7038733069309));
#49124=CARTESIAN_POINT('Ctrl Pts',(-30.8098570014971,57.5752750809247,16.5927354163629));
#49125=CARTESIAN_POINT('Ctrl Pts',(-30.5049158617185,55.5678330463115,16.4815975257948));
#49126=CARTESIAN_POINT('Ctrl Pts',(-32.0260978595029,54.2229100185152,16.3704596352268));
#49127=CARTESIAN_POINT('Ctrl Pts',(-33.9810478608982,54.7715292973545,16.2593217446587));
#49128=CARTESIAN_POINT('Ctrl Pts',(-34.580377958992,56.7115334351178,16.1481838540907));
#49129=CARTESIAN_POINT('Ctrl Pts',(-33.2755145181222,58.2672146434155,16.0370459635227));
#49130=CARTESIAN_POINT('Ctrl Pts',(-31.2608138438975,58.0146402695706,15.9259080729546));
#49131=CARTESIAN_POINT('Ctrl Pts',(-30.3803543116497,56.1849945025464,15.8147701823866));
#49132=CARTESIAN_POINT('Ctrl Pts',(-31.4400305164273,54.4529728621045,15.7036322918186));
#49133=CARTESIAN_POINT('Ctrl Pts',(-33.4699088102677,54.4039143989828,15.5924944012505));
#49134=CARTESIAN_POINT('Ctrl Pts',(-34.6120185708019,56.0827228792765,15.4813565106825));
#49135=CARTESIAN_POINT('Ctrl Pts',(-33.8209737810694,57.9527658651135,15.3702186201144));
#49136=CARTESIAN_POINT('Ctrl Pts',(-31.8208267096473,58.3023717975755,15.2590807295464));
#49137=CARTESIAN_POINT('Ctrl Pts',(-30.4423346512631,56.811542414391,15.1479428389783));
#49138=CARTESIAN_POINT('Ctrl Pts',(-30.9472470260343,54.8448507321039,15.0368049484103));
#49139=CARTESIAN_POINT('Ctrl Pts',(-32.873411799399,54.2024320014245,14.9256670578423));
#49140=CARTESIAN_POINT('Ctrl Pts',(-34.4577885337935,55.4722992717785,14.8145291672742));
#49141=CARTESIAN_POINT('Ctrl Pts',(-34.2501791887594,57.4921288300438,14.7033912767062));
#49142=CARTESIAN_POINT('Ctrl Pts',(-32.4406110471432,58.4131473734421,14.5922533861381));
#49143=CARTESIAN_POINT('Ctrl Pts',(-30.685402160969,57.3923369880037,14.4811154955701));
#49144=CARTESIAN_POINT('Ctrl Pts',(-30.5911155092112,55.3640553875343,14.3699776050021));
#49145=CARTESIAN_POINT('Ctrl Pts',(-32.2440519729435,54.1848149428223,14.258839714434));
#49146=CARTESIAN_POINT('Ctrl Pts',(-34.1312615834455,54.9339813630547,14.147701823866));
#49147=CARTESIAN_POINT('Ctrl Pts',(-34.5253569356325,56.9258470226862,14.0365639332979));
#49148=CARTESIAN_POINT('Ctrl Pts',(-33.0656241805903,58.3372088874948,13.9254260427299));
#49149=CARTESIAN_POINT('Ctrl Pts',(-31.0881610630665,57.8762830833115,13.8142881521618));
#49150=CARTESIAN_POINT('Ctrl Pts',(-30.4029864170935,55.964856866078,13.7031502615938));
#49151=CARTESIAN_POINT('Ctrl Pts',(-31.6371995019103,54.3526871828874,13.5920123710258));
#49152=CARTESIAN_POINT('Ctrl Pts',(-33.661208875352,54.5149972498541,13.4808744804577));
#49153=CARTESIAN_POINT('Ctrl Pts',(-34.6222201085763,56.3040513729488,13.3697365898897));
#49154=CARTESIAN_POINT('Ctrl Pts',(-33.6410001923652,58.0806490489849,13.2585986993216));
#49155=CARTESIAN_POINT('Ctrl Pts',(-31.6148898816497,58.2219813552109,13.1474608087536));
#49156=CARTESIAN_POINT('Ctrl Pts',(-30.3999497178981,56.5918847767849,13.0363229181856));
#49157=CARTESIAN_POINT('Ctrl Pts',(-30.8705832444619,55.3295607530454,12.9622309911402));
#49158=CARTESIAN_POINT('Ctrl Pts',(-31.320879066691,54.9374749902607,12.9251850276175));
#49159=CARTESIAN_POINT('Ctrl Pts',(-30.8911239915931,56.7241717536789,22.2244449171475));
#49160=CARTESIAN_POINT('Ctrl Pts',(-30.7473006326931,56.1891822041237,22.1873989536248));
#49161=CARTESIAN_POINT('Ctrl Pts',(-31.0382252657072,54.9735300058982,22.1133070265794));
#49162=CARTESIAN_POINT('Ctrl Pts',(-32.8174923591508,54.3470730060695,22.0021691360114));
#49163=CARTESIAN_POINT('Ctrl Pts',(-34.304571327466,55.5045615106007,21.8910312454433));
#49164=CARTESIAN_POINT('Ctrl Pts',(-34.1406566697445,57.3804999672191,21.7798933548753));
#49165=CARTESIAN_POINT('Ctrl Pts',(-32.474658653275,58.2607899676461,21.6687554643073));
#49166=CARTESIAN_POINT('Ctrl Pts',(-30.8320413354105,57.3382119657361,21.5576175737392));
#49167=CARTESIAN_POINT('Ctrl Pts',(-30.7160328400182,55.4579513902372,21.4464796831712));
#49168=CARTESIAN_POINT('Ctrl Pts',(-32.2329560159994,54.3406626672683,21.3353417926031));
#49169=CARTESIAN_POINT('Ctrl Pts',(-33.9942844449089,55.0091974164725,21.2242039020351));
#49170=CARTESIAN_POINT('Ctrl Pts',(-34.3878889346486,56.8515459694957,21.1130660114671));
#49171=CARTESIAN_POINT('Ctrl Pts',(-33.0534814963164,58.1814318877282,21.001928120899));
#49172=CARTESIAN_POINT('Ctrl Pts',(-31.2124690536731,57.7815724803175,20.890790230331));
#49173=CARTESIAN_POINT('Ctrl Pts',(-30.5499468456396,56.0179751041415,20.7796523397629));
#49174=CARTESIAN_POINT('Ctrl Pts',(-31.672331125513,54.504874688596,20.6685144491949));
#49175=CARTESIAN_POINT('Ctrl Pts',(-33.552289752533,54.6272320766892,20.5573765586268));
#49176=CARTESIAN_POINT('Ctrl Pts',(-34.4690758152034,56.2730507279312,20.4462386680588));
#49177=CARTESIAN_POINT('Ctrl Pts',(-33.5835443634768,57.9358948832952,20.3351007774908));
#49178=CARTESIAN_POINT('Ctrl Pts',(-31.7062325125535,58.0937440710183,20.2239628869227));
#49179=CARTESIAN_POINT('Ctrl Pts',(-30.5554650223787,56.602117318542,20.1128249963547));
#49180=CARTESIAN_POINT('Ctrl Pts',(-31.1845524609634,54.8263174191154,20.0016871057866));
#49181=CARTESIAN_POINT('Ctrl Pts',(-33.0176839446135,54.3917542043407,19.8905492152186));
#49182=CARTESIAN_POINT('Ctrl Pts',(-34.3769734456241,55.6961882906393,19.7794113246506));
#49183=CARTESIAN_POINT('Ctrl Pts',(-34.018247864129,57.5456563766984,19.6682734340825));
#49184=CARTESIAN_POINT('Ctrl Pts',(-32.2698527951939,58.2473193433743,19.5571355435145));
#49185=CARTESIAN_POINT('Ctrl Pts',(-30.7321140725153,57.1589371226573,19.4459976529464));
#49186=CARTESIAN_POINT('Ctrl Pts',(-30.812541388628,55.2767183028703,19.3348597623784));
#49187=CARTESIAN_POINT('Ctrl Pts',(-32.4375187087245,54.3234791162739,19.2237218718103));
#49188=CARTESIAN_POINT('Ctrl Pts',(-34.1196858633551,55.1717302004793,19.1125839812423));
#49189=CARTESIAN_POINT('Ctrl Pts',(-34.3193361787479,57.0450577184658,19.0014460906742));
#49190=CARTESIAN_POINT('Ctrl Pts',(-32.8537274570681,58.2287837479543,18.8903082001062));
#49191=CARTESIAN_POINT('Ctrl Pts',(-31.0643479823862,57.6394304298312,18.7791703095382));
#49192=CARTESIAN_POINT('Ctrl Pts',(-30.5890370808302,55.8164395398742,18.6680324189701));
#49193=CARTESIAN_POINT('Ctrl Pts',(-31.8628522109823,54.4284153137944,18.5568945284021));
#49194=CARTESIAN_POINT('Ctrl Pts',(-33.7198559381705,54.7458320669828,18.445756637834));
#49195=CARTESIAN_POINT('Ctrl Pts',(-34.4603116910435,56.4781546454978,18.334618747266));
#49196=CARTESIAN_POINT('Ctrl Pts',(-33.406471921658,58.039768547349,18.223480856698));
#49197=CARTESIAN_POINT('Ctrl Pts',(-31.522928122288,58.0013108582667,18.1123429661299));
#49198=CARTESIAN_POINT('Ctrl Pts',(-30.5337092933366,56.3979823372073,18.0012050755619));
#49199=CARTESIAN_POINT('Ctrl Pts',(-31.3442586474474,54.6973277624788,17.8900671849938));
#49200=CARTESIAN_POINT('Ctrl Pts',(-33.212671168548,54.4559755530648,17.7789292944258));
#49201=CARTESIAN_POINT('Ctrl Pts',(-34.4287676868359,55.8948381233621,17.6677914038578));
#49202=CARTESIAN_POINT('Ctrl Pts',(-33.8794412676495,57.6969082449663,17.5566535132897));
#49203=CARTESIAN_POINT('Ctrl Pts',(-32.0674966122556,58.2127306987079,17.4455156227217));
#49204=CARTESIAN_POINT('Ctrl Pts',(-30.6514272125861,56.9701673428525,17.3343777321536));
#49205=CARTESIAN_POINT('Ctrl Pts',(-30.9273774494778,55.1065505086418,17.2232398415856));
#49206=CARTESIAN_POINT('Ctrl Pts',(-32.6427669416152,54.3276698192808,17.1121019510175));
#49207=CARTESIAN_POINT('Ctrl Pts',(-34.2274802330049,55.3464436028498,17.0009640604495));
#49208=CARTESIAN_POINT('Ctrl Pts',(-34.231011276167,57.2303766615671,16.8898261698814));
#49209=CARTESIAN_POINT('Ctrl Pts',(-32.6501280672502,58.2550837015355,16.7786882793134));
#49210=CARTESIAN_POINT('Ctrl Pts',(-30.9318309358115,57.4826387481023,16.6675503887454));
#49211=CARTESIAN_POINT('Ctrl Pts',(-30.6488967330708,55.6200694272693,16.5564124981774));
#49212=CARTESIAN_POINT('Ctrl Pts',(-32.0602983434901,54.372206561362,16.4452746076093));
#49213=CARTESIAN_POINT('Ctrl Pts',(-33.8741638666671,54.8812331832842,16.3341367170413));
#49214=CARTESIAN_POINT('Ctrl Pts',(-34.4302416186091,56.6812314532133,16.2229988264732));
#49215=CARTESIAN_POINT('Ctrl Pts',(-33.2195473266022,58.1246425413596,16.1118609359052));
#49216=CARTESIAN_POINT('Ctrl Pts',(-31.3502432063489,57.8902959092574,16.0007230453371));
#49217=CARTESIAN_POINT('Ctrl Pts',(-30.5333245184248,56.1926916871221,15.8895851547691));
#49218=CARTESIAN_POINT('Ctrl Pts',(-31.5165262024604,54.5856662712538,15.778447264201));
#49219=CARTESIAN_POINT('Ctrl Pts',(-33.3999126066214,54.5401482504283,15.667309373633));
#49220=CARTESIAN_POINT('Ctrl Pts',(-34.4595987964669,56.0978007838681,15.556171483065));
#49221=CARTESIAN_POINT('Ctrl Pts',(-33.7256419840878,57.8328868456334,15.4450335924969));
#49222=CARTESIAN_POINT('Ctrl Pts',(-31.8698411648614,58.1572624803751,15.3338957019289));
#49223=CARTESIAN_POINT('Ctrl Pts',(-30.590831872096,56.7740230025534,15.2227578113608));
#49224=CARTESIAN_POINT('Ctrl Pts',(-31.0593058218999,54.9492631699881,15.1116199207928));
#49225=CARTESIAN_POINT('Ctrl Pts',(-32.8464634841781,54.353206398106,15.0004820302248));
#49226=CARTESIAN_POINT('Ctrl Pts',(-34.3164992048823,55.531430116903,14.8893441396567));
#49227=CARTESIAN_POINT('Ctrl Pts',(-34.123872573522,57.4054929808209,14.7782062490887));
#49228=CARTESIAN_POINT('Ctrl Pts',(-32.4448970183546,58.2600436245124,14.6670683585206));
#49229=CARTESIAN_POINT('Ctrl Pts',(-30.8163577297114,57.3129028983934,14.5559304679526));
#49230=CARTESIAN_POINT('Ctrl Pts',(-30.7288755399893,55.4309979577248,14.4447925773845));
#49231=CARTESIAN_POINT('Ctrl Pts',(-32.2625231838812,54.3368607242037,14.3336546868165));
#49232=CARTESIAN_POINT('Ctrl Pts',(-34.0135369924464,55.0319614376805,14.2225167962484));
#49233=CARTESIAN_POINT('Ctrl Pts',(-34.3791913425147,56.880078496545,14.1113789056804));
#49234=CARTESIAN_POINT('Ctrl Pts',(-33.0248043169983,58.1895854534881,14.0002410151124));
#49235=CARTESIAN_POINT('Ctrl Pts',(-31.1900504001867,57.7619236593993,13.8891031245443));
#49236=CARTESIAN_POINT('Ctrl Pts',(-30.5543233141752,55.9884409037984,13.7779652339763));
#49237=CARTESIAN_POINT('Ctrl Pts',(-31.69946593225,54.4926179908013,13.6668273434083));
#49238=CARTESIAN_POINT('Ctrl Pts',(-33.5774069631985,54.6432144942031,13.5556894528402));
#49239=CARTESIAN_POINT('Ctrl Pts',(-34.4690641115077,56.3031564828284,13.4445515622722));
#49240=CARTESIAN_POINT('Ctrl Pts',(-33.5586566967914,57.9515409790141,13.3334136717041));
#49241=CARTESIAN_POINT('Ctrl Pts',(-31.6787663486305,58.0826736409194,13.2222757811361));
#49242=CARTESIAN_POINT('Ctrl Pts',(-30.5515057669383,56.5702175776209,13.111137890568));
#49243=CARTESIAN_POINT('Ctrl Pts',(-30.9881746982542,55.3989927257806,13.0370459635227));
#49244=CARTESIAN_POINT('Ctrl Pts',(-31.4059736530045,55.03520293743,13.));
#49245=CARTESIAN_POINT('Ctrl Pts',(-31.6688940285233,54.8502492137286,21.3785196366098));
#49246=CARTESIAN_POINT('Ctrl Pts',(-31.8552973625104,54.7413392620857,21.3641270219409));
#49247=CARTESIAN_POINT('Ctrl Pts',(-32.0614196306261,54.6673572529872,21.349734407272));
#49248=CARTESIAN_POINT('Ctrl Pts',(-32.2736902248208,54.6382999126305,21.3353417926031));
#49249=CARTESIAN_POINT('Ctrl Pts',(-32.8200654923026,54.5635075836697,21.2982958290804));
#49250=CARTESIAN_POINT('Ctrl Pts',(-33.4071749686058,54.7863525000711,21.2612498655578));
#49251=CARTESIAN_POINT('Ctrl Pts',(-33.7663304550473,55.2048330504423,21.2242039020351));
#49252=CARTESIAN_POINT('Ctrl Pts',(-34.1254859414888,55.6233136008135,21.1871579385124));
#49253=CARTESIAN_POINT('Ctrl Pts',(-34.2566874380687,56.2374297851546,21.1501119749897));
#49254=CARTESIAN_POINT('Ctrl Pts',(-34.0998869466366,56.7661355303639,21.113066011467));
#49255=CARTESIAN_POINT('Ctrl Pts',(-33.9430864552046,57.2948412755732,21.0760200479444));
#49256=CARTESIAN_POINT('Ctrl Pts',(-33.4982839757605,57.7381365816507,21.0389740844217));
#49257=CARTESIAN_POINT('Ctrl Pts',(-32.9690473289312,57.893141000121,21.001928120899));
#49258=CARTESIAN_POINT('Ctrl Pts',(-32.4398106821019,58.0481454185913,20.9648821573763));
#49259=CARTESIAN_POINT('Ctrl Pts',(-31.8261398678875,57.9148589494544,20.9278361938536));
#49260=CARTESIAN_POINT('Ctrl Pts',(-31.4088840927747,57.5542828188566,20.890790230331));
#49261=CARTESIAN_POINT('Ctrl Pts',(-30.9916283176619,57.1937066882589,20.8537442668083));
#49262=CARTESIAN_POINT('Ctrl Pts',(-30.7707875816508,56.6058408962002,20.8166983032856));
#49263=CARTESIAN_POINT('Ctrl Pts',(-30.8474312602907,56.0597245975799,20.7796523397629));
#49264=CARTESIAN_POINT('Ctrl Pts',(-30.9171750925773,55.5627724129274,20.7459414387119));
#49265=CARTESIAN_POINT('Ctrl Pts',(-31.2332522390469,55.1003910850246,20.7122305376608));
#49266=CARTESIAN_POINT('Ctrl Pts',(-31.666645377609,54.8465106721999,20.6785196366098));
#49267=CARTESIAN_POINT('Ctrl Pts',(-30.5157034944334,56.8250975324092,22.));
#49268=CARTESIAN_POINT('Ctrl Pts',(-30.5033891751538,56.7529213757994,22.));
#49269=CARTESIAN_POINT('Ctrl Pts',(-30.4952952696159,56.6802754208432,22.));
#49270=CARTESIAN_POINT('Ctrl Pts',(-30.4912615438001,56.607470311302,22.));
#49271=CARTESIAN_POINT('Ctrl Pts',(-30.4871154839524,56.5326376738947,22.));
#49272=CARTESIAN_POINT('Ctrl Pts',(-30.487259104724,56.4576358814836,22.));
#49273=CARTESIAN_POINT('Ctrl Pts',(-30.4915726828735,56.3828069694704,22.));
#49274=CARTESIAN_POINT('Ctrl Pts',(-30.4952175802641,56.3195778597398,22.));
#49275=CARTESIAN_POINT('Ctrl Pts',(-30.5018408843279,56.2564719495607,22.));
#49276=CARTESIAN_POINT('Ctrl Pts',(-30.5113973391135,56.1937062820743,22.));
#49277=CARTESIAN_POINT('Ctrl Pts',(-30.5156431766697,56.1658201219624,22.));
#49278=CARTESIAN_POINT('Ctrl Pts',(-30.5204683060506,56.1380012967317,22.));
#49279=CARTESIAN_POINT('Ctrl Pts',(-30.5258701615125,56.1102698241508,22.));
#49280=CARTESIAN_POINT('Ctrl Pts',(-30.5288380312313,56.0950336893984,22.));
#49281=CARTESIAN_POINT('Ctrl Pts',(-30.5319800053069,56.079823934807,22.));
#49282=CARTESIAN_POINT('Ctrl Pts',(-30.5352957613589,56.0646439756259,22.));
#49283=CARTESIAN_POINT('Ctrl Pts',(-30.5383537435174,56.050644138601,22.));
#49284=CARTESIAN_POINT('Ctrl Pts',(-30.5415601340454,56.0366676410989,22.));
#49285=CARTESIAN_POINT('Ctrl Pts',(-30.5449092364481,56.0227386583762,22.));
#49286=CARTESIAN_POINT('Ctrl Pts',(-30.562023288202,55.9515609807379,22.));
#49287=CARTESIAN_POINT('Ctrl Pts',(-30.582885617709,55.8814985818673,22.));
#49288=CARTESIAN_POINT('Ctrl Pts',(-30.6073807784317,55.8128705897534,22.));
#49289=CARTESIAN_POINT('Ctrl Pts',(-30.6316859828533,55.744774797435,22.));
#49290=CARTESIAN_POINT('Ctrl Pts',(-30.6595684038256,55.6780903688681,22.));
#49291=CARTESIAN_POINT('Ctrl Pts',(-30.6909586479405,55.6131557366303,22.));
#49292=CARTESIAN_POINT('Ctrl Pts',(-30.717046572308,55.5591896136386,22.));
#49293=CARTESIAN_POINT('Ctrl Pts',(-30.7455582375738,55.5064323069469,22.));
#49294=CARTESIAN_POINT('Ctrl Pts',(-30.7764732244705,55.4550987628743,22.));
#49295=CARTESIAN_POINT('Ctrl Pts',(-30.7893770627354,55.4336722698765,22.));
#49296=CARTESIAN_POINT('Ctrl Pts',(-30.8026998040084,55.4124940848702,22.));
#49297=CARTESIAN_POINT('Ctrl Pts',(-30.8164407555073,55.3915810450032,22.));
#49298=CARTESIAN_POINT('Ctrl Pts',(-30.8228008343902,55.3819013235337,22.));
#49299=CARTESIAN_POINT('Ctrl Pts',(-30.8292505148999,55.3722784163222,22.));
#49300=CARTESIAN_POINT('Ctrl Pts',(-30.8357897592665,55.3627140504885,22.));
#49301=CARTESIAN_POINT('Ctrl Pts',(-30.842610586495,55.3527378386747,22.));
#49302=CARTESIAN_POINT('Ctrl Pts',(-30.8495241989623,55.342832182411,22.));
#49303=CARTESIAN_POINT('Ctrl Pts',(-30.8565275508905,55.3330023510939,22.));
#49304=CARTESIAN_POINT('Ctrl Pts',(-30.8964137687943,55.2770184739607,22.));
#49305=CARTESIAN_POINT('Ctrl Pts',(-30.9392347488862,55.223452024519,22.));
#49306=CARTESIAN_POINT('Ctrl Pts',(-30.9849250921345,55.1725987747036,22.));
#49307=CARTESIAN_POINT('Ctrl Pts',(-31.0263368675617,55.1265075613009,22.));
#49308=CARTESIAN_POINT('Ctrl Pts',(-31.070106455774,55.0826451744756,22.));
#49309=CARTESIAN_POINT('Ctrl Pts',(-31.1162077188352,55.0412612463575,22.));
#49310=CARTESIAN_POINT('Ctrl Pts',(-31.1707480896715,54.9923017464142,22.));
#49311=CARTESIAN_POINT('Ctrl Pts',(-31.2285529377195,54.9468098709297,22.));
#49312=CARTESIAN_POINT('Ctrl Pts',(-31.2892182914168,54.9049320829473,22.));
#49313=CARTESIAN_POINT('Ctrl Pts',(-31.3025747483259,54.8957120119093,22.));
#49314=CARTESIAN_POINT('Ctrl Pts',(-31.316069903986,54.8866673619299,22.));
#49315=CARTESIAN_POINT('Ctrl Pts',(-31.3296994894175,54.8778000986119,22.));
#49316=CARTESIAN_POINT('Ctrl Pts',(-31.3437625465174,54.8686508232369,22.));
#49317=CARTESIAN_POINT('Ctrl Pts',(-31.35797403863,54.8596873154124,22.));
#49318=CARTESIAN_POINT('Ctrl Pts',(-31.3723000273365,54.8509292655043,22.));
#49319=CARTESIAN_POINT('Ctrl Pts',(-31.4308133755576,54.8151577153162,22.));
#49320=CARTESIAN_POINT('Ctrl Pts',(-31.4913062998034,54.7827600287089,22.));
#49321=CARTESIAN_POINT('Ctrl Pts',(-31.5534255550724,54.7538008858545,22.));
#49322=CARTESIAN_POINT('Ctrl Pts',(-31.6155323755621,54.7248475399232,22.));
#49323=CARTESIAN_POINT('Ctrl Pts',(-31.6792660307875,54.6993312183976,22.));
#49324=CARTESIAN_POINT('Ctrl Pts',(-31.7442852730188,54.6773670392608,22.));
#49325=CARTESIAN_POINT('Ctrl Pts',(-31.791347955944,54.6614687734097,22.));
#49326=CARTESIAN_POINT('Ctrl Pts',(-31.8390844862475,54.6474326075963,22.));
#49327=CARTESIAN_POINT('Ctrl Pts',(-31.8873641955329,54.6353193456783,22.));
#49328=CARTESIAN_POINT('Ctrl Pts',(-31.9235796702862,54.6262329709327,22.));
#49329=CARTESIAN_POINT('Ctrl Pts',(-31.9601007697018,54.6182288634993,22.));
#49330=CARTESIAN_POINT('Ctrl Pts',(-31.9968706813336,54.6113381701107,22.));
#49331=CARTESIAN_POINT('Ctrl Pts',(-32.0090868552777,54.6090488551438,22.));
#49332=CARTESIAN_POINT('Ctrl Pts',(-32.0213209008061,54.6068842729294,22.));
#49333=CARTESIAN_POINT('Ctrl Pts',(-32.03357036514,54.6048451279784,22.));
#49334=CARTESIAN_POINT('Ctrl Pts',(-32.0985567096936,54.5940269752194,22.));
#49335=CARTESIAN_POINT('Ctrl Pts',(-32.1639811762486,54.5867347457029,22.));
#49336=CARTESIAN_POINT('Ctrl Pts',(-32.2295294708426,54.583092151071,22.));
#49337=CARTESIAN_POINT('Ctrl Pts',(-32.2756530618083,54.5805290097125,22.));
#49338=CARTESIAN_POINT('Ctrl Pts',(-32.3218379339147,54.5797739344473,22.));
#49339=CARTESIAN_POINT('Ctrl Pts',(-32.3679699516131,54.5808847307995,22.));
#49340=CARTESIAN_POINT('Ctrl Pts',(-32.3827771688533,54.5812412684867,22.));
#49341=CARTESIAN_POINT('Ctrl Pts',(-32.3975809348718,54.5817902377288,22.));
#49342=CARTESIAN_POINT('Ctrl Pts',(-32.4123708490685,54.5825334834863,22.));
#49343=CARTESIAN_POINT('Ctrl Pts',(-32.4753792589169,54.5856998800376,22.));
#49344=CARTESIAN_POINT('Ctrl Pts',(-32.5380109271213,54.5923812630455,22.));
#49345=CARTESIAN_POINT('Ctrl Pts',(-32.599975776176,54.6027055704928,22.));
#49346=CARTESIAN_POINT('Ctrl Pts',(-32.6570986727596,54.6122231333627,22.));
#49347=CARTESIAN_POINT('Ctrl Pts',(-32.7136552659116,54.6248370045788,22.));
#49348=CARTESIAN_POINT('Ctrl Pts',(-32.7694005056339,54.6406824777883,22.));
#49349=CARTESIAN_POINT('Ctrl Pts',(-32.7798334333406,54.6436480166809,22.));
#49350=CARTESIAN_POINT('Ctrl Pts',(-32.7902378797118,54.6467268441195,22.));
#49351=CARTESIAN_POINT('Ctrl Pts',(-32.8006124898339,54.6499179279034,22.));
#49352=CARTESIAN_POINT('Origin',(-32.5,56.2916512459885,17.));
#49353=CARTESIAN_POINT('Origin',(32.5,56.2916512459885,13.));
#49354=CARTESIAN_POINT('Ctrl Pts',(31.9588970197441,54.7159724828016,13.));
#49355=CARTESIAN_POINT('Ctrl Pts',(32.0152863485799,54.6890038458289,13.));
#49356=CARTESIAN_POINT('Ctrl Pts',(32.0731449906843,54.6655486354191,13.));
#49357=CARTESIAN_POINT('Ctrl Pts',(32.1321548891936,54.6454940895918,13.));
#49358=CARTESIAN_POINT('Ctrl Pts',(32.1695849277563,54.6327734708036,13.));
#49359=CARTESIAN_POINT('Ctrl Pts',(32.2074789471058,54.6214218413018,13.));
#49360=CARTESIAN_POINT('Ctrl Pts',(32.2457622247192,54.6114186950782,13.));
#49361=CARTESIAN_POINT('Ctrl Pts',(32.2719048889137,54.6045878041797,13.));
#49362=CARTESIAN_POINT('Ctrl Pts',(32.2982291704566,54.5983858679889,13.));
#49363=CARTESIAN_POINT('Ctrl Pts',(32.3247122732464,54.5928081200755,13.));
#49364=CARTESIAN_POINT('Ctrl Pts',(32.3387744982338,54.5898463996645,13.));
#49365=CARTESIAN_POINT('Ctrl Pts',(32.3528813591965,54.5870608477191,13.));
#49366=CARTESIAN_POINT('Ctrl Pts',(32.3670153450051,54.5844531528782,13.));
#49367=CARTESIAN_POINT('Ctrl Pts',(32.4318895160093,54.5724839855584,13.));
#49368=CARTESIAN_POINT('Ctrl Pts',(32.4974065808839,54.564242006131,13.));
#49369=CARTESIAN_POINT('Ctrl Pts',(32.5632274830034,54.5596289937387,13.));
#49370=CARTESIAN_POINT('Ctrl Pts',(32.6107070715096,54.5563014196231,13.));
#49371=CARTESIAN_POINT('Ctrl Pts',(32.6583455247626,54.5548630893557,13.));
#49372=CARTESIAN_POINT('Ctrl Pts',(32.7060224975765,54.5552923689741,13.));
#49373=CARTESIAN_POINT('Ctrl Pts',(32.7190852578705,54.5554099850144,13.));
#49374=CARTESIAN_POINT('Ctrl Pts',(32.7321509321603,54.555667872943,13.));
#49375=CARTESIAN_POINT('Ctrl Pts',(32.7452170875462,54.5560657581446,13.));
#49376=CARTESIAN_POINT('Ctrl Pts',(32.7585822784109,54.5564727494519,13.));
#49377=CARTESIAN_POINT('Ctrl Pts',(32.7719398790819,54.5570260108108,13.));
#49378=CARTESIAN_POINT('Ctrl Pts',(32.7852820453889,54.5577244070497,13.));
#49379=CARTESIAN_POINT('Ctrl Pts',(32.853041605873,54.561271284004,13.));
#49380=CARTESIAN_POINT('Ctrl Pts',(32.9204432863695,54.5685589035957,13.));
#49381=CARTESIAN_POINT('Ctrl Pts',(32.9871435056369,54.5794869269798,13.));
#49382=CARTESIAN_POINT('Ctrl Pts',(33.0548103384148,54.5905733182847,13.));
#49383=CARTESIAN_POINT('Ctrl Pts',(33.1217562800348,54.6054062113063,13.));
#49384=CARTESIAN_POINT('Ctrl Pts',(33.1876366469328,54.6239318015843,13.));
#49385=CARTESIAN_POINT('Ctrl Pts',(33.2284548198869,54.6354098910918,13.));
#49386=CARTESIAN_POINT('Ctrl Pts',(33.2688641590369,54.6483065465144,13.));
#49387=CARTESIAN_POINT('Ctrl Pts',(33.3087825622703,54.662619012904,13.));
#49388=CARTESIAN_POINT('Ctrl Pts',(33.3414809094137,54.6743427783,13.));
#49389=CARTESIAN_POINT('Ctrl Pts',(33.3738498710885,54.6870166551149,13.));
#49390=CARTESIAN_POINT('Ctrl Pts',(33.4058433876126,54.7006430223894,13.));
#49391=CARTESIAN_POINT('Ctrl Pts',(33.4189228879679,54.7062137159227,13.));
#49392=CARTESIAN_POINT('Ctrl Pts',(33.4319419054982,54.7119448243245,13.));
#49393=CARTESIAN_POINT('Ctrl Pts',(33.4448753978619,54.7178263149849,13.));
#49394=CARTESIAN_POINT('Ctrl Pts',(33.5090388472157,54.7470045692029,13.));
#49395=CARTESIAN_POINT('Ctrl Pts',(33.5712122520923,54.7799269958923,13.));
#49396=CARTESIAN_POINT('Ctrl Pts',(33.6310396925136,54.816520963373,13.));
#49397=CARTESIAN_POINT('Ctrl Pts',(33.6376901818306,54.8205887922503,13.));
#49398=CARTESIAN_POINT('Ctrl Pts',(33.6443116826016,54.8247020426775,13.));
#49399=CARTESIAN_POINT('Ctrl Pts',(33.6509037041525,54.8288606547027,13.));
#49400=CARTESIAN_POINT('Ctrl Pts',(33.7079313851622,54.8648368720406,13.));
#49401=CARTESIAN_POINT('Ctrl Pts',(33.7627542963076,54.9042038022191,13.));
#49402=CARTESIAN_POINT('Ctrl Pts',(33.815278351599,54.9466335926782,13.));
#49403=CARTESIAN_POINT('Ctrl Pts',(33.8717836154444,54.9922794684867,13.));
#49404=CARTESIAN_POINT('Ctrl Pts',(33.9256293125948,55.0414702768426,13.));
#49405=CARTESIAN_POINT('Ctrl Pts',(33.9766695218208,55.0938552564678,13.));
#49406=CARTESIAN_POINT('Ctrl Pts',(33.9860164683474,55.1034484695595,13.));
#49407=CARTESIAN_POINT('Ctrl Pts',(33.9952692319585,55.1131489427183,13.));
#49408=CARTESIAN_POINT('Ctrl Pts',(34.0044267784923,55.122954700519,13.));
#49409=CARTESIAN_POINT('Ctrl Pts',(34.0122933717197,55.1313781256821,13.));
#49410=CARTESIAN_POINT('Ctrl Pts',(34.0200833037881,55.1398724075814,13.));
#49411=CARTESIAN_POINT('Ctrl Pts',(34.0277952352549,55.1484347978079,13.));
#49412=CARTESIAN_POINT('Ctrl Pts',(34.0753570092449,55.2012416037971,13.));
#49413=CARTESIAN_POINT('Ctrl Pts',(34.1199659342344,55.2566479177833,13.));
#49414=CARTESIAN_POINT('Ctrl Pts',(34.1615258635099,55.3142853318928,13.));
#49415=CARTESIAN_POINT('Ctrl Pts',(34.203961681234,55.3731374724492,13.));
#49416=CARTESIAN_POINT('Ctrl Pts',(34.2432193073913,55.4343163955046,13.));
#49417=CARTESIAN_POINT('Ctrl Pts',(34.279168752062,55.4974776038552,13.));
#49418=CARTESIAN_POINT('Ctrl Pts',(34.3153358231695,55.5610211699543,13.));
#49419=CARTESIAN_POINT('Ctrl Pts',(34.3481552082549,55.6265719324186,13.));
#49420=CARTESIAN_POINT('Ctrl Pts',(34.3774567489378,55.6938154068255,13.));
#49421=CARTESIAN_POINT('Ctrl Pts',(34.3846992417049,55.7104360474361,13.));
#49422=CARTESIAN_POINT('Ctrl Pts',(34.3917266096341,55.7271602398749,13.));
#49423=CARTESIAN_POINT('Ctrl Pts',(34.3985358555223,55.7439834808493,13.));
#49424=CARTESIAN_POINT('Ctrl Pts',(34.4038603586493,55.7571384470005,13.));
#49425=CARTESIAN_POINT('Ctrl Pts',(34.4090519562624,55.7703555309735,13.));
#49426=CARTESIAN_POINT('Ctrl Pts',(34.4141017841657,55.78361234165,13.));
#49427=CARTESIAN_POINT('Ctrl Pts',(34.4409205170208,55.8540168922319,13.));
#49428=CARTESIAN_POINT('Ctrl Pts',(34.4637958508171,55.9256644804537,13.));
#49429=CARTESIAN_POINT('Ctrl Pts',(34.4826007269245,55.9981857629538,13.));
#49430=CARTESIAN_POINT('Ctrl Pts',(34.5014259920285,56.0707856759206,13.));
#49431=CARTESIAN_POINT('Ctrl Pts',(34.5161726006451,56.1442621127221,13.));
#49432=CARTESIAN_POINT('Ctrl Pts',(34.5266721187438,56.2182764863688,13.));
#49433=CARTESIAN_POINT('Ctrl Pts',(34.5369326971032,56.2906064993641,13.));
#49434=CARTESIAN_POINT('Ctrl Pts',(34.5431377093135,56.3634511943331,13.));
#49435=CARTESIAN_POINT('Ctrl Pts',(34.5450833843614,56.4365110275565,13.));
#49436=CARTESIAN_POINT('Ctrl Pts',(34.5455017158085,56.4522193164544,13.));
#49437=CARTESIAN_POINT('Ctrl Pts',(34.5457229607325,56.4679375826975,13.));
#49438=CARTESIAN_POINT('Ctrl Pts',(34.5457447745363,56.4836628867631,13.));
#49439=CARTESIAN_POINT('Ctrl Pts',(34.545763248735,56.4969807103663,13.));
#49440=CARTESIAN_POINT('Ctrl Pts',(34.5456386792457,56.5103035820178,13.));
#49441=CARTESIAN_POINT('Ctrl Pts',(34.5453721234943,56.52362996598,13.));
#49442=CARTESIAN_POINT('Ctrl Pts',(34.1542537360139,57.5104384051693,13.));
#49443=CARTESIAN_POINT('Ctrl Pts',(34.1045519887874,57.5661317580794,13.));
#49444=CARTESIAN_POINT('Ctrl Pts',(34.0516736631994,57.6187667032821,13.));
#49445=CARTESIAN_POINT('Ctrl Pts',(33.9959663128832,57.6682442041037,13.));
#49446=CARTESIAN_POINT('Ctrl Pts',(33.9417168531154,57.7164268528026,13.));
#49447=CARTESIAN_POINT('Ctrl Pts',(33.8847834892842,57.7616152150798,13.));
#49448=CARTESIAN_POINT('Ctrl Pts',(33.8254670336605,57.8036766866523,13.));
#49449=CARTESIAN_POINT('Ctrl Pts',(33.8122280670726,57.8130644764474,13.));
#49450=CARTESIAN_POINT('Ctrl Pts',(33.7988685443533,57.8222975377499,13.));
#49451=CARTESIAN_POINT('Ctrl Pts',(33.7853974830175,57.8313702492573,13.));
#49452=CARTESIAN_POINT('Ctrl Pts',(33.7235792094515,57.8730046348467,13.));
#49453=CARTESIAN_POINT('Ctrl Pts',(33.6595370839855,57.9111844300756,13.));
#49454=CARTESIAN_POINT('Ctrl Pts',(33.5936094996551,57.9457862388347,13.));
#49455=CARTESIAN_POINT('Ctrl Pts',(33.5473238504462,57.9700790625212,13.));
#49456=CARTESIAN_POINT('Ctrl Pts',(33.5001083178125,57.9926073121088,13.));
#49457=CARTESIAN_POINT('Ctrl Pts',(33.4520768825943,58.0133132482739,13.));
#49458=CARTESIAN_POINT('Ctrl Pts',(33.4338169281544,58.0211849566518,13.));
#49459=CARTESIAN_POINT('Ctrl Pts',(33.4154390450392,58.0287931599074,13.));
#49460=CARTESIAN_POINT('Ctrl Pts',(33.396949493977,58.036134191934,13.));
#49461=CARTESIAN_POINT('Ctrl Pts',(33.3793383499135,58.0431264640644,13.));
#49462=CARTESIAN_POINT('Ctrl Pts',(33.3616202465401,58.0498782555098,13.));
#49463=CARTESIAN_POINT('Ctrl Pts',(33.3438321782917,58.0563750966341,13.));
#49464=CARTESIAN_POINT('Ctrl Pts',(33.2756398801499,58.0812813720512,13.));
#49465=CARTESIAN_POINT('Ctrl Pts',(33.2063496366854,58.1024753903028,13.));
#49466=CARTESIAN_POINT('Ctrl Pts',(33.1362740500475,58.1198408416597,13.));
#49467=CARTESIAN_POINT('Ctrl Pts',(33.0677030438195,58.1368334425108,13.));
#49468=CARTESIAN_POINT('Ctrl Pts',(32.9983791190584,58.150160130782,13.));
#49469=CARTESIAN_POINT('Ctrl Pts',(32.9285938583003,58.1596629269119,13.));
#49470=CARTESIAN_POINT('Ctrl Pts',(32.860339265009,58.1689572890441,13.));
#49471=CARTESIAN_POINT('Ctrl Pts',(32.791642581611,58.1745936618249,13.));
#49472=CARTESIAN_POINT('Ctrl Pts',(32.7227877556981,58.1763767799635,13.));
#49473=CARTESIAN_POINT('Ctrl Pts',(32.7004157900083,58.1769561417917,13.));
#49474=CARTESIAN_POINT('Ctrl Pts',(32.6780272661526,58.1771283364136,13.));
#49475=CARTESIAN_POINT('Ctrl Pts',(32.6556323879924,58.1768855536512,13.));
#49476=CARTESIAN_POINT('Ctrl Pts',(32.6429970562573,58.176748574083,13.));
#49477=CARTESIAN_POINT('Ctrl Pts',(32.6303583960511,58.1764793454784,13.));
#49478=CARTESIAN_POINT('Ctrl Pts',(32.6177361302722,58.1760772493224,13.));
#49479=CARTESIAN_POINT('Ctrl Pts',(32.5494663659828,58.1739024409108,13.));
#49480=CARTESIAN_POINT('Ctrl Pts',(32.4815560589164,58.1678447148808,13.));
#49481=CARTESIAN_POINT('Ctrl Pts',(32.414274786044,58.1577646784655,13.));
#49482=CARTESIAN_POINT('Ctrl Pts',(32.4045647301645,58.1563099242274,13.));
#49483=CARTESIAN_POINT('Ctrl Pts',(32.3948677953976,58.1547713052596,13.));
#49484=CARTESIAN_POINT('Ctrl Pts',(32.3851848149706,58.1531483143848,13.));
#49485=CARTESIAN_POINT('Ctrl Pts',(32.3167654615574,58.141680359132,13.));
#49486=CARTESIAN_POINT('Ctrl Pts',(32.2490407706809,58.1260036975248,13.));
#49487=CARTESIAN_POINT('Ctrl Pts',(32.1823062478466,58.1063380403939,13.));
#49488=CARTESIAN_POINT('Ctrl Pts',(32.1200483333545,58.087991572208,13.));
#49489=CARTESIAN_POINT('Ctrl Pts',(32.0586518297553,58.0661723398642,13.));
#49490=CARTESIAN_POINT('Ctrl Pts',(31.9983820977037,58.041027736788,13.));
#49491=CARTESIAN_POINT('Ctrl Pts',(31.9850796184089,58.0354779267854,13.));
#49492=CARTESIAN_POINT('Ctrl Pts',(31.9718321459703,58.0297660234088,13.));
#49493=CARTESIAN_POINT('Ctrl Pts',(31.958642741509,58.0238934578502,13.));
#49494=CARTESIAN_POINT('Ctrl Pts',(31.9483333675334,58.0193032222019,13.));
#49495=CARTESIAN_POINT('Ctrl Pts',(31.9380601504676,58.0146150415553,13.));
#49496=CARTESIAN_POINT('Ctrl Pts',(31.9278362669042,58.0098353466313,13.));
#49497=CARTESIAN_POINT('Ctrl Pts',(31.8658980540082,57.9808790542455,13.));
#49498=CARTESIAN_POINT('Ctrl Pts',(31.8056527013631,57.9485169554678,13.));
#49499=CARTESIAN_POINT('Ctrl Pts',(31.7473720762079,57.9129741300425,13.));
#49500=CARTESIAN_POINT('Ctrl Pts',(31.6893603665029,57.8775953044864,13.));
#49501=CARTESIAN_POINT('Ctrl Pts',(31.6332945173391,57.8390642098787,13.));
#49502=CARTESIAN_POINT('Ctrl Pts',(31.5794782979512,57.797566170682,13.));
#49503=CARTESIAN_POINT('Ctrl Pts',(31.5268144518495,57.7569567340729,13.));
#49504=CARTESIAN_POINT('Ctrl Pts',(31.4763043636122,57.7135052606753,13.));
#49505=CARTESIAN_POINT('Ctrl Pts',(31.4282765727933,57.6673622960735,13.));
#49506=CARTESIAN_POINT('Ctrl Pts',(31.4181553624129,57.6576382874454,13.));
#49507=CARTESIAN_POINT('Ctrl Pts',(31.4081445655515,57.6477946903051,13.));
#49508=CARTESIAN_POINT('Ctrl Pts',(31.3982475480844,57.6378328286724,13.));
#49509=CARTESIAN_POINT('Ctrl Pts',(31.388870014372,57.6283938543947,13.));
#49510=CARTESIAN_POINT('Ctrl Pts',(31.3795934914324,57.6188473326524,13.));
#49511=CARTESIAN_POINT('Ctrl Pts',(31.3704354504481,57.6092101706513,13.));
#49512=CARTESIAN_POINT('Ctrl Pts',(31.3254237976821,57.5618436442967,13.));
#49513=CARTESIAN_POINT('Ctrl Pts',(31.2831878041685,57.5122078768965,13.));
#49514=CARTESIAN_POINT('Ctrl Pts',(31.2439955572223,57.4604767978076,13.));
#49515=CARTESIAN_POINT('Ctrl Pts',(31.2055484074953,57.4097291959668,13.));
#49516=CARTESIAN_POINT('Ctrl Pts',(31.1700298957995,57.356964452788,13.));
#49517=CARTESIAN_POINT('Ctrl Pts',(31.1377389872556,57.3023276232579,13.));
#49518=CARTESIAN_POINT('Ctrl Pts',(31.1064966595101,57.2494650123209,13.));
#49519=CARTESIAN_POINT('Ctrl Pts',(31.0782754670358,57.1948493079198,13.));
#49520=CARTESIAN_POINT('Ctrl Pts',(31.053394616225,57.1386036480321,13.));
#49521=CARTESIAN_POINT('Ctrl Pts',(31.0492539851721,57.1292433360518,13.));
#49522=CARTESIAN_POINT('Ctrl Pts',(31.045205981956,57.1198378750144,13.));
#49523=CARTESIAN_POINT('Ctrl Pts',(31.0412522209115,57.1103878272416,13.));
#49524=CARTESIAN_POINT('Ctrl Pts',(31.037066626976,57.1003836660893,13.));
#49525=CARTESIAN_POINT('Ctrl Pts',(31.0329866520609,57.090329535243,13.));
#49526=CARTESIAN_POINT('Ctrl Pts',(31.0290124456509,57.0802271145803,13.));
#49527=CARTESIAN_POINT('Origin',(32.5,56.2916512459885,23.5459252805377));
#49528=CARTESIAN_POINT('Ctrl Pts',(31.4704151231923,54.5113563798656,21.7959252805377));
#49529=CARTESIAN_POINT('Ctrl Pts',(31.3848836142506,54.5597932517276,21.7905813053169));
#49530=CARTESIAN_POINT('Ctrl Pts',(30.7359364258277,54.9934653968669,21.7481913665734));
#49531=CARTESIAN_POINT('Ctrl Pts',(30.0819661342964,56.5203533893187,21.6687554643073));
#49532=CARTESIAN_POINT('Ctrl Pts',(31.3808442960309,58.4469950837992,21.5576175737392));
#49533=CARTESIAN_POINT('Ctrl Pts',(33.7038051725687,58.4009643313194,21.4464796831712));
#49534=CARTESIAN_POINT('Ctrl Pts',(34.9250559921582,56.4241863460988,21.3353417926031));
#49535=CARTESIAN_POINT('Ctrl Pts',(33.9265523881077,54.326131973266,21.2242039020351));
#49536=CARTESIAN_POINT('Ctrl Pts',(32.2719558287363,54.111420270443,21.1443983980133));
#49537=CARTESIAN_POINT('Ctrl Pts',(31.5637955304719,54.4566153915593,21.1016388575141));
#49538=CARTESIAN_POINT('Ctrl Pts',(31.4731950477465,54.5099653993635,21.0959252805377));
#49539=CARTESIAN_POINT('Ctrl Pts',(31.4756555660462,54.5128362942924,21.8540747194623));
#49540=CARTESIAN_POINT('Ctrl Pts',(31.0702251268552,54.7510086370429,21.8286245525962));
#49541=CARTESIAN_POINT('Ctrl Pts',(30.2605073082537,55.6718001447715,21.7661284222074));
#49542=CARTESIAN_POINT('Ctrl Pts',(30.5464763025825,57.7337498950934,21.6665863282959));
#49543=CARTESIAN_POINT('Ctrl Pts',(32.6512600365403,58.7155097146097,21.5554484377278));
#49544=CARTESIAN_POINT('Ctrl Pts',(34.6188774786828,57.4788960204646,21.4443105471598));
#49545=CARTESIAN_POINT('Ctrl Pts',(34.6464212862449,55.1554778495401,21.3331726565918));
#49546=CARTESIAN_POINT('Ctrl Pts',(32.9604590994426,54.0382699285555,21.2364273806926));
#49547=CARTESIAN_POINT('Ctrl Pts',(31.8369684898523,54.3074066165865,21.1767280683161));
#49548=CARTESIAN_POINT('Ctrl Pts',(31.4729484072307,54.5150696468519,21.1540747194623));
#49549=CARTESIAN_POINT('Ctrl Pts',(32.1997834265915,57.930378193668,22.));
#49550=CARTESIAN_POINT('Ctrl Pts',(32.7446991236384,58.0302073467771,21.9629540364773));
#49551=CARTESIAN_POINT('Ctrl Pts',(33.932658940673,57.64135965021,21.888862109432));
#49552=CARTESIAN_POINT('Ctrl Pts',(34.4123083746051,55.8170344416491,21.7777242188639));
#49553=CARTESIAN_POINT('Ctrl Pts',(33.1376927310287,54.4290349887,21.6665863282959));
#49554=CARTESIAN_POINT('Ctrl Pts',(31.2813034436656,54.7450016890464,21.5554484377278));
#49555=CARTESIAN_POINT('Ctrl Pts',(30.5394479035103,56.4770839121465,21.4443105471598));
#49556=CARTESIAN_POINT('Ctrl Pts',(31.592583816614,58.0392131556089,21.3331726565918));
#49557=CARTESIAN_POINT('Ctrl Pts',(33.4760503309402,58.0018912265999,21.2220347660237));
#49558=CARTESIAN_POINT('Ctrl Pts',(34.4662456663514,56.3991112663237,21.1108968754557));
#49559=CARTESIAN_POINT('Ctrl Pts',(33.6566547164314,54.6979998974762,20.9997589848876));
#49560=CARTESIAN_POINT('Ctrl Pts',(31.7883942259045,54.4555617097706,20.8886210943196));
#49561=CARTESIAN_POINT('Ctrl Pts',(30.5714597638967,55.8937240769523,20.7774832037515));
#49562=CARTESIAN_POINT('Ctrl Pts',(31.1197474481277,57.6961102078823,20.6663453131835));
#49563=CARTESIAN_POINT('Ctrl Pts',(32.9313922508809,58.212980865287,20.5552074226155));
#49564=CARTESIAN_POINT('Ctrl Pts',(34.3481806801685,56.9712358625612,20.4440695320474));
#49565=CARTESIAN_POINT('Ctrl Pts',(34.07330745085,55.1074597880137,20.3329316414794));
#49566=CARTESIAN_POINT('Ctrl Pts',(32.3583685299806,54.3275873674106,20.2217937509113));
#49567=CARTESIAN_POINT('Ctrl Pts',(30.7730662696611,55.3454449973685,20.1106558603433));
#49568=CARTESIAN_POINT('Ctrl Pts',(30.7684461524674,57.2293758831938,19.9995179697753));
#49569=CARTESIAN_POINT('Ctrl Pts',(32.3487368516327,58.2549968011428,19.8883800792072));
#49570=CARTESIAN_POINT('Ctrl Pts',(34.0674804546367,57.4835452530785,19.7772421886392));
#49571=CARTESIAN_POINT('Ctrl Pts',(34.3514914067379,55.6211396100854,19.6661042980711));
#49572=CARTESIAN_POINT('Ctrl Pts',(32.9408112840734,54.3724608681775,19.5549664075031));
#49573=CARTESIAN_POINT('Ctrl Pts',(31.1266515903785,54.8804388458657,19.443828516935));
#49574=CARTESIAN_POINT('Ctrl Pts',(30.569533272628,56.680115536781,19.332690626367));
#49575=CARTESIAN_POINT('Ctrl Pts',(31.7793930425298,58.1242264572701,19.2215527357989));
#49576=CARTESIAN_POINT('Ctrl Pts',(33.6488325332889,57.8909605038465,19.1104148452309));
#49577=CARTESIAN_POINT('Ctrl Pts',(34.4667325774588,56.1938286494099,18.9992769546628));
#49578=CARTESIAN_POINT('Ctrl Pts',(33.4844599893276,54.586234926953,18.8881390640949));
#49579=CARTESIAN_POINT('Ctrl Pts',(31.6011000083735,54.539628102072,18.7770011735268));
#49580=CARTESIAN_POINT('Ctrl Pts',(30.5405133840023,56.0966679300985,18.6658632829588));
#49581=CARTESIAN_POINT('Ctrl Pts',(31.2734670813294,57.8321781984269,18.5547253923907));
#49582=CARTESIAN_POINT('Ctrl Pts',(33.1290802689521,58.1576266764213,18.4435875018227));
#49583=CARTESIAN_POINT('Ctrl Pts',(34.4088891521439,56.7751266813415,18.3324496112546));
#49584=CARTESIAN_POINT('Ctrl Pts',(33.9414701461048,54.9500961372979,18.2213117206866));
#49585=CARTESIAN_POINT('Ctrl Pts',(32.1546571679518,54.353006198509,18.1101738301185));
#49586=CARTESIAN_POINT('Ctrl Pts',(30.683940400427,55.5303800574079,17.9990359395505));
#49587=CARTESIAN_POINT('Ctrl Pts',(30.8754835799078,57.4045540686174,17.8878980489824));
#49588=CARTESIAN_POINT('Ctrl Pts',(32.5539650619684,58.260075505098,17.7767601584144));
#49589=CARTESIAN_POINT('Ctrl Pts',(34.1830517108038,57.3138758937664,17.6656222678464));
#49590=CARTESIAN_POINT('Ctrl Pts',(34.2716220416359,55.4320224695077,17.5544843772783));
#49591=CARTESIAN_POINT('Ctrl Pts',(32.7386066261983,54.3369970132152,17.4433464867103));
#49592=CARTESIAN_POINT('Ctrl Pts',(30.9871918598181,55.0310887434669,17.3322085961422));
#49593=CARTESIAN_POINT('Ctrl Pts',(30.6204675405577,56.8789876280276,17.2210707055742));
#49594=CARTESIAN_POINT('Ctrl Pts',(31.9741005967726,58.1892908612604,17.1099328150062));
#49595=CARTESIAN_POINT('Ctrl Pts',(33.8090953408664,57.7626630339378,16.9987949244381));
#49596=CARTESIAN_POINT('Ctrl Pts',(34.4458602733144,55.989601434697,16.8876570338701));
#49597=CARTESIAN_POINT('Ctrl Pts',(33.3015572300411,54.4930094532091,16.776519143302));
#49598=CARTESIAN_POINT('Ctrl Pts',(31.4235797638343,54.6427347026374,16.665381252734));
#49599=CARTESIAN_POINT('Ctrl Pts',(30.5308619472251,56.3017319641806,16.554243362166));
#49600=CARTESIAN_POINT('Ctrl Pts',(31.4405185218662,57.9515022300391,16.4431054715979));
#49601=CARTESIAN_POINT('Ctrl Pts',(33.3199305087784,58.0819920662063,16.3319675810299));
#49602=CARTESIAN_POINT('Ctrl Pts',(34.4488508023651,56.573762645781,16.2208296904618));
#49603=CARTESIAN_POINT('Ctrl Pts',(33.7939658550683,54.8073134617672,16.1096917998938));
#49604=CARTESIAN_POINT('Ctrl Pts',(31.9546992860713,54.3994954851817,15.9985539093257));
#49605=CARTESIAN_POINT('Ctrl Pts',(30.6145526446347,55.7235891349781,15.8874160187577));
#49606=CARTESIAN_POINT('Ctrl Pts',(31.0001773500497,57.5676364772256,15.7762781281896));
#49607=CARTESIAN_POINT('Ctrl Pts',(32.7586067359929,58.2437600667033,15.6651402376216));
#49608=CARTESIAN_POINT('Ctrl Pts',(34.2803304439162,57.1330963140847,15.5540023470536));
#49609=CARTESIAN_POINT('Ctrl Pts',(34.1724975057335,55.2522483481541,15.4428644564855));
#49610=CARTESIAN_POINT('Ctrl Pts',(32.5338086340801,54.3227776419367,15.3317265659175));
#49611=CARTESIAN_POINT('Ctrl Pts',(30.8641743343578,55.195439274664,15.2205886753495));
#49612=CARTESIAN_POINT('Ctrl Pts',(30.6918298216846,57.0714761554116,15.1094507847814));
#49613=CARTESIAN_POINT('Ctrl Pts',(32.1745239717376,58.2337304551949,14.9983128942134));
#49614=CARTESIAN_POINT('Ctrl Pts',(33.9551300366822,57.618377625218,14.8871750036453));
#49615=CARTESIAN_POINT('Ctrl Pts',(34.4038390465812,55.788657104035,14.7760371130773));
#49616=CARTESIAN_POINT('Ctrl Pts',(33.1099426465396,54.4193328057006,14.6648992225092));
#49617=CARTESIAN_POINT('Ctrl Pts',(31.2577587039999,54.7637628485765,14.5537613319412));
#49618=CARTESIAN_POINT('Ctrl Pts',(30.5426125496714,56.5066863904104,14.4426234413731));
#49619=CARTESIAN_POINT('Ctrl Pts',(31.6190848424819,58.0527859832773,14.3314855508051));
#49620=CARTESIAN_POINT('Ctrl Pts',(33.5018697389164,57.9868986634345,14.2203476602371));
#49621=CARTESIAN_POINT('Ctrl Pts',(34.4676299603036,56.3693327876154,14.109209769669));
#49622=CARTESIAN_POINT('Ctrl Pts',(33.6324000499911,54.680662853446,13.998071879101));
#49623=CARTESIAN_POINT('Ctrl Pts',(31.7606637541616,54.466551391645,13.886933988533));
#49624=CARTESIAN_POINT('Ctrl Pts',(30.5656658770528,55.9229694665903,13.7757960979649));
#49625=CARTESIAN_POINT('Ctrl Pts',(31.1411547963289,57.7168562799665,13.6646582073969));
#49626=CARTESIAN_POINT('Ctrl Pts',(32.9604725206547,58.2062164962561,13.5535203168288));
#49627=CARTESIAN_POINT('Ctrl Pts',(34.3581896580209,56.9431939941263,13.4423824262608));
#49628=CARTESIAN_POINT('Ctrl Pts',(34.0553346792797,55.0837258210724,13.3312445356927));
#49629=CARTESIAN_POINT('Ctrl Pts',(32.3283638467564,54.3300480294051,13.2201066451247));
#49630=CARTESIAN_POINT('Ctrl Pts',(30.7594958530051,55.3715226379038,13.1089687545567));
#49631=CARTESIAN_POINT('Ctrl Pts',(30.7817150891479,57.2558511192949,12.9978308639886));
#49632=CARTESIAN_POINT('Ctrl Pts',(32.3808507372123,58.2563466091157,12.8866929734206));
#49633=CARTESIAN_POINT('Ctrl Pts',(33.5126766583316,57.7258551932599,12.8126010463752));
#49634=CARTESIAN_POINT('Ctrl Pts',(33.8412759334222,57.2798490351089,12.7755550828525));
#49635=CARTESIAN_POINT('Ctrl Pts',(32.1764322475374,58.057840198652,22.0748149723825));
#49636=CARTESIAN_POINT('Ctrl Pts',(32.7637320936893,58.1654341743444,22.0377690088598));
#49637=CARTESIAN_POINT('Ctrl Pts',(34.0440927468328,57.7463414713666,21.9636770818144));
#49638=CARTESIAN_POINT('Ctrl Pts',(34.5610498473198,55.7801182186225,21.8525391912464));
#49639=CARTESIAN_POINT('Ctrl Pts',(33.1872931810462,54.2841586241499,21.7414013006783));
#49640=CARTESIAN_POINT('Ctrl Pts',(31.186511869781,54.624701565945,21.6302634101103));
#49641=CARTESIAN_POINT('Ctrl Pts',(30.3869539804389,56.4915070712039,21.5191255195423));
#49642=CARTESIAN_POINT('Ctrl Pts',(31.5220039764197,58.1751404650056,21.4079876289743));
#49643=CARTESIAN_POINT('Ctrl Pts',(33.551968611483,58.1349155948397,21.2968497384062));
#49644=CARTESIAN_POINT('Ctrl Pts',(34.6191824416203,56.4074696262487,21.1857118478381));
#49645=CARTESIAN_POINT('Ctrl Pts',(33.7466206069902,54.5740439227394,21.0745739572701));
#49646=CARTESIAN_POINT('Ctrl Pts',(31.7330447371731,54.312748623095,20.963436066702));
#49647=CARTESIAN_POINT('Ctrl Pts',(30.4214557589377,55.8627728590725,20.852298176134));
#49648=CARTESIAN_POINT('Ctrl Pts',(31.0123898691881,57.8053505883218,20.741160285566));
#49649=CARTESIAN_POINT('Ctrl Pts',(32.9649464200545,58.3624240204495,20.6300223949979));
#49650=CARTESIAN_POINT('Ctrl Pts',(34.4919342294714,57.0240947100387,20.5188845044299));
#49651=CARTESIAN_POINT('Ctrl Pts',(34.195681054595,55.0153520590646,20.4077466138619));
#49652=CARTESIAN_POINT('Ctrl Pts',(32.3473522766853,54.1748202940218,20.2966087232938));
#49653=CARTESIAN_POINT('Ctrl Pts',(30.6387434429966,55.2718480227484,20.1854708327258));
#49654=CARTESIAN_POINT('Ctrl Pts',(30.633763967948,57.3023131486426,20.0743329421578));
#49655=CARTESIAN_POINT('Ctrl Pts',(32.3369714356807,58.4077080025366,19.9631950515897));
#49656=CARTESIAN_POINT('Ctrl Pts',(34.1894008281341,57.5762520948665,19.8520571610217));
#49657=CARTESIAN_POINT('Ctrl Pts',(34.4955024680363,55.5689864691375,19.7409192704536));
#49658=CARTESIAN_POINT('Ctrl Pts',(32.9750980761269,54.2231841055976,19.6297813798856));
#49659=CARTESIAN_POINT('Ctrl Pts',(31.0198310233036,54.770673175488,19.5186434893175));
#49660=CARTESIAN_POINT('Ctrl Pts',(30.4193794230349,56.7103307214639,19.4075055987495));
#49661=CARTESIAN_POINT('Ctrl Pts',(31.7233434317421,58.2667661958427,19.2963677081815));
#49662=CARTESIAN_POINT('Ctrl Pts',(33.7381900057411,58.0153565570662,19.1852298176134));
#49663=CARTESIAN_POINT('Ctrl Pts',(34.6197072252154,56.1862198990258,19.0740919270454));
#49664=CARTESIAN_POINT('Ctrl Pts',(33.561032382455,54.4535857484765,18.9629540364773));
#49665=CARTESIAN_POINT('Ctrl Pts',(31.5311825670481,54.4033537929088,18.8518161459093));
#49666=CARTESIAN_POINT('Ctrl Pts',(30.3881023351889,56.0815019108803,18.7406782553412));
#49667=CARTESIAN_POINT('Ctrl Pts',(31.1780659864649,57.9520020985391,18.6295403647732));
#49668=CARTESIAN_POINT('Ctrl Pts',(33.1780108320884,58.3027643211953,18.5184024742051));
#49669=CARTESIAN_POINT('Ctrl Pts',(34.5573646739319,56.8127319385431,18.4072645836371));
#49670=CARTESIAN_POINT('Ctrl Pts',(34.053589297625,54.8457484885378,18.296126693069));
#49671=CARTESIAN_POINT('Ctrl Pts',(32.1277960183002,54.2022162300801,18.1849888025011));
#49672=CARTESIAN_POINT('Ctrl Pts',(30.5426852645059,55.4711675374879,18.073850911933));
#49673=CARTESIAN_POINT('Ctrl Pts',(30.7491268855679,57.4911168882046,17.962713021365));
#49674=CARTESIAN_POINT('Ctrl Pts',(32.5581625245214,58.4131817337352,17.8515751307969));
#49675=CARTESIAN_POINT('Ctrl Pts',(34.3139613451725,57.3933856640393,17.7404372402289));
#49676=CARTESIAN_POINT('Ctrl Pts',(34.4094207748664,55.3651595869833,17.6292993496608));
#49677=CARTESIAN_POINT('Ctrl Pts',(32.7571657150207,54.1849618325449,17.5181614590928));
#49678=CARTESIAN_POINT('Ctrl Pts',(30.869523959759,54.9330407897143,17.4070235685247));
#49679=CARTESIAN_POINT('Ctrl Pts',(30.4742754149858,56.924671305202,17.2958856779567));
#49680=CARTESIAN_POINT('Ctrl Pts',(31.9331955561555,58.3368913815559,17.1847477873886));
#49681=CARTESIAN_POINT('Ctrl Pts',(33.9109182327756,57.8770799672243,17.0736098968206));
#49682=CARTESIAN_POINT('Ctrl Pts',(34.5972114500352,55.9661076643609,16.9624720062525));
#49683=CARTESIAN_POINT('Ctrl Pts',(33.3639032430821,54.3531090936767,16.8513341156845));
#49684=CARTESIAN_POINT('Ctrl Pts',(31.339854600407,54.5144801395667,16.7401962251165));
#49685=CARTESIAN_POINT('Ctrl Pts',(30.3777001989226,56.3025160536559,16.6290583345484));
#49686=CARTESIAN_POINT('Ctrl Pts',(31.358110873882,58.0806072860715,16.5179204439804));
#49687=CARTESIAN_POINT('Ctrl Pts',(33.3837056158788,58.2212467668585,16.4067825534123));
#49688=CARTESIAN_POINT('Ctrl Pts',(34.6004345857622,56.5957055842903,16.2956446628443));
#49689=CARTESIAN_POINT('Ctrl Pts',(33.8946119587414,54.6918600176664,16.1845067722763));
#49690=CARTESIAN_POINT('Ctrl Pts',(31.9122851899249,54.252321505187,16.0733688817082));
#49691=CARTESIAN_POINT('Ctrl Pts',(30.467900451878,55.6794046320458,15.9622309911402));
#49692=CARTESIAN_POINT('Ctrl Pts',(30.8835194758665,57.6668840279746,15.8510931005722));
#49693=CARTESIAN_POINT('Ctrl Pts',(32.7787214556042,58.3955972623921,15.7399552100041));
#49694=CARTESIAN_POINT('Ctrl Pts',(34.4188065263637,57.1985448475426,15.6288173194361));
#49695=CARTESIAN_POINT('Ctrl Pts',(34.3025862222909,55.1714024344819,15.517679428868));
#49696=CARTESIAN_POINT('Ctrl Pts',(32.5364383072491,54.1696364627501,15.4065415383));
#49697=CARTESIAN_POINT('Ctrl Pts',(30.7369379943181,55.1101746880588,15.2954036477319));
#49698=CARTESIAN_POINT('Ctrl Pts',(30.5511883337254,57.1321318043788,15.1842657571639));
#49699=CARTESIAN_POINT('Ctrl Pts',(32.1492080841852,58.3847875365432,15.0731278665959));
#49700=CARTESIAN_POINT('Ctrl Pts',(34.0683116696875,57.7215718789046,14.9619899760278));
#49701=CARTESIAN_POINT('Ctrl Pts',(34.5519217655404,55.7495336601205,14.8508520854598));
#49702=CARTESIAN_POINT('Ctrl Pts',(33.1573846641151,54.2737017945638,14.7397141948917));
#49703=CARTESIAN_POINT('Ctrl Pts',(31.1611357940719,54.644921989334,14.6285763043237));
#49704=CARTESIAN_POINT('Ctrl Pts',(30.390364776299,56.5234120631583,14.5174384137557));
#49705=CARTESIAN_POINT('Ctrl Pts',(31.5505662815605,58.1897690023091,14.4063005231876));
#49706=CARTESIAN_POINT('Ctrl Pts',(33.5797962817342,58.1187568934329,14.2951626326196));
#49707=CARTESIAN_POINT('Ctrl Pts',(34.6206744074961,56.3753749443396,14.1840247420515));
#49708=CARTESIAN_POINT('Ctrl Pts',(33.7204793856121,54.555358384138,14.0728868514835));
#49709=CARTESIAN_POINT('Ctrl Pts',(31.7031573584894,54.324593094651,13.9617489609155));
#49710=CARTESIAN_POINT('Ctrl Pts',(30.4152112171297,55.8942929876505,13.8506110703474));
#49711=CARTESIAN_POINT('Ctrl Pts',(31.0354623047469,57.8277103129715,13.7394731797794));
#49712=CARTESIAN_POINT('Ctrl Pts',(32.9962885855616,58.3551335112704,13.6283352892113));
#49713=CARTESIAN_POINT('Ctrl Pts',(34.5027217167555,56.9938717138819,13.5171973986433));
#49714=CARTESIAN_POINT('Ctrl Pts',(34.1763103408583,54.9897720377719,13.4060595080752));
#49715=CARTESIAN_POINT('Ctrl Pts',(32.3150137958213,54.1774723490436,13.2949216175072));
#49716=CARTESIAN_POINT('Ctrl Pts',(30.6241175042368,55.2999540111744,13.1837837269392));
#49717=CARTESIAN_POINT('Ctrl Pts',(30.6480649772843,57.3308476580601,13.0726458363711));
#49718=CARTESIAN_POINT('Ctrl Pts',(32.3715831750057,58.4091628000752,12.9615079458031));
#49719=CARTESIAN_POINT('Ctrl Pts',(33.5914437753637,57.8374091717517,12.8874160187577));
#49720=CARTESIAN_POINT('Ctrl Pts',(33.9456018676194,57.3567121584624,12.850370055235));
#49721=CARTESIAN_POINT('Ctrl Pts',(32.1530810684833,58.1853022036361,22.149629944765));
#49722=CARTESIAN_POINT('Ctrl Pts',(32.7827650637402,58.3006610019118,22.1125839812423));
#49723=CARTESIAN_POINT('Ctrl Pts',(34.1555265529925,57.8513232925233,22.038492054197));
#49724=CARTESIAN_POINT('Ctrl Pts',(34.7097913200344,55.7432019955959,21.9273541636289));
#49725=CARTESIAN_POINT('Ctrl Pts',(33.2368936310637,54.1392822595999,21.8162162730609));
#49726=CARTESIAN_POINT('Ctrl Pts',(31.0917202958965,54.5044014428435,21.7050783824928));
#49727=CARTESIAN_POINT('Ctrl Pts',(30.2344600573676,56.5059302302613,21.5939404919248));
#49728=CARTESIAN_POINT('Ctrl Pts',(31.4514241362253,58.3110677744024,21.4828026013567));
#49729=CARTESIAN_POINT('Ctrl Pts',(33.6278868920259,58.2679399630795,21.3716647107887));
#49730=CARTESIAN_POINT('Ctrl Pts',(34.7721192168892,56.4158279861738,21.2605268202206));
#49731=CARTESIAN_POINT('Ctrl Pts',(33.836586497549,54.4500879480027,21.1493889296526));
#49732=CARTESIAN_POINT('Ctrl Pts',(31.6776952484416,54.1699355364193,21.0382510390845));
#49733=CARTESIAN_POINT('Ctrl Pts',(30.2714517539786,55.8318216411929,20.9271131485165));
#49734=CARTESIAN_POINT('Ctrl Pts',(30.9050322902485,57.9145909687611,20.8159752579484));
#49735=CARTESIAN_POINT('Ctrl Pts',(32.9985005892281,58.5118671756121,20.7048373673804));
#49736=CARTESIAN_POINT('Ctrl Pts',(34.6356877787742,57.0769535575161,20.5936994768124));
#49737=CARTESIAN_POINT('Ctrl Pts',(34.3180546583401,54.9232443301155,20.4825615862444));
#49738=CARTESIAN_POINT('Ctrl Pts',(32.3363360233899,54.022053220633,20.3714236956763));
#49739=CARTESIAN_POINT('Ctrl Pts',(30.5044206163321,55.1982510481284,20.2602858051083));
#49740=CARTESIAN_POINT('Ctrl Pts',(30.4990817834285,57.3752504140915,20.1491479145402));
#49741=CARTESIAN_POINT('Ctrl Pts',(32.3252060197288,58.5604192039304,20.0380100239722));
#49742=CARTESIAN_POINT('Ctrl Pts',(34.3113212016315,57.6689589366545,19.9268721334042));
#49743=CARTESIAN_POINT('Ctrl Pts',(34.6395135293347,55.5168333281896,19.8157342428361));
#49744=CARTESIAN_POINT('Ctrl Pts',(33.0093848681805,54.0739073430178,19.7045963522681));
#49745=CARTESIAN_POINT('Ctrl Pts',(30.9130104562287,54.6609075051103,19.5934584617));
#49746=CARTESIAN_POINT('Ctrl Pts',(30.269225573442,56.740545906147,19.482320571132));
#49747=CARTESIAN_POINT('Ctrl Pts',(31.6672938209545,58.4093059344153,19.3711826805639));
#49748=CARTESIAN_POINT('Ctrl Pts',(33.8275474781934,58.1397526102859,19.2600447899959));
#49749=CARTESIAN_POINT('Ctrl Pts',(34.7726818729719,56.1786111486417,19.1489068994278));
#49750=CARTESIAN_POINT('Ctrl Pts',(33.6376047755825,54.3209365700001,19.0377690088598));
#49751=CARTESIAN_POINT('Ctrl Pts',(31.4612651257226,54.2670794837456,18.9266311182918));
#49752=CARTESIAN_POINT('Ctrl Pts',(30.2356912863756,56.0663358916623,18.8154932277237));
#49753=CARTESIAN_POINT('Ctrl Pts',(31.0826648916003,58.0718259986511,18.7043553371557));
#49754=CARTESIAN_POINT('Ctrl Pts',(33.2269413952246,58.4479019659695,18.5932174465876));
#49755=CARTESIAN_POINT('Ctrl Pts',(34.7058401957198,56.8503371957446,18.4820795560196));
#49756=CARTESIAN_POINT('Ctrl Pts',(34.1657084491453,54.7414008397776,18.3709416654516));
#49757=CARTESIAN_POINT('Ctrl Pts',(32.1009348686486,54.0514262616511,18.2598037748835));
#49758=CARTESIAN_POINT('Ctrl Pts',(30.4014301285847,55.4119550175679,18.1486658843155));
#49759=CARTESIAN_POINT('Ctrl Pts',(30.622770191228,57.5776797077918,18.0375279937474));
#49760=CARTESIAN_POINT('Ctrl Pts',(32.5623599870745,58.5662879623725,17.9263901031794));
#49761=CARTESIAN_POINT('Ctrl Pts',(34.4448709795413,57.4728954343121,17.8152522126114));
#49762=CARTESIAN_POINT('Ctrl Pts',(34.5472195080969,55.2982967044589,17.7041143220433));
#49763=CARTESIAN_POINT('Ctrl Pts',(32.7757248038431,54.0329266518745,17.5929764314753));
#49764=CARTESIAN_POINT('Ctrl Pts',(30.7518560596998,54.8349928359617,17.4818385409072));
#49765=CARTESIAN_POINT('Ctrl Pts',(30.328083289414,56.9703549823765,17.3707006503392));
#49766=CARTESIAN_POINT('Ctrl Pts',(31.8922905155382,58.4844919018513,17.2595627597711));
#49767=CARTESIAN_POINT('Ctrl Pts',(34.0127411246847,57.9914969005107,17.1484248692031));
#49768=CARTESIAN_POINT('Ctrl Pts',(34.7485626267561,55.9426138940248,17.037286978635));
#49769=CARTESIAN_POINT('Ctrl Pts',(33.426249256123,54.2132087341443,16.926149088067));
#49770=CARTESIAN_POINT('Ctrl Pts',(31.2561294369797,54.3862255764958,16.815011197499));
#49771=CARTESIAN_POINT('Ctrl Pts',(30.2245384506201,56.3033001431311,16.7038733069309));
#49772=CARTESIAN_POINT('Ctrl Pts',(31.275703225898,58.2097123421038,16.5927354163629));
#49773=CARTESIAN_POINT('Ctrl Pts',(33.4474807229792,58.3605014675107,16.4815975257949));
#49774=CARTESIAN_POINT('Ctrl Pts',(34.7520183691595,56.6176485227996,16.3704596352268));
#49775=CARTESIAN_POINT('Ctrl Pts',(33.9952580624144,54.5764065735656,16.2593217446588));
#49776=CARTESIAN_POINT('Ctrl Pts',(31.8698710937785,54.1051475251923,16.1481838540907));
#49777=CARTESIAN_POINT('Ctrl Pts',(30.3212482591212,55.6352201291136,16.0370459635227));
#49778=CARTESIAN_POINT('Ctrl Pts',(30.7668616016832,57.7661315787236,15.9259080729546));
#49779=CARTESIAN_POINT('Ctrl Pts',(32.7988361752155,58.547434458081,15.8147701823866));
#49780=CARTESIAN_POINT('Ctrl Pts',(34.5572826088111,57.2639933810004,15.7036322918185));
#49781=CARTESIAN_POINT('Ctrl Pts',(34.4326749388484,55.0905565208099,15.5924944012505));
#49782=CARTESIAN_POINT('Ctrl Pts',(32.539067980418,54.0164952835633,15.4813565106825));
#49783=CARTESIAN_POINT('Ctrl Pts',(30.6097016542784,55.0249101014537,15.3702186201144));
#49784=CARTESIAN_POINT('Ctrl Pts',(30.4105468457662,57.192787453346,15.2590807295464));
#49785=CARTESIAN_POINT('Ctrl Pts',(32.1238921966328,58.5358446178915,15.1479428389784));
#49786=CARTESIAN_POINT('Ctrl Pts',(34.1814933026927,57.8247661325911,15.0368049484103));
#49787=CARTESIAN_POINT('Ctrl Pts',(34.7000044844997,55.710410216206,14.9256670578423));
#49788=CARTESIAN_POINT('Ctrl Pts',(33.2048266816905,54.128070783427,14.8145291672742));
#49789=CARTESIAN_POINT('Ctrl Pts',(31.064512884144,54.5260811300915,14.7033912767062));
#49790=CARTESIAN_POINT('Ctrl Pts',(30.2381170029266,56.5401377359063,14.5922533861381));
#49791=CARTESIAN_POINT('Ctrl Pts',(31.4820477206391,58.3267520213408,14.4811154955701));
#49792=CARTESIAN_POINT('Ctrl Pts',(33.6577228245521,58.2506151234314,14.369977605002));
#49793=CARTESIAN_POINT('Ctrl Pts',(34.7737188546885,56.3814171010637,14.258839714434));
#49794=CARTESIAN_POINT('Ctrl Pts',(33.8085587212332,54.4300539148302,14.147701823866));
#49795=CARTESIAN_POINT('Ctrl Pts',(31.6456509628172,54.182634797657,14.0365639332979));
#49796=CARTESIAN_POINT('Ctrl Pts',(30.2647565572066,55.8656165087107,13.9254260427299));
#49797=CARTESIAN_POINT('Ctrl Pts',(30.9297698131648,57.9385643459764,13.8142881521619));
#49798=CARTESIAN_POINT('Ctrl Pts',(33.0321046504684,58.5040505262847,13.7031502615938));
#49799=CARTESIAN_POINT('Ctrl Pts',(34.6472537754902,57.0445494336376,13.5920123710258));
#49800=CARTESIAN_POINT('Ctrl Pts',(34.2972860024369,54.8958182544712,13.4808744804577));
#49801=CARTESIAN_POINT('Ctrl Pts',(32.3016637448862,54.0248966686821,13.3697365898897));
#49802=CARTESIAN_POINT('Ctrl Pts',(30.4887391554684,55.2283853844451,13.2585986993216));
#49803=CARTESIAN_POINT('Ctrl Pts',(30.5144148654208,57.4058441968251,13.1474608087536));
#49804=CARTESIAN_POINT('Ctrl Pts',(32.3623156127991,58.5619789910347,13.0363229181856));
#49805=CARTESIAN_POINT('Ctrl Pts',(33.6702108923958,57.9489631502434,12.9622309911402));
#49806=CARTESIAN_POINT('Ctrl Pts',(34.0499278018167,57.4335752818158,12.9251850276175));
#49807=CARTESIAN_POINT('Ctrl Pts',(32.1297298894291,58.3127642086202,22.2244449171475));
#49808=CARTESIAN_POINT('Ctrl Pts',(32.8017980337912,58.4358878294791,22.1873989536248));
#49809=CARTESIAN_POINT('Ctrl Pts',(34.2669603591523,57.95630511368,22.1133070265794));
#49810=CARTESIAN_POINT('Ctrl Pts',(34.858532792749,55.7062857725693,22.0021691360114));
#49811=CARTESIAN_POINT('Ctrl Pts',(33.2864940810812,53.9944058950499,21.8910312454434));
#49812=CARTESIAN_POINT('Ctrl Pts',(30.9969287220119,54.384101319742,21.7798933548753));
#49813=CARTESIAN_POINT('Ctrl Pts',(30.0819661342964,56.5203533893187,21.6687554643073));
#49814=CARTESIAN_POINT('Ctrl Pts',(31.3808442960309,58.4469950837992,21.5576175737392));
#49815=CARTESIAN_POINT('Ctrl Pts',(33.7038051725687,58.4009643313194,21.4464796831712));
#49816=CARTESIAN_POINT('Ctrl Pts',(34.9250559921582,56.4241863460988,21.3353417926031));
#49817=CARTESIAN_POINT('Ctrl Pts',(33.9265523881077,54.326131973266,21.2242039020351));
#49818=CARTESIAN_POINT('Ctrl Pts',(31.6223457597102,54.0271224497437,21.113066011467));
#49819=CARTESIAN_POINT('Ctrl Pts',(30.1214477490197,55.8008704233132,21.001928120899));
#49820=CARTESIAN_POINT('Ctrl Pts',(30.7976747113088,58.0238313492005,20.890790230331));
#49821=CARTESIAN_POINT('Ctrl Pts',(33.0320547584019,58.6613103307746,20.7796523397629));
#49822=CARTESIAN_POINT('Ctrl Pts',(34.7794413280769,57.1298124049937,20.6685144491949));
#49823=CARTESIAN_POINT('Ctrl Pts',(34.4404282620852,54.8311366011664,20.5573765586268));
#49824=CARTESIAN_POINT('Ctrl Pts',(32.3253197700946,53.8692861472442,20.4462386680588));
#49825=CARTESIAN_POINT('Ctrl Pts',(30.3700977896676,55.1246540735083,20.3351007774907));
#49826=CARTESIAN_POINT('Ctrl Pts',(30.364399598909,57.4481876795404,20.2239628869227));
#49827=CARTESIAN_POINT('Ctrl Pts',(32.3134406037768,58.7131304053242,20.1128249963547));
#49828=CARTESIAN_POINT('Ctrl Pts',(34.4332415751289,57.7616657784424,20.0016871057866));
#49829=CARTESIAN_POINT('Ctrl Pts',(34.7835245906331,55.4646801872418,19.8905492152186));
#49830=CARTESIAN_POINT('Ctrl Pts',(33.043671660234,53.9246305804379,19.7794113246506));
#49831=CARTESIAN_POINT('Ctrl Pts',(30.8061898891538,54.5511418347326,19.6682734340825));
#49832=CARTESIAN_POINT('Ctrl Pts',(30.1190717238489,56.77076109083,19.5571355435145));
#49833=CARTESIAN_POINT('Ctrl Pts',(31.6112442101669,58.5518456729879,19.4459976529464));
#49834=CARTESIAN_POINT('Ctrl Pts',(33.9169049506455,58.2641486635057,19.3348597623784));
#49835=CARTESIAN_POINT('Ctrl Pts',(34.9256565207284,56.1710023982575,19.2237218718104));
#49836=CARTESIAN_POINT('Ctrl Pts',(33.71417716871,54.1882873915237,19.1125839812423));
#49837=CARTESIAN_POINT('Ctrl Pts',(31.3913476843971,54.1308051745824,19.0014460906743));
#49838=CARTESIAN_POINT('Ctrl Pts',(30.0832802375622,56.0511698724442,18.8903082001062));
#49839=CARTESIAN_POINT('Ctrl Pts',(30.9872637967357,58.1916498987633,18.7791703095382));
#49840=CARTESIAN_POINT('Ctrl Pts',(33.275871958361,58.5930396107435,18.6680324189701));
#49841=CARTESIAN_POINT('Ctrl Pts',(34.8543157175076,56.8879424529462,18.5568945284021));
#49842=CARTESIAN_POINT('Ctrl Pts',(34.2778276006656,54.6370531910173,18.445756637834));
#49843=CARTESIAN_POINT('Ctrl Pts',(32.0740737189969,53.9006362932223,18.334618747266));
#49844=CARTESIAN_POINT('Ctrl Pts',(30.2601749926635,55.3527424976477,18.223480856698));
#49845=CARTESIAN_POINT('Ctrl Pts',(30.4964134968881,57.664242527379,18.1123429661299));
#49846=CARTESIAN_POINT('Ctrl Pts',(32.5665574496276,58.7193941910096,18.0012050755619));
#49847=CARTESIAN_POINT('Ctrl Pts',(34.57578061391,57.552405204585,17.8900671849938));
#49848=CARTESIAN_POINT('Ctrl Pts',(34.6850182413274,55.2314338219344,17.7789292944258));
#49849=CARTESIAN_POINT('Ctrl Pts',(32.7942838926656,53.8808914712041,17.6677914038577));
#49850=CARTESIAN_POINT('Ctrl Pts',(30.6341881596407,54.7369448822092,17.5566535132897));
#49851=CARTESIAN_POINT('Ctrl Pts',(30.181891163842,57.0160386595509,17.4455156227217));
#49852=CARTESIAN_POINT('Ctrl Pts',(31.8513854749211,58.6320924221469,17.3343777321536));
#49853=CARTESIAN_POINT('Ctrl Pts',(34.1145640165938,58.105913833797,17.2232398415856));
#49854=CARTESIAN_POINT('Ctrl Pts',(34.899913803477,55.9191201236888,17.1121019510176));
#49855=CARTESIAN_POINT('Ctrl Pts',(33.4885952691639,54.0733083746118,17.0009640604495));
#49856=CARTESIAN_POINT('Ctrl Pts',(31.1724042735525,54.2579710134251,16.8898261698815));
#49857=CARTESIAN_POINT('Ctrl Pts',(30.0713767023175,56.3040842326063,16.7786882793134));
#49858=CARTESIAN_POINT('Ctrl Pts',(31.1932955779139,58.3388173981362,16.6675503887454));
#49859=CARTESIAN_POINT('Ctrl Pts',(33.5112558300795,58.4997561681628,16.5564124981773));
#49860=CARTESIAN_POINT('Ctrl Pts',(34.9036021525568,56.6395914613089,16.4452746076093));
#49861=CARTESIAN_POINT('Ctrl Pts',(34.0959041660874,54.4609531294646,16.3341367170413));
#49862=CARTESIAN_POINT('Ctrl Pts',(31.8274569976321,53.9579735451976,16.2229988264732));
#49863=CARTESIAN_POINT('Ctrl Pts',(30.1745960663645,55.5910356261813,16.1118609359052));
#49864=CARTESIAN_POINT('Ctrl Pts',(30.6502037274999,57.8653791294726,16.0007230453371));
#49865=CARTESIAN_POINT('Ctrl Pts',(32.8189508948268,58.6992716537698,15.8895851547691));
#49866=CARTESIAN_POINT('Ctrl Pts',(34.6957586912586,57.3294419144583,15.778447264201));
#49867=CARTESIAN_POINT('Ctrl Pts',(34.5627636554058,55.0097106071378,15.667309373633));
#49868=CARTESIAN_POINT('Ctrl Pts',(32.541697653587,53.8633541043766,15.556171483065));
#49869=CARTESIAN_POINT('Ctrl Pts',(30.4824653142387,54.9396455148486,15.4450335924969));
#49870=CARTESIAN_POINT('Ctrl Pts',(30.269905357807,57.2534431023133,15.3338957019289));
#49871=CARTESIAN_POINT('Ctrl Pts',(32.0985763090804,58.6869016992398,15.2227578113608));
#49872=CARTESIAN_POINT('Ctrl Pts',(34.2946749356979,57.9279603862777,15.1116199207928));
#49873=CARTESIAN_POINT('Ctrl Pts',(34.848087203459,55.6712867722916,15.0004820302248));
#49874=CARTESIAN_POINT('Ctrl Pts',(33.2522686992661,53.9824397722901,14.8893441396567));
#49875=CARTESIAN_POINT('Ctrl Pts',(30.9678899742159,54.4072402708491,14.7782062490887));
#49876=CARTESIAN_POINT('Ctrl Pts',(30.0858692295542,56.5568634086541,14.6670683585206));
#49877=CARTESIAN_POINT('Ctrl Pts',(31.4135291597177,58.4637350403728,14.5559304679526));
#49878=CARTESIAN_POINT('Ctrl Pts',(33.73564936737,58.3824733534297,14.4447925773845));
#49879=CARTESIAN_POINT('Ctrl Pts',(34.926763301881,56.387459257788,14.3336546868165));
#49880=CARTESIAN_POINT('Ctrl Pts',(33.8966380568543,54.3047494455222,14.2225167962484));
#49881=CARTESIAN_POINT('Ctrl Pts',(31.588144567145,54.040676500663,14.1113789056804));
#49882=CARTESIAN_POINT('Ctrl Pts',(30.1143018972834,55.8369400297709,14.0002410151124));
#49883=CARTESIAN_POINT('Ctrl Pts',(30.8240773215828,58.0494183789814,13.8891031245444));
#49884=CARTESIAN_POINT('Ctrl Pts',(33.0679207153753,58.652967541299,13.7779652339763));
#49885=CARTESIAN_POINT('Ctrl Pts',(34.7917858342248,57.0952271533931,13.6668273434083));
#49886=CARTESIAN_POINT('Ctrl Pts',(34.4182616640155,54.8018644711708,13.5556894528402));
#49887=CARTESIAN_POINT('Ctrl Pts',(32.2883136939512,53.8723209883206,13.4445515622722));
#49888=CARTESIAN_POINT('Ctrl Pts',(30.3533608067,55.1568167577159,13.3334136717041));
#49889=CARTESIAN_POINT('Ctrl Pts',(30.3807647535574,57.4808407355902,13.2222757811361));
#49890=CARTESIAN_POINT('Ctrl Pts',(32.3530480505924,58.7147951819942,13.1111378905681));
#49891=CARTESIAN_POINT('Ctrl Pts',(33.7489780094279,58.0605171287351,13.0370459635227));
#49892=CARTESIAN_POINT('Ctrl Pts',(34.1542537360139,57.5104384051693,13.));
#49893=CARTESIAN_POINT('Ctrl Pts',(32.1997834265915,57.930378193668,22.));
#49894=CARTESIAN_POINT('Ctrl Pts',(32.2590684210022,57.9484903047673,22.));
#49895=CARTESIAN_POINT('Ctrl Pts',(32.3192133660458,57.9629534896909,22.));
#49896=CARTESIAN_POINT('Ctrl Pts',(32.3799202087184,57.9739415995511,22.));
#49897=CARTESIAN_POINT('Ctrl Pts',(32.444639033103,57.9856558894244,22.));
#49898=CARTESIAN_POINT('Ctrl Pts',(32.5099970425744,57.9934211178934,22.));
#49899=CARTESIAN_POINT('Ctrl Pts',(32.5756660758642,57.9973955895089,22.));
#49900=CARTESIAN_POINT('Ctrl Pts',(32.6331264799928,58.0008732521725,22.));
#49901=CARTESIAN_POINT('Ctrl Pts',(32.6908259516985,58.0014477926639,22.));
#49902=CARTESIAN_POINT('Ctrl Pts',(32.7485570677748,57.9991916498582,22.));
#49903=CARTESIAN_POINT('Ctrl Pts',(32.7775225242247,57.9980596744068,22.));
#49904=CARTESIAN_POINT('Ctrl Pts',(32.8064960744379,57.9962146309829,22.));
#49905=CARTESIAN_POINT('Ctrl Pts',(32.835451944398,57.9936627183818,22.));
#49906=CARTESIAN_POINT('Ctrl Pts',(32.8486814477591,57.9924967877302,22.));
#49907=CARTESIAN_POINT('Ctrl Pts',(32.8619089919324,57.9911829627172,22.));
#49908=CARTESIAN_POINT('Ctrl Pts',(32.8751106150215,57.9897244385923,22.));
#49909=CARTESIAN_POINT('Ctrl Pts',(32.9416845684884,57.9823693038058,22.));
#49910=CARTESIAN_POINT('Ctrl Pts',(33.0077191568773,57.9713290351855,22.));
#49911=CARTESIAN_POINT('Ctrl Pts',(33.0728927906167,57.9567622281301,22.));
#49912=CARTESIAN_POINT('Ctrl Pts',(33.1392231872555,57.9419368756937,22.));
#49913=CARTESIAN_POINT('Ctrl Pts',(33.2046628033558,57.9234587511869,22.));
#49914=CARTESIAN_POINT('Ctrl Pts',(33.2688845825783,57.9014427391656,22.));
#49915=CARTESIAN_POINT('Ctrl Pts',(33.3226052862653,57.8830266243757,22.));
#49916=CARTESIAN_POINT('Ctrl Pts',(33.3754743938636,57.8621340596232,22.));
#49917=CARTESIAN_POINT('Ctrl Pts',(33.4272987060795,57.8388046347794,22.));
#49918=CARTESIAN_POINT('Ctrl Pts',(33.4511753909343,57.8280562176558,22.));
#49919=CARTESIAN_POINT('Ctrl Pts',(33.4748302313212,57.8167901903403,22.));
#49920=CARTESIAN_POINT('Ctrl Pts',(33.4982437788543,57.8050086614947,22.));
#49921=CARTESIAN_POINT('Ctrl Pts',(33.5084650463737,57.7998653931392,22.));
#49922=CARTESIAN_POINT('Ctrl Pts',(33.5186400681057,57.7946238947706,22.));
#49923=CARTESIAN_POINT('Ctrl Pts',(33.528754861639,57.7892910972011,22.));
#49924=CARTESIAN_POINT('Ctrl Pts',(33.5908341911969,57.7565611658687,22.));
#49925=CARTESIAN_POINT('Ctrl Pts',(33.6507646084389,57.7203369576125,22.));
#49926=CARTESIAN_POINT('Ctrl Pts',(33.7082063151528,57.6807516371278,22.));
#49927=CARTESIAN_POINT('Ctrl Pts',(33.759565116146,57.6453582842258,22.));
#49928=CARTESIAN_POINT('Ctrl Pts',(33.808935052041,57.6072772063167,22.));
#49929=CARTESIAN_POINT('Ctrl Pts',(33.8560671885274,57.566568812704,22.));
#49930=CARTESIAN_POINT('Ctrl Pts',(33.9074138354698,57.5222203135644,22.));
#49931=CARTESIAN_POINT('Ctrl Pts',(33.9561058514871,57.4747541508594,22.));
#49932=CARTESIAN_POINT('Ctrl Pts',(34.0020809130285,57.4244894418761,22.));
#49933=CARTESIAN_POINT('Ctrl Pts',(34.0198184128282,57.4050969661376,22.));
#49934=CARTESIAN_POINT('Ctrl Pts',(34.0371511842955,57.3852874792601,22.));
#49935=CARTESIAN_POINT('Ctrl Pts',(34.0540743682382,57.3650777298663,22.));
#49936=CARTESIAN_POINT('Ctrl Pts',(34.0614983915351,57.3562119247771,22.));
#49937=CARTESIAN_POINT('Ctrl Pts',(34.0688431367373,57.347269477393,22.));
#49938=CARTESIAN_POINT('Ctrl Pts',(34.0760999004165,57.3382624488906,22.));
#49939=CARTESIAN_POINT('Ctrl Pts',(34.1199740931949,57.2838062033321,22.));
#49940=CARTESIAN_POINT('Ctrl Pts',(34.1607162740126,57.2268964747805,22.));
#49941=CARTESIAN_POINT('Ctrl Pts',(34.1982933189745,57.1679133931306,22.));
#49942=CARTESIAN_POINT('Ctrl Pts',(34.2367405668772,57.107564391112,22.));
#49943=CARTESIAN_POINT('Ctrl Pts',(34.2718749445021,57.0450442239911,22.));
#49944=CARTESIAN_POINT('Ctrl Pts',(34.3036296838761,56.9807132904727,22.));
#49945=CARTESIAN_POINT('Ctrl Pts',(34.3279241124351,56.9314959673484,22.));
#49946=CARTESIAN_POINT('Ctrl Pts',(34.3502397773158,56.8812176908655,22.));
#49947=CARTESIAN_POINT('Ctrl Pts',(34.3705317464917,56.8300260001665,22.));
#49948=CARTESIAN_POINT('Ctrl Pts',(34.3831626883555,56.7981612134855,22.));
#49949=CARTESIAN_POINT('Ctrl Pts',(34.3950092682846,56.765942300049,22.));
#49950=CARTESIAN_POINT('Ctrl Pts',(34.4060577406907,56.7334031737725,22.));
#49951=CARTESIAN_POINT('Ctrl Pts',(34.4122566000748,56.7151467614053,22.));
#49952=CARTESIAN_POINT('Ctrl Pts',(34.4182059308302,56.6967833656075,22.));
#49953=CARTESIAN_POINT('Ctrl Pts',(34.4238930916556,56.6783523613184,22.));
#49954=CARTESIAN_POINT('Ctrl Pts',(34.4459473654135,56.6068786635096,22.));
#49955=CARTESIAN_POINT('Ctrl Pts',(34.4640895873943,56.5343189897469,22.));
#49956=CARTESIAN_POINT('Ctrl Pts',(34.4782337109615,56.4610520163694,22.));
#49957=CARTESIAN_POINT('Ctrl Pts',(34.4888128880618,56.4062515698597,22.));
#49958=CARTESIAN_POINT('Ctrl Pts',(34.4971546283919,56.3510545308308,22.));
#49959=CARTESIAN_POINT('Ctrl Pts',(34.5032062803039,56.2956100237494,22.));
#49960=CARTESIAN_POINT('Ctrl Pts',(34.5050941235412,56.27831383103,22.));
#49961=CARTESIAN_POINT('Ctrl Pts',(34.5067589921265,56.2609935141503,22.));
#49962=CARTESIAN_POINT('Ctrl Pts',(34.5081989725347,56.2436535052303,22.));
#49963=CARTESIAN_POINT('Ctrl Pts',(34.5095888645054,56.2269166530962,22.));
#49964=CARTESIAN_POINT('Ctrl Pts',(34.5107684790971,56.2101700013467,22.));
#49965=CARTESIAN_POINT('Ctrl Pts',(34.51173640528,56.1934236229305,22.));
#49966=CARTESIAN_POINT('Ctrl Pts',(34.5160829441441,56.118222862889,22.));
#49967=CARTESIAN_POINT('Ctrl Pts',(34.5161676811359,56.042991394141,22.));
#49968=CARTESIAN_POINT('Ctrl Pts',(34.511879539708,55.9680950252592,22.));
#49969=CARTESIAN_POINT('Ctrl Pts',(34.5085977311836,55.9107751942845,22.));
#49970=CARTESIAN_POINT('Ctrl Pts',(34.5027538123388,55.8536509962994,22.));
#49971=CARTESIAN_POINT('Ctrl Pts',(34.4942777735197,55.7968820122819,22.));
#49972=CARTESIAN_POINT('Ctrl Pts',(34.4923107028765,55.783707390942,22.));
#49973=CARTESIAN_POINT('Ctrl Pts',(34.4902017904221,55.7705518962168,22.));
#49974=CARTESIAN_POINT('Ctrl Pts',(34.4879524958972,55.7574168944054,22.));
#49975=CARTESIAN_POINT('Ctrl Pts',(31.6674621971265,54.8470528177236,20.8714803633902));
#49976=CARTESIAN_POINT('Ctrl Pts',(31.740921452131,54.8037964055072,20.8771939403667));
#49977=CARTESIAN_POINT('Ctrl Pts',(31.8176439327865,54.7663977740574,20.8829075173431));
#49978=CARTESIAN_POINT('Ctrl Pts',(31.896948563991,54.7356618022518,20.8886210943196));
#49979=CARTESIAN_POINT('Ctrl Pts',(32.4111477227468,54.5363744390058,20.9256670578423));
#49980=CARTESIAN_POINT('Ctrl Pts',(33.0339012195891,54.617187168241,20.9627130213649));
#49981=CARTESIAN_POINT('Ctrl Pts',(33.4802097929969,54.9411120943332,20.9997589848876));
#49982=CARTESIAN_POINT('Ctrl Pts',(33.9265183664047,55.2650370204254,21.0368049484103));
#49983=CARTESIAN_POINT('Ctrl Pts',(34.1963820163781,55.8320741433745,21.073850911933));
#49984=CARTESIAN_POINT('Ctrl Pts',(34.1662812854629,56.3827226982285,21.1108968754557));
#49985=CARTESIAN_POINT('Ctrl Pts',(34.1361805545477,56.9333712530824,21.1479428389783));
#49986=CARTESIAN_POINT('Ctrl Pts',(33.8061154427439,57.4676312398411,21.184988802501));
#49987=CARTESIAN_POINT('Ctrl Pts',(33.327171801121,57.740981554722,21.2220347660237));
#49988=CARTESIAN_POINT('Ctrl Pts',(32.8482281594981,58.0143318696029,21.2590807295464));
#49989=CARTESIAN_POINT('Ctrl Pts',(32.220405988056,58.0267725126059,21.2961266930691));
#49990=CARTESIAN_POINT('Ctrl Pts',(31.7309722501511,57.772637960197,21.3331726565918));
#49991=CARTESIAN_POINT('Ctrl Pts',(31.2415385122461,57.5185034077881,21.3702186201144));
#49992=CARTESIAN_POINT('Ctrl Pts',(30.8904932078782,56.9977936599673,21.4072645836371));
#49993=CARTESIAN_POINT('Ctrl Pts',(30.8386131457201,56.4487584155402,21.4443105471598));
#49994=CARTESIAN_POINT('Ctrl Pts',(30.786733083562,55.8997231711131,21.4813565106825));
#49995=CARTESIAN_POINT('Ctrl Pts',(31.0340182636138,55.3223624300798,21.5184024742052));
#49996=CARTESIAN_POINT('Ctrl Pts',(31.4670590682002,54.9810209428387,21.5554484377278));
#49997=CARTESIAN_POINT('Ctrl Pts',(31.5295263145409,54.9317815581341,21.5607924129486));
#49998=CARTESIAN_POINT('Ctrl Pts',(31.5958589129293,54.8874534513961,21.5661363881694));
#49999=CARTESIAN_POINT('Ctrl Pts',(31.6652082225275,54.8481806306042,21.5714803633902));
#50000=CARTESIAN_POINT('Ctrl Pts',(33.9541262883781,54.8399232067375,22.));
#50001=CARTESIAN_POINT('Ctrl Pts',(33.4713921772736,54.3563916207415,21.9629540364773));
#50002=CARTESIAN_POINT('Ctrl Pts',(31.9935412717563,53.9174716604953,21.8888621094319));
#50003=CARTESIAN_POINT('Ctrl Pts',(30.2271943832588,55.4316007569426,21.7777242188639));
#50004=CARTESIAN_POINT('Ctrl Pts',(30.5464763025825,57.7337498950934,21.6665863282959));
#50005=CARTESIAN_POINT('Ctrl Pts',(32.6512600365403,58.7155097146097,21.5554484377278));
#50006=CARTESIAN_POINT('Ctrl Pts',(34.6188774786828,57.4788960204646,21.4443105471598));
#50007=CARTESIAN_POINT('Ctrl Pts',(34.6464212862449,55.1554778495401,21.3331726565918));
#50008=CARTESIAN_POINT('Ctrl Pts',(32.7096416422032,53.872064985086,21.2220347660237));
#50009=CARTESIAN_POINT('Ctrl Pts',(30.5808145803544,54.8033004251176,21.1108968754557));
#50010=CARTESIAN_POINT('Ctrl Pts',(30.2087196709517,57.0968534624393,20.9997589848876));
#50011=CARTESIAN_POINT('Ctrl Pts',(31.9338196700205,58.6533891775714,20.8886210943196));
#50012=CARTESIAN_POINT('Ctrl Pts',(34.1771709144469,58.0482026788783,20.7774832037515));
#50013=CARTESIAN_POINT('Ctrl Pts',(34.8853786224564,55.8352230845946,20.6663453131835));
#50014=CARTESIAN_POINT('Ctrl Pts',(33.4102272112105,54.0400181863803,20.5552074226154));
#50015=CARTESIAN_POINT('Ctrl Pts',(31.1019320194545,54.3057581512874,20.4440695320474));
#50016=CARTESIAN_POINT('Ctrl Pts',(30.0733055503939,56.3892087930031,20.3329316414794));
#50017=CARTESIAN_POINT('Ctrl Pts',(31.2658594095642,58.3833638027877,20.2217937509113));
#50018=CARTESIAN_POINT('Ctrl Pts',(33.5880364581139,58.4629506390537,20.1106558603433));
#50019=CARTESIAN_POINT('Ctrl Pts',(34.914321242052,56.5551224909764,19.9995179697752));
#50020=CARTESIAN_POINT('Ctrl Pts',(34.0307504904903,54.406136137217,19.8883800792072));
#50021=CARTESIAN_POINT('Ctrl Pts',(31.7460664163078,53.9829831393046,19.7772421886392));
#50022=CARTESIAN_POINT('Ctrl Pts',(30.151466320847,55.6729802447186,19.6661042980711));
#50023=CARTESIAN_POINT('Ctrl Pts',(30.7065057264144,57.9292539322016,19.5549664075031));
#50024=CARTESIAN_POINT('Ctrl Pts',(32.9031507850421,58.6866113101155,19.443828516935));
#50025=CARTESIAN_POINT('Ctrl Pts',(34.7307873556619,57.2518345802401,19.332690626367));
#50026=CARTESIAN_POINT('Ctrl Pts',(34.5165589620033,54.9381911555042,19.221552735799));
#50027=CARTESIAN_POINT('Ctrl Pts',(32.4565512804853,53.8633851007703,19.1104148452309));
#50028=CARTESIAN_POINT('Ctrl Pts',(30.4363127049828,55.0111985872154,18.9992769546629));
#50029=CARTESIAN_POINT('Ctrl Pts',(30.3049905142645,57.3310249135316,18.8881390640948));
#50030=CARTESIAN_POINT('Ctrl Pts',(32.1827853990159,58.6995007346589,18.7770011735268));
#50031=CARTESIAN_POINT('Ctrl Pts',(34.3509304054687,57.8640446119295,18.6658632829587));
#50032=CARTESIAN_POINT('Ctrl Pts',(34.8248978208363,55.5893590092039,18.5547253923907));
#50033=CARTESIAN_POINT('Ctrl Pts',(33.1708598946486,53.9574894553413,18.4435875018226));
#50034=CARTESIAN_POINT('Ctrl Pts',(30.902776298825,54.462104659654,18.3324496112546));
#50035=CARTESIAN_POINT('Ctrl Pts',(30.0966496704334,56.6413246029078,18.2213117206866));
#50036=CARTESIAN_POINT('Ctrl Pts',(31.4903368545417,58.5004845570079,18.1101738301185));
#50037=CARTESIAN_POINT('Ctrl Pts',(33.8081801660464,58.3378743316585,17.9990359395505));
#50038=CARTESIAN_POINT('Ctrl Pts',(34.9286313357969,56.3023329102471,17.8878980489824));
#50039=CARTESIAN_POINT('Ctrl Pts',(33.8261287013398,54.2570144404017,17.7767601584144));
#50040=CARTESIAN_POINT('Ctrl Pts',(31.5098054272241,54.0740221130605,17.6656222678464));
#50041=CARTESIAN_POINT('Ctrl Pts',(30.0998184751403,55.9208508807133,17.5544843772783));
#50042=CARTESIAN_POINT('Ctrl Pts',(30.8867448926705,58.1070774278645,17.4433464867103));
#50043=CARTESIAN_POINT('Ctrl Pts',(33.1503020054966,58.6316238024116,17.3322085961423));
#50044=CARTESIAN_POINT('Ctrl Pts',(34.8186303177654,57.0143667589708,17.2210707055742));
#50045=CARTESIAN_POINT('Ctrl Pts',(34.3646900051272,54.7356000103461,17.1099328150062));
#50046=CARTESIAN_POINT('Ctrl Pts',(32.2039777837733,53.881104604526,16.9987949244381));
#50047=CARTESIAN_POINT('Ctrl Pts',(30.3142180540518,55.2330098770949,16.8876570338701));
#50048=CARTESIAN_POINT('Ctrl Pts',(30.4251293279101,57.5539016004218,16.776519143302));
#50049=CARTESIAN_POINT('Ctrl Pts',(32.4351932585659,58.7194412594432,16.665381252734));
#50050=CARTESIAN_POINT('Ctrl Pts',(34.5045755346152,57.6627971861383,16.554243362166));
#50051=CARTESIAN_POINT('Ctrl Pts',(34.7391470903975,55.3511276839614,16.4431054715979));
#50052=CARTESIAN_POINT('Ctrl Pts',(32.924201920686,53.9003300643712,16.3319675810299));
#50053=CARTESIAN_POINT('Ctrl Pts',(30.7209799221891,54.6383358417407,16.2208296904618));
#50054=CARTESIAN_POINT('Ctrl Pts',(30.1461151763815,56.8896399584928,16.1096917998938));
#50055=CARTESIAN_POINT('Ctrl Pts',(31.7257879044833,58.5935982250311,15.9985539093258));
#50056=CARTESIAN_POINT('Ctrl Pts',(34.0141057438103,58.1905583158083,15.8874160187577));
#50057=CARTESIAN_POINT('Ctrl Pts',(34.9165454246276,56.0494272304867,15.7762781281897));
#50058=CARTESIAN_POINT('Ctrl Pts',(33.6070936729406,54.130006533605,15.6651402376216));
#50059=CARTESIAN_POINT('Ctrl Pts',(31.284306526822,54.1891637565984,15.5540023470536));
#50060=CARTESIAN_POINT('Ctrl Pts',(30.074257404191,56.1727516226363,15.4428644564855));
#50061=CARTESIAN_POINT('Ctrl Pts',(31.0845179881232,58.2651696619898,15.3317265659175));
#50062=CARTESIAN_POINT('Ctrl Pts',(33.3903853125313,58.551203914661,15.2205886753495));
#50063=CARTESIAN_POINT('Ctrl Pts',(34.881272858026,56.7690439832157,15.1094507847814));
#50064=CARTESIAN_POINT('Ctrl Pts',(34.192554360499,54.5499210682071,14.9983128942134));
#50065=CARTESIAN_POINT('Ctrl Pts',(31.9546216431227,53.9250235318367,14.8871750036453));
#50066=CARTESIAN_POINT('Ctrl Pts',(30.2158799584561,55.4663271929179,14.7760371130773));
#50067=CARTESIAN_POINT('Ctrl Pts',(30.5678191761536,57.7630592969624,14.6648992225092));
#50068=CARTESIAN_POINT('Ctrl Pts',(32.6883055651204,58.7129949703237,14.5537613319412));
#50069=CARTESIAN_POINT('Ctrl Pts',(34.6364334330514,57.4466471822884,14.4426234413732));
#50070=CARTESIAN_POINT('Ctrl Pts',(34.6290601547835,55.1231186965397,14.3314855508051));
#50071=CARTESIAN_POINT('Ctrl Pts',(32.6729327631563,53.8691609424835,14.2203476602371));
#50072=CARTESIAN_POINT('Ctrl Pts',(30.5585204707244,54.8325367623412,14.109209769669));
#50073=CARTESIAN_POINT('Ctrl Pts',(30.2211615693062,57.1314551632494,13.998071879101));
#50074=CARTESIAN_POINT('Ctrl Pts',(31.969659013309,58.6616944230992,13.886933988533));
#50075=CARTESIAN_POINT('Ctrl Pts',(34.2035641928434,58.0226004643432,13.7757960979649));
#50076=CARTESIAN_POINT('Ctrl Pts',(34.8782165391171,55.7991607039093,13.6646582073969));
#50077=CARTESIAN_POINT('Ctrl Pts',(33.3759826838065,54.0264798110272,13.5535203168288));
#50078=CARTESIAN_POINT('Ctrl Pts',(31.072107305341,54.3271826722053,13.4423824262608));
#50079=CARTESIAN_POINT('Ctrl Pts',(30.0748873839319,56.4258925346357,13.3312445356927));
#50080=CARTESIAN_POINT('Ctrl Pts',(31.2980228170538,58.4019167094404,13.2201066451247));
#50081=CARTESIAN_POINT('Ctrl Pts',(33.6200956257376,58.4460163820148,13.1089687545567));
#50082=CARTESIAN_POINT('Ctrl Pts',(34.9194345180072,56.5189590291238,12.9978308639886));
#50083=CARTESIAN_POINT('Ctrl Pts',(33.9991195898382,54.3822352088321,12.8866929734206));
#50084=CARTESIAN_POINT('Ctrl Pts',(32.4788453194858,54.1263833506296,12.8126010463752));
#50085=CARTESIAN_POINT('Ctrl Pts',(31.8326342444893,54.3482983416318,12.7755550828525));
#50086=CARTESIAN_POINT('Ctrl Pts',(33.8624214427591,54.931476806163,22.0748149723825));
#50087=CARTESIAN_POINT('Ctrl Pts',(33.4101310816148,54.4784392630848,22.0377690088598));
#50088=CARTESIAN_POINT('Ctrl Pts',(32.0254812207533,54.067199902189,21.9636770818144));
#50089=CARTESIAN_POINT('Ctrl Pts',(30.3705294497321,55.4858400606075,21.8525391912464));
#50090=CARTESIAN_POINT('Ctrl Pts',(30.6696757733001,57.6428035756159,21.7414013006784));
#50091=CARTESIAN_POINT('Ctrl Pts',(32.6417207837188,58.5626484614684,21.6302634101103));
#50092=CARTESIAN_POINT('Ctrl Pts',(34.4852499295344,57.4040221256554,21.5191255195423));
#50093=CARTESIAN_POINT('Ctrl Pts',(34.5110566798406,55.2271309148553,21.4079876289742));
#50094=CARTESIAN_POINT('Ctrl Pts',(32.6964205385155,54.0246568103569,21.2968497384062));
#50095=CARTESIAN_POINT('Ctrl Pts',(30.7018484988177,54.8971636496158,21.1857118478381));
#50096=CARTESIAN_POINT('Ctrl Pts',(30.3532198498733,57.0460731790885,21.0745739572701));
#50097=CARTESIAN_POINT('Ctrl Pts',(31.969525977078,58.5044455719579,20.9634360667021));
#50098=CARTESIAN_POINT('Ctrl Pts',(34.0713997025409,57.9374253143107,20.852298176134));
#50099=CARTESIAN_POINT('Ctrl Pts',(34.7349441106375,55.8640078431202,20.741160285566));
#50100=CARTESIAN_POINT('Ctrl Pts',(33.352823499752,54.1820180001326,20.6300223949979));
#50101=CARTESIAN_POINT('Ctrl Pts',(31.1901015335782,54.4309990063087,20.5188845044299));
#50102=CARTESIAN_POINT('Ctrl Pts',(30.2263456554001,56.3830563013939,20.4077466138619));
#50103=CARTESIAN_POINT('Ctrl Pts',(31.3436908009795,58.2514494163732,20.2966087232938));
#50104=CARTESIAN_POINT('Ctrl Pts',(33.5194191611043,58.3260170884914,20.1854708327258));
#50105=CARTESIAN_POINT('Ctrl Pts',(34.7620614565391,56.5385066096463,20.0743329421577));
#50106=CARTESIAN_POINT('Ctrl Pts',(33.9342133200027,54.5250466289289,19.9631950515897));
#50107=CARTESIAN_POINT('Ctrl Pts',(31.7936134302447,54.1285798828619,19.8520571610216));
#50108=CARTESIAN_POINT('Ctrl Pts',(30.2995771969099,55.7119968893621,19.7409192704536));
#50109=CARTESIAN_POINT('Ctrl Pts',(30.8196129006621,57.8259781007111,19.6297813798856));
#50110=CARTESIAN_POINT('Ctrl Pts',(32.8777259778579,58.5355725422314,19.5186434893175));
#50111=CARTESIAN_POINT('Ctrl Pts',(34.5901021815509,57.1912803731282,19.4075055987495));
#50112=CARTESIAN_POINT('Ctrl Pts',(34.3893841562315,55.0235474616526,19.2963677081814));
#50113=CARTESIAN_POINT('Ctrl Pts',(32.4592913850741,54.0165243251615,19.1852298176134));
#50114=CARTESIAN_POINT('Ctrl Pts',(30.5664596711081,55.091950661044,19.0740919270453));
#50115=CARTESIAN_POINT('Ctrl Pts',(30.4434193478743,57.265476547833,18.9629540364773));
#50116=CARTESIAN_POINT('Ctrl Pts',(32.2027906188127,58.5476490919252,18.8518161459092));
#50117=CARTESIAN_POINT('Ctrl Pts',(34.2342010069002,57.7648812228701,18.7406782553413));
#50118=CARTESIAN_POINT('Ctrl Pts',(34.6782775462125,55.6336492484138,18.6295403647732));
#50119=CARTESIAN_POINT('Ctrl Pts',(33.1285519441202,54.1046939645864,18.5184024742052));
#50120=CARTESIAN_POINT('Ctrl Pts',(31.0035056193152,54.5774854822095,18.4072645836371));
#50121=CARTESIAN_POINT('Ctrl Pts',(30.2482175725494,56.6192723633811,18.2961266930691));
#50122=CARTESIAN_POINT('Ctrl Pts',(31.5540115185798,58.3611839203272,18.184988802501));
#50123=CARTESIAN_POINT('Ctrl Pts',(33.7256794498927,58.2088287503543,18.073850911933));
#50124=CARTESIAN_POINT('Ctrl Pts',(34.7754690805686,56.3016592683637,17.9627130213649));
#50125=CARTESIAN_POINT('Ctrl Pts',(33.7424960562255,54.3853293299944,17.8515751307969));
#50126=CARTESIAN_POINT('Ctrl Pts',(31.5722523007556,54.2138774604954,17.7404372402288));
#50127=CARTESIAN_POINT('Ctrl Pts',(30.2511865357786,55.9442355004157,17.6292993496608));
#50128=CARTESIAN_POINT('Ctrl Pts',(30.9884852378827,57.9925871122213,17.5181614590928));
#50129=CARTESIAN_POINT('Ctrl Pts',(33.1092905434961,58.4840528357393,17.4070235685247));
#50130=CARTESIAN_POINT('Ctrl Pts',(34.6724053048228,56.9687885206333,17.2958856779567));
#50131=CARTESIAN_POINT('Ctrl Pts',(34.2470928538934,54.833732778786,17.1847477873887));
#50132=CARTESIAN_POINT('Ctrl Pts',(32.2226465004149,54.0331263438891,17.0736098968206));
#50133=CARTESIAN_POINT('Ctrl Pts',(30.4520649505092,55.2997733652982,16.9624720062526));
#50134=CARTESIAN_POINT('Ctrl Pts',(30.5559815765657,57.4742974595635,16.8513341156845));
#50135=CARTESIAN_POINT('Ctrl Pts',(32.4392803122598,58.5663320624232,16.7401962251165));
#50136=CARTESIAN_POINT('Ctrl Pts',(34.3781564667511,57.5763255173654,16.6290583345484));
#50137=CARTESIAN_POINT('Ctrl Pts',(34.5979347074811,55.4104420425189,16.5179204439804));
#50138=CARTESIAN_POINT('Ctrl Pts',(32.897449518258,54.0511393452008,16.4067825534124));
#50139=CARTESIAN_POINT('Ctrl Pts',(30.833174277585,54.7426025998055,16.2956446628443));
#50140=CARTESIAN_POINT('Ctrl Pts',(30.2945635237363,56.8519276476706,16.1845067722763));
#50141=CARTESIAN_POINT('Ctrl Pts',(31.7746137879455,58.4484253511043,16.0733688817082));
#50142=CARTESIAN_POINT('Ctrl Pts',(33.9186182785215,58.070803256654,15.9622309911402));
#50143=CARTESIAN_POINT('Ctrl Pts',(34.7641453704728,56.0647031498647,15.8510931005722));
#50144=CARTESIAN_POINT('Ctrl Pts',(33.5372745278126,54.2663312092653,15.7399552100041));
#50145=CARTESIAN_POINT('Ctrl Pts',(31.3609745460778,54.3217576668876,15.6288173194361));
#50146=CARTESIAN_POINT('Ctrl Pts',(30.2272374802945,56.1802500577385,15.517679428868));
#50147=CARTESIAN_POINT('Ctrl Pts',(31.1737857225787,58.14070921924,15.4065415383));
#50148=CARTESIAN_POINT('Ctrl Pts',(33.3342329354787,58.4087046487412,15.2954036477319));
#50149=CARTESIAN_POINT('Ctrl Pts',(34.731097277289,56.7389370883627,15.1842657571639));
#50150=CARTESIAN_POINT('Ctrl Pts',(34.0858129876403,54.6597637265374,15.0731278665959));
#50151=CARTESIAN_POINT('Ctrl Pts',(31.9890160684358,54.0742755128362,14.9619899760278));
#50152=CARTESIAN_POINT('Ctrl Pts',(30.3599285720183,55.5183764650323,14.8508520854598));
#50153=CARTESIAN_POINT('Ctrl Pts',(30.6896726531005,57.6702645725732,14.7397141948917));
#50154=CARTESIAN_POINT('Ctrl Pts',(32.6764300265812,58.5602923101728,14.6285763043237));
#50155=CARTESIAN_POINT('Ctrl Pts',(34.5016987131585,57.373807068692,14.5174384137556));
#50156=CARTESIAN_POINT('Ctrl Pts',(34.4947904325672,55.1968125001003,14.4063005231876));
#50157=CARTESIAN_POINT('Ctrl Pts',(32.6620267142976,54.0219359119425,14.2951626326196));
#50158=CARTESIAN_POINT('Ctrl Pts',(30.6809603729032,54.9245561897684,14.1840247420515));
#50159=CARTESIAN_POINT('Ctrl Pts',(30.3648770967316,57.0784927148031,14.0728868514835));
#50160=CARTESIAN_POINT('Ctrl Pts',(32.0031051030322,58.5122270450561,13.9617489609154));
#50161=CARTESIAN_POINT('Ctrl Pts',(34.0961284820971,57.9134377099717,13.8506110703474));
#50162=CARTESIAN_POINT('Ctrl Pts',(34.7282337059124,55.8302197456797,13.7394731797794));
#50163=CARTESIAN_POINT('Ctrl Pts',(33.3207386122115,54.1693334258776,13.6283352892113));
#50164=CARTESIAN_POINT('Ctrl Pts',(31.1621577226746,54.4510723843451,13.5171973986433));
#50165=CARTESIAN_POINT('Ctrl Pts',(30.2278277302022,56.417426573495,13.4060595080752));
#50166=CARTESIAN_POINT('Ctrl Pts',(31.3738258149643,58.2688322792311,13.2949216175072));
#50167=CARTESIAN_POINT('Ctrl Pts',(33.549456509137,58.3101507946959,13.1837837269392));
#50168=CARTESIAN_POINT('Ctrl Pts',(34.7668522624408,56.5046238057481,13.0726458363711));
#50169=CARTESIAN_POINT('Ctrl Pts',(33.9045772301757,54.5026530186945,12.9615079458031));
#50170=CARTESIAN_POINT('Ctrl Pts',(32.4801794448133,54.2629365232493,12.8874160187577));
#50171=CARTESIAN_POINT('Ctrl Pts',(31.8747218362409,54.4708563886884,12.850370055235));
#50172=CARTESIAN_POINT('Ctrl Pts',(33.7707165971401,55.0230304055885,22.149629944765));
#50173=CARTESIAN_POINT('Ctrl Pts',(33.3488699859559,54.6004869054281,22.1125839812423));
#50174=CARTESIAN_POINT('Ctrl Pts',(32.0574211697503,54.2169281438828,22.0384920541969));
#50175=CARTESIAN_POINT('Ctrl Pts',(30.5138645162054,55.5400793642725,21.9273541636289));
#50176=CARTESIAN_POINT('Ctrl Pts',(30.7928752440177,57.5518572561383,21.8162162730608));
#50177=CARTESIAN_POINT('Ctrl Pts',(32.6321815308973,58.4097872083271,21.7050783824928));
#50178=CARTESIAN_POINT('Ctrl Pts',(34.351622380386,57.3291482308462,21.5939404919247));
#50179=CARTESIAN_POINT('Ctrl Pts',(34.3756920734363,55.2987839801705,21.4828026013567));
#50180=CARTESIAN_POINT('Ctrl Pts',(32.6831994348279,54.1772486356277,21.3716647107887));
#50181=CARTESIAN_POINT('Ctrl Pts',(30.8228824172809,54.9910268741142,21.2605268202206));
#50182=CARTESIAN_POINT('Ctrl Pts',(30.4977200287949,56.9952928957376,21.1493889296526));
#50183=CARTESIAN_POINT('Ctrl Pts',(32.0052322841356,58.3555019663445,21.0382510390846));
#50184=CARTESIAN_POINT('Ctrl Pts',(33.965628490635,57.826647949743,20.9271131485165));
#50185=CARTESIAN_POINT('Ctrl Pts',(34.5845095988185,55.8927926016459,20.8159752579485));
#50186=CARTESIAN_POINT('Ctrl Pts',(33.2954197882935,54.324017813885,20.7048373673804));
#50187=CARTESIAN_POINT('Ctrl Pts',(31.2782710477019,54.55623986133,20.5936994768124));
#50188=CARTESIAN_POINT('Ctrl Pts',(30.3793857604063,56.3769038097847,20.4825615862443));
#50189=CARTESIAN_POINT('Ctrl Pts',(31.4215221923948,58.1195350299587,20.3714236956763));
#50190=CARTESIAN_POINT('Ctrl Pts',(33.4508018640946,58.1890835379289,20.2602858051083));
#50191=CARTESIAN_POINT('Ctrl Pts',(34.6098016710262,56.5218907283163,20.1491479145402));
#50192=CARTESIAN_POINT('Ctrl Pts',(33.8376761495152,54.6439571206407,20.0380100239722));
#50193=CARTESIAN_POINT('Ctrl Pts',(31.8411604441815,54.2741766264192,19.9268721334041));
#50194=CARTESIAN_POINT('Ctrl Pts',(30.4476880729728,55.7510135340056,19.8157342428361));
#50195=CARTESIAN_POINT('Ctrl Pts',(30.9327200749098,57.7227022692206,19.7045963522681));
#50196=CARTESIAN_POINT('Ctrl Pts',(32.8523011706738,58.3845337743473,19.5934584617));
#50197=CARTESIAN_POINT('Ctrl Pts',(34.44941700744,57.1307261660161,19.482320571132));
#50198=CARTESIAN_POINT('Ctrl Pts',(34.2622093504597,55.1089037678012,19.3711826805639));
#50199=CARTESIAN_POINT('Ctrl Pts',(32.4620314896629,54.1696635495527,19.2600447899959));
#50200=CARTESIAN_POINT('Ctrl Pts',(30.6966066372334,55.1727027348726,19.1489068994278));
#50201=CARTESIAN_POINT('Ctrl Pts',(30.5818481814842,57.1999281821345,19.0377690088598));
#50202=CARTESIAN_POINT('Ctrl Pts',(32.2227958386095,58.3957974491916,18.9266311182918));
#50203=CARTESIAN_POINT('Ctrl Pts',(34.1174716083317,57.6657178338107,18.8154932277237));
#50204=CARTESIAN_POINT('Ctrl Pts',(34.5316572715886,55.6779394876238,18.7043553371557));
#50205=CARTESIAN_POINT('Ctrl Pts',(33.0862439935918,54.2518984738315,18.5932174465876));
#50206=CARTESIAN_POINT('Ctrl Pts',(31.1042349398054,54.692866304765,18.4820795560196));
#50207=CARTESIAN_POINT('Ctrl Pts',(30.3997854746655,56.5972201238544,18.3709416654515));
#50208=CARTESIAN_POINT('Ctrl Pts',(31.617686182618,58.2218832836466,18.2598037748835));
#50209=CARTESIAN_POINT('Ctrl Pts',(33.6431787337389,58.0797831690501,18.1486658843155));
#50210=CARTESIAN_POINT('Ctrl Pts',(34.6223068253404,56.3009856264801,18.0375279937474));
#50211=CARTESIAN_POINT('Ctrl Pts',(33.6588634111112,54.5136442195871,17.9263901031794));
#50212=CARTESIAN_POINT('Ctrl Pts',(31.6346991742871,54.3537328079304,17.8152522126114));
#50213=CARTESIAN_POINT('Ctrl Pts',(30.4025545964168,55.9676201201181,17.7041143220433));
#50214=CARTESIAN_POINT('Ctrl Pts',(31.0902255830949,57.878096796578,17.5929764314753));
#50215=CARTESIAN_POINT('Ctrl Pts',(33.0682790814955,58.336481869067,17.4818385409072));
#50216=CARTESIAN_POINT('Ctrl Pts',(34.5261802918802,56.9232102822958,17.3707006503392));
#50217=CARTESIAN_POINT('Ctrl Pts',(34.1294957026596,54.9318655472259,17.2595627597711));
#50218=CARTESIAN_POINT('Ctrl Pts',(32.2413152170565,54.1851480832521,17.1484248692031));
#50219=CARTESIAN_POINT('Ctrl Pts',(30.5899118469666,55.3665368535015,17.0372869786351));
#50220=CARTESIAN_POINT('Ctrl Pts',(30.6868338252212,57.3946933187051,16.926149088067));
#50221=CARTESIAN_POINT('Ctrl Pts',(32.4433673659537,58.4132228654032,16.815011197499));
#50222=CARTESIAN_POINT('Ctrl Pts',(34.2517373988869,57.4898538485926,16.7038733069309));
#50223=CARTESIAN_POINT('Ctrl Pts',(34.4567223245648,55.4697564010764,16.5927354163629));
#50224=CARTESIAN_POINT('Ctrl Pts',(32.87069711583,54.2019486260304,16.4815975257949));
#50225=CARTESIAN_POINT('Ctrl Pts',(30.9453686329808,54.8468693578704,16.3704596352268));
#50226=CARTESIAN_POINT('Ctrl Pts',(30.4430118710911,56.8142153368483,16.2593217446588));
#50227=CARTESIAN_POINT('Ctrl Pts',(31.8234396714077,58.3032524771776,16.1481838540907));
#50228=CARTESIAN_POINT('Ctrl Pts',(33.8231308132328,57.9510481974995,16.0370459635227));
#50229=CARTESIAN_POINT('Ctrl Pts',(34.611745316318,56.0799790692429,15.9259080729546));
#50230=CARTESIAN_POINT('Ctrl Pts',(33.4674553826844,54.4026558849256,15.8147701823866));
#50231=CARTESIAN_POINT('Ctrl Pts',(31.4376425653338,54.4543515771768,15.7036322918186));
#50232=CARTESIAN_POINT('Ctrl Pts',(30.3802175563979,56.1877484928406,15.5924944012505));
#50233=CARTESIAN_POINT('Ctrl Pts',(31.2630534570341,58.0162487764902,15.4813565106825));
#50234=CARTESIAN_POINT('Ctrl Pts',(33.278080558426,58.2662053828213,15.3702186201144));
#50235=CARTESIAN_POINT('Ctrl Pts',(34.5809216965521,56.7088301935099,15.2590807295464));
#50236=CARTESIAN_POINT('Ctrl Pts',(33.9790716147817,54.7696063848677,15.1479428389783));
#50237=CARTESIAN_POINT('Ctrl Pts',(32.0234104937489,54.2235274938358,15.0368049484103));
#50238=CARTESIAN_POINT('Ctrl Pts',(30.5039771855803,55.5704257371467,14.9256670578423));
#50239=CARTESIAN_POINT('Ctrl Pts',(30.8115261300475,57.577469848184,14.8145291672742));
#50240=CARTESIAN_POINT('Ctrl Pts',(32.6645544880419,58.4075896500218,14.7033912767062));
#50241=CARTESIAN_POINT('Ctrl Pts',(34.3669639932659,57.3009669550956,14.5922533861381));
#50242=CARTESIAN_POINT('Ctrl Pts',(34.3605207103508,55.2705063036608,14.4811154955701));
#50243=CARTESIAN_POINT('Ctrl Pts',(32.651120665439,54.1747108814015,14.3699776050021));
#50244=CARTESIAN_POINT('Ctrl Pts',(30.803400275082,55.0165756171955,14.258839714434));
#50245=CARTESIAN_POINT('Ctrl Pts',(30.5085926241571,57.0255302663568,14.147701823866));
#50246=CARTESIAN_POINT('Ctrl Pts',(32.0365511927554,58.3627596670131,14.0365639332979));
#50247=CARTESIAN_POINT('Ctrl Pts',(33.9886927713508,57.8042749556,13.9254260427299));
#50248=CARTESIAN_POINT('Ctrl Pts',(34.5782508727078,55.86127878745,13.8142881521619));
#50249=CARTESIAN_POINT('Ctrl Pts',(33.2654945406164,54.312187040728,13.7031502615938));
#50250=CARTESIAN_POINT('Ctrl Pts',(31.2522081400082,54.574962096485,13.5920123710258));
#50251=CARTESIAN_POINT('Ctrl Pts',(30.3807680764725,56.4089606123543,13.4808744804577));
#50252=CARTESIAN_POINT('Ctrl Pts',(31.4496288128749,58.135747849022,13.3697365898897));
#50253=CARTESIAN_POINT('Ctrl Pts',(33.4788173925363,58.1742852073771,13.2585986993216));
#50254=CARTESIAN_POINT('Ctrl Pts',(34.6142700068744,56.4902885823724,13.1474608087536));
#50255=CARTESIAN_POINT('Ctrl Pts',(33.8100348705131,54.6230708285569,13.0363229181856));
#50256=CARTESIAN_POINT('Ctrl Pts',(32.4815135701408,54.3994896958689,12.9622309911402));
#50257=CARTESIAN_POINT('Ctrl Pts',(31.9168094279925,54.593414435745,12.9251850276175));
#50258=CARTESIAN_POINT('Ctrl Pts',(33.6790117515211,55.1145840050141,22.2244449171475));
#50259=CARTESIAN_POINT('Ctrl Pts',(33.2876088902971,54.7225345477714,22.1873989536248));
#50260=CARTESIAN_POINT('Ctrl Pts',(32.0893611187473,54.3666563855765,22.1133070265794));
#50261=CARTESIAN_POINT('Ctrl Pts',(30.6571995826787,55.5943186679374,22.0021691360114));
#50262=CARTESIAN_POINT('Ctrl Pts',(30.9160747147354,57.4609109366607,21.8910312454433));
#50263=CARTESIAN_POINT('Ctrl Pts',(32.6226422780758,58.2569259551857,21.7798933548753));
#50264=CARTESIAN_POINT('Ctrl Pts',(34.2179948312376,57.2542743360371,21.6687554643072));
#50265=CARTESIAN_POINT('Ctrl Pts',(34.2403274670321,55.3704370454857,21.5576175737392));
#50266=CARTESIAN_POINT('Ctrl Pts',(32.6699783311403,54.3298404608986,21.4464796831711));
#50267=CARTESIAN_POINT('Ctrl Pts',(30.9439163357442,55.0848900986124,21.3353417926032));
#50268=CARTESIAN_POINT('Ctrl Pts',(30.6422202077165,56.9445126123869,21.2242039020351));
#50269=CARTESIAN_POINT('Ctrl Pts',(32.0409385911931,58.206558360731,21.1130660114671));
#50270=CARTESIAN_POINT('Ctrl Pts',(33.8598572787291,57.7158705851754,21.001928120899));
#50271=CARTESIAN_POINT('Ctrl Pts',(34.4340750869996,55.9215773601716,20.890790230331));
#50272=CARTESIAN_POINT('Ctrl Pts',(33.238016076835,54.4660176276373,20.7796523397629));
#50273=CARTESIAN_POINT('Ctrl Pts',(31.3664405618256,54.6814807163513,20.6685144491949));
#50274=CARTESIAN_POINT('Ctrl Pts',(30.5324258654125,56.3707513181755,20.5573765586268));
#50275=CARTESIAN_POINT('Ctrl Pts',(31.4993535838102,57.9876206435441,20.4462386680588));
#50276=CARTESIAN_POINT('Ctrl Pts',(33.3821845670849,58.0521499873667,20.3351007774907));
#50277=CARTESIAN_POINT('Ctrl Pts',(34.4575418855134,56.5052748469861,20.2239628869227));
#50278=CARTESIAN_POINT('Ctrl Pts',(33.7411389790275,54.7628676123527,20.1128249963547));
#50279=CARTESIAN_POINT('Ctrl Pts',(31.8887074581184,54.4197733699765,20.0016871057866));
#50280=CARTESIAN_POINT('Ctrl Pts',(30.5957989490357,55.7900301786492,19.8905492152186));
#50281=CARTESIAN_POINT('Ctrl Pts',(31.0458272491576,57.61942643773,19.7794113246505));
#50282=CARTESIAN_POINT('Ctrl Pts',(32.8268763634895,58.2334950064634,19.6682734340825));
#50283=CARTESIAN_POINT('Ctrl Pts',(34.308731833329,57.0701719589039,19.5571355435145));
#50284=CARTESIAN_POINT('Ctrl Pts',(34.1350345446879,55.1942600739497,19.4459976529464));
#50285=CARTESIAN_POINT('Ctrl Pts',(32.4647715942516,54.3228027739439,19.3348597623784));
#50286=CARTESIAN_POINT('Ctrl Pts',(30.8267536033587,55.2534548087013,19.2237218718103));
#50287=CARTESIAN_POINT('Ctrl Pts',(30.7202770150941,57.1343798164359,19.1125839812423));
#50288=CARTESIAN_POINT('Ctrl Pts',(32.2428010584064,58.2439458064581,19.0014460906742));
#50289=CARTESIAN_POINT('Ctrl Pts',(34.0007422097631,57.5665544447512,18.8903082001062));
#50290=CARTESIAN_POINT('Ctrl Pts',(34.3850369969648,55.7222297268338,18.7791703095382));
#50291=CARTESIAN_POINT('Ctrl Pts',(33.0439360430634,54.3991029830766,18.6680324189701));
#50292=CARTESIAN_POINT('Ctrl Pts',(31.2049642602956,54.8082471273204,18.5568945284021));
#50293=CARTESIAN_POINT('Ctrl Pts',(30.5513533767816,56.5751678843277,18.445756637834));
#50294=CARTESIAN_POINT('Ctrl Pts',(31.681360846656,58.0825826469659,18.334618747266));
#50295=CARTESIAN_POINT('Ctrl Pts',(33.5606780175853,57.9507375877459,18.223480856698));
#50296=CARTESIAN_POINT('Ctrl Pts',(34.469144570112,56.3003119845966,18.1123429661299));
#50297=CARTESIAN_POINT('Ctrl Pts',(33.5752307659969,54.6419591091798,18.0012050755619));
#50298=CARTESIAN_POINT('Ctrl Pts',(31.6971460478186,54.4935881553653,17.8900671849938));
#50299=CARTESIAN_POINT('Ctrl Pts',(30.5539226570551,55.9910047398206,17.7789292944258));
#50300=CARTESIAN_POINT('Ctrl Pts',(31.1919659283071,57.7636064809346,17.6677914038578));
#50301=CARTESIAN_POINT('Ctrl Pts',(33.027267619495,58.1889109023948,17.5566535132897));
#50302=CARTESIAN_POINT('Ctrl Pts',(34.3799552789376,56.8776320439583,17.4455156227217));
#50303=CARTESIAN_POINT('Ctrl Pts',(34.0118985514257,55.0299983156659,17.3343777321536));
#50304=CARTESIAN_POINT('Ctrl Pts',(32.2599839336981,54.3371698226151,17.2232398415856));
#50305=CARTESIAN_POINT('Ctrl Pts',(30.7277587434239,55.4333003417049,17.1121019510176));
#50306=CARTESIAN_POINT('Ctrl Pts',(30.8176860738768,57.3150891778467,17.0009640604495));
#50307=CARTESIAN_POINT('Ctrl Pts',(32.4474544196475,58.2601136683833,16.8898261698815));
#50308=CARTESIAN_POINT('Ctrl Pts',(34.1253183310228,57.4033821798196,16.7786882793134));
#50309=CARTESIAN_POINT('Ctrl Pts',(34.3155099416484,55.5290707596339,16.6675503887454));
#50310=CARTESIAN_POINT('Ctrl Pts',(32.843944713402,54.3527579068599,16.5564124981773));
#50311=CARTESIAN_POINT('Ctrl Pts',(31.0575629883768,54.9511361159353,16.4452746076093));
#50312=CARTESIAN_POINT('Ctrl Pts',(30.5914602184459,56.776503026026,16.3341367170413));
#50313=CARTESIAN_POINT('Ctrl Pts',(31.87226555487,58.158079603251,16.2229988264732));
#50314=CARTESIAN_POINT('Ctrl Pts',(33.727643347944,57.8312931383451,16.1118609359052));
#50315=CARTESIAN_POINT('Ctrl Pts',(34.4593452621631,56.095254988621,16.0007230453371));
#50316=CARTESIAN_POINT('Ctrl Pts',(33.3976362375564,54.5389805605859,15.8895851547691));
#50317=CARTESIAN_POINT('Ctrl Pts',(31.5143105845896,54.5869454874661,15.7784472642011));
#50318=CARTESIAN_POINT('Ctrl Pts',(30.5331976325014,56.1952469279427,15.667309373633));
#50319=CARTESIAN_POINT('Ctrl Pts',(31.3523211914896,57.8917883337404,15.556171483065));
#50320=CARTESIAN_POINT('Ctrl Pts',(33.2219281813735,58.1237061169015,15.4450335924969));
#50321=CARTESIAN_POINT('Ctrl Pts',(34.4307461158152,56.6787232986569,15.3338957019289));
#50322=CARTESIAN_POINT('Ctrl Pts',(33.872330241923,54.879449043198,15.2227578113608));
#50323=CARTESIAN_POINT('Ctrl Pts',(32.0578049190619,54.3727794748353,15.1116199207928));
#50324=CARTESIAN_POINT('Ctrl Pts',(30.6480257991425,55.6224750092611,15.0004820302248));
#50325=CARTESIAN_POINT('Ctrl Pts',(30.9333796069945,57.4846751237948,14.8893441396567));
#50326=CARTESIAN_POINT('Ctrl Pts',(32.6526789495027,58.254886989871,14.7782062490887));
#50327=CARTESIAN_POINT('Ctrl Pts',(34.2322292733731,57.2281268414992,14.6670683585206));
#50328=CARTESIAN_POINT('Ctrl Pts',(34.2262509881345,55.3442001072214,14.5559304679526));
#50329=CARTESIAN_POINT('Ctrl Pts',(32.6402146165803,54.3274858508605,14.4447925773845));
#50330=CARTESIAN_POINT('Ctrl Pts',(30.9258401772609,55.1085950446227,14.3336546868165));
#50331=CARTESIAN_POINT('Ctrl Pts',(30.6523081515825,56.9725678179105,14.2225167962485));
#50332=CARTESIAN_POINT('Ctrl Pts',(32.0699972824786,58.21329228897,14.1113789056804));
#50333=CARTESIAN_POINT('Ctrl Pts',(33.8812570606045,57.6951122012284,14.0002410151124));
#50334=CARTESIAN_POINT('Ctrl Pts',(34.4282680395032,55.8923378292205,13.8891031245443));
#50335=CARTESIAN_POINT('Ctrl Pts',(33.2102504690214,54.4550406555783,13.7779652339763));
#50336=CARTESIAN_POINT('Ctrl Pts',(31.3422585573418,54.6988518086249,13.6668273434082));
#50337=CARTESIAN_POINT('Ctrl Pts',(30.5337084227428,56.4004946512136,13.5556894528402));
#50338=CARTESIAN_POINT('Ctrl Pts',(31.5254318107855,58.0026634188128,13.4445515622722));
#50339=CARTESIAN_POINT('Ctrl Pts',(33.4081782759357,58.0384196200583,13.3334136717041));
#50340=CARTESIAN_POINT('Ctrl Pts',(34.4616877513079,56.4759533589966,13.2222757811361));
#50341=CARTESIAN_POINT('Ctrl Pts',(33.7154925108507,54.7434886384194,13.111137890568));
#50342=CARTESIAN_POINT('Ctrl Pts',(32.4828476954683,54.5360428684886,13.0370459635227));
#50343=CARTESIAN_POINT('Ctrl Pts',(31.9588970197441,54.7159724828016,13.));
#50344=CARTESIAN_POINT('Ctrl Pts',(31.667262219952,54.851191363199,21.3785196366098));
#50345=CARTESIAN_POINT('Ctrl Pts',(31.479741769716,54.9581664087852,21.3641270219409));
#50346=CARTESIAN_POINT('Ctrl Pts',(31.3126103376672,55.0996825231224,21.349734407272));
#50347=CARTESIAN_POINT('Ctrl Pts',(31.1813106469723,55.2689855779558,21.3353417926031));
#50348=CARTESIAN_POINT('Ctrl Pts',(30.843350959735,55.7047642698706,21.2982958290805));
#50349=CARTESIAN_POINT('Ctrl Pts',(30.7427855837258,56.3246384411287,21.2612498655578));
#50350=CARTESIAN_POINT('Ctrl Pts',(30.9256226263006,56.8449164848152,21.2242039020351));
#50351=CARTESIAN_POINT('Ctrl Pts',(31.1084596688754,57.3651945285016,21.1871579385124));
#50352=CARTESIAN_POINT('Ctrl Pts',(31.5746991300343,57.7858764446163,21.1501119749897));
#50353=CARTESIAN_POINT('Ctrl Pts',(32.110971975203,57.9144361067477,21.1130660114671));
#50354=CARTESIAN_POINT('Ctrl Pts',(32.6472448203718,58.0429957688791,21.0760200479444));
#50355=CARTESIAN_POINT('Ctrl Pts',(33.2535510495504,57.8794331770273,21.0389740844217));
#50356=CARTESIAN_POINT('Ctrl Pts',(33.6524071321848,57.4986030102674,21.001928120899));
#50357=CARTESIAN_POINT('Ctrl Pts',(34.0512632148192,57.1177728435075,20.9648821573763));
#50358=CARTESIAN_POINT('Ctrl Pts',(34.2426691509094,56.5196751018395,20.9278361938536));
#50359=CARTESIAN_POINT('Ctrl Pts',(34.1390289505937,55.9780329422498,20.890790230331));
#50360=CARTESIAN_POINT('Ctrl Pts',(34.035388750278,55.4363907826601,20.8537442668083));
#50361=CARTESIAN_POINT('Ctrl Pts',(33.6367024135565,54.9512042051487,20.8166983032856));
#50362=CARTESIAN_POINT('Ctrl Pts',(33.1254299926942,54.7445214311787,20.7796523397629));
#50363=CARTESIAN_POINT('Ctrl Pts',(32.6601848660756,54.5564452717343,20.7459414387119));
#50364=CARTESIAN_POINT('Ctrl Pts',(32.1017123235945,54.5989854456511,20.7122305376608));
#50365=CARTESIAN_POINT('Ctrl Pts',(31.6651488727496,54.8473747039336,20.6785196366098));
#50366=CARTESIAN_POINT('Ctrl Pts',(33.9541262883781,54.8399232067375,22.));
#50367=CARTESIAN_POINT('Ctrl Pts',(33.89777705666,54.7931706099734,22.));
#50368=CARTESIAN_POINT('Ctrl Pts',(33.8389107618346,54.7498380989977,22.));
#50369=CARTESIAN_POINT('Ctrl Pts',(33.7778765460594,54.7099422292599,22.));
#50370=CARTESIAN_POINT('Ctrl Pts',(33.715142612768,54.6689353153684,22.));
#50371=CARTESIAN_POINT('Ctrl Pts',(33.650117347963,54.6315587953775,22.));
#50372=CARTESIAN_POINT('Ctrl Pts',(33.5831568242514,54.5978800039331,22.));
#50373=CARTESIAN_POINT('Ctrl Pts',(33.5265763653167,54.5694220204725,22.));
#50374=CARTESIAN_POINT('Ctrl Pts',(33.4686133977542,54.5436050120003,22.));
#50375=CARTESIAN_POINT('Ctrl Pts',(33.4094785141808,54.5204983074666,22.));
#50376=CARTESIAN_POINT('Ctrl Pts',(33.3832054797345,54.5102322308723,22.));
#50377=CARTESIAN_POINT('Ctrl Pts',(33.3567011132798,54.5005015028803,22.));
#50378=CARTESIAN_POINT('Ctrl Pts',(33.3299840335543,54.4913139103876,22.));
#50379=CARTESIAN_POINT('Ctrl Pts',(33.3153052179449,54.4862660916334,22.));
#50380=CARTESIAN_POINT('Ctrl Pts',(33.3005621960478,54.4813822417937,22.));
#50381=CARTESIAN_POINT('Ctrl Pts',(33.2857580867441,54.4766637893069,22.));
#50382=CARTESIAN_POINT('Ctrl Pts',(33.2721048858946,54.4723121611084,22.));
#50383=CARTESIAN_POINT('Ctrl Pts',(33.2583976935292,54.4681007280097,22.));
#50384=CARTESIAN_POINT('Ctrl Pts',(33.2446602942607,54.4640366443286,22.));
#50385=CARTESIAN_POINT('Ctrl Pts',(33.1744615986776,54.4432690035566,22.));
#50386=CARTESIAN_POINT('Ctrl Pts',(33.1033546242792,54.4263051056874,22.));
#50387=CARTESIAN_POINT('Ctrl Pts',(33.0316734669243,54.4132045353738,22.));
#50388=CARTESIAN_POINT('Ctrl Pts',(32.9605481884268,54.4002055584262,22.));
#50389=CARTESIAN_POINT('Ctrl Pts',(32.8888565785142,54.3910102235798,22.));
#50390=CARTESIAN_POINT('Ctrl Pts',(32.8169264247183,54.385727650947,22.));
#50391=CARTESIAN_POINT('Ctrl Pts',(32.7571464345771,54.3813373900725,22.));
#50392=CARTESIAN_POINT('Ctrl Pts',(32.6972014393332,54.3796505588106,22.));
#50393=CARTESIAN_POINT('Ctrl Pts',(32.6372877973872,54.3807569468898,22.));
#50394=CARTESIAN_POINT('Ctrl Pts',(32.6122799917386,54.3812187505318,22.));
#50395=CARTESIAN_POINT('Ctrl Pts',(32.5872777755307,54.3821674889425,22.));
#50396=CARTESIAN_POINT('Ctrl Pts',(32.5622960765392,54.3836109807431,22.));
#50397=CARTESIAN_POINT('Ctrl Pts',(32.5507331510584,54.3842791093651,22.));
#50398=CARTESIAN_POINT('Ctrl Pts',(32.5391746273353,54.3850532424606,22.));
#50399=CARTESIAN_POINT('Ctrl Pts',(32.527622019984,54.3859342108815,22.));
#50400=CARTESIAN_POINT('Ctrl Pts',(32.515571956249,54.3868531138873,22.));
#50401=CARTESIAN_POINT('Ctrl Pts',(32.5035366027722,54.3878876490277,22.));
#50402=CARTESIAN_POINT('Ctrl Pts',(32.4915220458572,54.3890378132825,22.));
#50403=CARTESIAN_POINT('Ctrl Pts',(32.4230954842055,54.3955883490906,22.));
#50404=CARTESIAN_POINT('Ctrl Pts',(32.3552950943228,54.4058891778563,22.));
#50405=CARTESIAN_POINT('Ctrl Pts',(32.2884097213901,54.420031548574,22.));
#50406=CARTESIAN_POINT('Ctrl Pts',(32.2277876728082,54.4328495900548,22.));
#50407=CARTESIAN_POINT('Ctrl Pts',(32.1679169373136,54.448823971587,22.));
#50408=CARTESIAN_POINT('Ctrl Pts',(32.1090267714104,54.4680568733301,22.));
#50409=CARTESIAN_POINT('Ctrl Pts',(32.0393564154629,54.4908104704681,22.));
#50410=CARTESIAN_POINT('Ctrl Pts',(31.9710568700512,54.5181250014914,22.));
#50411=CARTESIAN_POINT('Ctrl Pts',(31.9044569620169,54.5497238479896,22.));
#50412=CARTESIAN_POINT('Ctrl Pts',(31.8897939177248,54.5566808438692,22.));
#50413=CARTESIAN_POINT('Ctrl Pts',(31.875213443077,54.5638456669608,22.));
#50414=CARTESIAN_POINT('Ctrl Pts',(31.8607193748282,54.571215603018,22.));
#50415=CARTESIAN_POINT('Ctrl Pts',(31.8457643400607,54.5788199310837,22.));
#50416=CARTESIAN_POINT('Ctrl Pts',(31.8308959671421,54.5866456914889,22.));
#50417=CARTESIAN_POINT('Ctrl Pts',(31.8161482776472,54.594673337877,22.));
#50418=CARTESIAN_POINT('Ctrl Pts',(31.7559125282455,54.6274616126968,22.));
#50419=CARTESIAN_POINT('Ctrl Pts',(31.6976088413824,54.6636511833295,22.));
#50420=CARTESIAN_POINT('Ctrl Pts',(31.6414698545344,54.702968470454,22.));
#50421=CARTESIAN_POINT('Ctrl Pts',(31.5853421058314,54.7422778868741,22.));
#50422=CARTESIAN_POINT('Ctrl Pts',(31.5313774894568,54.7847146962881,22.));
#50423=CARTESIAN_POINT('Ctrl Pts',(31.4798463246642,54.8300409282343,22.));
#50424=CARTESIAN_POINT('Ctrl Pts',(31.4425466815923,54.8628492740225,22.));
#50425=CARTESIAN_POINT('Ctrl Pts',(31.4065227401674,54.8971722385251,22.));
#50426=CARTESIAN_POINT('Ctrl Pts',(31.3718924923334,54.9329270614585,22.));
#50427=CARTESIAN_POINT('Ctrl Pts',(31.3459157227865,54.9597473949422,22.));
#50428=CARTESIAN_POINT('Ctrl Pts',(31.3207234116099,54.987373540647,22.));
#50429=CARTESIAN_POINT('Ctrl Pts',(31.2963709389138,55.0157718708887,22.));
#50430=CARTESIAN_POINT('Ctrl Pts',(31.2882802398916,55.0252067379589,22.));
#50431=CARTESIAN_POINT('Ctrl Pts',(31.2802886269196,55.0347194487898,22.));
#50432=CARTESIAN_POINT('Ctrl Pts',(31.2723979365543,55.0443082314195,22.));
#50433=CARTESIAN_POINT('Ctrl Pts',(31.2305359635494,55.0951789842957,22.));
#50434=CARTESIAN_POINT('Ctrl Pts',(31.1915084684126,55.1481921233583,22.));
#50435=CARTESIAN_POINT('Ctrl Pts',(31.1555797357851,55.2031373176633,22.));
#50436=CARTESIAN_POINT('Ctrl Pts',(31.130298191857,55.2417999489858,22.));
#50437=CARTESIAN_POINT('Ctrl Pts',(31.1065518383838,55.2814196840771,22.));
#50438=CARTESIAN_POINT('Ctrl Pts',(31.0844478042592,55.3219265813484,22.));
#50439=CARTESIAN_POINT('Ctrl Pts',(31.0773529644809,55.3349282779815,22.));
#50440=CARTESIAN_POINT('Ctrl Pts',(31.0704265009656,55.3480232015208,22.));
#50441=CARTESIAN_POINT('Ctrl Pts',(31.0636752117837,55.3612032672917,22.));
#50442=CARTESIAN_POINT('Ctrl Pts',(31.0349131819519,55.417353349843,22.));
#50443=CARTESIAN_POINT('Ctrl Pts',(31.0093835905525,55.4749346571281,22.));
#50444=CARTESIAN_POINT('Ctrl Pts',(30.9873422740719,55.5337599434685,22.));
#50445=CARTESIAN_POINT('Ctrl Pts',(30.9670232664277,55.5879886209558,22.));
#50446=CARTESIAN_POINT('Ctrl Pts',(30.9496688942649,55.6432750194153,22.));
#50447=CARTESIAN_POINT('Ctrl Pts',(30.9355188507018,55.6994745658575,22.));
#50448=CARTESIAN_POINT('Ctrl Pts',(30.9328706183904,55.7099925161458,22.));
#50449=CARTESIAN_POINT('Ctrl Pts',(30.9303347375364,55.7205424451195,22.));
#50450=CARTESIAN_POINT('Ctrl Pts',(30.9279109916838,55.7311226632894,22.));
#50451=CARTESIAN_POINT('Origin',(32.5,56.2916512459885,17.));
#50452=CARTESIAN_POINT('Origin',(32.5,-56.2916512459885,12.));
#50453=CARTESIAN_POINT('Origin',(-32.5,-56.2916512459885,12.));
#50454=CARTESIAN_POINT('Origin',(-65.,8.88178419700125E-15,12.));
#50455=CARTESIAN_POINT('Origin',(-32.5,56.2916512459885,12.));
#50456=CARTESIAN_POINT('Origin',(32.5,56.2916512459885,12.));
#50457=CARTESIAN_POINT('Origin',(65.,0.,7.));
#50458=CARTESIAN_POINT('Ctrl Pts',(66.6351293272515,-0.319230454628274,
7.));
#50459=CARTESIAN_POINT('Ctrl Pts',(66.6302897730466,-0.381554702499113,
7.));
#50460=CARTESIAN_POINT('Ctrl Pts',(66.6216732730344,-0.44339471174141,7.));
#50461=CARTESIAN_POINT('Ctrl Pts',(66.6095363361247,-0.504531338372354,
7.));
#50462=CARTESIAN_POINT('Ctrl Pts',(66.6018369189696,-0.543315126686597,
7.));
#50463=CARTESIAN_POINT('Ctrl Pts',(66.5927196857359,-0.581816142971907,
7.));
#50464=CARTESIAN_POINT('Ctrl Pts',(66.5822397317414,-0.619979888881646,
7.));
#50465=CARTESIAN_POINT('Ctrl Pts',(66.575055633828,-0.646141462444073,7.));
#50466=CARTESIAN_POINT('Ctrl Pts',(66.5672309976242,-0.672144564830664,
7.));
#50467=CARTESIAN_POINT('Ctrl Pts',(66.5587815172138,-0.69797162244664,7.));
#50468=CARTESIAN_POINT('Ctrl Pts',(66.5543304405506,-0.711576981338436,
7.));
#50469=CARTESIAN_POINT('Ctrl Pts',(66.5497059365671,-0.725133118782638,
7.));
#50470=CARTESIAN_POINT('Ctrl Pts',(66.5449151805486,-0.738624321418645,
7.));
#50471=CARTESIAN_POINT('Ctrl Pts',(66.5228385616516,-0.800794078740785,
7.));
#50472=CARTESIAN_POINT('Ctrl Pts',(66.4972129908327,-0.861656594198672,
7.));
#50473=CARTESIAN_POINT('Ctrl Pts',(66.4682928032974,-0.920967263964251,
7.));
#50474=CARTESIAN_POINT('Ctrl Pts',(66.4474370017557,-0.963739170488886,
7.));
#50475=CARTESIAN_POINT('Ctrl Pts',(66.4248666023715,-1.00570421528168,7.));
#50476=CARTESIAN_POINT('Ctrl Pts',(66.4006603561211,-1.04676903354864,7.));
#50477=CARTESIAN_POINT('Ctrl Pts',(66.3939846942071,-1.05809399655503,7.));
#50478=CARTESIAN_POINT('Ctrl Pts',(66.3871845393328,-1.06935047365006,7.));
#50479=CARTESIAN_POINT('Ctrl Pts',(66.3802613712345,-1.08053645690262,7.));
#50480=CARTESIAN_POINT('Ctrl Pts',(66.3732910164015,-1.09179868126564,7.));
#50481=CARTESIAN_POINT('Ctrl Pts',(66.366200339596,-1.10298231859776,7.));
#50482=CARTESIAN_POINT('Ctrl Pts',(66.3589938162138,-1.11408178950634,7.));
#50483=CARTESIAN_POINT('Ctrl Pts',(66.3220437716818,-1.17099216398268,7.));
#50484=CARTESIAN_POINT('Ctrl Pts',(66.2820328735632,-1.22572189932463,7.));
#50485=CARTESIAN_POINT('Ctrl Pts',(66.2392195753837,-1.27802354449959,7.));
#50486=CARTESIAN_POINT('Ctrl Pts',(66.1957886599383,-1.33107968419999,7.));
#50487=CARTESIAN_POINT('Ctrl Pts',(66.1494735385541,-1.38163817167118,7.));
#50488=CARTESIAN_POINT('Ctrl Pts',(66.1004928624473,-1.4294273768642,7.));
#50489=CARTESIAN_POINT('Ctrl Pts',(66.0701495070252,-1.45903262027388,7.));
#50490=CARTESIAN_POINT('Ctrl Pts',(66.0387821884129,-1.48757476196839,7.));
#50491=CARTESIAN_POINT('Ctrl Pts',(66.0064342586826,-1.51498409802404,7.));
#50492=CARTESIAN_POINT('Ctrl Pts',(65.9799267074793,-1.53744471250548,7.));
#50493=CARTESIAN_POINT('Ctrl Pts',(65.9527605447791,-1.55914459463409,7.));
#50494=CARTESIAN_POINT('Ctrl Pts',(65.9249567188516,-1.58004262988225,7.));
#50495=CARTESIAN_POINT('Ctrl Pts',(65.9136073282091,-1.58857310933178,7.));
#50496=CARTESIAN_POINT('Ctrl Pts',(65.9021495271597,-1.59697130994429,7.));
#50497=CARTESIAN_POINT('Ctrl Pts',(65.8906044505495,-1.60522061987257,7.));
#50498=CARTESIAN_POINT('Ctrl Pts',(65.8332561981394,-1.64619769814996,7.));
#50499=CARTESIAN_POINT('Ctrl Pts',(65.7736595595987,-1.68357914693718,7.));
#50500=CARTESIAN_POINT('Ctrl Pts',(65.7120551181349,-1.71709301891337,7.));
#50501=CARTESIAN_POINT('Ctrl Pts',(65.7052145748788,-1.7208143916827,7.));
#50502=CARTESIAN_POINT('Ctrl Pts',(65.6983492298898,-1.72448805150504,7.));
#50503=CARTESIAN_POINT('Ctrl Pts',(65.6914593790745,-1.72811360467692,7.));
#50504=CARTESIAN_POINT('Ctrl Pts',(65.6317930119872,-1.75951103144934,7.));
#50505=CARTESIAN_POINT('Ctrl Pts',(65.5702916681948,-1.78730397727615,7.));
#50506=CARTESIAN_POINT('Ctrl Pts',(65.5072864772923,-1.81157490046553,7.));
#50507=CARTESIAN_POINT('Ctrl Pts',(65.4395015551736,-1.83768707653506,7.));
#50508=CARTESIAN_POINT('Ctrl Pts',(65.3699753257072,-1.8597233626146,7.));
#50509=CARTESIAN_POINT('Ctrl Pts',(65.2990847711215,-1.87773280074392,7.));
#50510=CARTESIAN_POINT('Ctrl Pts',(65.2861211425482,-1.88102615439428,7.));
#50511=CARTESIAN_POINT('Ctrl Pts',(65.273111817892,-1.88418469346294,7.));
#50512=CARTESIAN_POINT('Ctrl Pts',(65.2600590170115,-1.88720850989751,7.));
#50513=CARTESIAN_POINT('Ctrl Pts',(65.2488130849708,-1.8898137464623,7.));
#50514=CARTESIAN_POINT('Ctrl Pts',(65.2375439537823,-1.89231686461017,7.));
#50515=CARTESIAN_POINT('Ctrl Pts',(65.2262547951763,-1.89471805491894,7.));
#50516=CARTESIAN_POINT('Ctrl Pts',(65.1567411013721,-1.90950353306807,7.));
#50517=CARTESIAN_POINT('Ctrl Pts',(65.0864519774429,-1.92043226303064,7.));
#50518=CARTESIAN_POINT('Ctrl Pts',(65.015754733485,-1.92760520158657,7.));
#50519=CARTESIAN_POINT('Ctrl Pts',(64.9435658003622,-1.93492948684464,7.));
#50520=CARTESIAN_POINT('Ctrl Pts',(64.8709504430061,-1.93833807716963,7.));
#50521=CARTESIAN_POINT('Ctrl Pts',(64.7982722133132,-1.93789067648535,7.));
#50522=CARTESIAN_POINT('Ctrl Pts',(64.7251526999959,-1.93744055929852,7.));
#50523=CARTESIAN_POINT('Ctrl Pts',(64.6519684871839,-1.93308764503148,7.));
#50524=CARTESIAN_POINT('Ctrl Pts',(64.5790772350591,-1.92484184820796,7.));
#50525=CARTESIAN_POINT('Ctrl Pts',(64.5610671587141,-1.92280446476361,7.));
#50526=CARTESIAN_POINT('Ctrl Pts',(64.5430749514638,-1.92052917538604,7.));
#50527=CARTESIAN_POINT('Ctrl Pts',(64.5251060094438,-1.918015636991,7.));
#50528=CARTESIAN_POINT('Ctrl Pts',(64.5110402167059,-1.91604808041119,7.));
#50529=CARTESIAN_POINT('Ctrl Pts',(64.4969870785069,-1.91393415852473,7.));
#50530=CARTESIAN_POINT('Ctrl Pts',(64.4829704724909,-1.91167739719604,7.));
#50531=CARTESIAN_POINT('Ctrl Pts',(64.4085834936561,-1.89970062785533,7.));
#50532=CARTESIAN_POINT('Ctrl Pts',(64.3350918230921,-1.88368734542449,7.));
#50533=CARTESIAN_POINT('Ctrl Pts',(64.2628790838146,-1.86371221650546,7.));
#50534=CARTESIAN_POINT('Ctrl Pts',(64.1905873443837,-1.84371523495678,7.));
#50535=CARTESIAN_POINT('Ctrl Pts',(64.1195762103623,-1.81974781469441,7.));
#50536=CARTESIAN_POINT('Ctrl Pts',(64.0502233636653,-1.79183341398573,7.));
#50537=CARTESIAN_POINT('Ctrl Pts',(63.9824494701887,-1.76455453921426,7.));
#50538=CARTESIAN_POINT('Ctrl Pts',(63.9162581817051,-1.73350624801242,7.));
#50539=CARTESIAN_POINT('Ctrl Pts',(63.8520110122706,-1.69866187357367,7.));
#50540=CARTESIAN_POINT('Ctrl Pts',(63.838191558037,-1.69116690932713,7.));
#50541=CARTESIAN_POINT('Ctrl Pts',(63.8244621192021,-1.6834961317264,7.));
#50542=CARTESIAN_POINT('Ctrl Pts',(63.8108264207747,-1.67564897964534,7.));
#50543=CARTESIAN_POINT('Ctrl Pts',(63.7992831576295,-1.66900599455042,7.));
#50544=CARTESIAN_POINT('Ctrl Pts',(63.7878070738684,-1.66223660984747,7.));
#50545=CARTESIAN_POINT('Ctrl Pts',(63.7763989699203,-1.65534250909262,7.));
#50546=CARTESIAN_POINT('Ctrl Pts',(63.1173724903363,-0.82323218010314,7.));
#50547=CARTESIAN_POINT('Ctrl Pts',(63.0939903977405,-0.752339169259015,
7.));
#50548=CARTESIAN_POINT('Ctrl Pts',(63.0748445296609,-0.680224887837059,
7.));
#50549=CARTESIAN_POINT('Ctrl Pts',(63.0598471165382,-0.607239755689072,
7.));
#50550=CARTESIAN_POINT('Ctrl Pts',(63.045242974325,-0.536168482222122,7.));
#50551=CARTESIAN_POINT('Ctrl Pts',(63.0345730321078,-0.464270523370859,
7.));
#50552=CARTESIAN_POINT('Ctrl Pts',(63.0278019508404,-0.391872562027795,
7.));
#50553=CARTESIAN_POINT('Ctrl Pts',(63.0262906434644,-0.37571331527496,7.));
#50554=CARTESIAN_POINT('Ctrl Pts',(63.0249735943724,-0.359527041219007,
7.));
#50555=CARTESIAN_POINT('Ctrl Pts',(63.0238511666502,-0.343324371082198,
7.));
#50556=CARTESIAN_POINT('Ctrl Pts',(63.0187005423293,-0.268973154322249,
7.));
#50557=CARTESIAN_POINT('Ctrl Pts',(63.01765302891,-0.194423668235733,6.99999999999999));
#50558=CARTESIAN_POINT('Ctrl Pts',(63.0206465481523,-0.12003052841074,6.99999999999999));
#50559=CARTESIAN_POINT('Ctrl Pts',(63.0227481861389,-0.0678018851499504,
6.99999999999999));
#50560=CARTESIAN_POINT('Ctrl Pts',(63.0268427413453,-0.0156503278706247,
7.));
#50561=CARTESIAN_POINT('Ctrl Pts',(63.0329233152646,0.0362966145553371,
7.));
#50562=CARTESIAN_POINT('Ctrl Pts',(63.0352354056611,0.0560490307420095,
7.));
#50563=CARTESIAN_POINT('Ctrl Pts',(63.0378347616354,0.0757718045552192,
7.));
#50564=CARTESIAN_POINT('Ctrl Pts',(63.0407214327064,0.0954576795021992,
7.));
#50565=CARTESIAN_POINT('Ctrl Pts',(63.0434693777868,0.114197501908112,7.));
#50566=CARTESIAN_POINT('Ctrl Pts',(63.0464788570236,0.132909725458142,7.));
#50567=CARTESIAN_POINT('Ctrl Pts',(63.0497439150678,0.151555112925564,7.));
#50568=CARTESIAN_POINT('Ctrl Pts',(63.0622655749108,0.223061100370353,7.));
#50569=CARTESIAN_POINT('Ctrl Pts',(63.0785510720888,0.293661818487745,7.));
#50570=CARTESIAN_POINT('Ctrl Pts',(63.0985450712042,0.363028530688884,7.));
#50571=CARTESIAN_POINT('Ctrl Pts',(63.1181095249786,0.430904988345293,7.));
#50572=CARTESIAN_POINT('Ctrl Pts',(63.1412253033662,0.497600711033835,7.));
#50573=CARTESIAN_POINT('Ctrl Pts',(63.1678836569475,0.562784339004564,6.99999999999999));
#50574=CARTESIAN_POINT('Ctrl Pts',(63.1939574715792,0.626538682555551,6.99999999999999));
#50575=CARTESIAN_POINT('Ctrl Pts',(63.2234205960509,0.688847180656012,7.));
#50576=CARTESIAN_POINT('Ctrl Pts',(63.2563003834741,0.749366435300762,7.));
#50577=CARTESIAN_POINT('Ctrl Pts',(63.2669864354346,0.769035415863878,7.));
#50578=CARTESIAN_POINT('Ctrl Pts',(63.2780336415092,0.788515094659923,7.));
#50579=CARTESIAN_POINT('Ctrl Pts',(63.2894436729518,0.807792724382841,7.));
#50580=CARTESIAN_POINT('Ctrl Pts',(63.295878298058,0.818664238701439,7.));
#50581=CARTESIAN_POINT('Ctrl Pts',(63.3024290949643,0.829472548346211,7.));
#50582=CARTESIAN_POINT('Ctrl Pts',(63.3090867443576,0.84020027364224,7.));
#50583=CARTESIAN_POINT('Ctrl Pts',(63.3451024516196,0.898233761293134,7.));
#50584=CARTESIAN_POINT('Ctrl Pts',(63.3843017903414,0.95401501249512,7.));
#50585=CARTESIAN_POINT('Ctrl Pts',(63.4266709047228,1.00724100891289,7.));
#50586=CARTESIAN_POINT('Ctrl Pts',(63.4327868740794,1.01492416603856,7.));
#50587=CARTESIAN_POINT('Ctrl Pts',(63.4389689569011,1.02255401965522,7.));
#50588=CARTESIAN_POINT('Ctrl Pts',(63.4452171764818,1.0301295944151,7.));
#50589=CARTESIAN_POINT('Ctrl Pts',(63.4893586672679,1.08364838631147,7.));
#50590=CARTESIAN_POINT('Ctrl Pts',(63.5367987510512,1.13446181353169,7.));
#50591=CARTESIAN_POINT('Ctrl Pts',(63.5871991852977,1.18242370280982,7.));
#50592=CARTESIAN_POINT('Ctrl Pts',(63.6342187269732,1.22716827863463,7.));
#50593=CARTESIAN_POINT('Ctrl Pts',(63.6838158179949,1.26943087720979,7.));
#50594=CARTESIAN_POINT('Ctrl Pts',(63.7357299599167,1.30905529564257,7.));
#50595=CARTESIAN_POINT('Ctrl Pts',(63.7471862227157,1.31779949778129,7.));
#50596=CARTESIAN_POINT('Ctrl Pts',(63.7587553478436,1.32641507643739,7.));
#50597=CARTESIAN_POINT('Ctrl Pts',(63.77043456489,1.33490009624518,7.));
#50598=CARTESIAN_POINT('Ctrl Pts',(63.7795655910972,1.34153384043588,7.));
#50599=CARTESIAN_POINT('Ctrl Pts',(63.7887633889848,1.34808730275802,7.));
#50600=CARTESIAN_POINT('Ctrl Pts',(63.7980157939078,1.35455228241838,7.));
#50601=CARTESIAN_POINT('Ctrl Pts',(63.8540658570817,1.39371642637854,7.));
#50602=CARTESIAN_POINT('Ctrl Pts',(63.9122195646569,1.42971188595968,7.));
#50603=CARTESIAN_POINT('Ctrl Pts',(63.972145843803,1.46241564583361,7.));
#50604=CARTESIAN_POINT('Ctrl Pts',(64.0317950323209,1.49496818815331,7.));
#50605=CARTESIAN_POINT('Ctrl Pts',(64.0932015439653,1.52425966109842,6.99999999999999));
#50606=CARTESIAN_POINT('Ctrl Pts',(64.1560527983145,1.5501195510723,6.99999999999999));
#50607=CARTESIAN_POINT('Ctrl Pts',(64.2175568100927,1.57542512363411,6.99999999999999));
#50608=CARTESIAN_POINT('Ctrl Pts',(64.2804452599182,1.59744473903897,7.));
#50609=CARTESIAN_POINT('Ctrl Pts',(64.3444233294929,1.615969062658,7.));
#50610=CARTESIAN_POINT('Ctrl Pts',(64.3578992521757,1.61987090518782,7.));
#50611=CARTESIAN_POINT('Ctrl Pts',(64.3714234816407,1.62361749280583,6.99999999999999));
#50612=CARTESIAN_POINT('Ctrl Pts',(64.3849931908178,1.62720657514001,6.99999999999999));
#50613=CARTESIAN_POINT('Ctrl Pts',(64.3978648606924,1.63061103151825,6.99999999999999));
#50614=CARTESIAN_POINT('Ctrl Pts',(64.4107792255323,1.63387407358145,7.));
#50615=CARTESIAN_POINT('Ctrl Pts',(64.4237128647624,1.63698901050256,7.));
#50616=CARTESIAN_POINT('Ctrl Pts',(64.4872431918316,1.65228965078473,7.));
#50617=CARTESIAN_POINT('Ctrl Pts',(64.5513507145775,1.66405191394776,6.99999999999999));
#50618=CARTESIAN_POINT('Ctrl Pts',(64.6157505858482,1.67213050415234,6.99999999999999));
#50619=CARTESIAN_POINT('Ctrl Pts',(64.6789248746032,1.68005535214111,6.99999999999999));
#50620=CARTESIAN_POINT('Ctrl Pts',(64.7423813716982,1.68443544216709,7.));
#50621=CARTESIAN_POINT('Ctrl Pts',(64.8058448174403,1.6850843166444,7.));
#50622=CARTESIAN_POINT('Ctrl Pts',(64.8672458808394,1.68571210453794,7.));
#50623=CARTESIAN_POINT('Ctrl Pts',(64.9286541091596,1.68284715375553,7.));
#50624=CARTESIAN_POINT('Ctrl Pts',(64.9898031296817,1.67627454332248,7.));
#50625=CARTESIAN_POINT('Ctrl Pts',(64.9999907153199,1.67517952935362,7.));
#50626=CARTESIAN_POINT('Ctrl Pts',(65.0101710540749,1.67398149897561,7.));
#50627=CARTESIAN_POINT('Ctrl Pts',(65.0203428468639,1.67267933134471,7.));
#50628=CARTESIAN_POINT('Ctrl Pts',(65.0310998269281,1.67130224949331,7.));
#50629=CARTESIAN_POINT('Ctrl Pts',(65.0418472497685,1.66980870242007,7.));
#50630=CARTESIAN_POINT('Ctrl Pts',(65.0525835864496,1.66819940096574,7.));
#50631=CARTESIAN_POINT('Origin',(65.,0.,-3.54592528053767));
#50632=CARTESIAN_POINT('Ctrl Pts',(67.0565599569794,0.00149374744778701,
-1.79592528053768));
#50633=CARTESIAN_POINT('Ctrl Pts',(67.0573792182402,0.0997825133646294,
-1.79058130531689));
#50634=CARTESIAN_POINT('Ctrl Pts',(67.0062893847297,0.87860858511394,-1.74819136657341));
#50635=CARTESIAN_POINT('Ctrl Pts',(66.0109392265833,2.20843178543789,-1.66875546430726));
#50636=CARTESIAN_POINT('Ctrl Pts',(63.6930089313552,2.04686416993215,-1.55761757373922));
#50637=CARTESIAN_POINT('Ctrl Pts',(62.5713939614548,0.0121365548742175,
-1.44647968317118));
#50638=CARTESIAN_POINT('Ctrl Pts',(63.67270376601,-2.03388137208553,-1.33534179260313));
#50639=CARTESIAN_POINT('Ctrl Pts',(65.9889058463299,-2.21817250383822,-1.22420390203509));
#50640=CARTESIAN_POINT('Ctrl Pts',(67.0021432190354,-0.892617277286194,
-1.14439839801327));
#50641=CARTESIAN_POINT('Ctrl Pts',(67.057275270459,-0.106740644746498,-1.10163885751414));
#50642=CARTESIAN_POINT('Ctrl Pts',(67.0563730581704,-0.00160407492545608,
-1.09592528053768));
#50643=CARTESIAN_POINT('Ctrl Pts',(67.052679279082,-0.0023836951352286,
-1.85407471946232));
#50644=CARTESIAN_POINT('Ctrl Pts',(67.0491241057456,0.467845902355832,-1.82862455259619));
#50645=CARTESIAN_POINT('Ctrl Pts',(66.6565276815742,1.62960580042267,-1.76612842220737));
#50646=CARTESIAN_POINT('Ctrl Pts',(64.7278715623352,2.41277602144419,-1.66658632829587));
#50647=CARTESIAN_POINT('Ctrl Pts',(62.8252644286755,1.08095990301173,-1.55544843772783));
#50648=CARTESIAN_POINT('Ctrl Pts',(62.9123886677794,-1.24138962897177,-1.44431054715979));
#50649=CARTESIAN_POINT('Ctrl Pts',(64.9107473342681,-2.42691462884512,-1.33317265659175));
#50650=CARTESIAN_POINT('Ctrl Pts',(66.7212428925551,-1.52545313603055,-1.23642738069259));
#50651=CARTESIAN_POINT('Ctrl Pts',(67.0499074437772,-0.417918813768391,
-1.17672806831612));
#50652=CARTESIAN_POINT('Ctrl Pts',(67.0520762837074,0.0011613687935982,
-1.15407471946233));
#50653=CARTESIAN_POINT('Ctrl Pts',(63.7309291201476,1.07935865304851,-2.));
#50654=CARTESIAN_POINT('Ctrl Pts',(63.3720166889934,0.657362393039509,-1.96295403647732));
#50655=CARTESIAN_POINT('Ctrl Pts',(63.1146663550338,-0.565736448038655,
-1.88886210943196));
#50656=CARTESIAN_POINT('Ctrl Pts',(64.4549392280646,-1.89346495741705,-1.77772421886392));
#50657=CARTESIAN_POINT('Ctrl Pts',(66.2941885938804,-1.48351678997984,-1.66658632829587));
#50658=CARTESIAN_POINT('Ctrl Pts',(66.9487863029052,0.282071400691234,-1.55544843772784));
#50659=CARTESIAN_POINT('Ctrl Pts',(65.8196738053231,1.79060584233582,-1.44431054715979));
#50660=CARTESIAN_POINT('Ctrl Pts',(63.9402861076227,1.65960613559166,-1.33317265659175));
#50661=CARTESIAN_POINT('Ctrl Pts',(63.0308759410067,0.00984037007930143,
-1.22203476602371));
#50662=CARTESIAN_POINT('Ctrl Pts',(63.9238225935869,-1.64907962812726,-1.11089687545567));
#50663=CARTESIAN_POINT('Ctrl Pts',(65.8018090473224,-1.79850365805791,-0.999758984887623));
#50664=CARTESIAN_POINT('Ctrl Pts',(66.9458893611786,-0.301774776475126,
-0.888621094319584));
#50665=CARTESIAN_POINT('Ctrl Pts',(66.3088756966202,1.47119119673887,-0.777483203751541));
#50666=CARTESIAN_POINT('Ctrl Pts',(64.4738329478959,1.89754943555687,-0.666345313183499));
#50667=CARTESIAN_POINT('Ctrl Pts',(63.1203970290852,0.587064100833473,-0.555207422615458));
#50668=CARTESIAN_POINT('Ctrl Pts',(63.4873829445486,-1.26077017125901,-0.444069532047416));
#50669=CARTESIAN_POINT('Ctrl Pts',(65.2388844462753,-1.95460593523975,-0.332931641479374));
#50670=CARTESIAN_POINT('Ctrl Pts',(66.7717322843115,-0.859369365311608,
-0.221793750911332));
#50671=CARTESIAN_POINT('Ctrl Pts',(66.6828934802986,1.02245805795664,-0.11065586034329));
#50672=CARTESIAN_POINT('Ctrl Pts',(65.0536831830854,1.96841785926001,0.000482030224751804));
#50673=CARTESIAN_POINT('Ctrl Pts',(63.3753360623109,1.1126625548375,0.111619920792793));
#50674=CARTESIAN_POINT('Ctrl Pts',(63.1840622672629,-0.761525447206207,
0.222757811360836));
#50675=CARTESIAN_POINT('Ctrl Pts',(64.654936873825,-1.93868054946276,0.333895701928877));
#50676=CARTESIAN_POINT('Ctrl Pts',(66.4416516727014,-1.34133936965715,0.445033592496918));
#50677=CARTESIAN_POINT('Ctrl Pts',(66.9088063462926,0.483744952595409,0.55617148306496));
#50678=CARTESIAN_POINT('Ctrl Pts',(65.6288089236944,1.86605203086771,0.667309373633002));
#50679=CARTESIAN_POINT('Ctrl Pts',(63.7732555621069,1.54034052425233,0.778447264201044));
#50680=CARTESIAN_POINT('Ctrl Pts',(63.0405552967276,-0.195262133588717,
0.889585154769085));
#50681=CARTESIAN_POINT('Ctrl Pts',(64.1013569898796,-1.7521391457636,1.00072304533713));
#50682=CARTESIAN_POINT('Ctrl Pts',(65.9846968214939,-1.70526332739895,1.11186093590517));
#50683=CARTESIAN_POINT('Ctrl Pts',(66.9667324851762,-0.0975406463695941,
1.22299882647321));
#50684=CARTESIAN_POINT('Ctrl Pts',(66.148595600912,1.59946209441983,1.33413671704125));
#50685=CARTESIAN_POINT('Ctrl Pts',(64.2791361371736,1.83245904107737,1.4452746076093));
#50686=CARTESIAN_POINT('Ctrl Pts',(63.0694915422322,0.38818544592543,1.55641249817734));
#50687=CARTESIAN_POINT('Ctrl Pts',(63.6268632321408,-1.41139869019814,1.66755038874538));
#50688=CARTESIAN_POINT('Ctrl Pts',(65.441082578101,-1.91911359883674,1.77868827931342));
#50689=CARTESIAN_POINT('Ctrl Pts',(66.8515740381086,-0.670242066229968,
1.88982616988146));
#50690=CARTESIAN_POINT('Ctrl Pts',(66.5672987827578,1.19210963065828,2.0009640604495));
#50691=CARTESIAN_POINT('Ctrl Pts',(64.8484571771716,1.9633098631627,2.11210195101754));
#50692=CARTESIAN_POINT('Ctrl Pts',(63.2683244359328,0.937470312465883,2.22323984158559));
#50693=CARTESIAN_POINT('Ctrl Pts',(63.2732139770213,-0.946446446867291,
2.33437773215363));
#50694=CARTESIAN_POINT('Ctrl Pts',(64.8586503480276,-1.96407003995016,2.44551562272167));
#50695=CARTESIAN_POINT('Ctrl Pts',(66.5734656584983,-1.18395805139742,2.55665351328971));
#50696=CARTESIAN_POINT('Ctrl Pts',(66.8480700074314,0.679844168596883,2.66779140385775));
#50697=CARTESIAN_POINT('Ctrl Pts',(65.4311149200231,1.92137731111722,2.7789292944258));
#50698=CARTESIAN_POINT('Ctrl Pts',(63.6195554571419,1.40425201087122,2.89006718499384));
#50699=CARTESIAN_POINT('Ctrl Pts',(63.0715325396447,-0.398201080226104,
3.00120507556188));
#50700=CARTESIAN_POINT('Ctrl Pts',(64.2886577589191,-1.83617620668518,3.11234296612993));
#50701=CARTESIAN_POINT('Ctrl Pts',(66.1568825986246,-1.59347842751063,3.22348085669796));
#50702=CARTESIAN_POINT('Ctrl Pts',(66.9661996758679,0.107748227638466,3.33461874726601));
#50703=CARTESIAN_POINT('Ctrl Pts',(65.9758318915686,1.71035170808285,3.44575663783405));
#50704=CARTESIAN_POINT('Ctrl Pts',(64.0922741102298,1.74745087340983,3.55689452840209));
#50705=CARTESIAN_POINT('Ctrl Pts',(63.0395681301103,0.185088436867106,3.66803241897013));
#50706=CARTESIAN_POINT('Ctrl Pts',(63.7812676733087,-1.54668754499179,3.77917030953817));
#50707=CARTESIAN_POINT('Ctrl Pts',(65.6384867364955,-1.86276287627795,3.89030820010621));
#50708=CARTESIAN_POINT('Ctrl Pts',(66.9112916488297,-0.473830221762714,
4.00144609067426));
#50709=CARTESIAN_POINT('Ctrl Pts',(66.4346696394808,1.34880460837872,4.11258398124229));
#50710=CARTESIAN_POINT('Ctrl Pts',(64.6448782388305,1.93686328389463,4.22372187181034));
#50711=CARTESIAN_POINT('Ctrl Pts',(63.1801338135814,0.752089030319261,4.33485976237838));
#50712=CARTESIAN_POINT('Ctrl Pts',(63.3811335473526,-1.12108084233401,4.44599765294643));
#50713=CARTESIAN_POINT('Ctrl Pts',(65.0639001046135,-1.96811270537376,4.55713554351446));
#50714=CARTESIAN_POINT('Ctrl Pts',(66.6881781710758,-1.0137086906561,4.66827343408251));
#50715=CARTESIAN_POINT('Ctrl Pts',(66.7672476130381,0.868554387592538,4.77941132465054));
#50716=CARTESIAN_POINT('Ctrl Pts',(65.2287352713998,1.95581977940926,4.8905492152186));
#50717=CARTESIAN_POINT('Ctrl Pts',(63.4808589446452,1.25290115725713,5.00168710578663));
#50718=CARTESIAN_POINT('Ctrl Pts',(63.1234696485087,-0.596812123952619,
5.11282499635468));
#50719=CARTESIAN_POINT('Ctrl Pts',(64.4836898753931,-1.90025645848877,5.22396288692272));
#50720=CARTESIAN_POINT('Ctrl Pts',(66.3164945930014,-1.46437458763454,5.33510077749075));
#50721=CARTESIAN_POINT('Ctrl Pts',(66.9442969223188,0.31186611096645,5.44623866805881));
#50722=CARTESIAN_POINT('Ctrl Pts',(65.7924621445391,1.80265190489436,5.55737655862683));
#50723=CARTESIAN_POINT('Ctrl Pts',(63.9152779448642,1.64345059076357,5.66851444919488));
#50724=CARTESIAN_POINT('Ctrl Pts',(63.0309518163246,-0.0200209171529675,
5.77965233976292));
#50725=CARTESIAN_POINT('Ctrl Pts',(63.9489184664916,-1.66516462760289,5.89079023033097));
#50726=CARTESIAN_POINT('Ctrl Pts',(65.8289506914941,-1.78616905068824,6.001928120899));
#50727=CARTESIAN_POINT('Ctrl Pts',(66.9502374569467,-0.272263260809144,
6.11306601146705));
#50728=CARTESIAN_POINT('Ctrl Pts',(66.2864448139981,1.49082960024053,6.22420390203509));
#50729=CARTESIAN_POINT('Ctrl Pts',(64.4451643957601,1.88938584790038,6.33534179260314));
#50730=CARTESIAN_POINT('Ctrl Pts',(63.1117120727514,0.558493595662749,6.44647968317117));
#50731=CARTESIAN_POINT('Ctrl Pts',(63.5066690059847,-1.28345183053528,6.55761757373921));
#50732=CARTESIAN_POINT('Ctrl Pts',(65.2684140085621,-1.95091987271333,6.66875546430726));
#50733=CARTESIAN_POINT('Ctrl Pts',(66.7846240008828,-0.832135508767304,
6.77989335487529));
#50734=CARTESIAN_POINT('Ctrl Pts',(66.6670561422041,1.04722013035562,6.89103124544334));
#50735=CARTESIAN_POINT('Ctrl Pts',(65.0241955006465,1.97020693527806,7.00216913601138));
#50736=CARTESIAN_POINT('Ctrl Pts',(63.3579443006206,1.08544634211747,7.11330702657943));
#50737=CARTESIAN_POINT('Ctrl Pts',(63.2516046182892,-0.159901738299191,
7.18739895362479));
#50738=CARTESIAN_POINT('Ctrl Pts',(63.4735576439471,-0.667480137268199,
7.22444491714747));
#50739=CARTESIAN_POINT('Ctrl Pts',(63.6322193753412,1.16331236980974,-2.07481497238249));
#50740=CARTESIAN_POINT('Ctrl Pts',(63.2453903360215,0.708492771249616,-2.03776900885981));
#50741=CARTESIAN_POINT('Ctrl Pts',(62.9680230067985,-0.609740058317773,
-1.96367708181445));
#50742=CARTESIAN_POINT('Ctrl Pts',(64.4125437948732,-2.04074076818053,-1.85253919124641));
#50743=CARTESIAN_POINT('Ctrl Pts',(66.3948520224261,-1.59890637623528,-1.74140130067836));
#50744=CARTESIAN_POINT('Ctrl Pts',(67.1003650694627,0.304011228025913,-1.63026341011032));
#50745=CARTESIAN_POINT('Ctrl Pts',(65.8834289457431,1.92988115670317,-1.51912551954228));
#50746=CARTESIAN_POINT('Ctrl Pts',(63.8578603822002,1.78869214703849,-1.40798762897424));
#50747=CARTESIAN_POINT('Ctrl Pts',(62.8777152811561,0.0106057650109386,
-1.2968497384062));
#50748=CARTESIAN_POINT('Ctrl Pts',(63.8401163177279,-1.77734687611335,-1.18571184783815));
#50749=CARTESIAN_POINT('Ctrl Pts',(65.8641746469915,-1.93839327331801,-1.07457395727011));
#50750=CARTESIAN_POINT('Ctrl Pts',(67.0972428003859,-0.325247154297195,
-0.963436066702072));
#50751=CARTESIAN_POINT('Ctrl Pts',(66.4106815043556,1.58562208464048,-0.852298176134029));
#50752=CARTESIAN_POINT('Ctrl Pts',(64.4329070892513,2.04514294157383,-0.741160285565989));
#50753=CARTESIAN_POINT('Ctrl Pts',(62.9741994190526,0.632726599672811,-0.630022394997946));
#50754=CARTESIAN_POINT('Ctrl Pts',(63.3697299072724,-1.35883427771699,-0.518884504429905));
#50755=CARTESIAN_POINT('Ctrl Pts',(65.2574651442524,-2.10663735927426,-0.407746613861863));
#50756=CARTESIAN_POINT('Ctrl Pts',(66.9095395923399,-0.926212070546681,
-0.296608723293821));
#50757=CARTESIAN_POINT('Ctrl Pts',(66.8137908073226,1.10198598313284,-0.185470832725779));
#50758=CARTESIAN_POINT('Ctrl Pts',(65.0578587207854,2.12152359010982,-0.0743329421577371));
#50759=CARTESIAN_POINT('Ctrl Pts',(63.2489678938882,1.19920668612863,0.036804948410304));
#50760=CARTESIAN_POINT('Ctrl Pts',(63.0428166102798,-0.820757743645065,
0.147942838978346));
#50761=CARTESIAN_POINT('Ctrl Pts',(64.6280974800075,-2.08947327927542,0.259080729546388));
#50762=CARTESIAN_POINT('Ctrl Pts',(66.5537849435622,-1.44567023799533,0.370218620114429));
#50763=CARTESIAN_POINT('Ctrl Pts',(67.0572754273494,0.521371173147926,0.481356510682472));
#50764=CARTESIAN_POINT('Ctrl Pts',(65.6777183812947,2.0111956337088,0.592494401250513));
#50765=CARTESIAN_POINT('Ctrl Pts',(63.6778380150419,1.66014992377277,0.703632291818555));
#50766=CARTESIAN_POINT('Ctrl Pts',(62.8881475079326,-0.210449839557629,
0.814770182386596));
#50767=CARTESIAN_POINT('Ctrl Pts',(64.0314595368616,-1.88842247767948,0.925908072954638));
#50768=CARTESIAN_POINT('Ctrl Pts',(66.0612876356907,-1.83790060601567,1.03704596352268));
#50769=CARTESIAN_POINT('Ctrl Pts',(67.1197071257548,-0.105127466352823,
1.14818385409072));
#50770=CARTESIAN_POINT('Ctrl Pts',(66.2379346445003,1.72387003543738,1.25932174465876));
#50771=CARTESIAN_POINT('Ctrl Pts',(64.2230665440017,1.97498974380222,1.37045963522681));
#50772=CARTESIAN_POINT('Ctrl Pts',(62.9193344468026,0.418378941744459,1.48159752579485));
#50773=CARTESIAN_POINT('Ctrl Pts',(63.5200591267976,-1.52117885042514,1.59273541636289));
#50774=CARTESIAN_POINT('Ctrl Pts',(65.4753904717057,-2.06838438946254,1.70387330693093));
#50775=CARTESIAN_POINT('Ctrl Pts',(66.995591526567,-0.722374239748755,1.81501119749897));
#50776=CARTESIAN_POINT('Ctrl Pts',(66.6892050256144,1.28483324388725,1.92614908806702));
#50777=CARTESIAN_POINT('Ctrl Pts',(64.8366700078289,2.11601828839369,2.03728697863506));
#50778=CARTESIAN_POINT('Ctrl Pts',(63.1336327841659,1.01038779625362,2.1484248692031));
#50779=CARTESIAN_POINT('Ctrl Pts',(63.1389026391995,-1.02006210437422,2.25956275977114));
#50780=CARTESIAN_POINT('Ctrl Pts',(64.8476560148535,-2.11683759257733,2.37070065033918));
#50781=CARTESIAN_POINT('Ctrl Pts',(66.6958515678104,-1.2760476257233,2.48183854090722));
#50782=CARTESIAN_POINT('Ctrl Pts',(66.9918149484855,0.732723204319577,2.59297643147526));
#50783=CARTESIAN_POINT('Ctrl Pts',(65.4646475180941,2.07082417580246,2.70411432204331));
#50784=CARTESIAN_POINT('Ctrl Pts',(63.5121829449299,1.51347629442987,2.81525221261135));
#50785=CARTESIAN_POINT('Ctrl Pts',(62.9215341952643,-0.429173603222882,
2.92639010317939));
#50786=CARTESIAN_POINT('Ctrl Pts',(64.2333287680788,-1.97899603468615,3.03752799374743));
#50787=CARTESIAN_POINT('Ctrl Pts',(66.2468662141139,-1.71742095225948,3.14866588431547));
#50788=CARTESIAN_POINT('Ctrl Pts',(67.1191328739459,0.116129004648158,3.25980377488352));
#50789=CARTESIAN_POINT('Ctrl Pts',(66.051733181654,1.84338476660971,3.37094166545155));
#50790=CARTESIAN_POINT('Ctrl Pts',(64.0216701807284,1.88336954628659,3.4820795560196));
#50791=CARTESIAN_POINT('Ctrl Pts',(62.8870835583976,0.199484821387334,3.59321744658764));
#50792=CARTESIAN_POINT('Ctrl Pts',(63.686473317166,-1.66699062284605,3.70435533715568));
#50793=CARTESIAN_POINT('Ctrl Pts',(65.6881489451415,-2.00765064501606,3.81549322772372));
#50794=CARTESIAN_POINT('Ctrl Pts',(67.0599540394824,-0.510685263521469,
3.92663111829177));
#50795=CARTESIAN_POINT('Ctrl Pts',(66.5462598400307,1.45371613128933,4.03776900885981));
#50796=CARTESIAN_POINT('Ctrl Pts',(64.6172564731933,2.08751466476979,4.14890689942785));
#50797=CARTESIAN_POINT('Ctrl Pts',(63.0385825971008,0.810587351755158,4.26004478999589));
#50798=CARTESIAN_POINT('Ctrl Pts',(63.2552163137658,-1.20827975739151,4.37118268056393));
#50799=CARTESIAN_POINT('Ctrl Pts',(65.0688703258357,-2.12119470101482,4.48232057113198));
#50800=CARTESIAN_POINT('Ctrl Pts',(66.8194865472274,-1.09255608031047,4.59345846170002));
#50801=CARTESIAN_POINT('Ctrl Pts',(66.9047060983459,0.936111514078455,4.70459635226806));
#50802=CARTESIAN_POINT('Ctrl Pts',(65.2465265552648,2.1079456175936,4.8157342428361));
#50803=CARTESIAN_POINT('Ctrl Pts',(63.3626984633988,1.35035320305219,4.92687213340414));
#50804=CARTESIAN_POINT('Ctrl Pts',(62.9775110302329,-0.643232834874305,
5.03801002397219));
#50805=CARTESIAN_POINT('Ctrl Pts',(64.4435306995345,-2.04806051976078,5.14914791454023));
#50806=CARTESIAN_POINT('Ctrl Pts',(66.4188930069729,-1.57827527209692,5.26028580510827));
#50807=CARTESIAN_POINT('Ctrl Pts',(67.0955264998601,0.336123404011309,5.37142369567631));
#50808=CARTESIAN_POINT('Ctrl Pts',(65.8541007317118,1.9428641754081,5.48256158624435));
#50809=CARTESIAN_POINT('Ctrl Pts',(63.8309070567223,1.77128000596152,5.5936994768124));
#50810=CARTESIAN_POINT('Ctrl Pts',(62.8777970581406,-0.021578166361293,
5.70483736738043));
#50811=CARTESIAN_POINT('Ctrl Pts',(63.867164175545,-1.79468298474187,5.81597525794848));
#50812=CARTESIAN_POINT('Ctrl Pts',(65.8934273984406,-1.92509926646556,5.92711314851651));
#50813=CARTESIAN_POINT('Ctrl Pts',(67.1019290958798,-0.293440200112777,
6.03825103908457));
#50814=CARTESIAN_POINT('Ctrl Pts',(66.3865059227299,1.60678798501315,6.14938892965259));
#50815=CARTESIAN_POINT('Ctrl Pts',(64.4020086652382,2.03634438098787,6.26052682022066));
#50816=CARTESIAN_POINT('Ctrl Pts',(62.9648389371536,0.601933848826794,6.37166471078868));
#50817=CARTESIAN_POINT('Ctrl Pts',(63.3905160600216,-1.38328014168385,6.48280260135673));
#50818=CARTESIAN_POINT('Ctrl Pts',(65.2892915487438,-2.10266459070399,6.59394049192477));
#50819=CARTESIAN_POINT('Ctrl Pts',(66.9234340409675,-0.896859934344193,
6.70507838249281));
#50820=CARTESIAN_POINT('Ctrl Pts',(66.796721623453,1.12867407706946,6.81621627306086));
#50821=CARTESIAN_POINT('Ctrl Pts',(65.026077453603,2.12345182245079,6.92735416362889));
#50822=CARTESIAN_POINT('Ctrl Pts',(63.2302233816263,1.1698735661067,7.03849205419693));
#50823=CARTESIAN_POINT('Ctrl Pts',(63.1156124805061,-0.172339073385988,
7.1125839812423));
#50824=CARTESIAN_POINT('Ctrl Pts',(63.3548292594101,-0.719397484879846,
7.14962994476498));
#50825=CARTESIAN_POINT('Ctrl Pts',(63.5335096305347,1.24726608657096,-2.14962994476498));
#50826=CARTESIAN_POINT('Ctrl Pts',(63.1187639830495,0.759623149459721,-2.1125839812423));
#50827=CARTESIAN_POINT('Ctrl Pts',(62.8213796585631,-0.653743668596888,
-2.03849205419694));
#50828=CARTESIAN_POINT('Ctrl Pts',(64.370148361682,-2.18801657894401,-1.9273541636289));
#50829=CARTESIAN_POINT('Ctrl Pts',(66.4955154509718,-1.71429596249071,-1.81621627306085));
#50830=CARTESIAN_POINT('Ctrl Pts',(67.2519438360201,0.32595105536059,-1.70507838249281));
#50831=CARTESIAN_POINT('Ctrl Pts',(65.9471840861633,2.06915647107053,-1.59394049192477));
#50832=CARTESIAN_POINT('Ctrl Pts',(63.7754346567777,1.91777815848532,-1.48280260135673));
#50833=CARTESIAN_POINT('Ctrl Pts',(62.7245546213054,0.0113711599425766,
-1.37166471078869));
#50834=CARTESIAN_POINT('Ctrl Pts',(63.756410041869,-1.90561412409944,-1.26052682022064));
#50835=CARTESIAN_POINT('Ctrl Pts',(65.9265402466607,-2.07828288857812,-1.1493889296526));
#50836=CARTESIAN_POINT('Ctrl Pts',(67.2485962395932,-0.348719532119266,
-1.03825103908456));
#50837=CARTESIAN_POINT('Ctrl Pts',(66.5124873120909,1.70005297254209,-0.927113148516519));
#50838=CARTESIAN_POINT('Ctrl Pts',(64.3919812306068,2.19273644759078,-0.815975257948477));
#50839=CARTESIAN_POINT('Ctrl Pts',(62.8280018090199,0.67838909851215,-0.704837367380436));
#50840=CARTESIAN_POINT('Ctrl Pts',(63.2520768699961,-1.45689838417496,-0.593699476812394));
#50841=CARTESIAN_POINT('Ctrl Pts',(65.2760458422295,-2.25866878330876,-0.482561586244352));
#50842=CARTESIAN_POINT('Ctrl Pts',(67.0473469003682,-0.993054775781753,
-0.37142369567631));
#50843=CARTESIAN_POINT('Ctrl Pts',(66.9446881343466,1.18151390830904,-0.260285805108268));
#50844=CARTESIAN_POINT('Ctrl Pts',(65.0620342584853,2.27462932095962,-0.149147914540226));
#50845=CARTESIAN_POINT('Ctrl Pts',(63.1225997254656,1.28575081741976,-0.0380100239721848));
#50846=CARTESIAN_POINT('Ctrl Pts',(62.9015709532967,-0.879990040083925,
0.0731278665958575));
#50847=CARTESIAN_POINT('Ctrl Pts',(64.6012580861897,-2.24026600908807,0.184265757163899));
#50848=CARTESIAN_POINT('Ctrl Pts',(66.6659182144232,-1.55000110633351,0.295403647731941));
#50849=CARTESIAN_POINT('Ctrl Pts',(67.2057445084059,0.55899739370044,0.406541538299982));
#50850=CARTESIAN_POINT('Ctrl Pts',(65.7266278388951,2.1563392365499,0.517679428868024));
#50851=CARTESIAN_POINT('Ctrl Pts',(63.5824204679768,1.77995932329319,0.628817319436066));
#50852=CARTESIAN_POINT('Ctrl Pts',(62.7357397191377,-0.225637545526539,
0.739955210004107));
#50853=CARTESIAN_POINT('Ctrl Pts',(63.9615620838435,-2.02470580959537,0.85109310057215));
#50854=CARTESIAN_POINT('Ctrl Pts',(66.1378784498875,-1.97053788463238,0.96223099114019));
#50855=CARTESIAN_POINT('Ctrl Pts',(67.2726817663336,-0.112714286336053,
1.07336888170823));
#50856=CARTESIAN_POINT('Ctrl Pts',(66.3272736880886,1.84827797645493,1.18450677227627));
#50857=CARTESIAN_POINT('Ctrl Pts',(64.1669969508297,2.11752044652708,1.29564466284432));
#50858=CARTESIAN_POINT('Ctrl Pts',(62.7691773513729,0.448572437563489,1.40678255341236));
#50859=CARTESIAN_POINT('Ctrl Pts',(63.4132550214545,-1.63095901065213,1.5179204439804));
#50860=CARTESIAN_POINT('Ctrl Pts',(65.5096983653104,-2.21765518008835,1.62905833454844));
#50861=CARTESIAN_POINT('Ctrl Pts',(67.1396090150254,-0.774506413267543,
1.74019622511649));
#50862=CARTESIAN_POINT('Ctrl Pts',(66.8111112684709,1.37755685711622,1.85133411568452));
#50863=CARTESIAN_POINT('Ctrl Pts',(64.8248828384863,2.26872671362468,1.96247200625257));
#50864=CARTESIAN_POINT('Ctrl Pts',(62.9989411323989,1.08330528004136,2.07360989682061));
#50865=CARTESIAN_POINT('Ctrl Pts',(63.0045913013778,-1.09367776188116,2.18474778738865));
#50866=CARTESIAN_POINT('Ctrl Pts',(64.8366616816794,-2.26960514520451,2.29588567795669));
#50867=CARTESIAN_POINT('Ctrl Pts',(66.8182374771223,-1.36813720004918,2.40702356852474));
#50868=CARTESIAN_POINT('Ctrl Pts',(67.1355598895398,0.785602240042274,2.51816145909277));
#50869=CARTESIAN_POINT('Ctrl Pts',(65.4981801161651,2.2202710404877,2.62929934966082));
#50870=CARTESIAN_POINT('Ctrl Pts',(63.4048104327177,1.62270057798853,2.74043724022886));
#50871=CARTESIAN_POINT('Ctrl Pts',(62.771535850884,-0.460146126219659,2.8515751307969));
#50872=CARTESIAN_POINT('Ctrl Pts',(64.1779997772384,-2.12181586268713,2.96271302136494));
#50873=CARTESIAN_POINT('Ctrl Pts',(66.3368498296032,-1.84136347700833,3.07385091193299));
#50874=CARTESIAN_POINT('Ctrl Pts',(67.2720660720238,0.124509781657855,3.18498880250102));
#50875=CARTESIAN_POINT('Ctrl Pts',(66.1276344717396,1.97641782513656,3.29612669306907));
#50876=CARTESIAN_POINT('Ctrl Pts',(63.9510662512269,2.01928821916336,3.40726458363711));
#50877=CARTESIAN_POINT('Ctrl Pts',(62.734598986685,0.213881205907557,3.51840247420515));
#50878=CARTESIAN_POINT('Ctrl Pts',(63.5916789610234,-1.7872937007003,3.62954036477319));
#50879=CARTESIAN_POINT('Ctrl Pts',(65.7378111537875,-2.15253841375417,3.74067825534123));
#50880=CARTESIAN_POINT('Ctrl Pts',(67.2086164301352,-0.547540305280222,
3.85181614590928));
#50881=CARTESIAN_POINT('Ctrl Pts',(66.6578500405806,1.55862765419994,3.96295403647732));
#50882=CARTESIAN_POINT('Ctrl Pts',(64.589634707556,2.23816604564495,4.07409192704536));
#50883=CARTESIAN_POINT('Ctrl Pts',(62.8970313806202,0.869085673191056,4.1852298176134));
#50884=CARTESIAN_POINT('Ctrl Pts',(63.1292990801791,-1.295478672449,4.29636770818144));
#50885=CARTESIAN_POINT('Ctrl Pts',(65.0738405470579,-2.27427669665589,4.40750559874948));
#50886=CARTESIAN_POINT('Ctrl Pts',(66.9507949233791,-1.17140346996484,4.51864348931753));
#50887=CARTESIAN_POINT('Ctrl Pts',(67.0421645836536,1.00366864056437,4.62978137988557));
#50888=CARTESIAN_POINT('Ctrl Pts',(65.2643178391297,2.26007145577795,4.74091927045361));
#50889=CARTESIAN_POINT('Ctrl Pts',(63.2445379821525,1.44780524884725,4.85205716102165));
#50890=CARTESIAN_POINT('Ctrl Pts',(62.8315524119571,-0.689653545795988,
4.96319505158969));
#50891=CARTESIAN_POINT('Ctrl Pts',(64.4033715236759,-2.19586458103279,5.07433294215774));
#50892=CARTESIAN_POINT('Ctrl Pts',(66.5212914209443,-1.69217595655929,5.18547083272578));
#50893=CARTESIAN_POINT('Ctrl Pts',(67.2467560774014,0.360380697056169,5.29660872329382));
#50894=CARTESIAN_POINT('Ctrl Pts',(65.9157393188846,2.08307644592185,5.40774661386186));
#50895=CARTESIAN_POINT('Ctrl Pts',(63.7465361685802,1.89910942115946,5.5188845044299));
#50896=CARTESIAN_POINT('Ctrl Pts',(62.7246422999565,-0.0231354155696212,
5.63002239499795));
#50897=CARTESIAN_POINT('Ctrl Pts',(63.7854098845984,-1.92420134188085,5.74116028556599));
#50898=CARTESIAN_POINT('Ctrl Pts',(65.957904105387,-2.06402948224289,5.85229817613403));
#50899=CARTESIAN_POINT('Ctrl Pts',(67.2536207348131,-0.314617139416408,
5.96343606670207));
#50900=CARTESIAN_POINT('Ctrl Pts',(66.4865670314617,1.72274636978576,6.07457395727011));
#50901=CARTESIAN_POINT('Ctrl Pts',(64.3588529347165,2.18330291407536,6.18571184783816));
#50902=CARTESIAN_POINT('Ctrl Pts',(62.8179658015557,0.645374101990838,6.29684973840619));
#50903=CARTESIAN_POINT('Ctrl Pts',(63.2743631140587,-1.48310845283243,6.40798762897424));
#50904=CARTESIAN_POINT('Ctrl Pts',(65.3101690889255,-2.25440930869464,6.51912551954228));
#50905=CARTESIAN_POINT('Ctrl Pts',(67.0622440810523,-0.961584359921082,
6.63026341011032));
#50906=CARTESIAN_POINT('Ctrl Pts',(66.9263871047018,1.21012802378329,6.74140130067837));
#50907=CARTESIAN_POINT('Ctrl Pts',(65.0279594065595,2.27669670962353,6.8525391912464));
#50908=CARTESIAN_POINT('Ctrl Pts',(63.1025024626319,1.25430079009593,6.96367708181444));
#50909=CARTESIAN_POINT('Ctrl Pts',(62.979620342723,-0.184776408472784,7.03776900885981));
#50910=CARTESIAN_POINT('Ctrl Pts',(63.2361008748732,-0.771314832491493,
7.07481497238249));
#50911=CARTESIAN_POINT('Ctrl Pts',(63.4347998857283,1.33121980333219,-2.22444491714747));
#50912=CARTESIAN_POINT('Ctrl Pts',(62.9921376300776,0.810753527669827,-2.18739895362479));
#50913=CARTESIAN_POINT('Ctrl Pts',(62.6747363103277,-0.697747278876005,
-2.11330702657943));
#50914=CARTESIAN_POINT('Ctrl Pts',(64.3277529284907,-2.33529238970749,-2.00216913601138));
#50915=CARTESIAN_POINT('Ctrl Pts',(66.5961788795174,-1.82968554874614,-1.89103124544334));
#50916=CARTESIAN_POINT('Ctrl Pts',(67.4035226025776,0.347890882695266,-1.7798933548753));
#50917=CARTESIAN_POINT('Ctrl Pts',(66.0109392265833,2.20843178543789,-1.66875546430726));
#50918=CARTESIAN_POINT('Ctrl Pts',(63.6930089313552,2.04686416993215,-1.55761757373922));
#50919=CARTESIAN_POINT('Ctrl Pts',(62.5713939614548,0.0121365548742175,
-1.44647968317118));
#50920=CARTESIAN_POINT('Ctrl Pts',(63.67270376601,-2.03388137208553,-1.33534179260313));
#50921=CARTESIAN_POINT('Ctrl Pts',(65.9889058463299,-2.21817250383822,-1.22420390203509));
#50922=CARTESIAN_POINT('Ctrl Pts',(67.3999496788005,-0.372191909941336,
-1.11306601146705));
#50923=CARTESIAN_POINT('Ctrl Pts',(66.6142931198262,1.8144838604437,-1.00192812089901));
#50924=CARTESIAN_POINT('Ctrl Pts',(64.3510553719621,2.34032995360773,-0.890790230330967));
#50925=CARTESIAN_POINT('Ctrl Pts',(62.6818041989874,0.724051597351488,-0.779652339762924));
#50926=CARTESIAN_POINT('Ctrl Pts',(63.1344238327198,-1.55496249063293,-0.668514449194883));
#50927=CARTESIAN_POINT('Ctrl Pts',(65.2946265402067,-2.41070020734327,-0.55737655862684));
#50928=CARTESIAN_POINT('Ctrl Pts',(67.1851542083967,-1.05989748101682,-0.446238668058799));
#50929=CARTESIAN_POINT('Ctrl Pts',(67.0755854613707,1.26104183348523,-0.335100777490757));
#50930=CARTESIAN_POINT('Ctrl Pts',(65.0662097961853,2.42773505180943,-0.223962886922715));
#50931=CARTESIAN_POINT('Ctrl Pts',(62.9962315570428,1.3722949487109,-0.112824996354674));
#50932=CARTESIAN_POINT('Ctrl Pts',(62.7603252963136,-0.939222336522784,
-0.00168710578663132));
#50933=CARTESIAN_POINT('Ctrl Pts',(64.5744186923722,-2.39105873890072,0.10945078478141));
#50934=CARTESIAN_POINT('Ctrl Pts',(66.778051485284,-1.65433197467169,0.220588675349452));
#50935=CARTESIAN_POINT('Ctrl Pts',(67.3542135894627,0.596623614252954,0.331726565917493));
#50936=CARTESIAN_POINT('Ctrl Pts',(65.7755372964953,2.301482839391,0.442864456485536));
#50937=CARTESIAN_POINT('Ctrl Pts',(63.4870029209119,1.89976872281362,0.554002347053577));
#50938=CARTESIAN_POINT('Ctrl Pts',(62.5833319303427,-0.24082525149545,0.665140237621619));
#50939=CARTESIAN_POINT('Ctrl Pts',(63.8916646308255,-2.16098914151125,0.77627812818966));
#50940=CARTESIAN_POINT('Ctrl Pts',(66.2144692640843,-2.1031751632491,0.887416018757702));
#50941=CARTESIAN_POINT('Ctrl Pts',(67.4256564069122,-0.120301106319279,
0.998553909325744));
#50942=CARTESIAN_POINT('Ctrl Pts',(66.416612731677,1.97268591747247,1.10969179989378));
#50943=CARTESIAN_POINT('Ctrl Pts',(64.1109273576576,2.26005114925193,1.22082969046183));
#50944=CARTESIAN_POINT('Ctrl Pts',(62.6190202559434,0.478765933382519,1.33196758102987));
#50945=CARTESIAN_POINT('Ctrl Pts',(63.3064509161112,-1.74073917087913,1.44310547159791));
#50946=CARTESIAN_POINT('Ctrl Pts',(65.5440062589152,-2.36692597071416,1.55424336216595));
#50947=CARTESIAN_POINT('Ctrl Pts',(67.2836265034836,-0.82663858678633,1.665381252734));
#50948=CARTESIAN_POINT('Ctrl Pts',(66.9330175113275,1.4702804703452,1.77651914330204));
#50949=CARTESIAN_POINT('Ctrl Pts',(64.8130956691436,2.42143513885567,1.88765703387008));
#50950=CARTESIAN_POINT('Ctrl Pts',(62.864249480632,1.15622276382909,1.99879492443812));
#50951=CARTESIAN_POINT('Ctrl Pts',(62.8702799635561,-1.16729341938809,2.10993281500616));
#50952=CARTESIAN_POINT('Ctrl Pts',(64.8256673485052,-2.42237269783168,2.2210707055742));
#50953=CARTESIAN_POINT('Ctrl Pts',(66.9406233864343,-1.46022677437506,2.33220859614225));
#50954=CARTESIAN_POINT('Ctrl Pts',(67.279304830594,0.838481275764972,2.44334648671029));
#50955=CARTESIAN_POINT('Ctrl Pts',(65.5317127142361,2.36971790517293,2.55448437727833));
#50956=CARTESIAN_POINT('Ctrl Pts',(63.2974379205056,1.7319248615472,2.66562226784637));
#50957=CARTESIAN_POINT('Ctrl Pts',(62.6215375065036,-0.491118649216439,
2.77676015841441));
#50958=CARTESIAN_POINT('Ctrl Pts',(64.122670786398,-2.2646356906881,2.88789804898245));
#50959=CARTESIAN_POINT('Ctrl Pts',(66.4268334450924,-1.96530600175718,2.9990359395505));
#50960=CARTESIAN_POINT('Ctrl Pts',(67.4249992701018,0.132890558667548,3.11017383011854));
#50961=CARTESIAN_POINT('Ctrl Pts',(66.2035357618251,2.10945088366341,3.22131172068658));
#50962=CARTESIAN_POINT('Ctrl Pts',(63.8804623217255,2.15520689204012,3.33244961125462));
#50963=CARTESIAN_POINT('Ctrl Pts',(62.5821144149725,0.228277590427784,3.44358750182266));
#50964=CARTESIAN_POINT('Ctrl Pts',(63.4968846048806,-1.90759677855456,3.55472539239071));
#50965=CARTESIAN_POINT('Ctrl Pts',(65.7874733624335,-2.29742618249227,3.66586328295874));
#50966=CARTESIAN_POINT('Ctrl Pts',(67.3572788207879,-0.584395347038978,
3.77700117352679));
#50967=CARTESIAN_POINT('Ctrl Pts',(66.7694402411304,1.66353917711055,3.88813906409483));
#50968=CARTESIAN_POINT('Ctrl Pts',(64.5620129419189,2.3888174265201,3.99927695466288));
#50969=CARTESIAN_POINT('Ctrl Pts',(62.7554801641395,0.927583994626953,4.11041484523091));
#50970=CARTESIAN_POINT('Ctrl Pts',(63.0033818465923,-1.38267758750649,4.22155273579896));
#50971=CARTESIAN_POINT('Ctrl Pts',(65.0788107682801,-2.42735869229696,4.33269062636699));
#50972=CARTESIAN_POINT('Ctrl Pts',(67.0821032995307,-1.25025085961922,4.44382851693504));
#50973=CARTESIAN_POINT('Ctrl Pts',(67.1796230689615,1.07122576705028,4.55496640750307));
#50974=CARTESIAN_POINT('Ctrl Pts',(65.2821091229946,2.41219729396229,4.66610429807113));
#50975=CARTESIAN_POINT('Ctrl Pts',(63.1263775009061,1.54525729464231,4.77724218863916));
#50976=CARTESIAN_POINT('Ctrl Pts',(62.6855937936814,-0.736074256717675,
4.88838007920721));
#50977=CARTESIAN_POINT('Ctrl Pts',(64.3632123478174,-2.3436686423048,4.99951796977525));
#50978=CARTESIAN_POINT('Ctrl Pts',(66.6236898349158,-1.80607664102166,5.11065586034329));
#50979=CARTESIAN_POINT('Ctrl Pts',(67.3979856549427,0.384637990101029,5.22179375091133));
#50980=CARTESIAN_POINT('Ctrl Pts',(65.9773779060574,2.22328871643559,5.33293164147938));
#50981=CARTESIAN_POINT('Ctrl Pts',(63.6621652804381,2.02693883635741,5.44406953204741));
#50982=CARTESIAN_POINT('Ctrl Pts',(62.5714875417724,-0.0246926647779473,
5.55520742261546));
#50983=CARTESIAN_POINT('Ctrl Pts',(63.7036555936518,-2.05371969901983,5.66634531318349));
#50984=CARTESIAN_POINT('Ctrl Pts',(66.0223808123334,-2.20295969802021,5.77748320375154));
#50985=CARTESIAN_POINT('Ctrl Pts',(67.4053123737463,-0.335794078720041,
5.88862109431958));
#50986=CARTESIAN_POINT('Ctrl Pts',(66.5866281401934,1.83870475455837,5.99975898488763));
#50987=CARTESIAN_POINT('Ctrl Pts',(64.3156972041947,2.33026144716285,6.11089687545566));
#50988=CARTESIAN_POINT('Ctrl Pts',(62.6710926659578,0.688814355154883,6.22203476602371));
#50989=CARTESIAN_POINT('Ctrl Pts',(63.1582101680956,-1.58293676398101,6.33317265659174));
#50990=CARTESIAN_POINT('Ctrl Pts',(65.3310466291073,-2.4061540266853,6.4443105471598));
#50991=CARTESIAN_POINT('Ctrl Pts',(67.2010541211369,-1.02630878549797,6.55544843772783));
#50992=CARTESIAN_POINT('Ctrl Pts',(67.0560525859507,1.29158197049713,6.66658632829588));
#50993=CARTESIAN_POINT('Ctrl Pts',(65.029841359516,2.42994159679627,6.77772421886392));
#50994=CARTESIAN_POINT('Ctrl Pts',(62.9747815436376,1.33872801408516,6.88886210943195));
#50995=CARTESIAN_POINT('Ctrl Pts',(62.8436282049399,-0.197213743559581,
6.96295403647732));
#50996=CARTESIAN_POINT('Ctrl Pts',(63.1173724903363,-0.82323218010314,7.));
#50997=CARTESIAN_POINT('Ctrl Pts',(63.7309291201476,1.07935865304851,-2.));
#50998=CARTESIAN_POINT('Ctrl Pts',(63.6855968419854,1.03706844878193,-2.));
#50999=CARTESIAN_POINT('Ctrl Pts',(63.6429944057469,0.992209355215868,-2.));
#51000=CARTESIAN_POINT('Ctrl Pts',(63.6031204505518,0.945126337776206,-2.));
#51001=CARTESIAN_POINT('Ctrl Pts',(63.5606157477665,0.894936943402905,-2.));
#51002=CARTESIAN_POINT('Ctrl Pts',(63.5212107097528,0.842220257206834,-2.));
#51003=CARTESIAN_POINT('Ctrl Pts',(63.4849325153228,0.787339414500543,-2.));
#51004=CARTESIAN_POINT('Ctrl Pts',(63.4531890951965,0.739318677132538,-2.));
#51005=CARTESIAN_POINT('Ctrl Pts',(63.4238399078534,0.689639781931255,-2.));
#51006=CARTESIAN_POINT('Ctrl Pts',(63.3969260537536,0.638518448144012,-2.));
#51007=CARTESIAN_POINT('Ctrl Pts',(63.3834208986394,0.612866174787509,-2.));
#51008=CARTESIAN_POINT('Ctrl Pts',(63.3705293094211,0.586850346511891,-2.));
#51009=CARTESIAN_POINT('Ctrl Pts',(63.3582588228011,0.560496376489487,-2.));
#51010=CARTESIAN_POINT('Ctrl Pts',(63.3526556403243,0.548462126537112,-2.));
#51011=CARTESIAN_POINT('Ctrl Pts',(63.3471814026121,0.536355708793655,-2.));
#51012=CARTESIAN_POINT('Ctrl Pts',(63.3418453144691,0.524199442929296,-2.));
#51013=CARTESIAN_POINT('Ctrl Pts',(63.3149230085512,0.462867114893175,-2.));
#51014=CARTESIAN_POINT('Ctrl Pts',(63.2914620509973,0.400159371536742,-2.));
#51015=CARTESIAN_POINT('Ctrl Pts',(63.2714860817372,0.336433888030266,-2.));
#51016=CARTESIAN_POINT('Ctrl Pts',(63.2511562856396,0.271579658979292,-2.));
#51017=CARTESIAN_POINT('Ctrl Pts',(63.234435470153,0.205670475363271,-2.));
#51018=CARTESIAN_POINT('Ctrl Pts',(63.2213878692259,0.139046848385531,-2.));
#51019=CARTESIAN_POINT('Ctrl Pts',(63.2104743799268,0.0833204168257664,
-2.));
#51020=CARTESIAN_POINT('Ctrl Pts',(63.2021313216505,0.0270932010885611,
-2.));
#51021=CARTESIAN_POINT('Ctrl Pts',(63.1964211149777,-0.0294478216180754,
-2.));
#51022=CARTESIAN_POINT('Ctrl Pts',(63.1937898542026,-0.0555019005259951,
-2.));
#51023=CARTESIAN_POINT('Ctrl Pts',(63.1917179786585,-0.0816227252280235,
-2.));
#51024=CARTESIAN_POINT('Ctrl Pts',(63.1902134007643,-0.107792402833692,
-2.));
#51025=CARTESIAN_POINT('Ctrl Pts',(63.1895569069983,-0.119211040759237,
-2.));
#51026=CARTESIAN_POINT('Ctrl Pts',(63.1890085369681,-0.130638731934728,
-2.));
#51027=CARTESIAN_POINT('Ctrl Pts',(63.188569278878,-0.142059931589906,-2.));
#51028=CARTESIAN_POINT('Ctrl Pts',(63.1858723378449,-0.212183402721495,
-2.));
#51029=CARTESIAN_POINT('Ctrl Pts',(63.1872764272312,-0.282193469637118,
-2.));
#51030=CARTESIAN_POINT('Ctrl Pts',(63.1928363192141,-0.351729486371673,
-2.));
#51031=CARTESIAN_POINT('Ctrl Pts',(63.1978071231062,-0.413897942825674,
-2.));
#51032=CARTESIAN_POINT('Ctrl Pts',(63.2061000911913,-0.475688445032767,
-2.));
#51033=CARTESIAN_POINT('Ctrl Pts',(63.2177875010733,-0.536855401025573,
-2.));
#51034=CARTESIAN_POINT('Ctrl Pts',(63.2305203455448,-0.603493719122339,
-2.));
#51035=CARTESIAN_POINT('Ctrl Pts',(63.2472809681187,-0.669392782961396,
-2.));
#51036=CARTESIAN_POINT('Ctrl Pts',(63.2678240437401,-0.734338936172354,
-2.));
#51037=CARTESIAN_POINT('Ctrl Pts',(63.2757504472629,-0.759397959810863,
-2.));
#51038=CARTESIAN_POINT('Ctrl Pts',(63.2842405167726,-0.784315071865798,
-2.));
#51039=CARTESIAN_POINT('Ctrl Pts',(63.2932821667432,-0.809077679604566,
-2.));
#51040=CARTESIAN_POINT('Ctrl Pts',(63.2972485928295,-0.819940636434083,
-2.));
#51041=CARTESIAN_POINT('Ctrl Pts',(63.301321059107,-0.830773275870266,-2.));
#51042=CARTESIAN_POINT('Ctrl Pts',(63.305493469376,-0.84156202494396,-2.));
#51043=CARTESIAN_POINT('Ctrl Pts',(63.3307175500488,-0.906784824105441,
-2.));
#51044=CARTESIAN_POINT('Ctrl Pts',(63.3596326694677,-0.970522726147455,
-2.));
#51045=CARTESIAN_POINT('Ctrl Pts',(63.3919260622372,-1.03255684531855,-2.));
#51046=CARTESIAN_POINT('Ctrl Pts',(63.4249680867708,-1.0960290516056,-2.));
#51047=CARTESIAN_POINT('Ctrl Pts',(63.4615471340283,-1.15771838394187,-2.));
#51048=CARTESIAN_POINT('Ctrl Pts',(63.5013843211809,-1.21738667180208,-2.));
#51049=CARTESIAN_POINT('Ctrl Pts',(63.5318674685179,-1.26304444385366,-2.));
#51050=CARTESIAN_POINT('Ctrl Pts',(63.5642595400749,-1.30751888441863,-2.));
#51051=CARTESIAN_POINT('Ctrl Pts',(63.5984551101011,-1.35069719140617,-2.));
#51052=CARTESIAN_POINT('Ctrl Pts',(63.6197386625932,-1.37757165972414,-2.));
#51053=CARTESIAN_POINT('Ctrl Pts',(63.6417211957122,-1.40394389607449,-2.));
#51054=CARTESIAN_POINT('Ctrl Pts',(63.6643801907515,-1.42978501718758,-2.));
#51055=CARTESIAN_POINT('Ctrl Pts',(63.6770896558904,-1.44427934173145,-2.));
#51056=CARTESIAN_POINT('Ctrl Pts',(63.6900164428935,-1.45861113921514,-2.));
#51057=CARTESIAN_POINT('Ctrl Pts',(63.7031327806133,-1.4727497841485,-2.));
#51058=CARTESIAN_POINT('Ctrl Pts',(63.7540080482783,-1.52759034717556,-2.));
#51059=CARTESIAN_POINT('Ctrl Pts',(63.8077798406958,-1.57958602567074,-2.));
#51060=CARTESIAN_POINT('Ctrl Pts',(63.864163060535,-1.62847278877981,-2.));
#51061=CARTESIAN_POINT('Ctrl Pts',(63.9063355382314,-1.6650382054542,-2.));
#51062=CARTESIAN_POINT('Ctrl Pts',(63.9499701263758,-1.69986415254484,-2.));
#51063=CARTESIAN_POINT('Ctrl Pts',(63.9949639294552,-1.73283039560955,-2.));
#51064=CARTESIAN_POINT('Ctrl Pts',(64.0089991299538,-1.74311376352765,-2.));
#51065=CARTESIAN_POINT('Ctrl Pts',(64.0231666801194,-1.7532160976543,-2.));
#51066=CARTESIAN_POINT('Ctrl Pts',(64.0374636965982,-1.76313352319509,-2.));
#51067=CARTESIAN_POINT('Ctrl Pts',(64.0512649018476,-1.7727070188707,-2.));
#51068=CARTESIAN_POINT('Ctrl Pts',(64.0651797317906,-1.78210327692406,-2.));
#51069=CARTESIAN_POINT('Ctrl Pts',(64.0792001599556,-1.7913160321663,-2.));
#51070=CARTESIAN_POINT('Ctrl Pts',(64.1421565047859,-1.83268434054044,-2.));
#51071=CARTESIAN_POINT('Ctrl Pts',(64.2072699652678,-1.87037681376273,-2.));
#51072=CARTESIAN_POINT('Ctrl Pts',(64.2742791023333,-1.90411417796279,-2.));
#51073=CARTESIAN_POINT('Ctrl Pts',(64.3255634213005,-1.92993450370516,-2.));
#51074=CARTESIAN_POINT('Ctrl Pts',(64.3779590786631,-1.95343777834749,-2.));
#51075=CARTESIAN_POINT('Ctrl Pts',(64.4313627927198,-1.97448349564832,-2.));
#51076=CARTESIAN_POINT('Ctrl Pts',(64.4437562344803,-1.97936759175068,-2.));
#51077=CARTESIAN_POINT('Ctrl Pts',(64.4562040109557,-1.98411926473272,-2.));
#51078=CARTESIAN_POINT('Ctrl Pts',(64.4687042096542,-1.98873909628092,-2.));
#51079=CARTESIAN_POINT('Ctrl Pts',(66.6673159824367,-0.00130059074131283,
-0.871480363390211));
#51080=CARTESIAN_POINT('Ctrl Pts',(66.6680474999804,-0.0865457667101108,
-0.877193940366669));
#51081=CARTESIAN_POINT('Ctrl Pts',(66.6620744628598,-0.171688078253662,
-0.882907517343126));
#51082=CARTESIAN_POINT('Ctrl Pts',(66.6490403647761,-0.255735261203256,
-0.888621094319584));
#51083=CARTESIAN_POINT('Ctrl Pts',(66.5645292565598,-0.800684403669386,
-0.925667057842264));
#51084=CARTESIAN_POINT('Ctrl Pts',(66.1831691519411,-1.29959403086365,-0.962713021364943));
#51085=CARTESIAN_POINT('Ctrl Pts',(65.6794913573425,-1.52414483947233,-0.999758984887624));
#51086=CARTESIAN_POINT('Ctrl Pts',(65.1758135627439,-1.74869564808102,-1.0368049484103));
#51087=CARTESIAN_POINT('Ctrl Pts',(64.5498180781654,-1.69888763810414,-1.07385091193299));
#51088=CARTESIAN_POINT('Ctrl Pts',(64.0879958937795,-1.39749696674794,-1.11089687545567));
#51089=CARTESIAN_POINT('Ctrl Pts',(63.6261737093935,-1.09610629539174,-1.14794283897835));
#51090=CARTESIAN_POINT('Ctrl Pts',(63.3285248252001,-0.54313296265622,-1.18498880250103));
#51091=CARTESIAN_POINT('Ctrl Pts',(63.3312687442061,0.00831466463026731,
-1.22203476602371));
#51092=CARTESIAN_POINT('Ctrl Pts',(63.3340126632121,0.559762291916755,-1.25908072954639));
#51093=CARTESIAN_POINT('Ctrl Pts',(63.6371493854174,1.10968421375421,-1.29612669306907));
#51094=CARTESIAN_POINT('Ctrl Pts',(64.1019490294701,1.40647845913029,-1.33317265659175));
#51095=CARTESIAN_POINT('Ctrl Pts',(64.5667486735228,1.70327270450638,-1.37021862011443));
#51096=CARTESIAN_POINT('Ctrl Pts',(65.193211239423,1.7469392734211,-1.40726458363711));
#51097=CARTESIAN_POINT('Ctrl Pts',(65.6946279386367,1.51735015093769,-1.44431054715979));
#51098=CARTESIAN_POINT('Ctrl Pts',(66.1960446378505,1.28776102845429,-1.48135651068247));
#51099=CARTESIAN_POINT('Ctrl Pts',(66.5724154703778,0.784916214572762,-1.51840247420515));
#51100=CARTESIAN_POINT('Ctrl Pts',(66.6515012684707,0.239229109186819,-1.55544843772783));
#51101=CARTESIAN_POINT('Ctrl Pts',(66.6629095976148,0.160512345140362,-1.56079241294863));
#51102=CARTESIAN_POINT('Ctrl Pts',(66.6681317812815,0.0809040843243828,
-1.56613638816942));
#51103=CARTESIAN_POINT('Ctrl Pts',(66.6674675207825,0.00121113675536799,
-1.57148036339021));
#51104=CARTESIAN_POINT('Ctrl Pts',(65.5301702171886,-1.98517432567172,-2.));
#51105=CARTESIAN_POINT('Ctrl Pts',(66.1902879097456,-1.80888011517988,-1.96295403647732));
#51106=CARTESIAN_POINT('Ctrl Pts',(67.3093622463653,-0.748693059830632,
-1.88886210943196));
#51107=CARTESIAN_POINT('Ctrl Pts',(66.8811995093437,1.53837321455301,-1.77772421886392));
#51108=CARTESIAN_POINT('Ctrl Pts',(64.7278715623352,2.41277602144419,-1.66658632829587));
#51109=CARTESIAN_POINT('Ctrl Pts',(62.8252644286755,1.08095990301173,-1.55544843772783));
#51110=CARTESIAN_POINT('Ctrl Pts',(62.9123886677794,-1.24138962897177,-1.44431054715979));
#51111=CARTESIAN_POINT('Ctrl Pts',(64.9107473342681,-2.42691462884512,-1.33317265659175));
#51112=CARTESIAN_POINT('Ctrl Pts',(66.9905869477348,-1.39134438721222,-1.22203476602371));
#51113=CARTESIAN_POINT('Ctrl Pts',(67.24852778644,0.917884815202477,-1.11089687545567));
#51114=CARTESIAN_POINT('Ctrl Pts',(65.4483108550045,2.38688976599863,-0.999758984887625));
#51115=CARTESIAN_POINT('Ctrl Pts',(63.2377776981899,1.67118490708906,-0.888621094319582));
#51116=CARTESIAN_POINT('Ctrl Pts',(62.6402125087857,-0.574193448178934,
-0.777483203751542));
#51117=CARTESIAN_POINT('Ctrl Pts',(64.2025947176117,-2.29399639382145,-0.666345313183498));
#51118=CARTESIAN_POINT('Ctrl Pts',(66.4948474007694,-1.91408331059475,-0.555207422615458));
#51119=CARTESIAN_POINT('Ctrl Pts',(67.4188511430454,0.217814411897158,-0.444069532047416));
#51120=CARTESIAN_POINT('Ctrl Pts',(66.1288520704621,2.15034287637184,-0.332931641479373));
#51121=CARTESIAN_POINT('Ctrl Pts',(63.8056023683761,2.11463875683278,-0.221793750911332));
#51122=CARTESIAN_POINT('Ctrl Pts',(62.5755981242121,0.143381478345983,-0.110655860343291));
#51123=CARTESIAN_POINT('Ctrl Pts',(63.5646765331008,-1.95911432942998,0.00048203022475183));
#51124=CARTESIAN_POINT('Ctrl Pts',(65.8675227272721,-2.26841065672895,0.111619920792793));
#51125=CARTESIAN_POINT('Ctrl Pts',(67.3763155620569,-0.501404942245515,
0.222757811360835));
#51126=CARTESIAN_POINT('Ctrl Pts',(66.7100397977853,1.72454238081742,0.333895701928876));
#51127=CARTESIAN_POINT('Ctrl Pts',(64.4785452214709,2.37199651591817,0.445033592496919));
#51128=CARTESIAN_POINT('Ctrl Pts',(62.7243441135659,0.848335334231218,0.55617148306496));
#51129=CARTESIAN_POINT('Ctrl Pts',(63.0530766482751,-1.45181679686653,0.667309373633002));
#51130=CARTESIAN_POINT('Ctrl Pts',(65.1638502053818,-2.42310455048396,0.778447264201043));
#51131=CARTESIAN_POINT('Ctrl Pts',(67.1246498118468,-1.17649722845176,0.889585154769086));
#51132=CARTESIAN_POINT('Ctrl Pts',(67.1407333500909,1.14697134880473,1.00072304533713));
#51133=CARTESIAN_POINT('Ctrl Pts',(65.1973793755662,2.42060404314488,1.11186093590517));
#51134=CARTESIAN_POINT('Ctrl Pts',(63.0733618200821,1.47863040518407,1.22299882647321));
#51135=CARTESIAN_POINT('Ctrl Pts',(62.7128180402749,-0.816750411403602,
1.33413671704125));
#51136=CARTESIAN_POINT('Ctrl Pts',(64.4457578465939,-2.36455031387796,1.4452746076093));
#51137=CARTESIAN_POINT('Ctrl Pts',(66.686001781468,-1.74805049822322,1.55641249817733));
#51138=CARTESIAN_POINT('Ctrl Pts',(67.3830291651992,0.468459762690022,1.66755038874538));
#51139=CARTESIAN_POINT('Ctrl Pts',(65.898842928637,2.25618349012117,1.77868827931342));
#51140=CARTESIAN_POINT('Ctrl Pts',(63.5919355659201,1.97879688218179,1.88982616988146));
#51141=CARTESIAN_POINT('Ctrl Pts',(62.5738455482538,-0.109804953100732,
2.0009640604495));
#51142=CARTESIAN_POINT('Ctrl Pts',(63.7764422147334,-2.09790106953769,2.11210195101754));
#51143=CARTESIAN_POINT('Ctrl Pts',(66.0989751981566,-2.1657645452103,2.22323984158559));
#51144=CARTESIAN_POINT('Ctrl Pts',(67.4156037194807,-0.25127917121156,2.33437773215363));
#51145=CARTESIAN_POINT('Ctrl Pts',(66.5212027615546,1.89320487789679,2.44551562272167));
#51146=CARTESIAN_POINT('Ctrl Pts',(64.234427664365,2.30481703186258,2.55665351328971));
#51147=CARTESIAN_POINT('Ctrl Pts',(62.6483896081628,0.606804018161656,2.66779140385776));
#51148=CARTESIAN_POINT('Ctrl Pts',(63.214807212685,-1.64662359498827,2.77892929442579));
#51149=CARTESIAN_POINT('Ctrl Pts',(65.4152320208998,-2.39287795766375,2.89006718499384));
#51150=CARTESIAN_POINT('Ctrl Pts',(67.2355902513335,-0.948903988607909,
3.00120507556188));
#51151=CARTESIAN_POINT('Ctrl Pts',(67.009687371404,1.36361256252398,3.11234296612992));
#51152=CARTESIAN_POINT('Ctrl Pts',(64.9442948490232,2.42799907075925,3.22348085669796));
#51153=CARTESIAN_POINT('Ctrl Pts',(62.9298898830713,1.27001049414665,3.334618747266));
#51154=CARTESIAN_POINT('Ctrl Pts',(62.8102801837889,-1.05043309065764,3.44575663783405));
#51155=CARTESIAN_POINT('Ctrl Pts',(64.6949458653977,-2.40940335486022,3.55689452840209));
#51156=CARTESIAN_POINT('Ctrl Pts',(66.8588310559543,-1.56301940386928,3.66803241897013));
#51157=CARTESIAN_POINT('Ctrl Pts',(67.3213071004237,0.714013933333857,3.77917030953817));
#51158=CARTESIAN_POINT('Ctrl Pts',(65.6590644304509,2.33750221987791,3.89030820010621));
#51159=CARTESIAN_POINT('Ctrl Pts',(63.39357261301,1.82144821550899,4.00144609067426));
#51160=CARTESIAN_POINT('Ctrl Pts',(62.5984620009619,-0.361797997181331,
4.1125839812423));
#51161=CARTESIAN_POINT('Ctrl Pts',(64.0015063548152,-2.21388639990766,4.22372187181034));
#51162=CARTESIAN_POINT('Ctrl Pts',(66.3184832656195,-2.03957947376811,4.33485976237838));
#51163=CARTESIAN_POINT('Ctrl Pts',(67.4286374911296,0.00157767540964959,
4.44599765294642));
#51164=CARTESIAN_POINT('Ctrl Pts',(66.3158322777071,2.04129075981349,4.55713554351446));
#51165=CARTESIAN_POINT('Ctrl Pts',(63.9986308592856,2.21258726309085,4.66827343408251));
#51166=CARTESIAN_POINT('Ctrl Pts',(62.5979939690176,0.358677549762036,4.77941132465055));
#51167=CARTESIAN_POINT('Ctrl Pts',(63.3959404447162,-1.82353378810157,4.89054921521859));
#51168=CARTESIAN_POINT('Ctrl Pts',(65.6621008123707,-2.33664397819607,5.00168710578663));
#51169=CARTESIAN_POINT('Ctrl Pts',(67.3222328179754,-0.710997418429188,
5.11282499635466));
#51170=CARTESIAN_POINT('Ctrl Pts',(66.8567987494513,1.56543310762405,5.22396288692272));
#51171=CARTESIAN_POINT('Ctrl Pts',(64.6918158067503,2.4090050242139,5.33510077749075));
#51172=CARTESIAN_POINT('Ctrl Pts',(62.8089171959401,1.04758718972752,5.4462386680588));
#51173=CARTESIAN_POINT('Ctrl Pts',(62.931541830362,-1.27269881881276,5.55737655862684));
#51174=CARTESIAN_POINT('Ctrl Pts',(64.9474490817621,-2.42806968006158,5.66851444919488));
#51175=CARTESIAN_POINT('Ctrl Pts',(67.0114579748176,-1.36099981154567,5.77965233976292));
#51176=CARTESIAN_POINT('Ctrl Pts',(67.234354225073,0.951806616989214,5.89079023033096));
#51177=CARTESIAN_POINT('Ctrl Pts',(65.4121253417219,2.39341760299657,6.001928120899));
#51178=CARTESIAN_POINT('Ctrl Pts',(63.2126643336617,1.64429852840487,6.11306601146706));
#51179=CARTESIAN_POINT('Ctrl Pts',(62.649189925264,-0.609850285121809,6.22420390203508));
#51180=CARTESIAN_POINT('Ctrl Pts',(64.2374031554985,-2.30582648807954,6.33534179260314));
#51181=CARTESIAN_POINT('Ctrl Pts',(66.5236998933488,-1.89119386508314,6.44647968317117));
#51182=CARTESIAN_POINT('Ctrl Pts',(67.4151988715152,0.25435224605703,6.55761757373922));
#51183=CARTESIAN_POINT('Ctrl Pts',(66.0963109962835,2.16731896239629,6.66875546430726));
#51184=CARTESIAN_POINT('Ctrl Pts',(63.7734206371606,2.09605634078856,6.77989335487529));
#51185=CARTESIAN_POINT('Ctrl Pts',(62.5742917867301,0.107152602938506,6.89103124544335));
#51186=CARTESIAN_POINT('Ctrl Pts',(63.5933356141608,-1.98161526205798,7.00216913601138));
#51187=CARTESIAN_POINT('Ctrl Pts',(65.9042541560964,-2.25300237548895,7.11330702657943));
#51188=CARTESIAN_POINT('Ctrl Pts',(66.8857543436368,-1.06431345694511,7.18739895362479));
#51189=CARTESIAN_POINT('Ctrl Pts',(67.0166758614465,-0.393720754290184,
7.22444491714747));
#51190=CARTESIAN_POINT('Ctrl Pts',(65.4967348970877,-1.85997880000276,-2.07481497238249));
#51191=CARTESIAN_POINT('Ctrl Pts',(66.1152220988337,-1.69480262890398,-2.03776900885981));
#51192=CARTESIAN_POINT('Ctrl Pts',(67.1637217267118,-0.701476540869014,
-1.96367708181445));
#51193=CARTESIAN_POINT('Ctrl Pts',(66.7625611820115,1.4413553150263,-1.8525391912464));
#51194=CARTESIAN_POINT('Ctrl Pts',(64.7450334117317,2.26061368566345,-1.74140130067836));
#51195=CARTESIAN_POINT('Ctrl Pts',(62.962414682697,1.01278889075625,-1.63026341011032));
#51196=CARTESIAN_POINT('Ctrl Pts',(63.0440444094189,-1.16310107509048,-1.51912551954228));
#51197=CARTESIAN_POINT('Ctrl Pts',(64.9163760764189,-2.27386063817902,-1.40798762897424));
#51198=CARTESIAN_POINT('Ctrl Pts',(66.8650500736736,-1.30359889821863,-1.2968497384062));
#51199=CARTESIAN_POINT('Ctrl Pts',(67.1067238075328,0.859998174993211,-1.18571184783815));
#51200=CARTESIAN_POINT('Ctrl Pts',(65.4200380164786,2.2363599535264,-1.07457395727011));
#51201=CARTESIAN_POINT('Ctrl Pts',(63.3489126975537,1.56579120426538,-0.963436066702071));
#51202=CARTESIAN_POINT('Ctrl Pts',(62.7890331093795,-0.53798179177636,-0.85229817613403));
#51203=CARTESIAN_POINT('Ctrl Pts',(64.2528832853252,-2.1493249255815,-0.741160285565987));
#51204=CARTESIAN_POINT('Ctrl Pts',(66.4005744678012,-1.79337115794136,-0.630022394997947));
#51205=CARTESIAN_POINT('Ctrl Pts',(67.2663056781698,0.204077890402244,-0.518884504429904));
#51206=CARTESIAN_POINT('Ctrl Pts',(66.0576607264394,2.014730953885,-0.407746613861862));
#51207=CARTESIAN_POINT('Ctrl Pts',(63.8809273599474,1.98127852376002,-0.296608723293821));
#51208=CARTESIAN_POINT('Ctrl Pts',(62.7284936474651,0.134339088808407,-0.185470832725779));
#51209=CARTESIAN_POINT('Ctrl Pts',(63.6551955739828,-1.83556228407719,-0.0743329421577371));
#51210=CARTESIAN_POINT('Ctrl Pts',(65.8128121849957,-2.12535275953085,0.0368049484103043));
#51211=CARTESIAN_POINT('Ctrl Pts',(67.2264526144558,-0.469783711552737,
0.147942838978346));
#51212=CARTESIAN_POINT('Ctrl Pts',(66.6021957013601,1.61578367529074,0.259080729546388));
#51213=CARTESIAN_POINT('Ctrl Pts',(64.5114309002076,2.22240595006455,0.37021862011443));
#51214=CARTESIAN_POINT('Ctrl Pts',(62.8678589330251,0.794834849795578,0.481356510682471));
#51215=CARTESIAN_POINT('Ctrl Pts',(63.1758598665065,-1.36025759991931,0.592494401250513));
#51216=CARTESIAN_POINT('Ctrl Pts',(65.153516950348,-2.27029084338243,0.703632291818555));
#51217=CARTESIAN_POINT('Ctrl Pts',(66.9906582290337,-1.10230113037647,0.814770182386596));
#51218=CARTESIAN_POINT('Ctrl Pts',(67.0057274548323,1.07463730786742,0.925908072954638));
#51219=CARTESIAN_POINT('Ctrl Pts',(65.1849315948547,2.26794803117707,1.03704596352268));
#51220=CARTESIAN_POINT('Ctrl Pts',(63.1948657487746,1.38538020118272,1.14818385409072));
#51221=CARTESIAN_POINT('Ctrl Pts',(62.8570597544889,-0.765241838189804,
1.25932174465876));
#51222=CARTESIAN_POINT('Ctrl Pts',(64.480711269498,-2.21542934465704,1.37045963522681));
#51223=CARTESIAN_POINT('Ctrl Pts',(66.5796736486789,-1.63780924727066,1.48159752579485));
#51224=CARTESIAN_POINT('Ctrl Pts',(67.232742822502,0.438916228156908,1.59273541636289));
#51225=CARTESIAN_POINT('Ctrl Pts',(65.8421571698655,2.11389670230683,1.70387330693093));
#51226=CARTESIAN_POINT('Ctrl Pts',(63.680735508938,1.8540035516147,1.81501119749897));
#51227=CARTESIAN_POINT('Ctrl Pts',(62.7268515981571,-0.102880075699926,
1.92614908806701));
#51228=CARTESIAN_POINT('Ctrl Pts',(63.8536061988389,-1.96559640298738,2.03728697863505));
#51229=CARTESIAN_POINT('Ctrl Pts',(66.0296680467136,-2.02918005124096,2.1484248692031));
#51230=CARTESIAN_POINT('Ctrl Pts',(67.2632630542012,-0.23543218612684,2.25956275977114));
#51231=CARTESIAN_POINT('Ctrl Pts',(66.42526772103,1.77380942893181,2.37070065033918));
#51232=CARTESIAN_POINT('Ctrl Pts',(64.2827086791644,2.15946315732203,2.48183854090722));
#51233=CARTESIAN_POINT('Ctrl Pts',(62.7966945178967,0.568535767837554,2.59297643147526));
#51234=CARTESIAN_POINT('Ctrl Pts',(63.3273908515816,-1.54277885758279,2.7041143220433));
#51235=CARTESIAN_POINT('Ctrl Pts',(65.3890453074919,-2.24197049835535,2.81525221261135));
#51236=CARTESIAN_POINT('Ctrl Pts',(67.0946021813807,-0.889061116308551,
2.92639010317939));
#51237=CARTESIAN_POINT('Ctrl Pts',(66.8829459242478,1.27761598813437,3.03752799374744));
#51238=CARTESIAN_POINT('Ctrl Pts',(64.9478079085913,2.27487668948697,3.14866588431547));
#51239=CARTESIAN_POINT('Ctrl Pts',(63.0604419061002,1.18991695809612,3.25980377488352));
#51240=CARTESIAN_POINT('Ctrl Pts',(62.9483754230397,-0.98418725961686,3.37094166545155));
#51241=CARTESIAN_POINT('Ctrl Pts',(64.7141841822776,-2.25745371715865,3.4820795560196));
#51242=CARTESIAN_POINT('Ctrl Pts',(66.7416034008459,-1.46444718612111,3.59321744658764));
#51243=CARTESIAN_POINT('Ctrl Pts',(67.1749132754993,0.668984462338435,3.70435533715568));
#51244=CARTESIAN_POINT('Ctrl Pts',(65.6175003638835,2.19008704561056,3.81549322772372));
#51245=CARTESIAN_POINT('Ctrl Pts',(63.4948823662959,1.70657811877717,3.92663111829177));
#51246=CARTESIAN_POINT('Ctrl Pts',(62.7499156079905,-0.338981114121067,
4.0377690088598));
#51247=CARTESIAN_POINT('Ctrl Pts',(64.0644766114669,-2.07426708888619,4.14890689942785));
#51248=CARTESIAN_POINT('Ctrl Pts',(66.2353327818609,-1.91095287354467,4.26004478999589));
#51249=CARTESIAN_POINT('Ctrl Pts',(67.2754748477136,0.00147817890715481,
4.37118268056393));
#51250=CARTESIAN_POINT('Ctrl Pts',(66.2328489791779,1.9125562368987,4.48232057113198));
#51251=CARTESIAN_POINT('Ctrl Pts',(64.061782459797,2.0730498824644,4.59345846170001));
#51252=CARTESIAN_POINT('Ctrl Pts',(62.7494770926002,0.336057458514928,4.70459635226806));
#51253=CARTESIAN_POINT('Ctrl Pts',(63.4971008700911,-1.70853216420175,4.8157342428361));
#51254=CARTESIAN_POINT('Ctrl Pts',(65.6203452556023,-2.18928292915949,4.92687213340414));
#51255=CARTESIAN_POINT('Ctrl Pts',(67.1757806124374,-0.666158184716354,
5.03801002397218));
#51256=CARTESIAN_POINT('Ctrl Pts',(66.7396992622713,1.46670866903236,5.14914791454023));
#51257=CARTESIAN_POINT('Ctrl Pts',(64.7112515215779,2.25708050733624,5.26028580510827));
#51258=CARTESIAN_POINT('Ctrl Pts',(62.9470983923676,0.981520836155458,5.3714236956763));
#51259=CARTESIAN_POINT('Ctrl Pts',(63.0619896729133,-1.19243574288082,5.48256158624435));
#51260=CARTESIAN_POINT('Ctrl Pts',(64.9507632188372,-2.27494284579562,5.59369947681239));
#51261=CARTESIAN_POINT('Ctrl Pts',(66.8846048641049,-1.27516801096354,5.70483736738043));
#51262=CARTESIAN_POINT('Ctrl Pts',(67.093444105432,0.891780689689939,5.81597525794848));
#51263=CARTESIAN_POINT('Ctrl Pts',(65.3861345518294,2.24247611081748,5.92711314851652));
#51264=CARTESIAN_POINT('Ctrl Pts',(63.3253831137711,1.54060042191708,6.03825103908456));
#51265=CARTESIAN_POINT('Ctrl Pts',(62.7974443627954,-0.571389921194146,
6.1493889296526));
#51266=CARTESIAN_POINT('Ctrl Pts',(64.2854965201902,-2.16040895192495,6.26052682022064));
#51267=CARTESIAN_POINT('Ctrl Pts',(66.4276073705699,-1.77192524115467,6.37166471078868));
#51268=CARTESIAN_POINT('Ctrl Pts',(67.2628837380762,0.238311456722616,6.48280260135673));
#51269=CARTESIAN_POINT('Ctrl Pts',(66.0271718634116,2.03063643871027,6.59394049192476));
#51270=CARTESIAN_POINT('Ctrl Pts',(63.8507751778273,1.96386801252778,6.70507838249281));
#51271=CARTESIAN_POINT('Ctrl Pts',(62.7272696944899,0.100394996677835,6.81621627306085));
#51272=CARTESIAN_POINT('Ctrl Pts',(63.6820472627792,-1.85664418964446,6.92735416362889));
#51273=CARTESIAN_POINT('Ctrl Pts',(65.8472271368835,-2.11091620548103,7.03849205419694));
#51274=CARTESIAN_POINT('Ctrl Pts',(66.7668287645171,-0.997192257060707,
7.1125839812423));
#51275=CARTESIAN_POINT('Ctrl Pts',(66.8894936833815,-0.368890654402881,
7.14962994476498));
#51276=CARTESIAN_POINT('Ctrl Pts',(65.4632995769868,-1.7347832743338,-2.14962994476498));
#51277=CARTESIAN_POINT('Ctrl Pts',(66.0401562879218,-1.58072514262809,-2.1125839812423));
#51278=CARTESIAN_POINT('Ctrl Pts',(67.0180812070583,-0.654260021907395,
-2.03849205419694));
#51279=CARTESIAN_POINT('Ctrl Pts',(66.6439228546792,1.3443374154996,-1.92735416362889));
#51280=CARTESIAN_POINT('Ctrl Pts',(64.7621952611282,2.10845134988271,-1.81621627306085));
#51281=CARTESIAN_POINT('Ctrl Pts',(63.0995649367186,0.944617878500777,-1.70507838249281));
#51282=CARTESIAN_POINT('Ctrl Pts',(63.1757001510583,-1.08481252120918,-1.59394049192477));
#51283=CARTESIAN_POINT('Ctrl Pts',(64.9220048185698,-2.12080664751291,-1.48280260135673));
#51284=CARTESIAN_POINT('Ctrl Pts',(66.7395131996123,-1.21585340922504,-1.37166471078869));
#51285=CARTESIAN_POINT('Ctrl Pts',(66.9649198286257,0.802111534783946,-1.26052682022064));
#51286=CARTESIAN_POINT('Ctrl Pts',(65.3917651779528,2.08583014105416,-1.1493889296526));
#51287=CARTESIAN_POINT('Ctrl Pts',(63.4600476969176,1.4603975014417,-1.03825103908456));
#51288=CARTESIAN_POINT('Ctrl Pts',(62.9378537099731,-0.501770135373788,
-0.927113148516519));
#51289=CARTESIAN_POINT('Ctrl Pts',(64.3031718530388,-2.00465345734156,-0.815975257948477));
#51290=CARTESIAN_POINT('Ctrl Pts',(66.306301534833,-1.67265900528796,-0.704837367380435));
#51291=CARTESIAN_POINT('Ctrl Pts',(67.1137602132943,0.190341368907332,-0.593699476812392));
#51292=CARTESIAN_POINT('Ctrl Pts',(65.9864693824166,1.87911903139815,-0.482561586244352));
#51293=CARTESIAN_POINT('Ctrl Pts',(63.9562523515188,1.84791829068726,-0.371423695676309));
#51294=CARTESIAN_POINT('Ctrl Pts',(62.8813891707182,0.125296699270833,-0.260285805108269));
#51295=CARTESIAN_POINT('Ctrl Pts',(63.7457146148648,-1.71201023872441,-0.149147914540226));
#51296=CARTESIAN_POINT('Ctrl Pts',(65.7581016427195,-1.98229486233275,-0.0380100239721847));
#51297=CARTESIAN_POINT('Ctrl Pts',(67.0765896668548,-0.438162480859964,
0.0731278665958569));
#51298=CARTESIAN_POINT('Ctrl Pts',(66.4943516049349,1.50702496976408,0.184265757163899));
#51299=CARTESIAN_POINT('Ctrl Pts',(64.5443165789444,2.07281538421093,0.295403647731941));
#51300=CARTESIAN_POINT('Ctrl Pts',(63.0113737524843,0.741334365359939,0.406541538299983));
#51301=CARTESIAN_POINT('Ctrl Pts',(63.298643084738,-1.2686984029721,0.517679428868024));
#51302=CARTESIAN_POINT('Ctrl Pts',(65.1431836953141,-2.11747713628089,0.628817319436066));
#51303=CARTESIAN_POINT('Ctrl Pts',(66.8566666462206,-1.02810503230118,0.739955210004107));
#51304=CARTESIAN_POINT('Ctrl Pts',(66.8707215595737,1.0023032669301,0.851093100572149));
#51305=CARTESIAN_POINT('Ctrl Pts',(65.1724838141431,2.11529201920926,0.96223099114019));
#51306=CARTESIAN_POINT('Ctrl Pts',(63.3163696774672,1.29212999718137,1.07336888170823));
#51307=CARTESIAN_POINT('Ctrl Pts',(63.0013014687028,-0.713733264976008,
1.18450677227627));
#51308=CARTESIAN_POINT('Ctrl Pts',(64.5156646924021,-2.06630837543612,1.29564466284432));
#51309=CARTESIAN_POINT('Ctrl Pts',(66.4733455158896,-1.52756799631811,1.40678255341236));
#51310=CARTESIAN_POINT('Ctrl Pts',(67.0824564798048,0.409372693623795,1.5179204439804));
#51311=CARTESIAN_POINT('Ctrl Pts',(65.7854714110939,1.97160991449248,1.62905833454844));
#51312=CARTESIAN_POINT('Ctrl Pts',(63.7695354519561,1.72921022104761,1.74019622511648));
#51313=CARTESIAN_POINT('Ctrl Pts',(62.8798576480604,-0.095955198299122,
1.85133411568453));
#51314=CARTESIAN_POINT('Ctrl Pts',(63.9307701829444,-1.83329173643707,1.96247200625256));
#51315=CARTESIAN_POINT('Ctrl Pts',(65.9603608952703,-1.89259555727162,2.07360989682061));
#51316=CARTESIAN_POINT('Ctrl Pts',(67.110922388922,-0.219585201042117,2.18474778738865));
#51317=CARTESIAN_POINT('Ctrl Pts',(66.3293326805052,1.65441397996683,2.29588567795669));
#51318=CARTESIAN_POINT('Ctrl Pts',(64.330989693964,2.01410928278149,2.40702356852474));
#51319=CARTESIAN_POINT('Ctrl Pts',(62.9449994276305,0.530267517513453,2.51816145909277));
#51320=CARTESIAN_POINT('Ctrl Pts',(63.4399744904782,-1.43893412017732,2.62929934966082));
#51321=CARTESIAN_POINT('Ctrl Pts',(65.362858594084,-2.09106303904695,2.74043724022886));
#51322=CARTESIAN_POINT('Ctrl Pts',(66.953614111428,-0.829218244009191,2.8515751307969));
#51323=CARTESIAN_POINT('Ctrl Pts',(66.7562044770915,1.19161941374475,2.96271302136494));
#51324=CARTESIAN_POINT('Ctrl Pts',(64.9513209681592,2.12175430821469,3.07385091193298));
#51325=CARTESIAN_POINT('Ctrl Pts',(63.1909939291292,1.10982342204558,3.18498880250103));
#51326=CARTESIAN_POINT('Ctrl Pts',(63.0864706622905,-0.917941428576071,
3.29612669306907));
#51327=CARTESIAN_POINT('Ctrl Pts',(64.7334224991575,-2.10550407945708,3.40726458363711));
#51328=CARTESIAN_POINT('Ctrl Pts',(66.6243757457373,-1.36587496837293,3.51840247420515));
#51329=CARTESIAN_POINT('Ctrl Pts',(67.0285194505751,0.623954991343011,3.6295403647732));
#51330=CARTESIAN_POINT('Ctrl Pts',(65.5759362973161,2.0426718713432,3.74067825534123));
#51331=CARTESIAN_POINT('Ctrl Pts',(63.5961921195818,1.59170802204535,3.85181614590928));
#51332=CARTESIAN_POINT('Ctrl Pts',(62.9013692150191,-0.316164231060802,
3.96295403647732));
#51333=CARTESIAN_POINT('Ctrl Pts',(64.1274468681187,-1.93464777786472,4.07409192704536));
#51334=CARTESIAN_POINT('Ctrl Pts',(66.1521822981021,-1.78232627332123,4.1852298176134));
#51335=CARTESIAN_POINT('Ctrl Pts',(67.1223122042977,0.00137868240466034,
4.29636770818144));
#51336=CARTESIAN_POINT('Ctrl Pts',(66.1498656806486,1.78382171398391,4.40750559874948));
#51337=CARTESIAN_POINT('Ctrl Pts',(64.1249340603086,1.93351250183796,4.51864348931753));
#51338=CARTESIAN_POINT('Ctrl Pts',(62.9009602161829,0.31343736726782,4.62978137988557));
#51339=CARTESIAN_POINT('Ctrl Pts',(63.5982612954659,-1.59353054030193,4.74091927045361));
#51340=CARTESIAN_POINT('Ctrl Pts',(65.578589698834,-2.04192188012291,4.85205716102165));
#51341=CARTESIAN_POINT('Ctrl Pts',(67.0293284068993,-0.621318951003518,
4.96319505158969));
#51342=CARTESIAN_POINT('Ctrl Pts',(66.6225997750914,1.36798423044066,5.07433294215773));
#51343=CARTESIAN_POINT('Ctrl Pts',(64.7306872364055,2.10515599045857,5.18547083272578));
#51344=CARTESIAN_POINT('Ctrl Pts',(63.0852795887951,0.915454482583398,5.29660872329381));
#51345=CARTESIAN_POINT('Ctrl Pts',(63.1924375154646,-1.11217266694888,5.40774661386187));
#51346=CARTESIAN_POINT('Ctrl Pts',(64.9540773559123,-2.12181601152966,5.5188845044299));
#51347=CARTESIAN_POINT('Ctrl Pts',(66.7577517533922,-1.18933621038142,5.63002239499795));
#51348=CARTESIAN_POINT('Ctrl Pts',(66.9525339857911,0.831754762390664,5.74116028556598));
#51349=CARTESIAN_POINT('Ctrl Pts',(65.360143761937,2.0915346186384,5.85229817613403));
#51350=CARTESIAN_POINT('Ctrl Pts',(63.4381018938805,1.43690231542928,5.96343606670207));
#51351=CARTESIAN_POINT('Ctrl Pts',(62.9456988003269,-0.532929557266482,
6.0745739572701));
#51352=CARTESIAN_POINT('Ctrl Pts',(64.3335898848817,-2.01499141577036,6.18571184783816));
#51353=CARTESIAN_POINT('Ctrl Pts',(66.3315148477911,-1.6526566172262,6.29684973840619));
#51354=CARTESIAN_POINT('Ctrl Pts',(67.1105686046372,0.2222706673882,6.40798762897424));
#51355=CARTESIAN_POINT('Ctrl Pts',(65.9580327305397,1.89395391502425,6.51912551954227));
#51356=CARTESIAN_POINT('Ctrl Pts',(63.9281297184939,1.83167968426699,6.63026341011033));
#51357=CARTESIAN_POINT('Ctrl Pts',(62.8802476022497,0.0936373904171628,
6.74140130067836));
#51358=CARTESIAN_POINT('Ctrl Pts',(63.7707589113974,-1.73167311723094,6.85253919124641));
#51359=CARTESIAN_POINT('Ctrl Pts',(65.7902001176707,-1.96883003547311,6.96367708181445));
#51360=CARTESIAN_POINT('Ctrl Pts',(66.6479031853974,-0.930071057176307,
7.03776900885981));
#51361=CARTESIAN_POINT('Ctrl Pts',(66.7623115053165,-0.344060554515578,
7.07481497238249));
#51362=CARTESIAN_POINT('Ctrl Pts',(65.4298642568859,-1.60958774866484,-2.22444491714747));
#51363=CARTESIAN_POINT('Ctrl Pts',(65.9650904770099,-1.4666476563522,-2.18739895362479));
#51364=CARTESIAN_POINT('Ctrl Pts',(66.8724406874047,-0.607043502945776,
-2.11330702657942));
#51365=CARTESIAN_POINT('Ctrl Pts',(66.5252845273471,1.2473195159729,-2.00216913601139));
#51366=CARTESIAN_POINT('Ctrl Pts',(64.7793571105247,1.95628901410197,-1.89103124544334));
#51367=CARTESIAN_POINT('Ctrl Pts',(63.2367151907402,0.876446866245303,-1.7798933548753));
#51368=CARTESIAN_POINT('Ctrl Pts',(63.3073558926977,-1.00652396732789,-1.66875546430726));
#51369=CARTESIAN_POINT('Ctrl Pts',(64.9276335607206,-1.9677526568468,-1.55761757373922));
#51370=CARTESIAN_POINT('Ctrl Pts',(66.6139763255511,-1.12810792023144,-1.44647968317117));
#51371=CARTESIAN_POINT('Ctrl Pts',(66.8231158497185,0.74422489457468,-1.33534179260313));
#51372=CARTESIAN_POINT('Ctrl Pts',(65.363492339427,1.93530032858193,-1.22420390203509));
#51373=CARTESIAN_POINT('Ctrl Pts',(63.5711826962814,1.35500379861802,-1.11306601146705));
#51374=CARTESIAN_POINT('Ctrl Pts',(63.0866743105668,-0.465558478971215,
-1.00192812089901));
#51375=CARTESIAN_POINT('Ctrl Pts',(64.3534604207524,-1.85998198910161,-0.890790230330965));
#51376=CARTESIAN_POINT('Ctrl Pts',(66.2120286018649,-1.55194685263456,-0.779652339762925));
#51377=CARTESIAN_POINT('Ctrl Pts',(66.9612147484188,0.176604847412417,-0.668514449194881));
#51378=CARTESIAN_POINT('Ctrl Pts',(65.915278038394,1.7435071089113,-0.55737655862684));
#51379=CARTESIAN_POINT('Ctrl Pts',(64.0315773430901,1.7145580576145,-0.446238668058799));
#51380=CARTESIAN_POINT('Ctrl Pts',(63.0342846939712,0.116254309733256,-0.335100777490757));
#51381=CARTESIAN_POINT('Ctrl Pts',(63.8362336557469,-1.58845819337162,-0.223962886922715));
#51382=CARTESIAN_POINT('Ctrl Pts',(65.703391100443,-1.83923696513465,-0.112824996354674));
#51383=CARTESIAN_POINT('Ctrl Pts',(66.9267267192538,-0.406541250167187,
-0.00168710578663183));
#51384=CARTESIAN_POINT('Ctrl Pts',(66.3865075085097,1.39826626423741,0.10945078478141));
#51385=CARTESIAN_POINT('Ctrl Pts',(64.5772022576811,1.92322481835731,0.220588675349452));
#51386=CARTESIAN_POINT('Ctrl Pts',(63.1548885719436,0.687833880924302,0.331726565917493));
#51387=CARTESIAN_POINT('Ctrl Pts',(63.4214263029693,-1.17713920602489,0.442864456485535));
#51388=CARTESIAN_POINT('Ctrl Pts',(65.1328504402804,-1.96466342917936,0.554002347053577));
#51389=CARTESIAN_POINT('Ctrl Pts',(66.7226750634076,-0.953908934225886,
0.665140237621619));
#51390=CARTESIAN_POINT('Ctrl Pts',(66.7357156643151,0.929969225992789,0.77627812818966));
#51391=CARTESIAN_POINT('Ctrl Pts',(65.1600360334315,1.96263600724145,0.887416018757702));
#51392=CARTESIAN_POINT('Ctrl Pts',(63.4378736061597,1.19887979318003,0.998553909325744));
#51393=CARTESIAN_POINT('Ctrl Pts',(63.1455431829167,-0.66222469176221,1.10969179989378));
#51394=CARTESIAN_POINT('Ctrl Pts',(64.5506181153062,-1.9171874062152,1.22082969046183));
#51395=CARTESIAN_POINT('Ctrl Pts',(66.3670173831005,-1.41732674536556,1.33196758102987));
#51396=CARTESIAN_POINT('Ctrl Pts',(66.9321701371076,0.379829159090682,1.44310547159791));
#51397=CARTESIAN_POINT('Ctrl Pts',(65.7287856523224,1.82932312667812,1.55424336216595));
#51398=CARTESIAN_POINT('Ctrl Pts',(63.858335394974,1.60441689048052,1.66538125273399));
#51399=CARTESIAN_POINT('Ctrl Pts',(63.0328636979636,-0.0890303208983184,
1.77651914330204));
#51400=CARTESIAN_POINT('Ctrl Pts',(64.00793416705,-1.70098706988675,1.88765703387008));
#51401=CARTESIAN_POINT('Ctrl Pts',(65.8910537438272,-1.75601106330228,1.99879492443812));
#51402=CARTESIAN_POINT('Ctrl Pts',(66.9585817236427,-0.203738215957396,
2.10993281500616));
#51403=CARTESIAN_POINT('Ctrl Pts',(66.2333976399805,1.53501853100185,2.2210707055742));
#51404=CARTESIAN_POINT('Ctrl Pts',(64.3792707087636,1.86875540824094,2.33220859614224));
#51405=CARTESIAN_POINT('Ctrl Pts',(63.0933043373643,0.491999267189351,2.44334648671029));
#51406=CARTESIAN_POINT('Ctrl Pts',(63.5525581293749,-1.33508938277185,2.55448437727833));
#51407=CARTESIAN_POINT('Ctrl Pts',(65.336671880676,-1.94015557973856,2.66562226784637));
#51408=CARTESIAN_POINT('Ctrl Pts',(66.8126260414754,-0.76937537170983,2.77676015841441));
#51409=CARTESIAN_POINT('Ctrl Pts',(66.6294630299351,1.10562283935513,2.88789804898245));
#51410=CARTESIAN_POINT('Ctrl Pts',(64.9548340277273,1.96863192694241,2.9990359395505));
#51411=CARTESIAN_POINT('Ctrl Pts',(63.3215459521581,1.02972988599504,3.11017383011853));
#51412=CARTESIAN_POINT('Ctrl Pts',(63.2245659015414,-0.851695597535288,
3.22131172068658));
#51413=CARTESIAN_POINT('Ctrl Pts',(64.7526608160373,-1.95355444175551,3.33244961125462));
#51414=CARTESIAN_POINT('Ctrl Pts',(66.507148090629,-1.26730275062476,3.44358750182267));
#51415=CARTESIAN_POINT('Ctrl Pts',(66.8821256256507,0.578925520347588,3.5547253923907));
#51416=CARTESIAN_POINT('Ctrl Pts',(65.5343722307488,1.89525669707585,3.66586328295875));
#51417=CARTESIAN_POINT('Ctrl Pts',(63.6975018728676,1.47683792531353,3.77700117352679));
#51418=CARTESIAN_POINT('Ctrl Pts',(63.0528228220477,-0.293347348000536,
3.88813906409483));
#51419=CARTESIAN_POINT('Ctrl Pts',(64.1904171247705,-1.79502846684324,3.99927695466287));
#51420=CARTESIAN_POINT('Ctrl Pts',(66.0690318143434,-1.65369967309779,4.11041484523092));
#51421=CARTESIAN_POINT('Ctrl Pts',(66.9691495608818,0.00127918590216747,
4.22155273579895));
#51422=CARTESIAN_POINT('Ctrl Pts',(66.0668823821194,1.65508719106912,4.332690626367));
#51423=CARTESIAN_POINT('Ctrl Pts',(64.18808566082,1.79397512121151,4.44382851693503));
#51424=CARTESIAN_POINT('Ctrl Pts',(63.0524433397656,0.290817276020709,4.55496640750308));
#51425=CARTESIAN_POINT('Ctrl Pts',(63.6994217208406,-1.4785289164021,4.66610429807112));
#51426=CARTESIAN_POINT('Ctrl Pts',(65.5368341420657,-1.89456083108634,4.77724218863916));
#51427=CARTESIAN_POINT('Ctrl Pts',(66.8828762013613,-0.576479717290682,
4.88838007920721));
#51428=CARTESIAN_POINT('Ctrl Pts',(66.5055002879113,1.26925979184897,4.99951796977524));
#51429=CARTESIAN_POINT('Ctrl Pts',(64.750122951233,1.9532314735809,5.11065586034329));
#51430=CARTESIAN_POINT('Ctrl Pts',(63.2234607852226,0.849388129011338,5.22179375091133));
#51431=CARTESIAN_POINT('Ctrl Pts',(63.3228853580158,-1.03190959101694,5.33293164147937));
#51432=CARTESIAN_POINT('Ctrl Pts',(64.9573914929873,-1.9686891772637,5.44406953204742));
#51433=CARTESIAN_POINT('Ctrl Pts',(66.6308986426796,-1.10350440979929,5.55520742261545));
#51434=CARTESIAN_POINT('Ctrl Pts',(66.8116238661501,0.771728835091389,5.6663453131835));
#51435=CARTESIAN_POINT('Ctrl Pts',(65.3341529720446,1.94059312645932,5.77748320375153));
#51436=CARTESIAN_POINT('Ctrl Pts',(63.5508206739898,1.33320420894149,5.88862109431959));
#51437=CARTESIAN_POINT('Ctrl Pts',(63.0939532378584,-0.494469193338818,
5.99975898488762));
#51438=CARTESIAN_POINT('Ctrl Pts',(64.3816832495733,-1.86957387961577,6.11089687545566));
#51439=CARTESIAN_POINT('Ctrl Pts',(66.2354223250123,-1.53338799329773,6.22203476602371));
#51440=CARTESIAN_POINT('Ctrl Pts',(66.9582534711982,0.206229878053785,6.33317265659175));
#51441=CARTESIAN_POINT('Ctrl Pts',(65.8888935976679,1.75727139133823,6.44431054715979));
#51442=CARTESIAN_POINT('Ctrl Pts',(64.0054842591604,1.6994913560062,6.55544843772783));
#51443=CARTESIAN_POINT('Ctrl Pts',(63.0332255100096,0.0868797841564908,
6.66658632829588));
#51444=CARTESIAN_POINT('Ctrl Pts',(63.8594705600156,-1.60670204481742,6.77772421886391));
#51445=CARTESIAN_POINT('Ctrl Pts',(65.7331730984579,-1.82674386546519,6.88886210943197));
#51446=CARTESIAN_POINT('Ctrl Pts',(66.5289776062776,-0.862949857291908,
6.96295403647732));
#51447=CARTESIAN_POINT('Ctrl Pts',(66.6351293272515,-0.319230454628274,
7.));
#51448=CARTESIAN_POINT('Ctrl Pts',(66.6638321395092,0.000941642735149761,
-1.3785196366098));
#51449=CARTESIAN_POINT('Ctrl Pts',(66.664949390616,0.216825623511906,-1.36412702194091));
#51450=CARTESIAN_POINT('Ctrl Pts',(66.625958965974,0.432322760104845,-1.34973440727202));
#51451=CARTESIAN_POINT('Ctrl Pts',(66.5449886773087,0.630681997774868,-1.33534179260313));
#51452=CARTESIAN_POINT('Ctrl Pts',(66.3365746796213,1.14125003924376,-1.29829582908045));
#51453=CARTESIAN_POINT('Ctrl Pts',(65.8500335095242,1.53827518391285,-1.26124986555777));
#51454=CARTESIAN_POINT('Ctrl Pts',(65.308044650618,1.64007166792007,-1.22420390203509));
#51455=CARTESIAN_POINT('Ctrl Pts',(64.7660557917118,1.74186815192729,-1.18715793851241));
#51456=CARTESIAN_POINT('Ctrl Pts',(64.1686192439966,1.54843597527265,-1.15011197498973));
#51457=CARTESIAN_POINT('Ctrl Pts',(63.7891495725199,1.14829284068046,-1.11306601146705));
#51458=CARTESIAN_POINT('Ctrl Pts',(63.4096799010432,0.748149706088272,-1.07602004794437));
#51459=CARTESIAN_POINT('Ctrl Pts',(63.248177105805,0.141295613558526,-1.03897408442169));
#51460=CARTESIAN_POINT('Ctrl Pts',(63.3785567265502,-0.394535351061412,
-1.00192812089901));
#51461=CARTESIAN_POINT('Ctrl Pts',(63.5089363472953,-0.93036631568135,-0.964882157376327));
#51462=CARTESIAN_POINT('Ctrl Pts',(63.9311983840238,-1.39517415239148,-0.927836193853646));
#51463=CARTESIAN_POINT('Ctrl Pts',(64.4520907659069,-1.57623888133537,-0.890790230330965));
#51464=CARTESIAN_POINT('Ctrl Pts',(64.9729831477899,-1.75730361027926,-0.853744266808285));
#51465=CARTESIAN_POINT('Ctrl Pts',(65.5925058748274,-1.65462523145691,-0.816698303285605));
#51466=CARTESIAN_POINT('Ctrl Pts',(66.0271315961051,-1.31519409203791,-0.779652339762925));
#51467=CARTESIAN_POINT('Ctrl Pts',(66.422630141453,-1.0063202373306,-0.745941438711882));
#51468=CARTESIAN_POINT('Ctrl Pts',(66.6650238854461,-0.501402189087533,
-0.712230537660838));
#51469=CARTESIAN_POINT('Ctrl Pts',(66.6681941903091,0.000864019930038266,
-0.678519636609795));
#51470=CARTESIAN_POINT('Ctrl Pts',(65.5301702171886,-1.98517432567172,-2.));
#51471=CARTESIAN_POINT('Ctrl Pts',(65.5988381452814,-1.95974913772664,-2.));
#51472=CARTESIAN_POINT('Ctrl Pts',(65.6658026948309,-1.93043476164875,-2.));
#51473=CARTESIAN_POINT('Ctrl Pts',(65.730874875774,-1.89752507621399,-2.));
#51474=CARTESIAN_POINT('Ctrl Pts',(65.7977553584727,-1.8637008580083,-2.));
#51475=CARTESIAN_POINT('Ctrl Pts',(65.8626376079646,-1.82607804419433,-2.));
#51476=CARTESIAN_POINT('Ctrl Pts',(65.9252852210981,-1.78493106183395,-2.));
#51477=CARTESIAN_POINT('Ctrl Pts',(65.9782205027354,-1.75016314345963,-2.));
#51478=CARTESIAN_POINT('Ctrl Pts',(66.0295599817184,-1.71287801549895,-2.));
#51479=CARTESIAN_POINT('Ctrl Pts',(66.0791382962118,-1.67322322119488,-2.));
#51480=CARTESIAN_POINT('Ctrl Pts',(66.1011632204631,-1.65560677235685,-2.));
#51481=CARTESIAN_POINT('Ctrl Pts',(66.1228402691625,-1.63752248214469,-2.));
#51482=CARTESIAN_POINT('Ctrl Pts',(66.1441533920278,-1.61898256263396,-2.));
#51483=CARTESIAN_POINT('Ctrl Pts',(66.1558656059004,-1.60879430895284,-2.));
#51484=CARTESIAN_POINT('Ctrl Pts',(66.167467902359,-1.59846845594872,-2.));
#51485=CARTESIAN_POINT('Ctrl Pts',(66.1789574836609,-1.58800698854278,-2.));
#51486=CARTESIAN_POINT('Ctrl Pts',(66.1895512887021,-1.57836114129822,-2.));
#51487=CARTESIAN_POINT('Ctrl Pts',(66.2000507028277,-1.56859848611489,-2.));
#51488=CARTESIAN_POINT('Ctrl Pts',(66.210437644616,-1.5587360337551,-2.));
#51489=CARTESIAN_POINT('Ctrl Pts',(66.2635229555623,-1.50833126968861,-2.));
#51490=CARTESIAN_POINT('Ctrl Pts',(66.3137682961291,-1.45523826476737,-2.));
#51491=CARTESIAN_POINT('Ctrl Pts',(66.3609549723778,-1.39971629736155,-2.));
#51492=CARTESIAN_POINT('Ctrl Pts',(66.4077748713701,-1.34462589658626,-2.));
#51493=CARTESIAN_POINT('Ctrl Pts',(66.4515839789298,-1.28714326375553,-2.));
#51494=CARTESIAN_POINT('Ctrl Pts',(66.4921238713265,-1.22749743717743,-2.));
#51495=CARTESIAN_POINT('Ctrl Pts',(66.5258166843524,-1.17792563113991,-2.));
#51496=CARTESIAN_POINT('Ctrl Pts',(66.5572507035796,-1.12685898699336,-2.));
#51497=CARTESIAN_POINT('Ctrl Pts',(66.5862499617206,-1.07442250689085,-2.));
#51498=CARTESIAN_POINT('Ctrl Pts',(66.5983545270528,-1.05253502286947,-2.));
#51499=CARTESIAN_POINT('Ctrl Pts',(66.6100345605391,-1.03040883225682,-2.));
#51500=CARTESIAN_POINT('Ctrl Pts',(66.6212758238085,-1.00805294268962,-2.));
#51501=CARTESIAN_POINT('Ctrl Pts',(66.6264792884302,-0.997704632392041,
-2.));
#51502=CARTESIAN_POINT('Ctrl Pts',(66.6315887267379,-0.987307105267063,
-2.));
#51503=CARTESIAN_POINT('Ctrl Pts',(66.6366026612151,-0.976861256677832,
-2.));
#51504=CARTESIAN_POINT('Ctrl Pts',(66.6418315207929,-0.965967640956889,
-2.));
#51505=CARTESIAN_POINT('Ctrl Pts',(66.6469528966202,-0.955028940819226,
-2.));
#51506=CARTESIAN_POINT('Ctrl Pts',(66.6519637514069,-0.944050420232592,
-2.));
#51507=CARTESIAN_POINT('Ctrl Pts',(66.6805038460038,-0.881520566661746,
-2.));
#51508=CARTESIAN_POINT('Ctrl Pts',(66.705483022792,-0.817657226321086,-2.));
#51509=CARTESIAN_POINT('Ctrl Pts',(66.726677809183,-0.752664675176916,-2.));
#51510=CARTESIAN_POINT('Ctrl Pts',(66.7458885398579,-0.693756112813037,
-2.));
#51511=CARTESIAN_POINT('Ctrl Pts',(66.7619899159167,-0.633919258272544,
-2.));
#51512=CARTESIAN_POINT('Ctrl Pts',(66.7747787781587,-0.573301385906257,
-2.));
#51513=CARTESIAN_POINT('Ctrl Pts',(66.7899084885612,-0.50158813755264,-2.));
#51514=CARTESIAN_POINT('Ctrl Pts',(66.8004026737972,-0.42878027311813,-2.));
#51515=CARTESIAN_POINT('Ctrl Pts',(66.8063365292405,-0.355301138761089,
-2.));
#51516=CARTESIAN_POINT('Ctrl Pts',(66.8076429326892,-0.339123900294128,
-2.));
#51517=CARTESIAN_POINT('Ctrl Pts',(66.8087280690516,-0.32291420665931,-2.));
#51518=CARTESIAN_POINT('Ctrl Pts',(66.809592371063,-0.306676740190648,-2.));
#51519=CARTESIAN_POINT('Ctrl Pts',(66.8104842013171,-0.289922106213089,
-2.));
#51520=CARTESIAN_POINT('Ctrl Pts',(66.8111409153901,-0.27313175447349,-2.));
#51521=CARTESIAN_POINT('Ctrl Pts',(66.8115624311269,-0.256344928177872,
-2.));
#51522=CARTESIAN_POINT('Ctrl Pts',(66.8132840454952,-0.187781790856896,
-2.));
#51523=CARTESIAN_POINT('Ctrl Pts',(66.8110938642257,-0.119190445643793,
-2.));
#51524=CARTESIAN_POINT('Ctrl Pts',(66.8051125395855,-0.0509093849216768,
-2.));
#51525=CARTESIAN_POINT('Ctrl Pts',(66.7991324434512,0.0173576515338734,
-2.));
#51526=CARTESIAN_POINT('Ctrl Pts',(66.7893623073071,0.0853156029745438,
-2.));
#51527=CARTESIAN_POINT('Ctrl Pts',(66.7758731021479,0.152611158122592,-2.));
#51528=CARTESIAN_POINT('Ctrl Pts',(66.7661100689037,0.201317418746942,-2.));
#51529=CARTESIAN_POINT('Ctrl Pts',(66.7543977966752,0.249676426140225,-2.));
#51530=CARTESIAN_POINT('Ctrl Pts',(66.7407489756663,0.29754456718097,-2.));
#51531=CARTESIAN_POINT('Ctrl Pts',(66.7305106872339,0.333451539247104,-2.));
#51532=CARTESIAN_POINT('Ctrl Pts',(66.7191824845939,0.369082153610466,-2.));
#51533=CARTESIAN_POINT('Ctrl Pts',(66.7067658074173,0.404371614546108,-2.));
#51534=CARTESIAN_POINT('Ctrl Pts',(66.7026385144614,0.4161018014119,-2.));
#51535=CARTESIAN_POINT('Ctrl Pts',(66.6983941580482,0.427785082937903,-2.));
#51536=CARTESIAN_POINT('Ctrl Pts',(66.6940333669607,0.439418945593974,-2.));
#51537=CARTESIAN_POINT('Ctrl Pts',(66.6709086373959,0.501111863762935,-2.));
#51538=CARTESIAN_POINT('Ctrl Pts',(66.6445114918184,0.561421289076099,-2.));
#51539=CARTESIAN_POINT('Ctrl Pts',(66.6148919774249,0.620012996701175,-2.));
#51540=CARTESIAN_POINT('Ctrl Pts',(66.5940505456268,0.661240380181596,-2.));
#51541=CARTESIAN_POINT('Ctrl Pts',(66.5716128408677,0.701616780460216,-2.));
#51542=CARTESIAN_POINT('Ctrl Pts',(66.5475858840223,0.741014396509355,-2.));
#51543=CARTESIAN_POINT('Ctrl Pts',(66.5398732603013,0.753660983009995,-2.));
#51544=CARTESIAN_POINT('Ctrl Pts',(66.5319957124855,0.766208337049959,-2.));
#51545=CARTESIAN_POINT('Ctrl Pts',(66.5239568319111,0.778646543700854,-2.));
#51546=CARTESIAN_POINT('Ctrl Pts',(66.4897115300548,0.831632794381773,-2.));
#51547=CARTESIAN_POINT('Ctrl Pts',(66.4526108600522,0.882535056499814,-2.));
#51548=CARTESIAN_POINT('Ctrl Pts',(66.4126890994678,0.931037995712848,-2.));
#51549=CARTESIAN_POINT('Ctrl Pts',(66.3758798548356,0.975759383966769,-2.));
#51550=CARTESIAN_POINT('Ctrl Pts',(66.336671680953,1.01844109085503,-2.));
#51551=CARTESIAN_POINT('Ctrl Pts',(66.295069969863,1.05880296618532,-2.));
#51552=CARTESIAN_POINT('Ctrl Pts',(66.2872852045854,1.0663557258525,-2.));
#51553=CARTESIAN_POINT('Ctrl Pts',(66.279416574172,1.07382715133634,-2.));
#51554=CARTESIAN_POINT('Ctrl Pts',(66.2714656498818,1.0812165860621,-2.));
#51555=CARTESIAN_POINT('Origin',(65.,0.,3.));
#51556=CARTESIAN_POINT('Origin',(65.,0.,8.));
#51557=CARTESIAN_POINT('Origin',(65.,0.,13.));
#51558=CARTESIAN_POINT('Ctrl Pts',(63.3648706727485,-0.319230454628301,
13.));
#51559=CARTESIAN_POINT('Ctrl Pts',(63.3697100624573,-0.381552584102801,
13.));
#51560=CARTESIAN_POINT('Ctrl Pts',(63.3783265672582,-0.443390469668827,
13.));
#51561=CARTESIAN_POINT('Ctrl Pts',(63.3904636088659,-0.504524999056366,
13.));
#51562=CARTESIAN_POINT('Ctrl Pts',(63.3981627172741,-0.543305567208763,
13.));
#51563=CARTESIAN_POINT('Ctrl Pts',(63.4072795438865,-0.581803401471875,
13.));
#51564=CARTESIAN_POINT('Ctrl Pts',(63.4177589835331,-0.619964019296847,
13.));
#51565=CARTESIAN_POINT('Ctrl Pts',(63.4249317271173,-0.646083385971169,
13.));
#51566=CARTESIAN_POINT('Ctrl Pts',(63.4327429984653,-0.672044791713898,
13.));
#51567=CARTESIAN_POINT('Ctrl Pts',(63.4411771706464,-0.69783074874542,13.));
#51568=CARTESIAN_POINT('Ctrl Pts',(63.445633981408,-0.711456642114301,13.));
#51569=CARTESIAN_POINT('Ctrl Pts',(63.4502647769864,-0.725033238750576,
13.));
#51570=CARTESIAN_POINT('Ctrl Pts',(63.4550623359318,-0.738544708545356,
13.));
#51571=CARTESIAN_POINT('Ctrl Pts',(63.4771367982206,-0.800713497682774,
13.));
#51572=CARTESIAN_POINT('Ctrl Pts',(63.5027603465155,-0.861575212002685,
13.));
#51573=CARTESIAN_POINT('Ctrl Pts',(63.5316785435928,-0.920885280767066,
13.));
#51574=CARTESIAN_POINT('Ctrl Pts',(63.552535208242,-0.963661468066429,13.));
#51575=CARTESIAN_POINT('Ctrl Pts',(63.5751068652181,-1.00563072000056,13.));
#51576=CARTESIAN_POINT('Ctrl Pts',(63.5993147001858,-1.04669965515685,13.));
#51577=CARTESIAN_POINT('Ctrl Pts',(63.6059727893565,-1.05799519780992,13.));
#51578=CARTESIAN_POINT('Ctrl Pts',(63.6127547257886,-1.06922261674128,13.));
#51579=CARTESIAN_POINT('Ctrl Pts',(63.6196590403468,-1.08037991992191,13.));
#51580=CARTESIAN_POINT('Ctrl Pts',(63.6266559377188,-1.09168683600231,13.));
#51581=CARTESIAN_POINT('Ctrl Pts',(63.6337742041172,-1.10291470718646,13.));
#51582=CARTESIAN_POINT('Ctrl Pts',(63.6410091869952,-1.11405768751354,13.));
#51583=CARTESIAN_POINT('Ctrl Pts',(63.6779597277015,-1.1709671723197,13.));
#51584=CARTESIAN_POINT('Ctrl Pts',(63.7179710366331,-1.2256961535147,13.));
#51585=CARTESIAN_POINT('Ctrl Pts',(63.7607845671631,-1.27799720826047,13.));
#51586=CARTESIAN_POINT('Ctrl Pts',(63.8042168531726,-1.33105413536263,13.));
#51587=CARTESIAN_POINT('Ctrl Pts',(63.8505333121816,-1.3816134481406,13.));
#51588=CARTESIAN_POINT('Ctrl Pts',(63.899515178467,-1.42940352766181,13.));
#51589=CARTESIAN_POINT('Ctrl Pts',(63.9298610021707,-1.45901100156839,13.));
#51590=CARTESIAN_POINT('Ctrl Pts',(63.9612308493175,-1.48755527136839,13.));
#51591=CARTESIAN_POINT('Ctrl Pts',(63.9935813335733,-1.51496662410822,13.));
#51592=CARTESIAN_POINT('Ctrl Pts',(64.0200865948567,-1.53742517714731,13.));
#51593=CARTESIAN_POINT('Ctrl Pts',(64.0472502674124,-1.55912317450051,13.));
#51594=CARTESIAN_POINT('Ctrl Pts',(64.0750513948299,-1.58001951679719,13.));
#51595=CARTESIAN_POINT('Ctrl Pts',(64.0864069562603,-1.58855477132336,13.));
#51596=CARTESIAN_POINT('Ctrl Pts',(64.0978710430034,-1.59695761736653,13.));
#51597=CARTESIAN_POINT('Ctrl Pts',(64.109422488797,-1.60521141817007,13.));
#51598=CARTESIAN_POINT('Ctrl Pts',(64.1667717342953,-1.64618890765761,13.));
#51599=CARTESIAN_POINT('Ctrl Pts',(64.2263690235154,-1.6835708134358,13.));
#51600=CARTESIAN_POINT('Ctrl Pts',(64.2879736625821,-1.71708519917631,13.));
#51601=CARTESIAN_POINT('Ctrl Pts',(64.2948173903715,-1.7208083495187,13.));
#51602=CARTESIAN_POINT('Ctrl Pts',(64.3016859372404,-1.7244837434876,13.));
#51603=CARTESIAN_POINT('Ctrl Pts',(64.3085790067212,-1.72811098684768,13.));
#51604=CARTESIAN_POINT('Ctrl Pts',(64.3682468605421,-1.75950916543644,13.));
#51605=CARTESIAN_POINT('Ctrl Pts',(64.4297493247371,-1.78730275834966,13.));
#51606=CARTESIAN_POINT('Ctrl Pts',(64.4927553331735,-1.81157421874288,13.));
#51607=CARTESIAN_POINT('Ctrl Pts',(64.5605395057602,-1.837686345206,13.));
#51608=CARTESIAN_POINT('Ctrl Pts',(64.630064551517,-1.85972265026457,13.));
#51609=CARTESIAN_POINT('Ctrl Pts',(64.7009535899412,-1.87773216280799,13.));
#51610=CARTESIAN_POINT('Ctrl Pts',(64.7139243245219,-1.88102740580073,13.));
#51611=CARTESIAN_POINT('Ctrl Pts',(64.7269407961053,-1.88418768246609,13.));
#51612=CARTESIAN_POINT('Ctrl Pts',(64.7400007816474,-1.88721308481341,13.));
#51613=CARTESIAN_POINT('Ctrl Pts',(64.7512396230459,-1.88981661121387,13.));
#51614=CARTESIAN_POINT('Ctrl Pts',(64.7625015972973,-1.89231813894598,13.));
#51615=CARTESIAN_POINT('Ctrl Pts',(64.7737835813128,-1.89471786802249,13.));
#51616=CARTESIAN_POINT('Ctrl Pts',(64.843296940848,-1.90950367430022,13.));
#51617=CARTESIAN_POINT('Ctrl Pts',(64.913585486576,-1.92043263344677,13.));
#51618=CARTESIAN_POINT('Ctrl Pts',(64.9842819831785,-1.92760569490766,13.));
#51619=CARTESIAN_POINT('Ctrl Pts',(65.05646946371,-1.93493003570874,13.));
#51620=CARTESIAN_POINT('Ctrl Pts',(65.1290831839004,-1.93833864552727,13.));
#51621=CARTESIAN_POINT('Ctrl Pts',(65.201759677652,-1.93789121633581,13.));
#51622=CARTESIAN_POINT('Ctrl Pts',(65.2748769215823,-1.93744107368796,13.));
#51623=CARTESIAN_POINT('Ctrl Pts',(65.3480587639425,-1.93308814116639,13.));
#51624=CARTESIAN_POINT('Ctrl Pts',(65.4209476367097,-1.9248423197926,13.));
#51625=CARTESIAN_POINT('Ctrl Pts',(65.4389597307297,-1.92280463551765,13.));
#51626=CARTESIAN_POINT('Ctrl Pts',(65.456953949934,-1.92052897608509,13.));
#51627=CARTESIAN_POINT('Ctrl Pts',(65.4749248972257,-1.91801499804223,13.));
#51628=CARTESIAN_POINT('Ctrl Pts',(65.4889862933804,-1.91604793194321,13.));
#51629=CARTESIAN_POINT('Ctrl Pts',(65.5030350340934,-1.91393458313286,13.));
#51630=CARTESIAN_POINT('Ctrl Pts',(65.5170472633766,-1.91167847471352,13.));
#51631=CARTESIAN_POINT('Ctrl Pts',(65.5914320406422,-1.89970178500425,13.));
#51632=CARTESIAN_POINT('Ctrl Pts',(65.6649215575059,-1.88368854669915,13.));
#51633=CARTESIAN_POINT('Ctrl Pts',(65.7371322844938,-1.86371341403934,13.));
#51634=CARTESIAN_POINT('Ctrl Pts',(65.8094217307119,-1.84371650584657,13.));
#51635=CARTESIAN_POINT('Ctrl Pts',(65.8804307229118,-1.81974914158094,13.));
#51636=CARTESIAN_POINT('Ctrl Pts',(65.9497816755116,-1.7918347663575,13.));
#51637=CARTESIAN_POINT('Ctrl Pts',(66.0175539940295,-1.76455580539227,13.));
#51638=CARTESIAN_POINT('Ctrl Pts',(66.0837439310439,-1.73350736821287,13.));
#51639=CARTESIAN_POINT('Ctrl Pts',(66.1479900592074,-1.69866277513519,13.));
#51640=CARTESIAN_POINT('Ctrl Pts',(66.161806917563,-1.69116905028708,13.));
#51641=CARTESIAN_POINT('Ctrl Pts',(66.1755338057728,-1.68349956906395,13.));
#51642=CARTESIAN_POINT('Ctrl Pts',(66.1891670016328,-1.67565377050185,13.));
#51643=CARTESIAN_POINT('Ctrl Pts',(66.2007100870974,-1.66901081427423,13.));
#51644=CARTESIAN_POINT('Ctrl Pts',(66.2121860050345,-1.66224145688859,13.));
#51645=CARTESIAN_POINT('Ctrl Pts',(66.2235939546713,-1.65534738192938,13.));
#51646=CARTESIAN_POINT('Ctrl Pts',(66.8826275096638,-0.823232180103057,
13.));
#51647=CARTESIAN_POINT('Ctrl Pts',(66.9060091418344,-0.75234056523854,13.));
#51648=CARTESIAN_POINT('Ctrl Pts',(66.9251542481804,-0.680227462783449,
13.));
#51649=CARTESIAN_POINT('Ctrl Pts',(66.9401506980288,-0.607243329607971,
13.));
#51650=CARTESIAN_POINT('Ctrl Pts',(66.9547542267031,-0.536171449771447,
13.));
#51651=CARTESIAN_POINT('Ctrl Pts',(66.9654231894067,-0.464272677050615,
13.));
#51652=CARTESIAN_POINT('Ctrl Pts',(66.9721930205229,-0.391873748622197,
13.));
#51653=CARTESIAN_POINT('Ctrl Pts',(66.973704025792,-0.375714532763298,13.));
#51654=CARTESIAN_POINT('Ctrl Pts',(66.9750207650907,-0.359528284183379,
13.));
#51655=CARTESIAN_POINT('Ctrl Pts',(66.9761428768562,-0.343325629457175,
13.));
#51656=CARTESIAN_POINT('Ctrl Pts',(66.9812921188373,-0.268973508318639,
13.));
#51657=CARTESIAN_POINT('Ctrl Pts',(66.982338009526,-0.194422973994401,13.));
#51658=CARTESIAN_POINT('Ctrl Pts',(66.9793427332316,-0.120028700216811,
13.));
#51659=CARTESIAN_POINT('Ctrl Pts',(66.9772398551,-0.0677990973105729,13.));
#51660=CARTESIAN_POINT('Ctrl Pts',(66.9731439809986,-0.0156465385725868,
13.));
#51661=CARTESIAN_POINT('Ctrl Pts',(66.9670620462467,0.036301425843876,13.));
#51662=CARTESIAN_POINT('Ctrl Pts',(66.9647496285227,0.0560526067661498,
13.));
#51663=CARTESIAN_POINT('Ctrl Pts',(66.9621499863883,0.0757741531518394,
13.));
#51664=CARTESIAN_POINT('Ctrl Pts',(66.959263072388,0.0954588091203112,13.));
#51665=CARTESIAN_POINT('Ctrl Pts',(66.9565142386985,0.114201953351662,13.));
#51666=CARTESIAN_POINT('Ctrl Pts',(66.9535037847261,0.132917493687503,13.));
#51667=CARTESIAN_POINT('Ctrl Pts',(66.9502376703079,0.151566178089532,13.));
#51668=CARTESIAN_POINT('Ctrl Pts',(66.9377139254721,0.223073582629113,13.));
#51669=CARTESIAN_POINT('Ctrl Pts',(66.9214263256521,0.293675712348292,13.));
#51670=CARTESIAN_POINT('Ctrl Pts',(66.9014303057997,0.363043772415116,13.));
#51671=CARTESIAN_POINT('Ctrl Pts',(66.8818637674727,0.430921920965692,13.));
#51672=CARTESIAN_POINT('Ctrl Pts',(66.8587459438609,0.497619260733484,13.));
#51673=CARTESIAN_POINT('Ctrl Pts',(66.832085679365,0.562804370291326,13.));
#51674=CARTESIAN_POINT('Ctrl Pts',(66.806010072774,0.626559974542009,13.));
#51675=CARTESIAN_POINT('Ctrl Pts',(66.7765453046617,0.688869612373866,13.));
#51676=CARTESIAN_POINT('Ctrl Pts',(66.7436641146812,0.749389827201452,13.));
#51677=CARTESIAN_POINT('Ctrl Pts',(66.7329788263453,0.769056875321275,13.));
#51678=CARTESIAN_POINT('Ctrl Pts',(66.7219324918104,0.78853464586851,13.));
#51679=CARTESIAN_POINT('Ctrl Pts',(66.7105234437382,0.807810393806577,13.));
#51680=CARTESIAN_POINT('Ctrl Pts',(66.7040881271314,0.818682952150557,13.));
#51681=CARTESIAN_POINT('Ctrl Pts',(66.6975366290266,0.829492290259307,13.));
#51682=CARTESIAN_POINT('Ctrl Pts',(66.6908782714334,0.840221024252215,13.));
#51683=CARTESIAN_POINT('Ctrl Pts',(66.6548614911017,0.898255524510526,13.));
#51684=CARTESIAN_POINT('Ctrl Pts',(66.6156613534594,0.95403757007839,13.));
#51685=CARTESIAN_POINT('Ctrl Pts',(66.5732918040599,1.00726408484869,13.));
#51686=CARTESIAN_POINT('Ctrl Pts',(66.5671762929795,1.01494666220588,13.));
#51687=CARTESIAN_POINT('Ctrl Pts',(66.5609946872862,1.02257593937887,13.));
#51688=CARTESIAN_POINT('Ctrl Pts',(66.5547469639699,1.0301509410887,13.));
#51689=CARTESIAN_POINT('Ctrl Pts',(66.5106056086045,1.0836697711388,13.));
#51690=CARTESIAN_POINT('Ctrl Pts',(66.4631661110399,1.13448299232108,13.));
#51691=CARTESIAN_POINT('Ctrl Pts',(66.4127666235202,1.18244447913167,13.));
#51692=CARTESIAN_POINT('Ctrl Pts',(66.365747970858,1.22718867397352,13.));
#51693=CARTESIAN_POINT('Ctrl Pts',(66.3161520834383,1.26945072111514,13.));
#51694=CARTESIAN_POINT('Ctrl Pts',(66.2642393874426,1.30907445582191,13.));
#51695=CARTESIAN_POINT('Ctrl Pts',(66.252782589871,1.31781915880565,13.));
#51696=CARTESIAN_POINT('Ctrl Pts',(66.2412129249471,1.32643521269063,13.));
#51697=CARTESIAN_POINT('Ctrl Pts',(66.2295331629191,1.33492068208728,13.));
#51698=CARTESIAN_POINT('Ctrl Pts',(66.220402595367,1.34155413500801,13.));
#51699=CARTESIAN_POINT('Ctrl Pts',(66.2112052676163,1.34810730470407,13.));
#51700=CARTESIAN_POINT('Ctrl Pts',(66.2019533412583,1.3545719924638,13.));
#51701=CARTESIAN_POINT('Ctrl Pts',(66.1459049969294,1.39373519280896,13.));
#51702=CARTESIAN_POINT('Ctrl Pts',(66.0877532410082,1.42972959280653,13.));
#51703=CARTESIAN_POINT('Ctrl Pts',(66.0278290561594,1.46243222395895,13.));
#51704=CARTESIAN_POINT('Ctrl Pts',(65.9681817043714,1.49498377805451,13.));
#51705=CARTESIAN_POINT('Ctrl Pts',(65.9067771564088,1.52427416708808,13.));
#51706=CARTESIAN_POINT('Ctrl Pts',(65.8439279085686,1.55013292120153,13.));
#51707=CARTESIAN_POINT('Ctrl Pts',(65.782425269513,1.57543762532004,13.));
#51708=CARTESIAN_POINT('Ctrl Pts',(65.71953820698,1.59745625939185,13.));
#51709=CARTESIAN_POINT('Ctrl Pts',(65.6555614668715,1.61597952404088,13.));
#51710=CARTESIAN_POINT('Ctrl Pts',(65.6420830163666,1.61988195647707,13.));
#51711=CARTESIAN_POINT('Ctrl Pts',(65.6285562363675,1.6236290658509,13.));
#51712=CARTESIAN_POINT('Ctrl Pts',(65.6149839550191,1.62721860069977,13.));
#51713=CARTESIAN_POINT('Ctrl Pts',(65.6021159145385,1.63062188114732,13.));
#51714=CARTESIAN_POINT('Ctrl Pts',(65.5892052052993,1.63388381687885,13.));
#51715=CARTESIAN_POINT('Ctrl Pts',(65.5762752295761,1.63699772300991,13.));
#51716=CARTESIAN_POINT('Ctrl Pts',(65.5127465219567,1.65229724378163,13.));
#51717=CARTESIAN_POINT('Ctrl Pts',(65.4486405341705,1.66405837364474,13.));
#51718=CARTESIAN_POINT('Ctrl Pts',(65.3842420392997,1.67213585465472,13.));
#51719=CARTESIAN_POINT('Ctrl Pts',(65.3210685723957,1.68005968082915,13.));
#51720=CARTESIAN_POINT('Ctrl Pts',(65.2576127399634,1.68443871292823,13.));
#51721=CARTESIAN_POINT('Ctrl Pts',(65.1941497362031,1.68508652435148,13.));
#51722=CARTESIAN_POINT('Ctrl Pts',(65.1327484538298,1.68571329033744,13.));
#51723=CARTESIAN_POINT('Ctrl Pts',(65.0713397979654,1.68284723930067,13.));
#51724=CARTESIAN_POINT('Ctrl Pts',(65.0101900871468,1.6762734709127,13.));
#51725=CARTESIAN_POINT('Ctrl Pts',(65.0000071662403,1.67517877786091,13.));
#51726=CARTESIAN_POINT('Ctrl Pts',(64.9898314781273,1.67398116343416,13.));
#51727=CARTESIAN_POINT('Ctrl Pts',(64.9796643197989,1.67267950846503,13.));
#51728=CARTESIAN_POINT('Ctrl Pts',(64.9689074729785,1.6713023583643,13.));
#51729=CARTESIAN_POINT('Ctrl Pts',(64.9581601737451,1.66980874798799,13.));
#51730=CARTESIAN_POINT('Ctrl Pts',(64.9474239513002,1.66819938802347,13.));
#51731=CARTESIAN_POINT('Origin',(65.,0.,23.5459252805377));
#51732=CARTESIAN_POINT('Ctrl Pts',(62.9434348764936,0.00149614206266632,
21.7959252805377));
#51733=CARTESIAN_POINT('Ctrl Pts',(62.9426160796481,0.0997858054225766,
21.7905813053169));
#51734=CARTESIAN_POINT('Ctrl Pts',(62.9937092272654,0.87861806824978,21.7481913665734));
#51735=CARTESIAN_POINT('Ctrl Pts',(63.9890540527047,2.20843040890228,21.6687554643073));
#51736=CARTESIAN_POINT('Ctrl Pts',(66.3069967286646,2.04687460564975,21.5576175737392));
#51737=CARTESIAN_POINT('Ctrl Pts',(67.428612079538,0.0121339679509602,21.4464796831712));
#51738=CARTESIAN_POINT('Ctrl Pts',(66.3273005244664,-2.03388573489,21.3353417926031));
#51739=CARTESIAN_POINT('Ctrl Pts',(64.0110910734901,-2.21817972145311,21.2242039020351));
#51740=CARTESIAN_POINT('Ctrl Pts',(62.9978510382059,-0.892619747709225,
21.1443983980133));
#51741=CARTESIAN_POINT('Ctrl Pts',(62.942718846502,-0.10674080247177,21.1016388575141));
#51742=CARTESIAN_POINT('Ctrl Pts',(62.9436210622307,-0.00160392935065416,
21.0959252805377));
#51743=CARTESIAN_POINT('Ctrl Pts',(62.9473239618077,-0.00235074752840471,
21.8540747194623));
#51744=CARTESIAN_POINT('Ctrl Pts',(62.9508762982104,0.467866578479434,21.8286245525962));
#51745=CARTESIAN_POINT('Ctrl Pts',(63.3434621334709,1.62957520615004,21.7661284222074));
#51746=CARTESIAN_POINT('Ctrl Pts',(65.2721300366129,2.41280623887489,21.6665863282959));
#51747=CARTESIAN_POINT('Ctrl Pts',(67.1747422685441,1.08094901338605,21.5554484377278));
#51748=CARTESIAN_POINT('Ctrl Pts',(67.0876157148515,-1.24138505016237,21.4443105471598));
#51749=CARTESIAN_POINT('Ctrl Pts',(65.0892538486775,-2.42692553227054,21.3331726565917));
#51750=CARTESIAN_POINT('Ctrl Pts',(63.2787520820962,-1.52545559952441,21.2364273806926));
#51751=CARTESIAN_POINT('Ctrl Pts',(62.9500869585733,-0.417919283968019,
21.1767280683161));
#51752=CARTESIAN_POINT('Ctrl Pts',(62.9479182248742,0.00116161895481415,
21.1540747194623));
#51753=CARTESIAN_POINT('Ctrl Pts',(66.2690708798524,1.07935865304855,22.));
#51754=CARTESIAN_POINT('Ctrl Pts',(66.6279833110066,0.657362393039556,21.9629540364773));
#51755=CARTESIAN_POINT('Ctrl Pts',(66.8852826717605,-0.565789777391214,
21.8888621094319));
#51756=CARTESIAN_POINT('Ctrl Pts',(65.5450879211412,-1.89344353213327,21.7777242188639));
#51757=CARTESIAN_POINT('Ctrl Pts',(63.7057951684468,-1.4835378033008,21.6665863282959));
#51758=CARTESIAN_POINT('Ctrl Pts',(63.0512142972679,0.282082603662779,21.5554484377278));
#51759=CARTESIAN_POINT('Ctrl Pts',(64.180320745495,1.79060472623492,21.4443105471598));
#51760=CARTESIAN_POINT('Ctrl Pts',(66.0597184815454,1.65961459691567,21.3331726565917));
#51761=CARTESIAN_POINT('Ctrl Pts',(66.9691289570557,0.009838272590972,21.2220347660237));
#51762=CARTESIAN_POINT('Ctrl Pts',(66.0761808851496,-1.6490831655076,21.1108968754557));
#51763=CARTESIAN_POINT('Ctrl Pts',(64.1981884552545,-1.79850951013062,20.9997589848876));
#51764=CARTESIAN_POINT('Ctrl Pts',(63.0541051349916,-0.301775268334271,
20.8886210943196));
#51765=CARTESIAN_POINT('Ctrl Pts',(63.6911204902705,1.47119522218438,20.7774832037516));
#51766=CARTESIAN_POINT('Ctrl Pts',(65.5261685894954,1.89755500871053,20.6663453131835));
#51767=CARTESIAN_POINT('Ctrl Pts',(66.8796083671824,0.587065728133533,20.5552074226155));
#51768=CARTESIAN_POINT('Ctrl Pts',(66.5126214133544,-1.26077376527147,20.4440695320474));
#51769=CARTESIAN_POINT('Ctrl Pts',(64.7611148635138,-1.95461157704262,20.3329316414794));
#51770=CARTESIAN_POINT('Ctrl Pts',(63.2282626195245,-0.859371828191345,
20.2217937509113));
#51771=CARTESIAN_POINT('Ctrl Pts',(63.3171016769871,1.02246099457515,20.1106558603433));
#51772=CARTESIAN_POINT('Ctrl Pts',(64.9463166628138,1.96842352553115,19.9995179697752));
#51773=CARTESIAN_POINT('Ctrl Pts',(66.6246686119733,1.11266575470347,19.8883800792072));
#51774=CARTESIAN_POINT('Ctrl Pts',(66.8159429576165,-0.761527637475687,
19.7772421886392));
#51775=CARTESIAN_POINT('Ctrl Pts',(65.3450641189423,-1.93868612782189,19.6661042980711));
#51776=CARTESIAN_POINT('Ctrl Pts',(63.5583441794198,-1.34134322872204,19.5549664075031));
#51777=CARTESIAN_POINT('Ctrl Pts',(63.0911881617047,0.483746344304433,19.443828516935));
#51778=CARTESIAN_POINT('Ctrl Pts',(64.3711892671104,1.86605739990808,19.332690626367));
#51779=CARTESIAN_POINT('Ctrl Pts',(66.2267479674628,1.54034495606735,19.221552735799));
#51780=CARTESIAN_POINT('Ctrl Pts',(66.9594503409616,-0.19526269537746,19.1104148452309));
#51781=CARTESIAN_POINT('Ctrl Pts',(65.8986455956832,-1.7521441870034,18.9992769546629));
#51782=CARTESIAN_POINT('Ctrl Pts',(64.0153003453502,-1.70526823375495,18.8881390640948));
#51783=CARTESIAN_POINT('Ctrl Pts',(63.0332618561676,-0.0975409270146879,
18.7770011735268));
#51784=CARTESIAN_POINT('Ctrl Pts',(63.8514010943644,1.59946669637175,18.6658632829587));
#51785=CARTESIAN_POINT('Ctrl Pts',(65.720865936886,1.83246431340309,18.5547253923907));
#51786=CARTESIAN_POINT('Ctrl Pts',(66.9305140122006,0.388186562807746,18.4435875018227));
#51787=CARTESIAN_POINT('Ctrl Pts',(66.3731407186298,-1.41140275105548,18.3324496112546));
#51788=CARTESIAN_POINT('Ctrl Pts',(64.5589161528223,-1.91911912048434,18.2213117206866));
#51789=CARTESIAN_POINT('Ctrl Pts',(63.1484206345677,-0.670243994641488,
18.1101738301185));
#51790=CARTESIAN_POINT('Ctrl Pts',(63.4326967078313,1.19211306057994,17.9990359395505));
#51791=CARTESIAN_POINT('Ctrl Pts',(65.1515432588453,1.96331551197126,17.8878980489824));
#51792=CARTESIAN_POINT('Ctrl Pts',(66.7316805464207,0.937473009742852,17.7767601584144));
#51793=CARTESIAN_POINT('Ctrl Pts',(66.7267909912641,-0.946449169970139,
17.6656222678463));
#51794=CARTESIAN_POINT('Ctrl Pts',(65.1413500586618,-1.96407569094589,17.5544843772784));
#51795=CARTESIAN_POINT('Ctrl Pts',(63.4265298143476,-1.18396145786556,17.4433464867103));
#51796=CARTESIAN_POINT('Ctrl Pts',(63.1519246753265,0.679846124635256,17.3322085961423));
#51797=CARTESIAN_POINT('Ctrl Pts',(64.5688838395789,1.921382839278,17.2210707055742));
#51798=CARTESIAN_POINT('Ctrl Pts',(66.3804485146544,1.40425605116615,17.1099328150062));
#51799=CARTESIAN_POINT('Ctrl Pts',(66.9284730089157,-0.398202225924797,
16.9987949244381));
#51800=CARTESIAN_POINT('Ctrl Pts',(65.7113442877452,-1.83618148970648,16.8876570338701));
#51801=CARTESIAN_POINT('Ctrl Pts',(63.8431140728085,-1.59348301224526,16.776519143302));
#51802=CARTESIAN_POINT('Ctrl Pts',(63.033794667009,0.107748537650188,16.665381252734));
#51803=CARTESIAN_POINT('Ctrl Pts',(64.024165300781,1.71035662908353,16.5542433621659));
#51804=CARTESIAN_POINT('Ctrl Pts',(65.9077285014668,1.74745590115203,16.4431054715979));
#51805=CARTESIAN_POINT('Ctrl Pts',(66.9604375104179,0.18508896940079,16.3319675810299));
#51806=CARTESIAN_POINT('Ctrl Pts',(66.2187358332113,-1.54669199509962,16.2208296904618));
#51807=CARTESIAN_POINT('Ctrl Pts',(64.3615114264595,-1.8627682357953,16.1096917998938));
#51808=CARTESIAN_POINT('Ctrl Pts',(63.0887028520271,-0.473831585058415,
15.9985539093257));
#51809=CARTESIAN_POINT('Ctrl Pts',(63.5653262327086,1.34880848913673,15.8874160187577));
#51810=CARTESIAN_POINT('Ctrl Pts',(65.3551227829179,1.9368688566197,15.7762781281897));
#51811=CARTESIAN_POINT('Ctrl Pts',(66.819871422519,0.752091194204021,15.6651402376216));
#51812=CARTESIAN_POINT('Ctrl Pts',(66.6188711104164,-1.12108406786278,15.5540023470536));
#51813=CARTESIAN_POINT('Ctrl Pts',(64.9360997115566,-1.96811836805763,15.4428644564855));
#51814=CARTESIAN_POINT('Ctrl Pts',(63.3118169716773,-1.01371160717774,15.3317265659175));
#51815=CARTESIAN_POINT('Ctrl Pts',(63.2327473023447,0.868556886382306,15.2205886753495));
#51816=CARTESIAN_POINT('Ctrl Pts',(64.771264070325,1.955825407051,15.1094507847814));
#51817=CARTESIAN_POINT('Ctrl Pts',(66.5191454265163,1.25290476136479,14.9983128942134));
#51818=CARTESIAN_POINT('Ctrl Pts',(66.8765357500253,-0.59681383973413,14.8871750036453));
#51819=CARTESIAN_POINT('Ctrl Pts',(65.516311611266,-1.90026192842665,14.7760371130773));
#51820=CARTESIAN_POINT('Ctrl Pts',(63.6835016170176,-1.46437879615621,14.6648992225092));
#51821=CARTESIAN_POINT('Ctrl Pts',(63.0556974877489,0.311866999404039,14.5537613319412));
#51822=CARTESIAN_POINT('Ctrl Pts',(64.2075355674246,1.80265710789545,14.4426234413732));
#51823=CARTESIAN_POINT('Ctrl Pts',(66.0847251913073,1.64345528891984,14.3314855508051));
#51824=CARTESIAN_POINT('Ctrl Pts',(66.969053819969,-0.0200209189642787,
14.2203476602371));
#51825=CARTESIAN_POINT('Ctrl Pts',(66.0510846129266,-1.66516952053625,14.109209769669));
#51826=CARTESIAN_POINT('Ctrl Pts',(64.1710468184079,-1.78617400482042,13.998071879101));
#51827=CARTESIAN_POINT('Ctrl Pts',(63.049757131241,-0.272264377212424,13.8869339885329));
#51828=CARTESIAN_POINT('Ctrl Pts',(63.7135511069036,1.49083448335769,13.7757960979649));
#51829=CARTESIAN_POINT('Ctrl Pts',(65.5548379149366,1.88939023827019,13.6646582073969));
#51830=CARTESIAN_POINT('Ctrl Pts',(66.8882920122399,0.558497016674507,13.5535203168288));
#51831=CARTESIAN_POINT('Ctrl Pts',(66.4933378285089,-1.28345860874756,13.4423824262608));
#51832=CARTESIAN_POINT('Ctrl Pts',(64.7315804519141,-1.95092037563962,13.3312445356927));
#51833=CARTESIAN_POINT('Ctrl Pts',(63.2153798048402,-0.832146062593809,
13.2201066451247));
#51834=CARTESIAN_POINT('Ctrl Pts',(63.3329222496525,1.04723556764185,13.1089687545567));
#51835=CARTESIAN_POINT('Ctrl Pts',(64.9758366741791,1.97019425053385,12.9978308639886));
#51836=CARTESIAN_POINT('Ctrl Pts',(66.6419915114447,1.08548270413877,12.8866929734206));
#51837=CARTESIAN_POINT('Ctrl Pts',(66.7483953817108,-0.159901738299113,
12.8126010463752));
#51838=CARTESIAN_POINT('Ctrl Pts',(66.526442356053,-0.667480137268131,12.7755550828525));
#51839=CARTESIAN_POINT('Ctrl Pts',(66.3677806246588,1.16331236980977,22.0748149723825));
#51840=CARTESIAN_POINT('Ctrl Pts',(66.7546096639785,0.708492771249666,22.0377690088598));
#51841=CARTESIAN_POINT('Ctrl Pts',(67.0319220552433,-0.6097975356867,21.9636770818144));
#51842=CARTESIAN_POINT('Ctrl Pts',(65.5874854660279,-2.04071767641435,21.8525391912464));
#51843=CARTESIAN_POINT('Ctrl Pts',(63.605130476917,-1.59892902399571,21.7414013006783));
#51844=CARTESIAN_POINT('Ctrl Pts',(62.8996355773925,0.304023302377046,21.6302634101103));
#51845=CARTESIAN_POINT('Ctrl Pts',(64.1165651812316,1.92987995379071,21.5191255195423));
#51846=CARTESIAN_POINT('Ctrl Pts',(66.1421445639184,1.7887012664937,21.4079876289742));
#51847=CARTESIAN_POINT('Ctrl Pts',(67.1222899978831,0.0106035043776343,
21.2968497384062));
#51848=CARTESIAN_POINT('Ctrl Pts',(66.1598874315886,-1.77735068863506,21.1857118478382));
#51849=CARTESIAN_POINT('Ctrl Pts',(64.135822661333,-1.93839958057145,21.0745739572701));
#51850=CARTESIAN_POINT('Ctrl Pts',(62.9027512676903,-0.325247684413694,
20.9634360667021));
#51851=CARTESIAN_POINT('Ctrl Pts',(63.5893143859473,1.58562642318962,20.852298176134));
#51852=CARTESIAN_POINT('Ctrl Pts',(65.56709456772,2.04514894821357,20.741160285566));
#51853=CARTESIAN_POINT('Ctrl Pts',(67.0258063969427,0.632728353546081,20.630022394998));
#51854=CARTESIAN_POINT('Ctrl Pts',(66.6302747895932,-1.35883815127573,20.5188845044299));
#51855=CARTESIAN_POINT('Ctrl Pts',(64.7425341118513,-2.10664343990283,20.4077466138619));
#51856=CARTESIAN_POINT('Ctrl Pts',(63.0904549151108,-0.926214724991942,
20.2966087232938));
#51857=CARTESIAN_POINT('Ctrl Pts',(63.1862039732913,1.1019891481648,20.1854708327258));
#51858=CARTESIAN_POINT('Ctrl Pts',(64.9421411131277,2.12152969710983,20.0743329421577));
#51859=CARTESIAN_POINT('Ctrl Pts',(66.7510371439672,1.19921013488374,19.9631950515897));
#51860=CARTESIAN_POINT('Ctrl Pts',(66.9571890209963,-0.820760104276143,
19.8520571610216));
#51861=CARTESIAN_POINT('Ctrl Pts',(65.3719035899786,-2.08947929152552,19.7409192704536));
#51862=CARTESIAN_POINT('Ctrl Pts',(63.4462105859322,-1.44567439722258,19.6297813798856));
#51863=CARTESIAN_POINT('Ctrl Pts',(62.942718653474,0.521372673105626,19.5186434893175));
#51864=CARTESIAN_POINT('Ctrl Pts',(64.3222796687888,2.01120142035911,19.4075055987495));
#51865=CARTESIAN_POINT('Ctrl Pts',(66.3221657890618,1.66015470029928,19.2963677081814));
#51866=CARTESIAN_POINT('Ctrl Pts',(67.1118585682622,-0.210450445042923,
19.1852298176134));
#51867=CARTESIAN_POINT('Ctrl Pts',(65.9685432498092,-1.88842791103253,19.0740919270454));
#51868=CARTESIAN_POINT('Ctrl Pts',(63.9387093107874,-1.83790589399349,18.9629540364773));
#51869=CARTESIAN_POINT('Ctrl Pts',(62.8802867754523,-0.105127768826806,
18.8518161459093));
#51870=CARTESIAN_POINT('Ctrl Pts',(63.762061793731,1.72387499533424,18.7406782553413));
#51871=CARTESIAN_POINT('Ctrl Pts',(65.7769356913807,1.9749954262153,18.6295403647732));
#51872=CARTESIAN_POINT('Ctrl Pts',(67.0806715396602,0.418380145499126,18.5184024742052));
#51873=CARTESIAN_POINT('Ctrl Pts',(66.4799451312683,-1.52118322714048,18.4072645836371));
#51874=CARTESIAN_POINT('Ctrl Pts',(64.5246081605074,-2.06839034059004,18.296126693069));
#51875=CARTESIAN_POINT('Ctrl Pts',(63.0044027317441,-0.722376318154269,
18.184988802501));
#51876=CARTESIAN_POINT('Ctrl Pts',(63.3107901142278,1.28483694059204,18.073850911933));
#51877=CARTESIAN_POINT('Ctrl Pts',(65.1633304621018,2.11602437657287,17.962713021365));
#51878=CARTESIAN_POINT('Ctrl Pts',(66.8663725857206,1.01039070332779,17.8515751307969));
#51879=CARTESIAN_POINT('Ctrl Pts',(66.8611027155246,-1.02006503928304,17.7404372402289));
#51880=CARTESIAN_POINT('Ctrl Pts',(65.1523444234686,-2.1168436831138,17.6292993496608));
#51881=CARTESIAN_POINT('Ctrl Pts',(63.3041435529085,-1.27605129715033,17.5181614590928));
#51882=CARTESIAN_POINT('Ctrl Pts',(63.0081793206914,0.732725312500794,17.4070235685247));
#51883=CARTESIAN_POINT('Ctrl Pts',(64.5353511450282,2.07083013394974,17.2958856779567));
#51884=CARTESIAN_POINT('Ctrl Pts',(66.4878213357972,1.51348064898345,17.1847477873886));
#51885=CARTESIAN_POINT('Ctrl Pts',(67.0784717848694,-0.429174838035294,
17.0736098968206));
#51886=CARTESIAN_POINT('Ctrl Pts',(65.7666734377774,-1.97900172862672,16.9624720062526));
#51887=CARTESIAN_POINT('Ctrl Pts',(63.7531301984196,-1.71742589359987,16.8513341156845));
#51888=CARTESIAN_POINT('Ctrl Pts',(62.8808610289137,0.11612933877294,16.7401962251165));
#51889=CARTESIAN_POINT('Ctrl Pts',(63.9482637923134,1.84339007037129,16.6290583345485));
#51890=CARTESIAN_POINT('Ctrl Pts',(65.9783326341088,1.88337496509218,16.5179204439804));
#51891=CARTESIAN_POINT('Ctrl Pts',(67.1129225208572,0.199485395342077,16.4067825534124));
#51892=CARTESIAN_POINT('Ctrl Pts',(66.3135304620949,-1.66699541908821,16.2956446628443));
#51893=CARTESIAN_POINT('Ctrl Pts',(64.3118490749262,-2.00765642140262,16.1845067722763));
#51894=CARTESIAN_POINT('Ctrl Pts',(62.9400400336448,-0.510686732855825,
16.0733688817082));
#51895=CARTESIAN_POINT('Ctrl Pts',(63.4537357110932,1.45372031389702,15.9622309911402));
#51896=CARTESIAN_POINT('Ctrl Pts',(65.3827446280278,2.08752067094762,15.8510931005722));
#51897=CARTESIAN_POINT('Ctrl Pts',(66.9614230462693,0.81058968394928,15.7399552100041));
#51898=CARTESIAN_POINT('Ctrl Pts',(66.7447887062896,-1.20828323380548,15.6288173194361));
#51899=CARTESIAN_POINT('Ctrl Pts',(64.931129476036,-2.12120080414854,15.517679428868));
#51900=CARTESIAN_POINT('Ctrl Pts',(63.1805082177236,-1.09255922368241,15.4065415383));
#51901=CARTESIAN_POINT('Ctrl Pts',(63.0952884215498,0.936114207226868,15.2954036477319));
#51902=CARTESIAN_POINT('Ctrl Pts',(64.7534727352587,2.10795168295958,15.1842657571639));
#51903=CARTESIAN_POINT('Ctrl Pts',(66.6373062477565,1.35035708749135,15.0731278665959));
#51904=CARTESIAN_POINT('Ctrl Pts',(67.022494788205,-0.643234684111208,14.9619899760278));
#51905=CARTESIAN_POINT('Ctrl Pts',(65.5564709027586,-2.04806641515651,14.8508520854598));
#51906=CARTESIAN_POINT('Ctrl Pts',(63.5811029082571,-1.57827980796208,14.7397141948917));
#51907=CARTESIAN_POINT('Ctrl Pts',(62.9044674754165,0.336124361552561,14.6285763043237));
#51908=CARTESIAN_POINT('Ctrl Pts',(64.1458968022858,1.9428697831044,14.5174384137556));
#51909=CARTESIAN_POINT('Ctrl Pts',(66.1690963233843,1.77128506954561,14.4063005231876));
#51910=CARTESIAN_POINT('Ctrl Pts',(67.1222090165502,-0.0215781683134909,
14.2951626326196));
#51911=CARTESIAN_POINT('Ctrl Pts',(66.1328391433939,-1.79468825825303,14.1840247420515));
#51912=CARTESIAN_POINT('Ctrl Pts',(64.1065699177788,-1.92510460593565,14.0728868514835));
#51913=CARTESIAN_POINT('Ctrl Pts',(62.8980650713711,-0.293441403351145,
13.9617489609155));
#51914=CARTESIAN_POINT('Ctrl Pts',(63.613489680895,1.60679324794459,13.8506110703474));
#51915=CARTESIAN_POINT('Ctrl Pts',(65.5979938251871,2.03634911284552,13.7394731797794));
#51916=CARTESIAN_POINT('Ctrl Pts',(67.0351654655728,0.601937535928652,13.6283352892113));
#51917=CARTESIAN_POINT('Ctrl Pts',(66.6094913060666,-1.38328744711302,13.5171973986433));
#51918=CARTESIAN_POINT('Ctrl Pts',(64.7107024808619,-2.10266513274845,13.4060595080752));
#51919=CARTESIAN_POINT('Ctrl Pts',(63.0765700607689,-0.896871309059063,
13.2949216175072));
#51920=CARTESIAN_POINT('Ctrl Pts',(63.2032550876981,1.12869071508499,13.1837837269391));
#51921=CARTESIAN_POINT('Ctrl Pts',(64.9739572238164,2.12343815107307,13.0726458363711));
#51922=CARTESIAN_POINT('Ctrl Pts',(66.7697074378301,1.16991275640646,12.9615079458031));
#51923=CARTESIAN_POINT('Ctrl Pts',(66.8843875194939,-0.172339073385905,
12.8874160187577));
#51924=CARTESIAN_POINT('Ctrl Pts',(66.6451707405899,-0.719397484879773,
12.850370055235));
#51925=CARTESIAN_POINT('Ctrl Pts',(66.4664903694652,1.247266086571,22.149629944765));
#51926=CARTESIAN_POINT('Ctrl Pts',(66.8812360169505,0.759623149459774,22.1125839812423));
#51927=CARTESIAN_POINT('Ctrl Pts',(67.1785614387261,-0.653805293982184,
22.0384920541969));
#51928=CARTESIAN_POINT('Ctrl Pts',(65.6298830109146,-2.18799182069543,21.9273541636289));
#51929=CARTESIAN_POINT('Ctrl Pts',(63.5044657853871,-1.71432024469062,21.8162162730608));
#51930=CARTESIAN_POINT('Ctrl Pts',(62.7480568575172,0.325964001091311,21.7050783824928));
#51931=CARTESIAN_POINT('Ctrl Pts',(64.0528096169681,2.06915518134649,21.5939404919247));
#51932=CARTESIAN_POINT('Ctrl Pts',(66.2245706462915,1.91778793607172,21.4828026013567));
#51933=CARTESIAN_POINT('Ctrl Pts',(67.2754510387106,0.0113687361642993,
21.3716647107886));
#51934=CARTESIAN_POINT('Ctrl Pts',(66.2435939780275,-1.90561821176253,21.2605268202207));
#51935=CARTESIAN_POINT('Ctrl Pts',(64.0734568674116,-2.07828965101228,21.1493889296526));
#51936=CARTESIAN_POINT('Ctrl Pts',(62.751397400389,-0.348720100493116,21.0382510390846));
#51937=CARTESIAN_POINT('Ctrl Pts',(63.4875082816241,1.70005762419486,20.9271131485165));
#51938=CARTESIAN_POINT('Ctrl Pts',(65.6080205459445,2.19274288771662,20.8159752579485));
#51939=CARTESIAN_POINT('Ctrl Pts',(67.172004426703,0.678390978958629,20.7048373673804));
#51940=CARTESIAN_POINT('Ctrl Pts',(66.7479281658321,-1.45690253727999,20.5936994768124));
#51941=CARTESIAN_POINT('Ctrl Pts',(64.7239533601888,-2.25867530276304,20.4825615862443));
#51942=CARTESIAN_POINT('Ctrl Pts',(62.9526472106971,-0.993057621792541,
20.3714236956763));
#51943=CARTESIAN_POINT('Ctrl Pts',(63.0553062695956,1.18151730175446,20.2602858051083));
#51944=CARTESIAN_POINT('Ctrl Pts',(64.9379655634416,2.2746358686885,20.1491479145402));
#51945=CARTESIAN_POINT('Ctrl Pts',(66.8774056759608,1.285754515064,20.0380100239722));
#51946=CARTESIAN_POINT('Ctrl Pts',(67.0984350843764,-0.879992571076597,
19.9268721334041));
#51947=CARTESIAN_POINT('Ctrl Pts',(65.3987430610147,-2.24027245522916,19.8157342428361));
#51948=CARTESIAN_POINT('Ctrl Pts',(63.3340769924447,-1.55000556572312,19.7045963522681));
#51949=CARTESIAN_POINT('Ctrl Pts',(62.7942491452433,0.558999001906815,19.5934584617));
#51950=CARTESIAN_POINT('Ctrl Pts',(64.2733700704672,2.15634544081014,19.482320571132));
#51951=CARTESIAN_POINT('Ctrl Pts',(66.4175836106607,1.77996444453121,19.3711826805639));
#51952=CARTESIAN_POINT('Ctrl Pts',(67.2642667955629,-0.225638194708385,
19.2600447899959));
#51953=CARTESIAN_POINT('Ctrl Pts',(66.0384409039352,-2.02471163506166,19.1489068994278));
#51954=CARTESIAN_POINT('Ctrl Pts',(63.8621182762245,-1.97054355423203,19.0377690088598));
#51955=CARTESIAN_POINT('Ctrl Pts',(62.727311694737,-0.112714610638923,18.9266311182918));
#51956=CARTESIAN_POINT('Ctrl Pts',(63.6727224930976,1.84828329429673,18.8154932277237));
#51957=CARTESIAN_POINT('Ctrl Pts',(65.8330054458753,2.11752653902752,18.7043553371557));
#51958=CARTESIAN_POINT('Ctrl Pts',(67.2308290671198,0.448573728190504,18.5932174465877));
#51959=CARTESIAN_POINT('Ctrl Pts',(66.5867495439068,-1.63096370322548,18.4820795560196));
#51960=CARTESIAN_POINT('Ctrl Pts',(64.4903001681923,-2.21766156069574,18.3709416654516));
#51961=CARTESIAN_POINT('Ctrl Pts',(62.8603848289206,-0.774508641667049,
18.2598037748835));
#51962=CARTESIAN_POINT('Ctrl Pts',(63.1888835206242,1.37756082060413,18.1486658843155));
#51963=CARTESIAN_POINT('Ctrl Pts',(65.1751176653583,2.26873324117447,18.0375279937474));
#51964=CARTESIAN_POINT('Ctrl Pts',(67.0010646250206,1.08330839691273,17.9263901031794));
#51965=CARTESIAN_POINT('Ctrl Pts',(66.9954144397851,-1.09368090859595,17.8152522126113));
#51966=CARTESIAN_POINT('Ctrl Pts',(65.1633387882755,-2.26961167528171,17.7041143220433));
#51967=CARTESIAN_POINT('Ctrl Pts',(63.1817572914694,-1.36814113643509,17.5929764314753));
#51968=CARTESIAN_POINT('Ctrl Pts',(62.8644339660562,0.785604500366333,17.4818385409072));
#51969=CARTESIAN_POINT('Ctrl Pts',(64.5018184504777,2.22027742862147,17.3707006503392));
#51970=CARTESIAN_POINT('Ctrl Pts',(66.5951941569401,1.62270524680075,17.2595627597711));
#51971=CARTESIAN_POINT('Ctrl Pts',(67.2284705608229,-0.460147450145792,
17.1484248692031));
#51972=CARTESIAN_POINT('Ctrl Pts',(65.8220025878096,-2.12182196754697,17.0372869786351));
#51973=CARTESIAN_POINT('Ctrl Pts',(63.6631463240307,-1.84136877495448,16.926149088067));
#51974=CARTESIAN_POINT('Ctrl Pts',(62.7279273908184,0.124510139895692,16.815011197499));
#51975=CARTESIAN_POINT('Ctrl Pts',(63.8723622838458,1.97642351165905,16.7038733069309));
#51976=CARTESIAN_POINT('Ctrl Pts',(66.0489367667509,2.01929402903232,16.5927354163629));
#51977=CARTESIAN_POINT('Ctrl Pts',(67.2654075312964,0.213881821283365,16.4815975257949));
#51978=CARTESIAN_POINT('Ctrl Pts',(66.4083250909786,-1.7872988430768,16.3704596352268));
#51979=CARTESIAN_POINT('Ctrl Pts',(64.2621867233928,-2.15254460700995,16.2593217446588));
#51980=CARTESIAN_POINT('Ctrl Pts',(62.7913772152625,-0.547541880653236,
16.1481838540907));
#51981=CARTESIAN_POINT('Ctrl Pts',(63.3421451894777,1.5586321386573,16.0370459635227));
#51982=CARTESIAN_POINT('Ctrl Pts',(65.4103664731376,2.23817248527553,15.9259080729546));
#51983=CARTESIAN_POINT('Ctrl Pts',(67.1029746700197,0.869088173694541,15.8147701823866));
#51984=CARTESIAN_POINT('Ctrl Pts',(66.8707063021627,-1.29548239974819,15.7036322918186));
#51985=CARTESIAN_POINT('Ctrl Pts',(64.9261592405154,-2.27428324023946,15.5924944012505));
#51986=CARTESIAN_POINT('Ctrl Pts',(63.0491994637699,-1.17140684018708,15.4813565106825));
#51987=CARTESIAN_POINT('Ctrl Pts',(62.9578295407548,1.00367152807143,15.3702186201144));
#51988=CARTESIAN_POINT('Ctrl Pts',(64.7356814001924,2.26007795886816,15.2590807295464));
#51989=CARTESIAN_POINT('Ctrl Pts',(66.7554670689966,1.44780941361792,15.1479428389783));
#51990=CARTESIAN_POINT('Ctrl Pts',(67.1684538263848,-0.689655528488287,
15.0368049484103));
#51991=CARTESIAN_POINT('Ctrl Pts',(65.5966301942511,-2.19587090188638,14.9256670578423));
#51992=CARTESIAN_POINT('Ctrl Pts',(63.4787041994968,-1.69218081976795,14.8145291672742));
#51993=CARTESIAN_POINT('Ctrl Pts',(62.753237463084,0.360381723701083,14.7033912767062));
#51994=CARTESIAN_POINT('Ctrl Pts',(64.084258037147,2.08308245831336,14.5922533861381));
#51995=CARTESIAN_POINT('Ctrl Pts',(66.2534674554613,1.89911485017137,14.4811154955701));
#51996=CARTESIAN_POINT('Ctrl Pts',(67.2753642131315,-0.0231354176627016,
14.3699776050021));
#51997=CARTESIAN_POINT('Ctrl Pts',(66.214593673861,-1.92420699596982,14.258839714434));
#51998=CARTESIAN_POINT('Ctrl Pts',(64.0420930171499,-2.06403520705088,14.147701823866));
#51999=CARTESIAN_POINT('Ctrl Pts',(62.746373011501,-0.314618429489868,14.0365639332979));
#52000=CARTESIAN_POINT('Ctrl Pts',(63.5134282548864,1.72275201253148,13.9254260427299));
#52001=CARTESIAN_POINT('Ctrl Pts',(65.6411497354375,2.18330798742086,13.8142881521618));
#52002=CARTESIAN_POINT('Ctrl Pts',(67.1820389189058,0.645378055182796,13.7031502615938));
#52003=CARTESIAN_POINT('Ctrl Pts',(66.7256447836243,-1.48311628547849,13.5920123710258));
#52004=CARTESIAN_POINT('Ctrl Pts',(64.6898245098097,-2.25440988985727,13.4808744804577));
#52005=CARTESIAN_POINT('Ctrl Pts',(62.9377603166977,-0.961596555524317,
13.3697365898897));
#52006=CARTESIAN_POINT('Ctrl Pts',(63.0735879257438,1.21014586252812,13.2585986993216));
#52007=CARTESIAN_POINT('Ctrl Pts',(64.9720777734537,2.2766820516123,13.1474608087536));
#52008=CARTESIAN_POINT('Ctrl Pts',(66.8974233642155,1.25434280867416,13.0363229181856));
#52009=CARTESIAN_POINT('Ctrl Pts',(67.020379657277,-0.184776408472694,12.9622309911402));
#52010=CARTESIAN_POINT('Ctrl Pts',(66.7638991251268,-0.771314832491415,
12.9251850276175));
#52011=CARTESIAN_POINT('Ctrl Pts',(66.5652001142717,1.33121980333223,22.2244449171475));
#52012=CARTESIAN_POINT('Ctrl Pts',(67.0078623699224,0.810753527669884,22.1873989536248));
#52013=CARTESIAN_POINT('Ctrl Pts',(67.3252008222088,-0.697813052277671,
22.1133070265794));
#52014=CARTESIAN_POINT('Ctrl Pts',(65.6722805558013,-2.3352659649765,22.0021691360114));
#52015=CARTESIAN_POINT('Ctrl Pts',(63.4038010938572,-1.82971146538554,21.8910312454434));
#52016=CARTESIAN_POINT('Ctrl Pts',(62.5964781376417,0.34790469980558,21.7798933548753));
#52017=CARTESIAN_POINT('Ctrl Pts',(63.9890540527047,2.20843040890228,21.6687554643073));
#52018=CARTESIAN_POINT('Ctrl Pts',(66.3069967286646,2.04687460564975,21.5576175737392));
#52019=CARTESIAN_POINT('Ctrl Pts',(67.428612079538,0.0121339679509602,21.4464796831712));
#52020=CARTESIAN_POINT('Ctrl Pts',(66.3273005244664,-2.03388573489,21.3353417926031));
#52021=CARTESIAN_POINT('Ctrl Pts',(64.0110910734901,-2.21817972145311,21.2242039020351));
#52022=CARTESIAN_POINT('Ctrl Pts',(62.6000435330876,-0.372192516572535,
21.1130660114671));
#52023=CARTESIAN_POINT('Ctrl Pts',(63.385702177301,1.8144888252001,21.001928120899));
#52024=CARTESIAN_POINT('Ctrl Pts',(65.6489465241691,2.34033682721966,20.8907902303309));
#52025=CARTESIAN_POINT('Ctrl Pts',(67.3182024564633,0.724053604371175,20.7796523397629));
#52026=CARTESIAN_POINT('Ctrl Pts',(66.865581542071,-1.55496692328425,20.6685144491949));
#52027=CARTESIAN_POINT('Ctrl Pts',(64.7053726085262,-2.41070716562325,20.5573765586268));
#52028=CARTESIAN_POINT('Ctrl Pts',(62.8148395062834,-1.05990051859314,20.4462386680588));
#52029=CARTESIAN_POINT('Ctrl Pts',(62.9244085658998,1.26104545534411,20.3351007774907));
#52030=CARTESIAN_POINT('Ctrl Pts',(64.9337900137556,2.42774204026718,20.2239628869227));
#52031=CARTESIAN_POINT('Ctrl Pts',(67.0037742079544,1.37229889524427,20.1128249963547));
#52032=CARTESIAN_POINT('Ctrl Pts',(67.2396811477566,-0.939225037877053,
20.0016871057866));
#52033=CARTESIAN_POINT('Ctrl Pts',(65.4255825320509,-2.39106561893279,19.8905492152186));
#52034=CARTESIAN_POINT('Ctrl Pts',(63.2219433989572,-1.65433673422366,19.7794113246505));
#52035=CARTESIAN_POINT('Ctrl Pts',(62.6457796370125,0.596625330708006,19.6682734340825));
#52036=CARTESIAN_POINT('Ctrl Pts',(64.2244604721458,2.30148946126118,19.5571355435145));
#52037=CARTESIAN_POINT('Ctrl Pts',(66.5130014322595,1.89977418876314,19.4459976529464));
#52038=CARTESIAN_POINT('Ctrl Pts',(67.4166750228635,-0.240825944373849,
19.3348597623784));
#52039=CARTESIAN_POINT('Ctrl Pts',(66.1083385580613,-2.16099535909078,19.2237218718103));
#52040=CARTESIAN_POINT('Ctrl Pts',(63.7855272416616,-2.10318121447058,19.1125839812423));
#52041=CARTESIAN_POINT('Ctrl Pts',(62.5743366140218,-0.12030145245104,19.0014460906743));
#52042=CARTESIAN_POINT('Ctrl Pts',(63.5833831924642,1.97269159325921,18.8903082001062));
#52043=CARTESIAN_POINT('Ctrl Pts',(65.88907520037,2.26005765183973,18.7791703095382));
#52044=CARTESIAN_POINT('Ctrl Pts',(67.3809865945794,0.478767310881884,18.6680324189701));
#52045=CARTESIAN_POINT('Ctrl Pts',(66.6935539565454,-1.74074417931048,18.5568945284021));
#52046=CARTESIAN_POINT('Ctrl Pts',(64.4559921758773,-2.36693278080144,18.445756637834));
#52047=CARTESIAN_POINT('Ctrl Pts',(62.7163669260972,-0.826640965179831,
18.334618747266));
#52048=CARTESIAN_POINT('Ctrl Pts',(63.0669769270206,1.47028470061623,18.2234808566979));
#52049=CARTESIAN_POINT('Ctrl Pts',(65.1869048686148,2.42144210577608,18.1123429661299));
#52050=CARTESIAN_POINT('Ctrl Pts',(67.1357566643205,1.15622609049767,18.0012050755618));
#52051=CARTESIAN_POINT('Ctrl Pts',(67.1297261640456,-1.16729677790885,17.8900671849939));
#52052=CARTESIAN_POINT('Ctrl Pts',(65.1743331530824,-2.42237966744962,17.7789292944258));
#52053=CARTESIAN_POINT('Ctrl Pts',(63.0593710300304,-1.46023097571985,17.6677914038578));
#52054=CARTESIAN_POINT('Ctrl Pts',(62.720688611421,0.838483688231869,17.5566535132897));
#52055=CARTESIAN_POINT('Ctrl Pts',(64.4682857559272,2.3697247232932,17.4455156227217));
#52056=CARTESIAN_POINT('Ctrl Pts',(66.7025669780829,1.73192984461804,17.3343777321536));
#52057=CARTESIAN_POINT('Ctrl Pts',(67.3784693367765,-0.491120062256288,
17.2232398415856));
#52058=CARTESIAN_POINT('Ctrl Pts',(65.8773317378418,-2.26464220646722,17.1121019510175));
#52059=CARTESIAN_POINT('Ctrl Pts',(63.5731624496418,-1.96531165630909,17.0009640604495));
#52060=CARTESIAN_POINT('Ctrl Pts',(62.5749937527231,0.132890941018443,16.8898261698815));
#52061=CARTESIAN_POINT('Ctrl Pts',(63.7964607753782,2.1094569529468,16.7786882793134));
#52062=CARTESIAN_POINT('Ctrl Pts',(66.119540899393,2.15521309297247,16.6675503887454));
#52063=CARTESIAN_POINT('Ctrl Pts',(67.4178925417354,0.228278247224652,16.5564124981773));
#52064=CARTESIAN_POINT('Ctrl Pts',(66.5031197198625,-1.90760226706539,16.4452746076093));
#52065=CARTESIAN_POINT('Ctrl Pts',(64.2125243718594,-2.29743279261728,16.3341367170413));
#52066=CARTESIAN_POINT('Ctrl Pts',(62.6427143968803,-0.584397028450647,
16.2229988264732));
#52067=CARTESIAN_POINT('Ctrl Pts',(63.2305546678621,1.66354396341759,16.1118609359052));
#52068=CARTESIAN_POINT('Ctrl Pts',(65.4379883182475,2.38882429960344,16.0007230453371));
#52069=CARTESIAN_POINT('Ctrl Pts',(67.24452629377,0.927586663439804,15.8895851547691));
#52070=CARTESIAN_POINT('Ctrl Pts',(66.996623898036,-1.3826815656909,15.7784472642011));
#52071=CARTESIAN_POINT('Ctrl Pts',(64.9211890049946,-2.42736567633038,15.667309373633));
#52072=CARTESIAN_POINT('Ctrl Pts',(62.9178907098163,-1.25025445669175,15.556171483065));
#52073=CARTESIAN_POINT('Ctrl Pts',(62.8203706599597,1.07122884891599,15.4450335924969));
#52074=CARTESIAN_POINT('Ctrl Pts',(64.7178900651262,2.41220423477674,15.3338957019289));
#52075=CARTESIAN_POINT('Ctrl Pts',(66.8736278902366,1.54526173974448,15.2227578113608));
#52076=CARTESIAN_POINT('Ctrl Pts',(67.3144128645646,-0.736076372865367,
15.1116199207928));
#52077=CARTESIAN_POINT('Ctrl Pts',(65.6367894857436,-2.34367538861624,15.0004820302248));
#52078=CARTESIAN_POINT('Ctrl Pts',(63.3763054907363,-1.80608183157382,14.8893441396567));
#52079=CARTESIAN_POINT('Ctrl Pts',(62.6020074507516,0.384639085849608,14.7782062490887));
#52080=CARTESIAN_POINT('Ctrl Pts',(64.0226192720082,2.22329513352231,14.6670683585206));
#52081=CARTESIAN_POINT('Ctrl Pts',(66.3378385875382,2.02694463079714,14.5559304679526));
#52082=CARTESIAN_POINT('Ctrl Pts',(67.4285194097127,-0.0246926670119161,
14.4447925773845));
#52083=CARTESIAN_POINT('Ctrl Pts',(66.2963482043283,-2.05372573368659,14.3336546868165));
#52084=CARTESIAN_POINT('Ctrl Pts',(63.9776161165208,-2.20296580816612,14.2225167962485));
#52085=CARTESIAN_POINT('Ctrl Pts',(62.5946809516312,-0.335795455628588,
14.1113789056804));
#52086=CARTESIAN_POINT('Ctrl Pts',(63.4133668288776,1.83871077711838,14.0002410151124));
#52087=CARTESIAN_POINT('Ctrl Pts',(65.684305645688,2.3302668619962,13.8891031245443));
#52088=CARTESIAN_POINT('Ctrl Pts',(67.3289123722387,0.688818574436941,13.7779652339763));
#52089=CARTESIAN_POINT('Ctrl Pts',(66.8417982611818,-1.58294512384396,13.6668273434083));
#52090=CARTESIAN_POINT('Ctrl Pts',(64.6689465387577,-2.4061546469661,13.5556894528402));
#52091=CARTESIAN_POINT('Ctrl Pts',(62.7989505726263,-1.02632180198957,13.4445515622722));
#52092=CARTESIAN_POINT('Ctrl Pts',(62.9439207637896,1.29160100997125,13.3334136717041));
#52093=CARTESIAN_POINT('Ctrl Pts',(64.970198323091,2.42992595215152,13.2222757811361));
#52094=CARTESIAN_POINT('Ctrl Pts',(67.0251392906009,1.33877286094185,13.111137890568));
#52095=CARTESIAN_POINT('Ctrl Pts',(67.1563717950601,-0.197213743559485,
13.0370459635227));
#52096=CARTESIAN_POINT('Ctrl Pts',(66.8826275096638,-0.823232180103057,
13.));
#52097=CARTESIAN_POINT('Ctrl Pts',(66.2690708798524,1.07935865304855,22.));
#52098=CARTESIAN_POINT('Ctrl Pts',(66.3144013959112,1.03707009263743,22.));
#52099=CARTESIAN_POINT('Ctrl Pts',(66.3570019677251,0.99221251338095,22.));
#52100=CARTESIAN_POINT('Ctrl Pts',(66.396874028036,0.945130914769627,22.));
#52101=CARTESIAN_POINT('Ctrl Pts',(66.439378556838,0.894940853142022,22.));
#52102=CARTESIAN_POINT('Ctrl Pts',(66.4787831170335,0.842223171997003,22.));
#52103=CARTESIAN_POINT('Ctrl Pts',(66.5150606107881,0.787341095409856,22.));
#52104=CARTESIAN_POINT('Ctrl Pts',(66.5468034178233,0.739319278396103,22.));
#52105=CARTESIAN_POINT('Ctrl Pts',(66.5761518212751,0.689639120405576,22.));
#52106=CARTESIAN_POINT('Ctrl Pts',(66.6030647719507,0.638516396532125,22.));
#52107=CARTESIAN_POINT('Ctrl Pts',(66.6165687845836,0.612864734723027,22.));
#52108=CARTESIAN_POINT('Ctrl Pts',(66.629459263796,0.586849522997877,22.));
#52109=CARTESIAN_POINT('Ctrl Pts',(66.6417286804043,0.560496177531073,22.));
#52110=CARTESIAN_POINT('Ctrl Pts',(66.647332630197,0.548459515187504,22.));
#52111=CARTESIAN_POINT('Ctrl Pts',(66.6528075873728,0.536350650701833,22.));
#52112=CARTESIAN_POINT('Ctrl Pts',(66.6581443433919,0.524191916046412,22.));
#52113=CARTESIAN_POINT('Ctrl Pts',(66.6850645452224,0.46285960297952,22.));
#52114=CARTESIAN_POINT('Ctrl Pts',(66.7085235016562,0.400151855797127,22.));
#52115=CARTESIAN_POINT('Ctrl Pts',(66.7284976532585,0.3364264028118,22.));
#52116=CARTESIAN_POINT('Ctrl Pts',(66.7488259022683,0.271571238880423,22.));
#52117=CARTESIAN_POINT('Ctrl Pts',(66.7655452530524,0.205661124541036,22.));
#52118=CARTESIAN_POINT('Ctrl Pts',(66.7785915546243,0.139036642052964,22.));
#52119=CARTESIAN_POINT('Ctrl Pts',(66.7895042319112,0.0833080914905487,
22.));
#52120=CARTESIAN_POINT('Ctrl Pts',(66.7978464644136,0.0270787841007689,
22.));
#52121=CARTESIAN_POINT('Ctrl Pts',(66.8035558761527,-0.0294642473876453,
22.));
#52122=CARTESIAN_POINT('Ctrl Pts',(66.8061865906747,-0.0555174698305799,
22.));
#52123=CARTESIAN_POINT('Ctrl Pts',(66.8082580030076,-0.081637411350437,
22.));
#52124=CARTESIAN_POINT('Ctrl Pts',(66.8097622067312,-0.107806177273391,
22.));
#52125=CARTESIAN_POINT('Ctrl Pts',(66.8104186759515,-0.119226830666176,
22.));
#52126=CARTESIAN_POINT('Ctrl Pts',(66.8109669930221,-0.130656542116141,
22.));
#52127=CARTESIAN_POINT('Ctrl Pts',(66.8114061694317,-0.14207975450712,22.));
#52128=CARTESIAN_POINT('Ctrl Pts',(66.8141021938362,-0.212204785620605,
22.));
#52129=CARTESIAN_POINT('Ctrl Pts',(66.8126973724661,-0.282216215137578,
22.));
#52130=CARTESIAN_POINT('Ctrl Pts',(66.80713701542,-0.351753309319936,22.));
#52131=CARTESIAN_POINT('Ctrl Pts',(66.80216566698,-0.413924339312757,22.));
#52132=CARTESIAN_POINT('Ctrl Pts',(66.7938721956305,-0.475717167669398,
22.));
#52133=CARTESIAN_POINT('Ctrl Pts',(66.7821843766151,-0.536886120776803,
22.));
#52134=CARTESIAN_POINT('Ctrl Pts',(66.7694512323358,-0.603525850935124,
22.));
#52135=CARTESIAN_POINT('Ctrl Pts',(66.7526905137876,-0.66942595359814,22.));
#52136=CARTESIAN_POINT('Ctrl Pts',(66.7321474941548,-0.734372824653469,
22.));
#52137=CARTESIAN_POINT('Ctrl Pts',(66.7242214209376,-0.759431149301895,
22.));
#52138=CARTESIAN_POINT('Ctrl Pts',(66.71573174826,-0.784347525586081,22.));
#52139=CARTESIAN_POINT('Ctrl Pts',(66.7066905572876,-0.80910936507284,22.));
#52140=CARTESIAN_POINT('Ctrl Pts',(66.7027243122815,-0.819972040411269,
22.));
#52141=CARTESIAN_POINT('Ctrl Pts',(66.6986520383784,-0.830804390701535,
22.));
#52142=CARTESIAN_POINT('Ctrl Pts',(66.6944798306678,-0.841592845083872,
22.));
#52143=CARTESIAN_POINT('Ctrl Pts',(66.6692560535682,-0.906816244172474,
22.));
#52144=CARTESIAN_POINT('Ctrl Pts',(66.6403413434903,-0.970554427372129,
22.));
#52145=CARTESIAN_POINT('Ctrl Pts',(66.6080484131008,-1.03258856567894,22.));
#52146=CARTESIAN_POINT('Ctrl Pts',(66.5750071922106,-1.09606015657544,22.));
#52147=CARTESIAN_POINT('Ctrl Pts',(66.5384290748914,-1.15774863483118,22.));
#52148=CARTESIAN_POINT('Ctrl Pts',(66.4985928798088,-1.21741589247309,22.));
#52149=CARTESIAN_POINT('Ctrl Pts',(66.4681126351482,-1.26306966556535,22.));
#52150=CARTESIAN_POINT('Ctrl Pts',(66.4357237709963,-1.30754017026296,22.));
#52151=CARTESIAN_POINT('Ctrl Pts',(66.4015316630724,-1.35071465500183,22.));
#52152=CARTESIAN_POINT('Ctrl Pts',(66.3802494925797,-1.37758772018966,22.));
#52153=CARTESIAN_POINT('Ctrl Pts',(66.3582683894734,-1.40395856097014,22.));
#52154=CARTESIAN_POINT('Ctrl Pts',(66.3356108635762,-1.42979830341358,22.));
#52155=CARTESIAN_POINT('Ctrl Pts',(66.3229007387176,-1.4442935468157,22.));
#52156=CARTESIAN_POINT('Ctrl Pts',(66.3099732536077,-1.45862623051675,22.));
#52157=CARTESIAN_POINT('Ctrl Pts',(66.2968561826132,-1.47276572508009,22.));
#52158=CARTESIAN_POINT('Ctrl Pts',(66.2459827546045,-1.52760453467751,22.));
#52159=CARTESIAN_POINT('Ctrl Pts',(66.1922128066828,-1.57959843575484,22.));
#52160=CARTESIAN_POINT('Ctrl Pts',(66.1358313615534,-1.62848347080716,22.));
#52161=CARTESIAN_POINT('Ctrl Pts',(66.0936603481041,-1.66504747632229,22.));
#52162=CARTESIAN_POINT('Ctrl Pts',(66.0500271947279,-1.69987205106308,22.));
#52163=CARTESIAN_POINT('Ctrl Pts',(66.00503476506,-1.73283699198631,22.));
#52164=CARTESIAN_POINT('Ctrl Pts',(65.9909996372083,-1.74312021438386,22.));
#52165=CARTESIAN_POINT('Ctrl Pts',(65.9768321470098,-1.75322240064489,22.));
#52166=CARTESIAN_POINT('Ctrl Pts',(65.9625351770669,-1.76313967663704,22.));
#52167=CARTESIAN_POINT('Ctrl Pts',(65.9487346475682,-1.77271259036793,22.));
#52168=CARTESIAN_POINT('Ctrl Pts',(65.9348204929495,-1.78210828001308,22.));
#52169=CARTESIAN_POINT('Ctrl Pts',(65.9208007360916,-1.79132048320785,22.));
#52170=CARTESIAN_POINT('Ctrl Pts',(65.8578459988918,-1.83268723707061,22.));
#52171=CARTESIAN_POINT('Ctrl Pts',(65.792733983974,-1.8703783102438,22.));
#52172=CARTESIAN_POINT('Ctrl Pts',(65.7257260555984,-1.90411450232551,22.));
#52173=CARTESIAN_POINT('Ctrl Pts',(65.6744429845571,-1.92993376845009,22.));
#52174=CARTESIAN_POINT('Ctrl Pts',(65.622048450405,-1.95343614609329,22.));
#52175=CARTESIAN_POINT('Ctrl Pts',(65.5686456989049,-1.97448116510364,22.));
#52176=CARTESIAN_POINT('Ctrl Pts',(65.5562524015237,-1.97936513028632,22.));
#52177=CARTESIAN_POINT('Ctrl Pts',(65.54380476008,-1.98411668136773,22.));
#52178=CARTESIAN_POINT('Ctrl Pts',(65.531304687333,-1.9887363997513,22.));
#52179=CARTESIAN_POINT('Ctrl Pts',(63.3326792503596,-0.00130047270866476,
20.8714803633902));
#52180=CARTESIAN_POINT('Ctrl Pts',(63.3319477300267,-0.086545894594441,
20.8771939403667));
#52181=CARTESIAN_POINT('Ctrl Pts',(63.3379207823453,-0.171688456696973,
20.8829075173431));
#52182=CARTESIAN_POINT('Ctrl Pts',(63.3509549142486,-0.25573589354722,20.8886210943196));
#52183=CARTESIAN_POINT('Ctrl Pts',(63.4354662417459,-0.800686682266386,
20.9256670578423));
#52184=CARTESIAN_POINT('Ctrl Pts',(63.8168273485002,-1.2995980961985,20.9627130213649));
#52185=CARTESIAN_POINT('Ctrl Pts',(64.3205066401932,-1.52414941239406,20.9997589848876));
#52186=CARTESIAN_POINT('Ctrl Pts',(64.8241859318862,-1.74870072858961,21.0368049484103));
#52187=CARTESIAN_POINT('Ctrl Pts',(65.4501834085179,-1.6988919470486,21.073850911933));
#52188=CARTESIAN_POINT('Ctrl Pts',(65.9120068254848,-1.39750064992834,21.1108968754557));
#52189=CARTESIAN_POINT('Ctrl Pts',(66.3738302424517,-1.09610935280807,21.1479428389783));
#52190=CARTESIAN_POINT('Ctrl Pts',(66.6714795997537,-0.543135540108549,
21.184988802501));
#52191=CARTESIAN_POINT('Ctrl Pts',(66.6687358658197,0.00831408696199361,
21.2220347660237));
#52192=CARTESIAN_POINT('Ctrl Pts',(66.6659921318856,0.559763714032539,21.2590807295464));
#52193=CARTESIAN_POINT('Ctrl Pts',(66.3628553067155,1.10968915547411,21.2961266930691));
#52194=CARTESIAN_POINT('Ctrl Pts',(65.898053938122,1.40648356441476,21.3331726565917));
#52195=CARTESIAN_POINT('Ctrl Pts',(65.4332525695286,1.70327797335542,21.3702186201144));
#52196=CARTESIAN_POINT('Ctrl Pts',(64.8067866575118,1.74694134979517,21.4072645836371));
#52197=CARTESIAN_POINT('Ctrl Pts',(64.3053692934656,1.51735268425302,21.4443105471598));
#52198=CARTESIAN_POINT('Ctrl Pts',(63.8039519294193,1.28776401871087,21.4813565106825));
#52199=CARTESIAN_POINT('Ctrl Pts',(63.4275831133436,0.784923311186826,21.5184024742051));
#52200=CARTESIAN_POINT('Ctrl Pts',(63.3484955171689,0.23923288959754,21.5554484377278));
#52201=CARTESIAN_POINT('Ctrl Pts',(63.337086928647,0.160515647180261,21.5607924129486));
#52202=CARTESIAN_POINT('Ctrl Pts',(63.3318644062264,0.0809067535388596,
21.5661363881694));
#52203=CARTESIAN_POINT('Ctrl Pts',(63.3325282901756,0.00121307831918299,
21.5714803633902));
#52204=CARTESIAN_POINT('Ctrl Pts',(64.4698297828114,-1.98517432567172,22.));
#52205=CARTESIAN_POINT('Ctrl Pts',(63.8097120902545,-1.80888011517989,21.9629540364773));
#52206=CARTESIAN_POINT('Ctrl Pts',(62.6906509614045,-0.748610048502898,
21.888862109432));
#52207=CARTESIAN_POINT('Ctrl Pts',(63.1187889329781,1.53833553624066,21.7777242188639));
#52208=CARTESIAN_POINT('Ctrl Pts',(65.2721300366129,2.41280623887489,21.6665863282959));
#52209=CARTESIAN_POINT('Ctrl Pts',(67.1747422685441,1.08094901338605,21.5554484377278));
#52210=CARTESIAN_POINT('Ctrl Pts',(67.0876157148515,-1.24138505016237,21.4443105471598));
#52211=CARTESIAN_POINT('Ctrl Pts',(65.0892538486775,-2.42692553227054,21.3331726565917));
#52212=CARTESIAN_POINT('Ctrl Pts',(63.0094071033202,-1.39134559511318,21.2220347660237));
#52213=CARTESIAN_POINT('Ctrl Pts',(62.7514666617416,0.917885875238371,21.1108968754557));
#52214=CARTESIAN_POINT('Ctrl Pts',(64.5516876929394,2.3868968681091,20.9997589848876));
#52215=CARTESIAN_POINT('Ctrl Pts',(66.7622271403759,1.67118893435552,20.8886210943196));
#52216=CARTESIAN_POINT('Ctrl Pts',(67.3597936726881,-0.574194749175797,
20.7774832037516));
#52217=CARTESIAN_POINT('Ctrl Pts',(65.7974074532359,-2.2940026123021,20.6663453131835));
#52218=CARTESIAN_POINT('Ctrl Pts',(63.5051485972519,-1.91408833219884,20.5552074226155));
#52219=CARTESIAN_POINT('Ctrl Pts',(62.5811424445442,0.217814955653713,20.4440695320474));
#52220=CARTESIAN_POINT('Ctrl Pts',(63.8711449203827,2.15034861017487,20.3329316414794));
#52221=CARTESIAN_POINT('Ctrl Pts',(66.1944008109328,2.11464436694832,20.2217937509113));
#52222=CARTESIAN_POINT('Ctrl Pts',(67.4244083164919,0.143381864737545,20.1106558603433));
#52223=CARTESIAN_POINT('Ctrl Pts',(66.4353272830534,-1.95911953903995,19.9995179697752));
#52224=CARTESIAN_POINT('Ctrl Pts',(64.132474966303,-2.26841668404625,19.8883800792072));
#52225=CARTESIAN_POINT('Ctrl Pts',(62.6236781227743,-0.50140627563105,19.7772421886392));
#52226=CARTESIAN_POINT('Ctrl Pts',(63.2899556571721,1.72454696459255,19.6661042980711));
#52227=CARTESIAN_POINT('Ctrl Pts',(65.5214561645339,2.37200281981328,19.5549664075031));
#52228=CARTESIAN_POINT('Ctrl Pts',(67.2756619344365,0.848337588988218,19.443828516935));
#52229=CARTESIAN_POINT('Ctrl Pts',(66.9469285261459,-1.45182065545646,19.332690626367));
#52230=CARTESIAN_POINT('Ctrl Pts',(64.8361493591312,-2.42311099039749,19.221552735799));
#52231=CARTESIAN_POINT('Ctrl Pts',(62.8753445414284,-1.17650035527426,19.1104148452309));
#52232=CARTESIAN_POINT('Ctrl Pts',(62.8592609604237,1.14697439714762,18.9992769546629));
#52233=CARTESIAN_POINT('Ctrl Pts',(64.8026200998564,2.42061047643986,18.8881390640948));
#52234=CARTESIAN_POINT('Ctrl Pts',(66.9266433003906,1.47863433497921,18.7770011735268));
#52235=CARTESIAN_POINT('Ctrl Pts',(67.2871880384261,-0.816752582102671,
18.6658632829587));
#52236=CARTESIAN_POINT('Ctrl Pts',(65.5542436264288,-2.36455659820143,18.5547253923907));
#52237=CARTESIAN_POINT('Ctrl Pts',(63.3139937376034,-1.7480551440608,18.4435875018227));
#52238=CARTESIAN_POINT('Ctrl Pts',(62.6169645013648,0.468461007727324,18.3324496112546));
#52239=CARTESIAN_POINT('Ctrl Pts',(64.1011546824859,2.25618948643599,18.2213117206866));
#52240=CARTESIAN_POINT('Ctrl Pts',(66.4080681763277,1.97880214127948,18.1101738301185));
#52241=CARTESIAN_POINT('Ctrl Pts',(67.4261608997972,-0.109805244932086,
17.9990359395505));
#52242=CARTESIAN_POINT('Ctrl Pts',(66.2235610371465,-2.09790664518147,17.8878980489825));
#52243=CARTESIAN_POINT('Ctrl Pts',(63.9010218810697,-2.16577030121656,17.7767601584144));
#52244=CARTESIAN_POINT('Ctrl Pts',(62.5843898605093,-0.251279839042475,
17.6656222678464));
#52245=CARTESIAN_POINT('Ctrl Pts',(63.478793195507,1.89320990951442,17.5544843772783));
#52246=CARTESIAN_POINT('Ctrl Pts',(65.7655743703156,2.30482315743208,17.4433464867103));
#52247=CARTESIAN_POINT('Ctrl Pts',(67.3516166417705,0.606805630879791,17.3322085961422));
#52248=CARTESIAN_POINT('Ctrl Pts',(66.7851975318663,-1.64662797126069,17.2210707055742));
#52249=CARTESIAN_POINT('Ctrl Pts',(64.5847668755277,-2.39288431727495,17.1099328150062));
#52250=CARTESIAN_POINT('Ctrl Pts',(62.7644038070828,-0.94890651053363,16.9987949244381));
#52251=CARTESIAN_POINT('Ctrl Pts',(62.9903072873999,1.36361618663094,16.8876570338701));
#52252=CARTESIAN_POINT('Ctrl Pts',(65.0557052990257,2.42800552371272,16.776519143302));
#52253=CARTESIAN_POINT('Ctrl Pts',(67.0701156187118,1.27001386948508,16.665381252734));
#52254=CARTESIAN_POINT('Ctrl Pts',(67.1897256358837,-1.05043588241968,16.5542433621659));
#52255=CARTESIAN_POINT('Ctrl Pts',(65.3050549453524,-2.40940975839149,16.4431054715979));
#52256=CARTESIAN_POINT('Ctrl Pts',(63.141164003784,-1.56302355794458,16.3319675810298));
#52257=CARTESIAN_POINT('Ctrl Pts',(62.6786867301813,0.714015830985959,16.2208296904619));
#52258=CARTESIAN_POINT('Ctrl Pts',(64.3409338179361,2.33750843231645,16.1096917998938));
#52259=CARTESIAN_POINT('Ctrl Pts',(66.6064316564341,1.82145305641563,15.9985539093258));
#52260=CARTESIAN_POINT('Ctrl Pts',(67.401544381661,-0.361798958737837,15.8874160187577));
#52261=CARTESIAN_POINT('Ctrl Pts',(65.9984962989145,-2.2138922838142,15.7762781281897));
#52262=CARTESIAN_POINT('Ctrl Pts',(63.6815132301988,-2.03958489439843,15.6651402376216));
#52263=CARTESIAN_POINT('Ctrl Pts',(62.5713560542506,0.00157767958230164,
15.5540023470536));
#52264=CARTESIAN_POINT('Ctrl Pts',(63.6841642251148,2.04129618504104,15.4428644564855));
#52265=CARTESIAN_POINT('Ctrl Pts',(66.0013718021885,2.21259314346663,15.3317265659175));
#52266=CARTESIAN_POINT('Ctrl Pts',(67.4020124146433,0.358678503164372,15.2205886753494));
#52267=CARTESIAN_POINT('Ctrl Pts',(66.6040638188323,-1.82353863480769,15.1094507847814));
#52268=CARTESIAN_POINT('Ctrl Pts',(64.3378974271891,-2.33665018787605,14.9983128942134));
#52269=CARTESIAN_POINT('Ctrl Pts',(62.6777610116057,-0.710999308952887,
14.8871750036453));
#52270=CARTESIAN_POINT('Ctrl Pts',(63.1431963129712,1.56543726976266,14.7760371130773));
#52271=CARTESIAN_POINT('Ctrl Pts',(65.308185017446,2.40901142364104,14.6648992225093));
#52272=CARTESIAN_POINT('Ctrl Pts',(67.1910886177016,1.04758997952522,14.5537613319412));
#52273=CARTESIAN_POINT('Ctrl Pts',(67.068463685159,-1.27270221153156,14.4426234413732));
#52274=CARTESIAN_POINT('Ctrl Pts',(65.0525510239567,-2.42807611461693,14.3314855508051));
#52275=CARTESIAN_POINT('Ctrl Pts',(62.9885367426501,-1.36100346218851,14.2203476602371));
#52276=CARTESIAN_POINT('Ctrl Pts',(62.7656397187534,0.951809206360665,14.109209769669));
#52277=CARTESIAN_POINT('Ctrl Pts',(64.5878737813476,2.39342385873018,13.998071879101));
#52278=CARTESIAN_POINT('Ctrl Pts',(66.7873400138256,1.64430308142019,13.8869339885329));
#52279=CARTESIAN_POINT('Ctrl Pts',(67.3508170614469,-0.609852217558742,
13.7757960979649));
#52280=CARTESIAN_POINT('Ctrl Pts',(65.7625975239189,-2.30583209920716,13.6646582073969));
#52281=CARTESIAN_POINT('Ctrl Pts',(63.4762984963492,-1.89119971793714,13.5535203168288));
#52282=CARTESIAN_POINT('Ctrl Pts',(62.5847903309572,0.254354168931206,13.4423824262608));
#52283=CARTESIAN_POINT('Ctrl Pts',(63.9036938704104,2.16732302296764,13.3312445356927));
#52284=CARTESIAN_POINT('Ctrl Pts',(66.2265689546786,2.09606376419022,13.2201066451247));
#52285=CARTESIAN_POINT('Ctrl Pts',(67.4257384694328,0.107152139943104,13.1089687545567));
#52286=CARTESIAN_POINT('Ctrl Pts',(66.4066260077932,-1.98162422647333,12.9978308639886));
#52287=CARTESIAN_POINT('Ctrl Pts',(64.0958295620755,-2.2529948526272,12.8866929734206));
#52288=CARTESIAN_POINT('Ctrl Pts',(63.1142456563632,-1.06431345694514,12.8126010463752));
#52289=CARTESIAN_POINT('Ctrl Pts',(62.9833241385535,-0.393720754290216,
12.7755550828525));
#52290=CARTESIAN_POINT('Ctrl Pts',(64.5032651029123,-1.85997880000276,22.0748149723825));
#52291=CARTESIAN_POINT('Ctrl Pts',(63.8847779011663,-1.694802628904,22.0377690088598));
#52292=CARTESIAN_POINT('Ctrl Pts',(62.8362906481067,-0.701398764671857,
21.9636770818144));
#52293=CARTESIAN_POINT('Ctrl Pts',(63.2374279891983,1.44132001290635,21.8525391912464));
#52294=CARTESIAN_POINT('Ctrl Pts',(65.2549680863783,2.26064199742416,21.7414013006783));
#52295=CARTESIAN_POINT('Ctrl Pts',(67.0375915921608,1.0127786878876,21.6302634101104));
#52296=CARTESIAN_POINT('Ctrl Pts',(66.9559596968202,-1.16309678504486,21.5191255195423));
#52297=CARTESIAN_POINT('Ctrl Pts',(65.0836250319239,-2.27387085397712,21.4079876289743));
#52298=CARTESIAN_POINT('Ctrl Pts',(63.1349443525531,-1.30360002994301,21.2968497384062));
#52299=CARTESIAN_POINT('Ctrl Pts',(62.8932709907757,0.859999168177673,21.1857118478382));
#52300=CARTESIAN_POINT('Ctrl Pts',(64.5799606230396,2.23636660774046,21.0745739572701));
#52301=CARTESIAN_POINT('Ctrl Pts',(66.6510918358667,1.56579497755125,20.9634360667021));
#52302=CARTESIAN_POINT('Ctrl Pts',(67.2109726822582,-0.537983010725524,
20.8522981761341));
#52303=CARTESIAN_POINT('Ctrl Pts',(65.7471187486173,-2.14933075189209,20.741160285566));
#52304=CARTESIAN_POINT('Ctrl Pts',(63.5994217826059,-1.7933758628567,20.630022394998));
#52305=CARTESIAN_POINT('Ctrl Pts',(62.73368831382,0.204078399866653,20.5188845044299));
#52306=CARTESIAN_POINT('Ctrl Pts',(63.9423364541786,2.01473632608427,20.4077466138619));
#52307=CARTESIAN_POINT('Ctrl Pts',(66.1190756188575,1.98128378007219,20.2966087232938));
#52308=CARTESIAN_POINT('Ctrl Pts',(67.2715123870543,0.134339450832088,20.1854708327258));
#52309=CARTESIAN_POINT('Ctrl Pts',(66.3448080015046,-1.83556716514178,20.0743329421578));
#52310=CARTESIAN_POINT('Ctrl Pts',(64.1871856540346,-2.12535840673385,19.9631950515897));
#52311=CARTESIAN_POINT('Ctrl Pts',(62.7735414686431,-0.469784960847975,
19.8520571610217));
#52312=CARTESIAN_POINT('Ctrl Pts',(63.3978000402315,1.61578796998894,19.7409192704536));
#52313=CARTESIAN_POINT('Ctrl Pts',(65.4885703983884,2.22241185640291,19.6297813798856));
#52314=CARTESIAN_POINT('Ctrl Pts',(67.1321467335585,0.794836962355754,19.5186434893175));
#52315=CARTESIAN_POINT('Ctrl Pts',(66.8241449815883,-1.36026121516629,19.4075055987495));
#52316=CARTESIAN_POINT('Ctrl Pts',(64.8464826416291,-2.27029687716116,19.2963677081814));
#52317=CARTESIAN_POINT('Ctrl Pts',(63.0093364803535,-1.10230406000511,19.1852298176134));
#52318=CARTESIAN_POINT('Ctrl Pts',(62.9942672144912,1.07464016396579,19.0740919270454));
#52319=CARTESIAN_POINT('Ctrl Pts',(64.8150679136506,2.26795405875467,18.9629540364773));
#52320=CARTESIAN_POINT('Ctrl Pts',(66.8051390487741,1.38538388314433,18.8518161459093));
#52321=CARTESIAN_POINT('Ctrl Pts',(67.1429459408574,-0.765243871993183,
18.7406782553413));
#52322=CARTESIAN_POINT('Ctrl Pts',(65.5192901106281,-2.21543523265805,18.6295403647732));
#52323=CARTESIAN_POINT('Ctrl Pts',(63.4203221529835,-1.63781360011732,18.5184024742052));
#52324=CARTESIAN_POINT('Ctrl Pts',(62.7672512434818,0.438917394675616,18.4072645836371));
#52325=CARTESIAN_POINT('Ctrl Pts',(64.1578405919126,2.11390232046252,18.2961266930691));
#52326=CARTESIAN_POINT('Ctrl Pts',(66.3192679973039,1.85400847904606,18.184988802501));
#52327=CARTESIAN_POINT('Ctrl Pts',(67.2731544432459,-0.102880349126863,
18.073850911933));
#52328=CARTESIAN_POINT('Ctrl Pts',(66.1463968479604,-1.96560162700175,17.9627130213649));
#52329=CARTESIAN_POINT('Ctrl Pts',(63.9703292167121,-2.02918544424321,17.8515751307969));
#52330=CARTESIAN_POINT('Ctrl Pts',(62.7367309306682,-0.235432811840826,
17.7404372402289));
#52331=CARTESIAN_POINT('Ctrl Pts',(63.5747284910006,1.77381414322919,17.6292993496608));
#52332=CARTESIAN_POINT('Ctrl Pts',(65.7172932271985,2.15946889658093,17.5181614590928));
#52333=CARTESIAN_POINT('Ctrl Pts',(67.2033113378831,0.568537278849208,17.4070235685247));
#52334=CARTESIAN_POINT('Ctrl Pts',(66.6726135937532,-1.54278295786448,17.2958856779567));
#52335=CARTESIAN_POINT('Ctrl Pts',(64.6109536585329,-2.24197645689605,17.1847477873887));
#52336=CARTESIAN_POINT('Ctrl Pts',(62.9053922517429,-0.889063479188381,
17.0736098968206));
#52337=CARTESIAN_POINT('Ctrl Pts',(63.1170490714002,1.27761938368609,16.9624720062526));
#52338=CARTESIAN_POINT('Ctrl Pts',(65.0521922301209,2.27488273548329,16.8513341156845));
#52339=CARTESIAN_POINT('Ctrl Pts',(66.9395632487115,1.18992012056796,16.7401962251165));
#52340=CARTESIAN_POINT('Ctrl Pts',(67.0516300296139,-0.984189875315707,
16.6290583345485));
#52341=CARTESIAN_POINT('Ctrl Pts',(65.2858165773424,-2.25745971684959,16.5179204439804));
#52342=CARTESIAN_POINT('Ctrl Pts',(63.2583919704513,-1.46445107821859,16.4067825534124));
#52343=CARTESIAN_POINT('Ctrl Pts',(62.8250809441801,0.66898624031462,16.2956446628443));
#52344=CARTESIAN_POINT('Ctrl Pts',(64.3824979949693,2.19009286626007,16.1845067722763));
#52345=CARTESIAN_POINT('Ctrl Pts',(66.5051216338947,1.70658265439079,16.0733688817082));
#52346=CARTESIAN_POINT('Ctrl Pts',(67.2500903721106,-0.338982015036762,
15.9622309911402));
#52347=CARTESIAN_POINT('Ctrl Pts',(65.9355258749046,-2.07427260172266,15.8510931005721));
#52348=CARTESIAN_POINT('Ctrl Pts',(63.7646639349497,-1.91095795232155,15.7399552100041));
#52349=CARTESIAN_POINT('Ctrl Pts',(62.7245191047287,0.00147818281665529,
15.6288173194361));
#52350=CARTESIAN_POINT('Ctrl Pts',(63.7671477441945,1.91256131998289,15.517679428868));
#52351=CARTESIAN_POINT('Ctrl Pts',(65.9382200338304,2.07305539199278,15.4065415383));
#52352=CARTESIAN_POINT('Ctrl Pts',(67.2505288884734,0.336058351790703,15.2954036477319));
#52353=CARTESIAN_POINT('Ctrl Pts',(66.5029031245757,-1.7085367052491,15.1842657571639));
#52354=CARTESIAN_POINT('Ctrl Pts',(64.3796530949801,-2.18928874722442,15.0731278665959));
#52355=CARTESIAN_POINT('Ctrl Pts',(62.8242136062828,-0.666159956013692,
14.9619899760278));
#52356=CARTESIAN_POINT('Ctrl Pts',(63.2602961115408,1.46671256868464,14.8508520854598));
#52357=CARTESIAN_POINT('Ctrl Pts',(65.2887492506402,2.25708650318186,14.7397141948917));
#52358=CARTESIAN_POINT('Ctrl Pts',(67.0529070546353,0.981523450013854,14.6285763043237));
#52359=CARTESIAN_POINT('Ctrl Pts',(66.93801549477,-1.19243892163694,14.5174384137556));
#52360=CARTESIAN_POINT('Ctrl Pts',(65.0492368802144,-2.27494887455409,14.4063005231876));
#52361=CARTESIAN_POINT('Ctrl Pts',(63.115390186507,-1.27517143137766,14.2951626326196));
#52362=CARTESIAN_POINT('Ctrl Pts',(62.9065502203286,0.891783115762019,14.1840247420515));
#52363=CARTESIAN_POINT('Ctrl Pts',(64.6138646265439,2.24248197203166,14.0728868514835));
#52364=CARTESIAN_POINT('Ctrl Pts',(66.6746209595408,1.54060468779532,13.9617489609154));
#52365=CARTESIAN_POINT('Ctrl Pts',(67.2025621832966,-0.571391731761448,
13.8506110703474));
#52366=CARTESIAN_POINT('Ctrl Pts',(65.7145041163797,-2.16041420918537,13.7394731797794));
#52367=CARTESIAN_POINT('Ctrl Pts',(63.5723911206821,-1.77193072489694,13.6283352892113));
#52368=CARTESIAN_POINT('Ctrl Pts',(62.7371061453451,0.23831325833024,13.5171973986433));
#52369=CARTESIAN_POINT('Ctrl Pts',(63.9728326963629,2.03064024320065,13.4060595080752));
#52370=CARTESIAN_POINT('Ctrl Pts',(66.1492150704054,1.96387496777071,13.2949216175072));
#52371=CARTESIAN_POINT('Ctrl Pts',(67.2727586535603,0.100394562881356,13.1837837269391));
#52372=CARTESIAN_POINT('Ctrl Pts',(66.3179167794963,-1.85665258871666,13.0726458363711));
#52373=CARTESIAN_POINT('Ctrl Pts',(64.1528513015804,-2.11090915705047,12.9615079458031));
#52374=CARTESIAN_POINT('Ctrl Pts',(63.2331712354829,-0.997192257060735,
12.8874160187577));
#52375=CARTESIAN_POINT('Ctrl Pts',(63.1105063166185,-0.368890654402911,
12.850370055235));
#52376=CARTESIAN_POINT('Ctrl Pts',(64.5367004230132,-1.7347832743338,22.149629944765));
#52377=CARTESIAN_POINT('Ctrl Pts',(63.9598437120782,-1.5807251426281,22.1125839812423));
#52378=CARTESIAN_POINT('Ctrl Pts',(62.9819303348089,-0.654187480840814,
22.0384920541969));
#52379=CARTESIAN_POINT('Ctrl Pts',(63.3560670454183,1.34430448957203,21.9273541636289));
#52380=CARTESIAN_POINT('Ctrl Pts',(65.2378061361438,2.10847775597344,21.8162162730608));
#52381=CARTESIAN_POINT('Ctrl Pts',(66.9004409157773,0.944608362389151,21.7050783824928));
#52382=CARTESIAN_POINT('Ctrl Pts',(66.8243036787891,-1.08480851992735,21.5939404919248));
#52383=CARTESIAN_POINT('Ctrl Pts',(65.0779962151703,-2.12081617568371,21.4828026013567));
#52384=CARTESIAN_POINT('Ctrl Pts',(63.260481601786,-1.21585446477283,21.3716647107887));
#52385=CARTESIAN_POINT('Ctrl Pts',(63.0350753198097,0.802112461116973,21.2605268202206));
#52386=CARTESIAN_POINT('Ctrl Pts',(64.6082335531397,2.08583634737181,21.1493889296526));
#52387=CARTESIAN_POINT('Ctrl Pts',(66.5399565313575,1.46040102074698,21.0382510390845));
#52388=CARTESIAN_POINT('Ctrl Pts',(67.0621516918282,-0.501771272275252,
20.9271131485165));
#52389=CARTESIAN_POINT('Ctrl Pts',(65.6968300439987,-2.00465889148207,20.8159752579485));
#52390=CARTESIAN_POINT('Ctrl Pts',(63.6936949679598,-1.67266339351456,20.7048373673804));
#52391=CARTESIAN_POINT('Ctrl Pts',(62.8862341830958,0.190341844079594,20.5936994768124));
#52392=CARTESIAN_POINT('Ctrl Pts',(64.0135279879744,1.87912404199367,20.4825615862443));
#52393=CARTESIAN_POINT('Ctrl Pts',(66.0437504267822,1.84792319319607,20.3714236956763));
#52394=CARTESIAN_POINT('Ctrl Pts',(67.1186164576166,0.125297036926629,20.2602858051083));
#52395=CARTESIAN_POINT('Ctrl Pts',(66.2542887199559,-1.71201479124362,20.1491479145402));
#52396=CARTESIAN_POINT('Ctrl Pts',(64.2418963417663,-1.98230012942144,20.0380100239722));
#52397=CARTESIAN_POINT('Ctrl Pts',(62.9234048145118,-0.438163646064901,
19.9268721334041));
#52398=CARTESIAN_POINT('Ctrl Pts',(63.505644423291,1.50702897538532,19.8157342428361));
#52399=CARTESIAN_POINT('Ctrl Pts',(65.4556846322429,2.07282089299253,19.7045963522681));
#52400=CARTESIAN_POINT('Ctrl Pts',(66.9886315326805,0.741336335723289,19.5934584617));
#52401=CARTESIAN_POINT('Ctrl Pts',(66.7013614370307,-1.26870177487612,19.482320571132));
#52402=CARTESIAN_POINT('Ctrl Pts',(64.856815924127,-2.11748276392483,19.3711826805639));
#52403=CARTESIAN_POINT('Ctrl Pts',(63.1433284192787,-1.02810776473596,19.2600447899959));
#52404=CARTESIAN_POINT('Ctrl Pts',(63.1292734685587,1.00230593078395,19.1489068994279));
#52405=CARTESIAN_POINT('Ctrl Pts',(64.8275157274446,2.11529764106946,19.0377690088598));
#52406=CARTESIAN_POINT('Ctrl Pts',(66.6836347971578,1.29213343130945,18.9266311182918));
#52407=CARTESIAN_POINT('Ctrl Pts',(66.9987038432886,-0.713735161883696,
18.8154932277237));
#52408=CARTESIAN_POINT('Ctrl Pts',(65.4843365948275,-2.06631386711466,18.7043553371557));
#52409=CARTESIAN_POINT('Ctrl Pts',(63.5266505683636,-1.52757205617383,18.5932174465876));
#52410=CARTESIAN_POINT('Ctrl Pts',(62.9175379855987,0.409373781623907,18.4820795560196));
#52411=CARTESIAN_POINT('Ctrl Pts',(64.2145265013393,1.97161515448904,18.3709416654516));
#52412=CARTESIAN_POINT('Ctrl Pts',(66.2304678182801,1.72921481681263,18.2598037748835));
#52413=CARTESIAN_POINT('Ctrl Pts',(67.1201479866946,-0.0959554533216394,
18.1486658843155));
#52414=CARTESIAN_POINT('Ctrl Pts',(66.0692326587742,-1.83329660882204,18.0375279937474));
#52415=CARTESIAN_POINT('Ctrl Pts',(64.0396365523547,-1.89260058726987,17.9263901031794));
#52416=CARTESIAN_POINT('Ctrl Pts',(62.8890720008271,-0.219585784639178,
17.8152522126113));
#52417=CARTESIAN_POINT('Ctrl Pts',(63.6706637864943,1.65441837694396,17.7041143220433));
#52418=CARTESIAN_POINT('Ctrl Pts',(65.6690120840812,2.01411463572978,17.5929764314753));
#52419=CARTESIAN_POINT('Ctrl Pts',(67.0550060339956,0.530268926818625,17.4818385409072));
#52420=CARTESIAN_POINT('Ctrl Pts',(66.5600296556403,-1.43893794446826,17.3707006503392));
#52421=CARTESIAN_POINT('Ctrl Pts',(64.6371404415378,-2.09106859651715,17.2595627597711));
#52422=CARTESIAN_POINT('Ctrl Pts',(63.0463806964032,-0.829220447843132,
17.1484248692031));
#52423=CARTESIAN_POINT('Ctrl Pts',(63.2437908554003,1.19162258074125,17.0372869786351));
#52424=CARTESIAN_POINT('Ctrl Pts',(65.0486791612162,2.12175994725385,16.926149088067));
#52425=CARTESIAN_POINT('Ctrl Pts',(66.8090108787112,1.10982637165085,16.815011197499));
#52426=CARTESIAN_POINT('Ctrl Pts',(66.9135344233438,-0.917943868211739,
16.7038733069309));
#52427=CARTESIAN_POINT('Ctrl Pts',(65.2665782093324,-2.10550967530768,16.5927354163629));
#52428=CARTESIAN_POINT('Ctrl Pts',(63.3756199371186,-1.3658785984926,16.4815975257949));
#52429=CARTESIAN_POINT('Ctrl Pts',(62.9714751581789,0.623956649643286,16.3704596352268));
#52430=CARTESIAN_POINT('Ctrl Pts',(64.4240621720026,2.04267730020369,16.2593217446588));
#52431=CARTESIAN_POINT('Ctrl Pts',(66.4038116113553,1.59171225236596,16.1481838540907));
#52432=CARTESIAN_POINT('Ctrl Pts',(67.0986363625603,-0.316165071335693,
16.0370459635227));
#52433=CARTESIAN_POINT('Ctrl Pts',(65.8725554508947,-1.93465291963112,15.9259080729547));
#52434=CARTESIAN_POINT('Ctrl Pts',(63.8478146397005,-1.78233101024467,15.8147701823866));
#52435=CARTESIAN_POINT('Ctrl Pts',(62.8776821552069,0.00137868605101399,
15.7036322918186));
#52436=CARTESIAN_POINT('Ctrl Pts',(63.8501312632742,1.78382645492474,15.5924944012505));
#52437=CARTESIAN_POINT('Ctrl Pts',(65.8750682654724,1.93351764051894,15.4813565106825));
#52438=CARTESIAN_POINT('Ctrl Pts',(67.0990453623036,0.313438200417032,15.3702186201144));
#52439=CARTESIAN_POINT('Ctrl Pts',(66.401742430319,-1.59353477569052,15.2590807295464));
#52440=CARTESIAN_POINT('Ctrl Pts',(64.4214087627711,-2.04192730657279,15.1479428389783));
#52441=CARTESIAN_POINT('Ctrl Pts',(62.9706662009597,-0.621320603074498,
15.0368049484103));
#52442=CARTESIAN_POINT('Ctrl Pts',(63.3773959101104,1.36798786760661,14.9256670578422));
#52443=CARTESIAN_POINT('Ctrl Pts',(65.2693134838344,2.10516158272269,14.8145291672742));
#52444=CARTESIAN_POINT('Ctrl Pts',(66.914725491569,0.91545692050249,14.7033912767062));
#52445=CARTESIAN_POINT('Ctrl Pts',(66.8075673043809,-1.11217563174233,14.5922533861381));
#52446=CARTESIAN_POINT('Ctrl Pts',(65.0459227364722,-2.12182163449126,14.4811154955701));
#52447=CARTESIAN_POINT('Ctrl Pts',(63.2422436303638,-1.18933940056681,14.3699776050021));
#52448=CARTESIAN_POINT('Ctrl Pts',(63.0474607219038,0.831757025163371,14.258839714434));
#52449=CARTESIAN_POINT('Ctrl Pts',(64.6398554717402,2.09154008533314,14.147701823866));
#52450=CARTESIAN_POINT('Ctrl Pts',(66.5619019052561,1.43690629417045,14.0365639332979));
#52451=CARTESIAN_POINT('Ctrl Pts',(67.0543073051464,-0.532931245964157,
13.9254260427299));
#52452=CARTESIAN_POINT('Ctrl Pts',(65.6664107088405,-2.01499631916359,13.8142881521618));
#52453=CARTESIAN_POINT('Ctrl Pts',(63.668483745015,-1.65266173185674,13.7031502615938));
#52454=CARTESIAN_POINT('Ctrl Pts',(62.889421959733,0.222272347729275,13.5920123710258));
#52455=CARTESIAN_POINT('Ctrl Pts',(64.0419715223154,1.89395746343366,13.4808744804577));
#52456=CARTESIAN_POINT('Ctrl Pts',(66.0718611861322,1.8316861713512,13.3697365898897));
#52457=CARTESIAN_POINT('Ctrl Pts',(67.1197788376878,0.093636985819607,13.2585986993216));
#52458=CARTESIAN_POINT('Ctrl Pts',(66.2292075511993,-1.73168095096,13.1474608087536));
#52459=CARTESIAN_POINT('Ctrl Pts',(64.2098730410853,-1.96882346147375,13.0363229181856));
#52460=CARTESIAN_POINT('Ctrl Pts',(63.3520968146026,-0.930071057176334,
12.9622309911402));
#52461=CARTESIAN_POINT('Ctrl Pts',(63.2376884946835,-0.344060554515606,
12.9251850276175));
#52462=CARTESIAN_POINT('Ctrl Pts',(64.5701357431142,-1.60958774866485,22.2244449171475));
#52463=CARTESIAN_POINT('Ctrl Pts',(64.0349095229901,-1.46664765635221,22.1873989536248));
#52464=CARTESIAN_POINT('Ctrl Pts',(63.1275700215111,-0.606976197009772,
22.1133070265794));
#52465=CARTESIAN_POINT('Ctrl Pts',(63.4747061016384,1.24728896623771,22.0021691360114));
#52466=CARTESIAN_POINT('Ctrl Pts',(65.2206441859093,1.95631351452272,21.8910312454434));
#52467=CARTESIAN_POINT('Ctrl Pts',(66.7632902393938,0.8764380368907,21.7798933548753));
#52468=CARTESIAN_POINT('Ctrl Pts',(66.692647660758,-1.00652025480984,21.6687554643073));
#52469=CARTESIAN_POINT('Ctrl Pts',(65.0723673984167,-1.9677614973903,21.5576175737392));
#52470=CARTESIAN_POINT('Ctrl Pts',(63.3860188510191,-1.12810889960266,21.4464796831712));
#52471=CARTESIAN_POINT('Ctrl Pts',(63.1768796488437,0.744225754056273,21.3353417926031));
#52472=CARTESIAN_POINT('Ctrl Pts',(64.6365064832399,1.93530608700317,21.2242039020351));
#52473=CARTESIAN_POINT('Ctrl Pts',(66.4288212268481,1.35500706394271,21.113066011467));
#52474=CARTESIAN_POINT('Ctrl Pts',(66.9133307013985,-0.46555953382498,21.001928120899));
#52475=CARTESIAN_POINT('Ctrl Pts',(65.6465413393799,-1.85998703107205,20.890790230331));
#52476=CARTESIAN_POINT('Ctrl Pts',(63.7879681533139,-1.55195092417241,20.7796523397629));
#52477=CARTESIAN_POINT('Ctrl Pts',(63.0387800523716,0.176605288292535,20.6685144491949));
#52478=CARTESIAN_POINT('Ctrl Pts',(64.0847195217704,1.74351175790307,20.5573765586268));
#52479=CARTESIAN_POINT('Ctrl Pts',(65.9684252347068,1.71456260631994,20.4462386680588));
#52480=CARTESIAN_POINT('Ctrl Pts',(66.965720528179,0.11625462302117,20.3351007774908));
#52481=CARTESIAN_POINT('Ctrl Pts',(66.163769438407,-1.58846241734545,20.2239628869227));
#52482=CARTESIAN_POINT('Ctrl Pts',(64.296607029498,-1.83924185210904,20.1128249963547));
#52483=CARTESIAN_POINT('Ctrl Pts',(63.0732681603805,-0.406542331281825,
20.0016871057866));
#52484=CARTESIAN_POINT('Ctrl Pts',(63.6134888063506,1.3982699807817,19.8905492152186));
#52485=CARTESIAN_POINT('Ctrl Pts',(65.4227988660973,1.92322992958215,19.7794113246506));
#52486=CARTESIAN_POINT('Ctrl Pts',(66.8451163318026,0.687835709090824,19.6682734340825));
#52487=CARTESIAN_POINT('Ctrl Pts',(66.5785778924731,-1.17714233458594,19.5571355435145));
#52488=CARTESIAN_POINT('Ctrl Pts',(64.8671492066249,-1.96466865068851,19.4459976529464));
#52489=CARTESIAN_POINT('Ctrl Pts',(63.277320358204,-0.953911469466806,19.3348597623784));
#52490=CARTESIAN_POINT('Ctrl Pts',(63.2642797226261,0.929971697602112,19.2237218718103));
#52491=CARTESIAN_POINT('Ctrl Pts',(64.8399635412389,1.96264122338426,19.1125839812423));
#52492=CARTESIAN_POINT('Ctrl Pts',(66.5621305455413,1.19888297947457,19.0014460906742));
#52493=CARTESIAN_POINT('Ctrl Pts',(66.8544617457199,-0.662226451774208,
18.8903082001062));
#52494=CARTESIAN_POINT('Ctrl Pts',(65.4493830790269,-1.91719250157128,18.7791703095382));
#52495=CARTESIAN_POINT('Ctrl Pts',(63.6329789837436,-1.41733051223035,18.6680324189701));
#52496=CARTESIAN_POINT('Ctrl Pts',(63.0678247277157,0.379830168572198,18.5568945284021));
#52497=CARTESIAN_POINT('Ctrl Pts',(64.271212410766,1.82932798851557,18.445756637834));
#52498=CARTESIAN_POINT('Ctrl Pts',(66.1416676392564,1.6044211545792,18.334618747266));
#52499=CARTESIAN_POINT('Ctrl Pts',(66.9671415301433,-0.089030557516416,
18.223480856698));
#52500=CARTESIAN_POINT('Ctrl Pts',(65.9920684695881,-1.70099159064233,18.1123429661299));
#52501=CARTESIAN_POINT('Ctrl Pts',(64.1089438879971,-1.75601573029652,18.0012050755619));
#52502=CARTESIAN_POINT('Ctrl Pts',(63.0414130709861,-0.203738757437529,
17.8900671849938));
#52503=CARTESIAN_POINT('Ctrl Pts',(63.7665990819878,1.53502261065873,17.7789292944258));
#52504=CARTESIAN_POINT('Ctrl Pts',(65.6207309409642,1.86876037487862,17.6677914038578));
#52505=CARTESIAN_POINT('Ctrl Pts',(66.906700730108,0.492000574788043,17.5566535132897));
#52506=CARTESIAN_POINT('Ctrl Pts',(66.4474457175273,-1.33509293107205,17.4455156227217));
#52507=CARTESIAN_POINT('Ctrl Pts',(64.6633272245428,-1.94016073613825,17.3343777321536));
#52508=CARTESIAN_POINT('Ctrl Pts',(63.1873691410633,-0.769377416497885,
17.2232398415856));
#52509=CARTESIAN_POINT('Ctrl Pts',(63.3705326394006,1.1056257777964,17.1121019510176));
#52510=CARTESIAN_POINT('Ctrl Pts',(65.0451660923113,1.96863715902441,17.0009640604495));
#52511=CARTESIAN_POINT('Ctrl Pts',(66.6784585087109,1.02973262273374,16.8898261698815));
#52512=CARTESIAN_POINT('Ctrl Pts',(66.7754388170738,-0.851697861107768,
16.7786882793134));
#52513=CARTESIAN_POINT('Ctrl Pts',(65.2473398413224,-1.95355963376578,16.6675503887454));
#52514=CARTESIAN_POINT('Ctrl Pts',(63.4928479037859,-1.2673061187666,16.5564124981773));
#52515=CARTESIAN_POINT('Ctrl Pts',(63.1178693721777,0.578927058971946,16.4452746076093));
#52516=CARTESIAN_POINT('Ctrl Pts',(64.4656263490358,1.89526173414732,16.3341367170413));
#52517=CARTESIAN_POINT('Ctrl Pts',(66.3025015888158,1.47684185034113,16.2229988264732));
#52518=CARTESIAN_POINT('Ctrl Pts',(66.9471823530099,-0.29334812763462,16.1118609359052));
#52519=CARTESIAN_POINT('Ctrl Pts',(65.8095850268849,-1.79503323753958,16.0007230453371));
#52520=CARTESIAN_POINT('Ctrl Pts',(63.9309653444512,-1.6537040681678,15.8895851547691));
#52521=CARTESIAN_POINT('Ctrl Pts',(63.0308452056851,0.00127918928536937,
15.778447264201));
#52522=CARTESIAN_POINT('Ctrl Pts',(63.9331147823537,1.65509158986659,15.667309373633));
#52523=CARTESIAN_POINT('Ctrl Pts',(65.8119164971145,1.79397988904509,15.556171483065));
#52524=CARTESIAN_POINT('Ctrl Pts',(66.9475618361337,0.290818049043361,15.4450335924969));
#52525=CARTESIAN_POINT('Ctrl Pts',(66.3005817360626,-1.47853284613194,15.3338957019289));
#52526=CARTESIAN_POINT('Ctrl Pts',(64.4631644305619,-1.89456586592116,15.2227578113608));
#52527=CARTESIAN_POINT('Ctrl Pts',(63.1171187956369,-0.5764812501353,15.1116199207928));
#52528=CARTESIAN_POINT('Ctrl Pts',(63.4944957086799,1.26926316652858,15.0004820302248));
#52529=CARTESIAN_POINT('Ctrl Pts',(65.2498777170288,1.95323666226352,14.8893441396567));
#52530=CARTESIAN_POINT('Ctrl Pts',(66.7765439285027,0.849390390991124,14.7782062490887));
#52531=CARTESIAN_POINT('Ctrl Pts',(66.6771191139918,-1.03191234184771,14.6670683585206));
#52532=CARTESIAN_POINT('Ctrl Pts',(65.0426085927299,-1.96869439442842,14.5559304679526));
#52533=CARTESIAN_POINT('Ctrl Pts',(63.3690970742208,-1.10350736975596,14.4447925773845));
#52534=CARTESIAN_POINT('Ctrl Pts',(63.1883712234789,0.771730934564724,14.3336546868165));
#52535=CARTESIAN_POINT('Ctrl Pts',(64.6658463169365,1.94059819863462,14.2225167962484));
#52536=CARTESIAN_POINT('Ctrl Pts',(66.4491828509713,1.33320790054559,14.1113789056804));
#52537=CARTESIAN_POINT('Ctrl Pts',(66.9060524269962,-0.494470760166863,
14.0002410151124));
#52538=CARTESIAN_POINT('Ctrl Pts',(65.6183173013013,-1.86957842914181,13.8891031245443));
#52539=CARTESIAN_POINT('Ctrl Pts',(63.764576369348,-1.53339273881653,13.7779652339763));
#52540=CARTESIAN_POINT('Ctrl Pts',(63.0417377741208,0.206231437128308,13.6668273434082));
#52541=CARTESIAN_POINT('Ctrl Pts',(64.111110348268,1.75727468366667,13.5556894528402));
#52542=CARTESIAN_POINT('Ctrl Pts',(65.9945073018589,1.69949737493169,13.4445515622722));
#52543=CARTESIAN_POINT('Ctrl Pts',(66.9667990218154,0.0868794087578594,
13.3334136717041));
#52544=CARTESIAN_POINT('Ctrl Pts',(66.1404983229023,-1.60670931320334,13.2222757811361));
#52545=CARTESIAN_POINT('Ctrl Pts',(64.2668947805903,-1.82673776589702,13.111137890568));
#52546=CARTESIAN_POINT('Ctrl Pts',(63.4710223937224,-0.862949857291932,
13.0370459635227));
#52547=CARTESIAN_POINT('Ctrl Pts',(63.3648706727485,-0.319230454628301,
13.));
#52548=CARTESIAN_POINT('Ctrl Pts',(63.3361634080255,0.000941845566869666,
21.3785196366098));
#52549=CARTESIAN_POINT('Ctrl Pts',(63.3350462116423,0.216826197428607,21.3641270219409));
#52550=CARTESIAN_POINT('Ctrl Pts',(63.3740367968513,0.432323693321034,21.349734407272));
#52551=CARTESIAN_POINT('Ctrl Pts',(63.4550073216056,0.630683367270934,21.3353417926031));
#52552=CARTESIAN_POINT('Ctrl Pts',(63.6634219269757,1.14125253170524,21.2982958290804));
#52553=CARTESIAN_POINT('Ctrl Pts',(64.1499642051078,1.5382793093542,21.2612498655578));
#52554=CARTESIAN_POINT('Ctrl Pts',(64.6919544681085,1.64007619433528,21.2242039020351));
#52555=CARTESIAN_POINT('Ctrl Pts',(65.2339447311093,1.74187307931635,21.1871579385124));
#52556=CARTESIAN_POINT('Ctrl Pts',(65.8313829789787,1.54844007162953,21.1501119749897));
#52557=CARTESIAN_POINT('Ctrl Pts',(66.2108536820051,1.14829580149151,21.113066011467));
#52558=CARTESIAN_POINT('Ctrl Pts',(66.5903243850316,0.748151531353484,21.0760200479444));
#52559=CARTESIAN_POINT('Ctrl Pts',(66.751827543215,0.141295998764253,21.0389740844217));
#52560=CARTESIAN_POINT('Ctrl Pts',(66.6214475619703,-0.394536350404874,
21.001928120899));
#52561=CARTESIAN_POINT('Ctrl Pts',(66.4910675807256,-0.930368699574004,
20.9648821573763));
#52562=CARTESIAN_POINT('Ctrl Pts',(66.0688044600528,-1.39517786532303,20.9278361938536));
#52563=CARTESIAN_POINT('Ctrl Pts',(65.5479107020387,-1.5762430970476,20.890790230331));
#52564=CARTESIAN_POINT('Ctrl Pts',(65.0270169440246,-1.75730832877217,20.8537442668083));
#52565=CARTESIAN_POINT('Ctrl Pts',(64.4074925486692,-1.65462962647229,20.8166983032856));
#52566=CARTESIAN_POINT('Ctrl Pts',(63.9728656675012,-1.31519757324486,20.7796523397629));
#52567=CARTESIAN_POINT('Ctrl Pts',(63.5773660666821,-1.00632288699472,20.7459414387119));
#52568=CARTESIAN_POINT('Ctrl Pts',(63.3349716882235,-0.501403518382676,
20.7122305376608));
#52569=CARTESIAN_POINT('Ctrl Pts',(63.3318013787731,0.000864016794202189,
20.6785196366098));
#52570=CARTESIAN_POINT('Ctrl Pts',(64.4698297828114,-1.98517432567172,22.));
#52571=CARTESIAN_POINT('Ctrl Pts',(64.4011635904062,-1.95974978038744,22.));
#52572=CARTESIAN_POINT('Ctrl Pts',(64.3342007656389,-1.93043577138037,22.));
#52573=CARTESIAN_POINT('Ctrl Pts',(64.2691302660868,-1.89752626078973,22.));
#52574=CARTESIAN_POINT('Ctrl Pts',(64.2022499741928,-1.86370144478953,22.));
#52575=CARTESIAN_POINT('Ctrl Pts',(64.1373679615241,-1.82607765547926,22.));
#52576=CARTESIAN_POINT('Ctrl Pts',(64.0747206099686,-1.78492942875554,22.));
#52577=CARTESIAN_POINT('Ctrl Pts',(64.0217852175793,-1.75016024101401,22.));
#52578=CARTESIAN_POINT('Ctrl Pts',(63.9704456655164,-1.71287362002848,22.));
#52579=CARTESIAN_POINT('Ctrl Pts',(63.9208673056513,-1.67321717698663,22.));
#52580=CARTESIAN_POINT('Ctrl Pts',(63.8988414814123,-1.65559929195053,22.));
#52581=CARTESIAN_POINT('Ctrl Pts',(63.8771635659827,-1.63751349743213,22.));
#52582=CARTESIAN_POINT('Ctrl Pts',(63.8558496107185,-1.61897201296707,22.));
#52583=CARTESIAN_POINT('Ctrl Pts',(63.8441378985453,-1.60878373366242,22.));
#52584=CARTESIAN_POINT('Ctrl Pts',(63.8325360961551,-1.59845785925709,22.));
#52585=CARTESIAN_POINT('Ctrl Pts',(63.8210470007987,-1.58799637542554,22.));
#52586=CARTESIAN_POINT('Ctrl Pts',(63.8104526359386,-1.57834959530466,22.));
#52587=CARTESIAN_POINT('Ctrl Pts',(63.7999526722266,-1.56858598843039,22.));
#52588=CARTESIAN_POINT('Ctrl Pts',(63.7895651937366,-1.55872256958869,22.));
#52589=CARTESIAN_POINT('Ctrl Pts',(63.7364801435476,-1.50831571822926,22.));
#52590=CARTESIAN_POINT('Ctrl Pts',(63.6862350752836,-1.45522053846986,22.));
#52591=CARTESIAN_POINT('Ctrl Pts',(63.6390486652555,-1.39969641403709,22.));
#52592=CARTESIAN_POINT('Ctrl Pts',(63.5922286928545,-1.34460347579517,22.));
#52593=CARTESIAN_POINT('Ctrl Pts',(63.5484195492904,-1.28711828832214,22.));
#52594=CARTESIAN_POINT('Ctrl Pts',(63.5078796466367,-1.22746999892659,22.));
#52595=CARTESIAN_POINT('Ctrl Pts',(63.474187130903,-1.17789659599779,22.));
#52596=CARTESIAN_POINT('Ctrl Pts',(63.4427533858128,-1.12682844545585,22.));
#52597=CARTESIAN_POINT('Ctrl Pts',(63.413754367488,-1.07439061084553,22.));
#52598=CARTESIAN_POINT('Ctrl Pts',(63.4016500392299,-1.05250280912221,22.));
#52599=CARTESIAN_POINT('Ctrl Pts',(63.3899702272242,-1.03037633270796,22.));
#52600=CARTESIAN_POINT('Ctrl Pts',(63.3787291685042,-1.0080201935721,22.));
#52601=CARTESIAN_POINT('Ctrl Pts',(63.3735259415771,-0.997672052170427,
22.));
#52602=CARTESIAN_POINT('Ctrl Pts',(63.3684167321672,-0.987274704411429,
22.));
#52603=CARTESIAN_POINT('Ctrl Pts',(63.3634030175311,-0.976829046022845,
22.));
#52604=CARTESIAN_POINT('Ctrl Pts',(63.358174016723,-0.965934856760109,22.));
#52605=CARTESIAN_POINT('Ctrl Pts',(63.3530525039999,-0.954995586455951,
22.));
#52606=CARTESIAN_POINT('Ctrl Pts',(63.3480415178783,-0.944016502304618,
22.));
#52607=CARTESIAN_POINT('Ctrl Pts',(63.3195013216542,-0.881484855151525,
22.));
#52608=CARTESIAN_POINT('Ctrl Pts',(63.2945220500079,-0.817619969382916,
22.));
#52609=CARTESIAN_POINT('Ctrl Pts',(63.273327165114,-0.752626219153232,22.));
#52610=CARTESIAN_POINT('Ctrl Pts',(63.2541166188605,-0.693717409257717,
22.));
#52611=CARTESIAN_POINT('Ctrl Pts',(63.2380153357376,-0.633880618069508,
22.));
#52612=CARTESIAN_POINT('Ctrl Pts',(63.2252264587662,-0.573263190512459,
22.));
#52613=CARTESIAN_POINT('Ctrl Pts',(63.2100966383573,-0.501550029564712,
22.));
#52614=CARTESIAN_POINT('Ctrl Pts',(63.199602249042,-0.428742773422565,22.));
#52615=CARTESIAN_POINT('Ctrl Pts',(63.1936681155555,-0.355264662039538,
22.));
#52616=CARTESIAN_POINT('Ctrl Pts',(63.1923616383022,-0.339087492895166,
22.));
#52617=CARTESIAN_POINT('Ctrl Pts',(63.1912764288138,-0.322877888063042,
22.));
#52618=CARTESIAN_POINT('Ctrl Pts',(63.1904120545576,-0.30664052888322,22.));
#52619=CARTESIAN_POINT('Ctrl Pts',(63.1895201663096,-0.289886316543617,
22.));
#52620=CARTESIAN_POINT('Ctrl Pts',(63.1888633864282,-0.273096407549196,
22.));
#52621=CARTESIAN_POINT('Ctrl Pts',(63.188441797465,-0.256310042477455,22.));
#52622=CARTESIAN_POINT('Ctrl Pts',(63.1867198704084,-0.187748247168369,
22.));
#52623=CARTESIAN_POINT('Ctrl Pts',(63.188909677006,-0.119158552195863,22.));
#52624=CARTESIAN_POINT('Ctrl Pts',(63.1948905827395,-0.050879356588759,
22.));
#52625=CARTESIAN_POINT('Ctrl Pts',(63.2008702728731,0.0173859614913684,
22.));
#52626=CARTESIAN_POINT('Ctrl Pts',(63.210639974989,0.085341978217158,22.));
#52627=CARTESIAN_POINT('Ctrl Pts',(63.2241287349543,0.152635471609117,22.));
#52628=CARTESIAN_POINT('Ctrl Pts',(63.2338917748096,0.201341880477173,22.));
#52629=CARTESIAN_POINT('Ctrl Pts',(63.2456041790461,0.24970094617825,22.));
#52630=CARTESIAN_POINT('Ctrl Pts',(63.2592532629239,0.297569075157063,22.));
#52631=CARTESIAN_POINT('Ctrl Pts',(63.2694917264659,0.333475960759386,22.));
#52632=CARTESIAN_POINT('Ctrl Pts',(63.2808201731862,0.369106450237582,22.));
#52633=CARTESIAN_POINT('Ctrl Pts',(63.2932371663357,0.404395756317229,22.));
#52634=CARTESIAN_POINT('Ctrl Pts',(63.2973637241668,0.416123503977368,22.));
#52635=CARTESIAN_POINT('Ctrl Pts',(63.3016073023584,0.427804353006757,22.));
#52636=CARTESIAN_POINT('Ctrl Pts',(63.3059672772102,0.439435804940296,22.));
#52637=CARTESIAN_POINT('Ctrl Pts',(63.3290918712259,0.501127124940676,22.));
#52638=CARTESIAN_POINT('Ctrl Pts',(63.3554889558721,0.561434936807572,22.));
#52639=CARTESIAN_POINT('Ctrl Pts',(63.3851084989831,0.620025088710617,22.));
#52640=CARTESIAN_POINT('Ctrl Pts',(63.4059501828543,0.66125183617762,22.));
#52641=CARTESIAN_POINT('Ctrl Pts',(63.4283882196152,0.701627610099956,22.));
#52642=CARTESIAN_POINT('Ctrl Pts',(63.4524155940489,0.741024631059141,22.));
#52643=CARTESIAN_POINT('Ctrl Pts',(63.4601281158537,0.753670639636949,22.));
#52644=CARTESIAN_POINT('Ctrl Pts',(63.4680055619147,0.766217427182377,22.));
#52645=CARTESIAN_POINT('Ctrl Pts',(63.4760443363961,0.778655072840915,22.));
#52646=CARTESIAN_POINT('Ctrl Pts',(63.510290079392,0.831640315514542,22.));
#52647=CARTESIAN_POINT('Ctrl Pts',(63.547391322875,0.882541662758466,22.));
#52648=CARTESIAN_POINT('Ctrl Pts',(63.5873138038049,0.931043840582933,22.));
#52649=CARTESIAN_POINT('Ctrl Pts',(63.6241208989844,0.975761108498468,22.));
#52650=CARTESIAN_POINT('Ctrl Pts',(63.6633266817943,1.01843913679488,22.));
#52651=CARTESIAN_POINT('Ctrl Pts',(63.7049257741094,1.05879788933142,22.));
#52652=CARTESIAN_POINT('Ctrl Pts',(63.7127105119291,1.06635051343316,22.));
#52653=CARTESIAN_POINT('Ctrl Pts',(63.7205791168681,1.07382181318669,22.));
#52654=CARTESIAN_POINT('Ctrl Pts',(63.7285300176229,1.08121113172718,22.));
#52655=CARTESIAN_POINT('Origin',(65.,0.,17.));
#52656=CARTESIAN_POINT('Origin',(65.,0.,12.));
#52657=CARTESIAN_POINT('Origin',(0.,0.,-2.));
#52658=CARTESIAN_POINT('',(-60.,-7.34788079488412E-15,22.));
#52659=CARTESIAN_POINT('Origin',(0.,0.,22.));
#52660=CARTESIAN_POINT('',(-60.,-7.34788079488412E-15,-2.));
#52661=CARTESIAN_POINT('',(-60.,-7.34788079488412E-15,-2.));
#52662=CARTESIAN_POINT('Origin',(0.,0.,-2.));
#52663=CARTESIAN_POINT('Origin',(0.,0.,-2.));
#52664=CARTESIAN_POINT('',(-70.,-8.57252759403147E-15,22.));
#52665=CARTESIAN_POINT('Origin',(0.,0.,22.));
#52666=CARTESIAN_POINT('',(-70.,-8.57252759403147E-15,-2.));
#52667=CARTESIAN_POINT('',(-70.,-8.57252759403147E-15,-2.));
#52668=CARTESIAN_POINT('Origin',(0.,0.,-2.));
#52669=CARTESIAN_POINT('Origin',(0.,0.,22.));
#52670=CARTESIAN_POINT('Origin',(0.,0.,-2.));
#52671=CARTESIAN_POINT('',(0.,0.,0.));
#52672=CARTESIAN_POINT('Origin',(53.1951359564886,14.3971354987959,15.5));
#52673=CARTESIAN_POINT('',(51.9326028526449,14.3970877066932,14.1934196736194));
#52674=CARTESIAN_POINT('',(51.9314232360955,14.3954626592386,14.0565803263806));
#52675=CARTESIAN_POINT('',(51.9306359564886,14.3971354987959,15.5));
#52676=CARTESIAN_POINT('',(52.2370198037663,15.2223467977324,14.));
#52677=CARTESIAN_POINT('Ctrl Pts',(51.9314232360955,14.3954626592386,14.0565803263806));
#52678=CARTESIAN_POINT('Ctrl Pts',(51.9340308380707,14.6945947257524,14.0377202175871));
#52679=CARTESIAN_POINT('Ctrl Pts',(52.0414421537953,14.9952702831595,14.0188601087935));
#52680=CARTESIAN_POINT('Ctrl Pts',(52.2370198037663,15.2223467977324,14.));
#52681=CARTESIAN_POINT('',(51.9306359564886,14.3971354987959,14.));
#52682=CARTESIAN_POINT('Origin',(53.1951359564886,14.3971354987959,14.));
#52683=CARTESIAN_POINT('',(51.9306359564886,14.3971354987959,13.));
#52684=CARTESIAN_POINT('',(51.9306359564886,14.3971354987959,15.5));
#52685=CARTESIAN_POINT('',(52.6278006430704,15.5272199611918,13.));
#52686=CARTESIAN_POINT('Origin',(53.1951359564886,14.3971354987959,13.));
#52687=CARTESIAN_POINT('',(53.7624712699068,13.2670510364,13.));
#52688=CARTESIAN_POINT('Origin',(53.1951359564886,14.3971354987959,13.));
#52689=CARTESIAN_POINT('Origin',(53.1951359564886,14.3971354987959,13.));
#52690=CARTESIAN_POINT('',(54.1550391816747,15.2234704396199,14.));
#52691=CARTESIAN_POINT('Origin',(53.1951359564886,14.3971354987959,14.));
#52692=CARTESIAN_POINT('Ctrl Pts',(54.1550492157916,15.2234767486837,14.));
#52693=CARTESIAN_POINT('Ctrl Pts',(53.8967914626893,15.5213134049997,14.024908160387));
#52694=CARTESIAN_POINT('Ctrl Pts',(53.487740680999,15.6908539055355,14.049816320774));
#52695=CARTESIAN_POINT('Ctrl Pts',(53.0948318338552,15.6595885868543,14.074724481161));
#52696=CARTESIAN_POINT('Ctrl Pts',(52.6820419543228,15.626741255404,14.1008929846199));
#52697=CARTESIAN_POINT('Ctrl Pts',(52.2870688888724,15.3722525873919,14.1270614880789));
#52698=CARTESIAN_POINT('Ctrl Pts',(52.0867822938008,15.0099588798403,14.1532299915378));
#52699=CARTESIAN_POINT('Ctrl Pts',(51.9842486685495,14.8244882185226,14.1666265522317));
#52700=CARTESIAN_POINT('Ctrl Pts',(51.9327378835252,14.6107643391081,14.1800231129255));
#52701=CARTESIAN_POINT('Ctrl Pts',(51.9326028526449,14.3970877066932,14.1934196736194));
#52702=CARTESIAN_POINT('Origin',(53.1951359564886,14.3971354987959,15.5));
#52703=CARTESIAN_POINT('',(51.9293004715569,14.396357843321,14.6934196736194));
#52704=CARTESIAN_POINT('',(51.9290361749446,14.3977594574901,14.5565803263806));
#52705=CARTESIAN_POINT('',(51.9306359564886,14.3971354987959,15.5));
#52706=CARTESIAN_POINT('Ctrl Pts',(51.9290361749446,14.3977594574901,14.5565803263806));
#52707=CARTESIAN_POINT('Ctrl Pts',(51.9288104788003,14.4349272053691,14.5542330751329));
#52708=CARTESIAN_POINT('Ctrl Pts',(51.9303086019301,14.4720763914416,14.5518858238852));
#52709=CARTESIAN_POINT('Ctrl Pts',(51.9335904462524,14.5090671744586,14.5495385726375));
#52710=CARTESIAN_POINT('Ctrl Pts',(51.9701783294547,14.9214616440634,14.5233700691785));
#52711=CARTESIAN_POINT('Ctrl Pts',(52.228466159159,15.3141680878373,14.4972015657196));
#52712=CARTESIAN_POINT('Ctrl Pts',(52.5926396873008,15.5111367764164,14.4710330622607));
#52713=CARTESIAN_POINT('Ctrl Pts',(52.9568132154426,15.7081054649956,14.4448645588018));
#52714=CARTESIAN_POINT('Ctrl Pts',(53.4268724420219,15.7093363983799,14.4186960553428));
#52715=CARTESIAN_POINT('Ctrl Pts',(53.7920269612472,15.514187779113,14.3925275518839));
#52716=CARTESIAN_POINT('Ctrl Pts',(54.1571814804725,15.3190391598462,14.366359048425));
#52717=CARTESIAN_POINT('Ctrl Pts',(54.417431292344,14.9275109879282,14.340190544966));
#52718=CARTESIAN_POINT('Ctrl Pts',(54.4560979757245,14.5153505128056,14.3140220415071));
#52719=CARTESIAN_POINT('Ctrl Pts',(54.4947646591051,14.103190037683,14.2878535380482));
#52720=CARTESIAN_POINT('Ctrl Pts',(54.3118482139948,13.6703972593558,14.2616850345893));
#52721=CARTESIAN_POINT('Ctrl Pts',(53.9893291901183,13.4106746119161,14.2355165311303));
#52722=CARTESIAN_POINT('Ctrl Pts',(53.6668101662417,13.1509519644765,14.2093480276714));
#52723=CARTESIAN_POINT('Ctrl Pts',(53.2046885635989,13.0642994479243,14.1831795242125));
#52724=CARTESIAN_POINT('Ctrl Pts',(52.8102658096442,13.1903246291658,14.1570110207536));
#52725=CARTESIAN_POINT('Ctrl Pts',(52.4158430556895,13.3163498104073,14.1308425172946));
#52726=CARTESIAN_POINT('Ctrl Pts',(52.089119150423,13.6550526894425,14.1046740138357));
#52727=CARTESIAN_POINT('Ctrl Pts',(51.976572074359,14.0527844617314,14.0785055103768));
#52728=CARTESIAN_POINT('Ctrl Pts',(51.9451396903252,14.163863827329,14.0711971157114));
#52729=CARTESIAN_POINT('Ctrl Pts',(51.9304127761573,14.2795473576308,14.063888721046));
#52730=CARTESIAN_POINT('Ctrl Pts',(51.9314232360955,14.3954626592386,14.0565803263806));
#52731=CARTESIAN_POINT('Ctrl Pts',(51.9326028526449,14.3970877066932,14.1934196736194));
#52732=CARTESIAN_POINT('Ctrl Pts',(51.9324741176125,14.1933737996841,14.2061916163845));
#52733=CARTESIAN_POINT('Ctrl Pts',(51.9790420088886,13.9897028365794,14.2189635591495));
#52734=CARTESIAN_POINT('Ctrl Pts',(52.0726123421383,13.8105984338676,14.2317355019146));
#52735=CARTESIAN_POINT('Ctrl Pts',(52.2643291102402,13.4436304425376,14.2579040053735));
#52736=CARTESIAN_POINT('Ctrl Pts',(52.6533627711367,13.1797932069689,14.2840725088324));
#52737=CARTESIAN_POINT('Ctrl Pts',(53.0652069371965,13.1373261840987,14.3102410122914));
#52738=CARTESIAN_POINT('Ctrl Pts',(53.4770511032563,13.0948591612284,14.3364095157503));
#52739=CARTESIAN_POINT('Ctrl Pts',(53.9117057744794,13.2737623510566,14.3625780192092));
#52740=CARTESIAN_POINT('Ctrl Pts',(54.174295890408,13.5938472660216,14.3887465226681));
#52741=CARTESIAN_POINT('Ctrl Pts',(54.4368860063367,13.9139321809865,14.4149150261271));
#52742=CARTESIAN_POINT('Ctrl Pts',(54.5274115669709,14.3751988210882,14.441083529586));
#52743=CARTESIAN_POINT('Ctrl Pts',(54.4052653400132,14.7707929840486,14.4672520330449));
#52744=CARTESIAN_POINT('Ctrl Pts',(54.2831191130554,15.1663871470091,14.4934205365038));
#52745=CARTESIAN_POINT('Ctrl Pts',(53.9483010985055,15.4963088328283,14.5195890399628));
#52746=CARTESIAN_POINT('Ctrl Pts',(53.550954854306,15.6126255371819,14.5457575434217));
#52747=CARTESIAN_POINT('Ctrl Pts',(53.1536086101064,15.7289422415355,14.5719260468806));
#52748=CARTESIAN_POINT('Ctrl Pts',(52.6937341362572,15.6316539644235,14.5980945503396));
#52749=CARTESIAN_POINT('Ctrl Pts',(52.3775410563803,15.3643818135364,14.6242630537985));
#52750=CARTESIAN_POINT('Ctrl Pts',(52.0990020785416,15.1289379773151,14.6473152604055));
#52751=CARTESIAN_POINT('Ctrl Pts',(51.9319612775611,14.7615849808525,14.6703674670124));
#52752=CARTESIAN_POINT('Ctrl Pts',(51.9293004715569,14.396357843321,14.6934196736194));
#52753=CARTESIAN_POINT('Origin',(53.1951359564886,14.3971354987959,15.5));
#52754=CARTESIAN_POINT('',(51.9308136275137,14.3982246453427,15.1934196736194));
#52755=CARTESIAN_POINT('',(51.932525975067,14.3974029423036,15.0565803263806));
#52756=CARTESIAN_POINT('',(51.9306359564886,14.3971354987959,15.5));
#52757=CARTESIAN_POINT('Ctrl Pts',(51.932525975067,14.3974029423036,15.0565803263806));
#52758=CARTESIAN_POINT('Ctrl Pts',(51.9321561072822,14.5888155966727,15.0445774292198));
#52759=CARTESIAN_POINT('Ctrl Pts',(51.9730705675611,14.7800782049927,15.0325745320589));
#52760=CARTESIAN_POINT('Ctrl Pts',(52.0560982976485,14.9508677919232,15.0205716348981));
#52761=CARTESIAN_POINT('Ctrl Pts',(52.2371138818755,15.323220219546,14.9944031314392));
#52762=CARTESIAN_POINT('Ctrl Pts',(52.6183020364058,15.5982603906742,14.9682346279803));
#52763=CARTESIAN_POINT('Ctrl Pts',(53.028733536876,15.6526576817852,14.9420661245214));
#52764=CARTESIAN_POINT('Ctrl Pts',(53.4391650373463,15.7070549728961,14.9158976210624));
#52765=CARTESIAN_POINT('Ctrl Pts',(53.8788398837565,15.5408093839899,14.8897291176035));
#52766=CARTESIAN_POINT('Ctrl Pts',(54.1506024967829,15.2284660841227,14.8635606141446));
#52767=CARTESIAN_POINT('Ctrl Pts',(54.4223651098093,14.9161227842554,14.8373921106856));
#52768=CARTESIAN_POINT('Ctrl Pts',(54.5262154894519,14.4576817734273,14.8112236072267));
#52769=CARTESIAN_POINT('Ctrl Pts',(54.4155861975138,14.0587161328242,14.7850551037678));
#52770=CARTESIAN_POINT('Ctrl Pts',(54.3049569055756,13.6597504922211,14.7588866003089));
#52771=CARTESIAN_POINT('Ctrl Pts',(53.9798479420568,13.320260221843,14.7327180968499));
#52772=CARTESIAN_POINT('Ctrl Pts',(53.5860414121493,13.1924713804069,14.706549593391));
#52773=CARTESIAN_POINT('Ctrl Pts',(53.1922348822418,13.0646825389707,14.6803810899321));
#52774=CARTESIAN_POINT('Ctrl Pts',(52.7297307859455,13.1485951264765,14.6542125864732));
#52775=CARTESIAN_POINT('Ctrl Pts',(52.4059227061476,13.4065926679472,14.6280440830142));
#52776=CARTESIAN_POINT('Ctrl Pts',(52.1111594252056,13.6414484561238,14.604222830803));
#52777=CARTESIAN_POINT('Ctrl Pts',(51.9313266688913,14.0205598299628,14.5804015785918));
#52778=CARTESIAN_POINT('Ctrl Pts',(51.9290361749446,14.3977594574901,14.5565803263806));
#52779=CARTESIAN_POINT('Ctrl Pts',(51.9293004715569,14.396357843321,14.6934196736194));
#52780=CARTESIAN_POINT('Ctrl Pts',(51.9289407723092,14.3469848614482,14.6965359704714));
#52781=CARTESIAN_POINT('Ctrl Pts',(51.9315850846113,14.2976507292224,14.6996522673233));
#52782=CARTESIAN_POINT('Ctrl Pts',(51.9373640512186,14.2486865756559,14.7027685641753));
#52783=CARTESIAN_POINT('Ctrl Pts',(51.985891811838,13.8375195133245,14.7289370676342));
#52784=CARTESIAN_POINT('Ctrl Pts',(52.2554590189813,13.452441413324,14.7551055710931));
#52785=CARTESIAN_POINT('Ctrl Pts',(52.6251876598399,13.2661248639499,14.781274074552));
#52786=CARTESIAN_POINT('Ctrl Pts',(52.9949163006986,13.0798083145759,14.807442578011));
#52787=CARTESIAN_POINT('Ctrl Pts',(53.4648063752726,13.0922533158284,14.8336110814699));
#52788=CARTESIAN_POINT('Ctrl Pts',(53.8241540209967,13.2978798810904,14.8597795849288));
#52789=CARTESIAN_POINT('Ctrl Pts',(54.1835016667209,13.5035064463524,14.8859480883877));
#52790=CARTESIAN_POINT('Ctrl Pts',(54.4323068835952,13.902314575624,14.9121165918467));
#52791=CARTESIAN_POINT('Ctrl Pts',(54.4590022406867,14.3154737155563,14.9382850953056));
#52792=CARTESIAN_POINT('Ctrl Pts',(54.4856975977781,14.7286328554886,14.9644535987645));
#52793=CARTESIAN_POINT('Ctrl Pts',(54.2902830950867,15.1561430060816,14.9906221022235));
#52794=CARTESIAN_POINT('Ctrl Pts',(53.9603850245763,15.4063036567383,15.0167906056824));
#52795=CARTESIAN_POINT('Ctrl Pts',(53.6304869540658,15.656464307395,15.0429591091413));
#52796=CARTESIAN_POINT('Ctrl Pts',(53.1661053157362,15.7292754581154,15.0691276126002));
#52797=CARTESIAN_POINT('Ctrl Pts',(52.7754743036767,15.592087662659,15.0952961160592));
#52798=CARTESIAN_POINT('Ctrl Pts',(52.3848432916172,15.4548998672026,15.1214646195181));
#52799=CARTESIAN_POINT('Ctrl Pts',(52.0679629058276,15.1077131255694,15.147633122977));
#52800=CARTESIAN_POINT('Ctrl Pts',(51.966926104032,14.7062101297548,15.1738016264359));
#52801=CARTESIAN_POINT('Ctrl Pts',(51.9416776248439,14.6058769852609,15.1803409754971));
#52802=CARTESIAN_POINT('Ctrl Pts',(51.9299079202419,14.502151956084,15.1868803245583));
#52803=CARTESIAN_POINT('Ctrl Pts',(51.9308136275137,14.3982246453427,15.1934196736194));
#52804=CARTESIAN_POINT('Origin',(53.1951359564886,14.3971354987959,15.5));
#52805=CARTESIAN_POINT('',(51.9321336144334,14.3964211293814,15.6934196736194));
#52806=CARTESIAN_POINT('',(51.9298800777713,14.396145855272,15.5565803263806));
#52807=CARTESIAN_POINT('',(51.9306359564886,14.3971354987959,15.5));
#52808=CARTESIAN_POINT('Ctrl Pts',(51.9298800777713,14.396145855272,15.5565803263806));
#52809=CARTESIAN_POINT('Ctrl Pts',(51.9328341793634,14.7397024926117,15.5349217833067));
#52810=CARTESIAN_POINT('Ctrl Pts',(52.0781516403077,15.0854616424501,15.5132632402327));
#52811=CARTESIAN_POINT('Ctrl Pts',(52.3278732854,15.32010983553,15.4916046971588));
#52812=CARTESIAN_POINT('Ctrl Pts',(52.6295944912569,15.6036188430973,15.4654361936999));
#52813=CARTESIAN_POINT('Ctrl Pts',(53.0837270081696,15.7249258591405,15.439267690241));
#52814=CARTESIAN_POINT('Ctrl Pts',(53.4866324184766,15.629635385456,15.413099186782));
#52815=CARTESIAN_POINT('Ctrl Pts',(53.8895378287836,15.5343449117715,15.3869306833231));
#52816=CARTESIAN_POINT('Ctrl Pts',(54.2412161324849,15.2224569483592,15.3607621798642));
#52817=CARTESIAN_POINT('Ctrl Pts',(54.3839705956172,14.8338257457023,15.3345936764052));
#52818=CARTESIAN_POINT('Ctrl Pts',(54.5267250587495,14.4451945430454,15.3084251729463));
#52819=CARTESIAN_POINT('Ctrl Pts',(54.460555681313,13.9798201011439,15.2822566694874));
#52820=CARTESIAN_POINT('Ctrl Pts',(54.2151336032284,13.6463818912608,15.2560881660285));
#52821=CARTESIAN_POINT('Ctrl Pts',(53.9697115251439,13.3129436813777,15.2299196625695));
#52822=CARTESIAN_POINT('Ctrl Pts',(53.5450367464114,13.111441703513,15.2037511591106));
#52823=CARTESIAN_POINT('Ctrl Pts',(53.1315384766945,13.1322317596502,15.1775826556517));
#52824=CARTESIAN_POINT('Ctrl Pts',(52.7180402069775,13.1530218157874,15.1514141521928));
#52825=CARTESIAN_POINT('Ctrl Pts',(52.3157184462761,13.3961039059265,15.1252456487338));
#52826=CARTESIAN_POINT('Ctrl Pts',(52.1049790728871,13.7524772930548,15.0990771452749));
#52827=CARTESIAN_POINT('Ctrl Pts',(51.99090105541,13.9453903155784,15.0849115389768));
#52828=CARTESIAN_POINT('Ctrl Pts',(51.9329624864653,14.1715011232728,15.0707459326787));
#52829=CARTESIAN_POINT('Ctrl Pts',(51.932525975067,14.3974029423036,15.0565803263806));
#52830=CARTESIAN_POINT('Ctrl Pts',(51.9308136275137,14.3982246453427,15.1934196736194));
#52831=CARTESIAN_POINT('Ctrl Pts',(51.9335322876909,14.0862661905168,15.2130488280172));
#52832=CARTESIAN_POINT('Ctrl Pts',(52.0504588679335,13.7724851395516,15.232677982415));
#52833=CARTESIAN_POINT('Ctrl Pts',(52.2598657119041,13.5431471347949,15.2523071368127));
#52834=CARTESIAN_POINT('Ctrl Pts',(52.5390353393737,13.2374063856457,15.2784756402716));
#52835=CARTESIAN_POINT('Ctrl Pts',(52.9825678121147,13.0817441373434,15.3046441437306));
#52836=CARTESIAN_POINT('Ctrl Pts',(53.3915779035484,13.1459611997424,15.3308126471895));
#52837=CARTESIAN_POINT('Ctrl Pts',(53.8005879949821,13.2101782621413,15.3569811506484));
#52838=CARTESIAN_POINT('Ctrl Pts',(54.1750757051085,13.4942746352416,15.3831496541074));
#52839=CARTESIAN_POINT('Ctrl Pts',(54.3471162900744,13.8708581246834,15.4093181575663));
#52840=CARTESIAN_POINT('Ctrl Pts',(54.5191568750402,14.2474416141252,15.4354866610252));
#52841=CARTESIAN_POINT('Ctrl Pts',(54.4887503348454,14.7165122199085,15.4616551644841));
#52842=CARTESIAN_POINT('Ctrl Pts',(54.2695313251181,15.0677331084555,15.4878236679431));
#52843=CARTESIAN_POINT('Ctrl Pts',(54.0503123153908,15.4189539970025,15.513992171402));
#52844=CARTESIAN_POINT('Ctrl Pts',(53.642280836131,15.6523251683133,15.5401606748609));
#52845=CARTESIAN_POINT('Ctrl Pts',(53.2284030520588,15.6632002142321,15.5663291783198));
#52846=CARTESIAN_POINT('Ctrl Pts',(52.8145252679866,15.6740752601509,15.5924976817788));
#52847=CARTESIAN_POINT('Ctrl Pts',(52.3948011791021,15.4624541806777,15.6186661852377));
#52848=CARTESIAN_POINT('Ctrl Pts',(52.1574400564301,15.1232303837968,15.6448346886966));
#52849=CARTESIAN_POINT('Ctrl Pts',(52.010543532722,14.9132937439633,15.6610296836709));
#52850=CARTESIAN_POINT('Ctrl Pts',(51.9334928433345,14.6544846908102,15.6772246786452));
#52851=CARTESIAN_POINT('Ctrl Pts',(51.9321336144334,14.3964211293814,15.6934196736194));
#52852=CARTESIAN_POINT('Origin',(53.1951359564886,14.3971354987959,15.5));
#52853=CARTESIAN_POINT('',(51.9286427349006,14.3970459914357,16.1934196736194));
#52854=CARTESIAN_POINT('',(51.9301690580704,14.3981838623804,16.0565803263806));
#52855=CARTESIAN_POINT('',(51.9306359564886,14.3971354987959,15.5));
#52856=CARTESIAN_POINT('Ctrl Pts',(51.9301690580704,14.3981838623804,16.0565803263806));
#52857=CARTESIAN_POINT('Ctrl Pts',(51.9294463895002,14.4798551199685,16.0514346408525));
#52858=CARTESIAN_POINT('Ctrl Pts',(51.9366958070815,14.5613987134005,16.0462889553244));
#52859=CARTESIAN_POINT('Ctrl Pts',(51.9523897974866,14.6412833003865,16.0411432697963));
#52860=CARTESIAN_POINT('Ctrl Pts',(52.0322019507863,15.0475382258844,16.0149747663373));
#52861=CARTESIAN_POINT('Ctrl Pts',(52.3304122644718,15.4108870194284,15.9888062628784));
#52862=CARTESIAN_POINT('Ctrl Pts',(52.7132996891177,15.5683997628469,15.9626377594195));
#52863=CARTESIAN_POINT('Ctrl Pts',(53.0961871137635,15.7259125062655,15.9364692559606));
#52864=CARTESIAN_POINT('Ctrl Pts',(53.5637516493698,15.6775891995586,15.9103007525016));
#52865=CARTESIAN_POINT('Ctrl Pts',(53.9063318003261,15.4450985880149,15.8841322490427));
#52866=CARTESIAN_POINT('Ctrl Pts',(54.2489119512824,15.2126079764712,15.8579637455838));
#52867=CARTESIAN_POINT('Ctrl Pts',(54.4665077175887,14.7959500600907,15.8317952421249));
#52868=CARTESIAN_POINT('Ctrl Pts',(54.4615465710813,14.3819592010216,15.8056267386659));
#52869=CARTESIAN_POINT('Ctrl Pts',(54.4565854245739,13.9679683419524,15.779458235207));
#52870=CARTESIAN_POINT('Ctrl Pts',(54.2290673652527,13.5566445401947,15.7532897317481));
#52871=CARTESIAN_POINT('Ctrl Pts',(53.8810141954492,13.3324302783772,15.7271212282891));
#52872=CARTESIAN_POINT('Ctrl Pts',(53.5329610256457,13.1082160165598,15.7009527248302));
#52873=CARTESIAN_POINT('Ctrl Pts',(53.0643727453599,13.0711112946827,15.6747842213713));
#52874=CARTESIAN_POINT('Ctrl Pts',(52.6853699093616,13.2377543099066,15.6486157179124));
#52875=CARTESIAN_POINT('Ctrl Pts',(52.3063670733632,13.4043973251305,15.6224472144534));
#52876=CARTESIAN_POINT('Ctrl Pts',(52.0169496816522,13.7747880774553,15.5962787109945));
#52877=CARTESIAN_POINT('Ctrl Pts',(51.9468959331972,14.1828389531634,15.5701102075356));
#52878=CARTESIAN_POINT('Ctrl Pts',(51.9348226546909,14.2531636963187,15.5656002471506));
#52879=CARTESIAN_POINT('Ctrl Pts',(51.9292649449293,14.324607025577,15.5610902867656));
#52880=CARTESIAN_POINT('Ctrl Pts',(51.9298800777713,14.396145855272,15.5565803263806));
#52881=CARTESIAN_POINT('Ctrl Pts',(51.9321336144334,14.3964211293814,15.6934196736194));
#52882=CARTESIAN_POINT('Ctrl Pts',(51.9312965483521,14.2374955401126,15.7033931821041));
#52883=CARTESIAN_POINT('Ctrl Pts',(51.9591660436084,14.0788526842429,15.7133666905887));
#52884=CARTESIAN_POINT('Ctrl Pts',(52.0171074139709,13.932081398796,15.7233401990734));
#52885=CARTESIAN_POINT('Ctrl Pts',(52.1691340506433,13.5469827249647,15.7495087025323));
#52886=CARTESIAN_POINT('Ctrl Pts',(52.5281854804477,13.2436118915905,15.7756772059913));
#52887=CARTESIAN_POINT('Ctrl Pts',(52.9332587743737,13.1580039865908,15.8018457094502));
#52888=CARTESIAN_POINT('Ctrl Pts',(53.3383320682997,13.072396081591,15.8280142129091));
#52889=CARTESIAN_POINT('Ctrl Pts',(53.7894272263473,13.2045511049655,15.854182716368));
#52890=CARTESIAN_POINT('Ctrl Pts',(54.0842678175164,13.4952091732588,15.880351219827));
#52891=CARTESIAN_POINT('Ctrl Pts',(54.3791084086854,13.7858672415521,15.9065197232859));
#52892=CARTESIAN_POINT('Ctrl Pts',(54.517694432976,14.2350283547642,15.9326882267448));
#52893=CARTESIAN_POINT('Ctrl Pts',(54.4378822697682,14.6412833306956,15.9588567302037));
#52894=CARTESIAN_POINT('Ctrl Pts',(54.3580701065605,15.047538306627,15.9850252336627));
#52895=CARTESIAN_POINT('Ctrl Pts',(54.0598597558545,15.4108871452777,16.0111937371216));
#52896=CARTESIAN_POINT('Ctrl Pts',(53.676972283676,15.5683999082504,16.0373622405805));
#52897=CARTESIAN_POINT('Ctrl Pts',(53.2940848114976,15.7259126712231,16.0635307440394));
#52898=CARTESIAN_POINT('Ctrl Pts',(52.8265202178467,15.6775893585178,16.0896992474984));
#52899=CARTESIAN_POINT('Ctrl Pts',(52.4839400243616,15.4450987181119,16.1158677509573));
#52900=CARTESIAN_POINT('Ctrl Pts',(52.1455210707975,15.2154320860769,16.1417183918447));
#52901=CARTESIAN_POINT('Ctrl Pts',(51.9290686466627,14.8060450268197,16.167569032732));
#52902=CARTESIAN_POINT('Ctrl Pts',(51.9286427349006,14.3970459914357,16.1934196736194));
#52903=CARTESIAN_POINT('Origin',(53.1951359564886,14.3971354987959,15.5));
#52904=CARTESIAN_POINT('',(51.9319412138059,14.397962888141,16.6934196736194));
#52905=CARTESIAN_POINT('',(51.9324421154971,14.3967173588992,16.5565803263806));
#52906=CARTESIAN_POINT('',(51.9306359564886,14.3971354987959,15.5));
#52907=CARTESIAN_POINT('Ctrl Pts',(51.9324421154971,14.3967173588992,16.5565803263806));
#52908=CARTESIAN_POINT('Ctrl Pts',(51.9331582847598,14.6327178878915,16.5417789949394));
#52909=CARTESIAN_POINT('Ctrl Pts',(51.9967468970028,14.8690767992861,16.5269776634981));
#52910=CARTESIAN_POINT('Ctrl Pts',(52.1207407212383,15.0677330252045,16.5121763320569));
#52911=CARTESIAN_POINT('Ctrl Pts',(52.339959703752,15.4189538701487,16.486007828598));
#52912=CARTESIAN_POINT('Ctrl Pts',(52.747991132356,15.652325012491,16.4598393251391));
#52913=CARTESIAN_POINT('Ctrl Pts',(53.1618688650479,15.6632000570604,16.4336708216802));
#52914=CARTESIAN_POINT('Ctrl Pts',(53.5757465977399,15.6740751016298,16.4075023182212));
#52915=CARTESIAN_POINT('Ctrl Pts',(53.9954706345197,15.4624540484263,16.3813338147623));
#52916=CARTESIAN_POINT('Ctrl Pts',(54.2328317277253,15.1232302936571,16.3551653113034));
#52917=CARTESIAN_POINT('Ctrl Pts',(54.470192820931,14.784006538888,16.3289968078444));
#52918=CARTESIAN_POINT('Ctrl Pts',(54.5251909705625,14.3171800825532,16.3028283043855));
#52919=CARTESIAN_POINT('Ctrl Pts',(54.3731643527629,13.9320814565291,16.2766598009266));
#52920=CARTESIAN_POINT('Ctrl Pts',(54.2211377349633,13.546982830505,16.2504912974677));
#52921=CARTESIAN_POINT('Ctrl Pts',(53.8620863497326,13.2436120347917,16.2243227940088));
#52922=CARTESIAN_POINT('Ctrl Pts',(53.4570131060934,13.1580041404195,16.1981542905498));
#52923=CARTESIAN_POINT('Ctrl Pts',(53.0519398624543,13.0723962460472,16.1719857870909));
#52924=CARTESIAN_POINT('Ctrl Pts',(52.6008447604067,13.204551253016,16.145817283632));
#52925=CARTESIAN_POINT('Ctrl Pts',(52.3060042058399,13.4952092852263,16.119648780173));
#52926=CARTESIAN_POINT('Ctrl Pts',(52.0691400952495,13.7287133104327,16.0986259622422));
#52927=CARTESIAN_POINT('Ctrl Pts',(51.9331215373257,14.0645140395593,16.0776031443114));
#52928=CARTESIAN_POINT('Ctrl Pts',(51.9301690580704,14.3981838623804,16.0565803263806));
#52929=CARTESIAN_POINT('Ctrl Pts',(51.9286427349006,14.3970459914357,16.1934196736194));
#52930=CARTESIAN_POINT('Ctrl Pts',(51.9286374978387,14.3920168903888,16.193737536191));
#52931=CARTESIAN_POINT('Ctrl Pts',(51.9286649228095,14.386987848009,16.1940553987625));
#52932=CARTESIAN_POINT('Ctrl Pts',(51.9287251846806,14.3819591991371,16.1943732613341));
#52933=CARTESIAN_POINT('Ctrl Pts',(51.9336863318039,13.9679682886746,16.220541764793));
#52934=CARTESIAN_POINT('Ctrl Pts',(52.1612044193698,13.5566444358558,16.2467102682519));
#52935=CARTESIAN_POINT('Ctrl Pts',(52.5092576323814,13.332430146203,16.2728787717108));
#52936=CARTESIAN_POINT('Ctrl Pts',(52.857310845393,13.1082158565502,16.2990472751698));
#52937=CARTESIAN_POINT('Ctrl Pts',(53.3258991838504,13.0711111300635,16.3252157786287));
#52938=CARTESIAN_POINT('Ctrl Pts',(53.7049020668992,13.2377541659764,16.3513842820876));
#52939=CARTESIAN_POINT('Ctrl Pts',(54.083904949948,13.4043972018893,16.3775527855466));
#52940=CARTESIAN_POINT('Ctrl Pts',(54.3733223775883,13.7747880002018,16.4037212890055));
#52941=CARTESIAN_POINT('Ctrl Pts',(54.4433761347398,14.1828389265634,16.4298897924644));
#52942=CARTESIAN_POINT('Ctrl Pts',(54.5134298918913,14.5908898529249,16.4560582959233));
#52943=CARTESIAN_POINT('Ctrl Pts',(54.3641199785539,15.0366009073353,16.4822267993823));
#52944=CARTESIAN_POINT('Ctrl Pts',(54.0623987352411,15.3201099501039,16.5083953028412));
#52945=CARTESIAN_POINT('Ctrl Pts',(53.7606774919283,15.6036189928724,16.5345638063001));
#52946=CARTESIAN_POINT('Ctrl Pts',(53.30654491864,15.724926023999,16.560732309759));
#52947=CARTESIAN_POINT('Ctrl Pts',(52.9036394583144,15.6296355384739,16.586900813218));
#52948=CARTESIAN_POINT('Ctrl Pts',(52.5007339979887,15.5343450529489,16.6130693166769));
#52949=CARTESIAN_POINT('Ctrl Pts',(52.1490556506257,15.2224570507722,16.6392378201358));
#52950=CARTESIAN_POINT('Ctrl Pts',(52.0063011697735,14.8338257998906,16.6654063235947));
#52951=CARTESIAN_POINT('Ctrl Pts',(51.9553616723993,14.6951493782073,16.6747441069363));
#52952=CARTESIAN_POINT('Ctrl Pts',(51.9310243942125,14.5467012595068,16.6840818902779));
#52953=CARTESIAN_POINT('Ctrl Pts',(51.9319412138059,14.397962888141,16.6934196736194));
#52954=CARTESIAN_POINT('Origin',(53.1951359564886,14.3971354987959,15.5));
#52955=CARTESIAN_POINT('',(51.9310991161132,14.3960665614756,17.1934196736194));
#52956=CARTESIAN_POINT('',(51.9288577112775,14.3966710926088,17.0565803263806));
#52957=CARTESIAN_POINT('',(51.9306359564886,14.3971354987959,15.5));
#52958=CARTESIAN_POINT('Ctrl Pts',(51.9288577112775,14.3966710926088,17.0565803263806));
#52959=CARTESIAN_POINT('Ctrl Pts',(51.9307115507732,14.783795951987,17.0321233490263));
#52960=CARTESIAN_POINT('Ctrl Pts',(52.121565621024,15.1725044294775,17.0076663716719));
#52961=CARTESIAN_POINT('Ctrl Pts',(52.4298869834431,15.406303531382,16.9832093943176));
#52962=CARTESIAN_POINT('Ctrl Pts',(52.7597850130333,15.6564641509158,16.9570408908587));
#52963=CARTESIAN_POINT('Ctrl Pts',(53.2241665936333,15.7292752927444,16.9308723873998));
#52964=CARTESIAN_POINT('Ctrl Pts',(53.6147975571804,15.5920875143541,16.9047038839408));
#52965=CARTESIAN_POINT('Ctrl Pts',(54.0054285207274,15.4548997359638,16.8785353804819));
#52966=CARTESIAN_POINT('Ctrl Pts',(54.3223088672216,15.1077130373545,16.852366877023));
#52967=CARTESIAN_POINT('Ctrl Pts',(54.4233456564843,14.706210091365,16.8261983735641));
#52968=CARTESIAN_POINT('Ctrl Pts',(54.524382445747,14.3047071453755,16.8000298701051));
#52969=CARTESIAN_POINT('Ctrl Pts',(54.4095756777782,13.8488879520058,16.7738613666462));
#52970=CARTESIAN_POINT('Ctrl Pts',(54.13040608496,13.5431472408216,16.7476928631873));
#52971=CARTESIAN_POINT('Ctrl Pts',(53.8512364921418,13.2374065296375,16.7215243597283));
#52972=CARTESIAN_POINT('Ctrl Pts',(53.4077040744743,13.0817443006388,16.6953558562694));
#52973=CARTESIAN_POINT('Ctrl Pts',(52.998694033819,13.1459613550608,16.6691873528105));
#52974=CARTESIAN_POINT('Ctrl Pts',(52.5896839931637,13.2101784094827,16.6430188493516));
#52975=CARTESIAN_POINT('Ctrl Pts',(52.2151963295206,13.4942747473253,16.6168503458927));
#52976=CARTESIAN_POINT('Ctrl Pts',(52.0431557659108,13.8708581900196,16.5906818424337));
#52977=CARTESIAN_POINT('Ctrl Pts',(51.9684241449892,14.0344399087392,16.579314670416));
#52978=CARTESIAN_POINT('Ctrl Pts',(51.9318921096253,14.2154729472068,16.5679474983983));
#52979=CARTESIAN_POINT('Ctrl Pts',(51.9324421154971,14.3967173588992,16.5565803263806));
#52980=CARTESIAN_POINT('Ctrl Pts',(51.9319412138059,14.397962888141,16.6934196736194));
#52981=CARTESIAN_POINT('Ctrl Pts',(51.9335937188396,14.1298720781913,16.7102503937368));
#52982=CARTESIAN_POINT('Ctrl Pts',(52.0172907607076,13.8608383066004,16.7270811138542));
#52983=CARTESIAN_POINT('Ctrl Pts',(52.1751381831274,13.6463817981057,16.7439118339715));
#52984=CARTESIAN_POINT('Ctrl Pts',(52.4205602916747,13.3129435467891,16.7700803374305));
#52985=CARTESIAN_POINT('Ctrl Pts',(52.8452351231106,13.1114415437426,16.7962488408894));
#52986=CARTESIAN_POINT('Ctrl Pts',(53.25873344417,13.1322316025356,16.8224173443483));
#52987=CARTESIAN_POINT('Ctrl Pts',(53.6722317652293,13.1530216613285,16.8485858478072));
#52988=CARTESIAN_POINT('Ctrl Pts',(54.0745535759121,13.3961037819609,16.8747543512662));
#52989=CARTESIAN_POINT('Ctrl Pts',(54.285292975442,13.7524772131894,16.9009228547251));
#52990=CARTESIAN_POINT('Ctrl Pts',(54.496032374972,14.108850644418,16.927091358184));
#52991=CARTESIAN_POINT('Ctrl Pts',(54.515189363349,14.5785153862427,16.9532598616429));
#52992=CARTESIAN_POINT('Ctrl Pts',(54.3341737566947,14.9508678603537,16.9794283651019));
#52993=CARTESIAN_POINT('Ctrl Pts',(54.1531581500404,15.3232203344646,17.0055968685608));
#52994=CARTESIAN_POINT('Ctrl Pts',(53.7719699483548,15.5982605408617,17.0317653720197));
#52995=CARTESIAN_POINT('Ctrl Pts',(53.3615383968383,15.652657838236,17.0579338754786));
#52996=CARTESIAN_POINT('Ctrl Pts',(52.9511068453218,15.7070551356103,17.0841023789376));
#52997=CARTESIAN_POINT('Ctrl Pts',(52.5114319439746,15.5408095239618,17.1102708823965));
#52998=CARTESIAN_POINT('Ctrl Pts',(52.2396692974107,15.2284661862235,17.1364393858554));
#52999=CARTESIAN_POINT('Ctrl Pts',(52.0424205472225,15.0017634594966,17.1554328151101));
#53000=CARTESIAN_POINT('Ctrl Pts',(51.9336286302043,14.6980958787159,17.1744262443648));
#53001=CARTESIAN_POINT('Ctrl Pts',(51.9310991161132,14.3960665614756,17.1934196736194));
#53002=CARTESIAN_POINT('Origin',(53.1951359564886,14.3971354987959,15.5));
#53003=CARTESIAN_POINT('',(51.929081218047,14.3977505022101,17.6934196736194));
#53004=CARTESIAN_POINT('',(51.9314271328212,14.3981451355535,17.5565803263806));
#53005=CARTESIAN_POINT('',(51.9306359564886,14.3971354987959,15.5));
#53006=CARTESIAN_POINT('',(54.1532521092111,15.2223467977324,18.));
#53007=CARTESIAN_POINT('Ctrl Pts',(51.929081218047,14.3977505022101,17.6934196736194));
#53008=CARTESIAN_POINT('Ctrl Pts',(51.9314396049108,14.022694300038,17.7171076053695));
#53009=CARTESIAN_POINT('Ctrl Pts',(52.1089957350005,13.6457772873263,17.7407955371196));
#53010=CARTESIAN_POINT('Ctrl Pts',(52.4009425562916,13.4106743694811,17.7644834688697));
#53011=CARTESIAN_POINT('Ctrl Pts',(52.7234616974046,13.1509517569817,17.7906519723286));
#53012=CARTESIAN_POINT('Ctrl Pts',(53.1855836521257,13.0642995791891,17.8168204757875));
#53013=CARTESIAN_POINT('Ctrl Pts',(53.5800062339574,13.190324595469,17.8429889792464));
#53014=CARTESIAN_POINT('Ctrl Pts',(53.974428815789,13.3163496117488,17.8691574827054));
#53015=CARTESIAN_POINT('Ctrl Pts',(54.3011520247311,13.6550518221011,17.8953259861643));
#53016=CARTESIAN_POINT('Ctrl Pts',(54.4136991111698,14.0527836440546,17.9214944896232));
#53017=CARTESIAN_POINT('Ctrl Pts',(54.5262461976084,14.4505154660081,17.9476629930821));
#53018=CARTESIAN_POINT('Ctrl Pts',(54.4246171615437,14.9072768995628,17.9738314965411));
#53019=CARTESIAN_POINT('Ctrl Pts',(54.1532521092111,15.2223467977324,18.));
#53020=CARTESIAN_POINT('',(52.2352328551172,15.2234705191483,18.));
#53021=CARTESIAN_POINT('Origin',(53.1951359564886,14.3971354987959,18.));
#53022=CARTESIAN_POINT('Ctrl Pts',(52.2352228301846,15.2234768233202,18.));
#53023=CARTESIAN_POINT('Ctrl Pts',(52.4934806168631,15.521313638849,17.975091839613));
#53024=CARTESIAN_POINT('Ctrl Pts',(52.9025313044196,15.6908537017463,17.950183679226));
#53025=CARTESIAN_POINT('Ctrl Pts',(53.295440078112,15.6595882927142,17.925275518839));
#53026=CARTESIAN_POINT('Ctrl Pts',(53.7082298804764,15.6267408663411,17.8991070153801));
#53027=CARTESIAN_POINT('Ctrl Pts',(54.1032028915872,15.3722524867281,17.8729385119211));
#53028=CARTESIAN_POINT('Ctrl Pts',(54.3034894678616,15.0099588806278,17.8467700084622));
#53029=CARTESIAN_POINT('Ctrl Pts',(54.5037760441361,14.6476652745274,17.8206015050033));
#53030=CARTESIAN_POINT('Ctrl Pts',(54.5093761855741,14.1775664419396,17.7944330015443));
#53031=CARTESIAN_POINT('Ctrl Pts',(54.3176594419829,13.8105984641279,17.7682644980854));
#53032=CARTESIAN_POINT('Ctrl Pts',(54.1259426983917,13.4436304863162,17.7420959946265));
#53033=CARTESIAN_POINT('Ctrl Pts',(53.7369090697714,13.1797933632805,17.7159274911676));
#53034=CARTESIAN_POINT('Ctrl Pts',(53.3250649526276,13.1373263636934,17.6897589877086));
#53035=CARTESIAN_POINT('Ctrl Pts',(52.9132208354839,13.0948593641063,17.6635904842497));
#53036=CARTESIAN_POINT('Ctrl Pts',(52.4785662298169,13.2737624879677,17.6374219807908));
#53037=CARTESIAN_POINT('Ctrl Pts',(52.2159761485057,13.5938473532064,17.6112534773319));
#53038=CARTESIAN_POINT('Ctrl Pts',(52.0331020154043,13.8167622552358,17.5930290936814));
#53039=CARTESIAN_POINT('Ctrl Pts',(51.9336803654542,14.1081512772947,17.574804710031));
#53040=CARTESIAN_POINT('Ctrl Pts',(51.9314271328212,14.3981451355535,17.5565803263806));
#53041=CARTESIAN_POINT('Origin',(53.1951359564886,14.3971354987959,19.1042117235887));
#53042=CARTESIAN_POINT('',(51.6501838308085,14.3978968813702,14.3957882764113));
#53043=CARTESIAN_POINT('',(51.654536051996,14.3970771807141,14.3542117235887));
#53044=CARTESIAN_POINT('',(51.6521359564886,14.397135498796,19.1042117235887));
#53045=CARTESIAN_POINT('',(53.5936497983458,12.9064860705774,14.));
#53046=CARTESIAN_POINT('Ctrl Pts',(51.654536051996,14.3970771807141,14.3542117235887));
#53047=CARTESIAN_POINT('Ctrl Pts',(51.6547008227736,14.6578150564091,14.3408151628949));
#53048=CARTESIAN_POINT('Ctrl Pts',(51.8403375140876,15.4280419867602,14.3012500987421));
#53049=CARTESIAN_POINT('Ctrl Pts',(53.0509994556171,16.2080945317645,14.2355165311303));
#53050=CARTESIAN_POINT('Ctrl Pts',(54.6273366519326,15.5169696210012,14.1570110207535));
#53051=CARTESIAN_POINT('Ctrl Pts',(54.9168336227569,13.8187144824051,14.0785055103768));
#53052=CARTESIAN_POINT('Ctrl Pts',(54.0838395965459,13.0375346028627,14.0261685034589));
#53053=CARTESIAN_POINT('Ctrl Pts',(53.5936497983458,12.9064860705774,14.));
#53054=CARTESIAN_POINT('',(52.7955932879501,12.9041246312965,14.));
#53055=CARTESIAN_POINT('Origin',(53.1951359564886,14.3971354987959,14.));
#53056=CARTESIAN_POINT('Ctrl Pts',(51.6501838308085,14.3978968813702,14.3957882764113));
#53057=CARTESIAN_POINT('Ctrl Pts',(51.6499084261818,14.443250645686,14.3934410251636));
#53058=CARTESIAN_POINT('Ctrl Pts',(51.6721169602754,14.9939590280816,14.3649252704569));
#53059=CARTESIAN_POINT('Ctrl Pts',(52.3307362917628,15.9953382094595,14.3102410122914));
#53060=CARTESIAN_POINT('Ctrl Pts',(54.0514987748276,15.9998443309588,14.2317355019146));
#53061=CARTESIAN_POINT('Ctrl Pts',(55.0042044918326,14.5665632650764,14.1532299915378));
#53062=CARTESIAN_POINT('Ctrl Pts',(54.3453458049291,13.0076586982508,14.0759848242329));
#53063=CARTESIAN_POINT('Ctrl Pts',(53.2607152655111,12.7814238100544,14.024908160387));
#53064=CARTESIAN_POINT('Ctrl Pts',(52.7955875161457,12.9041113834231,14.));
#53065=CARTESIAN_POINT('Origin',(53.1951359564886,14.3971354987959,19.1042117235887));
#53066=CARTESIAN_POINT('',(51.654442242504,14.3974618454408,14.8957882764113));
#53067=CARTESIAN_POINT('',(51.6505063374695,14.3961865684695,14.8542117235887));
#53068=CARTESIAN_POINT('',(51.6521359564886,14.397135498796,19.1042117235887));
#53069=CARTESIAN_POINT('Ctrl Pts',(51.6505063374695,14.3961865684695,14.8542117235887));
#53070=CARTESIAN_POINT('Ctrl Pts',(51.6537531731077,14.8418532139508,14.8311595169817));
#53071=CARTESIAN_POINT('Ctrl Pts',(52.0889693478695,15.798972462477,14.7819388069158));
#53072=CARTESIAN_POINT('Ctrl Pts',(53.7056220123855,16.1409817745025,14.706549593391));
#53073=CARTESIAN_POINT('Ctrl Pts',(54.9313021937626,14.9332257573755,14.6280440830142));
#53074=CARTESIAN_POINT('Ctrl Pts',(54.5999120631369,13.2446506074896,14.5495385726375));
#53075=CARTESIAN_POINT('Ctrl Pts',(53.0087562916135,12.5897333550461,14.4710330622607));
#53076=CARTESIAN_POINT('Ctrl Pts',(51.8276307116252,13.3907563492144,14.4059241125778));
#53077=CARTESIAN_POINT('Ctrl Pts',(51.6543789636963,14.148496272438,14.3669836663538));
#53078=CARTESIAN_POINT('Ctrl Pts',(51.654536051996,14.3970771807141,14.3542117235887));
#53079=CARTESIAN_POINT('Ctrl Pts',(51.654442242504,14.3974618454408,14.8957882764113));
#53080=CARTESIAN_POINT('Ctrl Pts',(51.6539909131311,14.6310322097678,14.8837853792505));
#53081=CARTESIAN_POINT('Ctrl Pts',(51.8127636494607,15.3732462698704,14.8456139786307));
#53082=CARTESIAN_POINT('Ctrl Pts',(52.9564001587445,16.1984187666638,14.781274074552));
#53083=CARTESIAN_POINT('Ctrl Pts',(54.5659334636339,15.5898376428623,14.7027685641752));
#53084=CARTESIAN_POINT('Ctrl Pts',(54.9461022318155,13.911606374279,14.6242630537985));
#53085=CARTESIAN_POINT('Ctrl Pts',(53.7559643179138,12.6688223002735,14.5457575434217));
#53086=CARTESIAN_POINT('Ctrl Pts',(52.1134816424644,12.9668195987494,14.4695992842926));
#53087=CARTESIAN_POINT('Ctrl Pts',(51.6529787949523,13.9376208629641,14.4196095286225));
#53088=CARTESIAN_POINT('Ctrl Pts',(51.6501838308085,14.3978968813702,14.3957882764113));
#53089=CARTESIAN_POINT('Origin',(53.1951359564886,14.3971354987959,19.1042117235887));
#53090=CARTESIAN_POINT('',(51.6512135991451,14.3959278910795,15.3957882764113));
#53091=CARTESIAN_POINT('',(51.6523527586964,14.3984645245941,15.3542117235887));
#53092=CARTESIAN_POINT('',(51.6521359564886,14.397135498796,19.1042117235887));
#53093=CARTESIAN_POINT('Ctrl Pts',(51.6523527586964,14.3984645245941,15.3542117235887));
#53094=CARTESIAN_POINT('Ctrl Pts',(51.651247573785,14.5252813221218,15.3476723745276));
#53095=CARTESIAN_POINT('Ctrl Pts',(51.7230815929517,15.1583461258636,15.3149645220075));
#53096=CARTESIAN_POINT('Ctrl Pts',(52.5930520129352,16.1115202855033,15.2560881660285));
#53097=CARTESIAN_POINT('Ctrl Pts',(54.2930303473182,15.8449779235543,15.1775826556517));
#53098=CARTESIAN_POINT('Ctrl Pts',(55.0083911483926,14.2799763521069,15.0990771452749));
#53099=CARTESIAN_POINT('Ctrl Pts',(54.0975810662168,12.8200452881305,15.0205716348981));
#53100=CARTESIAN_POINT('Ctrl Pts',(52.3774378038973,12.7744874306393,14.9420661245214));
#53101=CARTESIAN_POINT('Ctrl Pts',(51.6803897960552,13.7702239867045,14.8866128207515));
#53102=CARTESIAN_POINT('Ctrl Pts',(51.6500674162048,14.3359394264926,14.8573280204407));
#53103=CARTESIAN_POINT('Ctrl Pts',(51.6505063374695,14.3961865684695,14.8542117235887));
#53104=CARTESIAN_POINT('Ctrl Pts',(51.6512135991451,14.3959278910795,15.3957882764113));
#53105=CARTESIAN_POINT('Ctrl Pts',(51.6548183273038,14.8151512136696,15.3741297333373));
#53106=CARTESIAN_POINT('Ctrl Pts',(52.0463881522717,15.7468276199562,15.3263026868045));
#53107=CARTESIAN_POINT('Ctrl Pts',(53.6133427309768,16.1653895531783,15.2523071368127));
#53108=CARTESIAN_POINT('Ctrl Pts',(54.9007439708605,15.0236502232965,15.1738016264359));
#53109=CARTESIAN_POINT('Ctrl Pts',(54.6585153839456,13.3200374976642,15.0952961160592));
#53110=CARTESIAN_POINT('Ctrl Pts',(53.1038933588347,12.5823920603089,15.0167906056824));
#53111=CARTESIAN_POINT('Ctrl Pts',(51.8562787823209,13.3361985618968,14.9502879924664));
#53112=CARTESIAN_POINT('Ctrl Pts',(51.6549748934233,14.1218062449943,14.9099538827094));
#53113=CARTESIAN_POINT('Ctrl Pts',(51.654442242504,14.3974618454408,14.8957882764113));
#53114=CARTESIAN_POINT('Origin',(53.1951359564886,14.3971354987959,19.1042117235887));
#53115=CARTESIAN_POINT('',(51.6515662259554,14.3984147593818,15.8957882764113));
#53116=CARTESIAN_POINT('',(51.6539634663413,14.3962637929782,15.8542117235887));
#53117=CARTESIAN_POINT('',(51.6521359564886,14.397135498796,19.1042117235887));
#53118=CARTESIAN_POINT('Ctrl Pts',(51.6539634663413,14.3962637929782,15.8542117235887));
#53119=CARTESIAN_POINT('Ctrl Pts',(51.6556220588242,14.7111646038003,15.8380167286145));
#53120=CARTESIAN_POINT('Ctrl Pts',(51.9015651465378,15.5372739892809,15.7956532301813));
#53121=CARTESIAN_POINT('Ctrl Pts',(53.2428638938474,16.2135446545079,15.7271212282891));
#53122=CARTESIAN_POINT('Ctrl Pts',(54.7365592022647,15.3592345303502,15.6486157179124));
#53123=CARTESIAN_POINT('Ctrl Pts',(54.8478695024322,13.6420911264981,15.5701102075356));
#53124=CARTESIAN_POINT('Ctrl Pts',(53.4769690594307,12.6020894569994,15.4916046971588));
#53125=CARTESIAN_POINT('Ctrl Pts',(51.9885611628802,13.1244613999964,15.4196385358432));
#53126=CARTESIAN_POINT('Ctrl Pts',(51.6556701906089,14.0177987311608,15.3738408779865));
#53127=CARTESIAN_POINT('Ctrl Pts',(51.6523527586964,14.3984645245941,15.3542117235887));
#53128=CARTESIAN_POINT('Ctrl Pts',(51.6515662259554,14.3984147593818,15.8957882764113));
#53129=CARTESIAN_POINT('Ctrl Pts',(51.6506843931331,14.4980737158535,15.8906425908832));
#53130=CARTESIAN_POINT('Ctrl Pts',(51.7045173377561,15.1036026015034,15.8593284018961));
#53131=CARTESIAN_POINT('Ctrl Pts',(52.503850750664,16.077535486755,15.8018457094502));
#53132=CARTESIAN_POINT('Ctrl Pts',(54.2154808300007,15.9006366439348,15.7233401990734));
#53133=CARTESIAN_POINT('Ctrl Pts',(55.0120413695279,14.3753622311824,15.6448346886966));
#53134=CARTESIAN_POINT('Ctrl Pts',(54.1791579400318,12.8696146010229,15.5663291783198));
#53135=CARTESIAN_POINT('Ctrl Pts',(52.4637802022359,12.7337840295962,15.4878236679431));
#53136=CARTESIAN_POINT('Ctrl Pts',(51.6965951513912,13.7156125454117,15.4309767006402));
#53137=CARTESIAN_POINT('Ctrl Pts',(51.6504629862743,14.3086329806648,15.4002982367963));
#53138=CARTESIAN_POINT('Ctrl Pts',(51.6512135991451,14.3959278910795,15.3957882764113));
#53139=CARTESIAN_POINT('Origin',(53.1951359564886,14.3971354987959,19.1042117235887));
#53140=CARTESIAN_POINT('',(51.65433991327,14.3966252656123,16.3957882764113));
#53141=CARTESIAN_POINT('',(51.6497037375007,14.3970262778732,16.3542117235887));
#53142=CARTESIAN_POINT('',(51.6521359564886,14.397135498796,19.1042117235887));
#53143=CARTESIAN_POINT('Ctrl Pts',(51.6497037375007,14.3970262778732,16.3542117235887));
#53144=CARTESIAN_POINT('Ctrl Pts',(51.6502234542653,14.8961053696862,16.3283610827013));
#53145=CARTESIAN_POINT('Ctrl Pts',(52.1817212113122,15.9013530800272,16.2763419383551));
#53146=CARTESIAN_POINT('Ctrl Pts',(53.8864212481313,16.0775356953633,16.1981542905498));
#53147=CARTESIAN_POINT('Ctrl Pts',(54.9780904560539,14.7474117142528,16.119648780173));
#53148=CARTESIAN_POINT('Ctrl Pts',(54.4707636814861,13.1031516960174,16.0411432697963));
#53149=CARTESIAN_POINT('Ctrl Pts',(52.8194236367236,12.6193671146013,15.9626377594195));
#53150=CARTESIAN_POINT('Ctrl Pts',(51.7761788820818,13.5008286667841,15.900327244017));
#53151=CARTESIAN_POINT('Ctrl Pts',(51.6529420405103,14.2023356124785,15.8641852320734));
#53152=CARTESIAN_POINT('Ctrl Pts',(51.6539634663413,14.3962637929782,15.8542117235887));
#53153=CARTESIAN_POINT('Ctrl Pts',(51.65433991327,14.3966252656123,16.3957882764113));
#53154=CARTESIAN_POINT('Ctrl Pts',(51.6552138153438,14.684603767973,16.38098694497));
#53155=CARTESIAN_POINT('Ctrl Pts',(51.869991852728,15.4829338669789,16.3400171100699));
#53156=CARTESIAN_POINT('Ctrl Pts',(53.1474080250528,16.2135444290179,16.2728787717109));
#53157=CARTESIAN_POINT('Ctrl Pts',(54.6839066935017,15.4388557336608,16.1943732613341));
#53158=CARTESIAN_POINT('Ctrl Pts',(54.8852403705633,13.7299275672916,16.1158677509573));
#53159=CARTESIAN_POINT('Ctrl Pts',(53.5708482296119,12.6193673352972,16.0373622405805));
#53160=CARTESIAN_POINT('Ctrl Pts',(52.0277463399597,13.0714419423033,15.9640024157318));
#53161=CARTESIAN_POINT('Ctrl Pts',(51.6551689744653,13.9912557743182,15.9168110943421));
#53162=CARTESIAN_POINT('Ctrl Pts',(51.6515662259554,14.3984147593818,15.8957882764113));
#53163=CARTESIAN_POINT('Origin',(53.1951359564886,14.3971354987959,19.1042117235887));
#53164=CARTESIAN_POINT('',(51.6499660613832,14.3965688093956,16.8957882764113));
#53165=CARTESIAN_POINT('',(51.6537286904076,14.3981451166365,16.8542117235887));
#53166=CARTESIAN_POINT('',(51.6521359564886,14.397135498796,19.1042117235887));
#53167=CARTESIAN_POINT('Ctrl Pts',(51.6537286904076,14.3981451166365,16.8542117235887));
#53168=CARTESIAN_POINT('Ctrl Pts',(51.6526099457397,14.579642393835,16.8448739402472));
#53169=CARTESIAN_POINT('Ctrl Pts',(51.7655324660037,15.2684267173499,16.8093676534467));
#53170=CARTESIAN_POINT('Ctrl Pts',(52.7769291300874,16.1653897727513,16.7476928631873));
#53171=CARTESIAN_POINT('Ctrl Pts',(54.4393883485545,15.72131682132,16.6691873528105));
#53172=CARTESIAN_POINT('Ctrl Pts',(54.9859724441168,14.0896865557083,16.5906818424337));
#53173=CARTESIAN_POINT('Ctrl Pts',(53.9264918015332,12.7337838230954,16.5121763320569));
#53174=CARTESIAN_POINT('Ctrl Pts',(52.2111138507866,12.869614411397,16.4336708216802));
#53175=CARTESIAN_POINT('Ctrl Pts',(51.6524858829683,13.8795429426784,16.3810159521908));
#53176=CARTESIAN_POINT('Ctrl Pts',(51.6496973470012,14.3908895416808,16.3545295861603));
#53177=CARTESIAN_POINT('Ctrl Pts',(51.6497037375007,14.3970262778732,16.3542117235887));
#53178=CARTESIAN_POINT('Ctrl Pts',(51.6499660613832,14.3965688093956,16.8957882764113));
#53179=CARTESIAN_POINT('Ctrl Pts',(51.6522282000482,14.8689560438919,16.8713312990569));
#53180=CARTESIAN_POINT('Ctrl Pts',(52.1343035201105,15.8507887260607,16.8207058182437));
#53181=CARTESIAN_POINT('Ctrl Pts',(53.7972198251956,16.11152007286,16.7439118339715));
#53182=CARTESIAN_POINT('Ctrl Pts',(54.9572349488979,14.8405614110472,16.6654063235948));
#53183=CARTESIAN_POINT('Ctrl Pts',(54.5369577413632,13.1719279226262,16.586900813218));
#53184=CARTESIAN_POINT('Ctrl Pts',(52.9133028885494,12.602089679815,16.5083953028412));
#53185=CARTESIAN_POINT('Ctrl Pts',(51.8008704508192,13.4460106212472,16.4446911239056));
#53186=CARTESIAN_POINT('Ctrl Pts',(51.6536687712691,14.1754626501585,16.407155448429));
#53187=CARTESIAN_POINT('Ctrl Pts',(51.65433991327,14.3966252656123,16.3957882764113));
#53188=CARTESIAN_POINT('Origin',(53.1951359564886,14.3971354987959,19.1042117235887));
#53189=CARTESIAN_POINT('',(51.6531013855762,14.3983675031589,17.3957882764113));
#53190=CARTESIAN_POINT('',(51.6527011247771,14.3958311332086,17.3542117235887));
#53191=CARTESIAN_POINT('',(51.6521359564886,14.397135498796,19.1042117235887));
#53192=CARTESIAN_POINT('Ctrl Pts',(51.6527011247771,14.3958311332086,17.3542117235887));
#53193=CARTESIAN_POINT('Ctrl Pts',(51.6557877520943,14.7643809445978,17.3352182943341));
#53194=CARTESIAN_POINT('Ctrl Pts',(51.9714428864125,15.6454595543576,17.2900563616205));
#53195=CARTESIAN_POINT('Ctrl Pts',(53.4338717842849,16.1984189929661,17.2187259254479));
#53196=CARTESIAN_POINT('Ctrl Pts',(54.8293009543941,15.1915695541269,17.1402204150712));
#53197=CARTESIAN_POINT('Ctrl Pts',(54.7591722875712,13.4722511753948,17.0617149046944));
#53198=CARTESIAN_POINT('Ctrl Pts',(53.2863785654276,12.582391834622,16.9832093943176));
#53199=CARTESIAN_POINT('Ctrl Pts',(51.9166698060744,13.232298629585,16.9140416672824));
#53200=CARTESIAN_POINT('Ctrl Pts',(51.6557451516705,14.0710086043769,16.8710424437061));
#53201=CARTESIAN_POINT('Ctrl Pts',(51.6537286904076,14.3981451166365,16.8542117235887));
#53202=CARTESIAN_POINT('Ctrl Pts',(51.6531013855762,14.3983675031589,17.3957882764113));
#53203=CARTESIAN_POINT('Ctrl Pts',(51.6519028634372,14.5526188015874,17.3878441566028));
#53204=CARTESIAN_POINT('Ctrl Pts',(51.7435010772427,15.2135959185484,17.3537315333353));
#53205=CARTESIAN_POINT('Ctrl Pts',(52.6846499703254,16.1409815416267,17.293450406609));
#53206=CARTESIAN_POINT('Ctrl Pts',(54.36812854879,15.7848349642755,17.2149448962322));
#53207=CARTESIAN_POINT('Ctrl Pts',(54.9996481235109,14.1841565112764,17.1364393858554));
#53208=CARTESIAN_POINT('Ctrl Pts',(54.0128340063977,12.7744876345319,17.0579338754786));
#53209=CARTESIAN_POINT('Ctrl Pts',(52.292690959438,12.8200454826231,16.9794283651019));
#53210=CARTESIAN_POINT('Ctrl Pts',(51.6656274258073,13.8251612032116,16.9253798320794));
#53211=CARTESIAN_POINT('Ctrl Pts',(51.6498077544378,14.3635106325159,16.8974998025159));
#53212=CARTESIAN_POINT('Ctrl Pts',(51.6499660613832,14.3965688093956,16.8957882764113));
#53213=CARTESIAN_POINT('Origin',(53.1951359564886,14.3971354987959,19.1042117235887));
#53214=CARTESIAN_POINT('',(51.6537934596096,14.3955992295121,17.8957882764113));
#53215=CARTESIAN_POINT('',(51.650238794436,14.3978859537331,17.8542117235887));
#53216=CARTESIAN_POINT('',(51.6521359564886,14.397135498796,19.1042117235887));
#53217=CARTESIAN_POINT('',(52.7966221146313,12.9064860705774,18.));
#53218=CARTESIAN_POINT('Ctrl Pts',(52.7966221146313,12.9064860705774,18.));
#53219=CARTESIAN_POINT('Ctrl Pts',(52.3064323164312,13.0375346028627,17.9738314965411));
#53220=CARTESIAN_POINT('Ctrl Pts',(51.7535553056072,13.5560194656624,17.9390942553448));
#53221=CARTESIAN_POINT('Ctrl Pts',(51.6526562271057,14.2291272515896,17.9043570141486));
#53222=CARTESIAN_POINT('Ctrl Pts',(51.6537934596096,14.3955992295121,17.8957882764113));
#53223=CARTESIAN_POINT('',(53.5946788045247,12.9041246263415,18.));
#53224=CARTESIAN_POINT('Origin',(53.1951359564886,14.3971354987959,18.));
#53225=CARTESIAN_POINT('Ctrl Pts',(53.5946845822246,12.9041113672218,18.));
#53226=CARTESIAN_POINT('Ctrl Pts',(53.1295569761736,12.7814239312717,17.975091839613));
#53227=CARTESIAN_POINT('Ctrl Pts',(52.0976014587089,12.9966708391238,17.9264957474759));
#53228=CARTESIAN_POINT('Ctrl Pts',(51.6531166045831,13.9402254397343,17.8778996553388));
#53229=CARTESIAN_POINT('Ctrl Pts',(51.650238794436,14.3978859537331,17.8542117235887));
#53230=CARTESIAN_POINT('Origin',(53.1951359564886,14.3971354987959,4.5));
#53231=CARTESIAN_POINT('',(54.457664959728,14.3970890371748,5.80658032638058));
#53232=CARTESIAN_POINT('',(54.4588632108481,14.3954785432618,5.94341967361942));
#53233=CARTESIAN_POINT('',(54.4596359564886,14.3971354987959,4.5));
#53234=CARTESIAN_POINT('',(54.153252109211,15.2223467977324,6.));
#53235=CARTESIAN_POINT('Ctrl Pts',(54.4588632108481,14.3954785432618,5.94341967361942));
#53236=CARTESIAN_POINT('Ctrl Pts',(54.4562503558692,14.6946046444959,5.96227978241295));
#53237=CARTESIAN_POINT('Ctrl Pts',(54.348829759182,14.9952702831595,5.98113989120648));
#53238=CARTESIAN_POINT('Ctrl Pts',(54.153252109211,15.2223467977324,6.00000000000001));
#53239=CARTESIAN_POINT('',(54.4596359564886,14.3971354987959,6.));
#53240=CARTESIAN_POINT('Origin',(53.1951359564886,14.3971354987959,6.));
#53241=CARTESIAN_POINT('',(54.4596359564886,14.3971354987959,7.));
#53242=CARTESIAN_POINT('',(54.4596359564886,14.3971354987959,4.5));
#53243=CARTESIAN_POINT('',(52.6278006430704,15.5272199611918,7.));
#53244=CARTESIAN_POINT('Origin',(53.1951359564886,14.3971354987959,7.));
#53245=CARTESIAN_POINT('',(53.7624712699068,13.2670510364,7.));
#53246=CARTESIAN_POINT('Origin',(53.1951359564886,14.3971354987959,7.));
#53247=CARTESIAN_POINT('Origin',(53.1951359564886,14.3971354987959,7.));
#53248=CARTESIAN_POINT('',(52.2352360662266,15.2234730828751,6.));
#53249=CARTESIAN_POINT('Origin',(53.1951359564886,14.3971354987959,6.));
#53250=CARTESIAN_POINT('Ctrl Pts',(52.2352263046383,15.223479246524,6.));
#53251=CARTESIAN_POINT('Ctrl Pts',(52.4934849626836,15.5213201221341,5.97509183961299));
#53252=CARTESIAN_POINT('Ctrl Pts',(52.9025331767737,15.6908484929834,5.95018367922598));
#53253=CARTESIAN_POINT('Ctrl Pts',(53.2954400519545,15.6595806594193,5.92527551883897));
#53254=CARTESIAN_POINT('Ctrl Pts',(53.7082278597432,15.6267306858339,5.89910701538004));
#53255=CARTESIAN_POINT('Ctrl Pts',(54.1031995108901,15.3722499881178,5.87293851192112));
#53256=CARTESIAN_POINT('Ctrl Pts',(54.3034856243485,15.009959026203,5.84677000846219));
#53257=CARTESIAN_POINT('Ctrl Pts',(54.4060190030454,14.8244897704715,5.83337344776832));
#53258=CARTESIAN_POINT('Ctrl Pts',(54.457529785952,14.6107659273806,5.81997688707445));
#53259=CARTESIAN_POINT('Ctrl Pts',(54.457664959728,14.3970890371748,5.80658032638058));
#53260=CARTESIAN_POINT('Origin',(53.1951359564886,14.3971354987959,4.5));
#53261=CARTESIAN_POINT('',(54.4609673117159,14.396357828719,5.30658032638058));
#53262=CARTESIAN_POINT('',(54.4612320294125,14.3977598345137,5.44341967361942));
#53263=CARTESIAN_POINT('',(54.4596359564886,14.3971354987959,4.5));
#53264=CARTESIAN_POINT('Ctrl Pts',(54.4612320294125,14.3977598345137,5.44341967361942));
#53265=CARTESIAN_POINT('Ctrl Pts',(54.4614577199909,14.4349274614079,5.44576692486713));
#53266=CARTESIAN_POINT('Ctrl Pts',(54.4599595944507,14.4720765205797,5.44811417611484));
#53267=CARTESIAN_POINT('Ctrl Pts',(54.4566777507412,14.5090671702315,5.45046142736255));
#53268=CARTESIAN_POINT('Ctrl Pts',(54.4200898743707,14.9214601530044,5.47662993082147));
#53269=CARTESIAN_POINT('Ctrl Pts',(54.1618024272562,15.3141643064504,5.5027984342804));
#53270=CARTESIAN_POINT('Ctrl Pts',(53.7976302145161,15.5111328144605,5.52896693773933));
#53271=CARTESIAN_POINT('Ctrl Pts',(53.4334580017759,15.7081013224707,5.55513544119826));
#53272=CARTESIAN_POINT('Ctrl Pts',(52.9634010234101,15.709334185045,5.58130394465719));
#53273=CARTESIAN_POINT('Ctrl Pts',(52.598247155701,15.5141854678806,5.60747244811611));
#53274=CARTESIAN_POINT('Ctrl Pts',(52.2330932879918,15.3190367507161,5.63364095157504));
#53275=CARTESIAN_POINT('Ctrl Pts',(51.9728425309394,14.9275064538129,5.65980945503396));
#53276=CARTESIAN_POINT('Ctrl Pts',(51.9341769083662,14.5153483233265,5.68597795849289));
#53277=CARTESIAN_POINT('Ctrl Pts',(51.8955112857929,14.1031901928401,5.71214646195181));
#53278=CARTESIAN_POINT('Ctrl Pts',(52.0784307976988,13.6704042287705,5.73831496541074));
#53279=CARTESIAN_POINT('Ctrl Pts',(52.4009468670997,13.4106806439539,5.76448346886967));
#53280=CARTESIAN_POINT('Ctrl Pts',(52.7234629365007,13.1509570591374,5.7906519723286));
#53281=CARTESIAN_POINT('Ctrl Pts',(53.1855755633968,13.0642958535739,5.81682047578752));
#53282=CARTESIAN_POINT('Ctrl Pts',(53.5800025789138,13.1903251026303,5.84298897924645));
#53283=CARTESIAN_POINT('Ctrl Pts',(53.9744295944309,13.3163543516866,5.86915748270537));
#53284=CARTESIAN_POINT('Ctrl Pts',(54.3011709985689,13.6550740553627,5.8953259861643));
#53285=CARTESIAN_POINT('Ctrl Pts',(54.4137178903471,14.0528046923318,5.92149448962323));
#53286=CARTESIAN_POINT('Ctrl Pts',(54.4451502229132,14.1638837408548,5.92880288428863));
#53287=CARTESIAN_POINT('Ctrl Pts',(54.4598757063537,14.2795655532322,5.93611127895402));
#53288=CARTESIAN_POINT('Ctrl Pts',(54.4588632108481,14.3954785432618,5.94341967361942));
#53289=CARTESIAN_POINT('Ctrl Pts',(54.457664959728,14.3970890371748,5.80658032638058));
#53290=CARTESIAN_POINT('Ctrl Pts',(54.4577938309935,14.1933748843944,5.79380838361552));
#53291=CARTESIAN_POINT('Ctrl Pts',(54.4112262077565,13.9897034081911,5.78103644085047));
#53292=CARTESIAN_POINT('Ctrl Pts',(54.3176561881973,13.8105991567174,5.76826449808541));
#53293=CARTESIAN_POINT('Ctrl Pts',(54.1259400628177,13.4436314752601,5.74209599462648));
#53294=CARTESIAN_POINT('Ctrl Pts',(53.7369072362884,13.1797973384592,5.71592749116756));
#53295=CARTESIAN_POINT('Ctrl Pts',(53.3250643574771,13.1373309568652,5.68975898770863));
#53296=CARTESIAN_POINT('Ctrl Pts',(52.9132214786658,13.0948645752712,5.6635904842497));
#53297=CARTESIAN_POINT('Ctrl Pts',(52.4785685475723,13.2737659488842,5.63742198079078));
#53298=CARTESIAN_POINT('Ctrl Pts',(52.2159793451474,13.5938495375153,5.61125347733185));
#53299=CARTESIAN_POINT('Ctrl Pts',(51.9533901427224,13.9139331261464,5.58508497387292));
#53300=CARTESIAN_POINT('Ctrl Pts',(51.8628646689658,14.3751989297955,5.558916470414));
#53301=CARTESIAN_POINT('Ctrl Pts',(51.9850104565428,14.7707919534968,5.53274796695507));
#53302=CARTESIAN_POINT('Ctrl Pts',(52.1071562441199,15.1663849771981,5.50657946349614));
#53303=CARTESIAN_POINT('Ctrl Pts',(52.4419732930305,15.4963052209516,5.48041096003722));
#53304=CARTESIAN_POINT('Ctrl Pts',(52.8393182643656,15.6126214609836,5.45424245657829));
#53305=CARTESIAN_POINT('Ctrl Pts',(53.2366632357006,15.7289377010156,5.42807395311936));
#53306=CARTESIAN_POINT('Ctrl Pts',(53.69653612946,15.6316499373263,5.40190544966044));
#53307=CARTESIAN_POINT('Ctrl Pts',(54.0127281594174,15.3643787057253,5.37573694620151));
#53308=CARTESIAN_POINT('Ctrl Pts',(54.2912662123671,15.1289356793162,5.35268473959453));
#53309=CARTESIAN_POINT('Ctrl Pts',(54.4583064998761,14.7615838076199,5.32963253298755));
#53310=CARTESIAN_POINT('Ctrl Pts',(54.4609673117159,14.396357828719,5.30658032638058));
#53311=CARTESIAN_POINT('Origin',(53.1951359564886,14.3971354987959,4.5));
#53312=CARTESIAN_POINT('',(54.4594541523146,14.3982246410602,4.80658032638058));
#53313=CARTESIAN_POINT('',(54.4577421278041,14.3974029482829,4.94341967361942));
#53314=CARTESIAN_POINT('',(54.4596359564886,14.3971354987959,4.5));
#53315=CARTESIAN_POINT('Ctrl Pts',(54.4577421278041,14.3974029482829,4.94341967361942));
#53316=CARTESIAN_POINT('Ctrl Pts',(54.4581119948619,14.5888150279108,4.95542257078024));
#53317=CARTESIAN_POINT('Ctrl Pts',(54.4171976582396,14.7800770605195,4.96742546794106));
#53318=CARTESIAN_POINT('Ctrl Pts',(54.3341701782111,14.9508661287462,4.97942836510187));
#53319=CARTESIAN_POINT('Ctrl Pts',(54.1531551391583,15.3232174255002,5.0055968685608));
#53320=CARTESIAN_POINT('Ctrl Pts',(53.7719681306168,15.5982567367276,5.03176537201973));
#53321=CARTESIAN_POINT('Ctrl Pts',(53.3615378715941,15.6526538764831,5.05793387547865));
#53322=CARTESIAN_POINT('Ctrl Pts',(52.9511076125715,15.7070510162386,5.08410237893758));
#53323=CARTESIAN_POINT('Ctrl Pts',(52.5114341030678,15.5408059845222,5.11027088239651));
#53324=CARTESIAN_POINT('Ctrl Pts',(52.2396723049569,15.2284636038326,5.13643938585543));
#53325=CARTESIAN_POINT('Ctrl Pts',(51.9679105068461,14.9161212231431,5.16260788931436));
#53326=CARTESIAN_POINT('Ctrl Pts',(51.8640604201282,14.4576814934805,5.18877639277329));
#53327=CARTESIAN_POINT('Ctrl Pts',(51.974689389455,14.0587171002307,5.21494489623222));
#53328=CARTESIAN_POINT('Ctrl Pts',(52.0853183587818,13.659752706981,5.24111339969114));
#53329=CARTESIAN_POINT('Ctrl Pts',(52.4104263841535,13.3202636501442,5.26728190315006));
#53330=CARTESIAN_POINT('Ctrl Pts',(52.804231701646,13.1924751167177,5.29345040660899));
#53331=CARTESIAN_POINT('Ctrl Pts',(53.1980370191385,13.0646865832913,5.31961891006791));
#53332=CARTESIAN_POINT('Ctrl Pts',(53.6605396287519,13.1485985732751,5.34578741352685));
#53333=CARTESIAN_POINT('Ctrl Pts',(53.9843467807452,13.406595474317,5.37195591698577));
#53334=CARTESIAN_POINT('Ctrl Pts',(54.2791092171044,13.6414506795096,5.39577716919699));
#53335=CARTESIAN_POINT('Ctrl Pts',(54.4589415919506,14.0205614348097,5.4195984214082));
#53336=CARTESIAN_POINT('Ctrl Pts',(54.4612320294125,14.3977598345137,5.44341967361942));
#53337=CARTESIAN_POINT('Ctrl Pts',(54.4609673117159,14.396357828719,5.30658032638058));
#53338=CARTESIAN_POINT('Ctrl Pts',(54.4613270117525,14.3469850034748,5.30346402952863));
#53339=CARTESIAN_POINT('Ctrl Pts',(54.4586827097295,14.2976510284966,5.30034773267668));
#53340=CARTESIAN_POINT('Ctrl Pts',(54.4529037631581,14.2486870321021,5.29723143582473));
#53341=CARTESIAN_POINT('Ctrl Pts',(54.4043761707862,13.8375212895923,5.27106293236581));
#53342=CARTESIAN_POINT('Ctrl Pts',(54.134809819887,13.4524445040854,5.24489442890688));
#53343=CARTESIAN_POINT('Ctrl Pts',(53.7650823822708,13.2661285769126,5.21872592544795));
#53344=CARTESIAN_POINT('Ctrl Pts',(53.3953549446545,13.0798126497399,5.19255742198903));
#53345=CARTESIAN_POINT('Ctrl Pts',(52.9254664203212,13.0922575809014,5.1663889185301));
#53346=CARTESIAN_POINT('Ctrl Pts',(52.5661199525803,13.2978834669457,5.14022041507117));
#53347=CARTESIAN_POINT('Ctrl Pts',(52.2067734848394,13.5035093529901,5.11405191161225));
#53348=CARTESIAN_POINT('Ctrl Pts',(51.9579690736908,13.9023161939173,5.08788340815332));
#53349=CARTESIAN_POINT('Ctrl Pts',(51.9312738021255,14.315473986753,5.06171490469439));
#53350=CARTESIAN_POINT('Ctrl Pts',(51.9045785305602,14.7286317795887,5.03554640123547));
#53351=CARTESIAN_POINT('Ctrl Pts',(52.0999923985782,15.1561405243328,5.00937789777654));
#53352=CARTESIAN_POINT('Ctrl Pts',(52.4298893914915,15.4063003551787,4.98320939431761));
#53353=CARTESIAN_POINT('Ctrl Pts',(52.7597863844047,15.6564601860247,4.95704089085869));
#53354=CARTESIAN_POINT('Ctrl Pts',(53.2241665022132,15.7292711029725,4.93087238739976));
#53355=CARTESIAN_POINT('Ctrl Pts',(53.6147962366242,15.5920837570554,4.90470388394083));
#53356=CARTESIAN_POINT('Ctrl Pts',(54.0054259710351,15.4548964111382,4.87853538048191));
#53357=CARTESIAN_POINT('Ctrl Pts',(54.3223053220485,15.107710802356,4.85236687702298));
#53358=CARTESIAN_POINT('Ctrl Pts',(54.4233417938017,14.706209118673,4.82619837356406));
#53359=CARTESIAN_POINT('Ctrl Pts',(54.4485901905141,14.6058763020728,4.8196590245029));
#53360=CARTESIAN_POINT('Ctrl Pts',(54.460359856649,14.5021516119852,4.81311967544174));
#53361=CARTESIAN_POINT('Ctrl Pts',(54.4594541523146,14.3982246410602,4.80658032638058));
#53362=CARTESIAN_POINT('Origin',(53.1951359564886,14.3971354987959,4.5));
#53363=CARTESIAN_POINT('',(54.4581341693109,14.3964211317122,4.30658032638058));
#53364=CARTESIAN_POINT('',(54.4603880160508,14.3961458582298,4.44341967361942));
#53365=CARTESIAN_POINT('',(54.4596359564886,14.3971354987959,4.5));
#53366=CARTESIAN_POINT('Ctrl Pts',(54.4603880160508,14.3961458582298,4.44341967361942));
#53367=CARTESIAN_POINT('Ctrl Pts',(54.4574339233842,14.7397014586706,4.46507821669335));
#53368=CARTESIAN_POINT('Ctrl Pts',(54.312116901092,15.0854595650489,4.48673675976727));
#53369=CARTESIAN_POINT('Ctrl Pts',(54.0623960097695,15.3201070497197,4.50839530284119));
#53370=CARTESIAN_POINT('Ctrl Pts',(53.7606757146401,15.6036152013657,4.53456380630012));
#53371=CARTESIAN_POINT('Ctrl Pts',(53.3065445684699,15.7249218506019,4.56073230975905));
#53372=CARTESIAN_POINT('Ctrl Pts',(52.9036403743547,15.6296316648431,4.58690081321798));
#53373=CARTESIAN_POINT('Ctrl Pts',(52.5007361802396,15.5343414790843,4.6130693166769));
#53374=CARTESIAN_POINT('Ctrl Pts',(52.1490589381795,15.2224544583304,4.63923782013583));
#53375=CARTESIAN_POINT('Ctrl Pts',(52.0063049058888,14.8338244281946,4.66540632359475));
#53376=CARTESIAN_POINT('Ctrl Pts',(51.863550873598,14.4451943980587,4.69157482705368));
#53377=CARTESIAN_POINT('Ctrl Pts',(51.9297200510767,13.9798213585408,4.71774333051261));
#53378=CARTESIAN_POINT('Ctrl Pts',(52.1751413884872,13.6463841561873,4.74391183397154));
#53379=CARTESIAN_POINT('Ctrl Pts',(52.4205627258978,13.3129469538339,4.77008033743046));
#53380=CARTESIAN_POINT('Ctrl Pts',(52.8452362232402,13.111445588645,4.79624884088939));
#53381=CARTESIAN_POINT('Ctrl Pts',(53.2587332445463,13.1322355800464,4.82241734434831));
#53382=CARTESIAN_POINT('Ctrl Pts',(53.6722302658525,13.1530255714477,4.84858584780724));
#53383=CARTESIAN_POINT('Ctrl Pts',(54.0745508111225,13.3961069194393,4.87475435126617));
#53384=CARTESIAN_POINT('Ctrl Pts',(54.2852895489753,13.7524792345754,4.90092285472509));
#53385=CARTESIAN_POINT('Ctrl Pts',(54.3993672224223,13.9453916768054,4.9150884610232));
#53386=CARTESIAN_POINT('Ctrl Pts',(54.4573056172638,14.1715018075515,4.92925406732131));
#53387=CARTESIAN_POINT('Ctrl Pts',(54.4577421278041,14.3974029482829,4.94341967361942));
#53388=CARTESIAN_POINT('Ctrl Pts',(54.4594541523146,14.3982246410602,4.80658032638058));
#53389=CARTESIAN_POINT('Ctrl Pts',(54.4567355009545,14.0862672062605,4.78695117198281));
#53390=CARTESIAN_POINT('Ctrl Pts',(54.3398093025916,13.7724871818732,4.76732201758504));
#53391=CARTESIAN_POINT('Ctrl Pts',(54.1304031431366,13.5431499271195,4.74769286318727));
#53392=CARTESIAN_POINT('Ctrl Pts',(53.8512344282254,13.2374101778329,4.72152435972835));
#53393=CARTESIAN_POINT('Ctrl Pts',(53.4077034059102,13.0817484378434,4.69535585626942));
#53394=CARTESIAN_POINT('Ctrl Pts',(52.9986946517684,13.1459652901465,4.66918735281049));
#53395=CARTESIAN_POINT('Ctrl Pts',(52.5896858976267,13.2101821424497,4.64301884935157));
#53396=CARTESIAN_POINT('Ctrl Pts',(52.2151994116584,13.4942775870456,4.61685034589264));
#53397=CARTESIAN_POINT('Ctrl Pts',(52.0431593891151,13.8708598453683,4.59068184243372));
#53398=CARTESIAN_POINT('Ctrl Pts',(51.8711193665719,14.247442103691,4.56451333897479));
#53399=CARTESIAN_POINT('Ctrl Pts',(51.9015258074537,14.7165111757404,4.53834483551586));
#53400=CARTESIAN_POINT('Ctrl Pts',(52.1207441004937,15.0677309159732,4.51217633205694));
#53401=CARTESIAN_POINT('Ctrl Pts',(52.3399623935336,15.4189506562059,4.48600782859801));
#53402=CARTESIAN_POINT('Ctrl Pts',(52.7479925387317,15.6523210646219,4.45983932513909));
#53403=CARTESIAN_POINT('Ctrl Pts',(53.1618689696675,15.6631960750064,4.43367082168016));
#53404=CARTESIAN_POINT('Ctrl Pts',(53.5757454006032,15.6740710853908,4.40750231822123));
#53405=CARTESIAN_POINT('Ctrl Pts',(53.9954681172766,15.4624506977437,4.38133381476231));
#53406=CARTESIAN_POINT('Ctrl Pts',(54.2328284639311,15.1232280099042,4.35516531130338));
#53407=CARTESIAN_POINT('Ctrl Pts',(54.3797245073824,14.9132920564272,4.33897031632911));
#53408=CARTESIAN_POINT('Ctrl Pts',(54.4567749448579,14.6544838494259,4.32277532135484));
#53409=CARTESIAN_POINT('Ctrl Pts',(54.4581341693109,14.3964211317122,4.30658032638058));
#53410=CARTESIAN_POINT('Origin',(53.1951359564886,14.3971354987959,4.5));
#53411=CARTESIAN_POINT('',(54.461625037427,14.3970459917425,3.80658032638058));
#53412=CARTESIAN_POINT('',(54.4600990366243,14.3981838592136,3.94341967361942));
#53413=CARTESIAN_POINT('',(54.4596359564886,14.3971354987959,4.5));
#53414=CARTESIAN_POINT('Ctrl Pts',(54.4600990366243,14.3981838592136,3.94341967361942));
#53415=CARTESIAN_POINT('Ctrl Pts',(54.460821703013,14.4798548702781,3.94856535914753));
#53416=CARTESIAN_POINT('Ctrl Pts',(54.4535723073139,14.5613982175719,3.95371104467563));
#53417=CARTESIAN_POINT('Ctrl Pts',(54.4378783642807,14.6412825634277,3.95885673020374));
#53418=CARTESIAN_POINT('Ctrl Pts',(54.3580664518924,15.0475362626526,3.98502523366266));
#53419=CARTESIAN_POINT('Ctrl Pts',(54.0598570383511,15.410883959442,4.0111937371216));
#53420=CARTESIAN_POINT('Ctrl Pts',(53.6769707694449,15.5683962274082,4.03736224058052));
#53421=CARTESIAN_POINT('Ctrl Pts',(53.2940845005387,15.7259084953743,4.06353074403945));
#53422=CARTESIAN_POINT('Ctrl Pts',(52.8265213762676,15.6775853345172,4.08969924749837));
#53423=CARTESIAN_POINT('Ctrl Pts',(52.4839422593842,15.4450954247484,4.1158677509573));
#53424=CARTESIAN_POINT('Ctrl Pts',(52.1413631425007,15.2126055149797,4.14203625441622));
#53425=CARTESIAN_POINT('Ctrl Pts',(51.9237680330049,14.7959488562993,4.16820475787515));
#53426=CARTESIAN_POINT('Ctrl Pts',(51.9287291645367,14.3819592468436,4.19437326133408));
#53427=CARTESIAN_POINT('Ctrl Pts',(51.9336902960684,13.967969637388,4.22054176479301));
#53428=CARTESIAN_POINT('Ctrl Pts',(52.1612076686277,13.5566470771571,4.24671026825193));
#53429=CARTESIAN_POINT('Ctrl Pts',(52.5092597878395,13.3324334921487,4.27287877171086));
#53430=CARTESIAN_POINT('Ctrl Pts',(52.8573119070513,13.1082199071402,4.29904727516979));
#53431=CARTESIAN_POINT('Ctrl Pts',(53.3258987729157,13.0711152973543,4.32521577862871));
#53432=CARTESIAN_POINT('Ctrl Pts',(53.7049004648973,13.2377578095269,4.35138428208764));
#53433=CARTESIAN_POINT('Ctrl Pts',(54.0839021568789,13.4044003216995,4.37755278554656));
#53434=CARTESIAN_POINT('Ctrl Pts',(54.3733186749776,13.7747899558306,4.40372128900549));
#53435=CARTESIAN_POINT('Ctrl Pts',(54.4433722119826,14.1828395999241,4.42988979246442));
#53436=CARTESIAN_POINT('Ctrl Pts',(54.4554454540469,14.2531641308192,4.43439975284942));
#53437=CARTESIAN_POINT('Ctrl Pts',(54.4610031470343,14.3246072444484,4.43890971323442));
#53438=CARTESIAN_POINT('Ctrl Pts',(54.4603880160508,14.3961458582298,4.44341967361942));
#53439=CARTESIAN_POINT('Ctrl Pts',(54.4581341693109,14.3964211317122,4.30658032638058));
#53440=CARTESIAN_POINT('Ctrl Pts',(54.4589712326528,14.237496062036,4.29660681789592));
#53441=CARTESIAN_POINT('Ctrl Pts',(54.4311018285097,14.0788537248349,4.28663330941126));
#53442=CARTESIAN_POINT('Ctrl Pts',(54.3731606475783,13.9320829192412,4.2766598009266));
#53443=CARTESIAN_POINT('Ctrl Pts',(54.2211345079355,13.5469855044494,4.25049129746767));
#53444=CARTESIAN_POINT('Ctrl Pts',(53.8620842520145,13.2436156628976,4.22432279400875));
#53445=CARTESIAN_POINT('Ctrl Pts',(53.4570122824292,13.1580080377804,4.19815429054982));
#53446=CARTESIAN_POINT('Ctrl Pts',(53.0519403128439,13.0724004126631,4.17198578709089));
#53447=CARTESIAN_POINT('Ctrl Pts',(52.6008466295945,13.2045550039804,4.14581728363197));
#53448=CARTESIAN_POINT('Ctrl Pts',(52.3060070023708,13.4952121220022,4.11964878017304));
#53449=CARTESIAN_POINT('Ctrl Pts',(52.0111673751471,13.7858692400241,4.09348027671411));
#53450=CARTESIAN_POINT('Ctrl Pts',(51.8725818039492,14.2350288847506,4.06731177325519));
#53451=CARTESIAN_POINT('Ctrl Pts',(51.9523937062209,14.6412825324807,4.04114326979626));
#53452=CARTESIAN_POINT('Ctrl Pts',(52.0322056084927,15.0475361802107,4.01497476633734));
#53453=CARTESIAN_POINT('Ctrl Pts',(52.3304149842342,15.4108838309442,3.98880626287841));
#53454=CARTESIAN_POINT('Ctrl Pts',(52.7133012046075,15.5683960789447,3.96263775941948));
#53455=CARTESIAN_POINT('Ctrl Pts',(53.0961874249807,15.7259083269452,3.93646925596055));
#53456=CARTESIAN_POINT('Ctrl Pts',(53.5637504899858,15.6775851722127,3.91030075250163));
#53457=CARTESIAN_POINT('Ctrl Pts',(53.9063295634455,15.4450952919135,3.8841322490427));
#53458=CARTESIAN_POINT('Ctrl Pts',(54.2447474105889,15.2154294107524,3.85828160815533));
#53459=CARTESIAN_POINT('Ctrl Pts',(54.4611991270569,14.8060436899639,3.83243096726795));
#53460=CARTESIAN_POINT('Ctrl Pts',(54.461625037427,14.3970459917425,3.80658032638058));
#53461=CARTESIAN_POINT('Origin',(53.1951359564886,14.3971354987959,4.5));
#53462=CARTESIAN_POINT('',(54.458326569365,14.3979628849946,3.30658032638058));
#53463=CARTESIAN_POINT('',(54.4578259861007,14.3967173602322,3.44341967361942));
#53464=CARTESIAN_POINT('',(54.4596359564886,14.3971354987959,4.5));
#53465=CARTESIAN_POINT('Ctrl Pts',(54.4578259861007,14.3967173602322,3.44341967361942));
#53466=CARTESIAN_POINT('Ctrl Pts',(54.4571098189798,14.6327171768276,3.45822100506063));
#53467=CARTESIAN_POINT('Ctrl Pts',(54.3935213986439,14.8690753747194,3.47302233650185));
#53468=CARTESIAN_POINT('Ctrl Pts',(54.2695279486697,15.0677310009766,3.48782366794306));
#53469=CARTESIAN_POINT('Ctrl Pts',(54.0503096278436,15.4189507857301,3.51399217140199));
#53470=CARTESIAN_POINT('Ctrl Pts',(53.6422794309233,15.6523212237234,3.54016067486092));
#53471=CARTESIAN_POINT('Ctrl Pts',(53.228402947526,15.6631962354854,3.56632917831984));
#53472=CARTESIAN_POINT('Ctrl Pts',(52.8145264641287,15.6740712472475,3.59249768177877));
#53473=CARTESIAN_POINT('Ctrl Pts',(52.3948036942543,15.4624508327782,3.61866618523769));
#53474=CARTESIAN_POINT('Ctrl Pts',(52.1574433175134,15.1232281019409,3.64483468869662));
#53475=CARTESIAN_POINT('Ctrl Pts',(51.9200829407725,14.7840053711036,3.67100319215555));
#53476=CARTESIAN_POINT('Ctrl Pts',(51.865084957165,14.3171803238982,3.69717169561448));
#53477=CARTESIAN_POINT('Ctrl Pts',(52.0171111160778,13.932082860293,3.7233401990734));
#53478=CARTESIAN_POINT('Ctrl Pts',(52.1691372749905,13.5469853966878,3.74950870253233));
#53479=CARTESIAN_POINT('Ctrl Pts',(52.5281875764236,13.2436155166828,3.77567720599125));
#53480=CARTESIAN_POINT('Ctrl Pts',(52.933259597354,13.1580078807144,3.80184570945018));
#53481=CARTESIAN_POINT('Ctrl Pts',(53.3383316182844,13.072400244746,3.82801421290911));
#53482=CARTESIAN_POINT('Ctrl Pts',(53.7894253587122,13.2045548528142,3.85418271636804));
#53483=CARTESIAN_POINT('Ctrl Pts',(54.0842650233083,13.4952120076785,3.88035121982696));
#53484=CARTESIAN_POINT('Ctrl Pts',(54.3211284189289,13.7287153280572,3.90137403775778));
#53485=CARTESIAN_POINT('Ctrl Pts',(54.4571465662818,14.0645150435707,3.9223968556886));
#53486=CARTESIAN_POINT('Ctrl Pts',(54.4600990366243,14.3981838592136,3.94341967361942));
#53487=CARTESIAN_POINT('Ctrl Pts',(54.461625037427,14.3970459917425,3.80658032638058));
#53488=CARTESIAN_POINT('Ctrl Pts',(54.4616302744719,14.3920169071375,3.80626246380903));
#53489=CARTESIAN_POINT('Ctrl Pts',(54.4616028495907,14.3869878811994,3.80594460123748));
#53490=CARTESIAN_POINT('Ctrl Pts',(54.4615425879167,14.3819592487679,3.80562673866592));
#53491=CARTESIAN_POINT('Ctrl Pts',(54.4565814570138,13.9679696917871,3.779458235207));
#53492=CARTESIAN_POINT('Ctrl Pts',(54.2290641132938,13.5566471836914,3.75328973174807));
#53493=CARTESIAN_POINT('Ctrl Pts',(53.8810120381993,13.3324336271042,3.72712122828914));
#53494=CARTESIAN_POINT('Ctrl Pts',(53.5329599631049,13.1082200705171,3.70095272483021));
#53495=CARTESIAN_POINT('Ctrl Pts',(53.0643731566361,13.0711154654387,3.67478422137129));
#53496=CARTESIAN_POINT('Ctrl Pts',(52.6853715126953,13.2377579564865,3.64861571791236));
#53497=CARTESIAN_POINT('Ctrl Pts',(52.3063698687544,13.4044004475342,3.62244721445344));
#53498=CARTESIAN_POINT('Ctrl Pts',(52.0169533873414,13.7747900347083,3.59627871099451));
#53499=CARTESIAN_POINT('Ctrl Pts',(51.9468998592157,14.182839627083,3.57011020753558));
#53500=CARTESIAN_POINT('Ctrl Pts',(51.8768463310901,14.5908892194578,3.54394170407666));
#53501=CARTESIAN_POINT('Ctrl Pts',(52.0261557562516,15.0365988170334,3.51777320061773));
#53502=CARTESIAN_POINT('Ctrl Pts',(52.327876013137,15.3201069327361,3.4916046971588));
#53503=CARTESIAN_POINT('Ctrl Pts',(52.6295962700224,15.6036150484389,3.46543619369988));
#53504=CARTESIAN_POINT('Ctrl Pts',(53.0837273586317,15.7249216822689,3.43926769024095));
#53505=CARTESIAN_POINT('Ctrl Pts',(53.4866315016751,15.6296315086021,3.41309918678203));
#53506=CARTESIAN_POINT('Ctrl Pts',(53.8895356447186,15.5343413349353,3.3869306833231));
#53507=CARTESIAN_POINT('Ctrl Pts',(54.2412128421963,15.2224543537718,3.36076217986417));
#53508=CARTESIAN_POINT('Ctrl Pts',(54.3839668563951,14.8338243728713,3.33459367640525));
#53509=CARTESIAN_POINT('Ctrl Pts',(54.4349061872521,14.6951484043591,3.32525589306369));
#53510=CARTESIAN_POINT('Ctrl Pts',(54.4592433859174,14.5467007705307,3.31591810972213));
#53511=CARTESIAN_POINT('Ctrl Pts',(54.458326569365,14.3979628849946,3.30658032638058));
#53512=CARTESIAN_POINT('Origin',(53.1951359564886,14.3971354987959,4.5));
#53513=CARTESIAN_POINT('',(54.4591686783466,14.3960664985434,2.80658032638058));
#53514=CARTESIAN_POINT('',(54.4614103817624,14.3966710984295,2.94341967361942));
#53515=CARTESIAN_POINT('',(54.4596359564886,14.3971354987959,4.5));
#53516=CARTESIAN_POINT('Ctrl Pts',(54.4614103817624,14.3966710984295,2.94341967361942));
#53517=CARTESIAN_POINT('Ctrl Pts',(54.4595565487343,14.7837947911815,2.96787665097374));
#53518=CARTESIAN_POINT('Ctrl Pts',(54.2687030511239,15.172502088678,2.99233362832806));
#53519=CARTESIAN_POINT('Ctrl Pts',(53.9603826185353,15.4063004831901,3.01679060568238));
#53520=CARTESIAN_POINT('Ctrl Pts',(53.6304855838459,15.6564603458274,3.04295910914131));
#53521=CARTESIAN_POINT('Ctrl Pts',(53.1661054070793,15.729271271822,3.06912761260024));
#53522=CARTESIAN_POINT('Ctrl Pts',(52.7754756231319,15.5920839084722,3.09529611605917));
#53523=CARTESIAN_POINT('Ctrl Pts',(52.3848458391846,15.4548965451224,3.12146461951809));
#53524=CARTESIAN_POINT('Ctrl Pts',(52.0679664480565,15.1077108924282,3.14763312297702));
#53525=CARTESIAN_POINT('Ctrl Pts',(51.9669299635083,14.7062091578755,3.17380162643594));
#53526=CARTESIAN_POINT('Ctrl Pts',(51.8658934789601,14.3047074233228,3.19997012989487));
#53527=CARTESIAN_POINT('Ctrl Pts',(51.980699900992,13.8488896069116,3.2261386333538));
#53528=CARTESIAN_POINT('Ctrl Pts',(52.2598686512828,13.5431498188588,3.25230713681273));
#53529=CARTESIAN_POINT('Ctrl Pts',(52.5390374015737,13.237410030806,3.27847564027165));
#53530=CARTESIAN_POINT('Ctrl Pts',(52.9825684801236,13.0817482711116,3.30464414373058));
#53531=CARTESIAN_POINT('Ctrl Pts',(53.3915772861129,13.1459651315609,3.3308126471895));
#53532=CARTESIAN_POINT('Ctrl Pts',(53.8005860921022,13.2101819920102,3.35698115064843));
#53533=CARTESIAN_POINT('Ctrl Pts',(54.1750726255309,13.4942774726031,3.38314965410736));
#53534=CARTESIAN_POINT('Ctrl Pts',(54.3471126698793,13.8708597786564,3.40931815756629));
#53535=CARTESIAN_POINT('Ctrl Pts',(54.4218440652422,14.0344410036375,3.420685329584));
#53536=CARTESIAN_POINT('Ctrl Pts',(54.4583759903277,14.2154734956486,3.43205250160171));
#53537=CARTESIAN_POINT('Ctrl Pts',(54.4578259861007,14.3967173602322,3.44341967361942));
#53538=CARTESIAN_POINT('Ctrl Pts',(54.458326569365,14.3979628849946,3.30658032638058));
#53539=CARTESIAN_POINT('Ctrl Pts',(54.4566740698126,14.1298729507199,3.28974960626321));
#53540=CARTESIAN_POINT('Ctrl Pts',(54.3729773016518,13.8608400579149,3.27291888614584));
#53541=CARTESIAN_POINT('Ctrl Pts',(54.2151303952057,13.6463842512931,3.25608816602847));
#53542=CARTESIAN_POINT('Ctrl Pts',(53.9697090888974,13.3129470912529,3.22991966256954));
#53543=CARTESIAN_POINT('Ctrl Pts',(53.5450356453608,13.11144575181,3.20375115911061));
#53544=CARTESIAN_POINT('Ctrl Pts',(53.1315386764807,13.1322357404855,3.17758265565169));
#53545=CARTESIAN_POINT('Ctrl Pts',(52.7180417076007,13.153025729161,3.15141415219276));
#53546=CARTESIAN_POINT('Ctrl Pts',(52.3157212133773,13.396107045955,3.12524564873383));
#53547=CARTESIAN_POINT('Ctrl Pts',(52.1049825022091,13.7524793160883,3.09907714527491));
#53548=CARTESIAN_POINT('Ctrl Pts',(51.8942437910409,14.1088515862216,3.07290864181598));
#53549=CARTESIAN_POINT('Ctrl Pts',(51.8750868629279,14.5785148096942,3.04674013835705));
#53550=CARTESIAN_POINT('Ctrl Pts',(52.0561018790939,14.9508660589359,3.02057163489813));
#53551=CARTESIAN_POINT('Ctrl Pts',(52.2371168952598,15.3232173081776,2.9944031314392));
#53552=CARTESIAN_POINT('Ctrl Pts',(52.6183038557047,15.5982565831885,2.96823462798028));
#53553=CARTESIAN_POINT('Ctrl Pts',(53.0287340625826,15.6526537166303,2.94206612452135));
#53554=CARTESIAN_POINT('Ctrl Pts',(53.4391642694604,15.7070508500722,2.91589762106242));
#53555=CARTESIAN_POINT('Ctrl Pts',(53.8788377227713,15.5408058419451,2.88972911760349));
#53556=CARTESIAN_POINT('Ctrl Pts',(54.150599486686,15.2284634997803,2.86356061414457));
#53557=CARTESIAN_POINT('Ctrl Pts',(54.3478475962364,15.0017614956533,2.8445671848899));
#53558=CARTESIAN_POINT('Ctrl Pts',(54.4566391704649,14.6980948440071,2.82557375563524));
#53559=CARTESIAN_POINT('Ctrl Pts',(54.4591686783466,14.3960664985434,2.80658032638058));
#53560=CARTESIAN_POINT('Origin',(53.1951359564886,14.3971354987959,4.5));
#53561=CARTESIAN_POINT('',(54.4611870990995,14.3977489718831,2.30658032638058));
#53562=CARTESIAN_POINT('',(54.4588409672492,14.3981450852038,2.44341967361942));
#53563=CARTESIAN_POINT('',(54.4596359564886,14.3971354987959,4.5));
#53564=CARTESIAN_POINT('',(52.2370198037663,15.2223467977324,2.));
#53565=CARTESIAN_POINT('Ctrl Pts',(54.4611870990995,14.3977489718831,2.30658032638058));
#53566=CARTESIAN_POINT('Ctrl Pts',(54.4588273697934,14.0226957918939,2.2828923946305));
#53567=CARTESIAN_POINT('Ctrl Pts',(54.2812687919142,13.6457847405029,2.25920446288042));
#53568=CARTESIAN_POINT('Ctrl Pts',(53.9893248675414,13.4106809034345,2.23551653113033));
#53569=CARTESIAN_POINT('Ctrl Pts',(53.6668089267086,13.1509572754522,2.20934802767141));
#53570=CARTESIAN_POINT('Ctrl Pts',(53.2046966949687,13.064295685136,2.18317952421248));
#53571=CARTESIAN_POINT('Ctrl Pts',(52.8102694972366,13.190325107422,2.15701102075355));
#53572=CARTESIAN_POINT('Ctrl Pts',(52.4158422995045,13.316354529708,2.13084251729463));
#53573=CARTESIAN_POINT('Ctrl Pts',(52.0891001357801,13.6550749645963,2.1046740138357));
#53574=CARTESIAN_POINT('Ctrl Pts',(51.9765532487624,14.05280555706,2.07850551037678));
#53575=CARTESIAN_POINT('Ctrl Pts',(51.8640063617447,14.4505361495237,2.05233700691785));
#53576=CARTESIAN_POINT('Ctrl Pts',(51.9656547514336,14.9072768995629,2.02616850345892));
#53577=CARTESIAN_POINT('Ctrl Pts',(52.2370198037663,15.2223467977324,2.));
#53578=CARTESIAN_POINT('',(54.1550359790163,15.2234729584199,2.));
#53579=CARTESIAN_POINT('Origin',(53.1951359564886,14.3971354987959,2.));
#53580=CARTESIAN_POINT('Ctrl Pts',(54.1550457523823,15.2234791283661,2.));
#53581=CARTESIAN_POINT('Ctrl Pts',(53.8967871302309,15.5213198394325,2.02490816038701));
#53582=CARTESIAN_POINT('Ctrl Pts',(53.4877388130256,15.6908487049404,2.04981632077402));
#53583=CARTESIAN_POINT('Ctrl Pts',(53.0948318598941,15.6595809742728,2.07472448116103));
#53584=CARTESIAN_POINT('Ctrl Pts',(52.6820439702103,15.6267311087904,2.10089298461996));
#53585=CARTESIAN_POINT('Ctrl Pts',(52.2870722649439,15.3722500867662,2.12706148807889));
#53586=CARTESIAN_POINT('Ctrl Pts',(52.0867861333633,15.0099590154002,2.15322999153781));
#53587=CARTESIAN_POINT('Ctrl Pts',(51.8865000017826,14.6476679440343,2.17939849499674));
#53588=CARTESIAN_POINT('Ctrl Pts',(51.8808994438879,14.1775668233265,2.20556699845567));
#53589=CARTESIAN_POINT('Ctrl Pts',(52.0726155940678,13.8105991317322,2.23173550191459));
#53590=CARTESIAN_POINT('Ctrl Pts',(52.2643317442477,13.4436314401379,2.25790400537352));
#53591=CARTESIAN_POINT('Ctrl Pts',(52.6533646025024,13.1797971776571,2.28407250883245));
#53592=CARTESIAN_POINT('Ctrl Pts',(53.065207531184,13.1373307700534,2.31024101229137));
#53593=CARTESIAN_POINT('Ctrl Pts',(53.4770504598656,13.0948643624498,2.3364095157503));
#53594=CARTESIAN_POINT('Ctrl Pts',(53.9117034589741,13.2737658097233,2.36257801920922));
#53595=CARTESIAN_POINT('Ctrl Pts',(54.1742926968884,13.5938494504631,2.38874652266815));
#53596=CARTESIAN_POINT('Ctrl Pts',(54.3571662426276,13.8167634997217,2.40697090631857));
#53597=CARTESIAN_POINT('Ctrl Pts',(54.456587675354,14.1081518882761,2.425195289969));
#53598=CARTESIAN_POINT('Ctrl Pts',(54.4588409672492,14.3981450852038,2.44341967361942));
#53599=CARTESIAN_POINT('Origin',(53.1951359564886,14.3971354987959,0.895788276411274));
#53600=CARTESIAN_POINT('',(54.7400835567429,14.3978973414314,5.60421172358873));
#53601=CARTESIAN_POINT('',(54.7357308572386,14.3970788042278,5.64578827641127));
#53602=CARTESIAN_POINT('',(54.7381359564886,14.3971354987959,0.895788276411274));
#53603=CARTESIAN_POINT('',(52.7966221146314,12.9064860705774,6.));
#53604=CARTESIAN_POINT('Ctrl Pts',(54.7357308572386,14.3970788042278,5.64578827641127));
#53605=CARTESIAN_POINT('Ctrl Pts',(54.7355659120932,14.6578169944908,5.65918483710514));
#53606=CARTESIAN_POINT('Ctrl Pts',(54.5499292284113,15.4280437939379,5.69874990125794));
#53607=CARTESIAN_POINT('Ctrl Pts',(53.3392716219708,16.2080719085829,5.76448346886966));
#53608=CARTESIAN_POINT('Ctrl Pts',(51.7629444164752,15.5169955192796,5.84298897924645));
#53609=CARTESIAN_POINT('Ctrl Pts',(51.4734277108623,13.8186461670281,5.92149448962322));
#53610=CARTESIAN_POINT('Ctrl Pts',(52.3064323164313,13.0375346028627,5.97383149654107));
#53611=CARTESIAN_POINT('Ctrl Pts',(52.7966221146314,12.9064860705774,6.));
#53612=CARTESIAN_POINT('',(53.5946738441132,12.904124289093,6.));
#53613=CARTESIAN_POINT('Origin',(53.1951359564886,14.3971354987959,6.));
#53614=CARTESIAN_POINT('Ctrl Pts',(54.7400835567429,14.3978973414314,5.60421172358873));
#53615=CARTESIAN_POINT('Ctrl Pts',(54.740358954578,14.443250958116,5.60655897483644));
#53616=CARTESIAN_POINT('Ctrl Pts',(54.7181503847516,14.9939574593074,5.63507472954307));
#53617=CARTESIAN_POINT('Ctrl Pts',(54.0595320288467,15.9953308004787,5.68975898770864));
#53618=CARTESIAN_POINT('Ctrl Pts',(52.3387777758966,15.9998439842325,5.76826449808541));
#53619=CARTESIAN_POINT('Ctrl Pts',(51.386068598834,14.5665551393412,5.8467700084622));
#53620=CARTESIAN_POINT('Ctrl Pts',(52.0449383322286,13.007675117235,5.92401517576705));
#53621=CARTESIAN_POINT('Ctrl Pts',(53.1295481846289,12.781420423434,5.97509183961299));
#53622=CARTESIAN_POINT('Ctrl Pts',(53.5946794545978,12.9041113494969,6.));
#53623=CARTESIAN_POINT('Origin',(53.1951359564886,14.3971354987959,0.895788276411274));
#53624=CARTESIAN_POINT('',(54.7358250212096,14.397461852737,5.10421172358873));
#53625=CARTESIAN_POINT('',(54.7397605362559,14.3961865506515,5.14578827641127));
#53626=CARTESIAN_POINT('',(54.7381359564886,14.3971354987959,0.895788276411274));
#53627=CARTESIAN_POINT('Ctrl Pts',(54.7397605362559,14.3961865506515,5.14578827641127));
#53628=CARTESIAN_POINT('Ctrl Pts',(54.7365136934968,14.8418517823193,5.16884048301825));
#53629=CARTESIAN_POINT('Ctrl Pts',(54.3012988565586,15.7989681003252,5.21806119308416));
#53630=CARTESIAN_POINT('Ctrl Pts',(52.6846517467245,16.1409756074537,5.29345040660899));
#53631=CARTESIAN_POINT('Ctrl Pts',(51.4589751002972,14.933224869348,5.37195591698576));
#53632=CARTESIAN_POINT('Ctrl Pts',(51.7903649128864,13.2446527814935,5.45046142736255));
#53633=CARTESIAN_POINT('Ctrl Pts',(53.3815143142557,12.5897421777335,5.52896693773932));
#53634=CARTESIAN_POINT('Ctrl Pts',(54.5626373610633,13.3907557638884,5.59407588742224));
#53635=CARTESIAN_POINT('Ctrl Pts',(54.7358881117761,14.1484975960505,5.63301633364622));
#53636=CARTESIAN_POINT('Ctrl Pts',(54.7357308572386,14.3970788042278,5.64578827641127));
#53637=CARTESIAN_POINT('Ctrl Pts',(54.7358250212096,14.397461852737,5.10421172358873));
#53638=CARTESIAN_POINT('Ctrl Pts',(54.7362763496954,14.6310315157388,5.11621462074954));
#53639=CARTESIAN_POINT('Ctrl Pts',(54.5775040932279,15.3732433417349,5.15438602136928));
#53640=CARTESIAN_POINT('Ctrl Pts',(53.4338710221273,16.1984132586634,5.21872592544796));
#53641=CARTESIAN_POINT('Ctrl Pts',(51.8243426112988,15.5898341745865,5.29723143582474));
#53642=CARTESIAN_POINT('Ctrl Pts',(51.4441749154368,13.9116075960113,5.37573694620152));
#53643=CARTESIAN_POINT('Ctrl Pts',(52.6343093950298,12.6688279644592,5.45424245657829));
#53644=CARTESIAN_POINT('Ctrl Pts',(54.2767867908486,12.9668231409662,5.53040071570737));
#53645=CARTESIAN_POINT('Ctrl Pts',(54.7372886615245,13.9376228212707,5.58039047137751));
#53646=CARTESIAN_POINT('Ctrl Pts',(54.7400835567429,14.3978973414314,5.60421172358873));
#53647=CARTESIAN_POINT('Origin',(53.1951359564886,14.3971354987959,0.895788276411274));
#53648=CARTESIAN_POINT('',(54.7390536535266,14.3959278946887,4.60421172358873));
#53649=CARTESIAN_POINT('',(54.7379141108259,14.3984645193683,4.64578827641127));
#53650=CARTESIAN_POINT('',(54.7381359564886,14.3971354987959,0.895788276411274));
#53651=CARTESIAN_POINT('Ctrl Pts',(54.7379141108259,14.3984645193683,4.64578827641127));
#53652=CARTESIAN_POINT('Ctrl Pts',(54.7390192921529,14.5252809022368,4.65232762547243));
#53653=CARTESIAN_POINT('Ctrl Pts',(54.6671855077626,15.158343636416,4.68503547799252));
#53654=CARTESIAN_POINT('Ctrl Pts',(53.7972179286764,16.1115146859015,4.74391183397153));
#53655=CARTESIAN_POINT('Ctrl Pts',(52.0972451605188,15.8449731797319,4.82241734434831));
#53656=CARTESIAN_POINT('Ctrl Pts',(51.3818866828157,14.2799767547255,4.90092285472509));
#53657=CARTESIAN_POINT('Ctrl Pts',(52.2926938154427,12.820050407037,4.97942836510186));
#53658=CARTESIAN_POINT('Ctrl Pts',(54.0128314027411,12.7744928061304,5.05793387547865));
#53659=CARTESIAN_POINT('Ctrl Pts',(54.7098771965036,13.7702259631725,5.11338717924845));
#53660=CARTESIAN_POINT('Ctrl Pts',(54.7401994584832,14.3359395997999,5.14267197955932));
#53661=CARTESIAN_POINT('Ctrl Pts',(54.7397605362559,14.3961865506515,5.14578827641127));
#53662=CARTESIAN_POINT('Ctrl Pts',(54.7390536535266,14.3959278946887,4.60421172358873));
#53663=CARTESIAN_POINT('Ctrl Pts',(54.7354489362591,14.815149952008,4.62587026666265));
#53664=CARTESIAN_POINT('Ctrl Pts',(54.3438802932754,15.7468235466057,4.6736973131955));
#53665=CARTESIAN_POINT('Ctrl Pts',(52.7769304442279,16.1653842141838,4.74769286318728));
#53666=CARTESIAN_POINT('Ctrl Pts',(51.4895330907317,15.0236483351255,4.82619837356406));
#53667=CARTESIAN_POINT('Ctrl Pts',(51.7317609456535,13.3200407432483,4.90470388394085));
#53668=CARTESIAN_POINT('Ctrl Pts',(53.2863782799342,12.5823975487372,4.98320939431761));
#53669=CARTESIAN_POINT('Ctrl Pts',(54.5339890873504,13.3362017488983,5.04971200753359));
#53670=CARTESIAN_POINT('Ctrl Pts',(54.7352923713373,14.1218070799821,5.09004611729062));
#53671=CARTESIAN_POINT('Ctrl Pts',(54.7358250212096,14.397461852737,5.10421172358873));
#53672=CARTESIAN_POINT('Origin',(53.1951359564886,14.3971354987959,0.895788276411274));
#53673=CARTESIAN_POINT('',(54.7387010277811,14.3984147555176,4.10421172358872));
#53674=CARTESIAN_POINT('',(54.7363034079594,14.3962637958223,4.14578827641127));
#53675=CARTESIAN_POINT('',(54.7381359564886,14.3971354987959,0.895788276411274));
#53676=CARTESIAN_POINT('Ctrl Pts',(54.7363034079594,14.3962637958223,4.14578827641127));
#53677=CARTESIAN_POINT('Ctrl Pts',(54.7346448209044,14.7111635771051,4.16198327138554));
#53678=CARTESIAN_POINT('Ctrl Pts',(54.4887025372849,15.537270261699,4.20434676981873));
#53679=CARTESIAN_POINT('Ctrl Pts',(53.147408175106,16.2135387160798,4.27287877171085));
#53680=CARTESIAN_POINT('Ctrl Pts',(51.6537177503359,15.3592313846778,4.35138428208763));
#53681=CARTESIAN_POINT('Ctrl Pts',(51.5424078137269,13.6420935954197,4.42988979246441));
#53682=CARTESIAN_POINT('Ctrl Pts',(52.9133037754092,12.6020953249299,4.50839530284119));
#53683=CARTESIAN_POINT('Ctrl Pts',(54.4017068046157,13.124465562129,4.58036146415681));
#53684=CARTESIAN_POINT('Ctrl Pts',(54.7345966896724,14.0177999706171,4.62615912201351));
#53685=CARTESIAN_POINT('Ctrl Pts',(54.7379141108259,14.3984645193683,4.64578827641127));
#53686=CARTESIAN_POINT('Ctrl Pts',(54.7387010277811,14.3984147555176,4.10421172358872));
#53687=CARTESIAN_POINT('Ctrl Pts',(54.7395828579414,14.49807341117,4.10935740911683));
#53688=CARTESIAN_POINT('Ctrl Pts',(54.6857500758113,15.1036004690399,4.14067159810387));
#53689=CARTESIAN_POINT('Ctrl Pts',(53.8864190756817,16.077530414512,4.19815429054983));
#53690=CARTESIAN_POINT('Ctrl Pts',(52.1747941628695,15.9006321056092,4.2766598009266));
#53691=CARTESIAN_POINT('Ctrl Pts',(51.3782360277522,14.3753622969642,4.35516531130339));
#53692=CARTESIAN_POINT('Ctrl Pts',(52.2111169431944,12.8696192117062,4.43367082168016));
#53693=CARTESIAN_POINT('Ctrl Pts',(53.9264895031678,12.7337890506155,4.51217633205695));
#53694=CARTESIAN_POINT('Ctrl Pts',(54.6936722382488,13.7156146023329,4.5690232993598));
#53695=CARTESIAN_POINT('Ctrl Pts',(54.7398042641295,14.3086332477416,4.59970176320372));
#53696=CARTESIAN_POINT('Ctrl Pts',(54.7390536535266,14.3959278946887,4.60421172358873));
#53697=CARTESIAN_POINT('Origin',(53.1951359564886,14.3971354987959,0.895788276411274));
#53698=CARTESIAN_POINT('',(54.7359273488899,14.3966252672389,3.60421172358873));
#53699=CARTESIAN_POINT('',(54.740563122869,14.3970262782475,3.64578827641127));
#53700=CARTESIAN_POINT('',(54.7381359564886,14.3971354987959,0.895788276411274));
#53701=CARTESIAN_POINT('Ctrl Pts',(54.740563122869,14.3970262782475,3.64578827641127));
#53702=CARTESIAN_POINT('Ctrl Pts',(54.7400434078029,14.8961037383943,3.67163891729865));
#53703=CARTESIAN_POINT('Ctrl Pts',(54.208547388428,15.9013481621327,3.72365806164495));
#53704=CARTESIAN_POINT('Ctrl Pts',(52.5038529249194,16.0775302015138,3.80184570945018));
#53705=CARTESIAN_POINT('Ctrl Pts',(51.4121872860838,14.7474105690538,3.88035121982695));
#53706=CARTESIAN_POINT('Ctrl Pts',(51.9195124019995,13.1031559265556,3.95885673020373));
#53707=CARTESIAN_POINT('Ctrl Pts',(53.5708470479161,12.6193729267869,4.03736224058052));
#53708=CARTESIAN_POINT('Ctrl Pts',(54.6140883917719,13.5008315971724,4.09967275598302));
#53709=CARTESIAN_POINT('Ctrl Pts',(54.7373248304478,14.202336249353,4.13581476792661));
#53710=CARTESIAN_POINT('Ctrl Pts',(54.7363034079594,14.3962637958223,4.14578827641127));
#53711=CARTESIAN_POINT('Ctrl Pts',(54.7359273488899,14.3966252672389,3.60421172358873));
#53712=CARTESIAN_POINT('Ctrl Pts',(54.7350534494295,14.6846029003007,3.61901305502994));
#53713=CARTESIAN_POINT('Ctrl Pts',(54.5202760602344,15.482930589367,3.65998288993008));
#53714=CARTESIAN_POINT('Ctrl Pts',(53.2428637439183,16.2135389463141,3.72712122828915));
#53715=CARTESIAN_POINT('Ctrl Pts',(51.7063697132749,15.4388525891942,3.80562673866593));
#53716=CARTESIAN_POINT('Ctrl Pts',(51.5050366439836,13.7299295812751,3.88413224904271));
#53717=CARTESIAN_POINT('Ctrl Pts',(52.8194248174382,12.6193727014466,3.96263775941949));
#53718=CARTESIAN_POINT('Ctrl Pts',(54.3625220492744,13.0714459438974,4.03599758426816));
#53719=CARTESIAN_POINT('Ctrl Pts',(54.7350982901468,13.9912569994582,4.0831889056579));
#53720=CARTESIAN_POINT('Ctrl Pts',(54.7387010277811,14.3984147555176,4.10421172358872));
#53721=CARTESIAN_POINT('Origin',(53.1951359564886,14.3971354987959,0.895788276411274));
#53722=CARTESIAN_POINT('',(54.740301190334,14.3965688164982,3.10421172358873));
#53723=CARTESIAN_POINT('',(54.7365381831935,14.3981451127971,3.14578827641127));
#53724=CARTESIAN_POINT('',(54.7381359564886,14.3971354987959,0.895788276411274));
#53725=CARTESIAN_POINT('Ctrl Pts',(54.7365381831935,14.3981451127971,3.14578827641127));
#53726=CARTESIAN_POINT('Ctrl Pts',(54.7376569241507,14.5796417971643,3.15512605975283));
#53727=CARTESIAN_POINT('Ctrl Pts',(54.6247347728585,15.2684238709215,3.19063234655331));
#53728=CARTESIAN_POINT('Ctrl Pts',(53.6133414157458,16.1653839899769,3.25230713681272));
#53729=CARTESIAN_POINT('Ctrl Pts',(51.9508876322963,15.7213124929433,3.3308126471895));
#53730=CARTESIAN_POINT('Ctrl Pts',(51.4043053238161,14.0896875604189,3.40931815756628));
#53731=CARTESIAN_POINT('Ctrl Pts',(52.4637825025118,12.7337892614639,3.48782366794306));
#53732=CARTESIAN_POINT('Ctrl Pts',(54.1791548450535,12.8696194053218,3.56632917831983));
#53733=CARTESIAN_POINT('Ctrl Pts',(54.737780986498,13.8795446348882,3.61898404780924));
#53734=CARTESIAN_POINT('Ctrl Pts',(54.7405695133476,14.3908895621182,3.64547041383972));
#53735=CARTESIAN_POINT('Ctrl Pts',(54.740563122869,14.3970262782475,3.64578827641127));
#53736=CARTESIAN_POINT('Ctrl Pts',(54.740301190334,14.3965688164982,3.10421172358873));
#53737=CARTESIAN_POINT('Ctrl Pts',(54.7380390595611,14.8689546274245,3.12866870094305));
#53738=CARTESIAN_POINT('Ctrl Pts',(54.2559651859222,15.850784329065,3.17929418175629));
#53739=CARTESIAN_POINT('Ctrl Pts',(52.5930539078611,16.1115149029784,3.25608816602847));
#53740=CARTESIAN_POINT('Ctrl Pts',(51.4330422815012,14.8405600699842,3.33459367640525));
#53741=CARTESIAN_POINT('Ctrl Pts',(51.8533182226522,13.1719316222439,3.41309918678203));
#53742=CARTESIAN_POINT('Ctrl Pts',(53.4769681733105,12.6020950974316,3.49160469715881));
#53743=CARTESIAN_POINT('Ctrl Pts',(54.5893972536881,13.4460134923652,3.55530887609438));
#53744=CARTESIAN_POINT('Ctrl Pts',(54.7365984888838,14.175463319392,3.59284455157101));
#53745=CARTESIAN_POINT('Ctrl Pts',(54.7359273488899,14.3966252672389,3.60421172358873));
#53746=CARTESIAN_POINT('Origin',(53.1951359564886,14.3971354987959,0.895788276411274));
#53747=CARTESIAN_POINT('',(54.73716587472,14.3983674417199,2.60421172358873));
#53748=CARTESIAN_POINT('',(54.7375657625992,14.3958310564158,2.64578827641127));
#53749=CARTESIAN_POINT('',(54.7381359564886,14.3971354987959,0.895788276411274));
#53750=CARTESIAN_POINT('Ctrl Pts',(54.7375657625992,14.3958310564158,2.64578827641127));
#53751=CARTESIAN_POINT('Ctrl Pts',(54.734479142859,14.7643796819994,2.66478170566593));
#53752=CARTESIAN_POINT('Ctrl Pts',(54.4188250031304,15.6454555959149,2.70994363837952));
#53753=CARTESIAN_POINT('Ctrl Pts',(52.9564009216582,16.198413027115,2.78127407455204));
#53754=CARTESIAN_POINT('Ctrl Pts',(51.5609762954032,15.1915669978344,2.85977958492882));
#53755=CARTESIAN_POINT('Ctrl Pts',(51.6311047416152,13.472254177388,2.9382850953056));
#53756=CARTESIAN_POINT('Ctrl Pts',(53.1038936445493,12.5823977792548,3.01679060568238));
#53757=CARTESIAN_POINT('Ctrl Pts',(54.4735979274945,13.2323024338895,3.0859583327176));
#53758=CARTESIAN_POINT('Ctrl Pts',(54.7345217286191,14.0710096690757,3.1289575562939));
#53759=CARTESIAN_POINT('Ctrl Pts',(54.7365381831935,14.3981451127971,3.14578827641127));
#53760=CARTESIAN_POINT('Ctrl Pts',(54.73716587472,14.3983674417199,2.60421172358873));
#53761=CARTESIAN_POINT('Ctrl Pts',(54.7383644283813,14.5526183883782,2.61215584339723));
#53762=CARTESIAN_POINT('Ctrl Pts',(54.6467666252149,15.2135939671077,2.64626846666466));
#53763=CARTESIAN_POINT('Ctrl Pts',(53.7056202382209,16.1409758479641,2.70654959339102));
#53764=CARTESIAN_POINT('Ctrl Pts',(52.0221470001078,15.7848310056966,2.78505510376779));
#53765=CARTESIAN_POINT('Ctrl Pts',(51.3906291820654,14.1841570315506,2.86356061414457));
#53766=CARTESIAN_POINT('Ctrl Pts',(52.3774404052229,12.7744925974775,2.94206612452135));
#53767=CARTESIAN_POINT('Ctrl Pts',(54.0975782126823,12.8200502087089,3.02057163489813));
#53768=CARTESIAN_POINT('Ctrl Pts',(54.7246398714755,13.8251629314517,3.07462016792059));
#53769=CARTESIAN_POINT('Ctrl Pts',(54.7404594967271,14.3635107392415,3.10250019748412));
#53770=CARTESIAN_POINT('Ctrl Pts',(54.740301190334,14.3965688164982,3.10421172358873));
#53771=CARTESIAN_POINT('Origin',(53.1951359564886,14.3971354987959,0.895788276411274));
#53772=CARTESIAN_POINT('',(54.7364807484814,14.3955730757723,2.10421172358873));
#53773=CARTESIAN_POINT('',(54.7400287307462,14.397884086359,2.14578827641127));
#53774=CARTESIAN_POINT('',(54.7381359564886,14.3971354987959,0.895788276411274));
#53775=CARTESIAN_POINT('',(53.5936497983459,12.9064860705774,2.));
#53776=CARTESIAN_POINT('Ctrl Pts',(53.5936497983459,12.9064860705774,2.));
#53777=CARTESIAN_POINT('Ctrl Pts',(54.083839596546,13.0375346028627,2.02616850345893));
#53778=CARTESIAN_POINT('Ctrl Pts',(54.6367230898564,13.5559776050111,2.06090574465517));
#53779=CARTESIAN_POINT('Ctrl Pts',(54.737618997593,14.2290968579424,2.09564298585141));
#53780=CARTESIAN_POINT('Ctrl Pts',(54.7364807484814,14.3955730757723,2.10421172358873));
#53781=CARTESIAN_POINT('',(52.7955982877704,12.9041242545674,2.));
#53782=CARTESIAN_POINT('Origin',(53.1951359564886,14.3971354987959,2.));
#53783=CARTESIAN_POINT('Ctrl Pts',(52.7955926848293,12.9041113294173,2.));
#53784=CARTESIAN_POINT('Ctrl Pts',(53.2607241041145,12.7814202621555,2.02490816038701));
#53785=CARTESIAN_POINT('Ctrl Pts',(54.2926583006945,12.9966875828164,2.0735042525241));
#53786=CARTESIAN_POINT('Ctrl Pts',(54.7371492824905,13.9402272601641,2.12210034466119));
#53787=CARTESIAN_POINT('Ctrl Pts',(54.7400287307462,14.397884086359,2.14578827641127));
#53788=CARTESIAN_POINT('Origin',(14.1292828945603,53.2669068454841,15.5));
#53789=CARTESIAN_POINT('',(13.4980577522811,52.1734972976428,14.1934196736194));
#53790=CARTESIAN_POINT('',(13.4988747128346,52.1716629874611,14.0565803263806));
#53791=CARTESIAN_POINT('',(13.4970328945603,52.1718177223987,15.5));
#53792=CARTESIAN_POINT('',(12.9355708698302,52.8497595669186,14.));
#53793=CARTESIAN_POINT('Ctrl Pts',(13.4988747128346,52.1716629874611,14.0565803263806));
#53794=CARTESIAN_POINT('Ctrl Pts',(13.2411227471438,52.3234873105789,14.0377202175871));
#53795=CARTESIAN_POINT('Ctrl Pts',(13.0344360750677,52.5668460963447,14.0188601087935));
#53796=CARTESIAN_POINT('Ctrl Pts',(12.9355708698302,52.8497595669186,14.));
#53797=CARTESIAN_POINT('',(13.4970328945603,52.1718177223987,14.));
#53798=CARTESIAN_POINT('Origin',(14.1292828945603,53.2669068454841,14.));
#53799=CARTESIAN_POINT('',(13.4970328945603,52.1718177223987,13.));
#53800=CARTESIAN_POINT('',(13.4970328945603,52.1718177223987,15.5));
#53801=CARTESIAN_POINT('',(12.8669333849943,53.3406222827979,13.));
#53802=CARTESIAN_POINT('Origin',(14.1292828945603,53.2669068454841,13.));
#53803=CARTESIAN_POINT('',(15.3916324041264,53.1931914081703,13.));
#53804=CARTESIAN_POINT('Origin',(14.1292828945603,53.2669068454841,13.));
#53805=CARTESIAN_POINT('Origin',(14.1292828945603,53.2669068454841,13.));
#53806=CARTESIAN_POINT('',(13.8936073831512,54.5113748561459,14.));
#53807=CARTESIAN_POINT('Origin',(14.1292828945603,53.2669068454841,14.));
#53808=CARTESIAN_POINT('Ctrl Pts',(13.893606936201,54.511386694654,14.));
#53809=CARTESIAN_POINT('Ctrl Pts',(13.5065438623108,54.43664727626,14.024908160387));
#53810=CARTESIAN_POINT('Ctrl Pts',(13.1551923299505,54.1671690811723,14.049816320774));
#53811=CARTESIAN_POINT('Ctrl Pts',(12.9858145310893,53.8112673891924,14.074724481161));
#53812=CARTESIAN_POINT('Ctrl Pts',(12.8078662825437,53.43735721225,14.10089298462));
#53813=CARTESIAN_POINT('Ctrl Pts',(12.8307732764863,52.9680562770306,14.1270614880789));
#53814=CARTESIAN_POINT('Ctrl Pts',(13.0443854893126,52.6134561814805,14.1532299915378));
#53815=CARTESIAN_POINT('Ctrl Pts',(13.1537409585151,52.4319241458582,14.1666265522317));
#53816=CARTESIAN_POINT('Ctrl Pts',(13.3130758736166,52.2804525587352,14.1800231129255));
#53817=CARTESIAN_POINT('Ctrl Pts',(13.4980577522811,52.1734972976428,14.1934196736194));
#53818=CARTESIAN_POINT('Origin',(14.1292828945603,53.2669068454841,15.5));
#53819=CARTESIAN_POINT('',(13.4970386657413,52.17027240687,14.6934196736194));
#53820=CARTESIAN_POINT('',(13.4956926805926,52.1707443397673,14.5565803263806));
#53821=CARTESIAN_POINT('',(13.4970328945603,52.1718177223987,15.5));
#53822=CARTESIAN_POINT('Ctrl Pts',(13.4956926805926,52.1707443397673,14.5565803263806));
#53823=CARTESIAN_POINT('Ctrl Pts',(13.4633916214762,52.1891327536446,14.5542330751329));
#53824=CARTESIAN_POINT('Ctrl Pts',(13.4319685470764,52.2090047577526,14.5518858238852));
#53825=CARTESIAN_POINT('Ctrl Pts',(13.4015745144389,52.230342308046,14.5495385726374));
#53826=CARTESIAN_POINT('Ctrl Pts',(13.0627244024285,52.4682255594459,14.5233700691785));
#53827=CARTESIAN_POINT('Ctrl Pts',(12.8517746061391,52.8882625646258,14.4972015657196));
#53828=CARTESIAN_POINT('Ctrl Pts',(12.8632814695834,53.3021304033103,14.4710330622607));
#53829=CARTESIAN_POINT('Ctrl Pts',(12.8747883330277,53.7159982419948,14.4448645588017));
#53830=CARTESIAN_POINT('Ctrl Pts',(13.1087518562058,54.1236969141838,14.4186960553428));
#53831=CARTESIAN_POINT('Ctrl Pts',(13.460332770227,54.3423556782116,14.3925275518839));
#53832=CARTESIAN_POINT('Ctrl Pts',(13.8119136842482,54.5610144422395,14.366359048425));
#53833=CARTESIAN_POINT('Ctrl Pts',(14.2811119891126,54.5906332981061,14.340190544966));
#53834=CARTESIAN_POINT('Ctrl Pts',(14.6573867068861,54.4180393977443,14.3140220415071));
#53835=CARTESIAN_POINT('Ctrl Pts',(15.0336614246596,54.2454454973824,14.2878535380482));
#53836=CARTESIAN_POINT('Ctrl Pts',(15.3170125553422,53.8706388407919,14.2616850345893));
#53837=CARTESIAN_POINT('Ctrl Pts',(15.3806795111647,53.461467903109,14.2355165311303));
#53838=CARTESIAN_POINT('Ctrl Pts',(15.4443464669872,53.052296965426,14.2093480276714));
#53839=CARTESIAN_POINT('Ctrl Pts',(15.2883292479495,52.6087617466505,14.1831795242125));
#53840=CARTESIAN_POINT('Ctrl Pts',(14.981976715725,52.3301941698058,14.1570110207536));
#53841=CARTESIAN_POINT('Ctrl Pts',(14.6756241835006,52.0516265929611,14.1308425172946));
#53842=CARTESIAN_POINT('Ctrl Pts',(14.2189363380893,51.938026658047,14.1046740138357));
#53843=CARTESIAN_POINT('Ctrl Pts',(13.8182170120758,52.0394239070104,14.0785055103768));
#53844=CARTESIAN_POINT('Ctrl Pts',(13.7063032761926,52.067742343889,14.0711971157114));
#53845=CARTESIAN_POINT('Ctrl Pts',(13.5987550004656,52.1128302370619,14.063888721046));
#53846=CARTESIAN_POINT('Ctrl Pts',(13.4988747128346,52.1716629874611,14.0565803263806));
#53847=CARTESIAN_POINT('Ctrl Pts',(13.4980577522811,52.1734972976428,14.1934196736194));
#53848=CARTESIAN_POINT('Ctrl Pts',(13.6744148054729,52.0715288518372,14.2061916163845));
#53849=CARTESIAN_POINT('Ctrl Pts',(13.8740829845723,52.0100223374604,14.2189635591495));
#53850=CARTESIAN_POINT('Ctrl Pts',(14.0759771073047,52.00150441778,14.2317355019146));
#53851=CARTESIAN_POINT('Ctrl Pts',(14.4896390807605,51.9840520055104,14.2579040053735));
#53852=CARTESIAN_POINT('Ctrl Pts',(14.9126455959621,52.1890464368519,14.2840725088324));
#53853=CARTESIAN_POINT('Ctrl Pts',(15.1553451745864,52.5244804183786,14.3102410122914));
#53854=CARTESIAN_POINT('Ctrl Pts',(15.3980447532108,52.8599143999052,14.3364095157503));
#53855=CARTESIAN_POINT('Ctrl Pts',(15.460437395258,53.325787931617,14.3625780192092));
#53856=CARTESIAN_POINT('Ctrl Pts',(15.3145307999442,53.7132400695012,14.3887465226681));
#53857=CARTESIAN_POINT('Ctrl Pts',(15.1686242046305,54.1006922073853,14.4149150261271));
#53858=CARTESIAN_POINT('Ctrl Pts',(14.8144183719558,54.409722951442,14.441083529586));
#53859=CARTESIAN_POINT('Ctrl Pts',(14.4107506896371,54.5017382932332,14.4672520330449));
#53860=CARTESIAN_POINT('Ctrl Pts',(14.0070830073184,54.5937536350245,14.4934205365039));
#53861=CARTESIAN_POINT('Ctrl Pts',(13.5539534753558,54.4687535745504,14.5195890399628));
#53862=CARTESIAN_POINT('Ctrl Pts',(13.2545471544402,54.1828000037796,14.5457575434217));
#53863=CARTESIAN_POINT('Ctrl Pts',(12.9551408335246,53.8968464330087,14.5719260468806));
#53864=CARTESIAN_POINT('Ctrl Pts',(12.8094577236562,53.4499393519412,14.5980945503396));
#53865=CARTESIAN_POINT('Ctrl Pts',(12.8828256503828,53.0424720659447,14.6242630537985));
#53866=CARTESIAN_POINT('Ctrl Pts',(12.9474564997503,52.6835283427349,14.6473152604055));
#53867=CARTESIAN_POINT('Ctrl Pts',(13.1820731109759,52.3551902889475,14.6703674670124));
#53868=CARTESIAN_POINT('Ctrl Pts',(13.4970386657413,52.17027240687,14.6934196736194));
#53869=CARTESIAN_POINT('Origin',(14.1292828945603,53.2669068454841,15.5));
#53870=CARTESIAN_POINT('',(13.4961785456119,52.1725162395268,15.1934196736194));
#53871=CARTESIAN_POINT('',(13.4977463410385,52.1735883352515,15.0565803263806));
#53872=CARTESIAN_POINT('',(13.4970328945603,52.1718177223987,15.5));
#53873=CARTESIAN_POINT('Ctrl Pts',(13.4977463410385,52.1735883352515,15.0565803263806));
#53874=CARTESIAN_POINT('Ctrl Pts',(13.3317931989842,52.2689743399829,15.0445774292198));
#53875=CARTESIAN_POINT('Ctrl Pts',(13.186612163033,52.4000385957214,15.0325745320589));
#53876=CARTESIAN_POINT('Ctrl Pts',(13.0802179156269,52.5573375001258,15.0205716348981));
#53877=CARTESIAN_POINT('Ctrl Pts',(12.8482590648635,52.9002777810297,14.9944031314392));
#53878=CARTESIAN_POINT('Ctrl Pts',(12.800661371336,53.3679164545856,14.9682346279803));
#53879=CARTESIAN_POINT('Ctrl Pts',(12.9587676726968,53.7505591757409,14.9420661245213));
#53880=CARTESIAN_POINT('Ctrl Pts',(13.1168739740577,54.1332018968962,14.9158976210624));
#53881=CARTESIAN_POINT('Ctrl Pts',(13.4806842703069,54.4308486656509,14.8897291176035));
#53882=CARTESIAN_POINT('Ctrl Pts',(13.887062777462,54.5100303359217,14.8635606141446));
#53883=CARTESIAN_POINT('Ctrl Pts',(14.2934412846171,54.5892120061924,14.8373921106856));
#53884=CARTESIAN_POINT('Ctrl Pts',(14.7423880026779,54.4499285779793,14.8112236072267));
#53885=CARTESIAN_POINT('Ctrl Pts',(15.0325877125755,54.1546380042325,14.7850551037678));
#53886=CARTESIAN_POINT('Ctrl Pts',(15.322787422473,53.8593474304858,14.7588866003089));
#53887=CARTESIAN_POINT('Ctrl Pts',(15.4542401242071,53.4080497112055,14.7327180968499));
#53888=CARTESIAN_POINT('Ctrl Pts',(15.3680052510694,53.0031088631455,14.706549593391));
#53889=CARTESIAN_POINT('Ctrl Pts',(15.2817703779317,52.5981680150856,14.6803810899321));
#53890=CARTESIAN_POINT('Ctrl Pts',(14.9778479299221,52.239584038246,14.6542125864732));
#53891=CARTESIAN_POINT('Ctrl Pts',(14.5925114920515,52.0881567986362,14.6280440830142));
#53892=CARTESIAN_POINT('Ctrl Pts',(14.2417387974228,51.9503122148961,14.604222830803));
#53893=CARTESIAN_POINT('Ctrl Pts',(13.8235023586795,51.9841281668449,14.5804015785918));
#53894=CARTESIAN_POINT('Ctrl Pts',(13.4956926805926,52.1707443397673,14.5565803263806));
#53895=CARTESIAN_POINT('Ctrl Pts',(13.4970386657413,52.17027240687,14.6934196736194));
#53896=CARTESIAN_POINT('Ctrl Pts',(13.5396170697753,52.1452744089077,14.6965359704714));
#53897=CARTESIAN_POINT('Ctrl Pts',(13.5836638346913,52.1228973859148,14.6996522673233));
#53898=CARTESIAN_POINT('Ctrl Pts',(13.6289575157408,52.1034200423295,14.7027685641753));
#53899=CARTESIAN_POINT('Ctrl Pts',(14.0093024910506,51.9398627956362,14.7289370676342));
#53900=CARTESIAN_POINT('Ctrl Pts',(14.4775734783483,51.9807757931753,14.7551055710931));
#53901=CARTESIAN_POINT('Ctrl Pts',(14.823792639393,52.2078118983851,14.781274074552));
#53902=CARTESIAN_POINT('Ctrl Pts',(15.1700118004377,52.434848003595,14.807442578011));
#53903=CARTESIAN_POINT('Ctrl Pts',(15.3941791352292,52.8480072164757,14.8336110814699));
#53904=CARTESIAN_POINT('Ctrl Pts',(15.3957751288567,53.2620246601267,14.8597795849288));
#53905=CARTESIAN_POINT('Ctrl Pts',(15.3973711224841,53.6760421037777,14.8859480883878));
#53906=CARTESIAN_POINT('Ctrl Pts',(15.1763957749473,54.0909177781991,14.9121165918467));
#53907=CARTESIAN_POINT('Ctrl Pts',(14.83193716646,54.3206161896323,14.9382850953056));
#53908=CARTESIAN_POINT('Ctrl Pts',(14.4874785579727,54.5503146010655,14.9644535987645));
#53909=CARTESIAN_POINT('Ctrl Pts',(14.0195366885348,54.5948357495104,14.9906221022235));
#53910=CARTESIAN_POINT('Ctrl Pts',(13.6379422013928,54.4342159762724,15.0167906056824));
#53911=CARTESIAN_POINT('Ctrl Pts',(13.2563477142507,54.2735962030343,15.0429591091413));
#53912=CARTESIAN_POINT('Ctrl Pts',(12.9611006094046,53.9078355081131,15.0691276126002));
#53913=CARTESIAN_POINT('Ctrl Pts',(12.8845932246477,53.5009452588027,15.0952961160592));
#53914=CARTESIAN_POINT('Ctrl Pts',(12.8080858398908,53.0940550094922,15.1214646195181));
#53915=CARTESIAN_POINT('Ctrl Pts',(12.9503181752231,52.6460352057925,15.147633122977));
#53916=CARTESIAN_POINT('Ctrl Pts',(13.2475115476967,52.3577832908858,15.1738016264359));
#53917=CARTESIAN_POINT('Ctrl Pts',(13.3217783549033,52.2857508992711,15.1803409754971));
#53918=CARTESIAN_POINT('Ctrl Pts',(13.4057220070296,52.2236955258253,15.1868803245583));
#53919=CARTESIAN_POINT('Ctrl Pts',(13.4961785456119,52.1725162395268,15.1934196736194));
#53920=CARTESIAN_POINT('Origin',(14.1292828945603,53.2669068454841,15.5));
#53921=CARTESIAN_POINT('',(13.4984004295476,52.1727576237481,15.6934196736194));
#53922=CARTESIAN_POINT('',(13.4975120618698,52.1706683776322,15.5565803263806));
#53923=CARTESIAN_POINT('',(13.4970328945603,52.1718177223987,15.5));
#53924=CARTESIAN_POINT('Ctrl Pts',(13.4975120618698,52.1706683776322,15.5565803263806));
#53925=CARTESIAN_POINT('Ctrl Pts',(13.2014603606288,52.3450050094651,15.5349217833067));
#53926=CARTESIAN_POINT('Ctrl Pts',(12.9746829017777,52.6437331734245,15.5132632402327));
#53927=CARTESIAN_POINT('Ctrl Pts',(12.8963324343973,52.9773225319626,15.4916046971588));
#53928=CARTESIAN_POINT('Ctrl Pts',(12.8016670421014,53.3803752328285,15.4654361936999));
#53929=CARTESIAN_POINT('Ctrl Pts',(12.9236783333193,53.8343190010791,15.439267690241));
#53930=CARTESIAN_POINT('Ctrl Pts',(13.2076549868354,54.1356000609316,15.413099186782));
#53931=CARTESIAN_POINT('Ctrl Pts',(13.4916316403516,54.4368811207841,15.3869306833231));
#53932=CARTESIAN_POINT('Ctrl Pts',(13.9375736561661,54.5854994722384,15.3607621798642));
#53933=CARTESIAN_POINT('Ctrl Pts',(14.3455153495113,54.5148128681013,15.3345936764052));
#53934=CARTESIAN_POINT('Ctrl Pts',(14.7534570428566,54.4441262639641,15.3084251729463));
#53935=CARTESIAN_POINT('Ctrl Pts',(15.1233984137326,54.1541347042354,15.2822566694874));
#53936=CARTESIAN_POINT('Ctrl Pts',(15.2894533218141,53.7748738751902,15.2560881660285));
#53937=CARTESIAN_POINT('Ctrl Pts',(15.4555082298957,53.3956130461449,15.2299196625695));
#53938=CARTESIAN_POINT('Ctrl Pts',(15.4176766751828,52.9270829477831,15.2037511591106));
#53939=CARTESIAN_POINT('Ctrl Pts',(15.1929228414795,52.579377997485,15.1775826556517));
#53940=CARTESIAN_POINT('Ctrl Pts',(14.9681690077762,52.2316730471868,15.1514141521927));
#53941=CARTESIAN_POINT('Ctrl Pts',(14.5564928950826,52.0047932449523,15.1252456487338));
#53942=CARTESIAN_POINT('Ctrl Pts',(14.1424948347361,52.0004742879611,15.0990771452749));
#53943=CARTESIAN_POINT('Ctrl Pts',(13.9183882655449,51.9981363382785,15.0849115389768));
#53944=CARTESIAN_POINT('Ctrl Pts',(13.6936012952866,52.0610154646128,15.0707459326787));
#53945=CARTESIAN_POINT('Ctrl Pts',(13.4977463410385,52.1735883352515,15.0565803263806));
#53946=CARTESIAN_POINT('Ctrl Pts',(13.4961785456119,52.1725162395268,15.1934196736194));
#53947=CARTESIAN_POINT('Ctrl Pts',(13.7677018035866,52.018891451597,15.2130488280172));
#53948=CARTESIAN_POINT('Ctrl Pts',(14.0979074320564,51.9632623188715,15.2326779824149));
#53949=CARTESIAN_POINT('Ctrl Pts',(14.4012233710795,52.0299449584561,15.2523071368127));
#53950=CARTESIAN_POINT('Ctrl Pts',(14.8055874123741,52.1188425670469,15.2784756402716));
#53951=CARTESIAN_POINT('Ctrl Pts',(15.1621610853483,52.4251218103423,15.3046441437306));
#53952=CARTESIAN_POINT('Ctrl Pts',(15.3110525132995,52.8114434442094,15.3308126471895));
#53953=CARTESIAN_POINT('Ctrl Pts',(15.4599439412506,53.1977650780765,15.3569811506484));
#53954=CARTESIAN_POINT('Ctrl Pts',(15.4011531241786,53.6641291025153,15.3831496541074));
#53955=CARTESIAN_POINT('Ctrl Pts',(15.161042564887,54.0014123408011,15.4093181575663));
#53956=CARTESIAN_POINT('Ctrl Pts',(14.9209320055955,54.338695579087,15.4354866610252));
#53957=CARTESIAN_POINT('Ctrl Pts',(14.4995017040844,54.5468980312199,15.4616551644841));
#53958=CARTESIAN_POINT('Ctrl Pts',(14.0857260162278,54.5326592450683,15.4878236679431));
#53959=CARTESIAN_POINT('Ctrl Pts',(13.6719503283713,54.5184204589168,15.513992171402));
#53960=CARTESIAN_POINT('Ctrl Pts',(13.2658292541693,54.2817404344808,15.5401606748609));
#53961=CARTESIAN_POINT('Ctrl Pts',(13.0494723111738,53.9287493069653,15.5663291783198));
#53962=CARTESIAN_POINT('Ctrl Pts',(12.8331153681783,53.5757581794499,15.5924976817788));
#53963=CARTESIAN_POINT('Ctrl Pts',(12.8065225563893,53.1064559488549,15.6186661852377));
#53964=CARTESIAN_POINT('Ctrl Pts',(12.9816184085214,52.7312833144481,15.6448346886966));
#53965=CARTESIAN_POINT('Ctrl Pts',(13.0899806023986,52.4990988894489,15.6610296836709));
#53966=CARTESIAN_POINT('Ctrl Pts',(13.2755904595332,52.3029665221486,15.6772246786452));
#53967=CARTESIAN_POINT('Ctrl Pts',(13.4984004295476,52.1727576237481,15.6934196736194));
#53968=CARTESIAN_POINT('Origin',(14.1292828945603,53.2669068454841,15.5));
#53969=CARTESIAN_POINT('',(13.4961138435273,52.1700468646075,16.1934196736194));
#53970=CARTESIAN_POINT('',(13.4958915862187,52.1719376453661,16.0565803263806));
#53971=CARTESIAN_POINT('',(13.4970328945603,52.1718177223987,15.5));
#53972=CARTESIAN_POINT('Ctrl Pts',(13.4958915862187,52.1719376453661,16.0565803263806));
#53973=CARTESIAN_POINT('Ctrl Pts',(13.424800873756,52.2121474216226,16.0514346408525));
#53974=CARTESIAN_POINT('Ctrl Pts',(13.3578067644457,52.2591973943854,16.0462889553244));
#53975=CARTESIAN_POINT('Ctrl Pts',(13.2964716828247,52.3127310779992,16.0411432697963));
#53976=CARTESIAN_POINT('Ctrl Pts',(12.9845506983831,52.5849778713888,16.0149747663373));
#53977=CARTESIAN_POINT('Ctrl Pts',(12.8189865827469,53.0249099405019,15.9888062628784));
#53978=CARTESIAN_POINT('Ctrl Pts',(12.8740202534737,53.4352565161154,15.9626377594195));
#53979=CARTESIAN_POINT('Ctrl Pts',(12.9290539242004,53.8456030917289,15.9364692559605));
#53980=CARTESIAN_POINT('Ctrl Pts',(13.20468538129,54.2263641738429,15.9103007525016));
#53981=CARTESIAN_POINT('Ctrl Pts',(13.5773182028765,54.4068019672842,15.8841322490427));
#53982=CARTESIAN_POINT('Ctrl Pts',(13.9499510244629,54.5872397607254,15.8579637455838));
#53983=CARTESIAN_POINT('Ctrl Pts',(14.4195852105461,54.5673542654938,15.8317952421248));
#53984=CARTESIAN_POINT('Ctrl Pts',(14.7756312098701,54.3560623738526,15.8056267386659));
#53985=CARTESIAN_POINT('Ctrl Pts',(15.1316772091941,54.1447704822114,15.779458235207));
#53986=CARTESIAN_POINT('Ctrl Pts',(15.3741350217589,53.7420721941606,15.7532897317481));
#53987=CARTESIAN_POINT('Ctrl Pts',(15.3942836818793,53.3285422092164,15.7271212282891));
#53988=CARTESIAN_POINT('Ctrl Pts',(15.4144323419997,52.9150122242722,15.7009527248302));
#53989=CARTESIAN_POINT('Ctrl Pts',(15.2122718496755,52.4906505424345,15.6747842213713));
#53990=CARTESIAN_POINT('Ctrl Pts',(14.8784533736736,52.2457459854386,15.6486157179124));
#53991=CARTESIAN_POINT('Ctrl Pts',(14.5446348976717,52.0008414284427,15.6224472144534));
#53992=CARTESIAN_POINT('Ctrl Pts',(14.0791584379921,51.9353939962885,15.5962787109945));
#53993=CARTESIAN_POINT('Ctrl Pts',(13.6907491702475,52.078751096952,15.5701102075356));
#53994=CARTESIAN_POINT('Ctrl Pts',(13.6238095222296,52.1034577006719,15.5656002471506));
#53995=CARTESIAN_POINT('Ctrl Pts',(13.5591589344204,52.1343662450031,15.5610902867656));
#53996=CARTESIAN_POINT('Ctrl Pts',(13.4975120618698,52.1706683776322,15.5565803263806));
#53997=CARTESIAN_POINT('Ctrl Pts',(13.4984004295476,52.1727576237481,15.6934196736194));
#53998=CARTESIAN_POINT('Ctrl Pts',(13.6356154845652,52.0925699142095,15.7033931821041));
#53999=CARTESIAN_POINT('Ctrl Pts',(13.7869389649625,52.0373841810022,15.7133666905887));
#54000=CARTESIAN_POINT('Ctrl Pts',(13.9430173010127,52.0141772385597,15.7233401990734));
#54001=CARTESIAN_POINT('Ctrl Pts',(14.352535825319,51.9532868352966,15.7495087025323));
#54002=CARTESIAN_POINT('Ctrl Pts',(14.7947883578784,52.1125490669891,15.7756772059912));
#54003=CARTESIAN_POINT('Ctrl Pts',(15.0714636060597,52.4205488559651,15.8018457094502));
#54004=CARTESIAN_POINT('Ctrl Pts',(15.3481388542411,52.728548644941,15.8280142129091));
#54005=CARTESIAN_POINT('Ctrl Pts',(15.4592368180444,53.1852859912004,15.854182716368));
#54006=CARTESIAN_POINT('Ctrl Pts',(15.3549398499385,53.5859544394514,15.880351219827));
#54007=CARTESIAN_POINT('Ctrl Pts',(15.2506428818326,53.9866228877023,15.9065197232859));
#54008=CARTESIAN_POINT('Ctrl Pts',(14.9309509818175,54.3312224379448,15.9326882267448));
#54009=CARTESIAN_POINT('Ctrl Pts',(14.5392177979356,54.4652305557052,15.9588567302037));
#54010=CARTESIAN_POINT('Ctrl Pts',(14.1474846140537,54.5992386734655,15.9850252336627));
#54011=CARTESIAN_POINT('Ctrl Pts',(13.6837101463051,54.5226553587437,16.0111937371216));
#54012=CARTESIAN_POINT('Ctrl Pts',(13.3558563789031,54.2698214801479,16.0373622405805));
#54013=CARTESIAN_POINT('Ctrl Pts',(13.0280026115012,54.016987601552,16.0635307440394));
#54014=CARTESIAN_POINT('Ctrl Pts',(12.836069544446,53.5879031590821,16.0896992474984));
#54015=CARTESIAN_POINT('Ctrl Pts',(12.8661222463432,53.174974717257,16.1158677509573));
#54016=CARTESIAN_POINT('Ctrl Pts',(12.8958099052365,52.7670620187505,16.1417183918447));
#54017=CARTESIAN_POINT('Ctrl Pts',(13.1421232693052,52.3749152184319,16.167569032732));
#54018=CARTESIAN_POINT('Ctrl Pts',(13.4961138435273,52.1700468646075,16.1934196736194));
#54019=CARTESIAN_POINT('Origin',(14.1292828945603,53.2669068454841,15.5));
#54020=CARTESIAN_POINT('',(13.4969690270882,52.1733618792496,16.6934196736194));
#54021=CARTESIAN_POINT('',(13.4982981440081,52.173172919003,16.5565803263806));
#54022=CARTESIAN_POINT('',(13.4970328945603,52.1718177223987,15.5));
#54023=CARTESIAN_POINT('Ctrl Pts',(13.4982981440081,52.173172919003,16.5565803263806));
#54024=CARTESIAN_POINT('Ctrl Pts',(13.2942737914494,52.291793394842,16.5417789949394));
#54025=CARTESIAN_POINT('Ctrl Pts',(13.121375289642,52.4650421903572,16.5269776634981));
#54026=CARTESIAN_POINT('Ctrl Pts',(13.0113308722452,52.6717520885803,16.5121763320569));
#54027=CARTESIAN_POINT('Ctrl Pts',(12.8167742049128,53.0372116898416,16.486007828598));
#54028=CARTESIAN_POINT('Ctrl Pts',(12.8186845812821,53.5072628063503,16.4598393251391));
#54029=CARTESIAN_POINT('Ctrl Pts',(13.0162053670574,53.8711289302741,16.4336708216802));
#54030=CARTESIAN_POINT('Ctrl Pts',(13.2137261528326,54.234995054198,16.4075023182212));
#54031=CARTESIAN_POINT('Ctrl Pts',(13.6068573480137,54.492676185537,16.3813338147623));
#54032=CARTESIAN_POINT('Ctrl Pts',(14.0193142510176,54.5286250418801,16.3551653113034));
#54033=CARTESIAN_POINT('Ctrl Pts',(14.4317711540215,54.5645738982232,16.3289968078444));
#54034=CARTESIAN_POINT('Ctrl Pts',(14.8635537648482,54.3787904795703,16.3028283043855));
#54035=CARTESIAN_POINT('Ctrl Pts',(15.1210456285731,54.0545822792718,16.2766598009266));
#54036=CARTESIAN_POINT('Ctrl Pts',(15.3785374922981,53.7303740789732,16.2504912974677));
#54037=CARTESIAN_POINT('Ctrl Pts',(15.4617386089214,53.267741097029,16.2243227940087));
#54038=CARTESIAN_POINT('Ctrl Pts',(15.3333406086023,52.8741334617557,16.1981542905498));
#54039=CARTESIAN_POINT('Ctrl Pts',(15.2049426082832,52.4805258264823,16.1719857870909));
#54040=CARTESIAN_POINT('Ctrl Pts',(14.8649454910218,52.1559435378799,16.145817283632));
#54041=CARTESIAN_POINT('Ctrl Pts',(14.4658080057675,52.0459331524117,16.119648780173));
#54042=CARTESIAN_POINT('Ctrl Pts',(14.1451555582542,51.9575548350262,16.0986259622422));
#54043=CARTESIAN_POINT('Ctrl Pts',(13.7863343457911,52.0076596690573,16.0776031443114));
#54044=CARTESIAN_POINT('Ctrl Pts',(13.4958915862187,52.1719376453661,16.0565803263806));
#54045=CARTESIAN_POINT('Ctrl Pts',(13.4961138435273,52.1700468646075,16.1934196736194));
#54046=CARTESIAN_POINT('Ctrl Pts',(13.5004665539579,52.1675277788309,16.193737536191));
#54047=CARTESIAN_POINT('Ctrl Pts',(13.5048355445965,52.1650370085359,16.1940553987625));
#54048=CARTESIAN_POINT('Ctrl Pts',(13.5092206128964,52.1625748725828,16.1943732613341));
#54049=CARTESIAN_POINT('Ctrl Pts',(13.8702278067029,51.9598759109143,16.220541764793));
#54050=CARTESIAN_POINT('Ctrl Pts',(14.3402037234666,51.9512504287578,16.2467102682519));
#54051=CARTESIAN_POINT('Ctrl Pts',(14.7084055750498,52.1405661950787,16.2728787717108));
#54052=CARTESIAN_POINT('Ctrl Pts',(15.076607426633,52.3298819613996,16.2990472751698));
#54053=CARTESIAN_POINT('Ctrl Pts',(15.3430352130359,52.7171389761979,16.3252157786287));
#54054=CARTESIAN_POINT('Ctrl Pts',(15.3882195489486,53.1286865903088,16.3513842820876));
#54055=CARTESIAN_POINT('Ctrl Pts',(15.4334038848614,53.5402342044196,16.3775527855466));
#54056=CARTESIAN_POINT('Ctrl Pts',(15.2573447702841,53.976072417843,16.4037212890055));
#54057=CARTESIAN_POINT('Ctrl Pts',(14.9389892027717,54.240766195907,16.4298897924644));
#54058=CARTESIAN_POINT('Ctrl Pts',(14.6206336352594,54.505459973971,16.4560582959233));
#54059=CARTESIAN_POINT('Ctrl Pts',(14.1599816148119,54.5990093166755,16.4822267993823));
#54060=CARTESIAN_POINT('Ctrl Pts',(13.7635949875347,54.4794655848163,16.5083953028412));
#54061=CARTESIAN_POINT('Ctrl Pts',(13.3672083602574,54.3599218529572,16.5345638063001));
#54062=CARTESIAN_POINT('Ctrl Pts',(13.0350871261504,54.0272850465344,16.560732309759));
#54063=CARTESIAN_POINT('Ctrl Pts',(12.916158385472,53.6307134674394,16.586900813218));
#54064=CARTESIAN_POINT('Ctrl Pts',(12.7972296447936,53.2341418883445,16.6130693166769));
#54065=CARTESIAN_POINT('Ctrl Pts',(12.891493397544,52.7736355365774,16.6392378201358));
#54066=CARTESIAN_POINT('Ctrl Pts',(13.1566806746197,52.4556909263592,16.6654063235948));
#54067=CARTESIAN_POINT('Ctrl Pts',(13.2513082234268,52.3422378246374,16.6747441069363));
#54068=CARTESIAN_POINT('Ctrl Pts',(13.3676994181703,52.2469370707529,16.6840818902779));
#54069=CARTESIAN_POINT('Ctrl Pts',(13.4969690270882,52.1733618792496,16.6934196736194));
#54070=CARTESIAN_POINT('Origin',(14.1292828945603,53.2669068454841,15.5));
#54071=CARTESIAN_POINT('',(13.498190246218,52.1716844371558,17.1934196736194));
#54072=CARTESIAN_POINT('',(13.4965460097018,52.1700456009992,17.0565803263806));
#54073=CARTESIAN_POINT('',(13.4970328945603,52.1718177223987,15.5));
#54074=CARTESIAN_POINT('Ctrl Pts',(13.4965460097018,52.1700456009992,17.0565803263806));
#54075=CARTESIAN_POINT('Ctrl Pts',(13.1622129933252,52.3652134872718,17.0321233490263));
#54076=CARTESIAN_POINT('Ctrl Pts',(12.9210086316388,52.724852170666,17.0076663716719));
#54077=CARTESIAN_POINT('Ctrl Pts',(12.8726933551042,53.1087658234733,16.9832093943176));
#54078=CARTESIAN_POINT('Ctrl Pts',(12.8209969225157,53.5195461748581,16.9570408908587));
#54079=CARTESIAN_POINT('Ctrl Pts',(12.9901314007569,53.9581179567514,16.9308723873998));
#54080=CARTESIAN_POINT('Ctrl Pts',(13.3042549587021,54.2278203840484,16.9047038839408));
#54081=CARTESIAN_POINT('Ctrl Pts',(13.6183785166473,54.4975228113455,16.8785353804819));
#54082=CARTESIAN_POINT('Ctrl Pts',(14.0774911542964,54.5983558840463,16.852366877023));
#54083=CARTESIAN_POINT('Ctrl Pts',(14.4757212681973,54.4851048462746,16.8261983735641));
#54084=CARTESIAN_POINT('Ctrl Pts',(14.8739513820981,54.371853808503,16.8000298701051));
#54085=CARTESIAN_POINT('Ctrl Pts',(15.2112989722506,54.0445186602589,16.7738613666462));
#54086=CARTESIAN_POINT('Ctrl Pts',(15.3364933887363,53.6498803767018,16.7476928631873));
#54087=CARTESIAN_POINT('Ctrl Pts',(15.4616878052219,53.2552420931447,16.7215243597283));
#54088=CARTESIAN_POINT('Ctrl Pts',(15.3747290480406,52.7933006742746,16.6953558562694));
#54089=CARTESIAN_POINT('Ctrl Pts',(15.1146104479144,52.4711961414872,16.6691873528105));
#54090=CARTESIAN_POINT('Ctrl Pts',(14.8544918477881,52.1490916086999,16.6430188493516));
#54091=CARTESIAN_POINT('Ctrl Pts',(14.4212134047168,51.9668239619953,16.6168503458926));
#54092=CARTESIAN_POINT('Ctrl Pts',(14.0090623276641,52.00612418165,16.5906818424337));
#54093=CARTESIAN_POINT('Ctrl Pts',(13.8300306074324,52.0231955574683,16.579314670416));
#54094=CARTESIAN_POINT('Ctrl Pts',(13.6549853934321,52.0820744013433,16.5679474983983));
#54095=CARTESIAN_POINT('Ctrl Pts',(13.4982981440081,52.173172919003,16.5565803263806));
#54096=CARTESIAN_POINT('Ctrl Pts',(13.4969690270882,52.1733618792496,16.6934196736194));
#54097=CARTESIAN_POINT('Ctrl Pts',(13.7299687153222,52.0407475948441,16.7102503937368));
#54098=CARTESIAN_POINT('Ctrl Pts',(14.0048072977942,51.9787144778412,16.7270811138542));
#54099=CARTESIAN_POINT('Ctrl Pts',(14.2694557749176,52.0081860992865,16.7439118339715));
#54100=CARTESIAN_POINT('Ctrl Pts',(14.6809327967389,52.0540087511013,16.7700803374305));
#54101=CARTESIAN_POINT('Ctrl Pts',(15.0677760389805,52.3210369234002,16.7962488408894));
#54102=CARTESIAN_POINT('Ctrl Pts',(15.2565204673329,52.6895319775572,16.8224173443483));
#54103=CARTESIAN_POINT('Ctrl Pts',(15.4452648956853,53.0580270317142,16.8485858478072));
#54104=CARTESIAN_POINT('Ctrl Pts',(15.4359105101485,53.5279889677293,16.8747543512661));
#54105=CARTESIAN_POINT('Ctrl Pts',(15.2326517793344,53.8886813318345,16.9009228547251));
#54106=CARTESIAN_POINT('Ctrl Pts',(15.0293930485204,54.2493736959397,16.927091358184));
#54107=CARTESIAN_POINT('Ctrl Pts',(14.6322299724291,54.500796488135,16.9532598616429));
#54108=CARTESIAN_POINT('Ctrl Pts',(14.2192554962477,54.5302086092019,16.9794283651019));
#54109=CARTESIAN_POINT('Ctrl Pts',(13.8062810200662,54.5596207302688,17.0055968685608));
#54110=CARTESIAN_POINT('Ctrl Pts',(13.3774951437946,54.3670221802074,17.0317653720197));
#54111=CARTESIAN_POINT('Ctrl Pts',(13.1251699439815,54.0387767018187,17.0579338754786));
#54112=CARTESIAN_POINT('Ctrl Pts',(12.8728447441683,53.7105312234301,17.0841023789376));
#54113=CARTESIAN_POINT('Ctrl Pts',(12.7969802208135,53.2466388167143,17.1102708823965));
#54114=CARTESIAN_POINT('Ctrl Pts',(12.9315961537198,52.8551138190488,17.1364393858554));
#54115=CARTESIAN_POINT('Ctrl Pts',(13.0293020925489,52.570940046702,17.1554328151101));
#54116=CARTESIAN_POINT('Ctrl Pts',(13.2378899597344,52.32488970875,17.1744262443648));
#54117=CARTESIAN_POINT('Ctrl Pts',(13.498190246218,52.1716844371558,17.1934196736194));
#54118=CARTESIAN_POINT('Origin',(14.1292828945603,53.2669068454841,15.5));
#54119=CARTESIAN_POINT('',(13.4957229821349,52.1707788329429,17.6934196736194));
#54120=CARTESIAN_POINT('',(13.4965541629804,52.1730078059394,17.5565803263806));
#54121=CARTESIAN_POINT('',(13.4970328945603,52.1718177223987,15.5));
#54122=CARTESIAN_POINT('',(13.8936870225526,54.5092654229862,18.));
#54123=CARTESIAN_POINT('Ctrl Pts',(13.4957229821349,52.1707788329429,17.6934196736194));
#54124=CARTESIAN_POINT('Ctrl Pts',(13.8217103338362,51.9852932094709,17.7171076053695));
#54125=CARTESIAN_POINT('Ctrl Pts',(14.2369080256434,51.9506029252058,17.7407955371196));
#54126=CARTESIAN_POINT('Ctrl Pts',(14.5864865212314,52.0858847696684,17.7644834688697));
#54127=CARTESIAN_POINT('Ctrl Pts',(14.9726724562246,52.2353331660965,17.7906519723286));
#54128=CARTESIAN_POINT('Ctrl Pts',(15.2787764866269,52.5922161636807,17.8168204757875));
#54129=CARTESIAN_POINT('Ctrl Pts',(15.3668468800596,52.9968087774221,17.8429889792464));
#54130=CARTESIAN_POINT('Ctrl Pts',(15.4549172734922,53.4014013911635,17.8691574827054));
#54131=CARTESIAN_POINT('Ctrl Pts',(15.3249540299554,53.8537036210623,17.8953259861643));
#54132=CARTESIAN_POINT('Ctrl Pts',(15.0367817327077,54.1500381490016,17.9214944896232));
#54133=CARTESIAN_POINT('Ctrl Pts',(14.74860943546,54.4463726769409,17.9476629930821));
#54134=CARTESIAN_POINT('Ctrl Pts',(14.3022280845015,54.5867395029208,17.9738314965411));
#54135=CARTESIAN_POINT('Ctrl Pts',(13.8936870225526,54.5092654229862,18.));
#54136=CARTESIAN_POINT('',(12.9337042190835,52.8487739793662,18.));
#54137=CARTESIAN_POINT('Origin',(14.1292828945603,53.2669068454841,18.));
#54138=CARTESIAN_POINT('Ctrl Pts',(12.9336937527447,52.848768453162,18.));
#54139=CARTESIAN_POINT('Ctrl Pts',(12.8048883200695,53.2213447345786,17.975091839613));
#54140=CARTESIAN_POINT('Ctrl Pts',(12.8625878757539,53.660362859942,17.950183679226));
#54141=CARTESIAN_POINT('Ctrl Pts',(13.0861189278269,53.984999064981,17.925275518839));
#54142=CARTESIAN_POINT('Ctrl Pts',(13.3209605627957,54.3260617336993,17.89910701538));
#54143=CARTESIAN_POINT('Ctrl Pts',(13.7388402922128,54.5408742678445,17.8729385119211));
#54144=CARTESIAN_POINT('Ctrl Pts',(14.1527389844808,54.5331807500212,17.8467700084622));
#54145=CARTESIAN_POINT('Ctrl Pts',(14.5666376767488,54.5254872321979,17.8206015050033));
#54146=CARTESIAN_POINT('Ctrl Pts',(14.9765553318677,54.2952876624062,17.7944330015443));
#54147=CARTESIAN_POINT('Ctrl Pts',(15.1985005516415,53.9457721211068,17.7682644980854));
#54148=CARTESIAN_POINT('Ctrl Pts',(15.4204457714153,53.5962565798076,17.7420959946265));
#54149=CARTESIAN_POINT('Ctrl Pts',(15.4544185558441,53.1274250670007,17.7159274911675));
#54150=CARTESIAN_POINT('Ctrl Pts',(15.2852740004506,52.7495241339714,17.6897589877086));
#54151=CARTESIAN_POINT('Ctrl Pts',(15.1161294450571,52.3716232009421,17.6635904842497));
#54152=CARTESIAN_POINT('Ctrl Pts',(14.7438675498413,52.0846528476904,17.6374219807908));
#54153=CARTESIAN_POINT('Ctrl Pts',(14.3353709232147,52.0172856023794,17.6112534773319));
#54154=CARTESIAN_POINT('Ctrl Pts',(14.0508839155709,51.9703694107086,17.5930290936814));
#54155=CARTESIAN_POINT('Ctrl Pts',(13.7488228128377,52.0299622436843,17.574804710031));
#54156=CARTESIAN_POINT('Ctrl Pts',(13.4965541629804,52.1730078059394,17.5565803263806));
#54157=CARTESIAN_POINT('Origin',(14.1292828945603,53.2669068454841,19.1042117235887));
#54158=CARTESIAN_POINT('',(13.3561475049578,51.9293198574881,14.3957882764113));
#54159=CARTESIAN_POINT('',(13.3590334722299,51.9326791410008,14.3542117235887));
#54160=CARTESIAN_POINT('',(13.3577828945603,51.9306296474448,19.1042117235887));
#54161=CARTESIAN_POINT('',(15.6194800884629,52.8667052421829,14.));
#54162=CARTESIAN_POINT('Ctrl Pts',(13.3590334722299,51.9326791410008,14.3542117235887));
#54163=CARTESIAN_POINT('Ctrl Pts',(13.1333102308069,52.0631907802776,14.3408151628948));
#54164=CARTESIAN_POINT('Ctrl Pts',(12.5590924929827,52.6090703324587,14.301250098742));
#54165=CARTESIAN_POINT('Ctrl Pts',(12.4888785260391,54.0475602728967,14.2355165311303));
#54166=CARTESIAN_POINT('Ctrl Pts',(13.875577901283,55.0671461874891,14.1570110207536));
#54167=CARTESIAN_POINT('Ctrl Pts',(15.4910603626305,54.4687297322861,14.0785055103768));
#54168=CARTESIAN_POINT('Ctrl Pts',(15.7510836294753,53.3567463262428,14.0261685034589));
#54169=CARTESIAN_POINT('Ctrl Pts',(15.6194800884629,52.8667052421829,14.));
#54170=CARTESIAN_POINT('',(15.2224969554152,52.1743874122524,14.));
#54171=CARTESIAN_POINT('Origin',(14.1292828945603,53.2669068454841,14.));
#54172=CARTESIAN_POINT('Ctrl Pts',(13.3561475049578,51.9293198574881,14.3957882764113));
#54173=CARTESIAN_POINT('Ctrl Pts',(13.3167322940313,51.9517582304519,14.3934410251636));
#54174=CARTESIAN_POINT('Ctrl Pts',(12.8509091548948,52.2463455523906,14.3649252704569));
#54175=CARTESIAN_POINT('Ctrl Pts',(12.312999126503,53.317416116839,14.3102410122914));
#54176=CARTESIAN_POINT('Ctrl Pts',(13.1694776941512,54.809893106608,14.2317355019146));
#54177=CARTESIAN_POINT('Ctrl Pts',(14.8870885705587,54.9183199028175,14.1532299915378));
#54178=CARTESIAN_POINT('Ctrl Pts',(15.9077095091603,53.5682793339942,14.0759848242329));
#54179=CARTESIAN_POINT('Ctrl Pts',(15.5613200902447,52.5158444925152,14.024908160387));
#54180=CARTESIAN_POINT('Ctrl Pts',(15.2225055381224,52.1743757967134,14.));
#54181=CARTESIAN_POINT('Origin',(14.1292828945603,53.2669068454841,19.1042117235887));
#54182=CARTESIAN_POINT('',(13.3586534741695,51.9327902292019,14.8957882764113));
#54183=CARTESIAN_POINT('',(13.3577899368159,51.928743983656,14.8542117235887));
#54184=CARTESIAN_POINT('',(13.3577828945603,51.9306296474448,19.1042117235887));
#54185=CARTESIAN_POINT('Ctrl Pts',(13.3577899368159,51.928743983656,14.8542117235887));
#54186=CARTESIAN_POINT('Ctrl Pts',(12.9734547442474,52.1543891335537,14.8311595169817));
#54187=CARTESIAN_POINT('Ctrl Pts',(12.3621732880177,53.0098569651208,14.7819388069158));
#54188=CARTESIAN_POINT('Ctrl Pts',(12.8743108410601,54.5809237767911,14.706549593391));
#54189=CARTESIAN_POINT('Ctrl Pts',(14.53309819057,55.0385159317414,14.6280440830142));
#54190=CARTESIAN_POINT('Ctrl Pts',(15.8297520454146,53.9072361260964,14.5495385726375));
#54191=CARTESIAN_POINT('Ctrl Pts',(15.6013490876951,52.2017963646938,14.4710330622607));
#54192=CARTESIAN_POINT('Ctrl Pts',(14.3170802291729,51.5794230562898,14.4059241125778));
#54193=CARTESIAN_POINT('Ctrl Pts',(13.5742323121468,51.8082526389225,14.3669836663538));
#54194=CARTESIAN_POINT('Ctrl Pts',(13.3590334722299,51.9326791410008,14.3542117235887));
#54195=CARTESIAN_POINT('Ctrl Pts',(13.3586534741695,51.9327902292019,14.8957882764113));
#54196=CARTESIAN_POINT('Ctrl Pts',(13.1561499564235,52.0491845394435,14.8837853792505));
#54197=CARTESIAN_POINT('Ctrl Pts',(12.5927601381537,52.5577927522065,14.8456139786307));
#54198=CARTESIAN_POINT('Ctrl Pts',(12.4499580614657,53.9607971579715,14.781274074552));
#54199=CARTESIAN_POINT('Ctrl Pts',(13.7817713167743,55.0504032414556,14.7027685641753));
#54200=CARTESIAN_POINT('Ctrl Pts',(15.4252464910755,54.5405234556122,14.6242630537985));
#54201=CARTESIAN_POINT('Ctrl Pts',(15.9064600587523,52.8884418877606,14.5457575434217));
#54202=CARTESIAN_POINT('Ctrl Pts',(14.8271456061161,51.6150089076652,14.4695992842926));
#54203=CARTESIAN_POINT('Ctrl Pts',(13.7561556767951,51.7016023764131,14.4196095286225));
#54204=CARTESIAN_POINT('Ctrl Pts',(13.3561475049578,51.9293198574881,14.3957882764113));
#54205=CARTESIAN_POINT('Origin',(14.1292828945603,53.2669068454841,19.1042117235887));
#54206=CARTESIAN_POINT('',(13.3583675961487,51.9292271650606,15.3957882764113));
#54207=CARTESIAN_POINT('',(13.3567403793943,51.9314820095869,15.3542117235887));
#54208=CARTESIAN_POINT('',(13.3577828945603,51.9306296474448,19.1042117235887));
#54209=CARTESIAN_POINT('Ctrl Pts',(13.3567403793943,51.9314820095869,15.3542117235887));
#54210=CARTESIAN_POINT('Ctrl Pts',(13.2463612263437,51.9939332857897,15.3476723745276));
#54211=CARTESIAN_POINT('Ctrl Pts',(12.7340280693376,52.3726757467305,15.3149645220075));
#54212=CARTESIAN_POINT('Ctrl Pts',(12.343540269987,53.6026792252177,15.2560881660285));
#54213=CARTESIAN_POINT('Ctrl Pts',(13.4243618186884,54.9416323741225,15.1775826556517));
#54214=CARTESIAN_POINT('Ctrl Pts',(15.1373732173661,54.7786522269087,15.0990771452749));
#54215=CARTESIAN_POINT('Ctrl Pts',(15.9463055097723,53.2599021305098,15.0205716348981));
#54216=CARTESIAN_POINT('Ctrl Pts',(15.1256881964072,51.7474355457531,14.9420661245214));
#54217=CARTESIAN_POINT('Ctrl Pts',(13.9148311256039,51.641642546183,14.8866128207515));
#54218=CARTESIAN_POINT('Ctrl Pts',(13.4097460280966,51.8982402977282,14.8573280204407));
#54219=CARTESIAN_POINT('Ctrl Pts',(13.3577899368159,51.928743983656,14.8542117235887));
#54220=CARTESIAN_POINT('Ctrl Pts',(13.3583675961486,51.9292271650606,15.3957882764113));
#54221=CARTESIAN_POINT('Ctrl Pts',(12.997111941728,52.141960595601,15.3741297333373));
#54222=CARTESIAN_POINT('Ctrl Pts',(12.3860414668385,52.9469081505226,15.3263026868045));
#54223=CARTESIAN_POINT('Ctrl Pts',(12.8070334555363,54.5132114643008,15.2523071368127));
#54224=CARTESIAN_POINT('Ctrl Pts',(14.4395092097517,55.0572639347494,15.1738016264359));
#54225=CARTESIAN_POINT('Ctrl Pts',(15.7937667074068,53.9956815464663,15.0952961160592));
#54226=CARTESIAN_POINT('Ctrl Pts',(15.6552753932384,52.2805167973031,15.0167906056824));
#54227=CARTESIAN_POINT('Ctrl Pts',(14.3786526271626,51.5769541863948,14.9502879924664));
#54228=CARTESIAN_POINT('Ctrl Pts',(13.5976445334062,51.7954237290868,14.9099538827094));
#54229=CARTESIAN_POINT('Ctrl Pts',(13.3586534741695,51.9327902292019,14.8957882764113));
#54230=CARTESIAN_POINT('Origin',(14.1292828945603,53.2669068454841,19.1042117235887));
#54231=CARTESIAN_POINT('',(13.3563902185847,51.9307759828649,15.8957882764113));
#54232=CARTESIAN_POINT('',(13.3594516225044,51.9317765575137,15.8542117235887));
#54233=CARTESIAN_POINT('',(13.3577828945603,51.9306296474448,19.1042117235887));
#54234=CARTESIAN_POINT('Ctrl Pts',(13.3594516225044,51.9317765575137,15.8542117235887));
#54235=CARTESIAN_POINT('Ctrl Pts',(13.0875688358439,52.0906633350794,15.8380167286145));
#54236=CARTESIAN_POINT('Ctrl Pts',(12.4951087068473,52.7167109460471,15.7956532301813));
#54237=CARTESIAN_POINT('Ctrl Pts',(12.5800904986591,54.2164449634099,15.7271212282891));
#54238=CARTESIAN_POINT('Ctrl Pts',(14.0667923195219,55.0828679235634,15.6486157179124));
#54239=CARTESIAN_POINT('Ctrl Pts',(15.6095371717915,54.3206938223985,15.5701102075356));
#54240=CARTESIAN_POINT('Ctrl Pts',(15.8247548010729,52.6134584968728,15.4916046971588));
#54241=CARTESIAN_POINT('Ctrl Pts',(14.6281635632835,51.5856454904132,15.4196385358432));
#54242=CARTESIAN_POINT('Ctrl Pts',(13.6880653197304,51.7440221062451,15.3738408779865));
#54243=CARTESIAN_POINT('Ctrl Pts',(13.3567403793943,51.9314820095869,15.3542117235887));
#54244=CARTESIAN_POINT('Ctrl Pts',(13.3563902185847,51.9307759828649,15.8957882764113));
#54245=CARTESIAN_POINT('Ctrl Pts',(13.2696421210522,51.9798417675732,15.8906425908832));
#54246=CARTESIAN_POINT('Ctrl Pts',(12.7721552352232,52.3292268802209,15.8593284018961));
#54247=CARTESIAN_POINT('Ctrl Pts',(12.3283713567551,53.5084362707541,15.8018457094502));
#54248=CARTESIAN_POINT('Ctrl Pts',(13.3373852079753,54.9023018690978,15.7233401990734));
#54249=CARTESIAN_POINT('Ctrl Pts',(15.0565917302206,54.8295063313936,15.6448346886966));
#54250=CARTESIAN_POINT('Ctrl Pts',(15.9441656443073,53.3553344251959,15.5663291783198));
#54251=CARTESIAN_POINT('Ctrl Pts',(15.2041095597138,51.8018585649929,15.4878236679431));
#54252=CARTESIAN_POINT('Ctrl Pts',(13.9702286955569,51.6283710932553,15.4309767006402));
#54253=CARTESIAN_POINT('Ctrl Pts',(13.4335918937727,51.8849296635608,15.4002982367963));
#54254=CARTESIAN_POINT('Ctrl Pts',(13.3583675961486,51.9292271650606,15.3957882764113));
#54255=CARTESIAN_POINT('Origin',(14.1292828945603,53.2669068454841,19.1042117235887));
#54256=CARTESIAN_POINT('',(13.3593268090703,51.9322833195368,16.3957882764113));
#54257=CARTESIAN_POINT('',(13.356661426989,51.9284687668027,16.3542117235887));
#54258=CARTESIAN_POINT('',(13.3577828945603,51.9306296474448,19.1042117235887));
#54259=CARTESIAN_POINT('Ctrl Pts',(13.356661426989,51.9284687668027,16.3542117235887));
#54260=CARTESIAN_POINT('Ctrl Pts',(12.9247061434582,52.1784583832132,16.3283610827014));
#54261=CARTESIAN_POINT('Ctrl Pts',(12.3198850098697,53.141372730953,16.2763419383551));
#54262=CARTESIAN_POINT('Ctrl Pts',(13.0196563589383,54.7057774673455,16.1981542905498));
#54263=CARTESIAN_POINT('Ctrl Pts',(14.7174120024405,54.9861287238479,16.1196487801731));
#54264=CARTESIAN_POINT('Ctrl Pts',(15.8877194798386,53.7246409278238,16.0411432697963));
#54265=CARTESIAN_POINT('Ctrl Pts',(15.4810192232586,52.0526463245539,15.9626377594195));
#54266=CARTESIAN_POINT('Ctrl Pts',(14.1960288388142,51.5899006730013,15.900327244017));
#54267=CARTESIAN_POINT('Ctrl Pts',(13.5268876287458,51.8339278933634,15.8641852320734));
#54268=CARTESIAN_POINT('Ctrl Pts',(13.3594516225044,51.9317765575137,15.8542117235887));
#54269=CARTESIAN_POINT('Ctrl Pts',(13.3593268090703,51.9322833195368,16.3957882764113));
#54270=CARTESIAN_POINT('Ctrl Pts',(13.1103670811162,52.0770293806041,16.3809869449701));
#54271=CARTESIAN_POINT('Ctrl Pts',(12.5263819999043,52.6621976201272,16.3400171100699));
#54272=CARTESIAN_POINT('Ctrl Pts',(12.5323627785853,54.1337776405724,16.2728787717109));
#54273=CARTESIAN_POINT('Ctrl Pts',(13.9715120885841,55.0770800976453,16.1943732613341));
#54274=CARTESIAN_POINT('Ctrl Pts',(15.5521540067467,54.3969761475115,16.1158677509573));
#54275=CARTESIAN_POINT('Ctrl Pts',(15.8567312853937,52.7033991815805,16.0373622405805));
#54276=CARTESIAN_POINT('Ctrl Pts',(14.6936723389742,51.5930711363043,15.9640024157319));
#54277=CARTESIAN_POINT('Ctrl Pts',(13.7108015891028,51.7303165780056,15.9168110943421));
#54278=CARTESIAN_POINT('Ctrl Pts',(13.3563902185847,51.9307759828649,15.8957882764113));
#54279=CARTESIAN_POINT('Origin',(14.1292828945603,53.2669068454841,19.1042117235887));
#54280=CARTESIAN_POINT('',(13.3571887756701,51.9284672248908,16.8957882764113));
#54281=CARTESIAN_POINT('',(13.3577049605868,51.9325138973624,16.8542117235887));
#54282=CARTESIAN_POINT('',(13.3577828945603,51.9306296474448,19.1042117235887));
#54283=CARTESIAN_POINT('Ctrl Pts',(13.3577049605868,51.9325138973624,16.8542117235887));
#54284=CARTESIAN_POINT('Ctrl Pts',(13.1999643464624,52.02229366841,16.8448739402472));
#54285=CARTESIAN_POINT('Ctrl Pts',(12.6599209222933,52.4644795705919,16.8093676534467));
#54286=CARTESIAN_POINT('Ctrl Pts',(12.38882648105,53.7888562103795,16.7476928631873));
#54287=CARTESIAN_POINT('Ctrl Pts',(13.6046344626092,55.0065515658014,16.6691873528105));
#54288=CARTESIAN_POINT('Ctrl Pts',(15.2909596525271,54.6640921689023,16.5906818424337));
#54289=CARTESIAN_POINT('Ctrl Pts',(15.9354654978243,53.0686037624672,16.512176332057));
#54290=CARTESIAN_POINT('Ctrl Pts',(14.9601438503283,51.6509582729447,16.4336708216802));
#54291=CARTESIAN_POINT('Ctrl Pts',(13.8062061827166,51.672136525716,16.3810159521908));
#54292=CARTESIAN_POINT('Ctrl Pts',(13.3619728008082,51.9253948645857,16.3545295861603));
#54293=CARTESIAN_POINT('Ctrl Pts',(13.356661426989,51.9284687668027,16.3542117235887));
#54294=CARTESIAN_POINT('Ctrl Pts',(13.3571887756701,51.9284672248908,16.8957882764113));
#54295=CARTESIAN_POINT('Ctrl Pts',(12.9492205318827,52.1666198927584,16.871331299057));
#54296=CARTESIAN_POINT('Ctrl Pts',(12.3399661957944,53.0750256353043,16.8207058182437));
#54297=CARTESIAN_POINT('Ctrl Pts',(12.9456243299004,54.6455189484075,16.7439118339715));
#54298=CARTESIAN_POINT('Ctrl Pts',(14.6263142466089,55.0146421540478,16.6654063235947));
#54299=CARTESIAN_POINT('Ctrl Pts',(15.8612545351151,53.8163547667627,16.586900813218));
#54300=CARTESIAN_POINT('Ctrl Pts',(15.5429215283993,52.1253094303059,16.5083953028412));
#54301=CARTESIAN_POINT('Ctrl Pts',(14.2558484377857,51.5838751930056,16.4446911239056));
#54302=CARTESIAN_POINT('Ctrl Pts',(13.5505236662164,51.8211207946266,16.407155448429));
#54303=CARTESIAN_POINT('Ctrl Pts',(13.3593268090703,51.9322833195368,16.3957882764113));
#54304=CARTESIAN_POINT('Origin',(14.1292828945603,53.2669068454841,19.1042117235887));
#54305=CARTESIAN_POINT('',(13.3571987246687,51.9320818411207,17.3957882764113));
#54306=CARTESIAN_POINT('',(13.3591951473145,51.9304670067728,17.3542117235887));
#54307=CARTESIAN_POINT('',(13.3577828945603,51.9306296474448,19.1042117235887));
#54308=CARTESIAN_POINT('Ctrl Pts',(13.3591951473145,51.9304670067728,17.3542117235887));
#54309=CARTESIAN_POINT('Ctrl Pts',(13.0415649835786,52.117414997338,17.3352182943341));
#54310=CARTESIAN_POINT('Ctrl Pts',(12.4363561313197,52.8313196200715,17.2900563616205));
#54311=CARTESIAN_POINT('Ctrl Pts',(12.6886936446445,54.3742998061272,17.2187259254479));
#54312=CARTESIAN_POINT('Ctrl Pts',(14.2583653103316,55.0793521495312,17.1402204150712));
#54313=CARTESIAN_POINT('Ctrl Pts',(15.7122742697831,54.1589598165365,17.0617149046944));
#54314=CARTESIAN_POINT('Ctrl Pts',(15.7465182007044,52.4385534884905,16.9832093943176));
#54315=CARTESIAN_POINT('Ctrl Pts',(14.4988281136715,51.5773043644133,16.9140416672824));
#54316=CARTESIAN_POINT('Ctrl Pts',(13.6420217015477,51.7706919591752,16.8710424437061));
#54317=CARTESIAN_POINT('Ctrl Pts',(13.3577049605868,51.9325138973624,16.8542117235887));
#54318=CARTESIAN_POINT('Ctrl Pts',(13.3571987246687,51.9320818411208,17.3957882764113));
#54319=CARTESIAN_POINT('Ctrl Pts',(13.2230139283874,52.0081695343042,17.3878441566028));
#54320=CARTESIAN_POINT('Ctrl Pts',(12.6963900910873,52.417984443011,17.3537315333353));
#54321=CARTESIAN_POINT('Ctrl Pts',(12.3638250796578,53.6967359986949,17.293450406609));
#54322=CARTESIAN_POINT('Ctrl Pts',(13.5139962436502,54.9765978264215,17.2149448962322));
#54323=CARTESIAN_POINT('Ctrl Pts',(15.2159841085891,54.7231706136823,17.1364393858554));
#54324=CARTESIAN_POINT('Ctrl Pts',(15.9433860453712,53.1637302055401,17.0579338754786));
#54325=CARTESIAN_POINT('Ctrl Pts',(15.043860342301,51.6968216692226,16.9794283651019));
#54326=CARTESIAN_POINT('Ctrl Pts',(13.8598729208803,51.6563265828795,16.9253798320794));
#54327=CARTESIAN_POINT('Ctrl Pts',(13.3857388409122,51.9118010399395,16.8974998025159));
#54328=CARTESIAN_POINT('Ctrl Pts',(13.3571887756701,51.9284672248908,16.8957882764113));
#54329=CARTESIAN_POINT('Origin',(14.1292828945603,53.2669068454841,19.1042117235887));
#54330=CARTESIAN_POINT('',(13.3599426557471,51.9312965605688,17.8957882764113));
#54331=CARTESIAN_POINT('',(13.3561844802682,51.9293619476186,17.8542117235887));
#54332=CARTESIAN_POINT('',(13.3577828945603,51.9306296474448,19.1042117235887));
#54333=CARTESIAN_POINT('',(15.2209662466057,52.1764590205668,18.));
#54334=CARTESIAN_POINT('Ctrl Pts',(15.2209662466057,52.1764590205668,18.));
#54335=CARTESIAN_POINT('Ctrl Pts',(14.8623799894179,51.8174664687922,17.9738314965411));
#54336=CARTESIAN_POINT('Ctrl Pts',(14.136921272848,51.597902680369,17.9390942553448));
#54337=CARTESIAN_POINT('Ctrl Pts',(13.5035430816838,51.8470756229631,17.9043570141486));
#54338=CARTESIAN_POINT('Ctrl Pts',(13.3599426557471,51.9312965605688,17.8957882764113));
#54339=CARTESIAN_POINT('',(15.6220396093989,52.866415579935,18.));
#54340=CARTESIAN_POINT('Origin',(14.1292828945603,53.2669068454841,18.));
#54341=CARTESIAN_POINT('Ctrl Pts',(15.6220539738783,52.8664139542998,18.));
#54342=CARTESIAN_POINT('Ctrl Pts',(15.4957406336878,52.4022578052826,17.975091839613));
#54343=CARTESIAN_POINT('Ctrl Pts',(14.7933534445257,51.6161821464323,17.9264957474759));
#54344=CARTESIAN_POINT('Ctrl Pts',(13.7539689671603,51.7030240140342,17.8778996553388));
#54345=CARTESIAN_POINT('Ctrl Pts',(13.3561844802682,51.9293619476186,17.8542117235887));
#54346=CARTESIAN_POINT('Origin',(-39.0658530619283,38.8697713466882,15.5));
#54347=CARTESIAN_POINT('',(-38.4345426068235,37.7764071067805,14.1934196736194));
#54348=CARTESIAN_POINT('',(-38.4325424620228,37.7762177647969,14.0565803263806));
#54349=CARTESIAN_POINT('',(-38.4336030619283,37.7746822236028,15.5));
#54350=CARTESIAN_POINT('',(-39.3014489339362,37.6274127691862,14.));
#54351=CARTESIAN_POINT('Ctrl Pts',(-38.4325424620228,37.7762177647969,14.0565803263806));
#54352=CARTESIAN_POINT('Ctrl Pts',(-38.6929044073908,37.6289035868348,14.0377202175871));
#54353=CARTESIAN_POINT('Ctrl Pts',(-39.0070060787276,37.5715758131853,14.0188601087935));
#54354=CARTESIAN_POINT('Ctrl Pts',(-39.3014489339362,37.6274127691862,14.));
#54355=CARTESIAN_POINT('',(-38.4336030619283,37.7746822236028,14.));
#54356=CARTESIAN_POINT('Origin',(-39.0658530619283,38.8697713466882,14.));
#54357=CARTESIAN_POINT('',(-38.4336030619283,37.7746822236028,13.));
#54358=CARTESIAN_POINT('',(-38.4336030619283,37.7746822236028,15.5));
#54359=CARTESIAN_POINT('',(-39.7608672580762,37.8134023216061,13.));
#54360=CARTESIAN_POINT('Origin',(-39.0658530619283,38.8697713466882,13.));
#54361=CARTESIAN_POINT('',(-38.3708388657805,39.9261403717704,13.));
#54362=CARTESIAN_POINT('Origin',(-39.0658530619283,38.8697713466882,13.));
#54363=CARTESIAN_POINT('Origin',(-39.0658530619283,38.8697713466882,13.));
#54364=CARTESIAN_POINT('',(-40.2614318702746,39.2879073628688,14.));
#54365=CARTESIAN_POINT('Origin',(-39.0658530619283,38.8697713466882,14.));
#54366=CARTESIAN_POINT('Ctrl Pts',(-40.261442519219,39.2879130030575,14.));
#54367=CARTESIAN_POINT('Ctrl Pts',(-40.3902451808538,38.9153391953948,14.024908160387));
#54368=CARTESIAN_POINT('Ctrl Pts',(-40.3325529350425,38.4763144202223,14.049816320774));
#54369=CARTESIAN_POINT('Ctrl Pts',(-40.109022770241,38.1516757839093,14.074724481161));
#54370=CARTESIAN_POINT('Ctrl Pts',(-39.8741820674394,37.8106105608956,14.10089298462));
#54371=CARTESIAN_POINT('Ctrl Pts',(-39.4562961811819,37.5958001287034,14.1270614880789));
#54372=CARTESIAN_POINT('Ctrl Pts',(-39.0423952919771,37.6034944064735,14.1532299915378));
#54373=CARTESIAN_POINT('Ctrl Pts',(-38.8305051320303,37.6074333729988,14.1666265522317));
#54374=CARTESIAN_POINT('Ctrl Pts',(-38.619659348036,37.6696856996876,14.1800231129255));
#54375=CARTESIAN_POINT('Ctrl Pts',(-38.4345426068235,37.7764071067805,14.1934196736194));
#54376=CARTESIAN_POINT('Origin',(-39.0658530619283,38.8697713466882,15.5));
#54377=CARTESIAN_POINT('',(-38.4322601856233,37.7739115851766,14.6934196736194));
#54378=CARTESIAN_POINT('',(-38.4333416483911,37.7729821125454,14.5565803263806));
#54379=CARTESIAN_POINT('',(-38.4336030619283,37.7746822236028,15.5));
#54380=CARTESIAN_POINT('Ctrl Pts',(-38.4333416483911,37.7729821125454,14.5565803263806));
#54381=CARTESIAN_POINT('Ctrl Pts',(-38.4654171032337,37.7542027235003,14.5542330751329));
#54382=CARTESIAN_POINT('Ctrl Pts',(-38.4983383982293,37.7369254869309,14.5518858238852));
#54383=CARTESIAN_POINT('Ctrl Pts',(-38.5320143785611,37.721272199783,14.5495385726375));
#54384=CARTESIAN_POINT('Ctrl Pts',(-38.9074535262253,37.5467603748252,14.5233700691785));
#54385=CARTESIAN_POINT('Ctrl Pts',(-39.3766930387427,37.5740903519378,14.4972015657196));
#54386=CARTESIAN_POINT('Ctrl Pts',(-39.7293604226538,37.7909904189904,14.4710330622607));
#54387=CARTESIAN_POINT('Ctrl Pts',(-40.0820278065649,38.007890486043,14.4448645588018));
#54388=CARTESIAN_POINT('Ctrl Pts',(-40.3181230618696,38.4143606430356,14.4186960553428));
#54389=CARTESIAN_POINT('Ctrl Pts',(-40.3316969948736,38.8281685539702,14.3925275518839));
#54390=CARTESIAN_POINT('Ctrl Pts',(-40.3452709278776,39.2419764649047,14.366359048425));
#54391=CARTESIAN_POINT('Ctrl Pts',(-40.1363235385809,39.6631221297811,14.340190544966));
#54392=CARTESIAN_POINT('Ctrl Pts',(-39.7987141516887,39.9026904288663,14.3140220415071));
#54393=CARTESIAN_POINT('Ctrl Pts',(-39.4611047647966,40.1422587279515,14.2878535380482));
#54394=CARTESIAN_POINT('Ctrl Pts',(-38.9948333803092,40.2002496612456,14.2616850345893));
#54395=CARTESIAN_POINT('Ctrl Pts',(-38.6086468373336,40.0507988707032,14.2355165311303));
#54396=CARTESIAN_POINT('Ctrl Pts',(-38.222460294358,39.9013480801608,14.2093480276714));
#54397=CARTESIAN_POINT('Ctrl Pts',(-37.9163585928944,39.5444555657821,14.1831795242125));
#54398=CARTESIAN_POINT('Ctrl Pts',(-37.8282870218578,39.139867719385,14.1570110207536));
#54399=CARTESIAN_POINT('Ctrl Pts',(-37.7402154508212,38.7352798729879,14.1308425172946));
#54400=CARTESIAN_POINT('Ctrl Pts',(-37.8701740102116,38.2829966945726,14.1046740138357));
#54401=CARTESIAN_POINT('Ctrl Pts',(-38.1583471155032,37.9866613986385,14.0785055103768));
#54402=CARTESIAN_POINT('Ctrl Pts',(-38.2388287062341,37.9039002541438,14.0711971157114));
#54403=CARTESIAN_POINT('Ctrl Pts',(-38.3316507930811,37.8333028094348,14.063888721046));
#54404=CARTESIAN_POINT('Ctrl Pts',(-38.4325424620228,37.7762177647969,14.0565803263806));
#54405=CARTESIAN_POINT('Ctrl Pts',(-38.4345426068235,37.7764071067805,14.1934196736194));
#54406=CARTESIAN_POINT('Ctrl Pts',(-38.2580569790832,37.8781526020867,14.2061916163845));
#54407=CARTESIAN_POINT('Ctrl Pts',(-38.1049570809751,38.0203170861652,14.2189635591495));
#54408=CARTESIAN_POINT('Ctrl Pts',(-37.9966332783609,38.1909038725226,14.2317355019146));
#54409=CARTESIAN_POINT('Ctrl Pts',(-37.7746880461016,38.5404200730694,14.2579040053735));
#54410=CARTESIAN_POINT('Ctrl Pts',(-37.7407134737351,39.0092534864306,14.2840725088324));
#54411=CARTESIAN_POINT('Ctrl Pts',(-37.909858143811,39.3871556515896,14.3102410122914));
#54412=CARTESIAN_POINT('Ctrl Pts',(-38.0790028138868,39.7650578167486,14.3364095157503));
#54413=CARTESIAN_POINT('Ctrl Pts',(-38.451266726405,40.0520287337055,14.3625780192092));
#54414=CARTESIAN_POINT('Ctrl Pts',(-38.8597647299447,40.1193961008256,14.3887465226681));
#54415=CARTESIAN_POINT('Ctrl Pts',(-39.2682627334845,40.1867634679457,14.4149150261271));
#54416=CARTESIAN_POINT('Ctrl Pts',(-39.7129948280458,40.034527285229,14.441083529586));
#54417=CARTESIAN_POINT('Ctrl Pts',(-39.9945169439557,39.7309476936789,14.4672520330449));
#54418=CARTESIAN_POINT('Ctrl Pts',(-40.2760390598657,39.4273681021289,14.4934205365039));
#54419=CARTESIAN_POINT('Ctrl Pts',(-40.3943511971242,38.9724451017455,14.5195890399628));
#54420=CARTESIAN_POINT('Ctrl Pts',(-40.2964110981384,38.570173729657,14.5457575434217));
#54421=CARTESIAN_POINT('Ctrl Pts',(-40.1984709991526,38.1679023575684,14.5719260468806));
#54422=CARTESIAN_POINT('Ctrl Pts',(-39.8842786639225,37.8182826137747,14.5980945503396));
#54423=CARTESIAN_POINT('Ctrl Pts',(-39.4947165862022,37.6780870841148,14.6242630537985));
#54424=CARTESIAN_POINT('Ctrl Pts',(-39.1515458154338,37.5545868495612,14.6473152604055));
#54425=CARTESIAN_POINT('Ctrl Pts',(-38.7498873821672,37.59360186782,14.6703674670124));
#54426=CARTESIAN_POINT('Ctrl Pts',(-38.4322601856233,37.7739115851766,14.6934196736194));
#54427=CARTESIAN_POINT('Origin',(-39.0658530619283,38.8697713466882,15.5));
#54428=CARTESIAN_POINT('',(-38.4346334551116,37.7742886171168,15.1934196736194));
#54429=CARTESIAN_POINT('',(-38.4347780105727,37.7761824162226,15.0565803263806));
#54430=CARTESIAN_POINT('',(-38.4336030619283,37.7746822236028,15.5));
#54431=CARTESIAN_POINT('Ctrl Pts',(-38.4347780105727,37.7761824162226,15.0565803263806));
#54432=CARTESIAN_POINT('Ctrl Pts',(-38.6003617341532,37.6801555214811,15.0445774292198));
#54433=CARTESIAN_POINT('Ctrl Pts',(-38.7864577331936,37.6199570207433,15.0325745320589));
#54434=CARTESIAN_POINT('Ctrl Pts',(-38.9758802222155,37.6064663135108,15.0205716348981));
#54435=CARTESIAN_POINT('Ctrl Pts',(-39.388855772431,37.5770541129273,14.9944031314392));
#54436=CARTESIAN_POINT('Ctrl Pts',(-39.8176427771529,37.7696531482711,14.9682346279803));
#54437=CARTESIAN_POINT('Ctrl Pts',(-40.0699686232679,38.097899483489,14.9420661245214));
#54438=CARTESIAN_POINT('Ctrl Pts',(-40.3222944693828,38.4261458187069,14.9158976210624));
#54439=CARTESIAN_POINT('Ctrl Pts',(-40.3981591568908,38.8900394537988,14.8897291176035));
#54440=CARTESIAN_POINT('Ctrl Pts',(-40.2635428887314,39.2815654536187,14.8635606141446));
#54441=CARTESIAN_POINT('Ctrl Pts',(-40.1289266205721,39.6730914534386,14.8373921106856));
#54442=CARTESIAN_POINT('Ctrl Pts',(-39.7838293967455,39.9922498179864,14.8112236072267));
#54443=CARTESIAN_POINT('Ctrl Pts',(-39.3829992856625,40.0959251593025,14.7850551037678));
#54444=CARTESIAN_POINT('Ctrl Pts',(-38.9821691745794,40.1996005006187,14.7588866003089));
#54445=CARTESIAN_POINT('Ctrl Pts',(-38.52560617624,40.0877928187031,14.7327180968499));
#54446=CARTESIAN_POINT('Ctrl Pts',(-38.2180337582993,39.8106400014137,14.706549593391));
#54447=CARTESIAN_POINT('Ctrl Pts',(-37.9104613403587,39.5334871841242,14.6803810899321));
#54448=CARTESIAN_POINT('Ctrl Pts',(-37.7518795028169,39.0909892314608,14.6542125864732));
#54449=CARTESIAN_POINT('Ctrl Pts',(-37.8134079754514,38.681563441615,14.6280440830142));
#54450=CARTESIAN_POINT('Ctrl Pts',(-37.869417493424,38.308862151417,14.604222830803));
#54451=CARTESIAN_POINT('Ctrl Pts',(-38.1078215318973,37.9635661257619,14.5804015785918));
#54452=CARTESIAN_POINT('Ctrl Pts',(-38.4333416483911,37.7729821125454,14.5565803263806));
#54453=CARTESIAN_POINT('Ctrl Pts',(-38.4322601856233,37.7739115851766,14.6934196736194));
#54454=CARTESIAN_POINT('Ctrl Pts',(-38.389321969358,37.7982866315292,14.6965359704714));
#54455=CARTESIAN_POINT('Ctrl Pts',(-38.3479194071466,37.825243810264,14.6996522673233));
#54456=CARTESIAN_POINT('Ctrl Pts',(-38.3084045871421,37.8547306967159,14.7027685641753));
#54457=CARTESIAN_POINT('Ctrl Pts',(-37.976586486013,38.1023411545029,14.7289370676342));
#54458=CARTESIAN_POINT('Ctrl Pts',(-37.7778821039656,38.528333385603,14.7551055710931));
#54459=CARTESIAN_POINT('Ctrl Pts',(-37.8013916118278,38.941687151427,14.781274074552));
#54460=CARTESIAN_POINT('Ctrl Pts',(-37.82490111969,39.355040917251,14.807442578011));
#54461=CARTESIAN_POINT('Ctrl Pts',(-38.0706245174618,39.755756217799,14.8336110814699));
#54462=CARTESIAN_POINT('Ctrl Pts',(-38.428377122171,39.9641476765194,14.8597795849288));
#54463=CARTESIAN_POINT('Ctrl Pts',(-38.7861297268802,40.1725391352398,14.8859480883877));
#54464=CARTESIAN_POINT('Ctrl Pts',(-39.2559115385268,40.1886067521326,14.9121165918467));
#54465=CARTESIAN_POINT('Ctrl Pts',(-39.6270665080505,40.005145553951,14.9382850953056));
#54466=CARTESIAN_POINT('Ctrl Pts',(-39.9982214775741,39.8216843557693,14.9644535987645));
#54467=CARTESIAN_POINT('Ctrl Pts',(-40.2707496049748,39.4386943425132,14.9906221022234));
#54468=CARTESIAN_POINT('Ctrl Pts',(-40.3224461866044,39.0279128196441,15.0167906056824));
#54469=CARTESIAN_POINT('Ctrl Pts',(-40.3741427682341,38.6171312967749,15.0429591091413));
#54470=CARTESIAN_POINT('Ctrl Pts',(-40.2050078040927,38.1785582642928,15.0691276126002));
#54471=CARTESIAN_POINT('Ctrl Pts',(-39.8908833495191,37.9088550679237,15.0952961160592));
#54472=CARTESIAN_POINT('Ctrl Pts',(-39.5767588949456,37.6391518715546,15.1214646195181));
#54473=CARTESIAN_POINT('Ctrl Pts',(-39.1176449499399,37.5383185112986,15.147633122977));
#54474=CARTESIAN_POINT('Ctrl Pts',(-38.7194137008706,37.6515698720153,15.1738016264359));
#54475=CARTESIAN_POINT('Ctrl Pts',(-38.61989814589,37.679870694817,15.1803409754971));
#54476=CARTESIAN_POINT('Ctrl Pts',(-38.5241845298854,37.7215404565648,15.1868803245583));
#54477=CARTESIAN_POINT('Ctrl Pts',(-38.4346334551116,37.7742886171168,15.1934196736194));
#54478=CARTESIAN_POINT('Origin',(-39.0658530619283,38.8697713466882,15.5));
#54479=CARTESIAN_POINT('',(-38.4337315549884,37.7763335227174,15.6934196736194));
#54480=CARTESIAN_POINT('',(-38.4323663903519,37.7745195378425,15.5565803263806));
#54481=CARTESIAN_POINT('',(-38.4336030619283,37.7746822236028,15.5));
#54482=CARTESIAN_POINT('Ctrl Pts',(-38.4323663903519,37.7745195378425,15.5565803263806));
#54483=CARTESIAN_POINT('Ctrl Pts',(-38.7313730076302,37.6052990985956,15.5349217833067));
#54484=CARTESIAN_POINT('Ctrl Pts',(-39.1034689296549,37.5582680121359,15.5132632402327));
#54485=CARTESIAN_POINT('Ctrl Pts',(-39.4315419163111,37.6572094658042,15.4916046971588));
#54486=CARTESIAN_POINT('Ctrl Pts',(-39.8279295706787,37.7767535073269,15.4654361936999));
#54487=CARTESIAN_POINT('Ctrl Pts',(-40.1600516656647,38.1093911753228,15.439267690241));
#54488=CARTESIAN_POINT('Ctrl Pts',(-40.2789807143,38.5059637820164,15.413099186782));
#54489=CARTESIAN_POINT('Ctrl Pts',(-40.3979097629354,38.9025363887101,15.3869306833231));
#54490=CARTESIAN_POINT('Ctrl Pts',(-40.3036457652202,39.3630439341015,15.3607621798642));
#54491=CARTESIAN_POINT('Ctrl Pts',(-40.0384578014032,39.6809893678464,15.3345936764052));
#54492=CARTESIAN_POINT('Ctrl Pts',(-39.7732698375861,39.9989348015912,15.3084251729463));
#54493=CARTESIAN_POINT('Ctrl Pts',(-39.3371579076672,40.1743181236895,15.2822566694874));
#54494=CARTESIAN_POINT('Ctrl Pts',(-38.9256798191233,40.1284953536109,15.2560881660285));
#54495=CARTESIAN_POINT('Ctrl Pts',(-38.5142017305794,40.0826725835323,15.2299196625695));
#54496=CARTESIAN_POINT('Ctrl Pts',(-38.1273574834104,39.8156437212769,15.2037511591106));
#54497=CARTESIAN_POINT('Ctrl Pts',(-37.938612567216,39.4471477114983,15.1775826556517));
#54498=CARTESIAN_POINT('Ctrl Pts',(-37.7498676510216,39.0786517017197,15.1514141521928));
#54499=CARTESIAN_POINT('Ctrl Pts',(-37.7592220658018,38.608688544418,15.1252456487338));
#54500=CARTESIAN_POINT('Ctrl Pts',(-37.9624813210464,38.2479952475117,15.0990771452749));
#54501=CARTESIAN_POINT('Ctrl Pts',(-38.0725101803872,38.0527437595402,15.0849115389768));
#54502=CARTESIAN_POINT('Ctrl Pts',(-38.239359037454,37.8895116538818,15.0707459326787));
#54503=CARTESIAN_POINT('Ctrl Pts',(-38.4347780105727,37.7761824162226,15.0565803263806));
#54504=CARTESIAN_POINT('Ctrl Pts',(-38.4346334551116,37.7742886171168,15.1934196736194));
#54505=CARTESIAN_POINT('Ctrl Pts',(-38.1658281265106,37.9326226925712,15.2130488280172));
#54506=CARTESIAN_POINT('Ctrl Pts',(-37.952548489957,38.1907752905067,15.232677982415));
#54507=CARTESIAN_POINT('Ctrl Pts',(-37.8586391249355,38.4867967233546,15.2523071368127));
#54508=CARTESIAN_POINT('Ctrl Pts',(-37.7334443512028,38.8814361322879,15.2784756402716));
#54509=CARTESIAN_POINT('Ctrl Pts',(-37.8204033568707,39.3433788684653,15.3046441437306));
#54510=CARTESIAN_POINT('Ctrl Pts',(-38.0805226988896,39.6654843197861,15.3308126471895));
#54511=CARTESIAN_POINT('Ctrl Pts',(-38.3406420409086,39.987589771107,15.3569811506484));
#54512=CARTESIAN_POINT('Ctrl Pts',(-38.7739217192785,40.1698579375712,15.3831496541074));
#54513=CARTESIAN_POINT('Ctrl Pts',(-39.1860739715826,40.1305576058447,15.4093181575663));
#54514=CARTESIAN_POINT('Ctrl Pts',(-39.5982262238866,40.0912572741182,15.4354866610252));
#54515=CARTESIAN_POINT('Ctrl Pts',(-39.9892510501248,39.8303884442009,15.4616551644841));
#54516=CARTESIAN_POINT('Ctrl Pts',(-40.1838082722999,39.4649278007734,15.4878236679431));
#54517=CARTESIAN_POINT('Ctrl Pts',(-40.378365494475,39.0994671573459,15.513992171402));
#54518=CARTESIAN_POINT('Ctrl Pts',(-40.3764551125872,38.6294147004082,15.5401606748609));
#54519=CARTESIAN_POINT('Ctrl Pts',(-40.1789337635325,38.2655475388609,15.5663291783198));
#54520=CARTESIAN_POINT('Ctrl Pts',(-39.9814124144779,37.9016803773136,15.5924976817788));
#54521=CARTESIAN_POINT('Ctrl Pts',(-39.5882800982565,37.6439985111567,15.6186661852377));
#54522=CARTESIAN_POINT('Ctrl Pts',(-39.1758220190741,37.6080495523,15.6448346886966));
#54523=CARTESIAN_POINT('Ctrl Pts',(-38.9205626180182,37.5858016920459,15.6610296836709));
#54524=CARTESIAN_POINT('Ctrl Pts',(-38.6579013630336,37.6484785302017,15.6772246786452));
#54525=CARTESIAN_POINT('Ctrl Pts',(-38.4337315549884,37.7763335227174,15.6934196736194));
#54526=CARTESIAN_POINT('Origin',(-39.0658530619283,38.8697713466882,15.5));
#54527=CARTESIAN_POINT('',(-38.4325272584341,37.7729978925048,16.1934196736194));
#54528=CARTESIAN_POINT('',(-38.4342758514651,37.7737507965446,16.0565803263806));
#54529=CARTESIAN_POINT('',(-38.4336030619283,37.7746822236028,15.5));
#54530=CARTESIAN_POINT('Ctrl Pts',(-38.4342758514651,37.7737507965446,16.0565803263806));
#54531=CARTESIAN_POINT('Ctrl Pts',(-38.5046440871601,37.732289208729,16.0514346408525));
#54532=CARTESIAN_POINT('Ctrl Pts',(-38.5788878157804,37.6977955005524,16.0462889553244));
#54533=CARTESIAN_POINT('Ctrl Pts',(-38.6559170964541,37.6714445317291,16.0411432697963));
#54534=CARTESIAN_POINT('Ctrl Pts',(-39.0476512952768,37.5374360667672,16.0149747663373));
#54535=CARTESIAN_POINT('Ctrl Pts',(-39.5114269646143,37.6140195799122,15.9888062628784));
#54536=CARTESIAN_POINT('Ctrl Pts',(-39.8392815814542,37.8668541135745,15.9626377594195));
#54537=CARTESIAN_POINT('Ctrl Pts',(-40.1671361982942,38.1196886472368,15.9364692559606));
#54538=CARTESIAN_POINT('Ctrl Pts',(-40.3590697626365,38.5487742014165,15.9103007525016));
#54539=CARTESIAN_POINT('Ctrl Pts',(-40.3290169828723,38.9617037131001,15.8841322490427));
#54540=CARTESIAN_POINT('Ctrl Pts',(-40.2989642031082,39.3746332247836,15.8579637455838));
#54541=CARTESIAN_POINT('Ctrl Pts',(-40.0469250792374,39.771406693971,15.8317952421249));
#54542=CARTESIAN_POINT('Ctrl Pts',(-39.6859169501041,39.974106180808,15.8056267386659));
#54543=CARTESIAN_POINT('Ctrl Pts',(-39.3249088209707,40.176805667645,15.779458235207));
#54544=CARTESIAN_POINT('Ctrl Pts',(-38.8549316865748,40.1854311721316,15.7532897317481));
#54545=CARTESIAN_POINT('Ctrl Pts',(-38.4867288810043,39.9961149153207,15.7271212282891));
#54546=CARTESIAN_POINT('Ctrl Pts',(-38.1185260754338,39.8067986585099,15.7009527248302));
#54547=CARTESIAN_POINT('Ctrl Pts',(-37.8520975986887,39.4195406404017,15.6747842213713));
#54548=CARTESIAN_POINT('Ctrl Pts',(-37.806913145733,39.0079919599958,15.6486157179124));
#54549=CARTESIAN_POINT('Ctrl Pts',(-37.7617286927774,38.5964432795898,15.6224472144534));
#54550=CARTESIAN_POINT('Ctrl Pts',(-37.9377882636113,38.1606039368861,15.5962787109945));
#54551=CARTESIAN_POINT('Ctrl Pts',(-38.2561446559028,37.8959094730591,15.5701102075356));
#54552=CARTESIAN_POINT('Ctrl Pts',(-38.3110111758702,37.8502912149167,15.5656002471506));
#54553=CARTESIAN_POINT('Ctrl Pts',(-38.3701042153675,37.8097563252262,15.5610902867656));
#54554=CARTESIAN_POINT('Ctrl Pts',(-38.4323663903519,37.7745195378425,15.5565803263806));
#54555=CARTESIAN_POINT('Ctrl Pts',(-38.4337315549884,37.7763335227174,15.6934196736194));
#54556=CARTESIAN_POINT('Ctrl Pts',(-38.2956790587637,37.8550716053588,15.7033931821041));
#54557=CARTESIAN_POINT('Ctrl Pts',(-38.1722247361697,37.9585289981308,15.7133666905887));
#54558=CARTESIAN_POINT('Ctrl Pts',(-38.0740874997393,38.0820936667169,15.7233401990734));
#54559=CARTESIAN_POINT('Ctrl Pts',(-37.8165949017303,38.4063027915471,15.7495087025323));
#54560=CARTESIAN_POINT('Ctrl Pts',(-37.7333935478559,38.868937092764,15.7756772059912));
#54561=CARTESIAN_POINT('Ctrl Pts',(-37.8617919143246,39.2625458504732,15.8018457094502));
#54562=CARTESIAN_POINT('Ctrl Pts',(-37.9901902807933,39.6561546081824,15.8280142129091));
#54563=CARTESIAN_POINT('Ctrl Pts',(-38.3301883676052,39.9807378223839,15.854182716368));
#54564=CARTESIAN_POINT('Ctrl Pts',(-38.7293269910635,40.0907485215641,15.880351219827));
#54565=CARTESIAN_POINT('Ctrl Pts',(-39.128465614522,40.2007592207442,15.9065197232859));
#54566=CARTESIAN_POINT('Ctrl Pts',(-39.5867447746269,40.0961974049031,15.9326882267448));
#54567=CARTESIAN_POINT('Ctrl Pts',(-39.898666648561,39.8239498351585,15.9588567302037));
#54568=CARTESIAN_POINT('Ctrl Pts',(-40.2105885224951,39.551702265414,15.9850252336627));
#54569=CARTESIAN_POINT('Ctrl Pts',(-40.3761531102584,39.1117689417661,16.0111937371216));
#54570=CARTESIAN_POINT('Ctrl Pts',(-40.3211192825961,38.701421195982,16.0373622405805));
#54571=CARTESIAN_POINT('Ctrl Pts',(-40.2660854549337,38.291073450198,16.0635307440394));
#54572=CARTESIAN_POINT('Ctrl Pts',(-39.9904532118458,37.9103112822778,16.0896992474984));
#54573=CARTESIAN_POINT('Ctrl Pts',(-39.617819327633,37.7298729742913,16.1158677509573));
#54574=CARTESIAN_POINT('Ctrl Pts',(-39.249711738356,37.5516264074058,16.1417183918447));
#54575=CARTESIAN_POINT('Ctrl Pts',(-38.7869447075706,37.5688666846833,16.167569032732));
#54576=CARTESIAN_POINT('Ctrl Pts',(-38.4325272584341,37.7729978925048,16.1934196736194));
#54577=CARTESIAN_POINT('Origin',(-39.0658530619283,38.8697713466882,15.5));
#54578=CARTESIAN_POINT('',(-38.4349705604869,37.7753960169021,16.6934196736194));
#54579=CARTESIAN_POINT('',(-38.4341423505256,37.7764525809616,16.5565803263806));
#54580=CARTESIAN_POINT('',(-38.4336030619283,37.7746822236028,15.5));
#54581=CARTESIAN_POINT('Ctrl Pts',(-38.4341423505256,37.7764525809616,16.5565803263806));
#54582=CARTESIAN_POINT('Ctrl Pts',(-38.6388834301988,37.6590722267018,16.5417789949394));
#54583=CARTESIAN_POINT('Ctrl Pts',(-38.8753711836181,37.5959619576061,16.5269776634982));
#54584=CARTESIAN_POINT('Ctrl Pts',(-39.1094100531277,37.604015667637,16.5121763320569));
#54585=CARTESIAN_POINT('Ctrl Pts',(-39.5231868130501,37.6182544906534,16.486007828598));
#54586=CARTESIAN_POINT('Ctrl Pts',(-39.929308939441,37.8549351283607,16.4598393251391));
#54587=CARTESIAN_POINT('Ctrl Pts',(-40.1456664429884,38.2079271704546,16.4336708216802));
#54588=CARTESIAN_POINT('Ctrl Pts',(-40.3620239465357,38.5609192125485,16.4075023182212));
#54589=CARTESIAN_POINT('Ctrl Pts',(-40.3886168272394,39.0302226590291,16.3813338147623));
#54590=CARTESIAN_POINT('Ctrl Pts',(-40.2135205214552,39.4053962654636,16.3551653113034));
#54591=CARTESIAN_POINT('Ctrl Pts',(-40.0384242156709,39.780569871898,16.3289968078445));
#54592=CARTESIAN_POINT('Ctrl Pts',(-39.6616387233988,40.0616136382864,16.3028283043855));
#54593=CARTESIAN_POINT('Ctrl Pts',(-39.2521191380692,40.122504199314,16.2766598009266));
#54594=CARTESIAN_POINT('Ctrl Pts',(-38.8425995527396,40.1833947603415,16.2504912974677));
#54595=CARTESIAN_POINT('Ctrl Pts',(-38.4003458743526,40.0241321160083,16.2243227940087));
#54596=CARTESIAN_POINT('Ctrl Pts',(-38.1236699093341,39.7161315290339,16.1981542905498));
#54597=CARTESIAN_POINT('Ctrl Pts',(-37.8469939443156,39.4081309420595,16.1719857870909));
#54598=CARTESIAN_POINT('Ctrl Pts',(-37.7358956926656,38.951392412444,16.145817283632));
#54599=CARTESIAN_POINT('Ctrl Pts',(-37.8401929309945,38.5507229261018,16.119648780173));
#54600=CARTESIAN_POINT('Ctrl Pts',(-37.9239815150654,38.2288397249847,16.0986259622422));
#54601=CARTESIAN_POINT('Ctrl Pts',(-38.1467847875343,37.9431430780994,16.0776031443114));
#54602=CARTESIAN_POINT('Ctrl Pts',(-38.4342758514651,37.7737507965446,16.0565803263806));
#54603=CARTESIAN_POINT('Ctrl Pts',(-38.4325272584341,37.7729978925048,16.1934196736194));
#54604=CARTESIAN_POINT('Ctrl Pts',(-38.4281692990986,37.775507914246,16.193737536191));
#54605=CARTESIAN_POINT('Ctrl Pts',(-38.42382772163,37.7780461928786,16.1940553987625));
#54606=CARTESIAN_POINT('Ctrl Pts',(-38.4195029034438,37.7806127124219,16.1943732613341));
#54607=CARTESIAN_POINT('Ctrl Pts',(-38.063455888805,37.9919052065918,16.220541764793));
#54608=CARTESIAN_POINT('Ctrl Pts',(-37.820997384865,38.3946046429843,16.2467102682519));
#54609=CARTESIAN_POINT('Ctrl Pts',(-37.8008486672723,38.8081358071838,16.2728787717109));
#54610=CARTESIAN_POINT('Ctrl Pts',(-37.7806999496796,39.2216669713833,16.2990472751698));
#54611=CARTESIAN_POINT('Ctrl Pts',(-37.9828610184341,39.6460298633898,16.3252157786287));
#54612=CARTESIAN_POINT('Ctrl Pts',(-38.3166804464026,39.8909351187555,16.3513842820876));
#54613=CARTESIAN_POINT('Ctrl Pts',(-38.6504998743712,40.1358403741212,16.3775527855465));
#54614=CARTESIAN_POINT('Ctrl Pts',(-39.1159776615536,40.2012879928461,16.4037212890055));
#54615=CARTESIAN_POINT('Ctrl Pts',(-39.5043880368528,40.0579304834052,16.4298897924644));
#54616=CARTESIAN_POINT('Ctrl Pts',(-39.8927984121519,39.9145729739643,16.4560582959233));
#54617=CARTESIAN_POINT('Ctrl Pts',(-40.2041413755678,39.5624103363577,16.4822267993823));
#54618=CARTESIAN_POINT('Ctrl Pts',(-40.2988070379275,39.1593564860685,16.5083953028412));
#54619=CARTESIAN_POINT('Ctrl Pts',(-40.3934727002873,38.7563026357793,16.5345638063001));
#54620=CARTESIAN_POINT('Ctrl Pts',(-40.271461061591,38.3023575728075,16.560732309759));
#54621=CARTESIAN_POINT('Ctrl Pts',(-39.9874835980573,38.001075653904,16.586900813218));
#54622=CARTESIAN_POINT('Ctrl Pts',(-39.7035061345237,37.6997937350004,16.6130693166769));
#54623=CARTESIAN_POINT('Ctrl Pts',(-39.2575628461526,37.5511749601651,16.6392378201358));
#54624=CARTESIAN_POINT('Ctrl Pts',(-38.849619989904,37.6218617656895,16.6654063235947));
#54625=CARTESIAN_POINT('Ctrl Pts',(-38.7040525518056,37.6470851444788,16.6747441069363));
#54626=CARTESIAN_POINT('Ctrl Pts',(-38.5633236984099,37.7002326432607,16.6840818902779));
#54627=CARTESIAN_POINT('Ctrl Pts',(-38.4349705604869,37.7753960169021,16.6934196736194));
#54628=CARTESIAN_POINT('Origin',(-39.0658530619283,38.8697713466882,15.5));
#54629=CARTESIAN_POINT('',(-38.4329072841441,37.7756148875603,17.1934196736194));
#54630=CARTESIAN_POINT('',(-38.4323100738575,37.7733715239653,17.0565803263806));
#54631=CARTESIAN_POINT('',(-38.4336030619283,37.7746822236028,15.5));
#54632=CARTESIAN_POINT('Ctrl Pts',(-38.4323100738575,37.7733715239653,17.0565803263806));
#54633=CARTESIAN_POINT('Ctrl Pts',(-38.7684978446967,37.5814140598882,17.0321233490263));
#54634=CARTESIAN_POINT('Ctrl Pts',(-39.2005574419278,37.5523442127138,17.0076663716719));
#54635=CARTESIAN_POINT('Ctrl Pts',(-39.5571950289671,37.7024591900708,16.9832093943176));
#54636=CARTESIAN_POINT('Ctrl Pts',(-39.9387905055794,37.8630793782195,16.9570408908587));
#54637=CARTESIAN_POINT('Ctrl Pts',(-40.2340383736987,38.2288410235792,16.9308723873998));
#54638=CARTESIAN_POINT('Ctrl Pts',(-40.3105459562687,38.6357323277609,16.9047038839408));
#54639=CARTESIAN_POINT('Ctrl Pts',(-40.3870535388386,39.0426236319427,16.8785353804819));
#54640=CARTESIAN_POINT('Ctrl Pts',(-40.2448208358592,39.4906445949467,16.852366877023));
#54641=CARTESIAN_POINT('Ctrl Pts',(-39.9476266935978,39.7788972563362,16.8261983735641));
#54642=CARTESIAN_POINT('Ctrl Pts',(-39.6504325513363,40.0671499177256,16.8000298701051));
#54643=CARTESIAN_POINT('Ctrl Pts',(-39.1982769697929,40.1956342775006,16.7738613666462));
#54644=CARTESIAN_POINT('Ctrl Pts',(-38.7939118807236,40.106736438769,16.7476928631873));
#54645=CARTESIAN_POINT('Ctrl Pts',(-38.3895467916544,40.0178386000373,16.7215243597283));
#54646=CARTESIAN_POINT('Ctrl Pts',(-38.0329721950595,39.711558562799,16.6953558562694));
#54647=CARTESIAN_POINT('Ctrl Pts',(-37.8840803814008,39.3252359279146,16.6691873528105));
#54648=CARTESIAN_POINT('Ctrl Pts',(-37.7351885677422,38.9389132930302,16.6430188493516));
#54649=CARTESIAN_POINT('Ctrl Pts',(-37.7939795370199,38.4725480604996,16.6168503458926));
#54650=CARTESIAN_POINT('Ctrl Pts',(-38.0340907183856,38.1352639483972,16.5906818424337));
#54651=CARTESIAN_POINT('Ctrl Pts',(-38.1383911078307,37.9887532193016,16.579314670416));
#54652=CARTESIAN_POINT('Ctrl Pts',(-38.2769046668091,37.8665987062389,16.5679474983983));
#54653=CARTESIAN_POINT('Ctrl Pts',(-38.4341423505256,37.7764525809616,16.5565803263806));
#54654=CARTESIAN_POINT('Ctrl Pts',(-38.4349705604869,37.7753960169021,16.6934196736194));
#54655=CARTESIAN_POINT('Ctrl Pts',(-38.2036227489616,37.9108728917195,16.7102503937368));
#54656=CARTESIAN_POINT('Ctrl Pts',(-38.0124806835606,38.1178740898994,16.7270811138542));
#54657=CARTESIAN_POINT('Ctrl Pts',(-37.9056793271332,38.3618028680121,16.7439118339715));
#54658=CARTESIAN_POINT('Ctrl Pts',(-37.7396239447374,38.7410647789261,16.7700803374305));
#54659=CARTESIAN_POINT('Ctrl Pts',(-37.7774556040718,39.2095962148701,16.7962488408894));
#54660=CARTESIAN_POINT('Ctrl Pts',(-38.0022100801908,39.5573021560724,16.8224173443483));
#54661=CARTESIAN_POINT('Ctrl Pts',(-38.2269645563097,39.9050080972747,16.8485858478072));
#54662=CARTESIAN_POINT('Ctrl Pts',(-38.6386418492131,40.1318885437353,16.8747543512662));
#54663=CARTESIAN_POINT('Ctrl Pts',(-39.0526410872976,40.1362075141882,16.9009228547251));
#54664=CARTESIAN_POINT('Ctrl Pts',(-39.4666403253822,40.1405264846412,16.927091358184));
#54665=CARTESIAN_POINT('Ctrl Pts',(-39.8829615086478,39.9222839790863,16.9532598616429));
#54666=CARTESIAN_POINT('Ctrl Pts',(-40.1149210262726,39.5793427181871,16.9794283651019));
#54667=CARTESIAN_POINT('Ctrl Pts',(-40.3468805438973,39.2364014572879,17.0055968685608));
#54668=CARTESIAN_POINT('Ctrl Pts',(-40.3944783958811,38.7687614410443,17.0317653720197));
#54669=CARTESIAN_POINT('Ctrl Pts',(-40.236371633473,38.3861176323113,17.0579338754786));
#54670=CARTESIAN_POINT('Ctrl Pts',(-40.0782648710649,38.0034738235784,17.0841023789376));
#54671=CARTESIAN_POINT('Ctrl Pts',(-39.714453494265,37.7058262223561,17.1102708823965));
#54672=CARTESIAN_POINT('Ctrl Pts',(-39.3080738473792,37.6266443201347,17.1364393858554));
#54673=CARTESIAN_POINT('Ctrl Pts',(-39.0131183836182,37.5691730986546,17.1554328151101));
#54674=CARTESIAN_POINT('Ctrl Pts',(-38.6957377885278,37.6267904626672,17.1744262443648));
#54675=CARTESIAN_POINT('Ctrl Pts',(-38.4329072841441,37.7756148875603,17.1934196736194));
#54676=CARTESIAN_POINT('Origin',(-39.0658530619283,38.8697713466882,15.5));
#54677=CARTESIAN_POINT('',(-38.4333577759012,37.7730251466967,17.6934196736194));
#54678=CARTESIAN_POINT('',(-38.4348713855213,37.7748596688486,17.5565803263806));
#54679=CARTESIAN_POINT('',(-38.4336030619283,37.7746822236028,15.5));
#54680=CARTESIAN_POINT('',(-40.2595650866584,39.2869186252538,18.));
#54681=CARTESIAN_POINT('Ctrl Pts',(-38.4333577759012,37.7730251466967,17.6934196736194));
#54682=CARTESIAN_POINT('Ctrl Pts',(-38.1097262681979,37.9625959827323,17.7171076053695));
#54683=CARTESIAN_POINT('Ctrl Pts',(-37.8720798795257,38.3048233518517,17.7407955371196));
#54684=CARTESIAN_POINT('Ctrl Pts',(-37.814449821825,38.6752097670202,17.7644834688697));
#54685=CARTESIAN_POINT('Ctrl Pts',(-37.7507848138289,39.0843826018939,17.7906519723286));
#54686=CARTESIAN_POINT('Ctrl Pts',(-37.9068123877648,39.5279208384947,17.8168204757875));
#54687=CARTESIAN_POINT('Ctrl Pts',(-38.2131597275407,39.8064869141386,17.8429889792464));
#54688=CARTESIAN_POINT('Ctrl Pts',(-38.5195070673165,40.0850529897826,17.8691574827054));
#54689=CARTESIAN_POINT('Ctrl Pts',(-38.9761741729324,40.1986469044696,17.8953259861643));
#54690=CARTESIAN_POINT('Ctrl Pts',(-39.3768946753638,40.0972493078634,17.9214944896232));
#54691=CARTESIAN_POINT('Ctrl Pts',(-39.7776151777952,39.9958517112573,17.9476629930821));
#54692=CARTESIAN_POINT('Ctrl Pts',(-40.1223890770422,39.6794626033579,17.9738314965411));
#54693=CARTESIAN_POINT('Ctrl Pts',(-40.2595650866584,39.2869186252538,18.));
#54694=CARTESIAN_POINT('',(-39.301526156426,37.6253017999342,18.));
#54695=CARTESIAN_POINT('Origin',(-39.0658530619283,38.8697713466882,18.));
#54696=CARTESIAN_POINT('Ctrl Pts',(-39.301526596644,37.6252897660473,18.));
#54697=CARTESIAN_POINT('Ctrl Pts',(-39.6885864653113,37.7000302410441,17.975091839613));
#54698=CARTESIAN_POINT('Ctrl Pts',(-40.03994654915,37.9695057059561,17.950183679226));
#54699=CARTESIAN_POINT('Ctrl Pts',(-40.2093266637559,38.3254078043634,17.925275518839));
#54700=CARTESIAN_POINT('Ctrl Pts',(-40.3872773452222,38.6993184082981,17.89910701538));
#54701=CARTESIAN_POINT('Ctrl Pts',(-40.3643659014498,39.1686232325653,17.8729385119211));
#54702=CARTESIAN_POINT('Ctrl Pts',(-40.1507520928544,39.5232247114421,17.8467700084622));
#54703=CARTESIAN_POINT('Ctrl Pts',(-39.9371382842589,39.8778261903188,17.8206015050033));
#54704=CARTESIAN_POINT('Ctrl Pts',(-39.5328221108402,40.1177243238052,17.7944330015443));
#54705=CARTESIAN_POINT('Ctrl Pts',(-39.1191596128741,40.1351764464735,17.7682644980854));
#54706=CARTESIAN_POINT('Ctrl Pts',(-38.705497114908,40.1526285691419,17.7420959946265));
#54707=CARTESIAN_POINT('Ctrl Pts',(-38.2824882923945,39.9476346809922,17.7159274911676));
#54708=CARTESIAN_POINT('Ctrl Pts',(-38.0397877964566,39.6122000494563,17.6897589877086));
#54709=CARTESIAN_POINT('Ctrl Pts',(-37.7970873005187,39.2767654179205,17.6635904842497));
#54710=CARTESIAN_POINT('Ctrl Pts',(-37.7346951311565,38.8108900429983,17.6374219807908));
#54711=CARTESIAN_POINT('Ctrl Pts',(-37.8806022560883,38.4234367664048,17.6112534773319));
#54712=CARTESIAN_POINT('Ctrl Pts',(-37.9822155342897,38.1536048606431,17.5930290936814));
#54713=CARTESIAN_POINT('Ctrl Pts',(-38.184855409418,37.9218082144096,17.574804710031));
#54714=CARTESIAN_POINT('Ctrl Pts',(-38.4348713855213,37.7748596688486,17.5565803263806));
#54715=CARTESIAN_POINT('Origin',(-39.0658530619283,38.8697713466882,19.1042117235887));
#54716=CARTESIAN_POINT('',(-38.2940340733258,37.531419596366,14.3957882764113));
#54717=CARTESIAN_POINT('',(-38.2954995370357,37.5355989289914,14.3542117235887));
#54718=CARTESIAN_POINT('',(-38.2943530619284,37.5334941486488,19.1042117235887));
#54719=CARTESIAN_POINT('',(-37.9741697098829,39.9602191716055,14.));
#54720=CARTESIAN_POINT('Ctrl Pts',(-38.2954995370357,37.5355989289914,14.3542117235887));
#54721=CARTESIAN_POINT('Ctrl Pts',(-38.5213873438296,37.4053726489247,14.3408151628949));
#54722=CARTESIAN_POINT('Ctrl Pts',(-39.2812420752165,37.1810251467921,14.301250098742));
#54723=CARTESIAN_POINT('Ctrl Pts',(-40.5621358440549,37.8394569175814,14.2355165311304));
#54724=CARTESIAN_POINT('Ctrl Pts',(-40.7517455388365,39.5501918673983,14.1570110207535));
#54725=CARTESIAN_POINT('Ctrl Pts',(-39.4258164610498,40.6499822516744,14.0785055103768));
#54726=CARTESIAN_POINT('Ctrl Pts',(-38.3327559670706,40.3192117233802,14.0261685034589));
#54727=CARTESIAN_POINT('Ctrl Pts',(-37.9741697098829,39.9602191716055,14.));
#54728=CARTESIAN_POINT('',(-37.5730942570913,39.2702598116582,14.));
#54729=CARTESIAN_POINT('Origin',(-39.0658530619283,38.8697713466882,14.));
#54730=CARTESIAN_POINT('Ctrl Pts',(-38.2940340733258,37.531419596366,14.3957882764113));
#54731=CARTESIAN_POINT('Ctrl Pts',(-38.33317399173,37.5085041378475,14.3934410251636));
#54732=CARTESIAN_POINT('Ctrl Pts',(-38.8212071098194,37.2523822679137,14.3649252704569));
#54733=CARTESIAN_POINT('Ctrl Pts',(-40.0177412802272,37.3220721610693,14.3102410122914));
#54734=CARTESIAN_POINT('Ctrl Pts',(-40.8820235552812,38.8100518816852,14.2317355019146));
#54735=CARTESIAN_POINT('Ctrl Pts',(-40.1171224362185,40.3517547545305,14.1532299915378));
#54736=CARTESIAN_POINT('Ctrl Pts',(-38.4376290919279,40.5606360835951,14.0759848242329));
#54737=CARTESIAN_POINT('Ctrl Pts',(-37.6993939872544,39.7344135992461,14.024908160387));
#54738=CARTESIAN_POINT('Ctrl Pts',(-37.573079654256,39.2702614469549,14.));
#54739=CARTESIAN_POINT('Origin',(-39.0658530619283,38.8697713466882,19.1042117235887));
#54740=CARTESIAN_POINT('',(-38.2957867873204,37.5353247514265,14.8957882764113));
#54741=CARTESIAN_POINT('',(-38.2927144236218,37.5325537808421,14.8542117235887));
#54742=CARTESIAN_POINT('',(-38.2943530619284,37.5334941486488,19.1042117235887));
#54743=CARTESIAN_POINT('Ctrl Pts',(-38.2927144236218,37.5325537808421,14.8542117235887));
#54744=CARTESIAN_POINT('Ctrl Pts',(-38.6802974716782,37.3125317216241,14.8311595169817));
#54745=CARTESIAN_POINT('Ctrl Pts',(-39.7267977629897,37.2108801077358,14.7819388069158));
#54746=CARTESIAN_POINT('Ctrl Pts',(-40.8313162888141,38.4399409113082,14.706549593391));
#54747=CARTESIAN_POINT('Ctrl Pts',(-40.3982068515902,40.1052936742774,14.6280440830142));
#54748=CARTESIAN_POINT('Ctrl Pts',(-38.7701602990205,40.6625900679474,14.5495385726375));
#54749=CARTESIAN_POINT('Ctrl Pts',(-37.4074005907986,39.6120654537968,14.4710330622607));
#54750=CARTESIAN_POINT('Ctrl Pts',(-37.5105490854526,38.1886638489126,14.4059241125778));
#54751=CARTESIAN_POINT('Ctrl Pts',(-38.0801438046488,37.6597533768028,14.3669836663538));
#54752=CARTESIAN_POINT('Ctrl Pts',(-38.2954995370357,37.5355989289914,14.3542117235887));
#54753=CARTESIAN_POINT('Ctrl Pts',(-38.2957867873204,37.5353247514265,14.8957882764113));
#54754=CARTESIAN_POINT('Ctrl Pts',(-38.4978395239631,37.4181483982544,14.8837853792505));
#54755=CARTESIAN_POINT('Ctrl Pts',(-39.2200040297691,37.1845419759791,14.8456139786307));
#54756=CARTESIAN_POINT('Ctrl Pts',(-40.5064460859517,37.7623754838001,14.781274074552));
#54757=CARTESIAN_POINT('Ctrl Pts',(-40.7841666383236,39.4605673674226,14.7027685641753));
#54758=CARTESIAN_POINT('Ctrl Pts',(-39.5208569909583,40.6289217126118,14.6242630537985));
#54759=CARTESIAN_POINT('Ctrl Pts',(-37.8495006293028,40.2196233657655,14.5457575434217));
#54760=CARTESIAN_POINT('Ctrl Pts',(-37.2863317343909,38.6481881568849,14.4695992842926));
#54761=CARTESIAN_POINT('Ctrl Pts',(-37.8968197279324,37.7639788153404,14.4196095286225));
#54762=CARTESIAN_POINT('Ctrl Pts',(-38.2940340733258,37.531419596366,14.3957882764113));
#54763=CARTESIAN_POINT('Origin',(-39.0658530619283,38.8697713466882,19.1042117235887));
#54764=CARTESIAN_POINT('',(-38.2928440194275,37.5332956321379,15.3957882764113));
#54765=CARTESIAN_POINT('',(-38.2956103942192,37.5330138522408,15.3542117235887));
#54766=CARTESIAN_POINT('',(-38.2943530619284,37.5334941486488,19.1042117235887));
#54767=CARTESIAN_POINT('Ctrl Pts',(-38.2956103942192,37.5330138522408,15.3542117235887));
#54768=CARTESIAN_POINT('Ctrl Pts',(-38.4048846594434,37.4686481648294,15.3476723745276));
#54769=CARTESIAN_POINT('Ctrl Pts',(-38.9890534180561,37.2143251749767,15.3149645220075));
#54770=CARTESIAN_POINT('Ctrl Pts',(-40.2495149974676,37.4911553124801,15.2560881660285));
#54771=CARTESIAN_POINT('Ctrl Pts',(-40.8686733596744,39.0966551680435,15.1775826556517));
#54772=CARTESIAN_POINT('Ctrl Pts',(-39.8710199775172,40.4986802936762,15.0990771452749));
#54773=CARTESIAN_POINT('Ctrl Pts',(-38.151273037136,40.4398609986214,15.0205716348981));
#54774=CARTESIAN_POINT('Ctrl Pts',(-37.2517446794564,38.9729482851087,14.9420661245214));
#54775=CARTESIAN_POINT('Ctrl Pts',(-37.765555298795,37.8714157983081,14.8866128207515));
#54776=CARTESIAN_POINT('Ctrl Pts',(-38.2403192732087,37.5622973130857,14.8573280204407));
#54777=CARTESIAN_POINT('Ctrl Pts',(-38.2927144236218,37.5325537808421,14.8542117235887));
#54778=CARTESIAN_POINT('Ctrl Pts',(-38.2928440194275,37.5332956321379,15.3957882764113));
#54779=CARTESIAN_POINT('Ctrl Pts',(-38.6577053958295,37.3268052108187,15.3741297333373));
#54780=CARTESIAN_POINT('Ctrl Pts',(-39.6603483962762,37.2000760884311,15.3263026868045));
#54781=CARTESIAN_POINT('Ctrl Pts',(-40.8063139857151,38.3478206288557,15.2523071368127));
#54782=CARTESIAN_POINT('Ctrl Pts',(-40.4612384258706,40.0336169338117,15.1738016264359));
#54783=CARTESIAN_POINT('Ctrl Pts',(-38.8647480157521,40.6756488816116,15.0952961160592));
#54784=CARTESIAN_POINT('Ctrl Pts',(-37.4486135593306,39.6981268544225,15.0167906056824));
#54785=CARTESIAN_POINT('Ctrl Pts',(-37.4776219436003,38.2407538193379,14.9502879924664));
#54786=CARTESIAN_POINT('Ctrl Pts',(-38.0573277319451,37.6736142047346,14.9099538827094));
#54787=CARTESIAN_POINT('Ctrl Pts',(-38.2957867873204,37.5353247514265,14.8957882764113));
#54788=CARTESIAN_POINT('Origin',(-39.0658530619283,38.8697713466882,19.1042117235887));
#54789=CARTESIAN_POINT('',(-38.2951740301017,37.5323575792927,15.8957882764113));
#54790=CARTESIAN_POINT('',(-38.2945098549625,37.5355091383948,15.8542117235887));
#54791=CARTESIAN_POINT('',(-38.2943530619284,37.5334941486488,19.1042117235887));
#54792=CARTESIAN_POINT('Ctrl Pts',(-38.2945098549625,37.5355091383948,15.8542117235887));
#54793=CARTESIAN_POINT('Ctrl Pts',(-38.5680519773933,37.379494703083,15.8380167286145));
#54794=CARTESIAN_POINT('Ctrl Pts',(-39.406457455491,37.1794324424244,15.7956532301813));
#54795=CARTESIAN_POINT('Ctrl Pts',(-40.6627777316899,38.0028980795747,15.7271212282892));
#54796=CARTESIAN_POINT('Ctrl Pts',(-40.6697711344255,39.7236357807725,15.6486157179124));
#54797=CARTESIAN_POINT('Ctrl Pts',(-39.2383326839261,40.6786075590939,15.5701102075356));
#54798=CARTESIAN_POINT('Ctrl Pts',(-37.6522103975089,40.0113720173278,15.4916046971588));
#54799=CARTESIAN_POINT('Ctrl Pts',(-37.3603930477839,38.4611828913061,15.4196385358432));
#54800=CARTESIAN_POINT('Ctrl Pts',(-37.9676019940363,37.7262202408736,15.3738408779865));
#54801=CARTESIAN_POINT('Ctrl Pts',(-38.2956103942192,37.5330138522408,15.3542117235887));
#54802=CARTESIAN_POINT('Ctrl Pts',(-38.2951740301017,37.5323575792927,15.8957882764113));
#54803=CARTESIAN_POINT('Ctrl Pts',(-38.3810405288581,37.4817642775928,15.8906425908832));
#54804=CARTESIAN_POINT('Ctrl Pts',(-38.9323618573136,37.2256198547756,15.8593284018961));
#54805=CARTESIAN_POINT('Ctrl Pts',(-40.1754824724718,37.4308969968639,15.8018457094502));
#54806=CARTESIAN_POINT('Ctrl Pts',(-40.8781004790679,39.0016657040982,15.7233401990734));
#54807=CARTESIAN_POINT('Ctrl Pts',(-39.9554519188483,40.454148415738,15.6448346886966));
#54808=CARTESIAN_POINT('Ctrl Pts',(-38.2349899535507,40.4857241059463,15.5663291783198));
#54809=CARTESIAN_POINT('Ctrl Pts',(-37.2596657788943,39.0680749435715,15.4878236679431));
#54810=CARTESIAN_POINT('Ctrl Pts',(-37.726362925197,37.9127558858067,15.4309767006402));
#54811=CARTESIAN_POINT('Ctrl Pts',(-38.2168689019889,37.5762931512624,15.4002982367963));
#54812=CARTESIAN_POINT('Ctrl Pts',(-38.2928440194275,37.5332956321379,15.3957882764113));
#54813=CARTESIAN_POINT('Origin',(-39.0658530619283,38.8697713466882,19.1042117235887));
#54814=CARTESIAN_POINT('',(-38.295011126227,37.5356544186406,16.3957882764113));
#54815=CARTESIAN_POINT('',(-38.2930403179255,37.531438851785,16.3542117235887));
#54816=CARTESIAN_POINT('',(-38.2943530619284,37.5334941486488,19.1042117235887));
#54817=CARTESIAN_POINT('Ctrl Pts',(-38.2930403179255,37.531438851785,16.3542117235887));
#54818=CARTESIAN_POINT('Ctrl Pts',(-38.7255164935029,37.2823487342141,16.3283610827013));
#54819=CARTESIAN_POINT('Ctrl Pts',(-39.8618384352914,37.240015326582,16.276341938355));
#54820=CARTESIAN_POINT('Ctrl Pts',(-40.8667697353107,38.628241232664,16.1981542905498));
#54821=CARTESIAN_POINT('Ctrl Pts',(-40.2606815765474,40.2387207543455,16.119648780173));
#54822=CARTESIAN_POINT('Ctrl Pts',(-38.5830428006473,40.6214939022527,16.0411432697963));
#54823=CARTESIAN_POINT('Ctrl Pts',(-37.3383997450109,39.4332806175246,15.9626377594195));
#54824=CARTESIAN_POINT('Ctrl Pts',(-37.5801461044556,38.0890698220828,15.900327244017));
#54825=CARTESIAN_POINT('Ctrl Pts',(-38.1260519651447,37.6315889023455,15.8641852320734));
#54826=CARTESIAN_POINT('Ctrl Pts',(-38.2945098549625,37.5355091383948,15.8542117235887));
#54827=CARTESIAN_POINT('Ctrl Pts',(-38.295011126227,37.5356544186406,16.3957882764113));
#54828=CARTESIAN_POINT('Ctrl Pts',(-38.544845436971,37.3924216099234,16.3809869449701));
#54829=CARTESIAN_POINT('Ctrl Pts',(-39.3436107151108,37.1792592329343,16.3400171100699));
#54830=CARTESIAN_POINT('Ctrl Pts',(-40.6150494715949,37.9202307686755,16.2728787717109));
#54831=CARTESIAN_POINT('Ctrl Pts',(-40.7123989731982,39.6382265407265,16.1943732613341));
#54832=CARTESIAN_POINT('Ctrl Pts',(-39.333086957597,40.6670534245635,16.1158677509573));
#54833=CARTESIAN_POINT('Ctrl Pts',(-37.7141132310224,40.0840350136354,16.0373622405805));
#54834=CARTESIAN_POINT('Ctrl Pts',(-37.3340693749042,38.521628139946,15.9640024157318));
#54835=CARTESIAN_POINT('Ctrl Pts',(-37.9443644518928,37.7390576903556,15.9168110943421));
#54836=CARTESIAN_POINT('Ctrl Pts',(-38.2951740301017,37.5323575792927,15.8957882764113));
#54837=CARTESIAN_POINT('Origin',(-39.0658530619283,38.8697713466882,19.1042117235887));
#54838=CARTESIAN_POINT('',(-38.2927752994979,37.5318947737649,16.8957882764113));
#54839=CARTESIAN_POINT('',(-38.2960217454206,37.5343651514648,16.8542117235887));
#54840=CARTESIAN_POINT('',(-38.2943530619284,37.5334941486488,19.1042117235887));
#54841=CARTESIAN_POINT('Ctrl Pts',(-38.2960217454206,37.5343651514648,16.8542117235887));
#54842=CARTESIAN_POINT('Ctrl Pts',(-38.4526440402526,37.4426474088561,16.8448739402472));
#54843=CARTESIAN_POINT('Ctrl Pts',(-39.1056117500068,37.1960483659351,16.8093676534467));
#54844=CARTESIAN_POINT('Ctrl Pts',(-40.3881062726607,37.6234631732891,16.7476928631873));
#54845=CARTESIAN_POINT('Ctrl Pts',(-40.834758606014,39.2852359660895,16.6691873528105));
#54846=CARTESIAN_POINT('Ctrl Pts',(-39.6950143769496,40.5744102242793,16.5906818424337));
#54847=CARTESIAN_POINT('Ctrl Pts',(-37.9910233315818,40.3348238050802,16.5121763320569));
#54848=CARTESIAN_POINT('Ctrl Pts',(-37.250965136829,38.7813435147693,16.4336708216802));
#54849=CARTESIAN_POINT('Ctrl Pts',(-37.8462764933252,37.7925906195586,16.3810159521908));
#54850=CARTESIAN_POINT('Ctrl Pts',(-38.2877225391555,37.5345016936567,16.3545295861603));
#54851=CARTESIAN_POINT('Ctrl Pts',(-38.2930403179255,37.531438851785,16.3542117235887));
#54852=CARTESIAN_POINT('Ctrl Pts',(-38.2927752994979,37.5318947737649,16.8957882764113));
#54853=CARTESIAN_POINT('Ctrl Pts',(-38.7030067984342,37.2976596080307,16.871331299057));
#54854=CARTESIAN_POINT('Ctrl Pts',(-39.7943393979825,37.2242325343385,16.8207058182437));
#54855=CARTESIAN_POINT('Ctrl Pts',(-40.8516003110939,38.5339981005298,16.7439118339715));
#54856=CARTESIAN_POINT('Ctrl Pts',(-40.3309240105073,40.1740843304588,16.6654063235948));
#54857=CARTESIAN_POINT('Ctrl Pts',(-38.6757020358417,40.644431583443,16.586900813218));
#54858=CARTESIAN_POINT('Ctrl Pts',(-37.3703767628973,39.5232213878114,16.5083953028412));
#54859=CARTESIAN_POINT('Ctrl Pts',(-37.5450179797371,38.1378625018882,16.4446911239056));
#54860=CARTESIAN_POINT('Ctrl Pts',(-38.1031426043017,37.6456547913594,16.407155448429));
#54861=CARTESIAN_POINT('Ctrl Pts',(-38.295011126227,37.5356544186406,16.3957882764113));
#54862=CARTESIAN_POINT('Origin',(-39.0658530619283,38.8697713466882,19.1042117235887));
#54863=CARTESIAN_POINT('',(-38.2959007276492,37.5337106753505,17.3957882764113));
#54864=CARTESIAN_POINT('',(-38.2935040424574,37.5346322273253,17.3542117235887));
#54865=CARTESIAN_POINT('',(-38.2943530619284,37.5334941486488,19.1042117235887));
#54866=CARTESIAN_POINT('Ctrl Pts',(-38.2935040424574,37.5346322273253,17.3542117235887));
#54867=CARTESIAN_POINT('Ctrl Pts',(-38.6142216923301,37.353029943727,17.3352182943341));
#54868=CARTESIAN_POINT('Ctrl Pts',(-39.5350880316607,37.1858556050909,17.2900563616205));
#54869=CARTESIAN_POINT('Ctrl Pts',(-40.7451827384013,38.1758790339381,17.218725925448));
#54870=CARTESIAN_POINT('Ctrl Pts',(-40.5709395934168,39.8877854279213,17.1402204150712));
#54871=CARTESIAN_POINT('Ctrl Pts',(-39.0468978715213,40.6867135087542,17.0617149046944));
#54872=CARTESIAN_POINT('Ctrl Pts',(-37.5398562037872,39.8561642112719,16.9832093943176));
#54873=CARTESIAN_POINT('Ctrl Pts',(-37.4178373052429,38.3450042264081,16.9140416672824));
#54874=CARTESIAN_POINT('Ctrl Pts',(-38.013720699012,37.6996801517363,16.8710424437061));
#54875=CARTESIAN_POINT('Ctrl Pts',(-38.2960217454206,37.5343651514648,16.8542117235887));
#54876=CARTESIAN_POINT('Ctrl Pts',(-38.2959007276492,37.5337106753505,17.3957882764113));
#54877=CARTESIAN_POINT('Ctrl Pts',(-38.4288872990661,37.4555469373629,17.3878441566028));
#54878=CARTESIAN_POINT('Ctrl Pts',(-39.0471107626292,37.2043843657908,17.3537315333353));
#54879=CARTESIAN_POINT('Ctrl Pts',(-40.3208285827552,37.5557507395872,17.293450406609));
#54880=CARTESIAN_POINT('Ctrl Pts',(-40.8541369642561,39.1917640019411,17.2149448962322));
#54881=CARTESIAN_POINT('Ctrl Pts',(-39.7836658898432,40.5390185509755,17.1364393858554));
#54882=CARTESIAN_POINT('Ctrl Pts',(-38.0694451486085,40.389246627264,17.0579338754786));
#54883=CARTESIAN_POINT('Ctrl Pts',(-37.248825754395,38.87677605618,16.9794283651019));
#54884=CARTESIAN_POINT('Ctrl Pts',(-37.8057511921981,37.8311625054488,16.9253798320794));
#54885=CARTESIAN_POINT('Ctrl Pts',(-38.2640668491777,37.5482868076194,16.8974998025159));
#54886=CARTESIAN_POINT('Ctrl Pts',(-38.2927752994979,37.5318947737649,16.8957882764113));
#54887=CARTESIAN_POINT('Origin',(-39.0658530619283,38.8697713466882,19.1042117235887));
#54888=CARTESIAN_POINT('',(-38.2938718037177,37.5356881270255,17.8957882764113));
#54889=CARTESIAN_POINT('',(-38.2940537528419,37.5314721085808,17.8542117235887));
#54890=CARTESIAN_POINT('',(-38.2943530619284,37.5334941486488,19.1042117235887));
#54891=CARTESIAN_POINT('',(-37.5756558680257,39.2699729499893,18.));
#54892=CARTESIAN_POINT('Ctrl Pts',(-37.5756558680257,39.2699729499893,18.));
#54893=CARTESIAN_POINT('Ctrl Pts',(-37.4440523270134,38.7799318659294,17.9738314965411));
#54894=CARTESIAN_POINT('Ctrl Pts',(-37.6166680705089,38.0418709533316,17.9390942553448));
#54895=CARTESIAN_POINT('Ctrl Pts',(-38.1491376523637,37.6179382396386,17.9043570141486));
#54896=CARTESIAN_POINT('Ctrl Pts',(-38.2938718037177,37.5356881270255,17.8957882764113));
#54897=CARTESIAN_POINT('',(-37.9726405222314,39.962294313691,18.));
#54898=CARTESIAN_POINT('Origin',(-39.0658530619283,38.8697713466882,18.));
#54899=CARTESIAN_POINT('Ctrl Pts',(-37.972631799081,39.9623061512025,18.));
#54900=CARTESIAN_POINT('Ctrl Pts',(-37.6338216029696,39.6208387086168,17.975091839613));
#54901=CARTESIAN_POINT('Ctrl Pts',(-37.3042322663879,38.6195093398435,17.9264957474759));
#54902=CARTESIAN_POINT('Ctrl Pts',(-37.899143973177,37.7627950030077,17.8778996553388));
#54903=CARTESIAN_POINT('Ctrl Pts',(-38.2940537528419,37.5314721085808,17.8542117235887));
#54904=CARTESIAN_POINT('Origin',(-53.1951359564886,-14.3971354987959,15.5));
#54905=CARTESIAN_POINT('',(-51.9326028526449,-14.3970877066932,14.1934196736194));
#54906=CARTESIAN_POINT('',(-51.9314232360955,-14.3954626592386,14.0565803263806));
#54907=CARTESIAN_POINT('',(-51.9306359564886,-14.3971354987959,15.5));
#54908=CARTESIAN_POINT('',(-52.2370198037663,-15.2223467977324,14.));
#54909=CARTESIAN_POINT('Ctrl Pts',(-51.9314232360955,-14.3954626592386,
14.0565803263806));
#54910=CARTESIAN_POINT('Ctrl Pts',(-51.9340308380707,-14.6945947257524,
14.0377202175871));
#54911=CARTESIAN_POINT('Ctrl Pts',(-52.0414421537953,-14.9952702831595,
14.0188601087935));
#54912=CARTESIAN_POINT('Ctrl Pts',(-52.2370198037663,-15.2223467977324,
14.));
#54913=CARTESIAN_POINT('',(-51.9306359564886,-14.3971354987959,14.));
#54914=CARTESIAN_POINT('Origin',(-53.1951359564886,-14.3971354987959,14.));
#54915=CARTESIAN_POINT('',(-51.9306359564886,-14.3971354987959,13.));
#54916=CARTESIAN_POINT('',(-51.9306359564886,-14.3971354987959,15.5));
#54917=CARTESIAN_POINT('',(-52.6278006430704,-15.5272199611918,13.));
#54918=CARTESIAN_POINT('Origin',(-53.1951359564886,-14.3971354987959,13.));
#54919=CARTESIAN_POINT('',(-53.7624712699068,-13.2670510364,13.));
#54920=CARTESIAN_POINT('Origin',(-53.1951359564886,-14.3971354987959,13.));
#54921=CARTESIAN_POINT('Origin',(-53.1951359564886,-14.3971354987959,13.));
#54922=CARTESIAN_POINT('',(-54.1550391816747,-15.22347043962,14.));
#54923=CARTESIAN_POINT('Origin',(-53.1951359564886,-14.3971354987959,14.));
#54924=CARTESIAN_POINT('Ctrl Pts',(-54.1550492157916,-15.2234767486838,
14.));
#54925=CARTESIAN_POINT('Ctrl Pts',(-53.8967914626892,-15.5213134049997,
14.024908160387));
#54926=CARTESIAN_POINT('Ctrl Pts',(-53.4877406809989,-15.6908539055355,
14.049816320774));
#54927=CARTESIAN_POINT('Ctrl Pts',(-53.0948318338551,-15.6595885868543,
14.074724481161));
#54928=CARTESIAN_POINT('Ctrl Pts',(-52.6820419543228,-15.626741255404,14.1008929846199));
#54929=CARTESIAN_POINT('Ctrl Pts',(-52.2870688888724,-15.3722525873919,
14.1270614880789));
#54930=CARTESIAN_POINT('Ctrl Pts',(-52.0867822938008,-15.0099588798403,
14.1532299915378));
#54931=CARTESIAN_POINT('Ctrl Pts',(-51.9842486685495,-14.8244882185226,
14.1666265522317));
#54932=CARTESIAN_POINT('Ctrl Pts',(-51.9327378835252,-14.6107643391081,
14.1800231129255));
#54933=CARTESIAN_POINT('Ctrl Pts',(-51.9326028526449,-14.3970877066932,
14.1934196736194));
#54934=CARTESIAN_POINT('Origin',(-53.1951359564886,-14.3971354987959,15.5));
#54935=CARTESIAN_POINT('',(-51.9293004715569,-14.396357843321,14.6934196736194));
#54936=CARTESIAN_POINT('',(-51.9290361749446,-14.3977594574901,14.5565803263806));
#54937=CARTESIAN_POINT('',(-51.9306359564886,-14.3971354987959,15.5));
#54938=CARTESIAN_POINT('Ctrl Pts',(-51.9290361749446,-14.3977594574901,
14.5565803263806));
#54939=CARTESIAN_POINT('Ctrl Pts',(-51.9288104788004,-14.4349272053691,
14.5542330751329));
#54940=CARTESIAN_POINT('Ctrl Pts',(-51.9303086019301,-14.4720763914416,
14.5518858238852));
#54941=CARTESIAN_POINT('Ctrl Pts',(-51.9335904462524,-14.5090671744586,
14.5495385726375));
#54942=CARTESIAN_POINT('Ctrl Pts',(-51.9701783294547,-14.9214616440634,
14.5233700691785));
#54943=CARTESIAN_POINT('Ctrl Pts',(-52.228466159159,-15.3141680878373,14.4972015657196));
#54944=CARTESIAN_POINT('Ctrl Pts',(-52.5926396873008,-15.5111367764164,
14.4710330622607));
#54945=CARTESIAN_POINT('Ctrl Pts',(-52.9568132154426,-15.7081054649955,
14.4448645588018));
#54946=CARTESIAN_POINT('Ctrl Pts',(-53.4268724420219,-15.7093363983798,
14.4186960553428));
#54947=CARTESIAN_POINT('Ctrl Pts',(-53.7920269612472,-15.514187779113,14.3925275518839));
#54948=CARTESIAN_POINT('Ctrl Pts',(-54.1571814804725,-15.3190391598462,
14.366359048425));
#54949=CARTESIAN_POINT('Ctrl Pts',(-54.4174312923439,-14.9275109879282,
14.340190544966));
#54950=CARTESIAN_POINT('Ctrl Pts',(-54.4560979757245,-14.5153505128056,
14.3140220415071));
#54951=CARTESIAN_POINT('Ctrl Pts',(-54.4947646591051,-14.103190037683,14.2878535380482));
#54952=CARTESIAN_POINT('Ctrl Pts',(-54.3118482139948,-13.6703972593558,
14.2616850345893));
#54953=CARTESIAN_POINT('Ctrl Pts',(-53.9893291901183,-13.4106746119161,
14.2355165311303));
#54954=CARTESIAN_POINT('Ctrl Pts',(-53.6668101662417,-13.1509519644764,
14.2093480276714));
#54955=CARTESIAN_POINT('Ctrl Pts',(-53.2046885635989,-13.0642994479243,
14.1831795242125));
#54956=CARTESIAN_POINT('Ctrl Pts',(-52.8102658096442,-13.1903246291658,
14.1570110207536));
#54957=CARTESIAN_POINT('Ctrl Pts',(-52.4158430556895,-13.3163498104073,
14.1308425172946));
#54958=CARTESIAN_POINT('Ctrl Pts',(-52.089119150423,-13.6550526894425,14.1046740138357));
#54959=CARTESIAN_POINT('Ctrl Pts',(-51.976572074359,-14.0527844617314,14.0785055103768));
#54960=CARTESIAN_POINT('Ctrl Pts',(-51.9451396903252,-14.163863827329,14.0711971157114));
#54961=CARTESIAN_POINT('Ctrl Pts',(-51.9304127761573,-14.2795473576308,
14.063888721046));
#54962=CARTESIAN_POINT('Ctrl Pts',(-51.9314232360955,-14.3954626592386,
14.0565803263806));
#54963=CARTESIAN_POINT('Ctrl Pts',(-51.9326028526449,-14.3970877066932,
14.1934196736194));
#54964=CARTESIAN_POINT('Ctrl Pts',(-51.9324741176124,-14.1933737996841,
14.2061916163845));
#54965=CARTESIAN_POINT('Ctrl Pts',(-51.9790420088886,-13.9897028365794,
14.2189635591495));
#54966=CARTESIAN_POINT('Ctrl Pts',(-52.0726123421383,-13.8105984338676,
14.2317355019146));
#54967=CARTESIAN_POINT('Ctrl Pts',(-52.2643291102402,-13.4436304425376,
14.2579040053735));
#54968=CARTESIAN_POINT('Ctrl Pts',(-52.6533627711367,-13.1797932069689,
14.2840725088324));
#54969=CARTESIAN_POINT('Ctrl Pts',(-53.0652069371965,-13.1373261840987,
14.3102410122914));
#54970=CARTESIAN_POINT('Ctrl Pts',(-53.4770511032563,-13.0948591612284,
14.3364095157503));
#54971=CARTESIAN_POINT('Ctrl Pts',(-53.9117057744794,-13.2737623510566,
14.3625780192092));
#54972=CARTESIAN_POINT('Ctrl Pts',(-54.174295890408,-13.5938472660216,14.3887465226681));
#54973=CARTESIAN_POINT('Ctrl Pts',(-54.4368860063367,-13.9139321809865,
14.4149150261271));
#54974=CARTESIAN_POINT('Ctrl Pts',(-54.5274115669709,-14.3751988210882,
14.441083529586));
#54975=CARTESIAN_POINT('Ctrl Pts',(-54.4052653400131,-14.7707929840487,
14.4672520330449));
#54976=CARTESIAN_POINT('Ctrl Pts',(-54.2831191130553,-15.1663871470091,
14.4934205365038));
#54977=CARTESIAN_POINT('Ctrl Pts',(-53.9483010985055,-15.4963088328283,
14.5195890399628));
#54978=CARTESIAN_POINT('Ctrl Pts',(-53.5509548543059,-15.6126255371819,
14.5457575434217));
#54979=CARTESIAN_POINT('Ctrl Pts',(-53.1536086101064,-15.7289422415355,
14.5719260468806));
#54980=CARTESIAN_POINT('Ctrl Pts',(-52.6937341362571,-15.6316539644235,
14.5980945503395));
#54981=CARTESIAN_POINT('Ctrl Pts',(-52.3775410563803,-15.3643818135364,
14.6242630537985));
#54982=CARTESIAN_POINT('Ctrl Pts',(-52.0990020785416,-15.1289379773151,
14.6473152604054));
#54983=CARTESIAN_POINT('Ctrl Pts',(-51.9319612775611,-14.7615849808525,
14.6703674670124));
#54984=CARTESIAN_POINT('Ctrl Pts',(-51.9293004715569,-14.396357843321,14.6934196736194));
#54985=CARTESIAN_POINT('Origin',(-53.1951359564886,-14.3971354987959,15.5));
#54986=CARTESIAN_POINT('',(-51.9308136275137,-14.3982246453427,15.1934196736194));
#54987=CARTESIAN_POINT('',(-51.932525975067,-14.3974029423036,15.0565803263806));
#54988=CARTESIAN_POINT('',(-51.9306359564886,-14.3971354987959,15.5));
#54989=CARTESIAN_POINT('Ctrl Pts',(-51.932525975067,-14.3974029423036,15.0565803263806));
#54990=CARTESIAN_POINT('Ctrl Pts',(-51.9321561072822,-14.5888155966727,
15.0445774292198));
#54991=CARTESIAN_POINT('Ctrl Pts',(-51.9730705675611,-14.7800782049927,
15.0325745320589));
#54992=CARTESIAN_POINT('Ctrl Pts',(-52.0560982976485,-14.9508677919232,
15.0205716348981));
#54993=CARTESIAN_POINT('Ctrl Pts',(-52.2371138818754,-15.3232202195459,
14.9944031314392));
#54994=CARTESIAN_POINT('Ctrl Pts',(-52.6183020364058,-15.5982603906742,
14.9682346279803));
#54995=CARTESIAN_POINT('Ctrl Pts',(-53.0287335368761,-15.6526576817852,
14.9420661245214));
#54996=CARTESIAN_POINT('Ctrl Pts',(-53.4391650373463,-15.7070549728962,
14.9158976210624));
#54997=CARTESIAN_POINT('Ctrl Pts',(-53.8788398837565,-15.5408093839899,
14.8897291176035));
#54998=CARTESIAN_POINT('Ctrl Pts',(-54.1506024967829,-15.2284660841227,
14.8635606141446));
#54999=CARTESIAN_POINT('Ctrl Pts',(-54.4223651098093,-14.9161227842554,
14.8373921106857));
#55000=CARTESIAN_POINT('Ctrl Pts',(-54.5262154894519,-14.4576817734273,
14.8112236072267));
#55001=CARTESIAN_POINT('Ctrl Pts',(-54.4155861975138,-14.0587161328242,
14.7850551037678));
#55002=CARTESIAN_POINT('Ctrl Pts',(-54.3049569055756,-13.6597504922211,
14.7588866003089));
#55003=CARTESIAN_POINT('Ctrl Pts',(-53.9798479420568,-13.320260221843,14.7327180968499));
#55004=CARTESIAN_POINT('Ctrl Pts',(-53.5860414121493,-13.1924713804069,
14.706549593391));
#55005=CARTESIAN_POINT('Ctrl Pts',(-53.1922348822418,-13.0646825389707,
14.6803810899321));
#55006=CARTESIAN_POINT('Ctrl Pts',(-52.7297307859455,-13.1485951264764,
14.6542125864732));
#55007=CARTESIAN_POINT('Ctrl Pts',(-52.4059227061476,-13.4065926679472,
14.6280440830142));
#55008=CARTESIAN_POINT('Ctrl Pts',(-52.1111594252055,-13.6414484561238,
14.604222830803));
#55009=CARTESIAN_POINT('Ctrl Pts',(-51.9313266688913,-14.0205598299628,
14.5804015785918));
#55010=CARTESIAN_POINT('Ctrl Pts',(-51.9290361749446,-14.3977594574901,
14.5565803263806));
#55011=CARTESIAN_POINT('Ctrl Pts',(-51.9293004715569,-14.396357843321,14.6934196736194));
#55012=CARTESIAN_POINT('Ctrl Pts',(-51.9289407723091,-14.3469848614482,
14.6965359704714));
#55013=CARTESIAN_POINT('Ctrl Pts',(-51.9315850846113,-14.2976507292223,
14.6996522673233));
#55014=CARTESIAN_POINT('Ctrl Pts',(-51.9373640512185,-14.2486865756559,
14.7027685641753));
#55015=CARTESIAN_POINT('Ctrl Pts',(-51.985891811838,-13.8375195133245,14.7289370676342));
#55016=CARTESIAN_POINT('Ctrl Pts',(-52.2554590189813,-13.452441413324,14.7551055710931));
#55017=CARTESIAN_POINT('Ctrl Pts',(-52.62518765984,-13.2661248639499,14.781274074552));
#55018=CARTESIAN_POINT('Ctrl Pts',(-52.9949163006986,-13.0798083145759,
14.807442578011));
#55019=CARTESIAN_POINT('Ctrl Pts',(-53.4648063752726,-13.0922533158284,
14.8336110814699));
#55020=CARTESIAN_POINT('Ctrl Pts',(-53.8241540209967,-13.2978798810904,
14.8597795849288));
#55021=CARTESIAN_POINT('Ctrl Pts',(-54.1835016667209,-13.5035064463524,
14.8859480883877));
#55022=CARTESIAN_POINT('Ctrl Pts',(-54.4323068835952,-13.902314575624,14.9121165918467));
#55023=CARTESIAN_POINT('Ctrl Pts',(-54.4590022406867,-14.3154737155563,
14.9382850953056));
#55024=CARTESIAN_POINT('Ctrl Pts',(-54.4856975977781,-14.7286328554886,
14.9644535987645));
#55025=CARTESIAN_POINT('Ctrl Pts',(-54.2902830950867,-15.1561430060817,
14.9906221022234));
#55026=CARTESIAN_POINT('Ctrl Pts',(-53.9603850245762,-15.4063036567383,
15.0167906056824));
#55027=CARTESIAN_POINT('Ctrl Pts',(-53.6304869540657,-15.656464307395,15.0429591091413));
#55028=CARTESIAN_POINT('Ctrl Pts',(-53.1661053157362,-15.7292754581154,
15.0691276126002));
#55029=CARTESIAN_POINT('Ctrl Pts',(-52.7754743036767,-15.592087662659,15.0952961160592));
#55030=CARTESIAN_POINT('Ctrl Pts',(-52.3848432916172,-15.4548998672026,
15.1214646195181));
#55031=CARTESIAN_POINT('Ctrl Pts',(-52.0679629058276,-15.1077131255694,
15.147633122977));
#55032=CARTESIAN_POINT('Ctrl Pts',(-51.9669261040319,-14.7062101297548,
15.1738016264359));
#55033=CARTESIAN_POINT('Ctrl Pts',(-51.9416776248439,-14.6058769852609,
15.1803409754971));
#55034=CARTESIAN_POINT('Ctrl Pts',(-51.9299079202419,-14.502151956084,15.1868803245583));
#55035=CARTESIAN_POINT('Ctrl Pts',(-51.9308136275137,-14.3982246453427,
15.1934196736194));
#55036=CARTESIAN_POINT('Origin',(-53.1951359564886,-14.3971354987959,15.5));
#55037=CARTESIAN_POINT('',(-51.9321336144333,-14.3964211293814,15.6934196736194));
#55038=CARTESIAN_POINT('',(-51.9298800777713,-14.396145855272,15.5565803263806));
#55039=CARTESIAN_POINT('',(-51.9306359564886,-14.3971354987959,15.5));
#55040=CARTESIAN_POINT('Ctrl Pts',(-51.9298800777713,-14.396145855272,15.5565803263806));
#55041=CARTESIAN_POINT('Ctrl Pts',(-51.9328341793634,-14.7397024926117,
15.5349217833067));
#55042=CARTESIAN_POINT('Ctrl Pts',(-52.0781516403077,-15.0854616424501,
15.5132632402327));
#55043=CARTESIAN_POINT('Ctrl Pts',(-52.3278732854,-15.32010983553,15.4916046971588));
#55044=CARTESIAN_POINT('Ctrl Pts',(-52.6295944912569,-15.6036188430972,
15.4654361936999));
#55045=CARTESIAN_POINT('Ctrl Pts',(-53.0837270081697,-15.7249258591405,
15.439267690241));
#55046=CARTESIAN_POINT('Ctrl Pts',(-53.4866324184767,-15.629635385456,15.413099186782));
#55047=CARTESIAN_POINT('Ctrl Pts',(-53.8895378287837,-15.5343449117715,
15.3869306833231));
#55048=CARTESIAN_POINT('Ctrl Pts',(-54.2412161324849,-15.2224569483592,
15.3607621798642));
#55049=CARTESIAN_POINT('Ctrl Pts',(-54.3839705956172,-14.8338257457023,
15.3345936764052));
#55050=CARTESIAN_POINT('Ctrl Pts',(-54.5267250587495,-14.4451945430454,
15.3084251729463));
#55051=CARTESIAN_POINT('Ctrl Pts',(-54.4605556813129,-13.9798201011439,
15.2822566694874));
#55052=CARTESIAN_POINT('Ctrl Pts',(-54.2151336032284,-13.6463818912608,
15.2560881660285));
#55053=CARTESIAN_POINT('Ctrl Pts',(-53.9697115251439,-13.3129436813777,
15.2299196625696));
#55054=CARTESIAN_POINT('Ctrl Pts',(-53.5450367464114,-13.111441703513,15.2037511591106));
#55055=CARTESIAN_POINT('Ctrl Pts',(-53.1315384766945,-13.1322317596502,
15.1775826556517));
#55056=CARTESIAN_POINT('Ctrl Pts',(-52.7180402069775,-13.1530218157874,
15.1514141521928));
#55057=CARTESIAN_POINT('Ctrl Pts',(-52.3157184462761,-13.3961039059265,
15.1252456487338));
#55058=CARTESIAN_POINT('Ctrl Pts',(-52.1049790728871,-13.7524772930548,
15.0990771452749));
#55059=CARTESIAN_POINT('Ctrl Pts',(-51.99090105541,-13.9453903155784,15.0849115389768));
#55060=CARTESIAN_POINT('Ctrl Pts',(-51.9329624864653,-14.1715011232728,
15.0707459326787));
#55061=CARTESIAN_POINT('Ctrl Pts',(-51.932525975067,-14.3974029423036,15.0565803263806));
#55062=CARTESIAN_POINT('Ctrl Pts',(-51.9308136275137,-14.3982246453427,
15.1934196736194));
#55063=CARTESIAN_POINT('Ctrl Pts',(-51.9335322876909,-14.0862661905168,
15.2130488280172));
#55064=CARTESIAN_POINT('Ctrl Pts',(-52.0504588679336,-13.7724851395516,
15.2326779824149));
#55065=CARTESIAN_POINT('Ctrl Pts',(-52.2598657119042,-13.5431471347949,
15.2523071368127));
#55066=CARTESIAN_POINT('Ctrl Pts',(-52.5390353393738,-13.2374063856457,
15.2784756402716));
#55067=CARTESIAN_POINT('Ctrl Pts',(-52.9825678121147,-13.0817441373434,
15.3046441437306));
#55068=CARTESIAN_POINT('Ctrl Pts',(-53.3915779035484,-13.1459611997424,
15.3308126471895));
#55069=CARTESIAN_POINT('Ctrl Pts',(-53.8005879949821,-13.2101782621413,
15.3569811506484));
#55070=CARTESIAN_POINT('Ctrl Pts',(-54.1750757051085,-13.4942746352416,
15.3831496541073));
#55071=CARTESIAN_POINT('Ctrl Pts',(-54.3471162900744,-13.8708581246834,
15.4093181575663));
#55072=CARTESIAN_POINT('Ctrl Pts',(-54.5191568750402,-14.2474416141252,
15.4354866610252));
#55073=CARTESIAN_POINT('Ctrl Pts',(-54.4887503348454,-14.7165122199085,
15.4616551644841));
#55074=CARTESIAN_POINT('Ctrl Pts',(-54.2695313251181,-15.0677331084555,
15.4878236679431));
#55075=CARTESIAN_POINT('Ctrl Pts',(-54.0503123153908,-15.4189539970025,
15.513992171402));
#55076=CARTESIAN_POINT('Ctrl Pts',(-53.642280836131,-15.6523251683133,15.5401606748609));
#55077=CARTESIAN_POINT('Ctrl Pts',(-53.2284030520588,-15.6632002142321,
15.5663291783198));
#55078=CARTESIAN_POINT('Ctrl Pts',(-52.8145252679866,-15.6740752601508,
15.5924976817788));
#55079=CARTESIAN_POINT('Ctrl Pts',(-52.3948011791021,-15.4624541806777,
15.6186661852377));
#55080=CARTESIAN_POINT('Ctrl Pts',(-52.1574400564301,-15.1232303837968,
15.6448346886966));
#55081=CARTESIAN_POINT('Ctrl Pts',(-52.010543532722,-14.9132937439633,15.6610296836709));
#55082=CARTESIAN_POINT('Ctrl Pts',(-51.9334928433345,-14.6544846908102,
15.6772246786452));
#55083=CARTESIAN_POINT('Ctrl Pts',(-51.9321336144333,-14.3964211293814,
15.6934196736194));
#55084=CARTESIAN_POINT('Origin',(-53.1951359564886,-14.3971354987959,15.5));
#55085=CARTESIAN_POINT('',(-51.9286427349007,-14.3970459914357,16.1934196736194));
#55086=CARTESIAN_POINT('',(-51.9301690580705,-14.3981838623804,16.0565803263806));
#55087=CARTESIAN_POINT('',(-51.9306359564886,-14.3971354987959,15.5));
#55088=CARTESIAN_POINT('Ctrl Pts',(-51.9301690580705,-14.3981838623804,
16.0565803263806));
#55089=CARTESIAN_POINT('Ctrl Pts',(-51.9294463895002,-14.4798551199685,
16.0514346408525));
#55090=CARTESIAN_POINT('Ctrl Pts',(-51.9366958070815,-14.5613987134005,
16.0462889553244));
#55091=CARTESIAN_POINT('Ctrl Pts',(-51.9523897974866,-14.6412833003864,
16.0411432697963));
#55092=CARTESIAN_POINT('Ctrl Pts',(-52.0322019507863,-15.0475382258844,
16.0149747663373));
#55093=CARTESIAN_POINT('Ctrl Pts',(-52.3304122644718,-15.4108870194283,
15.9888062628784));
#55094=CARTESIAN_POINT('Ctrl Pts',(-52.7132996891177,-15.5683997628469,
15.9626377594195));
#55095=CARTESIAN_POINT('Ctrl Pts',(-53.0961871137635,-15.7259125062655,
15.9364692559606));
#55096=CARTESIAN_POINT('Ctrl Pts',(-53.5637516493698,-15.6775891995586,
15.9103007525016));
#55097=CARTESIAN_POINT('Ctrl Pts',(-53.9063318003261,-15.4450985880149,
15.8841322490427));
#55098=CARTESIAN_POINT('Ctrl Pts',(-54.2489119512824,-15.2126079764712,
15.8579637455838));
#55099=CARTESIAN_POINT('Ctrl Pts',(-54.4665077175887,-14.7959500600907,
15.8317952421249));
#55100=CARTESIAN_POINT('Ctrl Pts',(-54.4615465710813,-14.3819592010216,
15.8056267386659));
#55101=CARTESIAN_POINT('Ctrl Pts',(-54.4565854245739,-13.9679683419524,
15.779458235207));
#55102=CARTESIAN_POINT('Ctrl Pts',(-54.2290673652527,-13.5566445401947,
15.7532897317481));
#55103=CARTESIAN_POINT('Ctrl Pts',(-53.8810141954492,-13.3324302783772,
15.7271212282891));
#55104=CARTESIAN_POINT('Ctrl Pts',(-53.5329610256457,-13.1082160165598,
15.7009527248302));
#55105=CARTESIAN_POINT('Ctrl Pts',(-53.0643727453599,-13.0711112946827,
15.6747842213713));
#55106=CARTESIAN_POINT('Ctrl Pts',(-52.6853699093616,-13.2377543099066,
15.6486157179124));
#55107=CARTESIAN_POINT('Ctrl Pts',(-52.3063670733632,-13.4043973251304,
15.6224472144534));
#55108=CARTESIAN_POINT('Ctrl Pts',(-52.0169496816522,-13.7747880774553,
15.5962787109945));
#55109=CARTESIAN_POINT('Ctrl Pts',(-51.9468959331972,-14.1828389531634,
15.5701102075356));
#55110=CARTESIAN_POINT('Ctrl Pts',(-51.9348226546909,-14.2531636963187,
15.5656002471506));
#55111=CARTESIAN_POINT('Ctrl Pts',(-51.9292649449293,-14.324607025577,15.5610902867656));
#55112=CARTESIAN_POINT('Ctrl Pts',(-51.9298800777713,-14.396145855272,15.5565803263806));
#55113=CARTESIAN_POINT('Ctrl Pts',(-51.9321336144333,-14.3964211293814,
15.6934196736194));
#55114=CARTESIAN_POINT('Ctrl Pts',(-51.9312965483521,-14.2374955401126,
15.7033931821041));
#55115=CARTESIAN_POINT('Ctrl Pts',(-51.9591660436084,-14.0788526842429,
15.7133666905887));
#55116=CARTESIAN_POINT('Ctrl Pts',(-52.0171074139709,-13.932081398796,15.7233401990734));
#55117=CARTESIAN_POINT('Ctrl Pts',(-52.1691340506433,-13.5469827249646,
15.7495087025323));
#55118=CARTESIAN_POINT('Ctrl Pts',(-52.5281854804478,-13.2436118915905,
15.7756772059912));
#55119=CARTESIAN_POINT('Ctrl Pts',(-52.9332587743738,-13.1580039865908,
15.8018457094502));
#55120=CARTESIAN_POINT('Ctrl Pts',(-53.3383320682997,-13.072396081591,15.8280142129091));
#55121=CARTESIAN_POINT('Ctrl Pts',(-53.7894272263473,-13.2045511049655,
15.854182716368));
#55122=CARTESIAN_POINT('Ctrl Pts',(-54.0842678175163,-13.4952091732588,
15.880351219827));
#55123=CARTESIAN_POINT('Ctrl Pts',(-54.3791084086854,-13.7858672415521,
15.9065197232859));
#55124=CARTESIAN_POINT('Ctrl Pts',(-54.517694432976,-14.2350283547642,15.9326882267448));
#55125=CARTESIAN_POINT('Ctrl Pts',(-54.4378822697683,-14.6412833306956,
15.9588567302037));
#55126=CARTESIAN_POINT('Ctrl Pts',(-54.3580701065605,-15.047538306627,15.9850252336626));
#55127=CARTESIAN_POINT('Ctrl Pts',(-54.0598597558545,-15.4108871452777,
16.0111937371216));
#55128=CARTESIAN_POINT('Ctrl Pts',(-53.676972283676,-15.5683999082504,16.0373622405805));
#55129=CARTESIAN_POINT('Ctrl Pts',(-53.2940848114975,-15.7259126712231,
16.0635307440394));
#55130=CARTESIAN_POINT('Ctrl Pts',(-52.8265202178467,-15.6775893585178,
16.0896992474984));
#55131=CARTESIAN_POINT('Ctrl Pts',(-52.4839400243616,-15.4450987181119,
16.1158677509573));
#55132=CARTESIAN_POINT('Ctrl Pts',(-52.1455210707975,-15.2154320860769,
16.1417183918447));
#55133=CARTESIAN_POINT('Ctrl Pts',(-51.9290686466627,-14.8060450268197,
16.167569032732));
#55134=CARTESIAN_POINT('Ctrl Pts',(-51.9286427349007,-14.3970459914357,
16.1934196736194));
#55135=CARTESIAN_POINT('Origin',(-53.1951359564886,-14.3971354987959,15.5));
#55136=CARTESIAN_POINT('',(-51.9319412138059,-14.3979628881409,16.6934196736194));
#55137=CARTESIAN_POINT('',(-51.9324421154971,-14.3967173588992,16.5565803263806));
#55138=CARTESIAN_POINT('',(-51.9306359564886,-14.3971354987959,15.5));
#55139=CARTESIAN_POINT('Ctrl Pts',(-51.9324421154971,-14.3967173588992,
16.5565803263806));
#55140=CARTESIAN_POINT('Ctrl Pts',(-51.9331582847598,-14.6327178878915,
16.5417789949394));
#55141=CARTESIAN_POINT('Ctrl Pts',(-51.9967468970028,-14.869076799286,16.5269776634982));
#55142=CARTESIAN_POINT('Ctrl Pts',(-52.1207407212382,-15.0677330252045,
16.5121763320569));
#55143=CARTESIAN_POINT('Ctrl Pts',(-52.339959703752,-15.4189538701487,16.486007828598));
#55144=CARTESIAN_POINT('Ctrl Pts',(-52.747991132356,-15.652325012491,16.4598393251391));
#55145=CARTESIAN_POINT('Ctrl Pts',(-53.1618688650479,-15.6632000570604,
16.4336708216802));
#55146=CARTESIAN_POINT('Ctrl Pts',(-53.5757465977398,-15.6740751016298,
16.4075023182212));
#55147=CARTESIAN_POINT('Ctrl Pts',(-53.9954706345197,-15.4624540484263,
16.3813338147623));
#55148=CARTESIAN_POINT('Ctrl Pts',(-54.2328317277253,-15.1232302936571,
16.3551653113034));
#55149=CARTESIAN_POINT('Ctrl Pts',(-54.470192820931,-14.784006538888,16.3289968078444));
#55150=CARTESIAN_POINT('Ctrl Pts',(-54.5251909705625,-14.3171800825531,
16.3028283043855));
#55151=CARTESIAN_POINT('Ctrl Pts',(-54.3731643527629,-13.9320814565291,
16.2766598009266));
#55152=CARTESIAN_POINT('Ctrl Pts',(-54.2211377349632,-13.546982830505,16.2504912974677));
#55153=CARTESIAN_POINT('Ctrl Pts',(-53.8620863497326,-13.2436120347917,
16.2243227940088));
#55154=CARTESIAN_POINT('Ctrl Pts',(-53.4570131060935,-13.1580041404195,
16.1981542905498));
#55155=CARTESIAN_POINT('Ctrl Pts',(-53.0519398624543,-13.0723962460472,
16.1719857870909));
#55156=CARTESIAN_POINT('Ctrl Pts',(-52.6008447604068,-13.204551253016,16.145817283632));
#55157=CARTESIAN_POINT('Ctrl Pts',(-52.3060042058399,-13.4952092852263,
16.119648780173));
#55158=CARTESIAN_POINT('Ctrl Pts',(-52.0691400952495,-13.7287133104327,
16.0986259622422));
#55159=CARTESIAN_POINT('Ctrl Pts',(-51.9331215373257,-14.0645140395593,
16.0776031443114));
#55160=CARTESIAN_POINT('Ctrl Pts',(-51.9301690580705,-14.3981838623804,
16.0565803263806));
#55161=CARTESIAN_POINT('Ctrl Pts',(-51.9286427349007,-14.3970459914357,
16.1934196736194));
#55162=CARTESIAN_POINT('Ctrl Pts',(-51.9286374978387,-14.3920168903888,
16.193737536191));
#55163=CARTESIAN_POINT('Ctrl Pts',(-51.9286649228095,-14.386987848009,16.1940553987625));
#55164=CARTESIAN_POINT('Ctrl Pts',(-51.9287251846806,-14.3819591991371,
16.1943732613341));
#55165=CARTESIAN_POINT('Ctrl Pts',(-51.9336863318039,-13.9679682886745,
16.220541764793));
#55166=CARTESIAN_POINT('Ctrl Pts',(-52.1612044193698,-13.5566444358558,
16.2467102682519));
#55167=CARTESIAN_POINT('Ctrl Pts',(-52.5092576323814,-13.332430146203,16.2728787717108));
#55168=CARTESIAN_POINT('Ctrl Pts',(-52.857310845393,-13.1082158565502,16.2990472751698));
#55169=CARTESIAN_POINT('Ctrl Pts',(-53.3258991838504,-13.0711111300635,
16.3252157786287));
#55170=CARTESIAN_POINT('Ctrl Pts',(-53.7049020668993,-13.2377541659764,
16.3513842820876));
#55171=CARTESIAN_POINT('Ctrl Pts',(-54.0839049499481,-13.4043972018893,
16.3775527855466));
#55172=CARTESIAN_POINT('Ctrl Pts',(-54.3733223775883,-13.7747880002018,
16.4037212890055));
#55173=CARTESIAN_POINT('Ctrl Pts',(-54.4433761347398,-14.1828389265634,
16.4298897924644));
#55174=CARTESIAN_POINT('Ctrl Pts',(-54.5134298918912,-14.5908898529249,
16.4560582959233));
#55175=CARTESIAN_POINT('Ctrl Pts',(-54.3641199785539,-15.0366009073354,
16.4822267993823));
#55176=CARTESIAN_POINT('Ctrl Pts',(-54.0623987352411,-15.3201099501039,
16.5083953028412));
#55177=CARTESIAN_POINT('Ctrl Pts',(-53.7606774919283,-15.6036189928724,
16.5345638063001));
#55178=CARTESIAN_POINT('Ctrl Pts',(-53.30654491864,-15.724926023999,16.560732309759));
#55179=CARTESIAN_POINT('Ctrl Pts',(-52.9036394583143,-15.6296355384739,
16.586900813218));
#55180=CARTESIAN_POINT('Ctrl Pts',(-52.5007339979887,-15.5343450529489,
16.6130693166769));
#55181=CARTESIAN_POINT('Ctrl Pts',(-52.1490556506257,-15.2224570507722,
16.6392378201358));
#55182=CARTESIAN_POINT('Ctrl Pts',(-52.0063011697735,-14.8338257998905,
16.6654063235947));
#55183=CARTESIAN_POINT('Ctrl Pts',(-51.9553616723993,-14.6951493782072,
16.6747441069363));
#55184=CARTESIAN_POINT('Ctrl Pts',(-51.9310243942125,-14.5467012595068,
16.6840818902779));
#55185=CARTESIAN_POINT('Ctrl Pts',(-51.9319412138059,-14.3979628881409,
16.6934196736194));
#55186=CARTESIAN_POINT('Origin',(-53.1951359564886,-14.3971354987959,15.5));
#55187=CARTESIAN_POINT('',(-51.9310991161132,-14.3960665614756,17.1934196736194));
#55188=CARTESIAN_POINT('',(-51.9288577112775,-14.3966710926088,17.0565803263806));
#55189=CARTESIAN_POINT('',(-51.9306359564886,-14.3971354987959,15.5));
#55190=CARTESIAN_POINT('Ctrl Pts',(-51.9288577112775,-14.3966710926088,
17.0565803263806));
#55191=CARTESIAN_POINT('Ctrl Pts',(-51.9307115507732,-14.7837959519869,
17.0321233490263));
#55192=CARTESIAN_POINT('Ctrl Pts',(-52.121565621024,-15.1725044294775,17.0076663716719));
#55193=CARTESIAN_POINT('Ctrl Pts',(-52.4298869834431,-15.406303531382,16.9832093943176));
#55194=CARTESIAN_POINT('Ctrl Pts',(-52.7597850130333,-15.6564641509158,
16.9570408908587));
#55195=CARTESIAN_POINT('Ctrl Pts',(-53.2241665936332,-15.7292752927444,
16.9308723873998));
#55196=CARTESIAN_POINT('Ctrl Pts',(-53.6147975571803,-15.5920875143541,
16.9047038839408));
#55197=CARTESIAN_POINT('Ctrl Pts',(-54.0054285207274,-15.4548997359637,
16.8785353804819));
#55198=CARTESIAN_POINT('Ctrl Pts',(-54.3223088672216,-15.1077130373545,
16.852366877023));
#55199=CARTESIAN_POINT('Ctrl Pts',(-54.4233456564843,-14.706210091365,16.8261983735641));
#55200=CARTESIAN_POINT('Ctrl Pts',(-54.524382445747,-14.3047071453755,16.8000298701051));
#55201=CARTESIAN_POINT('Ctrl Pts',(-54.4095756777782,-13.8488879520058,
16.7738613666462));
#55202=CARTESIAN_POINT('Ctrl Pts',(-54.13040608496,-13.5431472408217,16.7476928631873));
#55203=CARTESIAN_POINT('Ctrl Pts',(-53.8512364921418,-13.2374065296375,
16.7215243597284));
#55204=CARTESIAN_POINT('Ctrl Pts',(-53.4077040744743,-13.0817443006388,
16.6953558562694));
#55205=CARTESIAN_POINT('Ctrl Pts',(-52.9986940338189,-13.1459613550607,
16.6691873528105));
#55206=CARTESIAN_POINT('Ctrl Pts',(-52.5896839931636,-13.2101784094827,
16.6430188493516));
#55207=CARTESIAN_POINT('Ctrl Pts',(-52.2151963295206,-13.4942747473253,
16.6168503458927));
#55208=CARTESIAN_POINT('Ctrl Pts',(-52.0431557659108,-13.8708581900196,
16.5906818424337));
#55209=CARTESIAN_POINT('Ctrl Pts',(-51.9684241449893,-14.0344399087392,
16.579314670416));
#55210=CARTESIAN_POINT('Ctrl Pts',(-51.9318921096253,-14.2154729472068,
16.5679474983983));
#55211=CARTESIAN_POINT('Ctrl Pts',(-51.9324421154971,-14.3967173588992,
16.5565803263806));
#55212=CARTESIAN_POINT('Ctrl Pts',(-51.9319412138059,-14.3979628881409,
16.6934196736194));
#55213=CARTESIAN_POINT('Ctrl Pts',(-51.9335937188396,-14.1298720781913,
16.7102503937368));
#55214=CARTESIAN_POINT('Ctrl Pts',(-52.0172907607077,-13.8608383066004,
16.7270811138542));
#55215=CARTESIAN_POINT('Ctrl Pts',(-52.1751381831274,-13.6463817981057,
16.7439118339715));
#55216=CARTESIAN_POINT('Ctrl Pts',(-52.4205602916747,-13.3129435467891,
16.7700803374304));
#55217=CARTESIAN_POINT('Ctrl Pts',(-52.8452351231106,-13.1114415437426,
16.7962488408894));
#55218=CARTESIAN_POINT('Ctrl Pts',(-53.25873344417,-13.1322316025356,16.8224173443483));
#55219=CARTESIAN_POINT('Ctrl Pts',(-53.6722317652293,-13.1530216613285,
16.8485858478072));
#55220=CARTESIAN_POINT('Ctrl Pts',(-54.0745535759121,-13.3961037819609,
16.8747543512662));
#55221=CARTESIAN_POINT('Ctrl Pts',(-54.2852929754421,-13.7524772131894,
16.9009228547251));
#55222=CARTESIAN_POINT('Ctrl Pts',(-54.496032374972,-14.108850644418,16.927091358184));
#55223=CARTESIAN_POINT('Ctrl Pts',(-54.5151893633491,-14.5785153862427,
16.9532598616429));
#55224=CARTESIAN_POINT('Ctrl Pts',(-54.3341737566947,-14.9508678603537,
16.9794283651019));
#55225=CARTESIAN_POINT('Ctrl Pts',(-54.1531581500404,-15.3232203344646,
17.0055968685608));
#55226=CARTESIAN_POINT('Ctrl Pts',(-53.7719699483547,-15.5982605408617,
17.0317653720197));
#55227=CARTESIAN_POINT('Ctrl Pts',(-53.3615383968383,-15.652657838236,17.0579338754786));
#55228=CARTESIAN_POINT('Ctrl Pts',(-52.9511068453218,-15.7070551356103,
17.0841023789376));
#55229=CARTESIAN_POINT('Ctrl Pts',(-52.5114319439747,-15.5408095239618,
17.1102708823965));
#55230=CARTESIAN_POINT('Ctrl Pts',(-52.2396692974108,-15.2284661862234,
17.1364393858554));
#55231=CARTESIAN_POINT('Ctrl Pts',(-52.0424205472225,-15.0017634594966,
17.1554328151101));
#55232=CARTESIAN_POINT('Ctrl Pts',(-51.9336286302044,-14.6980958787158,
17.1744262443647));
#55233=CARTESIAN_POINT('Ctrl Pts',(-51.9310991161132,-14.3960665614756,
17.1934196736194));
#55234=CARTESIAN_POINT('Origin',(-53.1951359564886,-14.3971354987959,15.5));
#55235=CARTESIAN_POINT('',(-51.929081218047,-14.3977505022101,17.6934196736194));
#55236=CARTESIAN_POINT('',(-51.9314271328212,-14.3981451355535,17.5565803263806));
#55237=CARTESIAN_POINT('',(-51.9306359564886,-14.3971354987959,15.5));
#55238=CARTESIAN_POINT('',(-54.1532521092111,-15.2223467977324,18.));
#55239=CARTESIAN_POINT('Ctrl Pts',(-51.929081218047,-14.3977505022101,17.6934196736194));
#55240=CARTESIAN_POINT('Ctrl Pts',(-51.9314396049108,-14.022694300038,17.7171076053695));
#55241=CARTESIAN_POINT('Ctrl Pts',(-52.1089957350005,-13.6457772873263,
17.7407955371196));
#55242=CARTESIAN_POINT('Ctrl Pts',(-52.4009425562916,-13.4106743694811,
17.7644834688697));
#55243=CARTESIAN_POINT('Ctrl Pts',(-52.7234616974047,-13.1509517569817,
17.7906519723286));
#55244=CARTESIAN_POINT('Ctrl Pts',(-53.1855836521258,-13.0642995791891,
17.8168204757875));
#55245=CARTESIAN_POINT('Ctrl Pts',(-53.5800062339574,-13.190324595469,17.8429889792464));
#55246=CARTESIAN_POINT('Ctrl Pts',(-53.974428815789,-13.3163496117488,17.8691574827054));
#55247=CARTESIAN_POINT('Ctrl Pts',(-54.3011520247311,-13.6550518221011,
17.8953259861643));
#55248=CARTESIAN_POINT('Ctrl Pts',(-54.4136991111698,-14.0527836440546,
17.9214944896232));
#55249=CARTESIAN_POINT('Ctrl Pts',(-54.5262461976084,-14.4505154660081,
17.9476629930822));
#55250=CARTESIAN_POINT('Ctrl Pts',(-54.4246171615437,-14.9072768995629,
17.9738314965411));
#55251=CARTESIAN_POINT('Ctrl Pts',(-54.153252109211,-15.2223467977324,18.));
#55252=CARTESIAN_POINT('',(-52.2352328551172,-15.2234705191484,18.));
#55253=CARTESIAN_POINT('Origin',(-53.1951359564886,-14.3971354987959,18.));
#55254=CARTESIAN_POINT('Ctrl Pts',(-52.2352228301846,-15.2234768233202,
18.));
#55255=CARTESIAN_POINT('Ctrl Pts',(-52.4934806168631,-15.521313638849,17.975091839613));
#55256=CARTESIAN_POINT('Ctrl Pts',(-52.9025313044196,-15.6908537017463,
17.950183679226));
#55257=CARTESIAN_POINT('Ctrl Pts',(-53.295440078112,-15.6595882927142,17.925275518839));
#55258=CARTESIAN_POINT('Ctrl Pts',(-53.7082298804764,-15.6267408663411,
17.89910701538));
#55259=CARTESIAN_POINT('Ctrl Pts',(-54.1032028915872,-15.3722524867282,
17.8729385119211));
#55260=CARTESIAN_POINT('Ctrl Pts',(-54.3034894678617,-15.0099588806278,
17.8467700084622));
#55261=CARTESIAN_POINT('Ctrl Pts',(-54.5037760441361,-14.6476652745275,
17.8206015050033));
#55262=CARTESIAN_POINT('Ctrl Pts',(-54.5093761855741,-14.1775664419396,
17.7944330015443));
#55263=CARTESIAN_POINT('Ctrl Pts',(-54.3176594419829,-13.8105984641279,
17.7682644980854));
#55264=CARTESIAN_POINT('Ctrl Pts',(-54.1259426983918,-13.4436304863162,
17.7420959946265));
#55265=CARTESIAN_POINT('Ctrl Pts',(-53.7369090697714,-13.1797933632805,
17.7159274911676));
#55266=CARTESIAN_POINT('Ctrl Pts',(-53.3250649526277,-13.1373263636934,
17.6897589877086));
#55267=CARTESIAN_POINT('Ctrl Pts',(-52.9132208354839,-13.0948593641063,
17.6635904842497));
#55268=CARTESIAN_POINT('Ctrl Pts',(-52.4785662298169,-13.2737624879677,
17.6374219807908));
#55269=CARTESIAN_POINT('Ctrl Pts',(-52.2159761485057,-13.5938473532063,
17.6112534773319));
#55270=CARTESIAN_POINT('Ctrl Pts',(-52.0331020154043,-13.8167622552357,
17.5930290936814));
#55271=CARTESIAN_POINT('Ctrl Pts',(-51.9336803654543,-14.1081512772947,
17.574804710031));
#55272=CARTESIAN_POINT('Ctrl Pts',(-51.9314271328212,-14.3981451355535,
17.5565803263806));
#55273=CARTESIAN_POINT('Origin',(-53.1951359564886,-14.3971354987959,19.1042117235887));
#55274=CARTESIAN_POINT('',(-51.6501838308085,-14.3978968813702,14.3957882764113));
#55275=CARTESIAN_POINT('',(-51.654536051996,-14.3970771807141,14.3542117235887));
#55276=CARTESIAN_POINT('',(-51.6521359564886,-14.3971354987959,19.1042117235887));
#55277=CARTESIAN_POINT('',(-53.5936497983459,-12.9064860705774,14.));
#55278=CARTESIAN_POINT('Ctrl Pts',(-51.654536051996,-14.3970771807141,14.3542117235887));
#55279=CARTESIAN_POINT('Ctrl Pts',(-51.6547008227736,-14.657815056409,14.3408151628949));
#55280=CARTESIAN_POINT('Ctrl Pts',(-51.8403375140876,-15.4280419867602,
14.3012500987421));
#55281=CARTESIAN_POINT('Ctrl Pts',(-53.0509994556171,-16.2080945317645,
14.2355165311303));
#55282=CARTESIAN_POINT('Ctrl Pts',(-54.6273366519326,-15.5169696210013,
14.1570110207536));
#55283=CARTESIAN_POINT('Ctrl Pts',(-54.9168336227569,-13.8187144824051,
14.0785055103768));
#55284=CARTESIAN_POINT('Ctrl Pts',(-54.083839596546,-13.0375346028626,14.0261685034589));
#55285=CARTESIAN_POINT('Ctrl Pts',(-53.5936497983459,-12.9064860705774,
14.));
#55286=CARTESIAN_POINT('',(-52.7955932879502,-12.9041246312965,14.));
#55287=CARTESIAN_POINT('Origin',(-53.1951359564886,-14.3971354987959,14.));
#55288=CARTESIAN_POINT('Ctrl Pts',(-51.6501838308085,-14.3978968813702,
14.3957882764113));
#55289=CARTESIAN_POINT('Ctrl Pts',(-51.6499084261818,-14.443250645686,14.3934410251636));
#55290=CARTESIAN_POINT('Ctrl Pts',(-51.6721169602754,-14.9939590280816,
14.3649252704569));
#55291=CARTESIAN_POINT('Ctrl Pts',(-52.3307362917628,-15.9953382094595,
14.3102410122914));
#55292=CARTESIAN_POINT('Ctrl Pts',(-54.0514987748276,-15.9998443309588,
14.2317355019146));
#55293=CARTESIAN_POINT('Ctrl Pts',(-55.0042044918326,-14.5665632650764,
14.1532299915378));
#55294=CARTESIAN_POINT('Ctrl Pts',(-54.3453458049292,-13.0076586982508,
14.0759848242329));
#55295=CARTESIAN_POINT('Ctrl Pts',(-53.2607152655111,-12.7814238100544,
14.024908160387));
#55296=CARTESIAN_POINT('Ctrl Pts',(-52.7955875161457,-12.9041113834231,
14.));
#55297=CARTESIAN_POINT('Origin',(-53.1951359564886,-14.3971354987959,19.1042117235887));
#55298=CARTESIAN_POINT('',(-51.654442242504,-14.3974618454408,14.8957882764113));
#55299=CARTESIAN_POINT('',(-51.6505063374695,-14.3961865684695,14.8542117235887));
#55300=CARTESIAN_POINT('',(-51.6521359564886,-14.3971354987959,19.1042117235887));
#55301=CARTESIAN_POINT('Ctrl Pts',(-51.6505063374695,-14.3961865684695,
14.8542117235887));
#55302=CARTESIAN_POINT('Ctrl Pts',(-51.6537531731077,-14.8418532139508,
14.8311595169817));
#55303=CARTESIAN_POINT('Ctrl Pts',(-52.0889693478694,-15.7989724624769,
14.7819388069158));
#55304=CARTESIAN_POINT('Ctrl Pts',(-53.7056220123855,-16.1409817745025,
14.706549593391));
#55305=CARTESIAN_POINT('Ctrl Pts',(-54.9313021937626,-14.9332257573755,
14.6280440830142));
#55306=CARTESIAN_POINT('Ctrl Pts',(-54.599912063137,-13.2446506074896,14.5495385726375));
#55307=CARTESIAN_POINT('Ctrl Pts',(-53.0087562916135,-12.5897333550461,
14.4710330622607));
#55308=CARTESIAN_POINT('Ctrl Pts',(-51.8276307116252,-13.3907563492144,
14.4059241125778));
#55309=CARTESIAN_POINT('Ctrl Pts',(-51.6543789636963,-14.148496272438,14.3669836663538));
#55310=CARTESIAN_POINT('Ctrl Pts',(-51.654536051996,-14.3970771807141,14.3542117235887));
#55311=CARTESIAN_POINT('Ctrl Pts',(-51.654442242504,-14.3974618454408,14.8957882764113));
#55312=CARTESIAN_POINT('Ctrl Pts',(-51.6539909131311,-14.6310322097678,
14.8837853792504));
#55313=CARTESIAN_POINT('Ctrl Pts',(-51.8127636494606,-15.3732462698704,
14.8456139786307));
#55314=CARTESIAN_POINT('Ctrl Pts',(-52.9564001587445,-16.1984187666639,
14.7812740745521));
#55315=CARTESIAN_POINT('Ctrl Pts',(-54.5659334636339,-15.5898376428623,
14.7027685641752));
#55316=CARTESIAN_POINT('Ctrl Pts',(-54.9461022318155,-13.911606374279,14.6242630537985));
#55317=CARTESIAN_POINT('Ctrl Pts',(-53.7559643179139,-12.6688223002735,
14.5457575434217));
#55318=CARTESIAN_POINT('Ctrl Pts',(-52.1134816424643,-12.9668195987494,
14.4695992842926));
#55319=CARTESIAN_POINT('Ctrl Pts',(-51.6529787949523,-13.937620862964,14.4196095286225));
#55320=CARTESIAN_POINT('Ctrl Pts',(-51.6501838308085,-14.3978968813702,
14.3957882764113));
#55321=CARTESIAN_POINT('Origin',(-53.1951359564886,-14.3971354987959,19.1042117235887));
#55322=CARTESIAN_POINT('',(-51.6512135991451,-14.3959278910795,15.3957882764113));
#55323=CARTESIAN_POINT('',(-51.6523527586964,-14.398464524594,15.3542117235887));
#55324=CARTESIAN_POINT('',(-51.6521359564886,-14.3971354987959,19.1042117235887));
#55325=CARTESIAN_POINT('Ctrl Pts',(-51.6523527586964,-14.398464524594,15.3542117235887));
#55326=CARTESIAN_POINT('Ctrl Pts',(-51.651247573785,-14.5252813221218,15.3476723745276));
#55327=CARTESIAN_POINT('Ctrl Pts',(-51.7230815929517,-15.1583461258636,
15.3149645220075));
#55328=CARTESIAN_POINT('Ctrl Pts',(-52.5930520129352,-16.1115202855033,
15.2560881660285));
#55329=CARTESIAN_POINT('Ctrl Pts',(-54.2930303473181,-15.8449779235543,
15.1775826556517));
#55330=CARTESIAN_POINT('Ctrl Pts',(-55.0083911483927,-14.2799763521069,
15.0990771452749));
#55331=CARTESIAN_POINT('Ctrl Pts',(-54.0975810662168,-12.8200452881305,
15.0205716348981));
#55332=CARTESIAN_POINT('Ctrl Pts',(-52.3774378038974,-12.7744874306393,
14.9420661245214));
#55333=CARTESIAN_POINT('Ctrl Pts',(-51.6803897960553,-13.7702239867045,
14.8866128207516));
#55334=CARTESIAN_POINT('Ctrl Pts',(-51.6500674162048,-14.3359394264926,
14.8573280204407));
#55335=CARTESIAN_POINT('Ctrl Pts',(-51.6505063374695,-14.3961865684695,
14.8542117235887));
#55336=CARTESIAN_POINT('Ctrl Pts',(-51.6512135991451,-14.3959278910795,
15.3957882764113));
#55337=CARTESIAN_POINT('Ctrl Pts',(-51.6548183273038,-14.8151512136696,
15.3741297333373));
#55338=CARTESIAN_POINT('Ctrl Pts',(-52.0463881522716,-15.7468276199561,
15.3263026868045));
#55339=CARTESIAN_POINT('Ctrl Pts',(-53.6133427309768,-16.1653895531783,
15.2523071368127));
#55340=CARTESIAN_POINT('Ctrl Pts',(-54.9007439708605,-15.0236502232965,
15.1738016264359));
#55341=CARTESIAN_POINT('Ctrl Pts',(-54.6585153839456,-13.3200374976642,
15.0952961160592));
#55342=CARTESIAN_POINT('Ctrl Pts',(-53.1038933588347,-12.5823920603089,
15.0167906056824));
#55343=CARTESIAN_POINT('Ctrl Pts',(-51.856278782321,-13.3361985618968,14.9502879924664));
#55344=CARTESIAN_POINT('Ctrl Pts',(-51.6549748934233,-14.1218062449943,
14.9099538827094));
#55345=CARTESIAN_POINT('Ctrl Pts',(-51.654442242504,-14.3974618454408,14.8957882764113));
#55346=CARTESIAN_POINT('Origin',(-53.1951359564886,-14.3971354987959,19.1042117235887));
#55347=CARTESIAN_POINT('',(-51.6515662259554,-14.3984147593818,15.8957882764113));
#55348=CARTESIAN_POINT('',(-51.6539634663413,-14.3962637929782,15.8542117235887));
#55349=CARTESIAN_POINT('',(-51.6521359564886,-14.3971354987959,19.1042117235887));
#55350=CARTESIAN_POINT('Ctrl Pts',(-51.6539634663413,-14.3962637929782,
15.8542117235887));
#55351=CARTESIAN_POINT('Ctrl Pts',(-51.6556220588241,-14.7111646038003,
15.8380167286145));
#55352=CARTESIAN_POINT('Ctrl Pts',(-51.9015651465377,-15.5372739892809,
15.7956532301813));
#55353=CARTESIAN_POINT('Ctrl Pts',(-53.2428638938474,-16.2135446545079,
15.7271212282891));
#55354=CARTESIAN_POINT('Ctrl Pts',(-54.7365592022647,-15.3592345303502,
15.6486157179124));
#55355=CARTESIAN_POINT('Ctrl Pts',(-54.8478695024322,-13.6420911264981,
15.5701102075356));
#55356=CARTESIAN_POINT('Ctrl Pts',(-53.4769690594307,-12.6020894569994,
15.4916046971588));
#55357=CARTESIAN_POINT('Ctrl Pts',(-51.9885611628803,-13.1244613999964,
15.4196385358432));
#55358=CARTESIAN_POINT('Ctrl Pts',(-51.6556701906089,-14.0177987311608,
15.3738408779865));
#55359=CARTESIAN_POINT('Ctrl Pts',(-51.6523527586964,-14.398464524594,15.3542117235887));
#55360=CARTESIAN_POINT('Ctrl Pts',(-51.6515662259554,-14.3984147593818,
15.8957882764113));
#55361=CARTESIAN_POINT('Ctrl Pts',(-51.6506843931331,-14.4980737158535,
15.8906425908832));
#55362=CARTESIAN_POINT('Ctrl Pts',(-51.7045173377561,-15.1036026015034,
15.8593284018961));
#55363=CARTESIAN_POINT('Ctrl Pts',(-52.503850750664,-16.077535486755,15.8018457094502));
#55364=CARTESIAN_POINT('Ctrl Pts',(-54.2154808300007,-15.9006366439348,
15.7233401990734));
#55365=CARTESIAN_POINT('Ctrl Pts',(-55.0120413695279,-14.3753622311824,
15.6448346886966));
#55366=CARTESIAN_POINT('Ctrl Pts',(-54.1791579400319,-12.8696146010229,
15.5663291783198));
#55367=CARTESIAN_POINT('Ctrl Pts',(-52.4637802022359,-12.7337840295961,
15.4878236679431));
#55368=CARTESIAN_POINT('Ctrl Pts',(-51.6965951513913,-13.7156125454117,
15.4309767006402));
#55369=CARTESIAN_POINT('Ctrl Pts',(-51.6504629862743,-14.3086329806648,
15.4002982367963));
#55370=CARTESIAN_POINT('Ctrl Pts',(-51.6512135991451,-14.3959278910795,
15.3957882764113));
#55371=CARTESIAN_POINT('Origin',(-53.1951359564886,-14.3971354987959,19.1042117235887));
#55372=CARTESIAN_POINT('',(-51.65433991327,-14.3966252656123,16.3957882764113));
#55373=CARTESIAN_POINT('',(-51.6497037375007,-14.3970262778732,16.3542117235887));
#55374=CARTESIAN_POINT('',(-51.6521359564886,-14.3971354987959,19.1042117235887));
#55375=CARTESIAN_POINT('Ctrl Pts',(-51.6497037375007,-14.3970262778732,
16.3542117235887));
#55376=CARTESIAN_POINT('Ctrl Pts',(-51.6502234542653,-14.8961053696861,
16.3283610827014));
#55377=CARTESIAN_POINT('Ctrl Pts',(-52.1817212113122,-15.9013530800272,
16.2763419383551));
#55378=CARTESIAN_POINT('Ctrl Pts',(-53.8864212481312,-16.0775356953633,
16.1981542905498));
#55379=CARTESIAN_POINT('Ctrl Pts',(-54.978090456054,-14.7474117142528,16.119648780173));
#55380=CARTESIAN_POINT('Ctrl Pts',(-54.4707636814861,-13.1031516960174,
16.0411432697963));
#55381=CARTESIAN_POINT('Ctrl Pts',(-52.8194236367236,-12.6193671146013,
15.9626377594195));
#55382=CARTESIAN_POINT('Ctrl Pts',(-51.7761788820818,-13.5008286667841,
15.900327244017));
#55383=CARTESIAN_POINT('Ctrl Pts',(-51.6529420405103,-14.2023356124785,
15.8641852320734));
#55384=CARTESIAN_POINT('Ctrl Pts',(-51.6539634663413,-14.3962637929782,
15.8542117235887));
#55385=CARTESIAN_POINT('Ctrl Pts',(-51.65433991327,-14.3966252656123,16.3957882764113));
#55386=CARTESIAN_POINT('Ctrl Pts',(-51.6552138153438,-14.684603767973,16.3809869449701));
#55387=CARTESIAN_POINT('Ctrl Pts',(-51.869991852728,-15.4829338669789,16.3400171100699));
#55388=CARTESIAN_POINT('Ctrl Pts',(-53.1474080250528,-16.2135444290179,
16.2728787717108));
#55389=CARTESIAN_POINT('Ctrl Pts',(-54.6839066935018,-15.4388557336608,
16.1943732613341));
#55390=CARTESIAN_POINT('Ctrl Pts',(-54.8852403705632,-13.7299275672916,
16.1158677509573));
#55391=CARTESIAN_POINT('Ctrl Pts',(-53.570848229612,-12.6193673352972,16.0373622405805));
#55392=CARTESIAN_POINT('Ctrl Pts',(-52.0277463399596,-13.0714419423033,
15.9640024157318));
#55393=CARTESIAN_POINT('Ctrl Pts',(-51.6551689744654,-13.9912557743182,
15.9168110943421));
#55394=CARTESIAN_POINT('Ctrl Pts',(-51.6515662259554,-14.3984147593818,
15.8957882764113));
#55395=CARTESIAN_POINT('Origin',(-53.1951359564886,-14.3971354987959,19.1042117235887));
#55396=CARTESIAN_POINT('',(-51.6499660613832,-14.3965688093956,16.8957882764113));
#55397=CARTESIAN_POINT('',(-51.6537286904076,-14.3981451166365,16.8542117235887));
#55398=CARTESIAN_POINT('',(-51.6521359564886,-14.3971354987959,19.1042117235887));
#55399=CARTESIAN_POINT('Ctrl Pts',(-51.6537286904076,-14.3981451166365,
16.8542117235887));
#55400=CARTESIAN_POINT('Ctrl Pts',(-51.6526099457396,-14.5796423938349,
16.8448739402472));
#55401=CARTESIAN_POINT('Ctrl Pts',(-51.7655324660036,-15.2684267173499,
16.8093676534467));
#55402=CARTESIAN_POINT('Ctrl Pts',(-52.7769291300874,-16.1653897727513,
16.7476928631873));
#55403=CARTESIAN_POINT('Ctrl Pts',(-54.4393883485545,-15.72131682132,16.6691873528105));
#55404=CARTESIAN_POINT('Ctrl Pts',(-54.9859724441167,-14.0896865557083,
16.5906818424337));
#55405=CARTESIAN_POINT('Ctrl Pts',(-53.9264918015333,-12.7337838230954,
16.5121763320569));
#55406=CARTESIAN_POINT('Ctrl Pts',(-52.2111138507866,-12.8696144113969,
16.4336708216802));
#55407=CARTESIAN_POINT('Ctrl Pts',(-51.6524858829682,-13.8795429426784,
16.3810159521908));
#55408=CARTESIAN_POINT('Ctrl Pts',(-51.6496973470012,-14.3908895416808,
16.3545295861603));
#55409=CARTESIAN_POINT('Ctrl Pts',(-51.6497037375007,-14.3970262778732,
16.3542117235887));
#55410=CARTESIAN_POINT('Ctrl Pts',(-51.6499660613832,-14.3965688093956,
16.8957882764113));
#55411=CARTESIAN_POINT('Ctrl Pts',(-51.6522282000482,-14.8689560438918,
16.8713312990569));
#55412=CARTESIAN_POINT('Ctrl Pts',(-52.1343035201106,-15.8507887260607,
16.8207058182437));
#55413=CARTESIAN_POINT('Ctrl Pts',(-53.7972198251955,-16.11152007286,16.7439118339715));
#55414=CARTESIAN_POINT('Ctrl Pts',(-54.9572349488979,-14.8405614110472,
16.6654063235947));
#55415=CARTESIAN_POINT('Ctrl Pts',(-54.5369577413632,-13.1719279226262,
16.586900813218));
#55416=CARTESIAN_POINT('Ctrl Pts',(-52.9133028885493,-12.602089679815,16.5083953028412));
#55417=CARTESIAN_POINT('Ctrl Pts',(-51.8008704508192,-13.4460106212472,
16.4446911239056));
#55418=CARTESIAN_POINT('Ctrl Pts',(-51.6536687712691,-14.1754626501585,
16.407155448429));
#55419=CARTESIAN_POINT('Ctrl Pts',(-51.65433991327,-14.3966252656123,16.3957882764113));
#55420=CARTESIAN_POINT('Origin',(-53.1951359564886,-14.3971354987959,19.1042117235887));
#55421=CARTESIAN_POINT('',(-51.6531013855762,-14.3983675031589,17.3957882764113));
#55422=CARTESIAN_POINT('',(-51.652701124777,-14.3958311332085,17.3542117235887));
#55423=CARTESIAN_POINT('',(-51.6521359564886,-14.3971354987959,19.1042117235887));
#55424=CARTESIAN_POINT('Ctrl Pts',(-51.652701124777,-14.3958311332085,17.3542117235887));
#55425=CARTESIAN_POINT('Ctrl Pts',(-51.6557877520943,-14.7643809445978,
17.3352182943341));
#55426=CARTESIAN_POINT('Ctrl Pts',(-51.9714428864125,-15.6454595543576,
17.2900563616205));
#55427=CARTESIAN_POINT('Ctrl Pts',(-53.4338717842849,-16.1984189929661,
17.218725925448));
#55428=CARTESIAN_POINT('Ctrl Pts',(-54.829300954394,-15.1915695541269,17.1402204150712));
#55429=CARTESIAN_POINT('Ctrl Pts',(-54.7591722875713,-13.4722511753948,
17.0617149046944));
#55430=CARTESIAN_POINT('Ctrl Pts',(-53.2863785654275,-12.582391834622,16.9832093943176));
#55431=CARTESIAN_POINT('Ctrl Pts',(-51.9166698060745,-13.232298629585,16.9140416672824));
#55432=CARTESIAN_POINT('Ctrl Pts',(-51.6557451516705,-14.0710086043769,
16.8710424437061));
#55433=CARTESIAN_POINT('Ctrl Pts',(-51.6537286904076,-14.3981451166365,
16.8542117235887));
#55434=CARTESIAN_POINT('Ctrl Pts',(-51.6531013855762,-14.3983675031589,
17.3957882764113));
#55435=CARTESIAN_POINT('Ctrl Pts',(-51.6519028634371,-14.5526188015874,
17.3878441566028));
#55436=CARTESIAN_POINT('Ctrl Pts',(-51.7435010772427,-15.2135959185484,
17.3537315333353));
#55437=CARTESIAN_POINT('Ctrl Pts',(-52.6846499703254,-16.1409815416267,
17.293450406609));
#55438=CARTESIAN_POINT('Ctrl Pts',(-54.3681285487899,-15.7848349642756,
17.2149448962322));
#55439=CARTESIAN_POINT('Ctrl Pts',(-54.9996481235109,-14.1841565112764,
17.1364393858554));
#55440=CARTESIAN_POINT('Ctrl Pts',(-54.0128340063977,-12.7744876345319,
17.0579338754786));
#55441=CARTESIAN_POINT('Ctrl Pts',(-52.292690959438,-12.8200454826231,16.9794283651019));
#55442=CARTESIAN_POINT('Ctrl Pts',(-51.6656274258073,-13.8251612032116,
16.9253798320794));
#55443=CARTESIAN_POINT('Ctrl Pts',(-51.6498077544378,-14.3635106325159,
16.8974998025159));
#55444=CARTESIAN_POINT('Ctrl Pts',(-51.6499660613832,-14.3965688093956,
16.8957882764113));
#55445=CARTESIAN_POINT('Origin',(-53.1951359564886,-14.3971354987959,19.1042117235887));
#55446=CARTESIAN_POINT('',(-51.6537934596095,-14.3955992295121,17.8957882764113));
#55447=CARTESIAN_POINT('',(-51.650238794436,-14.3978859537331,17.8542117235887));
#55448=CARTESIAN_POINT('',(-51.6521359564886,-14.3971354987959,19.1042117235887));
#55449=CARTESIAN_POINT('',(-52.7966221146314,-12.9064860705774,18.));
#55450=CARTESIAN_POINT('Ctrl Pts',(-52.7966221146314,-12.9064860705774,
18.));
#55451=CARTESIAN_POINT('Ctrl Pts',(-52.3064323164313,-13.0375346028627,
17.9738314965411));
#55452=CARTESIAN_POINT('Ctrl Pts',(-51.7535553056072,-13.5560194656624,
17.9390942553448));
#55453=CARTESIAN_POINT('Ctrl Pts',(-51.6526562271057,-14.2291272515896,
17.9043570141486));
#55454=CARTESIAN_POINT('Ctrl Pts',(-51.6537934596095,-14.3955992295121,
17.8957882764113));
#55455=CARTESIAN_POINT('',(-53.5946788045247,-12.9041246263415,18.));
#55456=CARTESIAN_POINT('Origin',(-53.1951359564886,-14.3971354987959,18.));
#55457=CARTESIAN_POINT('Ctrl Pts',(-53.5946845822246,-12.9041113672218,
18.));
#55458=CARTESIAN_POINT('Ctrl Pts',(-53.1295569761736,-12.7814239312717,
17.975091839613));
#55459=CARTESIAN_POINT('Ctrl Pts',(-52.0976014587089,-12.9966708391238,
17.9264957474759));
#55460=CARTESIAN_POINT('Ctrl Pts',(-51.6531166045831,-13.9402254397343,
17.8778996553388));
#55461=CARTESIAN_POINT('Ctrl Pts',(-51.650238794436,-14.3978859537331,17.8542117235887));
#55462=CARTESIAN_POINT('Origin',(-14.1292828945604,-53.2669068454841,15.5));
#55463=CARTESIAN_POINT('',(-13.4980577522812,-52.1734972976427,14.1934196736194));
#55464=CARTESIAN_POINT('',(-13.4988747128346,-52.1716629874611,14.0565803263806));
#55465=CARTESIAN_POINT('',(-13.4970328945604,-52.1718177223987,15.5));
#55466=CARTESIAN_POINT('',(-12.9355708698302,-52.8497595669186,14.));
#55467=CARTESIAN_POINT('Ctrl Pts',(-13.4988747128346,-52.1716629874611,
14.0565803263806));
#55468=CARTESIAN_POINT('Ctrl Pts',(-13.2411227471438,-52.3234873105789,
14.0377202175871));
#55469=CARTESIAN_POINT('Ctrl Pts',(-13.0344360750677,-52.5668460963448,
14.0188601087935));
#55470=CARTESIAN_POINT('Ctrl Pts',(-12.9355708698302,-52.8497595669186,
14.));
#55471=CARTESIAN_POINT('',(-13.4970328945604,-52.1718177223987,14.));
#55472=CARTESIAN_POINT('Origin',(-14.1292828945604,-53.2669068454841,14.));
#55473=CARTESIAN_POINT('',(-13.4970328945604,-52.1718177223987,13.));
#55474=CARTESIAN_POINT('',(-13.4970328945604,-52.1718177223987,15.5));
#55475=CARTESIAN_POINT('',(-12.8669333849943,-53.3406222827979,13.));
#55476=CARTESIAN_POINT('Origin',(-14.1292828945604,-53.2669068454841,13.));
#55477=CARTESIAN_POINT('',(-15.3916324041264,-53.1931914081703,13.));
#55478=CARTESIAN_POINT('Origin',(-14.1292828945604,-53.2669068454841,13.));
#55479=CARTESIAN_POINT('Origin',(-14.1292828945604,-53.2669068454841,13.));
#55480=CARTESIAN_POINT('',(-13.8936073831511,-54.5113748561459,14.));
#55481=CARTESIAN_POINT('Origin',(-14.1292828945604,-53.2669068454841,14.));
#55482=CARTESIAN_POINT('Ctrl Pts',(-13.8936069362009,-54.5113866946539,
14.));
#55483=CARTESIAN_POINT('Ctrl Pts',(-13.5065438623107,-54.43664727626,14.024908160387));
#55484=CARTESIAN_POINT('Ctrl Pts',(-13.1551923299505,-54.1671690811723,
14.049816320774));
#55485=CARTESIAN_POINT('Ctrl Pts',(-12.9858145310894,-53.8112673891924,
14.074724481161));
#55486=CARTESIAN_POINT('Ctrl Pts',(-12.8078662825437,-53.43735721225,14.10089298462));
#55487=CARTESIAN_POINT('Ctrl Pts',(-12.8307732764863,-52.9680562770306,
14.1270614880789));
#55488=CARTESIAN_POINT('Ctrl Pts',(-13.0443854893126,-52.6134561814805,
14.1532299915378));
#55489=CARTESIAN_POINT('Ctrl Pts',(-13.1537409585152,-52.4319241458581,
14.1666265522317));
#55490=CARTESIAN_POINT('Ctrl Pts',(-13.3130758736166,-52.2804525587351,
14.1800231129255));
#55491=CARTESIAN_POINT('Ctrl Pts',(-13.4980577522812,-52.1734972976427,
14.1934196736194));
#55492=CARTESIAN_POINT('Origin',(-14.1292828945604,-53.2669068454841,15.5));
#55493=CARTESIAN_POINT('',(-13.4970386657413,-52.17027240687,14.6934196736194));
#55494=CARTESIAN_POINT('',(-13.4956926805926,-52.1707443397673,14.5565803263806));
#55495=CARTESIAN_POINT('',(-13.4970328945604,-52.1718177223987,15.5));
#55496=CARTESIAN_POINT('Ctrl Pts',(-13.4956926805926,-52.1707443397673,
14.5565803263806));
#55497=CARTESIAN_POINT('Ctrl Pts',(-13.4633916214762,-52.1891327536446,
14.5542330751329));
#55498=CARTESIAN_POINT('Ctrl Pts',(-13.4319685470764,-52.2090047577526,
14.5518858238852));
#55499=CARTESIAN_POINT('Ctrl Pts',(-13.4015745144389,-52.230342308046,14.5495385726375));
#55500=CARTESIAN_POINT('Ctrl Pts',(-13.0627244024285,-52.4682255594459,
14.5233700691785));
#55501=CARTESIAN_POINT('Ctrl Pts',(-12.8517746061391,-52.8882625646258,
14.4972015657196));
#55502=CARTESIAN_POINT('Ctrl Pts',(-12.8632814695834,-53.3021304033103,
14.4710330622607));
#55503=CARTESIAN_POINT('Ctrl Pts',(-12.8747883330278,-53.7159982419948,
14.4448645588017));
#55504=CARTESIAN_POINT('Ctrl Pts',(-13.1087518562058,-54.1236969141839,
14.4186960553428));
#55505=CARTESIAN_POINT('Ctrl Pts',(-13.460332770227,-54.3423556782117,14.3925275518839));
#55506=CARTESIAN_POINT('Ctrl Pts',(-13.8119136842483,-54.5610144422395,
14.366359048425));
#55507=CARTESIAN_POINT('Ctrl Pts',(-14.2811119891127,-54.5906332981061,
14.3401905449661));
#55508=CARTESIAN_POINT('Ctrl Pts',(-14.6573867068862,-54.4180393977442,
14.3140220415071));
#55509=CARTESIAN_POINT('Ctrl Pts',(-15.0336614246597,-54.2454454973823,
14.2878535380482));
#55510=CARTESIAN_POINT('Ctrl Pts',(-15.3170125553423,-53.8706388407919,
14.2616850345893));
#55511=CARTESIAN_POINT('Ctrl Pts',(-15.3806795111647,-53.4614679031089,
14.2355165311303));
#55512=CARTESIAN_POINT('Ctrl Pts',(-15.4443464669872,-53.052296965426,14.2093480276714));
#55513=CARTESIAN_POINT('Ctrl Pts',(-15.2883292479495,-52.6087617466505,
14.1831795242125));
#55514=CARTESIAN_POINT('Ctrl Pts',(-14.981976715725,-52.3301941698058,14.1570110207536));
#55515=CARTESIAN_POINT('Ctrl Pts',(-14.6756241835005,-52.0516265929611,
14.1308425172946));
#55516=CARTESIAN_POINT('Ctrl Pts',(-14.2189363380893,-51.938026658047,14.1046740138357));
#55517=CARTESIAN_POINT('Ctrl Pts',(-13.8182170120758,-52.0394239070104,
14.0785055103768));
#55518=CARTESIAN_POINT('Ctrl Pts',(-13.7063032761926,-52.067742343889,14.0711971157114));
#55519=CARTESIAN_POINT('Ctrl Pts',(-13.5987550004656,-52.1128302370619,
14.063888721046));
#55520=CARTESIAN_POINT('Ctrl Pts',(-13.4988747128346,-52.1716629874611,
14.0565803263806));
#55521=CARTESIAN_POINT('Ctrl Pts',(-13.4980577522812,-52.1734972976427,
14.1934196736194));
#55522=CARTESIAN_POINT('Ctrl Pts',(-13.6744148054729,-52.0715288518372,
14.2061916163845));
#55523=CARTESIAN_POINT('Ctrl Pts',(-13.8740829845724,-52.0100223374604,
14.2189635591495));
#55524=CARTESIAN_POINT('Ctrl Pts',(-14.0759771073047,-52.00150441778,14.2317355019146));
#55525=CARTESIAN_POINT('Ctrl Pts',(-14.4896390807605,-51.9840520055104,
14.2579040053735));
#55526=CARTESIAN_POINT('Ctrl Pts',(-14.9126455959621,-52.189046436852,14.2840725088324));
#55527=CARTESIAN_POINT('Ctrl Pts',(-15.1553451745865,-52.5244804183786,
14.3102410122914));
#55528=CARTESIAN_POINT('Ctrl Pts',(-15.3980447532108,-52.8599143999053,
14.3364095157503));
#55529=CARTESIAN_POINT('Ctrl Pts',(-15.460437395258,-53.325787931617,14.3625780192092));
#55530=CARTESIAN_POINT('Ctrl Pts',(-15.3145307999442,-53.7132400695012,
14.3887465226681));
#55531=CARTESIAN_POINT('Ctrl Pts',(-15.1686242046305,-54.1006922073853,
14.4149150261271));
#55532=CARTESIAN_POINT('Ctrl Pts',(-14.8144183719558,-54.4097229514419,
14.441083529586));
#55533=CARTESIAN_POINT('Ctrl Pts',(-14.4107506896372,-54.5017382932332,
14.4672520330449));
#55534=CARTESIAN_POINT('Ctrl Pts',(-14.0070830073185,-54.5937536350245,
14.4934205365038));
#55535=CARTESIAN_POINT('Ctrl Pts',(-13.5539534753558,-54.4687535745504,
14.5195890399628));
#55536=CARTESIAN_POINT('Ctrl Pts',(-13.2545471544402,-54.1828000037796,
14.5457575434217));
#55537=CARTESIAN_POINT('Ctrl Pts',(-12.9551408335246,-53.8968464330088,
14.5719260468806));
#55538=CARTESIAN_POINT('Ctrl Pts',(-12.8094577236562,-53.4499393519412,
14.5980945503396));
#55539=CARTESIAN_POINT('Ctrl Pts',(-12.8828256503828,-53.0424720659447,
14.6242630537985));
#55540=CARTESIAN_POINT('Ctrl Pts',(-12.9474564997503,-52.6835283427349,
14.6473152604055));
#55541=CARTESIAN_POINT('Ctrl Pts',(-13.1820731109759,-52.3551902889475,
14.6703674670124));
#55542=CARTESIAN_POINT('Ctrl Pts',(-13.4970386657413,-52.17027240687,14.6934196736194));
#55543=CARTESIAN_POINT('Origin',(-14.1292828945604,-53.2669068454841,15.5));
#55544=CARTESIAN_POINT('',(-13.496178545612,-52.1725162395268,15.1934196736194));
#55545=CARTESIAN_POINT('',(-13.4977463410386,-52.1735883352515,15.0565803263806));
#55546=CARTESIAN_POINT('',(-13.4970328945604,-52.1718177223987,15.5));
#55547=CARTESIAN_POINT('Ctrl Pts',(-13.4977463410386,-52.1735883352515,
15.0565803263806));
#55548=CARTESIAN_POINT('Ctrl Pts',(-13.3317931989842,-52.2689743399828,
15.0445774292198));
#55549=CARTESIAN_POINT('Ctrl Pts',(-13.186612163033,-52.4000385957214,15.0325745320589));
#55550=CARTESIAN_POINT('Ctrl Pts',(-13.080217915627,-52.5573375001258,15.0205716348981));
#55551=CARTESIAN_POINT('Ctrl Pts',(-12.8482590648636,-52.9002777810298,
14.9944031314392));
#55552=CARTESIAN_POINT('Ctrl Pts',(-12.800661371336,-53.3679164545857,14.9682346279803));
#55553=CARTESIAN_POINT('Ctrl Pts',(-12.9587676726969,-53.7505591757409,
14.9420661245214));
#55554=CARTESIAN_POINT('Ctrl Pts',(-13.1168739740577,-54.1332018968962,
14.9158976210624));
#55555=CARTESIAN_POINT('Ctrl Pts',(-13.480684270307,-54.4308486656509,14.8897291176035));
#55556=CARTESIAN_POINT('Ctrl Pts',(-13.887062777462,-54.5100303359216,14.8635606141446));
#55557=CARTESIAN_POINT('Ctrl Pts',(-14.2934412846171,-54.5892120061924,
14.8373921106856));
#55558=CARTESIAN_POINT('Ctrl Pts',(-14.742388002678,-54.4499285779793,14.8112236072267));
#55559=CARTESIAN_POINT('Ctrl Pts',(-15.0325877125755,-54.1546380042325,
14.7850551037678));
#55560=CARTESIAN_POINT('Ctrl Pts',(-15.322787422473,-53.8593474304858,14.7588866003089));
#55561=CARTESIAN_POINT('Ctrl Pts',(-15.4542401242072,-53.4080497112054,
14.7327180968499));
#55562=CARTESIAN_POINT('Ctrl Pts',(-15.3680052510694,-53.0031088631455,
14.706549593391));
#55563=CARTESIAN_POINT('Ctrl Pts',(-15.2817703779317,-52.5981680150855,
14.6803810899321));
#55564=CARTESIAN_POINT('Ctrl Pts',(-14.9778479299221,-52.239584038246,14.6542125864732));
#55565=CARTESIAN_POINT('Ctrl Pts',(-14.5925114920515,-52.0881567986362,
14.6280440830142));
#55566=CARTESIAN_POINT('Ctrl Pts',(-14.2417387974229,-51.9503122148962,
14.604222830803));
#55567=CARTESIAN_POINT('Ctrl Pts',(-13.8235023586796,-51.9841281668449,
14.5804015785918));
#55568=CARTESIAN_POINT('Ctrl Pts',(-13.4956926805926,-52.1707443397673,
14.5565803263806));
#55569=CARTESIAN_POINT('Ctrl Pts',(-13.4970386657413,-52.17027240687,14.6934196736194));
#55570=CARTESIAN_POINT('Ctrl Pts',(-13.5396170697753,-52.1452744089077,
14.6965359704714));
#55571=CARTESIAN_POINT('Ctrl Pts',(-13.5836638346913,-52.1228973859148,
14.6996522673233));
#55572=CARTESIAN_POINT('Ctrl Pts',(-13.6289575157408,-52.1034200423295,
14.7027685641752));
#55573=CARTESIAN_POINT('Ctrl Pts',(-14.0093024910506,-51.9398627956363,
14.7289370676342));
#55574=CARTESIAN_POINT('Ctrl Pts',(-14.4775734783483,-51.9807757931753,
14.7551055710931));
#55575=CARTESIAN_POINT('Ctrl Pts',(-14.823792639393,-52.2078118983851,14.781274074552));
#55576=CARTESIAN_POINT('Ctrl Pts',(-15.1700118004377,-52.434848003595,14.807442578011));
#55577=CARTESIAN_POINT('Ctrl Pts',(-15.3941791352293,-52.8480072164757,
14.8336110814699));
#55578=CARTESIAN_POINT('Ctrl Pts',(-15.3957751288567,-53.2620246601267,
14.8597795849288));
#55579=CARTESIAN_POINT('Ctrl Pts',(-15.3973711224841,-53.6760421037777,
14.8859480883877));
#55580=CARTESIAN_POINT('Ctrl Pts',(-15.1763957749473,-54.0909177781991,
14.9121165918467));
#55581=CARTESIAN_POINT('Ctrl Pts',(-14.83193716646,-54.3206161896323,14.9382850953056));
#55582=CARTESIAN_POINT('Ctrl Pts',(-14.4874785579727,-54.5503146010655,
14.9644535987645));
#55583=CARTESIAN_POINT('Ctrl Pts',(-14.0195366885349,-54.5948357495104,
14.9906221022235));
#55584=CARTESIAN_POINT('Ctrl Pts',(-13.6379422013928,-54.4342159762724,
15.0167906056824));
#55585=CARTESIAN_POINT('Ctrl Pts',(-13.2563477142508,-54.2735962030343,
15.0429591091413));
#55586=CARTESIAN_POINT('Ctrl Pts',(-12.9611006094046,-53.9078355081131,
15.0691276126002));
#55587=CARTESIAN_POINT('Ctrl Pts',(-12.8845932246477,-53.5009452588027,
15.0952961160591));
#55588=CARTESIAN_POINT('Ctrl Pts',(-12.8080858398908,-53.0940550094922,
15.1214646195181));
#55589=CARTESIAN_POINT('Ctrl Pts',(-12.9503181752232,-52.6460352057925,
15.147633122977));
#55590=CARTESIAN_POINT('Ctrl Pts',(-13.2475115476967,-52.3577832908858,
15.1738016264359));
#55591=CARTESIAN_POINT('Ctrl Pts',(-13.3217783549033,-52.2857508992711,
15.1803409754971));
#55592=CARTESIAN_POINT('Ctrl Pts',(-13.4057220070297,-52.2236955258253,
15.1868803245583));
#55593=CARTESIAN_POINT('Ctrl Pts',(-13.496178545612,-52.1725162395268,15.1934196736194));
#55594=CARTESIAN_POINT('Origin',(-14.1292828945604,-53.2669068454841,15.5));
#55595=CARTESIAN_POINT('',(-13.4984004295476,-52.1727576237481,15.6934196736194));
#55596=CARTESIAN_POINT('',(-13.4975120618698,-52.1706683776322,15.5565803263806));
#55597=CARTESIAN_POINT('',(-13.4970328945604,-52.1718177223987,15.5));
#55598=CARTESIAN_POINT('Ctrl Pts',(-13.4975120618698,-52.1706683776322,
15.5565803263806));
#55599=CARTESIAN_POINT('Ctrl Pts',(-13.2014603606288,-52.3450050094651,
15.5349217833067));
#55600=CARTESIAN_POINT('Ctrl Pts',(-12.9746829017777,-52.6437331734245,
15.5132632402327));
#55601=CARTESIAN_POINT('Ctrl Pts',(-12.8963324343974,-52.9773225319626,
15.4916046971588));
#55602=CARTESIAN_POINT('Ctrl Pts',(-12.8016670421015,-53.3803752328285,
15.4654361936999));
#55603=CARTESIAN_POINT('Ctrl Pts',(-12.9236783333193,-53.8343190010791,
15.439267690241));
#55604=CARTESIAN_POINT('Ctrl Pts',(-13.2076549868355,-54.1356000609316,
15.413099186782));
#55605=CARTESIAN_POINT('Ctrl Pts',(-13.4916316403516,-54.4368811207841,
15.3869306833231));
#55606=CARTESIAN_POINT('Ctrl Pts',(-13.9375736561661,-54.5854994722384,
15.3607621798642));
#55607=CARTESIAN_POINT('Ctrl Pts',(-14.3455153495114,-54.5148128681013,
15.3345936764052));
#55608=CARTESIAN_POINT('Ctrl Pts',(-14.7534570428566,-54.4441262639641,
15.3084251729463));
#55609=CARTESIAN_POINT('Ctrl Pts',(-15.1233984137326,-54.1541347042354,
15.2822566694874));
#55610=CARTESIAN_POINT('Ctrl Pts',(-15.2894533218141,-53.7748738751901,
15.2560881660285));
#55611=CARTESIAN_POINT('Ctrl Pts',(-15.4555082298957,-53.3956130461449,
15.2299196625696));
#55612=CARTESIAN_POINT('Ctrl Pts',(-15.4176766751828,-52.9270829477831,
15.2037511591106));
#55613=CARTESIAN_POINT('Ctrl Pts',(-15.1929228414795,-52.579377997485,15.1775826556517));
#55614=CARTESIAN_POINT('Ctrl Pts',(-14.9681690077762,-52.2316730471868,
15.1514141521928));
#55615=CARTESIAN_POINT('Ctrl Pts',(-14.5564928950826,-52.0047932449524,
15.1252456487338));
#55616=CARTESIAN_POINT('Ctrl Pts',(-14.1424948347361,-52.0004742879611,
15.0990771452749));
#55617=CARTESIAN_POINT('Ctrl Pts',(-13.9183882655449,-51.9981363382785,
15.0849115389768));
#55618=CARTESIAN_POINT('Ctrl Pts',(-13.6936012952867,-52.0610154646128,
15.0707459326787));
#55619=CARTESIAN_POINT('Ctrl Pts',(-13.4977463410386,-52.1735883352515,
15.0565803263806));
#55620=CARTESIAN_POINT('Ctrl Pts',(-13.496178545612,-52.1725162395268,15.1934196736194));
#55621=CARTESIAN_POINT('Ctrl Pts',(-13.7677018035866,-52.018891451597,15.2130488280172));
#55622=CARTESIAN_POINT('Ctrl Pts',(-14.0979074320564,-51.9632623188715,
15.2326779824149));
#55623=CARTESIAN_POINT('Ctrl Pts',(-14.4012233710796,-52.0299449584561,
15.2523071368127));
#55624=CARTESIAN_POINT('Ctrl Pts',(-14.8055874123741,-52.1188425670469,
15.2784756402716));
#55625=CARTESIAN_POINT('Ctrl Pts',(-15.1621610853483,-52.4251218103423,
15.3046441437306));
#55626=CARTESIAN_POINT('Ctrl Pts',(-15.3110525132995,-52.8114434442094,
15.3308126471895));
#55627=CARTESIAN_POINT('Ctrl Pts',(-15.4599439412506,-53.1977650780765,
15.3569811506484));
#55628=CARTESIAN_POINT('Ctrl Pts',(-15.4011531241786,-53.6641291025153,
15.3831496541074));
#55629=CARTESIAN_POINT('Ctrl Pts',(-15.1610425648871,-54.0014123408011,
15.4093181575663));
#55630=CARTESIAN_POINT('Ctrl Pts',(-14.9209320055955,-54.338695579087,15.4354866610252));
#55631=CARTESIAN_POINT('Ctrl Pts',(-14.4995017040844,-54.5468980312198,
15.4616551644841));
#55632=CARTESIAN_POINT('Ctrl Pts',(-14.0857260162278,-54.5326592450683,
15.487823667943));
#55633=CARTESIAN_POINT('Ctrl Pts',(-13.6719503283713,-54.5184204589168,
15.513992171402));
#55634=CARTESIAN_POINT('Ctrl Pts',(-13.2658292541693,-54.2817404344808,
15.5401606748609));
#55635=CARTESIAN_POINT('Ctrl Pts',(-13.0494723111738,-53.9287493069654,
15.5663291783198));
#55636=CARTESIAN_POINT('Ctrl Pts',(-12.8331153681783,-53.5757581794499,
15.5924976817788));
#55637=CARTESIAN_POINT('Ctrl Pts',(-12.8065225563893,-53.1064559488549,
15.6186661852377));
#55638=CARTESIAN_POINT('Ctrl Pts',(-12.9816184085214,-52.7312833144481,
15.6448346886966));
#55639=CARTESIAN_POINT('Ctrl Pts',(-13.0899806023986,-52.4990988894489,
15.6610296836709));
#55640=CARTESIAN_POINT('Ctrl Pts',(-13.2755904595332,-52.3029665221486,
15.6772246786451));
#55641=CARTESIAN_POINT('Ctrl Pts',(-13.4984004295476,-52.1727576237481,
15.6934196736194));
#55642=CARTESIAN_POINT('Origin',(-14.1292828945604,-53.2669068454841,15.5));
#55643=CARTESIAN_POINT('',(-13.4961138435274,-52.1700468646075,16.1934196736194));
#55644=CARTESIAN_POINT('',(-13.4958915862188,-52.1719376453661,16.0565803263806));
#55645=CARTESIAN_POINT('',(-13.4970328945604,-52.1718177223987,15.5));
#55646=CARTESIAN_POINT('Ctrl Pts',(-13.4958915862188,-52.1719376453661,
16.0565803263806));
#55647=CARTESIAN_POINT('Ctrl Pts',(-13.4248008737561,-52.2121474216226,
16.0514346408525));
#55648=CARTESIAN_POINT('Ctrl Pts',(-13.3578067644458,-52.2591973943854,
16.0462889553244));
#55649=CARTESIAN_POINT('Ctrl Pts',(-13.2964716828247,-52.3127310779993,
16.0411432697963));
#55650=CARTESIAN_POINT('Ctrl Pts',(-12.9845506983831,-52.5849778713889,
16.0149747663373));
#55651=CARTESIAN_POINT('Ctrl Pts',(-12.8189865827469,-53.0249099405019,
15.9888062628784));
#55652=CARTESIAN_POINT('Ctrl Pts',(-12.8740202534737,-53.4352565161154,
15.9626377594195));
#55653=CARTESIAN_POINT('Ctrl Pts',(-12.9290539242004,-53.845603091729,15.9364692559605));
#55654=CARTESIAN_POINT('Ctrl Pts',(-13.2046853812901,-54.226364173843,15.9103007525016));
#55655=CARTESIAN_POINT('Ctrl Pts',(-13.5773182028765,-54.4068019672842,
15.8841322490427));
#55656=CARTESIAN_POINT('Ctrl Pts',(-13.9499510244629,-54.5872397607254,
15.8579637455838));
#55657=CARTESIAN_POINT('Ctrl Pts',(-14.4195852105461,-54.5673542654938,
15.8317952421249));
#55658=CARTESIAN_POINT('Ctrl Pts',(-14.7756312098701,-54.3560623738526,
15.8056267386659));
#55659=CARTESIAN_POINT('Ctrl Pts',(-15.1316772091941,-54.1447704822114,
15.779458235207));
#55660=CARTESIAN_POINT('Ctrl Pts',(-15.374135021759,-53.7420721941606,15.7532897317481));
#55661=CARTESIAN_POINT('Ctrl Pts',(-15.3942836818793,-53.3285422092164,
15.7271212282891));
#55662=CARTESIAN_POINT('Ctrl Pts',(-15.4144323419997,-52.9150122242722,
15.7009527248302));
#55663=CARTESIAN_POINT('Ctrl Pts',(-15.2122718496755,-52.4906505424345,
15.6747842213713));
#55664=CARTESIAN_POINT('Ctrl Pts',(-14.8784533736736,-52.2457459854386,
15.6486157179124));
#55665=CARTESIAN_POINT('Ctrl Pts',(-14.5446348976717,-52.0008414284427,
15.6224472144534));
#55666=CARTESIAN_POINT('Ctrl Pts',(-14.0791584379921,-51.9353939962886,
15.5962787109945));
#55667=CARTESIAN_POINT('Ctrl Pts',(-13.6907491702475,-52.0787510969521,
15.5701102075356));
#55668=CARTESIAN_POINT('Ctrl Pts',(-13.6238095222296,-52.1034577006719,
15.5656002471506));
#55669=CARTESIAN_POINT('Ctrl Pts',(-13.5591589344204,-52.1343662450032,
15.5610902867656));
#55670=CARTESIAN_POINT('Ctrl Pts',(-13.4975120618698,-52.1706683776322,
15.5565803263806));
#55671=CARTESIAN_POINT('Ctrl Pts',(-13.4984004295476,-52.1727576237481,
15.6934196736194));
#55672=CARTESIAN_POINT('Ctrl Pts',(-13.6356154845653,-52.0925699142095,
15.7033931821041));
#55673=CARTESIAN_POINT('Ctrl Pts',(-13.7869389649625,-52.0373841810022,
15.7133666905887));
#55674=CARTESIAN_POINT('Ctrl Pts',(-13.9430173010127,-52.0141772385597,
15.7233401990734));
#55675=CARTESIAN_POINT('Ctrl Pts',(-14.352535825319,-51.9532868352966,15.7495087025323));
#55676=CARTESIAN_POINT('Ctrl Pts',(-14.7947883578784,-52.1125490669891,
15.7756772059912));
#55677=CARTESIAN_POINT('Ctrl Pts',(-15.0714636060598,-52.4205488559651,
15.8018457094502));
#55678=CARTESIAN_POINT('Ctrl Pts',(-15.3481388542411,-52.728548644941,15.8280142129091));
#55679=CARTESIAN_POINT('Ctrl Pts',(-15.4592368180444,-53.1852859912004,
15.854182716368));
#55680=CARTESIAN_POINT('Ctrl Pts',(-15.3549398499385,-53.5859544394514,
15.8803512198269));
#55681=CARTESIAN_POINT('Ctrl Pts',(-15.2506428818326,-53.9866228877023,
15.9065197232859));
#55682=CARTESIAN_POINT('Ctrl Pts',(-14.9309509818175,-54.3312224379448,
15.9326882267448));
#55683=CARTESIAN_POINT('Ctrl Pts',(-14.5392177979356,-54.4652305557052,
15.9588567302037));
#55684=CARTESIAN_POINT('Ctrl Pts',(-14.1474846140538,-54.5992386734655,
15.9850252336627));
#55685=CARTESIAN_POINT('Ctrl Pts',(-13.6837101463051,-54.5226553587437,
16.0111937371216));
#55686=CARTESIAN_POINT('Ctrl Pts',(-13.3558563789032,-54.2698214801478,
16.0373622405805));
#55687=CARTESIAN_POINT('Ctrl Pts',(-13.0280026115013,-54.016987601552,16.0635307440394));
#55688=CARTESIAN_POINT('Ctrl Pts',(-12.8360695444461,-53.5879031590822,
16.0896992474984));
#55689=CARTESIAN_POINT('Ctrl Pts',(-12.8661222463432,-53.174974717257,16.1158677509573));
#55690=CARTESIAN_POINT('Ctrl Pts',(-12.8958099052366,-52.7670620187505,
16.1417183918447));
#55691=CARTESIAN_POINT('Ctrl Pts',(-13.1421232693053,-52.3749152184319,
16.167569032732));
#55692=CARTESIAN_POINT('Ctrl Pts',(-13.4961138435274,-52.1700468646075,
16.1934196736194));
#55693=CARTESIAN_POINT('Origin',(-14.1292828945604,-53.2669068454841,15.5));
#55694=CARTESIAN_POINT('',(-13.4969690270882,-52.1733618792496,16.6934196736194));
#55695=CARTESIAN_POINT('',(-13.4982981440081,-52.1731729190029,16.5565803263806));
#55696=CARTESIAN_POINT('',(-13.4970328945604,-52.1718177223987,15.5));
#55697=CARTESIAN_POINT('Ctrl Pts',(-13.4982981440081,-52.1731729190029,
16.5565803263806));
#55698=CARTESIAN_POINT('Ctrl Pts',(-13.2942737914495,-52.2917933948419,
16.5417789949394));
#55699=CARTESIAN_POINT('Ctrl Pts',(-13.121375289642,-52.4650421903572,16.5269776634982));
#55700=CARTESIAN_POINT('Ctrl Pts',(-13.0113308722452,-52.6717520885803,
16.5121763320569));
#55701=CARTESIAN_POINT('Ctrl Pts',(-12.8167742049128,-53.0372116898416,
16.486007828598));
#55702=CARTESIAN_POINT('Ctrl Pts',(-12.8186845812822,-53.5072628063503,
16.4598393251391));
#55703=CARTESIAN_POINT('Ctrl Pts',(-13.0162053670574,-53.8711289302741,
16.4336708216802));
#55704=CARTESIAN_POINT('Ctrl Pts',(-13.2137261528326,-54.234995054198,16.4075023182212));
#55705=CARTESIAN_POINT('Ctrl Pts',(-13.6068573480138,-54.4926761855371,
16.3813338147623));
#55706=CARTESIAN_POINT('Ctrl Pts',(-14.0193142510177,-54.5286250418801,
16.3551653113034));
#55707=CARTESIAN_POINT('Ctrl Pts',(-14.4317711540216,-54.5645738982232,
16.3289968078445));
#55708=CARTESIAN_POINT('Ctrl Pts',(-14.8635537648482,-54.3787904795703,
16.3028283043855));
#55709=CARTESIAN_POINT('Ctrl Pts',(-15.1210456285732,-54.0545822792717,
16.2766598009266));
#55710=CARTESIAN_POINT('Ctrl Pts',(-15.3785374922981,-53.7303740789732,
16.2504912974677));
#55711=CARTESIAN_POINT('Ctrl Pts',(-15.4617386089214,-53.267741097029,16.2243227940088));
#55712=CARTESIAN_POINT('Ctrl Pts',(-15.3333406086023,-52.8741334617557,
16.1981542905498));
#55713=CARTESIAN_POINT('Ctrl Pts',(-15.2049426082832,-52.4805258264823,
16.1719857870909));
#55714=CARTESIAN_POINT('Ctrl Pts',(-14.8649454910218,-52.1559435378799,
16.145817283632));
#55715=CARTESIAN_POINT('Ctrl Pts',(-14.4658080057675,-52.0459331524117,
16.119648780173));
#55716=CARTESIAN_POINT('Ctrl Pts',(-14.1451555582543,-51.9575548350262,
16.0986259622422));
#55717=CARTESIAN_POINT('Ctrl Pts',(-13.7863343457911,-52.0076596690572,
16.0776031443114));
#55718=CARTESIAN_POINT('Ctrl Pts',(-13.4958915862188,-52.1719376453661,
16.0565803263806));
#55719=CARTESIAN_POINT('Ctrl Pts',(-13.4961138435274,-52.1700468646075,
16.1934196736194));
#55720=CARTESIAN_POINT('Ctrl Pts',(-13.5004665539579,-52.1675277788308,
16.193737536191));
#55721=CARTESIAN_POINT('Ctrl Pts',(-13.5048355445966,-52.1650370085359,
16.1940553987625));
#55722=CARTESIAN_POINT('Ctrl Pts',(-13.5092206128964,-52.1625748725828,
16.1943732613341));
#55723=CARTESIAN_POINT('Ctrl Pts',(-13.8702278067029,-51.9598759109143,
16.220541764793));
#55724=CARTESIAN_POINT('Ctrl Pts',(-14.3402037234666,-51.9512504287578,
16.2467102682519));
#55725=CARTESIAN_POINT('Ctrl Pts',(-14.7084055750498,-52.1405661950787,
16.2728787717108));
#55726=CARTESIAN_POINT('Ctrl Pts',(-15.076607426633,-52.3298819613996,16.2990472751698));
#55727=CARTESIAN_POINT('Ctrl Pts',(-15.3430352130359,-52.7171389761979,
16.3252157786287));
#55728=CARTESIAN_POINT('Ctrl Pts',(-15.3882195489487,-53.1286865903088,
16.3513842820876));
#55729=CARTESIAN_POINT('Ctrl Pts',(-15.4334038848614,-53.5402342044196,
16.3775527855465));
#55730=CARTESIAN_POINT('Ctrl Pts',(-15.2573447702841,-53.976072417843,16.4037212890055));
#55731=CARTESIAN_POINT('Ctrl Pts',(-14.9389892027718,-54.240766195907,16.4298897924644));
#55732=CARTESIAN_POINT('Ctrl Pts',(-14.6206336352594,-54.505459973971,16.4560582959233));
#55733=CARTESIAN_POINT('Ctrl Pts',(-14.159981614812,-54.5990093166755,16.4822267993823));
#55734=CARTESIAN_POINT('Ctrl Pts',(-13.7635949875347,-54.4794655848163,
16.5083953028412));
#55735=CARTESIAN_POINT('Ctrl Pts',(-13.3672083602575,-54.3599218529572,
16.5345638063001));
#55736=CARTESIAN_POINT('Ctrl Pts',(-13.0350871261504,-54.0272850465344,
16.560732309759));
#55737=CARTESIAN_POINT('Ctrl Pts',(-12.916158385472,-53.6307134674394,16.586900813218));
#55738=CARTESIAN_POINT('Ctrl Pts',(-12.7972296447937,-53.2341418883445,
16.6130693166769));
#55739=CARTESIAN_POINT('Ctrl Pts',(-12.891493397544,-52.7736355365774,16.6392378201358));
#55740=CARTESIAN_POINT('Ctrl Pts',(-13.1566806746197,-52.4556909263592,
16.6654063235947));
#55741=CARTESIAN_POINT('Ctrl Pts',(-13.2513082234268,-52.3422378246374,
16.6747441069363));
#55742=CARTESIAN_POINT('Ctrl Pts',(-13.3676994181703,-52.2469370707529,
16.6840818902779));
#55743=CARTESIAN_POINT('Ctrl Pts',(-13.4969690270882,-52.1733618792496,
16.6934196736194));
#55744=CARTESIAN_POINT('Origin',(-14.1292828945604,-53.2669068454841,15.5));
#55745=CARTESIAN_POINT('',(-13.498190246218,-52.1716844371558,17.1934196736194));
#55746=CARTESIAN_POINT('',(-13.4965460097018,-52.1700456009991,17.0565803263806));
#55747=CARTESIAN_POINT('',(-13.4970328945604,-52.1718177223987,15.5));
#55748=CARTESIAN_POINT('Ctrl Pts',(-13.4965460097018,-52.1700456009991,
17.0565803263806));
#55749=CARTESIAN_POINT('Ctrl Pts',(-13.1622129933252,-52.3652134872717,
17.0321233490263));
#55750=CARTESIAN_POINT('Ctrl Pts',(-12.9210086316388,-52.724852170666,17.0076663716719));
#55751=CARTESIAN_POINT('Ctrl Pts',(-12.8726933551042,-53.1087658234733,
16.9832093943176));
#55752=CARTESIAN_POINT('Ctrl Pts',(-12.8209969225157,-53.5195461748581,
16.9570408908587));
#55753=CARTESIAN_POINT('Ctrl Pts',(-12.9901314007569,-53.9581179567514,
16.9308723873998));
#55754=CARTESIAN_POINT('Ctrl Pts',(-13.3042549587021,-54.2278203840484,
16.9047038839408));
#55755=CARTESIAN_POINT('Ctrl Pts',(-13.6183785166473,-54.4975228113454,
16.8785353804819));
#55756=CARTESIAN_POINT('Ctrl Pts',(-14.0774911542965,-54.5983558840463,
16.852366877023));
#55757=CARTESIAN_POINT('Ctrl Pts',(-14.4757212681973,-54.4851048462747,
16.8261983735641));
#55758=CARTESIAN_POINT('Ctrl Pts',(-14.8739513820982,-54.371853808503,16.8000298701051));
#55759=CARTESIAN_POINT('Ctrl Pts',(-15.2112989722507,-54.0445186602589,
16.7738613666462));
#55760=CARTESIAN_POINT('Ctrl Pts',(-15.3364933887363,-53.6498803767017,
16.7476928631873));
#55761=CARTESIAN_POINT('Ctrl Pts',(-15.4616878052219,-53.2552420931446,
16.7215243597284));
#55762=CARTESIAN_POINT('Ctrl Pts',(-15.3747290480406,-52.7933006742746,
16.6953558562694));
#55763=CARTESIAN_POINT('Ctrl Pts',(-15.1146104479144,-52.4711961414872,
16.6691873528105));
#55764=CARTESIAN_POINT('Ctrl Pts',(-14.8544918477881,-52.1490916086999,
16.6430188493516));
#55765=CARTESIAN_POINT('Ctrl Pts',(-14.4212134047168,-51.9668239619953,
16.6168503458927));
#55766=CARTESIAN_POINT('Ctrl Pts',(-14.0090623276642,-52.00612418165,16.5906818424337));
#55767=CARTESIAN_POINT('Ctrl Pts',(-13.8300306074324,-52.0231955574683,
16.579314670416));
#55768=CARTESIAN_POINT('Ctrl Pts',(-13.6549853934321,-52.0820744013432,
16.5679474983983));
#55769=CARTESIAN_POINT('Ctrl Pts',(-13.4982981440081,-52.1731729190029,
16.5565803263806));
#55770=CARTESIAN_POINT('Ctrl Pts',(-13.4969690270882,-52.1733618792496,
16.6934196736194));
#55771=CARTESIAN_POINT('Ctrl Pts',(-13.7299687153222,-52.0407475948441,
16.7102503937368));
#55772=CARTESIAN_POINT('Ctrl Pts',(-14.0048072977942,-51.9787144778412,
16.7270811138541));
#55773=CARTESIAN_POINT('Ctrl Pts',(-14.2694557749176,-52.0081860992865,
16.7439118339715));
#55774=CARTESIAN_POINT('Ctrl Pts',(-14.6809327967389,-52.0540087511013,
16.7700803374304));
#55775=CARTESIAN_POINT('Ctrl Pts',(-15.0677760389806,-52.3210369234002,
16.7962488408894));
#55776=CARTESIAN_POINT('Ctrl Pts',(-15.256520467333,-52.6895319775572,16.8224173443483));
#55777=CARTESIAN_POINT('Ctrl Pts',(-15.4452648956854,-53.0580270317142,
16.8485858478072));
#55778=CARTESIAN_POINT('Ctrl Pts',(-15.4359105101485,-53.5279889677293,
16.8747543512661));
#55779=CARTESIAN_POINT('Ctrl Pts',(-15.2326517793345,-53.8886813318345,
16.9009228547251));
#55780=CARTESIAN_POINT('Ctrl Pts',(-15.0293930485204,-54.2493736959397,
16.927091358184));
#55781=CARTESIAN_POINT('Ctrl Pts',(-14.6322299724291,-54.500796488135,16.9532598616429));
#55782=CARTESIAN_POINT('Ctrl Pts',(-14.2192554962477,-54.5302086092019,
16.9794283651019));
#55783=CARTESIAN_POINT('Ctrl Pts',(-13.8062810200663,-54.5596207302688,
17.0055968685608));
#55784=CARTESIAN_POINT('Ctrl Pts',(-13.3774951437947,-54.3670221802074,
17.0317653720197));
#55785=CARTESIAN_POINT('Ctrl Pts',(-13.1251699439815,-54.0387767018188,
17.0579338754786));
#55786=CARTESIAN_POINT('Ctrl Pts',(-12.8728447441683,-53.7105312234301,
17.0841023789376));
#55787=CARTESIAN_POINT('Ctrl Pts',(-12.7969802208136,-53.2466388167143,
17.1102708823965));
#55788=CARTESIAN_POINT('Ctrl Pts',(-12.9315961537199,-52.8551138190488,
17.1364393858554));
#55789=CARTESIAN_POINT('Ctrl Pts',(-13.0293020925489,-52.570940046702,17.1554328151101));
#55790=CARTESIAN_POINT('Ctrl Pts',(-13.2378899597345,-52.32488970875,17.1744262443647));
#55791=CARTESIAN_POINT('Ctrl Pts',(-13.498190246218,-52.1716844371558,17.1934196736194));
#55792=CARTESIAN_POINT('Origin',(-14.1292828945604,-53.2669068454841,15.5));
#55793=CARTESIAN_POINT('',(-13.495722982135,-52.1707788329429,17.6934196736194));
#55794=CARTESIAN_POINT('',(-13.4965541629804,-52.1730078059394,17.5565803263806));
#55795=CARTESIAN_POINT('',(-13.4970328945604,-52.1718177223987,15.5));
#55796=CARTESIAN_POINT('',(-13.8936870225526,-54.5092654229862,18.));
#55797=CARTESIAN_POINT('Ctrl Pts',(-13.495722982135,-52.1707788329429,17.6934196736194));
#55798=CARTESIAN_POINT('Ctrl Pts',(-13.8217103338362,-51.9852932094709,
17.7171076053695));
#55799=CARTESIAN_POINT('Ctrl Pts',(-14.2369080256434,-51.9506029252058,
17.7407955371196));
#55800=CARTESIAN_POINT('Ctrl Pts',(-14.5864865212314,-52.0858847696684,
17.7644834688697));
#55801=CARTESIAN_POINT('Ctrl Pts',(-14.9726724562246,-52.2353331660965,
17.7906519723286));
#55802=CARTESIAN_POINT('Ctrl Pts',(-15.2787764866269,-52.5922161636806,
17.8168204757875));
#55803=CARTESIAN_POINT('Ctrl Pts',(-15.3668468800596,-52.9968087774221,
17.8429889792464));
#55804=CARTESIAN_POINT('Ctrl Pts',(-15.4549172734923,-53.4014013911635,
17.8691574827054));
#55805=CARTESIAN_POINT('Ctrl Pts',(-15.3249540299554,-53.8537036210623,
17.8953259861643));
#55806=CARTESIAN_POINT('Ctrl Pts',(-15.0367817327077,-54.1500381490016,
17.9214944896232));
#55807=CARTESIAN_POINT('Ctrl Pts',(-14.74860943546,-54.4463726769409,17.9476629930821));
#55808=CARTESIAN_POINT('Ctrl Pts',(-14.3022280845015,-54.5867395029208,
17.9738314965411));
#55809=CARTESIAN_POINT('Ctrl Pts',(-13.8936870225526,-54.5092654229862,
18.));
#55810=CARTESIAN_POINT('',(-12.9337042190834,-52.8487739793663,18.));
#55811=CARTESIAN_POINT('Origin',(-14.1292828945604,-53.2669068454841,18.));
#55812=CARTESIAN_POINT('Ctrl Pts',(-12.9336937527446,-52.8487684531621,
18.));
#55813=CARTESIAN_POINT('Ctrl Pts',(-12.8048883200695,-53.2213447345786,
17.975091839613));
#55814=CARTESIAN_POINT('Ctrl Pts',(-12.8625878757539,-53.660362859942,17.950183679226));
#55815=CARTESIAN_POINT('Ctrl Pts',(-13.0861189278269,-53.984999064981,17.925275518839));
#55816=CARTESIAN_POINT('Ctrl Pts',(-13.3209605627957,-54.3260617336993,
17.89910701538));
#55817=CARTESIAN_POINT('Ctrl Pts',(-13.7388402922128,-54.5408742678445,
17.8729385119211));
#55818=CARTESIAN_POINT('Ctrl Pts',(-14.1527389844809,-54.5331807500212,
17.8467700084622));
#55819=CARTESIAN_POINT('Ctrl Pts',(-14.5666376767489,-54.5254872321979,
17.8206015050033));
#55820=CARTESIAN_POINT('Ctrl Pts',(-14.9765553318677,-54.2952876624061,
17.7944330015443));
#55821=CARTESIAN_POINT('Ctrl Pts',(-15.1985005516416,-53.9457721211068,
17.7682644980854));
#55822=CARTESIAN_POINT('Ctrl Pts',(-15.4204457714154,-53.5962565798075,
17.7420959946265));
#55823=CARTESIAN_POINT('Ctrl Pts',(-15.4544185558441,-53.1274250670007,
17.7159274911676));
#55824=CARTESIAN_POINT('Ctrl Pts',(-15.2852740004506,-52.7495241339714,
17.6897589877086));
#55825=CARTESIAN_POINT('Ctrl Pts',(-15.1161294450571,-52.3716232009421,
17.6635904842497));
#55826=CARTESIAN_POINT('Ctrl Pts',(-14.7438675498413,-52.0846528476903,
17.6374219807908));
#55827=CARTESIAN_POINT('Ctrl Pts',(-14.3353709232148,-52.0172856023794,
17.6112534773319));
#55828=CARTESIAN_POINT('Ctrl Pts',(-14.050883915571,-51.9703694107086,17.5930290936814));
#55829=CARTESIAN_POINT('Ctrl Pts',(-13.7488228128377,-52.0299622436843,
17.574804710031));
#55830=CARTESIAN_POINT('Ctrl Pts',(-13.4965541629804,-52.1730078059394,
17.5565803263806));
#55831=CARTESIAN_POINT('Origin',(-14.1292828945604,-53.2669068454841,19.1042117235887));
#55832=CARTESIAN_POINT('',(-13.3561475049579,-51.9293198574881,14.3957882764113));
#55833=CARTESIAN_POINT('',(-13.3590334722299,-51.9326791410007,14.3542117235887));
#55834=CARTESIAN_POINT('',(-13.3577828945603,-51.9306296474448,19.1042117235887));
#55835=CARTESIAN_POINT('',(-15.619480088463,-52.8667052421829,14.));
#55836=CARTESIAN_POINT('Ctrl Pts',(-13.3590334722299,-51.9326791410007,
14.3542117235887));
#55837=CARTESIAN_POINT('Ctrl Pts',(-13.133310230807,-52.0631907802776,14.3408151628949));
#55838=CARTESIAN_POINT('Ctrl Pts',(-12.5590924929827,-52.6090703324587,
14.301250098742));
#55839=CARTESIAN_POINT('Ctrl Pts',(-12.4888785260391,-54.0475602728968,
14.2355165311304));
#55840=CARTESIAN_POINT('Ctrl Pts',(-13.8755779012831,-55.0671461874891,
14.1570110207535));
#55841=CARTESIAN_POINT('Ctrl Pts',(-15.4910603626305,-54.4687297322861,
14.0785055103768));
#55842=CARTESIAN_POINT('Ctrl Pts',(-15.7510836294753,-53.3567463262428,
14.0261685034589));
#55843=CARTESIAN_POINT('Ctrl Pts',(-15.619480088463,-52.8667052421829,14.));
#55844=CARTESIAN_POINT('',(-15.2224969554152,-52.1743874122524,14.));
#55845=CARTESIAN_POINT('Origin',(-14.1292828945604,-53.2669068454841,14.));
#55846=CARTESIAN_POINT('Ctrl Pts',(-13.3561475049579,-51.9293198574881,
14.3957882764113));
#55847=CARTESIAN_POINT('Ctrl Pts',(-13.3167322940314,-51.9517582304518,
14.3934410251636));
#55848=CARTESIAN_POINT('Ctrl Pts',(-12.8509091548949,-52.2463455523905,
14.3649252704569));
#55849=CARTESIAN_POINT('Ctrl Pts',(-12.312999126503,-53.317416116839,14.3102410122914));
#55850=CARTESIAN_POINT('Ctrl Pts',(-13.1694776941513,-54.8098931066082,
14.2317355019146));
#55851=CARTESIAN_POINT('Ctrl Pts',(-14.8870885705588,-54.9183199028175,
14.1532299915378));
#55852=CARTESIAN_POINT('Ctrl Pts',(-15.9077095091603,-53.5682793339942,
14.0759848242329));
#55853=CARTESIAN_POINT('Ctrl Pts',(-15.5613200902447,-52.5158444925152,
14.024908160387));
#55854=CARTESIAN_POINT('Ctrl Pts',(-15.2225055381225,-52.1743757967134,
14.));
#55855=CARTESIAN_POINT('Origin',(-14.1292828945604,-53.2669068454841,19.1042117235887));
#55856=CARTESIAN_POINT('',(-13.3586534741695,-51.9327902292019,14.8957882764113));
#55857=CARTESIAN_POINT('',(-13.3577899368159,-51.928743983656,14.8542117235887));
#55858=CARTESIAN_POINT('',(-13.3577828945603,-51.9306296474448,19.1042117235887));
#55859=CARTESIAN_POINT('Ctrl Pts',(-13.3577899368159,-51.928743983656,14.8542117235887));
#55860=CARTESIAN_POINT('Ctrl Pts',(-12.9734547442474,-52.1543891335537,
14.8311595169817));
#55861=CARTESIAN_POINT('Ctrl Pts',(-12.3621732880177,-53.0098569651208,
14.7819388069158));
#55862=CARTESIAN_POINT('Ctrl Pts',(-12.8743108410601,-54.5809237767912,
14.706549593391));
#55863=CARTESIAN_POINT('Ctrl Pts',(-14.53309819057,-55.0385159317414,14.6280440830142));
#55864=CARTESIAN_POINT('Ctrl Pts',(-15.8297520454146,-53.9072361260964,
14.5495385726375));
#55865=CARTESIAN_POINT('Ctrl Pts',(-15.6013490876951,-52.2017963646938,
14.4710330622607));
#55866=CARTESIAN_POINT('Ctrl Pts',(-14.317080229173,-51.5794230562898,14.4059241125778));
#55867=CARTESIAN_POINT('Ctrl Pts',(-13.5742323121468,-51.8082526389224,
14.3669836663538));
#55868=CARTESIAN_POINT('Ctrl Pts',(-13.3590334722299,-51.9326791410007,
14.3542117235887));
#55869=CARTESIAN_POINT('Ctrl Pts',(-13.3586534741695,-51.9327902292019,
14.8957882764113));
#55870=CARTESIAN_POINT('Ctrl Pts',(-13.1561499564235,-52.0491845394434,
14.8837853792505));
#55871=CARTESIAN_POINT('Ctrl Pts',(-12.5927601381537,-52.5577927522065,
14.8456139786307));
#55872=CARTESIAN_POINT('Ctrl Pts',(-12.4499580614657,-53.9607971579716,
14.781274074552));
#55873=CARTESIAN_POINT('Ctrl Pts',(-13.7817713167744,-55.0504032414555,
14.7027685641753));
#55874=CARTESIAN_POINT('Ctrl Pts',(-15.4252464910755,-54.5405234556122,
14.6242630537985));
#55875=CARTESIAN_POINT('Ctrl Pts',(-15.9064600587524,-52.8884418877605,
14.5457575434217));
#55876=CARTESIAN_POINT('Ctrl Pts',(-14.8271456061161,-51.6150089076653,
14.4695992842926));
#55877=CARTESIAN_POINT('Ctrl Pts',(-13.7561556767952,-51.7016023764131,
14.4196095286225));
#55878=CARTESIAN_POINT('Ctrl Pts',(-13.3561475049579,-51.9293198574881,
14.3957882764113));
#55879=CARTESIAN_POINT('Origin',(-14.1292828945604,-53.2669068454841,19.1042117235887));
#55880=CARTESIAN_POINT('',(-13.3583675961487,-51.9292271650606,15.3957882764113));
#55881=CARTESIAN_POINT('',(-13.3567403793944,-51.9314820095869,15.3542117235887));
#55882=CARTESIAN_POINT('',(-13.3577828945603,-51.9306296474448,19.1042117235887));
#55883=CARTESIAN_POINT('Ctrl Pts',(-13.3567403793944,-51.9314820095869,
15.3542117235887));
#55884=CARTESIAN_POINT('Ctrl Pts',(-13.2463612263438,-51.9939332857897,
15.3476723745276));
#55885=CARTESIAN_POINT('Ctrl Pts',(-12.7340280693376,-52.3726757467305,
15.3149645220075));
#55886=CARTESIAN_POINT('Ctrl Pts',(-12.343540269987,-53.6026792252177,15.2560881660285));
#55887=CARTESIAN_POINT('Ctrl Pts',(-13.4243618186885,-54.9416323741227,
15.1775826556517));
#55888=CARTESIAN_POINT('Ctrl Pts',(-15.1373732173662,-54.7786522269085,
15.0990771452749));
#55889=CARTESIAN_POINT('Ctrl Pts',(-15.9463055097723,-53.2599021305098,
15.0205716348981));
#55890=CARTESIAN_POINT('Ctrl Pts',(-15.1256881964072,-51.7474355457531,
14.9420661245214));
#55891=CARTESIAN_POINT('Ctrl Pts',(-13.9148311256039,-51.641642546183,14.8866128207515));
#55892=CARTESIAN_POINT('Ctrl Pts',(-13.4097460280966,-51.8982402977282,
14.8573280204407));
#55893=CARTESIAN_POINT('Ctrl Pts',(-13.3577899368159,-51.928743983656,14.8542117235887));
#55894=CARTESIAN_POINT('Ctrl Pts',(-13.3583675961487,-51.9292271650606,
15.3957882764113));
#55895=CARTESIAN_POINT('Ctrl Pts',(-12.9971119417281,-52.1419605956009,
15.3741297333373));
#55896=CARTESIAN_POINT('Ctrl Pts',(-12.3860414668385,-52.9469081505226,
15.3263026868045));
#55897=CARTESIAN_POINT('Ctrl Pts',(-12.8070334555363,-54.5132114643009,
15.2523071368127));
#55898=CARTESIAN_POINT('Ctrl Pts',(-14.4395092097517,-55.0572639347494,
15.1738016264359));
#55899=CARTESIAN_POINT('Ctrl Pts',(-15.7937667074069,-53.9956815464662,
15.0952961160592));
#55900=CARTESIAN_POINT('Ctrl Pts',(-15.6552753932384,-52.280516797303,15.0167906056824));
#55901=CARTESIAN_POINT('Ctrl Pts',(-14.3786526271626,-51.5769541863948,
14.9502879924664));
#55902=CARTESIAN_POINT('Ctrl Pts',(-13.5976445334062,-51.7954237290868,
14.9099538827094));
#55903=CARTESIAN_POINT('Ctrl Pts',(-13.3586534741695,-51.9327902292019,
14.8957882764113));
#55904=CARTESIAN_POINT('Origin',(-14.1292828945604,-53.2669068454841,19.1042117235887));
#55905=CARTESIAN_POINT('',(-13.3563902185848,-51.9307759828648,15.8957882764113));
#55906=CARTESIAN_POINT('',(-13.3594516225044,-51.9317765575136,15.8542117235887));
#55907=CARTESIAN_POINT('',(-13.3577828945603,-51.9306296474448,19.1042117235887));
#55908=CARTESIAN_POINT('Ctrl Pts',(-13.3594516225044,-51.9317765575136,
15.8542117235887));
#55909=CARTESIAN_POINT('Ctrl Pts',(-13.087568835844,-52.0906633350794,15.8380167286145));
#55910=CARTESIAN_POINT('Ctrl Pts',(-12.4951087068473,-52.7167109460471,
15.7956532301813));
#55911=CARTESIAN_POINT('Ctrl Pts',(-12.5800904986592,-54.21644496341,15.7271212282892));
#55912=CARTESIAN_POINT('Ctrl Pts',(-14.0667923195219,-55.0828679235634,
15.6486157179124));
#55913=CARTESIAN_POINT('Ctrl Pts',(-15.6095371717916,-54.3206938223985,
15.5701102075356));
#55914=CARTESIAN_POINT('Ctrl Pts',(-15.8247548010729,-52.6134584968727,
15.4916046971588));
#55915=CARTESIAN_POINT('Ctrl Pts',(-14.6281635632835,-51.5856454904132,
15.4196385358432));
#55916=CARTESIAN_POINT('Ctrl Pts',(-13.6880653197304,-51.7440221062451,
15.3738408779865));
#55917=CARTESIAN_POINT('Ctrl Pts',(-13.3567403793944,-51.9314820095869,
15.3542117235887));
#55918=CARTESIAN_POINT('Ctrl Pts',(-13.3563902185848,-51.9307759828648,
15.8957882764113));
#55919=CARTESIAN_POINT('Ctrl Pts',(-13.2696421210522,-51.9798417675732,
15.8906425908832));
#55920=CARTESIAN_POINT('Ctrl Pts',(-12.7721552352232,-52.3292268802208,
15.8593284018961));
#55921=CARTESIAN_POINT('Ctrl Pts',(-12.3283713567552,-53.5084362707541,
15.8018457094502));
#55922=CARTESIAN_POINT('Ctrl Pts',(-13.3373852079754,-54.9023018690979,
15.7233401990734));
#55923=CARTESIAN_POINT('Ctrl Pts',(-15.0565917302206,-54.8295063313936,
15.6448346886966));
#55924=CARTESIAN_POINT('Ctrl Pts',(-15.9441656443073,-53.3553344251958,
15.5663291783198));
#55925=CARTESIAN_POINT('Ctrl Pts',(-15.2041095597138,-51.8018585649929,
15.4878236679431));
#55926=CARTESIAN_POINT('Ctrl Pts',(-13.970228695557,-51.6283710932553,15.4309767006402));
#55927=CARTESIAN_POINT('Ctrl Pts',(-13.4335918937727,-51.8849296635607,
15.4002982367963));
#55928=CARTESIAN_POINT('Ctrl Pts',(-13.3583675961487,-51.9292271650606,
15.3957882764113));
#55929=CARTESIAN_POINT('Origin',(-14.1292828945604,-53.2669068454841,19.1042117235887));
#55930=CARTESIAN_POINT('',(-13.3593268090704,-51.9322833195368,16.3957882764113));
#55931=CARTESIAN_POINT('',(-13.3566614269891,-51.9284687668027,16.3542117235887));
#55932=CARTESIAN_POINT('',(-13.3577828945603,-51.9306296474448,19.1042117235887));
#55933=CARTESIAN_POINT('Ctrl Pts',(-13.3566614269891,-51.9284687668027,
16.3542117235887));
#55934=CARTESIAN_POINT('Ctrl Pts',(-12.9247061434582,-52.1784583832132,
16.3283610827014));
#55935=CARTESIAN_POINT('Ctrl Pts',(-12.3198850098697,-53.141372730953,16.2763419383551));
#55936=CARTESIAN_POINT('Ctrl Pts',(-13.0196563589383,-54.7057774673455,
16.1981542905498));
#55937=CARTESIAN_POINT('Ctrl Pts',(-14.7174120024405,-54.986128723848,16.1196487801731));
#55938=CARTESIAN_POINT('Ctrl Pts',(-15.8877194798387,-53.7246409278238,
16.0411432697963));
#55939=CARTESIAN_POINT('Ctrl Pts',(-15.4810192232586,-52.0526463245539,
15.9626377594195));
#55940=CARTESIAN_POINT('Ctrl Pts',(-14.1960288388143,-51.5899006730013,
15.900327244017));
#55941=CARTESIAN_POINT('Ctrl Pts',(-13.5268876287458,-51.8339278933634,
15.8641852320734));
#55942=CARTESIAN_POINT('Ctrl Pts',(-13.3594516225044,-51.9317765575136,
15.8542117235887));
#55943=CARTESIAN_POINT('Ctrl Pts',(-13.3593268090704,-51.9322833195368,
16.3957882764113));
#55944=CARTESIAN_POINT('Ctrl Pts',(-13.1103670811162,-52.077029380604,16.3809869449701));
#55945=CARTESIAN_POINT('Ctrl Pts',(-12.5263819999043,-52.6621976201272,
16.3400171100699));
#55946=CARTESIAN_POINT('Ctrl Pts',(-12.5323627785853,-54.1337776405725,
16.2728787717109));
#55947=CARTESIAN_POINT('Ctrl Pts',(-13.9715120885842,-55.0770800976454,
16.1943732613341));
#55948=CARTESIAN_POINT('Ctrl Pts',(-15.5521540067467,-54.3969761475115,
16.1158677509573));
#55949=CARTESIAN_POINT('Ctrl Pts',(-15.8567312853938,-52.7033991815804,
16.0373622405805));
#55950=CARTESIAN_POINT('Ctrl Pts',(-14.6936723389742,-51.5930711363043,
15.9640024157318));
#55951=CARTESIAN_POINT('Ctrl Pts',(-13.7108015891029,-51.7303165780055,
15.9168110943421));
#55952=CARTESIAN_POINT('Ctrl Pts',(-13.3563902185848,-51.9307759828648,
15.8957882764113));
#55953=CARTESIAN_POINT('Origin',(-14.1292828945604,-53.2669068454841,19.1042117235887));
#55954=CARTESIAN_POINT('',(-13.3571887756701,-51.9284672248907,16.8957882764113));
#55955=CARTESIAN_POINT('',(-13.3577049605869,-51.9325138973624,16.8542117235887));
#55956=CARTESIAN_POINT('',(-13.3577828945603,-51.9306296474448,19.1042117235887));
#55957=CARTESIAN_POINT('Ctrl Pts',(-13.3577049605869,-51.9325138973624,
16.8542117235887));
#55958=CARTESIAN_POINT('Ctrl Pts',(-13.1999643464624,-52.0222936684099,
16.8448739402472));
#55959=CARTESIAN_POINT('Ctrl Pts',(-12.6599209222933,-52.4644795705918,
16.8093676534467));
#55960=CARTESIAN_POINT('Ctrl Pts',(-12.38882648105,-53.7888562103795,16.7476928631873));
#55961=CARTESIAN_POINT('Ctrl Pts',(-13.6046344626093,-55.0065515658013,
16.6691873528105));
#55962=CARTESIAN_POINT('Ctrl Pts',(-15.2909596525272,-54.6640921689023,
16.5906818424337));
#55963=CARTESIAN_POINT('Ctrl Pts',(-15.9354654978244,-53.0686037624671,
16.5121763320569));
#55964=CARTESIAN_POINT('Ctrl Pts',(-14.9601438503283,-51.6509582729447,
16.4336708216802));
#55965=CARTESIAN_POINT('Ctrl Pts',(-13.8062061827166,-51.672136525716,16.3810159521908));
#55966=CARTESIAN_POINT('Ctrl Pts',(-13.3619728008082,-51.9253948645857,
16.3545295861603));
#55967=CARTESIAN_POINT('Ctrl Pts',(-13.3566614269891,-51.9284687668027,
16.3542117235887));
#55968=CARTESIAN_POINT('Ctrl Pts',(-13.3571887756701,-51.9284672248907,
16.8957882764113));
#55969=CARTESIAN_POINT('Ctrl Pts',(-12.9492205318827,-52.1666198927584,
16.8713312990569));
#55970=CARTESIAN_POINT('Ctrl Pts',(-12.3399661957944,-53.0750256353043,
16.8207058182437));
#55971=CARTESIAN_POINT('Ctrl Pts',(-12.9456243299004,-54.6455189484075,
16.7439118339715));
#55972=CARTESIAN_POINT('Ctrl Pts',(-14.626314246609,-55.0146421540478,16.6654063235948));
#55973=CARTESIAN_POINT('Ctrl Pts',(-15.8612545351151,-53.8163547667627,
16.586900813218));
#55974=CARTESIAN_POINT('Ctrl Pts',(-15.5429215283994,-52.1253094303059,
16.5083953028412));
#55975=CARTESIAN_POINT('Ctrl Pts',(-14.2558484377858,-51.5838751930056,
16.4446911239056));
#55976=CARTESIAN_POINT('Ctrl Pts',(-13.5505236662165,-51.8211207946266,
16.407155448429));
#55977=CARTESIAN_POINT('Ctrl Pts',(-13.3593268090704,-51.9322833195368,
16.3957882764113));
#55978=CARTESIAN_POINT('Origin',(-14.1292828945604,-53.2669068454841,19.1042117235887));
#55979=CARTESIAN_POINT('',(-13.3571987246687,-51.9320818411208,17.3957882764113));
#55980=CARTESIAN_POINT('',(-13.3591951473146,-51.9304670067727,17.3542117235887));
#55981=CARTESIAN_POINT('',(-13.3577828945603,-51.9306296474448,19.1042117235887));
#55982=CARTESIAN_POINT('Ctrl Pts',(-13.3591951473146,-51.9304670067727,
17.3542117235887));
#55983=CARTESIAN_POINT('Ctrl Pts',(-13.0415649835786,-52.117414997338,17.3352182943341));
#55984=CARTESIAN_POINT('Ctrl Pts',(-12.4363561313197,-52.8313196200714,
17.2900563616205));
#55985=CARTESIAN_POINT('Ctrl Pts',(-12.6886936446445,-54.3742998061273,
17.2187259254479));
#55986=CARTESIAN_POINT('Ctrl Pts',(-14.2583653103316,-55.0793521495312,
17.1402204150712));
#55987=CARTESIAN_POINT('Ctrl Pts',(-15.7122742697832,-54.1589598165365,
17.0617149046944));
#55988=CARTESIAN_POINT('Ctrl Pts',(-15.7465182007045,-52.4385534884905,
16.9832093943176));
#55989=CARTESIAN_POINT('Ctrl Pts',(-14.4988281136715,-51.5773043644132,
16.9140416672824));
#55990=CARTESIAN_POINT('Ctrl Pts',(-13.6420217015477,-51.7706919591752,
16.8710424437061));
#55991=CARTESIAN_POINT('Ctrl Pts',(-13.3577049605869,-51.9325138973624,
16.8542117235887));
#55992=CARTESIAN_POINT('Ctrl Pts',(-13.3571987246687,-51.9320818411208,
17.3957882764113));
#55993=CARTESIAN_POINT('Ctrl Pts',(-13.2230139283874,-52.0081695343042,
17.3878441566028));
#55994=CARTESIAN_POINT('Ctrl Pts',(-12.6963900910874,-52.417984443011,17.3537315333353));
#55995=CARTESIAN_POINT('Ctrl Pts',(-12.3638250796578,-53.6967359986948,
17.293450406609));
#55996=CARTESIAN_POINT('Ctrl Pts',(-13.5139962436503,-54.9765978264216,
17.2149448962322));
#55997=CARTESIAN_POINT('Ctrl Pts',(-15.2159841085892,-54.7231706136822,
17.1364393858554));
#55998=CARTESIAN_POINT('Ctrl Pts',(-15.9433860453713,-53.1637302055401,
17.0579338754786));
#55999=CARTESIAN_POINT('Ctrl Pts',(-15.043860342301,-51.6968216692226,16.9794283651019));
#56000=CARTESIAN_POINT('Ctrl Pts',(-13.8598729208803,-51.6563265828795,
16.9253798320794));
#56001=CARTESIAN_POINT('Ctrl Pts',(-13.3857388409123,-51.9118010399394,
16.8974998025159));
#56002=CARTESIAN_POINT('Ctrl Pts',(-13.3571887756701,-51.9284672248907,
16.8957882764113));
#56003=CARTESIAN_POINT('Origin',(-14.1292828945604,-53.2669068454841,19.1042117235887));
#56004=CARTESIAN_POINT('',(-13.3599426557471,-51.9312965605688,17.8957882764113));
#56005=CARTESIAN_POINT('',(-13.3561844802682,-51.9293619476186,17.8542117235887));
#56006=CARTESIAN_POINT('',(-13.3577828945603,-51.9306296474448,19.1042117235887));
#56007=CARTESIAN_POINT('',(-15.2209662466057,-52.1764590205667,18.));
#56008=CARTESIAN_POINT('Ctrl Pts',(-15.2209662466057,-52.1764590205667,
18.));
#56009=CARTESIAN_POINT('Ctrl Pts',(-14.8623799894179,-51.8174664687921,
17.9738314965411));
#56010=CARTESIAN_POINT('Ctrl Pts',(-14.136921272848,-51.597902680369,17.9390942553448));
#56011=CARTESIAN_POINT('Ctrl Pts',(-13.5035430816839,-51.8470756229631,
17.9043570141486));
#56012=CARTESIAN_POINT('Ctrl Pts',(-13.3599426557471,-51.9312965605688,
17.8957882764113));
#56013=CARTESIAN_POINT('',(-15.6220396093989,-52.866415579935,18.));
#56014=CARTESIAN_POINT('Origin',(-14.1292828945604,-53.2669068454841,18.));
#56015=CARTESIAN_POINT('Ctrl Pts',(-15.6220539738783,-52.8664139542998,
18.));
#56016=CARTESIAN_POINT('Ctrl Pts',(-15.4957406336878,-52.4022578052826,
17.975091839613));
#56017=CARTESIAN_POINT('Ctrl Pts',(-14.7933534445258,-51.6161821464322,
17.9264957474759));
#56018=CARTESIAN_POINT('Ctrl Pts',(-13.7539689671603,-51.7030240140342,
17.8778996553388));
#56019=CARTESIAN_POINT('Ctrl Pts',(-13.3561844802682,-51.9293619476186,
17.8542117235887));
#56020=CARTESIAN_POINT('Origin',(39.0658530619283,-38.8697713466883,15.5));
#56021=CARTESIAN_POINT('',(38.4345426068235,-37.7764071067806,14.1934196736194));
#56022=CARTESIAN_POINT('',(38.4325424620227,-37.7762177647969,14.0565803263806));
#56023=CARTESIAN_POINT('',(38.4336030619283,-37.7746822236028,15.5));
#56024=CARTESIAN_POINT('',(39.3014489339361,-37.6274127691862,14.));
#56025=CARTESIAN_POINT('Ctrl Pts',(38.4325424620227,-37.7762177647969,14.0565803263806));
#56026=CARTESIAN_POINT('Ctrl Pts',(38.6929044073907,-37.6289035868348,14.0377202175871));
#56027=CARTESIAN_POINT('Ctrl Pts',(39.0070060787276,-37.5715758131853,14.0188601087935));
#56028=CARTESIAN_POINT('Ctrl Pts',(39.3014489339361,-37.6274127691862,14.));
#56029=CARTESIAN_POINT('',(38.4336030619283,-37.7746822236028,14.));
#56030=CARTESIAN_POINT('Origin',(39.0658530619283,-38.8697713466883,14.));
#56031=CARTESIAN_POINT('',(38.4336030619283,-37.7746822236028,13.));
#56032=CARTESIAN_POINT('',(38.4336030619283,-37.7746822236028,15.5));
#56033=CARTESIAN_POINT('',(39.7608672580761,-37.8134023216062,13.));
#56034=CARTESIAN_POINT('Origin',(39.0658530619283,-38.8697713466883,13.));
#56035=CARTESIAN_POINT('',(38.3708388657804,-39.9261403717704,13.));
#56036=CARTESIAN_POINT('Origin',(39.0658530619283,-38.8697713466883,13.));
#56037=CARTESIAN_POINT('Origin',(39.0658530619283,-38.8697713466883,13.));
#56038=CARTESIAN_POINT('',(40.2614318702746,-39.2879073628688,14.));
#56039=CARTESIAN_POINT('Origin',(39.0658530619283,-38.8697713466883,14.));
#56040=CARTESIAN_POINT('Ctrl Pts',(40.261442519219,-39.2879130030575,14.));
#56041=CARTESIAN_POINT('Ctrl Pts',(40.3902451808538,-38.9153391953948,14.024908160387));
#56042=CARTESIAN_POINT('Ctrl Pts',(40.3325529350425,-38.4763144202222,14.049816320774));
#56043=CARTESIAN_POINT('Ctrl Pts',(40.109022770241,-38.1516757839093,14.074724481161));
#56044=CARTESIAN_POINT('Ctrl Pts',(39.8741820674393,-37.8106105608956,14.10089298462));
#56045=CARTESIAN_POINT('Ctrl Pts',(39.4562961811818,-37.5958001287034,14.1270614880789));
#56046=CARTESIAN_POINT('Ctrl Pts',(39.042395291977,-37.6034944064735,14.1532299915378));
#56047=CARTESIAN_POINT('Ctrl Pts',(38.8305051320303,-37.6074333729988,14.1666265522317));
#56048=CARTESIAN_POINT('Ctrl Pts',(38.619659348036,-37.6696856996876,14.1800231129255));
#56049=CARTESIAN_POINT('Ctrl Pts',(38.4345426068235,-37.7764071067806,14.1934196736194));
#56050=CARTESIAN_POINT('Origin',(39.0658530619283,-38.8697713466883,15.5));
#56051=CARTESIAN_POINT('',(38.4322601856233,-37.7739115851766,14.6934196736194));
#56052=CARTESIAN_POINT('',(38.4333416483911,-37.7729821125454,14.5565803263806));
#56053=CARTESIAN_POINT('',(38.4336030619283,-37.7746822236028,15.5));
#56054=CARTESIAN_POINT('Ctrl Pts',(38.4333416483911,-37.7729821125454,14.5565803263806));
#56055=CARTESIAN_POINT('Ctrl Pts',(38.4654171032337,-37.7542027235003,14.5542330751329));
#56056=CARTESIAN_POINT('Ctrl Pts',(38.4983383982293,-37.7369254869309,14.5518858238852));
#56057=CARTESIAN_POINT('Ctrl Pts',(38.532014378561,-37.721272199783,14.5495385726375));
#56058=CARTESIAN_POINT('Ctrl Pts',(38.9074535262252,-37.5467603748252,14.5233700691785));
#56059=CARTESIAN_POINT('Ctrl Pts',(39.3766930387427,-37.5740903519378,14.4972015657196));
#56060=CARTESIAN_POINT('Ctrl Pts',(39.7293604226538,-37.7909904189904,14.4710330622607));
#56061=CARTESIAN_POINT('Ctrl Pts',(40.0820278065648,-38.007890486043,14.4448645588017));
#56062=CARTESIAN_POINT('Ctrl Pts',(40.3181230618696,-38.4143606430357,14.4186960553428));
#56063=CARTESIAN_POINT('Ctrl Pts',(40.3316969948736,-38.8281685539702,14.3925275518839));
#56064=CARTESIAN_POINT('Ctrl Pts',(40.3452709278776,-39.2419764649047,14.366359048425));
#56065=CARTESIAN_POINT('Ctrl Pts',(40.1363235385808,-39.6631221297811,14.340190544966));
#56066=CARTESIAN_POINT('Ctrl Pts',(39.7987141516887,-39.9026904288663,14.3140220415071));
#56067=CARTESIAN_POINT('Ctrl Pts',(39.4611047647966,-40.1422587279515,14.2878535380482));
#56068=CARTESIAN_POINT('Ctrl Pts',(38.9948333803092,-40.2002496612456,14.2616850345893));
#56069=CARTESIAN_POINT('Ctrl Pts',(38.6086468373336,-40.0507988707032,14.2355165311303));
#56070=CARTESIAN_POINT('Ctrl Pts',(38.222460294358,-39.9013480801609,14.2093480276714));
#56071=CARTESIAN_POINT('Ctrl Pts',(37.9163585928943,-39.5444555657821,14.1831795242125));
#56072=CARTESIAN_POINT('Ctrl Pts',(37.8282870218577,-39.1398677193851,14.1570110207535));
#56073=CARTESIAN_POINT('Ctrl Pts',(37.7402154508211,-38.735279872988,14.1308425172946));
#56074=CARTESIAN_POINT('Ctrl Pts',(37.8701740102116,-38.2829966945726,14.1046740138357));
#56075=CARTESIAN_POINT('Ctrl Pts',(38.1583471155031,-37.9866613986385,14.0785055103768));
#56076=CARTESIAN_POINT('Ctrl Pts',(38.2388287062341,-37.9039002541439,14.0711971157114));
#56077=CARTESIAN_POINT('Ctrl Pts',(38.3316507930811,-37.8333028094348,14.063888721046));
#56078=CARTESIAN_POINT('Ctrl Pts',(38.4325424620227,-37.7762177647969,14.0565803263806));
#56079=CARTESIAN_POINT('Ctrl Pts',(38.4345426068235,-37.7764071067806,14.1934196736194));
#56080=CARTESIAN_POINT('Ctrl Pts',(38.2580569790832,-37.8781526020867,14.2061916163845));
#56081=CARTESIAN_POINT('Ctrl Pts',(38.104957080975,-38.0203170861652,14.2189635591495));
#56082=CARTESIAN_POINT('Ctrl Pts',(37.9966332783609,-38.1909038725227,14.2317355019146));
#56083=CARTESIAN_POINT('Ctrl Pts',(37.7746880461016,-38.5404200730695,14.2579040053735));
#56084=CARTESIAN_POINT('Ctrl Pts',(37.7407134737351,-39.0092534864306,14.2840725088324));
#56085=CARTESIAN_POINT('Ctrl Pts',(37.9098581438109,-39.3871556515897,14.3102410122914));
#56086=CARTESIAN_POINT('Ctrl Pts',(38.0790028138868,-39.7650578167487,14.3364095157503));
#56087=CARTESIAN_POINT('Ctrl Pts',(38.451266726405,-40.0520287337056,14.3625780192092));
#56088=CARTESIAN_POINT('Ctrl Pts',(38.8597647299447,-40.1193961008257,14.3887465226681));
#56089=CARTESIAN_POINT('Ctrl Pts',(39.2682627334845,-40.1867634679457,14.4149150261271));
#56090=CARTESIAN_POINT('Ctrl Pts',(39.7129948280458,-40.034527285229,14.441083529586));
#56091=CARTESIAN_POINT('Ctrl Pts',(39.9945169439557,-39.730947693679,14.4672520330449));
#56092=CARTESIAN_POINT('Ctrl Pts',(40.2760390598657,-39.4273681021289,14.4934205365039));
#56093=CARTESIAN_POINT('Ctrl Pts',(40.3943511971241,-38.9724451017455,14.5195890399628));
#56094=CARTESIAN_POINT('Ctrl Pts',(40.2964110981383,-38.570173729657,14.5457575434217));
#56095=CARTESIAN_POINT('Ctrl Pts',(40.1984709991525,-38.1679023575684,14.5719260468806));
#56096=CARTESIAN_POINT('Ctrl Pts',(39.8842786639224,-37.8182826137747,14.5980945503396));
#56097=CARTESIAN_POINT('Ctrl Pts',(39.4947165862021,-37.6780870841148,14.6242630537985));
#56098=CARTESIAN_POINT('Ctrl Pts',(39.1515458154337,-37.5545868495612,14.6473152604055));
#56099=CARTESIAN_POINT('Ctrl Pts',(38.7498873821672,-37.5936018678201,14.6703674670124));
#56100=CARTESIAN_POINT('Ctrl Pts',(38.4322601856233,-37.7739115851766,14.6934196736194));
#56101=CARTESIAN_POINT('Origin',(39.0658530619283,-38.8697713466883,15.5));
#56102=CARTESIAN_POINT('',(38.4346334551116,-37.7742886171168,15.1934196736194));
#56103=CARTESIAN_POINT('',(38.4347780105726,-37.7761824162226,15.0565803263806));
#56104=CARTESIAN_POINT('',(38.4336030619283,-37.7746822236028,15.5));
#56105=CARTESIAN_POINT('Ctrl Pts',(38.4347780105726,-37.7761824162226,15.0565803263806));
#56106=CARTESIAN_POINT('Ctrl Pts',(38.6003617341531,-37.6801555214811,15.0445774292198));
#56107=CARTESIAN_POINT('Ctrl Pts',(38.7864577331935,-37.6199570207433,15.032574532059));
#56108=CARTESIAN_POINT('Ctrl Pts',(38.9758802222154,-37.6064663135108,15.0205716348981));
#56109=CARTESIAN_POINT('Ctrl Pts',(39.3888557724309,-37.5770541129272,14.9944031314392));
#56110=CARTESIAN_POINT('Ctrl Pts',(39.8176427771529,-37.7696531482711,14.9682346279803));
#56111=CARTESIAN_POINT('Ctrl Pts',(40.0699686232679,-38.097899483489,14.9420661245214));
#56112=CARTESIAN_POINT('Ctrl Pts',(40.3222944693828,-38.4261458187069,14.9158976210624));
#56113=CARTESIAN_POINT('Ctrl Pts',(40.3981591568908,-38.8900394537989,14.8897291176035));
#56114=CARTESIAN_POINT('Ctrl Pts',(40.2635428887314,-39.2815654536187,14.8635606141446));
#56115=CARTESIAN_POINT('Ctrl Pts',(40.1289266205721,-39.6730914534386,14.8373921106856));
#56116=CARTESIAN_POINT('Ctrl Pts',(39.7838293967455,-39.9922498179864,14.8112236072267));
#56117=CARTESIAN_POINT('Ctrl Pts',(39.3829992856624,-40.0959251593026,14.7850551037678));
#56118=CARTESIAN_POINT('Ctrl Pts',(38.9821691745794,-40.1996005006187,14.7588866003089));
#56119=CARTESIAN_POINT('Ctrl Pts',(38.5256061762399,-40.0877928187031,14.7327180968499));
#56120=CARTESIAN_POINT('Ctrl Pts',(38.2180337582993,-39.8106400014137,14.706549593391));
#56121=CARTESIAN_POINT('Ctrl Pts',(37.9104613403587,-39.5334871841242,14.6803810899321));
#56122=CARTESIAN_POINT('Ctrl Pts',(37.7518795028168,-39.0909892314609,14.6542125864732));
#56123=CARTESIAN_POINT('Ctrl Pts',(37.8134079754514,-38.6815634416151,14.6280440830142));
#56124=CARTESIAN_POINT('Ctrl Pts',(37.869417493424,-38.308862151417,14.604222830803));
#56125=CARTESIAN_POINT('Ctrl Pts',(38.1078215318972,-37.963566125762,14.5804015785918));
#56126=CARTESIAN_POINT('Ctrl Pts',(38.4333416483911,-37.7729821125454,14.5565803263806));
#56127=CARTESIAN_POINT('Ctrl Pts',(38.4322601856233,-37.7739115851766,14.6934196736194));
#56128=CARTESIAN_POINT('Ctrl Pts',(38.389321969358,-37.7982866315292,14.6965359704714));
#56129=CARTESIAN_POINT('Ctrl Pts',(38.3479194071466,-37.825243810264,14.6996522673233));
#56130=CARTESIAN_POINT('Ctrl Pts',(38.308404587142,-37.854730696716,14.7027685641753));
#56131=CARTESIAN_POINT('Ctrl Pts',(37.976586486013,-38.102341154503,14.7289370676342));
#56132=CARTESIAN_POINT('Ctrl Pts',(37.7778821039655,-38.528333385603,14.7551055710931));
#56133=CARTESIAN_POINT('Ctrl Pts',(37.8013916118277,-38.941687151427,14.781274074552));
#56134=CARTESIAN_POINT('Ctrl Pts',(37.8249011196899,-39.355040917251,14.807442578011));
#56135=CARTESIAN_POINT('Ctrl Pts',(38.0706245174618,-39.7557562177991,14.8336110814699));
#56136=CARTESIAN_POINT('Ctrl Pts',(38.428377122171,-39.9641476765195,14.8597795849288));
#56137=CARTESIAN_POINT('Ctrl Pts',(38.7861297268802,-40.1725391352399,14.8859480883877));
#56138=CARTESIAN_POINT('Ctrl Pts',(39.2559115385268,-40.1886067521326,14.9121165918467));
#56139=CARTESIAN_POINT('Ctrl Pts',(39.6270665080505,-40.005145553951,14.9382850953056));
#56140=CARTESIAN_POINT('Ctrl Pts',(39.9982214775741,-39.8216843557693,14.9644535987645));
#56141=CARTESIAN_POINT('Ctrl Pts',(40.2707496049748,-39.4386943425132,14.9906221022235));
#56142=CARTESIAN_POINT('Ctrl Pts',(40.3224461866044,-39.0279128196441,15.0167906056824));
#56143=CARTESIAN_POINT('Ctrl Pts',(40.3741427682341,-38.6171312967749,15.0429591091413));
#56144=CARTESIAN_POINT('Ctrl Pts',(40.2050078040926,-38.1785582642928,15.0691276126002));
#56145=CARTESIAN_POINT('Ctrl Pts',(39.8908833495191,-37.9088550679237,15.0952961160591));
#56146=CARTESIAN_POINT('Ctrl Pts',(39.5767588949455,-37.6391518715546,15.1214646195181));
#56147=CARTESIAN_POINT('Ctrl Pts',(39.1176449499399,-37.5383185112986,15.147633122977));
#56148=CARTESIAN_POINT('Ctrl Pts',(38.7194137008705,-37.6515698720153,15.1738016264359));
#56149=CARTESIAN_POINT('Ctrl Pts',(38.6198981458899,-37.679870694817,15.1803409754971));
#56150=CARTESIAN_POINT('Ctrl Pts',(38.5241845298854,-37.7215404565648,15.1868803245583));
#56151=CARTESIAN_POINT('Ctrl Pts',(38.4346334551116,-37.7742886171168,15.1934196736194));
#56152=CARTESIAN_POINT('Origin',(39.0658530619283,-38.8697713466883,15.5));
#56153=CARTESIAN_POINT('',(38.4337315549884,-37.7763335227174,15.6934196736194));
#56154=CARTESIAN_POINT('',(38.4323663903519,-37.7745195378426,15.5565803263806));
#56155=CARTESIAN_POINT('',(38.4336030619283,-37.7746822236028,15.5));
#56156=CARTESIAN_POINT('Ctrl Pts',(38.4323663903519,-37.7745195378426,15.5565803263806));
#56157=CARTESIAN_POINT('Ctrl Pts',(38.7313730076301,-37.6052990985956,15.5349217833067));
#56158=CARTESIAN_POINT('Ctrl Pts',(39.1034689296549,-37.5582680121359,15.5132632402327));
#56159=CARTESIAN_POINT('Ctrl Pts',(39.4315419163111,-37.6572094658042,15.4916046971588));
#56160=CARTESIAN_POINT('Ctrl Pts',(39.8279295706787,-37.7767535073269,15.4654361936999));
#56161=CARTESIAN_POINT('Ctrl Pts',(40.1600516656646,-38.1093911753228,15.439267690241));
#56162=CARTESIAN_POINT('Ctrl Pts',(40.2789807143,-38.5059637820165,15.413099186782));
#56163=CARTESIAN_POINT('Ctrl Pts',(40.3979097629354,-38.9025363887101,15.3869306833231));
#56164=CARTESIAN_POINT('Ctrl Pts',(40.3036457652202,-39.3630439341015,15.3607621798642));
#56165=CARTESIAN_POINT('Ctrl Pts',(40.0384578014032,-39.6809893678464,15.3345936764052));
#56166=CARTESIAN_POINT('Ctrl Pts',(39.7732698375861,-39.9989348015912,15.3084251729463));
#56167=CARTESIAN_POINT('Ctrl Pts',(39.3371579076672,-40.1743181236895,15.2822566694874));
#56168=CARTESIAN_POINT('Ctrl Pts',(38.9256798191233,-40.1284953536109,15.2560881660285));
#56169=CARTESIAN_POINT('Ctrl Pts',(38.5142017305793,-40.0826725835323,15.2299196625696));
#56170=CARTESIAN_POINT('Ctrl Pts',(38.1273574834104,-39.8156437212769,15.2037511591106));
#56171=CARTESIAN_POINT('Ctrl Pts',(37.938612567216,-39.4471477114983,15.1775826556517));
#56172=CARTESIAN_POINT('Ctrl Pts',(37.7498676510216,-39.0786517017197,15.1514141521928));
#56173=CARTESIAN_POINT('Ctrl Pts',(37.7592220658018,-38.6086885444181,15.1252456487338));
#56174=CARTESIAN_POINT('Ctrl Pts',(37.9624813210464,-38.2479952475117,15.0990771452749));
#56175=CARTESIAN_POINT('Ctrl Pts',(38.0725101803872,-38.0527437595403,15.0849115389768));
#56176=CARTESIAN_POINT('Ctrl Pts',(38.239359037454,-37.8895116538819,15.0707459326787));
#56177=CARTESIAN_POINT('Ctrl Pts',(38.4347780105726,-37.7761824162226,15.0565803263806));
#56178=CARTESIAN_POINT('Ctrl Pts',(38.4346334551116,-37.7742886171168,15.1934196736194));
#56179=CARTESIAN_POINT('Ctrl Pts',(38.1658281265106,-37.9326226925712,15.2130488280172));
#56180=CARTESIAN_POINT('Ctrl Pts',(37.9525484899569,-38.1907752905068,15.2326779824149));
#56181=CARTESIAN_POINT('Ctrl Pts',(37.8586391249354,-38.4867967233546,15.2523071368127));
#56182=CARTESIAN_POINT('Ctrl Pts',(37.7334443512028,-38.881436132288,15.2784756402716));
#56183=CARTESIAN_POINT('Ctrl Pts',(37.8204033568707,-39.3433788684654,15.3046441437306));
#56184=CARTESIAN_POINT('Ctrl Pts',(38.0805226988896,-39.6654843197862,15.3308126471895));
#56185=CARTESIAN_POINT('Ctrl Pts',(38.3406420409085,-39.987589771107,15.3569811506484));
#56186=CARTESIAN_POINT('Ctrl Pts',(38.7739217192785,-40.1698579375713,15.3831496541074));
#56187=CARTESIAN_POINT('Ctrl Pts',(39.1860739715826,-40.1305576058448,15.4093181575663));
#56188=CARTESIAN_POINT('Ctrl Pts',(39.5982262238866,-40.0912572741182,15.4354866610252));
#56189=CARTESIAN_POINT('Ctrl Pts',(39.9892510501248,-39.8303884442009,15.4616551644841));
#56190=CARTESIAN_POINT('Ctrl Pts',(40.1838082722999,-39.4649278007734,15.4878236679431));
#56191=CARTESIAN_POINT('Ctrl Pts',(40.378365494475,-39.0994671573459,15.513992171402));
#56192=CARTESIAN_POINT('Ctrl Pts',(40.3764551125871,-38.6294147004082,15.5401606748609));
#56193=CARTESIAN_POINT('Ctrl Pts',(40.1789337635325,-38.2655475388609,15.5663291783198));
#56194=CARTESIAN_POINT('Ctrl Pts',(39.9814124144778,-37.9016803773136,15.5924976817788));
#56195=CARTESIAN_POINT('Ctrl Pts',(39.5882800982564,-37.6439985111568,15.6186661852377));
#56196=CARTESIAN_POINT('Ctrl Pts',(39.175822019074,-37.6080495523001,15.6448346886966));
#56197=CARTESIAN_POINT('Ctrl Pts',(38.9205626180181,-37.5858016920459,15.6610296836709));
#56198=CARTESIAN_POINT('Ctrl Pts',(38.6579013630336,-37.6484785302017,15.6772246786452));
#56199=CARTESIAN_POINT('Ctrl Pts',(38.4337315549884,-37.7763335227174,15.6934196736194));
#56200=CARTESIAN_POINT('Origin',(39.0658530619283,-38.8697713466883,15.5));
#56201=CARTESIAN_POINT('',(38.4325272584341,-37.7729978925048,16.1934196736194));
#56202=CARTESIAN_POINT('',(38.4342758514651,-37.7737507965446,16.0565803263806));
#56203=CARTESIAN_POINT('',(38.4336030619283,-37.7746822236028,15.5));
#56204=CARTESIAN_POINT('Ctrl Pts',(38.4342758514651,-37.7737507965446,16.0565803263806));
#56205=CARTESIAN_POINT('Ctrl Pts',(38.5046440871601,-37.732289208729,16.0514346408525));
#56206=CARTESIAN_POINT('Ctrl Pts',(38.5788878157804,-37.6977955005524,16.0462889553244));
#56207=CARTESIAN_POINT('Ctrl Pts',(38.655917096454,-37.6714445317292,16.0411432697963));
#56208=CARTESIAN_POINT('Ctrl Pts',(39.0476512952768,-37.5374360667673,16.0149747663373));
#56209=CARTESIAN_POINT('Ctrl Pts',(39.5114269646143,-37.6140195799122,15.9888062628784));
#56210=CARTESIAN_POINT('Ctrl Pts',(39.8392815814542,-37.8668541135745,15.9626377594195));
#56211=CARTESIAN_POINT('Ctrl Pts',(40.1671361982941,-38.1196886472368,15.9364692559606));
#56212=CARTESIAN_POINT('Ctrl Pts',(40.3590697626365,-38.5487742014165,15.9103007525016));
#56213=CARTESIAN_POINT('Ctrl Pts',(40.3290169828723,-38.9617037131001,15.8841322490427));
#56214=CARTESIAN_POINT('Ctrl Pts',(40.2989642031081,-39.3746332247836,15.8579637455838));
#56215=CARTESIAN_POINT('Ctrl Pts',(40.0469250792374,-39.771406693971,15.8317952421249));
#56216=CARTESIAN_POINT('Ctrl Pts',(39.685916950104,-39.974106180808,15.8056267386659));
#56217=CARTESIAN_POINT('Ctrl Pts',(39.3249088209707,-40.176805667645,15.779458235207));
#56218=CARTESIAN_POINT('Ctrl Pts',(38.8549316865748,-40.1854311721316,15.7532897317481));
#56219=CARTESIAN_POINT('Ctrl Pts',(38.4867288810042,-39.9961149153208,15.7271212282891));
#56220=CARTESIAN_POINT('Ctrl Pts',(38.1185260754337,-39.80679865851,15.7009527248302));
#56221=CARTESIAN_POINT('Ctrl Pts',(37.8520975986886,-39.4195406404018,15.6747842213713));
#56222=CARTESIAN_POINT('Ctrl Pts',(37.806913145733,-39.0079919599958,15.6486157179124));
#56223=CARTESIAN_POINT('Ctrl Pts',(37.7617286927774,-38.5964432795899,15.6224472144534));
#56224=CARTESIAN_POINT('Ctrl Pts',(37.9377882636112,-38.1606039368862,15.5962787109945));
#56225=CARTESIAN_POINT('Ctrl Pts',(38.2561446559027,-37.8959094730591,15.5701102075356));
#56226=CARTESIAN_POINT('Ctrl Pts',(38.3110111758702,-37.8502912149167,15.5656002471506));
#56227=CARTESIAN_POINT('Ctrl Pts',(38.3701042153674,-37.8097563252262,15.5610902867656));
#56228=CARTESIAN_POINT('Ctrl Pts',(38.4323663903519,-37.7745195378426,15.5565803263806));
#56229=CARTESIAN_POINT('Ctrl Pts',(38.4337315549884,-37.7763335227174,15.6934196736194));
#56230=CARTESIAN_POINT('Ctrl Pts',(38.2956790587637,-37.8550716053588,15.7033931821041));
#56231=CARTESIAN_POINT('Ctrl Pts',(38.1722247361697,-37.9585289981308,15.7133666905887));
#56232=CARTESIAN_POINT('Ctrl Pts',(38.0740874997392,-38.082093666717,15.7233401990734));
#56233=CARTESIAN_POINT('Ctrl Pts',(37.8165949017303,-38.4063027915471,15.7495087025323));
#56234=CARTESIAN_POINT('Ctrl Pts',(37.7333935478558,-38.868937092764,15.7756772059912));
#56235=CARTESIAN_POINT('Ctrl Pts',(37.8617919143246,-39.2625458504732,15.8018457094502));
#56236=CARTESIAN_POINT('Ctrl Pts',(37.9901902807933,-39.6561546081824,15.8280142129091));
#56237=CARTESIAN_POINT('Ctrl Pts',(38.3301883676052,-39.9807378223839,15.854182716368));
#56238=CARTESIAN_POINT('Ctrl Pts',(38.7293269910636,-40.0907485215641,15.8803512198269));
#56239=CARTESIAN_POINT('Ctrl Pts',(39.128465614522,-40.2007592207443,15.9065197232859));
#56240=CARTESIAN_POINT('Ctrl Pts',(39.5867447746269,-40.0961974049031,15.9326882267448));
#56241=CARTESIAN_POINT('Ctrl Pts',(39.898666648561,-39.8239498351585,15.9588567302037));
#56242=CARTESIAN_POINT('Ctrl Pts',(40.2105885224951,-39.551702265414,15.9850252336627));
#56243=CARTESIAN_POINT('Ctrl Pts',(40.3761531102584,-39.1117689417661,16.0111937371216));
#56244=CARTESIAN_POINT('Ctrl Pts',(40.321119282596,-38.701421195982,16.0373622405805));
#56245=CARTESIAN_POINT('Ctrl Pts',(40.2660854549337,-38.291073450198,16.0635307440394));
#56246=CARTESIAN_POINT('Ctrl Pts',(39.9904532118457,-37.9103112822778,16.0896992474984));
#56247=CARTESIAN_POINT('Ctrl Pts',(39.6178193276329,-37.7298729742913,16.1158677509573));
#56248=CARTESIAN_POINT('Ctrl Pts',(39.2497117383559,-37.5516264074059,16.1417183918447));
#56249=CARTESIAN_POINT('Ctrl Pts',(38.7869447075705,-37.5688666846834,16.167569032732));
#56250=CARTESIAN_POINT('Ctrl Pts',(38.4325272584341,-37.7729978925048,16.1934196736194));
#56251=CARTESIAN_POINT('Origin',(39.0658530619283,-38.8697713466883,15.5));
#56252=CARTESIAN_POINT('',(38.4349705604869,-37.7753960169021,16.6934196736194));
#56253=CARTESIAN_POINT('',(38.4341423505256,-37.7764525809616,16.5565803263806));
#56254=CARTESIAN_POINT('',(38.4336030619283,-37.7746822236028,15.5));
#56255=CARTESIAN_POINT('Ctrl Pts',(38.4341423505256,-37.7764525809616,16.5565803263806));
#56256=CARTESIAN_POINT('Ctrl Pts',(38.6388834301988,-37.6590722267018,16.5417789949394));
#56257=CARTESIAN_POINT('Ctrl Pts',(38.8753711836181,-37.5959619576061,16.5269776634982));
#56258=CARTESIAN_POINT('Ctrl Pts',(39.1094100531276,-37.604015667637,16.5121763320569));
#56259=CARTESIAN_POINT('Ctrl Pts',(39.52318681305,-37.6182544906534,16.486007828598));
#56260=CARTESIAN_POINT('Ctrl Pts',(39.929308939441,-37.8549351283607,16.4598393251391));
#56261=CARTESIAN_POINT('Ctrl Pts',(40.1456664429883,-38.2079271704546,16.4336708216802));
#56262=CARTESIAN_POINT('Ctrl Pts',(40.3620239465357,-38.5609192125485,16.4075023182212));
#56263=CARTESIAN_POINT('Ctrl Pts',(40.3886168272394,-39.0302226590291,16.3813338147623));
#56264=CARTESIAN_POINT('Ctrl Pts',(40.2135205214552,-39.4053962654636,16.3551653113034));
#56265=CARTESIAN_POINT('Ctrl Pts',(40.0384242156709,-39.780569871898,16.3289968078445));
#56266=CARTESIAN_POINT('Ctrl Pts',(39.6616387233988,-40.0616136382864,16.3028283043855));
#56267=CARTESIAN_POINT('Ctrl Pts',(39.2521191380692,-40.122504199314,16.2766598009266));
#56268=CARTESIAN_POINT('Ctrl Pts',(38.8425995527396,-40.1833947603416,16.2504912974677));
#56269=CARTESIAN_POINT('Ctrl Pts',(38.4003458743526,-40.0241321160084,16.2243227940088));
#56270=CARTESIAN_POINT('Ctrl Pts',(38.1236699093341,-39.716131529034,16.1981542905498));
#56271=CARTESIAN_POINT('Ctrl Pts',(37.8469939443156,-39.4081309420596,16.1719857870909));
#56272=CARTESIAN_POINT('Ctrl Pts',(37.7358956926655,-38.951392412444,16.145817283632));
#56273=CARTESIAN_POINT('Ctrl Pts',(37.8401929309945,-38.5507229261019,16.119648780173));
#56274=CARTESIAN_POINT('Ctrl Pts',(37.9239815150653,-38.2288397249847,16.0986259622422));
#56275=CARTESIAN_POINT('Ctrl Pts',(38.1467847875343,-37.9431430780994,16.0776031443114));
#56276=CARTESIAN_POINT('Ctrl Pts',(38.4342758514651,-37.7737507965446,16.0565803263806));
#56277=CARTESIAN_POINT('Ctrl Pts',(38.4325272584341,-37.7729978925048,16.1934196736194));
#56278=CARTESIAN_POINT('Ctrl Pts',(38.4281692990986,-37.775507914246,16.193737536191));
#56279=CARTESIAN_POINT('Ctrl Pts',(38.42382772163,-37.7780461928786,16.1940553987625));
#56280=CARTESIAN_POINT('Ctrl Pts',(38.4195029034437,-37.7806127124219,16.1943732613341));
#56281=CARTESIAN_POINT('Ctrl Pts',(38.0634558888049,-37.9919052065918,16.220541764793));
#56282=CARTESIAN_POINT('Ctrl Pts',(37.8209973848649,-38.3946046429843,16.2467102682519));
#56283=CARTESIAN_POINT('Ctrl Pts',(37.8008486672722,-38.8081358071838,16.2728787717108));
#56284=CARTESIAN_POINT('Ctrl Pts',(37.7806999496795,-39.2216669713833,16.2990472751698));
#56285=CARTESIAN_POINT('Ctrl Pts',(37.9828610184341,-39.6460298633899,16.3252157786287));
#56286=CARTESIAN_POINT('Ctrl Pts',(38.3166804464026,-39.8909351187556,16.3513842820876));
#56287=CARTESIAN_POINT('Ctrl Pts',(38.6504998743712,-40.1358403741212,16.3775527855466));
#56288=CARTESIAN_POINT('Ctrl Pts',(39.1159776615536,-40.2012879928461,16.4037212890055));
#56289=CARTESIAN_POINT('Ctrl Pts',(39.5043880368528,-40.0579304834052,16.4298897924644));
#56290=CARTESIAN_POINT('Ctrl Pts',(39.8927984121519,-39.9145729739643,16.4560582959233));
#56291=CARTESIAN_POINT('Ctrl Pts',(40.2041413755678,-39.5624103363577,16.4822267993823));
#56292=CARTESIAN_POINT('Ctrl Pts',(40.2988070379275,-39.1593564860685,16.5083953028412));
#56293=CARTESIAN_POINT('Ctrl Pts',(40.3934727002873,-38.7563026357793,16.5345638063001));
#56294=CARTESIAN_POINT('Ctrl Pts',(40.271461061591,-38.3023575728076,16.560732309759));
#56295=CARTESIAN_POINT('Ctrl Pts',(39.9874835980573,-38.001075653904,16.586900813218));
#56296=CARTESIAN_POINT('Ctrl Pts',(39.7035061345236,-37.6997937350005,16.6130693166769));
#56297=CARTESIAN_POINT('Ctrl Pts',(39.2575628461526,-37.5511749601651,16.6392378201358));
#56298=CARTESIAN_POINT('Ctrl Pts',(38.849619989904,-37.6218617656895,16.6654063235948));
#56299=CARTESIAN_POINT('Ctrl Pts',(38.7040525518055,-37.6470851444788,16.6747441069363));
#56300=CARTESIAN_POINT('Ctrl Pts',(38.5633236984099,-37.7002326432607,16.6840818902779));
#56301=CARTESIAN_POINT('Ctrl Pts',(38.4349705604869,-37.7753960169021,16.6934196736194));
#56302=CARTESIAN_POINT('Origin',(39.0658530619283,-38.8697713466883,15.5));
#56303=CARTESIAN_POINT('',(38.4329072841441,-37.7756148875603,17.1934196736194));
#56304=CARTESIAN_POINT('',(38.4323100738575,-37.7733715239653,17.0565803263806));
#56305=CARTESIAN_POINT('',(38.4336030619283,-37.7746822236028,15.5));
#56306=CARTESIAN_POINT('Ctrl Pts',(38.4323100738575,-37.7733715239653,17.0565803263806));
#56307=CARTESIAN_POINT('Ctrl Pts',(38.7684978446967,-37.5814140598882,17.0321233490263));
#56308=CARTESIAN_POINT('Ctrl Pts',(39.2005574419278,-37.5523442127138,17.0076663716719));
#56309=CARTESIAN_POINT('Ctrl Pts',(39.5571950289671,-37.7024591900708,16.9832093943176));
#56310=CARTESIAN_POINT('Ctrl Pts',(39.9387905055794,-37.8630793782195,16.9570408908587));
#56311=CARTESIAN_POINT('Ctrl Pts',(40.2340383736987,-38.2288410235792,16.9308723873998));
#56312=CARTESIAN_POINT('Ctrl Pts',(40.3105459562687,-38.635732327761,16.9047038839408));
#56313=CARTESIAN_POINT('Ctrl Pts',(40.3870535388386,-39.0426236319427,16.8785353804819));
#56314=CARTESIAN_POINT('Ctrl Pts',(40.2448208358592,-39.4906445949467,16.852366877023));
#56315=CARTESIAN_POINT('Ctrl Pts',(39.9476266935978,-39.7788972563362,16.8261983735641));
#56316=CARTESIAN_POINT('Ctrl Pts',(39.6504325513363,-40.0671499177256,16.8000298701051));
#56317=CARTESIAN_POINT('Ctrl Pts',(39.1982769697929,-40.1956342775007,16.7738613666462));
#56318=CARTESIAN_POINT('Ctrl Pts',(38.7939118807236,-40.1067364387691,16.7476928631873));
#56319=CARTESIAN_POINT('Ctrl Pts',(38.3895467916544,-40.0178386000374,16.7215243597284));
#56320=CARTESIAN_POINT('Ctrl Pts',(38.0329721950594,-39.7115585627991,16.6953558562694));
#56321=CARTESIAN_POINT('Ctrl Pts',(37.8840803814008,-39.3252359279146,16.6691873528105));
#56322=CARTESIAN_POINT('Ctrl Pts',(37.7351885677422,-38.9389132930302,16.6430188493516));
#56323=CARTESIAN_POINT('Ctrl Pts',(37.7939795370199,-38.4725480604997,16.6168503458927));
#56324=CARTESIAN_POINT('Ctrl Pts',(38.0340907183856,-38.1352639483972,16.5906818424337));
#56325=CARTESIAN_POINT('Ctrl Pts',(38.1383911078307,-37.9887532193016,16.579314670416));
#56326=CARTESIAN_POINT('Ctrl Pts',(38.2769046668091,-37.8665987062389,16.5679474983983));
#56327=CARTESIAN_POINT('Ctrl Pts',(38.4341423505256,-37.7764525809616,16.5565803263806));
#56328=CARTESIAN_POINT('Ctrl Pts',(38.4349705604869,-37.7753960169021,16.6934196736194));
#56329=CARTESIAN_POINT('Ctrl Pts',(38.2036227489615,-37.9108728917196,16.7102503937368));
#56330=CARTESIAN_POINT('Ctrl Pts',(38.0124806835606,-38.1178740898995,16.7270811138542));
#56331=CARTESIAN_POINT('Ctrl Pts',(37.9056793271332,-38.3618028680121,16.7439118339715));
#56332=CARTESIAN_POINT('Ctrl Pts',(37.7396239447373,-38.7410647789262,16.7700803374304));
#56333=CARTESIAN_POINT('Ctrl Pts',(37.7774556040718,-39.2095962148701,16.7962488408894));
#56334=CARTESIAN_POINT('Ctrl Pts',(38.0022100801907,-39.5573021560724,16.8224173443483));
#56335=CARTESIAN_POINT('Ctrl Pts',(38.2269645563097,-39.9050080972747,16.8485858478072));
#56336=CARTESIAN_POINT('Ctrl Pts',(38.6386418492131,-40.1318885437354,16.8747543512661));
#56337=CARTESIAN_POINT('Ctrl Pts',(39.0526410872976,-40.1362075141883,16.9009228547251));
#56338=CARTESIAN_POINT('Ctrl Pts',(39.4666403253821,-40.1405264846412,16.927091358184));
#56339=CARTESIAN_POINT('Ctrl Pts',(39.8829615086478,-39.9222839790864,16.9532598616429));
#56340=CARTESIAN_POINT('Ctrl Pts',(40.1149210262726,-39.5793427181871,16.9794283651019));
#56341=CARTESIAN_POINT('Ctrl Pts',(40.3468805438973,-39.2364014572879,17.0055968685608));
#56342=CARTESIAN_POINT('Ctrl Pts',(40.3944783958811,-38.7687614410443,17.0317653720197));
#56343=CARTESIAN_POINT('Ctrl Pts',(40.236371633473,-38.3861176323113,17.0579338754786));
#56344=CARTESIAN_POINT('Ctrl Pts',(40.0782648710649,-38.0034738235784,17.0841023789376));
#56345=CARTESIAN_POINT('Ctrl Pts',(39.7144534942649,-37.7058262223562,17.1102708823965));
#56346=CARTESIAN_POINT('Ctrl Pts',(39.3080738473792,-37.6266443201348,17.1364393858554));
#56347=CARTESIAN_POINT('Ctrl Pts',(39.0131183836182,-37.5691730986546,17.1554328151101));
#56348=CARTESIAN_POINT('Ctrl Pts',(38.6957377885278,-37.6267904626672,17.1744262443648));
#56349=CARTESIAN_POINT('Ctrl Pts',(38.4329072841441,-37.7756148875603,17.1934196736194));
#56350=CARTESIAN_POINT('Origin',(39.0658530619283,-38.8697713466883,15.5));
#56351=CARTESIAN_POINT('',(38.4333577759012,-37.7730251466968,17.6934196736194));
#56352=CARTESIAN_POINT('',(38.4348713855213,-37.7748596688487,17.5565803263806));
#56353=CARTESIAN_POINT('',(38.4336030619283,-37.7746822236028,15.5));
#56354=CARTESIAN_POINT('',(40.2595650866584,-39.2869186252539,18.));
#56355=CARTESIAN_POINT('Ctrl Pts',(38.4333577759012,-37.7730251466968,17.6934196736194));
#56356=CARTESIAN_POINT('Ctrl Pts',(38.1097262681979,-37.9625959827323,17.7171076053695));
#56357=CARTESIAN_POINT('Ctrl Pts',(37.8720798795256,-38.3048233518517,17.7407955371196));
#56358=CARTESIAN_POINT('Ctrl Pts',(37.8144498218249,-38.6752097670202,17.7644834688697));
#56359=CARTESIAN_POINT('Ctrl Pts',(37.7507848138289,-39.084382601894,17.7906519723286));
#56360=CARTESIAN_POINT('Ctrl Pts',(37.9068123877648,-39.5279208384948,17.8168204757875));
#56361=CARTESIAN_POINT('Ctrl Pts',(38.2131597275406,-39.8064869141387,17.8429889792464));
#56362=CARTESIAN_POINT('Ctrl Pts',(38.5195070673165,-40.0850529897826,17.8691574827054));
#56363=CARTESIAN_POINT('Ctrl Pts',(38.9761741729324,-40.1986469044696,17.8953259861643));
#56364=CARTESIAN_POINT('Ctrl Pts',(39.3768946753638,-40.0972493078634,17.9214944896232));
#56365=CARTESIAN_POINT('Ctrl Pts',(39.7776151777952,-39.9958517112573,17.9476629930822));
#56366=CARTESIAN_POINT('Ctrl Pts',(40.1223890770422,-39.679462603358,17.9738314965411));
#56367=CARTESIAN_POINT('Ctrl Pts',(40.2595650866584,-39.2869186252539,18.));
#56368=CARTESIAN_POINT('',(39.301526156426,-37.6253017999342,18.));
#56369=CARTESIAN_POINT('Origin',(39.0658530619283,-38.8697713466883,18.));
#56370=CARTESIAN_POINT('Ctrl Pts',(39.301526596644,-37.6252897660473,18.));
#56371=CARTESIAN_POINT('Ctrl Pts',(39.6885864653113,-37.7000302410441,17.975091839613));
#56372=CARTESIAN_POINT('Ctrl Pts',(40.0399465491499,-37.9695057059562,17.950183679226));
#56373=CARTESIAN_POINT('Ctrl Pts',(40.2093266637559,-38.3254078043634,17.925275518839));
#56374=CARTESIAN_POINT('Ctrl Pts',(40.3872773452222,-38.6993184082982,17.89910701538));
#56375=CARTESIAN_POINT('Ctrl Pts',(40.3643659014498,-39.1686232325653,17.8729385119211));
#56376=CARTESIAN_POINT('Ctrl Pts',(40.1507520928543,-39.5232247114421,17.8467700084622));
#56377=CARTESIAN_POINT('Ctrl Pts',(39.9371382842589,-39.8778261903189,17.8206015050033));
#56378=CARTESIAN_POINT('Ctrl Pts',(39.5328221108402,-40.1177243238052,17.7944330015443));
#56379=CARTESIAN_POINT('Ctrl Pts',(39.1191596128741,-40.1351764464736,17.7682644980854));
#56380=CARTESIAN_POINT('Ctrl Pts',(38.705497114908,-40.1526285691419,17.7420959946265));
#56381=CARTESIAN_POINT('Ctrl Pts',(38.2824882923945,-39.9476346809923,17.7159274911676));
#56382=CARTESIAN_POINT('Ctrl Pts',(38.0397877964566,-39.6122000494564,17.6897589877086));
#56383=CARTESIAN_POINT('Ctrl Pts',(37.7970873005187,-39.2767654179205,17.6635904842497));
#56384=CARTESIAN_POINT('Ctrl Pts',(37.7346951311564,-38.8108900429983,17.6374219807908));
#56385=CARTESIAN_POINT('Ctrl Pts',(37.8806022560882,-38.4234367664048,17.6112534773319));
#56386=CARTESIAN_POINT('Ctrl Pts',(37.9822155342897,-38.1536048606431,17.5930290936814));
#56387=CARTESIAN_POINT('Ctrl Pts',(38.184855409418,-37.9218082144096,17.574804710031));
#56388=CARTESIAN_POINT('Ctrl Pts',(38.4348713855213,-37.7748596688487,17.5565803263806));
#56389=CARTESIAN_POINT('Origin',(39.0658530619283,-38.8697713466883,19.1042117235887));
#56390=CARTESIAN_POINT('',(38.2940340733258,-37.531419596366,14.3957882764113));
#56391=CARTESIAN_POINT('',(38.2954995370357,-37.5355989289915,14.3542117235887));
#56392=CARTESIAN_POINT('',(38.2943530619283,-37.5334941486488,19.1042117235887));
#56393=CARTESIAN_POINT('',(37.9741697098829,-39.9602191716056,14.));
#56394=CARTESIAN_POINT('Ctrl Pts',(38.2954995370357,-37.5355989289915,14.3542117235887));
#56395=CARTESIAN_POINT('Ctrl Pts',(38.5213873438295,-37.4053726489247,14.3408151628949));
#56396=CARTESIAN_POINT('Ctrl Pts',(39.2812420752165,-37.1810251467922,14.3012500987421));
#56397=CARTESIAN_POINT('Ctrl Pts',(40.5621358440548,-37.8394569175814,14.2355165311303));
#56398=CARTESIAN_POINT('Ctrl Pts',(40.7517455388365,-39.5501918673983,14.1570110207536));
#56399=CARTESIAN_POINT('Ctrl Pts',(39.4258164610498,-40.6499822516745,14.0785055103768));
#56400=CARTESIAN_POINT('Ctrl Pts',(38.3327559670706,-40.3192117233802,14.0261685034589));
#56401=CARTESIAN_POINT('Ctrl Pts',(37.9741697098829,-39.9602191716056,14.));
#56402=CARTESIAN_POINT('',(37.5730942570913,-39.2702598116583,14.));
#56403=CARTESIAN_POINT('Origin',(39.0658530619283,-38.8697713466883,14.));
#56404=CARTESIAN_POINT('Ctrl Pts',(38.2940340733258,-37.531419596366,14.3957882764113));
#56405=CARTESIAN_POINT('Ctrl Pts',(38.33317399173,-37.5085041378476,14.3934410251636));
#56406=CARTESIAN_POINT('Ctrl Pts',(38.8212071098193,-37.2523822679137,14.3649252704569));
#56407=CARTESIAN_POINT('Ctrl Pts',(40.0177412802272,-37.3220721610692,14.3102410122913));
#56408=CARTESIAN_POINT('Ctrl Pts',(40.8820235552811,-38.8100518816853,14.2317355019146));
#56409=CARTESIAN_POINT('Ctrl Pts',(40.1171224362185,-40.3517547545304,14.1532299915378));
#56410=CARTESIAN_POINT('Ctrl Pts',(38.4376290919279,-40.5606360835952,14.075984824233));
#56411=CARTESIAN_POINT('Ctrl Pts',(37.6993939872544,-39.7344135992462,14.024908160387));
#56412=CARTESIAN_POINT('Ctrl Pts',(37.5730796542559,-39.270261446955,14.));
#56413=CARTESIAN_POINT('Origin',(39.0658530619283,-38.8697713466883,19.1042117235887));
#56414=CARTESIAN_POINT('',(38.2957867873204,-37.5353247514265,14.8957882764113));
#56415=CARTESIAN_POINT('',(38.2927144236218,-37.5325537808421,14.8542117235887));
#56416=CARTESIAN_POINT('',(38.2943530619283,-37.5334941486488,19.1042117235887));
#56417=CARTESIAN_POINT('Ctrl Pts',(38.2927144236218,-37.5325537808421,14.8542117235887));
#56418=CARTESIAN_POINT('Ctrl Pts',(38.6802974716781,-37.3125317216241,14.8311595169817));
#56419=CARTESIAN_POINT('Ctrl Pts',(39.7267977629897,-37.2108801077358,14.7819388069158));
#56420=CARTESIAN_POINT('Ctrl Pts',(40.831316288814,-38.4399409113081,14.706549593391));
#56421=CARTESIAN_POINT('Ctrl Pts',(40.3982068515902,-40.1052936742774,14.6280440830142));
#56422=CARTESIAN_POINT('Ctrl Pts',(38.7701602990205,-40.6625900679474,14.5495385726375));
#56423=CARTESIAN_POINT('Ctrl Pts',(37.4074005907985,-39.6120654537969,14.4710330622607));
#56424=CARTESIAN_POINT('Ctrl Pts',(37.5105490854526,-38.1886638489127,14.4059241125778));
#56425=CARTESIAN_POINT('Ctrl Pts',(38.0801438046487,-37.6597533768028,14.3669836663538));
#56426=CARTESIAN_POINT('Ctrl Pts',(38.2954995370357,-37.5355989289915,14.3542117235887));
#56427=CARTESIAN_POINT('Ctrl Pts',(38.2957867873204,-37.5353247514265,14.8957882764113));
#56428=CARTESIAN_POINT('Ctrl Pts',(38.4978395239631,-37.4181483982544,14.8837853792504));
#56429=CARTESIAN_POINT('Ctrl Pts',(39.2200040297691,-37.1845419759791,14.8456139786307));
#56430=CARTESIAN_POINT('Ctrl Pts',(40.5064460859517,-37.7623754838001,14.7812740745521));
#56431=CARTESIAN_POINT('Ctrl Pts',(40.7841666383236,-39.4605673674226,14.7027685641753));
#56432=CARTESIAN_POINT('Ctrl Pts',(39.5208569909583,-40.6289217126118,14.6242630537985));
#56433=CARTESIAN_POINT('Ctrl Pts',(37.8495006293029,-40.2196233657656,14.5457575434217));
#56434=CARTESIAN_POINT('Ctrl Pts',(37.2863317343909,-38.6481881568849,14.4695992842926));
#56435=CARTESIAN_POINT('Ctrl Pts',(37.8968197279323,-37.7639788153404,14.4196095286225));
#56436=CARTESIAN_POINT('Ctrl Pts',(38.2940340733258,-37.531419596366,14.3957882764113));
#56437=CARTESIAN_POINT('Origin',(39.0658530619283,-38.8697713466883,19.1042117235887));
#56438=CARTESIAN_POINT('',(38.2928440194274,-37.5332956321379,15.3957882764113));
#56439=CARTESIAN_POINT('',(38.2956103942191,-37.5330138522408,15.3542117235887));
#56440=CARTESIAN_POINT('',(38.2943530619283,-37.5334941486488,19.1042117235887));
#56441=CARTESIAN_POINT('Ctrl Pts',(38.2956103942191,-37.5330138522408,15.3542117235887));
#56442=CARTESIAN_POINT('Ctrl Pts',(38.4048846594434,-37.4686481648294,15.3476723745276));
#56443=CARTESIAN_POINT('Ctrl Pts',(38.9890534180561,-37.2143251749767,15.3149645220075));
#56444=CARTESIAN_POINT('Ctrl Pts',(40.2495149974675,-37.4911553124802,15.2560881660285));
#56445=CARTESIAN_POINT('Ctrl Pts',(40.8686733596745,-39.0966551680434,15.1775826556517));
#56446=CARTESIAN_POINT('Ctrl Pts',(39.8710199775172,-40.4986802936762,15.0990771452749));
#56447=CARTESIAN_POINT('Ctrl Pts',(38.151273037136,-40.4398609986215,15.0205716348981));
#56448=CARTESIAN_POINT('Ctrl Pts',(37.2517446794564,-38.9729482851088,14.9420661245214));
#56449=CARTESIAN_POINT('Ctrl Pts',(37.7655552987949,-37.8714157983081,14.8866128207516));
#56450=CARTESIAN_POINT('Ctrl Pts',(38.2403192732087,-37.5622973130857,14.8573280204407));
#56451=CARTESIAN_POINT('Ctrl Pts',(38.2927144236218,-37.5325537808421,14.8542117235887));
#56452=CARTESIAN_POINT('Ctrl Pts',(38.2928440194274,-37.5332956321379,15.3957882764113));
#56453=CARTESIAN_POINT('Ctrl Pts',(38.6577053958294,-37.3268052108188,15.3741297333373));
#56454=CARTESIAN_POINT('Ctrl Pts',(39.6603483962762,-37.2000760884312,15.3263026868045));
#56455=CARTESIAN_POINT('Ctrl Pts',(40.8063139857151,-38.3478206288557,15.2523071368127));
#56456=CARTESIAN_POINT('Ctrl Pts',(40.4612384258705,-40.0336169338117,15.1738016264359));
#56457=CARTESIAN_POINT('Ctrl Pts',(38.8647480157521,-40.6756488816116,15.0952961160592));
#56458=CARTESIAN_POINT('Ctrl Pts',(37.4486135593306,-39.6981268544226,15.0167906056824));
#56459=CARTESIAN_POINT('Ctrl Pts',(37.4776219436003,-38.2407538193379,14.9502879924664));
#56460=CARTESIAN_POINT('Ctrl Pts',(38.057327731945,-37.6736142047347,14.9099538827094));
#56461=CARTESIAN_POINT('Ctrl Pts',(38.2957867873204,-37.5353247514265,14.8957882764113));
#56462=CARTESIAN_POINT('Origin',(39.0658530619283,-38.8697713466883,19.1042117235887));
#56463=CARTESIAN_POINT('',(38.2951740301017,-37.5323575792927,15.8957882764113));
#56464=CARTESIAN_POINT('',(38.2945098549624,-37.5355091383948,15.8542117235887));
#56465=CARTESIAN_POINT('',(38.2943530619283,-37.5334941486488,19.1042117235887));
#56466=CARTESIAN_POINT('Ctrl Pts',(38.2945098549624,-37.5355091383948,15.8542117235887));
#56467=CARTESIAN_POINT('Ctrl Pts',(38.5680519773933,-37.379494703083,15.8380167286145));
#56468=CARTESIAN_POINT('Ctrl Pts',(39.406457455491,-37.1794324424244,15.7956532301813));
#56469=CARTESIAN_POINT('Ctrl Pts',(40.6627777316899,-38.0028980795747,15.7271212282892));
#56470=CARTESIAN_POINT('Ctrl Pts',(40.6697711344255,-39.7236357807726,15.6486157179124));
#56471=CARTESIAN_POINT('Ctrl Pts',(39.2383326839261,-40.6786075590939,15.5701102075356));
#56472=CARTESIAN_POINT('Ctrl Pts',(37.6522103975089,-40.0113720173278,15.4916046971588));
#56473=CARTESIAN_POINT('Ctrl Pts',(37.3603930477839,-38.4611828913061,15.4196385358432));
#56474=CARTESIAN_POINT('Ctrl Pts',(37.9676019940362,-37.7262202408736,15.3738408779865));
#56475=CARTESIAN_POINT('Ctrl Pts',(38.2956103942191,-37.5330138522408,15.3542117235887));
#56476=CARTESIAN_POINT('Ctrl Pts',(38.2951740301017,-37.5323575792927,15.8957882764113));
#56477=CARTESIAN_POINT('Ctrl Pts',(38.381040528858,-37.4817642775928,15.8906425908832));
#56478=CARTESIAN_POINT('Ctrl Pts',(38.9323618573136,-37.2256198547756,15.8593284018961));
#56479=CARTESIAN_POINT('Ctrl Pts',(40.1754824724718,-37.430896996864,15.8018457094502));
#56480=CARTESIAN_POINT('Ctrl Pts',(40.8781004790678,-39.0016657040982,15.7233401990734));
#56481=CARTESIAN_POINT('Ctrl Pts',(39.9554519188484,-40.454148415738,15.6448346886966));
#56482=CARTESIAN_POINT('Ctrl Pts',(38.2349899535507,-40.4857241059463,15.5663291783198));
#56483=CARTESIAN_POINT('Ctrl Pts',(37.2596657788943,-39.0680749435716,15.4878236679431));
#56484=CARTESIAN_POINT('Ctrl Pts',(37.7263629251969,-37.9127558858068,15.4309767006402));
#56485=CARTESIAN_POINT('Ctrl Pts',(38.2168689019888,-37.5762931512624,15.4002982367963));
#56486=CARTESIAN_POINT('Ctrl Pts',(38.2928440194274,-37.5332956321379,15.3957882764113));
#56487=CARTESIAN_POINT('Origin',(39.0658530619283,-38.8697713466883,19.1042117235887));
#56488=CARTESIAN_POINT('',(38.295011126227,-37.5356544186406,16.3957882764113));
#56489=CARTESIAN_POINT('',(38.2930403179255,-37.5314388517851,16.3542117235887));
#56490=CARTESIAN_POINT('',(38.2943530619283,-37.5334941486488,19.1042117235887));
#56491=CARTESIAN_POINT('Ctrl Pts',(38.2930403179255,-37.5314388517851,16.3542117235887));
#56492=CARTESIAN_POINT('Ctrl Pts',(38.7255164935028,-37.2823487342141,16.3283610827014));
#56493=CARTESIAN_POINT('Ctrl Pts',(39.8618384352913,-37.240015326582,16.276341938355));
#56494=CARTESIAN_POINT('Ctrl Pts',(40.8667697353107,-38.6282412326641,16.1981542905498));
#56495=CARTESIAN_POINT('Ctrl Pts',(40.2606815765474,-40.2387207543454,16.119648780173));
#56496=CARTESIAN_POINT('Ctrl Pts',(38.5830428006472,-40.6214939022528,16.0411432697963));
#56497=CARTESIAN_POINT('Ctrl Pts',(37.3383997450109,-39.4332806175246,15.9626377594195));
#56498=CARTESIAN_POINT('Ctrl Pts',(37.5801461044556,-38.0890698220828,15.900327244017));
#56499=CARTESIAN_POINT('Ctrl Pts',(38.1260519651446,-37.6315889023455,15.8641852320734));
#56500=CARTESIAN_POINT('Ctrl Pts',(38.2945098549624,-37.5355091383948,15.8542117235887));
#56501=CARTESIAN_POINT('Ctrl Pts',(38.295011126227,-37.5356544186406,16.3957882764113));
#56502=CARTESIAN_POINT('Ctrl Pts',(38.5448454369709,-37.3924216099234,16.3809869449701));
#56503=CARTESIAN_POINT('Ctrl Pts',(39.3436107151107,-37.1792592329343,16.3400171100699));
#56504=CARTESIAN_POINT('Ctrl Pts',(40.6150494715948,-37.9202307686755,16.2728787717108));
#56505=CARTESIAN_POINT('Ctrl Pts',(40.7123989731982,-39.6382265407265,16.1943732613341));
#56506=CARTESIAN_POINT('Ctrl Pts',(39.333086957597,-40.6670534245635,16.1158677509573));
#56507=CARTESIAN_POINT('Ctrl Pts',(37.7141132310224,-40.0840350136355,16.0373622405805));
#56508=CARTESIAN_POINT('Ctrl Pts',(37.3340693749042,-38.521628139946,15.9640024157318));
#56509=CARTESIAN_POINT('Ctrl Pts',(37.9443644518927,-37.7390576903556,15.9168110943421));
#56510=CARTESIAN_POINT('Ctrl Pts',(38.2951740301017,-37.5323575792927,15.8957882764113));
#56511=CARTESIAN_POINT('Origin',(39.0658530619283,-38.8697713466883,19.1042117235887));
#56512=CARTESIAN_POINT('',(38.2927752994979,-37.531894773765,16.8957882764113));
#56513=CARTESIAN_POINT('',(38.2960217454205,-37.5343651514648,16.8542117235887));
#56514=CARTESIAN_POINT('',(38.2943530619283,-37.5334941486488,19.1042117235887));
#56515=CARTESIAN_POINT('Ctrl Pts',(38.2960217454205,-37.5343651514648,16.8542117235887));
#56516=CARTESIAN_POINT('Ctrl Pts',(38.4526440402526,-37.4426474088561,16.8448739402472));
#56517=CARTESIAN_POINT('Ctrl Pts',(39.1056117500068,-37.1960483659351,16.8093676534467));
#56518=CARTESIAN_POINT('Ctrl Pts',(40.3881062726606,-37.623463173289,16.7476928631873));
#56519=CARTESIAN_POINT('Ctrl Pts',(40.834758606014,-39.2852359660895,16.6691873528105));
#56520=CARTESIAN_POINT('Ctrl Pts',(39.6950143769496,-40.5744102242793,16.5906818424337));
#56521=CARTESIAN_POINT('Ctrl Pts',(37.9910233315818,-40.3348238050803,16.5121763320569));
#56522=CARTESIAN_POINT('Ctrl Pts',(37.2509651368289,-38.7813435147692,16.4336708216802));
#56523=CARTESIAN_POINT('Ctrl Pts',(37.8462764933252,-37.7925906195587,16.3810159521908));
#56524=CARTESIAN_POINT('Ctrl Pts',(38.2877225391554,-37.5345016936567,16.3545295861603));
#56525=CARTESIAN_POINT('Ctrl Pts',(38.2930403179255,-37.5314388517851,16.3542117235887));
#56526=CARTESIAN_POINT('Ctrl Pts',(38.2927752994979,-37.531894773765,16.8957882764113));
#56527=CARTESIAN_POINT('Ctrl Pts',(38.7030067984342,-37.2976596080307,16.8713312990569));
#56528=CARTESIAN_POINT('Ctrl Pts',(39.7943393979825,-37.2242325343386,16.8207058182437));
#56529=CARTESIAN_POINT('Ctrl Pts',(40.8516003110939,-38.5339981005298,16.7439118339715));
#56530=CARTESIAN_POINT('Ctrl Pts',(40.3309240105073,-40.1740843304588,16.6654063235947));
#56531=CARTESIAN_POINT('Ctrl Pts',(38.6757020358417,-40.644431583443,16.586900813218));
#56532=CARTESIAN_POINT('Ctrl Pts',(37.3703767628973,-39.5232213878114,16.5083953028412));
#56533=CARTESIAN_POINT('Ctrl Pts',(37.5450179797371,-38.1378625018882,16.4446911239056));
#56534=CARTESIAN_POINT('Ctrl Pts',(38.1031426043017,-37.6456547913594,16.407155448429));
#56535=CARTESIAN_POINT('Ctrl Pts',(38.295011126227,-37.5356544186406,16.3957882764113));
#56536=CARTESIAN_POINT('Origin',(39.0658530619283,-38.8697713466883,19.1042117235887));
#56537=CARTESIAN_POINT('',(38.2959007276492,-37.5337106753506,17.3957882764113));
#56538=CARTESIAN_POINT('',(38.2935040424574,-37.5346322273253,17.3542117235887));
#56539=CARTESIAN_POINT('',(38.2943530619283,-37.5334941486488,19.1042117235887));
#56540=CARTESIAN_POINT('Ctrl Pts',(38.2935040424574,-37.5346322273253,17.3542117235887));
#56541=CARTESIAN_POINT('Ctrl Pts',(38.6142216923301,-37.353029943727,17.3352182943341));
#56542=CARTESIAN_POINT('Ctrl Pts',(39.5350880316606,-37.1858556050909,17.2900563616205));
#56543=CARTESIAN_POINT('Ctrl Pts',(40.7451827384013,-38.1758790339381,17.218725925448));
#56544=CARTESIAN_POINT('Ctrl Pts',(40.5709395934168,-39.8877854279213,17.1402204150712));
#56545=CARTESIAN_POINT('Ctrl Pts',(39.0468978715213,-40.6867135087542,17.0617149046944));
#56546=CARTESIAN_POINT('Ctrl Pts',(37.5398562037872,-39.856164211272,16.9832093943176));
#56547=CARTESIAN_POINT('Ctrl Pts',(37.4178373052428,-38.3450042264081,16.9140416672824));
#56548=CARTESIAN_POINT('Ctrl Pts',(38.0137206990119,-37.6996801517363,16.8710424437061));
#56549=CARTESIAN_POINT('Ctrl Pts',(38.2960217454205,-37.5343651514648,16.8542117235887));
#56550=CARTESIAN_POINT('Ctrl Pts',(38.2959007276492,-37.5337106753506,17.3957882764113));
#56551=CARTESIAN_POINT('Ctrl Pts',(38.4288872990661,-37.455546937363,17.3878441566028));
#56552=CARTESIAN_POINT('Ctrl Pts',(39.0471107626292,-37.2043843657909,17.3537315333353));
#56553=CARTESIAN_POINT('Ctrl Pts',(40.3208285827551,-37.5557507395872,17.293450406609));
#56554=CARTESIAN_POINT('Ctrl Pts',(40.8541369642562,-39.1917640019411,17.2149448962322));
#56555=CARTESIAN_POINT('Ctrl Pts',(39.7836658898431,-40.5390185509755,17.1364393858554));
#56556=CARTESIAN_POINT('Ctrl Pts',(38.0694451486085,-40.389246627264,17.0579338754786));
#56557=CARTESIAN_POINT('Ctrl Pts',(37.2488257543949,-38.87677605618,16.9794283651019));
#56558=CARTESIAN_POINT('Ctrl Pts',(37.8057511921981,-37.8311625054488,16.9253798320794));
#56559=CARTESIAN_POINT('Ctrl Pts',(38.2640668491777,-37.5482868076194,16.8974998025159));
#56560=CARTESIAN_POINT('Ctrl Pts',(38.2927752994979,-37.531894773765,16.8957882764113));
#56561=CARTESIAN_POINT('Origin',(39.0658530619283,-38.8697713466883,19.1042117235887));
#56562=CARTESIAN_POINT('',(38.2938718037176,-37.5356881270256,17.8957882764113));
#56563=CARTESIAN_POINT('',(38.2940537528419,-37.5314721085808,17.8542117235887));
#56564=CARTESIAN_POINT('',(38.2943530619283,-37.5334941486488,19.1042117235887));
#56565=CARTESIAN_POINT('',(37.5756558680257,-39.2699729499894,18.));
#56566=CARTESIAN_POINT('Ctrl Pts',(37.5756558680257,-39.2699729499894,18.));
#56567=CARTESIAN_POINT('Ctrl Pts',(37.4440523270134,-38.7799318659295,17.9738314965411));
#56568=CARTESIAN_POINT('Ctrl Pts',(37.6166680705089,-38.0418709533316,17.9390942553448));
#56569=CARTESIAN_POINT('Ctrl Pts',(38.1491376523636,-37.6179382396386,17.9043570141486));
#56570=CARTESIAN_POINT('Ctrl Pts',(38.2938718037176,-37.5356881270256,17.8957882764113));
#56571=CARTESIAN_POINT('',(37.9726405222314,-39.962294313691,18.));
#56572=CARTESIAN_POINT('Origin',(39.0658530619283,-38.8697713466883,18.));
#56573=CARTESIAN_POINT('Ctrl Pts',(37.972631799081,-39.9623061512025,18.));
#56574=CARTESIAN_POINT('Ctrl Pts',(37.6338216029695,-39.6208387086169,17.975091839613));
#56575=CARTESIAN_POINT('Ctrl Pts',(37.3042322663879,-38.6195093398435,17.9264957474759));
#56576=CARTESIAN_POINT('Ctrl Pts',(37.899143973177,-37.7627950030077,17.8778996553388));
#56577=CARTESIAN_POINT('Ctrl Pts',(38.2940537528419,-37.5314721085808,17.8542117235887));
#56578=CARTESIAN_POINT('Origin',(14.1292828945603,53.2669068454841,4.5));
#56579=CARTESIAN_POINT('',(14.7605875520818,54.3602657339262,5.80658032638059));
#56580=CARTESIAN_POINT('',(14.7625813317603,54.3604987677494,5.94341967361941));
#56581=CARTESIAN_POINT('',(14.7615328945603,54.3619959685696,4.5));
#56582=CARTESIAN_POINT('',(13.8936870225526,54.5092654229862,6.));
#56583=CARTESIAN_POINT('Ctrl Pts',(14.7625813317603,54.3604987677494,5.94341967361941));
#56584=CARTESIAN_POINT('Ctrl Pts',(14.5022241622972,54.5077988388625,5.96227978241294));
#56585=CARTESIAN_POINT('Ctrl Pts',(14.1881298777611,54.5651023789871,5.98113989120647));
#56586=CARTESIAN_POINT('Ctrl Pts',(13.8936870225526,54.5092654229862,6.));
#56587=CARTESIAN_POINT('',(14.7615328945603,54.3619959685696,6.));
#56588=CARTESIAN_POINT('Origin',(14.1292828945603,53.2669068454841,6.));
#56589=CARTESIAN_POINT('',(14.7615328945603,54.3619959685696,7.));
#56590=CARTESIAN_POINT('',(14.7615328945603,54.3619959685696,4.5));
#56591=CARTESIAN_POINT('',(12.8669333849943,53.3406222827979,7.));
#56592=CARTESIAN_POINT('Origin',(14.1292828945603,53.2669068454841,7.));
#56593=CARTESIAN_POINT('',(15.3916324041264,53.1931914081703,7.));
#56594=CARTESIAN_POINT('Origin',(14.1292828945603,53.2669068454841,7.));
#56595=CARTESIAN_POINT('Origin',(14.1292828945603,53.2669068454841,7.));
#56596=CARTESIAN_POINT('',(12.9337035820666,52.8487780612894,6.));
#56597=CARTESIAN_POINT('Origin',(14.1292828945603,53.2669068454841,6.));
#56598=CARTESIAN_POINT('Ctrl Pts',(12.9336933707122,52.8487726938778,6.));
#56599=CARTESIAN_POINT('Ctrl Pts',(12.8048848553781,53.2213517629532,5.97509183961299));
#56600=CARTESIAN_POINT('Ctrl Pts',(12.8625933288288,53.6603618768577,5.95018367922598));
#56601=CARTESIAN_POINT('Ctrl Pts',(13.0861255368911,53.9849952189361,5.92527551883898));
#56602=CARTESIAN_POINT('Ctrl Pts',(13.3209683863418,54.3260548798291,5.89910701538005));
#56603=CARTESIAN_POINT('Ctrl Pts',(13.7388407631054,54.540870088853,5.87293851192112));
#56604=CARTESIAN_POINT('Ctrl Pts',(14.1527369297938,54.5331774952646,5.8467700084622));
#56605=CARTESIAN_POINT('Ctrl Pts',(14.3646246721213,54.5292393909301,5.83337344776833));
#56606=CARTESIAN_POINT('Ctrl Pts',(14.5754703413608,54.4669871159197,5.81997688707446));
#56607=CARTESIAN_POINT('Ctrl Pts',(14.7605875520818,54.3602657339262,5.80658032638059));
#56608=CARTESIAN_POINT('Origin',(14.1292828945603,53.2669068454841,4.5));
#56609=CARTESIAN_POINT('',(14.7628720032994,54.3627600319775,5.30658032638059));
#56610=CARTESIAN_POINT('',(14.761790188637,54.3636903053853,5.44341967361941));
#56611=CARTESIAN_POINT('',(14.7615328945603,54.3619959685696,4.5));
#56612=CARTESIAN_POINT('Ctrl Pts',(14.761790188637,54.3636903053853,5.44341967361941));
#56613=CARTESIAN_POINT('Ctrl Pts',(14.7297149272464,54.3824695710557,5.44576692486712));
#56614=CARTESIAN_POINT('Ctrl Pts',(14.6967938380796,54.3997466843015,5.44811417611483));
#56615=CARTESIAN_POINT('Ctrl Pts',(14.6631180766711,54.4153998475156,5.45046142736254));
#56616=CARTESIAN_POINT('Ctrl Pts',(14.2876813696889,54.5899102907896,5.47662993082147));
#56617=CARTESIAN_POINT('Ctrl Pts',(13.8184459253802,54.5625788561695,5.50279843428039));
#56618=CARTESIAN_POINT('Ctrl Pts',(13.4657801062202,54.3456807478706,5.52896693773932));
#56619=CARTESIAN_POINT('Ctrl Pts',(13.1131142870602,54.1287826395717,5.55513544119824));
#56620=CARTESIAN_POINT('Ctrl Pts',(12.8770180930488,53.7223178575942,5.58130394465717));
#56621=CARTESIAN_POINT('Ctrl Pts',(12.8634449158406,53.308510984467,5.6074724481161));
#56622=CARTESIAN_POINT('Ctrl Pts',(12.8498717386324,52.8947041113399,5.63364095157503));
#56623=CARTESIAN_POINT('Ctrl Pts',(13.0588215782272,52.4735551470632,5.65980945503395));
#56624=CARTESIAN_POINT('Ctrl Pts',(13.3964281425195,52.2339907213231,5.68597795849288));
#56625=CARTESIAN_POINT('Ctrl Pts',(13.7340347068117,51.9944262955831,5.7121464619518));
#56626=CARTESIAN_POINT('Ctrl Pts',(14.2002979958013,51.9364464083796,5.73831496541073));
#56627=CARTESIAN_POINT('Ctrl Pts',(14.5864832378068,52.0858916506601,5.76448346886966));
#56628=CARTESIAN_POINT('Ctrl Pts',(14.9726684798122,52.2353368929405,5.79065197232859));
#56629=CARTESIAN_POINT('Ctrl Pts',(15.2787756748334,52.592207264705,5.81682047578751));
#56630=CARTESIAN_POINT('Ctrl Pts',(15.3668446182304,52.9968058417406,5.84298897924644));
#56631=CARTESIAN_POINT('Ctrl Pts',(15.4549135616273,53.4014044187763,5.86915748270536));
#56632=CARTESIAN_POINT('Ctrl Pts',(15.3249442534001,53.8537312010832,5.89532598616429));
#56633=CARTESIAN_POINT('Ctrl Pts',(15.0367728841186,54.1500649721194,5.92149448962322));
#56634=CARTESIAN_POINT('Ctrl Pts',(14.9562917782241,54.2328256907373,5.92880288428862));
#56635=CARTESIAN_POINT('Ctrl Pts',(14.8634711500129,54.3034191895921,5.93611127895402));
#56636=CARTESIAN_POINT('Ctrl Pts',(14.7625813317603,54.3604987677494,5.94341967361941));
#56637=CARTESIAN_POINT('Ctrl Pts',(14.7605875520818,54.3602657339262,5.80658032638059));
#56638=CARTESIAN_POINT('Ctrl Pts',(14.9370736274398,54.2585202625491,5.79380838361553));
#56639=CARTESIAN_POINT('Ctrl Pts',(15.0901745042163,54.1163557782414,5.78103644085048));
#56640=CARTESIAN_POINT('Ctrl Pts',(15.1984983273048,53.9457696468095,5.76826449808542));
#56641=CARTESIAN_POINT('Ctrl Pts',(15.4204436015143,53.5962547881435,5.74209599462649));
#56642=CARTESIAN_POINT('Ctrl Pts',(15.4544141933199,53.1274254670123,5.71592749116756));
#56643=CARTESIAN_POINT('Ctrl Pts',(15.2852697206798,52.7495259168145,5.68975898770864));
#56644=CARTESIAN_POINT('Ctrl Pts',(15.1161252480396,52.3716263666167,5.66359048424971));
#56645=CARTESIAN_POINT('Ctrl Pts',(14.7438657109537,52.0846565873524,5.63742198079079));
#56646=CARTESIAN_POINT('Ctrl Pts',(14.3353706309513,52.0172894645935,5.61125347733186));
#56647=CARTESIAN_POINT('Ctrl Pts',(13.9268755509488,51.9499223418345,5.58508497387293));
#56648=CARTESIAN_POINT('Ctrl Pts',(13.4821449280297,52.1021578755809,5.558916470414));
#56649=CARTESIAN_POINT('Ctrl Pts',(13.2006242325166,52.4057357189425,5.53274796695508));
#56650=CARTESIAN_POINT('Ctrl Pts',(12.9191035370036,52.7093135623041,5.50657946349615));
#56651=CARTESIAN_POINT('Ctrl Pts',(12.8007927688965,53.1642337152808,5.48041096003723));
#56652=CARTESIAN_POINT('Ctrl Pts',(12.8987324301598,53.5665026413488,5.4542424565783));
#56653=CARTESIAN_POINT('Ctrl Pts',(12.9966720914231,53.9687715674169,5.42807395311937));
#56654=CARTESIAN_POINT('Ctrl Pts',(13.3108621820568,54.3183892665762,5.40190544966045));
#56655=CARTESIAN_POINT('Ctrl Pts',(13.7004218404058,54.4585839700534,5.37573694620152));
#56656=CARTESIAN_POINT('Ctrl Pts',(14.0435904799155,54.5820834768109,5.35268473959454));
#56657=CARTESIAN_POINT('Ctrl Pts',(14.4452466462963,54.5430686762864,5.32963253298757));
#56658=CARTESIAN_POINT('Ctrl Pts',(14.7628720032994,54.3627600319775,5.30658032638059));
#56659=CARTESIAN_POINT('Origin',(14.1292828945603,53.2669068454841,4.5));
#56660=CARTESIAN_POINT('',(14.7604987163791,54.3623830037273,4.80658032638059));
#56661=CARTESIAN_POINT('',(14.7603543171395,54.3604895118786,4.94341967361941));
#56662=CARTESIAN_POINT('',(14.7615328945603,54.3619959685696,4.5));
#56663=CARTESIAN_POINT('Ctrl Pts',(14.7603543171395,54.3604895118786,4.94341967361941));
#56664=CARTESIAN_POINT('Ctrl Pts',(14.5947715388364,54.4565158591777,4.95542257078023));
#56665=CARTESIAN_POINT('Ctrl Pts',(14.4086766047111,54.5167140163305,4.96742546794105));
#56666=CARTESIAN_POINT('Ctrl Pts',(14.2192552064615,54.5302046425139,4.97942836510187));
#56667=CARTESIAN_POINT('Ctrl Pts',(13.8062820343284,54.5596166663956,5.00559686856079));
#56668=CARTESIAN_POINT('Ctrl Pts',(13.3774975305931,54.3670187022342,5.03176537201972));
#56669=CARTESIAN_POINT('Ctrl Pts',(13.1251731138615,54.0387742648884,5.05793387547865));
#56670=CARTESIAN_POINT('Ctrl Pts',(12.8728486971299,53.7105298275425,5.08410237893757));
#56671=CARTESIAN_POINT('Ctrl Pts',(12.796984367402,53.2466389170122,5.1102708823965));
#56672=CARTESIAN_POINT('Ctrl Pts',(12.9315998955733,52.8551151331566,5.13643938585542));
#56673=CARTESIAN_POINT('Ctrl Pts',(13.0662154237445,52.4635913493009,5.16260788931435));
#56674=CARTESIAN_POINT('Ctrl Pts',(13.411310809815,52.14443469212,5.18877639277328));
#56675=CARTESIAN_POINT('Ctrl Pts',(13.81213856493,52.0407600014986,5.2149448962322));
#56676=CARTESIAN_POINT('Ctrl Pts',(14.212966320045,51.9370853108772,5.24111339969113));
#56677=CARTESIAN_POINT('Ctrl Pts',(14.6695264442046,52.0488925868152,5.26728190315006));
#56678=CARTESIAN_POINT('Ctrl Pts',(14.9770971987178,52.3260437079763,5.29345040660898));
#56679=CARTESIAN_POINT('Ctrl Pts',(15.284667953231,52.6031948291373,5.31961891006791));
#56680=CARTESIAN_POINT('Ctrl Pts',(15.4432493380979,53.0456897955214,5.34578741352683));
#56681=CARTESIAN_POINT('Ctrl Pts',(15.3817210457035,53.4551134392974,5.37195591698576));
#56682=CARTESIAN_POINT('Ctrl Pts',(15.3257116918039,53.827812775923,5.39577716919698));
#56683=CARTESIAN_POINT('Ctrl Pts',(15.087308341869,54.1731075442457,5.4195984214082));
#56684=CARTESIAN_POINT('Ctrl Pts',(14.761790188637,54.3636903053853,5.44341967361941));
#56685=CARTESIAN_POINT('Ctrl Pts',(14.7628720032994,54.3627600319775,5.30658032638059));
#56686=CARTESIAN_POINT('Ctrl Pts',(14.8058099708876,54.3383851306841,5.30346402952864));
#56687=CARTESIAN_POINT('Ctrl Pts',(14.8472122922316,54.3114281126392,5.30034773267669));
#56688=CARTESIAN_POINT('Ctrl Pts',(14.8867268805692,54.2819414022849,5.29723143582474));
#56689=CARTESIAN_POINT('Ctrl Pts',(15.2185430363193,54.0343324232445,5.27106293236581));
#56690=CARTESIAN_POINT('Ctrl Pts',(15.4172461217553,53.6083427573686,5.24489442890689));
#56691=CARTESIAN_POINT('Ctrl Pts',(15.393736730538,53.1949914739395,5.21872592544796));
#56692=CARTESIAN_POINT('Ctrl Pts',(15.3702273393206,52.7816401905105,5.19255742198903));
#56693=CARTESIAN_POINT('Ctrl Pts',(15.12450547145,52.3809272895283,5.16638891853011));
#56694=CARTESIAN_POINT('Ctrl Pts',(14.7667550258397,52.1725370796236,5.14022041507118));
#56695=CARTESIAN_POINT('Ctrl Pts',(14.4090045802295,51.9641468697189,5.11405191161226));
#56696=CARTESIAN_POINT('Ctrl Pts',(13.9392255568796,51.9480793508917,5.08788340815333));
#56697=CARTESIAN_POINT('Ctrl Pts',(13.5680728067532,52.1315394490878,5.0617149046944));
#56698=CARTESIAN_POINT('Ctrl Pts',(13.1969200566268,52.3149995472839,5.03554640123547));
#56699=CARTESIAN_POINT('Ctrl Pts',(12.9243935797239,52.6979872625031,5.00937789777655));
#56700=CARTESIAN_POINT('Ctrl Pts',(12.8726973119175,53.1087663210662,4.98320939431762));
#56701=CARTESIAN_POINT('Ctrl Pts',(12.8210010441111,53.5195453796293,4.9570408908587));
#56702=CARTESIAN_POINT('Ctrl Pts',(12.9901349854012,53.9581157815362,4.93087238739977));
#56703=CARTESIAN_POINT('Ctrl Pts',(13.3042575537142,54.227817360156,4.90470388394084));
#56704=CARTESIAN_POINT('Ctrl Pts',(13.6183801220271,54.4975189387757,4.87853538048192));
#56705=CARTESIAN_POINT('Ctrl Pts',(14.0774913173628,54.5983516941084,4.85236687702299));
#56706=CARTESIAN_POINT('Ctrl Pts',(14.4757201786558,54.4851010127079,4.82619837356406));
#56707=CARTESIAN_POINT('Ctrl Pts',(14.5752351369457,54.4568003596631,4.81965902450291));
#56708=CARTESIAN_POINT('Ctrl Pts',(14.6709481788587,54.4151308478692,4.81311967544175));
#56709=CARTESIAN_POINT('Ctrl Pts',(14.7604987163791,54.3623830037273,4.80658032638059));
#56710=CARTESIAN_POINT('Origin',(14.1292828945603,53.2669068454841,4.5));
#56711=CARTESIAN_POINT('',(14.7614006096927,54.3603381104062,4.30658032638059));
#56712=CARTESIAN_POINT('',(14.7627659331487,54.3621523730593,4.44341967361941));
#56713=CARTESIAN_POINT('',(14.7615328945603,54.3619959685696,4.5));
#56714=CARTESIAN_POINT('Ctrl Pts',(14.7627659331487,54.3621523730593,4.44341967361941));
#56715=CARTESIAN_POINT('Ctrl Pts',(14.463761030489,54.5313718419492,4.46507821669334));
#56716=CARTESIAN_POINT('Ctrl Pts',(14.0916672421201,54.5784026588885,4.48673675976726));
#56717=CARTESIAN_POINT('Ctrl Pts',(13.7635961371407,54.4794617725194,4.50839530284119));
#56718=CARTESIAN_POINT('Ctrl Pts',(13.3672107562715,54.3599184164247,4.53456380630012));
#56719=CARTESIAN_POINT('Ctrl Pts',(13.0350905669399,54.0272826554628,4.56073230975904));
#56720=CARTESIAN_POINT('Ctrl Pts',(12.9161621999348,53.6307123234038,4.58690081321797));
#56721=CARTESIAN_POINT('Ctrl Pts',(12.7972338329298,53.2341419913447,4.61306931667689));
#56722=CARTESIAN_POINT('Ctrl Pts',(12.8914972882514,52.7736370881886,4.63923782013582));
#56723=CARTESIAN_POINT('Ctrl Pts',(13.1566837320242,52.4556934772733,4.66540632359475));
#56724=CARTESIAN_POINT('Ctrl Pts',(13.421870175797,52.1377498663579,4.69157482705367));
#56725=CARTESIAN_POINT('Ctrl Pts',(13.8579796080209,51.9623675476834,4.7177433305126));
#56726=CARTESIAN_POINT('Ctrl Pts',(14.2694553352381,52.0081900560918,4.74391183397153));
#56727=CARTESIAN_POINT('Ctrl Pts',(14.6809310624553,52.0540125645002,4.77008033743045));
#56728=CARTESIAN_POINT('Ctrl Pts',(15.0677730846659,52.3210398999916,4.79624884088938));
#56729=CARTESIAN_POINT('Ctrl Pts',(15.2565169212345,52.6895337942872,4.82241734434831));
#56730=CARTESIAN_POINT('Ctrl Pts',(15.4452607578031,53.0580276885828,4.84858584780723));
#56731=CARTESIAN_POINT('Ctrl Pts',(15.4359064087297,53.5279881416827,4.87475435126616));
#56732=CARTESIAN_POINT('Ctrl Pts',(15.2326483139276,53.888679374195,4.90092285472508));
#56733=CARTESIAN_POINT('Ctrl Pts',(15.1226200827607,54.0839297446631,4.91508846102319));
#56734=CARTESIAN_POINT('Ctrl Pts',(14.9557721746585,54.2471609203011,4.9292540673213));
#56735=CARTESIAN_POINT('Ctrl Pts',(14.7603543171395,54.3604895118786,4.94341967361941));
#56736=CARTESIAN_POINT('Ctrl Pts',(14.7604987163791,54.3623830037273,4.80658032638059));
#56737=CARTESIAN_POINT('Ctrl Pts',(15.0293024323073,54.2040498780404,4.78695117198282));
#56738=CARTESIAN_POINT('Ctrl Pts',(15.242580788107,53.945898828656,4.76732201758505));
#56739=CARTESIAN_POINT('Ctrl Pts',(15.3364895893995,53.649879171516,4.74769286318729));
#56740=CARTESIAN_POINT('Ctrl Pts',(15.4616836115997,53.2552421298582,4.72152435972836));
#56741=CARTESIAN_POINT('Ctrl Pts',(15.3747251287497,52.7933021646762,4.69535585626943));
#56742=CARTESIAN_POINT('Ctrl Pts',(15.1146073473565,52.471198645522,4.66918735281051));
#56743=CARTESIAN_POINT('Ctrl Pts',(14.8544895659633,52.1490951263678,4.64301884935158));
#56744=CARTESIAN_POINT('Ctrl Pts',(14.4212124860269,51.9668280532413,4.61685034589265));
#56745=CARTESIAN_POINT('Ctrl Pts',(14.0090627058929,52.0061281492218,4.59068184243372));
#56746=CARTESIAN_POINT('Ctrl Pts',(13.596912925759,52.0454282452023,4.5645133389748));
#56747=CARTESIAN_POINT('Ctrl Pts',(13.2058904454275,52.3062955102899,4.53834483551587));
#56748=CARTESIAN_POINT('Ctrl Pts',(13.0113343903925,52.6717539614819,4.51217633205695));
#56749=CARTESIAN_POINT('Ctrl Pts',(12.8167783353574,53.0372124126739,4.48600782859802));
#56750=CARTESIAN_POINT('Ctrl Pts',(12.8186887056188,53.5072620499704,4.45983932513909));
#56751=CARTESIAN_POINT('Ctrl Pts',(13.0162088697902,53.8711270288388,4.43367082168017));
#56752=CARTESIAN_POINT('Ctrl Pts',(13.2137290339615,54.2349920077072,4.40750231822124));
#56753=CARTESIAN_POINT('Ctrl Pts',(13.606858992043,54.4926723281474,4.38133381476231));
#56754=CARTESIAN_POINT('Ctrl Pts',(14.0193145970927,54.5286210713629,4.35516531130339));
#56755=CARTESIAN_POINT('Ctrl Pts',(14.2745724669733,54.5508687981624,4.33897031632912));
#56756=CARTESIAN_POINT('Ctrl Pts',(14.5372321463568,54.4881923359769,4.32277532135485));
#56757=CARTESIAN_POINT('Ctrl Pts',(14.7614006096927,54.3603381104062,4.30658032638059));
#56758=CARTESIAN_POINT('Origin',(14.1292828945603,53.2669068454841,4.5));
#56759=CARTESIAN_POINT('',(14.7626048989925,54.3636737206204,3.80658032638058));
#56760=CARTESIAN_POINT('',(14.7608564829457,54.3629211099724,3.94341967361941));
#56761=CARTESIAN_POINT('',(14.7615328945603,54.3619959685696,4.5));
#56762=CARTESIAN_POINT('Ctrl Pts',(14.7608564829457,54.3629211099724,3.94341967361941));
#56763=CARTESIAN_POINT('Ctrl Pts',(14.6904886508112,54.4043824600063,3.94856535914752));
#56764=CARTESIAN_POINT('Ctrl Pts',(14.6162453479771,54.4388759703619,3.95371104467562));
#56765=CARTESIAN_POINT('Ctrl Pts',(14.5392165090643,54.465226788063,3.95885673020373));
#56766=CARTESIAN_POINT('Ctrl Pts',(14.1474845568267,54.5992344844895,3.98502523366266));
#56767=CARTESIAN_POINT('Ctrl Pts',(13.6837115472212,54.5226514105579,4.01119373712158));
#56768=CARTESIAN_POINT('Ctrl Pts',(13.3558588106244,54.2698183268938,4.03736224058051));
#56769=CARTESIAN_POINT('Ctrl Pts',(13.0280060740275,54.0169852432297,4.06353074403944));
#56770=CARTESIAN_POINT('Ctrl Pts',(12.8360736104392,53.5879021498331,4.08969924749836));
#56771=CARTESIAN_POINT('Ctrl Pts',(12.8661262178428,53.1749750062962,4.11586775095729));
#56772=CARTESIAN_POINT('Ctrl Pts',(12.8961788252464,52.7620478627593,4.14203625441622));
#56773=CARTESIAN_POINT('Ctrl Pts',(13.1482165036419,52.3652766690821,4.16820475787515));
#56774=CARTESIAN_POINT('Ctrl Pts',(13.5092225624184,52.1625783447115,4.19437326133407));
#56775=CARTESIAN_POINT('Ctrl Pts',(13.8702286211949,51.959880020341,4.220541764793));
#56776=CARTESIAN_POINT('Ctrl Pts',(14.3402030603525,51.951254565277,4.24671026825192));
#56777=CARTESIAN_POINT('Ctrl Pts',(14.708403754256,52.1405697363842,4.27287877171085));
#56778=CARTESIAN_POINT('Ctrl Pts',(15.0766044481595,52.3298849074914,4.29904727516978));
#56779=CARTESIAN_POINT('Ctrl Pts',(15.343031396809,52.7171407047698,4.3252157786287));
#56780=CARTESIAN_POINT('Ctrl Pts',(15.3882155906945,53.1286870249125,4.35138428208763));
#56781=CARTESIAN_POINT('Ctrl Pts',(15.43339978458,53.5402333450552,4.37755278554656));
#56782=CARTESIAN_POINT('Ctrl Pts',(15.2573412237015,53.9760701880622,4.40372128900548));
#56783=CARTESIAN_POINT('Ctrl Pts',(14.938986657059,54.2407631339519,4.42988979246441));
#56784=CARTESIAN_POINT('Ctrl Pts',(14.8841204517295,54.2863811304883,4.43439975284941));
#56785=CARTESIAN_POINT('Ctrl Pts',(14.825027751098,54.3269157877332,4.43890971323441));
#56786=CARTESIAN_POINT('Ctrl Pts',(14.7627659331487,54.3621523730593,4.44341967361941));
#56787=CARTESIAN_POINT('Ctrl Pts',(14.7614006096927,54.3603381104062,4.30658032638059));
#56788=CARTESIAN_POINT('Ctrl Pts',(14.899452277793,54.2816005000793,4.29660681789593));
#56789=CARTESIAN_POINT('Ctrl Pts',(15.0229058598302,54.178143727902,4.28663330941127));
#56790=CARTESIAN_POINT('Ctrl Pts',(15.1210425075748,54.0545798005254,4.27665980092661));
#56791=CARTESIAN_POINT('Ctrl Pts',(15.3785335609892,53.7303726204816,4.25049129746768));
#56792=CARTESIAN_POINT('Ctrl Pts',(15.4617344158,53.2677410944033,4.22432279400875));
#56793=CARTESIAN_POINT('Ctrl Pts',(15.3333368195411,52.8741346977794,4.19815429054983));
#56794=CARTESIAN_POINT('Ctrl Pts',(15.2049392232822,52.4805283011554,4.1719857870909));
#56795=CARTESIAN_POINT('Ctrl Pts',(14.8649431759537,52.1559470339858,4.14581728363197));
#56796=CARTESIAN_POINT('Ctrl Pts',(14.4658069467496,52.0459369947103,4.11964878017305));
#56797=CARTESIAN_POINT('Ctrl Pts',(14.0666707175455,51.9359269554348,4.09348027671412));
#56798=CARTESIAN_POINT('Ctrl Pts',(13.6083943064658,52.0404881440534,4.06731177325519));
#56799=CARTESIAN_POINT('Ctrl Pts',(13.2964743036118,52.3127340807067,4.04114326979627));
#56800=CARTESIAN_POINT('Ctrl Pts',(12.9845543007579,52.5849800173601,4.01497476633734));
#56801=CARTESIAN_POINT('Ctrl Pts',(12.8189907061297,53.0249107020483,3.98880626287841));
#56802=CARTESIAN_POINT('Ctrl Pts',(12.8740242036727,53.4352559863353,3.96263775941949));
#56803=CARTESIAN_POINT('Ctrl Pts',(12.9290577012157,53.8456012706222,3.93646925596056));
#56804=CARTESIAN_POINT('Ctrl Pts',(13.2046882909297,54.2263611545079,3.91030075250164));
#56805=CARTESIAN_POINT('Ctrl Pts',(13.5773199398677,54.4067983801299,3.88413224904271));
#56806=CARTESIAN_POINT('Ctrl Pts',(13.9454253210212,54.5850438777981,3.85828160815533));
#56807=CARTESIAN_POINT('Ctrl Pts',(14.4081895758327,54.5678037039579,3.83243096726796));
#56808=CARTESIAN_POINT('Ctrl Pts',(14.7626048989925,54.3636737206204,3.80658032638058));
#56809=CARTESIAN_POINT('Origin',(14.1292828945603,53.2669068454841,4.5));
#56810=CARTESIAN_POINT('',(14.7601616123225,54.3612756103012,3.30658032638059));
#56811=CARTESIAN_POINT('',(14.7609899830458,54.3602193411782,3.44341967361941));
#56812=CARTESIAN_POINT('',(14.7615328945603,54.3619959685696,4.5));
#56813=CARTESIAN_POINT('Ctrl Pts',(14.7609899830458,54.3602193411782,3.44341967361941));
#56814=CARTESIAN_POINT('Ctrl Pts',(14.5562500775904,54.4775990222049,3.45822100506063));
#56815=CARTESIAN_POINT('Ctrl Pts',(14.3197636804793,54.5407089292625,3.47302233650184));
#56816=CARTESIAN_POINT('Ctrl Pts',(14.0857261531979,54.532655265383,3.48782366794306));
#56817=CARTESIAN_POINT('Ctrl Pts',(13.671951766312,54.5184165239613,3.51399217140198));
#56818=CARTESIAN_POINT('Ctrl Pts',(13.2658319689464,54.2817372437526,3.54016067486091));
#56819=CARTESIAN_POINT('Ctrl Pts',(13.0494757061861,53.9287472260938,3.56632917831983));
#56820=CARTESIAN_POINT('Ctrl Pts',(12.8331194434257,53.575757208435,3.59249768177876));
#56821=CARTESIAN_POINT('Ctrl Pts',(12.8065267152706,53.1064564533261,3.61866618523769));
#56822=CARTESIAN_POINT('Ctrl Pts',(12.9816220168908,52.7312849984863,3.64483468869661));
#56823=CARTESIAN_POINT('Ctrl Pts',(13.1567173185109,52.3561135436466,3.67100319215554));
#56824=CARTESIAN_POINT('Ctrl Pts',(13.5335006499062,52.0750713890761,3.69717169561447));
#56825=CARTESIAN_POINT('Ctrl Pts',(13.9430178866457,52.0141811772634,3.72334019907339));
#56826=CARTESIAN_POINT('Ctrl Pts',(14.3525351233851,51.9532909654507,3.74950870253232));
#56827=CARTESIAN_POINT('Ctrl Pts',(14.7947862654686,52.1125526963959,3.77567720599125));
#56828=CARTESIAN_POINT('Ctrl Pts',(15.0714606437586,52.4205515169895,3.80184570945017));
#56829=CARTESIAN_POINT('Ctrl Pts',(15.3481350220485,52.7285503375831,3.8280142129091));
#56830=CARTESIAN_POINT('Ctrl Pts',(15.4592326365448,53.185286247825,3.85418271636802));
#56831=CARTESIAN_POINT('Ctrl Pts',(15.3549359963582,53.5859534363384,3.88035121982695));
#56832=CARTESIAN_POINT('Ctrl Pts',(15.271147892813,53.907834791464,3.90137403775777));
#56833=CARTESIAN_POINT('Ctrl Pts',(15.0483458981207,54.1935297998804,3.92239685568859));
#56834=CARTESIAN_POINT('Ctrl Pts',(14.7608564829457,54.3629211099724,3.94341967361941));
#56835=CARTESIAN_POINT('Ctrl Pts',(14.7626048989925,54.3636737206204,3.80658032638058));
#56836=CARTESIAN_POINT('Ctrl Pts',(14.7669628321868,54.3611637139356,3.80626246380903));
#56837=CARTESIAN_POINT('Ctrl Pts',(14.7713043836124,54.3586254505289,3.80594460123748));
#56838=CARTESIAN_POINT('Ctrl Pts',(14.7756291758562,54.3560589463809,3.80562673866593));
#56839=CARTESIAN_POINT('Ctrl Pts',(15.131674054745,54.1447677196515,3.779458235207));
#56840=CARTESIAN_POINT('Ctrl Pts',(15.3741311043607,53.7420706988344,3.75328973174808));
#56841=CARTESIAN_POINT('Ctrl Pts',(15.3942797010543,53.3285420152435,3.72712122828915));
#56842=CARTESIAN_POINT('Ctrl Pts',(15.414428297748,52.9150133316526,3.70095272483022));
#56843=CARTESIAN_POINT('Ctrl Pts',(15.2122684415196,52.4906529852878,3.6747842213713));
#56844=CARTESIAN_POINT('Ctrl Pts',(14.8784510160553,52.2457491989657,3.64861571791237));
#56845=CARTESIAN_POINT('Ctrl Pts',(14.544633590591,52.0008454126437,3.62244721445344));
#56846=CARTESIAN_POINT('Ctrl Pts',(14.0791585958908,51.9353981863644,3.59627871099452));
#56847=CARTESIAN_POINT('Ctrl Pts',(13.6907505503598,52.0787548359323,3.57011020753559));
#56848=CARTESIAN_POINT('Ctrl Pts',(13.3023425048288,52.2221114855002,3.54394170407667));
#56849=CARTESIAN_POINT('Ctrl Pts',(12.9910014084669,52.5742720109151,3.51777320061774));
#56850=CARTESIAN_POINT('Ctrl Pts',(12.896336314222,52.9773234433404,3.49160469715881));
#56851=CARTESIAN_POINT('Ctrl Pts',(12.801671219977,53.3803748757656,3.46543619369988));
#56852=CARTESIAN_POINT('Ctrl Pts',(12.9236821278488,53.8343172152012,3.43926769024096));
#56853=CARTESIAN_POINT('Ctrl Pts',(13.2076578874333,54.1355973270763,3.41309918678203));
#56854=CARTESIAN_POINT('Ctrl Pts',(13.4916336470178,54.4368774389515,3.38693068332311));
#56855=CARTESIAN_POINT('Ctrl Pts',(13.9375742583148,54.5854953232664,3.36076217986418));
#56856=CARTESIAN_POINT('Ctrl Pts',(14.3455146684413,54.5148089413369,3.33459367640525));
#56857=CARTESIAN_POINT('Ctrl Pts',(14.4910812336828,54.4895857137002,3.32525589306369));
#56858=CARTESIAN_POINT('Ctrl Pts',(14.6318092436286,54.436438533397,3.31591810972214));
#56859=CARTESIAN_POINT('Ctrl Pts',(14.7601616123225,54.3612756103012,3.30658032638059));
#56860=CARTESIAN_POINT('Origin',(14.1292828945603,53.2669068454841,4.5));
#56861=CARTESIAN_POINT('',(14.7622249872189,54.3610567043162,2.80658032638059));
#56862=CARTESIAN_POINT('',(14.7628222445741,54.3633003878638,2.94341967361941));
#56863=CARTESIAN_POINT('',(14.7615328945603,54.3619959685696,4.5));
#56864=CARTESIAN_POINT('Ctrl Pts',(14.7628222445741,54.3633003878638,2.94341967361941));
#56865=CARTESIAN_POINT('Ctrl Pts',(14.4266363996141,54.5552567541312,2.96787665097373));
#56866=CARTESIAN_POINT('Ctrl Pts',(13.9945792873817,54.5843264233177,2.99233362832806));
#56867=CARTESIAN_POINT('Ctrl Pts',(13.6379437474727,54.4342123040851,3.01679060568238));
#56868=CARTESIAN_POINT('Ctrl Pts',(13.256350461251,54.2735930341132,3.04295910914131));
#56869=CARTESIAN_POINT('Ctrl Pts',(12.9611042822246,53.9078334931332,3.06912761260023));
#56870=CARTESIAN_POINT('Ctrl Pts',(12.8845971374177,53.5009445240528,3.09529611605916));
#56871=CARTESIAN_POINT('Ctrl Pts',(12.8080899926107,53.0940555549725,3.12146461951808));
#56872=CARTESIAN_POINT('Ctrl Pts',(12.9503218820233,52.6460371577917,3.14763312297701));
#56873=CARTESIAN_POINT('Ctrl Pts',(13.2475143204016,52.3577861486808,3.17380162643594));
#56874=CARTESIAN_POINT('Ctrl Pts',(13.54470675878,52.0695351395699,3.19997012989486));
#56875=CARTESIAN_POINT('Ctrl Pts',(13.9968597461241,51.9410515185289,3.22613863335379));
#56876=CARTESIAN_POINT('Ctrl Pts',(14.4012225159017,52.0299488478797,3.25230713681272));
#56877=CARTESIAN_POINT('Ctrl Pts',(14.8055852856792,52.1188461772305,3.27847564027164));
#56878=CARTESIAN_POINT('Ctrl Pts',(15.1621578378903,52.4251244569731,3.30464414373057));
#56879=CARTESIAN_POINT('Ctrl Pts',(15.3110487977949,52.8114448760708,3.3308126471895));
#56880=CARTESIAN_POINT('Ctrl Pts',(15.4599397576996,53.1977652951685,3.35698115064842));
#56881=CARTESIAN_POINT('Ctrl Pts',(15.4011491252979,53.6641278536213,3.38314965410735));
#56882=CARTESIAN_POINT('Ctrl Pts',(15.1610393208939,54.0014100315303,3.40931815756628));
#56883=CARTESIAN_POINT('Ctrl Pts',(15.0567395295787,54.1479199204438,3.42068532958399));
#56884=CARTESIAN_POINT('Ctrl Pts',(14.918226764983,54.2700737329326,3.4320525016017));
#56885=CARTESIAN_POINT('Ctrl Pts',(14.7609899830458,54.3602193411782,3.44341967361941));
#56886=CARTESIAN_POINT('Ctrl Pts',(14.7601616123225,54.3612756103012,3.30658032638059));
#56887=CARTESIAN_POINT('Ctrl Pts',(14.9915080373649,54.2257995475618,3.28974960626321));
#56888=CARTESIAN_POINT('Ctrl Pts',(15.1826489574086,54.0187995905144,3.27291888614585));
#56889=CARTESIAN_POINT('Ctrl Pts',(15.2894496720194,53.7748722761244,3.25608816602848));
#56890=CARTESIAN_POINT('Ctrl Pts',(15.455504056515,53.395612641015,3.22991966256955));
#56891=CARTESIAN_POINT('Ctrl Pts',(15.4176726165505,52.9270840189701,3.20375115911062));
#56892=CARTESIAN_POINT('Ctrl Pts',(15.1929194920754,52.5793801620778,3.17758265565169));
#56893=CARTESIAN_POINT('Ctrl Pts',(14.9681663676002,52.2316763051856,3.15141415219277));
#56894=CARTESIAN_POINT('Ctrl Pts',(14.5564915586145,52.004797213446,3.12524564873384));
#56895=CARTESIAN_POINT('Ctrl Pts',(14.1424947973993,52.00047827147,3.09907714527492));
#56896=CARTESIAN_POINT('Ctrl Pts',(13.7284980361841,51.9961593294939,3.07290864181599));
#56897=CARTESIAN_POINT('Ctrl Pts',(13.3121793227393,52.2144005372813,3.04674013835706));
#56898=CARTESIAN_POINT('Ctrl Pts',(13.0802212088747,52.5573397364563,3.02057163489813));
#56899=CARTESIAN_POINT('Ctrl Pts',(12.8482630950101,52.9002789356314,2.99440313143921));
#56900=CARTESIAN_POINT('Ctrl Pts',(12.8006655807257,53.3679161261941,2.96823462798028));
#56901=CARTESIAN_POINT('Ctrl Pts',(12.9587713715113,53.7505576476053,2.94206612452136));
#56902=CARTESIAN_POINT('Ctrl Pts',(13.116877162297,54.1331991690165,2.91589762106243));
#56903=CARTESIAN_POINT('Ctrl Pts',(13.4806862581528,54.4308450212763,2.8897291176035));
#56904=CARTESIAN_POINT('Ctrl Pts',(13.8870635107844,54.5100264348898,2.86356061414458));
#56905=CARTESIAN_POINT('Ctrl Pts',(14.1820172367656,54.5674973017321,2.84456718488991));
#56906=CARTESIAN_POINT('Ctrl Pts',(14.499396034384,54.5098802470415,2.82557375563525));
#56907=CARTESIAN_POINT('Ctrl Pts',(14.7622249872189,54.3610567043162,2.80658032638059));
#56908=CARTESIAN_POINT('Origin',(14.1292828945603,53.2669068454841,4.5));
#56909=CARTESIAN_POINT('',(14.7617771735939,54.3636459375188,2.30658032638059));
#56910=CARTESIAN_POINT('',(14.7602610286104,54.3618122024717,2.44341967361941));
#56911=CARTESIAN_POINT('',(14.7615328945603,54.3619959685696,4.5));
#56912=CARTESIAN_POINT('',(12.9355708698302,52.8497595669186,2.));
#56913=CARTESIAN_POINT('Ctrl Pts',(14.7617771735939,54.3636459375188,2.30658032638059));
#56914=CARTESIAN_POINT('Ctrl Pts',(15.0854028058299,54.1740757700734,2.2828923946305));
#56915=CARTESIAN_POINT('Ctrl Pts',(15.3230378955527,53.8318500257242,2.25920446288042));
#56916=CARTESIAN_POINT('Ctrl Pts',(15.3806718879601,53.4614673043247,2.23551653113034));
#56917=CARTESIAN_POINT('Ctrl Pts',(15.4443412427006,53.0522985500271,2.20934802767141));
#56918=CARTESIAN_POINT('Ctrl Pts',(15.2883366067183,52.6087669190161,2.18317952421249));
#56919=CARTESIAN_POINT('Ctrl Pts',(14.981978171922,52.3301976113127,2.15701102075356));
#56920=CARTESIAN_POINT('Ctrl Pts',(14.6756197371256,52.0516283036092,2.13084251729463));
#56921=CARTESIAN_POINT('Ctrl Pts',(14.2189075035153,51.9380213192133,2.10467401383571));
#56922=CARTESIAN_POINT('Ctrl Pts',(13.8181892890955,52.0394181405146,2.07850551037678));
#56923=CARTESIAN_POINT('Ctrl Pts',(13.4174710746757,52.140814961816,2.05233700691785));
#56924=CARTESIAN_POINT('Ctrl Pts',(13.0727468794464,52.4572155888145,2.02616850345893));
#56925=CARTESIAN_POINT('Ctrl Pts',(12.9355708698302,52.8497595669186,2.));
#56926=CARTESIAN_POINT('',(13.8936035762985,54.5113733504501,2.));
#56927=CARTESIAN_POINT('Origin',(14.1292828945603,53.2669068454841,2.));
#56928=CARTESIAN_POINT('Ctrl Pts',(13.8936031194075,54.5113848919291,2.));
#56929=CARTESIAN_POINT('Ctrl Pts',(13.5065360962338,54.4366467486623,2.02490816038701));
#56930=CARTESIAN_POINT('Ctrl Pts',(13.1551959025419,54.1671648587472,2.04981632077402));
#56931=CARTESIAN_POINT('Ctrl Pts',(12.9858211468817,53.8112635997049,2.07472448116103));
#56932=CARTESIAN_POINT('Ctrl Pts',(12.8078760955218,53.4373538776067,2.10089298461995));
#56933=CARTESIAN_POINT('Ctrl Pts',(12.830777130449,52.9680579532916,2.12706148807888));
#56934=CARTESIAN_POINT('Ctrl Pts',(13.0443872879449,52.6134595791442,2.15322999153781));
#56935=CARTESIAN_POINT('Ctrl Pts',(13.2579974454408,52.2588612049968,2.17939849499673));
#56936=CARTESIAN_POINT('Ctrl Pts',(13.6623167255053,52.0189603810172,2.20556699845566));
#56937=CARTESIAN_POINT('Ctrl Pts',(14.0759781319804,52.0015075823912,2.23173550191458));
#56938=CARTESIAN_POINT('Ctrl Pts',(14.4896395384554,51.9840547837652,2.25790400537351));
#56939=CARTESIAN_POINT('Ctrl Pts',(14.9126430713409,52.1890500104929,2.28407250883244));
#56940=CARTESIAN_POINT('Ctrl Pts',(15.1553414968488,52.5244832283522,2.31024101229136));
#56941=CARTESIAN_POINT('Ctrl Pts',(15.3980399223566,52.8599164462115,2.33640951575029));
#56942=CARTESIAN_POINT('Ctrl Pts',(15.4604332404868,53.3257876552024,2.36257801920922));
#56943=CARTESIAN_POINT('Ctrl Pts',(15.3145273105893,53.7132383944998,2.38874652266814));
#56944=CARTESIAN_POINT('Ctrl Pts',(15.2129148646388,53.9830685332266,2.40697090631857));
#56945=CARTESIAN_POINT('Ctrl Pts',(15.010275844201,54.2148642023246,2.42519528996899));
#56946=CARTESIAN_POINT('Ctrl Pts',(14.7602610286104,54.3618122024717,2.44341967361941));
#56947=CARTESIAN_POINT('Origin',(14.1292828945603,53.2669068454841,0.895788276411274));
#56948=CARTESIAN_POINT('',(14.9010968564111,54.6052515498159,5.60421172358873));
#56949=CARTESIAN_POINT('',(14.89962934498,54.6010727330809,5.64578827641128));
#56950=CARTESIAN_POINT('',(14.9007828945603,54.6031840435236,0.895788276411274));
#56951=CARTESIAN_POINT('',(15.2209662466057,52.1764590205668,6.));
#56952=CARTESIAN_POINT('Ctrl Pts',(14.89962934498,54.6010727330809,5.64578827641128));
#56953=CARTESIAN_POINT('Ctrl Pts',(14.6737409652706,54.7312989825202,5.65918483710515));
#56954=CARTESIAN_POINT('Ctrl Pts',(13.9138866474417,54.955646298412,5.69874990125794));
#56955=CARTESIAN_POINT('Ctrl Pts',(12.6330342875793,54.2971998857928,5.76448346886966));
#56956=CARTESIAN_POINT('Ctrl Pts',(12.4433594214855,52.5865231455987,5.84298897924644));
#56957=CARTESIAN_POINT('Ctrl Pts',(13.7694165995699,51.486617996264,5.92149448962322));
#56958=CARTESIAN_POINT('Ctrl Pts',(14.8623799894179,51.8174664687921,5.97383149654107));
#56959=CARTESIAN_POINT('Ctrl Pts',(15.2209662466057,52.1764590205668,6.));
#56960=CARTESIAN_POINT('',(15.6220374293776,52.8664110852719,6.));
#56961=CARTESIAN_POINT('Origin',(14.1292828945603,53.2669068454841,6.));
#56962=CARTESIAN_POINT('Ctrl Pts',(14.9010968564111,54.6052515498159,5.60421172358873));
#56963=CARTESIAN_POINT('Ctrl Pts',(14.8619571740658,54.628166857787,5.60655897483644));
#56964=CARTESIAN_POINT('Ctrl Pts',(14.3739271072306,54.8842868995419,5.63507472954308));
#56965=CARTESIAN_POINT('Ctrl Pts',(13.1774033105245,54.8145932898247,5.68975898770864));
#56966=CARTESIAN_POINT('Ctrl Pts',(12.3131175991141,53.326633245717,5.76826449808541));
#56967=CARTESIAN_POINT('Ctrl Pts',(13.0780276880699,51.7849182946399,5.8467700084622));
#56968=CARTESIAN_POINT('Ctrl Pts',(14.7574918726583,51.5760767532103,5.92401517576705));
#56969=CARTESIAN_POINT('Ctrl Pts',(15.4957392820493,52.402248403584,5.97509183961299));
#56970=CARTESIAN_POINT('Ctrl Pts',(15.6220514315181,52.8664094746825,6.));
#56971=CARTESIAN_POINT('Origin',(14.1292828945603,53.2669068454841,0.895788276411274));
#56972=CARTESIAN_POINT('',(14.8993447411713,54.6013457970434,5.10421172358873));
#56973=CARTESIAN_POINT('',(14.9024169355128,54.6041163881961,5.14578827641128));
#56974=CARTESIAN_POINT('',(14.9007828945603,54.6031840435236,0.895788276411274));
#56975=CARTESIAN_POINT('Ctrl Pts',(14.9024169355127,54.6041163881961,5.14578827641128));
#56976=CARTESIAN_POINT('Ctrl Pts',(14.5148361321472,54.8241371380329,5.16884048301826));
#56977=CARTESIAN_POINT('Ctrl Pts',(13.4683417470894,54.9257881846255,5.21806119308415));
#56978=CARTESIAN_POINT('Ctrl Pts',(12.3638311119676,53.696734568805,5.29345040660898));
#56979=CARTESIAN_POINT('Ctrl Pts',(12.7969355370903,52.0313922294383,5.37195591698577));
#56980=CARTESIAN_POINT('Ctrl Pts',(14.424976702367,51.4740982114769,5.45046142736254));
#56981=CARTESIAN_POINT('Ctrl Pts',(15.7877203932888,52.5246186608361,5.52896693773932));
#56982=CARTESIAN_POINT('Ctrl Pts',(15.6845839838159,53.9480078415062,5.59407588742224));
#56983=CARTESIAN_POINT('Ctrl Pts',(15.1149856235702,54.4769183144689,5.63301633364622));
#56984=CARTESIAN_POINT('Ctrl Pts',(14.89962934498,54.6010727330809,5.64578827641128));
#56985=CARTESIAN_POINT('Ctrl Pts',(14.8993447411713,54.6013457970434,5.10421172358873));
#56986=CARTESIAN_POINT('Ctrl Pts',(14.6972931579988,54.7185214822016,5.11621462074955));
#56987=CARTESIAN_POINT('Ctrl Pts',(13.9751327847045,54.9521265711601,5.15438602136929));
#56988=CARTESIAN_POINT('Ctrl Pts',(12.6886982319545,54.374296277089,5.21872592544795));
#56989=CARTESIAN_POINT('Ctrl Pts',(12.4109789893207,52.6761143673659,5.29723143582474));
#56990=CARTESIAN_POINT('Ctrl Pts',(13.6742819091468,51.5077662723951,5.37573694620152));
#56991=CARTESIAN_POINT('Ctrl Pts',(15.3456277491901,51.9170631330653,5.4542424565783));
#56992=CARTESIAN_POINT('Ctrl Pts',(15.9087950365255,53.4884877368246,5.53040071570737));
#56993=CARTESIAN_POINT('Ctrl Pts',(15.2983088061438,54.3726938586823,5.58039047137751));
#56994=CARTESIAN_POINT('Ctrl Pts',(14.9010968564111,54.6052515498159,5.60421172358873));
#56995=CARTESIAN_POINT('Origin',(14.1292828945603,53.2669068454841,0.895788276411274));
#56996=CARTESIAN_POINT('',(14.9022875039252,54.6033748953446,4.60421172358873));
#56997=CARTESIAN_POINT('',(14.899520943644,54.6036563213,4.64578827641127));
#56998=CARTESIAN_POINT('',(14.9007828945603,54.6031840435236,0.895788276411274));
#56999=CARTESIAN_POINT('Ctrl Pts',(14.899520943644,54.6036563213,4.64578827641127));
#57000=CARTESIAN_POINT('Ctrl Pts',(14.7902473340007,54.6680216226135,4.65232762547243));
#57001=CARTESIAN_POINT('Ctrl Pts',(14.20608207924,54.9223430869235,4.68503547799252));
#57002=CARTESIAN_POINT('Ctrl Pts',(12.9456280488333,54.6455146101901,4.74391183397153));
#57003=CARTESIAN_POINT('Ctrl Pts',(12.3264734310144,53.0400243844668,4.8224173443483));
#57004=CARTESIAN_POINT('Ctrl Pts',(13.3241207711359,51.6380076713391,4.90092285472509));
#57005=CARTESIAN_POINT('Ctrl Pts',(15.0438575043004,51.6968266074015,4.97942836510187));
#57006=CARTESIAN_POINT('Ctrl Pts',(15.9433802614164,53.1637305367386,5.05793387547864));
#57007=CARTESIAN_POINT('Ctrl Pts',(15.4295729948612,54.265256390372,5.11338717924845));
#57008=CARTESIAN_POINT('Ctrl Pts',(14.9548117824789,54.5743730329603,5.14267197955933));
#57009=CARTESIAN_POINT('Ctrl Pts',(14.9024169355127,54.6041163881961,5.14578827641128));
#57010=CARTESIAN_POINT('Ctrl Pts',(14.9022875039252,54.6033748953446,4.60421172358873));
#57011=CARTESIAN_POINT('Ctrl Pts',(14.5374282197781,54.8098641325902,4.62587026666265));
#57012=CARTESIAN_POINT('Ctrl Pts',(13.5347909686423,54.9365925287331,4.6736973131955));
#57013=CARTESIAN_POINT('Ctrl Pts',(12.3888319545388,53.7888545684046,4.74769286318728));
#57014=CARTESIAN_POINT('Ctrl Pts',(12.7339055288242,52.1030679359729,4.82619837356406));
#57015=CARTESIAN_POINT('Ctrl Pts',(14.3303867955418,51.461039661442,4.90470388394084));
#57016=CARTESIAN_POINT('Ctrl Pts',(15.7465131069793,52.4385560995514,4.98320939431762));
#57017=CARTESIAN_POINT('Ctrl Pts',(15.7175049264688,53.8959207488069,5.04971200753358));
#57018=CARTESIAN_POINT('Ctrl Pts',(15.1378024352416,54.4630571321133,5.09004611729062));
#57019=CARTESIAN_POINT('Ctrl Pts',(14.8993447411713,54.6013457970434,5.10421172358873));
#57020=CARTESIAN_POINT('Origin',(14.1292828945603,53.2669068454841,0.895788276411274));
#57021=CARTESIAN_POINT('',(14.899957506564,54.6043129428392,4.10421172358873));
#57022=CARTESIAN_POINT('',(14.9006214745914,54.60116105013,4.14578827641127));
#57023=CARTESIAN_POINT('',(14.9007828945603,54.6031840435236,0.895788276411274));
#57024=CARTESIAN_POINT('Ctrl Pts',(14.9006214745914,54.60116105013,4.14578827641127));
#57025=CARTESIAN_POINT('Ctrl Pts',(14.6270809930356,54.7571745495808,4.16198327138554));
#57026=CARTESIAN_POINT('Ctrl Pts',(13.7886805442009,54.9572356101558,4.20434676981873));
#57027=CARTESIAN_POINT('Ctrl Pts',(12.5323678038339,54.1337749126023,4.27287877171085));
#57028=CARTESIAN_POINT('Ctrl Pts',(12.5253744436601,52.413047533365,4.35138428208763));
#57029=CARTESIAN_POINT('Ctrl Pts',(13.9568043064156,51.4580814834716,4.42988979246441));
#57030=CARTESIAN_POINT('Ctrl Pts',(15.5429170806551,52.1253130228171,4.50839530284119));
#57031=CARTESIAN_POINT('Ctrl Pts',(15.8347326759058,53.6754928499224,4.58036146415681));
#57032=CARTESIAN_POINT('Ctrl Pts',(15.2275273759708,54.4104510916165,4.62615912201351));
#57033=CARTESIAN_POINT('Ctrl Pts',(14.899520943644,54.6036563213,4.64578827641127));
#57034=CARTESIAN_POINT('Ctrl Pts',(14.899957506564,54.6043129428392,4.10421172358873));
#57035=CARTESIAN_POINT('Ctrl Pts',(14.8140915002504,54.654905954387,4.10935740911683));
#57036=CARTESIAN_POINT('Ctrl Pts',(14.2627733336105,54.9110489082196,4.14067159810387));
#57037=CARTESIAN_POINT('Ctrl Pts',(13.0196598476916,54.705772943414,4.19815429054983));
#57038=CARTESIAN_POINT('Ctrl Pts',(12.317045870665,53.1350132444558,4.2766598009266));
#57039=CARTESIAN_POINT('Ctrl Pts',(13.239689139382,51.6825388628568,4.35516531130338));
#57040=CARTESIAN_POINT('Ctrl Pts',(14.9601412381249,51.6509633535716,4.43367082168016));
#57041=CARTESIAN_POINT('Ctrl Pts',(15.9354598188275,53.0686043860759,4.51217633205695));
#57042=CARTESIAN_POINT('Ctrl Pts',(15.4687653497055,54.223916817667,4.5690232993598));
#57043=CARTESIAN_POINT('Ctrl Pts',(14.9782621856933,54.5603776227797,4.59970176320372));
#57044=CARTESIAN_POINT('Ctrl Pts',(14.9022875039252,54.6033748953446,4.60421172358873));
#57045=CARTESIAN_POINT('Origin',(14.1292828945603,53.2669068454841,0.895788276411274));
#57046=CARTESIAN_POINT('',(14.9001204094145,54.6010161225549,3.60421172358873));
#57047=CARTESIAN_POINT('',(14.9020910027761,54.6052313123369,3.64578827641127));
#57048=CARTESIAN_POINT('',(14.9007828945603,54.6031840435236,0.895788276411274));
#57049=CARTESIAN_POINT('Ctrl Pts',(14.9020910027761,54.6052313123369,3.64578827641127));
#57050=CARTESIAN_POINT('Ctrl Pts',(14.4696174214114,54.8543199357372,3.67163891729864));
#57051=CARTESIAN_POINT('Ctrl Pts',(13.3333022960118,54.8966530893797,3.72365806164495));
#57052=CARTESIAN_POINT('Ctrl Pts',(12.3283770240505,53.5084355106896,3.80184570945017));
#57053=CARTESIAN_POINT('Ctrl Pts',(12.9344615472089,51.8979656495417,3.88035121982696));
#57054=CARTESIAN_POINT('Ctrl Pts',(14.6120902596549,51.5151947977303,3.95885673020373));
#57055=CARTESIAN_POINT('Ctrl Pts',(15.8567258492822,52.7034009548899,4.03736224058051));
#57056=CARTESIAN_POINT('Ctrl Pts',(15.614980939896,54.0476036870055,4.09967275598302));
#57057=CARTESIAN_POINT('Ctrl Pts',(15.0690783538945,54.5050818625188,4.13581476792661));
#57058=CARTESIAN_POINT('Ctrl Pts',(14.9006214745914,54.60116105013,4.14578827641127));
#57059=CARTESIAN_POINT('Ctrl Pts',(14.9001204094145,54.6010161225549,3.60421172358873));
#57060=CARTESIAN_POINT('Ctrl Pts',(14.6502875315041,54.7442481097626,3.61901305502994));
#57061=CARTESIAN_POINT('Ctrl Pts',(13.8515268344552,54.9574092639254,3.65998288993008));
#57062=CARTESIAN_POINT('Ctrl Pts',(12.5800953694062,54.216441978079,3.72712122828915));
#57063=CARTESIAN_POINT('Ctrl Pts',(12.482746426243,52.4984560584277,3.80562673866593));
#57064=CARTESIAN_POINT('Ctrl Pts',(13.8620505314459,51.4696350750293,3.88413224904271));
#57065=CARTESIAN_POINT('Ctrl Pts',(15.4810149732843,52.0526501422855,3.96263775941949));
#57066=CARTESIAN_POINT('Ctrl Pts',(15.8610566498332,53.6150480556463,4.03599758426816));
#57067=CARTESIAN_POINT('Ctrl Pts',(15.2507650728867,54.3976140171991,4.08318890565791));
#57068=CARTESIAN_POINT('Ctrl Pts',(14.899957506564,54.6043129428392,4.10421172358873));
#57069=CARTESIAN_POINT('Origin',(14.1292828945603,53.2669068454841,0.895788276411274));
#57070=CARTESIAN_POINT('',(14.9023562176693,54.604775754849,3.10421172358873));
#57071=CARTESIAN_POINT('',(14.8991095940519,54.6023050298359,3.14578827641127));
#57072=CARTESIAN_POINT('',(14.9007828945603,54.6031840435236,0.895788276411274));
#57073=CARTESIAN_POINT('Ctrl Pts',(14.8991095940519,54.6023050298359,3.14578827641127));
#57074=CARTESIAN_POINT('Ctrl Pts',(14.7424882378679,54.6940222226684,3.15512605975283));
#57075=CARTESIAN_POINT('Ctrl Pts',(14.0895244416362,54.9406197878808,3.19063234655331));
#57076=CARTESIAN_POINT('Ctrl Pts',(12.8070376180166,54.5132075415872,3.25230713681272));
#57077=CARTESIAN_POINT('Ctrl Pts',(12.3603879600183,52.8514447189324,3.3308126471895));
#57078=CARTESIAN_POINT('Ctrl Pts',(13.5001253542918,51.5622781929174,3.40931815756628));
#57079=CARTESIAN_POINT('Ctrl Pts',(15.2041061771209,51.8018631754771,3.48782366794306));
#57080=CARTESIAN_POINT('Ctrl Pts',(15.944159933136,53.3553341468671,3.56632917831984));
#57081=CARTESIAN_POINT('Ctrl Pts',(15.3488521474601,54.3440811110856,3.61898404780924));
#57082=CARTESIAN_POINT('Ctrl Pts',(14.9074087496474,54.6021684888377,3.64547041383972));
#57083=CARTESIAN_POINT('Ctrl Pts',(14.9020910027761,54.6052313123369,3.64578827641127));
#57084=CARTESIAN_POINT('Ctrl Pts',(14.9023562176693,54.604775754849,3.10421172358873));
#57085=CARTESIAN_POINT('Ctrl Pts',(14.4921270687778,54.8390095809862,3.12866870094305));
#57086=CARTESIAN_POINT('Ctrl Pts',(13.4008007460488,54.9124362051017,3.1792941817563));
#57087=CARTESIAN_POINT('Ctrl Pts',(12.3435458814549,53.6026781745395,3.25608816602847));
#57088=CARTESIAN_POINT('Ctrl Pts',(12.8642192037884,51.9626013374103,3.33459367640525));
#57089=CARTESIAN_POINT('Ctrl Pts',(14.5194316817765,51.4922567887357,3.41309918678203));
#57090=CARTESIAN_POINT('Ctrl Pts',(15.824749470772,52.6134605506407,3.49160469715881));
#57091=CARTESIAN_POINT('Ctrl Pts',(15.6501092546376,53.9988114930956,3.55530887609437));
#57092=CARTESIAN_POINT('Ctrl Pts',(15.091987830948,54.4910163807415,3.59284455157101));
#57093=CARTESIAN_POINT('Ctrl Pts',(14.9001204094145,54.6010161225549,3.60421172358873));
#57094=CARTESIAN_POINT('Origin',(14.1292828945603,53.2669068454841,0.895788276411274));
#57095=CARTESIAN_POINT('',(14.8992309062956,54.6029598038327,2.60421172358873));
#57096=CARTESIAN_POINT('',(14.9016274172746,54.6020379108679,2.64578827641127));
#57097=CARTESIAN_POINT('',(14.9007828945603,54.6031840435236,0.895788276411274));
#57098=CARTESIAN_POINT('Ctrl Pts',(14.9016274172746,54.6020379108679,2.64578827641127));
#57099=CARTESIAN_POINT('Ctrl Pts',(14.5809116606718,54.7836391180053,2.66478170566594));
#57100=CARTESIAN_POINT('Ctrl Pts',(13.6600505366298,54.9508125591569,2.70994363837953));
#57101=CARTESIAN_POINT('Ctrl Pts',(12.4499634166736,53.9607949476381,2.78127407455204));
#57102=CARTESIAN_POINT('Ctrl Pts',(12.6242053254301,52.2488988977253,2.85977958492882));
#57103=CARTESIAN_POINT('Ctrl Pts',(14.1482380059646,51.4499755676755,2.9382850953056));
#57104=CARTESIAN_POINT('Ctrl Pts',(15.6552705807332,52.2805199058823,3.01679060568238));
#57105=CARTESIAN_POINT('Ctrl Pts',(15.777288771741,53.7916708150444,3.08595833271761));
#57106=CARTESIAN_POINT('Ctrl Pts',(15.1814089486113,54.4369910204986,3.1289575562939));
#57107=CARTESIAN_POINT('Ctrl Pts',(14.8991095940519,54.6023050298359,3.14578827641127));
#57108=CARTESIAN_POINT('Ctrl Pts',(14.8992309062956,54.6029598038327,2.60421172358873));
#57109=CARTESIAN_POINT('Ctrl Pts',(14.7662449521696,54.681123251708,2.61215584339723));
#57110=CARTESIAN_POINT('Ctrl Pts',(14.1480244437874,54.9322850073565,2.64626846666466));
#57111=CARTESIAN_POINT('Ctrl Pts',(12.8743150895914,54.5809192738243,2.70654959339101));
#57112=CARTESIAN_POINT('Ctrl Pts',(12.3410089780029,52.9449163922479,2.78505510376779));
#57113=CARTESIAN_POINT('Ctrl Pts',(13.4114743235374,51.5976690199096,2.86356061414457));
#57114=CARTESIAN_POINT('Ctrl Pts',(15.125685020798,51.7474403844543,2.94206612452135));
#57115=CARTESIAN_POINT('Ctrl Pts',(15.9462998191018,53.2599021194416,3.02057163489813));
#57116=CARTESIAN_POINT('Ctrl Pts',(15.3893775359764,54.3055097335425,3.07462016792059));
#57117=CARTESIAN_POINT('Ctrl Pts',(14.9310645035309,54.588383814741,3.10250019748412));
#57118=CARTESIAN_POINT('Ctrl Pts',(14.9023562176693,54.604775754849,3.10421172358873));
#57119=CARTESIAN_POINT('Origin',(14.1292828945603,53.2669068454841,0.895788276411274));
#57120=CARTESIAN_POINT('',(14.9013089558621,54.600969116598,2.10421172358873));
#57121=CARTESIAN_POINT('',(14.9010809748678,54.6051974101417,2.14578827641127));
#57122=CARTESIAN_POINT('',(14.9007828945603,54.6031840435236,0.895788276411274));
#57123=CARTESIAN_POINT('',(15.6194800884629,52.866705242183,2.));
#57124=CARTESIAN_POINT('Ctrl Pts',(15.6194800884629,52.866705242183,2.));
#57125=CARTESIAN_POINT('Ctrl Pts',(15.7510836294753,53.3567463262429,2.02616850345893));
#57126=CARTESIAN_POINT('Ctrl Pts',(15.5785415188313,54.0947786094125,2.06090574465517));
#57127=CARTESIAN_POINT('Ctrl Pts',(15.0460508163988,54.5187167298269,2.09564298585141));
#57128=CARTESIAN_POINT('Ctrl Pts',(14.9013089558621,54.600969116598,2.10421172358873));
#57129=CARTESIAN_POINT('',(15.2224998162609,52.1743915631094,2.));
#57130=CARTESIAN_POINT('Origin',(14.1292828945603,53.2669068454841,2.));
#57131=CARTESIAN_POINT('Ctrl Pts',(15.2225082026616,52.1743802571171,2.));
#57132=CARTESIAN_POINT('Ctrl Pts',(15.5613276195564,52.5158503863372,2.02490816038701));
#57133=CARTESIAN_POINT('Ctrl Pts',(15.8908670066042,53.5171650620887,2.0735042525241));
#57134=CARTESIAN_POINT('Ctrl Pts',(15.2959835850222,54.3738753315586,2.12210034466119));
#57135=CARTESIAN_POINT('Ctrl Pts',(14.9010809748678,54.6051974101417,2.14578827641127));
#57136=CARTESIAN_POINT('Origin',(-39.0658530619283,38.8697713466882,4.5));
#57137=CARTESIAN_POINT('',(-39.6970780592613,39.9631802546368,5.80658032638059));
#57138=CARTESIAN_POINT('',(-39.6962628554159,39.9650155589839,5.94341967361941));
#57139=CARTESIAN_POINT('',(-39.6981030619283,39.9648604697737,4.5));
#57140=CARTESIAN_POINT('',(-40.2595650866585,39.2869186252538,6.));
#57141=CARTESIAN_POINT('Ctrl Pts',(-39.6962628554159,39.9650155589839,5.94341967361941));
#57142=CARTESIAN_POINT('Ctrl Pts',(-39.9540142218038,39.8131911161898,5.96227978241294));
#57143=CARTESIAN_POINT('Ctrl Pts',(-40.160699881421,39.5698320958276,5.98113989120647));
#57144=CARTESIAN_POINT('Ctrl Pts',(-40.2595650866585,39.2869186252538,6.));
#57145=CARTESIAN_POINT('',(-39.6981030619283,39.9648604697737,6.));
#57146=CARTESIAN_POINT('Origin',(-39.0658530619283,38.8697713466882,6.));
#57147=CARTESIAN_POINT('',(-39.6981030619283,39.9648604697737,7.));
#57148=CARTESIAN_POINT('',(-39.6981030619283,39.9648604697737,4.5));
#57149=CARTESIAN_POINT('',(-39.7608672580762,37.8134023216061,7.));
#57150=CARTESIAN_POINT('Origin',(-39.0658530619283,38.8697713466882,7.));
#57151=CARTESIAN_POINT('',(-38.3708388657805,39.9261403717704,7.));
#57152=CARTESIAN_POINT('Origin',(-39.0658530619283,38.8697713466882,7.));
#57153=CARTESIAN_POINT('Origin',(-39.0658530619283,38.8697713466882,7.));
#57154=CARTESIAN_POINT('',(-39.3015291113282,37.6253036020567,6.));
#57155=CARTESIAN_POINT('Origin',(-39.0658530619283,38.8697713466882,6.));
#57156=CARTESIAN_POINT('Ctrl Pts',(-39.3015295597333,37.6252918061955,6.));
#57157=CARTESIAN_POINT('Ctrl Pts',(-39.6885932560667,37.7000310216234,5.97509183961299));
#57158=CARTESIAN_POINT('Ctrl Pts',(-40.0399430624791,37.9695097738977,5.95018367922598));
#57159=CARTESIAN_POINT('Ctrl Pts',(-40.2093203959796,38.3254113926459,5.92527551883898));
#57160=CARTESIAN_POINT('Ctrl Pts',(-40.3872681556177,38.6993214926512,5.89910701538005));
#57161=CARTESIAN_POINT('Ctrl Pts',(-40.3643620641528,39.1686216551033,5.87293851192112));
#57162=CARTESIAN_POINT('Ctrl Pts',(-40.1507501683313,39.5232214807692,5.8467700084622));
#57163=CARTESIAN_POINT('Ctrl Pts',(-40.0413948614145,39.7047533782285,5.83337344776833));
#57164=CARTESIAN_POINT('Ctrl Pts',(-39.8820599551598,39.8562249589825,5.81997688707446));
#57165=CARTESIAN_POINT('Ctrl Pts',(-39.6970780592613,39.9631802546368,5.80658032638059));
#57166=CARTESIAN_POINT('Origin',(-39.0658530619283,38.8697713466882,4.5));
#57167=CARTESIAN_POINT('',(-39.6980969738519,39.9664052404927,5.30658032638059));
#57168=CARTESIAN_POINT('',(-39.6994431549996,39.9659335873643,5.44341967361941));
#57169=CARTESIAN_POINT('',(-39.6981030619283,39.9648604697737,4.5));
#57170=CARTESIAN_POINT('Ctrl Pts',(-39.6994431549996,39.9659335873643,5.44341967361941));
#57171=CARTESIAN_POINT('Ctrl Pts',(-39.7317442057588,39.9475451778338,5.44576692486712));
#57172=CARTESIAN_POINT('Ctrl Pts',(-39.7631672715511,39.9276731785137,5.44811417611483));
#57173=CARTESIAN_POINT('Ctrl Pts',(-39.7935612952929,39.9063356334612,5.45046142736254));
#57174=CARTESIAN_POINT('Ctrl Pts',(-40.1324113081289,39.6684524404899,5.47662993082147));
#57175=CARTESIAN_POINT('Ctrl Pts',(-40.3433609694206,39.2484155500404,5.50279843428039));
#57176=CARTESIAN_POINT('Ctrl Pts',(-40.3318541433896,38.8345478072092,5.52896693773932));
#57177=CARTESIAN_POINT('Ctrl Pts',(-40.3203473173587,38.420680064378,5.55513544119825));
#57178=CARTESIAN_POINT('Ctrl Pts',(-40.086384004005,38.0129814691651,5.58130394465717));
#57179=CARTESIAN_POINT('Ctrl Pts',(-39.7348031115542,37.7943227533549,5.6074724481161));
#57180=CARTESIAN_POINT('Ctrl Pts',(-39.3832222191033,37.5756640375447,5.63364095157503));
#57181=CARTESIAN_POINT('Ctrl Pts',(-38.9140237475553,37.5460452011372,5.65980945503395));
#57182=CARTESIAN_POINT('Ctrl Pts',(-38.5377492251912,37.7186390805662,5.68597795849288));
#57183=CARTESIAN_POINT('Ctrl Pts',(-38.1614747028271,37.8912329599952,5.7121464619518));
#57184=CARTESIAN_POINT('Ctrl Pts',(-37.8781241296468,38.2660395552607,5.73831496541073));
#57185=CARTESIAN_POINT('Ctrl Pts',(-37.814457003614,38.6752103329024,5.76448346886966));
#57186=CARTESIAN_POINT('Ctrl Pts',(-37.7507898775812,39.0843811105442,5.79065197232858));
#57187=CARTESIAN_POINT('Ctrl Pts',(-37.9068061986959,39.5279160705621,5.81682047578751));
#57188=CARTESIAN_POINT('Ctrl Pts',(-38.2131591663055,39.8064837741936,5.84298897924644));
#57189=CARTESIAN_POINT('Ctrl Pts',(-38.5195121339152,40.0850514778251,5.86915748270536));
#57190=CARTESIAN_POINT('Ctrl Pts',(-38.9762017480197,40.1986519250703,5.89532598616429));
#57191=CARTESIAN_POINT('Ctrl Pts',(-39.3769209838015,40.0972547064535,5.92149448962322));
#57192=CARTESIAN_POINT('Ctrl Pts',(-39.4888346944845,40.0689362780501,5.92880288428861));
#57193=CARTESIAN_POINT('Ctrl Pts',(-39.5963828000181,40.0238483557584,5.93611127895401));
#57194=CARTESIAN_POINT('Ctrl Pts',(-39.6962628554159,39.9650155589839,5.94341967361941));
#57195=CARTESIAN_POINT('Ctrl Pts',(-39.6970780592613,39.9631802546368,5.80658032638059));
#57196=CARTESIAN_POINT('Ctrl Pts',(-39.520720989639,40.0651487333929,5.79380838361554));
#57197=CARTESIAN_POINT('Ctrl Pts',(-39.3210527704035,40.1266553179232,5.78103644085048));
#57198=CARTESIAN_POINT('Ctrl Pts',(-39.1191586941911,40.1351732662231,5.76826449808542));
#57199=CARTESIAN_POINT('Ctrl Pts',(-38.7054968160504,40.1526257371314,5.7420959946265));
#57200=CARTESIAN_POINT('Ctrl Pts',(-38.2824907599468,39.9476311900682,5.71592749116757));
#57201=CARTESIAN_POINT('Ctrl Pts',(-38.0397913612151,39.6121973316471,5.68975898770864));
#57202=CARTESIAN_POINT('Ctrl Pts',(-37.7970919624834,39.2767634732261,5.66359048424972));
#57203=CARTESIAN_POINT('Ctrl Pts',(-37.7346992211236,38.8108903034471,5.63742198079079));
#57204=CARTESIAN_POINT('Ctrl Pts',(-37.8806057126089,38.4234383862029,5.61125347733186));
#57205=CARTESIAN_POINT('Ctrl Pts',(-38.0265122040943,38.0359864689587,5.58508497387294));
#57206=CARTESIAN_POINT('Ctrl Pts',(-38.3807179284248,37.7269558042492,5.55891647041401));
#57207=CARTESIAN_POINT('Ctrl Pts',(-38.7843854256714,37.6349404921318,5.53274796695508));
#57208=CARTESIAN_POINT('Ctrl Pts',(-39.188052922918,37.5429251800145,5.50657946349616));
#57209=CARTESIAN_POINT('Ctrl Pts',(-39.6411821930806,37.6679252204893,5.48041096003723));
#57210=CARTESIAN_POINT('Ctrl Pts',(-39.9405883560671,37.9538786579723,5.4542424565783));
#57211=CARTESIAN_POINT('Ctrl Pts',(-40.2399945190536,38.2398320954553,5.42807395311938));
#57212=CARTESIAN_POINT('Ctrl Pts',(-40.3856775748639,38.6867389299465,5.40190544966045));
#57213=CARTESIAN_POINT('Ctrl Pts',(-40.312309689211,39.0942060073491,5.37573694620152));
#57214=CARTESIAN_POINT('Ctrl Pts',(-40.2476788760258,39.4531495468055,5.35268473959455));
#57215=CARTESIAN_POINT('Ctrl Pts',(-40.0130623748058,39.7814874463141,5.32963253298757));
#57216=CARTESIAN_POINT('Ctrl Pts',(-39.6980969738519,39.9664052404927,5.30658032638059));
#57217=CARTESIAN_POINT('Origin',(-39.0658530619283,38.8697713466882,4.5));
#57218=CARTESIAN_POINT('',(-39.6989570949589,39.9641614067485,4.80658032638059));
#57219=CARTESIAN_POINT('',(-39.697389467188,39.9630895992609,4.94341967361941));
#57220=CARTESIAN_POINT('',(-39.6981030619283,39.9648604697737,4.5));
#57221=CARTESIAN_POINT('Ctrl Pts',(-39.697389467188,39.9630895992609,4.94341967361941));
#57222=CARTESIAN_POINT('Ctrl Pts',(-39.8633425703643,39.8677036169061,4.95542257078023));
#57223=CARTESIAN_POINT('Ctrl Pts',(-40.0085235722312,39.7366393919841,4.96742546794105));
#57224=CARTESIAN_POINT('Ctrl Pts',(-40.1149177943607,39.5793405247057,4.97942836510186));
#57225=CARTESIAN_POINT('Ctrl Pts',(-40.3468765900167,39.2364003247431,5.00559686856079));
#57226=CARTESIAN_POINT('Ctrl Pts',(-40.3944742703016,38.7687617621182,5.03176537201971));
#57227=CARTESIAN_POINT('Ctrl Pts',(-40.2363680070802,38.3861191307629,5.05793387547864));
#57228=CARTESIAN_POINT('Ctrl Pts',(-40.0782617438588,38.0034764994076,5.08410237893757));
#57229=CARTESIAN_POINT('Ctrl Pts',(-39.7144515371312,37.705829799322,5.1102708823965));
#57230=CARTESIAN_POINT('Ctrl Pts',(-39.3080731239833,37.626648148232,5.13643938585542));
#57231=CARTESIAN_POINT('Ctrl Pts',(-38.9016947108354,37.5474664971421,5.16260788931435));
#57232=CARTESIAN_POINT('Ctrl Pts',(-38.4527480912673,37.6867498950478,5.18877639277327));
#57233=CARTESIAN_POINT('Ctrl Pts',(-38.1625484528667,37.982040398373,5.2149448962322));
#57234=CARTESIAN_POINT('Ctrl Pts',(-37.8723488144662,38.2773309016981,5.24111339969112));
#57235=CARTESIAN_POINT('Ctrl Pts',(-37.7408961572331,38.7286285104427,5.26728190315005));
#57236=CARTESIAN_POINT('Ctrl Pts',(-37.8271310042327,39.1335692645202,5.29345040660898));
#57237=CARTESIAN_POINT('Ctrl Pts',(-37.9133658512322,39.5385100185978,5.31961891006791));
#57238=CARTESIAN_POINT('Ctrl Pts',(-38.2172882024643,39.8970939180084,5.34578741352683));
#57239=CARTESIAN_POINT('Ctrl Pts',(-38.6026245602705,40.0485211199671,5.37195591698576));
#57240=CARTESIAN_POINT('Ctrl Pts',(-38.9533971820163,40.1863656694332,5.39577716919697));
#57241=CARTESIAN_POINT('Ctrl Pts',(-39.3716335617261,40.1525497161724,5.41959842140819));
#57242=CARTESIAN_POINT('Ctrl Pts',(-39.6994431549996,39.9659335873643,5.44341967361941));
#57243=CARTESIAN_POINT('Ctrl Pts',(-39.6980969738519,39.9664052404927,5.30658032638059));
#57244=CARTESIAN_POINT('Ctrl Pts',(-39.6555185906107,39.9914032265725,5.30346402952864));
#57245=CARTESIAN_POINT('Ctrl Pts',(-39.6114718472881,40.0137802388959,5.30034773267669));
#57246=CARTESIAN_POINT('Ctrl Pts',(-39.5661781885584,40.033257573116,5.29723143582475));
#57247=CARTESIAN_POINT('Ctrl Pts',(-39.1858334006749,40.1968147411666,5.27106293236582));
#57248=CARTESIAN_POINT('Ctrl Pts',(-38.7175626520242,40.1559017569539,5.24489442890689));
#57249=CARTESIAN_POINT('Ctrl Pts',(-38.3713436649215,39.928865763386,5.21872592544796));
#57250=CARTESIAN_POINT('Ctrl Pts',(-38.0251246778187,39.701829769818,5.19255742198904));
#57251=CARTESIAN_POINT('Ctrl Pts',(-37.8009574522638,39.2886707668948,5.16638891853011));
#57252=CARTESIAN_POINT('Ctrl Pts',(-37.7993614588042,38.8746535306862,5.14022041507118));
#57253=CARTESIAN_POINT('Ctrl Pts',(-37.7977654653446,38.4606362944776,5.11405191161226));
#57254=CARTESIAN_POINT('Ctrl Pts',(-38.0187407039802,38.0457608249837,5.08788340815333));
#57255=CARTESIAN_POINT('Ctrl Pts',(-38.3631991409408,37.8160625276688,5.06171490469441));
#57256=CARTESIAN_POINT('Ctrl Pts',(-38.7076575779013,37.5863642303539,5.03554640123548));
#57257=CARTESIAN_POINT('Ctrl Pts',(-39.1755992131868,37.5418431052181,5.00937789777655));
#57258=CARTESIAN_POINT('Ctrl Pts',(-39.5571935097812,37.7024627985795,4.98320939431763));
#57259=CARTESIAN_POINT('Ctrl Pts',(-39.9387878063755,37.863082491941,4.9570408908587));
#57260=CARTESIAN_POINT('Ctrl Pts',(-40.2340347642788,38.2288430037995,4.93087238739978));
#57261=CARTESIAN_POINT('Ctrl Pts',(-40.3105421109526,38.635733049973,4.90470388394085));
#57262=CARTESIAN_POINT('Ctrl Pts',(-40.3870494576263,39.0426230961465,4.87853538048192));
#57263=CARTESIAN_POINT('Ctrl Pts',(-40.2448171930705,39.4906426766349,4.85236687702299));
#57264=CARTESIAN_POINT('Ctrl Pts',(-39.9476239688235,39.7788944478041,4.82619837356406));
#57265=CARTESIAN_POINT('Ctrl Pts',(-39.8733571986579,39.8509268034996,4.81965902450291));
#57266=CARTESIAN_POINT('Ctrl Pts',(-39.789413588409,39.9129821459892,4.81311967544175));
#57267=CARTESIAN_POINT('Ctrl Pts',(-39.6989570949589,39.9641614067485,4.80658032638059));
#57268=CARTESIAN_POINT('Origin',(-39.0658530619283,38.8697713466882,4.5));
#57269=CARTESIAN_POINT('',(-39.6967352121902,39.9639200225483,4.30658032638059));
#57270=CARTESIAN_POINT('',(-39.6976237458347,39.9660095563765,4.44341967361941));
#57271=CARTESIAN_POINT('',(-39.6981030619283,39.9648604697737,4.5));
#57272=CARTESIAN_POINT('Ctrl Pts',(-39.6976237458347,39.9660095563765,4.44341967361941));
#57273=CARTESIAN_POINT('Ctrl Pts',(-39.9936753773632,39.7916729655961,4.46507821669334));
#57274=CARTESIAN_POINT('Ctrl Pts',(-40.2204527828214,39.4929448719807,4.48673675976726));
#57275=CARTESIAN_POINT('Ctrl Pts',(-40.2988032317419,39.159355592007,4.50839530284118));
#57276=CARTESIAN_POINT('Ctrl Pts',(-40.3934686017341,38.756302986065,4.53456380630011));
#57277=CARTESIAN_POINT('Ctrl Pts',(-40.2714573392084,38.3023593247386,4.56073230975904));
#57278=CARTESIAN_POINT('Ctrl Pts',(-39.9874807525881,38.0010783358291,4.58690081321797));
#57279=CARTESIAN_POINT('Ctrl Pts',(-39.7035041659678,37.6997973469195,4.61306931667689));
#57280=CARTESIAN_POINT('Ctrl Pts',(-39.2575622552529,37.5511790304267,4.63923782013582));
#57281=CARTESIAN_POINT('Ctrl Pts',(-38.8496206579413,37.6218656179337,4.66540632359474));
#57282=CARTESIAN_POINT('Ctrl Pts',(-38.4416790606296,37.6925522054406,4.69157482705367));
#57283=CARTESIAN_POINT('Ctrl Pts',(-38.0717377767213,37.9825436969474,4.7177433305126));
#57284=CARTESIAN_POINT('Ctrl Pts',(-37.9056829078162,38.361804436646,4.74391183397152));
#57285=CARTESIAN_POINT('Ctrl Pts',(-37.739628038911,38.7410651763447,4.77008033743045));
#57286=CARTESIAN_POINT('Ctrl Pts',(-37.777459585009,39.2095951642353,4.79624884088937));
#57287=CARTESIAN_POINT('Ctrl Pts',(-38.0022133656486,39.5573000327044,4.8224173443483));
#57288=CARTESIAN_POINT('Ctrl Pts',(-38.2269671462881,39.9050049011735,4.84858584780723));
#57289=CARTESIAN_POINT('Ctrl Pts',(-38.6386431614694,40.1318846502211,4.87475435126616));
#57290=CARTESIAN_POINT('Ctrl Pts',(-39.0526411245735,40.1362036060948,4.90092285472508));
#57291=CARTESIAN_POINT('Ctrl Pts',(-39.2767476411253,40.1385415551724,4.91508846102319));
#57292=CARTESIAN_POINT('Ctrl Pts',(-39.5015345588232,40.0756624434911,4.9292540673213));
#57293=CARTESIAN_POINT('Ctrl Pts',(-39.697389467188,39.9630895992609,4.94341967361941));
#57294=CARTESIAN_POINT('Ctrl Pts',(-39.6989570949589,39.9641614067485,4.80658032638059));
#57295=CARTESIAN_POINT('Ctrl Pts',(-39.4274339724573,40.1177861180174,4.78695117198282));
#57296=CARTESIAN_POINT('Ctrl Pts',(-39.0972285087862,40.1734152228909,4.76732201758506));
#57297=CARTESIAN_POINT('Ctrl Pts',(-38.7939127211062,40.1067326165456,4.74769286318729));
#57298=CARTESIAN_POINT('Ctrl Pts',(-38.389548881574,40.0178350522677,4.72152435972836));
#57299=CARTESIAN_POINT('Ctrl Pts',(-38.0329753864478,39.7115559618618,4.69535585626944));
#57300=CARTESIAN_POINT('Ctrl Pts',(-37.8840840327676,39.3252345207529,4.66918735281051));
#57301=CARTESIAN_POINT('Ctrl Pts',(-37.7351926790873,38.9389130796439,4.64301884935158));
#57302=CARTESIAN_POINT('Ctrl Pts',(-37.7939834668531,38.472549287832,4.61685034589266));
#57303=CARTESIAN_POINT('Ctrl Pts',(-38.0340939063583,38.1352662178079,4.59068184243373));
#57304=CARTESIAN_POINT('Ctrl Pts',(-38.2742043458636,37.7979831477837,4.5645133389748));
#57305=CARTESIAN_POINT('Ctrl Pts',(-38.6956344371082,37.5897807995474,4.53834483551588));
#57306=CARTESIAN_POINT('Ctrl Pts',(-39.1094099185268,37.6040195786007,4.51217633205695));
#57307=CARTESIAN_POINT('Ctrl Pts',(-39.5231853999454,37.618258357654,4.48600782859802));
#57308=CARTESIAN_POINT('Ctrl Pts',(-39.929306271538,37.854938263997,4.4598393251391));
#57309=CARTESIAN_POINT('Ctrl Pts',(-40.1456631065935,38.2079292154005,4.43367082168017));
#57310=CARTESIAN_POINT('Ctrl Pts',(-40.3620199416489,38.560920166804,4.40750231822124));
#57311=CARTESIAN_POINT('Ctrl Pts',(-40.3886127401672,39.0302221632679,4.38133381476232));
#57312=CARTESIAN_POINT('Ctrl Pts',(-40.2135169753906,39.4053946105006,4.35516531130339));
#57313=CARTESIAN_POINT('Ctrl Pts',(-40.1051548355753,39.6375789196628,4.33897031632912));
#57314=CARTESIAN_POINT('Ctrl Pts',(-39.919545071043,39.8337111891107,4.32277532135486));
#57315=CARTESIAN_POINT('Ctrl Pts',(-39.6967352121902,39.9639200225483,4.30658032638059));
#57316=CARTESIAN_POINT('Origin',(-39.0658530619283,38.8697713466882,4.5));
#57317=CARTESIAN_POINT('',(-39.6990217970716,39.9666307803347,3.80658032638059));
#57318=CARTESIAN_POINT('',(-39.6992442211058,39.9647402889406,3.94341967361941));
#57319=CARTESIAN_POINT('',(-39.6981030619283,39.9648604697737,4.5));
#57320=CARTESIAN_POINT('Ctrl Pts',(-39.6992442211058,39.9647402889406,3.94341967361941));
#57321=CARTESIAN_POINT('Ctrl Pts',(-39.7703349168266,39.9245305221536,3.94856535914752));
#57322=CARTESIAN_POINT('Ctrl Pts',(-39.8373290103598,39.877480560471,3.95371104467563));
#57323=CARTESIAN_POINT('Ctrl Pts',(-39.8986640775364,39.8239468894644,3.95885673020373));
#57324=CARTESIAN_POINT('Ctrl Pts',(-40.2105849885205,39.551700160189,3.98502523366266));
#57325=CARTESIAN_POINT('Ctrl Pts',(-40.3761490651667,39.1117681946799,4.01119373712159));
#57326=CARTESIAN_POINT('Ctrl Pts',(-40.3211154074003,38.7014217157033,4.03736224058051));
#57327=CARTESIAN_POINT('Ctrl Pts',(-40.2660817496338,38.2910752367267,4.06353074403944));
#57328=CARTESIAN_POINT('Ctrl Pts',(-39.9904503574547,37.9103142442825,4.08969924749836));
#57329=CARTESIAN_POINT('Ctrl Pts',(-39.6178176236238,37.7298764933343,4.11586775095729));
#57330=CARTESIAN_POINT('Ctrl Pts',(-39.245184889793,37.5494387423861,4.14203625441622));
#57331=CARTESIAN_POINT('Ctrl Pts',(-38.7755508143104,37.5693242329338,4.16820475787514));
#57332=CARTESIAN_POINT('Ctrl Pts',(-38.4195048988347,37.780616074816,4.19437326133407));
#57333=CARTESIAN_POINT('Ctrl Pts',(-38.0634589833589,37.9919079166982,4.220541764793));
#57334=CARTESIAN_POINT('Ctrl Pts',(-37.82100122789,38.3946061099149,4.24671026825192));
#57335=CARTESIAN_POINT('Ctrl Pts',(-37.8008525725161,38.8081359974719,4.27287877171085));
#57336=CARTESIAN_POINT('Ctrl Pts',(-37.7807039171422,39.221665885029,4.29904727516978));
#57337=CARTESIAN_POINT('Ctrl Pts',(-37.9828643618632,39.6460274669263,4.3252157786287));
#57338=CARTESIAN_POINT('Ctrl Pts',(-38.3166827592479,39.8909319662484,4.35138428208763));
#57339=CARTESIAN_POINT('Ctrl Pts',(-38.6505011566327,40.1358364655705,4.37755278554655));
#57340=CARTESIAN_POINT('Ctrl Pts',(-39.1159775066813,40.2012838823174,4.40372128900548));
#57341=CARTESIAN_POINT('Ctrl Pts',(-39.5043866829606,40.057926815412,4.42988979246441));
#57342=CARTESIAN_POINT('Ctrl Pts',(-39.571326315215,40.0332202175102,4.43439975284941));
#57343=CARTESIAN_POINT('Ctrl Pts',(-39.6359768878004,40.0023116804572,4.43890971323441));
#57344=CARTESIAN_POINT('Ctrl Pts',(-39.6976237458347,39.9660095563765,4.44341967361941));
#57345=CARTESIAN_POINT('Ctrl Pts',(-39.6967352121902,39.9639200225483,4.30658032638059));
#57346=CARTESIAN_POINT('Ctrl Pts',(-39.5595202256302,40.0441076920801,4.29660681789593));
#57347=CARTESIAN_POINT('Ctrl Pts',(-39.4081968207293,40.0992933977544,4.28663330941127));
#57348=CARTESIAN_POINT('Ctrl Pts',(-39.2521185625475,40.1225003286185,4.27665980092661));
#57349=CARTESIAN_POINT('Ctrl Pts',(-38.8426002425525,40.1833907015023,4.25049129746768));
#57350=CARTESIAN_POINT('Ctrl Pts',(-38.4003479306342,40.0241285492682,4.22432279400876));
#57351=CARTESIAN_POINT('Ctrl Pts',(-38.1236728204874,39.7161289139554,4.19815429054983));
#57352=CARTESIAN_POINT('Ctrl Pts',(-37.8469977103406,39.4081292786425,4.17198578709091));
#57353=CARTESIAN_POINT('Ctrl Pts',(-37.7358998019654,38.9513921602507,4.14581728363198));
#57354=CARTESIAN_POINT('Ctrl Pts',(-37.840196718037,38.5507239118952,4.11964878017305));
#57355=CARTESIAN_POINT('Ctrl Pts',(-37.9444936341086,38.1500556635396,4.09348027671412));
#57356=CARTESIAN_POINT('Ctrl Pts',(-38.2641853746271,37.8054562852203,4.0673117732552));
#57357=CARTESIAN_POINT('Ctrl Pts',(-38.6559183630715,37.6714482343173,4.04114326979627));
#57358=CARTESIAN_POINT('Ctrl Pts',(-39.0476513515158,37.5374401834144,4.01497476633735));
#57359=CARTESIAN_POINT('Ctrl Pts',(-39.5114255878859,37.6140234599276,3.98880626287842));
#57360=CARTESIAN_POINT('Ctrl Pts',(-39.8392791917195,37.8668572123835,3.9626377594195));
#57361=CARTESIAN_POINT('Ctrl Pts',(-40.1671327955531,38.1196909648394,3.93646925596057));
#57362=CARTESIAN_POINT('Ctrl Pts',(-40.3590657668502,38.548775193238,3.91030075250164));
#57363=CARTESIAN_POINT('Ctrl Pts',(-40.3290130799472,38.9617034290506,3.88413224904271));
#57364=CARTESIAN_POINT('Ctrl Pts',(-40.2993254358659,39.3696159240468,3.85828160815534));
#57365=CARTESIAN_POINT('Ctrl Pts',(-40.0530121946873,39.7617625287194,3.83243096726797));
#57366=CARTESIAN_POINT('Ctrl Pts',(-39.6990217970716,39.9666307803347,3.80658032638059));
#57367=CARTESIAN_POINT('Origin',(-39.0658530619283,38.8697713466882,4.5));
#57368=CARTESIAN_POINT('',(-39.6981666138854,39.9633157673857,3.30658032638059));
#57369=CARTESIAN_POINT('',(-39.6968376638892,39.9635050155947,3.44341967361941));
#57370=CARTESIAN_POINT('',(-39.6981030619283,39.9648604697737,4.5));
#57371=CARTESIAN_POINT('Ctrl Pts',(-39.6968376638892,39.9635050155947,3.44341967361941));
#57372=CARTESIAN_POINT('Ctrl Pts',(-39.9008619683973,39.8448845676908,3.45822100506062));
#57373=CARTESIAN_POINT('Ctrl Pts',(-40.0737604294823,39.6716358129756,3.47302233650184));
#57374=CARTESIAN_POINT('Ctrl Pts',(-40.1838048209619,39.4649259634328,3.48782366794305));
#57375=CARTESIAN_POINT('Ctrl Pts',(-40.3783614424731,39.0994664482373,3.51399217140198));
#57376=CARTESIAN_POINT('Ctrl Pts',(-40.3764510665601,38.6294154424261,3.54016067486091));
#57377=CARTESIAN_POINT('Ctrl Pts',(-40.1789303273027,38.265549404193,3.56632917831983));
#57378=CARTESIAN_POINT('Ctrl Pts',(-39.9814095880453,37.9016833659598,3.59249768177876));
#57379=CARTESIAN_POINT('Ctrl Pts',(-39.5882784854434,37.6440022953046,3.61866618523768));
#57380=CARTESIAN_POINT('Ctrl Pts',(-39.1758216795725,37.6080534474274,3.64483468869661));
#57381=CARTESIAN_POINT('Ctrl Pts',(-38.7633648737016,37.5721045995503,3.67100319215554));
#57382=CARTESIAN_POINT('Ctrl Pts',(-38.3315823645617,37.7578879744511,3.69717169561447));
#57383=CARTESIAN_POINT('Ctrl Pts',(-38.0740905614766,38.0820960983985,3.72334019907339));
#57384=CARTESIAN_POINT('Ctrl Pts',(-37.8165987583915,38.4063042223459,3.74950870253232));
#57385=CARTESIAN_POINT('Ctrl Pts',(-37.7333976613612,38.8689370953399,3.77567720599125));
#57386=CARTESIAN_POINT('Ctrl Pts',(-37.8617956314422,39.2625446379184,3.80184570945017));
#57387=CARTESIAN_POINT('Ctrl Pts',(-37.9901936015233,39.6561521804969,3.8280142129091));
#57388=CARTESIAN_POINT('Ctrl Pts',(-38.3301906387158,39.9807343926601,3.85418271636802));
#57389=CARTESIAN_POINT('Ctrl Pts',(-38.7293280299731,40.0907447522208,3.88035121982695));
#57390=CARTESIAN_POINT('Ctrl Pts',(-39.0499804019726,40.1791230487932,3.90137403775777));
#57391=CARTESIAN_POINT('Ctrl Pts',(-39.408801529933,40.1290182265619,3.92239685568859));
#57392=CARTESIAN_POINT('Ctrl Pts',(-39.6992442211058,39.9647402889406,3.94341967361941));
#57393=CARTESIAN_POINT('Ctrl Pts',(-39.6990217970716,39.9666307803347,3.80658032638059));
#57394=CARTESIAN_POINT('Ctrl Pts',(-39.6946690888126,39.9691498648546,3.80626246380904));
#57395=CARTESIAN_POINT('Ctrl Pts',(-39.6903001003537,39.9716406339069,3.80594460123749));
#57396=CARTESIAN_POINT('Ctrl Pts',(-39.6859150342415,39.9741027686317,3.80562673866594));
#57397=CARTESIAN_POINT('Ctrl Pts',(-39.3249080205419,40.1768016291735,3.77945823520701));
#57398=CARTESIAN_POINT('Ctrl Pts',(-38.8549323382457,40.1854271070305,3.75328973174808));
#57399=CARTESIAN_POINT('Ctrl Pts',(-38.486730670363,39.9961114351584,3.72712122828915));
#57400=CARTESIAN_POINT('Ctrl Pts',(-38.1185290024804,39.8067957632863,3.70095272483023));
#57401=CARTESIAN_POINT('Ctrl Pts',(-37.8521013490113,39.4195389416852,3.6747842213713));
#57402=CARTESIAN_POINT('Ctrl Pts',(-37.806917035636,39.007991532901,3.64861571791238));
#57403=CARTESIAN_POINT('Ctrl Pts',(-37.7617327222606,38.5964441241169,3.62244721445345));
#57404=CARTESIAN_POINT('Ctrl Pts',(-37.9377917489789,38.1606061281498,3.59627871099452));
#57405=CARTESIAN_POINT('Ctrl Pts',(-38.2561471576722,37.8959124821361,3.57011020753559));
#57406=CARTESIAN_POINT('Ctrl Pts',(-38.5745025663655,37.6312188361224,3.54394170407667));
#57407=CARTESIAN_POINT('Ctrl Pts',(-39.0351543570338,37.5376695400622,3.51777320061774));
#57408=CARTESIAN_POINT('Ctrl Pts',(-39.4315407865323,37.6572132122937,3.49160469715882));
#57409=CARTESIAN_POINT('Ctrl Pts',(-39.8279272160309,37.7767568845251,3.46543619369989));
#57410=CARTESIAN_POINT('Ctrl Pts',(-40.1600482843597,38.1093935250483,3.43926769024096));
#57411=CARTESIAN_POINT('Ctrl Pts',(-40.2789769657406,38.5059649062658,3.41309918678203));
#57412=CARTESIAN_POINT('Ctrl Pts',(-40.3979056471215,38.9025362874833,3.38693068332311));
#57413=CARTESIAN_POINT('Ctrl Pts',(-40.3036419415545,39.3630424093952,3.36076217986418));
#57414=CARTESIAN_POINT('Ctrl Pts',(-40.0384547967127,39.6809868610392,3.33459367640526));
#57415=CARTESIAN_POINT('Ctrl Pts',(-39.943827295091,39.7944399061765,3.3252558930637));
#57416=CARTESIAN_POINT('Ctrl Pts',(-39.8274361583624,39.8897406125527,3.31591810972215));
#57417=CARTESIAN_POINT('Ctrl Pts',(-39.6981666138854,39.9633157673857,3.30658032638059));
#57418=CARTESIAN_POINT('Origin',(-39.0658530619283,38.8697713466882,4.5));
#57419=CARTESIAN_POINT('',(-39.696945388151,39.9649932150637,2.80658032638059));
#57420=CARTESIAN_POINT('',(-39.6985897981371,39.9666323328488,2.94341967361941));
#57421=CARTESIAN_POINT('',(-39.6981030619283,39.9648604697737,4.5));
#57422=CARTESIAN_POINT('Ctrl Pts',(-39.6985897981371,39.9666323328488,2.94341967361941));
#57423=CARTESIAN_POINT('Ctrl Pts',(-40.0329227359304,39.771464492525,2.96787665097373));
#57424=CARTESIAN_POINT('Ctrl Pts',(-40.2741270402692,39.4118258938478,2.99233362832805));
#57425=CARTESIAN_POINT('Ctrl Pts',(-40.3224423052902,39.0279123314598,3.01679060568238));
#57426=CARTESIAN_POINT('Ctrl Pts',(-40.3741387255592,38.617132076822,3.0429591091413));
#57427=CARTESIAN_POINT('Ctrl Pts',(-40.2050042874718,38.1785603982041,3.06912761260023));
#57428=CARTESIAN_POINT('Ctrl Pts',(-39.8908808035795,37.908858034419,3.09529611605915));
#57429=CARTESIAN_POINT('Ctrl Pts',(-39.5767573196872,37.6391556706339,3.12146461951808));
#57430=CARTESIAN_POINT('Ctrl Pts',(-39.11764478999,37.5383226216818,3.14763312297701));
#57431=CARTESIAN_POINT('Ctrl Pts',(-38.7194147698321,37.6515736327838,3.17380162643593));
#57432=CARTESIAN_POINT('Ctrl Pts',(-38.3211847496743,37.7648246438858,3.19997012989486));
#57433=CARTESIAN_POINT('Ctrl Pts',(-37.9838372390559,38.092159715042,3.22613863335379));
#57434=CARTESIAN_POINT('Ctrl Pts',(-37.8586428520748,38.4867979056613,3.25230713681271));
#57435=CARTESIAN_POINT('Ctrl Pts',(-37.7334484650937,38.8814360962806,3.27847564027164));
#57436=CARTESIAN_POINT('Ctrl Pts',(-37.8204072017499,39.343377406363,3.30464414373057));
#57437=CARTESIAN_POINT('Ctrl Pts',(-38.080525740607,39.6654818632946,3.33081264718949));
#57438=CARTESIAN_POINT('Ctrl Pts',(-38.3406442794642,39.9875863202263,3.35698115064842));
#57439=CARTESIAN_POINT('Ctrl Pts',(-38.7739226205222,40.1698539240071,3.38314965410735));
#57440=CARTESIAN_POINT('Ctrl Pts',(-39.1860736005189,40.1305537136076,3.40931815756627));
#57441=CARTESIAN_POINT('Ctrl Pts',(-39.3651052785911,40.1134823418097,3.42068532958398));
#57442=CARTESIAN_POINT('Ctrl Pts',(-39.5401504513672,40.0546035118007,3.4320525016017));
#57443=CARTESIAN_POINT('Ctrl Pts',(-39.6968376638892,39.9635050155947,3.44341967361941));
#57444=CARTESIAN_POINT('Ctrl Pts',(-39.6981666138854,39.9633157673857,3.30658032638059));
#57445=CARTESIAN_POINT('Ctrl Pts',(-39.4651670418018,40.0959299856956,3.28974960626322));
#57446=CARTESIAN_POINT('Ctrl Pts',(-39.1903285963568,40.157963071813,3.27291888614585));
#57447=CARTESIAN_POINT('Ctrl Pts',(-38.9256802513517,40.1284914650089,3.25608816602848));
#57448=CARTESIAN_POINT('Ctrl Pts',(-38.5142034349489,40.0826688359585,3.22991966256955));
#57449=CARTESIAN_POINT('Ctrl Pts',(-38.1273603862597,39.8156407964813,3.20375115911062));
#57450=CARTESIAN_POINT('Ctrl Pts',(-37.9386160518288,39.4471459263554,3.1775826556517));
#57451=CARTESIAN_POINT('Ctrl Pts',(-37.749871717398,39.0786510562295,3.15141415219277));
#57452=CARTESIAN_POINT('Ctrl Pts',(-37.7592260972255,38.6086893554548,3.12524564873384));
#57453=CARTESIAN_POINT('Ctrl Pts',(-37.9624847270864,38.2479971709405,3.09907714527492));
#57454=CARTESIAN_POINT('Ctrl Pts',(-38.1657433569474,37.8873049864262,3.07290864181599));
#57455=CARTESIAN_POINT('Ctrl Pts',(-38.5629062368417,37.6358823181722,3.04674013835707));
#57456=CARTESIAN_POINT('Ctrl Pts',(-38.9758805061506,37.6064702124723,3.02057163489814));
#57457=CARTESIAN_POINT('Ctrl Pts',(-39.3888547754595,37.5770581067724,2.99440313143921));
#57458=CARTESIAN_POINT('Ctrl Pts',(-39.817640434183,37.7696565636265,2.96823462798029));
#57459=CARTESIAN_POINT('Ctrl Pts',(-40.0699655096421,38.0979018769219,2.94206612452136));
#57460=CARTESIAN_POINT('Ctrl Pts',(-40.3222905851012,38.4261471902174,2.91589762106243));
#57461=CARTESIAN_POINT('Ctrl Pts',(-40.398155077296,38.8900393599541,2.88972911760351));
#57462=CARTESIAN_POINT('Ctrl Pts',(-40.2635392087761,39.2815641648304,2.86356061414458));
#57463=CARTESIAN_POINT('Ctrl Pts',(-40.1658333166795,39.5657377972484,2.84456718488992));
#57464=CARTESIAN_POINT('Ctrl Pts',(-39.9572455465607,39.811788018551,2.82557375563525));
#57465=CARTESIAN_POINT('Ctrl Pts',(-39.696945388151,39.9649932150637,2.80658032638059));
#57466=CARTESIAN_POINT('Origin',(-39.0658530619283,38.8697713466882,4.5));
#57467=CARTESIAN_POINT('',(-39.6994125047665,39.9658989902663,2.30658032638059));
#57468=CARTESIAN_POINT('',(-39.6985816414592,39.9636701304732,2.44341967361941));
#57469=CARTESIAN_POINT('',(-39.6981030619283,39.9648604697737,4.5));
#57470=CARTESIAN_POINT('',(-39.3014489339361,37.6274127691862,2.));
#57471=CARTESIAN_POINT('Ctrl Pts',(-39.6994125047665,39.9658989902663,2.30658032638059));
#57472=CARTESIAN_POINT('Ctrl Pts',(-39.3734254452085,40.1513842194032,2.28289239463051));
#57473=CARTESIAN_POINT('Ctrl Pts',(-38.9582283391778,40.1860737601752,2.25920446288042));
#57474=CARTESIAN_POINT('Ctrl Pts',(-38.6086499461796,40.0507923518177,2.23551653113034));
#57475=CARTESIAN_POINT('Ctrl Pts',(-38.2224641245192,39.9013444371629,2.20934802767141));
#57476=CARTESIAN_POINT('Ctrl Pts',(-37.9163596177671,39.5444633609379,2.18317952421249));
#57477=CARTESIAN_POINT('Ctrl Pts',(-37.8282894528998,39.1398698141335,2.15701102075356));
#57478=CARTESIAN_POINT('Ctrl Pts',(-37.7402192880325,38.7352762673292,2.13084251729463));
#57479=CARTESIAN_POINT('Ctrl Pts',(-37.8701834650499,38.2829702499457,2.10467401383571));
#57480=CARTESIAN_POINT('Ctrl Pts',(-38.1583556110386,37.9866358554263,2.07850551037678));
#57481=CARTESIAN_POINT('Ctrl Pts',(-38.4465277570273,37.6903014609068,2.05233700691785));
#57482=CARTESIAN_POINT('Ctrl Pts',(-38.8929078719872,37.5499386892516,2.02616850345893));
#57483=CARTESIAN_POINT('Ctrl Pts',(-39.3014489339361,37.6274127691862,2.));
#57484=CARTESIAN_POINT('',(-40.2614317556684,39.2879039300605,2.00000000000001));
#57485=CARTESIAN_POINT('Origin',(-39.0658530619283,38.8697713466882,2.));
#57486=CARTESIAN_POINT('Ctrl Pts',(-40.261442204914,39.2879094456028,2.00000000000001));
#57487=CARTESIAN_POINT('Ctrl Pts',(-40.3902478674696,38.9153329576354,2.02490816038701));
#57488=CARTESIAN_POINT('Ctrl Pts',(-40.3325476766157,38.4763154063561,2.04981632077402));
#57489=CARTESIAN_POINT('Ctrl Pts',(-40.1090165446371,38.1516794088468,2.07472448116103));
#57490=CARTESIAN_POINT('Ctrl Pts',(-39.8741748257196,37.8106169581592,2.10089298461995));
#57491=CARTESIAN_POINT('Ctrl Pts',(-39.4562956252315,37.5958042374567,2.12706148807888));
#57492=CARTESIAN_POINT('Ctrl Pts',(-39.042397118114,37.6034976893836,2.1532299915378));
#57493=CARTESIAN_POINT('Ctrl Pts',(-38.6284986109964,37.6111911413105,2.17939849499673));
#57494=CARTESIAN_POINT('Ctrl Pts',(-38.2185807972492,37.841390765867,2.20556699845566));
#57495=CARTESIAN_POINT('Ctrl Pts',(-37.996635575997,38.1909062543644,2.23173550191458));
#57496=CARTESIAN_POINT('Ctrl Pts',(-37.7746903547448,38.5404217428618,2.25790400537351));
#57497=CARTESIAN_POINT('Ctrl Pts',(-37.7407177259875,39.0092530953003,2.28407250883244));
#57498=CARTESIAN_POINT('Ctrl Pts',(-37.909862273516,39.3871539257345,2.31024101229136));
#57499=CARTESIAN_POINT('Ctrl Pts',(-38.0790068210445,39.7650547561687,2.33640951575029));
#57500=CARTESIAN_POINT('Ctrl Pts',(-38.4512685448588,40.0520250645987,2.36257801920921));
#57501=CARTESIAN_POINT('Ctrl Pts',(-38.8597650567826,40.1193923002797,2.38874652266814));
#57502=CARTESIAN_POINT('Ctrl Pts',(-39.1442519845446,40.1663084852441,2.40697090631856));
#57503=CARTESIAN_POINT('Ctrl Pts',(-39.4463130348953,40.1067156626302,2.42519528996899));
#57504=CARTESIAN_POINT('Ctrl Pts',(-39.6985816414592,39.9636701304732,2.44341967361941));
#57505=CARTESIAN_POINT('Origin',(-39.0658530619283,38.8697713466882,0.895788276411275));
#57506=CARTESIAN_POINT('',(-39.8389883040075,40.2073580112695,5.60421172358873));
#57507=CARTESIAN_POINT('',(-39.8361023073888,40.2039982703455,5.64578827641128));
#57508=CARTESIAN_POINT('',(-39.8373530619284,40.2060485447276,0.895788276411275));
#57509=CARTESIAN_POINT('',(-37.5756558680257,39.2699729499894,6.));
#57510=CARTESIAN_POINT('Ctrl Pts',(-39.8361023073888,40.2039982703455,5.64578827641127));
#57511=CARTESIAN_POINT('Ctrl Pts',(-40.0618255698415,40.0734865888946,5.65918483710514));
#57512=CARTESIAN_POINT('Ctrl Pts',(-40.6360432757834,39.5276070596663,5.69874990125794));
#57513=CARTESIAN_POINT('Ctrl Pts',(-40.7062544764741,38.0891194878961,5.76448346886966));
#57514=CARTESIAN_POINT('Ctrl Pts',(-39.3195619844849,37.0695313077001,5.84298897924644));
#57515=CARTESIAN_POINT('Ctrl Pts',(-37.7040659529861,37.6679522088103,5.92149448962322));
#57516=CARTESIAN_POINT('Ctrl Pts',(-37.4440523270134,38.7799318659295,5.97383149654107));
#57517=CARTESIAN_POINT('Ctrl Pts',(-37.5756558680257,39.2699729499894,6.));
#57518=CARTESIAN_POINT('',(-37.9726388313436,39.9622904787117,6.));
#57519=CARTESIAN_POINT('Origin',(-39.0658530619283,38.8697713466882,6.));
#57520=CARTESIAN_POINT('Ctrl Pts',(-39.8389883040075,40.2073580112695,5.60421172358873));
#57521=CARTESIAN_POINT('Ctrl Pts',(-39.8784035047362,40.18491964361,5.60655897483644));
#57522=CARTESIAN_POINT('Ctrl Pts',(-40.3442265162732,39.8903323926484,5.63507472954307));
#57523=CARTESIAN_POINT('Ctrl Pts',(-40.8821362004287,38.8192621207561,5.68975898770863));
#57524=CARTESIAN_POINT('Ctrl Pts',(-40.0256584008921,37.3267854127763,5.76826449808542));
#57525=CARTESIAN_POINT('Ctrl Pts',(-38.3080469142999,37.2183586878016,5.84677000846219));
#57526=CARTESIAN_POINT('Ctrl Pts',(-37.2874279838024,38.5683990357347,5.92401517576706));
#57527=CARTESIAN_POINT('Ctrl Pts',(-37.6338153475925,39.6208332722494,5.97509183961299));
#57528=CARTESIAN_POINT('Ctrl Pts',(-37.972630261787,39.962302073481,6.));
#57529=CARTESIAN_POINT('Origin',(-39.0658530619283,38.8697713466882,0.895788276411275));
#57530=CARTESIAN_POINT('',(-39.8364823014031,40.2038876485621,5.10421172358873));
#57531=CARTESIAN_POINT('',(-39.8373456329825,40.207933543715,5.14578827641127));
#57532=CARTESIAN_POINT('',(-39.8373530619284,40.2060485447276,0.895788276411275));
#57533=CARTESIAN_POINT('Ctrl Pts',(-39.8373456329825,40.207933543715,5.14578827641127));
#57534=CARTESIAN_POINT('Ctrl Pts',(-40.2216806378635,39.9822885010755,5.16884048301825));
#57535=CARTESIAN_POINT('Ctrl Pts',(-40.8329618074793,39.1268210714738,5.21806119308415));
#57536=CARTESIAN_POINT('Ctrl Pts',(-40.3208244444739,37.5557551266231,5.29345040660899));
#57537=CARTESIAN_POINT('Ctrl Pts',(-38.6620380533448,37.0981630448849,5.37195591698576));
#57538=CARTESIAN_POINT('Ctrl Pts',(-37.3653845951193,38.2294425600612,5.45046142736254));
#57539=CARTESIAN_POINT('Ctrl Pts',(-37.5937879163964,39.9348809965236,5.52896693773932));
#57540=CARTESIAN_POINT('Ctrl Pts',(-38.8780553810739,40.5572546562641,5.59407588742223));
#57541=CARTESIAN_POINT('Ctrl Pts',(-39.6209034474226,40.3284248126315,5.63301633364622));
#57542=CARTESIAN_POINT('Ctrl Pts',(-39.8361023073888,40.2039982703455,5.64578827641127));
#57543=CARTESIAN_POINT('Ctrl Pts',(-39.8364823014031,40.2038876485621,5.10421172358873));
#57544=CARTESIAN_POINT('Ctrl Pts',(-40.0389857717083,40.0874933656255,5.11621462074954));
#57545=CARTESIAN_POINT('Ctrl Pts',(-40.6023754577107,39.5788852724494,5.15438602136929));
#57546=CARTESIAN_POINT('Ctrl Pts',(-40.7451774946681,38.1758811994982,5.21872592544796));
#57547=CARTESIAN_POINT('Ctrl Pts',(-39.4133645670745,37.0862753673933,5.29723143582474));
#57548=CARTESIAN_POINT('Ctrl Pts',(-37.7698897533292,37.5961550422892,5.37573694620152));
#57549=CARTESIAN_POINT('Ctrl Pts',(-37.2886763485593,39.2482362054987,5.4542424565783));
#57550=CARTESIAN_POINT('Ctrl Pts',(-38.3679904575111,40.521668910622,5.53040071570737));
#57551=CARTESIAN_POINT('Ctrl Pts',(-39.4389802356634,40.4350754385143,5.58039047137751));
#57552=CARTESIAN_POINT('Ctrl Pts',(-39.8389883040075,40.2073580112695,5.60421172358873));
#57553=CARTESIAN_POINT('Origin',(-39.0658530619283,38.8697713466882,0.895788276411275));
#57554=CARTESIAN_POINT('',(-39.8367681787868,40.2074507120888,4.60421172358873));
#57555=CARTESIAN_POINT('',(-39.838395191597,40.2051955164573,4.64578827641127));
#57556=CARTESIAN_POINT('',(-39.8373530619284,40.2060485447276,0.895788276411275));
#57557=CARTESIAN_POINT('Ctrl Pts',(-39.838395191597,40.2051955164573,4.64578827641127));
#57558=CARTESIAN_POINT('Ctrl Pts',(-39.9487742895753,40.1427442714185,4.65232762547243));
#57559=CARTESIAN_POINT('Ctrl Pts',(-40.461107190991,39.7640019994127,4.68503547799252));
#57560=CARTESIAN_POINT('Ctrl Pts',(-40.8515947960302,38.533999133735,4.74391183397153));
#57561=CARTESIAN_POINT('Ctrl Pts',(-39.7707737852476,37.1950466549738,4.82241734434831));
#57562=CARTESIAN_POINT('Ctrl Pts',(-38.05776324374,37.3580267168588,4.90092285472509));
#57563=CARTESIAN_POINT('Ctrl Pts',(-37.248831349992,38.8767760630727,4.97942836510187));
#57564=CARTESIAN_POINT('Ctrl Pts',(-38.0694482634705,40.3892418792306,5.05793387547865));
#57565=CARTESIAN_POINT('Ctrl Pts',(-39.280304717179,40.4950348443414,5.11338717924845));
#57566=CARTESIAN_POINT('Ctrl Pts',(-39.7853895670742,40.2384372151433,5.14267197955933));
#57567=CARTESIAN_POINT('Ctrl Pts',(-39.8373456329825,40.207933543715,5.14578827641127));
#57568=CARTESIAN_POINT('Ctrl Pts',(-39.8367681787868,40.2074507120888,4.60421172358873));
#57569=CARTESIAN_POINT('Ctrl Pts',(-40.1980237481411,39.9947173316426,4.62587026666265));
#57570=CARTESIAN_POINT('Ctrl Pts',(-40.8090940791592,39.1897699662685,4.6736973131955));
#57571=CARTESIAN_POINT('Ctrl Pts',(-40.3881021894619,37.6234670214254,4.74769286318728));
#57572=CARTESIAN_POINT('Ctrl Pts',(-38.7556268199881,37.0794146789619,4.82619837356406));
#57573=CARTESIAN_POINT('Ctrl Pts',(-37.4013696406987,38.1409968175026,4.90470388394084));
#57574=CARTESIAN_POINT('Ctrl Pts',(-37.5398609233301,39.8561611622598,4.98320939431762));
#57575=CARTESIAN_POINT('Ctrl Pts',(-38.8164833870163,40.5597236082337,5.04971200753358));
#57576=CARTESIAN_POINT('Ctrl Pts',(-39.5974912981552,40.3412541164524,5.09004611729062));
#57577=CARTESIAN_POINT('Ctrl Pts',(-39.8364823014031,40.2038876485621,5.10421172358873));
#57578=CARTESIAN_POINT('Origin',(-39.0658530619283,38.8697713466882,0.895788276411275));
#57579=CARTESIAN_POINT('',(-39.8387455558871,40.2059018946482,4.10421172358873));
#57580=CARTESIAN_POINT('',(-39.835683949911,40.2049009685562,4.14578827641127));
#57581=CARTESIAN_POINT('',(-39.8373530619284,40.2060485447276,0.895788276411275));
#57582=CARTESIAN_POINT('Ctrl Pts',(-39.835683949911,40.2049009685562,4.14578827641127));
#57583=CARTESIAN_POINT('Ctrl Pts',(-40.1075666009271,40.0460142702611,4.16198327138554));
#57584=CARTESIAN_POINT('Ctrl Pts',(-40.7000264343407,39.4199669716347,4.20434676981873));
#57585=CARTESIAN_POINT('Ctrl Pts',(-40.6150446849375,37.9202337024768,4.27287877171085));
#57586=CARTESIAN_POINT('Ctrl Pts',(-39.1283436057741,37.0538111746305,4.35138428208763));
#57587=CARTESIAN_POINT('Ctrl Pts',(-37.5855995232345,37.8159848954577,4.42988979246441));
#57588=CARTESIAN_POINT('Ctrl Pts',(-37.3703820012353,39.5232193693979,4.50839530284119));
#57589=CARTESIAN_POINT('Ctrl Pts',(-38.5669726422018,40.5510318627906,4.58036146415681));
#57590=CARTESIAN_POINT('Ctrl Pts',(-39.5070704165714,40.3926553262541,4.6261591220135));
#57591=CARTESIAN_POINT('Ctrl Pts',(-39.838395191597,40.2051955164573,4.64578827641127));
#57592=CARTESIAN_POINT('Ctrl Pts',(-39.8387455558872,40.2059018946482,4.10421172358873));
#57593=CARTESIAN_POINT('Ctrl Pts',(-39.9254936329904,40.1568361214949,4.10935740911683));
#57594=CARTESIAN_POINT('Ctrl Pts',(-40.4229804016609,39.8074510911275,4.14067159810387));
#57595=CARTESIAN_POINT('Ctrl Pts',(-40.8667641756192,38.6282419782981,4.19815429054983));
#57596=CARTESIAN_POINT('Ctrl Pts',(-39.8577505620191,37.2343767082119,4.2766598009266));
#57597=CARTESIAN_POINT('Ctrl Pts',(-38.1385444446535,37.3071722287696,4.35516531130339));
#57598=CARTESIAN_POINT('Ctrl Pts',(-37.2509707395799,38.781343787805,4.43367082168017));
#57599=CARTESIAN_POINT('Ctrl Pts',(-37.9910266499109,40.3348192821528,4.51217633205694));
#57600=CARTESIAN_POINT('Ctrl Pts',(-39.2249072234587,40.508306713049,4.5690232993598));
#57601=CARTESIAN_POINT('Ctrl Pts',(-39.7615438988762,40.2517482031576,4.59970176320373));
#57602=CARTESIAN_POINT('Ctrl Pts',(-39.8367681787868,40.2074507120888,4.60421172358873));
#57603=CARTESIAN_POINT('Origin',(-39.0658530619283,38.8697713466882,0.895788276411275));
#57604=CARTESIAN_POINT('',(-39.8358089661004,40.2043945583313,3.60421172358873));
#57605=CARTESIAN_POINT('',(-39.8384741440368,40.2082087576148,3.64578827641127));
#57606=CARTESIAN_POINT('',(-39.8373530619284,40.2060485447276,0.895788276411275));
#57607=CARTESIAN_POINT('Ctrl Pts',(-39.8384741440368,40.2082087576148,3.64578827641127));
#57608=CARTESIAN_POINT('Ctrl Pts',(-40.2704292120645,39.9582192659243,3.67163891729865));
#57609=CARTESIAN_POINT('Ctrl Pts',(-40.875250043897,38.9953053985923,3.72365806164495));
#57610=CARTESIAN_POINT('Ctrl Pts',(-40.1754790439541,37.4309014426854,3.80184570945018));
#57611=CARTESIAN_POINT('Ctrl Pts',(-38.4777242474675,37.1505503260543,3.88035121982696));
#57612=CARTESIAN_POINT('Ctrl Pts',(-37.3074173539442,38.412037492713,3.95885673020373));
#57613=CARTESIAN_POINT('Ctrl Pts',(-37.7141174076169,40.0840312618198,4.03736224058051));
#57614=CARTESIAN_POINT('Ctrl Pts',(-38.9991071509758,40.5467766825012,4.09967275598303));
#57615=CARTESIAN_POINT('Ctrl Pts',(-39.6682480272047,40.3027495838885,4.13581476792661));
#57616=CARTESIAN_POINT('Ctrl Pts',(-39.835683949911,40.2049009685562,4.14578827641127));
#57617=CARTESIAN_POINT('Ctrl Pts',(-39.8358089661004,40.2043945583313,3.60421172358873));
#57618=CARTESIAN_POINT('Ctrl Pts',(-40.0847686354211,40.0596485313516,3.61901305502994));
#57619=CARTESIAN_POINT('Ctrl Pts',(-40.6687535790882,39.4744804296355,3.65998288993008));
#57620=CARTESIAN_POINT('Ctrl Pts',(-40.662772801836,38.0029007557487,3.72712122828915));
#57621=CARTESIAN_POINT('Ctrl Pts',(-39.2236238307452,37.0595985208235,3.80562673866593));
#57622=CARTESIAN_POINT('Ctrl Pts',(-37.642982284831,37.7397023107928,3.88413224904271));
#57623=CARTESIAN_POINT('Ctrl Pts',(-37.3384050779085,39.4332788778856,3.96263775941949));
#57624=CARTESIAN_POINT('Ctrl Pts',(-38.5014637504291,40.5436066616789,4.03599758426816));
#57625=CARTESIAN_POINT('Ctrl Pts',(-39.4843342688332,40.4063612522992,4.08318890565791));
#57626=CARTESIAN_POINT('Ctrl Pts',(-39.8387455558872,40.2059018946482,4.10421172358873));
#57627=CARTESIAN_POINT('Origin',(-39.0658530619283,38.8697713466882,0.895788276411275));
#57628=CARTESIAN_POINT('',(-39.8379469994295,40.2082106520625,3.10421172358873));
#57629=CARTESIAN_POINT('',(-39.8374306108962,40.204163629121,3.14578827641127));
#57630=CARTESIAN_POINT('',(-39.8373530619284,40.2060485447276,0.895788276411275));
#57631=CARTESIAN_POINT('Ctrl Pts',(-39.8374306108962,40.204163629121,3.14578827641127));
#57632=CARTESIAN_POINT('Ctrl Pts',(-39.9951711463869,40.1143839028202,3.15512605975283));
#57633=CARTESIAN_POINT('Ctrl Pts',(-40.5352143013727,39.6721982210719,3.19063234655331));
#57634=CARTESIAN_POINT('Ctrl Pts',(-40.8063086069208,38.3478222423284,3.25230713681272));
#57635=CARTESIAN_POINT('Ctrl Pts',(-39.590501232232,37.1301274942208,3.3308126471895));
#57636=CARTESIAN_POINT('Ctrl Pts',(-37.9041768834746,37.4725867203679,3.40931815756627));
#57637=CARTESIAN_POINT('Ctrl Pts',(-37.259671359806,39.0680743307528,3.48782366794306));
#57638=CARTESIAN_POINT('Ctrl Pts',(-38.2349925206666,40.4857191130317,3.56632917831984));
#57639=CARTESIAN_POINT('Ctrl Pts',(-39.3889296125877,40.4645408708171,3.61898404780924));
#57640=CARTESIAN_POINT('Ctrl Pts',(-39.8331627728674,40.2112826582981,3.64547041383972));
#57641=CARTESIAN_POINT('Ctrl Pts',(-39.8384741440368,40.2082087576148,3.64578827641127));
#57642=CARTESIAN_POINT('Ctrl Pts',(-39.8379469994295,40.2082106520625,3.10421172358873));
#57643=CARTESIAN_POINT('Ctrl Pts',(-40.2459151473258,39.9700580402636,3.12866870094305));
#57644=CARTESIAN_POINT('Ctrl Pts',(-40.855169338561,39.0616525117032,3.1792941817563));
#57645=CARTESIAN_POINT('Ctrl Pts',(-40.249511348243,37.4911595684212,3.25608816602847));
#57646=CARTESIAN_POINT('Ctrl Pts',(-38.5688218267178,37.1220364497186,3.33459367640525));
#57647=CARTESIAN_POINT('Ctrl Pts',(-37.333881829365,38.3203235548052,3.41309918678203));
#57648=CARTESIAN_POINT('Ctrl Pts',(-37.6522147609439,40.011368493019,3.49160469715881));
#57649=CARTESIAN_POINT('Ctrl Pts',(-38.9392875485226,40.5528026028124,3.55530887609438));
#57650=CARTESIAN_POINT('Ctrl Pts',(-39.6446121539839,40.3155570570627,3.59284455157102));
#57651=CARTESIAN_POINT('Ctrl Pts',(-39.8358089661004,40.2043945583313,3.60421172358873));
#57652=CARTESIAN_POINT('Origin',(-39.0658530619283,38.8697713466882,0.895788276411275));
#57653=CARTESIAN_POINT('',(-39.8379370462828,40.204596038962,2.60421172358873));
#57654=CARTESIAN_POINT('',(-39.8359404161091,40.2062105265248,2.64578827641127));
#57655=CARTESIAN_POINT('',(-39.8373530619284,40.2060485447276,0.895788276411275));
#57656=CARTESIAN_POINT('Ctrl Pts',(-39.8359404161091,40.2062105265248,2.64578827641127));
#57657=CARTESIAN_POINT('Ctrl Pts',(-40.1535704235636,40.0192626275773,2.66478170566594));
#57658=CARTESIAN_POINT('Ctrl Pts',(-40.7587789941875,39.3053583432972,2.70994363837953));
#57659=CARTESIAN_POINT('Ctrl Pts',(-40.5064415845058,37.7623789454716,2.78127407455204));
#57660=CARTESIAN_POINT('Ctrl Pts',(-38.936770715205,37.0573269432749,2.85977958492882));
#57661=CARTESIAN_POINT('Ctrl Pts',(-37.4828624739785,37.9777188225534,2.9382850953056));
#57662=CARTESIAN_POINT('Ctrl Pts',(-37.4486185639574,39.6981242894461,3.01679060568238));
#57663=CARTESIAN_POINT('Ctrl Pts',(-38.6963080267235,40.5593729851321,3.0859583327176));
#57664=CARTESIAN_POINT('Ctrl Pts',(-39.5531140116672,40.3659854866553,3.1289575562939));
#57665=CARTESIAN_POINT('Ctrl Pts',(-39.8374306108962,40.204163629121,3.14578827641127));
#57666=CARTESIAN_POINT('Ctrl Pts',(-39.8379370462828,40.204596038962,2.60421172358873));
#57667=CARTESIAN_POINT('Ctrl Pts',(-39.9721218195358,40.1285083617881,2.61215584339723));
#57668=CARTESIAN_POINT('Ctrl Pts',(-40.4987455670004,39.7186935414776,2.64626846666466));
#57669=CARTESIAN_POINT('Ctrl Pts',(-40.8313104277201,38.439942299895,2.70654959339101));
#57670=CARTESIAN_POINT('Ctrl Pts',(-39.6811395860238,37.1600807661057,2.78505510376779));
#57671=CARTESIAN_POINT('Ctrl Pts',(-37.9791520940816,37.4135079224236,2.86356061414458));
#57672=CARTESIAN_POINT('Ctrl Pts',(-37.2517503435483,38.9729479619195,2.94206612452135));
#57673=CARTESIAN_POINT('Ctrl Pts',(-38.1512758267995,40.4398561533634,3.02057163489813));
#57674=CARTESIAN_POINT('Ctrl Pts',(-39.3352629723092,40.4803512300078,3.07462016792059));
#57675=CARTESIAN_POINT('Ctrl Pts',(-39.8093969408979,40.2248768330901,3.10250019748412));
#57676=CARTESIAN_POINT('Ctrl Pts',(-39.8379469994295,40.2082106520625,3.10421172358873));
#57677=CARTESIAN_POINT('Origin',(-39.0658530619283,38.8697713466882,0.895788276411275));
#57678=CARTESIAN_POINT('',(-39.8351916364771,40.2053827942122,2.10421172358873));
#57679=CARTESIAN_POINT('',(-39.838950903209,40.2073157943284,2.14578827641127));
#57680=CARTESIAN_POINT('',(-39.8373530619284,40.2060485447276,0.895788276411275));
#57681=CARTESIAN_POINT('',(-37.9741697098829,39.9602191716056,2.));
#57682=CARTESIAN_POINT('Ctrl Pts',(-37.9741697098829,39.9602191716056,2.));
#57683=CARTESIAN_POINT('Ctrl Pts',(-38.3327559670707,40.3192117233802,2.02616850345893));
#57684=CARTESIAN_POINT('Ctrl Pts',(-39.0582121561479,40.5387775404138,2.06090574465517));
#57685=CARTESIAN_POINT('Ctrl Pts',(-39.6915909718076,40.2896039589219,2.09564298585141));
#57686=CARTESIAN_POINT('Ctrl Pts',(-39.8351916364771,40.2053827942122,2.10421172358873));
#57687=CARTESIAN_POINT('',(-37.5730967199607,39.2702632425652,2.));
#57688=CARTESIAN_POINT('Origin',(-39.0658530619283,38.8697713466882,2.));
#57689=CARTESIAN_POINT('Ctrl Pts',(-37.5730824075077,39.2702648660737,2.));
#57690=CARTESIAN_POINT('Ctrl Pts',(-37.6993955576028,39.7344217910383,2.02490816038701));
#57691=CARTESIAN_POINT('Ctrl Pts',(-38.4017837618403,40.520493253107,2.0735042525241));
#57692=CARTESIAN_POINT('Ctrl Pts',(-39.4411667728032,40.4336532467271,2.12210034466119));
#57693=CARTESIAN_POINT('Ctrl Pts',(-39.838950903209,40.2073157943283,2.14578827641127));
#57694=CARTESIAN_POINT('Origin',(-53.1951359564886,-14.3971354987959,4.5));
#57695=CARTESIAN_POINT('',(-54.457664959728,-14.3970890371748,5.80658032638058));
#57696=CARTESIAN_POINT('',(-54.4588632108481,-14.3954785432618,5.94341967361942));
#57697=CARTESIAN_POINT('',(-54.4596359564886,-14.3971354987959,4.5));
#57698=CARTESIAN_POINT('',(-54.153252109211,-15.2223467977324,6.));
#57699=CARTESIAN_POINT('Ctrl Pts',(-54.4588632108481,-14.3954785432618,
5.94341967361942));
#57700=CARTESIAN_POINT('Ctrl Pts',(-54.4562503558692,-14.6946046444958,
5.96227978241294));
#57701=CARTESIAN_POINT('Ctrl Pts',(-54.348829759182,-14.9952702831595,5.98113989120647));
#57702=CARTESIAN_POINT('Ctrl Pts',(-54.153252109211,-15.2223467977324,6.));
#57703=CARTESIAN_POINT('',(-54.4596359564886,-14.3971354987959,6.));
#57704=CARTESIAN_POINT('Origin',(-53.1951359564886,-14.3971354987959,6.));
#57705=CARTESIAN_POINT('',(-54.4596359564886,-14.3971354987959,7.));
#57706=CARTESIAN_POINT('',(-54.4596359564886,-14.3971354987959,4.5));
#57707=CARTESIAN_POINT('',(-52.6278006430704,-15.5272199611918,7.));
#57708=CARTESIAN_POINT('Origin',(-53.1951359564886,-14.3971354987959,7.));
#57709=CARTESIAN_POINT('',(-53.7624712699068,-13.2670510364,7.));
#57710=CARTESIAN_POINT('Origin',(-53.1951359564886,-14.3971354987959,7.));
#57711=CARTESIAN_POINT('Origin',(-53.1951359564886,-14.3971354987959,7.));
#57712=CARTESIAN_POINT('',(-52.2352360662266,-15.2234730828751,6.));
#57713=CARTESIAN_POINT('Origin',(-53.1951359564886,-14.3971354987959,6.));
#57714=CARTESIAN_POINT('Ctrl Pts',(-52.2352263046383,-15.223479246524,6.));
#57715=CARTESIAN_POINT('Ctrl Pts',(-52.4934849626836,-15.5213201221341,
5.97509183961299));
#57716=CARTESIAN_POINT('Ctrl Pts',(-52.9025331767738,-15.6908484929834,
5.95018367922598));
#57717=CARTESIAN_POINT('Ctrl Pts',(-53.2954400519545,-15.6595806594193,
5.92527551883898));
#57718=CARTESIAN_POINT('Ctrl Pts',(-53.7082278597432,-15.6267306858339,
5.89910701538005));
#57719=CARTESIAN_POINT('Ctrl Pts',(-54.1031995108901,-15.3722499881178,
5.87293851192112));
#57720=CARTESIAN_POINT('Ctrl Pts',(-54.3034856243485,-15.009959026203,5.84677000846219));
#57721=CARTESIAN_POINT('Ctrl Pts',(-54.4060190030454,-14.8244897704715,
5.83337344776832));
#57722=CARTESIAN_POINT('Ctrl Pts',(-54.457529785952,-14.6107659273806,5.81997688707445));
#57723=CARTESIAN_POINT('Ctrl Pts',(-54.457664959728,-14.3970890371748,5.80658032638058));
#57724=CARTESIAN_POINT('Origin',(-53.1951359564886,-14.3971354987959,4.5));
#57725=CARTESIAN_POINT('',(-54.4609673117159,-14.396357828719,5.30658032638058));
#57726=CARTESIAN_POINT('',(-54.4612320294125,-14.3977598345137,5.44341967361941));
#57727=CARTESIAN_POINT('',(-54.4596359564886,-14.3971354987959,4.5));
#57728=CARTESIAN_POINT('Ctrl Pts',(-54.4612320294125,-14.3977598345137,
5.44341967361941));
#57729=CARTESIAN_POINT('Ctrl Pts',(-54.4614577199909,-14.4349274614079,
5.44576692486712));
#57730=CARTESIAN_POINT('Ctrl Pts',(-54.4599595944507,-14.4720765205797,
5.44811417611483));
#57731=CARTESIAN_POINT('Ctrl Pts',(-54.4566777507412,-14.5090671702315,
5.45046142736254));
#57732=CARTESIAN_POINT('Ctrl Pts',(-54.4200898743707,-14.9214601530044,
5.47662993082147));
#57733=CARTESIAN_POINT('Ctrl Pts',(-54.1618024272562,-15.3141643064504,
5.5027984342804));
#57734=CARTESIAN_POINT('Ctrl Pts',(-53.7976302145161,-15.5111328144605,
5.52896693773933));
#57735=CARTESIAN_POINT('Ctrl Pts',(-53.4334580017759,-15.7081013224707,
5.55513544119825));
#57736=CARTESIAN_POINT('Ctrl Pts',(-52.9634010234101,-15.709334185045,5.58130394465718));
#57737=CARTESIAN_POINT('Ctrl Pts',(-52.598247155701,-15.5141854678805,5.60747244811611));
#57738=CARTESIAN_POINT('Ctrl Pts',(-52.2330932879918,-15.3190367507161,
5.63364095157503));
#57739=CARTESIAN_POINT('Ctrl Pts',(-51.9728425309394,-14.9275064538129,
5.65980945503395));
#57740=CARTESIAN_POINT('Ctrl Pts',(-51.9341769083662,-14.5153483233265,
5.68597795849288));
#57741=CARTESIAN_POINT('Ctrl Pts',(-51.8955112857929,-14.1031901928401,
5.71214646195181));
#57742=CARTESIAN_POINT('Ctrl Pts',(-52.0784307976988,-13.6704042287704,
5.73831496541074));
#57743=CARTESIAN_POINT('Ctrl Pts',(-52.4009468670997,-13.4106806439539,
5.76448346886967));
#57744=CARTESIAN_POINT('Ctrl Pts',(-52.7234629365007,-13.1509570591374,
5.79065197232859));
#57745=CARTESIAN_POINT('Ctrl Pts',(-53.1855755633968,-13.0642958535739,
5.81682047578752));
#57746=CARTESIAN_POINT('Ctrl Pts',(-53.5800025789138,-13.1903251026302,
5.84298897924644));
#57747=CARTESIAN_POINT('Ctrl Pts',(-53.9744295944308,-13.3163543516866,
5.86915748270537));
#57748=CARTESIAN_POINT('Ctrl Pts',(-54.3011709985689,-13.6550740553627,
5.89532598616429));
#57749=CARTESIAN_POINT('Ctrl Pts',(-54.4137178903471,-14.0528046923317,
5.92149448962322));
#57750=CARTESIAN_POINT('Ctrl Pts',(-54.4451502229132,-14.1638837408548,
5.92880288428862));
#57751=CARTESIAN_POINT('Ctrl Pts',(-54.4598757063537,-14.2795655532322,
5.93611127895402));
#57752=CARTESIAN_POINT('Ctrl Pts',(-54.4588632108481,-14.3954785432618,
5.94341967361942));
#57753=CARTESIAN_POINT('Ctrl Pts',(-54.457664959728,-14.3970890371748,5.80658032638058));
#57754=CARTESIAN_POINT('Ctrl Pts',(-54.4577938309935,-14.1933748843943,
5.79380838361553));
#57755=CARTESIAN_POINT('Ctrl Pts',(-54.4112262077565,-13.989703408191,5.78103644085047));
#57756=CARTESIAN_POINT('Ctrl Pts',(-54.3176561881973,-13.8105991567173,
5.76826449808541));
#57757=CARTESIAN_POINT('Ctrl Pts',(-54.1259400628177,-13.4436314752601,
5.74209599462649));
#57758=CARTESIAN_POINT('Ctrl Pts',(-53.7369072362884,-13.1797973384592,
5.71592749116756));
#57759=CARTESIAN_POINT('Ctrl Pts',(-53.3250643574771,-13.1373309568652,
5.68975898770863));
#57760=CARTESIAN_POINT('Ctrl Pts',(-52.9132214786657,-13.0948645752712,
5.66359048424971));
#57761=CARTESIAN_POINT('Ctrl Pts',(-52.4785685475723,-13.2737659488842,
5.63742198079078));
#57762=CARTESIAN_POINT('Ctrl Pts',(-52.2159793451473,-13.5938495375153,
5.61125347733185));
#57763=CARTESIAN_POINT('Ctrl Pts',(-51.9533901427223,-13.9139331261463,
5.58508497387293));
#57764=CARTESIAN_POINT('Ctrl Pts',(-51.8628646689658,-14.3751989297955,
5.558916470414));
#57765=CARTESIAN_POINT('Ctrl Pts',(-51.9850104565428,-14.7707919534968,
5.53274796695507));
#57766=CARTESIAN_POINT('Ctrl Pts',(-52.1071562441199,-15.1663849771981,
5.50657946349615));
#57767=CARTESIAN_POINT('Ctrl Pts',(-52.4419732930306,-15.4963052209516,
5.48041096003722));
#57768=CARTESIAN_POINT('Ctrl Pts',(-52.8393182643656,-15.6126214609836,
5.4542424565783));
#57769=CARTESIAN_POINT('Ctrl Pts',(-53.2366632357006,-15.7289377010156,
5.42807395311937));
#57770=CARTESIAN_POINT('Ctrl Pts',(-53.69653612946,-15.6316499373263,5.40190544966044));
#57771=CARTESIAN_POINT('Ctrl Pts',(-54.0127281594173,-15.3643787057253,
5.37573694620152));
#57772=CARTESIAN_POINT('Ctrl Pts',(-54.291266212367,-15.1289356793162,5.35268473959454));
#57773=CARTESIAN_POINT('Ctrl Pts',(-54.4583064998761,-14.7615838076199,
5.32963253298756));
#57774=CARTESIAN_POINT('Ctrl Pts',(-54.4609673117159,-14.396357828719,5.30658032638058));
#57775=CARTESIAN_POINT('Origin',(-53.1951359564886,-14.3971354987959,4.5));
#57776=CARTESIAN_POINT('',(-54.4594541523146,-14.3982246410602,4.80658032638058));
#57777=CARTESIAN_POINT('',(-54.4577421278041,-14.3974029482829,4.94341967361941));
#57778=CARTESIAN_POINT('',(-54.4596359564886,-14.3971354987959,4.5));
#57779=CARTESIAN_POINT('Ctrl Pts',(-54.4577421278041,-14.3974029482829,
4.94341967361941));
#57780=CARTESIAN_POINT('Ctrl Pts',(-54.4581119948619,-14.5888150279108,
4.95542257078023));
#57781=CARTESIAN_POINT('Ctrl Pts',(-54.4171976582397,-14.7800770605195,
4.96742546794105));
#57782=CARTESIAN_POINT('Ctrl Pts',(-54.3341701782111,-14.9508661287461,
4.97942836510187));
#57783=CARTESIAN_POINT('Ctrl Pts',(-54.1531551391583,-15.3232174255002,
5.00559686856079));
#57784=CARTESIAN_POINT('Ctrl Pts',(-53.7719681306167,-15.5982567367276,
5.03176537201972));
#57785=CARTESIAN_POINT('Ctrl Pts',(-53.3615378715941,-15.6526538764831,
5.05793387547865));
#57786=CARTESIAN_POINT('Ctrl Pts',(-52.9511076125715,-15.7070510162386,
5.08410237893757));
#57787=CARTESIAN_POINT('Ctrl Pts',(-52.5114341030678,-15.5408059845222,
5.1102708823965));
#57788=CARTESIAN_POINT('Ctrl Pts',(-52.239672304957,-15.2284636038326,5.13643938585543));
#57789=CARTESIAN_POINT('Ctrl Pts',(-51.9679105068461,-14.9161212231431,
5.16260788931435));
#57790=CARTESIAN_POINT('Ctrl Pts',(-51.8640604201282,-14.4576814934805,
5.18877639277328));
#57791=CARTESIAN_POINT('Ctrl Pts',(-51.974689389455,-14.0587171002307,5.21494489623221));
#57792=CARTESIAN_POINT('Ctrl Pts',(-52.0853183587818,-13.659752706981,5.24111339969114));
#57793=CARTESIAN_POINT('Ctrl Pts',(-52.4104263841535,-13.3202636501442,
5.26728190315006));
#57794=CARTESIAN_POINT('Ctrl Pts',(-52.804231701646,-13.1924751167177,5.29345040660898));
#57795=CARTESIAN_POINT('Ctrl Pts',(-53.1980370191385,-13.0646865832913,
5.31961891006791));
#57796=CARTESIAN_POINT('Ctrl Pts',(-53.6605396287519,-13.1485985732751,
5.34578741352684));
#57797=CARTESIAN_POINT('Ctrl Pts',(-53.9843467807452,-13.406595474317,5.37195591698577));
#57798=CARTESIAN_POINT('Ctrl Pts',(-54.2791092171045,-13.6414506795096,
5.39577716919699));
#57799=CARTESIAN_POINT('Ctrl Pts',(-54.4589415919507,-14.0205614348097,
5.4195984214082));
#57800=CARTESIAN_POINT('Ctrl Pts',(-54.4612320294125,-14.3977598345137,
5.44341967361941));
#57801=CARTESIAN_POINT('Ctrl Pts',(-54.4609673117159,-14.396357828719,5.30658032638058));
#57802=CARTESIAN_POINT('Ctrl Pts',(-54.4613270117525,-14.3469850034748,
5.30346402952863));
#57803=CARTESIAN_POINT('Ctrl Pts',(-54.4586827097295,-14.2976510284966,
5.30034773267668));
#57804=CARTESIAN_POINT('Ctrl Pts',(-54.4529037631581,-14.2486870321021,
5.29723143582474));
#57805=CARTESIAN_POINT('Ctrl Pts',(-54.4043761707862,-13.8375212895923,
5.27106293236581));
#57806=CARTESIAN_POINT('Ctrl Pts',(-54.134809819887,-13.4524445040854,5.24489442890688));
#57807=CARTESIAN_POINT('Ctrl Pts',(-53.7650823822708,-13.2661285769126,
5.21872592544796));
#57808=CARTESIAN_POINT('Ctrl Pts',(-53.3953549446545,-13.0798126497399,
5.19255742198903));
#57809=CARTESIAN_POINT('Ctrl Pts',(-52.9254664203213,-13.0922575809014,
5.1663889185301));
#57810=CARTESIAN_POINT('Ctrl Pts',(-52.5661199525803,-13.2978834669457,
5.14022041507118));
#57811=CARTESIAN_POINT('Ctrl Pts',(-52.2067734848394,-13.5035093529901,
5.11405191161225));
#57812=CARTESIAN_POINT('Ctrl Pts',(-51.9579690736908,-13.9023161939173,
5.08788340815333));
#57813=CARTESIAN_POINT('Ctrl Pts',(-51.9312738021255,-14.315473986753,5.0617149046944));
#57814=CARTESIAN_POINT('Ctrl Pts',(-51.9045785305602,-14.7286317795886,
5.03554640123547));
#57815=CARTESIAN_POINT('Ctrl Pts',(-52.0999923985782,-15.1561405243328,
5.00937789777654));
#57816=CARTESIAN_POINT('Ctrl Pts',(-52.4298893914915,-15.4063003551787,
4.98320939431762));
#57817=CARTESIAN_POINT('Ctrl Pts',(-52.7597863844047,-15.6564601860247,
4.95704089085869));
#57818=CARTESIAN_POINT('Ctrl Pts',(-53.2241665022132,-15.7292711029725,
4.93087238739976));
#57819=CARTESIAN_POINT('Ctrl Pts',(-53.6147962366241,-15.5920837570553,
4.90470388394084));
#57820=CARTESIAN_POINT('Ctrl Pts',(-54.0054259710351,-15.4548964111382,
4.87853538048191));
#57821=CARTESIAN_POINT('Ctrl Pts',(-54.3223053220485,-15.107710802356,4.85236687702299));
#57822=CARTESIAN_POINT('Ctrl Pts',(-54.4233417938017,-14.706209118673,4.82619837356406));
#57823=CARTESIAN_POINT('Ctrl Pts',(-54.4485901905141,-14.6058763020728,
4.8196590245029));
#57824=CARTESIAN_POINT('Ctrl Pts',(-54.460359856649,-14.5021516119852,4.81311967544174));
#57825=CARTESIAN_POINT('Ctrl Pts',(-54.4594541523146,-14.3982246410602,
4.80658032638058));
#57826=CARTESIAN_POINT('Origin',(-53.1951359564886,-14.3971354987959,4.5));
#57827=CARTESIAN_POINT('',(-54.458134169311,-14.3964211317122,4.30658032638058));
#57828=CARTESIAN_POINT('',(-54.4603880160508,-14.3961458582298,4.44341967361942));
#57829=CARTESIAN_POINT('',(-54.4596359564886,-14.3971354987959,4.5));
#57830=CARTESIAN_POINT('Ctrl Pts',(-54.4603880160508,-14.3961458582298,
4.44341967361942));
#57831=CARTESIAN_POINT('Ctrl Pts',(-54.4574339233842,-14.7397014586706,
4.46507821669334));
#57832=CARTESIAN_POINT('Ctrl Pts',(-54.312116901092,-15.0854595650489,4.48673675976727));
#57833=CARTESIAN_POINT('Ctrl Pts',(-54.0623960097695,-15.3201070497197,
4.50839530284119));
#57834=CARTESIAN_POINT('Ctrl Pts',(-53.7606757146401,-15.6036152013657,
4.53456380630012));
#57835=CARTESIAN_POINT('Ctrl Pts',(-53.3065445684699,-15.7249218506019,
4.56073230975904));
#57836=CARTESIAN_POINT('Ctrl Pts',(-52.9036403743547,-15.6296316648431,
4.58690081321797));
#57837=CARTESIAN_POINT('Ctrl Pts',(-52.5007361802396,-15.5343414790842,
4.6130693166769));
#57838=CARTESIAN_POINT('Ctrl Pts',(-52.1490589381795,-15.2224544583304,
4.63923782013582));
#57839=CARTESIAN_POINT('Ctrl Pts',(-52.0063049058888,-14.8338244281946,
4.66540632359475));
#57840=CARTESIAN_POINT('Ctrl Pts',(-51.8635508735981,-14.4451943980587,
4.69157482705368));
#57841=CARTESIAN_POINT('Ctrl Pts',(-51.9297200510767,-13.9798213585407,
4.7177433305126));
#57842=CARTESIAN_POINT('Ctrl Pts',(-52.1751413884873,-13.6463841561873,
4.74391183397153));
#57843=CARTESIAN_POINT('Ctrl Pts',(-52.4205627258978,-13.3129469538339,
4.77008033743046));
#57844=CARTESIAN_POINT('Ctrl Pts',(-52.8452362232402,-13.111445588645,4.79624884088938));
#57845=CARTESIAN_POINT('Ctrl Pts',(-53.2587332445463,-13.1322355800464,
4.82241734434831));
#57846=CARTESIAN_POINT('Ctrl Pts',(-53.6722302658525,-13.1530255714477,
4.84858584780724));
#57847=CARTESIAN_POINT('Ctrl Pts',(-54.0745508111225,-13.3961069194393,
4.87475435126616));
#57848=CARTESIAN_POINT('Ctrl Pts',(-54.2852895489753,-13.7524792345754,
4.90092285472509));
#57849=CARTESIAN_POINT('Ctrl Pts',(-54.3993672224223,-13.9453916768054,
4.9150884610232));
#57850=CARTESIAN_POINT('Ctrl Pts',(-54.4573056172638,-14.1715018075515,
4.92925406732131));
#57851=CARTESIAN_POINT('Ctrl Pts',(-54.4577421278041,-14.3974029482829,
4.94341967361941));
#57852=CARTESIAN_POINT('Ctrl Pts',(-54.4594541523146,-14.3982246410602,
4.80658032638058));
#57853=CARTESIAN_POINT('Ctrl Pts',(-54.4567355009545,-14.0862672062605,
4.78695117198282));
#57854=CARTESIAN_POINT('Ctrl Pts',(-54.3398093025916,-13.7724871818732,
4.76732201758505));
#57855=CARTESIAN_POINT('Ctrl Pts',(-54.1304031431366,-13.5431499271195,
4.74769286318728));
#57856=CARTESIAN_POINT('Ctrl Pts',(-53.8512344282254,-13.2374101778329,
4.72152435972836));
#57857=CARTESIAN_POINT('Ctrl Pts',(-53.4077034059102,-13.0817484378433,
4.69535585626943));
#57858=CARTESIAN_POINT('Ctrl Pts',(-52.9986946517684,-13.1459652901465,
4.6691873528105));
#57859=CARTESIAN_POINT('Ctrl Pts',(-52.5896858976267,-13.2101821424497,
4.64301884935157));
#57860=CARTESIAN_POINT('Ctrl Pts',(-52.2151994116584,-13.4942775870456,
4.61685034589265));
#57861=CARTESIAN_POINT('Ctrl Pts',(-52.0431593891151,-13.8708598453683,
4.59068184243372));
#57862=CARTESIAN_POINT('Ctrl Pts',(-51.8711193665719,-14.247442103691,4.56451333897479));
#57863=CARTESIAN_POINT('Ctrl Pts',(-51.9015258074537,-14.7165111757404,
4.53834483551587));
#57864=CARTESIAN_POINT('Ctrl Pts',(-52.1207441004937,-15.0677309159732,
4.51217633205694));
#57865=CARTESIAN_POINT('Ctrl Pts',(-52.3399623935336,-15.4189506562059,
4.48600782859801));
#57866=CARTESIAN_POINT('Ctrl Pts',(-52.7479925387317,-15.6523210646219,
4.45983932513909));
#57867=CARTESIAN_POINT('Ctrl Pts',(-53.1618689696675,-15.6631960750064,
4.43367082168017));
#57868=CARTESIAN_POINT('Ctrl Pts',(-53.5757454006032,-15.6740710853908,
4.40750231822124));
#57869=CARTESIAN_POINT('Ctrl Pts',(-53.9954681172766,-15.4624506977437,
4.38133381476231));
#57870=CARTESIAN_POINT('Ctrl Pts',(-54.2328284639311,-15.1232280099042,
4.35516531130338));
#57871=CARTESIAN_POINT('Ctrl Pts',(-54.3797245073824,-14.9132920564272,
4.33897031632912));
#57872=CARTESIAN_POINT('Ctrl Pts',(-54.4567749448579,-14.6544838494259,
4.32277532135485));
#57873=CARTESIAN_POINT('Ctrl Pts',(-54.458134169311,-14.3964211317122,4.30658032638058));
#57874=CARTESIAN_POINT('Origin',(-53.1951359564886,-14.3971354987959,4.5));
#57875=CARTESIAN_POINT('',(-54.4616250374271,-14.3970459917425,3.80658032638058));
#57876=CARTESIAN_POINT('',(-54.4600990366243,-14.3981838592136,3.94341967361941));
#57877=CARTESIAN_POINT('',(-54.4596359564886,-14.3971354987959,4.5));
#57878=CARTESIAN_POINT('Ctrl Pts',(-54.4600990366243,-14.3981838592136,
3.94341967361941));
#57879=CARTESIAN_POINT('Ctrl Pts',(-54.460821703013,-14.4798548702781,3.94856535914752));
#57880=CARTESIAN_POINT('Ctrl Pts',(-54.4535723073139,-14.561398217572,3.95371104467563));
#57881=CARTESIAN_POINT('Ctrl Pts',(-54.4378783642807,-14.6412825634277,
3.95885673020373));
#57882=CARTESIAN_POINT('Ctrl Pts',(-54.3580664518923,-15.0475362626526,
3.98502523366266));
#57883=CARTESIAN_POINT('Ctrl Pts',(-54.0598570383511,-15.410883959442,4.01119373712159));
#57884=CARTESIAN_POINT('Ctrl Pts',(-53.6769707694449,-15.5683962274082,
4.03736224058052));
#57885=CARTESIAN_POINT('Ctrl Pts',(-53.2940845005388,-15.7259084953743,
4.06353074403944));
#57886=CARTESIAN_POINT('Ctrl Pts',(-52.8265213762676,-15.6775853345172,
4.08969924749837));
#57887=CARTESIAN_POINT('Ctrl Pts',(-52.4839422593842,-15.4450954247484,
4.11586775095729));
#57888=CARTESIAN_POINT('Ctrl Pts',(-52.1413631425007,-15.2126055149797,
4.14203625441622));
#57889=CARTESIAN_POINT('Ctrl Pts',(-51.9237680330049,-14.7959488562993,
4.16820475787515));
#57890=CARTESIAN_POINT('Ctrl Pts',(-51.9287291645367,-14.3819592468436,
4.19437326133407));
#57891=CARTESIAN_POINT('Ctrl Pts',(-51.9336902960684,-13.967969637388,4.220541764793));
#57892=CARTESIAN_POINT('Ctrl Pts',(-52.1612076686276,-13.5566470771571,
4.24671026825193));
#57893=CARTESIAN_POINT('Ctrl Pts',(-52.5092597878395,-13.3324334921486,
4.27287877171085));
#57894=CARTESIAN_POINT('Ctrl Pts',(-52.8573119070513,-13.1082199071402,
4.29904727516978));
#57895=CARTESIAN_POINT('Ctrl Pts',(-53.3258987729158,-13.0711152973543,
4.3252157786287));
#57896=CARTESIAN_POINT('Ctrl Pts',(-53.7049004648973,-13.2377578095269,
4.35138428208763));
#57897=CARTESIAN_POINT('Ctrl Pts',(-54.0839021568789,-13.4044003216995,
4.37755278554656));
#57898=CARTESIAN_POINT('Ctrl Pts',(-54.3733186749775,-13.7747899558306,
4.40372128900549));
#57899=CARTESIAN_POINT('Ctrl Pts',(-54.4433722119826,-14.1828395999241,
4.42988979246441));
#57900=CARTESIAN_POINT('Ctrl Pts',(-54.4554454540469,-14.2531641308192,
4.43439975284941));
#57901=CARTESIAN_POINT('Ctrl Pts',(-54.4610031470342,-14.3246072444484,
4.43890971323442));
#57902=CARTESIAN_POINT('Ctrl Pts',(-54.4603880160508,-14.3961458582298,
4.44341967361942));
#57903=CARTESIAN_POINT('Ctrl Pts',(-54.458134169311,-14.3964211317122,4.30658032638058));
#57904=CARTESIAN_POINT('Ctrl Pts',(-54.4589712326528,-14.237496062036,4.29660681789592));
#57905=CARTESIAN_POINT('Ctrl Pts',(-54.4311018285097,-14.0788537248348,
4.28663330941126));
#57906=CARTESIAN_POINT('Ctrl Pts',(-54.3731606475783,-13.9320829192412,
4.27665980092661));
#57907=CARTESIAN_POINT('Ctrl Pts',(-54.2211345079355,-13.5469855044494,
4.25049129746768));
#57908=CARTESIAN_POINT('Ctrl Pts',(-53.8620842520144,-13.2436156628976,
4.22432279400875));
#57909=CARTESIAN_POINT('Ctrl Pts',(-53.4570122824291,-13.1580080377804,
4.19815429054982));
#57910=CARTESIAN_POINT('Ctrl Pts',(-53.0519403128439,-13.0724004126631,
4.1719857870909));
#57911=CARTESIAN_POINT('Ctrl Pts',(-52.6008466295945,-13.2045550039804,
4.14581728363197));
#57912=CARTESIAN_POINT('Ctrl Pts',(-52.3060070023708,-13.4952121220022,
4.11964878017305));
#57913=CARTESIAN_POINT('Ctrl Pts',(-52.0111673751472,-13.7858692400241,
4.09348027671412));
#57914=CARTESIAN_POINT('Ctrl Pts',(-51.8725818039491,-14.2350288847506,
4.06731177325519));
#57915=CARTESIAN_POINT('Ctrl Pts',(-51.9523937062209,-14.6412825324806,
4.04114326979627));
#57916=CARTESIAN_POINT('Ctrl Pts',(-52.0322056084927,-15.0475361802107,
4.01497476633734));
#57917=CARTESIAN_POINT('Ctrl Pts',(-52.3304149842342,-15.4108838309442,
3.98880626287841));
#57918=CARTESIAN_POINT('Ctrl Pts',(-52.7133012046075,-15.5683960789447,
3.96263775941949));
#57919=CARTESIAN_POINT('Ctrl Pts',(-53.0961874249808,-15.7259083269452,
3.93646925596056));
#57920=CARTESIAN_POINT('Ctrl Pts',(-53.5637504899858,-15.6775851722127,
3.91030075250163));
#57921=CARTESIAN_POINT('Ctrl Pts',(-53.9063295634455,-15.4450952919135,
3.88413224904271));
#57922=CARTESIAN_POINT('Ctrl Pts',(-54.2447474105889,-15.2154294107524,
3.85828160815533));
#57923=CARTESIAN_POINT('Ctrl Pts',(-54.4611991270569,-14.8060436899639,
3.83243096726796));
#57924=CARTESIAN_POINT('Ctrl Pts',(-54.4616250374271,-14.3970459917425,
3.80658032638058));
#57925=CARTESIAN_POINT('Origin',(-53.1951359564886,-14.3971354987959,4.5));
#57926=CARTESIAN_POINT('',(-54.458326569365,-14.3979628849946,3.30658032638058));
#57927=CARTESIAN_POINT('',(-54.4578259861007,-14.3967173602322,3.44341967361941));
#57928=CARTESIAN_POINT('',(-54.4596359564886,-14.3971354987959,4.5));
#57929=CARTESIAN_POINT('Ctrl Pts',(-54.4578259861007,-14.3967173602322,
3.44341967361941));
#57930=CARTESIAN_POINT('Ctrl Pts',(-54.4571098189797,-14.6327171768276,
3.45822100506063));
#57931=CARTESIAN_POINT('Ctrl Pts',(-54.3935213986439,-14.8690753747194,
3.47302233650184));
#57932=CARTESIAN_POINT('Ctrl Pts',(-54.2695279486697,-15.0677310009766,
3.48782366794306));
#57933=CARTESIAN_POINT('Ctrl Pts',(-54.0503096278436,-15.4189507857301,
3.51399217140198));
#57934=CARTESIAN_POINT('Ctrl Pts',(-53.6422794309233,-15.6523212237234,
3.54016067486091));
#57935=CARTESIAN_POINT('Ctrl Pts',(-53.228402947526,-15.6631962354854,3.56632917831984));
#57936=CARTESIAN_POINT('Ctrl Pts',(-52.8145264641287,-15.6740712472475,
3.59249768177877));
#57937=CARTESIAN_POINT('Ctrl Pts',(-52.3948036942543,-15.4624508327782,
3.61866618523769));
#57938=CARTESIAN_POINT('Ctrl Pts',(-52.1574433175134,-15.1232281019409,
3.64483468869661));
#57939=CARTESIAN_POINT('Ctrl Pts',(-51.9200829407725,-14.7840053711036,
3.67100319215554));
#57940=CARTESIAN_POINT('Ctrl Pts',(-51.865084957165,-14.3171803238982,3.69717169561447));
#57941=CARTESIAN_POINT('Ctrl Pts',(-52.0171111160778,-13.932082860293,3.7233401990734));
#57942=CARTESIAN_POINT('Ctrl Pts',(-52.1691372749906,-13.5469853966878,
3.74950870253232));
#57943=CARTESIAN_POINT('Ctrl Pts',(-52.5281875764236,-13.2436155166828,
3.77567720599125));
#57944=CARTESIAN_POINT('Ctrl Pts',(-52.933259597354,-13.1580078807144,3.80184570945017));
#57945=CARTESIAN_POINT('Ctrl Pts',(-53.3383316182844,-13.072400244746,3.8280142129091));
#57946=CARTESIAN_POINT('Ctrl Pts',(-53.7894253587122,-13.2045548528142,
3.85418271636803));
#57947=CARTESIAN_POINT('Ctrl Pts',(-54.0842650233083,-13.4952120076785,
3.88035121982696));
#57948=CARTESIAN_POINT('Ctrl Pts',(-54.3211284189289,-13.7287153280572,
3.90137403775778));
#57949=CARTESIAN_POINT('Ctrl Pts',(-54.4571465662818,-14.0645150435707,
3.9223968556886));
#57950=CARTESIAN_POINT('Ctrl Pts',(-54.4600990366243,-14.3981838592136,
3.94341967361941));
#57951=CARTESIAN_POINT('Ctrl Pts',(-54.4616250374271,-14.3970459917425,
3.80658032638058));
#57952=CARTESIAN_POINT('Ctrl Pts',(-54.4616302744719,-14.3920169071375,
3.80626246380903));
#57953=CARTESIAN_POINT('Ctrl Pts',(-54.4616028495907,-14.3869878811994,
3.80594460123748));
#57954=CARTESIAN_POINT('Ctrl Pts',(-54.4615425879167,-14.3819592487679,
3.80562673866593));
#57955=CARTESIAN_POINT('Ctrl Pts',(-54.4565814570138,-13.9679696917871,
3.779458235207));
#57956=CARTESIAN_POINT('Ctrl Pts',(-54.2290641132938,-13.5566471836914,
3.75328973174807));
#57957=CARTESIAN_POINT('Ctrl Pts',(-53.8810120381994,-13.3324336271042,
3.72712122828915));
#57958=CARTESIAN_POINT('Ctrl Pts',(-53.532959963105,-13.1082200705171,3.70095272483022));
#57959=CARTESIAN_POINT('Ctrl Pts',(-53.0643731566361,-13.0711154654387,
3.67478422137129));
#57960=CARTESIAN_POINT('Ctrl Pts',(-52.6853715126953,-13.2377579564864,
3.64861571791237));
#57961=CARTESIAN_POINT('Ctrl Pts',(-52.3063698687544,-13.4044004475342,
3.62244721445344));
#57962=CARTESIAN_POINT('Ctrl Pts',(-52.0169533873414,-13.7747900347082,
3.59627871099452));
#57963=CARTESIAN_POINT('Ctrl Pts',(-51.9468998592157,-14.182839627083,3.57011020753559));
#57964=CARTESIAN_POINT('Ctrl Pts',(-51.87684633109,-14.5908892194578,3.54394170407666));
#57965=CARTESIAN_POINT('Ctrl Pts',(-52.0261557562516,-15.0365988170333,
3.51777320061773));
#57966=CARTESIAN_POINT('Ctrl Pts',(-52.327876013137,-15.3201069327361,3.49160469715881));
#57967=CARTESIAN_POINT('Ctrl Pts',(-52.6295962700224,-15.6036150484389,
3.46543619369988));
#57968=CARTESIAN_POINT('Ctrl Pts',(-53.0837273586317,-15.7249216822689,
3.43926769024096));
#57969=CARTESIAN_POINT('Ctrl Pts',(-53.4866315016752,-15.6296315086021,
3.41309918678203));
#57970=CARTESIAN_POINT('Ctrl Pts',(-53.8895356447186,-15.5343413349353,
3.38693068332311));
#57971=CARTESIAN_POINT('Ctrl Pts',(-54.2412128421963,-15.2224543537718,
3.36076217986418));
#57972=CARTESIAN_POINT('Ctrl Pts',(-54.3839668563951,-14.8338243728713,
3.33459367640525));
#57973=CARTESIAN_POINT('Ctrl Pts',(-54.4349061872521,-14.6951484043591,
3.32525589306369));
#57974=CARTESIAN_POINT('Ctrl Pts',(-54.4592433859174,-14.5467007705307,
3.31591810972214));
#57975=CARTESIAN_POINT('Ctrl Pts',(-54.458326569365,-14.3979628849946,3.30658032638058));
#57976=CARTESIAN_POINT('Origin',(-53.1951359564886,-14.3971354987959,4.5));
#57977=CARTESIAN_POINT('',(-54.4591686783466,-14.3960664985434,2.80658032638058));
#57978=CARTESIAN_POINT('',(-54.4614103817624,-14.3966710984295,2.94341967361941));
#57979=CARTESIAN_POINT('',(-54.4596359564886,-14.3971354987959,4.5));
#57980=CARTESIAN_POINT('Ctrl Pts',(-54.4614103817624,-14.3966710984295,
2.94341967361941));
#57981=CARTESIAN_POINT('Ctrl Pts',(-54.4595565487343,-14.7837947911815,
2.96787665097374));
#57982=CARTESIAN_POINT('Ctrl Pts',(-54.2687030511239,-15.172502088678,2.99233362832806));
#57983=CARTESIAN_POINT('Ctrl Pts',(-53.9603826185353,-15.4063004831901,
3.01679060568238));
#57984=CARTESIAN_POINT('Ctrl Pts',(-53.6304855838459,-15.6564603458274,
3.04295910914131));
#57985=CARTESIAN_POINT('Ctrl Pts',(-53.1661054070793,-15.729271271822,3.06912761260023));
#57986=CARTESIAN_POINT('Ctrl Pts',(-52.7754756231319,-15.5920839084722,
3.09529611605916));
#57987=CARTESIAN_POINT('Ctrl Pts',(-52.3848458391845,-15.4548965451224,
3.12146461951809));
#57988=CARTESIAN_POINT('Ctrl Pts',(-52.0679664480565,-15.1077108924282,
3.14763312297701));
#57989=CARTESIAN_POINT('Ctrl Pts',(-51.9669299635083,-14.7062091578755,
3.17380162643594));
#57990=CARTESIAN_POINT('Ctrl Pts',(-51.8658934789602,-14.3047074233228,
3.19997012989487));
#57991=CARTESIAN_POINT('Ctrl Pts',(-51.980699900992,-13.8488896069116,3.22613863335379));
#57992=CARTESIAN_POINT('Ctrl Pts',(-52.2598686512828,-13.5431498188588,
3.25230713681272));
#57993=CARTESIAN_POINT('Ctrl Pts',(-52.5390374015737,-13.237410030806,3.27847564027165));
#57994=CARTESIAN_POINT('Ctrl Pts',(-52.9825684801236,-13.0817482711116,
3.30464414373057));
#57995=CARTESIAN_POINT('Ctrl Pts',(-53.3915772861129,-13.1459651315609,
3.3308126471895));
#57996=CARTESIAN_POINT('Ctrl Pts',(-53.8005860921022,-13.2101819920102,
3.35698115064842));
#57997=CARTESIAN_POINT('Ctrl Pts',(-54.1750726255309,-13.4942774726031,
3.38314965410735));
#57998=CARTESIAN_POINT('Ctrl Pts',(-54.3471126698793,-13.8708597786564,
3.40931815756628));
#57999=CARTESIAN_POINT('Ctrl Pts',(-54.4218440652422,-14.0344410036375,
3.42068532958399));
#58000=CARTESIAN_POINT('Ctrl Pts',(-54.4583759903277,-14.2154734956486,
3.4320525016017));
#58001=CARTESIAN_POINT('Ctrl Pts',(-54.4578259861007,-14.3967173602322,
3.44341967361941));
#58002=CARTESIAN_POINT('Ctrl Pts',(-54.458326569365,-14.3979628849946,3.30658032638058));
#58003=CARTESIAN_POINT('Ctrl Pts',(-54.4566740698126,-14.1298729507199,
3.28974960626321));
#58004=CARTESIAN_POINT('Ctrl Pts',(-54.3729773016518,-13.8608400579149,
3.27291888614584));
#58005=CARTESIAN_POINT('Ctrl Pts',(-54.2151303952057,-13.6463842512931,
3.25608816602847));
#58006=CARTESIAN_POINT('Ctrl Pts',(-53.9697090888974,-13.3129470912529,
3.22991966256955));
#58007=CARTESIAN_POINT('Ctrl Pts',(-53.5450356453608,-13.1114457518099,
3.20375115911062));
#58008=CARTESIAN_POINT('Ctrl Pts',(-53.1315386764808,-13.1322357404855,
3.17758265565169));
#58009=CARTESIAN_POINT('Ctrl Pts',(-52.7180417076007,-13.153025729161,3.15141415219276));
#58010=CARTESIAN_POINT('Ctrl Pts',(-52.3157212133773,-13.396107045955,3.12524564873384));
#58011=CARTESIAN_POINT('Ctrl Pts',(-52.1049825022091,-13.7524793160883,
3.09907714527491));
#58012=CARTESIAN_POINT('Ctrl Pts',(-51.8942437910409,-14.1088515862216,
3.07290864181599));
#58013=CARTESIAN_POINT('Ctrl Pts',(-51.8750868629279,-14.5785148096942,
3.04674013835706));
#58014=CARTESIAN_POINT('Ctrl Pts',(-52.0561018790939,-14.9508660589359,
3.02057163489813));
#58015=CARTESIAN_POINT('Ctrl Pts',(-52.2371168952598,-15.3232173081776,
2.99440313143921));
#58016=CARTESIAN_POINT('Ctrl Pts',(-52.6183038557047,-15.5982565831885,
2.96823462798028));
#58017=CARTESIAN_POINT('Ctrl Pts',(-53.0287340625826,-15.6526537166303,
2.94206612452135));
#58018=CARTESIAN_POINT('Ctrl Pts',(-53.4391642694604,-15.7070508500722,
2.91589762106243));
#58019=CARTESIAN_POINT('Ctrl Pts',(-53.8788377227712,-15.5408058419451,
2.8897291176035));
#58020=CARTESIAN_POINT('Ctrl Pts',(-54.150599486686,-15.2284634997803,2.86356061414457));
#58021=CARTESIAN_POINT('Ctrl Pts',(-54.3478475962364,-15.0017614956533,
2.84456718488991));
#58022=CARTESIAN_POINT('Ctrl Pts',(-54.4566391704649,-14.6980948440071,
2.82557375563525));
#58023=CARTESIAN_POINT('Ctrl Pts',(-54.4591686783466,-14.3960664985434,
2.80658032638058));
#58024=CARTESIAN_POINT('Origin',(-53.1951359564886,-14.3971354987959,4.5));
#58025=CARTESIAN_POINT('',(-54.4611870990995,-14.3977489718831,2.30658032638058));
#58026=CARTESIAN_POINT('',(-54.4588409672492,-14.3981450852038,2.44341967361942));
#58027=CARTESIAN_POINT('',(-54.4596359564886,-14.3971354987959,4.5));
#58028=CARTESIAN_POINT('',(-52.2370198037663,-15.2223467977324,2.));
#58029=CARTESIAN_POINT('Ctrl Pts',(-54.4611870990995,-14.3977489718831,
2.30658032638058));
#58030=CARTESIAN_POINT('Ctrl Pts',(-54.4588273697935,-14.0226957918939,
2.2828923946305));
#58031=CARTESIAN_POINT('Ctrl Pts',(-54.2812687919142,-13.6457847405029,
2.25920446288042));
#58032=CARTESIAN_POINT('Ctrl Pts',(-53.9893248675415,-13.4106809034345,
2.23551653113034));
#58033=CARTESIAN_POINT('Ctrl Pts',(-53.6668089267087,-13.1509572754522,
2.20934802767141));
#58034=CARTESIAN_POINT('Ctrl Pts',(-53.2046966949687,-13.064295685136,2.18317952421249));
#58035=CARTESIAN_POINT('Ctrl Pts',(-52.8102694972366,-13.190325107422,2.15701102075356));
#58036=CARTESIAN_POINT('Ctrl Pts',(-52.4158422995045,-13.316354529708,2.13084251729463));
#58037=CARTESIAN_POINT('Ctrl Pts',(-52.0891001357801,-13.6550749645962,
2.10467401383571));
#58038=CARTESIAN_POINT('Ctrl Pts',(-51.9765532487624,-14.05280555706,2.07850551037678));
#58039=CARTESIAN_POINT('Ctrl Pts',(-51.8640063617447,-14.4505361495237,
2.05233700691785));
#58040=CARTESIAN_POINT('Ctrl Pts',(-51.9656547514336,-14.9072768995629,
2.02616850345893));
#58041=CARTESIAN_POINT('Ctrl Pts',(-52.2370198037663,-15.2223467977324,
2.));
#58042=CARTESIAN_POINT('',(-54.1550359790162,-15.2234729584201,2.));
#58043=CARTESIAN_POINT('Origin',(-53.1951359564886,-14.3971354987959,2.));
#58044=CARTESIAN_POINT('Ctrl Pts',(-54.1550457523822,-15.2234791283661,
2.));
#58045=CARTESIAN_POINT('Ctrl Pts',(-53.8967871302308,-15.5213198394326,
2.02490816038701));
#58046=CARTESIAN_POINT('Ctrl Pts',(-53.4877388130256,-15.6908487049404,
2.04981632077402));
#58047=CARTESIAN_POINT('Ctrl Pts',(-53.0948318598941,-15.6595809742728,
2.07472448116103));
#58048=CARTESIAN_POINT('Ctrl Pts',(-52.6820439702103,-15.6267311087904,
2.10089298461995));
#58049=CARTESIAN_POINT('Ctrl Pts',(-52.2870722649439,-15.3722500867662,
2.12706148807888));
#58050=CARTESIAN_POINT('Ctrl Pts',(-52.0867861333632,-15.0099590154002,
2.15322999153781));
#58051=CARTESIAN_POINT('Ctrl Pts',(-51.8865000017826,-14.6476679440343,
2.17939849499673));
#58052=CARTESIAN_POINT('Ctrl Pts',(-51.8808994438879,-14.1775668233264,
2.20556699845566));
#58053=CARTESIAN_POINT('Ctrl Pts',(-52.0726155940678,-13.8105991317322,
2.23173550191459));
#58054=CARTESIAN_POINT('Ctrl Pts',(-52.2643317442477,-13.4436314401379,
2.25790400537351));
#58055=CARTESIAN_POINT('Ctrl Pts',(-52.6533646025024,-13.1797971776571,
2.28407250883244));
#58056=CARTESIAN_POINT('Ctrl Pts',(-53.065207531184,-13.1373307700534,2.31024101229137));
#58057=CARTESIAN_POINT('Ctrl Pts',(-53.4770504598656,-13.0948643624498,
2.33640951575029));
#58058=CARTESIAN_POINT('Ctrl Pts',(-53.9117034589741,-13.2737658097233,
2.36257801920922));
#58059=CARTESIAN_POINT('Ctrl Pts',(-54.1742926968884,-13.5938494504631,
2.38874652266814));
#58060=CARTESIAN_POINT('Ctrl Pts',(-54.3571662426276,-13.8167634997217,
2.40697090631857));
#58061=CARTESIAN_POINT('Ctrl Pts',(-54.456587675354,-14.108151888276,2.42519528996899));
#58062=CARTESIAN_POINT('Ctrl Pts',(-54.4588409672492,-14.3981450852038,
2.44341967361942));
#58063=CARTESIAN_POINT('Origin',(-53.1951359564886,-14.3971354987959,0.895788276411275));
#58064=CARTESIAN_POINT('',(-54.7400835567429,-14.3978973414314,5.60421172358873));
#58065=CARTESIAN_POINT('',(-54.7357308572386,-14.3970788042278,5.64578827641128));
#58066=CARTESIAN_POINT('',(-54.7381359564886,-14.3971354987959,0.895788276411275));
#58067=CARTESIAN_POINT('',(-52.7966221146314,-12.9064860705774,6.));
#58068=CARTESIAN_POINT('Ctrl Pts',(-54.7357308572386,-14.3970788042278,
5.64578827641128));
#58069=CARTESIAN_POINT('Ctrl Pts',(-54.7355659120932,-14.6578169944908,
5.65918483710515));
#58070=CARTESIAN_POINT('Ctrl Pts',(-54.5499292284113,-15.4280437939379,
5.69874990125794));
#58071=CARTESIAN_POINT('Ctrl Pts',(-53.3392716219708,-16.2080719085829,
5.76448346886966));
#58072=CARTESIAN_POINT('Ctrl Pts',(-51.7629444164752,-15.5169955192796,
5.84298897924644));
#58073=CARTESIAN_POINT('Ctrl Pts',(-51.4734277108623,-13.8186461670281,
5.92149448962322));
#58074=CARTESIAN_POINT('Ctrl Pts',(-52.3064323164313,-13.0375346028627,
5.97383149654107));
#58075=CARTESIAN_POINT('Ctrl Pts',(-52.7966221146314,-12.9064860705774,
6.));
#58076=CARTESIAN_POINT('',(-53.5946738441133,-12.904124289093,6.));
#58077=CARTESIAN_POINT('Origin',(-53.1951359564886,-14.3971354987959,6.));
#58078=CARTESIAN_POINT('Ctrl Pts',(-54.7400835567429,-14.3978973414314,
5.60421172358873));
#58079=CARTESIAN_POINT('Ctrl Pts',(-54.740358954578,-14.4432509581161,5.60655897483644));
#58080=CARTESIAN_POINT('Ctrl Pts',(-54.7181503847516,-14.9939574593074,
5.63507472954307));
#58081=CARTESIAN_POINT('Ctrl Pts',(-54.0595320288467,-15.9953308004788,
5.68975898770864));
#58082=CARTESIAN_POINT('Ctrl Pts',(-52.3387777758965,-15.9998439842325,
5.76826449808541));
#58083=CARTESIAN_POINT('Ctrl Pts',(-51.386068598834,-14.5665551393412,5.8467700084622));
#58084=CARTESIAN_POINT('Ctrl Pts',(-52.0449383322286,-13.007675117235,5.92401517576705));
#58085=CARTESIAN_POINT('Ctrl Pts',(-53.1295481846289,-12.781420423434,5.97509183961299));
#58086=CARTESIAN_POINT('Ctrl Pts',(-53.5946794545979,-12.9041113494969,
6.));
#58087=CARTESIAN_POINT('Origin',(-53.1951359564886,-14.3971354987959,0.895788276411275));
#58088=CARTESIAN_POINT('',(-54.7358250212096,-14.397461852737,5.10421172358873));
#58089=CARTESIAN_POINT('',(-54.7397605362559,-14.3961865506515,5.14578827641127));
#58090=CARTESIAN_POINT('',(-54.7381359564886,-14.3971354987959,0.895788276411275));
#58091=CARTESIAN_POINT('Ctrl Pts',(-54.7397605362559,-14.3961865506515,
5.14578827641127));
#58092=CARTESIAN_POINT('Ctrl Pts',(-54.7365136934968,-14.8418517823194,
5.16884048301825));
#58093=CARTESIAN_POINT('Ctrl Pts',(-54.3012988565586,-15.7989681003252,
5.21806119308415));
#58094=CARTESIAN_POINT('Ctrl Pts',(-52.6846517467245,-16.1409756074536,
5.29345040660899));
#58095=CARTESIAN_POINT('Ctrl Pts',(-51.4589751002972,-14.933224869348,5.37195591698576));
#58096=CARTESIAN_POINT('Ctrl Pts',(-51.7903649128864,-13.2446527814935,
5.45046142736255));
#58097=CARTESIAN_POINT('Ctrl Pts',(-53.3815143142557,-12.5897421777335,
5.52896693773931));
#58098=CARTESIAN_POINT('Ctrl Pts',(-54.5626373610633,-13.3907557638884,
5.59407588742224));
#58099=CARTESIAN_POINT('Ctrl Pts',(-54.7358881117761,-14.1484975960505,
5.63301633364622));
#58100=CARTESIAN_POINT('Ctrl Pts',(-54.7357308572386,-14.3970788042278,
5.64578827641128));
#58101=CARTESIAN_POINT('Ctrl Pts',(-54.7358250212096,-14.397461852737,5.10421172358873));
#58102=CARTESIAN_POINT('Ctrl Pts',(-54.7362763496954,-14.6310315157388,
5.11621462074955));
#58103=CARTESIAN_POINT('Ctrl Pts',(-54.5775040932279,-15.3732433417349,
5.15438602136928));
#58104=CARTESIAN_POINT('Ctrl Pts',(-53.4338710221273,-16.1984132586634,
5.21872592544796));
#58105=CARTESIAN_POINT('Ctrl Pts',(-51.8243426112988,-15.5898341745865,
5.29723143582474));
#58106=CARTESIAN_POINT('Ctrl Pts',(-51.4441749154368,-13.9116075960113,
5.37573694620152));
#58107=CARTESIAN_POINT('Ctrl Pts',(-52.6343093950298,-12.6688279644592,
5.45424245657829));
#58108=CARTESIAN_POINT('Ctrl Pts',(-54.2767867908486,-12.9668231409662,
5.53040071570738));
#58109=CARTESIAN_POINT('Ctrl Pts',(-54.7372886615245,-13.9376228212707,
5.58039047137751));
#58110=CARTESIAN_POINT('Ctrl Pts',(-54.7400835567429,-14.3978973414314,
5.60421172358873));
#58111=CARTESIAN_POINT('Origin',(-53.1951359564886,-14.3971354987959,0.895788276411275));
#58112=CARTESIAN_POINT('',(-54.7390536535266,-14.3959278946888,4.60421172358873));
#58113=CARTESIAN_POINT('',(-54.7379141108259,-14.3984645193683,4.64578827641127));
#58114=CARTESIAN_POINT('',(-54.7381359564886,-14.3971354987959,0.895788276411275));
#58115=CARTESIAN_POINT('Ctrl Pts',(-54.7379141108259,-14.3984645193683,
4.64578827641127));
#58116=CARTESIAN_POINT('Ctrl Pts',(-54.7390192921529,-14.5252809022368,
4.65232762547243));
#58117=CARTESIAN_POINT('Ctrl Pts',(-54.6671855077626,-15.158343636416,4.68503547799252));
#58118=CARTESIAN_POINT('Ctrl Pts',(-53.7972179286764,-16.1115146859015,
4.74391183397153));
#58119=CARTESIAN_POINT('Ctrl Pts',(-52.0972451605187,-15.8449731797319,
4.8224173443483));
#58120=CARTESIAN_POINT('Ctrl Pts',(-51.3818866828157,-14.2799767547255,
4.90092285472509));
#58121=CARTESIAN_POINT('Ctrl Pts',(-52.2926938154427,-12.820050407037,4.97942836510186));
#58122=CARTESIAN_POINT('Ctrl Pts',(-54.0128314027411,-12.7744928061304,
5.05793387547865));
#58123=CARTESIAN_POINT('Ctrl Pts',(-54.7098771965036,-13.7702259631725,
5.11338717924845));
#58124=CARTESIAN_POINT('Ctrl Pts',(-54.7401994584832,-14.3359395997999,
5.14267197955932));
#58125=CARTESIAN_POINT('Ctrl Pts',(-54.7397605362559,-14.3961865506515,
5.14578827641127));
#58126=CARTESIAN_POINT('Ctrl Pts',(-54.7390536535266,-14.3959278946888,
4.60421172358873));
#58127=CARTESIAN_POINT('Ctrl Pts',(-54.7354489362591,-14.815149952008,4.62587026666265));
#58128=CARTESIAN_POINT('Ctrl Pts',(-54.3438802932755,-15.7468235466057,
4.6736973131955));
#58129=CARTESIAN_POINT('Ctrl Pts',(-52.7769304442279,-16.1653842141838,
4.74769286318728));
#58130=CARTESIAN_POINT('Ctrl Pts',(-51.4895330907316,-15.0236483351254,
4.82619837356406));
#58131=CARTESIAN_POINT('Ctrl Pts',(-51.7317609456535,-13.3200407432483,
4.90470388394085));
#58132=CARTESIAN_POINT('Ctrl Pts',(-53.2863782799341,-12.5823975487372,
4.98320939431761));
#58133=CARTESIAN_POINT('Ctrl Pts',(-54.5339890873504,-13.3362017488983,
5.04971200753359));
#58134=CARTESIAN_POINT('Ctrl Pts',(-54.7352923713373,-14.1218070799821,
5.09004611729062));
#58135=CARTESIAN_POINT('Ctrl Pts',(-54.7358250212096,-14.397461852737,5.10421172358873));
#58136=CARTESIAN_POINT('Origin',(-53.1951359564886,-14.3971354987959,0.895788276411275));
#58137=CARTESIAN_POINT('',(-54.7387010277811,-14.3984147555176,4.10421172358873));
#58138=CARTESIAN_POINT('',(-54.7363034079594,-14.3962637958223,4.14578827641127));
#58139=CARTESIAN_POINT('',(-54.7381359564886,-14.3971354987959,0.895788276411275));
#58140=CARTESIAN_POINT('Ctrl Pts',(-54.7363034079594,-14.3962637958223,
4.14578827641127));
#58141=CARTESIAN_POINT('Ctrl Pts',(-54.7346448209045,-14.7111635771051,
4.16198327138554));
#58142=CARTESIAN_POINT('Ctrl Pts',(-54.488702537285,-15.5372702616991,4.20434676981873));
#58143=CARTESIAN_POINT('Ctrl Pts',(-53.147408175106,-16.2135387160798,4.27287877171085));
#58144=CARTESIAN_POINT('Ctrl Pts',(-51.6537177503358,-15.3592313846778,
4.35138428208763));
#58145=CARTESIAN_POINT('Ctrl Pts',(-51.5424078137269,-13.6420935954197,
4.42988979246441));
#58146=CARTESIAN_POINT('Ctrl Pts',(-52.9133037754093,-12.6020953249298,
4.50839530284119));
#58147=CARTESIAN_POINT('Ctrl Pts',(-54.4017068046157,-13.124465562129,4.58036146415681));
#58148=CARTESIAN_POINT('Ctrl Pts',(-54.7345966896724,-14.0177999706171,
4.62615912201351));
#58149=CARTESIAN_POINT('Ctrl Pts',(-54.7379141108259,-14.3984645193683,
4.64578827641127));
#58150=CARTESIAN_POINT('Ctrl Pts',(-54.7387010277811,-14.3984147555176,
4.10421172358873));
#58151=CARTESIAN_POINT('Ctrl Pts',(-54.7395828579414,-14.49807341117,4.10935740911683));
#58152=CARTESIAN_POINT('Ctrl Pts',(-54.6857500758113,-15.1036004690399,
4.14067159810387));
#58153=CARTESIAN_POINT('Ctrl Pts',(-53.8864190756817,-16.0775304145121,
4.19815429054983));
#58154=CARTESIAN_POINT('Ctrl Pts',(-52.1747941628695,-15.9006321056092,
4.2766598009266));
#58155=CARTESIAN_POINT('Ctrl Pts',(-51.3782360277521,-14.3753622969642,
4.35516531130339));
#58156=CARTESIAN_POINT('Ctrl Pts',(-52.2111169431944,-12.8696192117061,
4.43367082168016));
#58157=CARTESIAN_POINT('Ctrl Pts',(-53.9264895031678,-12.7337890506155,
4.51217633205695));
#58158=CARTESIAN_POINT('Ctrl Pts',(-54.6936722382488,-13.7156146023329,
4.5690232993598));
#58159=CARTESIAN_POINT('Ctrl Pts',(-54.7398042641295,-14.3086332477416,
4.59970176320373));
#58160=CARTESIAN_POINT('Ctrl Pts',(-54.7390536535266,-14.3959278946888,
4.60421172358873));
#58161=CARTESIAN_POINT('Origin',(-53.1951359564886,-14.3971354987959,0.895788276411275));
#58162=CARTESIAN_POINT('',(-54.7359273488899,-14.3966252672389,3.60421172358873));
#58163=CARTESIAN_POINT('',(-54.740563122869,-14.3970262782475,3.64578827641127));
#58164=CARTESIAN_POINT('',(-54.7381359564886,-14.3971354987959,0.895788276411275));
#58165=CARTESIAN_POINT('Ctrl Pts',(-54.740563122869,-14.3970262782475,3.64578827641127));
#58166=CARTESIAN_POINT('Ctrl Pts',(-54.7400434078029,-14.8961037383943,
3.67163891729865));
#58167=CARTESIAN_POINT('Ctrl Pts',(-54.208547388428,-15.9013481621327,3.72365806164495));
#58168=CARTESIAN_POINT('Ctrl Pts',(-52.5038529249194,-16.0775302015137,
3.80184570945018));
#58169=CARTESIAN_POINT('Ctrl Pts',(-51.4121872860838,-14.7474105690538,
3.88035121982695));
#58170=CARTESIAN_POINT('Ctrl Pts',(-51.9195124019995,-13.1031559265556,
3.95885673020374));
#58171=CARTESIAN_POINT('Ctrl Pts',(-53.5708470479161,-12.6193729267869,
4.03736224058051));
#58172=CARTESIAN_POINT('Ctrl Pts',(-54.6140883917719,-13.5008315971724,
4.09967275598302));
#58173=CARTESIAN_POINT('Ctrl Pts',(-54.7373248304478,-14.202336249353,4.13581476792661));
#58174=CARTESIAN_POINT('Ctrl Pts',(-54.7363034079594,-14.3962637958223,
4.14578827641127));
#58175=CARTESIAN_POINT('Ctrl Pts',(-54.7359273488899,-14.3966252672389,
3.60421172358873));
#58176=CARTESIAN_POINT('Ctrl Pts',(-54.7350534494295,-14.6846029003008,
3.61901305502994));
#58177=CARTESIAN_POINT('Ctrl Pts',(-54.5202760602344,-15.482930589367,3.65998288993008));
#58178=CARTESIAN_POINT('Ctrl Pts',(-53.2428637439183,-16.2135389463141,
3.72712122828915));
#58179=CARTESIAN_POINT('Ctrl Pts',(-51.7063697132749,-15.4388525891942,
3.80562673866593));
#58180=CARTESIAN_POINT('Ctrl Pts',(-51.5050366439836,-13.7299295812751,
3.88413224904271));
#58181=CARTESIAN_POINT('Ctrl Pts',(-52.8194248174382,-12.6193727014466,
3.96263775941949));
#58182=CARTESIAN_POINT('Ctrl Pts',(-54.3625220492744,-13.0714459438974,
4.03599758426816));
#58183=CARTESIAN_POINT('Ctrl Pts',(-54.7350982901468,-13.9912569994582,
4.0831889056579));
#58184=CARTESIAN_POINT('Ctrl Pts',(-54.7387010277811,-14.3984147555176,
4.10421172358873));
#58185=CARTESIAN_POINT('Origin',(-53.1951359564886,-14.3971354987959,0.895788276411275));
#58186=CARTESIAN_POINT('',(-54.740301190334,-14.3965688164983,3.10421172358873));
#58187=CARTESIAN_POINT('',(-54.7365381831935,-14.3981451127971,3.14578827641127));
#58188=CARTESIAN_POINT('',(-54.7381359564886,-14.3971354987959,0.895788276411275));
#58189=CARTESIAN_POINT('Ctrl Pts',(-54.7365381831935,-14.3981451127971,
3.14578827641127));
#58190=CARTESIAN_POINT('Ctrl Pts',(-54.7376569241507,-14.5796417971643,
3.15512605975283));
#58191=CARTESIAN_POINT('Ctrl Pts',(-54.6247347728585,-15.2684238709215,
3.19063234655331));
#58192=CARTESIAN_POINT('Ctrl Pts',(-53.6133414157459,-16.165383989977,3.25230713681272));
#58193=CARTESIAN_POINT('Ctrl Pts',(-51.9508876322962,-15.7213124929433,
3.3308126471895));
#58194=CARTESIAN_POINT('Ctrl Pts',(-51.4043053238161,-14.0896875604189,
3.40931815756628));
#58195=CARTESIAN_POINT('Ctrl Pts',(-52.4637825025118,-12.7337892614639,
3.48782366794306));
#58196=CARTESIAN_POINT('Ctrl Pts',(-54.1791548450535,-12.8696194053218,
3.56632917831984));
#58197=CARTESIAN_POINT('Ctrl Pts',(-54.7377809864981,-13.8795446348882,
3.61898404780924));
#58198=CARTESIAN_POINT('Ctrl Pts',(-54.7405695133476,-14.3908895621182,
3.64547041383972));
#58199=CARTESIAN_POINT('Ctrl Pts',(-54.740563122869,-14.3970262782475,3.64578827641127));
#58200=CARTESIAN_POINT('Ctrl Pts',(-54.740301190334,-14.3965688164983,3.10421172358873));
#58201=CARTESIAN_POINT('Ctrl Pts',(-54.7380390595611,-14.8689546274246,
3.12866870094305));
#58202=CARTESIAN_POINT('Ctrl Pts',(-54.2559651859222,-15.850784329065,3.17929418175629));
#58203=CARTESIAN_POINT('Ctrl Pts',(-52.5930539078611,-16.1115149029785,
3.25608816602847));
#58204=CARTESIAN_POINT('Ctrl Pts',(-51.4330422815012,-14.8405600699842,
3.33459367640525));
#58205=CARTESIAN_POINT('Ctrl Pts',(-51.8533182226522,-13.1719316222439,
3.41309918678203));
#58206=CARTESIAN_POINT('Ctrl Pts',(-53.4769681733105,-12.6020950974316,
3.49160469715881));
#58207=CARTESIAN_POINT('Ctrl Pts',(-54.5893972536881,-13.4460134923652,
3.55530887609438));
#58208=CARTESIAN_POINT('Ctrl Pts',(-54.7365984888838,-14.175463319392,3.59284455157102));
#58209=CARTESIAN_POINT('Ctrl Pts',(-54.7359273488899,-14.3966252672389,
3.60421172358873));
#58210=CARTESIAN_POINT('Origin',(-53.1951359564886,-14.3971354987959,0.895788276411275));
#58211=CARTESIAN_POINT('',(-54.73716587472,-14.3983674417199,2.60421172358873));
#58212=CARTESIAN_POINT('',(-54.7375657625992,-14.3958310564158,2.64578827641127));
#58213=CARTESIAN_POINT('',(-54.7381359564886,-14.3971354987959,0.895788276411275));
#58214=CARTESIAN_POINT('Ctrl Pts',(-54.7375657625992,-14.3958310564158,
2.64578827641127));
#58215=CARTESIAN_POINT('Ctrl Pts',(-54.734479142859,-14.7643796819994,2.66478170566594));
#58216=CARTESIAN_POINT('Ctrl Pts',(-54.4188250031304,-15.6454555959149,
2.70994363837953));
#58217=CARTESIAN_POINT('Ctrl Pts',(-52.9564009216581,-16.198413027115,2.78127407455204));
#58218=CARTESIAN_POINT('Ctrl Pts',(-51.5609762954032,-15.1915669978344,
2.85977958492882));
#58219=CARTESIAN_POINT('Ctrl Pts',(-51.6311047416152,-13.472254177388,2.9382850953056));
#58220=CARTESIAN_POINT('Ctrl Pts',(-53.1038936445493,-12.5823977792547,
3.01679060568238));
#58221=CARTESIAN_POINT('Ctrl Pts',(-54.4735979274945,-13.2323024338895,
3.0859583327176));
#58222=CARTESIAN_POINT('Ctrl Pts',(-54.7345217286191,-14.0710096690757,
3.1289575562939));
#58223=CARTESIAN_POINT('Ctrl Pts',(-54.7365381831935,-14.3981451127971,
3.14578827641127));
#58224=CARTESIAN_POINT('Ctrl Pts',(-54.73716587472,-14.3983674417199,2.60421172358873));
#58225=CARTESIAN_POINT('Ctrl Pts',(-54.7383644283813,-14.5526183883782,
2.61215584339723));
#58226=CARTESIAN_POINT('Ctrl Pts',(-54.6467666252149,-15.2135939671077,
2.64626846666466));
#58227=CARTESIAN_POINT('Ctrl Pts',(-53.7056202382209,-16.1409758479641,
2.70654959339102));
#58228=CARTESIAN_POINT('Ctrl Pts',(-52.0221470001079,-15.7848310056966,
2.78505510376779));
#58229=CARTESIAN_POINT('Ctrl Pts',(-51.3906291820653,-14.1841570315506,
2.86356061414457));
#58230=CARTESIAN_POINT('Ctrl Pts',(-52.377440405223,-12.7744925974775,2.94206612452135));
#58231=CARTESIAN_POINT('Ctrl Pts',(-54.0975782126822,-12.8200502087089,
3.02057163489813));
#58232=CARTESIAN_POINT('Ctrl Pts',(-54.7246398714755,-13.8251629314517,
3.07462016792059));
#58233=CARTESIAN_POINT('Ctrl Pts',(-54.7404594967271,-14.3635107392415,
3.10250019748412));
#58234=CARTESIAN_POINT('Ctrl Pts',(-54.740301190334,-14.3965688164983,3.10421172358873));
#58235=CARTESIAN_POINT('Origin',(-53.1951359564886,-14.3971354987959,0.895788276411275));
#58236=CARTESIAN_POINT('',(-54.7364807484814,-14.3955730757723,2.10421172358873));
#58237=CARTESIAN_POINT('',(-54.7400287307462,-14.397884086359,2.14578827641127));
#58238=CARTESIAN_POINT('',(-54.7381359564886,-14.3971354987959,0.895788276411275));
#58239=CARTESIAN_POINT('',(-53.5936497983459,-12.9064860705774,2.));
#58240=CARTESIAN_POINT('Ctrl Pts',(-53.5936497983459,-12.9064860705774,
2.));
#58241=CARTESIAN_POINT('Ctrl Pts',(-54.083839596546,-13.0375346028627,2.02616850345893));
#58242=CARTESIAN_POINT('Ctrl Pts',(-54.6367230898564,-13.5559776050111,
2.06090574465517));
#58243=CARTESIAN_POINT('Ctrl Pts',(-54.737618997593,-14.2290968579424,2.09564298585141));
#58244=CARTESIAN_POINT('Ctrl Pts',(-54.7364807484814,-14.3955730757723,
2.10421172358873));
#58245=CARTESIAN_POINT('',(-52.7955982877703,-12.9041242545674,2.));
#58246=CARTESIAN_POINT('Origin',(-53.1951359564886,-14.3971354987959,2.));
#58247=CARTESIAN_POINT('Ctrl Pts',(-52.7955926848293,-12.9041113294173,
2.));
#58248=CARTESIAN_POINT('Ctrl Pts',(-53.2607241041144,-12.7814202621555,
2.02490816038701));
#58249=CARTESIAN_POINT('Ctrl Pts',(-54.2926583006945,-12.9966875828164,
2.0735042525241));
#58250=CARTESIAN_POINT('Ctrl Pts',(-54.7371492824905,-13.9402272601641,
2.12210034466119));
#58251=CARTESIAN_POINT('Ctrl Pts',(-54.7400287307462,-14.397884086359,2.14578827641127));
#58252=CARTESIAN_POINT('Origin',(-14.1292828945604,-53.2669068454841,4.5));
#58253=CARTESIAN_POINT('',(-14.7605875520818,-54.3602657339262,5.80658032638058));
#58254=CARTESIAN_POINT('',(-14.7625813317604,-54.3604987677495,5.94341967361942));
#58255=CARTESIAN_POINT('',(-14.7615328945604,-54.3619959685696,4.5));
#58256=CARTESIAN_POINT('',(-13.8936870225526,-54.5092654229862,6.));
#58257=CARTESIAN_POINT('Ctrl Pts',(-14.7625813317604,-54.3604987677495,
5.94341967361942));
#58258=CARTESIAN_POINT('Ctrl Pts',(-14.5022241622972,-54.5077988388626,
5.96227978241295));
#58259=CARTESIAN_POINT('Ctrl Pts',(-14.1881298777611,-54.5651023789871,
5.98113989120648));
#58260=CARTESIAN_POINT('Ctrl Pts',(-13.8936870225526,-54.5092654229862,
6.00000000000001));
#58261=CARTESIAN_POINT('',(-14.7615328945604,-54.3619959685696,6.));
#58262=CARTESIAN_POINT('Origin',(-14.1292828945604,-53.2669068454841,6.));
#58263=CARTESIAN_POINT('',(-14.7615328945604,-54.3619959685696,7.));
#58264=CARTESIAN_POINT('',(-14.7615328945604,-54.3619959685696,4.5));
#58265=CARTESIAN_POINT('',(-12.8669333849943,-53.3406222827979,7.));
#58266=CARTESIAN_POINT('Origin',(-14.1292828945604,-53.2669068454841,7.));
#58267=CARTESIAN_POINT('',(-15.3916324041264,-53.1931914081703,7.));
#58268=CARTESIAN_POINT('Origin',(-14.1292828945604,-53.2669068454841,7.));
#58269=CARTESIAN_POINT('Origin',(-14.1292828945604,-53.2669068454841,7.));
#58270=CARTESIAN_POINT('',(-12.9337035820667,-52.8487780612892,6.));
#58271=CARTESIAN_POINT('Origin',(-14.1292828945604,-53.2669068454841,6.));
#58272=CARTESIAN_POINT('Ctrl Pts',(-12.9336933707122,-52.8487726938777,
6.));
#58273=CARTESIAN_POINT('Ctrl Pts',(-12.8048848553781,-53.2213517629531,
5.97509183961299));
#58274=CARTESIAN_POINT('Ctrl Pts',(-12.8625933288288,-53.6603618768577,
5.95018367922598));
#58275=CARTESIAN_POINT('Ctrl Pts',(-13.0861255368911,-53.9849952189361,
5.92527551883897));
#58276=CARTESIAN_POINT('Ctrl Pts',(-13.3209683863418,-54.3260548798291,
5.89910701538004));
#58277=CARTESIAN_POINT('Ctrl Pts',(-13.7388407631054,-54.540870088853,5.87293851192112));
#58278=CARTESIAN_POINT('Ctrl Pts',(-14.1527369297938,-54.5331774952646,
5.84677000846219));
#58279=CARTESIAN_POINT('Ctrl Pts',(-14.3646246721213,-54.5292393909301,
5.83337344776832));
#58280=CARTESIAN_POINT('Ctrl Pts',(-14.5754703413608,-54.4669871159197,
5.81997688707445));
#58281=CARTESIAN_POINT('Ctrl Pts',(-14.7605875520818,-54.3602657339262,
5.80658032638058));
#58282=CARTESIAN_POINT('Origin',(-14.1292828945604,-53.2669068454841,4.5));
#58283=CARTESIAN_POINT('',(-14.7628720032994,-54.3627600319775,5.30658032638058));
#58284=CARTESIAN_POINT('',(-14.761790188637,-54.3636903053853,5.44341967361943));
#58285=CARTESIAN_POINT('',(-14.7615328945604,-54.3619959685696,4.5));
#58286=CARTESIAN_POINT('Ctrl Pts',(-14.761790188637,-54.3636903053853,5.44341967361943));
#58287=CARTESIAN_POINT('Ctrl Pts',(-14.7297149272464,-54.3824695710557,
5.44576692486714));
#58288=CARTESIAN_POINT('Ctrl Pts',(-14.6967938380796,-54.3997466843014,
5.44811417611484));
#58289=CARTESIAN_POINT('Ctrl Pts',(-14.6631180766711,-54.4153998475156,
5.45046142736255));
#58290=CARTESIAN_POINT('Ctrl Pts',(-14.2876813696889,-54.5899102907896,
5.47662993082148));
#58291=CARTESIAN_POINT('Ctrl Pts',(-13.8184459253802,-54.5625788561695,
5.5027984342804));
#58292=CARTESIAN_POINT('Ctrl Pts',(-13.4657801062202,-54.3456807478706,
5.52896693773933));
#58293=CARTESIAN_POINT('Ctrl Pts',(-13.1131142870602,-54.1287826395717,
5.55513544119826));
#58294=CARTESIAN_POINT('Ctrl Pts',(-12.8770180930488,-53.7223178575942,
5.58130394465719));
#58295=CARTESIAN_POINT('Ctrl Pts',(-12.8634449158406,-53.308510984467,5.60747244811611));
#58296=CARTESIAN_POINT('Ctrl Pts',(-12.8498717386324,-52.8947041113399,
5.63364095157504));
#58297=CARTESIAN_POINT('Ctrl Pts',(-13.0588215782272,-52.4735551470632,
5.65980945503396));
#58298=CARTESIAN_POINT('Ctrl Pts',(-13.3964281425195,-52.2339907213231,
5.68597795849289));
#58299=CARTESIAN_POINT('Ctrl Pts',(-13.7340347068117,-51.994426295583,5.71214646195181));
#58300=CARTESIAN_POINT('Ctrl Pts',(-14.2002979958014,-51.9364464083796,
5.73831496541074));
#58301=CARTESIAN_POINT('Ctrl Pts',(-14.5864832378068,-52.0858916506601,
5.76448346886967));
#58302=CARTESIAN_POINT('Ctrl Pts',(-14.9726684798122,-52.2353368929406,
5.7906519723286));
#58303=CARTESIAN_POINT('Ctrl Pts',(-15.2787756748334,-52.5922072647049,
5.81682047578752));
#58304=CARTESIAN_POINT('Ctrl Pts',(-15.3668446182304,-52.9968058417406,
5.84298897924645));
#58305=CARTESIAN_POINT('Ctrl Pts',(-15.4549135616273,-53.4014044187763,
5.86915748270538));
#58306=CARTESIAN_POINT('Ctrl Pts',(-15.3249442534001,-53.8537312010833,
5.8953259861643));
#58307=CARTESIAN_POINT('Ctrl Pts',(-15.0367728841186,-54.1500649721194,
5.92149448962323));
#58308=CARTESIAN_POINT('Ctrl Pts',(-14.9562917782242,-54.2328256907374,
5.92880288428863));
#58309=CARTESIAN_POINT('Ctrl Pts',(-14.8634711500129,-54.3034191895921,
5.93611127895402));
#58310=CARTESIAN_POINT('Ctrl Pts',(-14.7625813317604,-54.3604987677495,
5.94341967361942));
#58311=CARTESIAN_POINT('Ctrl Pts',(-14.7605875520818,-54.3602657339262,
5.80658032638058));
#58312=CARTESIAN_POINT('Ctrl Pts',(-14.9370736274398,-54.2585202625491,
5.79380838361552));
#58313=CARTESIAN_POINT('Ctrl Pts',(-15.0901745042163,-54.1163557782414,
5.78103644085047));
#58314=CARTESIAN_POINT('Ctrl Pts',(-15.1984983273049,-53.9457696468095,
5.76826449808541));
#58315=CARTESIAN_POINT('Ctrl Pts',(-15.4204436015143,-53.5962547881436,
5.74209599462648));
#58316=CARTESIAN_POINT('Ctrl Pts',(-15.4544141933199,-53.1274254670123,
5.71592749116756));
#58317=CARTESIAN_POINT('Ctrl Pts',(-15.2852697206798,-52.7495259168145,
5.68975898770863));
#58318=CARTESIAN_POINT('Ctrl Pts',(-15.1161252480397,-52.3716263666168,
5.6635904842497));
#58319=CARTESIAN_POINT('Ctrl Pts',(-14.7438657109538,-52.0846565873524,
5.63742198079078));
#58320=CARTESIAN_POINT('Ctrl Pts',(-14.3353706309513,-52.0172894645935,
5.61125347733185));
#58321=CARTESIAN_POINT('Ctrl Pts',(-13.9268755509488,-51.9499223418345,
5.58508497387292));
#58322=CARTESIAN_POINT('Ctrl Pts',(-13.4821449280297,-52.1021578755809,
5.558916470414));
#58323=CARTESIAN_POINT('Ctrl Pts',(-13.2006242325167,-52.4057357189425,
5.53274796695507));
#58324=CARTESIAN_POINT('Ctrl Pts',(-12.9191035370036,-52.7093135623041,
5.50657946349614));
#58325=CARTESIAN_POINT('Ctrl Pts',(-12.8007927688965,-53.1642337152808,
5.48041096003722));
#58326=CARTESIAN_POINT('Ctrl Pts',(-12.8987324301598,-53.5665026413488,
5.45424245657829));
#58327=CARTESIAN_POINT('Ctrl Pts',(-12.9966720914232,-53.9687715674168,
5.42807395311936));
#58328=CARTESIAN_POINT('Ctrl Pts',(-13.3108621820569,-54.3183892665762,
5.40190544966044));
#58329=CARTESIAN_POINT('Ctrl Pts',(-13.7004218404059,-54.4585839700533,
5.37573694620151));
#58330=CARTESIAN_POINT('Ctrl Pts',(-14.0435904799156,-54.5820834768108,
5.35268473959454));
#58331=CARTESIAN_POINT('Ctrl Pts',(-14.4452466462963,-54.5430686762864,
5.32963253298756));
#58332=CARTESIAN_POINT('Ctrl Pts',(-14.7628720032994,-54.3627600319775,
5.30658032638058));
#58333=CARTESIAN_POINT('Origin',(-14.1292828945604,-53.2669068454841,4.5));
#58334=CARTESIAN_POINT('',(-14.7604987163791,-54.3623830037273,4.80658032638058));
#58335=CARTESIAN_POINT('',(-14.7603543171395,-54.3604895118786,4.94341967361942));
#58336=CARTESIAN_POINT('',(-14.7615328945604,-54.3619959685696,4.5));
#58337=CARTESIAN_POINT('Ctrl Pts',(-14.7603543171395,-54.3604895118786,
4.94341967361942));
#58338=CARTESIAN_POINT('Ctrl Pts',(-14.5947715388364,-54.4565158591777,
4.95542257078024));
#58339=CARTESIAN_POINT('Ctrl Pts',(-14.4086766047112,-54.5167140163305,
4.96742546794106));
#58340=CARTESIAN_POINT('Ctrl Pts',(-14.2192552064615,-54.5302046425139,
4.97942836510188));
#58341=CARTESIAN_POINT('Ctrl Pts',(-13.8062820343284,-54.5596166663956,
5.00559686856081));
#58342=CARTESIAN_POINT('Ctrl Pts',(-13.3774975305931,-54.3670187022342,
5.03176537201973));
#58343=CARTESIAN_POINT('Ctrl Pts',(-13.1251731138615,-54.0387742648884,
5.05793387547866));
#58344=CARTESIAN_POINT('Ctrl Pts',(-12.8728486971299,-53.7105298275425,
5.08410237893758));
#58345=CARTESIAN_POINT('Ctrl Pts',(-12.796984367402,-53.2466389170122,5.11027088239651));
#58346=CARTESIAN_POINT('Ctrl Pts',(-12.9315998955733,-52.8551151331565,
5.13643938585543));
#58347=CARTESIAN_POINT('Ctrl Pts',(-13.0662154237446,-52.4635913493009,
5.16260788931436));
#58348=CARTESIAN_POINT('Ctrl Pts',(-13.411310809815,-52.14443469212,5.18877639277329));
#58349=CARTESIAN_POINT('Ctrl Pts',(-13.81213856493,-52.0407600014986,5.21494489623221));
#58350=CARTESIAN_POINT('Ctrl Pts',(-14.212966320045,-51.9370853108772,5.24111339969114));
#58351=CARTESIAN_POINT('Ctrl Pts',(-14.6695264442046,-52.0488925868152,
5.26728190315007));
#58352=CARTESIAN_POINT('Ctrl Pts',(-14.9770971987178,-52.3260437079763,
5.29345040660899));
#58353=CARTESIAN_POINT('Ctrl Pts',(-15.2846679532311,-52.6031948291373,
5.31961891006792));
#58354=CARTESIAN_POINT('Ctrl Pts',(-15.4432493380979,-53.0456897955214,
5.34578741352684));
#58355=CARTESIAN_POINT('Ctrl Pts',(-15.3817210457035,-53.4551134392974,
5.37195591698577));
#58356=CARTESIAN_POINT('Ctrl Pts',(-15.3257116918039,-53.827812775923,5.39577716919699));
#58357=CARTESIAN_POINT('Ctrl Pts',(-15.087308341869,-54.1731075442456,5.41959842140821));
#58358=CARTESIAN_POINT('Ctrl Pts',(-14.761790188637,-54.3636903053853,5.44341967361943));
#58359=CARTESIAN_POINT('Ctrl Pts',(-14.7628720032994,-54.3627600319775,
5.30658032638058));
#58360=CARTESIAN_POINT('Ctrl Pts',(-14.8058099708877,-54.3383851306842,
5.30346402952863));
#58361=CARTESIAN_POINT('Ctrl Pts',(-14.8472122922316,-54.3114281126392,
5.30034773267668));
#58362=CARTESIAN_POINT('Ctrl Pts',(-14.8867268805692,-54.281941402285,5.29723143582473));
#58363=CARTESIAN_POINT('Ctrl Pts',(-15.2185430363193,-54.0343324232445,
5.27106293236581));
#58364=CARTESIAN_POINT('Ctrl Pts',(-15.4172461217553,-53.6083427573686,
5.24489442890688));
#58365=CARTESIAN_POINT('Ctrl Pts',(-15.393736730538,-53.1949914739396,5.21872592544795));
#58366=CARTESIAN_POINT('Ctrl Pts',(-15.3702273393206,-52.7816401905105,
5.19255742198903));
#58367=CARTESIAN_POINT('Ctrl Pts',(-15.12450547145,-52.3809272895283,5.1663889185301));
#58368=CARTESIAN_POINT('Ctrl Pts',(-14.7667550258398,-52.1725370796236,
5.14022041507117));
#58369=CARTESIAN_POINT('Ctrl Pts',(-14.4090045802295,-51.9641468697189,
5.11405191161225));
#58370=CARTESIAN_POINT('Ctrl Pts',(-13.9392255568797,-51.9480793508917,
5.08788340815332));
#58371=CARTESIAN_POINT('Ctrl Pts',(-13.5680728067533,-52.1315394490878,
5.0617149046944));
#58372=CARTESIAN_POINT('Ctrl Pts',(-13.1969200566269,-52.3149995472838,
5.03554640123547));
#58373=CARTESIAN_POINT('Ctrl Pts',(-12.9243935797239,-52.6979872625031,
5.00937789777654));
#58374=CARTESIAN_POINT('Ctrl Pts',(-12.8726973119175,-53.1087663210662,
4.98320939431761));
#58375=CARTESIAN_POINT('Ctrl Pts',(-12.8210010441111,-53.5195453796293,
4.95704089085869));
#58376=CARTESIAN_POINT('Ctrl Pts',(-12.9901349854012,-53.9581157815361,
4.93087238739976));
#58377=CARTESIAN_POINT('Ctrl Pts',(-13.3042575537142,-54.2278173601559,
4.90470388394083));
#58378=CARTESIAN_POINT('Ctrl Pts',(-13.6183801220271,-54.4975189387757,
4.87853538048191));
#58379=CARTESIAN_POINT('Ctrl Pts',(-14.0774913173628,-54.5983516941084,
4.85236687702298));
#58380=CARTESIAN_POINT('Ctrl Pts',(-14.4757201786558,-54.4851010127079,
4.82619837356405));
#58381=CARTESIAN_POINT('Ctrl Pts',(-14.5752351369457,-54.4568003596631,
4.8196590245029));
#58382=CARTESIAN_POINT('Ctrl Pts',(-14.6709481788587,-54.4151308478692,
4.81311967544174));
#58383=CARTESIAN_POINT('Ctrl Pts',(-14.7604987163791,-54.3623830037273,
4.80658032638058));
#58384=CARTESIAN_POINT('Origin',(-14.1292828945604,-53.2669068454841,4.5));
#58385=CARTESIAN_POINT('',(-14.7614006096927,-54.3603381104062,4.30658032638058));
#58386=CARTESIAN_POINT('',(-14.7627659331487,-54.3621523730593,4.44341967361942));
#58387=CARTESIAN_POINT('',(-14.7615328945604,-54.3619959685696,4.5));
#58388=CARTESIAN_POINT('Ctrl Pts',(-14.7627659331487,-54.3621523730593,
4.44341967361942));
#58389=CARTESIAN_POINT('Ctrl Pts',(-14.463761030489,-54.5313718419493,4.46507821669335));
#58390=CARTESIAN_POINT('Ctrl Pts',(-14.0916672421201,-54.5784026588885,
4.48673675976727));
#58391=CARTESIAN_POINT('Ctrl Pts',(-13.7635961371407,-54.4794617725194,
4.5083953028412));
#58392=CARTESIAN_POINT('Ctrl Pts',(-13.3672107562715,-54.3599184164247,
4.53456380630013));
#58393=CARTESIAN_POINT('Ctrl Pts',(-13.0350905669399,-54.0272826554628,
4.56073230975905));
#58394=CARTESIAN_POINT('Ctrl Pts',(-12.9161621999348,-53.6307123234038,
4.58690081321798));
#58395=CARTESIAN_POINT('Ctrl Pts',(-12.7972338329298,-53.2341419913447,
4.61306931667691));
#58396=CARTESIAN_POINT('Ctrl Pts',(-12.8914972882515,-52.7736370881886,
4.63923782013583));
#58397=CARTESIAN_POINT('Ctrl Pts',(-13.1566837320242,-52.4556934772733,
4.66540632359475));
#58398=CARTESIAN_POINT('Ctrl Pts',(-13.421870175797,-52.1377498663579,4.69157482705368));
#58399=CARTESIAN_POINT('Ctrl Pts',(-13.8579796080209,-51.9623675476834,
4.71774333051261));
#58400=CARTESIAN_POINT('Ctrl Pts',(-14.2694553352381,-52.0081900560918,
4.74391183397154));
#58401=CARTESIAN_POINT('Ctrl Pts',(-14.6809310624553,-52.0540125645002,
4.77008033743047));
#58402=CARTESIAN_POINT('Ctrl Pts',(-15.0677730846659,-52.3210398999916,
4.79624884088939));
#58403=CARTESIAN_POINT('Ctrl Pts',(-15.2565169212345,-52.6895337942872,
4.82241734434832));
#58404=CARTESIAN_POINT('Ctrl Pts',(-15.4452607578031,-53.0580276885828,
4.84858584780724));
#58405=CARTESIAN_POINT('Ctrl Pts',(-15.4359064087297,-53.5279881416827,
4.87475435126617));
#58406=CARTESIAN_POINT('Ctrl Pts',(-15.2326483139276,-53.888679374195,4.90092285472509));
#58407=CARTESIAN_POINT('Ctrl Pts',(-15.1226200827607,-54.0839297446631,
4.9150884610232));
#58408=CARTESIAN_POINT('Ctrl Pts',(-14.9557721746586,-54.2471609203011,
4.92925406732131));
#58409=CARTESIAN_POINT('Ctrl Pts',(-14.7603543171395,-54.3604895118786,
4.94341967361942));
#58410=CARTESIAN_POINT('Ctrl Pts',(-14.7604987163791,-54.3623830037273,
4.80658032638058));
#58411=CARTESIAN_POINT('Ctrl Pts',(-15.0293024323073,-54.2040498780404,
4.78695117198281));
#58412=CARTESIAN_POINT('Ctrl Pts',(-15.2425807881071,-53.945898828656,4.76732201758504));
#58413=CARTESIAN_POINT('Ctrl Pts',(-15.3364895893995,-53.6498791715159,
4.74769286318727));
#58414=CARTESIAN_POINT('Ctrl Pts',(-15.4616836115997,-53.2552421298581,
4.72152435972835));
#58415=CARTESIAN_POINT('Ctrl Pts',(-15.3747251287498,-52.7933021646762,
4.69535585626942));
#58416=CARTESIAN_POINT('Ctrl Pts',(-15.1146073473566,-52.471198645522,4.6691873528105));
#58417=CARTESIAN_POINT('Ctrl Pts',(-14.8544895659634,-52.1490951263678,
4.64301884935157));
#58418=CARTESIAN_POINT('Ctrl Pts',(-14.4212124860269,-51.9668280532413,
4.61685034589264));
#58419=CARTESIAN_POINT('Ctrl Pts',(-14.009062705893,-52.0061281492218,4.59068184243372));
#58420=CARTESIAN_POINT('Ctrl Pts',(-13.596912925759,-52.0454282452023,4.56451333897479));
#58421=CARTESIAN_POINT('Ctrl Pts',(-13.2058904454275,-52.3062955102899,
4.53834483551586));
#58422=CARTESIAN_POINT('Ctrl Pts',(-13.0113343903925,-52.6717539614819,
4.51217633205694));
#58423=CARTESIAN_POINT('Ctrl Pts',(-12.8167783353574,-53.037212412674,4.48600782859801));
#58424=CARTESIAN_POINT('Ctrl Pts',(-12.8186887056188,-53.5072620499705,
4.45983932513909));
#58425=CARTESIAN_POINT('Ctrl Pts',(-13.0162088697902,-53.8711270288388,
4.43367082168016));
#58426=CARTESIAN_POINT('Ctrl Pts',(-13.2137290339616,-54.2349920077072,
4.40750231822123));
#58427=CARTESIAN_POINT('Ctrl Pts',(-13.606858992043,-54.4926723281474,4.38133381476231));
#58428=CARTESIAN_POINT('Ctrl Pts',(-14.0193145970927,-54.5286210713629,
4.35516531130338));
#58429=CARTESIAN_POINT('Ctrl Pts',(-14.2745724669733,-54.5508687981624,
4.33897031632911));
#58430=CARTESIAN_POINT('Ctrl Pts',(-14.5372321463568,-54.4881923359769,
4.32277532135484));
#58431=CARTESIAN_POINT('Ctrl Pts',(-14.7614006096927,-54.3603381104062,
4.30658032638058));
#58432=CARTESIAN_POINT('Origin',(-14.1292828945604,-53.2669068454841,4.5));
#58433=CARTESIAN_POINT('',(-14.7626048989925,-54.3636737206204,3.80658032638058));
#58434=CARTESIAN_POINT('',(-14.7608564829457,-54.3629211099724,3.94341967361942));
#58435=CARTESIAN_POINT('',(-14.7615328945604,-54.3619959685696,4.5));
#58436=CARTESIAN_POINT('Ctrl Pts',(-14.7608564829457,-54.3629211099724,
3.94341967361942));
#58437=CARTESIAN_POINT('Ctrl Pts',(-14.6904886508113,-54.4043824600063,
3.94856535914753));
#58438=CARTESIAN_POINT('Ctrl Pts',(-14.6162453479771,-54.4388759703619,
3.95371104467564));
#58439=CARTESIAN_POINT('Ctrl Pts',(-14.5392165090643,-54.465226788063,3.95885673020374));
#58440=CARTESIAN_POINT('Ctrl Pts',(-14.1474845568268,-54.5992344844895,
3.98502523366267));
#58441=CARTESIAN_POINT('Ctrl Pts',(-13.6837115472213,-54.5226514105579,
4.0111937371216));
#58442=CARTESIAN_POINT('Ctrl Pts',(-13.3558588106244,-54.2698183268938,
4.03736224058052));
#58443=CARTESIAN_POINT('Ctrl Pts',(-13.0280060740275,-54.0169852432297,
4.06353074403945));
#58444=CARTESIAN_POINT('Ctrl Pts',(-12.8360736104392,-53.5879021498332,
4.08969924749838));
#58445=CARTESIAN_POINT('Ctrl Pts',(-12.8661262178428,-53.1749750062963,
4.1158677509573));
#58446=CARTESIAN_POINT('Ctrl Pts',(-12.8961788252464,-52.7620478627593,
4.14203625441623));
#58447=CARTESIAN_POINT('Ctrl Pts',(-13.1482165036419,-52.3652766690821,
4.16820475787516));
#58448=CARTESIAN_POINT('Ctrl Pts',(-13.5092225624184,-52.1625783447115,
4.19437326133408));
#58449=CARTESIAN_POINT('Ctrl Pts',(-13.8702286211949,-51.959880020341,4.22054176479301));
#58450=CARTESIAN_POINT('Ctrl Pts',(-14.3402030603525,-51.951254565277,4.24671026825193));
#58451=CARTESIAN_POINT('Ctrl Pts',(-14.708403754256,-52.1405697363842,4.27287877171086));
#58452=CARTESIAN_POINT('Ctrl Pts',(-15.0766044481595,-52.3298849074914,
4.29904727516979));
#58453=CARTESIAN_POINT('Ctrl Pts',(-15.343031396809,-52.7171407047698,4.32521577862871));
#58454=CARTESIAN_POINT('Ctrl Pts',(-15.3882155906945,-53.1286870249125,
4.35138428208764));
#58455=CARTESIAN_POINT('Ctrl Pts',(-15.43339978458,-53.5402333450552,4.37755278554657));
#58456=CARTESIAN_POINT('Ctrl Pts',(-15.2573412237015,-53.9760701880622,
4.40372128900549));
#58457=CARTESIAN_POINT('Ctrl Pts',(-14.938986657059,-54.2407631339519,4.42988979246442));
#58458=CARTESIAN_POINT('Ctrl Pts',(-14.8841204517295,-54.2863811304883,
4.43439975284942));
#58459=CARTESIAN_POINT('Ctrl Pts',(-14.8250277510981,-54.3269157877332,
4.43890971323442));
#58460=CARTESIAN_POINT('Ctrl Pts',(-14.7627659331487,-54.3621523730593,
4.44341967361942));
#58461=CARTESIAN_POINT('Ctrl Pts',(-14.7614006096927,-54.3603381104062,
4.30658032638058));
#58462=CARTESIAN_POINT('Ctrl Pts',(-14.8994522777931,-54.2816005000793,
4.29660681789592));
#58463=CARTESIAN_POINT('Ctrl Pts',(-15.0229058598302,-54.178143727902,4.28663330941126));
#58464=CARTESIAN_POINT('Ctrl Pts',(-15.1210425075748,-54.0545798005254,
4.2766598009266));
#58465=CARTESIAN_POINT('Ctrl Pts',(-15.3785335609892,-53.7303726204816,
4.25049129746767));
#58466=CARTESIAN_POINT('Ctrl Pts',(-15.4617344158,-53.2677410944033,4.22432279400875));
#58467=CARTESIAN_POINT('Ctrl Pts',(-15.3333368195411,-52.8741346977794,
4.19815429054982));
#58468=CARTESIAN_POINT('Ctrl Pts',(-15.2049392232823,-52.4805283011554,
4.17198578709089));
#58469=CARTESIAN_POINT('Ctrl Pts',(-14.8649431759538,-52.1559470339858,
4.14581728363197));
#58470=CARTESIAN_POINT('Ctrl Pts',(-14.4658069467496,-52.0459369947103,
4.11964878017304));
#58471=CARTESIAN_POINT('Ctrl Pts',(-14.0666707175455,-51.9359269554348,
4.09348027671411));
#58472=CARTESIAN_POINT('Ctrl Pts',(-13.6083943064658,-52.0404881440534,
4.06731177325519));
#58473=CARTESIAN_POINT('Ctrl Pts',(-13.2964743036119,-52.3127340807067,
4.04114326979626));
#58474=CARTESIAN_POINT('Ctrl Pts',(-12.9845543007579,-52.5849800173601,
4.01497476633733));
#58475=CARTESIAN_POINT('Ctrl Pts',(-12.8189907061298,-53.0249107020483,
3.98880626287841));
#58476=CARTESIAN_POINT('Ctrl Pts',(-12.8740242036727,-53.4352559863353,
3.96263775941948));
#58477=CARTESIAN_POINT('Ctrl Pts',(-12.9290577012157,-53.8456012706222,
3.93646925596056));
#58478=CARTESIAN_POINT('Ctrl Pts',(-13.2046882909298,-54.2263611545079,
3.91030075250163));
#58479=CARTESIAN_POINT('Ctrl Pts',(-13.5773199398677,-54.4067983801299,
3.8841322490427));
#58480=CARTESIAN_POINT('Ctrl Pts',(-13.9454253210212,-54.5850438777981,
3.85828160815533));
#58481=CARTESIAN_POINT('Ctrl Pts',(-14.4081895758327,-54.5678037039579,
3.83243096726795));
#58482=CARTESIAN_POINT('Ctrl Pts',(-14.7626048989925,-54.3636737206204,
3.80658032638058));
#58483=CARTESIAN_POINT('Origin',(-14.1292828945604,-53.2669068454841,4.5));
#58484=CARTESIAN_POINT('',(-14.7601616123226,-54.3612756103012,3.30658032638058));
#58485=CARTESIAN_POINT('',(-14.7609899830459,-54.3602193411783,3.44341967361942));
#58486=CARTESIAN_POINT('',(-14.7615328945604,-54.3619959685696,4.5));
#58487=CARTESIAN_POINT('Ctrl Pts',(-14.7609899830459,-54.3602193411783,
3.44341967361942));
#58488=CARTESIAN_POINT('Ctrl Pts',(-14.5562500775905,-54.4775990222049,
3.45822100506064));
#58489=CARTESIAN_POINT('Ctrl Pts',(-14.3197636804794,-54.5407089292625,
3.47302233650185));
#58490=CARTESIAN_POINT('Ctrl Pts',(-14.0857261531979,-54.532655265383,3.48782366794307));
#58491=CARTESIAN_POINT('Ctrl Pts',(-13.671951766312,-54.5184165239613,3.51399217140199));
#58492=CARTESIAN_POINT('Ctrl Pts',(-13.2658319689464,-54.2817372437526,
3.54016067486092));
#58493=CARTESIAN_POINT('Ctrl Pts',(-13.0494757061861,-53.9287472260938,
3.56632917831984));
#58494=CARTESIAN_POINT('Ctrl Pts',(-12.8331194434257,-53.575757208435,3.59249768177877));
#58495=CARTESIAN_POINT('Ctrl Pts',(-12.8065267152706,-53.1064564533261,
3.6186661852377));
#58496=CARTESIAN_POINT('Ctrl Pts',(-12.9816220168908,-52.7312849984863,
3.64483468869663));
#58497=CARTESIAN_POINT('Ctrl Pts',(-13.1567173185109,-52.3561135436466,
3.67100319215555));
#58498=CARTESIAN_POINT('Ctrl Pts',(-13.5335006499063,-52.075071389076,3.69717169561448));
#58499=CARTESIAN_POINT('Ctrl Pts',(-13.9430178866457,-52.0141811772634,
3.72334019907341));
#58500=CARTESIAN_POINT('Ctrl Pts',(-14.3525351233851,-51.9532909654507,
3.74950870253233));
#58501=CARTESIAN_POINT('Ctrl Pts',(-14.7947862654687,-52.1125526963959,
3.77567720599126));
#58502=CARTESIAN_POINT('Ctrl Pts',(-15.0714606437586,-52.4205515169895,
3.80184570945019));
#58503=CARTESIAN_POINT('Ctrl Pts',(-15.3481350220485,-52.7285503375831,
3.82801421290911));
#58504=CARTESIAN_POINT('Ctrl Pts',(-15.4592326365449,-53.185286247825,3.85418271636804));
#58505=CARTESIAN_POINT('Ctrl Pts',(-15.3549359963582,-53.5859534363384,
3.88035121982696));
#58506=CARTESIAN_POINT('Ctrl Pts',(-15.271147892813,-53.907834791464,3.90137403775778));
#58507=CARTESIAN_POINT('Ctrl Pts',(-15.0483458981207,-54.1935297998804,
3.9223968556886));
#58508=CARTESIAN_POINT('Ctrl Pts',(-14.7608564829457,-54.3629211099724,
3.94341967361942));
#58509=CARTESIAN_POINT('Ctrl Pts',(-14.7626048989925,-54.3636737206204,
3.80658032638058));
#58510=CARTESIAN_POINT('Ctrl Pts',(-14.7669628321868,-54.3611637139356,
3.80626246380903));
#58511=CARTESIAN_POINT('Ctrl Pts',(-14.7713043836124,-54.3586254505289,
3.80594460123748));
#58512=CARTESIAN_POINT('Ctrl Pts',(-14.7756291758562,-54.3560589463809,
3.80562673866593));
#58513=CARTESIAN_POINT('Ctrl Pts',(-15.131674054745,-54.1447677196515,3.779458235207));
#58514=CARTESIAN_POINT('Ctrl Pts',(-15.3741311043607,-53.7420706988344,
3.75328973174807));
#58515=CARTESIAN_POINT('Ctrl Pts',(-15.3942797010543,-53.3285420152435,
3.72712122828914));
#58516=CARTESIAN_POINT('Ctrl Pts',(-15.414428297748,-52.9150133316526,3.70095272483022));
#58517=CARTESIAN_POINT('Ctrl Pts',(-15.2122684415196,-52.4906529852878,
3.67478422137129));
#58518=CARTESIAN_POINT('Ctrl Pts',(-14.8784510160553,-52.2457491989657,
3.64861571791236));
#58519=CARTESIAN_POINT('Ctrl Pts',(-14.544633590591,-52.0008454126437,3.62244721445344));
#58520=CARTESIAN_POINT('Ctrl Pts',(-14.0791585958908,-51.9353981863644,
3.59627871099451));
#58521=CARTESIAN_POINT('Ctrl Pts',(-13.6907505503598,-52.0787548359323,
3.57011020753558));
#58522=CARTESIAN_POINT('Ctrl Pts',(-13.3023425048288,-52.2221114855001,
3.54394170407666));
#58523=CARTESIAN_POINT('Ctrl Pts',(-12.991001408467,-52.5742720109151,3.51777320061773));
#58524=CARTESIAN_POINT('Ctrl Pts',(-12.896336314222,-52.9773234433404,3.49160469715881));
#58525=CARTESIAN_POINT('Ctrl Pts',(-12.801671219977,-53.3803748757656,3.46543619369988));
#58526=CARTESIAN_POINT('Ctrl Pts',(-12.9236821278489,-53.8343172152012,
3.43926769024095));
#58527=CARTESIAN_POINT('Ctrl Pts',(-13.2076578874333,-54.1355973270763,
3.41309918678203));
#58528=CARTESIAN_POINT('Ctrl Pts',(-13.4916336470178,-54.4368774389515,
3.3869306833231));
#58529=CARTESIAN_POINT('Ctrl Pts',(-13.9375742583148,-54.5854953232663,
3.36076217986417));
#58530=CARTESIAN_POINT('Ctrl Pts',(-14.3455146684413,-54.5148089413369,
3.33459367640524));
#58531=CARTESIAN_POINT('Ctrl Pts',(-14.4910812336828,-54.4895857137002,
3.32525589306369));
#58532=CARTESIAN_POINT('Ctrl Pts',(-14.6318092436287,-54.436438533397,3.31591810972213));
#58533=CARTESIAN_POINT('Ctrl Pts',(-14.7601616123226,-54.3612756103012,
3.30658032638058));
#58534=CARTESIAN_POINT('Origin',(-14.1292828945604,-53.2669068454841,4.5));
#58535=CARTESIAN_POINT('',(-14.7622249872189,-54.3610567043161,2.80658032638058));
#58536=CARTESIAN_POINT('',(-14.7628222445742,-54.3633003878638,2.94341967361942));
#58537=CARTESIAN_POINT('',(-14.7615328945604,-54.3619959685696,4.5));
#58538=CARTESIAN_POINT('Ctrl Pts',(-14.7628222445742,-54.3633003878638,
2.94341967361942));
#58539=CARTESIAN_POINT('Ctrl Pts',(-14.4266363996141,-54.5552567541312,
2.96787665097375));
#58540=CARTESIAN_POINT('Ctrl Pts',(-13.9945792873817,-54.5843264233178,
2.99233362832807));
#58541=CARTESIAN_POINT('Ctrl Pts',(-13.6379437474727,-54.4342123040852,
3.01679060568239));
#58542=CARTESIAN_POINT('Ctrl Pts',(-13.256350461251,-54.2735930341132,3.04295910914132));
#58543=CARTESIAN_POINT('Ctrl Pts',(-12.9611042822246,-53.9078334931332,
3.06912761260024));
#58544=CARTESIAN_POINT('Ctrl Pts',(-12.8845971374177,-53.5009445240528,
3.09529611605917));
#58545=CARTESIAN_POINT('Ctrl Pts',(-12.8080899926108,-53.0940555549725,
3.12146461951809));
#58546=CARTESIAN_POINT('Ctrl Pts',(-12.9503218820233,-52.6460371577917,
3.14763312297702));
#58547=CARTESIAN_POINT('Ctrl Pts',(-13.2475143204017,-52.3577861486808,
3.17380162643595));
#58548=CARTESIAN_POINT('Ctrl Pts',(-13.54470675878,-52.0695351395699,3.19997012989488));
#58549=CARTESIAN_POINT('Ctrl Pts',(-13.9968597461241,-51.9410515185288,
3.2261386333538));
#58550=CARTESIAN_POINT('Ctrl Pts',(-14.4012225159017,-52.0299488478796,
3.25230713681273));
#58551=CARTESIAN_POINT('Ctrl Pts',(-14.8055852856793,-52.1188461772304,
3.27847564027165));
#58552=CARTESIAN_POINT('Ctrl Pts',(-15.1621578378903,-52.4251244569732,
3.30464414373058));
#58553=CARTESIAN_POINT('Ctrl Pts',(-15.3110487977949,-52.8114448760709,
3.33081264718951));
#58554=CARTESIAN_POINT('Ctrl Pts',(-15.4599397576996,-53.1977652951686,
3.35698115064843));
#58555=CARTESIAN_POINT('Ctrl Pts',(-15.4011491252979,-53.6641278536213,
3.38314965410736));
#58556=CARTESIAN_POINT('Ctrl Pts',(-15.161039320894,-54.0014100315303,3.40931815756629));
#58557=CARTESIAN_POINT('Ctrl Pts',(-15.0567395295787,-54.1479199204438,
3.420685329584));
#58558=CARTESIAN_POINT('Ctrl Pts',(-14.918226764983,-54.2700737329326,3.43205250160171));
#58559=CARTESIAN_POINT('Ctrl Pts',(-14.7609899830459,-54.3602193411783,
3.44341967361942));
#58560=CARTESIAN_POINT('Ctrl Pts',(-14.7601616123226,-54.3612756103012,
3.30658032638058));
#58561=CARTESIAN_POINT('Ctrl Pts',(-14.9915080373649,-54.2257995475618,
3.28974960626321));
#58562=CARTESIAN_POINT('Ctrl Pts',(-15.1826489574086,-54.0187995905144,
3.27291888614584));
#58563=CARTESIAN_POINT('Ctrl Pts',(-15.2894496720194,-53.7748722761244,
3.25608816602847));
#58564=CARTESIAN_POINT('Ctrl Pts',(-15.4555040565151,-53.395612641015,3.22991966256954));
#58565=CARTESIAN_POINT('Ctrl Pts',(-15.4176726165505,-52.9270840189701,
3.20375115911061));
#58566=CARTESIAN_POINT('Ctrl Pts',(-15.1929194920754,-52.5793801620778,
3.17758265565168));
#58567=CARTESIAN_POINT('Ctrl Pts',(-14.9681663676002,-52.2316763051856,
3.15141415219276));
#58568=CARTESIAN_POINT('Ctrl Pts',(-14.5564915586145,-52.004797213446,3.12524564873383));
#58569=CARTESIAN_POINT('Ctrl Pts',(-14.1424947973993,-52.0004782714699,
3.09907714527491));
#58570=CARTESIAN_POINT('Ctrl Pts',(-13.7284980361841,-51.9961593294939,
3.07290864181598));
#58571=CARTESIAN_POINT('Ctrl Pts',(-13.3121793227393,-52.2144005372813,
3.04674013835705));
#58572=CARTESIAN_POINT('Ctrl Pts',(-13.0802212088747,-52.5573397364563,
3.02057163489813));
#58573=CARTESIAN_POINT('Ctrl Pts',(-12.8482630950101,-52.9002789356314,
2.9944031314392));
#58574=CARTESIAN_POINT('Ctrl Pts',(-12.8006655807257,-53.3679161261941,
2.96823462798027));
#58575=CARTESIAN_POINT('Ctrl Pts',(-12.9587713715114,-53.7505576476053,
2.94206612452135));
#58576=CARTESIAN_POINT('Ctrl Pts',(-13.116877162297,-54.1331991690165,2.91589762106242));
#58577=CARTESIAN_POINT('Ctrl Pts',(-13.4806862581528,-54.4308450212763,
2.88972911760349));
#58578=CARTESIAN_POINT('Ctrl Pts',(-13.8870635107844,-54.5100264348898,
2.86356061414457));
#58579=CARTESIAN_POINT('Ctrl Pts',(-14.1820172367656,-54.5674973017321,
2.8445671848899));
#58580=CARTESIAN_POINT('Ctrl Pts',(-14.4993960343841,-54.5098802470415,
2.82557375563524));
#58581=CARTESIAN_POINT('Ctrl Pts',(-14.7622249872189,-54.3610567043161,
2.80658032638058));
#58582=CARTESIAN_POINT('Origin',(-14.1292828945604,-53.2669068454841,4.5));
#58583=CARTESIAN_POINT('',(-14.7617771735939,-54.3636459375188,2.30658032638058));
#58584=CARTESIAN_POINT('',(-14.7602610286104,-54.3618122024717,2.44341967361942));
#58585=CARTESIAN_POINT('',(-14.7615328945604,-54.3619959685696,4.5));
#58586=CARTESIAN_POINT('',(-12.9355708698302,-52.8497595669186,2.));
#58587=CARTESIAN_POINT('Ctrl Pts',(-14.7617771735939,-54.3636459375188,
2.30658032638058));
#58588=CARTESIAN_POINT('Ctrl Pts',(-15.08540280583,-54.1740757700734,2.28289239463049));
#58589=CARTESIAN_POINT('Ctrl Pts',(-15.3230378955527,-53.8318500257242,
2.25920446288041));
#58590=CARTESIAN_POINT('Ctrl Pts',(-15.3806718879601,-53.4614673043247,
2.23551653113033));
#58591=CARTESIAN_POINT('Ctrl Pts',(-15.4443412427006,-53.0522985500271,
2.2093480276714));
#58592=CARTESIAN_POINT('Ctrl Pts',(-15.2883366067183,-52.6087669190161,
2.18317952421248));
#58593=CARTESIAN_POINT('Ctrl Pts',(-14.981978171922,-52.3301976113127,2.15701102075355));
#58594=CARTESIAN_POINT('Ctrl Pts',(-14.6756197371256,-52.0516283036092,
2.13084251729463));
#58595=CARTESIAN_POINT('Ctrl Pts',(-14.2189075035153,-51.9380213192134,
2.1046740138357));
#58596=CARTESIAN_POINT('Ctrl Pts',(-13.8181892890955,-52.0394181405147,
2.07850551037677));
#58597=CARTESIAN_POINT('Ctrl Pts',(-13.4174710746757,-52.140814961816,2.05233700691785));
#58598=CARTESIAN_POINT('Ctrl Pts',(-13.0727468794465,-52.4572155888145,
2.02616850345892));
#58599=CARTESIAN_POINT('Ctrl Pts',(-12.9355708698302,-52.8497595669186,
1.99999999999999));
#58600=CARTESIAN_POINT('',(-13.8936035762987,-54.5113733504501,2.));
#58601=CARTESIAN_POINT('Origin',(-14.1292828945604,-53.2669068454841,2.));
#58602=CARTESIAN_POINT('Ctrl Pts',(-13.8936031194076,-54.5113848919291,
2.));
#58603=CARTESIAN_POINT('Ctrl Pts',(-13.5065360962339,-54.4366467486624,
2.02490816038701));
#58604=CARTESIAN_POINT('Ctrl Pts',(-13.1551959025419,-54.1671648587472,
2.04981632077402));
#58605=CARTESIAN_POINT('Ctrl Pts',(-12.9858211468817,-53.8112635997049,
2.07472448116103));
#58606=CARTESIAN_POINT('Ctrl Pts',(-12.8078760955218,-53.4373538776067,
2.10089298461996));
#58607=CARTESIAN_POINT('Ctrl Pts',(-12.830777130449,-52.9680579532915,2.12706148807889));
#58608=CARTESIAN_POINT('Ctrl Pts',(-13.0443872879449,-52.6134595791442,
2.15322999153781));
#58609=CARTESIAN_POINT('Ctrl Pts',(-13.2579974454408,-52.2588612049968,
2.17939849499674));
#58610=CARTESIAN_POINT('Ctrl Pts',(-13.6623167255054,-52.0189603810172,
2.20556699845567));
#58611=CARTESIAN_POINT('Ctrl Pts',(-14.0759781319804,-52.0015075823912,
2.23173550191459));
#58612=CARTESIAN_POINT('Ctrl Pts',(-14.4896395384555,-51.9840547837653,
2.25790400537352));
#58613=CARTESIAN_POINT('Ctrl Pts',(-14.9126430713409,-52.1890500104929,
2.28407250883245));
#58614=CARTESIAN_POINT('Ctrl Pts',(-15.1553414968488,-52.5244832283522,
2.31024101229137));
#58615=CARTESIAN_POINT('Ctrl Pts',(-15.3980399223566,-52.8599164462115,
2.3364095157503));
#58616=CARTESIAN_POINT('Ctrl Pts',(-15.4604332404868,-53.3257876552024,
2.36257801920923));
#58617=CARTESIAN_POINT('Ctrl Pts',(-15.3145273105893,-53.7132383944998,
2.38874652266815));
#58618=CARTESIAN_POINT('Ctrl Pts',(-15.2129148646389,-53.9830685332266,
2.40697090631858));
#58619=CARTESIAN_POINT('Ctrl Pts',(-15.010275844201,-54.2148642023245,2.425195289969));
#58620=CARTESIAN_POINT('Ctrl Pts',(-14.7602610286104,-54.3618122024717,
2.44341967361942));
#58621=CARTESIAN_POINT('Origin',(-14.1292828945604,-53.2669068454841,0.895788276411274));
#58622=CARTESIAN_POINT('',(-14.9010968564111,-54.6052515498159,5.60421172358873));
#58623=CARTESIAN_POINT('',(-14.89962934498,-54.6010727330809,5.64578827641128));
#58624=CARTESIAN_POINT('',(-14.9007828945603,-54.6031840435235,0.895788276411274));
#58625=CARTESIAN_POINT('',(-15.2209662466057,-52.1764590205668,6.));
#58626=CARTESIAN_POINT('Ctrl Pts',(-14.89962934498,-54.6010727330809,5.64578827641128));
#58627=CARTESIAN_POINT('Ctrl Pts',(-14.6737409652706,-54.7312989825202,
5.65918483710515));
#58628=CARTESIAN_POINT('Ctrl Pts',(-13.9138866474417,-54.955646298412,5.69874990125794));
#58629=CARTESIAN_POINT('Ctrl Pts',(-12.6330342875793,-54.2971998857928,
5.76448346886966));
#58630=CARTESIAN_POINT('Ctrl Pts',(-12.4433594214856,-52.5865231455987,
5.84298897924644));
#58631=CARTESIAN_POINT('Ctrl Pts',(-13.76941659957,-51.486617996264,5.92149448962323));
#58632=CARTESIAN_POINT('Ctrl Pts',(-14.8623799894179,-51.8174664687922,
5.97383149654107));
#58633=CARTESIAN_POINT('Ctrl Pts',(-15.2209662466057,-52.1764590205668,
6.));
#58634=CARTESIAN_POINT('',(-15.6220374293776,-52.8664110852719,6.));
#58635=CARTESIAN_POINT('Origin',(-14.1292828945604,-53.2669068454841,6.));
#58636=CARTESIAN_POINT('Ctrl Pts',(-14.9010968564111,-54.6052515498159,
5.60421172358873));
#58637=CARTESIAN_POINT('Ctrl Pts',(-14.8619571740658,-54.628166857787,5.60655897483644));
#58638=CARTESIAN_POINT('Ctrl Pts',(-14.3739271072306,-54.8842868995418,
5.63507472954307));
#58639=CARTESIAN_POINT('Ctrl Pts',(-13.1774033105245,-54.8145932898247,
5.68975898770864));
#58640=CARTESIAN_POINT('Ctrl Pts',(-12.3131175991141,-53.3266332457169,
5.76826449808541));
#58641=CARTESIAN_POINT('Ctrl Pts',(-13.07802768807,-51.78491829464,5.84677000846219));
#58642=CARTESIAN_POINT('Ctrl Pts',(-14.7574918726583,-51.5760767532103,
5.92401517576706));
#58643=CARTESIAN_POINT('Ctrl Pts',(-15.4957392820493,-52.402248403584,5.97509183961299));
#58644=CARTESIAN_POINT('Ctrl Pts',(-15.6220514315181,-52.8664094746825,
6.));
#58645=CARTESIAN_POINT('Origin',(-14.1292828945604,-53.2669068454841,0.895788276411274));
#58646=CARTESIAN_POINT('',(-14.8993447411713,-54.6013457970434,5.10421172358873));
#58647=CARTESIAN_POINT('',(-14.9024169355128,-54.6041163881961,5.14578827641127));
#58648=CARTESIAN_POINT('',(-14.9007828945603,-54.6031840435235,0.895788276411274));
#58649=CARTESIAN_POINT('Ctrl Pts',(-14.9024169355128,-54.6041163881961,
5.14578827641127));
#58650=CARTESIAN_POINT('Ctrl Pts',(-14.5148361321472,-54.8241371380329,
5.16884048301825));
#58651=CARTESIAN_POINT('Ctrl Pts',(-13.4683417470894,-54.9257881846255,
5.21806119308415));
#58652=CARTESIAN_POINT('Ctrl Pts',(-12.3638311119676,-53.696734568805,5.29345040660899));
#58653=CARTESIAN_POINT('Ctrl Pts',(-12.7969355370903,-52.0313922294383,
5.37195591698576));
#58654=CARTESIAN_POINT('Ctrl Pts',(-14.424976702367,-51.4740982114769,5.45046142736254));
#58655=CARTESIAN_POINT('Ctrl Pts',(-15.7877203932888,-52.5246186608361,
5.52896693773933));
#58656=CARTESIAN_POINT('Ctrl Pts',(-15.6845839838159,-53.9480078415062,
5.59407588742224));
#58657=CARTESIAN_POINT('Ctrl Pts',(-15.1149856235702,-54.4769183144689,
5.63301633364622));
#58658=CARTESIAN_POINT('Ctrl Pts',(-14.89962934498,-54.6010727330809,5.64578827641128));
#58659=CARTESIAN_POINT('Ctrl Pts',(-14.8993447411713,-54.6013457970434,
5.10421172358873));
#58660=CARTESIAN_POINT('Ctrl Pts',(-14.6972931579988,-54.7185214822016,
5.11621462074955));
#58661=CARTESIAN_POINT('Ctrl Pts',(-13.9751327847045,-54.9521265711601,
5.15438602136929));
#58662=CARTESIAN_POINT('Ctrl Pts',(-12.6886982319545,-54.374296277089,5.21872592544796));
#58663=CARTESIAN_POINT('Ctrl Pts',(-12.4109789893208,-52.6761143673659,
5.29723143582474));
#58664=CARTESIAN_POINT('Ctrl Pts',(-13.6742819091468,-51.5077662723951,
5.37573694620152));
#58665=CARTESIAN_POINT('Ctrl Pts',(-15.3456277491901,-51.9170631330653,
5.4542424565783));
#58666=CARTESIAN_POINT('Ctrl Pts',(-15.9087950365254,-53.4884877368246,
5.53040071570737));
#58667=CARTESIAN_POINT('Ctrl Pts',(-15.2983088061438,-54.3726938586823,
5.58039047137751));
#58668=CARTESIAN_POINT('Ctrl Pts',(-14.9010968564111,-54.6052515498159,
5.60421172358873));
#58669=CARTESIAN_POINT('Origin',(-14.1292828945604,-53.2669068454841,0.895788276411274));
#58670=CARTESIAN_POINT('',(-14.9022875039252,-54.6033748953446,4.60421172358873));
#58671=CARTESIAN_POINT('',(-14.899520943644,-54.6036563213,4.64578827641127));
#58672=CARTESIAN_POINT('',(-14.9007828945603,-54.6031840435235,0.895788276411274));
#58673=CARTESIAN_POINT('Ctrl Pts',(-14.899520943644,-54.6036563213,4.64578827641127));
#58674=CARTESIAN_POINT('Ctrl Pts',(-14.7902473340007,-54.6680216226135,
4.65232762547243));
#58675=CARTESIAN_POINT('Ctrl Pts',(-14.20608207924,-54.9223430869235,4.68503547799252));
#58676=CARTESIAN_POINT('Ctrl Pts',(-12.9456280488333,-54.64551461019,4.74391183397153));
#58677=CARTESIAN_POINT('Ctrl Pts',(-12.3264734310144,-53.0400243844669,
4.82241734434831));
#58678=CARTESIAN_POINT('Ctrl Pts',(-13.324120771136,-51.638007671339,4.90092285472508));
#58679=CARTESIAN_POINT('Ctrl Pts',(-15.0438575043005,-51.6968266074015,
4.97942836510187));
#58680=CARTESIAN_POINT('Ctrl Pts',(-15.9433802614164,-53.1637305367386,
5.05793387547864));
#58681=CARTESIAN_POINT('Ctrl Pts',(-15.4295729948612,-54.2652563903719,
5.11338717924845));
#58682=CARTESIAN_POINT('Ctrl Pts',(-14.9548117824789,-54.5743730329603,
5.14267197955932));
#58683=CARTESIAN_POINT('Ctrl Pts',(-14.9024169355128,-54.6041163881961,
5.14578827641127));
#58684=CARTESIAN_POINT('Ctrl Pts',(-14.9022875039252,-54.6033748953446,
4.60421172358873));
#58685=CARTESIAN_POINT('Ctrl Pts',(-14.5374282197782,-54.8098641325902,
4.62587026666265));
#58686=CARTESIAN_POINT('Ctrl Pts',(-13.5347909686423,-54.936592528733,4.6736973131955));
#58687=CARTESIAN_POINT('Ctrl Pts',(-12.3888319545389,-53.7888545684045,
4.74769286318728));
#58688=CARTESIAN_POINT('Ctrl Pts',(-12.7339055288242,-52.1030679359729,
4.82619837356406));
#58689=CARTESIAN_POINT('Ctrl Pts',(-14.3303867955418,-51.461039661442,4.90470388394084));
#58690=CARTESIAN_POINT('Ctrl Pts',(-15.7465131069793,-52.4385560995515,
4.98320939431762));
#58691=CARTESIAN_POINT('Ctrl Pts',(-15.7175049264688,-53.8959207488069,
5.04971200753358));
#58692=CARTESIAN_POINT('Ctrl Pts',(-15.1378024352416,-54.4630571321133,
5.09004611729062));
#58693=CARTESIAN_POINT('Ctrl Pts',(-14.8993447411713,-54.6013457970434,
5.10421172358873));
#58694=CARTESIAN_POINT('Origin',(-14.1292828945604,-53.2669068454841,0.895788276411274));
#58695=CARTESIAN_POINT('',(-14.899957506564,-54.6043129428392,4.10421172358872));
#58696=CARTESIAN_POINT('',(-14.9006214745914,-54.60116105013,4.14578827641127));
#58697=CARTESIAN_POINT('',(-14.9007828945603,-54.6031840435235,0.895788276411274));
#58698=CARTESIAN_POINT('Ctrl Pts',(-14.9006214745914,-54.60116105013,4.14578827641127));
#58699=CARTESIAN_POINT('Ctrl Pts',(-14.6270809930356,-54.7571745495808,
4.16198327138554));
#58700=CARTESIAN_POINT('Ctrl Pts',(-13.7886805442009,-54.9572356101558,
4.20434676981873));
#58701=CARTESIAN_POINT('Ctrl Pts',(-12.5323678038339,-54.1337749126023,
4.27287877171085));
#58702=CARTESIAN_POINT('Ctrl Pts',(-12.5253744436601,-52.413047533365,4.35138428208763));
#58703=CARTESIAN_POINT('Ctrl Pts',(-13.9568043064156,-51.4580814834715,
4.42988979246441));
#58704=CARTESIAN_POINT('Ctrl Pts',(-15.5429170806551,-52.1253130228172,
4.50839530284119));
#58705=CARTESIAN_POINT('Ctrl Pts',(-15.8347326759058,-53.6754928499223,
4.58036146415681));
#58706=CARTESIAN_POINT('Ctrl Pts',(-15.2275273759708,-54.4104510916165,
4.62615912201351));
#58707=CARTESIAN_POINT('Ctrl Pts',(-14.899520943644,-54.6036563213,4.64578827641127));
#58708=CARTESIAN_POINT('Ctrl Pts',(-14.899957506564,-54.6043129428392,4.10421172358873));
#58709=CARTESIAN_POINT('Ctrl Pts',(-14.8140915002505,-54.654905954387,4.10935740911683));
#58710=CARTESIAN_POINT('Ctrl Pts',(-14.2627733336105,-54.9110489082195,
4.14067159810386));
#58711=CARTESIAN_POINT('Ctrl Pts',(-13.0196598476917,-54.705772943414,4.19815429054983));
#58712=CARTESIAN_POINT('Ctrl Pts',(-12.3170458706651,-53.1350132444558,
4.2766598009266));
#58713=CARTESIAN_POINT('Ctrl Pts',(-13.239689139382,-51.6825388628568,4.35516531130339));
#58714=CARTESIAN_POINT('Ctrl Pts',(-14.9601412381249,-51.6509633535717,
4.43367082168016));
#58715=CARTESIAN_POINT('Ctrl Pts',(-15.9354598188275,-53.0686043860759,
4.51217633205695));
#58716=CARTESIAN_POINT('Ctrl Pts',(-15.4687653497055,-54.223916817667,4.5690232993598));
#58717=CARTESIAN_POINT('Ctrl Pts',(-14.9782621856933,-54.5603776227797,
4.59970176320373));
#58718=CARTESIAN_POINT('Ctrl Pts',(-14.9022875039252,-54.6033748953446,
4.60421172358873));
#58719=CARTESIAN_POINT('Origin',(-14.1292828945604,-53.2669068454841,0.895788276411274));
#58720=CARTESIAN_POINT('',(-14.9001204094146,-54.6010161225549,3.60421172358873));
#58721=CARTESIAN_POINT('',(-14.9020910027761,-54.6052313123369,3.64578827641127));
#58722=CARTESIAN_POINT('',(-14.9007828945603,-54.6031840435235,0.895788276411274));
#58723=CARTESIAN_POINT('Ctrl Pts',(-14.9020910027761,-54.6052313123369,
3.64578827641127));
#58724=CARTESIAN_POINT('Ctrl Pts',(-14.4696174214115,-54.8543199357372,
3.67163891729865));
#58725=CARTESIAN_POINT('Ctrl Pts',(-13.3333022960118,-54.8966530893797,
3.72365806164495));
#58726=CARTESIAN_POINT('Ctrl Pts',(-12.3283770240505,-53.5084355106897,
3.80184570945017));
#58727=CARTESIAN_POINT('Ctrl Pts',(-12.9344615472089,-51.8979656495417,
3.88035121982696));
#58728=CARTESIAN_POINT('Ctrl Pts',(-14.612090259655,-51.5151947977304,3.95885673020373));
#58729=CARTESIAN_POINT('Ctrl Pts',(-15.8567258492822,-52.7034009548898,
4.03736224058051));
#58730=CARTESIAN_POINT('Ctrl Pts',(-15.614980939896,-54.0476036870055,4.09967275598303));
#58731=CARTESIAN_POINT('Ctrl Pts',(-15.0690783538945,-54.5050818625188,
4.13581476792661));
#58732=CARTESIAN_POINT('Ctrl Pts',(-14.9006214745914,-54.60116105013,4.14578827641127));
#58733=CARTESIAN_POINT('Ctrl Pts',(-14.9001204094146,-54.6010161225549,
3.60421172358873));
#58734=CARTESIAN_POINT('Ctrl Pts',(-14.6502875315042,-54.7442481097626,
3.61901305502994));
#58735=CARTESIAN_POINT('Ctrl Pts',(-13.8515268344553,-54.9574092639254,
3.65998288993008));
#58736=CARTESIAN_POINT('Ctrl Pts',(-12.5800953694062,-54.216441978079,3.72712122828915));
#58737=CARTESIAN_POINT('Ctrl Pts',(-12.482746426243,-52.4984560584276,3.80562673866593));
#58738=CARTESIAN_POINT('Ctrl Pts',(-13.8620505314459,-51.4696350750294,
3.88413224904271));
#58739=CARTESIAN_POINT('Ctrl Pts',(-15.4810149732843,-52.0526501422855,
3.96263775941948));
#58740=CARTESIAN_POINT('Ctrl Pts',(-15.8610566498332,-53.6150480556464,
4.03599758426816));
#58741=CARTESIAN_POINT('Ctrl Pts',(-15.2507650728867,-54.397614017199,4.0831889056579));
#58742=CARTESIAN_POINT('Ctrl Pts',(-14.899957506564,-54.6043129428392,4.10421172358873));
#58743=CARTESIAN_POINT('Origin',(-14.1292828945604,-53.2669068454841,0.895788276411274));
#58744=CARTESIAN_POINT('',(-14.9023562176693,-54.604775754849,3.10421172358873));
#58745=CARTESIAN_POINT('',(-14.8991095940519,-54.6023050298359,3.14578827641127));
#58746=CARTESIAN_POINT('',(-14.9007828945603,-54.6031840435235,0.895788276411274));
#58747=CARTESIAN_POINT('Ctrl Pts',(-14.8991095940519,-54.6023050298359,
3.14578827641127));
#58748=CARTESIAN_POINT('Ctrl Pts',(-14.7424882378679,-54.6940222226685,
3.15512605975283));
#58749=CARTESIAN_POINT('Ctrl Pts',(-14.0895244416362,-54.9406197878808,
3.19063234655331));
#58750=CARTESIAN_POINT('Ctrl Pts',(-12.8070376180166,-54.5132075415871,
3.25230713681272));
#58751=CARTESIAN_POINT('Ctrl Pts',(-12.3603879600184,-52.8514447189325,
3.3308126471895));
#58752=CARTESIAN_POINT('Ctrl Pts',(-13.5001253542918,-51.5622781929174,
3.40931815756628));
#58753=CARTESIAN_POINT('Ctrl Pts',(-15.2041061771209,-51.8018631754771,
3.48782366794306));
#58754=CARTESIAN_POINT('Ctrl Pts',(-15.944159933136,-53.3553341468671,3.56632917831984));
#58755=CARTESIAN_POINT('Ctrl Pts',(-15.3488521474601,-54.3440811110855,
3.61898404780924));
#58756=CARTESIAN_POINT('Ctrl Pts',(-14.9074087496474,-54.6021684888377,
3.64547041383972));
#58757=CARTESIAN_POINT('Ctrl Pts',(-14.9020910027761,-54.6052313123369,
3.64578827641127));
#58758=CARTESIAN_POINT('Ctrl Pts',(-14.9023562176693,-54.604775754849,3.10421172358873));
#58759=CARTESIAN_POINT('Ctrl Pts',(-14.4921270687778,-54.8390095809862,
3.12866870094305));
#58760=CARTESIAN_POINT('Ctrl Pts',(-13.4008007460488,-54.9124362051017,
3.1792941817563));
#58761=CARTESIAN_POINT('Ctrl Pts',(-12.3435458814549,-53.6026781745395,
3.25608816602847));
#58762=CARTESIAN_POINT('Ctrl Pts',(-12.8642192037885,-51.9626013374103,
3.33459367640525));
#58763=CARTESIAN_POINT('Ctrl Pts',(-14.5194316817766,-51.4922567887358,
3.41309918678203));
#58764=CARTESIAN_POINT('Ctrl Pts',(-15.824749470772,-52.6134605506407,3.49160469715881));
#58765=CARTESIAN_POINT('Ctrl Pts',(-15.6501092546376,-53.9988114930956,
3.55530887609438));
#58766=CARTESIAN_POINT('Ctrl Pts',(-15.091987830948,-54.4910163807415,3.59284455157101));
#58767=CARTESIAN_POINT('Ctrl Pts',(-14.9001204094146,-54.6010161225549,
3.60421172358873));
#58768=CARTESIAN_POINT('Origin',(-14.1292828945604,-53.2669068454841,0.895788276411274));
#58769=CARTESIAN_POINT('',(-14.8992309062956,-54.6029598038327,2.60421172358873));
#58770=CARTESIAN_POINT('',(-14.9016274172746,-54.6020379108679,2.64578827641127));
#58771=CARTESIAN_POINT('',(-14.9007828945603,-54.6031840435235,0.895788276411274));
#58772=CARTESIAN_POINT('Ctrl Pts',(-14.9016274172746,-54.6020379108679,
2.64578827641127));
#58773=CARTESIAN_POINT('Ctrl Pts',(-14.5809116606719,-54.7836391180053,
2.66478170566594));
#58774=CARTESIAN_POINT('Ctrl Pts',(-13.6600505366298,-54.9508125591569,
2.70994363837953));
#58775=CARTESIAN_POINT('Ctrl Pts',(-12.4499634166736,-53.960794947638,2.78127407455204));
#58776=CARTESIAN_POINT('Ctrl Pts',(-12.6242053254302,-52.2488988977254,
2.85977958492882));
#58777=CARTESIAN_POINT('Ctrl Pts',(-14.1482380059646,-51.4499755676755,
2.93828509530561));
#58778=CARTESIAN_POINT('Ctrl Pts',(-15.6552705807332,-52.2805199058824,
3.01679060568238));
#58779=CARTESIAN_POINT('Ctrl Pts',(-15.777288771741,-53.7916708150444,3.08595833271761));
#58780=CARTESIAN_POINT('Ctrl Pts',(-15.1814089486113,-54.4369910204986,
3.1289575562939));
#58781=CARTESIAN_POINT('Ctrl Pts',(-14.8991095940519,-54.6023050298359,
3.14578827641127));
#58782=CARTESIAN_POINT('Ctrl Pts',(-14.8992309062956,-54.6029598038327,
2.60421172358873));
#58783=CARTESIAN_POINT('Ctrl Pts',(-14.7662449521696,-54.681123251708,2.61215584339723));
#58784=CARTESIAN_POINT('Ctrl Pts',(-14.1480244437874,-54.9322850073565,
2.64626846666466));
#58785=CARTESIAN_POINT('Ctrl Pts',(-12.8743150895914,-54.5809192738243,
2.70654959339101));
#58786=CARTESIAN_POINT('Ctrl Pts',(-12.3410089780029,-52.9449163922479,
2.7850551037678));
#58787=CARTESIAN_POINT('Ctrl Pts',(-13.4114743235374,-51.5976690199096,
2.86356061414457));
#58788=CARTESIAN_POINT('Ctrl Pts',(-15.125685020798,-51.7474403844543,2.94206612452135));
#58789=CARTESIAN_POINT('Ctrl Pts',(-15.9462998191018,-53.2599021194416,
3.02057163489813));
#58790=CARTESIAN_POINT('Ctrl Pts',(-15.3893775359764,-54.3055097335425,
3.07462016792059));
#58791=CARTESIAN_POINT('Ctrl Pts',(-14.9310645035309,-54.5883838147409,
3.10250019748412));
#58792=CARTESIAN_POINT('Ctrl Pts',(-14.9023562176693,-54.604775754849,3.10421172358873));
#58793=CARTESIAN_POINT('Origin',(-14.1292828945604,-53.2669068454841,0.895788276411274));
#58794=CARTESIAN_POINT('',(-14.9013089558621,-54.6009691165979,2.10421172358873));
#58795=CARTESIAN_POINT('',(-14.9010809748678,-54.6051974101417,2.14578827641127));
#58796=CARTESIAN_POINT('',(-14.9007828945603,-54.6031840435235,0.895788276411274));
#58797=CARTESIAN_POINT('',(-15.6194800884629,-52.866705242183,2.));
#58798=CARTESIAN_POINT('Ctrl Pts',(-15.6194800884629,-52.866705242183,2.));
#58799=CARTESIAN_POINT('Ctrl Pts',(-15.7510836294753,-53.3567463262429,
2.02616850345893));
#58800=CARTESIAN_POINT('Ctrl Pts',(-15.5785415188313,-54.0947786094125,
2.06090574465517));
#58801=CARTESIAN_POINT('Ctrl Pts',(-15.0460508163988,-54.5187167298269,
2.09564298585141));
#58802=CARTESIAN_POINT('Ctrl Pts',(-14.9013089558621,-54.6009691165979,
2.10421172358873));
#58803=CARTESIAN_POINT('',(-15.2224998162609,-52.1743915631094,2.));
#58804=CARTESIAN_POINT('Origin',(-14.1292828945604,-53.2669068454841,2.));
#58805=CARTESIAN_POINT('Ctrl Pts',(-15.2225082026616,-52.1743802571171,
2.));
#58806=CARTESIAN_POINT('Ctrl Pts',(-15.5613276195564,-52.5158503863372,
2.02490816038701));
#58807=CARTESIAN_POINT('Ctrl Pts',(-15.8908670066042,-53.5171650620887,
2.0735042525241));
#58808=CARTESIAN_POINT('Ctrl Pts',(-15.2959835850222,-54.3738753315586,
2.12210034466119));
#58809=CARTESIAN_POINT('Ctrl Pts',(-14.9010809748678,-54.6051974101417,
2.14578827641127));
#58810=CARTESIAN_POINT('Origin',(39.0658530619283,-38.8697713466883,4.5));
#58811=CARTESIAN_POINT('',(39.6970780592612,-39.9631802546368,5.80658032638059));
#58812=CARTESIAN_POINT('',(39.6962628554159,-39.965015558984,5.94341967361942));
#58813=CARTESIAN_POINT('',(39.6981030619283,-39.9648604697737,4.5));
#58814=CARTESIAN_POINT('',(40.2595650866584,-39.2869186252538,6.));
#58815=CARTESIAN_POINT('Ctrl Pts',(39.6962628554159,-39.965015558984,5.94341967361942));
#58816=CARTESIAN_POINT('Ctrl Pts',(39.9540142218037,-39.8131911161898,5.96227978241295));
#58817=CARTESIAN_POINT('Ctrl Pts',(40.160699881421,-39.5698320958276,5.98113989120648));
#58818=CARTESIAN_POINT('Ctrl Pts',(40.2595650866584,-39.2869186252538,6.00000000000001));
#58819=CARTESIAN_POINT('',(39.6981030619283,-39.9648604697737,6.));
#58820=CARTESIAN_POINT('Origin',(39.0658530619283,-38.8697713466883,6.));
#58821=CARTESIAN_POINT('',(39.6981030619283,-39.9648604697737,7.));
#58822=CARTESIAN_POINT('',(39.6981030619283,-39.9648604697737,4.5));
#58823=CARTESIAN_POINT('',(39.7608672580761,-37.8134023216062,7.));
#58824=CARTESIAN_POINT('Origin',(39.0658530619283,-38.8697713466883,7.));
#58825=CARTESIAN_POINT('',(38.3708388657804,-39.9261403717704,7.));
#58826=CARTESIAN_POINT('Origin',(39.0658530619283,-38.8697713466883,7.));
#58827=CARTESIAN_POINT('Origin',(39.0658530619283,-38.8697713466883,7.));
#58828=CARTESIAN_POINT('',(39.3015291113281,-37.6253036020567,6.));
#58829=CARTESIAN_POINT('Origin',(39.0658530619283,-38.8697713466883,6.));
#58830=CARTESIAN_POINT('Ctrl Pts',(39.3015295597332,-37.6252918061955,6.));
#58831=CARTESIAN_POINT('Ctrl Pts',(39.6885932560667,-37.7000310216234,5.97509183961299));
#58832=CARTESIAN_POINT('Ctrl Pts',(40.039943062479,-37.9695097738977,5.95018367922598));
#58833=CARTESIAN_POINT('Ctrl Pts',(40.2093203959796,-38.325411392646,5.92527551883897));
#58834=CARTESIAN_POINT('Ctrl Pts',(40.3872681556176,-38.6993214926512,5.89910701538004));
#58835=CARTESIAN_POINT('Ctrl Pts',(40.3643620641527,-39.1686216551033,5.87293851192112));
#58836=CARTESIAN_POINT('Ctrl Pts',(40.1507501683313,-39.5232214807692,5.84677000846219));
#58837=CARTESIAN_POINT('Ctrl Pts',(40.0413948614145,-39.7047533782285,5.83337344776832));
#58838=CARTESIAN_POINT('Ctrl Pts',(39.8820599551598,-39.8562249589825,5.81997688707446));
#58839=CARTESIAN_POINT('Ctrl Pts',(39.6970780592612,-39.9631802546368,5.80658032638059));
#58840=CARTESIAN_POINT('Origin',(39.0658530619283,-38.8697713466883,4.5));
#58841=CARTESIAN_POINT('',(39.6980969738518,-39.9664052404928,5.30658032638059));
#58842=CARTESIAN_POINT('',(39.6994431549996,-39.9659335873643,5.44341967361942));
#58843=CARTESIAN_POINT('',(39.6981030619283,-39.9648604697737,4.5));
#58844=CARTESIAN_POINT('Ctrl Pts',(39.6994431549996,-39.9659335873643,5.44341967361942));
#58845=CARTESIAN_POINT('Ctrl Pts',(39.7317442057588,-39.9475451778339,5.44576692486713));
#58846=CARTESIAN_POINT('Ctrl Pts',(39.7631672715511,-39.9276731785138,5.44811417611484));
#58847=CARTESIAN_POINT('Ctrl Pts',(39.7935612952928,-39.9063356334613,5.45046142736255));
#58848=CARTESIAN_POINT('Ctrl Pts',(40.1324113081288,-39.6684524404899,5.47662993082147));
#58849=CARTESIAN_POINT('Ctrl Pts',(40.3433609694206,-39.2484155500404,5.5027984342804));
#58850=CARTESIAN_POINT('Ctrl Pts',(40.3318541433896,-38.8345478072092,5.52896693773932));
#58851=CARTESIAN_POINT('Ctrl Pts',(40.3203473173586,-38.420680064378,5.55513544119825));
#58852=CARTESIAN_POINT('Ctrl Pts',(40.086384004005,-38.0129814691652,5.58130394465718));
#58853=CARTESIAN_POINT('Ctrl Pts',(39.7348031115542,-37.794322753355,5.60747244811611));
#58854=CARTESIAN_POINT('Ctrl Pts',(39.3832222191033,-37.5756640375447,5.63364095157504));
#58855=CARTESIAN_POINT('Ctrl Pts',(38.9140237475553,-37.5460452011372,5.65980945503396));
#58856=CARTESIAN_POINT('Ctrl Pts',(38.5377492251912,-37.7186390805662,5.68597795849288));
#58857=CARTESIAN_POINT('Ctrl Pts',(38.161474702827,-37.8912329599952,5.71214646195181));
#58858=CARTESIAN_POINT('Ctrl Pts',(37.8781241296467,-38.2660395552607,5.73831496541074));
#58859=CARTESIAN_POINT('Ctrl Pts',(37.814457003614,-38.6752103329025,5.76448346886967));
#58860=CARTESIAN_POINT('Ctrl Pts',(37.7507898775812,-39.0843811105442,5.79065197232859));
#58861=CARTESIAN_POINT('Ctrl Pts',(37.9068061986959,-39.5279160705621,5.81682047578752));
#58862=CARTESIAN_POINT('Ctrl Pts',(38.2131591663055,-39.8064837741936,5.84298897924645));
#58863=CARTESIAN_POINT('Ctrl Pts',(38.5195121339151,-40.0850514778251,5.86915748270537));
#58864=CARTESIAN_POINT('Ctrl Pts',(38.9762017480197,-40.1986519250703,5.8953259861643));
#58865=CARTESIAN_POINT('Ctrl Pts',(39.3769209838014,-40.0972547064535,5.92149448962322));
#58866=CARTESIAN_POINT('Ctrl Pts',(39.4888346944845,-40.0689362780501,5.92880288428862));
#58867=CARTESIAN_POINT('Ctrl Pts',(39.596382800018,-40.0238483557585,5.93611127895402));
#58868=CARTESIAN_POINT('Ctrl Pts',(39.6962628554159,-39.965015558984,5.94341967361942));
#58869=CARTESIAN_POINT('Ctrl Pts',(39.6970780592612,-39.9631802546368,5.80658032638059));
#58870=CARTESIAN_POINT('Ctrl Pts',(39.5207209896389,-40.0651487333929,5.79380838361553));
#58871=CARTESIAN_POINT('Ctrl Pts',(39.3210527704035,-40.1266553179232,5.78103644085048));
#58872=CARTESIAN_POINT('Ctrl Pts',(39.1191586941911,-40.1351732662231,5.76826449808542));
#58873=CARTESIAN_POINT('Ctrl Pts',(38.7054968160504,-40.1526257371314,5.74209599462649));
#58874=CARTESIAN_POINT('Ctrl Pts',(38.2824907599468,-39.9476311900682,5.71592749116756));
#58875=CARTESIAN_POINT('Ctrl Pts',(38.0397913612151,-39.6121973316472,5.68975898770864));
#58876=CARTESIAN_POINT('Ctrl Pts',(37.7970919624834,-39.2767634732261,5.66359048424971));
#58877=CARTESIAN_POINT('Ctrl Pts',(37.7346992211236,-38.8108903034472,5.63742198079078));
#58878=CARTESIAN_POINT('Ctrl Pts',(37.8806057126089,-38.4234383862029,5.61125347733185));
#58879=CARTESIAN_POINT('Ctrl Pts',(38.0265122040942,-38.0359864689587,5.58508497387293));
#58880=CARTESIAN_POINT('Ctrl Pts',(38.3807179284248,-37.7269558042492,5.558916470414));
#58881=CARTESIAN_POINT('Ctrl Pts',(38.7843854256713,-37.6349404921319,5.53274796695507));
#58882=CARTESIAN_POINT('Ctrl Pts',(39.1880529229179,-37.5429251800145,5.50657946349615));
#58883=CARTESIAN_POINT('Ctrl Pts',(39.6411821930806,-37.6679252204893,5.48041096003722));
#58884=CARTESIAN_POINT('Ctrl Pts',(39.9405883560671,-37.9538786579723,5.4542424565783));
#58885=CARTESIAN_POINT('Ctrl Pts',(40.2399945190535,-38.2398320954553,5.42807395311937));
#58886=CARTESIAN_POINT('Ctrl Pts',(40.3856775748639,-38.6867389299466,5.40190544966044));
#58887=CARTESIAN_POINT('Ctrl Pts',(40.3123096892109,-39.0942060073491,5.37573694620152));
#58888=CARTESIAN_POINT('Ctrl Pts',(40.2476788760258,-39.4531495468055,5.35268473959454));
#58889=CARTESIAN_POINT('Ctrl Pts',(40.0130623748058,-39.7814874463141,5.32963253298756));
#58890=CARTESIAN_POINT('Ctrl Pts',(39.6980969738518,-39.9664052404928,5.30658032638059));
#58891=CARTESIAN_POINT('Origin',(39.0658530619283,-38.8697713466883,4.5));
#58892=CARTESIAN_POINT('',(39.6989570949588,-39.9641614067485,4.80658032638058));
#58893=CARTESIAN_POINT('',(39.697389467188,-39.9630895992609,4.94341967361942));
#58894=CARTESIAN_POINT('',(39.6981030619283,-39.9648604697737,4.5));
#58895=CARTESIAN_POINT('Ctrl Pts',(39.697389467188,-39.9630895992609,4.94341967361942));
#58896=CARTESIAN_POINT('Ctrl Pts',(39.8633425703643,-39.8677036169061,4.95542257078024));
#58897=CARTESIAN_POINT('Ctrl Pts',(40.0085235722312,-39.7366393919842,4.96742546794105));
#58898=CARTESIAN_POINT('Ctrl Pts',(40.1149177943607,-39.5793405247057,4.97942836510187));
#58899=CARTESIAN_POINT('Ctrl Pts',(40.3468765900167,-39.2364003247431,5.0055968685608));
#58900=CARTESIAN_POINT('Ctrl Pts',(40.3944742703015,-38.7687617621182,5.03176537201972));
#58901=CARTESIAN_POINT('Ctrl Pts',(40.2363680070802,-38.3861191307629,5.05793387547865));
#58902=CARTESIAN_POINT('Ctrl Pts',(40.0782617438588,-38.0034764994076,5.08410237893758));
#58903=CARTESIAN_POINT('Ctrl Pts',(39.7144515371312,-37.705829799322,5.11027088239651));
#58904=CARTESIAN_POINT('Ctrl Pts',(39.3080731239833,-37.626648148232,5.13643938585543));
#58905=CARTESIAN_POINT('Ctrl Pts',(38.9016947108354,-37.5474664971421,5.16260788931436));
#58906=CARTESIAN_POINT('Ctrl Pts',(38.4527480912673,-37.6867498950479,5.18877639277328));
#58907=CARTESIAN_POINT('Ctrl Pts',(38.1625484528667,-37.982040398373,5.21494489623221));
#58908=CARTESIAN_POINT('Ctrl Pts',(37.8723488144661,-38.2773309016981,5.24111339969114));
#58909=CARTESIAN_POINT('Ctrl Pts',(37.7408961572331,-38.7286285104427,5.26728190315006));
#58910=CARTESIAN_POINT('Ctrl Pts',(37.8271310042327,-39.1335692645202,5.29345040660899));
#58911=CARTESIAN_POINT('Ctrl Pts',(37.9133658512322,-39.5385100185978,5.31961891006792));
#58912=CARTESIAN_POINT('Ctrl Pts',(38.2172882024643,-39.8970939180085,5.34578741352684));
#58913=CARTESIAN_POINT('Ctrl Pts',(38.6026245602704,-40.0485211199672,5.37195591698577));
#58914=CARTESIAN_POINT('Ctrl Pts',(38.9533971820163,-40.1863656694333,5.39577716919699));
#58915=CARTESIAN_POINT('Ctrl Pts',(39.3716335617261,-40.1525497161724,5.4195984214082));
#58916=CARTESIAN_POINT('Ctrl Pts',(39.6994431549996,-39.9659335873643,5.44341967361942));
#58917=CARTESIAN_POINT('Ctrl Pts',(39.6980969738518,-39.9664052404928,5.30658032638059));
#58918=CARTESIAN_POINT('Ctrl Pts',(39.6555185906107,-39.9914032265725,5.30346402952864));
#58919=CARTESIAN_POINT('Ctrl Pts',(39.6114718472881,-40.0137802388959,5.30034773267669));
#58920=CARTESIAN_POINT('Ctrl Pts',(39.5661781885583,-40.0332575731161,5.29723143582474));
#58921=CARTESIAN_POINT('Ctrl Pts',(39.1858334006749,-40.1968147411666,5.27106293236581));
#58922=CARTESIAN_POINT('Ctrl Pts',(38.7175626520242,-40.1559017569539,5.24489442890688));
#58923=CARTESIAN_POINT('Ctrl Pts',(38.3713436649214,-39.928865763386,5.21872592544795));
#58924=CARTESIAN_POINT('Ctrl Pts',(38.0251246778187,-39.701829769818,5.19255742198903));
#58925=CARTESIAN_POINT('Ctrl Pts',(37.8009574522638,-39.2886707668948,5.1663889185301));
#58926=CARTESIAN_POINT('Ctrl Pts',(37.7993614588042,-38.8746535306862,5.14022041507118));
#58927=CARTESIAN_POINT('Ctrl Pts',(37.7977654653446,-38.4606362944777,5.11405191161225));
#58928=CARTESIAN_POINT('Ctrl Pts',(38.0187407039802,-38.0457608249837,5.08788340815333));
#58929=CARTESIAN_POINT('Ctrl Pts',(38.3631991409407,-37.8160625276688,5.0617149046944));
#58930=CARTESIAN_POINT('Ctrl Pts',(38.7076575779013,-37.5863642303539,5.03554640123547));
#58931=CARTESIAN_POINT('Ctrl Pts',(39.1755992131867,-37.5418431052182,5.00937789777654));
#58932=CARTESIAN_POINT('Ctrl Pts',(39.5571935097811,-37.7024627985796,4.98320939431762));
#58933=CARTESIAN_POINT('Ctrl Pts',(39.9387878063755,-37.863082491941,4.95704089085869));
#58934=CARTESIAN_POINT('Ctrl Pts',(40.2340347642788,-38.2288430037996,4.93087238739977));
#58935=CARTESIAN_POINT('Ctrl Pts',(40.3105421109525,-38.635733049973,4.90470388394084));
#58936=CARTESIAN_POINT('Ctrl Pts',(40.3870494576263,-39.0426230961465,4.87853538048192));
#58937=CARTESIAN_POINT('Ctrl Pts',(40.2448171930704,-39.4906426766349,4.85236687702299));
#58938=CARTESIAN_POINT('Ctrl Pts',(39.9476239688235,-39.7788944478041,4.82619837356406));
#58939=CARTESIAN_POINT('Ctrl Pts',(39.8733571986578,-39.8509268034997,4.8196590245029));
#58940=CARTESIAN_POINT('Ctrl Pts',(39.7894135884089,-39.9129821459893,4.81311967544174));
#58941=CARTESIAN_POINT('Ctrl Pts',(39.6989570949588,-39.9641614067485,4.80658032638058));
#58942=CARTESIAN_POINT('Origin',(39.0658530619283,-38.8697713466883,4.5));
#58943=CARTESIAN_POINT('',(39.6967352121902,-39.9639200225483,4.30658032638058));
#58944=CARTESIAN_POINT('',(39.6976237458347,-39.9660095563765,4.44341967361942));
#58945=CARTESIAN_POINT('',(39.6981030619283,-39.9648604697737,4.5));
#58946=CARTESIAN_POINT('Ctrl Pts',(39.6976237458347,-39.9660095563765,4.44341967361942));
#58947=CARTESIAN_POINT('Ctrl Pts',(39.9936753773632,-39.7916729655961,4.46507821669334));
#58948=CARTESIAN_POINT('Ctrl Pts',(40.2204527828214,-39.4929448719807,4.48673675976727));
#58949=CARTESIAN_POINT('Ctrl Pts',(40.2988032317419,-39.159355592007,4.50839530284119));
#58950=CARTESIAN_POINT('Ctrl Pts',(40.393468601734,-38.756302986065,4.53456380630012));
#58951=CARTESIAN_POINT('Ctrl Pts',(40.2714573392084,-38.3023593247387,4.56073230975905));
#58952=CARTESIAN_POINT('Ctrl Pts',(39.9874807525881,-38.0010783358291,4.58690081321797));
#58953=CARTESIAN_POINT('Ctrl Pts',(39.7035041659678,-37.6997973469195,4.6130693166769));
#58954=CARTESIAN_POINT('Ctrl Pts',(39.2575622552528,-37.5511790304267,4.63923782013583));
#58955=CARTESIAN_POINT('Ctrl Pts',(38.8496206579412,-37.6218656179337,4.66540632359475));
#58956=CARTESIAN_POINT('Ctrl Pts',(38.4416790606296,-37.6925522054406,4.69157482705368));
#58957=CARTESIAN_POINT('Ctrl Pts',(38.0717377767213,-37.9825436969474,4.71774333051261));
#58958=CARTESIAN_POINT('Ctrl Pts',(37.9056829078162,-38.3618044366461,4.74391183397153));
#58959=CARTESIAN_POINT('Ctrl Pts',(37.739628038911,-38.7410651763447,4.77008033743046));
#58960=CARTESIAN_POINT('Ctrl Pts',(37.7774595850089,-39.2095951642353,4.79624884088938));
#58961=CARTESIAN_POINT('Ctrl Pts',(38.0022133656485,-39.5573000327044,4.82241734434831));
#58962=CARTESIAN_POINT('Ctrl Pts',(38.2269671462881,-39.9050049011735,4.84858584780724));
#58963=CARTESIAN_POINT('Ctrl Pts',(38.6386431614693,-40.1318846502211,4.87475435126617));
#58964=CARTESIAN_POINT('Ctrl Pts',(39.0526411245735,-40.1362036060948,4.90092285472509));
#58965=CARTESIAN_POINT('Ctrl Pts',(39.2767476411253,-40.1385415551725,4.9150884610232));
#58966=CARTESIAN_POINT('Ctrl Pts',(39.5015345588232,-40.0756624434911,4.92925406732131));
#58967=CARTESIAN_POINT('Ctrl Pts',(39.697389467188,-39.9630895992609,4.94341967361942));
#58968=CARTESIAN_POINT('Ctrl Pts',(39.6989570949588,-39.9641614067485,4.80658032638058));
#58969=CARTESIAN_POINT('Ctrl Pts',(39.4274339724573,-40.1177861180175,4.78695117198281));
#58970=CARTESIAN_POINT('Ctrl Pts',(39.0972285087862,-40.1734152228909,4.76732201758505));
#58971=CARTESIAN_POINT('Ctrl Pts',(38.7939127211062,-40.1067326165456,4.74769286318728));
#58972=CARTESIAN_POINT('Ctrl Pts',(38.389548881574,-40.0178350522677,4.72152435972836));
#58973=CARTESIAN_POINT('Ctrl Pts',(38.0329753864477,-39.7115559618618,4.69535585626943));
#58974=CARTESIAN_POINT('Ctrl Pts',(37.8840840327675,-39.3252345207529,4.6691873528105));
#58975=CARTESIAN_POINT('Ctrl Pts',(37.7351926790873,-38.938913079644,4.64301884935158));
#58976=CARTESIAN_POINT('Ctrl Pts',(37.7939834668531,-38.472549287832,4.61685034589265));
#58977=CARTESIAN_POINT('Ctrl Pts',(38.0340939063583,-38.1352662178079,4.59068184243372));
#58978=CARTESIAN_POINT('Ctrl Pts',(38.2742043458635,-37.7979831477838,4.56451333897479));
#58979=CARTESIAN_POINT('Ctrl Pts',(38.6956344371082,-37.5897807995474,4.53834483551587));
#58980=CARTESIAN_POINT('Ctrl Pts',(39.1094099185268,-37.6040195786007,4.51217633205694));
#58981=CARTESIAN_POINT('Ctrl Pts',(39.5231853999454,-37.6182583576541,4.48600782859802));
#58982=CARTESIAN_POINT('Ctrl Pts',(39.929306271538,-37.854938263997,4.45983932513909));
#58983=CARTESIAN_POINT('Ctrl Pts',(40.1456631065934,-38.2079292154005,4.43367082168016));
#58984=CARTESIAN_POINT('Ctrl Pts',(40.3620199416489,-38.560920166804,4.40750231822124));
#58985=CARTESIAN_POINT('Ctrl Pts',(40.3886127401672,-39.030222163268,4.38133381476231));
#58986=CARTESIAN_POINT('Ctrl Pts',(40.2135169753906,-39.4053946105007,4.35516531130339));
#58987=CARTESIAN_POINT('Ctrl Pts',(40.1051548355753,-39.6375789196628,4.33897031632912));
#58988=CARTESIAN_POINT('Ctrl Pts',(39.9195450710429,-39.8337111891107,4.32277532135485));
#58989=CARTESIAN_POINT('Ctrl Pts',(39.6967352121902,-39.9639200225483,4.30658032638058));
#58990=CARTESIAN_POINT('Origin',(39.0658530619283,-38.8697713466883,4.5));
#58991=CARTESIAN_POINT('',(39.6990217970716,-39.9666307803348,3.80658032638058));
#58992=CARTESIAN_POINT('',(39.6992442211058,-39.9647402889406,3.94341967361942));
#58993=CARTESIAN_POINT('',(39.6981030619283,-39.9648604697737,4.5));
#58994=CARTESIAN_POINT('Ctrl Pts',(39.6992442211058,-39.9647402889406,3.94341967361942));
#58995=CARTESIAN_POINT('Ctrl Pts',(39.7703349168266,-39.9245305221536,3.94856535914752));
#58996=CARTESIAN_POINT('Ctrl Pts',(39.8373290103597,-39.877480560471,3.95371104467563));
#58997=CARTESIAN_POINT('Ctrl Pts',(39.8986640775363,-39.8239468894644,3.95885673020374));
#58998=CARTESIAN_POINT('Ctrl Pts',(40.2105849885204,-39.551700160189,3.98502523366267));
#58999=CARTESIAN_POINT('Ctrl Pts',(40.3761490651667,-39.1117681946799,4.01119373712159));
#59000=CARTESIAN_POINT('Ctrl Pts',(40.3211154074002,-38.7014217157033,4.03736224058052));
#59001=CARTESIAN_POINT('Ctrl Pts',(40.2660817496338,-38.2910752367267,4.06353074403944));
#59002=CARTESIAN_POINT('Ctrl Pts',(39.9904503574547,-37.9103142442825,4.08969924749837));
#59003=CARTESIAN_POINT('Ctrl Pts',(39.6178176236238,-37.7298764933343,4.1158677509573));
#59004=CARTESIAN_POINT('Ctrl Pts',(39.245184889793,-37.5494387423861,4.14203625441622));
#59005=CARTESIAN_POINT('Ctrl Pts',(38.7755508143104,-37.5693242329338,4.16820475787515));
#59006=CARTESIAN_POINT('Ctrl Pts',(38.4195048988346,-37.780616074816,4.19437326133408));
#59007=CARTESIAN_POINT('Ctrl Pts',(38.0634589833589,-37.9919079166982,4.220541764793));
#59008=CARTESIAN_POINT('Ctrl Pts',(37.82100122789,-38.3946061099149,4.24671026825193));
#59009=CARTESIAN_POINT('Ctrl Pts',(37.8008525725161,-38.8081359974719,4.27287877171085));
#59010=CARTESIAN_POINT('Ctrl Pts',(37.7807039171421,-39.221665885029,4.29904727516978));
#59011=CARTESIAN_POINT('Ctrl Pts',(37.9828643618631,-39.6460274669263,4.32521577862871));
#59012=CARTESIAN_POINT('Ctrl Pts',(38.3166827592479,-39.8909319662484,4.35138428208763));
#59013=CARTESIAN_POINT('Ctrl Pts',(38.6505011566327,-40.1358364655705,4.37755278554656));
#59014=CARTESIAN_POINT('Ctrl Pts',(39.1159775066813,-40.2012838823174,4.40372128900549));
#59015=CARTESIAN_POINT('Ctrl Pts',(39.5043866829606,-40.057926815412,4.42988979246442));
#59016=CARTESIAN_POINT('Ctrl Pts',(39.571326315215,-40.0332202175102,4.43439975284942));
#59017=CARTESIAN_POINT('Ctrl Pts',(39.6359768878004,-40.0023116804572,4.43890971323442));
#59018=CARTESIAN_POINT('Ctrl Pts',(39.6976237458347,-39.9660095563765,4.44341967361942));
#59019=CARTESIAN_POINT('Ctrl Pts',(39.6967352121902,-39.9639200225483,4.30658032638058));
#59020=CARTESIAN_POINT('Ctrl Pts',(39.5595202256301,-40.0441076920802,4.29660681789592));
#59021=CARTESIAN_POINT('Ctrl Pts',(39.4081968207292,-40.0992933977544,4.28663330941126));
#59022=CARTESIAN_POINT('Ctrl Pts',(39.2521185625475,-40.1225003286186,4.2766598009266));
#59023=CARTESIAN_POINT('Ctrl Pts',(38.8426002425525,-40.1833907015023,4.25049129746768));
#59024=CARTESIAN_POINT('Ctrl Pts',(38.4003479306342,-40.0241285492683,4.22432279400875));
#59025=CARTESIAN_POINT('Ctrl Pts',(38.1236728204874,-39.7161289139554,4.19815429054983));
#59026=CARTESIAN_POINT('Ctrl Pts',(37.8469977103406,-39.4081292786425,4.1719857870909));
#59027=CARTESIAN_POINT('Ctrl Pts',(37.7358998019653,-38.9513921602507,4.14581728363197));
#59028=CARTESIAN_POINT('Ctrl Pts',(37.840196718037,-38.5507239118952,4.11964878017305));
#59029=CARTESIAN_POINT('Ctrl Pts',(37.9444936341086,-38.1500556635397,4.09348027671412));
#59030=CARTESIAN_POINT('Ctrl Pts',(38.2641853746271,-37.8054562852204,4.06731177325519));
#59031=CARTESIAN_POINT('Ctrl Pts',(38.6559183630714,-37.6714482343174,4.04114326979627));
#59032=CARTESIAN_POINT('Ctrl Pts',(39.0476513515157,-37.5374401834144,4.01497476633734));
#59033=CARTESIAN_POINT('Ctrl Pts',(39.5114255878859,-37.6140234599277,3.98880626287842));
#59034=CARTESIAN_POINT('Ctrl Pts',(39.8392791917195,-37.8668572123836,3.96263775941949));
#59035=CARTESIAN_POINT('Ctrl Pts',(40.1671327955531,-38.1196909648395,3.93646925596056));
#59036=CARTESIAN_POINT('Ctrl Pts',(40.3590657668502,-38.548775193238,3.91030075250163));
#59037=CARTESIAN_POINT('Ctrl Pts',(40.3290130799472,-38.9617034290506,3.88413224904271));
#59038=CARTESIAN_POINT('Ctrl Pts',(40.2993254358659,-39.3696159240468,3.85828160815533));
#59039=CARTESIAN_POINT('Ctrl Pts',(40.0530121946873,-39.7617625287194,3.83243096726796));
#59040=CARTESIAN_POINT('Ctrl Pts',(39.6990217970716,-39.9666307803348,3.80658032638058));
#59041=CARTESIAN_POINT('Origin',(39.0658530619283,-38.8697713466883,4.5));
#59042=CARTESIAN_POINT('',(39.6981666138854,-39.9633157673858,3.30658032638058));
#59043=CARTESIAN_POINT('',(39.6968376638891,-39.9635050155947,3.44341967361942));
#59044=CARTESIAN_POINT('',(39.6981030619283,-39.9648604697737,4.5));
#59045=CARTESIAN_POINT('Ctrl Pts',(39.6968376638891,-39.9635050155947,3.44341967361942));
#59046=CARTESIAN_POINT('Ctrl Pts',(39.9008619683972,-39.8448845676908,3.45822100506063));
#59047=CARTESIAN_POINT('Ctrl Pts',(40.0737604294822,-39.6716358129756,3.47302233650185));
#59048=CARTESIAN_POINT('Ctrl Pts',(40.1838048209619,-39.4649259634328,3.48782366794306));
#59049=CARTESIAN_POINT('Ctrl Pts',(40.378361442473,-39.0994664482373,3.51399217140199));
#59050=CARTESIAN_POINT('Ctrl Pts',(40.3764510665601,-38.6294154424262,3.54016067486091));
#59051=CARTESIAN_POINT('Ctrl Pts',(40.1789303273027,-38.265549404193,3.56632917831984));
#59052=CARTESIAN_POINT('Ctrl Pts',(39.9814095880453,-37.9016833659598,3.59249768177876));
#59053=CARTESIAN_POINT('Ctrl Pts',(39.5882784854434,-37.6440022953046,3.61866618523769));
#59054=CARTESIAN_POINT('Ctrl Pts',(39.1758216795725,-37.6080534474275,3.64483468869662));
#59055=CARTESIAN_POINT('Ctrl Pts',(38.7633648737015,-37.5721045995503,3.67100319215554));
#59056=CARTESIAN_POINT('Ctrl Pts',(38.3315823645617,-37.7578879744512,3.69717169561447));
#59057=CARTESIAN_POINT('Ctrl Pts',(38.0740905614766,-38.0820960983986,3.7233401990734));
#59058=CARTESIAN_POINT('Ctrl Pts',(37.8165987583915,-38.406304222346,3.74950870253232));
#59059=CARTESIAN_POINT('Ctrl Pts',(37.7333976613611,-38.8689370953399,3.77567720599125));
#59060=CARTESIAN_POINT('Ctrl Pts',(37.8617956314422,-39.2625446379184,3.80184570945018));
#59061=CARTESIAN_POINT('Ctrl Pts',(37.9901936015233,-39.6561521804969,3.82801421290911));
#59062=CARTESIAN_POINT('Ctrl Pts',(38.3301906387158,-39.9807343926601,3.85418271636803));
#59063=CARTESIAN_POINT('Ctrl Pts',(38.729328029973,-40.0907447522208,3.88035121982696));
#59064=CARTESIAN_POINT('Ctrl Pts',(39.0499804019726,-40.1791230487932,3.90137403775778));
#59065=CARTESIAN_POINT('Ctrl Pts',(39.4088015299329,-40.129018226562,3.9223968556886));
#59066=CARTESIAN_POINT('Ctrl Pts',(39.6992442211058,-39.9647402889406,3.94341967361942));
#59067=CARTESIAN_POINT('Ctrl Pts',(39.6990217970716,-39.9666307803348,3.80658032638058));
#59068=CARTESIAN_POINT('Ctrl Pts',(39.6946690888126,-39.9691498648546,3.80626246380903));
#59069=CARTESIAN_POINT('Ctrl Pts',(39.6903001003537,-39.9716406339069,3.80594460123748));
#59070=CARTESIAN_POINT('Ctrl Pts',(39.6859150342415,-39.9741027686317,3.80562673866593));
#59071=CARTESIAN_POINT('Ctrl Pts',(39.3249080205419,-40.1768016291736,3.779458235207));
#59072=CARTESIAN_POINT('Ctrl Pts',(38.8549323382456,-40.1854271070305,3.75328973174807));
#59073=CARTESIAN_POINT('Ctrl Pts',(38.486730670363,-39.9961114351584,3.72712122828915));
#59074=CARTESIAN_POINT('Ctrl Pts',(38.1185290024803,-39.8067957632863,3.70095272483022));
#59075=CARTESIAN_POINT('Ctrl Pts',(37.8521013490113,-39.4195389416852,3.6747842213713));
#59076=CARTESIAN_POINT('Ctrl Pts',(37.8069170356359,-39.007991532901,3.64861571791237));
#59077=CARTESIAN_POINT('Ctrl Pts',(37.7617327222606,-38.5964441241169,3.62244721445344));
#59078=CARTESIAN_POINT('Ctrl Pts',(37.9377917489788,-38.1606061281498,3.59627871099451));
#59079=CARTESIAN_POINT('Ctrl Pts',(38.2561471576721,-37.8959124821361,3.57011020753559));
#59080=CARTESIAN_POINT('Ctrl Pts',(38.5745025663654,-37.6312188361225,3.54394170407666));
#59081=CARTESIAN_POINT('Ctrl Pts',(39.0351543570337,-37.5376695400622,3.51777320061774));
#59082=CARTESIAN_POINT('Ctrl Pts',(39.4315407865323,-37.6572132122937,3.49160469715881));
#59083=CARTESIAN_POINT('Ctrl Pts',(39.8279272160309,-37.7767568845252,3.46543619369988));
#59084=CARTESIAN_POINT('Ctrl Pts',(40.1600482843597,-38.1093935250484,3.43926769024095));
#59085=CARTESIAN_POINT('Ctrl Pts',(40.2789769657405,-38.5059649062659,3.41309918678203));
#59086=CARTESIAN_POINT('Ctrl Pts',(40.3979056471214,-38.9025362874834,3.3869306833231));
#59087=CARTESIAN_POINT('Ctrl Pts',(40.3036419415544,-39.3630424093952,3.36076217986418));
#59088=CARTESIAN_POINT('Ctrl Pts',(40.0384547967127,-39.6809868610392,3.33459367640525));
#59089=CARTESIAN_POINT('Ctrl Pts',(39.943827295091,-39.7944399061765,3.32525589306369));
#59090=CARTESIAN_POINT('Ctrl Pts',(39.8274361583624,-39.8897406125527,3.31591810972214));
#59091=CARTESIAN_POINT('Ctrl Pts',(39.6981666138854,-39.9633157673858,3.30658032638058));
#59092=CARTESIAN_POINT('Origin',(39.0658530619283,-38.8697713466883,4.5));
#59093=CARTESIAN_POINT('',(39.696945388151,-39.9649932150637,2.80658032638058));
#59094=CARTESIAN_POINT('',(39.6985897981371,-39.9666323328489,2.94341967361942));
#59095=CARTESIAN_POINT('',(39.6981030619283,-39.9648604697737,4.5));
#59096=CARTESIAN_POINT('Ctrl Pts',(39.6985897981371,-39.9666323328489,2.94341967361942));
#59097=CARTESIAN_POINT('Ctrl Pts',(40.0329227359303,-39.771464492525,2.96787665097374));
#59098=CARTESIAN_POINT('Ctrl Pts',(40.2741270402692,-39.4118258938478,2.99233362832806));
#59099=CARTESIAN_POINT('Ctrl Pts',(40.3224423052901,-39.0279123314598,3.01679060568238));
#59100=CARTESIAN_POINT('Ctrl Pts',(40.3741387255592,-38.6171320768221,3.04295910914131));
#59101=CARTESIAN_POINT('Ctrl Pts',(40.2050042874718,-38.1785603982041,3.06912761260023));
#59102=CARTESIAN_POINT('Ctrl Pts',(39.8908808035795,-37.908858034419,3.09529611605916));
#59103=CARTESIAN_POINT('Ctrl Pts',(39.5767573196872,-37.6391556706339,3.12146461951809));
#59104=CARTESIAN_POINT('Ctrl Pts',(39.1176447899899,-37.5383226216818,3.14763312297702));
#59105=CARTESIAN_POINT('Ctrl Pts',(38.7194147698321,-37.6515736327838,3.17380162643594));
#59106=CARTESIAN_POINT('Ctrl Pts',(38.3211847496743,-37.7648246438858,3.19997012989487));
#59107=CARTESIAN_POINT('Ctrl Pts',(37.9838372390559,-38.092159715042,3.22613863335379));
#59108=CARTESIAN_POINT('Ctrl Pts',(37.8586428520748,-38.4867979056613,3.25230713681272));
#59109=CARTESIAN_POINT('Ctrl Pts',(37.7334484650937,-38.8814360962806,3.27847564027165));
#59110=CARTESIAN_POINT('Ctrl Pts',(37.8204072017498,-39.343377406363,3.30464414373057));
#59111=CARTESIAN_POINT('Ctrl Pts',(38.080525740607,-39.6654818632946,3.3308126471895));
#59112=CARTESIAN_POINT('Ctrl Pts',(38.3406442794641,-39.9875863202263,3.35698115064843));
#59113=CARTESIAN_POINT('Ctrl Pts',(38.7739226205222,-40.1698539240072,3.38314965410735));
#59114=CARTESIAN_POINT('Ctrl Pts',(39.1860736005189,-40.1305537136077,3.40931815756628));
#59115=CARTESIAN_POINT('Ctrl Pts',(39.3651052785911,-40.1134823418097,3.42068532958399));
#59116=CARTESIAN_POINT('Ctrl Pts',(39.5401504513672,-40.0546035118007,3.43205250160171));
#59117=CARTESIAN_POINT('Ctrl Pts',(39.6968376638891,-39.9635050155947,3.44341967361942));
#59118=CARTESIAN_POINT('Ctrl Pts',(39.6981666138854,-39.9633157673858,3.30658032638058));
#59119=CARTESIAN_POINT('Ctrl Pts',(39.4651670418018,-40.0959299856956,3.28974960626321));
#59120=CARTESIAN_POINT('Ctrl Pts',(39.1903285963567,-40.157963071813,3.27291888614584));
#59121=CARTESIAN_POINT('Ctrl Pts',(38.9256802513517,-40.128491465009,3.25608816602847));
#59122=CARTESIAN_POINT('Ctrl Pts',(38.5142034349489,-40.0826688359585,3.22991966256954));
#59123=CARTESIAN_POINT('Ctrl Pts',(38.1273603862596,-39.8156407964813,3.20375115911062));
#59124=CARTESIAN_POINT('Ctrl Pts',(37.9386160518288,-39.4471459263554,3.17758265565169));
#59125=CARTESIAN_POINT('Ctrl Pts',(37.7498717173979,-39.0786510562295,3.15141415219276));
#59126=CARTESIAN_POINT('Ctrl Pts',(37.7592260972255,-38.6086893554548,3.12524564873384));
#59127=CARTESIAN_POINT('Ctrl Pts',(37.9624847270864,-38.2479971709405,3.09907714527491));
#59128=CARTESIAN_POINT('Ctrl Pts',(38.1657433569474,-37.8873049864262,3.07290864181599));
#59129=CARTESIAN_POINT('Ctrl Pts',(38.5629062368417,-37.6358823181722,3.04674013835706));
#59130=CARTESIAN_POINT('Ctrl Pts',(38.9758805061506,-37.6064702124723,3.02057163489813));
#59131=CARTESIAN_POINT('Ctrl Pts',(39.3888547754595,-37.5770581067724,2.99440313143921));
#59132=CARTESIAN_POINT('Ctrl Pts',(39.8176404341829,-37.7696565636265,2.96823462798028));
#59133=CARTESIAN_POINT('Ctrl Pts',(40.069965509642,-38.0979018769219,2.94206612452135));
#59134=CARTESIAN_POINT('Ctrl Pts',(40.3222905851012,-38.4261471902174,2.91589762106243));
#59135=CARTESIAN_POINT('Ctrl Pts',(40.3981550772959,-38.8900393599541,2.8897291176035));
#59136=CARTESIAN_POINT('Ctrl Pts',(40.263539208776,-39.2815641648305,2.86356061414457));
#59137=CARTESIAN_POINT('Ctrl Pts',(40.1658333166794,-39.5657377972484,2.84456718488991));
#59138=CARTESIAN_POINT('Ctrl Pts',(39.9572455465606,-39.811788018551,2.82557375563525));
#59139=CARTESIAN_POINT('Ctrl Pts',(39.696945388151,-39.9649932150637,2.80658032638058));
#59140=CARTESIAN_POINT('Origin',(39.0658530619283,-38.8697713466883,4.5));
#59141=CARTESIAN_POINT('',(39.6994125047665,-39.9658989902663,2.30658032638058));
#59142=CARTESIAN_POINT('',(39.6985816414592,-39.9636701304733,2.44341967361942));
#59143=CARTESIAN_POINT('',(39.6981030619283,-39.9648604697737,4.5));
#59144=CARTESIAN_POINT('',(39.301448933936,-37.6274127691862,2.));
#59145=CARTESIAN_POINT('Ctrl Pts',(39.6994125047665,-39.9658989902663,2.30658032638058));
#59146=CARTESIAN_POINT('Ctrl Pts',(39.3734254452084,-40.1513842194032,2.2828923946305));
#59147=CARTESIAN_POINT('Ctrl Pts',(38.9582283391778,-40.1860737601753,2.25920446288042));
#59148=CARTESIAN_POINT('Ctrl Pts',(38.6086499461795,-40.0507923518177,2.23551653113034));
#59149=CARTESIAN_POINT('Ctrl Pts',(38.2224641245192,-39.901344437163,2.20934802767141));
#59150=CARTESIAN_POINT('Ctrl Pts',(37.9163596177671,-39.5444633609379,2.18317952421248));
#59151=CARTESIAN_POINT('Ctrl Pts',(37.8282894528998,-39.1398698141336,2.15701102075356));
#59152=CARTESIAN_POINT('Ctrl Pts',(37.7402192880324,-38.7352762673292,2.13084251729463));
#59153=CARTESIAN_POINT('Ctrl Pts',(37.8701834650499,-38.2829702499457,2.10467401383571));
#59154=CARTESIAN_POINT('Ctrl Pts',(38.1583556110386,-37.9866358554263,2.07850551037678));
#59155=CARTESIAN_POINT('Ctrl Pts',(38.4465277570273,-37.6903014609069,2.05233700691785));
#59156=CARTESIAN_POINT('Ctrl Pts',(38.8929078719872,-37.5499386892516,2.02616850345893));
#59157=CARTESIAN_POINT('Ctrl Pts',(39.301448933936,-37.6274127691862,2.));
#59158=CARTESIAN_POINT('',(40.2614317556683,-39.2879039300607,2.));
#59159=CARTESIAN_POINT('Origin',(39.0658530619283,-38.8697713466883,2.));
#59160=CARTESIAN_POINT('Ctrl Pts',(40.2614422049139,-39.287909445603,2.));
#59161=CARTESIAN_POINT('Ctrl Pts',(40.3902478674695,-38.9153329576355,2.02490816038701));
#59162=CARTESIAN_POINT('Ctrl Pts',(40.3325476766157,-38.4763154063562,2.04981632077402));
#59163=CARTESIAN_POINT('Ctrl Pts',(40.1090165446371,-38.1516794088469,2.07472448116103));
#59164=CARTESIAN_POINT('Ctrl Pts',(39.8741748257196,-37.8106169581592,2.10089298461995));
#59165=CARTESIAN_POINT('Ctrl Pts',(39.4562956252315,-37.5958042374567,2.12706148807888));
#59166=CARTESIAN_POINT('Ctrl Pts',(39.042397118114,-37.6034976893836,2.15322999153781));
#59167=CARTESIAN_POINT('Ctrl Pts',(38.6284986109964,-37.6111911413106,2.17939849499673));
#59168=CARTESIAN_POINT('Ctrl Pts',(38.2185807972492,-37.841390765867,2.20556699845566));
#59169=CARTESIAN_POINT('Ctrl Pts',(37.996635575997,-38.1909062543644,2.23173550191459));
#59170=CARTESIAN_POINT('Ctrl Pts',(37.7746903547448,-38.5404217428618,2.25790400537351));
#59171=CARTESIAN_POINT('Ctrl Pts',(37.7407177259875,-39.0092530953003,2.28407250883244));
#59172=CARTESIAN_POINT('Ctrl Pts',(37.909862273516,-39.3871539257345,2.31024101229137));
#59173=CARTESIAN_POINT('Ctrl Pts',(38.0790068210445,-39.7650547561687,2.33640951575029));
#59174=CARTESIAN_POINT('Ctrl Pts',(38.4512685448588,-40.0520250645987,2.36257801920922));
#59175=CARTESIAN_POINT('Ctrl Pts',(38.8597650567826,-40.1193923002797,2.38874652266815));
#59176=CARTESIAN_POINT('Ctrl Pts',(39.1442519845445,-40.1663084852441,2.40697090631857));
#59177=CARTESIAN_POINT('Ctrl Pts',(39.4463130348952,-40.1067156626302,2.42519528996899));
#59178=CARTESIAN_POINT('Ctrl Pts',(39.6985816414592,-39.9636701304733,2.44341967361942));
#59179=CARTESIAN_POINT('Origin',(39.0658530619283,-38.8697713466883,0.895788276411275));
#59180=CARTESIAN_POINT('',(39.8389883040074,-40.2073580112696,5.60421172358873));
#59181=CARTESIAN_POINT('',(39.8361023073888,-40.2039982703455,5.64578827641128));
#59182=CARTESIAN_POINT('',(39.8373530619283,-40.2060485447276,0.895788276411275));
#59183=CARTESIAN_POINT('',(37.5756558680257,-39.2699729499894,6.));
#59184=CARTESIAN_POINT('Ctrl Pts',(39.8361023073888,-40.2039982703455,5.64578827641128));
#59185=CARTESIAN_POINT('Ctrl Pts',(40.0618255698415,-40.0734865888946,5.65918483710515));
#59186=CARTESIAN_POINT('Ctrl Pts',(40.6360432757833,-39.5276070596663,5.69874990125794));
#59187=CARTESIAN_POINT('Ctrl Pts',(40.706254476474,-38.0891194878961,5.76448346886966));
#59188=CARTESIAN_POINT('Ctrl Pts',(39.3195619844849,-37.0695313077001,5.84298897924644));
#59189=CARTESIAN_POINT('Ctrl Pts',(37.7040659529861,-37.6679522088103,5.92149448962322));
#59190=CARTESIAN_POINT('Ctrl Pts',(37.4440523270134,-38.7799318659295,5.97383149654107));
#59191=CARTESIAN_POINT('Ctrl Pts',(37.5756558680257,-39.2699729499894,6.));
#59192=CARTESIAN_POINT('',(37.9726388313436,-39.9622904787117,6.));
#59193=CARTESIAN_POINT('Origin',(39.0658530619283,-38.8697713466883,6.));
#59194=CARTESIAN_POINT('Ctrl Pts',(39.8389883040074,-40.2073580112696,5.60421172358873));
#59195=CARTESIAN_POINT('Ctrl Pts',(39.8784035047361,-40.1849196436101,5.60655897483644));
#59196=CARTESIAN_POINT('Ctrl Pts',(40.3442265162732,-39.8903323926485,5.63507472954307));
#59197=CARTESIAN_POINT('Ctrl Pts',(40.8821362004287,-38.8192621207562,5.68975898770864));
#59198=CARTESIAN_POINT('Ctrl Pts',(40.025658400892,-37.3267854127763,5.76826449808541));
#59199=CARTESIAN_POINT('Ctrl Pts',(38.3080469143,-37.2183586878016,5.8467700084622));
#59200=CARTESIAN_POINT('Ctrl Pts',(37.2874279838023,-38.5683990357347,5.92401517576705));
#59201=CARTESIAN_POINT('Ctrl Pts',(37.6338153475925,-39.6208332722494,5.97509183961299));
#59202=CARTESIAN_POINT('Ctrl Pts',(37.972630261787,-39.9623020734811,6.));
#59203=CARTESIAN_POINT('Origin',(39.0658530619283,-38.8697713466883,0.895788276411275));
#59204=CARTESIAN_POINT('',(39.836482301403,-40.2038876485621,5.10421172358873));
#59205=CARTESIAN_POINT('',(39.8373456329824,-40.2079335437151,5.14578827641127));
#59206=CARTESIAN_POINT('',(39.8373530619283,-40.2060485447276,0.895788276411275));
#59207=CARTESIAN_POINT('Ctrl Pts',(39.8373456329825,-40.2079335437151,5.14578827641127));
#59208=CARTESIAN_POINT('Ctrl Pts',(40.2216806378634,-39.9822885010756,5.16884048301825));
#59209=CARTESIAN_POINT('Ctrl Pts',(40.8329618074792,-39.1268210714738,5.21806119308415));
#59210=CARTESIAN_POINT('Ctrl Pts',(40.3208244444739,-37.5557551266231,5.29345040660899));
#59211=CARTESIAN_POINT('Ctrl Pts',(38.6620380533447,-37.098163044885,5.37195591698576));
#59212=CARTESIAN_POINT('Ctrl Pts',(37.3653845951192,-38.2294425600612,5.45046142736254));
#59213=CARTESIAN_POINT('Ctrl Pts',(37.5937879163964,-39.9348809965236,5.52896693773932));
#59214=CARTESIAN_POINT('Ctrl Pts',(38.8780553810739,-40.5572546562641,5.59407588742224));
#59215=CARTESIAN_POINT('Ctrl Pts',(39.6209034474226,-40.3284248126315,5.63301633364622));
#59216=CARTESIAN_POINT('Ctrl Pts',(39.8361023073888,-40.2039982703455,5.64578827641128));
#59217=CARTESIAN_POINT('Ctrl Pts',(39.836482301403,-40.2038876485621,5.10421172358873));
#59218=CARTESIAN_POINT('Ctrl Pts',(40.0389857717083,-40.0874933656255,5.11621462074955));
#59219=CARTESIAN_POINT('Ctrl Pts',(40.6023754577107,-39.5788852724495,5.15438602136929));
#59220=CARTESIAN_POINT('Ctrl Pts',(40.745177494668,-38.1758811994982,5.21872592544796));
#59221=CARTESIAN_POINT('Ctrl Pts',(39.4133645670745,-37.0862753673934,5.29723143582474));
#59222=CARTESIAN_POINT('Ctrl Pts',(37.7698897533292,-37.5961550422893,5.37573694620152));
#59223=CARTESIAN_POINT('Ctrl Pts',(37.2886763485592,-39.2482362054987,5.4542424565783));
#59224=CARTESIAN_POINT('Ctrl Pts',(38.3679904575112,-40.5216689106221,5.53040071570737));
#59225=CARTESIAN_POINT('Ctrl Pts',(39.4389802356634,-40.4350754385143,5.58039047137751));
#59226=CARTESIAN_POINT('Ctrl Pts',(39.8389883040074,-40.2073580112696,5.60421172358873));
#59227=CARTESIAN_POINT('Origin',(39.0658530619283,-38.8697713466883,0.895788276411275));
#59228=CARTESIAN_POINT('',(39.8367681787868,-40.2074507120888,4.60421172358873));
#59229=CARTESIAN_POINT('',(39.838395191597,-40.2051955164573,4.64578827641127));
#59230=CARTESIAN_POINT('',(39.8373530619283,-40.2060485447276,0.895788276411275));
#59231=CARTESIAN_POINT('Ctrl Pts',(39.838395191597,-40.2051955164573,4.64578827641127));
#59232=CARTESIAN_POINT('Ctrl Pts',(39.9487742895753,-40.1427442714186,4.65232762547243));
#59233=CARTESIAN_POINT('Ctrl Pts',(40.461107190991,-39.7640019994127,4.68503547799252));
#59234=CARTESIAN_POINT('Ctrl Pts',(40.85159479603,-38.533999133735,4.74391183397153));
#59235=CARTESIAN_POINT('Ctrl Pts',(39.7707737852476,-37.1950466549739,4.82241734434831));
#59236=CARTESIAN_POINT('Ctrl Pts',(38.05776324374,-37.3580267168588,4.90092285472509));
#59237=CARTESIAN_POINT('Ctrl Pts',(37.248831349992,-38.8767760630728,4.97942836510187));
#59238=CARTESIAN_POINT('Ctrl Pts',(38.0694482634704,-40.3892418792306,5.05793387547864));
#59239=CARTESIAN_POINT('Ctrl Pts',(39.280304717179,-40.4950348443414,5.11338717924845));
#59240=CARTESIAN_POINT('Ctrl Pts',(39.7853895670741,-40.2384372151433,5.14267197955933));
#59241=CARTESIAN_POINT('Ctrl Pts',(39.8373456329825,-40.2079335437151,5.14578827641127));
#59242=CARTESIAN_POINT('Ctrl Pts',(39.8367681787868,-40.2074507120888,4.60421172358873));
#59243=CARTESIAN_POINT('Ctrl Pts',(40.1980237481411,-39.9947173316426,4.62587026666265));
#59244=CARTESIAN_POINT('Ctrl Pts',(40.8090940791592,-39.1897699662685,4.6736973131955));
#59245=CARTESIAN_POINT('Ctrl Pts',(40.3881021894618,-37.6234670214255,4.74769286318729));
#59246=CARTESIAN_POINT('Ctrl Pts',(38.7556268199881,-37.0794146789619,4.82619837356406));
#59247=CARTESIAN_POINT('Ctrl Pts',(37.4013696406987,-38.1409968175026,4.90470388394084));
#59248=CARTESIAN_POINT('Ctrl Pts',(37.5398609233301,-39.8561611622599,4.98320939431763));
#59249=CARTESIAN_POINT('Ctrl Pts',(38.8164833870163,-40.5597236082337,5.04971200753358));
#59250=CARTESIAN_POINT('Ctrl Pts',(39.5974912981551,-40.3412541164524,5.09004611729062));
#59251=CARTESIAN_POINT('Ctrl Pts',(39.836482301403,-40.2038876485621,5.10421172358873));
#59252=CARTESIAN_POINT('Origin',(39.0658530619283,-38.8697713466883,0.895788276411275));
#59253=CARTESIAN_POINT('',(39.8387455558871,-40.2059018946483,4.10421172358873));
#59254=CARTESIAN_POINT('',(39.835683949911,-40.2049009685562,4.14578827641127));
#59255=CARTESIAN_POINT('',(39.8373530619283,-40.2060485447276,0.895788276411275));
#59256=CARTESIAN_POINT('Ctrl Pts',(39.8356839499109,-40.2049009685562,4.14578827641127));
#59257=CARTESIAN_POINT('Ctrl Pts',(40.107566600927,-40.0460142702611,4.16198327138554));
#59258=CARTESIAN_POINT('Ctrl Pts',(40.7000264343407,-39.4199669716347,4.20434676981874));
#59259=CARTESIAN_POINT('Ctrl Pts',(40.6150446849375,-37.9202337024769,4.27287877171085));
#59260=CARTESIAN_POINT('Ctrl Pts',(39.1283436057741,-37.0538111746305,4.35138428208763));
#59261=CARTESIAN_POINT('Ctrl Pts',(37.5855995232344,-37.8159848954578,4.42988979246441));
#59262=CARTESIAN_POINT('Ctrl Pts',(37.3703820012353,-39.5232193693979,4.50839530284119));
#59263=CARTESIAN_POINT('Ctrl Pts',(38.5669726422017,-40.5510318627907,4.58036146415681));
#59264=CARTESIAN_POINT('Ctrl Pts',(39.5070704165714,-40.3926553262541,4.6261591220135));
#59265=CARTESIAN_POINT('Ctrl Pts',(39.838395191597,-40.2051955164573,4.64578827641127));
#59266=CARTESIAN_POINT('Ctrl Pts',(39.8387455558871,-40.2059018946483,4.10421172358873));
#59267=CARTESIAN_POINT('Ctrl Pts',(39.9254936329904,-40.1568361214949,4.10935740911683));
#59268=CARTESIAN_POINT('Ctrl Pts',(40.4229804016609,-39.8074510911276,4.14067159810387));
#59269=CARTESIAN_POINT('Ctrl Pts',(40.8667641756191,-38.6282419782981,4.19815429054982));
#59270=CARTESIAN_POINT('Ctrl Pts',(39.8577505620191,-37.2343767082119,4.27665980092661));
#59271=CARTESIAN_POINT('Ctrl Pts',(38.1385444446534,-37.3071722287697,4.35516531130338));
#59272=CARTESIAN_POINT('Ctrl Pts',(37.2509707395799,-38.781343787805,4.43367082168017));
#59273=CARTESIAN_POINT('Ctrl Pts',(37.9910266499109,-40.3348192821528,4.51217633205694));
#59274=CARTESIAN_POINT('Ctrl Pts',(39.2249072234587,-40.508306713049,4.5690232993598));
#59275=CARTESIAN_POINT('Ctrl Pts',(39.7615438988762,-40.2517482031576,4.59970176320373));
#59276=CARTESIAN_POINT('Ctrl Pts',(39.8367681787868,-40.2074507120888,4.60421172358873));
#59277=CARTESIAN_POINT('Origin',(39.0658530619283,-38.8697713466883,0.895788276411275));
#59278=CARTESIAN_POINT('',(39.8358089661004,-40.2043945583313,3.60421172358873));
#59279=CARTESIAN_POINT('',(39.8384741440367,-40.2082087576147,3.64578827641127));
#59280=CARTESIAN_POINT('',(39.8373530619283,-40.2060485447276,0.895788276411275));
#59281=CARTESIAN_POINT('Ctrl Pts',(39.8384741440367,-40.2082087576148,3.64578827641127));
#59282=CARTESIAN_POINT('Ctrl Pts',(40.2704292120644,-39.9582192659243,3.67163891729865));
#59283=CARTESIAN_POINT('Ctrl Pts',(40.8752500438969,-38.9953053985924,3.72365806164495));
#59284=CARTESIAN_POINT('Ctrl Pts',(40.1754790439541,-37.4309014426854,3.80184570945018));
#59285=CARTESIAN_POINT('Ctrl Pts',(38.4777242474675,-37.1505503260543,3.88035121982696));
#59286=CARTESIAN_POINT('Ctrl Pts',(37.3074173539442,-38.4120374927131,3.95885673020373));
#59287=CARTESIAN_POINT('Ctrl Pts',(37.7141174076169,-40.0840312618198,4.03736224058051));
#59288=CARTESIAN_POINT('Ctrl Pts',(38.9991071509757,-40.5467766825013,4.09967275598303));
#59289=CARTESIAN_POINT('Ctrl Pts',(39.6682480272046,-40.3027495838885,4.13581476792661));
#59290=CARTESIAN_POINT('Ctrl Pts',(39.8356839499109,-40.2049009685562,4.14578827641127));
#59291=CARTESIAN_POINT('Ctrl Pts',(39.8358089661004,-40.2043945583313,3.60421172358873));
#59292=CARTESIAN_POINT('Ctrl Pts',(40.0847686354211,-40.0596485313517,3.61901305502994));
#59293=CARTESIAN_POINT('Ctrl Pts',(40.6687535790882,-39.4744804296356,3.65998288993008));
#59294=CARTESIAN_POINT('Ctrl Pts',(40.662772801836,-38.0029007557487,3.72712122828915));
#59295=CARTESIAN_POINT('Ctrl Pts',(39.2236238307452,-37.0595985208236,3.80562673866593));
#59296=CARTESIAN_POINT('Ctrl Pts',(37.642982284831,-37.7397023107928,3.88413224904271));
#59297=CARTESIAN_POINT('Ctrl Pts',(37.3384050779085,-39.4332788778856,3.96263775941949));
#59298=CARTESIAN_POINT('Ctrl Pts',(38.501463750429,-40.5436066616789,4.03599758426816));
#59299=CARTESIAN_POINT('Ctrl Pts',(39.4843342688331,-40.4063612522993,4.08318890565791));
#59300=CARTESIAN_POINT('Ctrl Pts',(39.8387455558871,-40.2059018946483,4.10421172358873));
#59301=CARTESIAN_POINT('Origin',(39.0658530619283,-38.8697713466883,0.895788276411275));
#59302=CARTESIAN_POINT('',(39.8379469994295,-40.2082106520626,3.10421172358873));
#59303=CARTESIAN_POINT('',(39.8374306108961,-40.204163629121,3.14578827641127));
#59304=CARTESIAN_POINT('',(39.8373530619283,-40.2060485447276,0.895788276411275));
#59305=CARTESIAN_POINT('Ctrl Pts',(39.8374306108961,-40.204163629121,3.14578827641127));
#59306=CARTESIAN_POINT('Ctrl Pts',(39.9951711463868,-40.1143839028202,3.15512605975283));
#59307=CARTESIAN_POINT('Ctrl Pts',(40.5352143013727,-39.6721982210719,3.19063234655331));
#59308=CARTESIAN_POINT('Ctrl Pts',(40.8063086069208,-38.3478222423284,3.25230713681272));
#59309=CARTESIAN_POINT('Ctrl Pts',(39.5905012322319,-37.1301274942209,3.3308126471895));
#59310=CARTESIAN_POINT('Ctrl Pts',(37.9041768834746,-37.472586720368,3.40931815756627));
#59311=CARTESIAN_POINT('Ctrl Pts',(37.259671359806,-39.0680743307528,3.48782366794306));
#59312=CARTESIAN_POINT('Ctrl Pts',(38.2349925206666,-40.4857191130318,3.56632917831984));
#59313=CARTESIAN_POINT('Ctrl Pts',(39.3889296125876,-40.4645408708171,3.61898404780924));
#59314=CARTESIAN_POINT('Ctrl Pts',(39.8331627728674,-40.2112826582981,3.64547041383972));
#59315=CARTESIAN_POINT('Ctrl Pts',(39.8384741440367,-40.2082087576148,3.64578827641127));
#59316=CARTESIAN_POINT('Ctrl Pts',(39.8379469994295,-40.2082106520626,3.10421172358873));
#59317=CARTESIAN_POINT('Ctrl Pts',(40.2459151473258,-39.9700580402637,3.12866870094305));
#59318=CARTESIAN_POINT('Ctrl Pts',(40.8551693385609,-39.0616525117033,3.1792941817563));
#59319=CARTESIAN_POINT('Ctrl Pts',(40.249511348243,-37.4911595684212,3.25608816602847));
#59320=CARTESIAN_POINT('Ctrl Pts',(38.5688218267177,-37.1220364497186,3.33459367640525));
#59321=CARTESIAN_POINT('Ctrl Pts',(37.333881829365,-38.3203235548052,3.41309918678203));
#59322=CARTESIAN_POINT('Ctrl Pts',(37.6522147609438,-40.0113684930191,3.49160469715881));
#59323=CARTESIAN_POINT('Ctrl Pts',(38.9392875485226,-40.5528026028124,3.55530887609437));
#59324=CARTESIAN_POINT('Ctrl Pts',(39.6446121539838,-40.3155570570627,3.59284455157101));
#59325=CARTESIAN_POINT('Ctrl Pts',(39.8358089661004,-40.2043945583313,3.60421172358873));
#59326=CARTESIAN_POINT('Origin',(39.0658530619283,-38.8697713466883,0.895788276411275));
#59327=CARTESIAN_POINT('',(39.8379370462827,-40.2045960389621,2.60421172358873));
#59328=CARTESIAN_POINT('',(39.8359404161091,-40.2062105265248,2.64578827641127));
#59329=CARTESIAN_POINT('',(39.8373530619283,-40.2060485447276,0.895788276411275));
#59330=CARTESIAN_POINT('Ctrl Pts',(39.8359404161091,-40.2062105265248,2.64578827641127));
#59331=CARTESIAN_POINT('Ctrl Pts',(40.1535704235635,-40.0192626275773,2.66478170566594));
#59332=CARTESIAN_POINT('Ctrl Pts',(40.7587789941875,-39.3053583432972,2.70994363837953));
#59333=CARTESIAN_POINT('Ctrl Pts',(40.5064415845057,-37.7623789454716,2.78127407455204));
#59334=CARTESIAN_POINT('Ctrl Pts',(38.936770715205,-37.057326943275,2.85977958492882));
#59335=CARTESIAN_POINT('Ctrl Pts',(37.4828624739785,-37.9777188225534,2.9382850953056));
#59336=CARTESIAN_POINT('Ctrl Pts',(37.4486185639574,-39.6981242894462,3.01679060568238));
#59337=CARTESIAN_POINT('Ctrl Pts',(38.6963080267235,-40.5593729851321,3.0859583327176));
#59338=CARTESIAN_POINT('Ctrl Pts',(39.5531140116671,-40.3659854866553,3.1289575562939));
#59339=CARTESIAN_POINT('Ctrl Pts',(39.8374306108961,-40.204163629121,3.14578827641127));
#59340=CARTESIAN_POINT('Ctrl Pts',(39.8379370462827,-40.2045960389621,2.60421172358873));
#59341=CARTESIAN_POINT('Ctrl Pts',(39.9721218195358,-40.1285083617881,2.61215584339723));
#59342=CARTESIAN_POINT('Ctrl Pts',(40.4987455670004,-39.7186935414777,2.64626846666466));
#59343=CARTESIAN_POINT('Ctrl Pts',(40.8313104277201,-38.439942299895,2.70654959339101));
#59344=CARTESIAN_POINT('Ctrl Pts',(39.6811395860237,-37.1600807661057,2.78505510376779));
#59345=CARTESIAN_POINT('Ctrl Pts',(37.9791520940816,-37.4135079224237,2.86356061414458));
#59346=CARTESIAN_POINT('Ctrl Pts',(37.2517503435483,-38.9729479619196,2.94206612452135));
#59347=CARTESIAN_POINT('Ctrl Pts',(38.1512758267994,-40.4398561533634,3.02057163489813));
#59348=CARTESIAN_POINT('Ctrl Pts',(39.3352629723092,-40.4803512300078,3.07462016792059));
#59349=CARTESIAN_POINT('Ctrl Pts',(39.8093969408979,-40.2248768330901,3.10250019748412));
#59350=CARTESIAN_POINT('Ctrl Pts',(39.8379469994295,-40.2082106520626,3.10421172358873));
#59351=CARTESIAN_POINT('Origin',(39.0658530619283,-38.8697713466883,0.895788276411275));
#59352=CARTESIAN_POINT('',(39.835191636477,-40.2053827942122,2.10421172358873));
#59353=CARTESIAN_POINT('',(39.8389509032089,-40.2073157943284,2.14578827641127));
#59354=CARTESIAN_POINT('',(39.8373530619283,-40.2060485447276,0.895788276411275));
#59355=CARTESIAN_POINT('',(37.9741697098829,-39.9602191716056,2.));
#59356=CARTESIAN_POINT('Ctrl Pts',(37.9741697098829,-39.9602191716056,2.));
#59357=CARTESIAN_POINT('Ctrl Pts',(38.3327559670707,-40.3192117233802,2.02616850345893));
#59358=CARTESIAN_POINT('Ctrl Pts',(39.0582121561479,-40.5387775404138,2.06090574465517));
#59359=CARTESIAN_POINT('Ctrl Pts',(39.6915909718076,-40.2896039589219,2.09564298585141));
#59360=CARTESIAN_POINT('Ctrl Pts',(39.835191636477,-40.2053827942122,2.10421172358873));
#59361=CARTESIAN_POINT('',(37.5730967199607,-39.2702632425652,2.));
#59362=CARTESIAN_POINT('Origin',(39.0658530619283,-38.8697713466883,2.));
#59363=CARTESIAN_POINT('Ctrl Pts',(37.5730824075077,-39.2702648660738,2.));
#59364=CARTESIAN_POINT('Ctrl Pts',(37.6993955576028,-39.7344217910383,2.02490816038701));
#59365=CARTESIAN_POINT('Ctrl Pts',(38.4017837618403,-40.520493253107,2.0735042525241));
#59366=CARTESIAN_POINT('Ctrl Pts',(39.4411667728031,-40.4336532467271,2.12210034466119));
#59367=CARTESIAN_POINT('Ctrl Pts',(39.8389509032089,-40.2073157943284,2.14578827641127));
#59368=CARTESIAN_POINT('Origin',(13.,-3.,18.));
#59369=CARTESIAN_POINT('',(9.53939201416946,-3.,18.));
#59370=CARTESIAN_POINT('',(9.53939201416946,-3.,2.));
#59371=CARTESIAN_POINT('',(9.53939201416946,-3.,0.));
#59372=CARTESIAN_POINT('',(13.,-3.,18.));
#59373=CARTESIAN_POINT('',(6.5,-3.,18.));
#59374=CARTESIAN_POINT('',(13.,-3.,2.));
#59375=CARTESIAN_POINT('',(13.,-3.,18.));
#59376=CARTESIAN_POINT('',(6.5,-3.,2.));
#59377=CARTESIAN_POINT('Origin',(13.,3.,18.));
#59378=CARTESIAN_POINT('',(13.,3.,18.));
#59379=CARTESIAN_POINT('',(13.,1.5,18.));
#59380=CARTESIAN_POINT('',(13.,3.,2.));
#59381=CARTESIAN_POINT('',(13.,3.,18.));
#59382=CARTESIAN_POINT('',(13.,1.5,2.));
#59383=CARTESIAN_POINT('Origin',(7.,3.,18.));
#59384=CARTESIAN_POINT('',(9.53939201416946,3.,2.));
#59385=CARTESIAN_POINT('',(9.53939201416946,3.,18.));
#59386=CARTESIAN_POINT('',(9.53939201416946,3.,0.));
#59387=CARTESIAN_POINT('',(3.5,3.,2.));
#59388=CARTESIAN_POINT('',(3.5,3.,18.));
#59389=CARTESIAN_POINT('Origin',(0.,0.,18.));
#59390=CARTESIAN_POINT('',(46.0449384185095,-16.7589870229578,18.));
#59391=CARTESIAN_POINT('',(34.5017338047181,-32.2758373034865,18.));
#59392=CARTESIAN_POINT('Ctrl Pts',(46.0449384185095,-16.7589870229578,18.));
#59393=CARTESIAN_POINT('Ctrl Pts',(45.8743956437238,-17.1218851168881,18.));
#59394=CARTESIAN_POINT('Ctrl Pts',(45.6995171721829,-17.4824839536868,18.));
#59395=CARTESIAN_POINT('Ctrl Pts',(45.5203598455,-17.8406806900323,18.));
#59396=CARTESIAN_POINT('Ctrl Pts',(45.1531768081802,-18.5748050936752,18.));
#59397=CARTESIAN_POINT('Ctrl Pts',(44.7680194870699,-19.2988348495882,18.));
#59398=CARTESIAN_POINT('Ctrl Pts',(44.3654220486085,-20.0118834338741,18.));
#59399=CARTESIAN_POINT('Ctrl Pts',(43.9631822808423,-20.7242985402524,18.));
#59400=CARTESIAN_POINT('Ctrl Pts',(43.5435334515142,-21.425751826585,18.));
#59401=CARTESIAN_POINT('Ctrl Pts',(43.1070531396035,-22.1153854338476,18.));
#59402=CARTESIAN_POINT('Ctrl Pts',(42.6709588293944,-22.8044091630961,18.));
#59403=CARTESIAN_POINT('Ctrl Pts',(42.2180628840101,-23.4816339600163,18.));
#59404=CARTESIAN_POINT('Ctrl Pts',(41.7489848299194,-24.1462327731379,18.));
#59405=CARTESIAN_POINT('Ctrl Pts',(41.2803227785336,-24.8102421856223,18.));
#59406=CARTESIAN_POINT('Ctrl Pts',(40.7955074062862,-25.4616478541608,18.));
#59407=CARTESIAN_POINT('Ctrl Pts',(40.295198597365,-26.0996556279412,18.));
#59408=CARTESIAN_POINT('Ctrl Pts',(39.7955319525129,-26.736844496156,18.));
#59409=CARTESIAN_POINT('Ctrl Pts',(39.2804117264143,-27.360669703197,18.));
#59410=CARTESIAN_POINT('Ctrl Pts',(38.7505356300951,-27.9703729038242,18.));
#59411=CARTESIAN_POINT('Ctrl Pts',(38.2210732096325,-28.5796001073353,18.));
#59412=CARTESIAN_POINT('Ctrl Pts',(37.6768780617941,-29.1747272108444,18.));
#59413=CARTESIAN_POINT('Ctrl Pts',(37.1186849480847,-29.7550324141308,18.));
#59414=CARTESIAN_POINT('Ctrl Pts',(36.5611161547233,-30.3346885654357,18.));
#59415=CARTESIAN_POINT('Ctrl Pts',(35.9895808113595,-30.899555826196,18.));
#59416=CARTESIAN_POINT('Ctrl Pts',(35.4048480816292,-31.4489514860585,18.));
#59417=CARTESIAN_POINT('Ctrl Pts',(35.107194183748,-31.7286173082753,18.));
#59418=CARTESIAN_POINT('Ctrl Pts',(34.8061210997365,-32.0042746598847,18.));
#59419=CARTESIAN_POINT('Ctrl Pts',(34.5017338047268,-32.2758373034788,18.));
#59420=CARTESIAN_POINT('',(44.1555553153094,-16.0713078122675,18.));
#59421=CARTESIAN_POINT('',(21.6129302780759,-7.86646329649042,18.));
#59422=CARTESIAN_POINT('',(43.5508185339833,-14.8096659320883,18.));
#59423=CARTESIAN_POINT('Origin',(44.4975754586351,-15.1316151914816,18.));
#59424=CARTESIAN_POINT('',(46.,0.,18.));
#59425=CARTESIAN_POINT('Origin',(1.83021655258307E-13,-3.27857114887026E-14,
18.));
#59426=CARTESIAN_POINT('',(46.0771487394572,7.40158428109252,18.));
#59427=CARTESIAN_POINT('Ctrl Pts',(46.0771487393634,7.40158428108604,18.));
#59428=CARTESIAN_POINT('Ctrl Pts',(46.2472869475148,4.94053945592452,18.));
#59429=CARTESIAN_POINT('Ctrl Pts',(46.2231469368338,2.46578847026075,18.));
#59430=CARTESIAN_POINT('Ctrl Pts',(46.,0.,18.));
#59431=CARTESIAN_POINT('',(46.4996348579608,6.56002729234549,18.));
#59432=CARTESIAN_POINT('',(43.358988599418,12.8159317895946,18.));
#59433=CARTESIAN_POINT('',(58.1177432099948,12.3926560582107,18.));
#59434=CARTESIAN_POINT('',(46.4996348579608,6.56002729234549,18.));
#59435=CARTESIAN_POINT('',(54.977096951452,18.6485605554598,18.));
#59436=CARTESIAN_POINT('',(58.1177432099948,12.3926560582107,18.));
#59437=CARTESIAN_POINT('',(45.2025619355918,13.741459297751,18.));
#59438=CARTESIAN_POINT('',(54.977096951452,18.6485605554598,18.));
#59439=CARTESIAN_POINT('',(37.5361777128299,31.4965928746404,18.));
#59440=CARTESIAN_POINT('Ctrl Pts',(37.5361777128299,31.4965928746404,18.));
#59441=CARTESIAN_POINT('Ctrl Pts',(37.7651853233442,31.1674494097669,18.));
#59442=CARTESIAN_POINT('Ctrl Pts',(37.9900338693208,30.8357007492528,18.));
#59443=CARTESIAN_POINT('Ctrl Pts',(38.2106627066136,30.5014475410796,18.));
#59444=CARTESIAN_POINT('Ctrl Pts',(38.6628417256667,29.8163952621406,18.));
#59445=CARTESIAN_POINT('Ctrl Pts',(39.0972913691121,29.1208241134464,18.));
#59446=CARTESIAN_POINT('Ctrl Pts',(39.5135109674438,28.4156399596004,18.));
#59447=CARTESIAN_POINT('Ctrl Pts',(39.9293606088442,27.7110826089289,18.));
#59448=CARTESIAN_POINT('Ctrl Pts',(40.327012508134,26.9969294809322,18.));
#59449=CARTESIAN_POINT('Ctrl Pts',(40.706012527242,26.2741097029318,18.));
#59450=CARTESIAN_POINT('Ctrl Pts',(41.0846776773738,25.5519285790389,18.));
#59451=CARTESIAN_POINT('Ctrl Pts',(41.444723808721,24.8210962666709,18.));
#59452=CARTESIAN_POINT('Ctrl Pts',(41.7857444361162,24.0825628192227,18.));
#59453=CARTESIAN_POINT('Ctrl Pts',(42.1264631259329,23.3446832647734,18.));
#59454=CARTESIAN_POINT('Ctrl Pts',(42.4481899106077,22.5991163638997,18.));
#59455=CARTESIAN_POINT('Ctrl Pts',(42.7505669752443,21.8468306747833,18.));
#59456=CARTESIAN_POINT('Ctrl Pts',(43.0525553238862,21.095512074491,18.));
#59457=CARTESIAN_POINT('Ctrl Pts',(43.3352436048344,20.3374921118706,18.));
#59458=CARTESIAN_POINT('Ctrl Pts',(43.5983239273765,19.573754195526,18.));
#59459=CARTESIAN_POINT('Ctrl Pts',(43.86119868316,18.8106130517806,18.));
#59460=CARTESIAN_POINT('Ctrl Pts',(44.104496050171,18.0417630511784,18.));
#59461=CARTESIAN_POINT('Ctrl Pts',(44.3279583123957,17.2682014144259,18.));
#59462=CARTESIAN_POINT('Ctrl Pts',(44.5511707711369,16.4955045249897,18.));
#59463=CARTESIAN_POINT('Ctrl Pts',(44.7545923968601,15.7181066959427,18.));
#59464=CARTESIAN_POINT('Ctrl Pts',(44.93801652698,14.9370153979336,18.));
#59465=CARTESIAN_POINT('Ctrl Pts',(45.0313867007029,14.539408877238,18.));
#59466=CARTESIAN_POINT('Ctrl Pts',(45.1195759021844,14.1408455013228,18.));
#59467=CARTESIAN_POINT('Ctrl Pts',(45.2025619355895,13.7414592977624,18.));
#59468=CARTESIAN_POINT('',(35.9959384951176,30.2041787151333,18.));
#59469=CARTESIAN_POINT('',(17.6190221917365,14.7841150227904,18.));
#59470=CARTESIAN_POINT('',(34.6009561857411,30.3112822399915,18.));
#59471=CARTESIAN_POINT('Origin',(35.3531508854311,30.9702231582522,18.));
#59472=CARTESIAN_POINT('',(23.,39.8371685740842,18.));
#59473=CARTESIAN_POINT('Origin',(1.19904086659517E-13,1.4210854715202E-13,
18.));
#59474=CARTESIAN_POINT('',(16.6286143540509,43.6047734828703,18.));
#59475=CARTESIAN_POINT('Ctrl Pts',(16.6286143540096,43.6047734827858,18.));
#59476=CARTESIAN_POINT('Ctrl Pts',(18.8450107965664,42.5215950805994,18.));
#59477=CARTESIAN_POINT('Ctrl Pts',(20.9761380121528,41.2633137257534,18.));
#59478=CARTESIAN_POINT('Ctrl Pts',(23.,39.8371685740842,18.));
#59479=CARTESIAN_POINT('',(17.56866714429,43.5498786998672,18.));
#59480=CARTESIAN_POINT('',(10.5805717967515,43.9579515042931,18.));
#59481=CARTESIAN_POINT('',(18.3265166382238,56.5277700595814,18.));
#59482=CARTESIAN_POINT('',(17.56866714429,43.5498786998672,18.));
#59483=CARTESIAN_POINT('',(11.3384212906854,56.9358428640073,18.));
#59484=CARTESIAN_POINT('',(18.3265166382238,56.5277700595814,18.));
#59485=CARTESIAN_POINT('',(10.7008281308737,46.0172966012375,18.));
#59486=CARTESIAN_POINT('',(11.3384212906854,56.9358428640073,18.));
#59487=CARTESIAN_POINT('',(-8.50876070567958,48.2555798975982,18.));
#59488=CARTESIAN_POINT('Ctrl Pts',(-8.50876070567958,48.2555798975982,18.));
#59489=CARTESIAN_POINT('Ctrl Pts',(-8.10921023867559,48.2893345785684,18.));
#59490=CARTESIAN_POINT('Ctrl Pts',(-7.70948313828089,48.3181848047075,18.));
#59491=CARTESIAN_POINT('Ctrl Pts',(-7.30969689033073,48.3421283806345,18.));
#59492=CARTESIAN_POINT('Ctrl Pts',(-6.49033472635619,48.3912007543976,18.));
#59493=CARTESIAN_POINT('Ctrl Pts',(-5.67072764184703,48.4196596047247,18.));
#59494=CARTESIAN_POINT('Ctrl Pts',(-4.85191047323153,48.4275242714055,18.));
#59495=CARTESIAN_POINT('Ctrl Pts',(-4.03382065662236,48.4353819519344,18.));
#59496=CARTESIAN_POINT('Ctrl Pts',(-3.21651952501596,48.4226820151353,18.));
#59497=CARTESIAN_POINT('Ctrl Pts',(-2.40103879694537,48.3894957296891,18.));
#59498=CARTESIAN_POINT('Ctrl Pts',(-1.58627997520921,48.3563388224843,18.));
#59499=CARTESIAN_POINT('Ctrl Pts',(-0.773338510221561,48.3027318255699,
18.));
#59500=CARTESIAN_POINT('Ctrl Pts',(0.0367595886500608,48.2287977387298,
18.));
#59501=CARTESIAN_POINT('Ctrl Pts',(0.846140753505449,48.1549290833008,18.));
#59502=CARTESIAN_POINT('Ctrl Pts',(1.65268340805356,48.0607693134724,18.));
#59503=CARTESIAN_POINT('Ctrl Pts',(2.4553698511975,47.9464928310905,18.));
#59504=CARTESIAN_POINT('Ctrl Pts',(3.25702489039038,47.8323631871365,18.));
#59505=CARTESIAN_POINT('Ctrl Pts',(4.05483344847245,47.6981685198292,18.));
#59506=CARTESIAN_POINT('Ctrl Pts',(4.84778992376607,47.5441338920999,18.));
#59507=CARTESIAN_POINT('Ctrl Pts',(5.64012898520712,47.3902191992169,18.));
#59508=CARTESIAN_POINT('Ctrl Pts',(6.42762334377131,47.2164954589048,18.));
#59509=CARTESIAN_POINT('Ctrl Pts',(7.20928051527433,47.023238095029,18.));
#59510=CARTESIAN_POINT('Ctrl Pts',(7.99006081195724,46.8301975301827,18.));
#59511=CARTESIAN_POINT('Ctrl Pts',(8.76501683998239,46.6176671844283,18.));
#59512=CARTESIAN_POINT('Ctrl Pts',(9.53317277684725,46.3859718167405,18.));
#59513=CARTESIAN_POINT('Ctrl Pts',(9.924195445201,46.2680294347701,18.));
#59514=CARTESIAN_POINT('Ctrl Pts',(10.3134562863487,46.145121765699,18.));
#59515=CARTESIAN_POINT('Ctrl Pts',(10.7008281308626,46.0172966012412,18.));
#59516=CARTESIAN_POINT('',(-8.1596168201918,46.2754865274007,18.));
#59517=CARTESIAN_POINT('',(-3.99390808633937,22.6505783192808,18.));
#59518=CARTESIAN_POINT('',(-8.94986234824223,45.1209481720799,18.));
#59519=CARTESIAN_POINT('Origin',(-9.14442457320401,46.1018383497338,18.));
#59520=CARTESIAN_POINT('',(-23.,39.8371685740842,18.));
#59521=CARTESIAN_POINT('Origin',(-6.31175685987896E-14,1.74894258640722E-13,
18.));
#59522=CARTESIAN_POINT('',(-29.4485343854063,36.2031892017778,18.));
#59523=CARTESIAN_POINT('Ctrl Pts',(-29.4485343853538,36.2031892016998,18.));
#59524=CARTESIAN_POINT('Ctrl Pts',(-27.4022761513372,37.5810556244599,18.));
#59525=CARTESIAN_POINT('Ctrl Pts',(-25.2470089259271,38.7975252541457,18.));
#59526=CARTESIAN_POINT('Ctrl Pts',(-23.,39.8371685740842,18.));
#59527=CARTESIAN_POINT('',(-28.9309677136708,36.9898514075217,18.));
#59528=CARTESIAN_POINT('',(-32.7784168026664,31.1420197146986,18.));
#59529=CARTESIAN_POINT('',(-39.791226571771,44.1351140013707,18.));
#59530=CARTESIAN_POINT('',(-28.9309677136708,36.9898514075217,18.));
#59531=CARTESIAN_POINT('',(-43.6386756607666,38.2872823085476,18.));
#59532=CARTESIAN_POINT('',(-39.791226571771,44.1351140013707,18.));
#59533=CARTESIAN_POINT('',(-34.5017338047182,32.2758373034865,18.));
#59534=CARTESIAN_POINT('',(-43.6386756607666,38.2872823085476,18.));
#59535=CARTESIAN_POINT('',(-46.0449384185095,16.7589870229578,18.));
#59536=CARTESIAN_POINT('Ctrl Pts',(-46.0449384185095,16.7589870229578,18.));
#59537=CARTESIAN_POINT('Ctrl Pts',(-43.6587293356143,21.8366030579606,18.));
#59538=CARTESIAN_POINT('Ctrl Pts',(-40.4224569853479,26.4671498428742,18.));
#59539=CARTESIAN_POINT('Ctrl Pts',(-35.8215879134419,31.0643477170003,18.));
#59540=CARTESIAN_POINT('Ctrl Pts',(-35.1697987101644,31.6798154760653,18.));
#59541=CARTESIAN_POINT('Ctrl Pts',(-34.5017338047181,32.2758373034865,18.));
#59542=CARTESIAN_POINT('',(-44.1555553153094,16.0713078122674,18.));
#59543=CARTESIAN_POINT('',(-21.6129302780759,7.86646329649041,18.));
#59544=CARTESIAN_POINT('',(-43.5508185339833,14.8096659320883,18.));
#59545=CARTESIAN_POINT('Origin',(-44.4975754586351,15.1316151914815,18.));
#59546=CARTESIAN_POINT('',(-46.,1.33226762955019E-14,18.));
#59547=CARTESIAN_POINT('Origin',(-1.83021655258307E-13,3.27857114887025E-14,
18.));
#59548=CARTESIAN_POINT('',(-46.0771487394572,-7.40158428109254,18.));
#59549=CARTESIAN_POINT('Ctrl Pts',(-46.0771487393634,-7.40158428108605,
18.));
#59550=CARTESIAN_POINT('Ctrl Pts',(-46.2472869474355,-4.94053945706959,
18.));
#59551=CARTESIAN_POINT('Ctrl Pts',(-46.2231469370949,-2.46578847314652,
18.));
#59552=CARTESIAN_POINT('Ctrl Pts',(-46.,6.66133814775094E-15,18.));
#59553=CARTESIAN_POINT('',(-46.4996348579608,-6.56002729234549,18.));
#59554=CARTESIAN_POINT('',(-43.358988599418,-12.8159317895946,18.));
#59555=CARTESIAN_POINT('',(-58.1177432099948,-12.3926560582107,18.));
#59556=CARTESIAN_POINT('',(-46.4996348579608,-6.56002729234549,18.));
#59557=CARTESIAN_POINT('',(-54.977096951452,-18.6485605554598,18.));
#59558=CARTESIAN_POINT('',(-58.1177432099948,-12.3926560582107,18.));
#59559=CARTESIAN_POINT('',(-45.2025619355918,-13.741459297751,18.));
#59560=CARTESIAN_POINT('',(-54.977096951452,-18.6485605554598,18.));
#59561=CARTESIAN_POINT('',(-37.5361777128299,-31.4965928746404,18.));
#59562=CARTESIAN_POINT('Ctrl Pts',(-37.5361777128299,-31.4965928746404,
18.));
#59563=CARTESIAN_POINT('Ctrl Pts',(-37.7651856275755,-31.1674489725069,
18.));
#59564=CARTESIAN_POINT('Ctrl Pts',(-37.9900344667344,-30.8356998678088,
18.));
#59565=CARTESIAN_POINT('Ctrl Pts',(-38.2106635859155,-30.5014462089352,
18.));
#59566=CARTESIAN_POINT('Ctrl Pts',(-38.6628429613237,-29.8163933416692,
18.));
#59567=CARTESIAN_POINT('Ctrl Pts',(-39.0972929310332,-29.1208215875746,
18.));
#59568=CARTESIAN_POINT('Ctrl Pts',(-39.5135128243241,-28.4156368135623,
18.));
#59569=CARTESIAN_POINT('Ctrl Pts',(-39.9293625109982,-27.7110792658639,
18.));
#59570=CARTESIAN_POINT('Ctrl Pts',(-40.3270144461478,-26.9969259376149,
18.));
#59571=CARTESIAN_POINT('Ctrl Pts',(-40.7060144914488,-26.274105956843,18.));
#59572=CARTESIAN_POINT('Ctrl Pts',(-41.0846796011326,-25.5519247574101,
18.));
#59573=CARTESIAN_POINT('Ctrl Pts',(-41.4447256889349,-24.8210923700318,
18.));
#59574=CARTESIAN_POINT('Ctrl Pts',(-41.7857462696941,-24.0825588483227,
18.));
#59575=CARTESIAN_POINT('Ctrl Pts',(-42.1264645145938,-23.3446800823079,
18.));
#59576=CARTESIAN_POINT('Ctrl Pts',(-42.448190895681,-22.5991139885945,18.));
#59577=CARTESIAN_POINT('Ctrl Pts',(-42.7505675993063,-21.8468291221756,
18.));
#59578=CARTESIAN_POINT('Ctrl Pts',(-43.0525558732906,-21.0955106322569,
18.));
#59579=CARTESIAN_POINT('Ctrl Pts',(-43.3352440854983,-20.3374907828153,
18.));
#59580=CARTESIAN_POINT('Ctrl Pts',(-43.598324345394,-19.5737529819962,18.));
#59581=CARTESIAN_POINT('Ctrl Pts',(-43.8611990228663,-18.810611999304,18.));
#59582=CARTESIAN_POINT('Ctrl Pts',(-44.1044963199916,-18.0417621627802,
18.));
#59583=CARTESIAN_POINT('Ctrl Pts',(-44.3279585209467,-17.2682006924827,
18.));
#59584=CARTESIAN_POINT('Ctrl Pts',(-44.5511707886356,-16.4955044188226,
18.));
#59585=CARTESIAN_POINT('Ctrl Pts',(-44.7545922549351,-15.7181072133933,
18.));
#59586=CARTESIAN_POINT('Ctrl Pts',(-44.9380162577493,-14.9370165444224,
18.));
#59587=CARTESIAN_POINT('Ctrl Pts',(-45.0313865311743,-14.5394096434031,
18.));
#59588=CARTESIAN_POINT('Ctrl Pts',(-45.1195758224217,-14.1408458851963,
18.));
#59589=CARTESIAN_POINT('Ctrl Pts',(-45.2025619355895,-13.7414592977624,
18.));
#59590=CARTESIAN_POINT('',(-35.9959384951176,-30.2041787151332,18.));
#59591=CARTESIAN_POINT('',(-17.6190221917365,-14.7841150227904,18.));
#59592=CARTESIAN_POINT('',(-34.6009561857411,-30.3112822399915,18.));
#59593=CARTESIAN_POINT('Origin',(-35.3531508854311,-30.9702231582522,18.));
#59594=CARTESIAN_POINT('',(-23.,-39.8371685740842,18.));
#59595=CARTESIAN_POINT('Origin',(-1.19904086659517E-13,-1.4210854715202E-13,
18.));
#59596=CARTESIAN_POINT('',(-16.6286143540509,-43.6047734828703,18.));
#59597=CARTESIAN_POINT('Ctrl Pts',(-16.6286143540096,-43.6047734827858,
18.));
#59598=CARTESIAN_POINT('Ctrl Pts',(-18.8450107961508,-42.5215950808033,
18.));
#59599=CARTESIAN_POINT('Ctrl Pts',(-20.976138011788,-41.2633137260105,18.));
#59600=CARTESIAN_POINT('Ctrl Pts',(-23.,-39.8371685740842,18.));
#59601=CARTESIAN_POINT('',(-17.56866714429,-43.5498786998672,18.));
#59602=CARTESIAN_POINT('',(-10.5805717967516,-43.9579515042931,18.));
#59603=CARTESIAN_POINT('',(-18.3265166382238,-56.5277700595814,18.));
#59604=CARTESIAN_POINT('',(-17.56866714429,-43.5498786998672,18.));
#59605=CARTESIAN_POINT('',(-11.3384212906854,-56.9358428640073,18.));
#59606=CARTESIAN_POINT('',(-18.3265166382238,-56.5277700595814,18.));
#59607=CARTESIAN_POINT('',(-10.7008281308737,-46.0172966012375,18.));
#59608=CARTESIAN_POINT('',(-11.3384212906854,-56.9358428640073,18.));
#59609=CARTESIAN_POINT('',(8.50876070567956,-48.2555798975982,18.));
#59610=CARTESIAN_POINT('Ctrl Pts',(8.50876070567956,-48.2555798975982,18.));
#59611=CARTESIAN_POINT('Ctrl Pts',(8.10921021903483,-48.2893345802281,18.));
#59612=CARTESIAN_POINT('Ctrl Pts',(7.70948309898196,-48.318184807544,18.));
#59613=CARTESIAN_POINT('Ctrl Pts',(7.30969683137374,-48.3421283841655,18.));
#59614=CARTESIAN_POINT('Ctrl Pts',(6.4903344600815,-48.3912007693555,18.));
#59615=CARTESIAN_POINT('Ctrl Pts',(5.67072716815546,-48.4196596206763,18.));
#59616=CARTESIAN_POINT('Ctrl Pts',(4.85190979280955,-48.4275242779409,18.));
#59617=CARTESIAN_POINT('Ctrl Pts',(4.0338208098616,-48.4353819390708,18.));
#59618=CARTESIAN_POINT('Ctrl Pts',(3.21652051059572,-48.4226820247691,18.));
#59619=CARTESIAN_POINT('Ctrl Pts',(2.40104061039322,-48.389495803488,18.));
#59620=CARTESIAN_POINT('Ctrl Pts',(1.58628269750797,-48.3563389637169,18.));
#59621=CARTESIAN_POINT('Ctrl Pts',(0.773342136541099,-48.3027320799326,
18.));
#59622=CARTESIAN_POINT('Ctrl Pts',(-0.0367550665778552,-48.2287981514392,
18.));
#59623=CARTESIAN_POINT('Ctrl Pts',(-0.846137205569798,-48.1549294836327,
18.));
#59624=CARTESIAN_POINT('Ctrl Pts',(-1.65268082939617,-48.0607696528264,
18.));
#59625=CARTESIAN_POINT('Ctrl Pts',(-2.45536823331685,-47.9464930614241,
18.));
#59626=CARTESIAN_POINT('Ctrl Pts',(-3.25702327991691,-47.832363444143,18.));
#59627=CARTESIAN_POINT('Ctrl Pts',(-4.0548318460644,-47.6981688032625,18.));
#59628=CARTESIAN_POINT('Ctrl Pts',(-4.8477883300669,-47.5441342016816,18.));
#59629=CARTESIAN_POINT('Ctrl Pts',(-5.64012748982834,-47.390219517518,18.));
#59630=CARTESIAN_POINT('Ctrl Pts',(-6.42762194625921,-47.2164957811652,
18.));
#59631=CARTESIAN_POINT('Ctrl Pts',(-7.20927921482277,-47.0232384165534,
18.));
#59632=CARTESIAN_POINT('Ctrl Pts',(-7.99005956714217,-46.8301978611867,
18.));
#59633=CARTESIAN_POINT('Ctrl Pts',(-8.76501565061606,-46.6176675222901,
18.));
#59634=CARTESIAN_POINT('Ctrl Pts',(-9.53317164254934,-46.3859721588735,
18.));
#59635=CARTESIAN_POINT('Ctrl Pts',(-9.92419469240932,-46.2680296724606,
18.));
#59636=CARTESIAN_POINT('Ctrl Pts',(-10.3134559117797,-46.1451218892995,
18.));
#59637=CARTESIAN_POINT('Ctrl Pts',(-10.7008281308626,-46.0172966012412,
18.));
#59638=CARTESIAN_POINT('',(8.15961682019179,-46.2754865274007,18.));
#59639=CARTESIAN_POINT('',(3.99390808633936,-22.6505783192808,18.));
#59640=CARTESIAN_POINT('',(8.94986234824221,-45.1209481720799,18.));
#59641=CARTESIAN_POINT('Origin',(9.144424573204,-46.1018383497338,18.));
#59642=CARTESIAN_POINT('',(23.,-39.8371685740842,18.));
#59643=CARTESIAN_POINT('Origin',(6.31175685987895E-14,-1.74894258640722E-13,
18.));
#59644=CARTESIAN_POINT('',(29.4485343854062,-36.2031892017778,18.));
#59645=CARTESIAN_POINT('Ctrl Pts',(29.4485343853537,-36.2031892016999,18.));
#59646=CARTESIAN_POINT('Ctrl Pts',(27.40227615007,-37.5810556253112,18.));
#59647=CARTESIAN_POINT('Ctrl Pts',(25.2470089248039,-38.797525254667,18.));
#59648=CARTESIAN_POINT('Ctrl Pts',(23.,-39.8371685740842,18.));
#59649=CARTESIAN_POINT('',(28.9309677136708,-36.9898514075217,18.));
#59650=CARTESIAN_POINT('',(32.7784168026664,-31.1420197146986,18.));
#59651=CARTESIAN_POINT('',(39.7912265717709,-44.1351140013707,18.));
#59652=CARTESIAN_POINT('',(28.9309677136708,-36.9898514075217,18.));
#59653=CARTESIAN_POINT('',(43.6386756607666,-38.2872823085476,18.));
#59654=CARTESIAN_POINT('',(39.7912265717709,-44.1351140013707,18.));
#59655=CARTESIAN_POINT('',(43.6386756607666,-38.2872823085476,18.));
#59656=CARTESIAN_POINT('Ctrl Pts',(52.7966221146313,12.9064860705774,18.));
#59657=CARTESIAN_POINT('Ctrl Pts',(52.7391846522721,12.9274734829174,18.));
#59658=CARTESIAN_POINT('Ctrl Pts',(52.6833098509988,12.9520735040296,18.));
#59659=CARTESIAN_POINT('Ctrl Pts',(52.6291956963058,12.9799861915281,18.));
#59660=CARTESIAN_POINT('Ctrl Pts',(52.575396618885,13.0077363586382,18.));
#59661=CARTESIAN_POINT('Ctrl Pts',(52.5233370565323,13.0387617569737,18.));
#59662=CARTESIAN_POINT('Ctrl Pts',(52.4732434855936,13.0728123808106,18.));
#59663=CARTESIAN_POINT('Ctrl Pts',(52.4354166035921,13.0985248406297,18.));
#59664=CARTESIAN_POINT('Ctrl Pts',(52.3987113360342,13.1259633238972,18.));
#59665=CARTESIAN_POINT('Ctrl Pts',(52.3632409515082,13.1550320009626,18.));
#59666=CARTESIAN_POINT('Ctrl Pts',(52.34482728488,13.1701223625688,18.));
#59667=CARTESIAN_POINT('Ctrl Pts',(52.3267466539926,13.1856521912727,18.));
#59668=CARTESIAN_POINT('Ctrl Pts',(52.3090166072819,13.2016088137114,18.));
#59669=CARTESIAN_POINT('Ctrl Pts',(52.2996792306519,13.2100122316992,18.));
#59670=CARTESIAN_POINT('Ctrl Pts',(52.290437736064,13.2185355104073,18.));
#59671=CARTESIAN_POINT('Ctrl Pts',(52.2813109131323,13.227161085094,18.));
#59672=CARTESIAN_POINT('Ctrl Pts',(52.2382824916349,13.2678263709279,18.));
#59673=CARTESIAN_POINT('Ctrl Pts',(52.1977162889855,13.3108358032842,18.));
#59674=CARTESIAN_POINT('Ctrl Pts',(52.1598201080567,13.3559496827387,18.));
#59675=CARTESIAN_POINT('Ctrl Pts',(52.1226978380937,13.4001422523101,18.));
#59676=CARTESIAN_POINT('Ctrl Pts',(52.0881372055927,13.4463551316942,18.));
#59677=CARTESIAN_POINT('Ctrl Pts',(52.0563765963043,13.4943859943979,18.));
#59678=CARTESIAN_POINT('Ctrl Pts',(52.0333851347596,13.5291554700963,18.));
#59679=CARTESIAN_POINT('Ctrl Pts',(52.0118618266788,13.5648781300802,18.));
#59680=CARTESIAN_POINT('Ctrl Pts',(51.9919136247933,13.6014809507274,18.));
#59681=CARTESIAN_POINT('Ctrl Pts',(51.9814876879778,13.6206114316362,18.));
#59682=CARTESIAN_POINT('Ctrl Pts',(51.9714922558871,13.6399823727779,18.));
#59683=CARTESIAN_POINT('Ctrl Pts',(51.9619442850847,13.6595834362837,18.));
#59684=CARTESIAN_POINT('Ctrl Pts',(51.9575038197887,13.6686992834163,18.));
#59685=CARTESIAN_POINT('Ctrl Pts',(51.9531624130337,13.6778603944405,18.));
#59686=CARTESIAN_POINT('Ctrl Pts',(51.948924721729,13.6870583249534,18.));
#59687=CARTESIAN_POINT('Ctrl Pts',(51.9255871022594,13.7377127466136,18.));
#59688=CARTESIAN_POINT('Ctrl Pts',(51.9053583908605,13.7895496677192,18.));
#59689=CARTESIAN_POINT('Ctrl Pts',(51.8884515319674,13.8423787830974,18.));
#59690=CARTESIAN_POINT('Ctrl Pts',(51.8771391871495,13.877726636496,18.));
#59691=CARTESIAN_POINT('Ctrl Pts',(51.8673149503303,13.9135190517323,18.));
#59692=CARTESIAN_POINT('Ctrl Pts',(51.8590555816082,13.9497009999509,18.));
#59693=CARTESIAN_POINT('Ctrl Pts',(51.8468310253394,14.0032533084619,18.));
#59694=CARTESIAN_POINT('Ctrl Pts',(51.8380328718691,14.0576598787871,18.));
#59695=CARTESIAN_POINT('Ctrl Pts',(51.8326065611663,14.1126100767572,18.));
#59696=CARTESIAN_POINT('Ctrl Pts',(51.830930637981,14.1295815175501,18.));
#59697=CARTESIAN_POINT('Ctrl Pts',(51.8295766661961,14.1466047249362,18.));
#59698=CARTESIAN_POINT('Ctrl Pts',(51.828543856078,14.1636702346734,18.));
#59699=CARTESIAN_POINT('Ctrl Pts',(51.8276375355829,14.1786457088329,18.));
#59700=CARTESIAN_POINT('Ctrl Pts',(51.8269785320498,14.1936603247014,18.));
#59701=CARTESIAN_POINT('Ctrl Pts',(51.826566991848,14.2086715965765,18.));
#59702=CARTESIAN_POINT('Ctrl Pts',(51.8250409572498,14.2643349804729,18.));
#59703=CARTESIAN_POINT('Ctrl Pts',(51.8269058844663,14.3200271043436,18.));
#59704=CARTESIAN_POINT('Ctrl Pts',(51.8320579502604,14.3754301634831,18.));
#59705=CARTESIAN_POINT('Ctrl Pts',(51.8372038210242,14.4307666039798,18.));
#59706=CARTESIAN_POINT('Ctrl Pts',(51.8456293850989,14.4858158153881,18.));
#59707=CARTESIAN_POINT('Ctrl Pts',(51.8572803743357,14.5402457976327,18.));
#59708=CARTESIAN_POINT('Ctrl Pts',(51.8647273765295,14.5750359934649,18.));
#59709=CARTESIAN_POINT('Ctrl Pts',(51.8734930706666,14.6095728457467,18.));
#59710=CARTESIAN_POINT('Ctrl Pts',(51.8835725601024,14.6437631510401,18.));
#59711=CARTESIAN_POINT('Ctrl Pts',(51.8887663989076,14.6613810011831,18.));
#59712=CARTESIAN_POINT('Ctrl Pts',(51.8943091902133,14.6789067372084,18.));
#59713=CARTESIAN_POINT('Ctrl Pts',(51.9002009421238,14.6963268927931,18.));
#59714=CARTESIAN_POINT('Ctrl Pts',(51.9037544840207,14.7068336577858,18.));
#59715=CARTESIAN_POINT('Ctrl Pts',(51.9074348703348,14.7173013531614,18.));
#59716=CARTESIAN_POINT('Ctrl Pts',(51.9112372618813,14.7277145312037,18.));
#59717=CARTESIAN_POINT('Ctrl Pts',(51.9296249995619,14.7780709408272,18.));
#59718=CARTESIAN_POINT('Ctrl Pts',(51.950888554962,14.827232989418,18.));
#59719=CARTESIAN_POINT('Ctrl Pts',(51.9749870630625,14.8748868070182,18.));
#59720=CARTESIAN_POINT('Ctrl Pts',(51.9901200745184,14.9048117204051,18.));
#59721=CARTESIAN_POINT('Ctrl Pts',(52.006371831386,14.9341413324084,18.));
#59722=CARTESIAN_POINT('Ctrl Pts',(52.0237395591854,14.9627903220902,18.));
#59723=CARTESIAN_POINT('Ctrl Pts',(52.0300897392709,14.9732652815005,18.));
#59724=CARTESIAN_POINT('Ctrl Pts',(52.036590534633,14.9836512987207,18.));
#59725=CARTESIAN_POINT('Ctrl Pts',(52.0432374284802,14.9939369612961,18.));
#59726=CARTESIAN_POINT('Ctrl Pts',(52.071139405187,15.0371135674213,18.));
#59727=CARTESIAN_POINT('Ctrl Pts',(52.1015680157944,15.078457457165,18.));
#59728=CARTESIAN_POINT('Ctrl Pts',(52.1344986678541,15.1176697568719,18.));
#59729=CARTESIAN_POINT('Ctrl Pts',(52.1528947874596,15.1395750065495,18.));
#59730=CARTESIAN_POINT('Ctrl Pts',(52.1720723161451,15.160814400533,18.));
#59731=CARTESIAN_POINT('Ctrl Pts',(52.1920310817112,15.1813299718051,18.));
#59732=CARTESIAN_POINT('Ctrl Pts',(52.2060486090393,15.1957385573463,18.));
#59733=CARTESIAN_POINT('Ctrl Pts',(52.2204515743704,15.2097900005096,18.));
#59734=CARTESIAN_POINT('Ctrl Pts',(52.2352228301846,15.2234768233201,18.));
#59735=CARTESIAN_POINT('Ctrl Pts',(54.1532521092111,15.2223467977324,18.));
#59736=CARTESIAN_POINT('Ctrl Pts',(54.1901305933404,15.1879071947037,18.));
#59737=CARTESIAN_POINT('Ctrl Pts',(54.2246310285467,15.1512289528612,18.));
#59738=CARTESIAN_POINT('Ctrl Pts',(54.2567513295154,15.1126319834755,18.));
#59739=CARTESIAN_POINT('Ctrl Pts',(54.2903114638431,15.0723048558287,18.));
#59740=CARTESIAN_POINT('Ctrl Pts',(54.3212739167588,15.0298826695218,18.));
#59741=CARTESIAN_POINT('Ctrl Pts',(54.3496082931449,14.9856806062947,18.));
#59742=CARTESIAN_POINT('Ctrl Pts',(54.3723325448347,14.9502304239334,18.));
#59743=CARTESIAN_POINT('Ctrl Pts',(54.393365943357,14.9136342530605,18.));
#59744=CARTESIAN_POINT('Ctrl Pts',(54.4126765683611,14.8760367445277,18.));
#59745=CARTESIAN_POINT('Ctrl Pts',(54.4208393026161,14.8601440185936,18.));
#59746=CARTESIAN_POINT('Ctrl Pts',(54.4286940175273,14.8440722071043,18.));
#59747=CARTESIAN_POINT('Ctrl Pts',(54.4362374127529,14.8278315944995,18.));
#59748=CARTESIAN_POINT('Ctrl Pts',(54.4405190389662,14.8186134333707,18.));
#59749=CARTESIAN_POINT('Ctrl Pts',(54.4447005519148,14.8093401785886,18.));
#59750=CARTESIAN_POINT('Ctrl Pts',(54.4487750435515,14.8000286716828,18.));
#59751=CARTESIAN_POINT('Ctrl Pts',(54.4705983254202,14.7501555444453,18.));
#59752=CARTESIAN_POINT('Ctrl Pts',(54.4894011486138,14.6990895949691,18.));
#59753=CARTESIAN_POINT('Ctrl Pts',(54.5051559559802,14.6471623387574,18.));
#59754=CARTESIAN_POINT('Ctrl Pts',(54.5211994761642,14.5942834958898,18.));
#59755=CARTESIAN_POINT('Ctrl Pts',(54.5340828409905,14.540510565072,18.));
#59756=CARTESIAN_POINT('Ctrl Pts',(54.5437362577265,14.4861590282357,18.));
#59757=CARTESIAN_POINT('Ctrl Pts',(54.5506403107398,14.4472872067934,18.));
#59758=CARTESIAN_POINT('Ctrl Pts',(54.5558914111236,14.4081186550579,18.));
#59759=CARTESIAN_POINT('Ctrl Pts',(54.559449023704,14.3687624021492,18.));
#59760=CARTESIAN_POINT('Ctrl Pts',(54.5609614737352,14.3520308540687,18.));
#59761=CARTESIAN_POINT('Ctrl Pts',(54.5621676846347,14.3352653382879,18.));
#59762=CARTESIAN_POINT('Ctrl Pts',(54.5630637815993,14.3184741004755,18.));
#59763=CARTESIAN_POINT('Ctrl Pts',(54.5635976657008,14.3084700771749,18.));
#59764=CARTESIAN_POINT('Ctrl Pts',(54.5640211036069,14.2984625720653,18.));
#59765=CARTESIAN_POINT('Ctrl Pts',(54.5643335016801,14.2884609518038,18.));
#59766=CARTESIAN_POINT('Ctrl Pts',(54.5661075110382,14.2316649294805,18.));
#59767=CARTESIAN_POINT('Ctrl Pts',(54.5643085969182,14.1749865267886,18.));
#59768=CARTESIAN_POINT('Ctrl Pts',(54.5588768122569,14.1187579548823,18.));
#59769=CARTESIAN_POINT('Ctrl Pts',(54.555541323331,14.0842297490327,18.));
#59770=CARTESIAN_POINT('Ctrl Pts',(54.5508350741444,14.0498706203909,18.));
#59771=CARTESIAN_POINT('Ctrl Pts',(54.5447349150617,14.0157544413133,18.));
#59772=CARTESIAN_POINT('Ctrl Pts',(54.5350624849657,13.9616597279126,18.));
#59773=CARTESIAN_POINT('Ctrl Pts',(54.5218884030871,13.908175336948,18.));
#59774=CARTESIAN_POINT('Ctrl Pts',(54.5054388352982,13.8555057819067,18.));
#59775=CARTESIAN_POINT('Ctrl Pts',(54.5005174069387,13.8397479550029,18.));
#59776=CARTESIAN_POINT('Ctrl Pts',(54.4953024361436,13.8240630966687,18.));
#59777=CARTESIAN_POINT('Ctrl Pts',(54.4897991057291,13.8084568180236,18.));
#59778=CARTESIAN_POINT('Ctrl Pts',(54.4847109304732,13.7940278314178,18.));
#59779=CARTESIAN_POINT('Ctrl Pts',(54.4793736286687,13.7796597824156,18.));
#59780=CARTESIAN_POINT('Ctrl Pts',(54.4738049082136,13.765391301815,18.));
#59781=CARTESIAN_POINT('Ctrl Pts',(54.4531741179316,13.712529960814,18.));
#59782=CARTESIAN_POINT('Ctrl Pts',(54.4293497755018,13.6609649910116,18.));
#59783=CARTESIAN_POINT('Ctrl Pts',(54.4026149607928,13.6109069383257,18.));
#59784=CARTESIAN_POINT('Ctrl Pts',(54.3752481593716,13.5596655587876,18.));
#59785=CARTESIAN_POINT('Ctrl Pts',(54.3448313135357,13.5100022755867,18.));
#59786=CARTESIAN_POINT('Ctrl Pts',(54.3116127229013,13.4621485545139,18.));
#59787=CARTESIAN_POINT('Ctrl Pts',(54.2914450604171,13.4330956152779,18.));
#59788=CARTESIAN_POINT('Ctrl Pts',(54.270243640872,13.404709837219,18.));
#59789=CARTESIAN_POINT('Ctrl Pts',(54.248055329197,13.3770462315215,18.));
#59790=CARTESIAN_POINT('Ctrl Pts',(54.2358385422418,13.3618147717255,18.));
#59791=CARTESIAN_POINT('Ctrl Pts',(54.2233224644031,13.3468022959008,18.));
#59792=CARTESIAN_POINT('Ctrl Pts',(54.210514166911,13.3320184620734,18.));
#59793=CARTESIAN_POINT('Ctrl Pts',(54.2028017059937,13.3231164404993,18.));
#59794=CARTESIAN_POINT('Ctrl Pts',(54.1949819266705,13.3142958366262,18.));
#59795=CARTESIAN_POINT('Ctrl Pts',(54.1870606016122,13.3055635742289,18.));
#59796=CARTESIAN_POINT('Ctrl Pts',(54.146465975084,13.2608131154156,18.));
#59797=CARTESIAN_POINT('Ctrl Pts',(54.10333569294,13.2185196121713,18.));
#59798=CARTESIAN_POINT('Ctrl Pts',(54.0579299117865,13.1789337623729,18.));
#59799=CARTESIAN_POINT('Ctrl Pts',(54.0284074581576,13.1531953787278,18.));
#59800=CARTESIAN_POINT('Ctrl Pts',(53.9979219697629,13.1286019537641,18.));
#59801=CARTESIAN_POINT('Ctrl Pts',(53.966534783368,13.1052284206224,18.));
#59802=CARTESIAN_POINT('Ctrl Pts',(53.9535624126213,13.0955681046655,18.));
#59803=CARTESIAN_POINT('Ctrl Pts',(53.940435929729,13.0861162377761,18.));
#59804=CARTESIAN_POINT('Ctrl Pts',(53.9271593222801,13.0768784342968,18.));
#59805=CARTESIAN_POINT('Ctrl Pts',(53.9174397053042,13.0701155687181,18.));
#59806=CARTESIAN_POINT('Ctrl Pts',(53.9076405168284,13.0634681523302,18.));
#59807=CARTESIAN_POINT('Ctrl Pts',(53.897771829427,13.0569437429014,18.));
#59808=CARTESIAN_POINT('Ctrl Pts',(53.8470357673058,13.0234010002221,18.));
#59809=CARTESIAN_POINT('Ctrl Pts',(53.7944075338674,12.9930657400092,18.));
#59810=CARTESIAN_POINT('Ctrl Pts',(53.740123223725,12.9662046863981,18.));
#59811=CARTESIAN_POINT('Ctrl Pts',(53.7146984023412,12.9536239335351,18.));
#59812=CARTESIAN_POINT('Ctrl Pts',(53.6889097287653,12.941805763883,18.));
#59813=CARTESIAN_POINT('Ctrl Pts',(53.6627787780123,12.9307804983812,18.));
#59814=CARTESIAN_POINT('Ctrl Pts',(53.6403263881356,12.9213073046241,18.));
#59815=CARTESIAN_POINT('Ctrl Pts',(53.6176212739246,12.9124195098708,18.));
#59816=CARTESIAN_POINT('Ctrl Pts',(53.5946845822246,12.9041113672218,18.));
#59817=CARTESIAN_POINT('Origin',(0.,0.,18.));
#59818=CARTESIAN_POINT('Ctrl Pts',(15.2209662466057,52.1764590205668,18.));
#59819=CARTESIAN_POINT('Ctrl Pts',(15.1740718831799,52.1372104252047,18.));
#59820=CARTESIAN_POINT('Ctrl Pts',(15.1248302485577,52.1011214310192,18.));
#59821=CARTESIAN_POINT('Ctrl Pts',(15.0736000909597,52.0682135291378,18.));
#59822=CARTESIAN_POINT('Ctrl Pts',(15.0226682165857,52.0354972307088,18.));
#59823=CARTESIAN_POINT('Ctrl Pts',(14.9697696730429,52.0059250068959,18.));
#59824=CARTESIAN_POINT('Ctrl Pts',(14.9152342077278,51.9795679908667,18.));
#59825=CARTESIAN_POINT('Ctrl Pts',(14.8740531445005,51.9596651636458,18.));
#59826=CARTESIAN_POINT('Ctrl Pts',(14.831938111089,51.9415966925909,18.));
#59827=CARTESIAN_POINT('Ctrl Pts',(14.7890287317841,51.9254127571039,18.));
#59828=CARTESIAN_POINT('Ctrl Pts',(14.7667532709537,51.9170112228272,18.));
#59829=CARTESIAN_POINT('Ctrl Pts',(14.7442637387324,51.9091178393319,18.));
#59830=CARTESIAN_POINT('Ctrl Pts',(14.7215798846744,51.9017414674401,18.));
#59831=CARTESIAN_POINT('Ctrl Pts',(14.7096336326145,51.8978567661154,18.));
#59832=CARTESIAN_POINT('Ctrl Pts',(14.6976315192819,51.8941150313084,18.));
#59833=CARTESIAN_POINT('Ctrl Pts',(14.6855981509457,51.8905237529518,18.));
#59834=CARTESIAN_POINT('Ctrl Pts',(14.6288668056565,51.8735926621063,18.));
#59835=CARTESIAN_POINT('Ctrl Pts',(14.5713364809609,51.8599659874371,18.));
#59836=CARTESIAN_POINT('Ctrl Pts',(14.5133186620421,51.8497038434798,18.));
#59837=CARTESIAN_POINT('Ctrl Pts',(14.4564856885499,51.8396512740043,18.));
#59838=CARTESIAN_POINT('Ctrl Pts',(14.3991838939685,51.8328273015831,18.));
#59839=CARTESIAN_POINT('Ctrl Pts',(14.3417076889049,51.8293372126129,18.));
#59840=CARTESIAN_POINT('Ctrl Pts',(14.3001007306979,51.8268107412538,18.));
#59841=CARTESIAN_POINT('Ctrl Pts',(14.2584023661317,51.8260323215432,18.));
#59842=CARTESIAN_POINT('Ctrl Pts',(14.2167293111348,51.8270580660935,18.));
#59843=CARTESIAN_POINT('Ctrl Pts',(14.1949488647985,51.827594172077,18.));
#59844=CARTESIAN_POINT('Ctrl Pts',(14.1731754256014,51.8286233369707,18.));
#59845=CARTESIAN_POINT('Ctrl Pts',(14.1514264245833,51.8301550767572,18.));
#59846=CARTESIAN_POINT('Ctrl Pts',(14.1413116392164,51.8308674413925,18.));
#59847=CARTESIAN_POINT('Ctrl Pts',(14.1312071832961,51.8316882253561,18.));
#59848=CARTESIAN_POINT('Ctrl Pts',(14.1211226983366,51.8326172394596,18.));
#59849=CARTESIAN_POINT('Ctrl Pts',(14.0655859083915,51.8377334611929,18.));
#59850=CARTESIAN_POINT('Ctrl Pts',(14.010579492857,51.8461333286653,18.));
#59851=CARTESIAN_POINT('Ctrl Pts',(13.9563747310531,51.8579061060214,18.));
#59852=CARTESIAN_POINT('Ctrl Pts',(13.9201064161194,51.8657832515449,18.));
#59853=CARTESIAN_POINT('Ctrl Pts',(13.8841971505527,51.8751714207574,18.));
#59854=CARTESIAN_POINT('Ctrl Pts',(13.8487329702921,51.8861095759353,18.));
#59855=CARTESIAN_POINT('Ctrl Pts',(13.7962430344238,51.902298955179,18.));
#59856=CARTESIAN_POINT('Ctrl Pts',(13.7447264797303,51.9218828237725,18.));
#59857=CARTESIAN_POINT('Ctrl Pts',(13.6944250448181,51.9446586129267,18.));
#59858=CARTESIAN_POINT('Ctrl Pts',(13.6788893969321,51.9516929379165,18.));
#59859=CARTESIAN_POINT('Ctrl Pts',(13.6634698927207,51.9590319641544,18.));
#59860=CARTESIAN_POINT('Ctrl Pts',(13.6481743336116,51.9666702755676,18.));
#59861=CARTESIAN_POINT('Ctrl Pts',(13.6347520070389,51.9733731302669,18.));
#59862=CARTESIAN_POINT('Ctrl Pts',(13.6214194410696,51.9803097396806,18.));
#59863=CARTESIAN_POINT('Ctrl Pts',(13.6082135027491,51.9874589876079,18.));
#59864=CARTESIAN_POINT('Ctrl Pts',(13.5592445611088,52.0139691147967,18.));
#59865=CARTESIAN_POINT('Ctrl Pts',(13.5119462056412,52.0434302755537,18.));
#59866=CARTESIAN_POINT('Ctrl Pts',(13.4665417533877,52.0755936524918,18.));
#59867=CARTESIAN_POINT('Ctrl Pts',(13.4211918994935,52.1077183533193,18.));
#59868=CARTESIAN_POINT('Ctrl Pts',(13.3777306362705,52.1425397400705,18.));
#59869=CARTESIAN_POINT('Ctrl Pts',(13.336418351779,52.1798448137035,18.));
#59870=CARTESIAN_POINT('Ctrl Pts',(13.310012629919,52.2036892321482,18.));
#59871=CARTESIAN_POINT('Ctrl Pts',(13.284485655765,52.2285490007982,18.));
#59872=CARTESIAN_POINT('Ctrl Pts',(13.2599156980565,52.2543732768879,18.));
#59873=CARTESIAN_POINT('Ctrl Pts',(13.2472551099776,52.2676801993451,18.));
#59874=CARTESIAN_POINT('Ctrl Pts',(13.2348487708532,52.2812432661479,18.));
#59875=CARTESIAN_POINT('Ctrl Pts',(13.2227083469491,52.2950557511153,18.));
#59876=CARTESIAN_POINT('Ctrl Pts',(13.2153859887604,52.3033865938607,18.));
#59877=CARTESIAN_POINT('Ctrl Pts',(13.2081608879655,52.311807752205,18.));
#59878=CARTESIAN_POINT('Ctrl Pts',(13.2010440030961,52.3203073114271,18.));
#59879=CARTESIAN_POINT('Ctrl Pts',(13.1666279154686,52.3614097853814,18.));
#59880=CARTESIAN_POINT('Ctrl Pts',(13.1346840827622,52.4044056088251,18.));
#59881=CARTESIAN_POINT('Ctrl Pts',(13.1054638931938,52.4491024554233,18.));
#59882=CARTESIAN_POINT('Ctrl Pts',(13.087114648167,52.4771704933884,18.));
#59883=CARTESIAN_POINT('Ctrl Pts',(13.0698403219756,52.5059097415566,18.));
#59884=CARTESIAN_POINT('Ctrl Pts',(13.0537134178051,52.5352751363851,18.));
#59885=CARTESIAN_POINT('Ctrl Pts',(13.0478169296962,52.5460120205131,18.));
#59886=CARTESIAN_POINT('Ctrl Pts',(13.0420727750503,52.5568348697425,18.));
#59887=CARTESIAN_POINT('Ctrl Pts',(13.0364885788728,52.5677340663375,18.));
#59888=CARTESIAN_POINT('Ctrl Pts',(13.0130475064211,52.6134861941154,18.));
#59889=CARTESIAN_POINT('Ctrl Pts',(12.9924569304889,52.6605100892665,18.));
#59890=CARTESIAN_POINT('Ctrl Pts',(12.9749633881428,52.7086350162103,18.));
#59891=CARTESIAN_POINT('Ctrl Pts',(12.9651909077076,52.7355192171171,18.));
#59892=CARTESIAN_POINT('Ctrl Pts',(12.9563857854424,52.7627472106675,18.));
#59893=CARTESIAN_POINT('Ctrl Pts',(12.948598136759,52.7902898637941,18.));
#59894=CARTESIAN_POINT('Ctrl Pts',(12.9431286937976,52.8096336961118,18.));
#59895=CARTESIAN_POINT('Ctrl Pts',(12.9381612650277,52.82913275561,18.));
#59896=CARTESIAN_POINT('Ctrl Pts',(12.9336937527446,52.8487684531621,18.));
#59897=CARTESIAN_POINT('Ctrl Pts',(13.8936870225526,54.5092654229862,18.));
#59898=CARTESIAN_POINT('Ctrl Pts',(13.9419518764864,54.5239833380073,18.));
#59899=CARTESIAN_POINT('Ctrl Pts',(13.9909664228046,54.5355224856699,18.));
#59900=CARTESIAN_POINT('Ctrl Pts',(14.0404525674476,54.5440410140802,18.));
#59901=CARTESIAN_POINT('Ctrl Pts',(14.0921569775487,54.5529413939656,18.));
#59902=CARTESIAN_POINT('Ctrl Pts',(14.1443769192153,54.5585445895535,18.));
#59903=CARTESIAN_POINT('Ctrl Pts',(14.1968242396273,54.5609818668625,18.));
#59904=CARTESIAN_POINT('Ctrl Pts',(14.2388871088231,54.5629365687584,18.));
#59905=CARTESIAN_POINT('Ctrl Pts',(14.2810970053263,54.5628539586051,18.));
#59906=CARTESIAN_POINT('Ctrl Pts',(14.3233126980424,54.5607787169104,18.));
#59907=CARTESIAN_POINT('Ctrl Pts',(14.3411576908209,54.5599014916259,18.));
#59908=CARTESIAN_POINT('Ctrl Pts',(14.359003766426,54.5586679663763,18.));
#59909=CARTESIAN_POINT('Ctrl Pts',(14.3768403679013,54.5570804251692,18.));
#59910=CARTESIAN_POINT('Ctrl Pts',(14.3869641761631,54.5561793587407,18.));
#59911=CARTESIAN_POINT('Ctrl Pts',(14.3970856400397,54.5551640486899,18.));
#59912=CARTESIAN_POINT('Ctrl Pts',(14.4071867211758,54.554036933109,18.));
#59913=CARTESIAN_POINT('Ctrl Pts',(14.46128977502,54.5479999164633,18.));
#59914=CARTESIAN_POINT('Ctrl Pts',(14.5149156125182,54.53875069329,18.));
#59915=CARTESIAN_POINT('Ctrl Pts',(14.5677633543885,54.5264311541972,18.));
#59916=CARTESIAN_POINT('Ctrl Pts',(14.6215795301015,54.51388585979,18.));
#59917=CARTESIAN_POINT('Ctrl Pts',(14.6745899303726,54.498156745542,18.));
#59918=CARTESIAN_POINT('Ctrl Pts',(14.7264864439584,54.4793411079432,18.));
#59919=CARTESIAN_POINT('Ctrl Pts',(14.7636024302316,54.4658843090452,18.));
#59920=CARTESIAN_POINT('Ctrl Pts',(14.8001489167129,54.4508476461193,18.));
#59921=CARTESIAN_POINT('Ctrl Pts',(14.8360112141901,54.4342505283932,18.));
#59922=CARTESIAN_POINT('Ctrl Pts',(14.8512574582442,54.4271945468959,18.));
#59923=CARTESIAN_POINT('Ctrl Pts',(14.8663799984359,54.4198563674573,18.));
#59924=CARTESIAN_POINT('Ctrl Pts',(14.8813697562834,54.4122367571808,18.));
#59925=CARTESIAN_POINT('Ctrl Pts',(14.8903005158295,54.4076970636177,18.));
#59926=CARTESIAN_POINT('Ctrl Pts',(14.8991790662204,54.4030599782254,18.));
#59927=CARTESIAN_POINT('Ctrl Pts',(14.9079969993248,54.3983296699863,18.));
#59928=CARTESIAN_POINT('Ctrl Pts',(14.9580707729375,54.3714680028497,18.));
#59929=CARTESIAN_POINT('Ctrl Pts',(15.0062562237396,54.3415708986464,18.));
#59930=CARTESIAN_POINT('Ctrl Pts',(15.052235675618,54.3087525448002,18.));
#59931=CARTESIAN_POINT('Ctrl Pts',(15.080470042487,54.288599946092,18.));
#59932=CARTESIAN_POINT('Ctrl Pts',(15.1078726148529,54.2673447838712,18.));
#59933=CARTESIAN_POINT('Ctrl Pts',(15.1343678441299,54.245003945279,18.));
#59934=CARTESIAN_POINT('Ctrl Pts',(15.1763790053575,54.209580036988,18.));
#59935=CARTESIAN_POINT('Ctrl Pts',(15.2161107900716,54.1714287640077,18.));
#59936=CARTESIAN_POINT('Ctrl Pts',(15.2534991669625,54.1308482498305,18.));
#59937=CARTESIAN_POINT('Ctrl Pts',(15.2646851435514,54.1187072391929,18.));
#59938=CARTESIAN_POINT('Ctrl Pts',(15.2756611560254,54.1063484965527,18.));
#59939=CARTESIAN_POINT('Ctrl Pts',(15.2864249364023,54.0937793159867,18.));
#59940=CARTESIAN_POINT('Ctrl Pts',(15.296376721656,54.0821583258301,18.));
#59941=CARTESIAN_POINT('Ctrl Pts',(15.3061511701423,54.0703520539335,18.));
#59942=CARTESIAN_POINT('Ctrl Pts',(15.3157236805298,54.0583951512571,18.));
#59943=CARTESIAN_POINT('Ctrl Pts',(15.3511875377787,54.014097691919,18.));
#59944=CARTESIAN_POINT('Ctrl Pts',(15.3839319325097,53.9676827164785,18.));
#59945=CARTESIAN_POINT('Ctrl Pts',(15.4139160661048,53.9195006536869,18.));
#59946=CARTESIAN_POINT('Ctrl Pts',(15.4446090042121,53.8701795997215,18.));
#59947=CARTESIAN_POINT('Ctrl Pts',(15.4724102509795,53.8190061740294,18.));
#59948=CARTESIAN_POINT('Ctrl Pts',(15.497243500525,53.7663111449781,18.));
#59949=CARTESIAN_POINT('Ctrl Pts',(15.5123202613396,53.7343189424406,18.));
#59950=CARTESIAN_POINT('Ctrl Pts',(15.5263023651589,53.7017650594462,18.));
#59951=CARTESIAN_POINT('Ctrl Pts',(15.5391656032547,53.668717588239,18.));
#59952=CARTESIAN_POINT('Ctrl Pts',(15.5462480435936,53.6505218010325,18.));
#59953=CARTESIAN_POINT('Ctrl Pts',(15.5529911929917,53.6321763121665,18.));
#59954=CARTESIAN_POINT('Ctrl Pts',(15.5593902229536,53.6136920745805,18.));
#59955=CARTESIAN_POINT('Ctrl Pts',(15.5632433723038,53.6025618675853,18.));
#59956=CARTESIAN_POINT('Ctrl Pts',(15.5669723526287,53.5913794289557,18.));
#59957=CARTESIAN_POINT('Ctrl Pts',(15.5705740541365,53.5801532197423,18.));
#59958=CARTESIAN_POINT('Ctrl Pts',(15.5890317873762,53.5226219738838,18.));
#59959=CARTESIAN_POINT('Ctrl Pts',(15.6040939073564,53.4641232630989,18.));
#59960=CARTESIAN_POINT('Ctrl Pts',(15.6156733811598,53.4050077405015,18.));
#59961=CARTESIAN_POINT('Ctrl Pts',(15.6232022585969,53.3665713200026,18.));
#59962=CARTESIAN_POINT('Ctrl Pts',(15.6292580546325,53.3278733667412,18.));
#59963=CARTESIAN_POINT('Ctrl Pts',(15.6338065434899,53.2890044670766,18.));
#59964=CARTESIAN_POINT('Ctrl Pts',(15.6356864328875,53.2729399597947,18.));
#59965=CARTESIAN_POINT('Ctrl Pts',(15.6373087460133,53.2568462124372,18.));
#59966=CARTESIAN_POINT('Ctrl Pts',(15.6386706145235,53.2407294854927,18.));
#59967=CARTESIAN_POINT('Ctrl Pts',(15.6396676228531,53.2289306143917,18.));
#59968=CARTESIAN_POINT('Ctrl Pts',(15.6405248635805,53.2171205569137,18.));
#59969=CARTESIAN_POINT('Ctrl Pts',(15.6412408277512,53.205311815233,18.));
#59970=CARTESIAN_POINT('Ctrl Pts',(15.6449216835252,53.1446016892555,18.));
#59971=CARTESIAN_POINT('Ctrl Pts',(15.6448786914156,53.0838566394801,18.));
#59972=CARTESIAN_POINT('Ctrl Pts',(15.6409989084031,53.0234144938957,18.));
#59973=CARTESIAN_POINT('Ctrl Pts',(15.6391817516166,52.9951054738585,18.));
#59974=CARTESIAN_POINT('Ctrl Pts',(15.6365222466638,52.9668626417859,18.));
#59975=CARTESIAN_POINT('Ctrl Pts',(15.6330049221515,52.9387198431847,18.));
#59976=CARTESIAN_POINT('Ctrl Pts',(15.6299827554381,52.91453889859,18.));
#59977=CARTESIAN_POINT('Ctrl Pts',(15.6263272558779,52.8904317889029,18.));
#59978=CARTESIAN_POINT('Ctrl Pts',(15.6220539738783,52.8664139542998,18.));
#59979=CARTESIAN_POINT('Ctrl Pts',(-37.5756558680257,39.2699729499893,18.));
#59980=CARTESIAN_POINT('Ctrl Pts',(-37.5651127690922,39.2097369422873,18.));
#59981=CARTESIAN_POINT('Ctrl Pts',(-37.5584799714475,39.1490477940627,18.));
#59982=CARTESIAN_POINT('Ctrl Pts',(-37.5555966212126,39.0882269703887,18.));
#59983=CARTESIAN_POINT('Ctrl Pts',(-37.5527300631013,39.0277603564721,18.));
#59984=CARTESIAN_POINT('Ctrl Pts',(-37.553569953746,38.9671624857772,18.));
#59985=CARTESIAN_POINT('Ctrl Pts',(-37.5580129364599,38.9067545255738,18.));
#59986=CARTESIAN_POINT('Ctrl Pts',(-37.5613679468783,38.8611389225246,18.));
#59987=CARTESIAN_POINT('Ctrl Pts',(-37.5667786506927,38.8156316117443,18.));
#59988=CARTESIAN_POINT('Ctrl Pts',(-37.5742186551894,38.7703786151083,18.));
#59989=CARTESIAN_POINT('Ctrl Pts',(-37.5780809441846,38.7468866735401,18.));
#59990=CARTESIAN_POINT('Ctrl Pts',(-37.5824903524789,38.7234634071241,18.));
#59991=CARTESIAN_POINT('Ctrl Pts',(-37.5874446737534,38.7001303514373,18.));
#59992=CARTESIAN_POINT('Ctrl Pts',(-37.5900538576765,38.6878420418179,18.));
#59993=CARTESIAN_POINT('Ctrl Pts',(-37.5928147908849,38.6755768363574,18.));
#59994=CARTESIAN_POINT('Ctrl Pts',(-37.5957216552661,38.6633597908174,18.));
#59995=CARTESIAN_POINT('Ctrl Pts',(-37.6094259854369,38.605762874059,18.));
#59996=CARTESIAN_POINT('Ctrl Pts',(-37.6263915747065,38.5491262011484,18.));
#59997=CARTESIAN_POINT('Ctrl Pts',(-37.6465146580723,38.4937496146526,18.));
#59998=CARTESIAN_POINT('Ctrl Pts',(-37.6662269366984,38.439503519135,18.));
#59999=CARTESIAN_POINT('Ctrl Pts',(-37.6889696982612,38.3864657328387,18.));
#60000=CARTESIAN_POINT('Ctrl Pts',(-37.7146868377003,38.3349439029342,18.));
#60001=CARTESIAN_POINT('Ctrl Pts',(-37.7333032641332,38.2976476725983,18.));
#60002=CARTESIAN_POINT('Ctrl Pts',(-37.7534791916943,38.2611463231356,18.));
#60003=CARTESIAN_POINT('Ctrl Pts',(-37.7752048261667,38.2255690008542,18.));
#60004=CARTESIAN_POINT('Ctrl Pts',(-37.7865596505648,38.2069746418461,18.));
#60005=CARTESIAN_POINT('Ctrl Pts',(-37.7983379414309,38.188632883801,18.));
#60006=CARTESIAN_POINT('Ctrl Pts',(-37.8105392196984,38.1705635815837,18.));
#60007=CARTESIAN_POINT('Ctrl Pts',(-37.8162136717173,38.1621600859665,18.));
#60008=CARTESIAN_POINT('Ctrl Pts',(-37.8219768455385,38.1538197468508,18.));
#60009=CARTESIAN_POINT('Ctrl Pts',(-37.8278237560891,38.1455508194946,18.));
#60010=CARTESIAN_POINT('Ctrl Pts',(-37.8600240522425,38.1000119135318,18.));
#60011=CARTESIAN_POINT('Ctrl Pts',(-37.8948027203391,38.0565742506206,18.));
#60012=CARTESIAN_POINT('Ctrl Pts',(-37.932101350128,38.0155174319281,18.));
#60013=CARTESIAN_POINT('Ctrl Pts',(-37.9570573615923,37.9880468668221,18.));
#60014=CARTESIAN_POINT('Ctrl Pts',(-37.9831422874089,37.9616427832137,18.));
#60015=CARTESIAN_POINT('Ctrl Pts',(-38.0103468288125,37.9363991775294,18.));
#60016=CARTESIAN_POINT('Ctrl Pts',(-38.050612215002,37.8990361682947,18.));
#60017=CARTESIAN_POINT('Ctrl Pts',(-38.0933303033917,37.8642134925913,18.));
#60018=CARTESIAN_POINT('Ctrl Pts',(-38.1382048591451,37.8320391955257,18.));
#60019=CARTESIAN_POINT('Ctrl Pts',(-38.1520648967442,37.8221017831198,18.));
#60020=CARTESIAN_POINT('Ctrl Pts',(-38.1661307314527,37.8124173314208,18.));
#60021=CARTESIAN_POINT('Ctrl Pts',(-38.1803937730742,37.8029898884102,18.));
#60022=CARTESIAN_POINT('Ctrl Pts',(-38.1929089479187,37.7947177329509,18.));
#60023=CARTESIAN_POINT('Ctrl Pts',(-38.2055816457065,37.7866401763901,18.));
#60024=CARTESIAN_POINT('Ctrl Pts',(-38.2183751516207,37.7787785855269,18.));
#60025=CARTESIAN_POINT('Ctrl Pts',(-38.2658171634217,37.7496255379568,18.));
#60026=CARTESIAN_POINT('Ctrl Pts',(-38.3149793341025,37.723394852447,18.));
#60027=CARTESIAN_POINT('Ctrl Pts',(-38.365534594144,37.700155493664,18.));
#60028=CARTESIAN_POINT('Ctrl Pts',(-38.4160291498247,37.6769440396019,18.));
#60029=CARTESIAN_POINT('Ctrl Pts',(-38.4679146667789,37.6567165566507,18.));
#60030=CARTESIAN_POINT('Ctrl Pts',(-38.5208765564485,37.6395920241963,18.));
#60031=CARTESIAN_POINT('Ctrl Pts',(-38.5547280084067,37.6286466011514,18.));
#60032=CARTESIAN_POINT('Ctrl Pts',(-38.5890193652551,37.6189698569052,18.));
#60033=CARTESIAN_POINT('Ctrl Pts',(-38.6236674824541,37.6106041450253,18.));
#60034=CARTESIAN_POINT('Ctrl Pts',(-38.641521850756,37.6062932469711,18.));
#60035=CARTESIAN_POINT('Ctrl Pts',(-38.6594709236641,37.6023306259802,18.));
#60036=CARTESIAN_POINT('Ctrl Pts',(-38.677503044697,37.5987230218509,18.));
#60037=CARTESIAN_POINT('Ctrl Pts',(-38.6883788046389,37.5965471582126,18.));
#60038=CARTESIAN_POINT('Ctrl Pts',(-38.6992841521561,37.5945006838765,18.));
#60039=CARTESIAN_POINT('Ctrl Pts',(-38.7102032898677,37.5925871316739,18.));
#60040=CARTESIAN_POINT('Ctrl Pts',(-38.763006061038,37.583333575052,18.));
#60041=CARTESIAN_POINT('Ctrl Pts',(-38.8162124112958,37.5771677759252,18.));
#60042=CARTESIAN_POINT('Ctrl Pts',(-38.8695301449481,37.5742112603263,18.));
#60043=CARTESIAN_POINT('Ctrl Pts',(-38.9030118817427,37.5723546683385,18.));
#60044=CARTESIAN_POINT('Ctrl Pts',(-38.9365374743059,37.5717646060231,18.));
#60045=CARTESIAN_POINT('Ctrl Pts',(-38.970031659091,37.5724813268559,18.));
#60046=CARTESIAN_POINT('Ctrl Pts',(-38.9822787358886,37.5727433942905,18.));
#60047=CARTESIAN_POINT('Ctrl Pts',(-38.9945241009328,37.5731803873939,18.));
#60048=CARTESIAN_POINT('Ctrl Pts',(-39.006755607008,37.5737941004355,18.));
#60049=CARTESIAN_POINT('Ctrl Pts',(-39.05809813714,37.5763702002338,18.));
#60050=CARTESIAN_POINT('Ctrl Pts',(-39.109116914763,37.5820508279815,18.));
#60051=CARTESIAN_POINT('Ctrl Pts',(-39.1595408594659,37.5909641089067,18.));
#60052=CARTESIAN_POINT('Ctrl Pts',(-39.187706877111,37.5959429265953,18.));
#60053=CARTESIAN_POINT('Ctrl Pts',(-39.2156870323819,37.6019312274164,18.));
#60054=CARTESIAN_POINT('Ctrl Pts',(-39.2434310600143,37.6089578358496,18.));
#60055=CARTESIAN_POINT('Ctrl Pts',(-39.2629177980487,37.6138931566914,18.));
#60056=CARTESIAN_POINT('Ctrl Pts',(-39.2822879943277,37.6193408368567,18.));
#60057=CARTESIAN_POINT('Ctrl Pts',(-39.3015265966439,37.6252897660473,18.));
#60058=CARTESIAN_POINT('Ctrl Pts',(-40.2595650866584,39.2869186252538,18.));
#60059=CARTESIAN_POINT('Ctrl Pts',(-40.2481791157548,39.3360745846547,18.));
#60060=CARTESIAN_POINT('Ctrl Pts',(-40.233665287806,39.3842904001651,18.));
#60061=CARTESIAN_POINT('Ctrl Pts',(-40.2162996606326,39.4314043435469,18.));
#60062=CARTESIAN_POINT('Ctrl Pts',(-40.1981554153043,39.4806307226793,18.));
#60063=CARTESIAN_POINT('Ctrl Pts',(-40.1768978215462,39.5286549715329,18.));
#60064=CARTESIAN_POINT('Ctrl Pts',(-40.1527847010642,39.5752932074852,18.));
#60065=CARTESIAN_POINT('Ctrl Pts',(-40.1334453389403,39.6126983095988,18.));
#60066=CARTESIAN_POINT('Ctrl Pts',(-40.1122679418623,39.6492120507124,18.));
#60067=CARTESIAN_POINT('Ctrl Pts',(-40.089361863191,39.6847344690018,18.));
#60068=CARTESIAN_POINT('Ctrl Pts',(-40.0796819049363,39.6997460094353,18.));
#60069=CARTESIAN_POINT('Ctrl Pts',(-40.0696929904195,39.7145804305273,18.));
#60070=CARTESIAN_POINT('Ctrl Pts',(-40.0594023733884,39.7292297389137,18.));
#60071=CARTESIAN_POINT('Ctrl Pts',(-40.0535563601133,39.7375518882114,18.));
#60072=CARTESIAN_POINT('Ctrl Pts',(-40.0476124487805,39.7458148202868,18.));
#60073=CARTESIAN_POINT('Ctrl Pts',(-40.0415817907732,39.7540041063919,18.));
#60074=CARTESIAN_POINT('Ctrl Pts',(-40.0093013797014,39.7978390447242,18.));
#60075=CARTESIAN_POINT('Ctrl Pts',(-39.9744777462107,39.8396546716854,18.));
#60076=CARTESIAN_POINT('Ctrl Pts',(-39.9373842779719,39.8792613960026,18.));
#60077=CARTESIAN_POINT('Ctrl Pts',(-39.8996105080951,39.9195945155777,18.));
#60078=CARTESIAN_POINT('Ctrl Pts',(-39.8594823789697,39.9576379445105,18.));
#60079=CARTESIAN_POINT('Ctrl Pts',(-39.817238289424,39.9931735245898,18.));
#60080=CARTESIAN_POINT('Ctrl Pts',(-39.7870250053652,40.0185888332561,18.));
#60081=CARTESIAN_POINT('Ctrl Pts',(-39.7557282762375,40.0427209888158,18.));
#60082=CARTESIAN_POINT('Ctrl Pts',(-39.7234222902936,40.0654803762021,18.));
#60083=CARTESIAN_POINT('Ctrl Pts',(-39.7096908088931,40.0751541284635,18.));
#60084=CARTESIAN_POINT('Ctrl Pts',(-39.6957768723929,40.0845797514891,18.));
#60085=CARTESIAN_POINT('Ctrl Pts',(-39.6816856838153,40.0937497716388,18.));
#60086=CARTESIAN_POINT('Ctrl Pts',(-39.6732915903904,40.0992123346739,18.));
#60087=CARTESIAN_POINT('Ctrl Pts',(-39.6648392875157,40.104581065436,18.));
#60088=CARTESIAN_POINT('Ctrl Pts',(-39.6563366062018,40.1098507565136,18.));
#60089=CARTESIAN_POINT('Ctrl Pts',(-39.6080360371336,40.1397859109041,18.));
#60090=CARTESIAN_POINT('Ctrl Pts',(-39.5580510184926,40.1665680778016,18.));
#60091=CARTESIAN_POINT('Ctrl Pts',(-39.5066393729943,40.1899792587996,18.));
#60092=CARTESIAN_POINT('Ctrl Pts',(-39.4750618486744,40.2043586300522,18.));
#60093=CARTESIAN_POINT('Ctrl Pts',(-39.4429452140606,40.217465799326,18.));
#60094=CARTESIAN_POINT('Ctrl Pts',(-39.4103419265004,40.2292437480239,18.));
#60095=CARTESIAN_POINT('Ctrl Pts',(-39.3586573390136,40.2479148227972,18.));
#60096=CARTESIAN_POINT('Ctrl Pts',(-39.3057507659291,40.2632482055135,18.));
#60097=CARTESIAN_POINT('Ctrl Pts',(-39.2519123537495,40.2753374915748,18.));
#60098=CARTESIAN_POINT('Ctrl Pts',(-39.2358056778285,40.2789542069425,18.));
#60099=CARTESIAN_POINT('Ctrl Pts',(-39.2196154532535,40.2822802513834,18.));
#60100=CARTESIAN_POINT('Ctrl Pts',(-39.2033491283307,40.2853173071474,18.));
#60101=CARTESIAN_POINT('Ctrl Pts',(-39.1883094890373,40.2881253306819,18.));
#60102=CARTESIAN_POINT('Ctrl Pts',(-39.1731980803203,40.2906871462819,18.));
#60103=CARTESIAN_POINT('Ctrl Pts',(-39.1580572086001,40.2929987736051,18.));
#60104=CARTESIAN_POINT('Ctrl Pts',(-39.1019623295839,40.3015630397466,18.));
#60105=CARTESIAN_POINT('Ctrl Pts',(-39.0453935804777,40.3067133780786,18.));
#60106=CARTESIAN_POINT('Ctrl Pts',(-38.988674785285,40.3085896575269,18.));
#60107=CARTESIAN_POINT('Ctrl Pts',(-38.9306156897047,40.3105102746249,18.));
#60108=CARTESIAN_POINT('Ctrl Pts',(-38.8723984153787,40.3090004242116,18.));
#60109=CARTESIAN_POINT('Ctrl Pts',(-38.8143475050087,40.3041593897172,18.));
#60110=CARTESIAN_POINT('Ctrl Pts',(-38.7791040438476,40.3012203348411,18.));
#60111=CARTESIAN_POINT('Ctrl Pts',(-38.7439215217934,40.297052459211,18.));
#60112=CARTESIAN_POINT('Ctrl Pts',(-38.7088709965466,40.2916688390196,18.));
#60113=CARTESIAN_POINT('Ctrl Pts',(-38.6895721262637,40.2887046098962,18.));
#60114=CARTESIAN_POINT('Ctrl Pts',(-38.6703132641282,40.2853716920803,18.));
#60115=CARTESIAN_POINT('Ctrl Pts',(-38.6511063076066,40.2816713797398,18.));
#60116=CARTESIAN_POINT('Ctrl Pts',(-38.6395410469613,40.2794432767793,18.));
#60117=CARTESIAN_POINT('Ctrl Pts',(-38.627992637109,40.2770815256585,18.));
#60118=CARTESIAN_POINT('Ctrl Pts',(-38.6164699649865,40.2745876647122,18.));
#60119=CARTESIAN_POINT('Ctrl Pts',(-38.557419079826,40.2618072354178,18.));
#60120=CARTESIAN_POINT('Ctrl Pts',(-38.4992281803323,40.2456023804861,18.));
#60121=CARTESIAN_POINT('Ctrl Pts',(-38.4422443841854,40.2260730329326,18.));
#60122=CARTESIAN_POINT('Ctrl Pts',(-38.4051943363965,40.2133753309704,18.));
#60123=CARTESIAN_POINT('Ctrl Pts',(-38.368654306916,40.1992711514025,18.));
#60124=CARTESIAN_POINT('Ctrl Pts',(-38.3327198362902,40.183776140909,18.));
#60125=CARTESIAN_POINT('Ctrl Pts',(-38.3178657816824,40.1773710449659,18.));
#60126=CARTESIAN_POINT('Ctrl Pts',(-38.3031152165708,40.170728187765,18.));
#60127=CARTESIAN_POINT('Ctrl Pts',(-38.2884749985355,40.1638482153583,18.));
#60128=CARTESIAN_POINT('Ctrl Pts',(-38.2777585350481,40.1588121583192,18.));
#60129=CARTESIAN_POINT('Ctrl Pts',(-38.2671022703707,40.1536494636781,18.));
#60130=CARTESIAN_POINT('Ctrl Pts',(-38.2565177796711,40.148365072953,18.));
#60131=CARTESIAN_POINT('Ctrl Pts',(-38.2021024002753,40.121197764261,18.));
#60132=CARTESIAN_POINT('Ctrl Pts',(-38.149518572045,40.0907880130311,18.));
#60133=CARTESIAN_POINT('Ctrl Pts',(-38.0991152601742,40.0572068987011,18.));
#60134=CARTESIAN_POINT('Ctrl Pts',(-38.0755109333516,40.0414805591354,18.));
#60135=CARTESIAN_POINT('Ctrl Pts',(-38.0523849413559,40.0250579742236,18.));
#60136=CARTESIAN_POINT('Ctrl Pts',(-38.0297743098615,40.0079426645895,18.));
#60137=CARTESIAN_POINT('Ctrl Pts',(-38.0103443715311,39.9932350076725,18.));
#60138=CARTESIAN_POINT('Ctrl Pts',(-37.9912950014703,39.9780157739289,18.));
#60139=CARTESIAN_POINT('Ctrl Pts',(-37.9726317990811,39.9623061512025,18.));
#60140=CARTESIAN_POINT('Ctrl Pts',(-52.7966221146314,-12.9064860705774,
18.));
#60141=CARTESIAN_POINT('Ctrl Pts',(-52.7391846522721,-12.9274734829173,
18.));
#60142=CARTESIAN_POINT('Ctrl Pts',(-52.6833098509988,-12.9520735040296,
18.));
#60143=CARTESIAN_POINT('Ctrl Pts',(-52.6291956963058,-12.9799861915281,
18.));
#60144=CARTESIAN_POINT('Ctrl Pts',(-52.5753966188852,-13.0077363586381,
18.));
#60145=CARTESIAN_POINT('Ctrl Pts',(-52.5233370565326,-13.0387617569735,
18.));
#60146=CARTESIAN_POINT('Ctrl Pts',(-52.4732434855941,-13.0728123808102,
18.));
#60147=CARTESIAN_POINT('Ctrl Pts',(-52.4354166035925,-13.0985248406294,
18.));
#60148=CARTESIAN_POINT('Ctrl Pts',(-52.3987113360346,-13.1259633238969,
18.));
#60149=CARTESIAN_POINT('Ctrl Pts',(-52.3632409515086,-13.1550320009623,
18.));
#60150=CARTESIAN_POINT('Ctrl Pts',(-52.3448272848805,-13.1701223625684,
18.));
#60151=CARTESIAN_POINT('Ctrl Pts',(-52.3267466539931,-13.1856521912722,
18.));
#60152=CARTESIAN_POINT('Ctrl Pts',(-52.3090166072825,-13.2016088137109,
18.));
#60153=CARTESIAN_POINT('Ctrl Pts',(-52.2996792306588,-13.210012231693,18.));
#60154=CARTESIAN_POINT('Ctrl Pts',(-52.2904377360769,-13.2185355103954,
18.));
#60155=CARTESIAN_POINT('Ctrl Pts',(-52.2813109131512,-13.2271610850761,
18.));
#60156=CARTESIAN_POINT('Ctrl Pts',(-52.2382824916528,-13.2678263709096,
18.));
#60157=CARTESIAN_POINT('Ctrl Pts',(-52.1977162890024,-13.3108358032656,
18.));
#60158=CARTESIAN_POINT('Ctrl Pts',(-52.1598201080725,-13.3559496827199,
18.));
#60159=CARTESIAN_POINT('Ctrl Pts',(-52.1226978381087,-13.4001422522907,
18.));
#60160=CARTESIAN_POINT('Ctrl Pts',(-52.088137205607,-13.4463551316742,18.));
#60161=CARTESIAN_POINT('Ctrl Pts',(-52.0563765963178,-13.4943859943775,
18.));
#60162=CARTESIAN_POINT('Ctrl Pts',(-52.0333851347714,-13.5291554700772,
18.));
#60163=CARTESIAN_POINT('Ctrl Pts',(-52.0118618266889,-13.5648781300626,
18.));
#60164=CARTESIAN_POINT('Ctrl Pts',(-51.991913624802,-13.6014809507113,18.));
#60165=CARTESIAN_POINT('Ctrl Pts',(-51.9814876879865,-13.6206114316197,
18.));
#60166=CARTESIAN_POINT('Ctrl Pts',(-51.9714922558957,-13.6399823727608,
18.));
#60167=CARTESIAN_POINT('Ctrl Pts',(-51.9619442850932,-13.6595834362661,
18.));
#60168=CARTESIAN_POINT('Ctrl Pts',(-51.9575038197999,-13.6686992833929,
18.));
#60169=CARTESIAN_POINT('Ctrl Pts',(-51.9531624130475,-13.6778603944113,
18.));
#60170=CARTESIAN_POINT('Ctrl Pts',(-51.9489247217451,-13.6870583249183,
18.));
#60171=CARTESIAN_POINT('Ctrl Pts',(-51.925587102274,-13.7377127465782,18.));
#60172=CARTESIAN_POINT('Ctrl Pts',(-51.9053583908736,-13.7895496676836,
18.));
#60173=CARTESIAN_POINT('Ctrl Pts',(-51.8884515319789,-13.8423787830615,
18.));
#60174=CARTESIAN_POINT('Ctrl Pts',(-51.8771391871561,-13.8777266364718,
18.));
#60175=CARTESIAN_POINT('Ctrl Pts',(-51.867314950333,-13.91351905172,18.));
#60176=CARTESIAN_POINT('Ctrl Pts',(-51.8590555816082,-13.9497009999509,
18.));
#60177=CARTESIAN_POINT('Ctrl Pts',(-51.8468310253394,-14.0032533084619,
18.));
#60178=CARTESIAN_POINT('Ctrl Pts',(-51.8380328718691,-14.0576598787871,
18.));
#60179=CARTESIAN_POINT('Ctrl Pts',(-51.8326065611663,-14.1126100767572,
18.));
#60180=CARTESIAN_POINT('Ctrl Pts',(-51.830930637981,-14.1295815175498,18.));
#60181=CARTESIAN_POINT('Ctrl Pts',(-51.8295766661961,-14.1466047249358,
18.));
#60182=CARTESIAN_POINT('Ctrl Pts',(-51.828543856078,-14.1636702346728,18.));
#60183=CARTESIAN_POINT('Ctrl Pts',(-51.8276375355831,-14.1786457088294,
18.));
#60184=CARTESIAN_POINT('Ctrl Pts',(-51.8269785320501,-14.193660324695,18.));
#60185=CARTESIAN_POINT('Ctrl Pts',(-51.8265669918482,-14.2086715965672,
18.));
#60186=CARTESIAN_POINT('Ctrl Pts',(-51.8250409572497,-14.2643349804636,
18.));
#60187=CARTESIAN_POINT('Ctrl Pts',(-51.8269058844658,-14.3200271043344,
18.));
#60188=CARTESIAN_POINT('Ctrl Pts',(-51.8320579502595,-14.3754301634739,
18.));
#60189=CARTESIAN_POINT('Ctrl Pts',(-51.837203821023,-14.4307666039711,18.));
#60190=CARTESIAN_POINT('Ctrl Pts',(-51.8456293850974,-14.4858158153797,
18.));
#60191=CARTESIAN_POINT('Ctrl Pts',(-51.857280374334,-14.5402457976247,18.));
#60192=CARTESIAN_POINT('Ctrl Pts',(-51.8647273765276,-14.5750359934568,
18.));
#60193=CARTESIAN_POINT('Ctrl Pts',(-51.8734930706644,-14.6095728457385,
18.));
#60194=CARTESIAN_POINT('Ctrl Pts',(-51.8835725600999,-14.6437631510318,
18.));
#60195=CARTESIAN_POINT('Ctrl Pts',(-51.8887663989049,-14.6613810011742,
18.));
#60196=CARTESIAN_POINT('Ctrl Pts',(-51.8943091902103,-14.678906737199,18.));
#60197=CARTESIAN_POINT('Ctrl Pts',(-51.9002009421205,-14.6963268927831,
18.));
#60198=CARTESIAN_POINT('Ctrl Pts',(-51.9037544840212,-14.7068336577877,
18.));
#60199=CARTESIAN_POINT('Ctrl Pts',(-51.9074348703396,-14.7173013531751,
18.));
#60200=CARTESIAN_POINT('Ctrl Pts',(-51.9112372618906,-14.7277145312291,
18.));
#60201=CARTESIAN_POINT('Ctrl Pts',(-51.9296249995719,-14.7780709408516,
18.));
#60202=CARTESIAN_POINT('Ctrl Pts',(-51.9508885549727,-14.8272329894413,
18.));
#60203=CARTESIAN_POINT('Ctrl Pts',(-51.9749870630737,-14.8748868070404,
18.));
#60204=CARTESIAN_POINT('Ctrl Pts',(-51.9901200745311,-14.9048117204289,
18.));
#60205=CARTESIAN_POINT('Ctrl Pts',(-52.0063718314004,-14.9341413324336,
18.));
#60206=CARTESIAN_POINT('Ctrl Pts',(-52.0237395592016,-14.9627903221168,
18.));
#60207=CARTESIAN_POINT('Ctrl Pts',(-52.0300897392816,-14.9732652815175,
18.));
#60208=CARTESIAN_POINT('Ctrl Pts',(-52.0365905346379,-14.9836512987282,
18.));
#60209=CARTESIAN_POINT('Ctrl Pts',(-52.043237428479,-14.9939369612944,18.));
#60210=CARTESIAN_POINT('Ctrl Pts',(-52.0711394051858,-15.0371135674196,
18.));
#60211=CARTESIAN_POINT('Ctrl Pts',(-52.1015680157931,-15.0784574571633,
18.));
#60212=CARTESIAN_POINT('Ctrl Pts',(-52.1344986678528,-15.1176697568703,
18.));
#60213=CARTESIAN_POINT('Ctrl Pts',(-52.1528947874586,-15.1395750065485,
18.));
#60214=CARTESIAN_POINT('Ctrl Pts',(-52.1720723161447,-15.1608144005325,
18.));
#60215=CARTESIAN_POINT('Ctrl Pts',(-52.1920310817112,-15.1813299718051,
18.));
#60216=CARTESIAN_POINT('Ctrl Pts',(-52.2060486090393,-15.1957385573463,
18.));
#60217=CARTESIAN_POINT('Ctrl Pts',(-52.2204515743704,-15.2097900005096,
18.));
#60218=CARTESIAN_POINT('Ctrl Pts',(-52.2352228301845,-15.2234768233201,
18.));
#60219=CARTESIAN_POINT('Ctrl Pts',(-54.153252109211,-15.2223467977324,18.));
#60220=CARTESIAN_POINT('Ctrl Pts',(-54.1901305933404,-15.1879071947038,
18.));
#60221=CARTESIAN_POINT('Ctrl Pts',(-54.2246310285466,-15.1512289528613,
18.));
#60222=CARTESIAN_POINT('Ctrl Pts',(-54.2567513295153,-15.1126319834757,
18.));
#60223=CARTESIAN_POINT('Ctrl Pts',(-54.290311463843,-15.0723048558288,18.));
#60224=CARTESIAN_POINT('Ctrl Pts',(-54.3212739167588,-15.0298826695219,
18.));
#60225=CARTESIAN_POINT('Ctrl Pts',(-54.3496082931449,-14.9856806062948,
18.));
#60226=CARTESIAN_POINT('Ctrl Pts',(-54.3723325448346,-14.9502304239335,
18.));
#60227=CARTESIAN_POINT('Ctrl Pts',(-54.393365943357,-14.9136342530605,18.));
#60228=CARTESIAN_POINT('Ctrl Pts',(-54.412676568361,-14.8760367445278,18.));
#60229=CARTESIAN_POINT('Ctrl Pts',(-54.4208393026161,-14.8601440185936,
18.));
#60230=CARTESIAN_POINT('Ctrl Pts',(-54.4286940175272,-14.8440722071043,
18.));
#60231=CARTESIAN_POINT('Ctrl Pts',(-54.4362374127529,-14.8278315944995,
18.));
#60232=CARTESIAN_POINT('Ctrl Pts',(-54.4405190389689,-14.8186134333647,
18.));
#60233=CARTESIAN_POINT('Ctrl Pts',(-54.4447005519202,-14.8093401785766,
18.));
#60234=CARTESIAN_POINT('Ctrl Pts',(-54.4487750435594,-14.8000286716647,
18.));
#60235=CARTESIAN_POINT('Ctrl Pts',(-54.4705983254274,-14.7501555444271,
18.));
#60236=CARTESIAN_POINT('Ctrl Pts',(-54.4894011486202,-14.6990895949508,
18.));
#60237=CARTESIAN_POINT('Ctrl Pts',(-54.5051559559858,-14.647162338739,18.));
#60238=CARTESIAN_POINT('Ctrl Pts',(-54.521199476169,-14.5942834958713,18.));
#60239=CARTESIAN_POINT('Ctrl Pts',(-54.5340828409945,-14.5405105650536,
18.));
#60240=CARTESIAN_POINT('Ctrl Pts',(-54.5437362577297,-14.4861590282174,
18.));
#60241=CARTESIAN_POINT('Ctrl Pts',(-54.5506403107422,-14.4472872067766,
18.));
#60242=CARTESIAN_POINT('Ctrl Pts',(-54.5558914111254,-14.4081186550425,
18.));
#60243=CARTESIAN_POINT('Ctrl Pts',(-54.5594490237053,-14.3687624021353,
18.));
#60244=CARTESIAN_POINT('Ctrl Pts',(-54.560961473737,-14.3520308540468,18.));
#60245=CARTESIAN_POINT('Ctrl Pts',(-54.5621676846368,-14.3352653382578,
18.));
#60246=CARTESIAN_POINT('Ctrl Pts',(-54.5630637816013,-14.3184741004373,
18.));
#60247=CARTESIAN_POINT('Ctrl Pts',(-54.5635976657032,-14.3084700771252,
18.));
#60248=CARTESIAN_POINT('Ctrl Pts',(-54.5640211036094,-14.2984625720042,
18.));
#60249=CARTESIAN_POINT('Ctrl Pts',(-54.5643335016824,-14.2884609517312,
18.));
#60250=CARTESIAN_POINT('Ctrl Pts',(-54.5661075110375,-14.2316649294083,
18.));
#60251=CARTESIAN_POINT('Ctrl Pts',(-54.5643085969144,-14.1749865267171,
18.));
#60252=CARTESIAN_POINT('Ctrl Pts',(-54.5588768122501,-14.1187579548114,
18.));
#60253=CARTESIAN_POINT('Ctrl Pts',(-54.5555413233245,-14.0842297489857,
18.));
#60254=CARTESIAN_POINT('Ctrl Pts',(-54.5508350741402,-14.0498706203676,
18.));
#60255=CARTESIAN_POINT('Ctrl Pts',(-54.5447349150618,-14.0157544413133,
18.));
#60256=CARTESIAN_POINT('Ctrl Pts',(-54.5350624849658,-13.9616597279133,
18.));
#60257=CARTESIAN_POINT('Ctrl Pts',(-54.5218884030874,-13.9081753369494,
18.));
#60258=CARTESIAN_POINT('Ctrl Pts',(-54.5054388352989,-13.8555057819088,
18.));
#60259=CARTESIAN_POINT('Ctrl Pts',(-54.5005174069393,-13.8397479550047,
18.));
#60260=CARTESIAN_POINT('Ctrl Pts',(-54.4953024361441,-13.8240630966703,
18.));
#60261=CARTESIAN_POINT('Ctrl Pts',(-54.4897991057295,-13.8084568180249,
18.));
#60262=CARTESIAN_POINT('Ctrl Pts',(-54.4847109304735,-13.7940278314187,
18.));
#60263=CARTESIAN_POINT('Ctrl Pts',(-54.4793736286689,-13.7796597824161,
18.));
#60264=CARTESIAN_POINT('Ctrl Pts',(-54.4738049082137,-13.765391301815,18.));
#60265=CARTESIAN_POINT('Ctrl Pts',(-54.4531741179316,-13.7125299608138,
18.));
#60266=CARTESIAN_POINT('Ctrl Pts',(-54.4293497755017,-13.6609649910114,
18.));
#60267=CARTESIAN_POINT('Ctrl Pts',(-54.4026149607926,-13.6109069383254,
18.));
#60268=CARTESIAN_POINT('Ctrl Pts',(-54.3752481593715,-13.5596655587874,
18.));
#60269=CARTESIAN_POINT('Ctrl Pts',(-54.3448313135357,-13.5100022755867,
18.));
#60270=CARTESIAN_POINT('Ctrl Pts',(-54.3116127229013,-13.462148554514,18.));
#60271=CARTESIAN_POINT('Ctrl Pts',(-54.2914450604172,-13.433095615278,18.));
#60272=CARTESIAN_POINT('Ctrl Pts',(-54.2702436408721,-13.4047098372191,
18.));
#60273=CARTESIAN_POINT('Ctrl Pts',(-54.2480553291971,-13.3770462315216,
18.));
#60274=CARTESIAN_POINT('Ctrl Pts',(-54.235838542242,-13.3618147717258,18.));
#60275=CARTESIAN_POINT('Ctrl Pts',(-54.2233224644036,-13.3468022959013,
18.));
#60276=CARTESIAN_POINT('Ctrl Pts',(-54.2105141669117,-13.3320184620741,
18.));
#60277=CARTESIAN_POINT('Ctrl Pts',(-54.2028017059965,-13.3231164405025,
18.));
#60278=CARTESIAN_POINT('Ctrl Pts',(-54.1949819266755,-13.3142958366318,
18.));
#60279=CARTESIAN_POINT('Ctrl Pts',(-54.1870606016195,-13.3055635742368,
18.));
#60280=CARTESIAN_POINT('Ctrl Pts',(-54.146465975092,-13.2608131154237,18.));
#60281=CARTESIAN_POINT('Ctrl Pts',(-54.1033356929487,-13.2185196121795,
18.));
#60282=CARTESIAN_POINT('Ctrl Pts',(-54.057929911796,-13.1789337623811,18.));
#60283=CARTESIAN_POINT('Ctrl Pts',(-54.0284074581666,-13.1531953787351,
18.));
#60284=CARTESIAN_POINT('Ctrl Pts',(-53.9979219697712,-13.1286019537706,
18.));
#60285=CARTESIAN_POINT('Ctrl Pts',(-53.9665347833756,-13.105228420628,18.));
#60286=CARTESIAN_POINT('Ctrl Pts',(-53.9535624126434,-13.0955681046817,
18.));
#60287=CARTESIAN_POINT('Ctrl Pts',(-53.9404359297659,-13.0861162378026,
18.));
#60288=CARTESIAN_POINT('Ctrl Pts',(-53.9271593223322,-13.076878434333,18.));
#60289=CARTESIAN_POINT('Ctrl Pts',(-53.9174397053675,-13.0701155687616,
18.));
#60290=CARTESIAN_POINT('Ctrl Pts',(-53.9076405169031,-13.0634681523805,
18.));
#60291=CARTESIAN_POINT('Ctrl Pts',(-53.8977718295133,-13.0569437429584,
18.));
#60292=CARTESIAN_POINT('Ctrl Pts',(-53.8470357673936,-13.023401000275,18.));
#60293=CARTESIAN_POINT('Ctrl Pts',(-53.7944075339565,-12.993065740058,18.));
#60294=CARTESIAN_POINT('Ctrl Pts',(-53.7401232238152,-12.9662046864427,
18.));
#60295=CARTESIAN_POINT('Ctrl Pts',(-53.7146984024022,-12.953623933563,18.));
#60296=CARTESIAN_POINT('Ctrl Pts',(-53.6889097287962,-12.9418057638961,
18.));
#60297=CARTESIAN_POINT('Ctrl Pts',(-53.6627787780123,-12.9307804983812,
18.));
#60298=CARTESIAN_POINT('Ctrl Pts',(-53.6403263881356,-12.9213073046241,
18.));
#60299=CARTESIAN_POINT('Ctrl Pts',(-53.6176212739247,-12.9124195098708,
18.));
#60300=CARTESIAN_POINT('Ctrl Pts',(-53.5946845822246,-12.9041113672218,
18.));
#60301=CARTESIAN_POINT('Ctrl Pts',(-15.2209662466057,-52.1764590205667,
18.));
#60302=CARTESIAN_POINT('Ctrl Pts',(-15.1740718831799,-52.1372104252047,
18.));
#60303=CARTESIAN_POINT('Ctrl Pts',(-15.1248302485577,-52.1011214310192,
18.));
#60304=CARTESIAN_POINT('Ctrl Pts',(-15.0736000909597,-52.0682135291378,
18.));
#60305=CARTESIAN_POINT('Ctrl Pts',(-15.0226682165858,-52.0354972307089,
18.));
#60306=CARTESIAN_POINT('Ctrl Pts',(-14.969769673043,-52.005925006896,18.));
#60307=CARTESIAN_POINT('Ctrl Pts',(-14.915234207728,-51.9795679908668,18.));
#60308=CARTESIAN_POINT('Ctrl Pts',(-14.8740531445008,-51.9596651636459,
18.));
#60309=CARTESIAN_POINT('Ctrl Pts',(-14.8319381110892,-51.941596692591,18.));
#60310=CARTESIAN_POINT('Ctrl Pts',(-14.7890287317843,-51.925412757104,18.));
#60311=CARTESIAN_POINT('Ctrl Pts',(-14.766753270954,-51.9170112228273,18.));
#60312=CARTESIAN_POINT('Ctrl Pts',(-14.7442637387328,-51.909117839332,18.));
#60313=CARTESIAN_POINT('Ctrl Pts',(-14.721579884675,-51.9017414674402,18.));
#60314=CARTESIAN_POINT('Ctrl Pts',(-14.7096336326171,-51.8978567661162,
18.));
#60315=CARTESIAN_POINT('Ctrl Pts',(-14.6976315192865,-51.8941150313098,
18.));
#60316=CARTESIAN_POINT('Ctrl Pts',(-14.6855981509523,-51.8905237529537,
18.));
#60317=CARTESIAN_POINT('Ctrl Pts',(-14.628866805663,-51.873592662108,18.));
#60318=CARTESIAN_POINT('Ctrl Pts',(-14.5713364809672,-51.8599659874384,
18.));
#60319=CARTESIAN_POINT('Ctrl Pts',(-14.5133186620481,-51.8497038434808,
18.));
#60320=CARTESIAN_POINT('Ctrl Pts',(-14.4564856885559,-51.8396512740051,
18.));
#60321=CARTESIAN_POINT('Ctrl Pts',(-14.3991838939743,-51.8328273015837,
18.));
#60322=CARTESIAN_POINT('Ctrl Pts',(-14.3417076889107,-51.8293372126133,
18.));
#60323=CARTESIAN_POINT('Ctrl Pts',(-14.3001007307031,-51.826810741254,18.));
#60324=CARTESIAN_POINT('Ctrl Pts',(-14.2584023661364,-51.8260323215432,
18.));
#60325=CARTESIAN_POINT('Ctrl Pts',(-14.2167293111391,-51.8270580660934,
18.));
#60326=CARTESIAN_POINT('Ctrl Pts',(-14.1949488648028,-51.8275941720769,
18.));
#60327=CARTESIAN_POINT('Ctrl Pts',(-14.1731754256056,-51.8286233369704,
18.));
#60328=CARTESIAN_POINT('Ctrl Pts',(-14.1514264245875,-51.8301550767569,
18.));
#60329=CARTESIAN_POINT('Ctrl Pts',(-14.1413116392116,-51.8308674413928,
18.));
#60330=CARTESIAN_POINT('Ctrl Pts',(-14.1312071832823,-51.8316882253572,
18.));
#60331=CARTESIAN_POINT('Ctrl Pts',(-14.1211226983139,-51.8326172394617,
18.));
#60332=CARTESIAN_POINT('Ctrl Pts',(-14.065585908369,-51.8377334611959,18.));
#60333=CARTESIAN_POINT('Ctrl Pts',(-14.0105794928347,-51.8461333286692,
18.));
#60334=CARTESIAN_POINT('Ctrl Pts',(-13.9563747310311,-51.8579061060262,
18.));
#60335=CARTESIAN_POINT('Ctrl Pts',(-13.9201064161049,-51.8657832515487,
18.));
#60336=CARTESIAN_POINT('Ctrl Pts',(-13.8841971505455,-51.8751714207596,
18.));
#60337=CARTESIAN_POINT('Ctrl Pts',(-13.8487329702921,-51.8861095759353,
18.));
#60338=CARTESIAN_POINT('Ctrl Pts',(-13.7962430344237,-51.902298955179,18.));
#60339=CARTESIAN_POINT('Ctrl Pts',(-13.7447264797303,-51.9218828237725,
18.));
#60340=CARTESIAN_POINT('Ctrl Pts',(-13.6944250448181,-51.9446586129267,
18.));
#60341=CARTESIAN_POINT('Ctrl Pts',(-13.6788893969317,-51.9516929379167,
18.));
#60342=CARTESIAN_POINT('Ctrl Pts',(-13.6634698927199,-51.9590319641548,
18.));
#60343=CARTESIAN_POINT('Ctrl Pts',(-13.6481743336104,-51.9666702755682,
18.));
#60344=CARTESIAN_POINT('Ctrl Pts',(-13.634752007033,-51.9733731302699,18.));
#60345=CARTESIAN_POINT('Ctrl Pts',(-13.6214194410592,-51.9803097396861,
18.));
#60346=CARTESIAN_POINT('Ctrl Pts',(-13.6082135027341,-51.987458987616,18.));
#60347=CARTESIAN_POINT('Ctrl Pts',(-13.559244561094,-52.0139691148055,18.));
#60348=CARTESIAN_POINT('Ctrl Pts',(-13.5119462056266,-52.0434302755632,
18.));
#60349=CARTESIAN_POINT('Ctrl Pts',(-13.4665417533732,-52.075593652502,18.));
#60350=CARTESIAN_POINT('Ctrl Pts',(-13.4211918994788,-52.1077183533306,
18.));
#60351=CARTESIAN_POINT('Ctrl Pts',(-13.3777306362556,-52.1425397400829,
18.));
#60352=CARTESIAN_POINT('Ctrl Pts',(-13.3364183517639,-52.1798448137172,
18.));
#60353=CARTESIAN_POINT('Ctrl Pts',(-13.3100126299148,-52.2036892321527,
18.));
#60354=CARTESIAN_POINT('Ctrl Pts',(-13.284485655771,-52.2285490007927,18.));
#60355=CARTESIAN_POINT('Ctrl Pts',(-13.2599156980719,-52.2543732768717,
18.));
#60356=CARTESIAN_POINT('Ctrl Pts',(-13.247255109996,-52.2676801993254,18.));
#60357=CARTESIAN_POINT('Ctrl Pts',(-13.2348487708744,-52.2812432661245,
18.));
#60358=CARTESIAN_POINT('Ctrl Pts',(-13.222708346973,-52.2950557510881,18.));
#60359=CARTESIAN_POINT('Ctrl Pts',(-13.215385988776,-52.3033865938424,18.));
#60360=CARTESIAN_POINT('Ctrl Pts',(-13.2081608879731,-52.3118077521959,
18.));
#60361=CARTESIAN_POINT('Ctrl Pts',(-13.2010440030959,-52.3203073114272,
18.));
#60362=CARTESIAN_POINT('Ctrl Pts',(-13.1666279154692,-52.3614097853807,
18.));
#60363=CARTESIAN_POINT('Ctrl Pts',(-13.1346840827633,-52.4044056088235,
18.));
#60364=CARTESIAN_POINT('Ctrl Pts',(-13.1054638931954,-52.4491024554207,
18.));
#60365=CARTESIAN_POINT('Ctrl Pts',(-13.0871146481686,-52.4771704933859,
18.));
#60366=CARTESIAN_POINT('Ctrl Pts',(-13.069840321977,-52.5059097415541,18.));
#60367=CARTESIAN_POINT('Ctrl Pts',(-13.0537134178065,-52.5352751363827,
18.));
#60368=CARTESIAN_POINT('Ctrl Pts',(-13.0478169297015,-52.5460120205034,
18.));
#60369=CARTESIAN_POINT('Ctrl Pts',(-13.0420727750593,-52.5568348697255,
18.));
#60370=CARTESIAN_POINT('Ctrl Pts',(-13.0364885788853,-52.5677340663131,
18.));
#60371=CARTESIAN_POINT('Ctrl Pts',(-13.0130475064328,-52.61348619409,18.));
#60372=CARTESIAN_POINT('Ctrl Pts',(-12.9924569304998,-52.6605100892402,
18.));
#60373=CARTESIAN_POINT('Ctrl Pts',(-12.9749633881527,-52.708635016183,18.));
#60374=CARTESIAN_POINT('Ctrl Pts',(-12.9651909077135,-52.7355192170987,
18.));
#60375=CARTESIAN_POINT('Ctrl Pts',(-12.956385785445,-52.7627472106582,18.));
#60376=CARTESIAN_POINT('Ctrl Pts',(-12.948598136759,-52.7902898637941,18.));
#60377=CARTESIAN_POINT('Ctrl Pts',(-12.9431286937976,-52.8096336961118,
18.));
#60378=CARTESIAN_POINT('Ctrl Pts',(-12.9381612650277,-52.82913275561,18.));
#60379=CARTESIAN_POINT('Ctrl Pts',(-12.9336937527446,-52.8487684531621,
18.));
#60380=CARTESIAN_POINT('Ctrl Pts',(-13.8936870225526,-54.5092654229862,
18.));
#60381=CARTESIAN_POINT('Ctrl Pts',(-13.9419518764876,-54.5239833380077,
18.));
#60382=CARTESIAN_POINT('Ctrl Pts',(-13.9909664228071,-54.5355224856705,
18.));
#60383=CARTESIAN_POINT('Ctrl Pts',(-14.0404525674513,-54.5440410140809,
18.));
#60384=CARTESIAN_POINT('Ctrl Pts',(-14.0921569775524,-54.5529413939661,
18.));
#60385=CARTESIAN_POINT('Ctrl Pts',(-14.1443769192189,-54.5585445895538,
18.));
#60386=CARTESIAN_POINT('Ctrl Pts',(-14.1968242396308,-54.5609818668627,
18.));
#60387=CARTESIAN_POINT('Ctrl Pts',(-14.2388871088265,-54.5629365687585,
18.));
#60388=CARTESIAN_POINT('Ctrl Pts',(-14.2810970053295,-54.562853958605,18.));
#60389=CARTESIAN_POINT('Ctrl Pts',(-14.3233126980455,-54.5607787169103,
18.));
#60390=CARTESIAN_POINT('Ctrl Pts',(-14.3411576908261,-54.5599014916257,
18.));
#60391=CARTESIAN_POINT('Ctrl Pts',(-14.3590037664332,-54.5586679663758,
18.));
#60392=CARTESIAN_POINT('Ctrl Pts',(-14.3768403679106,-54.5570804251684,
18.));
#60393=CARTESIAN_POINT('Ctrl Pts',(-14.3869641761715,-54.5561793587399,
18.));
#60394=CARTESIAN_POINT('Ctrl Pts',(-14.3970856400472,-54.5551640486891,
18.));
#60395=CARTESIAN_POINT('Ctrl Pts',(-14.4071867211825,-54.5540369331083,
18.));
#60396=CARTESIAN_POINT('Ctrl Pts',(-14.4612897750273,-54.5479999164622,
18.));
#60397=CARTESIAN_POINT('Ctrl Pts',(-14.5149156125263,-54.5387506932885,
18.));
#60398=CARTESIAN_POINT('Ctrl Pts',(-14.5677633543972,-54.5264311541952,
18.));
#60399=CARTESIAN_POINT('Ctrl Pts',(-14.6215795301098,-54.5138858597877,
18.));
#60400=CARTESIAN_POINT('Ctrl Pts',(-14.6745899303805,-54.4981567455395,
18.));
#60401=CARTESIAN_POINT('Ctrl Pts',(-14.7264864439659,-54.4793411079406,
18.));
#60402=CARTESIAN_POINT('Ctrl Pts',(-14.7636024302384,-54.4658843090425,
18.));
#60403=CARTESIAN_POINT('Ctrl Pts',(-14.800148916719,-54.4508476461167,18.));
#60404=CARTESIAN_POINT('Ctrl Pts',(-14.8360112141955,-54.4342505283907,
18.));
#60405=CARTESIAN_POINT('Ctrl Pts',(-14.8512574582524,-54.427194546892,18.));
#60406=CARTESIAN_POINT('Ctrl Pts',(-14.8663799984467,-54.419856367452,18.));
#60407=CARTESIAN_POINT('Ctrl Pts',(-14.8813697562969,-54.412236757174,18.));
#60408=CARTESIAN_POINT('Ctrl Pts',(-14.8903005158607,-54.4076970636017,
18.));
#60409=CARTESIAN_POINT('Ctrl Pts',(-14.8991790662691,-54.4030599781999,
18.));
#60410=CARTESIAN_POINT('Ctrl Pts',(-14.9079969993907,-54.3983296699509,
18.));
#60411=CARTESIAN_POINT('Ctrl Pts',(-14.9580707730014,-54.3714680028119,
18.));
#60412=CARTESIAN_POINT('Ctrl Pts',(-15.0062562238015,-54.3415708986061,
18.));
#60413=CARTESIAN_POINT('Ctrl Pts',(-15.0522356756777,-54.3087525447577,
18.));
#60414=CARTESIAN_POINT('Ctrl Pts',(-15.0804700425257,-54.2885999460621,
18.));
#60415=CARTESIAN_POINT('Ctrl Pts',(-15.1078726148715,-54.2673447838554,
18.));
#60416=CARTESIAN_POINT('Ctrl Pts',(-15.1343678441299,-54.245003945279,18.));
#60417=CARTESIAN_POINT('Ctrl Pts',(-15.1763790053575,-54.2095800369881,
18.));
#60418=CARTESIAN_POINT('Ctrl Pts',(-15.2161107900716,-54.1714287640079,
18.));
#60419=CARTESIAN_POINT('Ctrl Pts',(-15.2534991669623,-54.1308482498307,
18.));
#60420=CARTESIAN_POINT('Ctrl Pts',(-15.2646851435512,-54.1187072391932,
18.));
#60421=CARTESIAN_POINT('Ctrl Pts',(-15.2756611560252,-54.1063484965531,
18.));
#60422=CARTESIAN_POINT('Ctrl Pts',(-15.286424936402,-54.0937793159871,18.));
#60423=CARTESIAN_POINT('Ctrl Pts',(-15.2963767216443,-54.0821583258439,
18.));
#60424=CARTESIAN_POINT('Ctrl Pts',(-15.3061511701195,-54.0703520539612,
18.));
#60425=CARTESIAN_POINT('Ctrl Pts',(-15.3157236804964,-54.0583951512989,
18.));
#60426=CARTESIAN_POINT('Ctrl Pts',(-15.3511875377467,-54.0140976919625,
18.));
#60427=CARTESIAN_POINT('Ctrl Pts',(-15.3839319324792,-53.9676827165237,
18.));
#60428=CARTESIAN_POINT('Ctrl Pts',(-15.4139160660758,-53.9195006537336,
18.));
#60429=CARTESIAN_POINT('Ctrl Pts',(-15.4446090041847,-53.8701795997696,
18.));
#60430=CARTESIAN_POINT('Ctrl Pts',(-15.4724102509539,-53.8190061740789,
18.));
#60431=CARTESIAN_POINT('Ctrl Pts',(-15.4972435005011,-53.7663111450288,
18.));
#60432=CARTESIAN_POINT('Ctrl Pts',(-15.5123202613179,-53.7343189424898,
18.));
#60433=CARTESIAN_POINT('Ctrl Pts',(-15.5263023651392,-53.7017650594938,
18.));
#60434=CARTESIAN_POINT('Ctrl Pts',(-15.5391656032369,-53.6687175882849,
18.));
#60435=CARTESIAN_POINT('Ctrl Pts',(-15.5462480435773,-53.6505218010762,
18.));
#60436=CARTESIAN_POINT('Ctrl Pts',(-15.5529911929768,-53.6321763122081,
18.));
#60437=CARTESIAN_POINT('Ctrl Pts',(-15.5593902229399,-53.61369207462,18.));
#60438=CARTESIAN_POINT('Ctrl Pts',(-15.5632433722998,-53.6025618675981,
18.));
#60439=CARTESIAN_POINT('Ctrl Pts',(-15.5669723526336,-53.5913794289415,
18.));
#60440=CARTESIAN_POINT('Ctrl Pts',(-15.5705740541498,-53.5801532197009,
18.));
#60441=CARTESIAN_POINT('Ctrl Pts',(-15.5890317873878,-53.5226219738424,
18.));
#60442=CARTESIAN_POINT('Ctrl Pts',(-15.6040939073662,-53.4641232630576,
18.));
#60443=CARTESIAN_POINT('Ctrl Pts',(-15.6156733811679,-53.4050077404603,
18.));
#60444=CARTESIAN_POINT('Ctrl Pts',(-15.6232022586033,-53.3665713199646,
18.));
#60445=CARTESIAN_POINT('Ctrl Pts',(-15.6292580546374,-53.3278733667065,
18.));
#60446=CARTESIAN_POINT('Ctrl Pts',(-15.6338065434936,-53.2890044670453,
18.));
#60447=CARTESIAN_POINT('Ctrl Pts',(-15.635686432893,-53.2729399597453,18.));
#60448=CARTESIAN_POINT('Ctrl Pts',(-15.63730874602,-53.2568462123695,18.));
#60449=CARTESIAN_POINT('Ctrl Pts',(-15.6386706145308,-53.2407294854068,
18.));
#60450=CARTESIAN_POINT('Ctrl Pts',(-15.6396676228601,-53.2289306143017,
18.));
#60451=CARTESIAN_POINT('Ctrl Pts',(-15.6405248635871,-53.2171205568196,
18.));
#60452=CARTESIAN_POINT('Ctrl Pts',(-15.6412408277572,-53.2053118151348,
18.));
#60453=CARTESIAN_POINT('Ctrl Pts',(-15.6449216835272,-53.1446016891568,
18.));
#60454=CARTESIAN_POINT('Ctrl Pts',(-15.6448786914135,-53.0838566393811,
18.));
#60455=CARTESIAN_POINT('Ctrl Pts',(-15.6409989083968,-53.0234144937966,
18.));
#60456=CARTESIAN_POINT('Ctrl Pts',(-15.6391817516104,-52.9951054737926,
18.));
#60457=CARTESIAN_POINT('Ctrl Pts',(-15.6365222466597,-52.966862641753,18.));
#60458=CARTESIAN_POINT('Ctrl Pts',(-15.6330049221515,-52.9387198431847,
18.));
#60459=CARTESIAN_POINT('Ctrl Pts',(-15.6299827554382,-52.9145388985899,
18.));
#60460=CARTESIAN_POINT('Ctrl Pts',(-15.626327255878,-52.8904317889028,18.));
#60461=CARTESIAN_POINT('Ctrl Pts',(-15.6220539738783,-52.8664139542998,
18.));
#60462=CARTESIAN_POINT('Ctrl Pts',(37.5756558680257,-39.2699729499894,18.));
#60463=CARTESIAN_POINT('Ctrl Pts',(37.5651127690921,-39.2097369422873,18.));
#60464=CARTESIAN_POINT('Ctrl Pts',(37.5584799714474,-39.1490477940628,18.));
#60465=CARTESIAN_POINT('Ctrl Pts',(37.5555966212125,-39.0882269703887,18.));
#60466=CARTESIAN_POINT('Ctrl Pts',(37.5527300631012,-39.0277603564722,18.));
#60467=CARTESIAN_POINT('Ctrl Pts',(37.5535699537459,-38.9671624857774,18.));
#60468=CARTESIAN_POINT('Ctrl Pts',(37.5580129364599,-38.906754525574,18.));
#60469=CARTESIAN_POINT('Ctrl Pts',(37.5613679468783,-38.8611389225248,18.));
#60470=CARTESIAN_POINT('Ctrl Pts',(37.5667786506926,-38.8156316117445,18.));
#60471=CARTESIAN_POINT('Ctrl Pts',(37.5742186551894,-38.7703786151086,18.));
#60472=CARTESIAN_POINT('Ctrl Pts',(37.5780809441845,-38.7468866735407,18.));
#60473=CARTESIAN_POINT('Ctrl Pts',(37.5824903524787,-38.7234634071251,18.));
#60474=CARTESIAN_POINT('Ctrl Pts',(37.5874446737531,-38.7001303514386,18.));
#60475=CARTESIAN_POINT('Ctrl Pts',(37.5900538576758,-38.6878420418208,18.));
#60476=CARTESIAN_POINT('Ctrl Pts',(37.5928147908839,-38.6755768363618,18.));
#60477=CARTESIAN_POINT('Ctrl Pts',(37.5957216552647,-38.6633597908234,18.));
#60478=CARTESIAN_POINT('Ctrl Pts',(37.6094259854351,-38.6057628740656,18.));
#60479=CARTESIAN_POINT('Ctrl Pts',(37.6263915747042,-38.5491262011556,18.));
#60480=CARTESIAN_POINT('Ctrl Pts',(37.6465146580695,-38.4937496146603,18.));
#60481=CARTESIAN_POINT('Ctrl Pts',(37.6662269366953,-38.4395035191427,18.));
#60482=CARTESIAN_POINT('Ctrl Pts',(37.6889696982578,-38.3864657328463,18.));
#60483=CARTESIAN_POINT('Ctrl Pts',(37.7146868376966,-38.3349439029418,18.));
#60484=CARTESIAN_POINT('Ctrl Pts',(37.7333032641295,-38.2976476726051,18.));
#60485=CARTESIAN_POINT('Ctrl Pts',(37.7534791916908,-38.2611463231416,18.));
#60486=CARTESIAN_POINT('Ctrl Pts',(37.7752048261634,-38.2255690008596,18.));
#60487=CARTESIAN_POINT('Ctrl Pts',(37.7865596505613,-38.2069746418515,18.));
#60488=CARTESIAN_POINT('Ctrl Pts',(37.7983379414274,-38.1886328838064,18.));
#60489=CARTESIAN_POINT('Ctrl Pts',(37.8105392196947,-38.1705635815892,18.));
#60490=CARTESIAN_POINT('Ctrl Pts',(37.816213671722,-38.1621600859593,18.));
#60491=CARTESIAN_POINT('Ctrl Pts',(37.821976845552,-38.1538197468311,18.));
#60492=CARTESIAN_POINT('Ctrl Pts',(37.8278237561117,-38.1455508194627,18.));
#60493=CARTESIAN_POINT('Ctrl Pts',(37.8600240522662,-38.1000119135009,18.));
#60494=CARTESIAN_POINT('Ctrl Pts',(37.8948027203639,-38.0565742505908,18.));
#60495=CARTESIAN_POINT('Ctrl Pts',(37.9321013501539,-38.0155174318995,18.));
#60496=CARTESIAN_POINT('Ctrl Pts',(37.9570573616103,-37.9880468668039,18.));
#60497=CARTESIAN_POINT('Ctrl Pts',(37.9831422874183,-37.961642783205,18.));
#60498=CARTESIAN_POINT('Ctrl Pts',(38.0103468288125,-37.9363991775295,18.));
#60499=CARTESIAN_POINT('Ctrl Pts',(38.0506122150019,-37.8990361682947,18.));
#60500=CARTESIAN_POINT('Ctrl Pts',(38.0933303033916,-37.8642134925913,18.));
#60501=CARTESIAN_POINT('Ctrl Pts',(38.1382048591451,-37.8320391955257,18.));
#60502=CARTESIAN_POINT('Ctrl Pts',(38.1520648967439,-37.82210178312,18.));
#60503=CARTESIAN_POINT('Ctrl Pts',(38.1661307314521,-37.8124173314212,18.));
#60504=CARTESIAN_POINT('Ctrl Pts',(38.1803937730732,-37.8029898884108,18.));
#60505=CARTESIAN_POINT('Ctrl Pts',(38.1929089479265,-37.7947177329458,18.));
#60506=CARTESIAN_POINT('Ctrl Pts',(38.2055816457233,-37.7866401763794,18.));
#60507=CARTESIAN_POINT('Ctrl Pts',(38.2183751516466,-37.778778585511,18.));
#60508=CARTESIAN_POINT('Ctrl Pts',(38.2658171634483,-37.7496255379419,18.));
#60509=CARTESIAN_POINT('Ctrl Pts',(38.3149793341298,-37.7233948524332,18.));
#60510=CARTESIAN_POINT('Ctrl Pts',(38.3655345941719,-37.7001554936512,18.));
#60511=CARTESIAN_POINT('Ctrl Pts',(38.4160291498531,-37.6769440395902,18.));
#60512=CARTESIAN_POINT('Ctrl Pts',(38.4679146668078,-37.6567165566401,18.));
#60513=CARTESIAN_POINT('Ctrl Pts',(38.5208765564778,-37.6395920241868,18.));
#60514=CARTESIAN_POINT('Ctrl Pts',(38.5547280084195,-37.6286466011481,18.));
#60515=CARTESIAN_POINT('Ctrl Pts',(38.5890193652508,-37.6189698569069,18.));
#60516=CARTESIAN_POINT('Ctrl Pts',(38.6236674824325,-37.6106041450305,18.));
#60517=CARTESIAN_POINT('Ctrl Pts',(38.641521850732,-37.6062932469766,18.));
#60518=CARTESIAN_POINT('Ctrl Pts',(38.6594709236377,-37.6023306259858,18.));
#60519=CARTESIAN_POINT('Ctrl Pts',(38.6775030446682,-37.5987230218566,18.));
#60520=CARTESIAN_POINT('Ctrl Pts',(38.6883788045946,-37.5965471582212,18.));
#60521=CARTESIAN_POINT('Ctrl Pts',(38.6992841520963,-37.5945006838876,18.));
#60522=CARTESIAN_POINT('Ctrl Pts',(38.7102032897924,-37.5925871316871,18.));
#60523=CARTESIAN_POINT('Ctrl Pts',(38.7630060609621,-37.5833335750623,18.));
#60524=CARTESIAN_POINT('Ctrl Pts',(38.8162124112195,-37.5771677759325,18.));
#60525=CARTESIAN_POINT('Ctrl Pts',(38.8695301448715,-37.5742112603306,18.));
#60526=CARTESIAN_POINT('Ctrl Pts',(38.9030118816576,-37.5723546683413,18.));
#60527=CARTESIAN_POINT('Ctrl Pts',(38.9365374742123,-37.5717646060238,18.));
#60528=CARTESIAN_POINT('Ctrl Pts',(38.9700316589891,-37.5724813268537,18.));
#60529=CARTESIAN_POINT('Ctrl Pts',(38.9822787357142,-37.5727433942858,18.));
#60530=CARTESIAN_POINT('Ctrl Pts',(38.994524100686,-37.5731803873846,18.));
#60531=CARTESIAN_POINT('Ctrl Pts',(39.0067556066892,-37.5737941004195,18.));
#60532=CARTESIAN_POINT('Ctrl Pts',(39.0580981368241,-37.576370200205,18.));
#60533=CARTESIAN_POINT('Ctrl Pts',(39.1091169144504,-37.5820508279399,18.));
#60534=CARTESIAN_POINT('Ctrl Pts',(39.1595408591573,-37.5909641088522,18.));
#60535=CARTESIAN_POINT('Ctrl Pts',(39.1877068769066,-37.5959429265516,18.));
#60536=CARTESIAN_POINT('Ctrl Pts',(39.2156870322805,-37.6019312273908,18.));
#60537=CARTESIAN_POINT('Ctrl Pts',(39.2434310600143,-37.6089578358496,18.));
#60538=CARTESIAN_POINT('Ctrl Pts',(39.2629177980487,-37.6138931566914,18.));
#60539=CARTESIAN_POINT('Ctrl Pts',(39.2822879943277,-37.6193408368567,18.));
#60540=CARTESIAN_POINT('Ctrl Pts',(39.3015265966439,-37.6252897660473,18.));
#60541=CARTESIAN_POINT('Ctrl Pts',(40.2595650866584,-39.2869186252539,18.));
#60542=CARTESIAN_POINT('Ctrl Pts',(40.248179115755,-39.3360745846542,18.));
#60543=CARTESIAN_POINT('Ctrl Pts',(40.2336652878063,-39.384290400164,18.));
#60544=CARTESIAN_POINT('Ctrl Pts',(40.2162996606332,-39.4314043435453,18.));
#60545=CARTESIAN_POINT('Ctrl Pts',(40.1981554153049,-39.4806307226778,18.));
#60546=CARTESIAN_POINT('Ctrl Pts',(40.1768978215469,-39.5286549715316,18.));
#60547=CARTESIAN_POINT('Ctrl Pts',(40.1527847010649,-39.575293207484,18.));
#60548=CARTESIAN_POINT('Ctrl Pts',(40.1334453389409,-39.6126983095976,18.));
#60549=CARTESIAN_POINT('Ctrl Pts',(40.112267941863,-39.6492120507113,18.));
#60550=CARTESIAN_POINT('Ctrl Pts',(40.0893618631916,-39.6847344690008,18.));
#60551=CARTESIAN_POINT('Ctrl Pts',(40.0796819049373,-39.6997460094337,18.));
#60552=CARTESIAN_POINT('Ctrl Pts',(40.0696929904209,-39.7145804305253,18.));
#60553=CARTESIAN_POINT('Ctrl Pts',(40.0594023733901,-39.7292297389113,18.));
#60554=CARTESIAN_POINT('Ctrl Pts',(40.0535563601261,-39.7375518881931,18.));
#60555=CARTESIAN_POINT('Ctrl Pts',(40.0476124488049,-39.7458148202529,18.));
#60556=CARTESIAN_POINT('Ctrl Pts',(40.0415817908095,-39.7540041063426,18.));
#60557=CARTESIAN_POINT('Ctrl Pts',(40.0093013797404,-39.7978390446753,18.));
#60558=CARTESIAN_POINT('Ctrl Pts',(39.9744777462525,-39.8396546716371,18.));
#60559=CARTESIAN_POINT('Ctrl Pts',(39.9373842780164,-39.8792613959551,18.));
#60560=CARTESIAN_POINT('Ctrl Pts',(39.899610508142,-39.9195945155313,18.));
#60561=CARTESIAN_POINT('Ctrl Pts',(39.8594823790191,-39.9576379444654,18.));
#60562=CARTESIAN_POINT('Ctrl Pts',(39.8172382894759,-39.9931735245461,18.));
#60563=CARTESIAN_POINT('Ctrl Pts',(39.787025005414,-40.0185888332176,18.));
#60564=CARTESIAN_POINT('Ctrl Pts',(39.7557282762828,-40.042720988782,18.));
#60565=CARTESIAN_POINT('Ctrl Pts',(39.7234222903352,-40.0654803761728,18.));
#60566=CARTESIAN_POINT('Ctrl Pts',(39.7096908089594,-40.0751541284175,18.));
#60567=CARTESIAN_POINT('Ctrl Pts',(39.6957768724846,-40.0845797514274,18.));
#60568=CARTESIAN_POINT('Ctrl Pts',(39.681685683933,-40.0937497715622,18.));
#60569=CARTESIAN_POINT('Ctrl Pts',(39.6732915905444,-40.0992123345749,18.));
#60570=CARTESIAN_POINT('Ctrl Pts',(39.6648392877063,-40.1045810653156,18.));
#60571=CARTESIAN_POINT('Ctrl Pts',(39.6563366064296,-40.1098507563725,18.));
#60572=CARTESIAN_POINT('Ctrl Pts',(39.6080360373664,-40.139785910773,18.));
#60573=CARTESIAN_POINT('Ctrl Pts',(39.55805101873,-40.1665680776809,18.));
#60574=CARTESIAN_POINT('Ctrl Pts',(39.5066393732359,-40.1899792586896,18.));
#60575=CARTESIAN_POINT('Ctrl Pts',(39.4750618488382,-40.2043586299853,18.));
#60576=CARTESIAN_POINT('Ctrl Pts',(39.4429452141437,-40.2174657992959,18.));
#60577=CARTESIAN_POINT('Ctrl Pts',(39.4103419265004,-40.2292437480239,18.));
#60578=CARTESIAN_POINT('Ctrl Pts',(39.3586573390129,-40.2479148227975,18.));
#60579=CARTESIAN_POINT('Ctrl Pts',(39.3057507659274,-40.263248205514,18.));
#60580=CARTESIAN_POINT('Ctrl Pts',(39.251912353747,-40.2753374915754,18.));
#60581=CARTESIAN_POINT('Ctrl Pts',(39.2358056778267,-40.2789542069429,18.));
#60582=CARTESIAN_POINT('Ctrl Pts',(39.2196154532522,-40.2822802513836,18.));
#60583=CARTESIAN_POINT('Ctrl Pts',(39.2033491283299,-40.2853173071475,18.));
#60584=CARTESIAN_POINT('Ctrl Pts',(39.1883094890343,-40.2881253306825,18.));
#60585=CARTESIAN_POINT('Ctrl Pts',(39.173198080315,-40.2906871462828,18.));
#60586=CARTESIAN_POINT('Ctrl Pts',(39.1580572085924,-40.2929987736063,18.));
#60587=CARTESIAN_POINT('Ctrl Pts',(39.101962329576,-40.3015630397475,18.));
#60588=CARTESIAN_POINT('Ctrl Pts',(39.0453935804695,-40.3067133780792,18.));
#60589=CARTESIAN_POINT('Ctrl Pts',(38.9886747852766,-40.3085896575272,18.));
#60590=CARTESIAN_POINT('Ctrl Pts',(38.9306156896966,-40.3105102746249,18.));
#60591=CARTESIAN_POINT('Ctrl Pts',(38.8723984153708,-40.3090004242113,18.));
#60592=CARTESIAN_POINT('Ctrl Pts',(38.8143475050011,-40.3041593897166,18.));
#60593=CARTESIAN_POINT('Ctrl Pts',(38.7791040438403,-40.3012203348404,18.));
#60594=CARTESIAN_POINT('Ctrl Pts',(38.7439215217865,-40.2970524592101,18.));
#60595=CARTESIAN_POINT('Ctrl Pts',(38.70887099654,-40.2916688390186,18.));
#60596=CARTESIAN_POINT('Ctrl Pts',(38.6895721262573,-40.2887046098952,18.));
#60597=CARTESIAN_POINT('Ctrl Pts',(38.670313264122,-40.2853716920792,18.));
#60598=CARTESIAN_POINT('Ctrl Pts',(38.6511063076007,-40.2816713797387,18.));
#60599=CARTESIAN_POINT('Ctrl Pts',(38.6395410469802,-40.279443276783,18.));
#60600=CARTESIAN_POINT('Ctrl Pts',(38.6279926371529,-40.2770815256674,18.));
#60601=CARTESIAN_POINT('Ctrl Pts',(38.6164699650551,-40.2745876647271,18.));
#60602=CARTESIAN_POINT('Ctrl Pts',(38.5574190798941,-40.2618072354354,18.));
#60603=CARTESIAN_POINT('Ctrl Pts',(38.4992281803999,-40.2456023805064,18.));
#60604=CARTESIAN_POINT('Ctrl Pts',(38.4422443842522,-40.2260730329555,18.));
#60605=CARTESIAN_POINT('Ctrl Pts',(38.4051943364571,-40.2133753309932,18.));
#60606=CARTESIAN_POINT('Ctrl Pts',(38.3686543069706,-40.1992711514246,18.));
#60607=CARTESIAN_POINT('Ctrl Pts',(38.3327198363388,-40.18377614093,18.));
#60608=CARTESIAN_POINT('Ctrl Pts',(38.317865781759,-40.1773710449996,18.));
#60609=CARTESIAN_POINT('Ctrl Pts',(38.3031152166749,-40.1707281878123,18.));
#60610=CARTESIAN_POINT('Ctrl Pts',(38.2884749986667,-40.16384821542,18.));
#60611=CARTESIAN_POINT('Ctrl Pts',(38.2777585351888,-40.1588121583866,18.));
#60612=CARTESIAN_POINT('Ctrl Pts',(38.2671022705206,-40.1536494637514,18.));
#60613=CARTESIAN_POINT('Ctrl Pts',(38.2565177798301,-40.1483650730324,18.));
#60614=CARTESIAN_POINT('Ctrl Pts',(38.2021024004308,-40.1211977643468,18.));
#60615=CARTESIAN_POINT('Ctrl Pts',(38.1495185721966,-40.0907880131231,18.));
#60616=CARTESIAN_POINT('Ctrl Pts',(38.0991152603216,-40.0572068987993,18.));
#60617=CARTESIAN_POINT('Ctrl Pts',(38.0755109334479,-40.0414805592038,18.));
#60618=CARTESIAN_POINT('Ctrl Pts',(38.052384941403,-40.0250579742592,18.));
#60619=CARTESIAN_POINT('Ctrl Pts',(38.0297743098615,-40.0079426645895,18.));
#60620=CARTESIAN_POINT('Ctrl Pts',(38.0103443715311,-39.9932350076725,18.));
#60621=CARTESIAN_POINT('Ctrl Pts',(37.9912950014703,-39.9780157739289,18.));
#60622=CARTESIAN_POINT('Ctrl Pts',(37.9726317990811,-39.9623061512026,18.));
#60623=CARTESIAN_POINT('Origin',(39.0658530619283,-38.8697713466883,6.));
#60624=CARTESIAN_POINT('Ctrl Pts',(40.2595650866584,-39.2869186252538,6.));
#60625=CARTESIAN_POINT('Ctrl Pts',(40.2480819791948,-39.3364939464152,6.));
#60626=CARTESIAN_POINT('Ctrl Pts',(40.2334065100538,-39.3851618422783,6.));
#60627=CARTESIAN_POINT('Ctrl Pts',(40.2158026351627,-39.4327533922897,6.));
#60628=CARTESIAN_POINT('Ctrl Pts',(40.2039391979306,-39.4648258405338,6.));
#60629=CARTESIAN_POINT('Ctrl Pts',(40.1907446643154,-39.4964096047557,6.));
#60630=CARTESIAN_POINT('Ctrl Pts',(40.1762870855587,-39.5274524412394,6.));
#60631=CARTESIAN_POINT('Ctrl Pts',(40.1696136376125,-39.5417814486659,6.));
#60632=CARTESIAN_POINT('Ctrl Pts',(40.1626709449276,-39.5559951858299,6.));
#60633=CARTESIAN_POINT('Ctrl Pts',(40.1554650290736,-39.570088378074,6.));
#60634=CARTESIAN_POINT('Ctrl Pts',(40.1494095391052,-39.5819315894,6.));
#60635=CARTESIAN_POINT('Ctrl Pts',(40.1431714820681,-39.5936830081332,6.));
#60636=CARTESIAN_POINT('Ctrl Pts',(40.1367585398276,-39.605333444489,6.));
#60637=CARTESIAN_POINT('Ctrl Pts',(40.1108375205575,-39.6524243388018,6.));
#60638=CARTESIAN_POINT('Ctrl Pts',(40.0820470672629,-39.6978983470909,6.));
#60639=CARTESIAN_POINT('Ctrl Pts',(40.0506487799103,-39.7415597566453,6.));
#60640=CARTESIAN_POINT('Ctrl Pts',(40.0386313329833,-39.7582708169074,6.));
#60641=CARTESIAN_POINT('Ctrl Pts',(40.0262313128012,-39.7747162396004,6.));
#60642=CARTESIAN_POINT('Ctrl Pts',(40.0134614554023,-39.7908844940545,6.));
#60643=CARTESIAN_POINT('Ctrl Pts',(40.0042845094336,-39.8025036682472,6.));
#60644=CARTESIAN_POINT('Ctrl Pts',(39.9949165410699,-39.8139796930435,6.));
#60645=CARTESIAN_POINT('Ctrl Pts',(39.9853619687249,-39.8253081417496,6.));
#60646=CARTESIAN_POINT('Ctrl Pts',(39.9779669485161,-39.8340761016426,6.));
#60647=CARTESIAN_POINT('Ctrl Pts',(39.9704598011529,-39.8427558568352,6.));
#60648=CARTESIAN_POINT('Ctrl Pts',(39.9628530938026,-39.8513338610346,6.));
#60649=CARTESIAN_POINT('Ctrl Pts',(39.9252574597059,-39.8937300637949,6.));
#60650=CARTESIAN_POINT('Ctrl Pts',(39.8851758120027,-39.9337126571768,6.));
#60651=CARTESIAN_POINT('Ctrl Pts',(39.8429000971153,-39.9710687869798,6.));
#60652=CARTESIAN_POINT('Ctrl Pts',(39.8012367830184,-40.0078837804949,6.));
#60653=CARTESIAN_POINT('Ctrl Pts',(39.7574416833394,-40.0421487782558,6.));
#60654=CARTESIAN_POINT('Ctrl Pts',(39.7117463596985,-40.0736370674475,6.));
#60655=CARTESIAN_POINT('Ctrl Pts',(39.6878846430625,-40.0900799892649,6.));
#60656=CARTESIAN_POINT('Ctrl Pts',(39.6635040440747,-40.1057652810295,6.));
#60657=CARTESIAN_POINT('Ctrl Pts',(39.6386333596699,-40.1206568258712,6.));
#60658=CARTESIAN_POINT('Ctrl Pts',(39.6252910649894,-40.1286456442042,6.));
#60659=CARTESIAN_POINT('Ctrl Pts',(39.6118076808574,-40.1364059738163,6.));
#60660=CARTESIAN_POINT('Ctrl Pts',(39.5981873691663,-40.143931847729,6.));
#60661=CARTESIAN_POINT('Ctrl Pts',(39.5885046151473,-40.1492820326239,6.));
#60662=CARTESIAN_POINT('Ctrl Pts',(39.578752655703,-40.1545137209881,6.));
#60663=CARTESIAN_POINT('Ctrl Pts',(39.5689329318771,-40.1596246754951,6.));
#60664=CARTESIAN_POINT('Ctrl Pts',(39.5602883880088,-40.1641239741748,6.));
#60665=CARTESIAN_POINT('Ctrl Pts',(39.5516000265252,-40.1685251724648,6.));
#60666=CARTESIAN_POINT('Ctrl Pts',(39.5428697391371,-40.1728269741578,6.));
#60667=CARTESIAN_POINT('Ctrl Pts',(39.4996812011881,-40.1941078916592,6.));
#60668=CARTESIAN_POINT('Ctrl Pts',(39.4554640760098,-40.2129597963733,6.));
#60669=CARTESIAN_POINT('Ctrl Pts',(39.4103710639643,-40.2292497271408,6.));
#60670=CARTESIAN_POINT('Ctrl Pts',(39.3590466351121,-40.2477907683078,6.));
#60671=CARTESIAN_POINT('Ctrl Pts',(39.3065877413209,-40.2630147095086,6.));
#60672=CARTESIAN_POINT('Ctrl Pts',(39.2532910929843,-40.2750393024531,6.));
#60673=CARTESIAN_POINT('Ctrl Pts',(39.2011942210274,-40.2867932062822,6.));
#60674=CARTESIAN_POINT('Ctrl Pts',(39.1482960037837,-40.2954900228406,6.));
#60675=CARTESIAN_POINT('Ctrl Pts',(39.0948540754971,-40.3011985092878,6.));
#60676=CARTESIAN_POINT('Ctrl Pts',(39.0817639227308,-40.3025967552354,6.));
#60677=CARTESIAN_POINT('Ctrl Pts',(39.068641090622,-40.3038155206653,6.));
#60678=CARTESIAN_POINT('Ctrl Pts',(39.0554892737728,-40.3048554432515,6.));
#60679=CARTESIAN_POINT('Ctrl Pts',(39.0455592029516,-40.3056406203147,6.));
#60680=CARTESIAN_POINT('Ctrl Pts',(39.0356145767473,-40.3063236056235,6.));
#60681=CARTESIAN_POINT('Ctrl Pts',(39.025668518601,-40.3069043036963,6.));
#60682=CARTESIAN_POINT('Ctrl Pts',(38.9681511418141,-40.3102624410974,6.));
#60683=CARTESIAN_POINT('Ctrl Pts',(38.9104821863231,-40.310212548994,6.));
#60684=CARTESIAN_POINT('Ctrl Pts',(38.8529878287072,-40.3068889012164,6.));
#60685=CARTESIAN_POINT('Ctrl Pts',(38.7942601300285,-40.3034939561593,6.));
#60686=CARTESIAN_POINT('Ctrl Pts',(38.7357135777964,-40.2966834251873,6.));
#60687=CARTESIAN_POINT('Ctrl Pts',(38.6776775931017,-40.286548962706,6.));
#60688=CARTESIAN_POINT('Ctrl Pts',(38.6191308062327,-40.2763253020229,6.));
#60689=CARTESIAN_POINT('Ctrl Pts',(38.5611024280606,-40.2627189747631,6.));
#60690=CARTESIAN_POINT('Ctrl Pts',(38.5039291822238,-40.2457711880671,6.));
#60691=CARTESIAN_POINT('Ctrl Pts',(38.4909781935321,-40.2419321442865,6.));
#60692=CARTESIAN_POINT('Ctrl Pts',(38.4780675596638,-40.2379201261483,6.));
#60693=CARTESIAN_POINT('Ctrl Pts',(38.4652269235143,-40.2337440112463,6.));
#60694=CARTESIAN_POINT('Ctrl Pts',(38.4073726900059,-40.2149282825016,6.));
#60695=CARTESIAN_POINT('Ctrl Pts',(38.350840226895,-40.1927581041523,6.));
#60696=CARTESIAN_POINT('Ctrl Pts',(38.2959735970115,-40.1673423639825,6.));
#60697=CARTESIAN_POINT('Ctrl Pts',(38.2415891997282,-40.1421500072882,6.));
#60698=CARTESIAN_POINT('Ctrl Pts',(38.188840316281,-40.1137687286488,6.));
#60699=CARTESIAN_POINT('Ctrl Pts',(38.1380651653058,-40.0822545047403,6.));
#60700=CARTESIAN_POINT('Ctrl Pts',(38.1008618421232,-40.0591638031984,6.));
#60701=CARTESIAN_POINT('Ctrl Pts',(38.0647181228192,-40.0343901126825,6.));
#60702=CARTESIAN_POINT('Ctrl Pts',(38.0297736279237,-40.0079388493487,6.));
#60703=CARTESIAN_POINT('Ctrl Pts',(38.0103531401622,-39.9932384956196,6.));
#60704=CARTESIAN_POINT('Ctrl Pts',(37.9913031820638,-39.978019748027,6.));
#60705=CARTESIAN_POINT('Ctrl Pts',(37.972630261787,-39.9623020734811,6.));
#60706=CARTESIAN_POINT('Ctrl Pts',(37.5756558680257,-39.2699729499894,6.));
#60707=CARTESIAN_POINT('Ctrl Pts',(37.5651290682188,-39.2098300642739,6.));
#60708=CARTESIAN_POINT('Ctrl Pts',(37.5584870272447,-39.1491583710679,6.));
#60709=CARTESIAN_POINT('Ctrl Pts',(37.5555980370803,-39.0882817362079,6.));
#60710=CARTESIAN_POINT('Ctrl Pts',(37.5529191835608,-39.0318330886643,6.));
#60711=CARTESIAN_POINT('Ctrl Pts',(37.5534681438704,-38.9752074993234,6.));
#60712=CARTESIAN_POINT('Ctrl Pts',(37.5571795337599,-38.9186719371964,6.));
#60713=CARTESIAN_POINT('Ctrl Pts',(37.5580753630152,-38.9050257798197,6.));
#60714=CARTESIAN_POINT('Ctrl Pts',(37.5591557658531,-38.8913844979576,6.));
#60715=CARTESIAN_POINT('Ctrl Pts',(37.5604183353149,-38.8777672141046,6.));
#60716=CARTESIAN_POINT('Ctrl Pts',(37.5659749115671,-38.8178374610373,6.));
#60717=CARTESIAN_POINT('Ctrl Pts',(37.5750599728567,-38.7582987523151,6.));
#60718=CARTESIAN_POINT('Ctrl Pts',(37.5875760422342,-38.6994723222252,6.));
#60719=CARTESIAN_POINT('Ctrl Pts',(37.5953014146649,-38.6631625138097,6.));
#60720=CARTESIAN_POINT('Ctrl Pts',(37.6043349305656,-38.6271243505865,6.));
#60721=CARTESIAN_POINT('Ctrl Pts',(37.6146623853249,-38.5914381458253,6.));
#60722=CARTESIAN_POINT('Ctrl Pts',(37.618196224716,-38.5792270716504,6.));
#60723=CARTESIAN_POINT('Ctrl Pts',(37.6218816204035,-38.5670572471734,6.));
#60724=CARTESIAN_POINT('Ctrl Pts',(37.6257181655967,-38.554932025581,6.));
#60725=CARTESIAN_POINT('Ctrl Pts',(37.6293072146005,-38.5435890041159,6.));
#60726=CARTESIAN_POINT('Ctrl Pts',(37.6330262982645,-38.5322922610371,6.));
#60727=CARTESIAN_POINT('Ctrl Pts',(37.6368725792164,-38.5210500434224,6.));
#60728=CARTESIAN_POINT('Ctrl Pts',(37.6559105737014,-38.4654042703705,6.));
#60729=CARTESIAN_POINT('Ctrl Pts',(37.6780754632223,-38.4110469589617,6.));
#60730=CARTESIAN_POINT('Ctrl Pts',(37.7032762357148,-38.3582791322986,6.));
#60731=CARTESIAN_POINT('Ctrl Pts',(37.7278335946554,-38.3068585474627,6.));
#60732=CARTESIAN_POINT('Ctrl Pts',(37.755274401204,-38.2569465430554,6.));
#60733=CARTESIAN_POINT('Ctrl Pts',(37.7855529342812,-38.2088521686951,6.));
#60734=CARTESIAN_POINT('Ctrl Pts',(37.8019690565572,-38.182776825868,6.));
#60735=CARTESIAN_POINT('Ctrl Pts',(37.8192199432064,-38.1572363736107,6.));
#60736=CARTESIAN_POINT('Ctrl Pts',(37.8373023126868,-38.1322851555329,6.));
#60737=CARTESIAN_POINT('Ctrl Pts',(37.8523464601752,-38.1115262718488,6.));
#60738=CARTESIAN_POINT('Ctrl Pts',(37.8679662045799,-38.0911753045124,6.));
#60739=CARTESIAN_POINT('Ctrl Pts',(37.8841609617823,-38.0712658190579,6.));
#60740=CARTESIAN_POINT('Ctrl Pts',(37.8910830994432,-38.0627558922124,6.));
#60741=CARTESIAN_POINT('Ctrl Pts',(37.8981112327975,-38.0543257382742,6.));
#60742=CARTESIAN_POINT('Ctrl Pts',(37.9052335275508,-38.045991446363,6.));
#60743=CARTESIAN_POINT('Ctrl Pts',(37.9382051680335,-38.0074090391343,6.));
#60744=CARTESIAN_POINT('Ctrl Pts',(37.9732473043207,-37.9708103555609,6.));
#60745=CARTESIAN_POINT('Ctrl Pts',(38.0103191942679,-37.9364107324676,6.));
#60746=CARTESIAN_POINT('Ctrl Pts',(38.051746090584,-37.8979700265518,6.));
#60747=CARTESIAN_POINT('Ctrl Pts',(38.0957081060154,-37.8622743231266,6.));
#60748=CARTESIAN_POINT('Ctrl Pts',(38.1418690155718,-37.8294138953185,6.));
#60749=CARTESIAN_POINT('Ctrl Pts',(38.1810411655061,-37.8015285347964,6.));
#60750=CARTESIAN_POINT('Ctrl Pts',(38.2217977223915,-37.7756856343115,6.));
#60751=CARTESIAN_POINT('Ctrl Pts',(38.2639408148781,-37.7519688192021,6.));
#60752=CARTESIAN_POINT('Ctrl Pts',(38.2755270772485,-37.7454484329125,6.));
#60753=CARTESIAN_POINT('Ctrl Pts',(38.2872181519006,-37.739088903714,6.));
#60754=CARTESIAN_POINT('Ctrl Pts',(38.2990099288398,-37.7328923323595,6.));
#60755=CARTESIAN_POINT('Ctrl Pts',(38.3081902154278,-37.7280680975397,6.));
#60756=CARTESIAN_POINT('Ctrl Pts',(38.3174331791898,-37.7233419166124,6.));
#60757=CARTESIAN_POINT('Ctrl Pts',(38.326721624664,-37.7187221448981,6.));
#60758=CARTESIAN_POINT('Ctrl Pts',(38.3764239790722,-37.6940018048084,6.));
#60759=CARTESIAN_POINT('Ctrl Pts',(38.4275178409774,-37.6722751485944,6.));
#60760=CARTESIAN_POINT('Ctrl Pts',(38.4796831985246,-37.6536175540612,6.));
#60761=CARTESIAN_POINT('Ctrl Pts',(38.5315566487786,-37.6350643638333,6.));
#60762=CARTESIAN_POINT('Ctrl Pts',(38.5844908269661,-37.6195458589746,6.));
#60763=CARTESIAN_POINT('Ctrl Pts',(38.638177242684,-37.6071867479532,6.));
#60764=CARTESIAN_POINT('Ctrl Pts',(38.687988216704,-37.5957197995686,6.));
#60765=CARTESIAN_POINT('Ctrl Pts',(38.7384475153595,-37.5869729725659,6.));
#60766=CARTESIAN_POINT('Ctrl Pts',(38.7893004136634,-37.5810866485362,6.));
#60767=CARTESIAN_POINT('Ctrl Pts',(38.802362818863,-37.5795746491778,6.));
#60768=CARTESIAN_POINT('Ctrl Pts',(38.8154556556125,-37.5782513512197,6.));
#60769=CARTESIAN_POINT('Ctrl Pts',(38.8285456601,-37.5771216020813,6.));
#60770=CARTESIAN_POINT('Ctrl Pts',(38.8814582148971,-37.572554918147,6.));
#60771=CARTESIAN_POINT('Ctrl Pts',(38.9344079183622,-37.5711349247241,6.));
#60772=CARTESIAN_POINT('Ctrl Pts',(38.9871128327977,-37.5729646742369,6.));
#60773=CARTESIAN_POINT('Ctrl Pts',(39.0380304487623,-37.5747323743462,6.));
#60774=CARTESIAN_POINT('Ctrl Pts',(39.0887204479042,-37.5795333200091,6.));
#60775=CARTESIAN_POINT('Ctrl Pts',(39.1389156304819,-37.5875063462533,6.));
#60776=CARTESIAN_POINT('Ctrl Pts',(39.174030172766,-37.5930839565499,6.));
#60777=CARTESIAN_POINT('Ctrl Pts',(39.2089023015724,-37.6002148717552,6.));
#60778=CARTESIAN_POINT('Ctrl Pts',(39.2434333426904,-37.6089601149436,6.));
#60779=CARTESIAN_POINT('Ctrl Pts',(39.2629126135314,-37.6138933852743,6.));
#60780=CARTESIAN_POINT('Ctrl Pts',(39.2822832137846,-37.6193406085393,6.));
#60781=CARTESIAN_POINT('Ctrl Pts',(39.3015295597332,-37.6252918061955,6.));
#60782=CARTESIAN_POINT('Origin',(39.0658530619283,-38.8697713466883,0.895788276411275));
#60783=CARTESIAN_POINT('Ctrl Pts',(39.8389509032089,-40.2073157943284,2.14578827641127));
#60784=CARTESIAN_POINT('Ctrl Pts',(39.8806063786858,-40.1836140086682,2.14826884812012));
#60785=CARTESIAN_POINT('Ctrl Pts',(40.3479144857801,-39.8865682523885,2.17691792328789));
#60786=CARTESIAN_POINT('Ctrl Pts',(40.8820206309179,-38.8100483503822,2.23173550191459));
#60787=CARTESIAN_POINT('Ctrl Pts',(40.0177367088944,-37.3220789090571,2.31024101229137));
#60788=CARTESIAN_POINT('Ctrl Pts',(38.2999828751462,-37.2220283999295,2.38874652266815));
#60789=CARTESIAN_POINT('Ctrl Pts',(37.2689794778045,-38.599756793647,2.46725203304492));
#60790=CARTESIAN_POINT('Ctrl Pts',(37.8495046941263,-40.2196189105814,2.5457575434217));
#60791=CARTESIAN_POINT('Ctrl Pts',(39.1164929505456,-40.5298919958252,2.60526962454382));
#60792=CARTESIAN_POINT('Ctrl Pts',(39.7159505584363,-40.2768331102243,2.63861320220701));
#60793=CARTESIAN_POINT('Ctrl Pts',(39.8359404161091,-40.2062105265248,2.64578827641127));
#60794=CARTESIAN_POINT('Ctrl Pts',(39.835191636477,-40.2053827942122,2.10421172358873));
#60795=CARTESIAN_POINT('Ctrl Pts',(40.1301403364055,-40.0323966656676,2.12181148931034));
#60796=CARTESIAN_POINT('Ctrl Pts',(40.7310614116501,-39.3634532239961,2.16557975849087));
#60797=CARTESIAN_POINT('Ctrl Pts',(40.5621188491035,-37.8394675163551,2.23551653113034));
#60798=CARTESIAN_POINT('Ctrl Pts',(39.0323736383015,-37.0530949705805,2.31402204150712));
#60799=CARTESIAN_POINT('Ctrl Pts',(37.5317729583208,-37.8957949010443,2.3925275518839));
#60800=CARTESIAN_POINT('Ctrl Pts',(37.4074081512686,-39.612062461691,2.47103306226068));
#60801=CARTESIAN_POINT('Ctrl Pts',(38.6322604476798,-40.5562805179572,2.54159445282895));
#60802=CARTESIAN_POINT('Ctrl Pts',(39.5301075010647,-40.379146656691,2.5859873399383));
#60803=CARTESIAN_POINT('Ctrl Pts',(39.8379370462827,-40.2045960389621,2.60421172358873));
#60804=CARTESIAN_POINT('Ctrl Pts',(39.301448933936,-37.6274127691862,2.));
#60805=CARTESIAN_POINT('Ctrl Pts',(38.8929078719872,-37.5499386892516,2.02616850345893));
#60806=CARTESIAN_POINT('Ctrl Pts',(38.0001476420674,-37.8306642325621,2.07850551037678));
#60807=CARTESIAN_POINT('Ctrl Pts',(37.6102551110149,-39.1875822847128,2.15701102075356));
#60808=CARTESIAN_POINT('Ctrl Pts',(38.5285686312713,-40.2582255133881,2.23551653113034));
#60809=CARTESIAN_POINT('Ctrl Pts',(39.927370040977,-40.0842697726412,2.31402204150712));
#60810=CARTESIAN_POINT('Ctrl Pts',(40.5542159206369,-38.8208279060992,2.3925275518839));
#60811=CARTESIAN_POINT('Ctrl Pts',(39.8459288050188,-37.6014258590767,2.47103306226067));
#60812=CARTESIAN_POINT('Ctrl Pts',(38.4382167358195,-37.5194337211688,2.54953857263746));
#60813=CARTESIAN_POINT('Ctrl Pts',(37.5933017676156,-38.6484924080488,2.62804408301423));
#60814=CARTESIAN_POINT('Ctrl Pts',(38.0690465090536,-39.975981485731,2.70654959339101));
#60815=CARTESIAN_POINT('Ctrl Pts',(39.4387308817871,-40.3114038497388,2.78505510376779));
#60816=CARTESIAN_POINT('Ctrl Pts',(40.4740195694907,-39.3539315296908,2.86356061414458));
#60817=CARTESIAN_POINT('Ctrl Pts',(40.2464260929064,-37.9622550204806,2.94206612452135));
#60818=CARTESIAN_POINT('Ctrl Pts',(38.9600691167361,-37.3844596499183,3.02057163489813));
#60819=CARTESIAN_POINT('Ctrl Pts',(37.768580477053,-38.1387276546802,3.09907714527491));
#60820=CARTESIAN_POINT('Ctrl Pts',(37.7405173375704,-39.5486127570041,3.17758265565169));
#60821=CARTESIAN_POINT('Ctrl Pts',(38.9010464836381,-40.3496968754357,3.25608816602847));
#60822=CARTESIAN_POINT('Ctrl Pts',(40.2093782359874,-39.823548531307,3.33459367640525));
#60823=CARTESIAN_POINT('Ctrl Pts',(40.4921693526885,-38.4420301655716,3.41309918678203));
#60824=CARTESIAN_POINT('Ctrl Pts',(39.4958061477021,-37.4441202440019,3.49160469715881));
#60825=CARTESIAN_POINT('Ctrl Pts',(38.1138507756971,-37.7247681321827,3.57011020753558));
#60826=CARTESIAN_POINT('Ctrl Pts',(37.5856736955423,-39.032282120084,3.64861571791237));
#60827=CARTESIAN_POINT('Ctrl Pts',(38.3849566559494,-40.1940525848875,3.72712122828914));
#60828=CARTESIAN_POINT('Ctrl Pts',(39.7948837028381,-40.1681761513166,3.80562673866593));
#60829=CARTESIAN_POINT('Ctrl Pts',(40.5509987381473,-38.9778594216365,3.8841322490427));
#60830=CARTESIAN_POINT('Ctrl Pts',(39.975199824256,-37.690606736441,3.96263775941949));
#60831=CARTESIAN_POINT('Ctrl Pts',(38.5838771151456,-37.4608569069011,4.04114326979626));
#60832=CARTESIAN_POINT('Ctrl Pts',(37.6248018935901,-38.4946550418589,4.11964878017305));
#60833=CARTESIAN_POINT('Ctrl Pts',(37.9580956187159,-39.8648663970343,4.19815429054983));
#60834=CARTESIAN_POINT('Ctrl Pts',(39.2848525544708,-40.3426528537363,4.2766598009266));
#60835=CARTESIAN_POINT('Ctrl Pts',(40.4152055386855,-39.4995241597319,4.35516531130339));
#60836=CARTESIAN_POINT('Ctrl Pts',(40.3354271431306,-38.09161817034,4.43367082168016));
#60837=CARTESIAN_POINT('Ctrl Pts',(39.1170645283528,-37.3815784513111,4.51217633205694));
#60838=CARTESIAN_POINT('Ctrl Pts',(37.8527742546189,-38.0061854960201,4.59068184243372));
#60839=CARTESIAN_POINT('Ctrl Pts',(37.6764018913215,-39.4052768714559,4.6691873528105));
#60840=CARTESIAN_POINT('Ctrl Pts',(38.7461223767003,-40.3241141426736,4.74769286318728));
#60841=CARTESIAN_POINT('Ctrl Pts',(40.1025849285146,-39.9386622571232,4.82619837356406));
#60842=CARTESIAN_POINT('Ctrl Pts',(40.5292817221821,-38.5946035156582,4.90470388394085));
#60843=CARTESIAN_POINT('Ctrl Pts',(39.6435408484722,-37.4973219800824,4.98320939431762));
#60844=CARTESIAN_POINT('Ctrl Pts',(38.2397159426158,-37.6308853554897,5.0617149046944));
#60845=CARTESIAN_POINT('Ctrl Pts',(37.5767902267089,-38.8755117639716,5.14022041507118));
#60846=CARTESIAN_POINT('Ctrl Pts',(38.2492919033735,-40.1149887727412,5.21872592544795));
#60847=CARTESIAN_POINT('Ctrl Pts',(39.6541041493255,-40.2377277253793,5.29723143582474));
#60848=CARTESIAN_POINT('Ctrl Pts',(40.5313606306742,-39.1336457644378,5.37573694620152));
#60849=CARTESIAN_POINT('Ctrl Pts',(40.0943114632432,-37.7929252609641,5.4542424565783));
#60850=CARTESIAN_POINT('Ctrl Pts',(38.7349236527553,-37.4179251395397,5.53274796695507));
#60851=CARTESIAN_POINT('Ctrl Pts',(37.6723064797637,-38.3450171336683,5.61125347733186));
#60852=CARTESIAN_POINT('Ctrl Pts',(37.8594847038433,-39.742636643005,5.68975898770863));
#60853=CARTESIAN_POINT('Ctrl Pts',(39.1285028721539,-40.3576202841946,5.76826449808542));
#60854=CARTESIAN_POINT('Ctrl Pts',(40.3414559726878,-39.6379218175554,5.84677000846219));
#60855=CARTESIAN_POINT('Ctrl Pts',(40.4101742470825,-38.2300213301991,5.92527551883897));
#60856=CARTESIAN_POINT('Ctrl Pts',(39.2737694148595,-37.394461217524,6.00378102921576));
#60857=CARTESIAN_POINT('Ctrl Pts',(37.9498583767322,-37.8848716060229,6.08228653959253));
#60858=CARTESIAN_POINT('Ctrl Pts',(37.7367752723626,-38.7961472226316,6.13462354651038));
#60859=CARTESIAN_POINT('Ctrl Pts',(37.8446253550651,-39.1977395433016,6.16079204996931));
#60860=CARTESIAN_POINT('Ctrl Pts',(39.3187452171453,-37.5362049495383,1.94640265001023));
#60861=CARTESIAN_POINT('Ctrl Pts',(38.8802110918636,-37.4530431059918,1.97257115346916));
#60862=CARTESIAN_POINT('Ctrl Pts',(37.9219088231848,-37.7543781296798,2.02490816038701));
#60863=CARTESIAN_POINT('Ctrl Pts',(37.5033923116662,-39.210914391274,2.10341367076379));
#60864=CARTESIAN_POINT('Ctrl Pts',(38.4891238668221,-40.360158948323,2.18191918114057));
#60865=CARTESIAN_POINT('Ctrl Pts',(39.9906183548468,-40.1734322378127,2.26042469151735));
#60866=CARTESIAN_POINT('Ctrl Pts',(40.6634841573972,-38.8172347208602,2.33893020189413));
#60867=CARTESIAN_POINT('Ctrl Pts',(39.9031981063107,-37.5083102090702,2.4174357122709));
#60868=CARTESIAN_POINT('Ctrl Pts',(38.3921387822617,-37.4202986140891,2.49594122264769));
#60869=CARTESIAN_POINT('Ctrl Pts',(37.4851943376786,-38.6322472032482,2.57444673302446));
#60870=CARTESIAN_POINT('Ctrl Pts',(37.9958659040779,-40.0571939606811,2.65295224340125));
#60871=CARTESIAN_POINT('Ctrl Pts',(39.4661057263451,-40.4172413750055,2.73145775377802));
#60872=CARTESIAN_POINT('Ctrl Pts',(40.5774001869564,-39.3894761747327,2.8099632641548));
#60873=CARTESIAN_POINT('Ctrl Pts',(40.3330979234395,-37.8956296621443,2.88846877453158));
#60874=CARTESIAN_POINT('Ctrl Pts',(38.9523029828924,-37.2754154143705,2.96697428490836));
#60875=CARTESIAN_POINT('Ctrl Pts',(37.6733411426948,-38.0850580439712,3.04547979528514));
#60876=CARTESIAN_POINT('Ctrl Pts',(37.6432177463661,-39.5984499344848,3.12398530566192));
#60877=CARTESIAN_POINT('Ctrl Pts',(38.8889472001127,-40.4583456851777,3.2024908160387));
#60878=CARTESIAN_POINT('Ctrl Pts',(40.293330196176,-39.893570132972,3.28099632641548));
#60879=CARTESIAN_POINT('Ctrl Pts',(40.5968824374325,-38.4106275244906,3.35950183679226));
#60880=CARTESIAN_POINT('Ctrl Pts',(39.5273711758787,-37.3394559940749,3.43800734716904));
#60881=CARTESIAN_POINT('Ctrl Pts',(38.0439594782896,-37.6407076615778,3.51651285754582));
#60882=CARTESIAN_POINT('Ctrl Pts',(37.4770062502969,-39.0442128569736,3.5950183679226));
#60883=CARTESIAN_POINT('Ctrl Pts',(38.3349686108551,-40.2912747609356,3.67352387829938));
#60884=CARTESIAN_POINT('Ctrl Pts',(39.8484055252959,-40.2634986076469,3.75202938867616));
#60885=CARTESIAN_POINT('Ctrl Pts',(40.6600307852876,-38.9857947132862,3.83053489905294));
#60886=CARTESIAN_POINT('Ctrl Pts',(40.0419595641553,-37.6040383051891,3.90904040942972));
#60887=CARTESIAN_POINT('Ctrl Pts',(38.5484928259196,-37.3574213799522,3.9875459198065));
#60888=CARTESIAN_POINT('Ctrl Pts',(37.5190070470414,-38.4671158588103,4.06605143018328));
#60889=CARTESIAN_POINT('Ctrl Pts',(37.8767695483495,-39.9379213519628,4.14455694056006));
#60890=CARTESIAN_POINT('Ctrl Pts',(39.3009304136176,-40.4507845262585,4.22306245093683));
#60891=CARTESIAN_POINT('Ctrl Pts',(40.5142683210176,-39.5457574952881,4.30156796131362));
#60892=CARTESIAN_POINT('Ctrl Pts',(40.4286329903996,-38.0344900143857,4.38007347169039));
#60893=CARTESIAN_POINT('Ctrl Pts',(39.1208242208265,-37.2723226924175,4.45857898206717));
#60894=CARTESIAN_POINT('Ctrl Pts',(37.7637160108241,-37.9427852958327,4.53708449244395));
#60895=CARTESIAN_POINT('Ctrl Pts',(37.5743952612927,-39.4445910374365,4.61559000282073));
#60896=CARTESIAN_POINT('Ctrl Pts',(38.7226493317982,-40.430884794758,4.69409551319751));
#60897=CARTESIAN_POINT('Ctrl Pts',(40.1786966524752,-40.0171349389622,4.77260102357429));
#60898=CARTESIAN_POINT('Ctrl Pts',(40.6367194134647,-38.5744020550171,4.85110653395107));
#60899=CARTESIAN_POINT('Ctrl Pts',(39.6859518273974,-37.3965635383795,4.92961204432785));
#60900=CARTESIAN_POINT('Ctrl Pts',(38.1790650429905,-37.5399324759461,5.00811755470463));
#60901=CARTESIAN_POINT('Ctrl Pts',(37.4674706011366,-38.8759331970053,5.08662306508141));
#60902=CARTESIAN_POINT('Ctrl Pts',(38.1893440234058,-40.2064064749044,5.16512857545819));
#60903=CARTESIAN_POINT('Ctrl Pts',(39.6972906335328,-40.3381563141405,5.24363408583496));
#60904=CARTESIAN_POINT('Ctrl Pts',(40.638950945132,-39.1530181185549,5.32213959621175));
#60905=CARTESIAN_POINT('Ctrl Pts',(40.1698157903201,-37.7138685495171,5.40064510658852));
#60906=CARTESIAN_POINT('Ctrl Pts',(38.7106284529518,-37.3113377746548,5.47915061696531));
#60907=CARTESIAN_POINT('Ctrl Pts',(37.5699991848822,-38.3064922757992,5.55765612734208));
#60908=CARTESIAN_POINT('Ctrl Pts',(37.7709191080277,-39.8067180941779,5.63616163771886));
#60909=CARTESIAN_POINT('Ctrl Pts',(39.1331023112333,-40.466850791403,5.71466714809565));
#60910=CARTESIAN_POINT('Ctrl Pts',(40.4351044267926,-39.6943156243661,5.79317265847242));
#60911=CARTESIAN_POINT('Ctrl Pts',(40.5088676568797,-38.1830540494315,5.8716781688492));
#60912=CARTESIAN_POINT('Ctrl Pts',(39.2890336047346,-37.2861512475827,5.95018367922599));
#60913=CARTESIAN_POINT('Ctrl Pts',(37.8679275688169,-37.8125651402854,6.02868918960276));
#60914=CARTESIAN_POINT('Ctrl Pts',(37.6392009572462,-38.7907421037309,6.08102619652061));
#60915=CARTESIAN_POINT('Ctrl Pts',(37.7549688593853,-39.2218173455308,6.10719469997954));
#60916=CARTESIAN_POINT('Ctrl Pts',(39.3360415003545,-37.4449971298904,1.89280530002046));
#60917=CARTESIAN_POINT('Ctrl Pts',(38.8675143117401,-37.356147522732,1.91897380347939));
#60918=CARTESIAN_POINT('Ctrl Pts',(37.8436700043021,-37.6780920267975,1.97131081039724));
#60919=CARTESIAN_POINT('Ctrl Pts',(37.3965295123176,-39.2342464978351,2.04981632077402));
#60920=CARTESIAN_POINT('Ctrl Pts',(38.4496791023729,-40.4620923832581,2.1283218311508));
#60921=CARTESIAN_POINT('Ctrl Pts',(40.0538666687167,-40.2625947029841,2.20682734152758));
#60922=CARTESIAN_POINT('Ctrl Pts',(40.7727523941575,-38.8136415356213,2.28533285190436));
#60923=CARTESIAN_POINT('Ctrl Pts',(39.9604674076026,-37.4151945590636,2.36383836228113));
#60924=CARTESIAN_POINT('Ctrl Pts',(38.3460608287039,-37.3211635070092,2.44234387265792));
#60925=CARTESIAN_POINT('Ctrl Pts',(37.3770869077416,-38.6160019984476,2.52084938303469));
#60926=CARTESIAN_POINT('Ctrl Pts',(37.9226852991021,-40.1384064356313,2.59935489341147));
#60927=CARTESIAN_POINT('Ctrl Pts',(39.4934805709031,-40.5230789002723,2.67786040378825));
#60928=CARTESIAN_POINT('Ctrl Pts',(40.6807808044221,-39.4250208197745,2.75636591416503));
#60929=CARTESIAN_POINT('Ctrl Pts',(40.4197697539726,-37.829004303808,2.83487142454181));
#60930=CARTESIAN_POINT('Ctrl Pts',(38.9445368490487,-37.1663711788227,2.91337693491859));
#60931=CARTESIAN_POINT('Ctrl Pts',(37.5781018083366,-38.0313884332623,2.99188244529537));
#60932=CARTESIAN_POINT('Ctrl Pts',(37.5459181551617,-39.6482871119655,3.07038795567215));
#60933=CARTESIAN_POINT('Ctrl Pts',(38.8768479165872,-40.5669944949197,3.14889346604893));
#60934=CARTESIAN_POINT('Ctrl Pts',(40.3772821563646,-39.963591734637,3.22739897642571));
#60935=CARTESIAN_POINT('Ctrl Pts',(40.7015955221767,-38.3792248834095,3.30590448680249));
#60936=CARTESIAN_POINT('Ctrl Pts',(39.5589362040553,-37.2347917441479,3.38440999717927));
#60937=CARTESIAN_POINT('Ctrl Pts',(37.9740681808821,-37.5566471909729,3.46291550755605));
#60938=CARTESIAN_POINT('Ctrl Pts',(37.3683388050514,-39.0561435938632,3.54142101793282));
#60939=CARTESIAN_POINT('Ctrl Pts',(38.2849805657608,-40.3884969369837,3.61992652830961));
#60940=CARTESIAN_POINT('Ctrl Pts',(39.9019273477536,-40.3588210639772,3.69843203868639));
#60941=CARTESIAN_POINT('Ctrl Pts',(40.769062832428,-38.9937300049359,3.77693754906317));
#60942=CARTESIAN_POINT('Ctrl Pts',(40.1087193040547,-37.5174698739373,3.85544305943995));
#60943=CARTESIAN_POINT('Ctrl Pts',(38.5131085366936,-37.2539858530032,3.93394856981672));
#60944=CARTESIAN_POINT('Ctrl Pts',(37.4132122004928,-38.4395766757617,4.01245408019351));
#60945=CARTESIAN_POINT('Ctrl Pts',(37.7954434779832,-40.0109763068913,4.09095959057028));
#60946=CARTESIAN_POINT('Ctrl Pts',(39.3170082727643,-40.5589161987807,4.16946510094707));
#60947=CARTESIAN_POINT('Ctrl Pts',(40.6133311033497,-39.5919908308444,4.24797061132384));
#60948=CARTESIAN_POINT('Ctrl Pts',(40.5218388376685,-37.9773618584313,4.32647612170062));
#60949=CARTESIAN_POINT('Ctrl Pts',(39.1245839133003,-37.163066933524,4.4049816320774));
#60950=CARTESIAN_POINT('Ctrl Pts',(37.6746577670293,-37.8793850956453,4.48348714245418));
#60951=CARTESIAN_POINT('Ctrl Pts',(37.472388631264,-39.4839052034172,4.56199265283096));
#60952=CARTESIAN_POINT('Ctrl Pts',(38.6991762868961,-40.5376554468423,4.64049816320774));
#60953=CARTESIAN_POINT('Ctrl Pts',(40.2548083764357,-40.0956076208012,4.71900367358451));
#60954=CARTESIAN_POINT('Ctrl Pts',(40.7441571047474,-38.554200594376,4.79750918396131));
#60955=CARTESIAN_POINT('Ctrl Pts',(39.7283628063224,-37.2958050966767,4.87601469433807));
#60956=CARTESIAN_POINT('Ctrl Pts',(38.1184141433653,-37.4489795964024,4.95452020471486));
#60957=CARTESIAN_POINT('Ctrl Pts',(37.3581509755643,-38.876354630039,5.03302571509164));
#60958=CARTESIAN_POINT('Ctrl Pts',(38.1293961434381,-40.2978241770675,5.11153122546842));
#60959=CARTESIAN_POINT('Ctrl Pts',(39.74047711774,-40.4385849029016,5.1900367358452));
#60960=CARTESIAN_POINT('Ctrl Pts',(40.7465412595899,-39.172390472672,5.26854224622198));
#60961=CARTESIAN_POINT('Ctrl Pts',(40.245320117397,-37.6348118380701,5.34704775659875));
#60962=CARTESIAN_POINT('Ctrl Pts',(38.6863332531482,-37.2047504097699,5.42555326697554));
#60963=CARTESIAN_POINT('Ctrl Pts',(37.4676918900007,-38.2679674179302,5.50405877735231));
#60964=CARTESIAN_POINT('Ctrl Pts',(37.682353512212,-39.8707995453507,5.5825642877291));
#60965=CARTESIAN_POINT('Ctrl Pts',(39.1377017503128,-40.5760812986116,5.66106979810587));
#60966=CARTESIAN_POINT('Ctrl Pts',(40.5287528808974,-39.7507094311768,5.73957530848265));
#60967=CARTESIAN_POINT('Ctrl Pts',(40.6075610666769,-38.1360867686638,5.81808081885943));
#60968=CARTESIAN_POINT('Ctrl Pts',(39.3042977946098,-37.1778412776414,5.89658632923621));
#60969=CARTESIAN_POINT('Ctrl Pts',(37.7859967609014,-37.7402586745479,5.97509183961299));
#60970=CARTESIAN_POINT('Ctrl Pts',(37.5416266421298,-38.7853369848302,6.02742884653084));
#60971=CARTESIAN_POINT('Ctrl Pts',(37.6653123637055,-39.2458951477601,6.05359734998977));
#60972=CARTESIAN_POINT('Ctrl Pts',(39.3533377835637,-37.3537893102425,1.83920795003069));
#60973=CARTESIAN_POINT('Ctrl Pts',(38.8548175316166,-37.2592519394722,1.86537645348962));
#60974=CARTESIAN_POINT('Ctrl Pts',(37.7654311854195,-37.6018059239151,1.91771346040747));
#60975=CARTESIAN_POINT('Ctrl Pts',(37.2896667129688,-39.2575786043963,1.99621897078425));
#60976=CARTESIAN_POINT('Ctrl Pts',(38.4102343379238,-40.564025818193,2.07472448116103));
#60977=CARTESIAN_POINT('Ctrl Pts',(40.1171149825864,-40.3517571681556,2.15322999153781));
#60978=CARTESIAN_POINT('Ctrl Pts',(40.8820206309179,-38.8100483503822,2.23173550191459));
#60979=CARTESIAN_POINT('Ctrl Pts',(40.0177367088944,-37.3220789090571,2.31024101229137));
#60980=CARTESIAN_POINT('Ctrl Pts',(38.2999828751462,-37.2220283999295,2.38874652266815));
#60981=CARTESIAN_POINT('Ctrl Pts',(37.2689794778045,-38.599756793647,2.46725203304492));
#60982=CARTESIAN_POINT('Ctrl Pts',(37.8495046941263,-40.2196189105814,2.5457575434217));
#60983=CARTESIAN_POINT('Ctrl Pts',(39.5208554154611,-40.6289164255391,2.62426305379848));
#60984=CARTESIAN_POINT('Ctrl Pts',(40.7841614218878,-39.4605654648164,2.70276856417526));
#60985=CARTESIAN_POINT('Ctrl Pts',(40.5064415845057,-37.7623789454716,2.78127407455204));
#60986=CARTESIAN_POINT('Ctrl Pts',(38.936770715205,-37.057326943275,2.85977958492882));
#60987=CARTESIAN_POINT('Ctrl Pts',(37.4828624739785,-37.9777188225534,2.9382850953056));
#60988=CARTESIAN_POINT('Ctrl Pts',(37.4486185639574,-39.6981242894462,3.01679060568238));
#60989=CARTESIAN_POINT('Ctrl Pts',(38.8647486330617,-40.6756433046616,3.09529611605916));
#60990=CARTESIAN_POINT('Ctrl Pts',(40.4612341165532,-40.033613336302,3.17380162643594));
#60991=CARTESIAN_POINT('Ctrl Pts',(40.8063086069208,-38.3478222423284,3.25230713681272));
#60992=CARTESIAN_POINT('Ctrl Pts',(39.5905012322319,-37.1301274942209,3.3308126471895));
#60993=CARTESIAN_POINT('Ctrl Pts',(37.9041768834746,-37.472586720368,3.40931815756627));
#60994=CARTESIAN_POINT('Ctrl Pts',(37.259671359806,-39.0680743307528,3.48782366794306));
#60995=CARTESIAN_POINT('Ctrl Pts',(38.2349925206666,-40.4857191130318,3.56632917831984));
#60996=CARTESIAN_POINT('Ctrl Pts',(39.9554491702113,-40.4541435203075,3.64483468869662));
#60997=CARTESIAN_POINT('Ctrl Pts',(40.8780948795684,-39.0016652965856,3.7233401990734));
#60998=CARTESIAN_POINT('Ctrl Pts',(40.1754790439541,-37.4309014426854,3.80184570945018));
#60999=CARTESIAN_POINT('Ctrl Pts',(38.4777242474675,-37.1505503260543,3.88035121982696));
#61000=CARTESIAN_POINT('Ctrl Pts',(37.3074173539442,-38.4120374927131,3.95885673020373));
#61001=CARTESIAN_POINT('Ctrl Pts',(37.7141174076169,-40.0840312618198,4.03736224058051));
#61002=CARTESIAN_POINT('Ctrl Pts',(39.333086131911,-40.6670478713029,4.11586775095729));
#61003=CARTESIAN_POINT('Ctrl Pts',(40.7123938856819,-39.6382241664006,4.19437326133408));
#61004=CARTESIAN_POINT('Ctrl Pts',(40.6150446849375,-37.9202337024769,4.27287877171085));
#61005=CARTESIAN_POINT('Ctrl Pts',(39.1283436057741,-37.0538111746305,4.35138428208763));
#61006=CARTESIAN_POINT('Ctrl Pts',(37.5855995232344,-37.8159848954578,4.42988979246441));
#61007=CARTESIAN_POINT('Ctrl Pts',(37.3703820012353,-39.5232193693979,4.50839530284119));
#61008=CARTESIAN_POINT('Ctrl Pts',(38.675703241994,-40.6444260989267,4.58690081321797));
#61009=CARTESIAN_POINT('Ctrl Pts',(40.3309201003962,-40.1740803026401,4.66540632359475));
#61010=CARTESIAN_POINT('Ctrl Pts',(40.85159479603,-38.533999133735,4.74391183397153));
#61011=CARTESIAN_POINT('Ctrl Pts',(39.7707737852476,-37.1950466549739,4.82241734434831));
#61012=CARTESIAN_POINT('Ctrl Pts',(38.05776324374,-37.3580267168588,4.90092285472509));
#61013=CARTESIAN_POINT('Ctrl Pts',(37.248831349992,-38.8767760630728,4.97942836510187));
#61014=CARTESIAN_POINT('Ctrl Pts',(38.0694482634704,-40.3892418792306,5.05793387547864));
#61015=CARTESIAN_POINT('Ctrl Pts',(39.7836636019472,-40.5390134916628,5.13643938585543));
#61016=CARTESIAN_POINT('Ctrl Pts',(40.8541315740477,-39.1917628267891,5.2149448962322));
#61017=CARTESIAN_POINT('Ctrl Pts',(40.3208244444739,-37.5557551266231,5.29345040660899));
#61018=CARTESIAN_POINT('Ctrl Pts',(38.6620380533447,-37.098163044885,5.37195591698576));
#61019=CARTESIAN_POINT('Ctrl Pts',(37.3653845951192,-38.2294425600612,5.45046142736254));
#61020=CARTESIAN_POINT('Ctrl Pts',(37.5937879163964,-39.9348809965236,5.52896693773932));
#61021=CARTESIAN_POINT('Ctrl Pts',(39.1423011893922,-40.6853118058201,5.6074724481161));
#61022=CARTESIAN_POINT('Ctrl Pts',(40.6224013350022,-39.8071032379875,5.68597795849288));
#61023=CARTESIAN_POINT('Ctrl Pts',(40.706254476474,-38.0891194878961,5.76448346886966));
#61024=CARTESIAN_POINT('Ctrl Pts',(39.3195619844849,-37.0695313077001,5.84298897924644));
#61025=CARTESIAN_POINT('Ctrl Pts',(37.7040659529861,-37.6679522088103,5.92149448962322));
#61026=CARTESIAN_POINT('Ctrl Pts',(37.4440523270134,-38.7799318659295,5.97383149654107));
#61027=CARTESIAN_POINT('Ctrl Pts',(37.5756558680257,-39.2699729499894,6.));
#61028=CARTESIAN_POINT('Ctrl Pts',(39.301448933936,-37.6274127691862,2.));
#61029=CARTESIAN_POINT('Ctrl Pts',(39.2531837869401,-37.6126947647985,2.));
#61030=CARTESIAN_POINT('Ctrl Pts',(39.2041689564388,-37.6011555074407,2.));
#61031=CARTESIAN_POINT('Ctrl Pts',(39.1546825373219,-37.5926368604753,2.));
#61032=CARTESIAN_POINT('Ctrl Pts',(39.1029779407392,-37.5837363739855,2.));
#61033=CARTESIAN_POINT('Ctrl Pts',(39.0507578251666,-37.5781330493143,2.));
#61034=CARTESIAN_POINT('Ctrl Pts',(38.9983103424736,-37.5756956341644,2.));
#61035=CARTESIAN_POINT('Ctrl Pts',(38.956247582128,-37.573740832827,2.));
#61036=CARTESIAN_POINT('Ctrl Pts',(38.9140378036175,-37.5738233147571,2.));
#61037=CARTESIAN_POINT('Ctrl Pts',(38.8718222352065,-37.5758984072385,2.));
#61038=CARTESIAN_POINT('Ctrl Pts',(38.8539763703747,-37.5767756148975,2.));
#61039=CARTESIAN_POINT('Ctrl Pts',(38.8361294237341,-37.5780091556835,2.));
#61040=CARTESIAN_POINT('Ctrl Pts',(38.8182919536747,-37.5795967458238,2.));
#61041=CARTESIAN_POINT('Ctrl Pts',(38.8081693423868,-37.5804976896136,2.));
#61042=CARTESIAN_POINT('Ctrl Pts',(38.7980490773275,-37.5815128494687,2.));
#61043=CARTESIAN_POINT('Ctrl Pts',(38.7879491906622,-37.5826397882183,2.));
#61044=CARTESIAN_POINT('Ctrl Pts',(38.7338460090748,-37.5886765858406,2.));
#61045=CARTESIAN_POINT('Ctrl Pts',(38.6802200536712,-37.5979256005399,2.));
#61046=CARTESIAN_POINT('Ctrl Pts',(38.6273722027161,-37.6102449557351,2.));
#61047=CARTESIAN_POINT('Ctrl Pts',(38.5735560674502,-37.6227900275514,2.));
#61048=CARTESIAN_POINT('Ctrl Pts',(38.5205457122249,-37.6385189267485,2.));
#61049=CARTESIAN_POINT('Ctrl Pts',(38.4686492447585,-37.6573343726379,2.));
#61050=CARTESIAN_POINT('Ctrl Pts',(38.4315334390211,-37.670790980931,2.));
#61051=CARTESIAN_POINT('Ctrl Pts',(38.3949871291052,-37.6858274526293,2.));
#61052=CARTESIAN_POINT('Ctrl Pts',(38.3591250016156,-37.7024243845644,2.));
#61053=CARTESIAN_POINT('Ctrl Pts',(38.3438782291838,-37.7094805650532,2.));
#61054=CARTESIAN_POINT('Ctrl Pts',(38.3287551691711,-37.7168189666978,2.));
#61055=CARTESIAN_POINT('Ctrl Pts',(38.3137649009327,-37.7244388227765,2.));
#61056=CARTESIAN_POINT('Ctrl Pts',(38.3048335703861,-37.7289787984644,2.));
#61057=CARTESIAN_POINT('Ctrl Pts',(38.2959544590328,-37.7336161783391,2.));
#61058=CARTESIAN_POINT('Ctrl Pts',(38.2871359717617,-37.7383467951532,2.));
#61059=CARTESIAN_POINT('Ctrl Pts',(38.2370624085326,-37.765208413578,2.));
#61060=CARTESIAN_POINT('Ctrl Pts',(38.1888771643904,-37.7951055006235,2.));
#61061=CARTESIAN_POINT('Ctrl Pts',(38.1428979102889,-37.8279238866627,2.));
#61062=CARTESIAN_POINT('Ctrl Pts',(38.1146649272205,-37.8480756041162,2.));
#61063=CARTESIAN_POINT('Ctrl Pts',(38.0872636609614,-37.869329805144,2.));
#61064=CARTESIAN_POINT('Ctrl Pts',(38.0607696487925,-37.891669608828,2.));
#61065=CARTESIAN_POINT('Ctrl Pts',(38.018758629417,-37.9270933838087,2.));
#61066=CARTESIAN_POINT('Ctrl Pts',(37.9790269569645,-37.9652445703221,2.));
#61067=CARTESIAN_POINT('Ctrl Pts',(37.941638665414,-38.0058250350943,2.));
#61068=CARTESIAN_POINT('Ctrl Pts',(37.9304525998642,-38.0179661552194,2.));
#61069=CARTESIAN_POINT('Ctrl Pts',(37.9194765003133,-38.030325015124,2.));
#61070=CARTESIAN_POINT('Ctrl Pts',(37.9087126348759,-38.0428943202534,2.));
#61071=CARTESIAN_POINT('Ctrl Pts',(37.8987608212084,-38.0545153669214,2.));
#61072=CARTESIAN_POINT('Ctrl Pts',(37.8889863441702,-38.0663216998073,2.));
#61073=CARTESIAN_POINT('Ctrl Pts',(37.8794138052933,-38.078278667435,2.));
#61074=CARTESIAN_POINT('Ctrl Pts',(37.8439500327395,-38.1225761297731,2.));
#61075=CARTESIAN_POINT('Ctrl Pts',(37.8112056943055,-38.1689911399599,2.));
#61076=CARTESIAN_POINT('Ctrl Pts',(37.7812215917711,-38.2171732589094,2.));
#61077=CARTESIAN_POINT('Ctrl Pts',(37.7505286360925,-38.2664944496879,2.));
#61078=CARTESIAN_POINT('Ctrl Pts',(37.7227273546034,-38.3176680405939,2.));
#61079=CARTESIAN_POINT('Ctrl Pts',(37.6978940563208,-38.3703632510374,2.));
#61080=CARTESIAN_POINT('Ctrl Pts',(37.6828172333397,-38.4023556328291,2.));
#61081=CARTESIAN_POINT('Ctrl Pts',(37.668835066908,-38.4349097034794,2.));
#61082=CARTESIAN_POINT('Ctrl Pts',(37.6559717665496,-38.4679573676399,2.));
#61083=CARTESIAN_POINT('Ctrl Pts',(37.6488893068041,-38.4861532228698,2.));
#61084=CARTESIAN_POINT('Ctrl Pts',(37.6421461366806,-38.5044987807375,2.));
#61085=CARTESIAN_POINT('Ctrl Pts',(37.6357470847774,-38.5229830878593,2.));
#61086=CARTESIAN_POINT('Ctrl Pts',(37.6318939139077,-38.5341133607227,2.));
#61087=CARTESIAN_POINT('Ctrl Pts',(37.6281649122475,-38.5452958653565,2.));
#61088=CARTESIAN_POINT('Ctrl Pts',(37.6245631893162,-38.556522141548,2.));
#61089=CARTESIAN_POINT('Ctrl Pts',(37.6061053671321,-38.6140536656795,2.));
#61090=CARTESIAN_POINT('Ctrl Pts',(37.5910431547266,-38.6725526585157,2.));
#61091=CARTESIAN_POINT('Ctrl Pts',(37.5794635885497,-38.7316684529324,2.));
#61092=CARTESIAN_POINT('Ctrl Pts',(37.5719346379231,-38.7701051171919,2.));
#61093=CARTESIAN_POINT('Ctrl Pts',(37.5658787738499,-38.8088033108132,2.));
#61094=CARTESIAN_POINT('Ctrl Pts',(37.5613302232313,-38.8476724431746,2.));
#61095=CARTESIAN_POINT('Ctrl Pts',(37.5594503644604,-38.8637365667855,2.));
#61096=CARTESIAN_POINT('Ctrl Pts',(37.557828067648,-38.8798299274171,2.));
#61097=CARTESIAN_POINT('Ctrl Pts',(37.5564662009589,-38.8959462648398,2.));
#61098=CARTESIAN_POINT('Ctrl Pts',(37.5554691679703,-38.9077451583699,2.));
#61099=CARTESIAN_POINT('Ctrl Pts',(37.5546119020137,-38.9195552385045,2.));
#61100=CARTESIAN_POINT('Ctrl Pts',(37.553895912205,-38.9313640017395,2.));
#61101=CARTESIAN_POINT('Ctrl Pts',(37.5502149156531,-38.9920743864676,2.));
#61102=CARTESIAN_POINT('Ctrl Pts',(37.5502577736837,-39.0528196704592,2.));
#61103=CARTESIAN_POINT('Ctrl Pts',(37.5541374325488,-39.1132620114035,2.));
#61104=CARTESIAN_POINT('Ctrl Pts',(37.5559545726128,-39.1415717682938,2.));
#61105=CARTESIAN_POINT('Ctrl Pts',(37.5586141014167,-39.1698153256793,2.));
#61106=CARTESIAN_POINT('Ctrl Pts',(37.5621314917739,-39.1979588342647,2.));
#61107=CARTESIAN_POINT('Ctrl Pts',(37.5651536457416,-39.2221398342386,2.));
#61108=CARTESIAN_POINT('Ctrl Pts',(37.5688091345127,-39.2462469913776,2.));
#61109=CARTESIAN_POINT('Ctrl Pts',(37.5730824075077,-39.2702648660738,2.));
#61110=CARTESIAN_POINT('Ctrl Pts',(39.696945388151,-39.9649932150637,2.80658032638058));
#61111=CARTESIAN_POINT('Ctrl Pts',(39.5986128055021,-40.0228689487565,2.79940525217632));
#61112=CARTESIAN_POINT('Ctrl Pts',(39.4929004903071,-40.0674950246048,2.79223017797206));
#61113=CARTESIAN_POINT('Ctrl Pts',(39.3829982676155,-40.0959214023961,2.78505510376779));
#61114=CARTESIAN_POINT('Ctrl Pts',(38.9821694242093,-40.1995963950695,2.75888660030887));
#61115=CARTESIAN_POINT('Ctrl Pts',(38.5256079666315,-40.0877889404002,2.73271809684994));
#61116=CARTESIAN_POINT('Ctrl Pts',(38.2180364476029,-39.8106370334519,2.70654959339101));
#61117=CARTESIAN_POINT('Ctrl Pts',(37.9104649285743,-39.5334851265036,2.68038108993209));
#61118=CARTESIAN_POINT('Ctrl Pts',(37.7518833480949,-39.0909887672762,2.65421258647316));
#61119=CARTESIAN_POINT('Ctrl Pts',(37.8134117192226,-38.6815641398492,2.62804408301423));
#61120=CARTESIAN_POINT('Ctrl Pts',(37.8749400903502,-38.2721395124221,2.60187557955531));
#61121=CARTESIAN_POINT('Ctrl Pts',(38.1565784130848,-37.8957866167955,2.57570707609638));
#61122=CARTESIAN_POINT('Ctrl Pts',(38.532016252652,-37.7212755253001,2.54953857263746));
#61123=CARTESIAN_POINT('Ctrl Pts',(38.9074540922192,-37.5467644338048,2.52337006917853));
#61124=CARTESIAN_POINT('Ctrl Pts',(39.376691448619,-37.5740951464408,2.4972015657196));
#61125=CARTESIAN_POINT('Ctrl Pts',(39.7293579794219,-37.7909941772625,2.47103306226067));
#61126=CARTESIAN_POINT('Ctrl Pts',(40.0820245102248,-38.0078932080842,2.44486455880175));
#61127=CARTESIAN_POINT('Ctrl Pts',(40.3181202154309,-38.4143605570917,2.41869605534282));
#61128=CARTESIAN_POINT('Ctrl Pts',(40.3316937547572,-38.8281678760191,2.3925275518839));
#61129=CARTESIAN_POINT('Ctrl Pts',(40.3452672940836,-39.2419751949465,2.36635904842497));
#61130=CARTESIAN_POINT('Ctrl Pts',(40.1363186675303,-39.6631224837939,2.34019054496604));
#61131=CARTESIAN_POINT('Ctrl Pts',(39.7987107859694,-39.9026887516754,2.31402204150712));
#61132=CARTESIAN_POINT('Ctrl Pts',(39.7667081702677,-39.9253977807734,2.31154146979827));
#61133=CARTESIAN_POINT('Ctrl Pts',(39.7335494773786,-39.9464752002681,2.30906089808943));
#61134=CARTESIAN_POINT('Ctrl Pts',(39.6994125047665,-39.9658989902663,2.30658032638058));
#61135=CARTESIAN_POINT('Ctrl Pts',(37.9741697098829,-39.9602191716056,2.));
#61136=CARTESIAN_POINT('Ctrl Pts',(38.3327559670707,-40.3192117233802,2.02616850345893));
#61137=CARTESIAN_POINT('Ctrl Pts',(39.4257675096925,-40.6500214621299,2.07850551037678));
#61138=CARTESIAN_POINT('Ctrl Pts',(40.7517604581817,-39.5501737910362,2.15701102075356));
#61139=CARTESIAN_POINT('Ctrl Pts',(40.5621188491035,-37.8394675163551,2.23551653113034));
#61140=CARTESIAN_POINT('Ctrl Pts',(39.0323736383015,-37.0530949705805,2.31402204150712));
#61141=CARTESIAN_POINT('Ctrl Pts',(37.5317729583208,-37.8957949010443,2.3925275518839));
#61142=CARTESIAN_POINT('Ctrl Pts',(37.4074081512686,-39.612062461691,2.47103306226068));
#61143=CARTESIAN_POINT('Ctrl Pts',(38.7701598472246,-40.6625848481854,2.54953857263746));
#61144=CARTESIAN_POINT('Ctrl Pts',(40.3982034912373,-40.1052897198446,2.62804408301424));
#61145=CARTESIAN_POINT('Ctrl Pts',(40.8313104277201,-38.439942299895,2.70654959339101));
#61146=CARTESIAN_POINT('Ctrl Pts',(39.6811395860237,-37.1600807661057,2.78505510376779));
#61147=CARTESIAN_POINT('Ctrl Pts',(37.9791520940816,-37.4135079224237,2.86356061414458));
#61148=CARTESIAN_POINT('Ctrl Pts',(37.2517503435483,-38.9729479619196,2.94206612452135));
#61149=CARTESIAN_POINT('Ctrl Pts',(38.1512758267994,-40.4398561533634,3.02057163489813));
#61150=CARTESIAN_POINT('Ctrl Pts',(39.8710175096896,-40.4986752642982,3.09907714527491));
#61151=CARTESIAN_POINT('Ctrl Pts',(40.868667784705,-39.0966544678461,3.17758265565169));
#61152=CARTESIAN_POINT('Ctrl Pts',(40.249511348243,-37.4911595684212,3.25608816602847));
#61153=CARTESIAN_POINT('Ctrl Pts',(38.5688218267177,-37.1220364497186,3.33459367640525));
#61154=CARTESIAN_POINT('Ctrl Pts',(37.333881829365,-38.3203235548052,3.41309918678203));
#61155=CARTESIAN_POINT('Ctrl Pts',(37.6522147609438,-40.0113684930191,3.49160469715881));
#61156=CARTESIAN_POINT('Ctrl Pts',(39.238332151816,-40.6786019749499,3.57011020753559));
#61157=CARTESIAN_POINT('Ctrl Pts',(40.6697661826987,-39.7236331447561,3.64861571791237));
#61158=CARTESIAN_POINT('Ctrl Pts',(40.662772801836,-38.0029007557487,3.72712122828915));
#61159=CARTESIAN_POINT('Ctrl Pts',(39.2236238307452,-37.0595985208236,3.80562673866593));
#61160=CARTESIAN_POINT('Ctrl Pts',(37.642982284831,-37.7397023107928,3.88413224904271));
#61161=CARTESIAN_POINT('Ctrl Pts',(37.3384050779085,-39.4332788778856,3.96263775941949));
#61162=CARTESIAN_POINT('Ctrl Pts',(38.5830442911661,-40.6214884944164,4.04114326979627));
#61163=CARTESIAN_POINT('Ctrl Pts',(40.26067788792,-40.2387165281926,4.11964878017305));
#61164=CARTESIAN_POINT('Ctrl Pts',(40.8667641756191,-38.6282419782981,4.19815429054982));
#61165=CARTESIAN_POINT('Ctrl Pts',(39.8577505620191,-37.2343767082119,4.27665980092661));
#61166=CARTESIAN_POINT('Ctrl Pts',(38.1385444446534,-37.3071722287697,4.35516531130338));
#61167=CARTESIAN_POINT('Ctrl Pts',(37.2509707395799,-38.781343787805,4.43367082168017));
#61168=CARTESIAN_POINT('Ctrl Pts',(37.9910266499109,-40.3348192821528,4.51217633205694));
#61169=CARTESIAN_POINT('Ctrl Pts',(39.6950124343117,-40.5744049619641,4.59068184243373));
#61170=CARTESIAN_POINT('Ctrl Pts',(40.8347531457538,-39.285234683173,4.6691873528105));
#61171=CARTESIAN_POINT('Ctrl Pts',(40.3881021894618,-37.6234670214255,4.74769286318729));
#61172=CARTESIAN_POINT('Ctrl Pts',(38.7556268199881,-37.0794146789619,4.82619837356406));
#61173=CARTESIAN_POINT('Ctrl Pts',(37.4013696406987,-38.1409968175026,4.90470388394084));
#61174=CARTESIAN_POINT('Ctrl Pts',(37.5398609233301,-39.8561611622599,4.98320939431763));
#61175=CARTESIAN_POINT('Ctrl Pts',(39.0468979136614,-40.6867079066975,5.0617149046944));
#61176=CARTESIAN_POINT('Ctrl Pts',(40.5709349782279,-39.8877822721679,5.14022041507118));
#61177=CARTESIAN_POINT('Ctrl Pts',(40.745177494668,-38.1758811994982,5.21872592544796));
#61178=CARTESIAN_POINT('Ctrl Pts',(39.4133645670745,-37.0862753673934,5.29723143582474));
#61179=CARTESIAN_POINT('Ctrl Pts',(37.7698897533292,-37.5961550422893,5.37573694620152));
#61180=CARTESIAN_POINT('Ctrl Pts',(37.2886763485592,-39.2482362054987,5.4542424565783));
#61181=CARTESIAN_POINT('Ctrl Pts',(38.4012556794041,-40.5609170045275,5.53274796695508));
#61182=CARTESIAN_POINT('Ctrl Pts',(40.1099052932563,-40.3569060637301,5.61125347733186));
#61183=CARTESIAN_POINT('Ctrl Pts',(40.8821362004287,-38.8192621207562,5.68975898770864));
#61184=CARTESIAN_POINT('Ctrl Pts',(40.025658400892,-37.3267854127763,5.76826449808541));
#61185=CARTESIAN_POINT('Ctrl Pts',(38.3080469143,-37.2183586878016,5.8467700084622));
#61186=CARTESIAN_POINT('Ctrl Pts',(37.2707754210207,-38.5904264849422,5.92527551883897));
#61187=CARTESIAN_POINT('Ctrl Pts',(37.8419099014003,-40.2140906446281,6.00378102921576));
#61188=CARTESIAN_POINT('Ctrl Pts',(39.5137297698779,-40.6299518311032,6.08228653959253));
#61189=CARTESIAN_POINT('Ctrl Pts',(40.3550860167094,-39.8577931806474,6.13462354651039));
#61190=CARTESIAN_POINT('Ctrl Pts',(40.5224743779889,-39.378793292775,6.16079204996931));
#61191=CARTESIAN_POINT('Ctrl Pts',(38.0398499461207,-39.8946132698472,1.94640265001023));
#61192=CARTESIAN_POINT('Ctrl Pts',(38.3768621543504,-40.2320073282822,1.97257115346916));
#61193=CARTESIAN_POINT('Ctrl Pts',(39.4041135512345,-40.5429141695936,2.02490816038701));
#61194=CARTESIAN_POINT('Ctrl Pts',(40.650329218204,-39.5092379343175,2.10341367076379));
#61195=CARTESIAN_POINT('Ctrl Pts',(40.4720972414715,-37.9014549038573,2.18191918114057));
#61196=CARTESIAN_POINT('Ctrl Pts',(39.0343879004488,-37.1623938193051,2.26042469151735));
#61197=CARTESIAN_POINT('Ctrl Pts',(37.6240696333812,-37.954393397504,2.33893020189413));
#61198=CARTESIAN_POINT('Ctrl Pts',(37.5071871332558,-39.567403123707,2.41743571227091));
#61199=CARTESIAN_POINT('Ctrl Pts',(38.7879499877074,-40.5547216897998,2.49594122264769));
#61200=CARTESIAN_POINT('Ctrl Pts',(40.3180437170825,-40.0309557671714,2.57444673302446));
#61201=CARTESIAN_POINT('Ctrl Pts',(40.7250931288709,-38.4658026130365,2.65295224340125));
#61202=CARTESIAN_POINT('Ctrl Pts',(39.6441213754036,-37.2629429019217,2.73145775377802));
#61203=CARTESIAN_POINT('Ctrl Pts',(38.044532569248,-37.5011228205998,2.80996326415481));
#61204=CARTESIAN_POINT('Ctrl Pts',(37.3608943502601,-38.9667404252288,2.88846877453158));
#61205=CARTESIAN_POINT('Ctrl Pts',(38.2063006183275,-40.3453932847829,2.96697428490837));
#61206=CARTESIAN_POINT('Ctrl Pts',(39.8225754490498,-40.400673592003,3.04547979528514));
#61207=CARTESIAN_POINT('Ctrl Pts',(40.7602029110188,-39.0830042303774,3.12398530566192));
#61208=CARTESIAN_POINT('Ctrl Pts',(40.1782975152901,-37.5741026188095,3.2024908160387));
#61209=CARTESIAN_POINT('Ctrl Pts',(38.598725304576,-37.2271874907223,3.28099632641548));
#61210=CARTESIAN_POINT('Ctrl Pts',(37.4380844623892,-38.3533806319362,3.35950183679226));
#61211=CARTESIAN_POINT('Ctrl Pts',(37.7372651534312,-39.9426852341612,3.43800734716904));
#61212=CARTESIAN_POINT('Ctrl Pts',(39.2279550884041,-40.5697751592293,3.51651285754582));
#61213=CARTESIAN_POINT('Ctrl Pts',(40.5732680612611,-39.6722612478536,3.5950183679226));
#61214=CARTESIAN_POINT('Ctrl Pts',(40.5666954314397,-38.0550553160375,3.67352387829937));
#61215=CARTESIAN_POINT('Ctrl Pts',(39.214131681444,-37.1685060887655,3.75202938867616));
#61216=CARTESIAN_POINT('Ctrl Pts',(37.7285881416946,-37.8076919903125,3.83053489905293));
#61217=CARTESIAN_POINT('Ctrl Pts',(37.4423355733826,-39.399375908035,3.90904040942972));
#61218=CARTESIAN_POINT('Ctrl Pts',(38.6120920860802,-40.516097864552,3.98754591980649));
#61219=CARTESIAN_POINT('Ctrl Pts',(40.188792229238,-40.1563550606944,4.06605143018328));
#61220=CARTESIAN_POINT('Ctrl Pts',(40.758413831017,-38.6427733952556,4.14455694056005));
#61221=CARTESIAN_POINT('Ctrl Pts',(39.8101066964379,-37.3327688894207,4.22306245093684));
#61222=CARTESIAN_POINT('Ctrl Pts',(38.1943352093782,-37.401184727007,4.30156796131362));
#61223=CARTESIAN_POINT('Ctrl Pts',(37.360161650527,-38.7866639595805,4.38007347169039));
#61224=CARTESIAN_POINT('Ctrl Pts',(38.0556927021353,-40.2466758710431,4.45857898206717));
#61225=CARTESIAN_POINT('Ctrl Pts',(39.6571595751178,-40.4718470743308,4.53708449244395));
#61226=CARTESIAN_POINT('Ctrl Pts',(40.7283287185891,-39.2602386712458,4.61559000282073));
#61227=CARTESIAN_POINT('Ctrl Pts',(40.3085501518688,-37.6984499020877,4.69409551319751));
#61228=CARTESIAN_POINT('Ctrl Pts',(38.7742913281713,-37.1871300239526,4.77260102357429));
#61229=CARTESIAN_POINT('Ctrl Pts',(37.5015119247368,-38.1848429411531,4.85110653395107));
#61230=CARTESIAN_POINT('Ctrl Pts',(37.631670992589,-39.7968158255486,4.92961204432785));
#61231=CARTESIAN_POINT('Ctrl Pts',(39.0480383346578,-40.5773934042213,5.00811755470463));
#61232=CARTESIAN_POINT('Ctrl Pts',(40.4803829553959,-39.8265344772346,5.08662306508141));
#61233=CARTESIAN_POINT('Ctrl Pts',(40.6441423133075,-38.2176285328299,5.16512857545819));
#61234=CARTESIAN_POINT('Ctrl Pts',(39.3924568215175,-37.1935779446744,5.24363408583497));
#61235=CARTESIAN_POINT('Ctrl Pts',(37.8478603261192,-37.6727811258441,5.32213959621175));
#61236=CARTESIAN_POINT('Ctrl Pts',(37.3955987323729,-39.2254661767282,5.40064510658853));
#61237=CARTESIAN_POINT('Ctrl Pts',(38.4412406375015,-40.4591706088247,5.47915061696531));
#61238=CARTESIAN_POINT('Ctrl Pts',(40.04709074445,-40.2674338194666,5.55765612734208));
#61239=CARTESIAN_POINT('Ctrl Pts',(40.7728610105231,-38.8223009670344,5.63616163771887));
#61240=CARTESIAN_POINT('Ctrl Pts',(39.9679124974785,-37.419617899835,5.71466714809565));
#61241=CARTESIAN_POINT('Ctrl Pts',(38.3536397015357,-37.3177145801109,5.79317265847242));
#61242=CARTESIAN_POINT('Ctrl Pts',(37.3787747995027,-38.6072330401369,5.87167816884921));
#61243=CARTESIAN_POINT('Ctrl Pts',(37.9155474408704,-40.1332107732787,5.95018367922598));
#61244=CARTESIAN_POINT('Ctrl Pts',(39.4867836339601,-40.5240520115073,6.02868918960276));
#61245=CARTESIAN_POINT('Ctrl Pts',(40.2775203701537,-39.7983496548842,6.08102619652062));
#61246=CARTESIAN_POINT('Ctrl Pts',(40.4348379475454,-39.3481684036012,6.10719469997954));
#61247=CARTESIAN_POINT('Ctrl Pts',(38.1055301823584,-39.8290073680889,1.89280530002046));
#61248=CARTESIAN_POINT('Ctrl Pts',(38.4209683416301,-40.1448029331842,1.91897380347939));
#61249=CARTESIAN_POINT('Ctrl Pts',(39.3824595927764,-40.4358068770573,1.97131081039724));
#61250=CARTESIAN_POINT('Ctrl Pts',(40.5488979782264,-39.4683020775988,2.04981632077402));
#61251=CARTESIAN_POINT('Ctrl Pts',(40.3820756338396,-37.9634422913595,2.1283218311508));
#61252=CARTESIAN_POINT('Ctrl Pts',(39.0364021625962,-37.2716926680296,2.20682734152758));
#61253=CARTESIAN_POINT('Ctrl Pts',(37.7163663084416,-38.0129918939637,2.28533285190436));
#61254=CARTESIAN_POINT('Ctrl Pts',(37.606966115243,-39.5227437857229,2.36383836228114));
#61255=CARTESIAN_POINT('Ctrl Pts',(38.8057401281902,-40.4468585314142,2.44234387265792));
#61256=CARTESIAN_POINT('Ctrl Pts',(40.2378839429277,-39.9566218144982,2.5208493830347));
#61257=CARTESIAN_POINT('Ctrl Pts',(40.6188758300216,-38.491662926178,2.59935489341147));
#61258=CARTESIAN_POINT('Ctrl Pts',(39.6071031647834,-37.3658050377377,2.67786040378825));
#61259=CARTESIAN_POINT('Ctrl Pts',(38.1099130444145,-37.5887377187761,2.75636591416503));
#61260=CARTESIAN_POINT('Ctrl Pts',(37.4700383569718,-38.9605328885379,2.83487142454181));
#61261=CARTESIAN_POINT('Ctrl Pts',(38.2613254098556,-40.2509304162025,2.91337693491859));
#61262=CARTESIAN_POINT('Ctrl Pts',(39.77413338841,-40.3026719197079,2.99188244529537));
#61263=CARTESIAN_POINT('Ctrl Pts',(40.6517380373327,-39.0693539929087,3.07038795567215));
#61264=CARTESIAN_POINT('Ctrl Pts',(40.1070836823373,-37.6570456691978,3.14889346604893));
#61265=CARTESIAN_POINT('Ctrl Pts',(38.6286287824343,-37.3323385317259,3.22739897642571));
#61266=CARTESIAN_POINT('Ctrl Pts',(37.5422870954134,-38.3864377090672,3.30590448680249));
#61267=CARTESIAN_POINT('Ctrl Pts',(37.8223155459186,-39.8740019753033,3.38440999717927));
#61268=CARTESIAN_POINT('Ctrl Pts',(39.2175780249922,-40.4609483435087,3.46291550755605));
#61269=CARTESIAN_POINT('Ctrl Pts',(40.4767699398235,-39.620889350951,3.54142101793283));
#61270=CARTESIAN_POINT('Ctrl Pts',(40.4706180610435,-38.1072098763263,3.61992652830961));
#61271=CARTESIAN_POINT('Ctrl Pts',(39.2046395321427,-37.2774136567075,3.69843203868639));
#61272=CARTESIAN_POINT('Ctrl Pts',(37.8141939985582,-37.8756816698323,3.77693754906317));
#61273=CARTESIAN_POINT('Ctrl Pts',(37.5462660688567,-39.3654729381844,3.85544305943995));
#61274=CARTESIAN_POINT('Ctrl Pts',(38.6411398809942,-40.4107072346876,3.93394856981672));
#61275=CARTESIAN_POINT('Ctrl Pts',(40.1169065705561,-40.0739935931963,4.01245408019351));
#61276=CARTESIAN_POINT('Ctrl Pts',(40.650063486415,-38.6573048122132,4.09095959057028));
#61277=CARTESIAN_POINT('Ctrl Pts',(39.7624628308567,-37.4311610706296,4.16946510094707));
#61278=CARTESIAN_POINT('Ctrl Pts',(38.250125974103,-37.4951972252442,4.24797061132384));
#61279=CARTESIAN_POINT('Ctrl Pts',(37.4693525614741,-38.7919841313561,4.32647612170063));
#61280=CARTESIAN_POINT('Ctrl Pts',(38.1203587543597,-40.1585324599333,4.4049816320774));
#61281=CARTESIAN_POINT('Ctrl Pts',(39.6193067159238,-40.3692891866976,4.48348714245418));
#61282=CARTESIAN_POINT('Ctrl Pts',(40.6219042914244,-39.2352426593185,4.56199265283096));
#61283=CARTESIAN_POINT('Ctrl Pts',(40.2289981142758,-37.77343278275,4.64049816320774));
#61284=CARTESIAN_POINT('Ctrl Pts',(38.7929558363546,-37.2948453689432,4.71900367358452));
#61285=CARTESIAN_POINT('Ctrl Pts',(37.601654208775,-38.2286890648036,4.7975091839613));
#61286=CARTESIAN_POINT('Ctrl Pts',(37.7234810618479,-39.7374704888372,4.87601469433808));
#61287=CARTESIAN_POINT('Ctrl Pts',(39.0491787556542,-40.468078901745,4.95452020471486));
#61288=CARTESIAN_POINT('Ctrl Pts',(40.3898309325639,-39.7652866823013,5.03302571509164));
#61289=CARTESIAN_POINT('Ctrl Pts',(40.5431071319469,-38.2593758661616,5.11153122546842));
#61290=CARTESIAN_POINT('Ctrl Pts',(39.3715490759606,-37.3008805219554,5.1900367358452));
#61291=CARTESIAN_POINT('Ctrl Pts',(37.9258308989092,-37.7494072093988,5.26854224622198));
#61292=CARTESIAN_POINT('Ctrl Pts',(37.5025211161865,-39.2026961479577,5.34704775659876));
#61293=CARTESIAN_POINT('Ctrl Pts',(38.4812255955989,-40.3574242131219,5.42555326697554));
#61294=CARTESIAN_POINT('Ctrl Pts',(39.9842761956435,-40.1779615752029,5.50405877735232));
#61295=CARTESIAN_POINT('Ctrl Pts',(40.6635858206177,-38.8253398133127,5.58256428772909));
#61296=CARTESIAN_POINT('Ctrl Pts',(39.9101665940649,-37.5124503868936,5.66106979810588));
#61297=CARTESIAN_POINT('Ctrl Pts',(38.3992324887715,-37.4170704724203,5.73957530848265));
#61298=CARTESIAN_POINT('Ctrl Pts',(37.4867741779846,-38.6240395953316,5.81808081885943));
#61299=CARTESIAN_POINT('Ctrl Pts',(37.9891849803405,-40.0523309019293,5.89658632923621));
#61300=CARTESIAN_POINT('Ctrl Pts',(39.4598374980421,-40.4181521919114,5.97509183961299));
#61301=CARTESIAN_POINT('Ctrl Pts',(40.1999547235979,-39.7389061291211,6.02742884653085));
#61302=CARTESIAN_POINT('Ctrl Pts',(40.3472015171019,-39.3175435144275,6.05359734998977));
#61303=CARTESIAN_POINT('Ctrl Pts',(38.1712104185962,-39.7634014663305,1.83920795003069));
#61304=CARTESIAN_POINT('Ctrl Pts',(38.4650745289099,-40.0575985380862,1.86537645348962));
#61305=CARTESIAN_POINT('Ctrl Pts',(39.3608056343184,-40.328699584521,1.91771346040747));
#61306=CARTESIAN_POINT('Ctrl Pts',(40.4474667382487,-39.42736622088,1.99621897078425));
#61307=CARTESIAN_POINT('Ctrl Pts',(40.2920540262076,-38.0254296788618,2.07472448116103));
#61308=CARTESIAN_POINT('Ctrl Pts',(39.0384164247435,-37.3809915167542,2.15322999153781));
#61309=CARTESIAN_POINT('Ctrl Pts',(37.8086629835021,-38.0715903904234,2.23173550191459));
#61310=CARTESIAN_POINT('Ctrl Pts',(37.7067450972302,-39.4780844477388,2.31024101229137));
#61311=CARTESIAN_POINT('Ctrl Pts',(38.8235302686731,-40.3389953730286,2.38874652266814));
#61312=CARTESIAN_POINT('Ctrl Pts',(40.1577241687729,-39.8822878618251,2.46725203304493));
#61313=CARTESIAN_POINT('Ctrl Pts',(40.5126585311724,-38.5175232393194,2.5457575434217));
#61314=CARTESIAN_POINT('Ctrl Pts',(39.5700849541633,-37.4686671735537,2.62426305379848));
#61315=CARTESIAN_POINT('Ctrl Pts',(38.1752935195809,-37.6763526169523,2.70276856417526));
#61316=CARTESIAN_POINT('Ctrl Pts',(37.5791823636836,-38.9543253518471,2.78127407455204));
#61317=CARTESIAN_POINT('Ctrl Pts',(38.3163502013836,-40.156467547622,2.85977958492882));
#61318=CARTESIAN_POINT('Ctrl Pts',(39.7256913277703,-40.2046702474127,2.9382850953056));
#61319=CARTESIAN_POINT('Ctrl Pts',(40.5432731636465,-39.05570375544,3.01679060568238));
#61320=CARTESIAN_POINT('Ctrl Pts',(40.0358698493845,-37.7399887195861,3.09529611605916));
#61321=CARTESIAN_POINT('Ctrl Pts',(38.6585322602926,-37.4374895727296,3.17380162643594));
#61322=CARTESIAN_POINT('Ctrl Pts',(37.6464897284375,-38.4194947861982,3.25230713681272));
#61323=CARTESIAN_POINT('Ctrl Pts',(37.907365938406,-39.8053187164454,3.3308126471895));
#61324=CARTESIAN_POINT('Ctrl Pts',(39.2072009615803,-40.3521215277881,3.40931815756628));
#61325=CARTESIAN_POINT('Ctrl Pts',(40.3802718183859,-39.5695174540484,3.48782366794306));
#61326=CARTESIAN_POINT('Ctrl Pts',(40.3745406906472,-38.159364436615,3.56632917831984));
#61327=CARTESIAN_POINT('Ctrl Pts',(39.1951473828414,-37.3863212246494,3.64483468869662));
#61328=CARTESIAN_POINT('Ctrl Pts',(37.8997998554218,-37.943671349352,3.7233401990734));
#61329=CARTESIAN_POINT('Ctrl Pts',(37.6501965643308,-39.3315699683338,3.80184570945018));
#61330=CARTESIAN_POINT('Ctrl Pts',(38.6701876759083,-40.3053166048232,3.88035121982695));
#61331=CARTESIAN_POINT('Ctrl Pts',(40.0450209118742,-39.9916321256981,3.95885673020374));
#61332=CARTESIAN_POINT('Ctrl Pts',(40.5417131418129,-38.6718362291708,4.03736224058051));
#61333=CARTESIAN_POINT('Ctrl Pts',(39.7148189652755,-37.5295532518384,4.11586775095729));
#61334=CARTESIAN_POINT('Ctrl Pts',(38.3059167388278,-37.5892097234815,4.19437326133407));
#61335=CARTESIAN_POINT('Ctrl Pts',(37.5785434724212,-38.7973043031316,4.27287877171085));
#61336=CARTESIAN_POINT('Ctrl Pts',(38.1850248065841,-40.0703890488237,4.35138428208763));
#61337=CARTESIAN_POINT('Ctrl Pts',(39.5814538567299,-40.2667312990643,4.42988979246441));
#61338=CARTESIAN_POINT('Ctrl Pts',(40.5154798642596,-39.2102466473914,4.50839530284119));
#61339=CARTESIAN_POINT('Ctrl Pts',(40.1494460766828,-37.8484156634123,4.58690081321798));
#61340=CARTESIAN_POINT('Ctrl Pts',(38.8116203445378,-37.4025607139339,4.66540632359475));
#61341=CARTESIAN_POINT('Ctrl Pts',(37.7017964928131,-38.2725351884542,4.74391183397153));
#61342=CARTESIAN_POINT('Ctrl Pts',(37.8152911311068,-39.6781251521259,4.82241734434831));
#61343=CARTESIAN_POINT('Ctrl Pts',(39.0503191766506,-40.3587643992688,4.90092285472509));
#61344=CARTESIAN_POINT('Ctrl Pts',(40.2992789097318,-39.7040388873681,4.97942836510187));
#61345=CARTESIAN_POINT('Ctrl Pts',(40.4420719505864,-38.3011231994933,5.05793387547865));
#61346=CARTESIAN_POINT('Ctrl Pts',(39.3506413304036,-37.4081830992363,5.13643938585543));
#61347=CARTESIAN_POINT('Ctrl Pts',(38.0038014716991,-37.8260332929536,5.21494489623221));
#61348=CARTESIAN_POINT('Ctrl Pts',(37.6094435000001,-39.1799261191872,5.29345040660899));
#61349=CARTESIAN_POINT('Ctrl Pts',(38.5212105536963,-40.2556778174191,5.37195591698577));
#61350=CARTESIAN_POINT('Ctrl Pts',(39.9214616468371,-40.0884893309394,5.45046142736255));
#61351=CARTESIAN_POINT('Ctrl Pts',(40.5543106307123,-38.8283786595909,5.52896693773932));
#61352=CARTESIAN_POINT('Ctrl Pts',(39.8524206906513,-37.6052828739523,5.60747244811611));
#61353=CARTESIAN_POINT('Ctrl Pts',(38.4448252760073,-37.5164263647296,5.68597795849288));
#61354=CARTESIAN_POINT('Ctrl Pts',(37.5947735564665,-38.6408461505263,5.76448346886966));
#61355=CARTESIAN_POINT('Ctrl Pts',(38.0628225198106,-39.97145103058,5.84298897924644));
#61356=CARTESIAN_POINT('Ctrl Pts',(39.4328913621242,-40.3122523723155,5.92149448962322));
#61357=CARTESIAN_POINT('Ctrl Pts',(40.1223890770422,-39.6794626033579,5.97383149654108));
#61358=CARTESIAN_POINT('Ctrl Pts',(40.2595650866584,-39.2869186252538,6.));
#61359=CARTESIAN_POINT('Ctrl Pts',(39.6985816414592,-39.9636701304733,2.44341967361942));
#61360=CARTESIAN_POINT('Ctrl Pts',(39.808547063221,-39.9013157119468,2.45136379342792));
#61361=CARTESIAN_POINT('Ctrl Pts',(39.9090512176556,-39.8231041003581,2.45930791323642));
#61362=CARTESIAN_POINT('Ctrl Pts',(39.9945142458228,-39.7309450099414,2.46725203304493));
#61363=CARTESIAN_POINT('Ctrl Pts',(40.2760356229061,-39.4273663209899,2.49342053650385));
#61364=CARTESIAN_POINT('Ctrl Pts',(40.3943470770392,-38.9724447801547,2.51958903996278));
#61365=CARTESIAN_POINT('Ctrl Pts',(40.2964072079376,-38.5701746654428,2.54575754342171));
#61366=CARTESIAN_POINT('Ctrl Pts',(40.1984673388361,-38.1679045507309,2.57192604688063));
#61367=CARTESIAN_POINT('Ctrl Pts',(39.8842761464997,-37.8182858621423,2.59809455033956));
#61368=CARTESIAN_POINT('Ctrl Pts',(39.4947153112344,-37.6780907584144,2.62426305379849));
#61369=CARTESIAN_POINT('Ctrl Pts',(39.1051544759692,-37.5378956546866,2.65043155725741));
#61370=CARTESIAN_POINT('Ctrl Pts',(38.640223997775,-37.6071241358194,2.67660006071634));
#61371=CARTESIAN_POINT('Ctrl Pts',(38.3084068993617,-37.8547338322017,2.70276856417527));
#61372=CARTESIAN_POINT('Ctrl Pts',(37.9765898009484,-38.1023435285839,2.72893706763419));
#61373=CARTESIAN_POINT('Ctrl Pts',(37.777886082316,-38.5283344402155,2.75510557109312));
#61374=CARTESIAN_POINT('Ctrl Pts',(37.8013955292832,-38.9416869286604,2.78127407455204));
#61375=CARTESIAN_POINT('Ctrl Pts',(37.8249049762503,-39.3550394171054,2.80744257801097));
#61376=CARTESIAN_POINT('Ctrl Pts',(38.0706275888169,-39.7557534823637,2.8336110814699));
#61377=CARTESIAN_POINT('Ctrl Pts',(38.4283790828314,-39.9641442982913,2.85977958492882));
#61378=CARTESIAN_POINT('Ctrl Pts',(38.7861305768458,-40.1725351142189,2.88594808838775));
#61379=CARTESIAN_POINT('Ctrl Pts',(39.2559109523081,-40.1886026808158,2.91211659184668));
#61380=CARTESIAN_POINT('Ctrl Pts',(39.6270647793519,-40.0051420487855,2.9382850953056));
#61381=CARTESIAN_POINT('Ctrl Pts',(39.6513397427561,-39.9931429804635,2.93999662141021));
#61382=CARTESIAN_POINT('Ctrl Pts',(39.6751928123865,-39.9802903924142,2.94170814751481));
#61383=CARTESIAN_POINT('Ctrl Pts',(39.6985897981371,-39.9666323328489,2.94341967361942));
#61384=CARTESIAN_POINT('Ctrl Pts',(37.9741697098829,-39.9602191716056,2.));
#61385=CARTESIAN_POINT('Ctrl Pts',(38.0210640733086,-39.9994677669677,2.));
#61386=CARTESIAN_POINT('Ctrl Pts',(38.0703056805301,-40.0355567831455,2.));
#61387=CARTESIAN_POINT('Ctrl Pts',(38.1215357900136,-40.0684647235096,2.));
#61388=CARTESIAN_POINT('Ctrl Pts',(38.1724676227797,-40.1011810641969,2.));
#61389=CARTESIAN_POINT('Ctrl Pts',(38.2253661047044,-40.1307533458139,2.));
#61390=CARTESIAN_POINT('Ctrl Pts',(38.2799014945801,-40.1571104299646,2.));
#61391=CARTESIAN_POINT('Ctrl Pts',(38.3210824949734,-40.1770133057898,2.));
#61392=CARTESIAN_POINT('Ctrl Pts',(38.3631974573972,-40.1950818318595,2.));
#61393=CARTESIAN_POINT('Ctrl Pts',(38.4061067602768,-40.2112658265379,2.));
#61394=CARTESIAN_POINT('Ctrl Pts',(38.4283821944254,-40.2196673964429,2.));
#61395=CARTESIAN_POINT('Ctrl Pts',(38.4508716987496,-40.2275608160991,2.));
#61396=CARTESIAN_POINT('Ctrl Pts',(38.4735555240459,-40.2349372243514,2.));
#61397=CARTESIAN_POINT('Ctrl Pts',(38.4855017473433,-40.2388219403974,2.));
#61398=CARTESIAN_POINT('Ctrl Pts',(38.4975038315133,-40.2425636903004,2.));
#61399=CARTESIAN_POINT('Ctrl Pts',(38.5095371704371,-40.2461549840666,2.));
#61400=CARTESIAN_POINT('Ctrl Pts',(38.5662684087361,-40.2630861570139,2.));
#61401=CARTESIAN_POINT('Ctrl Pts',(38.6237986216725,-40.2767129172189,2.));
#61402=CARTESIAN_POINT('Ctrl Pts',(38.6818163301316,-40.286975145154,2.));
#61403=CARTESIAN_POINT('Ctrl Pts',(38.7386491570057,-40.2970277900975,2.));
#61404=CARTESIAN_POINT('Ctrl Pts',(38.7959508055663,-40.3038518408626,2.));
#61405=CARTESIAN_POINT('Ctrl Pts',(38.8534268715921,-40.3073420065174,2.));
#61406=CARTESIAN_POINT('Ctrl Pts',(38.8950337651378,-40.3098685355737,2.));
#61407=CARTESIAN_POINT('Ctrl Pts',(38.936732068862,-40.3106470090916,2.));
#61408=CARTESIAN_POINT('Ctrl Pts',(38.9784050690609,-40.3096213125542,2.));
#61409=CARTESIAN_POINT('Ctrl Pts',(39.0001855019757,-40.3090852312902,2.));
#61410=CARTESIAN_POINT('Ctrl Pts',(39.0219589293942,-40.3080560888428,2.));
#61411=CARTESIAN_POINT('Ctrl Pts',(39.0437079205698,-40.3065243689253,2.));
#61412=CARTESIAN_POINT('Ctrl Pts',(39.0538226985479,-40.3058120137285,2.));
#61413=CARTESIAN_POINT('Ctrl Pts',(39.0639271475071,-40.304991238701,2.));
#61414=CARTESIAN_POINT('Ctrl Pts',(39.0740116259566,-40.3040622329977,2.));
#61415=CARTESIAN_POINT('Ctrl Pts',(39.1295483097952,-40.2989460639973,2.));
#61416=CARTESIAN_POINT('Ctrl Pts',(39.1845546342683,-40.290546241389,2.));
#61417=CARTESIAN_POINT('Ctrl Pts',(39.2387593260286,-40.2787734967498,2.));
#61418=CARTESIAN_POINT('Ctrl Pts',(39.2750276515461,-40.2708963606396,2.));
#61419=CARTESIAN_POINT('Ctrl Pts',(39.3109369359741,-40.2615081906175,2.));
#61420=CARTESIAN_POINT('Ctrl Pts',(39.3464011448467,-40.2505700228958,2.));
#61421=CARTESIAN_POINT('Ctrl Pts',(39.3988910752724,-40.2343806398264,2.));
#61422=CARTESIAN_POINT('Ctrl Pts',(39.4504076476632,-40.2147967478769,2.));
#61423=CARTESIAN_POINT('Ctrl Pts',(39.5007091188364,-40.1920209197932,2.));
#61424=CARTESIAN_POINT('Ctrl Pts',(39.5162447294003,-40.1849866047498,2.));
#61425=CARTESIAN_POINT('Ctrl Pts',(39.5316641987863,-40.1776475888755,2.));
#61426=CARTESIAN_POINT('Ctrl Pts',(39.5469597255065,-40.1700092883085,2.));
#61427=CARTESIAN_POINT('Ctrl Pts',(39.5603821271819,-40.1633063914287,2.));
#61428=CARTESIAN_POINT('Ctrl Pts',(39.5737147687383,-40.1563697366024,2.));
#61429=CARTESIAN_POINT('Ctrl Pts',(39.5869207826454,-40.1492204403541,2.));
#61430=CARTESIAN_POINT('Ctrl Pts',(39.6358897832549,-40.1227102537983,2.));
#61431=CARTESIAN_POINT('Ctrl Pts',(39.6831882130913,-40.0932490202941,2.));
#61432=CARTESIAN_POINT('Ctrl Pts',(39.7285927500286,-40.0610855616068,2.));
#61433=CARTESIAN_POINT('Ctrl Pts',(39.7739426813493,-40.0289607841969,2.));
#61434=CARTESIAN_POINT('Ctrl Pts',(39.8174040328982,-39.9941393127207,2.));
#61435=CARTESIAN_POINT('Ctrl Pts',(39.8587164117551,-39.9568341504056,2.));
#61436=CARTESIAN_POINT('Ctrl Pts',(39.8851222214917,-39.9329896503903,2.));
#61437=CARTESIAN_POINT('Ctrl Pts',(39.9106492841583,-39.9081297964333,2.));
#61438=CARTESIAN_POINT('Ctrl Pts',(39.9352193294799,-39.8823054325727,2.));
#61439=CARTESIAN_POINT('Ctrl Pts',(39.9478799225961,-39.8689985070443,2.));
#61440=CARTESIAN_POINT('Ctrl Pts',(39.9602862681286,-39.8554354381392,2.));
#61441=CARTESIAN_POINT('Ctrl Pts',(39.9724266997057,-39.8416229521515,2.));
#61442=CARTESIAN_POINT('Ctrl Pts',(39.9797490690336,-39.8332921013825,2.));
#61443=CARTESIAN_POINT('Ctrl Pts',(39.9869741812514,-39.8248709352525,2.));
#61444=CARTESIAN_POINT('Ctrl Pts',(39.9940910777987,-39.8163713685009,2.));
#61445=CARTESIAN_POINT('Ctrl Pts',(40.0285072441014,-39.7752688316186,2.));
#61446=CARTESIAN_POINT('Ctrl Pts',(40.0604511582512,-39.7322729488107,2.));
#61447=CARTESIAN_POINT('Ctrl Pts',(40.0896714279617,-39.6875760500101,2.));
#61448=CARTESIAN_POINT('Ctrl Pts',(40.1080207191928,-39.6595079855692,2.));
#61449=CARTESIAN_POINT('Ctrl Pts',(40.1252950915591,-39.6307687140534,2.));
#61450=CARTESIAN_POINT('Ctrl Pts',(40.1414220409055,-39.6014032999083,2.));
#61451=CARTESIAN_POINT('Ctrl Pts',(40.1473185206864,-39.5906664539592,2.));
#61452=CARTESIAN_POINT('Ctrl Pts',(40.1530626681065,-39.5798436442736,2.));
#61453=CARTESIAN_POINT('Ctrl Pts',(40.1586468583821,-39.568944488148,2.));
#61454=CARTESIAN_POINT('Ctrl Pts',(40.1820879992589,-39.5231923483445,2.));
#61455=CARTESIAN_POINT('Ctrl Pts',(40.2026786417518,-39.4761684518135,2.));
#61456=CARTESIAN_POINT('Ctrl Pts',(40.2201722454891,-39.4280435373081,2.));
#61457=CARTESIAN_POINT('Ctrl Pts',(40.2299448374458,-39.4011591309003,2.));
#61458=CARTESIAN_POINT('Ctrl Pts',(40.238750054338,-39.3739309307312,2.));
#61459=CARTESIAN_POINT('Ctrl Pts',(40.2465377789655,-39.3463880711444,2.));
#61460=CARTESIAN_POINT('Ctrl Pts',(40.2520072382766,-39.3270442246388,2.));
#61461=CARTESIAN_POINT('Ctrl Pts',(40.2569746809644,-39.3075451531312,2.));
#61462=CARTESIAN_POINT('Ctrl Pts',(40.2614422049139,-39.2879094456029,2.));
#61463=CARTESIAN_POINT('Origin',(39.0658530619283,-38.8697713466883,4.5));
#61464=CARTESIAN_POINT('Origin',(-14.1292828945604,-53.2669068454841,6.));
#61465=CARTESIAN_POINT('Ctrl Pts',(-13.8936870225526,-54.5092654229862,
6.));
#61466=CARTESIAN_POINT('Ctrl Pts',(-13.9423636521357,-54.5241089051337,
6.));
#61467=CARTESIAN_POINT('Ctrl Pts',(-13.9918505584128,-54.5357341393499,
6.));
#61468=CARTESIAN_POINT('Ctrl Pts',(-14.0418694708007,-54.5442851897484,
6.));
#61469=CARTESIAN_POINT('Ctrl Pts',(-14.0755804158032,-54.5500482896627,
6.));
#61470=CARTESIAN_POINT('Ctrl Pts',(-14.1095337101414,-54.5544140915419,
6.));
#61471=CARTESIAN_POINT('Ctrl Pts',(-14.1436500643641,-54.5574153942333,
6.));
#61472=CARTESIAN_POINT('Ctrl Pts',(-14.1594122637946,-54.5588020351172,
6.));
#61473=CARTESIAN_POINT('Ctrl Pts',(-14.175209321514,-54.5598972886034,6.));
#61474=CARTESIAN_POINT('Ctrl Pts',(-14.1910336359969,-54.5607037375781,
6.));
#61475=CARTESIAN_POINT('Ctrl Pts',(-14.2042983435535,-54.561379742205,6.));
#61476=CARTESIAN_POINT('Ctrl Pts',(-14.2175747324108,-54.5618523554147,
6.));
#61477=CARTESIAN_POINT('Ctrl Pts',(-14.23085113108,-54.5621236288021,6.));
#61478=CARTESIAN_POINT('Ctrl Pts',(-14.2845943079494,-54.5632217499118,
6.));
#61479=CARTESIAN_POINT('Ctrl Pts',(-14.3383718685971,-54.5610264739157,
6.));
#61480=CARTESIAN_POINT('Ctrl Pts',(-14.3918835284745,-54.5556664140613,
6.));
#61481=CARTESIAN_POINT('Ctrl Pts',(-14.4123675638329,-54.5536146059913,
6.));
#61482=CARTESIAN_POINT('Ctrl Pts',(-14.4328128170871,-54.5510985259743,
6.));
#61483=CARTESIAN_POINT('Ctrl Pts',(-14.4532029278842,-54.5481234358992,
6.));
#61484=CARTESIAN_POINT('Ctrl Pts',(-14.4678705661439,-54.5459833030943,
6.));
#61485=CARTESIAN_POINT('Ctrl Pts',(-14.4825096747515,-54.5436056260969,
6.));
#61486=CARTESIAN_POINT('Ctrl Pts',(-14.4971141905477,-54.5409920215199,
6.));
#61487=CARTESIAN_POINT('Ctrl Pts',(-14.5083899394825,-54.5389741285999,
6.));
#61488=CARTESIAN_POINT('Ctrl Pts',(-14.5196453771421,-54.5368154090892,
6.));
#61489=CARTESIAN_POINT('Ctrl Pts',(-14.530862572558,-54.5345199552341,6.));
#61490=CARTESIAN_POINT('Ctrl Pts',(-14.5863736835655,-54.5231603248594,
6.));
#61491=CARTESIAN_POINT('Ctrl Pts',(-14.6410375587487,-54.50844123275,6.));
#61492=CARTESIAN_POINT('Ctrl Pts',(-14.6945239554116,-54.4905089639425,
6.));
#61493=CARTESIAN_POINT('Ctrl Pts',(-14.7472373377701,-54.4728358619729,
6.));
#61494=CARTESIAN_POINT('Ctrl Pts',(-14.7988082442548,-54.4520415391379,
6.));
#61495=CARTESIAN_POINT('Ctrl Pts',(-14.8489245845884,-54.428213079953,6.));
#61496=CARTESIAN_POINT('Ctrl Pts',(-14.8750932856906,-54.4157708341309,
6.));
#61497=CARTESIAN_POINT('Ctrl Pts',(-14.9008653565699,-54.4025004732343,
6.));
#61498=CARTESIAN_POINT('Ctrl Pts',(-14.9261951332699,-54.3884088626685,
6.));
#61499=CARTESIAN_POINT('Ctrl Pts',(-14.9397870442971,-54.3808473306696,
6.));
#61500=CARTESIAN_POINT('Ctrl Pts',(-14.9532515802469,-54.3730492659014,
6.));
#61501=CARTESIAN_POINT('Ctrl Pts',(-14.9665814892698,-54.365015287363,6.));
#61502=CARTESIAN_POINT('Ctrl Pts',(-14.9760605318105,-54.3593022382938,
6.));
#61503=CARTESIAN_POINT('Ctrl Pts',(-14.9854714934371,-54.3534698862629,
6.));
#61504=CARTESIAN_POINT('Ctrl Pts',(-14.9948117124905,-54.3475183599598,
6.));
#61505=CARTESIAN_POINT('Ctrl Pts',(-15.0030222328171,-54.3422866702739,
6.));
#61506=CARTESIAN_POINT('Ctrl Pts',(-15.0111697862519,-54.3369681733363,
6.));
#61507=CARTESIAN_POINT('Ctrl Pts',(-15.0192523731614,-54.331563816082,6.));
#61508=CARTESIAN_POINT('Ctrl Pts',(-15.0592738168887,-54.3048037970243,
6.));
#61509=CARTESIAN_POINT('Ctrl Pts',(-15.0977061906147,-54.2759385109371,
6.));
#61510=CARTESIAN_POINT('Ctrl Pts',(-15.1343580440251,-54.2450336527683,
6.));
#61511=CARTESIAN_POINT('Ctrl Pts',(-15.1760762697673,-54.2098568273243,
6.));
#61512=CARTESIAN_POINT('Ctrl Pts',(-15.2154892262361,-54.17203873631,6.));
#61513=CARTESIAN_POINT('Ctrl Pts',(-15.2525505184471,-54.1318952661582,
6.));
#61514=CARTESIAN_POINT('Ctrl Pts',(-15.2887783562999,-54.0926545640469,
6.));
#61515=CARTESIAN_POINT('Ctrl Pts',(-15.3227594146245,-54.0511910495941,
6.));
#61516=CARTESIAN_POINT('Ctrl Pts',(-15.3544244053254,-54.0077622836715,
6.));
#61517=CARTESIAN_POINT('Ctrl Pts',(-15.3621778074591,-53.9971284360401,
6.));
#61518=CARTESIAN_POINT('Ctrl Pts',(-15.3697922131958,-53.9863766151879,
6.));
#61519=CARTESIAN_POINT('Ctrl Pts',(-15.3772663285991,-53.975510336868,6.));
#61520=CARTESIAN_POINT('Ctrl Pts',(-15.3829111783894,-53.9673035450824,
6.));
#61521=CARTESIAN_POINT('Ctrl Pts',(-15.3884748239273,-53.9590330393209,
6.));
#61522=CARTESIAN_POINT('Ctrl Pts',(-15.3939506112134,-53.9507101506706,
6.));
#61523=CARTESIAN_POINT('Ctrl Pts',(-15.4256178027139,-53.9025778009366,
6.));
#61524=CARTESIAN_POINT('Ctrl Pts',(-15.4544095035981,-53.852609994368,6.));
#61525=CARTESIAN_POINT('Ctrl Pts',(-15.4802788953647,-53.8011564089965,
6.));
#61526=CARTESIAN_POINT('Ctrl Pts',(-15.5067035063538,-53.7485985062167,
6.));
#61527=CARTESIAN_POINT('Ctrl Pts',(-15.5300796467437,-53.6944895430076,
6.));
#61528=CARTESIAN_POINT('Ctrl Pts',(-15.5503219669977,-53.6391607087766,
6.));
#61529=CARTESIAN_POINT('Ctrl Pts',(-15.5707432288232,-53.5833427691257,
6.));
#61530=CARTESIAN_POINT('Ctrl Pts',(-15.5879756421218,-53.5262822854476,
6.));
#61531=CARTESIAN_POINT('Ctrl Pts',(-15.6018865037253,-53.4682915822501,
6.));
#61532=CARTESIAN_POINT('Ctrl Pts',(-15.6050386064326,-53.4551512996596,
6.));
#61533=CARTESIAN_POINT('Ctrl Pts',(-15.6080206160618,-53.4419594370913,
6.));
#61534=CARTESIAN_POINT('Ctrl Pts',(-15.6108253927011,-53.4287461304568,
6.));
#61535=CARTESIAN_POINT('Ctrl Pts',(-15.6234580838913,-53.3692335047533,
6.));
#61536=CARTESIAN_POINT('Ctrl Pts',(-15.6325248597527,-53.3091883987973,
6.));
#61537=CARTESIAN_POINT('Ctrl Pts',(-15.6379479683267,-53.2489633020354,
6.));
#61538=CARTESIAN_POINT('Ctrl Pts',(-15.6433234244293,-53.1892673989372,
6.));
#61539=CARTESIAN_POINT('Ctrl Pts',(-15.6451194085378,-53.1293935642286,
6.));
#61540=CARTESIAN_POINT('Ctrl Pts',(-15.6432152689538,-53.0696627698792,
6.));
#61541=CARTESIAN_POINT('Ctrl Pts',(-15.6418200559649,-53.0258964510577,
6.));
#61542=CARTESIAN_POINT('Ctrl Pts',(-15.6384374018706,-52.9822063985564,
6.));
#61543=CARTESIAN_POINT('Ctrl Pts',(-15.6330021738796,-52.9387162761377,
6.));
#61544=CARTESIAN_POINT('Ctrl Pts',(-15.6299816095937,-52.9145471500616,
6.));
#61545=CARTESIAN_POINT('Ctrl Pts',(-15.626326826898,-52.8904397607359,6.));
#61546=CARTESIAN_POINT('Ctrl Pts',(-15.6220514315181,-52.8664094746825,
6.));
#61547=CARTESIAN_POINT('Ctrl Pts',(-15.2209662466057,-52.1764590205668,
6.));
#61548=CARTESIAN_POINT('Ctrl Pts',(-15.1741443796226,-52.1372711016556,
6.));
#61549=CARTESIAN_POINT('Ctrl Pts',(-15.1249225029807,-52.1011828129763,
6.));
#61550=CARTESIAN_POINT('Ctrl Pts',(-15.0736468678487,-52.0682420900143,
6.));
#61551=CARTESIAN_POINT('Ctrl Pts',(-15.0261004125905,-52.0376970834737,
6.));
#61552=CARTESIAN_POINT('Ctrl Pts',(-14.9767869967238,-52.0098588542083,
6.));
#61553=CARTESIAN_POINT('Ctrl Pts',(-14.9259704605544,-51.9848043154143,
6.));
#61554=CARTESIAN_POINT('Ctrl Pts',(-14.9137051793402,-51.9787570523153,
6.));
#61555=CARTESIAN_POINT('Ctrl Pts',(-14.9013518482974,-51.9728720566067,
6.));
#61556=CARTESIAN_POINT('Ctrl Pts',(-14.8889282287138,-51.9671568052641,
6.));
#61557=CARTESIAN_POINT('Ctrl Pts',(-14.8342503521426,-51.9420032817374,
6.));
#61558=CARTESIAN_POINT('Ctrl Pts',(-14.7781470458952,-51.9201009097871,
6.));
#61559=CARTESIAN_POINT('Ctrl Pts',(-14.7209451681374,-51.9015259517645,
6.));
#61560=CARTESIAN_POINT('Ctrl Pts',(-14.6856380616414,-51.8900608032978,
6.));
#61561=CARTESIAN_POINT('Ctrl Pts',(-14.6499121652624,-51.8798643401128,
6.));
#61562=CARTESIAN_POINT('Ctrl Pts',(-14.6138441165377,-51.8709644321812,
6.));
#61563=CARTESIAN_POINT('Ctrl Pts',(-14.6015017900197,-51.8679189231072,
6.));
#61564=CARTESIAN_POINT('Ctrl Pts',(-14.5891194062045,-51.8650253041639,
6.));
#61565=CARTESIAN_POINT('Ctrl Pts',(-14.5767000721463,-51.8622849004515,
6.));
#61566=CARTESIAN_POINT('Ctrl Pts',(-14.5650829788742,-51.8597215161847,
6.));
#61567=CARTESIAN_POINT('Ctrl Pts',(-14.5534409513892,-51.8572938728812,
6.));
#61568=CARTESIAN_POINT('Ctrl Pts',(-14.5417825459458,-51.8550036366081,
6.));
#61569=CARTESIAN_POINT('Ctrl Pts',(-14.4840742559295,-51.843667127538,6.));
#61570=CARTESIAN_POINT('Ctrl Pts',(-14.4259183529299,-51.8356828275257,
6.));
#61571=CARTESIAN_POINT('Ctrl Pts',(-14.367620963232,-51.8311224894044,6.));
#61572=CARTESIAN_POINT('Ctrl Pts',(-14.3108124222532,-51.8266786171078,
6.));
#61573=CARTESIAN_POINT('Ctrl Pts',(-14.2538685532984,-51.8254861890658,
6.));
#61574=CARTESIAN_POINT('Ctrl Pts',(-14.1970797852011,-51.8276601888203,
6.));
#61575=CARTESIAN_POINT('Ctrl Pts',(-14.1662905485282,-51.8288388689574,
6.));
#61576=CARTESIAN_POINT('Ctrl Pts',(-14.1355471145905,-51.8310079452929,
6.));
#61577=CARTESIAN_POINT('Ctrl Pts',(-14.1048981745618,-51.8341917567471,
6.));
#61578=CARTESIAN_POINT('Ctrl Pts',(-14.0793989212455,-51.8368406188189,
6.));
#61579=CARTESIAN_POINT('Ctrl Pts',(-14.0539650962438,-51.8401919425301,
6.));
#61580=CARTESIAN_POINT('Ctrl Pts',(-14.0286260526481,-51.8442620101075,
6.));
#61581=CARTESIAN_POINT('Ctrl Pts',(-14.0177944478155,-51.846001829666,6.));
#61582=CARTESIAN_POINT('Ctrl Pts',(-14.0069789239642,-51.8478733580626,
6.));
#61583=CARTESIAN_POINT('Ctrl Pts',(-13.996199334982,-51.8498743912714,6.));
#61584=CARTESIAN_POINT('Ctrl Pts',(-13.9463007654824,-51.8591371465399,
6.));
#61585=CARTESIAN_POINT('Ctrl Pts',(-13.8970847123908,-51.8711850123186,
6.));
#61586=CARTESIAN_POINT('Ctrl Pts',(-13.8487579820866,-51.8860904144816,
6.));
#61587=CARTESIAN_POINT('Ctrl Pts',(-13.7947539043117,-51.9027468796016,
6.));
#61588=CARTESIAN_POINT('Ctrl Pts',(-13.7418592133642,-51.9229715823675,
6.));
#61589=CARTESIAN_POINT('Ctrl Pts',(-13.6903202642367,-51.9465184249238,
6.));
#61590=CARTESIAN_POINT('Ctrl Pts',(-13.6465843618314,-51.9665002527537,
6.));
#61591=CARTESIAN_POINT('Ctrl Pts',(-13.6038249088342,-51.9888755884466,
6.));
#61592=CARTESIAN_POINT('Ctrl Pts',(-13.562213300163,-52.0135148505948,6.));
#61593=CARTESIAN_POINT('Ctrl Pts',(-13.5507734482976,-52.0202886696816,
6.));
#61594=CARTESIAN_POINT('Ctrl Pts',(-13.5394204822292,-52.0272336869077,
6.));
#61595=CARTESIAN_POINT('Ctrl Pts',(-13.5281582767465,-52.0343473928026,
6.));
#61596=CARTESIAN_POINT('Ctrl Pts',(-13.519389840783,-52.0398859238388,6.));
#61597=CARTESIAN_POINT('Ctrl Pts',(-13.5106749801112,-52.0455277717095,
6.));
#61598=CARTESIAN_POINT('Ctrl Pts',(-13.5020295300328,-52.0512622211197,
6.));
#61599=CARTESIAN_POINT('Ctrl Pts',(-13.4557689093827,-52.0819464754268,
6.));
#61600=CARTESIAN_POINT('Ctrl Pts',(-13.4114050031948,-52.1153327757811,
6.));
#61601=CARTESIAN_POINT('Ctrl Pts',(-13.3691631578584,-52.1511816195792,
6.));
#61602=CARTESIAN_POINT('Ctrl Pts',(-13.3271578443737,-52.1868297289317,
6.));
#61603=CARTESIAN_POINT('Ctrl Pts',(-13.2872501901036,-52.2249138499118,
6.));
#61604=CARTESIAN_POINT('Ctrl Pts',(-13.2497024980977,-52.2652291266103,
6.));
#61605=CARTESIAN_POINT('Ctrl Pts',(-13.2148651399623,-52.3026342947483,
6.));
#61606=CARTESIAN_POINT('Ctrl Pts',(-13.1820592966373,-52.3419610028466,
6.));
#61607=CARTESIAN_POINT('Ctrl Pts',(-13.1515339537958,-52.3830588008458,
6.));
#61608=CARTESIAN_POINT('Ctrl Pts',(-13.1436930287938,-52.3936154309067,
6.));
#61609=CARTESIAN_POINT('Ctrl Pts',(-13.1360003096902,-52.404292764071,6.));
#61610=CARTESIAN_POINT('Ctrl Pts',(-13.1284766278539,-52.415064415478,6.));
#61611=CARTESIAN_POINT('Ctrl Pts',(-13.09806445529,-52.4586055072624,6.));
#61612=CARTESIAN_POINT('Ctrl Pts',(-13.0703588458369,-52.5037520470482,
6.));
#61613=CARTESIAN_POINT('Ctrl Pts',(-13.0455900654096,-52.5503113513571,
6.));
#61614=CARTESIAN_POINT('Ctrl Pts',(-13.0216615115111,-52.595291233427,6.));
#61615=CARTESIAN_POINT('Ctrl Pts',(-13.0004736387158,-52.6415904794481,
6.));
#61616=CARTESIAN_POINT('Ctrl Pts',(-12.9822803194866,-52.6890470685693,
6.));
#61617=CARTESIAN_POINT('Ctrl Pts',(-12.9695523308543,-52.7222475483307,
6.));
#61618=CARTESIAN_POINT('Ctrl Pts',(-12.9582909257562,-52.7560147190405,
6.));
#61619=CARTESIAN_POINT('Ctrl Pts',(-12.9485983183411,-52.7902936156639,
6.));
#61620=CARTESIAN_POINT('Ctrl Pts',(-12.9431308250061,-52.8096299645733,
6.));
#61621=CARTESIAN_POINT('Ctrl Pts',(-12.9381627931205,-52.8291291517901,
6.));
#61622=CARTESIAN_POINT('Ctrl Pts',(-12.9336933707122,-52.8487726938777,
6.));
#61623=CARTESIAN_POINT('Origin',(-14.1292828945604,-53.2669068454841,0.895788276411274));
#61624=CARTESIAN_POINT('Ctrl Pts',(-14.9010809748678,-54.6051974101417,
2.14578827641127));
#61625=CARTESIAN_POINT('Ctrl Pts',(-14.8597272487244,-54.6294211798578,
2.14826884812012));
#61626=CARTESIAN_POINT('Ctrl Pts',(-14.3688277705329,-54.885598628679,2.17691792328789));
#61627=CARTESIAN_POINT('Ctrl Pts',(-13.1694755608909,-54.8098887390119,
2.23173550191459));
#61628=CARTESIAN_POINT('Ctrl Pts',(-12.3130077055018,-53.3174154968918,
2.31024101229136));
#61629=CARTESIAN_POINT('Ctrl Pts',(-13.0852322400692,-51.7797767714816,
2.38874652266815));
#61630=CARTESIAN_POINT('Ctrl Pts',(-14.7938791388703,-51.5757659053288,
2.46725203304492));
#61631=CARTESIAN_POINT('Ctrl Pts',(-15.9064540032169,-52.8884432158558,
2.5457575434217));
#61632=CARTESIAN_POINT('Ctrl Pts',(-15.5416657446855,-54.1408201433548,
2.60526962454382));
#61633=CARTESIAN_POINT('Ctrl Pts',(-15.0227829664514,-54.5334351262247,
2.63861320220701));
#61634=CARTESIAN_POINT('Ctrl Pts',(-14.9016274172746,-54.6020379108679,
2.64578827641127));
#61635=CARTESIAN_POINT('Ctrl Pts',(-14.9013089558621,-54.6009691165979,
2.10421172358873));
#61636=CARTESIAN_POINT('Ctrl Pts',(-14.6040162957702,-54.7699114721225,
2.12181148931034));
#61637=CARTESIAN_POINT('Ctrl Pts',(-13.7242010739632,-54.9558633776928,
2.16557975849087));
#61638=CARTESIAN_POINT('Ctrl Pts',(-12.4888977717378,-54.0475500892828,
2.23551653113034));
#61639=CARTESIAN_POINT('Ctrl Pts',(-12.5727324025626,-52.3295818538895,
2.31402204150712));
#61640=CARTESIAN_POINT('Ctrl Pts',(-14.0528383317196,-51.4513683986095,
2.3925275518839));
#61641=CARTESIAN_POINT('Ctrl Pts',(-15.6013423678816,-52.2018016959779,
2.47103306226067));
#61642=CARTESIAN_POINT('Ctrl Pts',(-15.8066350265236,-53.7346571674393,
2.54159445282895));
#61643=CARTESIAN_POINT('Ctrl Pts',(-15.2043102739953,-54.4236472184416,
2.5859873399383));
#61644=CARTESIAN_POINT('Ctrl Pts',(-14.8992309062956,-54.6029598038327,
2.60421172358873));
#61645=CARTESIAN_POINT('Ctrl Pts',(-12.9355708698302,-52.8497595669186,
2.));
#61646=CARTESIAN_POINT('Ctrl Pts',(-13.0727468794465,-52.4572155888145,
2.02616850345893));
#61647=CARTESIAN_POINT('Ctrl Pts',(-13.762195269905,-51.8244143348175,2.07850551037678));
#61648=CARTESIAN_POINT('Ctrl Pts',(-15.132331970736,-52.1652352880051,2.15701102075356));
#61649=CARTESIAN_POINT('Ctrl Pts',(-15.600345878683,-53.4958301810381,2.23551653113034));
#61650=CARTESIAN_POINT('Ctrl Pts',(-14.7503158422929,-54.6202478137908,
2.31402204150712));
#61651=CARTESIAN_POINT('Ctrl Pts',(-13.3427136311611,-54.5313920070952,
2.3925275518839));
#61652=CARTESIAN_POINT('Ctrl Pts',(-12.6408318404032,-53.3082990617544,
2.47103306226068));
#61653=CARTESIAN_POINT('Ctrl Pts',(-13.2736756018811,-52.0481926662385,
2.54953857263745));
#61654=CARTESIAN_POINT('Ctrl Pts',(-14.6739244700172,-51.8810042409304,
2.62804408301423));
#61655=CARTESIAN_POINT('Ctrl Pts',(-15.5856878633849,-52.9567530803092,
2.70654959339101));
#61656=CARTESIAN_POINT('Ctrl Pts',(-15.191331582231,-54.3106417984376,2.78505510376779));
#61657=CARTESIAN_POINT('Ctrl Pts',(-13.8444953540085,-54.7284908735361,
2.86356061414457));
#61658=CARTESIAN_POINT('Ctrl Pts',(-12.7530680664413,-53.8355533167568,
2.94206612452135));
#61659=CARTESIAN_POINT('Ctrl Pts',(-12.8958606092946,-52.4326417450687,
3.02057163489813));
#61660=CARTESIAN_POINT('Ctrl Pts',(-14.1448167496288,-51.7779181217065,
3.09907714527491));
#61661=CARTESIAN_POINT('Ctrl Pts',(-15.3798411765859,-52.4585553969251,
3.17758265565169));
#61662=CARTESIAN_POINT('Ctrl Pts',(-15.4933354964796,-53.86414126306,3.25608816602848));
#61663=CARTESIAN_POINT('Ctrl Pts',(-14.3835148696119,-54.7341132075812,
3.33459367640524));
#61664=CARTESIAN_POINT('Ctrl Pts',(-13.0456930357207,-54.2882595546367,
3.41309918678203));
#61665=CARTESIAN_POINT('Ctrl Pts',(-12.6796603121052,-52.9264325363301,
3.49160469715881));
#61666=CARTESIAN_POINT('Ctrl Pts',(-13.6136836011906,-51.8699509600852,
3.57011020753559));
#61667=CARTESIAN_POINT('Ctrl Pts',(-15.0101085852912,-52.066292638923,3.64861571791237));
#61668=CARTESIAN_POINT('Ctrl Pts',(-15.6165881539764,-53.3393736780174,
3.72712122828915));
#61669=CARTESIAN_POINT('Ctrl Pts',(-14.8892170051293,-54.5474647404685,
3.80562673866593));
#61670=CARTESIAN_POINT('Ctrl Pts',(-13.4803188806439,-54.6071210383936,
3.88413224904271));
#61671=CARTESIAN_POINT('Ctrl Pts',(-12.6534271115016,-53.4648413867365,
3.96263775941949));
#61672=CARTESIAN_POINT('Ctrl Pts',(-13.1501178953861,-52.1450493326719,
4.04114326979627));
#61673=CARTESIAN_POINT('Ctrl Pts',(-14.5249471286252,-51.8313657668163,
4.11964878017305));
#61674=CARTESIAN_POINT('Ctrl Pts',(-15.5449352706108,-52.805109568325,4.19815429054982));
#61675=CARTESIAN_POINT('Ctrl Pts',(-15.2953327061785,-54.1930041465599,
4.2766598009266));
#61676=CARTESIAN_POINT('Ctrl Pts',(-13.9999889501244,-54.7503526485876,
4.35516531130338));
#61677=CARTESIAN_POINT('Ctrl Pts',(-12.8205990758801,-53.977311687267,4.43367082168017));
#61678=CARTESIAN_POINT('Ctrl Pts',(-12.8148679650961,-52.5671627753774,
4.51217633205694));
#61679=CARTESIAN_POINT('Ctrl Pts',(-13.9879354060905,-51.7845609801147,
4.59068184243372));
#61680=CARTESIAN_POINT('Ctrl Pts',(-15.2877666458998,-52.3313621994943,
4.6691873528105));
#61681=CARTESIAN_POINT('Ctrl Pts',(-15.5486420944497,-53.7171820950401,
4.74769286318728));
#61682=CARTESIAN_POINT('Ctrl Pts',(-14.5366025126985,-54.6991844494411,
4.82619837356406));
#61683=CARTESIAN_POINT('Ctrl Pts',(-13.1592689266914,-54.396686183443,4.90470388394084));
#61684=CARTESIAN_POINT('Ctrl Pts',(-12.651867102821,-53.0809749777224,4.98320939431762));
#61685=CARTESIAN_POINT('Ctrl Pts',(-13.4694465335298,-51.9320118320645,
5.0617149046944));
#61686=CARTESIAN_POINT('Ctrl Pts',(-14.8787836035794,-51.9802143885461,
5.14022041507118));
#61687=CARTESIAN_POINT('Ctrl Pts',(-15.6159492071913,-53.1823530914927,
5.21872592544796));
#61688=CARTESIAN_POINT('Ctrl Pts',(-15.0198399508834,-54.4603220891204,
5.29723143582474));
#61689=CARTESIAN_POINT('Ctrl Pts',(-13.6250522726906,-54.6680069657355,
5.37573694620152));
#61690=CARTESIAN_POINT('Ctrl Pts',(-12.6824820007894,-53.6191538682575,
5.45424245657829));
#61691=CARTESIAN_POINT('Ctrl Pts',(-13.0374143051107,-52.2543934093274,
5.53274796695507));
#61692=CARTESIAN_POINT('Ctrl Pts',(-14.3716061738679,-51.7976868080881,
5.61125347733185));
#61693=CARTESIAN_POINT('Ctrl Pts',(-15.4883847851255,-52.6585961458811,
5.68975898770864));
#61694=CARTESIAN_POINT('Ctrl Pts',(-15.3864730097086,-54.0650841092748,
5.76826449808541));
#61695=CARTESIAN_POINT('Ctrl Pts',(-14.156713139869,-54.7556852978769,5.8467700084622));
#61696=CARTESIAN_POINT('Ctrl Pts',(-12.9030960095782,-54.1112396708051,
5.92527551883897));
#61697=CARTESIAN_POINT('Ctrl Pts',(-12.747656043165,-52.7093273325191,6.00378102921575));
#61698=CARTESIAN_POINT('Ctrl Pts',(-13.8343697837273,-51.8079468650312,
6.08228653959253));
#61699=CARTESIAN_POINT('Ctrl Pts',(-14.7300614275788,-52.0790796540862,
6.13462354651038));
#61700=CARTESIAN_POINT('Ctrl Pts',(-15.0239255378924,-52.3732767258419,
6.16079204996931));
#61701=CARTESIAN_POINT('Ctrl Pts',(-12.8479344393867,-52.8191346777449,
1.94640265001023));
#61702=CARTESIAN_POINT('Ctrl Pts',(-12.9951812328907,-52.3977720630513,
1.97257115346916));
#61703=CARTESIAN_POINT('Ctrl Pts',(-13.7352455128293,-51.7185136720468,
2.02490816038701));
#61704=CARTESIAN_POINT('Ctrl Pts',(-15.2059708708849,-52.0843560132568,
2.10341367076379));
#61705=CARTESIAN_POINT('Ctrl Pts',(-15.7083440442499,-53.5126365996361,
2.18191918114057));
#61706=CARTESIAN_POINT('Ctrl Pts',(-14.7959090084834,-54.7196034114377,
2.26042469151735));
#61707=CARTESIAN_POINT('Ctrl Pts',(-13.2849676077377,-54.6242242510674,
2.33893020189413));
#61708=CARTESIAN_POINT('Ctrl Pts',(-12.5315571287694,-53.3113378734669,
2.41743571227091));
#61709=CARTESIAN_POINT('Ctrl Pts',(-13.2108611479438,-51.9587207013195,
2.49594122264769));
#61710=CARTESIAN_POINT('Ctrl Pts',(-14.7139093596349,-51.7792581290633,
2.57444673302446));
#61711=CARTESIAN_POINT('Ctrl Pts',(-15.6926099099956,-52.9339831254913,
2.65295224340125));
#61712=CARTESIAN_POINT('Ctrl Pts',(-15.2693019419295,-54.3872676543484,
2.73145775377802));
#61713=CARTESIAN_POINT('Ctrl Pts',(-13.8235876618921,-54.8357931410496,
2.80996326415481));
#61714=CARTESIAN_POINT('Ctrl Pts',(-12.6520331831854,-53.8773005270505,
2.88846877453158));
#61715=CARTESIAN_POINT('Ctrl Pts',(-12.8053088480064,-52.3713941292876,
2.96697428490836));
#61716=CARTESIAN_POINT('Ctrl Pts',(-14.1459571684074,-51.6686039370295,
3.04547979528514));
#61717=CARTESIAN_POINT('Ctrl Pts',(-15.4716509779683,-52.3992102332442,
3.12398530566192));
#61718=CARTESIAN_POINT('Ctrl Pts',(-15.5934774892658,-53.90798725892,3.2024908160387));
#61719=CARTESIAN_POINT('Ctrl Pts',(-14.4021793232963,-54.8418282390413,
3.28099632641548));
#61720=CARTESIAN_POINT('Ctrl Pts',(-12.9661412298193,-54.3632422169535,
3.35950183679226));
#61721=CARTESIAN_POINT('Ctrl Pts',(-12.5732361947429,-52.9014365971976,
3.43800734716904));
#61722=CARTESIAN_POINT('Ctrl Pts',(-13.5758308522243,-51.7673933710292,
3.51651285754582));
#61723=CARTESIAN_POINT('Ctrl Pts',(-15.0747744492345,-51.9781494844411,
3.5950183679226));
#61724=CARTESIAN_POINT('Ctrl Pts',(-15.7257787470295,-53.3446938343006,
3.67352387829938));
#61725=CARTESIAN_POINT('Ctrl Pts',(-14.945007607421,-54.6414769649982,3.75202938867616));
#61726=CARTESIAN_POINT('Ctrl Pts',(-13.4326751537753,-54.7055129331413,
3.83053489905294));
#61727=CARTESIAN_POINT('Ctrl Pts',(-12.5450770823513,-53.4793727613876,
3.90904040942971));
#61728=CARTESIAN_POINT('Ctrl Pts',(-13.0782324459937,-52.0626881049618,
3.9875459198065));
#61729=CARTESIAN_POINT('Ctrl Pts',(-14.5539948389685,-51.7259754437876,
4.06605143018328));
#61730=CARTESIAN_POINT('Ctrl Pts',(-15.6488654635013,-52.77120669718,4.14455694056005));
#61731=CARTESIAN_POINT('Ctrl Pts',(-15.3809383138062,-54.2609936281335,
4.22306245093684));
#61732=CARTESIAN_POINT('Ctrl Pts',(-13.9904968284622,-54.8592598994547,
4.30156796131361));
#61733=CARTESIAN_POINT('Ctrl Pts',(-12.7245219851981,-54.0294660957121,
4.3800734716904));
#61734=CARTESIAN_POINT('Ctrl Pts',(-12.7183701246174,-52.5157910280399,
4.45857898206717));
#61735=CARTESIAN_POINT('Ctrl Pts',(-13.9775583728655,-51.6757344812337,
4.53708449244395));
#61736=CARTESIAN_POINT('Ctrl Pts',(-15.3728167908182,-52.2626791406019,
4.61559000282073));
#61737=CARTESIAN_POINT('Ctrl Pts',(-15.6528444240053,-53.7502390759288,
4.69409551319751));
#61738=CARTESIAN_POINT('Ctrl Pts',(-14.5665059036703,-54.8043351843038,
4.77260102357429));
#61739=CARTESIAN_POINT('Ctrl Pts',(-13.0880553007387,-54.4796289923587,
4.85110653395107));
#61740=CARTESIAN_POINT('Ctrl Pts',(-12.5434025455522,-53.0673247799705,
4.92961204432785));
#61741=CARTESIAN_POINT('Ctrl Pts',(-13.4210046127319,-51.8340104451561,
5.00811755470463));
#61742=CARTESIAN_POINT('Ctrl Pts',(-14.9338082371531,-51.8857517948312,
5.08662306508141));
#61743=CARTESIAN_POINT('Ctrl Pts',(-15.725092891933,-53.1761455732413,5.16512857545819));
#61744=CARTESIAN_POINT('Ctrl Pts',(-15.0852202435382,-54.5479367313644,
5.24363408583496));
#61745=CARTESIAN_POINT('Ctrl Pts',(-13.5880341553344,-54.7708688040089,
5.32213959621175));
#61746=CARTESIAN_POINT('Ctrl Pts',(-12.5762650378488,-53.6450141017733,
5.40064510658852));
#61747=CARTESIAN_POINT('Ctrl Pts',(-12.9572547157706,-52.1800596826976,
5.47915061696531));
#61748=CARTESIAN_POINT('Ctrl Pts',(-14.3893963500343,-51.689823942551,5.55765612734208));
#61749=CARTESIAN_POINT('Ctrl Pts',(-15.58816332118,-52.6139369841994,5.63616163771886));
#61750=CARTESIAN_POINT('Ctrl Pts',(-15.478769687465,-54.1236823346513,5.71466714809565));
#61751=CARTESIAN_POINT('Ctrl Pts',(-14.1587269327564,-54.8649840454692,
5.79317265847243));
#61752=CARTESIAN_POINT('Ctrl Pts',(-12.8130754355786,-54.1732264091344,
5.8716781688492));
#61753=CARTESIAN_POINT('Ctrl Pts',(-12.6462238359385,-52.6683926035455,
5.95018367922599));
#61754=CARTESIAN_POINT('Ctrl Pts',(-13.8127187223415,-51.7008372421089,
6.02868918960276));
#61755=CARTESIAN_POINT('Ctrl Pts',(-14.7741676148585,-51.9918752589882,
6.08102619652061));
#61756=CARTESIAN_POINT('Ctrl Pts',(-15.0896057741302,-52.3076708240835,
6.10719469997954));
#61757=CARTESIAN_POINT('Ctrl Pts',(-12.7602980089432,-52.7885097885712,
1.89280530002046));
#61758=CARTESIAN_POINT('Ctrl Pts',(-12.917615586335,-52.3383285372882,1.91897380347939));
#61759=CARTESIAN_POINT('Ctrl Pts',(-13.7082957557537,-51.6126130092761,
1.97131081039724));
#61760=CARTESIAN_POINT('Ctrl Pts',(-15.2796097710338,-52.0034767385084,
2.04981632077402));
#61761=CARTESIAN_POINT('Ctrl Pts',(-15.8163422098168,-53.5294430182342,
2.1283218311508));
#61762=CARTESIAN_POINT('Ctrl Pts',(-14.8415021746739,-54.8189590090846,
2.20682734152758));
#61763=CARTESIAN_POINT('Ctrl Pts',(-13.2272215843143,-54.7170564950396,
2.28533285190436));
#61764=CARTESIAN_POINT('Ctrl Pts',(-12.4222824171356,-53.3143766851794,
2.36383836228113));
#61765=CARTESIAN_POINT('Ctrl Pts',(-13.1480466940065,-51.8692487364006,
2.44234387265792));
#61766=CARTESIAN_POINT('Ctrl Pts',(-14.7538942492526,-51.677512017196,2.52084938303469));
#61767=CARTESIAN_POINT('Ctrl Pts',(-15.7995319566062,-52.9112131706736,
2.59935489341148));
#61768=CARTESIAN_POINT('Ctrl Pts',(-15.347272301628,-54.4638935102592,2.67786040378825));
#61769=CARTESIAN_POINT('Ctrl Pts',(-13.8026799697757,-54.9430954085631,
2.75636591416504));
#61770=CARTESIAN_POINT('Ctrl Pts',(-12.5509982999295,-53.9190477373443,
2.83487142454181));
#61771=CARTESIAN_POINT('Ctrl Pts',(-12.7147570867183,-52.3101465135064,
2.91337693491859));
#61772=CARTESIAN_POINT('Ctrl Pts',(-14.147097587186,-51.5592897523525,2.99188244529537));
#61773=CARTESIAN_POINT('Ctrl Pts',(-15.5634607793507,-52.3398650695632,
3.07038795567215));
#61774=CARTESIAN_POINT('Ctrl Pts',(-15.693619482052,-53.9518332547799,3.14889346604893));
#61775=CARTESIAN_POINT('Ctrl Pts',(-14.4208437769808,-54.9495432705015,
3.22739897642571));
#61776=CARTESIAN_POINT('Ctrl Pts',(-12.886589423918,-54.4382248792703,3.30590448680249));
#61777=CARTESIAN_POINT('Ctrl Pts',(-12.4668120773806,-52.876440658065,3.38440999717927));
#61778=CARTESIAN_POINT('Ctrl Pts',(-13.5379781032581,-51.6648357819733,
3.46291550755605));
#61779=CARTESIAN_POINT('Ctrl Pts',(-15.1394403131777,-51.8900063299591,
3.54142101793283));
#61780=CARTESIAN_POINT('Ctrl Pts',(-15.8349693400828,-53.3500139905838,
3.61992652830961));
#61781=CARTESIAN_POINT('Ctrl Pts',(-15.0007982097127,-54.7354891895279,
3.69843203868639));
#61782=CARTESIAN_POINT('Ctrl Pts',(-13.3850314269068,-54.8039048278889,
3.77693754906317));
#61783=CARTESIAN_POINT('Ctrl Pts',(-12.4367270532009,-53.4939041360386,
3.85544305943994));
#61784=CARTESIAN_POINT('Ctrl Pts',(-13.0063469966013,-51.9803268772517,
3.93394856981673));
#61785=CARTESIAN_POINT('Ctrl Pts',(-14.5830425493117,-51.6205851207591,
4.01245408019351));
#61786=CARTESIAN_POINT('Ctrl Pts',(-15.7527956563917,-52.7373038260349,
4.09095959057028));
#61787=CARTESIAN_POINT('Ctrl Pts',(-15.4665439214339,-54.3289831097072,
4.16946510094706));
#61788=CARTESIAN_POINT('Ctrl Pts',(-13.9810047068001,-54.9681671503218,
4.24797061132384));
#61789=CARTESIAN_POINT('Ctrl Pts',(-12.628444894516,-54.0816205041571,4.32647612170062));
#61790=CARTESIAN_POINT('Ctrl Pts',(-12.6218722841388,-52.4644192807025,
4.4049816320774));
#61791=CARTESIAN_POINT('Ctrl Pts',(-13.9671813396406,-51.5669079823526,
4.48348714245418));
#61792=CARTESIAN_POINT('Ctrl Pts',(-15.4578669357366,-52.1939960817095,
4.56199265283096));
#61793=CARTESIAN_POINT('Ctrl Pts',(-15.7570467535609,-53.7832960568175,
4.64049816320773));
#61794=CARTESIAN_POINT('Ctrl Pts',(-14.5964092946421,-54.9094859191667,
4.71900367358452));
#61795=CARTESIAN_POINT('Ctrl Pts',(-13.016841674786,-54.5625718012743,4.7975091839613));
#61796=CARTESIAN_POINT('Ctrl Pts',(-12.4349379882833,-53.0536745822187,
4.87601469433808));
#61797=CARTESIAN_POINT('Ctrl Pts',(-13.3725626919339,-51.7360090582476,
4.95452020471486));
#61798=CARTESIAN_POINT('Ctrl Pts',(-14.9888328707268,-51.7912892011163,
5.03302571509164));
#61799=CARTESIAN_POINT('Ctrl Pts',(-15.8342365766747,-53.16993805499,5.11153122546842));
#61800=CARTESIAN_POINT('Ctrl Pts',(-15.1506005361929,-54.6355513736084,
5.1900367358452));
#61801=CARTESIAN_POINT('Ctrl Pts',(-13.5510160379782,-54.8737306422823,
5.26854224622197));
#61802=CARTESIAN_POINT('Ctrl Pts',(-12.4700480749082,-53.6708743352892,
5.34704775659876));
#61803=CARTESIAN_POINT('Ctrl Pts',(-12.8770951264305,-52.105725956068,5.42555326697553));
#61804=CARTESIAN_POINT('Ctrl Pts',(-14.4071865262006,-51.581961077014,5.50405877735231));
#61805=CARTESIAN_POINT('Ctrl Pts',(-15.6879418572343,-52.5692778225178,
5.58256428772909));
#61806=CARTESIAN_POINT('Ctrl Pts',(-15.5710663652214,-54.1822805600277,
5.66106979810588));
#61807=CARTESIAN_POINT('Ctrl Pts',(-14.1607407256438,-54.9742827930615,
5.73957530848265));
#61808=CARTESIAN_POINT('Ctrl Pts',(-12.7230548615789,-54.2352131474636,
5.81808081885943));
#61809=CARTESIAN_POINT('Ctrl Pts',(-12.544791628712,-52.6274578745722,5.89658632923621));
#61810=CARTESIAN_POINT('Ctrl Pts',(-13.7910676609558,-51.5937276191864,
5.97509183961299));
#61811=CARTESIAN_POINT('Ctrl Pts',(-14.8182738021382,-51.9046708638902,
6.02742884653084));
#61812=CARTESIAN_POINT('Ctrl Pts',(-15.1552860103679,-52.2420649223251,
6.05359734998977));
#61813=CARTESIAN_POINT('Ctrl Pts',(-12.6726615784998,-52.7578848993974,
1.83920795003069));
#61814=CARTESIAN_POINT('Ctrl Pts',(-12.8400499397792,-52.278885011525,1.86537645348962));
#61815=CARTESIAN_POINT('Ctrl Pts',(-13.681345998678,-51.5067123465054,1.91771346040747));
#61816=CARTESIAN_POINT('Ctrl Pts',(-15.3532486711827,-51.92259746376,1.99621897078425));
#61817=CARTESIAN_POINT('Ctrl Pts',(-15.9243403753837,-53.5462494368323,
2.07472448116103));
#61818=CARTESIAN_POINT('Ctrl Pts',(-14.8870953408643,-54.9183146067314,
2.15322999153781));
#61819=CARTESIAN_POINT('Ctrl Pts',(-13.1694755608909,-54.8098887390119,
2.23173550191459));
#61820=CARTESIAN_POINT('Ctrl Pts',(-12.3130077055018,-53.3174154968918,
2.31024101229136));
#61821=CARTESIAN_POINT('Ctrl Pts',(-13.0852322400692,-51.7797767714816,
2.38874652266815));
#61822=CARTESIAN_POINT('Ctrl Pts',(-14.7938791388703,-51.5757659053288,
2.46725203304492));
#61823=CARTESIAN_POINT('Ctrl Pts',(-15.9064540032169,-52.8884432158558,
2.5457575434217));
#61824=CARTESIAN_POINT('Ctrl Pts',(-15.4252426613265,-54.5405193661699,
2.62426305379848));
#61825=CARTESIAN_POINT('Ctrl Pts',(-13.7817722776592,-55.0503976760766,
2.70276856417526));
#61826=CARTESIAN_POINT('Ctrl Pts',(-12.4499634166736,-53.960794947638,2.78127407455204));
#61827=CARTESIAN_POINT('Ctrl Pts',(-12.6242053254302,-52.2488988977254,
2.85977958492882));
#61828=CARTESIAN_POINT('Ctrl Pts',(-14.1482380059646,-51.4499755676755,
2.93828509530561));
#61829=CARTESIAN_POINT('Ctrl Pts',(-15.6552705807332,-52.2805199058824,
3.01679060568238));
#61830=CARTESIAN_POINT('Ctrl Pts',(-15.7937614748382,-53.9956792506399,
3.09529611605916));
#61831=CARTESIAN_POINT('Ctrl Pts',(-14.4395082306652,-55.0572583019617,
3.17380162643594));
#61832=CARTESIAN_POINT('Ctrl Pts',(-12.8070376180166,-54.5132075415871,
3.25230713681272));
#61833=CARTESIAN_POINT('Ctrl Pts',(-12.3603879600184,-52.8514447189325,
3.3308126471895));
#61834=CARTESIAN_POINT('Ctrl Pts',(-13.5001253542918,-51.5622781929174,
3.40931815756628));
#61835=CARTESIAN_POINT('Ctrl Pts',(-15.2041061771209,-51.8018631754771,
3.48782366794306));
#61836=CARTESIAN_POINT('Ctrl Pts',(-15.944159933136,-53.3553341468671,3.56632917831984));
#61837=CARTESIAN_POINT('Ctrl Pts',(-15.0565888120043,-54.8295014140574,
3.64483468869662));
#61838=CARTESIAN_POINT('Ctrl Pts',(-13.3373877000383,-54.9022967226366,
3.7233401990734));
#61839=CARTESIAN_POINT('Ctrl Pts',(-12.3283770240505,-53.5084355106897,
3.80184570945017));
#61840=CARTESIAN_POINT('Ctrl Pts',(-12.9344615472089,-51.8979656495417,
3.88035121982696));
#61841=CARTESIAN_POINT('Ctrl Pts',(-14.612090259655,-51.5151947977304,3.95885673020373));
#61842=CARTESIAN_POINT('Ctrl Pts',(-15.8567258492822,-52.7034009548898,
4.03736224058051));
#61843=CARTESIAN_POINT('Ctrl Pts',(-15.5521495290616,-54.3969725912808,
4.11586775095729));
#61844=CARTESIAN_POINT('Ctrl Pts',(-13.9715125851379,-55.0770744011889,
4.19437326133407));
#61845=CARTESIAN_POINT('Ctrl Pts',(-12.5323678038339,-54.1337749126023,
4.27287877171085));
#61846=CARTESIAN_POINT('Ctrl Pts',(-12.5253744436601,-52.413047533365,4.35138428208763));
#61847=CARTESIAN_POINT('Ctrl Pts',(-13.9568043064156,-51.4580814834715,
4.42988979246441));
#61848=CARTESIAN_POINT('Ctrl Pts',(-15.5429170806551,-52.1253130228172,
4.50839530284119));
#61849=CARTESIAN_POINT('Ctrl Pts',(-15.8612490831165,-53.8163530377063,
4.58690081321797));
#61850=CARTESIAN_POINT('Ctrl Pts',(-14.6263126856139,-55.0146366540294,
4.66540632359475));
#61851=CARTESIAN_POINT('Ctrl Pts',(-12.9456280488333,-54.64551461019,4.74391183397153));
#61852=CARTESIAN_POINT('Ctrl Pts',(-12.3264734310144,-53.0400243844669,
4.82241734434831));
#61853=CARTESIAN_POINT('Ctrl Pts',(-13.324120771136,-51.638007671339,4.90092285472508));
#61854=CARTESIAN_POINT('Ctrl Pts',(-15.0438575043005,-51.6968266074015,
4.97942836510187));
#61855=CARTESIAN_POINT('Ctrl Pts',(-15.9433802614164,-53.1637305367386,
5.05793387547864));
#61856=CARTESIAN_POINT('Ctrl Pts',(-15.2159808288477,-54.7231660158524,
5.13643938585543));
#61857=CARTESIAN_POINT('Ctrl Pts',(-13.513997920622,-54.9765924805557,5.2149448962322));
#61858=CARTESIAN_POINT('Ctrl Pts',(-12.3638311119676,-53.696734568805,5.29345040660899));
#61859=CARTESIAN_POINT('Ctrl Pts',(-12.7969355370903,-52.0313922294383,
5.37195591698576));
#61860=CARTESIAN_POINT('Ctrl Pts',(-14.424976702367,-51.4740982114769,5.45046142736254));
#61861=CARTESIAN_POINT('Ctrl Pts',(-15.7877203932888,-52.5246186608361,
5.52896693773933));
#61862=CARTESIAN_POINT('Ctrl Pts',(-15.6633630429778,-54.2408787854042,
5.60747244811611));
#61863=CARTESIAN_POINT('Ctrl Pts',(-14.1627545185313,-55.0835815406539,
5.68597795849288));
#61864=CARTESIAN_POINT('Ctrl Pts',(-12.6330342875793,-54.2971998857928,
5.76448346886966));
#61865=CARTESIAN_POINT('Ctrl Pts',(-12.4433594214856,-52.5865231455987,
5.84298897924644));
#61866=CARTESIAN_POINT('Ctrl Pts',(-13.76941659957,-51.486617996264,5.92149448962323));
#61867=CARTESIAN_POINT('Ctrl Pts',(-14.8623799894179,-51.8174664687922,
5.97383149654107));
#61868=CARTESIAN_POINT('Ctrl Pts',(-15.2209662466057,-52.1764590205668,
6.));
#61869=CARTESIAN_POINT('Ctrl Pts',(-12.9355708698302,-52.8497595669186,
2.));
#61870=CARTESIAN_POINT('Ctrl Pts',(-12.9469576730109,-52.8006000143783,
2.));
#61871=CARTESIAN_POINT('Ctrl Pts',(-12.9614720678986,-52.7523805759145,
2.));
#61872=CARTESIAN_POINT('Ctrl Pts',(-12.9788381112572,-52.7052630574535,
2.));
#61873=CARTESIAN_POINT('Ctrl Pts',(-12.9969823676714,-52.6560340926918,
2.));
#61874=CARTESIAN_POINT('Ctrl Pts',(-13.0182396625092,-52.608007253985,2.));
#61875=CARTESIAN_POINT('Ctrl Pts',(-13.0423523228529,-52.5613664966425,
2.));
#61876=CARTESIAN_POINT('Ctrl Pts',(-13.061689993281,-52.5239619306945,2.));
#61877=CARTESIAN_POINT('Ctrl Pts',(-13.0828653436285,-52.4874486478168,
2.));
#61878=CARTESIAN_POINT('Ctrl Pts',(-13.1057691188079,-52.4519266272348,
2.));
#61879=CARTESIAN_POINT('Ctrl Pts',(-13.1154541423153,-52.436905889314,2.));
#61880=CARTESIAN_POINT('Ctrl Pts',(-13.1254484616934,-52.4220624809487,
2.));
#61881=CARTESIAN_POINT('Ctrl Pts',(-13.1357448170118,-52.4074044118665,
2.));
#61882=CARTESIAN_POINT('Ctrl Pts',(-13.1415823490882,-52.3990940004831,
2.));
#61883=CARTESIAN_POINT('Ctrl Pts',(-13.1475174809115,-52.3908426597166,
2.));
#61884=CARTESIAN_POINT('Ctrl Pts',(-13.1535391079514,-52.3826647593396,
2.));
#61885=CARTESIAN_POINT('Ctrl Pts',(-13.185818005202,-52.3388271712184,2.));
#61886=CARTESIAN_POINT('Ctrl Pts',(-13.2206401757039,-52.2970090605309,
2.));
#61887=CARTESIAN_POINT('Ctrl Pts',(-13.2577323841666,-52.2574000923829,
2.));
#61888=CARTESIAN_POINT('Ctrl Pts',(-13.2955035907173,-52.2170660551502,
2.));
#61889=CARTESIAN_POINT('Ctrl Pts',(-13.3356292075146,-52.1790218018794,
2.));
#61890=CARTESIAN_POINT('Ctrl Pts',(-13.3778710217101,-52.1434855491502,
2.));
#61891=CARTESIAN_POINT('Ctrl Pts',(-13.4080812323503,-52.1180709759184,
2.));
#61892=CARTESIAN_POINT('Ctrl Pts',(-13.4393749054964,-52.0939395106298,
2.));
#61893=CARTESIAN_POINT('Ctrl Pts',(-13.4716779317663,-52.0711807776364,
2.));
#61894=CARTESIAN_POINT('Ctrl Pts',(-13.4854146711621,-52.0615027127549,
2.));
#61895=CARTESIAN_POINT('Ctrl Pts',(-13.4993340562618,-52.0520730061476,
2.));
#61896=CARTESIAN_POINT('Ctrl Pts',(-13.5134308827615,-52.0428991428661,
2.));
#61897=CARTESIAN_POINT('Ctrl Pts',(-13.52183136089,-52.0374323211065,2.));
#61898=CARTESIAN_POINT('Ctrl Pts',(-13.5302901169523,-52.0320595108122,
2.));
#61899=CARTESIAN_POINT('Ctrl Pts',(-13.538799357562,-52.0267858960231,2.));
#61900=CARTESIAN_POINT('Ctrl Pts',(-13.5870981541539,-51.9968526434936,
2.));
#61901=CARTESIAN_POINT('Ctrl Pts',(-13.6370817517559,-51.9700725295858,
2.));
#61902=CARTESIAN_POINT('Ctrl Pts',(-13.6884925442776,-51.9466636060488,
2.));
#61903=CARTESIAN_POINT('Ctrl Pts',(-13.7200525424512,-51.932293362996,2.));
#61904=CARTESIAN_POINT('Ctrl Pts',(-13.752151284848,-51.9191940299464,2.));
#61905=CARTESIAN_POINT('Ctrl Pts',(-13.7847364470979,-51.9074225450413,
2.));
#61906=CARTESIAN_POINT('Ctrl Pts',(-13.836418792392,-51.88875214706,2.));
#61907=CARTESIAN_POINT('Ctrl Pts',(-13.8893237899006,-51.8734194145919,
2.));
#61908=CARTESIAN_POINT('Ctrl Pts',(-13.9431611750089,-51.861330721175,2.));
#61909=CARTESIAN_POINT('Ctrl Pts',(-13.9592695284011,-51.8577137374523,
2.));
#61910=CARTESIAN_POINT('Ctrl Pts',(-13.9754615001947,-51.8543874911092,
2.));
#61911=CARTESIAN_POINT('Ctrl Pts',(-13.9917296362983,-51.8513502983977,
2.));
#61912=CARTESIAN_POINT('Ctrl Pts',(-14.0067700369073,-51.8485423187486,
2.));
#61913=CARTESIAN_POINT('Ctrl Pts',(-14.0218822544663,-51.8459805725654,
2.));
#61914=CARTESIAN_POINT('Ctrl Pts',(-14.0370239759629,-51.8436690391789,
2.));
#61915=CARTESIAN_POINT('Ctrl Pts',(-14.0931183782155,-51.8351056744626,
2.));
#61916=CARTESIAN_POINT('Ctrl Pts',(-14.149687152489,-51.8299561325424,2.));
#61917=CARTESIAN_POINT('Ctrl Pts',(-14.2064063479335,-51.828080515235,2.));
#61918=CARTESIAN_POINT('Ctrl Pts',(-14.2644669778174,-51.8261605387361,
2.));
#61919=CARTESIAN_POINT('Ctrl Pts',(-14.3226861857286,-51.8276710218953,
2.));
#61920=CARTESIAN_POINT('Ctrl Pts',(-14.3807392825943,-51.8325126403782,
2.));
#61921=CARTESIAN_POINT('Ctrl Pts',(-14.4159849881017,-51.8354521262703,
2.));
#61922=CARTESIAN_POINT('Ctrl Pts',(-14.4511698447364,-51.8396204788386,
2.));
#61923=CARTESIAN_POINT('Ctrl Pts',(-14.4862227576225,-51.8450046114987,
2.));
#61924=CARTESIAN_POINT('Ctrl Pts',(-14.5055224539648,-51.8479690477423,
2.));
#61925=CARTESIAN_POINT('Ctrl Pts',(-14.5247821602815,-51.8513021647932,
2.));
#61926=CARTESIAN_POINT('Ctrl Pts',(-14.5439899738547,-51.855002666883,2.));
#61927=CARTESIAN_POINT('Ctrl Pts',(-14.5555560513246,-51.8572309420422,
2.));
#61928=CARTESIAN_POINT('Ctrl Pts',(-14.5671052783022,-51.8595928681044,
2.));
#61929=CARTESIAN_POINT('Ctrl Pts',(-14.5786287782272,-51.8620869089405,
2.));
#61930=CARTESIAN_POINT('Ctrl Pts',(-14.6376831017684,-51.8748680861369,
2.));
#61931=CARTESIAN_POINT('Ctrl Pts',(-14.6958774997537,-51.8910736753997,
2.));
#61932=CARTESIAN_POINT('Ctrl Pts',(-14.7528646870875,-51.9106036961952,
2.));
#61933=CARTESIAN_POINT('Ctrl Pts',(-14.7899177177268,-51.9233021024998,
2.));
#61934=CARTESIAN_POINT('Ctrl Pts',(-14.8264606634567,-51.9374070196433,
2.));
#61935=CARTESIAN_POINT('Ctrl Pts',(-14.8623979324973,-51.9529027870108,
2.));
#61936=CARTESIAN_POINT('Ctrl Pts',(-14.8772478015739,-51.9593058922771,
2.));
#61937=CARTESIAN_POINT('Ctrl Pts',(-14.8919942354505,-51.9659465911414,
2.));
#61938=CARTESIAN_POINT('Ctrl Pts',(-14.9066303803289,-51.9728242372457,
2.));
#61939=CARTESIAN_POINT('Ctrl Pts',(-14.9173472276096,-51.9778601728396,
2.));
#61940=CARTESIAN_POINT('Ctrl Pts',(-14.9280038818557,-51.9830227414937,
2.));
#61941=CARTESIAN_POINT('Ctrl Pts',(-14.9385887530582,-51.988306995363,2.));
#61942=CARTESIAN_POINT('Ctrl Pts',(-14.9930076777083,-52.0154743937796,
2.));
#61943=CARTESIAN_POINT('Ctrl Pts',(-15.0455947546779,-52.0458841568081,
2.));
#61944=CARTESIAN_POINT('Ctrl Pts',(-15.0960008499165,-52.0794651524903,
2.));
#61945=CARTESIAN_POINT('Ctrl Pts',(-15.1196129598423,-52.095195753278,2.));
#61946=CARTESIAN_POINT('Ctrl Pts',(-15.1427463702698,-52.111622952968,2.));
#61947=CARTESIAN_POINT('Ctrl Pts',(-15.165364007469,-52.1287432229353,2.));
#61948=CARTESIAN_POINT('Ctrl Pts',(-15.1847945994588,-52.1434510802399,
2.));
#61949=CARTESIAN_POINT('Ctrl Pts',(-15.2038445286663,-52.1586704870383,
2.));
#61950=CARTESIAN_POINT('Ctrl Pts',(-15.2225082026616,-52.1743802571171,
2.));
#61951=CARTESIAN_POINT('Ctrl Pts',(-14.7622249872189,-54.3610567043161,
2.80658032638058));
#61952=CARTESIAN_POINT('Ctrl Pts',(-14.8615128627433,-54.3048362110035,
2.79940525217631));
#61953=CARTESIAN_POINT('Ctrl Pts',(-14.9530160801183,-54.235599890915,2.79223017797205));
#61954=CARTESIAN_POINT('Ctrl Pts',(-15.0325849243862,-54.1546351912659,
2.78505510376779));
#61955=CARTESIAN_POINT('Ctrl Pts',(-15.3227836759489,-53.8593455590615,
2.75888660030886));
#61956=CARTESIAN_POINT('Ctrl Pts',(-15.4542357696669,-53.4080493196853,
2.73271809684993));
#61957=CARTESIAN_POINT('Ctrl Pts',(-15.3680012509646,-53.0031097267674,
2.70654959339101));
#61958=CARTESIAN_POINT('Ctrl Pts',(-15.2817667322623,-52.5981701338496,
2.68038108993208));
#61959=CARTESIAN_POINT('Ctrl Pts',(-14.9778456011397,-52.23958718739,2.65421258647316));
#61960=CARTESIAN_POINT('Ctrl Pts',(-14.5925102242225,-52.0881604517115,
2.62804408301423));
#61961=CARTESIAN_POINT('Ctrl Pts',(-14.2071748473052,-51.9367337160331,
2.6018755795553));
#61962=CARTESIAN_POINT('Ctrl Pts',(-13.7404252245931,-51.9924631911358,
2.57570707609637));
#61963=CARTESIAN_POINT('Ctrl Pts',(-13.4015764529908,-52.2303456612731,
2.54953857263745));
#61964=CARTESIAN_POINT('Ctrl Pts',(-13.0627276813885,-52.4682281314104,
2.52337006917852));
#61965=CARTESIAN_POINT('Ctrl Pts',(-12.8517797608958,-52.8882635965824,
2.4972015657196));
#61966=CARTESIAN_POINT('Ctrl Pts',(-12.8632860991091,-53.3021301533919,
2.47103306226067));
#61967=CARTESIAN_POINT('Ctrl Pts',(-12.8747924373225,-53.7159967102013,
2.44486455880174));
#61968=CARTESIAN_POINT('Ctrl Pts',(-13.1087530342418,-54.1236943586483,
2.41869605534282));
#61969=CARTESIAN_POINT('Ctrl Pts',(-13.4603337012234,-54.3423524839877,
2.39252755188389));
#61970=CARTESIAN_POINT('Ctrl Pts',(-13.8119143682051,-54.5610106093271,
2.36635904842496));
#61971=CARTESIAN_POINT('Ctrl Pts',(-14.281115105249,-54.590629211559,2.34019054496604));
#61972=CARTESIAN_POINT('Ctrl Pts',(-14.6573871465026,-54.4180355738828,
2.31402204150711));
#61973=CARTESIAN_POINT('Ctrl Pts',(-14.6930548254675,-54.4016750320804,
2.31154146979827));
#61974=CARTESIAN_POINT('Ctrl Pts',(-14.7278874868095,-54.3834974973412,
2.30906089808942));
#61975=CARTESIAN_POINT('Ctrl Pts',(-14.7617771735939,-54.3636459375188,
2.30658032638058));
#61976=CARTESIAN_POINT('Ctrl Pts',(-15.6194800884629,-52.866705242183,2.));
#61977=CARTESIAN_POINT('Ctrl Pts',(-15.7510836294753,-53.3567463262429,
2.02616850345893));
#61978=CARTESIAN_POINT('Ctrl Pts',(-15.4911223508182,-54.468705692608,2.07850551037678));
#61979=CARTESIAN_POINT('Ctrl Pts',(-13.8755519245004,-55.0671510173417,
2.15701102075356));
#61980=CARTESIAN_POINT('Ctrl Pts',(-12.4888977717378,-54.0475500892828,
2.23551653113034));
#61981=CARTESIAN_POINT('Ctrl Pts',(-12.5727324025626,-52.3295818538895,
2.31402204150712));
#61982=CARTESIAN_POINT('Ctrl Pts',(-14.0528383317196,-51.4513683986095,
2.3925275518839));
#61983=CARTESIAN_POINT('Ctrl Pts',(-15.6013423678816,-52.2018016959779,
2.47103306226067));
#61984=CARTESIAN_POINT('Ctrl Pts',(-15.8297478005623,-53.907232954514,2.54953857263746));
#61985=CARTESIAN_POINT('Ctrl Pts',(-14.5330963425821,-55.0385110233129,
2.62804408301423));
#61986=CARTESIAN_POINT('Ctrl Pts',(-12.8743150895914,-54.5809192738243,
2.70654959339101));
#61987=CARTESIAN_POINT('Ctrl Pts',(-12.3410089780029,-52.9449163922479,
2.7850551037678));
#61988=CARTESIAN_POINT('Ctrl Pts',(-13.4114743235374,-51.5976690199096,
2.86356061414457));
#61989=CARTESIAN_POINT('Ctrl Pts',(-15.125685020798,-51.7474403844543,2.94206612452135));
#61990=CARTESIAN_POINT('Ctrl Pts',(-15.9462998191018,-53.2599021194416,
3.02057163489813));
#61991=CARTESIAN_POINT('Ctrl Pts',(-15.1373700363305,-54.7786474915821,
3.09907714527491));
#61992=CARTESIAN_POINT('Ctrl Pts',(-13.4243640409752,-54.9416270991707,
3.17758265565169));
#61993=CARTESIAN_POINT('Ctrl Pts',(-12.3435458814549,-53.6026781745395,
3.25608816602847));
#61994=CARTESIAN_POINT('Ctrl Pts',(-12.8642192037885,-51.9626013374103,
3.33459367640525));
#61995=CARTESIAN_POINT('Ctrl Pts',(-14.5194316817766,-51.4922567887358,
3.41309918678203));
#61996=CARTESIAN_POINT('Ctrl Pts',(-15.824749470772,-52.6134605506407,3.49160469715881));
#61997=CARTESIAN_POINT('Ctrl Pts',(-15.6095325175198,-54.3206905095792,
3.57011020753559));
#61998=CARTESIAN_POINT('Ctrl Pts',(-14.0667925161087,-55.0828622138133,
3.64861571791237));
#61999=CARTESIAN_POINT('Ctrl Pts',(-12.5800953694062,-54.216441978079,3.72712122828915));
#62000=CARTESIAN_POINT('Ctrl Pts',(-12.482746426243,-52.4984560584276,3.80562673866593));
#62001=CARTESIAN_POINT('Ctrl Pts',(-13.8620505314459,-51.4696350750294,
3.88413224904271));
#62002=CARTESIAN_POINT('Ctrl Pts',(-15.4810149732843,-52.0526501422855,
3.96263775941948));
#62003=CARTESIAN_POINT('Ctrl Pts',(-15.8877139511439,-53.7246394886754,
4.04114326979627));
#62004=CARTESIAN_POINT('Ctrl Pts',(-14.7174101533174,-54.9861233184472,
4.11964878017304));
#62005=CARTESIAN_POINT('Ctrl Pts',(-13.0196598476917,-54.705772943414,4.19815429054983));
#62006=CARTESIAN_POINT('Ctrl Pts',(-12.3170458706651,-53.1350132444558,
4.2766598009266));
#62007=CARTESIAN_POINT('Ctrl Pts',(-13.239689139382,-51.6825388628568,4.35516531130339));
#62008=CARTESIAN_POINT('Ctrl Pts',(-14.9601412381249,-51.6509633535717,
4.43367082168016));
#62009=CARTESIAN_POINT('Ctrl Pts',(-15.9354598188275,-53.0686043860759,
4.51217633205695));
#62010=CARTESIAN_POINT('Ctrl Pts',(-15.2909560004752,-54.6640877757789,
4.59068184243372));
#62011=CARTESIAN_POINT('Ctrl Pts',(-13.6046361114517,-55.0065460966708,
4.6691873528105));
#62012=CARTESIAN_POINT('Ctrl Pts',(-12.3888319545389,-53.7888545684045,
4.74769286318728));
#62013=CARTESIAN_POINT('Ctrl Pts',(-12.7339055288242,-52.1030679359729,
4.82619837356406));
#62014=CARTESIAN_POINT('Ctrl Pts',(-14.3303867955418,-51.461039661442,4.90470388394084));
#62015=CARTESIAN_POINT('Ctrl Pts',(-15.7465131069793,-52.4385560995515,
4.98320939431762));
#62016=CARTESIAN_POINT('Ctrl Pts',(-15.7122693095411,-54.1589569990369,
5.0617149046944));
#62017=CARTESIAN_POINT('Ctrl Pts',(-14.2583648731494,-55.0793464756679,
5.14022041507118));
#62018=CARTESIAN_POINT('Ctrl Pts',(-12.6886982319545,-54.374296277089,5.21872592544796));
#62019=CARTESIAN_POINT('Ctrl Pts',(-12.4109789893208,-52.6761143673659,
5.29723143582474));
#62020=CARTESIAN_POINT('Ctrl Pts',(-13.6742819091468,-51.5077662723951,
5.37573694620152));
#62021=CARTESIAN_POINT('Ctrl Pts',(-15.3456277491901,-51.9170631330653,
5.4542424565783));
#62022=CARTESIAN_POINT('Ctrl Pts',(-15.9261522494264,-53.5369201511686,
5.53274796695508));
#62023=CARTESIAN_POINT('Ctrl Pts',(-14.895150144613,-54.9146464419454,5.61125347733186));
#62024=CARTESIAN_POINT('Ctrl Pts',(-13.1774033105245,-54.8145932898247,
5.68975898770864));
#62025=CARTESIAN_POINT('Ctrl Pts',(-12.3131175991141,-53.3266332457169,
5.76826449808541));
#62026=CARTESIAN_POINT('Ctrl Pts',(-13.07802768807,-51.78491829464,5.84677000846219));
#62027=CARTESIAN_POINT('Ctrl Pts',(-14.7848942477639,-51.572669265091,5.92527551883898));
#62028=CARTESIAN_POINT('Ctrl Pts',(-15.9054717137608,-52.8790772926886,
6.00378102921575));
#62029=CARTESIAN_POINT('Ctrl Pts',(-15.4296884573085,-54.5349259880616,
6.08228653959253));
#62030=CARTESIAN_POINT('Ctrl Pts',(-14.340318424872,-54.8774262527002,6.13462354651039));
#62031=CARTESIAN_POINT('Ctrl Pts',(-13.8417981729249,-54.7828888819299,
6.16079204996931));
#62032=CARTESIAN_POINT('Ctrl Pts',(-15.5298235927831,-52.8907830444123,
1.94640265001023));
#62033=CARTESIAN_POINT('Ctrl Pts',(-15.6535093143589,-53.3513412073422,
1.97257115346916));
#62034=CARTESIAN_POINT('Ctrl Pts',(-15.4091883934694,-54.3964004476471,
2.02490816038701));
#62035=CARTESIAN_POINT('Ctrl Pts',(-13.8908174408455,-54.9588407987496,
2.10341367076379));
#62036=CARTESIAN_POINT('Ctrl Pts',(-12.5875902013567,-54.0005833268291,
2.18191918114057));
#62037=CARTESIAN_POINT('Ctrl Pts',(-12.6663809901671,-52.3859752455852,
2.26042469151735));
#62038=CARTESIAN_POINT('Ctrl Pts',(-14.0574375563364,-51.5605987847522,
2.33893020189413));
#62039=CARTESIAN_POINT('Ctrl Pts',(-15.5127771133299,-52.2658828763921,
2.41743571227091));
#62040=CARTESIAN_POINT('Ctrl Pts',(-15.7274407199139,-53.8687082577405,
2.49594122264768));
#62041=CARTESIAN_POINT('Ctrl Pts',(-14.5088012366685,-54.9319239065435,
2.57444673302446));
#62042=CARTESIAN_POINT('Ctrl Pts',(-12.9498192014264,-54.5018627905033,
2.65295224340125));
#62043=CARTESIAN_POINT('Ctrl Pts',(-12.4485990159725,-52.9642886845846,
2.73145775377802));
#62044=CARTESIAN_POINT('Ctrl Pts',(-13.4546606892816,-51.6980973487976,
2.8099632641548));
#62045=CARTESIAN_POINT('Ctrl Pts',(-15.0657373016022,-51.8388578416582,
2.88846877453159));
#62046=CARTESIAN_POINT('Ctrl Pts',(-15.8369804815592,-53.2603235530564,
2.96697428490836));
#62047=CARTESIAN_POINT('Ctrl Pts',(-15.0767192977297,-54.6876948517164,
3.04547979528514));
#62048=CARTESIAN_POINT('Ctrl Pts',(-13.4667749074093,-54.8408689244782,
3.12398530566192));
#62049=CARTESIAN_POINT('Ctrl Pts',(-12.4509832887027,-53.5824767670773,
3.2024908160387));
#62050=CARTESIAN_POINT('Ctrl Pts',(-12.9403307263376,-52.0410738118106,
3.28099632641548));
#62051=CARTESIAN_POINT('Ctrl Pts',(-14.4959586990071,-51.5990271583197,
3.35950183679226));
#62052=CARTESIAN_POINT('Ctrl Pts',(-15.7227431105485,-52.6527746126658,
3.43800734716904));
#62053=CARTESIAN_POINT('Ctrl Pts',(-15.5204745093119,-54.2572904770775,
3.51651285754582));
#62054=CARTESIAN_POINT('Ctrl Pts',(-14.0705521986317,-54.9736067439322,
3.5950183679226));
#62055=CARTESIAN_POINT('Ctrl Pts',(-12.6733009701311,-54.1593139732339,
3.67352387829938));
#62056=CARTESIAN_POINT('Ctrl Pts',(-12.5818089465339,-52.5446892716908,
3.75202938867616));
#62057=CARTESIAN_POINT('Ctrl Pts',(-13.8781283480645,-51.5777664615214,
3.83053489905294));
#62058=CARTESIAN_POINT('Ctrl Pts',(-15.3996891180402,-52.1257049039707,
3.90904040942972));
#62059=CARTESIAN_POINT('Ctrl Pts',(-15.781919384443,-53.6971003784726,3.9875459198065));
#62060=CARTESIAN_POINT('Ctrl Pts',(-14.682025957689,-54.8826880651052,4.06605143018327));
#62061=CARTESIAN_POINT('Ctrl Pts',(-13.0864194109997,-54.6192047411514,
4.14455694056006));
#62062=CARTESIAN_POINT('Ctrl Pts',(-12.4260776293937,-53.1429485151161,
4.22306245093684));
#62063=CARTESIAN_POINT('Ctrl Pts',(-13.2932108202671,-51.7778610670395,
4.30156796131361));
#62064=CARTESIAN_POINT('Ctrl Pts',(-14.9101533252533,-51.7481852724522,
4.38007347169039));
#62065=CARTESIAN_POINT('Ctrl Pts',(-15.8267926610378,-53.0805350913999,
4.45857898206717));
#62066=CARTESIAN_POINT('Ctrl Pts',(-15.2210648879245,-54.5800275275424,
4.53708449244395));
#62067=CARTESIAN_POINT('Ctrl Pts',(-13.6362010561689,-54.901882123576,4.61559000282073));
#62068=CARTESIAN_POINT('Ctrl Pts',(-12.4935447622286,-53.7574520104367,
4.69409551319751));
#62069=CARTESIAN_POINT('Ctrl Pts',(-12.8178572670739,-52.173089352326,4.77260102357429));
#62070=CARTESIAN_POINT('Ctrl Pts',(-14.3182875437761,-51.5696881839643,
4.85110653395107));
#62071=CARTESIAN_POINT('Ctrl Pts',(-15.6492137736117,-52.488393144862,4.92961204432785));
#62072=CARTESIAN_POINT('Ctrl Pts',(-15.6170302262462,-54.1052875309521,
5.00811755470463));
#62073=CARTESIAN_POINT('Ctrl Pts',(-14.2505987614542,-54.9703025272976,
5.08662306508141));
#62074=CARTESIAN_POINT('Ctrl Pts',(-12.7753698302556,-54.307671097417,5.16512857545819));
#62075=CARTESIAN_POINT('Ctrl Pts',(-12.5143593387719,-52.7116589137378,
5.24363408583497));
#62076=CARTESIAN_POINT('Ctrl Pts',(-13.7016566713931,-51.6136035265765,
5.32213959621175));
#62077=CARTESIAN_POINT('Ctrl Pts',(-15.2724473555814,-51.9982753762946,
5.40064510658853));
#62078=CARTESIAN_POINT('Ctrl Pts',(-15.8180450739392,-53.5206750214142,
5.4791506169653));
#62079=CARTESIAN_POINT('Ctrl Pts',(-14.8490723677412,-54.8155115364335,
5.55765612734209));
#62080=CARTESIAN_POINT('Ctrl Pts',(-13.2346723673735,-54.7214780003996,
5.63616163771886));
#62081=CARTESIAN_POINT('Ctrl Pts',(-12.4223856990886,-53.3230398556834,
5.71466714809565));
#62082=CARTESIAN_POINT('Ctrl Pts',(-13.1412755979873,-51.8740809240222,
5.79317265847242));
#62083=CARTESIAN_POINT('Ctrl Pts',(-14.745449926773,-51.674601683786,5.87167816884921));
#62084=CARTESIAN_POINT('Ctrl Pts',(-15.7986087657921,-52.9024107406155,
5.95018367922598));
#62085=CARTESIAN_POINT('Ctrl Pts',(-15.3514506199299,-54.4586366531711,
6.02868918960277));
#62086=CARTESIAN_POINT('Ctrl Pts',(-14.3276216447485,-54.7805306694404,
6.08102619652062));
#62087=CARTESIAN_POINT('Ctrl Pts',(-13.8590944561341,-54.691681062282,6.10719469997954));
#62088=CARTESIAN_POINT('Ctrl Pts',(-15.4401670971033,-52.9148608466415,
1.89280530002046));
#62089=CARTESIAN_POINT('Ctrl Pts',(-15.5559349992425,-53.3459360884415,
1.91897380347939));
#62090=CARTESIAN_POINT('Ctrl Pts',(-15.3272544361205,-54.3240952026862,
1.97131081039724));
#62091=CARTESIAN_POINT('Ctrl Pts',(-13.9060829571907,-54.8505305801576,
2.04981632077402));
#62092=CARTESIAN_POINT('Ctrl Pts',(-12.6862826309757,-53.9536165643755,
2.1283218311508));
#62093=CARTESIAN_POINT('Ctrl Pts',(-12.7600295777717,-52.4423686372808,
2.20682734152758));
#62094=CARTESIAN_POINT('Ctrl Pts',(-14.0620367809532,-51.6698291708949,
2.28533285190436));
#62095=CARTESIAN_POINT('Ctrl Pts',(-15.4242118587782,-52.3299640568063,
2.36383836228114));
#62096=CARTESIAN_POINT('Ctrl Pts',(-15.6251336392654,-53.8301835609669,
2.44234387265791));
#62097=CARTESIAN_POINT('Ctrl Pts',(-14.4845061307549,-54.8253367897741,
2.52084938303469));
#62098=CARTESIAN_POINT('Ctrl Pts',(-13.0253233132613,-54.4228063071824,
2.59935489341147));
#62099=CARTESIAN_POINT('Ctrl Pts',(-12.5561890539421,-52.9836609769212,
2.67786040378825));
#62100=CARTESIAN_POINT('Ctrl Pts',(-13.4978470550258,-51.7985256776856,
2.75636591416503));
#62101=CARTESIAN_POINT('Ctrl Pts',(-15.0057895824065,-51.9302752988621,
2.83487142454181));
#62102=CARTESIAN_POINT('Ctrl Pts',(-15.7276611440166,-53.2607449866711,
2.91337693491859));
#62103=CARTESIAN_POINT('Ctrl Pts',(-15.016068559129,-54.5967422118507,2.99188244529537));
#62104=CARTESIAN_POINT('Ctrl Pts',(-13.5091857738434,-54.7401107497856,
3.07038795567215));
#62105=CARTESIAN_POINT('Ctrl Pts',(-12.5584206959504,-53.5622753596153,
3.14889346604893));
#62106=CARTESIAN_POINT('Ctrl Pts',(-13.0164422488867,-52.1195462862107,
3.22739897642571));
#62107=CARTESIAN_POINT('Ctrl Pts',(-14.4724857162377,-51.7057975279038,
3.30590448680249));
#62108=CARTESIAN_POINT('Ctrl Pts',(-15.6207367503249,-52.6920886746908,
3.38440999717927));
#62109=CARTESIAN_POINT('Ctrl Pts',(-15.4314165011041,-54.1938904445758,
3.46291550755605));
#62110=CARTESIAN_POINT('Ctrl Pts',(-14.0743118811546,-54.864351274051,3.54142101793283));
#62111=CARTESIAN_POINT('Ctrl Pts',(-12.766506570856,-54.1021859683889,3.61992652830961));
#62112=CARTESIAN_POINT('Ctrl Pts',(-12.6808714668247,-52.5909224849539,
3.69843203868639));
#62113=CARTESIAN_POINT('Ctrl Pts',(-13.894206164683,-51.6858978480135,3.77693754906317));
#62114=CARTESIAN_POINT('Ctrl Pts',(-15.3183632627962,-52.1987596656559,
3.85544305943995));
#62115=CARTESIAN_POINT('Ctrl Pts',(-15.6761248177421,-53.6695612682698,
3.93394856981672));
#62116=CARTESIAN_POINT('Ctrl Pts',(-14.6466417620606,-54.7792528117632,
4.01245408019351));
#62117=CARTESIAN_POINT('Ctrl Pts',(-13.1531789743077,-54.5326365388889,
4.09095959057028));
#62118=CARTESIAN_POINT('Ctrl Pts',(-12.5351093881223,-53.1508837857763,
4.16946510094707));
#62119=CARTESIAN_POINT('Ctrl Pts',(-13.3467325011522,-51.8731832712222,
4.24797061132384));
#62120=CARTESIAN_POINT('Ctrl Pts',(-14.8601654123817,-51.8454071913326,
4.32647612170063));
#62121=CARTESIAN_POINT('Ctrl Pts',(-15.7181255032481,-53.092465796724,4.4049816320774));
#62122=CARTESIAN_POINT('Ctrl Pts',(-15.1511737753737,-54.4959672793058,
4.48348714245419));
#62123=CARTESIAN_POINT('Ctrl Pts',(-13.6677660008861,-54.7972181504813,
4.56199265283096));
#62124=CARTESIAN_POINT('Ctrl Pts',(-12.5982575699184,-53.7260494524687,
4.64049816320774));
#62125=CARTESIAN_POINT('Ctrl Pts',(-12.9018090053235,-52.2431107686793,
4.71900367358452));
#62126=CARTESIAN_POINT('Ctrl Pts',(-14.3061882920105,-51.6783367064866,
4.7975091839613));
#62127=CARTESIAN_POINT('Ctrl Pts',(-15.5519144402441,-52.5382301901725,
4.87601469433808));
#62128=CARTESIAN_POINT('Ctrl Pts',(-15.5217911429513,-54.0516180628673,
4.95452020471486));
#62129=CARTESIAN_POINT('Ctrl Pts',(-14.242832649759,-54.8612585789273,5.03302571509164));
#62130=CARTESIAN_POINT('Ctrl Pts',(-12.8620414285567,-54.2410459177449,
5.11153122546842));
#62131=CARTESIAN_POINT('Ctrl Pts',(-12.617739688223,-52.7472034601099,5.1900367358452));
#62132=CARTESIAN_POINT('Ctrl Pts',(-13.7290314336393,-51.7194407807578,
5.26854224622197));
#62133=CARTESIAN_POINT('Ctrl Pts',(-15.1992669619728,-52.079487619524,5.34704775659876));
#62134=CARTESIAN_POINT('Ctrl Pts',(-15.709937898452,-53.5044298916598,5.42555326697553));
#62135=CARTESIAN_POINT('Ctrl Pts',(-14.8029945908694,-54.7163766309217,
5.50405877735232));
#62136=CARTESIAN_POINT('Ctrl Pts',(-13.2919414242225,-54.6283627109744,
5.58256428772909));
#62137=CARTESIAN_POINT('Ctrl Pts',(-12.5316537990631,-53.31944646565,5.66106979810588));
#62138=CARTESIAN_POINT('Ctrl Pts',(-13.2045235079047,-51.9632435534043,
5.73957530848265));
#62139=CARTESIAN_POINT('Ctrl Pts',(-14.706005605782,-51.7765341024811,5.81808081885944));
#62140=CARTESIAN_POINT('Ctrl Pts',(-15.6917458178233,-52.9257441885424,
5.89658632923621));
#62141=CARTESIAN_POINT('Ctrl Pts',(-15.2732127825514,-54.3823473182807,
5.975091839613));
#62142=CARTESIAN_POINT('Ctrl Pts',(-14.314924864625,-54.6836350861806,6.02742884653085));
#62143=CARTESIAN_POINT('Ctrl Pts',(-13.8763907393433,-54.6004732426341,
6.05359734998977));
#62144=CARTESIAN_POINT('Ctrl Pts',(-15.3505106014235,-52.9389386488708,
1.83920795003069));
#62145=CARTESIAN_POINT('Ctrl Pts',(-15.4583606841261,-53.3405309695408,
1.86537645348962));
#62146=CARTESIAN_POINT('Ctrl Pts',(-15.2453204787717,-54.2517899577253,
1.91771346040747));
#62147=CARTESIAN_POINT('Ctrl Pts',(-13.9213484735358,-54.7422203615657,
1.99621897078425));
#62148=CARTESIAN_POINT('Ctrl Pts',(-12.7849750605946,-53.9066498019218,
2.07472448116103));
#62149=CARTESIAN_POINT('Ctrl Pts',(-12.8536781653762,-52.4987620289764,
2.15322999153781));
#62150=CARTESIAN_POINT('Ctrl Pts',(-14.06663600557,-51.7790595570376,2.23173550191459));
#62151=CARTESIAN_POINT('Ctrl Pts',(-15.3356466042264,-52.3940452372206,
2.31024101229137));
#62152=CARTESIAN_POINT('Ctrl Pts',(-15.522826558617,-53.7916588641933,2.38874652266814));
#62153=CARTESIAN_POINT('Ctrl Pts',(-14.4602110248413,-54.7187496730048,
2.46725203304492));
#62154=CARTESIAN_POINT('Ctrl Pts',(-13.1008274250962,-54.3437498238614,
2.5457575434217));
#62155=CARTESIAN_POINT('Ctrl Pts',(-12.6637790919117,-53.0030332692578,
2.62426305379848));
#62156=CARTESIAN_POINT('Ctrl Pts',(-13.54103342077,-51.8989540065736,2.70276856417526));
#62157=CARTESIAN_POINT('Ctrl Pts',(-14.9458418632107,-52.0216927560659,
2.78127407455204));
#62158=CARTESIAN_POINT('Ctrl Pts',(-15.618341806474,-53.2611664202859,2.85977958492882));
#62159=CARTESIAN_POINT('Ctrl Pts',(-14.9554178205282,-54.505789571985,2.9382850953056));
#62160=CARTESIAN_POINT('Ctrl Pts',(-13.5515966402775,-54.6393525750931,
3.01679060568238));
#62161=CARTESIAN_POINT('Ctrl Pts',(-12.6658581031982,-53.5420739521532,
3.09529611605916));
#62162=CARTESIAN_POINT('Ctrl Pts',(-13.0925537714359,-52.198018760611,3.17380162643594));
#62163=CARTESIAN_POINT('Ctrl Pts',(-14.4490127334682,-51.8125678974878,
3.25230713681272));
#62164=CARTESIAN_POINT('Ctrl Pts',(-15.5187303901013,-52.7314027367159,
3.3308126471895));
#62165=CARTESIAN_POINT('Ctrl Pts',(-15.3423584928962,-54.130490412074,3.40931815756628));
#62166=CARTESIAN_POINT('Ctrl Pts',(-14.0780715636776,-54.75509580417,3.48782366794306));
#62167=CARTESIAN_POINT('Ctrl Pts',(-12.8597121715808,-54.0450579635438,
3.56632917831983));
#62168=CARTESIAN_POINT('Ctrl Pts',(-12.7799339871156,-52.6371556982172,
3.64483468869662));
#62169=CARTESIAN_POINT('Ctrl Pts',(-13.9102839813016,-51.7940292345055,
3.7233401990734));
#62170=CARTESIAN_POINT('Ctrl Pts',(-15.2370374075522,-52.2718144273412,
3.80184570945018));
#62171=CARTESIAN_POINT('Ctrl Pts',(-15.5703302510412,-53.642022158067,3.88035121982695));
#62172=CARTESIAN_POINT('Ctrl Pts',(-14.6112575664322,-54.6758175584211,
3.95885673020374));
#62173=CARTESIAN_POINT('Ctrl Pts',(-13.2199385376158,-54.4460683366263,
4.03736224058051));
#62174=CARTESIAN_POINT('Ctrl Pts',(-12.644141146851,-53.1588190564366,4.1158677509573));
#62175=CARTESIAN_POINT('Ctrl Pts',(-13.4002541820374,-51.9685054754049,
4.19437326133407));
#62176=CARTESIAN_POINT('Ctrl Pts',(-14.8101774995101,-51.9426291102131,
4.27287877171085));
#62177=CARTESIAN_POINT('Ctrl Pts',(-15.6094583454585,-53.1043965020481,
4.35138428208763));
#62178=CARTESIAN_POINT('Ctrl Pts',(-15.081282662823,-54.4119070310692,4.42988979246441));
#62179=CARTESIAN_POINT('Ctrl Pts',(-13.6993309456032,-54.6925541773866,
4.50839530284119));
#62180=CARTESIAN_POINT('Ctrl Pts',(-12.7029703776082,-53.6946468945009,
4.58690081321797));
#62181=CARTESIAN_POINT('Ctrl Pts',(-12.9857607435731,-52.3131321850324,
4.66540632359475));
#62182=CARTESIAN_POINT('Ctrl Pts',(-14.2940890402448,-51.7869852290089,
4.74391183397153));
#62183=CARTESIAN_POINT('Ctrl Pts',(-15.4546151068764,-52.5880672354829,
4.82241734434831));
#62184=CARTESIAN_POINT('Ctrl Pts',(-15.4265520596564,-53.9979485947826,
4.90092285472509));
#62185=CARTESIAN_POINT('Ctrl Pts',(-14.2350665380638,-54.7522146305569,
4.97942836510187));
#62186=CARTESIAN_POINT('Ctrl Pts',(-12.9487130268578,-54.1744207380729,
5.05793387547865));
#62187=CARTESIAN_POINT('Ctrl Pts',(-12.7211200376741,-52.7827480064818,
5.13643938585543));
#62188=CARTESIAN_POINT('Ctrl Pts',(-13.7564061958854,-51.8252780349391,
5.2149448962322));
#62189=CARTESIAN_POINT('Ctrl Pts',(-15.1260865683642,-52.1606998627533,
5.29345040660899));
#62190=CARTESIAN_POINT('Ctrl Pts',(-15.6018307229648,-53.4881847619054,
5.37195591698576));
#62191=CARTESIAN_POINT('Ctrl Pts',(-14.7569168139975,-54.6172417254097,
5.45046142736255));
#62192=CARTESIAN_POINT('Ctrl Pts',(-13.3492104810715,-54.5352474215493,
5.52896693773932));
#62193=CARTESIAN_POINT('Ctrl Pts',(-12.6409218990375,-53.3158530756166,
5.60747244811611));
#62194=CARTESIAN_POINT('Ctrl Pts',(-13.2677714178221,-52.0524061827865,
5.68597795849288));
#62195=CARTESIAN_POINT('Ctrl Pts',(-14.666561284791,-51.8784665211762,5.76448346886966));
#62196=CARTESIAN_POINT('Ctrl Pts',(-15.5848828698546,-52.9490776364693,
5.84298897924644));
#62197=CARTESIAN_POINT('Ctrl Pts',(-15.1949749451728,-54.3060579833903,
5.92149448962322));
#62198=CARTESIAN_POINT('Ctrl Pts',(-14.3022280845015,-54.5867395029208,
5.97383149654108));
#62199=CARTESIAN_POINT('Ctrl Pts',(-13.8936870225526,-54.5092654229862,
6.));
#62200=CARTESIAN_POINT('Ctrl Pts',(-14.7602610286104,-54.3618122024717,
2.44341967361942));
#62201=CARTESIAN_POINT('Ctrl Pts',(-14.651278048058,-54.4258677305587,2.45136379342793));
#62202=CARTESIAN_POINT('Ctrl Pts',(-14.5332929975391,-54.473801003601,2.45930791323643));
#62203=CARTESIAN_POINT('Ctrl Pts',(-14.4107496805131,-54.5017345633457,
2.46725203304493));
#62204=CARTESIAN_POINT('Ctrl Pts',(-14.0070831582596,-54.5937497232903,
2.49342053650386));
#62205=CARTESIAN_POINT('Ctrl Pts',(-13.5539552916779,-54.4687497735759,
2.51958903996278));
#62206=CARTESIAN_POINT('Ctrl Pts',(-13.254549969523,-54.1827970396181,2.54575754342171));
#62207=CARTESIAN_POINT('Ctrl Pts',(-12.955144647368,-53.8968443056602,2.57192604688064));
#62208=CARTESIAN_POINT('Ctrl Pts',(-12.8094618696399,-53.449938787459,2.59809455033956));
#62209=CARTESIAN_POINT('Ctrl Pts',(-12.8828295355855,-53.042472817911,2.62426305379849));
#62210=CARTESIAN_POINT('Ctrl Pts',(-12.9561972015311,-52.6350068483631,
2.65043155725742));
#62211=CARTESIAN_POINT('Ctrl Pts',(-13.2486153111506,-52.2669804274683,
2.67660006071634));
#62212=CARTESIAN_POINT('Ctrl Pts',(-13.6289591063671,-52.1034236752697,
2.70276856417527));
#62213=CARTESIAN_POINT('Ctrl Pts',(-14.0093029015836,-51.939866923071,2.7289370676342));
#62214=CARTESIAN_POINT('Ctrl Pts',(-14.4775723823971,-51.9807798395685,
2.75510557109312));
#62215=CARTESIAN_POINT('Ctrl Pts',(-14.8237904466811,-52.2078152418539,
2.78127407455205));
#62216=CARTESIAN_POINT('Ctrl Pts',(-15.1700085109651,-52.4348506441393,
2.80744257801098));
#62217=CARTESIAN_POINT('Ctrl Pts',(-15.3941751587196,-52.8480085322126,
2.8336110814699));
#62218=CARTESIAN_POINT('Ctrl Pts',(-15.3957711516058,-53.2620246681991,
2.85977958492883));
#62219=CARTESIAN_POINT('Ctrl Pts',(-15.397367144492,-53.6760408041856,2.88594808838776));
#62220=CARTESIAN_POINT('Ctrl Pts',(-15.1763924825101,-54.0909151880853,
2.91211659184668));
#62221=CARTESIAN_POINT('Ctrl Pts',(-14.8319349548107,-54.3206128805532,
2.93828509530561));
#62222=CARTESIAN_POINT('Ctrl Pts',(-14.8094060374995,-54.3356360398807,
2.93999662141021));
#62223=CARTESIAN_POINT('Ctrl Pts',(-14.7863488988009,-54.3498670707759,
2.94170814751482));
#62224=CARTESIAN_POINT('Ctrl Pts',(-14.7628222445742,-54.3633003878638,
2.94341967361942));
#62225=CARTESIAN_POINT('Ctrl Pts',(-15.6194800884629,-52.866705242183,2.));
#62226=CARTESIAN_POINT('Ctrl Pts',(-15.6300231873965,-52.926941249885,2.));
#62227=CARTESIAN_POINT('Ctrl Pts',(-15.6366567833015,-52.987630087735,2.));
#62228=CARTESIAN_POINT('Ctrl Pts',(-15.6395415323775,-53.0484503647743,
2.));
#62229=CARTESIAN_POINT('Ctrl Pts',(-15.6424094897195,-53.1089166152119,
2.));
#62230=CARTESIAN_POINT('Ctrl Pts',(-15.6415715704011,-53.1695138895016,
2.));
#62231=CARTESIAN_POINT('Ctrl Pts',(-15.6371309452724,-53.2299210873137,
2.));
#62232=CARTESIAN_POINT('Ctrl Pts',(-15.6337777267599,-53.275535956418,2.));
#62233=CARTESIAN_POINT('Ctrl Pts',(-15.628369049543,-53.3210424392735,2.));
#62234=CARTESIAN_POINT('Ctrl Pts',(-15.6209312260544,-53.3662945441232,
2.));
#62235=CARTESIAN_POINT('Ctrl Pts',(-15.6170700144012,-53.3897863565925,
2.));
#62236=CARTESIAN_POINT('Ctrl Pts',(-15.6126617095028,-53.4132094747526,
2.));
#62237=CARTESIAN_POINT('Ctrl Pts',(-15.6077085063714,-53.4365423663737,
2.));
#62238=CARTESIAN_POINT('Ctrl Pts',(-15.6050999838096,-53.4488302480955,
2.));
#62239=CARTESIAN_POINT('Ctrl Pts',(-15.6023397247485,-53.4610950217813,
2.));
#62240=CARTESIAN_POINT('Ctrl Pts',(-15.5994335441816,-53.4733116340984,
2.));
#62241=CARTESIAN_POINT('Ctrl Pts',(-15.5857322512136,-53.5309072929295,
2.));
#62242=CARTESIAN_POINT('Ctrl Pts',(-15.5687698297262,-53.5875426491389,
2.));
#62243=CARTESIAN_POINT('Ctrl Pts',(-15.5486498653488,-53.6429179274305,
2.));
#62244=CARTESIAN_POINT('Ctrl Pts',(-15.5289409667849,-53.6971618476645,
2.));
#62245=CARTESIAN_POINT('Ctrl Pts',(-15.5062016386593,-53.750197506391,2.));
#62246=CARTESIAN_POINT('Ctrl Pts',(-15.4804878124321,-53.8017173359829,
2.));
#62247=CARTESIAN_POINT('Ctrl Pts',(-15.4618733917502,-53.8390129050285,
2.));
#62248=CARTESIAN_POINT('Ctrl Pts',(-15.4416993411965,-53.8755136264382,
2.));
#62249=CARTESIAN_POINT('Ctrl Pts',(-15.4199753876582,-53.9110903776553,
2.));
#62250=CARTESIAN_POINT('Ctrl Pts',(-15.4086212485557,-53.9296847546606,
2.));
#62251=CARTESIAN_POINT('Ctrl Pts',(-15.3968435749602,-53.9480265376898,
2.));
#62252=CARTESIAN_POINT('Ctrl Pts',(-15.3846428359465,-53.9660958743658,
2.));
#62253=CARTESIAN_POINT('Ctrl Pts',(-15.3789686731663,-53.9744993290676,
2.));
#62254=CARTESIAN_POINT('Ctrl Pts',(-15.373205772762,-53.9828396301787,2.));
#62255=CARTESIAN_POINT('Ctrl Pts',(-15.3673591188136,-53.9911085225216,
2.));
#62256=CARTESIAN_POINT('Ctrl Pts',(-15.3351612285807,-54.0366458316147,
2.));
#62257=CARTESIAN_POINT('Ctrl Pts',(-15.3003846168084,-54.0800821194251,
2.));
#62258=CARTESIAN_POINT('Ctrl Pts',(-15.2630875306082,-54.1211378587395,
2.));
#62259=CARTESIAN_POINT('Ctrl Pts',(-15.2381315874427,-54.1486087633418,
2.));
#62260=CARTESIAN_POINT('Ctrl Pts',(-15.212046413087,-54.1750132365444,2.));
#62261=CARTESIAN_POINT('Ctrl Pts',(-15.1848412564379,-54.2002572946035,
2.));
#62262=CARTESIAN_POINT('Ctrl Pts',(-15.1445758545731,-54.2376201429619,
2.));
#62263=CARTESIAN_POINT('Ctrl Pts',(-15.1018570560095,-54.2724429083026,
2.));
#62264=CARTESIAN_POINT('Ctrl Pts',(-15.0569812349608,-54.3046174971127,
2.));
#62265=CARTESIAN_POINT('Ctrl Pts',(-15.0431218621615,-54.3145542427936,
2.));
#62266=CARTESIAN_POINT('Ctrl Pts',(-15.0290566706306,-54.3242380855765,
2.));
#62267=CARTESIAN_POINT('Ctrl Pts',(-15.0147942526821,-54.3336649770066,
2.));
#62268=CARTESIAN_POINT('Ctrl Pts',(-15.0022772711832,-54.3419382043128,
2.));
#62269=CARTESIAN_POINT('Ctrl Pts',(-14.9896026925897,-54.3500168035422,
2.));
#62270=CARTESIAN_POINT('Ctrl Pts',(-14.9768072444657,-54.357879401603,2.));
#62271=CARTESIAN_POINT('Ctrl Pts',(-14.9293632591267,-54.3870329711781,
2.));
#62272=CARTESIAN_POINT('Ctrl Pts',(-14.8801986447078,-54.4132643407243,
2.));
#62273=CARTESIAN_POINT('Ctrl Pts',(-14.8296406252006,-54.4365044915624,
2.));
#62274=CARTESIAN_POINT('Ctrl Pts',(-14.779143507916,-54.4597166472999,2.));
#62275=CARTESIAN_POINT('Ctrl Pts',(-14.7272551246641,-54.4799449627967,
2.));
#62276=CARTESIAN_POINT('Ctrl Pts',(-14.6742902116631,-54.497070407063,2.));
#62277=CARTESIAN_POINT('Ctrl Pts',(-14.640435964457,-54.5080166918931,2.));
#62278=CARTESIAN_POINT('Ctrl Pts',(-14.6061417257406,-54.5176942656991,
2.));
#62279=CARTESIAN_POINT('Ctrl Pts',(-14.571490685658,-54.5260607579898,2.));
#62280=CARTESIAN_POINT('Ctrl Pts',(-14.5536361910117,-54.5303717250331,
2.));
#62281=CARTESIAN_POINT('Ctrl Pts',(-14.5356869955265,-54.5343344557627,
2.));
#62282=CARTESIAN_POINT('Ctrl Pts',(-14.5176547593652,-54.5379422095234,
2.));
#62283=CARTESIAN_POINT('Ctrl Pts',(-14.5067786943522,-54.540118210553,2.));
#62284=CARTESIAN_POINT('Ctrl Pts',(-14.4958730433407,-54.5421648311715,
2.));
#62285=CARTESIAN_POINT('Ctrl Pts',(-14.484953604442,-54.5440785381673,2.));
#62286=CARTESIAN_POINT('Ctrl Pts',(-14.432148545692,-54.5533329889941,2.));
#62287=CARTESIAN_POINT('Ctrl Pts',(-14.3789399495426,-54.5594997842154,
2.));
#62288=CARTESIAN_POINT('Ctrl Pts',(-14.3256201372965,-54.5624573557298,
2.));
#62289=CARTESIAN_POINT('Ctrl Pts',(-14.2921372782686,-54.5643146006433,
2.));
#62290=CARTESIAN_POINT('Ctrl Pts',(-14.2586106299683,-54.564905353366,2.));
#62291=CARTESIAN_POINT('Ctrl Pts',(-14.2251154868282,-54.5641893509547,
2.));
#62292=CARTESIAN_POINT('Ctrl Pts',(-14.2128693182197,-54.5639275731138,
2.));
#62293=CARTESIAN_POINT('Ctrl Pts',(-14.2006248767607,-54.5634909095273,
2.));
#62294=CARTESIAN_POINT('Ctrl Pts',(-14.1883942976858,-54.562877565248,2.));
#62295=CARTESIAN_POINT('Ctrl Pts',(-14.1370506806676,-54.5603027637126,
2.));
#62296=CARTESIAN_POINT('Ctrl Pts',(-14.0860310638802,-54.5546235246412,
2.));
#62297=CARTESIAN_POINT('Ctrl Pts',(-14.0356066350433,-54.5457116916821,
2.));
#62298=CARTESIAN_POINT('Ctrl Pts',(-14.0074349170479,-54.5407327231398,
2.));
#62299=CARTESIAN_POINT('Ctrl Pts',(-13.9794492438898,-54.5347439009261,
2.));
#62300=CARTESIAN_POINT('Ctrl Pts',(-13.9516999296066,-54.5277163783411,
2.));
#62301=CARTESIAN_POINT('Ctrl Pts',(-13.932212693117,-54.5227812295604,2.));
#62302=CARTESIAN_POINT('Ctrl Pts',(-13.9128420740716,-54.517333696643,2.));
#62303=CARTESIAN_POINT('Ctrl Pts',(-13.8936031194075,-54.5113848919291,
2.));
#62304=CARTESIAN_POINT('Origin',(-14.1292828945604,-53.2669068454841,4.5));
#62305=CARTESIAN_POINT('Origin',(-53.1951359564886,-14.3971354987959,6.));
#62306=CARTESIAN_POINT('Ctrl Pts',(-54.153252109211,-15.2223467977324,6.));
#62307=CARTESIAN_POINT('Ctrl Pts',(-54.1904452248526,-15.1876133706859,
6.));
#62308=CARTESIAN_POINT('Ctrl Pts',(-54.2252563920676,-15.1505690966151,
6.));
#62309=CARTESIAN_POINT('Ctrl Pts',(-54.2576712403365,-15.1115269977936,
6.));
#62310=CARTESIAN_POINT('Ctrl Pts',(-54.2795176350154,-15.0852140842524,
6.));
#62311=CARTESIAN_POINT('Ctrl Pts',(-54.3002751129523,-15.0579926438535,
6.));
#62312=CARTESIAN_POINT('Ctrl Pts',(-54.3199324346161,-15.0299477424349,
6.));
#62313=CARTESIAN_POINT('Ctrl Pts',(-54.3290141536918,-15.0169909459524,
6.));
#62314=CARTESIAN_POINT('Ctrl Pts',(-54.337860965377,-15.0038582766482,6.));
#62315=CARTESIAN_POINT('Ctrl Pts',(-54.3464713059304,-14.9905576084913,
6.));
#62316=CARTESIAN_POINT('Ctrl Pts',(-54.3536893846595,-14.9794076116576,
6.));
#62317=CARTESIAN_POINT('Ctrl Pts',(-54.360737149428,-14.9681457923566,6.));
#62318=CARTESIAN_POINT('Ctrl Pts',(-54.3676105396868,-14.9567832871792,
6.));
#62319=CARTESIAN_POINT('Ctrl Pts',(-54.3954330978975,-14.9107893962733,
6.));
#62320=CARTESIAN_POINT('Ctrl Pts',(-54.4204206822397,-14.8631190273978,
6.));
#62321=CARTESIAN_POINT('Ctrl Pts',(-54.4425345345564,-14.8140965424809,
6.));
#62322=CARTESIAN_POINT('Ctrl Pts',(-54.4509995916475,-14.7953310136339,
6.));
#62323=CARTESIAN_POINT('Ctrl Pts',(-54.4590431897372,-14.7763669364333,
6.));
#62324=CARTESIAN_POINT('Ctrl Pts',(-54.466661705721,-14.757221110189,6.));
#62325=CARTESIAN_POINT('Ctrl Pts',(-54.4721419467216,-14.7434489080701,
6.));
#62326=CARTESIAN_POINT('Ctrl Pts',(-54.4774022168759,-14.7295826467956,
6.));
#62327=CARTESIAN_POINT('Ctrl Pts',(-54.4824408848208,-14.7156283850094,
6.));
#62328=CARTESIAN_POINT('Ctrl Pts',(-54.4863313549552,-14.7048539820679,
6.));
#62329=CARTESIAN_POINT('Ctrl Pts',(-54.4900897012811,-14.6940267512127,
6.));
#62330=CARTESIAN_POINT('Ctrl Pts',(-54.4937105016092,-14.6831642693933,
6.));
#62331=CARTESIAN_POINT('Ctrl Pts',(-54.5116283442986,-14.6294103413058,
6.));
#62332=CARTESIAN_POINT('Ctrl Pts',(-54.5262131829608,-14.574710406265,6.));
#62333=CARTESIAN_POINT('Ctrl Pts',(-54.5374265846656,-14.5194236085091,
6.));
#62334=CARTESIAN_POINT('Ctrl Pts',(-54.5484779141294,-14.464935895228,6.));
#62335=CARTESIAN_POINT('Ctrl Pts',(-54.5562549501662,-14.4098769850162,
6.));
#62336=CARTESIAN_POINT('Ctrl Pts',(-54.5606770668673,-14.3545607001907,
6.));
#62337=CARTESIAN_POINT('Ctrl Pts',(-54.5629861190299,-14.3256767525837,
6.));
#62338=CARTESIAN_POINT('Ctrl Pts',(-54.5643796851133,-14.2967222396842,
6.));
#62339=CARTESIAN_POINT('Ctrl Pts',(-54.5648408789288,-14.2677401408304,
6.));
#62340=CARTESIAN_POINT('Ctrl Pts',(-54.565088353036,-14.2521885033312,6.));
#62341=CARTESIAN_POINT('Ctrl Pts',(-54.5650672991614,-14.2366289098601,
6.));
#62342=CARTESIAN_POINT('Ctrl Pts',(-54.564774627536,-14.2210679501474,6.));
#62343=CARTESIAN_POINT('Ctrl Pts',(-54.5645665072061,-14.2100024699717,
6.));
#62344=CARTESIAN_POINT('Ctrl Pts',(-54.5642210307075,-14.1989362982813,
6.));
#62345=CARTESIAN_POINT('Ctrl Pts',(-54.5637369787213,-14.1878718044098,
6.));
#62346=CARTESIAN_POINT('Ctrl Pts',(-54.5633114560902,-14.1781451785949,
6.));
#62347=CARTESIAN_POINT('Ctrl Pts',(-54.5627792671646,-14.1684296794191,
6.));
#62348=CARTESIAN_POINT('Ctrl Pts',(-54.5621402322801,-14.1587275142813,
6.));
#62349=CARTESIAN_POINT('Ctrl Pts',(-54.5589760897247,-14.1106878307941,
6.));
#62350=CARTESIAN_POINT('Ctrl Pts',(-54.553194193763,-14.0629716935933,6.));
#62351=CARTESIAN_POINT('Ctrl Pts',(-54.5447557136211,-14.0157777529758,
6.));
#62352=CARTESIAN_POINT('Ctrl Pts',(-54.5351507946184,-13.9620602624519,
6.));
#62353=CARTESIAN_POINT('Ctrl Pts',(-54.5221058408493,-13.9090185683991,
6.));
#62354=CARTESIAN_POINT('Ctrl Pts',(-54.5058712195205,-13.8568507922243,
6.));
#62355=CARTESIAN_POINT('Ctrl Pts',(-54.4900017008414,-13.8058562244003,
6.));
#62356=CARTESIAN_POINT('Ctrl Pts',(-54.4710837860606,-13.7556960237054,
6.));
#62357=CARTESIAN_POINT('Ctrl Pts',(-54.449305884132,-13.7065589746003,6.));
#62358=CARTESIAN_POINT('Ctrl Pts',(-54.4439733588473,-13.6945273033388,
6.));
#62359=CARTESIAN_POINT('Ctrl Pts',(-54.4384691647044,-13.6825570212273,
6.));
#62360=CARTESIAN_POINT('Ctrl Pts',(-54.4327956995134,-13.6706510067857,
6.));
#62361=CARTESIAN_POINT('Ctrl Pts',(-54.4285108294522,-13.6616590198587,
6.));
#62362=CARTESIAN_POINT('Ctrl Pts',(-54.4241301793919,-13.652705501481,6.));
#62363=CARTESIAN_POINT('Ctrl Pts',(-54.4196602351581,-13.6438018793311,
6.));
#62364=CARTESIAN_POINT('Ctrl Pts',(-54.3938099878638,-13.5923111173985,
6.));
#62365=CARTESIAN_POINT('Ctrl Pts',(-54.3649324447925,-13.5423928808473,
6.));
#62366=CARTESIAN_POINT('Ctrl Pts',(-54.3333070254867,-13.4942625535239,
6.));
#62367=CARTESIAN_POINT('Ctrl Pts',(-54.301002857855,-13.4450992476719,6.));
#62368=CARTESIAN_POINT('Ctrl Pts',(-54.2658311993318,-13.3978004684424,
6.));
#62369=CARTESIAN_POINT('Ctrl Pts',(-54.2280361920572,-13.3526057240926,
6.));
#62370=CARTESIAN_POINT('Ctrl Pts',(-54.1899071161637,-13.3070115051319,
6.));
#62371=CARTESIAN_POINT('Ctrl Pts',(-54.1491075472883,-13.2635576362936,
6.));
#62372=CARTESIAN_POINT('Ctrl Pts',(-54.1058416126673,-13.2225152020661,
6.));
#62373=CARTESIAN_POINT('Ctrl Pts',(-54.0960379392223,-13.2132153539042,
6.));
#62374=CARTESIAN_POINT('Ctrl Pts',(-54.0861045521206,-13.2040370185881,
6.));
#62375=CARTESIAN_POINT('Ctrl Pts',(-54.076063979376,-13.1950014469293,6.));
#62376=CARTESIAN_POINT('Ctrl Pts',(-54.0308409078756,-13.1543049335365,
6.));
#62377=CARTESIAN_POINT('Ctrl Pts',(-53.9833737358298,-13.1164303526698,
6.));
#62378=CARTESIAN_POINT('Ctrl Pts',(-53.9339288505494,-13.0816212827293,
6.));
#62379=CARTESIAN_POINT('Ctrl Pts',(-53.8849184368331,-13.0471180796338,
6.));
#62380=CARTESIAN_POINT('Ctrl Pts',(-53.8339641911266,-13.0156258219973,
6.));
#62381=CARTESIAN_POINT('Ctrl Pts',(-53.7812837559444,-12.9874094817676,
6.));
#62382=CARTESIAN_POINT('Ctrl Pts',(-53.7426834463104,-12.9667346436454,
6.));
#62383=CARTESIAN_POINT('Ctrl Pts',(-53.7031554636913,-12.9478191086954,
6.));
#62384=CARTESIAN_POINT('Ctrl Pts',(-53.6627743368928,-12.9307811146157,
6.));
#62385=CARTESIAN_POINT('Ctrl Pts',(-53.6403329837275,-12.921312442672,6.));
#62386=CARTESIAN_POINT('Ctrl Pts',(-53.6176279860555,-12.912423887492,6.));
#62387=CARTESIAN_POINT('Ctrl Pts',(-53.5946794545979,-12.9041113494969,
6.));
#62388=CARTESIAN_POINT('Ctrl Pts',(-52.7966221146314,-12.9064860705774,
6.));
#62389=CARTESIAN_POINT('Ctrl Pts',(-52.7392734478413,-12.9274410373818,
6.));
#62390=CARTESIAN_POINT('Ctrl Pts',(-52.6834091366923,-12.9520243011176,
6.));
#62391=CARTESIAN_POINT('Ctrl Pts',(-52.6292438196105,-12.9799599642101,
6.));
#62392=CARTESIAN_POINT('Ctrl Pts',(-52.579017857924,-13.0058639119715,6.));
#62393=CARTESIAN_POINT('Ctrl Pts',(-52.5302525542186,-13.0346514876413,
6.));
#62394=CARTESIAN_POINT('Ctrl Pts',(-52.4831464368575,-13.0661326532274,
6.));
#62395=CARTESIAN_POINT('Ctrl Pts',(-52.4717767044507,-13.0737310809607,
6.));
#62396=CARTESIAN_POINT('Ctrl Pts',(-52.4605034750011,-13.0814868963895,
6.));
#62397=CARTESIAN_POINT('Ctrl Pts',(-52.4493421044387,-13.0893884562007,
6.));
#62398=CARTESIAN_POINT('Ctrl Pts',(-52.4002195795838,-13.1241641646178,
6.));
#62399=CARTESIAN_POINT('Ctrl Pts',(-52.3531999207051,-13.1617999131249,
6.));
#62400=CARTESIAN_POINT('Ctrl Pts',(-52.308512601551,-13.2020507624865,6.));
#62401=CARTESIAN_POINT('Ctrl Pts',(-52.2809299424638,-13.2268950690355,
6.));
#62402=CARTESIAN_POINT('Ctrl Pts',(-52.2542366022566,-13.2527364020133,
6.));
#62403=CARTESIAN_POINT('Ctrl Pts',(-52.2284950356863,-13.2795223256619,
6.));
#62404=CARTESIAN_POINT('Ctrl Pts',(-52.2196863975423,-13.2886883376888,
6.));
#62405=CARTESIAN_POINT('Ctrl Pts',(-52.2109892711622,-13.2979649851678,
6.));
#62406=CARTESIAN_POINT('Ctrl Pts',(-52.2024063576282,-13.3073502398414,
6.));
#62407=CARTESIAN_POINT('Ctrl Pts',(-52.1943778462967,-13.3161292661239,
6.));
#62408=CARTESIAN_POINT('Ctrl Pts',(-52.1864544231925,-13.3249977568293,
6.));
#62409=CARTESIAN_POINT('Ctrl Pts',(-52.1786418093699,-13.3339491349468,
6.));
#62410=CARTESIAN_POINT('Ctrl Pts',(-52.1399699653664,-13.3782577755679,
6.));
#62411=CARTESIAN_POINT('Ctrl Pts',(-52.1039774129608,-13.4246301646367,
6.));
#62412=CARTESIAN_POINT('Ctrl Pts',(-52.0708793546133,-13.4728370626374,
6.));
#62413=CARTESIAN_POINT('Ctrl Pts',(-52.0386265755499,-13.5198128221889,
6.));
#62414=CARTESIAN_POINT('Ctrl Pts',(-52.009121966523,-13.5685314991956,6.));
#62415=CARTESIAN_POINT('Ctrl Pts',(-51.982610320354,-13.6187990638912,6.));
#62416=CARTESIAN_POINT('Ctrl Pts',(-51.968236469053,-13.6460526903011,6.));
#62417=CARTESIAN_POINT('Ctrl Pts',(-51.9547432274292,-13.6737618469832,
6.));
#62418=CARTESIAN_POINT('Ctrl Pts',(-51.9421760191472,-13.7018965351452,
6.));
#62419=CARTESIAN_POINT('Ctrl Pts',(-51.9317203742409,-13.7253039858987,
6.));
#62420=CARTESIAN_POINT('Ctrl Pts',(-51.9219057931392,-13.7490060035482,
6.));
#62421=CARTESIAN_POINT('Ctrl Pts',(-51.9127610531855,-13.7729853084091,
6.));
#62422=CARTESIAN_POINT('Ctrl Pts',(-51.9088519886743,-13.7832356435864,
6.));
#62423=CARTESIAN_POINT('Ctrl Pts',(-51.9050650272361,-13.7935379060622,
6.));
#62424=CARTESIAN_POINT('Ctrl Pts',(-51.9014081870189,-13.8038737999324,
6.));
#62425=CARTESIAN_POINT('Ctrl Pts',(-51.8844806830126,-13.8517186262041,
6.));
#62426=CARTESIAN_POINT('Ctrl Pts',(-51.8703064127133,-13.900364924046,6.));
#62427=CARTESIAN_POINT('Ctrl Pts',(-51.8590515016651,-13.9496698048621,
6.));
#62428=CARTESIAN_POINT('Ctrl Pts',(-51.8464743828166,-14.0047669391872,
6.));
#62429=CARTESIAN_POINT('Ctrl Pts',(-51.8375421395456,-14.0606874236398,
6.));
#62430=CARTESIAN_POINT('Ctrl Pts',(-51.8321648228283,-14.1170948620909,
6.));
#62431=CARTESIAN_POINT('Ctrl Pts',(-51.8276016369014,-14.1649621614985,
6.));
#62432=CARTESIAN_POINT('Ctrl Pts',(-51.8255995131662,-14.2131805783548,
6.));
#62433=CARTESIAN_POINT('Ctrl Pts',(-51.8261319285703,-14.2615368910676,
6.));
#62434=CARTESIAN_POINT('Ctrl Pts',(-51.826278300178,-14.2748310053593,6.));
#62435=CARTESIAN_POINT('Ctrl Pts',(-51.8266163768541,-14.2881354730497,
6.));
#62436=CARTESIAN_POINT('Ctrl Pts',(-51.8271459227333,-14.3014456837575,
6.));
#62437=CARTESIAN_POINT('Ctrl Pts',(-51.8275582116147,-14.3118086232139,
6.));
#62438=CARTESIAN_POINT('Ctrl Pts',(-51.8280867629368,-14.3221768232919,
6.));
#62439=CARTESIAN_POINT('Ctrl Pts',(-51.8287302146405,-14.3325312126322,
6.));
#62440=CARTESIAN_POINT('Ctrl Pts',(-51.8321732391036,-14.3879361724649,
6.));
#62441=CARTESIAN_POINT('Ctrl Pts',(-51.8389046601932,-14.4430495470179,
6.));
#62442=CARTESIAN_POINT('Ctrl Pts',(-51.8488297362242,-14.4975564316833,
6.));
#62443=CARTESIAN_POINT('Ctrl Pts',(-51.8586992382113,-14.5517581128431,
6.));
#62444=CARTESIAN_POINT('Ctrl Pts',(-51.8717272178035,-14.6053611705386,
6.));
#62445=CARTESIAN_POINT('Ctrl Pts',(-51.8878674165357,-14.65803601794,6.));
#62446=CARTESIAN_POINT('Ctrl Pts',(-51.9028425534804,-14.7069085917211,
6.));
#62447=CARTESIAN_POINT('Ctrl Pts',(-51.9204975501467,-14.7549825914389,
6.));
#62448=CARTESIAN_POINT('Ctrl Pts',(-51.9408266061655,-14.8019671660641,
6.));
#62449=CARTESIAN_POINT('Ctrl Pts',(-51.946048451174,-14.8140359097509,6.));
#62450=CARTESIAN_POINT('Ctrl Pts',(-51.9514489311129,-14.8260366549904,
6.));
#62451=CARTESIAN_POINT('Ctrl Pts',(-51.9570156117182,-14.8379381689157,
6.));
#62452=CARTESIAN_POINT('Ctrl Pts',(-51.9795172113314,-14.8860463899781,
6.));
#62453=CARTESIAN_POINT('Ctrl Pts',(-52.0047624527053,-14.9326133843135,
6.));
#62454=CARTESIAN_POINT('Ctrl Pts',(-52.0326996003995,-14.9773433960441,
6.));
#62455=CARTESIAN_POINT('Ctrl Pts',(-52.0596890512109,-15.0205560555688,
6.));
#62456=CARTESIAN_POINT('Ctrl Pts',(-52.0891914487675,-15.0620548998265,
6.));
#62457=CARTESIAN_POINT('Ctrl Pts',(-52.1211934155095,-15.1015390599239,
6.));
#62458=CARTESIAN_POINT('Ctrl Pts',(-52.1435818547289,-15.1291620096505,
6.));
#62459=CARTESIAN_POINT('Ctrl Pts',(-52.167194352484,-15.1557982112222,6.));
#62460=CARTESIAN_POINT('Ctrl Pts',(-52.1920344148669,-15.1813316631752,
6.));
#62461=CARTESIAN_POINT('Ctrl Pts',(-52.2060464360847,-15.1957348182485,
6.));
#62462=CARTESIAN_POINT('Ctrl Pts',(-52.2204492103834,-15.2097868473553,
6.));
#62463=CARTESIAN_POINT('Ctrl Pts',(-52.2352263046383,-15.223479246524,6.));
#62464=CARTESIAN_POINT('Origin',(-53.1951359564886,-14.3971354987959,0.895788276411275));
#62465=CARTESIAN_POINT('Ctrl Pts',(-54.7400287307462,-14.397884086359,2.14578827641127));
#62466=CARTESIAN_POINT('Ctrl Pts',(-54.7403302631026,-14.4458093584932,
2.14826884812012));
#62467=CARTESIAN_POINT('Ctrl Pts',(-54.7167366550282,-14.9990296040617,
2.17691792328789));
#62468=CARTESIAN_POINT('Ctrl Pts',(-54.0514939360651,-15.9998439808924,
2.23173550191459));
#62469=CARTESIAN_POINT('Ctrl Pts',(-52.3307400382945,-15.9953304824803,
2.31024101229136));
#62470=CARTESIAN_POINT('Ctrl Pts',(-51.3852180733225,-14.5577448223715,
2.38874652266815));
#62471=CARTESIAN_POINT('Ctrl Pts',(-52.0628629644955,-12.9760077060224,
2.46725203304492));
#62472=CARTESIAN_POINT('Ctrl Pts',(-53.7559624418889,-12.6688282037076,
2.54575754342171));
#62473=CARTESIAN_POINT('Ctrl Pts',(-54.658158616602,-13.6109326580654,2.60526962454382));
#62474=CARTESIAN_POINT('Ctrl Pts',(-54.7387317829834,-14.2566058695901,
2.63861320220701));
#62475=CARTESIAN_POINT('Ctrl Pts',(-54.7375657625992,-14.3958310564158,
2.64578827641127));
#62476=CARTESIAN_POINT('Ctrl Pts',(-54.7364807484814,-14.3955730757723,
2.10421172358873));
#62477=CARTESIAN_POINT('Ctrl Pts',(-54.7341428408094,-14.7375070363914,
2.12181148931034));
#62478=CARTESIAN_POINT('Ctrl Pts',(-54.4552744897983,-15.5924244351668,
2.16557975849088));
#62479=CARTESIAN_POINT('Ctrl Pts',(-53.0510002557363,-16.2080728204287,
2.23551653113034));
#62480=CARTESIAN_POINT('Ctrl Pts',(-51.605113325188,-15.2764851170283,2.31402204150712));
#62481=CARTESIAN_POINT('Ctrl Pts',(-51.5846111642588,-13.5555692706413,
2.3925275518839));
#62482=CARTESIAN_POINT('Ctrl Pts',(-53.0087575469087,-12.5897418281553,
2.47103306226068));
#62483=CARTESIAN_POINT('Ctrl Pts',(-54.4388957804213,-13.178381042198,2.54159445282895));
#62484=CARTESIAN_POINT('Ctrl Pts',(-54.7344163061994,-14.0445046478413,
2.5859873399383));
#62485=CARTESIAN_POINT('Ctrl Pts',(-54.73716587472,-14.3983674417199,2.60421172358873));
#62486=CARTESIAN_POINT('Ctrl Pts',(-52.2370198037663,-15.2223467977324,
2.));
#62487=CARTESIAN_POINT('Ctrl Pts',(-51.9656547514336,-14.9072768995629,
2.02616850345893));
#62488=CARTESIAN_POINT('Ctrl Pts',(-51.7623579720558,-13.9937953994845,
2.07850551037678));
#62489=CARTESIAN_POINT('Ctrl Pts',(-52.7425844632288,-12.9776340948197,
2.15701102075356));
#62490=CARTESIAN_POINT('Ctrl Pts',(-54.1289211584486,-13.2376188657684,
2.23551653113034));
#62491=CARTESIAN_POINT('Ctrl Pts',(-54.6776801082256,-14.5359758627139,
2.31402204150712));
#62492=CARTESIAN_POINT('Ctrl Pts',(-53.8969277031993,-15.7105670448821,
2.3925275518839));
#62493=CARTESIAN_POINT('Ctrl Pts',(-52.486757059174,-15.7068681992943,2.47103306226068));
#62494=CARTESIAN_POINT('Ctrl Pts',(-51.7118947618914,-14.5287560364896,
2.54953857263746));
#62495=CARTESIAN_POINT('Ctrl Pts',(-52.2672298007042,-13.2325106809332,
2.62804408301423));
#62496=CARTESIAN_POINT('Ctrl Pts',(-53.6547374411216,-12.9807747893732,
2.70654959339101));
#62497=CARTESIAN_POINT('Ctrl Pts',(-54.6300613996379,-13.9992418052107,
2.78505510376779));
#62498=CARTESIAN_POINT('Ctrl Pts',(-54.3185111760821,-15.374560833818,2.86356061414457));
#62499=CARTESIAN_POINT('Ctrl Pts',(-52.9994908161496,-15.8732958581993,
2.94206612452135));
#62500=CARTESIAN_POINT('Ctrl Pts',(-51.855929934815,-15.0481780331667,3.02057163489813));
#62501=CARTESIAN_POINT('Ctrl Pts',(-51.9134007191539,-13.639188362749,3.09907714527491));
#62502=CARTESIAN_POINT('Ctrl Pts',(-53.1203622018242,-12.909944412367,3.17758265565169));
#62503=CARTESIAN_POINT('Ctrl Pts',(-54.394382532434,-13.5144484306959,3.25608816602847));
#62504=CARTESIAN_POINT('Ctrl Pts',(-54.592890039674,-14.9105673726083,3.33459367640525));
#62505=CARTESIAN_POINT('Ctrl Pts',(-53.5378584472409,-15.8462283160989,
3.41309918678203));
#62506=CARTESIAN_POINT('Ctrl Pts',(-52.1754651814132,-15.4823084146089,
3.49160469715881));
#62507=CARTESIAN_POINT('Ctrl Pts',(-51.7275369059285,-14.1451796218823,
3.57011020753559));
#62508=CARTESIAN_POINT('Ctrl Pts',(-52.5957863501673,-13.0340108603602,
3.64861571791237));
#62509=CARTESIAN_POINT('Ctrl Pts',(-54.0015467695738,-13.1453246755956,
3.72712122828915));
#62510=CARTESIAN_POINT('Ctrl Pts',(-54.6840988007339,-14.3792921998829,
3.80562673866593));
#62511=CARTESIAN_POINT('Ctrl Pts',(-54.0313135549908,-15.6292620174801,
3.8841322490427));
#62512=CARTESIAN_POINT('Ctrl Pts',(-52.6286243599758,-15.7742314816778,
3.96263775941949));
#62513=CARTESIAN_POINT('Ctrl Pts',(-51.7339962327512,-14.6841885294771,
4.04114326979626));
#62514=CARTESIAN_POINT('Ctrl Pts',(-52.1497529463451,-13.3367095952976,
4.11964878017305));
#62515=CARTESIAN_POINT('Ctrl Pts',(-53.5030339960932,-12.9402458213458,
4.19815429054982));
#62516=CARTESIAN_POINT('Ctrl Pts',(-54.5801847638567,-13.8503553460012,
4.27665980092661));
#62517=CARTESIAN_POINT('Ctrl Pts',(-54.41519083395,-15.2508303100966,4.35516531130338));
#62518=CARTESIAN_POINT('Ctrl Pts',(-53.1560226839298,-15.8856914730379,
4.43367082168017));
#62519=CARTESIAN_POINT('Ctrl Pts',(-51.9319322483355,-15.1855802477899,
4.51217633205694));
#62520=CARTESIAN_POINT('Ctrl Pts',(-51.8407129256901,-13.7783730316415,
4.59068184243372));
#62521=CARTESIAN_POINT('Ctrl Pts',(-52.9641723835949,-12.9260866978538,
4.6691873528105));
#62522=CARTESIAN_POINT('Ctrl Pts',(-54.2947654505407,-13.3930719178224,
4.74769286318728));
#62523=CARTESIAN_POINT('Ctrl Pts',(-54.639184673062,-14.7605251935738,4.82619837356406));
#62524=CARTESIAN_POINT('Ctrl Pts',(-53.6885466200216,-15.8020820199203,
4.90470388394084));
#62525=CARTESIAN_POINT('Ctrl Pts',(-52.2954062665963,-15.5836492690769,
4.98320939431762));
#62526=CARTESIAN_POINT('Ctrl Pts',(-51.7091646625421,-14.3011230348445,
5.0617149046944));
#62527=CARTESIAN_POINT('Ctrl Pts',(-52.455577895988,-13.1047025120629,5.14022041507118));
#62528=CARTESIAN_POINT('Ctrl Pts',(-53.8652434689878,-13.0673677185784,
5.21872592544796));
#62529=CARTESIAN_POINT('Ctrl Pts',(-54.6739425216854,-14.2225980750992,
5.29723143582473));
#62530=CARTESIAN_POINT('Ctrl Pts',(-54.1564090232193,-15.5343621736369,
5.37573694620152));
#62531=CARTESIAN_POINT('Ctrl Pts',(-52.7767903419413,-15.826225464705,5.45424245657829));
#62532=CARTESIAN_POINT('Ctrl Pts',(-51.7723391952092,-14.8364647334447,
5.53274796695508));
#62533=CARTESIAN_POINT('Ctrl Pts',(-52.0439156164789,-13.4526673224972,
5.61125347733185));
#62534=CARTESIAN_POINT('Ctrl Pts',(-53.3478744097592,-12.9159632016583,
5.68975898770863));
#62535=CARTESIAN_POINT('Ctrl Pts',(-54.5149728893469,-13.707465612061,5.76826449808541));
#62536=CARTESIAN_POINT('Ctrl Pts',(-54.498171162037,-15.1177692904017,5.84677000846219));
#62537=CARTESIAN_POINT('Ctrl Pts',(-53.3132562085964,-15.88121138355,5.92527551883898));
#62538=CARTESIAN_POINT('Ctrl Pts',(-52.0214443153046,-15.3148691319142,
6.00378102921575));
#62539=CARTESIAN_POINT('Ctrl Pts',(-51.7841832172828,-13.9230591799233,
6.08228653959254));
#62540=CARTESIAN_POINT('Ctrl Pts',(-52.4668366999413,-13.2829324314546,
6.13462354651038));
#62541=CARTESIAN_POINT('Ctrl Pts',(-52.8685508929576,-13.1755371825403,
6.16079204996931));
#62542=CARTESIAN_POINT('Ctrl Pts',(-52.166679656532,-15.2829297282066,1.94640265001023));
#62543=CARTESIAN_POINT('Ctrl Pts',(-51.8753923247543,-14.9447289570595,
1.97257115346916));
#62544=CARTESIAN_POINT('Ctrl Pts',(-51.6571705017343,-13.9641841650946,
2.02490816038701));
#62545=CARTESIAN_POINT('Ctrl Pts',(-52.7093603717901,-12.8734213253437,
2.10341367076379));
#62546=CARTESIAN_POINT('Ctrl Pts',(-54.1974750476659,-13.152492891787,2.18191918114057));
#62547=CARTESIAN_POINT('Ctrl Pts',(-54.7865211643106,-14.5461688352594,
2.26042469151734));
#62548=CARTESIAN_POINT('Ctrl Pts',(-53.9484497808213,-15.8069926902189,
2.33893020189413));
#62549=CARTESIAN_POINT('Ctrl Pts',(-52.4347513855474,-15.8030222936896,
2.4174357122709));
#62550=CARTESIAN_POINT('Ctrl Pts',(-51.6030025323684,-14.5384189651169,
2.49594122264769));
#62551=CARTESIAN_POINT('Ctrl Pts',(-52.199107521968,-13.1470096892963,2.57444673302446));
#62552=CARTESIAN_POINT('Ctrl Pts',(-53.688479108044,-12.8767925941513,2.65295224340125));
#62553=CARTESIAN_POINT('Ctrl Pts',(-54.7354065257529,-13.9700304189807,
2.73145775377802));
#62554=CARTESIAN_POINT('Ctrl Pts',(-54.4009838263146,-15.4463185656761,
2.80996326415481));
#62555=CARTESIAN_POINT('Ctrl Pts',(-52.9851275179857,-15.9816682478379,
2.88846877453158));
#62556=CARTESIAN_POINT('Ctrl Pts',(-51.757612055011,-15.0959743547226,2.96697428490837));
#62557=CARTESIAN_POINT('Ctrl Pts',(-51.8193020599743,-13.5835436342954,
3.04547979528514));
#62558=CARTESIAN_POINT('Ctrl Pts',(-53.1148726827325,-12.8007622013296,
3.12398530566192));
#62559=CARTESIAN_POINT('Ctrl Pts',(-54.4824252822431,-13.4496459136362,
3.2024908160387));
#62560=CARTESIAN_POINT('Ctrl Pts',(-54.695506228462,-14.9482610003549,3.28099632641548));
#62561=CARTESIAN_POINT('Ctrl Pts',(-53.5630194367425,-15.9526135407249,
3.35950183679226));
#62562=CARTESIAN_POINT('Ctrl Pts',(-52.1006059983742,-15.5619764407204,
3.43800734716904));
#62563=CARTESIAN_POINT('Ctrl Pts',(-51.6197930452243,-14.1266822680611,
3.51651285754582));
#62564=CARTESIAN_POINT('Ctrl Pts',(-52.5517850676155,-12.9339369940614,
3.5950183679226));
#62565=CARTESIAN_POINT('Ctrl Pts',(-54.0607494614004,-13.0534229188377,
3.67352387829937));
#62566=CARTESIAN_POINT('Ctrl Pts',(-54.7934110854636,-14.3779822331642,
3.75202938867616));
#62567=CARTESIAN_POINT('Ctrl Pts',(-54.0927015769186,-15.7197186499972,
3.83053489905293));
#62568=CARTESIAN_POINT('Ctrl Pts',(-52.5870338816236,-15.8753310549564,
3.90904040942972));
#62569=CARTESIAN_POINT('Ctrl Pts',(-51.626726583862,-14.7052625426693,3.98754591980649));
#62570=CARTESIAN_POINT('Ctrl Pts',(-52.0730060982299,-13.2588583723836,
4.06605143018328));
#62571=CARTESIAN_POINT('Ctrl Pts',(-53.5256383467009,-12.8332881898262,
4.14455694056005));
#62572=CARTESIAN_POINT('Ctrl Pts',(-54.681868194159,-13.8102134526169,4.22306245093684));
#62573=CARTESIAN_POINT('Ctrl Pts',(-54.5047612262982,-15.3135043591139,
4.30156796131361));
#62574=CARTESIAN_POINT('Ctrl Pts',(-53.1531511809886,-15.9949738873852,
4.38007347169039));
#62575=CARTESIAN_POINT('Ctrl Pts',(-51.8391940823356,-15.2434639600858,
4.45857898206717));
#62576=CARTESIAN_POINT('Ctrl Pts',(-51.741277888369,-13.7329465529009,4.53708449244395));
#62577=CARTESIAN_POINT('Ctrl Pts',(-52.9472161808664,-12.8180895735458,
4.61559000282073));
#62578=CARTESIAN_POINT('Ctrl Pts',(-54.3754948070962,-13.3193585377509,
4.69409551319751));
#62579=CARTESIAN_POINT('Ctrl Pts',(-54.7451995847704,-14.787203466935,4.77260102357429));
#62580=CARTESIAN_POINT('Ctrl Pts',(-53.7247703895732,-15.905226241914,4.85110653395107));
#62581=CARTESIAN_POINT('Ctrl Pts',(-52.2293525645705,-15.6707572392952,
4.92961204432785));
#62582=CARTESIAN_POINT('Ctrl Pts',(-51.6000720026333,-14.2940742748049,
5.00811755470463));
#62583=CARTESIAN_POINT('Ctrl Pts',(-52.4012832024729,-13.0098184770542,
5.08662306508141));
#62584=CARTESIAN_POINT('Ctrl Pts',(-53.9144394469056,-12.9697427477624,
5.16512857545819));
#62585=CARTESIAN_POINT('Ctrl Pts',(-54.78250918266,-14.2097844010517,5.24363408583497));
#62586=CARTESIAN_POINT('Ctrl Pts',(-54.2269809354599,-15.6178517291775,
5.32213959621174));
#62587=CARTESIAN_POINT('Ctrl Pts',(-52.746077476869,-15.9311421789546,5.40064510658853));
#62588=CARTESIAN_POINT('Ctrl Pts',(-51.6678844969053,-14.8687181120791,
5.4791506169653));
#62589=CARTESIAN_POINT('Ctrl Pts',(-51.9593987152814,-13.3833291421626,
5.55765612734209));
#62590=CARTESIAN_POINT('Ctrl Pts',(-53.3590877112581,-12.80722286035,5.63616163771886));
#62591=CARTESIAN_POINT('Ctrl Pts',(-54.611868786487,-13.6568334614203,5.71466714809565));
#62592=CARTESIAN_POINT('Ctrl Pts',(-54.5938335594918,-15.1706746577306,
5.79317265847242));
#62593=CARTESIAN_POINT('Ctrl Pts',(-53.3219280130545,-15.9901648918943,
5.87167816884921));
#62594=CARTESIAN_POINT('Ctrl Pts',(-51.9352776823614,-15.3822445943693,
5.95018367922597));
#62595=CARTESIAN_POINT('Ctrl Pts',(-51.680598048476,-13.8882548422916,6.02868918960277));
#62596=CARTESIAN_POINT('Ctrl Pts',(-52.4133685721046,-13.2011331552573,
6.08102619652061));
#62597=CARTESIAN_POINT('Ctrl Pts',(-52.8445746335155,-13.0858534785527,
6.10719469997954));
#62598=CARTESIAN_POINT('Ctrl Pts',(-52.0963395092977,-15.3435126586808,
1.89280530002046));
#62599=CARTESIAN_POINT('Ctrl Pts',(-51.7851298980751,-14.9821810145562,
1.91897380347939));
#62600=CARTESIAN_POINT('Ctrl Pts',(-51.5519830314128,-13.9345729307046,
1.97131081039724));
#62601=CARTESIAN_POINT('Ctrl Pts',(-52.6761362803514,-12.7692085558677,
2.04981632077402));
#62602=CARTESIAN_POINT('Ctrl Pts',(-54.2660289368831,-13.0673669178057,
2.1283218311508));
#62603=CARTESIAN_POINT('Ctrl Pts',(-54.8953622203958,-14.5563618078048,
2.20682734152757));
#62604=CARTESIAN_POINT('Ctrl Pts',(-53.9999718584432,-15.9034183355557,
2.28533285190436));
#62605=CARTESIAN_POINT('Ctrl Pts',(-52.382745711921,-15.899176388085,2.36383836228113));
#62606=CARTESIAN_POINT('Ctrl Pts',(-51.4941103028454,-14.5480818937442,
2.44234387265792));
#62607=CARTESIAN_POINT('Ctrl Pts',(-52.1309852432317,-13.0615086976593,
2.52084938303469));
#62608=CARTESIAN_POINT('Ctrl Pts',(-53.7222207749664,-12.7728103989294,
2.59935489341148));
#62609=CARTESIAN_POINT('Ctrl Pts',(-54.8407516518678,-13.9408190327507,
2.67786040378825));
#62610=CARTESIAN_POINT('Ctrl Pts',(-54.483456476547,-15.5180762975342,2.75636591416503));
#62611=CARTESIAN_POINT('Ctrl Pts',(-52.9707642198219,-16.0900406374764,
2.83487142454181));
#62612=CARTESIAN_POINT('Ctrl Pts',(-51.6592941752071,-15.1437706762785,
2.91337693491859));
#62613=CARTESIAN_POINT('Ctrl Pts',(-51.7252034007948,-13.5278989058417,
2.99188244529537));
#62614=CARTESIAN_POINT('Ctrl Pts',(-53.1093831636409,-12.6915799902922,
3.07038795567215));
#62615=CARTESIAN_POINT('Ctrl Pts',(-54.5704680320522,-13.3848433965765,
3.14889346604893));
#62616=CARTESIAN_POINT('Ctrl Pts',(-54.7981224172499,-14.9859546281015,
3.22739897642571));
#62617=CARTESIAN_POINT('Ctrl Pts',(-53.5881804262442,-16.0589987653509,
3.30590448680249));
#62618=CARTESIAN_POINT('Ctrl Pts',(-52.0257468153352,-15.6416444668319,
3.38440999717927));
#62619=CARTESIAN_POINT('Ctrl Pts',(-51.5120491845202,-14.10818491424,3.46291550755605));
#62620=CARTESIAN_POINT('Ctrl Pts',(-52.5077837850636,-12.8338631277627,
3.54142101793282));
#62621=CARTESIAN_POINT('Ctrl Pts',(-54.1199521532269,-12.9615211620797,
3.61992652830961));
#62622=CARTESIAN_POINT('Ctrl Pts',(-54.9027233701933,-14.3766722664456,
3.69843203868638));
#62623=CARTESIAN_POINT('Ctrl Pts',(-54.1540895988463,-15.8101752825143,
3.77693754906317));
#62624=CARTESIAN_POINT('Ctrl Pts',(-52.5454434032715,-15.9764306282351,
3.85544305943994));
#62625=CARTESIAN_POINT('Ctrl Pts',(-51.5194569349729,-14.7263365558616,
3.93394856981673));
#62626=CARTESIAN_POINT('Ctrl Pts',(-51.9962592501148,-13.1810071494696,
4.0124540801935));
#62627=CARTESIAN_POINT('Ctrl Pts',(-53.5482426973085,-12.7263305583065,
4.09095959057029));
#62628=CARTESIAN_POINT('Ctrl Pts',(-54.7835516244614,-13.7700715592326,
4.16946510094706));
#62629=CARTESIAN_POINT('Ctrl Pts',(-54.5943316186465,-15.3761784081312,
4.24797061132385));
#62630=CARTESIAN_POINT('Ctrl Pts',(-53.1502796780473,-16.1042563017325,
4.32647612170062));
#62631=CARTESIAN_POINT('Ctrl Pts',(-51.7464559163358,-15.3013476723818,
4.4049816320774));
#62632=CARTESIAN_POINT('Ctrl Pts',(-51.6418428510479,-13.6875200741603,
4.48348714245418));
#62633=CARTESIAN_POINT('Ctrl Pts',(-52.9302599781378,-12.7100924492378,
4.56199265283096));
#62634=CARTESIAN_POINT('Ctrl Pts',(-54.4562241636517,-13.2456451576794,
4.64049816320774));
#62635=CARTESIAN_POINT('Ctrl Pts',(-54.8512144964788,-14.8138817402962,
4.71900367358453));
#62636=CARTESIAN_POINT('Ctrl Pts',(-53.7609941591247,-16.0083704639078,
4.79750918396129));
#62637=CARTESIAN_POINT('Ctrl Pts',(-52.1632988625446,-15.7578652095136,
4.87601469433808));
#62638=CARTESIAN_POINT('Ctrl Pts',(-51.4909793427245,-14.2870255147652,
4.95452020471486));
#62639=CARTESIAN_POINT('Ctrl Pts',(-52.3469885089578,-12.9149344420456,
5.03302571509164));
#62640=CARTESIAN_POINT('Ctrl Pts',(-53.9636354248233,-12.8721177769464,
5.11153122546841));
#62641=CARTESIAN_POINT('Ctrl Pts',(-54.8910758436347,-14.1969707270041,
5.1900367358452));
#62642=CARTESIAN_POINT('Ctrl Pts',(-54.2975528477005,-15.7013412847181,
5.26854224622197));
#62643=CARTESIAN_POINT('Ctrl Pts',(-52.7153646117968,-16.0360588932041,
5.34704775659876));
#62644=CARTESIAN_POINT('Ctrl Pts',(-51.5634297986012,-14.9009714907135,
5.42555326697554));
#62645=CARTESIAN_POINT('Ctrl Pts',(-51.8748818140839,-13.313990961828,5.50405877735231));
#62646=CARTESIAN_POINT('Ctrl Pts',(-53.3703010127568,-12.6984825190418,
5.58256428772909));
#62647=CARTESIAN_POINT('Ctrl Pts',(-54.7087646836272,-13.6062013107796,
5.66106979810588));
#62648=CARTESIAN_POINT('Ctrl Pts',(-54.6894959569467,-15.2235800250595,
5.73957530848265));
#62649=CARTESIAN_POINT('Ctrl Pts',(-53.3305998175127,-16.0991184002386,
5.81808081885943));
#62650=CARTESIAN_POINT('Ctrl Pts',(-51.8491110494183,-15.4496200568245,
5.89658632923621));
#62651=CARTESIAN_POINT('Ctrl Pts',(-51.5770128796692,-13.8534505046598,
5.97509183961299));
#62652=CARTESIAN_POINT('Ctrl Pts',(-52.359900444268,-13.11933387906,6.02742884653084));
#62653=CARTESIAN_POINT('Ctrl Pts',(-52.8205983740735,-12.996169774565,6.05359734998977));
#62654=CARTESIAN_POINT('Ctrl Pts',(-52.0259993620635,-15.4040955891549,
1.83920795003069));
#62655=CARTESIAN_POINT('Ctrl Pts',(-51.6948674713958,-15.0196330720529,
1.86537645348962));
#62656=CARTESIAN_POINT('Ctrl Pts',(-51.4467955610913,-13.9049616963147,
1.91771346040747));
#62657=CARTESIAN_POINT('Ctrl Pts',(-52.6429121889126,-12.6649957863916,
1.99621897078425));
#62658=CARTESIAN_POINT('Ctrl Pts',(-54.3345828261005,-12.9822409438244,
2.07472448116103));
#62659=CARTESIAN_POINT('Ctrl Pts',(-55.0042032764809,-14.5665547803503,
2.15322999153781));
#62660=CARTESIAN_POINT('Ctrl Pts',(-54.0514939360651,-15.9998439808924,
2.23173550191459));
#62661=CARTESIAN_POINT('Ctrl Pts',(-52.3307400382945,-15.9953304824803,
2.31024101229136));
#62662=CARTESIAN_POINT('Ctrl Pts',(-51.3852180733225,-14.5577448223715,
2.38874652266815));
#62663=CARTESIAN_POINT('Ctrl Pts',(-52.0628629644955,-12.9760077060224,
2.46725203304492));
#62664=CARTESIAN_POINT('Ctrl Pts',(-53.7559624418889,-12.6688282037076,
2.54575754342171));
#62665=CARTESIAN_POINT('Ctrl Pts',(-54.9460967779827,-13.9116076465207,
2.62426305379848));
#62666=CARTESIAN_POINT('Ctrl Pts',(-54.5659291267794,-15.5898340293922,
2.70276856417526));
#62667=CARTESIAN_POINT('Ctrl Pts',(-52.9564009216581,-16.198413027115,2.78127407455204));
#62668=CARTESIAN_POINT('Ctrl Pts',(-51.5609762954032,-15.1915669978344,
2.85977958492882));
#62669=CARTESIAN_POINT('Ctrl Pts',(-51.6311047416152,-13.472254177388,2.9382850953056));
#62670=CARTESIAN_POINT('Ctrl Pts',(-53.1038936445493,-12.5823977792547,
3.01679060568238));
#62671=CARTESIAN_POINT('Ctrl Pts',(-54.6585107818613,-13.3200408795168,
3.09529611605916));
#62672=CARTESIAN_POINT('Ctrl Pts',(-54.9007386060379,-15.0236482558481,
3.17380162643594));
#62673=CARTESIAN_POINT('Ctrl Pts',(-53.6133414157459,-16.165383989977,3.25230713681272));
#62674=CARTESIAN_POINT('Ctrl Pts',(-51.9508876322962,-15.7213124929433,
3.3308126471895));
#62675=CARTESIAN_POINT('Ctrl Pts',(-51.4043053238161,-14.0896875604189,
3.40931815756628));
#62676=CARTESIAN_POINT('Ctrl Pts',(-52.4637825025118,-12.7337892614639,
3.48782366794306));
#62677=CARTESIAN_POINT('Ctrl Pts',(-54.1791548450535,-12.8696194053218,
3.56632917831984));
#62678=CARTESIAN_POINT('Ctrl Pts',(-55.0120356549231,-14.3753622997269,
3.64483468869662));
#62679=CARTESIAN_POINT('Ctrl Pts',(-54.215477620774,-15.9006319150314,3.72334019907339));
#62680=CARTESIAN_POINT('Ctrl Pts',(-52.5038529249194,-16.0775302015137,
3.80184570945018));
#62681=CARTESIAN_POINT('Ctrl Pts',(-51.4121872860838,-14.7474105690538,
3.88035121982695));
#62682=CARTESIAN_POINT('Ctrl Pts',(-51.9195124019995,-13.1031559265556,
3.95885673020374));
#62683=CARTESIAN_POINT('Ctrl Pts',(-53.5708470479161,-12.6193729267869,
4.03736224058051));
#62684=CARTESIAN_POINT('Ctrl Pts',(-54.8852350547638,-13.7299296658483,
4.11586775095729));
#62685=CARTESIAN_POINT('Ctrl Pts',(-54.6839020109947,-15.4388524571486,
4.19437326133407));
#62686=CARTESIAN_POINT('Ctrl Pts',(-53.147408175106,-16.2135387160798,4.27287877171085));
#62687=CARTESIAN_POINT('Ctrl Pts',(-51.6537177503358,-15.3592313846778,
4.35138428208763));
#62688=CARTESIAN_POINT('Ctrl Pts',(-51.5424078137269,-13.6420935954197,
4.42988979246441));
#62689=CARTESIAN_POINT('Ctrl Pts',(-52.9133037754093,-12.6020953249298,
4.50839530284119));
#62690=CARTESIAN_POINT('Ctrl Pts',(-54.5369535202073,-13.171931777608,4.58690081321797));
#62691=CARTESIAN_POINT('Ctrl Pts',(-54.9572294081871,-14.8405600136574,
4.66540632359475));
#62692=CARTESIAN_POINT('Ctrl Pts',(-53.7972179286764,-16.1115146859015,
4.74391183397153));
#62693=CARTESIAN_POINT('Ctrl Pts',(-52.0972451605187,-15.8449731797319,
4.8224173443483));
#62694=CARTESIAN_POINT('Ctrl Pts',(-51.3818866828157,-14.2799767547255,
4.90092285472509));
#62695=CARTESIAN_POINT('Ctrl Pts',(-52.2926938154427,-12.820050407037,4.97942836510186));
#62696=CARTESIAN_POINT('Ctrl Pts',(-54.0128314027411,-12.7744928061304,
5.05793387547865));
#62697=CARTESIAN_POINT('Ctrl Pts',(-54.9996425046093,-14.1841570529565,
5.13643938585543));
#62698=CARTESIAN_POINT('Ctrl Pts',(-54.368124759941,-15.7848308402587,5.2149448962322));
#62699=CARTESIAN_POINT('Ctrl Pts',(-52.6846517467245,-16.1409756074536,
5.29345040660899));
#62700=CARTESIAN_POINT('Ctrl Pts',(-51.4589751002972,-14.933224869348,5.37195591698576));
#62701=CARTESIAN_POINT('Ctrl Pts',(-51.7903649128864,-13.2446527814935,
5.45046142736255));
#62702=CARTESIAN_POINT('Ctrl Pts',(-53.3815143142557,-12.5897421777335,
5.52896693773931));
#62703=CARTESIAN_POINT('Ctrl Pts',(-54.8056605807673,-13.5555691601388,
5.60747244811611));
#62704=CARTESIAN_POINT('Ctrl Pts',(-54.7851583544017,-15.2764853923884,
5.68597795849288));
#62705=CARTESIAN_POINT('Ctrl Pts',(-53.3392716219708,-16.2080719085829,
5.76448346886966));
#62706=CARTESIAN_POINT('Ctrl Pts',(-51.7629444164752,-15.5169955192796,
5.84298897924644));
#62707=CARTESIAN_POINT('Ctrl Pts',(-51.4734277108623,-13.8186461670281,
5.92149448962322));
#62708=CARTESIAN_POINT('Ctrl Pts',(-52.3064323164313,-13.0375346028627,
5.97383149654107));
#62709=CARTESIAN_POINT('Ctrl Pts',(-52.7966221146314,-12.9064860705774,
6.));
#62710=CARTESIAN_POINT('Ctrl Pts',(-52.2370198037663,-15.2223467977324,
2.));
#62711=CARTESIAN_POINT('Ctrl Pts',(-52.2001398221824,-15.1879057962803,
2.));
#62712=CARTESIAN_POINT('Ctrl Pts',(-52.1656378013748,-15.1512262749774,
2.));
#62713=CARTESIAN_POINT('Ctrl Pts',(-52.133515895996,-15.112628111497,2.));
#62714=CARTESIAN_POINT('Ctrl Pts',(-52.0999545216902,-15.0723002605552,
2.));
#62715=CARTESIAN_POINT('Ctrl Pts',(-52.0689907405509,-15.0298774985346,
2.));
#62716=CARTESIAN_POINT('Ctrl Pts',(-52.040655024137,-14.9856749556978,2.));
#62717=CARTESIAN_POINT('Ctrl Pts',(-52.0179305604283,-14.9502257344445,
2.));
#62718=CARTESIAN_POINT('Ctrl Pts',(-51.9968968139207,-14.9136306734534,
2.));
#62719=CARTESIAN_POINT('Ctrl Pts',(-51.9775857407058,-14.8760343811022,
2.));
#62720=CARTESIAN_POINT('Ctrl Pts',(-51.9694199887411,-14.8601366630044,
2.));
#62721=CARTESIAN_POINT('Ctrl Pts',(-51.9615624516271,-14.8440597542834,
2.));
#62722=CARTESIAN_POINT('Ctrl Pts',(-51.9540164358689,-14.8278139468956,
2.));
#62723=CARTESIAN_POINT('Ctrl Pts',(-51.9497380912329,-14.8186031043633,
2.));
#62724=CARTESIAN_POINT('Ctrl Pts',(-51.9455597070027,-14.809337270677,2.));
#62725=CARTESIAN_POINT('Ctrl Pts',(-51.9414881758912,-14.8000332485161,
2.));
#62726=CARTESIAN_POINT('Ctrl Pts',(-51.9196632025412,-14.750160109849,2.));
#62727=CARTESIAN_POINT('Ctrl Pts',(-51.9008587821636,-14.6990941701308,
2.));
#62728=CARTESIAN_POINT('Ctrl Pts',(-51.8851025499192,-14.6471668919688,
2.));
#62729=CARTESIAN_POINT('Ctrl Pts',(-51.8690578814023,-14.5942890242042,
2.));
#62730=CARTESIAN_POINT('Ctrl Pts',(-51.856173427568,-14.5405170693332,2.));
#62731=CARTESIAN_POINT('Ctrl Pts',(-51.8465190610514,-14.4861664358985,
2.));
#62732=CARTESIAN_POINT('Ctrl Pts',(-51.8396145127886,-14.4472962965663,
2.));
#62733=CARTESIAN_POINT('Ctrl Pts',(-51.8343629002831,-14.4081294057031,
2.));
#62734=CARTESIAN_POINT('Ctrl Pts',(-51.8308047851344,-14.368774756998,2.));
#62735=CARTESIAN_POINT('Ctrl Pts',(-51.8292917204625,-14.3520394558225,
2.));
#62736=CARTESIAN_POINT('Ctrl Pts',(-51.8280850590022,-14.3352701586909,
2.));
#62737=CARTESIAN_POINT('Ctrl Pts',(-51.8271886807144,-14.3184751150899,
2.));
#62738=CARTESIAN_POINT('Ctrl Pts',(-51.8266545203306,-14.3084667881852,
2.));
#62739=CARTESIAN_POINT('Ctrl Pts',(-51.8262309124811,-14.2984549964066,
2.));
#62740=CARTESIAN_POINT('Ctrl Pts',(-51.8259184500034,-14.2884490816797,
2.));
#62741=CARTESIAN_POINT('Ctrl Pts',(-51.8241448794411,-14.2316544356751,
2.));
#62742=CARTESIAN_POINT('Ctrl Pts',(-51.8259444031621,-14.1749772817713,
2.));
#62743=CARTESIAN_POINT('Ctrl Pts',(-51.831377054275,-14.1187497415498,2.));
#62744=CARTESIAN_POINT('Ctrl Pts',(-51.8347120697802,-14.0842325758864,
2.));
#62745=CARTESIAN_POINT('Ctrl Pts',(-51.8394171165311,-14.0498843037551,
2.));
#62746=CARTESIAN_POINT('Ctrl Pts',(-51.845515342272,-14.0157787106909,2.));
#62747=CARTESIAN_POINT('Ctrl Pts',(-51.8551874830705,-13.9616852559467,
2.));
#62748=CARTESIAN_POINT('Ctrl Pts',(-51.8683614486688,-13.9082017945064,
2.));
#62749=CARTESIAN_POINT('Ctrl Pts',(-51.8848110251026,-13.8555328884186,
2.));
#62750=CARTESIAN_POINT('Ctrl Pts',(-51.8897327932489,-13.8397741760089,
2.));
#62751=CARTESIAN_POINT('Ctrl Pts',(-51.8949481552399,-13.8240884170171,
2.));
#62752=CARTESIAN_POINT('Ctrl Pts',(-51.9004519259216,-13.8084812249409,
2.));
#62753=CARTESIAN_POINT('Ctrl Pts',(-51.9055403383158,-13.7940518756473,
2.));
#62754=CARTESIAN_POINT('Ctrl Pts',(-51.9108779029592,-13.7796834481853,
2.));
#62755=CARTESIAN_POINT('Ctrl Pts',(-51.9164469096078,-13.7654145762878,
2.));
#62756=CARTESIAN_POINT('Ctrl Pts',(-51.937078011076,-13.7125537049463,2.));
#62757=CARTESIAN_POINT('Ctrl Pts',(-51.9609027535564,-13.6609889337068,
2.));
#62758=CARTESIAN_POINT('Ctrl Pts',(-51.9876380075214,-13.6109308617714,
2.));
#62759=CARTESIAN_POINT('Ctrl Pts',(-52.0150055546465,-13.5596889081893,
2.));
#62760=CARTESIAN_POINT('Ctrl Pts',(-52.0454232532683,-13.5100248567806,
2.));
#62761=CARTESIAN_POINT('Ctrl Pts',(-52.078642743017,-13.4621702328318,2.));
#62762=CARTESIAN_POINT('Ctrl Pts',(-52.0988112436159,-13.4331163244463,
2.));
#62763=CARTESIAN_POINT('Ctrl Pts',(-52.1200135483417,-13.4047295468345,
2.));
#62764=CARTESIAN_POINT('Ctrl Pts',(-52.1422027768384,-13.3770649262843,
2.));
#62765=CARTESIAN_POINT('Ctrl Pts',(-52.1544198936712,-13.3618331257985,
2.));
#62766=CARTESIAN_POINT('Ctrl Pts',(-52.1669363024172,-13.3468202983724,
2.));
#62767=CARTESIAN_POINT('Ctrl Pts',(-52.1797449296066,-13.3320361041244,
2.));
#62768=CARTESIAN_POINT('Ctrl Pts',(-52.1874577031558,-13.3231337338192,
2.));
#62769=CARTESIAN_POINT('Ctrl Pts',(-52.1952777965008,-13.3143127818998,
2.));
#62770=CARTESIAN_POINT('Ctrl Pts',(-52.203199440933,-13.3055801677412,2.));
#62771=CARTESIAN_POINT('Ctrl Pts',(-52.2437953927146,-13.2608282495827,
2.));
#62772=CARTESIAN_POINT('Ctrl Pts',(-52.2869270093575,-13.2185332555895,
2.));
#62773=CARTESIAN_POINT('Ctrl Pts',(-52.3323340644277,-13.1789459514645,
2.));
#62774=CARTESIAN_POINT('Ctrl Pts',(-52.3618576920541,-13.1532063208296,
2.));
#62775=CARTESIAN_POINT('Ctrl Pts',(-52.3923443514376,-13.128611691001,2.));
#62776=CARTESIAN_POINT('Ctrl Pts',(-52.4237326847397,-13.1052370160425,
2.));
#62777=CARTESIAN_POINT('Ctrl Pts',(-52.4367029256792,-13.095578167222,2.));
#62778=CARTESIAN_POINT('Ctrl Pts',(-52.4498272128038,-13.0861276945749,
2.));
#62779=CARTESIAN_POINT('Ctrl Pts',(-52.4631015594291,-13.0768912105345,
2.));
#62780=CARTESIAN_POINT('Ctrl Pts',(-52.4728212296877,-13.0701281221689,
2.));
#62781=CARTESIAN_POINT('Ctrl Pts',(-52.4826204708896,-13.063480479123,2.));
#62782=CARTESIAN_POINT('Ctrl Pts',(-52.4924892032556,-13.0569558445777,
2.));
#62783=CARTESIAN_POINT('Ctrl Pts',(-52.5432262963862,-13.0234114157406,
2.));
#62784=CARTESIAN_POINT('Ctrl Pts',(-52.5958554389749,-12.9930745926173,
2.));
#62785=CARTESIAN_POINT('Ctrl Pts',(-52.6501404637806,-12.9662121664589,
2.));
#62786=CARTESIAN_POINT('Ctrl Pts',(-52.6755695105507,-12.9536288454861,
2.));
#62787=CARTESIAN_POINT('Ctrl Pts',(-52.7013624781742,-12.9418083828321,
2.));
#62788=CARTESIAN_POINT('Ctrl Pts',(-52.7274977743506,-12.930781120438,2.));
#62789=CARTESIAN_POINT('Ctrl Pts',(-52.7499504413758,-12.9213076693217,
2.));
#62790=CARTESIAN_POINT('Ctrl Pts',(-52.7726557928972,-12.9124196555961,
2.));
#62791=CARTESIAN_POINT('Ctrl Pts',(-52.7955926848293,-12.9041113294173,
2.));
#62792=CARTESIAN_POINT('Ctrl Pts',(-54.4591686783466,-14.3960664985434,
2.80658032638058));
#62793=CARTESIAN_POINT('Ctrl Pts',(-54.4601242407418,-14.2819704202925,
2.79940525217632));
#62794=CARTESIAN_POINT('Ctrl Pts',(-54.4459154362348,-14.1681081402059,
2.79223017797206));
#62795=CARTESIAN_POINT('Ctrl Pts',(-54.4155823692926,-14.0587171406723,
2.78505510376779));
#62796=CARTESIAN_POINT('Ctrl Pts',(-54.3049534134658,-13.6597527999316,
2.75888660030887));
#62797=CARTESIAN_POINT('Ctrl Pts',(-53.9798454272937,-13.3202637946524,
2.73271809684994));
#62798=CARTESIAN_POINT('Ctrl Pts',(-53.5860401608047,-13.1924752739395,
2.70654959339101));
#62799=CARTESIAN_POINT('Ctrl Pts',(-53.1922348943158,-13.0646867532265,
2.68038108993209));
#62800=CARTESIAN_POINT('Ctrl Pts',(-52.72973234751,-13.1485987170799,2.65421258647316));
#62801=CARTESIAN_POINT('Ctrl Pts',(-52.405925234305,-13.4065955915993,2.62804408301423));
#62802=CARTESIAN_POINT('Ctrl Pts',(-52.0821181210999,-13.6645924661187,
2.60187557955531));
#62803=CARTESIAN_POINT('Ctrl Pts',(-51.8970064414956,-14.0966742513041,
2.57570707609638));
#62804=CARTESIAN_POINT('Ctrl Pts',(-51.9335943179073,-14.509067171031,2.54953857263746));
#62805=CARTESIAN_POINT('Ctrl Pts',(-51.9701821943189,-14.9214600907578,
2.52337006917853));
#62806=CARTESIAN_POINT('Ctrl Pts',(-52.2284696267464,-15.314164145026,2.4972015657196));
#62807=CARTESIAN_POINT('Ctrl Pts',(-52.5926417836311,-15.5111326464248,
2.47103306226068));
#62808=CARTESIAN_POINT('Ctrl Pts',(-52.9568139405158,-15.7081011478235,
2.44486455880175));
#62809=CARTESIAN_POINT('Ctrl Pts',(-53.4268708218575,-15.7093340963528,
2.41869605534282));
#62810=CARTESIAN_POINT('Ctrl Pts',(-53.7920246633661,-15.5141853735895,
2.3925275518839));
#62811=CARTESIAN_POINT('Ctrl Pts',(-54.1571785048747,-15.3190366508261,
2.36635904842497));
#62812=CARTESIAN_POINT('Ctrl Pts',(-54.4174293065502,-14.92750625677,2.34019054496604));
#62813=CARTESIAN_POINT('Ctrl Pts',(-54.456094882425,-14.5153482269177,2.31402204150712));
#62814=CARTESIAN_POINT('Ctrl Pts',(-54.4597600799313,-14.4762788338196,
2.31154146979827));
#62815=CARTESIAN_POINT('Ctrl Pts',(-54.461434207113,-14.4370240895848,2.30906089808943));
#62816=CARTESIAN_POINT('Ctrl Pts',(-54.4611870990995,-14.3977489718831,
2.30658032638058));
#62817=CARTESIAN_POINT('Ctrl Pts',(-53.5936497983459,-12.9064860705774,
2.));
#62818=CARTESIAN_POINT('Ctrl Pts',(-54.083839596546,-13.0375346028627,2.02616850345893));
#62819=CARTESIAN_POINT('Ctrl Pts',(-54.9168437793101,-13.8186488783651,
2.07850551037678));
#62820=CARTESIAN_POINT('Ctrl Pts',(-54.6273278627067,-15.5169944524465,
2.15701102075356));
#62821=CARTESIAN_POINT('Ctrl Pts',(-53.0510002557363,-16.2080728204287,
2.23551653113034));
#62822=CARTESIAN_POINT('Ctrl Pts',(-51.605113325188,-15.2764851170283,2.31402204150712));
#62823=CARTESIAN_POINT('Ctrl Pts',(-51.5846111642588,-13.5555692706413,
2.3925275518839));
#62824=CARTESIAN_POINT('Ctrl Pts',(-53.0087575469087,-12.5897418281553,
2.47103306226068));
#62825=CARTESIAN_POINT('Ctrl Pts',(-54.5999071972633,-13.2446527015669,
2.54953857263746));
#62826=CARTESIAN_POINT('Ctrl Pts',(-54.9312970207009,-14.9332249012822,
2.62804408301423));
#62827=CARTESIAN_POINT('Ctrl Pts',(-53.7056202382209,-16.1409758479641,
2.70654959339102));
#62828=CARTESIAN_POINT('Ctrl Pts',(-52.0221470001079,-15.7848310056966,
2.78505510376779));
#62829=CARTESIAN_POINT('Ctrl Pts',(-51.3906291820653,-14.1841570315506,
2.86356061414457));
#62830=CARTESIAN_POINT('Ctrl Pts',(-52.377440405223,-12.7744925974775,2.94206612452135));
#62831=CARTESIAN_POINT('Ctrl Pts',(-54.0975782126822,-12.8200502087089,
3.02057163489813));
#62832=CARTESIAN_POINT('Ctrl Pts',(-55.0083854595842,-14.2799767390429,
3.09907714527492));
#62833=CARTESIAN_POINT('Ctrl Pts',(-54.293026891849,-15.8449733636912,3.17758265565169));
#62834=CARTESIAN_POINT('Ctrl Pts',(-52.5930539078611,-16.1115149029785,
3.25608816602847));
#62835=CARTESIAN_POINT('Ctrl Pts',(-51.4330422815012,-14.8405600699842,
3.33459367640525));
#62836=CARTESIAN_POINT('Ctrl Pts',(-51.8533182226522,-13.1719316222439,
3.41309918678203));
#62837=CARTESIAN_POINT('Ctrl Pts',(-53.4769681733105,-12.6020950974316,
3.49160469715881));
#62838=CARTESIAN_POINT('Ctrl Pts',(-54.8478643087328,-13.642093499697,3.57011020753559));
#62839=CARTESIAN_POINT('Ctrl Pts',(-54.7365543580298,-15.3592315066375,
3.64861571791237));
#62840=CARTESIAN_POINT('Ctrl Pts',(-53.2428637439183,-16.2135389463141,
3.72712122828915));
#62841=CARTESIAN_POINT('Ctrl Pts',(-51.7063697132749,-15.4388525891942,
3.80562673866593));
#62842=CARTESIAN_POINT('Ctrl Pts',(-51.5050366439836,-13.7299295812751,
3.88413224904271));
#62843=CARTESIAN_POINT('Ctrl Pts',(-52.8194248174382,-12.6193727014466,
3.96263775941949));
#62844=CARTESIAN_POINT('Ctrl Pts',(-54.4707596726698,-13.1031557625362,
4.04114326979626));
#62845=CARTESIAN_POINT('Ctrl Pts',(-54.978084852892,-14.7474106134536,4.11964878017304));
#62846=CARTESIAN_POINT('Ctrl Pts',(-53.8864190756817,-16.0775304145121,
4.19815429054983));
#62847=CARTESIAN_POINT('Ctrl Pts',(-52.1747941628695,-15.9006321056092,
4.2766598009266));
#62848=CARTESIAN_POINT('Ctrl Pts',(-51.3782360277521,-14.3753622969642,
4.35516531130339));
#62849=CARTESIAN_POINT('Ctrl Pts',(-52.2111169431944,-12.8696192117061,
4.43367082168016));
#62850=CARTESIAN_POINT('Ctrl Pts',(-53.9264895031678,-12.7337890506155,
4.51217633205695));
#62851=CARTESIAN_POINT('Ctrl Pts',(-54.9859668161601,-14.0896875214679,
4.59068184243372));
#62852=CARTESIAN_POINT('Ctrl Pts',(-54.4393844383933,-15.7213126607523,
4.6691873528105));
#62853=CARTESIAN_POINT('Ctrl Pts',(-52.7769304442279,-16.1653842141838,
4.74769286318728));
#62854=CARTESIAN_POINT('Ctrl Pts',(-51.4895330907316,-15.0236483351254,
4.82619837356406));
#62855=CARTESIAN_POINT('Ctrl Pts',(-51.7317609456535,-13.3200407432483,
4.90470388394085));
#62856=CARTESIAN_POINT('Ctrl Pts',(-53.2863782799341,-12.5823975487372,
4.98320939431761));
#62857=CARTESIAN_POINT('Ctrl Pts',(-54.7591673697362,-13.4722540610765,
5.06171490469441));
#62858=CARTESIAN_POINT('Ctrl Pts',(-54.8292958244512,-15.1915670968036,
5.14022041507117));
#62859=CARTESIAN_POINT('Ctrl Pts',(-53.4338710221273,-16.1984132586634,
5.21872592544796));
#62860=CARTESIAN_POINT('Ctrl Pts',(-51.8243426112988,-15.5898341745865,
5.29723143582474));
#62861=CARTESIAN_POINT('Ctrl Pts',(-51.4441749154368,-13.9116075960113,
5.37573694620152));
#62862=CARTESIAN_POINT('Ctrl Pts',(-52.6343093950298,-12.6688279644592,
5.45424245657829));
#62863=CARTESIAN_POINT('Ctrl Pts',(-54.3274091023452,-12.976007562431,5.53274796695508));
#62864=CARTESIAN_POINT('Ctrl Pts',(-55.0050540475836,-14.5577447773064,
5.61125347733185));
#62865=CARTESIAN_POINT('Ctrl Pts',(-54.0595320288467,-15.9953308004788,
5.68975898770864));
#62866=CARTESIAN_POINT('Ctrl Pts',(-52.3387777758965,-15.9998439842325,
5.76826449808541));
#62867=CARTESIAN_POINT('Ctrl Pts',(-51.386068598834,-14.5665551393412,5.8467700084622));
#62868=CARTESIAN_POINT('Ctrl Pts',(-52.0556885439603,-12.9822402103746,
5.92527551883896));
#62869=CARTESIAN_POINT('Ctrl Pts',(-53.7473606277104,-12.6649964614199,
6.00378102921576));
#62870=CARTESIAN_POINT('Ctrl Pts',(-54.943474474887,-13.9049596945687,6.08228653959253));
#62871=CARTESIAN_POINT('Ctrl Pts',(-54.6954044415815,-15.0196330720529,
6.13462354651039));
#62872=CARTESIAN_POINT('Ctrl Pts',(-54.3642725509138,-15.404095589155,6.16079204996931));
#62873=CARTESIAN_POINT('Ctrl Pts',(-53.5696735389038,-12.996169774565,1.94640265001023));
#62874=CARTESIAN_POINT('Ctrl Pts',(-54.0303714687093,-13.11933387906,1.97257115346916));
#62875=CARTESIAN_POINT('Ctrl Pts',(-54.813258635941,-13.8534530528714,2.02490816038701));
#62876=CARTESIAN_POINT('Ctrl Pts',(-54.5411612077312,-15.4496190541765,
2.10341367076379));
#62877=CARTESIAN_POINT('Ctrl Pts',(-53.0596720623164,-16.099119257224,2.18191918114057));
#62878=CARTESIAN_POINT('Ctrl Pts',(-51.7007757366844,-15.2235797662662,
2.26042469151735));
#62879=CARTESIAN_POINT('Ctrl Pts',(-51.6815070715035,-13.6062014146337,
2.33893020189412));
#62880=CARTESIAN_POINT('Ctrl Pts',(-53.0199708515249,-12.6984821904956,
2.41743571227091));
#62881=CARTESIAN_POINT('Ctrl Pts',(-54.5153902842031,-13.3139908867102,
2.49594122264768));
#62882=CARTESIAN_POINT('Ctrl Pts',(-54.8268423098815,-14.9009715207264,
2.57444673302447));
#62883=CARTESIAN_POINT('Ctrl Pts',(-53.6749073688187,-16.0360591192444,
2.65295224340125));
#62884=CARTESIAN_POINT('Ctrl Pts',(-52.0927189215492,-15.7013414402026,
2.73145775377802));
#62885=CARTESIAN_POINT('Ctrl Pts',(-51.4991958566553,-14.1969707068861,
2.8099632641548));
#62886=CARTESIAN_POINT('Ctrl Pts',(-52.4266363894587,-12.8721175808469,
2.88846877453159));
#62887=CARTESIAN_POINT('Ctrl Pts',(-54.0432835122394,-12.9149342556498,
2.96697428490836));
#62888=CARTESIAN_POINT('Ctrl Pts',(-54.8992927858724,-14.2870255000261,
3.04547979528514));
#62889=CARTESIAN_POINT('Ctrl Pts',(-54.2269731814369,-15.7578653824051,
3.12398530566192));
#62890=CARTESIAN_POINT('Ctrl Pts',(-52.6292776820116,-16.0083706679245,
3.2024908160387));
#62891=CARTESIAN_POINT('Ctrl Pts',(-51.5390572066436,-14.8138817932341,
3.28099632641548));
#62892=CARTESIAN_POINT('Ctrl Pts',(-51.9340475894427,-13.2456450116627,
3.35950183679226));
#62893=CARTESIAN_POINT('Ctrl Pts',(-53.4600119684315,-12.7100922354268,
3.43800734716904));
#62894=CARTESIAN_POINT('Ctrl Pts',(-54.7484292588084,-13.6875199841967,
3.51651285754582));
#62895=CARTESIAN_POINT('Ctrl Pts',(-54.6438161802745,-15.3013477870039,
3.5950183679226));
#62896=CARTESIAN_POINT('Ctrl Pts',(-53.2399922406132,-16.104256518115,3.67352387829938));
#62897=CARTESIAN_POINT('Ctrl Pts',(-51.7959401169765,-15.3761785322325,
3.75202938867615));
#62898=CARTESIAN_POINT('Ctrl Pts',(-51.6067200871749,-13.7700714797477,
3.83053489905294));
#62899=CARTESIAN_POINT('Ctrl Pts',(-52.8420291709109,-12.7263303465236,
3.90904040942972));
#62900=CARTESIAN_POINT('Ctrl Pts',(-54.3940128148265,-13.1810069953183,
3.9875459198065));
#62901=CARTESIAN_POINT('Ctrl Pts',(-54.8708151904059,-14.7263365975901,
4.06605143018327));
#62902=CARTESIAN_POINT('Ctrl Pts',(-53.8448285920578,-15.9764308284185,
4.14455694056006));
#62903=CARTESIAN_POINT('Ctrl Pts',(-52.2361821925785,-15.8101754616262,
4.22306245093683));
#62904=CARTESIAN_POINT('Ctrl Pts',(-51.4875483263378,-14.3766722638491,
4.30156796131362));
#62905=CARTESIAN_POINT('Ctrl Pts',(-52.2703196425253,-12.9615209801128,
4.38007347169039));
#62906=CARTESIAN_POINT('Ctrl Pts',(-53.8824882150386,-12.8338629295998,
4.45857898206717));
#62907=CARTESIAN_POINT('Ctrl Pts',(-54.8782229417988,-14.1081848776325,
4.53708449244395));
#62908=CARTESIAN_POINT('Ctrl Pts',(-54.3645252458656,-15.6416446245447,
4.61559000282073));
#62909=CARTESIAN_POINT('Ctrl Pts',(-52.8020914369185,-16.0589989760686,
4.69409551319751));
#62910=CARTESIAN_POINT('Ctrl Pts',(-51.5921492925276,-14.9859547026092,
4.77260102357429));
#62911=CARTESIAN_POINT('Ctrl Pts',(-51.8198037066208,-13.3848432685065,
4.85110653395107));
#62912=CARTESIAN_POINT('Ctrl Pts',(-53.2808887601503,-12.6915797736435,
4.92961204432785));
#62913=CARTESIAN_POINT('Ctrl Pts',(-54.6650686986216,-13.527898796528,5.00811755470463));
#62914=CARTESIAN_POINT('Ctrl Pts',(-54.7309779322007,-15.1437707692933,
5.08662306508141));
#62915=CARTESIAN_POINT('Ctrl Pts',(-53.41950772211,-16.090040855094,5.16512857545819));
#62916=CARTESIAN_POINT('Ctrl Pts',(-51.9068152720538,-15.5180764339929,
5.24363408583497));
#62917=CARTESIAN_POINT('Ctrl Pts',(-51.5495200547613,-13.9408189852801,
5.32213959621175));
#62918=CARTESIAN_POINT('Ctrl Pts',(-52.6680510665282,-12.7728101740752,
5.40064510658852));
#62919=CARTESIAN_POINT('Ctrl Pts',(-54.2592868143519,-13.061508562707,5.47915061696532));
#62920=CARTESIAN_POINT('Ctrl Pts',(-54.8961618055507,-14.5480818513904,
5.55765612734208));
#62921=CARTESIAN_POINT('Ctrl Pts',(-54.0075263459451,-15.8991766869513,
5.63616163771887));
#62922=CARTESIAN_POINT('Ctrl Pts',(-52.3902998656125,-15.9034183386947,
5.71466714809564));
#62923=CARTESIAN_POINT('Ctrl Pts',(-51.494909657185,-14.5563621451974,5.79317265847243));
#62924=CARTESIAN_POINT('Ctrl Pts',(-52.1242424658418,-13.0673662284834,
5.8716781688492));
#62925=CARTESIAN_POINT('Ctrl Pts',(-53.7141364819045,-12.7692091902835,
5.950183679226));
#62926=CARTESIAN_POINT('Ctrl Pts',(-54.8382871174937,-13.9345710493921,
6.02868918960275));
#62927=CARTESIAN_POINT('Ctrl Pts',(-54.6051420149022,-14.9821810145562,
6.08102619652062));
#62928=CARTESIAN_POINT('Ctrl Pts',(-54.2939324036795,-15.3435126586808,
6.10719469997954));
#62929=CARTESIAN_POINT('Ctrl Pts',(-53.5456972794618,-13.0858534785527,
1.89280530002046));
#62930=CARTESIAN_POINT('Ctrl Pts',(-53.9769033408726,-13.2011331552573,
1.91897380347939));
#62931=CARTESIAN_POINT('Ctrl Pts',(-54.7096734925719,-13.8882572273778,
1.97131081039724));
#62932=CARTESIAN_POINT('Ctrl Pts',(-54.4549945527556,-15.3822436559065,
2.04981632077402));
#62933=CARTESIAN_POINT('Ctrl Pts',(-53.0683438688966,-15.9901656940193,
2.1283218311508));
#62934=CARTESIAN_POINT('Ctrl Pts',(-51.7964381481809,-15.1706744155041,
2.20682734152758));
#62935=CARTESIAN_POINT('Ctrl Pts',(-51.7784029787483,-13.6568335586262,
2.28533285190436));
#62936=CARTESIAN_POINT('Ctrl Pts',(-53.0311841561409,-12.807222552836,2.36383836228114));
#62937=CARTESIAN_POINT('Ctrl Pts',(-54.4308733711429,-13.3833290718535,
2.44234387265792));
#62938=CARTESIAN_POINT('Ctrl Pts',(-54.722387599062,-14.8687181401707,2.5208493830347));
#62939=CARTESIAN_POINT('Ctrl Pts',(-53.6441944994167,-15.9311423905248,
2.59935489341147));
#62940=CARTESIAN_POINT('Ctrl Pts',(-52.1632908429905,-15.6178518747085,
2.67786040378825));
#62941=CARTESIAN_POINT('Ctrl Pts',(-51.6077625312453,-14.2097843822215,
2.75636591416503));
#62942=CARTESIAN_POINT('Ctrl Pts',(-52.4758323736945,-12.9697425642164,
2.83487142454181));
#62943=CARTESIAN_POINT('Ctrl Pts',(-53.9889888117967,-13.0098183025906,
2.91337693491859));
#62944=CARTESIAN_POINT('Ctrl Pts',(-54.7902001121605,-14.2940742610093,
2.99188244529538));
#62945=CARTESIAN_POINT('Ctrl Pts',(-54.1609194710247,-15.670757401119,3.07038795567215));
#62946=CARTESIAN_POINT('Ctrl Pts',(-52.6655014561621,-15.9052264328705,
3.14889346604893));
#62947=CARTESIAN_POINT('Ctrl Pts',(-51.645072131786,-14.7872035164841,3.22739897642571));
#62948=CARTESIAN_POINT('Ctrl Pts',(-52.0147769562333,-13.3193584010815,
3.30590448680249));
#62949=CARTESIAN_POINT('Ctrl Pts',(-53.4430557635525,-12.818089373422,3.38440999717927));
#62950=CARTESIAN_POINT('Ctrl Pts',(-54.648994208884,-13.7329464686964,3.46291550755605));
#62951=CARTESIAN_POINT('Ctrl Pts',(-54.5510780025192,-15.2434640673703,
3.54142101793283));
#62952=CARTESIAN_POINT('Ctrl Pts',(-53.2371207373081,-15.9949740899159,
3.61992652830961));
#62953=CARTESIAN_POINT('Ctrl Pts',(-51.8855105206782,-15.3135044752707,
3.69843203868638));
#62954=CARTESIAN_POINT('Ctrl Pts',(-51.7084035303663,-13.8102133782203,
3.77693754906317));
#62955=CARTESIAN_POINT('Ctrl Pts',(-52.8646335243837,-12.8332879916007,
3.85544305943994));
#62956=CARTESIAN_POINT('Ctrl Pts',(-54.3172659569833,-13.2588582281004,
3.93394856981673));
#62957=CARTESIAN_POINT('Ctrl Pts',(-54.7635455279197,-14.7052625817266,
4.0124540801935));
#62958=CARTESIAN_POINT('Ctrl Pts',(-53.8032381084339,-15.875331242325,4.09095959057029));
#62959=CARTESIAN_POINT('Ctrl Pts',(-52.2975702222875,-15.7197188176431,
4.16946510094706));
#62960=CARTESIAN_POINT('Ctrl Pts',(-51.5968606249236,-14.377982230734,4.24797061132384));
#62961=CARTESIAN_POINT('Ctrl Pts',(-52.329522341856,-13.0534227485195,4.32647612170062));
#62962=CARTESIAN_POINT('Ctrl Pts',(-53.8384869269094,-12.9339368085841,
4.4049816320774));
#62963=CARTESIAN_POINT('Ctrl Pts',(-54.7704790674375,-14.1266822337971,
4.48348714245418));
#62964=CARTESIAN_POINT('Ctrl Pts',(-54.289666053338,-15.5619765883372,4.56199265283096));
#62965=CARTESIAN_POINT('Ctrl Pts',(-52.827252429609,-15.9526137379533,4.64049816320774));
#62966=CARTESIAN_POINT('Ctrl Pts',(-51.6947654943235,-14.9482610700929,
4.71900367358452));
#62967=CARTESIAN_POINT('Ctrl Pts',(-51.9078464675881,-13.4496457937646,
4.7975091839613));
#62968=CARTESIAN_POINT('Ctrl Pts',(-53.2753992403664,-12.8007619985498,
4.87601469433808));
#62969=CARTESIAN_POINT('Ctrl Pts',(-54.570970027507,-13.5835435319795,4.95452020471486));
#62970=CARTESIAN_POINT('Ctrl Pts',(-54.6326600399502,-15.095974441783,5.03302571509164));
#62971=CARTESIAN_POINT('Ctrl Pts',(-53.4051444220927,-15.9816684515245,
5.11153122546842));
#62972=CARTESIAN_POINT('Ctrl Pts',(-51.9892879328089,-15.4463186933993,
5.19003673584519));
#62973=CARTESIAN_POINT('Ctrl Pts',(-51.6548651940858,-13.970030374549,5.26854224622198));
#62974=CARTESIAN_POINT('Ctrl Pts',(-52.7017927380266,-12.8767923836913,
5.34704775659875));
#62975=CARTESIAN_POINT('Ctrl Pts',(-54.1911645263586,-13.147009562983,5.42555326697554));
#62976=CARTESIAN_POINT('Ctrl Pts',(-54.7872695635179,-14.5384189254744,
5.50405877735231));
#62977=CARTESIAN_POINT('Ctrl Pts',(-53.9555206630435,-15.8030225734238,
5.5825642877291));
#62978=CARTESIAN_POINT('Ctrl Pts',(-52.4418219553284,-15.806992693157,5.66106979810587));
#62979=CARTESIAN_POINT('Ctrl Pts',(-51.603750715536,-14.5461691510535,5.73957530848265));
#62980=CARTESIAN_POINT('Ctrl Pts',(-52.1927963877232,-13.1524922465921,
5.81808081885944));
#62981=CARTESIAN_POINT('Ctrl Pts',(-53.6809123360987,-12.8734219191469,
5.89658632923621));
#62982=CARTESIAN_POINT('Ctrl Pts',(-54.7330997601003,-13.9641824042154,
5.97509183961299));
#62983=CARTESIAN_POINT('Ctrl Pts',(-54.5148795882229,-14.9447289570596,
6.02742884653085));
#62984=CARTESIAN_POINT('Ctrl Pts',(-54.2235922564453,-15.2829297282066,
6.05359734998977));
#62985=CARTESIAN_POINT('Ctrl Pts',(-53.5217210200197,-13.1755371825403,
1.83920795003069));
#62986=CARTESIAN_POINT('Ctrl Pts',(-53.923435213036,-13.2829324314546,1.86537645348962));
#62987=CARTESIAN_POINT('Ctrl Pts',(-54.6060883492027,-13.9230614018842,
1.91771346040747));
#62988=CARTESIAN_POINT('Ctrl Pts',(-54.36882789778,-15.3148682576366,1.99621897078425));
#62989=CARTESIAN_POINT('Ctrl Pts',(-53.0770156754767,-15.8812121308145,
2.07472448116103));
#62990=CARTESIAN_POINT('Ctrl Pts',(-51.8921005596774,-15.1177690647421,
2.15322999153781));
#62991=CARTESIAN_POINT('Ctrl Pts',(-51.8752988859931,-13.7074657026186,
2.23173550191459));
#62992=CARTESIAN_POINT('Ctrl Pts',(-53.042397460757,-12.9159629151763,2.31024101229137));
#62993=CARTESIAN_POINT('Ctrl Pts',(-54.3463564580827,-13.4526672569968,
2.38874652266814));
#62994=CARTESIAN_POINT('Ctrl Pts',(-54.6179328882426,-14.836464759615,2.46725203304492));
#62995=CARTESIAN_POINT('Ctrl Pts',(-53.6134816300145,-15.8262256618051,
2.5457575434217));
#62996=CARTESIAN_POINT('Ctrl Pts',(-52.2338627644319,-15.5343623092145,
2.62426305379848));
#62997=CARTESIAN_POINT('Ctrl Pts',(-51.7163292058353,-14.222598057557,2.70276856417526));
#62998=CARTESIAN_POINT('Ctrl Pts',(-52.5250283579302,-13.0673675475858,
2.78127407455204));
#62999=CARTESIAN_POINT('Ctrl Pts',(-53.9346941113538,-13.1047023495315,
2.85977958492882));
#63000=CARTESIAN_POINT('Ctrl Pts',(-54.6811074384486,-14.3011230219925,
2.9382850953056));
#63001=CARTESIAN_POINT('Ctrl Pts',(-54.0948657606126,-15.5836494198329,
3.01679060568238));
#63002=CARTESIAN_POINT('Ctrl Pts',(-52.7017252303126,-15.8020821978166,
3.09529611605916));
#63003=CARTESIAN_POINT('Ctrl Pts',(-51.7510870569284,-14.7605252397341,
3.17380162643594));
#63004=CARTESIAN_POINT('Ctrl Pts',(-52.0955063230238,-13.3930717905004,
3.25230713681272));
#63005=CARTESIAN_POINT('Ctrl Pts',(-53.4260995586735,-12.9260865114173,
3.33081264718949));
#63006=CARTESIAN_POINT('Ctrl Pts',(-54.5495591589596,-13.7783729531961,
3.40931815756628));
#63007=CARTESIAN_POINT('Ctrl Pts',(-54.4583398247639,-15.1855803477368,
3.48782366794305));
#63008=CARTESIAN_POINT('Ctrl Pts',(-53.234249234003,-15.8856916617167,3.56632917831984));
#63009=CARTESIAN_POINT('Ctrl Pts',(-51.9750809243799,-15.250830418309,3.64483468869661));
#63010=CARTESIAN_POINT('Ctrl Pts',(-51.8100869735576,-13.8503552766928,
3.7233401990734));
#63011=CARTESIAN_POINT('Ctrl Pts',(-52.8872378778566,-12.9402456366778,
3.80184570945017));
#63012=CARTESIAN_POINT('Ctrl Pts',(-54.24051909914,-13.3367094608825,3.88035121982696));
#63013=CARTESIAN_POINT('Ctrl Pts',(-54.6562758654336,-14.6841885658631,
3.95885673020373));
#63014=CARTESIAN_POINT('Ctrl Pts',(-53.7616476248099,-15.7742316562315,
4.03736224058052));
#63015=CARTESIAN_POINT('Ctrl Pts',(-52.3589582519965,-15.6292621736601,
4.11586775095729));
#63016=CARTESIAN_POINT('Ctrl Pts',(-51.7061729235092,-14.3792921976189,
4.19437326133407));
#63017=CARTESIAN_POINT('Ctrl Pts',(-52.3887250411869,-13.1453245169262,
4.27287877171085));
#63018=CARTESIAN_POINT('Ctrl Pts',(-53.7944856387802,-13.0340106875684,
4.35138428208763));
#63019=CARTESIAN_POINT('Ctrl Pts',(-54.6627351930762,-14.1451795899616,
4.42988979246442));
#63020=CARTESIAN_POINT('Ctrl Pts',(-54.2148068608104,-15.4823085521296,
4.50839530284119));
#63021=CARTESIAN_POINT('Ctrl Pts',(-52.8524134222996,-15.8462284998381,
4.58690081321797));
#63022=CARTESIAN_POINT('Ctrl Pts',(-51.7973816961194,-14.9105674375766,
4.66540632359475));
#63023=CARTESIAN_POINT('Ctrl Pts',(-51.9958892285554,-13.5144483190228,
4.74391183397153));
#63024=CARTESIAN_POINT('Ctrl Pts',(-53.2699097205826,-12.9099442234561,
4.82241734434831));
#63025=CARTESIAN_POINT('Ctrl Pts',(-54.4768713563924,-13.6391882674309,
4.90092285472509));
#63026=CARTESIAN_POINT('Ctrl Pts',(-54.5343421476998,-15.0481781142727,
4.97942836510187));
#63027=CARTESIAN_POINT('Ctrl Pts',(-53.3907811220752,-15.873296047955,5.05793387547865));
#63028=CARTESIAN_POINT('Ctrl Pts',(-52.0717605935641,-15.3745609528058,
5.13643938585542));
#63029=CARTESIAN_POINT('Ctrl Pts',(-51.7602103334102,-13.9992417638178,
5.21494489623221));
#63030=CARTESIAN_POINT('Ctrl Pts',(-52.7355344095251,-12.9807745933074,
5.29345040660898));
#63031=CARTESIAN_POINT('Ctrl Pts',(-54.1230422383652,-13.232510563259,5.37195591698577));
#63032=CARTESIAN_POINT('Ctrl Pts',(-54.6783773214851,-14.5287559995584,
5.45046142736254));
#63033=CARTESIAN_POINT('Ctrl Pts',(-53.9035149801418,-15.7068684598963,
5.52896693773933));
#63034=CARTESIAN_POINT('Ctrl Pts',(-52.4933440450442,-15.7105670476193,
5.60747244811611));
#63035=CARTESIAN_POINT('Ctrl Pts',(-51.712591773887,-14.5359761569097,5.68597795849288));
#63036=CARTESIAN_POINT('Ctrl Pts',(-52.2613503096046,-13.2376182647008,
5.76448346886967));
#63037=CARTESIAN_POINT('Ctrl Pts',(-53.6476881902928,-12.9776346480105,
5.84298897924644));
#63038=CARTESIAN_POINT('Ctrl Pts',(-54.6279124027069,-13.9937937590388,
5.92149448962322));
#63039=CARTESIAN_POINT('Ctrl Pts',(-54.4246171615437,-14.9072768995629,
5.97383149654108));
#63040=CARTESIAN_POINT('Ctrl Pts',(-54.153252109211,-15.2223467977324,6.));
#63041=CARTESIAN_POINT('Ctrl Pts',(-54.4588409672492,-14.3981450852038,
2.44341967361942));
#63042=CARTESIAN_POINT('Ctrl Pts',(-54.4598231909075,-14.5245548856247,
2.45136379342792));
#63043=CARTESIAN_POINT('Ctrl Pts',(-54.4423420959139,-14.6506995799382,
2.45930791323642));
#63044=CARTESIAN_POINT('Ctrl Pts',(-54.4052616068446,-14.770791992877,2.46725203304492));
#63045=CARTESIAN_POINT('Ctrl Pts',(-54.2831158021666,-15.166385060345,2.49342053650385));
#63046=CARTESIAN_POINT('Ctrl Pts',(-53.9482987160905,-15.4963053610751,
2.51958903996278));
#63047=CARTESIAN_POINT('Ctrl Pts',(-53.5509536954554,-15.6126216193417,
2.5457575434217));
#63048=CARTESIAN_POINT('Ctrl Pts',(-53.1536086748203,-15.7289378776082,
2.57192604688063));
#63049=CARTESIAN_POINT('Ctrl Pts',(-52.6937357196261,-15.6316500934114,
2.59809455033956));
#63050=CARTESIAN_POINT('Ctrl Pts',(-52.3775436489295,-15.3643788260367,
2.62426305379848));
#63051=CARTESIAN_POINT('Ctrl Pts',(-52.061351578233,-15.097107558662,2.65043155725741));
#63052=CARTESIAN_POINT('Ctrl Pts',(-51.8888403920341,-14.6598528081095,
2.67660006071634));
#63053=CARTESIAN_POINT('Ctrl Pts',(-51.9373679909505,-14.2486870145047,
2.70276856417526));
#63054=CARTESIAN_POINT('Ctrl Pts',(-51.9858955898669,-13.8375212208999,
2.72893706763419));
#63055=CARTESIAN_POINT('Ctrl Pts',(-52.2554619738986,-13.4524443842429,
2.75510557109312));
#63056=CARTESIAN_POINT('Ctrl Pts',(-52.6251894581517,-13.2661284329053,
2.78127407455204));
#63057=CARTESIAN_POINT('Ctrl Pts',(-52.9949169424048,-13.0798124815677,
2.80744257801097));
#63058=CARTESIAN_POINT('Ctrl Pts',(-53.4648055268793,-13.0922574155496,
2.8336110814699));
#63059=CARTESIAN_POINT('Ctrl Pts',(-53.824152040299,-13.2978833279507,2.85977958492882));
#63060=CARTESIAN_POINT('Ctrl Pts',(-54.1834985537188,-13.5035092403518,
2.88594808838775));
#63061=CARTESIAN_POINT('Ctrl Pts',(-54.4323029960837,-13.9023161311722,
2.91211659184667));
#63062=CARTESIAN_POINT('Ctrl Pts',(-54.4589982709601,-14.3154739762224,
2.9382850953056));
#63063=CARTESIAN_POINT('Ctrl Pts',(-54.4607442500488,-14.342496172514,2.93999662141021));
#63064=CARTESIAN_POINT('Ctrl Pts',(-54.4615401150314,-14.3695797577353,
2.94170814751481));
#63065=CARTESIAN_POINT('Ctrl Pts',(-54.4614103817624,-14.3966710984295,
2.94341967361941));
#63066=CARTESIAN_POINT('Ctrl Pts',(-53.5936497983459,-12.9064860705774,
2.));
#63067=CARTESIAN_POINT('Ctrl Pts',(-53.6510872607052,-12.9274734829173,
2.));
#63068=CARTESIAN_POINT('Ctrl Pts',(-53.7069621322555,-12.9520730502145,
2.));
#63069=CARTESIAN_POINT('Ctrl Pts',(-53.7610764088156,-12.9799849419358,
2.));
#63070=CARTESIAN_POINT('Ctrl Pts',(-53.8148756915178,-13.0077343612928,
2.));
#63071=CARTESIAN_POINT('Ctrl Pts',(-53.8669355047625,-13.0387586838187,
2.));
#63072=CARTESIAN_POINT('Ctrl Pts',(-53.9170293533882,-13.0728080082455,
2.));
#63073=CARTESIAN_POINT('Ctrl Pts',(-53.9548563761379,-13.098519439989,2.));
#63074=CARTESIAN_POINT('Ctrl Pts',(-53.9915618038204,-13.125956761284,2.));
#63075=CARTESIAN_POINT('Ctrl Pts',(-54.0270323602658,-13.1550241879182,
2.));
#63076=CARTESIAN_POINT('Ctrl Pts',(-54.0454462553227,-13.1701140144463,
2.));
#63077=CARTESIAN_POINT('Ctrl Pts',(-54.0635271127833,-13.1856432908818,
2.));
#63078=CARTESIAN_POINT('Ctrl Pts',(-54.0812573827313,-13.2015993500242,
2.));
#63079=CARTESIAN_POINT('Ctrl Pts',(-54.090594739605,-13.210002347776,2.));
#63080=CARTESIAN_POINT('Ctrl Pts',(-54.0998362160445,-13.2185251993375,
2.));
#63081=CARTESIAN_POINT('Ctrl Pts',(-54.1089630227178,-13.22715034206,2.));
#63082=CARTESIAN_POINT('Ctrl Pts',(-54.1519916743795,-13.2678138813483,
2.));
#63083=CARTESIAN_POINT('Ctrl Pts',(-54.1925581151182,-13.3108214912836,
2.));
#63084=CARTESIAN_POINT('Ctrl Pts',(-54.2304545251372,-13.3559335739759,
2.));
#63085=CARTESIAN_POINT('Ctrl Pts',(-54.2675766912808,-13.4001239927502,
2.));
#63086=CARTESIAN_POINT('Ctrl Pts',(-54.3021372565952,-13.4463347100088,
2.));
#63087=CARTESIAN_POINT('Ctrl Pts',(-54.3338978256666,-13.494363501403,2.));
#63088=CARTESIAN_POINT('Ctrl Pts',(-54.3568895198966,-13.5291318735784,
2.));
#63089=CARTESIAN_POINT('Ctrl Pts',(-54.3784130414151,-13.5648534993358,
2.));
#63090=CARTESIAN_POINT('Ctrl Pts',(-54.3983614304231,-13.6014553927541,
2.));
#63091=CARTESIAN_POINT('Ctrl Pts',(-54.4087875591048,-13.6205855616426,
2.));
#63092=CARTESIAN_POINT('Ctrl Pts',(-54.4187831681,-13.6399562243591,2.));
#63093=CARTESIAN_POINT('Ctrl Pts',(-54.4283312993198,-13.6595570483555,
2.));
#63094=CARTESIAN_POINT('Ctrl Pts',(-54.4327718218402,-13.6686727484199,
2.));
#63095=CARTESIAN_POINT('Ctrl Pts',(-54.4371132830006,-13.6778337205283,
2.));
#63096=CARTESIAN_POINT('Ctrl Pts',(-54.4413510256536,-13.6870315207414,
2.));
#63097=CARTESIAN_POINT('Ctrl Pts',(-54.4646885493226,-13.7376844031253,
2.));
#63098=CARTESIAN_POINT('Ctrl Pts',(-54.4849171741929,-13.7895200078225,
2.));
#63099=CARTESIAN_POINT('Ctrl Pts',(-54.5018239463819,-13.842348125432,2.));
#63100=CARTESIAN_POINT('Ctrl Pts',(-54.5131364715696,-13.877696056095,2.));
#63101=CARTESIAN_POINT('Ctrl Pts',(-54.5229608260229,-13.9134887100352,
2.));
#63102=CARTESIAN_POINT('Ctrl Pts',(-54.5312202420661,-13.9496710849604,
2.));
#63103=CARTESIAN_POINT('Ctrl Pts',(-54.5434447189016,-14.0032233702325,
2.));
#63104=CARTESIAN_POINT('Ctrl Pts',(-54.5522427226731,-14.0576303083872,
2.));
#63105=CARTESIAN_POINT('Ctrl Pts',(-54.5576688283951,-14.1125811869758,
2.));
#63106=CARTESIAN_POINT('Ctrl Pts',(-54.5593446193985,-14.1295521404892,
2.));
#63107=CARTESIAN_POINT('Ctrl Pts',(-54.5606984801866,-14.1465748861851,
2.));
#63108=CARTESIAN_POINT('Ctrl Pts',(-54.5617312008432,-14.1636399587011,
2.));
#63109=CARTESIAN_POINT('Ctrl Pts',(-54.5626375347856,-14.1786165686416,
2.));
#63110=CARTESIAN_POINT('Ctrl Pts',(-54.5632965181387,-14.1936323469849,
2.));
#63111=CARTESIAN_POINT('Ctrl Pts',(-54.563708005032,-14.2086448003678,2.));
#63112=CARTESIAN_POINT('Ctrl Pts',(-54.5652337512305,-14.264309255436,2.));
#63113=CARTESIAN_POINT('Ctrl Pts',(-54.5633684846619,-14.3200027126482,
2.));
#63114=CARTESIAN_POINT('Ctrl Pts',(-54.5582160449935,-14.3754072804874,
2.));
#63115=CARTESIAN_POINT('Ctrl Pts',(-54.553069811687,-14.4307451108539,2.));
#63116=CARTESIAN_POINT('Ctrl Pts',(-54.5446438644364,-14.4857958885223,
2.));
#63117=CARTESIAN_POINT('Ctrl Pts',(-54.5329924871079,-14.540227530455,2.));
#63118=CARTESIAN_POINT('Ctrl Pts',(-54.5255451328249,-14.5750192731178,
2.));
#63119=CARTESIAN_POINT('Ctrl Pts',(-54.5167790477671,-14.6095577033572,
2.));
#63120=CARTESIAN_POINT('Ctrl Pts',(-54.5066991329777,-14.6437495917827,
2.));
#63121=CARTESIAN_POINT('Ctrl Pts',(-54.501505292656,-14.6613675193633,2.));
#63122=CARTESIAN_POINT('Ctrl Pts',(-54.495962519931,-14.6788933419033,2.));
#63123=CARTESIAN_POINT('Ctrl Pts',(-54.4900708072911,-14.6963135911257,
2.));
#63124=CARTESIAN_POINT('Ctrl Pts',(-54.4865172473944,-14.706820535848,2.));
#63125=CARTESIAN_POINT('Ctrl Pts',(-54.4828368476645,-14.7172884125542,
2.));
#63126=CARTESIAN_POINT('Ctrl Pts',(-54.4790344473056,-14.7277017730835,
2.));
#63127=CARTESIAN_POINT('Ctrl Pts',(-54.4606465121879,-14.7780594891827,
2.));
#63128=CARTESIAN_POINT('Ctrl Pts',(-54.4393828187194,-14.8272228509927,
2.));
#63129=CARTESIAN_POINT('Ctrl Pts',(-54.4152842461416,-14.8748779184924,
2.));
#63130=CARTESIAN_POINT('Ctrl Pts',(-54.4001512378088,-14.9048035305279,
2.));
#63131=CARTESIAN_POINT('Ctrl Pts',(-54.3838995195653,-14.9341338196321,
2.));
#63132=CARTESIAN_POINT('Ctrl Pts',(-54.3665318698004,-14.9627834478566,
2.));
#63133=CARTESIAN_POINT('Ctrl Pts',(-54.3601820700066,-14.9732580604758,
2.));
#63134=CARTESIAN_POINT('Ctrl Pts',(-54.3536816777358,-14.9836437343855,
2.));
#63135=CARTESIAN_POINT('Ctrl Pts',(-54.347035206222,-14.9939290625586,2.));
#63136=CARTESIAN_POINT('Ctrl Pts',(-54.3191335463697,-15.0371065180788,
2.));
#63137=CARTESIAN_POINT('Ctrl Pts',(-54.2887053621836,-15.0784511646849,
2.));
#63138=CARTESIAN_POINT('Ctrl Pts',(-54.2557752605174,-15.1176640701704,
2.));
#63139=CARTESIAN_POINT('Ctrl Pts',(-54.2373775276085,-15.1395719454944,
2.));
#63140=CARTESIAN_POINT('Ctrl Pts',(-54.2181982612199,-15.1608137789775,
2.));
#63141=CARTESIAN_POINT('Ctrl Pts',(-54.1982376363281,-15.1813315747386,
2.));
#63142=CARTESIAN_POINT('Ctrl Pts',(-54.1842200551681,-15.1957404356268,
2.));
#63143=CARTESIAN_POINT('Ctrl Pts',(-54.1698170448365,-15.2097921118142,
2.));
#63144=CARTESIAN_POINT('Ctrl Pts',(-54.1550457523822,-15.2234791283661,
2.));
#63145=CARTESIAN_POINT('Origin',(-53.1951359564886,-14.3971354987959,4.5));
#63146=CARTESIAN_POINT('Origin',(-39.0658530619283,38.8697713466882,6.));
#63147=CARTESIAN_POINT('Ctrl Pts',(-40.2595650866585,39.2869186252538,6.));
#63148=CARTESIAN_POINT('Ctrl Pts',(-40.2480819791952,39.3364939464135,6.));
#63149=CARTESIAN_POINT('Ctrl Pts',(-40.2334065100549,39.3851618422748,6.));
#63150=CARTESIAN_POINT('Ctrl Pts',(-40.2158026351646,39.4327533922847,6.));
#63151=CARTESIAN_POINT('Ctrl Pts',(-40.2039391979396,39.46482584051,6.));
#63152=CARTESIAN_POINT('Ctrl Pts',(-40.1907446643331,39.4964096047136,6.));
#63153=CARTESIAN_POINT('Ctrl Pts',(-40.1762870855865,39.5274524411797,6.));
#63154=CARTESIAN_POINT('Ctrl Pts',(-40.1696136376379,39.5417814486133,6.));
#63155=CARTESIAN_POINT('Ctrl Pts',(-40.1626709449503,39.5559951857844,6.));
#63156=CARTESIAN_POINT('Ctrl Pts',(-40.1554650290934,39.5700883780353,6.));
#63157=CARTESIAN_POINT('Ctrl Pts',(-40.1494095391196,39.5819315893728,6.));
#63158=CARTESIAN_POINT('Ctrl Pts',(-40.1431714820768,39.5936830081174,6.));
#63159=CARTESIAN_POINT('Ctrl Pts',(-40.1367585398302,39.6053334444843,6.));
#63160=CARTESIAN_POINT('Ctrl Pts',(-40.1108375205617,39.6524243387947,6.));
#63161=CARTESIAN_POINT('Ctrl Pts',(-40.082047067269,39.6978983470816,6.));
#63162=CARTESIAN_POINT('Ctrl Pts',(-40.0506487799185,39.741559756634,6.));
#63163=CARTESIAN_POINT('Ctrl Pts',(-40.0386313329921,39.7582708168956,6.));
#63164=CARTESIAN_POINT('Ctrl Pts',(-40.0262313128106,39.7747162395881,6.));
#63165=CARTESIAN_POINT('Ctrl Pts',(-40.0134614554123,39.7908844940418,6.));
#63166=CARTESIAN_POINT('Ctrl Pts',(-40.0042845094518,39.8025036682244,6.));
#63167=CARTESIAN_POINT('Ctrl Pts',(-39.9949165410966,39.8139796930109,6.));
#63168=CARTESIAN_POINT('Ctrl Pts',(-39.9853619687604,39.8253081417074,6.));
#63169=CARTESIAN_POINT('Ctrl Pts',(-39.9779669485307,39.8340761016259,6.));
#63170=CARTESIAN_POINT('Ctrl Pts',(-39.970459801146,39.8427558568435,6.));
#63171=CARTESIAN_POINT('Ctrl Pts',(-39.9628530937736,39.8513338610673,6.));
#63172=CARTESIAN_POINT('Ctrl Pts',(-39.9252574596781,39.8937300638237,6.));
#63173=CARTESIAN_POINT('Ctrl Pts',(-39.8851758119764,39.9337126572018,6.));
#63174=CARTESIAN_POINT('Ctrl Pts',(-39.8429000970909,39.9710687870014,6.));
#63175=CARTESIAN_POINT('Ctrl Pts',(-39.8012367829931,40.0078837805156,6.));
#63176=CARTESIAN_POINT('Ctrl Pts',(-39.7574416833132,40.0421487782755,6.));
#63177=CARTESIAN_POINT('Ctrl Pts',(-39.7117463596714,40.0736370674662,6.));
#63178=CARTESIAN_POINT('Ctrl Pts',(-39.6878846430372,40.0900799892815,6.));
#63179=CARTESIAN_POINT('Ctrl Pts',(-39.6635040440514,40.1057652810441,6.));
#63180=CARTESIAN_POINT('Ctrl Pts',(-39.6386333596486,40.120656825884,6.));
#63181=CARTESIAN_POINT('Ctrl Pts',(-39.6252910649646,40.1286456442187,6.));
#63182=CARTESIAN_POINT('Ctrl Pts',(-39.6118076808291,40.1364059738324,6.));
#63183=CARTESIAN_POINT('Ctrl Pts',(-39.5981873691344,40.1439318477466,6.));
#63184=CARTESIAN_POINT('Ctrl Pts',(-39.5885046150635,40.1492820326699,6.));
#63185=CARTESIAN_POINT('Ctrl Pts',(-39.5787526555666,40.1545137210612,6.));
#63186=CARTESIAN_POINT('Ctrl Pts',(-39.5689329316873,40.1596246755939,6.));
#63187=CARTESIAN_POINT('Ctrl Pts',(-39.5602883878672,40.1641239742467,6.));
#63188=CARTESIAN_POINT('Ctrl Pts',(-39.5516000264324,40.1685251725109,6.));
#63189=CARTESIAN_POINT('Ctrl Pts',(-39.5428697390936,40.1728269741793,6.));
#63190=CARTESIAN_POINT('Ctrl Pts',(-39.4996812011584,40.1941078916718,6.));
#63191=CARTESIAN_POINT('Ctrl Pts',(-39.4554640759948,40.2129597963788,6.));
#63192=CARTESIAN_POINT('Ctrl Pts',(-39.4103710639644,40.2292497271407,6.));
#63193=CARTESIAN_POINT('Ctrl Pts',(-39.3590466351126,40.2477907683076,6.));
#63194=CARTESIAN_POINT('Ctrl Pts',(-39.3065877413218,40.2630147095083,6.));
#63195=CARTESIAN_POINT('Ctrl Pts',(-39.2532910929857,40.2750393024528,6.));
#63196=CARTESIAN_POINT('Ctrl Pts',(-39.2011942210287,40.286793206282,6.));
#63197=CARTESIAN_POINT('Ctrl Pts',(-39.148296003785,40.2954900228404,6.));
#63198=CARTESIAN_POINT('Ctrl Pts',(-39.0948540754983,40.3011985092876,6.));
#63199=CARTESIAN_POINT('Ctrl Pts',(-39.0817639227262,40.3025967552359,6.));
#63200=CARTESIAN_POINT('Ctrl Pts',(-39.0686410906115,40.3038155206662,6.));
#63201=CARTESIAN_POINT('Ctrl Pts',(-39.0554892737564,40.3048554432527,6.));
#63202=CARTESIAN_POINT('Ctrl Pts',(-39.0455592030118,40.3056406203098,6.));
#63203=CARTESIAN_POINT('Ctrl Pts',(-39.0356145768843,40.306323605614,6.));
#63204=CARTESIAN_POINT('Ctrl Pts',(-39.0256685188148,40.3069043036838,6.));
#63205=CARTESIAN_POINT('Ctrl Pts',(-38.9681511420326,40.3102624410931,6.));
#63206=CARTESIAN_POINT('Ctrl Pts',(-38.9104821865459,40.3102125489983,6.));
#63207=CARTESIAN_POINT('Ctrl Pts',(-38.8529878289339,40.3068889012295,6.));
#63208=CARTESIAN_POINT('Ctrl Pts',(-38.7942601302541,40.3034939561811,6.));
#63209=CARTESIAN_POINT('Ctrl Pts',(-38.7357135780205,40.2966834252177,6.));
#63210=CARTESIAN_POINT('Ctrl Pts',(-38.6776775933238,40.2865489627448,6.));
#63211=CARTESIAN_POINT('Ctrl Pts',(-38.6191308064349,40.276325302067,6.));
#63212=CARTESIAN_POINT('Ctrl Pts',(-38.561102428243,40.2627189748103,6.));
#63213=CARTESIAN_POINT('Ctrl Pts',(-38.5039291823866,40.2457711881153,6.));
#63214=CARTESIAN_POINT('Ctrl Pts',(-38.4909781937364,40.2419321443485,6.));
#63215=CARTESIAN_POINT('Ctrl Pts',(-38.4780675599091,40.2379201262253,6.));
#63216=CARTESIAN_POINT('Ctrl Pts',(-38.4652269238002,40.2337440113392,6.));
#63217=CARTESIAN_POINT('Ctrl Pts',(-38.4073726902873,40.2149282826056,6.));
#63218=CARTESIAN_POINT('Ctrl Pts',(-38.3508402271714,40.1927581042671,6.));
#63219=CARTESIAN_POINT('Ctrl Pts',(-38.2959735972823,40.1673423641079,6.));
#63220=CARTESIAN_POINT('Ctrl Pts',(-38.2415891999933,40.142150007424,6.));
#63221=CARTESIAN_POINT('Ctrl Pts',(-38.1888403165397,40.1137687287949,6.));
#63222=CARTESIAN_POINT('Ctrl Pts',(-38.1380651655577,40.0822545048966,6.));
#63223=CARTESIAN_POINT('Ctrl Pts',(-38.1008618422864,40.0591638033102,6.));
#63224=CARTESIAN_POINT('Ctrl Pts',(-38.0647181228981,40.0343901127421,6.));
#63225=CARTESIAN_POINT('Ctrl Pts',(-38.0297736279237,40.0079388493487,6.));
#63226=CARTESIAN_POINT('Ctrl Pts',(-38.0103531401622,39.9932384956196,6.));
#63227=CARTESIAN_POINT('Ctrl Pts',(-37.9913031820638,39.978019748027,6.));
#63228=CARTESIAN_POINT('Ctrl Pts',(-37.972630261787,39.9623020734811,6.));
#63229=CARTESIAN_POINT('Ctrl Pts',(-37.5756558680257,39.2699729499894,6.));
#63230=CARTESIAN_POINT('Ctrl Pts',(-37.5651290682188,39.2098300642739,6.));
#63231=CARTESIAN_POINT('Ctrl Pts',(-37.5584870272447,39.1491583710678,6.));
#63232=CARTESIAN_POINT('Ctrl Pts',(-37.5555980370803,39.0882817362078,6.));
#63233=CARTESIAN_POINT('Ctrl Pts',(-37.5529191835609,39.0318330886644,6.));
#63234=CARTESIAN_POINT('Ctrl Pts',(-37.5534681438705,38.9752074993239,6.));
#63235=CARTESIAN_POINT('Ctrl Pts',(-37.5571795337599,38.9186719371971,6.));
#63236=CARTESIAN_POINT('Ctrl Pts',(-37.5580753630163,38.9050257798038,6.));
#63237=CARTESIAN_POINT('Ctrl Pts',(-37.5591557658557,38.8913844979252,6.));
#63238=CARTESIAN_POINT('Ctrl Pts',(-37.5604183353195,38.8777672140557,6.));
#63239=CARTESIAN_POINT('Ctrl Pts',(-37.5659749115735,38.8178374609894,6.));
#63240=CARTESIAN_POINT('Ctrl Pts',(-37.5750599728648,38.7582987522682,6.));
#63241=CARTESIAN_POINT('Ctrl Pts',(-37.587576042244,38.6994723221795,6.));
#63242=CARTESIAN_POINT('Ctrl Pts',(-37.5953014146754,38.6631625137662,6.));
#63243=CARTESIAN_POINT('Ctrl Pts',(-37.6043349305766,38.6271243505451,6.));
#63244=CARTESIAN_POINT('Ctrl Pts',(-37.6146623853363,38.591438145786,6.));
#63245=CARTESIAN_POINT('Ctrl Pts',(-37.6181962247196,38.5792270716391,6.));
#63246=CARTESIAN_POINT('Ctrl Pts',(-37.6218816203987,38.56705724719,6.));
#63247=CARTESIAN_POINT('Ctrl Pts',(-37.6257181655827,38.5549320256251,6.));
#63248=CARTESIAN_POINT('Ctrl Pts',(-37.6293072145904,38.5435890041466,6.));
#63249=CARTESIAN_POINT('Ctrl Pts',(-37.6330262982585,38.5322922610546,6.));
#63250=CARTESIAN_POINT('Ctrl Pts',(-37.636872579215,38.5210500434267,6.));
#63251=CARTESIAN_POINT('Ctrl Pts',(-37.6559105736999,38.4654042703744,6.));
#63252=CARTESIAN_POINT('Ctrl Pts',(-37.6780754632208,38.4110469589651,6.));
#63253=CARTESIAN_POINT('Ctrl Pts',(-37.7032762357134,38.3582791323017,6.));
#63254=CARTESIAN_POINT('Ctrl Pts',(-37.7278335946531,38.3068585474672,6.));
#63255=CARTESIAN_POINT('Ctrl Pts',(-37.7552744012006,38.2569465430614,6.));
#63256=CARTESIAN_POINT('Ctrl Pts',(-37.7855529342765,38.2088521687025,6.));
#63257=CARTESIAN_POINT('Ctrl Pts',(-37.8019690565523,38.1827768258755,6.));
#63258=CARTESIAN_POINT('Ctrl Pts',(-37.8192199432012,38.1572363736183,6.));
#63259=CARTESIAN_POINT('Ctrl Pts',(-37.8373023126813,38.1322851555406,6.));
#63260=CARTESIAN_POINT('Ctrl Pts',(-37.8523464601685,38.1115262718578,6.));
#63261=CARTESIAN_POINT('Ctrl Pts',(-37.8679662045719,38.0911753045226,6.));
#63262=CARTESIAN_POINT('Ctrl Pts',(-37.884160961773,38.0712658190693,6.));
#63263=CARTESIAN_POINT('Ctrl Pts',(-37.8910830994387,38.0627558922177,6.));
#63264=CARTESIAN_POINT('Ctrl Pts',(-37.8981112327979,38.0543257382737,6.));
#63265=CARTESIAN_POINT('Ctrl Pts',(-37.9052335275561,38.0459914463568,6.));
#63266=CARTESIAN_POINT('Ctrl Pts',(-37.9382051680373,38.0074090391303,6.));
#63267=CARTESIAN_POINT('Ctrl Pts',(-37.9732473043227,37.970810355559,6.));
#63268=CARTESIAN_POINT('Ctrl Pts',(-38.0103191942679,37.9364107324676,6.));
#63269=CARTESIAN_POINT('Ctrl Pts',(-38.0517460905842,37.8979700265516,6.));
#63270=CARTESIAN_POINT('Ctrl Pts',(-38.0957081060159,37.8622743231261,6.));
#63271=CARTESIAN_POINT('Ctrl Pts',(-38.1418690155727,37.8294138953178,6.));
#63272=CARTESIAN_POINT('Ctrl Pts',(-38.181041165507,37.8015285347958,6.));
#63273=CARTESIAN_POINT('Ctrl Pts',(-38.2217977223924,37.775685634311,6.));
#63274=CARTESIAN_POINT('Ctrl Pts',(-38.2639408148789,37.7519688192016,6.));
#63275=CARTESIAN_POINT('Ctrl Pts',(-38.2755270772501,37.7454484329116,6.));
#63276=CARTESIAN_POINT('Ctrl Pts',(-38.287218151903,37.7390889037126,6.));
#63277=CARTESIAN_POINT('Ctrl Pts',(-38.299009928843,37.7328923323578,6.));
#63278=CARTESIAN_POINT('Ctrl Pts',(-38.3081902153401,37.7280680975859,6.));
#63279=CARTESIAN_POINT('Ctrl Pts',(-38.31743317901,37.7233419167043,6.));
#63280=CARTESIAN_POINT('Ctrl Pts',(-38.3267216243912,37.7187221450337,6.));
#63281=CARTESIAN_POINT('Ctrl Pts',(-38.3764239787938,37.6940018049334,6.));
#63282=CARTESIAN_POINT('Ctrl Pts',(-38.427517840694,37.6722751487084,6.));
#63283=CARTESIAN_POINT('Ctrl Pts',(-38.4796831982367,37.6536175541641,6.));
#63284=CARTESIAN_POINT('Ctrl Pts',(-38.5315566484918,37.6350643639232,6.));
#63285=CARTESIAN_POINT('Ctrl Pts',(-38.5844908266812,37.6195458590518,6.));
#63286=CARTESIAN_POINT('Ctrl Pts',(-38.6381772424017,37.6071867480182,6.));
#63287=CARTESIAN_POINT('Ctrl Pts',(-38.6879882164427,37.5957197996179,6.));
#63288=CARTESIAN_POINT('Ctrl Pts',(-38.7384475151204,37.5869729726017,6.));
#63289=CARTESIAN_POINT('Ctrl Pts',(-38.7893004134472,37.5810866485612,6.));
#63290=CARTESIAN_POINT('Ctrl Pts',(-38.8023628187198,37.5795746491922,6.));
#63291=CARTESIAN_POINT('Ctrl Pts',(-38.8154556555427,37.5782513512257,6.));
#63292=CARTESIAN_POINT('Ctrl Pts',(-38.8285456601036,37.577121602081,6.));
#63293=CARTESIAN_POINT('Ctrl Pts',(-38.8814582148995,37.5725549181469,6.));
#63294=CARTESIAN_POINT('Ctrl Pts',(-38.9344079183634,37.5711349247241,6.));
#63295=CARTESIAN_POINT('Ctrl Pts',(-38.9871128327976,37.5729646742369,6.));
#63296=CARTESIAN_POINT('Ctrl Pts',(-39.0380304487625,37.5747323743462,6.));
#63297=CARTESIAN_POINT('Ctrl Pts',(-39.0887204479045,37.5795333200091,6.));
#63298=CARTESIAN_POINT('Ctrl Pts',(-39.1389156304824,37.5875063462533,6.));
#63299=CARTESIAN_POINT('Ctrl Pts',(-39.1740301727663,37.5930839565499,6.));
#63300=CARTESIAN_POINT('Ctrl Pts',(-39.2089023015726,37.6002148717553,6.));
#63301=CARTESIAN_POINT('Ctrl Pts',(-39.2434333426905,37.6089601149435,6.));
#63302=CARTESIAN_POINT('Ctrl Pts',(-39.2629126135314,37.6138933852742,6.));
#63303=CARTESIAN_POINT('Ctrl Pts',(-39.2822832137847,37.6193406085392,6.));
#63304=CARTESIAN_POINT('Ctrl Pts',(-39.3015295597332,37.6252918061955,6.));
#63305=CARTESIAN_POINT('Origin',(-39.0658530619283,38.8697713466882,0.895788276411275));
#63306=CARTESIAN_POINT('Ctrl Pts',(-39.838950903209,40.2073157943283,2.14578827641127));
#63307=CARTESIAN_POINT('Ctrl Pts',(-39.8806063786858,40.1836140086682,2.14826884812012));
#63308=CARTESIAN_POINT('Ctrl Pts',(-40.3479144857802,39.8865682523885,2.17691792328789));
#63309=CARTESIAN_POINT('Ctrl Pts',(-40.8820206309179,38.8100483503822,2.23173550191459));
#63310=CARTESIAN_POINT('Ctrl Pts',(-40.0177367088945,37.3220789090571,2.31024101229137));
#63311=CARTESIAN_POINT('Ctrl Pts',(-38.2999828751462,37.2220283999294,2.38874652266815));
#63312=CARTESIAN_POINT('Ctrl Pts',(-37.2689794778046,38.599756793647,2.46725203304492));
#63313=CARTESIAN_POINT('Ctrl Pts',(-37.8495046941264,40.2196189105814,2.5457575434217));
#63314=CARTESIAN_POINT('Ctrl Pts',(-39.1164929505456,40.5298919958252,2.60526962454382));
#63315=CARTESIAN_POINT('Ctrl Pts',(-39.7159505584363,40.2768331102243,2.63861320220701));
#63316=CARTESIAN_POINT('Ctrl Pts',(-39.8359404161091,40.2062105265248,2.64578827641127));
#63317=CARTESIAN_POINT('Ctrl Pts',(-39.8351916364771,40.2053827942122,2.10421172358873));
#63318=CARTESIAN_POINT('Ctrl Pts',(-40.1301403364056,40.0323966656676,2.12181148931034));
#63319=CARTESIAN_POINT('Ctrl Pts',(-40.7310614116502,39.3634532239961,2.16557975849088));
#63320=CARTESIAN_POINT('Ctrl Pts',(-40.5621188491035,37.8394675163551,2.23551653113034));
#63321=CARTESIAN_POINT('Ctrl Pts',(-39.0323736383015,37.0530949705804,2.31402204150712));
#63322=CARTESIAN_POINT('Ctrl Pts',(-37.5317729583208,37.8957949010443,2.3925275518839));
#63323=CARTESIAN_POINT('Ctrl Pts',(-37.4074081512687,39.612062461691,2.47103306226068));
#63324=CARTESIAN_POINT('Ctrl Pts',(-38.6322604476799,40.5562805179572,2.54159445282895));
#63325=CARTESIAN_POINT('Ctrl Pts',(-39.5301075010648,40.379146656691,2.5859873399383));
#63326=CARTESIAN_POINT('Ctrl Pts',(-39.8379370462828,40.204596038962,2.60421172358873));
#63327=CARTESIAN_POINT('Ctrl Pts',(-39.3014489339361,37.6274127691862,2.));
#63328=CARTESIAN_POINT('Ctrl Pts',(-38.8929078719872,37.5499386892516,2.02616850345893));
#63329=CARTESIAN_POINT('Ctrl Pts',(-38.0001476420674,37.8306642325621,2.07850551037678));
#63330=CARTESIAN_POINT('Ctrl Pts',(-37.610255111015,39.1875822847128,2.15701102075356));
#63331=CARTESIAN_POINT('Ctrl Pts',(-38.5285686312713,40.258225513388,2.23551653113034));
#63332=CARTESIAN_POINT('Ctrl Pts',(-39.9273700409771,40.0842697726412,2.31402204150712));
#63333=CARTESIAN_POINT('Ctrl Pts',(-40.5542159206369,38.8208279060991,2.3925275518839));
#63334=CARTESIAN_POINT('Ctrl Pts',(-39.8459288050189,37.6014258590767,2.47103306226067));
#63335=CARTESIAN_POINT('Ctrl Pts',(-38.4382167358195,37.5194337211688,2.54953857263746));
#63336=CARTESIAN_POINT('Ctrl Pts',(-37.5933017676156,38.6484924080488,2.62804408301423));
#63337=CARTESIAN_POINT('Ctrl Pts',(-38.0690465090537,39.9759814857309,2.70654959339101));
#63338=CARTESIAN_POINT('Ctrl Pts',(-39.4387308817872,40.3114038497387,2.7850551037678));
#63339=CARTESIAN_POINT('Ctrl Pts',(-40.4740195694907,39.3539315296908,2.86356061414457));
#63340=CARTESIAN_POINT('Ctrl Pts',(-40.2464260929064,37.9622550204806,2.94206612452135));
#63341=CARTESIAN_POINT('Ctrl Pts',(-38.9600691167361,37.3844596499182,3.02057163489813));
#63342=CARTESIAN_POINT('Ctrl Pts',(-37.768580477053,38.1387276546801,3.09907714527491));
#63343=CARTESIAN_POINT('Ctrl Pts',(-37.7405173375704,39.5486127570041,3.17758265565169));
#63344=CARTESIAN_POINT('Ctrl Pts',(-38.9010464836382,40.3496968754357,3.25608816602847));
#63345=CARTESIAN_POINT('Ctrl Pts',(-40.2093782359874,39.823548531307,3.33459367640525));
#63346=CARTESIAN_POINT('Ctrl Pts',(-40.4921693526885,38.4420301655715,3.41309918678203));
#63347=CARTESIAN_POINT('Ctrl Pts',(-39.4958061477021,37.4441202440019,3.49160469715882));
#63348=CARTESIAN_POINT('Ctrl Pts',(-38.1138507756971,37.7247681321827,3.57011020753558));
#63349=CARTESIAN_POINT('Ctrl Pts',(-37.5856736955423,39.032282120084,3.64861571791237));
#63350=CARTESIAN_POINT('Ctrl Pts',(-38.3849566559494,40.1940525848875,3.72712122828914));
#63351=CARTESIAN_POINT('Ctrl Pts',(-39.7948837028381,40.1681761513166,3.80562673866593));
#63352=CARTESIAN_POINT('Ctrl Pts',(-40.5509987381473,38.9778594216365,3.8841322490427));
#63353=CARTESIAN_POINT('Ctrl Pts',(-39.975199824256,37.6906067364409,3.96263775941949));
#63354=CARTESIAN_POINT('Ctrl Pts',(-38.5838771151456,37.4608569069011,4.04114326979626));
#63355=CARTESIAN_POINT('Ctrl Pts',(-37.6248018935901,38.4946550418589,4.11964878017305));
#63356=CARTESIAN_POINT('Ctrl Pts',(-37.9580956187159,39.8648663970342,4.19815429054983));
#63357=CARTESIAN_POINT('Ctrl Pts',(-39.2848525544709,40.3426528537363,4.2766598009266));
#63358=CARTESIAN_POINT('Ctrl Pts',(-40.4152055386856,39.4995241597319,4.35516531130339));
#63359=CARTESIAN_POINT('Ctrl Pts',(-40.3354271431306,38.09161817034,4.43367082168016));
#63360=CARTESIAN_POINT('Ctrl Pts',(-39.1170645283528,37.381578451311,4.51217633205694));
#63361=CARTESIAN_POINT('Ctrl Pts',(-37.8527742546189,38.0061854960201,4.59068184243372));
#63362=CARTESIAN_POINT('Ctrl Pts',(-37.6764018913215,39.4052768714559,4.6691873528105));
#63363=CARTESIAN_POINT('Ctrl Pts',(-38.7461223767003,40.3241141426736,4.74769286318728));
#63364=CARTESIAN_POINT('Ctrl Pts',(-40.1025849285147,39.9386622571232,4.82619837356406));
#63365=CARTESIAN_POINT('Ctrl Pts',(-40.5292817221821,38.5946035156581,4.90470388394085));
#63366=CARTESIAN_POINT('Ctrl Pts',(-39.6435408484723,37.4973219800824,4.98320939431762));
#63367=CARTESIAN_POINT('Ctrl Pts',(-38.2397159426158,37.6308853554897,5.0617149046944));
#63368=CARTESIAN_POINT('Ctrl Pts',(-37.576790226709,38.8755117639716,5.14022041507117));
#63369=CARTESIAN_POINT('Ctrl Pts',(-38.2492919033736,40.1149887727412,5.21872592544796));
#63370=CARTESIAN_POINT('Ctrl Pts',(-39.6541041493256,40.2377277253793,5.29723143582474));
#63371=CARTESIAN_POINT('Ctrl Pts',(-40.5313606306742,39.1336457644378,5.37573694620152));
#63372=CARTESIAN_POINT('Ctrl Pts',(-40.0943114632433,37.792925260964,5.4542424565783));
#63373=CARTESIAN_POINT('Ctrl Pts',(-38.7349236527553,37.4179251395397,5.53274796695507));
#63374=CARTESIAN_POINT('Ctrl Pts',(-37.6723064797637,38.3450171336682,5.61125347733186));
#63375=CARTESIAN_POINT('Ctrl Pts',(-37.8594847038433,39.742636643005,5.68975898770863));
#63376=CARTESIAN_POINT('Ctrl Pts',(-39.1285028721539,40.3576202841945,5.76826449808542));
#63377=CARTESIAN_POINT('Ctrl Pts',(-40.3414559726879,39.6379218175554,5.84677000846219));
#63378=CARTESIAN_POINT('Ctrl Pts',(-40.4101742470826,38.2300213301991,5.92527551883897));
#63379=CARTESIAN_POINT('Ctrl Pts',(-39.2737694148596,37.3944612175239,6.00378102921576));
#63380=CARTESIAN_POINT('Ctrl Pts',(-37.9498583767322,37.8848716060229,6.08228653959253));
#63381=CARTESIAN_POINT('Ctrl Pts',(-37.7367752723626,38.7961472226316,6.13462354651038));
#63382=CARTESIAN_POINT('Ctrl Pts',(-37.8446253550652,39.1977395433015,6.16079204996931));
#63383=CARTESIAN_POINT('Ctrl Pts',(-39.3187452171453,37.5362049495383,1.94640265001023));
#63384=CARTESIAN_POINT('Ctrl Pts',(-38.8802110918637,37.4530431059918,1.97257115346916));
#63385=CARTESIAN_POINT('Ctrl Pts',(-37.9219088231848,37.7543781296798,2.02490816038701));
#63386=CARTESIAN_POINT('Ctrl Pts',(-37.5033923116663,39.2109143912739,2.10341367076379));
#63387=CARTESIAN_POINT('Ctrl Pts',(-38.4891238668221,40.3601589483231,2.18191918114057));
#63388=CARTESIAN_POINT('Ctrl Pts',(-39.9906183548469,40.1734322378127,2.26042469151735));
#63389=CARTESIAN_POINT('Ctrl Pts',(-40.6634841573972,38.8172347208602,2.33893020189413));
#63390=CARTESIAN_POINT('Ctrl Pts',(-39.9031981063108,37.5083102090701,2.4174357122709));
#63391=CARTESIAN_POINT('Ctrl Pts',(-38.3921387822617,37.420298614089,2.49594122264769));
#63392=CARTESIAN_POINT('Ctrl Pts',(-37.4851943376786,38.6322472032482,2.57444673302446));
#63393=CARTESIAN_POINT('Ctrl Pts',(-37.9958659040779,40.0571939606811,2.65295224340125));
#63394=CARTESIAN_POINT('Ctrl Pts',(-39.4661057263452,40.4172413750055,2.73145775377802));
#63395=CARTESIAN_POINT('Ctrl Pts',(-40.5774001869564,39.3894761747327,2.8099632641548));
#63396=CARTESIAN_POINT('Ctrl Pts',(-40.3330979234396,37.8956296621443,2.88846877453158));
#63397=CARTESIAN_POINT('Ctrl Pts',(-38.9523029828924,37.2754154143704,2.96697428490836));
#63398=CARTESIAN_POINT('Ctrl Pts',(-37.6733411426948,38.0850580439713,3.04547979528514));
#63399=CARTESIAN_POINT('Ctrl Pts',(-37.6432177463661,39.5984499344847,3.12398530566192));
#63400=CARTESIAN_POINT('Ctrl Pts',(-38.8889472001127,40.4583456851777,3.2024908160387));
#63401=CARTESIAN_POINT('Ctrl Pts',(-40.2933301961761,39.893570132972,3.28099632641548));
#63402=CARTESIAN_POINT('Ctrl Pts',(-40.5968824374326,38.4106275244905,3.35950183679226));
#63403=CARTESIAN_POINT('Ctrl Pts',(-39.5273711758787,37.3394559940749,3.43800734716904));
#63404=CARTESIAN_POINT('Ctrl Pts',(-38.0439594782896,37.6407076615778,3.51651285754582));
#63405=CARTESIAN_POINT('Ctrl Pts',(-37.4770062502969,39.0442128569736,3.5950183679226));
#63406=CARTESIAN_POINT('Ctrl Pts',(-38.3349686108551,40.2912747609356,3.67352387829938));
#63407=CARTESIAN_POINT('Ctrl Pts',(-39.8484055252959,40.2634986076469,3.75202938867616));
#63408=CARTESIAN_POINT('Ctrl Pts',(-40.6600307852877,38.9857947132862,3.83053489905294));
#63409=CARTESIAN_POINT('Ctrl Pts',(-40.0419595641554,37.6040383051891,3.90904040942972));
#63410=CARTESIAN_POINT('Ctrl Pts',(-38.5484928259196,37.3574213799521,3.9875459198065));
#63411=CARTESIAN_POINT('Ctrl Pts',(-37.5190070470414,38.4671158588103,4.06605143018328));
#63412=CARTESIAN_POINT('Ctrl Pts',(-37.8767695483496,39.9379213519627,4.14455694056006));
#63413=CARTESIAN_POINT('Ctrl Pts',(-39.3009304136176,40.4507845262585,4.22306245093683));
#63414=CARTESIAN_POINT('Ctrl Pts',(-40.5142683210177,39.5457574952881,4.30156796131362));
#63415=CARTESIAN_POINT('Ctrl Pts',(-40.4286329903996,38.0344900143857,4.38007347169039));
#63416=CARTESIAN_POINT('Ctrl Pts',(-39.1208242208266,37.2723226924175,4.45857898206717));
#63417=CARTESIAN_POINT('Ctrl Pts',(-37.7637160108241,37.9427852958327,4.53708449244395));
#63418=CARTESIAN_POINT('Ctrl Pts',(-37.5743952612928,39.4445910374365,4.61559000282073));
#63419=CARTESIAN_POINT('Ctrl Pts',(-38.7226493317982,40.430884794758,4.69409551319751));
#63420=CARTESIAN_POINT('Ctrl Pts',(-40.1786966524752,40.0171349389622,4.77260102357429));
#63421=CARTESIAN_POINT('Ctrl Pts',(-40.6367194134648,38.574402055017,4.85110653395107));
#63422=CARTESIAN_POINT('Ctrl Pts',(-39.6859518273974,37.3965635383795,4.92961204432785));
#63423=CARTESIAN_POINT('Ctrl Pts',(-38.1790650429906,37.539932475946,5.00811755470463));
#63424=CARTESIAN_POINT('Ctrl Pts',(-37.4674706011366,38.8759331970053,5.08662306508141));
#63425=CARTESIAN_POINT('Ctrl Pts',(-38.1893440234059,40.2064064749044,5.16512857545819));
#63426=CARTESIAN_POINT('Ctrl Pts',(-39.6972906335328,40.3381563141404,5.24363408583496));
#63427=CARTESIAN_POINT('Ctrl Pts',(-40.6389509451321,39.1530181185549,5.32213959621175));
#63428=CARTESIAN_POINT('Ctrl Pts',(-40.1698157903201,37.713868549517,5.40064510658852));
#63429=CARTESIAN_POINT('Ctrl Pts',(-38.7106284529518,37.3113377746548,5.47915061696531));
#63430=CARTESIAN_POINT('Ctrl Pts',(-37.5699991848822,38.3064922757992,5.55765612734208));
#63431=CARTESIAN_POINT('Ctrl Pts',(-37.7709191080277,39.8067180941779,5.63616163771886));
#63432=CARTESIAN_POINT('Ctrl Pts',(-39.1331023112333,40.4668507914031,5.71466714809565));
#63433=CARTESIAN_POINT('Ctrl Pts',(-40.4351044267927,39.694315624366,5.79317265847242));
#63434=CARTESIAN_POINT('Ctrl Pts',(-40.5088676568798,38.1830540494315,5.8716781688492));
#63435=CARTESIAN_POINT('Ctrl Pts',(-39.2890336047347,37.2861512475826,5.95018367922599));
#63436=CARTESIAN_POINT('Ctrl Pts',(-37.8679275688169,37.8125651402854,6.02868918960276));
#63437=CARTESIAN_POINT('Ctrl Pts',(-37.6392009572462,38.7907421037309,6.08102619652061));
#63438=CARTESIAN_POINT('Ctrl Pts',(-37.7549688593853,39.2218173455308,6.10719469997954));
#63439=CARTESIAN_POINT('Ctrl Pts',(-39.3360415003545,37.4449971298904,1.89280530002046));
#63440=CARTESIAN_POINT('Ctrl Pts',(-38.8675143117401,37.356147522732,1.91897380347939));
#63441=CARTESIAN_POINT('Ctrl Pts',(-37.8436700043022,37.6780920267975,1.97131081039724));
#63442=CARTESIAN_POINT('Ctrl Pts',(-37.3965295123175,39.2342464978351,2.04981632077402));
#63443=CARTESIAN_POINT('Ctrl Pts',(-38.449679102373,40.462092383258,2.1283218311508));
#63444=CARTESIAN_POINT('Ctrl Pts',(-40.0538666687167,40.2625947029841,2.20682734152758));
#63445=CARTESIAN_POINT('Ctrl Pts',(-40.7727523941575,38.8136415356212,2.28533285190436));
#63446=CARTESIAN_POINT('Ctrl Pts',(-39.9604674076027,37.4151945590636,2.36383836228113));
#63447=CARTESIAN_POINT('Ctrl Pts',(-38.3460608287039,37.3211635070092,2.44234387265792));
#63448=CARTESIAN_POINT('Ctrl Pts',(-37.3770869077416,38.6160019984476,2.52084938303469));
#63449=CARTESIAN_POINT('Ctrl Pts',(-37.9226852991021,40.1384064356312,2.59935489341147));
#63450=CARTESIAN_POINT('Ctrl Pts',(-39.4934805709032,40.5230789002723,2.67786040378825));
#63451=CARTESIAN_POINT('Ctrl Pts',(-40.6807808044221,39.4250208197745,2.75636591416503));
#63452=CARTESIAN_POINT('Ctrl Pts',(-40.4197697539727,37.829004303808,2.83487142454181));
#63453=CARTESIAN_POINT('Ctrl Pts',(-38.9445368490487,37.1663711788227,2.91337693491859));
#63454=CARTESIAN_POINT('Ctrl Pts',(-37.5781018083366,38.0313884332623,2.99188244529537));
#63455=CARTESIAN_POINT('Ctrl Pts',(-37.5459181551618,39.6482871119655,3.07038795567215));
#63456=CARTESIAN_POINT('Ctrl Pts',(-38.8768479165872,40.5669944949197,3.14889346604893));
#63457=CARTESIAN_POINT('Ctrl Pts',(-40.3772821563647,39.963591734637,3.22739897642571));
#63458=CARTESIAN_POINT('Ctrl Pts',(-40.7015955221767,38.3792248834095,3.30590448680249));
#63459=CARTESIAN_POINT('Ctrl Pts',(-39.5589362040553,37.2347917441478,3.38440999717927));
#63460=CARTESIAN_POINT('Ctrl Pts',(-37.9740681808821,37.5566471909729,3.46291550755605));
#63461=CARTESIAN_POINT('Ctrl Pts',(-37.3683388050514,39.0561435938632,3.54142101793282));
#63462=CARTESIAN_POINT('Ctrl Pts',(-38.2849805657609,40.3884969369837,3.61992652830961));
#63463=CARTESIAN_POINT('Ctrl Pts',(-39.9019273477536,40.3588210639771,3.69843203868638));
#63464=CARTESIAN_POINT('Ctrl Pts',(-40.7690628324281,38.9937300049359,3.77693754906317));
#63465=CARTESIAN_POINT('Ctrl Pts',(-40.1087193040547,37.5174698739372,3.85544305943995));
#63466=CARTESIAN_POINT('Ctrl Pts',(-38.5131085366936,37.2539858530032,3.93394856981672));
#63467=CARTESIAN_POINT('Ctrl Pts',(-37.4132122004928,38.4395766757617,4.01245408019351));
#63468=CARTESIAN_POINT('Ctrl Pts',(-37.7954434779833,40.0109763068912,4.09095959057028));
#63469=CARTESIAN_POINT('Ctrl Pts',(-39.3170082727643,40.5589161987807,4.16946510094707));
#63470=CARTESIAN_POINT('Ctrl Pts',(-40.6133311033498,39.5919908308443,4.24797061132384));
#63471=CARTESIAN_POINT('Ctrl Pts',(-40.5218388376685,37.9773618584313,4.32647612170062));
#63472=CARTESIAN_POINT('Ctrl Pts',(-39.1245839133004,37.163066933524,4.4049816320774));
#63473=CARTESIAN_POINT('Ctrl Pts',(-37.6746577670293,37.8793850956452,4.48348714245418));
#63474=CARTESIAN_POINT('Ctrl Pts',(-37.472388631264,39.4839052034172,4.56199265283096));
#63475=CARTESIAN_POINT('Ctrl Pts',(-38.6991762868962,40.5376554468423,4.64049816320775));
#63476=CARTESIAN_POINT('Ctrl Pts',(-40.2548083764357,40.0956076208012,4.71900367358451));
#63477=CARTESIAN_POINT('Ctrl Pts',(-40.7441571047475,38.554200594376,4.7975091839613));
#63478=CARTESIAN_POINT('Ctrl Pts',(-39.7283628063224,37.2958050966767,4.87601469433807));
#63479=CARTESIAN_POINT('Ctrl Pts',(-38.1184141433653,37.4489795964024,4.95452020471486));
#63480=CARTESIAN_POINT('Ctrl Pts',(-37.3581509755643,38.876354630039,5.03302571509164));
#63481=CARTESIAN_POINT('Ctrl Pts',(-38.1293961434382,40.2978241770675,5.11153122546842));
#63482=CARTESIAN_POINT('Ctrl Pts',(-39.7404771177401,40.4385849029016,5.1900367358452));
#63483=CARTESIAN_POINT('Ctrl Pts',(-40.7465412595899,39.172390472672,5.26854224622198));
#63484=CARTESIAN_POINT('Ctrl Pts',(-40.245320117397,37.63481183807,5.34704775659875));
#63485=CARTESIAN_POINT('Ctrl Pts',(-38.6863332531482,37.2047504097698,5.42555326697554));
#63486=CARTESIAN_POINT('Ctrl Pts',(-37.4676918900007,38.2679674179302,5.50405877735231));
#63487=CARTESIAN_POINT('Ctrl Pts',(-37.682353512212,39.8707995453507,5.5825642877291));
#63488=CARTESIAN_POINT('Ctrl Pts',(-39.1377017503128,40.5760812986115,5.66106979810587));
#63489=CARTESIAN_POINT('Ctrl Pts',(-40.5287528808974,39.7507094311768,5.73957530848266));
#63490=CARTESIAN_POINT('Ctrl Pts',(-40.6075610666769,38.1360867686637,5.81808081885943));
#63491=CARTESIAN_POINT('Ctrl Pts',(-39.3042977946098,37.1778412776413,5.89658632923621));
#63492=CARTESIAN_POINT('Ctrl Pts',(-37.7859967609015,37.7402586745478,5.97509183961299));
#63493=CARTESIAN_POINT('Ctrl Pts',(-37.5416266421298,38.7853369848302,6.02742884653084));
#63494=CARTESIAN_POINT('Ctrl Pts',(-37.6653123637055,39.2458951477601,6.05359734998977));
#63495=CARTESIAN_POINT('Ctrl Pts',(-39.3533377835637,37.3537893102425,1.83920795003069));
#63496=CARTESIAN_POINT('Ctrl Pts',(-38.8548175316166,37.2592519394721,1.86537645348962));
#63497=CARTESIAN_POINT('Ctrl Pts',(-37.7654311854196,37.6018059239151,1.91771346040747));
#63498=CARTESIAN_POINT('Ctrl Pts',(-37.2896667129688,39.2575786043963,1.99621897078425));
#63499=CARTESIAN_POINT('Ctrl Pts',(-38.4102343379238,40.564025818193,2.07472448116103));
#63500=CARTESIAN_POINT('Ctrl Pts',(-40.1171149825865,40.3517571681556,2.15322999153781));
#63501=CARTESIAN_POINT('Ctrl Pts',(-40.8820206309179,38.8100483503822,2.23173550191459));
#63502=CARTESIAN_POINT('Ctrl Pts',(-40.0177367088945,37.3220789090571,2.31024101229137));
#63503=CARTESIAN_POINT('Ctrl Pts',(-38.2999828751462,37.2220283999294,2.38874652266815));
#63504=CARTESIAN_POINT('Ctrl Pts',(-37.2689794778046,38.599756793647,2.46725203304492));
#63505=CARTESIAN_POINT('Ctrl Pts',(-37.8495046941264,40.2196189105814,2.5457575434217));
#63506=CARTESIAN_POINT('Ctrl Pts',(-39.5208554154611,40.6289164255391,2.62426305379848));
#63507=CARTESIAN_POINT('Ctrl Pts',(-40.7841614218878,39.4605654648164,2.70276856417526));
#63508=CARTESIAN_POINT('Ctrl Pts',(-40.5064415845058,37.7623789454716,2.78127407455204));
#63509=CARTESIAN_POINT('Ctrl Pts',(-38.936770715205,37.0573269432749,2.85977958492882));
#63510=CARTESIAN_POINT('Ctrl Pts',(-37.4828624739785,37.9777188225534,2.9382850953056));
#63511=CARTESIAN_POINT('Ctrl Pts',(-37.4486185639574,39.6981242894461,3.01679060568238));
#63512=CARTESIAN_POINT('Ctrl Pts',(-38.8647486330618,40.6756433046616,3.09529611605916));
#63513=CARTESIAN_POINT('Ctrl Pts',(-40.4612341165533,40.033613336302,3.17380162643594));
#63514=CARTESIAN_POINT('Ctrl Pts',(-40.8063086069208,38.3478222423284,3.25230713681272));
#63515=CARTESIAN_POINT('Ctrl Pts',(-39.590501232232,37.1301274942208,3.3308126471895));
#63516=CARTESIAN_POINT('Ctrl Pts',(-37.9041768834746,37.4725867203679,3.40931815756627));
#63517=CARTESIAN_POINT('Ctrl Pts',(-37.259671359806,39.0680743307528,3.48782366794306));
#63518=CARTESIAN_POINT('Ctrl Pts',(-38.2349925206666,40.4857191130317,3.56632917831984));
#63519=CARTESIAN_POINT('Ctrl Pts',(-39.9554491702114,40.4541435203075,3.64483468869662));
#63520=CARTESIAN_POINT('Ctrl Pts',(-40.8780948795684,39.0016652965855,3.7233401990734));
#63521=CARTESIAN_POINT('Ctrl Pts',(-40.1754790439541,37.4309014426854,3.80184570945018));
#63522=CARTESIAN_POINT('Ctrl Pts',(-38.4777242474675,37.1505503260543,3.88035121982696));
#63523=CARTESIAN_POINT('Ctrl Pts',(-37.3074173539442,38.412037492713,3.95885673020373));
#63524=CARTESIAN_POINT('Ctrl Pts',(-37.7141174076169,40.0840312618198,4.03736224058051));
#63525=CARTESIAN_POINT('Ctrl Pts',(-39.333086131911,40.6670478713028,4.11586775095729));
#63526=CARTESIAN_POINT('Ctrl Pts',(-40.7123938856819,39.6382241664006,4.19437326133407));
#63527=CARTESIAN_POINT('Ctrl Pts',(-40.6150446849375,37.9202337024768,4.27287877171085));
#63528=CARTESIAN_POINT('Ctrl Pts',(-39.1283436057741,37.0538111746305,4.35138428208763));
#63529=CARTESIAN_POINT('Ctrl Pts',(-37.5855995232345,37.8159848954577,4.42988979246441));
#63530=CARTESIAN_POINT('Ctrl Pts',(-37.3703820012353,39.5232193693979,4.50839530284119));
#63531=CARTESIAN_POINT('Ctrl Pts',(-38.6757032419941,40.6444260989267,4.58690081321797));
#63532=CARTESIAN_POINT('Ctrl Pts',(-40.3309201003962,40.1740803026401,4.66540632359475));
#63533=CARTESIAN_POINT('Ctrl Pts',(-40.8515947960302,38.533999133735,4.74391183397153));
#63534=CARTESIAN_POINT('Ctrl Pts',(-39.7707737852476,37.1950466549738,4.82241734434831));
#63535=CARTESIAN_POINT('Ctrl Pts',(-38.05776324374,37.3580267168588,4.90092285472509));
#63536=CARTESIAN_POINT('Ctrl Pts',(-37.248831349992,38.8767760630727,4.97942836510187));
#63537=CARTESIAN_POINT('Ctrl Pts',(-38.0694482634705,40.3892418792306,5.05793387547865));
#63538=CARTESIAN_POINT('Ctrl Pts',(-39.7836636019473,40.5390134916628,5.13643938585543));
#63539=CARTESIAN_POINT('Ctrl Pts',(-40.8541315740477,39.1917628267891,5.2149448962322));
#63540=CARTESIAN_POINT('Ctrl Pts',(-40.3208244444739,37.5557551266231,5.29345040660899));
#63541=CARTESIAN_POINT('Ctrl Pts',(-38.6620380533448,37.0981630448849,5.37195591698576));
#63542=CARTESIAN_POINT('Ctrl Pts',(-37.3653845951193,38.2294425600612,5.45046142736254));
#63543=CARTESIAN_POINT('Ctrl Pts',(-37.5937879163964,39.9348809965236,5.52896693773932));
#63544=CARTESIAN_POINT('Ctrl Pts',(-39.1423011893922,40.6853118058201,5.6074724481161));
#63545=CARTESIAN_POINT('Ctrl Pts',(-40.6224013350023,39.8071032379875,5.68597795849288));
#63546=CARTESIAN_POINT('Ctrl Pts',(-40.7062544764741,38.0891194878961,5.76448346886966));
#63547=CARTESIAN_POINT('Ctrl Pts',(-39.3195619844849,37.0695313077001,5.84298897924644));
#63548=CARTESIAN_POINT('Ctrl Pts',(-37.7040659529861,37.6679522088103,5.92149448962322));
#63549=CARTESIAN_POINT('Ctrl Pts',(-37.4440523270134,38.7799318659295,5.97383149654107));
#63550=CARTESIAN_POINT('Ctrl Pts',(-37.5756558680257,39.2699729499894,6.));
#63551=CARTESIAN_POINT('Ctrl Pts',(-39.3014489339361,37.6274127691862,2.));
#63552=CARTESIAN_POINT('Ctrl Pts',(-39.2531837869401,37.6126947647985,2.));
#63553=CARTESIAN_POINT('Ctrl Pts',(-39.204168956439,37.6011555074407,2.));
#63554=CARTESIAN_POINT('Ctrl Pts',(-39.1546825373221,37.5926368604753,2.));
#63555=CARTESIAN_POINT('Ctrl Pts',(-39.1029779407396,37.5837363739855,2.));
#63556=CARTESIAN_POINT('Ctrl Pts',(-39.0507578251671,37.5781330493143,2.));
#63557=CARTESIAN_POINT('Ctrl Pts',(-38.9983103424742,37.5756956341644,2.));
#63558=CARTESIAN_POINT('Ctrl Pts',(-38.9562475821286,37.573740832827,2.));
#63559=CARTESIAN_POINT('Ctrl Pts',(-38.914037803618,37.5738233147571,2.));
#63560=CARTESIAN_POINT('Ctrl Pts',(-38.871822235207,37.5758984072385,2.));
#63561=CARTESIAN_POINT('Ctrl Pts',(-38.8539763703757,37.5767756148974,2.));
#63562=CARTESIAN_POINT('Ctrl Pts',(-38.8361294237355,37.5780091556834,2.));
#63563=CARTESIAN_POINT('Ctrl Pts',(-38.8182919536766,37.5795967458236,2.));
#63564=CARTESIAN_POINT('Ctrl Pts',(-38.8081693423886,37.5804976896133,2.));
#63565=CARTESIAN_POINT('Ctrl Pts',(-38.7980490773292,37.5815128494685,2.));
#63566=CARTESIAN_POINT('Ctrl Pts',(-38.7879491906638,37.5826397882181,2.));
#63567=CARTESIAN_POINT('Ctrl Pts',(-38.7338460090771,37.5886765858403,2.));
#63568=CARTESIAN_POINT('Ctrl Pts',(-38.6802200536741,37.5979256005394,2.));
#63569=CARTESIAN_POINT('Ctrl Pts',(-38.6273722027196,37.6102449557342,2.));
#63570=CARTESIAN_POINT('Ctrl Pts',(-38.5735560674545,37.6227900275503,2.));
#63571=CARTESIAN_POINT('Ctrl Pts',(-38.5205457122299,37.6385189267469,2.));
#63572=CARTESIAN_POINT('Ctrl Pts',(-38.4686492447641,37.6573343726358,2.));
#63573=CARTESIAN_POINT('Ctrl Pts',(-38.4315334390262,37.6707909809289,2.));
#63574=CARTESIAN_POINT('Ctrl Pts',(-38.3949871291098,37.6858274526273,2.));
#63575=CARTESIAN_POINT('Ctrl Pts',(-38.3591250016197,37.7024243845625,2.));
#63576=CARTESIAN_POINT('Ctrl Pts',(-38.3438782291903,37.7094805650501,2.));
#63577=CARTESIAN_POINT('Ctrl Pts',(-38.32875516918,37.7168189666934,2.));
#63578=CARTESIAN_POINT('Ctrl Pts',(-38.3137649009439,37.7244388227708,2.));
#63579=CARTESIAN_POINT('Ctrl Pts',(-38.3048335703805,37.7289787984671,2.));
#63580=CARTESIAN_POINT('Ctrl Pts',(-38.2959544590106,37.7336161783506,2.));
#63581=CARTESIAN_POINT('Ctrl Pts',(-38.2871359717232,37.7383467951739,2.));
#63582=CARTESIAN_POINT('Ctrl Pts',(-38.2370624084947,37.7652084136004,2.));
#63583=CARTESIAN_POINT('Ctrl Pts',(-38.1888771643531,37.7951055006477,2.));
#63584=CARTESIAN_POINT('Ctrl Pts',(-38.1428979102524,37.8279238866887,2.));
#63585=CARTESIAN_POINT('Ctrl Pts',(-38.1146649271969,37.8480756041345,2.));
#63586=CARTESIAN_POINT('Ctrl Pts',(-38.0872636609501,37.8693298051536,2.));
#63587=CARTESIAN_POINT('Ctrl Pts',(-38.0607696487925,37.891669608828,2.));
#63588=CARTESIAN_POINT('Ctrl Pts',(-38.0187586294166,37.9270933838091,2.));
#63589=CARTESIAN_POINT('Ctrl Pts',(-37.9790269569637,37.9652445703229,2.));
#63590=CARTESIAN_POINT('Ctrl Pts',(-37.9416386654128,38.0058250350956,2.));
#63591=CARTESIAN_POINT('Ctrl Pts',(-37.9304525998634,38.0179661552202,2.));
#63592=CARTESIAN_POINT('Ctrl Pts',(-37.9194765003128,38.0303250151245,2.));
#63593=CARTESIAN_POINT('Ctrl Pts',(-37.9087126348758,38.0428943202534,2.));
#63594=CARTESIAN_POINT('Ctrl Pts',(-37.8987608212141,38.0545153669148,2.));
#63595=CARTESIAN_POINT('Ctrl Pts',(-37.8889863441815,38.0663216997937,2.));
#63596=CARTESIAN_POINT('Ctrl Pts',(-37.8794138053098,38.0782786674143,2.));
#63597=CARTESIAN_POINT('Ctrl Pts',(-37.8439500327557,38.1225761297512,2.));
#63598=CARTESIAN_POINT('Ctrl Pts',(-37.8112056943211,38.1689911399369,2.));
#63599=CARTESIAN_POINT('Ctrl Pts',(-37.7812215917862,38.2171732588852,2.));
#63600=CARTESIAN_POINT('Ctrl Pts',(-37.7505286361066,38.266494449663,2.));
#63601=CARTESIAN_POINT('Ctrl Pts',(-37.7227273546167,38.3176680405683,2.));
#63602=CARTESIAN_POINT('Ctrl Pts',(-37.6978940563331,38.3703632510113,2.));
#63603=CARTESIAN_POINT('Ctrl Pts',(-37.682817233351,38.4023556328038,2.));
#63604=CARTESIAN_POINT('Ctrl Pts',(-37.6688350669181,38.4349097034549,2.));
#63605=CARTESIAN_POINT('Ctrl Pts',(-37.6559717665588,38.4679573676163,2.));
#63606=CARTESIAN_POINT('Ctrl Pts',(-37.648889306812,38.4861532228486,2.));
#63607=CARTESIAN_POINT('Ctrl Pts',(-37.6421461366873,38.5044987807188,2.));
#63608=CARTESIAN_POINT('Ctrl Pts',(-37.635747084783,38.5229830878431,2.));
#63609=CARTESIAN_POINT('Ctrl Pts',(-37.6318939139123,38.534113360709,2.));
#63610=CARTESIAN_POINT('Ctrl Pts',(-37.6281649122512,38.5452958653453,2.));
#63611=CARTESIAN_POINT('Ctrl Pts',(-37.624563189319,38.5565221415394,2.));
#63612=CARTESIAN_POINT('Ctrl Pts',(-37.6061053671342,38.614053665672,2.));
#63613=CARTESIAN_POINT('Ctrl Pts',(-37.5910431547281,38.6725526585093,2.));
#63614=CARTESIAN_POINT('Ctrl Pts',(-37.5794635885507,38.7316684529271,2.));
#63615=CARTESIAN_POINT('Ctrl Pts',(-37.5719346379239,38.770105117187,2.));
#63616=CARTESIAN_POINT('Ctrl Pts',(-37.5658787738505,38.8088033108087,2.));
#63617=CARTESIAN_POINT('Ctrl Pts',(-37.5613302232318,38.8476724431706,2.));
#63618=CARTESIAN_POINT('Ctrl Pts',(-37.5594503644639,38.8637365667554,2.));
#63619=CARTESIAN_POINT('Ctrl Pts',(-37.5578280676537,38.8798299273607,2.));
#63620=CARTESIAN_POINT('Ctrl Pts',(-37.5564662009659,38.8959462647572,2.));
#63621=CARTESIAN_POINT('Ctrl Pts',(-37.5554691679745,38.9077451583122,2.));
#63622=CARTESIAN_POINT('Ctrl Pts',(-37.5546119020158,38.9195552384719,2.));
#63623=CARTESIAN_POINT('Ctrl Pts',(-37.5538959122054,38.931364001732,2.));
#63624=CARTESIAN_POINT('Ctrl Pts',(-37.5502149156534,38.9920743864587,2.));
#63625=CARTESIAN_POINT('Ctrl Pts',(-37.5502577736835,39.0528196704491,2.));
#63626=CARTESIAN_POINT('Ctrl Pts',(-37.5541374325481,39.1132620113921,2.));
#63627=CARTESIAN_POINT('Ctrl Pts',(-37.5559545726121,39.1415717682862,2.));
#63628=CARTESIAN_POINT('Ctrl Pts',(-37.5586141014162,39.1698153256755,2.));
#63629=CARTESIAN_POINT('Ctrl Pts',(-37.5621314917739,39.1979588342647,2.));
#63630=CARTESIAN_POINT('Ctrl Pts',(-37.5651536457416,39.2221398342386,2.));
#63631=CARTESIAN_POINT('Ctrl Pts',(-37.5688091345127,39.2462469913775,2.));
#63632=CARTESIAN_POINT('Ctrl Pts',(-37.5730824075077,39.2702648660737,2.));
#63633=CARTESIAN_POINT('Ctrl Pts',(-39.696945388151,39.9649932150637,2.80658032638059));
#63634=CARTESIAN_POINT('Ctrl Pts',(-39.5986128055021,40.0228689487565,2.79940525217633));
#63635=CARTESIAN_POINT('Ctrl Pts',(-39.4929004903071,40.0674950246048,2.79223017797206));
#63636=CARTESIAN_POINT('Ctrl Pts',(-39.3829982676155,40.0959214023961,2.7850551037678));
#63637=CARTESIAN_POINT('Ctrl Pts',(-38.9821694242093,40.1995963950695,2.75888660030887));
#63638=CARTESIAN_POINT('Ctrl Pts',(-38.5256079666315,40.0877889404002,2.73271809684995));
#63639=CARTESIAN_POINT('Ctrl Pts',(-38.2180364476029,39.8106370334519,2.70654959339102));
#63640=CARTESIAN_POINT('Ctrl Pts',(-37.9104649285743,39.5334851265035,2.68038108993209));
#63641=CARTESIAN_POINT('Ctrl Pts',(-37.751883348095,39.0909887672762,2.65421258647317));
#63642=CARTESIAN_POINT('Ctrl Pts',(-37.8134117192226,38.6815641398491,2.62804408301424));
#63643=CARTESIAN_POINT('Ctrl Pts',(-37.8749400903503,38.2721395124221,2.60187557955531));
#63644=CARTESIAN_POINT('Ctrl Pts',(-38.1565784130849,37.8957866167954,2.57570707609639));
#63645=CARTESIAN_POINT('Ctrl Pts',(-38.5320162526521,37.7212755253001,2.54953857263746));
#63646=CARTESIAN_POINT('Ctrl Pts',(-38.9074540922193,37.5467644338048,2.52337006917854));
#63647=CARTESIAN_POINT('Ctrl Pts',(-39.3766914486191,37.5740951464407,2.49720156571961));
#63648=CARTESIAN_POINT('Ctrl Pts',(-39.729357979422,37.7909941772624,2.47103306226068));
#63649=CARTESIAN_POINT('Ctrl Pts',(-40.0820245102249,38.0078932080842,2.44486455880175));
#63650=CARTESIAN_POINT('Ctrl Pts',(-40.3181202154309,38.4143605570917,2.41869605534283));
#63651=CARTESIAN_POINT('Ctrl Pts',(-40.3316937547573,38.8281678760191,2.3925275518839));
#63652=CARTESIAN_POINT('Ctrl Pts',(-40.3452672940836,39.2419751949465,2.36635904842498));
#63653=CARTESIAN_POINT('Ctrl Pts',(-40.1363186675303,39.6631224837939,2.34019054496605));
#63654=CARTESIAN_POINT('Ctrl Pts',(-39.7987107859694,39.9026887516753,2.31402204150712));
#63655=CARTESIAN_POINT('Ctrl Pts',(-39.7667081702678,39.9253977807734,2.31154146979828));
#63656=CARTESIAN_POINT('Ctrl Pts',(-39.7335494773786,39.9464752002681,2.30906089808943));
#63657=CARTESIAN_POINT('Ctrl Pts',(-39.6994125047665,39.9658989902663,2.30658032638059));
#63658=CARTESIAN_POINT('Ctrl Pts',(-37.9741697098829,39.9602191716056,2.));
#63659=CARTESIAN_POINT('Ctrl Pts',(-38.3327559670707,40.3192117233802,2.02616850345893));
#63660=CARTESIAN_POINT('Ctrl Pts',(-39.4257675096926,40.6500214621298,2.07850551037678));
#63661=CARTESIAN_POINT('Ctrl Pts',(-40.7517604581818,39.5501737910362,2.15701102075356));
#63662=CARTESIAN_POINT('Ctrl Pts',(-40.5621188491035,37.8394675163551,2.23551653113034));
#63663=CARTESIAN_POINT('Ctrl Pts',(-39.0323736383015,37.0530949705804,2.31402204150712));
#63664=CARTESIAN_POINT('Ctrl Pts',(-37.5317729583208,37.8957949010443,2.3925275518839));
#63665=CARTESIAN_POINT('Ctrl Pts',(-37.4074081512687,39.612062461691,2.47103306226068));
#63666=CARTESIAN_POINT('Ctrl Pts',(-38.7701598472246,40.6625848481854,2.54953857263746));
#63667=CARTESIAN_POINT('Ctrl Pts',(-40.3982034912373,40.1052897198445,2.62804408301424));
#63668=CARTESIAN_POINT('Ctrl Pts',(-40.8313104277201,38.439942299895,2.70654959339101));
#63669=CARTESIAN_POINT('Ctrl Pts',(-39.6811395860238,37.1600807661057,2.78505510376779));
#63670=CARTESIAN_POINT('Ctrl Pts',(-37.9791520940816,37.4135079224236,2.86356061414458));
#63671=CARTESIAN_POINT('Ctrl Pts',(-37.2517503435483,38.9729479619195,2.94206612452135));
#63672=CARTESIAN_POINT('Ctrl Pts',(-38.1512758267995,40.4398561533634,3.02057163489813));
#63673=CARTESIAN_POINT('Ctrl Pts',(-39.8710175096897,40.4986752642982,3.09907714527491));
#63674=CARTESIAN_POINT('Ctrl Pts',(-40.8686677847051,39.096654467846,3.17758265565169));
#63675=CARTESIAN_POINT('Ctrl Pts',(-40.249511348243,37.4911595684212,3.25608816602847));
#63676=CARTESIAN_POINT('Ctrl Pts',(-38.5688218267178,37.1220364497186,3.33459367640525));
#63677=CARTESIAN_POINT('Ctrl Pts',(-37.333881829365,38.3203235548052,3.41309918678203));
#63678=CARTESIAN_POINT('Ctrl Pts',(-37.6522147609439,40.011368493019,3.49160469715881));
#63679=CARTESIAN_POINT('Ctrl Pts',(-39.2383321518161,40.67860197495,3.57011020753559));
#63680=CARTESIAN_POINT('Ctrl Pts',(-40.6697661826987,39.7236331447561,3.64861571791237));
#63681=CARTESIAN_POINT('Ctrl Pts',(-40.662772801836,38.0029007557487,3.72712122828915));
#63682=CARTESIAN_POINT('Ctrl Pts',(-39.2236238307452,37.0595985208235,3.80562673866593));
#63683=CARTESIAN_POINT('Ctrl Pts',(-37.642982284831,37.7397023107928,3.88413224904271));
#63684=CARTESIAN_POINT('Ctrl Pts',(-37.3384050779085,39.4332788778856,3.96263775941949));
#63685=CARTESIAN_POINT('Ctrl Pts',(-38.5830442911661,40.6214884944165,4.04114326979627));
#63686=CARTESIAN_POINT('Ctrl Pts',(-40.26067788792,40.2387165281925,4.11964878017304));
#63687=CARTESIAN_POINT('Ctrl Pts',(-40.8667641756192,38.6282419782981,4.19815429054983));
#63688=CARTESIAN_POINT('Ctrl Pts',(-39.8577505620191,37.2343767082119,4.2766598009266));
#63689=CARTESIAN_POINT('Ctrl Pts',(-38.1385444446535,37.3071722287696,4.35516531130339));
#63690=CARTESIAN_POINT('Ctrl Pts',(-37.2509707395799,38.781343787805,4.43367082168017));
#63691=CARTESIAN_POINT('Ctrl Pts',(-37.9910266499109,40.3348192821528,4.51217633205694));
#63692=CARTESIAN_POINT('Ctrl Pts',(-39.6950124343118,40.5744049619641,4.59068184243373));
#63693=CARTESIAN_POINT('Ctrl Pts',(-40.8347531457538,39.2852346831729,4.6691873528105));
#63694=CARTESIAN_POINT('Ctrl Pts',(-40.3881021894619,37.6234670214254,4.74769286318728));
#63695=CARTESIAN_POINT('Ctrl Pts',(-38.7556268199881,37.0794146789619,4.82619837356406));
#63696=CARTESIAN_POINT('Ctrl Pts',(-37.4013696406987,38.1409968175026,4.90470388394084));
#63697=CARTESIAN_POINT('Ctrl Pts',(-37.5398609233301,39.8561611622598,4.98320939431762));
#63698=CARTESIAN_POINT('Ctrl Pts',(-39.0468979136614,40.6867079066975,5.0617149046944));
#63699=CARTESIAN_POINT('Ctrl Pts',(-40.570934978228,39.8877822721678,5.14022041507118));
#63700=CARTESIAN_POINT('Ctrl Pts',(-40.7451774946681,38.1758811994982,5.21872592544796));
#63701=CARTESIAN_POINT('Ctrl Pts',(-39.4133645670745,37.0862753673933,5.29723143582474));
#63702=CARTESIAN_POINT('Ctrl Pts',(-37.7698897533292,37.5961550422892,5.37573694620152));
#63703=CARTESIAN_POINT('Ctrl Pts',(-37.2886763485593,39.2482362054987,5.4542424565783));
#63704=CARTESIAN_POINT('Ctrl Pts',(-38.4012556794041,40.5609170045275,5.53274796695508));
#63705=CARTESIAN_POINT('Ctrl Pts',(-40.1099052932564,40.3569060637301,5.61125347733186));
#63706=CARTESIAN_POINT('Ctrl Pts',(-40.8821362004287,38.8192621207561,5.68975898770863));
#63707=CARTESIAN_POINT('Ctrl Pts',(-40.0256584008921,37.3267854127763,5.76826449808542));
#63708=CARTESIAN_POINT('Ctrl Pts',(-38.3080469142999,37.2183586878016,5.84677000846219));
#63709=CARTESIAN_POINT('Ctrl Pts',(-37.2707754210207,38.5904264849421,5.92527551883898));
#63710=CARTESIAN_POINT('Ctrl Pts',(-37.8419099014004,40.2140906446281,6.00378102921575));
#63711=CARTESIAN_POINT('Ctrl Pts',(-39.513729769878,40.6299518311032,6.08228653959253));
#63712=CARTESIAN_POINT('Ctrl Pts',(-40.3550860167095,39.8577931806473,6.13462354651039));
#63713=CARTESIAN_POINT('Ctrl Pts',(-40.5224743779889,39.3787932927749,6.16079204996931));
#63714=CARTESIAN_POINT('Ctrl Pts',(-38.0398499461207,39.8946132698472,1.94640265001023));
#63715=CARTESIAN_POINT('Ctrl Pts',(-38.3768621543504,40.2320073282822,1.97257115346916));
#63716=CARTESIAN_POINT('Ctrl Pts',(-39.4041135512345,40.5429141695936,2.02490816038701));
#63717=CARTESIAN_POINT('Ctrl Pts',(-40.6503292182041,39.5092379343174,2.10341367076379));
#63718=CARTESIAN_POINT('Ctrl Pts',(-40.4720972414715,37.9014549038573,2.18191918114057));
#63719=CARTESIAN_POINT('Ctrl Pts',(-39.0343879004488,37.162393819305,2.26042469151735));
#63720=CARTESIAN_POINT('Ctrl Pts',(-37.6240696333812,37.954393397504,2.33893020189413));
#63721=CARTESIAN_POINT('Ctrl Pts',(-37.5071871332559,39.5674031237069,2.41743571227091));
#63722=CARTESIAN_POINT('Ctrl Pts',(-38.7879499877075,40.5547216897998,2.49594122264769));
#63723=CARTESIAN_POINT('Ctrl Pts',(-40.3180437170825,40.0309557671714,2.57444673302447));
#63724=CARTESIAN_POINT('Ctrl Pts',(-40.7250931288709,38.4658026130364,2.65295224340124));
#63725=CARTESIAN_POINT('Ctrl Pts',(-39.6441213754037,37.2629429019217,2.73145775377803));
#63726=CARTESIAN_POINT('Ctrl Pts',(-38.044532569248,37.5011228205998,2.8099632641548));
#63727=CARTESIAN_POINT('Ctrl Pts',(-37.3608943502601,38.9667404252287,2.88846877453158));
#63728=CARTESIAN_POINT('Ctrl Pts',(-38.2063006183275,40.345393284783,2.96697428490836));
#63729=CARTESIAN_POINT('Ctrl Pts',(-39.8225754490499,40.400673592003,3.04547979528514));
#63730=CARTESIAN_POINT('Ctrl Pts',(-40.7602029110189,39.0830042303774,3.12398530566192));
#63731=CARTESIAN_POINT('Ctrl Pts',(-40.1782975152901,37.5741026188095,3.2024908160387));
#63732=CARTESIAN_POINT('Ctrl Pts',(-38.5987253045761,37.2271874907222,3.28099632641548));
#63733=CARTESIAN_POINT('Ctrl Pts',(-37.4380844623892,38.3533806319362,3.35950183679226));
#63734=CARTESIAN_POINT('Ctrl Pts',(-37.7372651534313,39.9426852341611,3.43800734716904));
#63735=CARTESIAN_POINT('Ctrl Pts',(-39.2279550884041,40.5697751592293,3.51651285754582));
#63736=CARTESIAN_POINT('Ctrl Pts',(-40.5732680612612,39.6722612478535,3.5950183679226));
#63737=CARTESIAN_POINT('Ctrl Pts',(-40.5666954314398,38.0550553160375,3.67352387829938));
#63738=CARTESIAN_POINT('Ctrl Pts',(-39.214131681444,37.1685060887655,3.75202938867616));
#63739=CARTESIAN_POINT('Ctrl Pts',(-37.7285881416946,37.8076919903125,3.83053489905294));
#63740=CARTESIAN_POINT('Ctrl Pts',(-37.4423355733826,39.399375908035,3.90904040942972));
#63741=CARTESIAN_POINT('Ctrl Pts',(-38.6120920860802,40.516097864552,3.9875459198065));
#63742=CARTESIAN_POINT('Ctrl Pts',(-40.1887922292381,40.1563550606944,4.06605143018328));
#63743=CARTESIAN_POINT('Ctrl Pts',(-40.7584138310171,38.6427733952556,4.14455694056006));
#63744=CARTESIAN_POINT('Ctrl Pts',(-39.8101066964379,37.3327688894207,4.22306245093684));
#63745=CARTESIAN_POINT('Ctrl Pts',(-38.1943352093783,37.4011847270069,4.30156796131362));
#63746=CARTESIAN_POINT('Ctrl Pts',(-37.360161650527,38.7866639595805,4.3800734716904));
#63747=CARTESIAN_POINT('Ctrl Pts',(-38.0556927021353,40.246675871043,4.45857898206717));
#63748=CARTESIAN_POINT('Ctrl Pts',(-39.6571595751178,40.4718470743308,4.53708449244396));
#63749=CARTESIAN_POINT('Ctrl Pts',(-40.7283287185891,39.2602386712457,4.61559000282073));
#63750=CARTESIAN_POINT('Ctrl Pts',(-40.3085501518689,37.6984499020877,4.69409551319751));
#63751=CARTESIAN_POINT('Ctrl Pts',(-38.7742913281713,37.1871300239525,4.77260102357429));
#63752=CARTESIAN_POINT('Ctrl Pts',(-37.5015119247369,38.1848429411531,4.85110653395107));
#63753=CARTESIAN_POINT('Ctrl Pts',(-37.631670992589,39.7968158255485,4.92961204432785));
#63754=CARTESIAN_POINT('Ctrl Pts',(-39.0480383346578,40.5773934042212,5.00811755470463));
#63755=CARTESIAN_POINT('Ctrl Pts',(-40.4803829553959,39.8265344772346,5.08662306508141));
#63756=CARTESIAN_POINT('Ctrl Pts',(-40.6441423133075,38.2176285328298,5.16512857545819));
#63757=CARTESIAN_POINT('Ctrl Pts',(-39.3924568215175,37.1935779446743,5.24363408583497));
#63758=CARTESIAN_POINT('Ctrl Pts',(-37.8478603261192,37.672781125844,5.32213959621175));
#63759=CARTESIAN_POINT('Ctrl Pts',(-37.3955987323729,39.2254661767282,5.40064510658853));
#63760=CARTESIAN_POINT('Ctrl Pts',(-38.4412406375015,40.4591706088247,5.47915061696531));
#63761=CARTESIAN_POINT('Ctrl Pts',(-40.04709074445,40.2674338194665,5.55765612734208));
#63762=CARTESIAN_POINT('Ctrl Pts',(-40.7728610105232,38.8223009670344,5.63616163771886));
#63763=CARTESIAN_POINT('Ctrl Pts',(-39.9679124974786,37.419617899835,5.71466714809565));
#63764=CARTESIAN_POINT('Ctrl Pts',(-38.3536397015357,37.3177145801109,5.79317265847242));
#63765=CARTESIAN_POINT('Ctrl Pts',(-37.3787747995027,38.6072330401369,5.87167816884921));
#63766=CARTESIAN_POINT('Ctrl Pts',(-37.9155474408704,40.1332107732787,5.95018367922598));
#63767=CARTESIAN_POINT('Ctrl Pts',(-39.4867836339601,40.5240520115073,6.02868918960276));
#63768=CARTESIAN_POINT('Ctrl Pts',(-40.2775203701537,39.7983496548842,6.08102619652062));
#63769=CARTESIAN_POINT('Ctrl Pts',(-40.4348379475454,39.3481684036012,6.10719469997954));
#63770=CARTESIAN_POINT('Ctrl Pts',(-38.1055301823585,39.8290073680889,1.89280530002046));
#63771=CARTESIAN_POINT('Ctrl Pts',(-38.4209683416302,40.1448029331842,1.91897380347939));
#63772=CARTESIAN_POINT('Ctrl Pts',(-39.3824595927765,40.4358068770573,1.97131081039724));
#63773=CARTESIAN_POINT('Ctrl Pts',(-40.5488979782264,39.4683020775987,2.04981632077402));
#63774=CARTESIAN_POINT('Ctrl Pts',(-40.3820756338396,37.9634422913595,2.12832183115079));
#63775=CARTESIAN_POINT('Ctrl Pts',(-39.0364021625962,37.2716926680296,2.20682734152758));
#63776=CARTESIAN_POINT('Ctrl Pts',(-37.7163663084416,38.0129918939637,2.28533285190435));
#63777=CARTESIAN_POINT('Ctrl Pts',(-37.6069661152431,39.5227437857229,2.36383836228114));
#63778=CARTESIAN_POINT('Ctrl Pts',(-38.8057401281902,40.4468585314142,2.44234387265791));
#63779=CARTESIAN_POINT('Ctrl Pts',(-40.2378839429278,39.9566218144982,2.5208493830347));
#63780=CARTESIAN_POINT('Ctrl Pts',(-40.6188758300216,38.4916629261779,2.59935489341147));
#63781=CARTESIAN_POINT('Ctrl Pts',(-39.6071031647836,37.3658050377377,2.67786040378825));
#63782=CARTESIAN_POINT('Ctrl Pts',(-38.1099130444144,37.588737718776,2.75636591416503));
#63783=CARTESIAN_POINT('Ctrl Pts',(-37.4700383569719,38.9605328885379,2.83487142454181));
#63784=CARTESIAN_POINT('Ctrl Pts',(-38.2613254098556,40.2509304162024,2.91337693491859));
#63785=CARTESIAN_POINT('Ctrl Pts',(-39.7741333884101,40.3026719197079,2.99188244529537));
#63786=CARTESIAN_POINT('Ctrl Pts',(-40.6517380373327,39.0693539929087,3.07038795567215));
#63787=CARTESIAN_POINT('Ctrl Pts',(-40.1070836823373,37.6570456691978,3.14889346604893));
#63788=CARTESIAN_POINT('Ctrl Pts',(-38.6286287824344,37.3323385317259,3.22739897642571));
#63789=CARTESIAN_POINT('Ctrl Pts',(-37.5422870954133,38.3864377090672,3.30590448680249));
#63790=CARTESIAN_POINT('Ctrl Pts',(-37.8223155459186,39.8740019753033,3.38440999717927));
#63791=CARTESIAN_POINT('Ctrl Pts',(-39.2175780249923,40.4609483435086,3.46291550755605));
#63792=CARTESIAN_POINT('Ctrl Pts',(-40.4767699398235,39.620889350951,3.54142101793282));
#63793=CARTESIAN_POINT('Ctrl Pts',(-40.4706180610436,38.1072098763262,3.61992652830961));
#63794=CARTESIAN_POINT('Ctrl Pts',(-39.2046395321427,37.2774136567074,3.69843203868638));
#63795=CARTESIAN_POINT('Ctrl Pts',(-37.8141939985582,37.8756816698323,3.77693754906317));
#63796=CARTESIAN_POINT('Ctrl Pts',(-37.5462660688567,39.3654729381844,3.85544305943995));
#63797=CARTESIAN_POINT('Ctrl Pts',(-38.6411398809943,40.4107072346876,3.93394856981673));
#63798=CARTESIAN_POINT('Ctrl Pts',(-40.1169065705561,40.0739935931962,4.01245408019351));
#63799=CARTESIAN_POINT('Ctrl Pts',(-40.6500634864151,38.6573048122132,4.09095959057029));
#63800=CARTESIAN_POINT('Ctrl Pts',(-39.7624628308567,37.4311610706295,4.16946510094706));
#63801=CARTESIAN_POINT('Ctrl Pts',(-38.2501259741031,37.4951972252442,4.24797061132385));
#63802=CARTESIAN_POINT('Ctrl Pts',(-37.4693525614741,38.7919841313561,4.32647612170062));
#63803=CARTESIAN_POINT('Ctrl Pts',(-38.1203587543597,40.1585324599333,4.40498163207741));
#63804=CARTESIAN_POINT('Ctrl Pts',(-39.6193067159239,40.3692891866976,4.48348714245418));
#63805=CARTESIAN_POINT('Ctrl Pts',(-40.6219042914244,39.2352426593185,4.56199265283096));
#63806=CARTESIAN_POINT('Ctrl Pts',(-40.2289981142758,37.77343278275,4.64049816320774));
#63807=CARTESIAN_POINT('Ctrl Pts',(-38.7929558363546,37.2948453689432,4.71900367358452));
#63808=CARTESIAN_POINT('Ctrl Pts',(-37.601654208775,38.2286890648036,4.7975091839613));
#63809=CARTESIAN_POINT('Ctrl Pts',(-37.7234810618479,39.7374704888372,4.87601469433808));
#63810=CARTESIAN_POINT('Ctrl Pts',(-39.0491787556542,40.468078901745,4.95452020471485));
#63811=CARTESIAN_POINT('Ctrl Pts',(-40.3898309325639,39.7652866823013,5.03302571509164));
#63812=CARTESIAN_POINT('Ctrl Pts',(-40.543107131947,38.2593758661615,5.11153122546841));
#63813=CARTESIAN_POINT('Ctrl Pts',(-39.3715490759605,37.3008805219553,5.1900367358452));
#63814=CARTESIAN_POINT('Ctrl Pts',(-37.9258308989092,37.7494072093988,5.26854224622198));
#63815=CARTESIAN_POINT('Ctrl Pts',(-37.5025211161865,39.2026961479577,5.34704775659876));
#63816=CARTESIAN_POINT('Ctrl Pts',(-38.4812255955989,40.3574242131219,5.42555326697554));
#63817=CARTESIAN_POINT('Ctrl Pts',(-39.9842761956436,40.1779615752029,5.50405877735232));
#63818=CARTESIAN_POINT('Ctrl Pts',(-40.6635858206177,38.8253398133127,5.58256428772909));
#63819=CARTESIAN_POINT('Ctrl Pts',(-39.910166594065,37.5124503868936,5.66106979810588));
#63820=CARTESIAN_POINT('Ctrl Pts',(-38.3992324887715,37.4170704724202,5.73957530848266));
#63821=CARTESIAN_POINT('Ctrl Pts',(-37.4867741779846,38.6240395953316,5.81808081885943));
#63822=CARTESIAN_POINT('Ctrl Pts',(-37.9891849803405,40.0523309019294,5.89658632923621));
#63823=CARTESIAN_POINT('Ctrl Pts',(-39.4598374980422,40.4181521919114,5.97509183961299));
#63824=CARTESIAN_POINT('Ctrl Pts',(-40.199954723598,39.738906129121,6.02742884653085));
#63825=CARTESIAN_POINT('Ctrl Pts',(-40.347201517102,39.3175435144275,6.05359734998977));
#63826=CARTESIAN_POINT('Ctrl Pts',(-38.1712104185962,39.7634014663305,1.83920795003069));
#63827=CARTESIAN_POINT('Ctrl Pts',(-38.4650745289099,40.0575985380862,1.86537645348962));
#63828=CARTESIAN_POINT('Ctrl Pts',(-39.3608056343184,40.328699584521,1.91771346040747));
#63829=CARTESIAN_POINT('Ctrl Pts',(-40.4474667382488,39.4273662208801,1.99621897078425));
#63830=CARTESIAN_POINT('Ctrl Pts',(-40.2920540262076,38.0254296788617,2.07472448116103));
#63831=CARTESIAN_POINT('Ctrl Pts',(-39.0384164247435,37.3809915167541,2.15322999153781));
#63832=CARTESIAN_POINT('Ctrl Pts',(-37.8086629835021,38.0715903904234,2.23173550191459));
#63833=CARTESIAN_POINT('Ctrl Pts',(-37.7067450972302,39.4780844477388,2.31024101229137));
#63834=CARTESIAN_POINT('Ctrl Pts',(-38.8235302686731,40.3389953730286,2.38874652266815));
#63835=CARTESIAN_POINT('Ctrl Pts',(-40.157724168773,39.882287861825,2.46725203304493));
#63836=CARTESIAN_POINT('Ctrl Pts',(-40.5126585311724,38.5175232393194,2.5457575434217));
#63837=CARTESIAN_POINT('Ctrl Pts',(-39.5700849541634,37.4686671735537,2.62426305379849));
#63838=CARTESIAN_POINT('Ctrl Pts',(-38.1752935195808,37.6763526169522,2.70276856417526));
#63839=CARTESIAN_POINT('Ctrl Pts',(-37.5791823636837,38.9543253518471,2.78127407455204));
#63840=CARTESIAN_POINT('Ctrl Pts',(-38.3163502013836,40.156467547622,2.85977958492882));
#63841=CARTESIAN_POINT('Ctrl Pts',(-39.7256913277703,40.2046702474127,2.9382850953056));
#63842=CARTESIAN_POINT('Ctrl Pts',(-40.5432731636466,39.05570375544,3.01679060568238));
#63843=CARTESIAN_POINT('Ctrl Pts',(-40.0358698493845,37.7399887195861,3.09529611605916));
#63844=CARTESIAN_POINT('Ctrl Pts',(-38.6585322602927,37.4374895727296,3.17380162643594));
#63845=CARTESIAN_POINT('Ctrl Pts',(-37.6464897284375,38.4194947861982,3.25230713681272));
#63846=CARTESIAN_POINT('Ctrl Pts',(-37.9073659384061,39.8053187164454,3.3308126471895));
#63847=CARTESIAN_POINT('Ctrl Pts',(-39.2072009615803,40.352121527788,3.40931815756628));
#63848=CARTESIAN_POINT('Ctrl Pts',(-40.380271818386,39.5695174540484,3.48782366794306));
#63849=CARTESIAN_POINT('Ctrl Pts',(-40.3745406906472,38.159364436615,3.56632917831983));
#63850=CARTESIAN_POINT('Ctrl Pts',(-39.1951473828414,37.3863212246494,3.64483468869662));
#63851=CARTESIAN_POINT('Ctrl Pts',(-37.8997998554218,37.943671349352,3.7233401990734));
#63852=CARTESIAN_POINT('Ctrl Pts',(-37.6501965643308,39.3315699683338,3.80184570945018));
#63853=CARTESIAN_POINT('Ctrl Pts',(-38.6701876759084,40.3053166048232,3.88035121982695));
#63854=CARTESIAN_POINT('Ctrl Pts',(-40.0450209118742,39.9916321256981,3.95885673020374));
#63855=CARTESIAN_POINT('Ctrl Pts',(-40.541713141813,38.6718362291708,4.03736224058052));
#63856=CARTESIAN_POINT('Ctrl Pts',(-39.7148189652756,37.5295532518384,4.11586775095729));
#63857=CARTESIAN_POINT('Ctrl Pts',(-38.3059167388278,37.5892097234815,4.19437326133407));
#63858=CARTESIAN_POINT('Ctrl Pts',(-37.5785434724212,38.7973043031316,4.27287877171086));
#63859=CARTESIAN_POINT('Ctrl Pts',(-38.1850248065841,40.0703890488236,4.35138428208763));
#63860=CARTESIAN_POINT('Ctrl Pts',(-39.5814538567299,40.2667312990643,4.42988979246442));
#63861=CARTESIAN_POINT('Ctrl Pts',(-40.5154798642597,39.2102466473913,4.50839530284119));
#63862=CARTESIAN_POINT('Ctrl Pts',(-40.1494460766828,37.8484156634123,4.58690081321797));
#63863=CARTESIAN_POINT('Ctrl Pts',(-38.8116203445379,37.4025607139339,4.66540632359475));
#63864=CARTESIAN_POINT('Ctrl Pts',(-37.701796492813,38.2725351884541,4.74391183397153));
#63865=CARTESIAN_POINT('Ctrl Pts',(-37.8152911311069,39.6781251521259,4.82241734434831));
#63866=CARTESIAN_POINT('Ctrl Pts',(-39.0503191766506,40.3587643992687,4.90092285472509));
#63867=CARTESIAN_POINT('Ctrl Pts',(-40.2992789097319,39.7040388873681,4.97942836510187));
#63868=CARTESIAN_POINT('Ctrl Pts',(-40.4420719505864,38.3011231994932,5.05793387547865));
#63869=CARTESIAN_POINT('Ctrl Pts',(-39.3506413304036,37.4081830992363,5.13643938585543));
#63870=CARTESIAN_POINT('Ctrl Pts',(-38.0038014716992,37.8260332929536,5.21494489623221));
#63871=CARTESIAN_POINT('Ctrl Pts',(-37.6094435000001,39.1799261191872,5.29345040660899));
#63872=CARTESIAN_POINT('Ctrl Pts',(-38.5212105536964,40.2556778174191,5.37195591698577));
#63873=CARTESIAN_POINT('Ctrl Pts',(-39.9214616468371,40.0884893309394,5.45046142736255));
#63874=CARTESIAN_POINT('Ctrl Pts',(-40.5543106307123,38.8283786595909,5.52896693773932));
#63875=CARTESIAN_POINT('Ctrl Pts',(-39.8524206906514,37.6052828739522,5.60747244811611));
#63876=CARTESIAN_POINT('Ctrl Pts',(-38.4448252760073,37.5164263647296,5.68597795849288));
#63877=CARTESIAN_POINT('Ctrl Pts',(-37.5947735564665,38.6408461505263,5.76448346886966));
#63878=CARTESIAN_POINT('Ctrl Pts',(-38.0628225198106,39.97145103058,5.84298897924644));
#63879=CARTESIAN_POINT('Ctrl Pts',(-39.4328913621243,40.3122523723154,5.92149448962322));
#63880=CARTESIAN_POINT('Ctrl Pts',(-40.1223890770422,39.6794626033579,5.97383149654108));
#63881=CARTESIAN_POINT('Ctrl Pts',(-40.2595650866585,39.2869186252538,6.));
#63882=CARTESIAN_POINT('Ctrl Pts',(-39.6985816414592,39.9636701304732,2.44341967361941));
#63883=CARTESIAN_POINT('Ctrl Pts',(-39.808547063221,39.9013157119467,2.45136379342791));
#63884=CARTESIAN_POINT('Ctrl Pts',(-39.9090512176557,39.823104100358,2.45930791323641));
#63885=CARTESIAN_POINT('Ctrl Pts',(-39.9945142458229,39.7309450099414,2.46725203304492));
#63886=CARTESIAN_POINT('Ctrl Pts',(-40.2760356229061,39.4273663209898,2.49342053650384));
#63887=CARTESIAN_POINT('Ctrl Pts',(-40.3943470770393,38.9724447801546,2.51958903996277));
#63888=CARTESIAN_POINT('Ctrl Pts',(-40.2964072079377,38.5701746654427,2.5457575434217));
#63889=CARTESIAN_POINT('Ctrl Pts',(-40.1984673388361,38.1679045507309,2.57192604688062));
#63890=CARTESIAN_POINT('Ctrl Pts',(-39.8842761464997,37.8182858621423,2.59809455033955));
#63891=CARTESIAN_POINT('Ctrl Pts',(-39.4947153112345,37.6780907584144,2.62426305379848));
#63892=CARTESIAN_POINT('Ctrl Pts',(-39.1051544759692,37.5378956546866,2.65043155725741));
#63893=CARTESIAN_POINT('Ctrl Pts',(-38.640223997775,37.6071241358194,2.67660006071633));
#63894=CARTESIAN_POINT('Ctrl Pts',(-38.3084068993617,37.8547338322016,2.70276856417526));
#63895=CARTESIAN_POINT('Ctrl Pts',(-37.9765898009484,38.1023435285838,2.72893706763418));
#63896=CARTESIAN_POINT('Ctrl Pts',(-37.7778860823161,38.5283344402155,2.75510557109311));
#63897=CARTESIAN_POINT('Ctrl Pts',(-37.8013955292832,38.9416869286604,2.78127407455204));
#63898=CARTESIAN_POINT('Ctrl Pts',(-37.8249049762503,39.3550394171054,2.80744257801096));
#63899=CARTESIAN_POINT('Ctrl Pts',(-38.070627588817,39.7557534823636,2.83361108146989));
#63900=CARTESIAN_POINT('Ctrl Pts',(-38.4283790828314,39.9641442982913,2.85977958492881));
#63901=CARTESIAN_POINT('Ctrl Pts',(-38.7861305768459,40.1725351142189,2.88594808838774));
#63902=CARTESIAN_POINT('Ctrl Pts',(-39.2559109523081,40.1886026808158,2.91211659184667));
#63903=CARTESIAN_POINT('Ctrl Pts',(-39.6270647793519,40.0051420487854,2.93828509530559));
#63904=CARTESIAN_POINT('Ctrl Pts',(-39.6513397427562,39.9931429804635,2.9399966214102));
#63905=CARTESIAN_POINT('Ctrl Pts',(-39.6751928123865,39.9802903924142,2.9417081475148));
#63906=CARTESIAN_POINT('Ctrl Pts',(-39.6985897981371,39.9666323328488,2.94341967361941));
#63907=CARTESIAN_POINT('Ctrl Pts',(-37.9741697098829,39.9602191716056,2.));
#63908=CARTESIAN_POINT('Ctrl Pts',(-38.0210640733087,39.9994677669677,2.));
#63909=CARTESIAN_POINT('Ctrl Pts',(-38.0703056805302,40.0355567831455,2.));
#63910=CARTESIAN_POINT('Ctrl Pts',(-38.1215357900136,40.0684647235096,2.));
#63911=CARTESIAN_POINT('Ctrl Pts',(-38.1724676227795,40.1011810641967,2.));
#63912=CARTESIAN_POINT('Ctrl Pts',(-38.2253661047038,40.1307533458135,2.));
#63913=CARTESIAN_POINT('Ctrl Pts',(-38.2799014945792,40.1571104299641,2.));
#63914=CARTESIAN_POINT('Ctrl Pts',(-38.3210824949725,40.1770133057894,2.));
#63915=CARTESIAN_POINT('Ctrl Pts',(-38.3631974573963,40.1950818318592,2.));
#63916=CARTESIAN_POINT('Ctrl Pts',(-38.4061067602759,40.2112658265376,2.));
#63917=CARTESIAN_POINT('Ctrl Pts',(-38.4283821944242,40.2196673964425,2.));
#63918=CARTESIAN_POINT('Ctrl Pts',(-38.450871698748,40.2275608160985,2.));
#63919=CARTESIAN_POINT('Ctrl Pts',(-38.4735555240439,40.2349372243507,2.));
#63920=CARTESIAN_POINT('Ctrl Pts',(-38.4855017473361,40.2388219403951,2.));
#63921=CARTESIAN_POINT('Ctrl Pts',(-38.4975038315009,40.2425636902965,2.));
#63922=CARTESIAN_POINT('Ctrl Pts',(-38.5095371704194,40.2461549840613,2.));
#63923=CARTESIAN_POINT('Ctrl Pts',(-38.5662684087183,40.2630861570093,2.));
#63924=CARTESIAN_POINT('Ctrl Pts',(-38.6237986216546,40.276712917215,2.));
#63925=CARTESIAN_POINT('Ctrl Pts',(-38.6818163301137,40.2869751451508,2.));
#63926=CARTESIAN_POINT('Ctrl Pts',(-38.7386491569881,40.2970277900951,2.));
#63927=CARTESIAN_POINT('Ctrl Pts',(-38.795950805549,40.3038518408609,2.));
#63928=CARTESIAN_POINT('Ctrl Pts',(-38.8534268715751,40.3073420065163,2.));
#63929=CARTESIAN_POINT('Ctrl Pts',(-38.8950337651222,40.3098685355732,2.));
#63930=CARTESIAN_POINT('Ctrl Pts',(-38.9367320688478,40.3106470090916,2.));
#63931=CARTESIAN_POINT('Ctrl Pts',(-38.9784050690481,40.3096213125545,2.));
#63932=CARTESIAN_POINT('Ctrl Pts',(-39.0001855019627,40.3090852312907,2.));
#63933=CARTESIAN_POINT('Ctrl Pts',(-39.021958929381,40.3080560888435,2.));
#63934=CARTESIAN_POINT('Ctrl Pts',(-39.0437079205564,40.3065243689262,2.));
#63935=CARTESIAN_POINT('Ctrl Pts',(-39.0538226985227,40.3058120137303,2.));
#63936=CARTESIAN_POINT('Ctrl Pts',(-39.0639271474701,40.304991238704,2.));
#63937=CARTESIAN_POINT('Ctrl Pts',(-39.0740116259078,40.3040622330021,2.));
#63938=CARTESIAN_POINT('Ctrl Pts',(-39.1295483097472,40.2989460640037,2.));
#63939=CARTESIAN_POINT('Ctrl Pts',(-39.1845546342211,40.2905462413972,2.));
#63940=CARTESIAN_POINT('Ctrl Pts',(-39.2387593259822,40.2787734967599,2.));
#63941=CARTESIAN_POINT('Ctrl Pts',(-39.2750276515155,40.2708963606476,2.));
#63942=CARTESIAN_POINT('Ctrl Pts',(-39.310936935959,40.2615081906221,2.));
#63943=CARTESIAN_POINT('Ctrl Pts',(-39.3464011448468,40.2505700228958,2.));
#63944=CARTESIAN_POINT('Ctrl Pts',(-39.3988910752724,40.2343806398264,2.));
#63945=CARTESIAN_POINT('Ctrl Pts',(-39.4504076476632,40.2147967478769,2.));
#63946=CARTESIAN_POINT('Ctrl Pts',(-39.5007091188364,40.1920209197932,2.));
#63947=CARTESIAN_POINT('Ctrl Pts',(-39.5162447293996,40.1849866047501,2.));
#63948=CARTESIAN_POINT('Ctrl Pts',(-39.5316641987849,40.1776475888762,2.));
#63949=CARTESIAN_POINT('Ctrl Pts',(-39.5469597255045,40.1700092883095,2.));
#63950=CARTESIAN_POINT('Ctrl Pts',(-39.5603821271851,40.1633063914271,2.));
#63951=CARTESIAN_POINT('Ctrl Pts',(-39.5737147687466,40.1563697365981,2.));
#63952=CARTESIAN_POINT('Ctrl Pts',(-39.5869207826588,40.1492204403469,2.));
#63953=CARTESIAN_POINT('Ctrl Pts',(-39.635889783268,40.1227102537904,2.));
#63954=CARTESIAN_POINT('Ctrl Pts',(-39.6831882131042,40.0932490202857,2.));
#63955=CARTESIAN_POINT('Ctrl Pts',(-39.7285927500411,40.0610855615979,2.));
#63956=CARTESIAN_POINT('Ctrl Pts',(-39.7739426813613,40.0289607841877,2.));
#63957=CARTESIAN_POINT('Ctrl Pts',(-39.8174040329096,39.9941393127112,2.));
#63958=CARTESIAN_POINT('Ctrl Pts',(-39.8587164117659,39.9568341503958,2.));
#63959=CARTESIAN_POINT('Ctrl Pts',(-39.8851222214993,39.9329896503829,2.));
#63960=CARTESIAN_POINT('Ctrl Pts',(-39.9106492841629,39.9081297964286,2.));
#63961=CARTESIAN_POINT('Ctrl Pts',(-39.9352193294817,39.8823054325709,2.));
#63962=CARTESIAN_POINT('Ctrl Pts',(-39.9478799226003,39.8689985070399,2.));
#63963=CARTESIAN_POINT('Ctrl Pts',(-39.9602862681352,39.855435438132,2.));
#63964=CARTESIAN_POINT('Ctrl Pts',(-39.9724266997145,39.8416229521415,2.));
#63965=CARTESIAN_POINT('Ctrl Pts',(-39.9797490690399,39.8332921013752,2.));
#63966=CARTESIAN_POINT('Ctrl Pts',(-39.9869741812552,39.824870935248,2.));
#63967=CARTESIAN_POINT('Ctrl Pts',(-39.9940910778001,39.8163713684992,2.));
#63968=CARTESIAN_POINT('Ctrl Pts',(-40.0285072441039,39.7752688316156,2.));
#63969=CARTESIAN_POINT('Ctrl Pts',(-40.0604511582545,39.7322729488062,2.));
#63970=CARTESIAN_POINT('Ctrl Pts',(-40.0896714279657,39.6875760500042,2.));
#63971=CARTESIAN_POINT('Ctrl Pts',(-40.1080207191978,39.6595079855614,2.));
#63972=CARTESIAN_POINT('Ctrl Pts',(-40.1252950915649,39.6307687140437,2.));
#63973=CARTESIAN_POINT('Ctrl Pts',(-40.141422040912,39.6014032998966,2.));
#63974=CARTESIAN_POINT('Ctrl Pts',(-40.1473185206672,39.5906664539939,2.));
#63975=CARTESIAN_POINT('Ctrl Pts',(-40.1530626680629,39.5798436443556,2.));
#63976=CARTESIAN_POINT('Ctrl Pts',(-40.1586468583156,39.5689444882778,2.));
#63977=CARTESIAN_POINT('Ctrl Pts',(-40.1820879991975,39.5231923484773,2.));
#63978=CARTESIAN_POINT('Ctrl Pts',(-40.2026786416958,39.4761684519491,2.));
#63979=CARTESIAN_POINT('Ctrl Pts',(-40.2201722454389,39.4280435374464,2.));
#63980=CARTESIAN_POINT('Ctrl Pts',(-40.2299448374156,39.4011591309937,2.));
#63981=CARTESIAN_POINT('Ctrl Pts',(-40.2387500543247,39.3739309307784,2.));
#63982=CARTESIAN_POINT('Ctrl Pts',(-40.2465377789656,39.3463880711444,2.));
#63983=CARTESIAN_POINT('Ctrl Pts',(-40.2520072382767,39.3270442246388,2.));
#63984=CARTESIAN_POINT('Ctrl Pts',(-40.2569746809645,39.3075451531312,2.));
#63985=CARTESIAN_POINT('Ctrl Pts',(-40.2614422049139,39.2879094456029,2.));
#63986=CARTESIAN_POINT('Origin',(-39.0658530619283,38.8697713466882,4.5));
#63987=CARTESIAN_POINT('Origin',(14.1292828945603,53.2669068454841,6.));
#63988=CARTESIAN_POINT('Ctrl Pts',(13.8936870225526,54.5092654229862,6.));
#63989=CARTESIAN_POINT('Ctrl Pts',(13.9423636521365,54.524108905134,6.));
#63990=CARTESIAN_POINT('Ctrl Pts',(13.9918505584143,54.5357341393502,6.));
#63991=CARTESIAN_POINT('Ctrl Pts',(14.041869470803,54.5442851897488,6.));
#63992=CARTESIAN_POINT('Ctrl Pts',(14.0755804158076,54.5500482896634,6.));
#63993=CARTESIAN_POINT('Ctrl Pts',(14.1095337101478,54.5544140915427,6.));
#63994=CARTESIAN_POINT('Ctrl Pts',(14.1436500643726,54.5574153942341,6.));
#63995=CARTESIAN_POINT('Ctrl Pts',(14.159412263785,54.5588020351163,6.));
#63996=CARTESIAN_POINT('Ctrl Pts',(14.1752093214863,54.5598972886015,6.));
#63997=CARTESIAN_POINT('Ctrl Pts',(14.191033635951,54.5607037375757,6.));
#63998=CARTESIAN_POINT('Ctrl Pts',(14.2042983435199,54.5613797422037,6.));
#63999=CARTESIAN_POINT('Ctrl Pts',(14.2175747323894,54.5618523554142,6.));
#64000=CARTESIAN_POINT('Ctrl Pts',(14.230851131071,54.5621236288019,6.));
#64001=CARTESIAN_POINT('Ctrl Pts',(14.2845943079395,54.5632217499119,6.));
#64002=CARTESIAN_POINT('Ctrl Pts',(14.3383718685865,54.5610264739163,6.));
#64003=CARTESIAN_POINT('Ctrl Pts',(14.3918835284631,54.5556664140625,6.));
#64004=CARTESIAN_POINT('Ctrl Pts',(14.4123675638192,54.5536146059928,6.));
#64005=CARTESIAN_POINT('Ctrl Pts',(14.4328128170711,54.5510985259764,6.));
#64006=CARTESIAN_POINT('Ctrl Pts',(14.4532029278659,54.5481234359019,6.));
#64007=CARTESIAN_POINT('Ctrl Pts',(14.4678705661123,54.5459833030991,6.));
#64008=CARTESIAN_POINT('Ctrl Pts',(14.4825096747067,54.5436056261043,6.));
#64009=CARTESIAN_POINT('Ctrl Pts',(14.4971141904897,54.5409920215303,6.));
#64010=CARTESIAN_POINT('Ctrl Pts',(14.5083899393717,54.5389741286202,6.));
#64011=CARTESIAN_POINT('Ctrl Pts',(14.5196453769788,54.5368154091208,6.));
#64012=CARTESIAN_POINT('Ctrl Pts',(14.5308625723425,54.5345199552782,6.));
#64013=CARTESIAN_POINT('Ctrl Pts',(14.5863736833702,54.5231603249085,6.));
#64014=CARTESIAN_POINT('Ctrl Pts',(14.6410375585735,54.5084412328018,6.));
#64015=CARTESIAN_POINT('Ctrl Pts',(14.6945239552559,54.4905089639947,6.));
#64016=CARTESIAN_POINT('Ctrl Pts',(14.7472373376177,54.4728358620309,6.));
#64017=CARTESIAN_POINT('Ctrl Pts',(14.7988082441058,54.4520415392015,6.));
#64018=CARTESIAN_POINT('Ctrl Pts',(14.8489245844431,54.4282130800221,6.));
#64019=CARTESIAN_POINT('Ctrl Pts',(14.8750932855581,54.4157708341977,6.));
#64020=CARTESIAN_POINT('Ctrl Pts',(14.9008653564499,54.402500473298,6.));
#64021=CARTESIAN_POINT('Ctrl Pts',(14.9261951331621,54.3884088627284,6.));
#64022=CARTESIAN_POINT('Ctrl Pts',(14.9397870441658,54.3808473307443,6.));
#64023=CARTESIAN_POINT('Ctrl Pts',(14.9532515800927,54.3730492659916,6.));
#64024=CARTESIAN_POINT('Ctrl Pts',(14.9665814890931,54.3650152874695,6.));
#64025=CARTESIAN_POINT('Ctrl Pts',(14.976060531546,54.3593022384552,6.));
#64026=CARTESIAN_POINT('Ctrl Pts',(14.9854714930861,54.3534698864814,6.));
#64027=CARTESIAN_POINT('Ctrl Pts',(14.9948117120544,54.3475183602377,6.));
#64028=CARTESIAN_POINT('Ctrl Pts',(15.003022232497,54.3422866704823,6.));
#64029=CARTESIAN_POINT('Ctrl Pts',(15.0111697860467,54.3369681734725,6.));
#64030=CARTESIAN_POINT('Ctrl Pts',(15.0192523730691,54.3315638161437,6.));
#64031=CARTESIAN_POINT('Ctrl Pts',(15.0592738168297,54.3048037970687,6.));
#64032=CARTESIAN_POINT('Ctrl Pts',(15.0977061905865,54.2759385109608,6.));
#64033=CARTESIAN_POINT('Ctrl Pts',(15.1343580440251,54.2450336527682,6.));
#64034=CARTESIAN_POINT('Ctrl Pts',(15.1760762697649,54.2098568273262,6.));
#64035=CARTESIAN_POINT('Ctrl Pts',(15.2154892262316,54.1720387363143,6.));
#64036=CARTESIAN_POINT('Ctrl Pts',(15.2525505184408,54.1318952661649,6.));
#64037=CARTESIAN_POINT('Ctrl Pts',(15.2887783562941,54.0926545640536,6.));
#64038=CARTESIAN_POINT('Ctrl Pts',(15.3227594146192,54.0511910496008,6.));
#64039=CARTESIAN_POINT('Ctrl Pts',(15.3544244053206,54.0077622836781,6.));
#64040=CARTESIAN_POINT('Ctrl Pts',(15.3621778074482,53.9971284360551,6.));
#64041=CARTESIAN_POINT('Ctrl Pts',(15.3697922131791,53.9863766152115,6.));
#64042=CARTESIAN_POINT('Ctrl Pts',(15.3772663285767,53.9755103369004,6.));
#64043=CARTESIAN_POINT('Ctrl Pts',(15.3829111783903,53.9673035450815,6.));
#64044=CARTESIAN_POINT('Ctrl Pts',(15.3884748239509,53.959033039286,6.));
#64045=CARTESIAN_POINT('Ctrl Pts',(15.3939506112589,53.9507101506015,6.));
#64046=CARTESIAN_POINT('Ctrl Pts',(15.4256178027551,53.9025778008681,6.));
#64047=CARTESIAN_POINT('Ctrl Pts',(15.4544095036352,53.8526099943005,6.));
#64048=CARTESIAN_POINT('Ctrl Pts',(15.4802788953979,53.8011564089304,6.));
#64049=CARTESIAN_POINT('Ctrl Pts',(15.5067035063861,53.748598506146,6.));
#64050=CARTESIAN_POINT('Ctrl Pts',(15.5300796467746,53.6944895429324,6.));
#64051=CARTESIAN_POINT('Ctrl Pts',(15.5503219670269,53.6391607086969,6.));
#64052=CARTESIAN_POINT('Ctrl Pts',(15.5707432288469,53.5833427690514,6.));
#64053=CARTESIAN_POINT('Ctrl Pts',(15.5879756421407,53.5262822853792,6.));
#64054=CARTESIAN_POINT('Ctrl Pts',(15.6018865037402,53.468291582188,6.));
#64055=CARTESIAN_POINT('Ctrl Pts',(15.6050386064391,53.4551512996301,6.));
#64056=CARTESIAN_POINT('Ctrl Pts',(15.6080206160607,53.4419594370947,6.));
#64057=CARTESIAN_POINT('Ctrl Pts',(15.6108253926933,53.4287461304931,6.));
#64058=CARTESIAN_POINT('Ctrl Pts',(15.6234580838842,53.3692335047938,6.));
#64059=CARTESIAN_POINT('Ctrl Pts',(15.6325248597468,53.3091883988419,6.));
#64060=CARTESIAN_POINT('Ctrl Pts',(15.6379479683223,53.2489633020841,6.));
#64061=CARTESIAN_POINT('Ctrl Pts',(15.643323424427,53.1892673989841,6.));
#64062=CARTESIAN_POINT('Ctrl Pts',(15.6451194085375,53.1293935642736,6.));
#64063=CARTESIAN_POINT('Ctrl Pts',(15.6432152689552,53.0696627699222,6.));
#64064=CARTESIAN_POINT('Ctrl Pts',(15.6418200559671,53.0258964510863,6.));
#64065=CARTESIAN_POINT('Ctrl Pts',(15.6384374018724,52.9822063985706,6.));
#64066=CARTESIAN_POINT('Ctrl Pts',(15.6330021738796,52.9387162761377,6.));
#64067=CARTESIAN_POINT('Ctrl Pts',(15.6299816095937,52.9145471500616,6.));
#64068=CARTESIAN_POINT('Ctrl Pts',(15.626326826898,52.8904397607359,6.));
#64069=CARTESIAN_POINT('Ctrl Pts',(15.6220514315181,52.8664094746825,6.));
#64070=CARTESIAN_POINT('Ctrl Pts',(15.2209662466057,52.1764590205668,6.));
#64071=CARTESIAN_POINT('Ctrl Pts',(15.1741443796226,52.1372711016556,6.));
#64072=CARTESIAN_POINT('Ctrl Pts',(15.1249225029807,52.1011828129762,6.));
#64073=CARTESIAN_POINT('Ctrl Pts',(15.0736468678487,52.0682420900143,6.));
#64074=CARTESIAN_POINT('Ctrl Pts',(15.0261004125926,52.0376970834751,6.));
#64075=CARTESIAN_POINT('Ctrl Pts',(14.9767869967282,52.0098588542107,6.));
#64076=CARTESIAN_POINT('Ctrl Pts',(14.9259704605611,51.9848043154176,6.));
#64077=CARTESIAN_POINT('Ctrl Pts',(14.9137051793975,51.9787570523434,6.));
#64078=CARTESIAN_POINT('Ctrl Pts',(14.901351848406,51.9728720566584,6.));
#64079=CARTESIAN_POINT('Ctrl Pts',(14.8889282288742,51.9671568053379,6.));
#64080=CARTESIAN_POINT('Ctrl Pts',(14.8342503523039,51.942003281804,6.));
#64081=CARTESIAN_POINT('Ctrl Pts',(14.7781470460569,51.9201009098466,6.));
#64082=CARTESIAN_POINT('Ctrl Pts',(14.7209451682992,51.901525951817,6.));
#64083=CARTESIAN_POINT('Ctrl Pts',(14.6856380617977,51.8900608033443,6.));
#64084=CARTESIAN_POINT('Ctrl Pts',(14.649912165413,51.8798643401536,6.));
#64085=CARTESIAN_POINT('Ctrl Pts',(14.6138441166823,51.8709644322168,6.));
#64086=CARTESIAN_POINT('Ctrl Pts',(14.6015017903692,51.8679189231921,6.));
#64087=CARTESIAN_POINT('Ctrl Pts',(14.5891194067602,51.8650253042931,6.));
#64088=CARTESIAN_POINT('Ctrl Pts',(14.5767000729095,51.8622849006199,6.));
#64089=CARTESIAN_POINT('Ctrl Pts',(14.5650829794111,51.859721516297,6.));
#64090=CARTESIAN_POINT('Ctrl Pts',(14.5534409516981,51.8572938729425,6.));
#64091=CARTESIAN_POINT('Ctrl Pts',(14.5417825460264,51.8550036366239,6.));
#64092=CARTESIAN_POINT('Ctrl Pts',(14.4840742560038,51.8436671275493,6.));
#64093=CARTESIAN_POINT('Ctrl Pts',(14.4259183529976,51.8356828275334,6.));
#64094=CARTESIAN_POINT('Ctrl Pts',(14.367620963293,51.8311224894092,6.));
#64095=CARTESIAN_POINT('Ctrl Pts',(14.3108124223156,51.8266786171104,6.));
#64096=CARTESIAN_POINT('Ctrl Pts',(14.2538685533622,51.8254861890659,6.));
#64097=CARTESIAN_POINT('Ctrl Pts',(14.1970797852662,51.8276601888178,6.));
#64098=CARTESIAN_POINT('Ctrl Pts',(14.1662905485933,51.8288388689535,6.));
#64099=CARTESIAN_POINT('Ctrl Pts',(14.1355471146555,51.8310079452875,6.));
#64100=CARTESIAN_POINT('Ctrl Pts',(14.1048981746267,51.8341917567403,6.));
#64101=CARTESIAN_POINT('Ctrl Pts',(14.0793989213186,51.8368406188101,6.));
#64102=CARTESIAN_POINT('Ctrl Pts',(14.0539650963251,51.8401919425187,6.));
#64103=CARTESIAN_POINT('Ctrl Pts',(14.0286260527374,51.8442620100932,6.));
#64104=CARTESIAN_POINT('Ctrl Pts',(14.0177944477837,51.8460018296703,6.));
#64105=CARTESIAN_POINT('Ctrl Pts',(14.0069789238117,51.8478733580886,6.));
#64106=CARTESIAN_POINT('Ctrl Pts',(13.9961993347096,51.8498743913219,6.));
#64107=CARTESIAN_POINT('Ctrl Pts',(13.9463007653032,51.8591371465837,6.));
#64108=CARTESIAN_POINT('Ctrl Pts',(13.8970847123029,51.8711850123457,6.));
#64109=CARTESIAN_POINT('Ctrl Pts',(13.8487579820866,51.8860904144816,6.));
#64110=CARTESIAN_POINT('Ctrl Pts',(13.7947539043108,51.9027468796019,6.));
#64111=CARTESIAN_POINT('Ctrl Pts',(13.7418592133624,51.9229715823681,6.));
#64112=CARTESIAN_POINT('Ctrl Pts',(13.6903202642341,51.946518424925,6.));
#64113=CARTESIAN_POINT('Ctrl Pts',(13.646584361829,51.9665002527549,6.));
#64114=CARTESIAN_POINT('Ctrl Pts',(13.6038249088318,51.9888755884478,6.));
#64115=CARTESIAN_POINT('Ctrl Pts',(13.5622133001607,52.0135148505961,6.));
#64116=CARTESIAN_POINT('Ctrl Pts',(13.5507734482952,52.020288669683,6.));
#64117=CARTESIAN_POINT('Ctrl Pts',(13.5394204822265,52.0272336869092,6.));
#64118=CARTESIAN_POINT('Ctrl Pts',(13.5281582767437,52.0343473928043,6.));
#64119=CARTESIAN_POINT('Ctrl Pts',(13.5193898407158,52.0398859238812,6.));
#64120=CARTESIAN_POINT('Ctrl Pts',(13.5106749799805,52.0455277717941,6.));
#64121=CARTESIAN_POINT('Ctrl Pts',(13.5020295298397,52.0512622212478,6.));
#64122=CARTESIAN_POINT('Ctrl Pts',(13.4557689091919,52.0819464755643,6.));
#64123=CARTESIAN_POINT('Ctrl Pts',(13.4114050030068,52.1153327759281,6.));
#64124=CARTESIAN_POINT('Ctrl Pts',(13.3691631576739,52.1511816197357,6.));
#64125=CARTESIAN_POINT('Ctrl Pts',(13.3271578441964,52.1868297290946,6.));
#64126=CARTESIAN_POINT('Ctrl Pts',(13.2872501899337,52.2249138500805,6.));
#64127=CARTESIAN_POINT('Ctrl Pts',(13.2497024979355,52.2652291267845,6.));
#64128=CARTESIAN_POINT('Ctrl Pts',(13.2148651398199,52.3026342949139,6.));
#64129=CARTESIAN_POINT('Ctrl Pts',(13.1820592965135,52.341961003002,6.));
#64130=CARTESIAN_POINT('Ctrl Pts',(13.1515339536892,52.3830588009893,6.));
#64131=CARTESIAN_POINT('Ctrl Pts',(13.1436930287378,52.393615430985,6.));
#64132=CARTESIAN_POINT('Ctrl Pts',(13.136000309683,52.4042927640824,6.));
#64133=CARTESIAN_POINT('Ctrl Pts',(13.1284766278933,52.4150644154215,6.));
#64134=CARTESIAN_POINT('Ctrl Pts',(13.0980644553258,52.4586055072062,6.));
#64135=CARTESIAN_POINT('Ctrl Pts',(13.0703588458694,52.5037520469927,6.));
#64136=CARTESIAN_POINT('Ctrl Pts',(13.0455900654387,52.5503113513023,6.));
#64137=CARTESIAN_POINT('Ctrl Pts',(13.0216615115385,52.5952912333701,6.));
#64138=CARTESIAN_POINT('Ctrl Pts',(13.0004736387414,52.641590479389,6.));
#64139=CARTESIAN_POINT('Ctrl Pts',(12.98228031951,52.6890470685081,6.));
#64140=CARTESIAN_POINT('Ctrl Pts',(12.9695523308681,52.7222475482892,6.));
#64141=CARTESIAN_POINT('Ctrl Pts',(12.9582909257621,52.7560147190195,6.));
#64142=CARTESIAN_POINT('Ctrl Pts',(12.9485983183411,52.7902936156639,6.));
#64143=CARTESIAN_POINT('Ctrl Pts',(12.943130825006,52.8096299645733,6.));
#64144=CARTESIAN_POINT('Ctrl Pts',(12.9381627931205,52.8291291517902,6.));
#64145=CARTESIAN_POINT('Ctrl Pts',(12.9336933707122,52.8487726938778,6.));
#64146=CARTESIAN_POINT('Origin',(14.1292828945603,53.2669068454841,0.895788276411274));
#64147=CARTESIAN_POINT('Ctrl Pts',(14.9010809748678,54.6051974101417,2.14578827641127));
#64148=CARTESIAN_POINT('Ctrl Pts',(14.8597272487244,54.6294211798578,2.14826884812012));
#64149=CARTESIAN_POINT('Ctrl Pts',(14.3688277705329,54.885598628679,2.17691792328789));
#64150=CARTESIAN_POINT('Ctrl Pts',(13.1694755608909,54.8098887390118,2.23173550191458));
#64151=CARTESIAN_POINT('Ctrl Pts',(12.3130077055018,53.3174154968919,2.31024101229137));
#64152=CARTESIAN_POINT('Ctrl Pts',(13.0852322400692,51.7797767714816,2.38874652266814));
#64153=CARTESIAN_POINT('Ctrl Pts',(14.7938791388702,51.5757659053288,2.46725203304493));
#64154=CARTESIAN_POINT('Ctrl Pts',(15.9064540032169,52.8884432158558,2.5457575434217));
#64155=CARTESIAN_POINT('Ctrl Pts',(15.5416657446855,54.1408201433548,2.60526962454382));
#64156=CARTESIAN_POINT('Ctrl Pts',(15.0227829664514,54.5334351262247,2.63861320220701));
#64157=CARTESIAN_POINT('Ctrl Pts',(14.9016274172746,54.6020379108679,2.64578827641127));
#64158=CARTESIAN_POINT('Ctrl Pts',(14.9013089558621,54.600969116598,2.10421172358873));
#64159=CARTESIAN_POINT('Ctrl Pts',(14.6040162957702,54.7699114721225,2.12181148931034));
#64160=CARTESIAN_POINT('Ctrl Pts',(13.7242010739631,54.9558633776928,2.16557975849087));
#64161=CARTESIAN_POINT('Ctrl Pts',(12.4888977717378,54.0475500892828,2.23551653113034));
#64162=CARTESIAN_POINT('Ctrl Pts',(12.5727324025626,52.3295818538895,2.31402204150712));
#64163=CARTESIAN_POINT('Ctrl Pts',(14.0528383317196,51.4513683986094,2.3925275518839));
#64164=CARTESIAN_POINT('Ctrl Pts',(15.6013423678816,52.2018016959779,2.47103306226067));
#64165=CARTESIAN_POINT('Ctrl Pts',(15.8066350265236,53.7346571674393,2.54159445282895));
#64166=CARTESIAN_POINT('Ctrl Pts',(15.2043102739953,54.4236472184416,2.5859873399383));
#64167=CARTESIAN_POINT('Ctrl Pts',(14.8992309062956,54.6029598038327,2.60421172358873));
#64168=CARTESIAN_POINT('Ctrl Pts',(12.9355708698302,52.8497595669186,2.));
#64169=CARTESIAN_POINT('Ctrl Pts',(13.0727468794464,52.4572155888145,2.02616850345893));
#64170=CARTESIAN_POINT('Ctrl Pts',(13.762195269905,51.8244143348174,2.07850551037678));
#64171=CARTESIAN_POINT('Ctrl Pts',(15.132331970736,52.1652352880051,2.15701102075356));
#64172=CARTESIAN_POINT('Ctrl Pts',(15.600345878683,53.4958301810381,2.23551653113034));
#64173=CARTESIAN_POINT('Ctrl Pts',(14.7503158422929,54.6202478137908,2.31402204150712));
#64174=CARTESIAN_POINT('Ctrl Pts',(13.3427136311611,54.5313920070952,2.3925275518839));
#64175=CARTESIAN_POINT('Ctrl Pts',(12.6408318404031,53.3082990617544,2.47103306226068));
#64176=CARTESIAN_POINT('Ctrl Pts',(13.2736756018811,52.0481926662384,2.54953857263746));
#64177=CARTESIAN_POINT('Ctrl Pts',(14.6739244700172,51.8810042409304,2.62804408301423));
#64178=CARTESIAN_POINT('Ctrl Pts',(15.5856878633849,52.9567530803091,2.70654959339101));
#64179=CARTESIAN_POINT('Ctrl Pts',(15.1913315822309,54.3106417984377,2.78505510376779));
#64180=CARTESIAN_POINT('Ctrl Pts',(13.8444953540085,54.7284908735361,2.86356061414457));
#64181=CARTESIAN_POINT('Ctrl Pts',(12.7530680664412,53.8355533167568,2.94206612452135));
#64182=CARTESIAN_POINT('Ctrl Pts',(12.8958606092945,52.4326417450687,3.02057163489813));
#64183=CARTESIAN_POINT('Ctrl Pts',(14.1448167496288,51.7779181217064,3.09907714527491));
#64184=CARTESIAN_POINT('Ctrl Pts',(15.3798411765859,52.4585553969251,3.17758265565169));
#64185=CARTESIAN_POINT('Ctrl Pts',(15.4933354964796,53.86414126306,3.25608816602848));
#64186=CARTESIAN_POINT('Ctrl Pts',(14.3835148696119,54.7341132075812,3.33459367640524));
#64187=CARTESIAN_POINT('Ctrl Pts',(13.0456930357207,54.2882595546367,3.41309918678203));
#64188=CARTESIAN_POINT('Ctrl Pts',(12.6796603121051,52.9264325363301,3.4916046971588));
#64189=CARTESIAN_POINT('Ctrl Pts',(13.6136836011906,51.8699509600852,3.57011020753559));
#64190=CARTESIAN_POINT('Ctrl Pts',(15.0101085852912,52.066292638923,3.64861571791237));
#64191=CARTESIAN_POINT('Ctrl Pts',(15.6165881539763,53.3393736780174,3.72712122828915));
#64192=CARTESIAN_POINT('Ctrl Pts',(14.8892170051293,54.5474647404685,3.80562673866593));
#64193=CARTESIAN_POINT('Ctrl Pts',(13.4803188806438,54.6071210383936,3.88413224904271));
#64194=CARTESIAN_POINT('Ctrl Pts',(12.6534271115016,53.4648413867365,3.96263775941949));
#64195=CARTESIAN_POINT('Ctrl Pts',(13.1501178953861,52.1450493326719,4.04114326979627));
#64196=CARTESIAN_POINT('Ctrl Pts',(14.5249471286252,51.8313657668162,4.11964878017305));
#64197=CARTESIAN_POINT('Ctrl Pts',(15.5449352706107,52.805109568325,4.19815429054982));
#64198=CARTESIAN_POINT('Ctrl Pts',(15.2953327061785,54.1930041465599,4.2766598009266));
#64199=CARTESIAN_POINT('Ctrl Pts',(13.9999889501244,54.7503526485877,4.35516531130338));
#64200=CARTESIAN_POINT('Ctrl Pts',(12.8205990758801,53.9773116872669,4.43367082168016));
#64201=CARTESIAN_POINT('Ctrl Pts',(12.8148679650961,52.5671627753774,4.51217633205694));
#64202=CARTESIAN_POINT('Ctrl Pts',(13.9879354060904,51.7845609801148,4.59068184243372));
#64203=CARTESIAN_POINT('Ctrl Pts',(15.2877666458998,52.3313621994942,4.6691873528105));
#64204=CARTESIAN_POINT('Ctrl Pts',(15.5486420944497,53.7171820950402,4.74769286318728));
#64205=CARTESIAN_POINT('Ctrl Pts',(14.5366025126985,54.699184449441,4.82619837356406));
#64206=CARTESIAN_POINT('Ctrl Pts',(13.1592689266914,54.3966861834431,4.90470388394084));
#64207=CARTESIAN_POINT('Ctrl Pts',(12.651867102821,53.0809749777223,4.98320939431762));
#64208=CARTESIAN_POINT('Ctrl Pts',(13.4694465335298,51.9320118320646,5.06171490469439));
#64209=CARTESIAN_POINT('Ctrl Pts',(14.8787836035794,51.980214388546,5.14022041507118));
#64210=CARTESIAN_POINT('Ctrl Pts',(15.6159492071913,53.1823530914927,5.21872592544796));
#64211=CARTESIAN_POINT('Ctrl Pts',(15.0198399508834,54.4603220891203,5.29723143582474));
#64212=CARTESIAN_POINT('Ctrl Pts',(13.6250522726906,54.6680069657356,5.37573694620152));
#64213=CARTESIAN_POINT('Ctrl Pts',(12.6824820007894,53.6191538682575,5.4542424565783));
#64214=CARTESIAN_POINT('Ctrl Pts',(13.0374143051106,52.2543934093273,5.53274796695507));
#64215=CARTESIAN_POINT('Ctrl Pts',(14.3716061738679,51.7976868080881,5.61125347733186));
#64216=CARTESIAN_POINT('Ctrl Pts',(15.4883847851255,52.6585961458811,5.68975898770863));
#64217=CARTESIAN_POINT('Ctrl Pts',(15.3864730097086,54.0650841092748,5.76826449808542));
#64218=CARTESIAN_POINT('Ctrl Pts',(14.156713139869,54.755685297877,5.84677000846219));
#64219=CARTESIAN_POINT('Ctrl Pts',(12.9030960095781,54.1112396708051,5.92527551883898));
#64220=CARTESIAN_POINT('Ctrl Pts',(12.7476560431649,52.7093273325191,6.00378102921575));
#64221=CARTESIAN_POINT('Ctrl Pts',(13.8343697837273,51.8079468650312,6.08228653959253));
#64222=CARTESIAN_POINT('Ctrl Pts',(14.7300614275787,52.0790796540862,6.13462354651038));
#64223=CARTESIAN_POINT('Ctrl Pts',(15.0239255378924,52.3732767258419,6.16079204996931));
#64224=CARTESIAN_POINT('Ctrl Pts',(12.8479344393867,52.8191346777449,1.94640265001023));
#64225=CARTESIAN_POINT('Ctrl Pts',(12.9951812328907,52.3977720630513,1.97257115346916));
#64226=CARTESIAN_POINT('Ctrl Pts',(13.7352455128293,51.7185136720468,2.02490816038701));
#64227=CARTESIAN_POINT('Ctrl Pts',(15.2059708708849,52.0843560132567,2.10341367076379));
#64228=CARTESIAN_POINT('Ctrl Pts',(15.7083440442499,53.5126365996361,2.18191918114057));
#64229=CARTESIAN_POINT('Ctrl Pts',(14.7959090084834,54.7196034114378,2.26042469151735));
#64230=CARTESIAN_POINT('Ctrl Pts',(13.2849676077377,54.6242242510673,2.33893020189412));
#64231=CARTESIAN_POINT('Ctrl Pts',(12.5315571287693,53.311337873467,2.41743571227091));
#64232=CARTESIAN_POINT('Ctrl Pts',(13.2108611479438,51.9587207013194,2.49594122264769));
#64233=CARTESIAN_POINT('Ctrl Pts',(14.7139093596349,51.7792581290633,2.57444673302446));
#64234=CARTESIAN_POINT('Ctrl Pts',(15.6926099099956,52.9339831254913,2.65295224340124));
#64235=CARTESIAN_POINT('Ctrl Pts',(15.2693019419295,54.3872676543484,2.73145775377802));
#64236=CARTESIAN_POINT('Ctrl Pts',(13.8235876618921,54.8357931410496,2.80996326415481));
#64237=CARTESIAN_POINT('Ctrl Pts',(12.6520331831853,53.8773005270505,2.88846877453158));
#64238=CARTESIAN_POINT('Ctrl Pts',(12.8053088480064,52.3713941292876,2.96697428490836));
#64239=CARTESIAN_POINT('Ctrl Pts',(14.1459571684074,51.6686039370295,3.04547979528514));
#64240=CARTESIAN_POINT('Ctrl Pts',(15.4716509779683,52.3992102332441,3.12398530566192));
#64241=CARTESIAN_POINT('Ctrl Pts',(15.5934774892658,53.90798725892,3.2024908160387));
#64242=CARTESIAN_POINT('Ctrl Pts',(14.4021793232963,54.8418282390413,3.28099632641548));
#64243=CARTESIAN_POINT('Ctrl Pts',(12.9661412298193,54.3632422169536,3.35950183679226));
#64244=CARTESIAN_POINT('Ctrl Pts',(12.5732361947429,52.9014365971975,3.43800734716904));
#64245=CARTESIAN_POINT('Ctrl Pts',(13.5758308522243,51.7673933710292,3.51651285754582));
#64246=CARTESIAN_POINT('Ctrl Pts',(15.0747744492344,51.978149484441,3.5950183679226));
#64247=CARTESIAN_POINT('Ctrl Pts',(15.7257787470296,53.3446938343006,3.67352387829938));
#64248=CARTESIAN_POINT('Ctrl Pts',(14.945007607421,54.6414769649982,3.75202938867616));
#64249=CARTESIAN_POINT('Ctrl Pts',(13.4326751537753,54.7055129331413,3.83053489905294));
#64250=CARTESIAN_POINT('Ctrl Pts',(12.5450770823512,53.4793727613876,3.90904040942971));
#64251=CARTESIAN_POINT('Ctrl Pts',(13.0782324459937,52.0626881049618,3.9875459198065));
#64252=CARTESIAN_POINT('Ctrl Pts',(14.5539948389685,51.7259754437876,4.06605143018328));
#64253=CARTESIAN_POINT('Ctrl Pts',(15.6488654635012,52.77120669718,4.14455694056005));
#64254=CARTESIAN_POINT('Ctrl Pts',(15.3809383138062,54.2609936281335,4.22306245093684));
#64255=CARTESIAN_POINT('Ctrl Pts',(13.9904968284622,54.8592598994548,4.30156796131361));
#64256=CARTESIAN_POINT('Ctrl Pts',(12.724521985198,54.029466095712,4.3800734716904));
#64257=CARTESIAN_POINT('Ctrl Pts',(12.7183701246174,52.51579102804,4.45857898206717));
#64258=CARTESIAN_POINT('Ctrl Pts',(13.9775583728655,51.6757344812336,4.53708449244395));
#64259=CARTESIAN_POINT('Ctrl Pts',(15.3728167908182,52.2626791406019,4.61559000282073));
#64260=CARTESIAN_POINT('Ctrl Pts',(15.6528444240053,53.7502390759288,4.69409551319751));
#64261=CARTESIAN_POINT('Ctrl Pts',(14.5665059036703,54.8043351843039,4.77260102357429));
#64262=CARTESIAN_POINT('Ctrl Pts',(13.0880553007387,54.4796289923587,4.85110653395107));
#64263=CARTESIAN_POINT('Ctrl Pts',(12.5434025455521,53.0673247799706,4.92961204432785));
#64264=CARTESIAN_POINT('Ctrl Pts',(13.4210046127318,51.834010445156,5.00811755470463));
#64265=CARTESIAN_POINT('Ctrl Pts',(14.9338082371531,51.8857517948312,5.08662306508141));
#64266=CARTESIAN_POINT('Ctrl Pts',(15.725092891933,53.1761455732414,5.16512857545819));
#64267=CARTESIAN_POINT('Ctrl Pts',(15.0852202435382,54.5479367313644,5.24363408583497));
#64268=CARTESIAN_POINT('Ctrl Pts',(13.5880341553344,54.770868804009,5.32213959621175));
#64269=CARTESIAN_POINT('Ctrl Pts',(12.5762650378488,53.6450141017733,5.40064510658853));
#64270=CARTESIAN_POINT('Ctrl Pts',(12.9572547157705,52.1800596826977,5.4791506169653));
#64271=CARTESIAN_POINT('Ctrl Pts',(14.3893963500342,51.6898239425509,5.55765612734209));
#64272=CARTESIAN_POINT('Ctrl Pts',(15.5881633211799,52.6139369841995,5.63616163771886));
#64273=CARTESIAN_POINT('Ctrl Pts',(15.478769687465,54.1236823346512,5.71466714809565));
#64274=CARTESIAN_POINT('Ctrl Pts',(14.1587269327564,54.8649840454693,5.79317265847242));
#64275=CARTESIAN_POINT('Ctrl Pts',(12.8130754355785,54.1732264091344,5.8716781688492));
#64276=CARTESIAN_POINT('Ctrl Pts',(12.6462238359385,52.6683926035456,5.95018367922598));
#64277=CARTESIAN_POINT('Ctrl Pts',(13.8127187223415,51.7008372421088,6.02868918960276));
#64278=CARTESIAN_POINT('Ctrl Pts',(14.7741676148585,51.9918752589882,6.08102619652061));
#64279=CARTESIAN_POINT('Ctrl Pts',(15.0896057741302,52.3076708240835,6.10719469997954));
#64280=CARTESIAN_POINT('Ctrl Pts',(12.7602980089432,52.7885097885711,1.89280530002046));
#64281=CARTESIAN_POINT('Ctrl Pts',(12.9176155863349,52.3383285372882,1.91897380347939));
#64282=CARTESIAN_POINT('Ctrl Pts',(13.7082957557536,51.6126130092761,1.97131081039724));
#64283=CARTESIAN_POINT('Ctrl Pts',(15.2796097710338,52.0034767385083,2.04981632077402));
#64284=CARTESIAN_POINT('Ctrl Pts',(15.8163422098168,53.5294430182342,2.1283218311508));
#64285=CARTESIAN_POINT('Ctrl Pts',(14.8415021746739,54.8189590090846,2.20682734152758));
#64286=CARTESIAN_POINT('Ctrl Pts',(13.2272215843143,54.7170564950396,2.28533285190435));
#64287=CARTESIAN_POINT('Ctrl Pts',(12.4222824171356,53.3143766851794,2.36383836228114));
#64288=CARTESIAN_POINT('Ctrl Pts',(13.1480466940064,51.8692487364006,2.44234387265791));
#64289=CARTESIAN_POINT('Ctrl Pts',(14.7538942492525,51.677512017196,2.52084938303469));
#64290=CARTESIAN_POINT('Ctrl Pts',(15.7995319566062,52.9112131706735,2.59935489341147));
#64291=CARTESIAN_POINT('Ctrl Pts',(15.347272301628,54.4638935102592,2.67786040378825));
#64292=CARTESIAN_POINT('Ctrl Pts',(13.8026799697756,54.9430954085631,2.75636591416504));
#64293=CARTESIAN_POINT('Ctrl Pts',(12.5509982999295,53.9190477373443,2.83487142454181));
#64294=CARTESIAN_POINT('Ctrl Pts',(12.7147570867183,52.3101465135065,2.91337693491859));
#64295=CARTESIAN_POINT('Ctrl Pts',(14.147097587186,51.5592897523524,2.99188244529537));
#64296=CARTESIAN_POINT('Ctrl Pts',(15.5634607793508,52.3398650695633,3.07038795567215));
#64297=CARTESIAN_POINT('Ctrl Pts',(15.693619482052,53.9518332547799,3.14889346604893));
#64298=CARTESIAN_POINT('Ctrl Pts',(14.4208437769808,54.9495432705015,3.22739897642571));
#64299=CARTESIAN_POINT('Ctrl Pts',(12.8865894239179,54.4382248792704,3.30590448680249));
#64300=CARTESIAN_POINT('Ctrl Pts',(12.4668120773806,52.876440658065,3.38440999717926));
#64301=CARTESIAN_POINT('Ctrl Pts',(13.5379781032581,51.6648357819733,3.46291550755605));
#64302=CARTESIAN_POINT('Ctrl Pts',(15.1394403131777,51.8900063299591,3.54142101793282));
#64303=CARTESIAN_POINT('Ctrl Pts',(15.8349693400828,53.3500139905838,3.61992652830961));
#64304=CARTESIAN_POINT('Ctrl Pts',(15.0007982097127,54.7354891895278,3.69843203868638));
#64305=CARTESIAN_POINT('Ctrl Pts',(13.3850314269068,54.8039048278889,3.77693754906317));
#64306=CARTESIAN_POINT('Ctrl Pts',(12.4367270532009,53.4939041360386,3.85544305943994));
#64307=CARTESIAN_POINT('Ctrl Pts',(13.0063469966013,51.9803268772517,3.93394856981673));
#64308=CARTESIAN_POINT('Ctrl Pts',(14.5830425493117,51.620585120759,4.0124540801935));
#64309=CARTESIAN_POINT('Ctrl Pts',(15.7527956563917,52.7373038260349,4.09095959057029));
#64310=CARTESIAN_POINT('Ctrl Pts',(15.4665439214339,54.3289831097072,4.16946510094706));
#64311=CARTESIAN_POINT('Ctrl Pts',(13.9810047068001,54.9681671503218,4.24797061132385));
#64312=CARTESIAN_POINT('Ctrl Pts',(12.628444894516,54.0816205041572,4.32647612170062));
#64313=CARTESIAN_POINT('Ctrl Pts',(12.6218722841387,52.4644192807024,4.40498163207741));
#64314=CARTESIAN_POINT('Ctrl Pts',(13.9671813396405,51.5669079823527,4.48348714245418));
#64315=CARTESIAN_POINT('Ctrl Pts',(15.4578669357366,52.1939960817095,4.56199265283096));
#64316=CARTESIAN_POINT('Ctrl Pts',(15.7570467535609,53.7832960568176,4.64049816320774));
#64317=CARTESIAN_POINT('Ctrl Pts',(14.5964092946421,54.9094859191667,4.71900367358452));
#64318=CARTESIAN_POINT('Ctrl Pts',(13.016841674786,54.5625718012743,4.7975091839613));
#64319=CARTESIAN_POINT('Ctrl Pts',(12.4349379882832,53.0536745822187,4.87601469433807));
#64320=CARTESIAN_POINT('Ctrl Pts',(13.3725626919339,51.7360090582476,4.95452020471486));
#64321=CARTESIAN_POINT('Ctrl Pts',(14.9888328707268,51.7912892011163,5.03302571509164));
#64322=CARTESIAN_POINT('Ctrl Pts',(15.8342365766747,53.16993805499,5.11153122546842));
#64323=CARTESIAN_POINT('Ctrl Pts',(15.150600536193,54.6355513736084,5.1900367358452));
#64324=CARTESIAN_POINT('Ctrl Pts',(13.5510160379782,54.8737306422823,5.26854224622198));
#64325=CARTESIAN_POINT('Ctrl Pts',(12.4700480749082,53.6708743352892,5.34704775659876));
#64326=CARTESIAN_POINT('Ctrl Pts',(12.8770951264304,52.105725956068,5.42555326697553));
#64327=CARTESIAN_POINT('Ctrl Pts',(14.4071865262006,51.581961077014,5.50405877735232));
#64328=CARTESIAN_POINT('Ctrl Pts',(15.6879418572343,52.5692778225177,5.58256428772909));
#64329=CARTESIAN_POINT('Ctrl Pts',(15.5710663652214,54.1822805600277,5.66106979810588));
#64330=CARTESIAN_POINT('Ctrl Pts',(14.1607407256438,54.9742827930615,5.73957530848265));
#64331=CARTESIAN_POINT('Ctrl Pts',(12.7230548615789,54.2352131474636,5.81808081885943));
#64332=CARTESIAN_POINT('Ctrl Pts',(12.544791628712,52.6274578745722,5.89658632923621));
#64333=CARTESIAN_POINT('Ctrl Pts',(13.7910676609557,51.5937276191864,5.97509183961299));
#64334=CARTESIAN_POINT('Ctrl Pts',(14.8182738021382,51.9046708638902,6.02742884653084));
#64335=CARTESIAN_POINT('Ctrl Pts',(15.1552860103679,52.2420649223251,6.05359734998977));
#64336=CARTESIAN_POINT('Ctrl Pts',(12.6726615784997,52.7578848993974,1.83920795003069));
#64337=CARTESIAN_POINT('Ctrl Pts',(12.8400499397792,52.278885011525,1.86537645348962));
#64338=CARTESIAN_POINT('Ctrl Pts',(13.681345998678,51.5067123465054,1.91771346040747));
#64339=CARTESIAN_POINT('Ctrl Pts',(15.3532486711827,51.92259746376,1.99621897078425));
#64340=CARTESIAN_POINT('Ctrl Pts',(15.9243403753838,53.5462494368323,2.07472448116102));
#64341=CARTESIAN_POINT('Ctrl Pts',(14.8870953408643,54.9183146067315,2.15322999153781));
#64342=CARTESIAN_POINT('Ctrl Pts',(13.1694755608909,54.8098887390118,2.23173550191458));
#64343=CARTESIAN_POINT('Ctrl Pts',(12.3130077055018,53.3174154968919,2.31024101229137));
#64344=CARTESIAN_POINT('Ctrl Pts',(13.0852322400692,51.7797767714816,2.38874652266814));
#64345=CARTESIAN_POINT('Ctrl Pts',(14.7938791388702,51.5757659053288,2.46725203304493));
#64346=CARTESIAN_POINT('Ctrl Pts',(15.9064540032169,52.8884432158558,2.5457575434217));
#64347=CARTESIAN_POINT('Ctrl Pts',(15.4252426613265,54.54051936617,2.62426305379848));
#64348=CARTESIAN_POINT('Ctrl Pts',(13.7817722776592,55.0503976760766,2.70276856417526));
#64349=CARTESIAN_POINT('Ctrl Pts',(12.4499634166736,53.9607949476381,2.78127407455204));
#64350=CARTESIAN_POINT('Ctrl Pts',(12.6242053254301,52.2488988977253,2.85977958492882));
#64351=CARTESIAN_POINT('Ctrl Pts',(14.1482380059646,51.4499755676755,2.9382850953056));
#64352=CARTESIAN_POINT('Ctrl Pts',(15.6552705807332,52.2805199058823,3.01679060568238));
#64353=CARTESIAN_POINT('Ctrl Pts',(15.7937614748382,53.9956792506399,3.09529611605916));
#64354=CARTESIAN_POINT('Ctrl Pts',(14.4395082306652,55.0572583019616,3.17380162643594));
#64355=CARTESIAN_POINT('Ctrl Pts',(12.8070376180166,54.5132075415872,3.25230713681272));
#64356=CARTESIAN_POINT('Ctrl Pts',(12.3603879600183,52.8514447189324,3.3308126471895));
#64357=CARTESIAN_POINT('Ctrl Pts',(13.5001253542918,51.5622781929174,3.40931815756628));
#64358=CARTESIAN_POINT('Ctrl Pts',(15.2041061771209,51.8018631754771,3.48782366794306));
#64359=CARTESIAN_POINT('Ctrl Pts',(15.944159933136,53.3553341468671,3.56632917831984));
#64360=CARTESIAN_POINT('Ctrl Pts',(15.0565888120043,54.8295014140575,3.64483468869661));
#64361=CARTESIAN_POINT('Ctrl Pts',(13.3373877000383,54.9022967226367,3.7233401990734));
#64362=CARTESIAN_POINT('Ctrl Pts',(12.3283770240505,53.5084355106896,3.80184570945017));
#64363=CARTESIAN_POINT('Ctrl Pts',(12.9344615472089,51.8979656495417,3.88035121982696));
#64364=CARTESIAN_POINT('Ctrl Pts',(14.6120902596549,51.5151947977303,3.95885673020373));
#64365=CARTESIAN_POINT('Ctrl Pts',(15.8567258492822,52.7034009548899,4.03736224058051));
#64366=CARTESIAN_POINT('Ctrl Pts',(15.5521495290616,54.3969725912808,4.11586775095729));
#64367=CARTESIAN_POINT('Ctrl Pts',(13.9715125851379,55.077074401189,4.19437326133407));
#64368=CARTESIAN_POINT('Ctrl Pts',(12.5323678038339,54.1337749126023,4.27287877171085));
#64369=CARTESIAN_POINT('Ctrl Pts',(12.5253744436601,52.413047533365,4.35138428208763));
#64370=CARTESIAN_POINT('Ctrl Pts',(13.9568043064156,51.4580814834716,4.42988979246441));
#64371=CARTESIAN_POINT('Ctrl Pts',(15.5429170806551,52.1253130228171,4.50839530284119));
#64372=CARTESIAN_POINT('Ctrl Pts',(15.8612490831165,53.8163530377063,4.58690081321797));
#64373=CARTESIAN_POINT('Ctrl Pts',(14.6263126856138,55.0146366540294,4.66540632359475));
#64374=CARTESIAN_POINT('Ctrl Pts',(12.9456280488333,54.6455146101901,4.74391183397153));
#64375=CARTESIAN_POINT('Ctrl Pts',(12.3264734310144,53.0400243844668,4.8224173443483));
#64376=CARTESIAN_POINT('Ctrl Pts',(13.3241207711359,51.6380076713391,4.90092285472509));
#64377=CARTESIAN_POINT('Ctrl Pts',(15.0438575043004,51.6968266074015,4.97942836510187));
#64378=CARTESIAN_POINT('Ctrl Pts',(15.9433802614164,53.1637305367386,5.05793387547864));
#64379=CARTESIAN_POINT('Ctrl Pts',(15.2159808288478,54.7231660158524,5.13643938585543));
#64380=CARTESIAN_POINT('Ctrl Pts',(13.513997920622,54.9765924805557,5.21494489623221));
#64381=CARTESIAN_POINT('Ctrl Pts',(12.3638311119676,53.696734568805,5.29345040660898));
#64382=CARTESIAN_POINT('Ctrl Pts',(12.7969355370903,52.0313922294383,5.37195591698577));
#64383=CARTESIAN_POINT('Ctrl Pts',(14.424976702367,51.4740982114769,5.45046142736254));
#64384=CARTESIAN_POINT('Ctrl Pts',(15.7877203932888,52.5246186608361,5.52896693773932));
#64385=CARTESIAN_POINT('Ctrl Pts',(15.6633630429778,54.2408787854042,5.60747244811611));
#64386=CARTESIAN_POINT('Ctrl Pts',(14.1627545185313,55.0835815406539,5.68597795849288));
#64387=CARTESIAN_POINT('Ctrl Pts',(12.6330342875793,54.2971998857928,5.76448346886966));
#64388=CARTESIAN_POINT('Ctrl Pts',(12.4433594214855,52.5865231455987,5.84298897924644));
#64389=CARTESIAN_POINT('Ctrl Pts',(13.7694165995699,51.486617996264,5.92149448962322));
#64390=CARTESIAN_POINT('Ctrl Pts',(14.8623799894179,51.8174664687921,5.97383149654107));
#64391=CARTESIAN_POINT('Ctrl Pts',(15.2209662466057,52.1764590205668,6.));
#64392=CARTESIAN_POINT('Ctrl Pts',(12.9355708698302,52.8497595669186,2.));
#64393=CARTESIAN_POINT('Ctrl Pts',(12.9469576730111,52.8006000143775,2.));
#64394=CARTESIAN_POINT('Ctrl Pts',(12.961472067899,52.7523805759131,2.));
#64395=CARTESIAN_POINT('Ctrl Pts',(12.978838111258,52.7052630574514,2.));
#64396=CARTESIAN_POINT('Ctrl Pts',(12.9969823676722,52.6560340926898,2.));
#64397=CARTESIAN_POINT('Ctrl Pts',(13.0182396625101,52.6080072539831,2.));
#64398=CARTESIAN_POINT('Ctrl Pts',(13.0423523228538,52.5613664966406,2.));
#64399=CARTESIAN_POINT('Ctrl Pts',(13.0616899932819,52.5239619306927,2.));
#64400=CARTESIAN_POINT('Ctrl Pts',(13.0828653436295,52.4874486478152,2.));
#64401=CARTESIAN_POINT('Ctrl Pts',(13.1057691188089,52.4519266272332,2.));
#64402=CARTESIAN_POINT('Ctrl Pts',(13.1154541423168,52.4369058893117,2.));
#64403=CARTESIAN_POINT('Ctrl Pts',(13.1254484616954,52.4220624809456,2.));
#64404=CARTESIAN_POINT('Ctrl Pts',(13.1357448170144,52.4074044118627,2.));
#64405=CARTESIAN_POINT('Ctrl Pts',(13.1415823490888,52.3990940004822,2.));
#64406=CARTESIAN_POINT('Ctrl Pts',(13.1475174809101,52.3908426597185,2.));
#64407=CARTESIAN_POINT('Ctrl Pts',(13.1535391079478,52.3826647593444,2.));
#64408=CARTESIAN_POINT('Ctrl Pts',(13.1858180051981,52.3388271712232,2.));
#64409=CARTESIAN_POINT('Ctrl Pts',(13.2206401756997,52.2970090605356,2.));
#64410=CARTESIAN_POINT('Ctrl Pts',(13.2577323841621,52.2574000923877,2.));
#64411=CARTESIAN_POINT('Ctrl Pts',(13.2955035907129,52.2170660551546,2.));
#64412=CARTESIAN_POINT('Ctrl Pts',(13.3356292075102,52.1790218018834,2.));
#64413=CARTESIAN_POINT('Ctrl Pts',(13.3778710217058,52.1434855491538,2.));
#64414=CARTESIAN_POINT('Ctrl Pts',(13.4080812323462,52.1180709759216,2.));
#64415=CARTESIAN_POINT('Ctrl Pts',(13.4393749054926,52.0939395106326,2.));
#64416=CARTESIAN_POINT('Ctrl Pts',(13.4716779317629,52.0711807776388,2.));
#64417=CARTESIAN_POINT('Ctrl Pts',(13.4854146711569,52.0615027127585,2.));
#64418=CARTESIAN_POINT('Ctrl Pts',(13.4993340562547,52.0520730061524,2.));
#64419=CARTESIAN_POINT('Ctrl Pts',(13.5134308827525,52.042899142872,2.));
#64420=CARTESIAN_POINT('Ctrl Pts',(13.521831360858,52.0374323211272,2.));
#64421=CARTESIAN_POINT('Ctrl Pts',(13.5302901168969,52.0320595108474,2.));
#64422=CARTESIAN_POINT('Ctrl Pts',(13.5387993574829,52.0267858960721,2.));
#64423=CARTESIAN_POINT('Ctrl Pts',(13.5870981540731,51.9968526435391,2.));
#64424=CARTESIAN_POINT('Ctrl Pts',(13.6370817516734,51.9700725296277,2.));
#64425=CARTESIAN_POINT('Ctrl Pts',(13.6884925441937,51.946663606087,2.));
#64426=CARTESIAN_POINT('Ctrl Pts',(13.7200525423943,51.9322933630192,2.));
#64427=CARTESIAN_POINT('Ctrl Pts',(13.7521512848191,51.9191940299568,2.));
#64428=CARTESIAN_POINT('Ctrl Pts',(13.7847364470978,51.9074225450413,2.));
#64429=CARTESIAN_POINT('Ctrl Pts',(13.8364187923908,51.8887521470605,2.));
#64430=CARTESIAN_POINT('Ctrl Pts',(13.889323789898,51.8734194145927,2.));
#64431=CARTESIAN_POINT('Ctrl Pts',(13.943161175005,51.8613307211758,2.));
#64432=CARTESIAN_POINT('Ctrl Pts',(13.9592695283984,51.8577137374528,2.));
#64433=CARTESIAN_POINT('Ctrl Pts',(13.9754615001933,51.8543874911094,2.));
#64434=CARTESIAN_POINT('Ctrl Pts',(13.9917296362982,51.8513502983977,2.));
#64435=CARTESIAN_POINT('Ctrl Pts',(14.0067700369102,51.848542318748,2.));
#64436=CARTESIAN_POINT('Ctrl Pts',(14.0218822544722,51.8459805725644,2.));
#64437=CARTESIAN_POINT('Ctrl Pts',(14.0370239759719,51.8436690391775,2.));
#64438=CARTESIAN_POINT('Ctrl Pts',(14.0931183782243,51.8351056744616,2.));
#64439=CARTESIAN_POINT('Ctrl Pts',(14.1496871524976,51.8299561325418,2.));
#64440=CARTESIAN_POINT('Ctrl Pts',(14.2064063479419,51.8280805152347,2.));
#64441=CARTESIAN_POINT('Ctrl Pts',(14.2644669778257,51.8261605387362,2.));
#64442=CARTESIAN_POINT('Ctrl Pts',(14.3226861857367,51.8276710218956,2.));
#64443=CARTESIAN_POINT('Ctrl Pts',(14.3807392826023,51.8325126403789,2.));
#64444=CARTESIAN_POINT('Ctrl Pts',(14.4159849881094,51.8354521262711,2.));
#64445=CARTESIAN_POINT('Ctrl Pts',(14.4511698447437,51.8396204788396,2.));
#64446=CARTESIAN_POINT('Ctrl Pts',(14.4862227576295,51.8450046114997,2.));
#64447=CARTESIAN_POINT('Ctrl Pts',(14.5055224539705,51.8479690477433,2.));
#64448=CARTESIAN_POINT('Ctrl Pts',(14.5247821602859,51.851302164794,2.));
#64449=CARTESIAN_POINT('Ctrl Pts',(14.5439899738579,51.8550026668836,2.));
#64450=CARTESIAN_POINT('Ctrl Pts',(14.5555560513146,51.8572309420403,2.));
#64451=CARTESIAN_POINT('Ctrl Pts',(14.567105278279,51.8595928680997,2.));
#64452=CARTESIAN_POINT('Ctrl Pts',(14.5786287781909,51.8620869089327,2.));
#64453=CARTESIAN_POINT('Ctrl Pts',(14.6376831017328,51.8748680861278,2.));
#64454=CARTESIAN_POINT('Ctrl Pts',(14.6958774997188,51.8910736753892,2.));
#64455=CARTESIAN_POINT('Ctrl Pts',(14.7528646870533,51.9106036961834,2.));
#64456=CARTESIAN_POINT('Ctrl Pts',(14.7899177176958,51.9233021024882,2.));
#64457=CARTESIAN_POINT('Ctrl Pts',(14.8264606634288,51.937407019632,2.));
#64458=CARTESIAN_POINT('Ctrl Pts',(14.8623979324725,51.9529027870001,2.));
#64459=CARTESIAN_POINT('Ctrl Pts',(14.8772478015379,51.9593058922613,2.));
#64460=CARTESIAN_POINT('Ctrl Pts',(14.8919942354036,51.9659465911201,2.));
#64461=CARTESIAN_POINT('Ctrl Pts',(14.9066303802712,51.9728242372186,2.));
#64462=CARTESIAN_POINT('Ctrl Pts',(14.9173472275455,51.977860172809,2.));
#64463=CARTESIAN_POINT('Ctrl Pts',(14.9280038817855,51.9830227414594,2.));
#64464=CARTESIAN_POINT('Ctrl Pts',(14.9385887529819,51.9883069953249,2.));
#64465=CARTESIAN_POINT('Ctrl Pts',(14.9930076776348,52.015474393739,2.));
#64466=CARTESIAN_POINT('Ctrl Pts',(15.0455947546072,52.0458841567652,2.));
#64467=CARTESIAN_POINT('Ctrl Pts',(15.0960008498488,52.0794651524452,2.));
#64468=CARTESIAN_POINT('Ctrl Pts',(15.1196129597981,52.0951957532466,2.));
#64469=CARTESIAN_POINT('Ctrl Pts',(15.1427463702482,52.1116229529516,2.));
#64470=CARTESIAN_POINT('Ctrl Pts',(15.1653640074689,52.1287432229353,2.));
#64471=CARTESIAN_POINT('Ctrl Pts',(15.1847945994588,52.1434510802399,2.));
#64472=CARTESIAN_POINT('Ctrl Pts',(15.2038445286663,52.1586704870383,2.));
#64473=CARTESIAN_POINT('Ctrl Pts',(15.2225082026616,52.1743802571171,2.));
#64474=CARTESIAN_POINT('Ctrl Pts',(14.7622249872189,54.3610567043162,2.80658032638059));
#64475=CARTESIAN_POINT('Ctrl Pts',(14.8615128627433,54.3048362110035,2.79940525217632));
#64476=CARTESIAN_POINT('Ctrl Pts',(14.9530160801183,54.235599890915,2.79223017797206));
#64477=CARTESIAN_POINT('Ctrl Pts',(15.0325849243862,54.154635191266,2.7850551037678));
#64478=CARTESIAN_POINT('Ctrl Pts',(15.3227836759489,53.8593455590615,2.75888660030887));
#64479=CARTESIAN_POINT('Ctrl Pts',(15.4542357696669,53.4080493196853,2.73271809684994));
#64480=CARTESIAN_POINT('Ctrl Pts',(15.3680012509646,53.0031097267674,2.70654959339102));
#64481=CARTESIAN_POINT('Ctrl Pts',(15.2817667322623,52.5981701338495,2.68038108993209));
#64482=CARTESIAN_POINT('Ctrl Pts',(14.9778456011397,52.23958718739,2.65421258647316));
#64483=CARTESIAN_POINT('Ctrl Pts',(14.5925102242224,52.0881604517115,2.62804408301424));
#64484=CARTESIAN_POINT('Ctrl Pts',(14.2071748473051,51.9367337160331,2.60187557955531));
#64485=CARTESIAN_POINT('Ctrl Pts',(13.7404252245931,51.9924631911358,2.57570707609639));
#64486=CARTESIAN_POINT('Ctrl Pts',(13.4015764529908,52.2303456612731,2.54953857263746));
#64487=CARTESIAN_POINT('Ctrl Pts',(13.0627276813884,52.4682281314104,2.52337006917853));
#64488=CARTESIAN_POINT('Ctrl Pts',(12.8517797608958,52.8882635965824,2.49720156571961));
#64489=CARTESIAN_POINT('Ctrl Pts',(12.8632860991091,53.3021301533919,2.47103306226068));
#64490=CARTESIAN_POINT('Ctrl Pts',(12.8747924373225,53.7159967102013,2.44486455880175));
#64491=CARTESIAN_POINT('Ctrl Pts',(13.1087530342418,54.1236943586483,2.41869605534283));
#64492=CARTESIAN_POINT('Ctrl Pts',(13.4603337012234,54.3423524839877,2.3925275518839));
#64493=CARTESIAN_POINT('Ctrl Pts',(13.811914368205,54.5610106093271,2.36635904842497));
#64494=CARTESIAN_POINT('Ctrl Pts',(14.281115105249,54.5906292115589,2.34019054496605));
#64495=CARTESIAN_POINT('Ctrl Pts',(14.6573871465026,54.4180355738828,2.31402204150712));
#64496=CARTESIAN_POINT('Ctrl Pts',(14.6930548254675,54.4016750320804,2.31154146979828));
#64497=CARTESIAN_POINT('Ctrl Pts',(14.7278874868095,54.3834974973412,2.30906089808943));
#64498=CARTESIAN_POINT('Ctrl Pts',(14.7617771735939,54.3636459375188,2.30658032638059));
#64499=CARTESIAN_POINT('Ctrl Pts',(15.6194800884629,52.866705242183,2.));
#64500=CARTESIAN_POINT('Ctrl Pts',(15.7510836294753,53.3567463262429,2.02616850345893));
#64501=CARTESIAN_POINT('Ctrl Pts',(15.4911223508182,54.468705692608,2.07850551037678));
#64502=CARTESIAN_POINT('Ctrl Pts',(13.8755519245003,55.0671510173416,2.15701102075356));
#64503=CARTESIAN_POINT('Ctrl Pts',(12.4888977717378,54.0475500892828,2.23551653113034));
#64504=CARTESIAN_POINT('Ctrl Pts',(12.5727324025626,52.3295818538895,2.31402204150712));
#64505=CARTESIAN_POINT('Ctrl Pts',(14.0528383317196,51.4513683986094,2.3925275518839));
#64506=CARTESIAN_POINT('Ctrl Pts',(15.6013423678816,52.2018016959779,2.47103306226067));
#64507=CARTESIAN_POINT('Ctrl Pts',(15.8297478005623,53.907232954514,2.54953857263746));
#64508=CARTESIAN_POINT('Ctrl Pts',(14.5330963425821,55.0385110233129,2.62804408301424));
#64509=CARTESIAN_POINT('Ctrl Pts',(12.8743150895914,54.5809192738243,2.70654959339101));
#64510=CARTESIAN_POINT('Ctrl Pts',(12.3410089780029,52.9449163922479,2.78505510376779));
#64511=CARTESIAN_POINT('Ctrl Pts',(13.4114743235374,51.5976690199096,2.86356061414457));
#64512=CARTESIAN_POINT('Ctrl Pts',(15.125685020798,51.7474403844543,2.94206612452135));
#64513=CARTESIAN_POINT('Ctrl Pts',(15.9462998191018,53.2599021194416,3.02057163489813));
#64514=CARTESIAN_POINT('Ctrl Pts',(15.1373700363305,54.7786474915821,3.09907714527491));
#64515=CARTESIAN_POINT('Ctrl Pts',(13.4243640409751,54.9416270991707,3.17758265565169));
#64516=CARTESIAN_POINT('Ctrl Pts',(12.3435458814549,53.6026781745395,3.25608816602847));
#64517=CARTESIAN_POINT('Ctrl Pts',(12.8642192037884,51.9626013374103,3.33459367640525));
#64518=CARTESIAN_POINT('Ctrl Pts',(14.5194316817765,51.4922567887357,3.41309918678203));
#64519=CARTESIAN_POINT('Ctrl Pts',(15.824749470772,52.6134605506407,3.49160469715881));
#64520=CARTESIAN_POINT('Ctrl Pts',(15.6095325175198,54.3206905095792,3.57011020753559));
#64521=CARTESIAN_POINT('Ctrl Pts',(14.0667925161087,55.0828622138133,3.64861571791237));
#64522=CARTESIAN_POINT('Ctrl Pts',(12.5800953694062,54.216441978079,3.72712122828915));
#64523=CARTESIAN_POINT('Ctrl Pts',(12.482746426243,52.4984560584277,3.80562673866593));
#64524=CARTESIAN_POINT('Ctrl Pts',(13.8620505314459,51.4696350750293,3.88413224904271));
#64525=CARTESIAN_POINT('Ctrl Pts',(15.4810149732843,52.0526501422855,3.96263775941949));
#64526=CARTESIAN_POINT('Ctrl Pts',(15.8877139511439,53.7246394886753,4.04114326979626));
#64527=CARTESIAN_POINT('Ctrl Pts',(14.7174101533174,54.9861233184473,4.11964878017305));
#64528=CARTESIAN_POINT('Ctrl Pts',(13.0196598476916,54.705772943414,4.19815429054983));
#64529=CARTESIAN_POINT('Ctrl Pts',(12.317045870665,53.1350132444558,4.2766598009266));
#64530=CARTESIAN_POINT('Ctrl Pts',(13.239689139382,51.6825388628568,4.35516531130338));
#64531=CARTESIAN_POINT('Ctrl Pts',(14.9601412381249,51.6509633535716,4.43367082168016));
#64532=CARTESIAN_POINT('Ctrl Pts',(15.9354598188275,53.0686043860759,4.51217633205695));
#64533=CARTESIAN_POINT('Ctrl Pts',(15.2909560004752,54.6640877757789,4.59068184243372));
#64534=CARTESIAN_POINT('Ctrl Pts',(13.6046361114517,55.0065460966708,4.6691873528105));
#64535=CARTESIAN_POINT('Ctrl Pts',(12.3888319545388,53.7888545684046,4.74769286318728));
#64536=CARTESIAN_POINT('Ctrl Pts',(12.7339055288242,52.1030679359729,4.82619837356406));
#64537=CARTESIAN_POINT('Ctrl Pts',(14.3303867955418,51.461039661442,4.90470388394084));
#64538=CARTESIAN_POINT('Ctrl Pts',(15.7465131069793,52.4385560995514,4.98320939431762));
#64539=CARTESIAN_POINT('Ctrl Pts',(15.7122693095411,54.1589569990369,5.0617149046944));
#64540=CARTESIAN_POINT('Ctrl Pts',(14.2583648731494,55.079346475668,5.14022041507118));
#64541=CARTESIAN_POINT('Ctrl Pts',(12.6886982319545,54.374296277089,5.21872592544795));
#64542=CARTESIAN_POINT('Ctrl Pts',(12.4109789893207,52.6761143673659,5.29723143582474));
#64543=CARTESIAN_POINT('Ctrl Pts',(13.6742819091468,51.5077662723951,5.37573694620152));
#64544=CARTESIAN_POINT('Ctrl Pts',(15.3456277491901,51.9170631330653,5.4542424565783));
#64545=CARTESIAN_POINT('Ctrl Pts',(15.9261522494264,53.5369201511685,5.53274796695508));
#64546=CARTESIAN_POINT('Ctrl Pts',(14.895150144613,54.9146464419454,5.61125347733186));
#64547=CARTESIAN_POINT('Ctrl Pts',(13.1774033105245,54.8145932898247,5.68975898770864));
#64548=CARTESIAN_POINT('Ctrl Pts',(12.3131175991141,53.326633245717,5.76826449808541));
#64549=CARTESIAN_POINT('Ctrl Pts',(13.0780276880699,51.7849182946399,5.8467700084622));
#64550=CARTESIAN_POINT('Ctrl Pts',(14.7848942477639,51.5726692650909,5.92527551883897));
#64551=CARTESIAN_POINT('Ctrl Pts',(15.9054717137609,52.8790772926886,6.00378102921575));
#64552=CARTESIAN_POINT('Ctrl Pts',(15.4296884573085,54.5349259880616,6.08228653959253));
#64553=CARTESIAN_POINT('Ctrl Pts',(14.340318424872,54.8774262527002,6.13462354651039));
#64554=CARTESIAN_POINT('Ctrl Pts',(13.8417981729249,54.7828888819299,6.16079204996931));
#64555=CARTESIAN_POINT('Ctrl Pts',(15.5298235927831,52.8907830444123,1.94640265001023));
#64556=CARTESIAN_POINT('Ctrl Pts',(15.6535093143589,53.3513412073422,1.97257115346916));
#64557=CARTESIAN_POINT('Ctrl Pts',(15.4091883934694,54.3964004476471,2.02490816038701));
#64558=CARTESIAN_POINT('Ctrl Pts',(13.8908174408455,54.9588407987497,2.10341367076379));
#64559=CARTESIAN_POINT('Ctrl Pts',(12.5875902013567,54.0005833268291,2.18191918114057));
#64560=CARTESIAN_POINT('Ctrl Pts',(12.6663809901671,52.3859752455852,2.26042469151735));
#64561=CARTESIAN_POINT('Ctrl Pts',(14.0574375563363,51.5605987847521,2.33893020189413));
#64562=CARTESIAN_POINT('Ctrl Pts',(15.5127771133299,52.2658828763921,2.4174357122709));
#64563=CARTESIAN_POINT('Ctrl Pts',(15.7274407199138,53.8687082577405,2.49594122264769));
#64564=CARTESIAN_POINT('Ctrl Pts',(14.5088012366685,54.9319239065435,2.57444673302447));
#64565=CARTESIAN_POINT('Ctrl Pts',(12.9498192014263,54.5018627905034,2.65295224340124));
#64566=CARTESIAN_POINT('Ctrl Pts',(12.4485990159725,52.9642886845845,2.73145775377802));
#64567=CARTESIAN_POINT('Ctrl Pts',(13.4546606892816,51.6980973487976,2.8099632641548));
#64568=CARTESIAN_POINT('Ctrl Pts',(15.0657373016022,51.8388578416581,2.88846877453159));
#64569=CARTESIAN_POINT('Ctrl Pts',(15.8369804815592,53.2603235530564,2.96697428490836));
#64570=CARTESIAN_POINT('Ctrl Pts',(15.0767192977297,54.6876948517164,3.04547979528514));
#64571=CARTESIAN_POINT('Ctrl Pts',(13.4667749074092,54.8408689244782,3.12398530566192));
#64572=CARTESIAN_POINT('Ctrl Pts',(12.4509832887027,53.5824767670773,3.2024908160387));
#64573=CARTESIAN_POINT('Ctrl Pts',(12.9403307263376,52.0410738118106,3.28099632641548));
#64574=CARTESIAN_POINT('Ctrl Pts',(14.4959586990071,51.5990271583197,3.35950183679226));
#64575=CARTESIAN_POINT('Ctrl Pts',(15.7227431105484,52.6527746126658,3.43800734716904));
#64576=CARTESIAN_POINT('Ctrl Pts',(15.5204745093119,54.2572904770774,3.51651285754582));
#64577=CARTESIAN_POINT('Ctrl Pts',(14.0705521986317,54.9736067439323,3.5950183679226));
#64578=CARTESIAN_POINT('Ctrl Pts',(12.6733009701311,54.1593139732339,3.67352387829938));
#64579=CARTESIAN_POINT('Ctrl Pts',(12.5818089465338,52.5446892716908,3.75202938867616));
#64580=CARTESIAN_POINT('Ctrl Pts',(13.8781283480644,51.5777664615214,3.83053489905293));
#64581=CARTESIAN_POINT('Ctrl Pts',(15.3996891180402,52.1257049039707,3.90904040942972));
#64582=CARTESIAN_POINT('Ctrl Pts',(15.781919384443,53.6971003784726,3.98754591980649));
#64583=CARTESIAN_POINT('Ctrl Pts',(14.682025957689,54.8826880651051,4.06605143018328));
#64584=CARTESIAN_POINT('Ctrl Pts',(13.0864194109997,54.6192047411515,4.14455694056005));
#64585=CARTESIAN_POINT('Ctrl Pts',(12.4260776293936,53.142948515116,4.22306245093684));
#64586=CARTESIAN_POINT('Ctrl Pts',(13.2932108202671,51.7778610670395,4.30156796131361));
#64587=CARTESIAN_POINT('Ctrl Pts',(14.9101533252533,51.7481852724521,4.38007347169039));
#64588=CARTESIAN_POINT('Ctrl Pts',(15.8267926610378,53.0805350914,4.45857898206717));
#64589=CARTESIAN_POINT('Ctrl Pts',(15.2210648879244,54.5800275275423,4.53708449244395));
#64590=CARTESIAN_POINT('Ctrl Pts',(13.6362010561689,54.9018821235761,4.61559000282073));
#64591=CARTESIAN_POINT('Ctrl Pts',(12.4935447622286,53.7574520104367,4.69409551319751));
#64592=CARTESIAN_POINT('Ctrl Pts',(12.8178572670738,52.1730893523261,4.77260102357429));
#64593=CARTESIAN_POINT('Ctrl Pts',(14.3182875437761,51.5696881839643,4.85110653395107));
#64594=CARTESIAN_POINT('Ctrl Pts',(15.6492137736117,52.488393144862,4.92961204432785));
#64595=CARTESIAN_POINT('Ctrl Pts',(15.6170302262462,54.1052875309521,5.00811755470463));
#64596=CARTESIAN_POINT('Ctrl Pts',(14.2505987614542,54.9703025272977,5.08662306508142));
#64597=CARTESIAN_POINT('Ctrl Pts',(12.7753698302556,54.3076710974169,5.16512857545818));
#64598=CARTESIAN_POINT('Ctrl Pts',(12.5143593387719,52.7116589137379,5.24363408583497));
#64599=CARTESIAN_POINT('Ctrl Pts',(13.701656671393,51.6136035265765,5.32213959621175));
#64600=CARTESIAN_POINT('Ctrl Pts',(15.2724473555814,51.9982753762946,5.40064510658853));
#64601=CARTESIAN_POINT('Ctrl Pts',(15.8180450739392,53.5206750214142,5.4791506169653));
#64602=CARTESIAN_POINT('Ctrl Pts',(14.8490723677412,54.8155115364335,5.55765612734209));
#64603=CARTESIAN_POINT('Ctrl Pts',(13.2346723673735,54.7214780003996,5.63616163771886));
#64604=CARTESIAN_POINT('Ctrl Pts',(12.4223856990886,53.3230398556835,5.71466714809565));
#64605=CARTESIAN_POINT('Ctrl Pts',(13.1412755979873,51.8740809240221,5.79317265847242));
#64606=CARTESIAN_POINT('Ctrl Pts',(14.7454499267729,51.674601683786,5.8716781688492));
#64607=CARTESIAN_POINT('Ctrl Pts',(15.7986087657921,52.9024107406156,5.95018367922598));
#64608=CARTESIAN_POINT('Ctrl Pts',(15.3514506199299,54.4586366531711,6.02868918960276));
#64609=CARTESIAN_POINT('Ctrl Pts',(14.3276216447485,54.7805306694404,6.08102619652062));
#64610=CARTESIAN_POINT('Ctrl Pts',(13.8590944561341,54.691681062282,6.10719469997954));
#64611=CARTESIAN_POINT('Ctrl Pts',(15.4401670971033,52.9148608466415,1.89280530002046));
#64612=CARTESIAN_POINT('Ctrl Pts',(15.5559349992425,53.3459360884415,1.91897380347939));
#64613=CARTESIAN_POINT('Ctrl Pts',(15.3272544361205,54.3240952026862,1.97131081039724));
#64614=CARTESIAN_POINT('Ctrl Pts',(13.9060829571906,54.8505305801576,2.04981632077402));
#64615=CARTESIAN_POINT('Ctrl Pts',(12.6862826309757,53.9536165643755,2.1283218311508));
#64616=CARTESIAN_POINT('Ctrl Pts',(12.7600295777716,52.4423686372807,2.20682734152758));
#64617=CARTESIAN_POINT('Ctrl Pts',(14.0620367809532,51.6698291708949,2.28533285190436));
#64618=CARTESIAN_POINT('Ctrl Pts',(15.4242118587781,52.3299640568063,2.36383836228113));
#64619=CARTESIAN_POINT('Ctrl Pts',(15.6251336392654,53.8301835609669,2.44234387265791));
#64620=CARTESIAN_POINT('Ctrl Pts',(14.4845061307549,54.8253367897741,2.5208493830347));
#64621=CARTESIAN_POINT('Ctrl Pts',(13.0253233132612,54.4228063071824,2.59935489341147));
#64622=CARTESIAN_POINT('Ctrl Pts',(12.5561890539421,52.9836609769212,2.67786040378825));
#64623=CARTESIAN_POINT('Ctrl Pts',(13.4978470550258,51.7985256776855,2.75636591416503));
#64624=CARTESIAN_POINT('Ctrl Pts',(15.0057895824064,51.9302752988621,2.83487142454181));
#64625=CARTESIAN_POINT('Ctrl Pts',(15.7276611440166,53.2607449866712,2.91337693491859));
#64626=CARTESIAN_POINT('Ctrl Pts',(15.016068559129,54.5967422118507,2.99188244529537));
#64627=CARTESIAN_POINT('Ctrl Pts',(13.5091857738433,54.7401107497857,3.07038795567215));
#64628=CARTESIAN_POINT('Ctrl Pts',(12.5584206959504,53.5622753596153,3.14889346604893));
#64629=CARTESIAN_POINT('Ctrl Pts',(13.0164422488867,52.1195462862108,3.22739897642571));
#64630=CARTESIAN_POINT('Ctrl Pts',(14.4724857162377,51.7057975279038,3.30590448680249));
#64631=CARTESIAN_POINT('Ctrl Pts',(15.6207367503249,52.6920886746908,3.38440999717927));
#64632=CARTESIAN_POINT('Ctrl Pts',(15.4314165011041,54.1938904445757,3.46291550755605));
#64633=CARTESIAN_POINT('Ctrl Pts',(14.0743118811546,54.8643512740511,3.54142101793283));
#64634=CARTESIAN_POINT('Ctrl Pts',(12.7665065708559,54.1021859683889,3.61992652830961));
#64635=CARTESIAN_POINT('Ctrl Pts',(12.6808714668247,52.590922484954,3.69843203868639));
#64636=CARTESIAN_POINT('Ctrl Pts',(13.894206164683,51.6858978480135,3.77693754906317));
#64637=CARTESIAN_POINT('Ctrl Pts',(15.3183632627962,52.1987596656559,3.85544305943995));
#64638=CARTESIAN_POINT('Ctrl Pts',(15.6761248177421,53.6695612682698,3.93394856981672));
#64639=CARTESIAN_POINT('Ctrl Pts',(14.6466417620606,54.7792528117632,4.01245408019351));
#64640=CARTESIAN_POINT('Ctrl Pts',(13.1531789743077,54.5326365388889,4.09095959057028));
#64641=CARTESIAN_POINT('Ctrl Pts',(12.5351093881223,53.1508837857763,4.16946510094706));
#64642=CARTESIAN_POINT('Ctrl Pts',(13.3467325011522,51.8731832712222,4.24797061132384));
#64643=CARTESIAN_POINT('Ctrl Pts',(14.8601654123817,51.8454071913326,4.32647612170062));
#64644=CARTESIAN_POINT('Ctrl Pts',(15.7181255032481,53.0924657967241,4.40498163207741));
#64645=CARTESIAN_POINT('Ctrl Pts',(15.1511737753737,54.4959672793057,4.48348714245418));
#64646=CARTESIAN_POINT('Ctrl Pts',(13.6677660008861,54.7972181504814,4.56199265283096));
#64647=CARTESIAN_POINT('Ctrl Pts',(12.5982575699184,53.7260494524688,4.64049816320774));
#64648=CARTESIAN_POINT('Ctrl Pts',(12.9018090053235,52.2431107686793,4.71900367358452));
#64649=CARTESIAN_POINT('Ctrl Pts',(14.3061882920104,51.6783367064865,4.7975091839613));
#64650=CARTESIAN_POINT('Ctrl Pts',(15.5519144402441,52.5382301901725,4.87601469433808));
#64651=CARTESIAN_POINT('Ctrl Pts',(15.5217911429513,54.0516180628673,4.95452020471485));
#64652=CARTESIAN_POINT('Ctrl Pts',(14.242832649759,54.8612585789273,5.03302571509164));
#64653=CARTESIAN_POINT('Ctrl Pts',(12.8620414285566,54.2410459177449,5.11153122546842));
#64654=CARTESIAN_POINT('Ctrl Pts',(12.617739688223,52.7472034601098,5.19003673584519));
#64655=CARTESIAN_POINT('Ctrl Pts',(13.7290314336392,51.7194407807578,5.26854224622198));
#64656=CARTESIAN_POINT('Ctrl Pts',(15.1992669619728,52.079487619524,5.34704775659876));
#64657=CARTESIAN_POINT('Ctrl Pts',(15.709937898452,53.5044298916597,5.42555326697553));
#64658=CARTESIAN_POINT('Ctrl Pts',(14.8029945908694,54.7163766309217,5.50405877735232));
#64659=CARTESIAN_POINT('Ctrl Pts',(13.2919414242225,54.6283627109744,5.5825642877291));
#64660=CARTESIAN_POINT('Ctrl Pts',(12.531653799063,53.3194464656501,5.66106979810587));
#64661=CARTESIAN_POINT('Ctrl Pts',(13.2045235079047,51.9632435534043,5.73957530848265));
#64662=CARTESIAN_POINT('Ctrl Pts',(14.706005605782,51.7765341024811,5.81808081885944));
#64663=CARTESIAN_POINT('Ctrl Pts',(15.6917458178233,52.9257441885424,5.89658632923621));
#64664=CARTESIAN_POINT('Ctrl Pts',(15.2732127825514,54.3823473182807,5.975091839613));
#64665=CARTESIAN_POINT('Ctrl Pts',(14.314924864625,54.6836350861806,6.02742884653084));
#64666=CARTESIAN_POINT('Ctrl Pts',(13.8763907393433,54.6004732426341,6.05359734998977));
#64667=CARTESIAN_POINT('Ctrl Pts',(15.3505106014235,52.9389386488708,1.83920795003069));
#64668=CARTESIAN_POINT('Ctrl Pts',(15.4583606841261,53.3405309695408,1.86537645348962));
#64669=CARTESIAN_POINT('Ctrl Pts',(15.2453204787717,54.2517899577253,1.91771346040747));
#64670=CARTESIAN_POINT('Ctrl Pts',(13.9213484735358,54.7422203615657,1.99621897078425));
#64671=CARTESIAN_POINT('Ctrl Pts',(12.7849750605946,53.9066498019219,2.07472448116103));
#64672=CARTESIAN_POINT('Ctrl Pts',(12.8536781653762,52.4987620289764,2.15322999153781));
#64673=CARTESIAN_POINT('Ctrl Pts',(14.0666360055699,51.7790595570376,2.23173550191458));
#64674=CARTESIAN_POINT('Ctrl Pts',(15.3356466042264,52.3940452372206,2.31024101229137));
#64675=CARTESIAN_POINT('Ctrl Pts',(15.522826558617,53.7916588641933,2.38874652266814));
#64676=CARTESIAN_POINT('Ctrl Pts',(14.4602110248413,54.7187496730049,2.46725203304493));
#64677=CARTESIAN_POINT('Ctrl Pts',(13.1008274250962,54.3437498238614,2.5457575434217));
#64678=CARTESIAN_POINT('Ctrl Pts',(12.6637790919117,53.0030332692579,2.62426305379848));
#64679=CARTESIAN_POINT('Ctrl Pts',(13.54103342077,51.8989540065735,2.70276856417526));
#64680=CARTESIAN_POINT('Ctrl Pts',(14.9458418632107,52.021692756066,2.78127407455204));
#64681=CARTESIAN_POINT('Ctrl Pts',(15.618341806474,53.2611664202859,2.85977958492882));
#64682=CARTESIAN_POINT('Ctrl Pts',(14.9554178205282,54.505789571985,2.9382850953056));
#64683=CARTESIAN_POINT('Ctrl Pts',(13.5515966402774,54.6393525750931,3.01679060568238));
#64684=CARTESIAN_POINT('Ctrl Pts',(12.6658581031982,53.5420739521532,3.09529611605916));
#64685=CARTESIAN_POINT('Ctrl Pts',(13.0925537714358,52.1980187606109,3.17380162643594));
#64686=CARTESIAN_POINT('Ctrl Pts',(14.4490127334682,51.8125678974878,3.25230713681272));
#64687=CARTESIAN_POINT('Ctrl Pts',(15.5187303901013,52.7314027367158,3.3308126471895));
#64688=CARTESIAN_POINT('Ctrl Pts',(15.3423584928962,54.130490412074,3.40931815756628));
#64689=CARTESIAN_POINT('Ctrl Pts',(14.0780715636776,54.75509580417,3.48782366794306));
#64690=CARTESIAN_POINT('Ctrl Pts',(12.8597121715808,54.0450579635439,3.56632917831984));
#64691=CARTESIAN_POINT('Ctrl Pts',(12.7799339871155,52.6371556982171,3.64483468869662));
#64692=CARTESIAN_POINT('Ctrl Pts',(13.9102839813016,51.7940292345055,3.7233401990734));
#64693=CARTESIAN_POINT('Ctrl Pts',(15.2370374075522,52.2718144273411,3.80184570945018));
#64694=CARTESIAN_POINT('Ctrl Pts',(15.5703302510412,53.642022158067,3.88035121982695));
#64695=CARTESIAN_POINT('Ctrl Pts',(14.6112575664322,54.6758175584211,3.95885673020374));
#64696=CARTESIAN_POINT('Ctrl Pts',(13.2199385376158,54.4460683366263,4.03736224058051));
#64697=CARTESIAN_POINT('Ctrl Pts',(12.6441411468509,53.1588190564366,4.11586775095729));
#64698=CARTESIAN_POINT('Ctrl Pts',(13.4002541820373,51.9685054754049,4.19437326133407));
#64699=CARTESIAN_POINT('Ctrl Pts',(14.81017749951,51.942629110213,4.27287877171085));
#64700=CARTESIAN_POINT('Ctrl Pts',(15.6094583454585,53.1043965020482,4.35138428208763));
#64701=CARTESIAN_POINT('Ctrl Pts',(15.081282662823,54.4119070310692,4.42988979246441));
#64702=CARTESIAN_POINT('Ctrl Pts',(13.6993309456032,54.6925541773866,4.50839530284119));
#64703=CARTESIAN_POINT('Ctrl Pts',(12.7029703776082,53.6946468945009,4.58690081321797));
#64704=CARTESIAN_POINT('Ctrl Pts',(12.9857607435731,52.3131321850324,4.66540632359475));
#64705=CARTESIAN_POINT('Ctrl Pts',(14.2940890402447,51.7869852290089,4.74391183397153));
#64706=CARTESIAN_POINT('Ctrl Pts',(15.4546151068764,52.5880672354829,4.82241734434831));
#64707=CARTESIAN_POINT('Ctrl Pts',(15.4265520596564,53.9979485947826,4.90092285472509));
#64708=CARTESIAN_POINT('Ctrl Pts',(14.2350665380638,54.752214630557,4.97942836510187));
#64709=CARTESIAN_POINT('Ctrl Pts',(12.9487130268577,54.1744207380728,5.05793387547865));
#64710=CARTESIAN_POINT('Ctrl Pts',(12.7211200376741,52.7827480064819,5.13643938585542));
#64711=CARTESIAN_POINT('Ctrl Pts',(13.7564061958854,51.8252780349391,5.21494489623221));
#64712=CARTESIAN_POINT('Ctrl Pts',(15.1260865683642,52.1606998627533,5.29345040660899));
#64713=CARTESIAN_POINT('Ctrl Pts',(15.6018307229648,53.4881847619054,5.37195591698577));
#64714=CARTESIAN_POINT('Ctrl Pts',(14.7569168139975,54.6172417254098,5.45046142736255));
#64715=CARTESIAN_POINT('Ctrl Pts',(13.3492104810715,54.5352474215493,5.52896693773932));
#64716=CARTESIAN_POINT('Ctrl Pts',(12.6409218990375,53.3158530756166,5.60747244811611));
#64717=CARTESIAN_POINT('Ctrl Pts',(13.2677714178221,52.0524061827865,5.68597795849288));
#64718=CARTESIAN_POINT('Ctrl Pts',(14.666561284791,51.8784665211761,5.76448346886967));
#64719=CARTESIAN_POINT('Ctrl Pts',(15.5848828698546,52.9490776364694,5.84298897924644));
#64720=CARTESIAN_POINT('Ctrl Pts',(15.1949749451728,54.3060579833902,5.92149448962322));
#64721=CARTESIAN_POINT('Ctrl Pts',(14.3022280845014,54.5867395029208,5.97383149654107));
#64722=CARTESIAN_POINT('Ctrl Pts',(13.8936870225526,54.5092654229862,6.));
#64723=CARTESIAN_POINT('Ctrl Pts',(14.7602610286104,54.3618122024717,2.44341967361941));
#64724=CARTESIAN_POINT('Ctrl Pts',(14.651278048058,54.4258677305587,2.45136379342792));
#64725=CARTESIAN_POINT('Ctrl Pts',(14.5332929975391,54.473801003601,2.45930791323642));
#64726=CARTESIAN_POINT('Ctrl Pts',(14.4107496805131,54.5017345633457,2.46725203304492));
#64727=CARTESIAN_POINT('Ctrl Pts',(14.0070831582596,54.5937497232904,2.49342053650385));
#64728=CARTESIAN_POINT('Ctrl Pts',(13.5539552916779,54.4687497735759,2.51958903996277));
#64729=CARTESIAN_POINT('Ctrl Pts',(13.2545499695229,54.182797039618,2.5457575434217));
#64730=CARTESIAN_POINT('Ctrl Pts',(12.955144647368,53.8968443056602,2.57192604688063));
#64731=CARTESIAN_POINT('Ctrl Pts',(12.8094618696398,53.449938787459,2.59809455033955));
#64732=CARTESIAN_POINT('Ctrl Pts',(12.8828295355855,53.0424728179111,2.62426305379848));
#64733=CARTESIAN_POINT('Ctrl Pts',(12.9561972015311,52.6350068483631,2.65043155725741));
#64734=CARTESIAN_POINT('Ctrl Pts',(13.2486153111506,52.2669804274683,2.67660006071633));
#64735=CARTESIAN_POINT('Ctrl Pts',(13.6289591063671,52.1034236752696,2.70276856417526));
#64736=CARTESIAN_POINT('Ctrl Pts',(14.0093029015836,51.939866923071,2.72893706763419));
#64737=CARTESIAN_POINT('Ctrl Pts',(14.4775723823971,51.9807798395685,2.75510557109311));
#64738=CARTESIAN_POINT('Ctrl Pts',(14.8237904466811,52.2078152418539,2.78127407455204));
#64739=CARTESIAN_POINT('Ctrl Pts',(15.1700085109651,52.4348506441393,2.80744257801097));
#64740=CARTESIAN_POINT('Ctrl Pts',(15.3941751587195,52.8480085322126,2.83361108146989));
#64741=CARTESIAN_POINT('Ctrl Pts',(15.3957711516058,53.2620246681991,2.85977958492882));
#64742=CARTESIAN_POINT('Ctrl Pts',(15.397367144492,53.6760408041856,2.88594808838775));
#64743=CARTESIAN_POINT('Ctrl Pts',(15.1763924825101,54.0909151880853,2.91211659184667));
#64744=CARTESIAN_POINT('Ctrl Pts',(14.8319349548107,54.3206128805532,2.9382850953056));
#64745=CARTESIAN_POINT('Ctrl Pts',(14.8094060374994,54.3356360398807,2.9399966214102));
#64746=CARTESIAN_POINT('Ctrl Pts',(14.7863488988009,54.3498670707759,2.94170814751481));
#64747=CARTESIAN_POINT('Ctrl Pts',(14.7628222445741,54.3633003878638,2.94341967361941));
#64748=CARTESIAN_POINT('Ctrl Pts',(15.6194800884629,52.866705242183,2.));
#64749=CARTESIAN_POINT('Ctrl Pts',(15.6300231873965,52.926941249885,2.));
#64750=CARTESIAN_POINT('Ctrl Pts',(15.6366567833015,52.987630087735,2.));
#64751=CARTESIAN_POINT('Ctrl Pts',(15.6395415323775,53.0484503647743,2.));
#64752=CARTESIAN_POINT('Ctrl Pts',(15.6424094897195,53.1089166152119,2.));
#64753=CARTESIAN_POINT('Ctrl Pts',(15.6415715704011,53.1695138895016,2.));
#64754=CARTESIAN_POINT('Ctrl Pts',(15.6371309452724,53.2299210873137,2.));
#64755=CARTESIAN_POINT('Ctrl Pts',(15.6337777267599,53.275535956418,2.));
#64756=CARTESIAN_POINT('Ctrl Pts',(15.628369049543,53.3210424392735,2.));
#64757=CARTESIAN_POINT('Ctrl Pts',(15.6209312260544,53.3662945441232,2.));
#64758=CARTESIAN_POINT('Ctrl Pts',(15.6170700144012,53.3897863565923,2.));
#64759=CARTESIAN_POINT('Ctrl Pts',(15.6126617095029,53.4132094747523,2.));
#64760=CARTESIAN_POINT('Ctrl Pts',(15.6077085063715,53.4365423663732,2.));
#64761=CARTESIAN_POINT('Ctrl Pts',(15.6050999838077,53.4488302481048,2.));
#64762=CARTESIAN_POINT('Ctrl Pts',(15.6023397247443,53.4610950218001,2.));
#64763=CARTESIAN_POINT('Ctrl Pts',(15.5994335441749,53.4733116341268,2.));
#64764=CARTESIAN_POINT('Ctrl Pts',(15.5857322512059,53.5309072929574,2.));
#64765=CARTESIAN_POINT('Ctrl Pts',(15.5687698297175,53.5875426491662,2.));
#64766=CARTESIAN_POINT('Ctrl Pts',(15.5486498653391,53.6429179274572,2.));
#64767=CARTESIAN_POINT('Ctrl Pts',(15.5289409667744,53.6971618476902,2.));
#64768=CARTESIAN_POINT('Ctrl Pts',(15.5062016386482,53.7501975064157,2.));
#64769=CARTESIAN_POINT('Ctrl Pts',(15.4804878124203,53.8017173360065,2.));
#64770=CARTESIAN_POINT('Ctrl Pts',(15.4618733917387,53.8390129050498,2.));
#64771=CARTESIAN_POINT('Ctrl Pts',(15.4416993411855,53.8755136264573,2.));
#64772=CARTESIAN_POINT('Ctrl Pts',(15.4199753876479,53.9110903776723,2.));
#64773=CARTESIAN_POINT('Ctrl Pts',(15.4086212485451,53.9296847546774,2.));
#64774=CARTESIAN_POINT('Ctrl Pts',(15.3968435749493,53.9480265377065,2.));
#64775=CARTESIAN_POINT('Ctrl Pts',(15.3846428359354,53.9660958743824,2.));
#64776=CARTESIAN_POINT('Ctrl Pts',(15.3789686731488,53.9744993290933,2.));
#64777=CARTESIAN_POINT('Ctrl Pts',(15.373205772738,53.9828396302133,2.));
#64778=CARTESIAN_POINT('Ctrl Pts',(15.3673591187829,53.9911085225651,2.));
#64779=CARTESIAN_POINT('Ctrl Pts',(15.3351612285484,54.0366458316568,2.));
#64780=CARTESIAN_POINT('Ctrl Pts',(15.3003846167745,54.0800821194656,2.));
#64781=CARTESIAN_POINT('Ctrl Pts',(15.2630875305729,54.1211378587784,2.));
#64782=CARTESIAN_POINT('Ctrl Pts',(15.238131587418,54.1486087633668,2.));
#64783=CARTESIAN_POINT('Ctrl Pts',(15.2120464130742,54.1750132365563,2.));
#64784=CARTESIAN_POINT('Ctrl Pts',(15.1848412564379,54.2002572946035,2.));
#64785=CARTESIAN_POINT('Ctrl Pts',(15.1445758545731,54.237620142962,2.));
#64786=CARTESIAN_POINT('Ctrl Pts',(15.1018570560095,54.2724429083027,2.));
#64787=CARTESIAN_POINT('Ctrl Pts',(15.0569812349608,54.3046174971127,2.));
#64788=CARTESIAN_POINT('Ctrl Pts',(15.0431218621612,54.3145542427938,2.));
#64789=CARTESIAN_POINT('Ctrl Pts',(15.0290566706299,54.324238085577,2.));
#64790=CARTESIAN_POINT('Ctrl Pts',(15.0147942526811,54.3336649770073,2.));
#64791=CARTESIAN_POINT('Ctrl Pts',(15.0022772711783,54.341938204316,2.));
#64792=CARTESIAN_POINT('Ctrl Pts',(14.9896026925807,54.3500168035479,2.));
#64793=CARTESIAN_POINT('Ctrl Pts',(14.9768072444527,54.3578794016111,2.));
#64794=CARTESIAN_POINT('Ctrl Pts',(14.9293632591135,54.3870329711855,2.));
#64795=CARTESIAN_POINT('Ctrl Pts',(14.8801986446945,54.413264340731,2.));
#64796=CARTESIAN_POINT('Ctrl Pts',(14.8296406251874,54.4365044915685,2.));
#64797=CARTESIAN_POINT('Ctrl Pts',(14.7791435079019,54.4597166473058,2.));
#64798=CARTESIAN_POINT('Ctrl Pts',(14.7272551246491,54.4799449628023,2.));
#64799=CARTESIAN_POINT('Ctrl Pts',(14.6742902116473,54.4970704070682,2.));
#64800=CARTESIAN_POINT('Ctrl Pts',(14.6404359644482,54.5080166918955,2.));
#64801=CARTESIAN_POINT('Ctrl Pts',(14.6061417257392,54.5176942656993,2.));
#64802=CARTESIAN_POINT('Ctrl Pts',(14.571490685664,54.5260607579884,2.));
#64803=CARTESIAN_POINT('Ctrl Pts',(14.5536361910167,54.530371725032,2.));
#64804=CARTESIAN_POINT('Ctrl Pts',(14.5356869955305,54.5343344557618,2.));
#64805=CARTESIAN_POINT('Ctrl Pts',(14.5176547593681,54.5379422095229,2.));
#64806=CARTESIAN_POINT('Ctrl Pts',(14.5067786943717,54.5401182105492,2.));
#64807=CARTESIAN_POINT('Ctrl Pts',(14.4958730433768,54.5421648311648,2.));
#64808=CARTESIAN_POINT('Ctrl Pts',(14.4849536044948,54.5440785381581,2.));
#64809=CARTESIAN_POINT('Ctrl Pts',(14.432148545745,54.5533329889869,2.));
#64810=CARTESIAN_POINT('Ctrl Pts',(14.3789399495959,54.5594997842103,2.));
#64811=CARTESIAN_POINT('Ctrl Pts',(14.3256201373498,54.5624573557269,2.));
#64812=CARTESIAN_POINT('Ctrl Pts',(14.2921372783298,54.5643146006412,2.));
#64813=CARTESIAN_POINT('Ctrl Pts',(14.2586106300373,54.5649053533655,2.));
#64814=CARTESIAN_POINT('Ctrl Pts',(14.225115486905,54.5641893509564,2.));
#64815=CARTESIAN_POINT('Ctrl Pts',(14.212869318331,54.5639275731169,2.));
#64816=CARTESIAN_POINT('Ctrl Pts',(14.2006248769065,54.5634909095329,2.));
#64817=CARTESIAN_POINT('Ctrl Pts',(14.1883942978659,54.562877565257,2.));
#64818=CARTESIAN_POINT('Ctrl Pts',(14.1370506808453,54.5603027637289,2.));
#64819=CARTESIAN_POINT('Ctrl Pts',(14.0860310640551,54.5546235246645,2.));
#64820=CARTESIAN_POINT('Ctrl Pts',(14.0356066352152,54.5457116917125,2.));
#64821=CARTESIAN_POINT('Ctrl Pts',(14.0074349171617,54.5407327231642,2.));
#64822=CARTESIAN_POINT('Ctrl Pts',(13.9794492439462,54.5347439009404,2.));
#64823=CARTESIAN_POINT('Ctrl Pts',(13.9516999296066,54.5277163783411,2.));
#64824=CARTESIAN_POINT('Ctrl Pts',(13.932212693117,54.5227812295604,2.));
#64825=CARTESIAN_POINT('Ctrl Pts',(13.9128420740716,54.517333696643,2.));
#64826=CARTESIAN_POINT('Ctrl Pts',(13.8936031194075,54.5113848919291,2.));
#64827=CARTESIAN_POINT('Origin',(14.1292828945603,53.2669068454841,4.5));
#64828=CARTESIAN_POINT('Origin',(39.0658530619283,-38.8697713466883,7.));
#64829=CARTESIAN_POINT('',(39.0658530619283,-38.8697713466882,7.));
#64830=CARTESIAN_POINT('Origin',(39.0658530619283,-38.8697713466883,7.));
#64831=CARTESIAN_POINT('',(39.0658530619283,-38.8697713466882,7.));
#64832=CARTESIAN_POINT('Origin',(-14.1292828945604,-53.2669068454841,7.));
#64833=CARTESIAN_POINT('',(-14.1292828945603,-53.2669068454841,7.));
#64834=CARTESIAN_POINT('Origin',(-14.1292828945604,-53.2669068454841,7.));
#64835=CARTESIAN_POINT('',(-14.1292828945603,-53.2669068454841,7.));
#64836=CARTESIAN_POINT('Origin',(-53.1951359564886,-14.3971354987959,7.));
#64837=CARTESIAN_POINT('',(-53.1951359564886,-14.3971354987959,7.));
#64838=CARTESIAN_POINT('Origin',(-53.1951359564886,-14.3971354987959,7.));
#64839=CARTESIAN_POINT('',(-53.1951359564886,-14.3971354987959,7.));
#64840=CARTESIAN_POINT('Origin',(-39.0658530619283,38.8697713466882,7.));
#64841=CARTESIAN_POINT('',(-39.0658530619283,38.8697713466882,7.));
#64842=CARTESIAN_POINT('Origin',(-39.0658530619283,38.8697713466882,7.));
#64843=CARTESIAN_POINT('',(-39.0658530619283,38.8697713466882,7.));
#64844=CARTESIAN_POINT('Origin',(14.1292828945603,53.2669068454841,7.));
#64845=CARTESIAN_POINT('',(14.1292828945603,53.2669068454841,7.));
#64846=CARTESIAN_POINT('Origin',(14.1292828945603,53.2669068454841,7.));
#64847=CARTESIAN_POINT('',(14.1292828945603,53.2669068454841,7.));
#64848=CARTESIAN_POINT('Origin',(39.0658530619283,-38.8697713466883,14.));
#64849=CARTESIAN_POINT('Ctrl Pts',(39.3014489339361,-37.6274127691862,14.));
#64850=CARTESIAN_POINT('Ctrl Pts',(39.2527755161121,-37.6125702664346,14.));
#64851=CARTESIAN_POINT('Ctrl Pts',(39.2032917181168,-37.6009462766898,14.));
#64852=CARTESIAN_POINT('Ctrl Pts',(39.1532758042432,-37.5923965983573,14.));
#64853=CARTESIAN_POINT('Ctrl Pts',(39.11957228402,-37.5866353469022,14.));
#64854=CARTESIAN_POINT('Ctrl Pts',(39.0856264423049,-37.5822710037892,14.));
#64855=CARTESIAN_POINT('Ctrl Pts',(39.0515175292276,-37.5792707431897,14.));
#64856=CARTESIAN_POINT('Ctrl Pts',(39.0357879604487,-37.5778871515945,14.));
#64857=CARTESIAN_POINT('Ctrl Pts',(39.020023659971,-37.5767937802474,14.));
#64858=CARTESIAN_POINT('Ctrl Pts',(39.0042321835127,-37.5759880571028,14.));
#64859=CARTESIAN_POINT('Ctrl Pts',(38.9909279654484,-37.5753092404992,14.));
#64860=CARTESIAN_POINT('Ctrl Pts',(38.9776118489143,-37.5748350538309,14.));
#64861=CARTESIAN_POINT('Ctrl Pts',(38.964295763777,-37.5745634329246,14.));
#64862=CARTESIAN_POINT('Ctrl Pts',(38.9105541147734,-37.5734672131832,14.));
#64863=CARTESIAN_POINT('Ctrl Pts',(38.8567779423384,-37.5756644894702,14.));
#64864=CARTESIAN_POINT('Ctrl Pts',(38.8032675464005,-37.581026481916,14.));
#64865=CARTESIAN_POINT('Ctrl Pts',(38.7827897374601,-37.5830784543397,14.));
#64866=CARTESIAN_POINT('Ctrl Pts',(38.7623506706579,-37.5855944285777,14.));
#64867=CARTESIAN_POINT('Ctrl Pts',(38.741966693386,-37.5885691376506,14.));
#64868=CARTESIAN_POINT('Ctrl Pts',(38.7273323755428,-37.5907047776921,14.));
#64869=CARTESIAN_POINT('Ctrl Pts',(38.7127264476943,-37.5930768844319,14.));
#64870=CARTESIAN_POINT('Ctrl Pts',(38.6981549324168,-37.5956838482276,14.));
#64871=CARTESIAN_POINT('Ctrl Pts',(38.6868487314646,-37.5977066204644,14.));
#64872=CARTESIAN_POINT('Ctrl Pts',(38.6755628687237,-37.5998709906565,14.));
#64873=CARTESIAN_POINT('Ctrl Pts',(38.6643154441843,-37.6021728300854,14.));
#64874=CARTESIAN_POINT('Ctrl Pts',(38.6087986246104,-37.6135346137375,14.));
#64875=CARTESIAN_POINT('Ctrl Pts',(38.5541290481433,-37.6282564371478,14.));
#64876=CARTESIAN_POINT('Ctrl Pts',(38.5006370918184,-37.646191772746,14.));
#64877=CARTESIAN_POINT('Ctrl Pts',(38.4479217174824,-37.6638667279142,14.));
#64878=CARTESIAN_POINT('Ctrl Pts',(38.396348804881,-37.6846628180258,14.));
#64879=CARTESIAN_POINT('Ctrl Pts',(38.3462305040151,-37.7084927625726,14.));
#64880=CARTESIAN_POINT('Ctrl Pts',(38.3200575603805,-37.7209373144561,14.));
#64881=CARTESIAN_POINT('Ctrl Pts',(38.2942813568713,-37.7342101082399,14.));
#64882=CARTESIAN_POINT('Ctrl Pts',(38.2689475825533,-37.7483042482809,14.));
#64883=CARTESIAN_POINT('Ctrl Pts',(38.2553600451045,-37.7558635109953,14.));
#64884=CARTESIAN_POINT('Ctrl Pts',(38.2418997994627,-37.7636591075236,14.));
#64885=CARTESIAN_POINT('Ctrl Pts',(38.2285740909778,-37.7716904151908,14.));
#64886=CARTESIAN_POINT('Ctrl Pts',(38.2191033712726,-37.7773983491343,14.));
#64887=CARTESIAN_POINT('Ctrl Pts',(38.2097006104897,-37.7832253493693,14.));
#64888=CARTESIAN_POINT('Ctrl Pts',(38.2003684633688,-37.7891712859343,14.));
#64889=CARTESIAN_POINT('Ctrl Pts',(38.1921418096808,-37.7944128622123,14.));
#64890=CARTESIAN_POINT('Ctrl Pts',(38.1839782827807,-37.799741616598,14.));
#64891=CARTESIAN_POINT('Ctrl Pts',(38.1758800165188,-37.805156517765,14.));
#64892=CARTESIAN_POINT('Ctrl Pts',(38.1358534009022,-37.8319202917141,14.));
#64893=CARTESIAN_POINT('Ctrl Pts',(38.0974162938763,-37.8607893617484,14.));
#64894=CARTESIAN_POINT('Ctrl Pts',(38.0607602397062,-37.8916978987796,14.));
#64895=CARTESIAN_POINT('Ctrl Pts',(38.0190399864289,-37.9268765895189,14.));
#64896=CARTESIAN_POINT('Ctrl Pts',(37.9796253872743,-37.9646960620489,14.));
#64897=CARTESIAN_POINT('Ctrl Pts',(37.9425628056484,-38.0048405338641,14.));
#64898=CARTESIAN_POINT('Ctrl Pts',(37.9063354033645,-38.0440803780985,14.));
#64899=CARTESIAN_POINT('Ctrl Pts',(37.8723549080301,-38.0855424637378,14.));
#64900=CARTESIAN_POINT('Ctrl Pts',(37.840690574833,-38.128969359293,14.));
#64901=CARTESIAN_POINT('Ctrl Pts',(37.8329319648795,-38.1396101121555,14.));
#64902=CARTESIAN_POINT('Ctrl Pts',(37.8253125495561,-38.150368975123,14.));
#64903=CARTESIAN_POINT('Ctrl Pts',(37.8178336250567,-38.1612424270076,14.));
#64904=CARTESIAN_POINT('Ctrl Pts',(37.8121884193454,-38.1694498735041,14.));
#64905=CARTESIAN_POINT('Ctrl Pts',(37.8066244559601,-38.1777210085551,14.));
#64906=CARTESIAN_POINT('Ctrl Pts',(37.8011483696327,-38.1860445283744,14.));
#64907=CARTESIAN_POINT('Ctrl Pts',(37.7694817125934,-38.234177087235,14.));
#64908=CARTESIAN_POINT('Ctrl Pts',(37.740690869399,-38.2841447569426,14.));
#64909=CARTESIAN_POINT('Ctrl Pts',(37.714822629006,-38.3355979876329,14.));
#64910=CARTESIAN_POINT('Ctrl Pts',(37.688399760224,-38.3881544020733,14.));
#64911=CARTESIAN_POINT('Ctrl Pts',(37.6650255379469,-38.4422615831566,14.));
#64912=CARTESIAN_POINT('Ctrl Pts',(37.6447852836523,-38.497588492234,14.));
#64913=CARTESIAN_POINT('Ctrl Pts',(37.6243676757527,-38.5534001989154,14.));
#64914=CARTESIAN_POINT('Ctrl Pts',(37.6071385772686,-38.6104541129556,14.));
#64915=CARTESIAN_POINT('Ctrl Pts',(37.5932306356489,-38.6684381301182,14.));
#64916=CARTESIAN_POINT('Ctrl Pts',(37.5900811837451,-38.6815686046512,14.));
#64917=CARTESIAN_POINT('Ctrl Pts',(37.5871015926663,-38.6947505762787,14.));
#64918=CARTESIAN_POINT('Ctrl Pts',(37.5842989888732,-38.7079539606268,14.));
#64919=CARTESIAN_POINT('Ctrl Pts',(37.5716672473774,-38.7674635275383,14.));
#64920=CARTESIAN_POINT('Ctrl Pts',(37.5626014399524,-38.8275056873519,14.));
#64921=CARTESIAN_POINT('Ctrl Pts',(37.5571792782293,-38.8877281078776,14.));
#64922=CARTESIAN_POINT('Ctrl Pts',(37.5518047857275,-38.9474210798112,14.));
#64923=CARTESIAN_POINT('Ctrl Pts',(37.5500097107535,-39.0072922465006,14.));
#64924=CARTESIAN_POINT('Ctrl Pts',(37.55191466572,-39.0670207918836,14.));
#64925=CARTESIAN_POINT('Ctrl Pts',(37.5533104035149,-39.1107831850594,14.));
#64926=CARTESIAN_POINT('Ctrl Pts',(37.5566933253821,-39.1544695447415,14.));
#64927=CARTESIAN_POINT('Ctrl Pts',(37.5621285378972,-39.1979562890069,14.));
#64928=CARTESIAN_POINT('Ctrl Pts',(37.565149248657,-39.2221247784535,14.));
#64929=CARTESIAN_POINT('Ctrl Pts',(37.5688041553789,-39.2462316220403,14.));
#64930=CARTESIAN_POINT('Ctrl Pts',(37.5730796542559,-39.2702614469549,14.));
#64931=CARTESIAN_POINT('Ctrl Pts',(37.9741697098829,-39.9602191716056,14.));
#64932=CARTESIAN_POINT('Ctrl Pts',(38.020991576866,-39.9994070905167,14.));
#64933=CARTESIAN_POINT('Ctrl Pts',(38.0702141503049,-40.0354948198824,14.));
#64934=CARTESIAN_POINT('Ctrl Pts',(38.1214910131339,-40.0684345608226,14.));
#64935=CARTESIAN_POINT('Ctrl Pts',(38.1690376391703,-40.0989780351658,14.));
#64936=CARTESIAN_POINT('Ctrl Pts',(38.2183516107569,-40.1268144785211,14.));
#64937=CARTESIAN_POINT('Ctrl Pts',(38.269168974583,-40.1518670892131,14.));
#64938=CARTESIAN_POINT('Ctrl Pts',(38.2814354208216,-40.1579143628033,14.));
#64939=CARTESIAN_POINT('Ctrl Pts',(38.2937899478069,-40.1637993357403,14.));
#64940=CARTESIAN_POINT('Ctrl Pts',(38.3062147884412,-40.1695145314963,14.));
#64941=CARTESIAN_POINT('Ctrl Pts',(38.3608949816838,-40.1946664040676,14.));
#64942=CARTESIAN_POINT('Ctrl Pts',(38.4170009394504,-40.2165668551763,14.));
#64943=CARTESIAN_POINT('Ctrl Pts',(38.4742056409767,-40.2351397541773,14.));
#64944=CARTESIAN_POINT('Ctrl Pts',(38.5095144293503,-40.2466036119165,14.));
#64945=CARTESIAN_POINT('Ctrl Pts',(38.5452420718463,-40.2567987360604,14.));
#64946=CARTESIAN_POINT('Ctrl Pts',(38.5813118928663,-40.2656972878978,14.));
#64947=CARTESIAN_POINT('Ctrl Pts',(38.5936535320381,-40.2687420137329,14.));
#64948=CARTESIAN_POINT('Ctrl Pts',(38.606035223169,-40.2716348792846,14.));
#64949=CARTESIAN_POINT('Ctrl Pts',(38.6184538586389,-40.2743745611435,14.));
#64950=CARTESIAN_POINT('Ctrl Pts',(38.6300726309494,-40.2769377847601,14.));
#64951=CARTESIAN_POINT('Ctrl Pts',(38.6417163481208,-40.2793652420776,14.));
#64952=CARTESIAN_POINT('Ctrl Pts',(38.6533764439016,-40.2816552664683,14.));
#64953=CARTESIAN_POINT('Ctrl Pts',(38.7110876105802,-40.2929896484314,14.));
#64954=CARTESIAN_POINT('Ctrl Pts',(38.7692463793663,-40.3009718362976,14.));
#64955=CARTESIAN_POINT('Ctrl Pts',(38.8275464696014,-40.3055302032883,14.));
#64956=CARTESIAN_POINT('Ctrl Pts',(38.884358538419,-40.3099722248722,14.));
#64957=CARTESIAN_POINT('Ctrl Pts',(38.9413057829595,-40.3111628333597,14.));
#64958=CARTESIAN_POINT('Ctrl Pts',(38.9980976135487,-40.3089871593233,14.));
#64959=CARTESIAN_POINT('Ctrl Pts',(39.0288884010392,-40.3078075756365,14.));
#64960=CARTESIAN_POINT('Ctrl Pts',(39.0596332939681,-40.3056376455304,14.));
#64961=CARTESIAN_POINT('Ctrl Pts',(39.0902835748068,-40.3024530490142,14.));
#64962=CARTESIAN_POINT('Ctrl Pts',(39.1157839679843,-40.2998035312594,14.));
#64963=CARTESIAN_POINT('Ctrl Pts',(39.1412188509075,-40.2964515980885,14.));
#64964=CARTESIAN_POINT('Ctrl Pts',(39.1665588545923,-40.2923809784595,14.));
#64965=CARTESIAN_POINT('Ctrl Pts',(39.177388964653,-40.2906412289651,14.));
#64966=CARTESIAN_POINT('Ctrl Pts',(39.1882029800145,-40.2887698277109,14.));
#64967=CARTESIAN_POINT('Ctrl Pts',(39.1989810533142,-40.2867689791834,14.));
#64968=CARTESIAN_POINT('Ctrl Pts',(39.2488808956908,-40.2775055400359,14.));
#64969=CARTESIAN_POINT('Ctrl Pts',(39.2980978217139,-40.2654572977741,14.));
#64970=CARTESIAN_POINT('Ctrl Pts',(39.3464249159924,-40.2505519130058,14.));
#64971=CARTESIAN_POINT('Ctrl Pts',(39.4004290144141,-40.2338955864035,14.));
#64972=CARTESIAN_POINT('Ctrl Pts',(39.453323106219,-40.213671565055,14.));
#64973=CARTESIAN_POINT('Ctrl Pts',(39.5048609693631,-40.1901258318535,14.));
#64974=CARTESIAN_POINT('Ctrl Pts',(39.5485960623522,-40.1701448941847,14.));
#64975=CARTESIAN_POINT('Ctrl Pts',(39.5913543500861,-40.1477707447876,14.));
#64976=CARTESIAN_POINT('Ctrl Pts',(39.6329645160386,-40.1231328973124,14.));
#64977=CARTESIAN_POINT('Ctrl Pts',(39.6444045721053,-40.1163591113871,14.));
#64978=CARTESIAN_POINT('Ctrl Pts',(39.6557577122762,-40.109414126601,14.));
#64979=CARTESIAN_POINT('Ctrl Pts',(39.6670200627834,-40.1023004514028,14.));
#64980=CARTESIAN_POINT('Ctrl Pts',(39.6757877124576,-40.0967625122316,14.));
#64981=CARTESIAN_POINT('Ctrl Pts',(39.6845017797731,-40.0911212766431,14.));
#64982=CARTESIAN_POINT('Ctrl Pts',(39.6931464328262,-40.0853874573566,14.));
#64983=CARTESIAN_POINT('Ctrl Pts',(39.7394049739124,-40.0547051253513,14.));
#64984=CARTESIAN_POINT('Ctrl Pts',(39.7837665094937,-40.0213210070133,14.));
#64985=CARTESIAN_POINT('Ctrl Pts',(39.8260058213226,-39.9854744939929,14.));
#64986=CARTESIAN_POINT('Ctrl Pts',(39.8680089351017,-39.9498284311244,14.));
#64987=CARTESIAN_POINT('Ctrl Pts',(39.9079141963546,-39.9117464670036,14.));
#64988=CARTESIAN_POINT('Ctrl Pts',(39.9454594213871,-39.871433353871,14.));
#64989=CARTESIAN_POINT('Ctrl Pts',(39.9802942732058,-39.8340304265716,14.));
#64990=CARTESIAN_POINT('Ctrl Pts',(40.0130975716486,-39.7947059892306,14.));
#64991=CARTESIAN_POINT('Ctrl Pts',(40.0436204335297,-39.7536104031421,14.));
#64992=CARTESIAN_POINT('Ctrl Pts',(40.0514607527674,-39.7430542988211,14.));
#64993=CARTESIAN_POINT('Ctrl Pts',(40.059152868768,-39.7323774869518,14.));
#64994=CARTESIAN_POINT('Ctrl Pts',(40.0666759532076,-39.7216063497953,14.));
#64995=CARTESIAN_POINT('Ctrl Pts',(40.0970859623337,-39.6780669768348,14.));
#64996=CARTESIAN_POINT('Ctrl Pts',(40.1247894553757,-39.6329220142745,14.));
#64997=CARTESIAN_POINT('Ctrl Pts',(40.1495562730571,-39.5863640526291,14.));
#64998=CARTESIAN_POINT('Ctrl Pts',(40.1734835191653,-39.54138436162,14.));
#64999=CARTESIAN_POINT('Ctrl Pts',(40.1946700927784,-39.4950850230299,14.));
#65000=CARTESIAN_POINT('Ctrl Pts',(40.2128622006869,-39.4476279812285,14.));
#65001=CARTESIAN_POINT('Ctrl Pts',(40.2255879517124,-39.4144308112573,14.));
#65002=CARTESIAN_POINT('Ctrl Pts',(40.2368474822756,-39.3806668978155,14.));
#65003=CARTESIAN_POINT('Ctrl Pts',(40.2465386396389,-39.3463911596944,14.));
#65004=CARTESIAN_POINT('Ctrl Pts',(40.2520057165832,-39.327055172195,14.));
#65005=CARTESIAN_POINT('Ctrl Pts',(40.2569733939395,-39.3075562909784,14.));
#65006=CARTESIAN_POINT('Ctrl Pts',(40.261442519219,-39.2879130030575,14.));
#65007=CARTESIAN_POINT('Origin',(39.0658530619283,-38.8697713466883,19.1042117235887));
#65008=CARTESIAN_POINT('Ctrl Pts',(38.2940537528419,-37.5314721085808,17.8542117235887));
#65009=CARTESIAN_POINT('Ctrl Pts',(38.3354082297679,-37.5072482534306,17.8517311518799));
#65010=CARTESIAN_POINT('Ctrl Pts',(38.8263155408625,-37.2510699656701,17.8230820767121));
#65011=CARTESIAN_POINT('Ctrl Pts',(40.0256568276714,-37.3267811177079,17.7682644980854));
#65012=CARTESIAN_POINT('Ctrl Pts',(40.8821443104935,-38.8192615374441,17.6897589877086));
#65013=CARTESIAN_POINT('Ctrl Pts',(40.1099071502118,-40.3569109628883,17.6112534773319));
#65014=CARTESIAN_POINT('Ctrl Pts',(38.4012543668155,-40.5609220251472,17.5327479669551));
#65015=CARTESIAN_POINT('Ctrl Pts',(37.2886704652103,-39.2482374965453,17.4542424565783));
#65016=CARTESIAN_POINT('Ctrl Pts',(37.6534618751482,-37.995852754822,17.3947303754562));
#65017=CARTESIAN_POINT('Ctrl Pts',(38.1723477780672,-37.603235418619,17.361386797793));
#65018=CARTESIAN_POINT('Ctrl Pts',(38.2935040424574,-37.5346322273253,17.3542117235887));
#65019=CARTESIAN_POINT('Ctrl Pts',(38.2938718037176,-37.5356881270256,17.8957882764113));
#65020=CARTESIAN_POINT('Ctrl Pts',(38.5911486295276,-37.3667504425096,17.8781885106897));
#65021=CARTESIAN_POINT('Ctrl Pts',(39.4708982524073,-37.1808200198998,17.8344202415091));
#65022=CARTESIAN_POINT('Ctrl Pts',(40.7062722211716,-38.0891100356719,17.7644834688697));
#65023=CARTESIAN_POINT('Ctrl Pts',(40.6223994863181,-39.8071108514352,17.6859779584929));
#65024=CARTESIAN_POINT('Ctrl Pts',(39.1423049297703,-40.6853144575312,17.6074724481161));
#65025=CARTESIAN_POINT('Ctrl Pts',(37.593781529679,-39.9348860603428,17.5289669377393));
#65026=CARTESIAN_POINT('Ctrl Pts',(37.3884926508269,-38.402016881723,17.458405547171));
#65027=CARTESIAN_POINT('Ctrl Pts',(37.9908199438394,-37.7130239262802,17.4140126600617));
#65028=CARTESIAN_POINT('Ctrl Pts',(38.2959007276492,-37.5337106753506,17.3957882764113));
#65029=CARTESIAN_POINT('Ctrl Pts',(40.2595650866584,-39.2869186252539,18.));
#65030=CARTESIAN_POINT('Ctrl Pts',(40.1223890770422,-39.679462603358,17.9738314965411));
#65031=CARTESIAN_POINT('Ctrl Pts',(39.4328412785483,-40.3122408191566,17.9214944896232));
#65032=CARTESIAN_POINT('Ctrl Pts',(38.0628399617007,-39.9714590750956,17.8429889792464));
#65033=CARTESIAN_POINT('Ctrl Pts',(37.5947572398929,-38.6408443652932,17.7644834688697));
#65034=CARTESIAN_POINT('Ctrl Pts',(38.4448300096771,-37.5164220658531,17.6859779584929));
#65035=CARTESIAN_POINT('Ctrl Pts',(39.8524194013853,-37.6052793541117,17.6074724481161));
#65036=CARTESIAN_POINT('Ctrl Pts',(40.5543172769709,-38.8283781815623,17.5289669377393));
#65037=CARTESIAN_POINT('Ctrl Pts',(39.9214631686259,-40.0884933458361,17.4504614273625));
#65038=CARTESIAN_POINT('Ctrl Pts',(38.5212094780202,-40.2556819318544,17.3719559169858));
#65039=CARTESIAN_POINT('Ctrl Pts',(37.6094386785518,-39.1799271772095,17.293450406609));
#65040=CARTESIAN_POINT('Ctrl Pts',(38.0037983665503,-37.8260300114723,17.2149448962322));
#65041=CARTESIAN_POINT('Ctrl Pts',(39.350642117465,-37.4081786211339,17.1364393858554));
#65042=CARTESIAN_POINT('Ctrl Pts',(40.4420762478648,-38.3011214248007,17.0579338754787));
#65043=CARTESIAN_POINT('Ctrl Pts',(40.2992826919135,-39.7040414735315,16.9794283651019));
#65044=CARTESIAN_POINT('Ctrl Pts',(39.0503191421164,-40.358768990196,16.9009228547251));
#65045=CARTESIAN_POINT('Ctrl Pts',(37.8152872634063,-39.6781276508141,16.8224173443483));
#65046=CARTESIAN_POINT('Ctrl Pts',(37.7017922854028,-38.2725333429822,16.7439118339715));
#65047=CARTESIAN_POINT('Ctrl Pts',(38.8116195577816,-37.4025561853298,16.6654063235948));
#65048=CARTESIAN_POINT('Ctrl Pts',(40.1494494228946,-37.8484125098358,16.586900813218));
#65049=CARTESIAN_POINT('Ctrl Pts',(40.5154843389836,-39.2102476987511,16.5083953028412));
#65050=CARTESIAN_POINT('Ctrl Pts',(39.5814554487361,-40.2667356115709,16.4298897924644));
#65051=CARTESIAN_POINT('Ctrl Pts',(38.1850220871887,-40.0703927553964,16.3513842820876));
#65052=CARTESIAN_POINT('Ctrl Pts',(37.5785388809249,-38.7973040793768,16.2728787717108));
#65053=CARTESIAN_POINT('Ctrl Pts',(38.3059143927449,-37.5892057701993,16.1943732613341));
#65054=CARTESIAN_POINT('Ctrl Pts',(39.7148209687577,-37.5295491143576,16.1158677509573));
#65055=CARTESIAN_POINT('Ctrl Pts',(40.5417176980217,-38.6718356181182,16.0373622405805));
#65056=CARTESIAN_POINT('Ctrl Pts',(40.0450239347318,-39.9916355890619,15.9588567302037));
#65057=CARTESIAN_POINT('Ctrl Pts',(38.6701864544171,-40.3053210365855,15.880351219827));
#65058=CARTESIAN_POINT('Ctrl Pts',(37.6501921939814,-39.3315713939809,15.8018457094502));
#65059=CARTESIAN_POINT('Ctrl Pts',(37.8997962556048,-37.9436684903302,15.7233401990734));
#65060=CARTESIAN_POINT('Ctrl Pts',(39.195147782035,-37.3863166449999,15.6448346886966));
#65061=CARTESIAN_POINT('Ctrl Pts',(40.3745447306992,-38.1593622434704,15.5663291783198));
#65062=CARTESIAN_POINT('Ctrl Pts',(40.3802758763629,-39.5695196142836,15.4878236679431));
#65063=CARTESIAN_POINT('Ctrl Pts',(39.2072013976485,-40.3521261040356,15.4093181575663));
#65064=CARTESIAN_POINT('Ctrl Pts',(37.9073623625386,-39.8053216046427,15.3308126471895));
#65065=CARTESIAN_POINT('Ctrl Pts',(37.6464853455349,-38.4194933961106,15.2523071368127));
#65066=CARTESIAN_POINT('Ctrl Pts',(38.6585310049342,-37.4374851510426,15.173801626436));
#65067=CARTESIAN_POINT('Ctrl Pts',(40.0358728399512,-37.7399852318106,15.0952961160591));
#65068=CARTESIAN_POINT('Ctrl Pts',(40.5432777323755,-39.0557043292571,15.0167906056824));
#65069=CARTESIAN_POINT('Ctrl Pts',(39.7256933501734,-40.2046743690254,14.9382850953056));
#65070=CARTESIAN_POINT('Ctrl Pts',(38.3163479152336,-40.1564715183471,14.8597795849288));
#65071=CARTESIAN_POINT('Ctrl Pts',(37.5791777219181,-38.954325616703,14.781274074552));
#65072=CARTESIAN_POINT('Ctrl Pts',(38.1752908680604,-37.676348923403,14.7027685641753));
#65073=CARTESIAN_POINT('Ctrl Pts',(39.5700863286924,-37.4686628699809,14.6242630537985));
#65074=CARTESIAN_POINT('Ctrl Pts',(40.5126633343826,-38.5175221013622,14.5457575434217));
#65075=CARTESIAN_POINT('Ctrl Pts',(40.1577269226072,-39.8822911025123,14.4672520330449));
#65076=CARTESIAN_POINT('Ctrl Pts',(38.8235306389232,-40.3389996506625,14.3887465226681));
#65077=CARTESIAN_POINT('Ctrl Pts',(37.7067389013686,-39.4780868997918,14.3102410122914));
#65078=CARTESIAN_POINT('Ctrl Pts',(37.8086626184681,-38.0715866597083,14.2317355019146));
#65079=CARTESIAN_POINT('Ctrl Pts',(39.0384102949243,-37.3809896965113,14.1532299915378));
#65080=CARTESIAN_POINT('Ctrl Pts',(40.2920679536969,-38.0254209930877,14.074724481161));
#65081=CARTESIAN_POINT('Ctrl Pts',(40.4474545117342,-39.4273810345935,13.9962189707842));
#65082=CARTESIAN_POINT('Ctrl Pts',(39.3608457503204,-40.3286674512605,13.9177134604075));
#65083=CARTESIAN_POINT('Ctrl Pts',(38.4650745289098,-40.0575985380862,13.8653764534896));
#65084=CARTESIAN_POINT('Ctrl Pts',(38.1712104185962,-39.7634014663305,13.8392079500307));
#65085=CARTESIAN_POINT('Ctrl Pts',(40.3472015171019,-39.3175435144276,18.0535973499898));
#65086=CARTESIAN_POINT('Ctrl Pts',(40.1999547235979,-39.7389061291211,18.0274288465308));
#65087=CARTESIAN_POINT('Ctrl Pts',(39.4597837375779,-40.4181397905768,17.975091839613));
#65088=CARTESIAN_POINT('Ctrl Pts',(37.9892037027278,-40.0523395370335,17.8965863292362));
#65089=CARTESIAN_POINT('Ctrl Pts',(37.4867566635289,-38.6240376790355,17.8180808188594));
#65090=CARTESIAN_POINT('Ctrl Pts',(38.3992375699639,-37.4170658579415,17.7395753084827));
#65091=CARTESIAN_POINT('Ctrl Pts',(39.9101652101474,-37.5124466086438,17.6610697981059));
#65092=CARTESIAN_POINT('Ctrl Pts',(40.6635929548117,-38.8253393001895,17.5825642877291));
#65093=CARTESIAN_POINT('Ctrl Pts',(39.9842778291545,-40.1779658848535,17.5040587773523));
#65094=CARTESIAN_POINT('Ctrl Pts',(38.481224440952,-40.3574286296186,17.4255532669755));
#65095=CARTESIAN_POINT('Ctrl Pts',(37.5025159407713,-39.2026972836548,17.3470477565988));
#65096=CARTESIAN_POINT('Ctrl Pts',(37.9258275657957,-37.7494036870074,17.268542246222));
#65097=CARTESIAN_POINT('Ctrl Pts',(39.3715499208041,-37.3008757150928,17.1900367358452));
#65098=CARTESIAN_POINT('Ctrl Pts',(40.5431117447103,-38.2593739611798,17.1115312254684));
#65099=CARTESIAN_POINT('Ctrl Pts',(40.3898349924146,-39.7652894583281,17.0330257150916));
#65100=CARTESIAN_POINT('Ctrl Pts',(39.0491787185847,-40.4680838297154,16.9545202047148));
#65101=CARTESIAN_POINT('Ctrl Pts',(37.7234769101999,-39.7374731709667,16.8760146943381));
#65102=CARTESIAN_POINT('Ctrl Pts',(37.6016496924775,-38.2286870838463,16.7975091839613));
#65103=CARTESIAN_POINT('Ctrl Pts',(38.7929549918386,-37.2948405078714,16.7190036735845));
#65104=CARTESIAN_POINT('Ctrl Pts',(40.22900170615,-37.7734293976536,16.6404981632077));
#65105=CARTESIAN_POINT('Ctrl Pts',(40.6219090946604,-39.2352437878639,16.561992652831));
#65106=CARTESIAN_POINT('Ctrl Pts',(39.6193084248072,-40.3692938158071,16.4834871424542));
#65107=CARTESIAN_POINT('Ctrl Pts',(38.1203558353197,-40.1585364386243,16.4049816320774));
#65108=CARTESIAN_POINT('Ctrl Pts',(37.469347632893,-38.7919838911743,16.3264761217006));
#65109=CARTESIAN_POINT('Ctrl Pts',(38.2501234557823,-37.4951929817316,16.2479706113238));
#65110=CARTESIAN_POINT('Ctrl Pts',(39.7624649814247,-37.4311566293954,16.1694651009471));
#65111=CARTESIAN_POINT('Ctrl Pts',(40.650068377118,-38.6573041563001,16.0909595905703));
#65112=CARTESIAN_POINT('Ctrl Pts',(40.116909815337,-40.0739973108231,16.0124540801935));
#65113=CARTESIAN_POINT('Ctrl Pts',(38.6411385698271,-40.4107119918079,15.9339485698167));
#65114=CARTESIAN_POINT('Ctrl Pts',(37.5462613776579,-39.3654744684955,15.8554430594399));
#65115=CARTESIAN_POINT('Ctrl Pts',(37.8141901344604,-37.8756786009153,15.7769375490632));
#65116=CARTESIAN_POINT('Ctrl Pts',(39.2046399606431,-37.2774087408428,15.6984320386864));
#65117=CARTESIAN_POINT('Ctrl Pts',(40.4706223976961,-38.1072075221718,15.6199265283096));
#65118=CARTESIAN_POINT('Ctrl Pts',(40.4767742957171,-39.6208916697799,15.5414210179328));
#65119=CARTESIAN_POINT('Ctrl Pts',(39.2175784930743,-40.4609532557217,15.462915507556));
#65120=CARTESIAN_POINT('Ctrl Pts',(37.8223117075287,-39.8740050755378,15.3844099971793));
#65121=CARTESIAN_POINT('Ctrl Pts',(37.5422823907398,-38.3864362169263,15.3059044868025));
#65122=CARTESIAN_POINT('Ctrl Pts',(38.6286274349137,-37.3323337854206,15.2273989764257));
#65123=CARTESIAN_POINT('Ctrl Pts',(40.1070868924566,-37.6570419253671,15.1488934660489));
#65124=CARTESIAN_POINT('Ctrl Pts',(40.6517429414752,-39.0693546088525,15.0703879556722));
#65125=CARTESIAN_POINT('Ctrl Pts',(39.774135559288,-40.302676343909,14.9918824452954));
#65126=CARTESIAN_POINT('Ctrl Pts',(38.2613229558678,-40.2509346784385,14.9133769349186));
#65127=CARTESIAN_POINT('Ctrl Pts',(37.4700333744308,-38.9605331728383,14.8348714245418));
#65128=CARTESIAN_POINT('Ctrl Pts',(38.1099101982325,-37.5887337540646,14.756365914165));
#65129=CARTESIAN_POINT('Ctrl Pts',(39.6071046402236,-37.3658004182179,14.6778604037883));
#65130=CARTESIAN_POINT('Ctrl Pts',(40.6188809858598,-38.4916617046775,14.5993548934115));
#65131=CARTESIAN_POINT('Ctrl Pts',(40.2378868989348,-39.9566252931007,14.5208493830347));
#65132=CARTESIAN_POINT('Ctrl Pts',(38.8057405256223,-40.4468631230908,14.4423438726579));
#65133=CARTESIAN_POINT('Ctrl Pts',(37.6069594645119,-39.5227464177935,14.3638383622811));
#65134=CARTESIAN_POINT('Ctrl Pts',(37.7163659166087,-38.0129878893579,14.2853328519043));
#65135=CARTESIAN_POINT('Ctrl Pts',(39.0363955827559,-37.2716907141535,14.2068273415276));
#65136=CARTESIAN_POINT('Ctrl Pts',(40.3820905838163,-37.9634329679189,14.1283218311508));
#65137=CARTESIAN_POINT('Ctrl Pts',(40.5488848541016,-39.4683179788618,14.049816320774));
#65138=CARTESIAN_POINT('Ctrl Pts',(39.3825026538969,-40.4357723847318,13.9713108103972));
#65139=CARTESIAN_POINT('Ctrl Pts',(38.4209683416301,-40.1448029331842,13.9189738034794));
#65140=CARTESIAN_POINT('Ctrl Pts',(38.1055301823584,-39.8290073680889,13.8928053000205));
#65141=CARTESIAN_POINT('Ctrl Pts',(40.4348379475454,-39.3481684036013,18.1071946999795));
#65142=CARTESIAN_POINT('Ctrl Pts',(40.2775203701536,-39.7983496548843,18.0810261965206));
#65143=CARTESIAN_POINT('Ctrl Pts',(39.4867261966074,-40.5240387619969,18.0286891896027));
#65144=CARTESIAN_POINT('Ctrl Pts',(37.915567443755,-40.1332199989714,17.950183679226));
#65145=CARTESIAN_POINT('Ctrl Pts',(37.378756087165,-38.6072309927778,17.8716781688492));
#65146=CARTESIAN_POINT('Ctrl Pts',(38.3536451302507,-37.3177096500299,17.7931726584724));
#65147=CARTESIAN_POINT('Ctrl Pts',(39.9679110189094,-37.4196138631759,17.7146671480956));
#65148=CARTESIAN_POINT('Ctrl Pts',(40.7728686326526,-38.8223004188168,17.6361616377189));
#65149=CARTESIAN_POINT('Ctrl Pts',(40.0470924896831,-40.2674384238709,17.5576561273421));
#65150=CARTESIAN_POINT('Ctrl Pts',(38.4412394038838,-40.459175327383,17.4791506169653));
#65151=CARTESIAN_POINT('Ctrl Pts',(37.3955932029908,-39.2254673901001,17.4006451065885));
#65152=CARTESIAN_POINT('Ctrl Pts',(37.8478567650411,-37.6727773625425,17.3221395962118));
#65153=CARTESIAN_POINT('Ctrl Pts',(39.3924577241432,-37.1935728090517,17.243634085835));
#65154=CARTESIAN_POINT('Ctrl Pts',(40.6441472415558,-38.2176264975589,17.1651285754582));
#65155=CARTESIAN_POINT('Ctrl Pts',(40.4803872929157,-39.8265374431247,17.0866230650814));
#65156=CARTESIAN_POINT('Ctrl Pts',(39.048038295053,-40.5773986692348,17.0081175547046));
#65157=CARTESIAN_POINT('Ctrl Pts',(37.6316665569935,-39.7968186911193,16.9296120443279));
#65158=CARTESIAN_POINT('Ctrl Pts',(37.5015070995521,-38.1848408247104,16.8511065339511));
#65159=CARTESIAN_POINT('Ctrl Pts',(38.7742904258956,-37.187124830413,16.7726010235743));
#65160=CARTESIAN_POINT('Ctrl Pts',(40.3085539894053,-37.6984462854713,16.6940955131975));
#65161=CARTESIAN_POINT('Ctrl Pts',(40.7283338503372,-39.2602398769767,16.6155900028207));
#65162=CARTESIAN_POINT('Ctrl Pts',(39.6571614008785,-40.4718520200432,16.5370844924439));
#65163=CARTESIAN_POINT('Ctrl Pts',(38.0556895834507,-40.2466801218523,16.4585789820672));
#65164=CARTESIAN_POINT('Ctrl Pts',(37.360156384861,-38.7866637029718,16.3800734716904));
#65165=CARTESIAN_POINT('Ctrl Pts',(38.1943325188197,-37.4011801932639,16.3015679613136));
#65166=CARTESIAN_POINT('Ctrl Pts',(39.8101089940916,-37.3327641444332,16.2230624509368));
#65167=CARTESIAN_POINT('Ctrl Pts',(40.7584190562143,-38.6427726944821,16.1445569405601));
#65168=CARTESIAN_POINT('Ctrl Pts',(40.1887956959422,-40.1563590325843,16.0660514301833));
#65169=CARTESIAN_POINT('Ctrl Pts',(38.6120906852372,-40.5161029470303,15.9875459198065));
#65170=CARTESIAN_POINT('Ctrl Pts',(37.4423305613344,-39.3993775430101,15.9090404094297));
#65171=CARTESIAN_POINT('Ctrl Pts',(37.728584013316,-37.8076887115003,15.830534899053));
#65172=CARTESIAN_POINT('Ctrl Pts',(39.2141321392512,-37.1685008366856,15.7520293886761));
#65173=CARTESIAN_POINT('Ctrl Pts',(40.566700064693,-38.0550528008733,15.6735238782994));
#65174=CARTESIAN_POINT('Ctrl Pts',(40.5732727150713,-39.6722637252762,15.5950183679226));
#65175=CARTESIAN_POINT('Ctrl Pts',(39.2279555885002,-40.5697804074078,15.5165128575458));
#65176=CARTESIAN_POINT('Ctrl Pts',(37.7372610525188,-39.9426885464328,15.4380073471691));
#65177=CARTESIAN_POINT('Ctrl Pts',(37.4380794359446,-38.3533790377419,15.3595018367922));
#65178=CARTESIAN_POINT('Ctrl Pts',(38.5987238648931,-37.2271824197985,15.2809963264155));
#65179=CARTESIAN_POINT('Ctrl Pts',(40.1783009449621,-37.5740986189236,15.2024908160387));
#65180=CARTESIAN_POINT('Ctrl Pts',(40.7602081505748,-39.083004888448,15.1239853056619));
#65181=CARTESIAN_POINT('Ctrl Pts',(39.8225777684026,-40.4006783187926,15.0454797952851));
#65182=CARTESIAN_POINT('Ctrl Pts',(38.2062979965018,-40.34539783853,14.9669742849084));
#65183=CARTESIAN_POINT('Ctrl Pts',(37.3608890269436,-38.9667407289735,14.8884687745316));
#65184=CARTESIAN_POINT('Ctrl Pts',(38.0445295284046,-37.5011185847263,14.8099632641548));
#65185=CARTESIAN_POINT('Ctrl Pts',(39.6441229517549,-37.2629379664549,14.731457753778));
#65186=CARTESIAN_POINT('Ctrl Pts',(40.7250986373369,-38.4658013079928,14.6529522434012));
#65187=CARTESIAN_POINT('Ctrl Pts',(40.3180468752625,-40.030959483689,14.5744467330245));
#65188=CARTESIAN_POINT('Ctrl Pts',(38.7879504123214,-40.554726595519,14.4959412226477));
#65189=CARTESIAN_POINT('Ctrl Pts',(37.5071800276552,-39.5674059357952,14.4174357122709));
#65190=CARTESIAN_POINT('Ctrl Pts',(37.6240692147493,-37.9543891190076,14.3389302018941));
#65191=CARTESIAN_POINT('Ctrl Pts',(39.0343808705876,-37.1623917317957,14.2604246915173));
#65192=CARTESIAN_POINT('Ctrl Pts',(40.4721132139355,-37.9014449427502,14.1819191811406));
#65193=CARTESIAN_POINT('Ctrl Pts',(40.6503151964691,-39.50925492313,14.1034136707638));
#65194=CARTESIAN_POINT('Ctrl Pts',(39.4041595574733,-40.5428773182031,14.024908160387));
#65195=CARTESIAN_POINT('Ctrl Pts',(38.3768621543504,-40.2320073282822,13.9725711534692));
#65196=CARTESIAN_POINT('Ctrl Pts',(38.0398499461206,-39.8946132698472,13.9464026500102));
#65197=CARTESIAN_POINT('Ctrl Pts',(40.5224743779889,-39.378793292775,18.1607920499693));
#65198=CARTESIAN_POINT('Ctrl Pts',(40.3550860167094,-39.8577931806474,18.1346235465104));
#65199=CARTESIAN_POINT('Ctrl Pts',(39.513668655637,-40.6299377334171,18.0822865395925));
#65200=CARTESIAN_POINT('Ctrl Pts',(37.8419311847822,-40.2141004609093,18.0037810292158));
#65201=CARTESIAN_POINT('Ctrl Pts',(37.2707555108009,-38.59042430652,17.925275518839));
#65202=CARTESIAN_POINT('Ctrl Pts',(38.3080526905375,-37.2183534421184,17.8467700084622));
#65203=CARTESIAN_POINT('Ctrl Pts',(40.0256568276714,-37.3267811177079,17.7682644980854));
#65204=CARTESIAN_POINT('Ctrl Pts',(40.8821443104935,-38.8192615374441,17.6897589877086));
#65205=CARTESIAN_POINT('Ctrl Pts',(40.1099071502118,-40.3569109628883,17.6112534773319));
#65206=CARTESIAN_POINT('Ctrl Pts',(38.4012543668155,-40.5609220251472,17.5327479669551));
#65207=CARTESIAN_POINT('Ctrl Pts',(37.2886704652103,-39.2482374965453,17.4542424565783));
#65208=CARTESIAN_POINT('Ctrl Pts',(37.7698859642864,-37.5961510380776,17.3757369462015));
#65209=CARTESIAN_POINT('Ctrl Pts',(39.4133655274823,-37.0862699030106,17.2972314358247));
#65210=CARTESIAN_POINT('Ctrl Pts',(40.7451827384013,-38.1758790339381,17.218725925448));
#65211=CARTESIAN_POINT('Ctrl Pts',(40.5709395934168,-39.8877854279213,17.1402204150712));
#65212=CARTESIAN_POINT('Ctrl Pts',(39.0468978715213,-40.6867135087542,17.0617149046944));
#65213=CARTESIAN_POINT('Ctrl Pts',(37.5398562037872,-39.856164211272,16.9832093943176));
#65214=CARTESIAN_POINT('Ctrl Pts',(37.4013645066268,-38.1409945655745,16.9047038839408));
#65215=CARTESIAN_POINT('Ctrl Pts',(38.7556258599525,-37.0794091529547,16.8261983735641));
#65216=CARTESIAN_POINT('Ctrl Pts',(40.3881062726606,-37.623463173289,16.7476928631873));
#65217=CARTESIAN_POINT('Ctrl Pts',(40.834758606014,-39.2852359660895,16.6691873528105));
#65218=CARTESIAN_POINT('Ctrl Pts',(39.6950143769496,-40.5744102242793,16.5906818424337));
#65219=CARTESIAN_POINT('Ctrl Pts',(37.9910233315818,-40.3348238050803,16.5121763320569));
#65220=CARTESIAN_POINT('Ctrl Pts',(37.2509651368289,-38.7813435147692,16.4336708216802));
#65221=CARTESIAN_POINT('Ctrl Pts',(38.1385415818571,-37.3071674047963,16.3551653113034));
#65222=CARTESIAN_POINT('Ctrl Pts',(39.8577530067585,-37.234371659471,16.2766598009266));
#65223=CARTESIAN_POINT('Ctrl Pts',(40.8667697353107,-38.6282412326641,16.1981542905498));
#65224=CARTESIAN_POINT('Ctrl Pts',(40.2606815765474,-40.2387207543454,16.119648780173));
#65225=CARTESIAN_POINT('Ctrl Pts',(38.5830428006472,-40.6214939022528,16.0411432697963));
#65226=CARTESIAN_POINT('Ctrl Pts',(37.3383997450109,-39.4332806175246,15.9626377594195));
#65227=CARTESIAN_POINT('Ctrl Pts',(37.6429778921717,-37.7396988220853,15.8841322490427));
#65228=CARTESIAN_POINT('Ctrl Pts',(39.2236243178593,-37.0595929325284,15.8056267386659));
#65229=CARTESIAN_POINT('Ctrl Pts',(40.6627777316899,-38.0028980795747,15.7271212282892));
#65230=CARTESIAN_POINT('Ctrl Pts',(40.6697711344255,-39.7236357807726,15.6486157179124));
#65231=CARTESIAN_POINT('Ctrl Pts',(39.2383326839261,-40.6786075590939,15.5701102075356));
#65232=CARTESIAN_POINT('Ctrl Pts',(37.6522103975089,-40.0113720173278,15.4916046971588));
#65233=CARTESIAN_POINT('Ctrl Pts',(37.3338764811494,-38.3203218585575,15.413099186782));
#65234=CARTESIAN_POINT('Ctrl Pts',(38.5688202948726,-37.1220310541764,15.3345936764053));
#65235=CARTESIAN_POINT('Ctrl Pts',(40.2495149974675,-37.4911553124802,15.2560881660285));
#65236=CARTESIAN_POINT('Ctrl Pts',(40.8686733596745,-39.0966551680434,15.1775826556517));
#65237=CARTESIAN_POINT('Ctrl Pts',(39.8710199775172,-40.4986802936762,15.0990771452749));
#65238=CARTESIAN_POINT('Ctrl Pts',(38.151273037136,-40.4398609986215,15.0205716348981));
#65239=CARTESIAN_POINT('Ctrl Pts',(37.2517446794564,-38.9729482851088,14.9420661245214));
#65240=CARTESIAN_POINT('Ctrl Pts',(37.9791488585767,-37.4135034153879,14.8635606141446));
#65241=CARTESIAN_POINT('Ctrl Pts',(39.6811412632861,-37.160075514692,14.7850551037678));
#65242=CARTESIAN_POINT('Ctrl Pts',(40.831316288814,-38.4399409113081,14.706549593391));
#65243=CARTESIAN_POINT('Ctrl Pts',(40.3982068515902,-40.1052936742774,14.6280440830142));
#65244=CARTESIAN_POINT('Ctrl Pts',(38.7701602990205,-40.6625900679474,14.5495385726375));
#65245=CARTESIAN_POINT('Ctrl Pts',(37.4074005907985,-39.6120654537969,14.4710330622607));
#65246=CARTESIAN_POINT('Ctrl Pts',(37.5317725128899,-37.8957903486573,14.3925275518839));
#65247=CARTESIAN_POINT('Ctrl Pts',(39.0323661584192,-37.0530927494379,14.3140220415071));
#65248=CARTESIAN_POINT('Ctrl Pts',(40.5621358440548,-37.8394569175814,14.2355165311303));
#65249=CARTESIAN_POINT('Ctrl Pts',(40.7517455388365,-39.5501918673983,14.1570110207536));
#65250=CARTESIAN_POINT('Ctrl Pts',(39.4258164610498,-40.6499822516745,14.0785055103768));
#65251=CARTESIAN_POINT('Ctrl Pts',(38.3327559670706,-40.3192117233802,14.0261685034589));
#65252=CARTESIAN_POINT('Ctrl Pts',(37.9741697098829,-39.9602191716056,14.));
#65253=CARTESIAN_POINT('Ctrl Pts',(38.4329072841441,-37.7756148875603,17.1934196736194));
#65254=CARTESIAN_POINT('Ctrl Pts',(38.3336188224971,-37.831835714126,17.2005947478237));
#65255=CARTESIAN_POINT('Ctrl Pts',(38.2421150540945,-37.9010724492168,17.2077698220279));
#65256=CARTESIAN_POINT('Ctrl Pts',(38.1625457103697,-37.9820376407054,17.2149448962322));
#65257=CARTESIAN_POINT('Ctrl Pts',(37.8723451372175,-38.2773290667181,17.2411133996911));
#65258=CARTESIAN_POINT('Ctrl Pts',(37.7408919078847,-38.7286281219638,17.26728190315));
#65259=CARTESIAN_POINT('Ctrl Pts',(37.8271270931296,-39.1335701086941,17.293450406609));
#65260=CARTESIAN_POINT('Ctrl Pts',(37.9133622783746,-39.5385120954245,17.3196189100679));
#65261=CARTESIAN_POINT('Ctrl Pts',(38.2172858781974,-39.8970970136394,17.3457874135268));
#65262=CARTESIAN_POINT('Ctrl Pts',(38.6026232932098,-40.0485247084105,17.3719559169858));
#65263=CARTESIAN_POINT('Ctrl Pts',(38.9879607082221,-40.1999524031816,17.3981244204447));
#65264=CARTESIAN_POINT('Ctrl Pts',(39.454711938424,-40.1442228745088,17.4242929239036));
#65265=CARTESIAN_POINT('Ctrl Pts',(39.7935632382491,-39.9063389161268,17.4504614273625));
#65266=CARTESIAN_POINT('Ctrl Pts',(40.1324145380743,-39.6684549577448,17.4766299308215));
#65267=CARTESIAN_POINT('Ctrl Pts',(40.3433659075226,-39.2484165696536,17.5027984342804));
#65268=CARTESIAN_POINT('Ctrl Pts',(40.3318586129825,-38.8345475710328,17.5289669377393));
#65269=CARTESIAN_POINT('Ctrl Pts',(40.3203513184423,-38.4206785724121,17.5551354411983));
#65270=CARTESIAN_POINT('Ctrl Pts',(40.0863853599138,-38.0129789632619,17.5813039446572));
#65271=CARTESIAN_POINT('Ctrl Pts',(39.7348041486982,-37.7943196106437,17.6074724481161));
#65272=CARTESIAN_POINT('Ctrl Pts',(39.3832229374826,-37.5756602580255,17.633640951575));
#65273=CARTESIAN_POINT('Ctrl Pts',(38.9140264735798,-37.5460411619393,17.659809455034));
#65274=CARTESIAN_POINT('Ctrl Pts',(38.5377494466644,-37.7186353304695,17.6859779584929));
#65275=CARTESIAN_POINT('Ctrl Pts',(38.5020812950974,-37.7349959225928,17.6884585302017));
#65276=CARTESIAN_POINT('Ctrl Pts',(38.4672480779576,-37.7531735168604,17.6909391019106));
#65277=CARTESIAN_POINT('Ctrl Pts',(38.4333577759012,-37.7730251466968,17.6934196736194));
#65278=CARTESIAN_POINT('Ctrl Pts',(37.5756558680257,-39.2699729499894,18.));
#65279=CARTESIAN_POINT('Ctrl Pts',(37.4440523270134,-38.7799318659295,17.9738314965411));
#65280=CARTESIAN_POINT('Ctrl Pts',(37.7041245449082,-37.6679293649188,17.9214944896232));
#65281=CARTESIAN_POINT('Ctrl Pts',(39.3195387437205,-37.0695352316426,17.8429889792464));
#65282=CARTESIAN_POINT('Ctrl Pts',(40.7062722211716,-38.0891100356719,17.7644834688697));
#65283=CARTESIAN_POINT('Ctrl Pts',(40.6223994863181,-39.8071108514352,17.6859779584929));
#65284=CARTESIAN_POINT('Ctrl Pts',(39.1423049297703,-40.6853144575312,17.6074724481161));
#65285=CARTESIAN_POINT('Ctrl Pts',(37.593781529679,-39.9348860603428,17.5289669377393));
#65286=CARTESIAN_POINT('Ctrl Pts',(37.365380302334,-38.2294395514345,17.4504614273625));
#65287=CARTESIAN_POINT('Ctrl Pts',(38.6620363043874,-37.0981581562678,17.3719559169858));
#65288=CARTESIAN_POINT('Ctrl Pts',(40.3208285827551,-37.5557507395872,17.293450406609));
#65289=CARTESIAN_POINT('Ctrl Pts',(40.8541369642562,-39.1917640019411,17.2149448962322));
#65290=CARTESIAN_POINT('Ctrl Pts',(39.7836658898431,-40.5390185509755,17.1364393858554));
#65291=CARTESIAN_POINT('Ctrl Pts',(38.0694451486085,-40.389246627264,17.0579338754786));
#65292=CARTESIAN_POINT('Ctrl Pts',(37.2488257543949,-38.87677605618,16.9794283651019));
#65293=CARTESIAN_POINT('Ctrl Pts',(38.0577601193366,-37.3580220610822,16.9009228547251));
#65294=CARTESIAN_POINT('Ctrl Pts',(39.7707759682514,-37.1950414723212,16.8224173443483));
#65295=CARTESIAN_POINT('Ctrl Pts',(40.8516003110939,-38.5339981005298,16.7439118339715));
#65296=CARTESIAN_POINT('Ctrl Pts',(40.3309240105073,-40.1740843304588,16.6654063235947));
#65297=CARTESIAN_POINT('Ctrl Pts',(38.6757020358417,-40.644431583443,16.586900813218));
#65298=CARTESIAN_POINT('Ctrl Pts',(37.3703767628973,-39.5232213878114,16.5083953028412));
#65299=CARTESIAN_POINT('Ctrl Pts',(37.5855949493635,-37.8159816397815,16.4298897924644));
#65300=CARTESIAN_POINT('Ctrl Pts',(39.1283437989466,-37.0538055634981,16.3513842820876));
#65301=CARTESIAN_POINT('Ctrl Pts',(40.6150494715948,-37.9202307686755,16.2728787717108));
#65302=CARTESIAN_POINT('Ctrl Pts',(40.7123989731982,-39.6382265407265,16.1943732613341));
#65303=CARTESIAN_POINT('Ctrl Pts',(39.333086957597,-40.6670534245635,16.1158677509573));
#65304=CARTESIAN_POINT('Ctrl Pts',(37.7141132310224,-40.0840350136355,16.0373622405805));
#65305=CARTESIAN_POINT('Ctrl Pts',(37.3074119207117,-38.4120360784117,15.9588567302037));
#65306=CARTESIAN_POINT('Ctrl Pts',(38.4777224302706,-37.150545013987,15.880351219827));
#65307=CARTESIAN_POINT('Ctrl Pts',(40.1754824724718,-37.430896996864,15.8018457094502));
#65308=CARTESIAN_POINT('Ctrl Pts',(40.8781004790678,-39.0016657040982,15.7233401990734));
#65309=CARTESIAN_POINT('Ctrl Pts',(39.9554519188484,-40.454148415738,15.6448346886966));
#65310=CARTESIAN_POINT('Ctrl Pts',(38.2349899535507,-40.4857241059463,15.5663291783198));
#65311=CARTESIAN_POINT('Ctrl Pts',(37.2596657788943,-39.0680749435716,15.4878236679431));
#65312=CARTESIAN_POINT('Ctrl Pts',(37.904173294426,-37.4725824031402,15.4093181575663));
#65313=CARTESIAN_POINT('Ctrl Pts',(39.5905028527061,-37.1301221194426,15.3308126471895));
#65314=CARTESIAN_POINT('Ctrl Pts',(40.8063139857151,-38.3478206288557,15.2523071368127));
#65315=CARTESIAN_POINT('Ctrl Pts',(40.4612384258705,-40.0336169338117,15.1738016264359));
#65316=CARTESIAN_POINT('Ctrl Pts',(38.8647480157521,-40.6756488816116,15.0952961160592));
#65317=CARTESIAN_POINT('Ctrl Pts',(37.4486135593306,-39.6981268544226,15.0167906056824));
#65318=CARTESIAN_POINT('Ctrl Pts',(37.482857597304,-37.9777160555697,14.9382850953056));
#65319=CARTESIAN_POINT('Ctrl Pts',(38.9367702893063,-37.0573213639055,14.8597795849288));
#65320=CARTESIAN_POINT('Ctrl Pts',(40.5064460859517,-37.7623754838001,14.7812740745521));
#65321=CARTESIAN_POINT('Ctrl Pts',(40.7841666383236,-39.4605673674226,14.7027685641753));
#65322=CARTESIAN_POINT('Ctrl Pts',(39.5208569909583,-40.6289217126118,14.6242630537985));
#65323=CARTESIAN_POINT('Ctrl Pts',(37.8495006293029,-40.2196233657656,14.5457575434217));
#65324=CARTESIAN_POINT('Ctrl Pts',(37.2689744719433,-38.5997554156836,14.4672520330449));
#65325=CARTESIAN_POINT('Ctrl Pts',(38.2999795535027,-37.2220243444981,14.3887465226682));
#65326=CARTESIAN_POINT('Ctrl Pts',(40.0177412802272,-37.3220721610692,14.3102410122913));
#65327=CARTESIAN_POINT('Ctrl Pts',(40.8820235552811,-38.8100518816853,14.2317355019146));
#65328=CARTESIAN_POINT('Ctrl Pts',(40.1171224362185,-40.3517547545304,14.1532299915378));
#65329=CARTESIAN_POINT('Ctrl Pts',(38.4102262410485,-40.5640442208952,14.074724481161));
#65330=CARTESIAN_POINT('Ctrl Pts',(37.2896688855125,-39.2575551350437,13.9962189707842));
#65331=CARTESIAN_POINT('Ctrl Pts',(37.7654127933167,-37.6018660619834,13.9177134604075));
#65332=CARTESIAN_POINT('Ctrl Pts',(38.8548175316166,-37.2592519394722,13.8653764534896));
#65333=CARTESIAN_POINT('Ctrl Pts',(39.3533377835638,-37.3537893102425,13.8392079500307));
#65334=CARTESIAN_POINT('Ctrl Pts',(37.6653123637055,-39.2458951477601,18.0535973499898));
#65335=CARTESIAN_POINT('Ctrl Pts',(37.5416266421298,-38.7853369848302,18.0274288465308));
#65336=CARTESIAN_POINT('Ctrl Pts',(37.7860518276885,-37.7402372050404,17.975091839613));
#65337=CARTESIAN_POINT('Ctrl Pts',(39.304275952107,-37.1778449655031,17.8965863292362));
#65338=CARTESIAN_POINT('Ctrl Pts',(40.6075777437792,-38.1360778851249,17.8180808188594));
#65339=CARTESIAN_POINT('Ctrl Pts',(40.528751143438,-39.7507165865677,17.7395753084826));
#65340=CARTESIAN_POINT('Ctrl Pts',(39.137705265654,-40.5760837907846,17.6610697981059));
#65341=CARTESIAN_POINT('Ctrl Pts',(37.6823475097464,-39.8708043045094,17.5825642877291));
#65342=CARTESIAN_POINT('Ctrl Pts',(37.4676878554874,-38.267964590315,17.5040587773523));
#65343=CARTESIAN_POINT('Ctrl Pts',(38.6863316094155,-37.2047458152724,17.4255532669755));
#65344=CARTESIAN_POINT('Ctrl Pts',(40.2453240067019,-37.6348077149766,17.3470477565988));
#65345=CARTESIAN_POINT('Ctrl Pts',(40.7465463255008,-39.172391577122,17.268542246222));
#65346=CARTESIAN_POINT('Ctrl Pts',(39.7404792679866,-40.4385896578249,17.1900367358452));
#65347=CARTESIAN_POINT('Ctrl Pts',(38.1293932159793,-40.2978286394393,17.1115312254684));
#65348=CARTESIAN_POINT('Ctrl Pts',(37.3581457166218,-38.876354623561,17.0330257150916));
#65349=CARTESIAN_POINT('Ctrl Pts',(38.118411206939,-37.4489752207369,16.9545202047148));
#65350=CARTESIAN_POINT('Ctrl Pts',(39.7283648579877,-37.2958002258341,16.8760146943381));
#65351=CARTESIAN_POINT('Ctrl Pts',(40.7441622880019,-38.5541996233328,16.7975091839613));
#65352=CARTESIAN_POINT('Ctrl Pts',(40.2548120512981,-40.0956114062894,16.7190036735845));
#65353=CARTESIAN_POINT('Ctrl Pts',(38.6991751533109,-40.5376606013873,16.6404981632077));
#65354=CARTESIAN_POINT('Ctrl Pts',(37.4723837080864,-39.4839071003945,16.561992652831));
#65355=CARTESIAN_POINT('Ctrl Pts',(37.6746534683415,-37.8793820358441,16.4834871424542));
#65356=CARTESIAN_POINT('Ctrl Pts',(39.1245840948508,-37.1630616599808,16.4049816320774));
#65357=CARTESIAN_POINT('Ctrl Pts',(40.5218433363406,-37.9773591011396,16.3264761217006));
#65358=CARTESIAN_POINT('Ctrl Pts',(40.6133358847798,-39.5919930623209,16.2479706113238));
#65359=CARTESIAN_POINT('Ctrl Pts',(39.3170090487735,-40.5589214179339,16.1694651009471));
#65360=CARTESIAN_POINT('Ctrl Pts',(37.7954395526701,-40.010979832982,16.0909595905703));
#65361=CARTESIAN_POINT('Ctrl Pts',(37.4132070941463,-38.4395753465506,16.0124540801935));
#65362=CARTESIAN_POINT('Ctrl Pts',(38.5131068288268,-37.2539808605321,15.9339485698167));
#65363=CARTESIAN_POINT('Ctrl Pts',(40.1087225262984,-37.517465695595,15.8554430594399));
#65364=CARTESIAN_POINT('Ctrl Pts',(40.7690680950382,-38.9937303879309,15.7769375490632));
#65365=CARTESIAN_POINT('Ctrl Pts',(39.9019299310211,-40.3588256648782,15.6984320386864));
#65366=CARTESIAN_POINT('Ctrl Pts',(38.2849781530934,-40.3885016295036,15.6199265283096));
#65367=CARTESIAN_POINT('Ctrl Pts',(37.3683335599107,-39.0561441698123,15.5414210179328));
#65368=CARTESIAN_POINT('Ctrl Pts',(37.9740648077657,-37.5566431334877,15.462915507556));
#65369=CARTESIAN_POINT('Ctrl Pts',(39.558937727035,-37.2347866927388,15.3844099971793));
#65370=CARTESIAN_POINT('Ctrl Pts',(40.7016005773602,-38.37922336701,15.3059044868025));
#65371=CARTESIAN_POINT('Ctrl Pts',(40.3772862064154,-39.9635951157055,15.2273989764257));
#65372=CARTESIAN_POINT('Ctrl Pts',(38.8768473364175,-40.566999736337,15.1488934660489));
#65373=CARTESIAN_POINT('Ctrl Pts',(37.5459134516342,-39.6482895226222,15.0703879556721));
#65374=CARTESIAN_POINT('Ctrl Pts',(37.5780972250634,-38.0313858327519,14.9918824452954));
#65375=CARTESIAN_POINT('Ctrl Pts',(38.9445364487738,-37.1663659351315,14.9133769349186));
#65376=CARTESIAN_POINT('Ctrl Pts',(40.4197739845928,-37.829001050405,14.8348714245418));
#65377=CARTESIAN_POINT('Ctrl Pts',(40.6807857070153,-39.425022607912,14.756365914165));
#65378=CARTESIAN_POINT('Ctrl Pts',(39.4934820516118,-40.5230838692526,14.6778604037882));
#65379=CARTESIAN_POINT('Ctrl Pts',(37.9226814788354,-40.1384106227729,14.5993548934115));
#65380=CARTESIAN_POINT('Ctrl Pts',(37.3770822030539,-38.6160007033882,14.5208493830347));
#65381=CARTESIAN_POINT('Ctrl Pts',(38.3460577069044,-37.3211596955696,14.4423438726579));
#65382=CARTESIAN_POINT('Ctrl Pts',(39.9604717039048,-37.4151882170629,14.3638383622811));
#65383=CARTESIAN_POINT('Ctrl Pts',(40.7727551425788,-38.8136448544663,14.2853328519044));
#65384=CARTESIAN_POINT('Ctrl Pts',(40.053873673907,-40.2625924345728,14.2068273415276));
#65385=CARTESIAN_POINT('Ctrl Pts',(38.4496714926396,-40.4621096787767,14.1283218311508));
#65386=CARTESIAN_POINT('Ctrl Pts',(37.3965315541519,-39.2342244404969,14.049816320774));
#65387=CARTESIAN_POINT('Ctrl Pts',(37.8436527187451,-37.6781485467081,13.9713108103972));
#65388=CARTESIAN_POINT('Ctrl Pts',(38.8675143117402,-37.356147522732,13.9189738034794));
#65389=CARTESIAN_POINT('Ctrl Pts',(39.3360415003545,-37.4449971298904,13.8928053000205));
#65390=CARTESIAN_POINT('Ctrl Pts',(37.7549688593853,-39.2218173455308,18.1071946999795));
#65391=CARTESIAN_POINT('Ctrl Pts',(37.6392009572462,-38.7907421037308,18.0810261965206));
#65392=CARTESIAN_POINT('Ctrl Pts',(37.8679791104688,-37.812545045162,18.0286891896028));
#65393=CARTESIAN_POINT('Ctrl Pts',(39.2890131604934,-37.2861546993636,17.950183679226));
#65394=CARTESIAN_POINT('Ctrl Pts',(40.5088832663869,-38.1830457345779,17.8716781688492));
#65395=CARTESIAN_POINT('Ctrl Pts',(40.4351028005577,-39.6943223217001,17.7931726584724));
#65396=CARTESIAN_POINT('Ctrl Pts',(39.1331056015378,-40.466853124038,17.7146671480956));
#65397=CARTESIAN_POINT('Ctrl Pts',(37.7709134898136,-39.8067225486761,17.6361616377189));
#65398=CARTESIAN_POINT('Ctrl Pts',(37.5699954086408,-38.3064896291956,17.5576561273421));
#65399=CARTESIAN_POINT('Ctrl Pts',(38.7106269144436,-37.3113334742769,17.4791506169653));
#65400=CARTESIAN_POINT('Ctrl Pts',(40.1698194306487,-37.713864690366,17.4006451065885));
#65401=CARTESIAN_POINT('Ctrl Pts',(40.6389556867455,-39.1530191523028,17.3221395962118));
#65402=CARTESIAN_POINT('Ctrl Pts',(39.6972926461299,-40.3381607646743,17.243634085835));
#65403=CARTESIAN_POINT('Ctrl Pts',(38.1893412833502,-40.2064106516147,17.1651285754582));
#65404=CARTESIAN_POINT('Ctrl Pts',(37.4674656788486,-38.875933190942,17.0866230650814));
#65405=CARTESIAN_POINT('Ctrl Pts',(38.1790622945415,-37.5399283803915,17.0081175547046));
#65406=CARTESIAN_POINT('Ctrl Pts',(39.6859537477239,-37.396558979347,16.9296120443278));
#65407=CARTESIAN_POINT('Ctrl Pts',(40.63672426491,-38.5744011461358,16.8511065339511));
#65408=CARTESIAN_POINT('Ctrl Pts',(40.1787000920889,-40.01713848212,16.7726010235743));
#65409=CARTESIAN_POINT('Ctrl Pts',(38.7226482707802,-40.4308896193315,16.6940955131975));
#65410=CARTESIAN_POINT('Ctrl Pts',(37.5743906532754,-39.4445928129776,16.6155900028207));
#65411=CARTESIAN_POINT('Ctrl Pts',(37.7637119873195,-37.9427824319066,16.537084492444));
#65412=CARTESIAN_POINT('Ctrl Pts',(39.1208243907549,-37.2723177564635,16.4585789820672));
#65413=CARTESIAN_POINT('Ctrl Pts',(40.4286372010862,-38.0344874336038,16.3800734716904));
#65414=CARTESIAN_POINT('Ctrl Pts',(40.5142727963614,-39.5457595839153,16.3015679613136));
#65415=CARTESIAN_POINT('Ctrl Pts',(39.3009311399501,-40.4507894113044,16.2230624509368));
#65416=CARTESIAN_POINT('Ctrl Pts',(37.8767658743178,-39.9379246523286,16.14455694056));
#65417=CARTESIAN_POINT('Ctrl Pts',(37.5190022675809,-38.4671146146895,16.0660514301833));
#65418=CARTESIAN_POINT('Ctrl Pts',(38.548491227383,-37.3574167070772,15.9875459198065));
#65419=CARTESIAN_POINT('Ctrl Pts',(40.0419625801251,-37.6040343943261,15.9090404094297));
#65420=CARTESIAN_POINT('Ctrl Pts',(40.6600357110085,-38.9857950717635,15.8305348990529));
#65421=CARTESIAN_POINT('Ctrl Pts',(39.8484079431939,-40.2635029140183,15.7520293886762));
#65422=CARTESIAN_POINT('Ctrl Pts',(38.3349663526361,-40.2912791530608,15.6735238782994));
#65423=CARTESIAN_POINT('Ctrl Pts',(37.4770013409271,-39.044213396053,15.5950183679226));
#65424=CARTESIAN_POINT('Ctrl Pts',(38.0439563211054,-37.640703863835,15.5165128575458));
#65425=CARTESIAN_POINT('Ctrl Pts',(39.5273726013638,-37.3394512660349,15.438007347169));
#65426=CARTESIAN_POINT('Ctrl Pts',(40.5968871690054,-38.4106261051643,15.3595018367923));
#65427=CARTESIAN_POINT('Ctrl Pts',(40.2933339869602,-39.8935732975993,15.2809963264155));
#65428=CARTESIAN_POINT('Ctrl Pts',(38.8889466570829,-40.4583505910623,15.2024908160387));
#65429=CARTESIAN_POINT('Ctrl Pts',(37.6432133439378,-39.5984521908219,15.1239853056619));
#65430=CARTESIAN_POINT('Ctrl Pts',(37.6733368528227,-38.0850556099341,15.0454797952851));
#65431=CARTESIAN_POINT('Ctrl Pts',(38.9523026082414,-37.2754105063575,14.9669742849084));
#65432=CARTESIAN_POINT('Ctrl Pts',(40.3331018832338,-37.89562661701,14.8884687745316));
#65433=CARTESIAN_POINT('Ctrl Pts',(40.577404775707,-39.3894778484014,14.8099632641548));
#65434=CARTESIAN_POINT('Ctrl Pts',(39.4661071122653,-40.4172460258934,14.731457753778));
#65435=CARTESIAN_POINT('Ctrl Pts',(37.9958623283679,-40.0571978797803,14.6529522434012));
#65436=CARTESIAN_POINT('Ctrl Pts',(37.4851899341644,-38.6322459910928,14.5744467330245));
#65437=CARTESIAN_POINT('Ctrl Pts',(38.3921358603061,-37.4202950466411,14.4959412226477));
#65438=CARTESIAN_POINT('Ctrl Pts',(39.9032021275825,-37.5083042730566,14.4174357122709));
#65439=CARTESIAN_POINT('Ctrl Pts',(40.6634867298766,-38.8172378272473,14.3389302018941));
#65440=CARTESIAN_POINT('Ctrl Pts',(39.9906249115955,-40.1734301146151,14.2604246915173));
#65441=CARTESIAN_POINT('Ctrl Pts',(38.4891167442306,-40.3601751366582,14.1819191811406));
#65442=CARTESIAN_POINT('Ctrl Pts',(37.5033942227913,-39.2108937459501,14.1034136707638));
#65443=CARTESIAN_POINT('Ctrl Pts',(37.9218926441736,-37.7544310314327,14.024908160387));
#65444=CARTESIAN_POINT('Ctrl Pts',(38.8802110918637,-37.4530431059918,13.9725711534692));
#65445=CARTESIAN_POINT('Ctrl Pts',(39.3187452171453,-37.5362049495383,13.9464026500102));
#65446=CARTESIAN_POINT('Ctrl Pts',(37.8446253550651,-39.1977395433015,18.1607920499693));
#65447=CARTESIAN_POINT('Ctrl Pts',(37.7367752723626,-38.7961472226316,18.1346235465104));
#65448=CARTESIAN_POINT('Ctrl Pts',(37.9499063932491,-37.8848528852836,18.0822865395925));
#65449=CARTESIAN_POINT('Ctrl Pts',(39.2737503688799,-37.3944644332241,18.0037810292158));
#65450=CARTESIAN_POINT('Ctrl Pts',(40.4101887889945,-38.230013584031,17.925275518839));
#65451=CARTESIAN_POINT('Ctrl Pts',(40.3414544576775,-39.6379280568325,17.8467700084622));
#65452=CARTESIAN_POINT('Ctrl Pts',(39.1285059374216,-40.3576224572915,17.7682644980854));
#65453=CARTESIAN_POINT('Ctrl Pts',(37.8594794698809,-39.7426407928426,17.6897589877086));
#65454=CARTESIAN_POINT('Ctrl Pts',(37.6723029617942,-38.3450146680762,17.6112534773319));
#65455=CARTESIAN_POINT('Ctrl Pts',(38.7349222194717,-37.4179211332815,17.5327479669551));
#65456=CARTESIAN_POINT('Ctrl Pts',(40.0943148545955,-37.7929216657554,17.4542424565783));
#65457=CARTESIAN_POINT('Ctrl Pts',(40.5313650479902,-39.1336467274836,17.3757369462015));
#65458=CARTESIAN_POINT('Ctrl Pts',(39.6541060242733,-40.2377318715238,17.2972314358247));
#65459=CARTESIAN_POINT('Ctrl Pts',(38.249289350721,-40.11499266379,17.218725925448));
#65460=CARTESIAN_POINT('Ctrl Pts',(37.5767856410754,-38.8755117583229,17.1402204150712));
#65461=CARTESIAN_POINT('Ctrl Pts',(38.2397133821439,-37.6308815400462,17.0617149046944));
#65462=CARTESIAN_POINT('Ctrl Pts',(39.6435426374601,-37.4973177328599,16.9832093943176));
#65463=CARTESIAN_POINT('Ctrl Pts',(40.529286241818,-38.5946026689388,16.9047038839408));
#65464=CARTESIAN_POINT('Ctrl Pts',(40.1025881328798,-39.9386655579506,16.8261983735641));
#65465=CARTESIAN_POINT('Ctrl Pts',(38.7461213882494,-40.3241186372758,16.7476928631873));
#65466=CARTESIAN_POINT('Ctrl Pts',(37.6763975984644,-39.4052785255607,16.6691873528105));
#65467=CARTESIAN_POINT('Ctrl Pts',(37.8527705062976,-38.0061828279691,16.5906818424337));
#65468=CARTESIAN_POINT('Ctrl Pts',(39.1170646866591,-37.3815738529462,16.5121763320569));
#65469=CARTESIAN_POINT('Ctrl Pts',(40.335431065832,-38.0916157660679,16.4336708216802));
#65470=CARTESIAN_POINT('Ctrl Pts',(40.4152097079431,-39.4995261055097,16.3551653113034));
#65471=CARTESIAN_POINT('Ctrl Pts',(39.2848532311266,-40.3426574046748,16.2766598009266));
#65472=CARTESIAN_POINT('Ctrl Pts',(37.9580921959656,-39.8648694716751,16.1981542905498));
#65473=CARTESIAN_POINT('Ctrl Pts',(37.6247974410155,-38.4946538828284,16.119648780173));
#65474=CARTESIAN_POINT('Ctrl Pts',(38.5838756259392,-37.4608525536223,16.0411432697963));
#65475=CARTESIAN_POINT('Ctrl Pts',(39.9752026339518,-37.6906030930571,15.9626377594195));
#65476=CARTESIAN_POINT('Ctrl Pts',(40.5510033269788,-38.9778597555962,15.8841322490427));
#65477=CARTESIAN_POINT('Ctrl Pts',(39.7948859553666,-40.1681801631584,15.8056267386659));
#65478=CARTESIAN_POINT('Ctrl Pts',(38.3849545521788,-40.1940566766182,15.7271212282891));
#65479=CARTESIAN_POINT('Ctrl Pts',(37.5856691219435,-39.0322826222936,15.6486157179124));
#65480=CARTESIAN_POINT('Ctrl Pts',(38.1138478344451,-37.7247645941825,15.5701102075356));
#65481=CARTESIAN_POINT('Ctrl Pts',(39.4958074756927,-37.4441158393311,15.4916046971588));
#65482=CARTESIAN_POINT('Ctrl Pts',(40.4921737606505,-38.4420288433187,15.413099186782));
#65483=CARTESIAN_POINT('Ctrl Pts',(40.2093817675051,-39.823551479493,15.3345936764052));
#65484=CARTESIAN_POINT('Ctrl Pts',(38.9010459777483,-40.3497014457878,15.2560881660285));
#65485=CARTESIAN_POINT('Ctrl Pts',(37.7405132362414,-39.5486148590214,15.1775826556517));
#65486=CARTESIAN_POINT('Ctrl Pts',(37.768576480582,-38.1387253871164,15.0990771452749));
#65487=CARTESIAN_POINT('Ctrl Pts',(38.9600687677089,-37.3844550775834,15.0205716348981));
#65488=CARTESIAN_POINT('Ctrl Pts',(40.2464297818749,-37.962252183615,14.9420661245214));
#65489=CARTESIAN_POINT('Ctrl Pts',(40.4740238443987,-39.3539330888908,14.8635606141446));
#65490=CARTESIAN_POINT('Ctrl Pts',(39.4387321729189,-40.3114081825343,14.7850551037678));
#65491=CARTESIAN_POINT('Ctrl Pts',(38.0690431779005,-39.9759851367875,14.706549593391));
#65492=CARTESIAN_POINT('Ctrl Pts',(37.593297665275,-38.6484912787976,14.6280440830142));
#65493=CARTESIAN_POINT('Ctrl Pts',(38.4382140137078,-37.5194303977126,14.5495385726375));
#65494=CARTESIAN_POINT('Ctrl Pts',(39.8459325512601,-37.6014203290504,14.4710330622607));
#65495=CARTESIAN_POINT('Ctrl Pts',(40.5542183171743,-38.8208308000283,14.3925275518839));
#65496=CARTESIAN_POINT('Ctrl Pts',(39.9273761492841,-40.0842677946575,14.3140220415071));
#65497=CARTESIAN_POINT('Ctrl Pts',(38.5285619958217,-40.2582405945397,14.2355165311304));
#65498=CARTESIAN_POINT('Ctrl Pts',(37.6102568914307,-39.1875630514034,14.1570110207535));
#65499=CARTESIAN_POINT('Ctrl Pts',(38.0001325696021,-37.8307135161573,14.0785055103768));
#65500=CARTESIAN_POINT('Ctrl Pts',(38.8929078719872,-37.5499386892516,14.0261685034589));
#65501=CARTESIAN_POINT('Ctrl Pts',(39.3014489339361,-37.6274127691862,14.));
#65502=CARTESIAN_POINT('Ctrl Pts',(38.4348713855213,-37.7748596688487,17.5565803263806));
#65503=CARTESIAN_POINT('Ctrl Pts',(38.5438548719482,-37.7108039030124,17.5486362065721));
#65504=CARTESIAN_POINT('Ctrl Pts',(38.6618404864523,-37.6628704742542,17.5406920867636));
#65505=CARTESIAN_POINT('Ctrl Pts',(38.7843844490461,-37.6349368111596,17.5327479669551));
#65506=CARTESIAN_POINT('Ctrl Pts',(39.1880530978463,-37.5429213107728,17.5065794634961));
#65507=CARTESIAN_POINT('Ctrl Pts',(39.6411839762209,-37.6679214882641,17.4804109600372));
#65508=CARTESIAN_POINT('Ctrl Pts',(39.9405911143073,-37.9538757539645,17.4542424565783));
#65509=CARTESIAN_POINT('Ctrl Pts',(40.2399982523938,-38.2398300196648,17.4280739531194));
#65510=CARTESIAN_POINT('Ctrl Pts',(40.385681650192,-38.6867383735742,17.4019054496604));
#65511=CARTESIAN_POINT('Ctrl Pts',(40.3123135118049,-39.0942067412023,17.3757369462015));
#65512=CARTESIAN_POINT('Ctrl Pts',(40.2389453734179,-39.5016751088304,17.3495684427426));
#65513=CARTESIAN_POINT('Ctrl Pts',(39.9465256988456,-39.8697034901771,17.3233999392837));
#65514=CARTESIAN_POINT('Ctrl Pts',(39.5661797493007,-40.0332611462281,17.2972314358247));
#65515=CARTESIAN_POINT('Ctrl Pts',(39.1858337997559,-40.1968188022792,17.2710629323658));
#65516=CARTESIAN_POINT('Ctrl Pts',(38.7175615752384,-40.1559057330346,17.2448944289069));
#65517=CARTESIAN_POINT('Ctrl Pts',(38.3713415113721,-39.9288690475011,17.218725925448));
#65518=CARTESIAN_POINT('Ctrl Pts',(38.0251214475058,-39.7018323619677,17.192557421989));
#65519=CARTESIAN_POINT('Ctrl Pts',(37.8009535442906,-39.2886720601453,17.1663889185301));
#65520=CARTESIAN_POINT('Ctrl Pts',(37.7993575495278,-38.8746535395213,17.1402204150712));
#65521=CARTESIAN_POINT('Ctrl Pts',(37.7977615547649,-38.4606350188973,17.1140519116123));
#65522=CARTESIAN_POINT('Ctrl Pts',(38.0187374684544,-38.0457582794717,17.0878834081533));
#65523=CARTESIAN_POINT('Ctrl Pts',(38.3631969678519,-37.8160592752279,17.0617149046944));
#65524=CARTESIAN_POINT('Ctrl Pts',(38.3857260141201,-37.8010360301049,17.0600033785898));
#65525=CARTESIAN_POINT('Ctrl Pts',(38.4087832848556,-37.7868049178791,17.0582918524852));
#65526=CARTESIAN_POINT('Ctrl Pts',(38.4323100738575,-37.7733715239653,17.0565803263806));
#65527=CARTESIAN_POINT('Origin',(39.0658530619283,-38.8697713466883,15.5));
#65528=CARTESIAN_POINT('Origin',(-14.1292828945604,-53.2669068454841,14.));
#65529=CARTESIAN_POINT('Ctrl Pts',(-12.9355708698302,-52.8497595669186,
14.));
#65530=CARTESIAN_POINT('Ctrl Pts',(-12.9470539462122,-52.8001843799443,
14.));
#65531=CARTESIAN_POINT('Ctrl Pts',(-12.9617293958119,-52.7515166200284,
14.));
#65532=CARTESIAN_POINT('Ctrl Pts',(-12.9793332579477,-52.703925204681,14.));
#65533=CARTESIAN_POINT('Ctrl Pts',(-12.9911966085512,-52.6718530581471,
14.));
#65534=CARTESIAN_POINT('Ctrl Pts',(-13.0043910411209,-52.6402695886307,
14.));
#65535=CARTESIAN_POINT('Ctrl Pts',(-13.0188485042637,-52.6092270378974,
14.));
#65536=CARTESIAN_POINT('Ctrl Pts',(-13.0255213915096,-52.5948992516997,
14.));
#65537=CARTESIAN_POINT('Ctrl Pts',(-13.0324634794559,-52.580686716332,14.));
#65538=CARTESIAN_POINT('Ctrl Pts',(-13.0396687478568,-52.5665947050473,
14.));
#65539=CARTESIAN_POINT('Ctrl Pts',(-13.0457249481659,-52.5547500327394,
14.));
#65540=CARTESIAN_POINT('Ctrl Pts',(-13.0519637639886,-52.5429971707098,
14.));
#65541=CARTESIAN_POINT('Ctrl Pts',(-13.058377507715,-52.5313453176613,14.));
#65542=CARTESIAN_POINT('Ctrl Pts',(-13.0842985632228,-52.4842545166369,
14.));
#65543=CARTESIAN_POINT('Ctrl Pts',(-13.1130890591351,-52.4387805987043,
14.));
#65544=CARTESIAN_POINT('Ctrl Pts',(-13.1444873892514,-52.3951192737037,
14.));
#65545=CARTESIAN_POINT('Ctrl Pts',(-13.1565047144364,-52.3784084378536,
14.));
#65546=CARTESIAN_POINT('Ctrl Pts',(-13.1689046041074,-52.3619632326173,
14.));
#65547=CARTESIAN_POINT('Ctrl Pts',(-13.1816743223107,-52.3457951881003,
14.));
#65548=CARTESIAN_POINT('Ctrl Pts',(-13.1908504260224,-52.3341771045262,
14.));
#65549=CARTESIAN_POINT('Ctrl Pts',(-13.2002175167485,-52.3227021433122,
14.));
#65550=CARTESIAN_POINT('Ctrl Pts',(-13.2097711771542,-52.3113747298545,
14.));
#65551=CARTESIAN_POINT('Ctrl Pts',(-13.2171669954176,-52.3026057881325,
14.));
#65552=CARTESIAN_POINT('Ctrl Pts',(-13.2246749676875,-52.2939250678948,
14.));
#65553=CARTESIAN_POINT('Ctrl Pts',(-13.232282522036,-52.2853461206881,14.));
#65554=CARTESIAN_POINT('Ctrl Pts',(-13.2698783495994,-52.2429497597705,
14.));
#65555=CARTESIAN_POINT('Ctrl Pts',(-13.3099602111104,-52.2029670203149,
14.));
#65556=CARTESIAN_POINT('Ctrl Pts',(-13.3522361487837,-52.1656107563157,
14.));
#65557=CARTESIAN_POINT('Ctrl Pts',(-13.3938995696844,-52.1287957301818,
14.));
#65558=CARTESIAN_POINT('Ctrl Pts',(-13.4376947734015,-52.094530697541,14.));
#65559=CARTESIAN_POINT('Ctrl Pts',(-13.4833901901288,-52.0630423693105,
14.));
#65560=CARTESIAN_POINT('Ctrl Pts',(-13.5072520755132,-52.0465993443205,
14.));
#65561=CARTESIAN_POINT('Ctrl Pts',(-13.5316328454894,-52.0309139558741,
14.));
#65562=CARTESIAN_POINT('Ctrl Pts',(-13.5565037015348,-52.0160223211125,
14.));
#65563=CARTESIAN_POINT('Ctrl Pts',(-13.5698458264541,-52.0080336113198,
14.));
#65564=CARTESIAN_POINT('Ctrl Pts',(-13.5833290354763,-52.0002733832278,
14.));
#65565=CARTESIAN_POINT('Ctrl Pts',(-13.5969491667113,-51.9927476035094,
14.));
#65566=CARTESIAN_POINT('Ctrl Pts',(-13.6066315694002,-51.9873976088197,
14.));
#65567=CARTESIAN_POINT('Ctrl Pts',(-13.6163831716242,-51.9821661014994,
14.));
#65568=CARTESIAN_POINT('Ctrl Pts',(-13.6262025324358,-51.9770553186038,
14.));
#65569=CARTESIAN_POINT('Ctrl Pts',(-13.6348477565866,-51.9725556505942,
14.));
#65570=CARTESIAN_POINT('Ctrl Pts',(-13.6435368082189,-51.9681540962248,
14.));
#65571=CARTESIAN_POINT('Ctrl Pts',(-13.6522677898872,-51.9638519547314,
14.));
#65572=CARTESIAN_POINT('Ctrl Pts',(-13.6954565667737,-51.9425709308842,
14.));
#65573=CARTESIAN_POINT('Ctrl Pts',(-13.7396739228985,-51.9237189359356,
14.));
#65574=CARTESIAN_POINT('Ctrl Pts',(-13.7847671512145,-51.9074289316259,
14.));
#65575=CARTESIAN_POINT('Ctrl Pts',(-13.8360916879565,-51.8888878567031,
14.));
#65576=CARTESIAN_POINT('Ctrl Pts',(-13.8885506645623,-51.8736638854944,
14.));
#65577=CARTESIAN_POINT('Ctrl Pts',(-13.941847374976,-51.8616392672994,14.));
#65578=CARTESIAN_POINT('Ctrl Pts',(-13.9939442075944,-51.849885361354,14.));
#65579=CARTESIAN_POINT('Ctrl Pts',(-14.0468423626068,-51.8411885354972,
14.));
#65580=CARTESIAN_POINT('Ctrl Pts',(-14.1002842110383,-51.8354800340536,
14.));
#65581=CARTESIAN_POINT('Ctrl Pts',(-14.1133747158346,-51.8340817447407,
14.));
#65582=CARTESIAN_POINT('Ctrl Pts',(-14.12649790077,-51.8328629457924,14.));
#65583=CARTESIAN_POINT('Ctrl Pts',(-14.1396500710028,-51.8318229995033,
14.));
#65584=CARTESIAN_POINT('Ctrl Pts',(-14.1495801723766,-51.8310378232252,
14.));
#65585=CARTESIAN_POINT('Ctrl Pts',(-14.1595248274499,-51.8303548395322,
14.));
#65586=CARTESIAN_POINT('Ctrl Pts',(-14.1694709141462,-51.8297741437814,
14.));
#65587=CARTESIAN_POINT('Ctrl Pts',(-14.2269882874541,-51.8264160296513,
14.));
#65588=CARTESIAN_POINT('Ctrl Pts',(-14.2846572205454,-51.82646594941,14.));
#65589=CARTESIAN_POINT('Ctrl Pts',(-14.3421515419977,-51.829789630806,14.));
#65590=CARTESIAN_POINT('Ctrl Pts',(-14.4008791521421,-51.83318460722,14.));
#65591=CARTESIAN_POINT('Ctrl Pts',(-14.4594256017928,-51.839995169772,14.));
#65592=CARTESIAN_POINT('Ctrl Pts',(-14.5174614757873,-51.8501296661509,
14.));
#65593=CARTESIAN_POINT('Ctrl Pts',(-14.5760079663998,-51.8603533287973,
14.));
#65594=CARTESIAN_POINT('Ctrl Pts',(-14.6340360433043,-51.8739596390729,
14.));
#65595=CARTESIAN_POINT('Ctrl Pts',(-14.6912089918265,-51.8909073923744,
14.));
#65596=CARTESIAN_POINT('Ctrl Pts',(-14.7041595778874,-51.8947463292028,
14.));
#65597=CARTESIAN_POINT('Ctrl Pts',(-14.7170698109426,-51.8987582304422,
14.));
#65598=CARTESIAN_POINT('Ctrl Pts',(-14.7299100502027,-51.9029342190779,
14.));
#65599=CARTESIAN_POINT('Ctrl Pts',(-14.7877641556196,-51.9217499188366,
14.));
#65600=CARTESIAN_POINT('Ctrl Pts',(-14.844296494245,-51.9439200711751,14.));
#65601=CARTESIAN_POINT('Ctrl Pts',(-14.89916300966,-51.9693357901013,14.));
#65602=CARTESIAN_POINT('Ctrl Pts',(-14.9535472830576,-51.9945281209106,
14.));
#65603=CARTESIAN_POINT('Ctrl Pts',(-15.0062960530717,-52.0229093771236,
14.));
#65604=CARTESIAN_POINT('Ctrl Pts',(-15.0570711074075,-52.0544235838658,
14.));
#65605=CARTESIAN_POINT('Ctrl Pts',(-15.0942742803416,-52.0775142235243,
14.));
#65606=CARTESIAN_POINT('Ctrl Pts',(-15.1304178629323,-52.1022878477978,
14.));
#65607=CARTESIAN_POINT('Ctrl Pts',(-15.1653622380934,-52.1287390412771,
14.));
#65608=CARTESIAN_POINT('Ctrl Pts',(-15.1847827002204,-52.1434393871498,
14.));
#65609=CARTESIAN_POINT('Ctrl Pts',(-15.2038326363704,-52.1586581279523,
14.));
#65610=CARTESIAN_POINT('Ctrl Pts',(-15.2225055381225,-52.1743757967134,
14.));
#65611=CARTESIAN_POINT('Ctrl Pts',(-15.619480088463,-52.8667052421829,14.));
#65612=CARTESIAN_POINT('Ctrl Pts',(-15.6300068882699,-52.9268481278985,
14.));
#65613=CARTESIAN_POINT('Ctrl Pts',(-15.636648860063,-52.9875198480058,14.));
#65614=CARTESIAN_POINT('Ctrl Pts',(-15.6395377285819,-53.0483965304075,
14.));
#65615=CARTESIAN_POINT('Ctrl Pts',(-15.6422164647752,-53.104845126599,14.));
#65616=CARTESIAN_POINT('Ctrl Pts',(-15.6416673528963,-53.1614706817463,
14.));
#65617=CARTESIAN_POINT('Ctrl Pts',(-15.6379557899095,-53.2180062233411,
14.));
#65618=CARTESIAN_POINT('Ctrl Pts',(-15.6370599130155,-53.2316524649873,
14.));
#65619=CARTESIAN_POINT('Ctrl Pts',(-15.635979458861,-53.2452938319618,14.));
#65620=CARTESIAN_POINT('Ctrl Pts',(-15.6347168346783,-53.2589112013707,
14.));
#65621=CARTESIAN_POINT('Ctrl Pts',(-15.6291600434172,-53.3188410525236,
14.));
#65622=CARTESIAN_POINT('Ctrl Pts',(-15.6200747337923,-53.3783798722155,
14.));
#65623=CARTESIAN_POINT('Ctrl Pts',(-15.6075583989801,-53.4372064199324,
14.));
#65624=CARTESIAN_POINT('Ctrl Pts',(-15.5998328638199,-53.4735162957514,
14.));
#65625=CARTESIAN_POINT('Ctrl Pts',(-15.5907991790431,-53.5095545289945,
14.));
#65626=CARTESIAN_POINT('Ctrl Pts',(-15.5804715530903,-53.5452408049524,
14.));
#65627=CARTESIAN_POINT('Ctrl Pts',(-15.5769376859793,-53.5574517968589,
14.));
#65628=CARTESIAN_POINT('Ctrl Pts',(-15.5732522649477,-53.5696215399255,
14.));
#65629=CARTESIAN_POINT('Ctrl Pts',(-15.5694156969316,-53.5817466809952,
14.));
#65630=CARTESIAN_POINT('Ctrl Pts',(-15.5658265665456,-53.5930898168563,
14.));
#65631=CARTESIAN_POINT('Ctrl Pts',(-15.5621073992277,-53.6043866740437,
14.));
#65632=CARTESIAN_POINT('Ctrl Pts',(-15.5582610327256,-53.6156290047355,
14.));
#65633=CARTESIAN_POINT('Ctrl Pts',(-15.5392227656906,-53.6712748964329,
14.));
#65634=CARTESIAN_POINT('Ctrl Pts',(-15.5170576051387,-53.7256323263301,
14.));
#65635=CARTESIAN_POINT('Ctrl Pts',(-15.4918565786129,-53.7784002654543,
14.));
#65636=CARTESIAN_POINT('Ctrl Pts',(-15.4672989399537,-53.8298210272427,
14.));
#65637=CARTESIAN_POINT('Ctrl Pts',(-15.4398578622449,-53.8797331989486,
14.));
#65638=CARTESIAN_POINT('Ctrl Pts',(-15.4095790814541,-53.9278277241228,
14.));
#65639=CARTESIAN_POINT('Ctrl Pts',(-15.3931628297317,-53.9539031410025,
14.));
#65640=CARTESIAN_POINT('Ctrl Pts',(-15.375911821029,-53.9794436627758,14.));
#65641=CARTESIAN_POINT('Ctrl Pts',(-15.3578293393444,-54.0043949447235,
14.));
#65642=CARTESIAN_POINT('Ctrl Pts',(-15.3427850973266,-54.0251538831713,
14.));
#65643=CARTESIAN_POINT('Ctrl Pts',(-15.3271652651206,-54.0455049012987,
14.));
#65644=CARTESIAN_POINT('Ctrl Pts',(-15.3109704283096,-54.0654144328928,
14.));
#65645=CARTESIAN_POINT('Ctrl Pts',(-15.3040483576438,-54.0739242552656,
14.));
#65646=CARTESIAN_POINT('Ctrl Pts',(-15.2970202959566,-54.0823543061125,
14.));
#65647=CARTESIAN_POINT('Ctrl Pts',(-15.2898980773051,-54.0906884968018,
14.));
#65648=CARTESIAN_POINT('Ctrl Pts',(-15.2569263347024,-54.1292709671884,
14.));
#65649=CARTESIAN_POINT('Ctrl Pts',(-15.2218841350179,-54.1658696979238,
14.));
#65650=CARTESIAN_POINT('Ctrl Pts',(-15.1848122311441,-54.2002693479339,
14.));
#65651=CARTESIAN_POINT('Ctrl Pts',(-15.1433853438147,-54.2387100611489,
14.));
#65652=CARTESIAN_POINT('Ctrl Pts',(-15.0994234021571,-54.2744057498397,
14.));
#65653=CARTESIAN_POINT('Ctrl Pts',(-15.0532626173756,-54.3072661456667,
14.));
#65654=CARTESIAN_POINT('Ctrl Pts',(-15.014090564972,-54.335151484996,14.));
#65655=CARTESIAN_POINT('Ctrl Pts',(-14.9733341416966,-54.3609943509891,
14.));
#65656=CARTESIAN_POINT('Ctrl Pts',(-14.9311912107729,-54.3847111211312,
14.));
#65657=CARTESIAN_POINT('Ctrl Pts',(-14.9196049423273,-54.391231523474,14.));
#65658=CARTESIAN_POINT('Ctrl Pts',(-14.9079138627992,-54.3975910665321,
14.));
#65659=CARTESIAN_POINT('Ctrl Pts',(-14.8961220820674,-54.4037876495833,
14.));
#65660=CARTESIAN_POINT('Ctrl Pts',(-14.8869418707018,-54.4086118524283,
14.));
#65661=CARTESIAN_POINT('Ctrl Pts',(-14.8776989839247,-54.4133380017209,
14.));
#65662=CARTESIAN_POINT('Ctrl Pts',(-14.8684106168714,-54.4179577422776,
14.));
#65663=CARTESIAN_POINT('Ctrl Pts',(-14.8187084869932,-54.4426780126799,
14.));
#65664=CARTESIAN_POINT('Ctrl Pts',(-14.7676148803933,-54.464404589055,14.));
#65665=CARTESIAN_POINT('Ctrl Pts',(-14.7154497956283,-54.4830620982051,
14.));
#65666=CARTESIAN_POINT('Ctrl Pts',(-14.6635765838803,-54.501615215241,14.));
#65667=CARTESIAN_POINT('Ctrl Pts',(-14.6106426601789,-54.5171336375863,
14.));
#65668=CARTESIAN_POINT('Ctrl Pts',(-14.5569565025172,-54.5294926610513,
14.));
#65669=CARTESIAN_POINT('Ctrl Pts',(-14.5071457936645,-54.5409595222745,
14.));
#65670=CARTESIAN_POINT('Ctrl Pts',(-14.456686763942,-54.5497062605737,14.));
#65671=CARTESIAN_POINT('Ctrl Pts',(-14.4058341277,-54.5555924980414,14.));
#65672=CARTESIAN_POINT('Ctrl Pts',(-14.3927717853308,-54.557104475684,14.));
#65673=CARTESIAN_POINT('Ctrl Pts',(-14.3796790109819,-54.5584277519287,
14.));
#65674=CARTESIAN_POINT('Ctrl Pts',(-14.3665890681527,-54.5595574794671,
14.));
#65675=CARTESIAN_POINT('Ctrl Pts',(-14.313676726872,-54.5641240791723,14.));
#65676=CARTESIAN_POINT('Ctrl Pts',(-14.2607272248055,-54.565543985866,14.));
#65677=CARTESIAN_POINT('Ctrl Pts',(-14.2080224885386,-54.5637141509322,
14.));
#65678=CARTESIAN_POINT('Ctrl Pts',(-14.1571049407467,-54.5619463646896,
14.));
#65679=CARTESIAN_POINT('Ctrl Pts',(-14.1064149890402,-54.557145321735,14.));
#65680=CARTESIAN_POINT('Ctrl Pts',(-14.0562198243703,-54.5491721895645,
14.));
#65681=CARTESIAN_POINT('Ctrl Pts',(-14.0211056129848,-54.543594555737,14.));
#65682=CARTESIAN_POINT('Ctrl Pts',(-13.986233796236,-54.5364636409164,14.));
#65683=CARTESIAN_POINT('Ctrl Pts',(-13.9517030424607,-54.5277184245241,
14.));
#65684=CARTESIAN_POINT('Ctrl Pts',(-13.93222381495,-54.5227851392317,14.));
#65685=CARTESIAN_POINT('Ctrl Pts',(-13.9128532514771,-54.5173379031513,
14.));
#65686=CARTESIAN_POINT('Ctrl Pts',(-13.8936069362009,-54.5113866946539,
14.));
#65687=CARTESIAN_POINT('Origin',(-14.1292828945604,-53.2669068454841,19.1042117235887));
#65688=CARTESIAN_POINT('Ctrl Pts',(-13.3561844802682,-51.9293619476186,
17.8542117235887));
#65689=CARTESIAN_POINT('Ctrl Pts',(-13.3145289674606,-51.9530637836679,
17.8517311518799));
#65690=CARTESIAN_POINT('Ctrl Pts',(-12.8472204745978,-52.2501100679509,
17.8230820767121));
#65691=CARTESIAN_POINT('Ctrl Pts',(-12.3131148719809,-53.3266292410367,
17.7682644980854));
#65692=CARTESIAN_POINT('Ctrl Pts',(-13.177398497422,-54.8146003900027,17.6897589877086));
#65693=CARTESIAN_POINT('Ctrl Pts',(-14.8951536251653,-54.9146504373755,
17.6112534773319));
#65694=CARTESIAN_POINT('Ctrl Pts',(-15.9261572824593,-53.5369216264006,
17.5327479669551));
#65695=CARTESIAN_POINT('Ctrl Pts',(-15.3456319213627,-51.9170585592589,
17.4542424565783));
#65696=CARTESIAN_POINT('Ctrl Pts',(-14.0786429713653,-51.6067853756627,
17.3947303754562));
#65697=CARTESIAN_POINT('Ctrl Pts',(-13.4791850640252,-51.8598443884631,
17.361386797793));
#65698=CARTESIAN_POINT('Ctrl Pts',(-13.3591951473146,-51.9304670067727,
17.3542117235887));
#65699=CARTESIAN_POINT('Ctrl Pts',(-13.3599426557471,-51.9312965605688,
17.8957882764113));
#65700=CARTESIAN_POINT('Ctrl Pts',(-13.0649944461637,-52.1042822226529,
17.8781885106897));
#65701=CARTESIAN_POINT('Ctrl Pts',(-12.4640754788204,-52.7732237750949,
17.8344202415091));
#65702=CARTESIAN_POINT('Ctrl Pts',(-12.6330157688953,-54.2972115132025,
17.7644834688697));
#65703=CARTESIAN_POINT('Ctrl Pts',(-14.1627629159668,-55.0835833760402,
17.6859779584929));
#65704=CARTESIAN_POINT('Ctrl Pts',(-15.6633630152513,-54.2408836460551,
17.6074724481161));
#65705=CARTESIAN_POINT('Ctrl Pts',(-15.7877283921755,-52.5246154983424,
17.5289669377393));
#65706=CARTESIAN_POINT('Ctrl Pts',(-14.5628755318023,-51.5803972945988,
17.458405547171));
#65707=CARTESIAN_POINT('Ctrl Pts',(-13.6650283227152,-51.7575311866648,
17.4140126600617));
#65708=CARTESIAN_POINT('Ctrl Pts',(-13.3571987246687,-51.9320818411208,
17.3957882764113));
#65709=CARTESIAN_POINT('Ctrl Pts',(-13.8936870225526,-54.5092654229862,
18.));
#65710=CARTESIAN_POINT('Ctrl Pts',(-14.3022280845015,-54.5867395029208,
17.9738314965411));
#65711=CARTESIAN_POINT('Ctrl Pts',(-15.1949907864185,-54.306005850961,17.9214944896232));
#65712=CARTESIAN_POINT('Ctrl Pts',(-15.5848805170292,-52.9490991612648,
17.8429889792464));
#65713=CARTESIAN_POINT('Ctrl Pts',(-14.6665684258224,-51.8784501685123,
17.7644834688696));
#65714=CARTESIAN_POINT('Ctrl Pts',(-13.2677649070697,-52.0524087826961,
17.6859779584929));
#65715=CARTESIAN_POINT('Ctrl Pts',(-12.6409196641315,-53.3158497937513,
17.6074724481161));
#65716=CARTESIAN_POINT('Ctrl Pts',(-13.3492065366981,-54.5352532401981,
17.5289669377393));
#65717=CARTESIAN_POINT('Ctrl Pts',(-14.7569196663361,-54.6172449996945,
17.4504614273625));
#65718=CARTESIAN_POINT('Ctrl Pts',(-15.6018348475728,-53.488185970869,17.3719559169858));
#65719=CARTESIAN_POINT('Ctrl Pts',(-15.1260899874907,-52.160696114485,17.293450406609));
#65720=CARTESIAN_POINT('Ctrl Pts',(-13.7564048649609,-51.8252736441527,
17.2149448962322));
#65721=CARTESIAN_POINT('Ctrl Pts',(-12.7211156974588,-52.7827464099985,
17.1364393858554));
#65722=CARTESIAN_POINT('Ctrl Pts',(-12.9487092675231,-54.174423630146,17.0579338754786));
#65723=CARTESIAN_POINT('Ctrl Pts',(-14.2350668963379,-54.7522192803303,
16.9794283651019));
#65724=CARTESIAN_POINT('Ctrl Pts',(-15.4265561246117,-53.9979509037444,
16.900922854725));
#65725=CARTESIAN_POINT('Ctrl Pts',(-15.4546192812222,-52.5880650956991,
16.8224173443483));
#65726=CARTESIAN_POINT('Ctrl Pts',(-14.2940895544972,-51.7869805788023,
16.7439118339715));
#65727=CARTESIAN_POINT('Ctrl Pts',(-12.9857571502944,-52.3131291848103,
16.6654063235948));
#65728=CARTESIAN_POINT('Ctrl Pts',(-12.7029658920433,-53.6946482401116,
16.586900813218));
#65729=CARTESIAN_POINT('Ctrl Pts',(-13.6993295943645,-54.69255865938,16.5083953028412));
#65730=CARTESIAN_POINT('Ctrl Pts',(-15.0812856557068,-54.4119106312665,
16.4298897924644));
#65731=CARTESIAN_POINT('Ctrl Pts',(-15.6094629994388,-53.1043959909962,
16.3513842820876));
#65732=CARTESIAN_POINT('Ctrl Pts',(-14.8101796402302,-51.9426249466013,
16.2728787717108));
#65733=CARTESIAN_POINT('Ctrl Pts',(-13.4002518899393,-51.9685013930707,
16.1943732613341));
#65734=CARTESIAN_POINT('Ctrl Pts',(-12.6441364773908,-53.1588187166123,
16.1158677509573));
#65735=CARTESIAN_POINT('Ctrl Pts',(-13.2199356785565,-54.4460720440219,
16.0373622405805));
#65736=CARTESIAN_POINT('Ctrl Pts',(-14.6112590818024,-54.6758219881874,
15.9588567302038));
#65737=CARTESIAN_POINT('Ctrl Pts',(-15.5703347818477,-53.6420233374598,
15.8803512198269));
#65738=CARTESIAN_POINT('Ctrl Pts',(-15.2370408904378,-52.2718112986816,
15.8018457094502));
#65739=CARTESIAN_POINT('Ctrl Pts',(-13.9102832927596,-51.7940246036041,
15.7233401990734));
#65740=CARTESIAN_POINT('Ctrl Pts',(-12.7799297446004,-52.6371537182599,
15.6448346886966));
#65741=CARTESIAN_POINT('Ctrl Pts',(-12.8597081799673,-54.0450604100449,
15.5663291783198));
#65742=CARTESIAN_POINT('Ctrl Pts',(-14.0780714025733,-54.7551004833527,
15.4878236679431));
#65743=CARTESIAN_POINT('Ctrl Pts',(-15.3423623071066,-54.1304931269541,
15.4093181575663));
#65744=CARTESIAN_POINT('Ctrl Pts',(-15.5187347583226,-52.7314010536376,
15.3308126471895));
#65745=CARTESIAN_POINT('Ctrl Pts',(-14.4490137393998,-51.8125633237516,
15.2523071368127));
#65746=CARTESIAN_POINT('Ctrl Pts',(-13.0925505105556,-52.1980154020928,
15.1738016264359));
#65747=CARTESIAN_POINT('Ctrl Pts',(-12.6658535045584,-53.5420748131919,
15.0952961160591));
#65748=CARTESIAN_POINT('Ctrl Pts',(-13.551594819097,-54.6393568979555,15.0167906056824));
#65749=CARTESIAN_POINT('Ctrl Pts',(-14.9554204274106,-54.5057934526205,
14.9382850953056));
#65750=CARTESIAN_POINT('Ctrl Pts',(-15.6183464700209,-53.2611664293564,
14.8597795849288));
#65751=CARTESIAN_POINT('Ctrl Pts',(-14.9458444656461,-52.0216887907143,
14.7812740745521));
#65752=CARTESIAN_POINT('Ctrl Pts',(-13.5410315037528,-51.8989497980972,
14.7027685641753));
#65753=CARTESIAN_POINT('Ctrl Pts',(-12.6637746137877,-53.0030322708737,
14.6242630537985));
#65754=CARTESIAN_POINT('Ctrl Pts',(-13.1008239433931,-54.3437535140763,
14.5457575434217));
#65755=CARTESIAN_POINT('Ctrl Pts',(-14.4602125392812,-54.7187536954986,
14.4672520330449));
#65756=CARTESIAN_POINT('Ctrl Pts',(-15.5228300373051,-53.7916614633287,
14.3887465226681));
#65757=CARTESIAN_POINT('Ctrl Pts',(-15.3356521111637,-52.3940408681935,
14.3102410122914));
#65758=CARTESIAN_POINT('Ctrl Pts',(-14.0666325655589,-51.7790575741688,
14.2317355019146));
#65759=CARTESIAN_POINT('Ctrl Pts',(-12.8536802704289,-52.4987553418111,
14.1532299915378));
#65760=CARTESIAN_POINT('Ctrl Pts',(-12.7849592886011,-53.9066581474695,
14.074724481161));
#65761=CARTESIAN_POINT('Ctrl Pts',(-13.9213697617029,-54.7422164034654,
13.9962189707842));
#65762=CARTESIAN_POINT('Ctrl Pts',(-15.2452696789899,-54.2518096584208,
13.9177134604075));
#65763=CARTESIAN_POINT('Ctrl Pts',(-15.4583606841261,-53.3405309695408,
13.8653764534896));
#65764=CARTESIAN_POINT('Ctrl Pts',(-15.3505106014235,-52.9389386488708,
13.8392079500307));
#65765=CARTESIAN_POINT('Ctrl Pts',(-13.8763907393434,-54.6004732426341,
18.0535973499898));
#65766=CARTESIAN_POINT('Ctrl Pts',(-14.3149248646251,-54.6836350861806,
18.0274288465308));
#65767=CARTESIAN_POINT('Ctrl Pts',(-15.2732297867829,-54.3822913585465,
17.975091839613));
#65768=CARTESIAN_POINT('Ctrl Pts',(-15.6917432922651,-52.9257672935819,
17.8965863292362));
#65769=CARTESIAN_POINT('Ctrl Pts',(-14.7060132710725,-51.7765165492856,
17.8180808188594));
#65770=CARTESIAN_POINT('Ctrl Pts',(-13.2045165191651,-51.9632463441864,
17.7395753084827));
#65771=CARTESIAN_POINT('Ctrl Pts',(-12.5316514000813,-53.3194429428464,
17.6610697981059));
#65772=CARTESIAN_POINT('Ctrl Pts',(-13.2919371902728,-54.6283689567997,
17.5825642877291));
#65773=CARTESIAN_POINT('Ctrl Pts',(-14.8029976526125,-54.7163801455882,
17.5040587773523));
#65774=CARTESIAN_POINT('Ctrl Pts',(-15.7099423258683,-53.5044311893795,
17.4255532669755));
#65775=CARTESIAN_POINT('Ctrl Pts',(-15.1992706321147,-52.0794835960763,
17.3470477565988));
#65776=CARTESIAN_POINT('Ctrl Pts',(-13.7290300050048,-51.7194360676216,
17.268542246222));
#65777=CARTESIAN_POINT('Ctrl Pts',(-12.6177350293705,-52.7472017464206,
17.1900367358452));
#65778=CARTESIAN_POINT('Ctrl Pts',(-12.8620373932302,-54.2410490221397,
17.1115312254684));
#65779=CARTESIAN_POINT('Ctrl Pts',(-14.2428330343358,-54.8612635700639,
17.0330257150916));
#65780=CARTESIAN_POINT('Ctrl Pts',(-15.5217955063355,-54.0516205413417,
16.9545202047148));
#65781=CARTESIAN_POINT('Ctrl Pts',(-15.5519189210496,-52.5382278932962,
16.8760146943381));
#65782=CARTESIAN_POINT('Ctrl Pts',(-14.3061888440168,-51.6783317148849,
16.7975091839613));
#65783=CARTESIAN_POINT('Ctrl Pts',(-12.901805148244,-52.2431075481956,16.7190036735845));
#65784=CARTESIAN_POINT('Ctrl Pts',(-12.5982527550455,-53.7260508968676,
16.6404981632077));
#65785=CARTESIAN_POINT('Ctrl Pts',(-13.6677645504461,-54.7972229615204,
16.561992652831));
#65786=CARTESIAN_POINT('Ctrl Pts',(-15.1511769879803,-54.4959711438118,
16.4834871424542));
#65787=CARTESIAN_POINT('Ctrl Pts',(-15.7181304989006,-53.0924652481532,
16.4049816320774));
#65788=CARTESIAN_POINT('Ctrl Pts',(-14.8601677102629,-51.8454027220491,
16.3264761217006));
#65789=CARTESIAN_POINT('Ctrl Pts',(-13.3467300407797,-51.8731788891832,
16.2479706113238));
#65790=CARTESIAN_POINT('Ctrl Pts',(-12.5351043758535,-53.1508834210038,
16.1694651009471));
#65791=CARTESIAN_POINT('Ctrl Pts',(-13.1531759053504,-54.5326405184631,
16.0909595905703));
#65792=CARTESIAN_POINT('Ctrl Pts',(-14.6466433886818,-54.7792575667409,
16.0124540801935));
#65793=CARTESIAN_POINT('Ctrl Pts',(-15.676129681178,-53.6695625342478,15.9339485698167));
#65794=CARTESIAN_POINT('Ctrl Pts',(-15.3183670013781,-52.1987563073057,
15.8554430594399));
#65795=CARTESIAN_POINT('Ctrl Pts',(-13.8942054255916,-51.6858928771342,
15.7769375490632));
#65796=CARTESIAN_POINT('Ctrl Pts',(-12.680866912845,-52.5909203596381,15.6984320386864));
#65797=CARTESIAN_POINT('Ctrl Pts',(-12.7665022861979,-54.1021885944999,
15.6199265283096));
#65798=CARTESIAN_POINT('Ctrl Pts',(-14.0743117082228,-54.8643562967563,
15.5414210179328));
#65799=CARTESIAN_POINT('Ctrl Pts',(-15.431420595335,-54.1938933587688,15.4629155075561));
#65800=CARTESIAN_POINT('Ctrl Pts',(-15.6207414392394,-52.6920868680494,
15.3844099971793));
#65801=CARTESIAN_POINT('Ctrl Pts',(-14.4724867960198,-51.7057926183865,
15.3059044868025));
#65802=CARTESIAN_POINT('Ctrl Pts',(-13.0164387486087,-52.1195426811267,
15.2273989764257));
#65803=CARTESIAN_POINT('Ctrl Pts',(-12.5584157597012,-53.5622762838672,
15.1488934660489));
#65804=CARTESIAN_POINT('Ctrl Pts',(-13.5091838189608,-54.7401153900112,
15.0703879556722));
#65805=CARTESIAN_POINT('Ctrl Pts',(-15.0160713573958,-54.5967463773831,
14.9918824452954));
#65806=CARTESIAN_POINT('Ctrl Pts',(-15.727666149938,-53.2607449964075,14.9133769349186));
#65807=CARTESIAN_POINT('Ctrl Pts',(-15.0057923758998,-51.9302710423938,
14.8348714245418));
#65808=CARTESIAN_POINT('Ctrl Pts',(-13.4978449972707,-51.7985211602437,
14.756365914165));
#65809=CARTESIAN_POINT('Ctrl Pts',(-12.5561842470564,-52.9836599052406,
14.6778604037882));
#65810=CARTESIAN_POINT('Ctrl Pts',(-13.0253195759487,-54.4228102683146,
14.5993548934115));
#65811=CARTESIAN_POINT('Ctrl Pts',(-14.4845077563775,-54.8253411075794,
14.5208493830347));
#65812=CARTESIAN_POINT('Ctrl Pts',(-15.6251373733416,-53.830186350918,14.4423438726579));
#65813=CARTESIAN_POINT('Ctrl Pts',(-15.4242177700075,-52.3299593670269,
14.3638383622811));
#65814=CARTESIAN_POINT('Ctrl Pts',(-14.0620330883935,-51.6698270424536,
14.2853328519044));
#65815=CARTESIAN_POINT('Ctrl Pts',(-12.7600318373669,-52.4423614591769,
14.2068273415276));
#65816=CARTESIAN_POINT('Ctrl Pts',(-12.6862657010804,-53.9536255226119,
14.1283218311508));
#65817=CARTESIAN_POINT('Ctrl Pts',(-13.9061058082296,-54.8505263314733,
14.049816320774));
#65818=CARTESIAN_POINT('Ctrl Pts',(-15.3271999068701,-54.3241163497093,
13.9713108103972));
#65819=CARTESIAN_POINT('Ctrl Pts',(-15.5559349992425,-53.3459360884415,
13.9189738034794));
#65820=CARTESIAN_POINT('Ctrl Pts',(-15.4401670971033,-52.9148608466415,
13.8928053000205));
#65821=CARTESIAN_POINT('Ctrl Pts',(-13.8590944561342,-54.691681062282,18.1071946999795));
#65822=CARTESIAN_POINT('Ctrl Pts',(-14.3276216447486,-54.7805306694404,
18.0810261965206));
#65823=CARTESIAN_POINT('Ctrl Pts',(-15.3514687871474,-54.4585768661319,
18.0286891896028));
#65824=CARTESIAN_POINT('Ctrl Pts',(-15.798606067501,-52.902435425899,17.950183679226));
#65825=CARTESIAN_POINT('Ctrl Pts',(-14.7454581163227,-51.6745829300588,
17.8716781688492));
#65826=CARTESIAN_POINT('Ctrl Pts',(-13.1412681312604,-51.8740839056767,
17.7931726584724));
#65827=CARTESIAN_POINT('Ctrl Pts',(-12.4223831360311,-53.3230360919416,
17.7146671480956));
#65828=CARTESIAN_POINT('Ctrl Pts',(-13.2346678438474,-54.7214846734011,
17.6361616377189));
#65829=CARTESIAN_POINT('Ctrl Pts',(-14.849075638889,-54.8155152914819,17.5576561273421));
#65830=CARTESIAN_POINT('Ctrl Pts',(-15.8180498041638,-53.52067640789,17.4791506169653));
#65831=CARTESIAN_POINT('Ctrl Pts',(-15.2724512767387,-51.9982710776676,
17.4006451065885));
#65832=CARTESIAN_POINT('Ctrl Pts',(-13.7016551450487,-51.6135984910905,
17.3221395962117));
#65833=CARTESIAN_POINT('Ctrl Pts',(-12.5143543612823,-52.7116570828427,
17.243634085835));
#65834=CARTESIAN_POINT('Ctrl Pts',(-12.7753655189374,-54.3076744141334,
17.1651285754582));
#65835=CARTESIAN_POINT('Ctrl Pts',(-14.2505991723337,-54.9703078597976,
17.0866230650814));
#65836=CARTESIAN_POINT('Ctrl Pts',(-15.6170348880593,-54.1052901789391,
17.0081175547046));
#65837=CARTESIAN_POINT('Ctrl Pts',(-15.6492185608771,-52.4883906908934,
16.9296120443279));
#65838=CARTESIAN_POINT('Ctrl Pts',(-14.3182881335364,-51.5696828509675,
16.851106533951));
#65839=CARTESIAN_POINT('Ctrl Pts',(-12.8178531461936,-52.173085911581,16.7726010235743));
#65840=CARTESIAN_POINT('Ctrl Pts',(-12.4935396180478,-53.7574535536235,
16.6940955131975));
#65841=CARTESIAN_POINT('Ctrl Pts',(-13.6361995065277,-54.9018872636609,
16.6155900028207));
#65842=CARTESIAN_POINT('Ctrl Pts',(-15.2210683202537,-54.580031656357,16.5370844924439));
#65843=CARTESIAN_POINT('Ctrl Pts',(-15.8267979983625,-53.0805345053102,
16.4585789820672));
#65844=CARTESIAN_POINT('Ctrl Pts',(-14.9101557802956,-51.7481804974968,
16.3800734716904));
#65845=CARTESIAN_POINT('Ctrl Pts',(-13.2932081916201,-51.7778563852958,
16.3015679613136));
#65846=CARTESIAN_POINT('Ctrl Pts',(-12.4260722743163,-53.1429481253953,
16.2230624509368));
#65847=CARTESIAN_POINT('Ctrl Pts',(-13.0864161321444,-54.6192089929043,
16.14455694056));
#65848=CARTESIAN_POINT('Ctrl Pts',(-14.6820276955612,-54.8826931452944,
16.0660514301833));
#65849=CARTESIAN_POINT('Ctrl Pts',(-15.7819245805084,-53.6971017310358,
15.9875459198065));
#65850=CARTESIAN_POINT('Ctrl Pts',(-15.3996931123184,-52.1257013159298,
15.9090404094297));
#65851=CARTESIAN_POINT('Ctrl Pts',(-13.8781275584237,-51.5777611506643,
15.8305348990529));
#65852=CARTESIAN_POINT('Ctrl Pts',(-12.5818040810897,-52.5446870010162,
15.7520293886761));
#65853=CARTESIAN_POINT('Ctrl Pts',(-12.6732963924285,-54.1593167789549,
15.6735238782994));
#65854=CARTESIAN_POINT('Ctrl Pts',(-14.0705520138724,-54.9736121101599,
15.5950183679226));
#65855=CARTESIAN_POINT('Ctrl Pts',(-15.5204788835633,-54.2572935905836,
15.5165128575458));
#65856=CARTESIAN_POINT('Ctrl Pts',(-15.7227481201562,-52.6527726824611,
15.438007347169));
#65857=CARTESIAN_POINT('Ctrl Pts',(-14.4959598526397,-51.5990219130214,
15.3595018367922));
#65858=CARTESIAN_POINT('Ctrl Pts',(-12.9403269866619,-52.0410699601608,
15.2809963264155));
#65859=CARTESIAN_POINT('Ctrl Pts',(-12.4509780148441,-53.5824777545425,
15.2024908160387));
#65860=CARTESIAN_POINT('Ctrl Pts',(-13.4667728188247,-54.8408738820669,
15.1239853056619));
#65861=CARTESIAN_POINT('Ctrl Pts',(-15.076722287381,-54.6876993021459,15.0454797952851));
#65862=CARTESIAN_POINT('Ctrl Pts',(-15.8369858298552,-53.2603235634587,
14.9669742849083));
#65863=CARTESIAN_POINT('Ctrl Pts',(-15.0657402861535,-51.8388532940734,
14.8884687745316));
#65864=CARTESIAN_POINT('Ctrl Pts',(-13.4546584907886,-51.6980925223903,
14.8099632641548));
#65865=CARTESIAN_POINT('Ctrl Pts',(-12.4485938803251,-52.9642875396075,
14.731457753778));
#65866=CARTESIAN_POINT('Ctrl Pts',(-12.9498152085044,-54.5018670225529,
14.6529522434012));
#65867=CARTESIAN_POINT('Ctrl Pts',(-14.5088029734737,-54.9319285196604,
14.5744467330245));
#65868=CARTESIAN_POINT('Ctrl Pts',(-15.7274447093781,-53.8687112385072,
14.4959412226477));
#65869=CARTESIAN_POINT('Ctrl Pts',(-15.5127834288513,-52.2658778658603,
14.4174357122709));
#65870=CARTESIAN_POINT('Ctrl Pts',(-14.0574336112281,-51.5605965107385,
14.3389302018941));
#65871=CARTESIAN_POINT('Ctrl Pts',(-12.666383404305,-52.3859675765427,14.2604246915173));
#65872=CARTESIAN_POINT('Ctrl Pts',(-12.5875721135598,-54.0005928977544,
14.1819191811406));
#65873=CARTESIAN_POINT('Ctrl Pts',(-13.8908418547563,-54.9588362594811,
14.1034136707638));
#65874=CARTESIAN_POINT('Ctrl Pts',(-15.4091301347503,-54.3964230409977,
14.024908160387));
#65875=CARTESIAN_POINT('Ctrl Pts',(-15.6535093143589,-53.3513412073421,
13.9725711534692));
#65876=CARTESIAN_POINT('Ctrl Pts',(-15.5298235927831,-52.8907830444122,
13.9464026500102));
#65877=CARTESIAN_POINT('Ctrl Pts',(-13.841798172925,-54.7828888819299,18.1607920499693));
#65878=CARTESIAN_POINT('Ctrl Pts',(-14.3403184248721,-54.8774262527002,
18.1346235465104));
#65879=CARTESIAN_POINT('Ctrl Pts',(-15.4297077875118,-54.5348623737173,
18.0822865395925));
#65880=CARTESIAN_POINT('Ctrl Pts',(-15.905468842737,-52.8791035582161,18.0037810292158));
#65881=CARTESIAN_POINT('Ctrl Pts',(-14.7849029615728,-51.572649310832,17.925275518839));
#65882=CARTESIAN_POINT('Ctrl Pts',(-13.0780197433558,-51.7849214671671,
17.8467700084622));
#65883=CARTESIAN_POINT('Ctrl Pts',(-12.3131148719809,-53.3266292410367,
17.7682644980854));
#65884=CARTESIAN_POINT('Ctrl Pts',(-13.177398497422,-54.8146003900027,17.6897589877086));
#65885=CARTESIAN_POINT('Ctrl Pts',(-14.8951536251653,-54.9146504373755,
17.6112534773319));
#65886=CARTESIAN_POINT('Ctrl Pts',(-15.9261572824593,-53.5369216264006,
17.5327479669551));
#65887=CARTESIAN_POINT('Ctrl Pts',(-15.3456319213627,-51.9170585592589,
17.4542424565783));
#65888=CARTESIAN_POINT('Ctrl Pts',(-13.6742802850926,-51.5077609145594,
17.3757369462015));
#65889=CARTESIAN_POINT('Ctrl Pts',(-12.410973693194,-52.6761124192647,17.2972314358248));
#65890=CARTESIAN_POINT('Ctrl Pts',(-12.6886936446445,-54.3742998061273,
17.2187259254479));
#65891=CARTESIAN_POINT('Ctrl Pts',(-14.2583653103316,-55.0793521495312,
17.1402204150712));
#65892=CARTESIAN_POINT('Ctrl Pts',(-15.7122742697832,-54.1589598165365,
17.0617149046944));
#65893=CARTESIAN_POINT('Ctrl Pts',(-15.7465182007045,-52.4385534884905,
16.9832093943176));
#65894=CARTESIAN_POINT('Ctrl Pts',(-14.3303874230559,-51.4610339870501,
16.9047038839408));
#65895=CARTESIAN_POINT('Ctrl Pts',(-12.7339011441433,-52.1030642749663,
16.8261983735641));
#65896=CARTESIAN_POINT('Ctrl Pts',(-12.38882648105,-53.7888562103795,16.7476928631873));
#65897=CARTESIAN_POINT('Ctrl Pts',(-13.6046344626093,-55.0065515658013,
16.6691873528105));
#65898=CARTESIAN_POINT('Ctrl Pts',(-15.2909596525272,-54.6640921689023,
16.5906818424337));
#65899=CARTESIAN_POINT('Ctrl Pts',(-15.9354654978244,-53.0686037624671,
16.5121763320569));
#65900=CARTESIAN_POINT('Ctrl Pts',(-14.9601438503283,-51.6509582729447,
16.4336708216802));
#65901=CARTESIAN_POINT('Ctrl Pts',(-13.2396863424605,-51.6825338814083,
16.3551653113034));
#65902=CARTESIAN_POINT('Ctrl Pts',(-12.317040172779,-53.1350128297868,16.2766598009266));
#65903=CARTESIAN_POINT('Ctrl Pts',(-13.0196563589383,-54.7057774673455,
16.1981542905498));
#65904=CARTESIAN_POINT('Ctrl Pts',(-14.7174120024405,-54.986128723848,16.1196487801731));
#65905=CARTESIAN_POINT('Ctrl Pts',(-15.8877194798387,-53.7246409278238,
16.0411432697963));
#65906=CARTESIAN_POINT('Ctrl Pts',(-15.4810192232586,-52.0526463245539,
15.9626377594195));
#65907=CARTESIAN_POINT('Ctrl Pts',(-13.8620496912558,-51.4696294241944,
15.8841322490427));
#65908=CARTESIAN_POINT('Ctrl Pts',(-12.4827412493343,-52.4984536423944,
15.8056267386659));
#65909=CARTESIAN_POINT('Ctrl Pts',(-12.5800904986592,-54.21644496341,15.7271212282892));
#65910=CARTESIAN_POINT('Ctrl Pts',(-14.0667923195219,-55.0828679235634,
15.6486157179124));
#65911=CARTESIAN_POINT('Ctrl Pts',(-15.6095371717916,-54.3206938223985,
15.5701102075356));
#65912=CARTESIAN_POINT('Ctrl Pts',(-15.8247548010729,-52.6134584968727,
15.4916046971588));
#65913=CARTESIAN_POINT('Ctrl Pts',(-14.5194329092597,-51.4922512076563,
15.413099186782));
#65914=CARTESIAN_POINT('Ctrl Pts',(-12.864215224715,-51.9625972391948,15.3345936764052));
#65915=CARTESIAN_POINT('Ctrl Pts',(-12.343540269987,-53.6026792252177,15.2560881660285));
#65916=CARTESIAN_POINT('Ctrl Pts',(-13.4243618186885,-54.9416323741227,
15.1775826556517));
#65917=CARTESIAN_POINT('Ctrl Pts',(-15.1373732173662,-54.7786522269085,
15.0990771452749));
#65918=CARTESIAN_POINT('Ctrl Pts',(-15.9463055097723,-53.2599021305098,
15.0205716348981));
#65919=CARTESIAN_POINT('Ctrl Pts',(-15.1256881964072,-51.7474355457531,
14.9420661245214));
#65920=CARTESIAN_POINT('Ctrl Pts',(-13.4114719843065,-51.5976638845367,
14.8635606141446));
#65921=CARTESIAN_POINT('Ctrl Pts',(-12.3410035135938,-52.9449151739745,
14.7850551037678));
#65922=CARTESIAN_POINT('Ctrl Pts',(-12.8743108410601,-54.5809237767912,
14.706549593391));
#65923=CARTESIAN_POINT('Ctrl Pts',(-14.53309819057,-55.0385159317414,14.6280440830142));
#65924=CARTESIAN_POINT('Ctrl Pts',(-15.8297520454146,-53.9072361260964,
14.5495385726375));
#65925=CARTESIAN_POINT('Ctrl Pts',(-15.6013490876951,-52.2017963646938,
14.4710330622607));
#65926=CARTESIAN_POINT('Ctrl Pts',(-14.0528341340627,-51.4513659790234,
14.3925275518839));
#65927=CARTESIAN_POINT('Ctrl Pts',(-12.572734971243,-52.3295736939085,14.3140220415071));
#65928=CARTESIAN_POINT('Ctrl Pts',(-12.4888785260391,-54.0475602728968,
14.2355165311304));
#65929=CARTESIAN_POINT('Ctrl Pts',(-13.8755779012831,-55.0671461874891,
14.1570110207535));
#65930=CARTESIAN_POINT('Ctrl Pts',(-15.4910603626305,-54.4687297322861,
14.0785055103768));
#65931=CARTESIAN_POINT('Ctrl Pts',(-15.7510836294753,-53.3567463262428,
14.0261685034589));
#65932=CARTESIAN_POINT('Ctrl Pts',(-15.619480088463,-52.8667052421829,14.));
#65933=CARTESIAN_POINT('Ctrl Pts',(-13.498190246218,-52.1716844371558,17.1934196736194));
#65934=CARTESIAN_POINT('Ctrl Pts',(-13.5965228772488,-52.1138086750997,
17.2005947478237));
#65935=CARTESIAN_POINT('Ctrl Pts',(-13.7022352452507,-52.0691825768203,
17.2077698220279));
#65936=CARTESIAN_POINT('Ctrl Pts',(-13.8121375241322,-52.0407561835157,
17.2149448962322));
#65937=CARTESIAN_POINT('Ctrl Pts',(-14.2129665724708,-51.9370811342635,
17.2411133996911));
#65938=CARTESIAN_POINT('Ctrl Pts',(-14.6695282799808,-52.0488886243742,
17.26728190315));
#65939=CARTESIAN_POINT('Ctrl Pts',(-14.9770999437494,-52.3260406788269,
17.293450406609));
#65940=CARTESIAN_POINT('Ctrl Pts',(-15.2846716075181,-52.6031927332796,
17.3196189100679));
#65941=CARTESIAN_POINT('Ctrl Pts',(-15.4432532275454,-53.0456893520743,
17.3457874135268));
#65942=CARTESIAN_POINT('Ctrl Pts',(-15.3817248406863,-53.4551141662759,
17.3719559169858));
#65943=CARTESIAN_POINT('Ctrl Pts',(-15.3201964538272,-53.8645389804775,
17.3981244204447));
#65944=CARTESIAN_POINT('Ctrl Pts',(-15.0385580600817,-54.240891990086,17.4242929239036));
#65945=CARTESIAN_POINT('Ctrl Pts',(-14.6631200082692,-54.4154032016409,
17.4504614273625));
#65946=CARTESIAN_POINT('Ctrl Pts',(-14.2876819564568,-54.5899144131957,
17.4766299308215));
#65947=CARTESIAN_POINT('Ctrl Pts',(-13.8184442465775,-54.5625838266969,
17.5027984342804));
#65948=CARTESIAN_POINT('Ctrl Pts',(-13.4657775795434,-54.3456846257064,
17.5289669377393));
#65949=CARTESIAN_POINT('Ctrl Pts',(-13.1131109125093,-54.1287854247158,
17.5551354411982));
#65950=CARTESIAN_POINT('Ctrl Pts',(-12.8770152883204,-53.7223176092336,
17.5813039446572));
#65951=CARTESIAN_POINT('Ctrl Pts',(-12.8634416833823,-53.3085101996499,
17.6074724481161));
#65952=CARTESIAN_POINT('Ctrl Pts',(-12.8498680784442,-52.8947027900662,
17.633640951575));
#65953=CARTESIAN_POINT('Ctrl Pts',(-13.058816492757,-52.4735557863811,17.659809455034));
#65954=CARTESIAN_POINT('Ctrl Pts',(-13.3964246197054,-52.2339891821747,
17.6859779584929));
#65955=CARTESIAN_POINT('Ctrl Pts',(-13.4284272586679,-52.2112801211956,
17.6884585302017));
#65956=CARTESIAN_POINT('Ctrl Pts',(-13.46158597893,-52.1902026642355,17.6909391019106));
#65957=CARTESIAN_POINT('Ctrl Pts',(-13.495722982135,-52.1707788329429,17.6934196736194));
#65958=CARTESIAN_POINT('Ctrl Pts',(-15.2209662466057,-52.1764590205667,
18.));
#65959=CARTESIAN_POINT('Ctrl Pts',(-14.8623799894179,-51.8174664687921,
17.9738314965411));
#65960=CARTESIAN_POINT('Ctrl Pts',(-13.7693646387388,-51.4866597864568,
17.9214944896232));
#65961=CARTESIAN_POINT('Ctrl Pts',(-12.4433767107148,-52.5865029592796,
17.8429889792464));
#65962=CARTESIAN_POINT('Ctrl Pts',(-12.6330157688953,-54.2972115132025,
17.7644834688697));
#65963=CARTESIAN_POINT('Ctrl Pts',(-14.1627629159668,-55.0835833760402,
17.6859779584929));
#65964=CARTESIAN_POINT('Ctrl Pts',(-15.6633630152513,-54.2408836460551,
17.6074724481161));
#65965=CARTESIAN_POINT('Ctrl Pts',(-15.7877283921755,-52.5246154983424,
17.5289669377393));
#65966=CARTESIAN_POINT('Ctrl Pts',(-14.4249760687641,-51.4740929477669,
17.4504614273625));
#65967=CARTESIAN_POINT('Ctrl Pts',(-12.7969322124135,-52.0313881696841,
17.3719559169858));
#65968=CARTESIAN_POINT('Ctrl Pts',(-12.3638250796578,-53.6967359986948,
17.293450406609));
#65969=CARTESIAN_POINT('Ctrl Pts',(-13.5139962436503,-54.9765978264216,
17.2149448962322));
#65970=CARTESIAN_POINT('Ctrl Pts',(-15.2159841085892,-54.7231706136822,
17.1364393858554));
#65971=CARTESIAN_POINT('Ctrl Pts',(-15.9433860453713,-53.1637302055401,
17.0579338754786));
#65972=CARTESIAN_POINT('Ctrl Pts',(-15.043860342301,-51.6968216692226,16.9794283651019));
#65973=CARTESIAN_POINT('Ctrl Pts',(-13.3241182586501,-51.6380025442003,
16.9009228547251));
#65974=CARTESIAN_POINT('Ctrl Pts',(-12.3264677464456,-53.0400236709193,
16.8224173443483));
#65975=CARTESIAN_POINT('Ctrl Pts',(-12.9456243299004,-54.6455189484075,
16.7439118339715));
#65976=CARTESIAN_POINT('Ctrl Pts',(-14.626314246609,-55.0146421540478,16.6654063235948));
#65977=CARTESIAN_POINT('Ctrl Pts',(-15.8612545351151,-53.8163547667627,
16.586900813218));
#65978=CARTESIAN_POINT('Ctrl Pts',(-15.5429215283994,-52.1253094303059,
16.5083953028412));
#65979=CARTESIAN_POINT('Ctrl Pts',(-13.9568037640838,-51.4580757912425,
16.4298897924644));
#65980=CARTESIAN_POINT('Ctrl Pts',(-12.5253693960519,-52.413044846331,16.3513842820876));
#65981=CARTESIAN_POINT('Ctrl Pts',(-12.5323627785853,-54.1337776405725,
16.2728787717109));
#65982=CARTESIAN_POINT('Ctrl Pts',(-13.9715120885842,-55.0770800976454,
16.1943732613341));
#65983=CARTESIAN_POINT('Ctrl Pts',(-15.5521540067467,-54.3969761475115,
16.1158677509573));
#65984=CARTESIAN_POINT('Ctrl Pts',(-15.8567312853938,-52.7033991815804,
16.0373622405805));
#65985=CARTESIAN_POINT('Ctrl Pts',(-14.612091779025,-51.5151892852255,15.9588567302037));
#65986=CARTESIAN_POINT('Ctrl Pts',(-12.934457787186,-51.8979613415929,15.880351219827));
#65987=CARTESIAN_POINT('Ctrl Pts',(-12.3283713567552,-53.5084362707541,
15.8018457094502));
#65988=CARTESIAN_POINT('Ctrl Pts',(-13.3373852079754,-54.9023018690979,
15.7233401990734));
#65989=CARTESIAN_POINT('Ctrl Pts',(-15.0565917302206,-54.8295063313936,
15.6448346886966));
#65990=CARTESIAN_POINT('Ctrl Pts',(-15.9441656443073,-53.3553344251958,
15.5663291783198));
#65991=CARTESIAN_POINT('Ctrl Pts',(-15.2041095597138,-51.8018585649929,
15.4878236679431));
#65992=CARTESIAN_POINT('Ctrl Pts',(-13.5001233739826,-51.5622728287798,
15.4093181575663));
#65993=CARTESIAN_POINT('Ctrl Pts',(-12.3603823942099,-52.8514434111319,
15.3308126471895));
#65994=CARTESIAN_POINT('Ctrl Pts',(-12.8070334555363,-54.5132114643009,
15.2523071368127));
#65995=CARTESIAN_POINT('Ctrl Pts',(-14.4395092097517,-55.0572639347494,
15.1738016264359));
#65996=CARTESIAN_POINT('Ctrl Pts',(-15.7937667074069,-53.9956815464662,
15.0952961160592));
#65997=CARTESIAN_POINT('Ctrl Pts',(-15.6552753932384,-52.280516797303,15.0167906056824));
#65998=CARTESIAN_POINT('Ctrl Pts',(-14.14823804594,-51.4499698581624,14.9382850953056));
#65999=CARTESIAN_POINT('Ctrl Pts',(-12.6242006263839,-52.248895679213,14.8597795849288));
#66000=CARTESIAN_POINT('Ctrl Pts',(-12.4499580614657,-53.9607971579716,
14.781274074552));
#66001=CARTESIAN_POINT('Ctrl Pts',(-13.7817713167744,-55.0504032414555,
14.7027685641753));
#66002=CARTESIAN_POINT('Ctrl Pts',(-15.4252464910755,-54.5405234556122,
14.6242630537985));
#66003=CARTESIAN_POINT('Ctrl Pts',(-15.9064600587524,-52.8884418877605,
14.5457575434217));
#66004=CARTESIAN_POINT('Ctrl Pts',(-14.7938803736306,-51.575760805285,14.4672520330449));
#66005=CARTESIAN_POINT('Ctrl Pts',(-13.0852305278661,-51.7797717538672,
14.3887465226681));
#66006=CARTESIAN_POINT('Ctrl Pts',(-12.312999126503,-53.317416116839,14.3102410122914));
#66007=CARTESIAN_POINT('Ctrl Pts',(-13.1694776941513,-54.8098931066082,
14.2317355019146));
#66008=CARTESIAN_POINT('Ctrl Pts',(-14.8870885705588,-54.9183199028175,
14.1532299915378));
#66009=CARTESIAN_POINT('Ctrl Pts',(-15.9243621047065,-53.5462518811827,
14.074724481161));
#66010=CARTESIAN_POINT('Ctrl Pts',(-15.3532243372684,-51.9225867742538,
13.9962189707843));
#66011=CARTESIAN_POINT('Ctrl Pts',(-13.681410943509,-51.5067274632874,13.9177134604075));
#66012=CARTESIAN_POINT('Ctrl Pts',(-12.8400499397792,-52.2788850115251,
13.8653764534896));
#66013=CARTESIAN_POINT('Ctrl Pts',(-12.6726615784997,-52.7578848993975,
13.8392079500307));
#66014=CARTESIAN_POINT('Ctrl Pts',(-15.1552860103679,-52.2420649223251,
18.0535973499898));
#66015=CARTESIAN_POINT('Ctrl Pts',(-14.8182738021382,-51.9046708638902,
18.0274288465308));
#66016=CARTESIAN_POINT('Ctrl Pts',(-13.7910188263055,-51.5937668951064,
17.975091839613));
#66017=CARTESIAN_POINT('Ctrl Pts',(-12.5448078777489,-52.6274389027464,
17.8965863292362));
#66018=CARTESIAN_POINT('Ctrl Pts',(-12.7230374570564,-54.2352240753197,
17.8180808188594));
#66019=CARTESIAN_POINT('Ctrl Pts',(-14.1607486178545,-54.9742845180233,
17.7395753084827));
#66020=CARTESIAN_POINT('Ctrl Pts',(-15.5710663391631,-54.1822851282416,
17.6610697981059));
#66021=CARTESIAN_POINT('Ctrl Pts',(-15.6879493748746,-52.5692748502928,
17.5825642877291));
#66022=CARTESIAN_POINT('Ctrl Pts',(-14.407185930718,-51.5819561299908,17.5040587773523));
#66023=CARTESIAN_POINT('Ctrl Pts',(-12.8770920017801,-52.1057221405655,
17.4255532669755));
#66024=CARTESIAN_POINT('Ctrl Pts',(-12.4700424055274,-53.6708756791509,
17.3470477565988));
#66025=CARTESIAN_POINT('Ctrl Pts',(-13.5510144619001,-54.8737356665186,
17.268542246222));
#66026=CARTESIAN_POINT('Ctrl Pts',(-15.1506036186114,-54.6355556948135,
17.1900367358452));
#66027=CARTESIAN_POINT('Ctrl Pts',(-15.8342420126427,-53.1699377437178,
17.1115312254684));
#66028=CARTESIAN_POINT('Ctrl Pts',(-14.9888355379813,-51.791284560039,17.0330257150916));
#66029=CARTESIAN_POINT('Ctrl Pts',(-13.3725603306097,-51.7360042395789,
16.9545202047149));
#66030=CARTESIAN_POINT('Ctrl Pts',(-12.4349326457219,-53.0536739116012,
16.8760146943381));
#66031=CARTESIAN_POINT('Ctrl Pts',(-13.0168381795997,-54.5625758784866,
16.7975091839613));
#66032=CARTESIAN_POINT('Ctrl Pts',(-14.5964107617212,-54.9094910882809,
16.7190036735845));
#66033=CARTESIAN_POINT('Ctrl Pts',(-15.7570518775445,-53.7832976818467,
16.6404981632077));
#66034=CARTESIAN_POINT('Ctrl Pts',(-15.457871115886,-52.1939927053388,16.561992652831));
#66035=CARTESIAN_POINT('Ctrl Pts',(-13.9671808299377,-51.5669026325919,
16.4834871424542));
#66036=CARTESIAN_POINT('Ctrl Pts',(-12.6218675402158,-52.4644167553317,
16.4049816320774));
#66037=CARTESIAN_POINT('Ctrl Pts',(-12.6284401716074,-54.0816230680013,
16.3264761217006));
#66038=CARTESIAN_POINT('Ctrl Pts',(-13.9810042401211,-54.9681725040556,
16.2479706113238));
#66039=CARTESIAN_POINT('Ctrl Pts',(-15.4665481297228,-54.3289864519802,
16.1694651009471));
#66040=CARTESIAN_POINT('Ctrl Pts',(-15.7528007654441,-52.7373021594152,
16.0909595905703));
#66041=CARTESIAN_POINT('Ctrl Pts',(-14.5830439772701,-51.6205799399095,
16.0124540801935));
#66042=CARTESIAN_POINT('Ctrl Pts',(-13.0063434627971,-51.9803228284872,
15.9339485698167));
#66043=CARTESIAN_POINT('Ctrl Pts',(-12.4367217268737,-53.4939048503744,
15.8554430594399));
#66044=CARTESIAN_POINT('Ctrl Pts',(-13.3850290847768,-54.8039096647176,
15.7769375490632));
#66045=CARTESIAN_POINT('Ctrl Pts',(-15.0008009523569,-54.7354938110165,
15.6984320386864));
#66046=CARTESIAN_POINT('Ctrl Pts',(-15.8349747076461,-53.3500142521672,
15.6199265283096));
#66047=CARTESIAN_POINT('Ctrl Pts',(-15.1394434922597,-51.8900019968609,
15.5414210179328));
#66048=CARTESIAN_POINT('Ctrl Pts',(-13.5379762420925,-51.6648307405647,
15.462915507556));
#66049=CARTESIAN_POINT('Ctrl Pts',(-12.4668068464345,-52.8764394289472,
15.3844099971793));
#66050=CARTESIAN_POINT('Ctrl Pts',(-12.8865855118699,-54.4382285659772,
15.3059044868025));
#66051=CARTESIAN_POINT('Ctrl Pts',(-14.4208446971614,-54.9495485643972,
15.2273989764257));
#66052=CARTESIAN_POINT('Ctrl Pts',(-15.6936243998074,-53.9518354124797,
15.1488934660489));
#66053=CARTESIAN_POINT('Ctrl Pts',(-15.5634653023156,-52.3398621480091,
15.0703879556722));
#66054=CARTESIAN_POINT('Ctrl Pts',(-14.1470976247563,-51.5592843863476,
14.9918824452954));
#66055=CARTESIAN_POINT('Ctrl Pts',(-12.7147526703863,-52.3101434886333,
14.9133769349186));
#66056=CARTESIAN_POINT('Ctrl Pts',(-12.5509932669133,-53.919049814695,14.8348714245418));
#66057=CARTESIAN_POINT('Ctrl Pts',(-13.8026790667016,-54.9431006391055,
14.756365914165));
#66058=CARTESIAN_POINT('Ctrl Pts',(-15.3472759009633,-54.4638973536635,
14.6778604037883));
#66059=CARTESIAN_POINT('Ctrl Pts',(-15.7995376478154,-52.9112119224821,
14.5993548934115));
#66060=CARTESIAN_POINT('Ctrl Pts',(-14.7538954097245,-51.6775072239921,
14.5208493830347));
#66061=CARTESIAN_POINT('Ctrl Pts',(-13.1480450848167,-51.8692440206668,
14.4423438726579));
#66062=CARTESIAN_POINT('Ctrl Pts',(-12.4222743542852,-53.3143772678279,
14.3638383622811));
#66063=CARTESIAN_POINT('Ctrl Pts',(-13.2272235892288,-54.7170605998631,
14.2853328519044));
#66064=CARTESIAN_POINT('Ctrl Pts',(-14.8414958116982,-54.8189639865359,
14.2068273415276));
#66065=CARTESIAN_POINT('Ctrl Pts',(-15.8163626318126,-53.5294453155223,
14.1283218311508));
#66066=CARTESIAN_POINT('Ctrl Pts',(-15.2795869011495,-52.0034666921275,
14.049816320774));
#66067=CARTESIAN_POINT('Ctrl Pts',(-13.708356793232,-51.6126272165693,13.9713108103972));
#66068=CARTESIAN_POINT('Ctrl Pts',(-12.9176155863349,-52.3383285372882,
13.9189738034794));
#66069=CARTESIAN_POINT('Ctrl Pts',(-12.7602980089432,-52.7885097885712,
13.8928053000205));
#66070=CARTESIAN_POINT('Ctrl Pts',(-15.0896057741301,-52.3076708240835,
18.1071946999795));
#66071=CARTESIAN_POINT('Ctrl Pts',(-14.7741676148584,-51.9918752589882,
18.0810261965206));
#66072=CARTESIAN_POINT('Ctrl Pts',(-13.8126730138722,-51.700874003756,18.0286891896028));
#66073=CARTESIAN_POINT('Ctrl Pts',(-12.646239044783,-52.6683748462133,17.950183679226));
#66074=CARTESIAN_POINT('Ctrl Pts',(-12.8130591452175,-54.1732366374368,
17.8716781688492));
#66075=CARTESIAN_POINT('Ctrl Pts',(-14.1587343197422,-54.8649856600065,
17.7931726584724));
#66076=CARTESIAN_POINT('Ctrl Pts',(-15.4787696630749,-54.123686610428,17.7146671480956));
#66077=CARTESIAN_POINT('Ctrl Pts',(-15.5881703575737,-52.6139342022434,
17.6361616377189));
#66078=CARTESIAN_POINT('Ctrl Pts',(-14.3893957926718,-51.6898193122147,
17.5576561273421));
#66079=CARTESIAN_POINT('Ctrl Pts',(-12.9572517911467,-52.1800561114469,
17.4791506169653));
#66080=CARTESIAN_POINT('Ctrl Pts',(-12.576259731397,-53.6450153596069,17.4006451065885));
#66081=CARTESIAN_POINT('Ctrl Pts',(-13.58803268015,-54.7708735066155,17.3221395962118));
#66082=CARTESIAN_POINT('Ctrl Pts',(-15.0852231286336,-54.547940775945,17.243634085835));
#66083=CARTESIAN_POINT('Ctrl Pts',(-15.725097979914,-53.1761452818954,17.1651285754582));
#66084=CARTESIAN_POINT('Ctrl Pts',(-14.9338107336617,-51.8857474508553,
17.0866230650814));
#66085=CARTESIAN_POINT('Ctrl Pts',(-13.4210024025693,-51.8340059349575,
17.0081175547046));
#66086=CARTESIAN_POINT('Ctrl Pts',(-12.5433975449982,-53.067324152283,16.9296120443279));
#66087=CARTESIAN_POINT('Ctrl Pts',(-13.0880520292989,-54.4796328085655,
16.8511065339511));
#66088=CARTESIAN_POINT('Ctrl Pts',(-14.5665072768334,-54.8043400225141,
16.7726010235743));
#66089=CARTESIAN_POINT('Ctrl Pts',(-15.6528492199738,-53.7502405969307,
16.6940955131975));
#66090=CARTESIAN_POINT('Ctrl Pts',(-15.3728207033727,-52.2626759803716,
16.6155900028207));
#66091=CARTESIAN_POINT('Ctrl Pts',(-13.9775578957916,-51.6757294739412,
16.5370844924439));
#66092=CARTESIAN_POINT('Ctrl Pts',(-12.7183656843796,-52.5157886643324,
16.4585789820672));
#66093=CARTESIAN_POINT('Ctrl Pts',(-12.7245175646294,-54.0294684954301,
16.3800734716904));
#66094=CARTESIAN_POINT('Ctrl Pts',(-13.990496391658,-54.8592649104658,16.3015679613136));
#66095=CARTESIAN_POINT('Ctrl Pts',(-15.3809422526988,-54.2609967564488,
16.2230624509368));
#66096=CARTESIAN_POINT('Ctrl Pts',(-15.6488702454944,-52.77120513725,16.1445569405601));
#66097=CARTESIAN_POINT('Ctrl Pts',(-14.5539961755152,-51.7259705945934,
16.0660514301833));
#66098=CARTESIAN_POINT('Ctrl Pts',(-13.0782291384082,-52.0626843153815,
15.9875459198065));
#66099=CARTESIAN_POINT('Ctrl Pts',(-12.5450720969922,-53.4793734299947,
15.9090404094297));
#66100=CARTESIAN_POINT('Ctrl Pts',(-13.4326729615783,-54.7055174603373,
15.8305348990529));
#66101=CARTESIAN_POINT('Ctrl Pts',(-14.9450101744931,-54.6414812906393,
15.7520293886762));
#66102=CARTESIAN_POINT('Ctrl Pts',(-15.725783770985,-53.3446940791386,15.6735238782994));
#66103=CARTESIAN_POINT('Ctrl Pts',(-15.0747774248056,-51.9781454287288,
15.5950183679226));
#66104=CARTESIAN_POINT('Ctrl Pts',(-13.5758291102025,-51.7673886523496,
15.5165128575458));
#66105=CARTESIAN_POINT('Ctrl Pts',(-12.5732312986591,-52.9014354467625,
15.438007347169));
#66106=CARTESIAN_POINT('Ctrl Pts',(-12.9661375682035,-54.3632456676534,
15.3595018367923));
#66107=CARTESIAN_POINT('Ctrl Pts',(-14.402180184571,-54.841833194045,15.2809963264155));
#66108=CARTESIAN_POINT('Ctrl Pts',(-15.593482092208,-53.9079892784932,15.2024908160387));
#66109=CARTESIAN_POINT('Ctrl Pts',(-15.4716552113927,-52.3992074987152,
15.1239853056619));
#66110=CARTESIAN_POINT('Ctrl Pts',(-14.1459572035726,-51.6685989145327,
15.0454797952851));
#66111=CARTESIAN_POINT('Ctrl Pts',(-12.8053047143887,-52.3713912980536,
14.9669742849084));
#66112=CARTESIAN_POINT('Ctrl Pts',(-12.6520284723609,-53.8773024714182,
14.8884687745316));
#66113=CARTESIAN_POINT('Ctrl Pts',(-13.8235868166289,-54.8357980367556,
14.8099632641548));
#66114=CARTESIAN_POINT('Ctrl Pts',(-15.2693053108511,-54.3872712517148,
14.731457753778));
#66115=CARTESIAN_POINT('Ctrl Pts',(-15.6926152368783,-52.9339819572036,
14.6529522434012));
#66116=CARTESIAN_POINT('Ctrl Pts',(-14.7139104458185,-51.7792536426992,
14.5744467330245));
#66117=CARTESIAN_POINT('Ctrl Pts',(-13.2108596417673,-51.9587162874664,
14.4959412226477));
#66118=CARTESIAN_POINT('Ctrl Pts',(-12.5315495820674,-53.3113384188168,
14.4174357122709));
#66119=CARTESIAN_POINT('Ctrl Pts',(-13.2849694843063,-54.624228093118,14.3389302018941));
#66120=CARTESIAN_POINT('Ctrl Pts',(-14.7959030528376,-54.7196080702543,
14.2604246915173));
#66121=CARTESIAN_POINT('Ctrl Pts',(-15.7083631589187,-53.5126387498619,
14.1819191811406));
#66122=CARTESIAN_POINT('Ctrl Pts',(-15.2059494650307,-52.0843466100013,
14.1034136707638));
#66123=CARTESIAN_POINT('Ctrl Pts',(-13.735302642955,-51.7185269698511,14.024908160387));
#66124=CARTESIAN_POINT('Ctrl Pts',(-12.9951812328907,-52.3977720630514,
13.9725711534692));
#66125=CARTESIAN_POINT('Ctrl Pts',(-12.8479344393867,-52.8191346777449,
13.9464026500102));
#66126=CARTESIAN_POINT('Ctrl Pts',(-15.0239255378924,-52.3732767258419,
18.1607920499693));
#66127=CARTESIAN_POINT('Ctrl Pts',(-14.7300614275787,-52.0790796540862,
18.1346235465104));
#66128=CARTESIAN_POINT('Ctrl Pts',(-13.834327201439,-51.8079811124057,18.0822865395925));
#66129=CARTESIAN_POINT('Ctrl Pts',(-12.7476702118172,-52.7093107896801,
18.0037810292157));
#66130=CARTESIAN_POINT('Ctrl Pts',(-12.9030808333786,-54.111249199554,17.925275518839));
#66131=CARTESIAN_POINT('Ctrl Pts',(-14.15672002163,-54.7556868019897,17.8467700084622));
#66132=CARTESIAN_POINT('Ctrl Pts',(-15.3864729869866,-54.0650880926144,
17.7682644980854));
#66133=CARTESIAN_POINT('Ctrl Pts',(-15.4883913402728,-52.6585935541939,
17.6897589877086));
#66134=CARTESIAN_POINT('Ctrl Pts',(-14.3716056546256,-51.7976824944385,
17.6112534773319));
#66135=CARTESIAN_POINT('Ctrl Pts',(-13.0374115805133,-52.2543900823285,
17.5327479669551));
#66136=CARTESIAN_POINT('Ctrl Pts',(-12.6824770572666,-53.6191550400628,
17.4542424565783));
#66137=CARTESIAN_POINT('Ctrl Pts',(-13.6250508983998,-54.6680113467125,
17.3757369462015));
#66138=CARTESIAN_POINT('Ctrl Pts',(-15.0198426386559,-54.4603258570761,
17.2972314358247));
#66139=CARTESIAN_POINT('Ctrl Pts',(-15.6159539471854,-53.1823528200732,
17.218725925448));
#66140=CARTESIAN_POINT('Ctrl Pts',(-14.878785929342,-51.9802103416716,17.1402204150712));
#66141=CARTESIAN_POINT('Ctrl Pts',(-13.4694444745289,-51.9320076303361,
17.0617149046944));
#66142=CARTESIAN_POINT('Ctrl Pts',(-12.6518624442745,-53.0809743929648,
16.9832093943176));
#66143=CARTESIAN_POINT('Ctrl Pts',(-13.1592658789981,-54.3966897386446,
16.9047038839409));
#66144=CARTESIAN_POINT('Ctrl Pts',(-14.5366037919456,-54.6991889567472,
16.8261983735641));
#66145=CARTESIAN_POINT('Ctrl Pts',(-15.5486465624032,-53.7171835120147,
16.7476928631873));
#66146=CARTESIAN_POINT('Ctrl Pts',(-15.2877702908594,-52.3313592554045,
16.6691873528105));
#66147=CARTESIAN_POINT('Ctrl Pts',(-13.9879349616455,-51.7845563152906,
16.5906818424337));
#66148=CARTESIAN_POINT('Ctrl Pts',(-12.8148638285435,-52.567160573333,16.5121763320569));
#66149=CARTESIAN_POINT('Ctrl Pts',(-12.8205949576515,-53.9773139228589,
16.4336708216802));
#66150=CARTESIAN_POINT('Ctrl Pts',(-13.9999885431949,-54.7503573168762,
16.3551653113034));
#66151=CARTESIAN_POINT('Ctrl Pts',(-15.2953363756749,-54.1930070609174,
16.2766598009266));
#66152=CARTESIAN_POINT('Ctrl Pts',(-15.5449397255447,-52.8051081150848,
16.1981542905498));
#66153=CARTESIAN_POINT('Ctrl Pts',(-14.5249483737603,-51.8313612492774,
16.119648780173));
#66154=CARTESIAN_POINT('Ctrl Pts',(-13.1501148140193,-52.1450458022758,
16.0411432697963));
#66155=CARTESIAN_POINT('Ctrl Pts',(-12.6534224671108,-53.464842009615,15.9626377594195));
#66156=CARTESIAN_POINT('Ctrl Pts',(-13.4803168383798,-54.607125255957,15.8841322490427));
#66157=CARTESIAN_POINT('Ctrl Pts',(-14.8892193966293,-54.5474687702622,
15.8056267386659));
#66158=CARTESIAN_POINT('Ctrl Pts',(-15.6165928343238,-53.3393739061099,
15.7271212282891));
#66159=CARTESIAN_POINT('Ctrl Pts',(-15.0101113573514,-52.0662888605968,
15.6486157179124));
#66160=CARTESIAN_POINT('Ctrl Pts',(-13.6136819783124,-51.8699465641345,
15.5701102075356));
#66161=CARTESIAN_POINT('Ctrl Pts',(-12.6796557508836,-52.9264314645779,
15.4916046971588));
#66162=CARTESIAN_POINT('Ctrl Pts',(-13.0456896245371,-54.2882627693297,
15.413099186782));
#66163=CARTESIAN_POINT('Ctrl Pts',(-14.3835156719806,-54.7341178236928,
15.3345936764052));
#66164=CARTESIAN_POINT('Ctrl Pts',(-15.4933397846086,-53.8641431445067,
15.2560881660285));
#66165=CARTESIAN_POINT('Ctrl Pts',(-15.3798451204699,-52.4585528494213,
15.1775826556517));
#66166=CARTESIAN_POINT('Ctrl Pts',(-14.1448167823889,-51.7779134427179,
15.0990771452749));
#66167=CARTESIAN_POINT('Ctrl Pts',(-12.8958567583911,-52.4326391074739,
15.0205716348981));
#66168=CARTESIAN_POINT('Ctrl Pts',(-12.7530636778084,-53.8355551281416,
14.9420661245214));
#66169=CARTESIAN_POINT('Ctrl Pts',(-13.8444945665562,-54.7284954344056,
14.8635606141446));
#66170=CARTESIAN_POINT('Ctrl Pts',(-15.1913347207389,-54.3106451497661,
14.7850551037678));
#66171=CARTESIAN_POINT('Ctrl Pts',(-15.5856928259413,-52.9567519919251,
14.706549593391));
#66172=CARTESIAN_POINT('Ctrl Pts',(-14.6739254819125,-51.8810000614065,
14.6280440830142));
#66173=CARTESIAN_POINT('Ctrl Pts',(-13.2736741987179,-52.048188554266,14.5495385726375));
#66174=CARTESIAN_POINT('Ctrl Pts',(-12.6408248098497,-53.3082995698058,
14.4710330622607));
#66175=CARTESIAN_POINT('Ctrl Pts',(-13.3427153793839,-54.5313955863729,
14.3925275518839));
#66176=CARTESIAN_POINT('Ctrl Pts',(-14.7503102939771,-54.6202521539727,
14.3140220415071));
#66177=CARTESIAN_POINT('Ctrl Pts',(-15.6003636860249,-53.4958321842015,
14.2355165311303));
#66178=CARTESIAN_POINT('Ctrl Pts',(-15.1323120289118,-52.1652265278751,
14.1570110207536));
#66179=CARTESIAN_POINT('Ctrl Pts',(-13.762248492678,-51.824426723133,14.0785055103768));
#66180=CARTESIAN_POINT('Ctrl Pts',(-13.0727468794464,-52.4572155888145,
14.0261685034589));
#66181=CARTESIAN_POINT('Ctrl Pts',(-12.9355708698302,-52.8497595669186,
14.));
#66182=CARTESIAN_POINT('Ctrl Pts',(-13.4965541629804,-52.1730078059394,
17.5565803263806));
#66183=CARTESIAN_POINT('Ctrl Pts',(-13.3865887223467,-52.2353622375859,
17.5486362065721));
#66184=CARTESIAN_POINT('Ctrl Pts',(-13.2860845507673,-52.3135738660447,
17.5406920867636));
#66185=CARTESIAN_POINT('Ctrl Pts',(-13.2006215056576,-52.4057329773026,
17.5327479669551));
#66186=CARTESIAN_POINT('Ctrl Pts',(-12.9191000727644,-52.7093117349066,
17.5065794634962));
#66187=CARTESIAN_POINT('Ctrl Pts',(-12.8007885650155,-53.1642333874847,
17.4804109600372));
#66188=CARTESIAN_POINT('Ctrl Pts',(-12.8987284513299,-53.5665035982154,
17.4542424565783));
#66189=CARTESIAN_POINT('Ctrl Pts',(-12.9966683376443,-53.968773808946,17.4280739531194));
#66190=CARTESIAN_POINT('Ctrl Pts',(-13.3108596180221,-54.3183925778293,
17.4019054496604));
#66191=CARTESIAN_POINT('Ctrl Pts',(-13.7004205482536,-54.4585877139982,
17.3757369462015));
#66192=CARTESIAN_POINT('Ctrl Pts',(-14.0899814784852,-54.5987828501671,
17.3495684427426));
#66193=CARTESIAN_POINT('Ctrl Pts',(-14.5549120585705,-54.5295543536216,
17.3233999392837));
#66194=CARTESIAN_POINT('Ctrl Pts',(-14.8867292333681,-54.2819445991817,
17.2972314358247));
#66195=CARTESIAN_POINT('Ctrl Pts',(-15.2185464081657,-54.0343348447418,
17.2710629323658));
#66196=CARTESIAN_POINT('Ctrl Pts',(-15.4172501776756,-53.6083438324075,
17.2448944289069));
#66197=CARTESIAN_POINT('Ctrl Pts',(-15.3937407261232,-53.1949912465067,
17.218725925448));
#66198=CARTESIAN_POINT('Ctrl Pts',(-15.3702312745709,-52.781638660606,17.192557421989));
#66199=CARTESIAN_POINT('Ctrl Pts',(-15.1245086019565,-52.3809245011388,
17.1663889185301));
#66200=CARTESIAN_POINT('Ctrl Pts',(-14.7667570231804,-52.1725336361826,
17.1402204150712));
#66201=CARTESIAN_POINT('Ctrl Pts',(-14.4090054444043,-51.9641427712264,
17.1140519116123));
#66202=CARTESIAN_POINT('Ctrl Pts',(-13.9392249594666,-51.9480752007813,
17.0878834081533));
#66203=CARTESIAN_POINT('Ctrl Pts',(-13.5680710452887,-52.1315358759968,
17.0617149046944));
#66204=CARTESIAN_POINT('Ctrl Pts',(-13.5437960761855,-52.1435349471433,
17.0600033785898));
#66205=CARTESIAN_POINT('Ctrl Pts',(-13.5199430009518,-52.1563875382182,
17.0582918524852));
#66206=CARTESIAN_POINT('Ctrl Pts',(-13.4965460097018,-52.1700456009991,
17.0565803263806));
#66207=CARTESIAN_POINT('Origin',(-14.1292828945604,-53.2669068454841,15.5));
#66208=CARTESIAN_POINT('Origin',(-53.1951359564886,-14.3971354987959,14.));
#66209=CARTESIAN_POINT('Ctrl Pts',(-52.2370198037663,-15.2223467977324,
14.));
#66210=CARTESIAN_POINT('Ctrl Pts',(-52.1998280045551,-15.187614600057,14.));
#66211=CARTESIAN_POINT('Ctrl Pts',(-52.1650182492936,-15.1505714365352,
14.));
#66212=CARTESIAN_POINT('Ctrl Pts',(-52.1326048428076,-15.1115303634521,
14.));
#66213=CARTESIAN_POINT('Ctrl Pts',(-52.1107612978768,-15.0852204032691,
14.));
#66214=CARTESIAN_POINT('Ctrl Pts',(-52.0900064961692,-15.0580020338226,
14.));
#66215=CARTESIAN_POINT('Ctrl Pts',(-52.0703516540902,-15.0299603099463,
14.));
#66216=CARTESIAN_POINT('Ctrl Pts',(-52.0612801328574,-15.017017896442,14.));
#66217=CARTESIAN_POINT('Ctrl Pts',(-52.0524430090281,-15.0038999832866,
14.));
#66218=CARTESIAN_POINT('Ctrl Pts',(-52.0438418390641,-14.9906144201694,
14.));
#66219=CARTESIAN_POINT('Ctrl Pts',(-52.036611845359,-14.9794468071462,14.));
#66220=CARTESIAN_POINT('Ctrl Pts',(-52.0295526827715,-14.9681669384272,
14.));
#66221=CARTESIAN_POINT('Ctrl Pts',(-52.022668475442,-14.956786074209,14.));
#66222=CARTESIAN_POINT('Ctrl Pts',(-51.9948472065506,-14.9107923862691,
14.));
#66223=CARTESIAN_POINT('Ctrl Pts',(-51.9698609199132,-14.8631221292342,
14.));
#66224=CARTESIAN_POINT('Ctrl Pts',(-51.947748300236,-14.8140997169745,14.));
#66225=CARTESIAN_POINT('Ctrl Pts',(-51.9392849994114,-14.7953370634237,
14.));
#66226=CARTESIAN_POINT('Ctrl Pts',(-51.9312430201854,-14.776375916002,14.));
#66227=CARTESIAN_POINT('Ctrl Pts',(-51.9236259797948,-14.757233069302,14.));
#66228=CARTESIAN_POINT('Ctrl Pts',(-51.918152652305,-14.7434777176558,14.));
#66229=CARTESIAN_POINT('Ctrl Pts',(-51.9128987520874,-14.7296285333462,
14.));
#66230=CARTESIAN_POINT('Ctrl Pts',(-51.9078659027834,-14.7156915540625,
14.));
#66231=CARTESIAN_POINT('Ctrl Pts',(-51.9039695335319,-14.7049017182738,
14.));
#66232=CARTESIAN_POINT('Ctrl Pts',(-51.9002056527562,-14.6940588600005,
14.));
#66233=CARTESIAN_POINT('Ctrl Pts',(-51.8965797112069,-14.6831806448979,
14.));
#66234=CARTESIAN_POINT('Ctrl Pts',(-51.8786612859968,-14.629423439747,14.));
#66235=CARTESIAN_POINT('Ctrl Pts',(-51.8640761421938,-14.5747200728836,
14.));
#66236=CARTESIAN_POINT('Ctrl Pts',(-51.8528626358983,-14.5194298174396,
14.));
#66237=CARTESIAN_POINT('Ctrl Pts',(-51.8418116070222,-14.4649406867982,
14.));
#66238=CARTESIAN_POINT('Ctrl Pts',(-51.8340348275742,-14.409880375256,14.));
#66239=CARTESIAN_POINT('Ctrl Pts',(-51.8296128481337,-14.354562785674,14.));
#66240=CARTESIAN_POINT('Ctrl Pts',(-51.8273037118427,-14.3256762077624,
14.));
#66241=CARTESIAN_POINT('Ctrl Pts',(-51.8259101526051,-14.2967190813249,
14.));
#66242=CARTESIAN_POINT('Ctrl Pts',(-51.8254490493326,-14.2677344056925,
14.));
#66243=CARTESIAN_POINT('Ctrl Pts',(-51.8252016892536,-14.2521854992281,
14.));
#66244=CARTESIAN_POINT('Ctrl Pts',(-51.8252227392431,-14.2366286515745,
14.));
#66245=CARTESIAN_POINT('Ctrl Pts',(-51.8255152855579,-14.2210704503188,
14.));
#66246=CARTESIAN_POINT('Ctrl Pts',(-51.8257232519346,-14.2100103802406,
14.));
#66247=CARTESIAN_POINT('Ctrl Pts',(-51.8260684275002,-14.1989496254671,
14.));
#66248=CARTESIAN_POINT('Ctrl Pts',(-51.8265520290651,-14.1878905523495,
14.));
#66249=CARTESIAN_POINT('Ctrl Pts',(-51.8269778211602,-14.1781534748575,
14.));
#66250=CARTESIAN_POINT('Ctrl Pts',(-51.8275105014082,-14.1684274978297,
14.));
#66251=CARTESIAN_POINT('Ctrl Pts',(-51.8281502461755,-14.1587149162952,
14.));
#66252=CARTESIAN_POINT('Ctrl Pts',(-51.8313147365973,-14.1106717390646,
14.));
#66253=CARTESIAN_POINT('Ctrl Pts',(-51.8370971206981,-14.0629523055729,
14.));
#66254=CARTESIAN_POINT('Ctrl Pts',(-51.8455361922423,-14.0157553469174,
14.));
#66255=CARTESIAN_POINT('Ctrl Pts',(-51.8551414270627,-13.9620364196248,
14.));
#66256=CARTESIAN_POINT('Ctrl Pts',(-51.8681865747697,-13.9089935983908,
14.));
#66257=CARTESIAN_POINT('Ctrl Pts',(-51.8844213082613,-13.8568249617529,
14.));
#66258=CARTESIAN_POINT('Ctrl Pts',(-51.9002905362141,-13.8058308393532,
14.));
#66259=CARTESIAN_POINT('Ctrl Pts',(-51.9192079284338,-13.7556712969149,
14.));
#66260=CARTESIAN_POINT('Ctrl Pts',(-51.9409851275907,-13.7065350685516,
14.));
#66261=CARTESIAN_POINT('Ctrl Pts',(-51.9463194725313,-13.6944991042717,
14.));
#66262=CARTESIAN_POINT('Ctrl Pts',(-51.9518256037611,-13.6825245847688,
14.));
#66263=CARTESIAN_POINT('Ctrl Pts',(-51.9575011215412,-13.6706143910813,
14.));
#66264=CARTESIAN_POINT('Ctrl Pts',(-51.9617861950524,-13.6616220739992,
14.));
#66265=CARTESIAN_POINT('Ctrl Pts',(-51.9661670467492,-13.6526682499682,
14.));
#66266=CARTESIAN_POINT('Ctrl Pts',(-51.9706371983683,-13.6437643302994,
14.));
#66267=CARTESIAN_POINT('Ctrl Pts',(-51.9964876791123,-13.5922737716888,
14.));
#66268=CARTESIAN_POINT('Ctrl Pts',(-52.0253653817646,-13.5423559816578,
14.));
#66269=CARTESIAN_POINT('Ctrl Pts',(-52.056990938761,-13.4942262955812,14.));
#66270=CARTESIAN_POINT('Ctrl Pts',(-52.0892948739252,-13.4450642125649,
14.));
#66271=CARTESIAN_POINT('Ctrl Pts',(-52.1244662109051,-13.3977668163443,
14.));
#66272=CARTESIAN_POINT('Ctrl Pts',(-52.1622608704981,-13.3525735612878,
14.));
#66273=CARTESIAN_POINT('Ctrl Pts',(-52.2003880180872,-13.3069827311511,
14.));
#66274=CARTESIAN_POINT('Ctrl Pts',(-52.2411854112278,-13.2635321825438,
14.));
#66275=CARTESIAN_POINT('Ctrl Pts',(-52.2844490105985,-13.2224929144395,
14.));
#66276=CARTESIAN_POINT('Ctrl Pts',(-52.2942488213998,-13.2131969458032,
14.));
#66277=CARTESIAN_POINT('Ctrl Pts',(-52.3041782446756,-13.204022403894,14.));
#66278=CARTESIAN_POINT('Ctrl Pts',(-52.3142147728346,-13.1949905193645,
14.));
#66279=CARTESIAN_POINT('Ctrl Pts',(-52.3594366695135,-13.154295276693,14.));
#66280=CARTESIAN_POINT('Ctrl Pts',(-52.4069027254174,-13.1164219433845,
14.));
#66281=CARTESIAN_POINT('Ctrl Pts',(-52.4563466159028,-13.081614036475,14.));
#66282=CARTESIAN_POINT('Ctrl Pts',(-52.5053559226553,-13.0471120713103,
14.));
#66283=CARTESIAN_POINT('Ctrl Pts',(-52.5563091708902,-13.0156209538648,
14.));
#66284=CARTESIAN_POINT('Ctrl Pts',(-52.6089887803891,-12.9874055955952,
14.));
#66285=CARTESIAN_POINT('Ctrl Pts',(-52.6475874040962,-12.9667320559282,
14.));
#66286=CARTESIAN_POINT('Ctrl Pts',(-52.6871137410699,-12.9478176360512,
14.));
#66287=CARTESIAN_POINT('Ctrl Pts',(-52.7274932936822,-12.9307805393251,
14.));
#66288=CARTESIAN_POINT('Ctrl Pts',(-52.7499343911042,-12.9213121048654,
14.));
#66289=CARTESIAN_POINT('Ctrl Pts',(-52.7726391696466,-12.9124237518852,
14.));
#66290=CARTESIAN_POINT('Ctrl Pts',(-52.7955875161457,-12.9041113834231,
14.));
#66291=CARTESIAN_POINT('Ctrl Pts',(-53.5936497983459,-12.9064860705774,
14.));
#66292=CARTESIAN_POINT('Ctrl Pts',(-53.6509984651359,-12.9274410373818,
14.));
#66293=CARTESIAN_POINT('Ctrl Pts',(-53.7068627003681,-12.9520247913344,
14.));
#66294=CARTESIAN_POINT('Ctrl Pts',(-53.7610278853563,-12.9799613169679,
14.));
#66295=CARTESIAN_POINT('Ctrl Pts',(-53.8112531574186,-13.0058657720292,
14.));
#66296=CARTESIAN_POINT('Ctrl Pts',(-53.8600177560829,-13.0346541103165,
14.));
#66297=CARTESIAN_POINT('Ctrl Pts',(-53.9071231753197,-13.0661362083695,
14.));
#66298=CARTESIAN_POINT('Ctrl Pts',(-53.9184932356252,-13.073735192928,14.));
#66299=CARTESIAN_POINT('Ctrl Pts',(-53.929766785557,-13.0814915892485,14.));
#66300=CARTESIAN_POINT('Ctrl Pts',(-53.9409284677904,-13.089393751099,14.));
#66301=CARTESIAN_POINT('Ctrl Pts',(-53.9900508425651,-13.1241710317841,
14.));
#66302=CARTESIAN_POINT('Ctrl Pts',(-54.0370703142149,-13.1618085881906,
14.));
#66303=CARTESIAN_POINT('Ctrl Pts',(-54.0817574272605,-13.2020613661078,
14.));
#66304=CARTESIAN_POINT('Ctrl Pts',(-54.10933993136,-13.2269068380179,14.));
#66305=CARTESIAN_POINT('Ctrl Pts',(-54.1360331111675,-13.2527493803639,
14.));
#66306=CARTESIAN_POINT('Ctrl Pts',(-54.1617745164173,-13.2795365303592,
14.));
#66307=CARTESIAN_POINT('Ctrl Pts',(-54.1705826003128,-13.2887024427169,
14.));
#66308=CARTESIAN_POINT('Ctrl Pts',(-54.1792791849711,-13.2979789799756,
14.));
#66309=CARTESIAN_POINT('Ctrl Pts',(-54.1878615699546,-13.3073641131248,
14.));
#66310=CARTESIAN_POINT('Ctrl Pts',(-54.195890456635,-13.3161439768432,14.));
#66311=CARTESIAN_POINT('Ctrl Pts',(-54.2038142461512,-13.3250133167635,
14.));
#66312=CARTESIAN_POINT('Ctrl Pts',(-54.2116272144904,-13.3339655513165,
14.));
#66313=CARTESIAN_POINT('Ctrl Pts',(-54.250298832142,-13.3782761611554,14.));
#66314=CARTESIAN_POINT('Ctrl Pts',(-54.286291162471,-13.4246505091249,14.));
#66315=CARTESIAN_POINT('Ctrl Pts',(-54.3193890208801,-13.4728592463024,
14.));
#66316=CARTESIAN_POINT('Ctrl Pts',(-54.3516418894012,-13.5198372121435,
14.));
#66317=CARTESIAN_POINT('Ctrl Pts',(-54.3811465604949,-13.5685580127126,
14.));
#66318=CARTESIAN_POINT('Ctrl Pts',(-54.4076582516214,-13.6188275090082,
14.));
#66319=CARTESIAN_POINT('Ctrl Pts',(-54.422032099109,-13.6460821292277,14.));
#66320=CARTESIAN_POINT('Ctrl Pts',(-54.4355253353237,-13.6737922214405,
14.));
#66321=CARTESIAN_POINT('Ctrl Pts',(-54.4480925383944,-13.7019277688883,
14.));
#66322=CARTESIAN_POINT('Ctrl Pts',(-54.4585481854562,-13.7253359490815,
14.));
#66323=CARTESIAN_POINT('Ctrl Pts',(-54.4683627680535,-13.7490386437541,
14.));
#66324=CARTESIAN_POINT('Ctrl Pts',(-54.4775075098049,-13.7730185624462,
14.));
#66325=CARTESIAN_POINT('Ctrl Pts',(-54.4814161888852,-13.7832681472993,
14.));
#66326=CARTESIAN_POINT('Ctrl Pts',(-54.4852027887794,-13.7935696368397,
14.));
#66327=CARTESIAN_POINT('Ctrl Pts',(-54.4888592933946,-13.8039047382203,
14.));
#66328=CARTESIAN_POINT('Ctrl Pts',(-54.5057868221325,-13.8517503569301,
14.));
#66329=CARTESIAN_POINT('Ctrl Pts',(-54.5199611541528,-13.9003971684769,
14.));
#66330=CARTESIAN_POINT('Ctrl Pts',(-54.5312161752957,-13.9497022076935,
14.));
#66331=CARTESIAN_POINT('Ctrl Pts',(-54.5437933673149,-14.0047993006149,
14.));
#66332=CARTESIAN_POINT('Ctrl Pts',(-54.5527257730479,-14.060719293395,14.));
#66333=CARTESIAN_POINT('Ctrl Pts',(-54.5581033230398,-14.1171258864099,
14.));
#66334=CARTESIAN_POINT('Ctrl Pts',(-54.5626667133147,-14.1649925354209,
14.));
#66335=CARTESIAN_POINT('Ctrl Pts',(-54.5646690852638,-14.2132100479209,
14.));
#66336=CARTESIAN_POINT('Ctrl Pts',(-54.564136951052,-14.2615652592475,14.));
#66337=CARTESIAN_POINT('Ctrl Pts',(-54.5639906524104,-14.2748594650661,
14.));
#66338=CARTESIAN_POINT('Ctrl Pts',(-54.5636526398204,-14.2881640100053,
14.));
#66339=CARTESIAN_POINT('Ctrl Pts',(-54.5631231489384,-14.3014742844609,
14.));
#66340=CARTESIAN_POINT('Ctrl Pts',(-54.5627109268488,-14.3118366709255,
14.));
#66341=CARTESIAN_POINT('Ctrl Pts',(-54.5621824503484,-14.322204308924,14.));
#66342=CARTESIAN_POINT('Ctrl Pts',(-54.5615390811975,-14.3325581294891,
14.));
#66343=CARTESIAN_POINT('Ctrl Pts',(-54.5580964056233,-14.3879615399713,
14.));
#66344=CARTESIAN_POINT('Ctrl Pts',(-54.551365377527,-14.4430731532169,14.));
#66345=CARTESIAN_POINT('Ctrl Pts',(-54.5414407207137,-14.4975781576669,
14.));
#66346=CARTESIAN_POINT('Ctrl Pts',(-54.5315715932723,-14.5517782015807,
14.));
#66347=CARTESIAN_POINT('Ctrl Pts',(-54.5185439871495,-14.6053794990709,
14.));
#66348=CARTESIAN_POINT('Ctrl Pts',(-54.5024041439982,-14.6580525500535,
14.));
#66349=CARTESIAN_POINT('Ctrl Pts',(-54.4874293906239,-14.7069232819772,
14.));
#66350=CARTESIAN_POINT('Ctrl Pts',(-54.4697747813372,-14.7549954142157,
14.));
#66351=CARTESIAN_POINT('Ctrl Pts',(-54.4494461021838,-14.8019781702512,
14.));
#66352=CARTESIAN_POINT('Ctrl Pts',(-54.4442243438061,-14.8140464703156,
14.));
#66353=CARTESIAN_POINT('Ctrl Pts',(-54.4388239492052,-14.8260467746001,
14.));
#66354=CARTESIAN_POINT('Ctrl Pts',(-54.43325735223,-14.8379478524605,14.));
#66355=CARTESIAN_POINT('Ctrl Pts',(-54.4107559776503,-14.8860545524844,
14.));
#66356=CARTESIAN_POINT('Ctrl Pts',(-54.3855109054517,-14.9326200894641,
14.));
#66357=CARTESIAN_POINT('Ctrl Pts',(-54.3575738558942,-14.9773487851076,
14.));
#66358=CARTESIAN_POINT('Ctrl Pts',(-54.3305841285965,-15.0205607676511,
14.));
#66359=CARTESIAN_POINT('Ctrl Pts',(-54.3010813191933,-15.0620590195604,
14.));
#66360=CARTESIAN_POINT('Ctrl Pts',(-54.2690787903782,-15.1015427316642,
14.));
#66361=CARTESIAN_POINT('Ctrl Pts',(-54.246691332214,-15.129163672434,14.));
#66362=CARTESIAN_POINT('Ctrl Pts',(-54.2230798921333,-15.1557980567137,
14.));
#66363=CARTESIAN_POINT('Ctrl Pts',(-54.1982409588253,-15.1813299258066,
14.));
#66364=CARTESIAN_POINT('Ctrl Pts',(-54.1842289958931,-15.1957327827604,
14.));
#66365=CARTESIAN_POINT('Ctrl Pts',(-54.1698262703445,-15.2097845594384,
14.));
#66366=CARTESIAN_POINT('Ctrl Pts',(-54.1550492157917,-15.2234767486837,
14.));
#66367=CARTESIAN_POINT('Origin',(-53.1951359564886,-14.3971354987959,19.1042117235887));
#66368=CARTESIAN_POINT('Ctrl Pts',(-51.650238794436,-14.3978859537331,17.8542117235887));
#66369=CARTESIAN_POINT('Ctrl Pts',(-51.6499374336204,-14.4458116120497,
17.8517311518799));
#66370=CARTESIAN_POINT('Ctrl Pts',(-51.673532852059,-14.9990358635577,17.8230820767121));
#66371=CARTESIAN_POINT('Ctrl Pts',(-52.3387729531489,-15.9998443555804,
17.7682644980854));
#66372=CARTESIAN_POINT('Ctrl Pts',(-54.0595357659418,-15.9953385078432,
17.6897589877087));
#66373=CARTESIAN_POINT('Ctrl Pts',(-55.0050592474358,-14.557743765663,17.6112534773318));
#66374=CARTESIAN_POINT('Ctrl Pts',(-54.3274128937127,-12.9760039404155,
17.5327479669551));
#66375=CARTESIAN_POINT('Ctrl Pts',(-52.6343075214603,-12.6688220685915,
17.4542424565783));
#66376=CARTESIAN_POINT('Ctrl Pts',(-51.7321085269852,-13.6109301706732,
17.3947303754562));
#66377=CARTESIAN_POINT('Ctrl Pts',(-51.6515351015305,-14.2566054984256,
17.361386797793));
#66378=CARTESIAN_POINT('Ctrl Pts',(-51.652701124777,-14.3958311332085,17.3542117235887));
#66379=CARTESIAN_POINT('Ctrl Pts',(-51.6537934596095,-14.3955992295121,
17.8957882764113));
#66380=CARTESIAN_POINT('Ctrl Pts',(-51.6561292792194,-14.73752448157,17.8781885106897));
#66381=CARTESIAN_POINT('Ctrl Pts',(-51.9349899776299,-15.5924054167524,
17.8344202415091));
#66382=CARTESIAN_POINT('Ctrl Pts',(-53.3392724282712,-16.2080937050947,
17.7644834688697));
#66383=CARTESIAN_POINT('Ctrl Pts',(-54.7851641391705,-15.2764790675083,
17.6859779584929));
#66384=CARTESIAN_POINT('Ctrl Pts',(-54.8056647755616,-13.5555715973232,
17.6074724481161));
#66385=CARTESIAN_POINT('Ctrl Pts',(-53.3815155728066,-12.5897336831025,
17.5289669377393));
#66386=CARTESIAN_POINT('Ctrl Pts',(-51.9513720532365,-13.1783784136204,
17.458405547171));
#66387=CARTESIAN_POINT('Ctrl Pts',(-51.6558508817824,-14.0445039022943,
17.4140126600617));
#66388=CARTESIAN_POINT('Ctrl Pts',(-51.6531013855762,-14.3983675031589,
17.3957882764113));
#66389=CARTESIAN_POINT('Ctrl Pts',(-54.153252109211,-15.2223467977324,18.));
#66390=CARTESIAN_POINT('Ctrl Pts',(-54.4246171615437,-14.9072768995629,
17.9738314965411));
#66391=CARTESIAN_POINT('Ctrl Pts',(-54.6278752336732,-13.9937540324533,
17.9214944896232));
#66392=CARTESIAN_POINT('Ctrl Pts',(-53.6477056068469,-12.9776474013965,
17.8429889792464));
#66393=CARTESIAN_POINT('Ctrl Pts',(-52.2613397426835,-13.2376039347744,
17.7644834688697));
#66394=CARTESIAN_POINT('Ctrl Pts',(-51.7125907601688,-14.5359830763925,
17.6859779584929));
#66395=CARTESIAN_POINT('Ctrl Pts',(-52.4933400927667,-15.7105673519417,
17.6074724481161));
#66396=CARTESIAN_POINT('Ctrl Pts',(-53.903518042719,-15.7068747761389,17.5289669377394));
#66397=CARTESIAN_POINT('Ctrl Pts',(-54.6783815828028,-14.5287551705091,
17.4504614273625));
#66398=CARTESIAN_POINT('Ctrl Pts',(-54.1230453454191,-13.2325075949904,
17.3719559169858));
#66399=CARTESIAN_POINT('Ctrl Pts',(-52.7355328741211,-12.9807697615999,
17.293450406609));
#66400=CARTESIAN_POINT('Ctrl Pts',(-51.7602058672859,-13.9992407208286,
17.2149448962322));
#66401=CARTESIAN_POINT('Ctrl Pts',(-52.0717570426275,-15.3745639123133,
17.1364393858554));
#66402=CARTESIAN_POINT('Ctrl Pts',(-53.390781746669,-15.8733007472588,17.0579338754786));
#66403=CARTESIAN_POINT('Ctrl Pts',(-54.5343463517261,-15.0481801280675,
16.9794283651019));
#66404=CARTESIAN_POINT('Ctrl Pts',(-54.4768753865949,-13.6391859025932,
16.9009228547251));
#66405=CARTESIAN_POINT('Ctrl Pts',(-53.2699099545465,-12.9099395406961,
16.8224173443483));
#66406=CARTESIAN_POINT('Ctrl Pts',(-51.9958854602389,-13.5144455498356,
16.7439118339715));
#66407=CARTESIAN_POINT('Ctrl Pts',(-51.7973773032626,-14.9105690485955,
16.6654063235948));
#66408=CARTESIAN_POINT('Ctrl Pts',(-52.8524123453517,-15.8462330551256,
16.586900813218));
#66409=CARTESIAN_POINT('Ctrl Pts',(-54.2148100652166,-15.4823119617458,
16.5083953028412));
#66410=CARTESIAN_POINT('Ctrl Pts',(-54.6627398052285,-14.1451787985144,
16.4298897924644));
#66411=CARTESIAN_POINT('Ctrl Pts',(-53.7944875223078,-13.0340064035767,
16.3513842820877));
#66412=CARTESIAN_POINT('Ctrl Pts',(-52.3887225069356,-13.145320583037,16.2728787717108));
#66413=CARTESIAN_POINT('Ctrl Pts',(-51.706168244238,-14.3792921414933,16.1943732613341));
#66414=CARTESIAN_POINT('Ctrl Pts',(-52.3589556241958,-15.6292660458124,
16.1158677509573));
#66415=CARTESIAN_POINT('Ctrl Pts',(-53.7616494051484,-15.7742359839284,
16.0373622405805));
#66416=CARTESIAN_POINT('Ctrl Pts',(-54.6562804572666,-14.6841894679763,
15.9588567302037));
#66417=CARTESIAN_POINT('Ctrl Pts',(-54.2405223843948,-13.33670612834,15.880351219827));
#66418=CARTESIAN_POINT('Ctrl Pts',(-52.8872369102522,-12.9402410582164,
15.8018457094502));
#66419=CARTESIAN_POINT('Ctrl Pts',(-51.8100826208389,-13.8503535583387,
15.7233401990734));
#66420=CARTESIAN_POINT('Ctrl Pts',(-51.9750770902176,-15.2508331012045,
15.6448346886966));
#66421=CARTESIAN_POINT('Ctrl Pts',(-53.2342493568711,-15.885696339624,15.5663291783198));
#66422=CARTESIAN_POINT('Ctrl Pts',(-54.4583437946506,-15.1855828256918,
15.4878236679431));
#66423=CARTESIAN_POINT('Ctrl Pts',(-54.549563415235,-13.7783710083418,15.4093181575663));
#66424=CARTESIAN_POINT('Ctrl Pts',(-53.4261002848556,-12.9260818890411,
15.3308126471895));
#66425=CARTESIAN_POINT('Ctrl Pts',(-52.0955028666328,-13.393068633948,15.2523071368127));
#66426=CARTESIAN_POINT('Ctrl Pts',(-51.751082520038,-14.7605263839362,15.1738016264359));
#66427=CARTESIAN_POINT('Ctrl Pts',(-52.7017236774067,-15.8020866088358,
15.0952961160592));
#66428=CARTESIAN_POINT('Ctrl Pts',(-54.0948685923953,-15.5836531566747,
15.0167906056824));
#66429=CARTESIAN_POINT('Ctrl Pts',(-54.6811121004696,-14.3011227048956,
14.9382850953056));
#66430=CARTESIAN_POINT('Ctrl Pts',(-53.9346964498466,-13.1046983170808,
14.8597795849288));
#66431=CARTESIAN_POINT('Ctrl Pts',(-52.5250262261246,-13.0673633133234,
14.781274074552));
#66432=CARTESIAN_POINT('Ctrl Pts',(-51.7163246046947,-14.2225976133251,
14.7027685641753));
#66433=CARTESIAN_POINT('Ctrl Pts',(-52.2338596624079,-15.5343656873115,
14.6242630537985));
#66434=CARTESIAN_POINT('Ctrl Pts',(-53.6134830839557,-15.8262305186475,
14.5457575434217));
#66435=CARTESIAN_POINT('Ctrl Pts',(-54.6179371276052,-14.8364654611899,
14.4672520330449));
#66436=CARTESIAN_POINT('Ctrl Pts',(-54.3463604457024,-13.4526655408848,
14.3887465226682));
#66437=CARTESIAN_POINT('Ctrl Pts',(-53.0423964320333,-12.9159559714002,
14.3102410122914));
#66438=CARTESIAN_POINT('Ctrl Pts',(-51.8752954493436,-13.7074676781063,
14.2317355019146));
#66439=CARTESIAN_POINT('Ctrl Pts',(-51.8920958234221,-15.1177639193799,
14.1532299915378));
#66440=CARTESIAN_POINT('Ctrl Pts',(-53.0770150197731,-15.881229923416,14.074724481161));
#66441=CARTESIAN_POINT('Ctrl Pts',(-54.3688351006163,-15.3148479080822,
13.9962189707843));
#66442=CARTESIAN_POINT('Ctrl Pts',(-54.6060800258316,-13.9231151648839,
13.9177134604075));
#66443=CARTESIAN_POINT('Ctrl Pts',(-53.9234352130359,-13.2829324314546,
13.8653764534896));
#66444=CARTESIAN_POINT('Ctrl Pts',(-53.5217210200197,-13.1755371825403,
13.8392079500307));
#66445=CARTESIAN_POINT('Ctrl Pts',(-54.2235922564453,-15.2829297282066,
18.0535973499898));
#66446=CARTESIAN_POINT('Ctrl Pts',(-54.514879588223,-14.9447289570595,18.0274288465308));
#66447=CARTESIAN_POINT('Ctrl Pts',(-54.7330598623,-13.9641397611006,17.975091839613));
#66448=CARTESIAN_POINT('Ctrl Pts',(-53.68093103129,-12.8734356088235,17.8965863292362));
#66449=CARTESIAN_POINT('Ctrl Pts',(-52.192785045031,-13.1524768646333,17.8180808188594));
#66450=CARTESIAN_POINT('Ctrl Pts',(-51.6037496273957,-14.5461765785306,
17.7395753084826));
#66451=CARTESIAN_POINT('Ctrl Pts',(-52.441817712894,-15.8069930198213,17.6610697981059));
#66452=CARTESIAN_POINT('Ctrl Pts',(-53.95552395046,-15.8030293533737,17.5825642877291));
#66453=CARTESIAN_POINT('Ctrl Pts',(-54.7872741376805,-14.5384180355604,
17.5040587773523));
#66454=CARTESIAN_POINT('Ctrl Pts',(-54.1911678615169,-13.1470063767988,
17.4255532669755));
#66455=CARTESIAN_POINT('Ctrl Pts',(-52.7017910899008,-12.8767871972638,
17.3470477565988));
#66456=CARTESIAN_POINT('Ctrl Pts',(-51.6548604000807,-13.9700292549886,
17.268542246222));
#66457=CARTESIAN_POINT('Ctrl Pts',(-51.9892841211801,-15.4463218701793,
17.1900367358452));
#66458=CARTESIAN_POINT('Ctrl Pts',(-53.405145092541,-15.9816734958279,17.1115312254684));
#66459=CARTESIAN_POINT('Ctrl Pts',(-54.6326645526155,-15.0959766034206,
17.0330257150916));
#66460=CARTESIAN_POINT('Ctrl Pts',(-54.5709743535871,-13.5835409935271,
16.9545202047149));
#66461=CARTESIAN_POINT('Ctrl Pts',(-53.2753994915068,-12.8007569720048,
16.8760146943381));
#66462=CARTESIAN_POINT('Ctrl Pts',(-51.9078424226205,-13.4496428212774,
16.7975091839613));
#66463=CARTESIAN_POINT('Ctrl Pts',(-51.6947607789649,-14.9482627993849,
16.7190036735845));
#66464=CARTESIAN_POINT('Ctrl Pts',(-52.8272512735969,-15.9526186276675,
16.6404981632078));
#66465=CARTESIAN_POINT('Ctrl Pts',(-54.2896694929959,-15.5619802482706,
16.5619926528309));
#66466=CARTESIAN_POINT('Ctrl Pts',(-54.7704840181913,-14.1266813842457,
16.4834871424542));
#66467=CARTESIAN_POINT('Ctrl Pts',(-53.8384889487163,-12.9339322100829,
16.4049816320774));
#66468=CARTESIAN_POINT('Ctrl Pts',(-52.3295196215526,-13.0534185258236,
16.3264761217006));
#66469=CARTESIAN_POINT('Ctrl Pts',(-51.5968556021234,-14.377982170488,16.2479706113238));
#66470=CARTESIAN_POINT('Ctrl Pts',(-52.2975674015667,-15.7197229740698,
16.1694651009471));
#66471=CARTESIAN_POINT('Ctrl Pts',(-53.803240019476,-15.8753358877401,16.0909595905703));
#66472=CARTESIAN_POINT('Ctrl Pts',(-54.7635504568624,-14.7052635500685,
16.0124540801935));
#66473=CARTESIAN_POINT('Ctrl Pts',(-54.3172694834252,-13.2588546508992,
15.9339485698167));
#66474=CARTESIAN_POINT('Ctrl Pts',(-52.8646324857427,-12.8332830770114,
15.8554430594399));
#66475=CARTESIAN_POINT('Ctrl Pts',(-51.7083988580924,-13.8102115337131,
15.7769375490632));
#66476=CARTESIAN_POINT('Ctrl Pts',(-51.8855064050308,-15.3135073551311,
15.6984320386864));
#66477=CARTESIAN_POINT('Ctrl Pts',(-53.2371208691966,-15.994979111252,15.6199265283096));
#66478=CARTESIAN_POINT('Ctrl Pts',(-54.5510822638553,-15.2434667272446,
15.5414210179328));
#66479=CARTESIAN_POINT('Ctrl Pts',(-54.6489987776341,-13.7329443810606,
15.4629155075561));
#66480=CARTESIAN_POINT('Ctrl Pts',(-53.4430565430473,-12.8180844116938,
15.3844099971793));
#66481=CARTESIAN_POINT('Ctrl Pts',(-52.0147732460912,-13.3193550127907,
15.3059044868025));
#66482=CARTESIAN_POINT('Ctrl Pts',(-51.6450672618196,-14.787204744688,15.2273989764257));
#66483=CARTESIAN_POINT('Ctrl Pts',(-52.6654997892495,-15.9052311677249,
15.1488934660489));
#66484=CARTESIAN_POINT('Ctrl Pts',(-54.160922510703,-15.6707614123012,15.0703879556721));
#66485=CARTESIAN_POINT('Ctrl Pts',(-54.7902051164439,-14.2940739206327,
14.9918824452954));
#66486=CARTESIAN_POINT('Ctrl Pts',(-53.9889913219701,-13.0098139740974,
14.9133769349186));
#66487=CARTESIAN_POINT('Ctrl Pts',(-52.4758300853821,-12.9697380190954,
14.8348714245418));
#66488=CARTESIAN_POINT('Ctrl Pts',(-51.6077575923118,-14.2097839053763,
14.756365914165));
#66489=CARTESIAN_POINT('Ctrl Pts',(-52.1632875132312,-15.6178555008087,
14.6778604037883));
#66490=CARTESIAN_POINT('Ctrl Pts',(-53.644196060099,-15.9311476039325,14.5993548934115));
#66491=CARTESIAN_POINT('Ctrl Pts',(-54.7223921496577,-14.8687188932518,
14.5208493830347));
#66492=CARTESIAN_POINT('Ctrl Pts',(-54.4308776515139,-13.3833272297531,
14.4423438726579));
#66493=CARTESIAN_POINT('Ctrl Pts',(-53.0311830518934,-12.8072150992822,
14.3638383622811));
#66494=CARTESIAN_POINT('Ctrl Pts',(-51.778399289797,-13.6568356791444,14.2853328519043));
#66495=CARTESIAN_POINT('Ctrl Pts',(-51.7964330642132,-15.1706688923949,
14.2068273415276));
#66496=CARTESIAN_POINT('Ctrl Pts',(-53.0683431650544,-15.9901847928655,
14.1283218311508));
#66497=CARTESIAN_POINT('Ctrl Pts',(-54.4550022843884,-15.3822218123885,
14.049816320774));
#66498=CARTESIAN_POINT('Ctrl Pts',(-54.70966455814,-13.888314937391,13.9713108103972));
#66499=CARTESIAN_POINT('Ctrl Pts',(-53.9769033408726,-13.2011331552573,
13.9189738034794));
#66500=CARTESIAN_POINT('Ctrl Pts',(-53.5456972794617,-13.0858534785527,
13.8928053000205));
#66501=CARTESIAN_POINT('Ctrl Pts',(-54.2939324036796,-15.3435126586807,
18.1071946999795));
#66502=CARTESIAN_POINT('Ctrl Pts',(-54.6051420149022,-14.9821810145562,
18.0810261965206));
#66503=CARTESIAN_POINT('Ctrl Pts',(-54.8382444909268,-13.934525489748,18.0286891896028));
#66504=CARTESIAN_POINT('Ctrl Pts',(-53.7141564557331,-12.7692238162505,
17.950183679226));
#66505=CARTESIAN_POINT('Ctrl Pts',(-52.1242303473785,-13.0673497944923,
17.8716781688492));
#66506=CARTESIAN_POINT('Ctrl Pts',(-51.4949084946225,-14.5563700806686,
17.7931726584724));
#66507=CARTESIAN_POINT('Ctrl Pts',(-52.3902953330214,-15.9034186877009,
17.7146671480956));
#66508=CARTESIAN_POINT('Ctrl Pts',(-54.0075298582009,-15.8991839306084,
17.6361616377189));
#66509=CARTESIAN_POINT('Ctrl Pts',(-54.8961666925581,-14.5480809006117,
17.5576561273421));
#66510=CARTESIAN_POINT('Ctrl Pts',(-54.2592903776148,-13.0615051586072,
17.4791506169653));
#66511=CARTESIAN_POINT('Ctrl Pts',(-52.6680493056806,-12.7728046329277,
17.4006451065885));
#66512=CARTESIAN_POINT('Ctrl Pts',(-51.5495149328755,-13.9408177891487,
17.3221395962117));
#66513=CARTESIAN_POINT('Ctrl Pts',(-51.9068111997328,-15.5180798280453,
17.243634085835));
#66514=CARTESIAN_POINT('Ctrl Pts',(-53.419508438413,-16.090046244397,17.1651285754582));
#66515=CARTESIAN_POINT('Ctrl Pts',(-54.7309827535048,-15.1437730787738,
17.0866230650814));
#66516=CARTESIAN_POINT('Ctrl Pts',(-54.6650733205792,-13.5278960844609,
17.0081175547046));
#66517=CARTESIAN_POINT('Ctrl Pts',(-53.2808890284672,-12.6915744033134,
16.9296120443278));
#66518=CARTESIAN_POINT('Ctrl Pts',(-51.819799385002,-13.3848400927192,16.8511065339511));
#66519=CARTESIAN_POINT('Ctrl Pts',(-51.5921442546672,-14.9859565501742,
16.7726010235743));
#66520=CARTESIAN_POINT('Ctrl Pts',(-52.8020902018422,-16.0590042002094,
16.6940955131975));
#66521=CARTESIAN_POINT('Ctrl Pts',(-54.3645289207752,-15.6416485347953,
16.6155900028207));
#66522=CARTESIAN_POINT('Ctrl Pts',(-54.878228231154,-14.108183969977,16.5370844924439));
#66523=CARTESIAN_POINT('Ctrl Pts',(-53.8824903751248,-12.8338580165892,
16.4585789820672));
#66524=CARTESIAN_POINT('Ctrl Pts',(-52.2703167361696,-12.9615164686102,
16.3800734716904));
#66525=CARTESIAN_POINT('Ctrl Pts',(-51.4875429600088,-14.3766721994827,
16.3015679613136));
#66526=CARTESIAN_POINT('Ctrl Pts',(-52.2361791789376,-15.8101799023271,
16.2230624509368));
#66527=CARTESIAN_POINT('Ctrl Pts',(-53.8448306338036,-15.9764357915517,
16.1445569405601));
#66528=CARTESIAN_POINT('Ctrl Pts',(-54.8708204564582,-14.7263376321606,
16.0660514301833));
#66529=CARTESIAN_POINT('Ctrl Pts',(-54.3940165824557,-13.1810031734583,
15.9875459198065));
#66530=CARTESIAN_POINT('Ctrl Pts',(-52.8420280612331,-12.7263250958063,
15.9090404094297));
#66531=CARTESIAN_POINT('Ctrl Pts',(-51.6067150953462,-13.7700695090875,
15.8305348990529));
#66532=CARTESIAN_POINT('Ctrl Pts',(-51.7959357198438,-15.3761816090578,
15.7520293886762));
#66533=CARTESIAN_POINT('Ctrl Pts',(-53.2399923815221,-16.1042618828799,
15.6735238782994));
#66534=CARTESIAN_POINT('Ctrl Pts',(-54.6438207330599,-15.3013506287974,
15.5950183679226));
#66535=CARTESIAN_POINT('Ctrl Pts',(-54.7484341400332,-13.6875177537793,
15.5165128575458));
#66536=CARTESIAN_POINT('Ctrl Pts',(-53.460012801239,-12.7100869343466,15.438007347169));
#66537=CARTESIAN_POINT('Ctrl Pts',(-51.9340436255495,-13.2456413916334,
15.3595018367923));
#66538=CARTESIAN_POINT('Ctrl Pts',(-51.5390520036012,-14.8138831054396,
15.2809963264155));
#66539=CARTESIAN_POINT('Ctrl Pts',(-52.6292759010924,-16.0083757266141,
15.2024908160387));
#66540=CARTESIAN_POINT('Ctrl Pts',(-54.2269764290105,-15.7578696679277,
15.1239853056619));
#66541=CARTESIAN_POINT('Ctrl Pts',(-54.8992981324183,-14.2870251363698,
15.0454797952851));
#66542=CARTESIAN_POINT('Ctrl Pts',(-54.0432861940934,-12.914929631114,14.9669742849084));
#66543=CARTESIAN_POINT('Ctrl Pts',(-52.4266339446397,-12.8721127248673,
14.8884687745316));
#66544=CARTESIAN_POINT('Ctrl Pts',(-51.4991905799289,-14.1969701974275,
14.8099632641548));
#66545=CARTESIAN_POINT('Ctrl Pts',(-52.0927153640546,-15.7013453143059,
14.731457753778));
#66546=CARTESIAN_POINT('Ctrl Pts',(-53.6749090362423,-16.0360646892175,
14.6529522434013));
#66547=CARTESIAN_POINT('Ctrl Pts',(-54.8268471717101,-14.9009723253137,
14.5744467330245));
#66548=CARTESIAN_POINT('Ctrl Pts',(-54.5153948573255,-13.3139889186213,
14.4959412226477));
#66549=CARTESIAN_POINT('Ctrl Pts',(-53.0199696717534,-12.6984742271642,
14.4174357122709));
#66550=CARTESIAN_POINT('Ctrl Pts',(-51.6815031302505,-13.6062036801825,
14.3389302018941));
#66551=CARTESIAN_POINT('Ctrl Pts',(-51.7007703050042,-15.22357386541,14.2604246915173));
#66552=CARTESIAN_POINT('Ctrl Pts',(-53.0596713103357,-16.099139662315,14.1819191811406));
#66553=CARTESIAN_POINT('Ctrl Pts',(-54.5411694681605,-15.4495957166949,
14.1034136707638));
#66554=CARTESIAN_POINT('Ctrl Pts',(-54.8132490904484,-13.853514709898,14.024908160387));
#66555=CARTESIAN_POINT('Ctrl Pts',(-54.0303714687093,-13.11933387906,13.9725711534692));
#66556=CARTESIAN_POINT('Ctrl Pts',(-53.5696735389038,-12.996169774565,13.9464026500102));
#66557=CARTESIAN_POINT('Ctrl Pts',(-54.3642725509138,-15.4040955891549,
18.1607920499693));
#66558=CARTESIAN_POINT('Ctrl Pts',(-54.6954044415815,-15.0196330720529,
18.1346235465104));
#66559=CARTESIAN_POINT('Ctrl Pts',(-54.9434291195537,-13.9049112183953,
18.0822865395925));
#66560=CARTESIAN_POINT('Ctrl Pts',(-53.7473818801761,-12.6650120236775,
18.0037810292157));
#66561=CARTESIAN_POINT('Ctrl Pts',(-52.055675649726,-12.9822227243512,17.925275518839));
#66562=CARTESIAN_POINT('Ctrl Pts',(-51.3860673618493,-14.5665635828067,
17.8467700084622));
#66563=CARTESIAN_POINT('Ctrl Pts',(-52.3387729531489,-15.9998443555804,
17.7682644980854));
#66564=CARTESIAN_POINT('Ctrl Pts',(-54.0595357659418,-15.9953385078432,
17.6897589877087));
#66565=CARTESIAN_POINT('Ctrl Pts',(-55.0050592474358,-14.557743765663,17.6112534773318));
#66566=CARTESIAN_POINT('Ctrl Pts',(-54.3274128937127,-12.9760039404155,
17.5327479669551));
#66567=CARTESIAN_POINT('Ctrl Pts',(-52.6343075214603,-12.6688220685915,
17.4542424565783));
#66568=CARTESIAN_POINT('Ctrl Pts',(-51.4441694656704,-13.9116063233087,
17.3757369462015));
#66569=CARTESIAN_POINT('Ctrl Pts',(-51.8243382782854,-15.5898377859113,
17.2972314358247));
#66570=CARTESIAN_POINT('Ctrl Pts',(-53.4338717842849,-16.1984189929661,
17.218725925448));
#66571=CARTESIAN_POINT('Ctrl Pts',(-54.829300954394,-15.1915695541269,17.1402204150712));
#66572=CARTESIAN_POINT('Ctrl Pts',(-54.7591722875713,-13.4722511753948,
17.0617149046944));
#66573=CARTESIAN_POINT('Ctrl Pts',(-53.2863785654275,-12.582391834622,16.9832093943176));
#66574=CARTESIAN_POINT('Ctrl Pts',(-51.7317563473836,-13.320037364161,16.9047038839409));
#66575=CARTESIAN_POINT('Ctrl Pts',(-51.4895277303695,-15.0236503009635,
16.8261983735641));
#66576=CARTESIAN_POINT('Ctrl Pts',(-52.7769291300874,-16.1653897727513,
16.7476928631873));
#66577=CARTESIAN_POINT('Ctrl Pts',(-54.4393883485545,-15.72131682132,16.6691873528105));
#66578=CARTESIAN_POINT('Ctrl Pts',(-54.9859724441167,-14.0896865557083,
16.5906818424337));
#66579=CARTESIAN_POINT('Ctrl Pts',(-53.9264918015333,-12.7337838230954,
16.5121763320569));
#66580=CARTESIAN_POINT('Ctrl Pts',(-52.2111138507866,-12.8696144113969,
16.4336708216802));
#66581=CARTESIAN_POINT('Ctrl Pts',(-51.3782303178942,-14.3753622284773,
16.3551653113034));
#66582=CARTESIAN_POINT('Ctrl Pts',(-52.1747909563085,-15.9006368305844,
16.2766598009266));
#66583=CARTESIAN_POINT('Ctrl Pts',(-53.8864212481312,-16.0775356953633,
16.1981542905498));
#66584=CARTESIAN_POINT('Ctrl Pts',(-54.978090456054,-14.7474117142528,16.119648780173));
#66585=CARTESIAN_POINT('Ctrl Pts',(-54.4707636814861,-13.1031516960174,
16.0411432697963));
#66586=CARTESIAN_POINT('Ctrl Pts',(-52.8194236367236,-12.6193671146013,
15.9626377594195));
#66587=CARTESIAN_POINT('Ctrl Pts',(-51.5050313325997,-13.7299274844619,
15.8841322490427));
#66588=CARTESIAN_POINT('Ctrl Pts',(-51.706365034657,-15.4388558629844,15.8056267386659));
#66589=CARTESIAN_POINT('Ctrl Pts',(-53.2428638938474,-16.2135446545079,
15.7271212282891));
#66590=CARTESIAN_POINT('Ctrl Pts',(-54.7365592022647,-15.3592345303502,
15.6486157179124));
#66591=CARTESIAN_POINT('Ctrl Pts',(-54.8478695024322,-13.6420911264981,
15.5701102075356));
#66592=CARTESIAN_POINT('Ctrl Pts',(-53.4769690594307,-12.6020894569994,
15.4916046971588));
#66593=CARTESIAN_POINT('Ctrl Pts',(-51.8533140050079,-13.1719277704761,
15.413099186782));
#66594=CARTESIAN_POINT('Ctrl Pts',(-51.4330367453828,-14.8405614661914,
15.3345936764053));
#66595=CARTESIAN_POINT('Ctrl Pts',(-52.5930520129352,-16.1115202855033,
15.2560881660285));
#66596=CARTESIAN_POINT('Ctrl Pts',(-54.2930303473181,-15.8449779235543,
15.1775826556517));
#66597=CARTESIAN_POINT('Ctrl Pts',(-55.0083911483927,-14.2799763521069,
15.0990771452749));
#66598=CARTESIAN_POINT('Ctrl Pts',(-54.0975810662168,-12.8200452881305,
15.0205716348981));
#66599=CARTESIAN_POINT('Ctrl Pts',(-52.3774378038974,-12.7744874306393,
14.9420661245214));
#66600=CARTESIAN_POINT('Ctrl Pts',(-51.3906235675459,-14.1841564894788,
14.8635606141446));
#66601=CARTESIAN_POINT('Ctrl Pts',(-52.0221432148781,-15.784835127803,14.7850551037678));
#66602=CARTESIAN_POINT('Ctrl Pts',(-53.7056220123855,-16.1409817745025,
14.706549593391));
#66603=CARTESIAN_POINT('Ctrl Pts',(-54.9313021937626,-14.9332257573755,
14.6280440830142));
#66604=CARTESIAN_POINT('Ctrl Pts',(-54.599912063137,-13.2446506074896,14.5495385726375));
#66605=CARTESIAN_POINT('Ctrl Pts',(-53.0087562916135,-12.5897333550461,
14.4710330622607));
#66606=CARTESIAN_POINT('Ctrl Pts',(-51.584606970704,-13.5555716812206,14.3925275518839));
#66607=CARTESIAN_POINT('Ctrl Pts',(-51.6051075457953,-15.276478838425,14.3140220415071));
#66608=CARTESIAN_POINT('Ctrl Pts',(-53.0509994556171,-16.2080945317645,
14.2355165311303));
#66609=CARTESIAN_POINT('Ctrl Pts',(-54.6273366519326,-15.5169696210013,
14.1570110207536));
#66610=CARTESIAN_POINT('Ctrl Pts',(-54.9168336227569,-13.8187144824051,
14.0785055103768));
#66611=CARTESIAN_POINT('Ctrl Pts',(-54.083839596546,-13.0375346028626,14.0261685034589));
#66612=CARTESIAN_POINT('Ctrl Pts',(-53.5936497983459,-12.9064860705774,
14.));
#66613=CARTESIAN_POINT('Ctrl Pts',(-51.9310991161132,-14.3960665614756,
17.1934196736194));
#66614=CARTESIAN_POINT('Ctrl Pts',(-51.9301435513723,-14.2819701161204,
17.2005947478237));
#66615=CARTESIAN_POINT('Ctrl Pts',(-51.944352401566,-14.1681074628443,17.2077698220279));
#66616=CARTESIAN_POINT('Ctrl Pts',(-51.9746855643153,-14.0587160928713,
17.2149448962322));
#66617=CARTESIAN_POINT('Ctrl Pts',(-52.0853148695643,-13.6597504010857,
17.2411133996911));
#66618=CARTESIAN_POINT('Ctrl Pts',(-52.4104238718427,-13.3202600813428,
17.26728190315));
#66619=CARTESIAN_POINT('Ctrl Pts',(-52.8042304515315,-13.1924712270364,
17.293450406609));
#66620=CARTESIAN_POINT('Ctrl Pts',(-53.1980370312204,-13.0646823727301,
17.3196189100679));
#66621=CARTESIAN_POINT('Ctrl Pts',(-53.6605411883197,-13.1485949838602,
17.3457874135268));
#66622=CARTESIAN_POINT('Ctrl Pts',(-53.9843493064334,-13.4065925520117,
17.3719559169858));
#66623=CARTESIAN_POINT('Ctrl Pts',(-54.308157424547,-13.6645901201633,17.3981244204447));
#66624=CARTESIAN_POINT('Ctrl Pts',(-54.4932695036749,-14.0966726453362,
17.4242929239036));
#66625=CARTESIAN_POINT('Ctrl Pts',(-54.4566816198916,-14.5090671755276,
17.4504614273625));
#66626=CARTESIAN_POINT('Ctrl Pts',(-54.4200937361082,-14.921461705719,17.4766299308214));
#66627=CARTESIAN_POINT('Ctrl Pts',(-54.1618058894136,-15.314168240929,17.5027984342804));
#66628=CARTESIAN_POINT('Ctrl Pts',(-53.7976323077409,-15.5111369378344,
17.5289669377393));
#66629=CARTESIAN_POINT('Ctrl Pts',(-53.4334587260682,-15.7081056347398,
17.5551354411983));
#66630=CARTESIAN_POINT('Ctrl Pts',(-52.9633994094174,-15.7093364933408,
17.5813039446572));
#66631=CARTESIAN_POINT('Ctrl Pts',(-52.5982448623257,-15.5141878767164,
17.6074724481161));
#66632=CARTESIAN_POINT('Ctrl Pts',(-52.233090315234,-15.319039260092,17.633640951575));
#66633=CARTESIAN_POINT('Ctrl Pts',(-51.9728405377014,-14.9275111682423,
17.659809455034));
#66634=CARTESIAN_POINT('Ctrl Pts',(-51.9341738126876,-14.5153505987144,
17.6859779584929));
#66635=CARTESIAN_POINT('Ctrl Pts',(-51.9305085062518,-14.4762809648747,
17.6884585302017));
#66636=CARTESIAN_POINT('Ctrl Pts',(-51.9288342506125,-14.4370259363911,
17.6909391019106));
#66637=CARTESIAN_POINT('Ctrl Pts',(-51.929081218047,-14.3977505022101,17.6934196736194));
#66638=CARTESIAN_POINT('Ctrl Pts',(-52.7966221146314,-12.9064860705774,
18.));
#66639=CARTESIAN_POINT('Ctrl Pts',(-52.3064323164313,-13.0375346028627,
17.9738314965411));
#66640=CARTESIAN_POINT('Ctrl Pts',(-51.4734379005318,-13.818711947887,17.9214944896232));
#66641=CARTESIAN_POINT('Ctrl Pts',(-51.7629355980163,-15.5169705450585,
17.8429889792465));
#66642=CARTESIAN_POINT('Ctrl Pts',(-53.3392724282712,-16.2080937050947,
17.7644834688697));
#66643=CARTESIAN_POINT('Ctrl Pts',(-54.7851641391705,-15.2764790675083,
17.6859779584929));
#66644=CARTESIAN_POINT('Ctrl Pts',(-54.8056647755616,-13.5555715973232,
17.6074724481161));
#66645=CARTESIAN_POINT('Ctrl Pts',(-53.3815155728066,-12.5897336831025,
17.5289669377393));
#66646=CARTESIAN_POINT('Ctrl Pts',(-51.7903600412662,-13.244650694059,17.4504614273625));
#66647=CARTESIAN_POINT('Ctrl Pts',(-51.4589699241079,-14.9332257213623,
17.3719559169858));
#66648=CARTESIAN_POINT('Ctrl Pts',(-52.6846499703254,-16.1409815416267,
17.293450406609));
#66649=CARTESIAN_POINT('Ctrl Pts',(-54.3681285487899,-15.7848349642756,
17.2149448962322));
#66650=CARTESIAN_POINT('Ctrl Pts',(-54.9996481235109,-14.1841565112764,
17.1364393858554));
#66651=CARTESIAN_POINT('Ctrl Pts',(-54.0128340063977,-12.7744876345319,
17.0579338754786));
#66652=CARTESIAN_POINT('Ctrl Pts',(-52.292690959438,-12.8200454826231,16.9794283651019));
#66653=CARTESIAN_POINT('Ctrl Pts',(-51.3818809893341,-14.2799763673288,
16.9009228547251));
#66654=CARTESIAN_POINT('Ctrl Pts',(-52.0972417021453,-15.8449777434614,
16.8224173443483));
#66655=CARTESIAN_POINT('Ctrl Pts',(-53.7972198251955,-16.11152007286,16.7439118339715));
#66656=CARTESIAN_POINT('Ctrl Pts',(-54.9572349488979,-14.8405614110472,
16.6654063235947));
#66657=CARTESIAN_POINT('Ctrl Pts',(-54.5369577413632,-13.1719279226262,
16.586900813218));
#66658=CARTESIAN_POINT('Ctrl Pts',(-52.9133028885493,-12.602089679815,16.5083953028412));
#66659=CARTESIAN_POINT('Ctrl Pts',(-51.5424026157113,-13.6420912202446,
16.4298897924644));
#66660=CARTESIAN_POINT('Ctrl Pts',(-51.6537129020729,-15.359234410906,16.3513842820876));
#66661=CARTESIAN_POINT('Ctrl Pts',(-53.1474080250528,-16.2135444290179,
16.2728787717108));
#66662=CARTESIAN_POINT('Ctrl Pts',(-54.6839066935018,-15.4388557336608,
16.1943732613341));
#66663=CARTESIAN_POINT('Ctrl Pts',(-54.8852403705632,-13.7299275672916,
16.1158677509573));
#66664=CARTESIAN_POINT('Ctrl Pts',(-53.570848229612,-12.6193673352972,16.0373622405805));
#66665=CARTESIAN_POINT('Ctrl Pts',(-51.9195083898505,-13.1031518566562,
15.9588567302037));
#66666=CARTESIAN_POINT('Ctrl Pts',(-51.4121816782638,-14.7474116707683,
15.8803512198269));
#66667=CARTESIAN_POINT('Ctrl Pts',(-52.503850750664,-16.077535486755,15.8018457094502));
#66668=CARTESIAN_POINT('Ctrl Pts',(-54.2154808300007,-15.9006366439348,
15.7233401990734));
#66669=CARTESIAN_POINT('Ctrl Pts',(-55.0120413695279,-14.3753622311824,
15.6448346886966));
#66670=CARTESIAN_POINT('Ctrl Pts',(-54.1791579400319,-12.8696146010229,
15.5663291783198));
#66671=CARTESIAN_POINT('Ctrl Pts',(-52.4637802022359,-12.7337840295961,
15.4878236679431));
#66672=CARTESIAN_POINT('Ctrl Pts',(-51.4042996911802,-14.0896865938602,
15.4093181575663));
#66673=CARTESIAN_POINT('Ctrl Pts',(-51.9508837188856,-15.7213166569629,
15.3308126471895));
#66674=CARTESIAN_POINT('Ctrl Pts',(-53.6133427309768,-16.1653895531783,
15.2523071368127));
#66675=CARTESIAN_POINT('Ctrl Pts',(-54.9007439708605,-15.0236502232965,
15.1738016264359));
#66676=CARTESIAN_POINT('Ctrl Pts',(-54.6585153839456,-13.3200374976642,
15.0952961160592));
#66677=CARTESIAN_POINT('Ctrl Pts',(-53.1038933588347,-12.5823920603089,
15.0167906056824));
#66678=CARTESIAN_POINT('Ctrl Pts',(-51.6310998196598,-13.4722512894541,
14.9382850953056));
#66679=CARTESIAN_POINT('Ctrl Pts',(-51.5609711612584,-15.1915694569347,
14.8597795849288));
#66680=CARTESIAN_POINT('Ctrl Pts',(-52.9564001587445,-16.1984187666639,
14.7812740745521));
#66681=CARTESIAN_POINT('Ctrl Pts',(-54.5659334636339,-15.5898376428623,
14.7027685641752));
#66682=CARTESIAN_POINT('Ctrl Pts',(-54.9461022318155,-13.911606374279,14.6242630537985));
#66683=CARTESIAN_POINT('Ctrl Pts',(-53.7559643179139,-12.6688223002735,
14.5457575434217));
#66684=CARTESIAN_POINT('Ctrl Pts',(-52.0628591682458,-12.9760040856147,
14.4672520330449));
#66685=CARTESIAN_POINT('Ctrl Pts',(-51.3852128724656,-14.5577438020024,
14.3887465226681));
#66686=CARTESIAN_POINT('Ctrl Pts',(-52.3307362917628,-15.9953382094595,
14.3102410122914));
#66687=CARTESIAN_POINT('Ctrl Pts',(-54.0514987748276,-15.9998443309588,
14.2317355019146));
#66688=CARTESIAN_POINT('Ctrl Pts',(-55.0042044918326,-14.5665632650764,
14.1532299915378));
#66689=CARTESIAN_POINT('Ctrl Pts',(-54.3345957734336,-12.9822233909153,
14.074724481161));
#66690=CARTESIAN_POINT('Ctrl Pts',(-52.642890831849,-12.6650114501325,13.9962189707843));
#66691=CARTESIAN_POINT('Ctrl Pts',(-51.4468410434119,-13.9049130927216,
13.9177134604075));
#66692=CARTESIAN_POINT('Ctrl Pts',(-51.6948674713958,-15.0196330720529,
13.8653764534896));
#66693=CARTESIAN_POINT('Ctrl Pts',(-52.0259993620635,-15.404095589155,13.8392079500307));
#66694=CARTESIAN_POINT('Ctrl Pts',(-52.8205983740734,-12.996169774565,18.0535973499898));
#66695=CARTESIAN_POINT('Ctrl Pts',(-52.359900444268,-13.11933387906,18.0274288465308));
#66696=CARTESIAN_POINT('Ctrl Pts',(-51.5770224562855,-13.8535123278671,
17.975091839613));
#66697=CARTESIAN_POINT('Ctrl Pts',(-51.8491027615148,-15.449596585157,17.8965863292362));
#66698=CARTESIAN_POINT('Ctrl Pts',(-53.3306005753026,-16.0991388853812,
17.8180808188594));
#66699=CARTESIAN_POINT('Ctrl Pts',(-54.6895013936797,-15.2235740807106,
17.7395753084826));
#66700=CARTESIAN_POINT('Ctrl Pts',(-54.7087686260451,-13.6062036013328,
17.6610697981059));
#66701=CARTESIAN_POINT('Ctrl Pts',(-53.370302195588,-12.6984745354833,17.5825642877291));
#66702=CARTESIAN_POINT('Ctrl Pts',(-51.8748772355608,-13.3139889999824,
17.5040587773523));
#66703=CARTESIAN_POINT('Ctrl Pts',(-51.5634249338331,-14.9009722914672,
17.4255532669756));
#66704=CARTESIAN_POINT('Ctrl Pts',(-52.7153629422732,-16.0360644703525,
17.3470477565987));
#66705=CARTESIAN_POINT('Ctrl Pts',(-54.2975564085964,-15.7013451606169,
17.268542246222));
#66706=CARTESIAN_POINT('Ctrl Pts',(-54.8910811244797,-14.1969702179137,
17.1900367358452));
#66707=CARTESIAN_POINT('Ctrl Pts',(-53.9636378718331,-12.8721129164929,
17.1115312254684));
#66708=CARTESIAN_POINT('Ctrl Pts',(-52.3469858247822,-12.9149298139051,
17.0330257150916));
#66709=CARTESIAN_POINT('Ctrl Pts',(-51.4909739917866,-14.2870251506759,
16.9545202047148));
#66710=CARTESIAN_POINT('Ctrl Pts',(-52.1632956122412,-15.75786949867,16.8760146943381));
#66711=CARTESIAN_POINT('Ctrl Pts',(-53.7609959415414,-16.0083755267644,
16.7975091839613));
#66712=CARTESIAN_POINT('Ctrl Pts',(-54.8512197038372,-14.8138830536132,
16.7190036735845));
#66713=CARTESIAN_POINT('Ctrl Pts',(-54.4562281308453,-13.2456415346295,
16.6404981632077));
#66714=CARTESIAN_POINT('Ctrl Pts',(-52.9302591446351,-12.7100871437567,
16.561992652831));
#66715=CARTESIAN_POINT('Ctrl Pts',(-51.6418379657667,-13.6875178418857,
16.4834871424542));
#66716=CARTESIAN_POINT('Ctrl Pts',(-51.7464513597646,-15.3013505165395,
16.4049816320774));
#66717=CARTESIAN_POINT('Ctrl Pts',(-53.1502795370219,-16.1042616709564,
16.3264761217006));
#66718=CARTESIAN_POINT('Ctrl Pts',(-54.5943360194343,-15.3761814875148,
16.2479706113238));
#66719=CARTESIAN_POINT('Ctrl Pts',(-54.7835566204401,-13.7700695869338,
16.1694651009471));
#66720=CARTESIAN_POINT('Ctrl Pts',(-53.5482438079087,-12.7263253032243,
16.0909595905703));
#66721=CARTESIAN_POINT('Ctrl Pts',(-51.9962554793534,-13.1810033244324,
16.0124540801935));
#66722=CARTESIAN_POINT('Ctrl Pts',(-51.5194516645429,-14.7263375912924,
15.9339485698167));
#66723=CARTESIAN_POINT('Ctrl Pts',(-52.5454413598283,-15.9764355954941,
15.8554430594399));
#66724=CARTESIAN_POINT('Ctrl Pts',(-54.1540926149925,-15.8101797269071,
15.7769375490632));
#66725=CARTESIAN_POINT('Ctrl Pts',(-54.9027287409836,-14.376672202025,15.6984320386864));
#66726=CARTESIAN_POINT('Ctrl Pts',(-54.1199550619985,-12.9615166468276,
15.6199265283096));
#66727=CARTESIAN_POINT('Ctrl Pts',(-52.507781623182,-12.8338582106659,15.5414210179328));
#66728=CARTESIAN_POINT('Ctrl Pts',(-51.5120438907672,-14.1081840058335,
15.462915507556));
#66729=CARTESIAN_POINT('Ctrl Pts',(-52.0257431373717,-15.6416483803266,
15.3844099971793));
#66730=CARTESIAN_POINT('Ctrl Pts',(-53.5881816623453,-16.0590039938468,
15.3059044868025));
#66731=CARTESIAN_POINT('Ctrl Pts',(-54.7981274593024,-14.98595647718,15.2273989764257));
#66732=CARTESIAN_POINT('Ctrl Pts',(-54.5704723572559,-13.3848402181903,
15.1488934660489));
#66733=CARTESIAN_POINT('Ctrl Pts',(-53.1093828951161,-12.691574615422,15.0703879556721));
#66734=CARTESIAN_POINT('Ctrl Pts',(-51.7251987749648,-13.5278961916579,
14.9918824452954));
#66735=CARTESIAN_POINT('Ctrl Pts',(-51.659289349954,-15.143772987429,14.9133769349186));
#66736=CARTESIAN_POINT('Ctrl Pts',(-52.9707635028084,-16.0900460317101,
14.8348714245418));
#66737=CARTESIAN_POINT('Ctrl Pts',(-54.4834605524782,-15.5180796936027,
14.756365914165));
#66738=CARTESIAN_POINT('Ctrl Pts',(-54.8407567775752,-13.9408178370524,
14.6778604037883));
#66739=CARTESIAN_POINT('Ctrl Pts',(-53.7222225381219,-12.7728048506706,
14.5993548934115));
#66740=CARTESIAN_POINT('Ctrl Pts',(-52.1309816753803,-13.0615052950706,
14.5208493830347));
#66741=CARTESIAN_POINT('Ctrl Pts',(-51.4941054148939,-14.5480809347647,
14.4423438726579));
#66742=CARTESIAN_POINT('Ctrl Pts',(-52.3827421907963,-15.8991836501767,
14.3638383622811));
#66743=CARTESIAN_POINT('Ctrl Pts',(-53.9999764060854,-15.9034186645606,
14.2853328519044));
#66744=CARTESIAN_POINT('Ctrl Pts',(-54.8953633626269,-14.5563697820543,
14.2068273415276));
#66745=CARTESIAN_POINT('Ctrl Pts',(-54.2660411052506,-13.0673504209531,
14.1283218311508));
#66746=CARTESIAN_POINT('Ctrl Pts',(-52.676116208218,-12.7692232772124,14.049816320774));
#66747=CARTESIAN_POINT('Ctrl Pts',(-51.5520257773267,-13.934527251307,13.9713108103972));
#66748=CARTESIAN_POINT('Ctrl Pts',(-51.7851298980751,-14.9821810145562,
13.9189738034794));
#66749=CARTESIAN_POINT('Ctrl Pts',(-52.0963395092977,-15.3435126586808,
13.8928053000205));
#66750=CARTESIAN_POINT('Ctrl Pts',(-52.8445746335155,-13.0858534785527,
18.1071946999795));
#66751=CARTESIAN_POINT('Ctrl Pts',(-52.4133685721046,-13.2011331552573,
18.0810261965206));
#66752=CARTESIAN_POINT('Ctrl Pts',(-51.6806070120392,-13.8883127078473,
18.0286891896027));
#66753=CARTESIAN_POINT('Ctrl Pts',(-51.9352699250133,-15.3822226252554,
17.950183679226));
#66754=CARTESIAN_POINT('Ctrl Pts',(-53.3219287223341,-15.9901840656676,
17.8716781688492));
#66755=CARTESIAN_POINT('Ctrl Pts',(-54.5938386481889,-15.1706690939129,
17.7931726584724));
#66756=CARTESIAN_POINT('Ctrl Pts',(-54.6118724765287,-13.6568356053423,
17.7146671480956));
#66757=CARTESIAN_POINT('Ctrl Pts',(-53.3590888183695,-12.8072153878641,
17.6361616377188));
#66758=CARTESIAN_POINT('Ctrl Pts',(-51.9593944298553,-13.3833273059057,
17.5576561273421));
#66759=CARTESIAN_POINT('Ctrl Pts',(-51.6678799435583,-14.868718861572,17.4791506169653));
#66760=CARTESIAN_POINT('Ctrl Pts',(-52.7460759142211,-15.9311473990782,
17.4006451065885));
#66761=CARTESIAN_POINT('Ctrl Pts',(-54.2269842684028,-15.6178553569582,
17.3221395962117));
#66762=CARTESIAN_POINT('Ctrl Pts',(-54.7825141254484,-14.2097839245511,
17.243634085835));
#66763=CARTESIAN_POINT('Ctrl Pts',(-53.9144417372685,-12.9697381984539,
17.1651285754582));
#66764=CARTESIAN_POINT('Ctrl Pts',(-52.4012806901265,-13.009814145187,17.0866230650814));
#66765=CARTESIAN_POINT('Ctrl Pts',(-51.6000669942391,-14.2940739340229,
17.0081175547046));
#66766=CARTESIAN_POINT('Ctrl Pts',(-52.2293495223373,-15.6707612538786,
16.9296120443279));
#66767=CARTESIAN_POINT('Ctrl Pts',(-53.7247720578873,-15.9052309806687,
16.8511065339511));
#66768=CARTESIAN_POINT('Ctrl Pts',(-54.7452044587765,-14.7872046961792,
16.7726010235743));
#66769=CARTESIAN_POINT('Ctrl Pts',(-54.3754985203273,-13.3193551466328,
16.6940955131975));
#66770=CARTESIAN_POINT('Ctrl Pts',(-52.9472154007209,-12.8180846076984,
16.6155900028207));
#66771=CARTESIAN_POINT('Ctrl Pts',(-51.7412733158222,-13.7329444635267,
16.5370844924439));
#66772=CARTESIAN_POINT('Ctrl Pts',(-51.8391898174562,-15.2434666221729,
16.4585789820672));
#66773=CARTESIAN_POINT('Ctrl Pts',(-53.153151048991,-15.9949789128949,16.3800734716904));
#66774=CARTESIAN_POINT('Ctrl Pts',(-54.5047653453669,-15.3135072413688,
16.3015679613136));
#66775=CARTESIAN_POINT('Ctrl Pts',(-54.6818728703171,-13.8102116065761,
16.2230624509368));
#66776=CARTESIAN_POINT('Ctrl Pts',(-53.5256393862053,-12.8332832711514,
16.1445569405601));
#66777=CARTESIAN_POINT('Ctrl Pts',(-52.0730025688563,-13.2588547922085,
16.0660514301833));
#66778=CARTESIAN_POINT('Ctrl Pts',(-51.6267216508218,-14.7052635118164,
15.9875459198065));
#66779=CARTESIAN_POINT('Ctrl Pts',(-52.5870319689928,-15.8753357042332,
15.9090404094297));
#66780=CARTESIAN_POINT('Ctrl Pts',(-54.0927043999843,-15.7197228098794,
15.8305348990529));
#66781=CARTESIAN_POINT('Ctrl Pts',(-54.7934161124393,-14.3779821728676,
15.7520293886762));
#66782=CARTESIAN_POINT('Ctrl Pts',(-54.060752183965,-13.0534186926322,15.6735238782994));
#66783=CARTESIAN_POINT('Ctrl Pts',(-52.551783044128,-12.9339323917357,15.5950183679226));
#66784=CARTESIAN_POINT('Ctrl Pts',(-51.6197880903543,-14.1266814178069,
15.5165128575458));
#66785=CARTESIAN_POINT('Ctrl Pts',(-52.1006025558578,-15.5619801036903,
15.438007347169));
#66786=CARTESIAN_POINT('Ctrl Pts',(-53.5630205937139,-15.9526184345153,
15.3595018367923));
#66787=CARTESIAN_POINT('Ctrl Pts',(-54.6955109477442,-14.9482627310635,
15.2809963264155));
#66788=CARTESIAN_POINT('Ctrl Pts',(-54.4824293305661,-13.4496429387163,
15.2024908160387));
#66789=CARTESIAN_POINT('Ctrl Pts',(-53.1148724313975,-12.8007571705351,
15.1239853056619));
#66790=CARTESIAN_POINT('Ctrl Pts',(-51.8192977302698,-13.5835410938618,
15.0454797952851));
#66791=CARTESIAN_POINT('Ctrl Pts',(-51.7576075386495,-15.0959765179234,
14.9669742849084));
#66792=CARTESIAN_POINT('Ctrl Pts',(-52.9851268468723,-15.9816732967562,
14.8884687745316));
#66793=CARTESIAN_POINT('Ctrl Pts',(-54.4009876413224,-15.4463217443432,
14.8099632641548));
#66794=CARTESIAN_POINT('Ctrl Pts',(-54.7354113233349,-13.9700292998257,
14.731457753778));
#66795=CARTESIAN_POINT('Ctrl Pts',(-53.6884807583299,-12.8767874010678,
14.6529522434012));
#66796=CARTESIAN_POINT('Ctrl Pts',(-52.1991041825148,-13.1470065045264,
14.5744467330245));
#66797=CARTESIAN_POINT('Ctrl Pts',(-51.6029979573221,-14.5384180675271,
14.4959412226477));
#66798=CARTESIAN_POINT('Ctrl Pts',(-52.4347480898299,-15.803029090894,14.4174357122709));
#66799=CARTESIAN_POINT('Ctrl Pts',(-53.9484540373432,-15.8069929981624,
14.3389302018941));
#66800=CARTESIAN_POINT('Ctrl Pts',(-54.7865222334212,-14.5461762990323,
14.2604246915174));
#66801=CARTESIAN_POINT('Ctrl Pts',(-54.1974864370675,-13.1524774509909,
14.1819191811406));
#66802=CARTESIAN_POINT('Ctrl Pts',(-52.709341584587,-12.8734351042922,14.1034136707638));
#66803=CARTESIAN_POINT('Ctrl Pts',(-51.6572105112416,-13.9641414098923,
14.024908160387));
#66804=CARTESIAN_POINT('Ctrl Pts',(-51.8753923247544,-14.9447289570596,
13.9725711534692));
#66805=CARTESIAN_POINT('Ctrl Pts',(-52.166679656532,-15.2829297282066,13.9464026500102));
#66806=CARTESIAN_POINT('Ctrl Pts',(-52.8685508929575,-13.1755371825403,
18.1607920499693));
#66807=CARTESIAN_POINT('Ctrl Pts',(-52.4668366999413,-13.2829324314546,
18.1346235465104));
#66808=CARTESIAN_POINT('Ctrl Pts',(-51.7841915677929,-13.9231130878274,
18.0822865395925));
#66809=CARTESIAN_POINT('Ctrl Pts',(-52.0214370885118,-15.3148486653539,
18.0037810292158));
#66810=CARTESIAN_POINT('Ctrl Pts',(-53.3132568693655,-15.881229245954,17.925275518839));
#66811=CARTESIAN_POINT('Ctrl Pts',(-54.4981759026981,-15.1177641071153,
17.8467700084622));
#66812=CARTESIAN_POINT('Ctrl Pts',(-54.5149763270121,-13.7074676093518,
17.7682644980854));
#66813=CARTESIAN_POINT('Ctrl Pts',(-53.347875441151,-12.9159562402448,17.6897589877086));
#66814=CARTESIAN_POINT('Ctrl Pts',(-52.0439116241499,-13.4526656118291,
17.6112534773319));
#66815=CARTESIAN_POINT('Ctrl Pts',(-51.7723349532836,-14.8364654316768,
17.5327479669551));
#66816=CARTESIAN_POINT('Ctrl Pts',(-52.7767888861688,-15.826230327804,17.4542424565783));
#66817=CARTESIAN_POINT('Ctrl Pts',(-54.1564121282093,-15.5343655532995,
17.3757369462015));
#66818=CARTESIAN_POINT('Ctrl Pts',(-54.6739471264171,-14.2225976311884,
17.2972314358247));
#66819=CARTESIAN_POINT('Ctrl Pts',(-53.8652456027039,-13.0673634804149,
17.218725925448));
#66820=CARTESIAN_POINT('Ctrl Pts',(-52.4555755554708,-13.104698476469,17.1402204150712));
#66821=CARTESIAN_POINT('Ctrl Pts',(-51.7091599966916,-14.30112271737,17.0617149046944));
#66822=CARTESIAN_POINT('Ctrl Pts',(-52.2954034324334,-15.5836530090872,
16.9832093943176));
#66823=CARTESIAN_POINT('Ctrl Pts',(-53.6885481742331,-15.802086434573,16.9047038839408));
#66824=CARTESIAN_POINT('Ctrl Pts',(-54.6391892137158,-14.7605263387452,
16.8261983735641));
#66825=CARTESIAN_POINT('Ctrl Pts',(-54.2947689098094,-13.3930687586361,
16.7476928631873));
#66826=CARTESIAN_POINT('Ctrl Pts',(-52.9641716568067,-12.9260820716401,
16.6691873528105));
#66827=CARTESIAN_POINT('Ctrl Pts',(-51.8407086658775,-13.7783710851678,
16.5906818424337));
#66828=CARTESIAN_POINT('Ctrl Pts',(-51.931928275148,-15.1855827278064,16.5121763320569));
#66829=CARTESIAN_POINT('Ctrl Pts',(-53.15602256096,-15.8856961548333,16.4336708216802));
#66830=CARTESIAN_POINT('Ctrl Pts',(-54.4151946712995,-15.2508329952228,
16.3551653113034));
#66831=CARTESIAN_POINT('Ctrl Pts',(-54.5801891201939,-13.8503536262183,
16.2766598009266));
#66832=CARTESIAN_POINT('Ctrl Pts',(-53.5030349645019,-12.9402412390784,
16.1981542905498));
#66833=CARTESIAN_POINT('Ctrl Pts',(-52.1497496583592,-13.3367062599847,
16.119648780173));
#66834=CARTESIAN_POINT('Ctrl Pts',(-51.7339916371008,-14.6841894323404,
16.0411432697963));
#66835=CARTESIAN_POINT('Ctrl Pts',(-52.6286225781573,-15.7742358129723,
15.9626377594195));
#66836=CARTESIAN_POINT('Ctrl Pts',(-54.031316184976,-15.6292658928517,15.8841322490427));
#66837=CARTESIAN_POINT('Ctrl Pts',(-54.6841034838951,-14.3792921437102,
15.8056267386659));
#66838=CARTESIAN_POINT('Ctrl Pts',(-54.0015493059316,-13.1453207384369,
15.7271212282891));
#66839=CARTESIAN_POINT('Ctrl Pts',(-52.5957844650741,-13.0340065728055,
15.6486157179124));
#66840=CARTESIAN_POINT('Ctrl Pts',(-51.7275322899413,-14.1451788297802,
15.5701102075356));
#66841=CARTESIAN_POINT('Ctrl Pts',(-52.1754619743441,-15.482311827054,15.4916046971588));
#66842=CARTESIAN_POINT('Ctrl Pts',(-53.5378595250825,-15.8462328751838,
15.413099186782));
#66843=CARTESIAN_POINT('Ctrl Pts',(-54.5928944361861,-14.9105689849469,
15.3345936764052));
#66844=CARTESIAN_POINT('Ctrl Pts',(-54.3943863038764,-13.5144456592424,
15.2560881660285));
#66845=CARTESIAN_POINT('Ctrl Pts',(-53.120361967679,-12.9099397256483,15.1775826556517));
#66846=CARTESIAN_POINT('Ctrl Pts',(-51.9133966855747,-13.6391859960657,
15.0990771452749));
#66847=CARTESIAN_POINT('Ctrl Pts',(-51.8559257273451,-15.0481800484177,
15.0205716348981));
#66848=CARTESIAN_POINT('Ctrl Pts',(-52.9994901909362,-15.8733005618024,
14.9420661245214));
#66849=CARTESIAN_POINT('Ctrl Pts',(-54.3185147301667,-15.3745637950836,
14.8635606141446));
#66850=CARTESIAN_POINT('Ctrl Pts',(-54.6300658690945,-13.9992407625991,
14.7850551037678));
#66851=CARTESIAN_POINT('Ctrl Pts',(-53.654738978538,-12.980769951465,14.706549593391));
#66852=CARTESIAN_POINT('Ctrl Pts',(-52.2672266896493,-13.2325077139822,
14.6280440830142));
#66853=CARTESIAN_POINT('Ctrl Pts',(-51.7118904997504,-14.5287552002895,
14.5495385726375));
#66854=CARTESIAN_POINT('Ctrl Pts',(-52.4867539888634,-15.7068745316112,
14.4710330622607));
#66855=CARTESIAN_POINT('Ctrl Pts',(-53.8969316686011,-15.7105673317642,
14.3925275518839));
#66856=CARTESIAN_POINT('Ctrl Pts',(-54.6776811042154,-14.5359828160102,
14.3140220415071));
#66857=CARTESIAN_POINT('Ctrl Pts',(-54.1289317688846,-13.2376044810286,
14.2355165311303));
#66858=CARTESIAN_POINT('Ctrl Pts',(-52.742566960956,-12.9776469313721,14.1570110207535));
#66859=CARTESIAN_POINT('Ctrl Pts',(-51.7623952451564,-13.9937555684777,
14.0785055103768));
#66860=CARTESIAN_POINT('Ctrl Pts',(-51.9656547514336,-14.9072768995629,
14.0261685034589));
#66861=CARTESIAN_POINT('Ctrl Pts',(-52.2370198037663,-15.2223467977324,
14.));
#66862=CARTESIAN_POINT('Ctrl Pts',(-51.9314271328212,-14.3981451355535,
17.5565803263806));
#66863=CARTESIAN_POINT('Ctrl Pts',(-51.9304449349957,-14.5245552242527,
17.5486362065721));
#66864=CARTESIAN_POINT('Ctrl Pts',(-51.9479261083582,-14.6507002121319,
17.5406920867636));
#66865=CARTESIAN_POINT('Ctrl Pts',(-51.9850067205755,-14.7707929443901,
17.5327479669551));
#66866=CARTESIAN_POINT('Ctrl Pts',(-52.107152930912,-15.1663870637192,17.5065794634962));
#66867=CARTESIAN_POINT('Ctrl Pts',(-52.4419709085404,-15.4963086957616,
17.4804109600372));
#66868=CARTESIAN_POINT('Ctrl Pts',(-52.8393171043614,-15.6126253826987,
17.4542424565783));
#66869=CARTESIAN_POINT('Ctrl Pts',(-53.2366633001823,-15.7289420696358,
17.4280739531194));
#66870=CARTESIAN_POINT('Ctrl Pts',(-53.6965377141958,-15.6316538114677,
17.4019054496604));
#66871=CARTESIAN_POINT('Ctrl Pts',(-54.0127307542372,-15.3643816953651,
17.3757369462015));
#66872=CARTESIAN_POINT('Ctrl Pts',(-54.3289237942786,-15.0971095792625,
17.3495684427426));
#66873=CARTESIAN_POINT('Ctrl Pts',(-54.5014354603478,-14.6598536052254,
17.3233999392837));
#66874=CARTESIAN_POINT('Ctrl Pts',(-54.4529077060969,-14.248686593078,17.2972314358247));
#66875=CARTESIAN_POINT('Ctrl Pts',(-54.404379951846,-13.8375195809306,17.2710629323658));
#66876=CARTESIAN_POINT('Ctrl Pts',(-54.134812777275,-13.4524415306728,17.2448944289069));
#66877=CARTESIAN_POINT('Ctrl Pts',(-53.7650841821172,-13.2661250048862,
17.218725925448));
#66878=CARTESIAN_POINT('Ctrl Pts',(-53.3953555869595,-13.0798084790996,
17.192557421989));
#66879=CARTESIAN_POINT('Ctrl Pts',(-52.9254655712151,-13.0922534777843,
17.1663889185301));
#66880=CARTESIAN_POINT('Ctrl Pts',(-52.5661179702131,-13.2978800172768,
17.1402204150712));
#66881=CARTESIAN_POINT('Ctrl Pts',(-52.206770369211,-13.5035065567693,17.1140519116123));
#66882=CARTESIAN_POINT('Ctrl Pts',(-51.9579651829513,-13.9023146370697,
17.0878834081533));
#66883=CARTESIAN_POINT('Ctrl Pts',(-51.9312698291117,-14.3154737258394,
17.0617149046944));
#66884=CARTESIAN_POINT('Ctrl Pts',(-51.9295238448586,-14.3424960034753,
17.0600033785898));
#66885=CARTESIAN_POINT('Ctrl Pts',(-51.9287279775559,-14.3695796702728,
17.0582918524852));
#66886=CARTESIAN_POINT('Ctrl Pts',(-51.9288577112775,-14.3966710926088,
17.0565803263806));
#66887=CARTESIAN_POINT('Origin',(-53.1951359564886,-14.3971354987959,15.5));
#66888=CARTESIAN_POINT('Origin',(-39.0658530619283,38.8697713466882,14.));
#66889=CARTESIAN_POINT('Ctrl Pts',(-39.3014489339361,37.6274127691862,14.));
#66890=CARTESIAN_POINT('Ctrl Pts',(-39.2527755161194,37.6125702664367,14.));
#66891=CARTESIAN_POINT('Ctrl Pts',(-39.2032917181315,37.6009462766933,14.));
#66892=CARTESIAN_POINT('Ctrl Pts',(-39.1532758042656,37.5923965983611,14.));
#66893=CARTESIAN_POINT('Ctrl Pts',(-39.1195722840575,37.586635346908,14.));
#66894=CARTESIAN_POINT('Ctrl Pts',(-39.0856264423578,37.5822710037957,14.));
#66895=CARTESIAN_POINT('Ctrl Pts',(-39.051517529296,37.5792707431957,14.));
#66896=CARTESIAN_POINT('Ctrl Pts',(-39.0357879605352,37.5778871516012,14.));
#66897=CARTESIAN_POINT('Ctrl Pts',(-39.0200236600756,37.5767937802542,14.));
#66898=CARTESIAN_POINT('Ctrl Pts',(-39.0042321836355,37.575988057109,14.));
#66899=CARTESIAN_POINT('Ctrl Pts',(-38.9909279655358,37.5753092405024,14.));
#66900=CARTESIAN_POINT('Ctrl Pts',(-38.9776118489662,37.5748350538321,14.));
#66901=CARTESIAN_POINT('Ctrl Pts',(-38.9642957637935,37.5745634329249,14.));
#66902=CARTESIAN_POINT('Ctrl Pts',(-38.9105541147896,37.5734672131828,14.));
#66903=CARTESIAN_POINT('Ctrl Pts',(-38.8567779423543,37.5756644894692,14.));
#66904=CARTESIAN_POINT('Ctrl Pts',(-38.8032675464162,37.5810264819144,14.));
#66905=CARTESIAN_POINT('Ctrl Pts',(-38.7827897374805,37.5830784543374,14.));
#66906=CARTESIAN_POINT('Ctrl Pts',(-38.762350670683,37.5855944285744,14.));
#66907=CARTESIAN_POINT('Ctrl Pts',(-38.7419666934157,37.5885691376463,14.));
#66908=CARTESIAN_POINT('Ctrl Pts',(-38.7273323755994,37.5907047776834,14.));
#66909=CARTESIAN_POINT('Ctrl Pts',(-38.7127264477777,37.5930768844181,14.));
#66910=CARTESIAN_POINT('Ctrl Pts',(-38.6981549325269,37.5956838482079,14.));
#66911=CARTESIAN_POINT('Ctrl Pts',(-38.6868487316631,37.5977066204279,14.));
#66912=CARTESIAN_POINT('Ctrl Pts',(-38.6755628690101,37.5998709906011,14.));
#66913=CARTESIAN_POINT('Ctrl Pts',(-38.664315444558,37.6021728300089,14.));
#66914=CARTESIAN_POINT('Ctrl Pts',(-38.6087986249492,37.6135346136523,14.));
#66915=CARTESIAN_POINT('Ctrl Pts',(-38.5541290484473,37.628256437058,14.));
#66916=CARTESIAN_POINT('Ctrl Pts',(-38.5006370920885,37.6461917726554,14.));
#66917=CARTESIAN_POINT('Ctrl Pts',(-38.4479217177469,37.6638667278135,14.));
#66918=CARTESIAN_POINT('Ctrl Pts',(-38.3963488051394,37.6846628179155,14.));
#66919=CARTESIAN_POINT('Ctrl Pts',(-38.3462305042669,37.7084927624528,14.));
#66920=CARTESIAN_POINT('Ctrl Pts',(-38.3200575606107,37.7209373143401,14.));
#66921=CARTESIAN_POINT('Ctrl Pts',(-38.2942813570802,37.7342101081289,14.));
#66922=CARTESIAN_POINT('Ctrl Pts',(-38.2689475827414,37.7483042481762,14.));
#66923=CARTESIAN_POINT('Ctrl Pts',(-38.2553600453312,37.7558635108663,14.));
#66924=CARTESIAN_POINT('Ctrl Pts',(-38.2418997997272,37.7636591073689,14.));
#66925=CARTESIAN_POINT('Ctrl Pts',(-38.2285740912793,37.7716904150091,14.));
#66926=CARTESIAN_POINT('Ctrl Pts',(-38.219103371651,37.7773983489029,14.));
#66927=CARTESIAN_POINT('Ctrl Pts',(-38.2097006109437,37.7832253490862,14.));
#66928=CARTESIAN_POINT('Ctrl Pts',(-38.2003684638973,37.7891712855976,14.));
#66929=CARTESIAN_POINT('Ctrl Pts',(-38.1921418100671,37.7944128619607,14.));
#66930=CARTESIAN_POINT('Ctrl Pts',(-38.1839782830262,37.799741616435,14.));
#66931=CARTESIAN_POINT('Ctrl Pts',(-38.1758800166261,37.8051565176932,14.));
#66932=CARTESIAN_POINT('Ctrl Pts',(-38.135853400971,37.8319202916625,14.));
#66933=CARTESIAN_POINT('Ctrl Pts',(-38.097416293909,37.8607893617207,14.));
#66934=CARTESIAN_POINT('Ctrl Pts',(-38.0607602397062,37.8916978987796,14.));
#66935=CARTESIAN_POINT('Ctrl Pts',(-38.0190399864272,37.9268765895204,14.));
#66936=CARTESIAN_POINT('Ctrl Pts',(-37.979625387271,37.964696062052,14.));
#66937=CARTESIAN_POINT('Ctrl Pts',(-37.9425628056437,38.0048405338692,14.));
#66938=CARTESIAN_POINT('Ctrl Pts',(-37.9063354033603,38.0440803781036,14.));
#66939=CARTESIAN_POINT('Ctrl Pts',(-37.8723549080262,38.0855424637427,14.));
#66940=CARTESIAN_POINT('Ctrl Pts',(-37.8406905748295,38.1289693592978,14.));
#66941=CARTESIAN_POINT('Ctrl Pts',(-37.8329319648674,38.1396101121722,14.));
#66942=CARTESIAN_POINT('Ctrl Pts',(-37.8253125495357,38.1503689751519,14.));
#66943=CARTESIAN_POINT('Ctrl Pts',(-37.8178336250283,38.1612424270489,14.));
#66944=CARTESIAN_POINT('Ctrl Pts',(-37.8121884193235,38.1694498735365,14.));
#66945=CARTESIAN_POINT('Ctrl Pts',(-37.8066244559446,38.1777210085785,14.));
#66946=CARTESIAN_POINT('Ctrl Pts',(-37.8011483696233,38.1860445283887,14.));
#66947=CARTESIAN_POINT('Ctrl Pts',(-37.7694817125821,38.2341770872534,14.));
#66948=CARTESIAN_POINT('Ctrl Pts',(-37.7406908693863,38.2841447569653,14.));
#66949=CARTESIAN_POINT('Ctrl Pts',(-37.7148226289923,38.3355979876602,14.));
#66950=CARTESIAN_POINT('Ctrl Pts',(-37.6883997602119,38.3881544021,14.));
#66951=CARTESIAN_POINT('Ctrl Pts',(-37.6650255379363,38.4422615831827,14.));
#66952=CARTESIAN_POINT('Ctrl Pts',(-37.6447852836431,38.4975884922593,14.));
#66953=CARTESIAN_POINT('Ctrl Pts',(-37.6243676757452,38.553400198939,14.));
#66954=CARTESIAN_POINT('Ctrl Pts',(-37.6071385772626,38.6104541129774,14.));
#66955=CARTESIAN_POINT('Ctrl Pts',(-37.5932306356442,38.6684381301379,14.));
#66956=CARTESIAN_POINT('Ctrl Pts',(-37.5900811837444,38.681568604655,14.));
#66957=CARTESIAN_POINT('Ctrl Pts',(-37.5871015926692,38.6947505762665,14.));
#66958=CARTESIAN_POINT('Ctrl Pts',(-37.5842989888792,38.7079539605985,14.));
#66959=CARTESIAN_POINT('Ctrl Pts',(-37.5716672473803,38.7674635275195,14.));
#66960=CARTESIAN_POINT('Ctrl Pts',(-37.5626014399533,38.8275056873427,14.));
#66961=CARTESIAN_POINT('Ctrl Pts',(-37.5571792782293,38.887728107878,14.));
#66962=CARTESIAN_POINT('Ctrl Pts',(-37.5518047857275,38.9474210798117,14.));
#66963=CARTESIAN_POINT('Ctrl Pts',(-37.5500097107535,39.0072922465011,14.));
#66964=CARTESIAN_POINT('Ctrl Pts',(-37.5519146657201,39.0670207918841,14.));
#66965=CARTESIAN_POINT('Ctrl Pts',(-37.553310403515,39.1107831850598,14.));
#66966=CARTESIAN_POINT('Ctrl Pts',(-37.5566933253822,39.1544695447416,14.));
#66967=CARTESIAN_POINT('Ctrl Pts',(-37.5621285378972,39.1979562890069,14.));
#66968=CARTESIAN_POINT('Ctrl Pts',(-37.565149248657,39.2221247784534,14.));
#66969=CARTESIAN_POINT('Ctrl Pts',(-37.568804155379,39.2462316220403,14.));
#66970=CARTESIAN_POINT('Ctrl Pts',(-37.573079654256,39.2702614469549,14.));
#66971=CARTESIAN_POINT('Ctrl Pts',(-37.9741697098829,39.9602191716055,14.));
#66972=CARTESIAN_POINT('Ctrl Pts',(-38.020991576866,39.9994070905167,14.));
#66973=CARTESIAN_POINT('Ctrl Pts',(-38.0702141503049,40.0354948198823,14.));
#66974=CARTESIAN_POINT('Ctrl Pts',(-38.1214910131339,40.0684345608225,14.));
#66975=CARTESIAN_POINT('Ctrl Pts',(-38.1690376391659,40.0989780351629,14.));
#66976=CARTESIAN_POINT('Ctrl Pts',(-38.2183516107479,40.126814478516,14.));
#66977=CARTESIAN_POINT('Ctrl Pts',(-38.2691689745691,40.1518670892062,14.));
#66978=CARTESIAN_POINT('Ctrl Pts',(-38.2814354207102,40.1579143627485,14.));
#66979=CARTESIAN_POINT('Ctrl Pts',(-38.2937899475964,40.1637993356401,14.));
#66980=CARTESIAN_POINT('Ctrl Pts',(-38.3062147881308,40.1695145313534,14.));
#66981=CARTESIAN_POINT('Ctrl Pts',(-38.360894981368,40.1946664039371,14.));
#66982=CARTESIAN_POINT('Ctrl Pts',(-38.4170009391299,40.2165668550583,14.));
#66983=CARTESIAN_POINT('Ctrl Pts',(-38.4742056406521,40.2351397540719,14.));
#66984=CARTESIAN_POINT('Ctrl Pts',(-38.5095144290366,40.2466036118232,14.));
#66985=CARTESIAN_POINT('Ctrl Pts',(-38.5452420715441,40.2567987359784,14.));
#66986=CARTESIAN_POINT('Ctrl Pts',(-38.581311892576,40.2656972878261,14.));
#66987=CARTESIAN_POINT('Ctrl Pts',(-38.5936535300867,40.268742013254,14.));
#66988=CARTESIAN_POINT('Ctrl Pts',(-38.6060352195458,40.2716348784393,14.));
#66989=CARTESIAN_POINT('Ctrl Pts',(-38.6184538533342,40.2743745599732,14.));
#66990=CARTESIAN_POINT('Ctrl Pts',(-38.6300726272152,40.2769377839793,14.));
#66991=CARTESIAN_POINT('Ctrl Pts',(-38.6417163459698,40.2793652416505,14.));
#66992=CARTESIAN_POINT('Ctrl Pts',(-38.653376443336,40.2816552663571,14.));
#66993=CARTESIAN_POINT('Ctrl Pts',(-38.7110876100587,40.2929896483515,14.));
#66994=CARTESIAN_POINT('Ctrl Pts',(-38.7692463788907,40.3009718362435,14.));
#66995=CARTESIAN_POINT('Ctrl Pts',(-38.8275464691728,40.3055302032547,14.));
#66996=CARTESIAN_POINT('Ctrl Pts',(-38.8843585379937,40.3099722248553,14.));
#66997=CARTESIAN_POINT('Ctrl Pts',(-38.9413057825382,40.3111628333593,14.));
#66998=CARTESIAN_POINT('Ctrl Pts',(-38.9980976131321,40.3089871593392,14.));
#66999=CARTESIAN_POINT('Ctrl Pts',(-39.0288884006191,40.3078075756615,14.));
#67000=CARTESIAN_POINT('Ctrl Pts',(-39.0596332935447,40.3056376455648,14.));
#67001=CARTESIAN_POINT('Ctrl Pts',(-39.0902835743803,40.3024530490585,14.));
#67002=CARTESIAN_POINT('Ctrl Pts',(-39.1157839675052,40.2998035313171,14.));
#67003=CARTESIAN_POINT('Ctrl Pts',(-39.1412188503762,40.2964515981625,14.));
#67004=CARTESIAN_POINT('Ctrl Pts',(-39.1665588540094,40.2923809785531,14.));
#67005=CARTESIAN_POINT('Ctrl Pts',(-39.1773889643725,40.290641229015,14.));
#67006=CARTESIAN_POINT('Ctrl Pts',(-39.1882029800359,40.2887698277096,14.));
#67007=CARTESIAN_POINT('Ctrl Pts',(-39.1989810536353,40.2867689791238,14.));
#67008=CARTESIAN_POINT('Ctrl Pts',(-39.2488808959019,40.2775055399842,14.));
#67009=CARTESIAN_POINT('Ctrl Pts',(-39.2980978218176,40.2654572977421,14.));
#67010=CARTESIAN_POINT('Ctrl Pts',(-39.3464249159924,40.2505519130058,14.));
#67011=CARTESIAN_POINT('Ctrl Pts',(-39.4004290144133,40.2338955864037,14.));
#67012=CARTESIAN_POINT('Ctrl Pts',(-39.4533231062175,40.2136715650556,14.));
#67013=CARTESIAN_POINT('Ctrl Pts',(-39.5048609693609,40.1901258318545,14.));
#67014=CARTESIAN_POINT('Ctrl Pts',(-39.5485960623501,40.1701448941857,14.));
#67015=CARTESIAN_POINT('Ctrl Pts',(-39.5913543500841,40.1477707447887,14.));
#67016=CARTESIAN_POINT('Ctrl Pts',(-39.6329645160367,40.1231328973135,14.));
#67017=CARTESIAN_POINT('Ctrl Pts',(-39.6444045721025,40.1163591113887,14.));
#67018=CARTESIAN_POINT('Ctrl Pts',(-39.6557577122726,40.1094141266032,14.));
#67019=CARTESIAN_POINT('Ctrl Pts',(-39.6670200627789,40.1023004514057,14.));
#67020=CARTESIAN_POINT('Ctrl Pts',(-39.6757877124543,40.0967625122337,14.));
#67021=CARTESIAN_POINT('Ctrl Pts',(-39.6845017797711,40.0911212766444,14.));
#67022=CARTESIAN_POINT('Ctrl Pts',(-39.6931464328254,40.0853874573571,14.));
#67023=CARTESIAN_POINT('Ctrl Pts',(-39.7394049739142,40.0547051253501,14.));
#67024=CARTESIAN_POINT('Ctrl Pts',(-39.7837665094979,40.0213210070101,14.));
#67025=CARTESIAN_POINT('Ctrl Pts',(-39.826005821329,39.9854744939875,14.));
#67026=CARTESIAN_POINT('Ctrl Pts',(-39.8680089351073,39.9498284311192,14.));
#67027=CARTESIAN_POINT('Ctrl Pts',(-39.9079141963595,39.9117464669987,14.));
#67028=CARTESIAN_POINT('Ctrl Pts',(-39.9454594213913,39.8714333538664,14.));
#67029=CARTESIAN_POINT('Ctrl Pts',(-39.9802942732095,39.8340304265673,14.));
#67030=CARTESIAN_POINT('Ctrl Pts',(-40.0130975716519,39.7947059892265,14.));
#67031=CARTESIAN_POINT('Ctrl Pts',(-40.0436204335325,39.7536104031384,14.));
#67032=CARTESIAN_POINT('Ctrl Pts',(-40.0514607527816,39.743054298802,14.));
#67033=CARTESIAN_POINT('Ctrl Pts',(-40.0591528687932,39.7323774869168,14.));
#67034=CARTESIAN_POINT('Ctrl Pts',(-40.0666759532432,39.7216063497443,14.));
#67035=CARTESIAN_POINT('Ctrl Pts',(-40.0970859623649,39.6780669767858,14.));
#67036=CARTESIAN_POINT('Ctrl Pts',(-40.1247894554028,39.6329220142279,14.));
#67037=CARTESIAN_POINT('Ctrl Pts',(-40.1495562730805,39.586364052585,14.));
#67038=CARTESIAN_POINT('Ctrl Pts',(-40.1734835191867,39.5413843615755,14.));
#67039=CARTESIAN_POINT('Ctrl Pts',(-40.1946700927978,39.4950850229851,14.));
#67040=CARTESIAN_POINT('Ctrl Pts',(-40.2128622007042,39.4476279811834,14.));
#67041=CARTESIAN_POINT('Ctrl Pts',(-40.2255879517226,39.4144308112267,14.));
#67042=CARTESIAN_POINT('Ctrl Pts',(-40.23684748228,39.3806668978,14.));
#67043=CARTESIAN_POINT('Ctrl Pts',(-40.2465386396389,39.3463911596944,14.));
#67044=CARTESIAN_POINT('Ctrl Pts',(-40.2520057165832,39.327055172195,14.));
#67045=CARTESIAN_POINT('Ctrl Pts',(-40.2569733939395,39.3075562909784,14.));
#67046=CARTESIAN_POINT('Ctrl Pts',(-40.261442519219,39.2879130030575,14.));
#67047=CARTESIAN_POINT('Origin',(-39.0658530619283,38.8697713466882,19.1042117235887));
#67048=CARTESIAN_POINT('Ctrl Pts',(-38.2940537528419,37.5314721085808,17.8542117235887));
#67049=CARTESIAN_POINT('Ctrl Pts',(-38.3354082297679,37.5072482534305,17.8517311518799));
#67050=CARTESIAN_POINT('Ctrl Pts',(-38.8263155408625,37.2510699656701,17.8230820767121));
#67051=CARTESIAN_POINT('Ctrl Pts',(-40.0256568276714,37.3267811177079,17.7682644980854));
#67052=CARTESIAN_POINT('Ctrl Pts',(-40.8821443104935,38.819261537444,17.6897589877086));
#67053=CARTESIAN_POINT('Ctrl Pts',(-40.1099071502118,40.3569109628884,17.6112534773319));
#67054=CARTESIAN_POINT('Ctrl Pts',(-38.4012543668155,40.5609220251471,17.5327479669551));
#67055=CARTESIAN_POINT('Ctrl Pts',(-37.2886704652103,39.2482374965454,17.4542424565783));
#67056=CARTESIAN_POINT('Ctrl Pts',(-37.6534618751483,37.995852754822,17.3947303754562));
#67057=CARTESIAN_POINT('Ctrl Pts',(-38.1723477780673,37.603235418619,17.361386797793));
#67058=CARTESIAN_POINT('Ctrl Pts',(-38.2935040424574,37.5346322273253,17.3542117235887));
#67059=CARTESIAN_POINT('Ctrl Pts',(-38.2938718037177,37.5356881270255,17.8957882764113));
#67060=CARTESIAN_POINT('Ctrl Pts',(-38.5911486295276,37.3667504425096,17.8781885106897));
#67061=CARTESIAN_POINT('Ctrl Pts',(-39.4708982524073,37.1808200198997,17.8344202415091));
#67062=CARTESIAN_POINT('Ctrl Pts',(-40.7062722211717,38.0891100356719,17.7644834688697));
#67063=CARTESIAN_POINT('Ctrl Pts',(-40.6223994863181,39.8071108514352,17.6859779584929));
#67064=CARTESIAN_POINT('Ctrl Pts',(-39.1423049297703,40.6853144575311,17.6074724481161));
#67065=CARTESIAN_POINT('Ctrl Pts',(-37.5937815296791,39.9348860603428,17.5289669377393));
#67066=CARTESIAN_POINT('Ctrl Pts',(-37.388492650827,38.4020168817229,17.4584055471711));
#67067=CARTESIAN_POINT('Ctrl Pts',(-37.9908199438395,37.7130239262801,17.4140126600617));
#67068=CARTESIAN_POINT('Ctrl Pts',(-38.2959007276492,37.5337106753505,17.3957882764113));
#67069=CARTESIAN_POINT('Ctrl Pts',(-40.2595650866584,39.2869186252538,18.));
#67070=CARTESIAN_POINT('Ctrl Pts',(-40.1223890770422,39.6794626033579,17.9738314965411));
#67071=CARTESIAN_POINT('Ctrl Pts',(-39.4328412785483,40.3122408191566,17.9214944896232));
#67072=CARTESIAN_POINT('Ctrl Pts',(-38.0628399617007,39.9714590750955,17.8429889792464));
#67073=CARTESIAN_POINT('Ctrl Pts',(-37.594757239893,38.6408443652931,17.7644834688697));
#67074=CARTESIAN_POINT('Ctrl Pts',(-38.4448300096771,37.516422065853,17.6859779584929));
#67075=CARTESIAN_POINT('Ctrl Pts',(-39.8524194013854,37.6052793541117,17.6074724481161));
#67076=CARTESIAN_POINT('Ctrl Pts',(-40.5543172769709,38.8283781815623,17.5289669377393));
#67077=CARTESIAN_POINT('Ctrl Pts',(-39.9214631686259,40.088493345836,17.4504614273626));
#67078=CARTESIAN_POINT('Ctrl Pts',(-38.5212094780202,40.2556819318544,17.3719559169858));
#67079=CARTESIAN_POINT('Ctrl Pts',(-37.6094386785518,39.1799271772095,17.293450406609));
#67080=CARTESIAN_POINT('Ctrl Pts',(-38.0037983665504,37.8260300114723,17.2149448962322));
#67081=CARTESIAN_POINT('Ctrl Pts',(-39.350642117465,37.4081786211339,17.1364393858554));
#67082=CARTESIAN_POINT('Ctrl Pts',(-40.4420762478649,38.3011214248006,17.0579338754786));
#67083=CARTESIAN_POINT('Ctrl Pts',(-40.2992826919135,39.7040414735315,16.9794283651019));
#67084=CARTESIAN_POINT('Ctrl Pts',(-39.0503191421165,40.358768990196,16.9009228547251));
#67085=CARTESIAN_POINT('Ctrl Pts',(-37.8152872634063,39.678127650814,16.8224173443483));
#67086=CARTESIAN_POINT('Ctrl Pts',(-37.7017922854029,38.2725333429822,16.7439118339715));
#67087=CARTESIAN_POINT('Ctrl Pts',(-38.8116195577816,37.4025561853298,16.6654063235948));
#67088=CARTESIAN_POINT('Ctrl Pts',(-40.1494494228947,37.8484125098358,16.586900813218));
#67089=CARTESIAN_POINT('Ctrl Pts',(-40.5154843389836,39.2102476987511,16.5083953028412));
#67090=CARTESIAN_POINT('Ctrl Pts',(-39.5814554487361,40.2667356115709,16.4298897924644));
#67091=CARTESIAN_POINT('Ctrl Pts',(-38.1850220871887,40.0703927553964,16.3513842820876));
#67092=CARTESIAN_POINT('Ctrl Pts',(-37.578538880925,38.7973040793768,16.2728787717109));
#67093=CARTESIAN_POINT('Ctrl Pts',(-38.305914392745,37.5892057701993,16.1943732613341));
#67094=CARTESIAN_POINT('Ctrl Pts',(-39.7148209687578,37.5295491143576,16.1158677509573));
#67095=CARTESIAN_POINT('Ctrl Pts',(-40.5417176980217,38.6718356181182,16.0373622405805));
#67096=CARTESIAN_POINT('Ctrl Pts',(-40.0450239347318,39.9916355890619,15.9588567302037));
#67097=CARTESIAN_POINT('Ctrl Pts',(-38.670186454417,40.3053210365854,15.880351219827));
#67098=CARTESIAN_POINT('Ctrl Pts',(-37.6501921939814,39.3315713939809,15.8018457094502));
#67099=CARTESIAN_POINT('Ctrl Pts',(-37.8997962556048,37.9436684903302,15.7233401990734));
#67100=CARTESIAN_POINT('Ctrl Pts',(-39.1951477820351,37.3863166449999,15.6448346886966));
#67101=CARTESIAN_POINT('Ctrl Pts',(-40.3745447306992,38.1593622434704,15.5663291783198));
#67102=CARTESIAN_POINT('Ctrl Pts',(-40.380275876363,39.5695196142836,15.4878236679431));
#67103=CARTESIAN_POINT('Ctrl Pts',(-39.2072013976484,40.3521261040355,15.4093181575663));
#67104=CARTESIAN_POINT('Ctrl Pts',(-37.9073623625386,39.8053216046427,15.3308126471895));
#67105=CARTESIAN_POINT('Ctrl Pts',(-37.646485345535,38.4194933961106,15.2523071368127));
#67106=CARTESIAN_POINT('Ctrl Pts',(-38.6585310049343,37.4374851510426,15.1738016264359));
#67107=CARTESIAN_POINT('Ctrl Pts',(-40.0358728399513,37.7399852318106,15.0952961160592));
#67108=CARTESIAN_POINT('Ctrl Pts',(-40.5432777323755,39.0557043292571,15.0167906056824));
#67109=CARTESIAN_POINT('Ctrl Pts',(-39.7256933501734,40.2046743690254,14.9382850953056));
#67110=CARTESIAN_POINT('Ctrl Pts',(-38.3163479152336,40.156471518347,14.8597795849288));
#67111=CARTESIAN_POINT('Ctrl Pts',(-37.5791777219181,38.954325616703,14.781274074552));
#67112=CARTESIAN_POINT('Ctrl Pts',(-38.1752908680605,37.6763489234029,14.7027685641753));
#67113=CARTESIAN_POINT('Ctrl Pts',(-39.5700863286924,37.468662869981,14.6242630537985));
#67114=CARTESIAN_POINT('Ctrl Pts',(-40.5126633343826,38.5175221013622,14.5457575434217));
#67115=CARTESIAN_POINT('Ctrl Pts',(-40.1577269226072,39.8822911025123,14.4672520330449));
#67116=CARTESIAN_POINT('Ctrl Pts',(-38.8235306389231,40.3389996506624,14.3887465226681));
#67117=CARTESIAN_POINT('Ctrl Pts',(-37.7067389013687,39.4780868997918,14.3102410122914));
#67118=CARTESIAN_POINT('Ctrl Pts',(-37.8086626184681,38.0715866597082,14.2317355019146));
#67119=CARTESIAN_POINT('Ctrl Pts',(-39.0384102949244,37.3809896965113,14.1532299915378));
#67120=CARTESIAN_POINT('Ctrl Pts',(-40.292067953697,38.0254209930878,14.074724481161));
#67121=CARTESIAN_POINT('Ctrl Pts',(-40.4474545117342,39.4273810345935,13.9962189707842));
#67122=CARTESIAN_POINT('Ctrl Pts',(-39.3608457503204,40.3286674512605,13.9177134604075));
#67123=CARTESIAN_POINT('Ctrl Pts',(-38.4650745289098,40.0575985380861,13.8653764534896));
#67124=CARTESIAN_POINT('Ctrl Pts',(-38.1712104185962,39.7634014663304,13.8392079500307));
#67125=CARTESIAN_POINT('Ctrl Pts',(-40.3472015171019,39.3175435144276,18.0535973499898));
#67126=CARTESIAN_POINT('Ctrl Pts',(-40.1999547235979,39.7389061291211,18.0274288465308));
#67127=CARTESIAN_POINT('Ctrl Pts',(-39.4597837375779,40.4181397905767,17.975091839613));
#67128=CARTESIAN_POINT('Ctrl Pts',(-37.9892037027278,40.0523395370335,17.8965863292362));
#67129=CARTESIAN_POINT('Ctrl Pts',(-37.486756663529,38.6240376790354,17.8180808188594));
#67130=CARTESIAN_POINT('Ctrl Pts',(-38.399237569964,37.4170658579415,17.7395753084826));
#67131=CARTESIAN_POINT('Ctrl Pts',(-39.9101652101474,37.5124466086439,17.6610697981059));
#67132=CARTESIAN_POINT('Ctrl Pts',(-40.6635929548118,38.8253393001895,17.5825642877291));
#67133=CARTESIAN_POINT('Ctrl Pts',(-39.9842778291546,40.1779658848535,17.5040587773523));
#67134=CARTESIAN_POINT('Ctrl Pts',(-38.481224440952,40.3574286296185,17.4255532669755));
#67135=CARTESIAN_POINT('Ctrl Pts',(-37.5025159407713,39.2026972836548,17.3470477565987));
#67136=CARTESIAN_POINT('Ctrl Pts',(-37.9258275657958,37.7494036870074,17.268542246222));
#67137=CARTESIAN_POINT('Ctrl Pts',(-39.3715499208041,37.3008757150928,17.1900367358452));
#67138=CARTESIAN_POINT('Ctrl Pts',(-40.5431117447104,38.2593739611798,17.1115312254684));
#67139=CARTESIAN_POINT('Ctrl Pts',(-40.3898349924146,39.7652894583281,17.0330257150916));
#67140=CARTESIAN_POINT('Ctrl Pts',(-39.0491787185848,40.4680838297154,16.9545202047148));
#67141=CARTESIAN_POINT('Ctrl Pts',(-37.7234769101999,39.7374731709667,16.8760146943381));
#67142=CARTESIAN_POINT('Ctrl Pts',(-37.6016496924775,38.2286870838463,16.7975091839613));
#67143=CARTESIAN_POINT('Ctrl Pts',(-38.7929549918386,37.2948405078714,16.7190036735845));
#67144=CARTESIAN_POINT('Ctrl Pts',(-40.22900170615,37.7734293976535,16.6404981632077));
#67145=CARTESIAN_POINT('Ctrl Pts',(-40.6219090946604,39.2352437878639,16.561992652831));
#67146=CARTESIAN_POINT('Ctrl Pts',(-39.6193084248073,40.369293815807,16.4834871424542));
#67147=CARTESIAN_POINT('Ctrl Pts',(-38.1203558353197,40.1585364386243,16.4049816320774));
#67148=CARTESIAN_POINT('Ctrl Pts',(-37.469347632893,38.7919838911743,16.3264761217006));
#67149=CARTESIAN_POINT('Ctrl Pts',(-38.2501234557824,37.4951929817316,16.2479706113238));
#67150=CARTESIAN_POINT('Ctrl Pts',(-39.7624649814247,37.4311566293954,16.1694651009471));
#67151=CARTESIAN_POINT('Ctrl Pts',(-40.6500683771181,38.6573041563001,16.0909595905703));
#67152=CARTESIAN_POINT('Ctrl Pts',(-40.116909815337,40.0739973108231,16.0124540801935));
#67153=CARTESIAN_POINT('Ctrl Pts',(-38.6411385698271,40.4107119918078,15.9339485698167));
#67154=CARTESIAN_POINT('Ctrl Pts',(-37.5462613776579,39.3654744684955,15.85544305944));
#67155=CARTESIAN_POINT('Ctrl Pts',(-37.8141901344604,37.8756786009152,15.7769375490632));
#67156=CARTESIAN_POINT('Ctrl Pts',(-39.2046399606432,37.2774087408428,15.6984320386864));
#67157=CARTESIAN_POINT('Ctrl Pts',(-40.4706223976961,38.1072075221719,15.6199265283096));
#67158=CARTESIAN_POINT('Ctrl Pts',(-40.4767742957171,39.6208916697799,15.5414210179328));
#67159=CARTESIAN_POINT('Ctrl Pts',(-39.2175784930743,40.4609532557217,15.462915507556));
#67160=CARTESIAN_POINT('Ctrl Pts',(-37.8223117075287,39.8740050755377,15.3844099971793));
#67161=CARTESIAN_POINT('Ctrl Pts',(-37.5422823907398,38.3864362169262,15.3059044868025));
#67162=CARTESIAN_POINT('Ctrl Pts',(-38.6286274349138,37.3323337854205,15.2273989764257));
#67163=CARTESIAN_POINT('Ctrl Pts',(-40.1070868924567,37.6570419253671,15.1488934660489));
#67164=CARTESIAN_POINT('Ctrl Pts',(-40.6517429414752,39.0693546088525,15.0703879556721));
#67165=CARTESIAN_POINT('Ctrl Pts',(-39.774135559288,40.302676343909,14.9918824452954));
#67166=CARTESIAN_POINT('Ctrl Pts',(-38.2613229558677,40.2509346784385,14.9133769349186));
#67167=CARTESIAN_POINT('Ctrl Pts',(-37.4700333744309,38.9605331728382,14.8348714245418));
#67168=CARTESIAN_POINT('Ctrl Pts',(-38.1099101982326,37.5887337540646,14.756365914165));
#67169=CARTESIAN_POINT('Ctrl Pts',(-39.6071046402237,37.3658004182179,14.6778604037883));
#67170=CARTESIAN_POINT('Ctrl Pts',(-40.6188809858598,38.4916617046775,14.5993548934115));
#67171=CARTESIAN_POINT('Ctrl Pts',(-40.2378868989348,39.9566252931006,14.5208493830347));
#67172=CARTESIAN_POINT('Ctrl Pts',(-38.8057405256223,40.4468631230907,14.4423438726579));
#67173=CARTESIAN_POINT('Ctrl Pts',(-37.6069594645119,39.5227464177934,14.3638383622811));
#67174=CARTESIAN_POINT('Ctrl Pts',(-37.7163659166087,38.0129878893579,14.2853328519043));
#67175=CARTESIAN_POINT('Ctrl Pts',(-39.036395582756,37.2716907141535,14.2068273415276));
#67176=CARTESIAN_POINT('Ctrl Pts',(-40.3820905838163,37.963432967919,14.1283218311508));
#67177=CARTESIAN_POINT('Ctrl Pts',(-40.5488848541016,39.4683179788618,14.049816320774));
#67178=CARTESIAN_POINT('Ctrl Pts',(-39.3825026538969,40.4357723847318,13.9713108103972));
#67179=CARTESIAN_POINT('Ctrl Pts',(-38.4209683416301,40.1448029331841,13.9189738034794));
#67180=CARTESIAN_POINT('Ctrl Pts',(-38.1055301823584,39.8290073680888,13.8928053000205));
#67181=CARTESIAN_POINT('Ctrl Pts',(-40.4348379475454,39.3481684036013,18.1071946999795));
#67182=CARTESIAN_POINT('Ctrl Pts',(-40.2775203701537,39.7983496548842,18.0810261965206));
#67183=CARTESIAN_POINT('Ctrl Pts',(-39.4867261966074,40.5240387619969,18.0286891896027));
#67184=CARTESIAN_POINT('Ctrl Pts',(-37.9155674437551,40.1332199989714,17.950183679226));
#67185=CARTESIAN_POINT('Ctrl Pts',(-37.3787560871649,38.6072309927777,17.8716781688492));
#67186=CARTESIAN_POINT('Ctrl Pts',(-38.3536451302508,37.3177096500299,17.7931726584724));
#67187=CARTESIAN_POINT('Ctrl Pts',(-39.9679110189094,37.4196138631759,17.7146671480956));
#67188=CARTESIAN_POINT('Ctrl Pts',(-40.7728686326527,38.8223004188168,17.6361616377188));
#67189=CARTESIAN_POINT('Ctrl Pts',(-40.0470924896831,40.2674384238709,17.5576561273421));
#67190=CARTESIAN_POINT('Ctrl Pts',(-38.4412394038838,40.4591753273829,17.4791506169653));
#67191=CARTESIAN_POINT('Ctrl Pts',(-37.3955932029908,39.2254673901001,17.4006451065885));
#67192=CARTESIAN_POINT('Ctrl Pts',(-37.8478567650412,37.6727773625425,17.3221395962117));
#67193=CARTESIAN_POINT('Ctrl Pts',(-39.3924577241432,37.1935728090517,17.243634085835));
#67194=CARTESIAN_POINT('Ctrl Pts',(-40.6441472415558,38.2176264975589,17.1651285754582));
#67195=CARTESIAN_POINT('Ctrl Pts',(-40.4803872929157,39.8265374431247,17.0866230650814));
#67196=CARTESIAN_POINT('Ctrl Pts',(-39.0480382950531,40.5773986692348,17.0081175547046));
#67197=CARTESIAN_POINT('Ctrl Pts',(-37.6316665569936,39.7968186911193,16.9296120443279));
#67198=CARTESIAN_POINT('Ctrl Pts',(-37.5015070995522,38.1848408247104,16.8511065339511));
#67199=CARTESIAN_POINT('Ctrl Pts',(-38.7742904258956,37.187124830413,16.7726010235743));
#67200=CARTESIAN_POINT('Ctrl Pts',(-40.3085539894054,37.6984462854713,16.6940955131975));
#67201=CARTESIAN_POINT('Ctrl Pts',(-40.7283338503372,39.2602398769767,16.6155900028207));
#67202=CARTESIAN_POINT('Ctrl Pts',(-39.6571614008785,40.4718520200432,16.5370844924439));
#67203=CARTESIAN_POINT('Ctrl Pts',(-38.0556895834507,40.2466801218523,16.4585789820672));
#67204=CARTESIAN_POINT('Ctrl Pts',(-37.360156384861,38.7866637029717,16.3800734716904));
#67205=CARTESIAN_POINT('Ctrl Pts',(-38.1943325188198,37.4011801932639,16.3015679613136));
#67206=CARTESIAN_POINT('Ctrl Pts',(-39.8101089940917,37.3327641444332,16.2230624509368));
#67207=CARTESIAN_POINT('Ctrl Pts',(-40.7584190562144,38.6427726944821,16.1445569405601));
#67208=CARTESIAN_POINT('Ctrl Pts',(-40.1887956959422,40.1563590325842,16.0660514301833));
#67209=CARTESIAN_POINT('Ctrl Pts',(-38.6120906852372,40.5161029470303,15.9875459198065));
#67210=CARTESIAN_POINT('Ctrl Pts',(-37.4423305613345,39.39937754301,15.9090404094297));
#67211=CARTESIAN_POINT('Ctrl Pts',(-37.7285840133161,37.8076887115003,15.8305348990529));
#67212=CARTESIAN_POINT('Ctrl Pts',(-39.2141321392513,37.1685008366855,15.7520293886762));
#67213=CARTESIAN_POINT('Ctrl Pts',(-40.566700064693,38.0550528008733,15.6735238782994));
#67214=CARTESIAN_POINT('Ctrl Pts',(-40.5732727150713,39.6722637252762,15.5950183679226));
#67215=CARTESIAN_POINT('Ctrl Pts',(-39.2279555885002,40.5697804074078,15.5165128575458));
#67216=CARTESIAN_POINT('Ctrl Pts',(-37.7372610525188,39.9426885464327,15.438007347169));
#67217=CARTESIAN_POINT('Ctrl Pts',(-37.4380794359446,38.3533790377419,15.3595018367923));
#67218=CARTESIAN_POINT('Ctrl Pts',(-38.5987238648932,37.2271824197985,15.2809963264155));
#67219=CARTESIAN_POINT('Ctrl Pts',(-40.1783009449622,37.5740986189236,15.2024908160387));
#67220=CARTESIAN_POINT('Ctrl Pts',(-40.7602081505748,39.083004888448,15.1239853056619));
#67221=CARTESIAN_POINT('Ctrl Pts',(-39.8225777684026,40.4006783187926,15.0454797952851));
#67222=CARTESIAN_POINT('Ctrl Pts',(-38.2062979965018,40.3453978385299,14.9669742849084));
#67223=CARTESIAN_POINT('Ctrl Pts',(-37.3608890269436,38.9667407289735,14.8884687745316));
#67224=CARTESIAN_POINT('Ctrl Pts',(-38.0445295284047,37.5011185847262,14.8099632641548));
#67225=CARTESIAN_POINT('Ctrl Pts',(-39.6441229517549,37.262937966455,14.731457753778));
#67226=CARTESIAN_POINT('Ctrl Pts',(-40.725098637337,38.4658013079928,14.6529522434012));
#67227=CARTESIAN_POINT('Ctrl Pts',(-40.3180468752625,40.030959483689,14.5744467330245));
#67228=CARTESIAN_POINT('Ctrl Pts',(-38.7879504123214,40.5547265955191,14.4959412226477));
#67229=CARTESIAN_POINT('Ctrl Pts',(-37.5071800276552,39.5674059357951,14.4174357122709));
#67230=CARTESIAN_POINT('Ctrl Pts',(-37.6240692147494,37.9543891190076,14.3389302018941));
#67231=CARTESIAN_POINT('Ctrl Pts',(-39.0343808705876,37.1623917317957,14.2604246915173));
#67232=CARTESIAN_POINT('Ctrl Pts',(-40.4721132139356,37.9014449427502,14.1819191811406));
#67233=CARTESIAN_POINT('Ctrl Pts',(-40.6503151964691,39.50925492313,14.1034136707638));
#67234=CARTESIAN_POINT('Ctrl Pts',(-39.4041595574733,40.5428773182031,14.024908160387));
#67235=CARTESIAN_POINT('Ctrl Pts',(-38.3768621543504,40.2320073282821,13.9725711534692));
#67236=CARTESIAN_POINT('Ctrl Pts',(-38.0398499461206,39.8946132698472,13.9464026500102));
#67237=CARTESIAN_POINT('Ctrl Pts',(-40.5224743779889,39.378793292775,18.1607920499693));
#67238=CARTESIAN_POINT('Ctrl Pts',(-40.3550860167094,39.8577931806474,18.1346235465104));
#67239=CARTESIAN_POINT('Ctrl Pts',(-39.513668655637,40.6299377334171,18.0822865395925));
#67240=CARTESIAN_POINT('Ctrl Pts',(-37.8419311847822,40.2141004609093,18.0037810292157));
#67241=CARTESIAN_POINT('Ctrl Pts',(-37.270755510801,38.59042430652,17.925275518839));
#67242=CARTESIAN_POINT('Ctrl Pts',(-38.3080526905376,37.2183534421183,17.8467700084622));
#67243=CARTESIAN_POINT('Ctrl Pts',(-40.0256568276714,37.3267811177079,17.7682644980854));
#67244=CARTESIAN_POINT('Ctrl Pts',(-40.8821443104935,38.819261537444,17.6897589877086));
#67245=CARTESIAN_POINT('Ctrl Pts',(-40.1099071502118,40.3569109628884,17.6112534773319));
#67246=CARTESIAN_POINT('Ctrl Pts',(-38.4012543668155,40.5609220251471,17.5327479669551));
#67247=CARTESIAN_POINT('Ctrl Pts',(-37.2886704652103,39.2482374965454,17.4542424565783));
#67248=CARTESIAN_POINT('Ctrl Pts',(-37.7698859642865,37.5961510380776,17.3757369462015));
#67249=CARTESIAN_POINT('Ctrl Pts',(-39.4133655274823,37.0862699030106,17.2972314358247));
#67250=CARTESIAN_POINT('Ctrl Pts',(-40.7451827384013,38.1758790339381,17.218725925448));
#67251=CARTESIAN_POINT('Ctrl Pts',(-40.5709395934168,39.8877854279213,17.1402204150712));
#67252=CARTESIAN_POINT('Ctrl Pts',(-39.0468978715213,40.6867135087542,17.0617149046944));
#67253=CARTESIAN_POINT('Ctrl Pts',(-37.5398562037872,39.8561642112719,16.9832093943176));
#67254=CARTESIAN_POINT('Ctrl Pts',(-37.4013645066268,38.1409945655744,16.9047038839409));
#67255=CARTESIAN_POINT('Ctrl Pts',(-38.7556258599526,37.0794091529546,16.826198373564));
#67256=CARTESIAN_POINT('Ctrl Pts',(-40.3881062726607,37.6234631732891,16.7476928631873));
#67257=CARTESIAN_POINT('Ctrl Pts',(-40.834758606014,39.2852359660895,16.6691873528105));
#67258=CARTESIAN_POINT('Ctrl Pts',(-39.6950143769496,40.5744102242793,16.5906818424337));
#67259=CARTESIAN_POINT('Ctrl Pts',(-37.9910233315818,40.3348238050802,16.5121763320569));
#67260=CARTESIAN_POINT('Ctrl Pts',(-37.250965136829,38.7813435147693,16.4336708216802));
#67261=CARTESIAN_POINT('Ctrl Pts',(-38.1385415818572,37.3071674047962,16.3551653113034));
#67262=CARTESIAN_POINT('Ctrl Pts',(-39.8577530067586,37.234371659471,16.2766598009266));
#67263=CARTESIAN_POINT('Ctrl Pts',(-40.8667697353107,38.628241232664,16.1981542905498));
#67264=CARTESIAN_POINT('Ctrl Pts',(-40.2606815765474,40.2387207543455,16.119648780173));
#67265=CARTESIAN_POINT('Ctrl Pts',(-38.5830428006473,40.6214939022527,16.0411432697963));
#67266=CARTESIAN_POINT('Ctrl Pts',(-37.3383997450109,39.4332806175246,15.9626377594195));
#67267=CARTESIAN_POINT('Ctrl Pts',(-37.6429778921718,37.7396988220852,15.8841322490427));
#67268=CARTESIAN_POINT('Ctrl Pts',(-39.2236243178593,37.0595929325284,15.8056267386659));
#67269=CARTESIAN_POINT('Ctrl Pts',(-40.6627777316899,38.0028980795747,15.7271212282892));
#67270=CARTESIAN_POINT('Ctrl Pts',(-40.6697711344255,39.7236357807725,15.6486157179124));
#67271=CARTESIAN_POINT('Ctrl Pts',(-39.2383326839261,40.6786075590939,15.5701102075356));
#67272=CARTESIAN_POINT('Ctrl Pts',(-37.6522103975089,40.0113720173278,15.4916046971588));
#67273=CARTESIAN_POINT('Ctrl Pts',(-37.3338764811494,38.3203218585575,15.413099186782));
#67274=CARTESIAN_POINT('Ctrl Pts',(-38.5688202948727,37.1220310541764,15.3345936764052));
#67275=CARTESIAN_POINT('Ctrl Pts',(-40.2495149974676,37.4911553124801,15.2560881660285));
#67276=CARTESIAN_POINT('Ctrl Pts',(-40.8686733596744,39.0966551680435,15.1775826556517));
#67277=CARTESIAN_POINT('Ctrl Pts',(-39.8710199775172,40.4986802936762,15.0990771452749));
#67278=CARTESIAN_POINT('Ctrl Pts',(-38.151273037136,40.4398609986214,15.0205716348981));
#67279=CARTESIAN_POINT('Ctrl Pts',(-37.2517446794564,38.9729482851087,14.9420661245214));
#67280=CARTESIAN_POINT('Ctrl Pts',(-37.9791488585767,37.413503415388,14.8635606141446));
#67281=CARTESIAN_POINT('Ctrl Pts',(-39.6811412632862,37.1600755146919,14.7850551037678));
#67282=CARTESIAN_POINT('Ctrl Pts',(-40.8313162888141,38.4399409113082,14.706549593391));
#67283=CARTESIAN_POINT('Ctrl Pts',(-40.3982068515902,40.1052936742774,14.6280440830142));
#67284=CARTESIAN_POINT('Ctrl Pts',(-38.7701602990205,40.6625900679474,14.5495385726375));
#67285=CARTESIAN_POINT('Ctrl Pts',(-37.4074005907986,39.6120654537968,14.4710330622607));
#67286=CARTESIAN_POINT('Ctrl Pts',(-37.5317725128899,37.8957903486572,14.3925275518839));
#67287=CARTESIAN_POINT('Ctrl Pts',(-39.0323661584193,37.0530927494379,14.3140220415071));
#67288=CARTESIAN_POINT('Ctrl Pts',(-40.5621358440549,37.8394569175814,14.2355165311304));
#67289=CARTESIAN_POINT('Ctrl Pts',(-40.7517455388365,39.5501918673983,14.1570110207535));
#67290=CARTESIAN_POINT('Ctrl Pts',(-39.4258164610498,40.6499822516744,14.0785055103768));
#67291=CARTESIAN_POINT('Ctrl Pts',(-38.3327559670706,40.3192117233802,14.0261685034589));
#67292=CARTESIAN_POINT('Ctrl Pts',(-37.9741697098829,39.9602191716055,14.));
#67293=CARTESIAN_POINT('Ctrl Pts',(-38.4329072841441,37.7756148875603,17.1934196736194));
#67294=CARTESIAN_POINT('Ctrl Pts',(-38.3336188224971,37.831835714126,17.2005947478237));
#67295=CARTESIAN_POINT('Ctrl Pts',(-38.2421150540945,37.9010724492168,17.2077698220279));
#67296=CARTESIAN_POINT('Ctrl Pts',(-38.1625457103698,37.9820376407054,17.2149448962322));
#67297=CARTESIAN_POINT('Ctrl Pts',(-37.8723451372176,38.277329066718,17.2411133996911));
#67298=CARTESIAN_POINT('Ctrl Pts',(-37.7408919078847,38.7286281219637,17.2672819031501));
#67299=CARTESIAN_POINT('Ctrl Pts',(-37.8271270931297,39.1335701086941,17.293450406609));
#67300=CARTESIAN_POINT('Ctrl Pts',(-37.9133622783746,39.5385120954244,17.3196189100679));
#67301=CARTESIAN_POINT('Ctrl Pts',(-38.2172858781974,39.8970970136394,17.3457874135268));
#67302=CARTESIAN_POINT('Ctrl Pts',(-38.6026232932098,40.0485247084105,17.3719559169858));
#67303=CARTESIAN_POINT('Ctrl Pts',(-38.9879607082221,40.1999524031816,17.3981244204447));
#67304=CARTESIAN_POINT('Ctrl Pts',(-39.454711938424,40.1442228745088,17.4242929239036));
#67305=CARTESIAN_POINT('Ctrl Pts',(-39.7935632382492,39.9063389161268,17.4504614273625));
#67306=CARTESIAN_POINT('Ctrl Pts',(-40.1324145380743,39.6684549577448,17.4766299308215));
#67307=CARTESIAN_POINT('Ctrl Pts',(-40.3433659075226,39.2484165696535,17.5027984342804));
#67308=CARTESIAN_POINT('Ctrl Pts',(-40.3318586129825,38.8345475710328,17.5289669377393));
#67309=CARTESIAN_POINT('Ctrl Pts',(-40.3203513184424,38.4206785724121,17.5551354411982));
#67310=CARTESIAN_POINT('Ctrl Pts',(-40.0863853599139,38.0129789632619,17.5813039446572));
#67311=CARTESIAN_POINT('Ctrl Pts',(-39.7348041486982,37.7943196106437,17.6074724481161));
#67312=CARTESIAN_POINT('Ctrl Pts',(-39.3832229374826,37.5756602580255,17.633640951575));
#67313=CARTESIAN_POINT('Ctrl Pts',(-38.9140264735798,37.5460411619393,17.659809455034));
#67314=CARTESIAN_POINT('Ctrl Pts',(-38.5377494466644,37.7186353304695,17.6859779584929));
#67315=CARTESIAN_POINT('Ctrl Pts',(-38.5020812950974,37.7349959225928,17.6884585302017));
#67316=CARTESIAN_POINT('Ctrl Pts',(-38.4672480779576,37.7531735168604,17.6909391019106));
#67317=CARTESIAN_POINT('Ctrl Pts',(-38.4333577759012,37.7730251466967,17.6934196736194));
#67318=CARTESIAN_POINT('Ctrl Pts',(-37.5756558680257,39.2699729499893,18.));
#67319=CARTESIAN_POINT('Ctrl Pts',(-37.4440523270134,38.7799318659294,17.9738314965411));
#67320=CARTESIAN_POINT('Ctrl Pts',(-37.7041245449082,37.6679293649188,17.9214944896232));
#67321=CARTESIAN_POINT('Ctrl Pts',(-39.3195387437205,37.0695352316425,17.8429889792464));
#67322=CARTESIAN_POINT('Ctrl Pts',(-40.7062722211717,38.0891100356719,17.7644834688697));
#67323=CARTESIAN_POINT('Ctrl Pts',(-40.6223994863181,39.8071108514352,17.6859779584929));
#67324=CARTESIAN_POINT('Ctrl Pts',(-39.1423049297703,40.6853144575311,17.6074724481161));
#67325=CARTESIAN_POINT('Ctrl Pts',(-37.5937815296791,39.9348860603428,17.5289669377393));
#67326=CARTESIAN_POINT('Ctrl Pts',(-37.3653803023341,38.2294395514344,17.4504614273626));
#67327=CARTESIAN_POINT('Ctrl Pts',(-38.6620363043874,37.0981581562677,17.3719559169858));
#67328=CARTESIAN_POINT('Ctrl Pts',(-40.3208285827552,37.5557507395872,17.293450406609));
#67329=CARTESIAN_POINT('Ctrl Pts',(-40.8541369642561,39.1917640019411,17.2149448962322));
#67330=CARTESIAN_POINT('Ctrl Pts',(-39.7836658898432,40.5390185509755,17.1364393858554));
#67331=CARTESIAN_POINT('Ctrl Pts',(-38.0694451486085,40.389246627264,17.0579338754786));
#67332=CARTESIAN_POINT('Ctrl Pts',(-37.248825754395,38.87677605618,16.9794283651019));
#67333=CARTESIAN_POINT('Ctrl Pts',(-38.0577601193366,37.3580220610822,16.9009228547251));
#67334=CARTESIAN_POINT('Ctrl Pts',(-39.7707759682515,37.1950414723212,16.8224173443483));
#67335=CARTESIAN_POINT('Ctrl Pts',(-40.8516003110939,38.5339981005298,16.7439118339715));
#67336=CARTESIAN_POINT('Ctrl Pts',(-40.3309240105073,40.1740843304588,16.6654063235948));
#67337=CARTESIAN_POINT('Ctrl Pts',(-38.6757020358417,40.644431583443,16.586900813218));
#67338=CARTESIAN_POINT('Ctrl Pts',(-37.3703767628973,39.5232213878114,16.5083953028412));
#67339=CARTESIAN_POINT('Ctrl Pts',(-37.5855949493635,37.8159816397814,16.4298897924644));
#67340=CARTESIAN_POINT('Ctrl Pts',(-39.1283437989466,37.053805563498,16.3513842820876));
#67341=CARTESIAN_POINT('Ctrl Pts',(-40.6150494715949,37.9202307686755,16.2728787717109));
#67342=CARTESIAN_POINT('Ctrl Pts',(-40.7123989731982,39.6382265407265,16.1943732613341));
#67343=CARTESIAN_POINT('Ctrl Pts',(-39.333086957597,40.6670534245635,16.1158677509573));
#67344=CARTESIAN_POINT('Ctrl Pts',(-37.7141132310224,40.0840350136354,16.0373622405805));
#67345=CARTESIAN_POINT('Ctrl Pts',(-37.3074119207117,38.4120360784117,15.9588567302037));
#67346=CARTESIAN_POINT('Ctrl Pts',(-38.4777224302706,37.150545013987,15.8803512198269));
#67347=CARTESIAN_POINT('Ctrl Pts',(-40.1754824724718,37.4308969968639,15.8018457094502));
#67348=CARTESIAN_POINT('Ctrl Pts',(-40.8781004790679,39.0016657040982,15.7233401990734));
#67349=CARTESIAN_POINT('Ctrl Pts',(-39.9554519188483,40.454148415738,15.6448346886966));
#67350=CARTESIAN_POINT('Ctrl Pts',(-38.2349899535507,40.4857241059463,15.5663291783198));
#67351=CARTESIAN_POINT('Ctrl Pts',(-37.2596657788943,39.0680749435715,15.4878236679431));
#67352=CARTESIAN_POINT('Ctrl Pts',(-37.9041732944261,37.4725824031402,15.4093181575663));
#67353=CARTESIAN_POINT('Ctrl Pts',(-39.5905028527061,37.1301221194426,15.3308126471895));
#67354=CARTESIAN_POINT('Ctrl Pts',(-40.8063139857151,38.3478206288557,15.2523071368127));
#67355=CARTESIAN_POINT('Ctrl Pts',(-40.4612384258706,40.0336169338117,15.1738016264359));
#67356=CARTESIAN_POINT('Ctrl Pts',(-38.8647480157521,40.6756488816116,15.0952961160592));
#67357=CARTESIAN_POINT('Ctrl Pts',(-37.4486135593306,39.6981268544225,15.0167906056824));
#67358=CARTESIAN_POINT('Ctrl Pts',(-37.4828575973041,37.9777160555697,14.9382850953056));
#67359=CARTESIAN_POINT('Ctrl Pts',(-38.9367702893064,37.0573213639055,14.8597795849288));
#67360=CARTESIAN_POINT('Ctrl Pts',(-40.5064460859517,37.7623754838001,14.781274074552));
#67361=CARTESIAN_POINT('Ctrl Pts',(-40.7841666383236,39.4605673674226,14.7027685641753));
#67362=CARTESIAN_POINT('Ctrl Pts',(-39.5208569909583,40.6289217126118,14.6242630537985));
#67363=CARTESIAN_POINT('Ctrl Pts',(-37.8495006293028,40.2196233657655,14.5457575434217));
#67364=CARTESIAN_POINT('Ctrl Pts',(-37.2689744719433,38.5997554156835,14.4672520330449));
#67365=CARTESIAN_POINT('Ctrl Pts',(-38.2999795535027,37.2220243444981,14.3887465226681));
#67366=CARTESIAN_POINT('Ctrl Pts',(-40.0177412802272,37.3220721610693,14.3102410122914));
#67367=CARTESIAN_POINT('Ctrl Pts',(-40.8820235552812,38.8100518816852,14.2317355019146));
#67368=CARTESIAN_POINT('Ctrl Pts',(-40.1171224362185,40.3517547545305,14.1532299915378));
#67369=CARTESIAN_POINT('Ctrl Pts',(-38.4102262410485,40.5640442208951,14.074724481161));
#67370=CARTESIAN_POINT('Ctrl Pts',(-37.2896688855126,39.2575551350437,13.9962189707843));
#67371=CARTESIAN_POINT('Ctrl Pts',(-37.7654127933167,37.6018660619833,13.9177134604075));
#67372=CARTESIAN_POINT('Ctrl Pts',(-38.8548175316167,37.2592519394721,13.8653764534896));
#67373=CARTESIAN_POINT('Ctrl Pts',(-39.3533377835638,37.3537893102425,13.8392079500307));
#67374=CARTESIAN_POINT('Ctrl Pts',(-37.6653123637055,39.2458951477601,18.0535973499898));
#67375=CARTESIAN_POINT('Ctrl Pts',(-37.5416266421298,38.7853369848301,18.0274288465308));
#67376=CARTESIAN_POINT('Ctrl Pts',(-37.7860518276885,37.7402372050404,17.975091839613));
#67377=CARTESIAN_POINT('Ctrl Pts',(-39.304275952107,37.1778449655031,17.8965863292362));
#67378=CARTESIAN_POINT('Ctrl Pts',(-40.6075777437793,38.1360778851249,17.8180808188594));
#67379=CARTESIAN_POINT('Ctrl Pts',(-40.528751143438,39.7507165865677,17.7395753084826));
#67380=CARTESIAN_POINT('Ctrl Pts',(-39.1377052656541,40.5760837907846,17.6610697981059));
#67381=CARTESIAN_POINT('Ctrl Pts',(-37.6823475097464,39.8708043045094,17.5825642877291));
#67382=CARTESIAN_POINT('Ctrl Pts',(-37.4676878554875,38.267964590315,17.5040587773523));
#67383=CARTESIAN_POINT('Ctrl Pts',(-38.6863316094155,37.2047458152723,17.4255532669755));
#67384=CARTESIAN_POINT('Ctrl Pts',(-40.2453240067019,37.6348077149766,17.3470477565987));
#67385=CARTESIAN_POINT('Ctrl Pts',(-40.7465463255009,39.1723915771219,17.268542246222));
#67386=CARTESIAN_POINT('Ctrl Pts',(-39.7404792679866,40.4385896578249,17.1900367358452));
#67387=CARTESIAN_POINT('Ctrl Pts',(-38.1293932159794,40.2978286394393,17.1115312254684));
#67388=CARTESIAN_POINT('Ctrl Pts',(-37.3581457166218,38.876354623561,17.0330257150916));
#67389=CARTESIAN_POINT('Ctrl Pts',(-38.1184112069391,37.4489752207368,16.9545202047149));
#67390=CARTESIAN_POINT('Ctrl Pts',(-39.7283648579877,37.2958002258341,16.8760146943381));
#67391=CARTESIAN_POINT('Ctrl Pts',(-40.7441622880019,38.5541996233327,16.7975091839613));
#67392=CARTESIAN_POINT('Ctrl Pts',(-40.2548120512981,40.0956114062894,16.7190036735845));
#67393=CARTESIAN_POINT('Ctrl Pts',(-38.6991751533109,40.5376606013872,16.6404981632077));
#67394=CARTESIAN_POINT('Ctrl Pts',(-37.4723837080864,39.4839071003945,16.561992652831));
#67395=CARTESIAN_POINT('Ctrl Pts',(-37.6746534683415,37.8793820358439,16.4834871424542));
#67396=CARTESIAN_POINT('Ctrl Pts',(-39.1245840948508,37.1630616599808,16.4049816320774));
#67397=CARTESIAN_POINT('Ctrl Pts',(-40.5218433363406,37.9773591011396,16.3264761217006));
#67398=CARTESIAN_POINT('Ctrl Pts',(-40.6133358847799,39.5919930623209,16.2479706113239));
#67399=CARTESIAN_POINT('Ctrl Pts',(-39.3170090487735,40.5589214179339,16.1694651009471));
#67400=CARTESIAN_POINT('Ctrl Pts',(-37.7954395526702,40.010979832982,16.0909595905703));
#67401=CARTESIAN_POINT('Ctrl Pts',(-37.4132070941463,38.4395753465506,16.0124540801935));
#67402=CARTESIAN_POINT('Ctrl Pts',(-38.5131068288268,37.2539808605321,15.9339485698167));
#67403=CARTESIAN_POINT('Ctrl Pts',(-40.1087225262985,37.517465695595,15.85544305944));
#67404=CARTESIAN_POINT('Ctrl Pts',(-40.7690680950382,38.9937303879309,15.7769375490632));
#67405=CARTESIAN_POINT('Ctrl Pts',(-39.9019299310211,40.3588256648781,15.6984320386864));
#67406=CARTESIAN_POINT('Ctrl Pts',(-38.2849781530935,40.3885016295036,15.6199265283096));
#67407=CARTESIAN_POINT('Ctrl Pts',(-37.3683335599107,39.0561441698122,15.5414210179328));
#67408=CARTESIAN_POINT('Ctrl Pts',(-37.9740648077658,37.5566431334877,15.4629155075561));
#67409=CARTESIAN_POINT('Ctrl Pts',(-39.558937727035,37.2347866927387,15.3844099971793));
#67410=CARTESIAN_POINT('Ctrl Pts',(-40.7016005773603,38.37922336701,15.3059044868025));
#67411=CARTESIAN_POINT('Ctrl Pts',(-40.3772862064154,39.9635951157055,15.2273989764257));
#67412=CARTESIAN_POINT('Ctrl Pts',(-38.8768473364175,40.5669997363369,15.1488934660489));
#67413=CARTESIAN_POINT('Ctrl Pts',(-37.5459134516342,39.6482895226222,15.0703879556721));
#67414=CARTESIAN_POINT('Ctrl Pts',(-37.5780972250634,38.0313858327519,14.9918824452954));
#67415=CARTESIAN_POINT('Ctrl Pts',(-38.9445364487739,37.1663659351315,14.9133769349186));
#67416=CARTESIAN_POINT('Ctrl Pts',(-40.4197739845928,37.829001050405,14.8348714245418));
#67417=CARTESIAN_POINT('Ctrl Pts',(-40.6807857070153,39.425022607912,14.756365914165));
#67418=CARTESIAN_POINT('Ctrl Pts',(-39.4934820516118,40.5230838692526,14.6778604037883));
#67419=CARTESIAN_POINT('Ctrl Pts',(-37.9226814788354,40.1384106227729,14.5993548934115));
#67420=CARTESIAN_POINT('Ctrl Pts',(-37.3770822030539,38.6160007033882,14.5208493830347));
#67421=CARTESIAN_POINT('Ctrl Pts',(-38.3460577069044,37.3211596955696,14.4423438726579));
#67422=CARTESIAN_POINT('Ctrl Pts',(-39.9604717039049,37.415188217063,14.3638383622811));
#67423=CARTESIAN_POINT('Ctrl Pts',(-40.7727551425788,38.8136448544662,14.2853328519044));
#67424=CARTESIAN_POINT('Ctrl Pts',(-40.0538736739071,40.2625924345728,14.2068273415276));
#67425=CARTESIAN_POINT('Ctrl Pts',(-38.4496714926395,40.4621096787766,14.1283218311508));
#67426=CARTESIAN_POINT('Ctrl Pts',(-37.396531554152,39.2342244404969,14.049816320774));
#67427=CARTESIAN_POINT('Ctrl Pts',(-37.8436527187452,37.678148546708,13.9713108103972));
#67428=CARTESIAN_POINT('Ctrl Pts',(-38.8675143117402,37.356147522732,13.9189738034794));
#67429=CARTESIAN_POINT('Ctrl Pts',(-39.3360415003546,37.4449971298904,13.8928053000205));
#67430=CARTESIAN_POINT('Ctrl Pts',(-37.7549688593853,39.2218173455308,18.1071946999795));
#67431=CARTESIAN_POINT('Ctrl Pts',(-37.6392009572462,38.7907421037308,18.0810261965206));
#67432=CARTESIAN_POINT('Ctrl Pts',(-37.8679791104688,37.812545045162,18.0286891896028));
#67433=CARTESIAN_POINT('Ctrl Pts',(-39.2890131604935,37.2861546993635,17.950183679226));
#67434=CARTESIAN_POINT('Ctrl Pts',(-40.5088832663869,38.1830457345779,17.8716781688492));
#67435=CARTESIAN_POINT('Ctrl Pts',(-40.4351028005577,39.6943223217001,17.7931726584724));
#67436=CARTESIAN_POINT('Ctrl Pts',(-39.1331056015378,40.4668531240381,17.7146671480957));
#67437=CARTESIAN_POINT('Ctrl Pts',(-37.7709134898136,39.806722548676,17.6361616377188));
#67438=CARTESIAN_POINT('Ctrl Pts',(-37.5699954086408,38.3064896291956,17.5576561273421));
#67439=CARTESIAN_POINT('Ctrl Pts',(-38.7106269144436,37.3113334742769,17.4791506169653));
#67440=CARTESIAN_POINT('Ctrl Pts',(-40.1698194306487,37.713864690366,17.4006451065885));
#67441=CARTESIAN_POINT('Ctrl Pts',(-40.6389556867456,39.1530191523028,17.3221395962117));
#67442=CARTESIAN_POINT('Ctrl Pts',(-39.6972926461299,40.3381607646743,17.243634085835));
#67443=CARTESIAN_POINT('Ctrl Pts',(-38.1893412833502,40.2064106516146,17.1651285754582));
#67444=CARTESIAN_POINT('Ctrl Pts',(-37.4674656788486,38.8759331909419,17.0866230650814));
#67445=CARTESIAN_POINT('Ctrl Pts',(-38.1790622945415,37.5399283803915,17.0081175547046));
#67446=CARTESIAN_POINT('Ctrl Pts',(-39.6859537477239,37.396558979347,16.9296120443278));
#67447=CARTESIAN_POINT('Ctrl Pts',(-40.63672426491,38.5744011461357,16.8511065339511));
#67448=CARTESIAN_POINT('Ctrl Pts',(-40.1787000920889,40.01713848212,16.7726010235743));
#67449=CARTESIAN_POINT('Ctrl Pts',(-38.7226482707802,40.4308896193314,16.6940955131975));
#67450=CARTESIAN_POINT('Ctrl Pts',(-37.5743906532754,39.4445928129776,16.6155900028207));
#67451=CARTESIAN_POINT('Ctrl Pts',(-37.7637119873195,37.9427824319065,16.537084492444));
#67452=CARTESIAN_POINT('Ctrl Pts',(-39.120824390755,37.2723177564635,16.4585789820672));
#67453=CARTESIAN_POINT('Ctrl Pts',(-40.4286372010863,38.0344874336038,16.3800734716904));
#67454=CARTESIAN_POINT('Ctrl Pts',(-40.5142727963614,39.5457595839153,16.3015679613136));
#67455=CARTESIAN_POINT('Ctrl Pts',(-39.3009311399501,40.4507894113043,16.2230624509368));
#67456=CARTESIAN_POINT('Ctrl Pts',(-37.8767658743179,39.9379246523285,16.14455694056));
#67457=CARTESIAN_POINT('Ctrl Pts',(-37.5190022675809,38.4671146146895,16.0660514301833));
#67458=CARTESIAN_POINT('Ctrl Pts',(-38.5484912273831,37.3574167070772,15.9875459198065));
#67459=CARTESIAN_POINT('Ctrl Pts',(-40.0419625801251,37.604034394326,15.9090404094297));
#67460=CARTESIAN_POINT('Ctrl Pts',(-40.6600357110086,38.9857950717635,15.8305348990529));
#67461=CARTESIAN_POINT('Ctrl Pts',(-39.8484079431939,40.2635029140183,15.7520293886762));
#67462=CARTESIAN_POINT('Ctrl Pts',(-38.3349663526362,40.2912791530608,15.6735238782994));
#67463=CARTESIAN_POINT('Ctrl Pts',(-37.4770013409272,39.0442133960529,15.5950183679226));
#67464=CARTESIAN_POINT('Ctrl Pts',(-38.0439563211054,37.640703863835,15.5165128575458));
#67465=CARTESIAN_POINT('Ctrl Pts',(-39.5273726013639,37.3394512660349,15.438007347169));
#67466=CARTESIAN_POINT('Ctrl Pts',(-40.5968871690055,38.4106261051643,15.3595018367923));
#67467=CARTESIAN_POINT('Ctrl Pts',(-40.2933339869602,39.8935732975992,15.2809963264155));
#67468=CARTESIAN_POINT('Ctrl Pts',(-38.8889466570829,40.4583505910623,15.2024908160387));
#67469=CARTESIAN_POINT('Ctrl Pts',(-37.6432133439378,39.5984521908218,15.1239853056619));
#67470=CARTESIAN_POINT('Ctrl Pts',(-37.6733368528227,38.0850556099341,15.0454797952851));
#67471=CARTESIAN_POINT('Ctrl Pts',(-38.9523026082414,37.2754105063574,14.9669742849084));
#67472=CARTESIAN_POINT('Ctrl Pts',(-40.3331018832339,37.89562661701,14.8884687745316));
#67473=CARTESIAN_POINT('Ctrl Pts',(-40.577404775707,39.3894778484014,14.8099632641548));
#67474=CARTESIAN_POINT('Ctrl Pts',(-39.4661071122653,40.4172460258934,14.731457753778));
#67475=CARTESIAN_POINT('Ctrl Pts',(-37.995862328368,40.0571978797802,14.6529522434012));
#67476=CARTESIAN_POINT('Ctrl Pts',(-37.4851899341645,38.6322459910928,14.5744467330245));
#67477=CARTESIAN_POINT('Ctrl Pts',(-38.3921358603061,37.4202950466411,14.4959412226477));
#67478=CARTESIAN_POINT('Ctrl Pts',(-39.9032021275825,37.5083042730567,14.4174357122709));
#67479=CARTESIAN_POINT('Ctrl Pts',(-40.6634867298766,38.8172378272473,14.3389302018941));
#67480=CARTESIAN_POINT('Ctrl Pts',(-39.9906249115956,40.1734301146151,14.2604246915173));
#67481=CARTESIAN_POINT('Ctrl Pts',(-38.4891167442306,40.3601751366581,14.1819191811406));
#67482=CARTESIAN_POINT('Ctrl Pts',(-37.5033942227913,39.2108937459501,14.1034136707638));
#67483=CARTESIAN_POINT('Ctrl Pts',(-37.9218926441736,37.7544310314326,14.024908160387));
#67484=CARTESIAN_POINT('Ctrl Pts',(-38.8802110918637,37.4530431059918,13.9725711534692));
#67485=CARTESIAN_POINT('Ctrl Pts',(-39.3187452171454,37.5362049495383,13.9464026500102));
#67486=CARTESIAN_POINT('Ctrl Pts',(-37.8446253550651,39.1977395433015,18.1607920499693));
#67487=CARTESIAN_POINT('Ctrl Pts',(-37.7367752723626,38.7961472226315,18.1346235465104));
#67488=CARTESIAN_POINT('Ctrl Pts',(-37.9499063932492,37.8848528852835,18.0822865395925));
#67489=CARTESIAN_POINT('Ctrl Pts',(-39.2737503688799,37.3944644332241,18.0037810292158));
#67490=CARTESIAN_POINT('Ctrl Pts',(-40.4101887889945,38.2300135840309,17.925275518839));
#67491=CARTESIAN_POINT('Ctrl Pts',(-40.3414544576775,39.6379280568325,17.8467700084622));
#67492=CARTESIAN_POINT('Ctrl Pts',(-39.1285059374216,40.3576224572915,17.7682644980854));
#67493=CARTESIAN_POINT('Ctrl Pts',(-37.8594794698809,39.7426407928426,17.6897589877086));
#67494=CARTESIAN_POINT('Ctrl Pts',(-37.6723029617942,38.3450146680762,17.6112534773319));
#67495=CARTESIAN_POINT('Ctrl Pts',(-38.7349222194718,37.4179211332814,17.5327479669551));
#67496=CARTESIAN_POINT('Ctrl Pts',(-40.0943148545955,37.7929216657555,17.4542424565783));
#67497=CARTESIAN_POINT('Ctrl Pts',(-40.5313650479903,39.1336467274836,17.3757369462015));
#67498=CARTESIAN_POINT('Ctrl Pts',(-39.6541060242733,40.2377318715238,17.2972314358247));
#67499=CARTESIAN_POINT('Ctrl Pts',(-38.2492893507211,40.11499266379,17.218725925448));
#67500=CARTESIAN_POINT('Ctrl Pts',(-37.5767856410754,38.8755117583229,17.1402204150712));
#67501=CARTESIAN_POINT('Ctrl Pts',(-38.239713382144,37.6308815400461,17.0617149046944));
#67502=CARTESIAN_POINT('Ctrl Pts',(-39.6435426374601,37.4973177328599,16.9832093943176));
#67503=CARTESIAN_POINT('Ctrl Pts',(-40.5292862418181,38.5946026689388,16.9047038839408));
#67504=CARTESIAN_POINT('Ctrl Pts',(-40.1025881328798,39.9386655579506,16.8261983735641));
#67505=CARTESIAN_POINT('Ctrl Pts',(-38.7461213882494,40.3241186372757,16.7476928631873));
#67506=CARTESIAN_POINT('Ctrl Pts',(-37.6763975984645,39.4052785255607,16.6691873528105));
#67507=CARTESIAN_POINT('Ctrl Pts',(-37.8527705062975,38.0061828279691,16.5906818424337));
#67508=CARTESIAN_POINT('Ctrl Pts',(-39.1170646866591,37.3815738529462,16.5121763320569));
#67509=CARTESIAN_POINT('Ctrl Pts',(-40.335431065832,38.0916157660679,16.4336708216802));
#67510=CARTESIAN_POINT('Ctrl Pts',(-40.4152097079431,39.4995261055097,16.3551653113034));
#67511=CARTESIAN_POINT('Ctrl Pts',(-39.2848532311266,40.3426574046748,16.2766598009266));
#67512=CARTESIAN_POINT('Ctrl Pts',(-37.9580921959656,39.8648694716751,16.1981542905498));
#67513=CARTESIAN_POINT('Ctrl Pts',(-37.6247974410155,38.4946538828284,16.1196487801731));
#67514=CARTESIAN_POINT('Ctrl Pts',(-38.5838756259393,37.4608525536223,16.0411432697963));
#67515=CARTESIAN_POINT('Ctrl Pts',(-39.9752026339518,37.6906030930571,15.9626377594195));
#67516=CARTESIAN_POINT('Ctrl Pts',(-40.5510033269789,38.9778597555962,15.8841322490427));
#67517=CARTESIAN_POINT('Ctrl Pts',(-39.7948859553666,40.1681801631584,15.8056267386659));
#67518=CARTESIAN_POINT('Ctrl Pts',(-38.3849545521789,40.1940566766181,15.7271212282891));
#67519=CARTESIAN_POINT('Ctrl Pts',(-37.5856691219436,39.0322826222935,15.6486157179124));
#67520=CARTESIAN_POINT('Ctrl Pts',(-38.1138478344451,37.7247645941825,15.5701102075356));
#67521=CARTESIAN_POINT('Ctrl Pts',(-39.4958074756928,37.444115839331,15.4916046971588));
#67522=CARTESIAN_POINT('Ctrl Pts',(-40.4921737606506,38.4420288433187,15.413099186782));
#67523=CARTESIAN_POINT('Ctrl Pts',(-40.209381767505,39.823551479493,15.3345936764052));
#67524=CARTESIAN_POINT('Ctrl Pts',(-38.9010459777483,40.3497014457877,15.2560881660285));
#67525=CARTESIAN_POINT('Ctrl Pts',(-37.7405132362414,39.5486148590214,15.1775826556517));
#67526=CARTESIAN_POINT('Ctrl Pts',(-37.768576480582,38.1387253871163,15.0990771452749));
#67527=CARTESIAN_POINT('Ctrl Pts',(-38.960068767709,37.3844550775834,15.0205716348981));
#67528=CARTESIAN_POINT('Ctrl Pts',(-40.2464297818749,37.9622521836149,14.9420661245214));
#67529=CARTESIAN_POINT('Ctrl Pts',(-40.4740238443987,39.3539330888908,14.8635606141446));
#67530=CARTESIAN_POINT('Ctrl Pts',(-39.4387321729189,40.3114081825342,14.7850551037678));
#67531=CARTESIAN_POINT('Ctrl Pts',(-38.0690431779005,39.9759851367876,14.706549593391));
#67532=CARTESIAN_POINT('Ctrl Pts',(-37.5932976652751,38.6484912787975,14.6280440830142));
#67533=CARTESIAN_POINT('Ctrl Pts',(-38.4382140137078,37.5194303977126,14.5495385726375));
#67534=CARTESIAN_POINT('Ctrl Pts',(-39.8459325512601,37.6014203290504,14.4710330622607));
#67535=CARTESIAN_POINT('Ctrl Pts',(-40.5542183171743,38.8208308000283,14.3925275518839));
#67536=CARTESIAN_POINT('Ctrl Pts',(-39.9273761492841,40.0842677946574,14.3140220415071));
#67537=CARTESIAN_POINT('Ctrl Pts',(-38.5285619958217,40.2582405945396,14.2355165311303));
#67538=CARTESIAN_POINT('Ctrl Pts',(-37.6102568914307,39.1875630514033,14.1570110207536));
#67539=CARTESIAN_POINT('Ctrl Pts',(-38.0001325696021,37.8307135161573,14.0785055103768));
#67540=CARTESIAN_POINT('Ctrl Pts',(-38.8929078719873,37.5499386892516,14.0261685034589));
#67541=CARTESIAN_POINT('Ctrl Pts',(-39.3014489339362,37.6274127691862,14.));
#67542=CARTESIAN_POINT('Ctrl Pts',(-38.4348713855213,37.7748596688486,17.5565803263806));
#67543=CARTESIAN_POINT('Ctrl Pts',(-38.5438548719482,37.7108039030124,17.5486362065721));
#67544=CARTESIAN_POINT('Ctrl Pts',(-38.6618404864523,37.6628704742542,17.5406920867636));
#67545=CARTESIAN_POINT('Ctrl Pts',(-38.7843844490461,37.6349368111595,17.5327479669551));
#67546=CARTESIAN_POINT('Ctrl Pts',(-39.1880530978463,37.5429213107728,17.5065794634961));
#67547=CARTESIAN_POINT('Ctrl Pts',(-39.6411839762209,37.6679214882641,17.4804109600372));
#67548=CARTESIAN_POINT('Ctrl Pts',(-39.9405911143073,37.9538757539645,17.4542424565783));
#67549=CARTESIAN_POINT('Ctrl Pts',(-40.2399982523938,38.2398300196648,17.4280739531194));
#67550=CARTESIAN_POINT('Ctrl Pts',(-40.385681650192,38.6867383735742,17.4019054496604));
#67551=CARTESIAN_POINT('Ctrl Pts',(-40.312313511805,39.0942067412023,17.3757369462015));
#67552=CARTESIAN_POINT('Ctrl Pts',(-40.2389453734179,39.5016751088303,17.3495684427426));
#67553=CARTESIAN_POINT('Ctrl Pts',(-39.9465256988456,39.869703490177,17.3233999392837));
#67554=CARTESIAN_POINT('Ctrl Pts',(-39.5661797493007,40.0332611462281,17.2972314358247));
#67555=CARTESIAN_POINT('Ctrl Pts',(-39.1858337997559,40.1968188022792,17.2710629323658));
#67556=CARTESIAN_POINT('Ctrl Pts',(-38.7175615752385,40.1559057330346,17.2448944289069));
#67557=CARTESIAN_POINT('Ctrl Pts',(-38.3713415113722,39.9288690475011,17.218725925448));
#67558=CARTESIAN_POINT('Ctrl Pts',(-38.0251214475059,39.7018323619676,17.192557421989));
#67559=CARTESIAN_POINT('Ctrl Pts',(-37.8009535442906,39.2886720601453,17.1663889185301));
#67560=CARTESIAN_POINT('Ctrl Pts',(-37.7993575495278,38.8746535395213,17.1402204150712));
#67561=CARTESIAN_POINT('Ctrl Pts',(-37.797761554765,38.4606350188973,17.1140519116123));
#67562=CARTESIAN_POINT('Ctrl Pts',(-38.0187374684545,38.0457582794717,17.0878834081533));
#67563=CARTESIAN_POINT('Ctrl Pts',(-38.3631969678519,37.8160592752279,17.0617149046944));
#67564=CARTESIAN_POINT('Ctrl Pts',(-38.3857260141202,37.8010360301049,17.0600033785898));
#67565=CARTESIAN_POINT('Ctrl Pts',(-38.4087832848556,37.7868049178791,17.0582918524852));
#67566=CARTESIAN_POINT('Ctrl Pts',(-38.4323100738575,37.7733715239653,17.0565803263806));
#67567=CARTESIAN_POINT('Origin',(-39.0658530619283,38.8697713466882,15.5));
#67568=CARTESIAN_POINT('Origin',(14.1292828945603,53.2669068454841,14.));
#67569=CARTESIAN_POINT('Ctrl Pts',(12.9355708698302,52.8497595669186,14.));
#67570=CARTESIAN_POINT('Ctrl Pts',(12.9470539462111,52.800184379949,14.));
#67571=CARTESIAN_POINT('Ctrl Pts',(12.9617293958091,52.7515166200376,14.));
#67572=CARTESIAN_POINT('Ctrl Pts',(12.9793332579427,52.7039252046945,14.));
#67573=CARTESIAN_POINT('Ctrl Pts',(12.991196608558,52.6718530581276,14.));
#67574=CARTESIAN_POINT('Ctrl Pts',(13.0043910411423,52.640269588579,14.));
#67575=CARTESIAN_POINT('Ctrl Pts',(13.0188485043022,52.6092270378147,14.));
#67576=CARTESIAN_POINT('Ctrl Pts',(13.0255213915297,52.5948992516592,14.));
#67577=CARTESIAN_POINT('Ctrl Pts',(13.0324634794561,52.5806867163328,14.));
#67578=CARTESIAN_POINT('Ctrl Pts',(13.0396687478355,52.5665947050889,14.));
#67579=CARTESIAN_POINT('Ctrl Pts',(13.0457249481514,52.5547500327666,14.));
#67580=CARTESIAN_POINT('Ctrl Pts',(13.0519637639815,52.5429971707228,14.));
#67581=CARTESIAN_POINT('Ctrl Pts',(13.0583775077155,52.5313453176603,14.));
#67582=CARTESIAN_POINT('Ctrl Pts',(13.0842985632238,52.4842545166353,14.));
#67583=CARTESIAN_POINT('Ctrl Pts',(13.1130890591366,52.4387805987021,14.));
#67584=CARTESIAN_POINT('Ctrl Pts',(13.1444873892533,52.395119273701,14.));
#67585=CARTESIAN_POINT('Ctrl Pts',(13.1565047144307,52.3784084378615,14.));
#67586=CARTESIAN_POINT('Ctrl Pts',(13.1689046040936,52.3619632326356,14.));
#67587=CARTESIAN_POINT('Ctrl Pts',(13.1816743222884,52.3457951881286,14.));
#67588=CARTESIAN_POINT('Ctrl Pts',(13.1908504259838,52.3341771045746,14.));
#67589=CARTESIAN_POINT('Ctrl Pts',(13.2002175166929,52.32270214338,14.));
#67590=CARTESIAN_POINT('Ctrl Pts',(13.2097711770809,52.3113747299413,14.));
#67591=CARTESIAN_POINT('Ctrl Pts',(13.2171669953397,52.3026057882235,14.));
#67592=CARTESIAN_POINT('Ctrl Pts',(13.2246749676048,52.2939250679898,14.));
#67593=CARTESIAN_POINT('Ctrl Pts',(13.2322825219484,52.2853461207869,14.));
#67594=CARTESIAN_POINT('Ctrl Pts',(13.2698783495153,52.2429497598573,14.));
#67595=CARTESIAN_POINT('Ctrl Pts',(13.3099602110309,52.2029670203905,14.));
#67596=CARTESIAN_POINT('Ctrl Pts',(13.3522361487098,52.165610756381,14.));
#67597=CARTESIAN_POINT('Ctrl Pts',(13.393899569609,52.1287957302432,14.));
#67598=CARTESIAN_POINT('Ctrl Pts',(13.4376947733247,52.0945306975985,14.));
#67599=CARTESIAN_POINT('Ctrl Pts',(13.4833901900509,52.0630423693642,14.));
#67600=CARTESIAN_POINT('Ctrl Pts',(13.5072520754399,52.0465993443685,14.));
#67601=CARTESIAN_POINT('Ctrl Pts',(13.5316328454212,52.0309139559169,14.));
#67602=CARTESIAN_POINT('Ctrl Pts',(13.5565037014717,52.0160223211503,14.));
#67603=CARTESIAN_POINT('Ctrl Pts',(13.5698458263775,52.0080336113647,14.));
#67604=CARTESIAN_POINT('Ctrl Pts',(13.583329035386,52.0002733832793,14.));
#67605=CARTESIAN_POINT('Ctrl Pts',(13.5969491666071,51.9927476035671,14.));
#67606=CARTESIAN_POINT('Ctrl Pts',(13.606631569296,51.9873976088762,14.));
#67607=CARTESIAN_POINT('Ctrl Pts',(13.61638317152,51.9821661015547,14.));
#67608=CARTESIAN_POINT('Ctrl Pts',(13.6262025323318,51.977055318658,14.));
#67609=CARTESIAN_POINT('Ctrl Pts',(13.6348477565097,51.9725556506333,14.));
#67610=CARTESIAN_POINT('Ctrl Pts',(13.6435368081695,51.9681540962494,14.));
#67611=CARTESIAN_POINT('Ctrl Pts',(13.6522677898656,51.9638519547421,14.));
#67612=CARTESIAN_POINT('Ctrl Pts',(13.6954565667589,51.9425709308905,14.));
#67613=CARTESIAN_POINT('Ctrl Pts',(13.739673922891,51.9237189359383,14.));
#67614=CARTESIAN_POINT('Ctrl Pts',(13.7847671512145,51.9074289316259,14.));
#67615=CARTESIAN_POINT('Ctrl Pts',(13.8360916879594,51.888887856702,14.));
#67616=CARTESIAN_POINT('Ctrl Pts',(13.8885506645683,51.8736638854927,14.));
#67617=CARTESIAN_POINT('Ctrl Pts',(13.9418473749851,51.8616392672974,14.));
#67618=CARTESIAN_POINT('Ctrl Pts',(13.9939442076033,51.8498853613524,14.));
#67619=CARTESIAN_POINT('Ctrl Pts',(14.0468423626153,51.841188535496,14.));
#67620=CARTESIAN_POINT('Ctrl Pts',(14.1002842110465,51.8354800340528,14.));
#67621=CARTESIAN_POINT('Ctrl Pts',(14.1133747158556,51.8340817447386,14.));
#67622=CARTESIAN_POINT('Ctrl Pts',(14.1264979008037,51.8328629457893,14.));
#67623=CARTESIAN_POINT('Ctrl Pts',(14.1396500710493,51.8318229994997,14.));
#67624=CARTESIAN_POINT('Ctrl Pts',(14.1495801724506,51.8310378232197,14.));
#67625=CARTESIAN_POINT('Ctrl Pts',(14.1595248275512,51.8303548395254,14.));
#67626=CARTESIAN_POINT('Ctrl Pts',(14.169470914275,51.8297741437739,14.));
#67627=CARTESIAN_POINT('Ctrl Pts',(14.2269882875851,51.8264160296488,14.));
#67628=CARTESIAN_POINT('Ctrl Pts',(14.2846572206784,51.8264659494126,14.));
#67629=CARTESIAN_POINT('Ctrl Pts',(14.3421515421323,51.8297896308138,14.));
#67630=CARTESIAN_POINT('Ctrl Pts',(14.4008791522774,51.8331846072331,14.));
#67631=CARTESIAN_POINT('Ctrl Pts',(14.4594256019286,51.8399951697904,14.));
#67632=CARTESIAN_POINT('Ctrl Pts',(14.5174614759233,51.8501296661746,14.));
#67633=CARTESIAN_POINT('Ctrl Pts',(14.5760079665237,51.8603533288243,14.));
#67634=CARTESIAN_POINT('Ctrl Pts',(14.6340360434159,51.8739596391018,14.));
#67635=CARTESIAN_POINT('Ctrl Pts',(14.6912089919261,51.8909073924039,14.));
#67636=CARTESIAN_POINT('Ctrl Pts',(14.7041595779211,51.8947463292138,14.));
#67637=CARTESIAN_POINT('Ctrl Pts',(14.7170698109109,51.8987582304328,14.));
#67638=CARTESIAN_POINT('Ctrl Pts',(14.7299100501063,51.9029342190465,14.));
#67639=CARTESIAN_POINT('Ctrl Pts',(14.7877641555218,51.9217499188006,14.));
#67640=CARTESIAN_POINT('Ctrl Pts',(14.8442964941461,51.9439200711341,14.));
#67641=CARTESIAN_POINT('Ctrl Pts',(14.8991630095604,51.9693357900552,14.));
#67642=CARTESIAN_POINT('Ctrl Pts',(14.9535472829614,51.9945281208612,14.));
#67643=CARTESIAN_POINT('Ctrl Pts',(15.0062960529788,52.0229093770711,14.));
#67644=CARTESIAN_POINT('Ctrl Pts',(15.0570711073182,52.0544235838104,14.));
#67645=CARTESIAN_POINT('Ctrl Pts',(15.0942742802838,52.0775142234847,14.));
#67646=CARTESIAN_POINT('Ctrl Pts',(15.1304178629043,52.1022878477767,14.));
#67647=CARTESIAN_POINT('Ctrl Pts',(15.1653622380935,52.1287390412771,14.));
#67648=CARTESIAN_POINT('Ctrl Pts',(15.1847827002204,52.1434393871499,14.));
#67649=CARTESIAN_POINT('Ctrl Pts',(15.2038326363704,52.1586581279523,14.));
#67650=CARTESIAN_POINT('Ctrl Pts',(15.2225055381224,52.1743757967134,14.));
#67651=CARTESIAN_POINT('Ctrl Pts',(15.6194800884629,52.8667052421829,14.));
#67652=CARTESIAN_POINT('Ctrl Pts',(15.6300068882699,52.9268481278985,14.));
#67653=CARTESIAN_POINT('Ctrl Pts',(15.6366488600629,52.9875198480058,14.));
#67654=CARTESIAN_POINT('Ctrl Pts',(15.6395377285819,53.0483965304076,14.));
#67655=CARTESIAN_POINT('Ctrl Pts',(15.6422164647753,53.1048451266012,14.));
#67656=CARTESIAN_POINT('Ctrl Pts',(15.6416673528962,53.1614706817507,14.));
#67657=CARTESIAN_POINT('Ctrl Pts',(15.637955789909,53.2180062233477,14.));
#67658=CARTESIAN_POINT('Ctrl Pts',(15.6370599130148,53.2316524649969,14.));
#67659=CARTESIAN_POINT('Ctrl Pts',(15.63597945886,53.2452938319744,14.));
#67660=CARTESIAN_POINT('Ctrl Pts',(15.6347168346769,53.2589112013863,14.));
#67661=CARTESIAN_POINT('Ctrl Pts',(15.6291600434151,53.3188410525391,14.));
#67662=CARTESIAN_POINT('Ctrl Pts',(15.6200747337896,53.378379872231,14.));
#67663=CARTESIAN_POINT('Ctrl Pts',(15.6075583989768,53.4372064199478,14.));
#67664=CARTESIAN_POINT('Ctrl Pts',(15.5998328638163,53.473516295766,14.));
#67665=CARTESIAN_POINT('Ctrl Pts',(15.5907991790393,53.5095545290085,14.));
#67666=CARTESIAN_POINT('Ctrl Pts',(15.5804715530865,53.5452408049656,14.));
#67667=CARTESIAN_POINT('Ctrl Pts',(15.5769376859297,53.5574517970299,14.));
#67668=CARTESIAN_POINT('Ctrl Pts',(15.5732522648484,53.5696215402532,14.));
#67669=CARTESIAN_POINT('Ctrl Pts',(15.5694156967786,53.5817466814784,14.));
#67670=CARTESIAN_POINT('Ctrl Pts',(15.5658265664347,53.5930898171937,14.));
#67671=CARTESIAN_POINT('Ctrl Pts',(15.5621073991623,53.604386674236,14.));
#67672=CARTESIAN_POINT('Ctrl Pts',(15.5582610327089,53.6156290047843,14.));
#67673=CARTESIAN_POINT('Ctrl Pts',(15.5392227656735,53.6712748964768,14.));
#67674=CARTESIAN_POINT('Ctrl Pts',(15.5170576051216,53.7256323263693,14.));
#67675=CARTESIAN_POINT('Ctrl Pts',(15.4918565785963,53.778400265489,14.));
#67676=CARTESIAN_POINT('Ctrl Pts',(15.4672989399364,53.8298210272756,14.));
#67677=CARTESIAN_POINT('Ctrl Pts',(15.4398578622269,53.8797331989797,14.));
#67678=CARTESIAN_POINT('Ctrl Pts',(15.4095790814356,53.9278277241522,14.));
#67679=CARTESIAN_POINT('Ctrl Pts',(15.393162829712,53.9539031410322,14.));
#67680=CARTESIAN_POINT('Ctrl Pts',(15.3759118210083,53.9794436628058,14.));
#67681=CARTESIAN_POINT('Ctrl Pts',(15.3578293393225,54.0043949447537,14.));
#67682=CARTESIAN_POINT('Ctrl Pts',(15.3427850973017,54.0251538832043,14.));
#67683=CARTESIAN_POINT('Ctrl Pts',(15.3271652650927,54.0455049013344,14.));
#67684=CARTESIAN_POINT('Ctrl Pts',(15.3109704282784,54.0654144329311,14.));
#67685=CARTESIAN_POINT('Ctrl Pts',(15.3040483577008,54.0739242551948,14.));
#67686=CARTESIAN_POINT('Ctrl Pts',(15.2970202961045,54.0823543059347,14.));
#67687=CARTESIAN_POINT('Ctrl Pts',(15.2898980775462,54.0906884965195,14.));
#67688=CARTESIAN_POINT('Ctrl Pts',(15.2569263348732,54.1292709670099,14.));
#67689=CARTESIAN_POINT('Ctrl Pts',(15.2218841351082,54.1658696978399,14.));
#67690=CARTESIAN_POINT('Ctrl Pts',(15.1848122311441,54.2002693479339,14.));
#67691=CARTESIAN_POINT('Ctrl Pts',(15.1433853438138,54.2387100611496,14.));
#67692=CARTESIAN_POINT('Ctrl Pts',(15.0994234021552,54.2744057498411,14.));
#67693=CARTESIAN_POINT('Ctrl Pts',(15.0532626173727,54.3072661456687,14.));
#67694=CARTESIAN_POINT('Ctrl Pts',(15.0140905649692,54.3351514849978,14.));
#67695=CARTESIAN_POINT('Ctrl Pts',(14.9733341416939,54.3609943509907,14.));
#67696=CARTESIAN_POINT('Ctrl Pts',(14.9311912107702,54.3847111211327,14.));
#67697=CARTESIAN_POINT('Ctrl Pts',(14.9196049423228,54.3912315234765,14.));
#67698=CARTESIAN_POINT('Ctrl Pts',(14.9079138627929,54.3975910665355,14.));
#67699=CARTESIAN_POINT('Ctrl Pts',(14.8961220820593,54.4037876495875,14.));
#67700=CARTESIAN_POINT('Ctrl Pts',(14.8869418706782,54.4086118524406,14.));
#67701=CARTESIAN_POINT('Ctrl Pts',(14.8776989838853,54.4133380017409,14.));
#67702=CARTESIAN_POINT('Ctrl Pts',(14.8684106168162,54.417957742305,14.));
#67703=CARTESIAN_POINT('Ctrl Pts',(14.8187084869401,54.4426780127036,14.));
#67704=CARTESIAN_POINT('Ctrl Pts',(14.7676148803425,54.4644045890752,14.));
#67705=CARTESIAN_POINT('Ctrl Pts',(14.7154497955799,54.4830620982223,14.));
#67706=CARTESIAN_POINT('Ctrl Pts',(14.6635765838278,54.5016152152576,14.));
#67707=CARTESIAN_POINT('Ctrl Pts',(14.6106426601222,54.5171336376019,14.));
#67708=CARTESIAN_POINT('Ctrl Pts',(14.5569565024563,54.5294926610653,14.));
#67709=CARTESIAN_POINT('Ctrl Pts',(14.5071457936081,54.5409595222851,14.));
#67710=CARTESIAN_POINT('Ctrl Pts',(14.4566867638904,54.5497062605815,14.));
#67711=CARTESIAN_POINT('Ctrl Pts',(14.4058341276533,54.5555924980468,14.));
#67712=CARTESIAN_POINT('Ctrl Pts',(14.3927717853116,54.5571044756858,14.));
#67713=CARTESIAN_POINT('Ctrl Pts',(14.3796790109904,54.5584277519276,14.));
#67714=CARTESIAN_POINT('Ctrl Pts',(14.3665890681889,54.559557479464,14.));
#67715=CARTESIAN_POINT('Ctrl Pts',(14.313676726905,54.5641240791709,14.));
#67716=CARTESIAN_POINT('Ctrl Pts',(14.2607272248354,54.5655439858659,14.));
#67717=CARTESIAN_POINT('Ctrl Pts',(14.2080224885655,54.5637141509331,14.));
#67718=CARTESIAN_POINT('Ctrl Pts',(14.1571049407721,54.5619463646915,14.));
#67719=CARTESIAN_POINT('Ctrl Pts',(14.1064149890642,54.5571453217378,14.));
#67720=CARTESIAN_POINT('Ctrl Pts',(14.0562198243928,54.5491721895681,14.));
#67721=CARTESIAN_POINT('Ctrl Pts',(14.0211056129997,54.54359455574,14.));
#67722=CARTESIAN_POINT('Ctrl Pts',(13.9862337962434,54.5364636409183,14.));
#67723=CARTESIAN_POINT('Ctrl Pts',(13.9517030424607,54.5277184245241,14.));
#67724=CARTESIAN_POINT('Ctrl Pts',(13.93222381495,54.5227851392317,14.));
#67725=CARTESIAN_POINT('Ctrl Pts',(13.9128532514771,54.5173379031513,14.));
#67726=CARTESIAN_POINT('Ctrl Pts',(13.8936069362009,54.5113866946539,14.));
#67727=CARTESIAN_POINT('Origin',(14.1292828945603,53.2669068454841,19.1042117235887));
#67728=CARTESIAN_POINT('Ctrl Pts',(13.3561844802682,51.9293619476186,17.8542117235887));
#67729=CARTESIAN_POINT('Ctrl Pts',(13.3145289674605,51.9530637836679,17.8517311518799));
#67730=CARTESIAN_POINT('Ctrl Pts',(12.8472204745978,52.2501100679509,17.8230820767121));
#67731=CARTESIAN_POINT('Ctrl Pts',(12.3131148719809,53.3266292410367,17.7682644980854));
#67732=CARTESIAN_POINT('Ctrl Pts',(13.177398497422,54.8146003900027,17.6897589877087));
#67733=CARTESIAN_POINT('Ctrl Pts',(14.8951536251653,54.9146504373755,17.6112534773318));
#67734=CARTESIAN_POINT('Ctrl Pts',(15.9261572824593,53.5369216264007,17.5327479669551));
#67735=CARTESIAN_POINT('Ctrl Pts',(15.3456319213627,51.9170585592589,17.4542424565783));
#67736=CARTESIAN_POINT('Ctrl Pts',(14.0786429713653,51.6067853756627,17.3947303754562));
#67737=CARTESIAN_POINT('Ctrl Pts',(13.4791850640252,51.8598443884631,17.361386797793));
#67738=CARTESIAN_POINT('Ctrl Pts',(13.3591951473145,51.9304670067728,17.3542117235887));
#67739=CARTESIAN_POINT('Ctrl Pts',(13.3599426557471,51.9312965605688,17.8957882764113));
#67740=CARTESIAN_POINT('Ctrl Pts',(13.0649944461637,52.1042822226529,17.8781885106897));
#67741=CARTESIAN_POINT('Ctrl Pts',(12.4640754788204,52.7732237750949,17.8344202415091));
#67742=CARTESIAN_POINT('Ctrl Pts',(12.6330157688953,54.2972115132025,17.7644834688697));
#67743=CARTESIAN_POINT('Ctrl Pts',(14.1627629159667,55.0835833760401,17.6859779584929));
#67744=CARTESIAN_POINT('Ctrl Pts',(15.6633630152513,54.2408836460551,17.6074724481161));
#67745=CARTESIAN_POINT('Ctrl Pts',(15.7877283921754,52.5246154983423,17.5289669377393));
#67746=CARTESIAN_POINT('Ctrl Pts',(14.5628755318023,51.5803972945989,17.4584055471711));
#67747=CARTESIAN_POINT('Ctrl Pts',(13.6650283227152,51.7575311866648,17.4140126600617));
#67748=CARTESIAN_POINT('Ctrl Pts',(13.3571987246687,51.9320818411208,17.3957882764113));
#67749=CARTESIAN_POINT('Ctrl Pts',(13.8936870225526,54.5092654229862,18.));
#67750=CARTESIAN_POINT('Ctrl Pts',(14.3022280845015,54.5867395029208,17.9738314965411));
#67751=CARTESIAN_POINT('Ctrl Pts',(15.1949907864185,54.306005850961,17.9214944896232));
#67752=CARTESIAN_POINT('Ctrl Pts',(15.5848805170291,52.9490991612648,17.8429889792464));
#67753=CARTESIAN_POINT('Ctrl Pts',(14.6665684258223,51.8784501685123,17.7644834688696));
#67754=CARTESIAN_POINT('Ctrl Pts',(13.2677649070697,52.052408782696,17.6859779584929));
#67755=CARTESIAN_POINT('Ctrl Pts',(12.6409196641315,53.3158497937513,17.6074724481161));
#67756=CARTESIAN_POINT('Ctrl Pts',(13.3492065366981,54.5352532401981,17.5289669377393));
#67757=CARTESIAN_POINT('Ctrl Pts',(14.7569196663361,54.6172449996945,17.4504614273625));
#67758=CARTESIAN_POINT('Ctrl Pts',(15.6018348475728,53.488185970869,17.3719559169858));
#67759=CARTESIAN_POINT('Ctrl Pts',(15.1260899874907,52.1606961144849,17.293450406609));
#67760=CARTESIAN_POINT('Ctrl Pts',(13.7564048649609,51.8252736441527,17.2149448962322));
#67761=CARTESIAN_POINT('Ctrl Pts',(12.7211156974588,52.7827464099985,17.1364393858554));
#67762=CARTESIAN_POINT('Ctrl Pts',(12.948709267523,54.1744236301459,17.0579338754786));
#67763=CARTESIAN_POINT('Ctrl Pts',(14.2350668963378,54.7522192803303,16.9794283651019));
#67764=CARTESIAN_POINT('Ctrl Pts',(15.4265561246117,53.9979509037444,16.900922854725));
#67765=CARTESIAN_POINT('Ctrl Pts',(15.4546192812222,52.5880650956991,16.8224173443483));
#67766=CARTESIAN_POINT('Ctrl Pts',(14.2940895544972,51.7869805788024,16.7439118339715));
#67767=CARTESIAN_POINT('Ctrl Pts',(12.9857571502944,52.3131291848103,16.6654063235948));
#67768=CARTESIAN_POINT('Ctrl Pts',(12.7029658920433,53.6946482401115,16.586900813218));
#67769=CARTESIAN_POINT('Ctrl Pts',(13.6993295943645,54.69255865938,16.5083953028412));
#67770=CARTESIAN_POINT('Ctrl Pts',(15.0812856557068,54.4119106312665,16.4298897924644));
#67771=CARTESIAN_POINT('Ctrl Pts',(15.6094629994387,53.1043959909962,16.3513842820876));
#67772=CARTESIAN_POINT('Ctrl Pts',(14.8101796402302,51.9426249466013,16.2728787717108));
#67773=CARTESIAN_POINT('Ctrl Pts',(13.4002518899393,51.9685013930707,16.1943732613341));
#67774=CARTESIAN_POINT('Ctrl Pts',(12.6441364773908,53.1588187166123,16.1158677509573));
#67775=CARTESIAN_POINT('Ctrl Pts',(13.2199356785564,54.4460720440219,16.0373622405805));
#67776=CARTESIAN_POINT('Ctrl Pts',(14.6112590818024,54.6758219881873,15.9588567302037));
#67777=CARTESIAN_POINT('Ctrl Pts',(15.5703347818477,53.6420233374599,15.8803512198269));
#67778=CARTESIAN_POINT('Ctrl Pts',(15.2370408904378,52.2718112986816,15.8018457094502));
#67779=CARTESIAN_POINT('Ctrl Pts',(13.9102832927596,51.7940246036041,15.7233401990734));
#67780=CARTESIAN_POINT('Ctrl Pts',(12.7799297446004,52.6371537182599,15.6448346886966));
#67781=CARTESIAN_POINT('Ctrl Pts',(12.8597081799673,54.0450604100449,15.5663291783198));
#67782=CARTESIAN_POINT('Ctrl Pts',(14.0780714025732,54.7551004833527,15.4878236679431));
#67783=CARTESIAN_POINT('Ctrl Pts',(15.3423623071066,54.1304931269541,15.4093181575663));
#67784=CARTESIAN_POINT('Ctrl Pts',(15.5187347583226,52.7314010536377,15.3308126471895));
#67785=CARTESIAN_POINT('Ctrl Pts',(14.4490137393998,51.8125633237516,15.2523071368127));
#67786=CARTESIAN_POINT('Ctrl Pts',(13.0925505105556,52.1980154020928,15.1738016264359));
#67787=CARTESIAN_POINT('Ctrl Pts',(12.6658535045584,53.5420748131919,15.0952961160591));
#67788=CARTESIAN_POINT('Ctrl Pts',(13.551594819097,54.6393568979554,15.0167906056824));
#67789=CARTESIAN_POINT('Ctrl Pts',(14.9554204274106,54.5057934526205,14.9382850953056));
#67790=CARTESIAN_POINT('Ctrl Pts',(15.6183464700208,53.2611664293564,14.8597795849288));
#67791=CARTESIAN_POINT('Ctrl Pts',(14.9458444656461,52.0216887907143,14.781274074552));
#67792=CARTESIAN_POINT('Ctrl Pts',(13.5410315037528,51.8989497980972,14.7027685641753));
#67793=CARTESIAN_POINT('Ctrl Pts',(12.6637746137877,53.0030322708737,14.6242630537985));
#67794=CARTESIAN_POINT('Ctrl Pts',(13.1008239433931,54.3437535140763,14.5457575434217));
#67795=CARTESIAN_POINT('Ctrl Pts',(14.4602125392811,54.7187536954986,14.4672520330449));
#67796=CARTESIAN_POINT('Ctrl Pts',(15.5228300373051,53.7916614633287,14.3887465226681));
#67797=CARTESIAN_POINT('Ctrl Pts',(15.3356521111637,52.3940408681935,14.3102410122914));
#67798=CARTESIAN_POINT('Ctrl Pts',(14.0666325655588,51.7790575741688,14.2317355019146));
#67799=CARTESIAN_POINT('Ctrl Pts',(12.8536802704289,52.4987553418112,14.1532299915378));
#67800=CARTESIAN_POINT('Ctrl Pts',(12.7849592886011,53.9066581474694,14.074724481161));
#67801=CARTESIAN_POINT('Ctrl Pts',(13.9213697617028,54.7422164034654,13.9962189707843));
#67802=CARTESIAN_POINT('Ctrl Pts',(15.2452696789898,54.2518096584207,13.9177134604075));
#67803=CARTESIAN_POINT('Ctrl Pts',(15.4583606841261,53.3405309695408,13.8653764534896));
#67804=CARTESIAN_POINT('Ctrl Pts',(15.3505106014235,52.9389386488708,13.8392079500307));
#67805=CARTESIAN_POINT('Ctrl Pts',(13.8763907393434,54.6004732426341,18.0535973499898));
#67806=CARTESIAN_POINT('Ctrl Pts',(14.314924864625,54.6836350861806,18.0274288465308));
#67807=CARTESIAN_POINT('Ctrl Pts',(15.2732297867829,54.3822913585465,17.975091839613));
#67808=CARTESIAN_POINT('Ctrl Pts',(15.6917432922651,52.9257672935819,17.8965863292362));
#67809=CARTESIAN_POINT('Ctrl Pts',(14.7060132710725,51.7765165492856,17.8180808188594));
#67810=CARTESIAN_POINT('Ctrl Pts',(13.2045165191651,51.9632463441864,17.7395753084827));
#67811=CARTESIAN_POINT('Ctrl Pts',(12.5316514000813,53.3194429428464,17.6610697981059));
#67812=CARTESIAN_POINT('Ctrl Pts',(13.2919371902727,54.6283689567997,17.5825642877291));
#67813=CARTESIAN_POINT('Ctrl Pts',(14.8029976526125,54.7163801455881,17.5040587773523));
#67814=CARTESIAN_POINT('Ctrl Pts',(15.7099423258683,53.5044311893796,17.4255532669755));
#67815=CARTESIAN_POINT('Ctrl Pts',(15.1992706321147,52.0794835960762,17.3470477565988));
#67816=CARTESIAN_POINT('Ctrl Pts',(13.7290300050048,51.7194360676216,17.268542246222));
#67817=CARTESIAN_POINT('Ctrl Pts',(12.6177350293705,52.7472017464205,17.1900367358452));
#67818=CARTESIAN_POINT('Ctrl Pts',(12.8620373932302,54.2410490221397,17.1115312254684));
#67819=CARTESIAN_POINT('Ctrl Pts',(14.2428330343357,54.8612635700639,17.0330257150916));
#67820=CARTESIAN_POINT('Ctrl Pts',(15.5217955063355,54.0516205413418,16.9545202047148));
#67821=CARTESIAN_POINT('Ctrl Pts',(15.5519189210496,52.5382278932962,16.8760146943381));
#67822=CARTESIAN_POINT('Ctrl Pts',(14.3061888440168,51.678331714885,16.7975091839613));
#67823=CARTESIAN_POINT('Ctrl Pts',(12.901805148244,52.2431075481956,16.7190036735845));
#67824=CARTESIAN_POINT('Ctrl Pts',(12.5982527550455,53.7260508968675,16.6404981632077));
#67825=CARTESIAN_POINT('Ctrl Pts',(13.6677645504461,54.7972229615204,16.561992652831));
#67826=CARTESIAN_POINT('Ctrl Pts',(15.1511769879803,54.4959711438117,16.4834871424542));
#67827=CARTESIAN_POINT('Ctrl Pts',(15.7181304989006,53.0924652481532,16.4049816320774));
#67828=CARTESIAN_POINT('Ctrl Pts',(14.8601677102629,51.8454027220491,16.3264761217006));
#67829=CARTESIAN_POINT('Ctrl Pts',(13.3467300407797,51.8731788891832,16.2479706113238));
#67830=CARTESIAN_POINT('Ctrl Pts',(12.5351043758535,53.1508834210038,16.1694651009471));
#67831=CARTESIAN_POINT('Ctrl Pts',(13.1531759053504,54.5326405184631,16.0909595905703));
#67832=CARTESIAN_POINT('Ctrl Pts',(14.6466433886817,54.7792575667409,16.0124540801935));
#67833=CARTESIAN_POINT('Ctrl Pts',(15.676129681178,53.6695625342478,15.9339485698167));
#67834=CARTESIAN_POINT('Ctrl Pts',(15.318367001378,52.1987563073058,15.8554430594399));
#67835=CARTESIAN_POINT('Ctrl Pts',(13.8942054255916,51.6858928771342,15.7769375490632));
#67836=CARTESIAN_POINT('Ctrl Pts',(12.680866912845,52.5909203596381,15.6984320386864));
#67837=CARTESIAN_POINT('Ctrl Pts',(12.7665022861979,54.1021885944998,15.6199265283096));
#67838=CARTESIAN_POINT('Ctrl Pts',(14.0743117082228,54.8643562967563,15.5414210179328));
#67839=CARTESIAN_POINT('Ctrl Pts',(15.4314205953349,54.1938933587689,15.4629155075561));
#67840=CARTESIAN_POINT('Ctrl Pts',(15.6207414392393,52.6920868680493,15.3844099971793));
#67841=CARTESIAN_POINT('Ctrl Pts',(14.4724867960198,51.7057926183866,15.3059044868025));
#67842=CARTESIAN_POINT('Ctrl Pts',(13.0164387486087,52.1195426811267,15.2273989764257));
#67843=CARTESIAN_POINT('Ctrl Pts',(12.5584157597012,53.5622762838672,15.1488934660489));
#67844=CARTESIAN_POINT('Ctrl Pts',(13.5091838189608,54.7401153900111,15.0703879556721));
#67845=CARTESIAN_POINT('Ctrl Pts',(15.0160713573958,54.5967463773832,14.9918824452954));
#67846=CARTESIAN_POINT('Ctrl Pts',(15.727666149938,53.2607449964075,14.9133769349186));
#67847=CARTESIAN_POINT('Ctrl Pts',(15.0057923758998,51.930271042394,14.8348714245418));
#67848=CARTESIAN_POINT('Ctrl Pts',(13.4978449972707,51.7985211602437,14.756365914165));
#67849=CARTESIAN_POINT('Ctrl Pts',(12.5561842470564,52.9836599052407,14.6778604037882));
#67850=CARTESIAN_POINT('Ctrl Pts',(13.0253195759487,54.4228102683146,14.5993548934115));
#67851=CARTESIAN_POINT('Ctrl Pts',(14.4845077563774,54.8253411075795,14.5208493830347));
#67852=CARTESIAN_POINT('Ctrl Pts',(15.6251373733416,53.830186350918,14.4423438726579));
#67853=CARTESIAN_POINT('Ctrl Pts',(15.4242177700075,52.3299593670269,14.3638383622811));
#67854=CARTESIAN_POINT('Ctrl Pts',(14.0620330883935,51.6698270424536,14.2853328519044));
#67855=CARTESIAN_POINT('Ctrl Pts',(12.7600318373669,52.442361459177,14.2068273415276));
#67856=CARTESIAN_POINT('Ctrl Pts',(12.6862657010804,53.9536255226118,14.1283218311508));
#67857=CARTESIAN_POINT('Ctrl Pts',(13.9061058082296,54.8505263314733,14.049816320774));
#67858=CARTESIAN_POINT('Ctrl Pts',(15.32719990687,54.3241163497092,13.9713108103972));
#67859=CARTESIAN_POINT('Ctrl Pts',(15.5559349992425,53.3459360884415,13.9189738034794));
#67860=CARTESIAN_POINT('Ctrl Pts',(15.4401670971033,52.9148608466415,13.8928053000205));
#67861=CARTESIAN_POINT('Ctrl Pts',(13.8590944561342,54.691681062282,18.1071946999795));
#67862=CARTESIAN_POINT('Ctrl Pts',(14.3276216447486,54.7805306694404,18.0810261965206));
#67863=CARTESIAN_POINT('Ctrl Pts',(15.3514687871473,54.4585768661318,18.0286891896028));
#67864=CARTESIAN_POINT('Ctrl Pts',(15.798606067501,52.9024354258991,17.950183679226));
#67865=CARTESIAN_POINT('Ctrl Pts',(14.7454581163227,51.6745829300588,17.8716781688492));
#67866=CARTESIAN_POINT('Ctrl Pts',(13.1412681312604,51.8740839056768,17.7931726584724));
#67867=CARTESIAN_POINT('Ctrl Pts',(12.4223831360311,53.3230360919415,17.7146671480956));
#67868=CARTESIAN_POINT('Ctrl Pts',(13.2346678438474,54.7214846734012,17.6361616377189));
#67869=CARTESIAN_POINT('Ctrl Pts',(14.8490756388889,54.8155152914818,17.5576561273421));
#67870=CARTESIAN_POINT('Ctrl Pts',(15.8180498041638,53.5206764078901,17.4791506169653));
#67871=CARTESIAN_POINT('Ctrl Pts',(15.2724512767386,51.9982710776676,17.4006451065885));
#67872=CARTESIAN_POINT('Ctrl Pts',(13.7016551450487,51.6135984910905,17.3221395962117));
#67873=CARTESIAN_POINT('Ctrl Pts',(12.5143543612823,52.7116570828427,17.243634085835));
#67874=CARTESIAN_POINT('Ctrl Pts',(12.7753655189374,54.3076744141334,17.1651285754582));
#67875=CARTESIAN_POINT('Ctrl Pts',(14.2505991723336,54.9703078597976,17.0866230650814));
#67876=CARTESIAN_POINT('Ctrl Pts',(15.6170348880593,54.1052901789391,17.0081175547046));
#67877=CARTESIAN_POINT('Ctrl Pts',(15.649218560877,52.4883906908934,16.9296120443279));
#67878=CARTESIAN_POINT('Ctrl Pts',(14.3182881335363,51.5696828509675,16.8511065339511));
#67879=CARTESIAN_POINT('Ctrl Pts',(12.8178531461937,52.173085911581,16.7726010235743));
#67880=CARTESIAN_POINT('Ctrl Pts',(12.4935396180477,53.7574535536235,16.6940955131975));
#67881=CARTESIAN_POINT('Ctrl Pts',(13.6361995065277,54.9018872636609,16.6155900028207));
#67882=CARTESIAN_POINT('Ctrl Pts',(15.2210683202537,54.580031656357,16.5370844924439));
#67883=CARTESIAN_POINT('Ctrl Pts',(15.8267979983625,53.0805345053102,16.4585789820672));
#67884=CARTESIAN_POINT('Ctrl Pts',(14.9101557802956,51.7481804974969,16.3800734716904));
#67885=CARTESIAN_POINT('Ctrl Pts',(13.2932081916201,51.7778563852958,16.3015679613136));
#67886=CARTESIAN_POINT('Ctrl Pts',(12.4260722743162,53.1429481253953,16.2230624509368));
#67887=CARTESIAN_POINT('Ctrl Pts',(13.0864161321444,54.6192089929043,16.14455694056));
#67888=CARTESIAN_POINT('Ctrl Pts',(14.6820276955611,54.8826931452944,16.0660514301833));
#67889=CARTESIAN_POINT('Ctrl Pts',(15.7819245805083,53.6971017310358,15.9875459198065));
#67890=CARTESIAN_POINT('Ctrl Pts',(15.3996931123183,52.1257013159298,15.9090404094297));
#67891=CARTESIAN_POINT('Ctrl Pts',(13.8781275584237,51.5777611506643,15.8305348990529));
#67892=CARTESIAN_POINT('Ctrl Pts',(12.5818040810897,52.5446870010162,15.7520293886761));
#67893=CARTESIAN_POINT('Ctrl Pts',(12.6732963924285,54.1593167789549,15.6735238782994));
#67894=CARTESIAN_POINT('Ctrl Pts',(14.0705520138724,54.9736121101599,15.5950183679226));
#67895=CARTESIAN_POINT('Ctrl Pts',(15.5204788835632,54.2572935905837,15.5165128575458));
#67896=CARTESIAN_POINT('Ctrl Pts',(15.7227481201561,52.6527726824611,15.438007347169));
#67897=CARTESIAN_POINT('Ctrl Pts',(14.4959598526397,51.5990219130214,15.3595018367923));
#67898=CARTESIAN_POINT('Ctrl Pts',(12.9403269866619,52.0410699601607,15.2809963264155));
#67899=CARTESIAN_POINT('Ctrl Pts',(12.4509780148441,53.5824777545425,15.2024908160387));
#67900=CARTESIAN_POINT('Ctrl Pts',(13.4667728188246,54.8408738820669,15.1239853056619));
#67901=CARTESIAN_POINT('Ctrl Pts',(15.0767222873809,54.6876993021459,15.0454797952852));
#67902=CARTESIAN_POINT('Ctrl Pts',(15.8369858298551,53.2603235634587,14.9669742849083));
#67903=CARTESIAN_POINT('Ctrl Pts',(15.0657402861535,51.8388532940734,14.8884687745316));
#67904=CARTESIAN_POINT('Ctrl Pts',(13.4546584907886,51.6980925223903,14.8099632641548));
#67905=CARTESIAN_POINT('Ctrl Pts',(12.4485938803251,52.9642875396075,14.731457753778));
#67906=CARTESIAN_POINT('Ctrl Pts',(12.9498152085044,54.5018670225528,14.6529522434012));
#67907=CARTESIAN_POINT('Ctrl Pts',(14.5088029734737,54.9319285196604,14.5744467330245));
#67908=CARTESIAN_POINT('Ctrl Pts',(15.7274447093781,53.8687112385071,14.4959412226477));
#67909=CARTESIAN_POINT('Ctrl Pts',(15.5127834288513,52.2658778658604,14.4174357122709));
#67910=CARTESIAN_POINT('Ctrl Pts',(14.0574336112281,51.5605965107385,14.3389302018941));
#67911=CARTESIAN_POINT('Ctrl Pts',(12.666383404305,52.3859675765427,14.2604246915173));
#67912=CARTESIAN_POINT('Ctrl Pts',(12.5875721135598,54.0005928977544,14.1819191811406));
#67913=CARTESIAN_POINT('Ctrl Pts',(13.8908418547563,54.9588362594811,14.1034136707638));
#67914=CARTESIAN_POINT('Ctrl Pts',(15.4091301347503,54.3964230409977,14.024908160387));
#67915=CARTESIAN_POINT('Ctrl Pts',(15.6535093143589,53.3513412073422,13.9725711534692));
#67916=CARTESIAN_POINT('Ctrl Pts',(15.5298235927831,52.8907830444122,13.9464026500102));
#67917=CARTESIAN_POINT('Ctrl Pts',(13.841798172925,54.7828888819299,18.1607920499693));
#67918=CARTESIAN_POINT('Ctrl Pts',(14.3403184248721,54.8774262527002,18.1346235465104));
#67919=CARTESIAN_POINT('Ctrl Pts',(15.4297077875118,54.5348623737173,18.0822865395925));
#67920=CARTESIAN_POINT('Ctrl Pts',(15.905468842737,52.8791035582161,18.0037810292158));
#67921=CARTESIAN_POINT('Ctrl Pts',(14.7849029615728,51.5726493108321,17.925275518839));
#67922=CARTESIAN_POINT('Ctrl Pts',(13.0780197433558,51.7849214671671,17.8467700084622));
#67923=CARTESIAN_POINT('Ctrl Pts',(12.3131148719809,53.3266292410367,17.7682644980854));
#67924=CARTESIAN_POINT('Ctrl Pts',(13.177398497422,54.8146003900027,17.6897589877087));
#67925=CARTESIAN_POINT('Ctrl Pts',(14.8951536251653,54.9146504373755,17.6112534773318));
#67926=CARTESIAN_POINT('Ctrl Pts',(15.9261572824593,53.5369216264007,17.5327479669551));
#67927=CARTESIAN_POINT('Ctrl Pts',(15.3456319213627,51.9170585592589,17.4542424565783));
#67928=CARTESIAN_POINT('Ctrl Pts',(13.6742802850926,51.5077609145594,17.3757369462015));
#67929=CARTESIAN_POINT('Ctrl Pts',(12.410973693194,52.6761124192647,17.2972314358247));
#67930=CARTESIAN_POINT('Ctrl Pts',(12.6886936446445,54.3742998061272,17.2187259254479));
#67931=CARTESIAN_POINT('Ctrl Pts',(14.2583653103316,55.0793521495312,17.1402204150712));
#67932=CARTESIAN_POINT('Ctrl Pts',(15.7122742697831,54.1589598165365,17.0617149046944));
#67933=CARTESIAN_POINT('Ctrl Pts',(15.7465182007044,52.4385534884905,16.9832093943176));
#67934=CARTESIAN_POINT('Ctrl Pts',(14.3303874230559,51.4610339870501,16.9047038839408));
#67935=CARTESIAN_POINT('Ctrl Pts',(12.7339011441433,52.1030642749663,16.8261983735641));
#67936=CARTESIAN_POINT('Ctrl Pts',(12.38882648105,53.7888562103795,16.7476928631873));
#67937=CARTESIAN_POINT('Ctrl Pts',(13.6046344626092,55.0065515658014,16.6691873528105));
#67938=CARTESIAN_POINT('Ctrl Pts',(15.2909596525271,54.6640921689023,16.5906818424337));
#67939=CARTESIAN_POINT('Ctrl Pts',(15.9354654978243,53.0686037624672,16.512176332057));
#67940=CARTESIAN_POINT('Ctrl Pts',(14.9601438503283,51.6509582729447,16.4336708216802));
#67941=CARTESIAN_POINT('Ctrl Pts',(13.2396863424605,51.6825338814083,16.3551653113034));
#67942=CARTESIAN_POINT('Ctrl Pts',(12.317040172779,53.1350128297868,16.2766598009266));
#67943=CARTESIAN_POINT('Ctrl Pts',(13.0196563589383,54.7057774673455,16.1981542905498));
#67944=CARTESIAN_POINT('Ctrl Pts',(14.7174120024405,54.9861287238479,16.1196487801731));
#67945=CARTESIAN_POINT('Ctrl Pts',(15.8877194798386,53.7246409278238,16.0411432697963));
#67946=CARTESIAN_POINT('Ctrl Pts',(15.4810192232586,52.0526463245539,15.9626377594195));
#67947=CARTESIAN_POINT('Ctrl Pts',(13.8620496912558,51.4696294241944,15.8841322490427));
#67948=CARTESIAN_POINT('Ctrl Pts',(12.4827412493343,52.4984536423944,15.8056267386659));
#67949=CARTESIAN_POINT('Ctrl Pts',(12.5800904986591,54.2164449634099,15.7271212282891));
#67950=CARTESIAN_POINT('Ctrl Pts',(14.0667923195219,55.0828679235634,15.6486157179124));
#67951=CARTESIAN_POINT('Ctrl Pts',(15.6095371717915,54.3206938223985,15.5701102075356));
#67952=CARTESIAN_POINT('Ctrl Pts',(15.8247548010729,52.6134584968728,15.4916046971588));
#67953=CARTESIAN_POINT('Ctrl Pts',(14.5194329092597,51.4922512076563,15.413099186782));
#67954=CARTESIAN_POINT('Ctrl Pts',(12.864215224715,51.9625972391947,15.3345936764052));
#67955=CARTESIAN_POINT('Ctrl Pts',(12.343540269987,53.6026792252177,15.2560881660285));
#67956=CARTESIAN_POINT('Ctrl Pts',(13.4243618186884,54.9416323741225,15.1775826556517));
#67957=CARTESIAN_POINT('Ctrl Pts',(15.1373732173661,54.7786522269087,15.0990771452749));
#67958=CARTESIAN_POINT('Ctrl Pts',(15.9463055097723,53.2599021305098,15.0205716348981));
#67959=CARTESIAN_POINT('Ctrl Pts',(15.1256881964072,51.7474355457531,14.9420661245214));
#67960=CARTESIAN_POINT('Ctrl Pts',(13.4114719843064,51.5976638845367,14.8635606141446));
#67961=CARTESIAN_POINT('Ctrl Pts',(12.3410035135938,52.9449151739745,14.7850551037678));
#67962=CARTESIAN_POINT('Ctrl Pts',(12.8743108410601,54.5809237767911,14.706549593391));
#67963=CARTESIAN_POINT('Ctrl Pts',(14.53309819057,55.0385159317414,14.6280440830142));
#67964=CARTESIAN_POINT('Ctrl Pts',(15.8297520454146,53.9072361260964,14.5495385726375));
#67965=CARTESIAN_POINT('Ctrl Pts',(15.6013490876951,52.2017963646938,14.4710330622607));
#67966=CARTESIAN_POINT('Ctrl Pts',(14.0528341340627,51.4513659790234,14.3925275518839));
#67967=CARTESIAN_POINT('Ctrl Pts',(12.572734971243,52.3295736939085,14.3140220415071));
#67968=CARTESIAN_POINT('Ctrl Pts',(12.4888785260391,54.0475602728967,14.2355165311303));
#67969=CARTESIAN_POINT('Ctrl Pts',(13.875577901283,55.0671461874891,14.1570110207536));
#67970=CARTESIAN_POINT('Ctrl Pts',(15.4910603626305,54.4687297322861,14.0785055103768));
#67971=CARTESIAN_POINT('Ctrl Pts',(15.7510836294753,53.3567463262428,14.0261685034589));
#67972=CARTESIAN_POINT('Ctrl Pts',(15.6194800884629,52.8667052421829,14.));
#67973=CARTESIAN_POINT('Ctrl Pts',(13.498190246218,52.1716844371558,17.1934196736194));
#67974=CARTESIAN_POINT('Ctrl Pts',(13.5965228772488,52.1138086750997,17.2005947478237));
#67975=CARTESIAN_POINT('Ctrl Pts',(13.7022352452507,52.0691825768203,17.2077698220279));
#67976=CARTESIAN_POINT('Ctrl Pts',(13.8121375241322,52.0407561835157,17.2149448962322));
#67977=CARTESIAN_POINT('Ctrl Pts',(14.2129665724708,51.9370811342635,17.2411133996911));
#67978=CARTESIAN_POINT('Ctrl Pts',(14.6695282799807,52.0488886243742,17.2672819031501));
#67979=CARTESIAN_POINT('Ctrl Pts',(14.9770999437494,52.3260406788269,17.293450406609));
#67980=CARTESIAN_POINT('Ctrl Pts',(15.284671607518,52.6031927332796,17.3196189100679));
#67981=CARTESIAN_POINT('Ctrl Pts',(15.4432532275454,53.0456893520743,17.3457874135268));
#67982=CARTESIAN_POINT('Ctrl Pts',(15.3817248406863,53.4551141662759,17.3719559169858));
#67983=CARTESIAN_POINT('Ctrl Pts',(15.3201964538272,53.8645389804775,17.3981244204447));
#67984=CARTESIAN_POINT('Ctrl Pts',(15.0385580600817,54.240891990086,17.4242929239036));
#67985=CARTESIAN_POINT('Ctrl Pts',(14.6631200082692,54.4154032016409,17.4504614273625));
#67986=CARTESIAN_POINT('Ctrl Pts',(14.2876819564568,54.5899144131957,17.4766299308215));
#67987=CARTESIAN_POINT('Ctrl Pts',(13.8184442465774,54.5625838266969,17.5027984342804));
#67988=CARTESIAN_POINT('Ctrl Pts',(13.4657775795433,54.3456846257064,17.5289669377393));
#67989=CARTESIAN_POINT('Ctrl Pts',(13.1131109125092,54.1287854247159,17.5551354411982));
#67990=CARTESIAN_POINT('Ctrl Pts',(12.8770152883204,53.7223176092336,17.5813039446572));
#67991=CARTESIAN_POINT('Ctrl Pts',(12.8634416833823,53.3085101996499,17.6074724481161));
#67992=CARTESIAN_POINT('Ctrl Pts',(12.8498680784442,52.8947027900662,17.633640951575));
#67993=CARTESIAN_POINT('Ctrl Pts',(13.0588164927569,52.4735557863811,17.659809455034));
#67994=CARTESIAN_POINT('Ctrl Pts',(13.3964246197054,52.2339891821746,17.6859779584929));
#67995=CARTESIAN_POINT('Ctrl Pts',(13.4284272586679,52.2112801211956,17.6884585302017));
#67996=CARTESIAN_POINT('Ctrl Pts',(13.46158597893,52.1902026642355,17.6909391019106));
#67997=CARTESIAN_POINT('Ctrl Pts',(13.4957229821349,52.1707788329429,17.6934196736194));
#67998=CARTESIAN_POINT('Ctrl Pts',(15.2209662466057,52.1764590205668,18.));
#67999=CARTESIAN_POINT('Ctrl Pts',(14.8623799894179,51.8174664687922,17.9738314965411));
#68000=CARTESIAN_POINT('Ctrl Pts',(13.7693646387388,51.4866597864568,17.9214944896232));
#68001=CARTESIAN_POINT('Ctrl Pts',(12.4433767107148,52.5865029592797,17.8429889792465));
#68002=CARTESIAN_POINT('Ctrl Pts',(12.6330157688953,54.2972115132025,17.7644834688697));
#68003=CARTESIAN_POINT('Ctrl Pts',(14.1627629159667,55.0835833760401,17.6859779584929));
#68004=CARTESIAN_POINT('Ctrl Pts',(15.6633630152513,54.2408836460551,17.6074724481161));
#68005=CARTESIAN_POINT('Ctrl Pts',(15.7877283921754,52.5246154983423,17.5289669377393));
#68006=CARTESIAN_POINT('Ctrl Pts',(14.4249760687642,51.474092947767,17.4504614273626));
#68007=CARTESIAN_POINT('Ctrl Pts',(12.7969322124135,52.031388169684,17.3719559169858));
#68008=CARTESIAN_POINT('Ctrl Pts',(12.3638250796578,53.6967359986949,17.293450406609));
#68009=CARTESIAN_POINT('Ctrl Pts',(13.5139962436502,54.9765978264215,17.2149448962322));
#68010=CARTESIAN_POINT('Ctrl Pts',(15.2159841085891,54.7231706136823,17.1364393858554));
#68011=CARTESIAN_POINT('Ctrl Pts',(15.9433860453712,53.1637302055401,17.0579338754786));
#68012=CARTESIAN_POINT('Ctrl Pts',(15.043860342301,51.6968216692226,16.9794283651019));
#68013=CARTESIAN_POINT('Ctrl Pts',(13.3241182586501,51.6380025442004,16.9009228547251));
#68014=CARTESIAN_POINT('Ctrl Pts',(12.3264677464456,53.0400236709192,16.8224173443483));
#68015=CARTESIAN_POINT('Ctrl Pts',(12.9456243299004,54.6455189484075,16.7439118339715));
#68016=CARTESIAN_POINT('Ctrl Pts',(14.6263142466089,55.0146421540478,16.6654063235947));
#68017=CARTESIAN_POINT('Ctrl Pts',(15.8612545351151,53.8163547667627,16.586900813218));
#68018=CARTESIAN_POINT('Ctrl Pts',(15.5429215283993,52.1253094303059,16.5083953028412));
#68019=CARTESIAN_POINT('Ctrl Pts',(13.9568037640838,51.4580757912425,16.4298897924644));
#68020=CARTESIAN_POINT('Ctrl Pts',(12.5253693960519,52.413044846331,16.3513842820876));
#68021=CARTESIAN_POINT('Ctrl Pts',(12.5323627785853,54.1337776405724,16.2728787717109));
#68022=CARTESIAN_POINT('Ctrl Pts',(13.9715120885841,55.0770800976453,16.1943732613341));
#68023=CARTESIAN_POINT('Ctrl Pts',(15.5521540067467,54.3969761475115,16.1158677509573));
#68024=CARTESIAN_POINT('Ctrl Pts',(15.8567312853937,52.7033991815805,16.0373622405805));
#68025=CARTESIAN_POINT('Ctrl Pts',(14.612091779025,51.5151892852256,15.9588567302038));
#68026=CARTESIAN_POINT('Ctrl Pts',(12.934457787186,51.8979613415929,15.8803512198269));
#68027=CARTESIAN_POINT('Ctrl Pts',(12.3283713567551,53.5084362707541,15.8018457094502));
#68028=CARTESIAN_POINT('Ctrl Pts',(13.3373852079753,54.9023018690978,15.7233401990734));
#68029=CARTESIAN_POINT('Ctrl Pts',(15.0565917302206,54.8295063313936,15.6448346886966));
#68030=CARTESIAN_POINT('Ctrl Pts',(15.9441656443073,53.3553344251959,15.5663291783198));
#68031=CARTESIAN_POINT('Ctrl Pts',(15.2041095597138,51.8018585649929,15.4878236679431));
#68032=CARTESIAN_POINT('Ctrl Pts',(13.5001233739826,51.5622728287798,15.4093181575663));
#68033=CARTESIAN_POINT('Ctrl Pts',(12.3603823942099,52.8514434111319,15.3308126471895));
#68034=CARTESIAN_POINT('Ctrl Pts',(12.8070334555363,54.5132114643008,15.2523071368127));
#68035=CARTESIAN_POINT('Ctrl Pts',(14.4395092097517,55.0572639347494,15.1738016264359));
#68036=CARTESIAN_POINT('Ctrl Pts',(15.7937667074068,53.9956815464663,15.0952961160592));
#68037=CARTESIAN_POINT('Ctrl Pts',(15.6552753932384,52.2805167973031,15.0167906056824));
#68038=CARTESIAN_POINT('Ctrl Pts',(14.14823804594,51.4499698581624,14.9382850953056));
#68039=CARTESIAN_POINT('Ctrl Pts',(12.6242006263839,52.248895679213,14.8597795849288));
#68040=CARTESIAN_POINT('Ctrl Pts',(12.4499580614657,53.9607971579715,14.781274074552));
#68041=CARTESIAN_POINT('Ctrl Pts',(13.7817713167743,55.0504032414556,14.7027685641753));
#68042=CARTESIAN_POINT('Ctrl Pts',(15.4252464910755,54.5405234556122,14.6242630537985));
#68043=CARTESIAN_POINT('Ctrl Pts',(15.9064600587523,52.8884418877606,14.5457575434217));
#68044=CARTESIAN_POINT('Ctrl Pts',(14.7938803736306,51.575760805285,14.4672520330449));
#68045=CARTESIAN_POINT('Ctrl Pts',(13.0852305278661,51.7797717538672,14.3887465226681));
#68046=CARTESIAN_POINT('Ctrl Pts',(12.312999126503,53.317416116839,14.3102410122914));
#68047=CARTESIAN_POINT('Ctrl Pts',(13.1694776941512,54.809893106608,14.2317355019146));
#68048=CARTESIAN_POINT('Ctrl Pts',(14.8870885705587,54.9183199028175,14.1532299915378));
#68049=CARTESIAN_POINT('Ctrl Pts',(15.9243621047064,53.5462518811827,14.074724481161));
#68050=CARTESIAN_POINT('Ctrl Pts',(15.3532243372684,51.9225867742538,13.9962189707842));
#68051=CARTESIAN_POINT('Ctrl Pts',(13.6814109435091,51.5067274632874,13.9177134604075));
#68052=CARTESIAN_POINT('Ctrl Pts',(12.8400499397792,52.278885011525,13.8653764534896));
#68053=CARTESIAN_POINT('Ctrl Pts',(12.6726615784997,52.7578848993974,13.8392079500307));
#68054=CARTESIAN_POINT('Ctrl Pts',(15.1552860103679,52.2420649223251,18.0535973499898));
#68055=CARTESIAN_POINT('Ctrl Pts',(14.8182738021381,51.9046708638902,18.0274288465308));
#68056=CARTESIAN_POINT('Ctrl Pts',(13.7910188263055,51.5937668951064,17.975091839613));
#68057=CARTESIAN_POINT('Ctrl Pts',(12.5448078777489,52.6274389027465,17.8965863292362));
#68058=CARTESIAN_POINT('Ctrl Pts',(12.7230374570564,54.2352240753196,17.8180808188594));
#68059=CARTESIAN_POINT('Ctrl Pts',(14.1607486178545,54.9742845180234,17.7395753084826));
#68060=CARTESIAN_POINT('Ctrl Pts',(15.5710663391631,54.1822851282415,17.6610697981059));
#68061=CARTESIAN_POINT('Ctrl Pts',(15.6879493748746,52.5692748502929,17.5825642877291));
#68062=CARTESIAN_POINT('Ctrl Pts',(14.407185930718,51.5819561299908,17.5040587773523));
#68063=CARTESIAN_POINT('Ctrl Pts',(12.8770920017801,52.1057221405655,17.4255532669755));
#68064=CARTESIAN_POINT('Ctrl Pts',(12.4700424055274,53.6708756791509,17.3470477565988));
#68065=CARTESIAN_POINT('Ctrl Pts',(13.5510144619001,54.8737356665185,17.268542246222));
#68066=CARTESIAN_POINT('Ctrl Pts',(15.1506036186114,54.6355556948135,17.1900367358452));
#68067=CARTESIAN_POINT('Ctrl Pts',(15.8342420126426,53.1699377437178,17.1115312254684));
#68068=CARTESIAN_POINT('Ctrl Pts',(14.9888355379813,51.791284560039,17.0330257150916));
#68069=CARTESIAN_POINT('Ctrl Pts',(13.3725603306097,51.736004239579,16.9545202047149));
#68070=CARTESIAN_POINT('Ctrl Pts',(12.4349326457219,53.0536739116011,16.876014694338));
#68071=CARTESIAN_POINT('Ctrl Pts',(13.0168381795996,54.5625758784866,16.7975091839613));
#68072=CARTESIAN_POINT('Ctrl Pts',(14.5964107617212,54.9094910882809,16.7190036735845));
#68073=CARTESIAN_POINT('Ctrl Pts',(15.7570518775444,53.7832976818467,16.6404981632077));
#68074=CARTESIAN_POINT('Ctrl Pts',(15.457871115886,52.1939927053388,16.561992652831));
#68075=CARTESIAN_POINT('Ctrl Pts',(13.9671808299377,51.5669026325918,16.4834871424542));
#68076=CARTESIAN_POINT('Ctrl Pts',(12.6218675402158,52.4644167553317,16.4049816320774));
#68077=CARTESIAN_POINT('Ctrl Pts',(12.6284401716074,54.0816230680013,16.3264761217006));
#68078=CARTESIAN_POINT('Ctrl Pts',(13.981004240121,54.9681725040555,16.2479706113238));
#68079=CARTESIAN_POINT('Ctrl Pts',(15.4665481297227,54.3289864519802,16.1694651009471));
#68080=CARTESIAN_POINT('Ctrl Pts',(15.752800765444,52.7373021594152,16.0909595905703));
#68081=CARTESIAN_POINT('Ctrl Pts',(14.5830439772701,51.6205799399096,16.0124540801935));
#68082=CARTESIAN_POINT('Ctrl Pts',(13.0063434627971,51.9803228284871,15.9339485698167));
#68083=CARTESIAN_POINT('Ctrl Pts',(12.4367217268737,53.4939048503744,15.85544305944));
#68084=CARTESIAN_POINT('Ctrl Pts',(13.3850290847768,54.8039096647175,15.7769375490631));
#68085=CARTESIAN_POINT('Ctrl Pts',(15.0008009523568,54.7354938110165,15.6984320386864));
#68086=CARTESIAN_POINT('Ctrl Pts',(15.8349747076461,53.3500142521672,15.6199265283096));
#68087=CARTESIAN_POINT('Ctrl Pts',(15.1394434922597,51.8900019968609,15.5414210179329));
#68088=CARTESIAN_POINT('Ctrl Pts',(13.5379762420926,51.6648307405647,15.462915507556));
#68089=CARTESIAN_POINT('Ctrl Pts',(12.4668068464345,52.8764394289472,15.3844099971793));
#68090=CARTESIAN_POINT('Ctrl Pts',(12.8865855118699,54.4382285659771,15.3059044868025));
#68091=CARTESIAN_POINT('Ctrl Pts',(14.4208446971613,54.9495485643971,15.2273989764257));
#68092=CARTESIAN_POINT('Ctrl Pts',(15.6936243998074,53.9518354124798,15.1488934660489));
#68093=CARTESIAN_POINT('Ctrl Pts',(15.5634653023155,52.3398621480091,15.0703879556721));
#68094=CARTESIAN_POINT('Ctrl Pts',(14.1470976247563,51.5592843863476,14.9918824452954));
#68095=CARTESIAN_POINT('Ctrl Pts',(12.7147526703863,52.3101434886333,14.9133769349186));
#68096=CARTESIAN_POINT('Ctrl Pts',(12.5509932669133,53.9190498146948,14.8348714245418));
#68097=CARTESIAN_POINT('Ctrl Pts',(13.8026790667016,54.9431006391056,14.756365914165));
#68098=CARTESIAN_POINT('Ctrl Pts',(15.3472759009633,54.4638973536635,14.6778604037883));
#68099=CARTESIAN_POINT('Ctrl Pts',(15.7995376478153,52.9112119224821,14.5993548934115));
#68100=CARTESIAN_POINT('Ctrl Pts',(14.7538954097245,51.6775072239921,14.5208493830347));
#68101=CARTESIAN_POINT('Ctrl Pts',(13.1480450848167,51.8692440206669,14.4423438726579));
#68102=CARTESIAN_POINT('Ctrl Pts',(12.4222743542852,53.3143772678278,14.3638383622811));
#68103=CARTESIAN_POINT('Ctrl Pts',(13.2272235892287,54.7170605998631,14.2853328519043));
#68104=CARTESIAN_POINT('Ctrl Pts',(14.8414958116982,54.8189639865359,14.2068273415276));
#68105=CARTESIAN_POINT('Ctrl Pts',(15.8163626318126,53.5294453155223,14.1283218311508));
#68106=CARTESIAN_POINT('Ctrl Pts',(15.2795869011495,52.0034666921275,14.049816320774));
#68107=CARTESIAN_POINT('Ctrl Pts',(13.7083567932321,51.6126272165693,13.9713108103972));
#68108=CARTESIAN_POINT('Ctrl Pts',(12.9176155863349,52.3383285372882,13.9189738034794));
#68109=CARTESIAN_POINT('Ctrl Pts',(12.7602980089432,52.7885097885712,13.8928053000205));
#68110=CARTESIAN_POINT('Ctrl Pts',(15.0896057741301,52.3076708240835,18.1071946999795));
#68111=CARTESIAN_POINT('Ctrl Pts',(14.7741676148584,51.9918752589882,18.0810261965206));
#68112=CARTESIAN_POINT('Ctrl Pts',(13.8126730138722,51.700874003756,18.0286891896027));
#68113=CARTESIAN_POINT('Ctrl Pts',(12.646239044783,52.6683748462133,17.950183679226));
#68114=CARTESIAN_POINT('Ctrl Pts',(12.8130591452175,54.1732366374368,17.8716781688492));
#68115=CARTESIAN_POINT('Ctrl Pts',(14.1587343197422,54.8649856600065,17.7931726584724));
#68116=CARTESIAN_POINT('Ctrl Pts',(15.4787696630748,54.123686610428,17.7146671480956));
#68117=CARTESIAN_POINT('Ctrl Pts',(15.5881703575737,52.6139342022434,17.6361616377189));
#68118=CARTESIAN_POINT('Ctrl Pts',(14.3893957926718,51.6898193122148,17.5576561273421));
#68119=CARTESIAN_POINT('Ctrl Pts',(12.9572517911467,52.1800561114469,17.4791506169653));
#68120=CARTESIAN_POINT('Ctrl Pts',(12.576259731397,53.6450153596069,17.4006451065885));
#68121=CARTESIAN_POINT('Ctrl Pts',(13.5880326801499,54.7708735066155,17.3221395962118));
#68122=CARTESIAN_POINT('Ctrl Pts',(15.0852231286336,54.5479407759449,17.243634085835));
#68123=CARTESIAN_POINT('Ctrl Pts',(15.725097979914,53.1761452818955,17.1651285754582));
#68124=CARTESIAN_POINT('Ctrl Pts',(14.9338107336616,51.8857474508553,17.0866230650814));
#68125=CARTESIAN_POINT('Ctrl Pts',(13.4210024025693,51.8340059349576,17.0081175547046));
#68126=CARTESIAN_POINT('Ctrl Pts',(12.5433975449982,53.0673241522829,16.9296120443278));
#68127=CARTESIAN_POINT('Ctrl Pts',(13.0880520292989,54.4796328085656,16.8511065339511));
#68128=CARTESIAN_POINT('Ctrl Pts',(14.5665072768334,54.804340022514,16.7726010235743));
#68129=CARTESIAN_POINT('Ctrl Pts',(15.6528492199738,53.7502405969307,16.6940955131975));
#68130=CARTESIAN_POINT('Ctrl Pts',(15.3728207033727,52.2626759803717,16.6155900028207));
#68131=CARTESIAN_POINT('Ctrl Pts',(13.9775578957916,51.6757294739412,16.5370844924439));
#68132=CARTESIAN_POINT('Ctrl Pts',(12.7183656843797,52.5157886643324,16.4585789820672));
#68133=CARTESIAN_POINT('Ctrl Pts',(12.7245175646294,54.0294684954301,16.3800734716904));
#68134=CARTESIAN_POINT('Ctrl Pts',(13.990496391658,54.8592649104658,16.3015679613136));
#68135=CARTESIAN_POINT('Ctrl Pts',(15.3809422526988,54.2609967564488,16.2230624509369));
#68136=CARTESIAN_POINT('Ctrl Pts',(15.6488702454943,52.77120513725,16.14455694056));
#68137=CARTESIAN_POINT('Ctrl Pts',(14.5539961755152,51.7259705945935,16.0660514301833));
#68138=CARTESIAN_POINT('Ctrl Pts',(13.0782291384082,52.0626843153815,15.9875459198065));
#68139=CARTESIAN_POINT('Ctrl Pts',(12.5450720969922,53.4793734299947,15.9090404094297));
#68140=CARTESIAN_POINT('Ctrl Pts',(13.4326729615782,54.7055174603372,15.8305348990529));
#68141=CARTESIAN_POINT('Ctrl Pts',(14.9450101744931,54.6414812906394,15.7520293886762));
#68142=CARTESIAN_POINT('Ctrl Pts',(15.7257837709849,53.3446940791385,15.6735238782994));
#68143=CARTESIAN_POINT('Ctrl Pts',(15.0747774248056,51.9781454287288,15.5950183679226));
#68144=CARTESIAN_POINT('Ctrl Pts',(13.5758291102025,51.7673886523496,15.5165128575458));
#68145=CARTESIAN_POINT('Ctrl Pts',(12.5732312986591,52.9014354467625,15.438007347169));
#68146=CARTESIAN_POINT('Ctrl Pts',(12.9661375682035,54.3632456676534,15.3595018367923));
#68147=CARTESIAN_POINT('Ctrl Pts',(14.402180184571,54.841833194045,15.2809963264155));
#68148=CARTESIAN_POINT('Ctrl Pts',(15.593482092208,53.9079892784933,15.2024908160387));
#68149=CARTESIAN_POINT('Ctrl Pts',(15.4716552113927,52.3992074987152,15.1239853056619));
#68150=CARTESIAN_POINT('Ctrl Pts',(14.1459572035726,51.6685989145327,15.0454797952851));
#68151=CARTESIAN_POINT('Ctrl Pts',(12.8053047143887,52.3713912980536,14.9669742849084));
#68152=CARTESIAN_POINT('Ctrl Pts',(12.6520284723608,53.8773024714181,14.8884687745316));
#68153=CARTESIAN_POINT('Ctrl Pts',(13.8235868166289,54.8357980367556,14.8099632641548));
#68154=CARTESIAN_POINT('Ctrl Pts',(15.269305310851,54.3872712517148,14.731457753778));
#68155=CARTESIAN_POINT('Ctrl Pts',(15.6926152368783,52.9339819572036,14.6529522434012));
#68156=CARTESIAN_POINT('Ctrl Pts',(14.7139104458185,51.7792536426993,14.5744467330245));
#68157=CARTESIAN_POINT('Ctrl Pts',(13.2108596417673,51.9587162874664,14.4959412226477));
#68158=CARTESIAN_POINT('Ctrl Pts',(12.5315495820674,53.3113384188168,14.4174357122709));
#68159=CARTESIAN_POINT('Ctrl Pts',(13.2849694843063,54.6242280931179,14.3389302018941));
#68160=CARTESIAN_POINT('Ctrl Pts',(14.7959030528376,54.7196080702544,14.2604246915174));
#68161=CARTESIAN_POINT('Ctrl Pts',(15.7083631589187,53.5126387498619,14.1819191811406));
#68162=CARTESIAN_POINT('Ctrl Pts',(15.2059494650307,52.0843466100013,14.1034136707638));
#68163=CARTESIAN_POINT('Ctrl Pts',(13.7353026429551,51.7185269698512,14.024908160387));
#68164=CARTESIAN_POINT('Ctrl Pts',(12.9951812328907,52.3977720630513,13.9725711534692));
#68165=CARTESIAN_POINT('Ctrl Pts',(12.8479344393867,52.8191346777449,13.9464026500102));
#68166=CARTESIAN_POINT('Ctrl Pts',(15.0239255378924,52.3732767258419,18.1607920499693));
#68167=CARTESIAN_POINT('Ctrl Pts',(14.7300614275787,52.0790796540862,18.1346235465104));
#68168=CARTESIAN_POINT('Ctrl Pts',(13.8343272014389,51.8079811124056,18.0822865395925));
#68169=CARTESIAN_POINT('Ctrl Pts',(12.7476702118172,52.7093107896802,18.0037810292157));
#68170=CARTESIAN_POINT('Ctrl Pts',(12.9030808333786,54.111249199554,17.925275518839));
#68171=CARTESIAN_POINT('Ctrl Pts',(14.1567200216299,54.7556868019897,17.8467700084622));
#68172=CARTESIAN_POINT('Ctrl Pts',(15.3864729869866,54.0650880926144,17.7682644980854));
#68173=CARTESIAN_POINT('Ctrl Pts',(15.4883913402728,52.6585935541939,17.6897589877086));
#68174=CARTESIAN_POINT('Ctrl Pts',(14.3716056546256,51.7976824944386,17.6112534773319));
#68175=CARTESIAN_POINT('Ctrl Pts',(13.0374115805133,52.2543900823284,17.5327479669551));
#68176=CARTESIAN_POINT('Ctrl Pts',(12.6824770572666,53.6191550400629,17.4542424565783));
#68177=CARTESIAN_POINT('Ctrl Pts',(13.6250508983997,54.6680113467124,17.3757369462015));
#68178=CARTESIAN_POINT('Ctrl Pts',(15.0198426386559,54.4603258570762,17.2972314358247));
#68179=CARTESIAN_POINT('Ctrl Pts',(15.6159539471853,53.1823528200731,17.218725925448));
#68180=CARTESIAN_POINT('Ctrl Pts',(14.878785929342,51.9802103416717,17.1402204150712));
#68181=CARTESIAN_POINT('Ctrl Pts',(13.4694444745289,51.9320076303362,17.0617149046944));
#68182=CARTESIAN_POINT('Ctrl Pts',(12.6518624442745,53.0809743929648,16.9832093943176));
#68183=CARTESIAN_POINT('Ctrl Pts',(13.1592658789981,54.3966897386446,16.9047038839409));
#68184=CARTESIAN_POINT('Ctrl Pts',(14.5366037919456,54.6991889567471,16.8261983735641));
#68185=CARTESIAN_POINT('Ctrl Pts',(15.5486465624031,53.7171835120148,16.7476928631873));
#68186=CARTESIAN_POINT('Ctrl Pts',(15.2877702908594,52.3313592554045,16.6691873528105));
#68187=CARTESIAN_POINT('Ctrl Pts',(13.9879349616455,51.7845563152907,16.5906818424337));
#68188=CARTESIAN_POINT('Ctrl Pts',(12.8148638285435,52.567160573333,16.5121763320569));
#68189=CARTESIAN_POINT('Ctrl Pts',(12.8205949576515,53.9773139228589,16.4336708216802));
#68190=CARTESIAN_POINT('Ctrl Pts',(13.9999885431949,54.7503573168761,16.3551653113034));
#68191=CARTESIAN_POINT('Ctrl Pts',(15.2953363756748,54.1930070609175,16.2766598009266));
#68192=CARTESIAN_POINT('Ctrl Pts',(15.5449397255447,52.8051081150848,16.1981542905498));
#68193=CARTESIAN_POINT('Ctrl Pts',(14.5249483737603,51.8313612492774,16.119648780173));
#68194=CARTESIAN_POINT('Ctrl Pts',(13.1501148140193,52.1450458022758,16.0411432697963));
#68195=CARTESIAN_POINT('Ctrl Pts',(12.6534224671108,53.4648420096149,15.9626377594195));
#68196=CARTESIAN_POINT('Ctrl Pts',(13.4803168383797,54.6071252559569,15.8841322490427));
#68197=CARTESIAN_POINT('Ctrl Pts',(14.8892193966293,54.5474687702622,15.8056267386659));
#68198=CARTESIAN_POINT('Ctrl Pts',(15.6165928343238,53.3393739061099,15.7271212282891));
#68199=CARTESIAN_POINT('Ctrl Pts',(15.0101113573514,52.0662888605968,15.6486157179124));
#68200=CARTESIAN_POINT('Ctrl Pts',(13.6136819783124,51.8699465641344,15.5701102075356));
#68201=CARTESIAN_POINT('Ctrl Pts',(12.6796557508836,52.9264314645779,15.4916046971588));
#68202=CARTESIAN_POINT('Ctrl Pts',(13.0456896245371,54.2882627693297,15.413099186782));
#68203=CARTESIAN_POINT('Ctrl Pts',(14.3835156719806,54.7341178236928,15.3345936764053));
#68204=CARTESIAN_POINT('Ctrl Pts',(15.4933397846085,53.8641431445068,15.2560881660285));
#68205=CARTESIAN_POINT('Ctrl Pts',(15.3798451204699,52.4585528494213,15.1775826556517));
#68206=CARTESIAN_POINT('Ctrl Pts',(14.1448167823889,51.7779134427179,15.0990771452749));
#68207=CARTESIAN_POINT('Ctrl Pts',(12.8958567583911,52.4326391074739,15.0205716348981));
#68208=CARTESIAN_POINT('Ctrl Pts',(12.7530636778084,53.8355551281415,14.9420661245213));
#68209=CARTESIAN_POINT('Ctrl Pts',(13.8444945665562,54.7284954344056,14.8635606141446));
#68210=CARTESIAN_POINT('Ctrl Pts',(15.1913347207388,54.3106451497661,14.7850551037678));
#68211=CARTESIAN_POINT('Ctrl Pts',(15.5856928259413,52.9567519919252,14.706549593391));
#68212=CARTESIAN_POINT('Ctrl Pts',(14.6739254819125,51.8810000614065,14.6280440830142));
#68213=CARTESIAN_POINT('Ctrl Pts',(13.2736741987179,52.048188554266,14.5495385726375));
#68214=CARTESIAN_POINT('Ctrl Pts',(12.6408248098497,53.3082995698058,14.4710330622607));
#68215=CARTESIAN_POINT('Ctrl Pts',(13.3427153793838,54.5313955863728,14.3925275518839));
#68216=CARTESIAN_POINT('Ctrl Pts',(14.750310293977,54.6202521539728,14.3140220415071));
#68217=CARTESIAN_POINT('Ctrl Pts',(15.6003636860248,53.4958321842015,14.2355165311303));
#68218=CARTESIAN_POINT('Ctrl Pts',(15.1323120289118,52.1652265278751,14.1570110207536));
#68219=CARTESIAN_POINT('Ctrl Pts',(13.7622484926781,51.824426723133,14.0785055103768));
#68220=CARTESIAN_POINT('Ctrl Pts',(13.0727468794464,52.4572155888145,14.0261685034589));
#68221=CARTESIAN_POINT('Ctrl Pts',(12.9355708698302,52.8497595669186,14.));
#68222=CARTESIAN_POINT('Ctrl Pts',(13.4965541629804,52.1730078059394,17.5565803263806));
#68223=CARTESIAN_POINT('Ctrl Pts',(13.3865887223467,52.2353622375858,17.5486362065721));
#68224=CARTESIAN_POINT('Ctrl Pts',(13.2860845507673,52.3135738660446,17.5406920867636));
#68225=CARTESIAN_POINT('Ctrl Pts',(13.2006215056575,52.4057329773025,17.5327479669551));
#68226=CARTESIAN_POINT('Ctrl Pts',(12.9191000727644,52.7093117349065,17.5065794634961));
#68227=CARTESIAN_POINT('Ctrl Pts',(12.8007885650155,53.1642333874847,17.4804109600372));
#68228=CARTESIAN_POINT('Ctrl Pts',(12.8987284513299,53.5665035982154,17.4542424565783));
#68229=CARTESIAN_POINT('Ctrl Pts',(12.9966683376443,53.9687738089461,17.4280739531194));
#68230=CARTESIAN_POINT('Ctrl Pts',(13.310859618022,54.3183925778293,17.4019054496604));
#68231=CARTESIAN_POINT('Ctrl Pts',(13.7004205482536,54.4585877139982,17.3757369462015));
#68232=CARTESIAN_POINT('Ctrl Pts',(14.0899814784851,54.598782850167,17.3495684427426));
#68233=CARTESIAN_POINT('Ctrl Pts',(14.5549120585705,54.5295543536216,17.3233999392837));
#68234=CARTESIAN_POINT('Ctrl Pts',(14.8867292333681,54.2819445991817,17.2972314358247));
#68235=CARTESIAN_POINT('Ctrl Pts',(15.2185464081657,54.0343348447418,17.2710629323658));
#68236=CARTESIAN_POINT('Ctrl Pts',(15.4172501776755,53.6083438324075,17.2448944289069));
#68237=CARTESIAN_POINT('Ctrl Pts',(15.3937407261232,53.1949912465067,17.2187259254479));
#68238=CARTESIAN_POINT('Ctrl Pts',(15.3702312745709,52.7816386606059,17.192557421989));
#68239=CARTESIAN_POINT('Ctrl Pts',(15.1245086019564,52.3809245011388,17.1663889185301));
#68240=CARTESIAN_POINT('Ctrl Pts',(14.7667570231804,52.1725336361826,17.1402204150712));
#68241=CARTESIAN_POINT('Ctrl Pts',(14.4090054444043,51.9641427712265,17.1140519116122));
#68242=CARTESIAN_POINT('Ctrl Pts',(13.9392249594666,51.9480752007813,17.0878834081533));
#68243=CARTESIAN_POINT('Ctrl Pts',(13.5680710452887,52.1315358759968,17.0617149046944));
#68244=CARTESIAN_POINT('Ctrl Pts',(13.5437960761855,52.1435349471433,17.0600033785898));
#68245=CARTESIAN_POINT('Ctrl Pts',(13.5199430009518,52.1563875382183,17.0582918524852));
#68246=CARTESIAN_POINT('Ctrl Pts',(13.4965460097018,52.1700456009992,17.0565803263806));
#68247=CARTESIAN_POINT('Origin',(14.1292828945603,53.2669068454841,15.5));
#68248=CARTESIAN_POINT('Origin',(39.0658530619283,-38.8697713466883,13.));
#68249=CARTESIAN_POINT('',(39.0658530619283,-38.8697713466882,13.));
#68250=CARTESIAN_POINT('Origin',(39.0658530619283,-38.8697713466883,13.));
#68251=CARTESIAN_POINT('',(39.0658530619283,-38.8697713466882,13.));
#68252=CARTESIAN_POINT('Origin',(-14.1292828945604,-53.2669068454841,13.));
#68253=CARTESIAN_POINT('',(-14.1292828945603,-53.2669068454841,13.));
#68254=CARTESIAN_POINT('Origin',(-14.1292828945604,-53.2669068454841,13.));
#68255=CARTESIAN_POINT('',(-14.1292828945603,-53.2669068454841,13.));
#68256=CARTESIAN_POINT('Origin',(-53.1951359564886,-14.3971354987959,13.));
#68257=CARTESIAN_POINT('',(-53.1951359564886,-14.3971354987959,13.));
#68258=CARTESIAN_POINT('Origin',(-53.1951359564886,-14.3971354987959,13.));
#68259=CARTESIAN_POINT('',(-53.1951359564886,-14.3971354987959,13.));
#68260=CARTESIAN_POINT('Origin',(-39.0658530619283,38.8697713466882,13.));
#68261=CARTESIAN_POINT('',(-39.0658530619283,38.8697713466882,13.));
#68262=CARTESIAN_POINT('Origin',(-39.0658530619283,38.8697713466882,13.));
#68263=CARTESIAN_POINT('',(-39.0658530619283,38.8697713466882,13.));
#68264=CARTESIAN_POINT('Origin',(14.1292828945603,53.2669068454841,13.));
#68265=CARTESIAN_POINT('',(14.1292828945603,53.2669068454841,13.));
#68266=CARTESIAN_POINT('Origin',(14.1292828945603,53.2669068454841,13.));
#68267=CARTESIAN_POINT('',(14.1292828945603,53.2669068454841,13.));
#68268=CARTESIAN_POINT('Origin',(53.1951359564886,14.3971354987959,6.));
#68269=CARTESIAN_POINT('Ctrl Pts',(54.153252109211,15.2223467977324,6.));
#68270=CARTESIAN_POINT('Ctrl Pts',(54.1904452248552,15.1876133706834,6.));
#68271=CARTESIAN_POINT('Ctrl Pts',(54.2252563920727,15.1505690966098,6.));
#68272=CARTESIAN_POINT('Ctrl Pts',(54.2576712403435,15.1115269977852,6.));
#68273=CARTESIAN_POINT('Ctrl Pts',(54.2795176350337,15.08521408423,6.));
#68274=CARTESIAN_POINT('Ctrl Pts',(54.3002751129807,15.0579926438161,6.));
#68275=CARTESIAN_POINT('Ctrl Pts',(54.3199324346534,15.0299477423818,6.));
#68276=CARTESIAN_POINT('Ctrl Pts',(54.3290141536083,15.0169909460702,6.));
#68277=CARTESIAN_POINT('Ctrl Pts',(54.3378609651789,15.0038582769416,6.));
#68278=CARTESIAN_POINT('Ctrl Pts',(54.346471305624,14.9905576089646,6.));
#68279=CARTESIAN_POINT('Ctrl Pts',(54.3536893844502,14.9794076119916,6.));
#68280=CARTESIAN_POINT('Ctrl Pts',(54.3607371493116,14.9681457925481,6.));
#68281=CARTESIAN_POINT('Ctrl Pts',(54.3676105396587,14.9567832872257,6.));
#68282=CARTESIAN_POINT('Ctrl Pts',(54.395433097869,14.9107893963246,6.));
#68283=CARTESIAN_POINT('Ctrl Pts',(54.4204206822113,14.8631190274542,6.));
#68284=CARTESIAN_POINT('Ctrl Pts',(54.4425345345286,14.8140965425426,6.));
#68285=CARTESIAN_POINT('Ctrl Pts',(54.4509995916132,14.7953310137123,6.));
#68286=CARTESIAN_POINT('Ctrl Pts',(54.4590431896973,14.7763669365288,6.));
#68287=CARTESIAN_POINT('Ctrl Pts',(54.4666617056761,14.7572211103019,6.));
#68288=CARTESIAN_POINT('Ctrl Pts',(54.472141946642,14.7434489082736,6.));
#68289=CARTESIAN_POINT('Ctrl Pts',(54.4774022167645,14.7295826470911,6.));
#68290=CARTESIAN_POINT('Ctrl Pts',(54.4824408846806,14.7156283853978,6.));
#68291=CARTESIAN_POINT('Ctrl Pts',(54.4863313548671,14.7048539823218,6.));
#68292=CARTESIAN_POINT('Ctrl Pts',(54.4900897012419,14.6940267513306,6.));
#68293=CARTESIAN_POINT('Ctrl Pts',(54.4937105016155,14.6831642693743,6.));
#68294=CARTESIAN_POINT('Ctrl Pts',(54.5116283443036,14.6294103412881,6.));
#68295=CARTESIAN_POINT('Ctrl Pts',(54.5262131829647,14.5747104062488,6.));
#68296=CARTESIAN_POINT('Ctrl Pts',(54.5374265846686,14.5194236084943,6.));
#68297=CARTESIAN_POINT('Ctrl Pts',(54.5484779141318,14.464935895213,6.));
#68298=CARTESIAN_POINT('Ctrl Pts',(54.556254950168,14.4098769850011,6.));
#68299=CARTESIAN_POINT('Ctrl Pts',(54.5606770668685,14.3545607001755,6.));
#68300=CARTESIAN_POINT('Ctrl Pts',(54.5629861190308,14.3256767525692,6.));
#68301=CARTESIAN_POINT('Ctrl Pts',(54.5643796851138,14.2967222396706,6.));
#68302=CARTESIAN_POINT('Ctrl Pts',(54.564840878929,14.2677401408177,6.));
#68303=CARTESIAN_POINT('Ctrl Pts',(54.5650883530361,14.2521885033157,6.));
#68304=CARTESIAN_POINT('Ctrl Pts',(54.5650672991613,14.2366289098418,6.));
#68305=CARTESIAN_POINT('Ctrl Pts',(54.5647746275356,14.2210679501262,6.));
#68306=CARTESIAN_POINT('Ctrl Pts',(54.5645665072066,14.2100024700117,6.));
#68307=CARTESIAN_POINT('Ctrl Pts',(54.5642210307105,14.1989362983826,6.));
#68308=CARTESIAN_POINT('Ctrl Pts',(54.5637369787284,14.1878718045722,6.));
#68309=CARTESIAN_POINT('Ctrl Pts',(54.5633114560967,14.1781451787148,6.));
#68310=CARTESIAN_POINT('Ctrl Pts',(54.5627792671695,14.1684296794964,6.));
#68311=CARTESIAN_POINT('Ctrl Pts',(54.5621402322824,14.1587275143162,6.));
#68312=CARTESIAN_POINT('Ctrl Pts',(54.5589760897275,14.1106878308172,6.));
#68313=CARTESIAN_POINT('Ctrl Pts',(54.553194193765,14.0629716936048,6.));
#68314=CARTESIAN_POINT('Ctrl Pts',(54.5447557136211,14.0157777529758,6.));
#68315=CARTESIAN_POINT('Ctrl Pts',(54.5351507946179,13.9620602624492,6.));
#68316=CARTESIAN_POINT('Ctrl Pts',(54.522105840848,13.9090185683937,6.));
#68317=CARTESIAN_POINT('Ctrl Pts',(54.505871219518,13.8568507922163,6.));
#68318=CARTESIAN_POINT('Ctrl Pts',(54.4900017008387,13.8058562243927,6.));
#68319=CARTESIAN_POINT('Ctrl Pts',(54.4710837860578,13.7556960236983,6.));
#68320=CARTESIAN_POINT('Ctrl Pts',(54.449305884129,13.7065589745936,6.));
#68321=CARTESIAN_POINT('Ctrl Pts',(54.443973358842,13.6945273033271,6.));
#68322=CARTESIAN_POINT('Ctrl Pts',(54.4384691646966,13.6825570212106,6.));
#68323=CARTESIAN_POINT('Ctrl Pts',(54.432795699503,13.670651006764,6.));
#68324=CARTESIAN_POINT('Ctrl Pts',(54.428510829431,13.6616590198145,6.));
#68325=CARTESIAN_POINT('Ctrl Pts',(54.4241301793592,13.6527055014145,6.));
#68326=CARTESIAN_POINT('Ctrl Pts',(54.4196602351137,13.6438018792426,6.));
#68327=CARTESIAN_POINT('Ctrl Pts',(54.3938099878154,13.5923111173108,6.));
#68328=CARTESIAN_POINT('Ctrl Pts',(54.3649324447401,13.5423928807606,6.));
#68329=CARTESIAN_POINT('Ctrl Pts',(54.3333070254305,13.4942625534384,6.));
#68330=CARTESIAN_POINT('Ctrl Pts',(54.3010028577955,13.4450992475886,6.));
#68331=CARTESIAN_POINT('Ctrl Pts',(54.2658311992691,13.3978004683614,6.));
#68332=CARTESIAN_POINT('Ctrl Pts',(54.2280361919916,13.3526057240142,6.));
#68333=CARTESIAN_POINT('Ctrl Pts',(54.1899071161005,13.3070115050625,6.));
#68334=CARTESIAN_POINT('Ctrl Pts',(54.1491075472284,13.2635576362327,6.));
#68335=CARTESIAN_POINT('Ctrl Pts',(54.1058416126115,13.2225152020132,6.));
#68336=CARTESIAN_POINT('Ctrl Pts',(54.0960379392214,13.2132153539044,6.));
#68337=CARTESIAN_POINT('Ctrl Pts',(54.0861045521762,13.2040370186399,6.));
#68338=CARTESIAN_POINT('Ctrl Pts',(54.0760639794891,13.1950014470312,6.));
#68339=CARTESIAN_POINT('Ctrl Pts',(54.0308409079937,13.1543049336347,6.));
#68340=CARTESIAN_POINT('Ctrl Pts',(53.9833737359527,13.116430352764,6.));
#68341=CARTESIAN_POINT('Ctrl Pts',(53.9339288506769,13.0816212828191,6.));
#68342=CARTESIAN_POINT('Ctrl Pts',(53.8849184369623,13.0471180797172,6.));
#68343=CARTESIAN_POINT('Ctrl Pts',(53.8339641912571,13.0156258220742,6.));
#68344=CARTESIAN_POINT('Ctrl Pts',(53.781283756076,12.9874094818381,6.));
#68345=CARTESIAN_POINT('Ctrl Pts',(53.7426834464002,12.9667346436884,6.));
#68346=CARTESIAN_POINT('Ctrl Pts',(53.7031554637372,12.9478191087148,6.));
#68347=CARTESIAN_POINT('Ctrl Pts',(53.6627743368928,12.9307811146157,6.));
#68348=CARTESIAN_POINT('Ctrl Pts',(53.6403329837275,12.921312442672,6.));
#68349=CARTESIAN_POINT('Ctrl Pts',(53.6176279860555,12.912423887492,6.));
#68350=CARTESIAN_POINT('Ctrl Pts',(53.5946794545979,12.9041113494969,6.));
#68351=CARTESIAN_POINT('Ctrl Pts',(52.7966221146314,12.9064860705774,6.));
#68352=CARTESIAN_POINT('Ctrl Pts',(52.7392734478414,12.9274410373818,6.));
#68353=CARTESIAN_POINT('Ctrl Pts',(52.6834091366923,12.9520243011176,6.));
#68354=CARTESIAN_POINT('Ctrl Pts',(52.6292438196105,12.9799599642101,6.));
#68355=CARTESIAN_POINT('Ctrl Pts',(52.5790178579261,13.0058639119705,6.));
#68356=CARTESIAN_POINT('Ctrl Pts',(52.5302525542226,13.0346514876389,6.));
#68357=CARTESIAN_POINT('Ctrl Pts',(52.4831464368633,13.0661326532235,6.));
#68358=CARTESIAN_POINT('Ctrl Pts',(52.4717767044421,13.0737310809664,6.));
#68359=CARTESIAN_POINT('Ctrl Pts',(52.4605034749784,13.0814868964051,6.));
#68360=CARTESIAN_POINT('Ctrl Pts',(52.4493421044021,13.0893884562265,6.));
#68361=CARTESIAN_POINT('Ctrl Pts',(52.4002195795496,13.1241641646442,6.));
#68362=CARTESIAN_POINT('Ctrl Pts',(52.3531999206732,13.1617999131515,6.));
#68363=CARTESIAN_POINT('Ctrl Pts',(52.3085126015214,13.2020507625132,6.));
#68364=CARTESIAN_POINT('Ctrl Pts',(52.280929942436,13.2268950690618,6.));
#68365=CARTESIAN_POINT('Ctrl Pts',(52.2542366022306,13.2527364020391,6.));
#68366=CARTESIAN_POINT('Ctrl Pts',(52.2284950356621,13.2795223256871,6.));
#68367=CARTESIAN_POINT('Ctrl Pts',(52.2196863977047,13.2886883375202,6.));
#68368=CARTESIAN_POINT('Ctrl Pts',(52.2109892715066,13.2979649848007,6.));
#68369=CARTESIAN_POINT('Ctrl Pts',(52.2024063581496,13.3073502392712,6.));
#68370=CARTESIAN_POINT('Ctrl Pts',(52.1943778466578,13.3161292657201,6.));
#68371=CARTESIAN_POINT('Ctrl Pts',(52.1864544233969,13.3249977565961,6.));
#68372=CARTESIAN_POINT('Ctrl Pts',(52.178641809422,13.3339491348872,6.));
#68373=CARTESIAN_POINT('Ctrl Pts',(52.1399699654117,13.3782577755114,6.));
#68374=CARTESIAN_POINT('Ctrl Pts',(52.1039774129999,13.4246301645838,6.));
#68375=CARTESIAN_POINT('Ctrl Pts',(52.0708793546467,13.4728370625887,6.));
#68376=CARTESIAN_POINT('Ctrl Pts',(52.0386265755808,13.5198128221398,6.));
#68377=CARTESIAN_POINT('Ctrl Pts',(52.0091219665516,13.5685314991462,6.));
#68378=CARTESIAN_POINT('Ctrl Pts',(51.9826103203801,13.6187990638417,6.));
#68379=CARTESIAN_POINT('Ctrl Pts',(51.9682364690781,13.6460526902509,6.));
#68380=CARTESIAN_POINT('Ctrl Pts',(51.9547432274533,13.6737618469323,6.));
#68381=CARTESIAN_POINT('Ctrl Pts',(51.9421760191701,13.7018965350937,6.));
#68382=CARTESIAN_POINT('Ctrl Pts',(51.931720374266,13.72530398584,6.));
#68383=CARTESIAN_POINT('Ctrl Pts',(51.921905793166,13.7490060034822,6.));
#68384=CARTESIAN_POINT('Ctrl Pts',(51.9127610532135,13.7729853083355,6.));
#68385=CARTESIAN_POINT('Ctrl Pts',(51.9088519886793,13.7832356435714,6.));
#68386=CARTESIAN_POINT('Ctrl Pts',(51.9050650272194,13.7935379061066,6.));
#68387=CARTESIAN_POINT('Ctrl Pts',(51.9014081869821,13.8038738000364,6.));
#68388=CARTESIAN_POINT('Ctrl Pts',(51.884480682992,13.8517186262746,6.));
#68389=CARTESIAN_POINT('Ctrl Pts',(51.8703064127051,13.9003649240817,6.));
#68390=CARTESIAN_POINT('Ctrl Pts',(51.8590515016651,13.9496698048621,6.));
#68391=CARTESIAN_POINT('Ctrl Pts',(51.8464743828165,14.0047669391876,6.));
#68392=CARTESIAN_POINT('Ctrl Pts',(51.8375421395455,14.0606874236405,6.));
#68393=CARTESIAN_POINT('Ctrl Pts',(51.8321648228282,14.1170948620919,6.));
#68394=CARTESIAN_POINT('Ctrl Pts',(51.8276016369013,14.1649621614995,6.));
#68395=CARTESIAN_POINT('Ctrl Pts',(51.8255995131662,14.2131805783558,6.));
#68396=CARTESIAN_POINT('Ctrl Pts',(51.8261319285704,14.2615368910685,6.));
#68397=CARTESIAN_POINT('Ctrl Pts',(51.8262783001781,14.2748310053615,6.));
#68398=CARTESIAN_POINT('Ctrl Pts',(51.8266163768542,14.2881354730531,6.));
#68399=CARTESIAN_POINT('Ctrl Pts',(51.8271459227334,14.3014456837622,6.));
#68400=CARTESIAN_POINT('Ctrl Pts',(51.8275582116147,14.3118086232134,6.));
#68401=CARTESIAN_POINT('Ctrl Pts',(51.8280867629365,14.3221768232861,6.));
#68402=CARTESIAN_POINT('Ctrl Pts',(51.8287302146398,14.3325312126212,6.));
#68403=CARTESIAN_POINT('Ctrl Pts',(51.8321732391026,14.3879361724563,6.));
#68404=CARTESIAN_POINT('Ctrl Pts',(51.8389046601923,14.4430495470118,6.));
#68405=CARTESIAN_POINT('Ctrl Pts',(51.8488297362235,14.4975564316795,6.));
#68406=CARTESIAN_POINT('Ctrl Pts',(51.8586992382099,14.551758112836,6.));
#68407=CARTESIAN_POINT('Ctrl Pts',(51.8717272178009,14.6053611705282,6.));
#68408=CARTESIAN_POINT('Ctrl Pts',(51.8878674165316,14.6580360179265,6.));
#68409=CARTESIAN_POINT('Ctrl Pts',(51.9028425534762,14.7069085917089,6.));
#68410=CARTESIAN_POINT('Ctrl Pts',(51.9204975501424,14.754982591428,6.));
#68411=CARTESIAN_POINT('Ctrl Pts',(51.9408266061613,14.8019671660544,6.));
#68412=CARTESIAN_POINT('Ctrl Pts',(51.9460484511811,14.8140359097675,6.));
#68413=CARTESIAN_POINT('Ctrl Pts',(51.9514489311321,14.826036655033,6.));
#68414=CARTESIAN_POINT('Ctrl Pts',(51.9570156117501,14.837938168984,6.));
#68415=CARTESIAN_POINT('Ctrl Pts',(51.9795172113669,14.8860463900468,6.));
#68416=CARTESIAN_POINT('Ctrl Pts',(52.0047624527444,14.9326133843823,6.));
#68417=CARTESIAN_POINT('Ctrl Pts',(52.0326996004424,14.9773433961128,6.));
#68418=CARTESIAN_POINT('Ctrl Pts',(52.0596890512563,15.0205560556354,6.));
#68419=CARTESIAN_POINT('Ctrl Pts',(52.0891914488154,15.0620548998909,6.));
#68420=CARTESIAN_POINT('Ctrl Pts',(52.1211934155598,15.1015390599859,6.));
#68421=CARTESIAN_POINT('Ctrl Pts',(52.1435818547643,15.1291620096904,6.));
#68422=CARTESIAN_POINT('Ctrl Pts',(52.1671943525027,15.1557982112413,6.));
#68423=CARTESIAN_POINT('Ctrl Pts',(52.1920344148669,15.1813316631752,6.));
#68424=CARTESIAN_POINT('Ctrl Pts',(52.2060464360847,15.1957348182485,6.));
#68425=CARTESIAN_POINT('Ctrl Pts',(52.2204492103834,15.2097868473553,6.));
#68426=CARTESIAN_POINT('Ctrl Pts',(52.2352263046383,15.223479246524,6.));
#68427=CARTESIAN_POINT('Origin',(53.1951359564886,14.3971354987959,0.895788276411274));
#68428=CARTESIAN_POINT('Ctrl Pts',(54.7400287307462,14.397884086359,2.14578827641127));
#68429=CARTESIAN_POINT('Ctrl Pts',(54.7403302631026,14.4458093584932,2.14826884812012));
#68430=CARTESIAN_POINT('Ctrl Pts',(54.7167366550282,14.9990296040617,2.17691792328789));
#68431=CARTESIAN_POINT('Ctrl Pts',(54.0514939360652,15.9998439808924,2.23173550191458));
#68432=CARTESIAN_POINT('Ctrl Pts',(52.3307400382945,15.9953304824803,2.31024101229137));
#68433=CARTESIAN_POINT('Ctrl Pts',(51.3852180733224,14.5577448223715,2.38874652266814));
#68434=CARTESIAN_POINT('Ctrl Pts',(52.0628629644955,12.9760077060224,2.46725203304493));
#68435=CARTESIAN_POINT('Ctrl Pts',(53.7559624418889,12.6688282037076,2.5457575434217));
#68436=CARTESIAN_POINT('Ctrl Pts',(54.658158616602,13.6109326580654,2.60526962454382));
#68437=CARTESIAN_POINT('Ctrl Pts',(54.7387317829834,14.2566058695901,2.63861320220701));
#68438=CARTESIAN_POINT('Ctrl Pts',(54.7375657625992,14.3958310564158,2.64578827641127));
#68439=CARTESIAN_POINT('Ctrl Pts',(54.7364807484814,14.3955730757723,2.10421172358873));
#68440=CARTESIAN_POINT('Ctrl Pts',(54.7341428408094,14.7375070363914,2.12181148931034));
#68441=CARTESIAN_POINT('Ctrl Pts',(54.4552744897983,15.5924244351668,2.16557975849087));
#68442=CARTESIAN_POINT('Ctrl Pts',(53.0510002557363,16.2080728204287,2.23551653113034));
#68443=CARTESIAN_POINT('Ctrl Pts',(51.605113325188,15.2764851170283,2.31402204150712));
#68444=CARTESIAN_POINT('Ctrl Pts',(51.5846111642588,13.5555692706413,2.3925275518839));
#68445=CARTESIAN_POINT('Ctrl Pts',(53.0087575469087,12.5897418281553,2.47103306226068));
#68446=CARTESIAN_POINT('Ctrl Pts',(54.4388957804212,13.178381042198,2.54159445282895));
#68447=CARTESIAN_POINT('Ctrl Pts',(54.7344163061994,14.0445046478413,2.5859873399383));
#68448=CARTESIAN_POINT('Ctrl Pts',(54.73716587472,14.3983674417199,2.60421172358873));
#68449=CARTESIAN_POINT('Ctrl Pts',(52.2370198037663,15.2223467977324,2.));
#68450=CARTESIAN_POINT('Ctrl Pts',(51.9656547514336,14.9072768995629,2.02616850345893));
#68451=CARTESIAN_POINT('Ctrl Pts',(51.7623579720558,13.9937953994845,2.07850551037678));
#68452=CARTESIAN_POINT('Ctrl Pts',(52.7425844632288,12.9776340948198,2.15701102075356));
#68453=CARTESIAN_POINT('Ctrl Pts',(54.1289211584486,13.2376188657684,2.23551653113034));
#68454=CARTESIAN_POINT('Ctrl Pts',(54.6776801082256,14.5359758627139,2.31402204150712));
#68455=CARTESIAN_POINT('Ctrl Pts',(53.8969277031994,15.7105670448821,2.3925275518839));
#68456=CARTESIAN_POINT('Ctrl Pts',(52.4867570591739,15.7068681992943,2.47103306226068));
#68457=CARTESIAN_POINT('Ctrl Pts',(51.7118947618914,14.5287560364896,2.54953857263746));
#68458=CARTESIAN_POINT('Ctrl Pts',(52.2672298007042,13.2325106809332,2.62804408301423));
#68459=CARTESIAN_POINT('Ctrl Pts',(53.6547374411216,12.9807747893732,2.70654959339102));
#68460=CARTESIAN_POINT('Ctrl Pts',(54.6300613996379,13.9992418052107,2.7850551037678));
#68461=CARTESIAN_POINT('Ctrl Pts',(54.3185111760821,15.374560833818,2.86356061414457));
#68462=CARTESIAN_POINT('Ctrl Pts',(52.9994908161496,15.8732958581993,2.94206612452135));
#68463=CARTESIAN_POINT('Ctrl Pts',(51.855929934815,15.0481780331667,3.02057163489813));
#68464=CARTESIAN_POINT('Ctrl Pts',(51.9134007191539,13.6391883627491,3.09907714527491));
#68465=CARTESIAN_POINT('Ctrl Pts',(53.1203622018241,12.909944412367,3.17758265565169));
#68466=CARTESIAN_POINT('Ctrl Pts',(54.394382532434,13.5144484306959,3.25608816602847));
#68467=CARTESIAN_POINT('Ctrl Pts',(54.592890039674,14.9105673726083,3.33459367640525));
#68468=CARTESIAN_POINT('Ctrl Pts',(53.5378584472409,15.8462283160988,3.41309918678203));
#68469=CARTESIAN_POINT('Ctrl Pts',(52.1754651814132,15.4823084146089,3.49160469715881));
#68470=CARTESIAN_POINT('Ctrl Pts',(51.7275369059285,14.1451796218823,3.57011020753559));
#68471=CARTESIAN_POINT('Ctrl Pts',(52.5957863501673,13.0340108603602,3.64861571791237));
#68472=CARTESIAN_POINT('Ctrl Pts',(54.0015467695737,13.1453246755956,3.72712122828915));
#68473=CARTESIAN_POINT('Ctrl Pts',(54.6840988007338,14.3792921998829,3.80562673866593));
#68474=CARTESIAN_POINT('Ctrl Pts',(54.0313135549908,15.6292620174801,3.8841322490427));
#68475=CARTESIAN_POINT('Ctrl Pts',(52.6286243599757,15.7742314816778,3.96263775941949));
#68476=CARTESIAN_POINT('Ctrl Pts',(51.7339962327512,14.6841885294771,4.04114326979627));
#68477=CARTESIAN_POINT('Ctrl Pts',(52.149752946345,13.3367095952976,4.11964878017304));
#68478=CARTESIAN_POINT('Ctrl Pts',(53.5030339960934,12.9402458213459,4.19815429054983));
#68479=CARTESIAN_POINT('Ctrl Pts',(54.5801847638566,13.8503553460012,4.2766598009266));
#68480=CARTESIAN_POINT('Ctrl Pts',(54.41519083395,15.2508303100965,4.35516531130338));
#68481=CARTESIAN_POINT('Ctrl Pts',(53.1560226839298,15.885691473038,4.43367082168017));
#68482=CARTESIAN_POINT('Ctrl Pts',(51.9319322483355,15.1855802477898,4.51217633205694));
#68483=CARTESIAN_POINT('Ctrl Pts',(51.8407129256901,13.7783730316416,4.59068184243372));
#68484=CARTESIAN_POINT('Ctrl Pts',(52.9641723835949,12.9260866978538,4.6691873528105));
#68485=CARTESIAN_POINT('Ctrl Pts',(54.2947654505407,13.3930719178224,4.74769286318728));
#68486=CARTESIAN_POINT('Ctrl Pts',(54.6391846730619,14.7605251935738,4.82619837356406));
#68487=CARTESIAN_POINT('Ctrl Pts',(53.6885466200217,15.8020820199204,4.90470388394084));
#68488=CARTESIAN_POINT('Ctrl Pts',(52.2954062665962,15.5836492690769,4.98320939431762));
#68489=CARTESIAN_POINT('Ctrl Pts',(51.7091646625422,14.3011230348445,5.0617149046944));
#68490=CARTESIAN_POINT('Ctrl Pts',(52.455577895988,13.1047025120629,5.14022041507118));
#68491=CARTESIAN_POINT('Ctrl Pts',(53.8652434689878,13.0673677185785,5.21872592544796));
#68492=CARTESIAN_POINT('Ctrl Pts',(54.6739425216854,14.2225980750992,5.29723143582474));
#68493=CARTESIAN_POINT('Ctrl Pts',(54.1564090232194,15.5343621736369,5.37573694620152));
#68494=CARTESIAN_POINT('Ctrl Pts',(52.7767903419412,15.826225464705,5.4542424565783));
#68495=CARTESIAN_POINT('Ctrl Pts',(51.7723391952092,14.8364647334447,5.53274796695507));
#68496=CARTESIAN_POINT('Ctrl Pts',(52.0439156164789,13.4526673224972,5.61125347733186));
#68497=CARTESIAN_POINT('Ctrl Pts',(53.3478744097592,12.9159632016583,5.68975898770863));
#68498=CARTESIAN_POINT('Ctrl Pts',(54.5149728893469,13.7074656120611,5.76826449808541));
#68499=CARTESIAN_POINT('Ctrl Pts',(54.498171162037,15.1177692904017,5.84677000846219));
#68500=CARTESIAN_POINT('Ctrl Pts',(53.3132562085964,15.88121138355,5.92527551883897));
#68501=CARTESIAN_POINT('Ctrl Pts',(52.0214443153046,15.3148691319142,6.00378102921575));
#68502=CARTESIAN_POINT('Ctrl Pts',(51.7841832172828,13.9230591799233,6.08228653959253));
#68503=CARTESIAN_POINT('Ctrl Pts',(52.4668366999413,13.2829324314547,6.13462354651038));
#68504=CARTESIAN_POINT('Ctrl Pts',(52.8685508929576,13.1755371825404,6.16079204996931));
#68505=CARTESIAN_POINT('Ctrl Pts',(52.166679656532,15.2829297282066,1.94640265001023));
#68506=CARTESIAN_POINT('Ctrl Pts',(51.8753923247544,14.9447289570595,1.97257115346916));
#68507=CARTESIAN_POINT('Ctrl Pts',(51.6571705017343,13.9641841650946,2.02490816038701));
#68508=CARTESIAN_POINT('Ctrl Pts',(52.70936037179,12.8734213253438,2.10341367076379));
#68509=CARTESIAN_POINT('Ctrl Pts',(54.1974750476659,13.1524928917871,2.18191918114057));
#68510=CARTESIAN_POINT('Ctrl Pts',(54.7865211643106,14.5461688352594,2.26042469151735));
#68511=CARTESIAN_POINT('Ctrl Pts',(53.9484497808213,15.8069926902189,2.33893020189413));
#68512=CARTESIAN_POINT('Ctrl Pts',(52.4347513855474,15.8030222936896,2.4174357122709));
#68513=CARTESIAN_POINT('Ctrl Pts',(51.6030025323684,14.5384189651169,2.49594122264769));
#68514=CARTESIAN_POINT('Ctrl Pts',(52.199107521968,13.1470096892963,2.57444673302446));
#68515=CARTESIAN_POINT('Ctrl Pts',(53.688479108044,12.8767925941513,2.65295224340125));
#68516=CARTESIAN_POINT('Ctrl Pts',(54.7354065257528,13.9700304189807,2.73145775377802));
#68517=CARTESIAN_POINT('Ctrl Pts',(54.4009838263145,15.4463185656761,2.8099632641548));
#68518=CARTESIAN_POINT('Ctrl Pts',(52.9851275179858,15.9816682478379,2.88846877453158));
#68519=CARTESIAN_POINT('Ctrl Pts',(51.757612055011,15.0959743547226,2.96697428490836));
#68520=CARTESIAN_POINT('Ctrl Pts',(51.8193020599744,13.5835436342954,3.04547979528514));
#68521=CARTESIAN_POINT('Ctrl Pts',(53.1148726827324,12.8007622013296,3.12398530566192));
#68522=CARTESIAN_POINT('Ctrl Pts',(54.4824252822431,13.4496459136362,3.2024908160387));
#68523=CARTESIAN_POINT('Ctrl Pts',(54.695506228462,14.9482610003549,3.28099632641548));
#68524=CARTESIAN_POINT('Ctrl Pts',(53.5630194367425,15.9526135407249,3.35950183679226));
#68525=CARTESIAN_POINT('Ctrl Pts',(52.1006059983742,15.5619764407204,3.43800734716904));
#68526=CARTESIAN_POINT('Ctrl Pts',(51.6197930452243,14.1266822680612,3.51651285754582));
#68527=CARTESIAN_POINT('Ctrl Pts',(52.5517850676155,12.9339369940615,3.5950183679226));
#68528=CARTESIAN_POINT('Ctrl Pts',(54.0607494614003,13.0534229188377,3.67352387829937));
#68529=CARTESIAN_POINT('Ctrl Pts',(54.7934110854636,14.3779822331642,3.75202938867616));
#68530=CARTESIAN_POINT('Ctrl Pts',(54.0927015769186,15.7197186499972,3.83053489905293));
#68531=CARTESIAN_POINT('Ctrl Pts',(52.5870338816236,15.8753310549564,3.90904040942972));
#68532=CARTESIAN_POINT('Ctrl Pts',(51.6267265838621,14.7052625426694,3.98754591980649));
#68533=CARTESIAN_POINT('Ctrl Pts',(52.0730060982299,13.2588583723836,4.06605143018328));
#68534=CARTESIAN_POINT('Ctrl Pts',(53.525638346701,12.8332881898262,4.14455694056005));
#68535=CARTESIAN_POINT('Ctrl Pts',(54.681868194159,13.8102134526169,4.22306245093683));
#68536=CARTESIAN_POINT('Ctrl Pts',(54.5047612262982,15.3135043591139,4.30156796131361));
#68537=CARTESIAN_POINT('Ctrl Pts',(53.1531511809886,15.9949738873852,4.38007347169039));
#68538=CARTESIAN_POINT('Ctrl Pts',(51.8391940823356,15.2434639600858,4.45857898206717));
#68539=CARTESIAN_POINT('Ctrl Pts',(51.741277888369,13.7329465529009,4.53708449244395));
#68540=CARTESIAN_POINT('Ctrl Pts',(52.9472161808664,12.8180895735458,4.61559000282073));
#68541=CARTESIAN_POINT('Ctrl Pts',(54.3754948070961,13.3193585377509,4.69409551319751));
#68542=CARTESIAN_POINT('Ctrl Pts',(54.7451995847704,14.787203466935,4.77260102357429));
#68543=CARTESIAN_POINT('Ctrl Pts',(53.7247703895732,15.9052262419141,4.85110653395107));
#68544=CARTESIAN_POINT('Ctrl Pts',(52.2293525645705,15.6707572392952,4.92961204432785));
#68545=CARTESIAN_POINT('Ctrl Pts',(51.6000720026333,14.2940742748049,5.00811755470463));
#68546=CARTESIAN_POINT('Ctrl Pts',(52.4012832024729,13.0098184770543,5.08662306508141));
#68547=CARTESIAN_POINT('Ctrl Pts',(53.9144394469056,12.9697427477624,5.16512857545819));
#68548=CARTESIAN_POINT('Ctrl Pts',(54.78250918266,14.2097844010516,5.24363408583497));
#68549=CARTESIAN_POINT('Ctrl Pts',(54.2269809354599,15.6178517291775,5.32213959621174));
#68550=CARTESIAN_POINT('Ctrl Pts',(52.746077476869,15.9311421789545,5.40064510658853));
#68551=CARTESIAN_POINT('Ctrl Pts',(51.6678844969052,14.8687181120791,5.4791506169653));
#68552=CARTESIAN_POINT('Ctrl Pts',(51.9593987152815,13.3833291421626,5.5576561273421));
#68553=CARTESIAN_POINT('Ctrl Pts',(53.359087711258,12.80722286035,5.63616163771885));
#68554=CARTESIAN_POINT('Ctrl Pts',(54.611868786487,13.6568334614203,5.71466714809565));
#68555=CARTESIAN_POINT('Ctrl Pts',(54.5938335594919,15.1706746577306,5.79317265847242));
#68556=CARTESIAN_POINT('Ctrl Pts',(53.3219280130545,15.9901648918943,5.87167816884921));
#68557=CARTESIAN_POINT('Ctrl Pts',(51.9352776823615,15.3822445943694,5.95018367922598));
#68558=CARTESIAN_POINT('Ctrl Pts',(51.680598048476,13.8882548422916,6.02868918960276));
#68559=CARTESIAN_POINT('Ctrl Pts',(52.4133685721047,13.2011331552573,6.08102619652061));
#68560=CARTESIAN_POINT('Ctrl Pts',(52.8445746335155,13.0858534785527,6.10719469997954));
#68561=CARTESIAN_POINT('Ctrl Pts',(52.0963395092977,15.3435126586808,1.89280530002046));
#68562=CARTESIAN_POINT('Ctrl Pts',(51.7851298980751,14.9821810145562,1.91897380347939));
#68563=CARTESIAN_POINT('Ctrl Pts',(51.5519830314128,13.9345729307046,1.97131081039724));
#68564=CARTESIAN_POINT('Ctrl Pts',(52.6761362803514,12.7692085558677,2.04981632077402));
#68565=CARTESIAN_POINT('Ctrl Pts',(54.2660289368831,13.0673669178057,2.1283218311508));
#68566=CARTESIAN_POINT('Ctrl Pts',(54.8953622203958,14.5563618078048,2.20682734152758));
#68567=CARTESIAN_POINT('Ctrl Pts',(53.9999718584432,15.9034183355556,2.28533285190436));
#68568=CARTESIAN_POINT('Ctrl Pts',(52.382745711921,15.899176388085,2.36383836228113));
#68569=CARTESIAN_POINT('Ctrl Pts',(51.4941103028454,14.5480818937442,2.44234387265791));
#68570=CARTESIAN_POINT('Ctrl Pts',(52.1309852432318,13.0615086976594,2.52084938303469));
#68571=CARTESIAN_POINT('Ctrl Pts',(53.7222207749664,12.7728103989295,2.59935489341147));
#68572=CARTESIAN_POINT('Ctrl Pts',(54.8407516518678,13.9408190327507,2.67786040378825));
#68573=CARTESIAN_POINT('Ctrl Pts',(54.483456476547,15.5180762975341,2.75636591416503));
#68574=CARTESIAN_POINT('Ctrl Pts',(52.9707642198219,16.0900406374764,2.83487142454181));
#68575=CARTESIAN_POINT('Ctrl Pts',(51.6592941752072,15.1437706762785,2.91337693491859));
#68576=CARTESIAN_POINT('Ctrl Pts',(51.7252034007948,13.5278989058417,2.99188244529537));
#68577=CARTESIAN_POINT('Ctrl Pts',(53.1093831636409,12.6915799902922,3.07038795567215));
#68578=CARTESIAN_POINT('Ctrl Pts',(54.5704680320522,13.3848433965765,3.14889346604893));
#68579=CARTESIAN_POINT('Ctrl Pts',(54.7981224172499,14.9859546281015,3.22739897642571));
#68580=CARTESIAN_POINT('Ctrl Pts',(53.5881804262442,16.0589987653509,3.30590448680249));
#68581=CARTESIAN_POINT('Ctrl Pts',(52.0257468153352,15.6416444668319,3.38440999717927));
#68582=CARTESIAN_POINT('Ctrl Pts',(51.5120491845202,14.10818491424,3.46291550755605));
#68583=CARTESIAN_POINT('Ctrl Pts',(52.5077837850637,12.8338631277627,3.54142101793282));
#68584=CARTESIAN_POINT('Ctrl Pts',(54.1199521532269,12.9615211620797,3.61992652830961));
#68585=CARTESIAN_POINT('Ctrl Pts',(54.9027233701934,14.3766722664456,3.69843203868638));
#68586=CARTESIAN_POINT('Ctrl Pts',(54.1540895988462,15.8101752825143,3.77693754906317));
#68587=CARTESIAN_POINT('Ctrl Pts',(52.5454434032715,15.9764306282351,3.85544305943994));
#68588=CARTESIAN_POINT('Ctrl Pts',(51.5194569349729,14.7263365558616,3.93394856981673));
#68589=CARTESIAN_POINT('Ctrl Pts',(51.9962592501147,13.1810071494696,4.0124540801935));
#68590=CARTESIAN_POINT('Ctrl Pts',(53.5482426973085,12.7263305583065,4.09095959057029));
#68591=CARTESIAN_POINT('Ctrl Pts',(54.7835516244613,13.7700715592326,4.16946510094706));
#68592=CARTESIAN_POINT('Ctrl Pts',(54.5943316186464,15.3761784081312,4.24797061132384));
#68593=CARTESIAN_POINT('Ctrl Pts',(53.1502796780473,16.1042563017325,4.32647612170062));
#68594=CARTESIAN_POINT('Ctrl Pts',(51.7464559163357,15.3013476723818,4.4049816320774));
#68595=CARTESIAN_POINT('Ctrl Pts',(51.6418428510479,13.6875200741603,4.48348714245418));
#68596=CARTESIAN_POINT('Ctrl Pts',(52.9302599781379,12.7100924492379,4.56199265283096));
#68597=CARTESIAN_POINT('Ctrl Pts',(54.4562241636517,13.2456451576795,4.64049816320774));
#68598=CARTESIAN_POINT('Ctrl Pts',(54.8512144964787,14.8138817402962,4.71900367358452));
#68599=CARTESIAN_POINT('Ctrl Pts',(53.7609941591248,16.0083704639078,4.7975091839613));
#68600=CARTESIAN_POINT('Ctrl Pts',(52.1632988625446,15.7578652095136,4.87601469433808));
#68601=CARTESIAN_POINT('Ctrl Pts',(51.4909793427245,14.2870255147652,4.95452020471486));
#68602=CARTESIAN_POINT('Ctrl Pts',(52.3469885089579,12.9149344420457,5.03302571509164));
#68603=CARTESIAN_POINT('Ctrl Pts',(53.9636354248233,12.8721177769464,5.11153122546841));
#68604=CARTESIAN_POINT('Ctrl Pts',(54.8910758436347,14.1969707270041,5.1900367358452));
#68605=CARTESIAN_POINT('Ctrl Pts',(54.2975528477005,15.7013412847181,5.26854224622198));
#68606=CARTESIAN_POINT('Ctrl Pts',(52.7153646117967,16.0360588932041,5.34704775659875));
#68607=CARTESIAN_POINT('Ctrl Pts',(51.5634297986012,14.9009714907135,5.42555326697554));
#68608=CARTESIAN_POINT('Ctrl Pts',(51.874881814084,13.3139909618281,5.50405877735232));
#68609=CARTESIAN_POINT('Ctrl Pts',(53.3703010127568,12.6984825190418,5.58256428772909));
#68610=CARTESIAN_POINT('Ctrl Pts',(54.7087646836271,13.6062013107796,5.66106979810587));
#68611=CARTESIAN_POINT('Ctrl Pts',(54.6894959569468,15.2235800250595,5.73957530848266));
#68612=CARTESIAN_POINT('Ctrl Pts',(53.3305998175126,16.0991184002386,5.81808081885943));
#68613=CARTESIAN_POINT('Ctrl Pts',(51.8491110494184,15.4496200568245,5.89658632923621));
#68614=CARTESIAN_POINT('Ctrl Pts',(51.5770128796691,13.8534505046598,5.97509183961299));
#68615=CARTESIAN_POINT('Ctrl Pts',(52.359900444268,13.11933387906,6.02742884653084));
#68616=CARTESIAN_POINT('Ctrl Pts',(52.8205983740735,12.9961697745651,6.05359734998977));
#68617=CARTESIAN_POINT('Ctrl Pts',(52.0259993620635,15.4040955891549,1.83920795003069));
#68618=CARTESIAN_POINT('Ctrl Pts',(51.6948674713958,15.0196330720529,1.86537645348961));
#68619=CARTESIAN_POINT('Ctrl Pts',(51.4467955610913,13.9049616963147,1.91771346040747));
#68620=CARTESIAN_POINT('Ctrl Pts',(52.6429121889126,12.6649957863917,1.99621897078425));
#68621=CARTESIAN_POINT('Ctrl Pts',(54.3345828261004,12.9822409438244,2.07472448116103));
#68622=CARTESIAN_POINT('Ctrl Pts',(55.0042032764809,14.5665547803503,2.15322999153781));
#68623=CARTESIAN_POINT('Ctrl Pts',(54.0514939360652,15.9998439808924,2.23173550191458));
#68624=CARTESIAN_POINT('Ctrl Pts',(52.3307400382945,15.9953304824803,2.31024101229137));
#68625=CARTESIAN_POINT('Ctrl Pts',(51.3852180733224,14.5577448223715,2.38874652266814));
#68626=CARTESIAN_POINT('Ctrl Pts',(52.0628629644955,12.9760077060224,2.46725203304493));
#68627=CARTESIAN_POINT('Ctrl Pts',(53.7559624418889,12.6688282037076,2.5457575434217));
#68628=CARTESIAN_POINT('Ctrl Pts',(54.9460967779827,13.9116076465207,2.62426305379849));
#68629=CARTESIAN_POINT('Ctrl Pts',(54.5659291267794,15.5898340293922,2.70276856417526));
#68630=CARTESIAN_POINT('Ctrl Pts',(52.9564009216582,16.198413027115,2.78127407455204));
#68631=CARTESIAN_POINT('Ctrl Pts',(51.5609762954032,15.1915669978344,2.85977958492882));
#68632=CARTESIAN_POINT('Ctrl Pts',(51.6311047416152,13.472254177388,2.9382850953056));
#68633=CARTESIAN_POINT('Ctrl Pts',(53.1038936445493,12.5823977792548,3.01679060568238));
#68634=CARTESIAN_POINT('Ctrl Pts',(54.6585107818612,13.3200408795168,3.09529611605916));
#68635=CARTESIAN_POINT('Ctrl Pts',(54.9007386060379,15.0236482558482,3.17380162643594));
#68636=CARTESIAN_POINT('Ctrl Pts',(53.6133414157458,16.1653839899769,3.25230713681272));
#68637=CARTESIAN_POINT('Ctrl Pts',(51.9508876322963,15.7213124929433,3.3308126471895));
#68638=CARTESIAN_POINT('Ctrl Pts',(51.4043053238161,14.0896875604189,3.40931815756628));
#68639=CARTESIAN_POINT('Ctrl Pts',(52.4637825025118,12.7337892614639,3.48782366794306));
#68640=CARTESIAN_POINT('Ctrl Pts',(54.1791548450535,12.8696194053218,3.56632917831983));
#68641=CARTESIAN_POINT('Ctrl Pts',(55.0120356549231,14.3753622997269,3.64483468869662));
#68642=CARTESIAN_POINT('Ctrl Pts',(54.215477620774,15.9006319150314,3.72334019907339));
#68643=CARTESIAN_POINT('Ctrl Pts',(52.5038529249194,16.0775302015138,3.80184570945018));
#68644=CARTESIAN_POINT('Ctrl Pts',(51.4121872860838,14.7474105690538,3.88035121982695));
#68645=CARTESIAN_POINT('Ctrl Pts',(51.9195124019995,13.1031559265556,3.95885673020373));
#68646=CARTESIAN_POINT('Ctrl Pts',(53.5708470479161,12.6193729267869,4.03736224058052));
#68647=CARTESIAN_POINT('Ctrl Pts',(54.8852350547637,13.7299296658483,4.11586775095729));
#68648=CARTESIAN_POINT('Ctrl Pts',(54.6839020109947,15.4388524571485,4.19437326133407));
#68649=CARTESIAN_POINT('Ctrl Pts',(53.147408175106,16.2135387160798,4.27287877171085));
#68650=CARTESIAN_POINT('Ctrl Pts',(51.6537177503359,15.3592313846778,4.35138428208763));
#68651=CARTESIAN_POINT('Ctrl Pts',(51.5424078137269,13.6420935954197,4.42988979246441));
#68652=CARTESIAN_POINT('Ctrl Pts',(52.9133037754092,12.6020953249299,4.50839530284119));
#68653=CARTESIAN_POINT('Ctrl Pts',(54.5369535202073,13.171931777608,4.58690081321797));
#68654=CARTESIAN_POINT('Ctrl Pts',(54.9572294081871,14.8405600136574,4.66540632359475));
#68655=CARTESIAN_POINT('Ctrl Pts',(53.7972179286764,16.1115146859015,4.74391183397153));
#68656=CARTESIAN_POINT('Ctrl Pts',(52.0972451605188,15.8449731797319,4.82241734434831));
#68657=CARTESIAN_POINT('Ctrl Pts',(51.3818866828157,14.2799767547255,4.90092285472509));
#68658=CARTESIAN_POINT('Ctrl Pts',(52.2926938154427,12.820050407037,4.97942836510186));
#68659=CARTESIAN_POINT('Ctrl Pts',(54.0128314027411,12.7744928061304,5.05793387547865));
#68660=CARTESIAN_POINT('Ctrl Pts',(54.9996425046093,14.1841570529565,5.13643938585542));
#68661=CARTESIAN_POINT('Ctrl Pts',(54.368124759941,15.7848308402587,5.21494489623221));
#68662=CARTESIAN_POINT('Ctrl Pts',(52.6846517467245,16.1409756074537,5.29345040660899));
#68663=CARTESIAN_POINT('Ctrl Pts',(51.4589751002972,14.933224869348,5.37195591698576));
#68664=CARTESIAN_POINT('Ctrl Pts',(51.7903649128864,13.2446527814935,5.45046142736255));
#68665=CARTESIAN_POINT('Ctrl Pts',(53.3815143142557,12.5897421777335,5.52896693773932));
#68666=CARTESIAN_POINT('Ctrl Pts',(54.8056605807673,13.5555691601388,5.60747244811611));
#68667=CARTESIAN_POINT('Ctrl Pts',(54.7851583544017,15.2764853923884,5.68597795849288));
#68668=CARTESIAN_POINT('Ctrl Pts',(53.3392716219708,16.2080719085829,5.76448346886966));
#68669=CARTESIAN_POINT('Ctrl Pts',(51.7629444164752,15.5169955192796,5.84298897924645));
#68670=CARTESIAN_POINT('Ctrl Pts',(51.4734277108623,13.8186461670281,5.92149448962322));
#68671=CARTESIAN_POINT('Ctrl Pts',(52.3064323164313,13.0375346028627,5.97383149654107));
#68672=CARTESIAN_POINT('Ctrl Pts',(52.7966221146314,12.9064860705774,6.));
#68673=CARTESIAN_POINT('Ctrl Pts',(52.2370198037663,15.2223467977324,2.));
#68674=CARTESIAN_POINT('Ctrl Pts',(52.2001398221828,15.1879057962806,2.));
#68675=CARTESIAN_POINT('Ctrl Pts',(52.1656378013754,15.151226274978,2.));
#68676=CARTESIAN_POINT('Ctrl Pts',(52.1335158959969,15.112628111498,2.));
#68677=CARTESIAN_POINT('Ctrl Pts',(52.0999545216909,15.0723002605561,2.));
#68678=CARTESIAN_POINT('Ctrl Pts',(52.0689907405515,15.0298774985354,2.));
#68679=CARTESIAN_POINT('Ctrl Pts',(52.0406550241375,14.9856749556985,2.));
#68680=CARTESIAN_POINT('Ctrl Pts',(52.0179305604288,14.9502257344452,2.));
#68681=CARTESIAN_POINT('Ctrl Pts',(51.996896813921,14.9136306734541,2.));
#68682=CARTESIAN_POINT('Ctrl Pts',(51.9775857407062,14.8760343811028,2.));
#68683=CARTESIAN_POINT('Ctrl Pts',(51.9694199887415,14.8601366630052,2.));
#68684=CARTESIAN_POINT('Ctrl Pts',(51.9615624516275,14.8440597542843,2.));
#68685=CARTESIAN_POINT('Ctrl Pts',(51.9540164358694,14.8278139468967,2.));
#68686=CARTESIAN_POINT('Ctrl Pts',(51.949738091225,14.8186031043464,2.));
#68687=CARTESIAN_POINT('Ctrl Pts',(51.9455597069868,14.8093372706419,2.));
#68688=CARTESIAN_POINT('Ctrl Pts',(51.9414881758679,14.8000332484628,2.));
#68689=CARTESIAN_POINT('Ctrl Pts',(51.9196632025192,14.7501601097928,2.));
#68690=CARTESIAN_POINT('Ctrl Pts',(51.9008587821431,14.6990941700718,2.));
#68691=CARTESIAN_POINT('Ctrl Pts',(51.8851025499004,14.6471668919071,2.));
#68692=CARTESIAN_POINT('Ctrl Pts',(51.8690578813861,14.594289024142,2.));
#68693=CARTESIAN_POINT('Ctrl Pts',(51.8561734275543,14.5405170692708,2.));
#68694=CARTESIAN_POINT('Ctrl Pts',(51.8465190610403,14.486166435836,2.));
#68695=CARTESIAN_POINT('Ctrl Pts',(51.8396145127802,14.4472962965087,2.));
#68696=CARTESIAN_POINT('Ctrl Pts',(51.8343629002769,14.4081294056505,2.));
#68697=CARTESIAN_POINT('Ctrl Pts',(51.8308047851301,14.3687747569505,2.));
#68698=CARTESIAN_POINT('Ctrl Pts',(51.8292917204563,14.3520394557475,2.));
#68699=CARTESIAN_POINT('Ctrl Pts',(51.8280850589952,14.3352701585883,2.));
#68700=CARTESIAN_POINT('Ctrl Pts',(51.8271886807074,14.3184751149596,2.));
#68701=CARTESIAN_POINT('Ctrl Pts',(51.8266545203237,14.308466788039,2.));
#68702=CARTESIAN_POINT('Ctrl Pts',(51.8262309124747,14.2984549962446,2.));
#68703=CARTESIAN_POINT('Ctrl Pts',(51.8259184499979,14.288449081502,2.));
#68704=CARTESIAN_POINT('Ctrl Pts',(51.824144879443,14.2316544354973,2.));
#68705=CARTESIAN_POINT('Ctrl Pts',(51.8259444031715,14.1749772815937,2.));
#68706=CARTESIAN_POINT('Ctrl Pts',(51.8313770542921,14.1187497413728,2.));
#68707=CARTESIAN_POINT('Ctrl Pts',(51.8347120697962,14.084232575769,2.));
#68708=CARTESIAN_POINT('Ctrl Pts',(51.8394171165415,14.0498843036968,2.));
#68709=CARTESIAN_POINT('Ctrl Pts',(51.845515342272,14.0157787106909,2.));
#68710=CARTESIAN_POINT('Ctrl Pts',(51.8551874830705,13.961685255947,2.));
#68711=CARTESIAN_POINT('Ctrl Pts',(51.8683614486687,13.908201794507,2.));
#68712=CARTESIAN_POINT('Ctrl Pts',(51.8848110251023,13.8555328884195,2.));
#68713=CARTESIAN_POINT('Ctrl Pts',(51.8897327932487,13.8397741760092,2.));
#68714=CARTESIAN_POINT('Ctrl Pts',(51.89494815524,13.8240884170169,2.));
#68715=CARTESIAN_POINT('Ctrl Pts',(51.9004519259219,13.8084812249402,2.));
#68716=CARTESIAN_POINT('Ctrl Pts',(51.9055403383179,13.7940518756411,2.));
#68717=CARTESIAN_POINT('Ctrl Pts',(51.9108779029635,13.7796834481737,2.));
#68718=CARTESIAN_POINT('Ctrl Pts',(51.9164469096144,13.7654145762709,2.));
#68719=CARTESIAN_POINT('Ctrl Pts',(51.9370780110834,13.7125537049294,2.));
#68720=CARTESIAN_POINT('Ctrl Pts',(51.9609027535646,13.6609889336899,2.));
#68721=CARTESIAN_POINT('Ctrl Pts',(51.9876380075304,13.6109308617546,2.));
#68722=CARTESIAN_POINT('Ctrl Pts',(52.0150055546563,13.5596889081725,2.));
#68723=CARTESIAN_POINT('Ctrl Pts',(52.045423253279,13.5100248567638,2.));
#68724=CARTESIAN_POINT('Ctrl Pts',(52.0786427430285,13.4621702328152,2.));
#68725=CARTESIAN_POINT('Ctrl Pts',(52.0988112436273,13.4331163244306,2.));
#68726=CARTESIAN_POINT('Ctrl Pts',(52.120013548353,13.4047295468198,2.));
#68727=CARTESIAN_POINT('Ctrl Pts',(52.1422027768495,13.3770649262704,2.));
#68728=CARTESIAN_POINT('Ctrl Pts',(52.1544198936821,13.3618331257853,2.));
#68729=CARTESIAN_POINT('Ctrl Pts',(52.1669363024278,13.3468202983598,2.));
#68730=CARTESIAN_POINT('Ctrl Pts',(52.179744929617,13.3320361041125,2.));
#68731=CARTESIAN_POINT('Ctrl Pts',(52.1874577031776,13.3231337337943,2.));
#68732=CARTESIAN_POINT('Ctrl Pts',(52.1952777965343,13.3143127818621,2.));
#68733=CARTESIAN_POINT('Ctrl Pts',(52.2031994409785,13.305580167691,2.));
#68734=CARTESIAN_POINT('Ctrl Pts',(52.2437953927624,13.260828249534,2.));
#68735=CARTESIAN_POINT('Ctrl Pts',(52.2869270094075,13.2185332555424,2.));
#68736=CARTESIAN_POINT('Ctrl Pts',(52.3323340644797,13.1789459514192,2.));
#68737=CARTESIAN_POINT('Ctrl Pts',(52.361857692103,13.1532063207894,2.));
#68738=CARTESIAN_POINT('Ctrl Pts',(52.3923443514829,13.1286116909656,2.));
#68739=CARTESIAN_POINT('Ctrl Pts',(52.4237326847812,13.1052370160116,2.));
#68740=CARTESIAN_POINT('Ctrl Pts',(52.4367029257511,13.0955781671691,2.));
#68741=CARTESIAN_POINT('Ctrl Pts',(52.4498272129069,13.086127694501,2.));
#68742=CARTESIAN_POINT('Ctrl Pts',(52.463101559564,13.0768912104406,2.));
#68743=CARTESIAN_POINT('Ctrl Pts',(52.4728212298238,13.0701281220758,2.));
#68744=CARTESIAN_POINT('Ctrl Pts',(52.4826204710268,13.0634804790307,2.));
#68745=CARTESIAN_POINT('Ctrl Pts',(52.4924892033939,13.0569558444863,2.));
#68746=CARTESIAN_POINT('Ctrl Pts',(52.5432262965278,13.0234114156552,2.));
#68747=CARTESIAN_POINT('Ctrl Pts',(52.5958554391195,12.993074592538,2.));
#68748=CARTESIAN_POINT('Ctrl Pts',(52.6501404639279,12.966212166386,2.));
#68749=CARTESIAN_POINT('Ctrl Pts',(52.6755695106503,12.9536288454405,2.));
#68750=CARTESIAN_POINT('Ctrl Pts',(52.7013624782246,12.9418083828109,2.));
#68751=CARTESIAN_POINT('Ctrl Pts',(52.7274977743507,12.930781120438,2.));
#68752=CARTESIAN_POINT('Ctrl Pts',(52.7499504413758,12.9213076693218,2.));
#68753=CARTESIAN_POINT('Ctrl Pts',(52.7726557928972,12.9124196555961,2.));
#68754=CARTESIAN_POINT('Ctrl Pts',(52.7955926848293,12.9041113294173,2.));
#68755=CARTESIAN_POINT('Ctrl Pts',(54.4591686783466,14.3960664985434,2.80658032638058));
#68756=CARTESIAN_POINT('Ctrl Pts',(54.4601242407418,14.2819704202925,2.79940525217632));
#68757=CARTESIAN_POINT('Ctrl Pts',(54.4459154362348,14.1681081402059,2.79223017797205));
#68758=CARTESIAN_POINT('Ctrl Pts',(54.4155823692925,14.0587171406723,2.78505510376779));
#68759=CARTESIAN_POINT('Ctrl Pts',(54.3049534134658,13.6597527999315,2.75888660030886));
#68760=CARTESIAN_POINT('Ctrl Pts',(53.9798454272937,13.3202637946524,2.73271809684994));
#68761=CARTESIAN_POINT('Ctrl Pts',(53.5860401608047,13.1924752739395,2.70654959339101));
#68762=CARTESIAN_POINT('Ctrl Pts',(53.1922348943158,13.0646867532265,2.68038108993208));
#68763=CARTESIAN_POINT('Ctrl Pts',(52.72973234751,13.1485987170799,2.65421258647316));
#68764=CARTESIAN_POINT('Ctrl Pts',(52.405925234305,13.4065955915993,2.62804408301423));
#68765=CARTESIAN_POINT('Ctrl Pts',(52.0821181210999,13.6645924661187,2.6018755795553));
#68766=CARTESIAN_POINT('Ctrl Pts',(51.8970064414957,14.0966742513041,2.57570707609638));
#68767=CARTESIAN_POINT('Ctrl Pts',(51.9335943179073,14.509067171031,2.54953857263745));
#68768=CARTESIAN_POINT('Ctrl Pts',(51.9701821943189,14.9214600907578,2.52337006917852));
#68769=CARTESIAN_POINT('Ctrl Pts',(52.2284696267464,15.314164145026,2.4972015657196));
#68770=CARTESIAN_POINT('Ctrl Pts',(52.5926417836311,15.5111326464248,2.47103306226067));
#68771=CARTESIAN_POINT('Ctrl Pts',(52.9568139405157,15.7081011478236,2.44486455880174));
#68772=CARTESIAN_POINT('Ctrl Pts',(53.4268708218575,15.7093340963528,2.41869605534282));
#68773=CARTESIAN_POINT('Ctrl Pts',(53.7920246633662,15.5141853735895,2.39252755188389));
#68774=CARTESIAN_POINT('Ctrl Pts',(54.1571785048748,15.3190366508261,2.36635904842496));
#68775=CARTESIAN_POINT('Ctrl Pts',(54.4174293065502,14.92750625677,2.34019054496604));
#68776=CARTESIAN_POINT('Ctrl Pts',(54.456094882425,14.5153482269177,2.31402204150711));
#68777=CARTESIAN_POINT('Ctrl Pts',(54.4597600799313,14.4762788338196,2.31154146979827));
#68778=CARTESIAN_POINT('Ctrl Pts',(54.461434207113,14.4370240895848,2.30906089808942));
#68779=CARTESIAN_POINT('Ctrl Pts',(54.4611870990995,14.3977489718831,2.30658032638058));
#68780=CARTESIAN_POINT('Ctrl Pts',(53.5936497983459,12.9064860705774,2.));
#68781=CARTESIAN_POINT('Ctrl Pts',(54.083839596546,13.0375346028627,2.02616850345893));
#68782=CARTESIAN_POINT('Ctrl Pts',(54.9168437793101,13.8186488783651,2.07850551037678));
#68783=CARTESIAN_POINT('Ctrl Pts',(54.6273278627067,15.5169944524465,2.15701102075356));
#68784=CARTESIAN_POINT('Ctrl Pts',(53.0510002557363,16.2080728204287,2.23551653113034));
#68785=CARTESIAN_POINT('Ctrl Pts',(51.605113325188,15.2764851170283,2.31402204150712));
#68786=CARTESIAN_POINT('Ctrl Pts',(51.5846111642588,13.5555692706413,2.3925275518839));
#68787=CARTESIAN_POINT('Ctrl Pts',(53.0087575469087,12.5897418281553,2.47103306226068));
#68788=CARTESIAN_POINT('Ctrl Pts',(54.5999071972633,13.244652701567,2.54953857263746));
#68789=CARTESIAN_POINT('Ctrl Pts',(54.9312970207009,14.9332249012822,2.62804408301423));
#68790=CARTESIAN_POINT('Ctrl Pts',(53.7056202382209,16.1409758479641,2.70654959339102));
#68791=CARTESIAN_POINT('Ctrl Pts',(52.0221470001078,15.7848310056966,2.78505510376779));
#68792=CARTESIAN_POINT('Ctrl Pts',(51.3906291820654,14.1841570315506,2.86356061414457));
#68793=CARTESIAN_POINT('Ctrl Pts',(52.3774404052229,12.7744925974775,2.94206612452135));
#68794=CARTESIAN_POINT('Ctrl Pts',(54.0975782126823,12.8200502087089,3.02057163489813));
#68795=CARTESIAN_POINT('Ctrl Pts',(55.0083854595842,14.2799767390429,3.09907714527492));
#68796=CARTESIAN_POINT('Ctrl Pts',(54.293026891849,15.8449733636912,3.17758265565169));
#68797=CARTESIAN_POINT('Ctrl Pts',(52.5930539078611,16.1115149029784,3.25608816602847));
#68798=CARTESIAN_POINT('Ctrl Pts',(51.4330422815012,14.8405600699842,3.33459367640525));
#68799=CARTESIAN_POINT('Ctrl Pts',(51.8533182226522,13.1719316222439,3.41309918678203));
#68800=CARTESIAN_POINT('Ctrl Pts',(53.4769681733105,12.6020950974316,3.49160469715881));
#68801=CARTESIAN_POINT('Ctrl Pts',(54.8478643087328,13.642093499697,3.57011020753559));
#68802=CARTESIAN_POINT('Ctrl Pts',(54.7365543580298,15.3592315066375,3.64861571791237));
#68803=CARTESIAN_POINT('Ctrl Pts',(53.2428637439183,16.2135389463141,3.72712122828915));
#68804=CARTESIAN_POINT('Ctrl Pts',(51.7063697132749,15.4388525891942,3.80562673866593));
#68805=CARTESIAN_POINT('Ctrl Pts',(51.5050366439836,13.7299295812751,3.88413224904271));
#68806=CARTESIAN_POINT('Ctrl Pts',(52.8194248174382,12.6193727014466,3.96263775941949));
#68807=CARTESIAN_POINT('Ctrl Pts',(54.4707596726698,13.1031557625362,4.04114326979626));
#68808=CARTESIAN_POINT('Ctrl Pts',(54.978084852892,14.7474106134536,4.11964878017304));
#68809=CARTESIAN_POINT('Ctrl Pts',(53.8864190756817,16.077530414512,4.19815429054983));
#68810=CARTESIAN_POINT('Ctrl Pts',(52.1747941628695,15.9006321056092,4.2766598009266));
#68811=CARTESIAN_POINT('Ctrl Pts',(51.3782360277522,14.3753622969642,4.35516531130339));
#68812=CARTESIAN_POINT('Ctrl Pts',(52.2111169431944,12.8696192117062,4.43367082168016));
#68813=CARTESIAN_POINT('Ctrl Pts',(53.9264895031678,12.7337890506155,4.51217633205695));
#68814=CARTESIAN_POINT('Ctrl Pts',(54.9859668161601,14.0896875214679,4.59068184243372));
#68815=CARTESIAN_POINT('Ctrl Pts',(54.4393844383933,15.7213126607523,4.6691873528105));
#68816=CARTESIAN_POINT('Ctrl Pts',(52.7769304442279,16.1653842141838,4.74769286318728));
#68817=CARTESIAN_POINT('Ctrl Pts',(51.4895330907317,15.0236483351255,4.82619837356406));
#68818=CARTESIAN_POINT('Ctrl Pts',(51.7317609456535,13.3200407432483,4.90470388394085));
#68819=CARTESIAN_POINT('Ctrl Pts',(53.2863782799342,12.5823975487372,4.98320939431761));
#68820=CARTESIAN_POINT('Ctrl Pts',(54.7591673697362,13.4722540610765,5.06171490469441));
#68821=CARTESIAN_POINT('Ctrl Pts',(54.8292958244512,15.1915670968036,5.14022041507117));
#68822=CARTESIAN_POINT('Ctrl Pts',(53.4338710221273,16.1984132586634,5.21872592544796));
#68823=CARTESIAN_POINT('Ctrl Pts',(51.8243426112988,15.5898341745865,5.29723143582474));
#68824=CARTESIAN_POINT('Ctrl Pts',(51.4441749154368,13.9116075960113,5.37573694620152));
#68825=CARTESIAN_POINT('Ctrl Pts',(52.6343093950298,12.6688279644592,5.45424245657829));
#68826=CARTESIAN_POINT('Ctrl Pts',(54.3274091023452,12.976007562431,5.53274796695508));
#68827=CARTESIAN_POINT('Ctrl Pts',(55.0050540475836,14.5577447773064,5.61125347733185));
#68828=CARTESIAN_POINT('Ctrl Pts',(54.0595320288467,15.9953308004787,5.68975898770864));
#68829=CARTESIAN_POINT('Ctrl Pts',(52.3387777758966,15.9998439842325,5.76826449808541));
#68830=CARTESIAN_POINT('Ctrl Pts',(51.386068598834,14.5665551393412,5.8467700084622));
#68831=CARTESIAN_POINT('Ctrl Pts',(52.0556885439603,12.9822402103747,5.92527551883896));
#68832=CARTESIAN_POINT('Ctrl Pts',(53.7473606277103,12.6649964614199,6.00378102921576));
#68833=CARTESIAN_POINT('Ctrl Pts',(54.9434744748871,13.9049596945687,6.08228653959253));
#68834=CARTESIAN_POINT('Ctrl Pts',(54.6954044415815,15.0196330720529,6.13462354651039));
#68835=CARTESIAN_POINT('Ctrl Pts',(54.3642725509138,15.404095589155,6.16079204996931));
#68836=CARTESIAN_POINT('Ctrl Pts',(53.5696735389038,12.996169774565,1.94640265001023));
#68837=CARTESIAN_POINT('Ctrl Pts',(54.0303714687093,13.11933387906,1.97257115346916));
#68838=CARTESIAN_POINT('Ctrl Pts',(54.813258635941,13.8534530528714,2.02490816038701));
#68839=CARTESIAN_POINT('Ctrl Pts',(54.5411612077311,15.4496190541765,2.10341367076379));
#68840=CARTESIAN_POINT('Ctrl Pts',(53.0596720623164,16.099119257224,2.18191918114057));
#68841=CARTESIAN_POINT('Ctrl Pts',(51.7007757366845,15.2235797662663,2.26042469151735));
#68842=CARTESIAN_POINT('Ctrl Pts',(51.6815070715035,13.6062014146337,2.33893020189412));
#68843=CARTESIAN_POINT('Ctrl Pts',(53.0199708515249,12.6984821904957,2.41743571227091));
#68844=CARTESIAN_POINT('Ctrl Pts',(54.515390284203,13.3139908867102,2.49594122264768));
#68845=CARTESIAN_POINT('Ctrl Pts',(54.8268423098815,14.9009715207264,2.57444673302447));
#68846=CARTESIAN_POINT('Ctrl Pts',(53.6749073688187,16.0360591192445,2.65295224340125));
#68847=CARTESIAN_POINT('Ctrl Pts',(52.0927189215492,15.7013414402026,2.73145775377802));
#68848=CARTESIAN_POINT('Ctrl Pts',(51.4991958566553,14.1969707068861,2.8099632641548));
#68849=CARTESIAN_POINT('Ctrl Pts',(52.4266363894587,12.8721175808469,2.88846877453159));
#68850=CARTESIAN_POINT('Ctrl Pts',(54.0432835122395,12.9149342556498,2.96697428490836));
#68851=CARTESIAN_POINT('Ctrl Pts',(54.8992927858723,14.2870255000261,3.04547979528514));
#68852=CARTESIAN_POINT('Ctrl Pts',(54.2269731814369,15.7578653824051,3.12398530566192));
#68853=CARTESIAN_POINT('Ctrl Pts',(52.6292776820116,16.0083706679245,3.2024908160387));
#68854=CARTESIAN_POINT('Ctrl Pts',(51.5390572066436,14.8138817932341,3.28099632641548));
#68855=CARTESIAN_POINT('Ctrl Pts',(51.9340475894427,13.2456450116627,3.35950183679226));
#68856=CARTESIAN_POINT('Ctrl Pts',(53.4600119684315,12.7100922354268,3.43800734716904));
#68857=CARTESIAN_POINT('Ctrl Pts',(54.7484292588084,13.6875199841967,3.51651285754582));
#68858=CARTESIAN_POINT('Ctrl Pts',(54.6438161802745,15.3013477870039,3.5950183679226));
#68859=CARTESIAN_POINT('Ctrl Pts',(53.2399922406132,16.104256518115,3.67352387829938));
#68860=CARTESIAN_POINT('Ctrl Pts',(51.7959401169765,15.3761785322324,3.75202938867615));
#68861=CARTESIAN_POINT('Ctrl Pts',(51.606720087175,13.7700714797477,3.83053489905294));
#68862=CARTESIAN_POINT('Ctrl Pts',(52.8420291709109,12.7263303465236,3.90904040942971));
#68863=CARTESIAN_POINT('Ctrl Pts',(54.3940128148265,13.1810069953183,3.9875459198065));
#68864=CARTESIAN_POINT('Ctrl Pts',(54.8708151904059,14.7263365975901,4.06605143018327));
#68865=CARTESIAN_POINT('Ctrl Pts',(53.8448285920578,15.9764308284185,4.14455694056006));
#68866=CARTESIAN_POINT('Ctrl Pts',(52.2361821925785,15.8101754616261,4.22306245093683));
#68867=CARTESIAN_POINT('Ctrl Pts',(51.4875483263378,14.3766722638491,4.30156796131361));
#68868=CARTESIAN_POINT('Ctrl Pts',(52.2703196425253,12.9615209801128,4.38007347169039));
#68869=CARTESIAN_POINT('Ctrl Pts',(53.8824882150385,12.8338629295998,4.45857898206717));
#68870=CARTESIAN_POINT('Ctrl Pts',(54.8782229417988,14.1081848776325,4.53708449244395));
#68871=CARTESIAN_POINT('Ctrl Pts',(54.3645252458656,15.6416446245447,4.61559000282073));
#68872=CARTESIAN_POINT('Ctrl Pts',(52.8020914369185,16.0589989760686,4.69409551319751));
#68873=CARTESIAN_POINT('Ctrl Pts',(51.5921492925276,14.9859547026092,4.77260102357429));
#68874=CARTESIAN_POINT('Ctrl Pts',(51.8198037066208,13.3848432685065,4.85110653395107));
#68875=CARTESIAN_POINT('Ctrl Pts',(53.2808887601503,12.6915797736435,4.92961204432785));
#68876=CARTESIAN_POINT('Ctrl Pts',(54.6650686986216,13.527898796528,5.00811755470463));
#68877=CARTESIAN_POINT('Ctrl Pts',(54.7309779322007,15.1437707692933,5.08662306508141));
#68878=CARTESIAN_POINT('Ctrl Pts',(53.41950772211,16.0900408550939,5.16512857545819));
#68879=CARTESIAN_POINT('Ctrl Pts',(51.9068152720538,15.5180764339929,5.24363408583497));
#68880=CARTESIAN_POINT('Ctrl Pts',(51.5495200547613,13.9408189852801,5.32213959621175));
#68881=CARTESIAN_POINT('Ctrl Pts',(52.6680510665282,12.7728101740752,5.40064510658852));
#68882=CARTESIAN_POINT('Ctrl Pts',(54.2592868143519,13.061508562707,5.47915061696532));
#68883=CARTESIAN_POINT('Ctrl Pts',(54.8961618055507,14.5480818513904,5.55765612734208));
#68884=CARTESIAN_POINT('Ctrl Pts',(54.0075263459451,15.8991766869513,5.63616163771887));
#68885=CARTESIAN_POINT('Ctrl Pts',(52.3902998656124,15.9034183386948,5.71466714809564));
#68886=CARTESIAN_POINT('Ctrl Pts',(51.4949096571851,14.5563621451974,5.79317265847243));
#68887=CARTESIAN_POINT('Ctrl Pts',(52.1242424658418,13.0673662284834,5.8716781688492));
#68888=CARTESIAN_POINT('Ctrl Pts',(53.7141364819045,12.7692091902835,5.95018367922599));
#68889=CARTESIAN_POINT('Ctrl Pts',(54.8382871174936,13.9345710493921,6.02868918960276));
#68890=CARTESIAN_POINT('Ctrl Pts',(54.6051420149022,14.9821810145562,6.08102619652062));
#68891=CARTESIAN_POINT('Ctrl Pts',(54.2939324036795,15.3435126586808,6.10719469997954));
#68892=CARTESIAN_POINT('Ctrl Pts',(53.5456972794618,13.0858534785527,1.89280530002046));
#68893=CARTESIAN_POINT('Ctrl Pts',(53.9769033408726,13.2011331552573,1.91897380347939));
#68894=CARTESIAN_POINT('Ctrl Pts',(54.7096734925719,13.8882572273778,1.97131081039724));
#68895=CARTESIAN_POINT('Ctrl Pts',(54.4549945527556,15.3822436559065,2.04981632077402));
#68896=CARTESIAN_POINT('Ctrl Pts',(53.0683438688966,15.9901656940193,2.1283218311508));
#68897=CARTESIAN_POINT('Ctrl Pts',(51.7964381481809,15.1706744155041,2.20682734152758));
#68898=CARTESIAN_POINT('Ctrl Pts',(51.7784029787483,13.6568335586262,2.28533285190436));
#68899=CARTESIAN_POINT('Ctrl Pts',(53.0311841561409,12.807222552836,2.36383836228114));
#68900=CARTESIAN_POINT('Ctrl Pts',(54.4308733711429,13.3833290718535,2.44234387265792));
#68901=CARTESIAN_POINT('Ctrl Pts',(54.722387599062,14.8687181401707,2.5208493830347));
#68902=CARTESIAN_POINT('Ctrl Pts',(53.6441944994167,15.9311423905248,2.59935489341147));
#68903=CARTESIAN_POINT('Ctrl Pts',(52.1632908429905,15.6178518747085,2.67786040378825));
#68904=CARTESIAN_POINT('Ctrl Pts',(51.6077625312453,14.2097843822215,2.75636591416503));
#68905=CARTESIAN_POINT('Ctrl Pts',(52.4758323736945,12.9697425642164,2.83487142454181));
#68906=CARTESIAN_POINT('Ctrl Pts',(53.9889888117966,13.0098183025906,2.91337693491859));
#68907=CARTESIAN_POINT('Ctrl Pts',(54.7902001121604,14.2940742610093,2.99188244529538));
#68908=CARTESIAN_POINT('Ctrl Pts',(54.1609194710247,15.670757401119,3.07038795567215));
#68909=CARTESIAN_POINT('Ctrl Pts',(52.6655014561621,15.9052264328705,3.14889346604893));
#68910=CARTESIAN_POINT('Ctrl Pts',(51.645072131786,14.7872035164841,3.22739897642571));
#68911=CARTESIAN_POINT('Ctrl Pts',(52.0147769562332,13.3193584010816,3.30590448680249));
#68912=CARTESIAN_POINT('Ctrl Pts',(53.4430557635525,12.818089373422,3.38440999717927));
#68913=CARTESIAN_POINT('Ctrl Pts',(54.648994208884,13.7329464686964,3.46291550755605));
#68914=CARTESIAN_POINT('Ctrl Pts',(54.5510780025192,15.2434640673703,3.54142101793283));
#68915=CARTESIAN_POINT('Ctrl Pts',(53.2371207373081,15.9949740899159,3.61992652830961));
#68916=CARTESIAN_POINT('Ctrl Pts',(51.8855105206782,15.3135044752707,3.69843203868638));
#68917=CARTESIAN_POINT('Ctrl Pts',(51.7084035303663,13.8102133782203,3.77693754906317));
#68918=CARTESIAN_POINT('Ctrl Pts',(52.8646335243838,12.8332879916007,3.85544305943994));
#68919=CARTESIAN_POINT('Ctrl Pts',(54.3172659569832,13.2588582281004,3.93394856981673));
#68920=CARTESIAN_POINT('Ctrl Pts',(54.7635455279197,14.7052625817266,4.0124540801935));
#68921=CARTESIAN_POINT('Ctrl Pts',(53.8032381084338,15.875331242325,4.09095959057029));
#68922=CARTESIAN_POINT('Ctrl Pts',(52.2975702222875,15.7197188176431,4.16946510094706));
#68923=CARTESIAN_POINT('Ctrl Pts',(51.5968606249235,14.377982230734,4.24797061132384));
#68924=CARTESIAN_POINT('Ctrl Pts',(52.329522341856,13.0534227485195,4.32647612170062));
#68925=CARTESIAN_POINT('Ctrl Pts',(53.8384869269094,12.9339368085841,4.4049816320774));
#68926=CARTESIAN_POINT('Ctrl Pts',(54.7704790674375,14.1266822337971,4.48348714245418));
#68927=CARTESIAN_POINT('Ctrl Pts',(54.289666053338,15.5619765883372,4.56199265283096));
#68928=CARTESIAN_POINT('Ctrl Pts',(52.8272524296091,15.9526137379533,4.64049816320774));
#68929=CARTESIAN_POINT('Ctrl Pts',(51.6947654943235,14.9482610700929,4.71900367358452));
#68930=CARTESIAN_POINT('Ctrl Pts',(51.9078464675881,13.4496457937646,4.7975091839613));
#68931=CARTESIAN_POINT('Ctrl Pts',(53.2753992403664,12.8007619985498,4.87601469433808));
#68932=CARTESIAN_POINT('Ctrl Pts',(54.5709700275071,13.5835435319795,4.95452020471486));
#68933=CARTESIAN_POINT('Ctrl Pts',(54.6326600399502,15.095974441783,5.03302571509164));
#68934=CARTESIAN_POINT('Ctrl Pts',(53.4051444220927,15.9816684515245,5.11153122546842));
#68935=CARTESIAN_POINT('Ctrl Pts',(51.9892879328089,15.4463186933993,5.19003673584519));
#68936=CARTESIAN_POINT('Ctrl Pts',(51.6548651940858,13.970030374549,5.26854224622198));
#68937=CARTESIAN_POINT('Ctrl Pts',(52.7017927380267,12.8767923836913,5.34704775659875));
#68938=CARTESIAN_POINT('Ctrl Pts',(54.1911645263585,13.147009562983,5.42555326697554));
#68939=CARTESIAN_POINT('Ctrl Pts',(54.7872695635179,14.5384189254744,5.50405877735231));
#68940=CARTESIAN_POINT('Ctrl Pts',(53.9555206630434,15.8030225734238,5.5825642877291));
#68941=CARTESIAN_POINT('Ctrl Pts',(52.4418219553284,15.806992693157,5.66106979810588));
#68942=CARTESIAN_POINT('Ctrl Pts',(51.603750715536,14.5461691510535,5.73957530848265));
#68943=CARTESIAN_POINT('Ctrl Pts',(52.1927963877232,13.1524922465921,5.81808081885944));
#68944=CARTESIAN_POINT('Ctrl Pts',(53.6809123360987,12.873421919147,5.89658632923621));
#68945=CARTESIAN_POINT('Ctrl Pts',(54.7330997601003,13.9641824042154,5.975091839613));
#68946=CARTESIAN_POINT('Ctrl Pts',(54.5148795882229,14.9447289570596,6.02742884653085));
#68947=CARTESIAN_POINT('Ctrl Pts',(54.2235922564453,15.2829297282066,6.05359734998977));
#68948=CARTESIAN_POINT('Ctrl Pts',(53.5217210200197,13.1755371825404,1.83920795003069));
#68949=CARTESIAN_POINT('Ctrl Pts',(53.923435213036,13.2829324314546,1.86537645348962));
#68950=CARTESIAN_POINT('Ctrl Pts',(54.6060883492027,13.9230614018842,1.91771346040747));
#68951=CARTESIAN_POINT('Ctrl Pts',(54.36882789778,15.3148682576366,1.99621897078425));
#68952=CARTESIAN_POINT('Ctrl Pts',(53.0770156754767,15.8812121308145,2.07472448116103));
#68953=CARTESIAN_POINT('Ctrl Pts',(51.8921005596774,15.117769064742,2.15322999153781));
#68954=CARTESIAN_POINT('Ctrl Pts',(51.8752988859931,13.7074657026187,2.23173550191459));
#68955=CARTESIAN_POINT('Ctrl Pts',(53.042397460757,12.9159629151763,2.31024101229137));
#68956=CARTESIAN_POINT('Ctrl Pts',(54.3463564580827,13.4526672569968,2.38874652266814));
#68957=CARTESIAN_POINT('Ctrl Pts',(54.6179328882426,14.836464759615,2.46725203304492));
#68958=CARTESIAN_POINT('Ctrl Pts',(53.6134816300145,15.8262256618051,2.5457575434217));
#68959=CARTESIAN_POINT('Ctrl Pts',(52.2338627644319,15.5343623092145,2.62426305379848));
#68960=CARTESIAN_POINT('Ctrl Pts',(51.7163292058352,14.222598057557,2.70276856417526));
#68961=CARTESIAN_POINT('Ctrl Pts',(52.5250283579303,13.0673675475858,2.78127407455204));
#68962=CARTESIAN_POINT('Ctrl Pts',(53.9346941113537,13.1047023495315,2.85977958492882));
#68963=CARTESIAN_POINT('Ctrl Pts',(54.6811074384486,14.3011230219925,2.9382850953056));
#68964=CARTESIAN_POINT('Ctrl Pts',(54.0948657606125,15.5836494198329,3.01679060568238));
#68965=CARTESIAN_POINT('Ctrl Pts',(52.7017252303127,15.8020821978165,3.09529611605916));
#68966=CARTESIAN_POINT('Ctrl Pts',(51.7510870569283,14.7605252397341,3.17380162643594));
#68967=CARTESIAN_POINT('Ctrl Pts',(52.0955063230238,13.3930717905004,3.25230713681272));
#68968=CARTESIAN_POINT('Ctrl Pts',(53.4260995586735,12.9260865114173,3.33081264718949));
#68969=CARTESIAN_POINT('Ctrl Pts',(54.5495591589596,13.7783729531961,3.40931815756628));
#68970=CARTESIAN_POINT('Ctrl Pts',(54.4583398247639,15.1855803477368,3.48782366794305));
#68971=CARTESIAN_POINT('Ctrl Pts',(53.234249234003,15.8856916617167,3.56632917831984));
#68972=CARTESIAN_POINT('Ctrl Pts',(51.97508092438,15.250830418309,3.64483468869661));
#68973=CARTESIAN_POINT('Ctrl Pts',(51.8100869735575,13.8503552766928,3.7233401990734));
#68974=CARTESIAN_POINT('Ctrl Pts',(52.8872378778566,12.9402456366778,3.80184570945017));
#68975=CARTESIAN_POINT('Ctrl Pts',(54.2405190991399,13.3367094608825,3.88035121982696));
#68976=CARTESIAN_POINT('Ctrl Pts',(54.6562758654336,14.6841885658631,3.95885673020373));
#68977=CARTESIAN_POINT('Ctrl Pts',(53.7616476248098,15.7742316562315,4.03736224058052));
#68978=CARTESIAN_POINT('Ctrl Pts',(52.3589582519966,15.62926217366,4.11586775095729));
#68979=CARTESIAN_POINT('Ctrl Pts',(51.7061729235091,14.3792921976189,4.19437326133407));
#68980=CARTESIAN_POINT('Ctrl Pts',(52.3887250411869,13.1453245169262,4.27287877171086));
#68981=CARTESIAN_POINT('Ctrl Pts',(53.7944856387802,13.0340106875684,4.35138428208763));
#68982=CARTESIAN_POINT('Ctrl Pts',(54.6627351930762,14.1451795899617,4.42988979246442));
#68983=CARTESIAN_POINT('Ctrl Pts',(54.2148068608103,15.4823085521296,4.50839530284119));
#68984=CARTESIAN_POINT('Ctrl Pts',(52.8524134222997,15.8462284998381,4.58690081321797));
#68985=CARTESIAN_POINT('Ctrl Pts',(51.7973816961194,14.9105674375766,4.66540632359475));
#68986=CARTESIAN_POINT('Ctrl Pts',(51.9958892285554,13.5144483190228,4.74391183397153));
#68987=CARTESIAN_POINT('Ctrl Pts',(53.2699097205826,12.9099442234561,4.82241734434831));
#68988=CARTESIAN_POINT('Ctrl Pts',(54.4768713563924,13.6391882674309,4.90092285472509));
#68989=CARTESIAN_POINT('Ctrl Pts',(54.5343421476997,15.0481781142727,4.97942836510187));
#68990=CARTESIAN_POINT('Ctrl Pts',(53.3907811220753,15.873296047955,5.05793387547865));
#68991=CARTESIAN_POINT('Ctrl Pts',(52.0717605935641,15.3745609528057,5.13643938585542));
#68992=CARTESIAN_POINT('Ctrl Pts',(51.7602103334102,13.9992417638178,5.21494489623221));
#68993=CARTESIAN_POINT('Ctrl Pts',(52.7355344095251,12.9807745933074,5.29345040660898));
#68994=CARTESIAN_POINT('Ctrl Pts',(54.1230422383652,13.232510563259,5.37195591698578));
#68995=CARTESIAN_POINT('Ctrl Pts',(54.6783773214851,14.5287559995584,5.45046142736254));
#68996=CARTESIAN_POINT('Ctrl Pts',(53.9035149801418,15.7068684598963,5.52896693773933));
#68997=CARTESIAN_POINT('Ctrl Pts',(52.4933440450442,15.7105670476193,5.60747244811611));
#68998=CARTESIAN_POINT('Ctrl Pts',(51.7125917738871,14.5359761569097,5.68597795849288));
#68999=CARTESIAN_POINT('Ctrl Pts',(52.2613503096046,13.2376182647008,5.76448346886967));
#69000=CARTESIAN_POINT('Ctrl Pts',(53.6476881902928,12.9776346480105,5.84298897924644));
#69001=CARTESIAN_POINT('Ctrl Pts',(54.6279124027069,13.9937937590388,5.92149448962322));
#69002=CARTESIAN_POINT('Ctrl Pts',(54.4246171615437,14.9072768995629,5.97383149654108));
#69003=CARTESIAN_POINT('Ctrl Pts',(54.153252109211,15.2223467977324,6.));
#69004=CARTESIAN_POINT('Ctrl Pts',(54.4588409672492,14.3981450852038,2.44341967361942));
#69005=CARTESIAN_POINT('Ctrl Pts',(54.4598231909075,14.5245548856247,2.45136379342792));
#69006=CARTESIAN_POINT('Ctrl Pts',(54.4423420959139,14.6506995799382,2.45930791323643));
#69007=CARTESIAN_POINT('Ctrl Pts',(54.4052616068446,14.770791992877,2.46725203304493));
#69008=CARTESIAN_POINT('Ctrl Pts',(54.2831158021666,15.166385060345,2.49342053650386));
#69009=CARTESIAN_POINT('Ctrl Pts',(53.9482987160905,15.4963053610751,2.51958903996278));
#69010=CARTESIAN_POINT('Ctrl Pts',(53.5509536954554,15.6126216193417,2.54575754342171));
#69011=CARTESIAN_POINT('Ctrl Pts',(53.1536086748203,15.7289378776082,2.57192604688064));
#69012=CARTESIAN_POINT('Ctrl Pts',(52.6937357196261,15.6316500934114,2.59809455033956));
#69013=CARTESIAN_POINT('Ctrl Pts',(52.3775436489295,15.3643788260367,2.62426305379849));
#69014=CARTESIAN_POINT('Ctrl Pts',(52.061351578233,15.097107558662,2.65043155725741));
#69015=CARTESIAN_POINT('Ctrl Pts',(51.8888403920341,14.6598528081095,2.67660006071634));
#69016=CARTESIAN_POINT('Ctrl Pts',(51.9373679909505,14.2486870145047,2.70276856417527));
#69017=CARTESIAN_POINT('Ctrl Pts',(51.9858955898669,13.8375212208999,2.7289370676342));
#69018=CARTESIAN_POINT('Ctrl Pts',(52.2554619738986,13.4524443842429,2.75510557109312));
#69019=CARTESIAN_POINT('Ctrl Pts',(52.6251894581517,13.2661284329053,2.78127407455205));
#69020=CARTESIAN_POINT('Ctrl Pts',(52.9949169424048,13.0798124815677,2.80744257801097));
#69021=CARTESIAN_POINT('Ctrl Pts',(53.4648055268793,13.0922574155496,2.8336110814699));
#69022=CARTESIAN_POINT('Ctrl Pts',(53.824152040299,13.2978833279507,2.85977958492883));
#69023=CARTESIAN_POINT('Ctrl Pts',(54.1834985537187,13.5035092403518,2.88594808838775));
#69024=CARTESIAN_POINT('Ctrl Pts',(54.4323029960837,13.9023161311722,2.91211659184668));
#69025=CARTESIAN_POINT('Ctrl Pts',(54.4589982709602,14.3154739762224,2.93828509530561));
#69026=CARTESIAN_POINT('Ctrl Pts',(54.4607442500488,14.342496172514,2.93999662141021));
#69027=CARTESIAN_POINT('Ctrl Pts',(54.4615401150314,14.3695797577353,2.94170814751482));
#69028=CARTESIAN_POINT('Ctrl Pts',(54.4614103817624,14.3966710984295,2.94341967361942));
#69029=CARTESIAN_POINT('Ctrl Pts',(53.5936497983459,12.9064860705774,2.));
#69030=CARTESIAN_POINT('Ctrl Pts',(53.6510872607052,12.9274734829173,2.));
#69031=CARTESIAN_POINT('Ctrl Pts',(53.7069621322555,12.9520730502145,2.));
#69032=CARTESIAN_POINT('Ctrl Pts',(53.7610764088156,12.9799849419358,2.));
#69033=CARTESIAN_POINT('Ctrl Pts',(53.8148756915179,13.0077343612929,2.));
#69034=CARTESIAN_POINT('Ctrl Pts',(53.8669355047627,13.0387586838188,2.));
#69035=CARTESIAN_POINT('Ctrl Pts',(53.9170293533885,13.0728080082457,2.));
#69036=CARTESIAN_POINT('Ctrl Pts',(53.9548563761383,13.0985194399892,2.));
#69037=CARTESIAN_POINT('Ctrl Pts',(53.9915618038207,13.1259567612843,2.));
#69038=CARTESIAN_POINT('Ctrl Pts',(54.0270323602661,13.1550241879185,2.));
#69039=CARTESIAN_POINT('Ctrl Pts',(54.0454462553229,13.1701140144464,2.));
#69040=CARTESIAN_POINT('Ctrl Pts',(54.0635271127833,13.1856432908818,2.));
#69041=CARTESIAN_POINT('Ctrl Pts',(54.0812573827311,13.2015993500241,2.));
#69042=CARTESIAN_POINT('Ctrl Pts',(54.0905947396254,13.2100023477944,2.));
#69043=CARTESIAN_POINT('Ctrl Pts',(54.0998362160851,13.2185251993749,2.));
#69044=CARTESIAN_POINT('Ctrl Pts',(54.108963022778,13.2271503421169,2.));
#69045=CARTESIAN_POINT('Ctrl Pts',(54.1519916744371,13.2678138814072,2.));
#69046=CARTESIAN_POINT('Ctrl Pts',(54.1925581151732,13.3108214913442,2.));
#69047=CARTESIAN_POINT('Ctrl Pts',(54.2304545251895,13.3559335740381,2.));
#69048=CARTESIAN_POINT('Ctrl Pts',(54.2675766913303,13.4001239928139,2.));
#69049=CARTESIAN_POINT('Ctrl Pts',(54.3021372566419,13.4463347100738,2.));
#69050=CARTESIAN_POINT('Ctrl Pts',(54.3338978257104,13.4943635014692,2.));
#69051=CARTESIAN_POINT('Ctrl Pts',(54.3568895199349,13.5291318736403,2.));
#69052=CARTESIAN_POINT('Ctrl Pts',(54.3784130414483,13.5648534993931,2.));
#69053=CARTESIAN_POINT('Ctrl Pts',(54.3983614304516,13.6014553928064,2.));
#69054=CARTESIAN_POINT('Ctrl Pts',(54.4087875591326,13.6205855616955,2.));
#69055=CARTESIAN_POINT('Ctrl Pts',(54.418783168127,13.6399562244125,2.));
#69056=CARTESIAN_POINT('Ctrl Pts',(54.4283312993461,13.6595570484094,2.));
#69057=CARTESIAN_POINT('Ctrl Pts',(54.4327718218709,13.6686727484838,2.));
#69058=CARTESIAN_POINT('Ctrl Pts',(54.4371132830354,13.6778337206022,2.));
#69059=CARTESIAN_POINT('Ctrl Pts',(54.4413510256923,13.6870315208254,2.));
#69060=CARTESIAN_POINT('Ctrl Pts',(54.4646885493577,13.7376844032104,2.));
#69061=CARTESIAN_POINT('Ctrl Pts',(54.4849171742244,13.7895200079085,2.));
#69062=CARTESIAN_POINT('Ctrl Pts',(54.5018239464097,13.8423481255187,2.));
#69063=CARTESIAN_POINT('Ctrl Pts',(54.5131364715857,13.8776960561536,2.));
#69064=CARTESIAN_POINT('Ctrl Pts',(54.5229608260296,13.9134887100648,2.));
#69065=CARTESIAN_POINT('Ctrl Pts',(54.5312202420661,13.9496710849604,2.));
#69066=CARTESIAN_POINT('Ctrl Pts',(54.5434447189016,14.0032233702325,2.));
#69067=CARTESIAN_POINT('Ctrl Pts',(54.5522427226731,14.0576303083872,2.));
#69068=CARTESIAN_POINT('Ctrl Pts',(54.5576688283951,14.1125811869758,2.));
#69069=CARTESIAN_POINT('Ctrl Pts',(54.5593446193984,14.1295521404888,2.));
#69070=CARTESIAN_POINT('Ctrl Pts',(54.5606984801865,14.1465748861843,2.));
#69071=CARTESIAN_POINT('Ctrl Pts',(54.5617312008431,14.1636399586999,2.));
#69072=CARTESIAN_POINT('Ctrl Pts',(54.562637534785,14.1786165686302,2.));
#69073=CARTESIAN_POINT('Ctrl Pts',(54.5632965181378,14.1936323469634,2.));
#69074=CARTESIAN_POINT('Ctrl Pts',(54.5637080050311,14.2086448003361,2.));
#69075=CARTESIAN_POINT('Ctrl Pts',(54.5652337512309,14.2643092554044,2.));
#69076=CARTESIAN_POINT('Ctrl Pts',(54.5633684846636,14.3200027126169,2.));
#69077=CARTESIAN_POINT('Ctrl Pts',(54.5582160449964,14.3754072804563,2.));
#69078=CARTESIAN_POINT('Ctrl Pts',(54.553069811691,14.4307451108242,2.));
#69079=CARTESIAN_POINT('Ctrl Pts',(54.5446438644413,14.485795888494,2.));
#69080=CARTESIAN_POINT('Ctrl Pts',(54.5329924871137,14.5402275304281,2.));
#69081=CARTESIAN_POINT('Ctrl Pts',(54.5255451328294,14.5750192731003,2.));
#69082=CARTESIAN_POINT('Ctrl Pts',(54.5167790477696,14.6095577033489,2.));
#69083=CARTESIAN_POINT('Ctrl Pts',(54.5066991329774,14.6437495917835,2.));
#69084=CARTESIAN_POINT('Ctrl Pts',(54.501505292657,14.6613675193597,2.));
#69085=CARTESIAN_POINT('Ctrl Pts',(54.4959625199335,14.6788933418954,2.));
#69086=CARTESIAN_POINT('Ctrl Pts',(54.4900708072952,14.6963135911134,2.));
#69087=CARTESIAN_POINT('Ctrl Pts',(54.4865172473949,14.706820535847,2.));
#69088=CARTESIAN_POINT('Ctrl Pts',(54.482836847661,14.7172884125644,2.));
#69089=CARTESIAN_POINT('Ctrl Pts',(54.4790344472978,14.7277017731048,2.));
#69090=CARTESIAN_POINT('Ctrl Pts',(54.4606465121801,14.7780594892014,2.));
#69091=CARTESIAN_POINT('Ctrl Pts',(54.4393828187119,14.8272228510089,2.));
#69092=CARTESIAN_POINT('Ctrl Pts',(54.4152842461347,14.8748779185061,2.));
#69093=CARTESIAN_POINT('Ctrl Pts',(54.4001512378004,14.9048035305436,2.));
#69094=CARTESIAN_POINT('Ctrl Pts',(54.3838995195552,14.9341338196499,2.));
#69095=CARTESIAN_POINT('Ctrl Pts',(54.3665318697885,14.9627834478761,2.));
#69096=CARTESIAN_POINT('Ctrl Pts',(54.3601820699915,14.9732580605001,2.));
#69097=CARTESIAN_POINT('Ctrl Pts',(54.3536816777175,14.9836437344145,2.));
#69098=CARTESIAN_POINT('Ctrl Pts',(54.3470352062003,14.9939290625922,2.));
#69099=CARTESIAN_POINT('Ctrl Pts',(54.3191335463469,15.037106518111,2.));
#69100=CARTESIAN_POINT('Ctrl Pts',(54.2887053621599,15.0784511647158,2.));
#69101=CARTESIAN_POINT('Ctrl Pts',(54.2557752604927,15.1176640701999,2.));
#69102=CARTESIAN_POINT('Ctrl Pts',(54.2373775275913,15.1395719455134,2.));
#69103=CARTESIAN_POINT('Ctrl Pts',(54.218198261211,15.1608137789867,2.));
#69104=CARTESIAN_POINT('Ctrl Pts',(54.1982376363281,15.1813315747386,2.));
#69105=CARTESIAN_POINT('Ctrl Pts',(54.1842200551681,15.1957404356268,2.));
#69106=CARTESIAN_POINT('Ctrl Pts',(54.1698170448365,15.2097921118142,2.));
#69107=CARTESIAN_POINT('Ctrl Pts',(54.1550457523822,15.2234791283661,2.));
#69108=CARTESIAN_POINT('Origin',(53.1951359564886,14.3971354987959,4.5));
#69109=CARTESIAN_POINT('Origin',(53.1951359564886,14.3971354987959,7.));
#69110=CARTESIAN_POINT('',(53.1951359564886,14.3971354987959,7.));
#69111=CARTESIAN_POINT('Origin',(53.1951359564886,14.3971354987959,7.));
#69112=CARTESIAN_POINT('',(53.1951359564886,14.3971354987959,7.));
#69113=CARTESIAN_POINT('Origin',(53.1951359564886,14.3971354987959,14.));
#69114=CARTESIAN_POINT('Ctrl Pts',(52.2370198037663,15.2223467977324,14.));
#69115=CARTESIAN_POINT('Ctrl Pts',(52.1998280045505,15.1876146000526,14.));
#69116=CARTESIAN_POINT('Ctrl Pts',(52.1650182492849,15.1505714365259,14.));
#69117=CARTESIAN_POINT('Ctrl Pts',(52.1326048427955,15.1115303634374,14.));
#69118=CARTESIAN_POINT('Ctrl Pts',(52.1107612978531,15.0852204032398,14.));
#69119=CARTESIAN_POINT('Ctrl Pts',(52.0900064961352,15.0580020337776,14.));
#69120=CARTESIAN_POINT('Ctrl Pts',(52.0703516540471,15.0299603098848,14.));
#69121=CARTESIAN_POINT('Ctrl Pts',(52.0612801327296,15.0170178962581,14.));
#69122=CARTESIAN_POINT('Ctrl Pts',(52.0524430088201,15.0038999829769,14.));
#69123=CARTESIAN_POINT('Ctrl Pts',(52.0438418387803,14.990614419731,14.));
#69124=CARTESIAN_POINT('Ctrl Pts',(52.0366118451662,14.9794468068385,14.));
#69125=CARTESIAN_POINT('Ctrl Pts',(52.0295526826659,14.9681669382534,14.));
#69126=CARTESIAN_POINT('Ctrl Pts',(52.0226684754192,14.9567860741714,14.));
#69127=CARTESIAN_POINT('Ctrl Pts',(51.9948472065273,14.9107923862272,14.));
#69128=CARTESIAN_POINT('Ctrl Pts',(51.9698609198898,14.8631221291877,14.));
#69129=CARTESIAN_POINT('Ctrl Pts',(51.947748300213,14.8140997169234,14.));
#69130=CARTESIAN_POINT('Ctrl Pts',(51.9392849993811,14.7953370633544,14.));
#69131=CARTESIAN_POINT('Ctrl Pts',(51.9312430201486,14.7763759159143,14.));
#69132=CARTESIAN_POINT('Ctrl Pts',(51.9236259797524,14.7572330691954,14.));
#69133=CARTESIAN_POINT('Ctrl Pts',(51.9181526522308,14.743477717466,14.));
#69134=CARTESIAN_POINT('Ctrl Pts',(51.912898751984,14.729628533072,14.));
#69135=CARTESIAN_POINT('Ctrl Pts',(51.9078659026536,14.7156915537031,14.));
#69136=CARTESIAN_POINT('Ctrl Pts',(51.9039695334292,14.70490171798,14.));
#69137=CARTESIAN_POINT('Ctrl Pts',(51.900205652679,14.6940588597731,14.));
#69138=CARTESIAN_POINT('Ctrl Pts',(51.8965797111534,14.6831806447376,14.));
#69139=CARTESIAN_POINT('Ctrl Pts',(51.8786612859544,14.6294234395981,14.));
#69140=CARTESIAN_POINT('Ctrl Pts',(51.8640761421609,14.5747200727471,14.));
#69141=CARTESIAN_POINT('Ctrl Pts',(51.8528626358732,14.5194298173159,14.));
#69142=CARTESIAN_POINT('Ctrl Pts',(51.841811607002,14.4649406866733,14.));
#69143=CARTESIAN_POINT('Ctrl Pts',(51.834034827559,14.4098803751302,14.));
#69144=CARTESIAN_POINT('Ctrl Pts',(51.8296128481236,14.3545627855475,14.));
#69145=CARTESIAN_POINT('Ctrl Pts',(51.8273037118361,14.3256762076459,14.));
#69146=CARTESIAN_POINT('Ctrl Pts',(51.8259101526014,14.2967190812183,14.));
#69147=CARTESIAN_POINT('Ctrl Pts',(51.8254490493311,14.267734405596,14.));
#69148=CARTESIAN_POINT('Ctrl Pts',(51.8252016892528,14.2521854991105,14.));
#69149=CARTESIAN_POINT('Ctrl Pts',(51.8252227392438,14.2366286514356,14.));
#69150=CARTESIAN_POINT('Ctrl Pts',(51.8255152855609,14.2210704501588,14.));
#69151=CARTESIAN_POINT('Ctrl Pts',(51.8257232519385,14.210010380103,14.));
#69152=CARTESIAN_POINT('Ctrl Pts',(51.8260684275044,14.1989496253519,14.));
#69153=CARTESIAN_POINT('Ctrl Pts',(51.8265520290691,14.1878905522567,14.));
#69154=CARTESIAN_POINT('Ctrl Pts',(51.8269778211639,14.1781534747891,14.));
#69155=CARTESIAN_POINT('Ctrl Pts',(51.8275105014109,14.1684274977859,14.));
#69156=CARTESIAN_POINT('Ctrl Pts',(51.8281502461767,14.1587149162758,14.));
#69157=CARTESIAN_POINT('Ctrl Pts',(51.8313147365989,14.1106717390517,14.));
#69158=CARTESIAN_POINT('Ctrl Pts',(51.8370971206992,14.0629523055666,14.));
#69159=CARTESIAN_POINT('Ctrl Pts',(51.8455361922423,14.0157553469174,14.));
#69160=CARTESIAN_POINT('Ctrl Pts',(51.8551414270626,13.9620364196253,14.));
#69161=CARTESIAN_POINT('Ctrl Pts',(51.8681865747695,13.9089935983919,14.));
#69162=CARTESIAN_POINT('Ctrl Pts',(51.8844213082608,13.8568249617545,14.));
#69163=CARTESIAN_POINT('Ctrl Pts',(51.9002905362136,13.8058308393547,14.));
#69164=CARTESIAN_POINT('Ctrl Pts',(51.9192079284333,13.7556712969164,14.));
#69165=CARTESIAN_POINT('Ctrl Pts',(51.9409851275901,13.706535068553,14.));
#69166=CARTESIAN_POINT('Ctrl Pts',(51.9463194725345,13.6944991042644,14.));
#69167=CARTESIAN_POINT('Ctrl Pts',(51.9518256037684,13.682524584753,14.));
#69168=CARTESIAN_POINT('Ctrl Pts',(51.9575011215527,13.6706143910571,14.));
#69169=CARTESIAN_POINT('Ctrl Pts',(51.9617861950656,13.6616220739719,14.));
#69170=CARTESIAN_POINT('Ctrl Pts',(51.9661670467641,13.6526682499378,14.));
#69171=CARTESIAN_POINT('Ctrl Pts',(51.970637198385,13.6437643302661,14.));
#69172=CARTESIAN_POINT('Ctrl Pts',(51.9964876791319,13.5922737716532,14.));
#69173=CARTESIAN_POINT('Ctrl Pts',(52.0253653817872,13.5423559816202,14.));
#69174=CARTESIAN_POINT('Ctrl Pts',(52.0569909387869,13.4942262955418,14.));
#69175=CARTESIAN_POINT('Ctrl Pts',(52.0892948739529,13.445064212526,14.));
#69176=CARTESIAN_POINT('Ctrl Pts',(52.1244662109347,13.397766816306,14.));
#69177=CARTESIAN_POINT('Ctrl Pts',(52.1622608705295,13.3525735612502,14.));
#69178=CARTESIAN_POINT('Ctrl Pts',(52.2003880181175,13.3069827311179,14.));
#69179=CARTESIAN_POINT('Ctrl Pts',(52.2411854112565,13.2635321825146,14.));
#69180=CARTESIAN_POINT('Ctrl Pts',(52.2844490106252,13.2224929144142,14.));
#69181=CARTESIAN_POINT('Ctrl Pts',(52.2942488213751,13.2131969458271,14.));
#69182=CARTESIAN_POINT('Ctrl Pts',(52.3041782445982,13.2040224039658,14.));
#69183=CARTESIAN_POINT('Ctrl Pts',(52.3142147727034,13.1949905194826,14.));
#69184=CARTESIAN_POINT('Ctrl Pts',(52.3594366693831,13.154295276801,14.));
#69185=CARTESIAN_POINT('Ctrl Pts',(52.4069027252886,13.1164219434827,14.));
#69186=CARTESIAN_POINT('Ctrl Pts',(52.4563466157764,13.081614036564,14.));
#69187=CARTESIAN_POINT('Ctrl Pts',(52.5053559225274,13.0471120713928,14.));
#69188=CARTESIAN_POINT('Ctrl Pts',(52.5563091707611,13.0156209539409,14.));
#69189=CARTESIAN_POINT('Ctrl Pts',(52.608988780259,12.9874055956648,14.));
#69190=CARTESIAN_POINT('Ctrl Pts',(52.6475874040075,12.9667320559707,14.));
#69191=CARTESIAN_POINT('Ctrl Pts',(52.6871137410246,12.9478176360703,14.));
#69192=CARTESIAN_POINT('Ctrl Pts',(52.7274932936822,12.9307805393251,14.));
#69193=CARTESIAN_POINT('Ctrl Pts',(52.7499343911042,12.9213121048655,14.));
#69194=CARTESIAN_POINT('Ctrl Pts',(52.7726391696466,12.9124237518853,14.));
#69195=CARTESIAN_POINT('Ctrl Pts',(52.7955875161457,12.9041113834231,14.));
#69196=CARTESIAN_POINT('Ctrl Pts',(53.5936497983458,12.9064860705774,14.));
#69197=CARTESIAN_POINT('Ctrl Pts',(53.6509984651359,12.9274410373818,14.));
#69198=CARTESIAN_POINT('Ctrl Pts',(53.706862700368,12.9520247913344,14.));
#69199=CARTESIAN_POINT('Ctrl Pts',(53.7610278853563,12.9799613169679,14.));
#69200=CARTESIAN_POINT('Ctrl Pts',(53.811253157417,13.0058657720284,14.));
#69201=CARTESIAN_POINT('Ctrl Pts',(53.8600177560799,13.0346541103148,14.));
#69202=CARTESIAN_POINT('Ctrl Pts',(53.9071231753153,13.0661362083666,14.));
#69203=CARTESIAN_POINT('Ctrl Pts',(53.9184932356716,13.073735192959,14.));
#69204=CARTESIAN_POINT('Ctrl Pts',(53.9297667856534,13.0814915893148,14.));
#69205=CARTESIAN_POINT('Ctrl Pts',(53.9409284679357,13.0893937512018,14.));
#69206=CARTESIAN_POINT('Ctrl Pts',(53.9900508427055,13.1241710318921,14.));
#69207=CARTESIAN_POINT('Ctrl Pts',(54.0370703143504,13.1618085883035,14.));
#69208=CARTESIAN_POINT('Ctrl Pts',(54.0817574273909,13.2020613662253,14.));
#69209=CARTESIAN_POINT('Ctrl Pts',(54.1093399314821,13.2269068381337,14.));
#69210=CARTESIAN_POINT('Ctrl Pts',(54.1360331112816,13.2527493804774,14.));
#69211=CARTESIAN_POINT('Ctrl Pts',(54.1617745165237,13.2795365304701,14.));
#69212=CARTESIAN_POINT('Ctrl Pts',(54.1705826003212,13.2887024427274,14.));
#69213=CARTESIAN_POINT('Ctrl Pts',(54.1792791848838,13.2979789798834,14.));
#69214=CARTESIAN_POINT('Ctrl Pts',(54.1878615697741,13.3073641129274,14.));
#69215=CARTESIAN_POINT('Ctrl Pts',(54.1958904565107,13.3161439767043,14.));
#69216=CARTESIAN_POINT('Ctrl Pts',(54.2038142460818,13.3250133166843,14.));
#69217=CARTESIAN_POINT('Ctrl Pts',(54.2116272144744,13.3339655512983,14.));
#69218=CARTESIAN_POINT('Ctrl Pts',(54.2502988321281,13.3782761611381,14.));
#69219=CARTESIAN_POINT('Ctrl Pts',(54.286291162459,13.4246505091087,14.));
#69220=CARTESIAN_POINT('Ctrl Pts',(54.3193890208698,13.4728592462875,14.));
#69221=CARTESIAN_POINT('Ctrl Pts',(54.3516418893917,13.5198372121285,14.));
#69222=CARTESIAN_POINT('Ctrl Pts',(54.3811465604862,13.5685580126975,14.));
#69223=CARTESIAN_POINT('Ctrl Pts',(54.4076582516134,13.6188275089931,14.));
#69224=CARTESIAN_POINT('Ctrl Pts',(54.422032099101,13.6460821292118,14.));
#69225=CARTESIAN_POINT('Ctrl Pts',(54.4355253353158,13.6737922214238,14.));
#69226=CARTESIAN_POINT('Ctrl Pts',(54.4480925383866,13.7019277688707,14.));
#69227=CARTESIAN_POINT('Ctrl Pts',(54.4585481854474,13.7253359490609,14.));
#69228=CARTESIAN_POINT('Ctrl Pts',(54.4683627680438,13.7490386437303,14.));
#69229=CARTESIAN_POINT('Ctrl Pts',(54.4775075097945,13.7730185624192,14.));
#69230=CARTESIAN_POINT('Ctrl Pts',(54.4814161888883,13.7832681473069,14.));
#69231=CARTESIAN_POINT('Ctrl Pts',(54.4852027887952,13.7935696368824,14.));
#69232=CARTESIAN_POINT('Ctrl Pts',(54.4888592934221,13.8039047382981,14.));
#69233=CARTESIAN_POINT('Ctrl Pts',(54.5057868221478,13.8517503569829,14.));
#69234=CARTESIAN_POINT('Ctrl Pts',(54.5199611541589,13.9003971685037,14.));
#69235=CARTESIAN_POINT('Ctrl Pts',(54.5312161752957,13.9497022076934,14.));
#69236=CARTESIAN_POINT('Ctrl Pts',(54.5437933673147,14.0047993006142,14.));
#69237=CARTESIAN_POINT('Ctrl Pts',(54.5527257730476,14.0607192933935,14.));
#69238=CARTESIAN_POINT('Ctrl Pts',(54.5581033230396,14.1171258864077,14.));
#69239=CARTESIAN_POINT('Ctrl Pts',(54.5626667133145,14.1649925354187,14.));
#69240=CARTESIAN_POINT('Ctrl Pts',(54.5646690852637,14.2132100479189,14.));
#69241=CARTESIAN_POINT('Ctrl Pts',(54.564136951052,14.2615652592456,14.));
#69242=CARTESIAN_POINT('Ctrl Pts',(54.5639906524104,14.2748594650644,14.));
#69243=CARTESIAN_POINT('Ctrl Pts',(54.5636526398204,14.2881640100039,14.));
#69244=CARTESIAN_POINT('Ctrl Pts',(54.5631231489384,14.3014742844597,14.));
#69245=CARTESIAN_POINT('Ctrl Pts',(54.56271092685,14.3118366708953,14.));
#69246=CARTESIAN_POINT('Ctrl Pts',(54.5621824503514,14.3222043088647,14.));
#69247=CARTESIAN_POINT('Ctrl Pts',(54.5615390812029,14.3325581294009,14.));
#69248=CARTESIAN_POINT('Ctrl Pts',(54.5580964056323,14.3879615398826,14.));
#69249=CARTESIAN_POINT('Ctrl Pts',(54.5513653775396,14.4430731531279,14.));
#69250=CARTESIAN_POINT('Ctrl Pts',(54.5414407207299,14.4975781575777,14.));
#69251=CARTESIAN_POINT('Ctrl Pts',(54.5315715932928,14.5517782014875,14.));
#69252=CARTESIAN_POINT('Ctrl Pts',(54.5185439871748,14.6053794989741,14.));
#69253=CARTESIAN_POINT('Ctrl Pts',(54.5024041440289,14.6580525499533,14.));
#69254=CARTESIAN_POINT('Ctrl Pts',(54.4874293906556,14.7069232818865,14.));
#69255=CARTESIAN_POINT('Ctrl Pts',(54.4697747813692,14.7549954141343,14.));
#69256=CARTESIAN_POINT('Ctrl Pts',(54.4494461022151,14.801978170179,14.));
#69257=CARTESIAN_POINT('Ctrl Pts',(54.444224343838,14.8140464702437,14.));
#69258=CARTESIAN_POINT('Ctrl Pts',(54.4388239492377,14.8260467745287,14.));
#69259=CARTESIAN_POINT('Ctrl Pts',(54.4332573522632,14.8379478523894,14.));
#69260=CARTESIAN_POINT('Ctrl Pts',(54.4107559776874,14.8860545524122,14.));
#69261=CARTESIAN_POINT('Ctrl Pts',(54.385510905493,14.9326200893912,14.));
#69262=CARTESIAN_POINT('Ctrl Pts',(54.35757385594,14.9773487850342,14.));
#69263=CARTESIAN_POINT('Ctrl Pts',(54.3305841286444,15.0205607675808,14.));
#69264=CARTESIAN_POINT('Ctrl Pts',(54.3010813192433,15.0620590194932,14.));
#69265=CARTESIAN_POINT('Ctrl Pts',(54.26907879043,15.1015427316002,14.));
#69266=CARTESIAN_POINT('Ctrl Pts',(54.2466913322504,15.1291636723929,14.));
#69267=CARTESIAN_POINT('Ctrl Pts',(54.2230798921524,15.155798056694,14.));
#69268=CARTESIAN_POINT('Ctrl Pts',(54.1982409588252,15.1813299258066,14.));
#69269=CARTESIAN_POINT('Ctrl Pts',(54.184228995893,15.1957327827604,14.));
#69270=CARTESIAN_POINT('Ctrl Pts',(54.1698262703445,15.2097845594384,14.));
#69271=CARTESIAN_POINT('Ctrl Pts',(54.1550492157916,15.2234767486837,14.));
#69272=CARTESIAN_POINT('Origin',(53.1951359564886,14.3971354987959,19.1042117235887));
#69273=CARTESIAN_POINT('Ctrl Pts',(51.650238794436,14.3978859537331,17.8542117235887));
#69274=CARTESIAN_POINT('Ctrl Pts',(51.6499374336204,14.4458116120497,17.8517311518799));
#69275=CARTESIAN_POINT('Ctrl Pts',(51.673532852059,14.9990358635577,17.8230820767121));
#69276=CARTESIAN_POINT('Ctrl Pts',(52.3387729531489,15.9998443555804,17.7682644980854));
#69277=CARTESIAN_POINT('Ctrl Pts',(54.0595357659419,15.9953385078431,17.6897589877086));
#69278=CARTESIAN_POINT('Ctrl Pts',(55.0050592474358,14.557743765663,17.6112534773318));
#69279=CARTESIAN_POINT('Ctrl Pts',(54.3274128937127,12.9760039404156,17.5327479669551));
#69280=CARTESIAN_POINT('Ctrl Pts',(52.6343075214603,12.6688220685916,17.4542424565783));
#69281=CARTESIAN_POINT('Ctrl Pts',(51.7321085269852,13.6109301706732,17.3947303754562));
#69282=CARTESIAN_POINT('Ctrl Pts',(51.6515351015305,14.2566054984257,17.361386797793));
#69283=CARTESIAN_POINT('Ctrl Pts',(51.6527011247771,14.3958311332086,17.3542117235887));
#69284=CARTESIAN_POINT('Ctrl Pts',(51.6537934596096,14.3955992295121,17.8957882764113));
#69285=CARTESIAN_POINT('Ctrl Pts',(51.6561292792194,14.73752448157,17.8781885106897));
#69286=CARTESIAN_POINT('Ctrl Pts',(51.9349899776299,15.5924054167524,17.8344202415091));
#69287=CARTESIAN_POINT('Ctrl Pts',(53.3392724282712,16.2080937050947,17.7644834688697));
#69288=CARTESIAN_POINT('Ctrl Pts',(54.7851641391705,15.2764790675082,17.6859779584929));
#69289=CARTESIAN_POINT('Ctrl Pts',(54.8056647755616,13.5555715973232,17.6074724481161));
#69290=CARTESIAN_POINT('Ctrl Pts',(53.3815155728065,12.5897336831025,17.5289669377393));
#69291=CARTESIAN_POINT('Ctrl Pts',(51.9513720532365,13.1783784136204,17.458405547171));
#69292=CARTESIAN_POINT('Ctrl Pts',(51.6558508817824,14.0445039022943,17.4140126600617));
#69293=CARTESIAN_POINT('Ctrl Pts',(51.6531013855762,14.3983675031589,17.3957882764113));
#69294=CARTESIAN_POINT('Ctrl Pts',(54.1532521092111,15.2223467977324,18.));
#69295=CARTESIAN_POINT('Ctrl Pts',(54.4246171615437,14.9072768995628,17.9738314965411));
#69296=CARTESIAN_POINT('Ctrl Pts',(54.6278752336732,13.9937540324533,17.9214944896232));
#69297=CARTESIAN_POINT('Ctrl Pts',(53.6477056068469,12.9776474013965,17.8429889792464));
#69298=CARTESIAN_POINT('Ctrl Pts',(52.2613397426835,13.2376039347743,17.7644834688697));
#69299=CARTESIAN_POINT('Ctrl Pts',(51.7125907601688,14.5359830763926,17.6859779584929));
#69300=CARTESIAN_POINT('Ctrl Pts',(52.4933400927666,15.7105673519417,17.6074724481161));
#69301=CARTESIAN_POINT('Ctrl Pts',(53.9035180427191,15.7068747761389,17.5289669377393));
#69302=CARTESIAN_POINT('Ctrl Pts',(54.6783815828027,14.5287551705091,17.4504614273625));
#69303=CARTESIAN_POINT('Ctrl Pts',(54.1230453454192,13.2325075949904,17.3719559169858));
#69304=CARTESIAN_POINT('Ctrl Pts',(52.7355328741209,12.9807697615999,17.293450406609));
#69305=CARTESIAN_POINT('Ctrl Pts',(51.760205867286,13.9992407208286,17.2149448962322));
#69306=CARTESIAN_POINT('Ctrl Pts',(52.0717570426273,15.3745639123133,17.1364393858554));
#69307=CARTESIAN_POINT('Ctrl Pts',(53.3907817466691,15.8733007472588,17.0579338754786));
#69308=CARTESIAN_POINT('Ctrl Pts',(54.5343463517261,15.0481801280675,16.9794283651019));
#69309=CARTESIAN_POINT('Ctrl Pts',(54.4768753865949,13.6391859025932,16.9009228547251));
#69310=CARTESIAN_POINT('Ctrl Pts',(53.2699099545465,12.9099395406962,16.8224173443483));
#69311=CARTESIAN_POINT('Ctrl Pts',(51.9958854602388,13.5144455498356,16.7439118339715));
#69312=CARTESIAN_POINT('Ctrl Pts',(51.7973773032627,14.9105690485956,16.6654063235947));
#69313=CARTESIAN_POINT('Ctrl Pts',(52.8524123453517,15.8462330551256,16.586900813218));
#69314=CARTESIAN_POINT('Ctrl Pts',(54.2148100652166,15.4823119617458,16.5083953028412));
#69315=CARTESIAN_POINT('Ctrl Pts',(54.6627398052286,14.1451787985144,16.4298897924644));
#69316=CARTESIAN_POINT('Ctrl Pts',(53.7944875223078,13.0340064035767,16.3513842820876));
#69317=CARTESIAN_POINT('Ctrl Pts',(52.3887225069356,13.145320583037,16.2728787717108));
#69318=CARTESIAN_POINT('Ctrl Pts',(51.7061682442381,14.3792921414933,16.1943732613341));
#69319=CARTESIAN_POINT('Ctrl Pts',(52.3589556241958,15.6292660458125,16.1158677509573));
#69320=CARTESIAN_POINT('Ctrl Pts',(53.7616494051485,15.7742359839284,16.0373622405805));
#69321=CARTESIAN_POINT('Ctrl Pts',(54.6562804572665,14.6841894679762,15.9588567302037));
#69322=CARTESIAN_POINT('Ctrl Pts',(54.2405223843949,13.33670612834,15.880351219827));
#69323=CARTESIAN_POINT('Ctrl Pts',(52.8872369102521,12.9402410582164,15.8018457094502));
#69324=CARTESIAN_POINT('Ctrl Pts',(51.8100826208389,13.8503535583388,15.7233401990734));
#69325=CARTESIAN_POINT('Ctrl Pts',(51.9750770902176,15.2508331012045,15.6448346886966));
#69326=CARTESIAN_POINT('Ctrl Pts',(53.2342493568711,15.885696339624,15.5663291783198));
#69327=CARTESIAN_POINT('Ctrl Pts',(54.4583437946506,15.1855828256918,15.4878236679431));
#69328=CARTESIAN_POINT('Ctrl Pts',(54.549563415235,13.7783710083419,15.4093181575663));
#69329=CARTESIAN_POINT('Ctrl Pts',(53.4261002848556,12.9260818890411,15.3308126471895));
#69330=CARTESIAN_POINT('Ctrl Pts',(52.0955028666328,13.393068633948,15.2523071368127));
#69331=CARTESIAN_POINT('Ctrl Pts',(51.7510825200381,14.7605263839363,15.1738016264359));
#69332=CARTESIAN_POINT('Ctrl Pts',(52.7017236774067,15.8020866088358,15.0952961160592));
#69333=CARTESIAN_POINT('Ctrl Pts',(54.0948685923953,15.5836531566747,15.0167906056824));
#69334=CARTESIAN_POINT('Ctrl Pts',(54.6811121004696,14.3011227048956,14.9382850953056));
#69335=CARTESIAN_POINT('Ctrl Pts',(53.9346964498465,13.1046983170808,14.8597795849288));
#69336=CARTESIAN_POINT('Ctrl Pts',(52.5250262261246,13.0673633133234,14.7812740745521));
#69337=CARTESIAN_POINT('Ctrl Pts',(51.7163246046947,14.2225976133251,14.7027685641753));
#69338=CARTESIAN_POINT('Ctrl Pts',(52.2338596624079,15.5343656873115,14.6242630537985));
#69339=CARTESIAN_POINT('Ctrl Pts',(53.6134830839557,15.8262305186475,14.5457575434217));
#69340=CARTESIAN_POINT('Ctrl Pts',(54.6179371276052,14.8364654611899,14.4672520330449));
#69341=CARTESIAN_POINT('Ctrl Pts',(54.3463604457024,13.4526655408848,14.3887465226681));
#69342=CARTESIAN_POINT('Ctrl Pts',(53.0423964320332,12.9159559714002,14.3102410122914));
#69343=CARTESIAN_POINT('Ctrl Pts',(51.8752954493437,13.7074676781063,14.2317355019146));
#69344=CARTESIAN_POINT('Ctrl Pts',(51.892095823422,15.1177639193799,14.1532299915378));
#69345=CARTESIAN_POINT('Ctrl Pts',(53.0770150197732,15.881229923416,14.074724481161));
#69346=CARTESIAN_POINT('Ctrl Pts',(54.3688351006162,15.3148479080821,13.9962189707842));
#69347=CARTESIAN_POINT('Ctrl Pts',(54.6060800258316,13.9231151648839,13.9177134604075));
#69348=CARTESIAN_POINT('Ctrl Pts',(53.9234352130359,13.2829324314546,13.8653764534896));
#69349=CARTESIAN_POINT('Ctrl Pts',(53.5217210200197,13.1755371825403,13.8392079500307));
#69350=CARTESIAN_POINT('Ctrl Pts',(54.2235922564453,15.2829297282065,18.0535973499898));
#69351=CARTESIAN_POINT('Ctrl Pts',(54.514879588223,14.9447289570595,18.0274288465308));
#69352=CARTESIAN_POINT('Ctrl Pts',(54.7330598623,13.9641397611006,17.975091839613));
#69353=CARTESIAN_POINT('Ctrl Pts',(53.68093103129,12.8734356088235,17.8965863292362));
#69354=CARTESIAN_POINT('Ctrl Pts',(52.192785045031,13.1524768646333,17.8180808188594));
#69355=CARTESIAN_POINT('Ctrl Pts',(51.6037496273956,14.5461765785306,17.7395753084826));
#69356=CARTESIAN_POINT('Ctrl Pts',(52.441817712894,15.8069930198213,17.6610697981059));
#69357=CARTESIAN_POINT('Ctrl Pts',(53.95552395046,15.8030293533737,17.5825642877291));
#69358=CARTESIAN_POINT('Ctrl Pts',(54.7872741376804,14.5384180355604,17.5040587773523));
#69359=CARTESIAN_POINT('Ctrl Pts',(54.191167861517,13.1470063767988,17.4255532669756));
#69360=CARTESIAN_POINT('Ctrl Pts',(52.7017910899008,12.8767871972638,17.3470477565987));
#69361=CARTESIAN_POINT('Ctrl Pts',(51.6548604000808,13.9700292549887,17.268542246222));
#69362=CARTESIAN_POINT('Ctrl Pts',(51.9892841211801,15.4463218701793,17.1900367358452));
#69363=CARTESIAN_POINT('Ctrl Pts',(53.4051450925409,15.9816734958279,17.1115312254684));
#69364=CARTESIAN_POINT('Ctrl Pts',(54.6326645526155,15.0959766034206,17.0330257150917));
#69365=CARTESIAN_POINT('Ctrl Pts',(54.570974353587,13.5835409935271,16.9545202047148));
#69366=CARTESIAN_POINT('Ctrl Pts',(53.2753994915068,12.8007569720048,16.8760146943381));
#69367=CARTESIAN_POINT('Ctrl Pts',(51.9078424226204,13.4496428212774,16.7975091839613));
#69368=CARTESIAN_POINT('Ctrl Pts',(51.6947607789649,14.9482627993849,16.7190036735845));
#69369=CARTESIAN_POINT('Ctrl Pts',(52.827251273597,15.9526186276675,16.6404981632078));
#69370=CARTESIAN_POINT('Ctrl Pts',(54.2896694929959,15.5619802482706,16.561992652831));
#69371=CARTESIAN_POINT('Ctrl Pts',(54.7704840181913,14.1266813842457,16.4834871424542));
#69372=CARTESIAN_POINT('Ctrl Pts',(53.8384889487162,12.9339322100829,16.4049816320774));
#69373=CARTESIAN_POINT('Ctrl Pts',(52.3295196215527,13.0534185258236,16.3264761217006));
#69374=CARTESIAN_POINT('Ctrl Pts',(51.5968556021234,14.377982170488,16.2479706113238));
#69375=CARTESIAN_POINT('Ctrl Pts',(52.2975674015667,15.7197229740698,16.1694651009471));
#69376=CARTESIAN_POINT('Ctrl Pts',(53.803240019476,15.8753358877401,16.0909595905703));
#69377=CARTESIAN_POINT('Ctrl Pts',(54.7635504568624,14.7052635500684,16.0124540801935));
#69378=CARTESIAN_POINT('Ctrl Pts',(54.3172694834252,13.2588546508992,15.9339485698167));
#69379=CARTESIAN_POINT('Ctrl Pts',(52.8646324857426,12.8332830770114,15.8554430594399));
#69380=CARTESIAN_POINT('Ctrl Pts',(51.7083988580925,13.8102115337132,15.7769375490632));
#69381=CARTESIAN_POINT('Ctrl Pts',(51.8855064050308,15.3135073551311,15.6984320386864));
#69382=CARTESIAN_POINT('Ctrl Pts',(53.2371208691965,15.994979111252,15.6199265283096));
#69383=CARTESIAN_POINT('Ctrl Pts',(54.5510822638553,15.2434667272446,15.5414210179328));
#69384=CARTESIAN_POINT('Ctrl Pts',(54.6489987776341,13.7329443810606,15.4629155075561));
#69385=CARTESIAN_POINT('Ctrl Pts',(53.4430565430473,12.8180844116938,15.3844099971793));
#69386=CARTESIAN_POINT('Ctrl Pts',(52.0147732460911,13.3193550127907,15.3059044868025));
#69387=CARTESIAN_POINT('Ctrl Pts',(51.6450672618196,14.787204744688,15.2273989764257));
#69388=CARTESIAN_POINT('Ctrl Pts',(52.6654997892496,15.9052311677249,15.1488934660489));
#69389=CARTESIAN_POINT('Ctrl Pts',(54.1609225107029,15.6707614123012,15.0703879556721));
#69390=CARTESIAN_POINT('Ctrl Pts',(54.7902051164439,14.2940739206327,14.9918824452954));
#69391=CARTESIAN_POINT('Ctrl Pts',(53.9889913219699,13.0098139740974,14.9133769349186));
#69392=CARTESIAN_POINT('Ctrl Pts',(52.4758300853821,12.9697380190954,14.8348714245418));
#69393=CARTESIAN_POINT('Ctrl Pts',(51.6077575923118,14.2097839053763,14.756365914165));
#69394=CARTESIAN_POINT('Ctrl Pts',(52.1632875132313,15.6178555008087,14.6778604037883));
#69395=CARTESIAN_POINT('Ctrl Pts',(53.644196060099,15.9311476039325,14.5993548934115));
#69396=CARTESIAN_POINT('Ctrl Pts',(54.7223921496577,14.8687188932518,14.5208493830347));
#69397=CARTESIAN_POINT('Ctrl Pts',(54.4308776515139,13.3833272297531,14.4423438726579));
#69398=CARTESIAN_POINT('Ctrl Pts',(53.0311830518933,12.8072150992822,14.3638383622811));
#69399=CARTESIAN_POINT('Ctrl Pts',(51.7783992897971,13.6568356791444,14.2853328519044));
#69400=CARTESIAN_POINT('Ctrl Pts',(51.7964330642131,15.1706688923949,14.2068273415276));
#69401=CARTESIAN_POINT('Ctrl Pts',(53.0683431650545,15.9901847928655,14.1283218311508));
#69402=CARTESIAN_POINT('Ctrl Pts',(54.4550022843884,15.3822218123885,14.049816320774));
#69403=CARTESIAN_POINT('Ctrl Pts',(54.70966455814,13.888314937391,13.9713108103972));
#69404=CARTESIAN_POINT('Ctrl Pts',(53.9769033408726,13.2011331552573,13.9189738034794));
#69405=CARTESIAN_POINT('Ctrl Pts',(53.5456972794617,13.0858534785527,13.8928053000205));
#69406=CARTESIAN_POINT('Ctrl Pts',(54.2939324036796,15.3435126586807,18.1071946999795));
#69407=CARTESIAN_POINT('Ctrl Pts',(54.6051420149022,14.9821810145562,18.0810261965206));
#69408=CARTESIAN_POINT('Ctrl Pts',(54.8382444909268,13.934525489748,18.0286891896028));
#69409=CARTESIAN_POINT('Ctrl Pts',(53.714156455733,12.7692238162505,17.950183679226));
#69410=CARTESIAN_POINT('Ctrl Pts',(52.1242303473785,13.0673497944923,17.8716781688492));
#69411=CARTESIAN_POINT('Ctrl Pts',(51.4949084946224,14.5563700806686,17.7931726584724));
#69412=CARTESIAN_POINT('Ctrl Pts',(52.3902953330215,15.9034186877009,17.7146671480956));
#69413=CARTESIAN_POINT('Ctrl Pts',(54.0075298582009,15.8991839306084,17.6361616377189));
#69414=CARTESIAN_POINT('Ctrl Pts',(54.8961666925582,14.5480809006117,17.5576561273421));
#69415=CARTESIAN_POINT('Ctrl Pts',(54.2592903776148,13.0615051586072,17.4791506169653));
#69416=CARTESIAN_POINT('Ctrl Pts',(52.6680493056806,12.7728046329277,17.4006451065885));
#69417=CARTESIAN_POINT('Ctrl Pts',(51.5495149328755,13.9408177891487,17.3221395962118));
#69418=CARTESIAN_POINT('Ctrl Pts',(51.9068111997328,15.5180798280453,17.2436340858349));
#69419=CARTESIAN_POINT('Ctrl Pts',(53.4195084384129,16.090046244397,17.1651285754582));
#69420=CARTESIAN_POINT('Ctrl Pts',(54.7309827535048,15.1437730787738,17.0866230650814));
#69421=CARTESIAN_POINT('Ctrl Pts',(54.6650733205791,13.5278960844609,17.0081175547046));
#69422=CARTESIAN_POINT('Ctrl Pts',(53.2808890284672,12.6915744033134,16.9296120443278));
#69423=CARTESIAN_POINT('Ctrl Pts',(51.8197993850019,13.3848400927192,16.8511065339511));
#69424=CARTESIAN_POINT('Ctrl Pts',(51.5921442546672,14.9859565501742,16.7726010235743));
#69425=CARTESIAN_POINT('Ctrl Pts',(52.8020902018422,16.0590042002094,16.6940955131975));
#69426=CARTESIAN_POINT('Ctrl Pts',(54.3645289207752,15.6416485347953,16.6155900028207));
#69427=CARTESIAN_POINT('Ctrl Pts',(54.8782282311541,14.108183969977,16.5370844924439));
#69428=CARTESIAN_POINT('Ctrl Pts',(53.8824903751247,12.8338580165892,16.4585789820672));
#69429=CARTESIAN_POINT('Ctrl Pts',(52.2703167361696,12.9615164686103,16.3800734716904));
#69430=CARTESIAN_POINT('Ctrl Pts',(51.4875429600088,14.3766721994827,16.3015679613136));
#69431=CARTESIAN_POINT('Ctrl Pts',(52.2361791789377,15.8101799023271,16.2230624509368));
#69432=CARTESIAN_POINT('Ctrl Pts',(53.8448306338036,15.9764357915517,16.1445569405601));
#69433=CARTESIAN_POINT('Ctrl Pts',(54.8708204564582,14.7263376321606,16.0660514301832));
#69434=CARTESIAN_POINT('Ctrl Pts',(54.3940165824556,13.1810031734583,15.9875459198065));
#69435=CARTESIAN_POINT('Ctrl Pts',(52.8420280612332,12.7263250958063,15.9090404094297));
#69436=CARTESIAN_POINT('Ctrl Pts',(51.6067150953461,13.7700695090875,15.8305348990529));
#69437=CARTESIAN_POINT('Ctrl Pts',(51.7959357198439,15.3761816090578,15.7520293886761));
#69438=CARTESIAN_POINT('Ctrl Pts',(53.239992381522,16.1042618828799,15.6735238782994));
#69439=CARTESIAN_POINT('Ctrl Pts',(54.64382073306,15.3013506287974,15.5950183679226));
#69440=CARTESIAN_POINT('Ctrl Pts',(54.7484341400331,13.6875177537793,15.5165128575458));
#69441=CARTESIAN_POINT('Ctrl Pts',(53.460012801239,12.7100869343466,15.438007347169));
#69442=CARTESIAN_POINT('Ctrl Pts',(51.9340436255495,13.2456413916334,15.3595018367923));
#69443=CARTESIAN_POINT('Ctrl Pts',(51.5390520036012,14.8138831054397,15.2809963264155));
#69444=CARTESIAN_POINT('Ctrl Pts',(52.6292759010924,16.0083757266141,15.2024908160387));
#69445=CARTESIAN_POINT('Ctrl Pts',(54.2269764290105,15.7578696679277,15.1239853056619));
#69446=CARTESIAN_POINT('Ctrl Pts',(54.8992981324183,14.2870251363698,15.0454797952851));
#69447=CARTESIAN_POINT('Ctrl Pts',(54.0432861940933,12.9149296311139,14.9669742849084));
#69448=CARTESIAN_POINT('Ctrl Pts',(52.4266339446398,12.8721127248674,14.8884687745316));
#69449=CARTESIAN_POINT('Ctrl Pts',(51.4991905799288,14.1969701974276,14.8099632641548));
#69450=CARTESIAN_POINT('Ctrl Pts',(52.0927153640547,15.7013453143059,14.731457753778));
#69451=CARTESIAN_POINT('Ctrl Pts',(53.6749090362422,16.0360646892175,14.6529522434012));
#69452=CARTESIAN_POINT('Ctrl Pts',(54.8268471717102,14.9009723253136,14.5744467330245));
#69453=CARTESIAN_POINT('Ctrl Pts',(54.5153948573254,13.3139889186214,14.4959412226477));
#69454=CARTESIAN_POINT('Ctrl Pts',(53.0199696717534,12.6984742271641,14.4174357122709));
#69455=CARTESIAN_POINT('Ctrl Pts',(51.6815031302505,13.6062036801825,14.3389302018941));
#69456=CARTESIAN_POINT('Ctrl Pts',(51.7007703050042,15.22357386541,14.2604246915173));
#69457=CARTESIAN_POINT('Ctrl Pts',(53.0596713103358,16.099139662315,14.1819191811406));
#69458=CARTESIAN_POINT('Ctrl Pts',(54.5411694681605,15.4495957166949,14.1034136707638));
#69459=CARTESIAN_POINT('Ctrl Pts',(54.8132490904484,13.853514709898,14.024908160387));
#69460=CARTESIAN_POINT('Ctrl Pts',(54.0303714687093,13.11933387906,13.9725711534692));
#69461=CARTESIAN_POINT('Ctrl Pts',(53.5696735389038,12.996169774565,13.9464026500102));
#69462=CARTESIAN_POINT('Ctrl Pts',(54.3642725509139,15.4040955891549,18.1607920499693));
#69463=CARTESIAN_POINT('Ctrl Pts',(54.6954044415815,15.0196330720528,18.1346235465104));
#69464=CARTESIAN_POINT('Ctrl Pts',(54.9434291195537,13.9049112183953,18.0822865395925));
#69465=CARTESIAN_POINT('Ctrl Pts',(53.7473818801761,12.6650120236775,18.0037810292158));
#69466=CARTESIAN_POINT('Ctrl Pts',(52.055675649726,12.9822227243513,17.925275518839));
#69467=CARTESIAN_POINT('Ctrl Pts',(51.3860673618492,14.5665635828067,17.8467700084622));
#69468=CARTESIAN_POINT('Ctrl Pts',(52.3387729531489,15.9998443555804,17.7682644980854));
#69469=CARTESIAN_POINT('Ctrl Pts',(54.0595357659419,15.9953385078431,17.6897589877086));
#69470=CARTESIAN_POINT('Ctrl Pts',(55.0050592474358,14.557743765663,17.6112534773318));
#69471=CARTESIAN_POINT('Ctrl Pts',(54.3274128937127,12.9760039404156,17.5327479669551));
#69472=CARTESIAN_POINT('Ctrl Pts',(52.6343075214603,12.6688220685916,17.4542424565783));
#69473=CARTESIAN_POINT('Ctrl Pts',(51.4441694656704,13.9116063233088,17.3757369462015));
#69474=CARTESIAN_POINT('Ctrl Pts',(51.8243382782854,15.5898377859113,17.2972314358247));
#69475=CARTESIAN_POINT('Ctrl Pts',(53.4338717842849,16.1984189929661,17.2187259254479));
#69476=CARTESIAN_POINT('Ctrl Pts',(54.8293009543941,15.1915695541269,17.1402204150712));
#69477=CARTESIAN_POINT('Ctrl Pts',(54.7591722875712,13.4722511753948,17.0617149046944));
#69478=CARTESIAN_POINT('Ctrl Pts',(53.2863785654276,12.582391834622,16.9832093943176));
#69479=CARTESIAN_POINT('Ctrl Pts',(51.7317563473835,13.320037364161,16.9047038839408));
#69480=CARTESIAN_POINT('Ctrl Pts',(51.4895277303696,15.0236503009635,16.8261983735641));
#69481=CARTESIAN_POINT('Ctrl Pts',(52.7769291300874,16.1653897727513,16.7476928631873));
#69482=CARTESIAN_POINT('Ctrl Pts',(54.4393883485545,15.72131682132,16.6691873528105));
#69483=CARTESIAN_POINT('Ctrl Pts',(54.9859724441168,14.0896865557083,16.5906818424337));
#69484=CARTESIAN_POINT('Ctrl Pts',(53.9264918015332,12.7337838230954,16.5121763320569));
#69485=CARTESIAN_POINT('Ctrl Pts',(52.2111138507866,12.869614411397,16.4336708216802));
#69486=CARTESIAN_POINT('Ctrl Pts',(51.3782303178942,14.3753622284773,16.3551653113034));
#69487=CARTESIAN_POINT('Ctrl Pts',(52.1747909563085,15.9006368305844,16.2766598009266));
#69488=CARTESIAN_POINT('Ctrl Pts',(53.8864212481313,16.0775356953633,16.1981542905498));
#69489=CARTESIAN_POINT('Ctrl Pts',(54.9780904560539,14.7474117142528,16.119648780173));
#69490=CARTESIAN_POINT('Ctrl Pts',(54.4707636814861,13.1031516960174,16.0411432697963));
#69491=CARTESIAN_POINT('Ctrl Pts',(52.8194236367236,12.6193671146013,15.9626377594195));
#69492=CARTESIAN_POINT('Ctrl Pts',(51.5050313325997,13.7299274844619,15.8841322490427));
#69493=CARTESIAN_POINT('Ctrl Pts',(51.706365034657,15.4388558629845,15.8056267386659));
#69494=CARTESIAN_POINT('Ctrl Pts',(53.2428638938474,16.2135446545079,15.7271212282891));
#69495=CARTESIAN_POINT('Ctrl Pts',(54.7365592022647,15.3592345303502,15.6486157179124));
#69496=CARTESIAN_POINT('Ctrl Pts',(54.8478695024322,13.6420911264981,15.5701102075356));
#69497=CARTESIAN_POINT('Ctrl Pts',(53.4769690594307,12.6020894569994,15.4916046971588));
#69498=CARTESIAN_POINT('Ctrl Pts',(51.8533140050078,13.1719277704762,15.413099186782));
#69499=CARTESIAN_POINT('Ctrl Pts',(51.4330367453828,14.8405614661914,15.3345936764053));
#69500=CARTESIAN_POINT('Ctrl Pts',(52.5930520129352,16.1115202855033,15.2560881660285));
#69501=CARTESIAN_POINT('Ctrl Pts',(54.2930303473182,15.8449779235543,15.1775826556517));
#69502=CARTESIAN_POINT('Ctrl Pts',(55.0083911483926,14.2799763521069,15.0990771452749));
#69503=CARTESIAN_POINT('Ctrl Pts',(54.0975810662168,12.8200452881305,15.0205716348981));
#69504=CARTESIAN_POINT('Ctrl Pts',(52.3774378038973,12.7744874306393,14.9420661245214));
#69505=CARTESIAN_POINT('Ctrl Pts',(51.3906235675459,14.1841564894788,14.8635606141446));
#69506=CARTESIAN_POINT('Ctrl Pts',(52.0221432148781,15.7848351278031,14.7850551037678));
#69507=CARTESIAN_POINT('Ctrl Pts',(53.7056220123855,16.1409817745025,14.706549593391));
#69508=CARTESIAN_POINT('Ctrl Pts',(54.9313021937626,14.9332257573755,14.6280440830142));
#69509=CARTESIAN_POINT('Ctrl Pts',(54.5999120631369,13.2446506074896,14.5495385726375));
#69510=CARTESIAN_POINT('Ctrl Pts',(53.0087562916135,12.5897333550461,14.4710330622607));
#69511=CARTESIAN_POINT('Ctrl Pts',(51.584606970704,13.5555716812206,14.3925275518839));
#69512=CARTESIAN_POINT('Ctrl Pts',(51.6051075457953,15.2764788384251,14.3140220415071));
#69513=CARTESIAN_POINT('Ctrl Pts',(53.0509994556171,16.2080945317645,14.2355165311303));
#69514=CARTESIAN_POINT('Ctrl Pts',(54.6273366519326,15.5169696210012,14.1570110207535));
#69515=CARTESIAN_POINT('Ctrl Pts',(54.9168336227569,13.8187144824051,14.0785055103768));
#69516=CARTESIAN_POINT('Ctrl Pts',(54.0838395965459,13.0375346028627,14.0261685034589));
#69517=CARTESIAN_POINT('Ctrl Pts',(53.5936497983458,12.9064860705774,14.));
#69518=CARTESIAN_POINT('Ctrl Pts',(51.9310991161132,14.3960665614756,17.1934196736194));
#69519=CARTESIAN_POINT('Ctrl Pts',(51.9301435513723,14.2819701161205,17.2005947478237));
#69520=CARTESIAN_POINT('Ctrl Pts',(51.944352401566,14.1681074628443,17.2077698220279));
#69521=CARTESIAN_POINT('Ctrl Pts',(51.9746855643154,14.0587160928713,17.2149448962322));
#69522=CARTESIAN_POINT('Ctrl Pts',(52.0853148695643,13.6597504010857,17.2411133996911));
#69523=CARTESIAN_POINT('Ctrl Pts',(52.4104238718426,13.3202600813428,17.26728190315));
#69524=CARTESIAN_POINT('Ctrl Pts',(52.8042304515315,13.1924712270364,17.293450406609));
#69525=CARTESIAN_POINT('Ctrl Pts',(53.1980370312203,13.0646823727301,17.3196189100679));
#69526=CARTESIAN_POINT('Ctrl Pts',(53.6605411883198,13.1485949838602,17.3457874135268));
#69527=CARTESIAN_POINT('Ctrl Pts',(53.9843493064334,13.4065925520117,17.3719559169858));
#69528=CARTESIAN_POINT('Ctrl Pts',(54.308157424547,13.6645901201633,17.3981244204447));
#69529=CARTESIAN_POINT('Ctrl Pts',(54.4932695036749,14.0966726453362,17.4242929239036));
#69530=CARTESIAN_POINT('Ctrl Pts',(54.4566816198915,14.5090671755276,17.4504614273625));
#69531=CARTESIAN_POINT('Ctrl Pts',(54.4200937361082,14.921461705719,17.4766299308215));
#69532=CARTESIAN_POINT('Ctrl Pts',(54.1618058894136,15.314168240929,17.5027984342804));
#69533=CARTESIAN_POINT('Ctrl Pts',(53.7976323077409,15.5111369378344,17.5289669377393));
#69534=CARTESIAN_POINT('Ctrl Pts',(53.4334587260683,15.7081056347399,17.5551354411983));
#69535=CARTESIAN_POINT('Ctrl Pts',(52.9633994094174,15.7093364933408,17.5813039446572));
#69536=CARTESIAN_POINT('Ctrl Pts',(52.5982448623257,15.5141878767164,17.6074724481161));
#69537=CARTESIAN_POINT('Ctrl Pts',(52.233090315234,15.319039260092,17.633640951575));
#69538=CARTESIAN_POINT('Ctrl Pts',(51.9728405377014,14.9275111682423,17.6598094550339));
#69539=CARTESIAN_POINT('Ctrl Pts',(51.9341738126876,14.5153505987144,17.6859779584929));
#69540=CARTESIAN_POINT('Ctrl Pts',(51.9305085062518,14.4762809648747,17.6884585302017));
#69541=CARTESIAN_POINT('Ctrl Pts',(51.9288342506125,14.4370259363911,17.6909391019106));
#69542=CARTESIAN_POINT('Ctrl Pts',(51.929081218047,14.3977505022101,17.6934196736194));
#69543=CARTESIAN_POINT('Ctrl Pts',(52.7966221146313,12.9064860705774,18.));
#69544=CARTESIAN_POINT('Ctrl Pts',(52.3064323164312,13.0375346028627,17.9738314965411));
#69545=CARTESIAN_POINT('Ctrl Pts',(51.4734379005318,13.818711947887,17.9214944896232));
#69546=CARTESIAN_POINT('Ctrl Pts',(51.7629355980163,15.5169705450585,17.8429889792464));
#69547=CARTESIAN_POINT('Ctrl Pts',(53.3392724282712,16.2080937050947,17.7644834688697));
#69548=CARTESIAN_POINT('Ctrl Pts',(54.7851641391705,15.2764790675082,17.6859779584929));
#69549=CARTESIAN_POINT('Ctrl Pts',(54.8056647755616,13.5555715973232,17.6074724481161));
#69550=CARTESIAN_POINT('Ctrl Pts',(53.3815155728065,12.5897336831025,17.5289669377393));
#69551=CARTESIAN_POINT('Ctrl Pts',(51.7903600412662,13.244650694059,17.4504614273625));
#69552=CARTESIAN_POINT('Ctrl Pts',(51.458969924108,14.9332257213624,17.3719559169858));
#69553=CARTESIAN_POINT('Ctrl Pts',(52.6846499703254,16.1409815416267,17.293450406609));
#69554=CARTESIAN_POINT('Ctrl Pts',(54.36812854879,15.7848349642755,17.2149448962322));
#69555=CARTESIAN_POINT('Ctrl Pts',(54.9996481235109,14.1841565112764,17.1364393858554));
#69556=CARTESIAN_POINT('Ctrl Pts',(54.0128340063977,12.7744876345319,17.0579338754786));
#69557=CARTESIAN_POINT('Ctrl Pts',(52.292690959438,12.8200454826231,16.9794283651019));
#69558=CARTESIAN_POINT('Ctrl Pts',(51.3818809893341,14.2799763673289,16.9009228547251));
#69559=CARTESIAN_POINT('Ctrl Pts',(52.0972417021452,15.8449777434614,16.8224173443483));
#69560=CARTESIAN_POINT('Ctrl Pts',(53.7972198251956,16.11152007286,16.7439118339715));
#69561=CARTESIAN_POINT('Ctrl Pts',(54.9572349488979,14.8405614110472,16.6654063235948));
#69562=CARTESIAN_POINT('Ctrl Pts',(54.5369577413632,13.1719279226262,16.586900813218));
#69563=CARTESIAN_POINT('Ctrl Pts',(52.9133028885494,12.602089679815,16.5083953028412));
#69564=CARTESIAN_POINT('Ctrl Pts',(51.5424026157113,13.6420912202446,16.4298897924644));
#69565=CARTESIAN_POINT('Ctrl Pts',(51.6537129020729,15.359234410906,16.3513842820876));
#69566=CARTESIAN_POINT('Ctrl Pts',(53.1474080250528,16.2135444290179,16.2728787717109));
#69567=CARTESIAN_POINT('Ctrl Pts',(54.6839066935017,15.4388557336608,16.1943732613341));
#69568=CARTESIAN_POINT('Ctrl Pts',(54.8852403705633,13.7299275672916,16.1158677509573));
#69569=CARTESIAN_POINT('Ctrl Pts',(53.5708482296119,12.6193673352972,16.0373622405805));
#69570=CARTESIAN_POINT('Ctrl Pts',(51.9195083898506,13.1031518566562,15.9588567302037));
#69571=CARTESIAN_POINT('Ctrl Pts',(51.4121816782637,14.7474116707683,15.8803512198269));
#69572=CARTESIAN_POINT('Ctrl Pts',(52.503850750664,16.077535486755,15.8018457094502));
#69573=CARTESIAN_POINT('Ctrl Pts',(54.2154808300007,15.9006366439348,15.7233401990734));
#69574=CARTESIAN_POINT('Ctrl Pts',(55.0120413695279,14.3753622311824,15.6448346886966));
#69575=CARTESIAN_POINT('Ctrl Pts',(54.1791579400318,12.8696146010229,15.5663291783198));
#69576=CARTESIAN_POINT('Ctrl Pts',(52.4637802022359,12.7337840295962,15.4878236679431));
#69577=CARTESIAN_POINT('Ctrl Pts',(51.4042996911802,14.0896865938602,15.4093181575663));
#69578=CARTESIAN_POINT('Ctrl Pts',(51.9508837188856,15.721316656963,15.3308126471895));
#69579=CARTESIAN_POINT('Ctrl Pts',(53.6133427309768,16.1653895531783,15.2523071368127));
#69580=CARTESIAN_POINT('Ctrl Pts',(54.9007439708605,15.0236502232965,15.1738016264359));
#69581=CARTESIAN_POINT('Ctrl Pts',(54.6585153839456,13.3200374976642,15.0952961160592));
#69582=CARTESIAN_POINT('Ctrl Pts',(53.1038933588347,12.5823920603089,15.0167906056824));
#69583=CARTESIAN_POINT('Ctrl Pts',(51.6310998196597,13.4722512894541,14.9382850953056));
#69584=CARTESIAN_POINT('Ctrl Pts',(51.5609711612585,15.1915694569347,14.8597795849288));
#69585=CARTESIAN_POINT('Ctrl Pts',(52.9564001587445,16.1984187666638,14.781274074552));
#69586=CARTESIAN_POINT('Ctrl Pts',(54.5659334636339,15.5898376428623,14.7027685641752));
#69587=CARTESIAN_POINT('Ctrl Pts',(54.9461022318155,13.911606374279,14.6242630537985));
#69588=CARTESIAN_POINT('Ctrl Pts',(53.7559643179138,12.6688223002735,14.5457575434217));
#69589=CARTESIAN_POINT('Ctrl Pts',(52.0628591682458,12.9760040856148,14.4672520330449));
#69590=CARTESIAN_POINT('Ctrl Pts',(51.3852128724656,14.5577438020024,14.3887465226681));
#69591=CARTESIAN_POINT('Ctrl Pts',(52.3307362917628,15.9953382094595,14.3102410122914));
#69592=CARTESIAN_POINT('Ctrl Pts',(54.0514987748276,15.9998443309588,14.2317355019146));
#69593=CARTESIAN_POINT('Ctrl Pts',(55.0042044918326,14.5665632650764,14.1532299915378));
#69594=CARTESIAN_POINT('Ctrl Pts',(54.3345957734335,12.9822233909154,14.074724481161));
#69595=CARTESIAN_POINT('Ctrl Pts',(52.6428908318491,12.6650114501325,13.9962189707842));
#69596=CARTESIAN_POINT('Ctrl Pts',(51.4468410434118,13.9049130927216,13.9177134604075));
#69597=CARTESIAN_POINT('Ctrl Pts',(51.6948674713958,15.0196330720529,13.8653764534896));
#69598=CARTESIAN_POINT('Ctrl Pts',(52.0259993620635,15.404095589155,13.8392079500307));
#69599=CARTESIAN_POINT('Ctrl Pts',(52.8205983740734,12.9961697745651,18.0535973499898));
#69600=CARTESIAN_POINT('Ctrl Pts',(52.3599004442679,13.11933387906,18.0274288465308));
#69601=CARTESIAN_POINT('Ctrl Pts',(51.5770224562856,13.8535123278672,17.975091839613));
#69602=CARTESIAN_POINT('Ctrl Pts',(51.8491027615147,15.449596585157,17.8965863292362));
#69603=CARTESIAN_POINT('Ctrl Pts',(53.3306005753027,16.0991388853812,17.8180808188594));
#69604=CARTESIAN_POINT('Ctrl Pts',(54.6895013936796,15.2235740807106,17.7395753084826));
#69605=CARTESIAN_POINT('Ctrl Pts',(54.7087686260452,13.6062036013327,17.6610697981059));
#69606=CARTESIAN_POINT('Ctrl Pts',(53.370302195588,12.6984745354833,17.5825642877291));
#69607=CARTESIAN_POINT('Ctrl Pts',(51.8748772355608,13.3139889999824,17.5040587773523));
#69608=CARTESIAN_POINT('Ctrl Pts',(51.5634249338332,14.9009722914672,17.4255532669755));
#69609=CARTESIAN_POINT('Ctrl Pts',(52.7153629422732,16.0360644703525,17.3470477565987));
#69610=CARTESIAN_POINT('Ctrl Pts',(54.2975564085964,15.7013451606169,17.268542246222));
#69611=CARTESIAN_POINT('Ctrl Pts',(54.8910811244797,14.1969702179137,17.1900367358452));
#69612=CARTESIAN_POINT('Ctrl Pts',(53.9636378718331,12.8721129164929,17.1115312254684));
#69613=CARTESIAN_POINT('Ctrl Pts',(52.3469858247822,12.9149298139051,17.0330257150916));
#69614=CARTESIAN_POINT('Ctrl Pts',(51.4909739917867,14.2870251506759,16.9545202047149));
#69615=CARTESIAN_POINT('Ctrl Pts',(52.1632956122413,15.75786949867,16.8760146943381));
#69616=CARTESIAN_POINT('Ctrl Pts',(53.7609959415415,16.0083755267644,16.7975091839613));
#69617=CARTESIAN_POINT('Ctrl Pts',(54.8512197038372,14.8138830536132,16.7190036735845));
#69618=CARTESIAN_POINT('Ctrl Pts',(54.4562281308452,13.2456415346295,16.6404981632077));
#69619=CARTESIAN_POINT('Ctrl Pts',(52.9302591446352,12.7100871437567,16.561992652831));
#69620=CARTESIAN_POINT('Ctrl Pts',(51.6418379657667,13.6875178418857,16.4834871424542));
#69621=CARTESIAN_POINT('Ctrl Pts',(51.7464513597646,15.3013505165395,16.4049816320774));
#69622=CARTESIAN_POINT('Ctrl Pts',(53.1502795370219,16.1042616709564,16.3264761217006));
#69623=CARTESIAN_POINT('Ctrl Pts',(54.5943360194344,15.3761814875148,16.2479706113238));
#69624=CARTESIAN_POINT('Ctrl Pts',(54.7835566204401,13.7700695869339,16.1694651009471));
#69625=CARTESIAN_POINT('Ctrl Pts',(53.5482438079086,12.7263253032243,16.0909595905703));
#69626=CARTESIAN_POINT('Ctrl Pts',(51.9962554793534,13.1810033244324,16.0124540801935));
#69627=CARTESIAN_POINT('Ctrl Pts',(51.5194516645429,14.7263375912924,15.9339485698167));
#69628=CARTESIAN_POINT('Ctrl Pts',(52.5454413598284,15.9764355954941,15.85544305944));
#69629=CARTESIAN_POINT('Ctrl Pts',(54.1540926149925,15.8101797269071,15.7769375490631));
#69630=CARTESIAN_POINT('Ctrl Pts',(54.9027287409836,14.376672202025,15.6984320386864));
#69631=CARTESIAN_POINT('Ctrl Pts',(54.1199550619984,12.9615166468276,15.6199265283096));
#69632=CARTESIAN_POINT('Ctrl Pts',(52.507781623182,12.8338582106659,15.5414210179328));
#69633=CARTESIAN_POINT('Ctrl Pts',(51.5120438907673,14.1081840058336,15.462915507556));
#69634=CARTESIAN_POINT('Ctrl Pts',(52.0257431373717,15.6416483803266,15.3844099971793));
#69635=CARTESIAN_POINT('Ctrl Pts',(53.5881816623453,16.0590039938468,15.3059044868025));
#69636=CARTESIAN_POINT('Ctrl Pts',(54.7981274593024,14.98595647718,15.2273989764257));
#69637=CARTESIAN_POINT('Ctrl Pts',(54.5704723572558,13.3848402181903,15.1488934660489));
#69638=CARTESIAN_POINT('Ctrl Pts',(53.1093828951162,12.691574615422,15.0703879556721));
#69639=CARTESIAN_POINT('Ctrl Pts',(51.7251987749646,13.5278961916579,14.9918824452954));
#69640=CARTESIAN_POINT('Ctrl Pts',(51.6592893499541,15.143772987429,14.9133769349186));
#69641=CARTESIAN_POINT('Ctrl Pts',(52.9707635028083,16.0900460317101,14.8348714245418));
#69642=CARTESIAN_POINT('Ctrl Pts',(54.4834605524781,15.5180796936027,14.756365914165));
#69643=CARTESIAN_POINT('Ctrl Pts',(54.8407567775752,13.9408178370524,14.6778604037883));
#69644=CARTESIAN_POINT('Ctrl Pts',(53.7222225381219,12.7728048506706,14.5993548934115));
#69645=CARTESIAN_POINT('Ctrl Pts',(52.1309816753803,13.0615052950706,14.5208493830347));
#69646=CARTESIAN_POINT('Ctrl Pts',(51.4941054148939,14.5480809347647,14.4423438726579));
#69647=CARTESIAN_POINT('Ctrl Pts',(52.3827421907963,15.8991836501767,14.3638383622811));
#69648=CARTESIAN_POINT('Ctrl Pts',(53.9999764060855,15.9034186645606,14.2853328519044));
#69649=CARTESIAN_POINT('Ctrl Pts',(54.8953633626268,14.5563697820544,14.2068273415276));
#69650=CARTESIAN_POINT('Ctrl Pts',(54.2660411052506,13.0673504209531,14.1283218311508));
#69651=CARTESIAN_POINT('Ctrl Pts',(52.676116208218,12.7692232772124,14.049816320774));
#69652=CARTESIAN_POINT('Ctrl Pts',(51.5520257773267,13.934527251307,13.9713108103972));
#69653=CARTESIAN_POINT('Ctrl Pts',(51.7851298980751,14.9821810145562,13.9189738034794));
#69654=CARTESIAN_POINT('Ctrl Pts',(52.0963395092977,15.3435126586808,13.8928053000205));
#69655=CARTESIAN_POINT('Ctrl Pts',(52.8445746335154,13.0858534785527,18.1071946999795));
#69656=CARTESIAN_POINT('Ctrl Pts',(52.4133685721046,13.2011331552574,18.0810261965206));
#69657=CARTESIAN_POINT('Ctrl Pts',(51.6806070120392,13.8883127078473,18.0286891896028));
#69658=CARTESIAN_POINT('Ctrl Pts',(51.9352699250133,15.3822226252555,17.950183679226));
#69659=CARTESIAN_POINT('Ctrl Pts',(53.3219287223341,15.9901840656676,17.8716781688492));
#69660=CARTESIAN_POINT('Ctrl Pts',(54.5938386481888,15.1706690939129,17.7931726584724));
#69661=CARTESIAN_POINT('Ctrl Pts',(54.6118724765286,13.6568356053423,17.7146671480956));
#69662=CARTESIAN_POINT('Ctrl Pts',(53.3590888183695,12.8072153878641,17.6361616377189));
#69663=CARTESIAN_POINT('Ctrl Pts',(51.9593944298553,13.3833273059057,17.5576561273421));
#69664=CARTESIAN_POINT('Ctrl Pts',(51.6678799435584,14.868718861572,17.4791506169653));
#69665=CARTESIAN_POINT('Ctrl Pts',(52.746075914221,15.9311473990782,17.4006451065885));
#69666=CARTESIAN_POINT('Ctrl Pts',(54.2269842684029,15.6178553569582,17.3221395962117));
#69667=CARTESIAN_POINT('Ctrl Pts',(54.7825141254484,14.2097839245511,17.243634085835));
#69668=CARTESIAN_POINT('Ctrl Pts',(53.9144417372685,12.9697381984539,17.1651285754582));
#69669=CARTESIAN_POINT('Ctrl Pts',(52.4012806901265,13.009814145187,17.0866230650814));
#69670=CARTESIAN_POINT('Ctrl Pts',(51.6000669942391,14.294073934023,17.0081175547046));
#69671=CARTESIAN_POINT('Ctrl Pts',(52.2293495223373,15.6707612538786,16.9296120443278));
#69672=CARTESIAN_POINT('Ctrl Pts',(53.7247720578873,15.9052309806687,16.8511065339511));
#69673=CARTESIAN_POINT('Ctrl Pts',(54.7452044587765,14.7872046961792,16.7726010235743));
#69674=CARTESIAN_POINT('Ctrl Pts',(54.3754985203273,13.3193551466328,16.6940955131975));
#69675=CARTESIAN_POINT('Ctrl Pts',(52.9472154007209,12.8180846076984,16.6155900028207));
#69676=CARTESIAN_POINT('Ctrl Pts',(51.7412733158221,13.7329444635267,16.5370844924439));
#69677=CARTESIAN_POINT('Ctrl Pts',(51.8391898174563,15.243466622173,16.4585789820672));
#69678=CARTESIAN_POINT('Ctrl Pts',(53.153151048991,15.9949789128949,16.3800734716904));
#69679=CARTESIAN_POINT('Ctrl Pts',(54.5047653453669,15.3135072413688,16.3015679613136));
#69680=CARTESIAN_POINT('Ctrl Pts',(54.6818728703171,13.8102116065761,16.2230624509368));
#69681=CARTESIAN_POINT('Ctrl Pts',(53.5256393862053,12.8332832711514,16.14455694056));
#69682=CARTESIAN_POINT('Ctrl Pts',(52.0730025688563,13.2588547922086,16.0660514301833));
#69683=CARTESIAN_POINT('Ctrl Pts',(51.6267216508219,14.7052635118164,15.9875459198065));
#69684=CARTESIAN_POINT('Ctrl Pts',(52.5870319689928,15.8753357042332,15.9090404094297));
#69685=CARTESIAN_POINT('Ctrl Pts',(54.0927043999843,15.7197228098794,15.8305348990529));
#69686=CARTESIAN_POINT('Ctrl Pts',(54.7934161124393,14.3779821728676,15.7520293886762));
#69687=CARTESIAN_POINT('Ctrl Pts',(54.060752183965,13.0534186926323,15.6735238782993));
#69688=CARTESIAN_POINT('Ctrl Pts',(52.551783044128,12.9339323917357,15.5950183679226));
#69689=CARTESIAN_POINT('Ctrl Pts',(51.6197880903543,14.1266814178069,15.5165128575458));
#69690=CARTESIAN_POINT('Ctrl Pts',(52.1006025558579,15.5619801036903,15.438007347169));
#69691=CARTESIAN_POINT('Ctrl Pts',(53.5630205937139,15.9526184345153,15.3595018367923));
#69692=CARTESIAN_POINT('Ctrl Pts',(54.6955109477442,14.9482627310635,15.2809963264155));
#69693=CARTESIAN_POINT('Ctrl Pts',(54.4824293305661,13.4496429387163,15.2024908160387));
#69694=CARTESIAN_POINT('Ctrl Pts',(53.1148724313975,12.8007571705352,15.1239853056619));
#69695=CARTESIAN_POINT('Ctrl Pts',(51.8192977302697,13.5835410938618,15.0454797952851));
#69696=CARTESIAN_POINT('Ctrl Pts',(51.7576075386496,15.0959765179234,14.9669742849084));
#69697=CARTESIAN_POINT('Ctrl Pts',(52.9851268468722,15.9816732967562,14.8884687745316));
#69698=CARTESIAN_POINT('Ctrl Pts',(54.4009876413224,15.4463217443432,14.8099632641548));
#69699=CARTESIAN_POINT('Ctrl Pts',(54.7354113233349,13.9700292998257,14.731457753778));
#69700=CARTESIAN_POINT('Ctrl Pts',(53.6884807583299,12.8767874010678,14.6529522434012));
#69701=CARTESIAN_POINT('Ctrl Pts',(52.1991041825149,13.1470065045264,14.5744467330245));
#69702=CARTESIAN_POINT('Ctrl Pts',(51.602997957322,14.5384180675271,14.4959412226477));
#69703=CARTESIAN_POINT('Ctrl Pts',(52.4347480898299,15.803029090894,14.4174357122709));
#69704=CARTESIAN_POINT('Ctrl Pts',(53.9484540373433,15.8069929981624,14.3389302018941));
#69705=CARTESIAN_POINT('Ctrl Pts',(54.7865222334211,14.5461762990323,14.2604246915173));
#69706=CARTESIAN_POINT('Ctrl Pts',(54.1974864370675,13.1524774509909,14.1819191811406));
#69707=CARTESIAN_POINT('Ctrl Pts',(52.7093415845871,12.8734351042922,14.1034136707638));
#69708=CARTESIAN_POINT('Ctrl Pts',(51.6572105112416,13.9641414098923,14.024908160387));
#69709=CARTESIAN_POINT('Ctrl Pts',(51.8753923247544,14.9447289570596,13.9725711534692));
#69710=CARTESIAN_POINT('Ctrl Pts',(52.166679656532,15.2829297282066,13.9464026500102));
#69711=CARTESIAN_POINT('Ctrl Pts',(52.8685508929575,13.1755371825404,18.1607920499693));
#69712=CARTESIAN_POINT('Ctrl Pts',(52.4668366999413,13.2829324314547,18.1346235465104));
#69713=CARTESIAN_POINT('Ctrl Pts',(51.7841915677929,13.9231130878275,18.0822865395925));
#69714=CARTESIAN_POINT('Ctrl Pts',(52.0214370885118,15.3148486653539,18.0037810292157));
#69715=CARTESIAN_POINT('Ctrl Pts',(53.3132568693655,15.881229245954,17.925275518839));
#69716=CARTESIAN_POINT('Ctrl Pts',(54.498175902698,15.1177641071152,17.8467700084622));
#69717=CARTESIAN_POINT('Ctrl Pts',(54.5149763270121,13.7074676093518,17.7682644980854));
#69718=CARTESIAN_POINT('Ctrl Pts',(53.347875441151,12.9159562402449,17.6897589877086));
#69719=CARTESIAN_POINT('Ctrl Pts',(52.0439116241498,13.4526656118291,17.6112534773318));
#69720=CARTESIAN_POINT('Ctrl Pts',(51.7723349532836,14.8364654316769,17.5327479669551));
#69721=CARTESIAN_POINT('Ctrl Pts',(52.7767888861689,15.826230327804,17.4542424565783));
#69722=CARTESIAN_POINT('Ctrl Pts',(54.1564121282093,15.5343655532995,17.3757369462015));
#69723=CARTESIAN_POINT('Ctrl Pts',(54.6739471264171,14.2225976311884,17.2972314358247));
#69724=CARTESIAN_POINT('Ctrl Pts',(53.8652456027039,13.0673634804149,17.218725925448));
#69725=CARTESIAN_POINT('Ctrl Pts',(52.4555755554707,13.104698476469,17.1402204150712));
#69726=CARTESIAN_POINT('Ctrl Pts',(51.7091599966917,14.3011227173701,17.0617149046944));
#69727=CARTESIAN_POINT('Ctrl Pts',(52.2954034324334,15.5836530090872,16.9832093943176));
#69728=CARTESIAN_POINT('Ctrl Pts',(53.6885481742333,15.802086434573,16.9047038839408));
#69729=CARTESIAN_POINT('Ctrl Pts',(54.6391892137158,14.7605263387452,16.8261983735641));
#69730=CARTESIAN_POINT('Ctrl Pts',(54.2947689098094,13.3930687586361,16.7476928631873));
#69731=CARTESIAN_POINT('Ctrl Pts',(52.9641716568067,12.9260820716401,16.6691873528105));
#69732=CARTESIAN_POINT('Ctrl Pts',(51.8407086658775,13.7783710851678,16.5906818424337));
#69733=CARTESIAN_POINT('Ctrl Pts',(51.931928275148,15.1855827278064,16.5121763320569));
#69734=CARTESIAN_POINT('Ctrl Pts',(53.15602256096,15.8856961548334,16.4336708216802));
#69735=CARTESIAN_POINT('Ctrl Pts',(54.4151946712995,15.2508329952228,16.3551653113034));
#69736=CARTESIAN_POINT('Ctrl Pts',(54.5801891201939,13.8503536262184,16.2766598009266));
#69737=CARTESIAN_POINT('Ctrl Pts',(53.5030349645019,12.9402412390784,16.1981542905498));
#69738=CARTESIAN_POINT('Ctrl Pts',(52.1497496583591,13.3367062599848,16.119648780173));
#69739=CARTESIAN_POINT('Ctrl Pts',(51.7339916371008,14.6841894323404,16.0411432697963));
#69740=CARTESIAN_POINT('Ctrl Pts',(52.6286225781573,15.7742358129723,15.9626377594195));
#69741=CARTESIAN_POINT('Ctrl Pts',(54.031316184976,15.6292658928517,15.8841322490427));
#69742=CARTESIAN_POINT('Ctrl Pts',(54.6841034838951,14.3792921437102,15.8056267386659));
#69743=CARTESIAN_POINT('Ctrl Pts',(54.0015493059315,13.1453207384369,15.7271212282891));
#69744=CARTESIAN_POINT('Ctrl Pts',(52.5957844650742,13.0340065728056,15.6486157179124));
#69745=CARTESIAN_POINT('Ctrl Pts',(51.7275322899413,14.1451788297802,15.5701102075356));
#69746=CARTESIAN_POINT('Ctrl Pts',(52.1754619743441,15.482311827054,15.4916046971588));
#69747=CARTESIAN_POINT('Ctrl Pts',(53.5378595250824,15.8462328751838,15.413099186782));
#69748=CARTESIAN_POINT('Ctrl Pts',(54.5928944361861,14.9105689849469,15.3345936764052));
#69749=CARTESIAN_POINT('Ctrl Pts',(54.3943863038764,13.5144456592424,15.2560881660285));
#69750=CARTESIAN_POINT('Ctrl Pts',(53.120361967679,12.9099397256483,15.1775826556517));
#69751=CARTESIAN_POINT('Ctrl Pts',(51.9133966855747,13.6391859960657,15.0990771452749));
#69752=CARTESIAN_POINT('Ctrl Pts',(51.8559257273451,15.0481800484177,15.0205716348981));
#69753=CARTESIAN_POINT('Ctrl Pts',(52.9994901909361,15.8733005618024,14.9420661245214));
#69754=CARTESIAN_POINT('Ctrl Pts',(54.3185147301667,15.3745637950836,14.8635606141446));
#69755=CARTESIAN_POINT('Ctrl Pts',(54.6300658690945,13.9992407625991,14.7850551037678));
#69756=CARTESIAN_POINT('Ctrl Pts',(53.654738978538,12.980769951465,14.706549593391));
#69757=CARTESIAN_POINT('Ctrl Pts',(52.2672266896493,13.2325077139822,14.6280440830142));
#69758=CARTESIAN_POINT('Ctrl Pts',(51.7118904997504,14.5287552002895,14.5495385726374));
#69759=CARTESIAN_POINT('Ctrl Pts',(52.4867539888634,15.7068745316113,14.4710330622607));
#69760=CARTESIAN_POINT('Ctrl Pts',(53.8969316686011,15.7105673317642,14.3925275518839));
#69761=CARTESIAN_POINT('Ctrl Pts',(54.6776811042154,14.5359828160102,14.3140220415071));
#69762=CARTESIAN_POINT('Ctrl Pts',(54.1289317688846,13.2376044810286,14.2355165311303));
#69763=CARTESIAN_POINT('Ctrl Pts',(52.742566960956,12.9776469313721,14.1570110207535));
#69764=CARTESIAN_POINT('Ctrl Pts',(51.7623952451565,13.9937555684777,14.0785055103768));
#69765=CARTESIAN_POINT('Ctrl Pts',(51.9656547514336,14.9072768995629,14.0261685034589));
#69766=CARTESIAN_POINT('Ctrl Pts',(52.2370198037663,15.2223467977324,14.));
#69767=CARTESIAN_POINT('Ctrl Pts',(51.9314271328212,14.3981451355535,17.5565803263806));
#69768=CARTESIAN_POINT('Ctrl Pts',(51.9304449349957,14.5245552242527,17.5486362065721));
#69769=CARTESIAN_POINT('Ctrl Pts',(51.9479261083582,14.6507002121319,17.5406920867636));
#69770=CARTESIAN_POINT('Ctrl Pts',(51.9850067205755,14.7707929443901,17.5327479669551));
#69771=CARTESIAN_POINT('Ctrl Pts',(52.107152930912,15.1663870637192,17.5065794634962));
#69772=CARTESIAN_POINT('Ctrl Pts',(52.4419709085405,15.4963086957616,17.4804109600372));
#69773=CARTESIAN_POINT('Ctrl Pts',(52.8393171043614,15.6126253826987,17.4542424565783));
#69774=CARTESIAN_POINT('Ctrl Pts',(53.2366633001824,15.7289420696358,17.4280739531194));
#69775=CARTESIAN_POINT('Ctrl Pts',(53.6965377141958,15.6316538114677,17.4019054496604));
#69776=CARTESIAN_POINT('Ctrl Pts',(54.0127307542372,15.3643816953651,17.3757369462015));
#69777=CARTESIAN_POINT('Ctrl Pts',(54.3289237942786,15.0971095792624,17.3495684427426));
#69778=CARTESIAN_POINT('Ctrl Pts',(54.5014354603479,14.6598536052254,17.3233999392837));
#69779=CARTESIAN_POINT('Ctrl Pts',(54.452907706097,14.248686593078,17.2972314358247));
#69780=CARTESIAN_POINT('Ctrl Pts',(54.4043799518461,13.8375195809306,17.2710629323658));
#69781=CARTESIAN_POINT('Ctrl Pts',(54.134812777275,13.4524415306728,17.2448944289069));
#69782=CARTESIAN_POINT('Ctrl Pts',(53.7650841821172,13.2661250048862,17.218725925448));
#69783=CARTESIAN_POINT('Ctrl Pts',(53.3953555869595,13.0798084790996,17.192557421989));
#69784=CARTESIAN_POINT('Ctrl Pts',(52.9254655712151,13.0922534777843,17.1663889185301));
#69785=CARTESIAN_POINT('Ctrl Pts',(52.5661179702131,13.2978800172768,17.1402204150712));
#69786=CARTESIAN_POINT('Ctrl Pts',(52.206770369211,13.5035065567693,17.1140519116122));
#69787=CARTESIAN_POINT('Ctrl Pts',(51.9579651829513,13.9023146370697,17.0878834081533));
#69788=CARTESIAN_POINT('Ctrl Pts',(51.9312698291118,14.3154737258394,17.0617149046944));
#69789=CARTESIAN_POINT('Ctrl Pts',(51.9295238448586,14.3424960034753,17.0600033785898));
#69790=CARTESIAN_POINT('Ctrl Pts',(51.9287279775559,14.3695796702729,17.0582918524852));
#69791=CARTESIAN_POINT('Ctrl Pts',(51.9288577112775,14.3966710926088,17.0565803263806));
#69792=CARTESIAN_POINT('Origin',(53.1951359564886,14.3971354987959,15.5));
#69793=CARTESIAN_POINT('Origin',(53.1951359564886,14.3971354987959,13.));
#69794=CARTESIAN_POINT('',(53.1951359564886,14.3971354987959,13.));
#69795=CARTESIAN_POINT('Origin',(53.1951359564886,14.3971354987959,13.));
#69796=CARTESIAN_POINT('',(53.1951359564886,14.3971354987959,13.));
#69797=CARTESIAN_POINT('Origin',(38.7910352698572,-39.2874736104613,10.));
#69798=CARTESIAN_POINT('',(37.4169463095016,-41.3759849293267,8.5));
#69799=CARTESIAN_POINT('Origin',(37.4169463095016,-41.3759849293267,10.));
#69800=CARTESIAN_POINT('',(36.8673107253594,-42.2113894568729,8.5));
#69801=CARTESIAN_POINT('',(38.7910352698572,-39.2874736104613,8.5));
#69802=CARTESIAN_POINT('Origin',(36.8673107253594,-42.2113894568729,10.));
#69803=CARTESIAN_POINT('Origin',(39.0658530619283,-38.8697713466882,10.));
#69804=CARTESIAN_POINT('',(40.714759814355,-36.3635577640498,7.));
#69805=CARTESIAN_POINT('Origin',(40.714759814355,-36.3635577640498,10.));
#69806=CARTESIAN_POINT('',(39.0658530619283,-38.8697713466882,7.));
#69807=CARTESIAN_POINT('',(37.4169463095016,-41.3759849293267,7.));
#69808=CARTESIAN_POINT('',(39.0658530619283,-38.8697713466882,7.));
#69809=CARTESIAN_POINT('Origin',(37.4169463095016,-41.3759849293267,10.));
#69810=CARTESIAN_POINT('Origin',(37.4169463095016,-41.3759849293267,10.));
#69811=CARTESIAN_POINT('Origin',(-14.6284325622417,-53.2377587880251,10.));
#69812=CARTESIAN_POINT('',(-17.2116250730252,-54.5894675037741,10.));
#69813=CARTESIAN_POINT('Origin',(-17.1241809006482,-53.0920185007302,10.));
#69814=CARTESIAN_POINT('',(-18.2099244083879,-54.5311713888561,10.));
#69815=CARTESIAN_POINT('',(-14.7158767346186,-54.7352077910691,10.));
#69816=CARTESIAN_POINT('Origin',(-18.1224802360109,-53.0337223858122,10.));
#69817=CARTESIAN_POINT('Origin',(-14.1292828945603,-53.2669068454841,10.));
#69818=CARTESIAN_POINT('',(-11.1343848884725,-53.4417951902381,7.));
#69819=CARTESIAN_POINT('Origin',(-11.1343848884725,-53.4417951902381,10.));
#69820=CARTESIAN_POINT('',(-14.1292828945603,-53.2669068454841,7.));
#69821=CARTESIAN_POINT('',(-17.1241809006482,-53.0920185007302,7.));
#69822=CARTESIAN_POINT('',(-14.1292828945603,-53.2669068454841,7.));
#69823=CARTESIAN_POINT('Origin',(-17.1241809006482,-53.0920185007302,10.));
#69824=CARTESIAN_POINT('Origin',(-17.1241809006482,-53.0920185007302,10.));
#69825=CARTESIAN_POINT('Origin',(-53.4194678320988,-13.9502851775638,10.));
#69826=CARTESIAN_POINT('',(-54.5411272101499,-11.7160335714034,11.5));
#69827=CARTESIAN_POINT('Origin',(-54.5411272101499,-11.7160335714034,10.));
#69828=CARTESIAN_POINT('',(-54.9897909613702,-10.8223329289393,11.5));
#69829=CARTESIAN_POINT('',(-53.4194678320988,-13.9502851775638,11.5));
#69830=CARTESIAN_POINT('Origin',(-54.9897909613702,-10.8223329289393,10.));
#69831=CARTESIAN_POINT('Origin',(-53.1951359564886,-14.3971354987959,10.));
#69832=CARTESIAN_POINT('',(-51.8491447028274,-17.0782374261884,7.));
#69833=CARTESIAN_POINT('Origin',(-51.8491447028274,-17.0782374261884,10.));
#69834=CARTESIAN_POINT('',(-53.1951359564886,-14.3971354987959,7.));
#69835=CARTESIAN_POINT('',(-54.5411272101499,-11.7160335714034,7.));
#69836=CARTESIAN_POINT('',(-53.1951359564886,-14.3971354987959,7.));
#69837=CARTESIAN_POINT('Origin',(-54.5411272101499,-11.7160335714034,10.));
#69838=CARTESIAN_POINT('Origin',(-54.5411272101499,-11.7160335714034,10.));
#69839=CARTESIAN_POINT('Origin',(-38.7910352698572,39.2874736104613,10.));
#69840=CARTESIAN_POINT('',(-37.4169463095016,41.3759849293267,11.5));
#69841=CARTESIAN_POINT('Origin',(-37.4169463095016,41.3759849293267,10.));
#69842=CARTESIAN_POINT('',(-36.8673107253594,42.2113894568729,11.5));
#69843=CARTESIAN_POINT('',(-38.7910352698572,39.2874736104613,11.5));
#69844=CARTESIAN_POINT('Origin',(-36.8673107253594,42.2113894568729,10.));
#69845=CARTESIAN_POINT('Origin',(-39.0658530619283,38.8697713466882,10.));
#69846=CARTESIAN_POINT('',(-40.714759814355,36.3635577640498,7.));
#69847=CARTESIAN_POINT('Origin',(-40.714759814355,36.3635577640498,10.));
#69848=CARTESIAN_POINT('',(-39.0658530619283,38.8697713466882,7.));
#69849=CARTESIAN_POINT('',(-37.4169463095016,41.3759849293267,7.));
#69850=CARTESIAN_POINT('',(-39.0658530619283,38.8697713466882,7.));
#69851=CARTESIAN_POINT('Origin',(-37.4169463095016,41.3759849293267,10.));
#69852=CARTESIAN_POINT('Origin',(-37.4169463095016,41.3759849293267,10.));
#69853=CARTESIAN_POINT('Origin',(14.6284325622417,53.2377587880251,10.));
#69854=CARTESIAN_POINT('',(17.2116250730252,54.5894675037741,10.));
#69855=CARTESIAN_POINT('Origin',(17.1241809006482,53.0920185007302,10.));
#69856=CARTESIAN_POINT('',(18.2099244083878,54.5311713888561,10.));
#69857=CARTESIAN_POINT('',(14.7158767346186,54.7352077910691,10.));
#69858=CARTESIAN_POINT('Origin',(18.1224802360108,53.0337223858122,10.));
#69859=CARTESIAN_POINT('Origin',(14.1292828945603,53.2669068454841,10.));
#69860=CARTESIAN_POINT('',(11.1343848884724,53.4417951902381,7.));
#69861=CARTESIAN_POINT('Origin',(11.1343848884724,53.4417951902381,10.));
#69862=CARTESIAN_POINT('',(14.1292828945603,53.2669068454841,7.));
#69863=CARTESIAN_POINT('',(17.1241809006482,53.0920185007302,7.));
#69864=CARTESIAN_POINT('',(14.1292828945603,53.2669068454841,7.));
#69865=CARTESIAN_POINT('Origin',(17.1241809006482,53.0920185007302,10.));
#69866=CARTESIAN_POINT('Origin',(17.1241809006482,53.0920185007302,10.));
#69867=CARTESIAN_POINT('Origin',(53.4194678320988,13.9502851775638,10.));
#69868=CARTESIAN_POINT('',(54.5411272101499,11.7160335714034,8.5));
#69869=CARTESIAN_POINT('Origin',(54.5411272101499,11.7160335714034,10.));
#69870=CARTESIAN_POINT('',(54.9897909613702,10.8223329289393,8.5));
#69871=CARTESIAN_POINT('',(53.4194678320988,13.9502851775638,8.5));
#69872=CARTESIAN_POINT('Origin',(54.9897909613702,10.8223329289393,10.));
#69873=CARTESIAN_POINT('Origin',(53.1951359564886,14.3971354987959,10.));
#69874=CARTESIAN_POINT('',(51.8491447028274,17.0782374261884,7.));
#69875=CARTESIAN_POINT('Origin',(51.8491447028274,17.0782374261884,10.));
#69876=CARTESIAN_POINT('',(53.1951359564886,14.3971354987959,7.));
#69877=CARTESIAN_POINT('',(54.5411272101499,11.7160335714034,7.));
#69878=CARTESIAN_POINT('',(53.1951359564886,14.3971354987959,7.));
#69879=CARTESIAN_POINT('Origin',(54.5411272101499,11.7160335714034,10.));
#69880=CARTESIAN_POINT('Origin',(54.5411272101499,11.7160335714034,10.));
#69881=CARTESIAN_POINT('Origin',(32.7784168026664,-31.1420197146986,2.));
#69882=CARTESIAN_POINT('',(29.4485343854062,-36.2031892017778,2.));
#69883=CARTESIAN_POINT('Ctrl Pts',(29.4485343857591,-36.2031892014269,2.));
#69884=CARTESIAN_POINT('Ctrl Pts',(29.4485343857591,-36.2031892014269,4.66666666666667));
#69885=CARTESIAN_POINT('Ctrl Pts',(29.4485343857591,-36.2031892014269,7.33333333333333));
#69886=CARTESIAN_POINT('Ctrl Pts',(29.4485343857591,-36.2031892014269,12.6666666666667));
#69887=CARTESIAN_POINT('Ctrl Pts',(29.4485343857591,-36.2031892014269,15.3333333333333));
#69888=CARTESIAN_POINT('Ctrl Pts',(29.4485343857591,-36.2031892014269,18.));
#69889=CARTESIAN_POINT('',(28.9309677136708,-36.9898514075217,2.));
#69890=CARTESIAN_POINT('',(32.7784168026664,-31.1420197146986,2.));
#69891=CARTESIAN_POINT('',(28.9309677136708,-36.9898514075217,2.));
#69892=CARTESIAN_POINT('Origin',(43.6386756607666,-38.2872823085476,2.));
#69893=CARTESIAN_POINT('',(34.5017338047181,-32.2758373034865,2.));
#69894=CARTESIAN_POINT('Ctrl Pts',(34.5017338047181,-32.2758373034865,18.));
#69895=CARTESIAN_POINT('Ctrl Pts',(34.5017338047181,-32.2758373034865,15.3333333333333));
#69896=CARTESIAN_POINT('Ctrl Pts',(34.5017338047181,-32.2758373034865,12.6666666666667));
#69897=CARTESIAN_POINT('Ctrl Pts',(34.5017338047181,-32.2758373034865,7.33333333333333));
#69898=CARTESIAN_POINT('Ctrl Pts',(34.5017338047181,-32.2758373034865,4.66666666666667));
#69899=CARTESIAN_POINT('Ctrl Pts',(34.5017338047181,-32.2758373034865,2.));
#69900=CARTESIAN_POINT('',(43.6386756607666,-38.2872823085476,2.));
#69901=CARTESIAN_POINT('',(43.6386756607666,-38.2872823085476,2.));
#69902=CARTESIAN_POINT('',(43.6386756607666,-38.2872823085476,2.));
#69903=CARTESIAN_POINT('Origin',(39.7912265717709,-44.1351140013707,2.));
#69904=CARTESIAN_POINT('',(39.7912265717709,-44.1351140013707,2.));
#69905=CARTESIAN_POINT('',(39.7912265717709,-44.1351140013707,2.));
#69906=CARTESIAN_POINT('',(39.7912265717709,-44.1351140013707,2.));
#69907=CARTESIAN_POINT('Origin',(28.9309677136708,-36.9898514075217,2.));
#69908=CARTESIAN_POINT('',(28.9309677136708,-36.9898514075217,2.));
#69909=CARTESIAN_POINT('Origin',(-11.3384212906854,-56.9358428640073,2.));
#69910=CARTESIAN_POINT('',(-10.7008281308737,-46.0172966012375,2.));
#69911=CARTESIAN_POINT('Ctrl Pts',(-10.7008281308737,-46.0172966012375,
18.));
#69912=CARTESIAN_POINT('Ctrl Pts',(-10.7008281308737,-46.0172966012375,
15.3333333333333));
#69913=CARTESIAN_POINT('Ctrl Pts',(-10.7008281308737,-46.0172966012375,
12.6666666666667));
#69914=CARTESIAN_POINT('Ctrl Pts',(-10.7008281308737,-46.0172966012375,
7.33333333333333));
#69915=CARTESIAN_POINT('Ctrl Pts',(-10.7008281308737,-46.0172966012375,
4.66666666666667));
#69916=CARTESIAN_POINT('Ctrl Pts',(-10.7008281308737,-46.0172966012375,
2.));
#69917=CARTESIAN_POINT('',(-11.3384212906854,-56.9358428640073,2.));
#69918=CARTESIAN_POINT('',(-11.3384212906854,-56.9358428640073,2.));
#69919=CARTESIAN_POINT('',(-11.3384212906854,-56.9358428640073,2.));
#69920=CARTESIAN_POINT('Origin',(-18.3265166382238,-56.5277700595814,2.));
#69921=CARTESIAN_POINT('',(-18.3265166382238,-56.5277700595814,2.));
#69922=CARTESIAN_POINT('',(-18.3265166382238,-56.5277700595814,2.));
#69923=CARTESIAN_POINT('',(-18.3265166382238,-56.5277700595814,2.));
#69924=CARTESIAN_POINT('Origin',(-17.56866714429,-43.5498786998672,2.));
#69925=CARTESIAN_POINT('',(-17.56866714429,-43.5498786998672,2.));
#69926=CARTESIAN_POINT('',(-17.56866714429,-43.5498786998672,2.));
#69927=CARTESIAN_POINT('',(-17.56866714429,-43.5498786998672,2.));
#69928=CARTESIAN_POINT('Origin',(-10.5805717967516,-43.9579515042931,2.));
#69929=CARTESIAN_POINT('',(-16.6286143535706,-43.6047734830004,2.));
#69930=CARTESIAN_POINT('Ctrl Pts',(-16.6286143535706,-43.6047734830004,
2.));
#69931=CARTESIAN_POINT('Ctrl Pts',(-16.6286143535706,-43.6047734830004,
4.66666666666667));
#69932=CARTESIAN_POINT('Ctrl Pts',(-16.6286143535706,-43.6047734830004,
7.33333333333333));
#69933=CARTESIAN_POINT('Ctrl Pts',(-16.6286143535706,-43.6047734830004,
12.6666666666667));
#69934=CARTESIAN_POINT('Ctrl Pts',(-16.6286143535706,-43.6047734830004,
15.3333333333333));
#69935=CARTESIAN_POINT('Ctrl Pts',(-16.6286143535706,-43.6047734830004,
18.));
#69936=CARTESIAN_POINT('',(-10.5805717967516,-43.9579515042931,2.));
#69937=CARTESIAN_POINT('Origin',(-54.977096951452,-18.6485605554598,2.));
#69938=CARTESIAN_POINT('',(-45.2025619355918,-13.741459297751,2.));
#69939=CARTESIAN_POINT('Ctrl Pts',(-45.2025619355918,-13.741459297751,18.));
#69940=CARTESIAN_POINT('Ctrl Pts',(-45.2025619355918,-13.741459297751,15.3333333333333));
#69941=CARTESIAN_POINT('Ctrl Pts',(-45.2025619355918,-13.741459297751,12.6666666666667));
#69942=CARTESIAN_POINT('Ctrl Pts',(-45.2025619355918,-13.741459297751,7.33333333333333));
#69943=CARTESIAN_POINT('Ctrl Pts',(-45.2025619355918,-13.741459297751,4.66666666666667));
#69944=CARTESIAN_POINT('Ctrl Pts',(-45.2025619355918,-13.741459297751,2.));
#69945=CARTESIAN_POINT('',(-54.977096951452,-18.6485605554598,2.));
#69946=CARTESIAN_POINT('',(-54.977096951452,-18.6485605554598,2.));
#69947=CARTESIAN_POINT('',(-54.977096951452,-18.6485605554598,2.));
#69948=CARTESIAN_POINT('Origin',(-58.1177432099948,-12.3926560582107,2.));
#69949=CARTESIAN_POINT('',(-58.1177432099948,-12.3926560582107,2.));
#69950=CARTESIAN_POINT('',(-58.1177432099948,-12.3926560582107,2.));
#69951=CARTESIAN_POINT('',(-58.1177432099948,-12.3926560582107,2.));
#69952=CARTESIAN_POINT('Origin',(-46.4996348579608,-6.56002729234549,2.));
#69953=CARTESIAN_POINT('',(-46.4996348579608,-6.56002729234549,2.));
#69954=CARTESIAN_POINT('',(-46.4996348579608,-6.56002729234549,2.));
#69955=CARTESIAN_POINT('',(-46.4996348579608,-6.56002729234549,2.));
#69956=CARTESIAN_POINT('Origin',(-43.358988599418,-12.8159317895946,2.));
#69957=CARTESIAN_POINT('',(-46.0771487393297,-7.40158428157358,2.));
#69958=CARTESIAN_POINT('Ctrl Pts',(-46.0771487393297,-7.40158428157357,
2.));
#69959=CARTESIAN_POINT('Ctrl Pts',(-46.0771487393297,-7.40158428157357,
4.66666666666667));
#69960=CARTESIAN_POINT('Ctrl Pts',(-46.0771487393297,-7.40158428157357,
7.33333333333333));
#69961=CARTESIAN_POINT('Ctrl Pts',(-46.0771487393297,-7.40158428157357,
12.6666666666667));
#69962=CARTESIAN_POINT('Ctrl Pts',(-46.0771487393297,-7.40158428157357,
15.3333333333333));
#69963=CARTESIAN_POINT('Ctrl Pts',(-46.0771487393297,-7.40158428157357,
18.));
#69964=CARTESIAN_POINT('',(-43.358988599418,-12.8159317895946,2.));
#69965=CARTESIAN_POINT('Origin',(-43.6386756607666,38.2872823085476,2.));
#69966=CARTESIAN_POINT('',(-34.5017338047182,32.2758373034865,2.));
#69967=CARTESIAN_POINT('Ctrl Pts',(-34.5017338047182,32.2758373034865,18.));
#69968=CARTESIAN_POINT('Ctrl Pts',(-34.5017338047182,32.2758373034865,15.3333333333333));
#69969=CARTESIAN_POINT('Ctrl Pts',(-34.5017338047182,32.2758373034865,12.6666666666667));
#69970=CARTESIAN_POINT('Ctrl Pts',(-34.5017338047182,32.2758373034865,7.33333333333333));
#69971=CARTESIAN_POINT('Ctrl Pts',(-34.5017338047182,32.2758373034865,4.66666666666667));
#69972=CARTESIAN_POINT('Ctrl Pts',(-34.5017338047182,32.2758373034865,2.));
#69973=CARTESIAN_POINT('',(-43.6386756607666,38.2872823085476,2.));
#69974=CARTESIAN_POINT('',(-43.6386756607666,38.2872823085476,2.));
#69975=CARTESIAN_POINT('',(-43.6386756607666,38.2872823085476,2.));
#69976=CARTESIAN_POINT('Origin',(-39.791226571771,44.1351140013707,2.));
#69977=CARTESIAN_POINT('',(-39.791226571771,44.1351140013707,2.));
#69978=CARTESIAN_POINT('',(-39.791226571771,44.1351140013707,2.));
#69979=CARTESIAN_POINT('',(-39.791226571771,44.1351140013707,2.));
#69980=CARTESIAN_POINT('Origin',(-28.9309677136708,36.9898514075217,2.));
#69981=CARTESIAN_POINT('',(-28.9309677136708,36.9898514075217,2.));
#69982=CARTESIAN_POINT('',(-28.9309677136708,36.9898514075217,2.));
#69983=CARTESIAN_POINT('',(-28.9309677136708,36.9898514075217,2.));
#69984=CARTESIAN_POINT('Origin',(-32.7784168026664,31.1420197146986,2.));
#69985=CARTESIAN_POINT('',(-29.4485343857591,36.2031892014269,2.));
#69986=CARTESIAN_POINT('Ctrl Pts',(-29.4485343857591,36.2031892014269,2.));
#69987=CARTESIAN_POINT('Ctrl Pts',(-29.4485343857591,36.2031892014269,4.66666666666667));
#69988=CARTESIAN_POINT('Ctrl Pts',(-29.4485343857591,36.2031892014269,7.33333333333333));
#69989=CARTESIAN_POINT('Ctrl Pts',(-29.4485343857591,36.2031892014269,12.6666666666667));
#69990=CARTESIAN_POINT('Ctrl Pts',(-29.4485343857591,36.2031892014269,15.3333333333333));
#69991=CARTESIAN_POINT('Ctrl Pts',(-29.4485343857591,36.2031892014269,18.));
#69992=CARTESIAN_POINT('',(-32.7784168026664,31.1420197146986,2.));
#69993=CARTESIAN_POINT('Origin',(10.5805717967515,43.9579515042931,2.));
#69994=CARTESIAN_POINT('',(16.6286143540509,43.6047734828703,2.));
#69995=CARTESIAN_POINT('Ctrl Pts',(16.6286143535706,43.6047734830004,2.));
#69996=CARTESIAN_POINT('Ctrl Pts',(16.6286143535706,43.6047734830004,4.66666666666667));
#69997=CARTESIAN_POINT('Ctrl Pts',(16.6286143535706,43.6047734830004,7.33333333333333));
#69998=CARTESIAN_POINT('Ctrl Pts',(16.6286143535706,43.6047734830004,12.6666666666667));
#69999=CARTESIAN_POINT('Ctrl Pts',(16.6286143535706,43.6047734830004,15.3333333333333));
#70000=CARTESIAN_POINT('Ctrl Pts',(16.6286143535706,43.6047734830004,18.));
#70001=CARTESIAN_POINT('',(17.56866714429,43.5498786998672,2.));
#70002=CARTESIAN_POINT('',(10.5805717967515,43.9579515042931,2.));
#70003=CARTESIAN_POINT('',(17.56866714429,43.5498786998672,2.));
#70004=CARTESIAN_POINT('Origin',(11.3384212906854,56.9358428640073,2.));
#70005=CARTESIAN_POINT('',(10.7008281308737,46.0172966012375,2.));
#70006=CARTESIAN_POINT('Ctrl Pts',(10.7008281308737,46.0172966012375,18.));
#70007=CARTESIAN_POINT('Ctrl Pts',(10.7008281308737,46.0172966012375,15.3333333333333));
#70008=CARTESIAN_POINT('Ctrl Pts',(10.7008281308737,46.0172966012375,12.6666666666667));
#70009=CARTESIAN_POINT('Ctrl Pts',(10.7008281308737,46.0172966012375,7.33333333333333));
#70010=CARTESIAN_POINT('Ctrl Pts',(10.7008281308737,46.0172966012375,4.66666666666667));
#70011=CARTESIAN_POINT('Ctrl Pts',(10.7008281308737,46.0172966012375,2.));
#70012=CARTESIAN_POINT('',(11.3384212906854,56.9358428640073,2.));
#70013=CARTESIAN_POINT('',(11.3384212906854,56.9358428640073,2.));
#70014=CARTESIAN_POINT('',(11.3384212906854,56.9358428640073,2.));
#70015=CARTESIAN_POINT('Origin',(18.3265166382238,56.5277700595814,2.));
#70016=CARTESIAN_POINT('',(18.3265166382238,56.5277700595814,2.));
#70017=CARTESIAN_POINT('',(18.3265166382238,56.5277700595814,2.));
#70018=CARTESIAN_POINT('',(18.3265166382238,56.5277700595814,2.));
#70019=CARTESIAN_POINT('Origin',(17.56866714429,43.5498786998672,2.));
#70020=CARTESIAN_POINT('',(17.56866714429,43.5498786998672,2.));
#70021=CARTESIAN_POINT('Ctrl Pts',(46.0449384185095,-16.7589870229578,0.));
#70022=CARTESIAN_POINT('Ctrl Pts',(46.0449384185095,-16.7589870229578,20.));
#70023=CARTESIAN_POINT('Ctrl Pts',(46.0420594924752,-16.7651130917503,0.));
#70024=CARTESIAN_POINT('Ctrl Pts',(46.0420594924752,-16.7651130917503,20.));
#70025=CARTESIAN_POINT('Ctrl Pts',(46.0362995834799,-16.7773641333857,0.));
#70026=CARTESIAN_POINT('Ctrl Pts',(46.0362995834799,-16.7773641333857,20.));
#70027=CARTESIAN_POINT('Ctrl Pts',(46.0276535492064,-16.79573740799,0.));
#70028=CARTESIAN_POINT('Ctrl Pts',(46.0276535492064,-16.79573740799,20.));
#70029=CARTESIAN_POINT('Ctrl Pts',(46.0161131619282,-16.8202285317553,0.));
#70030=CARTESIAN_POINT('Ctrl Pts',(46.0161131619282,-16.8202285317553,20.));
#70031=CARTESIAN_POINT('Ctrl Pts',(46.0016671088634,-16.8508314760754,0.));
#70032=CARTESIAN_POINT('Ctrl Pts',(46.0016671088634,-16.8508314760754,20.));
#70033=CARTESIAN_POINT('Ctrl Pts',(45.9872004880192,-16.8814234574889,0.));
#70034=CARTESIAN_POINT('Ctrl Pts',(45.9872004880192,-16.8814234574889,20.));
#70035=CARTESIAN_POINT('Ctrl Pts',(45.9727133019197,-16.9120044710149,0.));
#70036=CARTESIAN_POINT('Ctrl Pts',(45.9727133019197,-16.9120044710149,20.));
#70037=CARTESIAN_POINT('Ctrl Pts',(45.9582055548827,-16.9425745084438,0.));
#70038=CARTESIAN_POINT('Ctrl Pts',(45.9582055548827,-16.9425745084438,20.));
#70039=CARTESIAN_POINT('Ctrl Pts',(45.9436772535459,-16.9731335574459,0.));
#70040=CARTESIAN_POINT('Ctrl Pts',(45.9436772535459,-16.9731335574459,20.));
#70041=CARTESIAN_POINT('Ctrl Pts',(45.9291284062576,-17.0036816026634,0.));
#70042=CARTESIAN_POINT('Ctrl Pts',(45.9291284062576,-17.0036816026634,20.));
#70043=CARTESIAN_POINT('Ctrl Pts',(45.91455902239,-17.0342186269342,0.));
#70044=CARTESIAN_POINT('Ctrl Pts',(45.91455902239,-17.0342186269342,20.));
#70045=CARTESIAN_POINT('Ctrl Pts',(45.8999691116666,-17.0647446124944,0.));
#70046=CARTESIAN_POINT('Ctrl Pts',(45.8999691116666,-17.0647446124944,20.));
#70047=CARTESIAN_POINT('Ctrl Pts',(45.8853586835176,-17.09525954213,0.));
#70048=CARTESIAN_POINT('Ctrl Pts',(45.8853586835176,-17.09525954213,20.));
#70049=CARTESIAN_POINT('Ctrl Pts',(45.8707277463338,-17.1257634005084,0.));
#70050=CARTESIAN_POINT('Ctrl Pts',(45.8707277463338,-17.1257634005084,20.));
#70051=CARTESIAN_POINT('Ctrl Pts',(45.8560763076625,-17.1562561738292,0.));
#70052=CARTESIAN_POINT('Ctrl Pts',(45.8560763076625,-17.1562561738292,20.));
#70053=CARTESIAN_POINT('Ctrl Pts',(45.8414043745501,-17.1867378492105,0.));
#70054=CARTESIAN_POINT('Ctrl Pts',(45.8414043745501,-17.1867378492105,20.));
#70055=CARTESIAN_POINT('Ctrl Pts',(45.8267119538424,-17.2172084141516,0.));
#70056=CARTESIAN_POINT('Ctrl Pts',(45.8267119538424,-17.2172084141516,20.));
#70057=CARTESIAN_POINT('Ctrl Pts',(45.8119990524823,-17.247667856,0.));
#70058=CARTESIAN_POINT('Ctrl Pts',(45.8119990524823,-17.247667856,20.));
#70059=CARTESIAN_POINT('Ctrl Pts',(45.7972656778619,-17.2781161613228,0.));
#70060=CARTESIAN_POINT('Ctrl Pts',(45.7972656778619,-17.2781161613228,20.));
#70061=CARTESIAN_POINT('Ctrl Pts',(45.7825118377706,-17.3085533159982,0.));
#70062=CARTESIAN_POINT('Ctrl Pts',(45.7825118377706,-17.3085533159982,20.));
#70063=CARTESIAN_POINT('Ctrl Pts',(45.7677375402375,-17.3389793054985,0.));
#70064=CARTESIAN_POINT('Ctrl Pts',(45.7677375402375,-17.3389793054985,20.));
#70065=CARTESIAN_POINT('Ctrl Pts',(45.7529427934047,-17.3693941151172,0.));
#70066=CARTESIAN_POINT('Ctrl Pts',(45.7529427934047,-17.3693941151172,20.));
#70067=CARTESIAN_POINT('Ctrl Pts',(45.7381276053971,-17.3997977302007,0.));
#70068=CARTESIAN_POINT('Ctrl Pts',(45.7381276053971,-17.3997977302007,20.));
#70069=CARTESIAN_POINT('Ctrl Pts',(45.7232919841685,-17.4301901364248,0.));
#70070=CARTESIAN_POINT('Ctrl Pts',(45.7232919841685,-17.4301901364248,20.));
#70071=CARTESIAN_POINT('Ctrl Pts',(45.7084359375081,-17.460571319782,0.));
#70072=CARTESIAN_POINT('Ctrl Pts',(45.7084359375081,-17.460571319782,20.));
#70073=CARTESIAN_POINT('Ctrl Pts',(45.6935594731126,-17.490941266452,0.));
#70074=CARTESIAN_POINT('Ctrl Pts',(45.6935594731126,-17.490941266452,20.));
#70075=CARTESIAN_POINT('Ctrl Pts',(45.67866259864,-17.5212999627071,0.));
#70076=CARTESIAN_POINT('Ctrl Pts',(45.67866259864,-17.5212999627071,20.));
#70077=CARTESIAN_POINT('Ctrl Pts',(45.6637453217655,-17.5516473948116,0.));
#70078=CARTESIAN_POINT('Ctrl Pts',(45.6637453217655,-17.5516473948116,20.));
#70079=CARTESIAN_POINT('Ctrl Pts',(45.6488076502485,-17.5819835489016,0.));
#70080=CARTESIAN_POINT('Ctrl Pts',(45.6488076502485,-17.5819835489016,20.));
#70081=CARTESIAN_POINT('Ctrl Pts',(45.6338495919363,-17.6123084109794,0.));
#70082=CARTESIAN_POINT('Ctrl Pts',(45.6338495919363,-17.6123084109794,20.));
#70083=CARTESIAN_POINT('Ctrl Pts',(45.6188711547313,-17.6426219669712,0.));
#70084=CARTESIAN_POINT('Ctrl Pts',(45.6188711547313,-17.6426219669712,20.));
#70085=CARTESIAN_POINT('Ctrl Pts',(45.6038723465685,-17.672924202767,0.));
#70086=CARTESIAN_POINT('Ctrl Pts',(45.6038723465685,-17.672924202767,20.));
#70087=CARTESIAN_POINT('Ctrl Pts',(45.5888531753911,-17.7032151042646,0.));
#70088=CARTESIAN_POINT('Ctrl Pts',(45.5888531753911,-17.7032151042646,20.));
#70089=CARTESIAN_POINT('Ctrl Pts',(45.5738136491221,-17.7334946574206,0.));
#70090=CARTESIAN_POINT('Ctrl Pts',(45.5738136491221,-17.7334946574206,20.));
#70091=CARTESIAN_POINT('Ctrl Pts',(45.5587537756595,-17.7637628482589,0.));
#70092=CARTESIAN_POINT('Ctrl Pts',(45.5587537756595,-17.7637628482589,20.));
#70093=CARTESIAN_POINT('Ctrl Pts',(45.5436735628911,-17.7940196628443,0.));
#70094=CARTESIAN_POINT('Ctrl Pts',(45.5436735628911,-17.7940196628443,20.));
#70095=CARTESIAN_POINT('Ctrl Pts',(45.528573018704,-17.8242650872661,0.));
#70096=CARTESIAN_POINT('Ctrl Pts',(45.528573018704,-17.8242650872661,20.));
#70097=CARTESIAN_POINT('Ctrl Pts',(45.5134521509949,-17.8544991076192,0.));
#70098=CARTESIAN_POINT('Ctrl Pts',(45.5134521509949,-17.8544991076192,20.));
#70099=CARTESIAN_POINT('Ctrl Pts',(45.498310967683,-17.8847217099814,0.));
#70100=CARTESIAN_POINT('Ctrl Pts',(45.498310967683,-17.8847217099814,20.));
#70101=CARTESIAN_POINT('Ctrl Pts',(45.4831494767122,-17.9149328804084,0.));
#70102=CARTESIAN_POINT('Ctrl Pts',(45.4831494767122,-17.9149328804084,20.));
#70103=CARTESIAN_POINT('Ctrl Pts',(45.4679676860453,-17.9451326049449,0.));
#70104=CARTESIAN_POINT('Ctrl Pts',(45.4679676860453,-17.9451326049449,20.));
#70105=CARTESIAN_POINT('Ctrl Pts',(45.4527656036598,-17.9753208696316,0.));
#70106=CARTESIAN_POINT('Ctrl Pts',(45.4527656036598,-17.9753208696316,20.));
#70107=CARTESIAN_POINT('Ctrl Pts',(45.4375432375433,-18.0054976605138,0.));
#70108=CARTESIAN_POINT('Ctrl Pts',(45.4375432375433,-18.0054976605138,20.));
#70109=CARTESIAN_POINT('Ctrl Pts',(45.4223005956881,-18.0356629636502,0.));
#70110=CARTESIAN_POINT('Ctrl Pts',(45.4223005956881,-18.0356629636502,20.));
#70111=CARTESIAN_POINT('Ctrl Pts',(45.4070376860893,-18.0658167651176,0.));
#70112=CARTESIAN_POINT('Ctrl Pts',(45.4070376860893,-18.0658167651176,20.));
#70113=CARTESIAN_POINT('Ctrl Pts',(45.3917545167484,-18.0959590510046,0.));
#70114=CARTESIAN_POINT('Ctrl Pts',(45.3917545167484,-18.0959590510046,20.));
#70115=CARTESIAN_POINT('Ctrl Pts',(45.3764510956741,-18.1260898074095,0.));
#70116=CARTESIAN_POINT('Ctrl Pts',(45.3764510956741,-18.1260898074095,20.));
#70117=CARTESIAN_POINT('Ctrl Pts',(45.3611274308852,-18.156209020436,0.));
#70118=CARTESIAN_POINT('Ctrl Pts',(45.3611274308852,-18.156209020436,20.));
#70119=CARTESIAN_POINT('Ctrl Pts',(45.3457835304119,-18.1863166761898,0.));
#70120=CARTESIAN_POINT('Ctrl Pts',(45.3457835304119,-18.1863166761898,20.));
#70121=CARTESIAN_POINT('Ctrl Pts',(45.3304194022976,-18.2164127607761,0.));
#70122=CARTESIAN_POINT('Ctrl Pts',(45.3304194022976,-18.2164127607761,20.));
#70123=CARTESIAN_POINT('Ctrl Pts',(45.3150350545965,-18.2464972603023,0.));
#70124=CARTESIAN_POINT('Ctrl Pts',(45.3150350545965,-18.2464972603023,20.));
#70125=CARTESIAN_POINT('Ctrl Pts',(45.299630495374,-18.276570160879,0.));
#70126=CARTESIAN_POINT('Ctrl Pts',(45.299630495374,-18.276570160879,20.));
#70127=CARTESIAN_POINT('Ctrl Pts',(45.2842057327048,-18.3066314486215,0.));
#70128=CARTESIAN_POINT('Ctrl Pts',(45.2842057327048,-18.3066314486215,20.));
#70129=CARTESIAN_POINT('Ctrl Pts',(45.2687607746732,-18.3366811096519,0.));
#70130=CARTESIAN_POINT('Ctrl Pts',(45.2687607746732,-18.3366811096519,20.));
#70131=CARTESIAN_POINT('Ctrl Pts',(45.2532956293718,-18.3667191300999,0.));
#70132=CARTESIAN_POINT('Ctrl Pts',(45.2532956293718,-18.3667191300999,20.));
#70133=CARTESIAN_POINT('Ctrl Pts',(45.2378103049022,-18.3967454961017,0.));
#70134=CARTESIAN_POINT('Ctrl Pts',(45.2378103049022,-18.3967454961017,20.));
#70135=CARTESIAN_POINT('Ctrl Pts',(45.2223048093755,-18.4267601937997,0.));
#70136=CARTESIAN_POINT('Ctrl Pts',(45.2223048093755,-18.4267601937997,20.));
#70137=CARTESIAN_POINT('Ctrl Pts',(45.2067791509123,-18.456763209342,0.));
#70138=CARTESIAN_POINT('Ctrl Pts',(45.2067791509123,-18.456763209342,20.));
#70139=CARTESIAN_POINT('Ctrl Pts',(45.1912333376434,-18.4867545288811,0.));
#70140=CARTESIAN_POINT('Ctrl Pts',(45.1912333376434,-18.4867545288811,20.));
#70141=CARTESIAN_POINT('Ctrl Pts',(45.1756673777099,-18.5167341385735,0.));
#70142=CARTESIAN_POINT('Ctrl Pts',(45.1756673777099,-18.5167341385735,20.));
#70143=CARTESIAN_POINT('Ctrl Pts',(45.1600812792631,-18.5467020245809,0.));
#70144=CARTESIAN_POINT('Ctrl Pts',(45.1600812792631,-18.5467020245809,20.));
#70145=CARTESIAN_POINT('Ctrl Pts',(45.144475050464,-18.5766581730695,0.));
#70146=CARTESIAN_POINT('Ctrl Pts',(45.144475050464,-18.5766581730695,20.));
#70147=CARTESIAN_POINT('Ctrl Pts',(45.1288486994834,-18.6066025702107,0.));
#70148=CARTESIAN_POINT('Ctrl Pts',(45.1288486994834,-18.6066025702107,20.));
#70149=CARTESIAN_POINT('Ctrl Pts',(45.1132022345013,-18.6365352021814,0.));
#70150=CARTESIAN_POINT('Ctrl Pts',(45.1132022345013,-18.6365352021814,20.));
#70151=CARTESIAN_POINT('Ctrl Pts',(45.097535663708,-18.6664560551643,0.));
#70152=CARTESIAN_POINT('Ctrl Pts',(45.097535663708,-18.6664560551643,20.));
#70153=CARTESIAN_POINT('Ctrl Pts',(45.081848995303,-18.6963651153477,0.));
#70154=CARTESIAN_POINT('Ctrl Pts',(45.081848995303,-18.6963651153477,20.));
#70155=CARTESIAN_POINT('Ctrl Pts',(45.0661422374956,-18.7262623689254,0.));
#70156=CARTESIAN_POINT('Ctrl Pts',(45.0661422374956,-18.7262623689254,20.));
#70157=CARTESIAN_POINT('Ctrl Pts',(45.050415398505,-18.7561478020964,0.));
#70158=CARTESIAN_POINT('Ctrl Pts',(45.050415398505,-18.7561478020964,20.));
#70159=CARTESIAN_POINT('Ctrl Pts',(45.0346684865594,-18.7860214010651,0.));
#70160=CARTESIAN_POINT('Ctrl Pts',(45.0346684865594,-18.7860214010651,20.));
#70161=CARTESIAN_POINT('Ctrl Pts',(45.0189015098976,-18.815883152041,0.));
#70162=CARTESIAN_POINT('Ctrl Pts',(45.0189015098976,-18.815883152041,20.));
#70163=CARTESIAN_POINT('Ctrl Pts',(45.0031144767678,-18.8457330412389,0.));
#70164=CARTESIAN_POINT('Ctrl Pts',(45.0031144767678,-18.8457330412389,20.));
#70165=CARTESIAN_POINT('Ctrl Pts',(44.987307395428,-18.8755710548788,0.));
#70166=CARTESIAN_POINT('Ctrl Pts',(44.987307395428,-18.8755710548788,20.));
#70167=CARTESIAN_POINT('Ctrl Pts',(44.971480274146,-18.9053971791858,0.));
#70168=CARTESIAN_POINT('Ctrl Pts',(44.971480274146,-18.9053971791858,20.));
#70169=CARTESIAN_POINT('Ctrl Pts',(44.9556331211993,-18.9352114003906,0.));
#70170=CARTESIAN_POINT('Ctrl Pts',(44.9556331211993,-18.9352114003906,20.));
#70171=CARTESIAN_POINT('Ctrl Pts',(44.9397659448752,-18.9650137047294,0.));
#70172=CARTESIAN_POINT('Ctrl Pts',(44.9397659448752,-18.9650137047294,20.));
#70173=CARTESIAN_POINT('Ctrl Pts',(44.9238787534705,-18.9948040784434,0.));
#70174=CARTESIAN_POINT('Ctrl Pts',(44.9238787534705,-18.9948040784434,20.));
#70175=CARTESIAN_POINT('Ctrl Pts',(44.9079715552916,-19.0245825077798,0.));
#70176=CARTESIAN_POINT('Ctrl Pts',(44.9079715552916,-19.0245825077798,20.));
#70177=CARTESIAN_POINT('Ctrl Pts',(44.8920443586544,-19.0543489789907,0.));
#70178=CARTESIAN_POINT('Ctrl Pts',(44.8920443586544,-19.0543489789907,20.));
#70179=CARTESIAN_POINT('Ctrl Pts',(44.8760971718851,-19.0841034783341,0.));
#70180=CARTESIAN_POINT('Ctrl Pts',(44.8760971718851,-19.0841034783341,20.));
#70181=CARTESIAN_POINT('Ctrl Pts',(44.8601300033192,-19.1138459920731,0.));
#70182=CARTESIAN_POINT('Ctrl Pts',(44.8601300033192,-19.1138459920731,20.));
#70183=CARTESIAN_POINT('Ctrl Pts',(44.8441428613021,-19.143576506476,0.));
#70184=CARTESIAN_POINT('Ctrl Pts',(44.8441428613021,-19.143576506476,20.));
#70185=CARTESIAN_POINT('Ctrl Pts',(44.8281357541891,-19.1732950078169,0.));
#70186=CARTESIAN_POINT('Ctrl Pts',(44.8281357541891,-19.1732950078169,20.));
#70187=CARTESIAN_POINT('Ctrl Pts',(44.8121086903447,-19.2030014823748,0.));
#70188=CARTESIAN_POINT('Ctrl Pts',(44.8121086903447,-19.2030014823748,20.));
#70189=CARTESIAN_POINT('Ctrl Pts',(44.7960616781431,-19.2326959164344,0.));
#70190=CARTESIAN_POINT('Ctrl Pts',(44.7960616781431,-19.2326959164344,20.));
#70191=CARTESIAN_POINT('Ctrl Pts',(44.7799947259683,-19.2623782962859,0.));
#70192=CARTESIAN_POINT('Ctrl Pts',(44.7799947259683,-19.2623782962859,20.));
#70193=CARTESIAN_POINT('Ctrl Pts',(44.7639078422139,-19.2920486082247,0.));
#70194=CARTESIAN_POINT('Ctrl Pts',(44.7639078422139,-19.2920486082247,20.));
#70195=CARTESIAN_POINT('Ctrl Pts',(44.7478010352831,-19.321706838552,0.));
#70196=CARTESIAN_POINT('Ctrl Pts',(44.7478010352831,-19.321706838552,20.));
#70197=CARTESIAN_POINT('Ctrl Pts',(44.731674313589,-19.3513529735741,0.));
#70198=CARTESIAN_POINT('Ctrl Pts',(44.731674313589,-19.3513529735741,20.));
#70199=CARTESIAN_POINT('Ctrl Pts',(44.7155276855546,-19.3809869996033,0.));
#70200=CARTESIAN_POINT('Ctrl Pts',(44.7155276855546,-19.3809869996033,20.));
#70201=CARTESIAN_POINT('Ctrl Pts',(44.6993611596123,-19.4106089029568,0.));
#70202=CARTESIAN_POINT('Ctrl Pts',(44.6993611596123,-19.4106089029568,20.));
#70203=CARTESIAN_POINT('Ctrl Pts',(44.6831747442042,-19.4402186699576,0.));
#70204=CARTESIAN_POINT('Ctrl Pts',(44.6831747442042,-19.4402186699576,20.));
#70205=CARTESIAN_POINT('Ctrl Pts',(44.6669684477819,-19.4698162869338,0.));
#70206=CARTESIAN_POINT('Ctrl Pts',(44.6669684477819,-19.4698162869338,20.));
#70207=CARTESIAN_POINT('Ctrl Pts',(44.6507422788067,-19.4994017402193,0.));
#70208=CARTESIAN_POINT('Ctrl Pts',(44.6507422788067,-19.4994017402193,20.));
#70209=CARTESIAN_POINT('Ctrl Pts',(44.6344962457493,-19.5289750161534,0.));
#70210=CARTESIAN_POINT('Ctrl Pts',(44.6344962457493,-19.5289750161534,20.));
#70211=CARTESIAN_POINT('Ctrl Pts',(44.6182303570903,-19.5585361010809,0.));
#70212=CARTESIAN_POINT('Ctrl Pts',(44.6182303570903,-19.5585361010809,20.));
#70213=CARTESIAN_POINT('Ctrl Pts',(44.60194462132,-19.5880849813526,0.));
#70214=CARTESIAN_POINT('Ctrl Pts',(44.60194462132,-19.5880849813526,20.));
#70215=CARTESIAN_POINT('Ctrl Pts',(44.5856390469384,-19.6176216433241,0.));
#70216=CARTESIAN_POINT('Ctrl Pts',(44.5856390469384,-19.6176216433241,20.));
#70217=CARTESIAN_POINT('Ctrl Pts',(44.5693136424548,-19.6471460733569,0.));
#70218=CARTESIAN_POINT('Ctrl Pts',(44.5693136424548,-19.6471460733569,20.));
#70219=CARTESIAN_POINT('Ctrl Pts',(44.5529684163885,-19.6766582578175,0.));
#70220=CARTESIAN_POINT('Ctrl Pts',(44.5529684163885,-19.6766582578175,20.));
#70221=CARTESIAN_POINT('Ctrl Pts',(44.5366033772681,-19.7061581830785,0.));
#70222=CARTESIAN_POINT('Ctrl Pts',(44.5366033772681,-19.7061581830785,20.));
#70223=CARTESIAN_POINT('Ctrl Pts',(44.5202185336324,-19.7356458355178,0.));
#70224=CARTESIAN_POINT('Ctrl Pts',(44.5202185336324,-19.7356458355178,20.));
#70225=CARTESIAN_POINT('Ctrl Pts',(44.5038138940293,-19.7651212015191,0.));
#70226=CARTESIAN_POINT('Ctrl Pts',(44.5038138940293,-19.7651212015191,20.));
#70227=CARTESIAN_POINT('Ctrl Pts',(44.4873894670167,-19.7945842674717,0.));
#70228=CARTESIAN_POINT('Ctrl Pts',(44.4873894670167,-19.7945842674717,20.));
#70229=CARTESIAN_POINT('Ctrl Pts',(44.4709452611615,-19.8240350197702,0.));
#70230=CARTESIAN_POINT('Ctrl Pts',(44.4709452611615,-19.8240350197702,20.));
#70231=CARTESIAN_POINT('Ctrl Pts',(44.4544812850403,-19.8534734448147,0.));
#70232=CARTESIAN_POINT('Ctrl Pts',(44.4544812850403,-19.8534734448147,20.));
#70233=CARTESIAN_POINT('Ctrl Pts',(44.4379975472397,-19.8828995290107,0.));
#70234=CARTESIAN_POINT('Ctrl Pts',(44.4379975472397,-19.8828995290107,20.));
#70235=CARTESIAN_POINT('Ctrl Pts',(44.4214940563556,-19.9123132587698,0.));
#70236=CARTESIAN_POINT('Ctrl Pts',(44.4214940563556,-19.9123132587698,20.));
#70237=CARTESIAN_POINT('Ctrl Pts',(44.4049708209939,-19.9417146205087,0.));
#70238=CARTESIAN_POINT('Ctrl Pts',(44.4049708209939,-19.9417146205087,20.));
#70239=CARTESIAN_POINT('Ctrl Pts',(44.3884278497697,-19.9711036006504,0.));
#70240=CARTESIAN_POINT('Ctrl Pts',(44.3884278497697,-19.9711036006504,20.));
#70241=CARTESIAN_POINT('Ctrl Pts',(44.371865151308,-20.0004801856229,0.));
#70242=CARTESIAN_POINT('Ctrl Pts',(44.371865151308,-20.0004801856229,20.));
#70243=CARTESIAN_POINT('Ctrl Pts',(44.3552827342435,-20.0298443618602,0.));
#70244=CARTESIAN_POINT('Ctrl Pts',(44.3552827342435,-20.0298443618602,20.));
#70245=CARTESIAN_POINT('Ctrl Pts',(44.3386806072204,-20.0591961158019,0.));
#70246=CARTESIAN_POINT('Ctrl Pts',(44.3386806072204,-20.0591961158019,20.));
#70247=CARTESIAN_POINT('Ctrl Pts',(44.3220587788923,-20.0885354338929,0.));
#70248=CARTESIAN_POINT('Ctrl Pts',(44.3220587788923,-20.0885354338929,20.));
#70249=CARTESIAN_POINT('Ctrl Pts',(44.3054172579221,-20.117862302584,0.));
#70250=CARTESIAN_POINT('Ctrl Pts',(44.3054172579221,-20.117862302584,20.));
#70251=CARTESIAN_POINT('Ctrl Pts',(44.2887560529826,-20.1471767083313,0.));
#70252=CARTESIAN_POINT('Ctrl Pts',(44.2887560529826,-20.1471767083313,20.));
#70253=CARTESIAN_POINT('Ctrl Pts',(44.2720751727557,-20.1764786375963,0.));
#70254=CARTESIAN_POINT('Ctrl Pts',(44.2720751727557,-20.1764786375963,20.));
#70255=CARTESIAN_POINT('Ctrl Pts',(44.2553746259333,-20.2057680768465,0.));
#70256=CARTESIAN_POINT('Ctrl Pts',(44.2553746259333,-20.2057680768465,20.));
#70257=CARTESIAN_POINT('Ctrl Pts',(44.238654421217,-20.2350450125552,0.));
#70258=CARTESIAN_POINT('Ctrl Pts',(44.238654421217,-20.2350450125552,20.));
#70259=CARTESIAN_POINT('Ctrl Pts',(44.221914567318,-20.2643094312016,0.));
#70260=CARTESIAN_POINT('Ctrl Pts',(44.221914567318,-20.2643094312016,20.));
#70261=CARTESIAN_POINT('Ctrl Pts',(44.205155072957,-20.2935613192706,0.));
#70262=CARTESIAN_POINT('Ctrl Pts',(44.205155072957,-20.2935613192706,20.));
#70263=CARTESIAN_POINT('Ctrl Pts',(44.1883759468646,-20.3228006632528,0.));
#70264=CARTESIAN_POINT('Ctrl Pts',(44.1883759468646,-20.3228006632528,20.));
#70265=CARTESIAN_POINT('Ctrl Pts',(44.1715771977807,-20.3520274496444,0.));
#70266=CARTESIAN_POINT('Ctrl Pts',(44.1715771977807,-20.3520274496444,20.));
#70267=CARTESIAN_POINT('Ctrl Pts',(44.1547588344544,-20.3812416649468,0.));
#70268=CARTESIAN_POINT('Ctrl Pts',(44.1547588344544,-20.3812416649468,20.));
#70269=CARTESIAN_POINT('Ctrl Pts',(44.1379208656442,-20.4104432956673,0.));
#70270=CARTESIAN_POINT('Ctrl Pts',(44.1379208656442,-20.4104432956673,20.));
#70271=CARTESIAN_POINT('Ctrl Pts',(44.1210633001184,-20.4396323283186,0.));
#70272=CARTESIAN_POINT('Ctrl Pts',(44.1210633001184,-20.4396323283186,20.));
#70273=CARTESIAN_POINT('Ctrl Pts',(44.1041861466545,-20.4688087494191,0.));
#70274=CARTESIAN_POINT('Ctrl Pts',(44.1041861466545,-20.4688087494191,20.));
#70275=CARTESIAN_POINT('Ctrl Pts',(44.0872894140398,-20.4979725454933,0.));
#70276=CARTESIAN_POINT('Ctrl Pts',(44.0872894140398,-20.4979725454933,20.));
#70277=CARTESIAN_POINT('Ctrl Pts',(44.0703731110714,-20.5271237030716,0.));
#70278=CARTESIAN_POINT('Ctrl Pts',(44.0703731110714,-20.5271237030716,20.));
#70279=CARTESIAN_POINT('Ctrl Pts',(44.053437246556,-20.5562622086905,0.));
#70280=CARTESIAN_POINT('Ctrl Pts',(44.053437246556,-20.5562622086905,20.));
#70281=CARTESIAN_POINT('Ctrl Pts',(44.03648182931,-20.5853880488919,0.));
#70282=CARTESIAN_POINT('Ctrl Pts',(44.03648182931,-20.5853880488919,20.));
#70283=CARTESIAN_POINT('Ctrl Pts',(44.0195068681592,-20.6145012102233,0.));
#70284=CARTESIAN_POINT('Ctrl Pts',(44.0195068681592,-20.6145012102233,20.));
#70285=CARTESIAN_POINT('Ctrl Pts',(44.0025123719387,-20.6436016792381,0.));
#70286=CARTESIAN_POINT('Ctrl Pts',(44.0025123719387,-20.6436016792381,20.));
#70287=CARTESIAN_POINT('Ctrl Pts',(43.9854983494929,-20.6726894424949,0.));
#70288=CARTESIAN_POINT('Ctrl Pts',(43.9854983494929,-20.6726894424949,20.));
#70289=CARTESIAN_POINT('Ctrl Pts',(43.9684648096756,-20.7017644865585,0.));
#70290=CARTESIAN_POINT('Ctrl Pts',(43.9684648096756,-20.7017644865585,20.));
#70291=CARTESIAN_POINT('Ctrl Pts',(43.9514117613501,-20.7308267979991,0.));
#70292=CARTESIAN_POINT('Ctrl Pts',(43.9514117613501,-20.7308267979991,20.));
#70293=CARTESIAN_POINT('Ctrl Pts',(43.9343392133895,-20.7598763633934,0.));
#70294=CARTESIAN_POINT('Ctrl Pts',(43.9343392133895,-20.7598763633934,20.));
#70295=CARTESIAN_POINT('Ctrl Pts',(43.9172471746767,-20.7889131693233,0.));
#70296=CARTESIAN_POINT('Ctrl Pts',(43.9172471746767,-20.7889131693233,20.));
#70297=CARTESIAN_POINT('Ctrl Pts',(43.9001356541037,-20.817937202377,0.));
#70298=CARTESIAN_POINT('Ctrl Pts',(43.9001356541037,-20.817937202377,20.));
#70299=CARTESIAN_POINT('Ctrl Pts',(43.8830046605723,-20.8469484491482,0.));
#70300=CARTESIAN_POINT('Ctrl Pts',(43.8830046605723,-20.8469484491482,20.));
#70301=CARTESIAN_POINT('Ctrl Pts',(43.8658542029936,-20.8759468962364,0.));
#70302=CARTESIAN_POINT('Ctrl Pts',(43.8658542029936,-20.8759468962364,20.));
#70303=CARTESIAN_POINT('Ctrl Pts',(43.8486842902882,-20.9049325302471,0.));
#70304=CARTESIAN_POINT('Ctrl Pts',(43.8486842902882,-20.9049325302471,20.));
#70305=CARTESIAN_POINT('Ctrl Pts',(43.8314949313861,-20.9339053377914,0.));
#70306=CARTESIAN_POINT('Ctrl Pts',(43.8314949313861,-20.9339053377914,20.));
#70307=CARTESIAN_POINT('Ctrl Pts',(43.8142861352268,-20.9628653054863,0.));
#70308=CARTESIAN_POINT('Ctrl Pts',(43.8142861352268,-20.9628653054863,20.));
#70309=CARTESIAN_POINT('Ctrl Pts',(43.7970579107591,-20.9918124199547,0.));
#70310=CARTESIAN_POINT('Ctrl Pts',(43.7970579107591,-20.9918124199547,20.));
#70311=CARTESIAN_POINT('Ctrl Pts',(43.7798102669417,-21.0207466678254,0.));
#70312=CARTESIAN_POINT('Ctrl Pts',(43.7798102669417,-21.0207466678254,20.));
#70313=CARTESIAN_POINT('Ctrl Pts',(43.7625432127426,-21.0496680357328,0.));
#70314=CARTESIAN_POINT('Ctrl Pts',(43.7625432127426,-21.0496680357328,20.));
#70315=CARTESIAN_POINT('Ctrl Pts',(43.7452567571393,-21.0785765103173,0.));
#70316=CARTESIAN_POINT('Ctrl Pts',(43.7452567571393,-21.0785765103173,20.));
#70317=CARTESIAN_POINT('Ctrl Pts',(43.7279509091188,-21.1074720782252,0.));
#70318=CARTESIAN_POINT('Ctrl Pts',(43.7279509091188,-21.1074720782252,20.));
#70319=CARTESIAN_POINT('Ctrl Pts',(43.7106256776774,-21.1363547261089,0.));
#70320=CARTESIAN_POINT('Ctrl Pts',(43.7106256776774,-21.1363547261089,20.));
#70321=CARTESIAN_POINT('Ctrl Pts',(43.6932810718209,-21.1652244406266,0.));
#70322=CARTESIAN_POINT('Ctrl Pts',(43.6932810718209,-21.1652244406266,20.));
#70323=CARTESIAN_POINT('Ctrl Pts',(43.6759171005641,-21.1940812084419,0.));
#70324=CARTESIAN_POINT('Ctrl Pts',(43.6759171005641,-21.1940812084419,20.));
#70325=CARTESIAN_POINT('Ctrl Pts',(43.658533772932,-21.2229250162246,0.));
#70326=CARTESIAN_POINT('Ctrl Pts',(43.658533772932,-21.2229250162246,20.));
#70327=CARTESIAN_POINT('Ctrl Pts',(43.6411310979584,-21.2517558506503,0.));
#70328=CARTESIAN_POINT('Ctrl Pts',(43.6411310979584,-21.2517558506503,20.));
#70329=CARTESIAN_POINT('Ctrl Pts',(43.6237090846874,-21.2805736984008,0.));
#70330=CARTESIAN_POINT('Ctrl Pts',(43.6237090846874,-21.2805736984008,20.));
#70331=CARTESIAN_POINT('Ctrl Pts',(43.6062677421718,-21.3093785461635,0.));
#70332=CARTESIAN_POINT('Ctrl Pts',(43.6062677421718,-21.3093785461635,20.));
#70333=CARTESIAN_POINT('Ctrl Pts',(43.5888070794743,-21.3381703806324,0.));
#70334=CARTESIAN_POINT('Ctrl Pts',(43.5888070794743,-21.3381703806324,20.));
#70335=CARTESIAN_POINT('Ctrl Pts',(43.571327105667,-21.3669491885068,0.));
#70336=CARTESIAN_POINT('Ctrl Pts',(43.571327105667,-21.3669491885068,20.));
#70337=CARTESIAN_POINT('Ctrl Pts',(43.5538278298311,-21.3957149564922,0.));
#70338=CARTESIAN_POINT('Ctrl Pts',(43.5538278298311,-21.3957149564922,20.));
#70339=CARTESIAN_POINT('Ctrl Pts',(43.5363092610574,-21.4244676712999,0.));
#70340=CARTESIAN_POINT('Ctrl Pts',(43.5363092610574,-21.4244676712999,20.));
#70341=CARTESIAN_POINT('Ctrl Pts',(43.5187714084458,-21.4532073196468,0.));
#70342=CARTESIAN_POINT('Ctrl Pts',(43.5187714084458,-21.4532073196468,20.));
#70343=CARTESIAN_POINT('Ctrl Pts',(43.5012142811058,-21.4819338882558,0.));
#70344=CARTESIAN_POINT('Ctrl Pts',(43.5012142811058,-21.4819338882558,20.));
#70345=CARTESIAN_POINT('Ctrl Pts',(43.4836378881563,-21.5106473638561,0.));
#70346=CARTESIAN_POINT('Ctrl Pts',(43.4836378881563,-21.5106473638561,20.));
#70347=CARTESIAN_POINT('Ctrl Pts',(43.4660422387257,-21.5393477331829,0.));
#70348=CARTESIAN_POINT('Ctrl Pts',(43.4660422387257,-21.5393477331829,20.));
#70349=CARTESIAN_POINT('Ctrl Pts',(43.4484273419519,-21.5680349829774,0.));
#70350=CARTESIAN_POINT('Ctrl Pts',(43.4484273419519,-21.5680349829774,20.));
#70351=CARTESIAN_POINT('Ctrl Pts',(43.4307932069823,-21.5967090999869,0.));
#70352=CARTESIAN_POINT('Ctrl Pts',(43.4307932069823,-21.5967090999869,20.));
#70353=CARTESIAN_POINT('Ctrl Pts',(43.4131398429739,-21.6253700709647,0.));
#70354=CARTESIAN_POINT('Ctrl Pts',(43.4131398429739,-21.6253700709647,20.));
#70355=CARTESIAN_POINT('Ctrl Pts',(43.3954672590924,-21.6540178826698,0.));
#70356=CARTESIAN_POINT('Ctrl Pts',(43.3954672590924,-21.6540178826698,20.));
#70357=CARTESIAN_POINT('Ctrl Pts',(43.3777754645132,-21.682652521867,0.));
#70358=CARTESIAN_POINT('Ctrl Pts',(43.3777754645132,-21.682652521867,20.));
#70359=CARTESIAN_POINT('Ctrl Pts',(43.3600644684208,-21.7112739753274,0.));
#70360=CARTESIAN_POINT('Ctrl Pts',(43.3600644684208,-21.7112739753274,20.));
#70361=CARTESIAN_POINT('Ctrl Pts',(43.3423342800096,-21.7398822298281,0.));
#70362=CARTESIAN_POINT('Ctrl Pts',(43.3423342800096,-21.7398822298281,20.));
#70363=CARTESIAN_POINT('Ctrl Pts',(43.3245849084831,-21.7684772721522,0.));
#70364=CARTESIAN_POINT('Ctrl Pts',(43.3245849084831,-21.7684772721522,20.));
#70365=CARTESIAN_POINT('Ctrl Pts',(43.3068163630542,-21.7970590890891,0.));
#70366=CARTESIAN_POINT('Ctrl Pts',(43.3068163630542,-21.7970590890891,20.));
#70367=CARTESIAN_POINT('Ctrl Pts',(43.2890286529453,-21.825627667434,0.));
#70368=CARTESIAN_POINT('Ctrl Pts',(43.2890286529453,-21.825627667434,20.));
#70369=CARTESIAN_POINT('Ctrl Pts',(43.271221787388,-21.854182993988,0.));
#70370=CARTESIAN_POINT('Ctrl Pts',(43.271221787388,-21.854182993988,20.));
#70371=CARTESIAN_POINT('Ctrl Pts',(43.2533957756234,-21.8827250555584,0.));
#70372=CARTESIAN_POINT('Ctrl Pts',(43.2533957756234,-21.8827250555584,20.));
#70373=CARTESIAN_POINT('Ctrl Pts',(43.2355506269018,-21.9112538389586,0.));
#70374=CARTESIAN_POINT('Ctrl Pts',(43.2355506269018,-21.9112538389586,20.));
#70375=CARTESIAN_POINT('Ctrl Pts',(43.217686350483,-21.939769331008,0.));
#70376=CARTESIAN_POINT('Ctrl Pts',(43.217686350483,-21.939769331008,20.));
#70377=CARTESIAN_POINT('Ctrl Pts',(43.1998029556363,-21.9682715185322,0.));
#70378=CARTESIAN_POINT('Ctrl Pts',(43.1998029556363,-21.9682715185322,20.));
#70379=CARTESIAN_POINT('Ctrl Pts',(43.1819004516401,-21.9967603883628,0.));
#70380=CARTESIAN_POINT('Ctrl Pts',(43.1819004516401,-21.9967603883628,20.));
#70381=CARTESIAN_POINT('Ctrl Pts',(43.1639788477821,-22.0252359273374,0.));
#70382=CARTESIAN_POINT('Ctrl Pts',(43.1639788477821,-22.0252359273374,20.));
#70383=CARTESIAN_POINT('Ctrl Pts',(43.1460381533593,-22.0536981222997,0.));
#70384=CARTESIAN_POINT('Ctrl Pts',(43.1460381533593,-22.0536981222997,20.));
#70385=CARTESIAN_POINT('Ctrl Pts',(43.1280783776784,-22.0821469600998,0.));
#70386=CARTESIAN_POINT('Ctrl Pts',(43.1280783776784,-22.0821469600998,20.));
#70387=CARTESIAN_POINT('Ctrl Pts',(43.1100995300552,-22.1105824275933,0.));
#70388=CARTESIAN_POINT('Ctrl Pts',(43.1100995300552,-22.1105824275933,20.));
#70389=CARTESIAN_POINT('Ctrl Pts',(43.0921016198148,-22.1390045116426,0.));
#70390=CARTESIAN_POINT('Ctrl Pts',(43.0921016198148,-22.1390045116426,20.));
#70391=CARTESIAN_POINT('Ctrl Pts',(43.0740846562917,-22.1674131991155,0.));
#70392=CARTESIAN_POINT('Ctrl Pts',(43.0740846562917,-22.1674131991155,20.));
#70393=CARTESIAN_POINT('Ctrl Pts',(43.0560486488298,-22.1958084768868,0.));
#70394=CARTESIAN_POINT('Ctrl Pts',(43.0560486488298,-22.1958084768868,20.));
#70395=CARTESIAN_POINT('Ctrl Pts',(43.0379936067822,-22.2241903318366,0.));
#70396=CARTESIAN_POINT('Ctrl Pts',(43.0379936067822,-22.2241903318366,20.));
#70397=CARTESIAN_POINT('Ctrl Pts',(43.0199195395114,-22.252558750852,0.));
#70398=CARTESIAN_POINT('Ctrl Pts',(43.0199195395114,-22.252558750852,20.));
#70399=CARTESIAN_POINT('Ctrl Pts',(43.0018264563892,-22.2809137208256,0.));
#70400=CARTESIAN_POINT('Ctrl Pts',(43.0018264563892,-22.2809137208256,20.));
#70401=CARTESIAN_POINT('Ctrl Pts',(42.9837143667967,-22.3092552286565,0.));
#70402=CARTESIAN_POINT('Ctrl Pts',(42.9837143667967,-22.3092552286565,20.));
#70403=CARTESIAN_POINT('Ctrl Pts',(42.965583280124,-22.3375832612492,0.));
#70404=CARTESIAN_POINT('Ctrl Pts',(42.965583280124,-22.3375832612492,20.));
#70405=CARTESIAN_POINT('Ctrl Pts',(42.947433205771,-22.3658978055149,0.));
#70406=CARTESIAN_POINT('Ctrl Pts',(42.947433205771,-22.3658978055149,20.));
#70407=CARTESIAN_POINT('Ctrl Pts',(42.9292641531465,-22.3941988483709,0.));
#70408=CARTESIAN_POINT('Ctrl Pts',(42.9292641531465,-22.3941988483709,20.));
#70409=CARTESIAN_POINT('Ctrl Pts',(42.9110761316689,-22.4224863767407,0.));
#70410=CARTESIAN_POINT('Ctrl Pts',(42.9110761316689,-22.4224863767407,20.));
#70411=CARTESIAN_POINT('Ctrl Pts',(42.8928691507659,-22.4507603775546,0.));
#70412=CARTESIAN_POINT('Ctrl Pts',(42.8928691507659,-22.4507603775546,20.));
#70413=CARTESIAN_POINT('Ctrl Pts',(42.8746432198743,-22.4790208377489,0.));
#70414=CARTESIAN_POINT('Ctrl Pts',(42.8746432198743,-22.4790208377489,20.));
#70415=CARTESIAN_POINT('Ctrl Pts',(42.8563983484404,-22.5072677442656,0.));
#70416=CARTESIAN_POINT('Ctrl Pts',(42.8563983484404,-22.5072677442656,20.));
#70417=CARTESIAN_POINT('Ctrl Pts',(42.8381345459193,-22.5355010840531,0.));
#70418=CARTESIAN_POINT('Ctrl Pts',(42.8381345459193,-22.5355010840531,20.));
#70419=CARTESIAN_POINT('Ctrl Pts',(42.8198518217756,-22.5637208440656,0.));
#70420=CARTESIAN_POINT('Ctrl Pts',(42.8198518217756,-22.5637208440656,20.));
#70421=CARTESIAN_POINT('Ctrl Pts',(42.8015501854832,-22.5919270112639,0.));
#70422=CARTESIAN_POINT('Ctrl Pts',(42.8015501854832,-22.5919270112639,20.));
#70423=CARTESIAN_POINT('Ctrl Pts',(42.7832296465255,-22.6201195726151,0.));
#70424=CARTESIAN_POINT('Ctrl Pts',(42.7832296465255,-22.6201195726151,20.));
#70425=CARTESIAN_POINT('Ctrl Pts',(42.7648902143955,-22.6482985150925,0.));
#70426=CARTESIAN_POINT('Ctrl Pts',(42.7648902143955,-22.6482985150925,20.));
#70427=CARTESIAN_POINT('Ctrl Pts',(42.7465318985949,-22.6764638256759,0.));
#70428=CARTESIAN_POINT('Ctrl Pts',(42.7465318985949,-22.6764638256759,20.));
#70429=CARTESIAN_POINT('Ctrl Pts',(42.7281547086347,-22.7046154913512,0.));
#70430=CARTESIAN_POINT('Ctrl Pts',(42.7281547086347,-22.7046154913512,20.));
#70431=CARTESIAN_POINT('Ctrl Pts',(42.7097586540349,-22.7327534991101,0.));
#70432=CARTESIAN_POINT('Ctrl Pts',(42.7097586540349,-22.7327534991101,20.));
#70433=CARTESIAN_POINT('Ctrl Pts',(42.6913437443248,-22.7608778359508,0.));
#70434=CARTESIAN_POINT('Ctrl Pts',(42.6913437443248,-22.7608778359508,20.));
#70435=CARTESIAN_POINT('Ctrl Pts',(42.6729099890431,-22.788988488878,0.));
#70436=CARTESIAN_POINT('Ctrl Pts',(42.6729099890431,-22.788988488878,20.));
#70437=CARTESIAN_POINT('Ctrl Pts',(42.6544573977378,-22.8170854449024,0.));
#70438=CARTESIAN_POINT('Ctrl Pts',(42.6544573977378,-22.8170854449024,20.));
#70439=CARTESIAN_POINT('Ctrl Pts',(42.6359859799663,-22.845168691041,0.));
#70440=CARTESIAN_POINT('Ctrl Pts',(42.6359859799663,-22.845168691041,20.));
#70441=CARTESIAN_POINT('Ctrl Pts',(42.6174957452953,-22.8732382143175,0.));
#70442=CARTESIAN_POINT('Ctrl Pts',(42.6174957452953,-22.8732382143175,20.));
#70443=CARTESIAN_POINT('Ctrl Pts',(42.5989867033005,-22.9012940017616,0.));
#70444=CARTESIAN_POINT('Ctrl Pts',(42.5989867033005,-22.9012940017616,20.));
#70445=CARTESIAN_POINT('Ctrl Pts',(42.5804588635669,-22.9293360404095,0.));
#70446=CARTESIAN_POINT('Ctrl Pts',(42.5804588635669,-22.9293360404095,20.));
#70447=CARTESIAN_POINT('Ctrl Pts',(42.5619122356886,-22.9573643173034,0.));
#70448=CARTESIAN_POINT('Ctrl Pts',(42.5619122356886,-22.9573643173034,20.));
#70449=CARTESIAN_POINT('Ctrl Pts',(42.5433468292689,-22.9853788194919,0.));
#70450=CARTESIAN_POINT('Ctrl Pts',(42.5433468292689,-22.9853788194919,20.));
#70451=CARTESIAN_POINT('Ctrl Pts',(42.5247626539203,-23.0133795340299,0.));
#70452=CARTESIAN_POINT('Ctrl Pts',(42.5247626539203,-23.0133795340299,20.));
#70453=CARTESIAN_POINT('Ctrl Pts',(42.5061597192647,-23.0413664479785,0.));
#70454=CARTESIAN_POINT('Ctrl Pts',(42.5061597192647,-23.0413664479785,20.));
#70455=CARTESIAN_POINT('Ctrl Pts',(42.4875380349329,-23.0693395484056,0.));
#70456=CARTESIAN_POINT('Ctrl Pts',(42.4875380349329,-23.0693395484056,20.));
#70457=CARTESIAN_POINT('Ctrl Pts',(42.4688976105654,-23.097298822385,0.));
#70458=CARTESIAN_POINT('Ctrl Pts',(42.4688976105654,-23.097298822385,20.));
#70459=CARTESIAN_POINT('Ctrl Pts',(42.4502384558115,-23.1252442569971,0.));
#70460=CARTESIAN_POINT('Ctrl Pts',(42.4502384558115,-23.1252442569971,20.));
#70461=CARTESIAN_POINT('Ctrl Pts',(42.4315605803297,-23.1531758393284,0.));
#70462=CARTESIAN_POINT('Ctrl Pts',(42.4315605803297,-23.1531758393284,20.));
#70463=CARTESIAN_POINT('Ctrl Pts',(42.4128639937879,-23.1810935564721,0.));
#70464=CARTESIAN_POINT('Ctrl Pts',(42.4128639937879,-23.1810935564721,20.));
#70465=CARTESIAN_POINT('Ctrl Pts',(42.3941487058631,-23.2089973955278,0.));
#70466=CARTESIAN_POINT('Ctrl Pts',(42.3941487058631,-23.2089973955278,20.));
#70467=CARTESIAN_POINT('Ctrl Pts',(42.3754147262417,-23.2368873436013,0.));
#70468=CARTESIAN_POINT('Ctrl Pts',(42.3754147262417,-23.2368873436013,20.));
#70469=CARTESIAN_POINT('Ctrl Pts',(42.3566620646188,-23.2647633878047,0.));
#70470=CARTESIAN_POINT('Ctrl Pts',(42.3566620646188,-23.2647633878047,20.));
#70471=CARTESIAN_POINT('Ctrl Pts',(42.3378907306988,-23.2926255152563,0.));
#70472=CARTESIAN_POINT('Ctrl Pts',(42.3378907306988,-23.2926255152563,20.));
#70473=CARTESIAN_POINT('Ctrl Pts',(42.3191007341954,-23.320473713081,0.));
#70474=CARTESIAN_POINT('Ctrl Pts',(42.3191007341954,-23.320473713081,20.));
#70475=CARTESIAN_POINT('Ctrl Pts',(42.3002920848317,-23.3483079684104,0.));
#70476=CARTESIAN_POINT('Ctrl Pts',(42.3002920848317,-23.3483079684104,20.));
#70477=CARTESIAN_POINT('Ctrl Pts',(42.2814647923395,-23.3761282683822,0.));
#70478=CARTESIAN_POINT('Ctrl Pts',(42.2814647923395,-23.3761282683822,20.));
#70479=CARTESIAN_POINT('Ctrl Pts',(42.2626188664603,-23.4039346001409,0.));
#70480=CARTESIAN_POINT('Ctrl Pts',(42.2626188664603,-23.4039346001409,20.));
#70481=CARTESIAN_POINT('Ctrl Pts',(42.2437543169442,-23.4317269508371,0.));
#70482=CARTESIAN_POINT('Ctrl Pts',(42.2437543169442,-23.4317269508371,20.));
#70483=CARTESIAN_POINT('Ctrl Pts',(42.2248711535508,-23.4595053076278,0.));
#70484=CARTESIAN_POINT('Ctrl Pts',(42.2248711535508,-23.4595053076278,20.));
#70485=CARTESIAN_POINT('Ctrl Pts',(42.2059693860486,-23.4872696576759,0.));
#70486=CARTESIAN_POINT('Ctrl Pts',(42.2059693860486,-23.4872696576759,20.));
#70487=CARTESIAN_POINT('Ctrl Pts',(42.1870490242153,-23.5150199881515,0.));
#70488=CARTESIAN_POINT('Ctrl Pts',(42.1870490242153,-23.5150199881515,20.));
#70489=CARTESIAN_POINT('Ctrl Pts',(42.1681100778379,-23.5427562862308,0.));
#70490=CARTESIAN_POINT('Ctrl Pts',(42.1681100778379,-23.5427562862308,20.));
#70491=CARTESIAN_POINT('Ctrl Pts',(42.1491525567126,-23.5704785390969,0.));
#70492=CARTESIAN_POINT('Ctrl Pts',(42.1491525567126,-23.5704785390969,20.));
#70493=CARTESIAN_POINT('Ctrl Pts',(42.1301764706447,-23.5981867339395,0.));
#70494=CARTESIAN_POINT('Ctrl Pts',(42.1301764706447,-23.5981867339395,20.));
#70495=CARTESIAN_POINT('Ctrl Pts',(42.1111818294483,-23.6258808579543,0.));
#70496=CARTESIAN_POINT('Ctrl Pts',(42.1111818294483,-23.6258808579543,20.));
#70497=CARTESIAN_POINT('Ctrl Pts',(42.0921686429469,-23.6535608983436,0.));
#70498=CARTESIAN_POINT('Ctrl Pts',(42.0921686429469,-23.6535608983436,20.));
#70499=CARTESIAN_POINT('Ctrl Pts',(42.0731369209731,-23.6812268423159,0.));
#70500=CARTESIAN_POINT('Ctrl Pts',(42.0731369209731,-23.6812268423159,20.));
#70501=CARTESIAN_POINT('Ctrl Pts',(42.0540866733685,-23.7088786770864,0.));
#70502=CARTESIAN_POINT('Ctrl Pts',(42.0540866733685,-23.7088786770864,20.));
#70503=CARTESIAN_POINT('Ctrl Pts',(42.0350179099839,-23.7365163898768,0.));
#70504=CARTESIAN_POINT('Ctrl Pts',(42.0350179099839,-23.7365163898768,20.));
#70505=CARTESIAN_POINT('Ctrl Pts',(42.0159306406794,-23.7641399679152,0.));
#70506=CARTESIAN_POINT('Ctrl Pts',(42.0159306406794,-23.7641399679152,20.));
#70507=CARTESIAN_POINT('Ctrl Pts',(41.9968248753238,-23.7917493984363,0.));
#70508=CARTESIAN_POINT('Ctrl Pts',(41.9968248753238,-23.7917493984363,20.));
#70509=CARTESIAN_POINT('Ctrl Pts',(41.9777006237952,-23.8193446686815,0.));
#70510=CARTESIAN_POINT('Ctrl Pts',(41.9777006237952,-23.8193446686815,20.));
#70511=CARTESIAN_POINT('Ctrl Pts',(41.9585578959806,-23.8469257658985,0.));
#70512=CARTESIAN_POINT('Ctrl Pts',(41.9585578959806,-23.8469257658985,20.));
#70513=CARTESIAN_POINT('Ctrl Pts',(41.9393967017767,-23.8744926773418,0.));
#70514=CARTESIAN_POINT('Ctrl Pts',(41.9393967017767,-23.8744926773418,20.));
#70515=CARTESIAN_POINT('Ctrl Pts',(41.9202170510888,-23.9020453902722,0.));
#70516=CARTESIAN_POINT('Ctrl Pts',(41.9202170510888,-23.9020453902722,20.));
#70517=CARTESIAN_POINT('Ctrl Pts',(41.9010189538314,-23.9295838919573,0.));
#70518=CARTESIAN_POINT('Ctrl Pts',(41.9010189538314,-23.9295838919573,20.));
#70519=CARTESIAN_POINT('Ctrl Pts',(41.8818024199281,-23.9571081696708,0.));
#70520=CARTESIAN_POINT('Ctrl Pts',(41.8818024199281,-23.9571081696708,20.));
#70521=CARTESIAN_POINT('Ctrl Pts',(41.8625674593112,-23.9846182106931,0.));
#70522=CARTESIAN_POINT('Ctrl Pts',(41.8625674593112,-23.9846182106931,20.));
#70523=CARTESIAN_POINT('Ctrl Pts',(41.8433140819226,-24.0121140023113,0.));
#70524=CARTESIAN_POINT('Ctrl Pts',(41.8433140819226,-24.0121140023113,20.));
#70525=CARTESIAN_POINT('Ctrl Pts',(41.824042297713,-24.0395955318191,0.));
#70526=CARTESIAN_POINT('Ctrl Pts',(41.824042297713,-24.0395955318191,20.));
#70527=CARTESIAN_POINT('Ctrl Pts',(41.8047521166422,-24.0670627865166,0.));
#70528=CARTESIAN_POINT('Ctrl Pts',(41.8047521166422,-24.0670627865166,20.));
#70529=CARTESIAN_POINT('Ctrl Pts',(41.785443548679,-24.0945157537107,0.));
#70530=CARTESIAN_POINT('Ctrl Pts',(41.785443548679,-24.0945157537107,20.));
#70531=CARTESIAN_POINT('Ctrl Pts',(41.7661166038015,-24.1219544207148,0.));
#70532=CARTESIAN_POINT('Ctrl Pts',(41.7661166038015,-24.1219544207148,20.));
#70533=CARTESIAN_POINT('Ctrl Pts',(41.7467712919966,-24.1493787748488,0.));
#70534=CARTESIAN_POINT('Ctrl Pts',(41.7467712919966,-24.1493787748488,20.));
#70535=CARTESIAN_POINT('Ctrl Pts',(41.7274076232604,-24.1767888034393,0.));
#70536=CARTESIAN_POINT('Ctrl Pts',(41.7274076232604,-24.1767888034393,20.));
#70537=CARTESIAN_POINT('Ctrl Pts',(41.7080256075983,-24.2041844938197,0.));
#70538=CARTESIAN_POINT('Ctrl Pts',(41.7080256075983,-24.2041844938197,20.));
#70539=CARTESIAN_POINT('Ctrl Pts',(41.688625255024,-24.2315658333297,0.));
#70540=CARTESIAN_POINT('Ctrl Pts',(41.688625255024,-24.2315658333297,20.));
#70541=CARTESIAN_POINT('Ctrl Pts',(41.6692065755608,-24.2589328093159,0.));
#70542=CARTESIAN_POINT('Ctrl Pts',(41.6692065755608,-24.2589328093159,20.));
#70543=CARTESIAN_POINT('Ctrl Pts',(41.6497695792407,-24.2862854091312,0.));
#70544=CARTESIAN_POINT('Ctrl Pts',(41.6497695792407,-24.2862854091312,20.));
#70545=CARTESIAN_POINT('Ctrl Pts',(41.630314276105,-24.3136236201351,0.));
#70546=CARTESIAN_POINT('Ctrl Pts',(41.630314276105,-24.3136236201351,20.));
#70547=CARTESIAN_POINT('Ctrl Pts',(41.610840676204,-24.3409474296941,0.));
#70548=CARTESIAN_POINT('Ctrl Pts',(41.610840676204,-24.3409474296941,20.));
#70549=CARTESIAN_POINT('Ctrl Pts',(41.5913487895971,-24.368256825181,0.));
#70550=CARTESIAN_POINT('Ctrl Pts',(41.5913487895971,-24.368256825181,20.));
#70551=CARTESIAN_POINT('Ctrl Pts',(41.5718386263526,-24.3955517939757,0.));
#70552=CARTESIAN_POINT('Ctrl Pts',(41.5718386263526,-24.3955517939757,20.));
#70553=CARTESIAN_POINT('Ctrl Pts',(41.5523101965477,-24.4228323234645,0.));
#70554=CARTESIAN_POINT('Ctrl Pts',(41.5523101965477,-24.4228323234645,20.));
#70555=CARTESIAN_POINT('Ctrl Pts',(41.5327635102685,-24.4500984010406,0.));
#70556=CARTESIAN_POINT('Ctrl Pts',(41.5327635102685,-24.4500984010406,20.));
#70557=CARTESIAN_POINT('Ctrl Pts',(41.5131985776101,-24.4773500141037,0.));
#70558=CARTESIAN_POINT('Ctrl Pts',(41.5131985776101,-24.4773500141037,20.));
#70559=CARTESIAN_POINT('Ctrl Pts',(41.4936154086768,-24.5045871500598,0.));
#70560=CARTESIAN_POINT('Ctrl Pts',(41.4936154086768,-24.5045871500598,20.));
#70561=CARTESIAN_POINT('Ctrl Pts',(41.4740140135823,-24.5318097963223,0.));
#70562=CARTESIAN_POINT('Ctrl Pts',(41.4740140135823,-24.5318097963223,20.));
#70563=CARTESIAN_POINT('Ctrl Pts',(41.4543944024488,-24.5590179403106,0.));
#70564=CARTESIAN_POINT('Ctrl Pts',(41.4543944024488,-24.5590179403106,20.));
#70565=CARTESIAN_POINT('Ctrl Pts',(41.4347565854076,-24.5862115694513,0.));
#70566=CARTESIAN_POINT('Ctrl Pts',(41.4347565854076,-24.5862115694513,20.));
#70567=CARTESIAN_POINT('Ctrl Pts',(41.4151005725989,-24.6133906711774,0.));
#70568=CARTESIAN_POINT('Ctrl Pts',(41.4151005725989,-24.6133906711774,20.));
#70569=CARTESIAN_POINT('Ctrl Pts',(41.3954263741717,-24.6405552329289,0.));
#70570=CARTESIAN_POINT('Ctrl Pts',(41.3954263741717,-24.6405552329289,20.));
#70571=CARTESIAN_POINT('Ctrl Pts',(41.3757340002844,-24.6677052421523,0.));
#70572=CARTESIAN_POINT('Ctrl Pts',(41.3757340002844,-24.6677052421523,20.));
#70573=CARTESIAN_POINT('Ctrl Pts',(41.3560234611038,-24.694840686301,0.));
#70574=CARTESIAN_POINT('Ctrl Pts',(41.3560234611038,-24.694840686301,20.));
#70575=CARTESIAN_POINT('Ctrl Pts',(41.3362947668064,-24.7219615528352,0.));
#70576=CARTESIAN_POINT('Ctrl Pts',(41.3362947668064,-24.7219615528352,20.));
#70577=CARTESIAN_POINT('Ctrl Pts',(41.3165479275773,-24.7490678292217,0.));
#70578=CARTESIAN_POINT('Ctrl Pts',(41.3165479275773,-24.7490678292217,20.));
#70579=CARTESIAN_POINT('Ctrl Pts',(41.2967829536105,-24.7761595029341,0.));
#70580=CARTESIAN_POINT('Ctrl Pts',(41.2967829536105,-24.7761595029341,20.));
#70581=CARTESIAN_POINT('Ctrl Pts',(41.276999855109,-24.8032365614526,0.));
#70582=CARTESIAN_POINT('Ctrl Pts',(41.276999855109,-24.8032365614526,20.));
#70583=CARTESIAN_POINT('Ctrl Pts',(41.2571986422843,-24.8302989922639,0.));
#70584=CARTESIAN_POINT('Ctrl Pts',(41.2571986422843,-24.8302989922639,20.));
#70585=CARTESIAN_POINT('Ctrl Pts',(41.2373793253577,-24.8573467828623,0.));
#70586=CARTESIAN_POINT('Ctrl Pts',(41.2373793253577,-24.8573467828623,20.));
#70587=CARTESIAN_POINT('Ctrl Pts',(41.2175419145588,-24.8843799207483,0.));
#70588=CARTESIAN_POINT('Ctrl Pts',(41.2175419145588,-24.8843799207483,20.));
#70589=CARTESIAN_POINT('Ctrl Pts',(41.1976864201268,-24.9113983934294,0.));
#70590=CARTESIAN_POINT('Ctrl Pts',(41.1976864201268,-24.9113983934294,20.));
#70591=CARTESIAN_POINT('Ctrl Pts',(41.1778128523092,-24.9384021884197,0.));
#70592=CARTESIAN_POINT('Ctrl Pts',(41.1778128523092,-24.9384021884197,20.));
#70593=CARTESIAN_POINT('Ctrl Pts',(41.1579212213625,-24.9653912932403,0.));
#70594=CARTESIAN_POINT('Ctrl Pts',(41.1579212213625,-24.9653912932403,20.));
#70595=CARTESIAN_POINT('Ctrl Pts',(41.1380115375521,-24.9923656954187,0.));
#70596=CARTESIAN_POINT('Ctrl Pts',(41.1380115375521,-24.9923656954187,20.));
#70597=CARTESIAN_POINT('Ctrl Pts',(41.1180838111525,-25.0193253824897,0.));
#70598=CARTESIAN_POINT('Ctrl Pts',(41.1180838111525,-25.0193253824897,20.));
#70599=CARTESIAN_POINT('Ctrl Pts',(41.0981380524472,-25.0462703419947,0.));
#70600=CARTESIAN_POINT('Ctrl Pts',(41.0981380524472,-25.0462703419947,20.));
#70601=CARTESIAN_POINT('Ctrl Pts',(41.0781742717283,-25.0732005614819,0.));
#70602=CARTESIAN_POINT('Ctrl Pts',(41.0781742717283,-25.0732005614819,20.));
#70603=CARTESIAN_POINT('Ctrl Pts',(41.058192479297,-25.1001160285063,0.));
#70604=CARTESIAN_POINT('Ctrl Pts',(41.058192479297,-25.1001160285063,20.));
#70605=CARTESIAN_POINT('Ctrl Pts',(41.0381926854635,-25.1270167306298,0.));
#70606=CARTESIAN_POINT('Ctrl Pts',(41.0381926854635,-25.1270167306298,20.));
#70607=CARTESIAN_POINT('Ctrl Pts',(41.0181749005471,-25.1539026554213,0.));
#70608=CARTESIAN_POINT('Ctrl Pts',(41.0181749005471,-25.1539026554213,20.));
#70609=CARTESIAN_POINT('Ctrl Pts',(40.9981391348755,-25.1807737904566,0.));
#70610=CARTESIAN_POINT('Ctrl Pts',(40.9981391348755,-25.1807737904566,20.));
#70611=CARTESIAN_POINT('Ctrl Pts',(40.9780853987856,-25.2076301233182,0.));
#70612=CARTESIAN_POINT('Ctrl Pts',(40.9780853987856,-25.2076301233182,20.));
#70613=CARTESIAN_POINT('Ctrl Pts',(40.9580137026228,-25.2344716415952,0.));
#70614=CARTESIAN_POINT('Ctrl Pts',(40.9580137026228,-25.2344716415952,20.));
#70615=CARTESIAN_POINT('Ctrl Pts',(40.9379240567416,-25.2612983328836,0.));
#70616=CARTESIAN_POINT('Ctrl Pts',(40.9379240567416,-25.2612983328836,20.));
#70617=CARTESIAN_POINT('Ctrl Pts',(40.9178164715051,-25.2881101847862,0.));
#70618=CARTESIAN_POINT('Ctrl Pts',(40.9178164715051,-25.2881101847862,20.));
#70619=CARTESIAN_POINT('Ctrl Pts',(40.8976909572856,-25.3149071849127,0.));
#70620=CARTESIAN_POINT('Ctrl Pts',(40.8976909572856,-25.3149071849127,20.));
#70621=CARTESIAN_POINT('Ctrl Pts',(40.8775475244644,-25.3416893208803,0.));
#70622=CARTESIAN_POINT('Ctrl Pts',(40.8775475244644,-25.3416893208803,20.));
#70623=CARTESIAN_POINT('Ctrl Pts',(40.8573861834315,-25.3684565803126,0.));
#70624=CARTESIAN_POINT('Ctrl Pts',(40.8573861834315,-25.3684565803126,20.));
#70625=CARTESIAN_POINT('Ctrl Pts',(40.8372069445861,-25.3952089508407,0.));
#70626=CARTESIAN_POINT('Ctrl Pts',(40.8372069445861,-25.3952089508407,20.));
#70627=CARTESIAN_POINT('Ctrl Pts',(40.8170098183361,-25.4219464201024,0.));
#70628=CARTESIAN_POINT('Ctrl Pts',(40.8170098183361,-25.4219464201024,20.));
#70629=CARTESIAN_POINT('Ctrl Pts',(40.796794815098,-25.4486689757422,0.));
#70630=CARTESIAN_POINT('Ctrl Pts',(40.796794815098,-25.4486689757422,20.));
#70631=CARTESIAN_POINT('Ctrl Pts',(40.7765619452973,-25.4753766054114,0.));
#70632=CARTESIAN_POINT('Ctrl Pts',(40.7765619452973,-25.4753766054114,20.));
#70633=CARTESIAN_POINT('Ctrl Pts',(40.7563112193678,-25.5020692967677,0.));
#70634=CARTESIAN_POINT('Ctrl Pts',(40.7563112193678,-25.5020692967677,20.));
#70635=CARTESIAN_POINT('Ctrl Pts',(40.7360426477524,-25.528747037476,0.));
#70636=CARTESIAN_POINT('Ctrl Pts',(40.7360426477524,-25.528747037476,20.));
#70637=CARTESIAN_POINT('Ctrl Pts',(40.715756240903,-25.5554098152083,0.));
#70638=CARTESIAN_POINT('Ctrl Pts',(40.715756240903,-25.5554098152083,20.));
#70639=CARTESIAN_POINT('Ctrl Pts',(40.6954520092804,-25.5820576176439,0.));
#70640=CARTESIAN_POINT('Ctrl Pts',(40.6954520092804,-25.5820576176439,20.));
#70641=CARTESIAN_POINT('Ctrl Pts',(40.6751299633542,-25.6086904324689,0.));
#70642=CARTESIAN_POINT('Ctrl Pts',(40.6751299633542,-25.6086904324689,20.));
#70643=CARTESIAN_POINT('Ctrl Pts',(40.6547901136033,-25.6353082473769,0.));
#70644=CARTESIAN_POINT('Ctrl Pts',(40.6547901136033,-25.6353082473769,20.));
#70645=CARTESIAN_POINT('Ctrl Pts',(40.6344324705148,-25.6619110500678,0.));
#70646=CARTESIAN_POINT('Ctrl Pts',(40.6344324705148,-25.6619110500678,20.));
#70647=CARTESIAN_POINT('Ctrl Pts',(40.6140570445846,-25.6884988282486,0.));
#70648=CARTESIAN_POINT('Ctrl Pts',(40.6140570445846,-25.6884988282486,20.));
#70649=CARTESIAN_POINT('Ctrl Pts',(40.5936638463177,-25.7150715696333,0.));
#70650=CARTESIAN_POINT('Ctrl Pts',(40.5936638463177,-25.7150715696333,20.));
#70651=CARTESIAN_POINT('Ctrl Pts',(40.5732528862276,-25.7416292619425,0.));
#70652=CARTESIAN_POINT('Ctrl Pts',(40.5732528862276,-25.7416292619425,20.));
#70653=CARTESIAN_POINT('Ctrl Pts',(40.5528241748366,-25.768171892904,0.));
#70654=CARTESIAN_POINT('Ctrl Pts',(40.5528241748366,-25.768171892904,20.));
#70655=CARTESIAN_POINT('Ctrl Pts',(40.5323777226757,-25.7946994502526,0.));
#70656=CARTESIAN_POINT('Ctrl Pts',(40.5323777226757,-25.7946994502526,20.));
#70657=CARTESIAN_POINT('Ctrl Pts',(40.5119135402852,-25.8212119217304,0.));
#70658=CARTESIAN_POINT('Ctrl Pts',(40.5119135402852,-25.8212119217304,20.));
#70659=CARTESIAN_POINT('Ctrl Pts',(40.491431638214,-25.8477092950863,0.));
#70660=CARTESIAN_POINT('Ctrl Pts',(40.491431638214,-25.8477092950863,20.));
#70661=CARTESIAN_POINT('Ctrl Pts',(40.4709320270197,-25.8741915580762,0.));
#70662=CARTESIAN_POINT('Ctrl Pts',(40.4709320270197,-25.8741915580762,20.));
#70663=CARTESIAN_POINT('Ctrl Pts',(40.4504147172684,-25.9006586984631,0.));
#70664=CARTESIAN_POINT('Ctrl Pts',(40.4504147172684,-25.9006586984631,20.));
#70665=CARTESIAN_POINT('Ctrl Pts',(40.4298797195352,-25.9271107040169,0.));
#70666=CARTESIAN_POINT('Ctrl Pts',(40.4298797195352,-25.9271107040169,20.));
#70667=CARTESIAN_POINT('Ctrl Pts',(40.4093270444043,-25.953547562515,0.));
#70668=CARTESIAN_POINT('Ctrl Pts',(40.4093270444043,-25.953547562515,20.));
#70669=CARTESIAN_POINT('Ctrl Pts',(40.3887567024682,-25.9799692617416,0.));
#70670=CARTESIAN_POINT('Ctrl Pts',(40.3887567024682,-25.9799692617416,20.));
#70671=CARTESIAN_POINT('Ctrl Pts',(40.3681687043283,-26.0063757894875,0.));
#70672=CARTESIAN_POINT('Ctrl Pts',(40.3681687043283,-26.0063757894875,20.));
#70673=CARTESIAN_POINT('Ctrl Pts',(40.347563060595,-26.0327671335511,0.));
#70674=CARTESIAN_POINT('Ctrl Pts',(40.347563060595,-26.0327671335511,20.));
#70675=CARTESIAN_POINT('Ctrl Pts',(40.326939781887,-26.0591432817373,0.));
#70676=CARTESIAN_POINT('Ctrl Pts',(40.326939781887,-26.0591432817373,20.));
#70677=CARTESIAN_POINT('Ctrl Pts',(40.3062988788318,-26.0855042218584,0.));
#70678=CARTESIAN_POINT('Ctrl Pts',(40.3062988788318,-26.0855042218584,20.));
#70679=CARTESIAN_POINT('Ctrl Pts',(40.2856403620657,-26.1118499417334,0.));
#70680=CARTESIAN_POINT('Ctrl Pts',(40.2856403620657,-26.1118499417334,20.));
#70681=CARTESIAN_POINT('Ctrl Pts',(40.2649642422341,-26.1381804291893,0.));
#70682=CARTESIAN_POINT('Ctrl Pts',(40.2649642422341,-26.1381804291893,20.));
#70683=CARTESIAN_POINT('Ctrl Pts',(40.2442705299908,-26.1644956720595,0.));
#70684=CARTESIAN_POINT('Ctrl Pts',(40.2442705299908,-26.1644956720595,20.));
#70685=CARTESIAN_POINT('Ctrl Pts',(40.2235592359986,-26.1907956581852,0.));
#70686=CARTESIAN_POINT('Ctrl Pts',(40.2235592359986,-26.1907956581852,20.));
#70687=CARTESIAN_POINT('Ctrl Pts',(40.2028303709288,-26.217080375414,0.));
#70688=CARTESIAN_POINT('Ctrl Pts',(40.2028303709288,-26.217080375414,20.));
#70689=CARTESIAN_POINT('Ctrl Pts',(40.1820839454613,-26.2433498116008,0.));
#70690=CARTESIAN_POINT('Ctrl Pts',(40.1820839454613,-26.2433498116008,20.));
#70691=CARTESIAN_POINT('Ctrl Pts',(40.161319970285,-26.2696039546074,0.));
#70692=CARTESIAN_POINT('Ctrl Pts',(40.161319970285,-26.2696039546074,20.));
#70693=CARTESIAN_POINT('Ctrl Pts',(40.1405384560971,-26.2958427923028,0.));
#70694=CARTESIAN_POINT('Ctrl Pts',(40.1405384560971,-26.2958427923028,20.));
#70695=CARTESIAN_POINT('Ctrl Pts',(40.1197394136039,-26.3220663125631,0.));
#70696=CARTESIAN_POINT('Ctrl Pts',(40.1197394136039,-26.3220663125631,20.));
#70697=CARTESIAN_POINT('Ctrl Pts',(40.0989228535202,-26.3482745032719,0.));
#70698=CARTESIAN_POINT('Ctrl Pts',(40.0989228535202,-26.3482745032719,20.));
#70699=CARTESIAN_POINT('Ctrl Pts',(40.0780887865696,-26.3744673523197,0.));
#70700=CARTESIAN_POINT('Ctrl Pts',(40.0780887865696,-26.3744673523197,20.));
#70701=CARTESIAN_POINT('Ctrl Pts',(40.0572372234843,-26.4006448476042,0.));
#70702=CARTESIAN_POINT('Ctrl Pts',(40.0572372234843,-26.4006448476042,20.));
#70703=CARTESIAN_POINT('Ctrl Pts',(40.0363681750052,-26.4268069770299,0.));
#70704=CARTESIAN_POINT('Ctrl Pts',(40.0363681750052,-26.4268069770299,20.));
#70705=CARTESIAN_POINT('Ctrl Pts',(40.015481651882,-26.4529537285089,0.));
#70706=CARTESIAN_POINT('Ctrl Pts',(40.015481651882,-26.4529537285089,20.));
#70707=CARTESIAN_POINT('Ctrl Pts',(39.994577664873,-26.4790850899607,0.));
#70708=CARTESIAN_POINT('Ctrl Pts',(39.994577664873,-26.4790850899607,20.));
#70709=CARTESIAN_POINT('Ctrl Pts',(39.9736562247456,-26.5052010493117,0.));
#70710=CARTESIAN_POINT('Ctrl Pts',(39.9736562247456,-26.5052010493117,20.));
#70711=CARTESIAN_POINT('Ctrl Pts',(39.9527173422752,-26.5313015944953,0.));
#70712=CARTESIAN_POINT('Ctrl Pts',(39.9527173422752,-26.5313015944953,20.));
#70713=CARTESIAN_POINT('Ctrl Pts',(39.9317610282459,-26.5573867134521,0.));
#70714=CARTESIAN_POINT('Ctrl Pts',(39.9317610282459,-26.5573867134521,20.));
#70715=CARTESIAN_POINT('Ctrl Pts',(39.9107872934506,-26.5834563941296,0.));
#70716=CARTESIAN_POINT('Ctrl Pts',(39.9107872934506,-26.5834563941296,20.));
#70717=CARTESIAN_POINT('Ctrl Pts',(39.8897961486907,-26.6095106244829,0.));
#70718=CARTESIAN_POINT('Ctrl Pts',(39.8897961486907,-26.6095106244829,20.));
#70719=CARTESIAN_POINT('Ctrl Pts',(39.8687876047769,-26.6355493924744,0.));
#70720=CARTESIAN_POINT('Ctrl Pts',(39.8687876047769,-26.6355493924744,20.));
#70721=CARTESIAN_POINT('Ctrl Pts',(39.847761672528,-26.6615726860735,0.));
#70722=CARTESIAN_POINT('Ctrl Pts',(39.847761672528,-26.6615726860735,20.));
#70723=CARTESIAN_POINT('Ctrl Pts',(39.8267183627717,-26.687580493257,0.));
#70724=CARTESIAN_POINT('Ctrl Pts',(39.8267183627717,-26.687580493257,20.));
#70725=CARTESIAN_POINT('Ctrl Pts',(39.8056576863443,-26.713572802009,0.));
#70726=CARTESIAN_POINT('Ctrl Pts',(39.8056576863443,-26.713572802009,20.));
#70727=CARTESIAN_POINT('Ctrl Pts',(39.7845796540903,-26.7395496003209,0.));
#70728=CARTESIAN_POINT('Ctrl Pts',(39.7845796540903,-26.7395496003209,20.));
#70729=CARTESIAN_POINT('Ctrl Pts',(39.7634842768631,-26.7655108761908,0.));
#70730=CARTESIAN_POINT('Ctrl Pts',(39.7634842768631,-26.7655108761908,20.));
#70731=CARTESIAN_POINT('Ctrl Pts',(39.7423715655248,-26.7914566176244,0.));
#70732=CARTESIAN_POINT('Ctrl Pts',(39.7423715655248,-26.7914566176244,20.));
#70733=CARTESIAN_POINT('Ctrl Pts',(39.7212415309462,-26.8173868126345,0.));
#70734=CARTESIAN_POINT('Ctrl Pts',(39.7212415309462,-26.8173868126345,20.));
#70735=CARTESIAN_POINT('Ctrl Pts',(39.7000941840065,-26.843301449241,0.));
#70736=CARTESIAN_POINT('Ctrl Pts',(39.7000941840065,-26.843301449241,20.));
#70737=CARTESIAN_POINT('Ctrl Pts',(39.6789295355942,-26.8692005154716,0.));
#70738=CARTESIAN_POINT('Ctrl Pts',(39.6789295355942,-26.8692005154716,20.));
#70739=CARTESIAN_POINT('Ctrl Pts',(39.6577475966055,-26.8950839993609,0.));
#70740=CARTESIAN_POINT('Ctrl Pts',(39.6577475966055,-26.8950839993609,20.));
#70741=CARTESIAN_POINT('Ctrl Pts',(39.6365483779457,-26.9209518889509,0.));
#70742=CARTESIAN_POINT('Ctrl Pts',(39.6365483779457,-26.9209518889509,20.));
#70743=CARTESIAN_POINT('Ctrl Pts',(39.6153318905282,-26.9468041722907,0.));
#70744=CARTESIAN_POINT('Ctrl Pts',(39.6153318905282,-26.9468041722907,20.));
#70745=CARTESIAN_POINT('Ctrl Pts',(39.5940981452753,-26.9726408374371,0.));
#70746=CARTESIAN_POINT('Ctrl Pts',(39.5940981452753,-26.9726408374371,20.));
#70747=CARTESIAN_POINT('Ctrl Pts',(39.5728471531177,-26.9984618724537,0.));
#70748=CARTESIAN_POINT('Ctrl Pts',(39.5728471531177,-26.9984618724537,20.));
#70749=CARTESIAN_POINT('Ctrl Pts',(39.5515789249952,-27.0242672654118,0.));
#70750=CARTESIAN_POINT('Ctrl Pts',(39.5515789249952,-27.0242672654118,20.));
#70751=CARTESIAN_POINT('Ctrl Pts',(39.5302934718558,-27.0500570043898,0.));
#70752=CARTESIAN_POINT('Ctrl Pts',(39.5302934718558,-27.0500570043898,20.));
#70753=CARTESIAN_POINT('Ctrl Pts',(39.5089908046561,-27.0758310774732,0.));
#70754=CARTESIAN_POINT('Ctrl Pts',(39.5089908046561,-27.0758310774732,20.));
#70755=CARTESIAN_POINT('Ctrl Pts',(39.4876709343614,-27.1015894727552,0.));
#70756=CARTESIAN_POINT('Ctrl Pts',(39.4876709343614,-27.1015894727552,20.));
#70757=CARTESIAN_POINT('Ctrl Pts',(39.4663338719455,-27.1273321783362,0.));
#70758=CARTESIAN_POINT('Ctrl Pts',(39.4663338719455,-27.1273321783362,20.));
#70759=CARTESIAN_POINT('Ctrl Pts',(39.4449796283908,-27.153059182324,0.));
#70760=CARTESIAN_POINT('Ctrl Pts',(39.4449796283908,-27.153059182324,20.));
#70761=CARTESIAN_POINT('Ctrl Pts',(39.4236082146882,-27.1787704728337,0.));
#70762=CARTESIAN_POINT('Ctrl Pts',(39.4236082146882,-27.1787704728337,20.));
#70763=CARTESIAN_POINT('Ctrl Pts',(39.4022196418372,-27.2044660379877,0.));
#70764=CARTESIAN_POINT('Ctrl Pts',(39.4022196418372,-27.2044660379877,20.));
#70765=CARTESIAN_POINT('Ctrl Pts',(39.3808139208456,-27.2301458659158,0.));
#70766=CARTESIAN_POINT('Ctrl Pts',(39.3808139208456,-27.2301458659158,20.));
#70767=CARTESIAN_POINT('Ctrl Pts',(39.3593910627297,-27.2558099447548,0.));
#70768=CARTESIAN_POINT('Ctrl Pts',(39.3593910627297,-27.2558099447548,20.));
#70769=CARTESIAN_POINT('Ctrl Pts',(39.3379510785145,-27.2814582626493,0.));
#70770=CARTESIAN_POINT('Ctrl Pts',(39.3379510785145,-27.2814582626493,20.));
#70771=CARTESIAN_POINT('Ctrl Pts',(39.3164939792334,-27.3070908077508,0.));
#70772=CARTESIAN_POINT('Ctrl Pts',(39.3164939792334,-27.3070908077508,20.));
#70773=CARTESIAN_POINT('Ctrl Pts',(39.2950197759285,-27.3327075682187,0.));
#70774=CARTESIAN_POINT('Ctrl Pts',(39.2950197759285,-27.3327075682187,20.));
#70775=CARTESIAN_POINT('Ctrl Pts',(39.2735284796508,-27.3583085322198,0.));
#70776=CARTESIAN_POINT('Ctrl Pts',(39.2735284796508,-27.3583085322198,20.));
#70777=CARTESIAN_POINT('Ctrl Pts',(39.25202010146,-27.3838936879286,0.));
#70778=CARTESIAN_POINT('Ctrl Pts',(39.25202010146,-27.3838936879286,20.));
#70779=CARTESIAN_POINT('Ctrl Pts',(39.2304946524241,-27.4094630235266,0.));
#70780=CARTESIAN_POINT('Ctrl Pts',(39.2304946524241,-27.4094630235266,20.));
#70781=CARTESIAN_POINT('Ctrl Pts',(39.2089521436188,-27.4350165272023,0.));
#70782=CARTESIAN_POINT('Ctrl Pts',(39.2089521436188,-27.4350165272023,20.));
#70783=CARTESIAN_POINT('Ctrl Pts',(39.1873925861285,-27.4605541871518,0.));
#70784=CARTESIAN_POINT('Ctrl Pts',(39.1873925861285,-27.4605541871518,20.));
#70785=CARTESIAN_POINT('Ctrl Pts',(39.1658159910457,-27.4860759915783,0.));
#70786=CARTESIAN_POINT('Ctrl Pts',(39.1658159910457,-27.4860759915783,20.));
#70787=CARTESIAN_POINT('Ctrl Pts',(39.1442223694722,-27.5115819286927,0.));
#70788=CARTESIAN_POINT('Ctrl Pts',(39.1442223694722,-27.5115819286927,20.));
#70789=CARTESIAN_POINT('Ctrl Pts',(39.1226117325183,-27.5370719867137,0.));
#70790=CARTESIAN_POINT('Ctrl Pts',(39.1226117325183,-27.5370719867137,20.));
#70791=CARTESIAN_POINT('Ctrl Pts',(39.100984091303,-27.5625461538676,0.));
#70792=CARTESIAN_POINT('Ctrl Pts',(39.100984091303,-27.5625461538676,20.));
#70793=CARTESIAN_POINT('Ctrl Pts',(39.0793394569537,-27.5880044183879,0.));
#70794=CARTESIAN_POINT('Ctrl Pts',(39.0793394569537,-27.5880044183879,20.));
#70795=CARTESIAN_POINT('Ctrl Pts',(39.057677840606,-27.6134467685156,0.));
#70796=CARTESIAN_POINT('Ctrl Pts',(39.057677840606,-27.6134467685156,20.));
#70797=CARTESIAN_POINT('Ctrl Pts',(39.0359992534037,-27.6388731924983,0.));
#70798=CARTESIAN_POINT('Ctrl Pts',(39.0359992534037,-27.6388731924983,20.));
#70799=CARTESIAN_POINT('Ctrl Pts',(39.0143037064988,-27.6642836785915,0.));
#70800=CARTESIAN_POINT('Ctrl Pts',(39.0143037064988,-27.6642836785915,20.));
#70801=CARTESIAN_POINT('Ctrl Pts',(38.9925912110523,-27.6896782150583,0.));
#70802=CARTESIAN_POINT('Ctrl Pts',(38.9925912110523,-27.6896782150583,20.));
#70803=CARTESIAN_POINT('Ctrl Pts',(38.9708617782339,-27.7150567901695,0.));
#70804=CARTESIAN_POINT('Ctrl Pts',(38.9708617782339,-27.7150567901695,20.));
#70805=CARTESIAN_POINT('Ctrl Pts',(38.9491154192216,-27.7404193922036,0.));
#70806=CARTESIAN_POINT('Ctrl Pts',(38.9491154192216,-27.7404193922036,20.));
#70807=CARTESIAN_POINT('Ctrl Pts',(38.9273521452022,-27.7657660094467,0.));
#70808=CARTESIAN_POINT('Ctrl Pts',(38.9273521452022,-27.7657660094467,20.));
#70809=CARTESIAN_POINT('Ctrl Pts',(38.9055719673706,-27.7910966301919,0.));
#70810=CARTESIAN_POINT('Ctrl Pts',(38.9055719673706,-27.7910966301919,20.));
#70811=CARTESIAN_POINT('Ctrl Pts',(38.8837748969299,-27.8164112427396,0.));
#70812=CARTESIAN_POINT('Ctrl Pts',(38.8837748969299,-27.8164112427396,20.));
#70813=CARTESIAN_POINT('Ctrl Pts',(38.8619609450912,-27.8417098353976,0.));
#70814=CARTESIAN_POINT('Ctrl Pts',(38.8619609450912,-27.8417098353976,20.));
#70815=CARTESIAN_POINT('Ctrl Pts',(38.8401301230745,-27.866992396481,0.));
#70816=CARTESIAN_POINT('Ctrl Pts',(38.8401301230745,-27.866992396481,20.));
#70817=CARTESIAN_POINT('Ctrl Pts',(38.8182824421081,-27.8922589143132,0.));
#70818=CARTESIAN_POINT('Ctrl Pts',(38.8182824421081,-27.8922589143132,20.));
#70819=CARTESIAN_POINT('Ctrl Pts',(38.7964179134294,-27.917509377225,0.));
#70820=CARTESIAN_POINT('Ctrl Pts',(38.7964179134294,-27.917509377225,20.));
#70821=CARTESIAN_POINT('Ctrl Pts',(38.7745365482837,-27.9427437735547,0.));
#70822=CARTESIAN_POINT('Ctrl Pts',(38.7745365482837,-27.9427437735547,20.));
#70823=CARTESIAN_POINT('Ctrl Pts',(38.752638357925,-27.9679620916479,0.));
#70824=CARTESIAN_POINT('Ctrl Pts',(38.752638357925,-27.9679620916479,20.));
#70825=CARTESIAN_POINT('Ctrl Pts',(38.7307233536152,-27.9931643198581,0.));
#70826=CARTESIAN_POINT('Ctrl Pts',(38.7307233536152,-27.9931643198581,20.));
#70827=CARTESIAN_POINT('Ctrl Pts',(38.7087915466246,-28.0183504465459,0.));
#70828=CARTESIAN_POINT('Ctrl Pts',(38.7087915466246,-28.0183504465459,20.));
#70829=CARTESIAN_POINT('Ctrl Pts',(38.6868429482324,-28.0435204600798,0.));
#70830=CARTESIAN_POINT('Ctrl Pts',(38.6868429482324,-28.0435204600798,20.));
#70831=CARTESIAN_POINT('Ctrl Pts',(38.6648775697261,-28.0686743488362,0.));
#70832=CARTESIAN_POINT('Ctrl Pts',(38.6648775697261,-28.0686743488362,20.));
#70833=CARTESIAN_POINT('Ctrl Pts',(38.6428954224012,-28.0938121011982,0.));
#70834=CARTESIAN_POINT('Ctrl Pts',(38.6428954224012,-28.0938121011982,20.));
#70835=CARTESIAN_POINT('Ctrl Pts',(38.6208965175619,-28.1189337055566,0.));
#70836=CARTESIAN_POINT('Ctrl Pts',(38.6208965175619,-28.1189337055566,20.));
#70837=CARTESIAN_POINT('Ctrl Pts',(38.5988808665205,-28.14403915031,0.));
#70838=CARTESIAN_POINT('Ctrl Pts',(38.5988808665205,-28.14403915031,20.));
#70839=CARTESIAN_POINT('Ctrl Pts',(38.5768484805978,-28.1691284238645,0.));
#70840=CARTESIAN_POINT('Ctrl Pts',(38.5768484805978,-28.1691284238645,20.));
#70841=CARTESIAN_POINT('Ctrl Pts',(38.5547993711231,-28.1942015146341,0.));
#70842=CARTESIAN_POINT('Ctrl Pts',(38.5547993711231,-28.1942015146341,20.));
#70843=CARTESIAN_POINT('Ctrl Pts',(38.5327335494334,-28.2192584110398,0.));
#70844=CARTESIAN_POINT('Ctrl Pts',(38.5327335494334,-28.2192584110398,20.));
#70845=CARTESIAN_POINT('Ctrl Pts',(38.5106510268752,-28.2442991015113,0.));
#70846=CARTESIAN_POINT('Ctrl Pts',(38.5106510268752,-28.2442991015113,20.));
#70847=CARTESIAN_POINT('Ctrl Pts',(38.4885518148031,-28.2693235744854,0.));
#70848=CARTESIAN_POINT('Ctrl Pts',(38.4885518148031,-28.2693235744854,20.));
#70849=CARTESIAN_POINT('Ctrl Pts',(38.4664359245797,-28.2943318184066,0.));
#70850=CARTESIAN_POINT('Ctrl Pts',(38.4664359245797,-28.2943318184066,20.));
#70851=CARTESIAN_POINT('Ctrl Pts',(38.4443033675759,-28.3193238217266,0.));
#70852=CARTESIAN_POINT('Ctrl Pts',(38.4443033675759,-28.3193238217266,20.));
#70853=CARTESIAN_POINT('Ctrl Pts',(38.4221541551709,-28.344299572905,0.));
#70854=CARTESIAN_POINT('Ctrl Pts',(38.4221541551709,-28.344299572905,20.));
#70855=CARTESIAN_POINT('Ctrl Pts',(38.3999882987522,-28.3692590604082,0.));
#70856=CARTESIAN_POINT('Ctrl Pts',(38.3999882987522,-28.3692590604082,20.));
#70857=CARTESIAN_POINT('Ctrl Pts',(38.3778058097152,-28.3942022727108,0.));
#70858=CARTESIAN_POINT('Ctrl Pts',(38.3778058097152,-28.3942022727108,20.));
#70859=CARTESIAN_POINT('Ctrl Pts',(38.3556066994642,-28.4191291982951,0.));
#70860=CARTESIAN_POINT('Ctrl Pts',(38.3556066994642,-28.4191291982951,20.));
#70861=CARTESIAN_POINT('Ctrl Pts',(38.3333909794119,-28.4440398256512,0.));
#70862=CARTESIAN_POINT('Ctrl Pts',(38.3333909794119,-28.4440398256512,20.));
#70863=CARTESIAN_POINT('Ctrl Pts',(38.3111586609794,-28.4689341432774,0.));
#70864=CARTESIAN_POINT('Ctrl Pts',(38.3111586609794,-28.4689341432774,20.));
#70865=CARTESIAN_POINT('Ctrl Pts',(38.2889097555964,-28.4938121396793,0.));
#70866=CARTESIAN_POINT('Ctrl Pts',(38.2889097555964,-28.4938121396793,20.));
#70867=CARTESIAN_POINT('Ctrl Pts',(38.2666442747002,-28.5186738033704,0.));
#70868=CARTESIAN_POINT('Ctrl Pts',(38.2666442747002,-28.5186738033704,20.));
#70869=CARTESIAN_POINT('Ctrl Pts',(38.2443622297368,-28.5435191228711,0.));
#70870=CARTESIAN_POINT('Ctrl Pts',(38.2443622297368,-28.5435191228711,20.));
#70871=CARTESIAN_POINT('Ctrl Pts',(38.2220636321601,-28.5683480867098,0.));
#70872=CARTESIAN_POINT('Ctrl Pts',(38.2220636321601,-28.5683480867098,20.));
#70873=CARTESIAN_POINT('Ctrl Pts',(38.1997484934321,-28.5931606834224,0.));
#70874=CARTESIAN_POINT('Ctrl Pts',(38.1997484934321,-28.5931606834224,20.));
#70875=CARTESIAN_POINT('Ctrl Pts',(38.1774168250235,-28.6179569015525,0.));
#70876=CARTESIAN_POINT('Ctrl Pts',(38.1774168250235,-28.6179569015525,20.));
#70877=CARTESIAN_POINT('Ctrl Pts',(38.1550686384134,-28.6427367296518,0.));
#70878=CARTESIAN_POINT('Ctrl Pts',(38.1550686384134,-28.6427367296518,20.));
#70879=CARTESIAN_POINT('Ctrl Pts',(38.1327039450889,-28.6675001562794,0.));
#70880=CARTESIAN_POINT('Ctrl Pts',(38.1327039450889,-28.6675001562794,20.));
#70881=CARTESIAN_POINT('Ctrl Pts',(38.1103227565456,-28.6922471700024,0.));
#70882=CARTESIAN_POINT('Ctrl Pts',(38.1103227565456,-28.6922471700024,20.));
#70883=CARTESIAN_POINT('Ctrl Pts',(38.0879250842874,-28.7169777593956,0.));
#70884=CARTESIAN_POINT('Ctrl Pts',(38.0879250842874,-28.7169777593956,20.));
#70885=CARTESIAN_POINT('Ctrl Pts',(38.0655109398262,-28.7416919130413,0.));
#70886=CARTESIAN_POINT('Ctrl Pts',(38.0655109398262,-28.7416919130413,20.));
#70887=CARTESIAN_POINT('Ctrl Pts',(38.0430803346823,-28.76638961953,0.));
#70888=CARTESIAN_POINT('Ctrl Pts',(38.0430803346823,-28.76638961953,20.));
#70889=CARTESIAN_POINT('Ctrl Pts',(38.020633280384,-28.7910708674595,0.));
#70890=CARTESIAN_POINT('Ctrl Pts',(38.020633280384,-28.7910708674595,20.));
#70891=CARTESIAN_POINT('Ctrl Pts',(37.9981697884679,-28.8157356454354,0.));
#70892=CARTESIAN_POINT('Ctrl Pts',(37.9981697884679,-28.8157356454354,20.));
#70893=CARTESIAN_POINT('Ctrl Pts',(37.975689870479,-28.8403839420709,0.));
#70894=CARTESIAN_POINT('Ctrl Pts',(37.975689870479,-28.8403839420709,20.));
#70895=CARTESIAN_POINT('Ctrl Pts',(37.9531935379708,-28.8650157459872,0.));
#70896=CARTESIAN_POINT('Ctrl Pts',(37.9531935379708,-28.8650157459872,20.));
#70897=CARTESIAN_POINT('Ctrl Pts',(37.9306808025048,-28.8896310458131,0.));
#70898=CARTESIAN_POINT('Ctrl Pts',(37.9306808025048,-28.8896310458131,20.));
#70899=CARTESIAN_POINT('Ctrl Pts',(37.9081516756509,-28.9142298301853,0.));
#70900=CARTESIAN_POINT('Ctrl Pts',(37.9081516756509,-28.9142298301853,20.));
#70901=CARTESIAN_POINT('Ctrl Pts',(37.8856061689868,-28.9388120877484,0.));
#70902=CARTESIAN_POINT('Ctrl Pts',(37.8856061689868,-28.9388120877484,20.));
#70903=CARTESIAN_POINT('Ctrl Pts',(37.8630442940985,-28.9633778071544,0.));
#70904=CARTESIAN_POINT('Ctrl Pts',(37.8630442940985,-28.9633778071544,20.));
#70905=CARTESIAN_POINT('Ctrl Pts',(37.8404660625803,-28.9879269770638,0.));
#70906=CARTESIAN_POINT('Ctrl Pts',(37.8404660625803,-28.9879269770638,20.));
#70907=CARTESIAN_POINT('Ctrl Pts',(37.8178714860345,-29.0124595861442,0.));
#70908=CARTESIAN_POINT('Ctrl Pts',(37.8178714860345,-29.0124595861442,20.));
#70909=CARTESIAN_POINT('Ctrl Pts',(37.7952605760716,-29.0369756230713,0.));
#70910=CARTESIAN_POINT('Ctrl Pts',(37.7952605760716,-29.0369756230713,20.));
#70911=CARTESIAN_POINT('Ctrl Pts',(37.7726333443105,-29.0614750765285,0.));
#70912=CARTESIAN_POINT('Ctrl Pts',(37.7726333443105,-29.0614750765285,20.));
#70913=CARTESIAN_POINT('Ctrl Pts',(37.7499898023784,-29.0859579352069,0.));
#70914=CARTESIAN_POINT('Ctrl Pts',(37.7499898023784,-29.0859579352069,20.));
#70915=CARTESIAN_POINT('Ctrl Pts',(37.7273299619109,-29.1104241878056,0.));
#70916=CARTESIAN_POINT('Ctrl Pts',(37.7273299619109,-29.1104241878056,20.));
#70917=CARTESIAN_POINT('Ctrl Pts',(37.7046538345516,-29.1348738230316,0.));
#70918=CARTESIAN_POINT('Ctrl Pts',(37.7046538345516,-29.1348738230316,20.));
#70919=CARTESIAN_POINT('Ctrl Pts',(37.6819614319522,-29.1593068295998,0.));
#70920=CARTESIAN_POINT('Ctrl Pts',(37.6819614319522,-29.1593068295998,20.));
#70921=CARTESIAN_POINT('Ctrl Pts',(37.6592527657727,-29.1837231962329,0.));
#70922=CARTESIAN_POINT('Ctrl Pts',(37.6592527657727,-29.1837231962329,20.));
#70923=CARTESIAN_POINT('Ctrl Pts',(37.6365278476807,-29.208122911661,0.));
#70924=CARTESIAN_POINT('Ctrl Pts',(37.6365278476807,-29.208122911661,20.));
#70925=CARTESIAN_POINT('Ctrl Pts',(37.6137866893519,-29.2325059646225,0.));
#70926=CARTESIAN_POINT('Ctrl Pts',(37.6137866893519,-29.2325059646225,20.));
#70927=CARTESIAN_POINT('Ctrl Pts',(37.5910293024705,-29.2568723438632,0.));
#70928=CARTESIAN_POINT('Ctrl Pts',(37.5910293024705,-29.2568723438632,20.));
#70929=CARTESIAN_POINT('Ctrl Pts',(37.5682556987287,-29.2812220381373,0.));
#70930=CARTESIAN_POINT('Ctrl Pts',(37.5682556987287,-29.2812220381373,20.));
#70931=CARTESIAN_POINT('Ctrl Pts',(37.5454658898273,-29.3055550362068,0.));
#70932=CARTESIAN_POINT('Ctrl Pts',(37.5454658898273,-29.3055550362068,20.));
#70933=CARTESIAN_POINT('Ctrl Pts',(37.5226598874754,-29.3298713268414,0.));
#70934=CARTESIAN_POINT('Ctrl Pts',(37.5226598874754,-29.3298713268414,20.));
#70935=CARTESIAN_POINT('Ctrl Pts',(37.4998377033899,-29.3541708988191,0.));
#70936=CARTESIAN_POINT('Ctrl Pts',(37.4998377033899,-29.3541708988191,20.));
#70937=CARTESIAN_POINT('Ctrl Pts',(37.4769993492958,-29.3784537409251,0.));
#70938=CARTESIAN_POINT('Ctrl Pts',(37.4769993492958,-29.3784537409251,20.));
#70939=CARTESIAN_POINT('Ctrl Pts',(37.4541448369259,-29.4027198419524,0.));
#70940=CARTESIAN_POINT('Ctrl Pts',(37.4541448369259,-29.4027198419524,20.));
#70941=CARTESIAN_POINT('Ctrl Pts',(37.4312741780212,-29.4269691907023,0.));
#70942=CARTESIAN_POINT('Ctrl Pts',(37.4312741780212,-29.4269691907023,20.));
#70943=CARTESIAN_POINT('Ctrl Pts',(37.4083873843312,-29.4512017759842,0.));
#70944=CARTESIAN_POINT('Ctrl Pts',(37.4083873843312,-29.4512017759842,20.));
#70945=CARTESIAN_POINT('Ctrl Pts',(37.3854844676135,-29.4754175866156,0.));
#70946=CARTESIAN_POINT('Ctrl Pts',(37.3854844676135,-29.4754175866156,20.));
#70947=CARTESIAN_POINT('Ctrl Pts',(37.3625654396334,-29.4996166114217,0.));
#70948=CARTESIAN_POINT('Ctrl Pts',(37.3625654396334,-29.4996166114217,20.));
#70949=CARTESIAN_POINT('Ctrl Pts',(37.3396303121646,-29.5237988392353,0.));
#70950=CARTESIAN_POINT('Ctrl Pts',(37.3396303121646,-29.5237988392353,20.));
#70951=CARTESIAN_POINT('Ctrl Pts',(37.3166790969884,-29.5479642588972,0.));
#70952=CARTESIAN_POINT('Ctrl Pts',(37.3166790969884,-29.5479642588972,20.));
#70953=CARTESIAN_POINT('Ctrl Pts',(37.2937118058947,-29.5721128592559,0.));
#70954=CARTESIAN_POINT('Ctrl Pts',(37.2937118058947,-29.5721128592559,20.));
#70955=CARTESIAN_POINT('Ctrl Pts',(37.2707284506814,-29.5962446291683,0.));
#70956=CARTESIAN_POINT('Ctrl Pts',(37.2707284506814,-29.5962446291683,20.));
#70957=CARTESIAN_POINT('Ctrl Pts',(37.2477290431548,-29.6203595574991,0.));
#70958=CARTESIAN_POINT('Ctrl Pts',(37.2477290431548,-29.6203595574991,20.));
#70959=CARTESIAN_POINT('Ctrl Pts',(37.2247135951292,-29.6444576331215,0.));
#70960=CARTESIAN_POINT('Ctrl Pts',(37.2247135951292,-29.6444576331215,20.));
#70961=CARTESIAN_POINT('Ctrl Pts',(37.2016821184267,-29.668538844916,0.));
#70962=CARTESIAN_POINT('Ctrl Pts',(37.2016821184267,-29.668538844916,20.));
#70963=CARTESIAN_POINT('Ctrl Pts',(37.1786346248774,-29.6926031817715,0.));
#70964=CARTESIAN_POINT('Ctrl Pts',(37.1786346248774,-29.6926031817715,20.));
#70965=CARTESIAN_POINT('Ctrl Pts',(37.155571126319,-29.7166506325841,0.));
#70966=CARTESIAN_POINT('Ctrl Pts',(37.155571126319,-29.7166506325841,20.));
#70967=CARTESIAN_POINT('Ctrl Pts',(37.1324916345976,-29.7406811862582,0.));
#70968=CARTESIAN_POINT('Ctrl Pts',(37.1324916345976,-29.7406811862582,20.));
#70969=CARTESIAN_POINT('Ctrl Pts',(37.1093961615672,-29.7646948317062,0.));
#70970=CARTESIAN_POINT('Ctrl Pts',(37.1093961615672,-29.7646948317062,20.));
#70971=CARTESIAN_POINT('Ctrl Pts',(37.0862847190902,-29.7886915578486,0.));
#70972=CARTESIAN_POINT('Ctrl Pts',(37.0862847190902,-29.7886915578486,20.));
#70973=CARTESIAN_POINT('Ctrl Pts',(37.0631573190373,-29.8126713536142,0.));
#70974=CARTESIAN_POINT('Ctrl Pts',(37.0631573190373,-29.8126713536142,20.));
#70975=CARTESIAN_POINT('Ctrl Pts',(37.0400139732874,-29.8366342079401,0.));
#70976=CARTESIAN_POINT('Ctrl Pts',(37.0400139732874,-29.8366342079401,20.));
#70977=CARTESIAN_POINT('Ctrl Pts',(37.0168546937273,-29.8605801097708,0.));
#70978=CARTESIAN_POINT('Ctrl Pts',(37.0168546937273,-29.8605801097708,20.));
#70979=CARTESIAN_POINT('Ctrl Pts',(36.9936794922513,-29.884509048059,0.));
#70980=CARTESIAN_POINT('Ctrl Pts',(36.9936794922513,-29.884509048059,20.));
#70981=CARTESIAN_POINT('Ctrl Pts',(36.9704883807614,-29.9084210117647,0.));
#70982=CARTESIAN_POINT('Ctrl Pts',(36.9704883807614,-29.9084210117647,20.));
#70983=CARTESIAN_POINT('Ctrl Pts',(36.9472813711676,-29.9323159898562,0.));
#70984=CARTESIAN_POINT('Ctrl Pts',(36.9472813711676,-29.9323159898562,20.));
#70985=CARTESIAN_POINT('Ctrl Pts',(36.9240584753882,-29.9561939713103,0.));
#70986=CARTESIAN_POINT('Ctrl Pts',(36.9240584753882,-29.9561939713103,20.));
#70987=CARTESIAN_POINT('Ctrl Pts',(36.9008197053507,-29.9800549451122,0.));
#70988=CARTESIAN_POINT('Ctrl Pts',(36.9008197053507,-29.9800549451122,20.));
#70989=CARTESIAN_POINT('Ctrl Pts',(36.8775650729895,-30.003898900255,0.));
#70990=CARTESIAN_POINT('Ctrl Pts',(36.8775650729895,-30.003898900255,20.));
#70991=CARTESIAN_POINT('Ctrl Pts',(36.8542945902472,-30.0277258257394,0.));
#70992=CARTESIAN_POINT('Ctrl Pts',(36.8542945902472,-30.0277258257394,20.));
#70993=CARTESIAN_POINT('Ctrl Pts',(36.8310082690741,-30.051535710574,0.));
#70994=CARTESIAN_POINT('Ctrl Pts',(36.8310082690741,-30.051535710574,20.));
#70995=CARTESIAN_POINT('Ctrl Pts',(36.8077061214283,-30.0753285437754,0.));
#70996=CARTESIAN_POINT('Ctrl Pts',(36.8077061214283,-30.0753285437754,20.));
#70997=CARTESIAN_POINT('Ctrl Pts',(36.7843881592759,-30.0991043143685,0.));
#70998=CARTESIAN_POINT('Ctrl Pts',(36.7843881592759,-30.0991043143685,20.));
#70999=CARTESIAN_POINT('Ctrl Pts',(36.7610543945915,-30.1228630113862,0.));
#71000=CARTESIAN_POINT('Ctrl Pts',(36.7610543945915,-30.1228630113862,20.));
#71001=CARTESIAN_POINT('Ctrl Pts',(36.7377048393574,-30.1466046238701,0.));
#71002=CARTESIAN_POINT('Ctrl Pts',(36.7377048393574,-30.1466046238701,20.));
#71003=CARTESIAN_POINT('Ctrl Pts',(36.7143395055641,-30.1703291408693,0.));
#71004=CARTESIAN_POINT('Ctrl Pts',(36.7143395055641,-30.1703291408693,20.));
#71005=CARTESIAN_POINT('Ctrl Pts',(36.6909584052099,-30.1940365514414,0.));
#71006=CARTESIAN_POINT('Ctrl Pts',(36.6909584052099,-30.1940365514414,20.));
#71007=CARTESIAN_POINT('Ctrl Pts',(36.6675615503012,-30.2177268446518,0.));
#71008=CARTESIAN_POINT('Ctrl Pts',(36.6675615503012,-30.2177268446518,20.));
#71009=CARTESIAN_POINT('Ctrl Pts',(36.6441489528521,-30.2414000095742,0.));
#71010=CARTESIAN_POINT('Ctrl Pts',(36.6441489528521,-30.2414000095742,20.));
#71011=CARTESIAN_POINT('Ctrl Pts',(36.6207206248848,-30.2650560352902,0.));
#71012=CARTESIAN_POINT('Ctrl Pts',(36.6207206248848,-30.2650560352902,20.));
#71013=CARTESIAN_POINT('Ctrl Pts',(36.5972765784293,-30.2886949108895,0.));
#71014=CARTESIAN_POINT('Ctrl Pts',(36.5972765784293,-30.2886949108895,20.));
#71015=CARTESIAN_POINT('Ctrl Pts',(36.5738168255233,-30.3123166254701,0.));
#71016=CARTESIAN_POINT('Ctrl Pts',(36.5738168255233,-30.3123166254701,20.));
#71017=CARTESIAN_POINT('Ctrl Pts',(36.5503413782123,-30.3359211681376,0.));
#71018=CARTESIAN_POINT('Ctrl Pts',(36.5503413782123,-30.3359211681376,20.));
#71019=CARTESIAN_POINT('Ctrl Pts',(36.5268502485502,-30.3595085280059,0.));
#71020=CARTESIAN_POINT('Ctrl Pts',(36.5268502485502,-30.3595085280059,20.));
#71021=CARTESIAN_POINT('Ctrl Pts',(36.5033434485984,-30.3830786941972,0.));
#71022=CARTESIAN_POINT('Ctrl Pts',(36.5033434485984,-30.3830786941972,20.));
#71023=CARTESIAN_POINT('Ctrl Pts',(36.4798209904267,-30.4066316558424,0.));
#71024=CARTESIAN_POINT('Ctrl Pts',(36.4798209904267,-30.4066316558424,20.));
#71025=CARTESIAN_POINT('Ctrl Pts',(36.456282886113,-30.4301674020802,0.));
#71026=CARTESIAN_POINT('Ctrl Pts',(36.456282886113,-30.4301674020802,20.));
#71027=CARTESIAN_POINT('Ctrl Pts',(36.4327291477428,-30.4536859220576,0.));
#71028=CARTESIAN_POINT('Ctrl Pts',(36.4327291477428,-30.4536859220576,20.));
#71029=CARTESIAN_POINT('Ctrl Pts',(36.4091597874097,-30.4771872049299,0.));
#71030=CARTESIAN_POINT('Ctrl Pts',(36.4091597874097,-30.4771872049299,20.));
#71031=CARTESIAN_POINT('Ctrl Pts',(36.3855748172148,-30.5006712398601,0.));
#71032=CARTESIAN_POINT('Ctrl Pts',(36.3855748172148,-30.5006712398601,20.));
#71033=CARTESIAN_POINT('Ctrl Pts',(36.3619742492671,-30.5241380160195,0.));
#71034=CARTESIAN_POINT('Ctrl Pts',(36.3619742492671,-30.5241380160195,20.));
#71035=CARTESIAN_POINT('Ctrl Pts',(36.3383580956832,-30.5475875225872,0.));
#71036=CARTESIAN_POINT('Ctrl Pts',(36.3383580956832,-30.5475875225872,20.));
#71037=CARTESIAN_POINT('Ctrl Pts',(36.3147263685874,-30.5710197487502,0.));
#71038=CARTESIAN_POINT('Ctrl Pts',(36.3147263685874,-30.5710197487502,20.));
#71039=CARTESIAN_POINT('Ctrl Pts',(36.2910790801119,-30.5944346837039,0.));
#71040=CARTESIAN_POINT('Ctrl Pts',(36.2910790801119,-30.5944346837039,20.));
#71041=CARTESIAN_POINT('Ctrl Pts',(36.2674162423973,-30.6178323166527,0.));
#71042=CARTESIAN_POINT('Ctrl Pts',(36.2674162423973,-30.6178323166527,20.));
#71043=CARTESIAN_POINT('Ctrl Pts',(36.2437378675924,-30.6412126368095,0.));
#71044=CARTESIAN_POINT('Ctrl Pts',(36.2437378675924,-30.6412126368095,20.));
#71045=CARTESIAN_POINT('Ctrl Pts',(36.2200439678542,-30.6645756333955,0.));
#71046=CARTESIAN_POINT('Ctrl Pts',(36.2200439678542,-30.6645756333955,20.));
#71047=CARTESIAN_POINT('Ctrl Pts',(36.196334555347,-30.6879212956392,0.));
#71048=CARTESIAN_POINT('Ctrl Pts',(36.196334555347,-30.6879212956392,20.));
#71049=CARTESIAN_POINT('Ctrl Pts',(36.1726096422428,-30.7112496127774,0.));
#71050=CARTESIAN_POINT('Ctrl Pts',(36.1726096422428,-30.7112496127774,20.));
#71051=CARTESIAN_POINT('Ctrl Pts',(36.1488692407204,-30.7345605740545,0.));
#71052=CARTESIAN_POINT('Ctrl Pts',(36.1488692407204,-30.7345605740545,20.));
#71053=CARTESIAN_POINT('Ctrl Pts',(36.1251133629669,-30.7578541687236,0.));
#71054=CARTESIAN_POINT('Ctrl Pts',(36.1251133629669,-30.7578541687236,20.));
#71055=CARTESIAN_POINT('Ctrl Pts',(36.1013420211777,-30.7811303860468,0.));
#71056=CARTESIAN_POINT('Ctrl Pts',(36.1013420211777,-30.7811303860468,20.));
#71057=CARTESIAN_POINT('Ctrl Pts',(36.0775552275565,-30.8043892152943,0.));
#71058=CARTESIAN_POINT('Ctrl Pts',(36.0775552275565,-30.8043892152943,20.));
#71059=CARTESIAN_POINT('Ctrl Pts',(36.0537529943146,-30.8276306457446,0.));
#71060=CARTESIAN_POINT('Ctrl Pts',(36.0537529943146,-30.8276306457446,20.));
#71061=CARTESIAN_POINT('Ctrl Pts',(36.0299353336712,-30.8508546666841,0.));
#71062=CARTESIAN_POINT('Ctrl Pts',(36.0299353336712,-30.8508546666841,20.));
#71063=CARTESIAN_POINT('Ctrl Pts',(36.0061022578528,-30.8740612674075,0.));
#71064=CARTESIAN_POINT('Ctrl Pts',(36.0061022578528,-30.8740612674075,20.));
#71065=CARTESIAN_POINT('Ctrl Pts',(35.9822537790931,-30.8972504372171,0.));
#71066=CARTESIAN_POINT('Ctrl Pts',(35.9822537790931,-30.8972504372171,20.));
#71067=CARTESIAN_POINT('Ctrl Pts',(35.9583899096339,-30.9204221654236,0.));
#71068=CARTESIAN_POINT('Ctrl Pts',(35.9583899096339,-30.9204221654236,20.));
#71069=CARTESIAN_POINT('Ctrl Pts',(35.9345106617251,-30.9435764413467,0.));
#71070=CARTESIAN_POINT('Ctrl Pts',(35.9345106617251,-30.9435764413467,20.));
#71071=CARTESIAN_POINT('Ctrl Pts',(35.9106160476245,-30.9667132543142,0.));
#71072=CARTESIAN_POINT('Ctrl Pts',(35.9106160476245,-30.9667132543142,20.));
#71073=CARTESIAN_POINT('Ctrl Pts',(35.886706079598,-30.9898325936627,0.));
#71074=CARTESIAN_POINT('Ctrl Pts',(35.886706079598,-30.9898325936627,20.));
#71075=CARTESIAN_POINT('Ctrl Pts',(35.8627807699193,-31.0129344487367,0.));
#71076=CARTESIAN_POINT('Ctrl Pts',(35.8627807699193,-31.0129344487367,20.));
#71077=CARTESIAN_POINT('Ctrl Pts',(35.8388401308696,-31.036018808889,0.));
#71078=CARTESIAN_POINT('Ctrl Pts',(35.8388401308696,-31.036018808889,20.));
#71079=CARTESIAN_POINT('Ctrl Pts',(35.8148841747376,-31.0590856634804,0.));
#71080=CARTESIAN_POINT('Ctrl Pts',(35.8148841747376,-31.0590856634804,20.));
#71081=CARTESIAN_POINT('Ctrl Pts',(35.7909129138202,-31.082135001881,0.));
#71082=CARTESIAN_POINT('Ctrl Pts',(35.7909129138202,-31.082135001881,20.));
#71083=CARTESIAN_POINT('Ctrl Pts',(35.7669263604212,-31.1051668134678,0.));
#71084=CARTESIAN_POINT('Ctrl Pts',(35.7669263604212,-31.1051668134678,20.));
#71085=CARTESIAN_POINT('Ctrl Pts',(35.7429245268523,-31.1281810876267,0.));
#71086=CARTESIAN_POINT('Ctrl Pts',(35.7429245268523,-31.1281810876267,20.));
#71087=CARTESIAN_POINT('Ctrl Pts',(35.7189074254331,-31.1511778137516,0.));
#71088=CARTESIAN_POINT('Ctrl Pts',(35.7189074254331,-31.1511778137516,20.));
#71089=CARTESIAN_POINT('Ctrl Pts',(35.6948750684911,-31.1741569812451,0.));
#71090=CARTESIAN_POINT('Ctrl Pts',(35.6948750684911,-31.1741569812451,20.));
#71091=CARTESIAN_POINT('Ctrl Pts',(35.6708274683619,-31.1971185795181,0.));
#71092=CARTESIAN_POINT('Ctrl Pts',(35.6708274683619,-31.1971185795181,20.));
#71093=CARTESIAN_POINT('Ctrl Pts',(35.6467646373883,-31.2200625979904,0.));
#71094=CARTESIAN_POINT('Ctrl Pts',(35.6467646373883,-31.2200625979904,20.));
#71095=CARTESIAN_POINT('Ctrl Pts',(35.6226865879214,-31.24298902609,0.));
#71096=CARTESIAN_POINT('Ctrl Pts',(35.6226865879214,-31.24298902609,20.));
#71097=CARTESIAN_POINT('Ctrl Pts',(35.5985933323194,-31.2658978532533,0.));
#71098=CARTESIAN_POINT('Ctrl Pts',(35.5985933323194,-31.2658978532533,20.));
#71099=CARTESIAN_POINT('Ctrl Pts',(35.5744848829487,-31.288789068925,0.));
#71100=CARTESIAN_POINT('Ctrl Pts',(35.5744848829487,-31.288789068925,20.));
#71101=CARTESIAN_POINT('Ctrl Pts',(35.5503612521832,-31.3116626625581,0.));
#71102=CARTESIAN_POINT('Ctrl Pts',(35.5503612521832,-31.3116626625581,20.));
#71103=CARTESIAN_POINT('Ctrl Pts',(35.5262224524039,-31.3345186236135,0.));
#71104=CARTESIAN_POINT('Ctrl Pts',(35.5262224524039,-31.3345186236135,20.));
#71105=CARTESIAN_POINT('Ctrl Pts',(35.502068496,-31.3573569415606,0.));
#71106=CARTESIAN_POINT('Ctrl Pts',(35.502068496,-31.3573569415606,20.));
#71107=CARTESIAN_POINT('Ctrl Pts',(35.4778993953681,-31.3801776058768,0.));
#71108=CARTESIAN_POINT('Ctrl Pts',(35.4778993953681,-31.3801776058768,20.));
#71109=CARTESIAN_POINT('Ctrl Pts',(35.4537151629126,-31.4029806060482,0.));
#71110=CARTESIAN_POINT('Ctrl Pts',(35.4537151629126,-31.4029806060482,20.));
#71111=CARTESIAN_POINT('Ctrl Pts',(35.4295158110454,-31.4257659315696,0.));
#71112=CARTESIAN_POINT('Ctrl Pts',(35.4295158110454,-31.4257659315696,20.));
#71113=CARTESIAN_POINT('Ctrl Pts',(35.4053013521866,-31.4485335719447,0.));
#71114=CARTESIAN_POINT('Ctrl Pts',(35.4053013521866,-31.4485335719447,20.));
#71115=CARTESIAN_POINT('Ctrl Pts',(35.3810717987641,-31.4712835166857,0.));
#71116=CARTESIAN_POINT('Ctrl Pts',(35.3810717987641,-31.4712835166857,20.));
#71117=CARTESIAN_POINT('Ctrl Pts',(35.3568271632136,-31.4940157553136,0.));
#71118=CARTESIAN_POINT('Ctrl Pts',(35.3568271632136,-31.4940157553136,20.));
#71119=CARTESIAN_POINT('Ctrl Pts',(35.3325674579779,-31.516730277357,0.));
#71120=CARTESIAN_POINT('Ctrl Pts',(35.3325674579779,-31.516730277357,20.));
#71121=CARTESIAN_POINT('Ctrl Pts',(35.3082926955072,-31.5394270723526,0.));
#71122=CARTESIAN_POINT('Ctrl Pts',(35.3082926955072,-31.5394270723526,20.));
#71123=CARTESIAN_POINT('Ctrl Pts',(35.2840028882593,-31.5621061298453,0.));
#71124=CARTESIAN_POINT('Ctrl Pts',(35.2840028882593,-31.5621061298453,20.));
#71125=CARTESIAN_POINT('Ctrl Pts',(35.2596980486996,-31.5847674393885,0.));
#71126=CARTESIAN_POINT('Ctrl Pts',(35.2596980486996,-31.5847674393885,20.));
#71127=CARTESIAN_POINT('Ctrl Pts',(35.2353781893014,-31.6074109905439,0.));
#71128=CARTESIAN_POINT('Ctrl Pts',(35.2353781893014,-31.6074109905439,20.));
#71129=CARTESIAN_POINT('Ctrl Pts',(35.2110433225458,-31.6300367728827,0.));
#71130=CARTESIAN_POINT('Ctrl Pts',(35.2110433225458,-31.6300367728827,20.));
#71131=CARTESIAN_POINT('Ctrl Pts',(35.1866934609214,-31.652644775984,0.));
#71132=CARTESIAN_POINT('Ctrl Pts',(35.1866934609214,-31.652644775984,20.));
#71133=CARTESIAN_POINT('Ctrl Pts',(35.1623286169245,-31.6752349894358,0.));
#71134=CARTESIAN_POINT('Ctrl Pts',(35.1623286169245,-31.6752349894358,20.));
#71135=CARTESIAN_POINT('Ctrl Pts',(35.1379488030591,-31.6978074028349,0.));
#71136=CARTESIAN_POINT('Ctrl Pts',(35.1379488030591,-31.6978074028349,20.));
#71137=CARTESIAN_POINT('Ctrl Pts',(35.1135540318367,-31.7203620057864,0.));
#71138=CARTESIAN_POINT('Ctrl Pts',(35.1135540318367,-31.7203620057864,20.));
#71139=CARTESIAN_POINT('Ctrl Pts',(35.0891443157764,-31.7428987879035,0.));
#71140=CARTESIAN_POINT('Ctrl Pts',(35.0891443157764,-31.7428987879035,20.));
#71141=CARTESIAN_POINT('Ctrl Pts',(35.0647196674043,-31.7654177388073,0.));
#71142=CARTESIAN_POINT('Ctrl Pts',(35.0647196674043,-31.7654177388073,20.));
#71143=CARTESIAN_POINT('Ctrl Pts',(35.0402800992547,-31.7879188481278,0.));
#71144=CARTESIAN_POINT('Ctrl Pts',(35.0402800992547,-31.7879188481278,20.));
#71145=CARTESIAN_POINT('Ctrl Pts',(35.0158256238691,-31.8104021055033,0.));
#71146=CARTESIAN_POINT('Ctrl Pts',(35.0158256238691,-31.8104021055033,20.));
#71147=CARTESIAN_POINT('Ctrl Pts',(34.991356253797,-31.8328675005809,0.));
#71148=CARTESIAN_POINT('Ctrl Pts',(34.991356253797,-31.8328675005809,20.));
#71149=CARTESIAN_POINT('Ctrl Pts',(34.9668720015954,-31.8553150230168,0.));
#71150=CARTESIAN_POINT('Ctrl Pts',(34.9668720015954,-31.8553150230168,20.));
#71151=CARTESIAN_POINT('Ctrl Pts',(34.9423728798289,-31.8777446624754,0.));
#71152=CARTESIAN_POINT('Ctrl Pts',(34.9423728798289,-31.8777446624754,20.));
#71153=CARTESIAN_POINT('Ctrl Pts',(34.9178589010694,-31.9001564086295,0.));
#71154=CARTESIAN_POINT('Ctrl Pts',(34.9178589010694,-31.9001564086295,20.));
#71155=CARTESIAN_POINT('Ctrl Pts',(34.8933300778963,-31.9225502511603,0.));
#71156=CARTESIAN_POINT('Ctrl Pts',(34.8933300778963,-31.9225502511603,20.));
#71157=CARTESIAN_POINT('Ctrl Pts',(34.8687864228965,-31.9449261797574,0.));
#71158=CARTESIAN_POINT('Ctrl Pts',(34.8687864228965,-31.9449261797574,20.));
#71159=CARTESIAN_POINT('Ctrl Pts',(34.8442279486644,-31.967284184119,0.));
#71160=CARTESIAN_POINT('Ctrl Pts',(34.8442279486644,-31.967284184119,20.));
#71161=CARTESIAN_POINT('Ctrl Pts',(34.8196546678026,-31.9896242539524,0.));
#71162=CARTESIAN_POINT('Ctrl Pts',(34.8196546678026,-31.9896242539524,20.));
#71163=CARTESIAN_POINT('Ctrl Pts',(34.7950665929206,-32.011946378973,0.));
#71164=CARTESIAN_POINT('Ctrl Pts',(34.7950665929206,-32.011946378973,20.));
#71165=CARTESIAN_POINT('Ctrl Pts',(34.7704637366357,-32.0342505489048,0.));
#71166=CARTESIAN_POINT('Ctrl Pts',(34.7704637366357,-32.0342505489048,20.));
#71167=CARTESIAN_POINT('Ctrl Pts',(34.7458461115727,-32.0565367534806,0.));
#71168=CARTESIAN_POINT('Ctrl Pts',(34.7458461115727,-32.0565367534806,20.));
#71169=CARTESIAN_POINT('Ctrl Pts',(34.7212137303638,-32.0788049824416,0.));
#71170=CARTESIAN_POINT('Ctrl Pts',(34.7212137303638,-32.0788049824416,20.));
#71171=CARTESIAN_POINT('Ctrl Pts',(34.6965666056491,-32.1010552255379,0.));
#71172=CARTESIAN_POINT('Ctrl Pts',(34.6965666056491,-32.1010552255379,20.));
#71173=CARTESIAN_POINT('Ctrl Pts',(34.6719047500757,-32.1232874725277,0.));
#71174=CARTESIAN_POINT('Ctrl Pts',(34.6719047500757,-32.1232874725277,20.));
#71175=CARTESIAN_POINT('Ctrl Pts',(34.6472281762982,-32.145501713178,0.));
#71176=CARTESIAN_POINT('Ctrl Pts',(34.6472281762982,-32.145501713178,20.));
#71177=CARTESIAN_POINT('Ctrl Pts',(34.6225368969784,-32.167697937264,0.));
#71178=CARTESIAN_POINT('Ctrl Pts',(34.6225368969784,-32.167697937264,20.));
#71179=CARTESIAN_POINT('Ctrl Pts',(34.5978309247855,-32.1898761345694,0.));
#71180=CARTESIAN_POINT('Ctrl Pts',(34.5978309247855,-32.1898761345694,20.));
#71181=CARTESIAN_POINT('Ctrl Pts',(34.5731102723969,-32.212036294887,0.));
#71182=CARTESIAN_POINT('Ctrl Pts',(34.5731102723969,-32.212036294887,20.));
#71183=CARTESIAN_POINT('Ctrl Pts',(34.5483749524972,-32.2341784080184,0.));
#71184=CARTESIAN_POINT('Ctrl Pts',(34.5483749524972,-32.2341784080184,20.));
#71185=CARTESIAN_POINT('Ctrl Pts',(34.5236249777791,-32.2563024637739,0.));
#71186=CARTESIAN_POINT('Ctrl Pts',(34.5236249777791,-32.2563024637739,20.));
#71187=CARTESIAN_POINT('Ctrl Pts',(34.4988603609426,-32.2784084519728,0.));
#71188=CARTESIAN_POINT('Ctrl Pts',(34.4988603609426,-32.2784084519728,20.));
#71189=CARTESIAN_POINT('Ctrl Pts',(34.474081114695,-32.3004963624427,0.));
#71190=CARTESIAN_POINT('Ctrl Pts',(34.474081114695,-32.3004963624427,20.));
#71191=CARTESIAN_POINT('Ctrl Pts',(34.4492872517507,-32.3225661850195,0.));
#71192=CARTESIAN_POINT('Ctrl Pts',(34.4492872517507,-32.3225661850195,20.));
#71193=CARTESIAN_POINT('Ctrl Pts',(34.4244787848311,-32.3446179095474,0.));
#71194=CARTESIAN_POINT('Ctrl Pts',(34.4244787848311,-32.3446179095474,20.));
#71195=CARTESIAN_POINT('Ctrl Pts',(34.3996557266651,-32.3666515258788,0.));
#71196=CARTESIAN_POINT('Ctrl Pts',(34.3996557266651,-32.3666515258788,20.));
#71197=CARTESIAN_POINT('Ctrl Pts',(34.3748180899889,-32.388667023875,0.));
#71198=CARTESIAN_POINT('Ctrl Pts',(34.3748180899889,-32.388667023875,20.));
#71199=CARTESIAN_POINT('Ctrl Pts',(34.3499658875467,-32.4106643934066,0.));
#71200=CARTESIAN_POINT('Ctrl Pts',(34.3499658875467,-32.4106643934066,20.));
#71201=CARTESIAN_POINT('Ctrl Pts',(34.3250991320904,-32.4326436243533,0.));
#71202=CARTESIAN_POINT('Ctrl Pts',(34.3250991320904,-32.4326436243533,20.));
#71203=CARTESIAN_POINT('Ctrl Pts',(34.3002178363797,-32.4546047066034,0.));
#71204=CARTESIAN_POINT('Ctrl Pts',(34.3002178363797,-32.4546047066034,20.));
#71205=CARTESIAN_POINT('Ctrl Pts',(34.2753220131812,-32.4765476300538,0.));
#71206=CARTESIAN_POINT('Ctrl Pts',(34.2753220131812,-32.4765476300538,20.));
#71207=CARTESIAN_POINT('Ctrl Pts',(34.2504116752689,-32.4984723846098,0.));
#71208=CARTESIAN_POINT('Ctrl Pts',(34.2504116752689,-32.4984723846098,20.));
#71209=CARTESIAN_POINT('Ctrl Pts',(34.2254868354237,-32.5203789601849,0.));
#71210=CARTESIAN_POINT('Ctrl Pts',(34.2254868354237,-32.5203789601849,20.));
#71211=CARTESIAN_POINT('Ctrl Pts',(34.2005475064343,-32.542267346702,0.));
#71212=CARTESIAN_POINT('Ctrl Pts',(34.2005475064343,-32.542267346702,20.));
#71213=CARTESIAN_POINT('Ctrl Pts',(34.1755937010962,-32.564137534092,0.));
#71214=CARTESIAN_POINT('Ctrl Pts',(34.1755937010962,-32.564137534092,20.));
#71215=CARTESIAN_POINT('Ctrl Pts',(34.1506254322131,-32.585989512295,0.));
#71216=CARTESIAN_POINT('Ctrl Pts',(34.1506254322131,-32.585989512295,20.));
#71217=CARTESIAN_POINT('Ctrl Pts',(34.1256427125955,-32.6078232712594,0.));
#71218=CARTESIAN_POINT('Ctrl Pts',(34.1256427125955,-32.6078232712594,20.));
#71219=CARTESIAN_POINT('Ctrl Pts',(34.1006455550618,-32.6296388009428,0.));
#71220=CARTESIAN_POINT('Ctrl Pts',(34.1006455550618,-32.6296388009428,20.));
#71221=CARTESIAN_POINT('Ctrl Pts',(34.0756339724376,-32.6514360913116,0.));
#71222=CARTESIAN_POINT('Ctrl Pts',(34.0756339724376,-32.6514360913116,20.));
#71223=CARTESIAN_POINT('Ctrl Pts',(34.0506079775557,-32.6732151323407,0.));
#71224=CARTESIAN_POINT('Ctrl Pts',(34.0506079775557,-32.6732151323407,20.));
#71225=CARTESIAN_POINT('Ctrl Pts',(34.0255675832564,-32.694975914014,0.));
#71226=CARTESIAN_POINT('Ctrl Pts',(34.0255675832564,-32.694975914014,20.));
#71227=CARTESIAN_POINT('Ctrl Pts',(34.0005128023871,-32.7167184263237,0.));
#71228=CARTESIAN_POINT('Ctrl Pts',(34.0005128023871,-32.7167184263237,20.));
#71229=CARTESIAN_POINT('Ctrl Pts',(33.9754436478026,-32.7384426592708,0.));
#71230=CARTESIAN_POINT('Ctrl Pts',(33.9754436478026,-32.7384426592708,20.));
#71231=CARTESIAN_POINT('Ctrl Pts',(33.950360132365,-32.7601486028652,0.));
#71232=CARTESIAN_POINT('Ctrl Pts',(33.950360132365,-32.7601486028652,20.));
#71233=CARTESIAN_POINT('Ctrl Pts',(33.9252622689445,-32.781836247126,0.));
#71234=CARTESIAN_POINT('Ctrl Pts',(33.9252622689445,-32.781836247126,20.));
#71235=CARTESIAN_POINT('Ctrl Pts',(33.9001500704179,-32.8035055820806,0.));
#71236=CARTESIAN_POINT('Ctrl Pts',(33.9001500704179,-32.8035055820806,20.));
#71237=CARTESIAN_POINT('Ctrl Pts',(33.8750235496691,-32.8251565977646,0.));
#71238=CARTESIAN_POINT('Ctrl Pts',(33.8750235496691,-32.8251565977646,20.));
#71239=CARTESIAN_POINT('Ctrl Pts',(33.8498827195893,-32.8467892842227,0.));
#71240=CARTESIAN_POINT('Ctrl Pts',(33.8498827195893,-32.8467892842227,20.));
#71241=CARTESIAN_POINT('Ctrl Pts',(33.8247275930774,-32.8684036315086,0.));
#71242=CARTESIAN_POINT('Ctrl Pts',(33.8247275930774,-32.8684036315086,20.));
#71243=CARTESIAN_POINT('Ctrl Pts',(33.7995581830395,-32.8899996296849,0.));
#71244=CARTESIAN_POINT('Ctrl Pts',(33.7995581830395,-32.8899996296849,20.));
#71245=CARTESIAN_POINT('Ctrl Pts',(33.7743745023893,-32.9115772688235,0.));
#71246=CARTESIAN_POINT('Ctrl Pts',(33.7743745023893,-32.9115772688235,20.));
#71247=CARTESIAN_POINT('Ctrl Pts',(33.7491765640476,-32.9331365390046,0.));
#71248=CARTESIAN_POINT('Ctrl Pts',(33.7491765640476,-32.9331365390046,20.));
#71249=CARTESIAN_POINT('Ctrl Pts',(33.723964380943,-32.9546774303179,0.));
#71250=CARTESIAN_POINT('Ctrl Pts',(33.723964380943,-32.9546774303179,20.));
#71251=CARTESIAN_POINT('Ctrl Pts',(33.6987379660104,-32.9761999328605,0.));
#71252=CARTESIAN_POINT('Ctrl Pts',(33.6987379660104,-32.9761999328605,20.));
#71253=CARTESIAN_POINT('Ctrl Pts',(33.6734973321919,-32.9977040367383,0.));
#71254=CARTESIAN_POINT('Ctrl Pts',(33.6734973321919,-32.9977040367383,20.));
#71255=CARTESIAN_POINT('Ctrl Pts',(33.6482424924372,-33.0191897320665,0.));
#71256=CARTESIAN_POINT('Ctrl Pts',(33.6482424924372,-33.0191897320665,20.));
#71257=CARTESIAN_POINT('Ctrl Pts',(33.6229734597032,-33.0406570089692,0.));
#71258=CARTESIAN_POINT('Ctrl Pts',(33.6229734597032,-33.0406570089692,20.));
#71259=CARTESIAN_POINT('Ctrl Pts',(33.5976902469543,-33.0621058575797,0.));
#71260=CARTESIAN_POINT('Ctrl Pts',(33.5976902469543,-33.0621058575797,20.));
#71261=CARTESIAN_POINT('Ctrl Pts',(33.572392867162,-33.0835362680399,0.));
#71262=CARTESIAN_POINT('Ctrl Pts',(33.572392867162,-33.0835362680399,20.));
#71263=CARTESIAN_POINT('Ctrl Pts',(33.5470813333053,-33.1049482305004,0.));
#71264=CARTESIAN_POINT('Ctrl Pts',(33.5470813333053,-33.1049482305004,20.));
#71265=CARTESIAN_POINT('Ctrl Pts',(33.5217556583703,-33.1263417351208,0.));
#71266=CARTESIAN_POINT('Ctrl Pts',(33.5217556583703,-33.1263417351208,20.));
#71267=CARTESIAN_POINT('Ctrl Pts',(33.4964158553505,-33.1477167720697,0.));
#71268=CARTESIAN_POINT('Ctrl Pts',(33.4964158553505,-33.1477167720697,20.));
#71269=CARTESIAN_POINT('Ctrl Pts',(33.4710619372468,-33.1690733315248,0.));
#71270=CARTESIAN_POINT('Ctrl Pts',(33.4710619372468,-33.1690733315248,20.));
#71271=CARTESIAN_POINT('Ctrl Pts',(33.4456939170666,-33.1904114036721,0.));
#71272=CARTESIAN_POINT('Ctrl Pts',(33.4456939170666,-33.1904114036721,20.));
#71273=CARTESIAN_POINT('Ctrl Pts',(33.4203118078248,-33.2117309787064,0.));
#71274=CARTESIAN_POINT('Ctrl Pts',(33.4203118078248,-33.2117309787064,20.));
#71275=CARTESIAN_POINT('Ctrl Pts',(33.3949156225429,-33.233032046831,0.));
#71276=CARTESIAN_POINT('Ctrl Pts',(33.3949156225429,-33.233032046831,20.));
#71277=CARTESIAN_POINT('Ctrl Pts',(33.3695053742505,-33.2543145982587,0.));
#71278=CARTESIAN_POINT('Ctrl Pts',(33.3695053742505,-33.2543145982587,20.));
#71279=CARTESIAN_POINT('Ctrl Pts',(33.3440810759838,-33.2755786232108,0.));
#71280=CARTESIAN_POINT('Ctrl Pts',(33.3440810759838,-33.2755786232108,20.));
#71281=CARTESIAN_POINT('Ctrl Pts',(33.3186427407863,-33.2968241119177,0.));
#71282=CARTESIAN_POINT('Ctrl Pts',(33.3186427407863,-33.2968241119177,20.));
#71283=CARTESIAN_POINT('Ctrl Pts',(33.2931903817093,-33.318051054619,0.));
#71284=CARTESIAN_POINT('Ctrl Pts',(33.2931903817093,-33.318051054619,20.));
#71285=CARTESIAN_POINT('Ctrl Pts',(33.2677240118112,-33.3392594415636,0.));
#71286=CARTESIAN_POINT('Ctrl Pts',(33.2677240118112,-33.3392594415636,20.));
#71287=CARTESIAN_POINT('Ctrl Pts',(33.2422436441578,-33.3604492630093,0.));
#71288=CARTESIAN_POINT('Ctrl Pts',(33.2422436441578,-33.3604492630093,20.));
#71289=CARTESIAN_POINT('Ctrl Pts',(33.2167492918215,-33.3816205092222,0.));
#71290=CARTESIAN_POINT('Ctrl Pts',(33.2167492918215,-33.3816205092222,20.));
#71291=CARTESIAN_POINT('Ctrl Pts',(33.1912409678819,-33.4027731704774,0.));
#71292=CARTESIAN_POINT('Ctrl Pts',(33.1912409678819,-33.4027731704774,20.));
#71293=CARTESIAN_POINT('Ctrl Pts',(33.1657186854252,-33.4239072370581,0.));
#71294=CARTESIAN_POINT('Ctrl Pts',(33.1657186854252,-33.4239072370581,20.));
#71295=CARTESIAN_POINT('Ctrl Pts',(33.1401824575448,-33.4450226992568,0.));
#71296=CARTESIAN_POINT('Ctrl Pts',(33.1401824575448,-33.4450226992568,20.));
#71297=CARTESIAN_POINT('Ctrl Pts',(33.1146322973416,-33.4661195473749,0.));
#71298=CARTESIAN_POINT('Ctrl Pts',(33.1146322973416,-33.4661195473749,20.));
#71299=CARTESIAN_POINT('Ctrl Pts',(33.0890682179238,-33.4871977717238,0.));
#71300=CARTESIAN_POINT('Ctrl Pts',(33.0890682179238,-33.4871977717238,20.));
#71301=CARTESIAN_POINT('Ctrl Pts',(33.063490232407,-33.5082573626235,0.));
#71302=CARTESIAN_POINT('Ctrl Pts',(33.063490232407,-33.5082573626235,20.));
#71303=CARTESIAN_POINT('Ctrl Pts',(33.0378983539137,-33.5292983104032,0.));
#71304=CARTESIAN_POINT('Ctrl Pts',(33.0378983539137,-33.5292983104032,20.));
#71305=CARTESIAN_POINT('Ctrl Pts',(33.0122925955738,-33.5503206054004,0.));
#71306=CARTESIAN_POINT('Ctrl Pts',(33.0122925955738,-33.5503206054004,20.));
#71307=CARTESIAN_POINT('Ctrl Pts',(32.986672970524,-33.5713242379612,0.));
#71308=CARTESIAN_POINT('Ctrl Pts',(32.986672970524,-33.5713242379612,20.));
#71309=CARTESIAN_POINT('Ctrl Pts',(32.9610394919081,-33.5923091984411,0.));
#71310=CARTESIAN_POINT('Ctrl Pts',(32.9610394919081,-33.5923091984411,20.));
#71311=CARTESIAN_POINT('Ctrl Pts',(32.935392172877,-33.6132754772046,0.));
#71312=CARTESIAN_POINT('Ctrl Pts',(32.935392172877,-33.6132754772046,20.));
#71313=CARTESIAN_POINT('Ctrl Pts',(32.9097310265884,-33.6342230646254,0.));
#71314=CARTESIAN_POINT('Ctrl Pts',(32.9097310265884,-33.6342230646254,20.));
#71315=CARTESIAN_POINT('Ctrl Pts',(32.8840560662069,-33.6551519510862,0.));
#71316=CARTESIAN_POINT('Ctrl Pts',(32.8840560662069,-33.6551519510862,20.));
#71317=CARTESIAN_POINT('Ctrl Pts',(32.8583673049046,-33.6760621269785,0.));
#71318=CARTESIAN_POINT('Ctrl Pts',(32.8583673049046,-33.6760621269785,20.));
#71319=CARTESIAN_POINT('Ctrl Pts',(32.8326647558605,-33.6969535827028,0.));
#71320=CARTESIAN_POINT('Ctrl Pts',(32.8326647558605,-33.6969535827028,20.));
#71321=CARTESIAN_POINT('Ctrl Pts',(32.8069484322617,-33.717826308669,0.));
#71322=CARTESIAN_POINT('Ctrl Pts',(32.8069484322617,-33.717826308669,20.));
#71323=CARTESIAN_POINT('Ctrl Pts',(32.7812183473018,-33.7386802952956,0.));
#71324=CARTESIAN_POINT('Ctrl Pts',(32.7812183473018,-33.7386802952956,20.));
#71325=CARTESIAN_POINT('Ctrl Pts',(32.755474514181,-33.7595155330097,0.));
#71326=CARTESIAN_POINT('Ctrl Pts',(32.755474514181,-33.7595155330097,20.));
#71327=CARTESIAN_POINT('Ctrl Pts',(32.7297169461064,-33.7803320122473,0.));
#71328=CARTESIAN_POINT('Ctrl Pts',(32.7297169461064,-33.7803320122473,20.));
#71329=CARTESIAN_POINT('Ctrl Pts',(32.7039456562922,-33.8011297234537,0.));
#71330=CARTESIAN_POINT('Ctrl Pts',(32.7039456562922,-33.8011297234537,20.));
#71331=CARTESIAN_POINT('Ctrl Pts',(32.6781606579597,-33.8219086570836,0.));
#71332=CARTESIAN_POINT('Ctrl Pts',(32.6781606579597,-33.8219086570836,20.));
#71333=CARTESIAN_POINT('Ctrl Pts',(32.652361964338,-33.8426688036011,0.));
#71334=CARTESIAN_POINT('Ctrl Pts',(32.652361964338,-33.8426688036011,20.));
#71335=CARTESIAN_POINT('Ctrl Pts',(32.6265495886629,-33.8634101534794,0.));
#71336=CARTESIAN_POINT('Ctrl Pts',(32.6265495886629,-33.8634101534794,20.));
#71337=CARTESIAN_POINT('Ctrl Pts',(32.6007235441777,-33.8841326972008,0.));
#71338=CARTESIAN_POINT('Ctrl Pts',(32.6007235441777,-33.8841326972008,20.));
#71339=CARTESIAN_POINT('Ctrl Pts',(32.5748838441319,-33.9048364252556,0.));
#71340=CARTESIAN_POINT('Ctrl Pts',(32.5748838441319,-33.9048364252556,20.));
#71341=CARTESIAN_POINT('Ctrl Pts',(32.5490305017817,-33.9255213281434,0.));
#71342=CARTESIAN_POINT('Ctrl Pts',(32.5490305017817,-33.9255213281434,20.));
#71343=CARTESIAN_POINT('Ctrl Pts',(32.5231635303904,-33.9461873963724,0.));
#71344=CARTESIAN_POINT('Ctrl Pts',(32.5231635303904,-33.9461873963724,20.));
#71345=CARTESIAN_POINT('Ctrl Pts',(32.4972829432285,-33.9668346204605,0.));
#71346=CARTESIAN_POINT('Ctrl Pts',(32.4972829432285,-33.9668346204605,20.));
#71347=CARTESIAN_POINT('Ctrl Pts',(32.4713887535741,-33.987462990935,0.));
#71348=CARTESIAN_POINT('Ctrl Pts',(32.4713887535741,-33.987462990935,20.));
#71349=CARTESIAN_POINT('Ctrl Pts',(32.4454809747123,-34.0080724983324,0.));
#71350=CARTESIAN_POINT('Ctrl Pts',(32.4454809747123,-34.0080724983324,20.));
#71351=CARTESIAN_POINT('Ctrl Pts',(32.4195596199344,-34.0286631331978,0.));
#71352=CARTESIAN_POINT('Ctrl Pts',(32.4195596199344,-34.0286631331978,20.));
#71353=CARTESIAN_POINT('Ctrl Pts',(32.3936247025392,-34.0492348860855,0.));
#71354=CARTESIAN_POINT('Ctrl Pts',(32.3936247025392,-34.0492348860855,20.));
#71355=CARTESIAN_POINT('Ctrl Pts',(32.3676762358321,-34.0697877475586,0.));
#71356=CARTESIAN_POINT('Ctrl Pts',(32.3676762358321,-34.0697877475586,20.));
#71357=CARTESIAN_POINT('Ctrl Pts',(32.3417142331256,-34.0903217081898,0.));
#71358=CARTESIAN_POINT('Ctrl Pts',(32.3417142331256,-34.0903217081898,20.));
#71359=CARTESIAN_POINT('Ctrl Pts',(32.3157387077392,-34.1108367585604,0.));
#71360=CARTESIAN_POINT('Ctrl Pts',(32.3157387077392,-34.1108367585604,20.));
#71361=CARTESIAN_POINT('Ctrl Pts',(32.289749672999,-34.131332889261,0.));
#71362=CARTESIAN_POINT('Ctrl Pts',(32.289749672999,-34.131332889261,20.));
#71363=CARTESIAN_POINT('Ctrl Pts',(32.2637471422388,-34.1518100908915,0.));
#71364=CARTESIAN_POINT('Ctrl Pts',(32.2637471422388,-34.1518100908915,20.));
#71365=CARTESIAN_POINT('Ctrl Pts',(32.2377311287994,-34.1722683540613,0.));
#71366=CARTESIAN_POINT('Ctrl Pts',(32.2377311287994,-34.1722683540613,20.));
#71367=CARTESIAN_POINT('Ctrl Pts',(32.2117016460282,-34.1927076693884,0.));
#71368=CARTESIAN_POINT('Ctrl Pts',(32.2117016460282,-34.1927076693884,20.));
#71369=CARTESIAN_POINT('Ctrl Pts',(32.1856587072789,-34.2131280274994,0.));
#71370=CARTESIAN_POINT('Ctrl Pts',(32.1856587072789,-34.2131280274994,20.));
#71371=CARTESIAN_POINT('Ctrl Pts',(32.1596023259127,-34.233529419031,0.));
#71372=CARTESIAN_POINT('Ctrl Pts',(32.1596023259127,-34.233529419031,20.));
#71373=CARTESIAN_POINT('Ctrl Pts',(32.1335325152974,-34.2539118346284,0.));
#71374=CARTESIAN_POINT('Ctrl Pts',(32.1335325152974,-34.2539118346284,20.));
#71375=CARTESIAN_POINT('Ctrl Pts',(32.1074492888083,-34.2742752649465,0.));
#71376=CARTESIAN_POINT('Ctrl Pts',(32.1074492888083,-34.2742752649465,20.));
#71377=CARTESIAN_POINT('Ctrl Pts',(32.081352659827,-34.2946197006486,0.));
#71378=CARTESIAN_POINT('Ctrl Pts',(32.081352659827,-34.2946197006486,20.));
#71379=CARTESIAN_POINT('Ctrl Pts',(32.0552426417428,-34.3149451324082,0.));
#71380=CARTESIAN_POINT('Ctrl Pts',(32.0552426417428,-34.3149451324082,20.));
#71381=CARTESIAN_POINT('Ctrl Pts',(32.0291192479513,-34.335251550907,0.));
#71382=CARTESIAN_POINT('Ctrl Pts',(32.0291192479513,-34.335251550907,20.));
#71383=CARTESIAN_POINT('Ctrl Pts',(32.0029824918551,-34.3555389468366,0.));
#71384=CARTESIAN_POINT('Ctrl Pts',(32.0029824918551,-34.3555389468366,20.));
#71385=CARTESIAN_POINT('Ctrl Pts',(31.9768323868632,-34.3758073108972,0.));
#71386=CARTESIAN_POINT('Ctrl Pts',(31.9768323868632,-34.3758073108972,20.));
#71387=CARTESIAN_POINT('Ctrl Pts',(31.9506689463919,-34.3960566337983,0.));
#71388=CARTESIAN_POINT('Ctrl Pts',(31.9506689463919,-34.3960566337983,20.));
#71389=CARTESIAN_POINT('Ctrl Pts',(31.9244921838641,-34.4162869062584,0.));
#71390=CARTESIAN_POINT('Ctrl Pts',(31.9244921838641,-34.4162869062584,20.));
#71391=CARTESIAN_POINT('Ctrl Pts',(31.8983021127101,-34.4364981190057,0.));
#71392=CARTESIAN_POINT('Ctrl Pts',(31.8983021127101,-34.4364981190057,20.));
#71393=CARTESIAN_POINT('Ctrl Pts',(31.8720987463673,-34.4566902627777,0.));
#71394=CARTESIAN_POINT('Ctrl Pts',(31.8720987463673,-34.4566902627777,20.));
#71395=CARTESIAN_POINT('Ctrl Pts',(31.8458820982794,-34.4768633283209,0.));
#71396=CARTESIAN_POINT('Ctrl Pts',(31.8458820982794,-34.4768633283209,20.));
#71397=CARTESIAN_POINT('Ctrl Pts',(31.819652181897,-34.4970173063908,0.));
#71398=CARTESIAN_POINT('Ctrl Pts',(31.819652181897,-34.4970173063908,20.));
#71399=CARTESIAN_POINT('Ctrl Pts',(31.7934090106771,-34.5171521877519,0.));
#71400=CARTESIAN_POINT('Ctrl Pts',(31.7934090106771,-34.5171521877519,20.));
#71401=CARTESIAN_POINT('Ctrl Pts',(31.7671525980837,-34.5372679631778,0.));
#71402=CARTESIAN_POINT('Ctrl Pts',(31.7671525980837,-34.5372679631778,20.));
#71403=CARTESIAN_POINT('Ctrl Pts',(31.7408829575878,-34.5573646234518,0.));
#71404=CARTESIAN_POINT('Ctrl Pts',(31.7408829575878,-34.5573646234518,20.));
#71405=CARTESIAN_POINT('Ctrl Pts',(31.7146001026678,-34.5774421593669,0.));
#71406=CARTESIAN_POINT('Ctrl Pts',(31.7146001026678,-34.5774421593669,20.));
#71407=CARTESIAN_POINT('Ctrl Pts',(31.6883040468088,-34.5975005617252,0.));
#71408=CARTESIAN_POINT('Ctrl Pts',(31.6883040468088,-34.5975005617252,20.));
#71409=CARTESIAN_POINT('Ctrl Pts',(31.6619948035026,-34.6175398213376,0.));
#71410=CARTESIAN_POINT('Ctrl Pts',(31.6619948035026,-34.6175398213376,20.));
#71411=CARTESIAN_POINT('Ctrl Pts',(31.6356723862475,-34.6375599290243,0.));
#71412=CARTESIAN_POINT('Ctrl Pts',(31.6356723862475,-34.6375599290243,20.));
#71413=CARTESIAN_POINT('Ctrl Pts',(31.609336808548,-34.6575608756141,0.));
#71414=CARTESIAN_POINT('Ctrl Pts',(31.609336808548,-34.6575608756141,20.));
#71415=CARTESIAN_POINT('Ctrl Pts',(31.5829880839157,-34.6775426519456,0.));
#71416=CARTESIAN_POINT('Ctrl Pts',(31.5829880839157,-34.6775426519456,20.));
#71417=CARTESIAN_POINT('Ctrl Pts',(31.556626225869,-34.6975052488666,0.));
#71418=CARTESIAN_POINT('Ctrl Pts',(31.556626225869,-34.6975052488666,20.));
#71419=CARTESIAN_POINT('Ctrl Pts',(31.5302512479332,-34.7174486572342,0.));
#71420=CARTESIAN_POINT('Ctrl Pts',(31.5302512479332,-34.7174486572342,20.));
#71421=CARTESIAN_POINT('Ctrl Pts',(31.5038631636409,-34.7373728679152,0.));
#71422=CARTESIAN_POINT('Ctrl Pts',(31.5038631636409,-34.7373728679152,20.));
#71423=CARTESIAN_POINT('Ctrl Pts',(31.4774619865312,-34.7572778717853,0.));
#71424=CARTESIAN_POINT('Ctrl Pts',(31.4774619865312,-34.7572778717853,20.));
#71425=CARTESIAN_POINT('Ctrl Pts',(31.4510477301503,-34.7771636597296,0.));
#71426=CARTESIAN_POINT('Ctrl Pts',(31.4510477301503,-34.7771636597296,20.));
#71427=CARTESIAN_POINT('Ctrl Pts',(31.4246204080513,-34.7970302226433,0.));
#71428=CARTESIAN_POINT('Ctrl Pts',(31.4246204080513,-34.7970302226433,20.));
#71429=CARTESIAN_POINT('Ctrl Pts',(31.3981800337935,-34.8168775514299,0.));
#71430=CARTESIAN_POINT('Ctrl Pts',(31.3981800337935,-34.8168775514299,20.));
#71431=CARTESIAN_POINT('Ctrl Pts',(31.3717266209433,-34.8367056370027,0.));
#71432=CARTESIAN_POINT('Ctrl Pts',(31.3717266209433,-34.8367056370027,20.));
#71433=CARTESIAN_POINT('Ctrl Pts',(31.3452601830725,-34.856514470283,0.));
#71434=CARTESIAN_POINT('Ctrl Pts',(31.3452601830725,-34.856514470283,20.));
#71435=CARTESIAN_POINT('Ctrl Pts',(31.3187807337598,-34.8763040422018,0.));
#71436=CARTESIAN_POINT('Ctrl Pts',(31.3187807337598,-34.8763040422018,20.));
#71437=CARTESIAN_POINT('Ctrl Pts',(31.2922882865907,-34.8960743436995,0.));
#71438=CARTESIAN_POINT('Ctrl Pts',(31.2922882865907,-34.8960743436995,20.));
#71439=CARTESIAN_POINT('Ctrl Pts',(31.2657828551579,-34.9158253657263,0.));
#71440=CARTESIAN_POINT('Ctrl Pts',(31.2657828551579,-34.9158253657263,20.));
#71441=CARTESIAN_POINT('Ctrl Pts',(31.2392644530613,-34.9355570992414,0.));
#71442=CARTESIAN_POINT('Ctrl Pts',(31.2392644530613,-34.9355570992414,20.));
#71443=CARTESIAN_POINT('Ctrl Pts',(31.2127330939085,-34.9552695352152,0.));
#71444=CARTESIAN_POINT('Ctrl Pts',(31.2127330939085,-34.9552695352152,20.));
#71445=CARTESIAN_POINT('Ctrl Pts',(31.1861887913133,-34.974962664626,0.));
#71446=CARTESIAN_POINT('Ctrl Pts',(31.1861887913133,-34.974962664626,20.));
#71447=CARTESIAN_POINT('Ctrl Pts',(31.1596315588953,-34.9946364784612,0.));
#71448=CARTESIAN_POINT('Ctrl Pts',(31.1596315588953,-34.9946364784612,20.));
#71449=CARTESIAN_POINT('Ctrl Pts',(31.1330614102809,-35.0142909677175,0.));
#71450=CARTESIAN_POINT('Ctrl Pts',(31.1330614102809,-35.0142909677175,20.));
#71451=CARTESIAN_POINT('Ctrl Pts',(31.1064783591027,-35.0339261234013,0.));
#71452=CARTESIAN_POINT('Ctrl Pts',(31.1064783591027,-35.0339261234013,20.));
#71453=CARTESIAN_POINT('Ctrl Pts',(31.0798824190003,-35.0535419365277,0.));
#71454=CARTESIAN_POINT('Ctrl Pts',(31.0798824190003,-35.0535419365277,20.));
#71455=CARTESIAN_POINT('Ctrl Pts',(31.0532736036193,-35.0731383981212,0.));
#71456=CARTESIAN_POINT('Ctrl Pts',(31.0532736036193,-35.0731383981212,20.));
#71457=CARTESIAN_POINT('Ctrl Pts',(31.026651926612,-35.0927154992152,0.));
#71458=CARTESIAN_POINT('Ctrl Pts',(31.026651926612,-35.0927154992152,20.));
#71459=CARTESIAN_POINT('Ctrl Pts',(31.0000174016378,-35.1122732308527,0.));
#71460=CARTESIAN_POINT('Ctrl Pts',(31.0000174016378,-35.1122732308527,20.));
#71461=CARTESIAN_POINT('Ctrl Pts',(30.9733700423633,-35.131811584087,0.));
#71462=CARTESIAN_POINT('Ctrl Pts',(30.9733700423633,-35.131811584087,20.));
#71463=CARTESIAN_POINT('Ctrl Pts',(30.9467098624624,-35.1513305499814,0.));
#71464=CARTESIAN_POINT('Ctrl Pts',(30.9467098624624,-35.1513305499814,20.));
#71465=CARTESIAN_POINT('Ctrl Pts',(30.9200368756162,-35.170830119609,0.));
#71466=CARTESIAN_POINT('Ctrl Pts',(30.9200368756162,-35.170830119609,20.));
#71467=CARTESIAN_POINT('Ctrl Pts',(30.8933510955115,-35.1903102840519,0.));
#71468=CARTESIAN_POINT('Ctrl Pts',(30.8933510955115,-35.1903102840519,20.));
#71469=CARTESIAN_POINT('Ctrl Pts',(30.8666525358408,-35.2097710343998,0.));
#71470=CARTESIAN_POINT('Ctrl Pts',(30.8666525358408,-35.2097710343998,20.));
#71471=CARTESIAN_POINT('Ctrl Pts',(30.8399412103026,-35.2292123617517,0.));
#71472=CARTESIAN_POINT('Ctrl Pts',(30.8399412103026,-35.2292123617517,20.));
#71473=CARTESIAN_POINT('Ctrl Pts',(30.8132171326021,-35.2486342572162,0.));
#71474=CARTESIAN_POINT('Ctrl Pts',(30.8132171326021,-35.2486342572162,20.));
#71475=CARTESIAN_POINT('Ctrl Pts',(30.786480316451,-35.2680367119112,0.));
#71476=CARTESIAN_POINT('Ctrl Pts',(30.786480316451,-35.2680367119112,20.));
#71477=CARTESIAN_POINT('Ctrl Pts',(30.7597307755696,-35.2874197169657,0.));
#71478=CARTESIAN_POINT('Ctrl Pts',(30.7597307755696,-35.2874197169657,20.));
#71479=CARTESIAN_POINT('Ctrl Pts',(30.732968523684,-35.3067832635177,0.));
#71480=CARTESIAN_POINT('Ctrl Pts',(30.732968523684,-35.3067832635177,20.));
#71481=CARTESIAN_POINT('Ctrl Pts',(30.7061935745273,-35.3261273427148,0.));
#71482=CARTESIAN_POINT('Ctrl Pts',(30.7061935745273,-35.3261273427148,20.));
#71483=CARTESIAN_POINT('Ctrl Pts',(30.6794059418388,-35.3454519457137,0.));
#71484=CARTESIAN_POINT('Ctrl Pts',(30.6794059418388,-35.3454519457137,20.));
#71485=CARTESIAN_POINT('Ctrl Pts',(30.6526056393638,-35.3647570636798,0.));
#71486=CARTESIAN_POINT('Ctrl Pts',(30.6526056393638,-35.3647570636798,20.));
#71487=CARTESIAN_POINT('Ctrl Pts',(30.6257926808541,-35.3840426877879,0.));
#71488=CARTESIAN_POINT('Ctrl Pts',(30.6257926808541,-35.3840426877879,20.));
#71489=CARTESIAN_POINT('Ctrl Pts',(30.5989670800681,-35.4033088092226,0.));
#71490=CARTESIAN_POINT('Ctrl Pts',(30.5989670800681,-35.4033088092226,20.));
#71491=CARTESIAN_POINT('Ctrl Pts',(30.5721288507715,-35.4225554191786,0.));
#71492=CARTESIAN_POINT('Ctrl Pts',(30.5721288507715,-35.4225554191786,20.));
#71493=CARTESIAN_POINT('Ctrl Pts',(30.5452780067368,-35.4417825088605,0.));
#71494=CARTESIAN_POINT('Ctrl Pts',(30.5452780067368,-35.4417825088605,20.));
#71495=CARTESIAN_POINT('Ctrl Pts',(30.5184145617424,-35.4609900694812,0.));
#71496=CARTESIAN_POINT('Ctrl Pts',(30.5184145617424,-35.4609900694812,20.));
#71497=CARTESIAN_POINT('Ctrl Pts',(30.4915385295724,-35.4801780922626,0.));
#71498=CARTESIAN_POINT('Ctrl Pts',(30.4915385295724,-35.4801780922626,20.));
#71499=CARTESIAN_POINT('Ctrl Pts',(30.4646499240177,-35.4993465684362,0.));
#71500=CARTESIAN_POINT('Ctrl Pts',(30.4646499240177,-35.4993465684362,20.));
#71501=CARTESIAN_POINT('Ctrl Pts',(30.437748758876,-35.518495489243,0.));
#71502=CARTESIAN_POINT('Ctrl Pts',(30.437748758876,-35.518495489243,20.));
#71503=CARTESIAN_POINT('Ctrl Pts',(30.4108350479521,-35.5376248459348,0.));
#71504=CARTESIAN_POINT('Ctrl Pts',(30.4108350479521,-35.5376248459348,20.));
#71505=CARTESIAN_POINT('Ctrl Pts',(30.3839088050584,-35.5567346297737,0.));
#71506=CARTESIAN_POINT('Ctrl Pts',(30.3839088050584,-35.5567346297737,20.));
#71507=CARTESIAN_POINT('Ctrl Pts',(30.3569700440131,-35.5758248320301,0.));
#71508=CARTESIAN_POINT('Ctrl Pts',(30.3569700440131,-35.5758248320301,20.));
#71509=CARTESIAN_POINT('Ctrl Pts',(30.3300187786403,-35.5948954439837,0.));
#71510=CARTESIAN_POINT('Ctrl Pts',(30.3300187786403,-35.5948954439837,20.));
#71511=CARTESIAN_POINT('Ctrl Pts',(30.3030550227693,-35.6139464569223,0.));
#71512=CARTESIAN_POINT('Ctrl Pts',(30.3030550227693,-35.6139464569223,20.));
#71513=CARTESIAN_POINT('Ctrl Pts',(30.2760787902362,-35.6329778621436,0.));
#71514=CARTESIAN_POINT('Ctrl Pts',(30.2760787902362,-35.6329778621436,20.));
#71515=CARTESIAN_POINT('Ctrl Pts',(30.2490900948838,-35.6519896509552,0.));
#71516=CARTESIAN_POINT('Ctrl Pts',(30.2490900948838,-35.6519896509552,20.));
#71517=CARTESIAN_POINT('Ctrl Pts',(30.2220889505625,-35.6709818146751,0.));
#71518=CARTESIAN_POINT('Ctrl Pts',(30.2220889505625,-35.6709818146751,20.));
#71519=CARTESIAN_POINT('Ctrl Pts',(30.1950753711288,-35.6899543446309,0.));
#71520=CARTESIAN_POINT('Ctrl Pts',(30.1950753711288,-35.6899543446309,20.));
#71521=CARTESIAN_POINT('Ctrl Pts',(30.1680493704465,-35.7089072321597,0.));
#71522=CARTESIAN_POINT('Ctrl Pts',(30.1680493704465,-35.7089072321597,20.));
#71523=CARTESIAN_POINT('Ctrl Pts',(30.141010962385,-35.727840468608,0.));
#71524=CARTESIAN_POINT('Ctrl Pts',(30.141010962385,-35.727840468608,20.));
#71525=CARTESIAN_POINT('Ctrl Pts',(30.1139601608197,-35.7467540453308,0.));
#71526=CARTESIAN_POINT('Ctrl Pts',(30.1139601608197,-35.7467540453308,20.));
#71527=CARTESIAN_POINT('Ctrl Pts',(30.0868969796328,-35.7656479536939,0.));
#71528=CARTESIAN_POINT('Ctrl Pts',(30.0868969796328,-35.7656479536939,20.));
#71529=CARTESIAN_POINT('Ctrl Pts',(30.0598214327127,-35.7845221850715,0.));
#71530=CARTESIAN_POINT('Ctrl Pts',(30.0598214327127,-35.7845221850715,20.));
#71531=CARTESIAN_POINT('Ctrl Pts',(30.0327335339539,-35.8033767308478,0.));
#71532=CARTESIAN_POINT('Ctrl Pts',(30.0327335339539,-35.8033767308478,20.));
#71533=CARTESIAN_POINT('Ctrl Pts',(30.005633297258,-35.8222115824167,0.));
#71534=CARTESIAN_POINT('Ctrl Pts',(30.005633297258,-35.8222115824167,20.));
#71535=CARTESIAN_POINT('Ctrl Pts',(29.9785207365333,-35.841026731182,0.));
#71536=CARTESIAN_POINT('Ctrl Pts',(29.9785207365333,-35.841026731182,20.));
#71537=CARTESIAN_POINT('Ctrl Pts',(29.9513958656946,-35.8598221685576,0.));
#71538=CARTESIAN_POINT('Ctrl Pts',(29.9513958656946,-35.8598221685576,20.));
#71539=CARTESIAN_POINT('Ctrl Pts',(29.9242586986624,-35.8785978859658,0.));
#71540=CARTESIAN_POINT('Ctrl Pts',(29.9242586986624,-35.8785978859658,20.));
#71541=CARTESIAN_POINT('Ctrl Pts',(29.8971092493634,-35.8973538748387,0.));
#71542=CARTESIAN_POINT('Ctrl Pts',(29.8971092493634,-35.8973538748387,20.));
#71543=CARTESIAN_POINT('Ctrl Pts',(29.869947531731,-35.9160901266177,0.));
#71544=CARTESIAN_POINT('Ctrl Pts',(29.869947531731,-35.9160901266177,20.));
#71545=CARTESIAN_POINT('Ctrl Pts',(29.8427735597048,-35.934806632754,0.));
#71546=CARTESIAN_POINT('Ctrl Pts',(29.8427735597048,-35.934806632754,20.));
#71547=CARTESIAN_POINT('Ctrl Pts',(29.8155873472308,-35.9535033847082,0.));
#71548=CARTESIAN_POINT('Ctrl Pts',(29.8155873472308,-35.9535033847082,20.));
#71549=CARTESIAN_POINT('Ctrl Pts',(29.7883889082614,-35.9721803739509,0.));
#71550=CARTESIAN_POINT('Ctrl Pts',(29.7883889082614,-35.9721803739509,20.));
#71551=CARTESIAN_POINT('Ctrl Pts',(29.7611782567557,-35.9908375919623,0.));
#71552=CARTESIAN_POINT('Ctrl Pts',(29.7611782567557,-35.9908375919623,20.));
#71553=CARTESIAN_POINT('Ctrl Pts',(29.7339554066796,-36.0094750302331,0.));
#71554=CARTESIAN_POINT('Ctrl Pts',(29.7339554066796,-36.0094750302331,20.));
#71555=CARTESIAN_POINT('Ctrl Pts',(29.7067203720053,-36.0280926802632,0.));
#71556=CARTESIAN_POINT('Ctrl Pts',(29.7067203720053,-36.0280926802632,20.));
#71557=CARTESIAN_POINT('Ctrl Pts',(29.6794731667106,-36.0466905335617,0.));
#71558=CARTESIAN_POINT('Ctrl Pts',(29.6794731667106,-36.0466905335617,20.));
#71559=CARTESIAN_POINT('Ctrl Pts',(29.6522138047793,-36.0652685816464,0.));
#71560=CARTESIAN_POINT('Ctrl Pts',(29.6522138047793,-36.0652685816464,20.));
#71561=CARTESIAN_POINT('Ctrl Pts',(29.6249423002017,-36.0838268160451,0.));
#71562=CARTESIAN_POINT('Ctrl Pts',(29.6249423002017,-36.0838268160451,20.));
#71563=CARTESIAN_POINT('Ctrl Pts',(29.5976586669748,-36.1023652282957,0.));
#71564=CARTESIAN_POINT('Ctrl Pts',(29.5976586669748,-36.1023652282957,20.));
#71565=CARTESIAN_POINT('Ctrl Pts',(29.5703629191022,-36.1208838099461,0.));
#71566=CARTESIAN_POINT('Ctrl Pts',(29.5703629191022,-36.1208838099461,20.));
#71567=CARTESIAN_POINT('Ctrl Pts',(29.5430550705937,-36.1393825525541,0.));
#71568=CARTESIAN_POINT('Ctrl Pts',(29.5430550705937,-36.1393825525541,20.));
#71569=CARTESIAN_POINT('Ctrl Pts',(29.5157351354651,-36.1578614476865,0.));
#71570=CARTESIAN_POINT('Ctrl Pts',(29.5157351354651,-36.1578614476865,20.));
#71571=CARTESIAN_POINT('Ctrl Pts',(29.4884031277381,-36.1763204869193,0.));
#71572=CARTESIAN_POINT('Ctrl Pts',(29.4884031277381,-36.1763204869193,20.));
#71573=CARTESIAN_POINT('Ctrl Pts',(29.4610590614411,-36.1947596618382,0.));
#71574=CARTESIAN_POINT('Ctrl Pts',(29.4610590614411,-36.1947596618382,20.));
#71575=CARTESIAN_POINT('Ctrl Pts',(29.4337029506094,-36.2131789640397,0.));
#71576=CARTESIAN_POINT('Ctrl Pts',(29.4337029506094,-36.2131789640397,20.));
#71577=CARTESIAN_POINT('Ctrl Pts',(29.4063348092849,-36.2315783851295,0.));
#71578=CARTESIAN_POINT('Ctrl Pts',(29.4063348092849,-36.2315783851295,20.));
#71579=CARTESIAN_POINT('Ctrl Pts',(29.3789546515147,-36.2499579167227,0.));
#71580=CARTESIAN_POINT('Ctrl Pts',(29.3789546515147,-36.2499579167227,20.));
#71581=CARTESIAN_POINT('Ctrl Pts',(29.3515624913523,-36.2683175504441,0.));
#71582=CARTESIAN_POINT('Ctrl Pts',(29.3515624913523,-36.2683175504441,20.));
#71583=CARTESIAN_POINT('Ctrl Pts',(29.3241583428569,-36.286657277928,0.));
#71584=CARTESIAN_POINT('Ctrl Pts',(29.3241583428569,-36.286657277928,20.));
#71585=CARTESIAN_POINT('Ctrl Pts',(29.2967422200943,-36.3049770908188,0.));
#71586=CARTESIAN_POINT('Ctrl Pts',(29.2967422200943,-36.3049770908188,20.));
#71587=CARTESIAN_POINT('Ctrl Pts',(29.2693141371364,-36.3232769807701,0.));
#71588=CARTESIAN_POINT('Ctrl Pts',(29.2693141371364,-36.3232769807701,20.));
#71589=CARTESIAN_POINT('Ctrl Pts',(29.241874108062,-36.3415569394456,0.));
#71590=CARTESIAN_POINT('Ctrl Pts',(29.241874108062,-36.3415569394456,20.));
#71591=CARTESIAN_POINT('Ctrl Pts',(29.2144221469562,-36.3598169585187,0.));
#71592=CARTESIAN_POINT('Ctrl Pts',(29.2144221469562,-36.3598169585187,20.));
#71593=CARTESIAN_POINT('Ctrl Pts',(29.186958267911,-36.3780570296726,0.));
#71594=CARTESIAN_POINT('Ctrl Pts',(29.186958267911,-36.3780570296726,20.));
#71595=CARTESIAN_POINT('Ctrl Pts',(29.1594824850239,-36.3962771446002,0.));
#71596=CARTESIAN_POINT('Ctrl Pts',(29.1594824850239,-36.3962771446002,20.));
#71597=CARTESIAN_POINT('Ctrl Pts',(29.1319948123985,-36.4144772950043,0.));
#71598=CARTESIAN_POINT('Ctrl Pts',(29.1319948123985,-36.4144772950043,20.));
#71599=CARTESIAN_POINT('Ctrl Pts',(29.1044952641442,-36.4326574725969,0.));
#71600=CARTESIAN_POINT('Ctrl Pts',(29.1044952641442,-36.4326574725969,20.));
#71601=CARTESIAN_POINT('Ctrl Pts',(29.0769838543763,-36.4508176690994,0.));
#71602=CARTESIAN_POINT('Ctrl Pts',(29.0769838543763,-36.4508176690994,20.));
#71603=CARTESIAN_POINT('Ctrl Pts',(29.0494605972165,-36.4689578762435,0.));
#71604=CARTESIAN_POINT('Ctrl Pts',(29.0494605972165,-36.4689578762435,20.));
#71605=CARTESIAN_POINT('Ctrl Pts',(29.0219255067927,-36.4870780857703,0.));
#71606=CARTESIAN_POINT('Ctrl Pts',(29.0219255067927,-36.4870780857703,20.));
#71607=CARTESIAN_POINT('Ctrl Pts',(28.99437859724,-36.5051782894317,0.));
#71608=CARTESIAN_POINT('Ctrl Pts',(28.99437859724,-36.5051782894317,20.));
#71609=CARTESIAN_POINT('Ctrl Pts',(28.9668198826995,-36.5232584789886,0.));
#71610=CARTESIAN_POINT('Ctrl Pts',(28.9668198826995,-36.5232584789886,20.));
#71611=CARTESIAN_POINT('Ctrl Pts',(28.9392493773185,-36.5413186462123,0.));
#71612=CARTESIAN_POINT('Ctrl Pts',(28.9392493773185,-36.5413186462123,20.));
#71613=CARTESIAN_POINT('Ctrl Pts',(28.9116670952497,-36.5593587828826,0.));
#71614=CARTESIAN_POINT('Ctrl Pts',(28.9116670952497,-36.5593587828826,20.));
#71615=CARTESIAN_POINT('Ctrl Pts',(28.8840730506515,-36.577378880789,0.));
#71616=CARTESIAN_POINT('Ctrl Pts',(28.8840730506515,-36.577378880789,20.));
#71617=CARTESIAN_POINT('Ctrl Pts',(28.8564672576885,-36.5953789317306,0.));
#71618=CARTESIAN_POINT('Ctrl Pts',(28.8564672576885,-36.5953789317306,20.));
#71619=CARTESIAN_POINT('Ctrl Pts',(28.8288497305324,-36.6133589275174,0.));
#71620=CARTESIAN_POINT('Ctrl Pts',(28.8288497305324,-36.6133589275174,20.));
#71621=CARTESIAN_POINT('Ctrl Pts',(28.8012204833609,-36.6313188599694,0.));
#71622=CARTESIAN_POINT('Ctrl Pts',(28.8012204833609,-36.6313188599694,20.));
#71623=CARTESIAN_POINT('Ctrl Pts',(28.7735795303585,-36.6492587209168,0.));
#71624=CARTESIAN_POINT('Ctrl Pts',(28.7735795303585,-36.6492587209168,20.));
#71625=CARTESIAN_POINT('Ctrl Pts',(28.7459268857152,-36.6671785021988,0.));
#71626=CARTESIAN_POINT('Ctrl Pts',(28.7459268857152,-36.6671785021988,20.));
#71627=CARTESIAN_POINT('Ctrl Pts',(28.7182625636274,-36.6850781956649,0.));
#71628=CARTESIAN_POINT('Ctrl Pts',(28.7182625636274,-36.6850781956649,20.));
#71629=CARTESIAN_POINT('Ctrl Pts',(28.6905865782966,-36.7029577931733,0.));
#71630=CARTESIAN_POINT('Ctrl Pts',(28.6905865782966,-36.7029577931733,20.));
#71631=CARTESIAN_POINT('Ctrl Pts',(28.6628989439305,-36.7208172865919,0.));
#71632=CARTESIAN_POINT('Ctrl Pts',(28.6628989439305,-36.7208172865919,20.));
#71633=CARTESIAN_POINT('Ctrl Pts',(28.6351996747428,-36.7386566677981,0.));
#71634=CARTESIAN_POINT('Ctrl Pts',(28.6351996747428,-36.7386566677981,20.));
#71635=CARTESIAN_POINT('Ctrl Pts',(28.6074887849535,-36.7564759286795,0.));
#71636=CARTESIAN_POINT('Ctrl Pts',(28.6074887849535,-36.7564759286795,20.));
#71637=CARTESIAN_POINT('Ctrl Pts',(28.5797662887891,-36.774275061134,0.));
#71638=CARTESIAN_POINT('Ctrl Pts',(28.5797662887891,-36.774275061134,20.));
#71639=CARTESIAN_POINT('Ctrl Pts',(28.5520322004824,-36.7920540570698,0.));
#71640=CARTESIAN_POINT('Ctrl Pts',(28.5520322004824,-36.7920540570698,20.));
#71641=CARTESIAN_POINT('Ctrl Pts',(28.5242865342724,-36.8098129084051,0.));
#71642=CARTESIAN_POINT('Ctrl Pts',(28.5242865342724,-36.8098129084051,20.));
#71643=CARTESIAN_POINT('Ctrl Pts',(28.496529304404,-36.8275516070676,0.));
#71644=CARTESIAN_POINT('Ctrl Pts',(28.496529304404,-36.8275516070676,20.));
#71645=CARTESIAN_POINT('Ctrl Pts',(28.4687605251277,-36.8452701449948,0.));
#71646=CARTESIAN_POINT('Ctrl Pts',(28.4687605251277,-36.8452701449948,20.));
#71647=CARTESIAN_POINT('Ctrl Pts',(28.4409802107002,-36.8629685141338,0.));
#71648=CARTESIAN_POINT('Ctrl Pts',(28.4409802107002,-36.8629685141338,20.));
#71649=CARTESIAN_POINT('Ctrl Pts',(28.413188375384,-36.8806467064409,0.));
#71650=CARTESIAN_POINT('Ctrl Pts',(28.413188375384,-36.8806467064409,20.));
#71651=CARTESIAN_POINT('Ctrl Pts',(28.3853850334475,-36.8983047138822,0.));
#71652=CARTESIAN_POINT('Ctrl Pts',(28.3853850334475,-36.8983047138822,20.));
#71653=CARTESIAN_POINT('Ctrl Pts',(28.3575701991656,-36.9159425284342,0.));
#71654=CARTESIAN_POINT('Ctrl Pts',(28.3575701991656,-36.9159425284342,20.));
#71655=CARTESIAN_POINT('Ctrl Pts',(28.3297438868192,-36.9335601420835,0.));
#71656=CARTESIAN_POINT('Ctrl Pts',(28.3297438868192,-36.9335601420835,20.));
#71657=CARTESIAN_POINT('Ctrl Pts',(28.3019061106957,-36.9511575468269,0.));
#71658=CARTESIAN_POINT('Ctrl Pts',(28.3019061106957,-36.9511575468269,20.));
#71659=CARTESIAN_POINT('Ctrl Pts',(28.2740568850881,-36.968734734671,0.));
#71660=CARTESIAN_POINT('Ctrl Pts',(28.2740568850881,-36.968734734671,20.));
#71661=CARTESIAN_POINT('Ctrl Pts',(28.2461962242955,-36.9862916976318,0.));
#71662=CARTESIAN_POINT('Ctrl Pts',(28.2461962242955,-36.9862916976318,20.));
#71663=CARTESIAN_POINT('Ctrl Pts',(28.2183241426219,-37.0038284277349,0.));
#71664=CARTESIAN_POINT('Ctrl Pts',(28.2183241426219,-37.0038284277349,20.));
#71665=CARTESIAN_POINT('Ctrl Pts',(28.1904406543778,-37.0213449170157,0.));
#71666=CARTESIAN_POINT('Ctrl Pts',(28.1904406543778,-37.0213449170157,20.));
#71667=CARTESIAN_POINT('Ctrl Pts',(28.1625457738797,-37.0388411575197,0.));
#71668=CARTESIAN_POINT('Ctrl Pts',(28.1625457738797,-37.0388411575197,20.));
#71669=CARTESIAN_POINT('Ctrl Pts',(28.1346395154506,-37.0563171413026,0.));
#71670=CARTESIAN_POINT('Ctrl Pts',(28.1346395154506,-37.0563171413026,20.));
#71671=CARTESIAN_POINT('Ctrl Pts',(28.1067218934195,-37.0737728604298,0.));
#71672=CARTESIAN_POINT('Ctrl Pts',(28.1067218934195,-37.0737728604298,20.));
#71673=CARTESIAN_POINT('Ctrl Pts',(28.0787929221219,-37.0912083069772,0.));
#71674=CARTESIAN_POINT('Ctrl Pts',(28.0787929221219,-37.0912083069772,20.));
#71675=CARTESIAN_POINT('Ctrl Pts',(28.0508526158994,-37.1086234730312,0.));
#71676=CARTESIAN_POINT('Ctrl Pts',(28.0508526158994,-37.1086234730312,20.));
#71677=CARTESIAN_POINT('Ctrl Pts',(28.0229009890985,-37.1260183506872,0.));
#71678=CARTESIAN_POINT('Ctrl Pts',(28.0229009890985,-37.1260183506872,20.));
#71679=CARTESIAN_POINT('Ctrl Pts',(27.994938056072,-37.1433929320507,0.));
#71680=CARTESIAN_POINT('Ctrl Pts',(27.994938056072,-37.1433929320507,20.));
#71681=CARTESIAN_POINT('Ctrl Pts',(27.9669638311771,-37.1607472092352,0.));
#71682=CARTESIAN_POINT('Ctrl Pts',(27.9669638311771,-37.1607472092352,20.));
#71683=CARTESIAN_POINT('Ctrl Pts',(27.9389783287777,-37.1780811743652,0.));
#71684=CARTESIAN_POINT('Ctrl Pts',(27.9389783287777,-37.1780811743652,20.));
#71685=CARTESIAN_POINT('Ctrl Pts',(27.9109815632437,-37.1953948195748,0.));
#71686=CARTESIAN_POINT('Ctrl Pts',(27.9109815632437,-37.1953948195748,20.));
#71687=CARTESIAN_POINT('Ctrl Pts',(27.8829735489517,-37.2126881370093,0.));
#71688=CARTESIAN_POINT('Ctrl Pts',(27.8829735489517,-37.2126881370093,20.));
#71689=CARTESIAN_POINT('Ctrl Pts',(27.8549543002843,-37.2299611188238,0.));
#71690=CARTESIAN_POINT('Ctrl Pts',(27.8549543002843,-37.2299611188238,20.));
#71691=CARTESIAN_POINT('Ctrl Pts',(27.8269238316305,-37.2472137571842,0.));
#71692=CARTESIAN_POINT('Ctrl Pts',(27.8269238316305,-37.2472137571842,20.));
#71693=CARTESIAN_POINT('Ctrl Pts',(27.7988821573846,-37.2644460442654,0.));
#71694=CARTESIAN_POINT('Ctrl Pts',(27.7988821573846,-37.2644460442654,20.));
#71695=CARTESIAN_POINT('Ctrl Pts',(27.7708292919468,-37.2816579722525,0.));
#71696=CARTESIAN_POINT('Ctrl Pts',(27.7708292919468,-37.2816579722525,20.));
#71697=CARTESIAN_POINT('Ctrl Pts',(27.7427652497224,-37.2988495333397,0.));
#71698=CARTESIAN_POINT('Ctrl Pts',(27.7427652497224,-37.2988495333397,20.));
#71699=CARTESIAN_POINT('Ctrl Pts',(27.7146900451228,-37.3160207197314,0.));
#71700=CARTESIAN_POINT('Ctrl Pts',(27.7146900451228,-37.3160207197314,20.));
#71701=CARTESIAN_POINT('Ctrl Pts',(27.6866036925651,-37.3331715236414,0.));
#71702=CARTESIAN_POINT('Ctrl Pts',(27.6866036925651,-37.3331715236414,20.));
#71703=CARTESIAN_POINT('Ctrl Pts',(27.6585062064726,-37.3503019372939,0.));
#71704=CARTESIAN_POINT('Ctrl Pts',(27.6585062064726,-37.3503019372939,20.));
#71705=CARTESIAN_POINT('Ctrl Pts',(27.6303976012744,-37.3674119529234,0.));
#71706=CARTESIAN_POINT('Ctrl Pts',(27.6303976012744,-37.3674119529234,20.));
#71707=CARTESIAN_POINT('Ctrl Pts',(27.6022778914064,-37.384501562775,0.));
#71708=CARTESIAN_POINT('Ctrl Pts',(27.6022778914064,-37.384501562775,20.));
#71709=CARTESIAN_POINT('Ctrl Pts',(27.5741470913094,-37.4015707591036,0.));
#71710=CARTESIAN_POINT('Ctrl Pts',(27.5741470913094,-37.4015707591036,20.));
#71711=CARTESIAN_POINT('Ctrl Pts',(27.5460052154308,-37.4186195341741,0.));
#71712=CARTESIAN_POINT('Ctrl Pts',(27.5460052154308,-37.4186195341741,20.));
#71713=CARTESIAN_POINT('Ctrl Pts',(27.5178522782226,-37.4356478802604,0.));
#71714=CARTESIAN_POINT('Ctrl Pts',(27.5178522782226,-37.4356478802604,20.));
#71715=CARTESIAN_POINT('Ctrl Pts',(27.4896882941429,-37.4526557896465,0.));
#71716=CARTESIAN_POINT('Ctrl Pts',(27.4896882941429,-37.4526557896465,20.));
#71717=CARTESIAN_POINT('Ctrl Pts',(27.4615132776558,-37.4696432546267,0.));
#71718=CARTESIAN_POINT('Ctrl Pts',(27.4615132776558,-37.4696432546267,20.));
#71719=CARTESIAN_POINT('Ctrl Pts',(27.4333272432311,-37.4866102675048,0.));
#71720=CARTESIAN_POINT('Ctrl Pts',(27.4333272432311,-37.4866102675048,20.));
#71721=CARTESIAN_POINT('Ctrl Pts',(27.4051302053449,-37.5035568205959,0.));
#71722=CARTESIAN_POINT('Ctrl Pts',(27.4051302053449,-37.5035568205959,20.));
#71723=CARTESIAN_POINT('Ctrl Pts',(27.3769221784798,-37.5204829062256,0.));
#71724=CARTESIAN_POINT('Ctrl Pts',(27.3769221784798,-37.5204829062256,20.));
#71725=CARTESIAN_POINT('Ctrl Pts',(27.3487031771241,-37.5373885167297,0.));
#71726=CARTESIAN_POINT('Ctrl Pts',(27.3487031771241,-37.5373885167297,20.));
#71727=CARTESIAN_POINT('Ctrl Pts',(27.3204732157704,-37.5542736444521,0.));
#71728=CARTESIAN_POINT('Ctrl Pts',(27.3204732157704,-37.5542736444521,20.));
#71729=CARTESIAN_POINT('Ctrl Pts',(27.2922323089174,-37.571138281747,0.));
#71730=CARTESIAN_POINT('Ctrl Pts',(27.2922323089174,-37.571138281747,20.));
#71731=CARTESIAN_POINT('Ctrl Pts',(27.2639804710687,-37.5879824209777,0.));
#71732=CARTESIAN_POINT('Ctrl Pts',(27.2639804710687,-37.5879824209777,20.));
#71733=CARTESIAN_POINT('Ctrl Pts',(27.2357177167352,-37.6048060545189,0.));
#71734=CARTESIAN_POINT('Ctrl Pts',(27.2357177167352,-37.6048060545189,20.));
#71735=CARTESIAN_POINT('Ctrl Pts',(27.2074440604332,-37.6216091747552,0.));
#71736=CARTESIAN_POINT('Ctrl Pts',(27.2074440604332,-37.6216091747552,20.));
#71737=CARTESIAN_POINT('Ctrl Pts',(27.1791595166855,-37.6383917740821,0.));
#71738=CARTESIAN_POINT('Ctrl Pts',(27.1791595166855,-37.6383917740821,20.));
#71739=CARTESIAN_POINT('Ctrl Pts',(27.15086410002,-37.6551538449046,0.));
#71740=CARTESIAN_POINT('Ctrl Pts',(27.15086410002,-37.6551538449046,20.));
#71741=CARTESIAN_POINT('Ctrl Pts',(27.1225578249702,-37.6718953796384,0.));
#71742=CARTESIAN_POINT('Ctrl Pts',(27.1225578249702,-37.6718953796384,20.));
#71743=CARTESIAN_POINT('Ctrl Pts',(27.0942407060752,-37.6886163707084,0.));
#71744=CARTESIAN_POINT('Ctrl Pts',(27.0942407060752,-37.6886163707084,20.));
#71745=CARTESIAN_POINT('Ctrl Pts',(27.0659127578793,-37.705316810549,0.));
#71746=CARTESIAN_POINT('Ctrl Pts',(27.0659127578793,-37.705316810549,20.));
#71747=CARTESIAN_POINT('Ctrl Pts',(27.0375739949332,-37.7219966916053,0.));
#71748=CARTESIAN_POINT('Ctrl Pts',(27.0375739949332,-37.7219966916053,20.));
#71749=CARTESIAN_POINT('Ctrl Pts',(27.0092244317933,-37.7386560063324,0.));
#71750=CARTESIAN_POINT('Ctrl Pts',(27.0092244317933,-37.7386560063324,20.));
#71751=CARTESIAN_POINT('Ctrl Pts',(26.9808640830224,-37.755294747196,0.));
#71752=CARTESIAN_POINT('Ctrl Pts',(26.9808640830224,-37.755294747196,20.));
#71753=CARTESIAN_POINT('Ctrl Pts',(26.9524929631885,-37.7719129066716,0.));
#71754=CARTESIAN_POINT('Ctrl Pts',(26.9524929631885,-37.7719129066716,20.));
#71755=CARTESIAN_POINT('Ctrl Pts',(26.9241110868652,-37.7885104772446,0.));
#71756=CARTESIAN_POINT('Ctrl Pts',(26.9241110868652,-37.7885104772446,20.));
#71757=CARTESIAN_POINT('Ctrl Pts',(26.8957184686315,-37.8050874514106,0.));
#71758=CARTESIAN_POINT('Ctrl Pts',(26.8957184686315,-37.8050874514106,20.));
#71759=CARTESIAN_POINT('Ctrl Pts',(26.8673151230714,-37.8216438216745,0.));
#71760=CARTESIAN_POINT('Ctrl Pts',(26.8673151230714,-37.8216438216745,20.));
#71761=CARTESIAN_POINT('Ctrl Pts',(26.8389010647754,-37.8381795805523,0.));
#71762=CARTESIAN_POINT('Ctrl Pts',(26.8389010647754,-37.8381795805523,20.));
#71763=CARTESIAN_POINT('Ctrl Pts',(26.8104763083398,-37.8546947205707,0.));
#71764=CARTESIAN_POINT('Ctrl Pts',(26.8104763083398,-37.8546947205707,20.));
#71765=CARTESIAN_POINT('Ctrl Pts',(26.7820408683669,-37.8711892342661,0.));
#71766=CARTESIAN_POINT('Ctrl Pts',(26.7820408683669,-37.8711892342661,20.));
#71767=CARTESIAN_POINT('Ctrl Pts',(26.7535947594648,-37.887663114185,0.));
#71768=CARTESIAN_POINT('Ctrl Pts',(26.7535947594648,-37.887663114185,20.));
#71769=CARTESIAN_POINT('Ctrl Pts',(26.7251379962461,-37.904116352883,0.));
#71770=CARTESIAN_POINT('Ctrl Pts',(26.7251379962461,-37.904116352883,20.));
#71771=CARTESIAN_POINT('Ctrl Pts',(26.6966705933291,-37.9205489429259,0.));
#71772=CARTESIAN_POINT('Ctrl Pts',(26.6966705933291,-37.9205489429259,20.));
#71773=CARTESIAN_POINT('Ctrl Pts',(26.6681925653377,-37.9369608768897,0.));
#71774=CARTESIAN_POINT('Ctrl Pts',(26.6681925653377,-37.9369608768897,20.));
#71775=CARTESIAN_POINT('Ctrl Pts',(26.6397039269022,-37.9533521473617,0.));
#71776=CARTESIAN_POINT('Ctrl Pts',(26.6397039269022,-37.9533521473617,20.));
#71777=CARTESIAN_POINT('Ctrl Pts',(26.6112046926582,-37.9697227469389,0.));
#71778=CARTESIAN_POINT('Ctrl Pts',(26.6112046926582,-37.9697227469389,20.));
#71779=CARTESIAN_POINT('Ctrl Pts',(26.5826948772471,-37.9860726682287,0.));
#71780=CARTESIAN_POINT('Ctrl Pts',(26.5826948772471,-37.9860726682287,20.));
#71781=CARTESIAN_POINT('Ctrl Pts',(26.5541744953162,-38.0024019038486,0.));
#71782=CARTESIAN_POINT('Ctrl Pts',(26.5541744953162,-38.0024019038486,20.));
#71783=CARTESIAN_POINT('Ctrl Pts',(26.5256435615177,-38.0187104464255,0.));
#71784=CARTESIAN_POINT('Ctrl Pts',(26.5256435615177,-38.0187104464255,20.));
#71785=CARTESIAN_POINT('Ctrl Pts',(26.4971020905092,-38.0349982885963,0.));
#71786=CARTESIAN_POINT('Ctrl Pts',(26.4971020905092,-38.0349982885963,20.));
#71787=CARTESIAN_POINT('Ctrl Pts',(26.4685500969542,-38.0512654230086,0.));
#71788=CARTESIAN_POINT('Ctrl Pts',(26.4685500969542,-38.0512654230086,20.));
#71789=CARTESIAN_POINT('Ctrl Pts',(26.4399875955219,-38.0675118423201,0.));
#71790=CARTESIAN_POINT('Ctrl Pts',(26.4399875955219,-38.0675118423201,20.));
#71791=CARTESIAN_POINT('Ctrl Pts',(26.4114146008872,-38.0837375391992,0.));
#71792=CARTESIAN_POINT('Ctrl Pts',(26.4114146008872,-38.0837375391992,20.));
#71793=CARTESIAN_POINT('Ctrl Pts',(26.38283112773,-38.0999425063245,0.));
#71794=CARTESIAN_POINT('Ctrl Pts',(26.38283112773,-38.0999425063245,20.));
#71795=CARTESIAN_POINT('Ctrl Pts',(26.3542371907363,-38.1161267363846,0.));
#71796=CARTESIAN_POINT('Ctrl Pts',(26.3542371907363,-38.1161267363846,20.));
#71797=CARTESIAN_POINT('Ctrl Pts',(26.3256328045975,-38.1322902220784,0.));
#71798=CARTESIAN_POINT('Ctrl Pts',(26.3256328045975,-38.1322902220784,20.));
#71799=CARTESIAN_POINT('Ctrl Pts',(26.2970179840108,-38.1484329561142,0.));
#71800=CARTESIAN_POINT('Ctrl Pts',(26.2970179840108,-38.1484329561142,20.));
#71801=CARTESIAN_POINT('Ctrl Pts',(26.2683927436784,-38.1645549312104,0.));
#71802=CARTESIAN_POINT('Ctrl Pts',(26.2683927436784,-38.1645549312104,20.));
#71803=CARTESIAN_POINT('Ctrl Pts',(26.2397570983077,-38.1806561400953,0.));
#71804=CARTESIAN_POINT('Ctrl Pts',(26.2397570983077,-38.1806561400953,20.));
#71805=CARTESIAN_POINT('Ctrl Pts',(26.2111110626121,-38.1967365755081,0.));
#71806=CARTESIAN_POINT('Ctrl Pts',(26.2111110626121,-38.1967365755081,20.));
#71807=CARTESIAN_POINT('Ctrl Pts',(26.1824546513102,-38.2127962301983,0.));
#71808=CARTESIAN_POINT('Ctrl Pts',(26.1824546513102,-38.2127962301983,20.));
#71809=CARTESIAN_POINT('Ctrl Pts',(26.1537878791271,-38.2288350969267,0.));
#71810=CARTESIAN_POINT('Ctrl Pts',(26.1537878791271,-38.2288350969267,20.));
#71811=CARTESIAN_POINT('Ctrl Pts',(26.1251107607929,-38.244853168464,0.));
#71812=CARTESIAN_POINT('Ctrl Pts',(26.1251107607929,-38.244853168464,20.));
#71813=CARTESIAN_POINT('Ctrl Pts',(26.0964233110434,-38.2608504375907,0.));
#71814=CARTESIAN_POINT('Ctrl Pts',(26.0964233110434,-38.2608504375907,20.));
#71815=CARTESIAN_POINT('Ctrl Pts',(26.0677255446196,-38.276826897097,0.));
#71816=CARTESIAN_POINT('Ctrl Pts',(26.0677255446196,-38.276826897097,20.));
#71817=CARTESIAN_POINT('Ctrl Pts',(26.0390174762675,-38.2927825397833,0.));
#71818=CARTESIAN_POINT('Ctrl Pts',(26.0390174762675,-38.2927825397833,20.));
#71819=CARTESIAN_POINT('Ctrl Pts',(26.0102991207387,-38.30871735846,0.));
#71820=CARTESIAN_POINT('Ctrl Pts',(26.0102991207387,-38.30871735846,20.));
#71821=CARTESIAN_POINT('Ctrl Pts',(25.9815704927901,-38.3246313459476,0.));
#71822=CARTESIAN_POINT('Ctrl Pts',(25.9815704927901,-38.3246313459476,20.));
#71823=CARTESIAN_POINT('Ctrl Pts',(25.9528316071847,-38.3405244950781,0.));
#71824=CARTESIAN_POINT('Ctrl Pts',(25.9528316071847,-38.3405244950781,20.));
#71825=CARTESIAN_POINT('Ctrl Pts',(25.9240824786908,-38.3563967986932,0.));
#71826=CARTESIAN_POINT('Ctrl Pts',(25.9240824786908,-38.3563967986932,20.));
#71827=CARTESIAN_POINT('Ctrl Pts',(25.8953231220827,-38.3722482496454,0.));
#71828=CARTESIAN_POINT('Ctrl Pts',(25.8953231220827,-38.3722482496454,20.));
#71829=CARTESIAN_POINT('Ctrl Pts',(25.8665535521392,-38.3880788407969,0.));
#71830=CARTESIAN_POINT('Ctrl Pts',(25.8665535521392,-38.3880788407969,20.));
#71831=CARTESIAN_POINT('Ctrl Pts',(25.8377737836446,-38.4038885650199,0.));
#71832=CARTESIAN_POINT('Ctrl Pts',(25.8377737836446,-38.4038885650199,20.));
#71833=CARTESIAN_POINT('Ctrl Pts',(25.8089838313888,-38.419677415197,0.));
#71834=CARTESIAN_POINT('Ctrl Pts',(25.8089838313888,-38.419677415197,20.));
#71835=CARTESIAN_POINT('Ctrl Pts',(25.7801837101667,-38.4354453842206,0.));
#71836=CARTESIAN_POINT('Ctrl Pts',(25.7801837101667,-38.4354453842206,20.));
#71837=CARTESIAN_POINT('Ctrl Pts',(25.7513734347795,-38.4511924649945,0.));
#71838=CARTESIAN_POINT('Ctrl Pts',(25.7513734347795,-38.4511924649945,20.));
#71839=CARTESIAN_POINT('Ctrl Pts',(25.7225530200331,-38.4669186504318,0.));
#71840=CARTESIAN_POINT('Ctrl Pts',(25.7225530200331,-38.4669186504318,20.));
#71841=CARTESIAN_POINT('Ctrl Pts',(25.6937224807392,-38.4826239334567,0.));
#71842=CARTESIAN_POINT('Ctrl Pts',(25.6937224807392,-38.4826239334567,20.));
#71843=CARTESIAN_POINT('Ctrl Pts',(25.6648818317151,-38.4983083070042,0.));
#71844=CARTESIAN_POINT('Ctrl Pts',(25.6648818317151,-38.4983083070042,20.));
#71845=CARTESIAN_POINT('Ctrl Pts',(25.6360310877836,-38.5139717640192,0.));
#71846=CARTESIAN_POINT('Ctrl Pts',(25.6360310877836,-38.5139717640192,20.));
#71847=CARTESIAN_POINT('Ctrl Pts',(25.6071702637723,-38.5296142974561,0.));
#71848=CARTESIAN_POINT('Ctrl Pts',(25.6071702637723,-38.5296142974561,20.));
#71849=CARTESIAN_POINT('Ctrl Pts',(25.5782993745137,-38.5452359002793,0.));
#71850=CARTESIAN_POINT('Ctrl Pts',(25.5782993745137,-38.5452359002793,20.));
#71851=CARTESIAN_POINT('Ctrl Pts',(25.5494184348456,-38.5608365654634,0.));
#71852=CARTESIAN_POINT('Ctrl Pts',(25.5494184348456,-38.5608365654634,20.));
#71853=CARTESIAN_POINT('Ctrl Pts',(25.5205274596115,-38.576416285994,0.));
#71854=CARTESIAN_POINT('Ctrl Pts',(25.5205274596115,-38.576416285994,20.));
#71855=CARTESIAN_POINT('Ctrl Pts',(25.4916264636604,-38.591975054867,0.));
#71856=CARTESIAN_POINT('Ctrl Pts',(25.4916264636604,-38.591975054867,20.));
#71857=CARTESIAN_POINT('Ctrl Pts',(25.462715461847,-38.6075128650891,0.));
#71858=CARTESIAN_POINT('Ctrl Pts',(25.462715461847,-38.6075128650891,20.));
#71859=CARTESIAN_POINT('Ctrl Pts',(25.4337944690316,-38.6230297096774,0.));
#71860=CARTESIAN_POINT('Ctrl Pts',(25.4337944690316,-38.6230297096774,20.));
#71861=CARTESIAN_POINT('Ctrl Pts',(25.4048635000794,-38.6385255816593,0.));
#71862=CARTESIAN_POINT('Ctrl Pts',(25.4048635000794,-38.6385255816593,20.));
#71863=CARTESIAN_POINT('Ctrl Pts',(25.3759225698613,-38.6540004740723,0.));
#71864=CARTESIAN_POINT('Ctrl Pts',(25.3759225698613,-38.6540004740723,20.));
#71865=CARTESIAN_POINT('Ctrl Pts',(25.3469716932528,-38.6694543799641,0.));
#71866=CARTESIAN_POINT('Ctrl Pts',(25.3469716932528,-38.6694543799641,20.));
#71867=CARTESIAN_POINT('Ctrl Pts',(25.318010885134,-38.6848872923919,0.));
#71868=CARTESIAN_POINT('Ctrl Pts',(25.318010885134,-38.6848872923919,20.));
#71869=CARTESIAN_POINT('Ctrl Pts',(25.2890401603912,-38.7002992044242,0.));
#71870=CARTESIAN_POINT('Ctrl Pts',(25.2890401603912,-38.7002992044242,20.));
#71871=CARTESIAN_POINT('Ctrl Pts',(25.2600595339159,-38.7156901091392,0.));
#71872=CARTESIAN_POINT('Ctrl Pts',(25.2600595339159,-38.7156901091392,20.));
#71873=CARTESIAN_POINT('Ctrl Pts',(25.2310690206049,-38.7310599996258,0.));
#71874=CARTESIAN_POINT('Ctrl Pts',(25.2310690206049,-38.7310599996258,20.));
#71875=CARTESIAN_POINT('Ctrl Pts',(25.2020686353608,-38.7464088689837,0.));
#71876=CARTESIAN_POINT('Ctrl Pts',(25.2020686353608,-38.7464088689837,20.));
#71877=CARTESIAN_POINT('Ctrl Pts',(25.1730583930911,-38.7617367103229,0.));
#71878=CARTESIAN_POINT('Ctrl Pts',(25.1730583930911,-38.7617367103229,20.));
#71879=CARTESIAN_POINT('Ctrl Pts',(25.1440383087084,-38.7770435167639,0.));
#71880=CARTESIAN_POINT('Ctrl Pts',(25.1440383087084,-38.7770435167639,20.));
#71881=CARTESIAN_POINT('Ctrl Pts',(25.1150083971302,-38.7923292814368,0.));
#71882=CARTESIAN_POINT('Ctrl Pts',(25.1150083971302,-38.7923292814368,20.));
#71883=CARTESIAN_POINT('Ctrl Pts',(25.0859686732794,-38.8075939974829,0.));
#71884=CARTESIAN_POINT('Ctrl Pts',(25.0859686732794,-38.8075939974829,20.));
#71885=CARTESIAN_POINT('Ctrl Pts',(25.0569191520845,-38.8228376580533,0.));
#71886=CARTESIAN_POINT('Ctrl Pts',(25.0569191520845,-38.8228376580533,20.));
#71887=CARTESIAN_POINT('Ctrl Pts',(25.0278598484791,-38.8380602563098,0.));
#71888=CARTESIAN_POINT('Ctrl Pts',(25.0278598484791,-38.8380602563098,20.));
#71889=CARTESIAN_POINT('Ctrl Pts',(24.9987907774025,-38.8532617854245,0.));
#71890=CARTESIAN_POINT('Ctrl Pts',(24.9987907774025,-38.8532617854245,20.));
#71891=CARTESIAN_POINT('Ctrl Pts',(24.9697119537988,-38.8684422385799,0.));
#71892=CARTESIAN_POINT('Ctrl Pts',(24.9697119537988,-38.8684422385799,20.));
#71893=CARTESIAN_POINT('Ctrl Pts',(24.9406233926168,-38.883601608968,0.));
#71894=CARTESIAN_POINT('Ctrl Pts',(24.9406233926168,-38.883601608968,20.));
#71895=CARTESIAN_POINT('Ctrl Pts',(24.9115251088107,-38.8987398897918,0.));
#71896=CARTESIAN_POINT('Ctrl Pts',(24.9115251088107,-38.8987398897918,20.));
#71897=CARTESIAN_POINT('Ctrl Pts',(24.8824171173401,-38.9138570742648,0.));
#71898=CARTESIAN_POINT('Ctrl Pts',(24.8824171173401,-38.9138570742648,20.));
#71899=CARTESIAN_POINT('Ctrl Pts',(24.8532994331703,-38.9289531556118,0.));
#71900=CARTESIAN_POINT('Ctrl Pts',(24.8532994331703,-38.9289531556118,20.));
#71901=CARTESIAN_POINT('Ctrl Pts',(24.8241720712716,-38.9440281270684,0.));
#71902=CARTESIAN_POINT('Ctrl Pts',(24.8241720712716,-38.9440281270684,20.));
#71903=CARTESIAN_POINT('Ctrl Pts',(24.7950350466188,-38.9590819818798,0.));
#71904=CARTESIAN_POINT('Ctrl Pts',(24.7950350466188,-38.9590819818798,20.));
#71905=CARTESIAN_POINT('Ctrl Pts',(24.7658883741919,-38.9741147133012,0.));
#71906=CARTESIAN_POINT('Ctrl Pts',(24.7658883741919,-38.9741147133012,20.));
#71907=CARTESIAN_POINT('Ctrl Pts',(24.736732068976,-38.989126314598,0.));
#71908=CARTESIAN_POINT('Ctrl Pts',(24.736732068976,-38.989126314598,20.));
#71909=CARTESIAN_POINT('Ctrl Pts',(24.7075661459616,-39.0041167790461,0.));
#71910=CARTESIAN_POINT('Ctrl Pts',(24.7075661459616,-39.0041167790461,20.));
#71911=CARTESIAN_POINT('Ctrl Pts',(24.6783906201452,-39.019086099931,0.));
#71912=CARTESIAN_POINT('Ctrl Pts',(24.6783906201452,-39.019086099931,20.));
#71913=CARTESIAN_POINT('Ctrl Pts',(24.6492055065285,-39.0340342705498,0.));
#71914=CARTESIAN_POINT('Ctrl Pts',(24.6492055065285,-39.0340342705498,20.));
#71915=CARTESIAN_POINT('Ctrl Pts',(24.6200108201182,-39.0489612842096,0.));
#71916=CARTESIAN_POINT('Ctrl Pts',(24.6200108201182,-39.0489612842096,20.));
#71917=CARTESIAN_POINT('Ctrl Pts',(24.5908065759258,-39.0638671342286,0.));
#71918=CARTESIAN_POINT('Ctrl Pts',(24.5908065759258,-39.0638671342286,20.));
#71919=CARTESIAN_POINT('Ctrl Pts',(24.5615927889669,-39.0787518139362,0.));
#71920=CARTESIAN_POINT('Ctrl Pts',(24.5615927889669,-39.0787518139362,20.));
#71921=CARTESIAN_POINT('Ctrl Pts',(24.5323694742616,-39.0936153166722,0.));
#71922=CARTESIAN_POINT('Ctrl Pts',(24.5323694742616,-39.0936153166722,20.));
#71923=CARTESIAN_POINT('Ctrl Pts',(24.5031366468345,-39.1084576357872,0.));
#71924=CARTESIAN_POINT('Ctrl Pts',(24.5031366468345,-39.1084576357872,20.));
#71925=CARTESIAN_POINT('Ctrl Pts',(24.4738943217155,-39.1232787646414,0.));
#71926=CARTESIAN_POINT('Ctrl Pts',(24.4738943217155,-39.1232787646414,20.));
#71927=CARTESIAN_POINT('Ctrl Pts',(24.4446425139409,-39.1380786966047,0.));
#71928=CARTESIAN_POINT('Ctrl Pts',(24.4446425139409,-39.1380786966047,20.));
#71929=CARTESIAN_POINT('Ctrl Pts',(24.4153812385543,-39.1528574250569,0.));
#71930=CARTESIAN_POINT('Ctrl Pts',(24.4153812385543,-39.1528574250569,20.));
#71931=CARTESIAN_POINT('Ctrl Pts',(24.3861105106067,-39.1676149433869,0.));
#71932=CARTESIAN_POINT('Ctrl Pts',(24.3861105106067,-39.1676149433869,20.));
#71933=CARTESIAN_POINT('Ctrl Pts',(24.3568303451549,-39.1823512449951,0.));
#71934=CARTESIAN_POINT('Ctrl Pts',(24.3568303451549,-39.1823512449951,20.));
#71935=CARTESIAN_POINT('Ctrl Pts',(24.3275407572587,-39.197066323292,0.));
#71936=CARTESIAN_POINT('Ctrl Pts',(24.3275407572587,-39.197066323292,20.));
#71937=CARTESIAN_POINT('Ctrl Pts',(24.2982417619806,-39.2117601717005,0.));
#71938=CARTESIAN_POINT('Ctrl Pts',(24.2982417619806,-39.2117601717005,20.));
#71939=CARTESIAN_POINT('Ctrl Pts',(24.2689333743822,-39.2264327836562,0.));
#71940=CARTESIAN_POINT('Ctrl Pts',(24.2689333743822,-39.2264327836562,20.));
#71941=CARTESIAN_POINT('Ctrl Pts',(24.239615609526,-39.2410841526078,0.));
#71942=CARTESIAN_POINT('Ctrl Pts',(24.239615609526,-39.2410841526078,20.));
#71943=CARTESIAN_POINT('Ctrl Pts',(24.2102884824784,-39.2557142720138,0.));
#71944=CARTESIAN_POINT('Ctrl Pts',(24.2102884824784,-39.2557142720138,20.));
#71945=CARTESIAN_POINT('Ctrl Pts',(24.1809520083146,-39.2703231353422,0.));
#71946=CARTESIAN_POINT('Ctrl Pts',(24.1809520083146,-39.2703231353422,20.));
#71947=CARTESIAN_POINT('Ctrl Pts',(24.1516062021224,-39.2849107360681,0.));
#71948=CARTESIAN_POINT('Ctrl Pts',(24.1516062021224,-39.2849107360681,20.));
#71949=CARTESIAN_POINT('Ctrl Pts',(24.1222510790066,-39.2994770676712,0.));
#71950=CARTESIAN_POINT('Ctrl Pts',(24.1222510790066,-39.2994770676712,20.));
#71951=CARTESIAN_POINT('Ctrl Pts',(24.0928866540881,-39.3140221236369,0.));
#71952=CARTESIAN_POINT('Ctrl Pts',(24.0928866540881,-39.3140221236369,20.));
#71953=CARTESIAN_POINT('Ctrl Pts',(24.0635129424931,-39.3285458974613,0.));
#71954=CARTESIAN_POINT('Ctrl Pts',(24.0635129424931,-39.3285458974613,20.));
#71955=CARTESIAN_POINT('Ctrl Pts',(24.0341299593437,-39.3430483826555,0.));
#71956=CARTESIAN_POINT('Ctrl Pts',(24.0341299593437,-39.3430483826555,20.));
#71957=CARTESIAN_POINT('Ctrl Pts',(24.0047377197503,-39.3575295727493,0.));
#71958=CARTESIAN_POINT('Ctrl Pts',(24.0047377197503,-39.3575295727493,20.));
#71959=CARTESIAN_POINT('Ctrl Pts',(23.9753362387978,-39.3719894612957,0.));
#71960=CARTESIAN_POINT('Ctrl Pts',(23.9753362387978,-39.3719894612957,20.));
#71961=CARTESIAN_POINT('Ctrl Pts',(23.9459255315518,-39.3864280418676,0.));
#71962=CARTESIAN_POINT('Ctrl Pts',(23.9459255315518,-39.3864280418676,20.));
#71963=CARTESIAN_POINT('Ctrl Pts',(23.9165056130837,-39.4008453080481,0.));
#71964=CARTESIAN_POINT('Ctrl Pts',(23.9165056130837,-39.4008453080481,20.));
#71965=CARTESIAN_POINT('Ctrl Pts',(23.8870764984925,-39.4152412534209,0.));
#71966=CARTESIAN_POINT('Ctrl Pts',(23.8870764984925,-39.4152412534209,20.));
#71967=CARTESIAN_POINT('Ctrl Pts',(23.8576382029237,-39.4296158715627,0.));
#71968=CARTESIAN_POINT('Ctrl Pts',(23.8576382029237,-39.4296158715627,20.));
#71969=CARTESIAN_POINT('Ctrl Pts',(23.8281907416004,-39.4439691560298,0.));
#71970=CARTESIAN_POINT('Ctrl Pts',(23.8281907416004,-39.4439691560298,20.));
#71971=CARTESIAN_POINT('Ctrl Pts',(23.7987341298022,-39.4583011003674,0.));
#71972=CARTESIAN_POINT('Ctrl Pts',(23.7987341298022,-39.4583011003674,20.));
#71973=CARTESIAN_POINT('Ctrl Pts',(23.769268382808,-39.4726116981337,0.));
#71974=CARTESIAN_POINT('Ctrl Pts',(23.769268382808,-39.4726116981337,20.));
#71975=CARTESIAN_POINT('Ctrl Pts',(23.7397935158457,-39.4869009429217,0.));
#71976=CARTESIAN_POINT('Ctrl Pts',(23.7397935158457,-39.4869009429217,20.));
#71977=CARTESIAN_POINT('Ctrl Pts',(23.7103095440476,-39.5011688283778,0.));
#71978=CARTESIAN_POINT('Ctrl Pts',(23.7103095440476,-39.5011688283778,20.));
#71979=CARTESIAN_POINT('Ctrl Pts',(23.6808164823786,-39.5154153482324,0.));
#71980=CARTESIAN_POINT('Ctrl Pts',(23.6808164823786,-39.5154153482324,20.));
#71981=CARTESIAN_POINT('Ctrl Pts',(23.651314345698,-39.5296404962722,0.));
#71982=CARTESIAN_POINT('Ctrl Pts',(23.651314345698,-39.5296404962722,20.));
#71983=CARTESIAN_POINT('Ctrl Pts',(23.6218031488904,-39.5438442662853,0.));
#71984=CARTESIAN_POINT('Ctrl Pts',(23.6218031488904,-39.5438442662853,20.));
#71985=CARTESIAN_POINT('Ctrl Pts',(23.5922829069852,-39.5580266520107,0.));
#71986=CARTESIAN_POINT('Ctrl Pts',(23.5922829069852,-39.5580266520107,20.));
#71987=CARTESIAN_POINT('Ctrl Pts',(23.5627536352592,-39.5721876470956,0.));
#71988=CARTESIAN_POINT('Ctrl Pts',(23.5627536352592,-39.5721876470956,20.));
#71989=CARTESIAN_POINT('Ctrl Pts',(23.5332153494019,-39.5863272450268,0.));
#71990=CARTESIAN_POINT('Ctrl Pts',(23.5332153494019,-39.5863272450268,20.));
#71991=CARTESIAN_POINT('Ctrl Pts',(23.5036680653391,-39.6004454392038,0.));
#71992=CARTESIAN_POINT('Ctrl Pts',(23.5036680653391,-39.6004454392038,20.));
#71993=CARTESIAN_POINT('Ctrl Pts',(23.4741117989348,-39.6145422230651,0.));
#71994=CARTESIAN_POINT('Ctrl Pts',(23.4741117989348,-39.6145422230651,20.));
#71995=CARTESIAN_POINT('Ctrl Pts',(23.4445465657147,-39.6286175902046,0.));
#71996=CARTESIAN_POINT('Ctrl Pts',(23.4445465657147,-39.6286175902046,20.));
#71997=CARTESIAN_POINT('Ctrl Pts',(23.414972380622,-39.6426715344742,0.));
#71998=CARTESIAN_POINT('Ctrl Pts',(23.414972380622,-39.6426715344742,20.));
#71999=CARTESIAN_POINT('Ctrl Pts',(23.385389257652,-39.6567040501382,0.));
#72000=CARTESIAN_POINT('Ctrl Pts',(23.385389257652,-39.6567040501382,20.));
#72001=CARTESIAN_POINT('Ctrl Pts',(23.3557972103217,-39.6707151316771,0.));
#72002=CARTESIAN_POINT('Ctrl Pts',(23.3557972103217,-39.6707151316771,20.));
#72003=CARTESIAN_POINT('Ctrl Pts',(23.3261962523444,-39.6847047735001,0.));
#72004=CARTESIAN_POINT('Ctrl Pts',(23.3261962523444,-39.6847047735001,20.));
#72005=CARTESIAN_POINT('Ctrl Pts',(23.2965863982648,-39.6986729696788,0.));
#72006=CARTESIAN_POINT('Ctrl Pts',(23.2965863982648,-39.6986729696788,20.));
#72007=CARTESIAN_POINT('Ctrl Pts',(23.2669676640418,-39.7126197136991,0.));
#72008=CARTESIAN_POINT('Ctrl Pts',(23.2669676640418,-39.7126197136991,20.));
#72009=CARTESIAN_POINT('Ctrl Pts',(23.2373400678346,-39.7265449981305,0.));
#72010=CARTESIAN_POINT('Ctrl Pts',(23.2373400678346,-39.7265449981305,20.));
#72011=CARTESIAN_POINT('Ctrl Pts',(23.2077036288597,-39.7404488151086,0.));
#72012=CARTESIAN_POINT('Ctrl Pts',(23.2077036288597,-39.7404488151086,20.));
#72013=CARTESIAN_POINT('Ctrl Pts',(23.1780583659508,-39.7543311569459,0.));
#72014=CARTESIAN_POINT('Ctrl Pts',(23.1780583659508,-39.7543311569459,20.));
#72015=CARTESIAN_POINT('Ctrl Pts',(23.1484042962029,-39.7681920167058,0.));
#72016=CARTESIAN_POINT('Ctrl Pts',(23.1484042962029,-39.7681920167058,20.));
#72017=CARTESIAN_POINT('Ctrl Pts',(23.118741433625,-39.7820313887737,0.));
#72018=CARTESIAN_POINT('Ctrl Pts',(23.118741433625,-39.7820313887737,20.));
#72019=CARTESIAN_POINT('Ctrl Pts',(23.089069787673,-39.7958492694787,0.));
#72020=CARTESIAN_POINT('Ctrl Pts',(23.089069787673,-39.7958492694787,20.));
#72021=CARTESIAN_POINT('Ctrl Pts',(23.0593893640427,-39.8096456567259,0.));
#72022=CARTESIAN_POINT('Ctrl Pts',(23.0593893640427,-39.8096456567259,20.));
#72023=CARTESIAN_POINT('Ctrl Pts',(23.0356380053138,-39.8206655709904,0.));
#72024=CARTESIAN_POINT('Ctrl Pts',(23.0356380053138,-39.8206655709904,20.));
#72025=CARTESIAN_POINT('Ctrl Pts',(23.0178205380655,-39.8289208340947,0.));
#72026=CARTESIAN_POINT('Ctrl Pts',(23.0178205380655,-39.8289208340947,20.));
#72027=CARTESIAN_POINT('Ctrl Pts',(23.0059404718139,-39.8344200439082,0.));
#72028=CARTESIAN_POINT('Ctrl Pts',(23.0059404718139,-39.8344200439082,20.));
#72029=CARTESIAN_POINT('Ctrl Pts',(23.,-39.8371685740842,0.));
#72030=CARTESIAN_POINT('Ctrl Pts',(23.,-39.8371685740842,20.));
#72031=CARTESIAN_POINT('',(46.0449384185095,-16.7589870229578,2.));
#72032=CARTESIAN_POINT('Ctrl Pts',(34.5017338047269,-32.2758373034788,2.));
#72033=CARTESIAN_POINT('Ctrl Pts',(35.1012599438994,-31.7409631286146,2.));
#72034=CARTESIAN_POINT('Ctrl Pts',(35.6879267845883,-31.1902015741136,2.));
#72035=CARTESIAN_POINT('Ctrl Pts',(36.260940923753,-30.624221206043,2.));
#72036=CARTESIAN_POINT('Ctrl Pts',(36.8331140520758,-30.0590715253732,2.));
#72037=CARTESIAN_POINT('Ctrl Pts',(37.3916744157871,-29.4787478132684,2.));
#72038=CARTESIAN_POINT('Ctrl Pts',(37.9358682563863,-28.8839535575986,2.));
#72039=CARTESIAN_POINT('Ctrl Pts',(38.4805324906895,-28.2886451699188,2.));
#72040=CARTESIAN_POINT('Ctrl Pts',(39.0108052381929,-27.6788413440332,2.));
#72041=CARTESIAN_POINT('Ctrl Pts',(39.5259687462372,-27.0552833125806,2.));
#72042=CARTESIAN_POINT('Ctrl Pts',(40.0415783150755,-26.4311853655743,2.));
#72043=CARTESIAN_POINT('Ctrl Pts',(40.5420523586309,-25.793309522113,2.));
#72044=CARTESIAN_POINT('Ctrl Pts',(41.0267109660362,-25.1424328771062,2.));
#72045=CARTESIAN_POINT('Ctrl Pts',(41.5120532707873,-24.4906380545866,2.));
#72046=CARTESIAN_POINT('Ctrl Pts',(41.9815353808389,-23.8258058651361,2.));
#72047=CARTESIAN_POINT('Ctrl Pts',(42.4345159310068,-23.1487486269677,2.));
#72048=CARTESIAN_POINT('Ctrl Pts',(42.8878234627796,-22.4712026586269,2.));
#72049=CARTESIAN_POINT('Ctrl Pts',(43.32460550914,-21.7814141347634,2.));
#72050=CARTESIAN_POINT('Ctrl Pts',(43.7442622667776,-21.0802269103741,2.));
#72051=CARTESIAN_POINT('Ctrl Pts',(44.1624443435522,-20.3815036696152,2.));
#72052=CARTESIAN_POINT('Ctrl Pts',(44.5636212234609,-19.671461867878,2.));
#72053=CARTESIAN_POINT('Ctrl Pts',(44.9472430970921,-18.9509636362294,2.));
#72054=CARTESIAN_POINT('Ctrl Pts',(45.1999134416925,-18.47641161251,2.));
#72055=CARTESIAN_POINT('Ctrl Pts',(45.4449691102617,-17.9973240026997,2.));
#72056=CARTESIAN_POINT('Ctrl Pts',(45.6822635680233,-17.5139530963398,2.));
#72057=CARTESIAN_POINT('Ctrl Pts',(45.8052462319505,-17.2634363236775,2.));
#72058=CARTESIAN_POINT('Ctrl Pts',(45.9261440619272,-17.01176962033,2.));
#72059=CARTESIAN_POINT('Ctrl Pts',(46.0449384185095,-16.7589870229578,2.));
#72060=CARTESIAN_POINT('',(46.0449384185095,-16.7589870229578,0.));
#72061=CARTESIAN_POINT('Ctrl Pts',(8.50876070567956,-48.2555798975982,0.));
#72062=CARTESIAN_POINT('Ctrl Pts',(8.50876070567956,-48.2555798975982,20.));
#72063=CARTESIAN_POINT('Ctrl Pts',(8.5020159114628,-48.2561497089132,0.));
#72064=CARTESIAN_POINT('Ctrl Pts',(8.5020159114628,-48.2561497089132,20.));
#72065=CARTESIAN_POINT('Ctrl Pts',(8.48852624368607,-48.2572870022174,0.));
#72066=CARTESIAN_POINT('Ctrl Pts',(8.48852624368607,-48.2572870022174,20.));
#72067=CARTESIAN_POINT('Ctrl Pts',(8.46829150399132,-48.2589859541967,0.));
#72068=CARTESIAN_POINT('Ctrl Pts',(8.46829150399132,-48.2589859541967,20.));
#72069=CARTESIAN_POINT('Ctrl Pts',(8.4413113750042,-48.2612372475269,0.));
#72070=CARTESIAN_POINT('Ctrl Pts',(8.4413113750042,-48.2612372475269,20.));
#72071=CARTESIAN_POINT('Ctrl Pts',(8.40758542125999,-48.2640280707484,0.));
#72072=CARTESIAN_POINT('Ctrl Pts',(8.40758542125999,-48.2640280707484,20.));
#72073=CARTESIAN_POINT('Ctrl Pts',(8.37385867778169,-48.2667956002972,0.));
#72074=CARTESIAN_POINT('Ctrl Pts',(8.37385867778169,-48.2667956002972,20.));
#72075=CARTESIAN_POINT('Ctrl Pts',(8.34013115014496,-48.2695398358687,0.));
#72076=CARTESIAN_POINT('Ctrl Pts',(8.34013115014496,-48.2695398358687,20.));
#72077=CARTESIAN_POINT('Ctrl Pts',(8.30640284761835,-48.2722607770974,0.));
#72078=CARTESIAN_POINT('Ctrl Pts',(8.30640284761835,-48.2722607770974,20.));
#72079=CARTESIAN_POINT('Ctrl Pts',(8.27267378419868,-48.274958423567,0.));
#72080=CARTESIAN_POINT('Ctrl Pts',(8.27267378419868,-48.274958423567,20.));
#72081=CARTESIAN_POINT('Ctrl Pts',(8.23894397736021,-48.2776327748283,0.));
#72082=CARTESIAN_POINT('Ctrl Pts',(8.23894397736021,-48.2776327748283,20.));
#72083=CARTESIAN_POINT('Ctrl Pts',(8.20521344665193,-48.2802838304168,0.));
#72084=CARTESIAN_POINT('Ctrl Pts',(8.20521344665193,-48.2802838304168,20.));
#72085=CARTESIAN_POINT('Ctrl Pts',(8.17148221231953,-48.2829115898716,0.));
#72086=CARTESIAN_POINT('Ctrl Pts',(8.17148221231953,-48.2829115898716,20.));
#72087=CARTESIAN_POINT('Ctrl Pts',(8.13775029398593,-48.2855160527521,0.));
#72088=CARTESIAN_POINT('Ctrl Pts',(8.13775029398593,-48.2855160527521,20.));
#72089=CARTESIAN_POINT('Ctrl Pts',(8.10401770912491,-48.288097218659,0.));
#72090=CARTESIAN_POINT('Ctrl Pts',(8.10401770912491,-48.288097218659,20.));
#72091=CARTESIAN_POINT('Ctrl Pts',(8.07028447346157,-48.2906550872281,0.));
#72092=CARTESIAN_POINT('Ctrl Pts',(8.07028447346157,-48.2906550872281,20.));
#72093=CARTESIAN_POINT('Ctrl Pts',(8.03655060167523,-48.2931896581208,0.));
#72094=CARTESIAN_POINT('Ctrl Pts',(8.03655060167523,-48.2931896581208,20.));
#72095=CARTESIAN_POINT('Ctrl Pts',(8.00281610801472,-48.2957009310153,0.));
#72096=CARTESIAN_POINT('Ctrl Pts',(8.00281610801472,-48.2957009310153,20.));
#72097=CARTESIAN_POINT('Ctrl Pts',(7.96908100690892,-48.2981889055984,0.));
#72098=CARTESIAN_POINT('Ctrl Pts',(7.96908100690892,-48.2981889055984,20.));
#72099=CARTESIAN_POINT('Ctrl Pts',(7.93534531368689,-48.300653581555,0.));
#72100=CARTESIAN_POINT('Ctrl Pts',(7.93534531368689,-48.300653581555,20.));
#72101=CARTESIAN_POINT('Ctrl Pts',(7.90160904447351,-48.3030949585702,0.));
#72102=CARTESIAN_POINT('Ctrl Pts',(7.90160904447351,-48.3030949585702,20.));
#72103=CARTESIAN_POINT('Ctrl Pts',(7.86787221586445,-48.3055130363337,0.));
#72104=CARTESIAN_POINT('Ctrl Pts',(7.86787221586445,-48.3055130363337,20.));
#72105=CARTESIAN_POINT('Ctrl Pts',(7.83413484466693,-48.3079078145432,0.));
#72106=CARTESIAN_POINT('Ctrl Pts',(7.83413484466693,-48.3079078145432,20.));
#72107=CARTESIAN_POINT('Ctrl Pts',(7.80039694763397,-48.3102792929086,0.));
#72108=CARTESIAN_POINT('Ctrl Pts',(7.80039694763397,-48.3102792929086,20.));
#72109=CARTESIAN_POINT('Ctrl Pts',(7.76665854114745,-48.3126274711557,0.));
#72110=CARTESIAN_POINT('Ctrl Pts',(7.76665854114745,-48.3126274711557,20.));
#72111=CARTESIAN_POINT('Ctrl Pts',(7.73291964123288,-48.3149523490266,0.));
#72112=CARTESIAN_POINT('Ctrl Pts',(7.73291964123288,-48.3149523490266,20.));
#72113=CARTESIAN_POINT('Ctrl Pts',(7.69918026370735,-48.3172539262766,0.));
#72114=CARTESIAN_POINT('Ctrl Pts',(7.69918026370735,-48.3172539262766,20.));
#72115=CARTESIAN_POINT('Ctrl Pts',(7.66544042428832,-48.3195322026739,0.));
#72116=CARTESIAN_POINT('Ctrl Pts',(7.66544042428832,-48.3195322026739,20.));
#72117=CARTESIAN_POINT('Ctrl Pts',(7.63170013870892,-48.3217871779975,0.));
#72118=CARTESIAN_POINT('Ctrl Pts',(7.63170013870892,-48.3217871779975,20.));
#72119=CARTESIAN_POINT('Ctrl Pts',(7.59795942285539,-48.3240188520354,0.));
#72120=CARTESIAN_POINT('Ctrl Pts',(7.59795942285539,-48.3240188520354,20.));
#72121=CARTESIAN_POINT('Ctrl Pts',(7.56421829277369,-48.3262272245847,0.));
#72122=CARTESIAN_POINT('Ctrl Pts',(7.56421829277369,-48.3262272245847,20.));
#72123=CARTESIAN_POINT('Ctrl Pts',(7.53047676460326,-48.328412295452,0.));
#72124=CARTESIAN_POINT('Ctrl Pts',(7.53047676460326,-48.328412295452,20.));
#72125=CARTESIAN_POINT('Ctrl Pts',(7.49673485453118,-48.3305740644544,0.));
#72126=CARTESIAN_POINT('Ctrl Pts',(7.49673485453118,-48.3305740644544,20.));
#72127=CARTESIAN_POINT('Ctrl Pts',(7.46299257874208,-48.3327125314199,0.));
#72128=CARTESIAN_POINT('Ctrl Pts',(7.46299257874208,-48.3327125314199,20.));
#72129=CARTESIAN_POINT('Ctrl Pts',(7.42924995335917,-48.3348276961881,0.));
#72130=CARTESIAN_POINT('Ctrl Pts',(7.42924995335917,-48.3348276961881,20.));
#72131=CARTESIAN_POINT('Ctrl Pts',(7.39550699443533,-48.3369195586108,0.));
#72132=CARTESIAN_POINT('Ctrl Pts',(7.39550699443533,-48.3369195586108,20.));
#72133=CARTESIAN_POINT('Ctrl Pts',(7.36176371798261,-48.3389881185516,0.));
#72134=CARTESIAN_POINT('Ctrl Pts',(7.36176371798261,-48.3389881185516,20.));
#72135=CARTESIAN_POINT('Ctrl Pts',(7.32802013999146,-48.3410333758855,0.));
#72136=CARTESIAN_POINT('Ctrl Pts',(7.32802013999146,-48.3410333758855,20.));
#72137=CARTESIAN_POINT('Ctrl Pts',(7.29427627645269,-48.3430553304987,0.));
#72138=CARTESIAN_POINT('Ctrl Pts',(7.29427627645269,-48.3430553304987,20.));
#72139=CARTESIAN_POINT('Ctrl Pts',(7.26053214338256,-48.3450539822883,0.));
#72140=CARTESIAN_POINT('Ctrl Pts',(7.26053214338256,-48.3450539822883,20.));
#72141=CARTESIAN_POINT('Ctrl Pts',(7.22678775682931,-48.3470293311619,0.));
#72142=CARTESIAN_POINT('Ctrl Pts',(7.22678775682931,-48.3470293311619,20.));
#72143=CARTESIAN_POINT('Ctrl Pts',(7.19304313285997,-48.3489813770376,0.));
#72144=CARTESIAN_POINT('Ctrl Pts',(7.19304313285997,-48.3489813770376,20.));
#72145=CARTESIAN_POINT('Ctrl Pts',(7.15929828755239,-48.3509101198447,0.));
#72146=CARTESIAN_POINT('Ctrl Pts',(7.15929828755239,-48.3509101198447,20.));
#72147=CARTESIAN_POINT('Ctrl Pts',(7.12555323698548,-48.3528155595232,0.));
#72148=CARTESIAN_POINT('Ctrl Pts',(7.12555323698548,-48.3528155595232,20.));
#72149=CARTESIAN_POINT('Ctrl Pts',(7.0918079972288,-48.354697696024,0.));
#72150=CARTESIAN_POINT('Ctrl Pts',(7.0918079972288,-48.354697696024,20.));
#72151=CARTESIAN_POINT('Ctrl Pts',(7.05806258433801,-48.3565565293095,0.));
#72152=CARTESIAN_POINT('Ctrl Pts',(7.05806258433801,-48.3565565293095,20.));
#72153=CARTESIAN_POINT('Ctrl Pts',(7.02431701436125,-48.3583920593534,0.));
#72154=CARTESIAN_POINT('Ctrl Pts',(7.02431701436125,-48.3583920593534,20.));
#72155=CARTESIAN_POINT('Ctrl Pts',(6.99057130334226,-48.3602042861407,0.));
#72156=CARTESIAN_POINT('Ctrl Pts',(6.99057130334226,-48.3602042861407,20.));
#72157=CARTESIAN_POINT('Ctrl Pts',(6.95682546732483,-48.3619932096677,0.));
#72158=CARTESIAN_POINT('Ctrl Pts',(6.95682546732483,-48.3619932096677,20.));
#72159=CARTESIAN_POINT('Ctrl Pts',(6.92307952235708,-48.3637588299416,0.));
#72160=CARTESIAN_POINT('Ctrl Pts',(6.92307952235708,-48.3637588299416,20.));
#72161=CARTESIAN_POINT('Ctrl Pts',(6.8893334844937,-48.3655011469807,0.));
#72162=CARTESIAN_POINT('Ctrl Pts',(6.8893334844937,-48.3655011469807,20.));
#72163=CARTESIAN_POINT('Ctrl Pts',(6.85558736979328,-48.3672201608141,0.));
#72164=CARTESIAN_POINT('Ctrl Pts',(6.85558736979328,-48.3672201608141,20.));
#72165=CARTESIAN_POINT('Ctrl Pts',(6.82184119431717,-48.3689158714816,0.));
#72166=CARTESIAN_POINT('Ctrl Pts',(6.82184119431717,-48.3689158714816,20.));
#72167=CARTESIAN_POINT('Ctrl Pts',(6.78809497412713,-48.370588279034,0.));
#72168=CARTESIAN_POINT('Ctrl Pts',(6.78809497412713,-48.370588279034,20.));
#72169=CARTESIAN_POINT('Ctrl Pts',(6.75434872528384,-48.3722373835335,0.));
#72170=CARTESIAN_POINT('Ctrl Pts',(6.75434872528384,-48.3722373835335,20.));
#72171=CARTESIAN_POINT('Ctrl Pts',(6.72060246384579,-48.3738631850533,0.));
#72172=CARTESIAN_POINT('Ctrl Pts',(6.72060246384579,-48.3738631850533,20.));
#72173=CARTESIAN_POINT('Ctrl Pts',(6.68685620587014,-48.3754656836776,0.));
#72174=CARTESIAN_POINT('Ctrl Pts',(6.68685620587014,-48.3754656836776,20.));
#72175=CARTESIAN_POINT('Ctrl Pts',(6.65310996741333,-48.3770448795022,0.));
#72176=CARTESIAN_POINT('Ctrl Pts',(6.65310996741333,-48.3770448795022,20.));
#72177=CARTESIAN_POINT('Ctrl Pts',(6.61936376453194,-48.3786007726338,0.));
#72178=CARTESIAN_POINT('Ctrl Pts',(6.61936376453194,-48.3786007726338,20.));
#72179=CARTESIAN_POINT('Ctrl Pts',(6.58561761328367,-48.3801333631899,0.));
#72180=CARTESIAN_POINT('Ctrl Pts',(6.58561761328367,-48.3801333631899,20.));
#72181=CARTESIAN_POINT('Ctrl Pts',(6.55187152972771,-48.3816426512995,0.));
#72182=CARTESIAN_POINT('Ctrl Pts',(6.55187152972771,-48.3816426512995,20.));
#72183=CARTESIAN_POINT('Ctrl Pts',(6.51812552992423,-48.3831286371024,0.));
#72184=CARTESIAN_POINT('Ctrl Pts',(6.51812552992423,-48.3831286371024,20.));
#72185=CARTESIAN_POINT('Ctrl Pts',(6.48437962993405,-48.3845913207494,0.));
#72186=CARTESIAN_POINT('Ctrl Pts',(6.48437962993405,-48.3845913207494,20.));
#72187=CARTESIAN_POINT('Ctrl Pts',(6.45063384581844,-48.3860307024022,0.));
#72188=CARTESIAN_POINT('Ctrl Pts',(6.45063384581844,-48.3860307024022,20.));
#72189=CARTESIAN_POINT('Ctrl Pts',(6.41688819363864,-48.3874467822337,0.));
#72190=CARTESIAN_POINT('Ctrl Pts',(6.41688819363864,-48.3874467822337,20.));
#72191=CARTESIAN_POINT('Ctrl Pts',(6.38314268945587,-48.388839560428,0.));
#72192=CARTESIAN_POINT('Ctrl Pts',(6.38314268945587,-48.388839560428,20.));
#72193=CARTESIAN_POINT('Ctrl Pts',(6.34939734933121,-48.3902090371802,0.));
#72194=CARTESIAN_POINT('Ctrl Pts',(6.34939734933121,-48.3902090371802,20.));
#72195=CARTESIAN_POINT('Ctrl Pts',(6.31565218932588,-48.3915552126968,0.));
#72196=CARTESIAN_POINT('Ctrl Pts',(6.31565218932588,-48.3915552126968,20.));
#72197=CARTESIAN_POINT('Ctrl Pts',(6.28190722550132,-48.3928780871951,0.));
#72198=CARTESIAN_POINT('Ctrl Pts',(6.28190722550132,-48.3928780871951,20.));
#72199=CARTESIAN_POINT('Ctrl Pts',(6.24816247391919,-48.3941776609035,0.));
#72200=CARTESIAN_POINT('Ctrl Pts',(6.24816247391919,-48.3941776609035,20.));
#72201=CARTESIAN_POINT('Ctrl Pts',(6.21441795064167,-48.3954539340615,0.));
#72202=CARTESIAN_POINT('Ctrl Pts',(6.21441795064167,-48.3954539340615,20.));
#72203=CARTESIAN_POINT('Ctrl Pts',(6.18067367173123,-48.3967069069196,0.));
#72204=CARTESIAN_POINT('Ctrl Pts',(6.18067367173123,-48.3967069069196,20.));
#72205=CARTESIAN_POINT('Ctrl Pts',(6.14692965325078,-48.3979365797396,0.));
#72206=CARTESIAN_POINT('Ctrl Pts',(6.14692965325078,-48.3979365797396,20.));
#72207=CARTESIAN_POINT('Ctrl Pts',(6.11318591126342,-48.3991429527941,0.));
#72208=CARTESIAN_POINT('Ctrl Pts',(6.11318591126342,-48.3991429527941,20.));
#72209=CARTESIAN_POINT('Ctrl Pts',(6.07944246183266,-48.400326026367,0.));
#72210=CARTESIAN_POINT('Ctrl Pts',(6.07944246183266,-48.400326026367,20.));
#72211=CARTESIAN_POINT('Ctrl Pts',(6.04569932102199,-48.4014858007534,0.));
#72212=CARTESIAN_POINT('Ctrl Pts',(6.04569932102199,-48.4014858007534,20.));
#72213=CARTESIAN_POINT('Ctrl Pts',(6.01195650489504,-48.4026222762592,0.));
#72214=CARTESIAN_POINT('Ctrl Pts',(6.01195650489504,-48.4026222762592,20.));
#72215=CARTESIAN_POINT('Ctrl Pts',(5.97821402951547,-48.4037354532014,0.));
#72216=CARTESIAN_POINT('Ctrl Pts',(5.97821402951547,-48.4037354532014,20.));
#72217=CARTESIAN_POINT('Ctrl Pts',(5.94447191094721,-48.404825331908,0.));
#72218=CARTESIAN_POINT('Ctrl Pts',(5.94447191094721,-48.404825331908,20.));
#72219=CARTESIAN_POINT('Ctrl Pts',(5.91073016525425,-48.4058919127185,0.));
#72220=CARTESIAN_POINT('Ctrl Pts',(5.91073016525425,-48.4058919127185,20.));
#72221=CARTESIAN_POINT('Ctrl Pts',(5.87698880850095,-48.4069351959835,0.));
#72222=CARTESIAN_POINT('Ctrl Pts',(5.87698880850095,-48.4069351959835,20.));
#72223=CARTESIAN_POINT('Ctrl Pts',(5.84324785675189,-48.4079551820643,0.));
#72224=CARTESIAN_POINT('Ctrl Pts',(5.84324785675189,-48.4079551820643,20.));
#72225=CARTESIAN_POINT('Ctrl Pts',(5.80950732607177,-48.4089518713337,0.));
#72226=CARTESIAN_POINT('Ctrl Pts',(5.80950732607177,-48.4089518713337,20.));
#72227=CARTESIAN_POINT('Ctrl Pts',(5.77576723252552,-48.4099252641753,0.));
#72228=CARTESIAN_POINT('Ctrl Pts',(5.77576723252552,-48.4099252641753,20.));
#72229=CARTESIAN_POINT('Ctrl Pts',(5.74202759217812,-48.4108753609837,0.));
#72230=CARTESIAN_POINT('Ctrl Pts',(5.74202759217812,-48.4108753609837,20.));
#72231=CARTESIAN_POINT('Ctrl Pts',(5.70828842109459,-48.4118021621647,0.));
#72232=CARTESIAN_POINT('Ctrl Pts',(5.70828842109459,-48.4118021621647,20.));
#72233=CARTESIAN_POINT('Ctrl Pts',(5.67454973534013,-48.412705668135,0.));
#72234=CARTESIAN_POINT('Ctrl Pts',(5.67454973534013,-48.412705668135,20.));
#72235=CARTESIAN_POINT('Ctrl Pts',(5.64081155098004,-48.4135858793227,0.));
#72236=CARTESIAN_POINT('Ctrl Pts',(5.64081155098004,-48.4135858793227,20.));
#72237=CARTESIAN_POINT('Ctrl Pts',(5.6070738840798,-48.414442796167,0.));
#72238=CARTESIAN_POINT('Ctrl Pts',(5.6070738840798,-48.414442796167,20.));
#72239=CARTESIAN_POINT('Ctrl Pts',(5.57333675070491,-48.4152764191183,0.));
#72240=CARTESIAN_POINT('Ctrl Pts',(5.57333675070491,-48.4152764191183,20.));
#72241=CARTESIAN_POINT('Ctrl Pts',(5.53960016692117,-48.4160867486381,0.));
#72242=CARTESIAN_POINT('Ctrl Pts',(5.53960016692117,-48.4160867486381,20.));
#72243=CARTESIAN_POINT('Ctrl Pts',(5.50586414879429,-48.4168737851989,0.));
#72244=CARTESIAN_POINT('Ctrl Pts',(5.50586414879429,-48.4168737851989,20.));
#72245=CARTESIAN_POINT('Ctrl Pts',(5.47212871239029,-48.417637529284,0.));
#72246=CARTESIAN_POINT('Ctrl Pts',(5.47212871239029,-48.417637529284,20.));
#72247=CARTESIAN_POINT('Ctrl Pts',(5.43839387377497,-48.4183779813881,0.));
#72248=CARTESIAN_POINT('Ctrl Pts',(5.43839387377497,-48.4183779813881,20.));
#72249=CARTESIAN_POINT('Ctrl Pts',(5.40465964901424,-48.4190951420167,0.));
#72250=CARTESIAN_POINT('Ctrl Pts',(5.40465964901424,-48.4190951420167,20.));
#72251=CARTESIAN_POINT('Ctrl Pts',(5.37092605417401,-48.4197890116867,0.));
#72252=CARTESIAN_POINT('Ctrl Pts',(5.37092605417401,-48.4197890116867,20.));
#72253=CARTESIAN_POINT('Ctrl Pts',(5.33719310532026,-48.4204595909261,0.));
#72254=CARTESIAN_POINT('Ctrl Pts',(5.33719310532026,-48.4204595909261,20.));
#72255=CARTESIAN_POINT('Ctrl Pts',(5.30346081851908,-48.4211068802741,0.));
#72256=CARTESIAN_POINT('Ctrl Pts',(5.30346081851908,-48.4211068802741,20.));
#72257=CARTESIAN_POINT('Ctrl Pts',(5.26972920983669,-48.4217308802807,0.));
#72258=CARTESIAN_POINT('Ctrl Pts',(5.26972920983669,-48.4217308802807,20.));
#72259=CARTESIAN_POINT('Ctrl Pts',(5.23599829533944,-48.4223315915069,0.));
#72260=CARTESIAN_POINT('Ctrl Pts',(5.23599829533944,-48.4223315915069,20.));
#72261=CARTESIAN_POINT('Ctrl Pts',(5.2022680910935,-48.4229090145253,0.));
#72262=CARTESIAN_POINT('Ctrl Pts',(5.2022680910935,-48.4229090145253,20.));
#72263=CARTESIAN_POINT('Ctrl Pts',(5.1685386131652,-48.4234631499194,0.));
#72264=CARTESIAN_POINT('Ctrl Pts',(5.1685386131652,-48.4234631499194,20.));
#72265=CARTESIAN_POINT('Ctrl Pts',(5.1348098776207,-48.4239939982838,0.));
#72266=CARTESIAN_POINT('Ctrl Pts',(5.1348098776207,-48.4239939982838,20.));
#72267=CARTESIAN_POINT('Ctrl Pts',(5.10108190052607,-48.4245015602246,0.));
#72268=CARTESIAN_POINT('Ctrl Pts',(5.10108190052607,-48.4245015602246,20.));
#72269=CARTESIAN_POINT('Ctrl Pts',(5.06735469794741,-48.4249858363582,0.));
#72270=CARTESIAN_POINT('Ctrl Pts',(5.06735469794741,-48.4249858363582,20.));
#72271=CARTESIAN_POINT('Ctrl Pts',(5.03362828595092,-48.4254468273122,0.));
#72272=CARTESIAN_POINT('Ctrl Pts',(5.03362828595092,-48.4254468273122,20.));
#72273=CARTESIAN_POINT('Ctrl Pts',(4.99990268060291,-48.4258845337255,0.));
#72274=CARTESIAN_POINT('Ctrl Pts',(4.99990268060291,-48.4258845337255,20.));
#72275=CARTESIAN_POINT('Ctrl Pts',(4.96617789796952,-48.4262989562483,0.));
#72276=CARTESIAN_POINT('Ctrl Pts',(4.96617789796952,-48.4262989562483,20.));
#72277=CARTESIAN_POINT('Ctrl Pts',(4.93245395411684,-48.4266900955418,0.));
#72278=CARTESIAN_POINT('Ctrl Pts',(4.93245395411684,-48.4266900955418,20.));
#72279=CARTESIAN_POINT('Ctrl Pts',(4.89873086511076,-48.4270579522784,0.));
#72280=CARTESIAN_POINT('Ctrl Pts',(4.89873086511076,-48.4270579522784,20.));
#72281=CARTESIAN_POINT('Ctrl Pts',(4.8650086470173,-48.4274025271416,0.));
#72282=CARTESIAN_POINT('Ctrl Pts',(4.8650086470173,-48.4274025271416,20.));
#72283=CARTESIAN_POINT('Ctrl Pts',(4.83128731590228,-48.4277238208263,0.));
#72284=CARTESIAN_POINT('Ctrl Pts',(4.83128731590228,-48.4277238208263,20.));
#72285=CARTESIAN_POINT('Ctrl Pts',(4.79756688783168,-48.4280218340382,0.));
#72286=CARTESIAN_POINT('Ctrl Pts',(4.79756688783168,-48.4280218340382,20.));
#72287=CARTESIAN_POINT('Ctrl Pts',(4.76384737887105,-48.4282965674942,0.));
#72288=CARTESIAN_POINT('Ctrl Pts',(4.76384737887105,-48.4282965674942,20.));
#72289=CARTESIAN_POINT('Ctrl Pts',(4.730128805086,-48.4285480219221,0.));
#72290=CARTESIAN_POINT('Ctrl Pts',(4.730128805086,-48.4285480219221,20.));
#72291=CARTESIAN_POINT('Ctrl Pts',(4.69641118254225,-48.4287761980604,0.));
#72292=CARTESIAN_POINT('Ctrl Pts',(4.69641118254225,-48.4287761980604,20.));
#72293=CARTESIAN_POINT('Ctrl Pts',(4.66269452730542,-48.4289810966589,0.));
#72294=CARTESIAN_POINT('Ctrl Pts',(4.66269452730542,-48.4289810966589,20.));
#72295=CARTESIAN_POINT('Ctrl Pts',(4.62897885544097,-48.4291627184787,0.));
#72296=CARTESIAN_POINT('Ctrl Pts',(4.62897885544097,-48.4291627184787,20.));
#72297=CARTESIAN_POINT('Ctrl Pts',(4.59526418301408,-48.4293210642923,0.));
#72298=CARTESIAN_POINT('Ctrl Pts',(4.59526418301408,-48.4293210642923,20.));
#72299=CARTESIAN_POINT('Ctrl Pts',(4.5615505260898,-48.4294561348833,0.));
#72300=CARTESIAN_POINT('Ctrl Pts',(4.5615505260898,-48.4294561348833,20.));
#72301=CARTESIAN_POINT('Ctrl Pts',(4.52783790073293,-48.4295679310466,0.));
#72302=CARTESIAN_POINT('Ctrl Pts',(4.52783790073293,-48.4295679310466,20.));
#72303=CARTESIAN_POINT('Ctrl Pts',(4.49412632300814,-48.4296564535884,0.));
#72304=CARTESIAN_POINT('Ctrl Pts',(4.49412632300814,-48.4296564535884,20.));
#72305=CARTESIAN_POINT('Ctrl Pts',(4.46041580898011,-48.4297217033257,0.));
#72306=CARTESIAN_POINT('Ctrl Pts',(4.46041580898011,-48.4297217033257,20.));
#72307=CARTESIAN_POINT('Ctrl Pts',(4.4267063747134,-48.4297636810863,0.));
#72308=CARTESIAN_POINT('Ctrl Pts',(4.4267063747134,-48.4297636810863,20.));
#72309=CARTESIAN_POINT('Ctrl Pts',(4.39299803627246,-48.4297823877088,0.));
#72310=CARTESIAN_POINT('Ctrl Pts',(4.39299803627246,-48.4297823877088,20.));
#72311=CARTESIAN_POINT('Ctrl Pts',(4.35929080972166,-48.4297778240431,0.));
#72312=CARTESIAN_POINT('Ctrl Pts',(4.35929080972166,-48.4297778240431,20.));
#72313=CARTESIAN_POINT('Ctrl Pts',(4.32558471112516,-48.42974999095,0.));
#72314=CARTESIAN_POINT('Ctrl Pts',(4.32558471112516,-48.42974999095,20.));
#72315=CARTESIAN_POINT('Ctrl Pts',(4.29187975654677,-48.4296988893018,0.));
#72316=CARTESIAN_POINT('Ctrl Pts',(4.29187975654677,-48.4296988893018,20.));
#72317=CARTESIAN_POINT('Ctrl Pts',(4.25817596205,-48.4296245199823,0.));
#72318=CARTESIAN_POINT('Ctrl Pts',(4.25817596205,-48.4296245199823,20.));
#72319=CARTESIAN_POINT('Ctrl Pts',(4.22447334369801,-48.4295268838864,0.));
#72320=CARTESIAN_POINT('Ctrl Pts',(4.22447334369801,-48.4295268838864,20.));
#72321=CARTESIAN_POINT('Ctrl Pts',(4.19077191755405,-48.4294059819202,0.));
#72322=CARTESIAN_POINT('Ctrl Pts',(4.19077191755405,-48.4294059819202,20.));
#72323=CARTESIAN_POINT('Ctrl Pts',(4.15707169968115,-48.4292618150011,0.));
#72324=CARTESIAN_POINT('Ctrl Pts',(4.15707169968115,-48.4292618150011,20.));
#72325=CARTESIAN_POINT('Ctrl Pts',(4.1233727061421,-48.429094384057,0.));
#72326=CARTESIAN_POINT('Ctrl Pts',(4.1233727061421,-48.429094384057,20.));
#72327=CARTESIAN_POINT('Ctrl Pts',(4.08967495299951,-48.4289036900268,0.));
#72328=CARTESIAN_POINT('Ctrl Pts',(4.08967495299951,-48.4289036900268,20.));
#72329=CARTESIAN_POINT('Ctrl Pts',(4.05597845631568,-48.4286897338604,0.));
#72330=CARTESIAN_POINT('Ctrl Pts',(4.05597845631568,-48.4286897338604,20.));
#72331=CARTESIAN_POINT('Ctrl Pts',(4.02228323215259,-48.4284525165189,0.));
#72332=CARTESIAN_POINT('Ctrl Pts',(4.02228323215259,-48.4284525165189,20.));
#72333=CARTESIAN_POINT('Ctrl Pts',(3.988589296572,-48.4281920389749,0.));
#72334=CARTESIAN_POINT('Ctrl Pts',(3.988589296572,-48.4281920389749,20.));
#72335=CARTESIAN_POINT('Ctrl Pts',(3.95489666563548,-48.427908302212,0.));
#72336=CARTESIAN_POINT('Ctrl Pts',(3.95489666563548,-48.427908302212,20.));
#72337=CARTESIAN_POINT('Ctrl Pts',(3.9212053554042,-48.4276013072253,0.));
#72338=CARTESIAN_POINT('Ctrl Pts',(3.9212053554042,-48.4276013072253,20.));
#72339=CARTESIAN_POINT('Ctrl Pts',(3.88751538193919,-48.4272710550207,0.));
#72340=CARTESIAN_POINT('Ctrl Pts',(3.88751538193919,-48.4272710550207,20.));
#72341=CARTESIAN_POINT('Ctrl Pts',(3.85382676130114,-48.4269175466151,0.));
#72342=CARTESIAN_POINT('Ctrl Pts',(3.85382676130114,-48.4269175466151,20.));
#72343=CARTESIAN_POINT('Ctrl Pts',(3.82013950955042,-48.4265407830367,0.));
#72344=CARTESIAN_POINT('Ctrl Pts',(3.82013950955042,-48.4265407830367,20.));
#72345=CARTESIAN_POINT('Ctrl Pts',(3.78645364274706,-48.4261407653249,0.));
#72346=CARTESIAN_POINT('Ctrl Pts',(3.78645364274706,-48.4261407653249,20.));
#72347=CARTESIAN_POINT('Ctrl Pts',(3.75276917695084,-48.4257174945298,0.));
#72348=CARTESIAN_POINT('Ctrl Pts',(3.75276917695084,-48.4257174945298,20.));
#72349=CARTESIAN_POINT('Ctrl Pts',(3.71908612822108,-48.4252709717129,0.));
#72350=CARTESIAN_POINT('Ctrl Pts',(3.71908612822108,-48.4252709717129,20.));
#72351=CARTESIAN_POINT('Ctrl Pts',(3.68540451261695,-48.424801197947,0.));
#72352=CARTESIAN_POINT('Ctrl Pts',(3.68540451261695,-48.424801197947,20.));
#72353=CARTESIAN_POINT('Ctrl Pts',(3.6517243461974,-48.4243081743158,0.));
#72354=CARTESIAN_POINT('Ctrl Pts',(3.6517243461974,-48.4243081743158,20.));
#72355=CARTESIAN_POINT('Ctrl Pts',(3.61804564502096,-48.4237919019141,0.));
#72356=CARTESIAN_POINT('Ctrl Pts',(3.61804564502096,-48.4237919019141,20.));
#72357=CARTESIAN_POINT('Ctrl Pts',(3.58436842514564,-48.4232523818483,0.));
#72358=CARTESIAN_POINT('Ctrl Pts',(3.58436842514564,-48.4232523818483,20.));
#72359=CARTESIAN_POINT('Ctrl Pts',(3.55069270262907,-48.4226896152354,0.));
#72360=CARTESIAN_POINT('Ctrl Pts',(3.55069270262907,-48.4226896152354,20.));
#72361=CARTESIAN_POINT('Ctrl Pts',(3.51701849352853,-48.422103603204,0.));
#72362=CARTESIAN_POINT('Ctrl Pts',(3.51701849352853,-48.422103603204,20.));
#72363=CARTESIAN_POINT('Ctrl Pts',(3.483345813901,-48.4214943468927,0.));
#72364=CARTESIAN_POINT('Ctrl Pts',(3.483345813901,-48.4214943468927,20.));
#72365=CARTESIAN_POINT('Ctrl Pts',(3.44967467980323,-48.4208618474523,0.));
#72366=CARTESIAN_POINT('Ctrl Pts',(3.44967467980323,-48.4208618474523,20.));
#72367=CARTESIAN_POINT('Ctrl Pts',(3.41600510729148,-48.4202061060442,0.));
#72368=CARTESIAN_POINT('Ctrl Pts',(3.41600510729148,-48.4202061060442,20.));
#72369=CARTESIAN_POINT('Ctrl Pts',(3.38233711242167,-48.4195271238417,0.));
#72370=CARTESIAN_POINT('Ctrl Pts',(3.38233711242167,-48.4195271238417,20.));
#72371=CARTESIAN_POINT('Ctrl Pts',(3.34867071124917,-48.4188249020284,0.));
#72372=CARTESIAN_POINT('Ctrl Pts',(3.34867071124917,-48.4188249020284,20.));
#72373=CARTESIAN_POINT('Ctrl Pts',(3.31500591982887,-48.4180994417999,0.));
#72374=CARTESIAN_POINT('Ctrl Pts',(3.31500591982887,-48.4180994417999,20.));
#72375=CARTESIAN_POINT('Ctrl Pts',(3.28134275421531,-48.4173507443625,0.));
#72376=CARTESIAN_POINT('Ctrl Pts',(3.28134275421531,-48.4173507443625,20.));
#72377=CARTESIAN_POINT('Ctrl Pts',(3.24768123046264,-48.4165788109335,0.));
#72378=CARTESIAN_POINT('Ctrl Pts',(3.24768123046264,-48.4165788109335,20.));
#72379=CARTESIAN_POINT('Ctrl Pts',(3.21402136462457,-48.4157836427414,0.));
#72380=CARTESIAN_POINT('Ctrl Pts',(3.21402136462457,-48.4157836427414,20.));
#72381=CARTESIAN_POINT('Ctrl Pts',(3.18036317275453,-48.4149652410254,0.));
#72382=CARTESIAN_POINT('Ctrl Pts',(3.18036317275453,-48.4149652410254,20.));
#72383=CARTESIAN_POINT('Ctrl Pts',(3.14670667090555,-48.414123607036,0.));
#72384=CARTESIAN_POINT('Ctrl Pts',(3.14670667090555,-48.414123607036,20.));
#72385=CARTESIAN_POINT('Ctrl Pts',(3.11305187512999,-48.4132587420349,0.));
#72386=CARTESIAN_POINT('Ctrl Pts',(3.11305187512999,-48.4132587420349,20.));
#72387=CARTESIAN_POINT('Ctrl Pts',(3.07939880147968,-48.4123706472953,0.));
#72388=CARTESIAN_POINT('Ctrl Pts',(3.07939880147968,-48.4123706472953,20.));
#72389=CARTESIAN_POINT('Ctrl Pts',(3.04574746600607,-48.4114593241014,0.));
#72390=CARTESIAN_POINT('Ctrl Pts',(3.04574746600607,-48.4114593241014,20.));
#72391=CARTESIAN_POINT('Ctrl Pts',(3.01209788475993,-48.4105247737488,0.));
#72392=CARTESIAN_POINT('Ctrl Pts',(3.01209788475993,-48.4105247737488,20.));
#72393=CARTESIAN_POINT('Ctrl Pts',(2.97845007379181,-48.4095669975441,0.));
#72394=CARTESIAN_POINT('Ctrl Pts',(2.97845007379181,-48.4095669975441,20.));
#72395=CARTESIAN_POINT('Ctrl Pts',(2.94480404915164,-48.4085859968048,0.));
#72396=CARTESIAN_POINT('Ctrl Pts',(2.94480404915164,-48.4085859968048,20.));
#72397=CARTESIAN_POINT('Ctrl Pts',(2.91115982688903,-48.4075817728593,0.));
#72398=CARTESIAN_POINT('Ctrl Pts',(2.91115982688903,-48.4075817728593,20.));
#72399=CARTESIAN_POINT('Ctrl Pts',(2.87751742305292,-48.4065543270471,0.));
#72400=CARTESIAN_POINT('Ctrl Pts',(2.87751742305292,-48.4065543270471,20.));
#72401=CARTESIAN_POINT('Ctrl Pts',(2.8438768536918,-48.4055036607195,0.));
#72402=CARTESIAN_POINT('Ctrl Pts',(2.8438768536918,-48.4055036607195,20.));
#72403=CARTESIAN_POINT('Ctrl Pts',(2.81023813485355,-48.4044297752383,0.));
#72404=CARTESIAN_POINT('Ctrl Pts',(2.81023813485355,-48.4044297752383,20.));
#72405=CARTESIAN_POINT('Ctrl Pts',(2.77660128258546,-48.4033326719771,0.));
#72406=CARTESIAN_POINT('Ctrl Pts',(2.77660128258546,-48.4033326719771,20.));
#72407=CARTESIAN_POINT('Ctrl Pts',(2.74296631293436,-48.4022123523201,0.));
#72408=CARTESIAN_POINT('Ctrl Pts',(2.74296631293436,-48.4022123523201,20.));
#72409=CARTESIAN_POINT('Ctrl Pts',(2.7093332419466,-48.4010688176627,0.));
#72410=CARTESIAN_POINT('Ctrl Pts',(2.7093332419466,-48.4010688176627,20.));
#72411=CARTESIAN_POINT('Ctrl Pts',(2.67570208566793,-48.3999020694116,0.));
#72412=CARTESIAN_POINT('Ctrl Pts',(2.67570208566793,-48.3999020694116,20.));
#72413=CARTESIAN_POINT('Ctrl Pts',(2.64207286014349,-48.3987121089844,0.));
#72414=CARTESIAN_POINT('Ctrl Pts',(2.64207286014349,-48.3987121089844,20.));
#72415=CARTESIAN_POINT('Ctrl Pts',(2.60844558141789,-48.3974989378103,0.));
#72416=CARTESIAN_POINT('Ctrl Pts',(2.60844558141789,-48.3974989378103,20.));
#72417=CARTESIAN_POINT('Ctrl Pts',(2.57482026553515,-48.3962625573292,0.));
#72418=CARTESIAN_POINT('Ctrl Pts',(2.57482026553515,-48.3962625573292,20.));
#72419=CARTESIAN_POINT('Ctrl Pts',(2.5411969285386,-48.3950029689925,0.));
#72420=CARTESIAN_POINT('Ctrl Pts',(2.5411969285386,-48.3950029689925,20.));
#72421=CARTESIAN_POINT('Ctrl Pts',(2.50757558647119,-48.3937201742621,0.));
#72422=CARTESIAN_POINT('Ctrl Pts',(2.50757558647119,-48.3937201742621,20.));
#72423=CARTESIAN_POINT('Ctrl Pts',(2.47395625537494,-48.3924141746117,0.));
#72424=CARTESIAN_POINT('Ctrl Pts',(2.47395625537494,-48.3924141746117,20.));
#72425=CARTESIAN_POINT('Ctrl Pts',(2.44033895129153,-48.3910849715258,0.));
#72426=CARTESIAN_POINT('Ctrl Pts',(2.44033895129153,-48.3910849715258,20.));
#72427=CARTESIAN_POINT('Ctrl Pts',(2.40672369026195,-48.3897325665,0.));
#72428=CARTESIAN_POINT('Ctrl Pts',(2.40672369026195,-48.3897325665,20.));
#72429=CARTESIAN_POINT('Ctrl Pts',(2.37311048832664,-48.3883569610415,0.));
#72430=CARTESIAN_POINT('Ctrl Pts',(2.37311048832664,-48.3883569610415,20.));
#72431=CARTESIAN_POINT('Ctrl Pts',(2.33949936152533,-48.3869581566679,0.));
#72432=CARTESIAN_POINT('Ctrl Pts',(2.33949936152533,-48.3869581566679,20.));
#72433=CARTESIAN_POINT('Ctrl Pts',(2.30589032589699,-48.3855361549086,0.));
#72434=CARTESIAN_POINT('Ctrl Pts',(2.30589032589699,-48.3855361549086,20.));
#72435=CARTESIAN_POINT('Ctrl Pts',(2.27228339748008,-48.3840909573039,0.));
#72436=CARTESIAN_POINT('Ctrl Pts',(2.27228339748008,-48.3840909573039,20.));
#72437=CARTESIAN_POINT('Ctrl Pts',(2.2386785923122,-48.3826225654054,0.));
#72438=CARTESIAN_POINT('Ctrl Pts',(2.2386785923122,-48.3826225654054,20.));
#72439=CARTESIAN_POINT('Ctrl Pts',(2.20507592643041,-48.3811309807756,0.));
#72440=CARTESIAN_POINT('Ctrl Pts',(2.20507592643041,-48.3811309807756,20.));
#72441=CARTESIAN_POINT('Ctrl Pts',(2.17147541587102,-48.3796162049883,0.));
#72442=CARTESIAN_POINT('Ctrl Pts',(2.17147541587102,-48.3796162049883,20.));
#72443=CARTESIAN_POINT('Ctrl Pts',(2.13787707667012,-48.3780782396279,0.));
#72444=CARTESIAN_POINT('Ctrl Pts',(2.13787707667012,-48.3780782396279,20.));
#72445=CARTESIAN_POINT('Ctrl Pts',(2.10428092486293,-48.3765170862905,0.));
#72446=CARTESIAN_POINT('Ctrl Pts',(2.10428092486293,-48.3765170862905,20.));
#72447=CARTESIAN_POINT('Ctrl Pts',(2.07068697648387,-48.374932746583,0.));
#72448=CARTESIAN_POINT('Ctrl Pts',(2.07068697648387,-48.374932746583,20.));
#72449=CARTESIAN_POINT('Ctrl Pts',(2.03709524756654,-48.3733252221237,0.));
#72450=CARTESIAN_POINT('Ctrl Pts',(2.03709524756654,-48.3733252221237,20.));
#72451=CARTESIAN_POINT('Ctrl Pts',(2.00350575414355,-48.3716945145424,0.));
#72452=CARTESIAN_POINT('Ctrl Pts',(2.00350575414355,-48.3716945145424,20.));
#72453=CARTESIAN_POINT('Ctrl Pts',(1.96991851224691,-48.3700406254798,0.));
#72454=CARTESIAN_POINT('Ctrl Pts',(1.96991851224691,-48.3700406254798,20.));
#72455=CARTESIAN_POINT('Ctrl Pts',(1.93633353790811,-48.3683635565876,0.));
#72456=CARTESIAN_POINT('Ctrl Pts',(1.93633353790811,-48.3683635565876,20.));
#72457=CARTESIAN_POINT('Ctrl Pts',(1.90275084715795,-48.3666633095284,0.));
#72458=CARTESIAN_POINT('Ctrl Pts',(1.90275084715795,-48.3666633095284,20.));
#72459=CARTESIAN_POINT('Ctrl Pts',(1.86917045602651,-48.3649398859758,0.));
#72460=CARTESIAN_POINT('Ctrl Pts',(1.86917045602651,-48.3649398859758,20.));
#72461=CARTESIAN_POINT('Ctrl Pts',(1.83559238054322,-48.3631932876149,0.));
#72462=CARTESIAN_POINT('Ctrl Pts',(1.83559238054322,-48.3631932876149,20.));
#72463=CARTESIAN_POINT('Ctrl Pts',(1.80201663673655,-48.3614235161422,0.));
#72464=CARTESIAN_POINT('Ctrl Pts',(1.80201663673655,-48.3614235161422,20.));
#72465=CARTESIAN_POINT('Ctrl Pts',(1.76844324063425,-48.3596305732653,0.));
#72466=CARTESIAN_POINT('Ctrl Pts',(1.76844324063425,-48.3596305732653,20.));
#72467=CARTESIAN_POINT('Ctrl Pts',(1.73487220826325,-48.357814460703,0.));
#72468=CARTESIAN_POINT('Ctrl Pts',(1.73487220826325,-48.357814460703,20.));
#72469=CARTESIAN_POINT('Ctrl Pts',(1.70130355564956,-48.3559751801849,0.));
#72470=CARTESIAN_POINT('Ctrl Pts',(1.70130355564956,-48.3559751801849,20.));
#72471=CARTESIAN_POINT('Ctrl Pts',(1.66773729881855,-48.3541127334515,0.));
#72472=CARTESIAN_POINT('Ctrl Pts',(1.66773729881855,-48.3541127334515,20.));
#72473=CARTESIAN_POINT('Ctrl Pts',(1.63417345379481,-48.3522271222546,0.));
#72474=CARTESIAN_POINT('Ctrl Pts',(1.63417345379481,-48.3522271222546,20.));
#72475=CARTESIAN_POINT('Ctrl Pts',(1.60061203660205,-48.350318348357,0.));
#72476=CARTESIAN_POINT('Ctrl Pts',(1.60061203660205,-48.350318348357,20.));
#72477=CARTESIAN_POINT('Ctrl Pts',(1.56705306326331,-48.3483864135332,0.));
#72478=CARTESIAN_POINT('Ctrl Pts',(1.56705306326331,-48.3483864135332,20.));
#72479=CARTESIAN_POINT('Ctrl Pts',(1.53349654980076,-48.3464313195685,0.));
#72480=CARTESIAN_POINT('Ctrl Pts',(1.53349654980076,-48.3464313195685,20.));
#72481=CARTESIAN_POINT('Ctrl Pts',(1.4999425122357,-48.3444530682597,0.));
#72482=CARTESIAN_POINT('Ctrl Pts',(1.4999425122357,-48.3444530682597,20.));
#72483=CARTESIAN_POINT('Ctrl Pts',(1.46639096658851,-48.3424516614145,0.));
#72484=CARTESIAN_POINT('Ctrl Pts',(1.46639096658851,-48.3424516614145,20.));
#72485=CARTESIAN_POINT('Ctrl Pts',(1.43284192887878,-48.3404271008519,0.));
#72486=CARTESIAN_POINT('Ctrl Pts',(1.43284192887878,-48.3404271008519,20.));
#72487=CARTESIAN_POINT('Ctrl Pts',(1.39929541512519,-48.3383793884017,0.));
#72488=CARTESIAN_POINT('Ctrl Pts',(1.39929541512519,-48.3383793884017,20.));
#72489=CARTESIAN_POINT('Ctrl Pts',(1.3657514413457,-48.336308525905,0.));
#72490=CARTESIAN_POINT('Ctrl Pts',(1.3657514413457,-48.336308525905,20.));
#72491=CARTESIAN_POINT('Ctrl Pts',(1.33221002355742,-48.3342145152137,0.));
#72492=CARTESIAN_POINT('Ctrl Pts',(1.33221002355742,-48.3342145152137,20.));
#72493=CARTESIAN_POINT('Ctrl Pts',(1.29867117777651,-48.3320973581913,0.));
#72494=CARTESIAN_POINT('Ctrl Pts',(1.29867117777651,-48.3320973581913,20.));
#72495=CARTESIAN_POINT('Ctrl Pts',(1.26513492001821,-48.3299570567123,0.));
#72496=CARTESIAN_POINT('Ctrl Pts',(1.26513492001821,-48.3299570567123,20.));
#72497=CARTESIAN_POINT('Ctrl Pts',(1.23160126629692,-48.3277936126623,0.));
#72498=CARTESIAN_POINT('Ctrl Pts',(1.23160126629692,-48.3277936126623,20.));
#72499=CARTESIAN_POINT('Ctrl Pts',(1.19807023262611,-48.3256070279384,0.));
#72500=CARTESIAN_POINT('Ctrl Pts',(1.19807023262611,-48.3256070279384,20.));
#72501=CARTESIAN_POINT('Ctrl Pts',(1.16454183501838,-48.3233973044482,0.));
#72502=CARTESIAN_POINT('Ctrl Pts',(1.16454183501838,-48.3233973044482,20.));
#72503=CARTESIAN_POINT('Ctrl Pts',(1.13101608948534,-48.3211644441107,0.));
#72504=CARTESIAN_POINT('Ctrl Pts',(1.13101608948534,-48.3211644441107,20.));
#72505=CARTESIAN_POINT('Ctrl Pts',(1.09749301203762,-48.3189084488565,0.));
#72506=CARTESIAN_POINT('Ctrl Pts',(1.09749301203762,-48.3189084488565,20.));
#72507=CARTESIAN_POINT('Ctrl Pts',(1.063972618685,-48.3166293206271,0.));
#72508=CARTESIAN_POINT('Ctrl Pts',(1.063972618685,-48.3166293206271,20.));
#72509=CARTESIAN_POINT('Ctrl Pts',(1.0304549254364,-48.3143270613748,0.));
#72510=CARTESIAN_POINT('Ctrl Pts',(1.0304549254364,-48.3143270613748,20.));
#72511=CARTESIAN_POINT('Ctrl Pts',(0.996939948299849,-48.312001673063,0.));
#72512=CARTESIAN_POINT('Ctrl Pts',(0.996939948299849,-48.312001673063,20.));
#72513=CARTESIAN_POINT('Ctrl Pts',(0.963427703282353,-48.3096531576664,
0.));
#72514=CARTESIAN_POINT('Ctrl Pts',(0.963427703282353,-48.3096531576664,
20.));
#72515=CARTESIAN_POINT('Ctrl Pts',(0.929918206389826,-48.3072815171712,
0.));
#72516=CARTESIAN_POINT('Ctrl Pts',(0.929918206389826,-48.3072815171712,
20.));
#72517=CARTESIAN_POINT('Ctrl Pts',(0.896411473627223,-48.3048867535744,
0.));
#72518=CARTESIAN_POINT('Ctrl Pts',(0.896411473627223,-48.3048867535744,
20.));
#72519=CARTESIAN_POINT('Ctrl Pts',(0.862907520998486,-48.3024688688845,
0.));
#72520=CARTESIAN_POINT('Ctrl Pts',(0.862907520998486,-48.3024688688845,
20.));
#72521=CARTESIAN_POINT('Ctrl Pts',(0.829406364506662,-48.3000278651208,
0.));
#72522=CARTESIAN_POINT('Ctrl Pts',(0.829406364506662,-48.3000278651208,
20.));
#72523=CARTESIAN_POINT('Ctrl Pts',(0.795908020153888,-48.2975637443136,
0.));
#72524=CARTESIAN_POINT('Ctrl Pts',(0.795908020153888,-48.2975637443136,
20.));
#72525=CARTESIAN_POINT('Ctrl Pts',(0.762412503941521,-48.2950765085043,
0.));
#72526=CARTESIAN_POINT('Ctrl Pts',(0.762412503941521,-48.2950765085043,
20.));
#72527=CARTESIAN_POINT('Ctrl Pts',(0.728919831869645,-48.2925661597457,
0.));
#72528=CARTESIAN_POINT('Ctrl Pts',(0.728919831869645,-48.2925661597457,
20.));
#72529=CARTESIAN_POINT('Ctrl Pts',(0.69543001993734,-48.2900327001016,0.));
#72530=CARTESIAN_POINT('Ctrl Pts',(0.69543001993734,-48.2900327001016,20.));
#72531=CARTESIAN_POINT('Ctrl Pts',(0.661943084142442,-48.2874761316474,
0.));
#72532=CARTESIAN_POINT('Ctrl Pts',(0.661943084142442,-48.2874761316474,
20.));
#72533=CARTESIAN_POINT('Ctrl Pts',(0.628459040481828,-48.2848964564694,
0.));
#72534=CARTESIAN_POINT('Ctrl Pts',(0.628459040481828,-48.2848964564694,
20.));
#72535=CARTESIAN_POINT('Ctrl Pts',(0.594977904951266,-48.282293676665,0.));
#72536=CARTESIAN_POINT('Ctrl Pts',(0.594977904951266,-48.282293676665,20.));
#72537=CARTESIAN_POINT('Ctrl Pts',(0.561499693545673,-48.2796677943426,
0.));
#72538=CARTESIAN_POINT('Ctrl Pts',(0.561499693545673,-48.2796677943426,
20.));
#72539=CARTESIAN_POINT('Ctrl Pts',(0.528024422259019,-48.2770188116216,
0.));
#72540=CARTESIAN_POINT('Ctrl Pts',(0.528024422259019,-48.2770188116216,
20.));
#72541=CARTESIAN_POINT('Ctrl Pts',(0.49455210708421,-48.2743467306329,0.));
#72542=CARTESIAN_POINT('Ctrl Pts',(0.49455210708421,-48.2743467306329,20.));
#72543=CARTESIAN_POINT('Ctrl Pts',(0.461082764012986,-48.2716515535183,
0.));
#72544=CARTESIAN_POINT('Ctrl Pts',(0.461082764012986,-48.2716515535183,
20.));
#72545=CARTESIAN_POINT('Ctrl Pts',(0.427616409036036,-48.2689332824309,
0.));
#72546=CARTESIAN_POINT('Ctrl Pts',(0.427616409036036,-48.2689332824309,
20.));
#72547=CARTESIAN_POINT('Ctrl Pts',(0.394153058142903,-48.2661919195348,
0.));
#72548=CARTESIAN_POINT('Ctrl Pts',(0.394153058142903,-48.2661919195348,
20.));
#72549=CARTESIAN_POINT('Ctrl Pts',(0.360692727321981,-48.2634274670053,
0.));
#72550=CARTESIAN_POINT('Ctrl Pts',(0.360692727321981,-48.2634274670053,
20.));
#72551=CARTESIAN_POINT('Ctrl Pts',(0.327235432560538,-48.2606399270286,
0.));
#72552=CARTESIAN_POINT('Ctrl Pts',(0.327235432560538,-48.2606399270286,
20.));
#72553=CARTESIAN_POINT('Ctrl Pts',(0.293781189844817,-48.2578293018028,
0.));
#72554=CARTESIAN_POINT('Ctrl Pts',(0.293781189844817,-48.2578293018028,
20.));
#72555=CARTESIAN_POINT('Ctrl Pts',(0.260330015159931,-48.2549955935366,
0.));
#72556=CARTESIAN_POINT('Ctrl Pts',(0.260330015159931,-48.2549955935366,
20.));
#72557=CARTESIAN_POINT('Ctrl Pts',(0.226881924489848,-48.2521388044499,
0.));
#72558=CARTESIAN_POINT('Ctrl Pts',(0.226881924489848,-48.2521388044499,
20.));
#72559=CARTESIAN_POINT('Ctrl Pts',(0.193436933817455,-48.2492589367737,
0.));
#72560=CARTESIAN_POINT('Ctrl Pts',(0.193436933817455,-48.2492589367737,
20.));
#72561=CARTESIAN_POINT('Ctrl Pts',(0.159995059124558,-48.2463559927498,
0.));
#72562=CARTESIAN_POINT('Ctrl Pts',(0.159995059124558,-48.2463559927498,
20.));
#72563=CARTESIAN_POINT('Ctrl Pts',(0.126556316391659,-48.2434299746318,
0.));
#72564=CARTESIAN_POINT('Ctrl Pts',(0.126556316391659,-48.2434299746318,
20.));
#72565=CARTESIAN_POINT('Ctrl Pts',(0.0931207215982655,-48.2404808846839,
0.));
#72566=CARTESIAN_POINT('Ctrl Pts',(0.0931207215982655,-48.2404808846839,
20.));
#72567=CARTESIAN_POINT('Ctrl Pts',(0.0596882907225815,-48.2375087251817,
0.));
#72568=CARTESIAN_POINT('Ctrl Pts',(0.0596882907225815,-48.2375087251817,
20.));
#72569=CARTESIAN_POINT('Ctrl Pts',(0.0262590397416584,-48.234513498412,
0.));
#72570=CARTESIAN_POINT('Ctrl Pts',(0.0262590397416584,-48.234513498412,
20.));
#72571=CARTESIAN_POINT('Ctrl Pts',(-0.00716701536858544,-48.2314952066725,
0.));
#72572=CARTESIAN_POINT('Ctrl Pts',(-0.00716701536858544,-48.2314952066725,
20.));
#72573=CARTESIAN_POINT('Ctrl Pts',(-0.040589858633453,-48.2284538522724,
0.));
#72574=CARTESIAN_POINT('Ctrl Pts',(-0.040589858633453,-48.2284538522724,
20.));
#72575=CARTESIAN_POINT('Ctrl Pts',(-0.0740094740794106,-48.2253894375317,
0.));
#72576=CARTESIAN_POINT('Ctrl Pts',(-0.0740094740794106,-48.2253894375317,
20.));
#72577=CARTESIAN_POINT('Ctrl Pts',(-0.107425845734137,-48.2223019647818,
0.));
#72578=CARTESIAN_POINT('Ctrl Pts',(-0.107425845734137,-48.2223019647818,
20.));
#72579=CARTESIAN_POINT('Ctrl Pts',(-0.140838957626559,-48.2191914363652,
0.));
#72580=CARTESIAN_POINT('Ctrl Pts',(-0.140838957626559,-48.2191914363652,
20.));
#72581=CARTESIAN_POINT('Ctrl Pts',(-0.174248793786917,-48.2160578546352,
0.));
#72582=CARTESIAN_POINT('Ctrl Pts',(-0.174248793786917,-48.2160578546352,
20.));
#72583=CARTESIAN_POINT('Ctrl Pts',(-0.207655338246577,-48.2129012219564,
0.));
#72584=CARTESIAN_POINT('Ctrl Pts',(-0.207655338246577,-48.2129012219564,
20.));
#72585=CARTESIAN_POINT('Ctrl Pts',(-0.241058575037889,-48.2097215407045,
0.));
#72586=CARTESIAN_POINT('Ctrl Pts',(-0.241058575037889,-48.2097215407045,
20.));
#72587=CARTESIAN_POINT('Ctrl Pts',(-0.274458488194607,-48.2065188132665,
0.));
#72588=CARTESIAN_POINT('Ctrl Pts',(-0.274458488194607,-48.2065188132665,
20.));
#72589=CARTESIAN_POINT('Ctrl Pts',(-0.307855061751732,-48.2032930420408,
0.));
#72590=CARTESIAN_POINT('Ctrl Pts',(-0.307855061751732,-48.2032930420408,
20.));
#72591=CARTESIAN_POINT('Ctrl Pts',(-0.341248279745661,-48.2000442294364,
0.));
#72592=CARTESIAN_POINT('Ctrl Pts',(-0.341248279745661,-48.2000442294364,
20.));
#72593=CARTESIAN_POINT('Ctrl Pts',(-0.374638126214117,-48.1967723778737,
0.));
#72594=CARTESIAN_POINT('Ctrl Pts',(-0.374638126214117,-48.1967723778737,
20.));
#72595=CARTESIAN_POINT('Ctrl Pts',(-0.408024585196243,-48.1934774897842,
0.));
#72596=CARTESIAN_POINT('Ctrl Pts',(-0.408024585196243,-48.1934774897842,
20.));
#72597=CARTESIAN_POINT('Ctrl Pts',(-0.441407640732114,-48.1901595676102,
0.));
#72598=CARTESIAN_POINT('Ctrl Pts',(-0.441407640732114,-48.1901595676102,
20.));
#72599=CARTESIAN_POINT('Ctrl Pts',(-0.474787276863089,-48.1868186138054,
0.));
#72600=CARTESIAN_POINT('Ctrl Pts',(-0.474787276863089,-48.1868186138054,
20.));
#72601=CARTESIAN_POINT('Ctrl Pts',(-0.508163477631873,-48.1834546308352,
0.));
#72602=CARTESIAN_POINT('Ctrl Pts',(-0.508163477631873,-48.1834546308352,
20.));
#72603=CARTESIAN_POINT('Ctrl Pts',(-0.541536227082378,-48.1800676211754,
0.));
#72604=CARTESIAN_POINT('Ctrl Pts',(-0.541536227082378,-48.1800676211754,
20.));
#72605=CARTESIAN_POINT('Ctrl Pts',(-0.574905509259906,-48.1766575873132,
0.));
#72606=CARTESIAN_POINT('Ctrl Pts',(-0.574905509259906,-48.1766575873132,
20.));
#72607=CARTESIAN_POINT('Ctrl Pts',(-0.608271308211115,-48.1732245317468,
0.));
#72608=CARTESIAN_POINT('Ctrl Pts',(-0.608271308211115,-48.1732245317468,
20.));
#72609=CARTESIAN_POINT('Ctrl Pts',(-0.641633607984118,-48.1697684569855,
0.));
#72610=CARTESIAN_POINT('Ctrl Pts',(-0.641633607984118,-48.1697684569855,
20.));
#72611=CARTESIAN_POINT('Ctrl Pts',(-0.674992392628253,-48.16628936555,0.));
#72612=CARTESIAN_POINT('Ctrl Pts',(-0.674992392628253,-48.16628936555,20.));
#72613=CARTESIAN_POINT('Ctrl Pts',(-0.708347646194296,-48.1627872599717,
0.));
#72614=CARTESIAN_POINT('Ctrl Pts',(-0.708347646194296,-48.1627872599717,
20.));
#72615=CARTESIAN_POINT('Ctrl Pts',(-0.741699352734275,-48.1592621427937,
0.));
#72616=CARTESIAN_POINT('Ctrl Pts',(-0.741699352734275,-48.1592621427937,
20.));
#72617=CARTESIAN_POINT('Ctrl Pts',(-0.775047496301551,-48.1557140165701,
0.));
#72618=CARTESIAN_POINT('Ctrl Pts',(-0.775047496301551,-48.1557140165701,
20.));
#72619=CARTESIAN_POINT('Ctrl Pts',(-0.808392060950887,-48.1521428838659,
0.));
#72620=CARTESIAN_POINT('Ctrl Pts',(-0.808392060950887,-48.1521428838659,
20.));
#72621=CARTESIAN_POINT('Ctrl Pts',(-0.84173303073841,-48.1485487472572,
0.));
#72622=CARTESIAN_POINT('Ctrl Pts',(-0.84173303073841,-48.1485487472572,
20.));
#72623=CARTESIAN_POINT('Ctrl Pts',(-0.875070389721544,-48.144931609331,
0.));
#72624=CARTESIAN_POINT('Ctrl Pts',(-0.875070389721544,-48.144931609331,
20.));
#72625=CARTESIAN_POINT('Ctrl Pts',(-0.908404121959303,-48.1412914726861,
0.));
#72626=CARTESIAN_POINT('Ctrl Pts',(-0.908404121959303,-48.1412914726861,
20.));
#72627=CARTESIAN_POINT('Ctrl Pts',(-0.941734211511966,-48.137628339932,
0.));
#72628=CARTESIAN_POINT('Ctrl Pts',(-0.941734211511966,-48.137628339932,
20.));
#72629=CARTESIAN_POINT('Ctrl Pts',(-0.975060642441261,-48.1339422136897,
0.));
#72630=CARTESIAN_POINT('Ctrl Pts',(-0.975060642441261,-48.1339422136897,
20.));
#72631=CARTESIAN_POINT('Ctrl Pts',(-1.00838339881034,-48.130233096591,0.));
#72632=CARTESIAN_POINT('Ctrl Pts',(-1.00838339881034,-48.130233096591,20.));
#72633=CARTESIAN_POINT('Ctrl Pts',(-1.04170246468366,-48.1265009912787,
0.));
#72634=CARTESIAN_POINT('Ctrl Pts',(-1.04170246468366,-48.1265009912787,
20.));
#72635=CARTESIAN_POINT('Ctrl Pts',(-1.0750178241273,-48.1227459004068,0.));
#72636=CARTESIAN_POINT('Ctrl Pts',(-1.0750178241273,-48.1227459004068,20.));
#72637=CARTESIAN_POINT('Ctrl Pts',(-1.10832946120863,-48.1189678266406,
0.));
#72638=CARTESIAN_POINT('Ctrl Pts',(-1.10832946120863,-48.1189678266406,
20.));
#72639=CARTESIAN_POINT('Ctrl Pts',(-1.14163735999659,-48.1151667726565,
0.));
#72640=CARTESIAN_POINT('Ctrl Pts',(-1.14163735999659,-48.1151667726565,
20.));
#72641=CARTESIAN_POINT('Ctrl Pts',(-1.17494150456147,-48.111342741142,0.));
#72642=CARTESIAN_POINT('Ctrl Pts',(-1.17494150456147,-48.111342741142,20.));
#72643=CARTESIAN_POINT('Ctrl Pts',(-1.20824187897491,-48.1074957347955,
0.));
#72644=CARTESIAN_POINT('Ctrl Pts',(-1.20824187897491,-48.1074957347955,
20.));
#72645=CARTESIAN_POINT('Ctrl Pts',(-1.24153846731024,-48.1036257563271,
0.));
#72646=CARTESIAN_POINT('Ctrl Pts',(-1.24153846731024,-48.1036257563271,
20.));
#72647=CARTESIAN_POINT('Ctrl Pts',(-1.27483125364217,-48.0997328084577,
0.));
#72648=CARTESIAN_POINT('Ctrl Pts',(-1.27483125364217,-48.0997328084577,
20.));
#72649=CARTESIAN_POINT('Ctrl Pts',(-1.30812022204706,-48.0958168939195,
0.));
#72650=CARTESIAN_POINT('Ctrl Pts',(-1.30812022204706,-48.0958168939195,
20.));
#72651=CARTESIAN_POINT('Ctrl Pts',(-1.34140535660262,-48.0918780154556,
0.));
#72652=CARTESIAN_POINT('Ctrl Pts',(-1.34140535660262,-48.0918780154556,
20.));
#72653=CARTESIAN_POINT('Ctrl Pts',(-1.37468664138803,-48.0879161758201,
0.));
#72654=CARTESIAN_POINT('Ctrl Pts',(-1.37468664138803,-48.0879161758201,
20.));
#72655=CARTESIAN_POINT('Ctrl Pts',(-1.40796406048389,-48.0839313777781,
0.));
#72656=CARTESIAN_POINT('Ctrl Pts',(-1.40796406048389,-48.0839313777781,
20.));
#72657=CARTESIAN_POINT('Ctrl Pts',(-1.44123759797226,-48.0799236241059,
0.));
#72658=CARTESIAN_POINT('Ctrl Pts',(-1.44123759797226,-48.0799236241059,
20.));
#72659=CARTESIAN_POINT('Ctrl Pts',(-1.47450723793683,-48.0758929175908,
0.));
#72660=CARTESIAN_POINT('Ctrl Pts',(-1.47450723793683,-48.0758929175908,
20.));
#72661=CARTESIAN_POINT('Ctrl Pts',(-1.50777296446293,-48.071839261032,0.));
#72662=CARTESIAN_POINT('Ctrl Pts',(-1.50777296446293,-48.071839261032,20.));
#72663=CARTESIAN_POINT('Ctrl Pts',(-1.54103476163745,-48.0677626572394,
0.));
#72664=CARTESIAN_POINT('Ctrl Pts',(-1.54103476163745,-48.0677626572394,
20.));
#72665=CARTESIAN_POINT('Ctrl Pts',(-1.57429261354891,-48.0636631090342,
0.));
#72666=CARTESIAN_POINT('Ctrl Pts',(-1.57429261354891,-48.0636631090342,
20.));
#72667=CARTESIAN_POINT('Ctrl Pts',(-1.60754650428747,-48.0595406192492,
0.));
#72668=CARTESIAN_POINT('Ctrl Pts',(-1.60754650428747,-48.0595406192492,
20.));
#72669=CARTESIAN_POINT('Ctrl Pts',(-1.64079641794463,-48.0553951907273,
0.));
#72670=CARTESIAN_POINT('Ctrl Pts',(-1.64079641794463,-48.0553951907273,
20.));
#72671=CARTESIAN_POINT('Ctrl Pts',(-1.67404233861339,-48.0512268263229,
0.));
#72672=CARTESIAN_POINT('Ctrl Pts',(-1.67404233861339,-48.0512268263229,
20.));
#72673=CARTESIAN_POINT('Ctrl Pts',(-1.70728425038806,-48.0470355289011,
0.));
#72674=CARTESIAN_POINT('Ctrl Pts',(-1.70728425038806,-48.0470355289011,
20.));
#72675=CARTESIAN_POINT('Ctrl Pts',(-1.74052213736473,-48.0428213013379,
0.));
#72676=CARTESIAN_POINT('Ctrl Pts',(-1.74052213736473,-48.0428213013379,
20.));
#72677=CARTESIAN_POINT('Ctrl Pts',(-1.77375598364111,-48.038584146521,0.));
#72678=CARTESIAN_POINT('Ctrl Pts',(-1.77375598364111,-48.038584146521,20.));
#72679=CARTESIAN_POINT('Ctrl Pts',(-1.80698577331665,-48.0343240673492,
0.));
#72680=CARTESIAN_POINT('Ctrl Pts',(-1.80698577331665,-48.0343240673492,
20.));
#72681=CARTESIAN_POINT('Ctrl Pts',(-1.84021149049247,-48.0300410667328,
0.));
#72682=CARTESIAN_POINT('Ctrl Pts',(-1.84021149049247,-48.0300410667328,
20.));
#72683=CARTESIAN_POINT('Ctrl Pts',(-1.87343311927143,-48.0257351475934,
0.));
#72684=CARTESIAN_POINT('Ctrl Pts',(-1.87343311927143,-48.0257351475934,
20.));
#72685=CARTESIAN_POINT('Ctrl Pts',(-1.90665064375788,-48.0214063128629,
0.));
#72686=CARTESIAN_POINT('Ctrl Pts',(-1.90665064375788,-48.0214063128629,
20.));
#72687=CARTESIAN_POINT('Ctrl Pts',(-1.93986404805774,-48.0170545654849,
0.));
#72688=CARTESIAN_POINT('Ctrl Pts',(-1.93986404805774,-48.0170545654849,
20.));
#72689=CARTESIAN_POINT('Ctrl Pts',(-1.97307331627851,-48.0126799084137,
0.));
#72690=CARTESIAN_POINT('Ctrl Pts',(-1.97307331627851,-48.0126799084137,
20.));
#72691=CARTESIAN_POINT('Ctrl Pts',(-2.00627843252927,-48.0082823446147,
0.));
#72692=CARTESIAN_POINT('Ctrl Pts',(-2.00627843252927,-48.0082823446147,
20.));
#72693=CARTESIAN_POINT('Ctrl Pts',(-2.03947938092069,-48.0038618770642,
0.));
#72694=CARTESIAN_POINT('Ctrl Pts',(-2.03947938092069,-48.0038618770642,
20.));
#72695=CARTESIAN_POINT('Ctrl Pts',(-2.07267614556538,-47.9994185087499,
0.));
#72696=CARTESIAN_POINT('Ctrl Pts',(-2.07267614556538,-47.9994185087499,
20.));
#72697=CARTESIAN_POINT('Ctrl Pts',(-2.1058687105775,-47.994952242671,0.));
#72698=CARTESIAN_POINT('Ctrl Pts',(-2.1058687105775,-47.994952242671,20.));
#72699=CARTESIAN_POINT('Ctrl Pts',(-2.13905706007287,-47.9904630818375,
0.));
#72700=CARTESIAN_POINT('Ctrl Pts',(-2.13905706007287,-47.9904630818375,
20.));
#72701=CARTESIAN_POINT('Ctrl Pts',(-2.172241178169,-47.9859510292704,0.));
#72702=CARTESIAN_POINT('Ctrl Pts',(-2.172241178169,-47.9859510292704,20.));
#72703=CARTESIAN_POINT('Ctrl Pts',(-2.20542104898522,-47.9814160880019,
0.));
#72704=CARTESIAN_POINT('Ctrl Pts',(-2.20542104898522,-47.9814160880019,
20.));
#72705=CARTESIAN_POINT('Ctrl Pts',(-2.23859665664241,-47.9768582610752,
0.));
#72706=CARTESIAN_POINT('Ctrl Pts',(-2.23859665664241,-47.9768582610752,
20.));
#72707=CARTESIAN_POINT('Ctrl Pts',(-2.27176798526354,-47.9722775515452,
0.));
#72708=CARTESIAN_POINT('Ctrl Pts',(-2.27176798526354,-47.9722775515452,
20.));
#72709=CARTESIAN_POINT('Ctrl Pts',(-2.30493501897296,-47.9676739624772,
0.));
#72710=CARTESIAN_POINT('Ctrl Pts',(-2.30493501897296,-47.9676739624772,
20.));
#72711=CARTESIAN_POINT('Ctrl Pts',(-2.33809774189659,-47.9630474969481,
0.));
#72712=CARTESIAN_POINT('Ctrl Pts',(-2.33809774189659,-47.9630474969481,
20.));
#72713=CARTESIAN_POINT('Ctrl Pts',(-2.37125613816232,-47.9583981580454,
0.));
#72714=CARTESIAN_POINT('Ctrl Pts',(-2.37125613816232,-47.9583981580454,
20.));
#72715=CARTESIAN_POINT('Ctrl Pts',(-2.40441019189961,-47.9537259488681,
0.));
#72716=CARTESIAN_POINT('Ctrl Pts',(-2.40441019189961,-47.9537259488681,
20.));
#72717=CARTESIAN_POINT('Ctrl Pts',(-2.43755988723967,-47.9490308725257,
0.));
#72718=CARTESIAN_POINT('Ctrl Pts',(-2.43755988723967,-47.9490308725257,
20.));
#72719=CARTESIAN_POINT('Ctrl Pts',(-2.4707052083155,-47.9443129321394,0.));
#72720=CARTESIAN_POINT('Ctrl Pts',(-2.4707052083155,-47.9443129321394,20.));
#72721=CARTESIAN_POINT('Ctrl Pts',(-2.5038461392621,-47.9395721308414,0.));
#72722=CARTESIAN_POINT('Ctrl Pts',(-2.5038461392621,-47.9395721308414,20.));
#72723=CARTESIAN_POINT('Ctrl Pts',(-2.53698266421615,-47.9348084717752,
0.));
#72724=CARTESIAN_POINT('Ctrl Pts',(-2.53698266421615,-47.9348084717752,
20.));
#72725=CARTESIAN_POINT('Ctrl Pts',(-2.57011476731624,-47.9300219580955,
0.));
#72726=CARTESIAN_POINT('Ctrl Pts',(-2.57011476731624,-47.9300219580955,
20.));
#72727=CARTESIAN_POINT('Ctrl Pts',(-2.60324243270259,-47.9252125929679,
0.));
#72728=CARTESIAN_POINT('Ctrl Pts',(-2.60324243270259,-47.9252125929679,
20.));
#72729=CARTESIAN_POINT('Ctrl Pts',(-2.6363656445172,-47.9203803795688,0.));
#72730=CARTESIAN_POINT('Ctrl Pts',(-2.6363656445172,-47.9203803795688,20.));
#72731=CARTESIAN_POINT('Ctrl Pts',(-2.66948438690367,-47.9155253210858,
0.));
#72732=CARTESIAN_POINT('Ctrl Pts',(-2.66948438690367,-47.9155253210858,
20.));
#72733=CARTESIAN_POINT('Ctrl Pts',(-2.70259864400759,-47.9106474207177,
0.));
#72734=CARTESIAN_POINT('Ctrl Pts',(-2.70259864400759,-47.9106474207177,
20.));
#72735=CARTESIAN_POINT('Ctrl Pts',(-2.7357083999763,-47.9057466816743,0.));
#72736=CARTESIAN_POINT('Ctrl Pts',(-2.7357083999763,-47.9057466816743,20.));
#72737=CARTESIAN_POINT('Ctrl Pts',(-2.76881363895919,-47.9008231071768,
0.));
#72738=CARTESIAN_POINT('Ctrl Pts',(-2.76881363895919,-47.9008231071768,
20.));
#72739=CARTESIAN_POINT('Ctrl Pts',(-2.80191434510735,-47.8958767004573,
0.));
#72740=CARTESIAN_POINT('Ctrl Pts',(-2.80191434510735,-47.8958767004573,
20.));
#72741=CARTESIAN_POINT('Ctrl Pts',(-2.83501050257377,-47.8909074647592,
0.));
#72742=CARTESIAN_POINT('Ctrl Pts',(-2.83501050257377,-47.8909074647592,
20.));
#72743=CARTESIAN_POINT('Ctrl Pts',(-2.86810209551309,-47.8859154033363,
0.));
#72744=CARTESIAN_POINT('Ctrl Pts',(-2.86810209551309,-47.8859154033363,
20.));
#72745=CARTESIAN_POINT('Ctrl Pts',(-2.90118910808201,-47.8809005194543,
0.));
#72746=CARTESIAN_POINT('Ctrl Pts',(-2.90118910808201,-47.8809005194543,
20.));
#72747=CARTESIAN_POINT('Ctrl Pts',(-2.93427152443919,-47.8758628163901,
0.));
#72748=CARTESIAN_POINT('Ctrl Pts',(-2.93427152443919,-47.8758628163901,
20.));
#72749=CARTESIAN_POINT('Ctrl Pts',(-2.96734932874506,-47.8708022974315,
0.));
#72750=CARTESIAN_POINT('Ctrl Pts',(-2.96734932874506,-47.8708022974315,
20.));
#72751=CARTESIAN_POINT('Ctrl Pts',(-3.00042250516194,-47.8657189658771,
0.));
#72752=CARTESIAN_POINT('Ctrl Pts',(-3.00042250516194,-47.8657189658771,
20.));
#72753=CARTESIAN_POINT('Ctrl Pts',(-3.03349103785389,-47.8606128250365,
0.));
#72754=CARTESIAN_POINT('Ctrl Pts',(-3.03349103785389,-47.8606128250365,
20.));
#72755=CARTESIAN_POINT('Ctrl Pts',(-3.06655491098683,-47.8554838782302,
0.));
#72756=CARTESIAN_POINT('Ctrl Pts',(-3.06655491098683,-47.8554838782302,
20.));
#72757=CARTESIAN_POINT('Ctrl Pts',(-3.09961410872877,-47.8503321287903,
0.));
#72758=CARTESIAN_POINT('Ctrl Pts',(-3.09961410872877,-47.8503321287903,
20.));
#72759=CARTESIAN_POINT('Ctrl Pts',(-3.13266861524955,-47.8451575800601,
0.));
#72760=CARTESIAN_POINT('Ctrl Pts',(-3.13266861524955,-47.8451575800601,
20.));
#72761=CARTESIAN_POINT('Ctrl Pts',(-3.16571841472091,-47.8399602353939,
0.));
#72762=CARTESIAN_POINT('Ctrl Pts',(-3.16571841472091,-47.8399602353939,
20.));
#72763=CARTESIAN_POINT('Ctrl Pts',(-3.19876349131676,-47.834740098157,0.));
#72764=CARTESIAN_POINT('Ctrl Pts',(-3.19876349131676,-47.834740098157,20.));
#72765=CARTESIAN_POINT('Ctrl Pts',(-3.23180382921274,-47.829497171726,0.));
#72766=CARTESIAN_POINT('Ctrl Pts',(-3.23180382921274,-47.829497171726,20.));
#72767=CARTESIAN_POINT('Ctrl Pts',(-3.26483941258678,-47.8242314594881,
0.));
#72768=CARTESIAN_POINT('Ctrl Pts',(-3.26483941258678,-47.8242314594881,
20.));
#72769=CARTESIAN_POINT('Ctrl Pts',(-3.29787022561837,-47.818942964842,0.));
#72770=CARTESIAN_POINT('Ctrl Pts',(-3.29787022561837,-47.818942964842,20.));
#72771=CARTESIAN_POINT('Ctrl Pts',(-3.33089625248904,-47.813631691197,0.));
#72772=CARTESIAN_POINT('Ctrl Pts',(-3.33089625248904,-47.813631691197,20.));
#72773=CARTESIAN_POINT('Ctrl Pts',(-3.36391747738215,-47.8082976419741,
0.));
#72774=CARTESIAN_POINT('Ctrl Pts',(-3.36391747738215,-47.8082976419741,
20.));
#72775=CARTESIAN_POINT('Ctrl Pts',(-3.39693388448307,-47.802940820605,0.));
#72776=CARTESIAN_POINT('Ctrl Pts',(-3.39693388448307,-47.802940820605,20.));
#72777=CARTESIAN_POINT('Ctrl Pts',(-3.42994545797923,-47.797561230533,0.));
#72778=CARTESIAN_POINT('Ctrl Pts',(-3.42994545797923,-47.797561230533,20.));
#72779=CARTESIAN_POINT('Ctrl Pts',(-3.46295218206013,-47.7921588752121,
0.));
#72780=CARTESIAN_POINT('Ctrl Pts',(-3.46295218206013,-47.7921588752121,
20.));
#72781=CARTESIAN_POINT('Ctrl Pts',(-3.49595404091729,-47.7867337581073,
0.));
#72782=CARTESIAN_POINT('Ctrl Pts',(-3.49595404091729,-47.7867337581073,
20.));
#72783=CARTESIAN_POINT('Ctrl Pts',(-3.52895101874416,-47.7812858826946,
0.));
#72784=CARTESIAN_POINT('Ctrl Pts',(-3.52895101874416,-47.7812858826946,
20.));
#72785=CARTESIAN_POINT('Ctrl Pts',(-3.56194309973643,-47.7758152524613,
0.));
#72786=CARTESIAN_POINT('Ctrl Pts',(-3.56194309973643,-47.7758152524613,
20.));
#72787=CARTESIAN_POINT('Ctrl Pts',(-3.59493026809159,-47.7703218709055,
0.));
#72788=CARTESIAN_POINT('Ctrl Pts',(-3.59493026809159,-47.7703218709055,
20.));
#72789=CARTESIAN_POINT('Ctrl Pts',(-3.62791250800925,-47.764805741537,0.));
#72790=CARTESIAN_POINT('Ctrl Pts',(-3.62791250800925,-47.764805741537,20.));
#72791=CARTESIAN_POINT('Ctrl Pts',(-3.66088980369085,-47.7592668678762,
0.));
#72792=CARTESIAN_POINT('Ctrl Pts',(-3.66088980369085,-47.7592668678762,
20.));
#72793=CARTESIAN_POINT('Ctrl Pts',(-3.69386213933995,-47.7537052534546,
0.));
#72794=CARTESIAN_POINT('Ctrl Pts',(-3.69386213933995,-47.7537052534546,
20.));
#72795=CARTESIAN_POINT('Ctrl Pts',(-3.72682949916223,-47.7481209018149,
0.));
#72796=CARTESIAN_POINT('Ctrl Pts',(-3.72682949916223,-47.7481209018149,
20.));
#72797=CARTESIAN_POINT('Ctrl Pts',(-3.75979186736546,-47.7425138165111,
0.));
#72798=CARTESIAN_POINT('Ctrl Pts',(-3.75979186736546,-47.7425138165111,
20.));
#72799=CARTESIAN_POINT('Ctrl Pts',(-3.7927492281595,-47.7368840011081,0.));
#72800=CARTESIAN_POINT('Ctrl Pts',(-3.7927492281595,-47.7368840011081,20.));
#72801=CARTESIAN_POINT('Ctrl Pts',(-3.82570156575624,-47.7312314591817,
0.));
#72802=CARTESIAN_POINT('Ctrl Pts',(-3.82570156575624,-47.7312314591817,
20.));
#72803=CARTESIAN_POINT('Ctrl Pts',(-3.85864886436974,-47.7255561943191,
0.));
#72804=CARTESIAN_POINT('Ctrl Pts',(-3.85864886436974,-47.7255561943191,
20.));
#72805=CARTESIAN_POINT('Ctrl Pts',(-3.89159110821606,-47.719858210118,0.));
#72806=CARTESIAN_POINT('Ctrl Pts',(-3.89159110821606,-47.719858210118,20.));
#72807=CARTESIAN_POINT('Ctrl Pts',(-3.92452828151334,-47.7141375101875,
0.));
#72808=CARTESIAN_POINT('Ctrl Pts',(-3.92452828151334,-47.7141375101875,
20.));
#72809=CARTESIAN_POINT('Ctrl Pts',(-3.95746036848188,-47.7083940981477,
0.));
#72810=CARTESIAN_POINT('Ctrl Pts',(-3.95746036848188,-47.7083940981477,
20.));
#72811=CARTESIAN_POINT('Ctrl Pts',(-3.99038735334402,-47.7026279776294,
0.));
#72812=CARTESIAN_POINT('Ctrl Pts',(-3.99038735334402,-47.7026279776294,
20.));
#72813=CARTESIAN_POINT('Ctrl Pts',(-4.02330922032434,-47.6968391522753,
0.));
#72814=CARTESIAN_POINT('Ctrl Pts',(-4.02330922032434,-47.6968391522753,
20.));
#72815=CARTESIAN_POINT('Ctrl Pts',(-4.05622595364953,-47.6910276257391,
0.));
#72816=CARTESIAN_POINT('Ctrl Pts',(-4.05622595364953,-47.6910276257391,
20.));
#72817=CARTESIAN_POINT('Ctrl Pts',(-4.0891375375485,-47.6851934016861,0.));
#72818=CARTESIAN_POINT('Ctrl Pts',(-4.0891375375485,-47.6851934016861,20.));
#72819=CARTESIAN_POINT('Ctrl Pts',(-4.1220439562522,-47.6793364837921,0.));
#72820=CARTESIAN_POINT('Ctrl Pts',(-4.1220439562522,-47.6793364837921,20.));
#72821=CARTESIAN_POINT('Ctrl Pts',(-4.15494519399371,-47.6734568757434,
0.));
#72822=CARTESIAN_POINT('Ctrl Pts',(-4.15494519399371,-47.6734568757434,
20.));
#72823=CARTESIAN_POINT('Ctrl Pts',(-4.18784123500837,-47.6675545812371,
0.));
#72824=CARTESIAN_POINT('Ctrl Pts',(-4.18784123500837,-47.6675545812371,
20.));
#72825=CARTESIAN_POINT('Ctrl Pts',(-4.22073206353346,-47.6616296039816,
0.));
#72826=CARTESIAN_POINT('Ctrl Pts',(-4.22073206353346,-47.6616296039816,
20.));
#72827=CARTESIAN_POINT('Ctrl Pts',(-4.25361766380861,-47.6556819476964,
0.));
#72828=CARTESIAN_POINT('Ctrl Pts',(-4.25361766380861,-47.6556819476964,
20.));
#72829=CARTESIAN_POINT('Ctrl Pts',(-4.28649802007568,-47.6497116161128,
0.));
#72830=CARTESIAN_POINT('Ctrl Pts',(-4.28649802007568,-47.6497116161128,
20.));
#72831=CARTESIAN_POINT('Ctrl Pts',(-4.31937311657887,-47.6437186129734,
0.));
#72832=CARTESIAN_POINT('Ctrl Pts',(-4.31937311657887,-47.6437186129734,
20.));
#72833=CARTESIAN_POINT('Ctrl Pts',(-4.35224293756441,-47.6377029420315,
0.));
#72834=CARTESIAN_POINT('Ctrl Pts',(-4.35224293756441,-47.6377029420315,
20.));
#72835=CARTESIAN_POINT('Ctrl Pts',(-4.38510746728076,-47.6316646070511,
0.));
#72836=CARTESIAN_POINT('Ctrl Pts',(-4.38510746728076,-47.6316646070511,
20.));
#72837=CARTESIAN_POINT('Ctrl Pts',(-4.41796668997837,-47.6256036118071,
0.));
#72838=CARTESIAN_POINT('Ctrl Pts',(-4.41796668997837,-47.6256036118071,
20.));
#72839=CARTESIAN_POINT('Ctrl Pts',(-4.45082058991005,-47.6195199600851,
0.));
#72840=CARTESIAN_POINT('Ctrl Pts',(-4.45082058991005,-47.6195199600851,
20.));
#72841=CARTESIAN_POINT('Ctrl Pts',(-4.48366915133085,-47.6134136556823,
0.));
#72842=CARTESIAN_POINT('Ctrl Pts',(-4.48366915133085,-47.6134136556823,
20.));
#72843=CARTESIAN_POINT('Ctrl Pts',(-4.51651235849824,-47.6072847024073,
0.));
#72844=CARTESIAN_POINT('Ctrl Pts',(-4.51651235849824,-47.6072847024073,
20.));
#72845=CARTESIAN_POINT('Ctrl Pts',(-4.54935019567199,-47.6011331040799,
0.));
#72846=CARTESIAN_POINT('Ctrl Pts',(-4.54935019567199,-47.6011331040799,
20.));
#72847=CARTESIAN_POINT('Ctrl Pts',(-4.5821826471142,-47.5949588645311,0.));
#72848=CARTESIAN_POINT('Ctrl Pts',(-4.5821826471142,-47.5949588645311,20.));
#72849=CARTESIAN_POINT('Ctrl Pts',(-4.61500969708897,-47.5887619876026,
0.));
#72850=CARTESIAN_POINT('Ctrl Pts',(-4.61500969708897,-47.5887619876026,
20.));
#72851=CARTESIAN_POINT('Ctrl Pts',(-4.64783132986261,-47.5825424771468,
0.));
#72852=CARTESIAN_POINT('Ctrl Pts',(-4.64783132986261,-47.5825424771468,
20.));
#72853=CARTESIAN_POINT('Ctrl Pts',(-4.68064752970371,-47.5763003370265,
0.));
#72854=CARTESIAN_POINT('Ctrl Pts',(-4.68064752970371,-47.5763003370265,
20.));
#72855=CARTESIAN_POINT('Ctrl Pts',(-4.7134582808831,-47.5700355711162,0.));
#72856=CARTESIAN_POINT('Ctrl Pts',(-4.7134582808831,-47.5700355711162,20.));
#72857=CARTESIAN_POINT('Ctrl Pts',(-4.74626356767414,-47.5637481833017,
0.));
#72858=CARTESIAN_POINT('Ctrl Pts',(-4.74626356767414,-47.5637481833017,
20.));
#72859=CARTESIAN_POINT('Ctrl Pts',(-4.77906337435245,-47.5574381774801,
0.));
#72860=CARTESIAN_POINT('Ctrl Pts',(-4.77906337435245,-47.5574381774801,
20.));
#72861=CARTESIAN_POINT('Ctrl Pts',(-4.8118576851959,-47.5511055575592,0.));
#72862=CARTESIAN_POINT('Ctrl Pts',(-4.8118576851959,-47.5511055575592,20.));
#72863=CARTESIAN_POINT('Ctrl Pts',(-4.84464648448476,-47.5447503274583,
0.));
#72864=CARTESIAN_POINT('Ctrl Pts',(-4.84464648448476,-47.5447503274583,
20.));
#72865=CARTESIAN_POINT('Ctrl Pts',(-4.87742975650163,-47.538372491107,0.));
#72866=CARTESIAN_POINT('Ctrl Pts',(-4.87742975650163,-47.538372491107,20.));
#72867=CARTESIAN_POINT('Ctrl Pts',(-4.91020748553146,-47.5319720524462,
0.));
#72868=CARTESIAN_POINT('Ctrl Pts',(-4.91020748553146,-47.5319720524462,
20.));
#72869=CARTESIAN_POINT('Ctrl Pts',(-4.94297965586158,-47.5255490154281,
0.));
#72870=CARTESIAN_POINT('Ctrl Pts',(-4.94297965586158,-47.5255490154281,
20.));
#72871=CARTESIAN_POINT('Ctrl Pts',(-4.97574625178171,-47.519103384016,0.));
#72872=CARTESIAN_POINT('Ctrl Pts',(-4.97574625178171,-47.519103384016,20.));
#72873=CARTESIAN_POINT('Ctrl Pts',(-5.00850725758369,-47.5126351621839,
0.));
#72874=CARTESIAN_POINT('Ctrl Pts',(-5.00850725758369,-47.5126351621839,
20.));
#72875=CARTESIAN_POINT('Ctrl Pts',(-5.04126265756156,-47.5061443539168,
0.));
#72876=CARTESIAN_POINT('Ctrl Pts',(-5.04126265756156,-47.5061443539168,
20.));
#72877=CARTESIAN_POINT('Ctrl Pts',(-5.074012436012,-47.4996309632108,0.));
#72878=CARTESIAN_POINT('Ctrl Pts',(-5.074012436012,-47.4996309632108,20.));
#72879=CARTESIAN_POINT('Ctrl Pts',(-5.10675657723404,-47.4930949940731,
0.));
#72880=CARTESIAN_POINT('Ctrl Pts',(-5.10675657723404,-47.4930949940731,
20.));
#72881=CARTESIAN_POINT('Ctrl Pts',(-5.13949506552924,-47.4865364505219,
0.));
#72882=CARTESIAN_POINT('Ctrl Pts',(-5.13949506552924,-47.4865364505219,
20.));
#72883=CARTESIAN_POINT('Ctrl Pts',(-5.17222788520145,-47.4799553365862,
0.));
#72884=CARTESIAN_POINT('Ctrl Pts',(-5.17222788520145,-47.4799553365862,
20.));
#72885=CARTESIAN_POINT('Ctrl Pts',(-5.20495502055715,-47.4733516563069,
0.));
#72886=CARTESIAN_POINT('Ctrl Pts',(-5.20495502055715,-47.4733516563069,
20.));
#72887=CARTESIAN_POINT('Ctrl Pts',(-5.23767645590512,-47.4667254137359,
0.));
#72888=CARTESIAN_POINT('Ctrl Pts',(-5.23767645590512,-47.4667254137359,
20.));
#72889=CARTESIAN_POINT('Ctrl Pts',(-5.27039217555657,-47.4600766129357,
0.));
#72890=CARTESIAN_POINT('Ctrl Pts',(-5.27039217555657,-47.4600766129357,
20.));
#72891=CARTESIAN_POINT('Ctrl Pts',(-5.30310216382507,-47.4534052579797,
0.));
#72892=CARTESIAN_POINT('Ctrl Pts',(-5.30310216382507,-47.4534052579797,
20.));
#72893=CARTESIAN_POINT('Ctrl Pts',(-5.33580640502662,-47.4467113529523,
0.));
#72894=CARTESIAN_POINT('Ctrl Pts',(-5.33580640502662,-47.4467113529523,
20.));
#72895=CARTESIAN_POINT('Ctrl Pts',(-5.36850488347925,-47.4399949019487,
0.));
#72896=CARTESIAN_POINT('Ctrl Pts',(-5.36850488347925,-47.4399949019487,
20.));
#72897=CARTESIAN_POINT('Ctrl Pts',(-5.4011975835038,-47.4332559090748,0.));
#72898=CARTESIAN_POINT('Ctrl Pts',(-5.4011975835038,-47.4332559090748,20.));
#72899=CARTESIAN_POINT('Ctrl Pts',(-5.43388448942351,-47.4264943784481,
0.));
#72900=CARTESIAN_POINT('Ctrl Pts',(-5.43388448942351,-47.4264943784481,
20.));
#72901=CARTESIAN_POINT('Ctrl Pts',(-5.46656558556427,-47.4197103141976,
0.));
#72902=CARTESIAN_POINT('Ctrl Pts',(-5.46656558556427,-47.4197103141976,
20.));
#72903=CARTESIAN_POINT('Ctrl Pts',(-5.49924085625465,-47.4129037204631,
0.));
#72904=CARTESIAN_POINT('Ctrl Pts',(-5.49924085625465,-47.4129037204631,
20.));
#72905=CARTESIAN_POINT('Ctrl Pts',(-5.53191028582555,-47.4060746013959,
0.));
#72906=CARTESIAN_POINT('Ctrl Pts',(-5.53191028582555,-47.4060746013959,
20.));
#72907=CARTESIAN_POINT('Ctrl Pts',(-5.56457385861038,-47.3992229611579,
0.));
#72908=CARTESIAN_POINT('Ctrl Pts',(-5.56457385861038,-47.3992229611579,
20.));
#72909=CARTESIAN_POINT('Ctrl Pts',(-5.59723155894484,-47.3923488039217,
0.));
#72910=CARTESIAN_POINT('Ctrl Pts',(-5.59723155894484,-47.3923488039217,
20.));
#72911=CARTESIAN_POINT('Ctrl Pts',(-5.62988337116716,-47.3854521338708,
0.));
#72912=CARTESIAN_POINT('Ctrl Pts',(-5.62988337116716,-47.3854521338708,
20.));
#72913=CARTESIAN_POINT('Ctrl Pts',(-5.66252927961812,-47.3785329551997,
0.));
#72914=CARTESIAN_POINT('Ctrl Pts',(-5.66252927961812,-47.3785329551997,
20.));
#72915=CARTESIAN_POINT('Ctrl Pts',(-5.69516926864089,-47.3715912721141,
0.));
#72916=CARTESIAN_POINT('Ctrl Pts',(-5.69516926864089,-47.3715912721141,
20.));
#72917=CARTESIAN_POINT('Ctrl Pts',(-5.72780332258136,-47.3646270888308,
0.));
#72918=CARTESIAN_POINT('Ctrl Pts',(-5.72780332258136,-47.3646270888308,
20.));
#72919=CARTESIAN_POINT('Ctrl Pts',(-5.76043142578787,-47.3576404095777,
0.));
#72920=CARTESIAN_POINT('Ctrl Pts',(-5.76043142578787,-47.3576404095777,
20.));
#72921=CARTESIAN_POINT('Ctrl Pts',(-5.79305356261143,-47.3506312385939,
0.));
#72922=CARTESIAN_POINT('Ctrl Pts',(-5.79305356261143,-47.3506312385939,
20.));
#72923=CARTESIAN_POINT('Ctrl Pts',(-5.82566971740557,-47.3435995801292,
0.));
#72924=CARTESIAN_POINT('Ctrl Pts',(-5.82566971740557,-47.3435995801292,
20.));
#72925=CARTESIAN_POINT('Ctrl Pts',(-5.85827987452641,-47.3365454384446,
0.));
#72926=CARTESIAN_POINT('Ctrl Pts',(-5.85827987452641,-47.3365454384446,
20.));
#72927=CARTESIAN_POINT('Ctrl Pts',(-5.89088401833278,-47.3294688178121,
0.));
#72928=CARTESIAN_POINT('Ctrl Pts',(-5.89088401833278,-47.3294688178121,
20.));
#72929=CARTESIAN_POINT('Ctrl Pts',(-5.92348213318599,-47.3223697225143,
0.));
#72930=CARTESIAN_POINT('Ctrl Pts',(-5.92348213318599,-47.3223697225143,
20.));
#72931=CARTESIAN_POINT('Ctrl Pts',(-5.95607420344987,-47.3152481568452,
0.));
#72932=CARTESIAN_POINT('Ctrl Pts',(-5.95607420344987,-47.3152481568452,
20.));
#72933=CARTESIAN_POINT('Ctrl Pts',(-5.98866021349068,-47.3081041251096,
0.));
#72934=CARTESIAN_POINT('Ctrl Pts',(-5.98866021349068,-47.3081041251096,
20.));
#72935=CARTESIAN_POINT('Ctrl Pts',(-6.02124014767731,-47.3009376316237,
0.));
#72936=CARTESIAN_POINT('Ctrl Pts',(-6.02124014767731,-47.3009376316237,
20.));
#72937=CARTESIAN_POINT('Ctrl Pts',(-6.0538139903813,-47.2937486807145,0.));
#72938=CARTESIAN_POINT('Ctrl Pts',(-6.0538139903813,-47.2937486807145,20.));
#72939=CARTESIAN_POINT('Ctrl Pts',(-6.08638172597685,-47.2865372767199,
0.));
#72940=CARTESIAN_POINT('Ctrl Pts',(-6.08638172597685,-47.2865372767199,
20.));
#72941=CARTESIAN_POINT('Ctrl Pts',(-6.11894333884089,-47.2793034239892,
0.));
#72942=CARTESIAN_POINT('Ctrl Pts',(-6.11894333884089,-47.2793034239892,
20.));
#72943=CARTESIAN_POINT('Ctrl Pts',(-6.15149881335291,-47.272047126882,0.));
#72944=CARTESIAN_POINT('Ctrl Pts',(-6.15149881335291,-47.272047126882,20.));
#72945=CARTESIAN_POINT('Ctrl Pts',(-6.1840481338953,-47.2647683897693,0.));
#72946=CARTESIAN_POINT('Ctrl Pts',(-6.1840481338953,-47.2647683897693,20.));
#72947=CARTESIAN_POINT('Ctrl Pts',(-6.21659128485297,-47.2574672170331,
0.));
#72948=CARTESIAN_POINT('Ctrl Pts',(-6.21659128485297,-47.2574672170331,
20.));
#72949=CARTESIAN_POINT('Ctrl Pts',(-6.24912825061344,-47.2501436130661,
0.));
#72950=CARTESIAN_POINT('Ctrl Pts',(-6.24912825061344,-47.2501436130661,
20.));
#72951=CARTESIAN_POINT('Ctrl Pts',(-6.28165901556677,-47.2427975822723,
0.));
#72952=CARTESIAN_POINT('Ctrl Pts',(-6.28165901556677,-47.2427975822723,
20.));
#72953=CARTESIAN_POINT('Ctrl Pts',(-6.31418356410551,-47.2354291290667,
0.));
#72954=CARTESIAN_POINT('Ctrl Pts',(-6.31418356410551,-47.2354291290667,
20.));
#72955=CARTESIAN_POINT('Ctrl Pts',(-6.34670188062517,-47.2280382578755,
0.));
#72956=CARTESIAN_POINT('Ctrl Pts',(-6.34670188062517,-47.2280382578755,
20.));
#72957=CARTESIAN_POINT('Ctrl Pts',(-6.37921394952381,-47.2206249731358,
0.));
#72958=CARTESIAN_POINT('Ctrl Pts',(-6.37921394952381,-47.2206249731358,
20.));
#72959=CARTESIAN_POINT('Ctrl Pts',(-6.41171975520235,-47.213189279296,0.));
#72960=CARTESIAN_POINT('Ctrl Pts',(-6.41171975520235,-47.213189279296,20.));
#72961=CARTESIAN_POINT('Ctrl Pts',(-6.44421928206447,-47.205731180815,0.));
#72962=CARTESIAN_POINT('Ctrl Pts',(-6.44421928206447,-47.205731180815,20.));
#72963=CARTESIAN_POINT('Ctrl Pts',(-6.47671251451639,-47.1982506821625,
0.));
#72964=CARTESIAN_POINT('Ctrl Pts',(-6.47671251451639,-47.1982506821625,
20.));
#72965=CARTESIAN_POINT('Ctrl Pts',(-6.50919943696718,-47.190747787819,0.));
#72966=CARTESIAN_POINT('Ctrl Pts',(-6.50919943696718,-47.190747787819,20.));
#72967=CARTESIAN_POINT('Ctrl Pts',(-6.54168003382863,-47.1832225022762,
0.));
#72968=CARTESIAN_POINT('Ctrl Pts',(-6.54168003382863,-47.1832225022762,
20.));
#72969=CARTESIAN_POINT('Ctrl Pts',(-6.57415428951526,-47.1756748300372,
0.));
#72970=CARTESIAN_POINT('Ctrl Pts',(-6.57415428951526,-47.1756748300372,
20.));
#72971=CARTESIAN_POINT('Ctrl Pts',(-6.60662218844436,-47.168104775616,0.));
#72972=CARTESIAN_POINT('Ctrl Pts',(-6.60662218844436,-47.168104775616,20.));
#72973=CARTESIAN_POINT('Ctrl Pts',(-6.63908371503578,-47.1605123435378,
0.));
#72974=CARTESIAN_POINT('Ctrl Pts',(-6.63908371503578,-47.1605123435378,
20.));
#72975=CARTESIAN_POINT('Ctrl Pts',(-6.67153885371228,-47.1528975383387,
0.));
#72976=CARTESIAN_POINT('Ctrl Pts',(-6.67153885371228,-47.1528975383387,
20.));
#72977=CARTESIAN_POINT('Ctrl Pts',(-6.70398758889918,-47.1452603645656,
0.));
#72978=CARTESIAN_POINT('Ctrl Pts',(-6.70398758889918,-47.1452603645656,
20.));
#72979=CARTESIAN_POINT('Ctrl Pts',(-6.7364299050246,-47.1376008267758,0.));
#72980=CARTESIAN_POINT('Ctrl Pts',(-6.7364299050246,-47.1376008267758,20.));
#72981=CARTESIAN_POINT('Ctrl Pts',(-6.76886578651956,-47.129918929538,0.));
#72982=CARTESIAN_POINT('Ctrl Pts',(-6.76886578651956,-47.129918929538,20.));
#72983=CARTESIAN_POINT('Ctrl Pts',(-6.80129521781809,-47.1222146774323,
0.));
#72984=CARTESIAN_POINT('Ctrl Pts',(-6.80129521781809,-47.1222146774323,
20.));
#72985=CARTESIAN_POINT('Ctrl Pts',(-6.83371818335699,-47.1144880750497,
0.));
#72986=CARTESIAN_POINT('Ctrl Pts',(-6.83371818335699,-47.1144880750497,
20.));
#72987=CARTESIAN_POINT('Ctrl Pts',(-6.8661346675759,-47.1067391269919,0.));
#72988=CARTESIAN_POINT('Ctrl Pts',(-6.8661346675759,-47.1067391269919,20.));
#72989=CARTESIAN_POINT('Ctrl Pts',(-6.89854465491704,-47.0989678378717,
0.));
#72990=CARTESIAN_POINT('Ctrl Pts',(-6.89854465491704,-47.0989678378717,
20.));
#72991=CARTESIAN_POINT('Ctrl Pts',(-6.93094812982543,-47.0911742123123,
0.));
#72992=CARTESIAN_POINT('Ctrl Pts',(-6.93094812982543,-47.0911742123123,
20.));
#72993=CARTESIAN_POINT('Ctrl Pts',(-6.96334507674875,-47.0833582549484,
0.));
#72994=CARTESIAN_POINT('Ctrl Pts',(-6.96334507674875,-47.0833582549484,
20.));
#72995=CARTESIAN_POINT('Ctrl Pts',(-6.99573548013778,-47.0755199704256,
0.));
#72996=CARTESIAN_POINT('Ctrl Pts',(-6.99573548013778,-47.0755199704256,
20.));
#72997=CARTESIAN_POINT('Ctrl Pts',(-7.02811932444603,-47.0676593634011,
0.));
#72998=CARTESIAN_POINT('Ctrl Pts',(-7.02811932444603,-47.0676593634011,
20.));
#72999=CARTESIAN_POINT('Ctrl Pts',(-7.06049659413009,-47.0597764385426,
0.));
#73000=CARTESIAN_POINT('Ctrl Pts',(-7.06049659413009,-47.0597764385426,
20.));
#73001=CARTESIAN_POINT('Ctrl Pts',(-7.09286727364934,-47.0518712005288,
0.));
#73002=CARTESIAN_POINT('Ctrl Pts',(-7.09286727364934,-47.0518712005288,
20.));
#73003=CARTESIAN_POINT('Ctrl Pts',(-7.12523134746605,-47.0439436540493,
0.));
#73004=CARTESIAN_POINT('Ctrl Pts',(-7.12523134746605,-47.0439436540493,
20.));
#73005=CARTESIAN_POINT('Ctrl Pts',(-7.15758880004523,-47.0359938038039,
0.));
#73006=CARTESIAN_POINT('Ctrl Pts',(-7.15758880004523,-47.0359938038039,
20.));
#73007=CARTESIAN_POINT('Ctrl Pts',(-7.18993961585471,-47.0280216545038,
0.));
#73008=CARTESIAN_POINT('Ctrl Pts',(-7.18993961585471,-47.0280216545038,
20.));
#73009=CARTESIAN_POINT('Ctrl Pts',(-7.22228377936531,-47.020027210871,0.));
#73010=CARTESIAN_POINT('Ctrl Pts',(-7.22228377936531,-47.020027210871,20.));
#73011=CARTESIAN_POINT('Ctrl Pts',(-7.25462127505078,-47.012010477639,0.));
#73012=CARTESIAN_POINT('Ctrl Pts',(-7.25462127505078,-47.012010477639,20.));
#73013=CARTESIAN_POINT('Ctrl Pts',(-7.28695208738785,-47.0039714595526,
0.));
#73014=CARTESIAN_POINT('Ctrl Pts',(-7.28695208738785,-47.0039714595526,
20.));
#73015=CARTESIAN_POINT('Ctrl Pts',(-7.31927620085615,-46.9959101613675,
0.));
#73016=CARTESIAN_POINT('Ctrl Pts',(-7.31927620085615,-46.9959101613675,
20.));
#73017=CARTESIAN_POINT('Ctrl Pts',(-7.35159359993819,-46.9878265878505,
0.));
#73018=CARTESIAN_POINT('Ctrl Pts',(-7.35159359993819,-46.9878265878505,
20.));
#73019=CARTESIAN_POINT('Ctrl Pts',(-7.38390426911933,-46.9797207437786,
0.));
#73020=CARTESIAN_POINT('Ctrl Pts',(-7.38390426911933,-46.9797207437786,
20.));
#73021=CARTESIAN_POINT('Ctrl Pts',(-7.41620819288779,-46.9715926339391,
0.));
#73022=CARTESIAN_POINT('Ctrl Pts',(-7.41620819288779,-46.9715926339391,
20.));
#73023=CARTESIAN_POINT('Ctrl Pts',(-7.44850535573483,-46.9634422631307,
0.));
#73024=CARTESIAN_POINT('Ctrl Pts',(-7.44850535573483,-46.9634422631307,
20.));
#73025=CARTESIAN_POINT('Ctrl Pts',(-7.4807957421548,-46.9552696361634,0.));
#73026=CARTESIAN_POINT('Ctrl Pts',(-7.4807957421548,-46.9552696361634,20.));
#73027=CARTESIAN_POINT('Ctrl Pts',(-7.51307933664513,-46.9470747578592,
0.));
#73028=CARTESIAN_POINT('Ctrl Pts',(-7.51307933664513,-46.9470747578592,
20.));
#73029=CARTESIAN_POINT('Ctrl Pts',(-7.54535612370603,-46.9388576330501,
0.));
#73030=CARTESIAN_POINT('Ctrl Pts',(-7.54535612370603,-46.9388576330501,
20.));
#73031=CARTESIAN_POINT('Ctrl Pts',(-7.5776260878407,-46.9306182665792,0.));
#73032=CARTESIAN_POINT('Ctrl Pts',(-7.5776260878407,-46.9306182665792,20.));
#73033=CARTESIAN_POINT('Ctrl Pts',(-7.60988921355522,-46.9223566632999,
0.));
#73034=CARTESIAN_POINT('Ctrl Pts',(-7.60988921355522,-46.9223566632999,
20.));
#73035=CARTESIAN_POINT('Ctrl Pts',(-7.64214548535858,-46.9140728280766,
0.));
#73036=CARTESIAN_POINT('Ctrl Pts',(-7.64214548535858,-46.9140728280766,
20.));
#73037=CARTESIAN_POINT('Ctrl Pts',(-7.67439488776289,-46.9057667657847,
0.));
#73038=CARTESIAN_POINT('Ctrl Pts',(-7.67439488776289,-46.9057667657847,
20.));
#73039=CARTESIAN_POINT('Ctrl Pts',(-7.70663740528332,-46.8974384813109,
0.));
#73040=CARTESIAN_POINT('Ctrl Pts',(-7.70663740528332,-46.8974384813109,
20.));
#73041=CARTESIAN_POINT('Ctrl Pts',(-7.73887302243817,-46.8890879795531,
0.));
#73042=CARTESIAN_POINT('Ctrl Pts',(-7.73887302243817,-46.8890879795531,
20.));
#73043=CARTESIAN_POINT('Ctrl Pts',(-7.77110172374869,-46.8807152654198,
0.));
#73044=CARTESIAN_POINT('Ctrl Pts',(-7.77110172374869,-46.8807152654198,
20.));
#73045=CARTESIAN_POINT('Ctrl Pts',(-7.80332349373919,-46.8723203438306,
0.));
#73046=CARTESIAN_POINT('Ctrl Pts',(-7.80332349373919,-46.8723203438306,
20.));
#73047=CARTESIAN_POINT('Ctrl Pts',(-7.83553831693688,-46.8639032197162,
0.));
#73048=CARTESIAN_POINT('Ctrl Pts',(-7.83553831693688,-46.8639032197162,
20.));
#73049=CARTESIAN_POINT('Ctrl Pts',(-7.86774617787214,-46.855463898018,0.));
#73050=CARTESIAN_POINT('Ctrl Pts',(-7.86774617787214,-46.855463898018,20.));
#73051=CARTESIAN_POINT('Ctrl Pts',(-7.8999470610784,-46.8470023836881,0.));
#73052=CARTESIAN_POINT('Ctrl Pts',(-7.8999470610784,-46.8470023836881,20.));
#73053=CARTESIAN_POINT('Ctrl Pts',(-7.93214095109212,-46.8385186816898,
0.));
#73054=CARTESIAN_POINT('Ctrl Pts',(-7.93214095109212,-46.8385186816898,
20.));
#73055=CARTESIAN_POINT('Ctrl Pts',(-7.96432783245287,-46.8300127969969,
0.));
#73056=CARTESIAN_POINT('Ctrl Pts',(-7.96432783245287,-46.8300127969969,
20.));
#73057=CARTESIAN_POINT('Ctrl Pts',(-7.99650768970305,-46.8214847345942,
0.));
#73058=CARTESIAN_POINT('Ctrl Pts',(-7.99650768970305,-46.8214847345942,
20.));
#73059=CARTESIAN_POINT('Ctrl Pts',(-8.02868050738829,-46.8129344994773,
0.));
#73060=CARTESIAN_POINT('Ctrl Pts',(-8.02868050738829,-46.8129344994773,
20.));
#73061=CARTESIAN_POINT('Ctrl Pts',(-8.0608462700573,-46.8043620966531,0.));
#73062=CARTESIAN_POINT('Ctrl Pts',(-8.0608462700573,-46.8043620966531,20.));
#73063=CARTESIAN_POINT('Ctrl Pts',(-8.09300496226221,-46.7957675311395,
0.));
#73064=CARTESIAN_POINT('Ctrl Pts',(-8.09300496226221,-46.7957675311395,
20.));
#73065=CARTESIAN_POINT('Ctrl Pts',(-8.12515656855803,-46.7871508079658,
0.));
#73066=CARTESIAN_POINT('Ctrl Pts',(-8.12515656855803,-46.7871508079658,
20.));
#73067=CARTESIAN_POINT('Ctrl Pts',(-8.15730107350296,-46.7785119321719,
0.));
#73068=CARTESIAN_POINT('Ctrl Pts',(-8.15730107350296,-46.7785119321719,
20.));
#73069=CARTESIAN_POINT('Ctrl Pts',(-8.18943846165846,-46.7698509088086,
0.));
#73070=CARTESIAN_POINT('Ctrl Pts',(-8.18943846165846,-46.7698509088086,
20.));
#73071=CARTESIAN_POINT('Ctrl Pts',(-8.22156871758883,-46.7611677429374,
0.));
#73072=CARTESIAN_POINT('Ctrl Pts',(-8.22156871758883,-46.7611677429374,
20.));
#73073=CARTESIAN_POINT('Ctrl Pts',(-8.2536918258617,-46.7524624396307,0.));
#73074=CARTESIAN_POINT('Ctrl Pts',(-8.2536918258617,-46.7524624396307,20.));
#73075=CARTESIAN_POINT('Ctrl Pts',(-8.28580777104746,-46.7437350039712,
0.));
#73076=CARTESIAN_POINT('Ctrl Pts',(-8.28580777104746,-46.7437350039712,
20.));
#73077=CARTESIAN_POINT('Ctrl Pts',(-8.31791653771974,-46.7349854410525,
0.));
#73078=CARTESIAN_POINT('Ctrl Pts',(-8.31791653771974,-46.7349854410525,
20.));
#73079=CARTESIAN_POINT('Ctrl Pts',(-8.35001811045537,-46.7262137559789,
0.));
#73080=CARTESIAN_POINT('Ctrl Pts',(-8.35001811045537,-46.7262137559789,
20.));
#73081=CARTESIAN_POINT('Ctrl Pts',(-8.38211247383477,-46.7174199538668,
0.));
#73082=CARTESIAN_POINT('Ctrl Pts',(-8.38211247383477,-46.7174199538668,
20.));
#73083=CARTESIAN_POINT('Ctrl Pts',(-8.41419961244156,-46.7086040398438,
0.));
#73084=CARTESIAN_POINT('Ctrl Pts',(-8.41419961244156,-46.7086040398438,
20.));
#73085=CARTESIAN_POINT('Ctrl Pts',(-8.44627951086263,-46.6997660190488,
0.));
#73086=CARTESIAN_POINT('Ctrl Pts',(-8.44627951086263,-46.6997660190488,
20.));
#73087=CARTESIAN_POINT('Ctrl Pts',(-8.47835215368745,-46.6909058966306,
0.));
#73088=CARTESIAN_POINT('Ctrl Pts',(-8.47835215368745,-46.6909058966306,
20.));
#73089=CARTESIAN_POINT('Ctrl Pts',(-8.51041752550882,-46.6820236777489,
0.));
#73090=CARTESIAN_POINT('Ctrl Pts',(-8.51041752550882,-46.6820236777489,
20.));
#73091=CARTESIAN_POINT('Ctrl Pts',(-8.54247561092259,-46.673119367573,0.));
#73092=CARTESIAN_POINT('Ctrl Pts',(-8.54247561092259,-46.673119367573,20.));
#73093=CARTESIAN_POINT('Ctrl Pts',(-8.57452639452829,-46.6641929712839,
0.));
#73094=CARTESIAN_POINT('Ctrl Pts',(-8.57452639452829,-46.6641929712839,
20.));
#73095=CARTESIAN_POINT('Ctrl Pts',(-8.60656986092879,-46.6552444940739,
0.));
#73096=CARTESIAN_POINT('Ctrl Pts',(-8.60656986092879,-46.6552444940739,
20.));
#73097=CARTESIAN_POINT('Ctrl Pts',(-8.63860599473004,-46.6462739411471,
0.));
#73098=CARTESIAN_POINT('Ctrl Pts',(-8.63860599473004,-46.6462739411471,
20.));
#73099=CARTESIAN_POINT('Ctrl Pts',(-8.67063478054117,-46.6372813177181,
0.));
#73100=CARTESIAN_POINT('Ctrl Pts',(-8.67063478054117,-46.6372813177181,
20.));
#73101=CARTESIAN_POINT('Ctrl Pts',(-8.70265620297455,-46.6282666290119,
0.));
#73102=CARTESIAN_POINT('Ctrl Pts',(-8.70265620297455,-46.6282666290119,
20.));
#73103=CARTESIAN_POINT('Ctrl Pts',(-8.73467024664571,-46.6192298802645,
0.));
#73104=CARTESIAN_POINT('Ctrl Pts',(-8.73467024664571,-46.6192298802645,
20.));
#73105=CARTESIAN_POINT('Ctrl Pts',(-8.76667689617331,-46.6101710767218,
0.));
#73106=CARTESIAN_POINT('Ctrl Pts',(-8.76667689617331,-46.6101710767218,
20.));
#73107=CARTESIAN_POINT('Ctrl Pts',(-8.79867613617934,-46.6010902236408,
0.));
#73108=CARTESIAN_POINT('Ctrl Pts',(-8.79867613617934,-46.6010902236408,
20.));
#73109=CARTESIAN_POINT('Ctrl Pts',(-8.83066795128935,-46.59198732629,0.));
#73110=CARTESIAN_POINT('Ctrl Pts',(-8.83066795128935,-46.59198732629,20.));
#73111=CARTESIAN_POINT('Ctrl Pts',(-8.86265232613216,-46.582862389949,0.));
#73112=CARTESIAN_POINT('Ctrl Pts',(-8.86265232613216,-46.582862389949,20.));
#73113=CARTESIAN_POINT('Ctrl Pts',(-8.8946292453399,-46.5737154199087,0.));
#73114=CARTESIAN_POINT('Ctrl Pts',(-8.8946292453399,-46.5737154199087,20.));
#73115=CARTESIAN_POINT('Ctrl Pts',(-8.92659869354789,-46.5645464214705,
0.));
#73116=CARTESIAN_POINT('Ctrl Pts',(-8.92659869354789,-46.5645464214705,
20.));
#73117=CARTESIAN_POINT('Ctrl Pts',(-8.95856065539471,-46.5553553999467,
0.));
#73118=CARTESIAN_POINT('Ctrl Pts',(-8.95856065539471,-46.5553553999467,
20.));
#73119=CARTESIAN_POINT('Ctrl Pts',(-8.9905151155223,-46.5461423606602,0.));
#73120=CARTESIAN_POINT('Ctrl Pts',(-8.9905151155223,-46.5461423606602,20.));
#73121=CARTESIAN_POINT('Ctrl Pts',(-9.02246205857629,-46.5369073089453,
0.));
#73122=CARTESIAN_POINT('Ctrl Pts',(-9.02246205857629,-46.5369073089453,
20.));
#73123=CARTESIAN_POINT('Ctrl Pts',(-9.05440146920516,-46.5276502501459,
0.));
#73124=CARTESIAN_POINT('Ctrl Pts',(-9.05440146920516,-46.5276502501459,
20.));
#73125=CARTESIAN_POINT('Ctrl Pts',(-9.08633333206091,-46.5183711896174,
0.));
#73126=CARTESIAN_POINT('Ctrl Pts',(-9.08633333206091,-46.5183711896174,
20.));
#73127=CARTESIAN_POINT('Ctrl Pts',(-9.11825763179854,-46.5090701327255,
0.));
#73128=CARTESIAN_POINT('Ctrl Pts',(-9.11825763179854,-46.5090701327255,
20.));
#73129=CARTESIAN_POINT('Ctrl Pts',(-9.15017435307667,-46.4997470848477,
0.));
#73130=CARTESIAN_POINT('Ctrl Pts',(-9.15017435307667,-46.4997470848477,
20.));
#73131=CARTESIAN_POINT('Ctrl Pts',(-9.18208348055726,-46.4904020513722,
0.));
#73132=CARTESIAN_POINT('Ctrl Pts',(-9.18208348055726,-46.4904020513722,
20.));
#73133=CARTESIAN_POINT('Ctrl Pts',(-9.21398499890594,-46.4810350376983,
0.));
#73134=CARTESIAN_POINT('Ctrl Pts',(-9.21398499890594,-46.4810350376983,
20.));
#73135=CARTESIAN_POINT('Ctrl Pts',(-9.24587889279172,-46.4716460492361,
0.));
#73136=CARTESIAN_POINT('Ctrl Pts',(-9.24587889279172,-46.4716460492361,
20.));
#73137=CARTESIAN_POINT('Ctrl Pts',(-9.277765146887,-46.4622350914066,0.));
#73138=CARTESIAN_POINT('Ctrl Pts',(-9.277765146887,-46.4622350914066,20.));
#73139=CARTESIAN_POINT('Ctrl Pts',(-9.30964374586753,-46.4528021696416,
0.));
#73140=CARTESIAN_POINT('Ctrl Pts',(-9.30964374586753,-46.4528021696416,
20.));
#73141=CARTESIAN_POINT('Ctrl Pts',(-9.34151467441242,-46.4433472893837,
0.));
#73142=CARTESIAN_POINT('Ctrl Pts',(-9.34151467441242,-46.4433472893837,
20.));
#73143=CARTESIAN_POINT('Ctrl Pts',(-9.37337791720394,-46.4338704560856,
0.));
#73144=CARTESIAN_POINT('Ctrl Pts',(-9.37337791720394,-46.4338704560856,
20.));
#73145=CARTESIAN_POINT('Ctrl Pts',(-9.40523345892774,-46.4243716752115,
0.));
#73146=CARTESIAN_POINT('Ctrl Pts',(-9.40523345892774,-46.4243716752115,
20.));
#73147=CARTESIAN_POINT('Ctrl Pts',(-9.43708128427275,-46.4148509522358,
0.));
#73148=CARTESIAN_POINT('Ctrl Pts',(-9.43708128427275,-46.4148509522358,
20.));
#73149=CARTESIAN_POINT('Ctrl Pts',(-9.46892137793149,-46.405308292644,0.));
#73150=CARTESIAN_POINT('Ctrl Pts',(-9.46892137793149,-46.405308292644,20.));
#73151=CARTESIAN_POINT('Ctrl Pts',(-9.5007537246001,-46.3957437019326,0.));
#73152=CARTESIAN_POINT('Ctrl Pts',(-9.5007537246001,-46.3957437019326,20.));
#73153=CARTESIAN_POINT('Ctrl Pts',(-9.53257830897852,-46.3861571856095,
0.));
#73154=CARTESIAN_POINT('Ctrl Pts',(-9.53257830897852,-46.3861571856095,
20.));
#73155=CARTESIAN_POINT('Ctrl Pts',(-9.56439511577024,-46.3765487491938,
0.));
#73156=CARTESIAN_POINT('Ctrl Pts',(-9.56439511577024,-46.3765487491938,
20.));
#73157=CARTESIAN_POINT('Ctrl Pts',(-9.59620412968214,-46.3669183982155,
0.));
#73158=CARTESIAN_POINT('Ctrl Pts',(-9.59620412968214,-46.3669183982155,
20.));
#73159=CARTESIAN_POINT('Ctrl Pts',(-9.62800533542437,-46.3572661382147,
0.));
#73160=CARTESIAN_POINT('Ctrl Pts',(-9.62800533542437,-46.3572661382147,
20.));
#73161=CARTESIAN_POINT('Ctrl Pts',(-9.6597987177104,-46.347591974742,0.));
#73162=CARTESIAN_POINT('Ctrl Pts',(-9.6597987177104,-46.347591974742,20.));
#73163=CARTESIAN_POINT('Ctrl Pts',(-9.69158426125693,-46.3378959133587,
0.));
#73164=CARTESIAN_POINT('Ctrl Pts',(-9.69158426125693,-46.3378959133587,
20.));
#73165=CARTESIAN_POINT('Ctrl Pts',(-9.72336195078415,-46.3281779596367,
0.));
#73166=CARTESIAN_POINT('Ctrl Pts',(-9.72336195078415,-46.3281779596367,
20.));
#73167=CARTESIAN_POINT('Ctrl Pts',(-9.75513177101578,-46.3184381191592,
0.));
#73168=CARTESIAN_POINT('Ctrl Pts',(-9.75513177101578,-46.3184381191592,
20.));
#73169=CARTESIAN_POINT('Ctrl Pts',(-9.78689370667941,-46.3086763975205,
0.));
#73170=CARTESIAN_POINT('Ctrl Pts',(-9.78689370667941,-46.3086763975205,
20.));
#73171=CARTESIAN_POINT('Ctrl Pts',(-9.8186477425062,-46.2988928003257,0.));
#73172=CARTESIAN_POINT('Ctrl Pts',(-9.8186477425062,-46.2988928003257,20.));
#73173=CARTESIAN_POINT('Ctrl Pts',(-9.85039386323086,-46.289087333191,0.));
#73174=CARTESIAN_POINT('Ctrl Pts',(-9.85039386323086,-46.289087333191,20.));
#73175=CARTESIAN_POINT('Ctrl Pts',(-9.88213205359192,-46.2792600017436,
0.));
#73176=CARTESIAN_POINT('Ctrl Pts',(-9.88213205359192,-46.2792600017436,
20.));
#73177=CARTESIAN_POINT('Ctrl Pts',(-9.91386229833138,-46.2694108116213,
0.));
#73178=CARTESIAN_POINT('Ctrl Pts',(-9.91386229833138,-46.2694108116213,
20.));
#73179=CARTESIAN_POINT('Ctrl Pts',(-9.94558458219447,-46.2595397684724,
0.));
#73180=CARTESIAN_POINT('Ctrl Pts',(-9.94558458219447,-46.2595397684724,
20.));
#73181=CARTESIAN_POINT('Ctrl Pts',(-9.97729888992981,-46.2496468779557,
0.));
#73182=CARTESIAN_POINT('Ctrl Pts',(-9.97729888992981,-46.2496468779557,
20.));
#73183=CARTESIAN_POINT('Ctrl Pts',(-10.0090052062895,-46.2397321457408,
0.));
#73184=CARTESIAN_POINT('Ctrl Pts',(-10.0090052062895,-46.2397321457408,
20.));
#73185=CARTESIAN_POINT('Ctrl Pts',(-10.0407035160293,-46.2297955775084,
0.));
#73186=CARTESIAN_POINT('Ctrl Pts',(-10.0407035160293,-46.2297955775084,
20.));
#73187=CARTESIAN_POINT('Ctrl Pts',(-10.0723938039086,-46.2198371789501,
0.));
#73188=CARTESIAN_POINT('Ctrl Pts',(-10.0723938039086,-46.2198371789501,
20.));
#73189=CARTESIAN_POINT('Ctrl Pts',(-10.1040760546909,-46.2098569557688,
0.));
#73190=CARTESIAN_POINT('Ctrl Pts',(-10.1040760546909,-46.2098569557688,
20.));
#73191=CARTESIAN_POINT('Ctrl Pts',(-10.1357502531431,-46.1998549136779,
0.));
#73192=CARTESIAN_POINT('Ctrl Pts',(-10.1357502531431,-46.1998549136779,
20.));
#73193=CARTESIAN_POINT('Ctrl Pts',(-10.1674163840354,-46.1898310584014,
0.));
#73194=CARTESIAN_POINT('Ctrl Pts',(-10.1674163840354,-46.1898310584014,
20.));
#73195=CARTESIAN_POINT('Ctrl Pts',(-10.199074432142,-46.179785395674,0.));
#73196=CARTESIAN_POINT('Ctrl Pts',(-10.199074432142,-46.179785395674,20.));
#73197=CARTESIAN_POINT('Ctrl Pts',(-10.2307243822402,-46.169717931241,0.));
#73198=CARTESIAN_POINT('Ctrl Pts',(-10.2307243822402,-46.169717931241,20.));
#73199=CARTESIAN_POINT('Ctrl Pts',(-10.2623662191114,-46.1596286708586,
0.));
#73200=CARTESIAN_POINT('Ctrl Pts',(-10.2623662191114,-46.1596286708586,
20.));
#73201=CARTESIAN_POINT('Ctrl Pts',(-10.2939999275403,-46.1495176202946,
0.));
#73202=CARTESIAN_POINT('Ctrl Pts',(-10.2939999275403,-46.1495176202946,
20.));
#73203=CARTESIAN_POINT('Ctrl Pts',(-10.3256254923156,-46.139384785327,0.));
#73204=CARTESIAN_POINT('Ctrl Pts',(-10.3256254923156,-46.139384785327,20.));
#73205=CARTESIAN_POINT('Ctrl Pts',(-10.3572428982293,-46.1292301717445,
0.));
#73206=CARTESIAN_POINT('Ctrl Pts',(-10.3572428982293,-46.1292301717445,
20.));
#73207=CARTESIAN_POINT('Ctrl Pts',(-10.3888521300774,-46.119053785347,0.));
#73208=CARTESIAN_POINT('Ctrl Pts',(-10.3888521300774,-46.119053785347,20.));
#73209=CARTESIAN_POINT('Ctrl Pts',(-10.4204531726593,-46.1088556319449,
0.));
#73210=CARTESIAN_POINT('Ctrl Pts',(-10.4204531726593,-46.1088556319449,
20.));
#73211=CARTESIAN_POINT('Ctrl Pts',(-10.4520460107784,-46.0986357173598,
0.));
#73212=CARTESIAN_POINT('Ctrl Pts',(-10.4520460107784,-46.0986357173598,
20.));
#73213=CARTESIAN_POINT('Ctrl Pts',(-10.4836306292415,-46.0883940474237,
0.));
#73214=CARTESIAN_POINT('Ctrl Pts',(-10.4836306292415,-46.0883940474237,
20.));
#73215=CARTESIAN_POINT('Ctrl Pts',(-10.5152070128593,-46.0781306279792,
0.));
#73216=CARTESIAN_POINT('Ctrl Pts',(-10.5152070128593,-46.0781306279792,
20.));
#73217=CARTESIAN_POINT('Ctrl Pts',(-10.5467751464457,-46.0678454648793,
0.));
#73218=CARTESIAN_POINT('Ctrl Pts',(-10.5467751464457,-46.0678454648793,
20.));
#73219=CARTESIAN_POINT('Ctrl Pts',(-10.5783350148188,-46.0575385639878,
0.));
#73220=CARTESIAN_POINT('Ctrl Pts',(-10.5783350148188,-46.0575385639878,
20.));
#73221=CARTESIAN_POINT('Ctrl Pts',(-10.6098866028001,-46.0472099311799,
0.));
#73222=CARTESIAN_POINT('Ctrl Pts',(-10.6098866028001,-46.0472099311799,
20.));
#73223=CARTESIAN_POINT('Ctrl Pts',(-10.6414298952151,-46.0368595723418,
0.));
#73224=CARTESIAN_POINT('Ctrl Pts',(-10.6414298952151,-46.0368595723418,
20.));
#73225=CARTESIAN_POINT('Ctrl Pts',(-10.6729648768932,-46.0264874933706,
0.));
#73226=CARTESIAN_POINT('Ctrl Pts',(-10.6729648768932,-46.0264874933706,
20.));
#73227=CARTESIAN_POINT('Ctrl Pts',(-10.7044915326674,-46.0160937001747,
0.));
#73228=CARTESIAN_POINT('Ctrl Pts',(-10.7044915326674,-46.0160937001747,
20.));
#73229=CARTESIAN_POINT('Ctrl Pts',(-10.7360098473747,-46.0056781986726,
0.));
#73230=CARTESIAN_POINT('Ctrl Pts',(-10.7360098473747,-46.0056781986726,
20.));
#73231=CARTESIAN_POINT('Ctrl Pts',(-10.7675198058554,-45.9952409947932,
0.));
#73232=CARTESIAN_POINT('Ctrl Pts',(-10.7675198058554,-45.9952409947932,
20.));
#73233=CARTESIAN_POINT('Ctrl Pts',(-10.7990213929536,-45.9847820944759,
0.));
#73234=CARTESIAN_POINT('Ctrl Pts',(-10.7990213929536,-45.9847820944759,
20.));
#73235=CARTESIAN_POINT('Ctrl Pts',(-10.8305145935168,-45.9743015036702,
0.));
#73236=CARTESIAN_POINT('Ctrl Pts',(-10.8305145935168,-45.9743015036702,
20.));
#73237=CARTESIAN_POINT('Ctrl Pts',(-10.8619993923967,-45.9637992283368,
0.));
#73238=CARTESIAN_POINT('Ctrl Pts',(-10.8619993923967,-45.9637992283368,
20.));
#73239=CARTESIAN_POINT('Ctrl Pts',(-10.8934757744485,-45.9532752744476,
0.));
#73240=CARTESIAN_POINT('Ctrl Pts',(-10.8934757744485,-45.9532752744476,
20.));
#73241=CARTESIAN_POINT('Ctrl Pts',(-10.9249437245321,-45.9427296479861,
0.));
#73242=CARTESIAN_POINT('Ctrl Pts',(-10.9249437245321,-45.9427296479861,
20.));
#73243=CARTESIAN_POINT('Ctrl Pts',(-10.9564032275107,-45.9321623549466,
0.));
#73244=CARTESIAN_POINT('Ctrl Pts',(-10.9564032275107,-45.9321623549466,
20.));
#73245=CARTESIAN_POINT('Ctrl Pts',(-10.9878542682513,-45.9215734013338,
0.));
#73246=CARTESIAN_POINT('Ctrl Pts',(-10.9878542682513,-45.9215734013338,
20.));
#73247=CARTESIAN_POINT('Ctrl Pts',(-11.0192968316247,-45.9109627931629,
0.));
#73248=CARTESIAN_POINT('Ctrl Pts',(-11.0192968316247,-45.9109627931629,
20.));
#73249=CARTESIAN_POINT('Ctrl Pts',(-11.0507309025053,-45.9003305364593,
0.));
#73250=CARTESIAN_POINT('Ctrl Pts',(-11.0507309025053,-45.9003305364593,
20.));
#73251=CARTESIAN_POINT('Ctrl Pts',(-11.0821564657716,-45.8896766372596,
0.));
#73252=CARTESIAN_POINT('Ctrl Pts',(-11.0821564657716,-45.8896766372596,
20.));
#73253=CARTESIAN_POINT('Ctrl Pts',(-11.1135735063059,-45.8790011016108,
0.));
#73254=CARTESIAN_POINT('Ctrl Pts',(-11.1135735063059,-45.8790011016108,
20.));
#73255=CARTESIAN_POINT('Ctrl Pts',(-11.1449820089942,-45.868303935571,0.));
#73256=CARTESIAN_POINT('Ctrl Pts',(-11.1449820089942,-45.868303935571,20.));
#73257=CARTESIAN_POINT('Ctrl Pts',(-11.1763819587263,-45.8575851452088,
0.));
#73258=CARTESIAN_POINT('Ctrl Pts',(-11.1763819587263,-45.8575851452088,
20.));
#73259=CARTESIAN_POINT('Ctrl Pts',(-11.207773340396,-45.8468447366038,0.));
#73260=CARTESIAN_POINT('Ctrl Pts',(-11.207773340396,-45.8468447366038,20.));
#73261=CARTESIAN_POINT('Ctrl Pts',(-11.2391561389011,-45.8360827158468,
0.));
#73262=CARTESIAN_POINT('Ctrl Pts',(-11.2391561389011,-45.8360827158468,
20.));
#73263=CARTESIAN_POINT('Ctrl Pts',(-11.2705303391434,-45.8252990890386,
0.));
#73264=CARTESIAN_POINT('Ctrl Pts',(-11.2705303391434,-45.8252990890386,
20.));
#73265=CARTESIAN_POINT('Ctrl Pts',(-11.3018959260283,-45.8144938622913,
0.));
#73266=CARTESIAN_POINT('Ctrl Pts',(-11.3018959260283,-45.8144938622913,
20.));
#73267=CARTESIAN_POINT('Ctrl Pts',(-11.3332528844652,-45.8036670417272,
0.));
#73268=CARTESIAN_POINT('Ctrl Pts',(-11.3332528844652,-45.8036670417272,
20.));
#73269=CARTESIAN_POINT('Ctrl Pts',(-11.3646011993674,-45.7928186334791,
0.));
#73270=CARTESIAN_POINT('Ctrl Pts',(-11.3646011993674,-45.7928186334791,
20.));
#73271=CARTESIAN_POINT('Ctrl Pts',(-11.395940855652,-45.7819486436912,0.));
#73272=CARTESIAN_POINT('Ctrl Pts',(-11.395940855652,-45.7819486436912,20.));
#73273=CARTESIAN_POINT('Ctrl Pts',(-11.4272718382404,-45.7710570785186,
0.));
#73274=CARTESIAN_POINT('Ctrl Pts',(-11.4272718382404,-45.7710570785186,
20.));
#73275=CARTESIAN_POINT('Ctrl Pts',(-11.4585941320575,-45.760143944127,0.));
#73276=CARTESIAN_POINT('Ctrl Pts',(-11.4585941320575,-45.760143944127,20.));
#73277=CARTESIAN_POINT('Ctrl Pts',(-11.489907722032,-45.7492092466918,0.));
#73278=CARTESIAN_POINT('Ctrl Pts',(-11.489907722032,-45.7492092466918,20.));
#73279=CARTESIAN_POINT('Ctrl Pts',(-11.5212125930967,-45.7382529923996,
0.));
#73280=CARTESIAN_POINT('Ctrl Pts',(-11.5212125930967,-45.7382529923996,
20.));
#73281=CARTESIAN_POINT('Ctrl Pts',(-11.5525087301884,-45.7272751874478,
0.));
#73282=CARTESIAN_POINT('Ctrl Pts',(-11.5525087301884,-45.7272751874478,
20.));
#73283=CARTESIAN_POINT('Ctrl Pts',(-11.5837961182482,-45.7162758380449,
0.));
#73284=CARTESIAN_POINT('Ctrl Pts',(-11.5837961182482,-45.7162758380449,
20.));
#73285=CARTESIAN_POINT('Ctrl Pts',(-11.615074742221,-45.7052549504103,0.));
#73286=CARTESIAN_POINT('Ctrl Pts',(-11.615074742221,-45.7052549504103,20.));
#73287=CARTESIAN_POINT('Ctrl Pts',(-11.6463445870557,-45.694212530774,0.));
#73288=CARTESIAN_POINT('Ctrl Pts',(-11.6463445870557,-45.694212530774,20.));
#73289=CARTESIAN_POINT('Ctrl Pts',(-11.6776056377055,-45.6831485853771,
0.));
#73290=CARTESIAN_POINT('Ctrl Pts',(-11.6776056377055,-45.6831485853771,
20.));
#73291=CARTESIAN_POINT('Ctrl Pts',(-11.7088578791267,-45.6720631204703,
0.));
#73292=CARTESIAN_POINT('Ctrl Pts',(-11.7088578791267,-45.6720631204703,
20.));
#73293=CARTESIAN_POINT('Ctrl Pts',(-11.7401012962797,-45.6609561423149,
0.));
#73294=CARTESIAN_POINT('Ctrl Pts',(-11.7401012962797,-45.6609561423149,
20.));
#73295=CARTESIAN_POINT('Ctrl Pts',(-11.7713358741293,-45.6498276571829,
0.));
#73296=CARTESIAN_POINT('Ctrl Pts',(-11.7713358741293,-45.6498276571829,
20.));
#73297=CARTESIAN_POINT('Ctrl Pts',(-11.8025615976441,-45.6386776713575,
0.));
#73298=CARTESIAN_POINT('Ctrl Pts',(-11.8025615976441,-45.6386776713575,
20.));
#73299=CARTESIAN_POINT('Ctrl Pts',(-11.8337784517972,-45.627506191133,0.));
#73300=CARTESIAN_POINT('Ctrl Pts',(-11.8337784517972,-45.627506191133,20.));
#73301=CARTESIAN_POINT('Ctrl Pts',(-11.8649864215653,-45.6163132228138,
0.));
#73302=CARTESIAN_POINT('Ctrl Pts',(-11.8649864215653,-45.6163132228138,
20.));
#73303=CARTESIAN_POINT('Ctrl Pts',(-11.8961854919294,-45.6050987727153,
0.));
#73304=CARTESIAN_POINT('Ctrl Pts',(-11.8961854919294,-45.6050987727153,
20.));
#73305=CARTESIAN_POINT('Ctrl Pts',(-11.9273756478741,-45.5938628471638,
0.));
#73306=CARTESIAN_POINT('Ctrl Pts',(-11.9273756478741,-45.5938628471638,
20.));
#73307=CARTESIAN_POINT('Ctrl Pts',(-11.9585568743886,-45.5826054524963,
0.));
#73308=CARTESIAN_POINT('Ctrl Pts',(-11.9585568743886,-45.5826054524963,
20.));
#73309=CARTESIAN_POINT('Ctrl Pts',(-11.989729156466,-45.5713265950605,0.));
#73310=CARTESIAN_POINT('Ctrl Pts',(-11.989729156466,-45.5713265950605,20.));
#73311=CARTESIAN_POINT('Ctrl Pts',(-12.0208924791035,-45.5600262812144,
0.));
#73312=CARTESIAN_POINT('Ctrl Pts',(-12.0208924791035,-45.5600262812144,
20.));
#73313=CARTESIAN_POINT('Ctrl Pts',(-12.0520468273019,-45.5487045173265,
0.));
#73314=CARTESIAN_POINT('Ctrl Pts',(-12.0520468273019,-45.5487045173265,
20.));
#73315=CARTESIAN_POINT('Ctrl Pts',(-12.0831921860666,-45.5373613097755,
0.));
#73316=CARTESIAN_POINT('Ctrl Pts',(-12.0831921860666,-45.5373613097755,
20.));
#73317=CARTESIAN_POINT('Ctrl Pts',(-12.1143285404065,-45.5259966649516,
0.));
#73318=CARTESIAN_POINT('Ctrl Pts',(-12.1143285404065,-45.5259966649516,
20.));
#73319=CARTESIAN_POINT('Ctrl Pts',(-12.1454558753351,-45.5146105892553,
0.));
#73320=CARTESIAN_POINT('Ctrl Pts',(-12.1454558753351,-45.5146105892553,
20.));
#73321=CARTESIAN_POINT('Ctrl Pts',(-12.1765741758697,-45.5032030890978,
0.));
#73322=CARTESIAN_POINT('Ctrl Pts',(-12.1765741758697,-45.5032030890978,
20.));
#73323=CARTESIAN_POINT('Ctrl Pts',(-12.2076834270323,-45.4917741709015,
0.));
#73324=CARTESIAN_POINT('Ctrl Pts',(-12.2076834270323,-45.4917741709015,
20.));
#73325=CARTESIAN_POINT('Ctrl Pts',(-12.2387836138487,-45.4803238410999,
0.));
#73326=CARTESIAN_POINT('Ctrl Pts',(-12.2387836138487,-45.4803238410999,
20.));
#73327=CARTESIAN_POINT('Ctrl Pts',(-12.269874721349,-45.4688521061371,0.));
#73328=CARTESIAN_POINT('Ctrl Pts',(-12.269874721349,-45.4688521061371,20.));
#73329=CARTESIAN_POINT('Ctrl Pts',(-12.3009567345673,-45.4573589724673,
0.));
#73330=CARTESIAN_POINT('Ctrl Pts',(-12.3009567345673,-45.4573589724673,
20.));
#73331=CARTESIAN_POINT('Ctrl Pts',(-12.3320296385418,-45.4458444465552,
0.));
#73332=CARTESIAN_POINT('Ctrl Pts',(-12.3320296385418,-45.4458444465552,
20.));
#73333=CARTESIAN_POINT('Ctrl Pts',(-12.3630934183143,-45.4343085348755,
0.));
#73334=CARTESIAN_POINT('Ctrl Pts',(-12.3630934183143,-45.4343085348755,
20.));
#73335=CARTESIAN_POINT('Ctrl Pts',(-12.3941480589311,-45.4227512439136,
0.));
#73336=CARTESIAN_POINT('Ctrl Pts',(-12.3941480589311,-45.4227512439136,
20.));
#73337=CARTESIAN_POINT('Ctrl Pts',(-12.4251935454428,-45.4111725801659,
0.));
#73338=CARTESIAN_POINT('Ctrl Pts',(-12.4251935454428,-45.4111725801659,
20.));
#73339=CARTESIAN_POINT('Ctrl Pts',(-12.4562298629045,-45.3995725501402,
0.));
#73340=CARTESIAN_POINT('Ctrl Pts',(-12.4562298629045,-45.3995725501402,
20.));
#73341=CARTESIAN_POINT('Ctrl Pts',(-12.4872569963754,-45.3879511603549,
0.));
#73342=CARTESIAN_POINT('Ctrl Pts',(-12.4872569963754,-45.3879511603549,
20.));
#73343=CARTESIAN_POINT('Ctrl Pts',(-12.5182749309189,-45.376308417339,0.));
#73344=CARTESIAN_POINT('Ctrl Pts',(-12.5182749309189,-45.376308417339,20.));
#73345=CARTESIAN_POINT('Ctrl Pts',(-12.5492836516023,-45.364644327632,0.));
#73346=CARTESIAN_POINT('Ctrl Pts',(-12.5492836516023,-45.364644327632,20.));
#73347=CARTESIAN_POINT('Ctrl Pts',(-12.5802831434966,-45.3529588977839,
0.));
#73348=CARTESIAN_POINT('Ctrl Pts',(-12.5802831434966,-45.3529588977839,
20.));
#73349=CARTESIAN_POINT('Ctrl Pts',(-12.6112733916776,-45.3412521343551,
0.));
#73350=CARTESIAN_POINT('Ctrl Pts',(-12.6112733916776,-45.3412521343551,
20.));
#73351=CARTESIAN_POINT('Ctrl Pts',(-12.6422543812252,-45.3295240439169,
0.));
#73352=CARTESIAN_POINT('Ctrl Pts',(-12.6422543812252,-45.3295240439169,
20.));
#73353=CARTESIAN_POINT('Ctrl Pts',(-12.6732260972239,-45.3177746330512,
0.));
#73354=CARTESIAN_POINT('Ctrl Pts',(-12.6732260972239,-45.3177746330512,
20.));
#73355=CARTESIAN_POINT('Ctrl Pts',(-12.7041885247626,-45.3060039083501,
0.));
#73356=CARTESIAN_POINT('Ctrl Pts',(-12.7041885247626,-45.3060039083501,
20.));
#73357=CARTESIAN_POINT('Ctrl Pts',(-12.7351416489341,-45.2942118764167,
0.));
#73358=CARTESIAN_POINT('Ctrl Pts',(-12.7351416489341,-45.2942118764167,
20.));
#73359=CARTESIAN_POINT('Ctrl Pts',(-12.7660854548354,-45.2823985438647,
0.));
#73360=CARTESIAN_POINT('Ctrl Pts',(-12.7660854548354,-45.2823985438647,
20.));
#73361=CARTESIAN_POINT('Ctrl Pts',(-12.7970199275678,-45.2705639173192,
0.));
#73362=CARTESIAN_POINT('Ctrl Pts',(-12.7970199275678,-45.2705639173192,
20.));
#73363=CARTESIAN_POINT('Ctrl Pts',(-12.8279450522366,-45.2587080034157,
0.));
#73364=CARTESIAN_POINT('Ctrl Pts',(-12.8279450522366,-45.2587080034157,
20.));
#73365=CARTESIAN_POINT('Ctrl Pts',(-12.8588608139512,-45.2468308087994,
0.));
#73366=CARTESIAN_POINT('Ctrl Pts',(-12.8588608139512,-45.2468308087994,
20.));
#73367=CARTESIAN_POINT('Ctrl Pts',(-12.8897671978257,-45.2349323401259,
0.));
#73368=CARTESIAN_POINT('Ctrl Pts',(-12.8897671978257,-45.2349323401259,
20.));
#73369=CARTESIAN_POINT('Ctrl Pts',(-12.9206641889781,-45.2230126040617,
0.));
#73370=CARTESIAN_POINT('Ctrl Pts',(-12.9206641889781,-45.2230126040617,
20.));
#73371=CARTESIAN_POINT('Ctrl Pts',(-12.9515517725313,-45.2110716072841,
0.));
#73372=CARTESIAN_POINT('Ctrl Pts',(-12.9515517725313,-45.2110716072841,
20.));
#73373=CARTESIAN_POINT('Ctrl Pts',(-12.9824299336127,-45.199109356482,0.));
#73374=CARTESIAN_POINT('Ctrl Pts',(-12.9824299336127,-45.199109356482,20.));
#73375=CARTESIAN_POINT('Ctrl Pts',(-13.0132986573536,-45.1871258583545,
0.));
#73376=CARTESIAN_POINT('Ctrl Pts',(-13.0132986573536,-45.1871258583545,
20.));
#73377=CARTESIAN_POINT('Ctrl Pts',(-13.0441579288899,-45.1751211196118,
0.));
#73378=CARTESIAN_POINT('Ctrl Pts',(-13.0441579288899,-45.1751211196118,
20.));
#73379=CARTESIAN_POINT('Ctrl Pts',(-13.0750077333614,-45.1630951469733,
0.));
#73380=CARTESIAN_POINT('Ctrl Pts',(-13.0750077333614,-45.1630951469733,
20.));
#73381=CARTESIAN_POINT('Ctrl Pts',(-13.1058480559121,-45.1510479471692,
0.));
#73382=CARTESIAN_POINT('Ctrl Pts',(-13.1058480559121,-45.1510479471692,
20.));
#73383=CARTESIAN_POINT('Ctrl Pts',(-13.1366788816904,-45.1389795269399,
0.));
#73384=CARTESIAN_POINT('Ctrl Pts',(-13.1366788816904,-45.1389795269399,
20.));
#73385=CARTESIAN_POINT('Ctrl Pts',(-13.1675001958493,-45.1268898930368,
0.));
#73386=CARTESIAN_POINT('Ctrl Pts',(-13.1675001958493,-45.1268898930368,
20.));
#73387=CARTESIAN_POINT('Ctrl Pts',(-13.198311983546,-45.114779052223,0.));
#73388=CARTESIAN_POINT('Ctrl Pts',(-13.198311983546,-45.114779052223,20.));
#73389=CARTESIAN_POINT('Ctrl Pts',(-13.2291142299426,-45.1026470112717,
0.));
#73390=CARTESIAN_POINT('Ctrl Pts',(-13.2291142299426,-45.1026470112717,
20.));
#73391=CARTESIAN_POINT('Ctrl Pts',(-13.259906920205,-45.0904937769663,0.));
#73392=CARTESIAN_POINT('Ctrl Pts',(-13.259906920205,-45.0904937769663,20.));
#73393=CARTESIAN_POINT('Ctrl Pts',(-13.2906900395037,-45.0783193561008,
0.));
#73394=CARTESIAN_POINT('Ctrl Pts',(-13.2906900395037,-45.0783193561008,
20.));
#73395=CARTESIAN_POINT('Ctrl Pts',(-13.3214635730135,-45.0661237554798,
0.));
#73396=CARTESIAN_POINT('Ctrl Pts',(-13.3214635730135,-45.0661237554798,
20.));
#73397=CARTESIAN_POINT('Ctrl Pts',(-13.3522275059137,-45.0539069819185,
0.));
#73398=CARTESIAN_POINT('Ctrl Pts',(-13.3522275059137,-45.0539069819185,
20.));
#73399=CARTESIAN_POINT('Ctrl Pts',(-13.3829818233878,-45.0416690422424,
0.));
#73400=CARTESIAN_POINT('Ctrl Pts',(-13.3829818233878,-45.0416690422424,
20.));
#73401=CARTESIAN_POINT('Ctrl Pts',(-13.4137265106238,-45.0294099432879,
0.));
#73402=CARTESIAN_POINT('Ctrl Pts',(-13.4137265106238,-45.0294099432879,
20.));
#73403=CARTESIAN_POINT('Ctrl Pts',(-13.4444615528144,-45.0171296919022,
0.));
#73404=CARTESIAN_POINT('Ctrl Pts',(-13.4444615528144,-45.0171296919022,
20.));
#73405=CARTESIAN_POINT('Ctrl Pts',(-13.4751869351564,-45.0048282949433,
0.));
#73406=CARTESIAN_POINT('Ctrl Pts',(-13.4751869351564,-45.0048282949433,
20.));
#73407=CARTESIAN_POINT('Ctrl Pts',(-13.5059026428512,-44.9925057592796,
0.));
#73408=CARTESIAN_POINT('Ctrl Pts',(-13.5059026428512,-44.9925057592796,
20.));
#73409=CARTESIAN_POINT('Ctrl Pts',(-13.5366086611044,-44.9801620917891,
0.));
#73410=CARTESIAN_POINT('Ctrl Pts',(-13.5366086611044,-44.9801620917891,
20.));
#73411=CARTESIAN_POINT('Ctrl Pts',(-13.5673049751264,-44.967797299361,0.));
#73412=CARTESIAN_POINT('Ctrl Pts',(-13.5673049751264,-44.967797299361,20.));
#73413=CARTESIAN_POINT('Ctrl Pts',(-13.5979915701319,-44.955411388895,0.));
#73414=CARTESIAN_POINT('Ctrl Pts',(-13.5979915701319,-44.955411388895,20.));
#73415=CARTESIAN_POINT('Ctrl Pts',(-13.6286684313402,-44.9430043673018,
0.));
#73416=CARTESIAN_POINT('Ctrl Pts',(-13.6286684313402,-44.9430043673018,
20.));
#73417=CARTESIAN_POINT('Ctrl Pts',(-13.6593355439745,-44.9305762415019,
0.));
#73418=CARTESIAN_POINT('Ctrl Pts',(-13.6593355439745,-44.9305762415019,
20.));
#73419=CARTESIAN_POINT('Ctrl Pts',(-13.6899928932632,-44.9181270184275,
0.));
#73420=CARTESIAN_POINT('Ctrl Pts',(-13.6899928932632,-44.9181270184275,
20.));
#73421=CARTESIAN_POINT('Ctrl Pts',(-13.7206404644388,-44.9056567050204,
0.));
#73422=CARTESIAN_POINT('Ctrl Pts',(-13.7206404644388,-44.9056567050204,
20.));
#73423=CARTESIAN_POINT('Ctrl Pts',(-13.7512782427386,-44.8931653082334,
0.));
#73424=CARTESIAN_POINT('Ctrl Pts',(-13.7512782427386,-44.8931653082334,
20.));
#73425=CARTESIAN_POINT('Ctrl Pts',(-13.7819062134042,-44.8806528350291,
0.));
#73426=CARTESIAN_POINT('Ctrl Pts',(-13.7819062134042,-44.8806528350291,
20.));
#73427=CARTESIAN_POINT('Ctrl Pts',(-13.8125243616816,-44.8681192923811,
0.));
#73428=CARTESIAN_POINT('Ctrl Pts',(-13.8125243616816,-44.8681192923811,
20.));
#73429=CARTESIAN_POINT('Ctrl Pts',(-13.8431326728214,-44.8555646872732,
0.));
#73430=CARTESIAN_POINT('Ctrl Pts',(-13.8431326728214,-44.8555646872732,
20.));
#73431=CARTESIAN_POINT('Ctrl Pts',(-13.8737311320789,-44.8429890267007,
0.));
#73432=CARTESIAN_POINT('Ctrl Pts',(-13.8737311320789,-44.8429890267007,
20.));
#73433=CARTESIAN_POINT('Ctrl Pts',(-13.9043197247138,-44.8303923176691,
0.));
#73434=CARTESIAN_POINT('Ctrl Pts',(-13.9043197247138,-44.8303923176691,
20.));
#73435=CARTESIAN_POINT('Ctrl Pts',(-13.9348984359903,-44.8177745671945,
0.));
#73436=CARTESIAN_POINT('Ctrl Pts',(-13.9348984359903,-44.8177745671945,
20.));
#73437=CARTESIAN_POINT('Ctrl Pts',(-13.9654672511774,-44.8051357823031,
0.));
#73438=CARTESIAN_POINT('Ctrl Pts',(-13.9654672511774,-44.8051357823031,
20.));
#73439=CARTESIAN_POINT('Ctrl Pts',(-13.9960261555481,-44.7924759700314,
0.));
#73440=CARTESIAN_POINT('Ctrl Pts',(-13.9960261555481,-44.7924759700314,
20.));
#73441=CARTESIAN_POINT('Ctrl Pts',(-14.0265751343805,-44.7797951374262,
0.));
#73442=CARTESIAN_POINT('Ctrl Pts',(-14.0265751343805,-44.7797951374262,
20.));
#73443=CARTESIAN_POINT('Ctrl Pts',(-14.057114172957,-44.7670932915455,0.));
#73444=CARTESIAN_POINT('Ctrl Pts',(-14.057114172957,-44.7670932915455,20.));
#73445=CARTESIAN_POINT('Ctrl Pts',(-14.0876432565649,-44.7543704394583,
0.));
#73446=CARTESIAN_POINT('Ctrl Pts',(-14.0876432565649,-44.7543704394583,
20.));
#73447=CARTESIAN_POINT('Ctrl Pts',(-14.118162370496,-44.7416265882442,0.));
#73448=CARTESIAN_POINT('Ctrl Pts',(-14.118162370496,-44.7416265882442,20.));
#73449=CARTESIAN_POINT('Ctrl Pts',(-14.1486715000464,-44.728861744993,0.));
#73450=CARTESIAN_POINT('Ctrl Pts',(-14.1486715000464,-44.728861744993,20.));
#73451=CARTESIAN_POINT('Ctrl Pts',(-14.1791706305171,-44.7160759168044,
0.));
#73452=CARTESIAN_POINT('Ctrl Pts',(-14.1791706305171,-44.7160759168044,
20.));
#73453=CARTESIAN_POINT('Ctrl Pts',(-14.2096597472134,-44.7032691107881,
0.));
#73454=CARTESIAN_POINT('Ctrl Pts',(-14.2096597472134,-44.7032691107881,
20.));
#73455=CARTESIAN_POINT('Ctrl Pts',(-14.2401388354454,-44.690441334065,0.));
#73456=CARTESIAN_POINT('Ctrl Pts',(-14.2401388354454,-44.690441334065,20.));
#73457=CARTESIAN_POINT('Ctrl Pts',(-14.2706078805279,-44.6775925937661,
0.));
#73458=CARTESIAN_POINT('Ctrl Pts',(-14.2706078805279,-44.6775925937661,
20.));
#73459=CARTESIAN_POINT('Ctrl Pts',(-14.3010668677802,-44.6647228970333,
0.));
#73460=CARTESIAN_POINT('Ctrl Pts',(-14.3010668677802,-44.6647228970333,
20.));
#73461=CARTESIAN_POINT('Ctrl Pts',(-14.3315157825264,-44.6518322510194,
0.));
#73462=CARTESIAN_POINT('Ctrl Pts',(-14.3315157825264,-44.6518322510194,
20.));
#73463=CARTESIAN_POINT('Ctrl Pts',(-14.3619546100951,-44.6389206628876,
0.));
#73464=CARTESIAN_POINT('Ctrl Pts',(-14.3619546100951,-44.6389206628876,
20.));
#73465=CARTESIAN_POINT('Ctrl Pts',(-14.3923833358197,-44.6259881398118,
0.));
#73466=CARTESIAN_POINT('Ctrl Pts',(-14.3923833358197,-44.6259881398118,
20.));
#73467=CARTESIAN_POINT('Ctrl Pts',(-14.4228019450383,-44.6130346889769,
0.));
#73468=CARTESIAN_POINT('Ctrl Pts',(-14.4228019450383,-44.6130346889769,
20.));
#73469=CARTESIAN_POINT('Ctrl Pts',(-14.4532104230937,-44.6000603175775,
0.));
#73470=CARTESIAN_POINT('Ctrl Pts',(-14.4532104230937,-44.6000603175775,
20.));
#73471=CARTESIAN_POINT('Ctrl Pts',(-14.4836087553332,-44.5870650328188,
0.));
#73472=CARTESIAN_POINT('Ctrl Pts',(-14.4836087553332,-44.5870650328188,
20.));
#73473=CARTESIAN_POINT('Ctrl Pts',(-14.5139969271087,-44.5740488419152,
0.));
#73474=CARTESIAN_POINT('Ctrl Pts',(-14.5139969271087,-44.5740488419152,
20.));
#73475=CARTESIAN_POINT('Ctrl Pts',(-14.5443749237768,-44.5610117520915,
0.));
#73476=CARTESIAN_POINT('Ctrl Pts',(-14.5443749237768,-44.5610117520915,
20.));
#73477=CARTESIAN_POINT('Ctrl Pts',(-14.5747427306988,-44.5479537705835,
0.));
#73478=CARTESIAN_POINT('Ctrl Pts',(-14.5747427306988,-44.5479537705835,
20.));
#73479=CARTESIAN_POINT('Ctrl Pts',(-14.6051003332411,-44.5348749046378,
0.));
#73480=CARTESIAN_POINT('Ctrl Pts',(-14.6051003332411,-44.5348749046378,
20.));
#73481=CARTESIAN_POINT('Ctrl Pts',(-14.6354477167742,-44.521775161512,0.));
#73482=CARTESIAN_POINT('Ctrl Pts',(-14.6354477167742,-44.521775161512,20.));
#73483=CARTESIAN_POINT('Ctrl Pts',(-14.6657848666744,-44.5086545484757,
0.));
#73484=CARTESIAN_POINT('Ctrl Pts',(-14.6657848666744,-44.5086545484757,
20.));
#73485=CARTESIAN_POINT('Ctrl Pts',(-14.6961117683217,-44.4955130728078,
0.));
#73486=CARTESIAN_POINT('Ctrl Pts',(-14.6961117683217,-44.4955130728078,
20.));
#73487=CARTESIAN_POINT('Ctrl Pts',(-14.7264284071013,-44.4823507417973,
0.));
#73488=CARTESIAN_POINT('Ctrl Pts',(-14.7264284071013,-44.4823507417973,
20.));
#73489=CARTESIAN_POINT('Ctrl Pts',(-14.756734768403,-44.469167562743,0.));
#73490=CARTESIAN_POINT('Ctrl Pts',(-14.756734768403,-44.469167562743,20.));
#73491=CARTESIAN_POINT('Ctrl Pts',(-14.7870308376214,-44.4559635429545,
0.));
#73492=CARTESIAN_POINT('Ctrl Pts',(-14.7870308376214,-44.4559635429545,
20.));
#73493=CARTESIAN_POINT('Ctrl Pts',(-14.817316600156,-44.4427386897515,0.));
#73494=CARTESIAN_POINT('Ctrl Pts',(-14.817316600156,-44.4427386897515,20.));
#73495=CARTESIAN_POINT('Ctrl Pts',(-14.8475920414108,-44.4294930104636,
0.));
#73496=CARTESIAN_POINT('Ctrl Pts',(-14.8475920414108,-44.4294930104636,
20.));
#73497=CARTESIAN_POINT('Ctrl Pts',(-14.8778571467943,-44.416226512431,0.));
#73498=CARTESIAN_POINT('Ctrl Pts',(-14.8778571467943,-44.416226512431,20.));
#73499=CARTESIAN_POINT('Ctrl Pts',(-14.9081119017199,-44.4029392030043,
0.));
#73500=CARTESIAN_POINT('Ctrl Pts',(-14.9081119017199,-44.4029392030043,
20.));
#73501=CARTESIAN_POINT('Ctrl Pts',(-14.9383562916061,-44.389631089546,0.));
#73502=CARTESIAN_POINT('Ctrl Pts',(-14.9383562916061,-44.389631089546,20.));
#73503=CARTESIAN_POINT('Ctrl Pts',(-14.9685903018767,-44.3763021794296,
0.));
#73504=CARTESIAN_POINT('Ctrl Pts',(-14.9685903018767,-44.3763021794296,
20.));
#73505=CARTESIAN_POINT('Ctrl Pts',(-14.9988139179602,-44.3629524800397,
0.));
#73506=CARTESIAN_POINT('Ctrl Pts',(-14.9988139179602,-44.3629524800397,
20.));
#73507=CARTESIAN_POINT('Ctrl Pts',(-15.0290271252899,-44.3495819987707,
0.));
#73508=CARTESIAN_POINT('Ctrl Pts',(-15.0290271252899,-44.3495819987707,
20.));
#73509=CARTESIAN_POINT('Ctrl Pts',(-15.0592299093033,-44.3361907430254,
0.));
#73510=CARTESIAN_POINT('Ctrl Pts',(-15.0592299093033,-44.3361907430254,
20.));
#73511=CARTESIAN_POINT('Ctrl Pts',(-15.0894222554425,-44.3227787202166,
0.));
#73512=CARTESIAN_POINT('Ctrl Pts',(-15.0894222554425,-44.3227787202166,
20.));
#73513=CARTESIAN_POINT('Ctrl Pts',(-15.1196041491546,-44.3093459377674,
0.));
#73514=CARTESIAN_POINT('Ctrl Pts',(-15.1196041491546,-44.3093459377674,
20.));
#73515=CARTESIAN_POINT('Ctrl Pts',(-15.1497755758918,-44.2958924031118,
0.));
#73516=CARTESIAN_POINT('Ctrl Pts',(-15.1497755758918,-44.2958924031118,
20.));
#73517=CARTESIAN_POINT('Ctrl Pts',(-15.1799365211114,-44.2824181236961,
0.));
#73518=CARTESIAN_POINT('Ctrl Pts',(-15.1799365211114,-44.2824181236961,
20.));
#73519=CARTESIAN_POINT('Ctrl Pts',(-15.2100869702755,-44.2689231069767,
0.));
#73520=CARTESIAN_POINT('Ctrl Pts',(-15.2100869702755,-44.2689231069767,
20.));
#73521=CARTESIAN_POINT('Ctrl Pts',(-15.2402269088514,-44.2554073604206,
0.));
#73522=CARTESIAN_POINT('Ctrl Pts',(-15.2402269088514,-44.2554073604206,
20.));
#73523=CARTESIAN_POINT('Ctrl Pts',(-15.2703563223108,-44.2418708915045,
0.));
#73524=CARTESIAN_POINT('Ctrl Pts',(-15.2703563223108,-44.2418708915045,
20.));
#73525=CARTESIAN_POINT('Ctrl Pts',(-15.30047519613,-44.2283137077152,0.));
#73526=CARTESIAN_POINT('Ctrl Pts',(-15.30047519613,-44.2283137077152,20.));
#73527=CARTESIAN_POINT('Ctrl Pts',(-15.3305835157903,-44.2147358165492,
0.));
#73528=CARTESIAN_POINT('Ctrl Pts',(-15.3305835157903,-44.2147358165492,
20.));
#73529=CARTESIAN_POINT('Ctrl Pts',(-15.3606812667781,-44.201137225514,0.));
#73530=CARTESIAN_POINT('Ctrl Pts',(-15.3606812667781,-44.201137225514,20.));
#73531=CARTESIAN_POINT('Ctrl Pts',(-15.390768434585,-44.1875179421286,0.));
#73532=CARTESIAN_POINT('Ctrl Pts',(-15.390768434585,-44.1875179421286,20.));
#73533=CARTESIAN_POINT('Ctrl Pts',(-15.4208450047077,-44.1738779739224,
0.));
#73534=CARTESIAN_POINT('Ctrl Pts',(-15.4208450047077,-44.1738779739224,
20.));
#73535=CARTESIAN_POINT('Ctrl Pts',(-15.4509109626472,-44.1602173284345,
0.));
#73536=CARTESIAN_POINT('Ctrl Pts',(-15.4509109626472,-44.1602173284345,
20.));
#73537=CARTESIAN_POINT('Ctrl Pts',(-15.4809662939093,-44.146536013213,0.));
#73538=CARTESIAN_POINT('Ctrl Pts',(-15.4809662939093,-44.146536013213,20.));
#73539=CARTESIAN_POINT('Ctrl Pts',(-15.5110109840048,-44.1328340358171,
0.));
#73540=CARTESIAN_POINT('Ctrl Pts',(-15.5110109840048,-44.1328340358171,
20.));
#73541=CARTESIAN_POINT('Ctrl Pts',(-15.5410450184494,-44.1191114038164,
0.));
#73542=CARTESIAN_POINT('Ctrl Pts',(-15.5410450184494,-44.1191114038164,
20.));
#73543=CARTESIAN_POINT('Ctrl Pts',(-15.5710683827646,-44.1053681247921,
0.));
#73544=CARTESIAN_POINT('Ctrl Pts',(-15.5710683827646,-44.1053681247921,
20.));
#73545=CARTESIAN_POINT('Ctrl Pts',(-15.6010810624766,-44.0916042063371,
0.));
#73546=CARTESIAN_POINT('Ctrl Pts',(-15.6010810624766,-44.0916042063371,
20.));
#73547=CARTESIAN_POINT('Ctrl Pts',(-15.6310830431167,-44.0778196560536,
0.));
#73548=CARTESIAN_POINT('Ctrl Pts',(-15.6310830431167,-44.0778196560536,
20.));
#73549=CARTESIAN_POINT('Ctrl Pts',(-15.6610743102207,-44.0640144815534,
0.));
#73550=CARTESIAN_POINT('Ctrl Pts',(-15.6610743102207,-44.0640144815534,
20.));
#73551=CARTESIAN_POINT('Ctrl Pts',(-15.6910548493289,-44.050188690457,0.));
#73552=CARTESIAN_POINT('Ctrl Pts',(-15.6910548493289,-44.050188690457,20.));
#73553=CARTESIAN_POINT('Ctrl Pts',(-15.7210246459868,-44.0363422903955,
0.));
#73554=CARTESIAN_POINT('Ctrl Pts',(-15.7210246459868,-44.0363422903955,
20.));
#73555=CARTESIAN_POINT('Ctrl Pts',(-15.7509836857452,-44.0224752890112,
0.));
#73556=CARTESIAN_POINT('Ctrl Pts',(-15.7509836857452,-44.0224752890112,
20.));
#73557=CARTESIAN_POINT('Ctrl Pts',(-15.7809319541602,-44.0085876939576,
0.));
#73558=CARTESIAN_POINT('Ctrl Pts',(-15.7809319541602,-44.0085876939576,
20.));
#73559=CARTESIAN_POINT('Ctrl Pts',(-15.8108694367927,-43.9946795128988,
0.));
#73560=CARTESIAN_POINT('Ctrl Pts',(-15.8108694367927,-43.9946795128988,
20.));
#73561=CARTESIAN_POINT('Ctrl Pts',(-15.8407961192089,-43.9807507535096,
0.));
#73562=CARTESIAN_POINT('Ctrl Pts',(-15.8407961192089,-43.9807507535096,
20.));
#73563=CARTESIAN_POINT('Ctrl Pts',(-15.8707119869797,-43.9668014234746,
0.));
#73564=CARTESIAN_POINT('Ctrl Pts',(-15.8707119869797,-43.9668014234746,
20.));
#73565=CARTESIAN_POINT('Ctrl Pts',(-15.9006170256808,-43.9528315304878,
0.));
#73566=CARTESIAN_POINT('Ctrl Pts',(-15.9006170256808,-43.9528315304878,
20.));
#73567=CARTESIAN_POINT('Ctrl Pts',(-15.9305112208934,-43.9388410822542,
0.));
#73568=CARTESIAN_POINT('Ctrl Pts',(-15.9305112208934,-43.9388410822542,
20.));
#73569=CARTESIAN_POINT('Ctrl Pts',(-15.9603945582034,-43.9248300864889,
0.));
#73570=CARTESIAN_POINT('Ctrl Pts',(-15.9603945582034,-43.9248300864889,
20.));
#73571=CARTESIAN_POINT('Ctrl Pts',(-15.9902670232019,-43.9107985509168,
0.));
#73572=CARTESIAN_POINT('Ctrl Pts',(-15.9902670232019,-43.9107985509168,
20.));
#73573=CARTESIAN_POINT('Ctrl Pts',(-16.020128601485,-43.896746483274,0.));
#73574=CARTESIAN_POINT('Ctrl Pts',(-16.020128601485,-43.896746483274,20.));
#73575=CARTESIAN_POINT('Ctrl Pts',(-16.0499792786541,-43.8826738913074,
0.));
#73576=CARTESIAN_POINT('Ctrl Pts',(-16.0499792786541,-43.8826738913074,
20.));
#73577=CARTESIAN_POINT('Ctrl Pts',(-16.0798190403159,-43.8685807827745,
0.));
#73578=CARTESIAN_POINT('Ctrl Pts',(-16.0798190403159,-43.8685807827745,
20.));
#73579=CARTESIAN_POINT('Ctrl Pts',(-16.1096478720818,-43.854467165442,0.));
#73580=CARTESIAN_POINT('Ctrl Pts',(-16.1096478720818,-43.854467165442,20.));
#73581=CARTESIAN_POINT('Ctrl Pts',(-16.1394657595683,-43.8403330470868,
0.));
#73582=CARTESIAN_POINT('Ctrl Pts',(-16.1394657595683,-43.8403330470868,
20.));
#73583=CARTESIAN_POINT('Ctrl Pts',(-16.1692726883968,-43.8261784354962,
0.));
#73584=CARTESIAN_POINT('Ctrl Pts',(-16.1692726883968,-43.8261784354962,
20.));
#73585=CARTESIAN_POINT('Ctrl Pts',(-16.199068644194,-43.8120033384679,0.));
#73586=CARTESIAN_POINT('Ctrl Pts',(-16.199068644194,-43.8120033384679,20.));
#73587=CARTESIAN_POINT('Ctrl Pts',(-16.2288536125917,-43.7978077638098,
0.));
#73588=CARTESIAN_POINT('Ctrl Pts',(-16.2288536125917,-43.7978077638098,
20.));
#73589=CARTESIAN_POINT('Ctrl Pts',(-16.2586275792268,-43.7835917193404,
0.));
#73590=CARTESIAN_POINT('Ctrl Pts',(-16.2586275792268,-43.7835917193404,
20.));
#73591=CARTESIAN_POINT('Ctrl Pts',(-16.2883905297415,-43.7693552128887,
0.));
#73592=CARTESIAN_POINT('Ctrl Pts',(-16.2883905297415,-43.7693552128887,
20.));
#73593=CARTESIAN_POINT('Ctrl Pts',(-16.3181424497834,-43.7550982522947,
0.));
#73594=CARTESIAN_POINT('Ctrl Pts',(-16.3181424497834,-43.7550982522947,
20.));
#73595=CARTESIAN_POINT('Ctrl Pts',(-16.3478833250055,-43.7408208454089,
0.));
#73596=CARTESIAN_POINT('Ctrl Pts',(-16.3478833250055,-43.7408208454089,
20.));
#73597=CARTESIAN_POINT('Ctrl Pts',(-16.3776131410651,-43.7265230000909,
0.));
#73598=CARTESIAN_POINT('Ctrl Pts',(-16.3776131410651,-43.7265230000909,
20.));
#73599=CARTESIAN_POINT('Ctrl Pts',(-16.4073318836249,-43.7122047242097,
0.));
#73600=CARTESIAN_POINT('Ctrl Pts',(-16.4073318836249,-43.7122047242097,
20.));
#73601=CARTESIAN_POINT('Ctrl Pts',(-16.4370395383524,-43.6978660256455,
0.));
#73602=CARTESIAN_POINT('Ctrl Pts',(-16.4370395383524,-43.6978660256455,
20.));
#73603=CARTESIAN_POINT('Ctrl Pts',(-16.4667360909207,-43.6835069122887,
0.));
#73604=CARTESIAN_POINT('Ctrl Pts',(-16.4667360909207,-43.6835069122887,
20.));
#73605=CARTESIAN_POINT('Ctrl Pts',(-16.4964215270082,-43.6691273920409,
0.));
#73606=CARTESIAN_POINT('Ctrl Pts',(-16.4964215270082,-43.6691273920409,
20.));
#73607=CARTESIAN_POINT('Ctrl Pts',(-16.5260958322991,-43.6547274728139,
0.));
#73608=CARTESIAN_POINT('Ctrl Pts',(-16.5260958322991,-43.6547274728139,
20.));
#73609=CARTESIAN_POINT('Ctrl Pts',(-16.5557589924819,-43.640307162529,0.));
#73610=CARTESIAN_POINT('Ctrl Pts',(-16.5557589924819,-43.640307162529,20.));
#73611=CARTESIAN_POINT('Ctrl Pts',(-16.5854109932504,-43.6258664691173,
0.));
#73612=CARTESIAN_POINT('Ctrl Pts',(-16.5854109932504,-43.6258664691173,
20.));
#73613=CARTESIAN_POINT('Ctrl Pts',(-16.6150518203036,-43.6114054005208,
0.));
#73614=CARTESIAN_POINT('Ctrl Pts',(-16.6150518203036,-43.6114054005208,
20.));
#73615=CARTESIAN_POINT('Ctrl Pts',(-16.6446814593459,-43.5969239646926,
0.));
#73616=CARTESIAN_POINT('Ctrl Pts',(-16.6446814593459,-43.5969239646926,
20.));
#73617=CARTESIAN_POINT('Ctrl Pts',(-16.6742998960869,-43.5824221695961,
0.));
#73618=CARTESIAN_POINT('Ctrl Pts',(-16.6742998960869,-43.5824221695961,
20.));
#73619=CARTESIAN_POINT('Ctrl Pts',(-16.7039071162413,-43.5679000232041,
0.));
#73620=CARTESIAN_POINT('Ctrl Pts',(-16.7039071162413,-43.5679000232041,
20.));
#73621=CARTESIAN_POINT('Ctrl Pts',(-16.7335031055295,-43.5533575334996,
0.));
#73622=CARTESIAN_POINT('Ctrl Pts',(-16.7335031055295,-43.5533575334996,
20.));
#73623=CARTESIAN_POINT('Ctrl Pts',(-16.7630878496767,-43.5387947084755,
0.));
#73624=CARTESIAN_POINT('Ctrl Pts',(-16.7630878496767,-43.5387947084755,
20.));
#73625=CARTESIAN_POINT('Ctrl Pts',(-16.792661334414,-43.5242115561352,0.));
#73626=CARTESIAN_POINT('Ctrl Pts',(-16.792661334414,-43.5242115561352,20.));
#73627=CARTESIAN_POINT('Ctrl Pts',(-16.8222235454772,-43.5096080844922,
0.));
#73628=CARTESIAN_POINT('Ctrl Pts',(-16.8222235454772,-43.5096080844922,
20.));
#73629=CARTESIAN_POINT('Ctrl Pts',(-16.8517744686076,-43.4949843015709,
0.));
#73630=CARTESIAN_POINT('Ctrl Pts',(-16.8517744686076,-43.4949843015709,
20.));
#73631=CARTESIAN_POINT('Ctrl Pts',(-16.8813140895513,-43.4803402154062,
0.));
#73632=CARTESIAN_POINT('Ctrl Pts',(-16.8813140895513,-43.4803402154062,
20.));
#73633=CARTESIAN_POINT('Ctrl Pts',(-16.91084239406,-43.4656758340435,0.));
#73634=CARTESIAN_POINT('Ctrl Pts',(-16.91084239406,-43.4656758340435,20.));
#73635=CARTESIAN_POINT('Ctrl Pts',(-16.9403593678908,-43.4509911655382,
0.));
#73636=CARTESIAN_POINT('Ctrl Pts',(-16.9403593678908,-43.4509911655382,
20.));
#73637=CARTESIAN_POINT('Ctrl Pts',(-16.9698649968061,-43.4362862179557,
0.));
#73638=CARTESIAN_POINT('Ctrl Pts',(-16.9698649968061,-43.4362862179557,
20.));
#73639=CARTESIAN_POINT('Ctrl Pts',(-16.9993592665737,-43.4215609993712,
0.));
#73640=CARTESIAN_POINT('Ctrl Pts',(-16.9993592665737,-43.4215609993712,
20.));
#73641=CARTESIAN_POINT('Ctrl Pts',(-17.0288421629666,-43.4068155178695,
0.));
#73642=CARTESIAN_POINT('Ctrl Pts',(-17.0288421629666,-43.4068155178695,
20.));
#73643=CARTESIAN_POINT('Ctrl Pts',(-17.0583136717632,-43.3920497815463,
0.));
#73644=CARTESIAN_POINT('Ctrl Pts',(-17.0583136717632,-43.3920497815463,
20.));
#73645=CARTESIAN_POINT('Ctrl Pts',(-17.0877737787472,-43.3772637985072,
0.));
#73646=CARTESIAN_POINT('Ctrl Pts',(-17.0877737787472,-43.3772637985072,
20.));
#73647=CARTESIAN_POINT('Ctrl Pts',(-17.1172224697079,-43.3624575768695,
0.));
#73648=CARTESIAN_POINT('Ctrl Pts',(-17.1172224697079,-43.3624575768695,
20.));
#73649=CARTESIAN_POINT('Ctrl Pts',(-17.1466597304397,-43.3476311247602,
0.));
#73650=CARTESIAN_POINT('Ctrl Pts',(-17.1466597304397,-43.3476311247602,
20.));
#73651=CARTESIAN_POINT('Ctrl Pts',(-17.1760855467426,-43.332784450317,0.));
#73652=CARTESIAN_POINT('Ctrl Pts',(-17.1760855467426,-43.332784450317,20.));
#73653=CARTESIAN_POINT('Ctrl Pts',(-17.2054999044213,-43.3179175616862,
0.));
#73654=CARTESIAN_POINT('Ctrl Pts',(-17.2054999044213,-43.3179175616862,
20.));
#73655=CARTESIAN_POINT('Ctrl Pts',(-17.2349027892859,-43.3030304670242,
0.));
#73656=CARTESIAN_POINT('Ctrl Pts',(-17.2349027892859,-43.3030304670242,
20.));
#73657=CARTESIAN_POINT('Ctrl Pts',(-17.2642941871522,-43.2881231744974,
0.));
#73658=CARTESIAN_POINT('Ctrl Pts',(-17.2642941871522,-43.2881231744974,
20.));
#73659=CARTESIAN_POINT('Ctrl Pts',(-17.2936740838416,-43.2731956922839,
0.));
#73660=CARTESIAN_POINT('Ctrl Pts',(-17.2936740838416,-43.2731956922839,
20.));
#73661=CARTESIAN_POINT('Ctrl Pts',(-17.3230424651811,-43.258248028572,0.));
#73662=CARTESIAN_POINT('Ctrl Pts',(-17.3230424651811,-43.258248028572,20.));
#73663=CARTESIAN_POINT('Ctrl Pts',(-17.3523993170031,-43.2432801915607,
0.));
#73664=CARTESIAN_POINT('Ctrl Pts',(-17.3523993170031,-43.2432801915607,
20.));
#73665=CARTESIAN_POINT('Ctrl Pts',(-17.3817446251452,-43.2282921894589,
0.));
#73666=CARTESIAN_POINT('Ctrl Pts',(-17.3817446251452,-43.2282921894589,
20.));
#73667=CARTESIAN_POINT('Ctrl Pts',(-17.4110783754507,-43.2132840304854,
0.));
#73668=CARTESIAN_POINT('Ctrl Pts',(-17.4110783754507,-43.2132840304854,
20.));
#73669=CARTESIAN_POINT('Ctrl Pts',(-17.4404005537678,-43.1982557228684,
0.));
#73670=CARTESIAN_POINT('Ctrl Pts',(-17.4404005537678,-43.1982557228684,
20.));
#73671=CARTESIAN_POINT('Ctrl Pts',(-17.4697111459501,-43.1832072748459,
0.));
#73672=CARTESIAN_POINT('Ctrl Pts',(-17.4697111459501,-43.1832072748459,
20.));
#73673=CARTESIAN_POINT('Ctrl Pts',(-17.4990101378563,-43.1681386946662,
0.));
#73674=CARTESIAN_POINT('Ctrl Pts',(-17.4990101378563,-43.1681386946662,
20.));
#73675=CARTESIAN_POINT('Ctrl Pts',(-17.5282975153509,-43.1530499905879,
0.));
#73676=CARTESIAN_POINT('Ctrl Pts',(-17.5282975153509,-43.1530499905879,
20.));
#73677=CARTESIAN_POINT('Ctrl Pts',(-17.557573264304,-43.1379411708804,0.));
#73678=CARTESIAN_POINT('Ctrl Pts',(-17.557573264304,-43.1379411708804,20.));
#73679=CARTESIAN_POINT('Ctrl Pts',(-17.5868373705916,-43.122812243824,0.));
#73680=CARTESIAN_POINT('Ctrl Pts',(-17.5868373705916,-43.122812243824,20.));
#73681=CARTESIAN_POINT('Ctrl Pts',(-17.6160898200949,-43.1076632177088,
0.));
#73682=CARTESIAN_POINT('Ctrl Pts',(-17.6160898200949,-43.1076632177088,
20.));
#73683=CARTESIAN_POINT('Ctrl Pts',(-17.645330598701,-43.0924941008354,0.));
#73684=CARTESIAN_POINT('Ctrl Pts',(-17.645330598701,-43.0924941008354,20.));
#73685=CARTESIAN_POINT('Ctrl Pts',(-17.674559692302,-43.0773049015136,0.));
#73686=CARTESIAN_POINT('Ctrl Pts',(-17.674559692302,-43.0773049015136,20.));
#73687=CARTESIAN_POINT('Ctrl Pts',(-17.7037770867956,-43.0620956280638,
0.));
#73688=CARTESIAN_POINT('Ctrl Pts',(-17.7037770867956,-43.0620956280638,
20.));
#73689=CARTESIAN_POINT('Ctrl Pts',(-17.7329827680847,-43.0468662888157,
0.));
#73690=CARTESIAN_POINT('Ctrl Pts',(-17.7329827680847,-43.0468662888157,
20.));
#73691=CARTESIAN_POINT('Ctrl Pts',(-17.7621767220773,-43.0316168921093,
0.));
#73692=CARTESIAN_POINT('Ctrl Pts',(-17.7621767220773,-43.0316168921093,
20.));
#73693=CARTESIAN_POINT('Ctrl Pts',(-17.7913589346876,-43.0163474462951,
0.));
#73694=CARTESIAN_POINT('Ctrl Pts',(-17.7913589346876,-43.0163474462951,
20.));
#73695=CARTESIAN_POINT('Ctrl Pts',(-17.8205293918351,-43.0010579597341,
0.));
#73696=CARTESIAN_POINT('Ctrl Pts',(-17.8205293918351,-43.0010579597341,
20.));
#73697=CARTESIAN_POINT('Ctrl Pts',(-17.8496880794454,-42.9857484407979,
0.));
#73698=CARTESIAN_POINT('Ctrl Pts',(-17.8496880794454,-42.9857484407979,
20.));
#73699=CARTESIAN_POINT('Ctrl Pts',(-17.8788349834491,-42.9704188978681,
0.));
#73700=CARTESIAN_POINT('Ctrl Pts',(-17.8788349834491,-42.9704188978681,
20.));
#73701=CARTESIAN_POINT('Ctrl Pts',(-17.9079700897828,-42.9550693393359,
0.));
#73702=CARTESIAN_POINT('Ctrl Pts',(-17.9079700897828,-42.9550693393359,
20.));
#73703=CARTESIAN_POINT('Ctrl Pts',(-17.9370933843882,-42.9396997736018,
0.));
#73704=CARTESIAN_POINT('Ctrl Pts',(-17.9370933843882,-42.9396997736018,
20.));
#73705=CARTESIAN_POINT('Ctrl Pts',(-17.9662048532126,-42.9243102090766,
0.));
#73706=CARTESIAN_POINT('Ctrl Pts',(-17.9662048532126,-42.9243102090766,
20.));
#73707=CARTESIAN_POINT('Ctrl Pts',(-17.9953044822088,-42.9089006541818,
0.));
#73708=CARTESIAN_POINT('Ctrl Pts',(-17.9953044822088,-42.9089006541818,
20.));
#73709=CARTESIAN_POINT('Ctrl Pts',(-18.0243922573354,-42.893471117349,0.));
#73710=CARTESIAN_POINT('Ctrl Pts',(-18.0243922573354,-42.893471117349,20.));
#73711=CARTESIAN_POINT('Ctrl Pts',(-18.0534681645565,-42.8780216070204,
0.));
#73712=CARTESIAN_POINT('Ctrl Pts',(-18.0534681645565,-42.8780216070204,
20.));
#73713=CARTESIAN_POINT('Ctrl Pts',(-18.0825321898416,-42.8625521316488,
0.));
#73714=CARTESIAN_POINT('Ctrl Pts',(-18.0825321898416,-42.8625521316488,
20.));
#73715=CARTESIAN_POINT('Ctrl Pts',(-18.1115843191668,-42.8470626996976,
0.));
#73716=CARTESIAN_POINT('Ctrl Pts',(-18.1115843191668,-42.8470626996976,
20.));
#73717=CARTESIAN_POINT('Ctrl Pts',(-18.1406245385131,-42.831553319639,0.));
#73718=CARTESIAN_POINT('Ctrl Pts',(-18.1406245385131,-42.831553319639,20.));
#73719=CARTESIAN_POINT('Ctrl Pts',(-18.1696528338673,-42.8160239999555,
0.));
#73720=CARTESIAN_POINT('Ctrl Pts',(-18.1696528338673,-42.8160239999555,
20.));
#73721=CARTESIAN_POINT('Ctrl Pts',(-18.1986691912208,-42.8004747491375,
0.));
#73722=CARTESIAN_POINT('Ctrl Pts',(-18.1986691912208,-42.8004747491375,
20.));
#73723=CARTESIAN_POINT('Ctrl Pts',(-18.2276735965714,-42.7849055756869,
0.));
#73724=CARTESIAN_POINT('Ctrl Pts',(-18.2276735965714,-42.7849055756869,
20.));
#73725=CARTESIAN_POINT('Ctrl Pts',(-18.256666035922,-42.7693164881155,0.));
#73726=CARTESIAN_POINT('Ctrl Pts',(-18.256666035922,-42.7693164881155,20.));
#73727=CARTESIAN_POINT('Ctrl Pts',(-18.285646495282,-42.7537074949463,0.));
#73728=CARTESIAN_POINT('Ctrl Pts',(-18.285646495282,-42.7537074949463,20.));
#73729=CARTESIAN_POINT('Ctrl Pts',(-18.3146149606662,-42.7380786047127,
0.));
#73730=CARTESIAN_POINT('Ctrl Pts',(-18.3146149606662,-42.7380786047127,
20.));
#73731=CARTESIAN_POINT('Ctrl Pts',(-18.3435714180954,-42.7224298259587,
0.));
#73732=CARTESIAN_POINT('Ctrl Pts',(-18.3435714180954,-42.7224298259587,
20.));
#73733=CARTESIAN_POINT('Ctrl Pts',(-18.372515853596,-42.7067611672378,0.));
#73734=CARTESIAN_POINT('Ctrl Pts',(-18.372515853596,-42.7067611672378,20.));
#73735=CARTESIAN_POINT('Ctrl Pts',(-18.4014482531999,-42.6910726371132,
0.));
#73736=CARTESIAN_POINT('Ctrl Pts',(-18.4014482531999,-42.6910726371132,
20.));
#73737=CARTESIAN_POINT('Ctrl Pts',(-18.4303686029444,-42.6753642441576,
0.));
#73738=CARTESIAN_POINT('Ctrl Pts',(-18.4303686029444,-42.6753642441576,
20.));
#73739=CARTESIAN_POINT('Ctrl Pts',(-18.4592768888724,-42.6596359969538,
0.));
#73740=CARTESIAN_POINT('Ctrl Pts',(-18.4592768888724,-42.6596359969538,
20.));
#73741=CARTESIAN_POINT('Ctrl Pts',(-18.4881730970326,-42.6438879040941,
0.));
#73742=CARTESIAN_POINT('Ctrl Pts',(-18.4881730970326,-42.6438879040941,
20.));
#73743=CARTESIAN_POINT('Ctrl Pts',(-18.5170572134793,-42.6281199741818,
0.));
#73744=CARTESIAN_POINT('Ctrl Pts',(-18.5170572134793,-42.6281199741818,
20.));
#73745=CARTESIAN_POINT('Ctrl Pts',(-18.5459292242727,-42.61233221583,0.));
#73746=CARTESIAN_POINT('Ctrl Pts',(-18.5459292242727,-42.61233221583,20.));
#73747=CARTESIAN_POINT('Ctrl Pts',(-18.574789115479,-42.596524637663,0.));
#73748=CARTESIAN_POINT('Ctrl Pts',(-18.574789115479,-42.596524637663,20.));
#73749=CARTESIAN_POINT('Ctrl Pts',(-18.6036368731702,-42.5806972483146,
0.));
#73750=CARTESIAN_POINT('Ctrl Pts',(-18.6036368731702,-42.5806972483146,
20.));
#73751=CARTESIAN_POINT('Ctrl Pts',(-18.632472483424,-42.5648500564287,0.));
#73752=CARTESIAN_POINT('Ctrl Pts',(-18.632472483424,-42.5648500564287,20.));
#73753=CARTESIAN_POINT('Ctrl Pts',(-18.6612959323233,-42.5489830706585,
0.));
#73754=CARTESIAN_POINT('Ctrl Pts',(-18.6612959323233,-42.5489830706585,
20.));
#73755=CARTESIAN_POINT('Ctrl Pts',(-18.6901072059568,-42.5330962996668,
0.));
#73756=CARTESIAN_POINT('Ctrl Pts',(-18.6901072059568,-42.5330962996668,
20.));
#73757=CARTESIAN_POINT('Ctrl Pts',(-18.718906290419,-42.5171897521269,0.));
#73758=CARTESIAN_POINT('Ctrl Pts',(-18.718906290419,-42.5171897521269,20.));
#73759=CARTESIAN_POINT('Ctrl Pts',(-18.7476931718101,-42.5012634367222,
0.));
#73760=CARTESIAN_POINT('Ctrl Pts',(-18.7476931718101,-42.5012634367222,
20.));
#73761=CARTESIAN_POINT('Ctrl Pts',(-18.7764678362368,-42.4853173621469,
0.));
#73762=CARTESIAN_POINT('Ctrl Pts',(-18.7764678362368,-42.4853173621469,
20.));
#73763=CARTESIAN_POINT('Ctrl Pts',(-18.8052302698113,-42.4693515371059,
0.));
#73764=CARTESIAN_POINT('Ctrl Pts',(-18.8052302698113,-42.4693515371059,
20.));
#73765=CARTESIAN_POINT('Ctrl Pts',(-18.8339804586522,-42.4533659703145,
0.));
#73766=CARTESIAN_POINT('Ctrl Pts',(-18.8339804586522,-42.4533659703145,
20.));
#73767=CARTESIAN_POINT('Ctrl Pts',(-18.8627183888827,-42.4373606704956,
0.));
#73768=CARTESIAN_POINT('Ctrl Pts',(-18.8627183888827,-42.4373606704956,
20.));
#73769=CARTESIAN_POINT('Ctrl Pts',(-18.8914440466322,-42.4213356463824,
0.));
#73770=CARTESIAN_POINT('Ctrl Pts',(-18.8914440466322,-42.4213356463824,
20.));
#73771=CARTESIAN_POINT('Ctrl Pts',(-18.9201574180352,-42.4052909067172,
0.));
#73772=CARTESIAN_POINT('Ctrl Pts',(-18.9201574180352,-42.4052909067172,
20.));
#73773=CARTESIAN_POINT('Ctrl Pts',(-18.9488584892326,-42.389226460254,0.));
#73774=CARTESIAN_POINT('Ctrl Pts',(-18.9488584892326,-42.389226460254,20.));
#73775=CARTESIAN_POINT('Ctrl Pts',(-18.9775472463711,-42.3731423157568,
0.));
#73776=CARTESIAN_POINT('Ctrl Pts',(-18.9775472463711,-42.3731423157568,
20.));
#73777=CARTESIAN_POINT('Ctrl Pts',(-19.0062236756035,-42.3570384820003,
0.));
#73778=CARTESIAN_POINT('Ctrl Pts',(-19.0062236756035,-42.3570384820003,
20.));
#73779=CARTESIAN_POINT('Ctrl Pts',(-19.0348877630887,-42.3409149677685,
0.));
#73780=CARTESIAN_POINT('Ctrl Pts',(-19.0348877630887,-42.3409149677685,
20.));
#73781=CARTESIAN_POINT('Ctrl Pts',(-19.0635394949913,-42.3247717818558,
0.));
#73782=CARTESIAN_POINT('Ctrl Pts',(-19.0635394949913,-42.3247717818558,
20.));
#73783=CARTESIAN_POINT('Ctrl Pts',(-19.0921788574819,-42.3086089330657,
0.));
#73784=CARTESIAN_POINT('Ctrl Pts',(-19.0921788574819,-42.3086089330657,
20.));
#73785=CARTESIAN_POINT('Ctrl Pts',(-19.1208058367362,-42.2924264302113,
0.));
#73786=CARTESIAN_POINT('Ctrl Pts',(-19.1208058367362,-42.2924264302113,
20.));
#73787=CARTESIAN_POINT('Ctrl Pts',(-19.1494204189361,-42.2762242821163,
0.));
#73788=CARTESIAN_POINT('Ctrl Pts',(-19.1494204189361,-42.2762242821163,
20.));
#73789=CARTESIAN_POINT('Ctrl Pts',(-19.1780225902694,-42.2600024976146,
0.));
#73790=CARTESIAN_POINT('Ctrl Pts',(-19.1780225902694,-42.2600024976146,
20.));
#73791=CARTESIAN_POINT('Ctrl Pts',(-19.2066123369297,-42.2437610855506,
0.));
#73792=CARTESIAN_POINT('Ctrl Pts',(-19.2066123369297,-42.2437610855506,
20.));
#73793=CARTESIAN_POINT('Ctrl Pts',(-19.2351896451166,-42.2275000547783,
0.));
#73794=CARTESIAN_POINT('Ctrl Pts',(-19.2351896451166,-42.2275000547783,
20.));
#73795=CARTESIAN_POINT('Ctrl Pts',(-19.2637545010356,-42.2112194141618,
0.));
#73796=CARTESIAN_POINT('Ctrl Pts',(-19.2637545010356,-42.2112194141618,
20.));
#73797=CARTESIAN_POINT('Ctrl Pts',(-19.2923068908981,-42.1949191725745,
0.));
#73798=CARTESIAN_POINT('Ctrl Pts',(-19.2923068908981,-42.1949191725745,
20.));
#73799=CARTESIAN_POINT('Ctrl Pts',(-19.3208468009212,-42.1785993388989,
0.));
#73800=CARTESIAN_POINT('Ctrl Pts',(-19.3208468009212,-42.1785993388989,
20.));
#73801=CARTESIAN_POINT('Ctrl Pts',(-19.3493742173283,-42.1622599220289,
0.));
#73802=CARTESIAN_POINT('Ctrl Pts',(-19.3493742173283,-42.1622599220289,
20.));
#73803=CARTESIAN_POINT('Ctrl Pts',(-19.377889126349,-42.1459009308685,0.));
#73804=CARTESIAN_POINT('Ctrl Pts',(-19.377889126349,-42.1459009308685,20.));
#73805=CARTESIAN_POINT('Ctrl Pts',(-19.4063915142187,-42.1295223743319,
0.));
#73806=CARTESIAN_POINT('Ctrl Pts',(-19.4063915142187,-42.1295223743319,
20.));
#73807=CARTESIAN_POINT('Ctrl Pts',(-19.4348813671785,-42.1131242613432,
0.));
#73808=CARTESIAN_POINT('Ctrl Pts',(-19.4348813671785,-42.1131242613432,
20.));
#73809=CARTESIAN_POINT('Ctrl Pts',(-19.4633586714748,-42.0967066008354,
0.));
#73810=CARTESIAN_POINT('Ctrl Pts',(-19.4633586714748,-42.0967066008354,
20.));
#73811=CARTESIAN_POINT('Ctrl Pts',(-19.4918234133604,-42.080269401751,0.));
#73812=CARTESIAN_POINT('Ctrl Pts',(-19.4918234133604,-42.080269401751,20.));
#73813=CARTESIAN_POINT('Ctrl Pts',(-19.520275579094,-42.0638126730426,0.));
#73814=CARTESIAN_POINT('Ctrl Pts',(-19.520275579094,-42.0638126730426,20.));
#73815=CARTESIAN_POINT('Ctrl Pts',(-19.5487151549408,-42.0473364236742,
0.));
#73816=CARTESIAN_POINT('Ctrl Pts',(-19.5487151549408,-42.0473364236742,
20.));
#73817=CARTESIAN_POINT('Ctrl Pts',(-19.5771421271718,-42.0308406626191,
0.));
#73818=CARTESIAN_POINT('Ctrl Pts',(-19.5771421271718,-42.0308406626191,
20.));
#73819=CARTESIAN_POINT('Ctrl Pts',(-19.6055564820642,-42.0143253988608,
0.));
#73820=CARTESIAN_POINT('Ctrl Pts',(-19.6055564820642,-42.0143253988608,
20.));
#73821=CARTESIAN_POINT('Ctrl Pts',(-19.6339582059009,-41.997790641393,0.));
#73822=CARTESIAN_POINT('Ctrl Pts',(-19.6339582059009,-41.997790641393,20.));
#73823=CARTESIAN_POINT('Ctrl Pts',(-19.6623472849704,-41.9812363992182,
0.));
#73824=CARTESIAN_POINT('Ctrl Pts',(-19.6623472849704,-41.9812363992182,
20.));
#73825=CARTESIAN_POINT('Ctrl Pts',(-19.6907237055675,-41.9646626813489,
0.));
#73826=CARTESIAN_POINT('Ctrl Pts',(-19.6907237055675,-41.9646626813489,
20.));
#73827=CARTESIAN_POINT('Ctrl Pts',(-19.7190874539927,-41.9480694968077,
0.));
#73828=CARTESIAN_POINT('Ctrl Pts',(-19.7190874539927,-41.9480694968077,
20.));
#73829=CARTESIAN_POINT('Ctrl Pts',(-19.7474385165532,-41.9314568546275,
0.));
#73830=CARTESIAN_POINT('Ctrl Pts',(-19.7474385165532,-41.9314568546275,
20.));
#73831=CARTESIAN_POINT('Ctrl Pts',(-19.775776879562,-41.9148247638512,0.));
#73832=CARTESIAN_POINT('Ctrl Pts',(-19.775776879562,-41.9148247638512,20.));
#73833=CARTESIAN_POINT('Ctrl Pts',(-19.8041025293385,-41.8981732335313,
0.));
#73834=CARTESIAN_POINT('Ctrl Pts',(-19.8041025293385,-41.8981732335313,
20.));
#73835=CARTESIAN_POINT('Ctrl Pts',(-19.8324154522082,-41.8815022727306,
0.));
#73836=CARTESIAN_POINT('Ctrl Pts',(-19.8324154522082,-41.8815022727306,
20.));
#73837=CARTESIAN_POINT('Ctrl Pts',(-19.8607156345021,-41.8648118905217,
0.));
#73838=CARTESIAN_POINT('Ctrl Pts',(-19.8607156345021,-41.8648118905217,
20.));
#73839=CARTESIAN_POINT('Ctrl Pts',(-19.889003062557,-41.8481020959867,0.));
#73840=CARTESIAN_POINT('Ctrl Pts',(-19.889003062557,-41.8481020959867,20.));
#73841=CARTESIAN_POINT('Ctrl Pts',(-19.9172777227157,-41.8313728982175,
0.));
#73842=CARTESIAN_POINT('Ctrl Pts',(-19.9172777227157,-41.8313728982175,
20.));
#73843=CARTESIAN_POINT('Ctrl Pts',(-19.945539601327,-41.8146243063151,0.));
#73844=CARTESIAN_POINT('Ctrl Pts',(-19.945539601327,-41.8146243063151,20.));
#73845=CARTESIAN_POINT('Ctrl Pts',(-19.9737886847462,-41.7978563293914,
0.));
#73846=CARTESIAN_POINT('Ctrl Pts',(-19.9737886847462,-41.7978563293914,
20.));
#73847=CARTESIAN_POINT('Ctrl Pts',(-20.0020249593348,-41.7810689765678,
0.));
#73848=CARTESIAN_POINT('Ctrl Pts',(-20.0020249593348,-41.7810689765678,
20.));
#73849=CARTESIAN_POINT('Ctrl Pts',(-20.0302484114611,-41.7642622569769,
0.));
#73850=CARTESIAN_POINT('Ctrl Pts',(-20.0302484114611,-41.7642622569769,
20.));
#73851=CARTESIAN_POINT('Ctrl Pts',(-20.0584590274992,-41.7474361797609,
0.));
#73852=CARTESIAN_POINT('Ctrl Pts',(-20.0584590274992,-41.7474361797609,
20.));
#73853=CARTESIAN_POINT('Ctrl Pts',(-20.0866567938288,-41.7305907540713,
0.));
#73854=CARTESIAN_POINT('Ctrl Pts',(-20.0866567938288,-41.7305907540713,
20.));
#73855=CARTESIAN_POINT('Ctrl Pts',(-20.1148416968357,-41.7137259890696,
0.));
#73856=CARTESIAN_POINT('Ctrl Pts',(-20.1148416968357,-41.7137259890696,
20.));
#73857=CARTESIAN_POINT('Ctrl Pts',(-20.1430137229118,-41.6968418939263,
0.));
#73858=CARTESIAN_POINT('Ctrl Pts',(-20.1430137229118,-41.6968418939263,
20.));
#73859=CARTESIAN_POINT('Ctrl Pts',(-20.1711728584549,-41.6799384778218,
0.));
#73860=CARTESIAN_POINT('Ctrl Pts',(-20.1711728584549,-41.6799384778218,
20.));
#73861=CARTESIAN_POINT('Ctrl Pts',(-20.199319089869,-41.6630157499462,0.));
#73862=CARTESIAN_POINT('Ctrl Pts',(-20.199319089869,-41.6630157499462,20.));
#73863=CARTESIAN_POINT('Ctrl Pts',(-20.2274524035648,-41.6460737195007,
0.));
#73864=CARTESIAN_POINT('Ctrl Pts',(-20.2274524035648,-41.6460737195007,
20.));
#73865=CARTESIAN_POINT('Ctrl Pts',(-20.2555727859589,-41.6291123956959,
0.));
#73866=CARTESIAN_POINT('Ctrl Pts',(-20.2555727859589,-41.6291123956959,
20.));
#73867=CARTESIAN_POINT('Ctrl Pts',(-20.2836802234745,-41.6121317877528,
0.));
#73868=CARTESIAN_POINT('Ctrl Pts',(-20.2836802234745,-41.6121317877528,
20.));
#73869=CARTESIAN_POINT('Ctrl Pts',(-20.3117747025404,-41.5951319049016,
0.));
#73870=CARTESIAN_POINT('Ctrl Pts',(-20.3117747025404,-41.5951319049016,
20.));
#73871=CARTESIAN_POINT('Ctrl Pts',(-20.3398562095917,-41.5781127563818,
0.));
#73872=CARTESIAN_POINT('Ctrl Pts',(-20.3398562095917,-41.5781127563818,
20.));
#73873=CARTESIAN_POINT('Ctrl Pts',(-20.3679247310694,-41.561074351443,0.));
#73874=CARTESIAN_POINT('Ctrl Pts',(-20.3679247310694,-41.561074351443,20.));
#73875=CARTESIAN_POINT('Ctrl Pts',(-20.3959802534211,-41.5440166993445,
0.));
#73876=CARTESIAN_POINT('Ctrl Pts',(-20.3959802534211,-41.5440166993445,
20.));
#73877=CARTESIAN_POINT('Ctrl Pts',(-20.4240227631002,-41.5269398093561,
0.));
#73878=CARTESIAN_POINT('Ctrl Pts',(-20.4240227631002,-41.5269398093561,
20.));
#73879=CARTESIAN_POINT('Ctrl Pts',(-20.4520522465668,-41.5098436907568,
0.));
#73880=CARTESIAN_POINT('Ctrl Pts',(-20.4520522465668,-41.5098436907568,
20.));
#73881=CARTESIAN_POINT('Ctrl Pts',(-20.4800686902869,-41.4927283528358,
0.));
#73882=CARTESIAN_POINT('Ctrl Pts',(-20.4800686902869,-41.4927283528358,
20.));
#73883=CARTESIAN_POINT('Ctrl Pts',(-20.5080720807336,-41.4755938048931,
0.));
#73884=CARTESIAN_POINT('Ctrl Pts',(-20.5080720807336,-41.4755938048931,
20.));
#73885=CARTESIAN_POINT('Ctrl Pts',(-20.5360624043854,-41.4584400562379,
0.));
#73886=CARTESIAN_POINT('Ctrl Pts',(-20.5360624043854,-41.4584400562379,
20.));
#73887=CARTESIAN_POINT('Ctrl Pts',(-20.564039647727,-41.4412671161883,0.));
#73888=CARTESIAN_POINT('Ctrl Pts',(-20.564039647727,-41.4412671161883,20.));
#73889=CARTESIAN_POINT('Ctrl Pts',(-20.592003797249,-41.4240749940721,0.));
#73890=CARTESIAN_POINT('Ctrl Pts',(-20.592003797249,-41.4240749940721,20.));
#73891=CARTESIAN_POINT('Ctrl Pts',(-20.6199548394484,-41.4068636992265,
0.));
#73892=CARTESIAN_POINT('Ctrl Pts',(-20.6199548394484,-41.4068636992265,
20.));
#73893=CARTESIAN_POINT('Ctrl Pts',(-20.6478927608288,-41.3896332409988,
0.));
#73894=CARTESIAN_POINT('Ctrl Pts',(-20.6478927608288,-41.3896332409988,
20.));
#73895=CARTESIAN_POINT('Ctrl Pts',(-20.6758175479,-41.372383628747,0.));
#73896=CARTESIAN_POINT('Ctrl Pts',(-20.6758175479,-41.372383628747,20.));
#73897=CARTESIAN_POINT('Ctrl Pts',(-20.7037291871782,-41.3551148718389,
0.));
#73898=CARTESIAN_POINT('Ctrl Pts',(-20.7037291871782,-41.3551148718389,
20.));
#73899=CARTESIAN_POINT('Ctrl Pts',(-20.731627665186,-41.3378269796522,0.));
#73900=CARTESIAN_POINT('Ctrl Pts',(-20.731627665186,-41.3378269796522,20.));
#73901=CARTESIAN_POINT('Ctrl Pts',(-20.7595129684521,-41.3205199615745,
0.));
#73902=CARTESIAN_POINT('Ctrl Pts',(-20.7595129684521,-41.3205199615745,
20.));
#73903=CARTESIAN_POINT('Ctrl Pts',(-20.7873850835117,-41.303193827003,0.));
#73904=CARTESIAN_POINT('Ctrl Pts',(-20.7873850835117,-41.303193827003,20.));
#73905=CARTESIAN_POINT('Ctrl Pts',(-20.8152439969059,-41.285848585344,0.));
#73906=CARTESIAN_POINT('Ctrl Pts',(-20.8152439969059,-41.285848585344,20.));
#73907=CARTESIAN_POINT('Ctrl Pts',(-20.8430896951822,-41.268484246013,0.));
#73908=CARTESIAN_POINT('Ctrl Pts',(-20.8430896951822,-41.268484246013,20.));
#73909=CARTESIAN_POINT('Ctrl Pts',(-20.8709221648944,-41.2511008184358,
0.));
#73910=CARTESIAN_POINT('Ctrl Pts',(-20.8709221648944,-41.2511008184358,
20.));
#73911=CARTESIAN_POINT('Ctrl Pts',(-20.8987413926025,-41.2336983120481,
0.));
#73912=CARTESIAN_POINT('Ctrl Pts',(-20.8987413926025,-41.2336983120481,
20.));
#73913=CARTESIAN_POINT('Ctrl Pts',(-20.9265473648728,-41.2162767362953,
0.));
#73914=CARTESIAN_POINT('Ctrl Pts',(-20.9265473648728,-41.2162767362953,
20.));
#73915=CARTESIAN_POINT('Ctrl Pts',(-20.9543400682781,-41.1988361006333,
0.));
#73916=CARTESIAN_POINT('Ctrl Pts',(-20.9543400682781,-41.1988361006333,
20.));
#73917=CARTESIAN_POINT('Ctrl Pts',(-20.9821194893979,-41.1813764145274,
0.));
#73918=CARTESIAN_POINT('Ctrl Pts',(-20.9821194893979,-41.1813764145274,
20.));
#73919=CARTESIAN_POINT('Ctrl Pts',(-21.009885614818,-41.1638976874526,0.));
#73920=CARTESIAN_POINT('Ctrl Pts',(-21.009885614818,-41.1638976874526,20.));
#73921=CARTESIAN_POINT('Ctrl Pts',(-21.0376384311301,-41.1463999288927,
0.));
#73922=CARTESIAN_POINT('Ctrl Pts',(-21.0376384311301,-41.1463999288927,
20.));
#73923=CARTESIAN_POINT('Ctrl Pts',(-21.0653779249329,-41.128883148342,0.));
#73924=CARTESIAN_POINT('Ctrl Pts',(-21.0653779249329,-41.128883148342,20.));
#73925=CARTESIAN_POINT('Ctrl Pts',(-21.0931040828311,-41.1113473553046,
0.));
#73926=CARTESIAN_POINT('Ctrl Pts',(-21.0931040828311,-41.1113473553046,
20.));
#73927=CARTESIAN_POINT('Ctrl Pts',(-21.1208168914355,-41.0937925592943,
0.));
#73928=CARTESIAN_POINT('Ctrl Pts',(-21.1208168914355,-41.0937925592943,
20.));
#73929=CARTESIAN_POINT('Ctrl Pts',(-21.1485163373635,-41.076218769835,0.));
#73930=CARTESIAN_POINT('Ctrl Pts',(-21.1485163373635,-41.076218769835,20.));
#73931=CARTESIAN_POINT('Ctrl Pts',(-21.1762024072388,-41.0586259964597,
0.));
#73932=CARTESIAN_POINT('Ctrl Pts',(-21.1762024072388,-41.0586259964597,
20.));
#73933=CARTESIAN_POINT('Ctrl Pts',(-21.2038750876913,-41.0410142487106,
0.));
#73934=CARTESIAN_POINT('Ctrl Pts',(-21.2038750876913,-41.0410142487106,
20.));
#73935=CARTESIAN_POINT('Ctrl Pts',(-21.2315343653574,-41.0233835361399,
0.));
#73936=CARTESIAN_POINT('Ctrl Pts',(-21.2315343653574,-41.0233835361399,
20.));
#73937=CARTESIAN_POINT('Ctrl Pts',(-21.25918022688,-41.0057338683097,0.));
#73938=CARTESIAN_POINT('Ctrl Pts',(-21.25918022688,-41.0057338683097,20.));
#73939=CARTESIAN_POINT('Ctrl Pts',(-21.286812658909,-40.9880652547927,0.));
#73940=CARTESIAN_POINT('Ctrl Pts',(-21.286812658909,-40.9880652547927,20.));
#73941=CARTESIAN_POINT('Ctrl Pts',(-21.3144316481012,-40.9703777051716,
0.));
#73942=CARTESIAN_POINT('Ctrl Pts',(-21.3144316481012,-40.9703777051716,
20.));
#73943=CARTESIAN_POINT('Ctrl Pts',(-21.342037181119,-40.9526712290373,0.));
#73944=CARTESIAN_POINT('Ctrl Pts',(-21.342037181119,-40.9526712290373,20.));
#73945=CARTESIAN_POINT('Ctrl Pts',(-21.3696292446317,-40.9349458359905,
0.));
#73946=CARTESIAN_POINT('Ctrl Pts',(-21.3696292446317,-40.9349458359905,
20.));
#73947=CARTESIAN_POINT('Ctrl Pts',(-21.3972078253142,-40.9172015356414,
0.));
#73948=CARTESIAN_POINT('Ctrl Pts',(-21.3972078253142,-40.9172015356414,
20.));
#73949=CARTESIAN_POINT('Ctrl Pts',(-21.424772909848,-40.8994383376102,0.));
#73950=CARTESIAN_POINT('Ctrl Pts',(-21.424772909848,-40.8994383376102,20.));
#73951=CARTESIAN_POINT('Ctrl Pts',(-21.45232448492,-40.8816562515268,0.));
#73952=CARTESIAN_POINT('Ctrl Pts',(-21.45232448492,-40.8816562515268,20.));
#73953=CARTESIAN_POINT('Ctrl Pts',(-21.4798625372243,-40.8638552870319,
0.));
#73954=CARTESIAN_POINT('Ctrl Pts',(-21.4798625372243,-40.8638552870319,
20.));
#73955=CARTESIAN_POINT('Ctrl Pts',(-21.5073870534614,-40.8460354537749,
0.));
#73956=CARTESIAN_POINT('Ctrl Pts',(-21.5073870534614,-40.8460354537749,
20.));
#73957=CARTESIAN_POINT('Ctrl Pts',(-21.5348980203391,-40.8281967614155,
0.));
#73958=CARTESIAN_POINT('Ctrl Pts',(-21.5348980203391,-40.8281967614155,
20.));
#73959=CARTESIAN_POINT('Ctrl Pts',(-21.5623954245725,-40.8103392196221,
0.));
#73960=CARTESIAN_POINT('Ctrl Pts',(-21.5623954245725,-40.8103392196221,
20.));
#73961=CARTESIAN_POINT('Ctrl Pts',(-21.5898792528837,-40.7924628380726,
0.));
#73962=CARTESIAN_POINT('Ctrl Pts',(-21.5898792528837,-40.7924628380726,
20.));
#73963=CARTESIAN_POINT('Ctrl Pts',(-21.6173494920019,-40.7745676264537,
0.));
#73964=CARTESIAN_POINT('Ctrl Pts',(-21.6173494920019,-40.7745676264537,
20.));
#73965=CARTESIAN_POINT('Ctrl Pts',(-21.6448061286619,-40.7566535944621,
0.));
#73966=CARTESIAN_POINT('Ctrl Pts',(-21.6448061286619,-40.7566535944621,
20.));
#73967=CARTESIAN_POINT('Ctrl Pts',(-21.6722491496038,-40.7387207518043,
0.));
#73968=CARTESIAN_POINT('Ctrl Pts',(-21.6722491496038,-40.7387207518043,
20.));
#73969=CARTESIAN_POINT('Ctrl Pts',(-21.6996785415723,-40.7207691081984,
0.));
#73970=CARTESIAN_POINT('Ctrl Pts',(-21.6996785415723,-40.7207691081984,
20.));
#73971=CARTESIAN_POINT('Ctrl Pts',(-21.7270942913167,-40.7027986733736,
0.));
#73972=CARTESIAN_POINT('Ctrl Pts',(-21.7270942913167,-40.7027986733736,
20.));
#73973=CARTESIAN_POINT('Ctrl Pts',(-21.7544963855931,-40.6848094570694,
0.));
#73974=CARTESIAN_POINT('Ctrl Pts',(-21.7544963855931,-40.6848094570694,
20.));
#73975=CARTESIAN_POINT('Ctrl Pts',(-21.781884811165,-40.6668014690334,0.));
#73976=CARTESIAN_POINT('Ctrl Pts',(-21.781884811165,-40.6668014690334,20.));
#73977=CARTESIAN_POINT('Ctrl Pts',(-21.8092595548052,-40.6487747190214,
0.));
#73978=CARTESIAN_POINT('Ctrl Pts',(-21.8092595548052,-40.6487747190214,
20.));
#73979=CARTESIAN_POINT('Ctrl Pts',(-21.8366206032979,-40.6307292167951,
0.));
#73980=CARTESIAN_POINT('Ctrl Pts',(-21.8366206032979,-40.6307292167951,
20.));
#73981=CARTESIAN_POINT('Ctrl Pts',(-21.8639679434382,-40.6126649721233,
0.));
#73982=CARTESIAN_POINT('Ctrl Pts',(-21.8639679434382,-40.6126649721233,
20.));
#73983=CARTESIAN_POINT('Ctrl Pts',(-21.8913015620281,-40.594581994783,0.));
#73984=CARTESIAN_POINT('Ctrl Pts',(-21.8913015620281,-40.594581994783,20.));
#73985=CARTESIAN_POINT('Ctrl Pts',(-21.9186214458728,-40.5764802945639,
0.));
#73986=CARTESIAN_POINT('Ctrl Pts',(-21.9186214458728,-40.5764802945639,
20.));
#73987=CARTESIAN_POINT('Ctrl Pts',(-21.9459275817778,-40.5583598812699,
0.));
#73988=CARTESIAN_POINT('Ctrl Pts',(-21.9459275817778,-40.5583598812699,
20.));
#73989=CARTESIAN_POINT('Ctrl Pts',(-21.9732199565439,-40.5402207647219,
0.));
#73990=CARTESIAN_POINT('Ctrl Pts',(-21.9732199565439,-40.5402207647219,
20.));
#73991=CARTESIAN_POINT('Ctrl Pts',(-22.0004985569689,-40.5220629547578,
0.));
#73992=CARTESIAN_POINT('Ctrl Pts',(-22.0004985569689,-40.5220629547578,
20.));
#73993=CARTESIAN_POINT('Ctrl Pts',(-22.0277633698572,-40.5038864612252,
0.));
#73994=CARTESIAN_POINT('Ctrl Pts',(-22.0277633698572,-40.5038864612252,
20.));
#73995=CARTESIAN_POINT('Ctrl Pts',(-22.0550143820281,-40.485691293976,0.));
#73996=CARTESIAN_POINT('Ctrl Pts',(-22.0550143820281,-40.485691293976,20.));
#73997=CARTESIAN_POINT('Ctrl Pts',(-22.0822515803231,-40.4674774628609,
0.));
#73998=CARTESIAN_POINT('Ctrl Pts',(-22.0822515803231,-40.4674774628609,
20.));
#73999=CARTESIAN_POINT('Ctrl Pts',(-22.1094749516164,-40.4492449777204,
0.));
#74000=CARTESIAN_POINT('Ctrl Pts',(-22.1094749516164,-40.4492449777204,
20.));
#74001=CARTESIAN_POINT('Ctrl Pts',(-22.1366844828092,-40.4309938483881,
0.));
#74002=CARTESIAN_POINT('Ctrl Pts',(-22.1366844828092,-40.4309938483881,
20.));
#74003=CARTESIAN_POINT('Ctrl Pts',(-22.1638801608087,-40.4127240847076,
0.));
#74004=CARTESIAN_POINT('Ctrl Pts',(-22.1638801608087,-40.4127240847076,
20.));
#74005=CARTESIAN_POINT('Ctrl Pts',(-22.1910619725087,-40.3944356965472,
0.));
#74006=CARTESIAN_POINT('Ctrl Pts',(-22.1910619725087,-40.3944356965472,
20.));
#74007=CARTESIAN_POINT('Ctrl Pts',(-22.2182299047735,-40.3761286938114,
0.));
#74008=CARTESIAN_POINT('Ctrl Pts',(-22.2182299047735,-40.3761286938114,
20.));
#74009=CARTESIAN_POINT('Ctrl Pts',(-22.2453839444114,-40.357803086462,0.));
#74010=CARTESIAN_POINT('Ctrl Pts',(-22.2453839444114,-40.357803086462,20.));
#74011=CARTESIAN_POINT('Ctrl Pts',(-22.2725240781926,-40.3394588845042,
0.));
#74012=CARTESIAN_POINT('Ctrl Pts',(-22.2725240781926,-40.3394588845042,
20.));
#74013=CARTESIAN_POINT('Ctrl Pts',(-22.2996502928986,-40.3210960979489,
0.));
#74014=CARTESIAN_POINT('Ctrl Pts',(-22.2996502928986,-40.3210960979489,
20.));
#74015=CARTESIAN_POINT('Ctrl Pts',(-22.3267625753671,-40.3027147367803,
0.));
#74016=CARTESIAN_POINT('Ctrl Pts',(-22.3267625753671,-40.3027147367803,
20.));
#74017=CARTESIAN_POINT('Ctrl Pts',(-22.3538609125294,-40.2843148109267,
0.));
#74018=CARTESIAN_POINT('Ctrl Pts',(-22.3538609125294,-40.2843148109267,
20.));
#74019=CARTESIAN_POINT('Ctrl Pts',(-22.3809452914735,-40.2658963302133,
0.));
#74020=CARTESIAN_POINT('Ctrl Pts',(-22.3809452914735,-40.2658963302133,
20.));
#74021=CARTESIAN_POINT('Ctrl Pts',(-22.4080156993888,-40.2474593044019,
0.));
#74022=CARTESIAN_POINT('Ctrl Pts',(-22.4080156993888,-40.2474593044019,
20.));
#74023=CARTESIAN_POINT('Ctrl Pts',(-22.4350721234534,-40.229003743277,0.));
#74024=CARTESIAN_POINT('Ctrl Pts',(-22.4350721234534,-40.229003743277,20.));
#74025=CARTESIAN_POINT('Ctrl Pts',(-22.4621145507305,-40.2105296567239,
0.));
#74026=CARTESIAN_POINT('Ctrl Pts',(-22.4621145507305,-40.2105296567239,
20.));
#74027=CARTESIAN_POINT('Ctrl Pts',(-22.4891429680799,-40.1920370547964,
0.));
#74028=CARTESIAN_POINT('Ctrl Pts',(-22.4891429680799,-40.1920370547964,
20.));
#74029=CARTESIAN_POINT('Ctrl Pts',(-22.5161573620162,-40.1735259478254,
0.));
#74030=CARTESIAN_POINT('Ctrl Pts',(-22.5161573620162,-40.1735259478254,
20.));
#74031=CARTESIAN_POINT('Ctrl Pts',(-22.5431577188606,-40.1549963463026,
0.));
#74032=CARTESIAN_POINT('Ctrl Pts',(-22.5431577188606,-40.1549963463026,
20.));
#74033=CARTESIAN_POINT('Ctrl Pts',(-22.5701440249982,-40.1364482606861,
0.));
#74034=CARTESIAN_POINT('Ctrl Pts',(-22.5701440249982,-40.1364482606861,
20.));
#74035=CARTESIAN_POINT('Ctrl Pts',(-22.5971162671187,-40.1178817012184,
0.));
#74036=CARTESIAN_POINT('Ctrl Pts',(-22.5971162671187,-40.1178817012184,
20.));
#74037=CARTESIAN_POINT('Ctrl Pts',(-22.6240744324259,-40.0992966777668,
0.));
#74038=CARTESIAN_POINT('Ctrl Pts',(-22.6240744324259,-40.0992966777668,
20.));
#74039=CARTESIAN_POINT('Ctrl Pts',(-22.6510185089549,-40.0806931995834,
0.));
#74040=CARTESIAN_POINT('Ctrl Pts',(-22.6510185089549,-40.0806931995834,
20.));
#74041=CARTESIAN_POINT('Ctrl Pts',(-22.6779484851672,-40.0620712756149,
0.));
#74042=CARTESIAN_POINT('Ctrl Pts',(-22.6779484851672,-40.0620712756149,
20.));
#74043=CARTESIAN_POINT('Ctrl Pts',(-22.7048643493645,-40.0434309149416,
0.));
#74044=CARTESIAN_POINT('Ctrl Pts',(-22.7048643493645,-40.0434309149416,
20.));
#74045=CARTESIAN_POINT('Ctrl Pts',(-22.73176608914,-40.0247721271957,0.));
#74046=CARTESIAN_POINT('Ctrl Pts',(-22.73176608914,-40.0247721271957,20.));
#74047=CARTESIAN_POINT('Ctrl Pts',(-22.7586536908732,-40.0060949229408,
0.));
#74048=CARTESIAN_POINT('Ctrl Pts',(-22.7586536908732,-40.0060949229408,
20.));
#74049=CARTESIAN_POINT('Ctrl Pts',(-22.7855271390494,-39.987399314188,0.));
#74050=CARTESIAN_POINT('Ctrl Pts',(-22.7855271390494,-39.987399314188,20.));
#74051=CARTESIAN_POINT('Ctrl Pts',(-22.8123864172494,-39.9686853136472,
0.));
#74052=CARTESIAN_POINT('Ctrl Pts',(-22.8123864172494,-39.9686853136472,
20.));
#74053=CARTESIAN_POINT('Ctrl Pts',(-22.839231509399,-39.9499529337848,0.));
#74054=CARTESIAN_POINT('Ctrl Pts',(-22.839231509399,-39.9499529337848,20.));
#74055=CARTESIAN_POINT('Ctrl Pts',(-22.8660624009432,-39.9312021859374,
0.));
#74056=CARTESIAN_POINT('Ctrl Pts',(-22.8660624009432,-39.9312021859374,
20.));
#74057=CARTESIAN_POINT('Ctrl Pts',(-22.8928790800155,-39.91243307943,0.));
#74058=CARTESIAN_POINT('Ctrl Pts',(-22.8928790800155,-39.91243307943,20.));
#74059=CARTESIAN_POINT('Ctrl Pts',(-22.9196815387084,-39.8936456206159,
0.));
#74060=CARTESIAN_POINT('Ctrl Pts',(-22.9196815387084,-39.8936456206159,
20.));
#74061=CARTESIAN_POINT('Ctrl Pts',(-22.9464697723601,-39.8748398133807,
0.));
#74062=CARTESIAN_POINT('Ctrl Pts',(-22.9464697723601,-39.8748398133807,
20.));
#74063=CARTESIAN_POINT('Ctrl Pts',(-22.9678889774251,-39.8597804904793,
0.));
#74064=CARTESIAN_POINT('Ctrl Pts',(-22.9678889774251,-39.8597804904793,
20.));
#74065=CARTESIAN_POINT('Ctrl Pts',(-22.9839469786126,-39.8484777427633,
0.));
#74066=CARTESIAN_POINT('Ctrl Pts',(-22.9839469786126,-39.8484777427633,
20.));
#74067=CARTESIAN_POINT('Ctrl Pts',(-22.9946494671375,-39.8409389084975,
0.));
#74068=CARTESIAN_POINT('Ctrl Pts',(-22.9946494671375,-39.8409389084975,
20.));
#74069=CARTESIAN_POINT('Ctrl Pts',(-23.,-39.8371685740842,0.));
#74070=CARTESIAN_POINT('Ctrl Pts',(-23.,-39.8371685740842,20.));
#74071=CARTESIAN_POINT('',(8.50876070567956,-48.2555798975982,2.));
#74072=CARTESIAN_POINT('Ctrl Pts',(-10.7008281308626,-46.0172966012412,
2.));
#74073=CARTESIAN_POINT('Ctrl Pts',(-9.9378504380159,-46.269064380565,2.));
#74074=CARTESIAN_POINT('Ctrl Pts',(-9.16754352004547,-46.5017519909094,
2.));
#74075=CARTESIAN_POINT('Ctrl Pts',(-8.39088307367083,-46.7150066081184,
2.));
#74076=CARTESIAN_POINT('Ctrl Pts',(-7.61536245946424,-46.9279482513967,
2.));
#74077=CARTESIAN_POINT('Ctrl Pts',(-6.83350712972477,-47.1215138755074,
2.));
#74078=CARTESIAN_POINT('Ctrl Pts',(-6.04630320233569,-47.295402450297,2.));
#74079=CARTESIAN_POINT('Ctrl Pts',(-5.25842029857172,-47.4694410068512,
2.));
#74080=CARTESIAN_POINT('Ctrl Pts',(-4.46517973963092,-47.6237685212337,
2.));
#74081=CARTESIAN_POINT('Ctrl Pts',(-3.66758232279066,-47.7581340190259,
2.));
#74082=CARTESIAN_POINT('Ctrl Pts',(-2.86929259445598,-47.8926161455541,
2.));
#74083=CARTESIAN_POINT('Ctrl Pts',(-2.06663861563481,-48.0071015607066,
2.));
#74084=CARTESIAN_POINT('Ctrl Pts',(-1.26063332675557,-48.1013899915641,
2.));
#74085=CARTESIAN_POINT('Ctrl Pts',(-0.453491517294757,-48.1958113753237,
2.));
#74086=CARTESIAN_POINT('Ctrl Pts',(0.35701088540252,-48.2699787547905,2.));
#74087=CARTESIAN_POINT('Ctrl Pts',(1.16984971133678,-48.3237428505666,2.));
#74088=CARTESIAN_POINT('Ctrl Pts',(1.98327626216417,-48.3775458205899,2.));
#74089=CARTESIAN_POINT('Ctrl Pts',(2.79904244044949,-48.4109159841017,2.));
#74090=CARTESIAN_POINT('Ctrl Pts',(3.61611754174313,-48.4237558233583,2.));
#74091=CARTESIAN_POINT('Ctrl Pts',(4.43032091679204,-48.4365505351801,2.));
#74092=CARTESIAN_POINT('Ctrl Pts',(5.24582385624142,-48.4289590209732,2.));
#74093=CARTESIAN_POINT('Ctrl Pts',(6.06160482699488,-48.4009361972841,2.));
#74094=CARTESIAN_POINT('Ctrl Pts',(6.59891438315241,-48.3824791217963,2.));
#74095=CARTESIAN_POINT('Ctrl Pts',(7.13634453433625,-48.3551597412747,2.));
#74096=CARTESIAN_POINT('Ctrl Pts',(7.67360352355697,-48.3189772976484,2.));
#74097=CARTESIAN_POINT('Ctrl Pts',(7.95204873082741,-48.3002250232013,2.));
#74098=CARTESIAN_POINT('Ctrl Pts',(8.23044739031116,-48.2790922644854,2.));
#74099=CARTESIAN_POINT('Ctrl Pts',(8.50876070567956,-48.2555798975982,2.));
#74100=CARTESIAN_POINT('',(8.50876070567956,-48.2555798975982,0.));
#74101=CARTESIAN_POINT('Ctrl Pts',(8.50876070567956,-48.2555798975982,0.));
#74102=CARTESIAN_POINT('Ctrl Pts',(8.50876070567956,-48.2555798975982,20.));
#74103=CARTESIAN_POINT('Ctrl Pts',(8.5020159114628,-48.2561497089132,0.));
#74104=CARTESIAN_POINT('Ctrl Pts',(8.5020159114628,-48.2561497089132,20.));
#74105=CARTESIAN_POINT('Ctrl Pts',(8.48852624368607,-48.2572870022174,0.));
#74106=CARTESIAN_POINT('Ctrl Pts',(8.48852624368607,-48.2572870022174,20.));
#74107=CARTESIAN_POINT('Ctrl Pts',(8.46829150399132,-48.2589859541967,0.));
#74108=CARTESIAN_POINT('Ctrl Pts',(8.46829150399132,-48.2589859541967,20.));
#74109=CARTESIAN_POINT('Ctrl Pts',(8.4413113750042,-48.2612372475269,0.));
#74110=CARTESIAN_POINT('Ctrl Pts',(8.4413113750042,-48.2612372475269,20.));
#74111=CARTESIAN_POINT('Ctrl Pts',(8.40758542125999,-48.2640280707484,0.));
#74112=CARTESIAN_POINT('Ctrl Pts',(8.40758542125999,-48.2640280707484,20.));
#74113=CARTESIAN_POINT('Ctrl Pts',(8.37385867778169,-48.2667956002972,0.));
#74114=CARTESIAN_POINT('Ctrl Pts',(8.37385867778169,-48.2667956002972,20.));
#74115=CARTESIAN_POINT('Ctrl Pts',(8.34013115014496,-48.2695398358687,0.));
#74116=CARTESIAN_POINT('Ctrl Pts',(8.34013115014496,-48.2695398358687,20.));
#74117=CARTESIAN_POINT('Ctrl Pts',(8.30640284761835,-48.2722607770974,0.));
#74118=CARTESIAN_POINT('Ctrl Pts',(8.30640284761835,-48.2722607770974,20.));
#74119=CARTESIAN_POINT('Ctrl Pts',(8.27267378419868,-48.274958423567,0.));
#74120=CARTESIAN_POINT('Ctrl Pts',(8.27267378419868,-48.274958423567,20.));
#74121=CARTESIAN_POINT('Ctrl Pts',(8.23894397736021,-48.2776327748283,0.));
#74122=CARTESIAN_POINT('Ctrl Pts',(8.23894397736021,-48.2776327748283,20.));
#74123=CARTESIAN_POINT('Ctrl Pts',(8.20521344665193,-48.2802838304168,0.));
#74124=CARTESIAN_POINT('Ctrl Pts',(8.20521344665193,-48.2802838304168,20.));
#74125=CARTESIAN_POINT('Ctrl Pts',(8.17148221231953,-48.2829115898716,0.));
#74126=CARTESIAN_POINT('Ctrl Pts',(8.17148221231953,-48.2829115898716,20.));
#74127=CARTESIAN_POINT('Ctrl Pts',(8.13775029398593,-48.2855160527521,0.));
#74128=CARTESIAN_POINT('Ctrl Pts',(8.13775029398593,-48.2855160527521,20.));
#74129=CARTESIAN_POINT('Ctrl Pts',(8.10401770912491,-48.288097218659,0.));
#74130=CARTESIAN_POINT('Ctrl Pts',(8.10401770912491,-48.288097218659,20.));
#74131=CARTESIAN_POINT('Ctrl Pts',(8.07028447346157,-48.2906550872281,0.));
#74132=CARTESIAN_POINT('Ctrl Pts',(8.07028447346157,-48.2906550872281,20.));
#74133=CARTESIAN_POINT('Ctrl Pts',(8.03655060167523,-48.2931896581208,0.));
#74134=CARTESIAN_POINT('Ctrl Pts',(8.03655060167523,-48.2931896581208,20.));
#74135=CARTESIAN_POINT('Ctrl Pts',(8.00281610801472,-48.2957009310153,0.));
#74136=CARTESIAN_POINT('Ctrl Pts',(8.00281610801472,-48.2957009310153,20.));
#74137=CARTESIAN_POINT('Ctrl Pts',(7.96908100690892,-48.2981889055984,0.));
#74138=CARTESIAN_POINT('Ctrl Pts',(7.96908100690892,-48.2981889055984,20.));
#74139=CARTESIAN_POINT('Ctrl Pts',(7.93534531368689,-48.300653581555,0.));
#74140=CARTESIAN_POINT('Ctrl Pts',(7.93534531368689,-48.300653581555,20.));
#74141=CARTESIAN_POINT('Ctrl Pts',(7.90160904447351,-48.3030949585702,0.));
#74142=CARTESIAN_POINT('Ctrl Pts',(7.90160904447351,-48.3030949585702,20.));
#74143=CARTESIAN_POINT('Ctrl Pts',(7.86787221586445,-48.3055130363337,0.));
#74144=CARTESIAN_POINT('Ctrl Pts',(7.86787221586445,-48.3055130363337,20.));
#74145=CARTESIAN_POINT('Ctrl Pts',(7.83413484466693,-48.3079078145432,0.));
#74146=CARTESIAN_POINT('Ctrl Pts',(7.83413484466693,-48.3079078145432,20.));
#74147=CARTESIAN_POINT('Ctrl Pts',(7.80039694763397,-48.3102792929086,0.));
#74148=CARTESIAN_POINT('Ctrl Pts',(7.80039694763397,-48.3102792929086,20.));
#74149=CARTESIAN_POINT('Ctrl Pts',(7.76665854114745,-48.3126274711557,0.));
#74150=CARTESIAN_POINT('Ctrl Pts',(7.76665854114745,-48.3126274711557,20.));
#74151=CARTESIAN_POINT('Ctrl Pts',(7.73291964123288,-48.3149523490266,0.));
#74152=CARTESIAN_POINT('Ctrl Pts',(7.73291964123288,-48.3149523490266,20.));
#74153=CARTESIAN_POINT('Ctrl Pts',(7.69918026370735,-48.3172539262766,0.));
#74154=CARTESIAN_POINT('Ctrl Pts',(7.69918026370735,-48.3172539262766,20.));
#74155=CARTESIAN_POINT('Ctrl Pts',(7.66544042428832,-48.3195322026739,0.));
#74156=CARTESIAN_POINT('Ctrl Pts',(7.66544042428832,-48.3195322026739,20.));
#74157=CARTESIAN_POINT('Ctrl Pts',(7.63170013870892,-48.3217871779975,0.));
#74158=CARTESIAN_POINT('Ctrl Pts',(7.63170013870892,-48.3217871779975,20.));
#74159=CARTESIAN_POINT('Ctrl Pts',(7.59795942285539,-48.3240188520354,0.));
#74160=CARTESIAN_POINT('Ctrl Pts',(7.59795942285539,-48.3240188520354,20.));
#74161=CARTESIAN_POINT('Ctrl Pts',(7.56421829277369,-48.3262272245847,0.));
#74162=CARTESIAN_POINT('Ctrl Pts',(7.56421829277369,-48.3262272245847,20.));
#74163=CARTESIAN_POINT('Ctrl Pts',(7.53047676460326,-48.328412295452,0.));
#74164=CARTESIAN_POINT('Ctrl Pts',(7.53047676460326,-48.328412295452,20.));
#74165=CARTESIAN_POINT('Ctrl Pts',(7.49673485453118,-48.3305740644544,0.));
#74166=CARTESIAN_POINT('Ctrl Pts',(7.49673485453118,-48.3305740644544,20.));
#74167=CARTESIAN_POINT('Ctrl Pts',(7.46299257874208,-48.3327125314199,0.));
#74168=CARTESIAN_POINT('Ctrl Pts',(7.46299257874208,-48.3327125314199,20.));
#74169=CARTESIAN_POINT('Ctrl Pts',(7.42924995335917,-48.3348276961881,0.));
#74170=CARTESIAN_POINT('Ctrl Pts',(7.42924995335917,-48.3348276961881,20.));
#74171=CARTESIAN_POINT('Ctrl Pts',(7.39550699443533,-48.3369195586108,0.));
#74172=CARTESIAN_POINT('Ctrl Pts',(7.39550699443533,-48.3369195586108,20.));
#74173=CARTESIAN_POINT('Ctrl Pts',(7.36176371798261,-48.3389881185516,0.));
#74174=CARTESIAN_POINT('Ctrl Pts',(7.36176371798261,-48.3389881185516,20.));
#74175=CARTESIAN_POINT('Ctrl Pts',(7.32802013999146,-48.3410333758855,0.));
#74176=CARTESIAN_POINT('Ctrl Pts',(7.32802013999146,-48.3410333758855,20.));
#74177=CARTESIAN_POINT('Ctrl Pts',(7.29427627645269,-48.3430553304987,0.));
#74178=CARTESIAN_POINT('Ctrl Pts',(7.29427627645269,-48.3430553304987,20.));
#74179=CARTESIAN_POINT('Ctrl Pts',(7.26053214338256,-48.3450539822883,0.));
#74180=CARTESIAN_POINT('Ctrl Pts',(7.26053214338256,-48.3450539822883,20.));
#74181=CARTESIAN_POINT('Ctrl Pts',(7.22678775682931,-48.3470293311619,0.));
#74182=CARTESIAN_POINT('Ctrl Pts',(7.22678775682931,-48.3470293311619,20.));
#74183=CARTESIAN_POINT('Ctrl Pts',(7.19304313285997,-48.3489813770376,0.));
#74184=CARTESIAN_POINT('Ctrl Pts',(7.19304313285997,-48.3489813770376,20.));
#74185=CARTESIAN_POINT('Ctrl Pts',(7.15929828755239,-48.3509101198447,0.));
#74186=CARTESIAN_POINT('Ctrl Pts',(7.15929828755239,-48.3509101198447,20.));
#74187=CARTESIAN_POINT('Ctrl Pts',(7.12555323698548,-48.3528155595232,0.));
#74188=CARTESIAN_POINT('Ctrl Pts',(7.12555323698548,-48.3528155595232,20.));
#74189=CARTESIAN_POINT('Ctrl Pts',(7.0918079972288,-48.354697696024,0.));
#74190=CARTESIAN_POINT('Ctrl Pts',(7.0918079972288,-48.354697696024,20.));
#74191=CARTESIAN_POINT('Ctrl Pts',(7.05806258433801,-48.3565565293095,0.));
#74192=CARTESIAN_POINT('Ctrl Pts',(7.05806258433801,-48.3565565293095,20.));
#74193=CARTESIAN_POINT('Ctrl Pts',(7.02431701436125,-48.3583920593534,0.));
#74194=CARTESIAN_POINT('Ctrl Pts',(7.02431701436125,-48.3583920593534,20.));
#74195=CARTESIAN_POINT('Ctrl Pts',(6.99057130334226,-48.3602042861407,0.));
#74196=CARTESIAN_POINT('Ctrl Pts',(6.99057130334226,-48.3602042861407,20.));
#74197=CARTESIAN_POINT('Ctrl Pts',(6.95682546732483,-48.3619932096677,0.));
#74198=CARTESIAN_POINT('Ctrl Pts',(6.95682546732483,-48.3619932096677,20.));
#74199=CARTESIAN_POINT('Ctrl Pts',(6.92307952235708,-48.3637588299416,0.));
#74200=CARTESIAN_POINT('Ctrl Pts',(6.92307952235708,-48.3637588299416,20.));
#74201=CARTESIAN_POINT('Ctrl Pts',(6.8893334844937,-48.3655011469807,0.));
#74202=CARTESIAN_POINT('Ctrl Pts',(6.8893334844937,-48.3655011469807,20.));
#74203=CARTESIAN_POINT('Ctrl Pts',(6.85558736979328,-48.3672201608141,0.));
#74204=CARTESIAN_POINT('Ctrl Pts',(6.85558736979328,-48.3672201608141,20.));
#74205=CARTESIAN_POINT('Ctrl Pts',(6.82184119431717,-48.3689158714816,0.));
#74206=CARTESIAN_POINT('Ctrl Pts',(6.82184119431717,-48.3689158714816,20.));
#74207=CARTESIAN_POINT('Ctrl Pts',(6.78809497412713,-48.370588279034,0.));
#74208=CARTESIAN_POINT('Ctrl Pts',(6.78809497412713,-48.370588279034,20.));
#74209=CARTESIAN_POINT('Ctrl Pts',(6.75434872528384,-48.3722373835335,0.));
#74210=CARTESIAN_POINT('Ctrl Pts',(6.75434872528384,-48.3722373835335,20.));
#74211=CARTESIAN_POINT('Ctrl Pts',(6.72060246384579,-48.3738631850533,0.));
#74212=CARTESIAN_POINT('Ctrl Pts',(6.72060246384579,-48.3738631850533,20.));
#74213=CARTESIAN_POINT('Ctrl Pts',(6.68685620587014,-48.3754656836776,0.));
#74214=CARTESIAN_POINT('Ctrl Pts',(6.68685620587014,-48.3754656836776,20.));
#74215=CARTESIAN_POINT('Ctrl Pts',(6.65310996741333,-48.3770448795022,0.));
#74216=CARTESIAN_POINT('Ctrl Pts',(6.65310996741333,-48.3770448795022,20.));
#74217=CARTESIAN_POINT('Ctrl Pts',(6.61936376453194,-48.3786007726338,0.));
#74218=CARTESIAN_POINT('Ctrl Pts',(6.61936376453194,-48.3786007726338,20.));
#74219=CARTESIAN_POINT('Ctrl Pts',(6.58561761328367,-48.3801333631899,0.));
#74220=CARTESIAN_POINT('Ctrl Pts',(6.58561761328367,-48.3801333631899,20.));
#74221=CARTESIAN_POINT('Ctrl Pts',(6.55187152972771,-48.3816426512995,0.));
#74222=CARTESIAN_POINT('Ctrl Pts',(6.55187152972771,-48.3816426512995,20.));
#74223=CARTESIAN_POINT('Ctrl Pts',(6.51812552992423,-48.3831286371024,0.));
#74224=CARTESIAN_POINT('Ctrl Pts',(6.51812552992423,-48.3831286371024,20.));
#74225=CARTESIAN_POINT('Ctrl Pts',(6.48437962993405,-48.3845913207494,0.));
#74226=CARTESIAN_POINT('Ctrl Pts',(6.48437962993405,-48.3845913207494,20.));
#74227=CARTESIAN_POINT('Ctrl Pts',(6.45063384581844,-48.3860307024022,0.));
#74228=CARTESIAN_POINT('Ctrl Pts',(6.45063384581844,-48.3860307024022,20.));
#74229=CARTESIAN_POINT('Ctrl Pts',(6.41688819363864,-48.3874467822337,0.));
#74230=CARTESIAN_POINT('Ctrl Pts',(6.41688819363864,-48.3874467822337,20.));
#74231=CARTESIAN_POINT('Ctrl Pts',(6.38314268945587,-48.388839560428,0.));
#74232=CARTESIAN_POINT('Ctrl Pts',(6.38314268945587,-48.388839560428,20.));
#74233=CARTESIAN_POINT('Ctrl Pts',(6.34939734933121,-48.3902090371802,0.));
#74234=CARTESIAN_POINT('Ctrl Pts',(6.34939734933121,-48.3902090371802,20.));
#74235=CARTESIAN_POINT('Ctrl Pts',(6.31565218932588,-48.3915552126968,0.));
#74236=CARTESIAN_POINT('Ctrl Pts',(6.31565218932588,-48.3915552126968,20.));
#74237=CARTESIAN_POINT('Ctrl Pts',(6.28190722550132,-48.3928780871951,0.));
#74238=CARTESIAN_POINT('Ctrl Pts',(6.28190722550132,-48.3928780871951,20.));
#74239=CARTESIAN_POINT('Ctrl Pts',(6.24816247391919,-48.3941776609035,0.));
#74240=CARTESIAN_POINT('Ctrl Pts',(6.24816247391919,-48.3941776609035,20.));
#74241=CARTESIAN_POINT('Ctrl Pts',(6.21441795064167,-48.3954539340615,0.));
#74242=CARTESIAN_POINT('Ctrl Pts',(6.21441795064167,-48.3954539340615,20.));
#74243=CARTESIAN_POINT('Ctrl Pts',(6.18067367173123,-48.3967069069196,0.));
#74244=CARTESIAN_POINT('Ctrl Pts',(6.18067367173123,-48.3967069069196,20.));
#74245=CARTESIAN_POINT('Ctrl Pts',(6.14692965325078,-48.3979365797396,0.));
#74246=CARTESIAN_POINT('Ctrl Pts',(6.14692965325078,-48.3979365797396,20.));
#74247=CARTESIAN_POINT('Ctrl Pts',(6.11318591126342,-48.3991429527941,0.));
#74248=CARTESIAN_POINT('Ctrl Pts',(6.11318591126342,-48.3991429527941,20.));
#74249=CARTESIAN_POINT('Ctrl Pts',(6.07944246183266,-48.400326026367,0.));
#74250=CARTESIAN_POINT('Ctrl Pts',(6.07944246183266,-48.400326026367,20.));
#74251=CARTESIAN_POINT('Ctrl Pts',(6.04569932102199,-48.4014858007534,0.));
#74252=CARTESIAN_POINT('Ctrl Pts',(6.04569932102199,-48.4014858007534,20.));
#74253=CARTESIAN_POINT('Ctrl Pts',(6.01195650489504,-48.4026222762592,0.));
#74254=CARTESIAN_POINT('Ctrl Pts',(6.01195650489504,-48.4026222762592,20.));
#74255=CARTESIAN_POINT('Ctrl Pts',(5.97821402951547,-48.4037354532014,0.));
#74256=CARTESIAN_POINT('Ctrl Pts',(5.97821402951547,-48.4037354532014,20.));
#74257=CARTESIAN_POINT('Ctrl Pts',(5.94447191094721,-48.404825331908,0.));
#74258=CARTESIAN_POINT('Ctrl Pts',(5.94447191094721,-48.404825331908,20.));
#74259=CARTESIAN_POINT('Ctrl Pts',(5.91073016525425,-48.4058919127185,0.));
#74260=CARTESIAN_POINT('Ctrl Pts',(5.91073016525425,-48.4058919127185,20.));
#74261=CARTESIAN_POINT('Ctrl Pts',(5.87698880850095,-48.4069351959835,0.));
#74262=CARTESIAN_POINT('Ctrl Pts',(5.87698880850095,-48.4069351959835,20.));
#74263=CARTESIAN_POINT('Ctrl Pts',(5.84324785675189,-48.4079551820643,0.));
#74264=CARTESIAN_POINT('Ctrl Pts',(5.84324785675189,-48.4079551820643,20.));
#74265=CARTESIAN_POINT('Ctrl Pts',(5.80950732607177,-48.4089518713337,0.));
#74266=CARTESIAN_POINT('Ctrl Pts',(5.80950732607177,-48.4089518713337,20.));
#74267=CARTESIAN_POINT('Ctrl Pts',(5.77576723252552,-48.4099252641753,0.));
#74268=CARTESIAN_POINT('Ctrl Pts',(5.77576723252552,-48.4099252641753,20.));
#74269=CARTESIAN_POINT('Ctrl Pts',(5.74202759217812,-48.4108753609837,0.));
#74270=CARTESIAN_POINT('Ctrl Pts',(5.74202759217812,-48.4108753609837,20.));
#74271=CARTESIAN_POINT('Ctrl Pts',(5.70828842109459,-48.4118021621647,0.));
#74272=CARTESIAN_POINT('Ctrl Pts',(5.70828842109459,-48.4118021621647,20.));
#74273=CARTESIAN_POINT('Ctrl Pts',(5.67454973534013,-48.412705668135,0.));
#74274=CARTESIAN_POINT('Ctrl Pts',(5.67454973534013,-48.412705668135,20.));
#74275=CARTESIAN_POINT('Ctrl Pts',(5.64081155098004,-48.4135858793227,0.));
#74276=CARTESIAN_POINT('Ctrl Pts',(5.64081155098004,-48.4135858793227,20.));
#74277=CARTESIAN_POINT('Ctrl Pts',(5.6070738840798,-48.414442796167,0.));
#74278=CARTESIAN_POINT('Ctrl Pts',(5.6070738840798,-48.414442796167,20.));
#74279=CARTESIAN_POINT('Ctrl Pts',(5.57333675070491,-48.4152764191183,0.));
#74280=CARTESIAN_POINT('Ctrl Pts',(5.57333675070491,-48.4152764191183,20.));
#74281=CARTESIAN_POINT('Ctrl Pts',(5.53960016692117,-48.4160867486381,0.));
#74282=CARTESIAN_POINT('Ctrl Pts',(5.53960016692117,-48.4160867486381,20.));
#74283=CARTESIAN_POINT('Ctrl Pts',(5.50586414879429,-48.4168737851989,0.));
#74284=CARTESIAN_POINT('Ctrl Pts',(5.50586414879429,-48.4168737851989,20.));
#74285=CARTESIAN_POINT('Ctrl Pts',(5.47212871239029,-48.417637529284,0.));
#74286=CARTESIAN_POINT('Ctrl Pts',(5.47212871239029,-48.417637529284,20.));
#74287=CARTESIAN_POINT('Ctrl Pts',(5.43839387377497,-48.4183779813881,0.));
#74288=CARTESIAN_POINT('Ctrl Pts',(5.43839387377497,-48.4183779813881,20.));
#74289=CARTESIAN_POINT('Ctrl Pts',(5.40465964901424,-48.4190951420167,0.));
#74290=CARTESIAN_POINT('Ctrl Pts',(5.40465964901424,-48.4190951420167,20.));
#74291=CARTESIAN_POINT('Ctrl Pts',(5.37092605417401,-48.4197890116867,0.));
#74292=CARTESIAN_POINT('Ctrl Pts',(5.37092605417401,-48.4197890116867,20.));
#74293=CARTESIAN_POINT('Ctrl Pts',(5.33719310532026,-48.4204595909261,0.));
#74294=CARTESIAN_POINT('Ctrl Pts',(5.33719310532026,-48.4204595909261,20.));
#74295=CARTESIAN_POINT('Ctrl Pts',(5.30346081851908,-48.4211068802741,0.));
#74296=CARTESIAN_POINT('Ctrl Pts',(5.30346081851908,-48.4211068802741,20.));
#74297=CARTESIAN_POINT('Ctrl Pts',(5.26972920983669,-48.4217308802807,0.));
#74298=CARTESIAN_POINT('Ctrl Pts',(5.26972920983669,-48.4217308802807,20.));
#74299=CARTESIAN_POINT('Ctrl Pts',(5.23599829533944,-48.4223315915069,0.));
#74300=CARTESIAN_POINT('Ctrl Pts',(5.23599829533944,-48.4223315915069,20.));
#74301=CARTESIAN_POINT('Ctrl Pts',(5.2022680910935,-48.4229090145253,0.));
#74302=CARTESIAN_POINT('Ctrl Pts',(5.2022680910935,-48.4229090145253,20.));
#74303=CARTESIAN_POINT('Ctrl Pts',(5.1685386131652,-48.4234631499194,0.));
#74304=CARTESIAN_POINT('Ctrl Pts',(5.1685386131652,-48.4234631499194,20.));
#74305=CARTESIAN_POINT('Ctrl Pts',(5.1348098776207,-48.4239939982838,0.));
#74306=CARTESIAN_POINT('Ctrl Pts',(5.1348098776207,-48.4239939982838,20.));
#74307=CARTESIAN_POINT('Ctrl Pts',(5.10108190052607,-48.4245015602246,0.));
#74308=CARTESIAN_POINT('Ctrl Pts',(5.10108190052607,-48.4245015602246,20.));
#74309=CARTESIAN_POINT('Ctrl Pts',(5.06735469794741,-48.4249858363582,0.));
#74310=CARTESIAN_POINT('Ctrl Pts',(5.06735469794741,-48.4249858363582,20.));
#74311=CARTESIAN_POINT('Ctrl Pts',(5.03362828595092,-48.4254468273122,0.));
#74312=CARTESIAN_POINT('Ctrl Pts',(5.03362828595092,-48.4254468273122,20.));
#74313=CARTESIAN_POINT('Ctrl Pts',(4.99990268060291,-48.4258845337255,0.));
#74314=CARTESIAN_POINT('Ctrl Pts',(4.99990268060291,-48.4258845337255,20.));
#74315=CARTESIAN_POINT('Ctrl Pts',(4.96617789796952,-48.4262989562483,0.));
#74316=CARTESIAN_POINT('Ctrl Pts',(4.96617789796952,-48.4262989562483,20.));
#74317=CARTESIAN_POINT('Ctrl Pts',(4.93245395411684,-48.4266900955418,0.));
#74318=CARTESIAN_POINT('Ctrl Pts',(4.93245395411684,-48.4266900955418,20.));
#74319=CARTESIAN_POINT('Ctrl Pts',(4.89873086511076,-48.4270579522784,0.));
#74320=CARTESIAN_POINT('Ctrl Pts',(4.89873086511076,-48.4270579522784,20.));
#74321=CARTESIAN_POINT('Ctrl Pts',(4.8650086470173,-48.4274025271416,0.));
#74322=CARTESIAN_POINT('Ctrl Pts',(4.8650086470173,-48.4274025271416,20.));
#74323=CARTESIAN_POINT('Ctrl Pts',(4.83128731590228,-48.4277238208263,0.));
#74324=CARTESIAN_POINT('Ctrl Pts',(4.83128731590228,-48.4277238208263,20.));
#74325=CARTESIAN_POINT('Ctrl Pts',(4.79756688783168,-48.4280218340382,0.));
#74326=CARTESIAN_POINT('Ctrl Pts',(4.79756688783168,-48.4280218340382,20.));
#74327=CARTESIAN_POINT('Ctrl Pts',(4.76384737887105,-48.4282965674942,0.));
#74328=CARTESIAN_POINT('Ctrl Pts',(4.76384737887105,-48.4282965674942,20.));
#74329=CARTESIAN_POINT('Ctrl Pts',(4.730128805086,-48.4285480219221,0.));
#74330=CARTESIAN_POINT('Ctrl Pts',(4.730128805086,-48.4285480219221,20.));
#74331=CARTESIAN_POINT('Ctrl Pts',(4.69641118254225,-48.4287761980604,0.));
#74332=CARTESIAN_POINT('Ctrl Pts',(4.69641118254225,-48.4287761980604,20.));
#74333=CARTESIAN_POINT('Ctrl Pts',(4.66269452730542,-48.4289810966589,0.));
#74334=CARTESIAN_POINT('Ctrl Pts',(4.66269452730542,-48.4289810966589,20.));
#74335=CARTESIAN_POINT('Ctrl Pts',(4.62897885544097,-48.4291627184787,0.));
#74336=CARTESIAN_POINT('Ctrl Pts',(4.62897885544097,-48.4291627184787,20.));
#74337=CARTESIAN_POINT('Ctrl Pts',(4.59526418301408,-48.4293210642923,0.));
#74338=CARTESIAN_POINT('Ctrl Pts',(4.59526418301408,-48.4293210642923,20.));
#74339=CARTESIAN_POINT('Ctrl Pts',(4.5615505260898,-48.4294561348833,0.));
#74340=CARTESIAN_POINT('Ctrl Pts',(4.5615505260898,-48.4294561348833,20.));
#74341=CARTESIAN_POINT('Ctrl Pts',(4.52783790073293,-48.4295679310466,0.));
#74342=CARTESIAN_POINT('Ctrl Pts',(4.52783790073293,-48.4295679310466,20.));
#74343=CARTESIAN_POINT('Ctrl Pts',(4.49412632300814,-48.4296564535884,0.));
#74344=CARTESIAN_POINT('Ctrl Pts',(4.49412632300814,-48.4296564535884,20.));
#74345=CARTESIAN_POINT('Ctrl Pts',(4.46041580898011,-48.4297217033257,0.));
#74346=CARTESIAN_POINT('Ctrl Pts',(4.46041580898011,-48.4297217033257,20.));
#74347=CARTESIAN_POINT('Ctrl Pts',(4.4267063747134,-48.4297636810863,0.));
#74348=CARTESIAN_POINT('Ctrl Pts',(4.4267063747134,-48.4297636810863,20.));
#74349=CARTESIAN_POINT('Ctrl Pts',(4.39299803627246,-48.4297823877088,0.));
#74350=CARTESIAN_POINT('Ctrl Pts',(4.39299803627246,-48.4297823877088,20.));
#74351=CARTESIAN_POINT('Ctrl Pts',(4.35929080972166,-48.4297778240431,0.));
#74352=CARTESIAN_POINT('Ctrl Pts',(4.35929080972166,-48.4297778240431,20.));
#74353=CARTESIAN_POINT('Ctrl Pts',(4.32558471112516,-48.42974999095,0.));
#74354=CARTESIAN_POINT('Ctrl Pts',(4.32558471112516,-48.42974999095,20.));
#74355=CARTESIAN_POINT('Ctrl Pts',(4.29187975654677,-48.4296988893018,0.));
#74356=CARTESIAN_POINT('Ctrl Pts',(4.29187975654677,-48.4296988893018,20.));
#74357=CARTESIAN_POINT('Ctrl Pts',(4.25817596205,-48.4296245199823,0.));
#74358=CARTESIAN_POINT('Ctrl Pts',(4.25817596205,-48.4296245199823,20.));
#74359=CARTESIAN_POINT('Ctrl Pts',(4.22447334369801,-48.4295268838864,0.));
#74360=CARTESIAN_POINT('Ctrl Pts',(4.22447334369801,-48.4295268838864,20.));
#74361=CARTESIAN_POINT('Ctrl Pts',(4.19077191755405,-48.4294059819202,0.));
#74362=CARTESIAN_POINT('Ctrl Pts',(4.19077191755405,-48.4294059819202,20.));
#74363=CARTESIAN_POINT('Ctrl Pts',(4.15707169968115,-48.4292618150011,0.));
#74364=CARTESIAN_POINT('Ctrl Pts',(4.15707169968115,-48.4292618150011,20.));
#74365=CARTESIAN_POINT('Ctrl Pts',(4.1233727061421,-48.429094384057,0.));
#74366=CARTESIAN_POINT('Ctrl Pts',(4.1233727061421,-48.429094384057,20.));
#74367=CARTESIAN_POINT('Ctrl Pts',(4.08967495299951,-48.4289036900268,0.));
#74368=CARTESIAN_POINT('Ctrl Pts',(4.08967495299951,-48.4289036900268,20.));
#74369=CARTESIAN_POINT('Ctrl Pts',(4.05597845631568,-48.4286897338604,0.));
#74370=CARTESIAN_POINT('Ctrl Pts',(4.05597845631568,-48.4286897338604,20.));
#74371=CARTESIAN_POINT('Ctrl Pts',(4.02228323215259,-48.4284525165189,0.));
#74372=CARTESIAN_POINT('Ctrl Pts',(4.02228323215259,-48.4284525165189,20.));
#74373=CARTESIAN_POINT('Ctrl Pts',(3.988589296572,-48.4281920389749,0.));
#74374=CARTESIAN_POINT('Ctrl Pts',(3.988589296572,-48.4281920389749,20.));
#74375=CARTESIAN_POINT('Ctrl Pts',(3.95489666563548,-48.427908302212,0.));
#74376=CARTESIAN_POINT('Ctrl Pts',(3.95489666563548,-48.427908302212,20.));
#74377=CARTESIAN_POINT('Ctrl Pts',(3.9212053554042,-48.4276013072253,0.));
#74378=CARTESIAN_POINT('Ctrl Pts',(3.9212053554042,-48.4276013072253,20.));
#74379=CARTESIAN_POINT('Ctrl Pts',(3.88751538193919,-48.4272710550207,0.));
#74380=CARTESIAN_POINT('Ctrl Pts',(3.88751538193919,-48.4272710550207,20.));
#74381=CARTESIAN_POINT('Ctrl Pts',(3.85382676130114,-48.4269175466151,0.));
#74382=CARTESIAN_POINT('Ctrl Pts',(3.85382676130114,-48.4269175466151,20.));
#74383=CARTESIAN_POINT('Ctrl Pts',(3.82013950955042,-48.4265407830367,0.));
#74384=CARTESIAN_POINT('Ctrl Pts',(3.82013950955042,-48.4265407830367,20.));
#74385=CARTESIAN_POINT('Ctrl Pts',(3.78645364274706,-48.4261407653249,0.));
#74386=CARTESIAN_POINT('Ctrl Pts',(3.78645364274706,-48.4261407653249,20.));
#74387=CARTESIAN_POINT('Ctrl Pts',(3.75276917695084,-48.4257174945298,0.));
#74388=CARTESIAN_POINT('Ctrl Pts',(3.75276917695084,-48.4257174945298,20.));
#74389=CARTESIAN_POINT('Ctrl Pts',(3.71908612822108,-48.4252709717129,0.));
#74390=CARTESIAN_POINT('Ctrl Pts',(3.71908612822108,-48.4252709717129,20.));
#74391=CARTESIAN_POINT('Ctrl Pts',(3.68540451261695,-48.424801197947,0.));
#74392=CARTESIAN_POINT('Ctrl Pts',(3.68540451261695,-48.424801197947,20.));
#74393=CARTESIAN_POINT('Ctrl Pts',(3.6517243461974,-48.4243081743158,0.));
#74394=CARTESIAN_POINT('Ctrl Pts',(3.6517243461974,-48.4243081743158,20.));
#74395=CARTESIAN_POINT('Ctrl Pts',(3.61804564502096,-48.4237919019141,0.));
#74396=CARTESIAN_POINT('Ctrl Pts',(3.61804564502096,-48.4237919019141,20.));
#74397=CARTESIAN_POINT('Ctrl Pts',(3.58436842514564,-48.4232523818483,0.));
#74398=CARTESIAN_POINT('Ctrl Pts',(3.58436842514564,-48.4232523818483,20.));
#74399=CARTESIAN_POINT('Ctrl Pts',(3.55069270262907,-48.4226896152354,0.));
#74400=CARTESIAN_POINT('Ctrl Pts',(3.55069270262907,-48.4226896152354,20.));
#74401=CARTESIAN_POINT('Ctrl Pts',(3.51701849352853,-48.422103603204,0.));
#74402=CARTESIAN_POINT('Ctrl Pts',(3.51701849352853,-48.422103603204,20.));
#74403=CARTESIAN_POINT('Ctrl Pts',(3.483345813901,-48.4214943468927,0.));
#74404=CARTESIAN_POINT('Ctrl Pts',(3.483345813901,-48.4214943468927,20.));
#74405=CARTESIAN_POINT('Ctrl Pts',(3.44967467980323,-48.4208618474523,0.));
#74406=CARTESIAN_POINT('Ctrl Pts',(3.44967467980323,-48.4208618474523,20.));
#74407=CARTESIAN_POINT('Ctrl Pts',(3.41600510729148,-48.4202061060442,0.));
#74408=CARTESIAN_POINT('Ctrl Pts',(3.41600510729148,-48.4202061060442,20.));
#74409=CARTESIAN_POINT('Ctrl Pts',(3.38233711242167,-48.4195271238417,0.));
#74410=CARTESIAN_POINT('Ctrl Pts',(3.38233711242167,-48.4195271238417,20.));
#74411=CARTESIAN_POINT('Ctrl Pts',(3.34867071124917,-48.4188249020284,0.));
#74412=CARTESIAN_POINT('Ctrl Pts',(3.34867071124917,-48.4188249020284,20.));
#74413=CARTESIAN_POINT('Ctrl Pts',(3.31500591982887,-48.4180994417999,0.));
#74414=CARTESIAN_POINT('Ctrl Pts',(3.31500591982887,-48.4180994417999,20.));
#74415=CARTESIAN_POINT('Ctrl Pts',(3.28134275421531,-48.4173507443625,0.));
#74416=CARTESIAN_POINT('Ctrl Pts',(3.28134275421531,-48.4173507443625,20.));
#74417=CARTESIAN_POINT('Ctrl Pts',(3.24768123046264,-48.4165788109335,0.));
#74418=CARTESIAN_POINT('Ctrl Pts',(3.24768123046264,-48.4165788109335,20.));
#74419=CARTESIAN_POINT('Ctrl Pts',(3.21402136462457,-48.4157836427414,0.));
#74420=CARTESIAN_POINT('Ctrl Pts',(3.21402136462457,-48.4157836427414,20.));
#74421=CARTESIAN_POINT('Ctrl Pts',(3.18036317275453,-48.4149652410254,0.));
#74422=CARTESIAN_POINT('Ctrl Pts',(3.18036317275453,-48.4149652410254,20.));
#74423=CARTESIAN_POINT('Ctrl Pts',(3.14670667090555,-48.414123607036,0.));
#74424=CARTESIAN_POINT('Ctrl Pts',(3.14670667090555,-48.414123607036,20.));
#74425=CARTESIAN_POINT('Ctrl Pts',(3.11305187512999,-48.4132587420349,0.));
#74426=CARTESIAN_POINT('Ctrl Pts',(3.11305187512999,-48.4132587420349,20.));
#74427=CARTESIAN_POINT('Ctrl Pts',(3.07939880147968,-48.4123706472953,0.));
#74428=CARTESIAN_POINT('Ctrl Pts',(3.07939880147968,-48.4123706472953,20.));
#74429=CARTESIAN_POINT('Ctrl Pts',(3.04574746600607,-48.4114593241014,0.));
#74430=CARTESIAN_POINT('Ctrl Pts',(3.04574746600607,-48.4114593241014,20.));
#74431=CARTESIAN_POINT('Ctrl Pts',(3.01209788475993,-48.4105247737488,0.));
#74432=CARTESIAN_POINT('Ctrl Pts',(3.01209788475993,-48.4105247737488,20.));
#74433=CARTESIAN_POINT('Ctrl Pts',(2.97845007379181,-48.4095669975441,0.));
#74434=CARTESIAN_POINT('Ctrl Pts',(2.97845007379181,-48.4095669975441,20.));
#74435=CARTESIAN_POINT('Ctrl Pts',(2.94480404915164,-48.4085859968048,0.));
#74436=CARTESIAN_POINT('Ctrl Pts',(2.94480404915164,-48.4085859968048,20.));
#74437=CARTESIAN_POINT('Ctrl Pts',(2.91115982688903,-48.4075817728593,0.));
#74438=CARTESIAN_POINT('Ctrl Pts',(2.91115982688903,-48.4075817728593,20.));
#74439=CARTESIAN_POINT('Ctrl Pts',(2.87751742305292,-48.4065543270471,0.));
#74440=CARTESIAN_POINT('Ctrl Pts',(2.87751742305292,-48.4065543270471,20.));
#74441=CARTESIAN_POINT('Ctrl Pts',(2.8438768536918,-48.4055036607195,0.));
#74442=CARTESIAN_POINT('Ctrl Pts',(2.8438768536918,-48.4055036607195,20.));
#74443=CARTESIAN_POINT('Ctrl Pts',(2.81023813485355,-48.4044297752383,0.));
#74444=CARTESIAN_POINT('Ctrl Pts',(2.81023813485355,-48.4044297752383,20.));
#74445=CARTESIAN_POINT('Ctrl Pts',(2.77660128258546,-48.4033326719771,0.));
#74446=CARTESIAN_POINT('Ctrl Pts',(2.77660128258546,-48.4033326719771,20.));
#74447=CARTESIAN_POINT('Ctrl Pts',(2.74296631293436,-48.4022123523201,0.));
#74448=CARTESIAN_POINT('Ctrl Pts',(2.74296631293436,-48.4022123523201,20.));
#74449=CARTESIAN_POINT('Ctrl Pts',(2.7093332419466,-48.4010688176627,0.));
#74450=CARTESIAN_POINT('Ctrl Pts',(2.7093332419466,-48.4010688176627,20.));
#74451=CARTESIAN_POINT('Ctrl Pts',(2.67570208566793,-48.3999020694116,0.));
#74452=CARTESIAN_POINT('Ctrl Pts',(2.67570208566793,-48.3999020694116,20.));
#74453=CARTESIAN_POINT('Ctrl Pts',(2.64207286014349,-48.3987121089844,0.));
#74454=CARTESIAN_POINT('Ctrl Pts',(2.64207286014349,-48.3987121089844,20.));
#74455=CARTESIAN_POINT('Ctrl Pts',(2.60844558141789,-48.3974989378103,0.));
#74456=CARTESIAN_POINT('Ctrl Pts',(2.60844558141789,-48.3974989378103,20.));
#74457=CARTESIAN_POINT('Ctrl Pts',(2.57482026553515,-48.3962625573292,0.));
#74458=CARTESIAN_POINT('Ctrl Pts',(2.57482026553515,-48.3962625573292,20.));
#74459=CARTESIAN_POINT('Ctrl Pts',(2.5411969285386,-48.3950029689925,0.));
#74460=CARTESIAN_POINT('Ctrl Pts',(2.5411969285386,-48.3950029689925,20.));
#74461=CARTESIAN_POINT('Ctrl Pts',(2.50757558647119,-48.3937201742621,0.));
#74462=CARTESIAN_POINT('Ctrl Pts',(2.50757558647119,-48.3937201742621,20.));
#74463=CARTESIAN_POINT('Ctrl Pts',(2.47395625537494,-48.3924141746117,0.));
#74464=CARTESIAN_POINT('Ctrl Pts',(2.47395625537494,-48.3924141746117,20.));
#74465=CARTESIAN_POINT('Ctrl Pts',(2.44033895129153,-48.3910849715258,0.));
#74466=CARTESIAN_POINT('Ctrl Pts',(2.44033895129153,-48.3910849715258,20.));
#74467=CARTESIAN_POINT('Ctrl Pts',(2.40672369026195,-48.3897325665,0.));
#74468=CARTESIAN_POINT('Ctrl Pts',(2.40672369026195,-48.3897325665,20.));
#74469=CARTESIAN_POINT('Ctrl Pts',(2.37311048832664,-48.3883569610415,0.));
#74470=CARTESIAN_POINT('Ctrl Pts',(2.37311048832664,-48.3883569610415,20.));
#74471=CARTESIAN_POINT('Ctrl Pts',(2.33949936152533,-48.3869581566679,0.));
#74472=CARTESIAN_POINT('Ctrl Pts',(2.33949936152533,-48.3869581566679,20.));
#74473=CARTESIAN_POINT('Ctrl Pts',(2.30589032589699,-48.3855361549086,0.));
#74474=CARTESIAN_POINT('Ctrl Pts',(2.30589032589699,-48.3855361549086,20.));
#74475=CARTESIAN_POINT('Ctrl Pts',(2.27228339748008,-48.3840909573039,0.));
#74476=CARTESIAN_POINT('Ctrl Pts',(2.27228339748008,-48.3840909573039,20.));
#74477=CARTESIAN_POINT('Ctrl Pts',(2.2386785923122,-48.3826225654054,0.));
#74478=CARTESIAN_POINT('Ctrl Pts',(2.2386785923122,-48.3826225654054,20.));
#74479=CARTESIAN_POINT('Ctrl Pts',(2.20507592643041,-48.3811309807756,0.));
#74480=CARTESIAN_POINT('Ctrl Pts',(2.20507592643041,-48.3811309807756,20.));
#74481=CARTESIAN_POINT('Ctrl Pts',(2.17147541587102,-48.3796162049883,0.));
#74482=CARTESIAN_POINT('Ctrl Pts',(2.17147541587102,-48.3796162049883,20.));
#74483=CARTESIAN_POINT('Ctrl Pts',(2.13787707667012,-48.3780782396279,0.));
#74484=CARTESIAN_POINT('Ctrl Pts',(2.13787707667012,-48.3780782396279,20.));
#74485=CARTESIAN_POINT('Ctrl Pts',(2.10428092486293,-48.3765170862905,0.));
#74486=CARTESIAN_POINT('Ctrl Pts',(2.10428092486293,-48.3765170862905,20.));
#74487=CARTESIAN_POINT('Ctrl Pts',(2.07068697648387,-48.374932746583,0.));
#74488=CARTESIAN_POINT('Ctrl Pts',(2.07068697648387,-48.374932746583,20.));
#74489=CARTESIAN_POINT('Ctrl Pts',(2.03709524756654,-48.3733252221237,0.));
#74490=CARTESIAN_POINT('Ctrl Pts',(2.03709524756654,-48.3733252221237,20.));
#74491=CARTESIAN_POINT('Ctrl Pts',(2.00350575414355,-48.3716945145424,0.));
#74492=CARTESIAN_POINT('Ctrl Pts',(2.00350575414355,-48.3716945145424,20.));
#74493=CARTESIAN_POINT('Ctrl Pts',(1.96991851224691,-48.3700406254798,0.));
#74494=CARTESIAN_POINT('Ctrl Pts',(1.96991851224691,-48.3700406254798,20.));
#74495=CARTESIAN_POINT('Ctrl Pts',(1.93633353790811,-48.3683635565876,0.));
#74496=CARTESIAN_POINT('Ctrl Pts',(1.93633353790811,-48.3683635565876,20.));
#74497=CARTESIAN_POINT('Ctrl Pts',(1.90275084715795,-48.3666633095284,0.));
#74498=CARTESIAN_POINT('Ctrl Pts',(1.90275084715795,-48.3666633095284,20.));
#74499=CARTESIAN_POINT('Ctrl Pts',(1.86917045602651,-48.3649398859758,0.));
#74500=CARTESIAN_POINT('Ctrl Pts',(1.86917045602651,-48.3649398859758,20.));
#74501=CARTESIAN_POINT('Ctrl Pts',(1.83559238054322,-48.3631932876149,0.));
#74502=CARTESIAN_POINT('Ctrl Pts',(1.83559238054322,-48.3631932876149,20.));
#74503=CARTESIAN_POINT('Ctrl Pts',(1.80201663673655,-48.3614235161422,0.));
#74504=CARTESIAN_POINT('Ctrl Pts',(1.80201663673655,-48.3614235161422,20.));
#74505=CARTESIAN_POINT('Ctrl Pts',(1.76844324063425,-48.3596305732653,0.));
#74506=CARTESIAN_POINT('Ctrl Pts',(1.76844324063425,-48.3596305732653,20.));
#74507=CARTESIAN_POINT('Ctrl Pts',(1.73487220826325,-48.357814460703,0.));
#74508=CARTESIAN_POINT('Ctrl Pts',(1.73487220826325,-48.357814460703,20.));
#74509=CARTESIAN_POINT('Ctrl Pts',(1.70130355564956,-48.3559751801849,0.));
#74510=CARTESIAN_POINT('Ctrl Pts',(1.70130355564956,-48.3559751801849,20.));
#74511=CARTESIAN_POINT('Ctrl Pts',(1.66773729881855,-48.3541127334515,0.));
#74512=CARTESIAN_POINT('Ctrl Pts',(1.66773729881855,-48.3541127334515,20.));
#74513=CARTESIAN_POINT('Ctrl Pts',(1.63417345379481,-48.3522271222546,0.));
#74514=CARTESIAN_POINT('Ctrl Pts',(1.63417345379481,-48.3522271222546,20.));
#74515=CARTESIAN_POINT('Ctrl Pts',(1.60061203660205,-48.350318348357,0.));
#74516=CARTESIAN_POINT('Ctrl Pts',(1.60061203660205,-48.350318348357,20.));
#74517=CARTESIAN_POINT('Ctrl Pts',(1.56705306326331,-48.3483864135332,0.));
#74518=CARTESIAN_POINT('Ctrl Pts',(1.56705306326331,-48.3483864135332,20.));
#74519=CARTESIAN_POINT('Ctrl Pts',(1.53349654980076,-48.3464313195685,0.));
#74520=CARTESIAN_POINT('Ctrl Pts',(1.53349654980076,-48.3464313195685,20.));
#74521=CARTESIAN_POINT('Ctrl Pts',(1.4999425122357,-48.3444530682597,0.));
#74522=CARTESIAN_POINT('Ctrl Pts',(1.4999425122357,-48.3444530682597,20.));
#74523=CARTESIAN_POINT('Ctrl Pts',(1.46639096658851,-48.3424516614145,0.));
#74524=CARTESIAN_POINT('Ctrl Pts',(1.46639096658851,-48.3424516614145,20.));
#74525=CARTESIAN_POINT('Ctrl Pts',(1.43284192887878,-48.3404271008519,0.));
#74526=CARTESIAN_POINT('Ctrl Pts',(1.43284192887878,-48.3404271008519,20.));
#74527=CARTESIAN_POINT('Ctrl Pts',(1.39929541512519,-48.3383793884017,0.));
#74528=CARTESIAN_POINT('Ctrl Pts',(1.39929541512519,-48.3383793884017,20.));
#74529=CARTESIAN_POINT('Ctrl Pts',(1.3657514413457,-48.336308525905,0.));
#74530=CARTESIAN_POINT('Ctrl Pts',(1.3657514413457,-48.336308525905,20.));
#74531=CARTESIAN_POINT('Ctrl Pts',(1.33221002355742,-48.3342145152137,0.));
#74532=CARTESIAN_POINT('Ctrl Pts',(1.33221002355742,-48.3342145152137,20.));
#74533=CARTESIAN_POINT('Ctrl Pts',(1.29867117777651,-48.3320973581913,0.));
#74534=CARTESIAN_POINT('Ctrl Pts',(1.29867117777651,-48.3320973581913,20.));
#74535=CARTESIAN_POINT('Ctrl Pts',(1.26513492001821,-48.3299570567123,0.));
#74536=CARTESIAN_POINT('Ctrl Pts',(1.26513492001821,-48.3299570567123,20.));
#74537=CARTESIAN_POINT('Ctrl Pts',(1.23160126629692,-48.3277936126623,0.));
#74538=CARTESIAN_POINT('Ctrl Pts',(1.23160126629692,-48.3277936126623,20.));
#74539=CARTESIAN_POINT('Ctrl Pts',(1.19807023262611,-48.3256070279384,0.));
#74540=CARTESIAN_POINT('Ctrl Pts',(1.19807023262611,-48.3256070279384,20.));
#74541=CARTESIAN_POINT('Ctrl Pts',(1.16454183501838,-48.3233973044482,0.));
#74542=CARTESIAN_POINT('Ctrl Pts',(1.16454183501838,-48.3233973044482,20.));
#74543=CARTESIAN_POINT('Ctrl Pts',(1.13101608948534,-48.3211644441107,0.));
#74544=CARTESIAN_POINT('Ctrl Pts',(1.13101608948534,-48.3211644441107,20.));
#74545=CARTESIAN_POINT('Ctrl Pts',(1.09749301203762,-48.3189084488565,0.));
#74546=CARTESIAN_POINT('Ctrl Pts',(1.09749301203762,-48.3189084488565,20.));
#74547=CARTESIAN_POINT('Ctrl Pts',(1.063972618685,-48.3166293206271,0.));
#74548=CARTESIAN_POINT('Ctrl Pts',(1.063972618685,-48.3166293206271,20.));
#74549=CARTESIAN_POINT('Ctrl Pts',(1.0304549254364,-48.3143270613748,0.));
#74550=CARTESIAN_POINT('Ctrl Pts',(1.0304549254364,-48.3143270613748,20.));
#74551=CARTESIAN_POINT('Ctrl Pts',(0.996939948299849,-48.312001673063,0.));
#74552=CARTESIAN_POINT('Ctrl Pts',(0.996939948299849,-48.312001673063,20.));
#74553=CARTESIAN_POINT('Ctrl Pts',(0.963427703282353,-48.3096531576664,
0.));
#74554=CARTESIAN_POINT('Ctrl Pts',(0.963427703282353,-48.3096531576664,
20.));
#74555=CARTESIAN_POINT('Ctrl Pts',(0.929918206389826,-48.3072815171712,
0.));
#74556=CARTESIAN_POINT('Ctrl Pts',(0.929918206389826,-48.3072815171712,
20.));
#74557=CARTESIAN_POINT('Ctrl Pts',(0.896411473627223,-48.3048867535744,
0.));
#74558=CARTESIAN_POINT('Ctrl Pts',(0.896411473627223,-48.3048867535744,
20.));
#74559=CARTESIAN_POINT('Ctrl Pts',(0.862907520998486,-48.3024688688845,
0.));
#74560=CARTESIAN_POINT('Ctrl Pts',(0.862907520998486,-48.3024688688845,
20.));
#74561=CARTESIAN_POINT('Ctrl Pts',(0.829406364506662,-48.3000278651208,
0.));
#74562=CARTESIAN_POINT('Ctrl Pts',(0.829406364506662,-48.3000278651208,
20.));
#74563=CARTESIAN_POINT('Ctrl Pts',(0.795908020153888,-48.2975637443136,
0.));
#74564=CARTESIAN_POINT('Ctrl Pts',(0.795908020153888,-48.2975637443136,
20.));
#74565=CARTESIAN_POINT('Ctrl Pts',(0.762412503941521,-48.2950765085043,
0.));
#74566=CARTESIAN_POINT('Ctrl Pts',(0.762412503941521,-48.2950765085043,
20.));
#74567=CARTESIAN_POINT('Ctrl Pts',(0.728919831869645,-48.2925661597457,
0.));
#74568=CARTESIAN_POINT('Ctrl Pts',(0.728919831869645,-48.2925661597457,
20.));
#74569=CARTESIAN_POINT('Ctrl Pts',(0.69543001993734,-48.2900327001016,0.));
#74570=CARTESIAN_POINT('Ctrl Pts',(0.69543001993734,-48.2900327001016,20.));
#74571=CARTESIAN_POINT('Ctrl Pts',(0.661943084142442,-48.2874761316474,
0.));
#74572=CARTESIAN_POINT('Ctrl Pts',(0.661943084142442,-48.2874761316474,
20.));
#74573=CARTESIAN_POINT('Ctrl Pts',(0.628459040481828,-48.2848964564694,
0.));
#74574=CARTESIAN_POINT('Ctrl Pts',(0.628459040481828,-48.2848964564694,
20.));
#74575=CARTESIAN_POINT('Ctrl Pts',(0.594977904951266,-48.282293676665,0.));
#74576=CARTESIAN_POINT('Ctrl Pts',(0.594977904951266,-48.282293676665,20.));
#74577=CARTESIAN_POINT('Ctrl Pts',(0.561499693545673,-48.2796677943426,
0.));
#74578=CARTESIAN_POINT('Ctrl Pts',(0.561499693545673,-48.2796677943426,
20.));
#74579=CARTESIAN_POINT('Ctrl Pts',(0.528024422259019,-48.2770188116216,
0.));
#74580=CARTESIAN_POINT('Ctrl Pts',(0.528024422259019,-48.2770188116216,
20.));
#74581=CARTESIAN_POINT('Ctrl Pts',(0.49455210708421,-48.2743467306329,0.));
#74582=CARTESIAN_POINT('Ctrl Pts',(0.49455210708421,-48.2743467306329,20.));
#74583=CARTESIAN_POINT('Ctrl Pts',(0.461082764012986,-48.2716515535183,
0.));
#74584=CARTESIAN_POINT('Ctrl Pts',(0.461082764012986,-48.2716515535183,
20.));
#74585=CARTESIAN_POINT('Ctrl Pts',(0.427616409036036,-48.2689332824309,
0.));
#74586=CARTESIAN_POINT('Ctrl Pts',(0.427616409036036,-48.2689332824309,
20.));
#74587=CARTESIAN_POINT('Ctrl Pts',(0.394153058142903,-48.2661919195348,
0.));
#74588=CARTESIAN_POINT('Ctrl Pts',(0.394153058142903,-48.2661919195348,
20.));
#74589=CARTESIAN_POINT('Ctrl Pts',(0.360692727321981,-48.2634274670053,
0.));
#74590=CARTESIAN_POINT('Ctrl Pts',(0.360692727321981,-48.2634274670053,
20.));
#74591=CARTESIAN_POINT('Ctrl Pts',(0.327235432560538,-48.2606399270286,
0.));
#74592=CARTESIAN_POINT('Ctrl Pts',(0.327235432560538,-48.2606399270286,
20.));
#74593=CARTESIAN_POINT('Ctrl Pts',(0.293781189844817,-48.2578293018028,
0.));
#74594=CARTESIAN_POINT('Ctrl Pts',(0.293781189844817,-48.2578293018028,
20.));
#74595=CARTESIAN_POINT('Ctrl Pts',(0.260330015159931,-48.2549955935366,
0.));
#74596=CARTESIAN_POINT('Ctrl Pts',(0.260330015159931,-48.2549955935366,
20.));
#74597=CARTESIAN_POINT('Ctrl Pts',(0.226881924489848,-48.2521388044499,
0.));
#74598=CARTESIAN_POINT('Ctrl Pts',(0.226881924489848,-48.2521388044499,
20.));
#74599=CARTESIAN_POINT('Ctrl Pts',(0.193436933817455,-48.2492589367737,
0.));
#74600=CARTESIAN_POINT('Ctrl Pts',(0.193436933817455,-48.2492589367737,
20.));
#74601=CARTESIAN_POINT('Ctrl Pts',(0.159995059124558,-48.2463559927498,
0.));
#74602=CARTESIAN_POINT('Ctrl Pts',(0.159995059124558,-48.2463559927498,
20.));
#74603=CARTESIAN_POINT('Ctrl Pts',(0.126556316391659,-48.2434299746318,
0.));
#74604=CARTESIAN_POINT('Ctrl Pts',(0.126556316391659,-48.2434299746318,
20.));
#74605=CARTESIAN_POINT('Ctrl Pts',(0.0931207215982655,-48.2404808846839,
0.));
#74606=CARTESIAN_POINT('Ctrl Pts',(0.0931207215982655,-48.2404808846839,
20.));
#74607=CARTESIAN_POINT('Ctrl Pts',(0.0596882907225815,-48.2375087251817,
0.));
#74608=CARTESIAN_POINT('Ctrl Pts',(0.0596882907225815,-48.2375087251817,
20.));
#74609=CARTESIAN_POINT('Ctrl Pts',(0.0262590397416584,-48.234513498412,
0.));
#74610=CARTESIAN_POINT('Ctrl Pts',(0.0262590397416584,-48.234513498412,
20.));
#74611=CARTESIAN_POINT('Ctrl Pts',(-0.00716701536858544,-48.2314952066725,
0.));
#74612=CARTESIAN_POINT('Ctrl Pts',(-0.00716701536858544,-48.2314952066725,
20.));
#74613=CARTESIAN_POINT('Ctrl Pts',(-0.040589858633453,-48.2284538522724,
0.));
#74614=CARTESIAN_POINT('Ctrl Pts',(-0.040589858633453,-48.2284538522724,
20.));
#74615=CARTESIAN_POINT('Ctrl Pts',(-0.0740094740794106,-48.2253894375317,
0.));
#74616=CARTESIAN_POINT('Ctrl Pts',(-0.0740094740794106,-48.2253894375317,
20.));
#74617=CARTESIAN_POINT('Ctrl Pts',(-0.107425845734137,-48.2223019647818,
0.));
#74618=CARTESIAN_POINT('Ctrl Pts',(-0.107425845734137,-48.2223019647818,
20.));
#74619=CARTESIAN_POINT('Ctrl Pts',(-0.140838957626559,-48.2191914363652,
0.));
#74620=CARTESIAN_POINT('Ctrl Pts',(-0.140838957626559,-48.2191914363652,
20.));
#74621=CARTESIAN_POINT('Ctrl Pts',(-0.174248793786917,-48.2160578546352,
0.));
#74622=CARTESIAN_POINT('Ctrl Pts',(-0.174248793786917,-48.2160578546352,
20.));
#74623=CARTESIAN_POINT('Ctrl Pts',(-0.207655338246577,-48.2129012219564,
0.));
#74624=CARTESIAN_POINT('Ctrl Pts',(-0.207655338246577,-48.2129012219564,
20.));
#74625=CARTESIAN_POINT('Ctrl Pts',(-0.241058575037889,-48.2097215407045,
0.));
#74626=CARTESIAN_POINT('Ctrl Pts',(-0.241058575037889,-48.2097215407045,
20.));
#74627=CARTESIAN_POINT('Ctrl Pts',(-0.274458488194607,-48.2065188132665,
0.));
#74628=CARTESIAN_POINT('Ctrl Pts',(-0.274458488194607,-48.2065188132665,
20.));
#74629=CARTESIAN_POINT('Ctrl Pts',(-0.307855061751732,-48.2032930420408,
0.));
#74630=CARTESIAN_POINT('Ctrl Pts',(-0.307855061751732,-48.2032930420408,
20.));
#74631=CARTESIAN_POINT('Ctrl Pts',(-0.341248279745661,-48.2000442294364,
0.));
#74632=CARTESIAN_POINT('Ctrl Pts',(-0.341248279745661,-48.2000442294364,
20.));
#74633=CARTESIAN_POINT('Ctrl Pts',(-0.374638126214117,-48.1967723778737,
0.));
#74634=CARTESIAN_POINT('Ctrl Pts',(-0.374638126214117,-48.1967723778737,
20.));
#74635=CARTESIAN_POINT('Ctrl Pts',(-0.408024585196243,-48.1934774897842,
0.));
#74636=CARTESIAN_POINT('Ctrl Pts',(-0.408024585196243,-48.1934774897842,
20.));
#74637=CARTESIAN_POINT('Ctrl Pts',(-0.441407640732114,-48.1901595676102,
0.));
#74638=CARTESIAN_POINT('Ctrl Pts',(-0.441407640732114,-48.1901595676102,
20.));
#74639=CARTESIAN_POINT('Ctrl Pts',(-0.474787276863089,-48.1868186138054,
0.));
#74640=CARTESIAN_POINT('Ctrl Pts',(-0.474787276863089,-48.1868186138054,
20.));
#74641=CARTESIAN_POINT('Ctrl Pts',(-0.508163477631873,-48.1834546308352,
0.));
#74642=CARTESIAN_POINT('Ctrl Pts',(-0.508163477631873,-48.1834546308352,
20.));
#74643=CARTESIAN_POINT('Ctrl Pts',(-0.541536227082378,-48.1800676211754,
0.));
#74644=CARTESIAN_POINT('Ctrl Pts',(-0.541536227082378,-48.1800676211754,
20.));
#74645=CARTESIAN_POINT('Ctrl Pts',(-0.574905509259906,-48.1766575873132,
0.));
#74646=CARTESIAN_POINT('Ctrl Pts',(-0.574905509259906,-48.1766575873132,
20.));
#74647=CARTESIAN_POINT('Ctrl Pts',(-0.608271308211115,-48.1732245317468,
0.));
#74648=CARTESIAN_POINT('Ctrl Pts',(-0.608271308211115,-48.1732245317468,
20.));
#74649=CARTESIAN_POINT('Ctrl Pts',(-0.641633607984118,-48.1697684569855,
0.));
#74650=CARTESIAN_POINT('Ctrl Pts',(-0.641633607984118,-48.1697684569855,
20.));
#74651=CARTESIAN_POINT('Ctrl Pts',(-0.674992392628253,-48.16628936555,0.));
#74652=CARTESIAN_POINT('Ctrl Pts',(-0.674992392628253,-48.16628936555,20.));
#74653=CARTESIAN_POINT('Ctrl Pts',(-0.708347646194296,-48.1627872599717,
0.));
#74654=CARTESIAN_POINT('Ctrl Pts',(-0.708347646194296,-48.1627872599717,
20.));
#74655=CARTESIAN_POINT('Ctrl Pts',(-0.741699352734275,-48.1592621427937,
0.));
#74656=CARTESIAN_POINT('Ctrl Pts',(-0.741699352734275,-48.1592621427937,
20.));
#74657=CARTESIAN_POINT('Ctrl Pts',(-0.775047496301551,-48.1557140165701,
0.));
#74658=CARTESIAN_POINT('Ctrl Pts',(-0.775047496301551,-48.1557140165701,
20.));
#74659=CARTESIAN_POINT('Ctrl Pts',(-0.808392060950887,-48.1521428838659,
0.));
#74660=CARTESIAN_POINT('Ctrl Pts',(-0.808392060950887,-48.1521428838659,
20.));
#74661=CARTESIAN_POINT('Ctrl Pts',(-0.84173303073841,-48.1485487472572,
0.));
#74662=CARTESIAN_POINT('Ctrl Pts',(-0.84173303073841,-48.1485487472572,
20.));
#74663=CARTESIAN_POINT('Ctrl Pts',(-0.875070389721544,-48.144931609331,
0.));
#74664=CARTESIAN_POINT('Ctrl Pts',(-0.875070389721544,-48.144931609331,
20.));
#74665=CARTESIAN_POINT('Ctrl Pts',(-0.908404121959303,-48.1412914726861,
0.));
#74666=CARTESIAN_POINT('Ctrl Pts',(-0.908404121959303,-48.1412914726861,
20.));
#74667=CARTESIAN_POINT('Ctrl Pts',(-0.941734211511966,-48.137628339932,
0.));
#74668=CARTESIAN_POINT('Ctrl Pts',(-0.941734211511966,-48.137628339932,
20.));
#74669=CARTESIAN_POINT('Ctrl Pts',(-0.975060642441261,-48.1339422136897,
0.));
#74670=CARTESIAN_POINT('Ctrl Pts',(-0.975060642441261,-48.1339422136897,
20.));
#74671=CARTESIAN_POINT('Ctrl Pts',(-1.00838339881034,-48.130233096591,0.));
#74672=CARTESIAN_POINT('Ctrl Pts',(-1.00838339881034,-48.130233096591,20.));
#74673=CARTESIAN_POINT('Ctrl Pts',(-1.04170246468366,-48.1265009912787,
0.));
#74674=CARTESIAN_POINT('Ctrl Pts',(-1.04170246468366,-48.1265009912787,
20.));
#74675=CARTESIAN_POINT('Ctrl Pts',(-1.0750178241273,-48.1227459004068,0.));
#74676=CARTESIAN_POINT('Ctrl Pts',(-1.0750178241273,-48.1227459004068,20.));
#74677=CARTESIAN_POINT('Ctrl Pts',(-1.10832946120863,-48.1189678266406,
0.));
#74678=CARTESIAN_POINT('Ctrl Pts',(-1.10832946120863,-48.1189678266406,
20.));
#74679=CARTESIAN_POINT('Ctrl Pts',(-1.14163735999659,-48.1151667726565,
0.));
#74680=CARTESIAN_POINT('Ctrl Pts',(-1.14163735999659,-48.1151667726565,
20.));
#74681=CARTESIAN_POINT('Ctrl Pts',(-1.17494150456147,-48.111342741142,0.));
#74682=CARTESIAN_POINT('Ctrl Pts',(-1.17494150456147,-48.111342741142,20.));
#74683=CARTESIAN_POINT('Ctrl Pts',(-1.20824187897491,-48.1074957347955,
0.));
#74684=CARTESIAN_POINT('Ctrl Pts',(-1.20824187897491,-48.1074957347955,
20.));
#74685=CARTESIAN_POINT('Ctrl Pts',(-1.24153846731024,-48.1036257563271,
0.));
#74686=CARTESIAN_POINT('Ctrl Pts',(-1.24153846731024,-48.1036257563271,
20.));
#74687=CARTESIAN_POINT('Ctrl Pts',(-1.27483125364217,-48.0997328084577,
0.));
#74688=CARTESIAN_POINT('Ctrl Pts',(-1.27483125364217,-48.0997328084577,
20.));
#74689=CARTESIAN_POINT('Ctrl Pts',(-1.30812022204706,-48.0958168939195,
0.));
#74690=CARTESIAN_POINT('Ctrl Pts',(-1.30812022204706,-48.0958168939195,
20.));
#74691=CARTESIAN_POINT('Ctrl Pts',(-1.34140535660262,-48.0918780154556,
0.));
#74692=CARTESIAN_POINT('Ctrl Pts',(-1.34140535660262,-48.0918780154556,
20.));
#74693=CARTESIAN_POINT('Ctrl Pts',(-1.37468664138803,-48.0879161758201,
0.));
#74694=CARTESIAN_POINT('Ctrl Pts',(-1.37468664138803,-48.0879161758201,
20.));
#74695=CARTESIAN_POINT('Ctrl Pts',(-1.40796406048389,-48.0839313777781,
0.));
#74696=CARTESIAN_POINT('Ctrl Pts',(-1.40796406048389,-48.0839313777781,
20.));
#74697=CARTESIAN_POINT('Ctrl Pts',(-1.44123759797226,-48.0799236241059,
0.));
#74698=CARTESIAN_POINT('Ctrl Pts',(-1.44123759797226,-48.0799236241059,
20.));
#74699=CARTESIAN_POINT('Ctrl Pts',(-1.47450723793683,-48.0758929175908,
0.));
#74700=CARTESIAN_POINT('Ctrl Pts',(-1.47450723793683,-48.0758929175908,
20.));
#74701=CARTESIAN_POINT('Ctrl Pts',(-1.50777296446293,-48.071839261032,0.));
#74702=CARTESIAN_POINT('Ctrl Pts',(-1.50777296446293,-48.071839261032,20.));
#74703=CARTESIAN_POINT('Ctrl Pts',(-1.54103476163745,-48.0677626572394,
0.));
#74704=CARTESIAN_POINT('Ctrl Pts',(-1.54103476163745,-48.0677626572394,
20.));
#74705=CARTESIAN_POINT('Ctrl Pts',(-1.57429261354891,-48.0636631090342,
0.));
#74706=CARTESIAN_POINT('Ctrl Pts',(-1.57429261354891,-48.0636631090342,
20.));
#74707=CARTESIAN_POINT('Ctrl Pts',(-1.60754650428747,-48.0595406192492,
0.));
#74708=CARTESIAN_POINT('Ctrl Pts',(-1.60754650428747,-48.0595406192492,
20.));
#74709=CARTESIAN_POINT('Ctrl Pts',(-1.64079641794463,-48.0553951907273,
0.));
#74710=CARTESIAN_POINT('Ctrl Pts',(-1.64079641794463,-48.0553951907273,
20.));
#74711=CARTESIAN_POINT('Ctrl Pts',(-1.67404233861339,-48.0512268263229,
0.));
#74712=CARTESIAN_POINT('Ctrl Pts',(-1.67404233861339,-48.0512268263229,
20.));
#74713=CARTESIAN_POINT('Ctrl Pts',(-1.70728425038806,-48.0470355289011,
0.));
#74714=CARTESIAN_POINT('Ctrl Pts',(-1.70728425038806,-48.0470355289011,
20.));
#74715=CARTESIAN_POINT('Ctrl Pts',(-1.74052213736473,-48.0428213013379,
0.));
#74716=CARTESIAN_POINT('Ctrl Pts',(-1.74052213736473,-48.0428213013379,
20.));
#74717=CARTESIAN_POINT('Ctrl Pts',(-1.77375598364111,-48.038584146521,0.));
#74718=CARTESIAN_POINT('Ctrl Pts',(-1.77375598364111,-48.038584146521,20.));
#74719=CARTESIAN_POINT('Ctrl Pts',(-1.80698577331665,-48.0343240673492,
0.));
#74720=CARTESIAN_POINT('Ctrl Pts',(-1.80698577331665,-48.0343240673492,
20.));
#74721=CARTESIAN_POINT('Ctrl Pts',(-1.84021149049247,-48.0300410667328,
0.));
#74722=CARTESIAN_POINT('Ctrl Pts',(-1.84021149049247,-48.0300410667328,
20.));
#74723=CARTESIAN_POINT('Ctrl Pts',(-1.87343311927143,-48.0257351475934,
0.));
#74724=CARTESIAN_POINT('Ctrl Pts',(-1.87343311927143,-48.0257351475934,
20.));
#74725=CARTESIAN_POINT('Ctrl Pts',(-1.90665064375788,-48.0214063128629,
0.));
#74726=CARTESIAN_POINT('Ctrl Pts',(-1.90665064375788,-48.0214063128629,
20.));
#74727=CARTESIAN_POINT('Ctrl Pts',(-1.93986404805774,-48.0170545654849,
0.));
#74728=CARTESIAN_POINT('Ctrl Pts',(-1.93986404805774,-48.0170545654849,
20.));
#74729=CARTESIAN_POINT('Ctrl Pts',(-1.97307331627851,-48.0126799084137,
0.));
#74730=CARTESIAN_POINT('Ctrl Pts',(-1.97307331627851,-48.0126799084137,
20.));
#74731=CARTESIAN_POINT('Ctrl Pts',(-2.00627843252927,-48.0082823446147,
0.));
#74732=CARTESIAN_POINT('Ctrl Pts',(-2.00627843252927,-48.0082823446147,
20.));
#74733=CARTESIAN_POINT('Ctrl Pts',(-2.03947938092069,-48.0038618770642,
0.));
#74734=CARTESIAN_POINT('Ctrl Pts',(-2.03947938092069,-48.0038618770642,
20.));
#74735=CARTESIAN_POINT('Ctrl Pts',(-2.07267614556538,-47.9994185087499,
0.));
#74736=CARTESIAN_POINT('Ctrl Pts',(-2.07267614556538,-47.9994185087499,
20.));
#74737=CARTESIAN_POINT('Ctrl Pts',(-2.1058687105775,-47.994952242671,0.));
#74738=CARTESIAN_POINT('Ctrl Pts',(-2.1058687105775,-47.994952242671,20.));
#74739=CARTESIAN_POINT('Ctrl Pts',(-2.13905706007287,-47.9904630818375,
0.));
#74740=CARTESIAN_POINT('Ctrl Pts',(-2.13905706007287,-47.9904630818375,
20.));
#74741=CARTESIAN_POINT('Ctrl Pts',(-2.172241178169,-47.9859510292704,0.));
#74742=CARTESIAN_POINT('Ctrl Pts',(-2.172241178169,-47.9859510292704,20.));
#74743=CARTESIAN_POINT('Ctrl Pts',(-2.20542104898522,-47.9814160880019,
0.));
#74744=CARTESIAN_POINT('Ctrl Pts',(-2.20542104898522,-47.9814160880019,
20.));
#74745=CARTESIAN_POINT('Ctrl Pts',(-2.23859665664241,-47.9768582610752,
0.));
#74746=CARTESIAN_POINT('Ctrl Pts',(-2.23859665664241,-47.9768582610752,
20.));
#74747=CARTESIAN_POINT('Ctrl Pts',(-2.27176798526354,-47.9722775515452,
0.));
#74748=CARTESIAN_POINT('Ctrl Pts',(-2.27176798526354,-47.9722775515452,
20.));
#74749=CARTESIAN_POINT('Ctrl Pts',(-2.30493501897296,-47.9676739624772,
0.));
#74750=CARTESIAN_POINT('Ctrl Pts',(-2.30493501897296,-47.9676739624772,
20.));
#74751=CARTESIAN_POINT('Ctrl Pts',(-2.33809774189659,-47.9630474969481,
0.));
#74752=CARTESIAN_POINT('Ctrl Pts',(-2.33809774189659,-47.9630474969481,
20.));
#74753=CARTESIAN_POINT('Ctrl Pts',(-2.37125613816232,-47.9583981580454,
0.));
#74754=CARTESIAN_POINT('Ctrl Pts',(-2.37125613816232,-47.9583981580454,
20.));
#74755=CARTESIAN_POINT('Ctrl Pts',(-2.40441019189961,-47.9537259488681,
0.));
#74756=CARTESIAN_POINT('Ctrl Pts',(-2.40441019189961,-47.9537259488681,
20.));
#74757=CARTESIAN_POINT('Ctrl Pts',(-2.43755988723967,-47.9490308725257,
0.));
#74758=CARTESIAN_POINT('Ctrl Pts',(-2.43755988723967,-47.9490308725257,
20.));
#74759=CARTESIAN_POINT('Ctrl Pts',(-2.4707052083155,-47.9443129321394,0.));
#74760=CARTESIAN_POINT('Ctrl Pts',(-2.4707052083155,-47.9443129321394,20.));
#74761=CARTESIAN_POINT('Ctrl Pts',(-2.5038461392621,-47.9395721308414,0.));
#74762=CARTESIAN_POINT('Ctrl Pts',(-2.5038461392621,-47.9395721308414,20.));
#74763=CARTESIAN_POINT('Ctrl Pts',(-2.53698266421615,-47.9348084717752,
0.));
#74764=CARTESIAN_POINT('Ctrl Pts',(-2.53698266421615,-47.9348084717752,
20.));
#74765=CARTESIAN_POINT('Ctrl Pts',(-2.57011476731624,-47.9300219580955,
0.));
#74766=CARTESIAN_POINT('Ctrl Pts',(-2.57011476731624,-47.9300219580955,
20.));
#74767=CARTESIAN_POINT('Ctrl Pts',(-2.60324243270259,-47.9252125929679,
0.));
#74768=CARTESIAN_POINT('Ctrl Pts',(-2.60324243270259,-47.9252125929679,
20.));
#74769=CARTESIAN_POINT('Ctrl Pts',(-2.6363656445172,-47.9203803795688,0.));
#74770=CARTESIAN_POINT('Ctrl Pts',(-2.6363656445172,-47.9203803795688,20.));
#74771=CARTESIAN_POINT('Ctrl Pts',(-2.66948438690367,-47.9155253210858,
0.));
#74772=CARTESIAN_POINT('Ctrl Pts',(-2.66948438690367,-47.9155253210858,
20.));
#74773=CARTESIAN_POINT('Ctrl Pts',(-2.70259864400759,-47.9106474207177,
0.));
#74774=CARTESIAN_POINT('Ctrl Pts',(-2.70259864400759,-47.9106474207177,
20.));
#74775=CARTESIAN_POINT('Ctrl Pts',(-2.7357083999763,-47.9057466816743,0.));
#74776=CARTESIAN_POINT('Ctrl Pts',(-2.7357083999763,-47.9057466816743,20.));
#74777=CARTESIAN_POINT('Ctrl Pts',(-2.76881363895919,-47.9008231071768,
0.));
#74778=CARTESIAN_POINT('Ctrl Pts',(-2.76881363895919,-47.9008231071768,
20.));
#74779=CARTESIAN_POINT('Ctrl Pts',(-2.80191434510735,-47.8958767004573,
0.));
#74780=CARTESIAN_POINT('Ctrl Pts',(-2.80191434510735,-47.8958767004573,
20.));
#74781=CARTESIAN_POINT('Ctrl Pts',(-2.83501050257377,-47.8909074647592,
0.));
#74782=CARTESIAN_POINT('Ctrl Pts',(-2.83501050257377,-47.8909074647592,
20.));
#74783=CARTESIAN_POINT('Ctrl Pts',(-2.86810209551309,-47.8859154033363,
0.));
#74784=CARTESIAN_POINT('Ctrl Pts',(-2.86810209551309,-47.8859154033363,
20.));
#74785=CARTESIAN_POINT('Ctrl Pts',(-2.90118910808201,-47.8809005194543,
0.));
#74786=CARTESIAN_POINT('Ctrl Pts',(-2.90118910808201,-47.8809005194543,
20.));
#74787=CARTESIAN_POINT('Ctrl Pts',(-2.93427152443919,-47.8758628163901,
0.));
#74788=CARTESIAN_POINT('Ctrl Pts',(-2.93427152443919,-47.8758628163901,
20.));
#74789=CARTESIAN_POINT('Ctrl Pts',(-2.96734932874506,-47.8708022974315,
0.));
#74790=CARTESIAN_POINT('Ctrl Pts',(-2.96734932874506,-47.8708022974315,
20.));
#74791=CARTESIAN_POINT('Ctrl Pts',(-3.00042250516194,-47.8657189658771,
0.));
#74792=CARTESIAN_POINT('Ctrl Pts',(-3.00042250516194,-47.8657189658771,
20.));
#74793=CARTESIAN_POINT('Ctrl Pts',(-3.03349103785389,-47.8606128250365,
0.));
#74794=CARTESIAN_POINT('Ctrl Pts',(-3.03349103785389,-47.8606128250365,
20.));
#74795=CARTESIAN_POINT('Ctrl Pts',(-3.06655491098683,-47.8554838782302,
0.));
#74796=CARTESIAN_POINT('Ctrl Pts',(-3.06655491098683,-47.8554838782302,
20.));
#74797=CARTESIAN_POINT('Ctrl Pts',(-3.09961410872877,-47.8503321287903,
0.));
#74798=CARTESIAN_POINT('Ctrl Pts',(-3.09961410872877,-47.8503321287903,
20.));
#74799=CARTESIAN_POINT('Ctrl Pts',(-3.13266861524955,-47.8451575800601,
0.));
#74800=CARTESIAN_POINT('Ctrl Pts',(-3.13266861524955,-47.8451575800601,
20.));
#74801=CARTESIAN_POINT('Ctrl Pts',(-3.16571841472091,-47.8399602353939,
0.));
#74802=CARTESIAN_POINT('Ctrl Pts',(-3.16571841472091,-47.8399602353939,
20.));
#74803=CARTESIAN_POINT('Ctrl Pts',(-3.19876349131676,-47.834740098157,0.));
#74804=CARTESIAN_POINT('Ctrl Pts',(-3.19876349131676,-47.834740098157,20.));
#74805=CARTESIAN_POINT('Ctrl Pts',(-3.23180382921274,-47.829497171726,0.));
#74806=CARTESIAN_POINT('Ctrl Pts',(-3.23180382921274,-47.829497171726,20.));
#74807=CARTESIAN_POINT('Ctrl Pts',(-3.26483941258678,-47.8242314594881,
0.));
#74808=CARTESIAN_POINT('Ctrl Pts',(-3.26483941258678,-47.8242314594881,
20.));
#74809=CARTESIAN_POINT('Ctrl Pts',(-3.29787022561837,-47.818942964842,0.));
#74810=CARTESIAN_POINT('Ctrl Pts',(-3.29787022561837,-47.818942964842,20.));
#74811=CARTESIAN_POINT('Ctrl Pts',(-3.33089625248904,-47.813631691197,0.));
#74812=CARTESIAN_POINT('Ctrl Pts',(-3.33089625248904,-47.813631691197,20.));
#74813=CARTESIAN_POINT('Ctrl Pts',(-3.36391747738215,-47.8082976419741,
0.));
#74814=CARTESIAN_POINT('Ctrl Pts',(-3.36391747738215,-47.8082976419741,
20.));
#74815=CARTESIAN_POINT('Ctrl Pts',(-3.39693388448307,-47.802940820605,0.));
#74816=CARTESIAN_POINT('Ctrl Pts',(-3.39693388448307,-47.802940820605,20.));
#74817=CARTESIAN_POINT('Ctrl Pts',(-3.42994545797923,-47.797561230533,0.));
#74818=CARTESIAN_POINT('Ctrl Pts',(-3.42994545797923,-47.797561230533,20.));
#74819=CARTESIAN_POINT('Ctrl Pts',(-3.46295218206013,-47.7921588752121,
0.));
#74820=CARTESIAN_POINT('Ctrl Pts',(-3.46295218206013,-47.7921588752121,
20.));
#74821=CARTESIAN_POINT('Ctrl Pts',(-3.49595404091729,-47.7867337581073,
0.));
#74822=CARTESIAN_POINT('Ctrl Pts',(-3.49595404091729,-47.7867337581073,
20.));
#74823=CARTESIAN_POINT('Ctrl Pts',(-3.52895101874416,-47.7812858826946,
0.));
#74824=CARTESIAN_POINT('Ctrl Pts',(-3.52895101874416,-47.7812858826946,
20.));
#74825=CARTESIAN_POINT('Ctrl Pts',(-3.56194309973643,-47.7758152524613,
0.));
#74826=CARTESIAN_POINT('Ctrl Pts',(-3.56194309973643,-47.7758152524613,
20.));
#74827=CARTESIAN_POINT('Ctrl Pts',(-3.59493026809159,-47.7703218709055,
0.));
#74828=CARTESIAN_POINT('Ctrl Pts',(-3.59493026809159,-47.7703218709055,
20.));
#74829=CARTESIAN_POINT('Ctrl Pts',(-3.62791250800925,-47.764805741537,0.));
#74830=CARTESIAN_POINT('Ctrl Pts',(-3.62791250800925,-47.764805741537,20.));
#74831=CARTESIAN_POINT('Ctrl Pts',(-3.66088980369085,-47.7592668678762,
0.));
#74832=CARTESIAN_POINT('Ctrl Pts',(-3.66088980369085,-47.7592668678762,
20.));
#74833=CARTESIAN_POINT('Ctrl Pts',(-3.69386213933995,-47.7537052534546,
0.));
#74834=CARTESIAN_POINT('Ctrl Pts',(-3.69386213933995,-47.7537052534546,
20.));
#74835=CARTESIAN_POINT('Ctrl Pts',(-3.72682949916223,-47.7481209018149,
0.));
#74836=CARTESIAN_POINT('Ctrl Pts',(-3.72682949916223,-47.7481209018149,
20.));
#74837=CARTESIAN_POINT('Ctrl Pts',(-3.75979186736546,-47.7425138165111,
0.));
#74838=CARTESIAN_POINT('Ctrl Pts',(-3.75979186736546,-47.7425138165111,
20.));
#74839=CARTESIAN_POINT('Ctrl Pts',(-3.7927492281595,-47.7368840011081,0.));
#74840=CARTESIAN_POINT('Ctrl Pts',(-3.7927492281595,-47.7368840011081,20.));
#74841=CARTESIAN_POINT('Ctrl Pts',(-3.82570156575624,-47.7312314591817,
0.));
#74842=CARTESIAN_POINT('Ctrl Pts',(-3.82570156575624,-47.7312314591817,
20.));
#74843=CARTESIAN_POINT('Ctrl Pts',(-3.85864886436974,-47.7255561943191,
0.));
#74844=CARTESIAN_POINT('Ctrl Pts',(-3.85864886436974,-47.7255561943191,
20.));
#74845=CARTESIAN_POINT('Ctrl Pts',(-3.89159110821606,-47.719858210118,0.));
#74846=CARTESIAN_POINT('Ctrl Pts',(-3.89159110821606,-47.719858210118,20.));
#74847=CARTESIAN_POINT('Ctrl Pts',(-3.92452828151334,-47.7141375101875,
0.));
#74848=CARTESIAN_POINT('Ctrl Pts',(-3.92452828151334,-47.7141375101875,
20.));
#74849=CARTESIAN_POINT('Ctrl Pts',(-3.95746036848188,-47.7083940981477,
0.));
#74850=CARTESIAN_POINT('Ctrl Pts',(-3.95746036848188,-47.7083940981477,
20.));
#74851=CARTESIAN_POINT('Ctrl Pts',(-3.99038735334402,-47.7026279776294,
0.));
#74852=CARTESIAN_POINT('Ctrl Pts',(-3.99038735334402,-47.7026279776294,
20.));
#74853=CARTESIAN_POINT('Ctrl Pts',(-4.02330922032434,-47.6968391522753,
0.));
#74854=CARTESIAN_POINT('Ctrl Pts',(-4.02330922032434,-47.6968391522753,
20.));
#74855=CARTESIAN_POINT('Ctrl Pts',(-4.05622595364953,-47.6910276257391,
0.));
#74856=CARTESIAN_POINT('Ctrl Pts',(-4.05622595364953,-47.6910276257391,
20.));
#74857=CARTESIAN_POINT('Ctrl Pts',(-4.0891375375485,-47.6851934016861,0.));
#74858=CARTESIAN_POINT('Ctrl Pts',(-4.0891375375485,-47.6851934016861,20.));
#74859=CARTESIAN_POINT('Ctrl Pts',(-4.1220439562522,-47.6793364837921,0.));
#74860=CARTESIAN_POINT('Ctrl Pts',(-4.1220439562522,-47.6793364837921,20.));
#74861=CARTESIAN_POINT('Ctrl Pts',(-4.15494519399371,-47.6734568757434,
0.));
#74862=CARTESIAN_POINT('Ctrl Pts',(-4.15494519399371,-47.6734568757434,
20.));
#74863=CARTESIAN_POINT('Ctrl Pts',(-4.18784123500837,-47.6675545812371,
0.));
#74864=CARTESIAN_POINT('Ctrl Pts',(-4.18784123500837,-47.6675545812371,
20.));
#74865=CARTESIAN_POINT('Ctrl Pts',(-4.22073206353346,-47.6616296039816,
0.));
#74866=CARTESIAN_POINT('Ctrl Pts',(-4.22073206353346,-47.6616296039816,
20.));
#74867=CARTESIAN_POINT('Ctrl Pts',(-4.25361766380861,-47.6556819476964,
0.));
#74868=CARTESIAN_POINT('Ctrl Pts',(-4.25361766380861,-47.6556819476964,
20.));
#74869=CARTESIAN_POINT('Ctrl Pts',(-4.28649802007568,-47.6497116161128,
0.));
#74870=CARTESIAN_POINT('Ctrl Pts',(-4.28649802007568,-47.6497116161128,
20.));
#74871=CARTESIAN_POINT('Ctrl Pts',(-4.31937311657887,-47.6437186129734,
0.));
#74872=CARTESIAN_POINT('Ctrl Pts',(-4.31937311657887,-47.6437186129734,
20.));
#74873=CARTESIAN_POINT('Ctrl Pts',(-4.35224293756441,-47.6377029420315,
0.));
#74874=CARTESIAN_POINT('Ctrl Pts',(-4.35224293756441,-47.6377029420315,
20.));
#74875=CARTESIAN_POINT('Ctrl Pts',(-4.38510746728076,-47.6316646070511,
0.));
#74876=CARTESIAN_POINT('Ctrl Pts',(-4.38510746728076,-47.6316646070511,
20.));
#74877=CARTESIAN_POINT('Ctrl Pts',(-4.41796668997837,-47.6256036118071,
0.));
#74878=CARTESIAN_POINT('Ctrl Pts',(-4.41796668997837,-47.6256036118071,
20.));
#74879=CARTESIAN_POINT('Ctrl Pts',(-4.45082058991005,-47.6195199600851,
0.));
#74880=CARTESIAN_POINT('Ctrl Pts',(-4.45082058991005,-47.6195199600851,
20.));
#74881=CARTESIAN_POINT('Ctrl Pts',(-4.48366915133085,-47.6134136556823,
0.));
#74882=CARTESIAN_POINT('Ctrl Pts',(-4.48366915133085,-47.6134136556823,
20.));
#74883=CARTESIAN_POINT('Ctrl Pts',(-4.51651235849824,-47.6072847024073,
0.));
#74884=CARTESIAN_POINT('Ctrl Pts',(-4.51651235849824,-47.6072847024073,
20.));
#74885=CARTESIAN_POINT('Ctrl Pts',(-4.54935019567199,-47.6011331040799,
0.));
#74886=CARTESIAN_POINT('Ctrl Pts',(-4.54935019567199,-47.6011331040799,
20.));
#74887=CARTESIAN_POINT('Ctrl Pts',(-4.5821826471142,-47.5949588645311,0.));
#74888=CARTESIAN_POINT('Ctrl Pts',(-4.5821826471142,-47.5949588645311,20.));
#74889=CARTESIAN_POINT('Ctrl Pts',(-4.61500969708897,-47.5887619876026,
0.));
#74890=CARTESIAN_POINT('Ctrl Pts',(-4.61500969708897,-47.5887619876026,
20.));
#74891=CARTESIAN_POINT('Ctrl Pts',(-4.64783132986261,-47.5825424771468,
0.));
#74892=CARTESIAN_POINT('Ctrl Pts',(-4.64783132986261,-47.5825424771468,
20.));
#74893=CARTESIAN_POINT('Ctrl Pts',(-4.68064752970371,-47.5763003370265,
0.));
#74894=CARTESIAN_POINT('Ctrl Pts',(-4.68064752970371,-47.5763003370265,
20.));
#74895=CARTESIAN_POINT('Ctrl Pts',(-4.7134582808831,-47.5700355711162,0.));
#74896=CARTESIAN_POINT('Ctrl Pts',(-4.7134582808831,-47.5700355711162,20.));
#74897=CARTESIAN_POINT('Ctrl Pts',(-4.74626356767414,-47.5637481833017,
0.));
#74898=CARTESIAN_POINT('Ctrl Pts',(-4.74626356767414,-47.5637481833017,
20.));
#74899=CARTESIAN_POINT('Ctrl Pts',(-4.77906337435245,-47.5574381774801,
0.));
#74900=CARTESIAN_POINT('Ctrl Pts',(-4.77906337435245,-47.5574381774801,
20.));
#74901=CARTESIAN_POINT('Ctrl Pts',(-4.8118576851959,-47.5511055575592,0.));
#74902=CARTESIAN_POINT('Ctrl Pts',(-4.8118576851959,-47.5511055575592,20.));
#74903=CARTESIAN_POINT('Ctrl Pts',(-4.84464648448476,-47.5447503274583,
0.));
#74904=CARTESIAN_POINT('Ctrl Pts',(-4.84464648448476,-47.5447503274583,
20.));
#74905=CARTESIAN_POINT('Ctrl Pts',(-4.87742975650163,-47.538372491107,0.));
#74906=CARTESIAN_POINT('Ctrl Pts',(-4.87742975650163,-47.538372491107,20.));
#74907=CARTESIAN_POINT('Ctrl Pts',(-4.91020748553146,-47.5319720524462,
0.));
#74908=CARTESIAN_POINT('Ctrl Pts',(-4.91020748553146,-47.5319720524462,
20.));
#74909=CARTESIAN_POINT('Ctrl Pts',(-4.94297965586158,-47.5255490154281,
0.));
#74910=CARTESIAN_POINT('Ctrl Pts',(-4.94297965586158,-47.5255490154281,
20.));
#74911=CARTESIAN_POINT('Ctrl Pts',(-4.97574625178171,-47.519103384016,0.));
#74912=CARTESIAN_POINT('Ctrl Pts',(-4.97574625178171,-47.519103384016,20.));
#74913=CARTESIAN_POINT('Ctrl Pts',(-5.00850725758369,-47.5126351621839,
0.));
#74914=CARTESIAN_POINT('Ctrl Pts',(-5.00850725758369,-47.5126351621839,
20.));
#74915=CARTESIAN_POINT('Ctrl Pts',(-5.04126265756156,-47.5061443539168,
0.));
#74916=CARTESIAN_POINT('Ctrl Pts',(-5.04126265756156,-47.5061443539168,
20.));
#74917=CARTESIAN_POINT('Ctrl Pts',(-5.074012436012,-47.4996309632108,0.));
#74918=CARTESIAN_POINT('Ctrl Pts',(-5.074012436012,-47.4996309632108,20.));
#74919=CARTESIAN_POINT('Ctrl Pts',(-5.10675657723404,-47.4930949940731,
0.));
#74920=CARTESIAN_POINT('Ctrl Pts',(-5.10675657723404,-47.4930949940731,
20.));
#74921=CARTESIAN_POINT('Ctrl Pts',(-5.13949506552924,-47.4865364505219,
0.));
#74922=CARTESIAN_POINT('Ctrl Pts',(-5.13949506552924,-47.4865364505219,
20.));
#74923=CARTESIAN_POINT('Ctrl Pts',(-5.17222788520145,-47.4799553365862,
0.));
#74924=CARTESIAN_POINT('Ctrl Pts',(-5.17222788520145,-47.4799553365862,
20.));
#74925=CARTESIAN_POINT('Ctrl Pts',(-5.20495502055715,-47.4733516563069,
0.));
#74926=CARTESIAN_POINT('Ctrl Pts',(-5.20495502055715,-47.4733516563069,
20.));
#74927=CARTESIAN_POINT('Ctrl Pts',(-5.23767645590512,-47.4667254137359,
0.));
#74928=CARTESIAN_POINT('Ctrl Pts',(-5.23767645590512,-47.4667254137359,
20.));
#74929=CARTESIAN_POINT('Ctrl Pts',(-5.27039217555657,-47.4600766129357,
0.));
#74930=CARTESIAN_POINT('Ctrl Pts',(-5.27039217555657,-47.4600766129357,
20.));
#74931=CARTESIAN_POINT('Ctrl Pts',(-5.30310216382507,-47.4534052579797,
0.));
#74932=CARTESIAN_POINT('Ctrl Pts',(-5.30310216382507,-47.4534052579797,
20.));
#74933=CARTESIAN_POINT('Ctrl Pts',(-5.33580640502662,-47.4467113529523,
0.));
#74934=CARTESIAN_POINT('Ctrl Pts',(-5.33580640502662,-47.4467113529523,
20.));
#74935=CARTESIAN_POINT('Ctrl Pts',(-5.36850488347925,-47.4399949019487,
0.));
#74936=CARTESIAN_POINT('Ctrl Pts',(-5.36850488347925,-47.4399949019487,
20.));
#74937=CARTESIAN_POINT('Ctrl Pts',(-5.4011975835038,-47.4332559090748,0.));
#74938=CARTESIAN_POINT('Ctrl Pts',(-5.4011975835038,-47.4332559090748,20.));
#74939=CARTESIAN_POINT('Ctrl Pts',(-5.43388448942351,-47.4264943784481,
0.));
#74940=CARTESIAN_POINT('Ctrl Pts',(-5.43388448942351,-47.4264943784481,
20.));
#74941=CARTESIAN_POINT('Ctrl Pts',(-5.46656558556427,-47.4197103141976,
0.));
#74942=CARTESIAN_POINT('Ctrl Pts',(-5.46656558556427,-47.4197103141976,
20.));
#74943=CARTESIAN_POINT('Ctrl Pts',(-5.49924085625465,-47.4129037204631,
0.));
#74944=CARTESIAN_POINT('Ctrl Pts',(-5.49924085625465,-47.4129037204631,
20.));
#74945=CARTESIAN_POINT('Ctrl Pts',(-5.53191028582555,-47.4060746013959,
0.));
#74946=CARTESIAN_POINT('Ctrl Pts',(-5.53191028582555,-47.4060746013959,
20.));
#74947=CARTESIAN_POINT('Ctrl Pts',(-5.56457385861038,-47.3992229611579,
0.));
#74948=CARTESIAN_POINT('Ctrl Pts',(-5.56457385861038,-47.3992229611579,
20.));
#74949=CARTESIAN_POINT('Ctrl Pts',(-5.59723155894484,-47.3923488039217,
0.));
#74950=CARTESIAN_POINT('Ctrl Pts',(-5.59723155894484,-47.3923488039217,
20.));
#74951=CARTESIAN_POINT('Ctrl Pts',(-5.62988337116716,-47.3854521338708,
0.));
#74952=CARTESIAN_POINT('Ctrl Pts',(-5.62988337116716,-47.3854521338708,
20.));
#74953=CARTESIAN_POINT('Ctrl Pts',(-5.66252927961812,-47.3785329551997,
0.));
#74954=CARTESIAN_POINT('Ctrl Pts',(-5.66252927961812,-47.3785329551997,
20.));
#74955=CARTESIAN_POINT('Ctrl Pts',(-5.69516926864089,-47.3715912721141,
0.));
#74956=CARTESIAN_POINT('Ctrl Pts',(-5.69516926864089,-47.3715912721141,
20.));
#74957=CARTESIAN_POINT('Ctrl Pts',(-5.72780332258136,-47.3646270888308,
0.));
#74958=CARTESIAN_POINT('Ctrl Pts',(-5.72780332258136,-47.3646270888308,
20.));
#74959=CARTESIAN_POINT('Ctrl Pts',(-5.76043142578787,-47.3576404095777,
0.));
#74960=CARTESIAN_POINT('Ctrl Pts',(-5.76043142578787,-47.3576404095777,
20.));
#74961=CARTESIAN_POINT('Ctrl Pts',(-5.79305356261143,-47.3506312385939,
0.));
#74962=CARTESIAN_POINT('Ctrl Pts',(-5.79305356261143,-47.3506312385939,
20.));
#74963=CARTESIAN_POINT('Ctrl Pts',(-5.82566971740557,-47.3435995801292,
0.));
#74964=CARTESIAN_POINT('Ctrl Pts',(-5.82566971740557,-47.3435995801292,
20.));
#74965=CARTESIAN_POINT('Ctrl Pts',(-5.85827987452641,-47.3365454384446,
0.));
#74966=CARTESIAN_POINT('Ctrl Pts',(-5.85827987452641,-47.3365454384446,
20.));
#74967=CARTESIAN_POINT('Ctrl Pts',(-5.89088401833278,-47.3294688178121,
0.));
#74968=CARTESIAN_POINT('Ctrl Pts',(-5.89088401833278,-47.3294688178121,
20.));
#74969=CARTESIAN_POINT('Ctrl Pts',(-5.92348213318599,-47.3223697225143,
0.));
#74970=CARTESIAN_POINT('Ctrl Pts',(-5.92348213318599,-47.3223697225143,
20.));
#74971=CARTESIAN_POINT('Ctrl Pts',(-5.95607420344987,-47.3152481568452,
0.));
#74972=CARTESIAN_POINT('Ctrl Pts',(-5.95607420344987,-47.3152481568452,
20.));
#74973=CARTESIAN_POINT('Ctrl Pts',(-5.98866021349068,-47.3081041251096,
0.));
#74974=CARTESIAN_POINT('Ctrl Pts',(-5.98866021349068,-47.3081041251096,
20.));
#74975=CARTESIAN_POINT('Ctrl Pts',(-6.02124014767731,-47.3009376316237,
0.));
#74976=CARTESIAN_POINT('Ctrl Pts',(-6.02124014767731,-47.3009376316237,
20.));
#74977=CARTESIAN_POINT('Ctrl Pts',(-6.0538139903813,-47.2937486807145,0.));
#74978=CARTESIAN_POINT('Ctrl Pts',(-6.0538139903813,-47.2937486807145,20.));
#74979=CARTESIAN_POINT('Ctrl Pts',(-6.08638172597685,-47.2865372767199,
0.));
#74980=CARTESIAN_POINT('Ctrl Pts',(-6.08638172597685,-47.2865372767199,
20.));
#74981=CARTESIAN_POINT('Ctrl Pts',(-6.11894333884089,-47.2793034239892,
0.));
#74982=CARTESIAN_POINT('Ctrl Pts',(-6.11894333884089,-47.2793034239892,
20.));
#74983=CARTESIAN_POINT('Ctrl Pts',(-6.15149881335291,-47.272047126882,0.));
#74984=CARTESIAN_POINT('Ctrl Pts',(-6.15149881335291,-47.272047126882,20.));
#74985=CARTESIAN_POINT('Ctrl Pts',(-6.1840481338953,-47.2647683897693,0.));
#74986=CARTESIAN_POINT('Ctrl Pts',(-6.1840481338953,-47.2647683897693,20.));
#74987=CARTESIAN_POINT('Ctrl Pts',(-6.21659128485297,-47.2574672170331,
0.));
#74988=CARTESIAN_POINT('Ctrl Pts',(-6.21659128485297,-47.2574672170331,
20.));
#74989=CARTESIAN_POINT('Ctrl Pts',(-6.24912825061344,-47.2501436130661,
0.));
#74990=CARTESIAN_POINT('Ctrl Pts',(-6.24912825061344,-47.2501436130661,
20.));
#74991=CARTESIAN_POINT('Ctrl Pts',(-6.28165901556677,-47.2427975822723,
0.));
#74992=CARTESIAN_POINT('Ctrl Pts',(-6.28165901556677,-47.2427975822723,
20.));
#74993=CARTESIAN_POINT('Ctrl Pts',(-6.31418356410551,-47.2354291290667,
0.));
#74994=CARTESIAN_POINT('Ctrl Pts',(-6.31418356410551,-47.2354291290667,
20.));
#74995=CARTESIAN_POINT('Ctrl Pts',(-6.34670188062517,-47.2280382578755,
0.));
#74996=CARTESIAN_POINT('Ctrl Pts',(-6.34670188062517,-47.2280382578755,
20.));
#74997=CARTESIAN_POINT('Ctrl Pts',(-6.37921394952381,-47.2206249731358,
0.));
#74998=CARTESIAN_POINT('Ctrl Pts',(-6.37921394952381,-47.2206249731358,
20.));
#74999=CARTESIAN_POINT('Ctrl Pts',(-6.41171975520235,-47.213189279296,0.));
#75000=CARTESIAN_POINT('Ctrl Pts',(-6.41171975520235,-47.213189279296,20.));
#75001=CARTESIAN_POINT('Ctrl Pts',(-6.44421928206447,-47.205731180815,0.));
#75002=CARTESIAN_POINT('Ctrl Pts',(-6.44421928206447,-47.205731180815,20.));
#75003=CARTESIAN_POINT('Ctrl Pts',(-6.47671251451639,-47.1982506821625,
0.));
#75004=CARTESIAN_POINT('Ctrl Pts',(-6.47671251451639,-47.1982506821625,
20.));
#75005=CARTESIAN_POINT('Ctrl Pts',(-6.50919943696718,-47.190747787819,0.));
#75006=CARTESIAN_POINT('Ctrl Pts',(-6.50919943696718,-47.190747787819,20.));
#75007=CARTESIAN_POINT('Ctrl Pts',(-6.54168003382863,-47.1832225022762,
0.));
#75008=CARTESIAN_POINT('Ctrl Pts',(-6.54168003382863,-47.1832225022762,
20.));
#75009=CARTESIAN_POINT('Ctrl Pts',(-6.57415428951526,-47.1756748300372,
0.));
#75010=CARTESIAN_POINT('Ctrl Pts',(-6.57415428951526,-47.1756748300372,
20.));
#75011=CARTESIAN_POINT('Ctrl Pts',(-6.60662218844436,-47.168104775616,0.));
#75012=CARTESIAN_POINT('Ctrl Pts',(-6.60662218844436,-47.168104775616,20.));
#75013=CARTESIAN_POINT('Ctrl Pts',(-6.63908371503578,-47.1605123435378,
0.));
#75014=CARTESIAN_POINT('Ctrl Pts',(-6.63908371503578,-47.1605123435378,
20.));
#75015=CARTESIAN_POINT('Ctrl Pts',(-6.67153885371228,-47.1528975383387,
0.));
#75016=CARTESIAN_POINT('Ctrl Pts',(-6.67153885371228,-47.1528975383387,
20.));
#75017=CARTESIAN_POINT('Ctrl Pts',(-6.70398758889918,-47.1452603645656,
0.));
#75018=CARTESIAN_POINT('Ctrl Pts',(-6.70398758889918,-47.1452603645656,
20.));
#75019=CARTESIAN_POINT('Ctrl Pts',(-6.7364299050246,-47.1376008267758,0.));
#75020=CARTESIAN_POINT('Ctrl Pts',(-6.7364299050246,-47.1376008267758,20.));
#75021=CARTESIAN_POINT('Ctrl Pts',(-6.76886578651956,-47.129918929538,0.));
#75022=CARTESIAN_POINT('Ctrl Pts',(-6.76886578651956,-47.129918929538,20.));
#75023=CARTESIAN_POINT('Ctrl Pts',(-6.80129521781809,-47.1222146774323,
0.));
#75024=CARTESIAN_POINT('Ctrl Pts',(-6.80129521781809,-47.1222146774323,
20.));
#75025=CARTESIAN_POINT('Ctrl Pts',(-6.83371818335699,-47.1144880750497,
0.));
#75026=CARTESIAN_POINT('Ctrl Pts',(-6.83371818335699,-47.1144880750497,
20.));
#75027=CARTESIAN_POINT('Ctrl Pts',(-6.8661346675759,-47.1067391269919,0.));
#75028=CARTESIAN_POINT('Ctrl Pts',(-6.8661346675759,-47.1067391269919,20.));
#75029=CARTESIAN_POINT('Ctrl Pts',(-6.89854465491704,-47.0989678378717,
0.));
#75030=CARTESIAN_POINT('Ctrl Pts',(-6.89854465491704,-47.0989678378717,
20.));
#75031=CARTESIAN_POINT('Ctrl Pts',(-6.93094812982543,-47.0911742123123,
0.));
#75032=CARTESIAN_POINT('Ctrl Pts',(-6.93094812982543,-47.0911742123123,
20.));
#75033=CARTESIAN_POINT('Ctrl Pts',(-6.96334507674875,-47.0833582549484,
0.));
#75034=CARTESIAN_POINT('Ctrl Pts',(-6.96334507674875,-47.0833582549484,
20.));
#75035=CARTESIAN_POINT('Ctrl Pts',(-6.99573548013778,-47.0755199704256,
0.));
#75036=CARTESIAN_POINT('Ctrl Pts',(-6.99573548013778,-47.0755199704256,
20.));
#75037=CARTESIAN_POINT('Ctrl Pts',(-7.02811932444603,-47.0676593634011,
0.));
#75038=CARTESIAN_POINT('Ctrl Pts',(-7.02811932444603,-47.0676593634011,
20.));
#75039=CARTESIAN_POINT('Ctrl Pts',(-7.06049659413009,-47.0597764385426,
0.));
#75040=CARTESIAN_POINT('Ctrl Pts',(-7.06049659413009,-47.0597764385426,
20.));
#75041=CARTESIAN_POINT('Ctrl Pts',(-7.09286727364934,-47.0518712005288,
0.));
#75042=CARTESIAN_POINT('Ctrl Pts',(-7.09286727364934,-47.0518712005288,
20.));
#75043=CARTESIAN_POINT('Ctrl Pts',(-7.12523134746605,-47.0439436540493,
0.));
#75044=CARTESIAN_POINT('Ctrl Pts',(-7.12523134746605,-47.0439436540493,
20.));
#75045=CARTESIAN_POINT('Ctrl Pts',(-7.15758880004523,-47.0359938038039,
0.));
#75046=CARTESIAN_POINT('Ctrl Pts',(-7.15758880004523,-47.0359938038039,
20.));
#75047=CARTESIAN_POINT('Ctrl Pts',(-7.18993961585471,-47.0280216545038,
0.));
#75048=CARTESIAN_POINT('Ctrl Pts',(-7.18993961585471,-47.0280216545038,
20.));
#75049=CARTESIAN_POINT('Ctrl Pts',(-7.22228377936531,-47.020027210871,0.));
#75050=CARTESIAN_POINT('Ctrl Pts',(-7.22228377936531,-47.020027210871,20.));
#75051=CARTESIAN_POINT('Ctrl Pts',(-7.25462127505078,-47.012010477639,0.));
#75052=CARTESIAN_POINT('Ctrl Pts',(-7.25462127505078,-47.012010477639,20.));
#75053=CARTESIAN_POINT('Ctrl Pts',(-7.28695208738785,-47.0039714595526,
0.));
#75054=CARTESIAN_POINT('Ctrl Pts',(-7.28695208738785,-47.0039714595526,
20.));
#75055=CARTESIAN_POINT('Ctrl Pts',(-7.31927620085615,-46.9959101613675,
0.));
#75056=CARTESIAN_POINT('Ctrl Pts',(-7.31927620085615,-46.9959101613675,
20.));
#75057=CARTESIAN_POINT('Ctrl Pts',(-7.35159359993819,-46.9878265878505,
0.));
#75058=CARTESIAN_POINT('Ctrl Pts',(-7.35159359993819,-46.9878265878505,
20.));
#75059=CARTESIAN_POINT('Ctrl Pts',(-7.38390426911933,-46.9797207437786,
0.));
#75060=CARTESIAN_POINT('Ctrl Pts',(-7.38390426911933,-46.9797207437786,
20.));
#75061=CARTESIAN_POINT('Ctrl Pts',(-7.41620819288779,-46.9715926339391,
0.));
#75062=CARTESIAN_POINT('Ctrl Pts',(-7.41620819288779,-46.9715926339391,
20.));
#75063=CARTESIAN_POINT('Ctrl Pts',(-7.44850535573483,-46.9634422631307,
0.));
#75064=CARTESIAN_POINT('Ctrl Pts',(-7.44850535573483,-46.9634422631307,
20.));
#75065=CARTESIAN_POINT('Ctrl Pts',(-7.4807957421548,-46.9552696361634,0.));
#75066=CARTESIAN_POINT('Ctrl Pts',(-7.4807957421548,-46.9552696361634,20.));
#75067=CARTESIAN_POINT('Ctrl Pts',(-7.51307933664513,-46.9470747578592,
0.));
#75068=CARTESIAN_POINT('Ctrl Pts',(-7.51307933664513,-46.9470747578592,
20.));
#75069=CARTESIAN_POINT('Ctrl Pts',(-7.54535612370603,-46.9388576330501,
0.));
#75070=CARTESIAN_POINT('Ctrl Pts',(-7.54535612370603,-46.9388576330501,
20.));
#75071=CARTESIAN_POINT('Ctrl Pts',(-7.5776260878407,-46.9306182665792,0.));
#75072=CARTESIAN_POINT('Ctrl Pts',(-7.5776260878407,-46.9306182665792,20.));
#75073=CARTESIAN_POINT('Ctrl Pts',(-7.60988921355522,-46.9223566632999,
0.));
#75074=CARTESIAN_POINT('Ctrl Pts',(-7.60988921355522,-46.9223566632999,
20.));
#75075=CARTESIAN_POINT('Ctrl Pts',(-7.64214548535858,-46.9140728280766,
0.));
#75076=CARTESIAN_POINT('Ctrl Pts',(-7.64214548535858,-46.9140728280766,
20.));
#75077=CARTESIAN_POINT('Ctrl Pts',(-7.67439488776289,-46.9057667657847,
0.));
#75078=CARTESIAN_POINT('Ctrl Pts',(-7.67439488776289,-46.9057667657847,
20.));
#75079=CARTESIAN_POINT('Ctrl Pts',(-7.70663740528332,-46.8974384813109,
0.));
#75080=CARTESIAN_POINT('Ctrl Pts',(-7.70663740528332,-46.8974384813109,
20.));
#75081=CARTESIAN_POINT('Ctrl Pts',(-7.73887302243817,-46.8890879795531,
0.));
#75082=CARTESIAN_POINT('Ctrl Pts',(-7.73887302243817,-46.8890879795531,
20.));
#75083=CARTESIAN_POINT('Ctrl Pts',(-7.77110172374869,-46.8807152654198,
0.));
#75084=CARTESIAN_POINT('Ctrl Pts',(-7.77110172374869,-46.8807152654198,
20.));
#75085=CARTESIAN_POINT('Ctrl Pts',(-7.80332349373919,-46.8723203438306,
0.));
#75086=CARTESIAN_POINT('Ctrl Pts',(-7.80332349373919,-46.8723203438306,
20.));
#75087=CARTESIAN_POINT('Ctrl Pts',(-7.83553831693688,-46.8639032197162,
0.));
#75088=CARTESIAN_POINT('Ctrl Pts',(-7.83553831693688,-46.8639032197162,
20.));
#75089=CARTESIAN_POINT('Ctrl Pts',(-7.86774617787214,-46.855463898018,0.));
#75090=CARTESIAN_POINT('Ctrl Pts',(-7.86774617787214,-46.855463898018,20.));
#75091=CARTESIAN_POINT('Ctrl Pts',(-7.8999470610784,-46.8470023836881,0.));
#75092=CARTESIAN_POINT('Ctrl Pts',(-7.8999470610784,-46.8470023836881,20.));
#75093=CARTESIAN_POINT('Ctrl Pts',(-7.93214095109212,-46.8385186816898,
0.));
#75094=CARTESIAN_POINT('Ctrl Pts',(-7.93214095109212,-46.8385186816898,
20.));
#75095=CARTESIAN_POINT('Ctrl Pts',(-7.96432783245287,-46.8300127969969,
0.));
#75096=CARTESIAN_POINT('Ctrl Pts',(-7.96432783245287,-46.8300127969969,
20.));
#75097=CARTESIAN_POINT('Ctrl Pts',(-7.99650768970305,-46.8214847345942,
0.));
#75098=CARTESIAN_POINT('Ctrl Pts',(-7.99650768970305,-46.8214847345942,
20.));
#75099=CARTESIAN_POINT('Ctrl Pts',(-8.02868050738829,-46.8129344994773,
0.));
#75100=CARTESIAN_POINT('Ctrl Pts',(-8.02868050738829,-46.8129344994773,
20.));
#75101=CARTESIAN_POINT('Ctrl Pts',(-8.0608462700573,-46.8043620966531,0.));
#75102=CARTESIAN_POINT('Ctrl Pts',(-8.0608462700573,-46.8043620966531,20.));
#75103=CARTESIAN_POINT('Ctrl Pts',(-8.09300496226221,-46.7957675311395,
0.));
#75104=CARTESIAN_POINT('Ctrl Pts',(-8.09300496226221,-46.7957675311395,
20.));
#75105=CARTESIAN_POINT('Ctrl Pts',(-8.12515656855803,-46.7871508079658,
0.));
#75106=CARTESIAN_POINT('Ctrl Pts',(-8.12515656855803,-46.7871508079658,
20.));
#75107=CARTESIAN_POINT('Ctrl Pts',(-8.15730107350296,-46.7785119321719,
0.));
#75108=CARTESIAN_POINT('Ctrl Pts',(-8.15730107350296,-46.7785119321719,
20.));
#75109=CARTESIAN_POINT('Ctrl Pts',(-8.18943846165846,-46.7698509088086,
0.));
#75110=CARTESIAN_POINT('Ctrl Pts',(-8.18943846165846,-46.7698509088086,
20.));
#75111=CARTESIAN_POINT('Ctrl Pts',(-8.22156871758883,-46.7611677429374,
0.));
#75112=CARTESIAN_POINT('Ctrl Pts',(-8.22156871758883,-46.7611677429374,
20.));
#75113=CARTESIAN_POINT('Ctrl Pts',(-8.2536918258617,-46.7524624396307,0.));
#75114=CARTESIAN_POINT('Ctrl Pts',(-8.2536918258617,-46.7524624396307,20.));
#75115=CARTESIAN_POINT('Ctrl Pts',(-8.28580777104746,-46.7437350039712,
0.));
#75116=CARTESIAN_POINT('Ctrl Pts',(-8.28580777104746,-46.7437350039712,
20.));
#75117=CARTESIAN_POINT('Ctrl Pts',(-8.31791653771974,-46.7349854410525,
0.));
#75118=CARTESIAN_POINT('Ctrl Pts',(-8.31791653771974,-46.7349854410525,
20.));
#75119=CARTESIAN_POINT('Ctrl Pts',(-8.35001811045537,-46.7262137559789,
0.));
#75120=CARTESIAN_POINT('Ctrl Pts',(-8.35001811045537,-46.7262137559789,
20.));
#75121=CARTESIAN_POINT('Ctrl Pts',(-8.38211247383477,-46.7174199538668,
0.));
#75122=CARTESIAN_POINT('Ctrl Pts',(-8.38211247383477,-46.7174199538668,
20.));
#75123=CARTESIAN_POINT('Ctrl Pts',(-8.41419961244156,-46.7086040398438,
0.));
#75124=CARTESIAN_POINT('Ctrl Pts',(-8.41419961244156,-46.7086040398438,
20.));
#75125=CARTESIAN_POINT('Ctrl Pts',(-8.44627951086263,-46.6997660190488,
0.));
#75126=CARTESIAN_POINT('Ctrl Pts',(-8.44627951086263,-46.6997660190488,
20.));
#75127=CARTESIAN_POINT('Ctrl Pts',(-8.47835215368745,-46.6909058966306,
0.));
#75128=CARTESIAN_POINT('Ctrl Pts',(-8.47835215368745,-46.6909058966306,
20.));
#75129=CARTESIAN_POINT('Ctrl Pts',(-8.51041752550882,-46.6820236777489,
0.));
#75130=CARTESIAN_POINT('Ctrl Pts',(-8.51041752550882,-46.6820236777489,
20.));
#75131=CARTESIAN_POINT('Ctrl Pts',(-8.54247561092259,-46.673119367573,0.));
#75132=CARTESIAN_POINT('Ctrl Pts',(-8.54247561092259,-46.673119367573,20.));
#75133=CARTESIAN_POINT('Ctrl Pts',(-8.57452639452829,-46.6641929712839,
0.));
#75134=CARTESIAN_POINT('Ctrl Pts',(-8.57452639452829,-46.6641929712839,
20.));
#75135=CARTESIAN_POINT('Ctrl Pts',(-8.60656986092879,-46.6552444940739,
0.));
#75136=CARTESIAN_POINT('Ctrl Pts',(-8.60656986092879,-46.6552444940739,
20.));
#75137=CARTESIAN_POINT('Ctrl Pts',(-8.63860599473004,-46.6462739411471,
0.));
#75138=CARTESIAN_POINT('Ctrl Pts',(-8.63860599473004,-46.6462739411471,
20.));
#75139=CARTESIAN_POINT('Ctrl Pts',(-8.67063478054117,-46.6372813177181,
0.));
#75140=CARTESIAN_POINT('Ctrl Pts',(-8.67063478054117,-46.6372813177181,
20.));
#75141=CARTESIAN_POINT('Ctrl Pts',(-8.70265620297455,-46.6282666290119,
0.));
#75142=CARTESIAN_POINT('Ctrl Pts',(-8.70265620297455,-46.6282666290119,
20.));
#75143=CARTESIAN_POINT('Ctrl Pts',(-8.73467024664571,-46.6192298802645,
0.));
#75144=CARTESIAN_POINT('Ctrl Pts',(-8.73467024664571,-46.6192298802645,
20.));
#75145=CARTESIAN_POINT('Ctrl Pts',(-8.76667689617331,-46.6101710767218,
0.));
#75146=CARTESIAN_POINT('Ctrl Pts',(-8.76667689617331,-46.6101710767218,
20.));
#75147=CARTESIAN_POINT('Ctrl Pts',(-8.79867613617934,-46.6010902236408,
0.));
#75148=CARTESIAN_POINT('Ctrl Pts',(-8.79867613617934,-46.6010902236408,
20.));
#75149=CARTESIAN_POINT('Ctrl Pts',(-8.83066795128935,-46.59198732629,0.));
#75150=CARTESIAN_POINT('Ctrl Pts',(-8.83066795128935,-46.59198732629,20.));
#75151=CARTESIAN_POINT('Ctrl Pts',(-8.86265232613216,-46.582862389949,0.));
#75152=CARTESIAN_POINT('Ctrl Pts',(-8.86265232613216,-46.582862389949,20.));
#75153=CARTESIAN_POINT('Ctrl Pts',(-8.8946292453399,-46.5737154199087,0.));
#75154=CARTESIAN_POINT('Ctrl Pts',(-8.8946292453399,-46.5737154199087,20.));
#75155=CARTESIAN_POINT('Ctrl Pts',(-8.92659869354789,-46.5645464214705,
0.));
#75156=CARTESIAN_POINT('Ctrl Pts',(-8.92659869354789,-46.5645464214705,
20.));
#75157=CARTESIAN_POINT('Ctrl Pts',(-8.95856065539471,-46.5553553999467,
0.));
#75158=CARTESIAN_POINT('Ctrl Pts',(-8.95856065539471,-46.5553553999467,
20.));
#75159=CARTESIAN_POINT('Ctrl Pts',(-8.9905151155223,-46.5461423606602,0.));
#75160=CARTESIAN_POINT('Ctrl Pts',(-8.9905151155223,-46.5461423606602,20.));
#75161=CARTESIAN_POINT('Ctrl Pts',(-9.02246205857629,-46.5369073089453,
0.));
#75162=CARTESIAN_POINT('Ctrl Pts',(-9.02246205857629,-46.5369073089453,
20.));
#75163=CARTESIAN_POINT('Ctrl Pts',(-9.05440146920516,-46.5276502501459,
0.));
#75164=CARTESIAN_POINT('Ctrl Pts',(-9.05440146920516,-46.5276502501459,
20.));
#75165=CARTESIAN_POINT('Ctrl Pts',(-9.08633333206091,-46.5183711896174,
0.));
#75166=CARTESIAN_POINT('Ctrl Pts',(-9.08633333206091,-46.5183711896174,
20.));
#75167=CARTESIAN_POINT('Ctrl Pts',(-9.11825763179854,-46.5090701327255,
0.));
#75168=CARTESIAN_POINT('Ctrl Pts',(-9.11825763179854,-46.5090701327255,
20.));
#75169=CARTESIAN_POINT('Ctrl Pts',(-9.15017435307667,-46.4997470848477,
0.));
#75170=CARTESIAN_POINT('Ctrl Pts',(-9.15017435307667,-46.4997470848477,
20.));
#75171=CARTESIAN_POINT('Ctrl Pts',(-9.18208348055726,-46.4904020513722,
0.));
#75172=CARTESIAN_POINT('Ctrl Pts',(-9.18208348055726,-46.4904020513722,
20.));
#75173=CARTESIAN_POINT('Ctrl Pts',(-9.21398499890594,-46.4810350376983,
0.));
#75174=CARTESIAN_POINT('Ctrl Pts',(-9.21398499890594,-46.4810350376983,
20.));
#75175=CARTESIAN_POINT('Ctrl Pts',(-9.24587889279172,-46.4716460492361,
0.));
#75176=CARTESIAN_POINT('Ctrl Pts',(-9.24587889279172,-46.4716460492361,
20.));
#75177=CARTESIAN_POINT('Ctrl Pts',(-9.277765146887,-46.4622350914066,0.));
#75178=CARTESIAN_POINT('Ctrl Pts',(-9.277765146887,-46.4622350914066,20.));
#75179=CARTESIAN_POINT('Ctrl Pts',(-9.30964374586753,-46.4528021696416,
0.));
#75180=CARTESIAN_POINT('Ctrl Pts',(-9.30964374586753,-46.4528021696416,
20.));
#75181=CARTESIAN_POINT('Ctrl Pts',(-9.34151467441242,-46.4433472893837,
0.));
#75182=CARTESIAN_POINT('Ctrl Pts',(-9.34151467441242,-46.4433472893837,
20.));
#75183=CARTESIAN_POINT('Ctrl Pts',(-9.37337791720394,-46.4338704560856,
0.));
#75184=CARTESIAN_POINT('Ctrl Pts',(-9.37337791720394,-46.4338704560856,
20.));
#75185=CARTESIAN_POINT('Ctrl Pts',(-9.40523345892774,-46.4243716752115,
0.));
#75186=CARTESIAN_POINT('Ctrl Pts',(-9.40523345892774,-46.4243716752115,
20.));
#75187=CARTESIAN_POINT('Ctrl Pts',(-9.43708128427275,-46.4148509522358,
0.));
#75188=CARTESIAN_POINT('Ctrl Pts',(-9.43708128427275,-46.4148509522358,
20.));
#75189=CARTESIAN_POINT('Ctrl Pts',(-9.46892137793149,-46.405308292644,0.));
#75190=CARTESIAN_POINT('Ctrl Pts',(-9.46892137793149,-46.405308292644,20.));
#75191=CARTESIAN_POINT('Ctrl Pts',(-9.5007537246001,-46.3957437019326,0.));
#75192=CARTESIAN_POINT('Ctrl Pts',(-9.5007537246001,-46.3957437019326,20.));
#75193=CARTESIAN_POINT('Ctrl Pts',(-9.53257830897852,-46.3861571856095,
0.));
#75194=CARTESIAN_POINT('Ctrl Pts',(-9.53257830897852,-46.3861571856095,
20.));
#75195=CARTESIAN_POINT('Ctrl Pts',(-9.56439511577024,-46.3765487491938,
0.));
#75196=CARTESIAN_POINT('Ctrl Pts',(-9.56439511577024,-46.3765487491938,
20.));
#75197=CARTESIAN_POINT('Ctrl Pts',(-9.59620412968214,-46.3669183982155,
0.));
#75198=CARTESIAN_POINT('Ctrl Pts',(-9.59620412968214,-46.3669183982155,
20.));
#75199=CARTESIAN_POINT('Ctrl Pts',(-9.62800533542437,-46.3572661382147,
0.));
#75200=CARTESIAN_POINT('Ctrl Pts',(-9.62800533542437,-46.3572661382147,
20.));
#75201=CARTESIAN_POINT('Ctrl Pts',(-9.6597987177104,-46.347591974742,0.));
#75202=CARTESIAN_POINT('Ctrl Pts',(-9.6597987177104,-46.347591974742,20.));
#75203=CARTESIAN_POINT('Ctrl Pts',(-9.69158426125693,-46.3378959133587,
0.));
#75204=CARTESIAN_POINT('Ctrl Pts',(-9.69158426125693,-46.3378959133587,
20.));
#75205=CARTESIAN_POINT('Ctrl Pts',(-9.72336195078415,-46.3281779596367,
0.));
#75206=CARTESIAN_POINT('Ctrl Pts',(-9.72336195078415,-46.3281779596367,
20.));
#75207=CARTESIAN_POINT('Ctrl Pts',(-9.75513177101578,-46.3184381191592,
0.));
#75208=CARTESIAN_POINT('Ctrl Pts',(-9.75513177101578,-46.3184381191592,
20.));
#75209=CARTESIAN_POINT('Ctrl Pts',(-9.78689370667941,-46.3086763975205,
0.));
#75210=CARTESIAN_POINT('Ctrl Pts',(-9.78689370667941,-46.3086763975205,
20.));
#75211=CARTESIAN_POINT('Ctrl Pts',(-9.8186477425062,-46.2988928003257,0.));
#75212=CARTESIAN_POINT('Ctrl Pts',(-9.8186477425062,-46.2988928003257,20.));
#75213=CARTESIAN_POINT('Ctrl Pts',(-9.85039386323086,-46.289087333191,0.));
#75214=CARTESIAN_POINT('Ctrl Pts',(-9.85039386323086,-46.289087333191,20.));
#75215=CARTESIAN_POINT('Ctrl Pts',(-9.88213205359192,-46.2792600017436,
0.));
#75216=CARTESIAN_POINT('Ctrl Pts',(-9.88213205359192,-46.2792600017436,
20.));
#75217=CARTESIAN_POINT('Ctrl Pts',(-9.91386229833138,-46.2694108116213,
0.));
#75218=CARTESIAN_POINT('Ctrl Pts',(-9.91386229833138,-46.2694108116213,
20.));
#75219=CARTESIAN_POINT('Ctrl Pts',(-9.94558458219447,-46.2595397684724,
0.));
#75220=CARTESIAN_POINT('Ctrl Pts',(-9.94558458219447,-46.2595397684724,
20.));
#75221=CARTESIAN_POINT('Ctrl Pts',(-9.97729888992981,-46.2496468779557,
0.));
#75222=CARTESIAN_POINT('Ctrl Pts',(-9.97729888992981,-46.2496468779557,
20.));
#75223=CARTESIAN_POINT('Ctrl Pts',(-10.0090052062895,-46.2397321457408,
0.));
#75224=CARTESIAN_POINT('Ctrl Pts',(-10.0090052062895,-46.2397321457408,
20.));
#75225=CARTESIAN_POINT('Ctrl Pts',(-10.0407035160293,-46.2297955775084,
0.));
#75226=CARTESIAN_POINT('Ctrl Pts',(-10.0407035160293,-46.2297955775084,
20.));
#75227=CARTESIAN_POINT('Ctrl Pts',(-10.0723938039086,-46.2198371789501,
0.));
#75228=CARTESIAN_POINT('Ctrl Pts',(-10.0723938039086,-46.2198371789501,
20.));
#75229=CARTESIAN_POINT('Ctrl Pts',(-10.1040760546909,-46.2098569557688,
0.));
#75230=CARTESIAN_POINT('Ctrl Pts',(-10.1040760546909,-46.2098569557688,
20.));
#75231=CARTESIAN_POINT('Ctrl Pts',(-10.1357502531431,-46.1998549136779,
0.));
#75232=CARTESIAN_POINT('Ctrl Pts',(-10.1357502531431,-46.1998549136779,
20.));
#75233=CARTESIAN_POINT('Ctrl Pts',(-10.1674163840354,-46.1898310584014,
0.));
#75234=CARTESIAN_POINT('Ctrl Pts',(-10.1674163840354,-46.1898310584014,
20.));
#75235=CARTESIAN_POINT('Ctrl Pts',(-10.199074432142,-46.179785395674,0.));
#75236=CARTESIAN_POINT('Ctrl Pts',(-10.199074432142,-46.179785395674,20.));
#75237=CARTESIAN_POINT('Ctrl Pts',(-10.2307243822402,-46.169717931241,0.));
#75238=CARTESIAN_POINT('Ctrl Pts',(-10.2307243822402,-46.169717931241,20.));
#75239=CARTESIAN_POINT('Ctrl Pts',(-10.2623662191114,-46.1596286708586,
0.));
#75240=CARTESIAN_POINT('Ctrl Pts',(-10.2623662191114,-46.1596286708586,
20.));
#75241=CARTESIAN_POINT('Ctrl Pts',(-10.2939999275403,-46.1495176202946,
0.));
#75242=CARTESIAN_POINT('Ctrl Pts',(-10.2939999275403,-46.1495176202946,
20.));
#75243=CARTESIAN_POINT('Ctrl Pts',(-10.3256254923156,-46.139384785327,0.));
#75244=CARTESIAN_POINT('Ctrl Pts',(-10.3256254923156,-46.139384785327,20.));
#75245=CARTESIAN_POINT('Ctrl Pts',(-10.3572428982293,-46.1292301717445,
0.));
#75246=CARTESIAN_POINT('Ctrl Pts',(-10.3572428982293,-46.1292301717445,
20.));
#75247=CARTESIAN_POINT('Ctrl Pts',(-10.3888521300774,-46.119053785347,0.));
#75248=CARTESIAN_POINT('Ctrl Pts',(-10.3888521300774,-46.119053785347,20.));
#75249=CARTESIAN_POINT('Ctrl Pts',(-10.4204531726593,-46.1088556319449,
0.));
#75250=CARTESIAN_POINT('Ctrl Pts',(-10.4204531726593,-46.1088556319449,
20.));
#75251=CARTESIAN_POINT('Ctrl Pts',(-10.4520460107784,-46.0986357173598,
0.));
#75252=CARTESIAN_POINT('Ctrl Pts',(-10.4520460107784,-46.0986357173598,
20.));
#75253=CARTESIAN_POINT('Ctrl Pts',(-10.4836306292415,-46.0883940474237,
0.));
#75254=CARTESIAN_POINT('Ctrl Pts',(-10.4836306292415,-46.0883940474237,
20.));
#75255=CARTESIAN_POINT('Ctrl Pts',(-10.5152070128593,-46.0781306279792,
0.));
#75256=CARTESIAN_POINT('Ctrl Pts',(-10.5152070128593,-46.0781306279792,
20.));
#75257=CARTESIAN_POINT('Ctrl Pts',(-10.5467751464457,-46.0678454648793,
0.));
#75258=CARTESIAN_POINT('Ctrl Pts',(-10.5467751464457,-46.0678454648793,
20.));
#75259=CARTESIAN_POINT('Ctrl Pts',(-10.5783350148188,-46.0575385639878,
0.));
#75260=CARTESIAN_POINT('Ctrl Pts',(-10.5783350148188,-46.0575385639878,
20.));
#75261=CARTESIAN_POINT('Ctrl Pts',(-10.6098866028001,-46.0472099311799,
0.));
#75262=CARTESIAN_POINT('Ctrl Pts',(-10.6098866028001,-46.0472099311799,
20.));
#75263=CARTESIAN_POINT('Ctrl Pts',(-10.6414298952151,-46.0368595723418,
0.));
#75264=CARTESIAN_POINT('Ctrl Pts',(-10.6414298952151,-46.0368595723418,
20.));
#75265=CARTESIAN_POINT('Ctrl Pts',(-10.6729648768932,-46.0264874933706,
0.));
#75266=CARTESIAN_POINT('Ctrl Pts',(-10.6729648768932,-46.0264874933706,
20.));
#75267=CARTESIAN_POINT('Ctrl Pts',(-10.7044915326674,-46.0160937001747,
0.));
#75268=CARTESIAN_POINT('Ctrl Pts',(-10.7044915326674,-46.0160937001747,
20.));
#75269=CARTESIAN_POINT('Ctrl Pts',(-10.7360098473747,-46.0056781986726,
0.));
#75270=CARTESIAN_POINT('Ctrl Pts',(-10.7360098473747,-46.0056781986726,
20.));
#75271=CARTESIAN_POINT('Ctrl Pts',(-10.7675198058554,-45.9952409947932,
0.));
#75272=CARTESIAN_POINT('Ctrl Pts',(-10.7675198058554,-45.9952409947932,
20.));
#75273=CARTESIAN_POINT('Ctrl Pts',(-10.7990213929536,-45.9847820944759,
0.));
#75274=CARTESIAN_POINT('Ctrl Pts',(-10.7990213929536,-45.9847820944759,
20.));
#75275=CARTESIAN_POINT('Ctrl Pts',(-10.8305145935168,-45.9743015036702,
0.));
#75276=CARTESIAN_POINT('Ctrl Pts',(-10.8305145935168,-45.9743015036702,
20.));
#75277=CARTESIAN_POINT('Ctrl Pts',(-10.8619993923967,-45.9637992283368,
0.));
#75278=CARTESIAN_POINT('Ctrl Pts',(-10.8619993923967,-45.9637992283368,
20.));
#75279=CARTESIAN_POINT('Ctrl Pts',(-10.8934757744485,-45.9532752744476,
0.));
#75280=CARTESIAN_POINT('Ctrl Pts',(-10.8934757744485,-45.9532752744476,
20.));
#75281=CARTESIAN_POINT('Ctrl Pts',(-10.9249437245321,-45.9427296479861,
0.));
#75282=CARTESIAN_POINT('Ctrl Pts',(-10.9249437245321,-45.9427296479861,
20.));
#75283=CARTESIAN_POINT('Ctrl Pts',(-10.9564032275107,-45.9321623549466,
0.));
#75284=CARTESIAN_POINT('Ctrl Pts',(-10.9564032275107,-45.9321623549466,
20.));
#75285=CARTESIAN_POINT('Ctrl Pts',(-10.9878542682513,-45.9215734013338,
0.));
#75286=CARTESIAN_POINT('Ctrl Pts',(-10.9878542682513,-45.9215734013338,
20.));
#75287=CARTESIAN_POINT('Ctrl Pts',(-11.0192968316247,-45.9109627931629,
0.));
#75288=CARTESIAN_POINT('Ctrl Pts',(-11.0192968316247,-45.9109627931629,
20.));
#75289=CARTESIAN_POINT('Ctrl Pts',(-11.0507309025053,-45.9003305364593,
0.));
#75290=CARTESIAN_POINT('Ctrl Pts',(-11.0507309025053,-45.9003305364593,
20.));
#75291=CARTESIAN_POINT('Ctrl Pts',(-11.0821564657716,-45.8896766372596,
0.));
#75292=CARTESIAN_POINT('Ctrl Pts',(-11.0821564657716,-45.8896766372596,
20.));
#75293=CARTESIAN_POINT('Ctrl Pts',(-11.1135735063059,-45.8790011016108,
0.));
#75294=CARTESIAN_POINT('Ctrl Pts',(-11.1135735063059,-45.8790011016108,
20.));
#75295=CARTESIAN_POINT('Ctrl Pts',(-11.1449820089942,-45.868303935571,0.));
#75296=CARTESIAN_POINT('Ctrl Pts',(-11.1449820089942,-45.868303935571,20.));
#75297=CARTESIAN_POINT('Ctrl Pts',(-11.1763819587263,-45.8575851452088,
0.));
#75298=CARTESIAN_POINT('Ctrl Pts',(-11.1763819587263,-45.8575851452088,
20.));
#75299=CARTESIAN_POINT('Ctrl Pts',(-11.207773340396,-45.8468447366038,0.));
#75300=CARTESIAN_POINT('Ctrl Pts',(-11.207773340396,-45.8468447366038,20.));
#75301=CARTESIAN_POINT('Ctrl Pts',(-11.2391561389011,-45.8360827158468,
0.));
#75302=CARTESIAN_POINT('Ctrl Pts',(-11.2391561389011,-45.8360827158468,
20.));
#75303=CARTESIAN_POINT('Ctrl Pts',(-11.2705303391434,-45.8252990890386,
0.));
#75304=CARTESIAN_POINT('Ctrl Pts',(-11.2705303391434,-45.8252990890386,
20.));
#75305=CARTESIAN_POINT('Ctrl Pts',(-11.3018959260283,-45.8144938622913,
0.));
#75306=CARTESIAN_POINT('Ctrl Pts',(-11.3018959260283,-45.8144938622913,
20.));
#75307=CARTESIAN_POINT('Ctrl Pts',(-11.3332528844652,-45.8036670417272,
0.));
#75308=CARTESIAN_POINT('Ctrl Pts',(-11.3332528844652,-45.8036670417272,
20.));
#75309=CARTESIAN_POINT('Ctrl Pts',(-11.3646011993674,-45.7928186334791,
0.));
#75310=CARTESIAN_POINT('Ctrl Pts',(-11.3646011993674,-45.7928186334791,
20.));
#75311=CARTESIAN_POINT('Ctrl Pts',(-11.395940855652,-45.7819486436912,0.));
#75312=CARTESIAN_POINT('Ctrl Pts',(-11.395940855652,-45.7819486436912,20.));
#75313=CARTESIAN_POINT('Ctrl Pts',(-11.4272718382404,-45.7710570785186,
0.));
#75314=CARTESIAN_POINT('Ctrl Pts',(-11.4272718382404,-45.7710570785186,
20.));
#75315=CARTESIAN_POINT('Ctrl Pts',(-11.4585941320575,-45.760143944127,0.));
#75316=CARTESIAN_POINT('Ctrl Pts',(-11.4585941320575,-45.760143944127,20.));
#75317=CARTESIAN_POINT('Ctrl Pts',(-11.489907722032,-45.7492092466918,0.));
#75318=CARTESIAN_POINT('Ctrl Pts',(-11.489907722032,-45.7492092466918,20.));
#75319=CARTESIAN_POINT('Ctrl Pts',(-11.5212125930967,-45.7382529923996,
0.));
#75320=CARTESIAN_POINT('Ctrl Pts',(-11.5212125930967,-45.7382529923996,
20.));
#75321=CARTESIAN_POINT('Ctrl Pts',(-11.5525087301884,-45.7272751874478,
0.));
#75322=CARTESIAN_POINT('Ctrl Pts',(-11.5525087301884,-45.7272751874478,
20.));
#75323=CARTESIAN_POINT('Ctrl Pts',(-11.5837961182482,-45.7162758380449,
0.));
#75324=CARTESIAN_POINT('Ctrl Pts',(-11.5837961182482,-45.7162758380449,
20.));
#75325=CARTESIAN_POINT('Ctrl Pts',(-11.615074742221,-45.7052549504103,0.));
#75326=CARTESIAN_POINT('Ctrl Pts',(-11.615074742221,-45.7052549504103,20.));
#75327=CARTESIAN_POINT('Ctrl Pts',(-11.6463445870557,-45.694212530774,0.));
#75328=CARTESIAN_POINT('Ctrl Pts',(-11.6463445870557,-45.694212530774,20.));
#75329=CARTESIAN_POINT('Ctrl Pts',(-11.6776056377055,-45.6831485853771,
0.));
#75330=CARTESIAN_POINT('Ctrl Pts',(-11.6776056377055,-45.6831485853771,
20.));
#75331=CARTESIAN_POINT('Ctrl Pts',(-11.7088578791267,-45.6720631204703,
0.));
#75332=CARTESIAN_POINT('Ctrl Pts',(-11.7088578791267,-45.6720631204703,
20.));
#75333=CARTESIAN_POINT('Ctrl Pts',(-11.7401012962797,-45.6609561423149,
0.));
#75334=CARTESIAN_POINT('Ctrl Pts',(-11.7401012962797,-45.6609561423149,
20.));
#75335=CARTESIAN_POINT('Ctrl Pts',(-11.7713358741293,-45.6498276571829,
0.));
#75336=CARTESIAN_POINT('Ctrl Pts',(-11.7713358741293,-45.6498276571829,
20.));
#75337=CARTESIAN_POINT('Ctrl Pts',(-11.8025615976441,-45.6386776713575,
0.));
#75338=CARTESIAN_POINT('Ctrl Pts',(-11.8025615976441,-45.6386776713575,
20.));
#75339=CARTESIAN_POINT('Ctrl Pts',(-11.8337784517972,-45.627506191133,0.));
#75340=CARTESIAN_POINT('Ctrl Pts',(-11.8337784517972,-45.627506191133,20.));
#75341=CARTESIAN_POINT('Ctrl Pts',(-11.8649864215653,-45.6163132228138,
0.));
#75342=CARTESIAN_POINT('Ctrl Pts',(-11.8649864215653,-45.6163132228138,
20.));
#75343=CARTESIAN_POINT('Ctrl Pts',(-11.8961854919294,-45.6050987727153,
0.));
#75344=CARTESIAN_POINT('Ctrl Pts',(-11.8961854919294,-45.6050987727153,
20.));
#75345=CARTESIAN_POINT('Ctrl Pts',(-11.9273756478741,-45.5938628471638,
0.));
#75346=CARTESIAN_POINT('Ctrl Pts',(-11.9273756478741,-45.5938628471638,
20.));
#75347=CARTESIAN_POINT('Ctrl Pts',(-11.9585568743886,-45.5826054524963,
0.));
#75348=CARTESIAN_POINT('Ctrl Pts',(-11.9585568743886,-45.5826054524963,
20.));
#75349=CARTESIAN_POINT('Ctrl Pts',(-11.989729156466,-45.5713265950605,0.));
#75350=CARTESIAN_POINT('Ctrl Pts',(-11.989729156466,-45.5713265950605,20.));
#75351=CARTESIAN_POINT('Ctrl Pts',(-12.0208924791035,-45.5600262812144,
0.));
#75352=CARTESIAN_POINT('Ctrl Pts',(-12.0208924791035,-45.5600262812144,
20.));
#75353=CARTESIAN_POINT('Ctrl Pts',(-12.0520468273019,-45.5487045173265,
0.));
#75354=CARTESIAN_POINT('Ctrl Pts',(-12.0520468273019,-45.5487045173265,
20.));
#75355=CARTESIAN_POINT('Ctrl Pts',(-12.0831921860666,-45.5373613097755,
0.));
#75356=CARTESIAN_POINT('Ctrl Pts',(-12.0831921860666,-45.5373613097755,
20.));
#75357=CARTESIAN_POINT('Ctrl Pts',(-12.1143285404065,-45.5259966649516,
0.));
#75358=CARTESIAN_POINT('Ctrl Pts',(-12.1143285404065,-45.5259966649516,
20.));
#75359=CARTESIAN_POINT('Ctrl Pts',(-12.1454558753351,-45.5146105892553,
0.));
#75360=CARTESIAN_POINT('Ctrl Pts',(-12.1454558753351,-45.5146105892553,
20.));
#75361=CARTESIAN_POINT('Ctrl Pts',(-12.1765741758697,-45.5032030890978,
0.));
#75362=CARTESIAN_POINT('Ctrl Pts',(-12.1765741758697,-45.5032030890978,
20.));
#75363=CARTESIAN_POINT('Ctrl Pts',(-12.2076834270323,-45.4917741709015,
0.));
#75364=CARTESIAN_POINT('Ctrl Pts',(-12.2076834270323,-45.4917741709015,
20.));
#75365=CARTESIAN_POINT('Ctrl Pts',(-12.2387836138487,-45.4803238410999,
0.));
#75366=CARTESIAN_POINT('Ctrl Pts',(-12.2387836138487,-45.4803238410999,
20.));
#75367=CARTESIAN_POINT('Ctrl Pts',(-12.269874721349,-45.4688521061371,0.));
#75368=CARTESIAN_POINT('Ctrl Pts',(-12.269874721349,-45.4688521061371,20.));
#75369=CARTESIAN_POINT('Ctrl Pts',(-12.3009567345673,-45.4573589724673,
0.));
#75370=CARTESIAN_POINT('Ctrl Pts',(-12.3009567345673,-45.4573589724673,
20.));
#75371=CARTESIAN_POINT('Ctrl Pts',(-12.3320296385418,-45.4458444465552,
0.));
#75372=CARTESIAN_POINT('Ctrl Pts',(-12.3320296385418,-45.4458444465552,
20.));
#75373=CARTESIAN_POINT('Ctrl Pts',(-12.3630934183143,-45.4343085348755,
0.));
#75374=CARTESIAN_POINT('Ctrl Pts',(-12.3630934183143,-45.4343085348755,
20.));
#75375=CARTESIAN_POINT('Ctrl Pts',(-12.3941480589311,-45.4227512439136,
0.));
#75376=CARTESIAN_POINT('Ctrl Pts',(-12.3941480589311,-45.4227512439136,
20.));
#75377=CARTESIAN_POINT('Ctrl Pts',(-12.4251935454428,-45.4111725801659,
0.));
#75378=CARTESIAN_POINT('Ctrl Pts',(-12.4251935454428,-45.4111725801659,
20.));
#75379=CARTESIAN_POINT('Ctrl Pts',(-12.4562298629045,-45.3995725501402,
0.));
#75380=CARTESIAN_POINT('Ctrl Pts',(-12.4562298629045,-45.3995725501402,
20.));
#75381=CARTESIAN_POINT('Ctrl Pts',(-12.4872569963754,-45.3879511603549,
0.));
#75382=CARTESIAN_POINT('Ctrl Pts',(-12.4872569963754,-45.3879511603549,
20.));
#75383=CARTESIAN_POINT('Ctrl Pts',(-12.5182749309189,-45.376308417339,0.));
#75384=CARTESIAN_POINT('Ctrl Pts',(-12.5182749309189,-45.376308417339,20.));
#75385=CARTESIAN_POINT('Ctrl Pts',(-12.5492836516023,-45.364644327632,0.));
#75386=CARTESIAN_POINT('Ctrl Pts',(-12.5492836516023,-45.364644327632,20.));
#75387=CARTESIAN_POINT('Ctrl Pts',(-12.5802831434966,-45.3529588977839,
0.));
#75388=CARTESIAN_POINT('Ctrl Pts',(-12.5802831434966,-45.3529588977839,
20.));
#75389=CARTESIAN_POINT('Ctrl Pts',(-12.6112733916776,-45.3412521343551,
0.));
#75390=CARTESIAN_POINT('Ctrl Pts',(-12.6112733916776,-45.3412521343551,
20.));
#75391=CARTESIAN_POINT('Ctrl Pts',(-12.6422543812252,-45.3295240439169,
0.));
#75392=CARTESIAN_POINT('Ctrl Pts',(-12.6422543812252,-45.3295240439169,
20.));
#75393=CARTESIAN_POINT('Ctrl Pts',(-12.6732260972239,-45.3177746330512,
0.));
#75394=CARTESIAN_POINT('Ctrl Pts',(-12.6732260972239,-45.3177746330512,
20.));
#75395=CARTESIAN_POINT('Ctrl Pts',(-12.7041885247626,-45.3060039083501,
0.));
#75396=CARTESIAN_POINT('Ctrl Pts',(-12.7041885247626,-45.3060039083501,
20.));
#75397=CARTESIAN_POINT('Ctrl Pts',(-12.7351416489341,-45.2942118764167,
0.));
#75398=CARTESIAN_POINT('Ctrl Pts',(-12.7351416489341,-45.2942118764167,
20.));
#75399=CARTESIAN_POINT('Ctrl Pts',(-12.7660854548354,-45.2823985438647,
0.));
#75400=CARTESIAN_POINT('Ctrl Pts',(-12.7660854548354,-45.2823985438647,
20.));
#75401=CARTESIAN_POINT('Ctrl Pts',(-12.7970199275678,-45.2705639173192,
0.));
#75402=CARTESIAN_POINT('Ctrl Pts',(-12.7970199275678,-45.2705639173192,
20.));
#75403=CARTESIAN_POINT('Ctrl Pts',(-12.8279450522366,-45.2587080034157,
0.));
#75404=CARTESIAN_POINT('Ctrl Pts',(-12.8279450522366,-45.2587080034157,
20.));
#75405=CARTESIAN_POINT('Ctrl Pts',(-12.8588608139512,-45.2468308087994,
0.));
#75406=CARTESIAN_POINT('Ctrl Pts',(-12.8588608139512,-45.2468308087994,
20.));
#75407=CARTESIAN_POINT('Ctrl Pts',(-12.8897671978257,-45.2349323401259,
0.));
#75408=CARTESIAN_POINT('Ctrl Pts',(-12.8897671978257,-45.2349323401259,
20.));
#75409=CARTESIAN_POINT('Ctrl Pts',(-12.9206641889781,-45.2230126040617,
0.));
#75410=CARTESIAN_POINT('Ctrl Pts',(-12.9206641889781,-45.2230126040617,
20.));
#75411=CARTESIAN_POINT('Ctrl Pts',(-12.9515517725313,-45.2110716072841,
0.));
#75412=CARTESIAN_POINT('Ctrl Pts',(-12.9515517725313,-45.2110716072841,
20.));
#75413=CARTESIAN_POINT('Ctrl Pts',(-12.9824299336127,-45.199109356482,0.));
#75414=CARTESIAN_POINT('Ctrl Pts',(-12.9824299336127,-45.199109356482,20.));
#75415=CARTESIAN_POINT('Ctrl Pts',(-13.0132986573536,-45.1871258583545,
0.));
#75416=CARTESIAN_POINT('Ctrl Pts',(-13.0132986573536,-45.1871258583545,
20.));
#75417=CARTESIAN_POINT('Ctrl Pts',(-13.0441579288899,-45.1751211196118,
0.));
#75418=CARTESIAN_POINT('Ctrl Pts',(-13.0441579288899,-45.1751211196118,
20.));
#75419=CARTESIAN_POINT('Ctrl Pts',(-13.0750077333614,-45.1630951469733,
0.));
#75420=CARTESIAN_POINT('Ctrl Pts',(-13.0750077333614,-45.1630951469733,
20.));
#75421=CARTESIAN_POINT('Ctrl Pts',(-13.1058480559121,-45.1510479471692,
0.));
#75422=CARTESIAN_POINT('Ctrl Pts',(-13.1058480559121,-45.1510479471692,
20.));
#75423=CARTESIAN_POINT('Ctrl Pts',(-13.1366788816904,-45.1389795269399,
0.));
#75424=CARTESIAN_POINT('Ctrl Pts',(-13.1366788816904,-45.1389795269399,
20.));
#75425=CARTESIAN_POINT('Ctrl Pts',(-13.1675001958493,-45.1268898930368,
0.));
#75426=CARTESIAN_POINT('Ctrl Pts',(-13.1675001958493,-45.1268898930368,
20.));
#75427=CARTESIAN_POINT('Ctrl Pts',(-13.198311983546,-45.114779052223,0.));
#75428=CARTESIAN_POINT('Ctrl Pts',(-13.198311983546,-45.114779052223,20.));
#75429=CARTESIAN_POINT('Ctrl Pts',(-13.2291142299426,-45.1026470112717,
0.));
#75430=CARTESIAN_POINT('Ctrl Pts',(-13.2291142299426,-45.1026470112717,
20.));
#75431=CARTESIAN_POINT('Ctrl Pts',(-13.259906920205,-45.0904937769663,0.));
#75432=CARTESIAN_POINT('Ctrl Pts',(-13.259906920205,-45.0904937769663,20.));
#75433=CARTESIAN_POINT('Ctrl Pts',(-13.2906900395037,-45.0783193561008,
0.));
#75434=CARTESIAN_POINT('Ctrl Pts',(-13.2906900395037,-45.0783193561008,
20.));
#75435=CARTESIAN_POINT('Ctrl Pts',(-13.3214635730135,-45.0661237554798,
0.));
#75436=CARTESIAN_POINT('Ctrl Pts',(-13.3214635730135,-45.0661237554798,
20.));
#75437=CARTESIAN_POINT('Ctrl Pts',(-13.3522275059137,-45.0539069819185,
0.));
#75438=CARTESIAN_POINT('Ctrl Pts',(-13.3522275059137,-45.0539069819185,
20.));
#75439=CARTESIAN_POINT('Ctrl Pts',(-13.3829818233878,-45.0416690422424,
0.));
#75440=CARTESIAN_POINT('Ctrl Pts',(-13.3829818233878,-45.0416690422424,
20.));
#75441=CARTESIAN_POINT('Ctrl Pts',(-13.4137265106238,-45.0294099432879,
0.));
#75442=CARTESIAN_POINT('Ctrl Pts',(-13.4137265106238,-45.0294099432879,
20.));
#75443=CARTESIAN_POINT('Ctrl Pts',(-13.4444615528144,-45.0171296919022,
0.));
#75444=CARTESIAN_POINT('Ctrl Pts',(-13.4444615528144,-45.0171296919022,
20.));
#75445=CARTESIAN_POINT('Ctrl Pts',(-13.4751869351564,-45.0048282949433,
0.));
#75446=CARTESIAN_POINT('Ctrl Pts',(-13.4751869351564,-45.0048282949433,
20.));
#75447=CARTESIAN_POINT('Ctrl Pts',(-13.5059026428512,-44.9925057592796,
0.));
#75448=CARTESIAN_POINT('Ctrl Pts',(-13.5059026428512,-44.9925057592796,
20.));
#75449=CARTESIAN_POINT('Ctrl Pts',(-13.5366086611044,-44.9801620917891,
0.));
#75450=CARTESIAN_POINT('Ctrl Pts',(-13.5366086611044,-44.9801620917891,
20.));
#75451=CARTESIAN_POINT('Ctrl Pts',(-13.5673049751264,-44.967797299361,0.));
#75452=CARTESIAN_POINT('Ctrl Pts',(-13.5673049751264,-44.967797299361,20.));
#75453=CARTESIAN_POINT('Ctrl Pts',(-13.5979915701319,-44.955411388895,0.));
#75454=CARTESIAN_POINT('Ctrl Pts',(-13.5979915701319,-44.955411388895,20.));
#75455=CARTESIAN_POINT('Ctrl Pts',(-13.6286684313402,-44.9430043673018,
0.));
#75456=CARTESIAN_POINT('Ctrl Pts',(-13.6286684313402,-44.9430043673018,
20.));
#75457=CARTESIAN_POINT('Ctrl Pts',(-13.6593355439745,-44.9305762415019,
0.));
#75458=CARTESIAN_POINT('Ctrl Pts',(-13.6593355439745,-44.9305762415019,
20.));
#75459=CARTESIAN_POINT('Ctrl Pts',(-13.6899928932632,-44.9181270184275,
0.));
#75460=CARTESIAN_POINT('Ctrl Pts',(-13.6899928932632,-44.9181270184275,
20.));
#75461=CARTESIAN_POINT('Ctrl Pts',(-13.7206404644388,-44.9056567050204,
0.));
#75462=CARTESIAN_POINT('Ctrl Pts',(-13.7206404644388,-44.9056567050204,
20.));
#75463=CARTESIAN_POINT('Ctrl Pts',(-13.7512782427386,-44.8931653082334,
0.));
#75464=CARTESIAN_POINT('Ctrl Pts',(-13.7512782427386,-44.8931653082334,
20.));
#75465=CARTESIAN_POINT('Ctrl Pts',(-13.7819062134042,-44.8806528350291,
0.));
#75466=CARTESIAN_POINT('Ctrl Pts',(-13.7819062134042,-44.8806528350291,
20.));
#75467=CARTESIAN_POINT('Ctrl Pts',(-13.8125243616816,-44.8681192923811,
0.));
#75468=CARTESIAN_POINT('Ctrl Pts',(-13.8125243616816,-44.8681192923811,
20.));
#75469=CARTESIAN_POINT('Ctrl Pts',(-13.8431326728214,-44.8555646872732,
0.));
#75470=CARTESIAN_POINT('Ctrl Pts',(-13.8431326728214,-44.8555646872732,
20.));
#75471=CARTESIAN_POINT('Ctrl Pts',(-13.8737311320789,-44.8429890267007,
0.));
#75472=CARTESIAN_POINT('Ctrl Pts',(-13.8737311320789,-44.8429890267007,
20.));
#75473=CARTESIAN_POINT('Ctrl Pts',(-13.9043197247138,-44.8303923176691,
0.));
#75474=CARTESIAN_POINT('Ctrl Pts',(-13.9043197247138,-44.8303923176691,
20.));
#75475=CARTESIAN_POINT('Ctrl Pts',(-13.9348984359903,-44.8177745671945,
0.));
#75476=CARTESIAN_POINT('Ctrl Pts',(-13.9348984359903,-44.8177745671945,
20.));
#75477=CARTESIAN_POINT('Ctrl Pts',(-13.9654672511774,-44.8051357823031,
0.));
#75478=CARTESIAN_POINT('Ctrl Pts',(-13.9654672511774,-44.8051357823031,
20.));
#75479=CARTESIAN_POINT('Ctrl Pts',(-13.9960261555481,-44.7924759700314,
0.));
#75480=CARTESIAN_POINT('Ctrl Pts',(-13.9960261555481,-44.7924759700314,
20.));
#75481=CARTESIAN_POINT('Ctrl Pts',(-14.0265751343805,-44.7797951374262,
0.));
#75482=CARTESIAN_POINT('Ctrl Pts',(-14.0265751343805,-44.7797951374262,
20.));
#75483=CARTESIAN_POINT('Ctrl Pts',(-14.057114172957,-44.7670932915455,0.));
#75484=CARTESIAN_POINT('Ctrl Pts',(-14.057114172957,-44.7670932915455,20.));
#75485=CARTESIAN_POINT('Ctrl Pts',(-14.0876432565649,-44.7543704394583,
0.));
#75486=CARTESIAN_POINT('Ctrl Pts',(-14.0876432565649,-44.7543704394583,
20.));
#75487=CARTESIAN_POINT('Ctrl Pts',(-14.118162370496,-44.7416265882442,0.));
#75488=CARTESIAN_POINT('Ctrl Pts',(-14.118162370496,-44.7416265882442,20.));
#75489=CARTESIAN_POINT('Ctrl Pts',(-14.1486715000464,-44.728861744993,0.));
#75490=CARTESIAN_POINT('Ctrl Pts',(-14.1486715000464,-44.728861744993,20.));
#75491=CARTESIAN_POINT('Ctrl Pts',(-14.1791706305171,-44.7160759168044,
0.));
#75492=CARTESIAN_POINT('Ctrl Pts',(-14.1791706305171,-44.7160759168044,
20.));
#75493=CARTESIAN_POINT('Ctrl Pts',(-14.2096597472134,-44.7032691107881,
0.));
#75494=CARTESIAN_POINT('Ctrl Pts',(-14.2096597472134,-44.7032691107881,
20.));
#75495=CARTESIAN_POINT('Ctrl Pts',(-14.2401388354454,-44.690441334065,0.));
#75496=CARTESIAN_POINT('Ctrl Pts',(-14.2401388354454,-44.690441334065,20.));
#75497=CARTESIAN_POINT('Ctrl Pts',(-14.2706078805279,-44.6775925937661,
0.));
#75498=CARTESIAN_POINT('Ctrl Pts',(-14.2706078805279,-44.6775925937661,
20.));
#75499=CARTESIAN_POINT('Ctrl Pts',(-14.3010668677802,-44.6647228970333,
0.));
#75500=CARTESIAN_POINT('Ctrl Pts',(-14.3010668677802,-44.6647228970333,
20.));
#75501=CARTESIAN_POINT('Ctrl Pts',(-14.3315157825264,-44.6518322510194,
0.));
#75502=CARTESIAN_POINT('Ctrl Pts',(-14.3315157825264,-44.6518322510194,
20.));
#75503=CARTESIAN_POINT('Ctrl Pts',(-14.3619546100951,-44.6389206628876,
0.));
#75504=CARTESIAN_POINT('Ctrl Pts',(-14.3619546100951,-44.6389206628876,
20.));
#75505=CARTESIAN_POINT('Ctrl Pts',(-14.3923833358197,-44.6259881398118,
0.));
#75506=CARTESIAN_POINT('Ctrl Pts',(-14.3923833358197,-44.6259881398118,
20.));
#75507=CARTESIAN_POINT('Ctrl Pts',(-14.4228019450383,-44.6130346889769,
0.));
#75508=CARTESIAN_POINT('Ctrl Pts',(-14.4228019450383,-44.6130346889769,
20.));
#75509=CARTESIAN_POINT('Ctrl Pts',(-14.4532104230937,-44.6000603175775,
0.));
#75510=CARTESIAN_POINT('Ctrl Pts',(-14.4532104230937,-44.6000603175775,
20.));
#75511=CARTESIAN_POINT('Ctrl Pts',(-14.4836087553332,-44.5870650328188,
0.));
#75512=CARTESIAN_POINT('Ctrl Pts',(-14.4836087553332,-44.5870650328188,
20.));
#75513=CARTESIAN_POINT('Ctrl Pts',(-14.5139969271087,-44.5740488419152,
0.));
#75514=CARTESIAN_POINT('Ctrl Pts',(-14.5139969271087,-44.5740488419152,
20.));
#75515=CARTESIAN_POINT('Ctrl Pts',(-14.5443749237768,-44.5610117520915,
0.));
#75516=CARTESIAN_POINT('Ctrl Pts',(-14.5443749237768,-44.5610117520915,
20.));
#75517=CARTESIAN_POINT('Ctrl Pts',(-14.5747427306988,-44.5479537705835,
0.));
#75518=CARTESIAN_POINT('Ctrl Pts',(-14.5747427306988,-44.5479537705835,
20.));
#75519=CARTESIAN_POINT('Ctrl Pts',(-14.6051003332411,-44.5348749046378,
0.));
#75520=CARTESIAN_POINT('Ctrl Pts',(-14.6051003332411,-44.5348749046378,
20.));
#75521=CARTESIAN_POINT('Ctrl Pts',(-14.6354477167742,-44.521775161512,0.));
#75522=CARTESIAN_POINT('Ctrl Pts',(-14.6354477167742,-44.521775161512,20.));
#75523=CARTESIAN_POINT('Ctrl Pts',(-14.6657848666744,-44.5086545484757,
0.));
#75524=CARTESIAN_POINT('Ctrl Pts',(-14.6657848666744,-44.5086545484757,
20.));
#75525=CARTESIAN_POINT('Ctrl Pts',(-14.6961117683217,-44.4955130728078,
0.));
#75526=CARTESIAN_POINT('Ctrl Pts',(-14.6961117683217,-44.4955130728078,
20.));
#75527=CARTESIAN_POINT('Ctrl Pts',(-14.7264284071013,-44.4823507417973,
0.));
#75528=CARTESIAN_POINT('Ctrl Pts',(-14.7264284071013,-44.4823507417973,
20.));
#75529=CARTESIAN_POINT('Ctrl Pts',(-14.756734768403,-44.469167562743,0.));
#75530=CARTESIAN_POINT('Ctrl Pts',(-14.756734768403,-44.469167562743,20.));
#75531=CARTESIAN_POINT('Ctrl Pts',(-14.7870308376214,-44.4559635429545,
0.));
#75532=CARTESIAN_POINT('Ctrl Pts',(-14.7870308376214,-44.4559635429545,
20.));
#75533=CARTESIAN_POINT('Ctrl Pts',(-14.817316600156,-44.4427386897515,0.));
#75534=CARTESIAN_POINT('Ctrl Pts',(-14.817316600156,-44.4427386897515,20.));
#75535=CARTESIAN_POINT('Ctrl Pts',(-14.8475920414108,-44.4294930104636,
0.));
#75536=CARTESIAN_POINT('Ctrl Pts',(-14.8475920414108,-44.4294930104636,
20.));
#75537=CARTESIAN_POINT('Ctrl Pts',(-14.8778571467943,-44.416226512431,0.));
#75538=CARTESIAN_POINT('Ctrl Pts',(-14.8778571467943,-44.416226512431,20.));
#75539=CARTESIAN_POINT('Ctrl Pts',(-14.9081119017199,-44.4029392030043,
0.));
#75540=CARTESIAN_POINT('Ctrl Pts',(-14.9081119017199,-44.4029392030043,
20.));
#75541=CARTESIAN_POINT('Ctrl Pts',(-14.9383562916061,-44.389631089546,0.));
#75542=CARTESIAN_POINT('Ctrl Pts',(-14.9383562916061,-44.389631089546,20.));
#75543=CARTESIAN_POINT('Ctrl Pts',(-14.9685903018767,-44.3763021794296,
0.));
#75544=CARTESIAN_POINT('Ctrl Pts',(-14.9685903018767,-44.3763021794296,
20.));
#75545=CARTESIAN_POINT('Ctrl Pts',(-14.9988139179602,-44.3629524800397,
0.));
#75546=CARTESIAN_POINT('Ctrl Pts',(-14.9988139179602,-44.3629524800397,
20.));
#75547=CARTESIAN_POINT('Ctrl Pts',(-15.0290271252899,-44.3495819987707,
0.));
#75548=CARTESIAN_POINT('Ctrl Pts',(-15.0290271252899,-44.3495819987707,
20.));
#75549=CARTESIAN_POINT('Ctrl Pts',(-15.0592299093033,-44.3361907430254,
0.));
#75550=CARTESIAN_POINT('Ctrl Pts',(-15.0592299093033,-44.3361907430254,
20.));
#75551=CARTESIAN_POINT('Ctrl Pts',(-15.0894222554425,-44.3227787202166,
0.));
#75552=CARTESIAN_POINT('Ctrl Pts',(-15.0894222554425,-44.3227787202166,
20.));
#75553=CARTESIAN_POINT('Ctrl Pts',(-15.1196041491546,-44.3093459377674,
0.));
#75554=CARTESIAN_POINT('Ctrl Pts',(-15.1196041491546,-44.3093459377674,
20.));
#75555=CARTESIAN_POINT('Ctrl Pts',(-15.1497755758918,-44.2958924031118,
0.));
#75556=CARTESIAN_POINT('Ctrl Pts',(-15.1497755758918,-44.2958924031118,
20.));
#75557=CARTESIAN_POINT('Ctrl Pts',(-15.1799365211114,-44.2824181236961,
0.));
#75558=CARTESIAN_POINT('Ctrl Pts',(-15.1799365211114,-44.2824181236961,
20.));
#75559=CARTESIAN_POINT('Ctrl Pts',(-15.2100869702755,-44.2689231069767,
0.));
#75560=CARTESIAN_POINT('Ctrl Pts',(-15.2100869702755,-44.2689231069767,
20.));
#75561=CARTESIAN_POINT('Ctrl Pts',(-15.2402269088514,-44.2554073604206,
0.));
#75562=CARTESIAN_POINT('Ctrl Pts',(-15.2402269088514,-44.2554073604206,
20.));
#75563=CARTESIAN_POINT('Ctrl Pts',(-15.2703563223108,-44.2418708915045,
0.));
#75564=CARTESIAN_POINT('Ctrl Pts',(-15.2703563223108,-44.2418708915045,
20.));
#75565=CARTESIAN_POINT('Ctrl Pts',(-15.30047519613,-44.2283137077152,0.));
#75566=CARTESIAN_POINT('Ctrl Pts',(-15.30047519613,-44.2283137077152,20.));
#75567=CARTESIAN_POINT('Ctrl Pts',(-15.3305835157903,-44.2147358165492,
0.));
#75568=CARTESIAN_POINT('Ctrl Pts',(-15.3305835157903,-44.2147358165492,
20.));
#75569=CARTESIAN_POINT('Ctrl Pts',(-15.3606812667781,-44.201137225514,0.));
#75570=CARTESIAN_POINT('Ctrl Pts',(-15.3606812667781,-44.201137225514,20.));
#75571=CARTESIAN_POINT('Ctrl Pts',(-15.390768434585,-44.1875179421286,0.));
#75572=CARTESIAN_POINT('Ctrl Pts',(-15.390768434585,-44.1875179421286,20.));
#75573=CARTESIAN_POINT('Ctrl Pts',(-15.4208450047077,-44.1738779739224,
0.));
#75574=CARTESIAN_POINT('Ctrl Pts',(-15.4208450047077,-44.1738779739224,
20.));
#75575=CARTESIAN_POINT('Ctrl Pts',(-15.4509109626472,-44.1602173284345,
0.));
#75576=CARTESIAN_POINT('Ctrl Pts',(-15.4509109626472,-44.1602173284345,
20.));
#75577=CARTESIAN_POINT('Ctrl Pts',(-15.4809662939093,-44.146536013213,0.));
#75578=CARTESIAN_POINT('Ctrl Pts',(-15.4809662939093,-44.146536013213,20.));
#75579=CARTESIAN_POINT('Ctrl Pts',(-15.5110109840048,-44.1328340358171,
0.));
#75580=CARTESIAN_POINT('Ctrl Pts',(-15.5110109840048,-44.1328340358171,
20.));
#75581=CARTESIAN_POINT('Ctrl Pts',(-15.5410450184494,-44.1191114038164,
0.));
#75582=CARTESIAN_POINT('Ctrl Pts',(-15.5410450184494,-44.1191114038164,
20.));
#75583=CARTESIAN_POINT('Ctrl Pts',(-15.5710683827646,-44.1053681247921,
0.));
#75584=CARTESIAN_POINT('Ctrl Pts',(-15.5710683827646,-44.1053681247921,
20.));
#75585=CARTESIAN_POINT('Ctrl Pts',(-15.6010810624766,-44.0916042063371,
0.));
#75586=CARTESIAN_POINT('Ctrl Pts',(-15.6010810624766,-44.0916042063371,
20.));
#75587=CARTESIAN_POINT('Ctrl Pts',(-15.6310830431167,-44.0778196560536,
0.));
#75588=CARTESIAN_POINT('Ctrl Pts',(-15.6310830431167,-44.0778196560536,
20.));
#75589=CARTESIAN_POINT('Ctrl Pts',(-15.6610743102207,-44.0640144815534,
0.));
#75590=CARTESIAN_POINT('Ctrl Pts',(-15.6610743102207,-44.0640144815534,
20.));
#75591=CARTESIAN_POINT('Ctrl Pts',(-15.6910548493289,-44.050188690457,0.));
#75592=CARTESIAN_POINT('Ctrl Pts',(-15.6910548493289,-44.050188690457,20.));
#75593=CARTESIAN_POINT('Ctrl Pts',(-15.7210246459868,-44.0363422903955,
0.));
#75594=CARTESIAN_POINT('Ctrl Pts',(-15.7210246459868,-44.0363422903955,
20.));
#75595=CARTESIAN_POINT('Ctrl Pts',(-15.7509836857452,-44.0224752890112,
0.));
#75596=CARTESIAN_POINT('Ctrl Pts',(-15.7509836857452,-44.0224752890112,
20.));
#75597=CARTESIAN_POINT('Ctrl Pts',(-15.7809319541602,-44.0085876939576,
0.));
#75598=CARTESIAN_POINT('Ctrl Pts',(-15.7809319541602,-44.0085876939576,
20.));
#75599=CARTESIAN_POINT('Ctrl Pts',(-15.8108694367927,-43.9946795128988,
0.));
#75600=CARTESIAN_POINT('Ctrl Pts',(-15.8108694367927,-43.9946795128988,
20.));
#75601=CARTESIAN_POINT('Ctrl Pts',(-15.8407961192089,-43.9807507535096,
0.));
#75602=CARTESIAN_POINT('Ctrl Pts',(-15.8407961192089,-43.9807507535096,
20.));
#75603=CARTESIAN_POINT('Ctrl Pts',(-15.8707119869797,-43.9668014234746,
0.));
#75604=CARTESIAN_POINT('Ctrl Pts',(-15.8707119869797,-43.9668014234746,
20.));
#75605=CARTESIAN_POINT('Ctrl Pts',(-15.9006170256808,-43.9528315304878,
0.));
#75606=CARTESIAN_POINT('Ctrl Pts',(-15.9006170256808,-43.9528315304878,
20.));
#75607=CARTESIAN_POINT('Ctrl Pts',(-15.9305112208934,-43.9388410822542,
0.));
#75608=CARTESIAN_POINT('Ctrl Pts',(-15.9305112208934,-43.9388410822542,
20.));
#75609=CARTESIAN_POINT('Ctrl Pts',(-15.9603945582034,-43.9248300864889,
0.));
#75610=CARTESIAN_POINT('Ctrl Pts',(-15.9603945582034,-43.9248300864889,
20.));
#75611=CARTESIAN_POINT('Ctrl Pts',(-15.9902670232019,-43.9107985509168,
0.));
#75612=CARTESIAN_POINT('Ctrl Pts',(-15.9902670232019,-43.9107985509168,
20.));
#75613=CARTESIAN_POINT('Ctrl Pts',(-16.020128601485,-43.896746483274,0.));
#75614=CARTESIAN_POINT('Ctrl Pts',(-16.020128601485,-43.896746483274,20.));
#75615=CARTESIAN_POINT('Ctrl Pts',(-16.0499792786541,-43.8826738913074,
0.));
#75616=CARTESIAN_POINT('Ctrl Pts',(-16.0499792786541,-43.8826738913074,
20.));
#75617=CARTESIAN_POINT('Ctrl Pts',(-16.0798190403159,-43.8685807827745,
0.));
#75618=CARTESIAN_POINT('Ctrl Pts',(-16.0798190403159,-43.8685807827745,
20.));
#75619=CARTESIAN_POINT('Ctrl Pts',(-16.1096478720818,-43.854467165442,0.));
#75620=CARTESIAN_POINT('Ctrl Pts',(-16.1096478720818,-43.854467165442,20.));
#75621=CARTESIAN_POINT('Ctrl Pts',(-16.1394657595683,-43.8403330470868,
0.));
#75622=CARTESIAN_POINT('Ctrl Pts',(-16.1394657595683,-43.8403330470868,
20.));
#75623=CARTESIAN_POINT('Ctrl Pts',(-16.1692726883968,-43.8261784354962,
0.));
#75624=CARTESIAN_POINT('Ctrl Pts',(-16.1692726883968,-43.8261784354962,
20.));
#75625=CARTESIAN_POINT('Ctrl Pts',(-16.199068644194,-43.8120033384679,0.));
#75626=CARTESIAN_POINT('Ctrl Pts',(-16.199068644194,-43.8120033384679,20.));
#75627=CARTESIAN_POINT('Ctrl Pts',(-16.2288536125917,-43.7978077638098,
0.));
#75628=CARTESIAN_POINT('Ctrl Pts',(-16.2288536125917,-43.7978077638098,
20.));
#75629=CARTESIAN_POINT('Ctrl Pts',(-16.2586275792268,-43.7835917193404,
0.));
#75630=CARTESIAN_POINT('Ctrl Pts',(-16.2586275792268,-43.7835917193404,
20.));
#75631=CARTESIAN_POINT('Ctrl Pts',(-16.2883905297415,-43.7693552128887,
0.));
#75632=CARTESIAN_POINT('Ctrl Pts',(-16.2883905297415,-43.7693552128887,
20.));
#75633=CARTESIAN_POINT('Ctrl Pts',(-16.3181424497834,-43.7550982522947,
0.));
#75634=CARTESIAN_POINT('Ctrl Pts',(-16.3181424497834,-43.7550982522947,
20.));
#75635=CARTESIAN_POINT('Ctrl Pts',(-16.3478833250055,-43.7408208454089,
0.));
#75636=CARTESIAN_POINT('Ctrl Pts',(-16.3478833250055,-43.7408208454089,
20.));
#75637=CARTESIAN_POINT('Ctrl Pts',(-16.3776131410651,-43.7265230000909,
0.));
#75638=CARTESIAN_POINT('Ctrl Pts',(-16.3776131410651,-43.7265230000909,
20.));
#75639=CARTESIAN_POINT('Ctrl Pts',(-16.4073318836249,-43.7122047242097,
0.));
#75640=CARTESIAN_POINT('Ctrl Pts',(-16.4073318836249,-43.7122047242097,
20.));
#75641=CARTESIAN_POINT('Ctrl Pts',(-16.4370395383524,-43.6978660256455,
0.));
#75642=CARTESIAN_POINT('Ctrl Pts',(-16.4370395383524,-43.6978660256455,
20.));
#75643=CARTESIAN_POINT('Ctrl Pts',(-16.4667360909207,-43.6835069122887,
0.));
#75644=CARTESIAN_POINT('Ctrl Pts',(-16.4667360909207,-43.6835069122887,
20.));
#75645=CARTESIAN_POINT('Ctrl Pts',(-16.4964215270082,-43.6691273920409,
0.));
#75646=CARTESIAN_POINT('Ctrl Pts',(-16.4964215270082,-43.6691273920409,
20.));
#75647=CARTESIAN_POINT('Ctrl Pts',(-16.5260958322991,-43.6547274728139,
0.));
#75648=CARTESIAN_POINT('Ctrl Pts',(-16.5260958322991,-43.6547274728139,
20.));
#75649=CARTESIAN_POINT('Ctrl Pts',(-16.5557589924819,-43.640307162529,0.));
#75650=CARTESIAN_POINT('Ctrl Pts',(-16.5557589924819,-43.640307162529,20.));
#75651=CARTESIAN_POINT('Ctrl Pts',(-16.5854109932504,-43.6258664691173,
0.));
#75652=CARTESIAN_POINT('Ctrl Pts',(-16.5854109932504,-43.6258664691173,
20.));
#75653=CARTESIAN_POINT('Ctrl Pts',(-16.6150518203036,-43.6114054005208,
0.));
#75654=CARTESIAN_POINT('Ctrl Pts',(-16.6150518203036,-43.6114054005208,
20.));
#75655=CARTESIAN_POINT('Ctrl Pts',(-16.6446814593459,-43.5969239646926,
0.));
#75656=CARTESIAN_POINT('Ctrl Pts',(-16.6446814593459,-43.5969239646926,
20.));
#75657=CARTESIAN_POINT('Ctrl Pts',(-16.6742998960869,-43.5824221695961,
0.));
#75658=CARTESIAN_POINT('Ctrl Pts',(-16.6742998960869,-43.5824221695961,
20.));
#75659=CARTESIAN_POINT('Ctrl Pts',(-16.7039071162413,-43.5679000232041,
0.));
#75660=CARTESIAN_POINT('Ctrl Pts',(-16.7039071162413,-43.5679000232041,
20.));
#75661=CARTESIAN_POINT('Ctrl Pts',(-16.7335031055295,-43.5533575334996,
0.));
#75662=CARTESIAN_POINT('Ctrl Pts',(-16.7335031055295,-43.5533575334996,
20.));
#75663=CARTESIAN_POINT('Ctrl Pts',(-16.7630878496767,-43.5387947084755,
0.));
#75664=CARTESIAN_POINT('Ctrl Pts',(-16.7630878496767,-43.5387947084755,
20.));
#75665=CARTESIAN_POINT('Ctrl Pts',(-16.792661334414,-43.5242115561352,0.));
#75666=CARTESIAN_POINT('Ctrl Pts',(-16.792661334414,-43.5242115561352,20.));
#75667=CARTESIAN_POINT('Ctrl Pts',(-16.8222235454772,-43.5096080844922,
0.));
#75668=CARTESIAN_POINT('Ctrl Pts',(-16.8222235454772,-43.5096080844922,
20.));
#75669=CARTESIAN_POINT('Ctrl Pts',(-16.8517744686076,-43.4949843015709,
0.));
#75670=CARTESIAN_POINT('Ctrl Pts',(-16.8517744686076,-43.4949843015709,
20.));
#75671=CARTESIAN_POINT('Ctrl Pts',(-16.8813140895513,-43.4803402154062,
0.));
#75672=CARTESIAN_POINT('Ctrl Pts',(-16.8813140895513,-43.4803402154062,
20.));
#75673=CARTESIAN_POINT('Ctrl Pts',(-16.91084239406,-43.4656758340435,0.));
#75674=CARTESIAN_POINT('Ctrl Pts',(-16.91084239406,-43.4656758340435,20.));
#75675=CARTESIAN_POINT('Ctrl Pts',(-16.9403593678908,-43.4509911655382,
0.));
#75676=CARTESIAN_POINT('Ctrl Pts',(-16.9403593678908,-43.4509911655382,
20.));
#75677=CARTESIAN_POINT('Ctrl Pts',(-16.9698649968061,-43.4362862179557,
0.));
#75678=CARTESIAN_POINT('Ctrl Pts',(-16.9698649968061,-43.4362862179557,
20.));
#75679=CARTESIAN_POINT('Ctrl Pts',(-16.9993592665737,-43.4215609993712,
0.));
#75680=CARTESIAN_POINT('Ctrl Pts',(-16.9993592665737,-43.4215609993712,
20.));
#75681=CARTESIAN_POINT('Ctrl Pts',(-17.0288421629666,-43.4068155178695,
0.));
#75682=CARTESIAN_POINT('Ctrl Pts',(-17.0288421629666,-43.4068155178695,
20.));
#75683=CARTESIAN_POINT('Ctrl Pts',(-17.0583136717632,-43.3920497815463,
0.));
#75684=CARTESIAN_POINT('Ctrl Pts',(-17.0583136717632,-43.3920497815463,
20.));
#75685=CARTESIAN_POINT('Ctrl Pts',(-17.0877737787472,-43.3772637985072,
0.));
#75686=CARTESIAN_POINT('Ctrl Pts',(-17.0877737787472,-43.3772637985072,
20.));
#75687=CARTESIAN_POINT('Ctrl Pts',(-17.1172224697079,-43.3624575768695,
0.));
#75688=CARTESIAN_POINT('Ctrl Pts',(-17.1172224697079,-43.3624575768695,
20.));
#75689=CARTESIAN_POINT('Ctrl Pts',(-17.1466597304397,-43.3476311247602,
0.));
#75690=CARTESIAN_POINT('Ctrl Pts',(-17.1466597304397,-43.3476311247602,
20.));
#75691=CARTESIAN_POINT('Ctrl Pts',(-17.1760855467426,-43.332784450317,0.));
#75692=CARTESIAN_POINT('Ctrl Pts',(-17.1760855467426,-43.332784450317,20.));
#75693=CARTESIAN_POINT('Ctrl Pts',(-17.2054999044213,-43.3179175616862,
0.));
#75694=CARTESIAN_POINT('Ctrl Pts',(-17.2054999044213,-43.3179175616862,
20.));
#75695=CARTESIAN_POINT('Ctrl Pts',(-17.2349027892859,-43.3030304670242,
0.));
#75696=CARTESIAN_POINT('Ctrl Pts',(-17.2349027892859,-43.3030304670242,
20.));
#75697=CARTESIAN_POINT('Ctrl Pts',(-17.2642941871522,-43.2881231744974,
0.));
#75698=CARTESIAN_POINT('Ctrl Pts',(-17.2642941871522,-43.2881231744974,
20.));
#75699=CARTESIAN_POINT('Ctrl Pts',(-17.2936740838416,-43.2731956922839,
0.));
#75700=CARTESIAN_POINT('Ctrl Pts',(-17.2936740838416,-43.2731956922839,
20.));
#75701=CARTESIAN_POINT('Ctrl Pts',(-17.3230424651811,-43.258248028572,0.));
#75702=CARTESIAN_POINT('Ctrl Pts',(-17.3230424651811,-43.258248028572,20.));
#75703=CARTESIAN_POINT('Ctrl Pts',(-17.3523993170031,-43.2432801915607,
0.));
#75704=CARTESIAN_POINT('Ctrl Pts',(-17.3523993170031,-43.2432801915607,
20.));
#75705=CARTESIAN_POINT('Ctrl Pts',(-17.3817446251452,-43.2282921894589,
0.));
#75706=CARTESIAN_POINT('Ctrl Pts',(-17.3817446251452,-43.2282921894589,
20.));
#75707=CARTESIAN_POINT('Ctrl Pts',(-17.4110783754507,-43.2132840304854,
0.));
#75708=CARTESIAN_POINT('Ctrl Pts',(-17.4110783754507,-43.2132840304854,
20.));
#75709=CARTESIAN_POINT('Ctrl Pts',(-17.4404005537678,-43.1982557228684,
0.));
#75710=CARTESIAN_POINT('Ctrl Pts',(-17.4404005537678,-43.1982557228684,
20.));
#75711=CARTESIAN_POINT('Ctrl Pts',(-17.4697111459501,-43.1832072748459,
0.));
#75712=CARTESIAN_POINT('Ctrl Pts',(-17.4697111459501,-43.1832072748459,
20.));
#75713=CARTESIAN_POINT('Ctrl Pts',(-17.4990101378563,-43.1681386946662,
0.));
#75714=CARTESIAN_POINT('Ctrl Pts',(-17.4990101378563,-43.1681386946662,
20.));
#75715=CARTESIAN_POINT('Ctrl Pts',(-17.5282975153509,-43.1530499905879,
0.));
#75716=CARTESIAN_POINT('Ctrl Pts',(-17.5282975153509,-43.1530499905879,
20.));
#75717=CARTESIAN_POINT('Ctrl Pts',(-17.557573264304,-43.1379411708804,0.));
#75718=CARTESIAN_POINT('Ctrl Pts',(-17.557573264304,-43.1379411708804,20.));
#75719=CARTESIAN_POINT('Ctrl Pts',(-17.5868373705916,-43.122812243824,0.));
#75720=CARTESIAN_POINT('Ctrl Pts',(-17.5868373705916,-43.122812243824,20.));
#75721=CARTESIAN_POINT('Ctrl Pts',(-17.6160898200949,-43.1076632177088,
0.));
#75722=CARTESIAN_POINT('Ctrl Pts',(-17.6160898200949,-43.1076632177088,
20.));
#75723=CARTESIAN_POINT('Ctrl Pts',(-17.645330598701,-43.0924941008354,0.));
#75724=CARTESIAN_POINT('Ctrl Pts',(-17.645330598701,-43.0924941008354,20.));
#75725=CARTESIAN_POINT('Ctrl Pts',(-17.674559692302,-43.0773049015136,0.));
#75726=CARTESIAN_POINT('Ctrl Pts',(-17.674559692302,-43.0773049015136,20.));
#75727=CARTESIAN_POINT('Ctrl Pts',(-17.7037770867956,-43.0620956280638,
0.));
#75728=CARTESIAN_POINT('Ctrl Pts',(-17.7037770867956,-43.0620956280638,
20.));
#75729=CARTESIAN_POINT('Ctrl Pts',(-17.7329827680847,-43.0468662888157,
0.));
#75730=CARTESIAN_POINT('Ctrl Pts',(-17.7329827680847,-43.0468662888157,
20.));
#75731=CARTESIAN_POINT('Ctrl Pts',(-17.7621767220773,-43.0316168921093,
0.));
#75732=CARTESIAN_POINT('Ctrl Pts',(-17.7621767220773,-43.0316168921093,
20.));
#75733=CARTESIAN_POINT('Ctrl Pts',(-17.7913589346876,-43.0163474462951,
0.));
#75734=CARTESIAN_POINT('Ctrl Pts',(-17.7913589346876,-43.0163474462951,
20.));
#75735=CARTESIAN_POINT('Ctrl Pts',(-17.8205293918351,-43.0010579597341,
0.));
#75736=CARTESIAN_POINT('Ctrl Pts',(-17.8205293918351,-43.0010579597341,
20.));
#75737=CARTESIAN_POINT('Ctrl Pts',(-17.8496880794454,-42.9857484407979,
0.));
#75738=CARTESIAN_POINT('Ctrl Pts',(-17.8496880794454,-42.9857484407979,
20.));
#75739=CARTESIAN_POINT('Ctrl Pts',(-17.8788349834491,-42.9704188978681,
0.));
#75740=CARTESIAN_POINT('Ctrl Pts',(-17.8788349834491,-42.9704188978681,
20.));
#75741=CARTESIAN_POINT('Ctrl Pts',(-17.9079700897828,-42.9550693393359,
0.));
#75742=CARTESIAN_POINT('Ctrl Pts',(-17.9079700897828,-42.9550693393359,
20.));
#75743=CARTESIAN_POINT('Ctrl Pts',(-17.9370933843882,-42.9396997736018,
0.));
#75744=CARTESIAN_POINT('Ctrl Pts',(-17.9370933843882,-42.9396997736018,
20.));
#75745=CARTESIAN_POINT('Ctrl Pts',(-17.9662048532126,-42.9243102090766,
0.));
#75746=CARTESIAN_POINT('Ctrl Pts',(-17.9662048532126,-42.9243102090766,
20.));
#75747=CARTESIAN_POINT('Ctrl Pts',(-17.9953044822088,-42.9089006541818,
0.));
#75748=CARTESIAN_POINT('Ctrl Pts',(-17.9953044822088,-42.9089006541818,
20.));
#75749=CARTESIAN_POINT('Ctrl Pts',(-18.0243922573354,-42.893471117349,0.));
#75750=CARTESIAN_POINT('Ctrl Pts',(-18.0243922573354,-42.893471117349,20.));
#75751=CARTESIAN_POINT('Ctrl Pts',(-18.0534681645565,-42.8780216070204,
0.));
#75752=CARTESIAN_POINT('Ctrl Pts',(-18.0534681645565,-42.8780216070204,
20.));
#75753=CARTESIAN_POINT('Ctrl Pts',(-18.0825321898416,-42.8625521316488,
0.));
#75754=CARTESIAN_POINT('Ctrl Pts',(-18.0825321898416,-42.8625521316488,
20.));
#75755=CARTESIAN_POINT('Ctrl Pts',(-18.1115843191668,-42.8470626996976,
0.));
#75756=CARTESIAN_POINT('Ctrl Pts',(-18.1115843191668,-42.8470626996976,
20.));
#75757=CARTESIAN_POINT('Ctrl Pts',(-18.1406245385131,-42.831553319639,0.));
#75758=CARTESIAN_POINT('Ctrl Pts',(-18.1406245385131,-42.831553319639,20.));
#75759=CARTESIAN_POINT('Ctrl Pts',(-18.1696528338673,-42.8160239999555,
0.));
#75760=CARTESIAN_POINT('Ctrl Pts',(-18.1696528338673,-42.8160239999555,
20.));
#75761=CARTESIAN_POINT('Ctrl Pts',(-18.1986691912208,-42.8004747491375,
0.));
#75762=CARTESIAN_POINT('Ctrl Pts',(-18.1986691912208,-42.8004747491375,
20.));
#75763=CARTESIAN_POINT('Ctrl Pts',(-18.2276735965714,-42.7849055756869,
0.));
#75764=CARTESIAN_POINT('Ctrl Pts',(-18.2276735965714,-42.7849055756869,
20.));
#75765=CARTESIAN_POINT('Ctrl Pts',(-18.256666035922,-42.7693164881155,0.));
#75766=CARTESIAN_POINT('Ctrl Pts',(-18.256666035922,-42.7693164881155,20.));
#75767=CARTESIAN_POINT('Ctrl Pts',(-18.285646495282,-42.7537074949463,0.));
#75768=CARTESIAN_POINT('Ctrl Pts',(-18.285646495282,-42.7537074949463,20.));
#75769=CARTESIAN_POINT('Ctrl Pts',(-18.3146149606662,-42.7380786047127,
0.));
#75770=CARTESIAN_POINT('Ctrl Pts',(-18.3146149606662,-42.7380786047127,
20.));
#75771=CARTESIAN_POINT('Ctrl Pts',(-18.3435714180954,-42.7224298259587,
0.));
#75772=CARTESIAN_POINT('Ctrl Pts',(-18.3435714180954,-42.7224298259587,
20.));
#75773=CARTESIAN_POINT('Ctrl Pts',(-18.372515853596,-42.7067611672378,0.));
#75774=CARTESIAN_POINT('Ctrl Pts',(-18.372515853596,-42.7067611672378,20.));
#75775=CARTESIAN_POINT('Ctrl Pts',(-18.4014482531999,-42.6910726371132,
0.));
#75776=CARTESIAN_POINT('Ctrl Pts',(-18.4014482531999,-42.6910726371132,
20.));
#75777=CARTESIAN_POINT('Ctrl Pts',(-18.4303686029444,-42.6753642441576,
0.));
#75778=CARTESIAN_POINT('Ctrl Pts',(-18.4303686029444,-42.6753642441576,
20.));
#75779=CARTESIAN_POINT('Ctrl Pts',(-18.4592768888724,-42.6596359969538,
0.));
#75780=CARTESIAN_POINT('Ctrl Pts',(-18.4592768888724,-42.6596359969538,
20.));
#75781=CARTESIAN_POINT('Ctrl Pts',(-18.4881730970326,-42.6438879040941,
0.));
#75782=CARTESIAN_POINT('Ctrl Pts',(-18.4881730970326,-42.6438879040941,
20.));
#75783=CARTESIAN_POINT('Ctrl Pts',(-18.5170572134793,-42.6281199741818,
0.));
#75784=CARTESIAN_POINT('Ctrl Pts',(-18.5170572134793,-42.6281199741818,
20.));
#75785=CARTESIAN_POINT('Ctrl Pts',(-18.5459292242727,-42.61233221583,0.));
#75786=CARTESIAN_POINT('Ctrl Pts',(-18.5459292242727,-42.61233221583,20.));
#75787=CARTESIAN_POINT('Ctrl Pts',(-18.574789115479,-42.596524637663,0.));
#75788=CARTESIAN_POINT('Ctrl Pts',(-18.574789115479,-42.596524637663,20.));
#75789=CARTESIAN_POINT('Ctrl Pts',(-18.6036368731702,-42.5806972483146,
0.));
#75790=CARTESIAN_POINT('Ctrl Pts',(-18.6036368731702,-42.5806972483146,
20.));
#75791=CARTESIAN_POINT('Ctrl Pts',(-18.632472483424,-42.5648500564287,0.));
#75792=CARTESIAN_POINT('Ctrl Pts',(-18.632472483424,-42.5648500564287,20.));
#75793=CARTESIAN_POINT('Ctrl Pts',(-18.6612959323233,-42.5489830706585,
0.));
#75794=CARTESIAN_POINT('Ctrl Pts',(-18.6612959323233,-42.5489830706585,
20.));
#75795=CARTESIAN_POINT('Ctrl Pts',(-18.6901072059568,-42.5330962996668,
0.));
#75796=CARTESIAN_POINT('Ctrl Pts',(-18.6901072059568,-42.5330962996668,
20.));
#75797=CARTESIAN_POINT('Ctrl Pts',(-18.718906290419,-42.5171897521269,0.));
#75798=CARTESIAN_POINT('Ctrl Pts',(-18.718906290419,-42.5171897521269,20.));
#75799=CARTESIAN_POINT('Ctrl Pts',(-18.7476931718101,-42.5012634367222,
0.));
#75800=CARTESIAN_POINT('Ctrl Pts',(-18.7476931718101,-42.5012634367222,
20.));
#75801=CARTESIAN_POINT('Ctrl Pts',(-18.7764678362368,-42.4853173621469,
0.));
#75802=CARTESIAN_POINT('Ctrl Pts',(-18.7764678362368,-42.4853173621469,
20.));
#75803=CARTESIAN_POINT('Ctrl Pts',(-18.8052302698113,-42.4693515371059,
0.));
#75804=CARTESIAN_POINT('Ctrl Pts',(-18.8052302698113,-42.4693515371059,
20.));
#75805=CARTESIAN_POINT('Ctrl Pts',(-18.8339804586522,-42.4533659703145,
0.));
#75806=CARTESIAN_POINT('Ctrl Pts',(-18.8339804586522,-42.4533659703145,
20.));
#75807=CARTESIAN_POINT('Ctrl Pts',(-18.8627183888827,-42.4373606704956,
0.));
#75808=CARTESIAN_POINT('Ctrl Pts',(-18.8627183888827,-42.4373606704956,
20.));
#75809=CARTESIAN_POINT('Ctrl Pts',(-18.8914440466322,-42.4213356463824,
0.));
#75810=CARTESIAN_POINT('Ctrl Pts',(-18.8914440466322,-42.4213356463824,
20.));
#75811=CARTESIAN_POINT('Ctrl Pts',(-18.9201574180352,-42.4052909067172,
0.));
#75812=CARTESIAN_POINT('Ctrl Pts',(-18.9201574180352,-42.4052909067172,
20.));
#75813=CARTESIAN_POINT('Ctrl Pts',(-18.9488584892326,-42.389226460254,0.));
#75814=CARTESIAN_POINT('Ctrl Pts',(-18.9488584892326,-42.389226460254,20.));
#75815=CARTESIAN_POINT('Ctrl Pts',(-18.9775472463711,-42.3731423157568,
0.));
#75816=CARTESIAN_POINT('Ctrl Pts',(-18.9775472463711,-42.3731423157568,
20.));
#75817=CARTESIAN_POINT('Ctrl Pts',(-19.0062236756035,-42.3570384820003,
0.));
#75818=CARTESIAN_POINT('Ctrl Pts',(-19.0062236756035,-42.3570384820003,
20.));
#75819=CARTESIAN_POINT('Ctrl Pts',(-19.0348877630887,-42.3409149677685,
0.));
#75820=CARTESIAN_POINT('Ctrl Pts',(-19.0348877630887,-42.3409149677685,
20.));
#75821=CARTESIAN_POINT('Ctrl Pts',(-19.0635394949913,-42.3247717818558,
0.));
#75822=CARTESIAN_POINT('Ctrl Pts',(-19.0635394949913,-42.3247717818558,
20.));
#75823=CARTESIAN_POINT('Ctrl Pts',(-19.0921788574819,-42.3086089330657,
0.));
#75824=CARTESIAN_POINT('Ctrl Pts',(-19.0921788574819,-42.3086089330657,
20.));
#75825=CARTESIAN_POINT('Ctrl Pts',(-19.1208058367362,-42.2924264302113,
0.));
#75826=CARTESIAN_POINT('Ctrl Pts',(-19.1208058367362,-42.2924264302113,
20.));
#75827=CARTESIAN_POINT('Ctrl Pts',(-19.1494204189361,-42.2762242821163,
0.));
#75828=CARTESIAN_POINT('Ctrl Pts',(-19.1494204189361,-42.2762242821163,
20.));
#75829=CARTESIAN_POINT('Ctrl Pts',(-19.1780225902694,-42.2600024976146,
0.));
#75830=CARTESIAN_POINT('Ctrl Pts',(-19.1780225902694,-42.2600024976146,
20.));
#75831=CARTESIAN_POINT('Ctrl Pts',(-19.2066123369297,-42.2437610855506,
0.));
#75832=CARTESIAN_POINT('Ctrl Pts',(-19.2066123369297,-42.2437610855506,
20.));
#75833=CARTESIAN_POINT('Ctrl Pts',(-19.2351896451166,-42.2275000547783,
0.));
#75834=CARTESIAN_POINT('Ctrl Pts',(-19.2351896451166,-42.2275000547783,
20.));
#75835=CARTESIAN_POINT('Ctrl Pts',(-19.2637545010356,-42.2112194141618,
0.));
#75836=CARTESIAN_POINT('Ctrl Pts',(-19.2637545010356,-42.2112194141618,
20.));
#75837=CARTESIAN_POINT('Ctrl Pts',(-19.2923068908981,-42.1949191725745,
0.));
#75838=CARTESIAN_POINT('Ctrl Pts',(-19.2923068908981,-42.1949191725745,
20.));
#75839=CARTESIAN_POINT('Ctrl Pts',(-19.3208468009212,-42.1785993388989,
0.));
#75840=CARTESIAN_POINT('Ctrl Pts',(-19.3208468009212,-42.1785993388989,
20.));
#75841=CARTESIAN_POINT('Ctrl Pts',(-19.3493742173283,-42.1622599220289,
0.));
#75842=CARTESIAN_POINT('Ctrl Pts',(-19.3493742173283,-42.1622599220289,
20.));
#75843=CARTESIAN_POINT('Ctrl Pts',(-19.377889126349,-42.1459009308685,0.));
#75844=CARTESIAN_POINT('Ctrl Pts',(-19.377889126349,-42.1459009308685,20.));
#75845=CARTESIAN_POINT('Ctrl Pts',(-19.4063915142187,-42.1295223743319,
0.));
#75846=CARTESIAN_POINT('Ctrl Pts',(-19.4063915142187,-42.1295223743319,
20.));
#75847=CARTESIAN_POINT('Ctrl Pts',(-19.4348813671785,-42.1131242613432,
0.));
#75848=CARTESIAN_POINT('Ctrl Pts',(-19.4348813671785,-42.1131242613432,
20.));
#75849=CARTESIAN_POINT('Ctrl Pts',(-19.4633586714748,-42.0967066008354,
0.));
#75850=CARTESIAN_POINT('Ctrl Pts',(-19.4633586714748,-42.0967066008354,
20.));
#75851=CARTESIAN_POINT('Ctrl Pts',(-19.4918234133604,-42.080269401751,0.));
#75852=CARTESIAN_POINT('Ctrl Pts',(-19.4918234133604,-42.080269401751,20.));
#75853=CARTESIAN_POINT('Ctrl Pts',(-19.520275579094,-42.0638126730426,0.));
#75854=CARTESIAN_POINT('Ctrl Pts',(-19.520275579094,-42.0638126730426,20.));
#75855=CARTESIAN_POINT('Ctrl Pts',(-19.5487151549408,-42.0473364236742,
0.));
#75856=CARTESIAN_POINT('Ctrl Pts',(-19.5487151549408,-42.0473364236742,
20.));
#75857=CARTESIAN_POINT('Ctrl Pts',(-19.5771421271718,-42.0308406626191,
0.));
#75858=CARTESIAN_POINT('Ctrl Pts',(-19.5771421271718,-42.0308406626191,
20.));
#75859=CARTESIAN_POINT('Ctrl Pts',(-19.6055564820642,-42.0143253988608,
0.));
#75860=CARTESIAN_POINT('Ctrl Pts',(-19.6055564820642,-42.0143253988608,
20.));
#75861=CARTESIAN_POINT('Ctrl Pts',(-19.6339582059009,-41.997790641393,0.));
#75862=CARTESIAN_POINT('Ctrl Pts',(-19.6339582059009,-41.997790641393,20.));
#75863=CARTESIAN_POINT('Ctrl Pts',(-19.6623472849704,-41.9812363992182,
0.));
#75864=CARTESIAN_POINT('Ctrl Pts',(-19.6623472849704,-41.9812363992182,
20.));
#75865=CARTESIAN_POINT('Ctrl Pts',(-19.6907237055675,-41.9646626813489,
0.));
#75866=CARTESIAN_POINT('Ctrl Pts',(-19.6907237055675,-41.9646626813489,
20.));
#75867=CARTESIAN_POINT('Ctrl Pts',(-19.7190874539927,-41.9480694968077,
0.));
#75868=CARTESIAN_POINT('Ctrl Pts',(-19.7190874539927,-41.9480694968077,
20.));
#75869=CARTESIAN_POINT('Ctrl Pts',(-19.7474385165532,-41.9314568546275,
0.));
#75870=CARTESIAN_POINT('Ctrl Pts',(-19.7474385165532,-41.9314568546275,
20.));
#75871=CARTESIAN_POINT('Ctrl Pts',(-19.775776879562,-41.9148247638512,0.));
#75872=CARTESIAN_POINT('Ctrl Pts',(-19.775776879562,-41.9148247638512,20.));
#75873=CARTESIAN_POINT('Ctrl Pts',(-19.8041025293385,-41.8981732335313,
0.));
#75874=CARTESIAN_POINT('Ctrl Pts',(-19.8041025293385,-41.8981732335313,
20.));
#75875=CARTESIAN_POINT('Ctrl Pts',(-19.8324154522082,-41.8815022727306,
0.));
#75876=CARTESIAN_POINT('Ctrl Pts',(-19.8324154522082,-41.8815022727306,
20.));
#75877=CARTESIAN_POINT('Ctrl Pts',(-19.8607156345021,-41.8648118905217,
0.));
#75878=CARTESIAN_POINT('Ctrl Pts',(-19.8607156345021,-41.8648118905217,
20.));
#75879=CARTESIAN_POINT('Ctrl Pts',(-19.889003062557,-41.8481020959867,0.));
#75880=CARTESIAN_POINT('Ctrl Pts',(-19.889003062557,-41.8481020959867,20.));
#75881=CARTESIAN_POINT('Ctrl Pts',(-19.9172777227157,-41.8313728982175,
0.));
#75882=CARTESIAN_POINT('Ctrl Pts',(-19.9172777227157,-41.8313728982175,
20.));
#75883=CARTESIAN_POINT('Ctrl Pts',(-19.945539601327,-41.8146243063151,0.));
#75884=CARTESIAN_POINT('Ctrl Pts',(-19.945539601327,-41.8146243063151,20.));
#75885=CARTESIAN_POINT('Ctrl Pts',(-19.9737886847462,-41.7978563293914,
0.));
#75886=CARTESIAN_POINT('Ctrl Pts',(-19.9737886847462,-41.7978563293914,
20.));
#75887=CARTESIAN_POINT('Ctrl Pts',(-20.0020249593348,-41.7810689765678,
0.));
#75888=CARTESIAN_POINT('Ctrl Pts',(-20.0020249593348,-41.7810689765678,
20.));
#75889=CARTESIAN_POINT('Ctrl Pts',(-20.0302484114611,-41.7642622569769,
0.));
#75890=CARTESIAN_POINT('Ctrl Pts',(-20.0302484114611,-41.7642622569769,
20.));
#75891=CARTESIAN_POINT('Ctrl Pts',(-20.0584590274992,-41.7474361797609,
0.));
#75892=CARTESIAN_POINT('Ctrl Pts',(-20.0584590274992,-41.7474361797609,
20.));
#75893=CARTESIAN_POINT('Ctrl Pts',(-20.0866567938288,-41.7305907540713,
0.));
#75894=CARTESIAN_POINT('Ctrl Pts',(-20.0866567938288,-41.7305907540713,
20.));
#75895=CARTESIAN_POINT('Ctrl Pts',(-20.1148416968357,-41.7137259890696,
0.));
#75896=CARTESIAN_POINT('Ctrl Pts',(-20.1148416968357,-41.7137259890696,
20.));
#75897=CARTESIAN_POINT('Ctrl Pts',(-20.1430137229118,-41.6968418939263,
0.));
#75898=CARTESIAN_POINT('Ctrl Pts',(-20.1430137229118,-41.6968418939263,
20.));
#75899=CARTESIAN_POINT('Ctrl Pts',(-20.1711728584549,-41.6799384778218,
0.));
#75900=CARTESIAN_POINT('Ctrl Pts',(-20.1711728584549,-41.6799384778218,
20.));
#75901=CARTESIAN_POINT('Ctrl Pts',(-20.199319089869,-41.6630157499462,0.));
#75902=CARTESIAN_POINT('Ctrl Pts',(-20.199319089869,-41.6630157499462,20.));
#75903=CARTESIAN_POINT('Ctrl Pts',(-20.2274524035648,-41.6460737195007,
0.));
#75904=CARTESIAN_POINT('Ctrl Pts',(-20.2274524035648,-41.6460737195007,
20.));
#75905=CARTESIAN_POINT('Ctrl Pts',(-20.2555727859589,-41.6291123956959,
0.));
#75906=CARTESIAN_POINT('Ctrl Pts',(-20.2555727859589,-41.6291123956959,
20.));
#75907=CARTESIAN_POINT('Ctrl Pts',(-20.2836802234745,-41.6121317877528,
0.));
#75908=CARTESIAN_POINT('Ctrl Pts',(-20.2836802234745,-41.6121317877528,
20.));
#75909=CARTESIAN_POINT('Ctrl Pts',(-20.3117747025404,-41.5951319049016,
0.));
#75910=CARTESIAN_POINT('Ctrl Pts',(-20.3117747025404,-41.5951319049016,
20.));
#75911=CARTESIAN_POINT('Ctrl Pts',(-20.3398562095917,-41.5781127563818,
0.));
#75912=CARTESIAN_POINT('Ctrl Pts',(-20.3398562095917,-41.5781127563818,
20.));
#75913=CARTESIAN_POINT('Ctrl Pts',(-20.3679247310694,-41.561074351443,0.));
#75914=CARTESIAN_POINT('Ctrl Pts',(-20.3679247310694,-41.561074351443,20.));
#75915=CARTESIAN_POINT('Ctrl Pts',(-20.3959802534211,-41.5440166993445,
0.));
#75916=CARTESIAN_POINT('Ctrl Pts',(-20.3959802534211,-41.5440166993445,
20.));
#75917=CARTESIAN_POINT('Ctrl Pts',(-20.4240227631002,-41.5269398093561,
0.));
#75918=CARTESIAN_POINT('Ctrl Pts',(-20.4240227631002,-41.5269398093561,
20.));
#75919=CARTESIAN_POINT('Ctrl Pts',(-20.4520522465668,-41.5098436907568,
0.));
#75920=CARTESIAN_POINT('Ctrl Pts',(-20.4520522465668,-41.5098436907568,
20.));
#75921=CARTESIAN_POINT('Ctrl Pts',(-20.4800686902869,-41.4927283528358,
0.));
#75922=CARTESIAN_POINT('Ctrl Pts',(-20.4800686902869,-41.4927283528358,
20.));
#75923=CARTESIAN_POINT('Ctrl Pts',(-20.5080720807336,-41.4755938048931,
0.));
#75924=CARTESIAN_POINT('Ctrl Pts',(-20.5080720807336,-41.4755938048931,
20.));
#75925=CARTESIAN_POINT('Ctrl Pts',(-20.5360624043854,-41.4584400562379,
0.));
#75926=CARTESIAN_POINT('Ctrl Pts',(-20.5360624043854,-41.4584400562379,
20.));
#75927=CARTESIAN_POINT('Ctrl Pts',(-20.564039647727,-41.4412671161883,0.));
#75928=CARTESIAN_POINT('Ctrl Pts',(-20.564039647727,-41.4412671161883,20.));
#75929=CARTESIAN_POINT('Ctrl Pts',(-20.592003797249,-41.4240749940721,0.));
#75930=CARTESIAN_POINT('Ctrl Pts',(-20.592003797249,-41.4240749940721,20.));
#75931=CARTESIAN_POINT('Ctrl Pts',(-20.6199548394484,-41.4068636992265,
0.));
#75932=CARTESIAN_POINT('Ctrl Pts',(-20.6199548394484,-41.4068636992265,
20.));
#75933=CARTESIAN_POINT('Ctrl Pts',(-20.6478927608288,-41.3896332409988,
0.));
#75934=CARTESIAN_POINT('Ctrl Pts',(-20.6478927608288,-41.3896332409988,
20.));
#75935=CARTESIAN_POINT('Ctrl Pts',(-20.6758175479,-41.372383628747,0.));
#75936=CARTESIAN_POINT('Ctrl Pts',(-20.6758175479,-41.372383628747,20.));
#75937=CARTESIAN_POINT('Ctrl Pts',(-20.7037291871782,-41.3551148718389,
0.));
#75938=CARTESIAN_POINT('Ctrl Pts',(-20.7037291871782,-41.3551148718389,
20.));
#75939=CARTESIAN_POINT('Ctrl Pts',(-20.731627665186,-41.3378269796522,0.));
#75940=CARTESIAN_POINT('Ctrl Pts',(-20.731627665186,-41.3378269796522,20.));
#75941=CARTESIAN_POINT('Ctrl Pts',(-20.7595129684521,-41.3205199615745,
0.));
#75942=CARTESIAN_POINT('Ctrl Pts',(-20.7595129684521,-41.3205199615745,
20.));
#75943=CARTESIAN_POINT('Ctrl Pts',(-20.7873850835117,-41.303193827003,0.));
#75944=CARTESIAN_POINT('Ctrl Pts',(-20.7873850835117,-41.303193827003,20.));
#75945=CARTESIAN_POINT('Ctrl Pts',(-20.8152439969059,-41.285848585344,0.));
#75946=CARTESIAN_POINT('Ctrl Pts',(-20.8152439969059,-41.285848585344,20.));
#75947=CARTESIAN_POINT('Ctrl Pts',(-20.8430896951822,-41.268484246013,0.));
#75948=CARTESIAN_POINT('Ctrl Pts',(-20.8430896951822,-41.268484246013,20.));
#75949=CARTESIAN_POINT('Ctrl Pts',(-20.8709221648944,-41.2511008184358,
0.));
#75950=CARTESIAN_POINT('Ctrl Pts',(-20.8709221648944,-41.2511008184358,
20.));
#75951=CARTESIAN_POINT('Ctrl Pts',(-20.8987413926025,-41.2336983120481,
0.));
#75952=CARTESIAN_POINT('Ctrl Pts',(-20.8987413926025,-41.2336983120481,
20.));
#75953=CARTESIAN_POINT('Ctrl Pts',(-20.9265473648728,-41.2162767362953,
0.));
#75954=CARTESIAN_POINT('Ctrl Pts',(-20.9265473648728,-41.2162767362953,
20.));
#75955=CARTESIAN_POINT('Ctrl Pts',(-20.9543400682781,-41.1988361006333,
0.));
#75956=CARTESIAN_POINT('Ctrl Pts',(-20.9543400682781,-41.1988361006333,
20.));
#75957=CARTESIAN_POINT('Ctrl Pts',(-20.9821194893979,-41.1813764145274,
0.));
#75958=CARTESIAN_POINT('Ctrl Pts',(-20.9821194893979,-41.1813764145274,
20.));
#75959=CARTESIAN_POINT('Ctrl Pts',(-21.009885614818,-41.1638976874526,0.));
#75960=CARTESIAN_POINT('Ctrl Pts',(-21.009885614818,-41.1638976874526,20.));
#75961=CARTESIAN_POINT('Ctrl Pts',(-21.0376384311301,-41.1463999288927,
0.));
#75962=CARTESIAN_POINT('Ctrl Pts',(-21.0376384311301,-41.1463999288927,
20.));
#75963=CARTESIAN_POINT('Ctrl Pts',(-21.0653779249329,-41.128883148342,0.));
#75964=CARTESIAN_POINT('Ctrl Pts',(-21.0653779249329,-41.128883148342,20.));
#75965=CARTESIAN_POINT('Ctrl Pts',(-21.0931040828311,-41.1113473553046,
0.));
#75966=CARTESIAN_POINT('Ctrl Pts',(-21.0931040828311,-41.1113473553046,
20.));
#75967=CARTESIAN_POINT('Ctrl Pts',(-21.1208168914355,-41.0937925592943,
0.));
#75968=CARTESIAN_POINT('Ctrl Pts',(-21.1208168914355,-41.0937925592943,
20.));
#75969=CARTESIAN_POINT('Ctrl Pts',(-21.1485163373635,-41.076218769835,0.));
#75970=CARTESIAN_POINT('Ctrl Pts',(-21.1485163373635,-41.076218769835,20.));
#75971=CARTESIAN_POINT('Ctrl Pts',(-21.1762024072388,-41.0586259964597,
0.));
#75972=CARTESIAN_POINT('Ctrl Pts',(-21.1762024072388,-41.0586259964597,
20.));
#75973=CARTESIAN_POINT('Ctrl Pts',(-21.2038750876913,-41.0410142487106,
0.));
#75974=CARTESIAN_POINT('Ctrl Pts',(-21.2038750876913,-41.0410142487106,
20.));
#75975=CARTESIAN_POINT('Ctrl Pts',(-21.2315343653574,-41.0233835361399,
0.));
#75976=CARTESIAN_POINT('Ctrl Pts',(-21.2315343653574,-41.0233835361399,
20.));
#75977=CARTESIAN_POINT('Ctrl Pts',(-21.25918022688,-41.0057338683097,0.));
#75978=CARTESIAN_POINT('Ctrl Pts',(-21.25918022688,-41.0057338683097,20.));
#75979=CARTESIAN_POINT('Ctrl Pts',(-21.286812658909,-40.9880652547927,0.));
#75980=CARTESIAN_POINT('Ctrl Pts',(-21.286812658909,-40.9880652547927,20.));
#75981=CARTESIAN_POINT('Ctrl Pts',(-21.3144316481012,-40.9703777051716,
0.));
#75982=CARTESIAN_POINT('Ctrl Pts',(-21.3144316481012,-40.9703777051716,
20.));
#75983=CARTESIAN_POINT('Ctrl Pts',(-21.342037181119,-40.9526712290373,0.));
#75984=CARTESIAN_POINT('Ctrl Pts',(-21.342037181119,-40.9526712290373,20.));
#75985=CARTESIAN_POINT('Ctrl Pts',(-21.3696292446317,-40.9349458359905,
0.));
#75986=CARTESIAN_POINT('Ctrl Pts',(-21.3696292446317,-40.9349458359905,
20.));
#75987=CARTESIAN_POINT('Ctrl Pts',(-21.3972078253142,-40.9172015356414,
0.));
#75988=CARTESIAN_POINT('Ctrl Pts',(-21.3972078253142,-40.9172015356414,
20.));
#75989=CARTESIAN_POINT('Ctrl Pts',(-21.424772909848,-40.8994383376102,0.));
#75990=CARTESIAN_POINT('Ctrl Pts',(-21.424772909848,-40.8994383376102,20.));
#75991=CARTESIAN_POINT('Ctrl Pts',(-21.45232448492,-40.8816562515268,0.));
#75992=CARTESIAN_POINT('Ctrl Pts',(-21.45232448492,-40.8816562515268,20.));
#75993=CARTESIAN_POINT('Ctrl Pts',(-21.4798625372243,-40.8638552870319,
0.));
#75994=CARTESIAN_POINT('Ctrl Pts',(-21.4798625372243,-40.8638552870319,
20.));
#75995=CARTESIAN_POINT('Ctrl Pts',(-21.5073870534614,-40.8460354537749,
0.));
#75996=CARTESIAN_POINT('Ctrl Pts',(-21.5073870534614,-40.8460354537749,
20.));
#75997=CARTESIAN_POINT('Ctrl Pts',(-21.5348980203391,-40.8281967614155,
0.));
#75998=CARTESIAN_POINT('Ctrl Pts',(-21.5348980203391,-40.8281967614155,
20.));
#75999=CARTESIAN_POINT('Ctrl Pts',(-21.5623954245725,-40.8103392196221,
0.));
#76000=CARTESIAN_POINT('Ctrl Pts',(-21.5623954245725,-40.8103392196221,
20.));
#76001=CARTESIAN_POINT('Ctrl Pts',(-21.5898792528837,-40.7924628380726,
0.));
#76002=CARTESIAN_POINT('Ctrl Pts',(-21.5898792528837,-40.7924628380726,
20.));
#76003=CARTESIAN_POINT('Ctrl Pts',(-21.6173494920019,-40.7745676264537,
0.));
#76004=CARTESIAN_POINT('Ctrl Pts',(-21.6173494920019,-40.7745676264537,
20.));
#76005=CARTESIAN_POINT('Ctrl Pts',(-21.6448061286619,-40.7566535944621,
0.));
#76006=CARTESIAN_POINT('Ctrl Pts',(-21.6448061286619,-40.7566535944621,
20.));
#76007=CARTESIAN_POINT('Ctrl Pts',(-21.6722491496038,-40.7387207518043,
0.));
#76008=CARTESIAN_POINT('Ctrl Pts',(-21.6722491496038,-40.7387207518043,
20.));
#76009=CARTESIAN_POINT('Ctrl Pts',(-21.6996785415723,-40.7207691081984,
0.));
#76010=CARTESIAN_POINT('Ctrl Pts',(-21.6996785415723,-40.7207691081984,
20.));
#76011=CARTESIAN_POINT('Ctrl Pts',(-21.7270942913167,-40.7027986733736,
0.));
#76012=CARTESIAN_POINT('Ctrl Pts',(-21.7270942913167,-40.7027986733736,
20.));
#76013=CARTESIAN_POINT('Ctrl Pts',(-21.7544963855931,-40.6848094570694,
0.));
#76014=CARTESIAN_POINT('Ctrl Pts',(-21.7544963855931,-40.6848094570694,
20.));
#76015=CARTESIAN_POINT('Ctrl Pts',(-21.781884811165,-40.6668014690334,0.));
#76016=CARTESIAN_POINT('Ctrl Pts',(-21.781884811165,-40.6668014690334,20.));
#76017=CARTESIAN_POINT('Ctrl Pts',(-21.8092595548052,-40.6487747190214,
0.));
#76018=CARTESIAN_POINT('Ctrl Pts',(-21.8092595548052,-40.6487747190214,
20.));
#76019=CARTESIAN_POINT('Ctrl Pts',(-21.8366206032979,-40.6307292167951,
0.));
#76020=CARTESIAN_POINT('Ctrl Pts',(-21.8366206032979,-40.6307292167951,
20.));
#76021=CARTESIAN_POINT('Ctrl Pts',(-21.8639679434382,-40.6126649721233,
0.));
#76022=CARTESIAN_POINT('Ctrl Pts',(-21.8639679434382,-40.6126649721233,
20.));
#76023=CARTESIAN_POINT('Ctrl Pts',(-21.8913015620281,-40.594581994783,0.));
#76024=CARTESIAN_POINT('Ctrl Pts',(-21.8913015620281,-40.594581994783,20.));
#76025=CARTESIAN_POINT('Ctrl Pts',(-21.9186214458728,-40.5764802945639,
0.));
#76026=CARTESIAN_POINT('Ctrl Pts',(-21.9186214458728,-40.5764802945639,
20.));
#76027=CARTESIAN_POINT('Ctrl Pts',(-21.9459275817778,-40.5583598812699,
0.));
#76028=CARTESIAN_POINT('Ctrl Pts',(-21.9459275817778,-40.5583598812699,
20.));
#76029=CARTESIAN_POINT('Ctrl Pts',(-21.9732199565439,-40.5402207647219,
0.));
#76030=CARTESIAN_POINT('Ctrl Pts',(-21.9732199565439,-40.5402207647219,
20.));
#76031=CARTESIAN_POINT('Ctrl Pts',(-22.0004985569689,-40.5220629547578,
0.));
#76032=CARTESIAN_POINT('Ctrl Pts',(-22.0004985569689,-40.5220629547578,
20.));
#76033=CARTESIAN_POINT('Ctrl Pts',(-22.0277633698572,-40.5038864612252,
0.));
#76034=CARTESIAN_POINT('Ctrl Pts',(-22.0277633698572,-40.5038864612252,
20.));
#76035=CARTESIAN_POINT('Ctrl Pts',(-22.0550143820281,-40.485691293976,0.));
#76036=CARTESIAN_POINT('Ctrl Pts',(-22.0550143820281,-40.485691293976,20.));
#76037=CARTESIAN_POINT('Ctrl Pts',(-22.0822515803231,-40.4674774628609,
0.));
#76038=CARTESIAN_POINT('Ctrl Pts',(-22.0822515803231,-40.4674774628609,
20.));
#76039=CARTESIAN_POINT('Ctrl Pts',(-22.1094749516164,-40.4492449777204,
0.));
#76040=CARTESIAN_POINT('Ctrl Pts',(-22.1094749516164,-40.4492449777204,
20.));
#76041=CARTESIAN_POINT('Ctrl Pts',(-22.1366844828092,-40.4309938483881,
0.));
#76042=CARTESIAN_POINT('Ctrl Pts',(-22.1366844828092,-40.4309938483881,
20.));
#76043=CARTESIAN_POINT('Ctrl Pts',(-22.1638801608087,-40.4127240847076,
0.));
#76044=CARTESIAN_POINT('Ctrl Pts',(-22.1638801608087,-40.4127240847076,
20.));
#76045=CARTESIAN_POINT('Ctrl Pts',(-22.1910619725087,-40.3944356965472,
0.));
#76046=CARTESIAN_POINT('Ctrl Pts',(-22.1910619725087,-40.3944356965472,
20.));
#76047=CARTESIAN_POINT('Ctrl Pts',(-22.2182299047735,-40.3761286938114,
0.));
#76048=CARTESIAN_POINT('Ctrl Pts',(-22.2182299047735,-40.3761286938114,
20.));
#76049=CARTESIAN_POINT('Ctrl Pts',(-22.2453839444114,-40.357803086462,0.));
#76050=CARTESIAN_POINT('Ctrl Pts',(-22.2453839444114,-40.357803086462,20.));
#76051=CARTESIAN_POINT('Ctrl Pts',(-22.2725240781926,-40.3394588845042,
0.));
#76052=CARTESIAN_POINT('Ctrl Pts',(-22.2725240781926,-40.3394588845042,
20.));
#76053=CARTESIAN_POINT('Ctrl Pts',(-22.2996502928986,-40.3210960979489,
0.));
#76054=CARTESIAN_POINT('Ctrl Pts',(-22.2996502928986,-40.3210960979489,
20.));
#76055=CARTESIAN_POINT('Ctrl Pts',(-22.3267625753671,-40.3027147367803,
0.));
#76056=CARTESIAN_POINT('Ctrl Pts',(-22.3267625753671,-40.3027147367803,
20.));
#76057=CARTESIAN_POINT('Ctrl Pts',(-22.3538609125294,-40.2843148109267,
0.));
#76058=CARTESIAN_POINT('Ctrl Pts',(-22.3538609125294,-40.2843148109267,
20.));
#76059=CARTESIAN_POINT('Ctrl Pts',(-22.3809452914735,-40.2658963302133,
0.));
#76060=CARTESIAN_POINT('Ctrl Pts',(-22.3809452914735,-40.2658963302133,
20.));
#76061=CARTESIAN_POINT('Ctrl Pts',(-22.4080156993888,-40.2474593044019,
0.));
#76062=CARTESIAN_POINT('Ctrl Pts',(-22.4080156993888,-40.2474593044019,
20.));
#76063=CARTESIAN_POINT('Ctrl Pts',(-22.4350721234534,-40.229003743277,0.));
#76064=CARTESIAN_POINT('Ctrl Pts',(-22.4350721234534,-40.229003743277,20.));
#76065=CARTESIAN_POINT('Ctrl Pts',(-22.4621145507305,-40.2105296567239,
0.));
#76066=CARTESIAN_POINT('Ctrl Pts',(-22.4621145507305,-40.2105296567239,
20.));
#76067=CARTESIAN_POINT('Ctrl Pts',(-22.4891429680799,-40.1920370547964,
0.));
#76068=CARTESIAN_POINT('Ctrl Pts',(-22.4891429680799,-40.1920370547964,
20.));
#76069=CARTESIAN_POINT('Ctrl Pts',(-22.5161573620162,-40.1735259478254,
0.));
#76070=CARTESIAN_POINT('Ctrl Pts',(-22.5161573620162,-40.1735259478254,
20.));
#76071=CARTESIAN_POINT('Ctrl Pts',(-22.5431577188606,-40.1549963463026,
0.));
#76072=CARTESIAN_POINT('Ctrl Pts',(-22.5431577188606,-40.1549963463026,
20.));
#76073=CARTESIAN_POINT('Ctrl Pts',(-22.5701440249982,-40.1364482606861,
0.));
#76074=CARTESIAN_POINT('Ctrl Pts',(-22.5701440249982,-40.1364482606861,
20.));
#76075=CARTESIAN_POINT('Ctrl Pts',(-22.5971162671187,-40.1178817012184,
0.));
#76076=CARTESIAN_POINT('Ctrl Pts',(-22.5971162671187,-40.1178817012184,
20.));
#76077=CARTESIAN_POINT('Ctrl Pts',(-22.6240744324259,-40.0992966777668,
0.));
#76078=CARTESIAN_POINT('Ctrl Pts',(-22.6240744324259,-40.0992966777668,
20.));
#76079=CARTESIAN_POINT('Ctrl Pts',(-22.6510185089549,-40.0806931995834,
0.));
#76080=CARTESIAN_POINT('Ctrl Pts',(-22.6510185089549,-40.0806931995834,
20.));
#76081=CARTESIAN_POINT('Ctrl Pts',(-22.6779484851672,-40.0620712756149,
0.));
#76082=CARTESIAN_POINT('Ctrl Pts',(-22.6779484851672,-40.0620712756149,
20.));
#76083=CARTESIAN_POINT('Ctrl Pts',(-22.7048643493645,-40.0434309149416,
0.));
#76084=CARTESIAN_POINT('Ctrl Pts',(-22.7048643493645,-40.0434309149416,
20.));
#76085=CARTESIAN_POINT('Ctrl Pts',(-22.73176608914,-40.0247721271957,0.));
#76086=CARTESIAN_POINT('Ctrl Pts',(-22.73176608914,-40.0247721271957,20.));
#76087=CARTESIAN_POINT('Ctrl Pts',(-22.7586536908732,-40.0060949229408,
0.));
#76088=CARTESIAN_POINT('Ctrl Pts',(-22.7586536908732,-40.0060949229408,
20.));
#76089=CARTESIAN_POINT('Ctrl Pts',(-22.7855271390494,-39.987399314188,0.));
#76090=CARTESIAN_POINT('Ctrl Pts',(-22.7855271390494,-39.987399314188,20.));
#76091=CARTESIAN_POINT('Ctrl Pts',(-22.8123864172494,-39.9686853136472,
0.));
#76092=CARTESIAN_POINT('Ctrl Pts',(-22.8123864172494,-39.9686853136472,
20.));
#76093=CARTESIAN_POINT('Ctrl Pts',(-22.839231509399,-39.9499529337848,0.));
#76094=CARTESIAN_POINT('Ctrl Pts',(-22.839231509399,-39.9499529337848,20.));
#76095=CARTESIAN_POINT('Ctrl Pts',(-22.8660624009432,-39.9312021859374,
0.));
#76096=CARTESIAN_POINT('Ctrl Pts',(-22.8660624009432,-39.9312021859374,
20.));
#76097=CARTESIAN_POINT('Ctrl Pts',(-22.8928790800155,-39.91243307943,0.));
#76098=CARTESIAN_POINT('Ctrl Pts',(-22.8928790800155,-39.91243307943,20.));
#76099=CARTESIAN_POINT('Ctrl Pts',(-22.9196815387084,-39.8936456206159,
0.));
#76100=CARTESIAN_POINT('Ctrl Pts',(-22.9196815387084,-39.8936456206159,
20.));
#76101=CARTESIAN_POINT('Ctrl Pts',(-22.9464697723601,-39.8748398133807,
0.));
#76102=CARTESIAN_POINT('Ctrl Pts',(-22.9464697723601,-39.8748398133807,
20.));
#76103=CARTESIAN_POINT('Ctrl Pts',(-22.9678889774251,-39.8597804904793,
0.));
#76104=CARTESIAN_POINT('Ctrl Pts',(-22.9678889774251,-39.8597804904793,
20.));
#76105=CARTESIAN_POINT('Ctrl Pts',(-22.9839469786126,-39.8484777427633,
0.));
#76106=CARTESIAN_POINT('Ctrl Pts',(-22.9839469786126,-39.8484777427633,
20.));
#76107=CARTESIAN_POINT('Ctrl Pts',(-22.9946494671375,-39.8409389084975,
0.));
#76108=CARTESIAN_POINT('Ctrl Pts',(-22.9946494671375,-39.8409389084975,
20.));
#76109=CARTESIAN_POINT('Ctrl Pts',(-23.,-39.8371685740842,0.));
#76110=CARTESIAN_POINT('Ctrl Pts',(-23.,-39.8371685740842,20.));
#76111=CARTESIAN_POINT('',(-23.,-39.8371685740842,2.));
#76112=CARTESIAN_POINT('',(-23.,-39.8371685740842,0.));
#76113=CARTESIAN_POINT('Ctrl Pts',(-23.,-39.8371685740842,2.));
#76114=CARTESIAN_POINT('Ctrl Pts',(-20.9761380116544,-41.2633137261046,
2.));
#76115=CARTESIAN_POINT('Ctrl Pts',(-18.8450107958689,-42.5215950809686,
2.));
#76116=CARTESIAN_POINT('Ctrl Pts',(-16.6286143535706,-43.6047734830004,
2.));
#76117=CARTESIAN_POINT('Ctrl Pts',(-37.5361777128299,-31.4965928746404,
0.));
#76118=CARTESIAN_POINT('Ctrl Pts',(-37.5361777128299,-31.4965928746404,
20.));
#76119=CARTESIAN_POINT('Ctrl Pts',(-37.5400435810124,-31.4910366171629,
0.));
#76120=CARTESIAN_POINT('Ctrl Pts',(-37.5400435810124,-31.4910366171629,
20.));
#76121=CARTESIAN_POINT('Ctrl Pts',(-37.5477733397939,-31.4799228688318,
0.));
#76122=CARTESIAN_POINT('Ctrl Pts',(-37.5477733397939,-31.4799228688318,
20.));
#76123=CARTESIAN_POINT('Ctrl Pts',(-37.5593620452151,-31.4632485462068,
0.));
#76124=CARTESIAN_POINT('Ctrl Pts',(-37.5593620452151,-31.4632485462068,
20.));
#76125=CARTESIAN_POINT('Ctrl Pts',(-37.574801786924,-31.4410087157717,0.));
#76126=CARTESIAN_POINT('Ctrl Pts',(-37.574801786924,-31.4410087157717,20.));
#76127=CARTESIAN_POINT('Ctrl Pts',(-37.5940816876034,-31.4131965946731,
0.));
#76128=CARTESIAN_POINT('Ctrl Pts',(-37.5940816876034,-31.4131965946731,
20.));
#76129=CARTESIAN_POINT('Ctrl Pts',(-37.6133418102375,-31.3853721428083,
0.));
#76130=CARTESIAN_POINT('Ctrl Pts',(-37.6133418102375,-31.3853721428083,
20.));
#76131=CARTESIAN_POINT('Ctrl Pts',(-37.6325821517747,-31.3575353648538,
0.));
#76132=CARTESIAN_POINT('Ctrl Pts',(-37.6325821517747,-31.3575353648538,
20.));
#76133=CARTESIAN_POINT('Ctrl Pts',(-37.6518027072643,-31.3296862686536,
0.));
#76134=CARTESIAN_POINT('Ctrl Pts',(-37.6518027072643,-31.3296862686536,
20.));
#76135=CARTESIAN_POINT('Ctrl Pts',(-37.6710034693473,-31.3018248661211,
0.));
#76136=CARTESIAN_POINT('Ctrl Pts',(-37.6710034693473,-31.3018248661211,
20.));
#76137=CARTESIAN_POINT('Ctrl Pts',(-37.6901844288974,-31.2739511721649,
0.));
#76138=CARTESIAN_POINT('Ctrl Pts',(-37.6901844288974,-31.2739511721649,
20.));
#76139=CARTESIAN_POINT('Ctrl Pts',(-37.7093455757381,-31.2460652034827,
0.));
#76140=CARTESIAN_POINT('Ctrl Pts',(-37.7093455757381,-31.2460652034827,
20.));
#76141=CARTESIAN_POINT('Ctrl Pts',(-37.7284868993471,-31.2181669773772,
0.));
#76142=CARTESIAN_POINT('Ctrl Pts',(-37.7284868993471,-31.2181669773772,
20.));
#76143=CARTESIAN_POINT('Ctrl Pts',(-37.7476083895316,-31.1902565106222,
0.));
#76144=CARTESIAN_POINT('Ctrl Pts',(-37.7476083895316,-31.1902565106222,
20.));
#76145=CARTESIAN_POINT('Ctrl Pts',(-37.7667100372089,-31.1623338181506,
0.));
#76146=CARTESIAN_POINT('Ctrl Pts',(-37.7667100372089,-31.1623338181506,
20.));
#76147=CARTESIAN_POINT('Ctrl Pts',(-37.7857918342009,-31.1343989133989,
0.));
#76148=CARTESIAN_POINT('Ctrl Pts',(-37.7857918342009,-31.1343989133989,
20.));
#76149=CARTESIAN_POINT('Ctrl Pts',(-37.8048537728749,-31.1064518089103,
0.));
#76150=CARTESIAN_POINT('Ctrl Pts',(-37.8048537728749,-31.1064518089103,
20.));
#76151=CARTESIAN_POINT('Ctrl Pts',(-37.8238958458276,-31.0784925168637,
0.));
#76152=CARTESIAN_POINT('Ctrl Pts',(-37.8238958458276,-31.0784925168637,
20.));
#76153=CARTESIAN_POINT('Ctrl Pts',(-37.8429180455734,-31.0505210495984,
0.));
#76154=CARTESIAN_POINT('Ctrl Pts',(-37.8429180455734,-31.0505210495984,
20.));
#76155=CARTESIAN_POINT('Ctrl Pts',(-37.861920364175,-31.0225374202321,0.));
#76156=CARTESIAN_POINT('Ctrl Pts',(-37.861920364175,-31.0225374202321,20.));
#76157=CARTESIAN_POINT('Ctrl Pts',(-37.8809027932971,-30.9945416425721,
0.));
#76158=CARTESIAN_POINT('Ctrl Pts',(-37.8809027932971,-30.9945416425721,
20.));
#76159=CARTESIAN_POINT('Ctrl Pts',(-37.8998653243731,-30.9665337308352,
0.));
#76160=CARTESIAN_POINT('Ctrl Pts',(-37.8998653243731,-30.9665337308352,
20.));
#76161=CARTESIAN_POINT('Ctrl Pts',(-37.9188079487378,-30.938513699426,0.));
#76162=CARTESIAN_POINT('Ctrl Pts',(-37.9188079487378,-30.938513699426,20.));
#76163=CARTESIAN_POINT('Ctrl Pts',(-37.9377306577632,-30.9104815627079,
0.));
#76164=CARTESIAN_POINT('Ctrl Pts',(-37.9377306577632,-30.9104815627079,
20.));
#76165=CARTESIAN_POINT('Ctrl Pts',(-37.9566334430211,-30.882437334731,0.));
#76166=CARTESIAN_POINT('Ctrl Pts',(-37.9566334430211,-30.882437334731,20.));
#76167=CARTESIAN_POINT('Ctrl Pts',(-37.9755162962752,-30.8543810292446,
0.));
#76168=CARTESIAN_POINT('Ctrl Pts',(-37.9755162962752,-30.8543810292446,
20.));
#76169=CARTESIAN_POINT('Ctrl Pts',(-37.9943792094053,-30.8263126598247,
0.));
#76170=CARTESIAN_POINT('Ctrl Pts',(-37.9943792094053,-30.8263126598247,
20.));
#76171=CARTESIAN_POINT('Ctrl Pts',(-38.0132221743517,-30.7982322399668,
0.));
#76172=CARTESIAN_POINT('Ctrl Pts',(-38.0132221743517,-30.7982322399668,
20.));
#76173=CARTESIAN_POINT('Ctrl Pts',(-38.0320451830565,-30.7701397831859,
0.));
#76174=CARTESIAN_POINT('Ctrl Pts',(-38.0320451830565,-30.7701397831859,
20.));
#76175=CARTESIAN_POINT('Ctrl Pts',(-38.0508482273931,-30.7420353031339,
0.));
#76176=CARTESIAN_POINT('Ctrl Pts',(-38.0508482273931,-30.7420353031339,
20.));
#76177=CARTESIAN_POINT('Ctrl Pts',(-38.0696312991626,-30.7139188136053,
0.));
#76178=CARTESIAN_POINT('Ctrl Pts',(-38.0696312991626,-30.7139188136053,
20.));
#76179=CARTESIAN_POINT('Ctrl Pts',(-38.088394390128,-30.6857903284809,0.));
#76180=CARTESIAN_POINT('Ctrl Pts',(-38.088394390128,-30.6857903284809,20.));
#76181=CARTESIAN_POINT('Ctrl Pts',(-38.1071374920373,-30.6576498616875,
0.));
#76182=CARTESIAN_POINT('Ctrl Pts',(-38.1071374920373,-30.6576498616875,
20.));
#76183=CARTESIAN_POINT('Ctrl Pts',(-38.125860596649,-30.6294974271553,0.));
#76184=CARTESIAN_POINT('Ctrl Pts',(-38.125860596649,-30.6294974271553,20.));
#76185=CARTESIAN_POINT('Ctrl Pts',(-38.1445636957629,-30.6013330387674,
0.));
#76186=CARTESIAN_POINT('Ctrl Pts',(-38.1445636957629,-30.6013330387674,
20.));
#76187=CARTESIAN_POINT('Ctrl Pts',(-38.1632467812242,-30.5731567103519,
0.));
#76188=CARTESIAN_POINT('Ctrl Pts',(-38.1632467812242,-30.5731567103519,
20.));
#76189=CARTESIAN_POINT('Ctrl Pts',(-38.1819098449085,-30.5449684557073,
0.));
#76190=CARTESIAN_POINT('Ctrl Pts',(-38.1819098449085,-30.5449684557073,
20.));
#76191=CARTESIAN_POINT('Ctrl Pts',(-38.2005528787125,-30.5167682886194,
0.));
#76192=CARTESIAN_POINT('Ctrl Pts',(-38.2005528787125,-30.5167682886194,
20.));
#76193=CARTESIAN_POINT('Ctrl Pts',(-38.2191758745422,-30.4885562228796,
0.));
#76194=CARTESIAN_POINT('Ctrl Pts',(-38.2191758745422,-30.4885562228796,
20.));
#76195=CARTESIAN_POINT('Ctrl Pts',(-38.2377788243005,-30.460332272307,0.));
#76196=CARTESIAN_POINT('Ctrl Pts',(-38.2377788243005,-30.460332272307,20.));
#76197=CARTESIAN_POINT('Ctrl Pts',(-38.2563617198829,-30.4320964507535,
0.));
#76198=CARTESIAN_POINT('Ctrl Pts',(-38.2563617198829,-30.4320964507535,
20.));
#76199=CARTESIAN_POINT('Ctrl Pts',(-38.2749245531853,-30.4038487720928,
0.));
#76200=CARTESIAN_POINT('Ctrl Pts',(-38.2749245531853,-30.4038487720928,
20.));
#76201=CARTESIAN_POINT('Ctrl Pts',(-38.2934673161074,-30.3755892502132,
0.));
#76202=CARTESIAN_POINT('Ctrl Pts',(-38.2934673161074,-30.3755892502132,
20.));
#76203=CARTESIAN_POINT('Ctrl Pts',(-38.3119900005578,-30.3473178990095,
0.));
#76204=CARTESIAN_POINT('Ctrl Pts',(-38.3119900005578,-30.3473178990095,
20.));
#76205=CARTESIAN_POINT('Ctrl Pts',(-38.3304925984593,-30.3190347323738,
0.));
#76206=CARTESIAN_POINT('Ctrl Pts',(-38.3304925984593,-30.3190347323738,
20.));
#76207=CARTESIAN_POINT('Ctrl Pts',(-38.3489751017513,-30.2907397641919,
0.));
#76208=CARTESIAN_POINT('Ctrl Pts',(-38.3489751017513,-30.2907397641919,
20.));
#76209=CARTESIAN_POINT('Ctrl Pts',(-38.3674375023871,-30.2624330083488,
0.));
#76210=CARTESIAN_POINT('Ctrl Pts',(-38.3674375023871,-30.2624330083488,
20.));
#76211=CARTESIAN_POINT('Ctrl Pts',(-38.3858797923318,-30.2341144787313,
0.));
#76212=CARTESIAN_POINT('Ctrl Pts',(-38.3858797923318,-30.2341144787313,
20.));
#76213=CARTESIAN_POINT('Ctrl Pts',(-38.4043019635603,-30.2057841892317,
0.));
#76214=CARTESIAN_POINT('Ctrl Pts',(-38.4043019635603,-30.2057841892317,
20.));
#76215=CARTESIAN_POINT('Ctrl Pts',(-38.4227040080549,-30.1774421537519,
0.));
#76216=CARTESIAN_POINT('Ctrl Pts',(-38.4227040080549,-30.1774421537519,
20.));
#76217=CARTESIAN_POINT('Ctrl Pts',(-38.4410859178039,-30.1490883862047,
0.));
#76218=CARTESIAN_POINT('Ctrl Pts',(-38.4410859178039,-30.1490883862047,
20.));
#76219=CARTESIAN_POINT('Ctrl Pts',(-38.4594476848032,-30.1207229005118,
0.));
#76220=CARTESIAN_POINT('Ctrl Pts',(-38.4594476848032,-30.1207229005118,
20.));
#76221=CARTESIAN_POINT('Ctrl Pts',(-38.4777893010568,-30.0923457106026,
0.));
#76222=CARTESIAN_POINT('Ctrl Pts',(-38.4777893010568,-30.0923457106026,
20.));
#76223=CARTESIAN_POINT('Ctrl Pts',(-38.4961107585777,-30.0639568304126,
0.));
#76224=CARTESIAN_POINT('Ctrl Pts',(-38.4961107585777,-30.0639568304126,
20.));
#76225=CARTESIAN_POINT('Ctrl Pts',(-38.5144120493894,-30.0355562738816,
0.));
#76226=CARTESIAN_POINT('Ctrl Pts',(-38.5144120493894,-30.0355562738816,
20.));
#76227=CARTESIAN_POINT('Ctrl Pts',(-38.532693165526,-30.0071440549534,0.));
#76228=CARTESIAN_POINT('Ctrl Pts',(-38.532693165526,-30.0071440549534,20.));
#76229=CARTESIAN_POINT('Ctrl Pts',(-38.5509540990321,-29.978720187576,0.));
#76230=CARTESIAN_POINT('Ctrl Pts',(-38.5509540990321,-29.978720187576,20.));
#76231=CARTESIAN_POINT('Ctrl Pts',(-38.5691948419622,-29.9502846857025,
0.));
#76232=CARTESIAN_POINT('Ctrl Pts',(-38.5691948419622,-29.9502846857025,
20.));
#76233=CARTESIAN_POINT('Ctrl Pts',(-38.5874153863803,-29.9218375632917,
0.));
#76234=CARTESIAN_POINT('Ctrl Pts',(-38.5874153863803,-29.9218375632917,
20.));
#76235=CARTESIAN_POINT('Ctrl Pts',(-38.6056157243597,-29.8933788343089,
0.));
#76236=CARTESIAN_POINT('Ctrl Pts',(-38.6056157243597,-29.8933788343089,
20.));
#76237=CARTESIAN_POINT('Ctrl Pts',(-38.6237958479822,-29.864908512726,0.));
#76238=CARTESIAN_POINT('Ctrl Pts',(-38.6237958479822,-29.864908512726,20.));
#76239=CARTESIAN_POINT('Ctrl Pts',(-38.6419557493389,-29.8364266125215,
0.));
#76240=CARTESIAN_POINT('Ctrl Pts',(-38.6419557493389,-29.8364266125215,
20.));
#76241=CARTESIAN_POINT('Ctrl Pts',(-38.66009542053,-29.8079331476799,0.));
#76242=CARTESIAN_POINT('Ctrl Pts',(-38.66009542053,-29.8079331476799,20.));
#76243=CARTESIAN_POINT('Ctrl Pts',(-38.6782148536649,-29.7794281321916,
0.));
#76244=CARTESIAN_POINT('Ctrl Pts',(-38.6782148536649,-29.7794281321916,
20.));
#76245=CARTESIAN_POINT('Ctrl Pts',(-38.6963140408627,-29.7509115800524,
0.));
#76246=CARTESIAN_POINT('Ctrl Pts',(-38.6963140408627,-29.7509115800524,
20.));
#76247=CARTESIAN_POINT('Ctrl Pts',(-38.7143929742521,-29.7223835052637,
0.));
#76248=CARTESIAN_POINT('Ctrl Pts',(-38.7143929742521,-29.7223835052637,
20.));
#76249=CARTESIAN_POINT('Ctrl Pts',(-38.7324516459718,-29.6938439218325,
0.));
#76250=CARTESIAN_POINT('Ctrl Pts',(-38.7324516459718,-29.6938439218325,
20.));
#76251=CARTESIAN_POINT('Ctrl Pts',(-38.7504900481697,-29.6652928437714,
0.));
#76252=CARTESIAN_POINT('Ctrl Pts',(-38.7504900481697,-29.6652928437714,
20.));
#76253=CARTESIAN_POINT('Ctrl Pts',(-38.7685081730036,-29.6367302850988,
0.));
#76254=CARTESIAN_POINT('Ctrl Pts',(-38.7685081730036,-29.6367302850988,
20.));
#76255=CARTESIAN_POINT('Ctrl Pts',(-38.7865060126402,-29.6081562598384,
0.));
#76256=CARTESIAN_POINT('Ctrl Pts',(-38.7865060126402,-29.6081562598384,
20.));
#76257=CARTESIAN_POINT('Ctrl Pts',(-38.8044835592559,-29.5795707820205,
0.));
#76258=CARTESIAN_POINT('Ctrl Pts',(-38.8044835592559,-29.5795707820205,
20.));
#76259=CARTESIAN_POINT('Ctrl Pts',(-38.8224408050366,-29.5509738656807,
0.));
#76260=CARTESIAN_POINT('Ctrl Pts',(-38.8224408050366,-29.5509738656807,
20.));
#76261=CARTESIAN_POINT('Ctrl Pts',(-38.8403777421773,-29.5223655248609,
0.));
#76262=CARTESIAN_POINT('Ctrl Pts',(-38.8403777421773,-29.5223655248609,
20.));
#76263=CARTESIAN_POINT('Ctrl Pts',(-38.8582943628826,-29.4937457736083,
0.));
#76264=CARTESIAN_POINT('Ctrl Pts',(-38.8582943628826,-29.4937457736083,
20.));
#76265=CARTESIAN_POINT('Ctrl Pts',(-38.8761906593666,-29.4651146259764,
0.));
#76266=CARTESIAN_POINT('Ctrl Pts',(-38.8761906593666,-29.4651146259764,
20.));
#76267=CARTESIAN_POINT('Ctrl Pts',(-38.8940666238533,-29.4364720960241,
0.));
#76268=CARTESIAN_POINT('Ctrl Pts',(-38.8940666238533,-29.4364720960241,
20.));
#76269=CARTESIAN_POINT('Ctrl Pts',(-38.9119222485755,-29.4078181978158,
0.));
#76270=CARTESIAN_POINT('Ctrl Pts',(-38.9119222485755,-29.4078181978158,
20.));
#76271=CARTESIAN_POINT('Ctrl Pts',(-38.9297575257761,-29.3791529454216,
0.));
#76272=CARTESIAN_POINT('Ctrl Pts',(-38.9297575257761,-29.3791529454216,
20.));
#76273=CARTESIAN_POINT('Ctrl Pts',(-38.9475724477072,-29.3504763529173,
0.));
#76274=CARTESIAN_POINT('Ctrl Pts',(-38.9475724477072,-29.3504763529173,
20.));
#76275=CARTESIAN_POINT('Ctrl Pts',(-38.9653670066308,-29.3217884343845,
0.));
#76276=CARTESIAN_POINT('Ctrl Pts',(-38.9653670066308,-29.3217884343845,
20.));
#76277=CARTESIAN_POINT('Ctrl Pts',(-38.9831411948183,-29.2930892039104,
0.));
#76278=CARTESIAN_POINT('Ctrl Pts',(-38.9831411948183,-29.2930892039104,
20.));
#76279=CARTESIAN_POINT('Ctrl Pts',(-39.0008950045503,-29.2643786755883,
0.));
#76280=CARTESIAN_POINT('Ctrl Pts',(-39.0008950045503,-29.2643786755883,
20.));
#76281=CARTESIAN_POINT('Ctrl Pts',(-39.0186284281173,-29.2356568635168,
0.));
#76282=CARTESIAN_POINT('Ctrl Pts',(-39.0186284281173,-29.2356568635168,
20.));
#76283=CARTESIAN_POINT('Ctrl Pts',(-39.0363414578191,-29.2069237818005,
0.));
#76284=CARTESIAN_POINT('Ctrl Pts',(-39.0363414578191,-29.2069237818005,
20.));
#76285=CARTESIAN_POINT('Ctrl Pts',(-39.054034085965,-29.1781794445493,0.));
#76286=CARTESIAN_POINT('Ctrl Pts',(-39.054034085965,-29.1781794445493,20.));
#76287=CARTESIAN_POINT('Ctrl Pts',(-39.0717063048737,-29.1494238658788,
0.));
#76288=CARTESIAN_POINT('Ctrl Pts',(-39.0717063048737,-29.1494238658788,
20.));
#76289=CARTESIAN_POINT('Ctrl Pts',(-39.0893581068737,-29.1206570599103,
0.));
#76290=CARTESIAN_POINT('Ctrl Pts',(-39.0893581068737,-29.1206570599103,
20.));
#76291=CARTESIAN_POINT('Ctrl Pts',(-39.106989484303,-29.0918790407708,0.));
#76292=CARTESIAN_POINT('Ctrl Pts',(-39.106989484303,-29.0918790407708,20.));
#76293=CARTESIAN_POINT('Ctrl Pts',(-39.1246004295092,-29.0630898225929,
0.));
#76294=CARTESIAN_POINT('Ctrl Pts',(-39.1246004295092,-29.0630898225929,
20.));
#76295=CARTESIAN_POINT('Ctrl Pts',(-39.1421909348497,-29.034289419515,0.));
#76296=CARTESIAN_POINT('Ctrl Pts',(-39.1421909348497,-29.034289419515,20.));
#76297=CARTESIAN_POINT('Ctrl Pts',(-39.1597609926911,-29.0054778456813,
0.));
#76298=CARTESIAN_POINT('Ctrl Pts',(-39.1597609926911,-29.0054778456813,
20.));
#76299=CARTESIAN_POINT('Ctrl Pts',(-39.1773105954099,-28.9766551152413,
0.));
#76300=CARTESIAN_POINT('Ctrl Pts',(-39.1773105954099,-28.9766551152413,
20.));
#76301=CARTESIAN_POINT('Ctrl Pts',(-39.1948397353917,-28.9478212423503,
0.));
#76302=CARTESIAN_POINT('Ctrl Pts',(-39.1948397353917,-28.9478212423503,
20.));
#76303=CARTESIAN_POINT('Ctrl Pts',(-39.2123484050317,-28.9189762411689,
0.));
#76304=CARTESIAN_POINT('Ctrl Pts',(-39.2123484050317,-28.9189762411689,
20.));
#76305=CARTESIAN_POINT('Ctrl Pts',(-39.2298365967351,-28.8901201258634,
0.));
#76306=CARTESIAN_POINT('Ctrl Pts',(-39.2298365967351,-28.8901201258634,
20.));
#76307=CARTESIAN_POINT('Ctrl Pts',(-39.2473043029163,-28.8612529106058,
0.));
#76308=CARTESIAN_POINT('Ctrl Pts',(-39.2473043029163,-28.8612529106058,
20.));
#76309=CARTESIAN_POINT('Ctrl Pts',(-39.2647515159997,-28.8323746095736,
0.));
#76310=CARTESIAN_POINT('Ctrl Pts',(-39.2647515159997,-28.8323746095736,
20.));
#76311=CARTESIAN_POINT('Ctrl Pts',(-39.2821782284193,-28.80348523695,0.));
#76312=CARTESIAN_POINT('Ctrl Pts',(-39.2821782284193,-28.80348523695,20.));
#76313=CARTESIAN_POINT('Ctrl Pts',(-39.2995844326181,-28.7745848069238,
0.));
#76314=CARTESIAN_POINT('Ctrl Pts',(-39.2995844326181,-28.7745848069238,
20.));
#76315=CARTESIAN_POINT('Ctrl Pts',(-39.316970121049,-28.7456733336894,0.));
#76316=CARTESIAN_POINT('Ctrl Pts',(-39.316970121049,-28.7456733336894,20.));
#76317=CARTESIAN_POINT('Ctrl Pts',(-39.3343352861746,-28.7167508314468,
0.));
#76318=CARTESIAN_POINT('Ctrl Pts',(-39.3343352861746,-28.7167508314468,
20.));
#76319=CARTESIAN_POINT('Ctrl Pts',(-39.3516799204672,-28.6878173144015,
0.));
#76320=CARTESIAN_POINT('Ctrl Pts',(-39.3516799204672,-28.6878173144015,
20.));
#76321=CARTESIAN_POINT('Ctrl Pts',(-39.3690040164086,-28.6588727967647,
0.));
#76322=CARTESIAN_POINT('Ctrl Pts',(-39.3690040164086,-28.6588727967647,
20.));
#76323=CARTESIAN_POINT('Ctrl Pts',(-39.3863075664906,-28.6299172927529,
0.));
#76324=CARTESIAN_POINT('Ctrl Pts',(-39.3863075664906,-28.6299172927529,
20.));
#76325=CARTESIAN_POINT('Ctrl Pts',(-39.4035905632141,-28.600950816588,0.));
#76326=CARTESIAN_POINT('Ctrl Pts',(-39.4035905632141,-28.600950816588,20.));
#76327=CARTESIAN_POINT('Ctrl Pts',(-39.4208529990894,-28.5719733824975,
0.));
#76328=CARTESIAN_POINT('Ctrl Pts',(-39.4208529990894,-28.5719733824975,
20.));
#76329=CARTESIAN_POINT('Ctrl Pts',(-39.4380948666368,-28.5429850047148,
0.));
#76330=CARTESIAN_POINT('Ctrl Pts',(-39.4380948666368,-28.5429850047148,
20.));
#76331=CARTESIAN_POINT('Ctrl Pts',(-39.4553161583861,-28.5139856974786,
0.));
#76332=CARTESIAN_POINT('Ctrl Pts',(-39.4553161583861,-28.5139856974786,
20.));
#76333=CARTESIAN_POINT('Ctrl Pts',(-39.4725168668771,-28.4849754750331,
0.));
#76334=CARTESIAN_POINT('Ctrl Pts',(-39.4725168668771,-28.4849754750331,
20.));
#76335=CARTESIAN_POINT('Ctrl Pts',(-39.4896969846589,-28.455954351628,0.));
#76336=CARTESIAN_POINT('Ctrl Pts',(-39.4896969846589,-28.455954351628,20.));
#76337=CARTESIAN_POINT('Ctrl Pts',(-39.5068565042907,-28.4269223415187,
0.));
#76338=CARTESIAN_POINT('Ctrl Pts',(-39.5068565042907,-28.4269223415187,
20.));
#76339=CARTESIAN_POINT('Ctrl Pts',(-39.5239954183412,-28.3978794589661,
0.));
#76340=CARTESIAN_POINT('Ctrl Pts',(-39.5239954183412,-28.3978794589661,
20.));
#76341=CARTESIAN_POINT('Ctrl Pts',(-39.5411137193887,-28.3688257182364,
0.));
#76342=CARTESIAN_POINT('Ctrl Pts',(-39.5411137193887,-28.3688257182364,
20.));
#76343=CARTESIAN_POINT('Ctrl Pts',(-39.5582114000212,-28.3397611336014,
0.));
#76344=CARTESIAN_POINT('Ctrl Pts',(-39.5582114000212,-28.3397611336014,
20.));
#76345=CARTESIAN_POINT('Ctrl Pts',(-39.5752884528361,-28.3106857193381,
0.));
#76346=CARTESIAN_POINT('Ctrl Pts',(-39.5752884528361,-28.3106857193381,
20.));
#76347=CARTESIAN_POINT('Ctrl Pts',(-39.5923448704403,-28.2815994897291,
0.));
#76348=CARTESIAN_POINT('Ctrl Pts',(-39.5923448704403,-28.2815994897291,
20.));
#76349=CARTESIAN_POINT('Ctrl Pts',(-39.6093806454502,-28.2525024590626,
0.));
#76350=CARTESIAN_POINT('Ctrl Pts',(-39.6093806454502,-28.2525024590626,
20.));
#76351=CARTESIAN_POINT('Ctrl Pts',(-39.6263957704923,-28.2233946416323,
0.));
#76352=CARTESIAN_POINT('Ctrl Pts',(-39.6263957704923,-28.2233946416323,
20.));
#76353=CARTESIAN_POINT('Ctrl Pts',(-39.6433902382029,-28.1942760517371,
0.));
#76354=CARTESIAN_POINT('Ctrl Pts',(-39.6433902382029,-28.1942760517371,
20.));
#76355=CARTESIAN_POINT('Ctrl Pts',(-39.6603640412281,-28.1651467036817,
0.));
#76356=CARTESIAN_POINT('Ctrl Pts',(-39.6603640412281,-28.1651467036817,
20.));
#76357=CARTESIAN_POINT('Ctrl Pts',(-39.6773171722241,-28.136006611776,0.));
#76358=CARTESIAN_POINT('Ctrl Pts',(-39.6773171722241,-28.136006611776,20.));
#76359=CARTESIAN_POINT('Ctrl Pts',(-39.6942496238565,-28.1068557903356,
0.));
#76360=CARTESIAN_POINT('Ctrl Pts',(-39.6942496238565,-28.1068557903356,
20.));
#76361=CARTESIAN_POINT('Ctrl Pts',(-39.7111613888006,-28.0776942536814,
0.));
#76362=CARTESIAN_POINT('Ctrl Pts',(-39.7111613888006,-28.0776942536814,
20.));
#76363=CARTESIAN_POINT('Ctrl Pts',(-39.728052459741,-28.0485220161395,0.));
#76364=CARTESIAN_POINT('Ctrl Pts',(-39.728052459741,-28.0485220161395,20.));
#76365=CARTESIAN_POINT('Ctrl Pts',(-39.7449228293718,-28.0193390920415,
0.));
#76366=CARTESIAN_POINT('Ctrl Pts',(-39.7449228293718,-28.0193390920415,
20.));
#76367=CARTESIAN_POINT('Ctrl Pts',(-39.7617724903968,-27.9901454957246,
0.));
#76368=CARTESIAN_POINT('Ctrl Pts',(-39.7617724903968,-27.9901454957246,
20.));
#76369=CARTESIAN_POINT('Ctrl Pts',(-39.7786014355293,-27.960941241531,0.));
#76370=CARTESIAN_POINT('Ctrl Pts',(-39.7786014355293,-27.960941241531,20.));
#76371=CARTESIAN_POINT('Ctrl Pts',(-39.795409657493,-27.9317263438086,0.));
#76372=CARTESIAN_POINT('Ctrl Pts',(-39.795409657493,-27.9317263438086,20.));
#76373=CARTESIAN_POINT('Ctrl Pts',(-39.8121971490214,-27.9025008169107,
0.));
#76374=CARTESIAN_POINT('Ctrl Pts',(-39.8121971490214,-27.9025008169107,
20.));
#76375=CARTESIAN_POINT('Ctrl Pts',(-39.828963902858,-27.8732646751959,0.));
#76376=CARTESIAN_POINT('Ctrl Pts',(-39.828963902858,-27.8732646751959,20.));
#76377=CARTESIAN_POINT('Ctrl Pts',(-39.845709911756,-27.8440179330284,0.));
#76378=CARTESIAN_POINT('Ctrl Pts',(-39.845709911756,-27.8440179330284,20.));
#76379=CARTESIAN_POINT('Ctrl Pts',(-39.8624351684781,-27.8147606047778,
0.));
#76380=CARTESIAN_POINT('Ctrl Pts',(-39.8624351684781,-27.8147606047778,
20.));
#76381=CARTESIAN_POINT('Ctrl Pts',(-39.8791396657966,-27.785492704819,0.));
#76382=CARTESIAN_POINT('Ctrl Pts',(-39.8791396657966,-27.785492704819,20.));
#76383=CARTESIAN_POINT('Ctrl Pts',(-39.8958233964934,-27.7562142475319,
0.));
#76384=CARTESIAN_POINT('Ctrl Pts',(-39.8958233964934,-27.7562142475319,
20.));
#76385=CARTESIAN_POINT('Ctrl Pts',(-39.9124863533599,-27.726925247302,0.));
#76386=CARTESIAN_POINT('Ctrl Pts',(-39.9124863533599,-27.726925247302,20.));
#76387=CARTESIAN_POINT('Ctrl Pts',(-39.9291285291975,-27.6976257185198,
0.));
#76388=CARTESIAN_POINT('Ctrl Pts',(-39.9291285291975,-27.6976257185198,
20.));
#76389=CARTESIAN_POINT('Ctrl Pts',(-39.9457499168175,-27.6683156755815,
0.));
#76390=CARTESIAN_POINT('Ctrl Pts',(-39.9457499168175,-27.6683156755815,
20.));
#76391=CARTESIAN_POINT('Ctrl Pts',(-39.9623505090412,-27.6389951328887,
0.));
#76392=CARTESIAN_POINT('Ctrl Pts',(-39.9623505090412,-27.6389951328887,
20.));
#76393=CARTESIAN_POINT('Ctrl Pts',(-39.9789302986995,-27.6096641048483,
0.));
#76394=CARTESIAN_POINT('Ctrl Pts',(-39.9789302986995,-27.6096641048483,
20.));
#76395=CARTESIAN_POINT('Ctrl Pts',(-39.9954892786331,-27.5803226058724,
0.));
#76396=CARTESIAN_POINT('Ctrl Pts',(-39.9954892786331,-27.5803226058724,
20.));
#76397=CARTESIAN_POINT('Ctrl Pts',(-40.0120274416924,-27.5509706503786,
0.));
#76398=CARTESIAN_POINT('Ctrl Pts',(-40.0120274416924,-27.5509706503786,
20.));
#76399=CARTESIAN_POINT('Ctrl Pts',(-40.0285447807378,-27.5216082527897,
0.));
#76400=CARTESIAN_POINT('Ctrl Pts',(-40.0285447807378,-27.5216082527897,
20.));
#76401=CARTESIAN_POINT('Ctrl Pts',(-40.045041288639,-27.4922354275335,0.));
#76402=CARTESIAN_POINT('Ctrl Pts',(-40.045041288639,-27.4922354275335,20.));
#76403=CARTESIAN_POINT('Ctrl Pts',(-40.0615169582759,-27.4628521890436,
0.));
#76404=CARTESIAN_POINT('Ctrl Pts',(-40.0615169582759,-27.4628521890436,
20.));
#76405=CARTESIAN_POINT('Ctrl Pts',(-40.077971782538,-27.4334585517582,0.));
#76406=CARTESIAN_POINT('Ctrl Pts',(-40.077971782538,-27.4334585517582,20.));
#76407=CARTESIAN_POINT('Ctrl Pts',(-40.0944057543248,-27.4040545301216,
0.));
#76408=CARTESIAN_POINT('Ctrl Pts',(-40.0944057543248,-27.4040545301216,
20.));
#76409=CARTESIAN_POINT('Ctrl Pts',(-40.1108188665452,-27.374640138583,0.));
#76410=CARTESIAN_POINT('Ctrl Pts',(-40.1108188665452,-27.374640138583,20.));
#76411=CARTESIAN_POINT('Ctrl Pts',(-40.1272111121183,-27.3452153915969,
0.));
#76412=CARTESIAN_POINT('Ctrl Pts',(-40.1272111121183,-27.3452153915969,
20.));
#76413=CARTESIAN_POINT('Ctrl Pts',(-40.1435824839731,-27.3157803036231,
0.));
#76414=CARTESIAN_POINT('Ctrl Pts',(-40.1435824839731,-27.3157803036231,
20.));
#76415=CARTESIAN_POINT('Ctrl Pts',(-40.1599329750483,-27.2863348891265,
0.));
#76416=CARTESIAN_POINT('Ctrl Pts',(-40.1599329750483,-27.2863348891265,
20.));
#76417=CARTESIAN_POINT('Ctrl Pts',(-40.1762625782924,-27.2568791625774,
0.));
#76418=CARTESIAN_POINT('Ctrl Pts',(-40.1762625782924,-27.2568791625774,
20.));
#76419=CARTESIAN_POINT('Ctrl Pts',(-40.1925712866631,-27.2274131384508,
0.));
#76420=CARTESIAN_POINT('Ctrl Pts',(-40.1925712866631,-27.2274131384508,
20.));
#76421=CARTESIAN_POINT('Ctrl Pts',(-40.2088590931287,-27.1979368312277,
0.));
#76422=CARTESIAN_POINT('Ctrl Pts',(-40.2088590931287,-27.1979368312277,
20.));
#76423=CARTESIAN_POINT('Ctrl Pts',(-40.225125990667,-27.1684502553939,0.));
#76424=CARTESIAN_POINT('Ctrl Pts',(-40.225125990667,-27.1684502553939,20.));
#76425=CARTESIAN_POINT('Ctrl Pts',(-40.2413719722657,-27.1389534254409,
0.));
#76426=CARTESIAN_POINT('Ctrl Pts',(-40.2413719722657,-27.1389534254409,
20.));
#76427=CARTESIAN_POINT('Ctrl Pts',(-40.2575970309226,-27.1094463558649,
0.));
#76428=CARTESIAN_POINT('Ctrl Pts',(-40.2575970309226,-27.1094463558649,
20.));
#76429=CARTESIAN_POINT('Ctrl Pts',(-40.2738011596454,-27.0799290611676,
0.));
#76430=CARTESIAN_POINT('Ctrl Pts',(-40.2738011596454,-27.0799290611676,
20.));
#76431=CARTESIAN_POINT('Ctrl Pts',(-40.2899843514517,-27.0504015558557,
0.));
#76432=CARTESIAN_POINT('Ctrl Pts',(-40.2899843514517,-27.0504015558557,
20.));
#76433=CARTESIAN_POINT('Ctrl Pts',(-40.3061465993685,-27.0208638544413,
0.));
#76434=CARTESIAN_POINT('Ctrl Pts',(-40.3061465993685,-27.0208638544413,
20.));
#76435=CARTESIAN_POINT('Ctrl Pts',(-40.3222878964329,-26.9913159714415,
0.));
#76436=CARTESIAN_POINT('Ctrl Pts',(-40.3222878964329,-26.9913159714415,
20.));
#76437=CARTESIAN_POINT('Ctrl Pts',(-40.3384082356913,-26.9617579213786,
0.));
#76438=CARTESIAN_POINT('Ctrl Pts',(-40.3384082356913,-26.9617579213786,
20.));
#76439=CARTESIAN_POINT('Ctrl Pts',(-40.3545076102003,-26.9321897187802,
0.));
#76440=CARTESIAN_POINT('Ctrl Pts',(-40.3545076102003,-26.9321897187802,
20.));
#76441=CARTESIAN_POINT('Ctrl Pts',(-40.3705860130263,-26.9026113781788,
0.));
#76442=CARTESIAN_POINT('Ctrl Pts',(-40.3705860130263,-26.9026113781788,
20.));
#76443=CARTESIAN_POINT('Ctrl Pts',(-40.386643437246,-26.8730229141124,0.));
#76444=CARTESIAN_POINT('Ctrl Pts',(-40.386643437246,-26.8730229141124,20.));
#76445=CARTESIAN_POINT('Ctrl Pts',(-40.4026798759458,-26.8434243411241,
0.));
#76446=CARTESIAN_POINT('Ctrl Pts',(-40.4026798759458,-26.8434243411241,
20.));
#76447=CARTESIAN_POINT('Ctrl Pts',(-40.4186953222224,-26.8138156737619,
0.));
#76448=CARTESIAN_POINT('Ctrl Pts',(-40.4186953222224,-26.8138156737619,
20.));
#76449=CARTESIAN_POINT('Ctrl Pts',(-40.4346897691821,-26.7841969265794,
0.));
#76450=CARTESIAN_POINT('Ctrl Pts',(-40.4346897691821,-26.7841969265794,
20.));
#76451=CARTESIAN_POINT('Ctrl Pts',(-40.4506632099408,-26.754568114135,0.));
#76452=CARTESIAN_POINT('Ctrl Pts',(-40.4506632099408,-26.754568114135,20.));
#76453=CARTESIAN_POINT('Ctrl Pts',(-40.4666156376241,-26.7249292509923,
0.));
#76454=CARTESIAN_POINT('Ctrl Pts',(-40.4666156376241,-26.7249292509923,
20.));
#76455=CARTESIAN_POINT('Ctrl Pts',(-40.4825470453679,-26.6952803517197,
0.));
#76456=CARTESIAN_POINT('Ctrl Pts',(-40.4825470453679,-26.6952803517197,
20.));
#76457=CARTESIAN_POINT('Ctrl Pts',(-40.4984574263178,-26.6656214308914,
0.));
#76458=CARTESIAN_POINT('Ctrl Pts',(-40.4984574263178,-26.6656214308914,
20.));
#76459=CARTESIAN_POINT('Ctrl Pts',(-40.5143467736295,-26.6359525030862,
0.));
#76460=CARTESIAN_POINT('Ctrl Pts',(-40.5143467736295,-26.6359525030862,
20.));
#76461=CARTESIAN_POINT('Ctrl Pts',(-40.5302150804687,-26.606273582888,0.));
#76462=CARTESIAN_POINT('Ctrl Pts',(-40.5302150804687,-26.606273582888,20.));
#76463=CARTESIAN_POINT('Ctrl Pts',(-40.546062340011,-26.5765846848862,0.));
#76464=CARTESIAN_POINT('Ctrl Pts',(-40.546062340011,-26.5765846848862,20.));
#76465=CARTESIAN_POINT('Ctrl Pts',(-40.5618885454414,-26.5468858236748,
0.));
#76466=CARTESIAN_POINT('Ctrl Pts',(-40.5618885454414,-26.5468858236748,
20.));
#76467=CARTESIAN_POINT('Ctrl Pts',(-40.5776936899555,-26.5171770138532,
0.));
#76468=CARTESIAN_POINT('Ctrl Pts',(-40.5776936899555,-26.5171770138532,
20.));
#76469=CARTESIAN_POINT('Ctrl Pts',(-40.5934777667583,-26.4874582700259,
0.));
#76470=CARTESIAN_POINT('Ctrl Pts',(-40.5934777667583,-26.4874582700259,
20.));
#76471=CARTESIAN_POINT('Ctrl Pts',(-40.6092407690651,-26.4577296068023,
0.));
#76472=CARTESIAN_POINT('Ctrl Pts',(-40.6092407690651,-26.4577296068023,
20.));
#76473=CARTESIAN_POINT('Ctrl Pts',(-40.6249826901011,-26.427991038797,0.));
#76474=CARTESIAN_POINT('Ctrl Pts',(-40.6249826901011,-26.427991038797,20.));
#76475=CARTESIAN_POINT('Ctrl Pts',(-40.6407035231015,-26.3982425806297,
0.));
#76476=CARTESIAN_POINT('Ctrl Pts',(-40.6407035231015,-26.3982425806297,
20.));
#76477=CARTESIAN_POINT('Ctrl Pts',(-40.6564032613109,-26.3684842469248,
0.));
#76478=CARTESIAN_POINT('Ctrl Pts',(-40.6564032613109,-26.3684842469248,
20.));
#76479=CARTESIAN_POINT('Ctrl Pts',(-40.6720818979844,-26.338716052312,0.));
#76480=CARTESIAN_POINT('Ctrl Pts',(-40.6720818979844,-26.338716052312,20.));
#76481=CARTESIAN_POINT('Ctrl Pts',(-40.6877394263869,-26.308938011426,0.));
#76482=CARTESIAN_POINT('Ctrl Pts',(-40.6877394263869,-26.308938011426,20.));
#76483=CARTESIAN_POINT('Ctrl Pts',(-40.7033758397932,-26.2791501389067,
0.));
#76484=CARTESIAN_POINT('Ctrl Pts',(-40.7033758397932,-26.2791501389067,
20.));
#76485=CARTESIAN_POINT('Ctrl Pts',(-40.7189911314882,-26.2493524493989,
0.));
#76486=CARTESIAN_POINT('Ctrl Pts',(-40.7189911314882,-26.2493524493989,
20.));
#76487=CARTESIAN_POINT('Ctrl Pts',(-40.7345852947664,-26.2195449575524,
0.));
#76488=CARTESIAN_POINT('Ctrl Pts',(-40.7345852947664,-26.2195449575524,
20.));
#76489=CARTESIAN_POINT('Ctrl Pts',(-40.7501583229328,-26.1897276780219,
0.));
#76490=CARTESIAN_POINT('Ctrl Pts',(-40.7501583229328,-26.1897276780219,
20.));
#76491=CARTESIAN_POINT('Ctrl Pts',(-40.7657102093021,-26.1599006254674,
0.));
#76492=CARTESIAN_POINT('Ctrl Pts',(-40.7657102093021,-26.1599006254674,
20.));
#76493=CARTESIAN_POINT('Ctrl Pts',(-40.7812409471992,-26.1300638145535,
0.));
#76494=CARTESIAN_POINT('Ctrl Pts',(-40.7812409471992,-26.1300638145535,
20.));
#76495=CARTESIAN_POINT('Ctrl Pts',(-40.7967505299588,-26.1002172599501,
0.));
#76496=CARTESIAN_POINT('Ctrl Pts',(-40.7967505299588,-26.1002172599501,
20.));
#76497=CARTESIAN_POINT('Ctrl Pts',(-40.8122389509256,-26.0703609763318,
0.));
#76498=CARTESIAN_POINT('Ctrl Pts',(-40.8122389509256,-26.0703609763318,
20.));
#76499=CARTESIAN_POINT('Ctrl Pts',(-40.8277062034539,-26.0404949783787,
0.));
#76500=CARTESIAN_POINT('Ctrl Pts',(-40.8277062034539,-26.0404949783787,
20.));
#76501=CARTESIAN_POINT('Ctrl Pts',(-40.843152280908,-26.0106192807756,0.));
#76502=CARTESIAN_POINT('Ctrl Pts',(-40.843152280908,-26.0106192807756,20.));
#76503=CARTESIAN_POINT('Ctrl Pts',(-40.8585771766627,-25.9807338982121,
0.));
#76504=CARTESIAN_POINT('Ctrl Pts',(-40.8585771766627,-25.9807338982121,
20.));
#76505=CARTESIAN_POINT('Ctrl Pts',(-40.8739808841024,-25.950838845383,0.));
#76506=CARTESIAN_POINT('Ctrl Pts',(-40.8739808841024,-25.950838845383,20.));
#76507=CARTESIAN_POINT('Ctrl Pts',(-40.8893633966224,-25.9209341369879,
0.));
#76508=CARTESIAN_POINT('Ctrl Pts',(-40.8893633966224,-25.9209341369879,
20.));
#76509=CARTESIAN_POINT('Ctrl Pts',(-40.9047247076274,-25.891019787731,0.));
#76510=CARTESIAN_POINT('Ctrl Pts',(-40.9047247076274,-25.891019787731,20.));
#76511=CARTESIAN_POINT('Ctrl Pts',(-40.9200648105322,-25.861095812322,0.));
#76512=CARTESIAN_POINT('Ctrl Pts',(-40.9200648105322,-25.861095812322,20.));
#76513=CARTESIAN_POINT('Ctrl Pts',(-40.9353836987613,-25.8311622254754,
0.));
#76514=CARTESIAN_POINT('Ctrl Pts',(-40.9353836987613,-25.8311622254754,
20.));
#76515=CARTESIAN_POINT('Ctrl Pts',(-40.9506813657491,-25.8012190419102,
0.));
#76516=CARTESIAN_POINT('Ctrl Pts',(-40.9506813657491,-25.8012190419102,
20.));
#76517=CARTESIAN_POINT('Ctrl Pts',(-40.9659578049399,-25.7712662763511,
0.));
#76518=CARTESIAN_POINT('Ctrl Pts',(-40.9659578049399,-25.7712662763511,
20.));
#76519=CARTESIAN_POINT('Ctrl Pts',(-40.981213009789,-25.7413039435271,0.));
#76520=CARTESIAN_POINT('Ctrl Pts',(-40.981213009789,-25.7413039435271,20.));
#76521=CARTESIAN_POINT('Ctrl Pts',(-40.9964469737613,-25.7113320581728,
0.));
#76522=CARTESIAN_POINT('Ctrl Pts',(-40.9964469737613,-25.7113320581728,
20.));
#76523=CARTESIAN_POINT('Ctrl Pts',(-41.0116596903317,-25.6813506350271,
0.));
#76524=CARTESIAN_POINT('Ctrl Pts',(-41.0116596903317,-25.6813506350271,
20.));
#76525=CARTESIAN_POINT('Ctrl Pts',(-41.0268511529852,-25.6513596888338,
0.));
#76526=CARTESIAN_POINT('Ctrl Pts',(-41.0268511529852,-25.6513596888338,
20.));
#76527=CARTESIAN_POINT('Ctrl Pts',(-41.0420213552163,-25.6213592343415,
0.));
#76528=CARTESIAN_POINT('Ctrl Pts',(-41.0420213552163,-25.6213592343415,
20.));
#76529=CARTESIAN_POINT('Ctrl Pts',(-41.05717029053,-25.5913492863038,0.));
#76530=CARTESIAN_POINT('Ctrl Pts',(-41.05717029053,-25.5913492863038,20.));
#76531=CARTESIAN_POINT('Ctrl Pts',(-41.072297952441,-25.5613298594791,0.));
#76532=CARTESIAN_POINT('Ctrl Pts',(-41.072297952441,-25.5613298594791,20.));
#76533=CARTESIAN_POINT('Ctrl Pts',(-41.0874043344745,-25.5313009686309,
0.));
#76534=CARTESIAN_POINT('Ctrl Pts',(-41.0874043344745,-25.5313009686309,
20.));
#76535=CARTESIAN_POINT('Ctrl Pts',(-41.1024894301655,-25.5012626285275,
0.));
#76536=CARTESIAN_POINT('Ctrl Pts',(-41.1024894301655,-25.5012626285275,
20.));
#76537=CARTESIAN_POINT('Ctrl Pts',(-41.1175532330596,-25.4712148539422,
0.));
#76538=CARTESIAN_POINT('Ctrl Pts',(-41.1175532330596,-25.4712148539422,
20.));
#76539=CARTESIAN_POINT('Ctrl Pts',(-41.132595736712,-25.4411576596529,0.));
#76540=CARTESIAN_POINT('Ctrl Pts',(-41.132595736712,-25.4411576596529,20.));
#76541=CARTESIAN_POINT('Ctrl Pts',(-41.1476169346881,-25.4110910604425,
0.));
#76542=CARTESIAN_POINT('Ctrl Pts',(-41.1476169346881,-25.4110910604425,
20.));
#76543=CARTESIAN_POINT('Ctrl Pts',(-41.1626168205634,-25.3810150710984,
0.));
#76544=CARTESIAN_POINT('Ctrl Pts',(-41.1626168205634,-25.3810150710984,
20.));
#76545=CARTESIAN_POINT('Ctrl Pts',(-41.1775953879232,-25.3509297064131,
0.));
#76546=CARTESIAN_POINT('Ctrl Pts',(-41.1775953879232,-25.3509297064131,
20.));
#76547=CARTESIAN_POINT('Ctrl Pts',(-41.1925526303629,-25.3208349811839,
0.));
#76548=CARTESIAN_POINT('Ctrl Pts',(-41.1925526303629,-25.3208349811839,
20.));
#76549=CARTESIAN_POINT('Ctrl Pts',(-41.2074885414881,-25.2907309102128,
0.));
#76550=CARTESIAN_POINT('Ctrl Pts',(-41.2074885414881,-25.2907309102128,
20.));
#76551=CARTESIAN_POINT('Ctrl Pts',(-41.2224031149147,-25.2606175083067,
0.));
#76552=CARTESIAN_POINT('Ctrl Pts',(-41.2224031149147,-25.2606175083067,
20.));
#76553=CARTESIAN_POINT('Ctrl Pts',(-41.2372963442684,-25.2304947902774,
0.));
#76554=CARTESIAN_POINT('Ctrl Pts',(-41.2372963442684,-25.2304947902774,
20.));
#76555=CARTESIAN_POINT('Ctrl Pts',(-41.2521682231854,-25.2003627709414,
0.));
#76556=CARTESIAN_POINT('Ctrl Pts',(-41.2521682231854,-25.2003627709414,
20.));
#76557=CARTESIAN_POINT('Ctrl Pts',(-41.2670187453114,-25.1702214651198,
0.));
#76558=CARTESIAN_POINT('Ctrl Pts',(-41.2670187453114,-25.1702214651198,
20.));
#76559=CARTESIAN_POINT('Ctrl Pts',(-41.2818479043026,-25.1400708876386,
0.));
#76560=CARTESIAN_POINT('Ctrl Pts',(-41.2818479043026,-25.1400708876386,
20.));
#76561=CARTESIAN_POINT('Ctrl Pts',(-41.2966556938255,-25.1099110533288,
0.));
#76562=CARTESIAN_POINT('Ctrl Pts',(-41.2966556938255,-25.1099110533288,
20.));
#76563=CARTESIAN_POINT('Ctrl Pts',(-41.3114421075567,-25.0797419770258,
0.));
#76564=CARTESIAN_POINT('Ctrl Pts',(-41.3114421075567,-25.0797419770258,
20.));
#76565=CARTESIAN_POINT('Ctrl Pts',(-41.3262071391823,-25.0495636735701,
0.));
#76566=CARTESIAN_POINT('Ctrl Pts',(-41.3262071391823,-25.0495636735701,
20.));
#76567=CARTESIAN_POINT('Ctrl Pts',(-41.3409507823989,-25.0193761578067,
0.));
#76568=CARTESIAN_POINT('Ctrl Pts',(-41.3409507823989,-25.0193761578067,
20.));
#76569=CARTESIAN_POINT('Ctrl Pts',(-41.3556730309131,-24.9891794445855,
0.));
#76570=CARTESIAN_POINT('Ctrl Pts',(-41.3556730309131,-24.9891794445855,
20.));
#76571=CARTESIAN_POINT('Ctrl Pts',(-41.3703738784418,-24.9589735487609,
0.));
#76572=CARTESIAN_POINT('Ctrl Pts',(-41.3703738784418,-24.9589735487609,
20.));
#76573=CARTESIAN_POINT('Ctrl Pts',(-41.3850533187123,-24.9287584851923,
0.));
#76574=CARTESIAN_POINT('Ctrl Pts',(-41.3850533187123,-24.9287584851923,
20.));
#76575=CARTESIAN_POINT('Ctrl Pts',(-41.3997113454618,-24.8985342687436,
0.));
#76576=CARTESIAN_POINT('Ctrl Pts',(-41.3997113454618,-24.8985342687436,
20.));
#76577=CARTESIAN_POINT('Ctrl Pts',(-41.4143479524375,-24.8683009142837,
0.));
#76578=CARTESIAN_POINT('Ctrl Pts',(-41.4143479524375,-24.8683009142837,
20.));
#76579=CARTESIAN_POINT('Ctrl Pts',(-41.4289631333969,-24.8380584366858,
0.));
#76580=CARTESIAN_POINT('Ctrl Pts',(-41.4289631333969,-24.8380584366858,
20.));
#76581=CARTESIAN_POINT('Ctrl Pts',(-41.4435568821071,-24.8078068508284,
0.));
#76582=CARTESIAN_POINT('Ctrl Pts',(-41.4435568821071,-24.8078068508284,
20.));
#76583=CARTESIAN_POINT('Ctrl Pts',(-41.4581291923457,-24.7775461715943,
0.));
#76584=CARTESIAN_POINT('Ctrl Pts',(-41.4581291923457,-24.7775461715943,
20.));
#76585=CARTESIAN_POINT('Ctrl Pts',(-41.4726800579006,-24.7472764138709,
0.));
#76586=CARTESIAN_POINT('Ctrl Pts',(-41.4726800579006,-24.7472764138709,
20.));
#76587=CARTESIAN_POINT('Ctrl Pts',(-41.4872094725702,-24.7169975925505,
0.));
#76588=CARTESIAN_POINT('Ctrl Pts',(-41.4872094725702,-24.7169975925505,
20.));
#76589=CARTESIAN_POINT('Ctrl Pts',(-41.5017174301628,-24.68670972253,0.));
#76590=CARTESIAN_POINT('Ctrl Pts',(-41.5017174301628,-24.68670972253,20.));
#76591=CARTESIAN_POINT('Ctrl Pts',(-41.516203924497,-24.6564128187107,0.));
#76592=CARTESIAN_POINT('Ctrl Pts',(-41.516203924497,-24.6564128187107,20.));
#76593=CARTESIAN_POINT('Ctrl Pts',(-41.5306689494012,-24.626106895999,0.));
#76594=CARTESIAN_POINT('Ctrl Pts',(-41.5306689494012,-24.626106895999,20.));
#76595=CARTESIAN_POINT('Ctrl Pts',(-41.545112498714,-24.5957919693057,0.));
#76596=CARTESIAN_POINT('Ctrl Pts',(-41.545112498714,-24.5957919693057,20.));
#76597=CARTESIAN_POINT('Ctrl Pts',(-41.5595345662842,-24.5654680535465,
0.));
#76598=CARTESIAN_POINT('Ctrl Pts',(-41.5595345662842,-24.5654680535465,
20.));
#76599=CARTESIAN_POINT('Ctrl Pts',(-41.5739351459709,-24.5351351636416,
0.));
#76600=CARTESIAN_POINT('Ctrl Pts',(-41.5739351459709,-24.5351351636416,
20.));
#76601=CARTESIAN_POINT('Ctrl Pts',(-41.5883142316433,-24.5047933145158,
0.));
#76602=CARTESIAN_POINT('Ctrl Pts',(-41.5883142316433,-24.5047933145158,
20.));
#76603=CARTESIAN_POINT('Ctrl Pts',(-41.6026718171809,-24.4744425210985,
0.));
#76604=CARTESIAN_POINT('Ctrl Pts',(-41.6026718171809,-24.4744425210985,
20.));
#76605=CARTESIAN_POINT('Ctrl Pts',(-41.6170078964732,-24.4440827983238,
0.));
#76606=CARTESIAN_POINT('Ctrl Pts',(-41.6170078964732,-24.4440827983238,
20.));
#76607=CARTESIAN_POINT('Ctrl Pts',(-41.6313224634201,-24.4137141611302,
0.));
#76608=CARTESIAN_POINT('Ctrl Pts',(-41.6313224634201,-24.4137141611302,
20.));
#76609=CARTESIAN_POINT('Ctrl Pts',(-41.6456155119319,-24.3833366244611,
0.));
#76610=CARTESIAN_POINT('Ctrl Pts',(-41.6456155119319,-24.3833366244611,
20.));
#76611=CARTESIAN_POINT('Ctrl Pts',(-41.6598870359289,-24.3529502032644,
0.));
#76612=CARTESIAN_POINT('Ctrl Pts',(-41.6598870359289,-24.3529502032644,
20.));
#76613=CARTESIAN_POINT('Ctrl Pts',(-41.6741370293416,-24.3225549124927,
0.));
#76614=CARTESIAN_POINT('Ctrl Pts',(-41.6741370293416,-24.3225549124927,
20.));
#76615=CARTESIAN_POINT('Ctrl Pts',(-41.6883654861106,-24.2921507671029,
0.));
#76616=CARTESIAN_POINT('Ctrl Pts',(-41.6883654861106,-24.2921507671029,
20.));
#76617=CARTESIAN_POINT('Ctrl Pts',(-41.7025724001866,-24.2617377820568,
0.));
#76618=CARTESIAN_POINT('Ctrl Pts',(-41.7025724001866,-24.2617377820568,
20.));
#76619=CARTESIAN_POINT('Ctrl Pts',(-41.7167577655309,-24.2313159723205,
0.));
#76620=CARTESIAN_POINT('Ctrl Pts',(-41.7167577655309,-24.2313159723205,
20.));
#76621=CARTESIAN_POINT('Ctrl Pts',(-41.7309215761147,-24.2008853528648,
0.));
#76622=CARTESIAN_POINT('Ctrl Pts',(-41.7309215761147,-24.2008853528648,
20.));
#76623=CARTESIAN_POINT('Ctrl Pts',(-41.7450638259196,-24.1704459386651,
0.));
#76624=CARTESIAN_POINT('Ctrl Pts',(-41.7450638259196,-24.1704459386651,
20.));
#76625=CARTESIAN_POINT('Ctrl Pts',(-41.7591845089374,-24.1399977447013,
0.));
#76626=CARTESIAN_POINT('Ctrl Pts',(-41.7591845089374,-24.1399977447013,
20.));
#76627=CARTESIAN_POINT('Ctrl Pts',(-41.7732836191701,-24.1095407859578,
0.));
#76628=CARTESIAN_POINT('Ctrl Pts',(-41.7732836191701,-24.1095407859578,
20.));
#76629=CARTESIAN_POINT('Ctrl Pts',(-41.78736115063,-24.0790750774236,0.));
#76630=CARTESIAN_POINT('Ctrl Pts',(-41.78736115063,-24.0790750774236,20.));
#76631=CARTESIAN_POINT('Ctrl Pts',(-41.8014170973399,-24.0486006340924,
0.));
#76632=CARTESIAN_POINT('Ctrl Pts',(-41.8014170973399,-24.0486006340924,
20.));
#76633=CARTESIAN_POINT('Ctrl Pts',(-41.8154514533324,-24.0181174709622,
0.));
#76634=CARTESIAN_POINT('Ctrl Pts',(-41.8154514533324,-24.0181174709622,
20.));
#76635=CARTESIAN_POINT('Ctrl Pts',(-41.8294642126506,-23.9876256030355,
0.));
#76636=CARTESIAN_POINT('Ctrl Pts',(-41.8294642126506,-23.9876256030355,
20.));
#76637=CARTESIAN_POINT('Ctrl Pts',(-41.8434553693478,-23.9571250453194,
0.));
#76638=CARTESIAN_POINT('Ctrl Pts',(-41.8434553693478,-23.9571250453194,
20.));
#76639=CARTESIAN_POINT('Ctrl Pts',(-41.8574249174873,-23.9266158128252,
0.));
#76640=CARTESIAN_POINT('Ctrl Pts',(-41.8574249174873,-23.9266158128252,
20.));
#76641=CARTESIAN_POINT('Ctrl Pts',(-41.8713728511429,-23.8960979205694,
0.));
#76642=CARTESIAN_POINT('Ctrl Pts',(-41.8713728511429,-23.8960979205694,
20.));
#76643=CARTESIAN_POINT('Ctrl Pts',(-41.8852991643986,-23.8655713835725,
0.));
#76644=CARTESIAN_POINT('Ctrl Pts',(-41.8852991643986,-23.8655713835725,
20.));
#76645=CARTESIAN_POINT('Ctrl Pts',(-41.8992038513488,-23.8350362168598,
0.));
#76646=CARTESIAN_POINT('Ctrl Pts',(-41.8992038513488,-23.8350362168598,
20.));
#76647=CARTESIAN_POINT('Ctrl Pts',(-41.9130869060982,-23.8044924354607,
0.));
#76648=CARTESIAN_POINT('Ctrl Pts',(-41.9130869060982,-23.8044924354607,
20.));
#76649=CARTESIAN_POINT('Ctrl Pts',(-41.9269483227618,-23.7739400544092,
0.));
#76650=CARTESIAN_POINT('Ctrl Pts',(-41.9269483227618,-23.7739400544092,
20.));
#76651=CARTESIAN_POINT('Ctrl Pts',(-41.9407880954647,-23.7433790887435,
0.));
#76652=CARTESIAN_POINT('Ctrl Pts',(-41.9407880954647,-23.7433790887435,
20.));
#76653=CARTESIAN_POINT('Ctrl Pts',(-41.9546062183422,-23.7128095535066,
0.));
#76654=CARTESIAN_POINT('Ctrl Pts',(-41.9546062183422,-23.7128095535066,
20.));
#76655=CARTESIAN_POINT('Ctrl Pts',(-41.9684026855399,-23.6822314637457,
0.));
#76656=CARTESIAN_POINT('Ctrl Pts',(-41.9684026855399,-23.6822314637457,
20.));
#76657=CARTESIAN_POINT('Ctrl Pts',(-41.9821774912142,-23.651644834513,0.));
#76658=CARTESIAN_POINT('Ctrl Pts',(-41.9821774912142,-23.651644834513,20.));
#76659=CARTESIAN_POINT('Ctrl Pts',(-41.9959306295311,-23.6210496808648,
0.));
#76660=CARTESIAN_POINT('Ctrl Pts',(-41.9959306295311,-23.6210496808648,
20.));
#76661=CARTESIAN_POINT('Ctrl Pts',(-42.0096620946675,-23.5904460178619,
0.));
#76662=CARTESIAN_POINT('Ctrl Pts',(-42.0096620946675,-23.5904460178619,
20.));
#76663=CARTESIAN_POINT('Ctrl Pts',(-42.02337188081,-23.5598338605694,0.));
#76664=CARTESIAN_POINT('Ctrl Pts',(-42.02337188081,-23.5598338605694,20.));
#76665=CARTESIAN_POINT('Ctrl Pts',(-42.0370599821558,-23.5292132240566,
0.));
#76666=CARTESIAN_POINT('Ctrl Pts',(-42.0370599821558,-23.5292132240566,
20.));
#76667=CARTESIAN_POINT('Ctrl Pts',(-42.0507263929126,-23.4985841233977,
0.));
#76668=CARTESIAN_POINT('Ctrl Pts',(-42.0507263929126,-23.4985841233977,
20.));
#76669=CARTESIAN_POINT('Ctrl Pts',(-42.0643711072981,-23.4679465736707,
0.));
#76670=CARTESIAN_POINT('Ctrl Pts',(-42.0643711072981,-23.4679465736707,
20.));
#76671=CARTESIAN_POINT('Ctrl Pts',(-42.0779941195407,-23.4373005899585,
0.));
#76672=CARTESIAN_POINT('Ctrl Pts',(-42.0779941195407,-23.4373005899585,
20.));
#76673=CARTESIAN_POINT('Ctrl Pts',(-42.0915954238788,-23.4066461873484,
0.));
#76674=CARTESIAN_POINT('Ctrl Pts',(-42.0915954238788,-23.4066461873484,
20.));
#76675=CARTESIAN_POINT('Ctrl Pts',(-42.1051750145614,-23.3759833809318,
0.));
#76676=CARTESIAN_POINT('Ctrl Pts',(-42.1051750145614,-23.3759833809318,
20.));
#76677=CARTESIAN_POINT('Ctrl Pts',(-42.1187328858474,-23.3453121858047,
0.));
#76678=CARTESIAN_POINT('Ctrl Pts',(-42.1187328858474,-23.3453121858047,
20.));
#76679=CARTESIAN_POINT('Ctrl Pts',(-42.1322690320059,-23.3146326170671,
0.));
#76680=CARTESIAN_POINT('Ctrl Pts',(-42.1322690320059,-23.3146326170671,
20.));
#76681=CARTESIAN_POINT('Ctrl Pts',(-42.145783447317,-23.2839446898238,0.));
#76682=CARTESIAN_POINT('Ctrl Pts',(-42.145783447317,-23.2839446898238,20.));
#76683=CARTESIAN_POINT('Ctrl Pts',(-42.1592761260708,-23.2532484191837,
0.));
#76684=CARTESIAN_POINT('Ctrl Pts',(-42.1592761260708,-23.2532484191837,
20.));
#76685=CARTESIAN_POINT('Ctrl Pts',(-42.1727470625681,-23.2225438202604,
0.));
#76686=CARTESIAN_POINT('Ctrl Pts',(-42.1727470625681,-23.2225438202604,
20.));
#76687=CARTESIAN_POINT('Ctrl Pts',(-42.1861962511195,-23.1918309081713,
0.));
#76688=CARTESIAN_POINT('Ctrl Pts',(-42.1861962511195,-23.1918309081713,
20.));
#76689=CARTESIAN_POINT('Ctrl Pts',(-42.1996236860461,-23.1611096980384,
0.));
#76690=CARTESIAN_POINT('Ctrl Pts',(-42.1996236860461,-23.1611096980384,
20.));
#76691=CARTESIAN_POINT('Ctrl Pts',(-42.2130293616794,-23.1303802049881,
0.));
#76692=CARTESIAN_POINT('Ctrl Pts',(-42.2130293616794,-23.1303802049881,
20.));
#76693=CARTESIAN_POINT('Ctrl Pts',(-42.2264132723612,-23.0996424441509,
0.));
#76694=CARTESIAN_POINT('Ctrl Pts',(-42.2264132723612,-23.0996424441509,
20.));
#76695=CARTESIAN_POINT('Ctrl Pts',(-42.2397754124437,-23.0688964306618,
0.));
#76696=CARTESIAN_POINT('Ctrl Pts',(-42.2397754124437,-23.0688964306618,
20.));
#76697=CARTESIAN_POINT('Ctrl Pts',(-42.2531157762897,-23.0381421796601,
0.));
#76698=CARTESIAN_POINT('Ctrl Pts',(-42.2531157762897,-23.0381421796601,
20.));
#76699=CARTESIAN_POINT('Ctrl Pts',(-42.2664343582719,-23.0073797062893,
0.));
#76700=CARTESIAN_POINT('Ctrl Pts',(-42.2664343582719,-23.0073797062893,
20.));
#76701=CARTESIAN_POINT('Ctrl Pts',(-42.2797311527738,-22.9766090256973,
0.));
#76702=CARTESIAN_POINT('Ctrl Pts',(-42.2797311527738,-22.9766090256973,
20.));
#76703=CARTESIAN_POINT('Ctrl Pts',(-42.2930061541893,-22.9458301530364,
0.));
#76704=CARTESIAN_POINT('Ctrl Pts',(-42.2930061541893,-22.9458301530364,
20.));
#76705=CARTESIAN_POINT('Ctrl Pts',(-42.3062593569226,-22.9150431034629,
0.));
#76706=CARTESIAN_POINT('Ctrl Pts',(-42.3062593569226,-22.9150431034629,
20.));
#76707=CARTESIAN_POINT('Ctrl Pts',(-42.3194907553882,-22.8842478921374,
0.));
#76708=CARTESIAN_POINT('Ctrl Pts',(-42.3194907553882,-22.8842478921374,
20.));
#76709=CARTESIAN_POINT('Ctrl Pts',(-42.3327003440109,-22.8534445342249,
0.));
#76710=CARTESIAN_POINT('Ctrl Pts',(-42.3327003440109,-22.8534445342249,
20.));
#76711=CARTESIAN_POINT('Ctrl Pts',(-42.3458881172255,-22.8226330448945,
0.));
#76712=CARTESIAN_POINT('Ctrl Pts',(-42.3458881172255,-22.8226330448945,
20.));
#76713=CARTESIAN_POINT('Ctrl Pts',(-42.3590540694774,-22.7918134393197,
0.));
#76714=CARTESIAN_POINT('Ctrl Pts',(-42.3590540694774,-22.7918134393197,
20.));
#76715=CARTESIAN_POINT('Ctrl Pts',(-42.3721981952224,-22.7609857326781,
0.));
#76716=CARTESIAN_POINT('Ctrl Pts',(-42.3721981952224,-22.7609857326781,
20.));
#76717=CARTESIAN_POINT('Ctrl Pts',(-42.3853204889273,-22.7301499401517,
0.));
#76718=CARTESIAN_POINT('Ctrl Pts',(-42.3853204889273,-22.7301499401517,
20.));
#76719=CARTESIAN_POINT('Ctrl Pts',(-42.398420945069,-22.6993060769268,0.));
#76720=CARTESIAN_POINT('Ctrl Pts',(-42.398420945069,-22.6993060769268,20.));
#76721=CARTESIAN_POINT('Ctrl Pts',(-42.411499558135,-22.6684541581936,0.));
#76722=CARTESIAN_POINT('Ctrl Pts',(-42.411499558135,-22.6684541581936,20.));
#76723=CARTESIAN_POINT('Ctrl Pts',(-42.4245563226236,-22.6375941991468,
0.));
#76724=CARTESIAN_POINT('Ctrl Pts',(-42.4245563226236,-22.6375941991468,
20.));
#76725=CARTESIAN_POINT('Ctrl Pts',(-42.4375912330427,-22.6067262149851,
0.));
#76726=CARTESIAN_POINT('Ctrl Pts',(-42.4375912330427,-22.6067262149851,
20.));
#76727=CARTESIAN_POINT('Ctrl Pts',(-42.4506042839107,-22.5758502209116,
0.));
#76728=CARTESIAN_POINT('Ctrl Pts',(-42.4506042839107,-22.5758502209116,
20.));
#76729=CARTESIAN_POINT('Ctrl Pts',(-42.4635954697559,-22.5449662321334,
0.));
#76730=CARTESIAN_POINT('Ctrl Pts',(-42.4635954697559,-22.5449662321334,
20.));
#76731=CARTESIAN_POINT('Ctrl Pts',(-42.4765647851171,-22.5140742638619,
0.));
#76732=CARTESIAN_POINT('Ctrl Pts',(-42.4765647851171,-22.5140742638619,
20.));
#76733=CARTESIAN_POINT('Ctrl Pts',(-42.4895122245441,-22.4831743313126,
0.));
#76734=CARTESIAN_POINT('Ctrl Pts',(-42.4895122245441,-22.4831743313126,
20.));
#76735=CARTESIAN_POINT('Ctrl Pts',(-42.502437782597,-22.4522664497054,0.));
#76736=CARTESIAN_POINT('Ctrl Pts',(-42.502437782597,-22.4522664497054,20.));
#76737=CARTESIAN_POINT('Ctrl Pts',(-42.5153414538467,-22.4213506342639,
0.));
#76738=CARTESIAN_POINT('Ctrl Pts',(-42.5153414538467,-22.4213506342639,
20.));
#76739=CARTESIAN_POINT('Ctrl Pts',(-42.5282232328748,-22.3904269002165,
0.));
#76740=CARTESIAN_POINT('Ctrl Pts',(-42.5282232328748,-22.3904269002165,
20.));
#76741=CARTESIAN_POINT('Ctrl Pts',(-42.5410831142727,-22.3594952627952,
0.));
#76742=CARTESIAN_POINT('Ctrl Pts',(-42.5410831142727,-22.3594952627952,
20.));
#76743=CARTESIAN_POINT('Ctrl Pts',(-42.5539210926424,-22.3285557372364,
0.));
#76744=CARTESIAN_POINT('Ctrl Pts',(-42.5539210926424,-22.3285557372364,
20.));
#76745=CARTESIAN_POINT('Ctrl Pts',(-42.5667371625962,-22.2976083387805,
0.));
#76746=CARTESIAN_POINT('Ctrl Pts',(-42.5667371625962,-22.2976083387805,
20.));
#76747=CARTESIAN_POINT('Ctrl Pts',(-42.5795313187569,-22.2666530826722,
0.));
#76748=CARTESIAN_POINT('Ctrl Pts',(-42.5795313187569,-22.2666530826722,
20.));
#76749=CARTESIAN_POINT('Ctrl Pts',(-42.5923035557573,-22.2356899841602,
0.));
#76750=CARTESIAN_POINT('Ctrl Pts',(-42.5923035557573,-22.2356899841602,
20.));
#76751=CARTESIAN_POINT('Ctrl Pts',(-42.6050538682411,-22.2047190584974,
0.));
#76752=CARTESIAN_POINT('Ctrl Pts',(-42.6050538682411,-22.2047190584974,
20.));
#76753=CARTESIAN_POINT('Ctrl Pts',(-42.6177822508627,-22.1737403209406,
0.));
#76754=CARTESIAN_POINT('Ctrl Pts',(-42.6177822508627,-22.1737403209406,
20.));
#76755=CARTESIAN_POINT('Ctrl Pts',(-42.6304886982869,-22.1427537867512,
0.));
#76756=CARTESIAN_POINT('Ctrl Pts',(-42.6304886982869,-22.1427537867512,
20.));
#76757=CARTESIAN_POINT('Ctrl Pts',(-42.6431732051887,-22.1117594711942,
0.));
#76758=CARTESIAN_POINT('Ctrl Pts',(-42.6431732051887,-22.1117594711942,
20.));
#76759=CARTESIAN_POINT('Ctrl Pts',(-42.6558357662536,-22.0807573895388,
0.));
#76760=CARTESIAN_POINT('Ctrl Pts',(-42.6558357662536,-22.0807573895388,
20.));
#76761=CARTESIAN_POINT('Ctrl Pts',(-42.6684763761777,-22.0497475570584,
0.));
#76762=CARTESIAN_POINT('Ctrl Pts',(-42.6684763761777,-22.0497475570584,
20.));
#76763=CARTESIAN_POINT('Ctrl Pts',(-42.6810950296678,-22.0187299890302,
0.));
#76764=CARTESIAN_POINT('Ctrl Pts',(-42.6810950296678,-22.0187299890302,
20.));
#76765=CARTESIAN_POINT('Ctrl Pts',(-42.6936917214411,-21.9877047007357,
0.));
#76766=CARTESIAN_POINT('Ctrl Pts',(-42.6936917214411,-21.9877047007357,
20.));
#76767=CARTESIAN_POINT('Ctrl Pts',(-42.7062664462249,-21.9566717074606,
0.));
#76768=CARTESIAN_POINT('Ctrl Pts',(-42.7062664462249,-21.9566717074606,
20.));
#76769=CARTESIAN_POINT('Ctrl Pts',(-42.7188191987573,-21.9256310244944,
0.));
#76770=CARTESIAN_POINT('Ctrl Pts',(-42.7188191987573,-21.9256310244944,
20.));
#76771=CARTESIAN_POINT('Ctrl Pts',(-42.7313499737866,-21.8945826671308,
0.));
#76772=CARTESIAN_POINT('Ctrl Pts',(-42.7313499737866,-21.8945826671308,
20.));
#76773=CARTESIAN_POINT('Ctrl Pts',(-42.7438587660714,-21.8635266506674,
0.));
#76774=CARTESIAN_POINT('Ctrl Pts',(-42.7438587660714,-21.8635266506674,
20.));
#76775=CARTESIAN_POINT('Ctrl Pts',(-42.7563455703812,-21.832462990406,0.));
#76776=CARTESIAN_POINT('Ctrl Pts',(-42.7563455703812,-21.832462990406,20.));
#76777=CARTESIAN_POINT('Ctrl Pts',(-42.7688103814962,-21.8013917016521,
0.));
#76778=CARTESIAN_POINT('Ctrl Pts',(-42.7688103814962,-21.8013917016521,
20.));
#76779=CARTESIAN_POINT('Ctrl Pts',(-42.7812531942069,-21.7703127997157,
0.));
#76780=CARTESIAN_POINT('Ctrl Pts',(-42.7812531942069,-21.7703127997157,
20.));
#76781=CARTESIAN_POINT('Ctrl Pts',(-42.7936740033148,-21.7392262999104,
0.));
#76782=CARTESIAN_POINT('Ctrl Pts',(-42.7936740033148,-21.7392262999104,
20.));
#76783=CARTESIAN_POINT('Ctrl Pts',(-42.8060728036314,-21.7081322175539,
0.));
#76784=CARTESIAN_POINT('Ctrl Pts',(-42.8060728036314,-21.7081322175539,
20.));
#76785=CARTESIAN_POINT('Ctrl Pts',(-42.8184495899785,-21.677030567968,0.));
#76786=CARTESIAN_POINT('Ctrl Pts',(-42.8184495899785,-21.677030567968,20.));
#76787=CARTESIAN_POINT('Ctrl Pts',(-42.8308043571887,-21.6459213664784,
0.));
#76788=CARTESIAN_POINT('Ctrl Pts',(-42.8308043571887,-21.6459213664784,
20.));
#76789=CARTESIAN_POINT('Ctrl Pts',(-42.8431371001047,-21.6148046284149,
0.));
#76790=CARTESIAN_POINT('Ctrl Pts',(-42.8431371001047,-21.6148046284149,
20.));
#76791=CARTESIAN_POINT('Ctrl Pts',(-42.8554478135801,-21.5836803691112,
0.));
#76792=CARTESIAN_POINT('Ctrl Pts',(-42.8554478135801,-21.5836803691112,
20.));
#76793=CARTESIAN_POINT('Ctrl Pts',(-42.8677364924794,-21.5525486039049,
0.));
#76794=CARTESIAN_POINT('Ctrl Pts',(-42.8677364924794,-21.5525486039049,
20.));
#76795=CARTESIAN_POINT('Ctrl Pts',(-42.8800031316769,-21.5214093481377,
0.));
#76796=CARTESIAN_POINT('Ctrl Pts',(-42.8800031316769,-21.5214093481377,
20.));
#76797=CARTESIAN_POINT('Ctrl Pts',(-42.8922477260581,-21.490262617155,0.));
#76798=CARTESIAN_POINT('Ctrl Pts',(-42.8922477260581,-21.490262617155,20.));
#76799=CARTESIAN_POINT('Ctrl Pts',(-42.9044702705183,-21.4591084263065,
0.));
#76800=CARTESIAN_POINT('Ctrl Pts',(-42.9044702705183,-21.4591084263065,
20.));
#76801=CARTESIAN_POINT('Ctrl Pts',(-42.916670759964,-21.4279467909454,0.));
#76802=CARTESIAN_POINT('Ctrl Pts',(-42.916670759964,-21.4279467909454,20.));
#76803=CARTESIAN_POINT('Ctrl Pts',(-42.9288491893122,-21.3967777264294,
0.));
#76804=CARTESIAN_POINT('Ctrl Pts',(-42.9288491893122,-21.3967777264294,
20.));
#76805=CARTESIAN_POINT('Ctrl Pts',(-42.9410055534907,-21.3656012481198,
0.));
#76806=CARTESIAN_POINT('Ctrl Pts',(-42.9410055534907,-21.3656012481198,
20.));
#76807=CARTESIAN_POINT('Ctrl Pts',(-42.9531398474371,-21.3344173713818,
0.));
#76808=CARTESIAN_POINT('Ctrl Pts',(-42.9531398474371,-21.3344173713818,
20.));
#76809=CARTESIAN_POINT('Ctrl Pts',(-42.9652520660998,-21.3032261115844,
0.));
#76810=CARTESIAN_POINT('Ctrl Pts',(-42.9652520660998,-21.3032261115844,
20.));
#76811=CARTESIAN_POINT('Ctrl Pts',(-42.9773422044374,-21.2720274841006,
0.));
#76812=CARTESIAN_POINT('Ctrl Pts',(-42.9773422044374,-21.2720274841006,
20.));
#76813=CARTESIAN_POINT('Ctrl Pts',(-42.9894102574195,-21.2408215043074,
0.));
#76814=CARTESIAN_POINT('Ctrl Pts',(-42.9894102574195,-21.2408215043074,
20.));
#76815=CARTESIAN_POINT('Ctrl Pts',(-43.0014562200264,-21.2096081875857,
0.));
#76816=CARTESIAN_POINT('Ctrl Pts',(-43.0014562200264,-21.2096081875857,
20.));
#76817=CARTESIAN_POINT('Ctrl Pts',(-43.0134800872489,-21.1783875493204,
0.));
#76818=CARTESIAN_POINT('Ctrl Pts',(-43.0134800872489,-21.1783875493204,
20.));
#76819=CARTESIAN_POINT('Ctrl Pts',(-43.0254818540885,-21.1471596049,0.));
#76820=CARTESIAN_POINT('Ctrl Pts',(-43.0254818540885,-21.1471596049,20.));
#76821=CARTESIAN_POINT('Ctrl Pts',(-43.037461515557,-21.1159243697169,0.));
#76822=CARTESIAN_POINT('Ctrl Pts',(-43.037461515557,-21.1159243697169,20.));
#76823=CARTESIAN_POINT('Ctrl Pts',(-43.0494190666771,-21.0846818591673,
0.));
#76824=CARTESIAN_POINT('Ctrl Pts',(-43.0494190666771,-21.0846818591673,
20.));
#76825=CARTESIAN_POINT('Ctrl Pts',(-43.0613545024815,-21.0534320886512,
0.));
#76826=CARTESIAN_POINT('Ctrl Pts',(-43.0613545024815,-21.0534320886512,
20.));
#76827=CARTESIAN_POINT('Ctrl Pts',(-43.0732678180139,-21.0221750735727,
0.));
#76828=CARTESIAN_POINT('Ctrl Pts',(-43.0732678180139,-21.0221750735727,
20.));
#76829=CARTESIAN_POINT('Ctrl Pts',(-43.0851590083283,-20.9909108293397,
0.));
#76830=CARTESIAN_POINT('Ctrl Pts',(-43.0851590083283,-20.9909108293397,
20.));
#76831=CARTESIAN_POINT('Ctrl Pts',(-43.0970280684896,-20.959639371364,0.));
#76832=CARTESIAN_POINT('Ctrl Pts',(-43.0970280684896,-20.959639371364,20.));
#76833=CARTESIAN_POINT('Ctrl Pts',(-43.1088749935734,-20.9283607150615,
0.));
#76834=CARTESIAN_POINT('Ctrl Pts',(-43.1088749935734,-20.9283607150615,
20.));
#76835=CARTESIAN_POINT('Ctrl Pts',(-43.1206997786657,-20.8970748758512,
0.));
#76836=CARTESIAN_POINT('Ctrl Pts',(-43.1206997786657,-20.8970748758512,
20.));
#76837=CARTESIAN_POINT('Ctrl Pts',(-43.132502418863,-20.8657818691565,0.));
#76838=CARTESIAN_POINT('Ctrl Pts',(-43.132502418863,-20.8657818691565,20.));
#76839=CARTESIAN_POINT('Ctrl Pts',(-43.1442829092724,-20.8344817104039,
0.));
#76840=CARTESIAN_POINT('Ctrl Pts',(-43.1442829092724,-20.8344817104039,
20.));
#76841=CARTESIAN_POINT('Ctrl Pts',(-43.1560412450117,-20.8031744150242,
0.));
#76842=CARTESIAN_POINT('Ctrl Pts',(-43.1560412450117,-20.8031744150242,
20.));
#76843=CARTESIAN_POINT('Ctrl Pts',(-43.1677774212093,-20.7718599984518,
0.));
#76844=CARTESIAN_POINT('Ctrl Pts',(-43.1677774212093,-20.7718599984518,
20.));
#76845=CARTESIAN_POINT('Ctrl Pts',(-43.1794914330045,-20.7405384761252,
0.));
#76846=CARTESIAN_POINT('Ctrl Pts',(-43.1794914330045,-20.7405384761252,
20.));
#76847=CARTESIAN_POINT('Ctrl Pts',(-43.1911832755467,-20.7092098634864,
0.));
#76848=CARTESIAN_POINT('Ctrl Pts',(-43.1911832755467,-20.7092098634864,
20.));
#76849=CARTESIAN_POINT('Ctrl Pts',(-43.202852943996,-20.6778741759814,0.));
#76850=CARTESIAN_POINT('Ctrl Pts',(-43.202852943996,-20.6778741759814,20.));
#76851=CARTESIAN_POINT('Ctrl Pts',(-43.2145004335236,-20.6465314290598,
0.));
#76852=CARTESIAN_POINT('Ctrl Pts',(-43.2145004335236,-20.6465314290598,
20.));
#76853=CARTESIAN_POINT('Ctrl Pts',(-43.2261257393109,-20.615181638175,0.));
#76854=CARTESIAN_POINT('Ctrl Pts',(-43.2261257393109,-20.615181638175,20.));
#76855=CARTESIAN_POINT('Ctrl Pts',(-43.2377288565503,-20.5838248187841,
0.));
#76856=CARTESIAN_POINT('Ctrl Pts',(-43.2377288565503,-20.5838248187841,
20.));
#76857=CARTESIAN_POINT('Ctrl Pts',(-43.2493097804445,-20.5524609863481,
0.));
#76858=CARTESIAN_POINT('Ctrl Pts',(-43.2493097804445,-20.5524609863481,
20.));
#76859=CARTESIAN_POINT('Ctrl Pts',(-43.2608685062069,-20.5210901563314,
0.));
#76860=CARTESIAN_POINT('Ctrl Pts',(-43.2608685062069,-20.5210901563314,
20.));
#76861=CARTESIAN_POINT('Ctrl Pts',(-43.2724050290617,-20.4897123442023,
0.));
#76862=CARTESIAN_POINT('Ctrl Pts',(-43.2724050290617,-20.4897123442023,
20.));
#76863=CARTESIAN_POINT('Ctrl Pts',(-43.283919344243,-20.4583275654327,0.));
#76864=CARTESIAN_POINT('Ctrl Pts',(-43.283919344243,-20.4583275654327,20.));
#76865=CARTESIAN_POINT('Ctrl Pts',(-43.2954114469964,-20.4269358354984,
0.));
#76866=CARTESIAN_POINT('Ctrl Pts',(-43.2954114469964,-20.4269358354984,
20.));
#76867=CARTESIAN_POINT('Ctrl Pts',(-43.3068813325774,-20.3955371698787,
0.));
#76868=CARTESIAN_POINT('Ctrl Pts',(-43.3068813325774,-20.3955371698787,
20.));
#76869=CARTESIAN_POINT('Ctrl Pts',(-43.3183289962528,-20.3641315840566,
0.));
#76870=CARTESIAN_POINT('Ctrl Pts',(-43.3183289962528,-20.3641315840566,
20.));
#76871=CARTESIAN_POINT('Ctrl Pts',(-43.3297544333003,-20.3327190935193,
0.));
#76872=CARTESIAN_POINT('Ctrl Pts',(-43.3297544333003,-20.3327190935193,
20.));
#76873=CARTESIAN_POINT('Ctrl Pts',(-43.3411576390085,-20.3012997137575,
0.));
#76874=CARTESIAN_POINT('Ctrl Pts',(-43.3411576390085,-20.3012997137575,
20.));
#76875=CARTESIAN_POINT('Ctrl Pts',(-43.3525386086763,-20.2698734602656,
0.));
#76876=CARTESIAN_POINT('Ctrl Pts',(-43.3525386086763,-20.2698734602656,
20.));
#76877=CARTESIAN_POINT('Ctrl Pts',(-43.3638973376125,-20.2384403485411,
0.));
#76878=CARTESIAN_POINT('Ctrl Pts',(-43.3638973376125,-20.2384403485411,
20.));
#76879=CARTESIAN_POINT('Ctrl Pts',(-43.3752338211368,-20.2070003940853,
0.));
#76880=CARTESIAN_POINT('Ctrl Pts',(-43.3752338211368,-20.2070003940853,
20.));
#76881=CARTESIAN_POINT('Ctrl Pts',(-43.3865480545792,-20.1755536124033,
0.));
#76882=CARTESIAN_POINT('Ctrl Pts',(-43.3865480545792,-20.1755536124033,
20.));
#76883=CARTESIAN_POINT('Ctrl Pts',(-43.3978400332808,-20.1441000190037,
0.));
#76884=CARTESIAN_POINT('Ctrl Pts',(-43.3978400332808,-20.1441000190037,
20.));
#76885=CARTESIAN_POINT('Ctrl Pts',(-43.409109752594,-20.1126396293992,0.));
#76886=CARTESIAN_POINT('Ctrl Pts',(-43.409109752594,-20.1126396293992,20.));
#76887=CARTESIAN_POINT('Ctrl Pts',(-43.4203572078819,-20.0811724591058,
0.));
#76888=CARTESIAN_POINT('Ctrl Pts',(-43.4203572078819,-20.0811724591058,
20.));
#76889=CARTESIAN_POINT('Ctrl Pts',(-43.4315823945181,-20.0496985236436,
0.));
#76890=CARTESIAN_POINT('Ctrl Pts',(-43.4315823945181,-20.0496985236436,
20.));
#76891=CARTESIAN_POINT('Ctrl Pts',(-43.4427853078868,-20.0182178385356,
0.));
#76892=CARTESIAN_POINT('Ctrl Pts',(-43.4427853078868,-20.0182178385356,
20.));
#76893=CARTESIAN_POINT('Ctrl Pts',(-43.4539659433821,-19.9867304193089,
0.));
#76894=CARTESIAN_POINT('Ctrl Pts',(-43.4539659433821,-19.9867304193089,
20.));
#76895=CARTESIAN_POINT('Ctrl Pts',(-43.4651242964088,-19.9552362814936,
0.));
#76896=CARTESIAN_POINT('Ctrl Pts',(-43.4651242964088,-19.9552362814936,
20.));
#76897=CARTESIAN_POINT('Ctrl Pts',(-43.4762603623832,-19.923735440624,0.));
#76898=CARTESIAN_POINT('Ctrl Pts',(-43.4762603623832,-19.923735440624,20.));
#76899=CARTESIAN_POINT('Ctrl Pts',(-43.4873741367321,-19.8922279122378,
0.));
#76900=CARTESIAN_POINT('Ctrl Pts',(-43.4873741367321,-19.8922279122378,
20.));
#76901=CARTESIAN_POINT('Ctrl Pts',(-43.4984656148936,-19.8607137118763,
0.));
#76902=CARTESIAN_POINT('Ctrl Pts',(-43.4984656148936,-19.8607137118763,
20.));
#76903=CARTESIAN_POINT('Ctrl Pts',(-43.5095347923164,-19.8291928550844,
0.));
#76904=CARTESIAN_POINT('Ctrl Pts',(-43.5095347923164,-19.8291928550844,
20.));
#76905=CARTESIAN_POINT('Ctrl Pts',(-43.5205816644596,-19.7976653574108,
0.));
#76906=CARTESIAN_POINT('Ctrl Pts',(-43.5205816644596,-19.7976653574108,
20.));
#76907=CARTESIAN_POINT('Ctrl Pts',(-43.5316062267925,-19.7661312344072,
0.));
#76908=CARTESIAN_POINT('Ctrl Pts',(-43.5316062267925,-19.7661312344072,
20.));
#76909=CARTESIAN_POINT('Ctrl Pts',(-43.542608474795,-19.734590501629,0.));
#76910=CARTESIAN_POINT('Ctrl Pts',(-43.542608474795,-19.734590501629,20.));
#76911=CARTESIAN_POINT('Ctrl Pts',(-43.5535884039576,-19.7030431746352,
0.));
#76912=CARTESIAN_POINT('Ctrl Pts',(-43.5535884039576,-19.7030431746352,
20.));
#76913=CARTESIAN_POINT('Ctrl Pts',(-43.5645460097823,-19.6714892689885,
0.));
#76914=CARTESIAN_POINT('Ctrl Pts',(-43.5645460097823,-19.6714892689885,
20.));
#76915=CARTESIAN_POINT('Ctrl Pts',(-43.5754812877819,-19.639928800255,0.));
#76916=CARTESIAN_POINT('Ctrl Pts',(-43.5754812877819,-19.639928800255,20.));
#76917=CARTESIAN_POINT('Ctrl Pts',(-43.5863942334797,-19.6083617840046,
0.));
#76918=CARTESIAN_POINT('Ctrl Pts',(-43.5863942334797,-19.6083617840046,
20.));
#76919=CARTESIAN_POINT('Ctrl Pts',(-43.5972848424097,-19.5767882358104,
0.));
#76920=CARTESIAN_POINT('Ctrl Pts',(-43.5972848424097,-19.5767882358104,
20.));
#76921=CARTESIAN_POINT('Ctrl Pts',(-43.6081531101168,-19.545208171249,0.));
#76922=CARTESIAN_POINT('Ctrl Pts',(-43.6081531101168,-19.545208171249,20.));
#76923=CARTESIAN_POINT('Ctrl Pts',(-43.6189990321561,-19.5136216059004,
0.));
#76924=CARTESIAN_POINT('Ctrl Pts',(-43.6189990321561,-19.5136216059004,
20.));
#76925=CARTESIAN_POINT('Ctrl Pts',(-43.629822604094,-19.4820285553483,0.));
#76926=CARTESIAN_POINT('Ctrl Pts',(-43.629822604094,-19.4820285553483,20.));
#76927=CARTESIAN_POINT('Ctrl Pts',(-43.6406238215078,-19.4504290351799,
0.));
#76928=CARTESIAN_POINT('Ctrl Pts',(-43.6406238215078,-19.4504290351799,
20.));
#76929=CARTESIAN_POINT('Ctrl Pts',(-43.6514026799849,-19.4188230609858,
0.));
#76930=CARTESIAN_POINT('Ctrl Pts',(-43.6514026799849,-19.4188230609858,
20.));
#76931=CARTESIAN_POINT('Ctrl Pts',(-43.6621591751234,-19.3872106483603,
0.));
#76932=CARTESIAN_POINT('Ctrl Pts',(-43.6621591751234,-19.3872106483603,
20.));
#76933=CARTESIAN_POINT('Ctrl Pts',(-43.6728933025325,-19.3555918129009,
0.));
#76934=CARTESIAN_POINT('Ctrl Pts',(-43.6728933025325,-19.3555918129009,
20.));
#76935=CARTESIAN_POINT('Ctrl Pts',(-43.6836050578319,-19.3239665702086,
0.));
#76936=CARTESIAN_POINT('Ctrl Pts',(-43.6836050578319,-19.3239665702086,
20.));
#76937=CARTESIAN_POINT('Ctrl Pts',(-43.6942944366523,-19.2923349358879,
0.));
#76938=CARTESIAN_POINT('Ctrl Pts',(-43.6942944366523,-19.2923349358879,
20.));
#76939=CARTESIAN_POINT('Ctrl Pts',(-43.7049614346349,-19.2606969255464,
0.));
#76940=CARTESIAN_POINT('Ctrl Pts',(-43.7049614346349,-19.2606969255464,
20.));
#76941=CARTESIAN_POINT('Ctrl Pts',(-43.7156060474324,-19.2290525547956,
0.));
#76942=CARTESIAN_POINT('Ctrl Pts',(-43.7156060474324,-19.2290525547956,
20.));
#76943=CARTESIAN_POINT('Ctrl Pts',(-43.7262282707082,-19.1974018392505,
0.));
#76944=CARTESIAN_POINT('Ctrl Pts',(-43.7262282707082,-19.1974018392505,
20.));
#76945=CARTESIAN_POINT('Ctrl Pts',(-43.7368281001363,-19.1657447945291,
0.));
#76946=CARTESIAN_POINT('Ctrl Pts',(-43.7368281001363,-19.1657447945291,
20.));
#76947=CARTESIAN_POINT('Ctrl Pts',(-43.747405531401,-19.1340814362531,0.));
#76948=CARTESIAN_POINT('Ctrl Pts',(-43.747405531401,-19.1340814362531,20.));
#76949=CARTESIAN_POINT('Ctrl Pts',(-43.7579605601976,-19.1024117800474,
0.));
#76950=CARTESIAN_POINT('Ctrl Pts',(-43.7579605601976,-19.1024117800474,
20.));
#76951=CARTESIAN_POINT('Ctrl Pts',(-43.7684931822314,-19.0707358415405,
0.));
#76952=CARTESIAN_POINT('Ctrl Pts',(-43.7684931822314,-19.0707358415405,
20.));
#76953=CARTESIAN_POINT('Ctrl Pts',(-43.779003393219,-19.039053636364,0.));
#76954=CARTESIAN_POINT('Ctrl Pts',(-43.779003393219,-19.039053636364,20.));
#76955=CARTESIAN_POINT('Ctrl Pts',(-43.7894911888877,-19.0073651801531,
0.));
#76956=CARTESIAN_POINT('Ctrl Pts',(-43.7894911888877,-19.0073651801531,
20.));
#76957=CARTESIAN_POINT('Ctrl Pts',(-43.7999565649762,-18.9756704885464,
0.));
#76958=CARTESIAN_POINT('Ctrl Pts',(-43.7999565649762,-18.9756704885464,
20.));
#76959=CARTESIAN_POINT('Ctrl Pts',(-43.8103995172341,-18.9439695771858,
0.));
#76960=CARTESIAN_POINT('Ctrl Pts',(-43.8103995172341,-18.9439695771858,
20.));
#76961=CARTESIAN_POINT('Ctrl Pts',(-43.8208200414219,-18.9122624617166,
0.));
#76962=CARTESIAN_POINT('Ctrl Pts',(-43.8208200414219,-18.9122624617166,
20.));
#76963=CARTESIAN_POINT('Ctrl Pts',(-43.8312181333106,-18.8805491577876,
0.));
#76964=CARTESIAN_POINT('Ctrl Pts',(-43.8312181333106,-18.8805491577876,
20.));
#76965=CARTESIAN_POINT('Ctrl Pts',(-43.8415937886817,-18.8488296810507,
0.));
#76966=CARTESIAN_POINT('Ctrl Pts',(-43.8415937886817,-18.8488296810507,
20.));
#76967=CARTESIAN_POINT('Ctrl Pts',(-43.8519470033272,-18.8171040471611,
0.));
#76968=CARTESIAN_POINT('Ctrl Pts',(-43.8519470033272,-18.8171040471611,
20.));
#76969=CARTESIAN_POINT('Ctrl Pts',(-43.8622777730502,-18.7853722717774,
0.));
#76970=CARTESIAN_POINT('Ctrl Pts',(-43.8622777730502,-18.7853722717774,
20.));
#76971=CARTESIAN_POINT('Ctrl Pts',(-43.8725860936644,-18.7536343705616,
0.));
#76972=CARTESIAN_POINT('Ctrl Pts',(-43.8725860936644,-18.7536343705616,
20.));
#76973=CARTESIAN_POINT('Ctrl Pts',(-43.8828719609947,-18.721890359179,0.));
#76974=CARTESIAN_POINT('Ctrl Pts',(-43.8828719609947,-18.721890359179,20.));
#76975=CARTESIAN_POINT('Ctrl Pts',(-43.8931353708767,-18.6901402532984,
0.));
#76976=CARTESIAN_POINT('Ctrl Pts',(-43.8931353708767,-18.6901402532984,
20.));
#76977=CARTESIAN_POINT('Ctrl Pts',(-43.903376319157,-18.6583840685915,0.));
#76978=CARTESIAN_POINT('Ctrl Pts',(-43.903376319157,-18.6583840685915,20.));
#76979=CARTESIAN_POINT('Ctrl Pts',(-43.913594801693,-18.6266218207337,0.));
#76980=CARTESIAN_POINT('Ctrl Pts',(-43.913594801693,-18.6266218207337,20.));
#76981=CARTESIAN_POINT('Ctrl Pts',(-43.9237908143526,-18.5948535254034,
0.));
#76982=CARTESIAN_POINT('Ctrl Pts',(-43.9237908143526,-18.5948535254034,
20.));
#76983=CARTESIAN_POINT('Ctrl Pts',(-43.9339643530151,-18.5630791982821,
0.));
#76984=CARTESIAN_POINT('Ctrl Pts',(-43.9339643530151,-18.5630791982821,
20.));
#76985=CARTESIAN_POINT('Ctrl Pts',(-43.94411541357,-18.5312988550549,0.));
#76986=CARTESIAN_POINT('Ctrl Pts',(-43.94411541357,-18.5312988550549,20.));
#76987=CARTESIAN_POINT('Ctrl Pts',(-43.9542439919177,-18.4995125114099,
0.));
#76988=CARTESIAN_POINT('Ctrl Pts',(-43.9542439919177,-18.4995125114099,
20.));
#76989=CARTESIAN_POINT('Ctrl Pts',(-43.9643500839697,-18.4677201830388,
0.));
#76990=CARTESIAN_POINT('Ctrl Pts',(-43.9643500839697,-18.4677201830388,
20.));
#76991=CARTESIAN_POINT('Ctrl Pts',(-43.9744336856481,-18.4359218856365,
0.));
#76992=CARTESIAN_POINT('Ctrl Pts',(-43.9744336856481,-18.4359218856365,
20.));
#76993=CARTESIAN_POINT('Ctrl Pts',(-43.9844947928861,-18.4041176349014,
0.));
#76994=CARTESIAN_POINT('Ctrl Pts',(-43.9844947928861,-18.4041176349014,
20.));
#76995=CARTESIAN_POINT('Ctrl Pts',(-43.9945334016277,-18.3723074465347,
0.));
#76996=CARTESIAN_POINT('Ctrl Pts',(-43.9945334016277,-18.3723074465347,
20.));
#76997=CARTESIAN_POINT('Ctrl Pts',(-44.0045495078276,-18.3404913362408,
0.));
#76998=CARTESIAN_POINT('Ctrl Pts',(-44.0045495078276,-18.3404913362408,
20.));
#76999=CARTESIAN_POINT('Ctrl Pts',(-44.0145431074514,-18.3086693197275,
0.));
#77000=CARTESIAN_POINT('Ctrl Pts',(-44.0145431074514,-18.3086693197275,
20.));
#77001=CARTESIAN_POINT('Ctrl Pts',(-44.0245141964756,-18.2768414127056,
0.));
#77002=CARTESIAN_POINT('Ctrl Pts',(-44.0245141964756,-18.2768414127056,
20.));
#77003=CARTESIAN_POINT('Ctrl Pts',(-44.0344627708874,-18.2450076308889,
0.));
#77004=CARTESIAN_POINT('Ctrl Pts',(-44.0344627708874,-18.2450076308889,
20.));
#77005=CARTESIAN_POINT('Ctrl Pts',(-44.044388826685,-18.2131679899948,0.));
#77006=CARTESIAN_POINT('Ctrl Pts',(-44.044388826685,-18.2131679899948,20.));
#77007=CARTESIAN_POINT('Ctrl Pts',(-44.0542923598773,-18.1813225057438,
0.));
#77008=CARTESIAN_POINT('Ctrl Pts',(-44.0542923598773,-18.1813225057438,
20.));
#77009=CARTESIAN_POINT('Ctrl Pts',(-44.0641733664839,-18.1494711938598,
0.));
#77010=CARTESIAN_POINT('Ctrl Pts',(-44.0641733664839,-18.1494711938598,
20.));
#77011=CARTESIAN_POINT('Ctrl Pts',(-44.0740318425361,-18.1176140700699,
0.));
#77012=CARTESIAN_POINT('Ctrl Pts',(-44.0740318425361,-18.1176140700699,
20.));
#77013=CARTESIAN_POINT('Ctrl Pts',(-44.0838677840754,-18.0857511501043,
0.));
#77014=CARTESIAN_POINT('Ctrl Pts',(-44.0838677840754,-18.0857511501043,
20.));
#77015=CARTESIAN_POINT('Ctrl Pts',(-44.0936811871546,-18.0538824496962,
0.));
#77016=CARTESIAN_POINT('Ctrl Pts',(-44.0936811871546,-18.0538824496962,
20.));
#77017=CARTESIAN_POINT('Ctrl Pts',(-44.1034720478372,-18.0220079845822,
0.));
#77018=CARTESIAN_POINT('Ctrl Pts',(-44.1034720478372,-18.0220079845822,
20.));
#77019=CARTESIAN_POINT('Ctrl Pts',(-44.1132403621971,-17.9901277705015,
0.));
#77020=CARTESIAN_POINT('Ctrl Pts',(-44.1132403621971,-17.9901277705015,
20.));
#77021=CARTESIAN_POINT('Ctrl Pts',(-44.1229861263191,-17.9582418231966,
0.));
#77022=CARTESIAN_POINT('Ctrl Pts',(-44.1229861263191,-17.9582418231966,
20.));
#77023=CARTESIAN_POINT('Ctrl Pts',(-44.1327093362991,-17.9263501584131,
0.));
#77024=CARTESIAN_POINT('Ctrl Pts',(-44.1327093362991,-17.9263501584131,
20.));
#77025=CARTESIAN_POINT('Ctrl Pts',(-44.142409988244,-17.8944527919,0.));
#77026=CARTESIAN_POINT('Ctrl Pts',(-44.142409988244,-17.8944527919,20.));
#77027=CARTESIAN_POINT('Ctrl Pts',(-44.1520880782717,-17.8625497394092,
0.));
#77028=CARTESIAN_POINT('Ctrl Pts',(-44.1520880782717,-17.8625497394092,
20.));
#77029=CARTESIAN_POINT('Ctrl Pts',(-44.1617436025112,-17.8306410166963,
0.));
#77030=CARTESIAN_POINT('Ctrl Pts',(-44.1617436025112,-17.8306410166963,
20.));
#77031=CARTESIAN_POINT('Ctrl Pts',(-44.1713765571021,-17.7987266395196,
0.));
#77032=CARTESIAN_POINT('Ctrl Pts',(-44.1713765571021,-17.7987266395196,
20.));
#77033=CARTESIAN_POINT('Ctrl Pts',(-44.1809869381949,-17.7668066236405,
0.));
#77034=CARTESIAN_POINT('Ctrl Pts',(-44.1809869381949,-17.7668066236405,
20.));
#77035=CARTESIAN_POINT('Ctrl Pts',(-44.1905747419505,-17.7348809848234,
0.));
#77036=CARTESIAN_POINT('Ctrl Pts',(-44.1905747419505,-17.7348809848234,
20.));
#77037=CARTESIAN_POINT('Ctrl Pts',(-44.2001399645408,-17.7029497388358,
0.));
#77038=CARTESIAN_POINT('Ctrl Pts',(-44.2001399645408,-17.7029497388358,
20.));
#77039=CARTESIAN_POINT('Ctrl Pts',(-44.2096826021493,-17.6710129014481,
0.));
#77040=CARTESIAN_POINT('Ctrl Pts',(-44.2096826021493,-17.6710129014481,
20.));
#77041=CARTESIAN_POINT('Ctrl Pts',(-44.2192026509705,-17.6390704884341,
0.));
#77042=CARTESIAN_POINT('Ctrl Pts',(-44.2192026509705,-17.6390704884341,
20.));
#77043=CARTESIAN_POINT('Ctrl Pts',(-44.2287001072093,-17.6071225155702,
0.));
#77044=CARTESIAN_POINT('Ctrl Pts',(-44.2287001072093,-17.6071225155702,
20.));
#77045=CARTESIAN_POINT('Ctrl Pts',(-44.2381749670816,-17.5751689986363,
0.));
#77046=CARTESIAN_POINT('Ctrl Pts',(-44.2381749670816,-17.5751689986363,
20.));
#77047=CARTESIAN_POINT('Ctrl Pts',(-44.2476272268138,-17.5432099534151,
0.));
#77048=CARTESIAN_POINT('Ctrl Pts',(-44.2476272268138,-17.5432099534151,
20.));
#77049=CARTESIAN_POINT('Ctrl Pts',(-44.2570568826434,-17.5112453956925,
0.));
#77050=CARTESIAN_POINT('Ctrl Pts',(-44.2570568826434,-17.5112453956925,
20.));
#77051=CARTESIAN_POINT('Ctrl Pts',(-44.2664639308192,-17.4792753412574,
0.));
#77052=CARTESIAN_POINT('Ctrl Pts',(-44.2664639308192,-17.4792753412574,
20.));
#77053=CARTESIAN_POINT('Ctrl Pts',(-44.2758483676008,-17.447299805902,0.));
#77054=CARTESIAN_POINT('Ctrl Pts',(-44.2758483676008,-17.447299805902,20.));
#77055=CARTESIAN_POINT('Ctrl Pts',(-44.2852101892593,-17.4153188054211,
0.));
#77056=CARTESIAN_POINT('Ctrl Pts',(-44.2852101892593,-17.4153188054211,
20.));
#77057=CARTESIAN_POINT('Ctrl Pts',(-44.2945493920761,-17.3833323556128,
0.));
#77058=CARTESIAN_POINT('Ctrl Pts',(-44.2945493920761,-17.3833323556128,
20.));
#77059=CARTESIAN_POINT('Ctrl Pts',(-44.3038659723435,-17.3513404722779,
0.));
#77060=CARTESIAN_POINT('Ctrl Pts',(-44.3038659723435,-17.3513404722779,
20.));
#77061=CARTESIAN_POINT('Ctrl Pts',(-44.3131599263643,-17.3193431712198,
0.));
#77062=CARTESIAN_POINT('Ctrl Pts',(-44.3131599263643,-17.3193431712198,
20.));
#77063=CARTESIAN_POINT('Ctrl Pts',(-44.3224312504523,-17.2873404682456,
0.));
#77064=CARTESIAN_POINT('Ctrl Pts',(-44.3224312504523,-17.2873404682456,
20.));
#77065=CARTESIAN_POINT('Ctrl Pts',(-44.3316799409325,-17.2553323791649,
0.));
#77066=CARTESIAN_POINT('Ctrl Pts',(-44.3316799409325,-17.2553323791649,
20.));
#77067=CARTESIAN_POINT('Ctrl Pts',(-44.340905994141,-17.2233189197905,0.));
#77068=CARTESIAN_POINT('Ctrl Pts',(-44.340905994141,-17.2233189197905,20.));
#77069=CARTESIAN_POINT('Ctrl Pts',(-44.3501094064252,-17.1913001059384,
0.));
#77070=CARTESIAN_POINT('Ctrl Pts',(-44.3501094064252,-17.1913001059384,
20.));
#77071=CARTESIAN_POINT('Ctrl Pts',(-44.3592901741436,-17.1592759534275,
0.));
#77072=CARTESIAN_POINT('Ctrl Pts',(-44.3592901741436,-17.1592759534275,
20.));
#77073=CARTESIAN_POINT('Ctrl Pts',(-44.3684482936655,-17.1272464780797,
0.));
#77074=CARTESIAN_POINT('Ctrl Pts',(-44.3684482936655,-17.1272464780797,
20.));
#77075=CARTESIAN_POINT('Ctrl Pts',(-44.3775837613707,-17.0952116957196,
0.));
#77076=CARTESIAN_POINT('Ctrl Pts',(-44.3775837613707,-17.0952116957196,
20.));
#77077=CARTESIAN_POINT('Ctrl Pts',(-44.3866965736492,-17.0631716221745,
0.));
#77078=CARTESIAN_POINT('Ctrl Pts',(-44.3866965736492,-17.0631716221745,
20.));
#77079=CARTESIAN_POINT('Ctrl Pts',(-44.3957867269024,-17.0311262732746,
0.));
#77080=CARTESIAN_POINT('Ctrl Pts',(-44.3957867269024,-17.0311262732746,
20.));
#77081=CARTESIAN_POINT('Ctrl Pts',(-44.404854217543,-16.9990756648532,0.));
#77082=CARTESIAN_POINT('Ctrl Pts',(-44.404854217543,-16.9990756648532,20.));
#77083=CARTESIAN_POINT('Ctrl Pts',(-44.4138990419958,-16.967019812747,0.));
#77084=CARTESIAN_POINT('Ctrl Pts',(-44.4138990419958,-16.967019812747,20.));
#77085=CARTESIAN_POINT('Ctrl Pts',(-44.4229211966955,-16.9349587327952,
0.));
#77086=CARTESIAN_POINT('Ctrl Pts',(-44.4229211966955,-16.9349587327952,
20.));
#77087=CARTESIAN_POINT('Ctrl Pts',(-44.431920678088,-16.9028924408399,0.));
#77088=CARTESIAN_POINT('Ctrl Pts',(-44.431920678088,-16.9028924408399,20.));
#77089=CARTESIAN_POINT('Ctrl Pts',(-44.4408974826294,-16.870820952726,0.));
#77090=CARTESIAN_POINT('Ctrl Pts',(-44.4408974826294,-16.870820952726,20.));
#77091=CARTESIAN_POINT('Ctrl Pts',(-44.4498516067869,-16.8387442843012,
0.));
#77092=CARTESIAN_POINT('Ctrl Pts',(-44.4498516067869,-16.8387442843012,
20.));
#77093=CARTESIAN_POINT('Ctrl Pts',(-44.4587830470388,-16.8066624514163,
0.));
#77094=CARTESIAN_POINT('Ctrl Pts',(-44.4587830470388,-16.8066624514163,
20.));
#77095=CARTESIAN_POINT('Ctrl Pts',(-44.4676917998748,-16.7745754699247,
0.));
#77096=CARTESIAN_POINT('Ctrl Pts',(-44.4676917998748,-16.7745754699247,
20.));
#77097=CARTESIAN_POINT('Ctrl Pts',(-44.4765778617956,-16.742483355683,0.));
#77098=CARTESIAN_POINT('Ctrl Pts',(-44.4765778617956,-16.742483355683,20.));
#77099=CARTESIAN_POINT('Ctrl Pts',(-44.4854412293128,-16.7103861245505,
0.));
#77100=CARTESIAN_POINT('Ctrl Pts',(-44.4854412293128,-16.7103861245505,
20.));
#77101=CARTESIAN_POINT('Ctrl Pts',(-44.4942818989491,-16.6782837923892,
0.));
#77102=CARTESIAN_POINT('Ctrl Pts',(-44.4942818989491,-16.6782837923892,
20.));
#77103=CARTESIAN_POINT('Ctrl Pts',(-44.5030998672381,-16.6461763750644,
0.));
#77104=CARTESIAN_POINT('Ctrl Pts',(-44.5030998672381,-16.6461763750644,
20.));
#77105=CARTESIAN_POINT('Ctrl Pts',(-44.5118951307243,-16.6140638884438,
0.));
#77106=CARTESIAN_POINT('Ctrl Pts',(-44.5118951307243,-16.6140638884438,
20.));
#77107=CARTESIAN_POINT('Ctrl Pts',(-44.5206676859633,-16.581946348398,0.));
#77108=CARTESIAN_POINT('Ctrl Pts',(-44.5206676859633,-16.581946348398,20.));
#77109=CARTESIAN_POINT('Ctrl Pts',(-44.5294175295214,-16.5498237708003,
0.));
#77110=CARTESIAN_POINT('Ctrl Pts',(-44.5294175295214,-16.5498237708003,
20.));
#77111=CARTESIAN_POINT('Ctrl Pts',(-44.5381446579761,-16.5176961715269,
0.));
#77112=CARTESIAN_POINT('Ctrl Pts',(-44.5381446579761,-16.5176961715269,
20.));
#77113=CARTESIAN_POINT('Ctrl Pts',(-44.5468490679154,-16.4855635664567,
0.));
#77114=CARTESIAN_POINT('Ctrl Pts',(-44.5468490679154,-16.4855635664567,
20.));
#77115=CARTESIAN_POINT('Ctrl Pts',(-44.5555307559385,-16.4534259714715,
0.));
#77116=CARTESIAN_POINT('Ctrl Pts',(-44.5555307559385,-16.4534259714715,
20.));
#77117=CARTESIAN_POINT('Ctrl Pts',(-44.5641897186557,-16.4212834024559,
0.));
#77118=CARTESIAN_POINT('Ctrl Pts',(-44.5641897186557,-16.4212834024559,
20.));
#77119=CARTESIAN_POINT('Ctrl Pts',(-44.5728259526889,-16.3891358752972,
0.));
#77120=CARTESIAN_POINT('Ctrl Pts',(-44.5728259526889,-16.3891358752972,
20.));
#77121=CARTESIAN_POINT('Ctrl Pts',(-44.581439454671,-16.3569834058857,0.));
#77122=CARTESIAN_POINT('Ctrl Pts',(-44.581439454671,-16.3569834058857,20.));
#77123=CARTESIAN_POINT('Ctrl Pts',(-44.5900302212458,-16.3248260101143,
0.));
#77124=CARTESIAN_POINT('Ctrl Pts',(-44.5900302212458,-16.3248260101143,
20.));
#77125=CARTESIAN_POINT('Ctrl Pts',(-44.5985982490682,-16.2926637038787,
0.));
#77126=CARTESIAN_POINT('Ctrl Pts',(-44.5985982490682,-16.2926637038787,
20.));
#77127=CARTESIAN_POINT('Ctrl Pts',(-44.6071435348036,-16.2604965030773,
0.));
#77128=CARTESIAN_POINT('Ctrl Pts',(-44.6071435348036,-16.2604965030773,
20.));
#77129=CARTESIAN_POINT('Ctrl Pts',(-44.6156660751288,-16.2283244236112,
0.));
#77130=CARTESIAN_POINT('Ctrl Pts',(-44.6156660751288,-16.2283244236112,
20.));
#77131=CARTESIAN_POINT('Ctrl Pts',(-44.6241658667307,-16.196147481384,0.));
#77132=CARTESIAN_POINT('Ctrl Pts',(-44.6241658667307,-16.196147481384,20.));
#77133=CARTESIAN_POINT('Ctrl Pts',(-44.6326429063072,-16.1639656923022,
0.));
#77134=CARTESIAN_POINT('Ctrl Pts',(-44.6326429063072,-16.1639656923022,
20.));
#77135=CARTESIAN_POINT('Ctrl Pts',(-44.6410971905673,-16.131779072275,0.));
#77136=CARTESIAN_POINT('Ctrl Pts',(-44.6410971905673,-16.131779072275,20.));
#77137=CARTESIAN_POINT('Ctrl Pts',(-44.649528716232,-16.0995876372141,0.));
#77138=CARTESIAN_POINT('Ctrl Pts',(-44.649528716232,-16.0995876372141,20.));
#77139=CARTESIAN_POINT('Ctrl Pts',(-44.6579374800339,-16.0673914030343,
0.));
#77140=CARTESIAN_POINT('Ctrl Pts',(-44.6579374800339,-16.0673914030343,
20.));
#77141=CARTESIAN_POINT('Ctrl Pts',(-44.6663234787169,-16.0351903856534,
0.));
#77142=CARTESIAN_POINT('Ctrl Pts',(-44.6663234787169,-16.0351903856534,
20.));
#77143=CARTESIAN_POINT('Ctrl Pts',(-44.6746867090345,-16.0029846009915,
0.));
#77144=CARTESIAN_POINT('Ctrl Pts',(-44.6746867090345,-16.0029846009915,
20.));
#77145=CARTESIAN_POINT('Ctrl Pts',(-44.6830271677516,-15.9707740649715,
0.));
#77146=CARTESIAN_POINT('Ctrl Pts',(-44.6830271677516,-15.9707740649715,
20.));
#77147=CARTESIAN_POINT('Ctrl Pts',(-44.691344851643,-15.9385587935186,0.));
#77148=CARTESIAN_POINT('Ctrl Pts',(-44.691344851643,-15.9385587935186,20.));
#77149=CARTESIAN_POINT('Ctrl Pts',(-44.6996397574952,-15.9063388025603,
0.));
#77150=CARTESIAN_POINT('Ctrl Pts',(-44.6996397574952,-15.9063388025603,
20.));
#77151=CARTESIAN_POINT('Ctrl Pts',(-44.7079118821065,-15.8741141080271,
0.));
#77152=CARTESIAN_POINT('Ctrl Pts',(-44.7079118821065,-15.8741141080271,
20.));
#77153=CARTESIAN_POINT('Ctrl Pts',(-44.7161612222865,-15.8418847258528,
0.));
#77154=CARTESIAN_POINT('Ctrl Pts',(-44.7161612222865,-15.8418847258528,
20.));
#77155=CARTESIAN_POINT('Ctrl Pts',(-44.7243877748558,-15.8096506719735,
0.));
#77156=CARTESIAN_POINT('Ctrl Pts',(-44.7243877748558,-15.8096506719735,
20.));
#77157=CARTESIAN_POINT('Ctrl Pts',(-44.7325915366458,-15.7774119623278,
0.));
#77158=CARTESIAN_POINT('Ctrl Pts',(-44.7325915366458,-15.7774119623278,
20.));
#77159=CARTESIAN_POINT('Ctrl Pts',(-44.7407725044985,-15.745168612857,0.));
#77160=CARTESIAN_POINT('Ctrl Pts',(-44.7407725044985,-15.745168612857,20.));
#77161=CARTESIAN_POINT('Ctrl Pts',(-44.7489306752664,-15.7129206395047,
0.));
#77162=CARTESIAN_POINT('Ctrl Pts',(-44.7489306752664,-15.7129206395047,
20.));
#77163=CARTESIAN_POINT('Ctrl Pts',(-44.7570660458133,-15.6806680582172,
0.));
#77164=CARTESIAN_POINT('Ctrl Pts',(-44.7570660458133,-15.6806680582172,
20.));
#77165=CARTESIAN_POINT('Ctrl Pts',(-44.7651786130144,-15.6484108849434,
0.));
#77166=CARTESIAN_POINT('Ctrl Pts',(-44.7651786130144,-15.6484108849434,
20.));
#77167=CARTESIAN_POINT('Ctrl Pts',(-44.7732683737566,-15.6161491356348,
0.));
#77168=CARTESIAN_POINT('Ctrl Pts',(-44.7732683737566,-15.6161491356348,
20.));
#77169=CARTESIAN_POINT('Ctrl Pts',(-44.7813353249379,-15.583882826246,0.));
#77170=CARTESIAN_POINT('Ctrl Pts',(-44.7813353249379,-15.583882826246,20.));
#77171=CARTESIAN_POINT('Ctrl Pts',(-44.7893794634672,-15.5516119727338,
0.));
#77172=CARTESIAN_POINT('Ctrl Pts',(-44.7893794634672,-15.5516119727338,
20.));
#77173=CARTESIAN_POINT('Ctrl Pts',(-44.7974007862643,-15.5193365910578,
0.));
#77174=CARTESIAN_POINT('Ctrl Pts',(-44.7974007862643,-15.5193365910578,
20.));
#77175=CARTESIAN_POINT('Ctrl Pts',(-44.8053992902599,-15.4870566971798,
0.));
#77176=CARTESIAN_POINT('Ctrl Pts',(-44.8053992902599,-15.4870566971798,
20.));
#77177=CARTESIAN_POINT('Ctrl Pts',(-44.8133749723964,-15.4547723070643,
0.));
#77178=CARTESIAN_POINT('Ctrl Pts',(-44.8133749723964,-15.4547723070643,
20.));
#77179=CARTESIAN_POINT('Ctrl Pts',(-44.8213278296263,-15.4224834366782,
0.));
#77180=CARTESIAN_POINT('Ctrl Pts',(-44.8213278296263,-15.4224834366782,
20.));
#77181=CARTESIAN_POINT('Ctrl Pts',(-44.8292578589132,-15.3901901019906,
0.));
#77182=CARTESIAN_POINT('Ctrl Pts',(-44.8292578589132,-15.3901901019906,
20.));
#77183=CARTESIAN_POINT('Ctrl Pts',(-44.8371650572316,-15.3578923189739,
0.));
#77184=CARTESIAN_POINT('Ctrl Pts',(-44.8371650572316,-15.3578923189739,
20.));
#77185=CARTESIAN_POINT('Ctrl Pts',(-44.8450494215678,-15.3255901036026,
0.));
#77186=CARTESIAN_POINT('Ctrl Pts',(-44.8450494215678,-15.3255901036026,
20.));
#77187=CARTESIAN_POINT('Ctrl Pts',(-44.8529109489191,-15.2932834718541,
0.));
#77188=CARTESIAN_POINT('Ctrl Pts',(-44.8529109489191,-15.2932834718541,
20.));
#77189=CARTESIAN_POINT('Ctrl Pts',(-44.8607496362943,-15.2609724397079,
0.));
#77190=CARTESIAN_POINT('Ctrl Pts',(-44.8607496362943,-15.2609724397079,
20.));
#77191=CARTESIAN_POINT('Ctrl Pts',(-44.8685654807131,-15.2286570231461,
0.));
#77192=CARTESIAN_POINT('Ctrl Pts',(-44.8685654807131,-15.2286570231461,
20.));
#77193=CARTESIAN_POINT('Ctrl Pts',(-44.8763584792064,-15.1963372381533,
0.));
#77194=CARTESIAN_POINT('Ctrl Pts',(-44.8763584792064,-15.1963372381533,
20.));
#77195=CARTESIAN_POINT('Ctrl Pts',(-44.8841286288163,-15.1640131007166,
0.));
#77196=CARTESIAN_POINT('Ctrl Pts',(-44.8841286288163,-15.1640131007166,
20.));
#77197=CARTESIAN_POINT('Ctrl Pts',(-44.8918759265956,-15.1316846268256,
0.));
#77198=CARTESIAN_POINT('Ctrl Pts',(-44.8918759265956,-15.1316846268256,
20.));
#77199=CARTESIAN_POINT('Ctrl Pts',(-44.8996003696078,-15.0993518324721,
0.));
#77200=CARTESIAN_POINT('Ctrl Pts',(-44.8996003696078,-15.0993518324721,
20.));
#77201=CARTESIAN_POINT('Ctrl Pts',(-44.9073019549277,-15.0670147336509,
0.));
#77202=CARTESIAN_POINT('Ctrl Pts',(-44.9073019549277,-15.0670147336509,
20.));
#77203=CARTESIAN_POINT('Ctrl Pts',(-44.9149806796409,-15.034673346359,0.));
#77204=CARTESIAN_POINT('Ctrl Pts',(-44.9149806796409,-15.034673346359,20.));
#77205=CARTESIAN_POINT('Ctrl Pts',(-44.9226365408441,-15.0023276865958,
0.));
#77206=CARTESIAN_POINT('Ctrl Pts',(-44.9226365408441,-15.0023276865958,
20.));
#77207=CARTESIAN_POINT('Ctrl Pts',(-44.9302695356455,-14.969977770363,0.));
#77208=CARTESIAN_POINT('Ctrl Pts',(-44.9302695356455,-14.969977770363,20.));
#77209=CARTESIAN_POINT('Ctrl Pts',(-44.9378796611651,-14.9376236136649,
0.));
#77210=CARTESIAN_POINT('Ctrl Pts',(-44.9378796611651,-14.9376236136649,
20.));
#77211=CARTESIAN_POINT('Ctrl Pts',(-44.9454669145344,-14.9052652325081,
0.));
#77212=CARTESIAN_POINT('Ctrl Pts',(-44.9454669145344,-14.9052652325081,
20.));
#77213=CARTESIAN_POINT('Ctrl Pts',(-44.9530312928958,-14.8729026429019,
0.));
#77214=CARTESIAN_POINT('Ctrl Pts',(-44.9530312928958,-14.8729026429019,
20.));
#77215=CARTESIAN_POINT('Ctrl Pts',(-44.9605727934022,-14.8405358608577,
0.));
#77216=CARTESIAN_POINT('Ctrl Pts',(-44.9605727934022,-14.8405358608577,
20.));
#77217=CARTESIAN_POINT('Ctrl Pts',(-44.9680914132176,-14.8081649023895,
0.));
#77218=CARTESIAN_POINT('Ctrl Pts',(-44.9680914132176,-14.8081649023895,
20.));
#77219=CARTESIAN_POINT('Ctrl Pts',(-44.9755871495162,-14.7757897835134,
0.));
#77220=CARTESIAN_POINT('Ctrl Pts',(-44.9755871495162,-14.7757897835134,
20.));
#77221=CARTESIAN_POINT('Ctrl Pts',(-44.9830599994838,-14.7434105202483,
0.));
#77222=CARTESIAN_POINT('Ctrl Pts',(-44.9830599994838,-14.7434105202483,
20.));
#77223=CARTESIAN_POINT('Ctrl Pts',(-44.9905099603172,-14.7110271286153,
0.));
#77224=CARTESIAN_POINT('Ctrl Pts',(-44.9905099603172,-14.7110271286153,
20.));
#77225=CARTESIAN_POINT('Ctrl Pts',(-44.9979370292253,-14.6786396246378,
0.));
#77226=CARTESIAN_POINT('Ctrl Pts',(-44.9979370292253,-14.6786396246378,
20.));
#77227=CARTESIAN_POINT('Ctrl Pts',(-45.0053412034276,-14.6462480243418,
0.));
#77228=CARTESIAN_POINT('Ctrl Pts',(-45.0053412034276,-14.6462480243418,
20.));
#77229=CARTESIAN_POINT('Ctrl Pts',(-45.0127224801553,-14.6138523437553,
0.));
#77230=CARTESIAN_POINT('Ctrl Pts',(-45.0127224801553,-14.6138523437553,
20.));
#77231=CARTESIAN_POINT('Ctrl Pts',(-45.020080856651,-14.5814525989087,0.));
#77232=CARTESIAN_POINT('Ctrl Pts',(-45.020080856651,-14.5814525989087,20.));
#77233=CARTESIAN_POINT('Ctrl Pts',(-45.0274163301681,-14.5490488058349,
0.));
#77234=CARTESIAN_POINT('Ctrl Pts',(-45.0274163301681,-14.5490488058349,
20.));
#77235=CARTESIAN_POINT('Ctrl Pts',(-45.0347288979708,-14.516640980569,0.));
#77236=CARTESIAN_POINT('Ctrl Pts',(-45.0347288979708,-14.516640980569,20.));
#77237=CARTESIAN_POINT('Ctrl Pts',(-45.0420185573342,-14.4842291391484,
0.));
#77238=CARTESIAN_POINT('Ctrl Pts',(-45.0420185573342,-14.4842291391484,
20.));
#77239=CARTESIAN_POINT('Ctrl Pts',(-45.0492853055441,-14.451813297613,0.));
#77240=CARTESIAN_POINT('Ctrl Pts',(-45.0492853055441,-14.451813297613,20.));
#77241=CARTESIAN_POINT('Ctrl Pts',(-45.0565291398984,-14.4193934720051,
0.));
#77242=CARTESIAN_POINT('Ctrl Pts',(-45.0565291398984,-14.4193934720051,
20.));
#77243=CARTESIAN_POINT('Ctrl Pts',(-45.0637500577056,-14.3869696783692,
0.));
#77244=CARTESIAN_POINT('Ctrl Pts',(-45.0637500577056,-14.3869696783692,
20.));
#77245=CARTESIAN_POINT('Ctrl Pts',(-45.0709480562863,-14.354541932752,0.));
#77246=CARTESIAN_POINT('Ctrl Pts',(-45.0709480562863,-14.354541932752,20.));
#77247=CARTESIAN_POINT('Ctrl Pts',(-45.078123132972,-14.3221102512025,0.));
#77248=CARTESIAN_POINT('Ctrl Pts',(-45.078123132972,-14.3221102512025,20.));
#77249=CARTESIAN_POINT('Ctrl Pts',(-45.0852752851048,-14.2896746497719,
0.));
#77250=CARTESIAN_POINT('Ctrl Pts',(-45.0852752851048,-14.2896746497719,
20.));
#77251=CARTESIAN_POINT('Ctrl Pts',(-45.0924045100383,-14.2572351445137,
0.));
#77252=CARTESIAN_POINT('Ctrl Pts',(-45.0924045100383,-14.2572351445137,
20.));
#77253=CARTESIAN_POINT('Ctrl Pts',(-45.0995108051367,-14.2247917514836,
0.));
#77254=CARTESIAN_POINT('Ctrl Pts',(-45.0995108051367,-14.2247917514836,
20.));
#77255=CARTESIAN_POINT('Ctrl Pts',(-45.1065941677758,-14.1923444867396,
0.));
#77256=CARTESIAN_POINT('Ctrl Pts',(-45.1065941677758,-14.1923444867396,
20.));
#77257=CARTESIAN_POINT('Ctrl Pts',(-45.1136545953429,-14.1598933663422,
0.));
#77258=CARTESIAN_POINT('Ctrl Pts',(-45.1136545953429,-14.1598933663422,
20.));
#77259=CARTESIAN_POINT('Ctrl Pts',(-45.1206920852361,-14.127438406354,0.));
#77260=CARTESIAN_POINT('Ctrl Pts',(-45.1206920852361,-14.127438406354,20.));
#77261=CARTESIAN_POINT('Ctrl Pts',(-45.127706634865,-14.0949796228398,0.));
#77262=CARTESIAN_POINT('Ctrl Pts',(-45.127706634865,-14.0949796228398,20.));
#77263=CARTESIAN_POINT('Ctrl Pts',(-45.1346982416501,-14.0625170318664,
0.));
#77264=CARTESIAN_POINT('Ctrl Pts',(-45.1346982416501,-14.0625170318664,
20.));
#77265=CARTESIAN_POINT('Ctrl Pts',(-45.1416669030232,-14.0300506495033,
0.));
#77266=CARTESIAN_POINT('Ctrl Pts',(-45.1416669030232,-14.0300506495033,
20.));
#77267=CARTESIAN_POINT('Ctrl Pts',(-45.1486126164275,-13.997580491822,0.));
#77268=CARTESIAN_POINT('Ctrl Pts',(-45.1486126164275,-13.997580491822,20.));
#77269=CARTESIAN_POINT('Ctrl Pts',(-45.1555353793172,-13.9651065748961,
0.));
#77270=CARTESIAN_POINT('Ctrl Pts',(-45.1555353793172,-13.9651065748961,
20.));
#77271=CARTESIAN_POINT('Ctrl Pts',(-45.1624351891574,-13.9326289148012,
0.));
#77272=CARTESIAN_POINT('Ctrl Pts',(-45.1624351891574,-13.9326289148012,
20.));
#77273=CARTESIAN_POINT('Ctrl Pts',(-45.1693120434241,-13.9001475276153,
0.));
#77274=CARTESIAN_POINT('Ctrl Pts',(-45.1693120434241,-13.9001475276153,
20.));
#77275=CARTESIAN_POINT('Ctrl Pts',(-45.1761659396043,-13.8676624294184,
0.));
#77276=CARTESIAN_POINT('Ctrl Pts',(-45.1761659396043,-13.8676624294184,
20.));
#77277=CARTESIAN_POINT('Ctrl Pts',(-45.1829968751969,-13.8351736362929,
0.));
#77278=CARTESIAN_POINT('Ctrl Pts',(-45.1829968751969,-13.8351736362929,
20.));
#77279=CARTESIAN_POINT('Ctrl Pts',(-45.1898048477123,-13.8026811643234,
0.));
#77280=CARTESIAN_POINT('Ctrl Pts',(-45.1898048477123,-13.8026811643234,
20.));
#77281=CARTESIAN_POINT('Ctrl Pts',(-45.1965898546723,-13.7701850295967,
0.));
#77282=CARTESIAN_POINT('Ctrl Pts',(-45.1965898546723,-13.7701850295967,
20.));
#77283=CARTESIAN_POINT('Ctrl Pts',(-45.2033518936101,-13.7376852482019,
0.));
#77284=CARTESIAN_POINT('Ctrl Pts',(-45.2033518936101,-13.7376852482019,
20.));
#77285=CARTESIAN_POINT('Ctrl Pts',(-45.2100909620697,-13.7051818362299,
0.));
#77286=CARTESIAN_POINT('Ctrl Pts',(-45.2100909620697,-13.7051818362299,
20.));
#77287=CARTESIAN_POINT('Ctrl Pts',(-45.2168070576061,-13.6726748097738,
0.));
#77288=CARTESIAN_POINT('Ctrl Pts',(-45.2168070576061,-13.6726748097738,
20.));
#77289=CARTESIAN_POINT('Ctrl Pts',(-45.2235001777847,-13.6401641849286,
0.));
#77290=CARTESIAN_POINT('Ctrl Pts',(-45.2235001777847,-13.6401641849286,
20.));
#77291=CARTESIAN_POINT('Ctrl Pts',(-45.2301703201819,-13.6076499777914,
0.));
#77292=CARTESIAN_POINT('Ctrl Pts',(-45.2301703201819,-13.6076499777914,
20.));
#77293=CARTESIAN_POINT('Ctrl Pts',(-45.2368174823856,-13.5751322044618,
0.));
#77294=CARTESIAN_POINT('Ctrl Pts',(-45.2368174823856,-13.5751322044618,
20.));
#77295=CARTESIAN_POINT('Ctrl Pts',(-45.2434416619952,-13.542610881041,0.));
#77296=CARTESIAN_POINT('Ctrl Pts',(-45.2434416619952,-13.542610881041,20.));
#77297=CARTESIAN_POINT('Ctrl Pts',(-45.2500428566225,-13.5100860236329,
0.));
#77298=CARTESIAN_POINT('Ctrl Pts',(-45.2500428566225,-13.5100860236329,
20.));
#77299=CARTESIAN_POINT('Ctrl Pts',(-45.2566210638904,-13.4775576483433,
0.));
#77300=CARTESIAN_POINT('Ctrl Pts',(-45.2566210638904,-13.4775576483433,
20.));
#77301=CARTESIAN_POINT('Ctrl Pts',(-45.2631762814325,-13.44502577128,0.));
#77302=CARTESIAN_POINT('Ctrl Pts',(-45.2631762814325,-13.44502577128,20.));
#77303=CARTESIAN_POINT('Ctrl Pts',(-45.2697085068935,-13.4124904085531,
0.));
#77304=CARTESIAN_POINT('Ctrl Pts',(-45.2697085068935,-13.4124904085531,
20.));
#77305=CARTESIAN_POINT('Ctrl Pts',(-45.276217737929,-13.3799515762744,0.));
#77306=CARTESIAN_POINT('Ctrl Pts',(-45.276217737929,-13.3799515762744,20.));
#77307=CARTESIAN_POINT('Ctrl Pts',(-45.2827039722059,-13.3474092905576,
0.));
#77308=CARTESIAN_POINT('Ctrl Pts',(-45.2827039722059,-13.3474092905576,
20.));
#77309=CARTESIAN_POINT('Ctrl Pts',(-45.2891672074022,-13.3148635675188,
0.));
#77310=CARTESIAN_POINT('Ctrl Pts',(-45.2891672074022,-13.3148635675188,
20.));
#77311=CARTESIAN_POINT('Ctrl Pts',(-45.2956074412073,-13.282314423276,0.));
#77312=CARTESIAN_POINT('Ctrl Pts',(-45.2956074412073,-13.282314423276,20.));
#77313=CARTESIAN_POINT('Ctrl Pts',(-45.3020246713218,-13.2497618739494,
0.));
#77314=CARTESIAN_POINT('Ctrl Pts',(-45.3020246713218,-13.2497618739494,
20.));
#77315=CARTESIAN_POINT('Ctrl Pts',(-45.3084188954577,-13.217205935661,0.));
#77316=CARTESIAN_POINT('Ctrl Pts',(-45.3084188954577,-13.217205935661,20.));
#77317=CARTESIAN_POINT('Ctrl Pts',(-45.3147901113387,-13.1846466245352,
0.));
#77318=CARTESIAN_POINT('Ctrl Pts',(-45.3147901113387,-13.1846466245352,
20.));
#77319=CARTESIAN_POINT('Ctrl Pts',(-45.321138316699,-13.1520839566979,0.));
#77320=CARTESIAN_POINT('Ctrl Pts',(-45.321138316699,-13.1520839566979,20.));
#77321=CARTESIAN_POINT('Ctrl Pts',(-45.3274635092846,-13.1195179482773,
0.));
#77322=CARTESIAN_POINT('Ctrl Pts',(-45.3274635092846,-13.1195179482773,
20.));
#77323=CARTESIAN_POINT('Ctrl Pts',(-45.3337656868523,-13.0869486154035,
0.));
#77324=CARTESIAN_POINT('Ctrl Pts',(-45.3337656868523,-13.0869486154035,
20.));
#77325=CARTESIAN_POINT('Ctrl Pts',(-45.3400448471699,-13.0543759742083,
0.));
#77326=CARTESIAN_POINT('Ctrl Pts',(-45.3400448471699,-13.0543759742083,
20.));
#77327=CARTESIAN_POINT('Ctrl Pts',(-45.3463009880171,-13.021800040826,0.));
#77328=CARTESIAN_POINT('Ctrl Pts',(-45.3463009880171,-13.021800040826,20.));
#77329=CARTESIAN_POINT('Ctrl Pts',(-45.3525341071849,-12.9892208313927,
0.));
#77330=CARTESIAN_POINT('Ctrl Pts',(-45.3525341071849,-12.9892208313927,
20.));
#77331=CARTESIAN_POINT('Ctrl Pts',(-45.3587442024753,-12.9566383620464,
0.));
#77332=CARTESIAN_POINT('Ctrl Pts',(-45.3587442024753,-12.9566383620464,
20.));
#77333=CARTESIAN_POINT('Ctrl Pts',(-45.3649312717011,-12.9240526489272,
0.));
#77334=CARTESIAN_POINT('Ctrl Pts',(-45.3649312717011,-12.9240526489272,
20.));
#77335=CARTESIAN_POINT('Ctrl Pts',(-45.371095312686,-12.8914637081769,0.));
#77336=CARTESIAN_POINT('Ctrl Pts',(-45.371095312686,-12.8914637081769,20.));
#77337=CARTESIAN_POINT('Ctrl Pts',(-45.3772363232658,-12.8588715559393,
0.));
#77338=CARTESIAN_POINT('Ctrl Pts',(-45.3772363232658,-12.8588715559393,
20.));
#77339=CARTESIAN_POINT('Ctrl Pts',(-45.3833543012877,-12.82627620836,0.));
#77340=CARTESIAN_POINT('Ctrl Pts',(-45.3833543012877,-12.82627620836,20.));
#77341=CARTESIAN_POINT('Ctrl Pts',(-45.3894492446102,-12.7936776815868,
0.));
#77342=CARTESIAN_POINT('Ctrl Pts',(-45.3894492446102,-12.7936776815868,
20.));
#77343=CARTESIAN_POINT('Ctrl Pts',(-45.3955211511034,-12.7610759917694,
0.));
#77344=CARTESIAN_POINT('Ctrl Pts',(-45.3955211511034,-12.7610759917694,
20.));
#77345=CARTESIAN_POINT('Ctrl Pts',(-45.4015700186485,-12.7284711550592,
0.));
#77346=CARTESIAN_POINT('Ctrl Pts',(-45.4015700186485,-12.7284711550592,
20.));
#77347=CARTESIAN_POINT('Ctrl Pts',(-45.407595845137,-12.6958631876099,0.));
#77348=CARTESIAN_POINT('Ctrl Pts',(-45.407595845137,-12.6958631876099,20.));
#77349=CARTESIAN_POINT('Ctrl Pts',(-45.4135986284717,-12.6632521055766,
0.));
#77350=CARTESIAN_POINT('Ctrl Pts',(-45.4135986284717,-12.6632521055766,
20.));
#77351=CARTESIAN_POINT('Ctrl Pts',(-45.4195783665665,-12.6306379251164,
0.));
#77352=CARTESIAN_POINT('Ctrl Pts',(-45.4195783665665,-12.6306379251164,
20.));
#77353=CARTESIAN_POINT('Ctrl Pts',(-45.4255350573473,-12.5980206623884,
0.));
#77354=CARTESIAN_POINT('Ctrl Pts',(-45.4255350573473,-12.5980206623884,
20.));
#77355=CARTESIAN_POINT('Ctrl Pts',(-45.4314686987515,-12.5654003335532,
0.));
#77356=CARTESIAN_POINT('Ctrl Pts',(-45.4314686987515,-12.5654003335532,
20.));
#77357=CARTESIAN_POINT('Ctrl Pts',(-45.4373792887274,-12.5327769547739,
0.));
#77358=CARTESIAN_POINT('Ctrl Pts',(-45.4373792887274,-12.5327769547739,
20.));
#77359=CARTESIAN_POINT('Ctrl Pts',(-45.4432668252347,-12.500150542215,0.));
#77360=CARTESIAN_POINT('Ctrl Pts',(-45.4432668252347,-12.500150542215,20.));
#77361=CARTESIAN_POINT('Ctrl Pts',(-45.4491313062444,-12.4675211120431,
0.));
#77362=CARTESIAN_POINT('Ctrl Pts',(-45.4491313062444,-12.4675211120431,
20.));
#77363=CARTESIAN_POINT('Ctrl Pts',(-45.4549727297392,-12.4348886804266,
0.));
#77364=CARTESIAN_POINT('Ctrl Pts',(-45.4549727297392,-12.4348886804266,
20.));
#77365=CARTESIAN_POINT('Ctrl Pts',(-45.4607910937128,-12.4022532635357,
0.));
#77366=CARTESIAN_POINT('Ctrl Pts',(-45.4607910937128,-12.4022532635357,
20.));
#77367=CARTESIAN_POINT('Ctrl Pts',(-45.4665863961701,-12.3696148775423,
0.));
#77368=CARTESIAN_POINT('Ctrl Pts',(-45.4665863961701,-12.3696148775423,
20.));
#77369=CARTESIAN_POINT('Ctrl Pts',(-45.4723586351267,-12.3369735386201,
0.));
#77370=CARTESIAN_POINT('Ctrl Pts',(-45.4723586351267,-12.3369735386201,
20.));
#77371=CARTESIAN_POINT('Ctrl Pts',(-45.4781078086095,-12.3043292629445,
0.));
#77372=CARTESIAN_POINT('Ctrl Pts',(-45.4781078086095,-12.3043292629445,
20.));
#77373=CARTESIAN_POINT('Ctrl Pts',(-45.483833914657,-12.2716820666929,0.));
#77374=CARTESIAN_POINT('Ctrl Pts',(-45.483833914657,-12.2716820666929,20.));
#77375=CARTESIAN_POINT('Ctrl Pts',(-45.4895369513189,-12.2390319660445,
0.));
#77376=CARTESIAN_POINT('Ctrl Pts',(-45.4895369513189,-12.2390319660445,
20.));
#77377=CARTESIAN_POINT('Ctrl Pts',(-45.4952169166561,-12.2063789771801,
0.));
#77378=CARTESIAN_POINT('Ctrl Pts',(-45.4952169166561,-12.2063789771801,
20.));
#77379=CARTESIAN_POINT('Ctrl Pts',(-45.5008738087416,-12.1737231162825,
0.));
#77380=CARTESIAN_POINT('Ctrl Pts',(-45.5008738087416,-12.1737231162825,
20.));
#77381=CARTESIAN_POINT('Ctrl Pts',(-45.5065076256599,-12.1410643995363,
0.));
#77382=CARTESIAN_POINT('Ctrl Pts',(-45.5065076256599,-12.1410643995363,
20.));
#77383=CARTESIAN_POINT('Ctrl Pts',(-45.5121183655068,-12.1084028431278,
0.));
#77384=CARTESIAN_POINT('Ctrl Pts',(-45.5121183655068,-12.1084028431278,
20.));
#77385=CARTESIAN_POINT('Ctrl Pts',(-45.5177060263888,-12.0757384632451,
0.));
#77386=CARTESIAN_POINT('Ctrl Pts',(-45.5177060263888,-12.0757384632451,
20.));
#77387=CARTESIAN_POINT('Ctrl Pts',(-45.5232706064237,-12.0430712760778,
0.));
#77388=CARTESIAN_POINT('Ctrl Pts',(-45.5232706064237,-12.0430712760778,
20.));
#77389=CARTESIAN_POINT('Ctrl Pts',(-45.5288121037395,-12.0104012978174,
0.));
#77390=CARTESIAN_POINT('Ctrl Pts',(-45.5288121037395,-12.0104012978174,
20.));
#77391=CARTESIAN_POINT('Ctrl Pts',(-45.5343305164759,-11.9777285446569,
0.));
#77392=CARTESIAN_POINT('Ctrl Pts',(-45.5343305164759,-11.9777285446569,
20.));
#77393=CARTESIAN_POINT('Ctrl Pts',(-45.5398258427845,-11.945053032791,0.));
#77394=CARTESIAN_POINT('Ctrl Pts',(-45.5398258427845,-11.945053032791,20.));
#77395=CARTESIAN_POINT('Ctrl Pts',(-45.5452980808284,-11.9123747784165,
0.));
#77396=CARTESIAN_POINT('Ctrl Pts',(-45.5452980808284,-11.9123747784165,
20.));
#77397=CARTESIAN_POINT('Ctrl Pts',(-45.5507472287824,-11.8796937977314,
0.));
#77398=CARTESIAN_POINT('Ctrl Pts',(-45.5507472287824,-11.8796937977314,
20.));
#77399=CARTESIAN_POINT('Ctrl Pts',(-45.5561732848327,-11.8470101069358,
0.));
#77400=CARTESIAN_POINT('Ctrl Pts',(-45.5561732848327,-11.8470101069358,
20.));
#77401=CARTESIAN_POINT('Ctrl Pts',(-45.5615762471761,-11.8143237222317,
0.));
#77402=CARTESIAN_POINT('Ctrl Pts',(-45.5615762471761,-11.8143237222317,
20.));
#77403=CARTESIAN_POINT('Ctrl Pts',(-45.5669561140206,-11.7816346598227,
0.));
#77404=CARTESIAN_POINT('Ctrl Pts',(-45.5669561140206,-11.7816346598227,
20.));
#77405=CARTESIAN_POINT('Ctrl Pts',(-45.5723128835857,-11.748942935914,0.));
#77406=CARTESIAN_POINT('Ctrl Pts',(-45.5723128835857,-11.748942935914,20.));
#77407=CARTESIAN_POINT('Ctrl Pts',(-45.5776465541021,-11.7162485667124,
0.));
#77408=CARTESIAN_POINT('Ctrl Pts',(-45.5776465541021,-11.7162485667124,
20.));
#77409=CARTESIAN_POINT('Ctrl Pts',(-45.5829571238122,-11.6835515684258,
0.));
#77410=CARTESIAN_POINT('Ctrl Pts',(-45.5829571238122,-11.6835515684258,
20.));
#77411=CARTESIAN_POINT('Ctrl Pts',(-45.5882445909695,-11.6508519572639,
0.));
#77412=CARTESIAN_POINT('Ctrl Pts',(-45.5882445909695,-11.6508519572639,
20.));
#77413=CARTESIAN_POINT('Ctrl Pts',(-45.5935089538387,-11.6181497494381,
0.));
#77414=CARTESIAN_POINT('Ctrl Pts',(-45.5935089538387,-11.6181497494381,
20.));
#77415=CARTESIAN_POINT('Ctrl Pts',(-45.598750210696,-11.5854449611619,0.));
#77416=CARTESIAN_POINT('Ctrl Pts',(-45.598750210696,-11.5854449611619,20.));
#77417=CARTESIAN_POINT('Ctrl Pts',(-45.6039683598295,-11.5527376086502,
0.));
#77418=CARTESIAN_POINT('Ctrl Pts',(-45.6039683598295,-11.5527376086502,
20.));
#77419=CARTESIAN_POINT('Ctrl Pts',(-45.6091633995383,-11.5200277081201,
0.));
#77420=CARTESIAN_POINT('Ctrl Pts',(-45.6091633995383,-11.5200277081201,
20.));
#77421=CARTESIAN_POINT('Ctrl Pts',(-45.6143353281323,-11.4873152757897,
0.));
#77422=CARTESIAN_POINT('Ctrl Pts',(-45.6143353281323,-11.4873152757897,
20.));
#77423=CARTESIAN_POINT('Ctrl Pts',(-45.6194841439321,-11.4546003278786,
0.));
#77424=CARTESIAN_POINT('Ctrl Pts',(-45.6194841439321,-11.4546003278786,
20.));
#77425=CARTESIAN_POINT('Ctrl Pts',(-45.6246098452703,-11.421882880608,0.));
#77426=CARTESIAN_POINT('Ctrl Pts',(-45.6246098452703,-11.421882880608,20.));
#77427=CARTESIAN_POINT('Ctrl Pts',(-45.6297124304911,-11.3891629502006,
0.));
#77428=CARTESIAN_POINT('Ctrl Pts',(-45.6297124304911,-11.3891629502006,
20.));
#77429=CARTESIAN_POINT('Ctrl Pts',(-45.6347918979506,-11.3564405528809,
0.));
#77430=CARTESIAN_POINT('Ctrl Pts',(-45.6347918979506,-11.3564405528809,
20.));
#77431=CARTESIAN_POINT('Ctrl Pts',(-45.6398482460165,-11.3237157048751,
0.));
#77432=CARTESIAN_POINT('Ctrl Pts',(-45.6398482460165,-11.3237157048751,
20.));
#77433=CARTESIAN_POINT('Ctrl Pts',(-45.6448814730677,-11.290988422411,0.));
#77434=CARTESIAN_POINT('Ctrl Pts',(-45.6448814730677,-11.290988422411,20.));
#77435=CARTESIAN_POINT('Ctrl Pts',(-45.6498915774933,-11.2582587217178,
0.));
#77436=CARTESIAN_POINT('Ctrl Pts',(-45.6498915774933,-11.2582587217178,
20.));
#77437=CARTESIAN_POINT('Ctrl Pts',(-45.6548785576938,-11.2255266190259,
0.));
#77438=CARTESIAN_POINT('Ctrl Pts',(-45.6548785576938,-11.2255266190259,
20.));
#77439=CARTESIAN_POINT('Ctrl Pts',(-45.6598424120808,-11.1927921305675,
0.));
#77440=CARTESIAN_POINT('Ctrl Pts',(-45.6598424120808,-11.1927921305675,
20.));
#77441=CARTESIAN_POINT('Ctrl Pts',(-45.6647831390778,-11.1600552725764,
0.));
#77442=CARTESIAN_POINT('Ctrl Pts',(-45.6647831390778,-11.1600552725764,
20.));
#77443=CARTESIAN_POINT('Ctrl Pts',(-45.6697007371202,-11.1273160612881,
0.));
#77444=CARTESIAN_POINT('Ctrl Pts',(-45.6697007371202,-11.1273160612881,
20.));
#77445=CARTESIAN_POINT('Ctrl Pts',(-45.6745952046549,-11.0945745129393,
0.));
#77446=CARTESIAN_POINT('Ctrl Pts',(-45.6745952046549,-11.0945745129393,
20.));
#77447=CARTESIAN_POINT('Ctrl Pts',(-45.6794665401395,-11.0618306437685,
0.));
#77448=CARTESIAN_POINT('Ctrl Pts',(-45.6794665401395,-11.0618306437685,
20.));
#77449=CARTESIAN_POINT('Ctrl Pts',(-45.684314742043,-11.0290844700154,0.));
#77450=CARTESIAN_POINT('Ctrl Pts',(-45.684314742043,-11.0290844700154,20.));
#77451=CARTESIAN_POINT('Ctrl Pts',(-45.6891398088456,-10.9963360079212,
0.));
#77452=CARTESIAN_POINT('Ctrl Pts',(-45.6891398088456,-10.9963360079212,
20.));
#77453=CARTESIAN_POINT('Ctrl Pts',(-45.6939417390393,-10.9635852737287,
0.));
#77454=CARTESIAN_POINT('Ctrl Pts',(-45.6939417390393,-10.9635852737287,
20.));
#77455=CARTESIAN_POINT('Ctrl Pts',(-45.698720531127,-10.930832283682,0.));
#77456=CARTESIAN_POINT('Ctrl Pts',(-45.698720531127,-10.930832283682,20.));
#77457=CARTESIAN_POINT('Ctrl Pts',(-45.7034761836229,-10.8980770540269,
0.));
#77458=CARTESIAN_POINT('Ctrl Pts',(-45.7034761836229,-10.8980770540269,
20.));
#77459=CARTESIAN_POINT('Ctrl Pts',(-45.7082086950532,-10.8653196010107,
0.));
#77460=CARTESIAN_POINT('Ctrl Pts',(-45.7082086950532,-10.8653196010107,
20.));
#77461=CARTESIAN_POINT('Ctrl Pts',(-45.7129180639559,-10.832559940882,0.));
#77462=CARTESIAN_POINT('Ctrl Pts',(-45.7129180639559,-10.832559940882,20.));
#77463=CARTESIAN_POINT('Ctrl Pts',(-45.7176042888794,-10.7997980898913,
0.));
#77464=CARTESIAN_POINT('Ctrl Pts',(-45.7176042888794,-10.7997980898913,
20.));
#77465=CARTESIAN_POINT('Ctrl Pts',(-45.7222673683833,-10.7670340642896,
0.));
#77466=CARTESIAN_POINT('Ctrl Pts',(-45.7222673683833,-10.7670340642896,
20.));
#77467=CARTESIAN_POINT('Ctrl Pts',(-45.7269073010391,-10.73426788033,0.));
#77468=CARTESIAN_POINT('Ctrl Pts',(-45.7269073010391,-10.73426788033,20.));
#77469=CARTESIAN_POINT('Ctrl Pts',(-45.7315240854293,-10.7014995542666,
0.));
#77470=CARTESIAN_POINT('Ctrl Pts',(-45.7315240854293,-10.7014995542666,
20.));
#77471=CARTESIAN_POINT('Ctrl Pts',(-45.7361177201484,-10.6687291023553,
0.));
#77472=CARTESIAN_POINT('Ctrl Pts',(-45.7361177201484,-10.6687291023553,
20.));
#77473=CARTESIAN_POINT('Ctrl Pts',(-45.7406882038015,-10.6359565408533,
0.));
#77474=CARTESIAN_POINT('Ctrl Pts',(-45.7406882038015,-10.6359565408533,
20.));
#77475=CARTESIAN_POINT('Ctrl Pts',(-45.745235535006,-10.6031818860194,0.));
#77476=CARTESIAN_POINT('Ctrl Pts',(-45.745235535006,-10.6031818860194,20.));
#77477=CARTESIAN_POINT('Ctrl Pts',(-45.7497597123901,-10.5704051541135,
0.));
#77478=CARTESIAN_POINT('Ctrl Pts',(-45.7497597123901,-10.5704051541135,
20.));
#77479=CARTESIAN_POINT('Ctrl Pts',(-45.7542607345937,-10.5376263613968,
0.));
#77480=CARTESIAN_POINT('Ctrl Pts',(-45.7542607345937,-10.5376263613968,
20.));
#77481=CARTESIAN_POINT('Ctrl Pts',(-45.7587386002674,-10.504845524132,0.));
#77482=CARTESIAN_POINT('Ctrl Pts',(-45.7587386002674,-10.504845524132,20.));
#77483=CARTESIAN_POINT('Ctrl Pts',(-45.7631933080735,-10.4720626585828,
0.));
#77484=CARTESIAN_POINT('Ctrl Pts',(-45.7631933080735,-10.4720626585828,
20.));
#77485=CARTESIAN_POINT('Ctrl Pts',(-45.7676248566855,-10.4392777810149,
0.));
#77486=CARTESIAN_POINT('Ctrl Pts',(-45.7676248566855,-10.4392777810149,
20.));
#77487=CARTESIAN_POINT('Ctrl Pts',(-45.772033244789,-10.406490907695,0.));
#77488=CARTESIAN_POINT('Ctrl Pts',(-45.772033244789,-10.406490907695,20.));
#77489=CARTESIAN_POINT('Ctrl Pts',(-45.7764184710811,-10.3737020548914,
0.));
#77490=CARTESIAN_POINT('Ctrl Pts',(-45.7764184710811,-10.3737020548914,
20.));
#77491=CARTESIAN_POINT('Ctrl Pts',(-45.7807805342697,-10.3409112388736,
0.));
#77492=CARTESIAN_POINT('Ctrl Pts',(-45.7807805342697,-10.3409112388736,
20.));
#77493=CARTESIAN_POINT('Ctrl Pts',(-45.7851194330743,-10.3081184759123,
0.));
#77494=CARTESIAN_POINT('Ctrl Pts',(-45.7851194330743,-10.3081184759123,
20.));
#77495=CARTESIAN_POINT('Ctrl Pts',(-45.7894351662253,-10.2753237822795,
0.));
#77496=CARTESIAN_POINT('Ctrl Pts',(-45.7894351662253,-10.2753237822795,
20.));
#77497=CARTESIAN_POINT('Ctrl Pts',(-45.7937277324643,-10.2425271742485,
0.));
#77498=CARTESIAN_POINT('Ctrl Pts',(-45.7937277324643,-10.2425271742485,
20.));
#77499=CARTESIAN_POINT('Ctrl Pts',(-45.7979971305449,-10.2097286680937,
0.));
#77500=CARTESIAN_POINT('Ctrl Pts',(-45.7979971305449,-10.2097286680937,
20.));
#77501=CARTESIAN_POINT('Ctrl Pts',(-45.8022433592327,-10.1769282800914,
0.));
#77502=CARTESIAN_POINT('Ctrl Pts',(-45.8022433592327,-10.1769282800914,
20.));
#77503=CARTESIAN_POINT('Ctrl Pts',(-45.8064664173048,-10.1441260265191,
0.));
#77504=CARTESIAN_POINT('Ctrl Pts',(-45.8064664173048,-10.1441260265191,
20.));
#77505=CARTESIAN_POINT('Ctrl Pts',(-45.8106663035491,-10.1113219236554,
0.));
#77506=CARTESIAN_POINT('Ctrl Pts',(-45.8106663035491,-10.1113219236554,
20.));
#77507=CARTESIAN_POINT('Ctrl Pts',(-45.8148430167647,-10.0785159877801,
0.));
#77508=CARTESIAN_POINT('Ctrl Pts',(-45.8148430167647,-10.0785159877801,
20.));
#77509=CARTESIAN_POINT('Ctrl Pts',(-45.8189965557614,-10.0457082351741,
0.));
#77510=CARTESIAN_POINT('Ctrl Pts',(-45.8189965557614,-10.0457082351741,
20.));
#77511=CARTESIAN_POINT('Ctrl Pts',(-45.8231269193611,-10.0128986821194,
0.));
#77512=CARTESIAN_POINT('Ctrl Pts',(-45.8231269193611,-10.0128986821194,
20.));
#77513=CARTESIAN_POINT('Ctrl Pts',(-45.8272341063969,-9.98008734489947,
0.));
#77514=CARTESIAN_POINT('Ctrl Pts',(-45.8272341063969,-9.98008734489947,
20.));
#77515=CARTESIAN_POINT('Ctrl Pts',(-45.8313181157134,-9.94727423979905,
0.));
#77516=CARTESIAN_POINT('Ctrl Pts',(-45.8313181157134,-9.94727423979905,
20.));
#77517=CARTESIAN_POINT('Ctrl Pts',(-45.8353789461673,-9.91445938310424,
0.));
#77518=CARTESIAN_POINT('Ctrl Pts',(-45.8353789461673,-9.91445938310424,
20.));
#77519=CARTESIAN_POINT('Ctrl Pts',(-45.8394165966264,-9.88164279110241,
0.));
#77520=CARTESIAN_POINT('Ctrl Pts',(-45.8394165966264,-9.88164279110241,
20.));
#77521=CARTESIAN_POINT('Ctrl Pts',(-45.84343106597,-9.84882448008225,0.));
#77522=CARTESIAN_POINT('Ctrl Pts',(-45.84343106597,-9.84882448008225,20.));
#77523=CARTESIAN_POINT('Ctrl Pts',(-45.8474223530896,-9.81600446633367,
0.));
#77524=CARTESIAN_POINT('Ctrl Pts',(-45.8474223530896,-9.81600446633367,
20.));
#77525=CARTESIAN_POINT('Ctrl Pts',(-45.8513904568872,-9.78318276614761,
0.));
#77526=CARTESIAN_POINT('Ctrl Pts',(-45.8513904568872,-9.78318276614761,
20.));
#77527=CARTESIAN_POINT('Ctrl Pts',(-45.8553353762765,-9.75035939581618,
0.));
#77528=CARTESIAN_POINT('Ctrl Pts',(-45.8553353762765,-9.75035939581618,
20.));
#77529=CARTESIAN_POINT('Ctrl Pts',(-45.8592571101813,-9.7175343716322,0.));
#77530=CARTESIAN_POINT('Ctrl Pts',(-45.8592571101813,-9.7175343716322,20.));
#77531=CARTESIAN_POINT('Ctrl Pts',(-45.8631556575366,-9.68470770988975,
0.));
#77532=CARTESIAN_POINT('Ctrl Pts',(-45.8631556575366,-9.68470770988975,
20.));
#77533=CARTESIAN_POINT('Ctrl Pts',(-45.8670310172895,-9.65187942688401,
0.));
#77534=CARTESIAN_POINT('Ctrl Pts',(-45.8670310172895,-9.65187942688401,
20.));
#77535=CARTESIAN_POINT('Ctrl Pts',(-45.870883188399,-9.61904953891159,0.));
#77536=CARTESIAN_POINT('Ctrl Pts',(-45.870883188399,-9.61904953891159,20.));
#77537=CARTESIAN_POINT('Ctrl Pts',(-45.8747121698355,-9.58621806227057,
0.));
#77538=CARTESIAN_POINT('Ctrl Pts',(-45.8747121698355,-9.58621806227057,
20.));
#77539=CARTESIAN_POINT('Ctrl Pts',(-45.8785179605829,-9.55338501326047,
0.));
#77540=CARTESIAN_POINT('Ctrl Pts',(-45.8785179605829,-9.55338501326047,
20.));
#77541=CARTESIAN_POINT('Ctrl Pts',(-45.882300559635,-9.52055040818184,0.));
#77542=CARTESIAN_POINT('Ctrl Pts',(-45.882300559635,-9.52055040818184,20.));
#77543=CARTESIAN_POINT('Ctrl Pts',(-45.8860599659967,-9.48771426333609,
0.));
#77544=CARTESIAN_POINT('Ctrl Pts',(-45.8860599659967,-9.48771426333609,
20.));
#77545=CARTESIAN_POINT('Ctrl Pts',(-45.8897961786838,-9.45487659502548,
0.));
#77546=CARTESIAN_POINT('Ctrl Pts',(-45.8897961786838,-9.45487659502548,
20.));
#77547=CARTESIAN_POINT('Ctrl Pts',(-45.8935091967241,-9.42203741955324,
0.));
#77548=CARTESIAN_POINT('Ctrl Pts',(-45.8935091967241,-9.42203741955324,
20.));
#77549=CARTESIAN_POINT('Ctrl Pts',(-45.8971990191563,-9.3891967532238,0.));
#77550=CARTESIAN_POINT('Ctrl Pts',(-45.8971990191563,-9.3891967532238,20.));
#77551=CARTESIAN_POINT('Ctrl Pts',(-45.90086564503,-9.35635461234246,0.));
#77552=CARTESIAN_POINT('Ctrl Pts',(-45.90086564503,-9.35635461234246,20.));
#77553=CARTESIAN_POINT('Ctrl Pts',(-45.9045090734063,-9.32351101321579,
0.));
#77554=CARTESIAN_POINT('Ctrl Pts',(-45.9045090734063,-9.32351101321579,
20.));
#77555=CARTESIAN_POINT('Ctrl Pts',(-45.9081293033577,-9.29066597215162,
0.));
#77556=CARTESIAN_POINT('Ctrl Pts',(-45.9081293033577,-9.29066597215162,
20.));
#77557=CARTESIAN_POINT('Ctrl Pts',(-45.9117263339694,-9.25781950545901,
0.));
#77558=CARTESIAN_POINT('Ctrl Pts',(-45.9117263339694,-9.25781950545901,
20.));
#77559=CARTESIAN_POINT('Ctrl Pts',(-45.9153001643391,-9.22497162944821,
0.));
#77560=CARTESIAN_POINT('Ctrl Pts',(-45.9153001643391,-9.22497162944821,
20.));
#77561=CARTESIAN_POINT('Ctrl Pts',(-45.9188507935764,-9.19212236043073,
0.));
#77562=CARTESIAN_POINT('Ctrl Pts',(-45.9188507935764,-9.19212236043073,
20.));
#77563=CARTESIAN_POINT('Ctrl Pts',(-45.9223782208015,-9.15927171471891,
0.));
#77564=CARTESIAN_POINT('Ctrl Pts',(-45.9223782208015,-9.15927171471891,
20.));
#77565=CARTESIAN_POINT('Ctrl Pts',(-45.9258824451441,-9.12641970862566,
0.));
#77566=CARTESIAN_POINT('Ctrl Pts',(-45.9258824451441,-9.12641970862566,
20.));
#77567=CARTESIAN_POINT('Ctrl Pts',(-45.9293634657451,-9.09356635846485,
0.));
#77568=CARTESIAN_POINT('Ctrl Pts',(-45.9293634657451,-9.09356635846485,
20.));
#77569=CARTESIAN_POINT('Ctrl Pts',(-45.9328212817567,-9.06071168055121,
0.));
#77570=CARTESIAN_POINT('Ctrl Pts',(-45.9328212817567,-9.06071168055121,
20.));
#77571=CARTESIAN_POINT('Ctrl Pts',(-45.9362558923428,-9.02785569120061,
0.));
#77572=CARTESIAN_POINT('Ctrl Pts',(-45.9362558923428,-9.02785569120061,
20.));
#77573=CARTESIAN_POINT('Ctrl Pts',(-45.939667296681,-8.99499840673046,0.));
#77574=CARTESIAN_POINT('Ctrl Pts',(-45.939667296681,-8.99499840673046,20.));
#77575=CARTESIAN_POINT('Ctrl Pts',(-45.9430554939595,-8.96213984345905,
0.));
#77576=CARTESIAN_POINT('Ctrl Pts',(-45.9430554939595,-8.96213984345905,
20.));
#77577=CARTESIAN_POINT('Ctrl Pts',(-45.9464204833787,-8.92928001770575,
0.));
#77578=CARTESIAN_POINT('Ctrl Pts',(-45.9464204833787,-8.92928001770575,
20.));
#77579=CARTESIAN_POINT('Ctrl Pts',(-45.9497622641496,-8.89641894579082,
0.));
#77580=CARTESIAN_POINT('Ctrl Pts',(-45.9497622641496,-8.89641894579082,
20.));
#77581=CARTESIAN_POINT('Ctrl Pts',(-45.9530808354938,-8.86355664403534,
0.));
#77582=CARTESIAN_POINT('Ctrl Pts',(-45.9530808354938,-8.86355664403534,
20.));
#77583=CARTESIAN_POINT('Ctrl Pts',(-45.9563761966444,-8.83069312876127,
0.));
#77584=CARTESIAN_POINT('Ctrl Pts',(-45.9563761966444,-8.83069312876127,
20.));
#77585=CARTESIAN_POINT('Ctrl Pts',(-45.9596483468462,-8.79782841629147,
0.));
#77586=CARTESIAN_POINT('Ctrl Pts',(-45.9596483468462,-8.79782841629147,
20.));
#77587=CARTESIAN_POINT('Ctrl Pts',(-45.9628972853566,-8.76496252295001,
0.));
#77588=CARTESIAN_POINT('Ctrl Pts',(-45.9628972853566,-8.76496252295001,
20.));
#77589=CARTESIAN_POINT('Ctrl Pts',(-45.9661230114446,-8.73209546506199,
0.));
#77590=CARTESIAN_POINT('Ctrl Pts',(-45.9661230114446,-8.73209546506199,
20.));
#77591=CARTESIAN_POINT('Ctrl Pts',(-45.9693255243897,-8.69922725895329,
0.));
#77592=CARTESIAN_POINT('Ctrl Pts',(-45.9693255243897,-8.69922725895329,
20.));
#77593=CARTESIAN_POINT('Ctrl Pts',(-45.9725048234817,-8.66635792095043,
0.));
#77594=CARTESIAN_POINT('Ctrl Pts',(-45.9725048234817,-8.66635792095043,
20.));
#77595=CARTESIAN_POINT('Ctrl Pts',(-45.9756609080225,-8.63348746738099,
0.));
#77596=CARTESIAN_POINT('Ctrl Pts',(-45.9756609080225,-8.63348746738099,
20.));
#77597=CARTESIAN_POINT('Ctrl Pts',(-45.9787937773254,-8.60061591457339,
0.));
#77598=CARTESIAN_POINT('Ctrl Pts',(-45.9787937773254,-8.60061591457339,
20.));
#77599=CARTESIAN_POINT('Ctrl Pts',(-45.9819034307166,-8.56774327885725,
0.));
#77600=CARTESIAN_POINT('Ctrl Pts',(-45.9819034307166,-8.56774327885725,
20.));
#77601=CARTESIAN_POINT('Ctrl Pts',(-45.9849898675351,-8.53486957656347,
0.));
#77602=CARTESIAN_POINT('Ctrl Pts',(-45.9849898675351,-8.53486957656347,
20.));
#77603=CARTESIAN_POINT('Ctrl Pts',(-45.9880530871298,-8.50199482402354,
0.));
#77604=CARTESIAN_POINT('Ctrl Pts',(-45.9880530871298,-8.50199482402354,
20.));
#77605=CARTESIAN_POINT('Ctrl Pts',(-45.991093088861,-8.46911903756973,0.));
#77606=CARTESIAN_POINT('Ctrl Pts',(-45.991093088861,-8.46911903756973,20.));
#77607=CARTESIAN_POINT('Ctrl Pts',(-45.9941098720982,-8.43624223353471,
0.));
#77608=CARTESIAN_POINT('Ctrl Pts',(-45.9941098720982,-8.43624223353471,
20.));
#77609=CARTESIAN_POINT('Ctrl Pts',(-45.9971034362229,-8.40336442825199,
0.));
#77610=CARTESIAN_POINT('Ctrl Pts',(-45.9971034362229,-8.40336442825199,
20.));
#77611=CARTESIAN_POINT('Ctrl Pts',(-46.000073780629,-8.37048563805605,0.));
#77612=CARTESIAN_POINT('Ctrl Pts',(-46.000073780629,-8.37048563805605,20.));
#77613=CARTESIAN_POINT('Ctrl Pts',(-46.0030209047226,-8.33760587928253,
0.));
#77614=CARTESIAN_POINT('Ctrl Pts',(-46.0030209047226,-8.33760587928253,
20.));
#77615=CARTESIAN_POINT('Ctrl Pts',(-46.0059448079215,-8.30472516826797,
0.));
#77616=CARTESIAN_POINT('Ctrl Pts',(-46.0059448079215,-8.30472516826797,
20.));
#77617=CARTESIAN_POINT('Ctrl Pts',(-46.0088454896554,-8.27184352134994,
0.));
#77618=CARTESIAN_POINT('Ctrl Pts',(-46.0088454896554,-8.27184352134994,
20.));
#77619=CARTESIAN_POINT('Ctrl Pts',(-46.0117229493647,-8.23896095486669,
0.));
#77620=CARTESIAN_POINT('Ctrl Pts',(-46.0117229493647,-8.23896095486669,
20.));
#77621=CARTESIAN_POINT('Ctrl Pts',(-46.0145771865005,-8.20607748515696,
0.));
#77622=CARTESIAN_POINT('Ctrl Pts',(-46.0145771865005,-8.20607748515696,
20.));
#77623=CARTESIAN_POINT('Ctrl Pts',(-46.0174082005262,-8.17319312856042,
0.));
#77624=CARTESIAN_POINT('Ctrl Pts',(-46.0174082005262,-8.17319312856042,
20.));
#77625=CARTESIAN_POINT('Ctrl Pts',(-46.0202159909161,-8.14030790141739,
0.));
#77626=CARTESIAN_POINT('Ctrl Pts',(-46.0202159909161,-8.14030790141739,
20.));
#77627=CARTESIAN_POINT('Ctrl Pts',(-46.0230005571558,-8.107421820069,0.));
#77628=CARTESIAN_POINT('Ctrl Pts',(-46.0230005571558,-8.107421820069,20.));
#77629=CARTESIAN_POINT('Ctrl Pts',(-46.025761898743,-8.07453490085736,0.));
#77630=CARTESIAN_POINT('Ctrl Pts',(-46.025761898743,-8.07453490085736,20.));
#77631=CARTESIAN_POINT('Ctrl Pts',(-46.0285000151874,-8.04164716012545,
0.));
#77632=CARTESIAN_POINT('Ctrl Pts',(-46.0285000151874,-8.04164716012545,
20.));
#77633=CARTESIAN_POINT('Ctrl Pts',(-46.0312149060105,-8.00875861421695,
0.));
#77634=CARTESIAN_POINT('Ctrl Pts',(-46.0312149060105,-8.00875861421695,
20.));
#77635=CARTESIAN_POINT('Ctrl Pts',(-46.0339065707442,-7.9758692794762,0.));
#77636=CARTESIAN_POINT('Ctrl Pts',(-46.0339065707442,-7.9758692794762,20.));
#77637=CARTESIAN_POINT('Ctrl Pts',(-46.0365750089318,-7.94297917224815,
0.));
#77638=CARTESIAN_POINT('Ctrl Pts',(-46.0365750089318,-7.94297917224815,
20.));
#77639=CARTESIAN_POINT('Ctrl Pts',(-46.0392202201279,-7.91008830887855,
0.));
#77640=CARTESIAN_POINT('Ctrl Pts',(-46.0392202201279,-7.91008830887855,
20.));
#77641=CARTESIAN_POINT('Ctrl Pts',(-46.0418422038989,-7.877196705714,0.));
#77642=CARTESIAN_POINT('Ctrl Pts',(-46.0418422038989,-7.877196705714,20.));
#77643=CARTESIAN_POINT('Ctrl Pts',(-46.0444409598224,-7.84430437910167,
0.));
#77644=CARTESIAN_POINT('Ctrl Pts',(-46.0444409598224,-7.84430437910167,
20.));
#77645=CARTESIAN_POINT('Ctrl Pts',(-46.0470164874882,-7.81141134538954,
0.));
#77646=CARTESIAN_POINT('Ctrl Pts',(-46.0470164874882,-7.81141134538954,
20.));
#77647=CARTESIAN_POINT('Ctrl Pts',(-46.0495687864972,-7.77851762092636,
0.));
#77648=CARTESIAN_POINT('Ctrl Pts',(-46.0495687864972,-7.77851762092636,
20.));
#77649=CARTESIAN_POINT('Ctrl Pts',(-46.052097856463,-7.74562322206167,0.));
#77650=CARTESIAN_POINT('Ctrl Pts',(-46.052097856463,-7.74562322206167,20.));
#77651=CARTESIAN_POINT('Ctrl Pts',(-46.0546036970108,-7.71272816514571,
0.));
#77652=CARTESIAN_POINT('Ctrl Pts',(-46.0546036970108,-7.71272816514571,
20.));
#77653=CARTESIAN_POINT('Ctrl Pts',(-46.0570863077758,-7.67983246652917,
0.));
#77654=CARTESIAN_POINT('Ctrl Pts',(-46.0570863077758,-7.67983246652917,
20.));
#77655=CARTESIAN_POINT('Ctrl Pts',(-46.0595456884042,-7.64693614256335,
0.));
#77656=CARTESIAN_POINT('Ctrl Pts',(-46.0595456884042,-7.64693614256335,
20.));
#77657=CARTESIAN_POINT('Ctrl Pts',(-46.0619818385541,-7.61403920960035,
0.));
#77658=CARTESIAN_POINT('Ctrl Pts',(-46.0619818385541,-7.61403920960035,
20.));
#77659=CARTESIAN_POINT('Ctrl Pts',(-46.0643947578955,-7.58114168399302,
0.));
#77660=CARTESIAN_POINT('Ctrl Pts',(-46.0643947578955,-7.58114168399302,
20.));
#77661=CARTESIAN_POINT('Ctrl Pts',(-46.0667844461104,-7.54824358209484,
0.));
#77662=CARTESIAN_POINT('Ctrl Pts',(-46.0667844461104,-7.54824358209484,
20.));
#77663=CARTESIAN_POINT('Ctrl Pts',(-46.0691509028928,-7.51534492025983,
0.));
#77664=CARTESIAN_POINT('Ctrl Pts',(-46.0691509028928,-7.51534492025983,
20.));
#77665=CARTESIAN_POINT('Ctrl Pts',(-46.0714941279471,-7.4824457148425,0.));
#77666=CARTESIAN_POINT('Ctrl Pts',(-46.0714941279471,-7.4824457148425,20.));
#77667=CARTESIAN_POINT('Ctrl Pts',(-46.0738141209885,-7.44954598219809,
0.));
#77668=CARTESIAN_POINT('Ctrl Pts',(-46.0738141209885,-7.44954598219809,
20.));
#77669=CARTESIAN_POINT('Ctrl Pts',(-46.0761108817447,-7.4166457386826,0.));
#77670=CARTESIAN_POINT('Ctrl Pts',(-46.0761108817447,-7.4166457386826,20.));
#77671=CARTESIAN_POINT('Ctrl Pts',(-46.0783844099553,-7.38374500065294,
0.));
#77672=CARTESIAN_POINT('Ctrl Pts',(-46.0783844099553,-7.38374500065294,
20.));
#77673=CARTESIAN_POINT('Ctrl Pts',(-46.0806347053718,-7.35084378446661,
0.));
#77674=CARTESIAN_POINT('Ctrl Pts',(-46.0806347053718,-7.35084378446661,
20.));
#77675=CARTESIAN_POINT('Ctrl Pts',(-46.0828617677561,-7.31794210648139,
0.));
#77676=CARTESIAN_POINT('Ctrl Pts',(-46.0828617677561,-7.31794210648139,
20.));
#77677=CARTESIAN_POINT('Ctrl Pts',(-46.0850655968817,-7.2850399830555,0.));
#77678=CARTESIAN_POINT('Ctrl Pts',(-46.0850655968817,-7.2850399830555,20.));
#77679=CARTESIAN_POINT('Ctrl Pts',(-46.0872461925336,-7.25213743054749,
0.));
#77680=CARTESIAN_POINT('Ctrl Pts',(-46.0872461925336,-7.25213743054749,
20.));
#77681=CARTESIAN_POINT('Ctrl Pts',(-46.0894035545083,-7.2192344653164,0.));
#77682=CARTESIAN_POINT('Ctrl Pts',(-46.0894035545083,-7.2192344653164,20.));
#77683=CARTESIAN_POINT('Ctrl Pts',(-46.0915376826137,-7.18633110372211,
0.));
#77684=CARTESIAN_POINT('Ctrl Pts',(-46.0915376826137,-7.18633110372211,
20.));
#77685=CARTESIAN_POINT('Ctrl Pts',(-46.0936485766695,-7.15342736212529,
0.));
#77686=CARTESIAN_POINT('Ctrl Pts',(-46.0936485766695,-7.15342736212529,
20.));
#77687=CARTESIAN_POINT('Ctrl Pts',(-46.0957362365075,-7.12052325688752,
0.));
#77688=CARTESIAN_POINT('Ctrl Pts',(-46.0957362365075,-7.12052325688752,
20.));
#77689=CARTESIAN_POINT('Ctrl Pts',(-46.097800661971,-7.08761880437093,0.));
#77690=CARTESIAN_POINT('Ctrl Pts',(-46.097800661971,-7.08761880437093,20.));
#77691=CARTESIAN_POINT('Ctrl Pts',(-46.0998418529147,-7.05471402093801,
0.));
#77692=CARTESIAN_POINT('Ctrl Pts',(-46.0998418529147,-7.05471402093801,
20.));
#77693=CARTESIAN_POINT('Ctrl Pts',(-46.1018598092046,-7.02180892295147,
0.));
#77694=CARTESIAN_POINT('Ctrl Pts',(-46.1018598092046,-7.02180892295147,
20.));
#77695=CARTESIAN_POINT('Ctrl Pts',(-46.103854530718,-6.98890352677438,0.));
#77696=CARTESIAN_POINT('Ctrl Pts',(-46.103854530718,-6.98890352677438,20.));
#77697=CARTESIAN_POINT('Ctrl Pts',(-46.1058260173429,-6.95599784877019,
0.));
#77698=CARTESIAN_POINT('Ctrl Pts',(-46.1058260173429,-6.95599784877019,
20.));
#77699=CARTESIAN_POINT('Ctrl Pts',(-46.1077742689797,-6.92309190530285,
0.));
#77700=CARTESIAN_POINT('Ctrl Pts',(-46.1077742689797,-6.92309190530285,
20.));
#77701=CARTESIAN_POINT('Ctrl Pts',(-46.1096992855399,-6.89018571273689,
0.));
#77702=CARTESIAN_POINT('Ctrl Pts',(-46.1096992855399,-6.89018571273689,
20.));
#77703=CARTESIAN_POINT('Ctrl Pts',(-46.111601066948,-6.85727928743787,0.));
#77704=CARTESIAN_POINT('Ctrl Pts',(-46.111601066948,-6.85727928743787,20.));
#77705=CARTESIAN_POINT('Ctrl Pts',(-46.1134796131392,-6.82437264577169,
0.));
#77706=CARTESIAN_POINT('Ctrl Pts',(-46.1134796131392,-6.82437264577169,
20.));
#77707=CARTESIAN_POINT('Ctrl Pts',(-46.1153349240611,-6.7914658041047,0.));
#77708=CARTESIAN_POINT('Ctrl Pts',(-46.1153349240611,-6.7914658041047,20.));
#77709=CARTESIAN_POINT('Ctrl Pts',(-46.1171669996709,-6.75855877880356,
0.));
#77710=CARTESIAN_POINT('Ctrl Pts',(-46.1171669996709,-6.75855877880356,
20.));
#77711=CARTESIAN_POINT('Ctrl Pts',(-46.1189758399374,-6.7256515862352,0.));
#77712=CARTESIAN_POINT('Ctrl Pts',(-46.1189758399374,-6.7256515862352,20.));
#77713=CARTESIAN_POINT('Ctrl Pts',(-46.1207614448407,-6.69274424276687,
0.));
#77714=CARTESIAN_POINT('Ctrl Pts',(-46.1207614448407,-6.69274424276687,
20.));
#77715=CARTESIAN_POINT('Ctrl Pts',(-46.122523814374,-6.65983676476652,0.));
#77716=CARTESIAN_POINT('Ctrl Pts',(-46.122523814374,-6.65983676476652,20.));
#77717=CARTESIAN_POINT('Ctrl Pts',(-46.124262948542,-6.62692916860257,0.));
#77718=CARTESIAN_POINT('Ctrl Pts',(-46.124262948542,-6.62692916860257,20.));
#77719=CARTESIAN_POINT('Ctrl Pts',(-46.1259788473615,-6.59402147064399,
0.));
#77720=CARTESIAN_POINT('Ctrl Pts',(-46.1259788473615,-6.59402147064399,
20.));
#77721=CARTESIAN_POINT('Ctrl Pts',(-46.1276715108604,-6.56111368726009,
0.));
#77722=CARTESIAN_POINT('Ctrl Pts',(-46.1276715108604,-6.56111368726009,
20.));
#77723=CARTESIAN_POINT('Ctrl Pts',(-46.1293409390781,-6.52820583482049,
0.));
#77724=CARTESIAN_POINT('Ctrl Pts',(-46.1293409390781,-6.52820583482049,
20.));
#77725=CARTESIAN_POINT('Ctrl Pts',(-46.1309871320644,-6.49529792969508,
0.));
#77726=CARTESIAN_POINT('Ctrl Pts',(-46.1309871320644,-6.49529792969508,
20.));
#77727=CARTESIAN_POINT('Ctrl Pts',(-46.1326100898806,-6.46238998825407,
0.));
#77728=CARTESIAN_POINT('Ctrl Pts',(-46.1326100898806,-6.46238998825407,
20.));
#77729=CARTESIAN_POINT('Ctrl Pts',(-46.1342098125991,-6.42948202686813,
0.));
#77730=CARTESIAN_POINT('Ctrl Pts',(-46.1342098125991,-6.42948202686813,
20.));
#77731=CARTESIAN_POINT('Ctrl Pts',(-46.1357863003044,-6.39657406190844,
0.));
#77732=CARTESIAN_POINT('Ctrl Pts',(-46.1357863003044,-6.39657406190844,
20.));
#77733=CARTESIAN_POINT('Ctrl Pts',(-46.1373395530931,-6.36366610974647,
0.));
#77734=CARTESIAN_POINT('Ctrl Pts',(-46.1373395530931,-6.36366610974647,
20.));
#77735=CARTESIAN_POINT('Ctrl Pts',(-46.138869571074,-6.33075818675419,0.));
#77736=CARTESIAN_POINT('Ctrl Pts',(-46.138869571074,-6.33075818675419,20.));
#77737=CARTESIAN_POINT('Ctrl Pts',(-46.1403763543673,-6.29785030930381,
0.));
#77738=CARTESIAN_POINT('Ctrl Pts',(-46.1403763543673,-6.29785030930381,
20.));
#77739=CARTESIAN_POINT('Ctrl Pts',(-46.141859903105,-6.26494249376777,0.));
#77740=CARTESIAN_POINT('Ctrl Pts',(-46.141859903105,-6.26494249376777,20.));
#77741=CARTESIAN_POINT('Ctrl Pts',(-46.1433202174297,-6.23203475651882,
0.));
#77742=CARTESIAN_POINT('Ctrl Pts',(-46.1433202174297,-6.23203475651882,
20.));
#77743=CARTESIAN_POINT('Ctrl Pts',(-46.1447572974959,-6.19912711393004,
0.));
#77744=CARTESIAN_POINT('Ctrl Pts',(-46.1447572974959,-6.19912711393004,
20.));
#77745=CARTESIAN_POINT('Ctrl Pts',(-46.1461711434687,-6.16621958237487,
0.));
#77746=CARTESIAN_POINT('Ctrl Pts',(-46.1461711434687,-6.16621958237487,
20.));
#77747=CARTESIAN_POINT('Ctrl Pts',(-46.1475617555249,-6.1333121782271,0.));
#77748=CARTESIAN_POINT('Ctrl Pts',(-46.1475617555249,-6.1333121782271,20.));
#77749=CARTESIAN_POINT('Ctrl Pts',(-46.1489291338532,-6.10040491786085,
0.));
#77750=CARTESIAN_POINT('Ctrl Pts',(-46.1489291338532,-6.10040491786085,
20.));
#77751=CARTESIAN_POINT('Ctrl Pts',(-46.1502732786543,-6.06749781765058,
0.));
#77752=CARTESIAN_POINT('Ctrl Pts',(-46.1502732786543,-6.06749781765058,
20.));
#77753=CARTESIAN_POINT('Ctrl Pts',(-46.151594190141,-6.03459089397104,0.));
#77754=CARTESIAN_POINT('Ctrl Pts',(-46.151594190141,-6.03459089397104,20.));
#77755=CARTESIAN_POINT('Ctrl Pts',(-46.1528918685373,-6.0016841631972,0.));
#77756=CARTESIAN_POINT('Ctrl Pts',(-46.1528918685373,-6.0016841631972,20.));
#77757=CARTESIAN_POINT('Ctrl Pts',(-46.1541663140783,-5.96877764170411,
0.));
#77758=CARTESIAN_POINT('Ctrl Pts',(-46.1541663140783,-5.96877764170411,
20.));
#77759=CARTESIAN_POINT('Ctrl Pts',(-46.1554175270101,-5.93587134586689,
0.));
#77760=CARTESIAN_POINT('Ctrl Pts',(-46.1554175270101,-5.93587134586689,
20.));
#77761=CARTESIAN_POINT('Ctrl Pts',(-46.1566455075904,-5.90296529206097,
0.));
#77762=CARTESIAN_POINT('Ctrl Pts',(-46.1566455075904,-5.90296529206097,
20.));
#77763=CARTESIAN_POINT('Ctrl Pts',(-46.1578502560886,-5.87005949666211,
0.));
#77764=CARTESIAN_POINT('Ctrl Pts',(-46.1578502560886,-5.87005949666211,
20.));
#77765=CARTESIAN_POINT('Ctrl Pts',(-46.1590317727861,-5.83715397604653,
0.));
#77766=CARTESIAN_POINT('Ctrl Pts',(-46.1590317727861,-5.83715397604653,
20.));
#77767=CARTESIAN_POINT('Ctrl Pts',(-46.160190057976,-5.80424874659071,0.));
#77768=CARTESIAN_POINT('Ctrl Pts',(-46.160190057976,-5.80424874659071,20.));
#77769=CARTESIAN_POINT('Ctrl Pts',(-46.1613251119636,-5.77134382467172,
0.));
#77770=CARTESIAN_POINT('Ctrl Pts',(-46.1613251119636,-5.77134382467172,
20.));
#77771=CARTESIAN_POINT('Ctrl Pts',(-46.1624369350662,-5.73843922666647,
0.));
#77772=CARTESIAN_POINT('Ctrl Pts',(-46.1624369350662,-5.73843922666647,
20.));
#77773=CARTESIAN_POINT('Ctrl Pts',(-46.1635255276116,-5.70553496895184,
0.));
#77774=CARTESIAN_POINT('Ctrl Pts',(-46.1635255276116,-5.70553496895184,
20.));
#77775=CARTESIAN_POINT('Ctrl Pts',(-46.1645908899393,-5.67263106790478,
0.));
#77776=CARTESIAN_POINT('Ctrl Pts',(-46.1645908899393,-5.67263106790478,
20.));
#77777=CARTESIAN_POINT('Ctrl Pts',(-46.1656330223979,-5.63972753990235,
0.));
#77778=CARTESIAN_POINT('Ctrl Pts',(-46.1656330223979,-5.63972753990235,
20.));
#77779=CARTESIAN_POINT('Ctrl Pts',(-46.166651925349,-5.60682440132181,0.));
#77780=CARTESIAN_POINT('Ctrl Pts',(-46.166651925349,-5.60682440132181,20.));
#77781=CARTESIAN_POINT('Ctrl Pts',(-46.1676475991657,-5.57392166854074,
0.));
#77782=CARTESIAN_POINT('Ctrl Pts',(-46.1676475991657,-5.57392166854074,
20.));
#77783=CARTESIAN_POINT('Ctrl Pts',(-46.1686200442337,-5.54101935793709,
0.));
#77784=CARTESIAN_POINT('Ctrl Pts',(-46.1686200442337,-5.54101935793709,
20.));
#77785=CARTESIAN_POINT('Ctrl Pts',(-46.1695692609505,-5.50811748588893,
0.));
#77786=CARTESIAN_POINT('Ctrl Pts',(-46.1695692609505,-5.50811748588893,
20.));
#77787=CARTESIAN_POINT('Ctrl Pts',(-46.170495249726,-5.47521606877459,0.));
#77788=CARTESIAN_POINT('Ctrl Pts',(-46.170495249726,-5.47521606877459,20.));
#77789=CARTESIAN_POINT('Ctrl Pts',(-46.1713980109807,-5.44231512297238,
0.));
#77790=CARTESIAN_POINT('Ctrl Pts',(-46.1713980109807,-5.44231512297238,
20.));
#77791=CARTESIAN_POINT('Ctrl Pts',(-46.1722775451467,-5.40941466486069,
0.));
#77792=CARTESIAN_POINT('Ctrl Pts',(-46.1722775451467,-5.40941466486069,
20.));
#77793=CARTESIAN_POINT('Ctrl Pts',(-46.1731338526667,-5.37651471081787,
0.));
#77794=CARTESIAN_POINT('Ctrl Pts',(-46.1731338526667,-5.37651471081787,
20.));
#77795=CARTESIAN_POINT('Ctrl Pts',(-46.1739669339953,-5.34361527722239,
0.));
#77796=CARTESIAN_POINT('Ctrl Pts',(-46.1739669339953,-5.34361527722239,
20.));
#77797=CARTESIAN_POINT('Ctrl Pts',(-46.1747767895978,-5.31071638045279,
0.));
#77798=CARTESIAN_POINT('Ctrl Pts',(-46.1747767895978,-5.31071638045279,
20.));
#77799=CARTESIAN_POINT('Ctrl Pts',(-46.1755634199519,-5.2778180368879,0.));
#77800=CARTESIAN_POINT('Ctrl Pts',(-46.1755634199519,-5.2778180368879,20.));
#77801=CARTESIAN_POINT('Ctrl Pts',(-46.1763268255471,-5.24492026290662,
0.));
#77802=CARTESIAN_POINT('Ctrl Pts',(-46.1763268255471,-5.24492026290662,
20.));
#77803=CARTESIAN_POINT('Ctrl Pts',(-46.1770670068854,-5.21202307488801,
0.));
#77804=CARTESIAN_POINT('Ctrl Pts',(-46.1770670068854,-5.21202307488801,
20.));
#77805=CARTESIAN_POINT('Ctrl Pts',(-46.1777839644797,-5.17912648921101,
0.));
#77806=CARTESIAN_POINT('Ctrl Pts',(-46.1777839644797,-5.17912648921101,
20.));
#77807=CARTESIAN_POINT('Ctrl Pts',(-46.1784776988548,-5.14623052225471,
0.));
#77808=CARTESIAN_POINT('Ctrl Pts',(-46.1784776988548,-5.14623052225471,
20.));
#77809=CARTESIAN_POINT('Ctrl Pts',(-46.1791482105459,-5.11333519039808,
0.));
#77810=CARTESIAN_POINT('Ctrl Pts',(-46.1791482105459,-5.11333519039808,
20.));
#77811=CARTESIAN_POINT('Ctrl Pts',(-46.1797955000997,-5.08044051002025,
0.));
#77812=CARTESIAN_POINT('Ctrl Pts',(-46.1797955000997,-5.08044051002025,
20.));
#77813=CARTESIAN_POINT('Ctrl Pts',(-46.1804195680748,-5.0475464975003,0.));
#77814=CARTESIAN_POINT('Ctrl Pts',(-46.1804195680748,-5.0475464975003,20.));
#77815=CARTESIAN_POINT('Ctrl Pts',(-46.1810204150412,-5.01465316921748,
0.));
#77816=CARTESIAN_POINT('Ctrl Pts',(-46.1810204150412,-5.01465316921748,
20.));
#77817=CARTESIAN_POINT('Ctrl Pts',(-46.1815980415817,-4.981760541551,0.));
#77818=CARTESIAN_POINT('Ctrl Pts',(-46.1815980415817,-4.981760541551,20.));
#77819=CARTESIAN_POINT('Ctrl Pts',(-46.182152448291,-4.94886863088032,0.));
#77820=CARTESIAN_POINT('Ctrl Pts',(-46.182152448291,-4.94886863088032,20.));
#77821=CARTESIAN_POINT('Ctrl Pts',(-46.1826836357763,-4.91597745358481,
0.));
#77822=CARTESIAN_POINT('Ctrl Pts',(-46.1826836357763,-4.91597745358481,
20.));
#77823=CARTESIAN_POINT('Ctrl Pts',(-46.1831916046531,-4.88308702604349,
0.));
#77824=CARTESIAN_POINT('Ctrl Pts',(-46.1831916046531,-4.88308702604349,
20.));
#77825=CARTESIAN_POINT('Ctrl Pts',(-46.1836763555496,-4.85019736463543,
0.));
#77826=CARTESIAN_POINT('Ctrl Pts',(-46.1836763555496,-4.85019736463543,
20.));
#77827=CARTESIAN_POINT('Ctrl Pts',(-46.1841378891039,-4.81730848573953,
0.));
#77828=CARTESIAN_POINT('Ctrl Pts',(-46.1841378891039,-4.81730848573953,
20.));
#77829=CARTESIAN_POINT('Ctrl Pts',(-46.1845762059678,-4.78442040573514,
0.));
#77830=CARTESIAN_POINT('Ctrl Pts',(-46.1845762059678,-4.78442040573514,
20.));
#77831=CARTESIAN_POINT('Ctrl Pts',(-46.1849913068043,-4.7515331410016,0.));
#77832=CARTESIAN_POINT('Ctrl Pts',(-46.1849913068043,-4.7515331410016,20.));
#77833=CARTESIAN_POINT('Ctrl Pts',(-46.1853831922891,-4.71864670791826,
0.));
#77834=CARTESIAN_POINT('Ctrl Pts',(-46.1853831922891,-4.71864670791826,
20.));
#77835=CARTESIAN_POINT('Ctrl Pts',(-46.1857518631086,-4.68576112286394,
0.));
#77836=CARTESIAN_POINT('Ctrl Pts',(-46.1857518631086,-4.68576112286394,
20.));
#77837=CARTESIAN_POINT('Ctrl Pts',(-46.1860973199616,-4.65287640221747,
0.));
#77838=CARTESIAN_POINT('Ctrl Pts',(-46.1860973199616,-4.65287640221747,
20.));
#77839=CARTESIAN_POINT('Ctrl Pts',(-46.1864195635571,-4.6199925623574,0.));
#77840=CARTESIAN_POINT('Ctrl Pts',(-46.1864195635571,-4.6199925623574,20.));
#77841=CARTESIAN_POINT('Ctrl Pts',(-46.1867185946155,-4.58710961966232,
0.));
#77842=CARTESIAN_POINT('Ctrl Pts',(-46.1867185946155,-4.58710961966232,
20.));
#77843=CARTESIAN_POINT('Ctrl Pts',(-46.1869944138693,-4.55422759051101,
0.));
#77844=CARTESIAN_POINT('Ctrl Pts',(-46.1869944138693,-4.55422759051101,
20.));
#77845=CARTESIAN_POINT('Ctrl Pts',(-46.1872470220627,-4.52134649128217,
0.));
#77846=CARTESIAN_POINT('Ctrl Pts',(-46.1872470220627,-4.52134649128217,
20.));
#77847=CARTESIAN_POINT('Ctrl Pts',(-46.1874764199521,-4.48846633835459,
0.));
#77848=CARTESIAN_POINT('Ctrl Pts',(-46.1874764199521,-4.48846633835459,
20.));
#77849=CARTESIAN_POINT('Ctrl Pts',(-46.1876826083051,-4.4555871481068,0.));
#77850=CARTESIAN_POINT('Ctrl Pts',(-46.1876826083051,-4.4555871481068,20.));
#77851=CARTESIAN_POINT('Ctrl Pts',(-46.1878655879008,-4.42270893691723,
0.));
#77852=CARTESIAN_POINT('Ctrl Pts',(-46.1878655879008,-4.42270893691723,
20.));
#77853=CARTESIAN_POINT('Ctrl Pts',(-46.1880253595297,-4.38983172116389,
0.));
#77854=CARTESIAN_POINT('Ctrl Pts',(-46.1880253595297,-4.38983172116389,
20.));
#77855=CARTESIAN_POINT('Ctrl Pts',(-46.1881619239926,-4.35695551722447,
0.));
#77856=CARTESIAN_POINT('Ctrl Pts',(-46.1881619239926,-4.35695551722447,
20.));
#77857=CARTESIAN_POINT('Ctrl Pts',(-46.1882752821036,-4.32408034147654,
0.));
#77858=CARTESIAN_POINT('Ctrl Pts',(-46.1882752821036,-4.32408034147654,
20.));
#77859=CARTESIAN_POINT('Ctrl Pts',(-46.1883654346888,-4.29120621029776,
0.));
#77860=CARTESIAN_POINT('Ctrl Pts',(-46.1883654346888,-4.29120621029776,
20.));
#77861=CARTESIAN_POINT('Ctrl Pts',(-46.1884323825857,-4.25833314006578,
0.));
#77862=CARTESIAN_POINT('Ctrl Pts',(-46.1884323825857,-4.25833314006578,
20.));
#77863=CARTESIAN_POINT('Ctrl Pts',(-46.1884761266433,-4.22546114715825,
0.));
#77864=CARTESIAN_POINT('Ctrl Pts',(-46.1884761266433,-4.22546114715825,
20.));
#77865=CARTESIAN_POINT('Ctrl Pts',(-46.1884966677209,-4.19259024795238,
0.));
#77866=CARTESIAN_POINT('Ctrl Pts',(-46.1884966677209,-4.19259024795238,
20.));
#77867=CARTESIAN_POINT('Ctrl Pts',(-46.1884940066895,-4.15972045882508,
0.));
#77868=CARTESIAN_POINT('Ctrl Pts',(-46.1884940066895,-4.15972045882508,
20.));
#77869=CARTESIAN_POINT('Ctrl Pts',(-46.1884681444317,-4.12685179615294,
0.));
#77870=CARTESIAN_POINT('Ctrl Pts',(-46.1884681444317,-4.12685179615294,
20.));
#77871=CARTESIAN_POINT('Ctrl Pts',(-46.188419081843,-4.09398427631254,0.));
#77872=CARTESIAN_POINT('Ctrl Pts',(-46.188419081843,-4.09398427631254,20.));
#77873=CARTESIAN_POINT('Ctrl Pts',(-46.18834681983,-4.06111791568023,0.));
#77874=CARTESIAN_POINT('Ctrl Pts',(-46.18834681983,-4.06111791568023,20.));
#77875=CARTESIAN_POINT('Ctrl Pts',(-46.1882513593113,-4.02825273063217,
0.));
#77876=CARTESIAN_POINT('Ctrl Pts',(-46.1882513593113,-4.02825273063217,
20.));
#77877=CARTESIAN_POINT('Ctrl Pts',(-46.1881327012171,-3.99538873754442,
0.));
#77878=CARTESIAN_POINT('Ctrl Pts',(-46.1881327012171,-3.99538873754442,
20.));
#77879=CARTESIAN_POINT('Ctrl Pts',(-46.1879908464881,-3.96252595279274,
0.));
#77880=CARTESIAN_POINT('Ctrl Pts',(-46.1879908464881,-3.96252595279274,
20.));
#77881=CARTESIAN_POINT('Ctrl Pts',(-46.1878257960766,-3.92966439275257,
0.));
#77882=CARTESIAN_POINT('Ctrl Pts',(-46.1878257960766,-3.92966439275257,
20.));
#77883=CARTESIAN_POINT('Ctrl Pts',(-46.1876375509469,-3.89680407379914,
0.));
#77884=CARTESIAN_POINT('Ctrl Pts',(-46.1876375509469,-3.89680407379914,
20.));
#77885=CARTESIAN_POINT('Ctrl Pts',(-46.1874261120751,-3.86394501230744,
0.));
#77886=CARTESIAN_POINT('Ctrl Pts',(-46.1874261120751,-3.86394501230744,
20.));
#77887=CARTESIAN_POINT('Ctrl Pts',(-46.1871914804492,-3.83108722465198,
0.));
#77888=CARTESIAN_POINT('Ctrl Pts',(-46.1871914804492,-3.83108722465198,
20.));
#77889=CARTESIAN_POINT('Ctrl Pts',(-46.1869336570686,-3.79823072720685,
0.));
#77890=CARTESIAN_POINT('Ctrl Pts',(-46.1869336570686,-3.79823072720685,
20.));
#77891=CARTESIAN_POINT('Ctrl Pts',(-46.1866526429445,-3.76537553634595,
0.));
#77892=CARTESIAN_POINT('Ctrl Pts',(-46.1866526429445,-3.76537553634595,
20.));
#77893=CARTESIAN_POINT('Ctrl Pts',(-46.1863484390996,-3.73252166844327,
0.));
#77894=CARTESIAN_POINT('Ctrl Pts',(-46.1863484390996,-3.73252166844327,
20.));
#77895=CARTESIAN_POINT('Ctrl Pts',(-46.1860210465678,-3.69966913987252,
0.));
#77896=CARTESIAN_POINT('Ctrl Pts',(-46.1860210465678,-3.69966913987252,
20.));
#77897=CARTESIAN_POINT('Ctrl Pts',(-46.185670466394,-3.66681796700709,0.));
#77898=CARTESIAN_POINT('Ctrl Pts',(-46.185670466394,-3.66681796700709,20.));
#77899=CARTESIAN_POINT('Ctrl Pts',(-46.1852966996347,-3.63396816621989,
0.));
#77900=CARTESIAN_POINT('Ctrl Pts',(-46.1852966996347,-3.63396816621989,
20.));
#77901=CARTESIAN_POINT('Ctrl Pts',(-46.1848997473582,-3.60111975388338,
0.));
#77902=CARTESIAN_POINT('Ctrl Pts',(-46.1848997473582,-3.60111975388338,
20.));
#77903=CARTESIAN_POINT('Ctrl Pts',(-46.1844796106451,-3.56827274636958,
0.));
#77904=CARTESIAN_POINT('Ctrl Pts',(-46.1844796106451,-3.56827274636958,
20.));
#77905=CARTESIAN_POINT('Ctrl Pts',(-46.1840362905882,-3.53542716005024,
0.));
#77906=CARTESIAN_POINT('Ctrl Pts',(-46.1840362905882,-3.53542716005024,
20.));
#77907=CARTESIAN_POINT('Ctrl Pts',(-46.1835697882921,-3.50258301129688,
0.));
#77908=CARTESIAN_POINT('Ctrl Pts',(-46.1835697882921,-3.50258301129688,
20.));
#77909=CARTESIAN_POINT('Ctrl Pts',(-46.1830801048722,-3.4697403164807,0.));
#77910=CARTESIAN_POINT('Ctrl Pts',(-46.1830801048722,-3.4697403164807,20.));
#77911=CARTESIAN_POINT('Ctrl Pts',(-46.1825672414553,-3.43689909197262,
0.));
#77912=CARTESIAN_POINT('Ctrl Pts',(-46.1825672414553,-3.43689909197262,
20.));
#77913=CARTESIAN_POINT('Ctrl Pts',(-46.1820311991793,-3.40405935414302,
0.));
#77914=CARTESIAN_POINT('Ctrl Pts',(-46.1820311991793,-3.40405935414302,
20.));
#77915=CARTESIAN_POINT('Ctrl Pts',(-46.1814719791936,-3.37122111936182,
0.));
#77916=CARTESIAN_POINT('Ctrl Pts',(-46.1814719791936,-3.37122111936182,
20.));
#77917=CARTESIAN_POINT('Ctrl Pts',(-46.1808895826591,-3.33838440399861,
0.));
#77918=CARTESIAN_POINT('Ctrl Pts',(-46.1808895826591,-3.33838440399861,
20.));
#77919=CARTESIAN_POINT('Ctrl Pts',(-46.1802840107495,-3.30554922442265,
0.));
#77920=CARTESIAN_POINT('Ctrl Pts',(-46.1802840107495,-3.30554922442265,
20.));
#77921=CARTESIAN_POINT('Ctrl Pts',(-46.1796552646498,-3.27271559700278,
0.));
#77922=CARTESIAN_POINT('Ctrl Pts',(-46.1796552646498,-3.27271559700278,
20.));
#77923=CARTESIAN_POINT('Ctrl Pts',(-46.1790033455572,-3.23988353810748,
0.));
#77924=CARTESIAN_POINT('Ctrl Pts',(-46.1790033455572,-3.23988353810748,
20.));
#77925=CARTESIAN_POINT('Ctrl Pts',(-46.1783282546796,-3.2070530641047,0.));
#77926=CARTESIAN_POINT('Ctrl Pts',(-46.1783282546796,-3.2070530641047,20.));
#77927=CARTESIAN_POINT('Ctrl Pts',(-46.1776299932363,-3.17422419136187,
0.));
#77928=CARTESIAN_POINT('Ctrl Pts',(-46.1776299932363,-3.17422419136187,
20.));
#77929=CARTESIAN_POINT('Ctrl Pts',(-46.1769085624582,-3.14139693624604,
0.));
#77930=CARTESIAN_POINT('Ctrl Pts',(-46.1769085624582,-3.14139693624604,
20.));
#77931=CARTESIAN_POINT('Ctrl Pts',(-46.1761639635878,-3.10857131512384,
0.));
#77932=CARTESIAN_POINT('Ctrl Pts',(-46.1761639635878,-3.10857131512384,
20.));
#77933=CARTESIAN_POINT('Ctrl Pts',(-46.1753961978798,-3.07574734436159,
0.));
#77934=CARTESIAN_POINT('Ctrl Pts',(-46.1753961978798,-3.07574734436159,
20.));
#77935=CARTESIAN_POINT('Ctrl Pts',(-46.1746052665999,-3.04292504032496,
0.));
#77936=CARTESIAN_POINT('Ctrl Pts',(-46.1746052665999,-3.04292504032496,
20.));
#77937=CARTESIAN_POINT('Ctrl Pts',(-46.1737911710261,-3.01010441937912,
0.));
#77938=CARTESIAN_POINT('Ctrl Pts',(-46.1737911710261,-3.01010441937912,
20.));
#77939=CARTESIAN_POINT('Ctrl Pts',(-46.1729539124487,-2.97728549788889,
0.));
#77940=CARTESIAN_POINT('Ctrl Pts',(-46.1729539124487,-2.97728549788889,
20.));
#77941=CARTESIAN_POINT('Ctrl Pts',(-46.172093492169,-2.94446829221864,0.));
#77942=CARTESIAN_POINT('Ctrl Pts',(-46.172093492169,-2.94446829221864,20.));
#77943=CARTESIAN_POINT('Ctrl Pts',(-46.1712099114993,-2.91165281873224,
0.));
#77944=CARTESIAN_POINT('Ctrl Pts',(-46.1712099114993,-2.91165281873224,
20.));
#77945=CARTESIAN_POINT('Ctrl Pts',(-46.1703031717627,-2.87883909379286,
0.));
#77946=CARTESIAN_POINT('Ctrl Pts',(-46.1703031717627,-2.87883909379286,
20.));
#77947=CARTESIAN_POINT('Ctrl Pts',(-46.169373274294,-2.84602713376308,0.));
#77948=CARTESIAN_POINT('Ctrl Pts',(-46.169373274294,-2.84602713376308,20.));
#77949=CARTESIAN_POINT('Ctrl Pts',(-46.1684202204402,-2.81321695500491,
0.));
#77950=CARTESIAN_POINT('Ctrl Pts',(-46.1684202204402,-2.81321695500491,
20.));
#77951=CARTESIAN_POINT('Ctrl Pts',(-46.1674440115603,-2.78040857388008,
0.));
#77952=CARTESIAN_POINT('Ctrl Pts',(-46.1674440115603,-2.78040857388008,
20.));
#77953=CARTESIAN_POINT('Ctrl Pts',(-46.1664446490252,-2.74760200674979,
0.));
#77954=CARTESIAN_POINT('Ctrl Pts',(-46.1664446490252,-2.74760200674979,
20.));
#77955=CARTESIAN_POINT('Ctrl Pts',(-46.1654221342175,-2.71479726997479,
0.));
#77956=CARTESIAN_POINT('Ctrl Pts',(-46.1654221342175,-2.71479726997479,
20.));
#77957=CARTESIAN_POINT('Ctrl Pts',(-46.1643764685316,-2.68199437991523,
0.));
#77958=CARTESIAN_POINT('Ctrl Pts',(-46.1643764685316,-2.68199437991523,
20.));
#77959=CARTESIAN_POINT('Ctrl Pts',(-46.163307653373,-2.64919335293067,0.));
#77960=CARTESIAN_POINT('Ctrl Pts',(-46.163307653373,-2.64919335293067,20.));
#77961=CARTESIAN_POINT('Ctrl Pts',(-46.1622156901587,-2.61639420537994,
0.));
#77962=CARTESIAN_POINT('Ctrl Pts',(-46.1622156901587,-2.61639420537994,
20.));
#77963=CARTESIAN_POINT('Ctrl Pts',(-46.1611005803162,-2.58359695362107,
0.));
#77964=CARTESIAN_POINT('Ctrl Pts',(-46.1611005803162,-2.58359695362107,
20.));
#77965=CARTESIAN_POINT('Ctrl Pts',(-46.1599623252856,-2.55080161401166,
0.));
#77966=CARTESIAN_POINT('Ctrl Pts',(-46.1599623252856,-2.55080161401166,
20.));
#77967=CARTESIAN_POINT('Ctrl Pts',(-46.1588009265184,-2.51800820290891,
0.));
#77968=CARTESIAN_POINT('Ctrl Pts',(-46.1588009265184,-2.51800820290891,
20.));
#77969=CARTESIAN_POINT('Ctrl Pts',(-46.1576163854777,-2.48521673666957,
0.));
#77970=CARTESIAN_POINT('Ctrl Pts',(-46.1576163854777,-2.48521673666957,
20.));
#77971=CARTESIAN_POINT('Ctrl Pts',(-46.1564087036389,-2.4524272316497,0.));
#77972=CARTESIAN_POINT('Ctrl Pts',(-46.1564087036389,-2.4524272316497,20.));
#77973=CARTESIAN_POINT('Ctrl Pts',(-46.155177882489,-2.41963970420457,0.));
#77974=CARTESIAN_POINT('Ctrl Pts',(-46.155177882489,-2.41963970420457,20.));
#77975=CARTESIAN_POINT('Ctrl Pts',(-46.1539239235264,-2.3868541706887,0.));
#77976=CARTESIAN_POINT('Ctrl Pts',(-46.1539239235264,-2.3868541706887,20.));
#77977=CARTESIAN_POINT('Ctrl Pts',(-46.1526468282604,-2.35407064745589,
0.));
#77978=CARTESIAN_POINT('Ctrl Pts',(-46.1526468282604,-2.35407064745589,
20.));
#77979=CARTESIAN_POINT('Ctrl Pts',(-46.1513465982124,-2.32128915085919,
0.));
#77980=CARTESIAN_POINT('Ctrl Pts',(-46.1513465982124,-2.32128915085919,
20.));
#77981=CARTESIAN_POINT('Ctrl Pts',(-46.1500232349155,-2.28850969725138,
0.));
#77982=CARTESIAN_POINT('Ctrl Pts',(-46.1500232349155,-2.28850969725138,
20.));
#77983=CARTESIAN_POINT('Ctrl Pts',(-46.1486767399146,-2.25573230298458,
0.));
#77984=CARTESIAN_POINT('Ctrl Pts',(-46.1486767399146,-2.25573230298458,
20.));
#77985=CARTESIAN_POINT('Ctrl Pts',(-46.147307114766,-2.22295698441049,0.));
#77986=CARTESIAN_POINT('Ctrl Pts',(-46.147307114766,-2.22295698441049,20.));
#77987=CARTESIAN_POINT('Ctrl Pts',(-46.1459143610377,-2.19018375787986,
0.));
#77988=CARTESIAN_POINT('Ctrl Pts',(-46.1459143610377,-2.19018375787986,
20.));
#77989=CARTESIAN_POINT('Ctrl Pts',(-46.1444984803082,-2.15741263974262,
0.));
#77990=CARTESIAN_POINT('Ctrl Pts',(-46.1444984803082,-2.15741263974262,
20.));
#77991=CARTESIAN_POINT('Ctrl Pts',(-46.1430594741682,-2.12464364634812,
0.));
#77992=CARTESIAN_POINT('Ctrl Pts',(-46.1430594741682,-2.12464364634812,
20.));
#77993=CARTESIAN_POINT('Ctrl Pts',(-46.1415973442202,-2.09187679404497,
0.));
#77994=CARTESIAN_POINT('Ctrl Pts',(-46.1415973442202,-2.09187679404497,
20.));
#77995=CARTESIAN_POINT('Ctrl Pts',(-46.1401120920793,-2.05911209918101,
0.));
#77996=CARTESIAN_POINT('Ctrl Pts',(-46.1401120920793,-2.05911209918101,
20.));
#77997=CARTESIAN_POINT('Ctrl Pts',(-46.1386037193727,-2.02634957810317,
0.));
#77998=CARTESIAN_POINT('Ctrl Pts',(-46.1386037193727,-2.02634957810317,
20.));
#77999=CARTESIAN_POINT('Ctrl Pts',(-46.1370722277379,-1.99358924715753,
0.));
#78000=CARTESIAN_POINT('Ctrl Pts',(-46.1370722277379,-1.99358924715753,
20.));
#78001=CARTESIAN_POINT('Ctrl Pts',(-46.1355176188236,-1.9608311226893,0.));
#78002=CARTESIAN_POINT('Ctrl Pts',(-46.1355176188236,-1.9608311226893,20.));
#78003=CARTESIAN_POINT('Ctrl Pts',(-46.1339398942902,-1.92807522104339,
0.));
#78004=CARTESIAN_POINT('Ctrl Pts',(-46.1339398942902,-1.92807522104339,
20.));
#78005=CARTESIAN_POINT('Ctrl Pts',(-46.1323390558096,-1.89532155856414,
0.));
#78006=CARTESIAN_POINT('Ctrl Pts',(-46.1323390558096,-1.89532155856414,
20.));
#78007=CARTESIAN_POINT('Ctrl Pts',(-46.1307151050651,-1.86257015159582,
0.));
#78008=CARTESIAN_POINT('Ctrl Pts',(-46.1307151050651,-1.86257015159582,
20.));
#78009=CARTESIAN_POINT('Ctrl Pts',(-46.1290680437528,-1.82982101648206,
0.));
#78010=CARTESIAN_POINT('Ctrl Pts',(-46.1290680437528,-1.82982101648206,
20.));
#78011=CARTESIAN_POINT('Ctrl Pts',(-46.1273978735796,-1.79707416956534,
0.));
#78012=CARTESIAN_POINT('Ctrl Pts',(-46.1273978735796,-1.79707416956534,
20.));
#78013=CARTESIAN_POINT('Ctrl Pts',(-46.1257045962649,-1.76432962718685,
0.));
#78014=CARTESIAN_POINT('Ctrl Pts',(-46.1257045962649,-1.76432962718685,
20.));
#78015=CARTESIAN_POINT('Ctrl Pts',(-46.1239882135394,-1.73158740568597,
0.));
#78016=CARTESIAN_POINT('Ctrl Pts',(-46.1239882135394,-1.73158740568597,
20.));
#78017=CARTESIAN_POINT('Ctrl Pts',(-46.1222487271454,-1.69884752140039,
0.));
#78018=CARTESIAN_POINT('Ctrl Pts',(-46.1222487271454,-1.69884752140039,
20.));
#78019=CARTESIAN_POINT('Ctrl Pts',(-46.1204861388364,-1.66610999066655,
0.));
#78020=CARTESIAN_POINT('Ctrl Pts',(-46.1204861388364,-1.66610999066655,
20.));
#78021=CARTESIAN_POINT('Ctrl Pts',(-46.1187004503775,-1.6333748298207,0.));
#78022=CARTESIAN_POINT('Ctrl Pts',(-46.1187004503775,-1.6333748298207,20.));
#78023=CARTESIAN_POINT('Ctrl Pts',(-46.1168916635447,-1.60064205519958,
0.));
#78024=CARTESIAN_POINT('Ctrl Pts',(-46.1168916635447,-1.60064205519958,
20.));
#78025=CARTESIAN_POINT('Ctrl Pts',(-46.1150597801266,-1.56791168314158,
0.));
#78026=CARTESIAN_POINT('Ctrl Pts',(-46.1150597801266,-1.56791168314158,
20.));
#78027=CARTESIAN_POINT('Ctrl Pts',(-46.1132048019234,-1.53518372998667,
0.));
#78028=CARTESIAN_POINT('Ctrl Pts',(-46.1132048019234,-1.53518372998667,
20.));
#78029=CARTESIAN_POINT('Ctrl Pts',(-46.111326730748,-1.5024582120743,0.));
#78030=CARTESIAN_POINT('Ctrl Pts',(-46.111326730748,-1.5024582120743,20.));
#78031=CARTESIAN_POINT('Ctrl Pts',(-46.1094255684237,-1.46973514574143,
0.));
#78032=CARTESIAN_POINT('Ctrl Pts',(-46.1094255684237,-1.46973514574143,
20.));
#78033=CARTESIAN_POINT('Ctrl Pts',(-46.1075013167858,-1.4370145473209,0.));
#78034=CARTESIAN_POINT('Ctrl Pts',(-46.1075013167858,-1.4370145473209,20.));
#78035=CARTESIAN_POINT('Ctrl Pts',(-46.1055539776802,-1.40429643313893,
0.));
#78036=CARTESIAN_POINT('Ctrl Pts',(-46.1055539776802,-1.40429643313893,
20.));
#78037=CARTESIAN_POINT('Ctrl Pts',(-46.1035835529643,-1.37158081951551,
0.));
#78038=CARTESIAN_POINT('Ctrl Pts',(-46.1035835529643,-1.37158081951551,
20.));
#78039=CARTESIAN_POINT('Ctrl Pts',(-46.1015900445065,-1.33886772276919,
0.));
#78040=CARTESIAN_POINT('Ctrl Pts',(-46.1015900445065,-1.33886772276919,
20.));
#78041=CARTESIAN_POINT('Ctrl Pts',(-46.0995734541875,-1.30615715922172,
0.));
#78042=CARTESIAN_POINT('Ctrl Pts',(-46.0995734541875,-1.30615715922172,
20.));
#78043=CARTESIAN_POINT('Ctrl Pts',(-46.0975337839002,-1.27344914520175,
0.));
#78044=CARTESIAN_POINT('Ctrl Pts',(-46.0975337839002,-1.27344914520175,
20.));
#78045=CARTESIAN_POINT('Ctrl Pts',(-46.0954710355506,-1.24074369705072,
0.));
#78046=CARTESIAN_POINT('Ctrl Pts',(-46.0954710355506,-1.24074369705072,
20.));
#78047=CARTESIAN_POINT('Ctrl Pts',(-46.0933852110571,-1.20804083112097,
0.));
#78048=CARTESIAN_POINT('Ctrl Pts',(-46.0933852110571,-1.20804083112097,
20.));
#78049=CARTESIAN_POINT('Ctrl Pts',(-46.0912763123502,-1.17534056376402,
0.));
#78050=CARTESIAN_POINT('Ctrl Pts',(-46.0912763123502,-1.17534056376402,
20.));
#78051=CARTESIAN_POINT('Ctrl Pts',(-46.0891443413718,-1.14264291132052,
0.));
#78052=CARTESIAN_POINT('Ctrl Pts',(-46.0891443413718,-1.14264291132052,
20.));
#78053=CARTESIAN_POINT('Ctrl Pts',(-46.0869893000734,-1.10994789011162,
0.));
#78054=CARTESIAN_POINT('Ctrl Pts',(-46.0869893000734,-1.10994789011162,
20.));
#78055=CARTESIAN_POINT('Ctrl Pts',(-46.0848111904142,-1.07725551642471,
0.));
#78056=CARTESIAN_POINT('Ctrl Pts',(-46.0848111904142,-1.07725551642471,
20.));
#78057=CARTESIAN_POINT('Ctrl Pts',(-46.0826100143611,-1.04456580652047,
0.));
#78058=CARTESIAN_POINT('Ctrl Pts',(-46.0826100143611,-1.04456580652047,
20.));
#78059=CARTESIAN_POINT('Ctrl Pts',(-46.0803857738924,-1.01187877665954,
0.));
#78060=CARTESIAN_POINT('Ctrl Pts',(-46.0803857738924,-1.01187877665954,
20.));
#78061=CARTESIAN_POINT('Ctrl Pts',(-46.0781384710012,-0.979194443126286,
0.));
#78062=CARTESIAN_POINT('Ctrl Pts',(-46.0781384710012,-0.979194443126286,
20.));
#78063=CARTESIAN_POINT('Ctrl Pts',(-46.0758681076973,-0.946512822248744,
0.));
#78064=CARTESIAN_POINT('Ctrl Pts',(-46.0758681076973,-0.946512822248744,
20.));
#78065=CARTESIAN_POINT('Ctrl Pts',(-46.0735746860119,-0.913833930432268,
0.));
#78066=CARTESIAN_POINT('Ctrl Pts',(-46.0735746860119,-0.913833930432268,
20.));
#78067=CARTESIAN_POINT('Ctrl Pts',(-46.0712582079948,-0.881157784136737,
0.));
#78068=CARTESIAN_POINT('Ctrl Pts',(-46.0712582079948,-0.881157784136737,
20.));
#78069=CARTESIAN_POINT('Ctrl Pts',(-46.0689186757066,-0.848484399815181,
0.));
#78070=CARTESIAN_POINT('Ctrl Pts',(-46.0689186757066,-0.848484399815181,
20.));
#78071=CARTESIAN_POINT('Ctrl Pts',(-46.0665560912128,-0.815813793858633,
0.));
#78072=CARTESIAN_POINT('Ctrl Pts',(-46.0665560912128,-0.815813793858633,
20.));
#78073=CARTESIAN_POINT('Ctrl Pts',(-46.064170456577,-0.78314598254893,0.));
#78074=CARTESIAN_POINT('Ctrl Pts',(-46.064170456577,-0.78314598254893,20.));
#78075=CARTESIAN_POINT('Ctrl Pts',(-46.0617617738521,-0.750480981980923,
0.));
#78076=CARTESIAN_POINT('Ctrl Pts',(-46.0617617738521,-0.750480981980923,
20.));
#78077=CARTESIAN_POINT('Ctrl Pts',(-46.0593300450868,-0.717818808129722,
0.));
#78078=CARTESIAN_POINT('Ctrl Pts',(-46.0593300450868,-0.717818808129722,
20.));
#78079=CARTESIAN_POINT('Ctrl Pts',(-46.0568752723439,-0.685159476991759,
0.));
#78080=CARTESIAN_POINT('Ctrl Pts',(-46.0568752723439,-0.685159476991759,
20.));
#78081=CARTESIAN_POINT('Ctrl Pts',(-46.0543974577158,-0.652503004713259,
0.));
#78082=CARTESIAN_POINT('Ctrl Pts',(-46.0543974577158,-0.652503004713259,
20.));
#78083=CARTESIAN_POINT('Ctrl Pts',(-46.0518966033391,-0.619849407700859,
0.));
#78084=CARTESIAN_POINT('Ctrl Pts',(-46.0518966033391,-0.619849407700859,
20.));
#78085=CARTESIAN_POINT('Ctrl Pts',(-46.0493727114182,-0.587198702798619,
0.));
#78086=CARTESIAN_POINT('Ctrl Pts',(-46.0493727114182,-0.587198702798619,
20.));
#78087=CARTESIAN_POINT('Ctrl Pts',(-46.0468257841997,-0.554550907098827,
0.));
#78088=CARTESIAN_POINT('Ctrl Pts',(-46.0468257841997,-0.554550907098827,
20.));
#78089=CARTESIAN_POINT('Ctrl Pts',(-46.044255823933,-0.521906037621043,
0.));
#78090=CARTESIAN_POINT('Ctrl Pts',(-46.044255823933,-0.521906037621043,
20.));
#78091=CARTESIAN_POINT('Ctrl Pts',(-46.0416628328334,-0.489264111013836,
0.));
#78092=CARTESIAN_POINT('Ctrl Pts',(-46.0416628328334,-0.489264111013836,
20.));
#78093=CARTESIAN_POINT('Ctrl Pts',(-46.0390468130479,-0.456625143292611,
0.));
#78094=CARTESIAN_POINT('Ctrl Pts',(-46.0390468130479,-0.456625143292611,
20.));
#78095=CARTESIAN_POINT('Ctrl Pts',(-46.0364077666069,-0.423989149445243,
0.));
#78096=CARTESIAN_POINT('Ctrl Pts',(-46.0364077666069,-0.423989149445243,
20.));
#78097=CARTESIAN_POINT('Ctrl Pts',(-46.0337456954889,-0.391356143937831,
0.));
#78098=CARTESIAN_POINT('Ctrl Pts',(-46.0337456954889,-0.391356143937831,
20.));
#78099=CARTESIAN_POINT('Ctrl Pts',(-46.0310606017089,-0.358726141441568,
0.));
#78100=CARTESIAN_POINT('Ctrl Pts',(-46.0310606017089,-0.358726141441568,
20.));
#78101=CARTESIAN_POINT('Ctrl Pts',(-46.0283524874048,-0.32609915751695,
0.));
#78102=CARTESIAN_POINT('Ctrl Pts',(-46.0283524874048,-0.32609915751695,
20.));
#78103=CARTESIAN_POINT('Ctrl Pts',(-46.025621354915,-0.293475209241787,
0.));
#78104=CARTESIAN_POINT('Ctrl Pts',(-46.025621354915,-0.293475209241787,
20.));
#78105=CARTESIAN_POINT('Ctrl Pts',(-46.022867206884,-0.260854316057531,
0.));
#78106=CARTESIAN_POINT('Ctrl Pts',(-46.022867206884,-0.260854316057531,
20.));
#78107=CARTESIAN_POINT('Ctrl Pts',(-46.0200900461091,-0.228236498538561,
0.));
#78108=CARTESIAN_POINT('Ctrl Pts',(-46.0200900461091,-0.228236498538561,
20.));
#78109=CARTESIAN_POINT('Ctrl Pts',(-46.0172898753497,-0.195621776838879,
0.));
#78110=CARTESIAN_POINT('Ctrl Pts',(-46.0172898753497,-0.195621776838879,
20.));
#78111=CARTESIAN_POINT('Ctrl Pts',(-46.0144666971462,-0.163010169231703,
0.));
#78112=CARTESIAN_POINT('Ctrl Pts',(-46.0144666971462,-0.163010169231703,
20.));
#78113=CARTESIAN_POINT('Ctrl Pts',(-46.0116205136405,-0.130401690656317,
0.));
#78114=CARTESIAN_POINT('Ctrl Pts',(-46.0116205136405,-0.130401690656317,
20.));
#78115=CARTESIAN_POINT('Ctrl Pts',(-46.0087513263814,-0.0977963511372804,
0.));
#78116=CARTESIAN_POINT('Ctrl Pts',(-46.0087513263814,-0.0977963511372804,
20.));
#78117=CARTESIAN_POINT('Ctrl Pts',(-46.0058591364029,-0.0651941566547531,
0.));
#78118=CARTESIAN_POINT('Ctrl Pts',(-46.0058591364029,-0.0651941566547531,
20.));
#78119=CARTESIAN_POINT('Ctrl Pts',(-46.0035269827389,-0.0391149194889384,
0.));
#78120=CARTESIAN_POINT('Ctrl Pts',(-46.0035269827389,-0.0391149194889384,
20.));
#78121=CARTESIAN_POINT('Ctrl Pts',(-46.0017675166781,-0.019556908668581,
0.));
#78122=CARTESIAN_POINT('Ctrl Pts',(-46.0017675166781,-0.019556908668581,
20.));
#78123=CARTESIAN_POINT('Ctrl Pts',(-46.0005899389515,-0.00651886458936213,
0.));
#78124=CARTESIAN_POINT('Ctrl Pts',(-46.0005899389515,-0.00651886458936213,
20.));
#78125=CARTESIAN_POINT('Ctrl Pts',(-46.,6.66133814775094E-15,0.));
#78126=CARTESIAN_POINT('Ctrl Pts',(-46.,6.66133814775094E-15,20.));
#78127=CARTESIAN_POINT('',(-37.5361777128299,-31.4965928746404,2.));
#78128=CARTESIAN_POINT('Ctrl Pts',(-45.2025619355895,-13.7414592977624,
2.));
#78129=CARTESIAN_POINT('Ctrl Pts',(-45.039110381915,-14.5281012519506,2.));
#78130=CARTESIAN_POINT('Ctrl Pts',(-44.8554703046336,-15.3115504167957,
2.));
#78131=CARTESIAN_POINT('Ctrl Pts',(-44.6518239974238,-16.0907854020754,
2.));
#78132=CARTESIAN_POINT('Ctrl Pts',(-44.4484766164816,-16.8688765718406,
2.));
#78133=CARTESIAN_POINT('Ctrl Pts',(-44.2251817634589,-17.6427657588129,
2.));
#78134=CARTESIAN_POINT('Ctrl Pts',(-43.9821717973476,-18.4114484455697,
2.));
#78135=CARTESIAN_POINT('Ctrl Pts',(-43.7389516037332,-19.1807961183945,
2.));
#78136=CARTESIAN_POINT('Ctrl Pts',(-43.4759822277029,-19.9449281117179,
2.));
#78137=CARTESIAN_POINT('Ctrl Pts',(-43.1935467196845,-20.7028522155842,
2.));
#78138=CARTESIAN_POINT('Ctrl Pts',(-42.910867002848,-21.4614316610926,2.));
#78139=CARTESIAN_POINT('Ctrl Pts',(-42.6086875412903,-22.2137923134146,
2.));
#78140=CARTESIAN_POINT('Ctrl Pts',(-42.2873413628421,-22.9589568069778,
2.));
#78141=CARTESIAN_POINT('Ctrl Pts',(-41.9655415151298,-23.7051733069134,
2.));
#78142=CARTESIAN_POINT('Ctrl Pts',(-41.6245208625705,-24.4441731529251,
2.));
#78143=CARTESIAN_POINT('Ctrl Pts',(-41.264662211266,-25.1749947461293,2.));
#78144=CARTESIAN_POINT('Ctrl Pts',(-40.9045440154532,-25.9063434372103,
2.));
#78145=CARTESIAN_POINT('Ctrl Pts',(-40.5255607195679,-26.6295019186582,
2.));
#78146=CARTESIAN_POINT('Ctrl Pts',(-40.1281432215925,-27.3435288185695,
2.));
#78147=CARTESIAN_POINT('Ctrl Pts',(-39.7321221742634,-28.0550467617012,
2.));
#78148=CARTESIAN_POINT('Ctrl Pts',(-39.3177963661132,-28.7574970523859,
2.));
#78149=CARTESIAN_POINT('Ctrl Pts',(-38.8856375198795,-29.4499724760943,
2.));
#78150=CARTESIAN_POINT('Ctrl Pts',(-38.6009983664357,-29.9060677755493,
2.));
#78151=CARTESIAN_POINT('Ctrl Pts',(-38.3086239303204,-30.3578363585341,
2.));
#78152=CARTESIAN_POINT('Ctrl Pts',(-38.0086594336355,-30.8050251768588,
2.));
#78153=CARTESIAN_POINT('Ctrl Pts',(-37.8531970881941,-31.0367893466863,
2.));
#78154=CARTESIAN_POINT('Ctrl Pts',(-37.6956964623238,-31.2673229660863,
2.));
#78155=CARTESIAN_POINT('Ctrl Pts',(-37.5361777128299,-31.4965928746404,
2.));
#78156=CARTESIAN_POINT('',(-37.5361777128299,-31.4965928746404,0.));
#78157=CARTESIAN_POINT('Ctrl Pts',(-37.5361777128299,-31.4965928746404,
0.));
#78158=CARTESIAN_POINT('Ctrl Pts',(-37.5361777128299,-31.4965928746404,
20.));
#78159=CARTESIAN_POINT('Ctrl Pts',(-37.5400435810124,-31.4910366171629,
0.));
#78160=CARTESIAN_POINT('Ctrl Pts',(-37.5400435810124,-31.4910366171629,
20.));
#78161=CARTESIAN_POINT('Ctrl Pts',(-37.5477733397939,-31.4799228688318,
0.));
#78162=CARTESIAN_POINT('Ctrl Pts',(-37.5477733397939,-31.4799228688318,
20.));
#78163=CARTESIAN_POINT('Ctrl Pts',(-37.5593620452151,-31.4632485462068,
0.));
#78164=CARTESIAN_POINT('Ctrl Pts',(-37.5593620452151,-31.4632485462068,
20.));
#78165=CARTESIAN_POINT('Ctrl Pts',(-37.574801786924,-31.4410087157717,0.));
#78166=CARTESIAN_POINT('Ctrl Pts',(-37.574801786924,-31.4410087157717,20.));
#78167=CARTESIAN_POINT('Ctrl Pts',(-37.5940816876034,-31.4131965946731,
0.));
#78168=CARTESIAN_POINT('Ctrl Pts',(-37.5940816876034,-31.4131965946731,
20.));
#78169=CARTESIAN_POINT('Ctrl Pts',(-37.6133418102375,-31.3853721428083,
0.));
#78170=CARTESIAN_POINT('Ctrl Pts',(-37.6133418102375,-31.3853721428083,
20.));
#78171=CARTESIAN_POINT('Ctrl Pts',(-37.6325821517747,-31.3575353648538,
0.));
#78172=CARTESIAN_POINT('Ctrl Pts',(-37.6325821517747,-31.3575353648538,
20.));
#78173=CARTESIAN_POINT('Ctrl Pts',(-37.6518027072643,-31.3296862686536,
0.));
#78174=CARTESIAN_POINT('Ctrl Pts',(-37.6518027072643,-31.3296862686536,
20.));
#78175=CARTESIAN_POINT('Ctrl Pts',(-37.6710034693473,-31.3018248661211,
0.));
#78176=CARTESIAN_POINT('Ctrl Pts',(-37.6710034693473,-31.3018248661211,
20.));
#78177=CARTESIAN_POINT('Ctrl Pts',(-37.6901844288974,-31.2739511721649,
0.));
#78178=CARTESIAN_POINT('Ctrl Pts',(-37.6901844288974,-31.2739511721649,
20.));
#78179=CARTESIAN_POINT('Ctrl Pts',(-37.7093455757381,-31.2460652034827,
0.));
#78180=CARTESIAN_POINT('Ctrl Pts',(-37.7093455757381,-31.2460652034827,
20.));
#78181=CARTESIAN_POINT('Ctrl Pts',(-37.7284868993471,-31.2181669773772,
0.));
#78182=CARTESIAN_POINT('Ctrl Pts',(-37.7284868993471,-31.2181669773772,
20.));
#78183=CARTESIAN_POINT('Ctrl Pts',(-37.7476083895316,-31.1902565106222,
0.));
#78184=CARTESIAN_POINT('Ctrl Pts',(-37.7476083895316,-31.1902565106222,
20.));
#78185=CARTESIAN_POINT('Ctrl Pts',(-37.7667100372089,-31.1623338181506,
0.));
#78186=CARTESIAN_POINT('Ctrl Pts',(-37.7667100372089,-31.1623338181506,
20.));
#78187=CARTESIAN_POINT('Ctrl Pts',(-37.7857918342009,-31.1343989133989,
0.));
#78188=CARTESIAN_POINT('Ctrl Pts',(-37.7857918342009,-31.1343989133989,
20.));
#78189=CARTESIAN_POINT('Ctrl Pts',(-37.8048537728749,-31.1064518089103,
0.));
#78190=CARTESIAN_POINT('Ctrl Pts',(-37.8048537728749,-31.1064518089103,
20.));
#78191=CARTESIAN_POINT('Ctrl Pts',(-37.8238958458276,-31.0784925168637,
0.));
#78192=CARTESIAN_POINT('Ctrl Pts',(-37.8238958458276,-31.0784925168637,
20.));
#78193=CARTESIAN_POINT('Ctrl Pts',(-37.8429180455734,-31.0505210495984,
0.));
#78194=CARTESIAN_POINT('Ctrl Pts',(-37.8429180455734,-31.0505210495984,
20.));
#78195=CARTESIAN_POINT('Ctrl Pts',(-37.861920364175,-31.0225374202321,0.));
#78196=CARTESIAN_POINT('Ctrl Pts',(-37.861920364175,-31.0225374202321,20.));
#78197=CARTESIAN_POINT('Ctrl Pts',(-37.8809027932971,-30.9945416425721,
0.));
#78198=CARTESIAN_POINT('Ctrl Pts',(-37.8809027932971,-30.9945416425721,
20.));
#78199=CARTESIAN_POINT('Ctrl Pts',(-37.8998653243731,-30.9665337308352,
0.));
#78200=CARTESIAN_POINT('Ctrl Pts',(-37.8998653243731,-30.9665337308352,
20.));
#78201=CARTESIAN_POINT('Ctrl Pts',(-37.9188079487378,-30.938513699426,0.));
#78202=CARTESIAN_POINT('Ctrl Pts',(-37.9188079487378,-30.938513699426,20.));
#78203=CARTESIAN_POINT('Ctrl Pts',(-37.9377306577632,-30.9104815627079,
0.));
#78204=CARTESIAN_POINT('Ctrl Pts',(-37.9377306577632,-30.9104815627079,
20.));
#78205=CARTESIAN_POINT('Ctrl Pts',(-37.9566334430211,-30.882437334731,0.));
#78206=CARTESIAN_POINT('Ctrl Pts',(-37.9566334430211,-30.882437334731,20.));
#78207=CARTESIAN_POINT('Ctrl Pts',(-37.9755162962752,-30.8543810292446,
0.));
#78208=CARTESIAN_POINT('Ctrl Pts',(-37.9755162962752,-30.8543810292446,
20.));
#78209=CARTESIAN_POINT('Ctrl Pts',(-37.9943792094053,-30.8263126598247,
0.));
#78210=CARTESIAN_POINT('Ctrl Pts',(-37.9943792094053,-30.8263126598247,
20.));
#78211=CARTESIAN_POINT('Ctrl Pts',(-38.0132221743517,-30.7982322399668,
0.));
#78212=CARTESIAN_POINT('Ctrl Pts',(-38.0132221743517,-30.7982322399668,
20.));
#78213=CARTESIAN_POINT('Ctrl Pts',(-38.0320451830565,-30.7701397831859,
0.));
#78214=CARTESIAN_POINT('Ctrl Pts',(-38.0320451830565,-30.7701397831859,
20.));
#78215=CARTESIAN_POINT('Ctrl Pts',(-38.0508482273931,-30.7420353031339,
0.));
#78216=CARTESIAN_POINT('Ctrl Pts',(-38.0508482273931,-30.7420353031339,
20.));
#78217=CARTESIAN_POINT('Ctrl Pts',(-38.0696312991626,-30.7139188136053,
0.));
#78218=CARTESIAN_POINT('Ctrl Pts',(-38.0696312991626,-30.7139188136053,
20.));
#78219=CARTESIAN_POINT('Ctrl Pts',(-38.088394390128,-30.6857903284809,0.));
#78220=CARTESIAN_POINT('Ctrl Pts',(-38.088394390128,-30.6857903284809,20.));
#78221=CARTESIAN_POINT('Ctrl Pts',(-38.1071374920373,-30.6576498616875,
0.));
#78222=CARTESIAN_POINT('Ctrl Pts',(-38.1071374920373,-30.6576498616875,
20.));
#78223=CARTESIAN_POINT('Ctrl Pts',(-38.125860596649,-30.6294974271553,0.));
#78224=CARTESIAN_POINT('Ctrl Pts',(-38.125860596649,-30.6294974271553,20.));
#78225=CARTESIAN_POINT('Ctrl Pts',(-38.1445636957629,-30.6013330387674,
0.));
#78226=CARTESIAN_POINT('Ctrl Pts',(-38.1445636957629,-30.6013330387674,
20.));
#78227=CARTESIAN_POINT('Ctrl Pts',(-38.1632467812242,-30.5731567103519,
0.));
#78228=CARTESIAN_POINT('Ctrl Pts',(-38.1632467812242,-30.5731567103519,
20.));
#78229=CARTESIAN_POINT('Ctrl Pts',(-38.1819098449085,-30.5449684557073,
0.));
#78230=CARTESIAN_POINT('Ctrl Pts',(-38.1819098449085,-30.5449684557073,
20.));
#78231=CARTESIAN_POINT('Ctrl Pts',(-38.2005528787125,-30.5167682886194,
0.));
#78232=CARTESIAN_POINT('Ctrl Pts',(-38.2005528787125,-30.5167682886194,
20.));
#78233=CARTESIAN_POINT('Ctrl Pts',(-38.2191758745422,-30.4885562228796,
0.));
#78234=CARTESIAN_POINT('Ctrl Pts',(-38.2191758745422,-30.4885562228796,
20.));
#78235=CARTESIAN_POINT('Ctrl Pts',(-38.2377788243005,-30.460332272307,0.));
#78236=CARTESIAN_POINT('Ctrl Pts',(-38.2377788243005,-30.460332272307,20.));
#78237=CARTESIAN_POINT('Ctrl Pts',(-38.2563617198829,-30.4320964507535,
0.));
#78238=CARTESIAN_POINT('Ctrl Pts',(-38.2563617198829,-30.4320964507535,
20.));
#78239=CARTESIAN_POINT('Ctrl Pts',(-38.2749245531853,-30.4038487720928,
0.));
#78240=CARTESIAN_POINT('Ctrl Pts',(-38.2749245531853,-30.4038487720928,
20.));
#78241=CARTESIAN_POINT('Ctrl Pts',(-38.2934673161074,-30.3755892502132,
0.));
#78242=CARTESIAN_POINT('Ctrl Pts',(-38.2934673161074,-30.3755892502132,
20.));
#78243=CARTESIAN_POINT('Ctrl Pts',(-38.3119900005578,-30.3473178990095,
0.));
#78244=CARTESIAN_POINT('Ctrl Pts',(-38.3119900005578,-30.3473178990095,
20.));
#78245=CARTESIAN_POINT('Ctrl Pts',(-38.3304925984593,-30.3190347323738,
0.));
#78246=CARTESIAN_POINT('Ctrl Pts',(-38.3304925984593,-30.3190347323738,
20.));
#78247=CARTESIAN_POINT('Ctrl Pts',(-38.3489751017513,-30.2907397641919,
0.));
#78248=CARTESIAN_POINT('Ctrl Pts',(-38.3489751017513,-30.2907397641919,
20.));
#78249=CARTESIAN_POINT('Ctrl Pts',(-38.3674375023871,-30.2624330083488,
0.));
#78250=CARTESIAN_POINT('Ctrl Pts',(-38.3674375023871,-30.2624330083488,
20.));
#78251=CARTESIAN_POINT('Ctrl Pts',(-38.3858797923318,-30.2341144787313,
0.));
#78252=CARTESIAN_POINT('Ctrl Pts',(-38.3858797923318,-30.2341144787313,
20.));
#78253=CARTESIAN_POINT('Ctrl Pts',(-38.4043019635603,-30.2057841892317,
0.));
#78254=CARTESIAN_POINT('Ctrl Pts',(-38.4043019635603,-30.2057841892317,
20.));
#78255=CARTESIAN_POINT('Ctrl Pts',(-38.4227040080549,-30.1774421537519,
0.));
#78256=CARTESIAN_POINT('Ctrl Pts',(-38.4227040080549,-30.1774421537519,
20.));
#78257=CARTESIAN_POINT('Ctrl Pts',(-38.4410859178039,-30.1490883862047,
0.));
#78258=CARTESIAN_POINT('Ctrl Pts',(-38.4410859178039,-30.1490883862047,
20.));
#78259=CARTESIAN_POINT('Ctrl Pts',(-38.4594476848032,-30.1207229005118,
0.));
#78260=CARTESIAN_POINT('Ctrl Pts',(-38.4594476848032,-30.1207229005118,
20.));
#78261=CARTESIAN_POINT('Ctrl Pts',(-38.4777893010568,-30.0923457106026,
0.));
#78262=CARTESIAN_POINT('Ctrl Pts',(-38.4777893010568,-30.0923457106026,
20.));
#78263=CARTESIAN_POINT('Ctrl Pts',(-38.4961107585777,-30.0639568304126,
0.));
#78264=CARTESIAN_POINT('Ctrl Pts',(-38.4961107585777,-30.0639568304126,
20.));
#78265=CARTESIAN_POINT('Ctrl Pts',(-38.5144120493894,-30.0355562738816,
0.));
#78266=CARTESIAN_POINT('Ctrl Pts',(-38.5144120493894,-30.0355562738816,
20.));
#78267=CARTESIAN_POINT('Ctrl Pts',(-38.532693165526,-30.0071440549534,0.));
#78268=CARTESIAN_POINT('Ctrl Pts',(-38.532693165526,-30.0071440549534,20.));
#78269=CARTESIAN_POINT('Ctrl Pts',(-38.5509540990321,-29.978720187576,0.));
#78270=CARTESIAN_POINT('Ctrl Pts',(-38.5509540990321,-29.978720187576,20.));
#78271=CARTESIAN_POINT('Ctrl Pts',(-38.5691948419622,-29.9502846857025,
0.));
#78272=CARTESIAN_POINT('Ctrl Pts',(-38.5691948419622,-29.9502846857025,
20.));
#78273=CARTESIAN_POINT('Ctrl Pts',(-38.5874153863803,-29.9218375632917,
0.));
#78274=CARTESIAN_POINT('Ctrl Pts',(-38.5874153863803,-29.9218375632917,
20.));
#78275=CARTESIAN_POINT('Ctrl Pts',(-38.6056157243597,-29.8933788343089,
0.));
#78276=CARTESIAN_POINT('Ctrl Pts',(-38.6056157243597,-29.8933788343089,
20.));
#78277=CARTESIAN_POINT('Ctrl Pts',(-38.6237958479822,-29.864908512726,0.));
#78278=CARTESIAN_POINT('Ctrl Pts',(-38.6237958479822,-29.864908512726,20.));
#78279=CARTESIAN_POINT('Ctrl Pts',(-38.6419557493389,-29.8364266125215,
0.));
#78280=CARTESIAN_POINT('Ctrl Pts',(-38.6419557493389,-29.8364266125215,
20.));
#78281=CARTESIAN_POINT('Ctrl Pts',(-38.66009542053,-29.8079331476799,0.));
#78282=CARTESIAN_POINT('Ctrl Pts',(-38.66009542053,-29.8079331476799,20.));
#78283=CARTESIAN_POINT('Ctrl Pts',(-38.6782148536649,-29.7794281321916,
0.));
#78284=CARTESIAN_POINT('Ctrl Pts',(-38.6782148536649,-29.7794281321916,
20.));
#78285=CARTESIAN_POINT('Ctrl Pts',(-38.6963140408627,-29.7509115800524,
0.));
#78286=CARTESIAN_POINT('Ctrl Pts',(-38.6963140408627,-29.7509115800524,
20.));
#78287=CARTESIAN_POINT('Ctrl Pts',(-38.7143929742521,-29.7223835052637,
0.));
#78288=CARTESIAN_POINT('Ctrl Pts',(-38.7143929742521,-29.7223835052637,
20.));
#78289=CARTESIAN_POINT('Ctrl Pts',(-38.7324516459718,-29.6938439218325,
0.));
#78290=CARTESIAN_POINT('Ctrl Pts',(-38.7324516459718,-29.6938439218325,
20.));
#78291=CARTESIAN_POINT('Ctrl Pts',(-38.7504900481697,-29.6652928437714,
0.));
#78292=CARTESIAN_POINT('Ctrl Pts',(-38.7504900481697,-29.6652928437714,
20.));
#78293=CARTESIAN_POINT('Ctrl Pts',(-38.7685081730036,-29.6367302850988,
0.));
#78294=CARTESIAN_POINT('Ctrl Pts',(-38.7685081730036,-29.6367302850988,
20.));
#78295=CARTESIAN_POINT('Ctrl Pts',(-38.7865060126402,-29.6081562598384,
0.));
#78296=CARTESIAN_POINT('Ctrl Pts',(-38.7865060126402,-29.6081562598384,
20.));
#78297=CARTESIAN_POINT('Ctrl Pts',(-38.8044835592559,-29.5795707820205,
0.));
#78298=CARTESIAN_POINT('Ctrl Pts',(-38.8044835592559,-29.5795707820205,
20.));
#78299=CARTESIAN_POINT('Ctrl Pts',(-38.8224408050366,-29.5509738656807,
0.));
#78300=CARTESIAN_POINT('Ctrl Pts',(-38.8224408050366,-29.5509738656807,
20.));
#78301=CARTESIAN_POINT('Ctrl Pts',(-38.8403777421773,-29.5223655248609,
0.));
#78302=CARTESIAN_POINT('Ctrl Pts',(-38.8403777421773,-29.5223655248609,
20.));
#78303=CARTESIAN_POINT('Ctrl Pts',(-38.8582943628826,-29.4937457736083,
0.));
#78304=CARTESIAN_POINT('Ctrl Pts',(-38.8582943628826,-29.4937457736083,
20.));
#78305=CARTESIAN_POINT('Ctrl Pts',(-38.8761906593666,-29.4651146259764,
0.));
#78306=CARTESIAN_POINT('Ctrl Pts',(-38.8761906593666,-29.4651146259764,
20.));
#78307=CARTESIAN_POINT('Ctrl Pts',(-38.8940666238533,-29.4364720960241,
0.));
#78308=CARTESIAN_POINT('Ctrl Pts',(-38.8940666238533,-29.4364720960241,
20.));
#78309=CARTESIAN_POINT('Ctrl Pts',(-38.9119222485755,-29.4078181978158,
0.));
#78310=CARTESIAN_POINT('Ctrl Pts',(-38.9119222485755,-29.4078181978158,
20.));
#78311=CARTESIAN_POINT('Ctrl Pts',(-38.9297575257761,-29.3791529454216,
0.));
#78312=CARTESIAN_POINT('Ctrl Pts',(-38.9297575257761,-29.3791529454216,
20.));
#78313=CARTESIAN_POINT('Ctrl Pts',(-38.9475724477072,-29.3504763529173,
0.));
#78314=CARTESIAN_POINT('Ctrl Pts',(-38.9475724477072,-29.3504763529173,
20.));
#78315=CARTESIAN_POINT('Ctrl Pts',(-38.9653670066308,-29.3217884343845,
0.));
#78316=CARTESIAN_POINT('Ctrl Pts',(-38.9653670066308,-29.3217884343845,
20.));
#78317=CARTESIAN_POINT('Ctrl Pts',(-38.9831411948183,-29.2930892039104,
0.));
#78318=CARTESIAN_POINT('Ctrl Pts',(-38.9831411948183,-29.2930892039104,
20.));
#78319=CARTESIAN_POINT('Ctrl Pts',(-39.0008950045503,-29.2643786755883,
0.));
#78320=CARTESIAN_POINT('Ctrl Pts',(-39.0008950045503,-29.2643786755883,
20.));
#78321=CARTESIAN_POINT('Ctrl Pts',(-39.0186284281173,-29.2356568635168,
0.));
#78322=CARTESIAN_POINT('Ctrl Pts',(-39.0186284281173,-29.2356568635168,
20.));
#78323=CARTESIAN_POINT('Ctrl Pts',(-39.0363414578191,-29.2069237818005,
0.));
#78324=CARTESIAN_POINT('Ctrl Pts',(-39.0363414578191,-29.2069237818005,
20.));
#78325=CARTESIAN_POINT('Ctrl Pts',(-39.054034085965,-29.1781794445493,0.));
#78326=CARTESIAN_POINT('Ctrl Pts',(-39.054034085965,-29.1781794445493,20.));
#78327=CARTESIAN_POINT('Ctrl Pts',(-39.0717063048737,-29.1494238658788,
0.));
#78328=CARTESIAN_POINT('Ctrl Pts',(-39.0717063048737,-29.1494238658788,
20.));
#78329=CARTESIAN_POINT('Ctrl Pts',(-39.0893581068737,-29.1206570599103,
0.));
#78330=CARTESIAN_POINT('Ctrl Pts',(-39.0893581068737,-29.1206570599103,
20.));
#78331=CARTESIAN_POINT('Ctrl Pts',(-39.106989484303,-29.0918790407708,0.));
#78332=CARTESIAN_POINT('Ctrl Pts',(-39.106989484303,-29.0918790407708,20.));
#78333=CARTESIAN_POINT('Ctrl Pts',(-39.1246004295092,-29.0630898225929,
0.));
#78334=CARTESIAN_POINT('Ctrl Pts',(-39.1246004295092,-29.0630898225929,
20.));
#78335=CARTESIAN_POINT('Ctrl Pts',(-39.1421909348497,-29.034289419515,0.));
#78336=CARTESIAN_POINT('Ctrl Pts',(-39.1421909348497,-29.034289419515,20.));
#78337=CARTESIAN_POINT('Ctrl Pts',(-39.1597609926911,-29.0054778456813,
0.));
#78338=CARTESIAN_POINT('Ctrl Pts',(-39.1597609926911,-29.0054778456813,
20.));
#78339=CARTESIAN_POINT('Ctrl Pts',(-39.1773105954099,-28.9766551152413,
0.));
#78340=CARTESIAN_POINT('Ctrl Pts',(-39.1773105954099,-28.9766551152413,
20.));
#78341=CARTESIAN_POINT('Ctrl Pts',(-39.1948397353917,-28.9478212423503,
0.));
#78342=CARTESIAN_POINT('Ctrl Pts',(-39.1948397353917,-28.9478212423503,
20.));
#78343=CARTESIAN_POINT('Ctrl Pts',(-39.2123484050317,-28.9189762411689,
0.));
#78344=CARTESIAN_POINT('Ctrl Pts',(-39.2123484050317,-28.9189762411689,
20.));
#78345=CARTESIAN_POINT('Ctrl Pts',(-39.2298365967351,-28.8901201258634,
0.));
#78346=CARTESIAN_POINT('Ctrl Pts',(-39.2298365967351,-28.8901201258634,
20.));
#78347=CARTESIAN_POINT('Ctrl Pts',(-39.2473043029163,-28.8612529106058,
0.));
#78348=CARTESIAN_POINT('Ctrl Pts',(-39.2473043029163,-28.8612529106058,
20.));
#78349=CARTESIAN_POINT('Ctrl Pts',(-39.2647515159997,-28.8323746095736,
0.));
#78350=CARTESIAN_POINT('Ctrl Pts',(-39.2647515159997,-28.8323746095736,
20.));
#78351=CARTESIAN_POINT('Ctrl Pts',(-39.2821782284193,-28.80348523695,0.));
#78352=CARTESIAN_POINT('Ctrl Pts',(-39.2821782284193,-28.80348523695,20.));
#78353=CARTESIAN_POINT('Ctrl Pts',(-39.2995844326181,-28.7745848069238,
0.));
#78354=CARTESIAN_POINT('Ctrl Pts',(-39.2995844326181,-28.7745848069238,
20.));
#78355=CARTESIAN_POINT('Ctrl Pts',(-39.316970121049,-28.7456733336894,0.));
#78356=CARTESIAN_POINT('Ctrl Pts',(-39.316970121049,-28.7456733336894,20.));
#78357=CARTESIAN_POINT('Ctrl Pts',(-39.3343352861746,-28.7167508314468,
0.));
#78358=CARTESIAN_POINT('Ctrl Pts',(-39.3343352861746,-28.7167508314468,
20.));
#78359=CARTESIAN_POINT('Ctrl Pts',(-39.3516799204672,-28.6878173144015,
0.));
#78360=CARTESIAN_POINT('Ctrl Pts',(-39.3516799204672,-28.6878173144015,
20.));
#78361=CARTESIAN_POINT('Ctrl Pts',(-39.3690040164086,-28.6588727967647,
0.));
#78362=CARTESIAN_POINT('Ctrl Pts',(-39.3690040164086,-28.6588727967647,
20.));
#78363=CARTESIAN_POINT('Ctrl Pts',(-39.3863075664906,-28.6299172927529,
0.));
#78364=CARTESIAN_POINT('Ctrl Pts',(-39.3863075664906,-28.6299172927529,
20.));
#78365=CARTESIAN_POINT('Ctrl Pts',(-39.4035905632141,-28.600950816588,0.));
#78366=CARTESIAN_POINT('Ctrl Pts',(-39.4035905632141,-28.600950816588,20.));
#78367=CARTESIAN_POINT('Ctrl Pts',(-39.4208529990894,-28.5719733824975,
0.));
#78368=CARTESIAN_POINT('Ctrl Pts',(-39.4208529990894,-28.5719733824975,
20.));
#78369=CARTESIAN_POINT('Ctrl Pts',(-39.4380948666368,-28.5429850047148,
0.));
#78370=CARTESIAN_POINT('Ctrl Pts',(-39.4380948666368,-28.5429850047148,
20.));
#78371=CARTESIAN_POINT('Ctrl Pts',(-39.4553161583861,-28.5139856974786,
0.));
#78372=CARTESIAN_POINT('Ctrl Pts',(-39.4553161583861,-28.5139856974786,
20.));
#78373=CARTESIAN_POINT('Ctrl Pts',(-39.4725168668771,-28.4849754750331,
0.));
#78374=CARTESIAN_POINT('Ctrl Pts',(-39.4725168668771,-28.4849754750331,
20.));
#78375=CARTESIAN_POINT('Ctrl Pts',(-39.4896969846589,-28.455954351628,0.));
#78376=CARTESIAN_POINT('Ctrl Pts',(-39.4896969846589,-28.455954351628,20.));
#78377=CARTESIAN_POINT('Ctrl Pts',(-39.5068565042907,-28.4269223415187,
0.));
#78378=CARTESIAN_POINT('Ctrl Pts',(-39.5068565042907,-28.4269223415187,
20.));
#78379=CARTESIAN_POINT('Ctrl Pts',(-39.5239954183412,-28.3978794589661,
0.));
#78380=CARTESIAN_POINT('Ctrl Pts',(-39.5239954183412,-28.3978794589661,
20.));
#78381=CARTESIAN_POINT('Ctrl Pts',(-39.5411137193887,-28.3688257182364,
0.));
#78382=CARTESIAN_POINT('Ctrl Pts',(-39.5411137193887,-28.3688257182364,
20.));
#78383=CARTESIAN_POINT('Ctrl Pts',(-39.5582114000212,-28.3397611336014,
0.));
#78384=CARTESIAN_POINT('Ctrl Pts',(-39.5582114000212,-28.3397611336014,
20.));
#78385=CARTESIAN_POINT('Ctrl Pts',(-39.5752884528361,-28.3106857193381,
0.));
#78386=CARTESIAN_POINT('Ctrl Pts',(-39.5752884528361,-28.3106857193381,
20.));
#78387=CARTESIAN_POINT('Ctrl Pts',(-39.5923448704403,-28.2815994897291,
0.));
#78388=CARTESIAN_POINT('Ctrl Pts',(-39.5923448704403,-28.2815994897291,
20.));
#78389=CARTESIAN_POINT('Ctrl Pts',(-39.6093806454502,-28.2525024590626,
0.));
#78390=CARTESIAN_POINT('Ctrl Pts',(-39.6093806454502,-28.2525024590626,
20.));
#78391=CARTESIAN_POINT('Ctrl Pts',(-39.6263957704923,-28.2233946416323,
0.));
#78392=CARTESIAN_POINT('Ctrl Pts',(-39.6263957704923,-28.2233946416323,
20.));
#78393=CARTESIAN_POINT('Ctrl Pts',(-39.6433902382029,-28.1942760517371,
0.));
#78394=CARTESIAN_POINT('Ctrl Pts',(-39.6433902382029,-28.1942760517371,
20.));
#78395=CARTESIAN_POINT('Ctrl Pts',(-39.6603640412281,-28.1651467036817,
0.));
#78396=CARTESIAN_POINT('Ctrl Pts',(-39.6603640412281,-28.1651467036817,
20.));
#78397=CARTESIAN_POINT('Ctrl Pts',(-39.6773171722241,-28.136006611776,0.));
#78398=CARTESIAN_POINT('Ctrl Pts',(-39.6773171722241,-28.136006611776,20.));
#78399=CARTESIAN_POINT('Ctrl Pts',(-39.6942496238565,-28.1068557903356,
0.));
#78400=CARTESIAN_POINT('Ctrl Pts',(-39.6942496238565,-28.1068557903356,
20.));
#78401=CARTESIAN_POINT('Ctrl Pts',(-39.7111613888006,-28.0776942536814,
0.));
#78402=CARTESIAN_POINT('Ctrl Pts',(-39.7111613888006,-28.0776942536814,
20.));
#78403=CARTESIAN_POINT('Ctrl Pts',(-39.728052459741,-28.0485220161395,0.));
#78404=CARTESIAN_POINT('Ctrl Pts',(-39.728052459741,-28.0485220161395,20.));
#78405=CARTESIAN_POINT('Ctrl Pts',(-39.7449228293718,-28.0193390920415,
0.));
#78406=CARTESIAN_POINT('Ctrl Pts',(-39.7449228293718,-28.0193390920415,
20.));
#78407=CARTESIAN_POINT('Ctrl Pts',(-39.7617724903968,-27.9901454957246,
0.));
#78408=CARTESIAN_POINT('Ctrl Pts',(-39.7617724903968,-27.9901454957246,
20.));
#78409=CARTESIAN_POINT('Ctrl Pts',(-39.7786014355293,-27.960941241531,0.));
#78410=CARTESIAN_POINT('Ctrl Pts',(-39.7786014355293,-27.960941241531,20.));
#78411=CARTESIAN_POINT('Ctrl Pts',(-39.795409657493,-27.9317263438086,0.));
#78412=CARTESIAN_POINT('Ctrl Pts',(-39.795409657493,-27.9317263438086,20.));
#78413=CARTESIAN_POINT('Ctrl Pts',(-39.8121971490214,-27.9025008169107,
0.));
#78414=CARTESIAN_POINT('Ctrl Pts',(-39.8121971490214,-27.9025008169107,
20.));
#78415=CARTESIAN_POINT('Ctrl Pts',(-39.828963902858,-27.8732646751959,0.));
#78416=CARTESIAN_POINT('Ctrl Pts',(-39.828963902858,-27.8732646751959,20.));
#78417=CARTESIAN_POINT('Ctrl Pts',(-39.845709911756,-27.8440179330284,0.));
#78418=CARTESIAN_POINT('Ctrl Pts',(-39.845709911756,-27.8440179330284,20.));
#78419=CARTESIAN_POINT('Ctrl Pts',(-39.8624351684781,-27.8147606047778,
0.));
#78420=CARTESIAN_POINT('Ctrl Pts',(-39.8624351684781,-27.8147606047778,
20.));
#78421=CARTESIAN_POINT('Ctrl Pts',(-39.8791396657966,-27.785492704819,0.));
#78422=CARTESIAN_POINT('Ctrl Pts',(-39.8791396657966,-27.785492704819,20.));
#78423=CARTESIAN_POINT('Ctrl Pts',(-39.8958233964934,-27.7562142475319,
0.));
#78424=CARTESIAN_POINT('Ctrl Pts',(-39.8958233964934,-27.7562142475319,
20.));
#78425=CARTESIAN_POINT('Ctrl Pts',(-39.9124863533599,-27.726925247302,0.));
#78426=CARTESIAN_POINT('Ctrl Pts',(-39.9124863533599,-27.726925247302,20.));
#78427=CARTESIAN_POINT('Ctrl Pts',(-39.9291285291975,-27.6976257185198,
0.));
#78428=CARTESIAN_POINT('Ctrl Pts',(-39.9291285291975,-27.6976257185198,
20.));
#78429=CARTESIAN_POINT('Ctrl Pts',(-39.9457499168175,-27.6683156755815,
0.));
#78430=CARTESIAN_POINT('Ctrl Pts',(-39.9457499168175,-27.6683156755815,
20.));
#78431=CARTESIAN_POINT('Ctrl Pts',(-39.9623505090412,-27.6389951328887,
0.));
#78432=CARTESIAN_POINT('Ctrl Pts',(-39.9623505090412,-27.6389951328887,
20.));
#78433=CARTESIAN_POINT('Ctrl Pts',(-39.9789302986995,-27.6096641048483,
0.));
#78434=CARTESIAN_POINT('Ctrl Pts',(-39.9789302986995,-27.6096641048483,
20.));
#78435=CARTESIAN_POINT('Ctrl Pts',(-39.9954892786331,-27.5803226058724,
0.));
#78436=CARTESIAN_POINT('Ctrl Pts',(-39.9954892786331,-27.5803226058724,
20.));
#78437=CARTESIAN_POINT('Ctrl Pts',(-40.0120274416924,-27.5509706503786,
0.));
#78438=CARTESIAN_POINT('Ctrl Pts',(-40.0120274416924,-27.5509706503786,
20.));
#78439=CARTESIAN_POINT('Ctrl Pts',(-40.0285447807378,-27.5216082527897,
0.));
#78440=CARTESIAN_POINT('Ctrl Pts',(-40.0285447807378,-27.5216082527897,
20.));
#78441=CARTESIAN_POINT('Ctrl Pts',(-40.045041288639,-27.4922354275335,0.));
#78442=CARTESIAN_POINT('Ctrl Pts',(-40.045041288639,-27.4922354275335,20.));
#78443=CARTESIAN_POINT('Ctrl Pts',(-40.0615169582759,-27.4628521890436,
0.));
#78444=CARTESIAN_POINT('Ctrl Pts',(-40.0615169582759,-27.4628521890436,
20.));
#78445=CARTESIAN_POINT('Ctrl Pts',(-40.077971782538,-27.4334585517582,0.));
#78446=CARTESIAN_POINT('Ctrl Pts',(-40.077971782538,-27.4334585517582,20.));
#78447=CARTESIAN_POINT('Ctrl Pts',(-40.0944057543248,-27.4040545301216,
0.));
#78448=CARTESIAN_POINT('Ctrl Pts',(-40.0944057543248,-27.4040545301216,
20.));
#78449=CARTESIAN_POINT('Ctrl Pts',(-40.1108188665452,-27.374640138583,0.));
#78450=CARTESIAN_POINT('Ctrl Pts',(-40.1108188665452,-27.374640138583,20.));
#78451=CARTESIAN_POINT('Ctrl Pts',(-40.1272111121183,-27.3452153915969,
0.));
#78452=CARTESIAN_POINT('Ctrl Pts',(-40.1272111121183,-27.3452153915969,
20.));
#78453=CARTESIAN_POINT('Ctrl Pts',(-40.1435824839731,-27.3157803036231,
0.));
#78454=CARTESIAN_POINT('Ctrl Pts',(-40.1435824839731,-27.3157803036231,
20.));
#78455=CARTESIAN_POINT('Ctrl Pts',(-40.1599329750483,-27.2863348891265,
0.));
#78456=CARTESIAN_POINT('Ctrl Pts',(-40.1599329750483,-27.2863348891265,
20.));
#78457=CARTESIAN_POINT('Ctrl Pts',(-40.1762625782924,-27.2568791625774,
0.));
#78458=CARTESIAN_POINT('Ctrl Pts',(-40.1762625782924,-27.2568791625774,
20.));
#78459=CARTESIAN_POINT('Ctrl Pts',(-40.1925712866631,-27.2274131384508,
0.));
#78460=CARTESIAN_POINT('Ctrl Pts',(-40.1925712866631,-27.2274131384508,
20.));
#78461=CARTESIAN_POINT('Ctrl Pts',(-40.2088590931287,-27.1979368312277,
0.));
#78462=CARTESIAN_POINT('Ctrl Pts',(-40.2088590931287,-27.1979368312277,
20.));
#78463=CARTESIAN_POINT('Ctrl Pts',(-40.225125990667,-27.1684502553939,0.));
#78464=CARTESIAN_POINT('Ctrl Pts',(-40.225125990667,-27.1684502553939,20.));
#78465=CARTESIAN_POINT('Ctrl Pts',(-40.2413719722657,-27.1389534254409,
0.));
#78466=CARTESIAN_POINT('Ctrl Pts',(-40.2413719722657,-27.1389534254409,
20.));
#78467=CARTESIAN_POINT('Ctrl Pts',(-40.2575970309226,-27.1094463558649,
0.));
#78468=CARTESIAN_POINT('Ctrl Pts',(-40.2575970309226,-27.1094463558649,
20.));
#78469=CARTESIAN_POINT('Ctrl Pts',(-40.2738011596454,-27.0799290611676,
0.));
#78470=CARTESIAN_POINT('Ctrl Pts',(-40.2738011596454,-27.0799290611676,
20.));
#78471=CARTESIAN_POINT('Ctrl Pts',(-40.2899843514517,-27.0504015558557,
0.));
#78472=CARTESIAN_POINT('Ctrl Pts',(-40.2899843514517,-27.0504015558557,
20.));
#78473=CARTESIAN_POINT('Ctrl Pts',(-40.3061465993685,-27.0208638544413,
0.));
#78474=CARTESIAN_POINT('Ctrl Pts',(-40.3061465993685,-27.0208638544413,
20.));
#78475=CARTESIAN_POINT('Ctrl Pts',(-40.3222878964329,-26.9913159714415,
0.));
#78476=CARTESIAN_POINT('Ctrl Pts',(-40.3222878964329,-26.9913159714415,
20.));
#78477=CARTESIAN_POINT('Ctrl Pts',(-40.3384082356913,-26.9617579213786,
0.));
#78478=CARTESIAN_POINT('Ctrl Pts',(-40.3384082356913,-26.9617579213786,
20.));
#78479=CARTESIAN_POINT('Ctrl Pts',(-40.3545076102003,-26.9321897187802,
0.));
#78480=CARTESIAN_POINT('Ctrl Pts',(-40.3545076102003,-26.9321897187802,
20.));
#78481=CARTESIAN_POINT('Ctrl Pts',(-40.3705860130263,-26.9026113781788,
0.));
#78482=CARTESIAN_POINT('Ctrl Pts',(-40.3705860130263,-26.9026113781788,
20.));
#78483=CARTESIAN_POINT('Ctrl Pts',(-40.386643437246,-26.8730229141124,0.));
#78484=CARTESIAN_POINT('Ctrl Pts',(-40.386643437246,-26.8730229141124,20.));
#78485=CARTESIAN_POINT('Ctrl Pts',(-40.4026798759458,-26.8434243411241,
0.));
#78486=CARTESIAN_POINT('Ctrl Pts',(-40.4026798759458,-26.8434243411241,
20.));
#78487=CARTESIAN_POINT('Ctrl Pts',(-40.4186953222224,-26.8138156737619,
0.));
#78488=CARTESIAN_POINT('Ctrl Pts',(-40.4186953222224,-26.8138156737619,
20.));
#78489=CARTESIAN_POINT('Ctrl Pts',(-40.4346897691821,-26.7841969265794,
0.));
#78490=CARTESIAN_POINT('Ctrl Pts',(-40.4346897691821,-26.7841969265794,
20.));
#78491=CARTESIAN_POINT('Ctrl Pts',(-40.4506632099408,-26.754568114135,0.));
#78492=CARTESIAN_POINT('Ctrl Pts',(-40.4506632099408,-26.754568114135,20.));
#78493=CARTESIAN_POINT('Ctrl Pts',(-40.4666156376241,-26.7249292509923,
0.));
#78494=CARTESIAN_POINT('Ctrl Pts',(-40.4666156376241,-26.7249292509923,
20.));
#78495=CARTESIAN_POINT('Ctrl Pts',(-40.4825470453679,-26.6952803517197,
0.));
#78496=CARTESIAN_POINT('Ctrl Pts',(-40.4825470453679,-26.6952803517197,
20.));
#78497=CARTESIAN_POINT('Ctrl Pts',(-40.4984574263178,-26.6656214308914,
0.));
#78498=CARTESIAN_POINT('Ctrl Pts',(-40.4984574263178,-26.6656214308914,
20.));
#78499=CARTESIAN_POINT('Ctrl Pts',(-40.5143467736295,-26.6359525030862,
0.));
#78500=CARTESIAN_POINT('Ctrl Pts',(-40.5143467736295,-26.6359525030862,
20.));
#78501=CARTESIAN_POINT('Ctrl Pts',(-40.5302150804687,-26.606273582888,0.));
#78502=CARTESIAN_POINT('Ctrl Pts',(-40.5302150804687,-26.606273582888,20.));
#78503=CARTESIAN_POINT('Ctrl Pts',(-40.546062340011,-26.5765846848862,0.));
#78504=CARTESIAN_POINT('Ctrl Pts',(-40.546062340011,-26.5765846848862,20.));
#78505=CARTESIAN_POINT('Ctrl Pts',(-40.5618885454414,-26.5468858236748,
0.));
#78506=CARTESIAN_POINT('Ctrl Pts',(-40.5618885454414,-26.5468858236748,
20.));
#78507=CARTESIAN_POINT('Ctrl Pts',(-40.5776936899555,-26.5171770138532,
0.));
#78508=CARTESIAN_POINT('Ctrl Pts',(-40.5776936899555,-26.5171770138532,
20.));
#78509=CARTESIAN_POINT('Ctrl Pts',(-40.5934777667583,-26.4874582700259,
0.));
#78510=CARTESIAN_POINT('Ctrl Pts',(-40.5934777667583,-26.4874582700259,
20.));
#78511=CARTESIAN_POINT('Ctrl Pts',(-40.6092407690651,-26.4577296068023,
0.));
#78512=CARTESIAN_POINT('Ctrl Pts',(-40.6092407690651,-26.4577296068023,
20.));
#78513=CARTESIAN_POINT('Ctrl Pts',(-40.6249826901011,-26.427991038797,0.));
#78514=CARTESIAN_POINT('Ctrl Pts',(-40.6249826901011,-26.427991038797,20.));
#78515=CARTESIAN_POINT('Ctrl Pts',(-40.6407035231015,-26.3982425806297,
0.));
#78516=CARTESIAN_POINT('Ctrl Pts',(-40.6407035231015,-26.3982425806297,
20.));
#78517=CARTESIAN_POINT('Ctrl Pts',(-40.6564032613109,-26.3684842469248,
0.));
#78518=CARTESIAN_POINT('Ctrl Pts',(-40.6564032613109,-26.3684842469248,
20.));
#78519=CARTESIAN_POINT('Ctrl Pts',(-40.6720818979844,-26.338716052312,0.));
#78520=CARTESIAN_POINT('Ctrl Pts',(-40.6720818979844,-26.338716052312,20.));
#78521=CARTESIAN_POINT('Ctrl Pts',(-40.6877394263869,-26.308938011426,0.));
#78522=CARTESIAN_POINT('Ctrl Pts',(-40.6877394263869,-26.308938011426,20.));
#78523=CARTESIAN_POINT('Ctrl Pts',(-40.7033758397932,-26.2791501389067,
0.));
#78524=CARTESIAN_POINT('Ctrl Pts',(-40.7033758397932,-26.2791501389067,
20.));
#78525=CARTESIAN_POINT('Ctrl Pts',(-40.7189911314882,-26.2493524493989,
0.));
#78526=CARTESIAN_POINT('Ctrl Pts',(-40.7189911314882,-26.2493524493989,
20.));
#78527=CARTESIAN_POINT('Ctrl Pts',(-40.7345852947664,-26.2195449575524,
0.));
#78528=CARTESIAN_POINT('Ctrl Pts',(-40.7345852947664,-26.2195449575524,
20.));
#78529=CARTESIAN_POINT('Ctrl Pts',(-40.7501583229328,-26.1897276780219,
0.));
#78530=CARTESIAN_POINT('Ctrl Pts',(-40.7501583229328,-26.1897276780219,
20.));
#78531=CARTESIAN_POINT('Ctrl Pts',(-40.7657102093021,-26.1599006254674,
0.));
#78532=CARTESIAN_POINT('Ctrl Pts',(-40.7657102093021,-26.1599006254674,
20.));
#78533=CARTESIAN_POINT('Ctrl Pts',(-40.7812409471992,-26.1300638145535,
0.));
#78534=CARTESIAN_POINT('Ctrl Pts',(-40.7812409471992,-26.1300638145535,
20.));
#78535=CARTESIAN_POINT('Ctrl Pts',(-40.7967505299588,-26.1002172599501,
0.));
#78536=CARTESIAN_POINT('Ctrl Pts',(-40.7967505299588,-26.1002172599501,
20.));
#78537=CARTESIAN_POINT('Ctrl Pts',(-40.8122389509256,-26.0703609763318,
0.));
#78538=CARTESIAN_POINT('Ctrl Pts',(-40.8122389509256,-26.0703609763318,
20.));
#78539=CARTESIAN_POINT('Ctrl Pts',(-40.8277062034539,-26.0404949783787,
0.));
#78540=CARTESIAN_POINT('Ctrl Pts',(-40.8277062034539,-26.0404949783787,
20.));
#78541=CARTESIAN_POINT('Ctrl Pts',(-40.843152280908,-26.0106192807756,0.));
#78542=CARTESIAN_POINT('Ctrl Pts',(-40.843152280908,-26.0106192807756,20.));
#78543=CARTESIAN_POINT('Ctrl Pts',(-40.8585771766627,-25.9807338982121,
0.));
#78544=CARTESIAN_POINT('Ctrl Pts',(-40.8585771766627,-25.9807338982121,
20.));
#78545=CARTESIAN_POINT('Ctrl Pts',(-40.8739808841024,-25.950838845383,0.));
#78546=CARTESIAN_POINT('Ctrl Pts',(-40.8739808841024,-25.950838845383,20.));
#78547=CARTESIAN_POINT('Ctrl Pts',(-40.8893633966224,-25.9209341369879,
0.));
#78548=CARTESIAN_POINT('Ctrl Pts',(-40.8893633966224,-25.9209341369879,
20.));
#78549=CARTESIAN_POINT('Ctrl Pts',(-40.9047247076274,-25.891019787731,0.));
#78550=CARTESIAN_POINT('Ctrl Pts',(-40.9047247076274,-25.891019787731,20.));
#78551=CARTESIAN_POINT('Ctrl Pts',(-40.9200648105322,-25.861095812322,0.));
#78552=CARTESIAN_POINT('Ctrl Pts',(-40.9200648105322,-25.861095812322,20.));
#78553=CARTESIAN_POINT('Ctrl Pts',(-40.9353836987613,-25.8311622254754,
0.));
#78554=CARTESIAN_POINT('Ctrl Pts',(-40.9353836987613,-25.8311622254754,
20.));
#78555=CARTESIAN_POINT('Ctrl Pts',(-40.9506813657491,-25.8012190419102,
0.));
#78556=CARTESIAN_POINT('Ctrl Pts',(-40.9506813657491,-25.8012190419102,
20.));
#78557=CARTESIAN_POINT('Ctrl Pts',(-40.9659578049399,-25.7712662763511,
0.));
#78558=CARTESIAN_POINT('Ctrl Pts',(-40.9659578049399,-25.7712662763511,
20.));
#78559=CARTESIAN_POINT('Ctrl Pts',(-40.981213009789,-25.7413039435271,0.));
#78560=CARTESIAN_POINT('Ctrl Pts',(-40.981213009789,-25.7413039435271,20.));
#78561=CARTESIAN_POINT('Ctrl Pts',(-40.9964469737613,-25.7113320581728,
0.));
#78562=CARTESIAN_POINT('Ctrl Pts',(-40.9964469737613,-25.7113320581728,
20.));
#78563=CARTESIAN_POINT('Ctrl Pts',(-41.0116596903317,-25.6813506350271,
0.));
#78564=CARTESIAN_POINT('Ctrl Pts',(-41.0116596903317,-25.6813506350271,
20.));
#78565=CARTESIAN_POINT('Ctrl Pts',(-41.0268511529852,-25.6513596888338,
0.));
#78566=CARTESIAN_POINT('Ctrl Pts',(-41.0268511529852,-25.6513596888338,
20.));
#78567=CARTESIAN_POINT('Ctrl Pts',(-41.0420213552163,-25.6213592343415,
0.));
#78568=CARTESIAN_POINT('Ctrl Pts',(-41.0420213552163,-25.6213592343415,
20.));
#78569=CARTESIAN_POINT('Ctrl Pts',(-41.05717029053,-25.5913492863038,0.));
#78570=CARTESIAN_POINT('Ctrl Pts',(-41.05717029053,-25.5913492863038,20.));
#78571=CARTESIAN_POINT('Ctrl Pts',(-41.072297952441,-25.5613298594791,0.));
#78572=CARTESIAN_POINT('Ctrl Pts',(-41.072297952441,-25.5613298594791,20.));
#78573=CARTESIAN_POINT('Ctrl Pts',(-41.0874043344745,-25.5313009686309,
0.));
#78574=CARTESIAN_POINT('Ctrl Pts',(-41.0874043344745,-25.5313009686309,
20.));
#78575=CARTESIAN_POINT('Ctrl Pts',(-41.1024894301655,-25.5012626285275,
0.));
#78576=CARTESIAN_POINT('Ctrl Pts',(-41.1024894301655,-25.5012626285275,
20.));
#78577=CARTESIAN_POINT('Ctrl Pts',(-41.1175532330596,-25.4712148539422,
0.));
#78578=CARTESIAN_POINT('Ctrl Pts',(-41.1175532330596,-25.4712148539422,
20.));
#78579=CARTESIAN_POINT('Ctrl Pts',(-41.132595736712,-25.4411576596529,0.));
#78580=CARTESIAN_POINT('Ctrl Pts',(-41.132595736712,-25.4411576596529,20.));
#78581=CARTESIAN_POINT('Ctrl Pts',(-41.1476169346881,-25.4110910604425,
0.));
#78582=CARTESIAN_POINT('Ctrl Pts',(-41.1476169346881,-25.4110910604425,
20.));
#78583=CARTESIAN_POINT('Ctrl Pts',(-41.1626168205634,-25.3810150710984,
0.));
#78584=CARTESIAN_POINT('Ctrl Pts',(-41.1626168205634,-25.3810150710984,
20.));
#78585=CARTESIAN_POINT('Ctrl Pts',(-41.1775953879232,-25.3509297064131,
0.));
#78586=CARTESIAN_POINT('Ctrl Pts',(-41.1775953879232,-25.3509297064131,
20.));
#78587=CARTESIAN_POINT('Ctrl Pts',(-41.1925526303629,-25.3208349811839,
0.));
#78588=CARTESIAN_POINT('Ctrl Pts',(-41.1925526303629,-25.3208349811839,
20.));
#78589=CARTESIAN_POINT('Ctrl Pts',(-41.2074885414881,-25.2907309102128,
0.));
#78590=CARTESIAN_POINT('Ctrl Pts',(-41.2074885414881,-25.2907309102128,
20.));
#78591=CARTESIAN_POINT('Ctrl Pts',(-41.2224031149147,-25.2606175083067,
0.));
#78592=CARTESIAN_POINT('Ctrl Pts',(-41.2224031149147,-25.2606175083067,
20.));
#78593=CARTESIAN_POINT('Ctrl Pts',(-41.2372963442684,-25.2304947902774,
0.));
#78594=CARTESIAN_POINT('Ctrl Pts',(-41.2372963442684,-25.2304947902774,
20.));
#78595=CARTESIAN_POINT('Ctrl Pts',(-41.2521682231854,-25.2003627709414,
0.));
#78596=CARTESIAN_POINT('Ctrl Pts',(-41.2521682231854,-25.2003627709414,
20.));
#78597=CARTESIAN_POINT('Ctrl Pts',(-41.2670187453114,-25.1702214651198,
0.));
#78598=CARTESIAN_POINT('Ctrl Pts',(-41.2670187453114,-25.1702214651198,
20.));
#78599=CARTESIAN_POINT('Ctrl Pts',(-41.2818479043026,-25.1400708876386,
0.));
#78600=CARTESIAN_POINT('Ctrl Pts',(-41.2818479043026,-25.1400708876386,
20.));
#78601=CARTESIAN_POINT('Ctrl Pts',(-41.2966556938255,-25.1099110533288,
0.));
#78602=CARTESIAN_POINT('Ctrl Pts',(-41.2966556938255,-25.1099110533288,
20.));
#78603=CARTESIAN_POINT('Ctrl Pts',(-41.3114421075567,-25.0797419770258,
0.));
#78604=CARTESIAN_POINT('Ctrl Pts',(-41.3114421075567,-25.0797419770258,
20.));
#78605=CARTESIAN_POINT('Ctrl Pts',(-41.3262071391823,-25.0495636735701,
0.));
#78606=CARTESIAN_POINT('Ctrl Pts',(-41.3262071391823,-25.0495636735701,
20.));
#78607=CARTESIAN_POINT('Ctrl Pts',(-41.3409507823989,-25.0193761578067,
0.));
#78608=CARTESIAN_POINT('Ctrl Pts',(-41.3409507823989,-25.0193761578067,
20.));
#78609=CARTESIAN_POINT('Ctrl Pts',(-41.3556730309131,-24.9891794445855,
0.));
#78610=CARTESIAN_POINT('Ctrl Pts',(-41.3556730309131,-24.9891794445855,
20.));
#78611=CARTESIAN_POINT('Ctrl Pts',(-41.3703738784418,-24.9589735487609,
0.));
#78612=CARTESIAN_POINT('Ctrl Pts',(-41.3703738784418,-24.9589735487609,
20.));
#78613=CARTESIAN_POINT('Ctrl Pts',(-41.3850533187123,-24.9287584851923,
0.));
#78614=CARTESIAN_POINT('Ctrl Pts',(-41.3850533187123,-24.9287584851923,
20.));
#78615=CARTESIAN_POINT('Ctrl Pts',(-41.3997113454618,-24.8985342687436,
0.));
#78616=CARTESIAN_POINT('Ctrl Pts',(-41.3997113454618,-24.8985342687436,
20.));
#78617=CARTESIAN_POINT('Ctrl Pts',(-41.4143479524375,-24.8683009142837,
0.));
#78618=CARTESIAN_POINT('Ctrl Pts',(-41.4143479524375,-24.8683009142837,
20.));
#78619=CARTESIAN_POINT('Ctrl Pts',(-41.4289631333969,-24.8380584366858,
0.));
#78620=CARTESIAN_POINT('Ctrl Pts',(-41.4289631333969,-24.8380584366858,
20.));
#78621=CARTESIAN_POINT('Ctrl Pts',(-41.4435568821071,-24.8078068508284,
0.));
#78622=CARTESIAN_POINT('Ctrl Pts',(-41.4435568821071,-24.8078068508284,
20.));
#78623=CARTESIAN_POINT('Ctrl Pts',(-41.4581291923457,-24.7775461715943,
0.));
#78624=CARTESIAN_POINT('Ctrl Pts',(-41.4581291923457,-24.7775461715943,
20.));
#78625=CARTESIAN_POINT('Ctrl Pts',(-41.4726800579006,-24.7472764138709,
0.));
#78626=CARTESIAN_POINT('Ctrl Pts',(-41.4726800579006,-24.7472764138709,
20.));
#78627=CARTESIAN_POINT('Ctrl Pts',(-41.4872094725702,-24.7169975925505,
0.));
#78628=CARTESIAN_POINT('Ctrl Pts',(-41.4872094725702,-24.7169975925505,
20.));
#78629=CARTESIAN_POINT('Ctrl Pts',(-41.5017174301628,-24.68670972253,0.));
#78630=CARTESIAN_POINT('Ctrl Pts',(-41.5017174301628,-24.68670972253,20.));
#78631=CARTESIAN_POINT('Ctrl Pts',(-41.516203924497,-24.6564128187107,0.));
#78632=CARTESIAN_POINT('Ctrl Pts',(-41.516203924497,-24.6564128187107,20.));
#78633=CARTESIAN_POINT('Ctrl Pts',(-41.5306689494012,-24.626106895999,0.));
#78634=CARTESIAN_POINT('Ctrl Pts',(-41.5306689494012,-24.626106895999,20.));
#78635=CARTESIAN_POINT('Ctrl Pts',(-41.545112498714,-24.5957919693057,0.));
#78636=CARTESIAN_POINT('Ctrl Pts',(-41.545112498714,-24.5957919693057,20.));
#78637=CARTESIAN_POINT('Ctrl Pts',(-41.5595345662842,-24.5654680535465,
0.));
#78638=CARTESIAN_POINT('Ctrl Pts',(-41.5595345662842,-24.5654680535465,
20.));
#78639=CARTESIAN_POINT('Ctrl Pts',(-41.5739351459709,-24.5351351636416,
0.));
#78640=CARTESIAN_POINT('Ctrl Pts',(-41.5739351459709,-24.5351351636416,
20.));
#78641=CARTESIAN_POINT('Ctrl Pts',(-41.5883142316433,-24.5047933145158,
0.));
#78642=CARTESIAN_POINT('Ctrl Pts',(-41.5883142316433,-24.5047933145158,
20.));
#78643=CARTESIAN_POINT('Ctrl Pts',(-41.6026718171809,-24.4744425210985,
0.));
#78644=CARTESIAN_POINT('Ctrl Pts',(-41.6026718171809,-24.4744425210985,
20.));
#78645=CARTESIAN_POINT('Ctrl Pts',(-41.6170078964732,-24.4440827983238,
0.));
#78646=CARTESIAN_POINT('Ctrl Pts',(-41.6170078964732,-24.4440827983238,
20.));
#78647=CARTESIAN_POINT('Ctrl Pts',(-41.6313224634201,-24.4137141611302,
0.));
#78648=CARTESIAN_POINT('Ctrl Pts',(-41.6313224634201,-24.4137141611302,
20.));
#78649=CARTESIAN_POINT('Ctrl Pts',(-41.6456155119319,-24.3833366244611,
0.));
#78650=CARTESIAN_POINT('Ctrl Pts',(-41.6456155119319,-24.3833366244611,
20.));
#78651=CARTESIAN_POINT('Ctrl Pts',(-41.6598870359289,-24.3529502032644,
0.));
#78652=CARTESIAN_POINT('Ctrl Pts',(-41.6598870359289,-24.3529502032644,
20.));
#78653=CARTESIAN_POINT('Ctrl Pts',(-41.6741370293416,-24.3225549124927,
0.));
#78654=CARTESIAN_POINT('Ctrl Pts',(-41.6741370293416,-24.3225549124927,
20.));
#78655=CARTESIAN_POINT('Ctrl Pts',(-41.6883654861106,-24.2921507671029,
0.));
#78656=CARTESIAN_POINT('Ctrl Pts',(-41.6883654861106,-24.2921507671029,
20.));
#78657=CARTESIAN_POINT('Ctrl Pts',(-41.7025724001866,-24.2617377820568,
0.));
#78658=CARTESIAN_POINT('Ctrl Pts',(-41.7025724001866,-24.2617377820568,
20.));
#78659=CARTESIAN_POINT('Ctrl Pts',(-41.7167577655309,-24.2313159723205,
0.));
#78660=CARTESIAN_POINT('Ctrl Pts',(-41.7167577655309,-24.2313159723205,
20.));
#78661=CARTESIAN_POINT('Ctrl Pts',(-41.7309215761147,-24.2008853528648,
0.));
#78662=CARTESIAN_POINT('Ctrl Pts',(-41.7309215761147,-24.2008853528648,
20.));
#78663=CARTESIAN_POINT('Ctrl Pts',(-41.7450638259196,-24.1704459386651,
0.));
#78664=CARTESIAN_POINT('Ctrl Pts',(-41.7450638259196,-24.1704459386651,
20.));
#78665=CARTESIAN_POINT('Ctrl Pts',(-41.7591845089374,-24.1399977447013,
0.));
#78666=CARTESIAN_POINT('Ctrl Pts',(-41.7591845089374,-24.1399977447013,
20.));
#78667=CARTESIAN_POINT('Ctrl Pts',(-41.7732836191701,-24.1095407859578,
0.));
#78668=CARTESIAN_POINT('Ctrl Pts',(-41.7732836191701,-24.1095407859578,
20.));
#78669=CARTESIAN_POINT('Ctrl Pts',(-41.78736115063,-24.0790750774236,0.));
#78670=CARTESIAN_POINT('Ctrl Pts',(-41.78736115063,-24.0790750774236,20.));
#78671=CARTESIAN_POINT('Ctrl Pts',(-41.8014170973399,-24.0486006340924,
0.));
#78672=CARTESIAN_POINT('Ctrl Pts',(-41.8014170973399,-24.0486006340924,
20.));
#78673=CARTESIAN_POINT('Ctrl Pts',(-41.8154514533324,-24.0181174709622,
0.));
#78674=CARTESIAN_POINT('Ctrl Pts',(-41.8154514533324,-24.0181174709622,
20.));
#78675=CARTESIAN_POINT('Ctrl Pts',(-41.8294642126506,-23.9876256030355,
0.));
#78676=CARTESIAN_POINT('Ctrl Pts',(-41.8294642126506,-23.9876256030355,
20.));
#78677=CARTESIAN_POINT('Ctrl Pts',(-41.8434553693478,-23.9571250453194,
0.));
#78678=CARTESIAN_POINT('Ctrl Pts',(-41.8434553693478,-23.9571250453194,
20.));
#78679=CARTESIAN_POINT('Ctrl Pts',(-41.8574249174873,-23.9266158128252,
0.));
#78680=CARTESIAN_POINT('Ctrl Pts',(-41.8574249174873,-23.9266158128252,
20.));
#78681=CARTESIAN_POINT('Ctrl Pts',(-41.8713728511429,-23.8960979205694,
0.));
#78682=CARTESIAN_POINT('Ctrl Pts',(-41.8713728511429,-23.8960979205694,
20.));
#78683=CARTESIAN_POINT('Ctrl Pts',(-41.8852991643986,-23.8655713835725,
0.));
#78684=CARTESIAN_POINT('Ctrl Pts',(-41.8852991643986,-23.8655713835725,
20.));
#78685=CARTESIAN_POINT('Ctrl Pts',(-41.8992038513488,-23.8350362168598,
0.));
#78686=CARTESIAN_POINT('Ctrl Pts',(-41.8992038513488,-23.8350362168598,
20.));
#78687=CARTESIAN_POINT('Ctrl Pts',(-41.9130869060982,-23.8044924354607,
0.));
#78688=CARTESIAN_POINT('Ctrl Pts',(-41.9130869060982,-23.8044924354607,
20.));
#78689=CARTESIAN_POINT('Ctrl Pts',(-41.9269483227618,-23.7739400544092,
0.));
#78690=CARTESIAN_POINT('Ctrl Pts',(-41.9269483227618,-23.7739400544092,
20.));
#78691=CARTESIAN_POINT('Ctrl Pts',(-41.9407880954647,-23.7433790887435,
0.));
#78692=CARTESIAN_POINT('Ctrl Pts',(-41.9407880954647,-23.7433790887435,
20.));
#78693=CARTESIAN_POINT('Ctrl Pts',(-41.9546062183422,-23.7128095535066,
0.));
#78694=CARTESIAN_POINT('Ctrl Pts',(-41.9546062183422,-23.7128095535066,
20.));
#78695=CARTESIAN_POINT('Ctrl Pts',(-41.9684026855399,-23.6822314637457,
0.));
#78696=CARTESIAN_POINT('Ctrl Pts',(-41.9684026855399,-23.6822314637457,
20.));
#78697=CARTESIAN_POINT('Ctrl Pts',(-41.9821774912142,-23.651644834513,0.));
#78698=CARTESIAN_POINT('Ctrl Pts',(-41.9821774912142,-23.651644834513,20.));
#78699=CARTESIAN_POINT('Ctrl Pts',(-41.9959306295311,-23.6210496808648,
0.));
#78700=CARTESIAN_POINT('Ctrl Pts',(-41.9959306295311,-23.6210496808648,
20.));
#78701=CARTESIAN_POINT('Ctrl Pts',(-42.0096620946675,-23.5904460178619,
0.));
#78702=CARTESIAN_POINT('Ctrl Pts',(-42.0096620946675,-23.5904460178619,
20.));
#78703=CARTESIAN_POINT('Ctrl Pts',(-42.02337188081,-23.5598338605694,0.));
#78704=CARTESIAN_POINT('Ctrl Pts',(-42.02337188081,-23.5598338605694,20.));
#78705=CARTESIAN_POINT('Ctrl Pts',(-42.0370599821558,-23.5292132240566,
0.));
#78706=CARTESIAN_POINT('Ctrl Pts',(-42.0370599821558,-23.5292132240566,
20.));
#78707=CARTESIAN_POINT('Ctrl Pts',(-42.0507263929126,-23.4985841233977,
0.));
#78708=CARTESIAN_POINT('Ctrl Pts',(-42.0507263929126,-23.4985841233977,
20.));
#78709=CARTESIAN_POINT('Ctrl Pts',(-42.0643711072981,-23.4679465736707,
0.));
#78710=CARTESIAN_POINT('Ctrl Pts',(-42.0643711072981,-23.4679465736707,
20.));
#78711=CARTESIAN_POINT('Ctrl Pts',(-42.0779941195407,-23.4373005899585,
0.));
#78712=CARTESIAN_POINT('Ctrl Pts',(-42.0779941195407,-23.4373005899585,
20.));
#78713=CARTESIAN_POINT('Ctrl Pts',(-42.0915954238788,-23.4066461873484,
0.));
#78714=CARTESIAN_POINT('Ctrl Pts',(-42.0915954238788,-23.4066461873484,
20.));
#78715=CARTESIAN_POINT('Ctrl Pts',(-42.1051750145614,-23.3759833809318,
0.));
#78716=CARTESIAN_POINT('Ctrl Pts',(-42.1051750145614,-23.3759833809318,
20.));
#78717=CARTESIAN_POINT('Ctrl Pts',(-42.1187328858474,-23.3453121858047,
0.));
#78718=CARTESIAN_POINT('Ctrl Pts',(-42.1187328858474,-23.3453121858047,
20.));
#78719=CARTESIAN_POINT('Ctrl Pts',(-42.1322690320059,-23.3146326170671,
0.));
#78720=CARTESIAN_POINT('Ctrl Pts',(-42.1322690320059,-23.3146326170671,
20.));
#78721=CARTESIAN_POINT('Ctrl Pts',(-42.145783447317,-23.2839446898238,0.));
#78722=CARTESIAN_POINT('Ctrl Pts',(-42.145783447317,-23.2839446898238,20.));
#78723=CARTESIAN_POINT('Ctrl Pts',(-42.1592761260708,-23.2532484191837,
0.));
#78724=CARTESIAN_POINT('Ctrl Pts',(-42.1592761260708,-23.2532484191837,
20.));
#78725=CARTESIAN_POINT('Ctrl Pts',(-42.1727470625681,-23.2225438202604,
0.));
#78726=CARTESIAN_POINT('Ctrl Pts',(-42.1727470625681,-23.2225438202604,
20.));
#78727=CARTESIAN_POINT('Ctrl Pts',(-42.1861962511195,-23.1918309081713,
0.));
#78728=CARTESIAN_POINT('Ctrl Pts',(-42.1861962511195,-23.1918309081713,
20.));
#78729=CARTESIAN_POINT('Ctrl Pts',(-42.1996236860461,-23.1611096980384,
0.));
#78730=CARTESIAN_POINT('Ctrl Pts',(-42.1996236860461,-23.1611096980384,
20.));
#78731=CARTESIAN_POINT('Ctrl Pts',(-42.2130293616794,-23.1303802049881,
0.));
#78732=CARTESIAN_POINT('Ctrl Pts',(-42.2130293616794,-23.1303802049881,
20.));
#78733=CARTESIAN_POINT('Ctrl Pts',(-42.2264132723612,-23.0996424441509,
0.));
#78734=CARTESIAN_POINT('Ctrl Pts',(-42.2264132723612,-23.0996424441509,
20.));
#78735=CARTESIAN_POINT('Ctrl Pts',(-42.2397754124437,-23.0688964306618,
0.));
#78736=CARTESIAN_POINT('Ctrl Pts',(-42.2397754124437,-23.0688964306618,
20.));
#78737=CARTESIAN_POINT('Ctrl Pts',(-42.2531157762897,-23.0381421796601,
0.));
#78738=CARTESIAN_POINT('Ctrl Pts',(-42.2531157762897,-23.0381421796601,
20.));
#78739=CARTESIAN_POINT('Ctrl Pts',(-42.2664343582719,-23.0073797062893,
0.));
#78740=CARTESIAN_POINT('Ctrl Pts',(-42.2664343582719,-23.0073797062893,
20.));
#78741=CARTESIAN_POINT('Ctrl Pts',(-42.2797311527738,-22.9766090256973,
0.));
#78742=CARTESIAN_POINT('Ctrl Pts',(-42.2797311527738,-22.9766090256973,
20.));
#78743=CARTESIAN_POINT('Ctrl Pts',(-42.2930061541893,-22.9458301530364,
0.));
#78744=CARTESIAN_POINT('Ctrl Pts',(-42.2930061541893,-22.9458301530364,
20.));
#78745=CARTESIAN_POINT('Ctrl Pts',(-42.3062593569226,-22.9150431034629,
0.));
#78746=CARTESIAN_POINT('Ctrl Pts',(-42.3062593569226,-22.9150431034629,
20.));
#78747=CARTESIAN_POINT('Ctrl Pts',(-42.3194907553882,-22.8842478921374,
0.));
#78748=CARTESIAN_POINT('Ctrl Pts',(-42.3194907553882,-22.8842478921374,
20.));
#78749=CARTESIAN_POINT('Ctrl Pts',(-42.3327003440109,-22.8534445342249,
0.));
#78750=CARTESIAN_POINT('Ctrl Pts',(-42.3327003440109,-22.8534445342249,
20.));
#78751=CARTESIAN_POINT('Ctrl Pts',(-42.3458881172255,-22.8226330448945,
0.));
#78752=CARTESIAN_POINT('Ctrl Pts',(-42.3458881172255,-22.8226330448945,
20.));
#78753=CARTESIAN_POINT('Ctrl Pts',(-42.3590540694774,-22.7918134393197,
0.));
#78754=CARTESIAN_POINT('Ctrl Pts',(-42.3590540694774,-22.7918134393197,
20.));
#78755=CARTESIAN_POINT('Ctrl Pts',(-42.3721981952224,-22.7609857326781,
0.));
#78756=CARTESIAN_POINT('Ctrl Pts',(-42.3721981952224,-22.7609857326781,
20.));
#78757=CARTESIAN_POINT('Ctrl Pts',(-42.3853204889273,-22.7301499401517,
0.));
#78758=CARTESIAN_POINT('Ctrl Pts',(-42.3853204889273,-22.7301499401517,
20.));
#78759=CARTESIAN_POINT('Ctrl Pts',(-42.398420945069,-22.6993060769268,0.));
#78760=CARTESIAN_POINT('Ctrl Pts',(-42.398420945069,-22.6993060769268,20.));
#78761=CARTESIAN_POINT('Ctrl Pts',(-42.411499558135,-22.6684541581936,0.));
#78762=CARTESIAN_POINT('Ctrl Pts',(-42.411499558135,-22.6684541581936,20.));
#78763=CARTESIAN_POINT('Ctrl Pts',(-42.4245563226236,-22.6375941991468,
0.));
#78764=CARTESIAN_POINT('Ctrl Pts',(-42.4245563226236,-22.6375941991468,
20.));
#78765=CARTESIAN_POINT('Ctrl Pts',(-42.4375912330427,-22.6067262149851,
0.));
#78766=CARTESIAN_POINT('Ctrl Pts',(-42.4375912330427,-22.6067262149851,
20.));
#78767=CARTESIAN_POINT('Ctrl Pts',(-42.4506042839107,-22.5758502209116,
0.));
#78768=CARTESIAN_POINT('Ctrl Pts',(-42.4506042839107,-22.5758502209116,
20.));
#78769=CARTESIAN_POINT('Ctrl Pts',(-42.4635954697559,-22.5449662321334,
0.));
#78770=CARTESIAN_POINT('Ctrl Pts',(-42.4635954697559,-22.5449662321334,
20.));
#78771=CARTESIAN_POINT('Ctrl Pts',(-42.4765647851171,-22.5140742638619,
0.));
#78772=CARTESIAN_POINT('Ctrl Pts',(-42.4765647851171,-22.5140742638619,
20.));
#78773=CARTESIAN_POINT('Ctrl Pts',(-42.4895122245441,-22.4831743313126,
0.));
#78774=CARTESIAN_POINT('Ctrl Pts',(-42.4895122245441,-22.4831743313126,
20.));
#78775=CARTESIAN_POINT('Ctrl Pts',(-42.502437782597,-22.4522664497054,0.));
#78776=CARTESIAN_POINT('Ctrl Pts',(-42.502437782597,-22.4522664497054,20.));
#78777=CARTESIAN_POINT('Ctrl Pts',(-42.5153414538467,-22.4213506342639,
0.));
#78778=CARTESIAN_POINT('Ctrl Pts',(-42.5153414538467,-22.4213506342639,
20.));
#78779=CARTESIAN_POINT('Ctrl Pts',(-42.5282232328748,-22.3904269002165,
0.));
#78780=CARTESIAN_POINT('Ctrl Pts',(-42.5282232328748,-22.3904269002165,
20.));
#78781=CARTESIAN_POINT('Ctrl Pts',(-42.5410831142727,-22.3594952627952,
0.));
#78782=CARTESIAN_POINT('Ctrl Pts',(-42.5410831142727,-22.3594952627952,
20.));
#78783=CARTESIAN_POINT('Ctrl Pts',(-42.5539210926424,-22.3285557372364,
0.));
#78784=CARTESIAN_POINT('Ctrl Pts',(-42.5539210926424,-22.3285557372364,
20.));
#78785=CARTESIAN_POINT('Ctrl Pts',(-42.5667371625962,-22.2976083387805,
0.));
#78786=CARTESIAN_POINT('Ctrl Pts',(-42.5667371625962,-22.2976083387805,
20.));
#78787=CARTESIAN_POINT('Ctrl Pts',(-42.5795313187569,-22.2666530826722,
0.));
#78788=CARTESIAN_POINT('Ctrl Pts',(-42.5795313187569,-22.2666530826722,
20.));
#78789=CARTESIAN_POINT('Ctrl Pts',(-42.5923035557573,-22.2356899841602,
0.));
#78790=CARTESIAN_POINT('Ctrl Pts',(-42.5923035557573,-22.2356899841602,
20.));
#78791=CARTESIAN_POINT('Ctrl Pts',(-42.6050538682411,-22.2047190584974,
0.));
#78792=CARTESIAN_POINT('Ctrl Pts',(-42.6050538682411,-22.2047190584974,
20.));
#78793=CARTESIAN_POINT('Ctrl Pts',(-42.6177822508627,-22.1737403209406,
0.));
#78794=CARTESIAN_POINT('Ctrl Pts',(-42.6177822508627,-22.1737403209406,
20.));
#78795=CARTESIAN_POINT('Ctrl Pts',(-42.6304886982869,-22.1427537867512,
0.));
#78796=CARTESIAN_POINT('Ctrl Pts',(-42.6304886982869,-22.1427537867512,
20.));
#78797=CARTESIAN_POINT('Ctrl Pts',(-42.6431732051887,-22.1117594711942,
0.));
#78798=CARTESIAN_POINT('Ctrl Pts',(-42.6431732051887,-22.1117594711942,
20.));
#78799=CARTESIAN_POINT('Ctrl Pts',(-42.6558357662536,-22.0807573895388,
0.));
#78800=CARTESIAN_POINT('Ctrl Pts',(-42.6558357662536,-22.0807573895388,
20.));
#78801=CARTESIAN_POINT('Ctrl Pts',(-42.6684763761777,-22.0497475570584,
0.));
#78802=CARTESIAN_POINT('Ctrl Pts',(-42.6684763761777,-22.0497475570584,
20.));
#78803=CARTESIAN_POINT('Ctrl Pts',(-42.6810950296678,-22.0187299890302,
0.));
#78804=CARTESIAN_POINT('Ctrl Pts',(-42.6810950296678,-22.0187299890302,
20.));
#78805=CARTESIAN_POINT('Ctrl Pts',(-42.6936917214411,-21.9877047007357,
0.));
#78806=CARTESIAN_POINT('Ctrl Pts',(-42.6936917214411,-21.9877047007357,
20.));
#78807=CARTESIAN_POINT('Ctrl Pts',(-42.7062664462249,-21.9566717074606,
0.));
#78808=CARTESIAN_POINT('Ctrl Pts',(-42.7062664462249,-21.9566717074606,
20.));
#78809=CARTESIAN_POINT('Ctrl Pts',(-42.7188191987573,-21.9256310244944,
0.));
#78810=CARTESIAN_POINT('Ctrl Pts',(-42.7188191987573,-21.9256310244944,
20.));
#78811=CARTESIAN_POINT('Ctrl Pts',(-42.7313499737866,-21.8945826671308,
0.));
#78812=CARTESIAN_POINT('Ctrl Pts',(-42.7313499737866,-21.8945826671308,
20.));
#78813=CARTESIAN_POINT('Ctrl Pts',(-42.7438587660714,-21.8635266506674,
0.));
#78814=CARTESIAN_POINT('Ctrl Pts',(-42.7438587660714,-21.8635266506674,
20.));
#78815=CARTESIAN_POINT('Ctrl Pts',(-42.7563455703812,-21.832462990406,0.));
#78816=CARTESIAN_POINT('Ctrl Pts',(-42.7563455703812,-21.832462990406,20.));
#78817=CARTESIAN_POINT('Ctrl Pts',(-42.7688103814962,-21.8013917016521,
0.));
#78818=CARTESIAN_POINT('Ctrl Pts',(-42.7688103814962,-21.8013917016521,
20.));
#78819=CARTESIAN_POINT('Ctrl Pts',(-42.7812531942069,-21.7703127997157,
0.));
#78820=CARTESIAN_POINT('Ctrl Pts',(-42.7812531942069,-21.7703127997157,
20.));
#78821=CARTESIAN_POINT('Ctrl Pts',(-42.7936740033148,-21.7392262999104,
0.));
#78822=CARTESIAN_POINT('Ctrl Pts',(-42.7936740033148,-21.7392262999104,
20.));
#78823=CARTESIAN_POINT('Ctrl Pts',(-42.8060728036314,-21.7081322175539,
0.));
#78824=CARTESIAN_POINT('Ctrl Pts',(-42.8060728036314,-21.7081322175539,
20.));
#78825=CARTESIAN_POINT('Ctrl Pts',(-42.8184495899785,-21.677030567968,0.));
#78826=CARTESIAN_POINT('Ctrl Pts',(-42.8184495899785,-21.677030567968,20.));
#78827=CARTESIAN_POINT('Ctrl Pts',(-42.8308043571887,-21.6459213664784,
0.));
#78828=CARTESIAN_POINT('Ctrl Pts',(-42.8308043571887,-21.6459213664784,
20.));
#78829=CARTESIAN_POINT('Ctrl Pts',(-42.8431371001047,-21.6148046284149,
0.));
#78830=CARTESIAN_POINT('Ctrl Pts',(-42.8431371001047,-21.6148046284149,
20.));
#78831=CARTESIAN_POINT('Ctrl Pts',(-42.8554478135801,-21.5836803691112,
0.));
#78832=CARTESIAN_POINT('Ctrl Pts',(-42.8554478135801,-21.5836803691112,
20.));
#78833=CARTESIAN_POINT('Ctrl Pts',(-42.8677364924794,-21.5525486039049,
0.));
#78834=CARTESIAN_POINT('Ctrl Pts',(-42.8677364924794,-21.5525486039049,
20.));
#78835=CARTESIAN_POINT('Ctrl Pts',(-42.8800031316769,-21.5214093481377,
0.));
#78836=CARTESIAN_POINT('Ctrl Pts',(-42.8800031316769,-21.5214093481377,
20.));
#78837=CARTESIAN_POINT('Ctrl Pts',(-42.8922477260581,-21.490262617155,0.));
#78838=CARTESIAN_POINT('Ctrl Pts',(-42.8922477260581,-21.490262617155,20.));
#78839=CARTESIAN_POINT('Ctrl Pts',(-42.9044702705183,-21.4591084263065,
0.));
#78840=CARTESIAN_POINT('Ctrl Pts',(-42.9044702705183,-21.4591084263065,
20.));
#78841=CARTESIAN_POINT('Ctrl Pts',(-42.916670759964,-21.4279467909454,0.));
#78842=CARTESIAN_POINT('Ctrl Pts',(-42.916670759964,-21.4279467909454,20.));
#78843=CARTESIAN_POINT('Ctrl Pts',(-42.9288491893122,-21.3967777264294,
0.));
#78844=CARTESIAN_POINT('Ctrl Pts',(-42.9288491893122,-21.3967777264294,
20.));
#78845=CARTESIAN_POINT('Ctrl Pts',(-42.9410055534907,-21.3656012481198,
0.));
#78846=CARTESIAN_POINT('Ctrl Pts',(-42.9410055534907,-21.3656012481198,
20.));
#78847=CARTESIAN_POINT('Ctrl Pts',(-42.9531398474371,-21.3344173713818,
0.));
#78848=CARTESIAN_POINT('Ctrl Pts',(-42.9531398474371,-21.3344173713818,
20.));
#78849=CARTESIAN_POINT('Ctrl Pts',(-42.9652520660998,-21.3032261115844,
0.));
#78850=CARTESIAN_POINT('Ctrl Pts',(-42.9652520660998,-21.3032261115844,
20.));
#78851=CARTESIAN_POINT('Ctrl Pts',(-42.9773422044374,-21.2720274841006,
0.));
#78852=CARTESIAN_POINT('Ctrl Pts',(-42.9773422044374,-21.2720274841006,
20.));
#78853=CARTESIAN_POINT('Ctrl Pts',(-42.9894102574195,-21.2408215043074,
0.));
#78854=CARTESIAN_POINT('Ctrl Pts',(-42.9894102574195,-21.2408215043074,
20.));
#78855=CARTESIAN_POINT('Ctrl Pts',(-43.0014562200264,-21.2096081875857,
0.));
#78856=CARTESIAN_POINT('Ctrl Pts',(-43.0014562200264,-21.2096081875857,
20.));
#78857=CARTESIAN_POINT('Ctrl Pts',(-43.0134800872489,-21.1783875493204,
0.));
#78858=CARTESIAN_POINT('Ctrl Pts',(-43.0134800872489,-21.1783875493204,
20.));
#78859=CARTESIAN_POINT('Ctrl Pts',(-43.0254818540885,-21.1471596049,0.));
#78860=CARTESIAN_POINT('Ctrl Pts',(-43.0254818540885,-21.1471596049,20.));
#78861=CARTESIAN_POINT('Ctrl Pts',(-43.037461515557,-21.1159243697169,0.));
#78862=CARTESIAN_POINT('Ctrl Pts',(-43.037461515557,-21.1159243697169,20.));
#78863=CARTESIAN_POINT('Ctrl Pts',(-43.0494190666771,-21.0846818591673,
0.));
#78864=CARTESIAN_POINT('Ctrl Pts',(-43.0494190666771,-21.0846818591673,
20.));
#78865=CARTESIAN_POINT('Ctrl Pts',(-43.0613545024815,-21.0534320886512,
0.));
#78866=CARTESIAN_POINT('Ctrl Pts',(-43.0613545024815,-21.0534320886512,
20.));
#78867=CARTESIAN_POINT('Ctrl Pts',(-43.0732678180139,-21.0221750735727,
0.));
#78868=CARTESIAN_POINT('Ctrl Pts',(-43.0732678180139,-21.0221750735727,
20.));
#78869=CARTESIAN_POINT('Ctrl Pts',(-43.0851590083283,-20.9909108293397,
0.));
#78870=CARTESIAN_POINT('Ctrl Pts',(-43.0851590083283,-20.9909108293397,
20.));
#78871=CARTESIAN_POINT('Ctrl Pts',(-43.0970280684896,-20.959639371364,0.));
#78872=CARTESIAN_POINT('Ctrl Pts',(-43.0970280684896,-20.959639371364,20.));
#78873=CARTESIAN_POINT('Ctrl Pts',(-43.1088749935734,-20.9283607150615,
0.));
#78874=CARTESIAN_POINT('Ctrl Pts',(-43.1088749935734,-20.9283607150615,
20.));
#78875=CARTESIAN_POINT('Ctrl Pts',(-43.1206997786657,-20.8970748758512,
0.));
#78876=CARTESIAN_POINT('Ctrl Pts',(-43.1206997786657,-20.8970748758512,
20.));
#78877=CARTESIAN_POINT('Ctrl Pts',(-43.132502418863,-20.8657818691565,0.));
#78878=CARTESIAN_POINT('Ctrl Pts',(-43.132502418863,-20.8657818691565,20.));
#78879=CARTESIAN_POINT('Ctrl Pts',(-43.1442829092724,-20.8344817104039,
0.));
#78880=CARTESIAN_POINT('Ctrl Pts',(-43.1442829092724,-20.8344817104039,
20.));
#78881=CARTESIAN_POINT('Ctrl Pts',(-43.1560412450117,-20.8031744150242,
0.));
#78882=CARTESIAN_POINT('Ctrl Pts',(-43.1560412450117,-20.8031744150242,
20.));
#78883=CARTESIAN_POINT('Ctrl Pts',(-43.1677774212093,-20.7718599984518,
0.));
#78884=CARTESIAN_POINT('Ctrl Pts',(-43.1677774212093,-20.7718599984518,
20.));
#78885=CARTESIAN_POINT('Ctrl Pts',(-43.1794914330045,-20.7405384761252,
0.));
#78886=CARTESIAN_POINT('Ctrl Pts',(-43.1794914330045,-20.7405384761252,
20.));
#78887=CARTESIAN_POINT('Ctrl Pts',(-43.1911832755467,-20.7092098634864,
0.));
#78888=CARTESIAN_POINT('Ctrl Pts',(-43.1911832755467,-20.7092098634864,
20.));
#78889=CARTESIAN_POINT('Ctrl Pts',(-43.202852943996,-20.6778741759814,0.));
#78890=CARTESIAN_POINT('Ctrl Pts',(-43.202852943996,-20.6778741759814,20.));
#78891=CARTESIAN_POINT('Ctrl Pts',(-43.2145004335236,-20.6465314290598,
0.));
#78892=CARTESIAN_POINT('Ctrl Pts',(-43.2145004335236,-20.6465314290598,
20.));
#78893=CARTESIAN_POINT('Ctrl Pts',(-43.2261257393109,-20.615181638175,0.));
#78894=CARTESIAN_POINT('Ctrl Pts',(-43.2261257393109,-20.615181638175,20.));
#78895=CARTESIAN_POINT('Ctrl Pts',(-43.2377288565503,-20.5838248187841,
0.));
#78896=CARTESIAN_POINT('Ctrl Pts',(-43.2377288565503,-20.5838248187841,
20.));
#78897=CARTESIAN_POINT('Ctrl Pts',(-43.2493097804445,-20.5524609863481,
0.));
#78898=CARTESIAN_POINT('Ctrl Pts',(-43.2493097804445,-20.5524609863481,
20.));
#78899=CARTESIAN_POINT('Ctrl Pts',(-43.2608685062069,-20.5210901563314,
0.));
#78900=CARTESIAN_POINT('Ctrl Pts',(-43.2608685062069,-20.5210901563314,
20.));
#78901=CARTESIAN_POINT('Ctrl Pts',(-43.2724050290617,-20.4897123442023,
0.));
#78902=CARTESIAN_POINT('Ctrl Pts',(-43.2724050290617,-20.4897123442023,
20.));
#78903=CARTESIAN_POINT('Ctrl Pts',(-43.283919344243,-20.4583275654327,0.));
#78904=CARTESIAN_POINT('Ctrl Pts',(-43.283919344243,-20.4583275654327,20.));
#78905=CARTESIAN_POINT('Ctrl Pts',(-43.2954114469964,-20.4269358354984,
0.));
#78906=CARTESIAN_POINT('Ctrl Pts',(-43.2954114469964,-20.4269358354984,
20.));
#78907=CARTESIAN_POINT('Ctrl Pts',(-43.3068813325774,-20.3955371698787,
0.));
#78908=CARTESIAN_POINT('Ctrl Pts',(-43.3068813325774,-20.3955371698787,
20.));
#78909=CARTESIAN_POINT('Ctrl Pts',(-43.3183289962528,-20.3641315840566,
0.));
#78910=CARTESIAN_POINT('Ctrl Pts',(-43.3183289962528,-20.3641315840566,
20.));
#78911=CARTESIAN_POINT('Ctrl Pts',(-43.3297544333003,-20.3327190935193,
0.));
#78912=CARTESIAN_POINT('Ctrl Pts',(-43.3297544333003,-20.3327190935193,
20.));
#78913=CARTESIAN_POINT('Ctrl Pts',(-43.3411576390085,-20.3012997137575,
0.));
#78914=CARTESIAN_POINT('Ctrl Pts',(-43.3411576390085,-20.3012997137575,
20.));
#78915=CARTESIAN_POINT('Ctrl Pts',(-43.3525386086763,-20.2698734602656,
0.));
#78916=CARTESIAN_POINT('Ctrl Pts',(-43.3525386086763,-20.2698734602656,
20.));
#78917=CARTESIAN_POINT('Ctrl Pts',(-43.3638973376125,-20.2384403485411,
0.));
#78918=CARTESIAN_POINT('Ctrl Pts',(-43.3638973376125,-20.2384403485411,
20.));
#78919=CARTESIAN_POINT('Ctrl Pts',(-43.3752338211368,-20.2070003940853,
0.));
#78920=CARTESIAN_POINT('Ctrl Pts',(-43.3752338211368,-20.2070003940853,
20.));
#78921=CARTESIAN_POINT('Ctrl Pts',(-43.3865480545792,-20.1755536124033,
0.));
#78922=CARTESIAN_POINT('Ctrl Pts',(-43.3865480545792,-20.1755536124033,
20.));
#78923=CARTESIAN_POINT('Ctrl Pts',(-43.3978400332808,-20.1441000190037,
0.));
#78924=CARTESIAN_POINT('Ctrl Pts',(-43.3978400332808,-20.1441000190037,
20.));
#78925=CARTESIAN_POINT('Ctrl Pts',(-43.409109752594,-20.1126396293992,0.));
#78926=CARTESIAN_POINT('Ctrl Pts',(-43.409109752594,-20.1126396293992,20.));
#78927=CARTESIAN_POINT('Ctrl Pts',(-43.4203572078819,-20.0811724591058,
0.));
#78928=CARTESIAN_POINT('Ctrl Pts',(-43.4203572078819,-20.0811724591058,
20.));
#78929=CARTESIAN_POINT('Ctrl Pts',(-43.4315823945181,-20.0496985236436,
0.));
#78930=CARTESIAN_POINT('Ctrl Pts',(-43.4315823945181,-20.0496985236436,
20.));
#78931=CARTESIAN_POINT('Ctrl Pts',(-43.4427853078868,-20.0182178385356,
0.));
#78932=CARTESIAN_POINT('Ctrl Pts',(-43.4427853078868,-20.0182178385356,
20.));
#78933=CARTESIAN_POINT('Ctrl Pts',(-43.4539659433821,-19.9867304193089,
0.));
#78934=CARTESIAN_POINT('Ctrl Pts',(-43.4539659433821,-19.9867304193089,
20.));
#78935=CARTESIAN_POINT('Ctrl Pts',(-43.4651242964088,-19.9552362814936,
0.));
#78936=CARTESIAN_POINT('Ctrl Pts',(-43.4651242964088,-19.9552362814936,
20.));
#78937=CARTESIAN_POINT('Ctrl Pts',(-43.4762603623832,-19.923735440624,0.));
#78938=CARTESIAN_POINT('Ctrl Pts',(-43.4762603623832,-19.923735440624,20.));
#78939=CARTESIAN_POINT('Ctrl Pts',(-43.4873741367321,-19.8922279122378,
0.));
#78940=CARTESIAN_POINT('Ctrl Pts',(-43.4873741367321,-19.8922279122378,
20.));
#78941=CARTESIAN_POINT('Ctrl Pts',(-43.4984656148936,-19.8607137118763,
0.));
#78942=CARTESIAN_POINT('Ctrl Pts',(-43.4984656148936,-19.8607137118763,
20.));
#78943=CARTESIAN_POINT('Ctrl Pts',(-43.5095347923164,-19.8291928550844,
0.));
#78944=CARTESIAN_POINT('Ctrl Pts',(-43.5095347923164,-19.8291928550844,
20.));
#78945=CARTESIAN_POINT('Ctrl Pts',(-43.5205816644596,-19.7976653574108,
0.));
#78946=CARTESIAN_POINT('Ctrl Pts',(-43.5205816644596,-19.7976653574108,
20.));
#78947=CARTESIAN_POINT('Ctrl Pts',(-43.5316062267925,-19.7661312344072,
0.));
#78948=CARTESIAN_POINT('Ctrl Pts',(-43.5316062267925,-19.7661312344072,
20.));
#78949=CARTESIAN_POINT('Ctrl Pts',(-43.542608474795,-19.734590501629,0.));
#78950=CARTESIAN_POINT('Ctrl Pts',(-43.542608474795,-19.734590501629,20.));
#78951=CARTESIAN_POINT('Ctrl Pts',(-43.5535884039576,-19.7030431746352,
0.));
#78952=CARTESIAN_POINT('Ctrl Pts',(-43.5535884039576,-19.7030431746352,
20.));
#78953=CARTESIAN_POINT('Ctrl Pts',(-43.5645460097823,-19.6714892689885,
0.));
#78954=CARTESIAN_POINT('Ctrl Pts',(-43.5645460097823,-19.6714892689885,
20.));
#78955=CARTESIAN_POINT('Ctrl Pts',(-43.5754812877819,-19.639928800255,0.));
#78956=CARTESIAN_POINT('Ctrl Pts',(-43.5754812877819,-19.639928800255,20.));
#78957=CARTESIAN_POINT('Ctrl Pts',(-43.5863942334797,-19.6083617840046,
0.));
#78958=CARTESIAN_POINT('Ctrl Pts',(-43.5863942334797,-19.6083617840046,
20.));
#78959=CARTESIAN_POINT('Ctrl Pts',(-43.5972848424097,-19.5767882358104,
0.));
#78960=CARTESIAN_POINT('Ctrl Pts',(-43.5972848424097,-19.5767882358104,
20.));
#78961=CARTESIAN_POINT('Ctrl Pts',(-43.6081531101168,-19.545208171249,0.));
#78962=CARTESIAN_POINT('Ctrl Pts',(-43.6081531101168,-19.545208171249,20.));
#78963=CARTESIAN_POINT('Ctrl Pts',(-43.6189990321561,-19.5136216059004,
0.));
#78964=CARTESIAN_POINT('Ctrl Pts',(-43.6189990321561,-19.5136216059004,
20.));
#78965=CARTESIAN_POINT('Ctrl Pts',(-43.629822604094,-19.4820285553483,0.));
#78966=CARTESIAN_POINT('Ctrl Pts',(-43.629822604094,-19.4820285553483,20.));
#78967=CARTESIAN_POINT('Ctrl Pts',(-43.6406238215078,-19.4504290351799,
0.));
#78968=CARTESIAN_POINT('Ctrl Pts',(-43.6406238215078,-19.4504290351799,
20.));
#78969=CARTESIAN_POINT('Ctrl Pts',(-43.6514026799849,-19.4188230609858,
0.));
#78970=CARTESIAN_POINT('Ctrl Pts',(-43.6514026799849,-19.4188230609858,
20.));
#78971=CARTESIAN_POINT('Ctrl Pts',(-43.6621591751234,-19.3872106483603,
0.));
#78972=CARTESIAN_POINT('Ctrl Pts',(-43.6621591751234,-19.3872106483603,
20.));
#78973=CARTESIAN_POINT('Ctrl Pts',(-43.6728933025325,-19.3555918129009,
0.));
#78974=CARTESIAN_POINT('Ctrl Pts',(-43.6728933025325,-19.3555918129009,
20.));
#78975=CARTESIAN_POINT('Ctrl Pts',(-43.6836050578319,-19.3239665702086,
0.));
#78976=CARTESIAN_POINT('Ctrl Pts',(-43.6836050578319,-19.3239665702086,
20.));
#78977=CARTESIAN_POINT('Ctrl Pts',(-43.6942944366523,-19.2923349358879,
0.));
#78978=CARTESIAN_POINT('Ctrl Pts',(-43.6942944366523,-19.2923349358879,
20.));
#78979=CARTESIAN_POINT('Ctrl Pts',(-43.7049614346349,-19.2606969255464,
0.));
#78980=CARTESIAN_POINT('Ctrl Pts',(-43.7049614346349,-19.2606969255464,
20.));
#78981=CARTESIAN_POINT('Ctrl Pts',(-43.7156060474324,-19.2290525547956,
0.));
#78982=CARTESIAN_POINT('Ctrl Pts',(-43.7156060474324,-19.2290525547956,
20.));
#78983=CARTESIAN_POINT('Ctrl Pts',(-43.7262282707082,-19.1974018392505,
0.));
#78984=CARTESIAN_POINT('Ctrl Pts',(-43.7262282707082,-19.1974018392505,
20.));
#78985=CARTESIAN_POINT('Ctrl Pts',(-43.7368281001363,-19.1657447945291,
0.));
#78986=CARTESIAN_POINT('Ctrl Pts',(-43.7368281001363,-19.1657447945291,
20.));
#78987=CARTESIAN_POINT('Ctrl Pts',(-43.747405531401,-19.1340814362531,0.));
#78988=CARTESIAN_POINT('Ctrl Pts',(-43.747405531401,-19.1340814362531,20.));
#78989=CARTESIAN_POINT('Ctrl Pts',(-43.7579605601976,-19.1024117800474,
0.));
#78990=CARTESIAN_POINT('Ctrl Pts',(-43.7579605601976,-19.1024117800474,
20.));
#78991=CARTESIAN_POINT('Ctrl Pts',(-43.7684931822314,-19.0707358415405,
0.));
#78992=CARTESIAN_POINT('Ctrl Pts',(-43.7684931822314,-19.0707358415405,
20.));
#78993=CARTESIAN_POINT('Ctrl Pts',(-43.779003393219,-19.039053636364,0.));
#78994=CARTESIAN_POINT('Ctrl Pts',(-43.779003393219,-19.039053636364,20.));
#78995=CARTESIAN_POINT('Ctrl Pts',(-43.7894911888877,-19.0073651801531,
0.));
#78996=CARTESIAN_POINT('Ctrl Pts',(-43.7894911888877,-19.0073651801531,
20.));
#78997=CARTESIAN_POINT('Ctrl Pts',(-43.7999565649762,-18.9756704885464,
0.));
#78998=CARTESIAN_POINT('Ctrl Pts',(-43.7999565649762,-18.9756704885464,
20.));
#78999=CARTESIAN_POINT('Ctrl Pts',(-43.8103995172341,-18.9439695771858,
0.));
#79000=CARTESIAN_POINT('Ctrl Pts',(-43.8103995172341,-18.9439695771858,
20.));
#79001=CARTESIAN_POINT('Ctrl Pts',(-43.8208200414219,-18.9122624617166,
0.));
#79002=CARTESIAN_POINT('Ctrl Pts',(-43.8208200414219,-18.9122624617166,
20.));
#79003=CARTESIAN_POINT('Ctrl Pts',(-43.8312181333106,-18.8805491577876,
0.));
#79004=CARTESIAN_POINT('Ctrl Pts',(-43.8312181333106,-18.8805491577876,
20.));
#79005=CARTESIAN_POINT('Ctrl Pts',(-43.8415937886817,-18.8488296810507,
0.));
#79006=CARTESIAN_POINT('Ctrl Pts',(-43.8415937886817,-18.8488296810507,
20.));
#79007=CARTESIAN_POINT('Ctrl Pts',(-43.8519470033272,-18.8171040471611,
0.));
#79008=CARTESIAN_POINT('Ctrl Pts',(-43.8519470033272,-18.8171040471611,
20.));
#79009=CARTESIAN_POINT('Ctrl Pts',(-43.8622777730502,-18.7853722717774,
0.));
#79010=CARTESIAN_POINT('Ctrl Pts',(-43.8622777730502,-18.7853722717774,
20.));
#79011=CARTESIAN_POINT('Ctrl Pts',(-43.8725860936644,-18.7536343705616,
0.));
#79012=CARTESIAN_POINT('Ctrl Pts',(-43.8725860936644,-18.7536343705616,
20.));
#79013=CARTESIAN_POINT('Ctrl Pts',(-43.8828719609947,-18.721890359179,0.));
#79014=CARTESIAN_POINT('Ctrl Pts',(-43.8828719609947,-18.721890359179,20.));
#79015=CARTESIAN_POINT('Ctrl Pts',(-43.8931353708767,-18.6901402532984,
0.));
#79016=CARTESIAN_POINT('Ctrl Pts',(-43.8931353708767,-18.6901402532984,
20.));
#79017=CARTESIAN_POINT('Ctrl Pts',(-43.903376319157,-18.6583840685915,0.));
#79018=CARTESIAN_POINT('Ctrl Pts',(-43.903376319157,-18.6583840685915,20.));
#79019=CARTESIAN_POINT('Ctrl Pts',(-43.913594801693,-18.6266218207337,0.));
#79020=CARTESIAN_POINT('Ctrl Pts',(-43.913594801693,-18.6266218207337,20.));
#79021=CARTESIAN_POINT('Ctrl Pts',(-43.9237908143526,-18.5948535254034,
0.));
#79022=CARTESIAN_POINT('Ctrl Pts',(-43.9237908143526,-18.5948535254034,
20.));
#79023=CARTESIAN_POINT('Ctrl Pts',(-43.9339643530151,-18.5630791982821,
0.));
#79024=CARTESIAN_POINT('Ctrl Pts',(-43.9339643530151,-18.5630791982821,
20.));
#79025=CARTESIAN_POINT('Ctrl Pts',(-43.94411541357,-18.5312988550549,0.));
#79026=CARTESIAN_POINT('Ctrl Pts',(-43.94411541357,-18.5312988550549,20.));
#79027=CARTESIAN_POINT('Ctrl Pts',(-43.9542439919177,-18.4995125114099,
0.));
#79028=CARTESIAN_POINT('Ctrl Pts',(-43.9542439919177,-18.4995125114099,
20.));
#79029=CARTESIAN_POINT('Ctrl Pts',(-43.9643500839697,-18.4677201830388,
0.));
#79030=CARTESIAN_POINT('Ctrl Pts',(-43.9643500839697,-18.4677201830388,
20.));
#79031=CARTESIAN_POINT('Ctrl Pts',(-43.9744336856481,-18.4359218856365,
0.));
#79032=CARTESIAN_POINT('Ctrl Pts',(-43.9744336856481,-18.4359218856365,
20.));
#79033=CARTESIAN_POINT('Ctrl Pts',(-43.9844947928861,-18.4041176349014,
0.));
#79034=CARTESIAN_POINT('Ctrl Pts',(-43.9844947928861,-18.4041176349014,
20.));
#79035=CARTESIAN_POINT('Ctrl Pts',(-43.9945334016277,-18.3723074465347,
0.));
#79036=CARTESIAN_POINT('Ctrl Pts',(-43.9945334016277,-18.3723074465347,
20.));
#79037=CARTESIAN_POINT('Ctrl Pts',(-44.0045495078276,-18.3404913362408,
0.));
#79038=CARTESIAN_POINT('Ctrl Pts',(-44.0045495078276,-18.3404913362408,
20.));
#79039=CARTESIAN_POINT('Ctrl Pts',(-44.0145431074514,-18.3086693197275,
0.));
#79040=CARTESIAN_POINT('Ctrl Pts',(-44.0145431074514,-18.3086693197275,
20.));
#79041=CARTESIAN_POINT('Ctrl Pts',(-44.0245141964756,-18.2768414127056,
0.));
#79042=CARTESIAN_POINT('Ctrl Pts',(-44.0245141964756,-18.2768414127056,
20.));
#79043=CARTESIAN_POINT('Ctrl Pts',(-44.0344627708874,-18.2450076308889,
0.));
#79044=CARTESIAN_POINT('Ctrl Pts',(-44.0344627708874,-18.2450076308889,
20.));
#79045=CARTESIAN_POINT('Ctrl Pts',(-44.044388826685,-18.2131679899948,0.));
#79046=CARTESIAN_POINT('Ctrl Pts',(-44.044388826685,-18.2131679899948,20.));
#79047=CARTESIAN_POINT('Ctrl Pts',(-44.0542923598773,-18.1813225057438,
0.));
#79048=CARTESIAN_POINT('Ctrl Pts',(-44.0542923598773,-18.1813225057438,
20.));
#79049=CARTESIAN_POINT('Ctrl Pts',(-44.0641733664839,-18.1494711938598,
0.));
#79050=CARTESIAN_POINT('Ctrl Pts',(-44.0641733664839,-18.1494711938598,
20.));
#79051=CARTESIAN_POINT('Ctrl Pts',(-44.0740318425361,-18.1176140700699,
0.));
#79052=CARTESIAN_POINT('Ctrl Pts',(-44.0740318425361,-18.1176140700699,
20.));
#79053=CARTESIAN_POINT('Ctrl Pts',(-44.0838677840754,-18.0857511501043,
0.));
#79054=CARTESIAN_POINT('Ctrl Pts',(-44.0838677840754,-18.0857511501043,
20.));
#79055=CARTESIAN_POINT('Ctrl Pts',(-44.0936811871546,-18.0538824496962,
0.));
#79056=CARTESIAN_POINT('Ctrl Pts',(-44.0936811871546,-18.0538824496962,
20.));
#79057=CARTESIAN_POINT('Ctrl Pts',(-44.1034720478372,-18.0220079845822,
0.));
#79058=CARTESIAN_POINT('Ctrl Pts',(-44.1034720478372,-18.0220079845822,
20.));
#79059=CARTESIAN_POINT('Ctrl Pts',(-44.1132403621971,-17.9901277705015,
0.));
#79060=CARTESIAN_POINT('Ctrl Pts',(-44.1132403621971,-17.9901277705015,
20.));
#79061=CARTESIAN_POINT('Ctrl Pts',(-44.1229861263191,-17.9582418231966,
0.));
#79062=CARTESIAN_POINT('Ctrl Pts',(-44.1229861263191,-17.9582418231966,
20.));
#79063=CARTESIAN_POINT('Ctrl Pts',(-44.1327093362991,-17.9263501584131,
0.));
#79064=CARTESIAN_POINT('Ctrl Pts',(-44.1327093362991,-17.9263501584131,
20.));
#79065=CARTESIAN_POINT('Ctrl Pts',(-44.142409988244,-17.8944527919,0.));
#79066=CARTESIAN_POINT('Ctrl Pts',(-44.142409988244,-17.8944527919,20.));
#79067=CARTESIAN_POINT('Ctrl Pts',(-44.1520880782717,-17.8625497394092,
0.));
#79068=CARTESIAN_POINT('Ctrl Pts',(-44.1520880782717,-17.8625497394092,
20.));
#79069=CARTESIAN_POINT('Ctrl Pts',(-44.1617436025112,-17.8306410166963,
0.));
#79070=CARTESIAN_POINT('Ctrl Pts',(-44.1617436025112,-17.8306410166963,
20.));
#79071=CARTESIAN_POINT('Ctrl Pts',(-44.1713765571021,-17.7987266395196,
0.));
#79072=CARTESIAN_POINT('Ctrl Pts',(-44.1713765571021,-17.7987266395196,
20.));
#79073=CARTESIAN_POINT('Ctrl Pts',(-44.1809869381949,-17.7668066236405,
0.));
#79074=CARTESIAN_POINT('Ctrl Pts',(-44.1809869381949,-17.7668066236405,
20.));
#79075=CARTESIAN_POINT('Ctrl Pts',(-44.1905747419505,-17.7348809848234,
0.));
#79076=CARTESIAN_POINT('Ctrl Pts',(-44.1905747419505,-17.7348809848234,
20.));
#79077=CARTESIAN_POINT('Ctrl Pts',(-44.2001399645408,-17.7029497388358,
0.));
#79078=CARTESIAN_POINT('Ctrl Pts',(-44.2001399645408,-17.7029497388358,
20.));
#79079=CARTESIAN_POINT('Ctrl Pts',(-44.2096826021493,-17.6710129014481,
0.));
#79080=CARTESIAN_POINT('Ctrl Pts',(-44.2096826021493,-17.6710129014481,
20.));
#79081=CARTESIAN_POINT('Ctrl Pts',(-44.2192026509705,-17.6390704884341,
0.));
#79082=CARTESIAN_POINT('Ctrl Pts',(-44.2192026509705,-17.6390704884341,
20.));
#79083=CARTESIAN_POINT('Ctrl Pts',(-44.2287001072093,-17.6071225155702,
0.));
#79084=CARTESIAN_POINT('Ctrl Pts',(-44.2287001072093,-17.6071225155702,
20.));
#79085=CARTESIAN_POINT('Ctrl Pts',(-44.2381749670816,-17.5751689986363,
0.));
#79086=CARTESIAN_POINT('Ctrl Pts',(-44.2381749670816,-17.5751689986363,
20.));
#79087=CARTESIAN_POINT('Ctrl Pts',(-44.2476272268138,-17.5432099534151,
0.));
#79088=CARTESIAN_POINT('Ctrl Pts',(-44.2476272268138,-17.5432099534151,
20.));
#79089=CARTESIAN_POINT('Ctrl Pts',(-44.2570568826434,-17.5112453956925,
0.));
#79090=CARTESIAN_POINT('Ctrl Pts',(-44.2570568826434,-17.5112453956925,
20.));
#79091=CARTESIAN_POINT('Ctrl Pts',(-44.2664639308192,-17.4792753412574,
0.));
#79092=CARTESIAN_POINT('Ctrl Pts',(-44.2664639308192,-17.4792753412574,
20.));
#79093=CARTESIAN_POINT('Ctrl Pts',(-44.2758483676008,-17.447299805902,0.));
#79094=CARTESIAN_POINT('Ctrl Pts',(-44.2758483676008,-17.447299805902,20.));
#79095=CARTESIAN_POINT('Ctrl Pts',(-44.2852101892593,-17.4153188054211,
0.));
#79096=CARTESIAN_POINT('Ctrl Pts',(-44.2852101892593,-17.4153188054211,
20.));
#79097=CARTESIAN_POINT('Ctrl Pts',(-44.2945493920761,-17.3833323556128,
0.));
#79098=CARTESIAN_POINT('Ctrl Pts',(-44.2945493920761,-17.3833323556128,
20.));
#79099=CARTESIAN_POINT('Ctrl Pts',(-44.3038659723435,-17.3513404722779,
0.));
#79100=CARTESIAN_POINT('Ctrl Pts',(-44.3038659723435,-17.3513404722779,
20.));
#79101=CARTESIAN_POINT('Ctrl Pts',(-44.3131599263643,-17.3193431712198,
0.));
#79102=CARTESIAN_POINT('Ctrl Pts',(-44.3131599263643,-17.3193431712198,
20.));
#79103=CARTESIAN_POINT('Ctrl Pts',(-44.3224312504523,-17.2873404682456,
0.));
#79104=CARTESIAN_POINT('Ctrl Pts',(-44.3224312504523,-17.2873404682456,
20.));
#79105=CARTESIAN_POINT('Ctrl Pts',(-44.3316799409325,-17.2553323791649,
0.));
#79106=CARTESIAN_POINT('Ctrl Pts',(-44.3316799409325,-17.2553323791649,
20.));
#79107=CARTESIAN_POINT('Ctrl Pts',(-44.340905994141,-17.2233189197905,0.));
#79108=CARTESIAN_POINT('Ctrl Pts',(-44.340905994141,-17.2233189197905,20.));
#79109=CARTESIAN_POINT('Ctrl Pts',(-44.3501094064252,-17.1913001059384,
0.));
#79110=CARTESIAN_POINT('Ctrl Pts',(-44.3501094064252,-17.1913001059384,
20.));
#79111=CARTESIAN_POINT('Ctrl Pts',(-44.3592901741436,-17.1592759534275,
0.));
#79112=CARTESIAN_POINT('Ctrl Pts',(-44.3592901741436,-17.1592759534275,
20.));
#79113=CARTESIAN_POINT('Ctrl Pts',(-44.3684482936655,-17.1272464780797,
0.));
#79114=CARTESIAN_POINT('Ctrl Pts',(-44.3684482936655,-17.1272464780797,
20.));
#79115=CARTESIAN_POINT('Ctrl Pts',(-44.3775837613707,-17.0952116957196,
0.));
#79116=CARTESIAN_POINT('Ctrl Pts',(-44.3775837613707,-17.0952116957196,
20.));
#79117=CARTESIAN_POINT('Ctrl Pts',(-44.3866965736492,-17.0631716221745,
0.));
#79118=CARTESIAN_POINT('Ctrl Pts',(-44.3866965736492,-17.0631716221745,
20.));
#79119=CARTESIAN_POINT('Ctrl Pts',(-44.3957867269024,-17.0311262732746,
0.));
#79120=CARTESIAN_POINT('Ctrl Pts',(-44.3957867269024,-17.0311262732746,
20.));
#79121=CARTESIAN_POINT('Ctrl Pts',(-44.404854217543,-16.9990756648532,0.));
#79122=CARTESIAN_POINT('Ctrl Pts',(-44.404854217543,-16.9990756648532,20.));
#79123=CARTESIAN_POINT('Ctrl Pts',(-44.4138990419958,-16.967019812747,0.));
#79124=CARTESIAN_POINT('Ctrl Pts',(-44.4138990419958,-16.967019812747,20.));
#79125=CARTESIAN_POINT('Ctrl Pts',(-44.4229211966955,-16.9349587327952,
0.));
#79126=CARTESIAN_POINT('Ctrl Pts',(-44.4229211966955,-16.9349587327952,
20.));
#79127=CARTESIAN_POINT('Ctrl Pts',(-44.431920678088,-16.9028924408399,0.));
#79128=CARTESIAN_POINT('Ctrl Pts',(-44.431920678088,-16.9028924408399,20.));
#79129=CARTESIAN_POINT('Ctrl Pts',(-44.4408974826294,-16.870820952726,0.));
#79130=CARTESIAN_POINT('Ctrl Pts',(-44.4408974826294,-16.870820952726,20.));
#79131=CARTESIAN_POINT('Ctrl Pts',(-44.4498516067869,-16.8387442843012,
0.));
#79132=CARTESIAN_POINT('Ctrl Pts',(-44.4498516067869,-16.8387442843012,
20.));
#79133=CARTESIAN_POINT('Ctrl Pts',(-44.4587830470388,-16.8066624514163,
0.));
#79134=CARTESIAN_POINT('Ctrl Pts',(-44.4587830470388,-16.8066624514163,
20.));
#79135=CARTESIAN_POINT('Ctrl Pts',(-44.4676917998748,-16.7745754699247,
0.));
#79136=CARTESIAN_POINT('Ctrl Pts',(-44.4676917998748,-16.7745754699247,
20.));
#79137=CARTESIAN_POINT('Ctrl Pts',(-44.4765778617956,-16.742483355683,0.));
#79138=CARTESIAN_POINT('Ctrl Pts',(-44.4765778617956,-16.742483355683,20.));
#79139=CARTESIAN_POINT('Ctrl Pts',(-44.4854412293128,-16.7103861245505,
0.));
#79140=CARTESIAN_POINT('Ctrl Pts',(-44.4854412293128,-16.7103861245505,
20.));
#79141=CARTESIAN_POINT('Ctrl Pts',(-44.4942818989491,-16.6782837923892,
0.));
#79142=CARTESIAN_POINT('Ctrl Pts',(-44.4942818989491,-16.6782837923892,
20.));
#79143=CARTESIAN_POINT('Ctrl Pts',(-44.5030998672381,-16.6461763750644,
0.));
#79144=CARTESIAN_POINT('Ctrl Pts',(-44.5030998672381,-16.6461763750644,
20.));
#79145=CARTESIAN_POINT('Ctrl Pts',(-44.5118951307243,-16.6140638884438,
0.));
#79146=CARTESIAN_POINT('Ctrl Pts',(-44.5118951307243,-16.6140638884438,
20.));
#79147=CARTESIAN_POINT('Ctrl Pts',(-44.5206676859633,-16.581946348398,0.));
#79148=CARTESIAN_POINT('Ctrl Pts',(-44.5206676859633,-16.581946348398,20.));
#79149=CARTESIAN_POINT('Ctrl Pts',(-44.5294175295214,-16.5498237708003,
0.));
#79150=CARTESIAN_POINT('Ctrl Pts',(-44.5294175295214,-16.5498237708003,
20.));
#79151=CARTESIAN_POINT('Ctrl Pts',(-44.5381446579761,-16.5176961715269,
0.));
#79152=CARTESIAN_POINT('Ctrl Pts',(-44.5381446579761,-16.5176961715269,
20.));
#79153=CARTESIAN_POINT('Ctrl Pts',(-44.5468490679154,-16.4855635664567,
0.));
#79154=CARTESIAN_POINT('Ctrl Pts',(-44.5468490679154,-16.4855635664567,
20.));
#79155=CARTESIAN_POINT('Ctrl Pts',(-44.5555307559385,-16.4534259714715,
0.));
#79156=CARTESIAN_POINT('Ctrl Pts',(-44.5555307559385,-16.4534259714715,
20.));
#79157=CARTESIAN_POINT('Ctrl Pts',(-44.5641897186557,-16.4212834024559,
0.));
#79158=CARTESIAN_POINT('Ctrl Pts',(-44.5641897186557,-16.4212834024559,
20.));
#79159=CARTESIAN_POINT('Ctrl Pts',(-44.5728259526889,-16.3891358752972,
0.));
#79160=CARTESIAN_POINT('Ctrl Pts',(-44.5728259526889,-16.3891358752972,
20.));
#79161=CARTESIAN_POINT('Ctrl Pts',(-44.581439454671,-16.3569834058857,0.));
#79162=CARTESIAN_POINT('Ctrl Pts',(-44.581439454671,-16.3569834058857,20.));
#79163=CARTESIAN_POINT('Ctrl Pts',(-44.5900302212458,-16.3248260101143,
0.));
#79164=CARTESIAN_POINT('Ctrl Pts',(-44.5900302212458,-16.3248260101143,
20.));
#79165=CARTESIAN_POINT('Ctrl Pts',(-44.5985982490682,-16.2926637038787,
0.));
#79166=CARTESIAN_POINT('Ctrl Pts',(-44.5985982490682,-16.2926637038787,
20.));
#79167=CARTESIAN_POINT('Ctrl Pts',(-44.6071435348036,-16.2604965030773,
0.));
#79168=CARTESIAN_POINT('Ctrl Pts',(-44.6071435348036,-16.2604965030773,
20.));
#79169=CARTESIAN_POINT('Ctrl Pts',(-44.6156660751288,-16.2283244236112,
0.));
#79170=CARTESIAN_POINT('Ctrl Pts',(-44.6156660751288,-16.2283244236112,
20.));
#79171=CARTESIAN_POINT('Ctrl Pts',(-44.6241658667307,-16.196147481384,0.));
#79172=CARTESIAN_POINT('Ctrl Pts',(-44.6241658667307,-16.196147481384,20.));
#79173=CARTESIAN_POINT('Ctrl Pts',(-44.6326429063072,-16.1639656923022,
0.));
#79174=CARTESIAN_POINT('Ctrl Pts',(-44.6326429063072,-16.1639656923022,
20.));
#79175=CARTESIAN_POINT('Ctrl Pts',(-44.6410971905673,-16.131779072275,0.));
#79176=CARTESIAN_POINT('Ctrl Pts',(-44.6410971905673,-16.131779072275,20.));
#79177=CARTESIAN_POINT('Ctrl Pts',(-44.649528716232,-16.0995876372141,0.));
#79178=CARTESIAN_POINT('Ctrl Pts',(-44.649528716232,-16.0995876372141,20.));
#79179=CARTESIAN_POINT('Ctrl Pts',(-44.6579374800339,-16.0673914030343,
0.));
#79180=CARTESIAN_POINT('Ctrl Pts',(-44.6579374800339,-16.0673914030343,
20.));
#79181=CARTESIAN_POINT('Ctrl Pts',(-44.6663234787169,-16.0351903856534,
0.));
#79182=CARTESIAN_POINT('Ctrl Pts',(-44.6663234787169,-16.0351903856534,
20.));
#79183=CARTESIAN_POINT('Ctrl Pts',(-44.6746867090345,-16.0029846009915,
0.));
#79184=CARTESIAN_POINT('Ctrl Pts',(-44.6746867090345,-16.0029846009915,
20.));
#79185=CARTESIAN_POINT('Ctrl Pts',(-44.6830271677516,-15.9707740649715,
0.));
#79186=CARTESIAN_POINT('Ctrl Pts',(-44.6830271677516,-15.9707740649715,
20.));
#79187=CARTESIAN_POINT('Ctrl Pts',(-44.691344851643,-15.9385587935186,0.));
#79188=CARTESIAN_POINT('Ctrl Pts',(-44.691344851643,-15.9385587935186,20.));
#79189=CARTESIAN_POINT('Ctrl Pts',(-44.6996397574952,-15.9063388025603,
0.));
#79190=CARTESIAN_POINT('Ctrl Pts',(-44.6996397574952,-15.9063388025603,
20.));
#79191=CARTESIAN_POINT('Ctrl Pts',(-44.7079118821065,-15.8741141080271,
0.));
#79192=CARTESIAN_POINT('Ctrl Pts',(-44.7079118821065,-15.8741141080271,
20.));
#79193=CARTESIAN_POINT('Ctrl Pts',(-44.7161612222865,-15.8418847258528,
0.));
#79194=CARTESIAN_POINT('Ctrl Pts',(-44.7161612222865,-15.8418847258528,
20.));
#79195=CARTESIAN_POINT('Ctrl Pts',(-44.7243877748558,-15.8096506719735,
0.));
#79196=CARTESIAN_POINT('Ctrl Pts',(-44.7243877748558,-15.8096506719735,
20.));
#79197=CARTESIAN_POINT('Ctrl Pts',(-44.7325915366458,-15.7774119623278,
0.));
#79198=CARTESIAN_POINT('Ctrl Pts',(-44.7325915366458,-15.7774119623278,
20.));
#79199=CARTESIAN_POINT('Ctrl Pts',(-44.7407725044985,-15.745168612857,0.));
#79200=CARTESIAN_POINT('Ctrl Pts',(-44.7407725044985,-15.745168612857,20.));
#79201=CARTESIAN_POINT('Ctrl Pts',(-44.7489306752664,-15.7129206395047,
0.));
#79202=CARTESIAN_POINT('Ctrl Pts',(-44.7489306752664,-15.7129206395047,
20.));
#79203=CARTESIAN_POINT('Ctrl Pts',(-44.7570660458133,-15.6806680582172,
0.));
#79204=CARTESIAN_POINT('Ctrl Pts',(-44.7570660458133,-15.6806680582172,
20.));
#79205=CARTESIAN_POINT('Ctrl Pts',(-44.7651786130144,-15.6484108849434,
0.));
#79206=CARTESIAN_POINT('Ctrl Pts',(-44.7651786130144,-15.6484108849434,
20.));
#79207=CARTESIAN_POINT('Ctrl Pts',(-44.7732683737566,-15.6161491356348,
0.));
#79208=CARTESIAN_POINT('Ctrl Pts',(-44.7732683737566,-15.6161491356348,
20.));
#79209=CARTESIAN_POINT('Ctrl Pts',(-44.7813353249379,-15.583882826246,0.));
#79210=CARTESIAN_POINT('Ctrl Pts',(-44.7813353249379,-15.583882826246,20.));
#79211=CARTESIAN_POINT('Ctrl Pts',(-44.7893794634672,-15.5516119727338,
0.));
#79212=CARTESIAN_POINT('Ctrl Pts',(-44.7893794634672,-15.5516119727338,
20.));
#79213=CARTESIAN_POINT('Ctrl Pts',(-44.7974007862643,-15.5193365910578,
0.));
#79214=CARTESIAN_POINT('Ctrl Pts',(-44.7974007862643,-15.5193365910578,
20.));
#79215=CARTESIAN_POINT('Ctrl Pts',(-44.8053992902599,-15.4870566971798,
0.));
#79216=CARTESIAN_POINT('Ctrl Pts',(-44.8053992902599,-15.4870566971798,
20.));
#79217=CARTESIAN_POINT('Ctrl Pts',(-44.8133749723964,-15.4547723070643,
0.));
#79218=CARTESIAN_POINT('Ctrl Pts',(-44.8133749723964,-15.4547723070643,
20.));
#79219=CARTESIAN_POINT('Ctrl Pts',(-44.8213278296263,-15.4224834366782,
0.));
#79220=CARTESIAN_POINT('Ctrl Pts',(-44.8213278296263,-15.4224834366782,
20.));
#79221=CARTESIAN_POINT('Ctrl Pts',(-44.8292578589132,-15.3901901019906,
0.));
#79222=CARTESIAN_POINT('Ctrl Pts',(-44.8292578589132,-15.3901901019906,
20.));
#79223=CARTESIAN_POINT('Ctrl Pts',(-44.8371650572316,-15.3578923189739,
0.));
#79224=CARTESIAN_POINT('Ctrl Pts',(-44.8371650572316,-15.3578923189739,
20.));
#79225=CARTESIAN_POINT('Ctrl Pts',(-44.8450494215678,-15.3255901036026,
0.));
#79226=CARTESIAN_POINT('Ctrl Pts',(-44.8450494215678,-15.3255901036026,
20.));
#79227=CARTESIAN_POINT('Ctrl Pts',(-44.8529109489191,-15.2932834718541,
0.));
#79228=CARTESIAN_POINT('Ctrl Pts',(-44.8529109489191,-15.2932834718541,
20.));
#79229=CARTESIAN_POINT('Ctrl Pts',(-44.8607496362943,-15.2609724397079,
0.));
#79230=CARTESIAN_POINT('Ctrl Pts',(-44.8607496362943,-15.2609724397079,
20.));
#79231=CARTESIAN_POINT('Ctrl Pts',(-44.8685654807131,-15.2286570231461,
0.));
#79232=CARTESIAN_POINT('Ctrl Pts',(-44.8685654807131,-15.2286570231461,
20.));
#79233=CARTESIAN_POINT('Ctrl Pts',(-44.8763584792064,-15.1963372381533,
0.));
#79234=CARTESIAN_POINT('Ctrl Pts',(-44.8763584792064,-15.1963372381533,
20.));
#79235=CARTESIAN_POINT('Ctrl Pts',(-44.8841286288163,-15.1640131007166,
0.));
#79236=CARTESIAN_POINT('Ctrl Pts',(-44.8841286288163,-15.1640131007166,
20.));
#79237=CARTESIAN_POINT('Ctrl Pts',(-44.8918759265956,-15.1316846268256,
0.));
#79238=CARTESIAN_POINT('Ctrl Pts',(-44.8918759265956,-15.1316846268256,
20.));
#79239=CARTESIAN_POINT('Ctrl Pts',(-44.8996003696078,-15.0993518324721,
0.));
#79240=CARTESIAN_POINT('Ctrl Pts',(-44.8996003696078,-15.0993518324721,
20.));
#79241=CARTESIAN_POINT('Ctrl Pts',(-44.9073019549277,-15.0670147336509,
0.));
#79242=CARTESIAN_POINT('Ctrl Pts',(-44.9073019549277,-15.0670147336509,
20.));
#79243=CARTESIAN_POINT('Ctrl Pts',(-44.9149806796409,-15.034673346359,0.));
#79244=CARTESIAN_POINT('Ctrl Pts',(-44.9149806796409,-15.034673346359,20.));
#79245=CARTESIAN_POINT('Ctrl Pts',(-44.9226365408441,-15.0023276865958,
0.));
#79246=CARTESIAN_POINT('Ctrl Pts',(-44.9226365408441,-15.0023276865958,
20.));
#79247=CARTESIAN_POINT('Ctrl Pts',(-44.9302695356455,-14.969977770363,0.));
#79248=CARTESIAN_POINT('Ctrl Pts',(-44.9302695356455,-14.969977770363,20.));
#79249=CARTESIAN_POINT('Ctrl Pts',(-44.9378796611651,-14.9376236136649,
0.));
#79250=CARTESIAN_POINT('Ctrl Pts',(-44.9378796611651,-14.9376236136649,
20.));
#79251=CARTESIAN_POINT('Ctrl Pts',(-44.9454669145344,-14.9052652325081,
0.));
#79252=CARTESIAN_POINT('Ctrl Pts',(-44.9454669145344,-14.9052652325081,
20.));
#79253=CARTESIAN_POINT('Ctrl Pts',(-44.9530312928958,-14.8729026429019,
0.));
#79254=CARTESIAN_POINT('Ctrl Pts',(-44.9530312928958,-14.8729026429019,
20.));
#79255=CARTESIAN_POINT('Ctrl Pts',(-44.9605727934022,-14.8405358608577,
0.));
#79256=CARTESIAN_POINT('Ctrl Pts',(-44.9605727934022,-14.8405358608577,
20.));
#79257=CARTESIAN_POINT('Ctrl Pts',(-44.9680914132176,-14.8081649023895,
0.));
#79258=CARTESIAN_POINT('Ctrl Pts',(-44.9680914132176,-14.8081649023895,
20.));
#79259=CARTESIAN_POINT('Ctrl Pts',(-44.9755871495162,-14.7757897835134,
0.));
#79260=CARTESIAN_POINT('Ctrl Pts',(-44.9755871495162,-14.7757897835134,
20.));
#79261=CARTESIAN_POINT('Ctrl Pts',(-44.9830599994838,-14.7434105202483,
0.));
#79262=CARTESIAN_POINT('Ctrl Pts',(-44.9830599994838,-14.7434105202483,
20.));
#79263=CARTESIAN_POINT('Ctrl Pts',(-44.9905099603172,-14.7110271286153,
0.));
#79264=CARTESIAN_POINT('Ctrl Pts',(-44.9905099603172,-14.7110271286153,
20.));
#79265=CARTESIAN_POINT('Ctrl Pts',(-44.9979370292253,-14.6786396246378,
0.));
#79266=CARTESIAN_POINT('Ctrl Pts',(-44.9979370292253,-14.6786396246378,
20.));
#79267=CARTESIAN_POINT('Ctrl Pts',(-45.0053412034276,-14.6462480243418,
0.));
#79268=CARTESIAN_POINT('Ctrl Pts',(-45.0053412034276,-14.6462480243418,
20.));
#79269=CARTESIAN_POINT('Ctrl Pts',(-45.0127224801553,-14.6138523437553,
0.));
#79270=CARTESIAN_POINT('Ctrl Pts',(-45.0127224801553,-14.6138523437553,
20.));
#79271=CARTESIAN_POINT('Ctrl Pts',(-45.020080856651,-14.5814525989087,0.));
#79272=CARTESIAN_POINT('Ctrl Pts',(-45.020080856651,-14.5814525989087,20.));
#79273=CARTESIAN_POINT('Ctrl Pts',(-45.0274163301681,-14.5490488058349,
0.));
#79274=CARTESIAN_POINT('Ctrl Pts',(-45.0274163301681,-14.5490488058349,
20.));
#79275=CARTESIAN_POINT('Ctrl Pts',(-45.0347288979708,-14.516640980569,0.));
#79276=CARTESIAN_POINT('Ctrl Pts',(-45.0347288979708,-14.516640980569,20.));
#79277=CARTESIAN_POINT('Ctrl Pts',(-45.0420185573342,-14.4842291391484,
0.));
#79278=CARTESIAN_POINT('Ctrl Pts',(-45.0420185573342,-14.4842291391484,
20.));
#79279=CARTESIAN_POINT('Ctrl Pts',(-45.0492853055441,-14.451813297613,0.));
#79280=CARTESIAN_POINT('Ctrl Pts',(-45.0492853055441,-14.451813297613,20.));
#79281=CARTESIAN_POINT('Ctrl Pts',(-45.0565291398984,-14.4193934720051,
0.));
#79282=CARTESIAN_POINT('Ctrl Pts',(-45.0565291398984,-14.4193934720051,
20.));
#79283=CARTESIAN_POINT('Ctrl Pts',(-45.0637500577056,-14.3869696783692,
0.));
#79284=CARTESIAN_POINT('Ctrl Pts',(-45.0637500577056,-14.3869696783692,
20.));
#79285=CARTESIAN_POINT('Ctrl Pts',(-45.0709480562863,-14.354541932752,0.));
#79286=CARTESIAN_POINT('Ctrl Pts',(-45.0709480562863,-14.354541932752,20.));
#79287=CARTESIAN_POINT('Ctrl Pts',(-45.078123132972,-14.3221102512025,0.));
#79288=CARTESIAN_POINT('Ctrl Pts',(-45.078123132972,-14.3221102512025,20.));
#79289=CARTESIAN_POINT('Ctrl Pts',(-45.0852752851048,-14.2896746497719,
0.));
#79290=CARTESIAN_POINT('Ctrl Pts',(-45.0852752851048,-14.2896746497719,
20.));
#79291=CARTESIAN_POINT('Ctrl Pts',(-45.0924045100383,-14.2572351445137,
0.));
#79292=CARTESIAN_POINT('Ctrl Pts',(-45.0924045100383,-14.2572351445137,
20.));
#79293=CARTESIAN_POINT('Ctrl Pts',(-45.0995108051367,-14.2247917514836,
0.));
#79294=CARTESIAN_POINT('Ctrl Pts',(-45.0995108051367,-14.2247917514836,
20.));
#79295=CARTESIAN_POINT('Ctrl Pts',(-45.1065941677758,-14.1923444867396,
0.));
#79296=CARTESIAN_POINT('Ctrl Pts',(-45.1065941677758,-14.1923444867396,
20.));
#79297=CARTESIAN_POINT('Ctrl Pts',(-45.1136545953429,-14.1598933663422,
0.));
#79298=CARTESIAN_POINT('Ctrl Pts',(-45.1136545953429,-14.1598933663422,
20.));
#79299=CARTESIAN_POINT('Ctrl Pts',(-45.1206920852361,-14.127438406354,0.));
#79300=CARTESIAN_POINT('Ctrl Pts',(-45.1206920852361,-14.127438406354,20.));
#79301=CARTESIAN_POINT('Ctrl Pts',(-45.127706634865,-14.0949796228398,0.));
#79302=CARTESIAN_POINT('Ctrl Pts',(-45.127706634865,-14.0949796228398,20.));
#79303=CARTESIAN_POINT('Ctrl Pts',(-45.1346982416501,-14.0625170318664,
0.));
#79304=CARTESIAN_POINT('Ctrl Pts',(-45.1346982416501,-14.0625170318664,
20.));
#79305=CARTESIAN_POINT('Ctrl Pts',(-45.1416669030232,-14.0300506495033,
0.));
#79306=CARTESIAN_POINT('Ctrl Pts',(-45.1416669030232,-14.0300506495033,
20.));
#79307=CARTESIAN_POINT('Ctrl Pts',(-45.1486126164275,-13.997580491822,0.));
#79308=CARTESIAN_POINT('Ctrl Pts',(-45.1486126164275,-13.997580491822,20.));
#79309=CARTESIAN_POINT('Ctrl Pts',(-45.1555353793172,-13.9651065748961,
0.));
#79310=CARTESIAN_POINT('Ctrl Pts',(-45.1555353793172,-13.9651065748961,
20.));
#79311=CARTESIAN_POINT('Ctrl Pts',(-45.1624351891574,-13.9326289148012,
0.));
#79312=CARTESIAN_POINT('Ctrl Pts',(-45.1624351891574,-13.9326289148012,
20.));
#79313=CARTESIAN_POINT('Ctrl Pts',(-45.1693120434241,-13.9001475276153,
0.));
#79314=CARTESIAN_POINT('Ctrl Pts',(-45.1693120434241,-13.9001475276153,
20.));
#79315=CARTESIAN_POINT('Ctrl Pts',(-45.1761659396043,-13.8676624294184,
0.));
#79316=CARTESIAN_POINT('Ctrl Pts',(-45.1761659396043,-13.8676624294184,
20.));
#79317=CARTESIAN_POINT('Ctrl Pts',(-45.1829968751969,-13.8351736362929,
0.));
#79318=CARTESIAN_POINT('Ctrl Pts',(-45.1829968751969,-13.8351736362929,
20.));
#79319=CARTESIAN_POINT('Ctrl Pts',(-45.1898048477123,-13.8026811643234,
0.));
#79320=CARTESIAN_POINT('Ctrl Pts',(-45.1898048477123,-13.8026811643234,
20.));
#79321=CARTESIAN_POINT('Ctrl Pts',(-45.1965898546723,-13.7701850295967,
0.));
#79322=CARTESIAN_POINT('Ctrl Pts',(-45.1965898546723,-13.7701850295967,
20.));
#79323=CARTESIAN_POINT('Ctrl Pts',(-45.2033518936101,-13.7376852482019,
0.));
#79324=CARTESIAN_POINT('Ctrl Pts',(-45.2033518936101,-13.7376852482019,
20.));
#79325=CARTESIAN_POINT('Ctrl Pts',(-45.2100909620697,-13.7051818362299,
0.));
#79326=CARTESIAN_POINT('Ctrl Pts',(-45.2100909620697,-13.7051818362299,
20.));
#79327=CARTESIAN_POINT('Ctrl Pts',(-45.2168070576061,-13.6726748097738,
0.));
#79328=CARTESIAN_POINT('Ctrl Pts',(-45.2168070576061,-13.6726748097738,
20.));
#79329=CARTESIAN_POINT('Ctrl Pts',(-45.2235001777847,-13.6401641849286,
0.));
#79330=CARTESIAN_POINT('Ctrl Pts',(-45.2235001777847,-13.6401641849286,
20.));
#79331=CARTESIAN_POINT('Ctrl Pts',(-45.2301703201819,-13.6076499777914,
0.));
#79332=CARTESIAN_POINT('Ctrl Pts',(-45.2301703201819,-13.6076499777914,
20.));
#79333=CARTESIAN_POINT('Ctrl Pts',(-45.2368174823856,-13.5751322044618,
0.));
#79334=CARTESIAN_POINT('Ctrl Pts',(-45.2368174823856,-13.5751322044618,
20.));
#79335=CARTESIAN_POINT('Ctrl Pts',(-45.2434416619952,-13.542610881041,0.));
#79336=CARTESIAN_POINT('Ctrl Pts',(-45.2434416619952,-13.542610881041,20.));
#79337=CARTESIAN_POINT('Ctrl Pts',(-45.2500428566225,-13.5100860236329,
0.));
#79338=CARTESIAN_POINT('Ctrl Pts',(-45.2500428566225,-13.5100860236329,
20.));
#79339=CARTESIAN_POINT('Ctrl Pts',(-45.2566210638904,-13.4775576483433,
0.));
#79340=CARTESIAN_POINT('Ctrl Pts',(-45.2566210638904,-13.4775576483433,
20.));
#79341=CARTESIAN_POINT('Ctrl Pts',(-45.2631762814325,-13.44502577128,0.));
#79342=CARTESIAN_POINT('Ctrl Pts',(-45.2631762814325,-13.44502577128,20.));
#79343=CARTESIAN_POINT('Ctrl Pts',(-45.2697085068935,-13.4124904085531,
0.));
#79344=CARTESIAN_POINT('Ctrl Pts',(-45.2697085068935,-13.4124904085531,
20.));
#79345=CARTESIAN_POINT('Ctrl Pts',(-45.276217737929,-13.3799515762744,0.));
#79346=CARTESIAN_POINT('Ctrl Pts',(-45.276217737929,-13.3799515762744,20.));
#79347=CARTESIAN_POINT('Ctrl Pts',(-45.2827039722059,-13.3474092905576,
0.));
#79348=CARTESIAN_POINT('Ctrl Pts',(-45.2827039722059,-13.3474092905576,
20.));
#79349=CARTESIAN_POINT('Ctrl Pts',(-45.2891672074022,-13.3148635675188,
0.));
#79350=CARTESIAN_POINT('Ctrl Pts',(-45.2891672074022,-13.3148635675188,
20.));
#79351=CARTESIAN_POINT('Ctrl Pts',(-45.2956074412073,-13.282314423276,0.));
#79352=CARTESIAN_POINT('Ctrl Pts',(-45.2956074412073,-13.282314423276,20.));
#79353=CARTESIAN_POINT('Ctrl Pts',(-45.3020246713218,-13.2497618739494,
0.));
#79354=CARTESIAN_POINT('Ctrl Pts',(-45.3020246713218,-13.2497618739494,
20.));
#79355=CARTESIAN_POINT('Ctrl Pts',(-45.3084188954577,-13.217205935661,0.));
#79356=CARTESIAN_POINT('Ctrl Pts',(-45.3084188954577,-13.217205935661,20.));
#79357=CARTESIAN_POINT('Ctrl Pts',(-45.3147901113387,-13.1846466245352,
0.));
#79358=CARTESIAN_POINT('Ctrl Pts',(-45.3147901113387,-13.1846466245352,
20.));
#79359=CARTESIAN_POINT('Ctrl Pts',(-45.321138316699,-13.1520839566979,0.));
#79360=CARTESIAN_POINT('Ctrl Pts',(-45.321138316699,-13.1520839566979,20.));
#79361=CARTESIAN_POINT('Ctrl Pts',(-45.3274635092846,-13.1195179482773,
0.));
#79362=CARTESIAN_POINT('Ctrl Pts',(-45.3274635092846,-13.1195179482773,
20.));
#79363=CARTESIAN_POINT('Ctrl Pts',(-45.3337656868523,-13.0869486154035,
0.));
#79364=CARTESIAN_POINT('Ctrl Pts',(-45.3337656868523,-13.0869486154035,
20.));
#79365=CARTESIAN_POINT('Ctrl Pts',(-45.3400448471699,-13.0543759742083,
0.));
#79366=CARTESIAN_POINT('Ctrl Pts',(-45.3400448471699,-13.0543759742083,
20.));
#79367=CARTESIAN_POINT('Ctrl Pts',(-45.3463009880171,-13.021800040826,0.));
#79368=CARTESIAN_POINT('Ctrl Pts',(-45.3463009880171,-13.021800040826,20.));
#79369=CARTESIAN_POINT('Ctrl Pts',(-45.3525341071849,-12.9892208313927,
0.));
#79370=CARTESIAN_POINT('Ctrl Pts',(-45.3525341071849,-12.9892208313927,
20.));
#79371=CARTESIAN_POINT('Ctrl Pts',(-45.3587442024753,-12.9566383620464,
0.));
#79372=CARTESIAN_POINT('Ctrl Pts',(-45.3587442024753,-12.9566383620464,
20.));
#79373=CARTESIAN_POINT('Ctrl Pts',(-45.3649312717011,-12.9240526489272,
0.));
#79374=CARTESIAN_POINT('Ctrl Pts',(-45.3649312717011,-12.9240526489272,
20.));
#79375=CARTESIAN_POINT('Ctrl Pts',(-45.371095312686,-12.8914637081769,0.));
#79376=CARTESIAN_POINT('Ctrl Pts',(-45.371095312686,-12.8914637081769,20.));
#79377=CARTESIAN_POINT('Ctrl Pts',(-45.3772363232658,-12.8588715559393,
0.));
#79378=CARTESIAN_POINT('Ctrl Pts',(-45.3772363232658,-12.8588715559393,
20.));
#79379=CARTESIAN_POINT('Ctrl Pts',(-45.3833543012877,-12.82627620836,0.));
#79380=CARTESIAN_POINT('Ctrl Pts',(-45.3833543012877,-12.82627620836,20.));
#79381=CARTESIAN_POINT('Ctrl Pts',(-45.3894492446102,-12.7936776815868,
0.));
#79382=CARTESIAN_POINT('Ctrl Pts',(-45.3894492446102,-12.7936776815868,
20.));
#79383=CARTESIAN_POINT('Ctrl Pts',(-45.3955211511034,-12.7610759917694,
0.));
#79384=CARTESIAN_POINT('Ctrl Pts',(-45.3955211511034,-12.7610759917694,
20.));
#79385=CARTESIAN_POINT('Ctrl Pts',(-45.4015700186485,-12.7284711550592,
0.));
#79386=CARTESIAN_POINT('Ctrl Pts',(-45.4015700186485,-12.7284711550592,
20.));
#79387=CARTESIAN_POINT('Ctrl Pts',(-45.407595845137,-12.6958631876099,0.));
#79388=CARTESIAN_POINT('Ctrl Pts',(-45.407595845137,-12.6958631876099,20.));
#79389=CARTESIAN_POINT('Ctrl Pts',(-45.4135986284717,-12.6632521055766,
0.));
#79390=CARTESIAN_POINT('Ctrl Pts',(-45.4135986284717,-12.6632521055766,
20.));
#79391=CARTESIAN_POINT('Ctrl Pts',(-45.4195783665665,-12.6306379251164,
0.));
#79392=CARTESIAN_POINT('Ctrl Pts',(-45.4195783665665,-12.6306379251164,
20.));
#79393=CARTESIAN_POINT('Ctrl Pts',(-45.4255350573473,-12.5980206623884,
0.));
#79394=CARTESIAN_POINT('Ctrl Pts',(-45.4255350573473,-12.5980206623884,
20.));
#79395=CARTESIAN_POINT('Ctrl Pts',(-45.4314686987515,-12.5654003335532,
0.));
#79396=CARTESIAN_POINT('Ctrl Pts',(-45.4314686987515,-12.5654003335532,
20.));
#79397=CARTESIAN_POINT('Ctrl Pts',(-45.4373792887274,-12.5327769547739,
0.));
#79398=CARTESIAN_POINT('Ctrl Pts',(-45.4373792887274,-12.5327769547739,
20.));
#79399=CARTESIAN_POINT('Ctrl Pts',(-45.4432668252347,-12.500150542215,0.));
#79400=CARTESIAN_POINT('Ctrl Pts',(-45.4432668252347,-12.500150542215,20.));
#79401=CARTESIAN_POINT('Ctrl Pts',(-45.4491313062444,-12.4675211120431,
0.));
#79402=CARTESIAN_POINT('Ctrl Pts',(-45.4491313062444,-12.4675211120431,
20.));
#79403=CARTESIAN_POINT('Ctrl Pts',(-45.4549727297392,-12.4348886804266,
0.));
#79404=CARTESIAN_POINT('Ctrl Pts',(-45.4549727297392,-12.4348886804266,
20.));
#79405=CARTESIAN_POINT('Ctrl Pts',(-45.4607910937128,-12.4022532635357,
0.));
#79406=CARTESIAN_POINT('Ctrl Pts',(-45.4607910937128,-12.4022532635357,
20.));
#79407=CARTESIAN_POINT('Ctrl Pts',(-45.4665863961701,-12.3696148775423,
0.));
#79408=CARTESIAN_POINT('Ctrl Pts',(-45.4665863961701,-12.3696148775423,
20.));
#79409=CARTESIAN_POINT('Ctrl Pts',(-45.4723586351267,-12.3369735386201,
0.));
#79410=CARTESIAN_POINT('Ctrl Pts',(-45.4723586351267,-12.3369735386201,
20.));
#79411=CARTESIAN_POINT('Ctrl Pts',(-45.4781078086095,-12.3043292629445,
0.));
#79412=CARTESIAN_POINT('Ctrl Pts',(-45.4781078086095,-12.3043292629445,
20.));
#79413=CARTESIAN_POINT('Ctrl Pts',(-45.483833914657,-12.2716820666929,0.));
#79414=CARTESIAN_POINT('Ctrl Pts',(-45.483833914657,-12.2716820666929,20.));
#79415=CARTESIAN_POINT('Ctrl Pts',(-45.4895369513189,-12.2390319660445,
0.));
#79416=CARTESIAN_POINT('Ctrl Pts',(-45.4895369513189,-12.2390319660445,
20.));
#79417=CARTESIAN_POINT('Ctrl Pts',(-45.4952169166561,-12.2063789771801,
0.));
#79418=CARTESIAN_POINT('Ctrl Pts',(-45.4952169166561,-12.2063789771801,
20.));
#79419=CARTESIAN_POINT('Ctrl Pts',(-45.5008738087416,-12.1737231162825,
0.));
#79420=CARTESIAN_POINT('Ctrl Pts',(-45.5008738087416,-12.1737231162825,
20.));
#79421=CARTESIAN_POINT('Ctrl Pts',(-45.5065076256599,-12.1410643995363,
0.));
#79422=CARTESIAN_POINT('Ctrl Pts',(-45.5065076256599,-12.1410643995363,
20.));
#79423=CARTESIAN_POINT('Ctrl Pts',(-45.5121183655068,-12.1084028431278,
0.));
#79424=CARTESIAN_POINT('Ctrl Pts',(-45.5121183655068,-12.1084028431278,
20.));
#79425=CARTESIAN_POINT('Ctrl Pts',(-45.5177060263888,-12.0757384632451,
0.));
#79426=CARTESIAN_POINT('Ctrl Pts',(-45.5177060263888,-12.0757384632451,
20.));
#79427=CARTESIAN_POINT('Ctrl Pts',(-45.5232706064237,-12.0430712760778,
0.));
#79428=CARTESIAN_POINT('Ctrl Pts',(-45.5232706064237,-12.0430712760778,
20.));
#79429=CARTESIAN_POINT('Ctrl Pts',(-45.5288121037395,-12.0104012978174,
0.));
#79430=CARTESIAN_POINT('Ctrl Pts',(-45.5288121037395,-12.0104012978174,
20.));
#79431=CARTESIAN_POINT('Ctrl Pts',(-45.5343305164759,-11.9777285446569,
0.));
#79432=CARTESIAN_POINT('Ctrl Pts',(-45.5343305164759,-11.9777285446569,
20.));
#79433=CARTESIAN_POINT('Ctrl Pts',(-45.5398258427845,-11.945053032791,0.));
#79434=CARTESIAN_POINT('Ctrl Pts',(-45.5398258427845,-11.945053032791,20.));
#79435=CARTESIAN_POINT('Ctrl Pts',(-45.5452980808284,-11.9123747784165,
0.));
#79436=CARTESIAN_POINT('Ctrl Pts',(-45.5452980808284,-11.9123747784165,
20.));
#79437=CARTESIAN_POINT('Ctrl Pts',(-45.5507472287824,-11.8796937977314,
0.));
#79438=CARTESIAN_POINT('Ctrl Pts',(-45.5507472287824,-11.8796937977314,
20.));
#79439=CARTESIAN_POINT('Ctrl Pts',(-45.5561732848327,-11.8470101069358,
0.));
#79440=CARTESIAN_POINT('Ctrl Pts',(-45.5561732848327,-11.8470101069358,
20.));
#79441=CARTESIAN_POINT('Ctrl Pts',(-45.5615762471761,-11.8143237222317,
0.));
#79442=CARTESIAN_POINT('Ctrl Pts',(-45.5615762471761,-11.8143237222317,
20.));
#79443=CARTESIAN_POINT('Ctrl Pts',(-45.5669561140206,-11.7816346598227,
0.));
#79444=CARTESIAN_POINT('Ctrl Pts',(-45.5669561140206,-11.7816346598227,
20.));
#79445=CARTESIAN_POINT('Ctrl Pts',(-45.5723128835857,-11.748942935914,0.));
#79446=CARTESIAN_POINT('Ctrl Pts',(-45.5723128835857,-11.748942935914,20.));
#79447=CARTESIAN_POINT('Ctrl Pts',(-45.5776465541021,-11.7162485667124,
0.));
#79448=CARTESIAN_POINT('Ctrl Pts',(-45.5776465541021,-11.7162485667124,
20.));
#79449=CARTESIAN_POINT('Ctrl Pts',(-45.5829571238122,-11.6835515684258,
0.));
#79450=CARTESIAN_POINT('Ctrl Pts',(-45.5829571238122,-11.6835515684258,
20.));
#79451=CARTESIAN_POINT('Ctrl Pts',(-45.5882445909695,-11.6508519572639,
0.));
#79452=CARTESIAN_POINT('Ctrl Pts',(-45.5882445909695,-11.6508519572639,
20.));
#79453=CARTESIAN_POINT('Ctrl Pts',(-45.5935089538387,-11.6181497494381,
0.));
#79454=CARTESIAN_POINT('Ctrl Pts',(-45.5935089538387,-11.6181497494381,
20.));
#79455=CARTESIAN_POINT('Ctrl Pts',(-45.598750210696,-11.5854449611619,0.));
#79456=CARTESIAN_POINT('Ctrl Pts',(-45.598750210696,-11.5854449611619,20.));
#79457=CARTESIAN_POINT('Ctrl Pts',(-45.6039683598295,-11.5527376086502,
0.));
#79458=CARTESIAN_POINT('Ctrl Pts',(-45.6039683598295,-11.5527376086502,
20.));
#79459=CARTESIAN_POINT('Ctrl Pts',(-45.6091633995383,-11.5200277081201,
0.));
#79460=CARTESIAN_POINT('Ctrl Pts',(-45.6091633995383,-11.5200277081201,
20.));
#79461=CARTESIAN_POINT('Ctrl Pts',(-45.6143353281323,-11.4873152757897,
0.));
#79462=CARTESIAN_POINT('Ctrl Pts',(-45.6143353281323,-11.4873152757897,
20.));
#79463=CARTESIAN_POINT('Ctrl Pts',(-45.6194841439321,-11.4546003278786,
0.));
#79464=CARTESIAN_POINT('Ctrl Pts',(-45.6194841439321,-11.4546003278786,
20.));
#79465=CARTESIAN_POINT('Ctrl Pts',(-45.6246098452703,-11.421882880608,0.));
#79466=CARTESIAN_POINT('Ctrl Pts',(-45.6246098452703,-11.421882880608,20.));
#79467=CARTESIAN_POINT('Ctrl Pts',(-45.6297124304911,-11.3891629502006,
0.));
#79468=CARTESIAN_POINT('Ctrl Pts',(-45.6297124304911,-11.3891629502006,
20.));
#79469=CARTESIAN_POINT('Ctrl Pts',(-45.6347918979506,-11.3564405528809,
0.));
#79470=CARTESIAN_POINT('Ctrl Pts',(-45.6347918979506,-11.3564405528809,
20.));
#79471=CARTESIAN_POINT('Ctrl Pts',(-45.6398482460165,-11.3237157048751,
0.));
#79472=CARTESIAN_POINT('Ctrl Pts',(-45.6398482460165,-11.3237157048751,
20.));
#79473=CARTESIAN_POINT('Ctrl Pts',(-45.6448814730677,-11.290988422411,0.));
#79474=CARTESIAN_POINT('Ctrl Pts',(-45.6448814730677,-11.290988422411,20.));
#79475=CARTESIAN_POINT('Ctrl Pts',(-45.6498915774933,-11.2582587217178,
0.));
#79476=CARTESIAN_POINT('Ctrl Pts',(-45.6498915774933,-11.2582587217178,
20.));
#79477=CARTESIAN_POINT('Ctrl Pts',(-45.6548785576938,-11.2255266190259,
0.));
#79478=CARTESIAN_POINT('Ctrl Pts',(-45.6548785576938,-11.2255266190259,
20.));
#79479=CARTESIAN_POINT('Ctrl Pts',(-45.6598424120808,-11.1927921305675,
0.));
#79480=CARTESIAN_POINT('Ctrl Pts',(-45.6598424120808,-11.1927921305675,
20.));
#79481=CARTESIAN_POINT('Ctrl Pts',(-45.6647831390778,-11.1600552725764,
0.));
#79482=CARTESIAN_POINT('Ctrl Pts',(-45.6647831390778,-11.1600552725764,
20.));
#79483=CARTESIAN_POINT('Ctrl Pts',(-45.6697007371202,-11.1273160612881,
0.));
#79484=CARTESIAN_POINT('Ctrl Pts',(-45.6697007371202,-11.1273160612881,
20.));
#79485=CARTESIAN_POINT('Ctrl Pts',(-45.6745952046549,-11.0945745129393,
0.));
#79486=CARTESIAN_POINT('Ctrl Pts',(-45.6745952046549,-11.0945745129393,
20.));
#79487=CARTESIAN_POINT('Ctrl Pts',(-45.6794665401395,-11.0618306437685,
0.));
#79488=CARTESIAN_POINT('Ctrl Pts',(-45.6794665401395,-11.0618306437685,
20.));
#79489=CARTESIAN_POINT('Ctrl Pts',(-45.684314742043,-11.0290844700154,0.));
#79490=CARTESIAN_POINT('Ctrl Pts',(-45.684314742043,-11.0290844700154,20.));
#79491=CARTESIAN_POINT('Ctrl Pts',(-45.6891398088456,-10.9963360079212,
0.));
#79492=CARTESIAN_POINT('Ctrl Pts',(-45.6891398088456,-10.9963360079212,
20.));
#79493=CARTESIAN_POINT('Ctrl Pts',(-45.6939417390393,-10.9635852737287,
0.));
#79494=CARTESIAN_POINT('Ctrl Pts',(-45.6939417390393,-10.9635852737287,
20.));
#79495=CARTESIAN_POINT('Ctrl Pts',(-45.698720531127,-10.930832283682,0.));
#79496=CARTESIAN_POINT('Ctrl Pts',(-45.698720531127,-10.930832283682,20.));
#79497=CARTESIAN_POINT('Ctrl Pts',(-45.7034761836229,-10.8980770540269,
0.));
#79498=CARTESIAN_POINT('Ctrl Pts',(-45.7034761836229,-10.8980770540269,
20.));
#79499=CARTESIAN_POINT('Ctrl Pts',(-45.7082086950532,-10.8653196010107,
0.));
#79500=CARTESIAN_POINT('Ctrl Pts',(-45.7082086950532,-10.8653196010107,
20.));
#79501=CARTESIAN_POINT('Ctrl Pts',(-45.7129180639559,-10.832559940882,0.));
#79502=CARTESIAN_POINT('Ctrl Pts',(-45.7129180639559,-10.832559940882,20.));
#79503=CARTESIAN_POINT('Ctrl Pts',(-45.7176042888794,-10.7997980898913,
0.));
#79504=CARTESIAN_POINT('Ctrl Pts',(-45.7176042888794,-10.7997980898913,
20.));
#79505=CARTESIAN_POINT('Ctrl Pts',(-45.7222673683833,-10.7670340642896,
0.));
#79506=CARTESIAN_POINT('Ctrl Pts',(-45.7222673683833,-10.7670340642896,
20.));
#79507=CARTESIAN_POINT('Ctrl Pts',(-45.7269073010391,-10.73426788033,0.));
#79508=CARTESIAN_POINT('Ctrl Pts',(-45.7269073010391,-10.73426788033,20.));
#79509=CARTESIAN_POINT('Ctrl Pts',(-45.7315240854293,-10.7014995542666,
0.));
#79510=CARTESIAN_POINT('Ctrl Pts',(-45.7315240854293,-10.7014995542666,
20.));
#79511=CARTESIAN_POINT('Ctrl Pts',(-45.7361177201484,-10.6687291023553,
0.));
#79512=CARTESIAN_POINT('Ctrl Pts',(-45.7361177201484,-10.6687291023553,
20.));
#79513=CARTESIAN_POINT('Ctrl Pts',(-45.7406882038015,-10.6359565408533,
0.));
#79514=CARTESIAN_POINT('Ctrl Pts',(-45.7406882038015,-10.6359565408533,
20.));
#79515=CARTESIAN_POINT('Ctrl Pts',(-45.745235535006,-10.6031818860194,0.));
#79516=CARTESIAN_POINT('Ctrl Pts',(-45.745235535006,-10.6031818860194,20.));
#79517=CARTESIAN_POINT('Ctrl Pts',(-45.7497597123901,-10.5704051541135,
0.));
#79518=CARTESIAN_POINT('Ctrl Pts',(-45.7497597123901,-10.5704051541135,
20.));
#79519=CARTESIAN_POINT('Ctrl Pts',(-45.7542607345937,-10.5376263613968,
0.));
#79520=CARTESIAN_POINT('Ctrl Pts',(-45.7542607345937,-10.5376263613968,
20.));
#79521=CARTESIAN_POINT('Ctrl Pts',(-45.7587386002674,-10.504845524132,0.));
#79522=CARTESIAN_POINT('Ctrl Pts',(-45.7587386002674,-10.504845524132,20.));
#79523=CARTESIAN_POINT('Ctrl Pts',(-45.7631933080735,-10.4720626585828,
0.));
#79524=CARTESIAN_POINT('Ctrl Pts',(-45.7631933080735,-10.4720626585828,
20.));
#79525=CARTESIAN_POINT('Ctrl Pts',(-45.7676248566855,-10.4392777810149,
0.));
#79526=CARTESIAN_POINT('Ctrl Pts',(-45.7676248566855,-10.4392777810149,
20.));
#79527=CARTESIAN_POINT('Ctrl Pts',(-45.772033244789,-10.406490907695,0.));
#79528=CARTESIAN_POINT('Ctrl Pts',(-45.772033244789,-10.406490907695,20.));
#79529=CARTESIAN_POINT('Ctrl Pts',(-45.7764184710811,-10.3737020548914,
0.));
#79530=CARTESIAN_POINT('Ctrl Pts',(-45.7764184710811,-10.3737020548914,
20.));
#79531=CARTESIAN_POINT('Ctrl Pts',(-45.7807805342697,-10.3409112388736,
0.));
#79532=CARTESIAN_POINT('Ctrl Pts',(-45.7807805342697,-10.3409112388736,
20.));
#79533=CARTESIAN_POINT('Ctrl Pts',(-45.7851194330743,-10.3081184759123,
0.));
#79534=CARTESIAN_POINT('Ctrl Pts',(-45.7851194330743,-10.3081184759123,
20.));
#79535=CARTESIAN_POINT('Ctrl Pts',(-45.7894351662253,-10.2753237822795,
0.));
#79536=CARTESIAN_POINT('Ctrl Pts',(-45.7894351662253,-10.2753237822795,
20.));
#79537=CARTESIAN_POINT('Ctrl Pts',(-45.7937277324643,-10.2425271742485,
0.));
#79538=CARTESIAN_POINT('Ctrl Pts',(-45.7937277324643,-10.2425271742485,
20.));
#79539=CARTESIAN_POINT('Ctrl Pts',(-45.7979971305449,-10.2097286680937,
0.));
#79540=CARTESIAN_POINT('Ctrl Pts',(-45.7979971305449,-10.2097286680937,
20.));
#79541=CARTESIAN_POINT('Ctrl Pts',(-45.8022433592327,-10.1769282800914,
0.));
#79542=CARTESIAN_POINT('Ctrl Pts',(-45.8022433592327,-10.1769282800914,
20.));
#79543=CARTESIAN_POINT('Ctrl Pts',(-45.8064664173048,-10.1441260265191,
0.));
#79544=CARTESIAN_POINT('Ctrl Pts',(-45.8064664173048,-10.1441260265191,
20.));
#79545=CARTESIAN_POINT('Ctrl Pts',(-45.8106663035491,-10.1113219236554,
0.));
#79546=CARTESIAN_POINT('Ctrl Pts',(-45.8106663035491,-10.1113219236554,
20.));
#79547=CARTESIAN_POINT('Ctrl Pts',(-45.8148430167647,-10.0785159877801,
0.));
#79548=CARTESIAN_POINT('Ctrl Pts',(-45.8148430167647,-10.0785159877801,
20.));
#79549=CARTESIAN_POINT('Ctrl Pts',(-45.8189965557614,-10.0457082351741,
0.));
#79550=CARTESIAN_POINT('Ctrl Pts',(-45.8189965557614,-10.0457082351741,
20.));
#79551=CARTESIAN_POINT('Ctrl Pts',(-45.8231269193611,-10.0128986821194,
0.));
#79552=CARTESIAN_POINT('Ctrl Pts',(-45.8231269193611,-10.0128986821194,
20.));
#79553=CARTESIAN_POINT('Ctrl Pts',(-45.8272341063969,-9.98008734489947,
0.));
#79554=CARTESIAN_POINT('Ctrl Pts',(-45.8272341063969,-9.98008734489947,
20.));
#79555=CARTESIAN_POINT('Ctrl Pts',(-45.8313181157134,-9.94727423979905,
0.));
#79556=CARTESIAN_POINT('Ctrl Pts',(-45.8313181157134,-9.94727423979905,
20.));
#79557=CARTESIAN_POINT('Ctrl Pts',(-45.8353789461673,-9.91445938310424,
0.));
#79558=CARTESIAN_POINT('Ctrl Pts',(-45.8353789461673,-9.91445938310424,
20.));
#79559=CARTESIAN_POINT('Ctrl Pts',(-45.8394165966264,-9.88164279110241,
0.));
#79560=CARTESIAN_POINT('Ctrl Pts',(-45.8394165966264,-9.88164279110241,
20.));
#79561=CARTESIAN_POINT('Ctrl Pts',(-45.84343106597,-9.84882448008225,0.));
#79562=CARTESIAN_POINT('Ctrl Pts',(-45.84343106597,-9.84882448008225,20.));
#79563=CARTESIAN_POINT('Ctrl Pts',(-45.8474223530896,-9.81600446633367,
0.));
#79564=CARTESIAN_POINT('Ctrl Pts',(-45.8474223530896,-9.81600446633367,
20.));
#79565=CARTESIAN_POINT('Ctrl Pts',(-45.8513904568872,-9.78318276614761,
0.));
#79566=CARTESIAN_POINT('Ctrl Pts',(-45.8513904568872,-9.78318276614761,
20.));
#79567=CARTESIAN_POINT('Ctrl Pts',(-45.8553353762765,-9.75035939581618,
0.));
#79568=CARTESIAN_POINT('Ctrl Pts',(-45.8553353762765,-9.75035939581618,
20.));
#79569=CARTESIAN_POINT('Ctrl Pts',(-45.8592571101813,-9.7175343716322,0.));
#79570=CARTESIAN_POINT('Ctrl Pts',(-45.8592571101813,-9.7175343716322,20.));
#79571=CARTESIAN_POINT('Ctrl Pts',(-45.8631556575366,-9.68470770988975,
0.));
#79572=CARTESIAN_POINT('Ctrl Pts',(-45.8631556575366,-9.68470770988975,
20.));
#79573=CARTESIAN_POINT('Ctrl Pts',(-45.8670310172895,-9.65187942688401,
0.));
#79574=CARTESIAN_POINT('Ctrl Pts',(-45.8670310172895,-9.65187942688401,
20.));
#79575=CARTESIAN_POINT('Ctrl Pts',(-45.870883188399,-9.61904953891159,0.));
#79576=CARTESIAN_POINT('Ctrl Pts',(-45.870883188399,-9.61904953891159,20.));
#79577=CARTESIAN_POINT('Ctrl Pts',(-45.8747121698355,-9.58621806227057,
0.));
#79578=CARTESIAN_POINT('Ctrl Pts',(-45.8747121698355,-9.58621806227057,
20.));
#79579=CARTESIAN_POINT('Ctrl Pts',(-45.8785179605829,-9.55338501326047,
0.));
#79580=CARTESIAN_POINT('Ctrl Pts',(-45.8785179605829,-9.55338501326047,
20.));
#79581=CARTESIAN_POINT('Ctrl Pts',(-45.882300559635,-9.52055040818184,0.));
#79582=CARTESIAN_POINT('Ctrl Pts',(-45.882300559635,-9.52055040818184,20.));
#79583=CARTESIAN_POINT('Ctrl Pts',(-45.8860599659967,-9.48771426333609,
0.));
#79584=CARTESIAN_POINT('Ctrl Pts',(-45.8860599659967,-9.48771426333609,
20.));
#79585=CARTESIAN_POINT('Ctrl Pts',(-45.8897961786838,-9.45487659502548,
0.));
#79586=CARTESIAN_POINT('Ctrl Pts',(-45.8897961786838,-9.45487659502548,
20.));
#79587=CARTESIAN_POINT('Ctrl Pts',(-45.8935091967241,-9.42203741955324,
0.));
#79588=CARTESIAN_POINT('Ctrl Pts',(-45.8935091967241,-9.42203741955324,
20.));
#79589=CARTESIAN_POINT('Ctrl Pts',(-45.8971990191563,-9.3891967532238,0.));
#79590=CARTESIAN_POINT('Ctrl Pts',(-45.8971990191563,-9.3891967532238,20.));
#79591=CARTESIAN_POINT('Ctrl Pts',(-45.90086564503,-9.35635461234246,0.));
#79592=CARTESIAN_POINT('Ctrl Pts',(-45.90086564503,-9.35635461234246,20.));
#79593=CARTESIAN_POINT('Ctrl Pts',(-45.9045090734063,-9.32351101321579,
0.));
#79594=CARTESIAN_POINT('Ctrl Pts',(-45.9045090734063,-9.32351101321579,
20.));
#79595=CARTESIAN_POINT('Ctrl Pts',(-45.9081293033577,-9.29066597215162,
0.));
#79596=CARTESIAN_POINT('Ctrl Pts',(-45.9081293033577,-9.29066597215162,
20.));
#79597=CARTESIAN_POINT('Ctrl Pts',(-45.9117263339694,-9.25781950545901,
0.));
#79598=CARTESIAN_POINT('Ctrl Pts',(-45.9117263339694,-9.25781950545901,
20.));
#79599=CARTESIAN_POINT('Ctrl Pts',(-45.9153001643391,-9.22497162944821,
0.));
#79600=CARTESIAN_POINT('Ctrl Pts',(-45.9153001643391,-9.22497162944821,
20.));
#79601=CARTESIAN_POINT('Ctrl Pts',(-45.9188507935764,-9.19212236043073,
0.));
#79602=CARTESIAN_POINT('Ctrl Pts',(-45.9188507935764,-9.19212236043073,
20.));
#79603=CARTESIAN_POINT('Ctrl Pts',(-45.9223782208015,-9.15927171471891,
0.));
#79604=CARTESIAN_POINT('Ctrl Pts',(-45.9223782208015,-9.15927171471891,
20.));
#79605=CARTESIAN_POINT('Ctrl Pts',(-45.9258824451441,-9.12641970862566,
0.));
#79606=CARTESIAN_POINT('Ctrl Pts',(-45.9258824451441,-9.12641970862566,
20.));
#79607=CARTESIAN_POINT('Ctrl Pts',(-45.9293634657451,-9.09356635846485,
0.));
#79608=CARTESIAN_POINT('Ctrl Pts',(-45.9293634657451,-9.09356635846485,
20.));
#79609=CARTESIAN_POINT('Ctrl Pts',(-45.9328212817567,-9.06071168055121,
0.));
#79610=CARTESIAN_POINT('Ctrl Pts',(-45.9328212817567,-9.06071168055121,
20.));
#79611=CARTESIAN_POINT('Ctrl Pts',(-45.9362558923428,-9.02785569120061,
0.));
#79612=CARTESIAN_POINT('Ctrl Pts',(-45.9362558923428,-9.02785569120061,
20.));
#79613=CARTESIAN_POINT('Ctrl Pts',(-45.939667296681,-8.99499840673046,0.));
#79614=CARTESIAN_POINT('Ctrl Pts',(-45.939667296681,-8.99499840673046,20.));
#79615=CARTESIAN_POINT('Ctrl Pts',(-45.9430554939595,-8.96213984345905,
0.));
#79616=CARTESIAN_POINT('Ctrl Pts',(-45.9430554939595,-8.96213984345905,
20.));
#79617=CARTESIAN_POINT('Ctrl Pts',(-45.9464204833787,-8.92928001770575,
0.));
#79618=CARTESIAN_POINT('Ctrl Pts',(-45.9464204833787,-8.92928001770575,
20.));
#79619=CARTESIAN_POINT('Ctrl Pts',(-45.9497622641496,-8.89641894579082,
0.));
#79620=CARTESIAN_POINT('Ctrl Pts',(-45.9497622641496,-8.89641894579082,
20.));
#79621=CARTESIAN_POINT('Ctrl Pts',(-45.9530808354938,-8.86355664403534,
0.));
#79622=CARTESIAN_POINT('Ctrl Pts',(-45.9530808354938,-8.86355664403534,
20.));
#79623=CARTESIAN_POINT('Ctrl Pts',(-45.9563761966444,-8.83069312876127,
0.));
#79624=CARTESIAN_POINT('Ctrl Pts',(-45.9563761966444,-8.83069312876127,
20.));
#79625=CARTESIAN_POINT('Ctrl Pts',(-45.9596483468462,-8.79782841629147,
0.));
#79626=CARTESIAN_POINT('Ctrl Pts',(-45.9596483468462,-8.79782841629147,
20.));
#79627=CARTESIAN_POINT('Ctrl Pts',(-45.9628972853566,-8.76496252295001,
0.));
#79628=CARTESIAN_POINT('Ctrl Pts',(-45.9628972853566,-8.76496252295001,
20.));
#79629=CARTESIAN_POINT('Ctrl Pts',(-45.9661230114446,-8.73209546506199,
0.));
#79630=CARTESIAN_POINT('Ctrl Pts',(-45.9661230114446,-8.73209546506199,
20.));
#79631=CARTESIAN_POINT('Ctrl Pts',(-45.9693255243897,-8.69922725895329,
0.));
#79632=CARTESIAN_POINT('Ctrl Pts',(-45.9693255243897,-8.69922725895329,
20.));
#79633=CARTESIAN_POINT('Ctrl Pts',(-45.9725048234817,-8.66635792095043,
0.));
#79634=CARTESIAN_POINT('Ctrl Pts',(-45.9725048234817,-8.66635792095043,
20.));
#79635=CARTESIAN_POINT('Ctrl Pts',(-45.9756609080225,-8.63348746738099,
0.));
#79636=CARTESIAN_POINT('Ctrl Pts',(-45.9756609080225,-8.63348746738099,
20.));
#79637=CARTESIAN_POINT('Ctrl Pts',(-45.9787937773254,-8.60061591457339,
0.));
#79638=CARTESIAN_POINT('Ctrl Pts',(-45.9787937773254,-8.60061591457339,
20.));
#79639=CARTESIAN_POINT('Ctrl Pts',(-45.9819034307166,-8.56774327885725,
0.));
#79640=CARTESIAN_POINT('Ctrl Pts',(-45.9819034307166,-8.56774327885725,
20.));
#79641=CARTESIAN_POINT('Ctrl Pts',(-45.9849898675351,-8.53486957656347,
0.));
#79642=CARTESIAN_POINT('Ctrl Pts',(-45.9849898675351,-8.53486957656347,
20.));
#79643=CARTESIAN_POINT('Ctrl Pts',(-45.9880530871298,-8.50199482402354,
0.));
#79644=CARTESIAN_POINT('Ctrl Pts',(-45.9880530871298,-8.50199482402354,
20.));
#79645=CARTESIAN_POINT('Ctrl Pts',(-45.991093088861,-8.46911903756973,0.));
#79646=CARTESIAN_POINT('Ctrl Pts',(-45.991093088861,-8.46911903756973,20.));
#79647=CARTESIAN_POINT('Ctrl Pts',(-45.9941098720982,-8.43624223353471,
0.));
#79648=CARTESIAN_POINT('Ctrl Pts',(-45.9941098720982,-8.43624223353471,
20.));
#79649=CARTESIAN_POINT('Ctrl Pts',(-45.9971034362229,-8.40336442825199,
0.));
#79650=CARTESIAN_POINT('Ctrl Pts',(-45.9971034362229,-8.40336442825199,
20.));
#79651=CARTESIAN_POINT('Ctrl Pts',(-46.000073780629,-8.37048563805605,0.));
#79652=CARTESIAN_POINT('Ctrl Pts',(-46.000073780629,-8.37048563805605,20.));
#79653=CARTESIAN_POINT('Ctrl Pts',(-46.0030209047226,-8.33760587928253,
0.));
#79654=CARTESIAN_POINT('Ctrl Pts',(-46.0030209047226,-8.33760587928253,
20.));
#79655=CARTESIAN_POINT('Ctrl Pts',(-46.0059448079215,-8.30472516826797,
0.));
#79656=CARTESIAN_POINT('Ctrl Pts',(-46.0059448079215,-8.30472516826797,
20.));
#79657=CARTESIAN_POINT('Ctrl Pts',(-46.0088454896554,-8.27184352134994,
0.));
#79658=CARTESIAN_POINT('Ctrl Pts',(-46.0088454896554,-8.27184352134994,
20.));
#79659=CARTESIAN_POINT('Ctrl Pts',(-46.0117229493647,-8.23896095486669,
0.));
#79660=CARTESIAN_POINT('Ctrl Pts',(-46.0117229493647,-8.23896095486669,
20.));
#79661=CARTESIAN_POINT('Ctrl Pts',(-46.0145771865005,-8.20607748515696,
0.));
#79662=CARTESIAN_POINT('Ctrl Pts',(-46.0145771865005,-8.20607748515696,
20.));
#79663=CARTESIAN_POINT('Ctrl Pts',(-46.0174082005262,-8.17319312856042,
0.));
#79664=CARTESIAN_POINT('Ctrl Pts',(-46.0174082005262,-8.17319312856042,
20.));
#79665=CARTESIAN_POINT('Ctrl Pts',(-46.0202159909161,-8.14030790141739,
0.));
#79666=CARTESIAN_POINT('Ctrl Pts',(-46.0202159909161,-8.14030790141739,
20.));
#79667=CARTESIAN_POINT('Ctrl Pts',(-46.0230005571558,-8.107421820069,0.));
#79668=CARTESIAN_POINT('Ctrl Pts',(-46.0230005571558,-8.107421820069,20.));
#79669=CARTESIAN_POINT('Ctrl Pts',(-46.025761898743,-8.07453490085736,0.));
#79670=CARTESIAN_POINT('Ctrl Pts',(-46.025761898743,-8.07453490085736,20.));
#79671=CARTESIAN_POINT('Ctrl Pts',(-46.0285000151874,-8.04164716012545,
0.));
#79672=CARTESIAN_POINT('Ctrl Pts',(-46.0285000151874,-8.04164716012545,
20.));
#79673=CARTESIAN_POINT('Ctrl Pts',(-46.0312149060105,-8.00875861421695,
0.));
#79674=CARTESIAN_POINT('Ctrl Pts',(-46.0312149060105,-8.00875861421695,
20.));
#79675=CARTESIAN_POINT('Ctrl Pts',(-46.0339065707442,-7.9758692794762,0.));
#79676=CARTESIAN_POINT('Ctrl Pts',(-46.0339065707442,-7.9758692794762,20.));
#79677=CARTESIAN_POINT('Ctrl Pts',(-46.0365750089318,-7.94297917224815,
0.));
#79678=CARTESIAN_POINT('Ctrl Pts',(-46.0365750089318,-7.94297917224815,
20.));
#79679=CARTESIAN_POINT('Ctrl Pts',(-46.0392202201279,-7.91008830887855,
0.));
#79680=CARTESIAN_POINT('Ctrl Pts',(-46.0392202201279,-7.91008830887855,
20.));
#79681=CARTESIAN_POINT('Ctrl Pts',(-46.0418422038989,-7.877196705714,0.));
#79682=CARTESIAN_POINT('Ctrl Pts',(-46.0418422038989,-7.877196705714,20.));
#79683=CARTESIAN_POINT('Ctrl Pts',(-46.0444409598224,-7.84430437910167,
0.));
#79684=CARTESIAN_POINT('Ctrl Pts',(-46.0444409598224,-7.84430437910167,
20.));
#79685=CARTESIAN_POINT('Ctrl Pts',(-46.0470164874882,-7.81141134538954,
0.));
#79686=CARTESIAN_POINT('Ctrl Pts',(-46.0470164874882,-7.81141134538954,
20.));
#79687=CARTESIAN_POINT('Ctrl Pts',(-46.0495687864972,-7.77851762092636,
0.));
#79688=CARTESIAN_POINT('Ctrl Pts',(-46.0495687864972,-7.77851762092636,
20.));
#79689=CARTESIAN_POINT('Ctrl Pts',(-46.052097856463,-7.74562322206167,0.));
#79690=CARTESIAN_POINT('Ctrl Pts',(-46.052097856463,-7.74562322206167,20.));
#79691=CARTESIAN_POINT('Ctrl Pts',(-46.0546036970108,-7.71272816514571,
0.));
#79692=CARTESIAN_POINT('Ctrl Pts',(-46.0546036970108,-7.71272816514571,
20.));
#79693=CARTESIAN_POINT('Ctrl Pts',(-46.0570863077758,-7.67983246652917,
0.));
#79694=CARTESIAN_POINT('Ctrl Pts',(-46.0570863077758,-7.67983246652917,
20.));
#79695=CARTESIAN_POINT('Ctrl Pts',(-46.0595456884042,-7.64693614256335,
0.));
#79696=CARTESIAN_POINT('Ctrl Pts',(-46.0595456884042,-7.64693614256335,
20.));
#79697=CARTESIAN_POINT('Ctrl Pts',(-46.0619818385541,-7.61403920960035,
0.));
#79698=CARTESIAN_POINT('Ctrl Pts',(-46.0619818385541,-7.61403920960035,
20.));
#79699=CARTESIAN_POINT('Ctrl Pts',(-46.0643947578955,-7.58114168399302,
0.));
#79700=CARTESIAN_POINT('Ctrl Pts',(-46.0643947578955,-7.58114168399302,
20.));
#79701=CARTESIAN_POINT('Ctrl Pts',(-46.0667844461104,-7.54824358209484,
0.));
#79702=CARTESIAN_POINT('Ctrl Pts',(-46.0667844461104,-7.54824358209484,
20.));
#79703=CARTESIAN_POINT('Ctrl Pts',(-46.0691509028928,-7.51534492025983,
0.));
#79704=CARTESIAN_POINT('Ctrl Pts',(-46.0691509028928,-7.51534492025983,
20.));
#79705=CARTESIAN_POINT('Ctrl Pts',(-46.0714941279471,-7.4824457148425,0.));
#79706=CARTESIAN_POINT('Ctrl Pts',(-46.0714941279471,-7.4824457148425,20.));
#79707=CARTESIAN_POINT('Ctrl Pts',(-46.0738141209885,-7.44954598219809,
0.));
#79708=CARTESIAN_POINT('Ctrl Pts',(-46.0738141209885,-7.44954598219809,
20.));
#79709=CARTESIAN_POINT('Ctrl Pts',(-46.0761108817447,-7.4166457386826,0.));
#79710=CARTESIAN_POINT('Ctrl Pts',(-46.0761108817447,-7.4166457386826,20.));
#79711=CARTESIAN_POINT('Ctrl Pts',(-46.0783844099553,-7.38374500065294,
0.));
#79712=CARTESIAN_POINT('Ctrl Pts',(-46.0783844099553,-7.38374500065294,
20.));
#79713=CARTESIAN_POINT('Ctrl Pts',(-46.0806347053718,-7.35084378446661,
0.));
#79714=CARTESIAN_POINT('Ctrl Pts',(-46.0806347053718,-7.35084378446661,
20.));
#79715=CARTESIAN_POINT('Ctrl Pts',(-46.0828617677561,-7.31794210648139,
0.));
#79716=CARTESIAN_POINT('Ctrl Pts',(-46.0828617677561,-7.31794210648139,
20.));
#79717=CARTESIAN_POINT('Ctrl Pts',(-46.0850655968817,-7.2850399830555,0.));
#79718=CARTESIAN_POINT('Ctrl Pts',(-46.0850655968817,-7.2850399830555,20.));
#79719=CARTESIAN_POINT('Ctrl Pts',(-46.0872461925336,-7.25213743054749,
0.));
#79720=CARTESIAN_POINT('Ctrl Pts',(-46.0872461925336,-7.25213743054749,
20.));
#79721=CARTESIAN_POINT('Ctrl Pts',(-46.0894035545083,-7.2192344653164,0.));
#79722=CARTESIAN_POINT('Ctrl Pts',(-46.0894035545083,-7.2192344653164,20.));
#79723=CARTESIAN_POINT('Ctrl Pts',(-46.0915376826137,-7.18633110372211,
0.));
#79724=CARTESIAN_POINT('Ctrl Pts',(-46.0915376826137,-7.18633110372211,
20.));
#79725=CARTESIAN_POINT('Ctrl Pts',(-46.0936485766695,-7.15342736212529,
0.));
#79726=CARTESIAN_POINT('Ctrl Pts',(-46.0936485766695,-7.15342736212529,
20.));
#79727=CARTESIAN_POINT('Ctrl Pts',(-46.0957362365075,-7.12052325688752,
0.));
#79728=CARTESIAN_POINT('Ctrl Pts',(-46.0957362365075,-7.12052325688752,
20.));
#79729=CARTESIAN_POINT('Ctrl Pts',(-46.097800661971,-7.08761880437093,0.));
#79730=CARTESIAN_POINT('Ctrl Pts',(-46.097800661971,-7.08761880437093,20.));
#79731=CARTESIAN_POINT('Ctrl Pts',(-46.0998418529147,-7.05471402093801,
0.));
#79732=CARTESIAN_POINT('Ctrl Pts',(-46.0998418529147,-7.05471402093801,
20.));
#79733=CARTESIAN_POINT('Ctrl Pts',(-46.1018598092046,-7.02180892295147,
0.));
#79734=CARTESIAN_POINT('Ctrl Pts',(-46.1018598092046,-7.02180892295147,
20.));
#79735=CARTESIAN_POINT('Ctrl Pts',(-46.103854530718,-6.98890352677438,0.));
#79736=CARTESIAN_POINT('Ctrl Pts',(-46.103854530718,-6.98890352677438,20.));
#79737=CARTESIAN_POINT('Ctrl Pts',(-46.1058260173429,-6.95599784877019,
0.));
#79738=CARTESIAN_POINT('Ctrl Pts',(-46.1058260173429,-6.95599784877019,
20.));
#79739=CARTESIAN_POINT('Ctrl Pts',(-46.1077742689797,-6.92309190530285,
0.));
#79740=CARTESIAN_POINT('Ctrl Pts',(-46.1077742689797,-6.92309190530285,
20.));
#79741=CARTESIAN_POINT('Ctrl Pts',(-46.1096992855399,-6.89018571273689,
0.));
#79742=CARTESIAN_POINT('Ctrl Pts',(-46.1096992855399,-6.89018571273689,
20.));
#79743=CARTESIAN_POINT('Ctrl Pts',(-46.111601066948,-6.85727928743787,0.));
#79744=CARTESIAN_POINT('Ctrl Pts',(-46.111601066948,-6.85727928743787,20.));
#79745=CARTESIAN_POINT('Ctrl Pts',(-46.1134796131392,-6.82437264577169,
0.));
#79746=CARTESIAN_POINT('Ctrl Pts',(-46.1134796131392,-6.82437264577169,
20.));
#79747=CARTESIAN_POINT('Ctrl Pts',(-46.1153349240611,-6.7914658041047,0.));
#79748=CARTESIAN_POINT('Ctrl Pts',(-46.1153349240611,-6.7914658041047,20.));
#79749=CARTESIAN_POINT('Ctrl Pts',(-46.1171669996709,-6.75855877880356,
0.));
#79750=CARTESIAN_POINT('Ctrl Pts',(-46.1171669996709,-6.75855877880356,
20.));
#79751=CARTESIAN_POINT('Ctrl Pts',(-46.1189758399374,-6.7256515862352,0.));
#79752=CARTESIAN_POINT('Ctrl Pts',(-46.1189758399374,-6.7256515862352,20.));
#79753=CARTESIAN_POINT('Ctrl Pts',(-46.1207614448407,-6.69274424276687,
0.));
#79754=CARTESIAN_POINT('Ctrl Pts',(-46.1207614448407,-6.69274424276687,
20.));
#79755=CARTESIAN_POINT('Ctrl Pts',(-46.122523814374,-6.65983676476652,0.));
#79756=CARTESIAN_POINT('Ctrl Pts',(-46.122523814374,-6.65983676476652,20.));
#79757=CARTESIAN_POINT('Ctrl Pts',(-46.124262948542,-6.62692916860257,0.));
#79758=CARTESIAN_POINT('Ctrl Pts',(-46.124262948542,-6.62692916860257,20.));
#79759=CARTESIAN_POINT('Ctrl Pts',(-46.1259788473615,-6.59402147064399,
0.));
#79760=CARTESIAN_POINT('Ctrl Pts',(-46.1259788473615,-6.59402147064399,
20.));
#79761=CARTESIAN_POINT('Ctrl Pts',(-46.1276715108604,-6.56111368726009,
0.));
#79762=CARTESIAN_POINT('Ctrl Pts',(-46.1276715108604,-6.56111368726009,
20.));
#79763=CARTESIAN_POINT('Ctrl Pts',(-46.1293409390781,-6.52820583482049,
0.));
#79764=CARTESIAN_POINT('Ctrl Pts',(-46.1293409390781,-6.52820583482049,
20.));
#79765=CARTESIAN_POINT('Ctrl Pts',(-46.1309871320644,-6.49529792969508,
0.));
#79766=CARTESIAN_POINT('Ctrl Pts',(-46.1309871320644,-6.49529792969508,
20.));
#79767=CARTESIAN_POINT('Ctrl Pts',(-46.1326100898806,-6.46238998825407,
0.));
#79768=CARTESIAN_POINT('Ctrl Pts',(-46.1326100898806,-6.46238998825407,
20.));
#79769=CARTESIAN_POINT('Ctrl Pts',(-46.1342098125991,-6.42948202686813,
0.));
#79770=CARTESIAN_POINT('Ctrl Pts',(-46.1342098125991,-6.42948202686813,
20.));
#79771=CARTESIAN_POINT('Ctrl Pts',(-46.1357863003044,-6.39657406190844,
0.));
#79772=CARTESIAN_POINT('Ctrl Pts',(-46.1357863003044,-6.39657406190844,
20.));
#79773=CARTESIAN_POINT('Ctrl Pts',(-46.1373395530931,-6.36366610974647,
0.));
#79774=CARTESIAN_POINT('Ctrl Pts',(-46.1373395530931,-6.36366610974647,
20.));
#79775=CARTESIAN_POINT('Ctrl Pts',(-46.138869571074,-6.33075818675419,0.));
#79776=CARTESIAN_POINT('Ctrl Pts',(-46.138869571074,-6.33075818675419,20.));
#79777=CARTESIAN_POINT('Ctrl Pts',(-46.1403763543673,-6.29785030930381,
0.));
#79778=CARTESIAN_POINT('Ctrl Pts',(-46.1403763543673,-6.29785030930381,
20.));
#79779=CARTESIAN_POINT('Ctrl Pts',(-46.141859903105,-6.26494249376777,0.));
#79780=CARTESIAN_POINT('Ctrl Pts',(-46.141859903105,-6.26494249376777,20.));
#79781=CARTESIAN_POINT('Ctrl Pts',(-46.1433202174297,-6.23203475651882,
0.));
#79782=CARTESIAN_POINT('Ctrl Pts',(-46.1433202174297,-6.23203475651882,
20.));
#79783=CARTESIAN_POINT('Ctrl Pts',(-46.1447572974959,-6.19912711393004,
0.));
#79784=CARTESIAN_POINT('Ctrl Pts',(-46.1447572974959,-6.19912711393004,
20.));
#79785=CARTESIAN_POINT('Ctrl Pts',(-46.1461711434687,-6.16621958237487,
0.));
#79786=CARTESIAN_POINT('Ctrl Pts',(-46.1461711434687,-6.16621958237487,
20.));
#79787=CARTESIAN_POINT('Ctrl Pts',(-46.1475617555249,-6.1333121782271,0.));
#79788=CARTESIAN_POINT('Ctrl Pts',(-46.1475617555249,-6.1333121782271,20.));
#79789=CARTESIAN_POINT('Ctrl Pts',(-46.1489291338532,-6.10040491786085,
0.));
#79790=CARTESIAN_POINT('Ctrl Pts',(-46.1489291338532,-6.10040491786085,
20.));
#79791=CARTESIAN_POINT('Ctrl Pts',(-46.1502732786543,-6.06749781765058,
0.));
#79792=CARTESIAN_POINT('Ctrl Pts',(-46.1502732786543,-6.06749781765058,
20.));
#79793=CARTESIAN_POINT('Ctrl Pts',(-46.151594190141,-6.03459089397104,0.));
#79794=CARTESIAN_POINT('Ctrl Pts',(-46.151594190141,-6.03459089397104,20.));
#79795=CARTESIAN_POINT('Ctrl Pts',(-46.1528918685373,-6.0016841631972,0.));
#79796=CARTESIAN_POINT('Ctrl Pts',(-46.1528918685373,-6.0016841631972,20.));
#79797=CARTESIAN_POINT('Ctrl Pts',(-46.1541663140783,-5.96877764170411,
0.));
#79798=CARTESIAN_POINT('Ctrl Pts',(-46.1541663140783,-5.96877764170411,
20.));
#79799=CARTESIAN_POINT('Ctrl Pts',(-46.1554175270101,-5.93587134586689,
0.));
#79800=CARTESIAN_POINT('Ctrl Pts',(-46.1554175270101,-5.93587134586689,
20.));
#79801=CARTESIAN_POINT('Ctrl Pts',(-46.1566455075904,-5.90296529206097,
0.));
#79802=CARTESIAN_POINT('Ctrl Pts',(-46.1566455075904,-5.90296529206097,
20.));
#79803=CARTESIAN_POINT('Ctrl Pts',(-46.1578502560886,-5.87005949666211,
0.));
#79804=CARTESIAN_POINT('Ctrl Pts',(-46.1578502560886,-5.87005949666211,
20.));
#79805=CARTESIAN_POINT('Ctrl Pts',(-46.1590317727861,-5.83715397604653,
0.));
#79806=CARTESIAN_POINT('Ctrl Pts',(-46.1590317727861,-5.83715397604653,
20.));
#79807=CARTESIAN_POINT('Ctrl Pts',(-46.160190057976,-5.80424874659071,0.));
#79808=CARTESIAN_POINT('Ctrl Pts',(-46.160190057976,-5.80424874659071,20.));
#79809=CARTESIAN_POINT('Ctrl Pts',(-46.1613251119636,-5.77134382467172,
0.));
#79810=CARTESIAN_POINT('Ctrl Pts',(-46.1613251119636,-5.77134382467172,
20.));
#79811=CARTESIAN_POINT('Ctrl Pts',(-46.1624369350662,-5.73843922666647,
0.));
#79812=CARTESIAN_POINT('Ctrl Pts',(-46.1624369350662,-5.73843922666647,
20.));
#79813=CARTESIAN_POINT('Ctrl Pts',(-46.1635255276116,-5.70553496895184,
0.));
#79814=CARTESIAN_POINT('Ctrl Pts',(-46.1635255276116,-5.70553496895184,
20.));
#79815=CARTESIAN_POINT('Ctrl Pts',(-46.1645908899393,-5.67263106790478,
0.));
#79816=CARTESIAN_POINT('Ctrl Pts',(-46.1645908899393,-5.67263106790478,
20.));
#79817=CARTESIAN_POINT('Ctrl Pts',(-46.1656330223979,-5.63972753990235,
0.));
#79818=CARTESIAN_POINT('Ctrl Pts',(-46.1656330223979,-5.63972753990235,
20.));
#79819=CARTESIAN_POINT('Ctrl Pts',(-46.166651925349,-5.60682440132181,0.));
#79820=CARTESIAN_POINT('Ctrl Pts',(-46.166651925349,-5.60682440132181,20.));
#79821=CARTESIAN_POINT('Ctrl Pts',(-46.1676475991657,-5.57392166854074,
0.));
#79822=CARTESIAN_POINT('Ctrl Pts',(-46.1676475991657,-5.57392166854074,
20.));
#79823=CARTESIAN_POINT('Ctrl Pts',(-46.1686200442337,-5.54101935793709,
0.));
#79824=CARTESIAN_POINT('Ctrl Pts',(-46.1686200442337,-5.54101935793709,
20.));
#79825=CARTESIAN_POINT('Ctrl Pts',(-46.1695692609505,-5.50811748588893,
0.));
#79826=CARTESIAN_POINT('Ctrl Pts',(-46.1695692609505,-5.50811748588893,
20.));
#79827=CARTESIAN_POINT('Ctrl Pts',(-46.170495249726,-5.47521606877459,0.));
#79828=CARTESIAN_POINT('Ctrl Pts',(-46.170495249726,-5.47521606877459,20.));
#79829=CARTESIAN_POINT('Ctrl Pts',(-46.1713980109807,-5.44231512297238,
0.));
#79830=CARTESIAN_POINT('Ctrl Pts',(-46.1713980109807,-5.44231512297238,
20.));
#79831=CARTESIAN_POINT('Ctrl Pts',(-46.1722775451467,-5.40941466486069,
0.));
#79832=CARTESIAN_POINT('Ctrl Pts',(-46.1722775451467,-5.40941466486069,
20.));
#79833=CARTESIAN_POINT('Ctrl Pts',(-46.1731338526667,-5.37651471081787,
0.));
#79834=CARTESIAN_POINT('Ctrl Pts',(-46.1731338526667,-5.37651471081787,
20.));
#79835=CARTESIAN_POINT('Ctrl Pts',(-46.1739669339953,-5.34361527722239,
0.));
#79836=CARTESIAN_POINT('Ctrl Pts',(-46.1739669339953,-5.34361527722239,
20.));
#79837=CARTESIAN_POINT('Ctrl Pts',(-46.1747767895978,-5.31071638045279,
0.));
#79838=CARTESIAN_POINT('Ctrl Pts',(-46.1747767895978,-5.31071638045279,
20.));
#79839=CARTESIAN_POINT('Ctrl Pts',(-46.1755634199519,-5.2778180368879,0.));
#79840=CARTESIAN_POINT('Ctrl Pts',(-46.1755634199519,-5.2778180368879,20.));
#79841=CARTESIAN_POINT('Ctrl Pts',(-46.1763268255471,-5.24492026290662,
0.));
#79842=CARTESIAN_POINT('Ctrl Pts',(-46.1763268255471,-5.24492026290662,
20.));
#79843=CARTESIAN_POINT('Ctrl Pts',(-46.1770670068854,-5.21202307488801,
0.));
#79844=CARTESIAN_POINT('Ctrl Pts',(-46.1770670068854,-5.21202307488801,
20.));
#79845=CARTESIAN_POINT('Ctrl Pts',(-46.1777839644797,-5.17912648921101,
0.));
#79846=CARTESIAN_POINT('Ctrl Pts',(-46.1777839644797,-5.17912648921101,
20.));
#79847=CARTESIAN_POINT('Ctrl Pts',(-46.1784776988548,-5.14623052225471,
0.));
#79848=CARTESIAN_POINT('Ctrl Pts',(-46.1784776988548,-5.14623052225471,
20.));
#79849=CARTESIAN_POINT('Ctrl Pts',(-46.1791482105459,-5.11333519039808,
0.));
#79850=CARTESIAN_POINT('Ctrl Pts',(-46.1791482105459,-5.11333519039808,
20.));
#79851=CARTESIAN_POINT('Ctrl Pts',(-46.1797955000997,-5.08044051002025,
0.));
#79852=CARTESIAN_POINT('Ctrl Pts',(-46.1797955000997,-5.08044051002025,
20.));
#79853=CARTESIAN_POINT('Ctrl Pts',(-46.1804195680748,-5.0475464975003,0.));
#79854=CARTESIAN_POINT('Ctrl Pts',(-46.1804195680748,-5.0475464975003,20.));
#79855=CARTESIAN_POINT('Ctrl Pts',(-46.1810204150412,-5.01465316921748,
0.));
#79856=CARTESIAN_POINT('Ctrl Pts',(-46.1810204150412,-5.01465316921748,
20.));
#79857=CARTESIAN_POINT('Ctrl Pts',(-46.1815980415817,-4.981760541551,0.));
#79858=CARTESIAN_POINT('Ctrl Pts',(-46.1815980415817,-4.981760541551,20.));
#79859=CARTESIAN_POINT('Ctrl Pts',(-46.182152448291,-4.94886863088032,0.));
#79860=CARTESIAN_POINT('Ctrl Pts',(-46.182152448291,-4.94886863088032,20.));
#79861=CARTESIAN_POINT('Ctrl Pts',(-46.1826836357763,-4.91597745358481,
0.));
#79862=CARTESIAN_POINT('Ctrl Pts',(-46.1826836357763,-4.91597745358481,
20.));
#79863=CARTESIAN_POINT('Ctrl Pts',(-46.1831916046531,-4.88308702604349,
0.));
#79864=CARTESIAN_POINT('Ctrl Pts',(-46.1831916046531,-4.88308702604349,
20.));
#79865=CARTESIAN_POINT('Ctrl Pts',(-46.1836763555496,-4.85019736463543,
0.));
#79866=CARTESIAN_POINT('Ctrl Pts',(-46.1836763555496,-4.85019736463543,
20.));
#79867=CARTESIAN_POINT('Ctrl Pts',(-46.1841378891039,-4.81730848573953,
0.));
#79868=CARTESIAN_POINT('Ctrl Pts',(-46.1841378891039,-4.81730848573953,
20.));
#79869=CARTESIAN_POINT('Ctrl Pts',(-46.1845762059678,-4.78442040573514,
0.));
#79870=CARTESIAN_POINT('Ctrl Pts',(-46.1845762059678,-4.78442040573514,
20.));
#79871=CARTESIAN_POINT('Ctrl Pts',(-46.1849913068043,-4.7515331410016,0.));
#79872=CARTESIAN_POINT('Ctrl Pts',(-46.1849913068043,-4.7515331410016,20.));
#79873=CARTESIAN_POINT('Ctrl Pts',(-46.1853831922891,-4.71864670791826,
0.));
#79874=CARTESIAN_POINT('Ctrl Pts',(-46.1853831922891,-4.71864670791826,
20.));
#79875=CARTESIAN_POINT('Ctrl Pts',(-46.1857518631086,-4.68576112286394,
0.));
#79876=CARTESIAN_POINT('Ctrl Pts',(-46.1857518631086,-4.68576112286394,
20.));
#79877=CARTESIAN_POINT('Ctrl Pts',(-46.1860973199616,-4.65287640221747,
0.));
#79878=CARTESIAN_POINT('Ctrl Pts',(-46.1860973199616,-4.65287640221747,
20.));
#79879=CARTESIAN_POINT('Ctrl Pts',(-46.1864195635571,-4.6199925623574,0.));
#79880=CARTESIAN_POINT('Ctrl Pts',(-46.1864195635571,-4.6199925623574,20.));
#79881=CARTESIAN_POINT('Ctrl Pts',(-46.1867185946155,-4.58710961966232,
0.));
#79882=CARTESIAN_POINT('Ctrl Pts',(-46.1867185946155,-4.58710961966232,
20.));
#79883=CARTESIAN_POINT('Ctrl Pts',(-46.1869944138693,-4.55422759051101,
0.));
#79884=CARTESIAN_POINT('Ctrl Pts',(-46.1869944138693,-4.55422759051101,
20.));
#79885=CARTESIAN_POINT('Ctrl Pts',(-46.1872470220627,-4.52134649128217,
0.));
#79886=CARTESIAN_POINT('Ctrl Pts',(-46.1872470220627,-4.52134649128217,
20.));
#79887=CARTESIAN_POINT('Ctrl Pts',(-46.1874764199521,-4.48846633835459,
0.));
#79888=CARTESIAN_POINT('Ctrl Pts',(-46.1874764199521,-4.48846633835459,
20.));
#79889=CARTESIAN_POINT('Ctrl Pts',(-46.1876826083051,-4.4555871481068,0.));
#79890=CARTESIAN_POINT('Ctrl Pts',(-46.1876826083051,-4.4555871481068,20.));
#79891=CARTESIAN_POINT('Ctrl Pts',(-46.1878655879008,-4.42270893691723,
0.));
#79892=CARTESIAN_POINT('Ctrl Pts',(-46.1878655879008,-4.42270893691723,
20.));
#79893=CARTESIAN_POINT('Ctrl Pts',(-46.1880253595297,-4.38983172116389,
0.));
#79894=CARTESIAN_POINT('Ctrl Pts',(-46.1880253595297,-4.38983172116389,
20.));
#79895=CARTESIAN_POINT('Ctrl Pts',(-46.1881619239926,-4.35695551722447,
0.));
#79896=CARTESIAN_POINT('Ctrl Pts',(-46.1881619239926,-4.35695551722447,
20.));
#79897=CARTESIAN_POINT('Ctrl Pts',(-46.1882752821036,-4.32408034147654,
0.));
#79898=CARTESIAN_POINT('Ctrl Pts',(-46.1882752821036,-4.32408034147654,
20.));
#79899=CARTESIAN_POINT('Ctrl Pts',(-46.1883654346888,-4.29120621029776,
0.));
#79900=CARTESIAN_POINT('Ctrl Pts',(-46.1883654346888,-4.29120621029776,
20.));
#79901=CARTESIAN_POINT('Ctrl Pts',(-46.1884323825857,-4.25833314006578,
0.));
#79902=CARTESIAN_POINT('Ctrl Pts',(-46.1884323825857,-4.25833314006578,
20.));
#79903=CARTESIAN_POINT('Ctrl Pts',(-46.1884761266433,-4.22546114715825,
0.));
#79904=CARTESIAN_POINT('Ctrl Pts',(-46.1884761266433,-4.22546114715825,
20.));
#79905=CARTESIAN_POINT('Ctrl Pts',(-46.1884966677209,-4.19259024795238,
0.));
#79906=CARTESIAN_POINT('Ctrl Pts',(-46.1884966677209,-4.19259024795238,
20.));
#79907=CARTESIAN_POINT('Ctrl Pts',(-46.1884940066895,-4.15972045882508,
0.));
#79908=CARTESIAN_POINT('Ctrl Pts',(-46.1884940066895,-4.15972045882508,
20.));
#79909=CARTESIAN_POINT('Ctrl Pts',(-46.1884681444317,-4.12685179615294,
0.));
#79910=CARTESIAN_POINT('Ctrl Pts',(-46.1884681444317,-4.12685179615294,
20.));
#79911=CARTESIAN_POINT('Ctrl Pts',(-46.188419081843,-4.09398427631254,0.));
#79912=CARTESIAN_POINT('Ctrl Pts',(-46.188419081843,-4.09398427631254,20.));
#79913=CARTESIAN_POINT('Ctrl Pts',(-46.18834681983,-4.06111791568023,0.));
#79914=CARTESIAN_POINT('Ctrl Pts',(-46.18834681983,-4.06111791568023,20.));
#79915=CARTESIAN_POINT('Ctrl Pts',(-46.1882513593113,-4.02825273063217,
0.));
#79916=CARTESIAN_POINT('Ctrl Pts',(-46.1882513593113,-4.02825273063217,
20.));
#79917=CARTESIAN_POINT('Ctrl Pts',(-46.1881327012171,-3.99538873754442,
0.));
#79918=CARTESIAN_POINT('Ctrl Pts',(-46.1881327012171,-3.99538873754442,
20.));
#79919=CARTESIAN_POINT('Ctrl Pts',(-46.1879908464881,-3.96252595279274,
0.));
#79920=CARTESIAN_POINT('Ctrl Pts',(-46.1879908464881,-3.96252595279274,
20.));
#79921=CARTESIAN_POINT('Ctrl Pts',(-46.1878257960766,-3.92966439275257,
0.));
#79922=CARTESIAN_POINT('Ctrl Pts',(-46.1878257960766,-3.92966439275257,
20.));
#79923=CARTESIAN_POINT('Ctrl Pts',(-46.1876375509469,-3.89680407379914,
0.));
#79924=CARTESIAN_POINT('Ctrl Pts',(-46.1876375509469,-3.89680407379914,
20.));
#79925=CARTESIAN_POINT('Ctrl Pts',(-46.1874261120751,-3.86394501230744,
0.));
#79926=CARTESIAN_POINT('Ctrl Pts',(-46.1874261120751,-3.86394501230744,
20.));
#79927=CARTESIAN_POINT('Ctrl Pts',(-46.1871914804492,-3.83108722465198,
0.));
#79928=CARTESIAN_POINT('Ctrl Pts',(-46.1871914804492,-3.83108722465198,
20.));
#79929=CARTESIAN_POINT('Ctrl Pts',(-46.1869336570686,-3.79823072720685,
0.));
#79930=CARTESIAN_POINT('Ctrl Pts',(-46.1869336570686,-3.79823072720685,
20.));
#79931=CARTESIAN_POINT('Ctrl Pts',(-46.1866526429445,-3.76537553634595,
0.));
#79932=CARTESIAN_POINT('Ctrl Pts',(-46.1866526429445,-3.76537553634595,
20.));
#79933=CARTESIAN_POINT('Ctrl Pts',(-46.1863484390996,-3.73252166844327,
0.));
#79934=CARTESIAN_POINT('Ctrl Pts',(-46.1863484390996,-3.73252166844327,
20.));
#79935=CARTESIAN_POINT('Ctrl Pts',(-46.1860210465678,-3.69966913987252,
0.));
#79936=CARTESIAN_POINT('Ctrl Pts',(-46.1860210465678,-3.69966913987252,
20.));
#79937=CARTESIAN_POINT('Ctrl Pts',(-46.185670466394,-3.66681796700709,0.));
#79938=CARTESIAN_POINT('Ctrl Pts',(-46.185670466394,-3.66681796700709,20.));
#79939=CARTESIAN_POINT('Ctrl Pts',(-46.1852966996347,-3.63396816621989,
0.));
#79940=CARTESIAN_POINT('Ctrl Pts',(-46.1852966996347,-3.63396816621989,
20.));
#79941=CARTESIAN_POINT('Ctrl Pts',(-46.1848997473582,-3.60111975388338,
0.));
#79942=CARTESIAN_POINT('Ctrl Pts',(-46.1848997473582,-3.60111975388338,
20.));
#79943=CARTESIAN_POINT('Ctrl Pts',(-46.1844796106451,-3.56827274636958,
0.));
#79944=CARTESIAN_POINT('Ctrl Pts',(-46.1844796106451,-3.56827274636958,
20.));
#79945=CARTESIAN_POINT('Ctrl Pts',(-46.1840362905882,-3.53542716005024,
0.));
#79946=CARTESIAN_POINT('Ctrl Pts',(-46.1840362905882,-3.53542716005024,
20.));
#79947=CARTESIAN_POINT('Ctrl Pts',(-46.1835697882921,-3.50258301129688,
0.));
#79948=CARTESIAN_POINT('Ctrl Pts',(-46.1835697882921,-3.50258301129688,
20.));
#79949=CARTESIAN_POINT('Ctrl Pts',(-46.1830801048722,-3.4697403164807,0.));
#79950=CARTESIAN_POINT('Ctrl Pts',(-46.1830801048722,-3.4697403164807,20.));
#79951=CARTESIAN_POINT('Ctrl Pts',(-46.1825672414553,-3.43689909197262,
0.));
#79952=CARTESIAN_POINT('Ctrl Pts',(-46.1825672414553,-3.43689909197262,
20.));
#79953=CARTESIAN_POINT('Ctrl Pts',(-46.1820311991793,-3.40405935414302,
0.));
#79954=CARTESIAN_POINT('Ctrl Pts',(-46.1820311991793,-3.40405935414302,
20.));
#79955=CARTESIAN_POINT('Ctrl Pts',(-46.1814719791936,-3.37122111936182,
0.));
#79956=CARTESIAN_POINT('Ctrl Pts',(-46.1814719791936,-3.37122111936182,
20.));
#79957=CARTESIAN_POINT('Ctrl Pts',(-46.1808895826591,-3.33838440399861,
0.));
#79958=CARTESIAN_POINT('Ctrl Pts',(-46.1808895826591,-3.33838440399861,
20.));
#79959=CARTESIAN_POINT('Ctrl Pts',(-46.1802840107495,-3.30554922442265,
0.));
#79960=CARTESIAN_POINT('Ctrl Pts',(-46.1802840107495,-3.30554922442265,
20.));
#79961=CARTESIAN_POINT('Ctrl Pts',(-46.1796552646498,-3.27271559700278,
0.));
#79962=CARTESIAN_POINT('Ctrl Pts',(-46.1796552646498,-3.27271559700278,
20.));
#79963=CARTESIAN_POINT('Ctrl Pts',(-46.1790033455572,-3.23988353810748,
0.));
#79964=CARTESIAN_POINT('Ctrl Pts',(-46.1790033455572,-3.23988353810748,
20.));
#79965=CARTESIAN_POINT('Ctrl Pts',(-46.1783282546796,-3.2070530641047,0.));
#79966=CARTESIAN_POINT('Ctrl Pts',(-46.1783282546796,-3.2070530641047,20.));
#79967=CARTESIAN_POINT('Ctrl Pts',(-46.1776299932363,-3.17422419136187,
0.));
#79968=CARTESIAN_POINT('Ctrl Pts',(-46.1776299932363,-3.17422419136187,
20.));
#79969=CARTESIAN_POINT('Ctrl Pts',(-46.1769085624582,-3.14139693624604,
0.));
#79970=CARTESIAN_POINT('Ctrl Pts',(-46.1769085624582,-3.14139693624604,
20.));
#79971=CARTESIAN_POINT('Ctrl Pts',(-46.1761639635878,-3.10857131512384,
0.));
#79972=CARTESIAN_POINT('Ctrl Pts',(-46.1761639635878,-3.10857131512384,
20.));
#79973=CARTESIAN_POINT('Ctrl Pts',(-46.1753961978798,-3.07574734436159,
0.));
#79974=CARTESIAN_POINT('Ctrl Pts',(-46.1753961978798,-3.07574734436159,
20.));
#79975=CARTESIAN_POINT('Ctrl Pts',(-46.1746052665999,-3.04292504032496,
0.));
#79976=CARTESIAN_POINT('Ctrl Pts',(-46.1746052665999,-3.04292504032496,
20.));
#79977=CARTESIAN_POINT('Ctrl Pts',(-46.1737911710261,-3.01010441937912,
0.));
#79978=CARTESIAN_POINT('Ctrl Pts',(-46.1737911710261,-3.01010441937912,
20.));
#79979=CARTESIAN_POINT('Ctrl Pts',(-46.1729539124487,-2.97728549788889,
0.));
#79980=CARTESIAN_POINT('Ctrl Pts',(-46.1729539124487,-2.97728549788889,
20.));
#79981=CARTESIAN_POINT('Ctrl Pts',(-46.172093492169,-2.94446829221864,0.));
#79982=CARTESIAN_POINT('Ctrl Pts',(-46.172093492169,-2.94446829221864,20.));
#79983=CARTESIAN_POINT('Ctrl Pts',(-46.1712099114993,-2.91165281873224,
0.));
#79984=CARTESIAN_POINT('Ctrl Pts',(-46.1712099114993,-2.91165281873224,
20.));
#79985=CARTESIAN_POINT('Ctrl Pts',(-46.1703031717627,-2.87883909379286,
0.));
#79986=CARTESIAN_POINT('Ctrl Pts',(-46.1703031717627,-2.87883909379286,
20.));
#79987=CARTESIAN_POINT('Ctrl Pts',(-46.169373274294,-2.84602713376308,0.));
#79988=CARTESIAN_POINT('Ctrl Pts',(-46.169373274294,-2.84602713376308,20.));
#79989=CARTESIAN_POINT('Ctrl Pts',(-46.1684202204402,-2.81321695500491,
0.));
#79990=CARTESIAN_POINT('Ctrl Pts',(-46.1684202204402,-2.81321695500491,
20.));
#79991=CARTESIAN_POINT('Ctrl Pts',(-46.1674440115603,-2.78040857388008,
0.));
#79992=CARTESIAN_POINT('Ctrl Pts',(-46.1674440115603,-2.78040857388008,
20.));
#79993=CARTESIAN_POINT('Ctrl Pts',(-46.1664446490252,-2.74760200674979,
0.));
#79994=CARTESIAN_POINT('Ctrl Pts',(-46.1664446490252,-2.74760200674979,
20.));
#79995=CARTESIAN_POINT('Ctrl Pts',(-46.1654221342175,-2.71479726997479,
0.));
#79996=CARTESIAN_POINT('Ctrl Pts',(-46.1654221342175,-2.71479726997479,
20.));
#79997=CARTESIAN_POINT('Ctrl Pts',(-46.1643764685316,-2.68199437991523,
0.));
#79998=CARTESIAN_POINT('Ctrl Pts',(-46.1643764685316,-2.68199437991523,
20.));
#79999=CARTESIAN_POINT('Ctrl Pts',(-46.163307653373,-2.64919335293067,0.));
#80000=CARTESIAN_POINT('Ctrl Pts',(-46.163307653373,-2.64919335293067,20.));
#80001=CARTESIAN_POINT('Ctrl Pts',(-46.1622156901587,-2.61639420537994,
0.));
#80002=CARTESIAN_POINT('Ctrl Pts',(-46.1622156901587,-2.61639420537994,
20.));
#80003=CARTESIAN_POINT('Ctrl Pts',(-46.1611005803162,-2.58359695362107,
0.));
#80004=CARTESIAN_POINT('Ctrl Pts',(-46.1611005803162,-2.58359695362107,
20.));
#80005=CARTESIAN_POINT('Ctrl Pts',(-46.1599623252856,-2.55080161401166,
0.));
#80006=CARTESIAN_POINT('Ctrl Pts',(-46.1599623252856,-2.55080161401166,
20.));
#80007=CARTESIAN_POINT('Ctrl Pts',(-46.1588009265184,-2.51800820290891,
0.));
#80008=CARTESIAN_POINT('Ctrl Pts',(-46.1588009265184,-2.51800820290891,
20.));
#80009=CARTESIAN_POINT('Ctrl Pts',(-46.1576163854777,-2.48521673666957,
0.));
#80010=CARTESIAN_POINT('Ctrl Pts',(-46.1576163854777,-2.48521673666957,
20.));
#80011=CARTESIAN_POINT('Ctrl Pts',(-46.1564087036389,-2.4524272316497,0.));
#80012=CARTESIAN_POINT('Ctrl Pts',(-46.1564087036389,-2.4524272316497,20.));
#80013=CARTESIAN_POINT('Ctrl Pts',(-46.155177882489,-2.41963970420457,0.));
#80014=CARTESIAN_POINT('Ctrl Pts',(-46.155177882489,-2.41963970420457,20.));
#80015=CARTESIAN_POINT('Ctrl Pts',(-46.1539239235264,-2.3868541706887,0.));
#80016=CARTESIAN_POINT('Ctrl Pts',(-46.1539239235264,-2.3868541706887,20.));
#80017=CARTESIAN_POINT('Ctrl Pts',(-46.1526468282604,-2.35407064745589,
0.));
#80018=CARTESIAN_POINT('Ctrl Pts',(-46.1526468282604,-2.35407064745589,
20.));
#80019=CARTESIAN_POINT('Ctrl Pts',(-46.1513465982124,-2.32128915085919,
0.));
#80020=CARTESIAN_POINT('Ctrl Pts',(-46.1513465982124,-2.32128915085919,
20.));
#80021=CARTESIAN_POINT('Ctrl Pts',(-46.1500232349155,-2.28850969725138,
0.));
#80022=CARTESIAN_POINT('Ctrl Pts',(-46.1500232349155,-2.28850969725138,
20.));
#80023=CARTESIAN_POINT('Ctrl Pts',(-46.1486767399146,-2.25573230298458,
0.));
#80024=CARTESIAN_POINT('Ctrl Pts',(-46.1486767399146,-2.25573230298458,
20.));
#80025=CARTESIAN_POINT('Ctrl Pts',(-46.147307114766,-2.22295698441049,0.));
#80026=CARTESIAN_POINT('Ctrl Pts',(-46.147307114766,-2.22295698441049,20.));
#80027=CARTESIAN_POINT('Ctrl Pts',(-46.1459143610377,-2.19018375787986,
0.));
#80028=CARTESIAN_POINT('Ctrl Pts',(-46.1459143610377,-2.19018375787986,
20.));
#80029=CARTESIAN_POINT('Ctrl Pts',(-46.1444984803082,-2.15741263974262,
0.));
#80030=CARTESIAN_POINT('Ctrl Pts',(-46.1444984803082,-2.15741263974262,
20.));
#80031=CARTESIAN_POINT('Ctrl Pts',(-46.1430594741682,-2.12464364634812,
0.));
#80032=CARTESIAN_POINT('Ctrl Pts',(-46.1430594741682,-2.12464364634812,
20.));
#80033=CARTESIAN_POINT('Ctrl Pts',(-46.1415973442202,-2.09187679404497,
0.));
#80034=CARTESIAN_POINT('Ctrl Pts',(-46.1415973442202,-2.09187679404497,
20.));
#80035=CARTESIAN_POINT('Ctrl Pts',(-46.1401120920793,-2.05911209918101,
0.));
#80036=CARTESIAN_POINT('Ctrl Pts',(-46.1401120920793,-2.05911209918101,
20.));
#80037=CARTESIAN_POINT('Ctrl Pts',(-46.1386037193727,-2.02634957810317,
0.));
#80038=CARTESIAN_POINT('Ctrl Pts',(-46.1386037193727,-2.02634957810317,
20.));
#80039=CARTESIAN_POINT('Ctrl Pts',(-46.1370722277379,-1.99358924715753,
0.));
#80040=CARTESIAN_POINT('Ctrl Pts',(-46.1370722277379,-1.99358924715753,
20.));
#80041=CARTESIAN_POINT('Ctrl Pts',(-46.1355176188236,-1.9608311226893,0.));
#80042=CARTESIAN_POINT('Ctrl Pts',(-46.1355176188236,-1.9608311226893,20.));
#80043=CARTESIAN_POINT('Ctrl Pts',(-46.1339398942902,-1.92807522104339,
0.));
#80044=CARTESIAN_POINT('Ctrl Pts',(-46.1339398942902,-1.92807522104339,
20.));
#80045=CARTESIAN_POINT('Ctrl Pts',(-46.1323390558096,-1.89532155856414,
0.));
#80046=CARTESIAN_POINT('Ctrl Pts',(-46.1323390558096,-1.89532155856414,
20.));
#80047=CARTESIAN_POINT('Ctrl Pts',(-46.1307151050651,-1.86257015159582,
0.));
#80048=CARTESIAN_POINT('Ctrl Pts',(-46.1307151050651,-1.86257015159582,
20.));
#80049=CARTESIAN_POINT('Ctrl Pts',(-46.1290680437528,-1.82982101648206,
0.));
#80050=CARTESIAN_POINT('Ctrl Pts',(-46.1290680437528,-1.82982101648206,
20.));
#80051=CARTESIAN_POINT('Ctrl Pts',(-46.1273978735796,-1.79707416956534,
0.));
#80052=CARTESIAN_POINT('Ctrl Pts',(-46.1273978735796,-1.79707416956534,
20.));
#80053=CARTESIAN_POINT('Ctrl Pts',(-46.1257045962649,-1.76432962718685,
0.));
#80054=CARTESIAN_POINT('Ctrl Pts',(-46.1257045962649,-1.76432962718685,
20.));
#80055=CARTESIAN_POINT('Ctrl Pts',(-46.1239882135394,-1.73158740568597,
0.));
#80056=CARTESIAN_POINT('Ctrl Pts',(-46.1239882135394,-1.73158740568597,
20.));
#80057=CARTESIAN_POINT('Ctrl Pts',(-46.1222487271454,-1.69884752140039,
0.));
#80058=CARTESIAN_POINT('Ctrl Pts',(-46.1222487271454,-1.69884752140039,
20.));
#80059=CARTESIAN_POINT('Ctrl Pts',(-46.1204861388364,-1.66610999066655,
0.));
#80060=CARTESIAN_POINT('Ctrl Pts',(-46.1204861388364,-1.66610999066655,
20.));
#80061=CARTESIAN_POINT('Ctrl Pts',(-46.1187004503775,-1.6333748298207,0.));
#80062=CARTESIAN_POINT('Ctrl Pts',(-46.1187004503775,-1.6333748298207,20.));
#80063=CARTESIAN_POINT('Ctrl Pts',(-46.1168916635447,-1.60064205519958,
0.));
#80064=CARTESIAN_POINT('Ctrl Pts',(-46.1168916635447,-1.60064205519958,
20.));
#80065=CARTESIAN_POINT('Ctrl Pts',(-46.1150597801266,-1.56791168314158,
0.));
#80066=CARTESIAN_POINT('Ctrl Pts',(-46.1150597801266,-1.56791168314158,
20.));
#80067=CARTESIAN_POINT('Ctrl Pts',(-46.1132048019234,-1.53518372998667,
0.));
#80068=CARTESIAN_POINT('Ctrl Pts',(-46.1132048019234,-1.53518372998667,
20.));
#80069=CARTESIAN_POINT('Ctrl Pts',(-46.111326730748,-1.5024582120743,0.));
#80070=CARTESIAN_POINT('Ctrl Pts',(-46.111326730748,-1.5024582120743,20.));
#80071=CARTESIAN_POINT('Ctrl Pts',(-46.1094255684237,-1.46973514574143,
0.));
#80072=CARTESIAN_POINT('Ctrl Pts',(-46.1094255684237,-1.46973514574143,
20.));
#80073=CARTESIAN_POINT('Ctrl Pts',(-46.1075013167858,-1.4370145473209,0.));
#80074=CARTESIAN_POINT('Ctrl Pts',(-46.1075013167858,-1.4370145473209,20.));
#80075=CARTESIAN_POINT('Ctrl Pts',(-46.1055539776802,-1.40429643313893,
0.));
#80076=CARTESIAN_POINT('Ctrl Pts',(-46.1055539776802,-1.40429643313893,
20.));
#80077=CARTESIAN_POINT('Ctrl Pts',(-46.1035835529643,-1.37158081951551,
0.));
#80078=CARTESIAN_POINT('Ctrl Pts',(-46.1035835529643,-1.37158081951551,
20.));
#80079=CARTESIAN_POINT('Ctrl Pts',(-46.1015900445065,-1.33886772276919,
0.));
#80080=CARTESIAN_POINT('Ctrl Pts',(-46.1015900445065,-1.33886772276919,
20.));
#80081=CARTESIAN_POINT('Ctrl Pts',(-46.0995734541875,-1.30615715922172,
0.));
#80082=CARTESIAN_POINT('Ctrl Pts',(-46.0995734541875,-1.30615715922172,
20.));
#80083=CARTESIAN_POINT('Ctrl Pts',(-46.0975337839002,-1.27344914520175,
0.));
#80084=CARTESIAN_POINT('Ctrl Pts',(-46.0975337839002,-1.27344914520175,
20.));
#80085=CARTESIAN_POINT('Ctrl Pts',(-46.0954710355506,-1.24074369705072,
0.));
#80086=CARTESIAN_POINT('Ctrl Pts',(-46.0954710355506,-1.24074369705072,
20.));
#80087=CARTESIAN_POINT('Ctrl Pts',(-46.0933852110571,-1.20804083112097,
0.));
#80088=CARTESIAN_POINT('Ctrl Pts',(-46.0933852110571,-1.20804083112097,
20.));
#80089=CARTESIAN_POINT('Ctrl Pts',(-46.0912763123502,-1.17534056376402,
0.));
#80090=CARTESIAN_POINT('Ctrl Pts',(-46.0912763123502,-1.17534056376402,
20.));
#80091=CARTESIAN_POINT('Ctrl Pts',(-46.0891443413718,-1.14264291132052,
0.));
#80092=CARTESIAN_POINT('Ctrl Pts',(-46.0891443413718,-1.14264291132052,
20.));
#80093=CARTESIAN_POINT('Ctrl Pts',(-46.0869893000734,-1.10994789011162,
0.));
#80094=CARTESIAN_POINT('Ctrl Pts',(-46.0869893000734,-1.10994789011162,
20.));
#80095=CARTESIAN_POINT('Ctrl Pts',(-46.0848111904142,-1.07725551642471,
0.));
#80096=CARTESIAN_POINT('Ctrl Pts',(-46.0848111904142,-1.07725551642471,
20.));
#80097=CARTESIAN_POINT('Ctrl Pts',(-46.0826100143611,-1.04456580652047,
0.));
#80098=CARTESIAN_POINT('Ctrl Pts',(-46.0826100143611,-1.04456580652047,
20.));
#80099=CARTESIAN_POINT('Ctrl Pts',(-46.0803857738924,-1.01187877665954,
0.));
#80100=CARTESIAN_POINT('Ctrl Pts',(-46.0803857738924,-1.01187877665954,
20.));
#80101=CARTESIAN_POINT('Ctrl Pts',(-46.0781384710012,-0.979194443126286,
0.));
#80102=CARTESIAN_POINT('Ctrl Pts',(-46.0781384710012,-0.979194443126286,
20.));
#80103=CARTESIAN_POINT('Ctrl Pts',(-46.0758681076973,-0.946512822248744,
0.));
#80104=CARTESIAN_POINT('Ctrl Pts',(-46.0758681076973,-0.946512822248744,
20.));
#80105=CARTESIAN_POINT('Ctrl Pts',(-46.0735746860119,-0.913833930432268,
0.));
#80106=CARTESIAN_POINT('Ctrl Pts',(-46.0735746860119,-0.913833930432268,
20.));
#80107=CARTESIAN_POINT('Ctrl Pts',(-46.0712582079948,-0.881157784136737,
0.));
#80108=CARTESIAN_POINT('Ctrl Pts',(-46.0712582079948,-0.881157784136737,
20.));
#80109=CARTESIAN_POINT('Ctrl Pts',(-46.0689186757066,-0.848484399815181,
0.));
#80110=CARTESIAN_POINT('Ctrl Pts',(-46.0689186757066,-0.848484399815181,
20.));
#80111=CARTESIAN_POINT('Ctrl Pts',(-46.0665560912128,-0.815813793858633,
0.));
#80112=CARTESIAN_POINT('Ctrl Pts',(-46.0665560912128,-0.815813793858633,
20.));
#80113=CARTESIAN_POINT('Ctrl Pts',(-46.064170456577,-0.78314598254893,0.));
#80114=CARTESIAN_POINT('Ctrl Pts',(-46.064170456577,-0.78314598254893,20.));
#80115=CARTESIAN_POINT('Ctrl Pts',(-46.0617617738521,-0.750480981980923,
0.));
#80116=CARTESIAN_POINT('Ctrl Pts',(-46.0617617738521,-0.750480981980923,
20.));
#80117=CARTESIAN_POINT('Ctrl Pts',(-46.0593300450868,-0.717818808129722,
0.));
#80118=CARTESIAN_POINT('Ctrl Pts',(-46.0593300450868,-0.717818808129722,
20.));
#80119=CARTESIAN_POINT('Ctrl Pts',(-46.0568752723439,-0.685159476991759,
0.));
#80120=CARTESIAN_POINT('Ctrl Pts',(-46.0568752723439,-0.685159476991759,
20.));
#80121=CARTESIAN_POINT('Ctrl Pts',(-46.0543974577158,-0.652503004713259,
0.));
#80122=CARTESIAN_POINT('Ctrl Pts',(-46.0543974577158,-0.652503004713259,
20.));
#80123=CARTESIAN_POINT('Ctrl Pts',(-46.0518966033391,-0.619849407700859,
0.));
#80124=CARTESIAN_POINT('Ctrl Pts',(-46.0518966033391,-0.619849407700859,
20.));
#80125=CARTESIAN_POINT('Ctrl Pts',(-46.0493727114182,-0.587198702798619,
0.));
#80126=CARTESIAN_POINT('Ctrl Pts',(-46.0493727114182,-0.587198702798619,
20.));
#80127=CARTESIAN_POINT('Ctrl Pts',(-46.0468257841997,-0.554550907098827,
0.));
#80128=CARTESIAN_POINT('Ctrl Pts',(-46.0468257841997,-0.554550907098827,
20.));
#80129=CARTESIAN_POINT('Ctrl Pts',(-46.044255823933,-0.521906037621043,
0.));
#80130=CARTESIAN_POINT('Ctrl Pts',(-46.044255823933,-0.521906037621043,
20.));
#80131=CARTESIAN_POINT('Ctrl Pts',(-46.0416628328334,-0.489264111013836,
0.));
#80132=CARTESIAN_POINT('Ctrl Pts',(-46.0416628328334,-0.489264111013836,
20.));
#80133=CARTESIAN_POINT('Ctrl Pts',(-46.0390468130479,-0.456625143292611,
0.));
#80134=CARTESIAN_POINT('Ctrl Pts',(-46.0390468130479,-0.456625143292611,
20.));
#80135=CARTESIAN_POINT('Ctrl Pts',(-46.0364077666069,-0.423989149445243,
0.));
#80136=CARTESIAN_POINT('Ctrl Pts',(-46.0364077666069,-0.423989149445243,
20.));
#80137=CARTESIAN_POINT('Ctrl Pts',(-46.0337456954889,-0.391356143937831,
0.));
#80138=CARTESIAN_POINT('Ctrl Pts',(-46.0337456954889,-0.391356143937831,
20.));
#80139=CARTESIAN_POINT('Ctrl Pts',(-46.0310606017089,-0.358726141441568,
0.));
#80140=CARTESIAN_POINT('Ctrl Pts',(-46.0310606017089,-0.358726141441568,
20.));
#80141=CARTESIAN_POINT('Ctrl Pts',(-46.0283524874048,-0.32609915751695,
0.));
#80142=CARTESIAN_POINT('Ctrl Pts',(-46.0283524874048,-0.32609915751695,
20.));
#80143=CARTESIAN_POINT('Ctrl Pts',(-46.025621354915,-0.293475209241787,
0.));
#80144=CARTESIAN_POINT('Ctrl Pts',(-46.025621354915,-0.293475209241787,
20.));
#80145=CARTESIAN_POINT('Ctrl Pts',(-46.022867206884,-0.260854316057531,
0.));
#80146=CARTESIAN_POINT('Ctrl Pts',(-46.022867206884,-0.260854316057531,
20.));
#80147=CARTESIAN_POINT('Ctrl Pts',(-46.0200900461091,-0.228236498538561,
0.));
#80148=CARTESIAN_POINT('Ctrl Pts',(-46.0200900461091,-0.228236498538561,
20.));
#80149=CARTESIAN_POINT('Ctrl Pts',(-46.0172898753497,-0.195621776838879,
0.));
#80150=CARTESIAN_POINT('Ctrl Pts',(-46.0172898753497,-0.195621776838879,
20.));
#80151=CARTESIAN_POINT('Ctrl Pts',(-46.0144666971462,-0.163010169231703,
0.));
#80152=CARTESIAN_POINT('Ctrl Pts',(-46.0144666971462,-0.163010169231703,
20.));
#80153=CARTESIAN_POINT('Ctrl Pts',(-46.0116205136405,-0.130401690656317,
0.));
#80154=CARTESIAN_POINT('Ctrl Pts',(-46.0116205136405,-0.130401690656317,
20.));
#80155=CARTESIAN_POINT('Ctrl Pts',(-46.0087513263814,-0.0977963511372804,
0.));
#80156=CARTESIAN_POINT('Ctrl Pts',(-46.0087513263814,-0.0977963511372804,
20.));
#80157=CARTESIAN_POINT('Ctrl Pts',(-46.0058591364029,-0.0651941566547531,
0.));
#80158=CARTESIAN_POINT('Ctrl Pts',(-46.0058591364029,-0.0651941566547531,
20.));
#80159=CARTESIAN_POINT('Ctrl Pts',(-46.0035269827389,-0.0391149194889384,
0.));
#80160=CARTESIAN_POINT('Ctrl Pts',(-46.0035269827389,-0.0391149194889384,
20.));
#80161=CARTESIAN_POINT('Ctrl Pts',(-46.0017675166781,-0.019556908668581,
0.));
#80162=CARTESIAN_POINT('Ctrl Pts',(-46.0017675166781,-0.019556908668581,
20.));
#80163=CARTESIAN_POINT('Ctrl Pts',(-46.0005899389515,-0.00651886458936213,
0.));
#80164=CARTESIAN_POINT('Ctrl Pts',(-46.0005899389515,-0.00651886458936213,
20.));
#80165=CARTESIAN_POINT('Ctrl Pts',(-46.,6.66133814775094E-15,0.));
#80166=CARTESIAN_POINT('Ctrl Pts',(-46.,6.66133814775094E-15,20.));
#80167=CARTESIAN_POINT('',(-46.,1.33226762955019E-14,2.));
#80168=CARTESIAN_POINT('',(-46.,1.33226762955019E-14,0.));
#80169=CARTESIAN_POINT('Ctrl Pts',(-46.,6.66133814775094E-15,2.));
#80170=CARTESIAN_POINT('Ctrl Pts',(-46.2231469371097,-2.46578847330934,
2.));
#80171=CARTESIAN_POINT('Ctrl Pts',(-46.2472869474438,-4.94053945739677,
2.));
#80172=CARTESIAN_POINT('Ctrl Pts',(-46.0771487393297,-7.40158428157358,
2.));
#80173=CARTESIAN_POINT('Ctrl Pts',(-46.0449384185095,16.7589870229578,0.));
#80174=CARTESIAN_POINT('Ctrl Pts',(-46.0449384185095,16.7589870229578,20.));
#80175=CARTESIAN_POINT('Ctrl Pts',(-46.0420594924752,16.7651130917503,0.));
#80176=CARTESIAN_POINT('Ctrl Pts',(-46.0420594924752,16.7651130917503,20.));
#80177=CARTESIAN_POINT('Ctrl Pts',(-46.0362995834799,16.7773641333857,0.));
#80178=CARTESIAN_POINT('Ctrl Pts',(-46.0362995834799,16.7773641333857,20.));
#80179=CARTESIAN_POINT('Ctrl Pts',(-46.0276535492065,16.7957374079899,0.));
#80180=CARTESIAN_POINT('Ctrl Pts',(-46.0276535492065,16.7957374079899,20.));
#80181=CARTESIAN_POINT('Ctrl Pts',(-46.0161131619282,16.8202285317553,0.));
#80182=CARTESIAN_POINT('Ctrl Pts',(-46.0161131619282,16.8202285317553,20.));
#80183=CARTESIAN_POINT('Ctrl Pts',(-46.0016671088634,16.8508314760754,0.));
#80184=CARTESIAN_POINT('Ctrl Pts',(-46.0016671088634,16.8508314760754,20.));
#80185=CARTESIAN_POINT('Ctrl Pts',(-45.9872004880192,16.8814234574888,0.));
#80186=CARTESIAN_POINT('Ctrl Pts',(-45.9872004880192,16.8814234574888,20.));
#80187=CARTESIAN_POINT('Ctrl Pts',(-45.9727133019197,16.9120044710149,0.));
#80188=CARTESIAN_POINT('Ctrl Pts',(-45.9727133019197,16.9120044710149,20.));
#80189=CARTESIAN_POINT('Ctrl Pts',(-45.9582055548827,16.9425745084438,0.));
#80190=CARTESIAN_POINT('Ctrl Pts',(-45.9582055548827,16.9425745084438,20.));
#80191=CARTESIAN_POINT('Ctrl Pts',(-45.9436772535459,16.9731335574459,0.));
#80192=CARTESIAN_POINT('Ctrl Pts',(-45.9436772535459,16.9731335574459,20.));
#80193=CARTESIAN_POINT('Ctrl Pts',(-45.9291284062576,17.0036816026634,0.));
#80194=CARTESIAN_POINT('Ctrl Pts',(-45.9291284062576,17.0036816026634,20.));
#80195=CARTESIAN_POINT('Ctrl Pts',(-45.91455902239,17.0342186269341,0.));
#80196=CARTESIAN_POINT('Ctrl Pts',(-45.91455902239,17.0342186269341,20.));
#80197=CARTESIAN_POINT('Ctrl Pts',(-45.8999691116667,17.0647446124944,0.));
#80198=CARTESIAN_POINT('Ctrl Pts',(-45.8999691116667,17.0647446124944,20.));
#80199=CARTESIAN_POINT('Ctrl Pts',(-45.8853586835176,17.0952595421299,0.));
#80200=CARTESIAN_POINT('Ctrl Pts',(-45.8853586835176,17.0952595421299,20.));
#80201=CARTESIAN_POINT('Ctrl Pts',(-45.8707277463338,17.1257634005083,0.));
#80202=CARTESIAN_POINT('Ctrl Pts',(-45.8707277463338,17.1257634005083,20.));
#80203=CARTESIAN_POINT('Ctrl Pts',(-45.8560763076625,17.1562561738292,0.));
#80204=CARTESIAN_POINT('Ctrl Pts',(-45.8560763076625,17.1562561738292,20.));
#80205=CARTESIAN_POINT('Ctrl Pts',(-45.8414043745501,17.1867378492105,0.));
#80206=CARTESIAN_POINT('Ctrl Pts',(-45.8414043745501,17.1867378492105,20.));
#80207=CARTESIAN_POINT('Ctrl Pts',(-45.8267119538424,17.2172084141516,0.));
#80208=CARTESIAN_POINT('Ctrl Pts',(-45.8267119538424,17.2172084141516,20.));
#80209=CARTESIAN_POINT('Ctrl Pts',(-45.8119990524824,17.247667856,0.));
#80210=CARTESIAN_POINT('Ctrl Pts',(-45.8119990524824,17.247667856,20.));
#80211=CARTESIAN_POINT('Ctrl Pts',(-45.7972656778619,17.2781161613228,0.));
#80212=CARTESIAN_POINT('Ctrl Pts',(-45.7972656778619,17.2781161613228,20.));
#80213=CARTESIAN_POINT('Ctrl Pts',(-45.7825118377706,17.3085533159981,0.));
#80214=CARTESIAN_POINT('Ctrl Pts',(-45.7825118377706,17.3085533159981,20.));
#80215=CARTESIAN_POINT('Ctrl Pts',(-45.7677375402376,17.3389793054984,0.));
#80216=CARTESIAN_POINT('Ctrl Pts',(-45.7677375402376,17.3389793054984,20.));
#80217=CARTESIAN_POINT('Ctrl Pts',(-45.7529427934047,17.3693941151172,0.));
#80218=CARTESIAN_POINT('Ctrl Pts',(-45.7529427934047,17.3693941151172,20.));
#80219=CARTESIAN_POINT('Ctrl Pts',(-45.7381276053972,17.3997977302007,0.));
#80220=CARTESIAN_POINT('Ctrl Pts',(-45.7381276053972,17.3997977302007,20.));
#80221=CARTESIAN_POINT('Ctrl Pts',(-45.7232919841685,17.4301901364248,0.));
#80222=CARTESIAN_POINT('Ctrl Pts',(-45.7232919841685,17.4301901364248,20.));
#80223=CARTESIAN_POINT('Ctrl Pts',(-45.7084359375081,17.460571319782,0.));
#80224=CARTESIAN_POINT('Ctrl Pts',(-45.7084359375081,17.460571319782,20.));
#80225=CARTESIAN_POINT('Ctrl Pts',(-45.6935594731126,17.4909412664519,0.));
#80226=CARTESIAN_POINT('Ctrl Pts',(-45.6935594731126,17.4909412664519,20.));
#80227=CARTESIAN_POINT('Ctrl Pts',(-45.6786625986401,17.5212999627071,0.));
#80228=CARTESIAN_POINT('Ctrl Pts',(-45.6786625986401,17.5212999627071,20.));
#80229=CARTESIAN_POINT('Ctrl Pts',(-45.6637453217655,17.5516473948116,0.));
#80230=CARTESIAN_POINT('Ctrl Pts',(-45.6637453217655,17.5516473948116,20.));
#80231=CARTESIAN_POINT('Ctrl Pts',(-45.6488076502485,17.5819835489016,0.));
#80232=CARTESIAN_POINT('Ctrl Pts',(-45.6488076502485,17.5819835489016,20.));
#80233=CARTESIAN_POINT('Ctrl Pts',(-45.6338495919363,17.6123084109793,0.));
#80234=CARTESIAN_POINT('Ctrl Pts',(-45.6338495919363,17.6123084109793,20.));
#80235=CARTESIAN_POINT('Ctrl Pts',(-45.6188711547313,17.6426219669711,0.));
#80236=CARTESIAN_POINT('Ctrl Pts',(-45.6188711547313,17.6426219669711,20.));
#80237=CARTESIAN_POINT('Ctrl Pts',(-45.6038723465685,17.672924202767,0.));
#80238=CARTESIAN_POINT('Ctrl Pts',(-45.6038723465685,17.672924202767,20.));
#80239=CARTESIAN_POINT('Ctrl Pts',(-45.5888531753912,17.7032151042645,0.));
#80240=CARTESIAN_POINT('Ctrl Pts',(-45.5888531753912,17.7032151042645,20.));
#80241=CARTESIAN_POINT('Ctrl Pts',(-45.5738136491221,17.7334946574206,0.));
#80242=CARTESIAN_POINT('Ctrl Pts',(-45.5738136491221,17.7334946574206,20.));
#80243=CARTESIAN_POINT('Ctrl Pts',(-45.5587537756595,17.7637628482589,0.));
#80244=CARTESIAN_POINT('Ctrl Pts',(-45.5587537756595,17.7637628482589,20.));
#80245=CARTESIAN_POINT('Ctrl Pts',(-45.5436735628911,17.7940196628442,0.));
#80246=CARTESIAN_POINT('Ctrl Pts',(-45.5436735628911,17.7940196628442,20.));
#80247=CARTESIAN_POINT('Ctrl Pts',(-45.528573018704,17.8242650872661,0.));
#80248=CARTESIAN_POINT('Ctrl Pts',(-45.528573018704,17.8242650872661,20.));
#80249=CARTESIAN_POINT('Ctrl Pts',(-45.5134521509949,17.8544991076191,0.));
#80250=CARTESIAN_POINT('Ctrl Pts',(-45.5134521509949,17.8544991076191,20.));
#80251=CARTESIAN_POINT('Ctrl Pts',(-45.498310967683,17.8847217099814,0.));
#80252=CARTESIAN_POINT('Ctrl Pts',(-45.498310967683,17.8847217099814,20.));
#80253=CARTESIAN_POINT('Ctrl Pts',(-45.4831494767122,17.9149328804084,0.));
#80254=CARTESIAN_POINT('Ctrl Pts',(-45.4831494767122,17.9149328804084,20.));
#80255=CARTESIAN_POINT('Ctrl Pts',(-45.4679676860453,17.9451326049449,0.));
#80256=CARTESIAN_POINT('Ctrl Pts',(-45.4679676860453,17.9451326049449,20.));
#80257=CARTESIAN_POINT('Ctrl Pts',(-45.4527656036598,17.9753208696315,0.));
#80258=CARTESIAN_POINT('Ctrl Pts',(-45.4527656036598,17.9753208696315,20.));
#80259=CARTESIAN_POINT('Ctrl Pts',(-45.4375432375433,18.0054976605137,0.));
#80260=CARTESIAN_POINT('Ctrl Pts',(-45.4375432375433,18.0054976605137,20.));
#80261=CARTESIAN_POINT('Ctrl Pts',(-45.4223005956881,18.0356629636502,0.));
#80262=CARTESIAN_POINT('Ctrl Pts',(-45.4223005956881,18.0356629636502,20.));
#80263=CARTESIAN_POINT('Ctrl Pts',(-45.4070376860893,18.0658167651176,0.));
#80264=CARTESIAN_POINT('Ctrl Pts',(-45.4070376860893,18.0658167651176,20.));
#80265=CARTESIAN_POINT('Ctrl Pts',(-45.3917545167484,18.0959590510046,0.));
#80266=CARTESIAN_POINT('Ctrl Pts',(-45.3917545167484,18.0959590510046,20.));
#80267=CARTESIAN_POINT('Ctrl Pts',(-45.3764510956741,18.1260898074095,0.));
#80268=CARTESIAN_POINT('Ctrl Pts',(-45.3764510956741,18.1260898074095,20.));
#80269=CARTESIAN_POINT('Ctrl Pts',(-45.3611274308852,18.156209020436,0.));
#80270=CARTESIAN_POINT('Ctrl Pts',(-45.3611274308852,18.156209020436,20.));
#80271=CARTESIAN_POINT('Ctrl Pts',(-45.345783530412,18.1863166761897,0.));
#80272=CARTESIAN_POINT('Ctrl Pts',(-45.345783530412,18.1863166761897,20.));
#80273=CARTESIAN_POINT('Ctrl Pts',(-45.3304194022976,18.216412760776,0.));
#80274=CARTESIAN_POINT('Ctrl Pts',(-45.3304194022976,18.216412760776,20.));
#80275=CARTESIAN_POINT('Ctrl Pts',(-45.3150350545965,18.2464972603023,0.));
#80276=CARTESIAN_POINT('Ctrl Pts',(-45.3150350545965,18.2464972603023,20.));
#80277=CARTESIAN_POINT('Ctrl Pts',(-45.299630495374,18.2765701608789,0.));
#80278=CARTESIAN_POINT('Ctrl Pts',(-45.299630495374,18.2765701608789,20.));
#80279=CARTESIAN_POINT('Ctrl Pts',(-45.2842057327049,18.3066314486214,0.));
#80280=CARTESIAN_POINT('Ctrl Pts',(-45.2842057327049,18.3066314486214,20.));
#80281=CARTESIAN_POINT('Ctrl Pts',(-45.2687607746732,18.3366811096519,0.));
#80282=CARTESIAN_POINT('Ctrl Pts',(-45.2687607746732,18.3366811096519,20.));
#80283=CARTESIAN_POINT('Ctrl Pts',(-45.2532956293718,18.3667191300999,0.));
#80284=CARTESIAN_POINT('Ctrl Pts',(-45.2532956293718,18.3667191300999,20.));
#80285=CARTESIAN_POINT('Ctrl Pts',(-45.2378103049023,18.3967454961016,0.));
#80286=CARTESIAN_POINT('Ctrl Pts',(-45.2378103049023,18.3967454961016,20.));
#80287=CARTESIAN_POINT('Ctrl Pts',(-45.2223048093755,18.4267601937997,0.));
#80288=CARTESIAN_POINT('Ctrl Pts',(-45.2223048093755,18.4267601937997,20.));
#80289=CARTESIAN_POINT('Ctrl Pts',(-45.2067791509123,18.456763209342,0.));
#80290=CARTESIAN_POINT('Ctrl Pts',(-45.2067791509123,18.456763209342,20.));
#80291=CARTESIAN_POINT('Ctrl Pts',(-45.1912333376434,18.4867545288811,0.));
#80292=CARTESIAN_POINT('Ctrl Pts',(-45.1912333376434,18.4867545288811,20.));
#80293=CARTESIAN_POINT('Ctrl Pts',(-45.1756673777099,18.5167341385735,0.));
#80294=CARTESIAN_POINT('Ctrl Pts',(-45.1756673777099,18.5167341385735,20.));
#80295=CARTESIAN_POINT('Ctrl Pts',(-45.1600812792631,18.5467020245809,0.));
#80296=CARTESIAN_POINT('Ctrl Pts',(-45.1600812792631,18.5467020245809,20.));
#80297=CARTESIAN_POINT('Ctrl Pts',(-45.144475050464,18.5766581730694,0.));
#80298=CARTESIAN_POINT('Ctrl Pts',(-45.144475050464,18.5766581730694,20.));
#80299=CARTESIAN_POINT('Ctrl Pts',(-45.1288486994834,18.6066025702106,0.));
#80300=CARTESIAN_POINT('Ctrl Pts',(-45.1288486994834,18.6066025702106,20.));
#80301=CARTESIAN_POINT('Ctrl Pts',(-45.1132022345013,18.6365352021813,0.));
#80302=CARTESIAN_POINT('Ctrl Pts',(-45.1132022345013,18.6365352021813,20.));
#80303=CARTESIAN_POINT('Ctrl Pts',(-45.097535663708,18.6664560551643,0.));
#80304=CARTESIAN_POINT('Ctrl Pts',(-45.097535663708,18.6664560551643,20.));
#80305=CARTESIAN_POINT('Ctrl Pts',(-45.081848995303,18.6963651153477,0.));
#80306=CARTESIAN_POINT('Ctrl Pts',(-45.081848995303,18.6963651153477,20.));
#80307=CARTESIAN_POINT('Ctrl Pts',(-45.0661422374956,18.7262623689254,0.));
#80308=CARTESIAN_POINT('Ctrl Pts',(-45.0661422374956,18.7262623689254,20.));
#80309=CARTESIAN_POINT('Ctrl Pts',(-45.050415398505,18.7561478020964,0.));
#80310=CARTESIAN_POINT('Ctrl Pts',(-45.050415398505,18.7561478020964,20.));
#80311=CARTESIAN_POINT('Ctrl Pts',(-45.0346684865594,18.7860214010651,0.));
#80312=CARTESIAN_POINT('Ctrl Pts',(-45.0346684865594,18.7860214010651,20.));
#80313=CARTESIAN_POINT('Ctrl Pts',(-45.0189015098976,18.815883152041,0.));
#80314=CARTESIAN_POINT('Ctrl Pts',(-45.0189015098976,18.815883152041,20.));
#80315=CARTESIAN_POINT('Ctrl Pts',(-45.0031144767678,18.8457330412389,0.));
#80316=CARTESIAN_POINT('Ctrl Pts',(-45.0031144767678,18.8457330412389,20.));
#80317=CARTESIAN_POINT('Ctrl Pts',(-44.9873073954281,18.8755710548787,0.));
#80318=CARTESIAN_POINT('Ctrl Pts',(-44.9873073954281,18.8755710548787,20.));
#80319=CARTESIAN_POINT('Ctrl Pts',(-44.971480274146,18.9053971791858,0.));
#80320=CARTESIAN_POINT('Ctrl Pts',(-44.971480274146,18.9053971791858,20.));
#80321=CARTESIAN_POINT('Ctrl Pts',(-44.9556331211993,18.9352114003906,0.));
#80322=CARTESIAN_POINT('Ctrl Pts',(-44.9556331211993,18.9352114003906,20.));
#80323=CARTESIAN_POINT('Ctrl Pts',(-44.9397659448753,18.9650137047293,0.));
#80324=CARTESIAN_POINT('Ctrl Pts',(-44.9397659448753,18.9650137047293,20.));
#80325=CARTESIAN_POINT('Ctrl Pts',(-44.9238787534705,18.9948040784434,0.));
#80326=CARTESIAN_POINT('Ctrl Pts',(-44.9238787534705,18.9948040784434,20.));
#80327=CARTESIAN_POINT('Ctrl Pts',(-44.9079715552916,19.0245825077797,0.));
#80328=CARTESIAN_POINT('Ctrl Pts',(-44.9079715552916,19.0245825077797,20.));
#80329=CARTESIAN_POINT('Ctrl Pts',(-44.8920443586544,19.0543489789907,0.));
#80330=CARTESIAN_POINT('Ctrl Pts',(-44.8920443586544,19.0543489789907,20.));
#80331=CARTESIAN_POINT('Ctrl Pts',(-44.8760971718851,19.0841034783341,0.));
#80332=CARTESIAN_POINT('Ctrl Pts',(-44.8760971718851,19.0841034783341,20.));
#80333=CARTESIAN_POINT('Ctrl Pts',(-44.8601300033192,19.1138459920731,0.));
#80334=CARTESIAN_POINT('Ctrl Pts',(-44.8601300033192,19.1138459920731,20.));
#80335=CARTESIAN_POINT('Ctrl Pts',(-44.8441428613021,19.143576506476,0.));
#80336=CARTESIAN_POINT('Ctrl Pts',(-44.8441428613021,19.143576506476,20.));
#80337=CARTESIAN_POINT('Ctrl Pts',(-44.8281357541891,19.1732950078168,0.));
#80338=CARTESIAN_POINT('Ctrl Pts',(-44.8281357541891,19.1732950078168,20.));
#80339=CARTESIAN_POINT('Ctrl Pts',(-44.8121086903447,19.2030014823748,0.));
#80340=CARTESIAN_POINT('Ctrl Pts',(-44.8121086903447,19.2030014823748,20.));
#80341=CARTESIAN_POINT('Ctrl Pts',(-44.7960616781431,19.2326959164344,0.));
#80342=CARTESIAN_POINT('Ctrl Pts',(-44.7960616781431,19.2326959164344,20.));
#80343=CARTESIAN_POINT('Ctrl Pts',(-44.7799947259683,19.2623782962858,0.));
#80344=CARTESIAN_POINT('Ctrl Pts',(-44.7799947259683,19.2623782962858,20.));
#80345=CARTESIAN_POINT('Ctrl Pts',(-44.7639078422139,19.2920486082247,0.));
#80346=CARTESIAN_POINT('Ctrl Pts',(-44.7639078422139,19.2920486082247,20.));
#80347=CARTESIAN_POINT('Ctrl Pts',(-44.7478010352831,19.3217068385519,0.));
#80348=CARTESIAN_POINT('Ctrl Pts',(-44.7478010352831,19.3217068385519,20.));
#80349=CARTESIAN_POINT('Ctrl Pts',(-44.731674313589,19.3513529735741,0.));
#80350=CARTESIAN_POINT('Ctrl Pts',(-44.731674313589,19.3513529735741,20.));
#80351=CARTESIAN_POINT('Ctrl Pts',(-44.7155276855546,19.3809869996033,0.));
#80352=CARTESIAN_POINT('Ctrl Pts',(-44.7155276855546,19.3809869996033,20.));
#80353=CARTESIAN_POINT('Ctrl Pts',(-44.6993611596123,19.4106089029568,0.));
#80354=CARTESIAN_POINT('Ctrl Pts',(-44.6993611596123,19.4106089029568,20.));
#80355=CARTESIAN_POINT('Ctrl Pts',(-44.6831747442042,19.4402186699576,0.));
#80356=CARTESIAN_POINT('Ctrl Pts',(-44.6831747442042,19.4402186699576,20.));
#80357=CARTESIAN_POINT('Ctrl Pts',(-44.666968447782,19.4698162869338,0.));
#80358=CARTESIAN_POINT('Ctrl Pts',(-44.666968447782,19.4698162869338,20.));
#80359=CARTESIAN_POINT('Ctrl Pts',(-44.6507422788067,19.4994017402193,0.));
#80360=CARTESIAN_POINT('Ctrl Pts',(-44.6507422788067,19.4994017402193,20.));
#80361=CARTESIAN_POINT('Ctrl Pts',(-44.6344962457493,19.5289750161533,0.));
#80362=CARTESIAN_POINT('Ctrl Pts',(-44.6344962457493,19.5289750161533,20.));
#80363=CARTESIAN_POINT('Ctrl Pts',(-44.6182303570903,19.5585361010809,0.));
#80364=CARTESIAN_POINT('Ctrl Pts',(-44.6182303570903,19.5585361010809,20.));
#80365=CARTESIAN_POINT('Ctrl Pts',(-44.60194462132,19.5880849813525,0.));
#80366=CARTESIAN_POINT('Ctrl Pts',(-44.60194462132,19.5880849813525,20.));
#80367=CARTESIAN_POINT('Ctrl Pts',(-44.5856390469384,19.6176216433241,0.));
#80368=CARTESIAN_POINT('Ctrl Pts',(-44.5856390469384,19.6176216433241,20.));
#80369=CARTESIAN_POINT('Ctrl Pts',(-44.5693136424549,19.6471460733568,0.));
#80370=CARTESIAN_POINT('Ctrl Pts',(-44.5693136424549,19.6471460733568,20.));
#80371=CARTESIAN_POINT('Ctrl Pts',(-44.5529684163885,19.6766582578175,0.));
#80372=CARTESIAN_POINT('Ctrl Pts',(-44.5529684163885,19.6766582578175,20.));
#80373=CARTESIAN_POINT('Ctrl Pts',(-44.5366033772682,19.7061581830785,0.));
#80374=CARTESIAN_POINT('Ctrl Pts',(-44.5366033772682,19.7061581830785,20.));
#80375=CARTESIAN_POINT('Ctrl Pts',(-44.5202185336324,19.7356458355178,0.));
#80376=CARTESIAN_POINT('Ctrl Pts',(-44.5202185336324,19.7356458355178,20.));
#80377=CARTESIAN_POINT('Ctrl Pts',(-44.5038138940293,19.7651212015191,0.));
#80378=CARTESIAN_POINT('Ctrl Pts',(-44.5038138940293,19.7651212015191,20.));
#80379=CARTESIAN_POINT('Ctrl Pts',(-44.4873894670167,19.7945842674717,0.));
#80380=CARTESIAN_POINT('Ctrl Pts',(-44.4873894670167,19.7945842674717,20.));
#80381=CARTESIAN_POINT('Ctrl Pts',(-44.4709452611615,19.8240350197702,0.));
#80382=CARTESIAN_POINT('Ctrl Pts',(-44.4709452611615,19.8240350197702,20.));
#80383=CARTESIAN_POINT('Ctrl Pts',(-44.4544812850403,19.8534734448146,0.));
#80384=CARTESIAN_POINT('Ctrl Pts',(-44.4544812850403,19.8534734448146,20.));
#80385=CARTESIAN_POINT('Ctrl Pts',(-44.4379975472397,19.8828995290107,0.));
#80386=CARTESIAN_POINT('Ctrl Pts',(-44.4379975472397,19.8828995290107,20.));
#80387=CARTESIAN_POINT('Ctrl Pts',(-44.4214940563557,19.9123132587697,0.));
#80388=CARTESIAN_POINT('Ctrl Pts',(-44.4214940563557,19.9123132587697,20.));
#80389=CARTESIAN_POINT('Ctrl Pts',(-44.4049708209939,19.9417146205087,0.));
#80390=CARTESIAN_POINT('Ctrl Pts',(-44.4049708209939,19.9417146205087,20.));
#80391=CARTESIAN_POINT('Ctrl Pts',(-44.3884278497697,19.9711036006503,0.));
#80392=CARTESIAN_POINT('Ctrl Pts',(-44.3884278497697,19.9711036006503,20.));
#80393=CARTESIAN_POINT('Ctrl Pts',(-44.371865151308,20.0004801856228,0.));
#80394=CARTESIAN_POINT('Ctrl Pts',(-44.371865151308,20.0004801856228,20.));
#80395=CARTESIAN_POINT('Ctrl Pts',(-44.3552827342435,20.0298443618602,0.));
#80396=CARTESIAN_POINT('Ctrl Pts',(-44.3552827342435,20.0298443618602,20.));
#80397=CARTESIAN_POINT('Ctrl Pts',(-44.3386806072204,20.0591961158018,0.));
#80398=CARTESIAN_POINT('Ctrl Pts',(-44.3386806072204,20.0591961158018,20.));
#80399=CARTESIAN_POINT('Ctrl Pts',(-44.3220587788923,20.0885354338929,0.));
#80400=CARTESIAN_POINT('Ctrl Pts',(-44.3220587788923,20.0885354338929,20.));
#80401=CARTESIAN_POINT('Ctrl Pts',(-44.3054172579222,20.117862302584,0.));
#80402=CARTESIAN_POINT('Ctrl Pts',(-44.3054172579222,20.117862302584,20.));
#80403=CARTESIAN_POINT('Ctrl Pts',(-44.2887560529826,20.1471767083313,0.));
#80404=CARTESIAN_POINT('Ctrl Pts',(-44.2887560529826,20.1471767083313,20.));
#80405=CARTESIAN_POINT('Ctrl Pts',(-44.2720751727557,20.1764786375963,0.));
#80406=CARTESIAN_POINT('Ctrl Pts',(-44.2720751727557,20.1764786375963,20.));
#80407=CARTESIAN_POINT('Ctrl Pts',(-44.2553746259333,20.2057680768465,0.));
#80408=CARTESIAN_POINT('Ctrl Pts',(-44.2553746259333,20.2057680768465,20.));
#80409=CARTESIAN_POINT('Ctrl Pts',(-44.238654421217,20.2350450125552,0.));
#80410=CARTESIAN_POINT('Ctrl Pts',(-44.238654421217,20.2350450125552,20.));
#80411=CARTESIAN_POINT('Ctrl Pts',(-44.221914567318,20.2643094312016,0.));
#80412=CARTESIAN_POINT('Ctrl Pts',(-44.221914567318,20.2643094312016,20.));
#80413=CARTESIAN_POINT('Ctrl Pts',(-44.205155072957,20.2935613192706,0.));
#80414=CARTESIAN_POINT('Ctrl Pts',(-44.205155072957,20.2935613192706,20.));
#80415=CARTESIAN_POINT('Ctrl Pts',(-44.1883759468646,20.3228006632528,0.));
#80416=CARTESIAN_POINT('Ctrl Pts',(-44.1883759468646,20.3228006632528,20.));
#80417=CARTESIAN_POINT('Ctrl Pts',(-44.1715771977807,20.3520274496443,0.));
#80418=CARTESIAN_POINT('Ctrl Pts',(-44.1715771977807,20.3520274496443,20.));
#80419=CARTESIAN_POINT('Ctrl Pts',(-44.1547588344544,20.3812416649468,0.));
#80420=CARTESIAN_POINT('Ctrl Pts',(-44.1547588344544,20.3812416649468,20.));
#80421=CARTESIAN_POINT('Ctrl Pts',(-44.1379208656442,20.4104432956673,0.));
#80422=CARTESIAN_POINT('Ctrl Pts',(-44.1379208656442,20.4104432956673,20.));
#80423=CARTESIAN_POINT('Ctrl Pts',(-44.1210633001184,20.4396323283186,0.));
#80424=CARTESIAN_POINT('Ctrl Pts',(-44.1210633001184,20.4396323283186,20.));
#80425=CARTESIAN_POINT('Ctrl Pts',(-44.1041861466545,20.468808749419,0.));
#80426=CARTESIAN_POINT('Ctrl Pts',(-44.1041861466545,20.468808749419,20.));
#80427=CARTESIAN_POINT('Ctrl Pts',(-44.0872894140398,20.4979725454932,0.));
#80428=CARTESIAN_POINT('Ctrl Pts',(-44.0872894140398,20.4979725454932,20.));
#80429=CARTESIAN_POINT('Ctrl Pts',(-44.0703731110714,20.5271237030716,0.));
#80430=CARTESIAN_POINT('Ctrl Pts',(-44.0703731110714,20.5271237030716,20.));
#80431=CARTESIAN_POINT('Ctrl Pts',(-44.053437246556,20.5562622086905,0.));
#80432=CARTESIAN_POINT('Ctrl Pts',(-44.053437246556,20.5562622086905,20.));
#80433=CARTESIAN_POINT('Ctrl Pts',(-44.03648182931,20.5853880488919,0.));
#80434=CARTESIAN_POINT('Ctrl Pts',(-44.03648182931,20.5853880488919,20.));
#80435=CARTESIAN_POINT('Ctrl Pts',(-44.0195068681592,20.6145012102233,0.));
#80436=CARTESIAN_POINT('Ctrl Pts',(-44.0195068681592,20.6145012102233,20.));
#80437=CARTESIAN_POINT('Ctrl Pts',(-44.0025123719387,20.6436016792381,0.));
#80438=CARTESIAN_POINT('Ctrl Pts',(-44.0025123719387,20.6436016792381,20.));
#80439=CARTESIAN_POINT('Ctrl Pts',(-43.9854983494929,20.6726894424949,0.));
#80440=CARTESIAN_POINT('Ctrl Pts',(-43.9854983494929,20.6726894424949,20.));
#80441=CARTESIAN_POINT('Ctrl Pts',(-43.9684648096756,20.7017644865584,0.));
#80442=CARTESIAN_POINT('Ctrl Pts',(-43.9684648096756,20.7017644865584,20.));
#80443=CARTESIAN_POINT('Ctrl Pts',(-43.9514117613501,20.7308267979991,0.));
#80444=CARTESIAN_POINT('Ctrl Pts',(-43.9514117613501,20.7308267979991,20.));
#80445=CARTESIAN_POINT('Ctrl Pts',(-43.9343392133895,20.7598763633934,0.));
#80446=CARTESIAN_POINT('Ctrl Pts',(-43.9343392133895,20.7598763633934,20.));
#80447=CARTESIAN_POINT('Ctrl Pts',(-43.9172471746767,20.7889131693233,0.));
#80448=CARTESIAN_POINT('Ctrl Pts',(-43.9172471746767,20.7889131693233,20.));
#80449=CARTESIAN_POINT('Ctrl Pts',(-43.9001356541037,20.817937202377,0.));
#80450=CARTESIAN_POINT('Ctrl Pts',(-43.9001356541037,20.817937202377,20.));
#80451=CARTESIAN_POINT('Ctrl Pts',(-43.8830046605723,20.8469484491482,0.));
#80452=CARTESIAN_POINT('Ctrl Pts',(-43.8830046605723,20.8469484491482,20.));
#80453=CARTESIAN_POINT('Ctrl Pts',(-43.8658542029936,20.8759468962364,0.));
#80454=CARTESIAN_POINT('Ctrl Pts',(-43.8658542029936,20.8759468962364,20.));
#80455=CARTESIAN_POINT('Ctrl Pts',(-43.8486842902882,20.9049325302471,0.));
#80456=CARTESIAN_POINT('Ctrl Pts',(-43.8486842902882,20.9049325302471,20.));
#80457=CARTESIAN_POINT('Ctrl Pts',(-43.8314949313861,20.9339053377913,0.));
#80458=CARTESIAN_POINT('Ctrl Pts',(-43.8314949313861,20.9339053377913,20.));
#80459=CARTESIAN_POINT('Ctrl Pts',(-43.8142861352268,20.9628653054863,0.));
#80460=CARTESIAN_POINT('Ctrl Pts',(-43.8142861352268,20.9628653054863,20.));
#80461=CARTESIAN_POINT('Ctrl Pts',(-43.7970579107591,20.9918124199547,0.));
#80462=CARTESIAN_POINT('Ctrl Pts',(-43.7970579107591,20.9918124199547,20.));
#80463=CARTESIAN_POINT('Ctrl Pts',(-43.7798102669417,21.0207466678254,0.));
#80464=CARTESIAN_POINT('Ctrl Pts',(-43.7798102669417,21.0207466678254,20.));
#80465=CARTESIAN_POINT('Ctrl Pts',(-43.7625432127426,21.0496680357328,0.));
#80466=CARTESIAN_POINT('Ctrl Pts',(-43.7625432127426,21.0496680357328,20.));
#80467=CARTESIAN_POINT('Ctrl Pts',(-43.7452567571393,21.0785765103172,0.));
#80468=CARTESIAN_POINT('Ctrl Pts',(-43.7452567571393,21.0785765103172,20.));
#80469=CARTESIAN_POINT('Ctrl Pts',(-43.7279509091188,21.1074720782252,0.));
#80470=CARTESIAN_POINT('Ctrl Pts',(-43.7279509091188,21.1074720782252,20.));
#80471=CARTESIAN_POINT('Ctrl Pts',(-43.7106256776774,21.1363547261089,0.));
#80472=CARTESIAN_POINT('Ctrl Pts',(-43.7106256776774,21.1363547261089,20.));
#80473=CARTESIAN_POINT('Ctrl Pts',(-43.6932810718209,21.1652244406266,0.));
#80474=CARTESIAN_POINT('Ctrl Pts',(-43.6932810718209,21.1652244406266,20.));
#80475=CARTESIAN_POINT('Ctrl Pts',(-43.6759171005642,21.1940812084419,0.));
#80476=CARTESIAN_POINT('Ctrl Pts',(-43.6759171005642,21.1940812084419,20.));
#80477=CARTESIAN_POINT('Ctrl Pts',(-43.658533772932,21.2229250162246,0.));
#80478=CARTESIAN_POINT('Ctrl Pts',(-43.658533772932,21.2229250162246,20.));
#80479=CARTESIAN_POINT('Ctrl Pts',(-43.6411310979585,21.2517558506503,0.));
#80480=CARTESIAN_POINT('Ctrl Pts',(-43.6411310979585,21.2517558506503,20.));
#80481=CARTESIAN_POINT('Ctrl Pts',(-43.6237090846874,21.2805736984007,0.));
#80482=CARTESIAN_POINT('Ctrl Pts',(-43.6237090846874,21.2805736984007,20.));
#80483=CARTESIAN_POINT('Ctrl Pts',(-43.6062677421718,21.3093785461635,0.));
#80484=CARTESIAN_POINT('Ctrl Pts',(-43.6062677421718,21.3093785461635,20.));
#80485=CARTESIAN_POINT('Ctrl Pts',(-43.5888070794743,21.3381703806323,0.));
#80486=CARTESIAN_POINT('Ctrl Pts',(-43.5888070794743,21.3381703806323,20.));
#80487=CARTESIAN_POINT('Ctrl Pts',(-43.571327105667,21.3669491885068,0.));
#80488=CARTESIAN_POINT('Ctrl Pts',(-43.571327105667,21.3669491885068,20.));
#80489=CARTESIAN_POINT('Ctrl Pts',(-43.5538278298311,21.3957149564922,0.));
#80490=CARTESIAN_POINT('Ctrl Pts',(-43.5538278298311,21.3957149564922,20.));
#80491=CARTESIAN_POINT('Ctrl Pts',(-43.5363092610574,21.4244676712999,0.));
#80492=CARTESIAN_POINT('Ctrl Pts',(-43.5363092610574,21.4244676712999,20.));
#80493=CARTESIAN_POINT('Ctrl Pts',(-43.5187714084458,21.4532073196468,0.));
#80494=CARTESIAN_POINT('Ctrl Pts',(-43.5187714084458,21.4532073196468,20.));
#80495=CARTESIAN_POINT('Ctrl Pts',(-43.5012142811058,21.4819338882558,0.));
#80496=CARTESIAN_POINT('Ctrl Pts',(-43.5012142811058,21.4819338882558,20.));
#80497=CARTESIAN_POINT('Ctrl Pts',(-43.4836378881563,21.5106473638561,0.));
#80498=CARTESIAN_POINT('Ctrl Pts',(-43.4836378881563,21.5106473638561,20.));
#80499=CARTESIAN_POINT('Ctrl Pts',(-43.4660422387257,21.5393477331829,0.));
#80500=CARTESIAN_POINT('Ctrl Pts',(-43.4660422387257,21.5393477331829,20.));
#80501=CARTESIAN_POINT('Ctrl Pts',(-43.4484273419519,21.5680349829773,0.));
#80502=CARTESIAN_POINT('Ctrl Pts',(-43.4484273419519,21.5680349829773,20.));
#80503=CARTESIAN_POINT('Ctrl Pts',(-43.4307932069824,21.5967090999869,0.));
#80504=CARTESIAN_POINT('Ctrl Pts',(-43.4307932069824,21.5967090999869,20.));
#80505=CARTESIAN_POINT('Ctrl Pts',(-43.4131398429739,21.6253700709647,0.));
#80506=CARTESIAN_POINT('Ctrl Pts',(-43.4131398429739,21.6253700709647,20.));
#80507=CARTESIAN_POINT('Ctrl Pts',(-43.3954672590924,21.6540178826698,0.));
#80508=CARTESIAN_POINT('Ctrl Pts',(-43.3954672590924,21.6540178826698,20.));
#80509=CARTESIAN_POINT('Ctrl Pts',(-43.3777754645132,21.682652521867,0.));
#80510=CARTESIAN_POINT('Ctrl Pts',(-43.3777754645132,21.682652521867,20.));
#80511=CARTESIAN_POINT('Ctrl Pts',(-43.3600644684208,21.7112739753274,0.));
#80512=CARTESIAN_POINT('Ctrl Pts',(-43.3600644684208,21.7112739753274,20.));
#80513=CARTESIAN_POINT('Ctrl Pts',(-43.3423342800096,21.7398822298281,0.));
#80514=CARTESIAN_POINT('Ctrl Pts',(-43.3423342800096,21.7398822298281,20.));
#80515=CARTESIAN_POINT('Ctrl Pts',(-43.3245849084831,21.7684772721522,0.));
#80516=CARTESIAN_POINT('Ctrl Pts',(-43.3245849084831,21.7684772721522,20.));
#80517=CARTESIAN_POINT('Ctrl Pts',(-43.3068163630542,21.7970590890891,0.));
#80518=CARTESIAN_POINT('Ctrl Pts',(-43.3068163630542,21.7970590890891,20.));
#80519=CARTESIAN_POINT('Ctrl Pts',(-43.2890286529453,21.8256276674339,0.));
#80520=CARTESIAN_POINT('Ctrl Pts',(-43.2890286529453,21.8256276674339,20.));
#80521=CARTESIAN_POINT('Ctrl Pts',(-43.271221787388,21.8541829939879,0.));
#80522=CARTESIAN_POINT('Ctrl Pts',(-43.271221787388,21.8541829939879,20.));
#80523=CARTESIAN_POINT('Ctrl Pts',(-43.2533957756234,21.8827250555583,0.));
#80524=CARTESIAN_POINT('Ctrl Pts',(-43.2533957756234,21.8827250555583,20.));
#80525=CARTESIAN_POINT('Ctrl Pts',(-43.2355506269018,21.9112538389585,0.));
#80526=CARTESIAN_POINT('Ctrl Pts',(-43.2355506269018,21.9112538389585,20.));
#80527=CARTESIAN_POINT('Ctrl Pts',(-43.217686350483,21.9397693310079,0.));
#80528=CARTESIAN_POINT('Ctrl Pts',(-43.217686350483,21.9397693310079,20.));
#80529=CARTESIAN_POINT('Ctrl Pts',(-43.1998029556363,21.9682715185322,0.));
#80530=CARTESIAN_POINT('Ctrl Pts',(-43.1998029556363,21.9682715185322,20.));
#80531=CARTESIAN_POINT('Ctrl Pts',(-43.1819004516401,21.9967603883628,0.));
#80532=CARTESIAN_POINT('Ctrl Pts',(-43.1819004516401,21.9967603883628,20.));
#80533=CARTESIAN_POINT('Ctrl Pts',(-43.1639788477821,22.0252359273373,0.));
#80534=CARTESIAN_POINT('Ctrl Pts',(-43.1639788477821,22.0252359273373,20.));
#80535=CARTESIAN_POINT('Ctrl Pts',(-43.1460381533594,22.0536981222997,0.));
#80536=CARTESIAN_POINT('Ctrl Pts',(-43.1460381533594,22.0536981222997,20.));
#80537=CARTESIAN_POINT('Ctrl Pts',(-43.1280783776785,22.0821469600997,0.));
#80538=CARTESIAN_POINT('Ctrl Pts',(-43.1280783776785,22.0821469600997,20.));
#80539=CARTESIAN_POINT('Ctrl Pts',(-43.1100995300552,22.1105824275933,0.));
#80540=CARTESIAN_POINT('Ctrl Pts',(-43.1100995300552,22.1105824275933,20.));
#80541=CARTESIAN_POINT('Ctrl Pts',(-43.0921016198148,22.1390045116426,0.));
#80542=CARTESIAN_POINT('Ctrl Pts',(-43.0921016198148,22.1390045116426,20.));
#80543=CARTESIAN_POINT('Ctrl Pts',(-43.0740846562917,22.1674131991155,0.));
#80544=CARTESIAN_POINT('Ctrl Pts',(-43.0740846562917,22.1674131991155,20.));
#80545=CARTESIAN_POINT('Ctrl Pts',(-43.0560486488298,22.1958084768867,0.));
#80546=CARTESIAN_POINT('Ctrl Pts',(-43.0560486488298,22.1958084768867,20.));
#80547=CARTESIAN_POINT('Ctrl Pts',(-43.0379936067822,22.2241903318366,0.));
#80548=CARTESIAN_POINT('Ctrl Pts',(-43.0379936067822,22.2241903318366,20.));
#80549=CARTESIAN_POINT('Ctrl Pts',(-43.0199195395115,22.252558750852,0.));
#80550=CARTESIAN_POINT('Ctrl Pts',(-43.0199195395115,22.252558750852,20.));
#80551=CARTESIAN_POINT('Ctrl Pts',(-43.0018264563892,22.2809137208256,0.));
#80552=CARTESIAN_POINT('Ctrl Pts',(-43.0018264563892,22.2809137208256,20.));
#80553=CARTESIAN_POINT('Ctrl Pts',(-42.9837143667966,22.3092552286564,0.));
#80554=CARTESIAN_POINT('Ctrl Pts',(-42.9837143667966,22.3092552286564,20.));
#80555=CARTESIAN_POINT('Ctrl Pts',(-42.965583280124,22.3375832612492,0.));
#80556=CARTESIAN_POINT('Ctrl Pts',(-42.965583280124,22.3375832612492,20.));
#80557=CARTESIAN_POINT('Ctrl Pts',(-42.947433205771,22.3658978055149,0.));
#80558=CARTESIAN_POINT('Ctrl Pts',(-42.947433205771,22.3658978055149,20.));
#80559=CARTESIAN_POINT('Ctrl Pts',(-42.9292641531465,22.3941988483709,0.));
#80560=CARTESIAN_POINT('Ctrl Pts',(-42.9292641531465,22.3941988483709,20.));
#80561=CARTESIAN_POINT('Ctrl Pts',(-42.9110761316689,22.4224863767407,0.));
#80562=CARTESIAN_POINT('Ctrl Pts',(-42.9110761316689,22.4224863767407,20.));
#80563=CARTESIAN_POINT('Ctrl Pts',(-42.8928691507659,22.4507603775546,0.));
#80564=CARTESIAN_POINT('Ctrl Pts',(-42.8928691507659,22.4507603775546,20.));
#80565=CARTESIAN_POINT('Ctrl Pts',(-42.8746432198744,22.4790208377488,0.));
#80566=CARTESIAN_POINT('Ctrl Pts',(-42.8746432198744,22.4790208377488,20.));
#80567=CARTESIAN_POINT('Ctrl Pts',(-42.8563983484404,22.5072677442656,0.));
#80568=CARTESIAN_POINT('Ctrl Pts',(-42.8563983484404,22.5072677442656,20.));
#80569=CARTESIAN_POINT('Ctrl Pts',(-42.8381345459193,22.535501084053,0.));
#80570=CARTESIAN_POINT('Ctrl Pts',(-42.8381345459193,22.535501084053,20.));
#80571=CARTESIAN_POINT('Ctrl Pts',(-42.8198518217756,22.5637208440656,0.));
#80572=CARTESIAN_POINT('Ctrl Pts',(-42.8198518217756,22.5637208440656,20.));
#80573=CARTESIAN_POINT('Ctrl Pts',(-42.8015501854832,22.5919270112639,0.));
#80574=CARTESIAN_POINT('Ctrl Pts',(-42.8015501854832,22.5919270112639,20.));
#80575=CARTESIAN_POINT('Ctrl Pts',(-42.7832296465255,22.620119572615,0.));
#80576=CARTESIAN_POINT('Ctrl Pts',(-42.7832296465255,22.620119572615,20.));
#80577=CARTESIAN_POINT('Ctrl Pts',(-42.7648902143955,22.6482985150925,0.));
#80578=CARTESIAN_POINT('Ctrl Pts',(-42.7648902143955,22.6482985150925,20.));
#80579=CARTESIAN_POINT('Ctrl Pts',(-42.7465318985949,22.6764638256759,0.));
#80580=CARTESIAN_POINT('Ctrl Pts',(-42.7465318985949,22.6764638256759,20.));
#80581=CARTESIAN_POINT('Ctrl Pts',(-42.7281547086347,22.7046154913511,0.));
#80582=CARTESIAN_POINT('Ctrl Pts',(-42.7281547086347,22.7046154913511,20.));
#80583=CARTESIAN_POINT('Ctrl Pts',(-42.7097586540349,22.73275349911,0.));
#80584=CARTESIAN_POINT('Ctrl Pts',(-42.7097586540349,22.73275349911,20.));
#80585=CARTESIAN_POINT('Ctrl Pts',(-42.6913437443248,22.7608778359508,0.));
#80586=CARTESIAN_POINT('Ctrl Pts',(-42.6913437443248,22.7608778359508,20.));
#80587=CARTESIAN_POINT('Ctrl Pts',(-42.6729099890431,22.788988488878,0.));
#80588=CARTESIAN_POINT('Ctrl Pts',(-42.6729099890431,22.788988488878,20.));
#80589=CARTESIAN_POINT('Ctrl Pts',(-42.6544573977378,22.8170854449023,0.));
#80590=CARTESIAN_POINT('Ctrl Pts',(-42.6544573977378,22.8170854449023,20.));
#80591=CARTESIAN_POINT('Ctrl Pts',(-42.6359859799663,22.845168691041,0.));
#80592=CARTESIAN_POINT('Ctrl Pts',(-42.6359859799663,22.845168691041,20.));
#80593=CARTESIAN_POINT('Ctrl Pts',(-42.6174957452953,22.8732382143174,0.));
#80594=CARTESIAN_POINT('Ctrl Pts',(-42.6174957452953,22.8732382143174,20.));
#80595=CARTESIAN_POINT('Ctrl Pts',(-42.5989867033005,22.9012940017616,0.));
#80596=CARTESIAN_POINT('Ctrl Pts',(-42.5989867033005,22.9012940017616,20.));
#80597=CARTESIAN_POINT('Ctrl Pts',(-42.5804588635669,22.9293360404094,0.));
#80598=CARTESIAN_POINT('Ctrl Pts',(-42.5804588635669,22.9293360404094,20.));
#80599=CARTESIAN_POINT('Ctrl Pts',(-42.5619122356886,22.9573643173033,0.));
#80600=CARTESIAN_POINT('Ctrl Pts',(-42.5619122356886,22.9573643173033,20.));
#80601=CARTESIAN_POINT('Ctrl Pts',(-42.5433468292689,22.9853788194919,0.));
#80602=CARTESIAN_POINT('Ctrl Pts',(-42.5433468292689,22.9853788194919,20.));
#80603=CARTESIAN_POINT('Ctrl Pts',(-42.5247626539203,23.0133795340298,0.));
#80604=CARTESIAN_POINT('Ctrl Pts',(-42.5247626539203,23.0133795340298,20.));
#80605=CARTESIAN_POINT('Ctrl Pts',(-42.5061597192647,23.0413664479785,0.));
#80606=CARTESIAN_POINT('Ctrl Pts',(-42.5061597192647,23.0413664479785,20.));
#80607=CARTESIAN_POINT('Ctrl Pts',(-42.4875380349329,23.0693395484056,0.));
#80608=CARTESIAN_POINT('Ctrl Pts',(-42.4875380349329,23.0693395484056,20.));
#80609=CARTESIAN_POINT('Ctrl Pts',(-42.4688976105654,23.0972988223849,0.));
#80610=CARTESIAN_POINT('Ctrl Pts',(-42.4688976105654,23.0972988223849,20.));
#80611=CARTESIAN_POINT('Ctrl Pts',(-42.4502384558115,23.125244256997,0.));
#80612=CARTESIAN_POINT('Ctrl Pts',(-42.4502384558115,23.125244256997,20.));
#80613=CARTESIAN_POINT('Ctrl Pts',(-42.4315605803298,23.1531758393284,0.));
#80614=CARTESIAN_POINT('Ctrl Pts',(-42.4315605803298,23.1531758393284,20.));
#80615=CARTESIAN_POINT('Ctrl Pts',(-42.4128639937879,23.1810935564721,0.));
#80616=CARTESIAN_POINT('Ctrl Pts',(-42.4128639937879,23.1810935564721,20.));
#80617=CARTESIAN_POINT('Ctrl Pts',(-42.3941487058631,23.2089973955278,0.));
#80618=CARTESIAN_POINT('Ctrl Pts',(-42.3941487058631,23.2089973955278,20.));
#80619=CARTESIAN_POINT('Ctrl Pts',(-42.3754147262417,23.2368873436013,0.));
#80620=CARTESIAN_POINT('Ctrl Pts',(-42.3754147262417,23.2368873436013,20.));
#80621=CARTESIAN_POINT('Ctrl Pts',(-42.3566620646188,23.2647633878047,0.));
#80622=CARTESIAN_POINT('Ctrl Pts',(-42.3566620646188,23.2647633878047,20.));
#80623=CARTESIAN_POINT('Ctrl Pts',(-42.3378907306988,23.2926255152563,0.));
#80624=CARTESIAN_POINT('Ctrl Pts',(-42.3378907306988,23.2926255152563,20.));
#80625=CARTESIAN_POINT('Ctrl Pts',(-42.3191007341954,23.320473713081,0.));
#80626=CARTESIAN_POINT('Ctrl Pts',(-42.3191007341954,23.320473713081,20.));
#80627=CARTESIAN_POINT('Ctrl Pts',(-42.3002920848317,23.3483079684103,0.));
#80628=CARTESIAN_POINT('Ctrl Pts',(-42.3002920848317,23.3483079684103,20.));
#80629=CARTESIAN_POINT('Ctrl Pts',(-42.2814647923395,23.3761282683822,0.));
#80630=CARTESIAN_POINT('Ctrl Pts',(-42.2814647923395,23.3761282683822,20.));
#80631=CARTESIAN_POINT('Ctrl Pts',(-42.2626188664603,23.4039346001409,0.));
#80632=CARTESIAN_POINT('Ctrl Pts',(-42.2626188664603,23.4039346001409,20.));
#80633=CARTESIAN_POINT('Ctrl Pts',(-42.2437543169442,23.4317269508371,0.));
#80634=CARTESIAN_POINT('Ctrl Pts',(-42.2437543169442,23.4317269508371,20.));
#80635=CARTESIAN_POINT('Ctrl Pts',(-42.2248711535508,23.4595053076277,0.));
#80636=CARTESIAN_POINT('Ctrl Pts',(-42.2248711535508,23.4595053076277,20.));
#80637=CARTESIAN_POINT('Ctrl Pts',(-42.2059693860486,23.4872696576759,0.));
#80638=CARTESIAN_POINT('Ctrl Pts',(-42.2059693860486,23.4872696576759,20.));
#80639=CARTESIAN_POINT('Ctrl Pts',(-42.1870490242153,23.5150199881514,0.));
#80640=CARTESIAN_POINT('Ctrl Pts',(-42.1870490242153,23.5150199881514,20.));
#80641=CARTESIAN_POINT('Ctrl Pts',(-42.1681100778379,23.5427562862307,0.));
#80642=CARTESIAN_POINT('Ctrl Pts',(-42.1681100778379,23.5427562862307,20.));
#80643=CARTESIAN_POINT('Ctrl Pts',(-42.1491525567126,23.5704785390969,0.));
#80644=CARTESIAN_POINT('Ctrl Pts',(-42.1491525567126,23.5704785390969,20.));
#80645=CARTESIAN_POINT('Ctrl Pts',(-42.1301764706447,23.5981867339394,0.));
#80646=CARTESIAN_POINT('Ctrl Pts',(-42.1301764706447,23.5981867339394,20.));
#80647=CARTESIAN_POINT('Ctrl Pts',(-42.1111818294483,23.6258808579542,0.));
#80648=CARTESIAN_POINT('Ctrl Pts',(-42.1111818294483,23.6258808579542,20.));
#80649=CARTESIAN_POINT('Ctrl Pts',(-42.0921686429469,23.6535608983435,0.));
#80650=CARTESIAN_POINT('Ctrl Pts',(-42.0921686429469,23.6535608983435,20.));
#80651=CARTESIAN_POINT('Ctrl Pts',(-42.0731369209731,23.6812268423159,0.));
#80652=CARTESIAN_POINT('Ctrl Pts',(-42.0731369209731,23.6812268423159,20.));
#80653=CARTESIAN_POINT('Ctrl Pts',(-42.0540866733685,23.7088786770864,0.));
#80654=CARTESIAN_POINT('Ctrl Pts',(-42.0540866733685,23.7088786770864,20.));
#80655=CARTESIAN_POINT('Ctrl Pts',(-42.0350179099839,23.7365163898767,0.));
#80656=CARTESIAN_POINT('Ctrl Pts',(-42.0350179099839,23.7365163898767,20.));
#80657=CARTESIAN_POINT('Ctrl Pts',(-42.0159306406794,23.7641399679152,0.));
#80658=CARTESIAN_POINT('Ctrl Pts',(-42.0159306406794,23.7641399679152,20.));
#80659=CARTESIAN_POINT('Ctrl Pts',(-41.9968248753238,23.7917493984363,0.));
#80660=CARTESIAN_POINT('Ctrl Pts',(-41.9968248753238,23.7917493984363,20.));
#80661=CARTESIAN_POINT('Ctrl Pts',(-41.9777006237952,23.8193446686815,0.));
#80662=CARTESIAN_POINT('Ctrl Pts',(-41.9777006237952,23.8193446686815,20.));
#80663=CARTESIAN_POINT('Ctrl Pts',(-41.9585578959807,23.8469257658985,0.));
#80664=CARTESIAN_POINT('Ctrl Pts',(-41.9585578959807,23.8469257658985,20.));
#80665=CARTESIAN_POINT('Ctrl Pts',(-41.9393967017767,23.8744926773418,0.));
#80666=CARTESIAN_POINT('Ctrl Pts',(-41.9393967017767,23.8744926773418,20.));
#80667=CARTESIAN_POINT('Ctrl Pts',(-41.9202170510888,23.9020453902722,0.));
#80668=CARTESIAN_POINT('Ctrl Pts',(-41.9202170510888,23.9020453902722,20.));
#80669=CARTESIAN_POINT('Ctrl Pts',(-41.9010189538314,23.9295838919572,0.));
#80670=CARTESIAN_POINT('Ctrl Pts',(-41.9010189538314,23.9295838919572,20.));
#80671=CARTESIAN_POINT('Ctrl Pts',(-41.8818024199281,23.9571081696707,0.));
#80672=CARTESIAN_POINT('Ctrl Pts',(-41.8818024199281,23.9571081696707,20.));
#80673=CARTESIAN_POINT('Ctrl Pts',(-41.8625674593112,23.984618210693,0.));
#80674=CARTESIAN_POINT('Ctrl Pts',(-41.8625674593112,23.984618210693,20.));
#80675=CARTESIAN_POINT('Ctrl Pts',(-41.8433140819226,24.0121140023113,0.));
#80676=CARTESIAN_POINT('Ctrl Pts',(-41.8433140819226,24.0121140023113,20.));
#80677=CARTESIAN_POINT('Ctrl Pts',(-41.824042297713,24.0395955318191,0.));
#80678=CARTESIAN_POINT('Ctrl Pts',(-41.824042297713,24.0395955318191,20.));
#80679=CARTESIAN_POINT('Ctrl Pts',(-41.8047521166422,24.0670627865166,0.));
#80680=CARTESIAN_POINT('Ctrl Pts',(-41.8047521166422,24.0670627865166,20.));
#80681=CARTESIAN_POINT('Ctrl Pts',(-41.785443548679,24.0945157537107,0.));
#80682=CARTESIAN_POINT('Ctrl Pts',(-41.785443548679,24.0945157537107,20.));
#80683=CARTESIAN_POINT('Ctrl Pts',(-41.7661166038015,24.1219544207148,0.));
#80684=CARTESIAN_POINT('Ctrl Pts',(-41.7661166038015,24.1219544207148,20.));
#80685=CARTESIAN_POINT('Ctrl Pts',(-41.7467712919966,24.1493787748488,0.));
#80686=CARTESIAN_POINT('Ctrl Pts',(-41.7467712919966,24.1493787748488,20.));
#80687=CARTESIAN_POINT('Ctrl Pts',(-41.7274076232605,24.1767888034393,0.));
#80688=CARTESIAN_POINT('Ctrl Pts',(-41.7274076232605,24.1767888034393,20.));
#80689=CARTESIAN_POINT('Ctrl Pts',(-41.7080256075983,24.2041844938197,0.));
#80690=CARTESIAN_POINT('Ctrl Pts',(-41.7080256075983,24.2041844938197,20.));
#80691=CARTESIAN_POINT('Ctrl Pts',(-41.688625255024,24.2315658333297,0.));
#80692=CARTESIAN_POINT('Ctrl Pts',(-41.688625255024,24.2315658333297,20.));
#80693=CARTESIAN_POINT('Ctrl Pts',(-41.6692065755608,24.2589328093159,0.));
#80694=CARTESIAN_POINT('Ctrl Pts',(-41.6692065755608,24.2589328093159,20.));
#80695=CARTESIAN_POINT('Ctrl Pts',(-41.6497695792407,24.2862854091312,0.));
#80696=CARTESIAN_POINT('Ctrl Pts',(-41.6497695792407,24.2862854091312,20.));
#80697=CARTESIAN_POINT('Ctrl Pts',(-41.630314276105,24.3136236201351,0.));
#80698=CARTESIAN_POINT('Ctrl Pts',(-41.630314276105,24.3136236201351,20.));
#80699=CARTESIAN_POINT('Ctrl Pts',(-41.610840676204,24.340947429694,0.));
#80700=CARTESIAN_POINT('Ctrl Pts',(-41.610840676204,24.340947429694,20.));
#80701=CARTESIAN_POINT('Ctrl Pts',(-41.5913487895971,24.368256825181,0.));
#80702=CARTESIAN_POINT('Ctrl Pts',(-41.5913487895971,24.368256825181,20.));
#80703=CARTESIAN_POINT('Ctrl Pts',(-41.5718386263526,24.3955517939756,0.));
#80704=CARTESIAN_POINT('Ctrl Pts',(-41.5718386263526,24.3955517939756,20.));
#80705=CARTESIAN_POINT('Ctrl Pts',(-41.5523101965477,24.4228323234645,0.));
#80706=CARTESIAN_POINT('Ctrl Pts',(-41.5523101965477,24.4228323234645,20.));
#80707=CARTESIAN_POINT('Ctrl Pts',(-41.5327635102685,24.4500984010406,0.));
#80708=CARTESIAN_POINT('Ctrl Pts',(-41.5327635102685,24.4500984010406,20.));
#80709=CARTESIAN_POINT('Ctrl Pts',(-41.5131985776101,24.4773500141036,0.));
#80710=CARTESIAN_POINT('Ctrl Pts',(-41.5131985776101,24.4773500141036,20.));
#80711=CARTESIAN_POINT('Ctrl Pts',(-41.4936154086768,24.5045871500598,0.));
#80712=CARTESIAN_POINT('Ctrl Pts',(-41.4936154086768,24.5045871500598,20.));
#80713=CARTESIAN_POINT('Ctrl Pts',(-41.4740140135823,24.5318097963222,0.));
#80714=CARTESIAN_POINT('Ctrl Pts',(-41.4740140135823,24.5318097963222,20.));
#80715=CARTESIAN_POINT('Ctrl Pts',(-41.4543944024488,24.5590179403106,0.));
#80716=CARTESIAN_POINT('Ctrl Pts',(-41.4543944024488,24.5590179403106,20.));
#80717=CARTESIAN_POINT('Ctrl Pts',(-41.4347565854076,24.5862115694513,0.));
#80718=CARTESIAN_POINT('Ctrl Pts',(-41.4347565854076,24.5862115694513,20.));
#80719=CARTESIAN_POINT('Ctrl Pts',(-41.4151005725989,24.6133906711774,0.));
#80720=CARTESIAN_POINT('Ctrl Pts',(-41.4151005725989,24.6133906711774,20.));
#80721=CARTESIAN_POINT('Ctrl Pts',(-41.3954263741717,24.6405552329288,0.));
#80722=CARTESIAN_POINT('Ctrl Pts',(-41.3954263741717,24.6405552329288,20.));
#80723=CARTESIAN_POINT('Ctrl Pts',(-41.3757340002844,24.6677052421523,0.));
#80724=CARTESIAN_POINT('Ctrl Pts',(-41.3757340002844,24.6677052421523,20.));
#80725=CARTESIAN_POINT('Ctrl Pts',(-41.3560234611038,24.694840686301,0.));
#80726=CARTESIAN_POINT('Ctrl Pts',(-41.3560234611038,24.694840686301,20.));
#80727=CARTESIAN_POINT('Ctrl Pts',(-41.3362947668064,24.7219615528352,0.));
#80728=CARTESIAN_POINT('Ctrl Pts',(-41.3362947668064,24.7219615528352,20.));
#80729=CARTESIAN_POINT('Ctrl Pts',(-41.3165479275773,24.7490678292217,0.));
#80730=CARTESIAN_POINT('Ctrl Pts',(-41.3165479275773,24.7490678292217,20.));
#80731=CARTESIAN_POINT('Ctrl Pts',(-41.2967829536105,24.776159502934,0.));
#80732=CARTESIAN_POINT('Ctrl Pts',(-41.2967829536105,24.776159502934,20.));
#80733=CARTESIAN_POINT('Ctrl Pts',(-41.276999855109,24.8032365614525,0.));
#80734=CARTESIAN_POINT('Ctrl Pts',(-41.276999855109,24.8032365614525,20.));
#80735=CARTESIAN_POINT('Ctrl Pts',(-41.2571986422843,24.8302989922639,0.));
#80736=CARTESIAN_POINT('Ctrl Pts',(-41.2571986422843,24.8302989922639,20.));
#80737=CARTESIAN_POINT('Ctrl Pts',(-41.2373793253577,24.8573467828623,0.));
#80738=CARTESIAN_POINT('Ctrl Pts',(-41.2373793253577,24.8573467828623,20.));
#80739=CARTESIAN_POINT('Ctrl Pts',(-41.2175419145589,24.8843799207482,0.));
#80740=CARTESIAN_POINT('Ctrl Pts',(-41.2175419145589,24.8843799207482,20.));
#80741=CARTESIAN_POINT('Ctrl Pts',(-41.1976864201268,24.9113983934293,0.));
#80742=CARTESIAN_POINT('Ctrl Pts',(-41.1976864201268,24.9113983934293,20.));
#80743=CARTESIAN_POINT('Ctrl Pts',(-41.1778128523092,24.9384021884197,0.));
#80744=CARTESIAN_POINT('Ctrl Pts',(-41.1778128523092,24.9384021884197,20.));
#80745=CARTESIAN_POINT('Ctrl Pts',(-41.1579212213625,24.9653912932402,0.));
#80746=CARTESIAN_POINT('Ctrl Pts',(-41.1579212213625,24.9653912932402,20.));
#80747=CARTESIAN_POINT('Ctrl Pts',(-41.1380115375521,24.9923656954187,0.));
#80748=CARTESIAN_POINT('Ctrl Pts',(-41.1380115375521,24.9923656954187,20.));
#80749=CARTESIAN_POINT('Ctrl Pts',(-41.1180838111525,25.0193253824897,0.));
#80750=CARTESIAN_POINT('Ctrl Pts',(-41.1180838111525,25.0193253824897,20.));
#80751=CARTESIAN_POINT('Ctrl Pts',(-41.0981380524472,25.0462703419947,0.));
#80752=CARTESIAN_POINT('Ctrl Pts',(-41.0981380524472,25.0462703419947,20.));
#80753=CARTESIAN_POINT('Ctrl Pts',(-41.0781742717283,25.0732005614819,0.));
#80754=CARTESIAN_POINT('Ctrl Pts',(-41.0781742717283,25.0732005614819,20.));
#80755=CARTESIAN_POINT('Ctrl Pts',(-41.058192479297,25.1001160285063,0.));
#80756=CARTESIAN_POINT('Ctrl Pts',(-41.058192479297,25.1001160285063,20.));
#80757=CARTESIAN_POINT('Ctrl Pts',(-41.0381926854636,25.1270167306298,0.));
#80758=CARTESIAN_POINT('Ctrl Pts',(-41.0381926854636,25.1270167306298,20.));
#80759=CARTESIAN_POINT('Ctrl Pts',(-41.0181749005471,25.1539026554213,0.));
#80760=CARTESIAN_POINT('Ctrl Pts',(-41.0181749005471,25.1539026554213,20.));
#80761=CARTESIAN_POINT('Ctrl Pts',(-40.9981391348755,25.1807737904566,0.));
#80762=CARTESIAN_POINT('Ctrl Pts',(-40.9981391348755,25.1807737904566,20.));
#80763=CARTESIAN_POINT('Ctrl Pts',(-40.9780853987856,25.2076301233182,0.));
#80764=CARTESIAN_POINT('Ctrl Pts',(-40.9780853987856,25.2076301233182,20.));
#80765=CARTESIAN_POINT('Ctrl Pts',(-40.9580137026228,25.2344716415952,0.));
#80766=CARTESIAN_POINT('Ctrl Pts',(-40.9580137026228,25.2344716415952,20.));
#80767=CARTESIAN_POINT('Ctrl Pts',(-40.9379240567416,25.2612983328836,0.));
#80768=CARTESIAN_POINT('Ctrl Pts',(-40.9379240567416,25.2612983328836,20.));
#80769=CARTESIAN_POINT('Ctrl Pts',(-40.9178164715051,25.2881101847861,0.));
#80770=CARTESIAN_POINT('Ctrl Pts',(-40.9178164715051,25.2881101847861,20.));
#80771=CARTESIAN_POINT('Ctrl Pts',(-40.8976909572856,25.3149071849127,0.));
#80772=CARTESIAN_POINT('Ctrl Pts',(-40.8976909572856,25.3149071849127,20.));
#80773=CARTESIAN_POINT('Ctrl Pts',(-40.8775475244644,25.3416893208802,0.));
#80774=CARTESIAN_POINT('Ctrl Pts',(-40.8775475244644,25.3416893208802,20.));
#80775=CARTESIAN_POINT('Ctrl Pts',(-40.8573861834316,25.3684565803126,0.));
#80776=CARTESIAN_POINT('Ctrl Pts',(-40.8573861834316,25.3684565803126,20.));
#80777=CARTESIAN_POINT('Ctrl Pts',(-40.8372069445862,25.3952089508407,0.));
#80778=CARTESIAN_POINT('Ctrl Pts',(-40.8372069445862,25.3952089508407,20.));
#80779=CARTESIAN_POINT('Ctrl Pts',(-40.8170098183362,25.4219464201024,0.));
#80780=CARTESIAN_POINT('Ctrl Pts',(-40.8170098183362,25.4219464201024,20.));
#80781=CARTESIAN_POINT('Ctrl Pts',(-40.7967948150981,25.4486689757422,0.));
#80782=CARTESIAN_POINT('Ctrl Pts',(-40.7967948150981,25.4486689757422,20.));
#80783=CARTESIAN_POINT('Ctrl Pts',(-40.7765619452973,25.4753766054114,0.));
#80784=CARTESIAN_POINT('Ctrl Pts',(-40.7765619452973,25.4753766054114,20.));
#80785=CARTESIAN_POINT('Ctrl Pts',(-40.7563112193678,25.5020692967677,0.));
#80786=CARTESIAN_POINT('Ctrl Pts',(-40.7563112193678,25.5020692967677,20.));
#80787=CARTESIAN_POINT('Ctrl Pts',(-40.7360426477524,25.528747037476,0.));
#80788=CARTESIAN_POINT('Ctrl Pts',(-40.7360426477524,25.528747037476,20.));
#80789=CARTESIAN_POINT('Ctrl Pts',(-40.715756240903,25.5554098152083,0.));
#80790=CARTESIAN_POINT('Ctrl Pts',(-40.715756240903,25.5554098152083,20.));
#80791=CARTESIAN_POINT('Ctrl Pts',(-40.6954520092804,25.5820576176439,0.));
#80792=CARTESIAN_POINT('Ctrl Pts',(-40.6954520092804,25.5820576176439,20.));
#80793=CARTESIAN_POINT('Ctrl Pts',(-40.6751299633543,25.6086904324689,0.));
#80794=CARTESIAN_POINT('Ctrl Pts',(-40.6751299633543,25.6086904324689,20.));
#80795=CARTESIAN_POINT('Ctrl Pts',(-40.6547901136033,25.6353082473768,0.));
#80796=CARTESIAN_POINT('Ctrl Pts',(-40.6547901136033,25.6353082473768,20.));
#80797=CARTESIAN_POINT('Ctrl Pts',(-40.6344324705148,25.6619110500677,0.));
#80798=CARTESIAN_POINT('Ctrl Pts',(-40.6344324705148,25.6619110500677,20.));
#80799=CARTESIAN_POINT('Ctrl Pts',(-40.6140570445847,25.6884988282486,0.));
#80800=CARTESIAN_POINT('Ctrl Pts',(-40.6140570445847,25.6884988282486,20.));
#80801=CARTESIAN_POINT('Ctrl Pts',(-40.5936638463177,25.7150715696332,0.));
#80802=CARTESIAN_POINT('Ctrl Pts',(-40.5936638463177,25.7150715696332,20.));
#80803=CARTESIAN_POINT('Ctrl Pts',(-40.5732528862276,25.7416292619425,0.));
#80804=CARTESIAN_POINT('Ctrl Pts',(-40.5732528862276,25.7416292619425,20.));
#80805=CARTESIAN_POINT('Ctrl Pts',(-40.5528241748366,25.768171892904,0.));
#80806=CARTESIAN_POINT('Ctrl Pts',(-40.5528241748366,25.768171892904,20.));
#80807=CARTESIAN_POINT('Ctrl Pts',(-40.5323777226758,25.7946994502526,0.));
#80808=CARTESIAN_POINT('Ctrl Pts',(-40.5323777226758,25.7946994502526,20.));
#80809=CARTESIAN_POINT('Ctrl Pts',(-40.5119135402853,25.8212119217304,0.));
#80810=CARTESIAN_POINT('Ctrl Pts',(-40.5119135402853,25.8212119217304,20.));
#80811=CARTESIAN_POINT('Ctrl Pts',(-40.4914316382141,25.8477092950863,0.));
#80812=CARTESIAN_POINT('Ctrl Pts',(-40.4914316382141,25.8477092950863,20.));
#80813=CARTESIAN_POINT('Ctrl Pts',(-40.4709320270197,25.8741915580762,0.));
#80814=CARTESIAN_POINT('Ctrl Pts',(-40.4709320270197,25.8741915580762,20.));
#80815=CARTESIAN_POINT('Ctrl Pts',(-40.4504147172684,25.900658698463,0.));
#80816=CARTESIAN_POINT('Ctrl Pts',(-40.4504147172684,25.900658698463,20.));
#80817=CARTESIAN_POINT('Ctrl Pts',(-40.4298797195353,25.9271107040168,0.));
#80818=CARTESIAN_POINT('Ctrl Pts',(-40.4298797195353,25.9271107040168,20.));
#80819=CARTESIAN_POINT('Ctrl Pts',(-40.4093270444043,25.953547562515,0.));
#80820=CARTESIAN_POINT('Ctrl Pts',(-40.4093270444043,25.953547562515,20.));
#80821=CARTESIAN_POINT('Ctrl Pts',(-40.3887567024682,25.9799692617416,0.));
#80822=CARTESIAN_POINT('Ctrl Pts',(-40.3887567024682,25.9799692617416,20.));
#80823=CARTESIAN_POINT('Ctrl Pts',(-40.3681687043284,26.0063757894875,0.));
#80824=CARTESIAN_POINT('Ctrl Pts',(-40.3681687043284,26.0063757894875,20.));
#80825=CARTESIAN_POINT('Ctrl Pts',(-40.347563060595,26.0327671335511,0.));
#80826=CARTESIAN_POINT('Ctrl Pts',(-40.347563060595,26.0327671335511,20.));
#80827=CARTESIAN_POINT('Ctrl Pts',(-40.326939781887,26.0591432817373,0.));
#80828=CARTESIAN_POINT('Ctrl Pts',(-40.326939781887,26.0591432817373,20.));
#80829=CARTESIAN_POINT('Ctrl Pts',(-40.3062988788318,26.0855042218583,0.));
#80830=CARTESIAN_POINT('Ctrl Pts',(-40.3062988788318,26.0855042218583,20.));
#80831=CARTESIAN_POINT('Ctrl Pts',(-40.2856403620657,26.1118499417334,0.));
#80832=CARTESIAN_POINT('Ctrl Pts',(-40.2856403620657,26.1118499417334,20.));
#80833=CARTESIAN_POINT('Ctrl Pts',(-40.2649642422341,26.1381804291892,0.));
#80834=CARTESIAN_POINT('Ctrl Pts',(-40.2649642422341,26.1381804291892,20.));
#80835=CARTESIAN_POINT('Ctrl Pts',(-40.2442705299908,26.1644956720595,0.));
#80836=CARTESIAN_POINT('Ctrl Pts',(-40.2442705299908,26.1644956720595,20.));
#80837=CARTESIAN_POINT('Ctrl Pts',(-40.2235592359986,26.1907956581851,0.));
#80838=CARTESIAN_POINT('Ctrl Pts',(-40.2235592359986,26.1907956581851,20.));
#80839=CARTESIAN_POINT('Ctrl Pts',(-40.2028303709288,26.217080375414,0.));
#80840=CARTESIAN_POINT('Ctrl Pts',(-40.2028303709288,26.217080375414,20.));
#80841=CARTESIAN_POINT('Ctrl Pts',(-40.1820839454613,26.2433498116008,0.));
#80842=CARTESIAN_POINT('Ctrl Pts',(-40.1820839454613,26.2433498116008,20.));
#80843=CARTESIAN_POINT('Ctrl Pts',(-40.161319970285,26.2696039546074,0.));
#80844=CARTESIAN_POINT('Ctrl Pts',(-40.161319970285,26.2696039546074,20.));
#80845=CARTESIAN_POINT('Ctrl Pts',(-40.1405384560971,26.2958427923028,0.));
#80846=CARTESIAN_POINT('Ctrl Pts',(-40.1405384560971,26.2958427923028,20.));
#80847=CARTESIAN_POINT('Ctrl Pts',(-40.1197394136039,26.3220663125631,0.));
#80848=CARTESIAN_POINT('Ctrl Pts',(-40.1197394136039,26.3220663125631,20.));
#80849=CARTESIAN_POINT('Ctrl Pts',(-40.0989228535202,26.3482745032719,0.));
#80850=CARTESIAN_POINT('Ctrl Pts',(-40.0989228535202,26.3482745032719,20.));
#80851=CARTESIAN_POINT('Ctrl Pts',(-40.0780887865696,26.3744673523197,0.));
#80852=CARTESIAN_POINT('Ctrl Pts',(-40.0780887865696,26.3744673523197,20.));
#80853=CARTESIAN_POINT('Ctrl Pts',(-40.0572372234844,26.4006448476041,0.));
#80854=CARTESIAN_POINT('Ctrl Pts',(-40.0572372234844,26.4006448476041,20.));
#80855=CARTESIAN_POINT('Ctrl Pts',(-40.0363681750053,26.4268069770299,0.));
#80856=CARTESIAN_POINT('Ctrl Pts',(-40.0363681750053,26.4268069770299,20.));
#80857=CARTESIAN_POINT('Ctrl Pts',(-40.015481651882,26.4529537285089,0.));
#80858=CARTESIAN_POINT('Ctrl Pts',(-40.015481651882,26.4529537285089,20.));
#80859=CARTESIAN_POINT('Ctrl Pts',(-39.9945776648731,26.4790850899607,0.));
#80860=CARTESIAN_POINT('Ctrl Pts',(-39.9945776648731,26.4790850899607,20.));
#80861=CARTESIAN_POINT('Ctrl Pts',(-39.9736562247456,26.5052010493117,0.));
#80862=CARTESIAN_POINT('Ctrl Pts',(-39.9736562247456,26.5052010493117,20.));
#80863=CARTESIAN_POINT('Ctrl Pts',(-39.9527173422752,26.5313015944953,0.));
#80864=CARTESIAN_POINT('Ctrl Pts',(-39.9527173422752,26.5313015944953,20.));
#80865=CARTESIAN_POINT('Ctrl Pts',(-39.9317610282459,26.5573867134521,0.));
#80866=CARTESIAN_POINT('Ctrl Pts',(-39.9317610282459,26.5573867134521,20.));
#80867=CARTESIAN_POINT('Ctrl Pts',(-39.9107872934506,26.5834563941296,0.));
#80868=CARTESIAN_POINT('Ctrl Pts',(-39.9107872934506,26.5834563941296,20.));
#80869=CARTESIAN_POINT('Ctrl Pts',(-39.8897961486907,26.6095106244829,0.));
#80870=CARTESIAN_POINT('Ctrl Pts',(-39.8897961486907,26.6095106244829,20.));
#80871=CARTESIAN_POINT('Ctrl Pts',(-39.8687876047769,26.6355493924743,0.));
#80872=CARTESIAN_POINT('Ctrl Pts',(-39.8687876047769,26.6355493924743,20.));
#80873=CARTESIAN_POINT('Ctrl Pts',(-39.847761672528,26.6615726860734,0.));
#80874=CARTESIAN_POINT('Ctrl Pts',(-39.847761672528,26.6615726860734,20.));
#80875=CARTESIAN_POINT('Ctrl Pts',(-39.8267183627717,26.687580493257,0.));
#80876=CARTESIAN_POINT('Ctrl Pts',(-39.8267183627717,26.687580493257,20.));
#80877=CARTESIAN_POINT('Ctrl Pts',(-39.8056576863443,26.713572802009,0.));
#80878=CARTESIAN_POINT('Ctrl Pts',(-39.8056576863443,26.713572802009,20.));
#80879=CARTESIAN_POINT('Ctrl Pts',(-39.7845796540903,26.7395496003209,0.));
#80880=CARTESIAN_POINT('Ctrl Pts',(-39.7845796540903,26.7395496003209,20.));
#80881=CARTESIAN_POINT('Ctrl Pts',(-39.7634842768632,26.7655108761908,0.));
#80882=CARTESIAN_POINT('Ctrl Pts',(-39.7634842768632,26.7655108761908,20.));
#80883=CARTESIAN_POINT('Ctrl Pts',(-39.7423715655248,26.7914566176244,0.));
#80884=CARTESIAN_POINT('Ctrl Pts',(-39.7423715655248,26.7914566176244,20.));
#80885=CARTESIAN_POINT('Ctrl Pts',(-39.7212415309462,26.8173868126344,0.));
#80886=CARTESIAN_POINT('Ctrl Pts',(-39.7212415309462,26.8173868126344,20.));
#80887=CARTESIAN_POINT('Ctrl Pts',(-39.7000941840066,26.843301449241,0.));
#80888=CARTESIAN_POINT('Ctrl Pts',(-39.7000941840066,26.843301449241,20.));
#80889=CARTESIAN_POINT('Ctrl Pts',(-39.6789295355942,26.8692005154716,0.));
#80890=CARTESIAN_POINT('Ctrl Pts',(-39.6789295355942,26.8692005154716,20.));
#80891=CARTESIAN_POINT('Ctrl Pts',(-39.6577475966055,26.8950839993609,0.));
#80892=CARTESIAN_POINT('Ctrl Pts',(-39.6577475966055,26.8950839993609,20.));
#80893=CARTESIAN_POINT('Ctrl Pts',(-39.6365483779458,26.9209518889509,0.));
#80894=CARTESIAN_POINT('Ctrl Pts',(-39.6365483779458,26.9209518889509,20.));
#80895=CARTESIAN_POINT('Ctrl Pts',(-39.6153318905283,26.9468041722907,0.));
#80896=CARTESIAN_POINT('Ctrl Pts',(-39.6153318905283,26.9468041722907,20.));
#80897=CARTESIAN_POINT('Ctrl Pts',(-39.5940981452753,26.972640837437,0.));
#80898=CARTESIAN_POINT('Ctrl Pts',(-39.5940981452753,26.972640837437,20.));
#80899=CARTESIAN_POINT('Ctrl Pts',(-39.5728471531178,26.9984618724537,0.));
#80900=CARTESIAN_POINT('Ctrl Pts',(-39.5728471531178,26.9984618724537,20.));
#80901=CARTESIAN_POINT('Ctrl Pts',(-39.5515789249953,27.0242672654118,0.));
#80902=CARTESIAN_POINT('Ctrl Pts',(-39.5515789249953,27.0242672654118,20.));
#80903=CARTESIAN_POINT('Ctrl Pts',(-39.5302934718558,27.0500570043898,0.));
#80904=CARTESIAN_POINT('Ctrl Pts',(-39.5302934718558,27.0500570043898,20.));
#80905=CARTESIAN_POINT('Ctrl Pts',(-39.5089908046561,27.0758310774732,0.));
#80906=CARTESIAN_POINT('Ctrl Pts',(-39.5089908046561,27.0758310774732,20.));
#80907=CARTESIAN_POINT('Ctrl Pts',(-39.4876709343614,27.1015894727552,0.));
#80908=CARTESIAN_POINT('Ctrl Pts',(-39.4876709343614,27.1015894727552,20.));
#80909=CARTESIAN_POINT('Ctrl Pts',(-39.4663338719455,27.1273321783362,0.));
#80910=CARTESIAN_POINT('Ctrl Pts',(-39.4663338719455,27.1273321783362,20.));
#80911=CARTESIAN_POINT('Ctrl Pts',(-39.4449796283908,27.153059182324,0.));
#80912=CARTESIAN_POINT('Ctrl Pts',(-39.4449796283908,27.153059182324,20.));
#80913=CARTESIAN_POINT('Ctrl Pts',(-39.4236082146882,27.1787704728336,0.));
#80914=CARTESIAN_POINT('Ctrl Pts',(-39.4236082146882,27.1787704728336,20.));
#80915=CARTESIAN_POINT('Ctrl Pts',(-39.4022196418372,27.2044660379877,0.));
#80916=CARTESIAN_POINT('Ctrl Pts',(-39.4022196418372,27.2044660379877,20.));
#80917=CARTESIAN_POINT('Ctrl Pts',(-39.3808139208456,27.2301458659157,0.));
#80918=CARTESIAN_POINT('Ctrl Pts',(-39.3808139208456,27.2301458659157,20.));
#80919=CARTESIAN_POINT('Ctrl Pts',(-39.3593910627297,27.2558099447548,0.));
#80920=CARTESIAN_POINT('Ctrl Pts',(-39.3593910627297,27.2558099447548,20.));
#80921=CARTESIAN_POINT('Ctrl Pts',(-39.3379510785145,27.2814582626492,0.));
#80922=CARTESIAN_POINT('Ctrl Pts',(-39.3379510785145,27.2814582626492,20.));
#80923=CARTESIAN_POINT('Ctrl Pts',(-39.3164939792334,27.3070908077508,0.));
#80924=CARTESIAN_POINT('Ctrl Pts',(-39.3164939792334,27.3070908077508,20.));
#80925=CARTESIAN_POINT('Ctrl Pts',(-39.2950197759285,27.3327075682187,0.));
#80926=CARTESIAN_POINT('Ctrl Pts',(-39.2950197759285,27.3327075682187,20.));
#80927=CARTESIAN_POINT('Ctrl Pts',(-39.2735284796508,27.3583085322198,0.));
#80928=CARTESIAN_POINT('Ctrl Pts',(-39.2735284796508,27.3583085322198,20.));
#80929=CARTESIAN_POINT('Ctrl Pts',(-39.25202010146,27.3838936879286,0.));
#80930=CARTESIAN_POINT('Ctrl Pts',(-39.25202010146,27.3838936879286,20.));
#80931=CARTESIAN_POINT('Ctrl Pts',(-39.2304946524241,27.4094630235265,0.));
#80932=CARTESIAN_POINT('Ctrl Pts',(-39.2304946524241,27.4094630235265,20.));
#80933=CARTESIAN_POINT('Ctrl Pts',(-39.2089521436188,27.4350165272023,0.));
#80934=CARTESIAN_POINT('Ctrl Pts',(-39.2089521436188,27.4350165272023,20.));
#80935=CARTESIAN_POINT('Ctrl Pts',(-39.1873925861285,27.4605541871518,0.));
#80936=CARTESIAN_POINT('Ctrl Pts',(-39.1873925861285,27.4605541871518,20.));
#80937=CARTESIAN_POINT('Ctrl Pts',(-39.1658159910458,27.4860759915783,0.));
#80938=CARTESIAN_POINT('Ctrl Pts',(-39.1658159910458,27.4860759915783,20.));
#80939=CARTESIAN_POINT('Ctrl Pts',(-39.1442223694722,27.5115819286926,0.));
#80940=CARTESIAN_POINT('Ctrl Pts',(-39.1442223694722,27.5115819286926,20.));
#80941=CARTESIAN_POINT('Ctrl Pts',(-39.1226117325183,27.5370719867136,0.));
#80942=CARTESIAN_POINT('Ctrl Pts',(-39.1226117325183,27.5370719867136,20.));
#80943=CARTESIAN_POINT('Ctrl Pts',(-39.100984091303,27.5625461538675,0.));
#80944=CARTESIAN_POINT('Ctrl Pts',(-39.100984091303,27.5625461538675,20.));
#80945=CARTESIAN_POINT('Ctrl Pts',(-39.0793394569537,27.5880044183879,0.));
#80946=CARTESIAN_POINT('Ctrl Pts',(-39.0793394569537,27.5880044183879,20.));
#80947=CARTESIAN_POINT('Ctrl Pts',(-39.057677840606,27.6134467685155,0.));
#80948=CARTESIAN_POINT('Ctrl Pts',(-39.057677840606,27.6134467685155,20.));
#80949=CARTESIAN_POINT('Ctrl Pts',(-39.0359992534037,27.6388731924983,0.));
#80950=CARTESIAN_POINT('Ctrl Pts',(-39.0359992534037,27.6388731924983,20.));
#80951=CARTESIAN_POINT('Ctrl Pts',(-39.0143037064988,27.6642836785915,0.));
#80952=CARTESIAN_POINT('Ctrl Pts',(-39.0143037064988,27.6642836785915,20.));
#80953=CARTESIAN_POINT('Ctrl Pts',(-38.9925912110523,27.6896782150583,0.));
#80954=CARTESIAN_POINT('Ctrl Pts',(-38.9925912110523,27.6896782150583,20.));
#80955=CARTESIAN_POINT('Ctrl Pts',(-38.9708617782339,27.7150567901695,0.));
#80956=CARTESIAN_POINT('Ctrl Pts',(-38.9708617782339,27.7150567901695,20.));
#80957=CARTESIAN_POINT('Ctrl Pts',(-38.9491154192216,27.7404193922036,0.));
#80958=CARTESIAN_POINT('Ctrl Pts',(-38.9491154192216,27.7404193922036,20.));
#80959=CARTESIAN_POINT('Ctrl Pts',(-38.9273521452022,27.7657660094466,0.));
#80960=CARTESIAN_POINT('Ctrl Pts',(-38.9273521452022,27.7657660094466,20.));
#80961=CARTESIAN_POINT('Ctrl Pts',(-38.9055719673706,27.7910966301919,0.));
#80962=CARTESIAN_POINT('Ctrl Pts',(-38.9055719673706,27.7910966301919,20.));
#80963=CARTESIAN_POINT('Ctrl Pts',(-38.8837748969299,27.8164112427396,0.));
#80964=CARTESIAN_POINT('Ctrl Pts',(-38.8837748969299,27.8164112427396,20.));
#80965=CARTESIAN_POINT('Ctrl Pts',(-38.8619609450913,27.8417098353975,0.));
#80966=CARTESIAN_POINT('Ctrl Pts',(-38.8619609450913,27.8417098353975,20.));
#80967=CARTESIAN_POINT('Ctrl Pts',(-38.8401301230745,27.866992396481,0.));
#80968=CARTESIAN_POINT('Ctrl Pts',(-38.8401301230745,27.866992396481,20.));
#80969=CARTESIAN_POINT('Ctrl Pts',(-38.8182824421082,27.8922589143132,0.));
#80970=CARTESIAN_POINT('Ctrl Pts',(-38.8182824421082,27.8922589143132,20.));
#80971=CARTESIAN_POINT('Ctrl Pts',(-38.7964179134294,27.917509377225,0.));
#80972=CARTESIAN_POINT('Ctrl Pts',(-38.7964179134294,27.917509377225,20.));
#80973=CARTESIAN_POINT('Ctrl Pts',(-38.7745365482838,27.9427437735546,0.));
#80974=CARTESIAN_POINT('Ctrl Pts',(-38.7745365482838,27.9427437735546,20.));
#80975=CARTESIAN_POINT('Ctrl Pts',(-38.752638357925,27.9679620916479,0.));
#80976=CARTESIAN_POINT('Ctrl Pts',(-38.752638357925,27.9679620916479,20.));
#80977=CARTESIAN_POINT('Ctrl Pts',(-38.7307233536152,27.993164319858,0.));
#80978=CARTESIAN_POINT('Ctrl Pts',(-38.7307233536152,27.993164319858,20.));
#80979=CARTESIAN_POINT('Ctrl Pts',(-38.7087915466247,28.0183504465458,0.));
#80980=CARTESIAN_POINT('Ctrl Pts',(-38.7087915466247,28.0183504465458,20.));
#80981=CARTESIAN_POINT('Ctrl Pts',(-38.6868429482325,28.0435204600798,0.));
#80982=CARTESIAN_POINT('Ctrl Pts',(-38.6868429482325,28.0435204600798,20.));
#80983=CARTESIAN_POINT('Ctrl Pts',(-38.6648775697261,28.0686743488361,0.));
#80984=CARTESIAN_POINT('Ctrl Pts',(-38.6648775697261,28.0686743488361,20.));
#80985=CARTESIAN_POINT('Ctrl Pts',(-38.6428954224012,28.0938121011982,0.));
#80986=CARTESIAN_POINT('Ctrl Pts',(-38.6428954224012,28.0938121011982,20.));
#80987=CARTESIAN_POINT('Ctrl Pts',(-38.6208965175619,28.1189337055566,0.));
#80988=CARTESIAN_POINT('Ctrl Pts',(-38.6208965175619,28.1189337055566,20.));
#80989=CARTESIAN_POINT('Ctrl Pts',(-38.5988808665205,28.14403915031,0.));
#80990=CARTESIAN_POINT('Ctrl Pts',(-38.5988808665205,28.14403915031,20.));
#80991=CARTESIAN_POINT('Ctrl Pts',(-38.5768484805979,28.1691284238645,0.));
#80992=CARTESIAN_POINT('Ctrl Pts',(-38.5768484805979,28.1691284238645,20.));
#80993=CARTESIAN_POINT('Ctrl Pts',(-38.5547993711231,28.194201514634,0.));
#80994=CARTESIAN_POINT('Ctrl Pts',(-38.5547993711231,28.194201514634,20.));
#80995=CARTESIAN_POINT('Ctrl Pts',(-38.5327335494335,28.2192584110398,0.));
#80996=CARTESIAN_POINT('Ctrl Pts',(-38.5327335494335,28.2192584110398,20.));
#80997=CARTESIAN_POINT('Ctrl Pts',(-38.5106510268752,28.2442991015113,0.));
#80998=CARTESIAN_POINT('Ctrl Pts',(-38.5106510268752,28.2442991015113,20.));
#80999=CARTESIAN_POINT('Ctrl Pts',(-38.4885518148031,28.2693235744854,0.));
#81000=CARTESIAN_POINT('Ctrl Pts',(-38.4885518148031,28.2693235744854,20.));
#81001=CARTESIAN_POINT('Ctrl Pts',(-38.4664359245797,28.2943318184065,0.));
#81002=CARTESIAN_POINT('Ctrl Pts',(-38.4664359245797,28.2943318184065,20.));
#81003=CARTESIAN_POINT('Ctrl Pts',(-38.444303367576,28.3193238217266,0.));
#81004=CARTESIAN_POINT('Ctrl Pts',(-38.444303367576,28.3193238217266,20.));
#81005=CARTESIAN_POINT('Ctrl Pts',(-38.422154155171,28.3442995729049,0.));
#81006=CARTESIAN_POINT('Ctrl Pts',(-38.422154155171,28.3442995729049,20.));
#81007=CARTESIAN_POINT('Ctrl Pts',(-38.3999882987522,28.3692590604082,0.));
#81008=CARTESIAN_POINT('Ctrl Pts',(-38.3999882987522,28.3692590604082,20.));
#81009=CARTESIAN_POINT('Ctrl Pts',(-38.3778058097152,28.3942022727108,0.));
#81010=CARTESIAN_POINT('Ctrl Pts',(-38.3778058097152,28.3942022727108,20.));
#81011=CARTESIAN_POINT('Ctrl Pts',(-38.3556066994642,28.419129198295,0.));
#81012=CARTESIAN_POINT('Ctrl Pts',(-38.3556066994642,28.419129198295,20.));
#81013=CARTESIAN_POINT('Ctrl Pts',(-38.333390979412,28.4440398256512,0.));
#81014=CARTESIAN_POINT('Ctrl Pts',(-38.333390979412,28.4440398256512,20.));
#81015=CARTESIAN_POINT('Ctrl Pts',(-38.3111586609795,28.4689341432774,0.));
#81016=CARTESIAN_POINT('Ctrl Pts',(-38.3111586609795,28.4689341432774,20.));
#81017=CARTESIAN_POINT('Ctrl Pts',(-38.2889097555964,28.4938121396793,0.));
#81018=CARTESIAN_POINT('Ctrl Pts',(-38.2889097555964,28.4938121396793,20.));
#81019=CARTESIAN_POINT('Ctrl Pts',(-38.2666442747002,28.5186738033703,0.));
#81020=CARTESIAN_POINT('Ctrl Pts',(-38.2666442747002,28.5186738033703,20.));
#81021=CARTESIAN_POINT('Ctrl Pts',(-38.2443622297368,28.543519122871,0.));
#81022=CARTESIAN_POINT('Ctrl Pts',(-38.2443622297368,28.543519122871,20.));
#81023=CARTESIAN_POINT('Ctrl Pts',(-38.2220636321601,28.5683480867097,0.));
#81024=CARTESIAN_POINT('Ctrl Pts',(-38.2220636321601,28.5683480867097,20.));
#81025=CARTESIAN_POINT('Ctrl Pts',(-38.1997484934321,28.5931606834223,0.));
#81026=CARTESIAN_POINT('Ctrl Pts',(-38.1997484934321,28.5931606834223,20.));
#81027=CARTESIAN_POINT('Ctrl Pts',(-38.1774168250235,28.6179569015525,0.));
#81028=CARTESIAN_POINT('Ctrl Pts',(-38.1774168250235,28.6179569015525,20.));
#81029=CARTESIAN_POINT('Ctrl Pts',(-38.1550686384134,28.6427367296518,0.));
#81030=CARTESIAN_POINT('Ctrl Pts',(-38.1550686384134,28.6427367296518,20.));
#81031=CARTESIAN_POINT('Ctrl Pts',(-38.1327039450889,28.6675001562794,0.));
#81032=CARTESIAN_POINT('Ctrl Pts',(-38.1327039450889,28.6675001562794,20.));
#81033=CARTESIAN_POINT('Ctrl Pts',(-38.1103227565456,28.6922471700024,0.));
#81034=CARTESIAN_POINT('Ctrl Pts',(-38.1103227565456,28.6922471700024,20.));
#81035=CARTESIAN_POINT('Ctrl Pts',(-38.0879250842874,28.7169777593955,0.));
#81036=CARTESIAN_POINT('Ctrl Pts',(-38.0879250842874,28.7169777593955,20.));
#81037=CARTESIAN_POINT('Ctrl Pts',(-38.0655109398262,28.7416919130413,0.));
#81038=CARTESIAN_POINT('Ctrl Pts',(-38.0655109398262,28.7416919130413,20.));
#81039=CARTESIAN_POINT('Ctrl Pts',(-38.0430803346823,28.76638961953,0.));
#81040=CARTESIAN_POINT('Ctrl Pts',(-38.0430803346823,28.76638961953,20.));
#81041=CARTESIAN_POINT('Ctrl Pts',(-38.020633280384,28.7910708674595,0.));
#81042=CARTESIAN_POINT('Ctrl Pts',(-38.020633280384,28.7910708674595,20.));
#81043=CARTESIAN_POINT('Ctrl Pts',(-37.9981697884679,28.8157356454354,0.));
#81044=CARTESIAN_POINT('Ctrl Pts',(-37.9981697884679,28.8157356454354,20.));
#81045=CARTESIAN_POINT('Ctrl Pts',(-37.975689870479,28.8403839420709,0.));
#81046=CARTESIAN_POINT('Ctrl Pts',(-37.975689870479,28.8403839420709,20.));
#81047=CARTESIAN_POINT('Ctrl Pts',(-37.9531935379708,28.8650157459871,0.));
#81048=CARTESIAN_POINT('Ctrl Pts',(-37.9531935379708,28.8650157459871,20.));
#81049=CARTESIAN_POINT('Ctrl Pts',(-37.9306808025049,28.8896310458131,0.));
#81050=CARTESIAN_POINT('Ctrl Pts',(-37.9306808025049,28.8896310458131,20.));
#81051=CARTESIAN_POINT('Ctrl Pts',(-37.9081516756509,28.9142298301853,0.));
#81052=CARTESIAN_POINT('Ctrl Pts',(-37.9081516756509,28.9142298301853,20.));
#81053=CARTESIAN_POINT('Ctrl Pts',(-37.8856061689868,28.9388120877483,0.));
#81054=CARTESIAN_POINT('Ctrl Pts',(-37.8856061689868,28.9388120877483,20.));
#81055=CARTESIAN_POINT('Ctrl Pts',(-37.8630442940985,28.9633778071544,0.));
#81056=CARTESIAN_POINT('Ctrl Pts',(-37.8630442940985,28.9633778071544,20.));
#81057=CARTESIAN_POINT('Ctrl Pts',(-37.8404660625803,28.9879269770637,0.));
#81058=CARTESIAN_POINT('Ctrl Pts',(-37.8404660625803,28.9879269770637,20.));
#81059=CARTESIAN_POINT('Ctrl Pts',(-37.8178714860345,29.0124595861441,0.));
#81060=CARTESIAN_POINT('Ctrl Pts',(-37.8178714860345,29.0124595861441,20.));
#81061=CARTESIAN_POINT('Ctrl Pts',(-37.7952605760716,29.0369756230713,0.));
#81062=CARTESIAN_POINT('Ctrl Pts',(-37.7952605760716,29.0369756230713,20.));
#81063=CARTESIAN_POINT('Ctrl Pts',(-37.7726333443105,29.0614750765285,0.));
#81064=CARTESIAN_POINT('Ctrl Pts',(-37.7726333443105,29.0614750765285,20.));
#81065=CARTESIAN_POINT('Ctrl Pts',(-37.7499898023785,29.0859579352069,0.));
#81066=CARTESIAN_POINT('Ctrl Pts',(-37.7499898023785,29.0859579352069,20.));
#81067=CARTESIAN_POINT('Ctrl Pts',(-37.7273299619109,29.1104241878056,0.));
#81068=CARTESIAN_POINT('Ctrl Pts',(-37.7273299619109,29.1104241878056,20.));
#81069=CARTESIAN_POINT('Ctrl Pts',(-37.7046538345516,29.1348738230316,0.));
#81070=CARTESIAN_POINT('Ctrl Pts',(-37.7046538345516,29.1348738230316,20.));
#81071=CARTESIAN_POINT('Ctrl Pts',(-37.6819614319523,29.1593068295997,0.));
#81072=CARTESIAN_POINT('Ctrl Pts',(-37.6819614319523,29.1593068295997,20.));
#81073=CARTESIAN_POINT('Ctrl Pts',(-37.6592527657727,29.1837231962328,0.));
#81074=CARTESIAN_POINT('Ctrl Pts',(-37.6592527657727,29.1837231962328,20.));
#81075=CARTESIAN_POINT('Ctrl Pts',(-37.6365278476807,29.208122911661,0.));
#81076=CARTESIAN_POINT('Ctrl Pts',(-37.6365278476807,29.208122911661,20.));
#81077=CARTESIAN_POINT('Ctrl Pts',(-37.613786689352,29.2325059646224,0.));
#81078=CARTESIAN_POINT('Ctrl Pts',(-37.613786689352,29.2325059646224,20.));
#81079=CARTESIAN_POINT('Ctrl Pts',(-37.5910293024705,29.2568723438631,0.));
#81080=CARTESIAN_POINT('Ctrl Pts',(-37.5910293024705,29.2568723438631,20.));
#81081=CARTESIAN_POINT('Ctrl Pts',(-37.5682556987287,29.2812220381372,0.));
#81082=CARTESIAN_POINT('Ctrl Pts',(-37.5682556987287,29.2812220381372,20.));
#81083=CARTESIAN_POINT('Ctrl Pts',(-37.5454658898274,29.3055550362067,0.));
#81084=CARTESIAN_POINT('Ctrl Pts',(-37.5454658898274,29.3055550362067,20.));
#81085=CARTESIAN_POINT('Ctrl Pts',(-37.5226598874754,29.3298713268414,0.));
#81086=CARTESIAN_POINT('Ctrl Pts',(-37.5226598874754,29.3298713268414,20.));
#81087=CARTESIAN_POINT('Ctrl Pts',(-37.4998377033899,29.3541708988191,0.));
#81088=CARTESIAN_POINT('Ctrl Pts',(-37.4998377033899,29.3541708988191,20.));
#81089=CARTESIAN_POINT('Ctrl Pts',(-37.4769993492958,29.378453740925,0.));
#81090=CARTESIAN_POINT('Ctrl Pts',(-37.4769993492958,29.378453740925,20.));
#81091=CARTESIAN_POINT('Ctrl Pts',(-37.4541448369259,29.4027198419524,0.));
#81092=CARTESIAN_POINT('Ctrl Pts',(-37.4541448369259,29.4027198419524,20.));
#81093=CARTESIAN_POINT('Ctrl Pts',(-37.4312741780213,29.4269691907023,0.));
#81094=CARTESIAN_POINT('Ctrl Pts',(-37.4312741780213,29.4269691907023,20.));
#81095=CARTESIAN_POINT('Ctrl Pts',(-37.4083873843313,29.4512017759842,0.));
#81096=CARTESIAN_POINT('Ctrl Pts',(-37.4083873843313,29.4512017759842,20.));
#81097=CARTESIAN_POINT('Ctrl Pts',(-37.3854844676135,29.4754175866156,0.));
#81098=CARTESIAN_POINT('Ctrl Pts',(-37.3854844676135,29.4754175866156,20.));
#81099=CARTESIAN_POINT('Ctrl Pts',(-37.3625654396335,29.4996166114217,0.));
#81100=CARTESIAN_POINT('Ctrl Pts',(-37.3625654396335,29.4996166114217,20.));
#81101=CARTESIAN_POINT('Ctrl Pts',(-37.3396303121646,29.5237988392353,0.));
#81102=CARTESIAN_POINT('Ctrl Pts',(-37.3396303121646,29.5237988392353,20.));
#81103=CARTESIAN_POINT('Ctrl Pts',(-37.3166790969884,29.5479642588972,0.));
#81104=CARTESIAN_POINT('Ctrl Pts',(-37.3166790969884,29.5479642588972,20.));
#81105=CARTESIAN_POINT('Ctrl Pts',(-37.2937118058947,29.5721128592559,0.));
#81106=CARTESIAN_POINT('Ctrl Pts',(-37.2937118058947,29.5721128592559,20.));
#81107=CARTESIAN_POINT('Ctrl Pts',(-37.2707284506814,29.5962446291682,0.));
#81108=CARTESIAN_POINT('Ctrl Pts',(-37.2707284506814,29.5962446291682,20.));
#81109=CARTESIAN_POINT('Ctrl Pts',(-37.2477290431548,29.6203595574991,0.));
#81110=CARTESIAN_POINT('Ctrl Pts',(-37.2477290431548,29.6203595574991,20.));
#81111=CARTESIAN_POINT('Ctrl Pts',(-37.2247135951292,29.6444576331214,0.));
#81112=CARTESIAN_POINT('Ctrl Pts',(-37.2247135951292,29.6444576331214,20.));
#81113=CARTESIAN_POINT('Ctrl Pts',(-37.2016821184267,29.668538844916,0.));
#81114=CARTESIAN_POINT('Ctrl Pts',(-37.2016821184267,29.668538844916,20.));
#81115=CARTESIAN_POINT('Ctrl Pts',(-37.1786346248774,29.6926031817715,0.));
#81116=CARTESIAN_POINT('Ctrl Pts',(-37.1786346248774,29.6926031817715,20.));
#81117=CARTESIAN_POINT('Ctrl Pts',(-37.155571126319,29.7166506325841,0.));
#81118=CARTESIAN_POINT('Ctrl Pts',(-37.155571126319,29.7166506325841,20.));
#81119=CARTESIAN_POINT('Ctrl Pts',(-37.1324916345976,29.7406811862582,0.));
#81120=CARTESIAN_POINT('Ctrl Pts',(-37.1324916345976,29.7406811862582,20.));
#81121=CARTESIAN_POINT('Ctrl Pts',(-37.1093961615672,29.7646948317061,0.));
#81122=CARTESIAN_POINT('Ctrl Pts',(-37.1093961615672,29.7646948317061,20.));
#81123=CARTESIAN_POINT('Ctrl Pts',(-37.0862847190902,29.7886915578485,0.));
#81124=CARTESIAN_POINT('Ctrl Pts',(-37.0862847190902,29.7886915578485,20.));
#81125=CARTESIAN_POINT('Ctrl Pts',(-37.0631573190374,29.8126713536142,0.));
#81126=CARTESIAN_POINT('Ctrl Pts',(-37.0631573190374,29.8126713536142,20.));
#81127=CARTESIAN_POINT('Ctrl Pts',(-37.0400139732874,29.83663420794,0.));
#81128=CARTESIAN_POINT('Ctrl Pts',(-37.0400139732874,29.83663420794,20.));
#81129=CARTESIAN_POINT('Ctrl Pts',(-37.0168546937273,29.8605801097708,0.));
#81130=CARTESIAN_POINT('Ctrl Pts',(-37.0168546937273,29.8605801097708,20.));
#81131=CARTESIAN_POINT('Ctrl Pts',(-36.9936794922513,29.884509048059,0.));
#81132=CARTESIAN_POINT('Ctrl Pts',(-36.9936794922513,29.884509048059,20.));
#81133=CARTESIAN_POINT('Ctrl Pts',(-36.9704883807614,29.9084210117647,0.));
#81134=CARTESIAN_POINT('Ctrl Pts',(-36.9704883807614,29.9084210117647,20.));
#81135=CARTESIAN_POINT('Ctrl Pts',(-36.9472813711676,29.9323159898562,0.));
#81136=CARTESIAN_POINT('Ctrl Pts',(-36.9472813711676,29.9323159898562,20.));
#81137=CARTESIAN_POINT('Ctrl Pts',(-36.9240584753883,29.9561939713102,0.));
#81138=CARTESIAN_POINT('Ctrl Pts',(-36.9240584753883,29.9561939713102,20.));
#81139=CARTESIAN_POINT('Ctrl Pts',(-36.9008197053507,29.9800549451122,0.));
#81140=CARTESIAN_POINT('Ctrl Pts',(-36.9008197053507,29.9800549451122,20.));
#81141=CARTESIAN_POINT('Ctrl Pts',(-36.8775650729895,30.0038989002549,0.));
#81142=CARTESIAN_POINT('Ctrl Pts',(-36.8775650729895,30.0038989002549,20.));
#81143=CARTESIAN_POINT('Ctrl Pts',(-36.8542945902473,30.0277258257393,0.));
#81144=CARTESIAN_POINT('Ctrl Pts',(-36.8542945902473,30.0277258257393,20.));
#81145=CARTESIAN_POINT('Ctrl Pts',(-36.8310082690741,30.0515357105739,0.));
#81146=CARTESIAN_POINT('Ctrl Pts',(-36.8310082690741,30.0515357105739,20.));
#81147=CARTESIAN_POINT('Ctrl Pts',(-36.8077061214283,30.0753285437754,0.));
#81148=CARTESIAN_POINT('Ctrl Pts',(-36.8077061214283,30.0753285437754,20.));
#81149=CARTESIAN_POINT('Ctrl Pts',(-36.784388159276,30.0991043143684,0.));
#81150=CARTESIAN_POINT('Ctrl Pts',(-36.784388159276,30.0991043143684,20.));
#81151=CARTESIAN_POINT('Ctrl Pts',(-36.7610543945915,30.1228630113862,0.));
#81152=CARTESIAN_POINT('Ctrl Pts',(-36.7610543945915,30.1228630113862,20.));
#81153=CARTESIAN_POINT('Ctrl Pts',(-36.7377048393574,30.14660462387,0.));
#81154=CARTESIAN_POINT('Ctrl Pts',(-36.7377048393574,30.14660462387,20.));
#81155=CARTESIAN_POINT('Ctrl Pts',(-36.7143395055641,30.1703291408693,0.));
#81156=CARTESIAN_POINT('Ctrl Pts',(-36.7143395055641,30.1703291408693,20.));
#81157=CARTESIAN_POINT('Ctrl Pts',(-36.6909584052099,30.1940365514414,0.));
#81158=CARTESIAN_POINT('Ctrl Pts',(-36.6909584052099,30.1940365514414,20.));
#81159=CARTESIAN_POINT('Ctrl Pts',(-36.6675615503012,30.2177268446518,0.));
#81160=CARTESIAN_POINT('Ctrl Pts',(-36.6675615503012,30.2177268446518,20.));
#81161=CARTESIAN_POINT('Ctrl Pts',(-36.6441489528521,30.2414000095742,0.));
#81162=CARTESIAN_POINT('Ctrl Pts',(-36.6441489528521,30.2414000095742,20.));
#81163=CARTESIAN_POINT('Ctrl Pts',(-36.6207206248849,30.2650560352902,0.));
#81164=CARTESIAN_POINT('Ctrl Pts',(-36.6207206248849,30.2650560352902,20.));
#81165=CARTESIAN_POINT('Ctrl Pts',(-36.5972765784293,30.2886949108895,0.));
#81166=CARTESIAN_POINT('Ctrl Pts',(-36.5972765784293,30.2886949108895,20.));
#81167=CARTESIAN_POINT('Ctrl Pts',(-36.5738168255233,30.3123166254701,0.));
#81168=CARTESIAN_POINT('Ctrl Pts',(-36.5738168255233,30.3123166254701,20.));
#81169=CARTESIAN_POINT('Ctrl Pts',(-36.5503413782123,30.3359211681375,0.));
#81170=CARTESIAN_POINT('Ctrl Pts',(-36.5503413782123,30.3359211681375,20.));
#81171=CARTESIAN_POINT('Ctrl Pts',(-36.5268502485502,30.3595085280058,0.));
#81172=CARTESIAN_POINT('Ctrl Pts',(-36.5268502485502,30.3595085280058,20.));
#81173=CARTESIAN_POINT('Ctrl Pts',(-36.5033434485984,30.3830786941972,0.));
#81174=CARTESIAN_POINT('Ctrl Pts',(-36.5033434485984,30.3830786941972,20.));
#81175=CARTESIAN_POINT('Ctrl Pts',(-36.4798209904267,30.4066316558423,0.));
#81176=CARTESIAN_POINT('Ctrl Pts',(-36.4798209904267,30.4066316558423,20.));
#81177=CARTESIAN_POINT('Ctrl Pts',(-36.456282886113,30.4301674020801,0.));
#81178=CARTESIAN_POINT('Ctrl Pts',(-36.456282886113,30.4301674020801,20.));
#81179=CARTESIAN_POINT('Ctrl Pts',(-36.4327291477429,30.4536859220576,0.));
#81180=CARTESIAN_POINT('Ctrl Pts',(-36.4327291477429,30.4536859220576,20.));
#81181=CARTESIAN_POINT('Ctrl Pts',(-36.4091597874097,30.4771872049298,0.));
#81182=CARTESIAN_POINT('Ctrl Pts',(-36.4091597874097,30.4771872049298,20.));
#81183=CARTESIAN_POINT('Ctrl Pts',(-36.3855748172148,30.5006712398601,0.));
#81184=CARTESIAN_POINT('Ctrl Pts',(-36.3855748172148,30.5006712398601,20.));
#81185=CARTESIAN_POINT('Ctrl Pts',(-36.3619742492671,30.5241380160195,0.));
#81186=CARTESIAN_POINT('Ctrl Pts',(-36.3619742492671,30.5241380160195,20.));
#81187=CARTESIAN_POINT('Ctrl Pts',(-36.3383580956833,30.5475875225872,0.));
#81188=CARTESIAN_POINT('Ctrl Pts',(-36.3383580956833,30.5475875225872,20.));
#81189=CARTESIAN_POINT('Ctrl Pts',(-36.3147263685875,30.5710197487502,0.));
#81190=CARTESIAN_POINT('Ctrl Pts',(-36.3147263685875,30.5710197487502,20.));
#81191=CARTESIAN_POINT('Ctrl Pts',(-36.2910790801119,30.5944346837039,0.));
#81192=CARTESIAN_POINT('Ctrl Pts',(-36.2910790801119,30.5944346837039,20.));
#81193=CARTESIAN_POINT('Ctrl Pts',(-36.2674162423973,30.6178323166527,0.));
#81194=CARTESIAN_POINT('Ctrl Pts',(-36.2674162423973,30.6178323166527,20.));
#81195=CARTESIAN_POINT('Ctrl Pts',(-36.2437378675924,30.6412126368094,0.));
#81196=CARTESIAN_POINT('Ctrl Pts',(-36.2437378675924,30.6412126368094,20.));
#81197=CARTESIAN_POINT('Ctrl Pts',(-36.2200439678543,30.6645756333954,0.));
#81198=CARTESIAN_POINT('Ctrl Pts',(-36.2200439678543,30.6645756333954,20.));
#81199=CARTESIAN_POINT('Ctrl Pts',(-36.1963345553471,30.6879212956391,0.));
#81200=CARTESIAN_POINT('Ctrl Pts',(-36.1963345553471,30.6879212956391,20.));
#81201=CARTESIAN_POINT('Ctrl Pts',(-36.1726096422428,30.7112496127774,0.));
#81202=CARTESIAN_POINT('Ctrl Pts',(-36.1726096422428,30.7112496127774,20.));
#81203=CARTESIAN_POINT('Ctrl Pts',(-36.1488692407204,30.7345605740544,0.));
#81204=CARTESIAN_POINT('Ctrl Pts',(-36.1488692407204,30.7345605740544,20.));
#81205=CARTESIAN_POINT('Ctrl Pts',(-36.125113362967,30.7578541687236,0.));
#81206=CARTESIAN_POINT('Ctrl Pts',(-36.125113362967,30.7578541687236,20.));
#81207=CARTESIAN_POINT('Ctrl Pts',(-36.1013420211777,30.7811303860468,0.));
#81208=CARTESIAN_POINT('Ctrl Pts',(-36.1013420211777,30.7811303860468,20.));
#81209=CARTESIAN_POINT('Ctrl Pts',(-36.0775552275565,30.8043892152943,0.));
#81210=CARTESIAN_POINT('Ctrl Pts',(-36.0775552275565,30.8043892152943,20.));
#81211=CARTESIAN_POINT('Ctrl Pts',(-36.0537529943146,30.8276306457446,0.));
#81212=CARTESIAN_POINT('Ctrl Pts',(-36.0537529943146,30.8276306457446,20.));
#81213=CARTESIAN_POINT('Ctrl Pts',(-36.0299353336712,30.8508546666841,0.));
#81214=CARTESIAN_POINT('Ctrl Pts',(-36.0299353336712,30.8508546666841,20.));
#81215=CARTESIAN_POINT('Ctrl Pts',(-36.0061022578528,30.8740612674075,0.));
#81216=CARTESIAN_POINT('Ctrl Pts',(-36.0061022578528,30.8740612674075,20.));
#81217=CARTESIAN_POINT('Ctrl Pts',(-35.9822537790931,30.8972504372171,0.));
#81218=CARTESIAN_POINT('Ctrl Pts',(-35.9822537790931,30.8972504372171,20.));
#81219=CARTESIAN_POINT('Ctrl Pts',(-35.9583899096339,30.9204221654236,0.));
#81220=CARTESIAN_POINT('Ctrl Pts',(-35.9583899096339,30.9204221654236,20.));
#81221=CARTESIAN_POINT('Ctrl Pts',(-35.9345106617251,30.9435764413467,0.));
#81222=CARTESIAN_POINT('Ctrl Pts',(-35.9345106617251,30.9435764413467,20.));
#81223=CARTESIAN_POINT('Ctrl Pts',(-35.9106160476245,30.9667132543142,0.));
#81224=CARTESIAN_POINT('Ctrl Pts',(-35.9106160476245,30.9667132543142,20.));
#81225=CARTESIAN_POINT('Ctrl Pts',(-35.886706079598,30.9898325936627,0.));
#81226=CARTESIAN_POINT('Ctrl Pts',(-35.886706079598,30.9898325936627,20.));
#81227=CARTESIAN_POINT('Ctrl Pts',(-35.8627807699193,31.0129344487367,0.));
#81228=CARTESIAN_POINT('Ctrl Pts',(-35.8627807699193,31.0129344487367,20.));
#81229=CARTESIAN_POINT('Ctrl Pts',(-35.8388401308696,31.036018808889,0.));
#81230=CARTESIAN_POINT('Ctrl Pts',(-35.8388401308696,31.036018808889,20.));
#81231=CARTESIAN_POINT('Ctrl Pts',(-35.8148841747376,31.0590856634804,0.));
#81232=CARTESIAN_POINT('Ctrl Pts',(-35.8148841747376,31.0590856634804,20.));
#81233=CARTESIAN_POINT('Ctrl Pts',(-35.7909129138202,31.0821350018809,0.));
#81234=CARTESIAN_POINT('Ctrl Pts',(-35.7909129138202,31.0821350018809,20.));
#81235=CARTESIAN_POINT('Ctrl Pts',(-35.7669263604212,31.1051668134678,0.));
#81236=CARTESIAN_POINT('Ctrl Pts',(-35.7669263604212,31.1051668134678,20.));
#81237=CARTESIAN_POINT('Ctrl Pts',(-35.7429245268523,31.1281810876267,0.));
#81238=CARTESIAN_POINT('Ctrl Pts',(-35.7429245268523,31.1281810876267,20.));
#81239=CARTESIAN_POINT('Ctrl Pts',(-35.7189074254331,31.1511778137516,0.));
#81240=CARTESIAN_POINT('Ctrl Pts',(-35.7189074254331,31.1511778137516,20.));
#81241=CARTESIAN_POINT('Ctrl Pts',(-35.6948750684911,31.1741569812451,0.));
#81242=CARTESIAN_POINT('Ctrl Pts',(-35.6948750684911,31.1741569812451,20.));
#81243=CARTESIAN_POINT('Ctrl Pts',(-35.6708274683619,31.1971185795181,0.));
#81244=CARTESIAN_POINT('Ctrl Pts',(-35.6708274683619,31.1971185795181,20.));
#81245=CARTESIAN_POINT('Ctrl Pts',(-35.6467646373884,31.2200625979904,0.));
#81246=CARTESIAN_POINT('Ctrl Pts',(-35.6467646373884,31.2200625979904,20.));
#81247=CARTESIAN_POINT('Ctrl Pts',(-35.6226865879214,31.24298902609,0.));
#81248=CARTESIAN_POINT('Ctrl Pts',(-35.6226865879214,31.24298902609,20.));
#81249=CARTESIAN_POINT('Ctrl Pts',(-35.5985933323195,31.2658978532533,0.));
#81250=CARTESIAN_POINT('Ctrl Pts',(-35.5985933323195,31.2658978532533,20.));
#81251=CARTESIAN_POINT('Ctrl Pts',(-35.5744848829488,31.288789068925,0.));
#81252=CARTESIAN_POINT('Ctrl Pts',(-35.5744848829488,31.288789068925,20.));
#81253=CARTESIAN_POINT('Ctrl Pts',(-35.5503612521832,31.3116626625581,0.));
#81254=CARTESIAN_POINT('Ctrl Pts',(-35.5503612521832,31.3116626625581,20.));
#81255=CARTESIAN_POINT('Ctrl Pts',(-35.5262224524039,31.3345186236135,0.));
#81256=CARTESIAN_POINT('Ctrl Pts',(-35.5262224524039,31.3345186236135,20.));
#81257=CARTESIAN_POINT('Ctrl Pts',(-35.502068496,31.3573569415605,0.));
#81258=CARTESIAN_POINT('Ctrl Pts',(-35.502068496,31.3573569415605,20.));
#81259=CARTESIAN_POINT('Ctrl Pts',(-35.4778993953681,31.3801776058767,0.));
#81260=CARTESIAN_POINT('Ctrl Pts',(-35.4778993953681,31.3801776058767,20.));
#81261=CARTESIAN_POINT('Ctrl Pts',(-35.4537151629127,31.4029806060482,0.));
#81262=CARTESIAN_POINT('Ctrl Pts',(-35.4537151629127,31.4029806060482,20.));
#81263=CARTESIAN_POINT('Ctrl Pts',(-35.4295158110455,31.4257659315696,0.));
#81264=CARTESIAN_POINT('Ctrl Pts',(-35.4295158110455,31.4257659315696,20.));
#81265=CARTESIAN_POINT('Ctrl Pts',(-35.4053013521866,31.4485335719446,0.));
#81266=CARTESIAN_POINT('Ctrl Pts',(-35.4053013521866,31.4485335719446,20.));
#81267=CARTESIAN_POINT('Ctrl Pts',(-35.3810717987641,31.4712835166857,0.));
#81268=CARTESIAN_POINT('Ctrl Pts',(-35.3810717987641,31.4712835166857,20.));
#81269=CARTESIAN_POINT('Ctrl Pts',(-35.3568271632136,31.4940157553136,0.));
#81270=CARTESIAN_POINT('Ctrl Pts',(-35.3568271632136,31.4940157553136,20.));
#81271=CARTESIAN_POINT('Ctrl Pts',(-35.3325674579779,31.5167302773569,0.));
#81272=CARTESIAN_POINT('Ctrl Pts',(-35.3325674579779,31.5167302773569,20.));
#81273=CARTESIAN_POINT('Ctrl Pts',(-35.3082926955072,31.5394270723526,0.));
#81274=CARTESIAN_POINT('Ctrl Pts',(-35.3082926955072,31.5394270723526,20.));
#81275=CARTESIAN_POINT('Ctrl Pts',(-35.2840028882593,31.5621061298453,0.));
#81276=CARTESIAN_POINT('Ctrl Pts',(-35.2840028882593,31.5621061298453,20.));
#81277=CARTESIAN_POINT('Ctrl Pts',(-35.2596980486997,31.5847674393884,0.));
#81278=CARTESIAN_POINT('Ctrl Pts',(-35.2596980486997,31.5847674393884,20.));
#81279=CARTESIAN_POINT('Ctrl Pts',(-35.2353781893015,31.6074109905439,0.));
#81280=CARTESIAN_POINT('Ctrl Pts',(-35.2353781893015,31.6074109905439,20.));
#81281=CARTESIAN_POINT('Ctrl Pts',(-35.2110433225459,31.6300367728826,0.));
#81282=CARTESIAN_POINT('Ctrl Pts',(-35.2110433225459,31.6300367728826,20.));
#81283=CARTESIAN_POINT('Ctrl Pts',(-35.1866934609214,31.6526447759839,0.));
#81284=CARTESIAN_POINT('Ctrl Pts',(-35.1866934609214,31.6526447759839,20.));
#81285=CARTESIAN_POINT('Ctrl Pts',(-35.1623286169245,31.6752349894358,0.));
#81286=CARTESIAN_POINT('Ctrl Pts',(-35.1623286169245,31.6752349894358,20.));
#81287=CARTESIAN_POINT('Ctrl Pts',(-35.1379488030591,31.6978074028349,0.));
#81288=CARTESIAN_POINT('Ctrl Pts',(-35.1379488030591,31.6978074028349,20.));
#81289=CARTESIAN_POINT('Ctrl Pts',(-35.1135540318367,31.7203620057864,0.));
#81290=CARTESIAN_POINT('Ctrl Pts',(-35.1135540318367,31.7203620057864,20.));
#81291=CARTESIAN_POINT('Ctrl Pts',(-35.0891443157764,31.7428987879034,0.));
#81292=CARTESIAN_POINT('Ctrl Pts',(-35.0891443157764,31.7428987879034,20.));
#81293=CARTESIAN_POINT('Ctrl Pts',(-35.0647196674044,31.7654177388073,0.));
#81294=CARTESIAN_POINT('Ctrl Pts',(-35.0647196674044,31.7654177388073,20.));
#81295=CARTESIAN_POINT('Ctrl Pts',(-35.0402800992547,31.7879188481277,0.));
#81296=CARTESIAN_POINT('Ctrl Pts',(-35.0402800992547,31.7879188481277,20.));
#81297=CARTESIAN_POINT('Ctrl Pts',(-35.0158256238691,31.8104021055032,0.));
#81298=CARTESIAN_POINT('Ctrl Pts',(-35.0158256238691,31.8104021055032,20.));
#81299=CARTESIAN_POINT('Ctrl Pts',(-34.991356253797,31.8328675005809,0.));
#81300=CARTESIAN_POINT('Ctrl Pts',(-34.991356253797,31.8328675005809,20.));
#81301=CARTESIAN_POINT('Ctrl Pts',(-34.9668720015954,31.8553150230168,0.));
#81302=CARTESIAN_POINT('Ctrl Pts',(-34.9668720015954,31.8553150230168,20.));
#81303=CARTESIAN_POINT('Ctrl Pts',(-34.9423728798289,31.8777446624754,0.));
#81304=CARTESIAN_POINT('Ctrl Pts',(-34.9423728798289,31.8777446624754,20.));
#81305=CARTESIAN_POINT('Ctrl Pts',(-34.9178589010694,31.9001564086295,0.));
#81306=CARTESIAN_POINT('Ctrl Pts',(-34.9178589010694,31.9001564086295,20.));
#81307=CARTESIAN_POINT('Ctrl Pts',(-34.8933300778963,31.9225502511603,0.));
#81308=CARTESIAN_POINT('Ctrl Pts',(-34.8933300778963,31.9225502511603,20.));
#81309=CARTESIAN_POINT('Ctrl Pts',(-34.8687864228965,31.9449261797574,0.));
#81310=CARTESIAN_POINT('Ctrl Pts',(-34.8687864228965,31.9449261797574,20.));
#81311=CARTESIAN_POINT('Ctrl Pts',(-34.8442279486644,31.967284184119,0.));
#81312=CARTESIAN_POINT('Ctrl Pts',(-34.8442279486644,31.967284184119,20.));
#81313=CARTESIAN_POINT('Ctrl Pts',(-34.8196546678026,31.9896242539524,0.));
#81314=CARTESIAN_POINT('Ctrl Pts',(-34.8196546678026,31.9896242539524,20.));
#81315=CARTESIAN_POINT('Ctrl Pts',(-34.7950665929206,32.0119463789729,0.));
#81316=CARTESIAN_POINT('Ctrl Pts',(-34.7950665929206,32.0119463789729,20.));
#81317=CARTESIAN_POINT('Ctrl Pts',(-34.7704637366357,32.0342505489048,0.));
#81318=CARTESIAN_POINT('Ctrl Pts',(-34.7704637366357,32.0342505489048,20.));
#81319=CARTESIAN_POINT('Ctrl Pts',(-34.7458461115727,32.0565367534806,0.));
#81320=CARTESIAN_POINT('Ctrl Pts',(-34.7458461115727,32.0565367534806,20.));
#81321=CARTESIAN_POINT('Ctrl Pts',(-34.7212137303638,32.0788049824416,0.));
#81322=CARTESIAN_POINT('Ctrl Pts',(-34.7212137303638,32.0788049824416,20.));
#81323=CARTESIAN_POINT('Ctrl Pts',(-34.6965666056491,32.1010552255378,0.));
#81324=CARTESIAN_POINT('Ctrl Pts',(-34.6965666056491,32.1010552255378,20.));
#81325=CARTESIAN_POINT('Ctrl Pts',(-34.6719047500757,32.1232874725276,0.));
#81326=CARTESIAN_POINT('Ctrl Pts',(-34.6719047500757,32.1232874725276,20.));
#81327=CARTESIAN_POINT('Ctrl Pts',(-34.6472281762982,32.145501713178,0.));
#81328=CARTESIAN_POINT('Ctrl Pts',(-34.6472281762982,32.145501713178,20.));
#81329=CARTESIAN_POINT('Ctrl Pts',(-34.6225368969784,32.167697937264,0.));
#81330=CARTESIAN_POINT('Ctrl Pts',(-34.6225368969784,32.167697937264,20.));
#81331=CARTESIAN_POINT('Ctrl Pts',(-34.5978309247855,32.1898761345694,0.));
#81332=CARTESIAN_POINT('Ctrl Pts',(-34.5978309247855,32.1898761345694,20.));
#81333=CARTESIAN_POINT('Ctrl Pts',(-34.5731102723969,32.212036294887,0.));
#81334=CARTESIAN_POINT('Ctrl Pts',(-34.5731102723969,32.212036294887,20.));
#81335=CARTESIAN_POINT('Ctrl Pts',(-34.5483749524972,32.2341784080183,0.));
#81336=CARTESIAN_POINT('Ctrl Pts',(-34.5483749524972,32.2341784080183,20.));
#81337=CARTESIAN_POINT('Ctrl Pts',(-34.5236249777791,32.2563024637739,0.));
#81338=CARTESIAN_POINT('Ctrl Pts',(-34.5236249777791,32.2563024637739,20.));
#81339=CARTESIAN_POINT('Ctrl Pts',(-34.4988603609427,32.2784084519728,0.));
#81340=CARTESIAN_POINT('Ctrl Pts',(-34.4988603609427,32.2784084519728,20.));
#81341=CARTESIAN_POINT('Ctrl Pts',(-34.474081114695,32.3004963624427,0.));
#81342=CARTESIAN_POINT('Ctrl Pts',(-34.474081114695,32.3004963624427,20.));
#81343=CARTESIAN_POINT('Ctrl Pts',(-34.4492872517507,32.3225661850195,0.));
#81344=CARTESIAN_POINT('Ctrl Pts',(-34.4492872517507,32.3225661850195,20.));
#81345=CARTESIAN_POINT('Ctrl Pts',(-34.4244787848311,32.3446179095473,0.));
#81346=CARTESIAN_POINT('Ctrl Pts',(-34.4244787848311,32.3446179095473,20.));
#81347=CARTESIAN_POINT('Ctrl Pts',(-34.3996557266651,32.3666515258787,0.));
#81348=CARTESIAN_POINT('Ctrl Pts',(-34.3996557266651,32.3666515258787,20.));
#81349=CARTESIAN_POINT('Ctrl Pts',(-34.3748180899889,32.388667023875,0.));
#81350=CARTESIAN_POINT('Ctrl Pts',(-34.3748180899889,32.388667023875,20.));
#81351=CARTESIAN_POINT('Ctrl Pts',(-34.3499658875467,32.4106643934066,0.));
#81352=CARTESIAN_POINT('Ctrl Pts',(-34.3499658875467,32.4106643934066,20.));
#81353=CARTESIAN_POINT('Ctrl Pts',(-34.3250991320905,32.4326436243532,0.));
#81354=CARTESIAN_POINT('Ctrl Pts',(-34.3250991320905,32.4326436243532,20.));
#81355=CARTESIAN_POINT('Ctrl Pts',(-34.3002178363797,32.4546047066033,0.));
#81356=CARTESIAN_POINT('Ctrl Pts',(-34.3002178363797,32.4546047066033,20.));
#81357=CARTESIAN_POINT('Ctrl Pts',(-34.2753220131812,32.4765476300538,0.));
#81358=CARTESIAN_POINT('Ctrl Pts',(-34.2753220131812,32.4765476300538,20.));
#81359=CARTESIAN_POINT('Ctrl Pts',(-34.2504116752689,32.4984723846097,0.));
#81360=CARTESIAN_POINT('Ctrl Pts',(-34.2504116752689,32.4984723846097,20.));
#81361=CARTESIAN_POINT('Ctrl Pts',(-34.2254868354237,32.5203789601849,0.));
#81362=CARTESIAN_POINT('Ctrl Pts',(-34.2254868354237,32.5203789601849,20.));
#81363=CARTESIAN_POINT('Ctrl Pts',(-34.2005475064343,32.542267346702,0.));
#81364=CARTESIAN_POINT('Ctrl Pts',(-34.2005475064343,32.542267346702,20.));
#81365=CARTESIAN_POINT('Ctrl Pts',(-34.1755937010963,32.564137534092,0.));
#81366=CARTESIAN_POINT('Ctrl Pts',(-34.1755937010963,32.564137534092,20.));
#81367=CARTESIAN_POINT('Ctrl Pts',(-34.1506254322131,32.585989512295,0.));
#81368=CARTESIAN_POINT('Ctrl Pts',(-34.1506254322131,32.585989512295,20.));
#81369=CARTESIAN_POINT('Ctrl Pts',(-34.1256427125956,32.6078232712594,0.));
#81370=CARTESIAN_POINT('Ctrl Pts',(-34.1256427125956,32.6078232712594,20.));
#81371=CARTESIAN_POINT('Ctrl Pts',(-34.1006455550618,32.6296388009428,0.));
#81372=CARTESIAN_POINT('Ctrl Pts',(-34.1006455550618,32.6296388009428,20.));
#81373=CARTESIAN_POINT('Ctrl Pts',(-34.0756339724376,32.6514360913116,0.));
#81374=CARTESIAN_POINT('Ctrl Pts',(-34.0756339724376,32.6514360913116,20.));
#81375=CARTESIAN_POINT('Ctrl Pts',(-34.0506079775557,32.6732151323407,0.));
#81376=CARTESIAN_POINT('Ctrl Pts',(-34.0506079775557,32.6732151323407,20.));
#81377=CARTESIAN_POINT('Ctrl Pts',(-34.0255675832564,32.694975914014,0.));
#81378=CARTESIAN_POINT('Ctrl Pts',(-34.0255675832564,32.694975914014,20.));
#81379=CARTESIAN_POINT('Ctrl Pts',(-34.0005128023872,32.7167184263237,0.));
#81380=CARTESIAN_POINT('Ctrl Pts',(-34.0005128023872,32.7167184263237,20.));
#81381=CARTESIAN_POINT('Ctrl Pts',(-33.9754436478026,32.7384426592708,0.));
#81382=CARTESIAN_POINT('Ctrl Pts',(-33.9754436478026,32.7384426592708,20.));
#81383=CARTESIAN_POINT('Ctrl Pts',(-33.9503601323651,32.7601486028652,0.));
#81384=CARTESIAN_POINT('Ctrl Pts',(-33.9503601323651,32.7601486028652,20.));
#81385=CARTESIAN_POINT('Ctrl Pts',(-33.9252622689445,32.781836247126,0.));
#81386=CARTESIAN_POINT('Ctrl Pts',(-33.9252622689445,32.781836247126,20.));
#81387=CARTESIAN_POINT('Ctrl Pts',(-33.9001500704179,32.8035055820805,0.));
#81388=CARTESIAN_POINT('Ctrl Pts',(-33.9001500704179,32.8035055820805,20.));
#81389=CARTESIAN_POINT('Ctrl Pts',(-33.8750235496691,32.8251565977646,0.));
#81390=CARTESIAN_POINT('Ctrl Pts',(-33.8750235496691,32.8251565977646,20.));
#81391=CARTESIAN_POINT('Ctrl Pts',(-33.8498827195893,32.8467892842227,0.));
#81392=CARTESIAN_POINT('Ctrl Pts',(-33.8498827195893,32.8467892842227,20.));
#81393=CARTESIAN_POINT('Ctrl Pts',(-33.8247275930774,32.8684036315085,0.));
#81394=CARTESIAN_POINT('Ctrl Pts',(-33.8247275930774,32.8684036315085,20.));
#81395=CARTESIAN_POINT('Ctrl Pts',(-33.7995581830395,32.8899996296849,0.));
#81396=CARTESIAN_POINT('Ctrl Pts',(-33.7995581830395,32.8899996296849,20.));
#81397=CARTESIAN_POINT('Ctrl Pts',(-33.7743745023893,32.9115772688235,0.));
#81398=CARTESIAN_POINT('Ctrl Pts',(-33.7743745023893,32.9115772688235,20.));
#81399=CARTESIAN_POINT('Ctrl Pts',(-33.7491765640476,32.9331365390046,0.));
#81400=CARTESIAN_POINT('Ctrl Pts',(-33.7491765640476,32.9331365390046,20.));
#81401=CARTESIAN_POINT('Ctrl Pts',(-33.723964380943,32.9546774303179,0.));
#81402=CARTESIAN_POINT('Ctrl Pts',(-33.723964380943,32.9546774303179,20.));
#81403=CARTESIAN_POINT('Ctrl Pts',(-33.6987379660104,32.9761999328604,0.));
#81404=CARTESIAN_POINT('Ctrl Pts',(-33.6987379660104,32.9761999328604,20.));
#81405=CARTESIAN_POINT('Ctrl Pts',(-33.673497332192,32.9977040367383,0.));
#81406=CARTESIAN_POINT('Ctrl Pts',(-33.673497332192,32.9977040367383,20.));
#81407=CARTESIAN_POINT('Ctrl Pts',(-33.6482424924373,33.0191897320665,0.));
#81408=CARTESIAN_POINT('Ctrl Pts',(-33.6482424924373,33.0191897320665,20.));
#81409=CARTESIAN_POINT('Ctrl Pts',(-33.6229734597032,33.0406570089692,0.));
#81410=CARTESIAN_POINT('Ctrl Pts',(-33.6229734597032,33.0406570089692,20.));
#81411=CARTESIAN_POINT('Ctrl Pts',(-33.5976902469543,33.0621058575797,0.));
#81412=CARTESIAN_POINT('Ctrl Pts',(-33.5976902469543,33.0621058575797,20.));
#81413=CARTESIAN_POINT('Ctrl Pts',(-33.572392867162,33.0835362680399,0.));
#81414=CARTESIAN_POINT('Ctrl Pts',(-33.572392867162,33.0835362680399,20.));
#81415=CARTESIAN_POINT('Ctrl Pts',(-33.5470813333053,33.1049482305003,0.));
#81416=CARTESIAN_POINT('Ctrl Pts',(-33.5470813333053,33.1049482305003,20.));
#81417=CARTESIAN_POINT('Ctrl Pts',(-33.5217556583704,33.1263417351207,0.));
#81418=CARTESIAN_POINT('Ctrl Pts',(-33.5217556583704,33.1263417351207,20.));
#81419=CARTESIAN_POINT('Ctrl Pts',(-33.4964158553506,33.1477167720697,0.));
#81420=CARTESIAN_POINT('Ctrl Pts',(-33.4964158553506,33.1477167720697,20.));
#81421=CARTESIAN_POINT('Ctrl Pts',(-33.4710619372468,33.1690733315248,0.));
#81422=CARTESIAN_POINT('Ctrl Pts',(-33.4710619372468,33.1690733315248,20.));
#81423=CARTESIAN_POINT('Ctrl Pts',(-33.4456939170666,33.1904114036721,0.));
#81424=CARTESIAN_POINT('Ctrl Pts',(-33.4456939170666,33.1904114036721,20.));
#81425=CARTESIAN_POINT('Ctrl Pts',(-33.4203118078248,33.2117309787063,0.));
#81426=CARTESIAN_POINT('Ctrl Pts',(-33.4203118078248,33.2117309787063,20.));
#81427=CARTESIAN_POINT('Ctrl Pts',(-33.3949156225429,33.233032046831,0.));
#81428=CARTESIAN_POINT('Ctrl Pts',(-33.3949156225429,33.233032046831,20.));
#81429=CARTESIAN_POINT('Ctrl Pts',(-33.3695053742505,33.2543145982587,0.));
#81430=CARTESIAN_POINT('Ctrl Pts',(-33.3695053742505,33.2543145982587,20.));
#81431=CARTESIAN_POINT('Ctrl Pts',(-33.3440810759838,33.2755786232108,0.));
#81432=CARTESIAN_POINT('Ctrl Pts',(-33.3440810759838,33.2755786232108,20.));
#81433=CARTESIAN_POINT('Ctrl Pts',(-33.3186427407863,33.2968241119176,0.));
#81434=CARTESIAN_POINT('Ctrl Pts',(-33.3186427407863,33.2968241119176,20.));
#81435=CARTESIAN_POINT('Ctrl Pts',(-33.2931903817093,33.318051054619,0.));
#81436=CARTESIAN_POINT('Ctrl Pts',(-33.2931903817093,33.318051054619,20.));
#81437=CARTESIAN_POINT('Ctrl Pts',(-33.2677240118112,33.3392594415636,0.));
#81438=CARTESIAN_POINT('Ctrl Pts',(-33.2677240118112,33.3392594415636,20.));
#81439=CARTESIAN_POINT('Ctrl Pts',(-33.2422436441578,33.3604492630093,0.));
#81440=CARTESIAN_POINT('Ctrl Pts',(-33.2422436441578,33.3604492630093,20.));
#81441=CARTESIAN_POINT('Ctrl Pts',(-33.2167492918215,33.3816205092222,0.));
#81442=CARTESIAN_POINT('Ctrl Pts',(-33.2167492918215,33.3816205092222,20.));
#81443=CARTESIAN_POINT('Ctrl Pts',(-33.1912409678819,33.4027731704774,0.));
#81444=CARTESIAN_POINT('Ctrl Pts',(-33.1912409678819,33.4027731704774,20.));
#81445=CARTESIAN_POINT('Ctrl Pts',(-33.1657186854252,33.4239072370581,0.));
#81446=CARTESIAN_POINT('Ctrl Pts',(-33.1657186854252,33.4239072370581,20.));
#81447=CARTESIAN_POINT('Ctrl Pts',(-33.1401824575448,33.4450226992567,0.));
#81448=CARTESIAN_POINT('Ctrl Pts',(-33.1401824575448,33.4450226992567,20.));
#81449=CARTESIAN_POINT('Ctrl Pts',(-33.1146322973416,33.4661195473749,0.));
#81450=CARTESIAN_POINT('Ctrl Pts',(-33.1146322973416,33.4661195473749,20.));
#81451=CARTESIAN_POINT('Ctrl Pts',(-33.0890682179239,33.4871977717238,0.));
#81452=CARTESIAN_POINT('Ctrl Pts',(-33.0890682179239,33.4871977717238,20.));
#81453=CARTESIAN_POINT('Ctrl Pts',(-33.063490232407,33.5082573626235,0.));
#81454=CARTESIAN_POINT('Ctrl Pts',(-33.063490232407,33.5082573626235,20.));
#81455=CARTESIAN_POINT('Ctrl Pts',(-33.0378983539138,33.5292983104032,0.));
#81456=CARTESIAN_POINT('Ctrl Pts',(-33.0378983539138,33.5292983104032,20.));
#81457=CARTESIAN_POINT('Ctrl Pts',(-33.0122925955739,33.5503206054003,0.));
#81458=CARTESIAN_POINT('Ctrl Pts',(-33.0122925955739,33.5503206054003,20.));
#81459=CARTESIAN_POINT('Ctrl Pts',(-32.986672970524,33.5713242379612,0.));
#81460=CARTESIAN_POINT('Ctrl Pts',(-32.986672970524,33.5713242379612,20.));
#81461=CARTESIAN_POINT('Ctrl Pts',(-32.9610394919081,33.5923091984411,0.));
#81462=CARTESIAN_POINT('Ctrl Pts',(-32.9610394919081,33.5923091984411,20.));
#81463=CARTESIAN_POINT('Ctrl Pts',(-32.935392172877,33.6132754772045,0.));
#81464=CARTESIAN_POINT('Ctrl Pts',(-32.935392172877,33.6132754772045,20.));
#81465=CARTESIAN_POINT('Ctrl Pts',(-32.9097310265884,33.6342230646254,0.));
#81466=CARTESIAN_POINT('Ctrl Pts',(-32.9097310265884,33.6342230646254,20.));
#81467=CARTESIAN_POINT('Ctrl Pts',(-32.8840560662069,33.6551519510862,0.));
#81468=CARTESIAN_POINT('Ctrl Pts',(-32.8840560662069,33.6551519510862,20.));
#81469=CARTESIAN_POINT('Ctrl Pts',(-32.8583673049046,33.6760621269785,0.));
#81470=CARTESIAN_POINT('Ctrl Pts',(-32.8583673049046,33.6760621269785,20.));
#81471=CARTESIAN_POINT('Ctrl Pts',(-32.8326647558606,33.6969535827028,0.));
#81472=CARTESIAN_POINT('Ctrl Pts',(-32.8326647558606,33.6969535827028,20.));
#81473=CARTESIAN_POINT('Ctrl Pts',(-32.8069484322617,33.717826308669,0.));
#81474=CARTESIAN_POINT('Ctrl Pts',(-32.8069484322617,33.717826308669,20.));
#81475=CARTESIAN_POINT('Ctrl Pts',(-32.7812183473018,33.7386802952956,0.));
#81476=CARTESIAN_POINT('Ctrl Pts',(-32.7812183473018,33.7386802952956,20.));
#81477=CARTESIAN_POINT('Ctrl Pts',(-32.7554745141811,33.7595155330097,0.));
#81478=CARTESIAN_POINT('Ctrl Pts',(-32.7554745141811,33.7595155330097,20.));
#81479=CARTESIAN_POINT('Ctrl Pts',(-32.7297169461065,33.7803320122473,0.));
#81480=CARTESIAN_POINT('Ctrl Pts',(-32.7297169461065,33.7803320122473,20.));
#81481=CARTESIAN_POINT('Ctrl Pts',(-32.7039456562922,33.8011297234537,0.));
#81482=CARTESIAN_POINT('Ctrl Pts',(-32.7039456562922,33.8011297234537,20.));
#81483=CARTESIAN_POINT('Ctrl Pts',(-32.6781606579598,33.8219086570836,0.));
#81484=CARTESIAN_POINT('Ctrl Pts',(-32.6781606579598,33.8219086570836,20.));
#81485=CARTESIAN_POINT('Ctrl Pts',(-32.652361964338,33.8426688036011,0.));
#81486=CARTESIAN_POINT('Ctrl Pts',(-32.652361964338,33.8426688036011,20.));
#81487=CARTESIAN_POINT('Ctrl Pts',(-32.6265495886629,33.8634101534794,0.));
#81488=CARTESIAN_POINT('Ctrl Pts',(-32.6265495886629,33.8634101534794,20.));
#81489=CARTESIAN_POINT('Ctrl Pts',(-32.6007235441777,33.8841326972007,0.));
#81490=CARTESIAN_POINT('Ctrl Pts',(-32.6007235441777,33.8841326972007,20.));
#81491=CARTESIAN_POINT('Ctrl Pts',(-32.5748838441319,33.9048364252556,0.));
#81492=CARTESIAN_POINT('Ctrl Pts',(-32.5748838441319,33.9048364252556,20.));
#81493=CARTESIAN_POINT('Ctrl Pts',(-32.5490305017817,33.9255213281433,0.));
#81494=CARTESIAN_POINT('Ctrl Pts',(-32.5490305017817,33.9255213281433,20.));
#81495=CARTESIAN_POINT('Ctrl Pts',(-32.5231635303904,33.9461873963724,0.));
#81496=CARTESIAN_POINT('Ctrl Pts',(-32.5231635303904,33.9461873963724,20.));
#81497=CARTESIAN_POINT('Ctrl Pts',(-32.4972829432285,33.9668346204604,0.));
#81498=CARTESIAN_POINT('Ctrl Pts',(-32.4972829432285,33.9668346204604,20.));
#81499=CARTESIAN_POINT('Ctrl Pts',(-32.4713887535742,33.987462990935,0.));
#81500=CARTESIAN_POINT('Ctrl Pts',(-32.4713887535742,33.987462990935,20.));
#81501=CARTESIAN_POINT('Ctrl Pts',(-32.4454809747123,34.0080724983324,0.));
#81502=CARTESIAN_POINT('Ctrl Pts',(-32.4454809747123,34.0080724983324,20.));
#81503=CARTESIAN_POINT('Ctrl Pts',(-32.4195596199345,34.0286631331978,0.));
#81504=CARTESIAN_POINT('Ctrl Pts',(-32.4195596199345,34.0286631331978,20.));
#81505=CARTESIAN_POINT('Ctrl Pts',(-32.3936247025393,34.0492348860854,0.));
#81506=CARTESIAN_POINT('Ctrl Pts',(-32.3936247025393,34.0492348860854,20.));
#81507=CARTESIAN_POINT('Ctrl Pts',(-32.3676762358321,34.0697877475586,0.));
#81508=CARTESIAN_POINT('Ctrl Pts',(-32.3676762358321,34.0697877475586,20.));
#81509=CARTESIAN_POINT('Ctrl Pts',(-32.3417142331257,34.0903217081898,0.));
#81510=CARTESIAN_POINT('Ctrl Pts',(-32.3417142331257,34.0903217081898,20.));
#81511=CARTESIAN_POINT('Ctrl Pts',(-32.3157387077392,34.1108367585604,0.));
#81512=CARTESIAN_POINT('Ctrl Pts',(-32.3157387077392,34.1108367585604,20.));
#81513=CARTESIAN_POINT('Ctrl Pts',(-32.2897496729991,34.131332889261,0.));
#81514=CARTESIAN_POINT('Ctrl Pts',(-32.2897496729991,34.131332889261,20.));
#81515=CARTESIAN_POINT('Ctrl Pts',(-32.2637471422389,34.1518100908915,0.));
#81516=CARTESIAN_POINT('Ctrl Pts',(-32.2637471422389,34.1518100908915,20.));
#81517=CARTESIAN_POINT('Ctrl Pts',(-32.2377311287994,34.1722683540613,0.));
#81518=CARTESIAN_POINT('Ctrl Pts',(-32.2377311287994,34.1722683540613,20.));
#81519=CARTESIAN_POINT('Ctrl Pts',(-32.2117016460282,34.1927076693883,0.));
#81520=CARTESIAN_POINT('Ctrl Pts',(-32.2117016460282,34.1927076693883,20.));
#81521=CARTESIAN_POINT('Ctrl Pts',(-32.1856587072789,34.2131280274994,0.));
#81522=CARTESIAN_POINT('Ctrl Pts',(-32.1856587072789,34.2131280274994,20.));
#81523=CARTESIAN_POINT('Ctrl Pts',(-32.1596023259127,34.233529419031,0.));
#81524=CARTESIAN_POINT('Ctrl Pts',(-32.1596023259127,34.233529419031,20.));
#81525=CARTESIAN_POINT('Ctrl Pts',(-32.1335325152974,34.2539118346284,0.));
#81526=CARTESIAN_POINT('Ctrl Pts',(-32.1335325152974,34.2539118346284,20.));
#81527=CARTESIAN_POINT('Ctrl Pts',(-32.1074492888083,34.2742752649465,0.));
#81528=CARTESIAN_POINT('Ctrl Pts',(-32.1074492888083,34.2742752649465,20.));
#81529=CARTESIAN_POINT('Ctrl Pts',(-32.081352659827,34.2946197006486,0.));
#81530=CARTESIAN_POINT('Ctrl Pts',(-32.081352659827,34.2946197006486,20.));
#81531=CARTESIAN_POINT('Ctrl Pts',(-32.0552426417428,34.3149451324081,0.));
#81532=CARTESIAN_POINT('Ctrl Pts',(-32.0552426417428,34.3149451324081,20.));
#81533=CARTESIAN_POINT('Ctrl Pts',(-32.0291192479513,34.335251550907,0.));
#81534=CARTESIAN_POINT('Ctrl Pts',(-32.0291192479513,34.335251550907,20.));
#81535=CARTESIAN_POINT('Ctrl Pts',(-32.0029824918551,34.3555389468366,0.));
#81536=CARTESIAN_POINT('Ctrl Pts',(-32.0029824918551,34.3555389468366,20.));
#81537=CARTESIAN_POINT('Ctrl Pts',(-31.9768323868632,34.3758073108972,0.));
#81538=CARTESIAN_POINT('Ctrl Pts',(-31.9768323868632,34.3758073108972,20.));
#81539=CARTESIAN_POINT('Ctrl Pts',(-31.9506689463919,34.3960566337982,0.));
#81540=CARTESIAN_POINT('Ctrl Pts',(-31.9506689463919,34.3960566337982,20.));
#81541=CARTESIAN_POINT('Ctrl Pts',(-31.9244921838641,34.4162869062583,0.));
#81542=CARTESIAN_POINT('Ctrl Pts',(-31.9244921838641,34.4162869062583,20.));
#81543=CARTESIAN_POINT('Ctrl Pts',(-31.8983021127102,34.4364981190057,0.));
#81544=CARTESIAN_POINT('Ctrl Pts',(-31.8983021127102,34.4364981190057,20.));
#81545=CARTESIAN_POINT('Ctrl Pts',(-31.8720987463673,34.4566902627777,0.));
#81546=CARTESIAN_POINT('Ctrl Pts',(-31.8720987463673,34.4566902627777,20.));
#81547=CARTESIAN_POINT('Ctrl Pts',(-31.8458820982794,34.4768633283209,0.));
#81548=CARTESIAN_POINT('Ctrl Pts',(-31.8458820982794,34.4768633283209,20.));
#81549=CARTESIAN_POINT('Ctrl Pts',(-31.819652181897,34.4970173063908,0.));
#81550=CARTESIAN_POINT('Ctrl Pts',(-31.819652181897,34.4970173063908,20.));
#81551=CARTESIAN_POINT('Ctrl Pts',(-31.7934090106771,34.5171521877518,0.));
#81552=CARTESIAN_POINT('Ctrl Pts',(-31.7934090106771,34.5171521877518,20.));
#81553=CARTESIAN_POINT('Ctrl Pts',(-31.7671525980838,34.5372679631777,0.));
#81554=CARTESIAN_POINT('Ctrl Pts',(-31.7671525980838,34.5372679631777,20.));
#81555=CARTESIAN_POINT('Ctrl Pts',(-31.7408829575879,34.5573646234518,0.));
#81556=CARTESIAN_POINT('Ctrl Pts',(-31.7408829575879,34.5573646234518,20.));
#81557=CARTESIAN_POINT('Ctrl Pts',(-31.7146001026678,34.5774421593669,0.));
#81558=CARTESIAN_POINT('Ctrl Pts',(-31.7146001026678,34.5774421593669,20.));
#81559=CARTESIAN_POINT('Ctrl Pts',(-31.6883040468088,34.5975005617252,0.));
#81560=CARTESIAN_POINT('Ctrl Pts',(-31.6883040468088,34.5975005617252,20.));
#81561=CARTESIAN_POINT('Ctrl Pts',(-31.6619948035027,34.6175398213376,0.));
#81562=CARTESIAN_POINT('Ctrl Pts',(-31.6619948035027,34.6175398213376,20.));
#81563=CARTESIAN_POINT('Ctrl Pts',(-31.6356723862475,34.6375599290242,0.));
#81564=CARTESIAN_POINT('Ctrl Pts',(-31.6356723862475,34.6375599290242,20.));
#81565=CARTESIAN_POINT('Ctrl Pts',(-31.609336808548,34.6575608756141,0.));
#81566=CARTESIAN_POINT('Ctrl Pts',(-31.609336808548,34.6575608756141,20.));
#81567=CARTESIAN_POINT('Ctrl Pts',(-31.5829880839157,34.6775426519456,0.));
#81568=CARTESIAN_POINT('Ctrl Pts',(-31.5829880839157,34.6775426519456,20.));
#81569=CARTESIAN_POINT('Ctrl Pts',(-31.556626225869,34.6975052488666,0.));
#81570=CARTESIAN_POINT('Ctrl Pts',(-31.556626225869,34.6975052488666,20.));
#81571=CARTESIAN_POINT('Ctrl Pts',(-31.5302512479332,34.7174486572342,0.));
#81572=CARTESIAN_POINT('Ctrl Pts',(-31.5302512479332,34.7174486572342,20.));
#81573=CARTESIAN_POINT('Ctrl Pts',(-31.5038631636409,34.7373728679152,0.));
#81574=CARTESIAN_POINT('Ctrl Pts',(-31.5038631636409,34.7373728679152,20.));
#81575=CARTESIAN_POINT('Ctrl Pts',(-31.4774619865312,34.7572778717852,0.));
#81576=CARTESIAN_POINT('Ctrl Pts',(-31.4774619865312,34.7572778717852,20.));
#81577=CARTESIAN_POINT('Ctrl Pts',(-31.4510477301503,34.7771636597296,0.));
#81578=CARTESIAN_POINT('Ctrl Pts',(-31.4510477301503,34.7771636597296,20.));
#81579=CARTESIAN_POINT('Ctrl Pts',(-31.4246204080513,34.7970302226433,0.));
#81580=CARTESIAN_POINT('Ctrl Pts',(-31.4246204080513,34.7970302226433,20.));
#81581=CARTESIAN_POINT('Ctrl Pts',(-31.3981800337935,34.8168775514299,0.));
#81582=CARTESIAN_POINT('Ctrl Pts',(-31.3981800337935,34.8168775514299,20.));
#81583=CARTESIAN_POINT('Ctrl Pts',(-31.3717266209434,34.8367056370026,0.));
#81584=CARTESIAN_POINT('Ctrl Pts',(-31.3717266209434,34.8367056370026,20.));
#81585=CARTESIAN_POINT('Ctrl Pts',(-31.3452601830726,34.856514470283,0.));
#81586=CARTESIAN_POINT('Ctrl Pts',(-31.3452601830726,34.856514470283,20.));
#81587=CARTESIAN_POINT('Ctrl Pts',(-31.3187807337598,34.8763040422018,0.));
#81588=CARTESIAN_POINT('Ctrl Pts',(-31.3187807337598,34.8763040422018,20.));
#81589=CARTESIAN_POINT('Ctrl Pts',(-31.2922882865907,34.8960743436995,0.));
#81590=CARTESIAN_POINT('Ctrl Pts',(-31.2922882865907,34.8960743436995,20.));
#81591=CARTESIAN_POINT('Ctrl Pts',(-31.2657828551579,34.9158253657262,0.));
#81592=CARTESIAN_POINT('Ctrl Pts',(-31.2657828551579,34.9158253657262,20.));
#81593=CARTESIAN_POINT('Ctrl Pts',(-31.2392644530613,34.9355570992414,0.));
#81594=CARTESIAN_POINT('Ctrl Pts',(-31.2392644530613,34.9355570992414,20.));
#81595=CARTESIAN_POINT('Ctrl Pts',(-31.2127330939086,34.9552695352152,0.));
#81596=CARTESIAN_POINT('Ctrl Pts',(-31.2127330939086,34.9552695352152,20.));
#81597=CARTESIAN_POINT('Ctrl Pts',(-31.1861887913133,34.9749626646259,0.));
#81598=CARTESIAN_POINT('Ctrl Pts',(-31.1861887913133,34.9749626646259,20.));
#81599=CARTESIAN_POINT('Ctrl Pts',(-31.1596315588953,34.9946364784612,0.));
#81600=CARTESIAN_POINT('Ctrl Pts',(-31.1596315588953,34.9946364784612,20.));
#81601=CARTESIAN_POINT('Ctrl Pts',(-31.1330614102809,35.0142909677175,0.));
#81602=CARTESIAN_POINT('Ctrl Pts',(-31.1330614102809,35.0142909677175,20.));
#81603=CARTESIAN_POINT('Ctrl Pts',(-31.1064783591027,35.0339261234012,0.));
#81604=CARTESIAN_POINT('Ctrl Pts',(-31.1064783591027,35.0339261234012,20.));
#81605=CARTESIAN_POINT('Ctrl Pts',(-31.0798824190004,35.0535419365277,0.));
#81606=CARTESIAN_POINT('Ctrl Pts',(-31.0798824190004,35.0535419365277,20.));
#81607=CARTESIAN_POINT('Ctrl Pts',(-31.0532736036193,35.0731383981212,0.));
#81608=CARTESIAN_POINT('Ctrl Pts',(-31.0532736036193,35.0731383981212,20.));
#81609=CARTESIAN_POINT('Ctrl Pts',(-31.026651926612,35.0927154992152,0.));
#81610=CARTESIAN_POINT('Ctrl Pts',(-31.026651926612,35.0927154992152,20.));
#81611=CARTESIAN_POINT('Ctrl Pts',(-31.0000174016378,35.1122732308527,0.));
#81612=CARTESIAN_POINT('Ctrl Pts',(-31.0000174016378,35.1122732308527,20.));
#81613=CARTESIAN_POINT('Ctrl Pts',(-30.9733700423633,35.131811584087,0.));
#81614=CARTESIAN_POINT('Ctrl Pts',(-30.9733700423633,35.131811584087,20.));
#81615=CARTESIAN_POINT('Ctrl Pts',(-30.9467098624624,35.1513305499814,0.));
#81616=CARTESIAN_POINT('Ctrl Pts',(-30.9467098624624,35.1513305499814,20.));
#81617=CARTESIAN_POINT('Ctrl Pts',(-30.9200368756162,35.170830119609,0.));
#81618=CARTESIAN_POINT('Ctrl Pts',(-30.9200368756162,35.170830119609,20.));
#81619=CARTESIAN_POINT('Ctrl Pts',(-30.8933510955116,35.1903102840518,0.));
#81620=CARTESIAN_POINT('Ctrl Pts',(-30.8933510955116,35.1903102840518,20.));
#81621=CARTESIAN_POINT('Ctrl Pts',(-30.8666525358408,35.2097710343997,0.));
#81622=CARTESIAN_POINT('Ctrl Pts',(-30.8666525358408,35.2097710343997,20.));
#81623=CARTESIAN_POINT('Ctrl Pts',(-30.8399412103027,35.2292123617517,0.));
#81624=CARTESIAN_POINT('Ctrl Pts',(-30.8399412103027,35.2292123617517,20.));
#81625=CARTESIAN_POINT('Ctrl Pts',(-30.8132171326021,35.2486342572162,0.));
#81626=CARTESIAN_POINT('Ctrl Pts',(-30.8132171326021,35.2486342572162,20.));
#81627=CARTESIAN_POINT('Ctrl Pts',(-30.7864803164511,35.2680367119112,0.));
#81628=CARTESIAN_POINT('Ctrl Pts',(-30.7864803164511,35.2680367119112,20.));
#81629=CARTESIAN_POINT('Ctrl Pts',(-30.7597307755696,35.2874197169657,0.));
#81630=CARTESIAN_POINT('Ctrl Pts',(-30.7597307755696,35.2874197169657,20.));
#81631=CARTESIAN_POINT('Ctrl Pts',(-30.732968523684,35.3067832635176,0.));
#81632=CARTESIAN_POINT('Ctrl Pts',(-30.732968523684,35.3067832635176,20.));
#81633=CARTESIAN_POINT('Ctrl Pts',(-30.7061935745273,35.3261273427148,0.));
#81634=CARTESIAN_POINT('Ctrl Pts',(-30.7061935745273,35.3261273427148,20.));
#81635=CARTESIAN_POINT('Ctrl Pts',(-30.6794059418388,35.3454519457137,0.));
#81636=CARTESIAN_POINT('Ctrl Pts',(-30.6794059418388,35.3454519457137,20.));
#81637=CARTESIAN_POINT('Ctrl Pts',(-30.6526056393639,35.3647570636798,0.));
#81638=CARTESIAN_POINT('Ctrl Pts',(-30.6526056393639,35.3647570636798,20.));
#81639=CARTESIAN_POINT('Ctrl Pts',(-30.6257926808542,35.3840426877879,0.));
#81640=CARTESIAN_POINT('Ctrl Pts',(-30.6257926808542,35.3840426877879,20.));
#81641=CARTESIAN_POINT('Ctrl Pts',(-30.5989670800681,35.4033088092225,0.));
#81642=CARTESIAN_POINT('Ctrl Pts',(-30.5989670800681,35.4033088092225,20.));
#81643=CARTESIAN_POINT('Ctrl Pts',(-30.5721288507715,35.4225554191786,0.));
#81644=CARTESIAN_POINT('Ctrl Pts',(-30.5721288507715,35.4225554191786,20.));
#81645=CARTESIAN_POINT('Ctrl Pts',(-30.5452780067369,35.4417825088605,0.));
#81646=CARTESIAN_POINT('Ctrl Pts',(-30.5452780067369,35.4417825088605,20.));
#81647=CARTESIAN_POINT('Ctrl Pts',(-30.5184145617425,35.4609900694812,0.));
#81648=CARTESIAN_POINT('Ctrl Pts',(-30.5184145617425,35.4609900694812,20.));
#81649=CARTESIAN_POINT('Ctrl Pts',(-30.4915385295724,35.4801780922625,0.));
#81650=CARTESIAN_POINT('Ctrl Pts',(-30.4915385295724,35.4801780922625,20.));
#81651=CARTESIAN_POINT('Ctrl Pts',(-30.4646499240178,35.4993465684361,0.));
#81652=CARTESIAN_POINT('Ctrl Pts',(-30.4646499240178,35.4993465684361,20.));
#81653=CARTESIAN_POINT('Ctrl Pts',(-30.437748758876,35.518495489243,0.));
#81654=CARTESIAN_POINT('Ctrl Pts',(-30.437748758876,35.518495489243,20.));
#81655=CARTESIAN_POINT('Ctrl Pts',(-30.4108350479521,35.5376248459348,0.));
#81656=CARTESIAN_POINT('Ctrl Pts',(-30.4108350479521,35.5376248459348,20.));
#81657=CARTESIAN_POINT('Ctrl Pts',(-30.3839088050584,35.5567346297736,0.));
#81658=CARTESIAN_POINT('Ctrl Pts',(-30.3839088050584,35.5567346297736,20.));
#81659=CARTESIAN_POINT('Ctrl Pts',(-30.3569700440131,35.5758248320301,0.));
#81660=CARTESIAN_POINT('Ctrl Pts',(-30.3569700440131,35.5758248320301,20.));
#81661=CARTESIAN_POINT('Ctrl Pts',(-30.3300187786403,35.5948954439837,0.));
#81662=CARTESIAN_POINT('Ctrl Pts',(-30.3300187786403,35.5948954439837,20.));
#81663=CARTESIAN_POINT('Ctrl Pts',(-30.3030550227693,35.6139464569223,0.));
#81664=CARTESIAN_POINT('Ctrl Pts',(-30.3030550227693,35.6139464569223,20.));
#81665=CARTESIAN_POINT('Ctrl Pts',(-30.2760787902362,35.6329778621436,0.));
#81666=CARTESIAN_POINT('Ctrl Pts',(-30.2760787902362,35.6329778621436,20.));
#81667=CARTESIAN_POINT('Ctrl Pts',(-30.2490900948838,35.6519896509552,0.));
#81668=CARTESIAN_POINT('Ctrl Pts',(-30.2490900948838,35.6519896509552,20.));
#81669=CARTESIAN_POINT('Ctrl Pts',(-30.2220889505625,35.6709818146751,0.));
#81670=CARTESIAN_POINT('Ctrl Pts',(-30.2220889505625,35.6709818146751,20.));
#81671=CARTESIAN_POINT('Ctrl Pts',(-30.1950753711288,35.6899543446308,0.));
#81672=CARTESIAN_POINT('Ctrl Pts',(-30.1950753711288,35.6899543446308,20.));
#81673=CARTESIAN_POINT('Ctrl Pts',(-30.1680493704465,35.7089072321597,0.));
#81674=CARTESIAN_POINT('Ctrl Pts',(-30.1680493704465,35.7089072321597,20.));
#81675=CARTESIAN_POINT('Ctrl Pts',(-30.141010962385,35.7278404686079,0.));
#81676=CARTESIAN_POINT('Ctrl Pts',(-30.141010962385,35.7278404686079,20.));
#81677=CARTESIAN_POINT('Ctrl Pts',(-30.1139601608197,35.7467540453308,0.));
#81678=CARTESIAN_POINT('Ctrl Pts',(-30.1139601608197,35.7467540453308,20.));
#81679=CARTESIAN_POINT('Ctrl Pts',(-30.0868969796328,35.7656479536938,0.));
#81680=CARTESIAN_POINT('Ctrl Pts',(-30.0868969796328,35.7656479536938,20.));
#81681=CARTESIAN_POINT('Ctrl Pts',(-30.0598214327127,35.7845221850715,0.));
#81682=CARTESIAN_POINT('Ctrl Pts',(-30.0598214327127,35.7845221850715,20.));
#81683=CARTESIAN_POINT('Ctrl Pts',(-30.0327335339539,35.8033767308478,0.));
#81684=CARTESIAN_POINT('Ctrl Pts',(-30.0327335339539,35.8033767308478,20.));
#81685=CARTESIAN_POINT('Ctrl Pts',(-30.005633297258,35.8222115824166,0.));
#81686=CARTESIAN_POINT('Ctrl Pts',(-30.005633297258,35.8222115824166,20.));
#81687=CARTESIAN_POINT('Ctrl Pts',(-29.9785207365333,35.841026731182,0.));
#81688=CARTESIAN_POINT('Ctrl Pts',(-29.9785207365333,35.841026731182,20.));
#81689=CARTESIAN_POINT('Ctrl Pts',(-29.9513958656946,35.8598221685576,0.));
#81690=CARTESIAN_POINT('Ctrl Pts',(-29.9513958656946,35.8598221685576,20.));
#81691=CARTESIAN_POINT('Ctrl Pts',(-29.9242586986624,35.8785978859658,0.));
#81692=CARTESIAN_POINT('Ctrl Pts',(-29.9242586986624,35.8785978859658,20.));
#81693=CARTESIAN_POINT('Ctrl Pts',(-29.8971092493635,35.8973538748387,0.));
#81694=CARTESIAN_POINT('Ctrl Pts',(-29.8971092493635,35.8973538748387,20.));
#81695=CARTESIAN_POINT('Ctrl Pts',(-29.869947531731,35.9160901266176,0.));
#81696=CARTESIAN_POINT('Ctrl Pts',(-29.869947531731,35.9160901266176,20.));
#81697=CARTESIAN_POINT('Ctrl Pts',(-29.8427735597049,35.9348066327539,0.));
#81698=CARTESIAN_POINT('Ctrl Pts',(-29.8427735597049,35.9348066327539,20.));
#81699=CARTESIAN_POINT('Ctrl Pts',(-29.8155873472308,35.9535033847081,0.));
#81700=CARTESIAN_POINT('Ctrl Pts',(-29.8155873472308,35.9535033847081,20.));
#81701=CARTESIAN_POINT('Ctrl Pts',(-29.7883889082614,35.9721803739509,0.));
#81702=CARTESIAN_POINT('Ctrl Pts',(-29.7883889082614,35.9721803739509,20.));
#81703=CARTESIAN_POINT('Ctrl Pts',(-29.7611782567557,35.9908375919623,0.));
#81704=CARTESIAN_POINT('Ctrl Pts',(-29.7611782567557,35.9908375919623,20.));
#81705=CARTESIAN_POINT('Ctrl Pts',(-29.7339554066796,36.009475030233,0.));
#81706=CARTESIAN_POINT('Ctrl Pts',(-29.7339554066796,36.009475030233,20.));
#81707=CARTESIAN_POINT('Ctrl Pts',(-29.7067203720053,36.0280926802632,0.));
#81708=CARTESIAN_POINT('Ctrl Pts',(-29.7067203720053,36.0280926802632,20.));
#81709=CARTESIAN_POINT('Ctrl Pts',(-29.6794731667107,36.0466905335617,0.));
#81710=CARTESIAN_POINT('Ctrl Pts',(-29.6794731667107,36.0466905335617,20.));
#81711=CARTESIAN_POINT('Ctrl Pts',(-29.6522138047794,36.0652685816464,0.));
#81712=CARTESIAN_POINT('Ctrl Pts',(-29.6522138047794,36.0652685816464,20.));
#81713=CARTESIAN_POINT('Ctrl Pts',(-29.6249423002017,36.0838268160451,0.));
#81714=CARTESIAN_POINT('Ctrl Pts',(-29.6249423002017,36.0838268160451,20.));
#81715=CARTESIAN_POINT('Ctrl Pts',(-29.5976586669748,36.1023652282957,0.));
#81716=CARTESIAN_POINT('Ctrl Pts',(-29.5976586669748,36.1023652282957,20.));
#81717=CARTESIAN_POINT('Ctrl Pts',(-29.5703629191022,36.120883809946,0.));
#81718=CARTESIAN_POINT('Ctrl Pts',(-29.5703629191022,36.120883809946,20.));
#81719=CARTESIAN_POINT('Ctrl Pts',(-29.5430550705938,36.1393825525541,0.));
#81720=CARTESIAN_POINT('Ctrl Pts',(-29.5430550705938,36.1393825525541,20.));
#81721=CARTESIAN_POINT('Ctrl Pts',(-29.5157351354652,36.1578614476865,0.));
#81722=CARTESIAN_POINT('Ctrl Pts',(-29.5157351354652,36.1578614476865,20.));
#81723=CARTESIAN_POINT('Ctrl Pts',(-29.4884031277381,36.1763204869192,0.));
#81724=CARTESIAN_POINT('Ctrl Pts',(-29.4884031277381,36.1763204869192,20.));
#81725=CARTESIAN_POINT('Ctrl Pts',(-29.4610590614411,36.1947596618382,0.));
#81726=CARTESIAN_POINT('Ctrl Pts',(-29.4610590614411,36.1947596618382,20.));
#81727=CARTESIAN_POINT('Ctrl Pts',(-29.4337029506094,36.2131789640396,0.));
#81728=CARTESIAN_POINT('Ctrl Pts',(-29.4337029506094,36.2131789640396,20.));
#81729=CARTESIAN_POINT('Ctrl Pts',(-29.4063348092849,36.2315783851295,0.));
#81730=CARTESIAN_POINT('Ctrl Pts',(-29.4063348092849,36.2315783851295,20.));
#81731=CARTESIAN_POINT('Ctrl Pts',(-29.3789546515147,36.2499579167227,0.));
#81732=CARTESIAN_POINT('Ctrl Pts',(-29.3789546515147,36.2499579167227,20.));
#81733=CARTESIAN_POINT('Ctrl Pts',(-29.3515624913523,36.2683175504441,0.));
#81734=CARTESIAN_POINT('Ctrl Pts',(-29.3515624913523,36.2683175504441,20.));
#81735=CARTESIAN_POINT('Ctrl Pts',(-29.3241583428569,36.286657277928,0.));
#81736=CARTESIAN_POINT('Ctrl Pts',(-29.3241583428569,36.286657277928,20.));
#81737=CARTESIAN_POINT('Ctrl Pts',(-29.2967422200943,36.3049770908188,0.));
#81738=CARTESIAN_POINT('Ctrl Pts',(-29.2967422200943,36.3049770908188,20.));
#81739=CARTESIAN_POINT('Ctrl Pts',(-29.2693141371364,36.3232769807701,0.));
#81740=CARTESIAN_POINT('Ctrl Pts',(-29.2693141371364,36.3232769807701,20.));
#81741=CARTESIAN_POINT('Ctrl Pts',(-29.241874108062,36.3415569394456,0.));
#81742=CARTESIAN_POINT('Ctrl Pts',(-29.241874108062,36.3415569394456,20.));
#81743=CARTESIAN_POINT('Ctrl Pts',(-29.2144221469563,36.3598169585186,0.));
#81744=CARTESIAN_POINT('Ctrl Pts',(-29.2144221469563,36.3598169585186,20.));
#81745=CARTESIAN_POINT('Ctrl Pts',(-29.186958267911,36.3780570296725,0.));
#81746=CARTESIAN_POINT('Ctrl Pts',(-29.186958267911,36.3780570296725,20.));
#81747=CARTESIAN_POINT('Ctrl Pts',(-29.1594824850239,36.3962771446002,0.));
#81748=CARTESIAN_POINT('Ctrl Pts',(-29.1594824850239,36.3962771446002,20.));
#81749=CARTESIAN_POINT('Ctrl Pts',(-29.1319948123985,36.4144772950043,0.));
#81750=CARTESIAN_POINT('Ctrl Pts',(-29.1319948123985,36.4144772950043,20.));
#81751=CARTESIAN_POINT('Ctrl Pts',(-29.1044952641443,36.4326574725969,0.));
#81752=CARTESIAN_POINT('Ctrl Pts',(-29.1044952641443,36.4326574725969,20.));
#81753=CARTESIAN_POINT('Ctrl Pts',(-29.0769838543763,36.4508176690994,0.));
#81754=CARTESIAN_POINT('Ctrl Pts',(-29.0769838543763,36.4508176690994,20.));
#81755=CARTESIAN_POINT('Ctrl Pts',(-29.0494605972165,36.4689578762435,0.));
#81756=CARTESIAN_POINT('Ctrl Pts',(-29.0494605972165,36.4689578762435,20.));
#81757=CARTESIAN_POINT('Ctrl Pts',(-29.0219255067927,36.4870780857703,0.));
#81758=CARTESIAN_POINT('Ctrl Pts',(-29.0219255067927,36.4870780857703,20.));
#81759=CARTESIAN_POINT('Ctrl Pts',(-28.99437859724,36.5051782894316,0.));
#81760=CARTESIAN_POINT('Ctrl Pts',(-28.99437859724,36.5051782894316,20.));
#81761=CARTESIAN_POINT('Ctrl Pts',(-28.9668198826995,36.5232584789885,0.));
#81762=CARTESIAN_POINT('Ctrl Pts',(-28.9668198826995,36.5232584789885,20.));
#81763=CARTESIAN_POINT('Ctrl Pts',(-28.9392493773185,36.5413186462123,0.));
#81764=CARTESIAN_POINT('Ctrl Pts',(-28.9392493773185,36.5413186462123,20.));
#81765=CARTESIAN_POINT('Ctrl Pts',(-28.9116670952497,36.5593587828826,0.));
#81766=CARTESIAN_POINT('Ctrl Pts',(-28.9116670952497,36.5593587828826,20.));
#81767=CARTESIAN_POINT('Ctrl Pts',(-28.8840730506515,36.577378880789,0.));
#81768=CARTESIAN_POINT('Ctrl Pts',(-28.8840730506515,36.577378880789,20.));
#81769=CARTESIAN_POINT('Ctrl Pts',(-28.8564672576885,36.5953789317305,0.));
#81770=CARTESIAN_POINT('Ctrl Pts',(-28.8564672576885,36.5953789317305,20.));
#81771=CARTESIAN_POINT('Ctrl Pts',(-28.8288497305324,36.6133589275174,0.));
#81772=CARTESIAN_POINT('Ctrl Pts',(-28.8288497305324,36.6133589275174,20.));
#81773=CARTESIAN_POINT('Ctrl Pts',(-28.8012204833609,36.6313188599694,0.));
#81774=CARTESIAN_POINT('Ctrl Pts',(-28.8012204833609,36.6313188599694,20.));
#81775=CARTESIAN_POINT('Ctrl Pts',(-28.7735795303585,36.6492587209167,0.));
#81776=CARTESIAN_POINT('Ctrl Pts',(-28.7735795303585,36.6492587209167,20.));
#81777=CARTESIAN_POINT('Ctrl Pts',(-28.7459268857152,36.6671785021988,0.));
#81778=CARTESIAN_POINT('Ctrl Pts',(-28.7459268857152,36.6671785021988,20.));
#81779=CARTESIAN_POINT('Ctrl Pts',(-28.7182625636274,36.6850781956649,0.));
#81780=CARTESIAN_POINT('Ctrl Pts',(-28.7182625636274,36.6850781956649,20.));
#81781=CARTESIAN_POINT('Ctrl Pts',(-28.6905865782966,36.7029577931733,0.));
#81782=CARTESIAN_POINT('Ctrl Pts',(-28.6905865782966,36.7029577931733,20.));
#81783=CARTESIAN_POINT('Ctrl Pts',(-28.6628989439305,36.7208172865919,0.));
#81784=CARTESIAN_POINT('Ctrl Pts',(-28.6628989439305,36.7208172865919,20.));
#81785=CARTESIAN_POINT('Ctrl Pts',(-28.6351996747428,36.738656667798,0.));
#81786=CARTESIAN_POINT('Ctrl Pts',(-28.6351996747428,36.738656667798,20.));
#81787=CARTESIAN_POINT('Ctrl Pts',(-28.6074887849535,36.7564759286795,0.));
#81788=CARTESIAN_POINT('Ctrl Pts',(-28.6074887849535,36.7564759286795,20.));
#81789=CARTESIAN_POINT('Ctrl Pts',(-28.5797662887891,36.774275061134,0.));
#81790=CARTESIAN_POINT('Ctrl Pts',(-28.5797662887891,36.774275061134,20.));
#81791=CARTESIAN_POINT('Ctrl Pts',(-28.5520322004825,36.7920540570698,0.));
#81792=CARTESIAN_POINT('Ctrl Pts',(-28.5520322004825,36.7920540570698,20.));
#81793=CARTESIAN_POINT('Ctrl Pts',(-28.5242865342725,36.809812908405,0.));
#81794=CARTESIAN_POINT('Ctrl Pts',(-28.5242865342725,36.809812908405,20.));
#81795=CARTESIAN_POINT('Ctrl Pts',(-28.496529304404,36.8275516070676,0.));
#81796=CARTESIAN_POINT('Ctrl Pts',(-28.496529304404,36.8275516070676,20.));
#81797=CARTESIAN_POINT('Ctrl Pts',(-28.4687605251277,36.8452701449948,0.));
#81798=CARTESIAN_POINT('Ctrl Pts',(-28.4687605251277,36.8452701449948,20.));
#81799=CARTESIAN_POINT('Ctrl Pts',(-28.4409802107003,36.8629685141338,0.));
#81800=CARTESIAN_POINT('Ctrl Pts',(-28.4409802107003,36.8629685141338,20.));
#81801=CARTESIAN_POINT('Ctrl Pts',(-28.4131883753841,36.8806467064409,0.));
#81802=CARTESIAN_POINT('Ctrl Pts',(-28.4131883753841,36.8806467064409,20.));
#81803=CARTESIAN_POINT('Ctrl Pts',(-28.3853850334476,36.8983047138822,0.));
#81804=CARTESIAN_POINT('Ctrl Pts',(-28.3853850334476,36.8983047138822,20.));
#81805=CARTESIAN_POINT('Ctrl Pts',(-28.3575701991656,36.9159425284342,0.));
#81806=CARTESIAN_POINT('Ctrl Pts',(-28.3575701991656,36.9159425284342,20.));
#81807=CARTESIAN_POINT('Ctrl Pts',(-28.3297438868192,36.9335601420835,0.));
#81808=CARTESIAN_POINT('Ctrl Pts',(-28.3297438868192,36.9335601420835,20.));
#81809=CARTESIAN_POINT('Ctrl Pts',(-28.3019061106957,36.9511575468269,0.));
#81810=CARTESIAN_POINT('Ctrl Pts',(-28.3019061106957,36.9511575468269,20.));
#81811=CARTESIAN_POINT('Ctrl Pts',(-28.2740568850882,36.9687347346709,0.));
#81812=CARTESIAN_POINT('Ctrl Pts',(-28.2740568850882,36.9687347346709,20.));
#81813=CARTESIAN_POINT('Ctrl Pts',(-28.2461962242955,36.9862916976318,0.));
#81814=CARTESIAN_POINT('Ctrl Pts',(-28.2461962242955,36.9862916976318,20.));
#81815=CARTESIAN_POINT('Ctrl Pts',(-28.2183241426219,37.0038284277349,0.));
#81816=CARTESIAN_POINT('Ctrl Pts',(-28.2183241426219,37.0038284277349,20.));
#81817=CARTESIAN_POINT('Ctrl Pts',(-28.1904406543778,37.0213449170157,0.));
#81818=CARTESIAN_POINT('Ctrl Pts',(-28.1904406543778,37.0213449170157,20.));
#81819=CARTESIAN_POINT('Ctrl Pts',(-28.1625457738798,37.0388411575197,0.));
#81820=CARTESIAN_POINT('Ctrl Pts',(-28.1625457738798,37.0388411575197,20.));
#81821=CARTESIAN_POINT('Ctrl Pts',(-28.1346395154507,37.0563171413025,0.));
#81822=CARTESIAN_POINT('Ctrl Pts',(-28.1346395154507,37.0563171413025,20.));
#81823=CARTESIAN_POINT('Ctrl Pts',(-28.1067218934195,37.0737728604297,0.));
#81824=CARTESIAN_POINT('Ctrl Pts',(-28.1067218934195,37.0737728604297,20.));
#81825=CARTESIAN_POINT('Ctrl Pts',(-28.0787929221219,37.0912083069771,0.));
#81826=CARTESIAN_POINT('Ctrl Pts',(-28.0787929221219,37.0912083069771,20.));
#81827=CARTESIAN_POINT('Ctrl Pts',(-28.0508526158994,37.1086234730311,0.));
#81828=CARTESIAN_POINT('Ctrl Pts',(-28.0508526158994,37.1086234730311,20.));
#81829=CARTESIAN_POINT('Ctrl Pts',(-28.0229009890986,37.1260183506872,0.));
#81830=CARTESIAN_POINT('Ctrl Pts',(-28.0229009890986,37.1260183506872,20.));
#81831=CARTESIAN_POINT('Ctrl Pts',(-27.994938056072,37.1433929320507,0.));
#81832=CARTESIAN_POINT('Ctrl Pts',(-27.994938056072,37.1433929320507,20.));
#81833=CARTESIAN_POINT('Ctrl Pts',(-27.9669638311771,37.1607472092352,0.));
#81834=CARTESIAN_POINT('Ctrl Pts',(-27.9669638311771,37.1607472092352,20.));
#81835=CARTESIAN_POINT('Ctrl Pts',(-27.9389783287777,37.1780811743651,0.));
#81836=CARTESIAN_POINT('Ctrl Pts',(-27.9389783287777,37.1780811743651,20.));
#81837=CARTESIAN_POINT('Ctrl Pts',(-27.9109815632437,37.1953948195748,0.));
#81838=CARTESIAN_POINT('Ctrl Pts',(-27.9109815632437,37.1953948195748,20.));
#81839=CARTESIAN_POINT('Ctrl Pts',(-27.8829735489517,37.2126881370093,0.));
#81840=CARTESIAN_POINT('Ctrl Pts',(-27.8829735489517,37.2126881370093,20.));
#81841=CARTESIAN_POINT('Ctrl Pts',(-27.8549543002843,37.2299611188238,0.));
#81842=CARTESIAN_POINT('Ctrl Pts',(-27.8549543002843,37.2299611188238,20.));
#81843=CARTESIAN_POINT('Ctrl Pts',(-27.8269238316305,37.2472137571841,0.));
#81844=CARTESIAN_POINT('Ctrl Pts',(-27.8269238316305,37.2472137571841,20.));
#81845=CARTESIAN_POINT('Ctrl Pts',(-27.7988821573847,37.2644460442654,0.));
#81846=CARTESIAN_POINT('Ctrl Pts',(-27.7988821573847,37.2644460442654,20.));
#81847=CARTESIAN_POINT('Ctrl Pts',(-27.7708292919468,37.2816579722525,0.));
#81848=CARTESIAN_POINT('Ctrl Pts',(-27.7708292919468,37.2816579722525,20.));
#81849=CARTESIAN_POINT('Ctrl Pts',(-27.7427652497224,37.2988495333397,0.));
#81850=CARTESIAN_POINT('Ctrl Pts',(-27.7427652497224,37.2988495333397,20.));
#81851=CARTESIAN_POINT('Ctrl Pts',(-27.7146900451229,37.3160207197314,0.));
#81852=CARTESIAN_POINT('Ctrl Pts',(-27.7146900451229,37.3160207197314,20.));
#81853=CARTESIAN_POINT('Ctrl Pts',(-27.6866036925651,37.3331715236413,0.));
#81854=CARTESIAN_POINT('Ctrl Pts',(-27.6866036925651,37.3331715236413,20.));
#81855=CARTESIAN_POINT('Ctrl Pts',(-27.6585062064726,37.3503019372939,0.));
#81856=CARTESIAN_POINT('Ctrl Pts',(-27.6585062064726,37.3503019372939,20.));
#81857=CARTESIAN_POINT('Ctrl Pts',(-27.6303976012745,37.3674119529233,0.));
#81858=CARTESIAN_POINT('Ctrl Pts',(-27.6303976012745,37.3674119529233,20.));
#81859=CARTESIAN_POINT('Ctrl Pts',(-27.6022778914064,37.384501562775,0.));
#81860=CARTESIAN_POINT('Ctrl Pts',(-27.6022778914064,37.384501562775,20.));
#81861=CARTESIAN_POINT('Ctrl Pts',(-27.5741470913095,37.4015707591036,0.));
#81862=CARTESIAN_POINT('Ctrl Pts',(-27.5741470913095,37.4015707591036,20.));
#81863=CARTESIAN_POINT('Ctrl Pts',(-27.5460052154308,37.418619534174,0.));
#81864=CARTESIAN_POINT('Ctrl Pts',(-27.5460052154308,37.418619534174,20.));
#81865=CARTESIAN_POINT('Ctrl Pts',(-27.5178522782226,37.4356478802604,0.));
#81866=CARTESIAN_POINT('Ctrl Pts',(-27.5178522782226,37.4356478802604,20.));
#81867=CARTESIAN_POINT('Ctrl Pts',(-27.489688294143,37.4526557896465,0.));
#81868=CARTESIAN_POINT('Ctrl Pts',(-27.489688294143,37.4526557896465,20.));
#81869=CARTESIAN_POINT('Ctrl Pts',(-27.4615132776558,37.4696432546266,0.));
#81870=CARTESIAN_POINT('Ctrl Pts',(-27.4615132776558,37.4696432546266,20.));
#81871=CARTESIAN_POINT('Ctrl Pts',(-27.4333272432311,37.4866102675047,0.));
#81872=CARTESIAN_POINT('Ctrl Pts',(-27.4333272432311,37.4866102675047,20.));
#81873=CARTESIAN_POINT('Ctrl Pts',(-27.4051302053449,37.5035568205959,0.));
#81874=CARTESIAN_POINT('Ctrl Pts',(-27.4051302053449,37.5035568205959,20.));
#81875=CARTESIAN_POINT('Ctrl Pts',(-27.3769221784798,37.5204829062256,0.));
#81876=CARTESIAN_POINT('Ctrl Pts',(-27.3769221784798,37.5204829062256,20.));
#81877=CARTESIAN_POINT('Ctrl Pts',(-27.3487031771241,37.5373885167297,0.));
#81878=CARTESIAN_POINT('Ctrl Pts',(-27.3487031771241,37.5373885167297,20.));
#81879=CARTESIAN_POINT('Ctrl Pts',(-27.3204732157704,37.5542736444521,0.));
#81880=CARTESIAN_POINT('Ctrl Pts',(-27.3204732157704,37.5542736444521,20.));
#81881=CARTESIAN_POINT('Ctrl Pts',(-27.2922323089174,37.571138281747,0.));
#81882=CARTESIAN_POINT('Ctrl Pts',(-27.2922323089174,37.571138281747,20.));
#81883=CARTESIAN_POINT('Ctrl Pts',(-27.2639804710687,37.5879824209777,0.));
#81884=CARTESIAN_POINT('Ctrl Pts',(-27.2639804710687,37.5879824209777,20.));
#81885=CARTESIAN_POINT('Ctrl Pts',(-27.2357177167352,37.6048060545188,0.));
#81886=CARTESIAN_POINT('Ctrl Pts',(-27.2357177167352,37.6048060545188,20.));
#81887=CARTESIAN_POINT('Ctrl Pts',(-27.2074440604332,37.6216091747552,0.));
#81888=CARTESIAN_POINT('Ctrl Pts',(-27.2074440604332,37.6216091747552,20.));
#81889=CARTESIAN_POINT('Ctrl Pts',(-27.1791595166856,37.6383917740821,0.));
#81890=CARTESIAN_POINT('Ctrl Pts',(-27.1791595166856,37.6383917740821,20.));
#81891=CARTESIAN_POINT('Ctrl Pts',(-27.15086410002,37.6551538449046,0.));
#81892=CARTESIAN_POINT('Ctrl Pts',(-27.15086410002,37.6551538449046,20.));
#81893=CARTESIAN_POINT('Ctrl Pts',(-27.1225578249703,37.6718953796384,0.));
#81894=CARTESIAN_POINT('Ctrl Pts',(-27.1225578249703,37.6718953796384,20.));
#81895=CARTESIAN_POINT('Ctrl Pts',(-27.0942407060752,37.6886163707084,0.));
#81896=CARTESIAN_POINT('Ctrl Pts',(-27.0942407060752,37.6886163707084,20.));
#81897=CARTESIAN_POINT('Ctrl Pts',(-27.0659127578793,37.705316810549,0.));
#81898=CARTESIAN_POINT('Ctrl Pts',(-27.0659127578793,37.705316810549,20.));
#81899=CARTESIAN_POINT('Ctrl Pts',(-27.0375739949332,37.7219966916053,0.));
#81900=CARTESIAN_POINT('Ctrl Pts',(-27.0375739949332,37.7219966916053,20.));
#81901=CARTESIAN_POINT('Ctrl Pts',(-27.0092244317934,37.7386560063324,0.));
#81902=CARTESIAN_POINT('Ctrl Pts',(-27.0092244317934,37.7386560063324,20.));
#81903=CARTESIAN_POINT('Ctrl Pts',(-26.9808640830224,37.755294747196,0.));
#81904=CARTESIAN_POINT('Ctrl Pts',(-26.9808640830224,37.755294747196,20.));
#81905=CARTESIAN_POINT('Ctrl Pts',(-26.9524929631885,37.7719129066715,0.));
#81906=CARTESIAN_POINT('Ctrl Pts',(-26.9524929631885,37.7719129066715,20.));
#81907=CARTESIAN_POINT('Ctrl Pts',(-26.9241110868652,37.7885104772446,0.));
#81908=CARTESIAN_POINT('Ctrl Pts',(-26.9241110868652,37.7885104772446,20.));
#81909=CARTESIAN_POINT('Ctrl Pts',(-26.8957184686315,37.8050874514106,0.));
#81910=CARTESIAN_POINT('Ctrl Pts',(-26.8957184686315,37.8050874514106,20.));
#81911=CARTESIAN_POINT('Ctrl Pts',(-26.8673151230714,37.8216438216745,0.));
#81912=CARTESIAN_POINT('Ctrl Pts',(-26.8673151230714,37.8216438216745,20.));
#81913=CARTESIAN_POINT('Ctrl Pts',(-26.8389010647754,37.8381795805523,0.));
#81914=CARTESIAN_POINT('Ctrl Pts',(-26.8389010647754,37.8381795805523,20.));
#81915=CARTESIAN_POINT('Ctrl Pts',(-26.8104763083398,37.8546947205707,0.));
#81916=CARTESIAN_POINT('Ctrl Pts',(-26.8104763083398,37.8546947205707,20.));
#81917=CARTESIAN_POINT('Ctrl Pts',(-26.782040868367,37.8711892342661,0.));
#81918=CARTESIAN_POINT('Ctrl Pts',(-26.782040868367,37.8711892342661,20.));
#81919=CARTESIAN_POINT('Ctrl Pts',(-26.7535947594648,37.887663114185,0.));
#81920=CARTESIAN_POINT('Ctrl Pts',(-26.7535947594648,37.887663114185,20.));
#81921=CARTESIAN_POINT('Ctrl Pts',(-26.7251379962461,37.904116352883,0.));
#81922=CARTESIAN_POINT('Ctrl Pts',(-26.7251379962461,37.904116352883,20.));
#81923=CARTESIAN_POINT('Ctrl Pts',(-26.6966705933291,37.9205489429259,0.));
#81924=CARTESIAN_POINT('Ctrl Pts',(-26.6966705933291,37.9205489429259,20.));
#81925=CARTESIAN_POINT('Ctrl Pts',(-26.6681925653377,37.9369608768896,0.));
#81926=CARTESIAN_POINT('Ctrl Pts',(-26.6681925653377,37.9369608768896,20.));
#81927=CARTESIAN_POINT('Ctrl Pts',(-26.6397039269022,37.9533521473617,0.));
#81928=CARTESIAN_POINT('Ctrl Pts',(-26.6397039269022,37.9533521473617,20.));
#81929=CARTESIAN_POINT('Ctrl Pts',(-26.6112046926582,37.9697227469388,0.));
#81930=CARTESIAN_POINT('Ctrl Pts',(-26.6112046926582,37.9697227469388,20.));
#81931=CARTESIAN_POINT('Ctrl Pts',(-26.5826948772472,37.9860726682286,0.));
#81932=CARTESIAN_POINT('Ctrl Pts',(-26.5826948772472,37.9860726682286,20.));
#81933=CARTESIAN_POINT('Ctrl Pts',(-26.5541744953163,38.0024019038486,0.));
#81934=CARTESIAN_POINT('Ctrl Pts',(-26.5541744953163,38.0024019038486,20.));
#81935=CARTESIAN_POINT('Ctrl Pts',(-26.5256435615177,38.0187104464255,0.));
#81936=CARTESIAN_POINT('Ctrl Pts',(-26.5256435615177,38.0187104464255,20.));
#81937=CARTESIAN_POINT('Ctrl Pts',(-26.4971020905092,38.0349982885963,0.));
#81938=CARTESIAN_POINT('Ctrl Pts',(-26.4971020905092,38.0349982885963,20.));
#81939=CARTESIAN_POINT('Ctrl Pts',(-26.4685500969542,38.0512654230085,0.));
#81940=CARTESIAN_POINT('Ctrl Pts',(-26.4685500969542,38.0512654230085,20.));
#81941=CARTESIAN_POINT('Ctrl Pts',(-26.439987595522,38.0675118423201,0.));
#81942=CARTESIAN_POINT('Ctrl Pts',(-26.439987595522,38.0675118423201,20.));
#81943=CARTESIAN_POINT('Ctrl Pts',(-26.4114146008872,38.0837375391992,0.));
#81944=CARTESIAN_POINT('Ctrl Pts',(-26.4114146008872,38.0837375391992,20.));
#81945=CARTESIAN_POINT('Ctrl Pts',(-26.3828311277301,38.0999425063245,0.));
#81946=CARTESIAN_POINT('Ctrl Pts',(-26.3828311277301,38.0999425063245,20.));
#81947=CARTESIAN_POINT('Ctrl Pts',(-26.3542371907363,38.1161267363846,0.));
#81948=CARTESIAN_POINT('Ctrl Pts',(-26.3542371907363,38.1161267363846,20.));
#81949=CARTESIAN_POINT('Ctrl Pts',(-26.3256328045976,38.1322902220784,0.));
#81950=CARTESIAN_POINT('Ctrl Pts',(-26.3256328045976,38.1322902220784,20.));
#81951=CARTESIAN_POINT('Ctrl Pts',(-26.2970179840108,38.1484329561142,0.));
#81952=CARTESIAN_POINT('Ctrl Pts',(-26.2970179840108,38.1484329561142,20.));
#81953=CARTESIAN_POINT('Ctrl Pts',(-26.2683927436784,38.1645549312104,0.));
#81954=CARTESIAN_POINT('Ctrl Pts',(-26.2683927436784,38.1645549312104,20.));
#81955=CARTESIAN_POINT('Ctrl Pts',(-26.2397570983077,38.1806561400953,0.));
#81956=CARTESIAN_POINT('Ctrl Pts',(-26.2397570983077,38.1806561400953,20.));
#81957=CARTESIAN_POINT('Ctrl Pts',(-26.2111110626121,38.196736575508,0.));
#81958=CARTESIAN_POINT('Ctrl Pts',(-26.2111110626121,38.196736575508,20.));
#81959=CARTESIAN_POINT('Ctrl Pts',(-26.1824546513102,38.2127962301983,0.));
#81960=CARTESIAN_POINT('Ctrl Pts',(-26.1824546513102,38.2127962301983,20.));
#81961=CARTESIAN_POINT('Ctrl Pts',(-26.1537878791271,38.2288350969267,0.));
#81962=CARTESIAN_POINT('Ctrl Pts',(-26.1537878791271,38.2288350969267,20.));
#81963=CARTESIAN_POINT('Ctrl Pts',(-26.1251107607929,38.244853168464,0.));
#81964=CARTESIAN_POINT('Ctrl Pts',(-26.1251107607929,38.244853168464,20.));
#81965=CARTESIAN_POINT('Ctrl Pts',(-26.0964233110434,38.2608504375906,0.));
#81966=CARTESIAN_POINT('Ctrl Pts',(-26.0964233110434,38.2608504375906,20.));
#81967=CARTESIAN_POINT('Ctrl Pts',(-26.0677255446196,38.276826897097,0.));
#81968=CARTESIAN_POINT('Ctrl Pts',(-26.0677255446196,38.276826897097,20.));
#81969=CARTESIAN_POINT('Ctrl Pts',(-26.0390174762676,38.2927825397833,0.));
#81970=CARTESIAN_POINT('Ctrl Pts',(-26.0390174762676,38.2927825397833,20.));
#81971=CARTESIAN_POINT('Ctrl Pts',(-26.0102991207387,38.3087173584599,0.));
#81972=CARTESIAN_POINT('Ctrl Pts',(-26.0102991207387,38.3087173584599,20.));
#81973=CARTESIAN_POINT('Ctrl Pts',(-25.9815704927901,38.3246313459476,0.));
#81974=CARTESIAN_POINT('Ctrl Pts',(-25.9815704927901,38.3246313459476,20.));
#81975=CARTESIAN_POINT('Ctrl Pts',(-25.9528316071847,38.3405244950781,0.));
#81976=CARTESIAN_POINT('Ctrl Pts',(-25.9528316071847,38.3405244950781,20.));
#81977=CARTESIAN_POINT('Ctrl Pts',(-25.9240824786909,38.3563967986931,0.));
#81978=CARTESIAN_POINT('Ctrl Pts',(-25.9240824786909,38.3563967986931,20.));
#81979=CARTESIAN_POINT('Ctrl Pts',(-25.8953231220827,38.3722482496454,0.));
#81980=CARTESIAN_POINT('Ctrl Pts',(-25.8953231220827,38.3722482496454,20.));
#81981=CARTESIAN_POINT('Ctrl Pts',(-25.8665535521392,38.3880788407969,0.));
#81982=CARTESIAN_POINT('Ctrl Pts',(-25.8665535521392,38.3880788407969,20.));
#81983=CARTESIAN_POINT('Ctrl Pts',(-25.8377737836446,38.4038885650199,0.));
#81984=CARTESIAN_POINT('Ctrl Pts',(-25.8377737836446,38.4038885650199,20.));
#81985=CARTESIAN_POINT('Ctrl Pts',(-25.8089838313888,38.4196774151969,0.));
#81986=CARTESIAN_POINT('Ctrl Pts',(-25.8089838313888,38.4196774151969,20.));
#81987=CARTESIAN_POINT('Ctrl Pts',(-25.7801837101667,38.4354453842206,0.));
#81988=CARTESIAN_POINT('Ctrl Pts',(-25.7801837101667,38.4354453842206,20.));
#81989=CARTESIAN_POINT('Ctrl Pts',(-25.7513734347795,38.4511924649945,0.));
#81990=CARTESIAN_POINT('Ctrl Pts',(-25.7513734347795,38.4511924649945,20.));
#81991=CARTESIAN_POINT('Ctrl Pts',(-25.7225530200332,38.4669186504318,0.));
#81992=CARTESIAN_POINT('Ctrl Pts',(-25.7225530200332,38.4669186504318,20.));
#81993=CARTESIAN_POINT('Ctrl Pts',(-25.6937224807392,38.4826239334567,0.));
#81994=CARTESIAN_POINT('Ctrl Pts',(-25.6937224807392,38.4826239334567,20.));
#81995=CARTESIAN_POINT('Ctrl Pts',(-25.6648818317151,38.4983083070042,0.));
#81996=CARTESIAN_POINT('Ctrl Pts',(-25.6648818317151,38.4983083070042,20.));
#81997=CARTESIAN_POINT('Ctrl Pts',(-25.6360310877836,38.5139717640192,0.));
#81998=CARTESIAN_POINT('Ctrl Pts',(-25.6360310877836,38.5139717640192,20.));
#81999=CARTESIAN_POINT('Ctrl Pts',(-25.6071702637723,38.5296142974561,0.));
#82000=CARTESIAN_POINT('Ctrl Pts',(-25.6071702637723,38.5296142974561,20.));
#82001=CARTESIAN_POINT('Ctrl Pts',(-25.5782993745137,38.5452359002793,0.));
#82002=CARTESIAN_POINT('Ctrl Pts',(-25.5782993745137,38.5452359002793,20.));
#82003=CARTESIAN_POINT('Ctrl Pts',(-25.5494184348457,38.5608365654634,0.));
#82004=CARTESIAN_POINT('Ctrl Pts',(-25.5494184348457,38.5608365654634,20.));
#82005=CARTESIAN_POINT('Ctrl Pts',(-25.5205274596115,38.5764162859939,0.));
#82006=CARTESIAN_POINT('Ctrl Pts',(-25.5205274596115,38.5764162859939,20.));
#82007=CARTESIAN_POINT('Ctrl Pts',(-25.4916264636604,38.591975054867,0.));
#82008=CARTESIAN_POINT('Ctrl Pts',(-25.4916264636604,38.591975054867,20.));
#82009=CARTESIAN_POINT('Ctrl Pts',(-25.462715461847,38.6075128650891,0.));
#82010=CARTESIAN_POINT('Ctrl Pts',(-25.462715461847,38.6075128650891,20.));
#82011=CARTESIAN_POINT('Ctrl Pts',(-25.4337944690316,38.6230297096774,0.));
#82012=CARTESIAN_POINT('Ctrl Pts',(-25.4337944690316,38.6230297096774,20.));
#82013=CARTESIAN_POINT('Ctrl Pts',(-25.4048635000795,38.6385255816593,0.));
#82014=CARTESIAN_POINT('Ctrl Pts',(-25.4048635000795,38.6385255816593,20.));
#82015=CARTESIAN_POINT('Ctrl Pts',(-25.3759225698613,38.6540004740723,0.));
#82016=CARTESIAN_POINT('Ctrl Pts',(-25.3759225698613,38.6540004740723,20.));
#82017=CARTESIAN_POINT('Ctrl Pts',(-25.3469716932528,38.6694543799641,0.));
#82018=CARTESIAN_POINT('Ctrl Pts',(-25.3469716932528,38.6694543799641,20.));
#82019=CARTESIAN_POINT('Ctrl Pts',(-25.3180108851341,38.6848872923919,0.));
#82020=CARTESIAN_POINT('Ctrl Pts',(-25.3180108851341,38.6848872923919,20.));
#82021=CARTESIAN_POINT('Ctrl Pts',(-25.2890401603913,38.7002992044241,0.));
#82022=CARTESIAN_POINT('Ctrl Pts',(-25.2890401603913,38.7002992044241,20.));
#82023=CARTESIAN_POINT('Ctrl Pts',(-25.2600595339159,38.7156901091392,0.));
#82024=CARTESIAN_POINT('Ctrl Pts',(-25.2600595339159,38.7156901091392,20.));
#82025=CARTESIAN_POINT('Ctrl Pts',(-25.231069020605,38.7310599996258,0.));
#82026=CARTESIAN_POINT('Ctrl Pts',(-25.231069020605,38.7310599996258,20.));
#82027=CARTESIAN_POINT('Ctrl Pts',(-25.2020686353608,38.7464088689836,0.));
#82028=CARTESIAN_POINT('Ctrl Pts',(-25.2020686353608,38.7464088689836,20.));
#82029=CARTESIAN_POINT('Ctrl Pts',(-25.1730583930911,38.7617367103228,0.));
#82030=CARTESIAN_POINT('Ctrl Pts',(-25.1730583930911,38.7617367103228,20.));
#82031=CARTESIAN_POINT('Ctrl Pts',(-25.1440383087085,38.7770435167639,0.));
#82032=CARTESIAN_POINT('Ctrl Pts',(-25.1440383087085,38.7770435167639,20.));
#82033=CARTESIAN_POINT('Ctrl Pts',(-25.1150083971302,38.7923292814368,0.));
#82034=CARTESIAN_POINT('Ctrl Pts',(-25.1150083971302,38.7923292814368,20.));
#82035=CARTESIAN_POINT('Ctrl Pts',(-25.0859686732795,38.8075939974829,0.));
#82036=CARTESIAN_POINT('Ctrl Pts',(-25.0859686732795,38.8075939974829,20.));
#82037=CARTESIAN_POINT('Ctrl Pts',(-25.0569191520845,38.8228376580533,0.));
#82038=CARTESIAN_POINT('Ctrl Pts',(-25.0569191520845,38.8228376580533,20.));
#82039=CARTESIAN_POINT('Ctrl Pts',(-25.0278598484791,38.8380602563098,0.));
#82040=CARTESIAN_POINT('Ctrl Pts',(-25.0278598484791,38.8380602563098,20.));
#82041=CARTESIAN_POINT('Ctrl Pts',(-24.9987907774025,38.8532617854245,0.));
#82042=CARTESIAN_POINT('Ctrl Pts',(-24.9987907774025,38.8532617854245,20.));
#82043=CARTESIAN_POINT('Ctrl Pts',(-24.9697119537989,38.8684422385799,0.));
#82044=CARTESIAN_POINT('Ctrl Pts',(-24.9697119537989,38.8684422385799,20.));
#82045=CARTESIAN_POINT('Ctrl Pts',(-24.9406233926168,38.883601608968,0.));
#82046=CARTESIAN_POINT('Ctrl Pts',(-24.9406233926168,38.883601608968,20.));
#82047=CARTESIAN_POINT('Ctrl Pts',(-24.9115251088108,38.8987398897918,0.));
#82048=CARTESIAN_POINT('Ctrl Pts',(-24.9115251088108,38.8987398897918,20.));
#82049=CARTESIAN_POINT('Ctrl Pts',(-24.8824171173402,38.9138570742648,0.));
#82050=CARTESIAN_POINT('Ctrl Pts',(-24.8824171173402,38.9138570742648,20.));
#82051=CARTESIAN_POINT('Ctrl Pts',(-24.8532994331703,38.9289531556117,0.));
#82052=CARTESIAN_POINT('Ctrl Pts',(-24.8532994331703,38.9289531556117,20.));
#82053=CARTESIAN_POINT('Ctrl Pts',(-24.8241720712716,38.9440281270684,0.));
#82054=CARTESIAN_POINT('Ctrl Pts',(-24.8241720712716,38.9440281270684,20.));
#82055=CARTESIAN_POINT('Ctrl Pts',(-24.7950350466188,38.9590819818797,0.));
#82056=CARTESIAN_POINT('Ctrl Pts',(-24.7950350466188,38.9590819818797,20.));
#82057=CARTESIAN_POINT('Ctrl Pts',(-24.7658883741919,38.9741147133012,0.));
#82058=CARTESIAN_POINT('Ctrl Pts',(-24.7658883741919,38.9741147133012,20.));
#82059=CARTESIAN_POINT('Ctrl Pts',(-24.736732068976,38.989126314598,0.));
#82060=CARTESIAN_POINT('Ctrl Pts',(-24.736732068976,38.989126314598,20.));
#82061=CARTESIAN_POINT('Ctrl Pts',(-24.7075661459617,39.0041167790461,0.));
#82062=CARTESIAN_POINT('Ctrl Pts',(-24.7075661459617,39.0041167790461,20.));
#82063=CARTESIAN_POINT('Ctrl Pts',(-24.6783906201452,39.019086099931,0.));
#82064=CARTESIAN_POINT('Ctrl Pts',(-24.6783906201452,39.019086099931,20.));
#82065=CARTESIAN_POINT('Ctrl Pts',(-24.6492055065285,39.0340342705498,0.));
#82066=CARTESIAN_POINT('Ctrl Pts',(-24.6492055065285,39.0340342705498,20.));
#82067=CARTESIAN_POINT('Ctrl Pts',(-24.6200108201182,39.0489612842095,0.));
#82068=CARTESIAN_POINT('Ctrl Pts',(-24.6200108201182,39.0489612842095,20.));
#82069=CARTESIAN_POINT('Ctrl Pts',(-24.5908065759258,39.0638671342286,0.));
#82070=CARTESIAN_POINT('Ctrl Pts',(-24.5908065759258,39.0638671342286,20.));
#82071=CARTESIAN_POINT('Ctrl Pts',(-24.5615927889669,39.0787518139362,0.));
#82072=CARTESIAN_POINT('Ctrl Pts',(-24.5615927889669,39.0787518139362,20.));
#82073=CARTESIAN_POINT('Ctrl Pts',(-24.5323694742617,39.0936153166722,0.));
#82074=CARTESIAN_POINT('Ctrl Pts',(-24.5323694742617,39.0936153166722,20.));
#82075=CARTESIAN_POINT('Ctrl Pts',(-24.5031366468345,39.1084576357871,0.));
#82076=CARTESIAN_POINT('Ctrl Pts',(-24.5031366468345,39.1084576357871,20.));
#82077=CARTESIAN_POINT('Ctrl Pts',(-24.4738943217155,39.1232787646414,0.));
#82078=CARTESIAN_POINT('Ctrl Pts',(-24.4738943217155,39.1232787646414,20.));
#82079=CARTESIAN_POINT('Ctrl Pts',(-24.4446425139409,39.1380786966047,0.));
#82080=CARTESIAN_POINT('Ctrl Pts',(-24.4446425139409,39.1380786966047,20.));
#82081=CARTESIAN_POINT('Ctrl Pts',(-24.4153812385543,39.1528574250568,0.));
#82082=CARTESIAN_POINT('Ctrl Pts',(-24.4153812385543,39.1528574250568,20.));
#82083=CARTESIAN_POINT('Ctrl Pts',(-24.3861105106067,39.1676149433869,0.));
#82084=CARTESIAN_POINT('Ctrl Pts',(-24.3861105106067,39.1676149433869,20.));
#82085=CARTESIAN_POINT('Ctrl Pts',(-24.3568303451549,39.1823512449951,0.));
#82086=CARTESIAN_POINT('Ctrl Pts',(-24.3568303451549,39.1823512449951,20.));
#82087=CARTESIAN_POINT('Ctrl Pts',(-24.3275407572588,39.197066323292,0.));
#82088=CARTESIAN_POINT('Ctrl Pts',(-24.3275407572588,39.197066323292,20.));
#82089=CARTESIAN_POINT('Ctrl Pts',(-24.2982417619806,39.2117601717005,0.));
#82090=CARTESIAN_POINT('Ctrl Pts',(-24.2982417619806,39.2117601717005,20.));
#82091=CARTESIAN_POINT('Ctrl Pts',(-24.2689333743823,39.2264327836562,0.));
#82092=CARTESIAN_POINT('Ctrl Pts',(-24.2689333743823,39.2264327836562,20.));
#82093=CARTESIAN_POINT('Ctrl Pts',(-24.2396156095261,39.2410841526077,0.));
#82094=CARTESIAN_POINT('Ctrl Pts',(-24.2396156095261,39.2410841526077,20.));
#82095=CARTESIAN_POINT('Ctrl Pts',(-24.2102884824784,39.2557142720138,0.));
#82096=CARTESIAN_POINT('Ctrl Pts',(-24.2102884824784,39.2557142720138,20.));
#82097=CARTESIAN_POINT('Ctrl Pts',(-24.1809520083147,39.2703231353422,0.));
#82098=CARTESIAN_POINT('Ctrl Pts',(-24.1809520083147,39.2703231353422,20.));
#82099=CARTESIAN_POINT('Ctrl Pts',(-24.1516062021224,39.2849107360681,0.));
#82100=CARTESIAN_POINT('Ctrl Pts',(-24.1516062021224,39.2849107360681,20.));
#82101=CARTESIAN_POINT('Ctrl Pts',(-24.1222510790066,39.2994770676712,0.));
#82102=CARTESIAN_POINT('Ctrl Pts',(-24.1222510790066,39.2994770676712,20.));
#82103=CARTESIAN_POINT('Ctrl Pts',(-24.0928866540882,39.3140221236369,0.));
#82104=CARTESIAN_POINT('Ctrl Pts',(-24.0928866540882,39.3140221236369,20.));
#82105=CARTESIAN_POINT('Ctrl Pts',(-24.0635129424931,39.3285458974612,0.));
#82106=CARTESIAN_POINT('Ctrl Pts',(-24.0635129424931,39.3285458974612,20.));
#82107=CARTESIAN_POINT('Ctrl Pts',(-24.0341299593437,39.3430483826555,0.));
#82108=CARTESIAN_POINT('Ctrl Pts',(-24.0341299593437,39.3430483826555,20.));
#82109=CARTESIAN_POINT('Ctrl Pts',(-24.0047377197503,39.3575295727493,0.));
#82110=CARTESIAN_POINT('Ctrl Pts',(-24.0047377197503,39.3575295727493,20.));
#82111=CARTESIAN_POINT('Ctrl Pts',(-23.9753362387978,39.3719894612957,0.));
#82112=CARTESIAN_POINT('Ctrl Pts',(-23.9753362387978,39.3719894612957,20.));
#82113=CARTESIAN_POINT('Ctrl Pts',(-23.9459255315518,39.3864280418676,0.));
#82114=CARTESIAN_POINT('Ctrl Pts',(-23.9459255315518,39.3864280418676,20.));
#82115=CARTESIAN_POINT('Ctrl Pts',(-23.9165056130837,39.4008453080481,0.));
#82116=CARTESIAN_POINT('Ctrl Pts',(-23.9165056130837,39.4008453080481,20.));
#82117=CARTESIAN_POINT('Ctrl Pts',(-23.8870764984925,39.4152412534209,0.));
#82118=CARTESIAN_POINT('Ctrl Pts',(-23.8870764984925,39.4152412534209,20.));
#82119=CARTESIAN_POINT('Ctrl Pts',(-23.8576382029238,39.4296158715627,0.));
#82120=CARTESIAN_POINT('Ctrl Pts',(-23.8576382029238,39.4296158715627,20.));
#82121=CARTESIAN_POINT('Ctrl Pts',(-23.8281907416005,39.4439691560298,0.));
#82122=CARTESIAN_POINT('Ctrl Pts',(-23.8281907416005,39.4439691560298,20.));
#82123=CARTESIAN_POINT('Ctrl Pts',(-23.7987341298022,39.4583011003674,0.));
#82124=CARTESIAN_POINT('Ctrl Pts',(-23.7987341298022,39.4583011003674,20.));
#82125=CARTESIAN_POINT('Ctrl Pts',(-23.7692683828081,39.4726116981337,0.));
#82126=CARTESIAN_POINT('Ctrl Pts',(-23.7692683828081,39.4726116981337,20.));
#82127=CARTESIAN_POINT('Ctrl Pts',(-23.7397935158457,39.4869009429217,0.));
#82128=CARTESIAN_POINT('Ctrl Pts',(-23.7397935158457,39.4869009429217,20.));
#82129=CARTESIAN_POINT('Ctrl Pts',(-23.7103095440476,39.5011688283778,0.));
#82130=CARTESIAN_POINT('Ctrl Pts',(-23.7103095440476,39.5011688283778,20.));
#82131=CARTESIAN_POINT('Ctrl Pts',(-23.6808164823786,39.5154153482324,0.));
#82132=CARTESIAN_POINT('Ctrl Pts',(-23.6808164823786,39.5154153482324,20.));
#82133=CARTESIAN_POINT('Ctrl Pts',(-23.651314345698,39.5296404962721,0.));
#82134=CARTESIAN_POINT('Ctrl Pts',(-23.651314345698,39.5296404962721,20.));
#82135=CARTESIAN_POINT('Ctrl Pts',(-23.6218031488905,39.5438442662853,0.));
#82136=CARTESIAN_POINT('Ctrl Pts',(-23.6218031488905,39.5438442662853,20.));
#82137=CARTESIAN_POINT('Ctrl Pts',(-23.5922829069852,39.5580266520107,0.));
#82138=CARTESIAN_POINT('Ctrl Pts',(-23.5922829069852,39.5580266520107,20.));
#82139=CARTESIAN_POINT('Ctrl Pts',(-23.5627536352592,39.5721876470956,0.));
#82140=CARTESIAN_POINT('Ctrl Pts',(-23.5627536352592,39.5721876470956,20.));
#82141=CARTESIAN_POINT('Ctrl Pts',(-23.533215349402,39.5863272450267,0.));
#82142=CARTESIAN_POINT('Ctrl Pts',(-23.533215349402,39.5863272450267,20.));
#82143=CARTESIAN_POINT('Ctrl Pts',(-23.5036680653391,39.6004454392038,0.));
#82144=CARTESIAN_POINT('Ctrl Pts',(-23.5036680653391,39.6004454392038,20.));
#82145=CARTESIAN_POINT('Ctrl Pts',(-23.4741117989348,39.6145422230651,0.));
#82146=CARTESIAN_POINT('Ctrl Pts',(-23.4741117989348,39.6145422230651,20.));
#82147=CARTESIAN_POINT('Ctrl Pts',(-23.4445465657147,39.6286175902046,0.));
#82148=CARTESIAN_POINT('Ctrl Pts',(-23.4445465657147,39.6286175902046,20.));
#82149=CARTESIAN_POINT('Ctrl Pts',(-23.4149723806221,39.6426715344742,0.));
#82150=CARTESIAN_POINT('Ctrl Pts',(-23.4149723806221,39.6426715344742,20.));
#82151=CARTESIAN_POINT('Ctrl Pts',(-23.385389257652,39.6567040501382,0.));
#82152=CARTESIAN_POINT('Ctrl Pts',(-23.385389257652,39.6567040501382,20.));
#82153=CARTESIAN_POINT('Ctrl Pts',(-23.3557972103217,39.670715131677,0.));
#82154=CARTESIAN_POINT('Ctrl Pts',(-23.3557972103217,39.670715131677,20.));
#82155=CARTESIAN_POINT('Ctrl Pts',(-23.3261962523444,39.6847047735001,0.));
#82156=CARTESIAN_POINT('Ctrl Pts',(-23.3261962523444,39.6847047735001,20.));
#82157=CARTESIAN_POINT('Ctrl Pts',(-23.2965863982648,39.6986729696788,0.));
#82158=CARTESIAN_POINT('Ctrl Pts',(-23.2965863982648,39.6986729696788,20.));
#82159=CARTESIAN_POINT('Ctrl Pts',(-23.2669676640418,39.712619713699,0.));
#82160=CARTESIAN_POINT('Ctrl Pts',(-23.2669676640418,39.712619713699,20.));
#82161=CARTESIAN_POINT('Ctrl Pts',(-23.2373400678346,39.7265449981305,0.));
#82162=CARTESIAN_POINT('Ctrl Pts',(-23.2373400678346,39.7265449981305,20.));
#82163=CARTESIAN_POINT('Ctrl Pts',(-23.2077036288598,39.7404488151086,0.));
#82164=CARTESIAN_POINT('Ctrl Pts',(-23.2077036288598,39.7404488151086,20.));
#82165=CARTESIAN_POINT('Ctrl Pts',(-23.1780583659508,39.7543311569459,0.));
#82166=CARTESIAN_POINT('Ctrl Pts',(-23.1780583659508,39.7543311569459,20.));
#82167=CARTESIAN_POINT('Ctrl Pts',(-23.1484042962029,39.7681920167058,0.));
#82168=CARTESIAN_POINT('Ctrl Pts',(-23.1484042962029,39.7681920167058,20.));
#82169=CARTESIAN_POINT('Ctrl Pts',(-23.1187414336251,39.7820313887737,0.));
#82170=CARTESIAN_POINT('Ctrl Pts',(-23.1187414336251,39.7820313887737,20.));
#82171=CARTESIAN_POINT('Ctrl Pts',(-23.089069787673,39.7958492694787,0.));
#82172=CARTESIAN_POINT('Ctrl Pts',(-23.089069787673,39.7958492694787,20.));
#82173=CARTESIAN_POINT('Ctrl Pts',(-23.0593893640427,39.8096456567259,0.));
#82174=CARTESIAN_POINT('Ctrl Pts',(-23.0593893640427,39.8096456567259,20.));
#82175=CARTESIAN_POINT('Ctrl Pts',(-23.0356380053139,39.8206655709903,0.));
#82176=CARTESIAN_POINT('Ctrl Pts',(-23.0356380053139,39.8206655709903,20.));
#82177=CARTESIAN_POINT('Ctrl Pts',(-23.0178205380655,39.8289208340947,0.));
#82178=CARTESIAN_POINT('Ctrl Pts',(-23.0178205380655,39.8289208340947,20.));
#82179=CARTESIAN_POINT('Ctrl Pts',(-23.005940471814,39.8344200439082,0.));
#82180=CARTESIAN_POINT('Ctrl Pts',(-23.005940471814,39.8344200439082,20.));
#82181=CARTESIAN_POINT('Ctrl Pts',(-23.,39.8371685740842,0.));
#82182=CARTESIAN_POINT('Ctrl Pts',(-23.,39.8371685740842,20.));
#82183=CARTESIAN_POINT('',(-46.0449384185095,16.7589870229578,2.));
#82184=CARTESIAN_POINT('Ctrl Pts',(-34.5017338047269,32.2758373034787,2.));
#82185=CARTESIAN_POINT('Ctrl Pts',(-35.1012599438994,31.7409631286146,2.));
#82186=CARTESIAN_POINT('Ctrl Pts',(-35.6879267845883,31.1902015741133,2.));
#82187=CARTESIAN_POINT('Ctrl Pts',(-36.260940923753,30.624221206043,2.));
#82188=CARTESIAN_POINT('Ctrl Pts',(-36.8331139940994,30.0590715826381,2.));
#82189=CARTESIAN_POINT('Ctrl Pts',(-37.3916743025935,29.4787479308737,2.));
#82190=CARTESIAN_POINT('Ctrl Pts',(-37.9358680909622,28.8839537384041,2.));
#82191=CARTESIAN_POINT('Ctrl Pts',(-38.4805318739963,28.288645850072,2.));
#82192=CARTESIAN_POINT('Ctrl Pts',(-39.0108041943122,27.6788425476408,2.));
#82193=CARTESIAN_POINT('Ctrl Pts',(-39.5259673010255,27.0552850618763,2.));
#82194=CARTESIAN_POINT('Ctrl Pts',(-40.0415776804199,26.4311861937323,2.));
#82195=CARTESIAN_POINT('Ctrl Pts',(-40.5420524892488,25.7933093866071,2.));
#82196=CARTESIAN_POINT('Ctrl Pts',(-41.0267118135419,25.1424317389406,2.));
#82197=CARTESIAN_POINT('Ctrl Pts',(-41.5120542721152,24.4906366698793,2.));
#82198=CARTESIAN_POINT('Ctrl Pts',(-41.9815365243414,23.8258042250936,2.));
#82199=CARTESIAN_POINT('Ctrl Pts',(-42.4345172043854,23.1487467236845,2.));
#82200=CARTESIAN_POINT('Ctrl Pts',(-42.8878253137778,22.4711998228236,2.));
#82201=CARTESIAN_POINT('Ctrl Pts',(-43.3246078927956,21.7814103343397,2.));
#82202=CARTESIAN_POINT('Ctrl Pts',(-43.7442651357813,21.0802221166732,2.));
#82203=CARTESIAN_POINT('Ctrl Pts',(-44.1624466566267,20.3814996231056,2.));
#82204=CARTESIAN_POINT('Ctrl Pts',(-44.5636230181975,19.6714585963912,2.));
#82205=CARTESIAN_POINT('Ctrl Pts',(-44.9472444130411,18.9509611646836,2.));
#82206=CARTESIAN_POINT('Ctrl Pts',(-45.1999149529739,18.4764087087029,2.));
#82207=CARTESIAN_POINT('Ctrl Pts',(-45.4449708032456,17.9973206591027,2.));
#82208=CARTESIAN_POINT('Ctrl Pts',(-45.6822654287125,17.5139493060988,2.));
#82209=CARTESIAN_POINT('Ctrl Pts',(-45.8052474513848,17.2634337852467,2.));
#82210=CARTESIAN_POINT('Ctrl Pts',(-45.926144661035,17.0117683454893,2.));
#82211=CARTESIAN_POINT('Ctrl Pts',(-46.0449384185095,16.7589870229578,2.));
#82212=CARTESIAN_POINT('',(-46.0449384185095,16.7589870229578,0.));
#82213=CARTESIAN_POINT('Ctrl Pts',(-46.0449384185095,16.7589870229578,0.));
#82214=CARTESIAN_POINT('Ctrl Pts',(-46.0449384185095,16.7589870229578,20.));
#82215=CARTESIAN_POINT('Ctrl Pts',(-46.0420594924752,16.7651130917503,0.));
#82216=CARTESIAN_POINT('Ctrl Pts',(-46.0420594924752,16.7651130917503,20.));
#82217=CARTESIAN_POINT('Ctrl Pts',(-46.0362995834799,16.7773641333857,0.));
#82218=CARTESIAN_POINT('Ctrl Pts',(-46.0362995834799,16.7773641333857,20.));
#82219=CARTESIAN_POINT('Ctrl Pts',(-46.0276535492065,16.7957374079899,0.));
#82220=CARTESIAN_POINT('Ctrl Pts',(-46.0276535492065,16.7957374079899,20.));
#82221=CARTESIAN_POINT('Ctrl Pts',(-46.0161131619282,16.8202285317553,0.));
#82222=CARTESIAN_POINT('Ctrl Pts',(-46.0161131619282,16.8202285317553,20.));
#82223=CARTESIAN_POINT('Ctrl Pts',(-46.0016671088634,16.8508314760754,0.));
#82224=CARTESIAN_POINT('Ctrl Pts',(-46.0016671088634,16.8508314760754,20.));
#82225=CARTESIAN_POINT('Ctrl Pts',(-45.9872004880192,16.8814234574888,0.));
#82226=CARTESIAN_POINT('Ctrl Pts',(-45.9872004880192,16.8814234574888,20.));
#82227=CARTESIAN_POINT('Ctrl Pts',(-45.9727133019197,16.9120044710149,0.));
#82228=CARTESIAN_POINT('Ctrl Pts',(-45.9727133019197,16.9120044710149,20.));
#82229=CARTESIAN_POINT('Ctrl Pts',(-45.9582055548827,16.9425745084438,0.));
#82230=CARTESIAN_POINT('Ctrl Pts',(-45.9582055548827,16.9425745084438,20.));
#82231=CARTESIAN_POINT('Ctrl Pts',(-45.9436772535459,16.9731335574459,0.));
#82232=CARTESIAN_POINT('Ctrl Pts',(-45.9436772535459,16.9731335574459,20.));
#82233=CARTESIAN_POINT('Ctrl Pts',(-45.9291284062576,17.0036816026634,0.));
#82234=CARTESIAN_POINT('Ctrl Pts',(-45.9291284062576,17.0036816026634,20.));
#82235=CARTESIAN_POINT('Ctrl Pts',(-45.91455902239,17.0342186269341,0.));
#82236=CARTESIAN_POINT('Ctrl Pts',(-45.91455902239,17.0342186269341,20.));
#82237=CARTESIAN_POINT('Ctrl Pts',(-45.8999691116667,17.0647446124944,0.));
#82238=CARTESIAN_POINT('Ctrl Pts',(-45.8999691116667,17.0647446124944,20.));
#82239=CARTESIAN_POINT('Ctrl Pts',(-45.8853586835176,17.0952595421299,0.));
#82240=CARTESIAN_POINT('Ctrl Pts',(-45.8853586835176,17.0952595421299,20.));
#82241=CARTESIAN_POINT('Ctrl Pts',(-45.8707277463338,17.1257634005083,0.));
#82242=CARTESIAN_POINT('Ctrl Pts',(-45.8707277463338,17.1257634005083,20.));
#82243=CARTESIAN_POINT('Ctrl Pts',(-45.8560763076625,17.1562561738292,0.));
#82244=CARTESIAN_POINT('Ctrl Pts',(-45.8560763076625,17.1562561738292,20.));
#82245=CARTESIAN_POINT('Ctrl Pts',(-45.8414043745501,17.1867378492105,0.));
#82246=CARTESIAN_POINT('Ctrl Pts',(-45.8414043745501,17.1867378492105,20.));
#82247=CARTESIAN_POINT('Ctrl Pts',(-45.8267119538424,17.2172084141516,0.));
#82248=CARTESIAN_POINT('Ctrl Pts',(-45.8267119538424,17.2172084141516,20.));
#82249=CARTESIAN_POINT('Ctrl Pts',(-45.8119990524824,17.247667856,0.));
#82250=CARTESIAN_POINT('Ctrl Pts',(-45.8119990524824,17.247667856,20.));
#82251=CARTESIAN_POINT('Ctrl Pts',(-45.7972656778619,17.2781161613228,0.));
#82252=CARTESIAN_POINT('Ctrl Pts',(-45.7972656778619,17.2781161613228,20.));
#82253=CARTESIAN_POINT('Ctrl Pts',(-45.7825118377706,17.3085533159981,0.));
#82254=CARTESIAN_POINT('Ctrl Pts',(-45.7825118377706,17.3085533159981,20.));
#82255=CARTESIAN_POINT('Ctrl Pts',(-45.7677375402376,17.3389793054984,0.));
#82256=CARTESIAN_POINT('Ctrl Pts',(-45.7677375402376,17.3389793054984,20.));
#82257=CARTESIAN_POINT('Ctrl Pts',(-45.7529427934047,17.3693941151172,0.));
#82258=CARTESIAN_POINT('Ctrl Pts',(-45.7529427934047,17.3693941151172,20.));
#82259=CARTESIAN_POINT('Ctrl Pts',(-45.7381276053972,17.3997977302007,0.));
#82260=CARTESIAN_POINT('Ctrl Pts',(-45.7381276053972,17.3997977302007,20.));
#82261=CARTESIAN_POINT('Ctrl Pts',(-45.7232919841685,17.4301901364248,0.));
#82262=CARTESIAN_POINT('Ctrl Pts',(-45.7232919841685,17.4301901364248,20.));
#82263=CARTESIAN_POINT('Ctrl Pts',(-45.7084359375081,17.460571319782,0.));
#82264=CARTESIAN_POINT('Ctrl Pts',(-45.7084359375081,17.460571319782,20.));
#82265=CARTESIAN_POINT('Ctrl Pts',(-45.6935594731126,17.4909412664519,0.));
#82266=CARTESIAN_POINT('Ctrl Pts',(-45.6935594731126,17.4909412664519,20.));
#82267=CARTESIAN_POINT('Ctrl Pts',(-45.6786625986401,17.5212999627071,0.));
#82268=CARTESIAN_POINT('Ctrl Pts',(-45.6786625986401,17.5212999627071,20.));
#82269=CARTESIAN_POINT('Ctrl Pts',(-45.6637453217655,17.5516473948116,0.));
#82270=CARTESIAN_POINT('Ctrl Pts',(-45.6637453217655,17.5516473948116,20.));
#82271=CARTESIAN_POINT('Ctrl Pts',(-45.6488076502485,17.5819835489016,0.));
#82272=CARTESIAN_POINT('Ctrl Pts',(-45.6488076502485,17.5819835489016,20.));
#82273=CARTESIAN_POINT('Ctrl Pts',(-45.6338495919363,17.6123084109793,0.));
#82274=CARTESIAN_POINT('Ctrl Pts',(-45.6338495919363,17.6123084109793,20.));
#82275=CARTESIAN_POINT('Ctrl Pts',(-45.6188711547313,17.6426219669711,0.));
#82276=CARTESIAN_POINT('Ctrl Pts',(-45.6188711547313,17.6426219669711,20.));
#82277=CARTESIAN_POINT('Ctrl Pts',(-45.6038723465685,17.672924202767,0.));
#82278=CARTESIAN_POINT('Ctrl Pts',(-45.6038723465685,17.672924202767,20.));
#82279=CARTESIAN_POINT('Ctrl Pts',(-45.5888531753912,17.7032151042645,0.));
#82280=CARTESIAN_POINT('Ctrl Pts',(-45.5888531753912,17.7032151042645,20.));
#82281=CARTESIAN_POINT('Ctrl Pts',(-45.5738136491221,17.7334946574206,0.));
#82282=CARTESIAN_POINT('Ctrl Pts',(-45.5738136491221,17.7334946574206,20.));
#82283=CARTESIAN_POINT('Ctrl Pts',(-45.5587537756595,17.7637628482589,0.));
#82284=CARTESIAN_POINT('Ctrl Pts',(-45.5587537756595,17.7637628482589,20.));
#82285=CARTESIAN_POINT('Ctrl Pts',(-45.5436735628911,17.7940196628442,0.));
#82286=CARTESIAN_POINT('Ctrl Pts',(-45.5436735628911,17.7940196628442,20.));
#82287=CARTESIAN_POINT('Ctrl Pts',(-45.528573018704,17.8242650872661,0.));
#82288=CARTESIAN_POINT('Ctrl Pts',(-45.528573018704,17.8242650872661,20.));
#82289=CARTESIAN_POINT('Ctrl Pts',(-45.5134521509949,17.8544991076191,0.));
#82290=CARTESIAN_POINT('Ctrl Pts',(-45.5134521509949,17.8544991076191,20.));
#82291=CARTESIAN_POINT('Ctrl Pts',(-45.498310967683,17.8847217099814,0.));
#82292=CARTESIAN_POINT('Ctrl Pts',(-45.498310967683,17.8847217099814,20.));
#82293=CARTESIAN_POINT('Ctrl Pts',(-45.4831494767122,17.9149328804084,0.));
#82294=CARTESIAN_POINT('Ctrl Pts',(-45.4831494767122,17.9149328804084,20.));
#82295=CARTESIAN_POINT('Ctrl Pts',(-45.4679676860453,17.9451326049449,0.));
#82296=CARTESIAN_POINT('Ctrl Pts',(-45.4679676860453,17.9451326049449,20.));
#82297=CARTESIAN_POINT('Ctrl Pts',(-45.4527656036598,17.9753208696315,0.));
#82298=CARTESIAN_POINT('Ctrl Pts',(-45.4527656036598,17.9753208696315,20.));
#82299=CARTESIAN_POINT('Ctrl Pts',(-45.4375432375433,18.0054976605137,0.));
#82300=CARTESIAN_POINT('Ctrl Pts',(-45.4375432375433,18.0054976605137,20.));
#82301=CARTESIAN_POINT('Ctrl Pts',(-45.4223005956881,18.0356629636502,0.));
#82302=CARTESIAN_POINT('Ctrl Pts',(-45.4223005956881,18.0356629636502,20.));
#82303=CARTESIAN_POINT('Ctrl Pts',(-45.4070376860893,18.0658167651176,0.));
#82304=CARTESIAN_POINT('Ctrl Pts',(-45.4070376860893,18.0658167651176,20.));
#82305=CARTESIAN_POINT('Ctrl Pts',(-45.3917545167484,18.0959590510046,0.));
#82306=CARTESIAN_POINT('Ctrl Pts',(-45.3917545167484,18.0959590510046,20.));
#82307=CARTESIAN_POINT('Ctrl Pts',(-45.3764510956741,18.1260898074095,0.));
#82308=CARTESIAN_POINT('Ctrl Pts',(-45.3764510956741,18.1260898074095,20.));
#82309=CARTESIAN_POINT('Ctrl Pts',(-45.3611274308852,18.156209020436,0.));
#82310=CARTESIAN_POINT('Ctrl Pts',(-45.3611274308852,18.156209020436,20.));
#82311=CARTESIAN_POINT('Ctrl Pts',(-45.345783530412,18.1863166761897,0.));
#82312=CARTESIAN_POINT('Ctrl Pts',(-45.345783530412,18.1863166761897,20.));
#82313=CARTESIAN_POINT('Ctrl Pts',(-45.3304194022976,18.216412760776,0.));
#82314=CARTESIAN_POINT('Ctrl Pts',(-45.3304194022976,18.216412760776,20.));
#82315=CARTESIAN_POINT('Ctrl Pts',(-45.3150350545965,18.2464972603023,0.));
#82316=CARTESIAN_POINT('Ctrl Pts',(-45.3150350545965,18.2464972603023,20.));
#82317=CARTESIAN_POINT('Ctrl Pts',(-45.299630495374,18.2765701608789,0.));
#82318=CARTESIAN_POINT('Ctrl Pts',(-45.299630495374,18.2765701608789,20.));
#82319=CARTESIAN_POINT('Ctrl Pts',(-45.2842057327049,18.3066314486214,0.));
#82320=CARTESIAN_POINT('Ctrl Pts',(-45.2842057327049,18.3066314486214,20.));
#82321=CARTESIAN_POINT('Ctrl Pts',(-45.2687607746732,18.3366811096519,0.));
#82322=CARTESIAN_POINT('Ctrl Pts',(-45.2687607746732,18.3366811096519,20.));
#82323=CARTESIAN_POINT('Ctrl Pts',(-45.2532956293718,18.3667191300999,0.));
#82324=CARTESIAN_POINT('Ctrl Pts',(-45.2532956293718,18.3667191300999,20.));
#82325=CARTESIAN_POINT('Ctrl Pts',(-45.2378103049023,18.3967454961016,0.));
#82326=CARTESIAN_POINT('Ctrl Pts',(-45.2378103049023,18.3967454961016,20.));
#82327=CARTESIAN_POINT('Ctrl Pts',(-45.2223048093755,18.4267601937997,0.));
#82328=CARTESIAN_POINT('Ctrl Pts',(-45.2223048093755,18.4267601937997,20.));
#82329=CARTESIAN_POINT('Ctrl Pts',(-45.2067791509123,18.456763209342,0.));
#82330=CARTESIAN_POINT('Ctrl Pts',(-45.2067791509123,18.456763209342,20.));
#82331=CARTESIAN_POINT('Ctrl Pts',(-45.1912333376434,18.4867545288811,0.));
#82332=CARTESIAN_POINT('Ctrl Pts',(-45.1912333376434,18.4867545288811,20.));
#82333=CARTESIAN_POINT('Ctrl Pts',(-45.1756673777099,18.5167341385735,0.));
#82334=CARTESIAN_POINT('Ctrl Pts',(-45.1756673777099,18.5167341385735,20.));
#82335=CARTESIAN_POINT('Ctrl Pts',(-45.1600812792631,18.5467020245809,0.));
#82336=CARTESIAN_POINT('Ctrl Pts',(-45.1600812792631,18.5467020245809,20.));
#82337=CARTESIAN_POINT('Ctrl Pts',(-45.144475050464,18.5766581730694,0.));
#82338=CARTESIAN_POINT('Ctrl Pts',(-45.144475050464,18.5766581730694,20.));
#82339=CARTESIAN_POINT('Ctrl Pts',(-45.1288486994834,18.6066025702106,0.));
#82340=CARTESIAN_POINT('Ctrl Pts',(-45.1288486994834,18.6066025702106,20.));
#82341=CARTESIAN_POINT('Ctrl Pts',(-45.1132022345013,18.6365352021813,0.));
#82342=CARTESIAN_POINT('Ctrl Pts',(-45.1132022345013,18.6365352021813,20.));
#82343=CARTESIAN_POINT('Ctrl Pts',(-45.097535663708,18.6664560551643,0.));
#82344=CARTESIAN_POINT('Ctrl Pts',(-45.097535663708,18.6664560551643,20.));
#82345=CARTESIAN_POINT('Ctrl Pts',(-45.081848995303,18.6963651153477,0.));
#82346=CARTESIAN_POINT('Ctrl Pts',(-45.081848995303,18.6963651153477,20.));
#82347=CARTESIAN_POINT('Ctrl Pts',(-45.0661422374956,18.7262623689254,0.));
#82348=CARTESIAN_POINT('Ctrl Pts',(-45.0661422374956,18.7262623689254,20.));
#82349=CARTESIAN_POINT('Ctrl Pts',(-45.050415398505,18.7561478020964,0.));
#82350=CARTESIAN_POINT('Ctrl Pts',(-45.050415398505,18.7561478020964,20.));
#82351=CARTESIAN_POINT('Ctrl Pts',(-45.0346684865594,18.7860214010651,0.));
#82352=CARTESIAN_POINT('Ctrl Pts',(-45.0346684865594,18.7860214010651,20.));
#82353=CARTESIAN_POINT('Ctrl Pts',(-45.0189015098976,18.815883152041,0.));
#82354=CARTESIAN_POINT('Ctrl Pts',(-45.0189015098976,18.815883152041,20.));
#82355=CARTESIAN_POINT('Ctrl Pts',(-45.0031144767678,18.8457330412389,0.));
#82356=CARTESIAN_POINT('Ctrl Pts',(-45.0031144767678,18.8457330412389,20.));
#82357=CARTESIAN_POINT('Ctrl Pts',(-44.9873073954281,18.8755710548787,0.));
#82358=CARTESIAN_POINT('Ctrl Pts',(-44.9873073954281,18.8755710548787,20.));
#82359=CARTESIAN_POINT('Ctrl Pts',(-44.971480274146,18.9053971791858,0.));
#82360=CARTESIAN_POINT('Ctrl Pts',(-44.971480274146,18.9053971791858,20.));
#82361=CARTESIAN_POINT('Ctrl Pts',(-44.9556331211993,18.9352114003906,0.));
#82362=CARTESIAN_POINT('Ctrl Pts',(-44.9556331211993,18.9352114003906,20.));
#82363=CARTESIAN_POINT('Ctrl Pts',(-44.9397659448753,18.9650137047293,0.));
#82364=CARTESIAN_POINT('Ctrl Pts',(-44.9397659448753,18.9650137047293,20.));
#82365=CARTESIAN_POINT('Ctrl Pts',(-44.9238787534705,18.9948040784434,0.));
#82366=CARTESIAN_POINT('Ctrl Pts',(-44.9238787534705,18.9948040784434,20.));
#82367=CARTESIAN_POINT('Ctrl Pts',(-44.9079715552916,19.0245825077797,0.));
#82368=CARTESIAN_POINT('Ctrl Pts',(-44.9079715552916,19.0245825077797,20.));
#82369=CARTESIAN_POINT('Ctrl Pts',(-44.8920443586544,19.0543489789907,0.));
#82370=CARTESIAN_POINT('Ctrl Pts',(-44.8920443586544,19.0543489789907,20.));
#82371=CARTESIAN_POINT('Ctrl Pts',(-44.8760971718851,19.0841034783341,0.));
#82372=CARTESIAN_POINT('Ctrl Pts',(-44.8760971718851,19.0841034783341,20.));
#82373=CARTESIAN_POINT('Ctrl Pts',(-44.8601300033192,19.1138459920731,0.));
#82374=CARTESIAN_POINT('Ctrl Pts',(-44.8601300033192,19.1138459920731,20.));
#82375=CARTESIAN_POINT('Ctrl Pts',(-44.8441428613021,19.143576506476,0.));
#82376=CARTESIAN_POINT('Ctrl Pts',(-44.8441428613021,19.143576506476,20.));
#82377=CARTESIAN_POINT('Ctrl Pts',(-44.8281357541891,19.1732950078168,0.));
#82378=CARTESIAN_POINT('Ctrl Pts',(-44.8281357541891,19.1732950078168,20.));
#82379=CARTESIAN_POINT('Ctrl Pts',(-44.8121086903447,19.2030014823748,0.));
#82380=CARTESIAN_POINT('Ctrl Pts',(-44.8121086903447,19.2030014823748,20.));
#82381=CARTESIAN_POINT('Ctrl Pts',(-44.7960616781431,19.2326959164344,0.));
#82382=CARTESIAN_POINT('Ctrl Pts',(-44.7960616781431,19.2326959164344,20.));
#82383=CARTESIAN_POINT('Ctrl Pts',(-44.7799947259683,19.2623782962858,0.));
#82384=CARTESIAN_POINT('Ctrl Pts',(-44.7799947259683,19.2623782962858,20.));
#82385=CARTESIAN_POINT('Ctrl Pts',(-44.7639078422139,19.2920486082247,0.));
#82386=CARTESIAN_POINT('Ctrl Pts',(-44.7639078422139,19.2920486082247,20.));
#82387=CARTESIAN_POINT('Ctrl Pts',(-44.7478010352831,19.3217068385519,0.));
#82388=CARTESIAN_POINT('Ctrl Pts',(-44.7478010352831,19.3217068385519,20.));
#82389=CARTESIAN_POINT('Ctrl Pts',(-44.731674313589,19.3513529735741,0.));
#82390=CARTESIAN_POINT('Ctrl Pts',(-44.731674313589,19.3513529735741,20.));
#82391=CARTESIAN_POINT('Ctrl Pts',(-44.7155276855546,19.3809869996033,0.));
#82392=CARTESIAN_POINT('Ctrl Pts',(-44.7155276855546,19.3809869996033,20.));
#82393=CARTESIAN_POINT('Ctrl Pts',(-44.6993611596123,19.4106089029568,0.));
#82394=CARTESIAN_POINT('Ctrl Pts',(-44.6993611596123,19.4106089029568,20.));
#82395=CARTESIAN_POINT('Ctrl Pts',(-44.6831747442042,19.4402186699576,0.));
#82396=CARTESIAN_POINT('Ctrl Pts',(-44.6831747442042,19.4402186699576,20.));
#82397=CARTESIAN_POINT('Ctrl Pts',(-44.666968447782,19.4698162869338,0.));
#82398=CARTESIAN_POINT('Ctrl Pts',(-44.666968447782,19.4698162869338,20.));
#82399=CARTESIAN_POINT('Ctrl Pts',(-44.6507422788067,19.4994017402193,0.));
#82400=CARTESIAN_POINT('Ctrl Pts',(-44.6507422788067,19.4994017402193,20.));
#82401=CARTESIAN_POINT('Ctrl Pts',(-44.6344962457493,19.5289750161533,0.));
#82402=CARTESIAN_POINT('Ctrl Pts',(-44.6344962457493,19.5289750161533,20.));
#82403=CARTESIAN_POINT('Ctrl Pts',(-44.6182303570903,19.5585361010809,0.));
#82404=CARTESIAN_POINT('Ctrl Pts',(-44.6182303570903,19.5585361010809,20.));
#82405=CARTESIAN_POINT('Ctrl Pts',(-44.60194462132,19.5880849813525,0.));
#82406=CARTESIAN_POINT('Ctrl Pts',(-44.60194462132,19.5880849813525,20.));
#82407=CARTESIAN_POINT('Ctrl Pts',(-44.5856390469384,19.6176216433241,0.));
#82408=CARTESIAN_POINT('Ctrl Pts',(-44.5856390469384,19.6176216433241,20.));
#82409=CARTESIAN_POINT('Ctrl Pts',(-44.5693136424549,19.6471460733568,0.));
#82410=CARTESIAN_POINT('Ctrl Pts',(-44.5693136424549,19.6471460733568,20.));
#82411=CARTESIAN_POINT('Ctrl Pts',(-44.5529684163885,19.6766582578175,0.));
#82412=CARTESIAN_POINT('Ctrl Pts',(-44.5529684163885,19.6766582578175,20.));
#82413=CARTESIAN_POINT('Ctrl Pts',(-44.5366033772682,19.7061581830785,0.));
#82414=CARTESIAN_POINT('Ctrl Pts',(-44.5366033772682,19.7061581830785,20.));
#82415=CARTESIAN_POINT('Ctrl Pts',(-44.5202185336324,19.7356458355178,0.));
#82416=CARTESIAN_POINT('Ctrl Pts',(-44.5202185336324,19.7356458355178,20.));
#82417=CARTESIAN_POINT('Ctrl Pts',(-44.5038138940293,19.7651212015191,0.));
#82418=CARTESIAN_POINT('Ctrl Pts',(-44.5038138940293,19.7651212015191,20.));
#82419=CARTESIAN_POINT('Ctrl Pts',(-44.4873894670167,19.7945842674717,0.));
#82420=CARTESIAN_POINT('Ctrl Pts',(-44.4873894670167,19.7945842674717,20.));
#82421=CARTESIAN_POINT('Ctrl Pts',(-44.4709452611615,19.8240350197702,0.));
#82422=CARTESIAN_POINT('Ctrl Pts',(-44.4709452611615,19.8240350197702,20.));
#82423=CARTESIAN_POINT('Ctrl Pts',(-44.4544812850403,19.8534734448146,0.));
#82424=CARTESIAN_POINT('Ctrl Pts',(-44.4544812850403,19.8534734448146,20.));
#82425=CARTESIAN_POINT('Ctrl Pts',(-44.4379975472397,19.8828995290107,0.));
#82426=CARTESIAN_POINT('Ctrl Pts',(-44.4379975472397,19.8828995290107,20.));
#82427=CARTESIAN_POINT('Ctrl Pts',(-44.4214940563557,19.9123132587697,0.));
#82428=CARTESIAN_POINT('Ctrl Pts',(-44.4214940563557,19.9123132587697,20.));
#82429=CARTESIAN_POINT('Ctrl Pts',(-44.4049708209939,19.9417146205087,0.));
#82430=CARTESIAN_POINT('Ctrl Pts',(-44.4049708209939,19.9417146205087,20.));
#82431=CARTESIAN_POINT('Ctrl Pts',(-44.3884278497697,19.9711036006503,0.));
#82432=CARTESIAN_POINT('Ctrl Pts',(-44.3884278497697,19.9711036006503,20.));
#82433=CARTESIAN_POINT('Ctrl Pts',(-44.371865151308,20.0004801856228,0.));
#82434=CARTESIAN_POINT('Ctrl Pts',(-44.371865151308,20.0004801856228,20.));
#82435=CARTESIAN_POINT('Ctrl Pts',(-44.3552827342435,20.0298443618602,0.));
#82436=CARTESIAN_POINT('Ctrl Pts',(-44.3552827342435,20.0298443618602,20.));
#82437=CARTESIAN_POINT('Ctrl Pts',(-44.3386806072204,20.0591961158018,0.));
#82438=CARTESIAN_POINT('Ctrl Pts',(-44.3386806072204,20.0591961158018,20.));
#82439=CARTESIAN_POINT('Ctrl Pts',(-44.3220587788923,20.0885354338929,0.));
#82440=CARTESIAN_POINT('Ctrl Pts',(-44.3220587788923,20.0885354338929,20.));
#82441=CARTESIAN_POINT('Ctrl Pts',(-44.3054172579222,20.117862302584,0.));
#82442=CARTESIAN_POINT('Ctrl Pts',(-44.3054172579222,20.117862302584,20.));
#82443=CARTESIAN_POINT('Ctrl Pts',(-44.2887560529826,20.1471767083313,0.));
#82444=CARTESIAN_POINT('Ctrl Pts',(-44.2887560529826,20.1471767083313,20.));
#82445=CARTESIAN_POINT('Ctrl Pts',(-44.2720751727557,20.1764786375963,0.));
#82446=CARTESIAN_POINT('Ctrl Pts',(-44.2720751727557,20.1764786375963,20.));
#82447=CARTESIAN_POINT('Ctrl Pts',(-44.2553746259333,20.2057680768465,0.));
#82448=CARTESIAN_POINT('Ctrl Pts',(-44.2553746259333,20.2057680768465,20.));
#82449=CARTESIAN_POINT('Ctrl Pts',(-44.238654421217,20.2350450125552,0.));
#82450=CARTESIAN_POINT('Ctrl Pts',(-44.238654421217,20.2350450125552,20.));
#82451=CARTESIAN_POINT('Ctrl Pts',(-44.221914567318,20.2643094312016,0.));
#82452=CARTESIAN_POINT('Ctrl Pts',(-44.221914567318,20.2643094312016,20.));
#82453=CARTESIAN_POINT('Ctrl Pts',(-44.205155072957,20.2935613192706,0.));
#82454=CARTESIAN_POINT('Ctrl Pts',(-44.205155072957,20.2935613192706,20.));
#82455=CARTESIAN_POINT('Ctrl Pts',(-44.1883759468646,20.3228006632528,0.));
#82456=CARTESIAN_POINT('Ctrl Pts',(-44.1883759468646,20.3228006632528,20.));
#82457=CARTESIAN_POINT('Ctrl Pts',(-44.1715771977807,20.3520274496443,0.));
#82458=CARTESIAN_POINT('Ctrl Pts',(-44.1715771977807,20.3520274496443,20.));
#82459=CARTESIAN_POINT('Ctrl Pts',(-44.1547588344544,20.3812416649468,0.));
#82460=CARTESIAN_POINT('Ctrl Pts',(-44.1547588344544,20.3812416649468,20.));
#82461=CARTESIAN_POINT('Ctrl Pts',(-44.1379208656442,20.4104432956673,0.));
#82462=CARTESIAN_POINT('Ctrl Pts',(-44.1379208656442,20.4104432956673,20.));
#82463=CARTESIAN_POINT('Ctrl Pts',(-44.1210633001184,20.4396323283186,0.));
#82464=CARTESIAN_POINT('Ctrl Pts',(-44.1210633001184,20.4396323283186,20.));
#82465=CARTESIAN_POINT('Ctrl Pts',(-44.1041861466545,20.468808749419,0.));
#82466=CARTESIAN_POINT('Ctrl Pts',(-44.1041861466545,20.468808749419,20.));
#82467=CARTESIAN_POINT('Ctrl Pts',(-44.0872894140398,20.4979725454932,0.));
#82468=CARTESIAN_POINT('Ctrl Pts',(-44.0872894140398,20.4979725454932,20.));
#82469=CARTESIAN_POINT('Ctrl Pts',(-44.0703731110714,20.5271237030716,0.));
#82470=CARTESIAN_POINT('Ctrl Pts',(-44.0703731110714,20.5271237030716,20.));
#82471=CARTESIAN_POINT('Ctrl Pts',(-44.053437246556,20.5562622086905,0.));
#82472=CARTESIAN_POINT('Ctrl Pts',(-44.053437246556,20.5562622086905,20.));
#82473=CARTESIAN_POINT('Ctrl Pts',(-44.03648182931,20.5853880488919,0.));
#82474=CARTESIAN_POINT('Ctrl Pts',(-44.03648182931,20.5853880488919,20.));
#82475=CARTESIAN_POINT('Ctrl Pts',(-44.0195068681592,20.6145012102233,0.));
#82476=CARTESIAN_POINT('Ctrl Pts',(-44.0195068681592,20.6145012102233,20.));
#82477=CARTESIAN_POINT('Ctrl Pts',(-44.0025123719387,20.6436016792381,0.));
#82478=CARTESIAN_POINT('Ctrl Pts',(-44.0025123719387,20.6436016792381,20.));
#82479=CARTESIAN_POINT('Ctrl Pts',(-43.9854983494929,20.6726894424949,0.));
#82480=CARTESIAN_POINT('Ctrl Pts',(-43.9854983494929,20.6726894424949,20.));
#82481=CARTESIAN_POINT('Ctrl Pts',(-43.9684648096756,20.7017644865584,0.));
#82482=CARTESIAN_POINT('Ctrl Pts',(-43.9684648096756,20.7017644865584,20.));
#82483=CARTESIAN_POINT('Ctrl Pts',(-43.9514117613501,20.7308267979991,0.));
#82484=CARTESIAN_POINT('Ctrl Pts',(-43.9514117613501,20.7308267979991,20.));
#82485=CARTESIAN_POINT('Ctrl Pts',(-43.9343392133895,20.7598763633934,0.));
#82486=CARTESIAN_POINT('Ctrl Pts',(-43.9343392133895,20.7598763633934,20.));
#82487=CARTESIAN_POINT('Ctrl Pts',(-43.9172471746767,20.7889131693233,0.));
#82488=CARTESIAN_POINT('Ctrl Pts',(-43.9172471746767,20.7889131693233,20.));
#82489=CARTESIAN_POINT('Ctrl Pts',(-43.9001356541037,20.817937202377,0.));
#82490=CARTESIAN_POINT('Ctrl Pts',(-43.9001356541037,20.817937202377,20.));
#82491=CARTESIAN_POINT('Ctrl Pts',(-43.8830046605723,20.8469484491482,0.));
#82492=CARTESIAN_POINT('Ctrl Pts',(-43.8830046605723,20.8469484491482,20.));
#82493=CARTESIAN_POINT('Ctrl Pts',(-43.8658542029936,20.8759468962364,0.));
#82494=CARTESIAN_POINT('Ctrl Pts',(-43.8658542029936,20.8759468962364,20.));
#82495=CARTESIAN_POINT('Ctrl Pts',(-43.8486842902882,20.9049325302471,0.));
#82496=CARTESIAN_POINT('Ctrl Pts',(-43.8486842902882,20.9049325302471,20.));
#82497=CARTESIAN_POINT('Ctrl Pts',(-43.8314949313861,20.9339053377913,0.));
#82498=CARTESIAN_POINT('Ctrl Pts',(-43.8314949313861,20.9339053377913,20.));
#82499=CARTESIAN_POINT('Ctrl Pts',(-43.8142861352268,20.9628653054863,0.));
#82500=CARTESIAN_POINT('Ctrl Pts',(-43.8142861352268,20.9628653054863,20.));
#82501=CARTESIAN_POINT('Ctrl Pts',(-43.7970579107591,20.9918124199547,0.));
#82502=CARTESIAN_POINT('Ctrl Pts',(-43.7970579107591,20.9918124199547,20.));
#82503=CARTESIAN_POINT('Ctrl Pts',(-43.7798102669417,21.0207466678254,0.));
#82504=CARTESIAN_POINT('Ctrl Pts',(-43.7798102669417,21.0207466678254,20.));
#82505=CARTESIAN_POINT('Ctrl Pts',(-43.7625432127426,21.0496680357328,0.));
#82506=CARTESIAN_POINT('Ctrl Pts',(-43.7625432127426,21.0496680357328,20.));
#82507=CARTESIAN_POINT('Ctrl Pts',(-43.7452567571393,21.0785765103172,0.));
#82508=CARTESIAN_POINT('Ctrl Pts',(-43.7452567571393,21.0785765103172,20.));
#82509=CARTESIAN_POINT('Ctrl Pts',(-43.7279509091188,21.1074720782252,0.));
#82510=CARTESIAN_POINT('Ctrl Pts',(-43.7279509091188,21.1074720782252,20.));
#82511=CARTESIAN_POINT('Ctrl Pts',(-43.7106256776774,21.1363547261089,0.));
#82512=CARTESIAN_POINT('Ctrl Pts',(-43.7106256776774,21.1363547261089,20.));
#82513=CARTESIAN_POINT('Ctrl Pts',(-43.6932810718209,21.1652244406266,0.));
#82514=CARTESIAN_POINT('Ctrl Pts',(-43.6932810718209,21.1652244406266,20.));
#82515=CARTESIAN_POINT('Ctrl Pts',(-43.6759171005642,21.1940812084419,0.));
#82516=CARTESIAN_POINT('Ctrl Pts',(-43.6759171005642,21.1940812084419,20.));
#82517=CARTESIAN_POINT('Ctrl Pts',(-43.658533772932,21.2229250162246,0.));
#82518=CARTESIAN_POINT('Ctrl Pts',(-43.658533772932,21.2229250162246,20.));
#82519=CARTESIAN_POINT('Ctrl Pts',(-43.6411310979585,21.2517558506503,0.));
#82520=CARTESIAN_POINT('Ctrl Pts',(-43.6411310979585,21.2517558506503,20.));
#82521=CARTESIAN_POINT('Ctrl Pts',(-43.6237090846874,21.2805736984007,0.));
#82522=CARTESIAN_POINT('Ctrl Pts',(-43.6237090846874,21.2805736984007,20.));
#82523=CARTESIAN_POINT('Ctrl Pts',(-43.6062677421718,21.3093785461635,0.));
#82524=CARTESIAN_POINT('Ctrl Pts',(-43.6062677421718,21.3093785461635,20.));
#82525=CARTESIAN_POINT('Ctrl Pts',(-43.5888070794743,21.3381703806323,0.));
#82526=CARTESIAN_POINT('Ctrl Pts',(-43.5888070794743,21.3381703806323,20.));
#82527=CARTESIAN_POINT('Ctrl Pts',(-43.571327105667,21.3669491885068,0.));
#82528=CARTESIAN_POINT('Ctrl Pts',(-43.571327105667,21.3669491885068,20.));
#82529=CARTESIAN_POINT('Ctrl Pts',(-43.5538278298311,21.3957149564922,0.));
#82530=CARTESIAN_POINT('Ctrl Pts',(-43.5538278298311,21.3957149564922,20.));
#82531=CARTESIAN_POINT('Ctrl Pts',(-43.5363092610574,21.4244676712999,0.));
#82532=CARTESIAN_POINT('Ctrl Pts',(-43.5363092610574,21.4244676712999,20.));
#82533=CARTESIAN_POINT('Ctrl Pts',(-43.5187714084458,21.4532073196468,0.));
#82534=CARTESIAN_POINT('Ctrl Pts',(-43.5187714084458,21.4532073196468,20.));
#82535=CARTESIAN_POINT('Ctrl Pts',(-43.5012142811058,21.4819338882558,0.));
#82536=CARTESIAN_POINT('Ctrl Pts',(-43.5012142811058,21.4819338882558,20.));
#82537=CARTESIAN_POINT('Ctrl Pts',(-43.4836378881563,21.5106473638561,0.));
#82538=CARTESIAN_POINT('Ctrl Pts',(-43.4836378881563,21.5106473638561,20.));
#82539=CARTESIAN_POINT('Ctrl Pts',(-43.4660422387257,21.5393477331829,0.));
#82540=CARTESIAN_POINT('Ctrl Pts',(-43.4660422387257,21.5393477331829,20.));
#82541=CARTESIAN_POINT('Ctrl Pts',(-43.4484273419519,21.5680349829773,0.));
#82542=CARTESIAN_POINT('Ctrl Pts',(-43.4484273419519,21.5680349829773,20.));
#82543=CARTESIAN_POINT('Ctrl Pts',(-43.4307932069824,21.5967090999869,0.));
#82544=CARTESIAN_POINT('Ctrl Pts',(-43.4307932069824,21.5967090999869,20.));
#82545=CARTESIAN_POINT('Ctrl Pts',(-43.4131398429739,21.6253700709647,0.));
#82546=CARTESIAN_POINT('Ctrl Pts',(-43.4131398429739,21.6253700709647,20.));
#82547=CARTESIAN_POINT('Ctrl Pts',(-43.3954672590924,21.6540178826698,0.));
#82548=CARTESIAN_POINT('Ctrl Pts',(-43.3954672590924,21.6540178826698,20.));
#82549=CARTESIAN_POINT('Ctrl Pts',(-43.3777754645132,21.682652521867,0.));
#82550=CARTESIAN_POINT('Ctrl Pts',(-43.3777754645132,21.682652521867,20.));
#82551=CARTESIAN_POINT('Ctrl Pts',(-43.3600644684208,21.7112739753274,0.));
#82552=CARTESIAN_POINT('Ctrl Pts',(-43.3600644684208,21.7112739753274,20.));
#82553=CARTESIAN_POINT('Ctrl Pts',(-43.3423342800096,21.7398822298281,0.));
#82554=CARTESIAN_POINT('Ctrl Pts',(-43.3423342800096,21.7398822298281,20.));
#82555=CARTESIAN_POINT('Ctrl Pts',(-43.3245849084831,21.7684772721522,0.));
#82556=CARTESIAN_POINT('Ctrl Pts',(-43.3245849084831,21.7684772721522,20.));
#82557=CARTESIAN_POINT('Ctrl Pts',(-43.3068163630542,21.7970590890891,0.));
#82558=CARTESIAN_POINT('Ctrl Pts',(-43.3068163630542,21.7970590890891,20.));
#82559=CARTESIAN_POINT('Ctrl Pts',(-43.2890286529453,21.8256276674339,0.));
#82560=CARTESIAN_POINT('Ctrl Pts',(-43.2890286529453,21.8256276674339,20.));
#82561=CARTESIAN_POINT('Ctrl Pts',(-43.271221787388,21.8541829939879,0.));
#82562=CARTESIAN_POINT('Ctrl Pts',(-43.271221787388,21.8541829939879,20.));
#82563=CARTESIAN_POINT('Ctrl Pts',(-43.2533957756234,21.8827250555583,0.));
#82564=CARTESIAN_POINT('Ctrl Pts',(-43.2533957756234,21.8827250555583,20.));
#82565=CARTESIAN_POINT('Ctrl Pts',(-43.2355506269018,21.9112538389585,0.));
#82566=CARTESIAN_POINT('Ctrl Pts',(-43.2355506269018,21.9112538389585,20.));
#82567=CARTESIAN_POINT('Ctrl Pts',(-43.217686350483,21.9397693310079,0.));
#82568=CARTESIAN_POINT('Ctrl Pts',(-43.217686350483,21.9397693310079,20.));
#82569=CARTESIAN_POINT('Ctrl Pts',(-43.1998029556363,21.9682715185322,0.));
#82570=CARTESIAN_POINT('Ctrl Pts',(-43.1998029556363,21.9682715185322,20.));
#82571=CARTESIAN_POINT('Ctrl Pts',(-43.1819004516401,21.9967603883628,0.));
#82572=CARTESIAN_POINT('Ctrl Pts',(-43.1819004516401,21.9967603883628,20.));
#82573=CARTESIAN_POINT('Ctrl Pts',(-43.1639788477821,22.0252359273373,0.));
#82574=CARTESIAN_POINT('Ctrl Pts',(-43.1639788477821,22.0252359273373,20.));
#82575=CARTESIAN_POINT('Ctrl Pts',(-43.1460381533594,22.0536981222997,0.));
#82576=CARTESIAN_POINT('Ctrl Pts',(-43.1460381533594,22.0536981222997,20.));
#82577=CARTESIAN_POINT('Ctrl Pts',(-43.1280783776785,22.0821469600997,0.));
#82578=CARTESIAN_POINT('Ctrl Pts',(-43.1280783776785,22.0821469600997,20.));
#82579=CARTESIAN_POINT('Ctrl Pts',(-43.1100995300552,22.1105824275933,0.));
#82580=CARTESIAN_POINT('Ctrl Pts',(-43.1100995300552,22.1105824275933,20.));
#82581=CARTESIAN_POINT('Ctrl Pts',(-43.0921016198148,22.1390045116426,0.));
#82582=CARTESIAN_POINT('Ctrl Pts',(-43.0921016198148,22.1390045116426,20.));
#82583=CARTESIAN_POINT('Ctrl Pts',(-43.0740846562917,22.1674131991155,0.));
#82584=CARTESIAN_POINT('Ctrl Pts',(-43.0740846562917,22.1674131991155,20.));
#82585=CARTESIAN_POINT('Ctrl Pts',(-43.0560486488298,22.1958084768867,0.));
#82586=CARTESIAN_POINT('Ctrl Pts',(-43.0560486488298,22.1958084768867,20.));
#82587=CARTESIAN_POINT('Ctrl Pts',(-43.0379936067822,22.2241903318366,0.));
#82588=CARTESIAN_POINT('Ctrl Pts',(-43.0379936067822,22.2241903318366,20.));
#82589=CARTESIAN_POINT('Ctrl Pts',(-43.0199195395115,22.252558750852,0.));
#82590=CARTESIAN_POINT('Ctrl Pts',(-43.0199195395115,22.252558750852,20.));
#82591=CARTESIAN_POINT('Ctrl Pts',(-43.0018264563892,22.2809137208256,0.));
#82592=CARTESIAN_POINT('Ctrl Pts',(-43.0018264563892,22.2809137208256,20.));
#82593=CARTESIAN_POINT('Ctrl Pts',(-42.9837143667966,22.3092552286564,0.));
#82594=CARTESIAN_POINT('Ctrl Pts',(-42.9837143667966,22.3092552286564,20.));
#82595=CARTESIAN_POINT('Ctrl Pts',(-42.965583280124,22.3375832612492,0.));
#82596=CARTESIAN_POINT('Ctrl Pts',(-42.965583280124,22.3375832612492,20.));
#82597=CARTESIAN_POINT('Ctrl Pts',(-42.947433205771,22.3658978055149,0.));
#82598=CARTESIAN_POINT('Ctrl Pts',(-42.947433205771,22.3658978055149,20.));
#82599=CARTESIAN_POINT('Ctrl Pts',(-42.9292641531465,22.3941988483709,0.));
#82600=CARTESIAN_POINT('Ctrl Pts',(-42.9292641531465,22.3941988483709,20.));
#82601=CARTESIAN_POINT('Ctrl Pts',(-42.9110761316689,22.4224863767407,0.));
#82602=CARTESIAN_POINT('Ctrl Pts',(-42.9110761316689,22.4224863767407,20.));
#82603=CARTESIAN_POINT('Ctrl Pts',(-42.8928691507659,22.4507603775546,0.));
#82604=CARTESIAN_POINT('Ctrl Pts',(-42.8928691507659,22.4507603775546,20.));
#82605=CARTESIAN_POINT('Ctrl Pts',(-42.8746432198744,22.4790208377488,0.));
#82606=CARTESIAN_POINT('Ctrl Pts',(-42.8746432198744,22.4790208377488,20.));
#82607=CARTESIAN_POINT('Ctrl Pts',(-42.8563983484404,22.5072677442656,0.));
#82608=CARTESIAN_POINT('Ctrl Pts',(-42.8563983484404,22.5072677442656,20.));
#82609=CARTESIAN_POINT('Ctrl Pts',(-42.8381345459193,22.535501084053,0.));
#82610=CARTESIAN_POINT('Ctrl Pts',(-42.8381345459193,22.535501084053,20.));
#82611=CARTESIAN_POINT('Ctrl Pts',(-42.8198518217756,22.5637208440656,0.));
#82612=CARTESIAN_POINT('Ctrl Pts',(-42.8198518217756,22.5637208440656,20.));
#82613=CARTESIAN_POINT('Ctrl Pts',(-42.8015501854832,22.5919270112639,0.));
#82614=CARTESIAN_POINT('Ctrl Pts',(-42.8015501854832,22.5919270112639,20.));
#82615=CARTESIAN_POINT('Ctrl Pts',(-42.7832296465255,22.620119572615,0.));
#82616=CARTESIAN_POINT('Ctrl Pts',(-42.7832296465255,22.620119572615,20.));
#82617=CARTESIAN_POINT('Ctrl Pts',(-42.7648902143955,22.6482985150925,0.));
#82618=CARTESIAN_POINT('Ctrl Pts',(-42.7648902143955,22.6482985150925,20.));
#82619=CARTESIAN_POINT('Ctrl Pts',(-42.7465318985949,22.6764638256759,0.));
#82620=CARTESIAN_POINT('Ctrl Pts',(-42.7465318985949,22.6764638256759,20.));
#82621=CARTESIAN_POINT('Ctrl Pts',(-42.7281547086347,22.7046154913511,0.));
#82622=CARTESIAN_POINT('Ctrl Pts',(-42.7281547086347,22.7046154913511,20.));
#82623=CARTESIAN_POINT('Ctrl Pts',(-42.7097586540349,22.73275349911,0.));
#82624=CARTESIAN_POINT('Ctrl Pts',(-42.7097586540349,22.73275349911,20.));
#82625=CARTESIAN_POINT('Ctrl Pts',(-42.6913437443248,22.7608778359508,0.));
#82626=CARTESIAN_POINT('Ctrl Pts',(-42.6913437443248,22.7608778359508,20.));
#82627=CARTESIAN_POINT('Ctrl Pts',(-42.6729099890431,22.788988488878,0.));
#82628=CARTESIAN_POINT('Ctrl Pts',(-42.6729099890431,22.788988488878,20.));
#82629=CARTESIAN_POINT('Ctrl Pts',(-42.6544573977378,22.8170854449023,0.));
#82630=CARTESIAN_POINT('Ctrl Pts',(-42.6544573977378,22.8170854449023,20.));
#82631=CARTESIAN_POINT('Ctrl Pts',(-42.6359859799663,22.845168691041,0.));
#82632=CARTESIAN_POINT('Ctrl Pts',(-42.6359859799663,22.845168691041,20.));
#82633=CARTESIAN_POINT('Ctrl Pts',(-42.6174957452953,22.8732382143174,0.));
#82634=CARTESIAN_POINT('Ctrl Pts',(-42.6174957452953,22.8732382143174,20.));
#82635=CARTESIAN_POINT('Ctrl Pts',(-42.5989867033005,22.9012940017616,0.));
#82636=CARTESIAN_POINT('Ctrl Pts',(-42.5989867033005,22.9012940017616,20.));
#82637=CARTESIAN_POINT('Ctrl Pts',(-42.5804588635669,22.9293360404094,0.));
#82638=CARTESIAN_POINT('Ctrl Pts',(-42.5804588635669,22.9293360404094,20.));
#82639=CARTESIAN_POINT('Ctrl Pts',(-42.5619122356886,22.9573643173033,0.));
#82640=CARTESIAN_POINT('Ctrl Pts',(-42.5619122356886,22.9573643173033,20.));
#82641=CARTESIAN_POINT('Ctrl Pts',(-42.5433468292689,22.9853788194919,0.));
#82642=CARTESIAN_POINT('Ctrl Pts',(-42.5433468292689,22.9853788194919,20.));
#82643=CARTESIAN_POINT('Ctrl Pts',(-42.5247626539203,23.0133795340298,0.));
#82644=CARTESIAN_POINT('Ctrl Pts',(-42.5247626539203,23.0133795340298,20.));
#82645=CARTESIAN_POINT('Ctrl Pts',(-42.5061597192647,23.0413664479785,0.));
#82646=CARTESIAN_POINT('Ctrl Pts',(-42.5061597192647,23.0413664479785,20.));
#82647=CARTESIAN_POINT('Ctrl Pts',(-42.4875380349329,23.0693395484056,0.));
#82648=CARTESIAN_POINT('Ctrl Pts',(-42.4875380349329,23.0693395484056,20.));
#82649=CARTESIAN_POINT('Ctrl Pts',(-42.4688976105654,23.0972988223849,0.));
#82650=CARTESIAN_POINT('Ctrl Pts',(-42.4688976105654,23.0972988223849,20.));
#82651=CARTESIAN_POINT('Ctrl Pts',(-42.4502384558115,23.125244256997,0.));
#82652=CARTESIAN_POINT('Ctrl Pts',(-42.4502384558115,23.125244256997,20.));
#82653=CARTESIAN_POINT('Ctrl Pts',(-42.4315605803298,23.1531758393284,0.));
#82654=CARTESIAN_POINT('Ctrl Pts',(-42.4315605803298,23.1531758393284,20.));
#82655=CARTESIAN_POINT('Ctrl Pts',(-42.4128639937879,23.1810935564721,0.));
#82656=CARTESIAN_POINT('Ctrl Pts',(-42.4128639937879,23.1810935564721,20.));
#82657=CARTESIAN_POINT('Ctrl Pts',(-42.3941487058631,23.2089973955278,0.));
#82658=CARTESIAN_POINT('Ctrl Pts',(-42.3941487058631,23.2089973955278,20.));
#82659=CARTESIAN_POINT('Ctrl Pts',(-42.3754147262417,23.2368873436013,0.));
#82660=CARTESIAN_POINT('Ctrl Pts',(-42.3754147262417,23.2368873436013,20.));
#82661=CARTESIAN_POINT('Ctrl Pts',(-42.3566620646188,23.2647633878047,0.));
#82662=CARTESIAN_POINT('Ctrl Pts',(-42.3566620646188,23.2647633878047,20.));
#82663=CARTESIAN_POINT('Ctrl Pts',(-42.3378907306988,23.2926255152563,0.));
#82664=CARTESIAN_POINT('Ctrl Pts',(-42.3378907306988,23.2926255152563,20.));
#82665=CARTESIAN_POINT('Ctrl Pts',(-42.3191007341954,23.320473713081,0.));
#82666=CARTESIAN_POINT('Ctrl Pts',(-42.3191007341954,23.320473713081,20.));
#82667=CARTESIAN_POINT('Ctrl Pts',(-42.3002920848317,23.3483079684103,0.));
#82668=CARTESIAN_POINT('Ctrl Pts',(-42.3002920848317,23.3483079684103,20.));
#82669=CARTESIAN_POINT('Ctrl Pts',(-42.2814647923395,23.3761282683822,0.));
#82670=CARTESIAN_POINT('Ctrl Pts',(-42.2814647923395,23.3761282683822,20.));
#82671=CARTESIAN_POINT('Ctrl Pts',(-42.2626188664603,23.4039346001409,0.));
#82672=CARTESIAN_POINT('Ctrl Pts',(-42.2626188664603,23.4039346001409,20.));
#82673=CARTESIAN_POINT('Ctrl Pts',(-42.2437543169442,23.4317269508371,0.));
#82674=CARTESIAN_POINT('Ctrl Pts',(-42.2437543169442,23.4317269508371,20.));
#82675=CARTESIAN_POINT('Ctrl Pts',(-42.2248711535508,23.4595053076277,0.));
#82676=CARTESIAN_POINT('Ctrl Pts',(-42.2248711535508,23.4595053076277,20.));
#82677=CARTESIAN_POINT('Ctrl Pts',(-42.2059693860486,23.4872696576759,0.));
#82678=CARTESIAN_POINT('Ctrl Pts',(-42.2059693860486,23.4872696576759,20.));
#82679=CARTESIAN_POINT('Ctrl Pts',(-42.1870490242153,23.5150199881514,0.));
#82680=CARTESIAN_POINT('Ctrl Pts',(-42.1870490242153,23.5150199881514,20.));
#82681=CARTESIAN_POINT('Ctrl Pts',(-42.1681100778379,23.5427562862307,0.));
#82682=CARTESIAN_POINT('Ctrl Pts',(-42.1681100778379,23.5427562862307,20.));
#82683=CARTESIAN_POINT('Ctrl Pts',(-42.1491525567126,23.5704785390969,0.));
#82684=CARTESIAN_POINT('Ctrl Pts',(-42.1491525567126,23.5704785390969,20.));
#82685=CARTESIAN_POINT('Ctrl Pts',(-42.1301764706447,23.5981867339394,0.));
#82686=CARTESIAN_POINT('Ctrl Pts',(-42.1301764706447,23.5981867339394,20.));
#82687=CARTESIAN_POINT('Ctrl Pts',(-42.1111818294483,23.6258808579542,0.));
#82688=CARTESIAN_POINT('Ctrl Pts',(-42.1111818294483,23.6258808579542,20.));
#82689=CARTESIAN_POINT('Ctrl Pts',(-42.0921686429469,23.6535608983435,0.));
#82690=CARTESIAN_POINT('Ctrl Pts',(-42.0921686429469,23.6535608983435,20.));
#82691=CARTESIAN_POINT('Ctrl Pts',(-42.0731369209731,23.6812268423159,0.));
#82692=CARTESIAN_POINT('Ctrl Pts',(-42.0731369209731,23.6812268423159,20.));
#82693=CARTESIAN_POINT('Ctrl Pts',(-42.0540866733685,23.7088786770864,0.));
#82694=CARTESIAN_POINT('Ctrl Pts',(-42.0540866733685,23.7088786770864,20.));
#82695=CARTESIAN_POINT('Ctrl Pts',(-42.0350179099839,23.7365163898767,0.));
#82696=CARTESIAN_POINT('Ctrl Pts',(-42.0350179099839,23.7365163898767,20.));
#82697=CARTESIAN_POINT('Ctrl Pts',(-42.0159306406794,23.7641399679152,0.));
#82698=CARTESIAN_POINT('Ctrl Pts',(-42.0159306406794,23.7641399679152,20.));
#82699=CARTESIAN_POINT('Ctrl Pts',(-41.9968248753238,23.7917493984363,0.));
#82700=CARTESIAN_POINT('Ctrl Pts',(-41.9968248753238,23.7917493984363,20.));
#82701=CARTESIAN_POINT('Ctrl Pts',(-41.9777006237952,23.8193446686815,0.));
#82702=CARTESIAN_POINT('Ctrl Pts',(-41.9777006237952,23.8193446686815,20.));
#82703=CARTESIAN_POINT('Ctrl Pts',(-41.9585578959807,23.8469257658985,0.));
#82704=CARTESIAN_POINT('Ctrl Pts',(-41.9585578959807,23.8469257658985,20.));
#82705=CARTESIAN_POINT('Ctrl Pts',(-41.9393967017767,23.8744926773418,0.));
#82706=CARTESIAN_POINT('Ctrl Pts',(-41.9393967017767,23.8744926773418,20.));
#82707=CARTESIAN_POINT('Ctrl Pts',(-41.9202170510888,23.9020453902722,0.));
#82708=CARTESIAN_POINT('Ctrl Pts',(-41.9202170510888,23.9020453902722,20.));
#82709=CARTESIAN_POINT('Ctrl Pts',(-41.9010189538314,23.9295838919572,0.));
#82710=CARTESIAN_POINT('Ctrl Pts',(-41.9010189538314,23.9295838919572,20.));
#82711=CARTESIAN_POINT('Ctrl Pts',(-41.8818024199281,23.9571081696707,0.));
#82712=CARTESIAN_POINT('Ctrl Pts',(-41.8818024199281,23.9571081696707,20.));
#82713=CARTESIAN_POINT('Ctrl Pts',(-41.8625674593112,23.984618210693,0.));
#82714=CARTESIAN_POINT('Ctrl Pts',(-41.8625674593112,23.984618210693,20.));
#82715=CARTESIAN_POINT('Ctrl Pts',(-41.8433140819226,24.0121140023113,0.));
#82716=CARTESIAN_POINT('Ctrl Pts',(-41.8433140819226,24.0121140023113,20.));
#82717=CARTESIAN_POINT('Ctrl Pts',(-41.824042297713,24.0395955318191,0.));
#82718=CARTESIAN_POINT('Ctrl Pts',(-41.824042297713,24.0395955318191,20.));
#82719=CARTESIAN_POINT('Ctrl Pts',(-41.8047521166422,24.0670627865166,0.));
#82720=CARTESIAN_POINT('Ctrl Pts',(-41.8047521166422,24.0670627865166,20.));
#82721=CARTESIAN_POINT('Ctrl Pts',(-41.785443548679,24.0945157537107,0.));
#82722=CARTESIAN_POINT('Ctrl Pts',(-41.785443548679,24.0945157537107,20.));
#82723=CARTESIAN_POINT('Ctrl Pts',(-41.7661166038015,24.1219544207148,0.));
#82724=CARTESIAN_POINT('Ctrl Pts',(-41.7661166038015,24.1219544207148,20.));
#82725=CARTESIAN_POINT('Ctrl Pts',(-41.7467712919966,24.1493787748488,0.));
#82726=CARTESIAN_POINT('Ctrl Pts',(-41.7467712919966,24.1493787748488,20.));
#82727=CARTESIAN_POINT('Ctrl Pts',(-41.7274076232605,24.1767888034393,0.));
#82728=CARTESIAN_POINT('Ctrl Pts',(-41.7274076232605,24.1767888034393,20.));
#82729=CARTESIAN_POINT('Ctrl Pts',(-41.7080256075983,24.2041844938197,0.));
#82730=CARTESIAN_POINT('Ctrl Pts',(-41.7080256075983,24.2041844938197,20.));
#82731=CARTESIAN_POINT('Ctrl Pts',(-41.688625255024,24.2315658333297,0.));
#82732=CARTESIAN_POINT('Ctrl Pts',(-41.688625255024,24.2315658333297,20.));
#82733=CARTESIAN_POINT('Ctrl Pts',(-41.6692065755608,24.2589328093159,0.));
#82734=CARTESIAN_POINT('Ctrl Pts',(-41.6692065755608,24.2589328093159,20.));
#82735=CARTESIAN_POINT('Ctrl Pts',(-41.6497695792407,24.2862854091312,0.));
#82736=CARTESIAN_POINT('Ctrl Pts',(-41.6497695792407,24.2862854091312,20.));
#82737=CARTESIAN_POINT('Ctrl Pts',(-41.630314276105,24.3136236201351,0.));
#82738=CARTESIAN_POINT('Ctrl Pts',(-41.630314276105,24.3136236201351,20.));
#82739=CARTESIAN_POINT('Ctrl Pts',(-41.610840676204,24.340947429694,0.));
#82740=CARTESIAN_POINT('Ctrl Pts',(-41.610840676204,24.340947429694,20.));
#82741=CARTESIAN_POINT('Ctrl Pts',(-41.5913487895971,24.368256825181,0.));
#82742=CARTESIAN_POINT('Ctrl Pts',(-41.5913487895971,24.368256825181,20.));
#82743=CARTESIAN_POINT('Ctrl Pts',(-41.5718386263526,24.3955517939756,0.));
#82744=CARTESIAN_POINT('Ctrl Pts',(-41.5718386263526,24.3955517939756,20.));
#82745=CARTESIAN_POINT('Ctrl Pts',(-41.5523101965477,24.4228323234645,0.));
#82746=CARTESIAN_POINT('Ctrl Pts',(-41.5523101965477,24.4228323234645,20.));
#82747=CARTESIAN_POINT('Ctrl Pts',(-41.5327635102685,24.4500984010406,0.));
#82748=CARTESIAN_POINT('Ctrl Pts',(-41.5327635102685,24.4500984010406,20.));
#82749=CARTESIAN_POINT('Ctrl Pts',(-41.5131985776101,24.4773500141036,0.));
#82750=CARTESIAN_POINT('Ctrl Pts',(-41.5131985776101,24.4773500141036,20.));
#82751=CARTESIAN_POINT('Ctrl Pts',(-41.4936154086768,24.5045871500598,0.));
#82752=CARTESIAN_POINT('Ctrl Pts',(-41.4936154086768,24.5045871500598,20.));
#82753=CARTESIAN_POINT('Ctrl Pts',(-41.4740140135823,24.5318097963222,0.));
#82754=CARTESIAN_POINT('Ctrl Pts',(-41.4740140135823,24.5318097963222,20.));
#82755=CARTESIAN_POINT('Ctrl Pts',(-41.4543944024488,24.5590179403106,0.));
#82756=CARTESIAN_POINT('Ctrl Pts',(-41.4543944024488,24.5590179403106,20.));
#82757=CARTESIAN_POINT('Ctrl Pts',(-41.4347565854076,24.5862115694513,0.));
#82758=CARTESIAN_POINT('Ctrl Pts',(-41.4347565854076,24.5862115694513,20.));
#82759=CARTESIAN_POINT('Ctrl Pts',(-41.4151005725989,24.6133906711774,0.));
#82760=CARTESIAN_POINT('Ctrl Pts',(-41.4151005725989,24.6133906711774,20.));
#82761=CARTESIAN_POINT('Ctrl Pts',(-41.3954263741717,24.6405552329288,0.));
#82762=CARTESIAN_POINT('Ctrl Pts',(-41.3954263741717,24.6405552329288,20.));
#82763=CARTESIAN_POINT('Ctrl Pts',(-41.3757340002844,24.6677052421523,0.));
#82764=CARTESIAN_POINT('Ctrl Pts',(-41.3757340002844,24.6677052421523,20.));
#82765=CARTESIAN_POINT('Ctrl Pts',(-41.3560234611038,24.694840686301,0.));
#82766=CARTESIAN_POINT('Ctrl Pts',(-41.3560234611038,24.694840686301,20.));
#82767=CARTESIAN_POINT('Ctrl Pts',(-41.3362947668064,24.7219615528352,0.));
#82768=CARTESIAN_POINT('Ctrl Pts',(-41.3362947668064,24.7219615528352,20.));
#82769=CARTESIAN_POINT('Ctrl Pts',(-41.3165479275773,24.7490678292217,0.));
#82770=CARTESIAN_POINT('Ctrl Pts',(-41.3165479275773,24.7490678292217,20.));
#82771=CARTESIAN_POINT('Ctrl Pts',(-41.2967829536105,24.776159502934,0.));
#82772=CARTESIAN_POINT('Ctrl Pts',(-41.2967829536105,24.776159502934,20.));
#82773=CARTESIAN_POINT('Ctrl Pts',(-41.276999855109,24.8032365614525,0.));
#82774=CARTESIAN_POINT('Ctrl Pts',(-41.276999855109,24.8032365614525,20.));
#82775=CARTESIAN_POINT('Ctrl Pts',(-41.2571986422843,24.8302989922639,0.));
#82776=CARTESIAN_POINT('Ctrl Pts',(-41.2571986422843,24.8302989922639,20.));
#82777=CARTESIAN_POINT('Ctrl Pts',(-41.2373793253577,24.8573467828623,0.));
#82778=CARTESIAN_POINT('Ctrl Pts',(-41.2373793253577,24.8573467828623,20.));
#82779=CARTESIAN_POINT('Ctrl Pts',(-41.2175419145589,24.8843799207482,0.));
#82780=CARTESIAN_POINT('Ctrl Pts',(-41.2175419145589,24.8843799207482,20.));
#82781=CARTESIAN_POINT('Ctrl Pts',(-41.1976864201268,24.9113983934293,0.));
#82782=CARTESIAN_POINT('Ctrl Pts',(-41.1976864201268,24.9113983934293,20.));
#82783=CARTESIAN_POINT('Ctrl Pts',(-41.1778128523092,24.9384021884197,0.));
#82784=CARTESIAN_POINT('Ctrl Pts',(-41.1778128523092,24.9384021884197,20.));
#82785=CARTESIAN_POINT('Ctrl Pts',(-41.1579212213625,24.9653912932402,0.));
#82786=CARTESIAN_POINT('Ctrl Pts',(-41.1579212213625,24.9653912932402,20.));
#82787=CARTESIAN_POINT('Ctrl Pts',(-41.1380115375521,24.9923656954187,0.));
#82788=CARTESIAN_POINT('Ctrl Pts',(-41.1380115375521,24.9923656954187,20.));
#82789=CARTESIAN_POINT('Ctrl Pts',(-41.1180838111525,25.0193253824897,0.));
#82790=CARTESIAN_POINT('Ctrl Pts',(-41.1180838111525,25.0193253824897,20.));
#82791=CARTESIAN_POINT('Ctrl Pts',(-41.0981380524472,25.0462703419947,0.));
#82792=CARTESIAN_POINT('Ctrl Pts',(-41.0981380524472,25.0462703419947,20.));
#82793=CARTESIAN_POINT('Ctrl Pts',(-41.0781742717283,25.0732005614819,0.));
#82794=CARTESIAN_POINT('Ctrl Pts',(-41.0781742717283,25.0732005614819,20.));
#82795=CARTESIAN_POINT('Ctrl Pts',(-41.058192479297,25.1001160285063,0.));
#82796=CARTESIAN_POINT('Ctrl Pts',(-41.058192479297,25.1001160285063,20.));
#82797=CARTESIAN_POINT('Ctrl Pts',(-41.0381926854636,25.1270167306298,0.));
#82798=CARTESIAN_POINT('Ctrl Pts',(-41.0381926854636,25.1270167306298,20.));
#82799=CARTESIAN_POINT('Ctrl Pts',(-41.0181749005471,25.1539026554213,0.));
#82800=CARTESIAN_POINT('Ctrl Pts',(-41.0181749005471,25.1539026554213,20.));
#82801=CARTESIAN_POINT('Ctrl Pts',(-40.9981391348755,25.1807737904566,0.));
#82802=CARTESIAN_POINT('Ctrl Pts',(-40.9981391348755,25.1807737904566,20.));
#82803=CARTESIAN_POINT('Ctrl Pts',(-40.9780853987856,25.2076301233182,0.));
#82804=CARTESIAN_POINT('Ctrl Pts',(-40.9780853987856,25.2076301233182,20.));
#82805=CARTESIAN_POINT('Ctrl Pts',(-40.9580137026228,25.2344716415952,0.));
#82806=CARTESIAN_POINT('Ctrl Pts',(-40.9580137026228,25.2344716415952,20.));
#82807=CARTESIAN_POINT('Ctrl Pts',(-40.9379240567416,25.2612983328836,0.));
#82808=CARTESIAN_POINT('Ctrl Pts',(-40.9379240567416,25.2612983328836,20.));
#82809=CARTESIAN_POINT('Ctrl Pts',(-40.9178164715051,25.2881101847861,0.));
#82810=CARTESIAN_POINT('Ctrl Pts',(-40.9178164715051,25.2881101847861,20.));
#82811=CARTESIAN_POINT('Ctrl Pts',(-40.8976909572856,25.3149071849127,0.));
#82812=CARTESIAN_POINT('Ctrl Pts',(-40.8976909572856,25.3149071849127,20.));
#82813=CARTESIAN_POINT('Ctrl Pts',(-40.8775475244644,25.3416893208802,0.));
#82814=CARTESIAN_POINT('Ctrl Pts',(-40.8775475244644,25.3416893208802,20.));
#82815=CARTESIAN_POINT('Ctrl Pts',(-40.8573861834316,25.3684565803126,0.));
#82816=CARTESIAN_POINT('Ctrl Pts',(-40.8573861834316,25.3684565803126,20.));
#82817=CARTESIAN_POINT('Ctrl Pts',(-40.8372069445862,25.3952089508407,0.));
#82818=CARTESIAN_POINT('Ctrl Pts',(-40.8372069445862,25.3952089508407,20.));
#82819=CARTESIAN_POINT('Ctrl Pts',(-40.8170098183362,25.4219464201024,0.));
#82820=CARTESIAN_POINT('Ctrl Pts',(-40.8170098183362,25.4219464201024,20.));
#82821=CARTESIAN_POINT('Ctrl Pts',(-40.7967948150981,25.4486689757422,0.));
#82822=CARTESIAN_POINT('Ctrl Pts',(-40.7967948150981,25.4486689757422,20.));
#82823=CARTESIAN_POINT('Ctrl Pts',(-40.7765619452973,25.4753766054114,0.));
#82824=CARTESIAN_POINT('Ctrl Pts',(-40.7765619452973,25.4753766054114,20.));
#82825=CARTESIAN_POINT('Ctrl Pts',(-40.7563112193678,25.5020692967677,0.));
#82826=CARTESIAN_POINT('Ctrl Pts',(-40.7563112193678,25.5020692967677,20.));
#82827=CARTESIAN_POINT('Ctrl Pts',(-40.7360426477524,25.528747037476,0.));
#82828=CARTESIAN_POINT('Ctrl Pts',(-40.7360426477524,25.528747037476,20.));
#82829=CARTESIAN_POINT('Ctrl Pts',(-40.715756240903,25.5554098152083,0.));
#82830=CARTESIAN_POINT('Ctrl Pts',(-40.715756240903,25.5554098152083,20.));
#82831=CARTESIAN_POINT('Ctrl Pts',(-40.6954520092804,25.5820576176439,0.));
#82832=CARTESIAN_POINT('Ctrl Pts',(-40.6954520092804,25.5820576176439,20.));
#82833=CARTESIAN_POINT('Ctrl Pts',(-40.6751299633543,25.6086904324689,0.));
#82834=CARTESIAN_POINT('Ctrl Pts',(-40.6751299633543,25.6086904324689,20.));
#82835=CARTESIAN_POINT('Ctrl Pts',(-40.6547901136033,25.6353082473768,0.));
#82836=CARTESIAN_POINT('Ctrl Pts',(-40.6547901136033,25.6353082473768,20.));
#82837=CARTESIAN_POINT('Ctrl Pts',(-40.6344324705148,25.6619110500677,0.));
#82838=CARTESIAN_POINT('Ctrl Pts',(-40.6344324705148,25.6619110500677,20.));
#82839=CARTESIAN_POINT('Ctrl Pts',(-40.6140570445847,25.6884988282486,0.));
#82840=CARTESIAN_POINT('Ctrl Pts',(-40.6140570445847,25.6884988282486,20.));
#82841=CARTESIAN_POINT('Ctrl Pts',(-40.5936638463177,25.7150715696332,0.));
#82842=CARTESIAN_POINT('Ctrl Pts',(-40.5936638463177,25.7150715696332,20.));
#82843=CARTESIAN_POINT('Ctrl Pts',(-40.5732528862276,25.7416292619425,0.));
#82844=CARTESIAN_POINT('Ctrl Pts',(-40.5732528862276,25.7416292619425,20.));
#82845=CARTESIAN_POINT('Ctrl Pts',(-40.5528241748366,25.768171892904,0.));
#82846=CARTESIAN_POINT('Ctrl Pts',(-40.5528241748366,25.768171892904,20.));
#82847=CARTESIAN_POINT('Ctrl Pts',(-40.5323777226758,25.7946994502526,0.));
#82848=CARTESIAN_POINT('Ctrl Pts',(-40.5323777226758,25.7946994502526,20.));
#82849=CARTESIAN_POINT('Ctrl Pts',(-40.5119135402853,25.8212119217304,0.));
#82850=CARTESIAN_POINT('Ctrl Pts',(-40.5119135402853,25.8212119217304,20.));
#82851=CARTESIAN_POINT('Ctrl Pts',(-40.4914316382141,25.8477092950863,0.));
#82852=CARTESIAN_POINT('Ctrl Pts',(-40.4914316382141,25.8477092950863,20.));
#82853=CARTESIAN_POINT('Ctrl Pts',(-40.4709320270197,25.8741915580762,0.));
#82854=CARTESIAN_POINT('Ctrl Pts',(-40.4709320270197,25.8741915580762,20.));
#82855=CARTESIAN_POINT('Ctrl Pts',(-40.4504147172684,25.900658698463,0.));
#82856=CARTESIAN_POINT('Ctrl Pts',(-40.4504147172684,25.900658698463,20.));
#82857=CARTESIAN_POINT('Ctrl Pts',(-40.4298797195353,25.9271107040168,0.));
#82858=CARTESIAN_POINT('Ctrl Pts',(-40.4298797195353,25.9271107040168,20.));
#82859=CARTESIAN_POINT('Ctrl Pts',(-40.4093270444043,25.953547562515,0.));
#82860=CARTESIAN_POINT('Ctrl Pts',(-40.4093270444043,25.953547562515,20.));
#82861=CARTESIAN_POINT('Ctrl Pts',(-40.3887567024682,25.9799692617416,0.));
#82862=CARTESIAN_POINT('Ctrl Pts',(-40.3887567024682,25.9799692617416,20.));
#82863=CARTESIAN_POINT('Ctrl Pts',(-40.3681687043284,26.0063757894875,0.));
#82864=CARTESIAN_POINT('Ctrl Pts',(-40.3681687043284,26.0063757894875,20.));
#82865=CARTESIAN_POINT('Ctrl Pts',(-40.347563060595,26.0327671335511,0.));
#82866=CARTESIAN_POINT('Ctrl Pts',(-40.347563060595,26.0327671335511,20.));
#82867=CARTESIAN_POINT('Ctrl Pts',(-40.326939781887,26.0591432817373,0.));
#82868=CARTESIAN_POINT('Ctrl Pts',(-40.326939781887,26.0591432817373,20.));
#82869=CARTESIAN_POINT('Ctrl Pts',(-40.3062988788318,26.0855042218583,0.));
#82870=CARTESIAN_POINT('Ctrl Pts',(-40.3062988788318,26.0855042218583,20.));
#82871=CARTESIAN_POINT('Ctrl Pts',(-40.2856403620657,26.1118499417334,0.));
#82872=CARTESIAN_POINT('Ctrl Pts',(-40.2856403620657,26.1118499417334,20.));
#82873=CARTESIAN_POINT('Ctrl Pts',(-40.2649642422341,26.1381804291892,0.));
#82874=CARTESIAN_POINT('Ctrl Pts',(-40.2649642422341,26.1381804291892,20.));
#82875=CARTESIAN_POINT('Ctrl Pts',(-40.2442705299908,26.1644956720595,0.));
#82876=CARTESIAN_POINT('Ctrl Pts',(-40.2442705299908,26.1644956720595,20.));
#82877=CARTESIAN_POINT('Ctrl Pts',(-40.2235592359986,26.1907956581851,0.));
#82878=CARTESIAN_POINT('Ctrl Pts',(-40.2235592359986,26.1907956581851,20.));
#82879=CARTESIAN_POINT('Ctrl Pts',(-40.2028303709288,26.217080375414,0.));
#82880=CARTESIAN_POINT('Ctrl Pts',(-40.2028303709288,26.217080375414,20.));
#82881=CARTESIAN_POINT('Ctrl Pts',(-40.1820839454613,26.2433498116008,0.));
#82882=CARTESIAN_POINT('Ctrl Pts',(-40.1820839454613,26.2433498116008,20.));
#82883=CARTESIAN_POINT('Ctrl Pts',(-40.161319970285,26.2696039546074,0.));
#82884=CARTESIAN_POINT('Ctrl Pts',(-40.161319970285,26.2696039546074,20.));
#82885=CARTESIAN_POINT('Ctrl Pts',(-40.1405384560971,26.2958427923028,0.));
#82886=CARTESIAN_POINT('Ctrl Pts',(-40.1405384560971,26.2958427923028,20.));
#82887=CARTESIAN_POINT('Ctrl Pts',(-40.1197394136039,26.3220663125631,0.));
#82888=CARTESIAN_POINT('Ctrl Pts',(-40.1197394136039,26.3220663125631,20.));
#82889=CARTESIAN_POINT('Ctrl Pts',(-40.0989228535202,26.3482745032719,0.));
#82890=CARTESIAN_POINT('Ctrl Pts',(-40.0989228535202,26.3482745032719,20.));
#82891=CARTESIAN_POINT('Ctrl Pts',(-40.0780887865696,26.3744673523197,0.));
#82892=CARTESIAN_POINT('Ctrl Pts',(-40.0780887865696,26.3744673523197,20.));
#82893=CARTESIAN_POINT('Ctrl Pts',(-40.0572372234844,26.4006448476041,0.));
#82894=CARTESIAN_POINT('Ctrl Pts',(-40.0572372234844,26.4006448476041,20.));
#82895=CARTESIAN_POINT('Ctrl Pts',(-40.0363681750053,26.4268069770299,0.));
#82896=CARTESIAN_POINT('Ctrl Pts',(-40.0363681750053,26.4268069770299,20.));
#82897=CARTESIAN_POINT('Ctrl Pts',(-40.015481651882,26.4529537285089,0.));
#82898=CARTESIAN_POINT('Ctrl Pts',(-40.015481651882,26.4529537285089,20.));
#82899=CARTESIAN_POINT('Ctrl Pts',(-39.9945776648731,26.4790850899607,0.));
#82900=CARTESIAN_POINT('Ctrl Pts',(-39.9945776648731,26.4790850899607,20.));
#82901=CARTESIAN_POINT('Ctrl Pts',(-39.9736562247456,26.5052010493117,0.));
#82902=CARTESIAN_POINT('Ctrl Pts',(-39.9736562247456,26.5052010493117,20.));
#82903=CARTESIAN_POINT('Ctrl Pts',(-39.9527173422752,26.5313015944953,0.));
#82904=CARTESIAN_POINT('Ctrl Pts',(-39.9527173422752,26.5313015944953,20.));
#82905=CARTESIAN_POINT('Ctrl Pts',(-39.9317610282459,26.5573867134521,0.));
#82906=CARTESIAN_POINT('Ctrl Pts',(-39.9317610282459,26.5573867134521,20.));
#82907=CARTESIAN_POINT('Ctrl Pts',(-39.9107872934506,26.5834563941296,0.));
#82908=CARTESIAN_POINT('Ctrl Pts',(-39.9107872934506,26.5834563941296,20.));
#82909=CARTESIAN_POINT('Ctrl Pts',(-39.8897961486907,26.6095106244829,0.));
#82910=CARTESIAN_POINT('Ctrl Pts',(-39.8897961486907,26.6095106244829,20.));
#82911=CARTESIAN_POINT('Ctrl Pts',(-39.8687876047769,26.6355493924743,0.));
#82912=CARTESIAN_POINT('Ctrl Pts',(-39.8687876047769,26.6355493924743,20.));
#82913=CARTESIAN_POINT('Ctrl Pts',(-39.847761672528,26.6615726860734,0.));
#82914=CARTESIAN_POINT('Ctrl Pts',(-39.847761672528,26.6615726860734,20.));
#82915=CARTESIAN_POINT('Ctrl Pts',(-39.8267183627717,26.687580493257,0.));
#82916=CARTESIAN_POINT('Ctrl Pts',(-39.8267183627717,26.687580493257,20.));
#82917=CARTESIAN_POINT('Ctrl Pts',(-39.8056576863443,26.713572802009,0.));
#82918=CARTESIAN_POINT('Ctrl Pts',(-39.8056576863443,26.713572802009,20.));
#82919=CARTESIAN_POINT('Ctrl Pts',(-39.7845796540903,26.7395496003209,0.));
#82920=CARTESIAN_POINT('Ctrl Pts',(-39.7845796540903,26.7395496003209,20.));
#82921=CARTESIAN_POINT('Ctrl Pts',(-39.7634842768632,26.7655108761908,0.));
#82922=CARTESIAN_POINT('Ctrl Pts',(-39.7634842768632,26.7655108761908,20.));
#82923=CARTESIAN_POINT('Ctrl Pts',(-39.7423715655248,26.7914566176244,0.));
#82924=CARTESIAN_POINT('Ctrl Pts',(-39.7423715655248,26.7914566176244,20.));
#82925=CARTESIAN_POINT('Ctrl Pts',(-39.7212415309462,26.8173868126344,0.));
#82926=CARTESIAN_POINT('Ctrl Pts',(-39.7212415309462,26.8173868126344,20.));
#82927=CARTESIAN_POINT('Ctrl Pts',(-39.7000941840066,26.843301449241,0.));
#82928=CARTESIAN_POINT('Ctrl Pts',(-39.7000941840066,26.843301449241,20.));
#82929=CARTESIAN_POINT('Ctrl Pts',(-39.6789295355942,26.8692005154716,0.));
#82930=CARTESIAN_POINT('Ctrl Pts',(-39.6789295355942,26.8692005154716,20.));
#82931=CARTESIAN_POINT('Ctrl Pts',(-39.6577475966055,26.8950839993609,0.));
#82932=CARTESIAN_POINT('Ctrl Pts',(-39.6577475966055,26.8950839993609,20.));
#82933=CARTESIAN_POINT('Ctrl Pts',(-39.6365483779458,26.9209518889509,0.));
#82934=CARTESIAN_POINT('Ctrl Pts',(-39.6365483779458,26.9209518889509,20.));
#82935=CARTESIAN_POINT('Ctrl Pts',(-39.6153318905283,26.9468041722907,0.));
#82936=CARTESIAN_POINT('Ctrl Pts',(-39.6153318905283,26.9468041722907,20.));
#82937=CARTESIAN_POINT('Ctrl Pts',(-39.5940981452753,26.972640837437,0.));
#82938=CARTESIAN_POINT('Ctrl Pts',(-39.5940981452753,26.972640837437,20.));
#82939=CARTESIAN_POINT('Ctrl Pts',(-39.5728471531178,26.9984618724537,0.));
#82940=CARTESIAN_POINT('Ctrl Pts',(-39.5728471531178,26.9984618724537,20.));
#82941=CARTESIAN_POINT('Ctrl Pts',(-39.5515789249953,27.0242672654118,0.));
#82942=CARTESIAN_POINT('Ctrl Pts',(-39.5515789249953,27.0242672654118,20.));
#82943=CARTESIAN_POINT('Ctrl Pts',(-39.5302934718558,27.0500570043898,0.));
#82944=CARTESIAN_POINT('Ctrl Pts',(-39.5302934718558,27.0500570043898,20.));
#82945=CARTESIAN_POINT('Ctrl Pts',(-39.5089908046561,27.0758310774732,0.));
#82946=CARTESIAN_POINT('Ctrl Pts',(-39.5089908046561,27.0758310774732,20.));
#82947=CARTESIAN_POINT('Ctrl Pts',(-39.4876709343614,27.1015894727552,0.));
#82948=CARTESIAN_POINT('Ctrl Pts',(-39.4876709343614,27.1015894727552,20.));
#82949=CARTESIAN_POINT('Ctrl Pts',(-39.4663338719455,27.1273321783362,0.));
#82950=CARTESIAN_POINT('Ctrl Pts',(-39.4663338719455,27.1273321783362,20.));
#82951=CARTESIAN_POINT('Ctrl Pts',(-39.4449796283908,27.153059182324,0.));
#82952=CARTESIAN_POINT('Ctrl Pts',(-39.4449796283908,27.153059182324,20.));
#82953=CARTESIAN_POINT('Ctrl Pts',(-39.4236082146882,27.1787704728336,0.));
#82954=CARTESIAN_POINT('Ctrl Pts',(-39.4236082146882,27.1787704728336,20.));
#82955=CARTESIAN_POINT('Ctrl Pts',(-39.4022196418372,27.2044660379877,0.));
#82956=CARTESIAN_POINT('Ctrl Pts',(-39.4022196418372,27.2044660379877,20.));
#82957=CARTESIAN_POINT('Ctrl Pts',(-39.3808139208456,27.2301458659157,0.));
#82958=CARTESIAN_POINT('Ctrl Pts',(-39.3808139208456,27.2301458659157,20.));
#82959=CARTESIAN_POINT('Ctrl Pts',(-39.3593910627297,27.2558099447548,0.));
#82960=CARTESIAN_POINT('Ctrl Pts',(-39.3593910627297,27.2558099447548,20.));
#82961=CARTESIAN_POINT('Ctrl Pts',(-39.3379510785145,27.2814582626492,0.));
#82962=CARTESIAN_POINT('Ctrl Pts',(-39.3379510785145,27.2814582626492,20.));
#82963=CARTESIAN_POINT('Ctrl Pts',(-39.3164939792334,27.3070908077508,0.));
#82964=CARTESIAN_POINT('Ctrl Pts',(-39.3164939792334,27.3070908077508,20.));
#82965=CARTESIAN_POINT('Ctrl Pts',(-39.2950197759285,27.3327075682187,0.));
#82966=CARTESIAN_POINT('Ctrl Pts',(-39.2950197759285,27.3327075682187,20.));
#82967=CARTESIAN_POINT('Ctrl Pts',(-39.2735284796508,27.3583085322198,0.));
#82968=CARTESIAN_POINT('Ctrl Pts',(-39.2735284796508,27.3583085322198,20.));
#82969=CARTESIAN_POINT('Ctrl Pts',(-39.25202010146,27.3838936879286,0.));
#82970=CARTESIAN_POINT('Ctrl Pts',(-39.25202010146,27.3838936879286,20.));
#82971=CARTESIAN_POINT('Ctrl Pts',(-39.2304946524241,27.4094630235265,0.));
#82972=CARTESIAN_POINT('Ctrl Pts',(-39.2304946524241,27.4094630235265,20.));
#82973=CARTESIAN_POINT('Ctrl Pts',(-39.2089521436188,27.4350165272023,0.));
#82974=CARTESIAN_POINT('Ctrl Pts',(-39.2089521436188,27.4350165272023,20.));
#82975=CARTESIAN_POINT('Ctrl Pts',(-39.1873925861285,27.4605541871518,0.));
#82976=CARTESIAN_POINT('Ctrl Pts',(-39.1873925861285,27.4605541871518,20.));
#82977=CARTESIAN_POINT('Ctrl Pts',(-39.1658159910458,27.4860759915783,0.));
#82978=CARTESIAN_POINT('Ctrl Pts',(-39.1658159910458,27.4860759915783,20.));
#82979=CARTESIAN_POINT('Ctrl Pts',(-39.1442223694722,27.5115819286926,0.));
#82980=CARTESIAN_POINT('Ctrl Pts',(-39.1442223694722,27.5115819286926,20.));
#82981=CARTESIAN_POINT('Ctrl Pts',(-39.1226117325183,27.5370719867136,0.));
#82982=CARTESIAN_POINT('Ctrl Pts',(-39.1226117325183,27.5370719867136,20.));
#82983=CARTESIAN_POINT('Ctrl Pts',(-39.100984091303,27.5625461538675,0.));
#82984=CARTESIAN_POINT('Ctrl Pts',(-39.100984091303,27.5625461538675,20.));
#82985=CARTESIAN_POINT('Ctrl Pts',(-39.0793394569537,27.5880044183879,0.));
#82986=CARTESIAN_POINT('Ctrl Pts',(-39.0793394569537,27.5880044183879,20.));
#82987=CARTESIAN_POINT('Ctrl Pts',(-39.057677840606,27.6134467685155,0.));
#82988=CARTESIAN_POINT('Ctrl Pts',(-39.057677840606,27.6134467685155,20.));
#82989=CARTESIAN_POINT('Ctrl Pts',(-39.0359992534037,27.6388731924983,0.));
#82990=CARTESIAN_POINT('Ctrl Pts',(-39.0359992534037,27.6388731924983,20.));
#82991=CARTESIAN_POINT('Ctrl Pts',(-39.0143037064988,27.6642836785915,0.));
#82992=CARTESIAN_POINT('Ctrl Pts',(-39.0143037064988,27.6642836785915,20.));
#82993=CARTESIAN_POINT('Ctrl Pts',(-38.9925912110523,27.6896782150583,0.));
#82994=CARTESIAN_POINT('Ctrl Pts',(-38.9925912110523,27.6896782150583,20.));
#82995=CARTESIAN_POINT('Ctrl Pts',(-38.9708617782339,27.7150567901695,0.));
#82996=CARTESIAN_POINT('Ctrl Pts',(-38.9708617782339,27.7150567901695,20.));
#82997=CARTESIAN_POINT('Ctrl Pts',(-38.9491154192216,27.7404193922036,0.));
#82998=CARTESIAN_POINT('Ctrl Pts',(-38.9491154192216,27.7404193922036,20.));
#82999=CARTESIAN_POINT('Ctrl Pts',(-38.9273521452022,27.7657660094466,0.));
#83000=CARTESIAN_POINT('Ctrl Pts',(-38.9273521452022,27.7657660094466,20.));
#83001=CARTESIAN_POINT('Ctrl Pts',(-38.9055719673706,27.7910966301919,0.));
#83002=CARTESIAN_POINT('Ctrl Pts',(-38.9055719673706,27.7910966301919,20.));
#83003=CARTESIAN_POINT('Ctrl Pts',(-38.8837748969299,27.8164112427396,0.));
#83004=CARTESIAN_POINT('Ctrl Pts',(-38.8837748969299,27.8164112427396,20.));
#83005=CARTESIAN_POINT('Ctrl Pts',(-38.8619609450913,27.8417098353975,0.));
#83006=CARTESIAN_POINT('Ctrl Pts',(-38.8619609450913,27.8417098353975,20.));
#83007=CARTESIAN_POINT('Ctrl Pts',(-38.8401301230745,27.866992396481,0.));
#83008=CARTESIAN_POINT('Ctrl Pts',(-38.8401301230745,27.866992396481,20.));
#83009=CARTESIAN_POINT('Ctrl Pts',(-38.8182824421082,27.8922589143132,0.));
#83010=CARTESIAN_POINT('Ctrl Pts',(-38.8182824421082,27.8922589143132,20.));
#83011=CARTESIAN_POINT('Ctrl Pts',(-38.7964179134294,27.917509377225,0.));
#83012=CARTESIAN_POINT('Ctrl Pts',(-38.7964179134294,27.917509377225,20.));
#83013=CARTESIAN_POINT('Ctrl Pts',(-38.7745365482838,27.9427437735546,0.));
#83014=CARTESIAN_POINT('Ctrl Pts',(-38.7745365482838,27.9427437735546,20.));
#83015=CARTESIAN_POINT('Ctrl Pts',(-38.752638357925,27.9679620916479,0.));
#83016=CARTESIAN_POINT('Ctrl Pts',(-38.752638357925,27.9679620916479,20.));
#83017=CARTESIAN_POINT('Ctrl Pts',(-38.7307233536152,27.993164319858,0.));
#83018=CARTESIAN_POINT('Ctrl Pts',(-38.7307233536152,27.993164319858,20.));
#83019=CARTESIAN_POINT('Ctrl Pts',(-38.7087915466247,28.0183504465458,0.));
#83020=CARTESIAN_POINT('Ctrl Pts',(-38.7087915466247,28.0183504465458,20.));
#83021=CARTESIAN_POINT('Ctrl Pts',(-38.6868429482325,28.0435204600798,0.));
#83022=CARTESIAN_POINT('Ctrl Pts',(-38.6868429482325,28.0435204600798,20.));
#83023=CARTESIAN_POINT('Ctrl Pts',(-38.6648775697261,28.0686743488361,0.));
#83024=CARTESIAN_POINT('Ctrl Pts',(-38.6648775697261,28.0686743488361,20.));
#83025=CARTESIAN_POINT('Ctrl Pts',(-38.6428954224012,28.0938121011982,0.));
#83026=CARTESIAN_POINT('Ctrl Pts',(-38.6428954224012,28.0938121011982,20.));
#83027=CARTESIAN_POINT('Ctrl Pts',(-38.6208965175619,28.1189337055566,0.));
#83028=CARTESIAN_POINT('Ctrl Pts',(-38.6208965175619,28.1189337055566,20.));
#83029=CARTESIAN_POINT('Ctrl Pts',(-38.5988808665205,28.14403915031,0.));
#83030=CARTESIAN_POINT('Ctrl Pts',(-38.5988808665205,28.14403915031,20.));
#83031=CARTESIAN_POINT('Ctrl Pts',(-38.5768484805979,28.1691284238645,0.));
#83032=CARTESIAN_POINT('Ctrl Pts',(-38.5768484805979,28.1691284238645,20.));
#83033=CARTESIAN_POINT('Ctrl Pts',(-38.5547993711231,28.194201514634,0.));
#83034=CARTESIAN_POINT('Ctrl Pts',(-38.5547993711231,28.194201514634,20.));
#83035=CARTESIAN_POINT('Ctrl Pts',(-38.5327335494335,28.2192584110398,0.));
#83036=CARTESIAN_POINT('Ctrl Pts',(-38.5327335494335,28.2192584110398,20.));
#83037=CARTESIAN_POINT('Ctrl Pts',(-38.5106510268752,28.2442991015113,0.));
#83038=CARTESIAN_POINT('Ctrl Pts',(-38.5106510268752,28.2442991015113,20.));
#83039=CARTESIAN_POINT('Ctrl Pts',(-38.4885518148031,28.2693235744854,0.));
#83040=CARTESIAN_POINT('Ctrl Pts',(-38.4885518148031,28.2693235744854,20.));
#83041=CARTESIAN_POINT('Ctrl Pts',(-38.4664359245797,28.2943318184065,0.));
#83042=CARTESIAN_POINT('Ctrl Pts',(-38.4664359245797,28.2943318184065,20.));
#83043=CARTESIAN_POINT('Ctrl Pts',(-38.444303367576,28.3193238217266,0.));
#83044=CARTESIAN_POINT('Ctrl Pts',(-38.444303367576,28.3193238217266,20.));
#83045=CARTESIAN_POINT('Ctrl Pts',(-38.422154155171,28.3442995729049,0.));
#83046=CARTESIAN_POINT('Ctrl Pts',(-38.422154155171,28.3442995729049,20.));
#83047=CARTESIAN_POINT('Ctrl Pts',(-38.3999882987522,28.3692590604082,0.));
#83048=CARTESIAN_POINT('Ctrl Pts',(-38.3999882987522,28.3692590604082,20.));
#83049=CARTESIAN_POINT('Ctrl Pts',(-38.3778058097152,28.3942022727108,0.));
#83050=CARTESIAN_POINT('Ctrl Pts',(-38.3778058097152,28.3942022727108,20.));
#83051=CARTESIAN_POINT('Ctrl Pts',(-38.3556066994642,28.419129198295,0.));
#83052=CARTESIAN_POINT('Ctrl Pts',(-38.3556066994642,28.419129198295,20.));
#83053=CARTESIAN_POINT('Ctrl Pts',(-38.333390979412,28.4440398256512,0.));
#83054=CARTESIAN_POINT('Ctrl Pts',(-38.333390979412,28.4440398256512,20.));
#83055=CARTESIAN_POINT('Ctrl Pts',(-38.3111586609795,28.4689341432774,0.));
#83056=CARTESIAN_POINT('Ctrl Pts',(-38.3111586609795,28.4689341432774,20.));
#83057=CARTESIAN_POINT('Ctrl Pts',(-38.2889097555964,28.4938121396793,0.));
#83058=CARTESIAN_POINT('Ctrl Pts',(-38.2889097555964,28.4938121396793,20.));
#83059=CARTESIAN_POINT('Ctrl Pts',(-38.2666442747002,28.5186738033703,0.));
#83060=CARTESIAN_POINT('Ctrl Pts',(-38.2666442747002,28.5186738033703,20.));
#83061=CARTESIAN_POINT('Ctrl Pts',(-38.2443622297368,28.543519122871,0.));
#83062=CARTESIAN_POINT('Ctrl Pts',(-38.2443622297368,28.543519122871,20.));
#83063=CARTESIAN_POINT('Ctrl Pts',(-38.2220636321601,28.5683480867097,0.));
#83064=CARTESIAN_POINT('Ctrl Pts',(-38.2220636321601,28.5683480867097,20.));
#83065=CARTESIAN_POINT('Ctrl Pts',(-38.1997484934321,28.5931606834223,0.));
#83066=CARTESIAN_POINT('Ctrl Pts',(-38.1997484934321,28.5931606834223,20.));
#83067=CARTESIAN_POINT('Ctrl Pts',(-38.1774168250235,28.6179569015525,0.));
#83068=CARTESIAN_POINT('Ctrl Pts',(-38.1774168250235,28.6179569015525,20.));
#83069=CARTESIAN_POINT('Ctrl Pts',(-38.1550686384134,28.6427367296518,0.));
#83070=CARTESIAN_POINT('Ctrl Pts',(-38.1550686384134,28.6427367296518,20.));
#83071=CARTESIAN_POINT('Ctrl Pts',(-38.1327039450889,28.6675001562794,0.));
#83072=CARTESIAN_POINT('Ctrl Pts',(-38.1327039450889,28.6675001562794,20.));
#83073=CARTESIAN_POINT('Ctrl Pts',(-38.1103227565456,28.6922471700024,0.));
#83074=CARTESIAN_POINT('Ctrl Pts',(-38.1103227565456,28.6922471700024,20.));
#83075=CARTESIAN_POINT('Ctrl Pts',(-38.0879250842874,28.7169777593955,0.));
#83076=CARTESIAN_POINT('Ctrl Pts',(-38.0879250842874,28.7169777593955,20.));
#83077=CARTESIAN_POINT('Ctrl Pts',(-38.0655109398262,28.7416919130413,0.));
#83078=CARTESIAN_POINT('Ctrl Pts',(-38.0655109398262,28.7416919130413,20.));
#83079=CARTESIAN_POINT('Ctrl Pts',(-38.0430803346823,28.76638961953,0.));
#83080=CARTESIAN_POINT('Ctrl Pts',(-38.0430803346823,28.76638961953,20.));
#83081=CARTESIAN_POINT('Ctrl Pts',(-38.020633280384,28.7910708674595,0.));
#83082=CARTESIAN_POINT('Ctrl Pts',(-38.020633280384,28.7910708674595,20.));
#83083=CARTESIAN_POINT('Ctrl Pts',(-37.9981697884679,28.8157356454354,0.));
#83084=CARTESIAN_POINT('Ctrl Pts',(-37.9981697884679,28.8157356454354,20.));
#83085=CARTESIAN_POINT('Ctrl Pts',(-37.975689870479,28.8403839420709,0.));
#83086=CARTESIAN_POINT('Ctrl Pts',(-37.975689870479,28.8403839420709,20.));
#83087=CARTESIAN_POINT('Ctrl Pts',(-37.9531935379708,28.8650157459871,0.));
#83088=CARTESIAN_POINT('Ctrl Pts',(-37.9531935379708,28.8650157459871,20.));
#83089=CARTESIAN_POINT('Ctrl Pts',(-37.9306808025049,28.8896310458131,0.));
#83090=CARTESIAN_POINT('Ctrl Pts',(-37.9306808025049,28.8896310458131,20.));
#83091=CARTESIAN_POINT('Ctrl Pts',(-37.9081516756509,28.9142298301853,0.));
#83092=CARTESIAN_POINT('Ctrl Pts',(-37.9081516756509,28.9142298301853,20.));
#83093=CARTESIAN_POINT('Ctrl Pts',(-37.8856061689868,28.9388120877483,0.));
#83094=CARTESIAN_POINT('Ctrl Pts',(-37.8856061689868,28.9388120877483,20.));
#83095=CARTESIAN_POINT('Ctrl Pts',(-37.8630442940985,28.9633778071544,0.));
#83096=CARTESIAN_POINT('Ctrl Pts',(-37.8630442940985,28.9633778071544,20.));
#83097=CARTESIAN_POINT('Ctrl Pts',(-37.8404660625803,28.9879269770637,0.));
#83098=CARTESIAN_POINT('Ctrl Pts',(-37.8404660625803,28.9879269770637,20.));
#83099=CARTESIAN_POINT('Ctrl Pts',(-37.8178714860345,29.0124595861441,0.));
#83100=CARTESIAN_POINT('Ctrl Pts',(-37.8178714860345,29.0124595861441,20.));
#83101=CARTESIAN_POINT('Ctrl Pts',(-37.7952605760716,29.0369756230713,0.));
#83102=CARTESIAN_POINT('Ctrl Pts',(-37.7952605760716,29.0369756230713,20.));
#83103=CARTESIAN_POINT('Ctrl Pts',(-37.7726333443105,29.0614750765285,0.));
#83104=CARTESIAN_POINT('Ctrl Pts',(-37.7726333443105,29.0614750765285,20.));
#83105=CARTESIAN_POINT('Ctrl Pts',(-37.7499898023785,29.0859579352069,0.));
#83106=CARTESIAN_POINT('Ctrl Pts',(-37.7499898023785,29.0859579352069,20.));
#83107=CARTESIAN_POINT('Ctrl Pts',(-37.7273299619109,29.1104241878056,0.));
#83108=CARTESIAN_POINT('Ctrl Pts',(-37.7273299619109,29.1104241878056,20.));
#83109=CARTESIAN_POINT('Ctrl Pts',(-37.7046538345516,29.1348738230316,0.));
#83110=CARTESIAN_POINT('Ctrl Pts',(-37.7046538345516,29.1348738230316,20.));
#83111=CARTESIAN_POINT('Ctrl Pts',(-37.6819614319523,29.1593068295997,0.));
#83112=CARTESIAN_POINT('Ctrl Pts',(-37.6819614319523,29.1593068295997,20.));
#83113=CARTESIAN_POINT('Ctrl Pts',(-37.6592527657727,29.1837231962328,0.));
#83114=CARTESIAN_POINT('Ctrl Pts',(-37.6592527657727,29.1837231962328,20.));
#83115=CARTESIAN_POINT('Ctrl Pts',(-37.6365278476807,29.208122911661,0.));
#83116=CARTESIAN_POINT('Ctrl Pts',(-37.6365278476807,29.208122911661,20.));
#83117=CARTESIAN_POINT('Ctrl Pts',(-37.613786689352,29.2325059646224,0.));
#83118=CARTESIAN_POINT('Ctrl Pts',(-37.613786689352,29.2325059646224,20.));
#83119=CARTESIAN_POINT('Ctrl Pts',(-37.5910293024705,29.2568723438631,0.));
#83120=CARTESIAN_POINT('Ctrl Pts',(-37.5910293024705,29.2568723438631,20.));
#83121=CARTESIAN_POINT('Ctrl Pts',(-37.5682556987287,29.2812220381372,0.));
#83122=CARTESIAN_POINT('Ctrl Pts',(-37.5682556987287,29.2812220381372,20.));
#83123=CARTESIAN_POINT('Ctrl Pts',(-37.5454658898274,29.3055550362067,0.));
#83124=CARTESIAN_POINT('Ctrl Pts',(-37.5454658898274,29.3055550362067,20.));
#83125=CARTESIAN_POINT('Ctrl Pts',(-37.5226598874754,29.3298713268414,0.));
#83126=CARTESIAN_POINT('Ctrl Pts',(-37.5226598874754,29.3298713268414,20.));
#83127=CARTESIAN_POINT('Ctrl Pts',(-37.4998377033899,29.3541708988191,0.));
#83128=CARTESIAN_POINT('Ctrl Pts',(-37.4998377033899,29.3541708988191,20.));
#83129=CARTESIAN_POINT('Ctrl Pts',(-37.4769993492958,29.378453740925,0.));
#83130=CARTESIAN_POINT('Ctrl Pts',(-37.4769993492958,29.378453740925,20.));
#83131=CARTESIAN_POINT('Ctrl Pts',(-37.4541448369259,29.4027198419524,0.));
#83132=CARTESIAN_POINT('Ctrl Pts',(-37.4541448369259,29.4027198419524,20.));
#83133=CARTESIAN_POINT('Ctrl Pts',(-37.4312741780213,29.4269691907023,0.));
#83134=CARTESIAN_POINT('Ctrl Pts',(-37.4312741780213,29.4269691907023,20.));
#83135=CARTESIAN_POINT('Ctrl Pts',(-37.4083873843313,29.4512017759842,0.));
#83136=CARTESIAN_POINT('Ctrl Pts',(-37.4083873843313,29.4512017759842,20.));
#83137=CARTESIAN_POINT('Ctrl Pts',(-37.3854844676135,29.4754175866156,0.));
#83138=CARTESIAN_POINT('Ctrl Pts',(-37.3854844676135,29.4754175866156,20.));
#83139=CARTESIAN_POINT('Ctrl Pts',(-37.3625654396335,29.4996166114217,0.));
#83140=CARTESIAN_POINT('Ctrl Pts',(-37.3625654396335,29.4996166114217,20.));
#83141=CARTESIAN_POINT('Ctrl Pts',(-37.3396303121646,29.5237988392353,0.));
#83142=CARTESIAN_POINT('Ctrl Pts',(-37.3396303121646,29.5237988392353,20.));
#83143=CARTESIAN_POINT('Ctrl Pts',(-37.3166790969884,29.5479642588972,0.));
#83144=CARTESIAN_POINT('Ctrl Pts',(-37.3166790969884,29.5479642588972,20.));
#83145=CARTESIAN_POINT('Ctrl Pts',(-37.2937118058947,29.5721128592559,0.));
#83146=CARTESIAN_POINT('Ctrl Pts',(-37.2937118058947,29.5721128592559,20.));
#83147=CARTESIAN_POINT('Ctrl Pts',(-37.2707284506814,29.5962446291682,0.));
#83148=CARTESIAN_POINT('Ctrl Pts',(-37.2707284506814,29.5962446291682,20.));
#83149=CARTESIAN_POINT('Ctrl Pts',(-37.2477290431548,29.6203595574991,0.));
#83150=CARTESIAN_POINT('Ctrl Pts',(-37.2477290431548,29.6203595574991,20.));
#83151=CARTESIAN_POINT('Ctrl Pts',(-37.2247135951292,29.6444576331214,0.));
#83152=CARTESIAN_POINT('Ctrl Pts',(-37.2247135951292,29.6444576331214,20.));
#83153=CARTESIAN_POINT('Ctrl Pts',(-37.2016821184267,29.668538844916,0.));
#83154=CARTESIAN_POINT('Ctrl Pts',(-37.2016821184267,29.668538844916,20.));
#83155=CARTESIAN_POINT('Ctrl Pts',(-37.1786346248774,29.6926031817715,0.));
#83156=CARTESIAN_POINT('Ctrl Pts',(-37.1786346248774,29.6926031817715,20.));
#83157=CARTESIAN_POINT('Ctrl Pts',(-37.155571126319,29.7166506325841,0.));
#83158=CARTESIAN_POINT('Ctrl Pts',(-37.155571126319,29.7166506325841,20.));
#83159=CARTESIAN_POINT('Ctrl Pts',(-37.1324916345976,29.7406811862582,0.));
#83160=CARTESIAN_POINT('Ctrl Pts',(-37.1324916345976,29.7406811862582,20.));
#83161=CARTESIAN_POINT('Ctrl Pts',(-37.1093961615672,29.7646948317061,0.));
#83162=CARTESIAN_POINT('Ctrl Pts',(-37.1093961615672,29.7646948317061,20.));
#83163=CARTESIAN_POINT('Ctrl Pts',(-37.0862847190902,29.7886915578485,0.));
#83164=CARTESIAN_POINT('Ctrl Pts',(-37.0862847190902,29.7886915578485,20.));
#83165=CARTESIAN_POINT('Ctrl Pts',(-37.0631573190374,29.8126713536142,0.));
#83166=CARTESIAN_POINT('Ctrl Pts',(-37.0631573190374,29.8126713536142,20.));
#83167=CARTESIAN_POINT('Ctrl Pts',(-37.0400139732874,29.83663420794,0.));
#83168=CARTESIAN_POINT('Ctrl Pts',(-37.0400139732874,29.83663420794,20.));
#83169=CARTESIAN_POINT('Ctrl Pts',(-37.0168546937273,29.8605801097708,0.));
#83170=CARTESIAN_POINT('Ctrl Pts',(-37.0168546937273,29.8605801097708,20.));
#83171=CARTESIAN_POINT('Ctrl Pts',(-36.9936794922513,29.884509048059,0.));
#83172=CARTESIAN_POINT('Ctrl Pts',(-36.9936794922513,29.884509048059,20.));
#83173=CARTESIAN_POINT('Ctrl Pts',(-36.9704883807614,29.9084210117647,0.));
#83174=CARTESIAN_POINT('Ctrl Pts',(-36.9704883807614,29.9084210117647,20.));
#83175=CARTESIAN_POINT('Ctrl Pts',(-36.9472813711676,29.9323159898562,0.));
#83176=CARTESIAN_POINT('Ctrl Pts',(-36.9472813711676,29.9323159898562,20.));
#83177=CARTESIAN_POINT('Ctrl Pts',(-36.9240584753883,29.9561939713102,0.));
#83178=CARTESIAN_POINT('Ctrl Pts',(-36.9240584753883,29.9561939713102,20.));
#83179=CARTESIAN_POINT('Ctrl Pts',(-36.9008197053507,29.9800549451122,0.));
#83180=CARTESIAN_POINT('Ctrl Pts',(-36.9008197053507,29.9800549451122,20.));
#83181=CARTESIAN_POINT('Ctrl Pts',(-36.8775650729895,30.0038989002549,0.));
#83182=CARTESIAN_POINT('Ctrl Pts',(-36.8775650729895,30.0038989002549,20.));
#83183=CARTESIAN_POINT('Ctrl Pts',(-36.8542945902473,30.0277258257393,0.));
#83184=CARTESIAN_POINT('Ctrl Pts',(-36.8542945902473,30.0277258257393,20.));
#83185=CARTESIAN_POINT('Ctrl Pts',(-36.8310082690741,30.0515357105739,0.));
#83186=CARTESIAN_POINT('Ctrl Pts',(-36.8310082690741,30.0515357105739,20.));
#83187=CARTESIAN_POINT('Ctrl Pts',(-36.8077061214283,30.0753285437754,0.));
#83188=CARTESIAN_POINT('Ctrl Pts',(-36.8077061214283,30.0753285437754,20.));
#83189=CARTESIAN_POINT('Ctrl Pts',(-36.784388159276,30.0991043143684,0.));
#83190=CARTESIAN_POINT('Ctrl Pts',(-36.784388159276,30.0991043143684,20.));
#83191=CARTESIAN_POINT('Ctrl Pts',(-36.7610543945915,30.1228630113862,0.));
#83192=CARTESIAN_POINT('Ctrl Pts',(-36.7610543945915,30.1228630113862,20.));
#83193=CARTESIAN_POINT('Ctrl Pts',(-36.7377048393574,30.14660462387,0.));
#83194=CARTESIAN_POINT('Ctrl Pts',(-36.7377048393574,30.14660462387,20.));
#83195=CARTESIAN_POINT('Ctrl Pts',(-36.7143395055641,30.1703291408693,0.));
#83196=CARTESIAN_POINT('Ctrl Pts',(-36.7143395055641,30.1703291408693,20.));
#83197=CARTESIAN_POINT('Ctrl Pts',(-36.6909584052099,30.1940365514414,0.));
#83198=CARTESIAN_POINT('Ctrl Pts',(-36.6909584052099,30.1940365514414,20.));
#83199=CARTESIAN_POINT('Ctrl Pts',(-36.6675615503012,30.2177268446518,0.));
#83200=CARTESIAN_POINT('Ctrl Pts',(-36.6675615503012,30.2177268446518,20.));
#83201=CARTESIAN_POINT('Ctrl Pts',(-36.6441489528521,30.2414000095742,0.));
#83202=CARTESIAN_POINT('Ctrl Pts',(-36.6441489528521,30.2414000095742,20.));
#83203=CARTESIAN_POINT('Ctrl Pts',(-36.6207206248849,30.2650560352902,0.));
#83204=CARTESIAN_POINT('Ctrl Pts',(-36.6207206248849,30.2650560352902,20.));
#83205=CARTESIAN_POINT('Ctrl Pts',(-36.5972765784293,30.2886949108895,0.));
#83206=CARTESIAN_POINT('Ctrl Pts',(-36.5972765784293,30.2886949108895,20.));
#83207=CARTESIAN_POINT('Ctrl Pts',(-36.5738168255233,30.3123166254701,0.));
#83208=CARTESIAN_POINT('Ctrl Pts',(-36.5738168255233,30.3123166254701,20.));
#83209=CARTESIAN_POINT('Ctrl Pts',(-36.5503413782123,30.3359211681375,0.));
#83210=CARTESIAN_POINT('Ctrl Pts',(-36.5503413782123,30.3359211681375,20.));
#83211=CARTESIAN_POINT('Ctrl Pts',(-36.5268502485502,30.3595085280058,0.));
#83212=CARTESIAN_POINT('Ctrl Pts',(-36.5268502485502,30.3595085280058,20.));
#83213=CARTESIAN_POINT('Ctrl Pts',(-36.5033434485984,30.3830786941972,0.));
#83214=CARTESIAN_POINT('Ctrl Pts',(-36.5033434485984,30.3830786941972,20.));
#83215=CARTESIAN_POINT('Ctrl Pts',(-36.4798209904267,30.4066316558423,0.));
#83216=CARTESIAN_POINT('Ctrl Pts',(-36.4798209904267,30.4066316558423,20.));
#83217=CARTESIAN_POINT('Ctrl Pts',(-36.456282886113,30.4301674020801,0.));
#83218=CARTESIAN_POINT('Ctrl Pts',(-36.456282886113,30.4301674020801,20.));
#83219=CARTESIAN_POINT('Ctrl Pts',(-36.4327291477429,30.4536859220576,0.));
#83220=CARTESIAN_POINT('Ctrl Pts',(-36.4327291477429,30.4536859220576,20.));
#83221=CARTESIAN_POINT('Ctrl Pts',(-36.4091597874097,30.4771872049298,0.));
#83222=CARTESIAN_POINT('Ctrl Pts',(-36.4091597874097,30.4771872049298,20.));
#83223=CARTESIAN_POINT('Ctrl Pts',(-36.3855748172148,30.5006712398601,0.));
#83224=CARTESIAN_POINT('Ctrl Pts',(-36.3855748172148,30.5006712398601,20.));
#83225=CARTESIAN_POINT('Ctrl Pts',(-36.3619742492671,30.5241380160195,0.));
#83226=CARTESIAN_POINT('Ctrl Pts',(-36.3619742492671,30.5241380160195,20.));
#83227=CARTESIAN_POINT('Ctrl Pts',(-36.3383580956833,30.5475875225872,0.));
#83228=CARTESIAN_POINT('Ctrl Pts',(-36.3383580956833,30.5475875225872,20.));
#83229=CARTESIAN_POINT('Ctrl Pts',(-36.3147263685875,30.5710197487502,0.));
#83230=CARTESIAN_POINT('Ctrl Pts',(-36.3147263685875,30.5710197487502,20.));
#83231=CARTESIAN_POINT('Ctrl Pts',(-36.2910790801119,30.5944346837039,0.));
#83232=CARTESIAN_POINT('Ctrl Pts',(-36.2910790801119,30.5944346837039,20.));
#83233=CARTESIAN_POINT('Ctrl Pts',(-36.2674162423973,30.6178323166527,0.));
#83234=CARTESIAN_POINT('Ctrl Pts',(-36.2674162423973,30.6178323166527,20.));
#83235=CARTESIAN_POINT('Ctrl Pts',(-36.2437378675924,30.6412126368094,0.));
#83236=CARTESIAN_POINT('Ctrl Pts',(-36.2437378675924,30.6412126368094,20.));
#83237=CARTESIAN_POINT('Ctrl Pts',(-36.2200439678543,30.6645756333954,0.));
#83238=CARTESIAN_POINT('Ctrl Pts',(-36.2200439678543,30.6645756333954,20.));
#83239=CARTESIAN_POINT('Ctrl Pts',(-36.1963345553471,30.6879212956391,0.));
#83240=CARTESIAN_POINT('Ctrl Pts',(-36.1963345553471,30.6879212956391,20.));
#83241=CARTESIAN_POINT('Ctrl Pts',(-36.1726096422428,30.7112496127774,0.));
#83242=CARTESIAN_POINT('Ctrl Pts',(-36.1726096422428,30.7112496127774,20.));
#83243=CARTESIAN_POINT('Ctrl Pts',(-36.1488692407204,30.7345605740544,0.));
#83244=CARTESIAN_POINT('Ctrl Pts',(-36.1488692407204,30.7345605740544,20.));
#83245=CARTESIAN_POINT('Ctrl Pts',(-36.125113362967,30.7578541687236,0.));
#83246=CARTESIAN_POINT('Ctrl Pts',(-36.125113362967,30.7578541687236,20.));
#83247=CARTESIAN_POINT('Ctrl Pts',(-36.1013420211777,30.7811303860468,0.));
#83248=CARTESIAN_POINT('Ctrl Pts',(-36.1013420211777,30.7811303860468,20.));
#83249=CARTESIAN_POINT('Ctrl Pts',(-36.0775552275565,30.8043892152943,0.));
#83250=CARTESIAN_POINT('Ctrl Pts',(-36.0775552275565,30.8043892152943,20.));
#83251=CARTESIAN_POINT('Ctrl Pts',(-36.0537529943146,30.8276306457446,0.));
#83252=CARTESIAN_POINT('Ctrl Pts',(-36.0537529943146,30.8276306457446,20.));
#83253=CARTESIAN_POINT('Ctrl Pts',(-36.0299353336712,30.8508546666841,0.));
#83254=CARTESIAN_POINT('Ctrl Pts',(-36.0299353336712,30.8508546666841,20.));
#83255=CARTESIAN_POINT('Ctrl Pts',(-36.0061022578528,30.8740612674075,0.));
#83256=CARTESIAN_POINT('Ctrl Pts',(-36.0061022578528,30.8740612674075,20.));
#83257=CARTESIAN_POINT('Ctrl Pts',(-35.9822537790931,30.8972504372171,0.));
#83258=CARTESIAN_POINT('Ctrl Pts',(-35.9822537790931,30.8972504372171,20.));
#83259=CARTESIAN_POINT('Ctrl Pts',(-35.9583899096339,30.9204221654236,0.));
#83260=CARTESIAN_POINT('Ctrl Pts',(-35.9583899096339,30.9204221654236,20.));
#83261=CARTESIAN_POINT('Ctrl Pts',(-35.9345106617251,30.9435764413467,0.));
#83262=CARTESIAN_POINT('Ctrl Pts',(-35.9345106617251,30.9435764413467,20.));
#83263=CARTESIAN_POINT('Ctrl Pts',(-35.9106160476245,30.9667132543142,0.));
#83264=CARTESIAN_POINT('Ctrl Pts',(-35.9106160476245,30.9667132543142,20.));
#83265=CARTESIAN_POINT('Ctrl Pts',(-35.886706079598,30.9898325936627,0.));
#83266=CARTESIAN_POINT('Ctrl Pts',(-35.886706079598,30.9898325936627,20.));
#83267=CARTESIAN_POINT('Ctrl Pts',(-35.8627807699193,31.0129344487367,0.));
#83268=CARTESIAN_POINT('Ctrl Pts',(-35.8627807699193,31.0129344487367,20.));
#83269=CARTESIAN_POINT('Ctrl Pts',(-35.8388401308696,31.036018808889,0.));
#83270=CARTESIAN_POINT('Ctrl Pts',(-35.8388401308696,31.036018808889,20.));
#83271=CARTESIAN_POINT('Ctrl Pts',(-35.8148841747376,31.0590856634804,0.));
#83272=CARTESIAN_POINT('Ctrl Pts',(-35.8148841747376,31.0590856634804,20.));
#83273=CARTESIAN_POINT('Ctrl Pts',(-35.7909129138202,31.0821350018809,0.));
#83274=CARTESIAN_POINT('Ctrl Pts',(-35.7909129138202,31.0821350018809,20.));
#83275=CARTESIAN_POINT('Ctrl Pts',(-35.7669263604212,31.1051668134678,0.));
#83276=CARTESIAN_POINT('Ctrl Pts',(-35.7669263604212,31.1051668134678,20.));
#83277=CARTESIAN_POINT('Ctrl Pts',(-35.7429245268523,31.1281810876267,0.));
#83278=CARTESIAN_POINT('Ctrl Pts',(-35.7429245268523,31.1281810876267,20.));
#83279=CARTESIAN_POINT('Ctrl Pts',(-35.7189074254331,31.1511778137516,0.));
#83280=CARTESIAN_POINT('Ctrl Pts',(-35.7189074254331,31.1511778137516,20.));
#83281=CARTESIAN_POINT('Ctrl Pts',(-35.6948750684911,31.1741569812451,0.));
#83282=CARTESIAN_POINT('Ctrl Pts',(-35.6948750684911,31.1741569812451,20.));
#83283=CARTESIAN_POINT('Ctrl Pts',(-35.6708274683619,31.1971185795181,0.));
#83284=CARTESIAN_POINT('Ctrl Pts',(-35.6708274683619,31.1971185795181,20.));
#83285=CARTESIAN_POINT('Ctrl Pts',(-35.6467646373884,31.2200625979904,0.));
#83286=CARTESIAN_POINT('Ctrl Pts',(-35.6467646373884,31.2200625979904,20.));
#83287=CARTESIAN_POINT('Ctrl Pts',(-35.6226865879214,31.24298902609,0.));
#83288=CARTESIAN_POINT('Ctrl Pts',(-35.6226865879214,31.24298902609,20.));
#83289=CARTESIAN_POINT('Ctrl Pts',(-35.5985933323195,31.2658978532533,0.));
#83290=CARTESIAN_POINT('Ctrl Pts',(-35.5985933323195,31.2658978532533,20.));
#83291=CARTESIAN_POINT('Ctrl Pts',(-35.5744848829488,31.288789068925,0.));
#83292=CARTESIAN_POINT('Ctrl Pts',(-35.5744848829488,31.288789068925,20.));
#83293=CARTESIAN_POINT('Ctrl Pts',(-35.5503612521832,31.3116626625581,0.));
#83294=CARTESIAN_POINT('Ctrl Pts',(-35.5503612521832,31.3116626625581,20.));
#83295=CARTESIAN_POINT('Ctrl Pts',(-35.5262224524039,31.3345186236135,0.));
#83296=CARTESIAN_POINT('Ctrl Pts',(-35.5262224524039,31.3345186236135,20.));
#83297=CARTESIAN_POINT('Ctrl Pts',(-35.502068496,31.3573569415605,0.));
#83298=CARTESIAN_POINT('Ctrl Pts',(-35.502068496,31.3573569415605,20.));
#83299=CARTESIAN_POINT('Ctrl Pts',(-35.4778993953681,31.3801776058767,0.));
#83300=CARTESIAN_POINT('Ctrl Pts',(-35.4778993953681,31.3801776058767,20.));
#83301=CARTESIAN_POINT('Ctrl Pts',(-35.4537151629127,31.4029806060482,0.));
#83302=CARTESIAN_POINT('Ctrl Pts',(-35.4537151629127,31.4029806060482,20.));
#83303=CARTESIAN_POINT('Ctrl Pts',(-35.4295158110455,31.4257659315696,0.));
#83304=CARTESIAN_POINT('Ctrl Pts',(-35.4295158110455,31.4257659315696,20.));
#83305=CARTESIAN_POINT('Ctrl Pts',(-35.4053013521866,31.4485335719446,0.));
#83306=CARTESIAN_POINT('Ctrl Pts',(-35.4053013521866,31.4485335719446,20.));
#83307=CARTESIAN_POINT('Ctrl Pts',(-35.3810717987641,31.4712835166857,0.));
#83308=CARTESIAN_POINT('Ctrl Pts',(-35.3810717987641,31.4712835166857,20.));
#83309=CARTESIAN_POINT('Ctrl Pts',(-35.3568271632136,31.4940157553136,0.));
#83310=CARTESIAN_POINT('Ctrl Pts',(-35.3568271632136,31.4940157553136,20.));
#83311=CARTESIAN_POINT('Ctrl Pts',(-35.3325674579779,31.5167302773569,0.));
#83312=CARTESIAN_POINT('Ctrl Pts',(-35.3325674579779,31.5167302773569,20.));
#83313=CARTESIAN_POINT('Ctrl Pts',(-35.3082926955072,31.5394270723526,0.));
#83314=CARTESIAN_POINT('Ctrl Pts',(-35.3082926955072,31.5394270723526,20.));
#83315=CARTESIAN_POINT('Ctrl Pts',(-35.2840028882593,31.5621061298453,0.));
#83316=CARTESIAN_POINT('Ctrl Pts',(-35.2840028882593,31.5621061298453,20.));
#83317=CARTESIAN_POINT('Ctrl Pts',(-35.2596980486997,31.5847674393884,0.));
#83318=CARTESIAN_POINT('Ctrl Pts',(-35.2596980486997,31.5847674393884,20.));
#83319=CARTESIAN_POINT('Ctrl Pts',(-35.2353781893015,31.6074109905439,0.));
#83320=CARTESIAN_POINT('Ctrl Pts',(-35.2353781893015,31.6074109905439,20.));
#83321=CARTESIAN_POINT('Ctrl Pts',(-35.2110433225459,31.6300367728826,0.));
#83322=CARTESIAN_POINT('Ctrl Pts',(-35.2110433225459,31.6300367728826,20.));
#83323=CARTESIAN_POINT('Ctrl Pts',(-35.1866934609214,31.6526447759839,0.));
#83324=CARTESIAN_POINT('Ctrl Pts',(-35.1866934609214,31.6526447759839,20.));
#83325=CARTESIAN_POINT('Ctrl Pts',(-35.1623286169245,31.6752349894358,0.));
#83326=CARTESIAN_POINT('Ctrl Pts',(-35.1623286169245,31.6752349894358,20.));
#83327=CARTESIAN_POINT('Ctrl Pts',(-35.1379488030591,31.6978074028349,0.));
#83328=CARTESIAN_POINT('Ctrl Pts',(-35.1379488030591,31.6978074028349,20.));
#83329=CARTESIAN_POINT('Ctrl Pts',(-35.1135540318367,31.7203620057864,0.));
#83330=CARTESIAN_POINT('Ctrl Pts',(-35.1135540318367,31.7203620057864,20.));
#83331=CARTESIAN_POINT('Ctrl Pts',(-35.0891443157764,31.7428987879034,0.));
#83332=CARTESIAN_POINT('Ctrl Pts',(-35.0891443157764,31.7428987879034,20.));
#83333=CARTESIAN_POINT('Ctrl Pts',(-35.0647196674044,31.7654177388073,0.));
#83334=CARTESIAN_POINT('Ctrl Pts',(-35.0647196674044,31.7654177388073,20.));
#83335=CARTESIAN_POINT('Ctrl Pts',(-35.0402800992547,31.7879188481277,0.));
#83336=CARTESIAN_POINT('Ctrl Pts',(-35.0402800992547,31.7879188481277,20.));
#83337=CARTESIAN_POINT('Ctrl Pts',(-35.0158256238691,31.8104021055032,0.));
#83338=CARTESIAN_POINT('Ctrl Pts',(-35.0158256238691,31.8104021055032,20.));
#83339=CARTESIAN_POINT('Ctrl Pts',(-34.991356253797,31.8328675005809,0.));
#83340=CARTESIAN_POINT('Ctrl Pts',(-34.991356253797,31.8328675005809,20.));
#83341=CARTESIAN_POINT('Ctrl Pts',(-34.9668720015954,31.8553150230168,0.));
#83342=CARTESIAN_POINT('Ctrl Pts',(-34.9668720015954,31.8553150230168,20.));
#83343=CARTESIAN_POINT('Ctrl Pts',(-34.9423728798289,31.8777446624754,0.));
#83344=CARTESIAN_POINT('Ctrl Pts',(-34.9423728798289,31.8777446624754,20.));
#83345=CARTESIAN_POINT('Ctrl Pts',(-34.9178589010694,31.9001564086295,0.));
#83346=CARTESIAN_POINT('Ctrl Pts',(-34.9178589010694,31.9001564086295,20.));
#83347=CARTESIAN_POINT('Ctrl Pts',(-34.8933300778963,31.9225502511603,0.));
#83348=CARTESIAN_POINT('Ctrl Pts',(-34.8933300778963,31.9225502511603,20.));
#83349=CARTESIAN_POINT('Ctrl Pts',(-34.8687864228965,31.9449261797574,0.));
#83350=CARTESIAN_POINT('Ctrl Pts',(-34.8687864228965,31.9449261797574,20.));
#83351=CARTESIAN_POINT('Ctrl Pts',(-34.8442279486644,31.967284184119,0.));
#83352=CARTESIAN_POINT('Ctrl Pts',(-34.8442279486644,31.967284184119,20.));
#83353=CARTESIAN_POINT('Ctrl Pts',(-34.8196546678026,31.9896242539524,0.));
#83354=CARTESIAN_POINT('Ctrl Pts',(-34.8196546678026,31.9896242539524,20.));
#83355=CARTESIAN_POINT('Ctrl Pts',(-34.7950665929206,32.0119463789729,0.));
#83356=CARTESIAN_POINT('Ctrl Pts',(-34.7950665929206,32.0119463789729,20.));
#83357=CARTESIAN_POINT('Ctrl Pts',(-34.7704637366357,32.0342505489048,0.));
#83358=CARTESIAN_POINT('Ctrl Pts',(-34.7704637366357,32.0342505489048,20.));
#83359=CARTESIAN_POINT('Ctrl Pts',(-34.7458461115727,32.0565367534806,0.));
#83360=CARTESIAN_POINT('Ctrl Pts',(-34.7458461115727,32.0565367534806,20.));
#83361=CARTESIAN_POINT('Ctrl Pts',(-34.7212137303638,32.0788049824416,0.));
#83362=CARTESIAN_POINT('Ctrl Pts',(-34.7212137303638,32.0788049824416,20.));
#83363=CARTESIAN_POINT('Ctrl Pts',(-34.6965666056491,32.1010552255378,0.));
#83364=CARTESIAN_POINT('Ctrl Pts',(-34.6965666056491,32.1010552255378,20.));
#83365=CARTESIAN_POINT('Ctrl Pts',(-34.6719047500757,32.1232874725276,0.));
#83366=CARTESIAN_POINT('Ctrl Pts',(-34.6719047500757,32.1232874725276,20.));
#83367=CARTESIAN_POINT('Ctrl Pts',(-34.6472281762982,32.145501713178,0.));
#83368=CARTESIAN_POINT('Ctrl Pts',(-34.6472281762982,32.145501713178,20.));
#83369=CARTESIAN_POINT('Ctrl Pts',(-34.6225368969784,32.167697937264,0.));
#83370=CARTESIAN_POINT('Ctrl Pts',(-34.6225368969784,32.167697937264,20.));
#83371=CARTESIAN_POINT('Ctrl Pts',(-34.5978309247855,32.1898761345694,0.));
#83372=CARTESIAN_POINT('Ctrl Pts',(-34.5978309247855,32.1898761345694,20.));
#83373=CARTESIAN_POINT('Ctrl Pts',(-34.5731102723969,32.212036294887,0.));
#83374=CARTESIAN_POINT('Ctrl Pts',(-34.5731102723969,32.212036294887,20.));
#83375=CARTESIAN_POINT('Ctrl Pts',(-34.5483749524972,32.2341784080183,0.));
#83376=CARTESIAN_POINT('Ctrl Pts',(-34.5483749524972,32.2341784080183,20.));
#83377=CARTESIAN_POINT('Ctrl Pts',(-34.5236249777791,32.2563024637739,0.));
#83378=CARTESIAN_POINT('Ctrl Pts',(-34.5236249777791,32.2563024637739,20.));
#83379=CARTESIAN_POINT('Ctrl Pts',(-34.4988603609427,32.2784084519728,0.));
#83380=CARTESIAN_POINT('Ctrl Pts',(-34.4988603609427,32.2784084519728,20.));
#83381=CARTESIAN_POINT('Ctrl Pts',(-34.474081114695,32.3004963624427,0.));
#83382=CARTESIAN_POINT('Ctrl Pts',(-34.474081114695,32.3004963624427,20.));
#83383=CARTESIAN_POINT('Ctrl Pts',(-34.4492872517507,32.3225661850195,0.));
#83384=CARTESIAN_POINT('Ctrl Pts',(-34.4492872517507,32.3225661850195,20.));
#83385=CARTESIAN_POINT('Ctrl Pts',(-34.4244787848311,32.3446179095473,0.));
#83386=CARTESIAN_POINT('Ctrl Pts',(-34.4244787848311,32.3446179095473,20.));
#83387=CARTESIAN_POINT('Ctrl Pts',(-34.3996557266651,32.3666515258787,0.));
#83388=CARTESIAN_POINT('Ctrl Pts',(-34.3996557266651,32.3666515258787,20.));
#83389=CARTESIAN_POINT('Ctrl Pts',(-34.3748180899889,32.388667023875,0.));
#83390=CARTESIAN_POINT('Ctrl Pts',(-34.3748180899889,32.388667023875,20.));
#83391=CARTESIAN_POINT('Ctrl Pts',(-34.3499658875467,32.4106643934066,0.));
#83392=CARTESIAN_POINT('Ctrl Pts',(-34.3499658875467,32.4106643934066,20.));
#83393=CARTESIAN_POINT('Ctrl Pts',(-34.3250991320905,32.4326436243532,0.));
#83394=CARTESIAN_POINT('Ctrl Pts',(-34.3250991320905,32.4326436243532,20.));
#83395=CARTESIAN_POINT('Ctrl Pts',(-34.3002178363797,32.4546047066033,0.));
#83396=CARTESIAN_POINT('Ctrl Pts',(-34.3002178363797,32.4546047066033,20.));
#83397=CARTESIAN_POINT('Ctrl Pts',(-34.2753220131812,32.4765476300538,0.));
#83398=CARTESIAN_POINT('Ctrl Pts',(-34.2753220131812,32.4765476300538,20.));
#83399=CARTESIAN_POINT('Ctrl Pts',(-34.2504116752689,32.4984723846097,0.));
#83400=CARTESIAN_POINT('Ctrl Pts',(-34.2504116752689,32.4984723846097,20.));
#83401=CARTESIAN_POINT('Ctrl Pts',(-34.2254868354237,32.5203789601849,0.));
#83402=CARTESIAN_POINT('Ctrl Pts',(-34.2254868354237,32.5203789601849,20.));
#83403=CARTESIAN_POINT('Ctrl Pts',(-34.2005475064343,32.542267346702,0.));
#83404=CARTESIAN_POINT('Ctrl Pts',(-34.2005475064343,32.542267346702,20.));
#83405=CARTESIAN_POINT('Ctrl Pts',(-34.1755937010963,32.564137534092,0.));
#83406=CARTESIAN_POINT('Ctrl Pts',(-34.1755937010963,32.564137534092,20.));
#83407=CARTESIAN_POINT('Ctrl Pts',(-34.1506254322131,32.585989512295,0.));
#83408=CARTESIAN_POINT('Ctrl Pts',(-34.1506254322131,32.585989512295,20.));
#83409=CARTESIAN_POINT('Ctrl Pts',(-34.1256427125956,32.6078232712594,0.));
#83410=CARTESIAN_POINT('Ctrl Pts',(-34.1256427125956,32.6078232712594,20.));
#83411=CARTESIAN_POINT('Ctrl Pts',(-34.1006455550618,32.6296388009428,0.));
#83412=CARTESIAN_POINT('Ctrl Pts',(-34.1006455550618,32.6296388009428,20.));
#83413=CARTESIAN_POINT('Ctrl Pts',(-34.0756339724376,32.6514360913116,0.));
#83414=CARTESIAN_POINT('Ctrl Pts',(-34.0756339724376,32.6514360913116,20.));
#83415=CARTESIAN_POINT('Ctrl Pts',(-34.0506079775557,32.6732151323407,0.));
#83416=CARTESIAN_POINT('Ctrl Pts',(-34.0506079775557,32.6732151323407,20.));
#83417=CARTESIAN_POINT('Ctrl Pts',(-34.0255675832564,32.694975914014,0.));
#83418=CARTESIAN_POINT('Ctrl Pts',(-34.0255675832564,32.694975914014,20.));
#83419=CARTESIAN_POINT('Ctrl Pts',(-34.0005128023872,32.7167184263237,0.));
#83420=CARTESIAN_POINT('Ctrl Pts',(-34.0005128023872,32.7167184263237,20.));
#83421=CARTESIAN_POINT('Ctrl Pts',(-33.9754436478026,32.7384426592708,0.));
#83422=CARTESIAN_POINT('Ctrl Pts',(-33.9754436478026,32.7384426592708,20.));
#83423=CARTESIAN_POINT('Ctrl Pts',(-33.9503601323651,32.7601486028652,0.));
#83424=CARTESIAN_POINT('Ctrl Pts',(-33.9503601323651,32.7601486028652,20.));
#83425=CARTESIAN_POINT('Ctrl Pts',(-33.9252622689445,32.781836247126,0.));
#83426=CARTESIAN_POINT('Ctrl Pts',(-33.9252622689445,32.781836247126,20.));
#83427=CARTESIAN_POINT('Ctrl Pts',(-33.9001500704179,32.8035055820805,0.));
#83428=CARTESIAN_POINT('Ctrl Pts',(-33.9001500704179,32.8035055820805,20.));
#83429=CARTESIAN_POINT('Ctrl Pts',(-33.8750235496691,32.8251565977646,0.));
#83430=CARTESIAN_POINT('Ctrl Pts',(-33.8750235496691,32.8251565977646,20.));
#83431=CARTESIAN_POINT('Ctrl Pts',(-33.8498827195893,32.8467892842227,0.));
#83432=CARTESIAN_POINT('Ctrl Pts',(-33.8498827195893,32.8467892842227,20.));
#83433=CARTESIAN_POINT('Ctrl Pts',(-33.8247275930774,32.8684036315085,0.));
#83434=CARTESIAN_POINT('Ctrl Pts',(-33.8247275930774,32.8684036315085,20.));
#83435=CARTESIAN_POINT('Ctrl Pts',(-33.7995581830395,32.8899996296849,0.));
#83436=CARTESIAN_POINT('Ctrl Pts',(-33.7995581830395,32.8899996296849,20.));
#83437=CARTESIAN_POINT('Ctrl Pts',(-33.7743745023893,32.9115772688235,0.));
#83438=CARTESIAN_POINT('Ctrl Pts',(-33.7743745023893,32.9115772688235,20.));
#83439=CARTESIAN_POINT('Ctrl Pts',(-33.7491765640476,32.9331365390046,0.));
#83440=CARTESIAN_POINT('Ctrl Pts',(-33.7491765640476,32.9331365390046,20.));
#83441=CARTESIAN_POINT('Ctrl Pts',(-33.723964380943,32.9546774303179,0.));
#83442=CARTESIAN_POINT('Ctrl Pts',(-33.723964380943,32.9546774303179,20.));
#83443=CARTESIAN_POINT('Ctrl Pts',(-33.6987379660104,32.9761999328604,0.));
#83444=CARTESIAN_POINT('Ctrl Pts',(-33.6987379660104,32.9761999328604,20.));
#83445=CARTESIAN_POINT('Ctrl Pts',(-33.673497332192,32.9977040367383,0.));
#83446=CARTESIAN_POINT('Ctrl Pts',(-33.673497332192,32.9977040367383,20.));
#83447=CARTESIAN_POINT('Ctrl Pts',(-33.6482424924373,33.0191897320665,0.));
#83448=CARTESIAN_POINT('Ctrl Pts',(-33.6482424924373,33.0191897320665,20.));
#83449=CARTESIAN_POINT('Ctrl Pts',(-33.6229734597032,33.0406570089692,0.));
#83450=CARTESIAN_POINT('Ctrl Pts',(-33.6229734597032,33.0406570089692,20.));
#83451=CARTESIAN_POINT('Ctrl Pts',(-33.5976902469543,33.0621058575797,0.));
#83452=CARTESIAN_POINT('Ctrl Pts',(-33.5976902469543,33.0621058575797,20.));
#83453=CARTESIAN_POINT('Ctrl Pts',(-33.572392867162,33.0835362680399,0.));
#83454=CARTESIAN_POINT('Ctrl Pts',(-33.572392867162,33.0835362680399,20.));
#83455=CARTESIAN_POINT('Ctrl Pts',(-33.5470813333053,33.1049482305003,0.));
#83456=CARTESIAN_POINT('Ctrl Pts',(-33.5470813333053,33.1049482305003,20.));
#83457=CARTESIAN_POINT('Ctrl Pts',(-33.5217556583704,33.1263417351207,0.));
#83458=CARTESIAN_POINT('Ctrl Pts',(-33.5217556583704,33.1263417351207,20.));
#83459=CARTESIAN_POINT('Ctrl Pts',(-33.4964158553506,33.1477167720697,0.));
#83460=CARTESIAN_POINT('Ctrl Pts',(-33.4964158553506,33.1477167720697,20.));
#83461=CARTESIAN_POINT('Ctrl Pts',(-33.4710619372468,33.1690733315248,0.));
#83462=CARTESIAN_POINT('Ctrl Pts',(-33.4710619372468,33.1690733315248,20.));
#83463=CARTESIAN_POINT('Ctrl Pts',(-33.4456939170666,33.1904114036721,0.));
#83464=CARTESIAN_POINT('Ctrl Pts',(-33.4456939170666,33.1904114036721,20.));
#83465=CARTESIAN_POINT('Ctrl Pts',(-33.4203118078248,33.2117309787063,0.));
#83466=CARTESIAN_POINT('Ctrl Pts',(-33.4203118078248,33.2117309787063,20.));
#83467=CARTESIAN_POINT('Ctrl Pts',(-33.3949156225429,33.233032046831,0.));
#83468=CARTESIAN_POINT('Ctrl Pts',(-33.3949156225429,33.233032046831,20.));
#83469=CARTESIAN_POINT('Ctrl Pts',(-33.3695053742505,33.2543145982587,0.));
#83470=CARTESIAN_POINT('Ctrl Pts',(-33.3695053742505,33.2543145982587,20.));
#83471=CARTESIAN_POINT('Ctrl Pts',(-33.3440810759838,33.2755786232108,0.));
#83472=CARTESIAN_POINT('Ctrl Pts',(-33.3440810759838,33.2755786232108,20.));
#83473=CARTESIAN_POINT('Ctrl Pts',(-33.3186427407863,33.2968241119176,0.));
#83474=CARTESIAN_POINT('Ctrl Pts',(-33.3186427407863,33.2968241119176,20.));
#83475=CARTESIAN_POINT('Ctrl Pts',(-33.2931903817093,33.318051054619,0.));
#83476=CARTESIAN_POINT('Ctrl Pts',(-33.2931903817093,33.318051054619,20.));
#83477=CARTESIAN_POINT('Ctrl Pts',(-33.2677240118112,33.3392594415636,0.));
#83478=CARTESIAN_POINT('Ctrl Pts',(-33.2677240118112,33.3392594415636,20.));
#83479=CARTESIAN_POINT('Ctrl Pts',(-33.2422436441578,33.3604492630093,0.));
#83480=CARTESIAN_POINT('Ctrl Pts',(-33.2422436441578,33.3604492630093,20.));
#83481=CARTESIAN_POINT('Ctrl Pts',(-33.2167492918215,33.3816205092222,0.));
#83482=CARTESIAN_POINT('Ctrl Pts',(-33.2167492918215,33.3816205092222,20.));
#83483=CARTESIAN_POINT('Ctrl Pts',(-33.1912409678819,33.4027731704774,0.));
#83484=CARTESIAN_POINT('Ctrl Pts',(-33.1912409678819,33.4027731704774,20.));
#83485=CARTESIAN_POINT('Ctrl Pts',(-33.1657186854252,33.4239072370581,0.));
#83486=CARTESIAN_POINT('Ctrl Pts',(-33.1657186854252,33.4239072370581,20.));
#83487=CARTESIAN_POINT('Ctrl Pts',(-33.1401824575448,33.4450226992567,0.));
#83488=CARTESIAN_POINT('Ctrl Pts',(-33.1401824575448,33.4450226992567,20.));
#83489=CARTESIAN_POINT('Ctrl Pts',(-33.1146322973416,33.4661195473749,0.));
#83490=CARTESIAN_POINT('Ctrl Pts',(-33.1146322973416,33.4661195473749,20.));
#83491=CARTESIAN_POINT('Ctrl Pts',(-33.0890682179239,33.4871977717238,0.));
#83492=CARTESIAN_POINT('Ctrl Pts',(-33.0890682179239,33.4871977717238,20.));
#83493=CARTESIAN_POINT('Ctrl Pts',(-33.063490232407,33.5082573626235,0.));
#83494=CARTESIAN_POINT('Ctrl Pts',(-33.063490232407,33.5082573626235,20.));
#83495=CARTESIAN_POINT('Ctrl Pts',(-33.0378983539138,33.5292983104032,0.));
#83496=CARTESIAN_POINT('Ctrl Pts',(-33.0378983539138,33.5292983104032,20.));
#83497=CARTESIAN_POINT('Ctrl Pts',(-33.0122925955739,33.5503206054003,0.));
#83498=CARTESIAN_POINT('Ctrl Pts',(-33.0122925955739,33.5503206054003,20.));
#83499=CARTESIAN_POINT('Ctrl Pts',(-32.986672970524,33.5713242379612,0.));
#83500=CARTESIAN_POINT('Ctrl Pts',(-32.986672970524,33.5713242379612,20.));
#83501=CARTESIAN_POINT('Ctrl Pts',(-32.9610394919081,33.5923091984411,0.));
#83502=CARTESIAN_POINT('Ctrl Pts',(-32.9610394919081,33.5923091984411,20.));
#83503=CARTESIAN_POINT('Ctrl Pts',(-32.935392172877,33.6132754772045,0.));
#83504=CARTESIAN_POINT('Ctrl Pts',(-32.935392172877,33.6132754772045,20.));
#83505=CARTESIAN_POINT('Ctrl Pts',(-32.9097310265884,33.6342230646254,0.));
#83506=CARTESIAN_POINT('Ctrl Pts',(-32.9097310265884,33.6342230646254,20.));
#83507=CARTESIAN_POINT('Ctrl Pts',(-32.8840560662069,33.6551519510862,0.));
#83508=CARTESIAN_POINT('Ctrl Pts',(-32.8840560662069,33.6551519510862,20.));
#83509=CARTESIAN_POINT('Ctrl Pts',(-32.8583673049046,33.6760621269785,0.));
#83510=CARTESIAN_POINT('Ctrl Pts',(-32.8583673049046,33.6760621269785,20.));
#83511=CARTESIAN_POINT('Ctrl Pts',(-32.8326647558606,33.6969535827028,0.));
#83512=CARTESIAN_POINT('Ctrl Pts',(-32.8326647558606,33.6969535827028,20.));
#83513=CARTESIAN_POINT('Ctrl Pts',(-32.8069484322617,33.717826308669,0.));
#83514=CARTESIAN_POINT('Ctrl Pts',(-32.8069484322617,33.717826308669,20.));
#83515=CARTESIAN_POINT('Ctrl Pts',(-32.7812183473018,33.7386802952956,0.));
#83516=CARTESIAN_POINT('Ctrl Pts',(-32.7812183473018,33.7386802952956,20.));
#83517=CARTESIAN_POINT('Ctrl Pts',(-32.7554745141811,33.7595155330097,0.));
#83518=CARTESIAN_POINT('Ctrl Pts',(-32.7554745141811,33.7595155330097,20.));
#83519=CARTESIAN_POINT('Ctrl Pts',(-32.7297169461065,33.7803320122473,0.));
#83520=CARTESIAN_POINT('Ctrl Pts',(-32.7297169461065,33.7803320122473,20.));
#83521=CARTESIAN_POINT('Ctrl Pts',(-32.7039456562922,33.8011297234537,0.));
#83522=CARTESIAN_POINT('Ctrl Pts',(-32.7039456562922,33.8011297234537,20.));
#83523=CARTESIAN_POINT('Ctrl Pts',(-32.6781606579598,33.8219086570836,0.));
#83524=CARTESIAN_POINT('Ctrl Pts',(-32.6781606579598,33.8219086570836,20.));
#83525=CARTESIAN_POINT('Ctrl Pts',(-32.652361964338,33.8426688036011,0.));
#83526=CARTESIAN_POINT('Ctrl Pts',(-32.652361964338,33.8426688036011,20.));
#83527=CARTESIAN_POINT('Ctrl Pts',(-32.6265495886629,33.8634101534794,0.));
#83528=CARTESIAN_POINT('Ctrl Pts',(-32.6265495886629,33.8634101534794,20.));
#83529=CARTESIAN_POINT('Ctrl Pts',(-32.6007235441777,33.8841326972007,0.));
#83530=CARTESIAN_POINT('Ctrl Pts',(-32.6007235441777,33.8841326972007,20.));
#83531=CARTESIAN_POINT('Ctrl Pts',(-32.5748838441319,33.9048364252556,0.));
#83532=CARTESIAN_POINT('Ctrl Pts',(-32.5748838441319,33.9048364252556,20.));
#83533=CARTESIAN_POINT('Ctrl Pts',(-32.5490305017817,33.9255213281433,0.));
#83534=CARTESIAN_POINT('Ctrl Pts',(-32.5490305017817,33.9255213281433,20.));
#83535=CARTESIAN_POINT('Ctrl Pts',(-32.5231635303904,33.9461873963724,0.));
#83536=CARTESIAN_POINT('Ctrl Pts',(-32.5231635303904,33.9461873963724,20.));
#83537=CARTESIAN_POINT('Ctrl Pts',(-32.4972829432285,33.9668346204604,0.));
#83538=CARTESIAN_POINT('Ctrl Pts',(-32.4972829432285,33.9668346204604,20.));
#83539=CARTESIAN_POINT('Ctrl Pts',(-32.4713887535742,33.987462990935,0.));
#83540=CARTESIAN_POINT('Ctrl Pts',(-32.4713887535742,33.987462990935,20.));
#83541=CARTESIAN_POINT('Ctrl Pts',(-32.4454809747123,34.0080724983324,0.));
#83542=CARTESIAN_POINT('Ctrl Pts',(-32.4454809747123,34.0080724983324,20.));
#83543=CARTESIAN_POINT('Ctrl Pts',(-32.4195596199345,34.0286631331978,0.));
#83544=CARTESIAN_POINT('Ctrl Pts',(-32.4195596199345,34.0286631331978,20.));
#83545=CARTESIAN_POINT('Ctrl Pts',(-32.3936247025393,34.0492348860854,0.));
#83546=CARTESIAN_POINT('Ctrl Pts',(-32.3936247025393,34.0492348860854,20.));
#83547=CARTESIAN_POINT('Ctrl Pts',(-32.3676762358321,34.0697877475586,0.));
#83548=CARTESIAN_POINT('Ctrl Pts',(-32.3676762358321,34.0697877475586,20.));
#83549=CARTESIAN_POINT('Ctrl Pts',(-32.3417142331257,34.0903217081898,0.));
#83550=CARTESIAN_POINT('Ctrl Pts',(-32.3417142331257,34.0903217081898,20.));
#83551=CARTESIAN_POINT('Ctrl Pts',(-32.3157387077392,34.1108367585604,0.));
#83552=CARTESIAN_POINT('Ctrl Pts',(-32.3157387077392,34.1108367585604,20.));
#83553=CARTESIAN_POINT('Ctrl Pts',(-32.2897496729991,34.131332889261,0.));
#83554=CARTESIAN_POINT('Ctrl Pts',(-32.2897496729991,34.131332889261,20.));
#83555=CARTESIAN_POINT('Ctrl Pts',(-32.2637471422389,34.1518100908915,0.));
#83556=CARTESIAN_POINT('Ctrl Pts',(-32.2637471422389,34.1518100908915,20.));
#83557=CARTESIAN_POINT('Ctrl Pts',(-32.2377311287994,34.1722683540613,0.));
#83558=CARTESIAN_POINT('Ctrl Pts',(-32.2377311287994,34.1722683540613,20.));
#83559=CARTESIAN_POINT('Ctrl Pts',(-32.2117016460282,34.1927076693883,0.));
#83560=CARTESIAN_POINT('Ctrl Pts',(-32.2117016460282,34.1927076693883,20.));
#83561=CARTESIAN_POINT('Ctrl Pts',(-32.1856587072789,34.2131280274994,0.));
#83562=CARTESIAN_POINT('Ctrl Pts',(-32.1856587072789,34.2131280274994,20.));
#83563=CARTESIAN_POINT('Ctrl Pts',(-32.1596023259127,34.233529419031,0.));
#83564=CARTESIAN_POINT('Ctrl Pts',(-32.1596023259127,34.233529419031,20.));
#83565=CARTESIAN_POINT('Ctrl Pts',(-32.1335325152974,34.2539118346284,0.));
#83566=CARTESIAN_POINT('Ctrl Pts',(-32.1335325152974,34.2539118346284,20.));
#83567=CARTESIAN_POINT('Ctrl Pts',(-32.1074492888083,34.2742752649465,0.));
#83568=CARTESIAN_POINT('Ctrl Pts',(-32.1074492888083,34.2742752649465,20.));
#83569=CARTESIAN_POINT('Ctrl Pts',(-32.081352659827,34.2946197006486,0.));
#83570=CARTESIAN_POINT('Ctrl Pts',(-32.081352659827,34.2946197006486,20.));
#83571=CARTESIAN_POINT('Ctrl Pts',(-32.0552426417428,34.3149451324081,0.));
#83572=CARTESIAN_POINT('Ctrl Pts',(-32.0552426417428,34.3149451324081,20.));
#83573=CARTESIAN_POINT('Ctrl Pts',(-32.0291192479513,34.335251550907,0.));
#83574=CARTESIAN_POINT('Ctrl Pts',(-32.0291192479513,34.335251550907,20.));
#83575=CARTESIAN_POINT('Ctrl Pts',(-32.0029824918551,34.3555389468366,0.));
#83576=CARTESIAN_POINT('Ctrl Pts',(-32.0029824918551,34.3555389468366,20.));
#83577=CARTESIAN_POINT('Ctrl Pts',(-31.9768323868632,34.3758073108972,0.));
#83578=CARTESIAN_POINT('Ctrl Pts',(-31.9768323868632,34.3758073108972,20.));
#83579=CARTESIAN_POINT('Ctrl Pts',(-31.9506689463919,34.3960566337982,0.));
#83580=CARTESIAN_POINT('Ctrl Pts',(-31.9506689463919,34.3960566337982,20.));
#83581=CARTESIAN_POINT('Ctrl Pts',(-31.9244921838641,34.4162869062583,0.));
#83582=CARTESIAN_POINT('Ctrl Pts',(-31.9244921838641,34.4162869062583,20.));
#83583=CARTESIAN_POINT('Ctrl Pts',(-31.8983021127102,34.4364981190057,0.));
#83584=CARTESIAN_POINT('Ctrl Pts',(-31.8983021127102,34.4364981190057,20.));
#83585=CARTESIAN_POINT('Ctrl Pts',(-31.8720987463673,34.4566902627777,0.));
#83586=CARTESIAN_POINT('Ctrl Pts',(-31.8720987463673,34.4566902627777,20.));
#83587=CARTESIAN_POINT('Ctrl Pts',(-31.8458820982794,34.4768633283209,0.));
#83588=CARTESIAN_POINT('Ctrl Pts',(-31.8458820982794,34.4768633283209,20.));
#83589=CARTESIAN_POINT('Ctrl Pts',(-31.819652181897,34.4970173063908,0.));
#83590=CARTESIAN_POINT('Ctrl Pts',(-31.819652181897,34.4970173063908,20.));
#83591=CARTESIAN_POINT('Ctrl Pts',(-31.7934090106771,34.5171521877518,0.));
#83592=CARTESIAN_POINT('Ctrl Pts',(-31.7934090106771,34.5171521877518,20.));
#83593=CARTESIAN_POINT('Ctrl Pts',(-31.7671525980838,34.5372679631777,0.));
#83594=CARTESIAN_POINT('Ctrl Pts',(-31.7671525980838,34.5372679631777,20.));
#83595=CARTESIAN_POINT('Ctrl Pts',(-31.7408829575879,34.5573646234518,0.));
#83596=CARTESIAN_POINT('Ctrl Pts',(-31.7408829575879,34.5573646234518,20.));
#83597=CARTESIAN_POINT('Ctrl Pts',(-31.7146001026678,34.5774421593669,0.));
#83598=CARTESIAN_POINT('Ctrl Pts',(-31.7146001026678,34.5774421593669,20.));
#83599=CARTESIAN_POINT('Ctrl Pts',(-31.6883040468088,34.5975005617252,0.));
#83600=CARTESIAN_POINT('Ctrl Pts',(-31.6883040468088,34.5975005617252,20.));
#83601=CARTESIAN_POINT('Ctrl Pts',(-31.6619948035027,34.6175398213376,0.));
#83602=CARTESIAN_POINT('Ctrl Pts',(-31.6619948035027,34.6175398213376,20.));
#83603=CARTESIAN_POINT('Ctrl Pts',(-31.6356723862475,34.6375599290242,0.));
#83604=CARTESIAN_POINT('Ctrl Pts',(-31.6356723862475,34.6375599290242,20.));
#83605=CARTESIAN_POINT('Ctrl Pts',(-31.609336808548,34.6575608756141,0.));
#83606=CARTESIAN_POINT('Ctrl Pts',(-31.609336808548,34.6575608756141,20.));
#83607=CARTESIAN_POINT('Ctrl Pts',(-31.5829880839157,34.6775426519456,0.));
#83608=CARTESIAN_POINT('Ctrl Pts',(-31.5829880839157,34.6775426519456,20.));
#83609=CARTESIAN_POINT('Ctrl Pts',(-31.556626225869,34.6975052488666,0.));
#83610=CARTESIAN_POINT('Ctrl Pts',(-31.556626225869,34.6975052488666,20.));
#83611=CARTESIAN_POINT('Ctrl Pts',(-31.5302512479332,34.7174486572342,0.));
#83612=CARTESIAN_POINT('Ctrl Pts',(-31.5302512479332,34.7174486572342,20.));
#83613=CARTESIAN_POINT('Ctrl Pts',(-31.5038631636409,34.7373728679152,0.));
#83614=CARTESIAN_POINT('Ctrl Pts',(-31.5038631636409,34.7373728679152,20.));
#83615=CARTESIAN_POINT('Ctrl Pts',(-31.4774619865312,34.7572778717852,0.));
#83616=CARTESIAN_POINT('Ctrl Pts',(-31.4774619865312,34.7572778717852,20.));
#83617=CARTESIAN_POINT('Ctrl Pts',(-31.4510477301503,34.7771636597296,0.));
#83618=CARTESIAN_POINT('Ctrl Pts',(-31.4510477301503,34.7771636597296,20.));
#83619=CARTESIAN_POINT('Ctrl Pts',(-31.4246204080513,34.7970302226433,0.));
#83620=CARTESIAN_POINT('Ctrl Pts',(-31.4246204080513,34.7970302226433,20.));
#83621=CARTESIAN_POINT('Ctrl Pts',(-31.3981800337935,34.8168775514299,0.));
#83622=CARTESIAN_POINT('Ctrl Pts',(-31.3981800337935,34.8168775514299,20.));
#83623=CARTESIAN_POINT('Ctrl Pts',(-31.3717266209434,34.8367056370026,0.));
#83624=CARTESIAN_POINT('Ctrl Pts',(-31.3717266209434,34.8367056370026,20.));
#83625=CARTESIAN_POINT('Ctrl Pts',(-31.3452601830726,34.856514470283,0.));
#83626=CARTESIAN_POINT('Ctrl Pts',(-31.3452601830726,34.856514470283,20.));
#83627=CARTESIAN_POINT('Ctrl Pts',(-31.3187807337598,34.8763040422018,0.));
#83628=CARTESIAN_POINT('Ctrl Pts',(-31.3187807337598,34.8763040422018,20.));
#83629=CARTESIAN_POINT('Ctrl Pts',(-31.2922882865907,34.8960743436995,0.));
#83630=CARTESIAN_POINT('Ctrl Pts',(-31.2922882865907,34.8960743436995,20.));
#83631=CARTESIAN_POINT('Ctrl Pts',(-31.2657828551579,34.9158253657262,0.));
#83632=CARTESIAN_POINT('Ctrl Pts',(-31.2657828551579,34.9158253657262,20.));
#83633=CARTESIAN_POINT('Ctrl Pts',(-31.2392644530613,34.9355570992414,0.));
#83634=CARTESIAN_POINT('Ctrl Pts',(-31.2392644530613,34.9355570992414,20.));
#83635=CARTESIAN_POINT('Ctrl Pts',(-31.2127330939086,34.9552695352152,0.));
#83636=CARTESIAN_POINT('Ctrl Pts',(-31.2127330939086,34.9552695352152,20.));
#83637=CARTESIAN_POINT('Ctrl Pts',(-31.1861887913133,34.9749626646259,0.));
#83638=CARTESIAN_POINT('Ctrl Pts',(-31.1861887913133,34.9749626646259,20.));
#83639=CARTESIAN_POINT('Ctrl Pts',(-31.1596315588953,34.9946364784612,0.));
#83640=CARTESIAN_POINT('Ctrl Pts',(-31.1596315588953,34.9946364784612,20.));
#83641=CARTESIAN_POINT('Ctrl Pts',(-31.1330614102809,35.0142909677175,0.));
#83642=CARTESIAN_POINT('Ctrl Pts',(-31.1330614102809,35.0142909677175,20.));
#83643=CARTESIAN_POINT('Ctrl Pts',(-31.1064783591027,35.0339261234012,0.));
#83644=CARTESIAN_POINT('Ctrl Pts',(-31.1064783591027,35.0339261234012,20.));
#83645=CARTESIAN_POINT('Ctrl Pts',(-31.0798824190004,35.0535419365277,0.));
#83646=CARTESIAN_POINT('Ctrl Pts',(-31.0798824190004,35.0535419365277,20.));
#83647=CARTESIAN_POINT('Ctrl Pts',(-31.0532736036193,35.0731383981212,0.));
#83648=CARTESIAN_POINT('Ctrl Pts',(-31.0532736036193,35.0731383981212,20.));
#83649=CARTESIAN_POINT('Ctrl Pts',(-31.026651926612,35.0927154992152,0.));
#83650=CARTESIAN_POINT('Ctrl Pts',(-31.026651926612,35.0927154992152,20.));
#83651=CARTESIAN_POINT('Ctrl Pts',(-31.0000174016378,35.1122732308527,0.));
#83652=CARTESIAN_POINT('Ctrl Pts',(-31.0000174016378,35.1122732308527,20.));
#83653=CARTESIAN_POINT('Ctrl Pts',(-30.9733700423633,35.131811584087,0.));
#83654=CARTESIAN_POINT('Ctrl Pts',(-30.9733700423633,35.131811584087,20.));
#83655=CARTESIAN_POINT('Ctrl Pts',(-30.9467098624624,35.1513305499814,0.));
#83656=CARTESIAN_POINT('Ctrl Pts',(-30.9467098624624,35.1513305499814,20.));
#83657=CARTESIAN_POINT('Ctrl Pts',(-30.9200368756162,35.170830119609,0.));
#83658=CARTESIAN_POINT('Ctrl Pts',(-30.9200368756162,35.170830119609,20.));
#83659=CARTESIAN_POINT('Ctrl Pts',(-30.8933510955116,35.1903102840518,0.));
#83660=CARTESIAN_POINT('Ctrl Pts',(-30.8933510955116,35.1903102840518,20.));
#83661=CARTESIAN_POINT('Ctrl Pts',(-30.8666525358408,35.2097710343997,0.));
#83662=CARTESIAN_POINT('Ctrl Pts',(-30.8666525358408,35.2097710343997,20.));
#83663=CARTESIAN_POINT('Ctrl Pts',(-30.8399412103027,35.2292123617517,0.));
#83664=CARTESIAN_POINT('Ctrl Pts',(-30.8399412103027,35.2292123617517,20.));
#83665=CARTESIAN_POINT('Ctrl Pts',(-30.8132171326021,35.2486342572162,0.));
#83666=CARTESIAN_POINT('Ctrl Pts',(-30.8132171326021,35.2486342572162,20.));
#83667=CARTESIAN_POINT('Ctrl Pts',(-30.7864803164511,35.2680367119112,0.));
#83668=CARTESIAN_POINT('Ctrl Pts',(-30.7864803164511,35.2680367119112,20.));
#83669=CARTESIAN_POINT('Ctrl Pts',(-30.7597307755696,35.2874197169657,0.));
#83670=CARTESIAN_POINT('Ctrl Pts',(-30.7597307755696,35.2874197169657,20.));
#83671=CARTESIAN_POINT('Ctrl Pts',(-30.732968523684,35.3067832635176,0.));
#83672=CARTESIAN_POINT('Ctrl Pts',(-30.732968523684,35.3067832635176,20.));
#83673=CARTESIAN_POINT('Ctrl Pts',(-30.7061935745273,35.3261273427148,0.));
#83674=CARTESIAN_POINT('Ctrl Pts',(-30.7061935745273,35.3261273427148,20.));
#83675=CARTESIAN_POINT('Ctrl Pts',(-30.6794059418388,35.3454519457137,0.));
#83676=CARTESIAN_POINT('Ctrl Pts',(-30.6794059418388,35.3454519457137,20.));
#83677=CARTESIAN_POINT('Ctrl Pts',(-30.6526056393639,35.3647570636798,0.));
#83678=CARTESIAN_POINT('Ctrl Pts',(-30.6526056393639,35.3647570636798,20.));
#83679=CARTESIAN_POINT('Ctrl Pts',(-30.6257926808542,35.3840426877879,0.));
#83680=CARTESIAN_POINT('Ctrl Pts',(-30.6257926808542,35.3840426877879,20.));
#83681=CARTESIAN_POINT('Ctrl Pts',(-30.5989670800681,35.4033088092225,0.));
#83682=CARTESIAN_POINT('Ctrl Pts',(-30.5989670800681,35.4033088092225,20.));
#83683=CARTESIAN_POINT('Ctrl Pts',(-30.5721288507715,35.4225554191786,0.));
#83684=CARTESIAN_POINT('Ctrl Pts',(-30.5721288507715,35.4225554191786,20.));
#83685=CARTESIAN_POINT('Ctrl Pts',(-30.5452780067369,35.4417825088605,0.));
#83686=CARTESIAN_POINT('Ctrl Pts',(-30.5452780067369,35.4417825088605,20.));
#83687=CARTESIAN_POINT('Ctrl Pts',(-30.5184145617425,35.4609900694812,0.));
#83688=CARTESIAN_POINT('Ctrl Pts',(-30.5184145617425,35.4609900694812,20.));
#83689=CARTESIAN_POINT('Ctrl Pts',(-30.4915385295724,35.4801780922625,0.));
#83690=CARTESIAN_POINT('Ctrl Pts',(-30.4915385295724,35.4801780922625,20.));
#83691=CARTESIAN_POINT('Ctrl Pts',(-30.4646499240178,35.4993465684361,0.));
#83692=CARTESIAN_POINT('Ctrl Pts',(-30.4646499240178,35.4993465684361,20.));
#83693=CARTESIAN_POINT('Ctrl Pts',(-30.437748758876,35.518495489243,0.));
#83694=CARTESIAN_POINT('Ctrl Pts',(-30.437748758876,35.518495489243,20.));
#83695=CARTESIAN_POINT('Ctrl Pts',(-30.4108350479521,35.5376248459348,0.));
#83696=CARTESIAN_POINT('Ctrl Pts',(-30.4108350479521,35.5376248459348,20.));
#83697=CARTESIAN_POINT('Ctrl Pts',(-30.3839088050584,35.5567346297736,0.));
#83698=CARTESIAN_POINT('Ctrl Pts',(-30.3839088050584,35.5567346297736,20.));
#83699=CARTESIAN_POINT('Ctrl Pts',(-30.3569700440131,35.5758248320301,0.));
#83700=CARTESIAN_POINT('Ctrl Pts',(-30.3569700440131,35.5758248320301,20.));
#83701=CARTESIAN_POINT('Ctrl Pts',(-30.3300187786403,35.5948954439837,0.));
#83702=CARTESIAN_POINT('Ctrl Pts',(-30.3300187786403,35.5948954439837,20.));
#83703=CARTESIAN_POINT('Ctrl Pts',(-30.3030550227693,35.6139464569223,0.));
#83704=CARTESIAN_POINT('Ctrl Pts',(-30.3030550227693,35.6139464569223,20.));
#83705=CARTESIAN_POINT('Ctrl Pts',(-30.2760787902362,35.6329778621436,0.));
#83706=CARTESIAN_POINT('Ctrl Pts',(-30.2760787902362,35.6329778621436,20.));
#83707=CARTESIAN_POINT('Ctrl Pts',(-30.2490900948838,35.6519896509552,0.));
#83708=CARTESIAN_POINT('Ctrl Pts',(-30.2490900948838,35.6519896509552,20.));
#83709=CARTESIAN_POINT('Ctrl Pts',(-30.2220889505625,35.6709818146751,0.));
#83710=CARTESIAN_POINT('Ctrl Pts',(-30.2220889505625,35.6709818146751,20.));
#83711=CARTESIAN_POINT('Ctrl Pts',(-30.1950753711288,35.6899543446308,0.));
#83712=CARTESIAN_POINT('Ctrl Pts',(-30.1950753711288,35.6899543446308,20.));
#83713=CARTESIAN_POINT('Ctrl Pts',(-30.1680493704465,35.7089072321597,0.));
#83714=CARTESIAN_POINT('Ctrl Pts',(-30.1680493704465,35.7089072321597,20.));
#83715=CARTESIAN_POINT('Ctrl Pts',(-30.141010962385,35.7278404686079,0.));
#83716=CARTESIAN_POINT('Ctrl Pts',(-30.141010962385,35.7278404686079,20.));
#83717=CARTESIAN_POINT('Ctrl Pts',(-30.1139601608197,35.7467540453308,0.));
#83718=CARTESIAN_POINT('Ctrl Pts',(-30.1139601608197,35.7467540453308,20.));
#83719=CARTESIAN_POINT('Ctrl Pts',(-30.0868969796328,35.7656479536938,0.));
#83720=CARTESIAN_POINT('Ctrl Pts',(-30.0868969796328,35.7656479536938,20.));
#83721=CARTESIAN_POINT('Ctrl Pts',(-30.0598214327127,35.7845221850715,0.));
#83722=CARTESIAN_POINT('Ctrl Pts',(-30.0598214327127,35.7845221850715,20.));
#83723=CARTESIAN_POINT('Ctrl Pts',(-30.0327335339539,35.8033767308478,0.));
#83724=CARTESIAN_POINT('Ctrl Pts',(-30.0327335339539,35.8033767308478,20.));
#83725=CARTESIAN_POINT('Ctrl Pts',(-30.005633297258,35.8222115824166,0.));
#83726=CARTESIAN_POINT('Ctrl Pts',(-30.005633297258,35.8222115824166,20.));
#83727=CARTESIAN_POINT('Ctrl Pts',(-29.9785207365333,35.841026731182,0.));
#83728=CARTESIAN_POINT('Ctrl Pts',(-29.9785207365333,35.841026731182,20.));
#83729=CARTESIAN_POINT('Ctrl Pts',(-29.9513958656946,35.8598221685576,0.));
#83730=CARTESIAN_POINT('Ctrl Pts',(-29.9513958656946,35.8598221685576,20.));
#83731=CARTESIAN_POINT('Ctrl Pts',(-29.9242586986624,35.8785978859658,0.));
#83732=CARTESIAN_POINT('Ctrl Pts',(-29.9242586986624,35.8785978859658,20.));
#83733=CARTESIAN_POINT('Ctrl Pts',(-29.8971092493635,35.8973538748387,0.));
#83734=CARTESIAN_POINT('Ctrl Pts',(-29.8971092493635,35.8973538748387,20.));
#83735=CARTESIAN_POINT('Ctrl Pts',(-29.869947531731,35.9160901266176,0.));
#83736=CARTESIAN_POINT('Ctrl Pts',(-29.869947531731,35.9160901266176,20.));
#83737=CARTESIAN_POINT('Ctrl Pts',(-29.8427735597049,35.9348066327539,0.));
#83738=CARTESIAN_POINT('Ctrl Pts',(-29.8427735597049,35.9348066327539,20.));
#83739=CARTESIAN_POINT('Ctrl Pts',(-29.8155873472308,35.9535033847081,0.));
#83740=CARTESIAN_POINT('Ctrl Pts',(-29.8155873472308,35.9535033847081,20.));
#83741=CARTESIAN_POINT('Ctrl Pts',(-29.7883889082614,35.9721803739509,0.));
#83742=CARTESIAN_POINT('Ctrl Pts',(-29.7883889082614,35.9721803739509,20.));
#83743=CARTESIAN_POINT('Ctrl Pts',(-29.7611782567557,35.9908375919623,0.));
#83744=CARTESIAN_POINT('Ctrl Pts',(-29.7611782567557,35.9908375919623,20.));
#83745=CARTESIAN_POINT('Ctrl Pts',(-29.7339554066796,36.009475030233,0.));
#83746=CARTESIAN_POINT('Ctrl Pts',(-29.7339554066796,36.009475030233,20.));
#83747=CARTESIAN_POINT('Ctrl Pts',(-29.7067203720053,36.0280926802632,0.));
#83748=CARTESIAN_POINT('Ctrl Pts',(-29.7067203720053,36.0280926802632,20.));
#83749=CARTESIAN_POINT('Ctrl Pts',(-29.6794731667107,36.0466905335617,0.));
#83750=CARTESIAN_POINT('Ctrl Pts',(-29.6794731667107,36.0466905335617,20.));
#83751=CARTESIAN_POINT('Ctrl Pts',(-29.6522138047794,36.0652685816464,0.));
#83752=CARTESIAN_POINT('Ctrl Pts',(-29.6522138047794,36.0652685816464,20.));
#83753=CARTESIAN_POINT('Ctrl Pts',(-29.6249423002017,36.0838268160451,0.));
#83754=CARTESIAN_POINT('Ctrl Pts',(-29.6249423002017,36.0838268160451,20.));
#83755=CARTESIAN_POINT('Ctrl Pts',(-29.5976586669748,36.1023652282957,0.));
#83756=CARTESIAN_POINT('Ctrl Pts',(-29.5976586669748,36.1023652282957,20.));
#83757=CARTESIAN_POINT('Ctrl Pts',(-29.5703629191022,36.120883809946,0.));
#83758=CARTESIAN_POINT('Ctrl Pts',(-29.5703629191022,36.120883809946,20.));
#83759=CARTESIAN_POINT('Ctrl Pts',(-29.5430550705938,36.1393825525541,0.));
#83760=CARTESIAN_POINT('Ctrl Pts',(-29.5430550705938,36.1393825525541,20.));
#83761=CARTESIAN_POINT('Ctrl Pts',(-29.5157351354652,36.1578614476865,0.));
#83762=CARTESIAN_POINT('Ctrl Pts',(-29.5157351354652,36.1578614476865,20.));
#83763=CARTESIAN_POINT('Ctrl Pts',(-29.4884031277381,36.1763204869192,0.));
#83764=CARTESIAN_POINT('Ctrl Pts',(-29.4884031277381,36.1763204869192,20.));
#83765=CARTESIAN_POINT('Ctrl Pts',(-29.4610590614411,36.1947596618382,0.));
#83766=CARTESIAN_POINT('Ctrl Pts',(-29.4610590614411,36.1947596618382,20.));
#83767=CARTESIAN_POINT('Ctrl Pts',(-29.4337029506094,36.2131789640396,0.));
#83768=CARTESIAN_POINT('Ctrl Pts',(-29.4337029506094,36.2131789640396,20.));
#83769=CARTESIAN_POINT('Ctrl Pts',(-29.4063348092849,36.2315783851295,0.));
#83770=CARTESIAN_POINT('Ctrl Pts',(-29.4063348092849,36.2315783851295,20.));
#83771=CARTESIAN_POINT('Ctrl Pts',(-29.3789546515147,36.2499579167227,0.));
#83772=CARTESIAN_POINT('Ctrl Pts',(-29.3789546515147,36.2499579167227,20.));
#83773=CARTESIAN_POINT('Ctrl Pts',(-29.3515624913523,36.2683175504441,0.));
#83774=CARTESIAN_POINT('Ctrl Pts',(-29.3515624913523,36.2683175504441,20.));
#83775=CARTESIAN_POINT('Ctrl Pts',(-29.3241583428569,36.286657277928,0.));
#83776=CARTESIAN_POINT('Ctrl Pts',(-29.3241583428569,36.286657277928,20.));
#83777=CARTESIAN_POINT('Ctrl Pts',(-29.2967422200943,36.3049770908188,0.));
#83778=CARTESIAN_POINT('Ctrl Pts',(-29.2967422200943,36.3049770908188,20.));
#83779=CARTESIAN_POINT('Ctrl Pts',(-29.2693141371364,36.3232769807701,0.));
#83780=CARTESIAN_POINT('Ctrl Pts',(-29.2693141371364,36.3232769807701,20.));
#83781=CARTESIAN_POINT('Ctrl Pts',(-29.241874108062,36.3415569394456,0.));
#83782=CARTESIAN_POINT('Ctrl Pts',(-29.241874108062,36.3415569394456,20.));
#83783=CARTESIAN_POINT('Ctrl Pts',(-29.2144221469563,36.3598169585186,0.));
#83784=CARTESIAN_POINT('Ctrl Pts',(-29.2144221469563,36.3598169585186,20.));
#83785=CARTESIAN_POINT('Ctrl Pts',(-29.186958267911,36.3780570296725,0.));
#83786=CARTESIAN_POINT('Ctrl Pts',(-29.186958267911,36.3780570296725,20.));
#83787=CARTESIAN_POINT('Ctrl Pts',(-29.1594824850239,36.3962771446002,0.));
#83788=CARTESIAN_POINT('Ctrl Pts',(-29.1594824850239,36.3962771446002,20.));
#83789=CARTESIAN_POINT('Ctrl Pts',(-29.1319948123985,36.4144772950043,0.));
#83790=CARTESIAN_POINT('Ctrl Pts',(-29.1319948123985,36.4144772950043,20.));
#83791=CARTESIAN_POINT('Ctrl Pts',(-29.1044952641443,36.4326574725969,0.));
#83792=CARTESIAN_POINT('Ctrl Pts',(-29.1044952641443,36.4326574725969,20.));
#83793=CARTESIAN_POINT('Ctrl Pts',(-29.0769838543763,36.4508176690994,0.));
#83794=CARTESIAN_POINT('Ctrl Pts',(-29.0769838543763,36.4508176690994,20.));
#83795=CARTESIAN_POINT('Ctrl Pts',(-29.0494605972165,36.4689578762435,0.));
#83796=CARTESIAN_POINT('Ctrl Pts',(-29.0494605972165,36.4689578762435,20.));
#83797=CARTESIAN_POINT('Ctrl Pts',(-29.0219255067927,36.4870780857703,0.));
#83798=CARTESIAN_POINT('Ctrl Pts',(-29.0219255067927,36.4870780857703,20.));
#83799=CARTESIAN_POINT('Ctrl Pts',(-28.99437859724,36.5051782894316,0.));
#83800=CARTESIAN_POINT('Ctrl Pts',(-28.99437859724,36.5051782894316,20.));
#83801=CARTESIAN_POINT('Ctrl Pts',(-28.9668198826995,36.5232584789885,0.));
#83802=CARTESIAN_POINT('Ctrl Pts',(-28.9668198826995,36.5232584789885,20.));
#83803=CARTESIAN_POINT('Ctrl Pts',(-28.9392493773185,36.5413186462123,0.));
#83804=CARTESIAN_POINT('Ctrl Pts',(-28.9392493773185,36.5413186462123,20.));
#83805=CARTESIAN_POINT('Ctrl Pts',(-28.9116670952497,36.5593587828826,0.));
#83806=CARTESIAN_POINT('Ctrl Pts',(-28.9116670952497,36.5593587828826,20.));
#83807=CARTESIAN_POINT('Ctrl Pts',(-28.8840730506515,36.577378880789,0.));
#83808=CARTESIAN_POINT('Ctrl Pts',(-28.8840730506515,36.577378880789,20.));
#83809=CARTESIAN_POINT('Ctrl Pts',(-28.8564672576885,36.5953789317305,0.));
#83810=CARTESIAN_POINT('Ctrl Pts',(-28.8564672576885,36.5953789317305,20.));
#83811=CARTESIAN_POINT('Ctrl Pts',(-28.8288497305324,36.6133589275174,0.));
#83812=CARTESIAN_POINT('Ctrl Pts',(-28.8288497305324,36.6133589275174,20.));
#83813=CARTESIAN_POINT('Ctrl Pts',(-28.8012204833609,36.6313188599694,0.));
#83814=CARTESIAN_POINT('Ctrl Pts',(-28.8012204833609,36.6313188599694,20.));
#83815=CARTESIAN_POINT('Ctrl Pts',(-28.7735795303585,36.6492587209167,0.));
#83816=CARTESIAN_POINT('Ctrl Pts',(-28.7735795303585,36.6492587209167,20.));
#83817=CARTESIAN_POINT('Ctrl Pts',(-28.7459268857152,36.6671785021988,0.));
#83818=CARTESIAN_POINT('Ctrl Pts',(-28.7459268857152,36.6671785021988,20.));
#83819=CARTESIAN_POINT('Ctrl Pts',(-28.7182625636274,36.6850781956649,0.));
#83820=CARTESIAN_POINT('Ctrl Pts',(-28.7182625636274,36.6850781956649,20.));
#83821=CARTESIAN_POINT('Ctrl Pts',(-28.6905865782966,36.7029577931733,0.));
#83822=CARTESIAN_POINT('Ctrl Pts',(-28.6905865782966,36.7029577931733,20.));
#83823=CARTESIAN_POINT('Ctrl Pts',(-28.6628989439305,36.7208172865919,0.));
#83824=CARTESIAN_POINT('Ctrl Pts',(-28.6628989439305,36.7208172865919,20.));
#83825=CARTESIAN_POINT('Ctrl Pts',(-28.6351996747428,36.738656667798,0.));
#83826=CARTESIAN_POINT('Ctrl Pts',(-28.6351996747428,36.738656667798,20.));
#83827=CARTESIAN_POINT('Ctrl Pts',(-28.6074887849535,36.7564759286795,0.));
#83828=CARTESIAN_POINT('Ctrl Pts',(-28.6074887849535,36.7564759286795,20.));
#83829=CARTESIAN_POINT('Ctrl Pts',(-28.5797662887891,36.774275061134,0.));
#83830=CARTESIAN_POINT('Ctrl Pts',(-28.5797662887891,36.774275061134,20.));
#83831=CARTESIAN_POINT('Ctrl Pts',(-28.5520322004825,36.7920540570698,0.));
#83832=CARTESIAN_POINT('Ctrl Pts',(-28.5520322004825,36.7920540570698,20.));
#83833=CARTESIAN_POINT('Ctrl Pts',(-28.5242865342725,36.809812908405,0.));
#83834=CARTESIAN_POINT('Ctrl Pts',(-28.5242865342725,36.809812908405,20.));
#83835=CARTESIAN_POINT('Ctrl Pts',(-28.496529304404,36.8275516070676,0.));
#83836=CARTESIAN_POINT('Ctrl Pts',(-28.496529304404,36.8275516070676,20.));
#83837=CARTESIAN_POINT('Ctrl Pts',(-28.4687605251277,36.8452701449948,0.));
#83838=CARTESIAN_POINT('Ctrl Pts',(-28.4687605251277,36.8452701449948,20.));
#83839=CARTESIAN_POINT('Ctrl Pts',(-28.4409802107003,36.8629685141338,0.));
#83840=CARTESIAN_POINT('Ctrl Pts',(-28.4409802107003,36.8629685141338,20.));
#83841=CARTESIAN_POINT('Ctrl Pts',(-28.4131883753841,36.8806467064409,0.));
#83842=CARTESIAN_POINT('Ctrl Pts',(-28.4131883753841,36.8806467064409,20.));
#83843=CARTESIAN_POINT('Ctrl Pts',(-28.3853850334476,36.8983047138822,0.));
#83844=CARTESIAN_POINT('Ctrl Pts',(-28.3853850334476,36.8983047138822,20.));
#83845=CARTESIAN_POINT('Ctrl Pts',(-28.3575701991656,36.9159425284342,0.));
#83846=CARTESIAN_POINT('Ctrl Pts',(-28.3575701991656,36.9159425284342,20.));
#83847=CARTESIAN_POINT('Ctrl Pts',(-28.3297438868192,36.9335601420835,0.));
#83848=CARTESIAN_POINT('Ctrl Pts',(-28.3297438868192,36.9335601420835,20.));
#83849=CARTESIAN_POINT('Ctrl Pts',(-28.3019061106957,36.9511575468269,0.));
#83850=CARTESIAN_POINT('Ctrl Pts',(-28.3019061106957,36.9511575468269,20.));
#83851=CARTESIAN_POINT('Ctrl Pts',(-28.2740568850882,36.9687347346709,0.));
#83852=CARTESIAN_POINT('Ctrl Pts',(-28.2740568850882,36.9687347346709,20.));
#83853=CARTESIAN_POINT('Ctrl Pts',(-28.2461962242955,36.9862916976318,0.));
#83854=CARTESIAN_POINT('Ctrl Pts',(-28.2461962242955,36.9862916976318,20.));
#83855=CARTESIAN_POINT('Ctrl Pts',(-28.2183241426219,37.0038284277349,0.));
#83856=CARTESIAN_POINT('Ctrl Pts',(-28.2183241426219,37.0038284277349,20.));
#83857=CARTESIAN_POINT('Ctrl Pts',(-28.1904406543778,37.0213449170157,0.));
#83858=CARTESIAN_POINT('Ctrl Pts',(-28.1904406543778,37.0213449170157,20.));
#83859=CARTESIAN_POINT('Ctrl Pts',(-28.1625457738798,37.0388411575197,0.));
#83860=CARTESIAN_POINT('Ctrl Pts',(-28.1625457738798,37.0388411575197,20.));
#83861=CARTESIAN_POINT('Ctrl Pts',(-28.1346395154507,37.0563171413025,0.));
#83862=CARTESIAN_POINT('Ctrl Pts',(-28.1346395154507,37.0563171413025,20.));
#83863=CARTESIAN_POINT('Ctrl Pts',(-28.1067218934195,37.0737728604297,0.));
#83864=CARTESIAN_POINT('Ctrl Pts',(-28.1067218934195,37.0737728604297,20.));
#83865=CARTESIAN_POINT('Ctrl Pts',(-28.0787929221219,37.0912083069771,0.));
#83866=CARTESIAN_POINT('Ctrl Pts',(-28.0787929221219,37.0912083069771,20.));
#83867=CARTESIAN_POINT('Ctrl Pts',(-28.0508526158994,37.1086234730311,0.));
#83868=CARTESIAN_POINT('Ctrl Pts',(-28.0508526158994,37.1086234730311,20.));
#83869=CARTESIAN_POINT('Ctrl Pts',(-28.0229009890986,37.1260183506872,0.));
#83870=CARTESIAN_POINT('Ctrl Pts',(-28.0229009890986,37.1260183506872,20.));
#83871=CARTESIAN_POINT('Ctrl Pts',(-27.994938056072,37.1433929320507,0.));
#83872=CARTESIAN_POINT('Ctrl Pts',(-27.994938056072,37.1433929320507,20.));
#83873=CARTESIAN_POINT('Ctrl Pts',(-27.9669638311771,37.1607472092352,0.));
#83874=CARTESIAN_POINT('Ctrl Pts',(-27.9669638311771,37.1607472092352,20.));
#83875=CARTESIAN_POINT('Ctrl Pts',(-27.9389783287777,37.1780811743651,0.));
#83876=CARTESIAN_POINT('Ctrl Pts',(-27.9389783287777,37.1780811743651,20.));
#83877=CARTESIAN_POINT('Ctrl Pts',(-27.9109815632437,37.1953948195748,0.));
#83878=CARTESIAN_POINT('Ctrl Pts',(-27.9109815632437,37.1953948195748,20.));
#83879=CARTESIAN_POINT('Ctrl Pts',(-27.8829735489517,37.2126881370093,0.));
#83880=CARTESIAN_POINT('Ctrl Pts',(-27.8829735489517,37.2126881370093,20.));
#83881=CARTESIAN_POINT('Ctrl Pts',(-27.8549543002843,37.2299611188238,0.));
#83882=CARTESIAN_POINT('Ctrl Pts',(-27.8549543002843,37.2299611188238,20.));
#83883=CARTESIAN_POINT('Ctrl Pts',(-27.8269238316305,37.2472137571841,0.));
#83884=CARTESIAN_POINT('Ctrl Pts',(-27.8269238316305,37.2472137571841,20.));
#83885=CARTESIAN_POINT('Ctrl Pts',(-27.7988821573847,37.2644460442654,0.));
#83886=CARTESIAN_POINT('Ctrl Pts',(-27.7988821573847,37.2644460442654,20.));
#83887=CARTESIAN_POINT('Ctrl Pts',(-27.7708292919468,37.2816579722525,0.));
#83888=CARTESIAN_POINT('Ctrl Pts',(-27.7708292919468,37.2816579722525,20.));
#83889=CARTESIAN_POINT('Ctrl Pts',(-27.7427652497224,37.2988495333397,0.));
#83890=CARTESIAN_POINT('Ctrl Pts',(-27.7427652497224,37.2988495333397,20.));
#83891=CARTESIAN_POINT('Ctrl Pts',(-27.7146900451229,37.3160207197314,0.));
#83892=CARTESIAN_POINT('Ctrl Pts',(-27.7146900451229,37.3160207197314,20.));
#83893=CARTESIAN_POINT('Ctrl Pts',(-27.6866036925651,37.3331715236413,0.));
#83894=CARTESIAN_POINT('Ctrl Pts',(-27.6866036925651,37.3331715236413,20.));
#83895=CARTESIAN_POINT('Ctrl Pts',(-27.6585062064726,37.3503019372939,0.));
#83896=CARTESIAN_POINT('Ctrl Pts',(-27.6585062064726,37.3503019372939,20.));
#83897=CARTESIAN_POINT('Ctrl Pts',(-27.6303976012745,37.3674119529233,0.));
#83898=CARTESIAN_POINT('Ctrl Pts',(-27.6303976012745,37.3674119529233,20.));
#83899=CARTESIAN_POINT('Ctrl Pts',(-27.6022778914064,37.384501562775,0.));
#83900=CARTESIAN_POINT('Ctrl Pts',(-27.6022778914064,37.384501562775,20.));
#83901=CARTESIAN_POINT('Ctrl Pts',(-27.5741470913095,37.4015707591036,0.));
#83902=CARTESIAN_POINT('Ctrl Pts',(-27.5741470913095,37.4015707591036,20.));
#83903=CARTESIAN_POINT('Ctrl Pts',(-27.5460052154308,37.418619534174,0.));
#83904=CARTESIAN_POINT('Ctrl Pts',(-27.5460052154308,37.418619534174,20.));
#83905=CARTESIAN_POINT('Ctrl Pts',(-27.5178522782226,37.4356478802604,0.));
#83906=CARTESIAN_POINT('Ctrl Pts',(-27.5178522782226,37.4356478802604,20.));
#83907=CARTESIAN_POINT('Ctrl Pts',(-27.489688294143,37.4526557896465,0.));
#83908=CARTESIAN_POINT('Ctrl Pts',(-27.489688294143,37.4526557896465,20.));
#83909=CARTESIAN_POINT('Ctrl Pts',(-27.4615132776558,37.4696432546266,0.));
#83910=CARTESIAN_POINT('Ctrl Pts',(-27.4615132776558,37.4696432546266,20.));
#83911=CARTESIAN_POINT('Ctrl Pts',(-27.4333272432311,37.4866102675047,0.));
#83912=CARTESIAN_POINT('Ctrl Pts',(-27.4333272432311,37.4866102675047,20.));
#83913=CARTESIAN_POINT('Ctrl Pts',(-27.4051302053449,37.5035568205959,0.));
#83914=CARTESIAN_POINT('Ctrl Pts',(-27.4051302053449,37.5035568205959,20.));
#83915=CARTESIAN_POINT('Ctrl Pts',(-27.3769221784798,37.5204829062256,0.));
#83916=CARTESIAN_POINT('Ctrl Pts',(-27.3769221784798,37.5204829062256,20.));
#83917=CARTESIAN_POINT('Ctrl Pts',(-27.3487031771241,37.5373885167297,0.));
#83918=CARTESIAN_POINT('Ctrl Pts',(-27.3487031771241,37.5373885167297,20.));
#83919=CARTESIAN_POINT('Ctrl Pts',(-27.3204732157704,37.5542736444521,0.));
#83920=CARTESIAN_POINT('Ctrl Pts',(-27.3204732157704,37.5542736444521,20.));
#83921=CARTESIAN_POINT('Ctrl Pts',(-27.2922323089174,37.571138281747,0.));
#83922=CARTESIAN_POINT('Ctrl Pts',(-27.2922323089174,37.571138281747,20.));
#83923=CARTESIAN_POINT('Ctrl Pts',(-27.2639804710687,37.5879824209777,0.));
#83924=CARTESIAN_POINT('Ctrl Pts',(-27.2639804710687,37.5879824209777,20.));
#83925=CARTESIAN_POINT('Ctrl Pts',(-27.2357177167352,37.6048060545188,0.));
#83926=CARTESIAN_POINT('Ctrl Pts',(-27.2357177167352,37.6048060545188,20.));
#83927=CARTESIAN_POINT('Ctrl Pts',(-27.2074440604332,37.6216091747552,0.));
#83928=CARTESIAN_POINT('Ctrl Pts',(-27.2074440604332,37.6216091747552,20.));
#83929=CARTESIAN_POINT('Ctrl Pts',(-27.1791595166856,37.6383917740821,0.));
#83930=CARTESIAN_POINT('Ctrl Pts',(-27.1791595166856,37.6383917740821,20.));
#83931=CARTESIAN_POINT('Ctrl Pts',(-27.15086410002,37.6551538449046,0.));
#83932=CARTESIAN_POINT('Ctrl Pts',(-27.15086410002,37.6551538449046,20.));
#83933=CARTESIAN_POINT('Ctrl Pts',(-27.1225578249703,37.6718953796384,0.));
#83934=CARTESIAN_POINT('Ctrl Pts',(-27.1225578249703,37.6718953796384,20.));
#83935=CARTESIAN_POINT('Ctrl Pts',(-27.0942407060752,37.6886163707084,0.));
#83936=CARTESIAN_POINT('Ctrl Pts',(-27.0942407060752,37.6886163707084,20.));
#83937=CARTESIAN_POINT('Ctrl Pts',(-27.0659127578793,37.705316810549,0.));
#83938=CARTESIAN_POINT('Ctrl Pts',(-27.0659127578793,37.705316810549,20.));
#83939=CARTESIAN_POINT('Ctrl Pts',(-27.0375739949332,37.7219966916053,0.));
#83940=CARTESIAN_POINT('Ctrl Pts',(-27.0375739949332,37.7219966916053,20.));
#83941=CARTESIAN_POINT('Ctrl Pts',(-27.0092244317934,37.7386560063324,0.));
#83942=CARTESIAN_POINT('Ctrl Pts',(-27.0092244317934,37.7386560063324,20.));
#83943=CARTESIAN_POINT('Ctrl Pts',(-26.9808640830224,37.755294747196,0.));
#83944=CARTESIAN_POINT('Ctrl Pts',(-26.9808640830224,37.755294747196,20.));
#83945=CARTESIAN_POINT('Ctrl Pts',(-26.9524929631885,37.7719129066715,0.));
#83946=CARTESIAN_POINT('Ctrl Pts',(-26.9524929631885,37.7719129066715,20.));
#83947=CARTESIAN_POINT('Ctrl Pts',(-26.9241110868652,37.7885104772446,0.));
#83948=CARTESIAN_POINT('Ctrl Pts',(-26.9241110868652,37.7885104772446,20.));
#83949=CARTESIAN_POINT('Ctrl Pts',(-26.8957184686315,37.8050874514106,0.));
#83950=CARTESIAN_POINT('Ctrl Pts',(-26.8957184686315,37.8050874514106,20.));
#83951=CARTESIAN_POINT('Ctrl Pts',(-26.8673151230714,37.8216438216745,0.));
#83952=CARTESIAN_POINT('Ctrl Pts',(-26.8673151230714,37.8216438216745,20.));
#83953=CARTESIAN_POINT('Ctrl Pts',(-26.8389010647754,37.8381795805523,0.));
#83954=CARTESIAN_POINT('Ctrl Pts',(-26.8389010647754,37.8381795805523,20.));
#83955=CARTESIAN_POINT('Ctrl Pts',(-26.8104763083398,37.8546947205707,0.));
#83956=CARTESIAN_POINT('Ctrl Pts',(-26.8104763083398,37.8546947205707,20.));
#83957=CARTESIAN_POINT('Ctrl Pts',(-26.782040868367,37.8711892342661,0.));
#83958=CARTESIAN_POINT('Ctrl Pts',(-26.782040868367,37.8711892342661,20.));
#83959=CARTESIAN_POINT('Ctrl Pts',(-26.7535947594648,37.887663114185,0.));
#83960=CARTESIAN_POINT('Ctrl Pts',(-26.7535947594648,37.887663114185,20.));
#83961=CARTESIAN_POINT('Ctrl Pts',(-26.7251379962461,37.904116352883,0.));
#83962=CARTESIAN_POINT('Ctrl Pts',(-26.7251379962461,37.904116352883,20.));
#83963=CARTESIAN_POINT('Ctrl Pts',(-26.6966705933291,37.9205489429259,0.));
#83964=CARTESIAN_POINT('Ctrl Pts',(-26.6966705933291,37.9205489429259,20.));
#83965=CARTESIAN_POINT('Ctrl Pts',(-26.6681925653377,37.9369608768896,0.));
#83966=CARTESIAN_POINT('Ctrl Pts',(-26.6681925653377,37.9369608768896,20.));
#83967=CARTESIAN_POINT('Ctrl Pts',(-26.6397039269022,37.9533521473617,0.));
#83968=CARTESIAN_POINT('Ctrl Pts',(-26.6397039269022,37.9533521473617,20.));
#83969=CARTESIAN_POINT('Ctrl Pts',(-26.6112046926582,37.9697227469388,0.));
#83970=CARTESIAN_POINT('Ctrl Pts',(-26.6112046926582,37.9697227469388,20.));
#83971=CARTESIAN_POINT('Ctrl Pts',(-26.5826948772472,37.9860726682286,0.));
#83972=CARTESIAN_POINT('Ctrl Pts',(-26.5826948772472,37.9860726682286,20.));
#83973=CARTESIAN_POINT('Ctrl Pts',(-26.5541744953163,38.0024019038486,0.));
#83974=CARTESIAN_POINT('Ctrl Pts',(-26.5541744953163,38.0024019038486,20.));
#83975=CARTESIAN_POINT('Ctrl Pts',(-26.5256435615177,38.0187104464255,0.));
#83976=CARTESIAN_POINT('Ctrl Pts',(-26.5256435615177,38.0187104464255,20.));
#83977=CARTESIAN_POINT('Ctrl Pts',(-26.4971020905092,38.0349982885963,0.));
#83978=CARTESIAN_POINT('Ctrl Pts',(-26.4971020905092,38.0349982885963,20.));
#83979=CARTESIAN_POINT('Ctrl Pts',(-26.4685500969542,38.0512654230085,0.));
#83980=CARTESIAN_POINT('Ctrl Pts',(-26.4685500969542,38.0512654230085,20.));
#83981=CARTESIAN_POINT('Ctrl Pts',(-26.439987595522,38.0675118423201,0.));
#83982=CARTESIAN_POINT('Ctrl Pts',(-26.439987595522,38.0675118423201,20.));
#83983=CARTESIAN_POINT('Ctrl Pts',(-26.4114146008872,38.0837375391992,0.));
#83984=CARTESIAN_POINT('Ctrl Pts',(-26.4114146008872,38.0837375391992,20.));
#83985=CARTESIAN_POINT('Ctrl Pts',(-26.3828311277301,38.0999425063245,0.));
#83986=CARTESIAN_POINT('Ctrl Pts',(-26.3828311277301,38.0999425063245,20.));
#83987=CARTESIAN_POINT('Ctrl Pts',(-26.3542371907363,38.1161267363846,0.));
#83988=CARTESIAN_POINT('Ctrl Pts',(-26.3542371907363,38.1161267363846,20.));
#83989=CARTESIAN_POINT('Ctrl Pts',(-26.3256328045976,38.1322902220784,0.));
#83990=CARTESIAN_POINT('Ctrl Pts',(-26.3256328045976,38.1322902220784,20.));
#83991=CARTESIAN_POINT('Ctrl Pts',(-26.2970179840108,38.1484329561142,0.));
#83992=CARTESIAN_POINT('Ctrl Pts',(-26.2970179840108,38.1484329561142,20.));
#83993=CARTESIAN_POINT('Ctrl Pts',(-26.2683927436784,38.1645549312104,0.));
#83994=CARTESIAN_POINT('Ctrl Pts',(-26.2683927436784,38.1645549312104,20.));
#83995=CARTESIAN_POINT('Ctrl Pts',(-26.2397570983077,38.1806561400953,0.));
#83996=CARTESIAN_POINT('Ctrl Pts',(-26.2397570983077,38.1806561400953,20.));
#83997=CARTESIAN_POINT('Ctrl Pts',(-26.2111110626121,38.196736575508,0.));
#83998=CARTESIAN_POINT('Ctrl Pts',(-26.2111110626121,38.196736575508,20.));
#83999=CARTESIAN_POINT('Ctrl Pts',(-26.1824546513102,38.2127962301983,0.));
#84000=CARTESIAN_POINT('Ctrl Pts',(-26.1824546513102,38.2127962301983,20.));
#84001=CARTESIAN_POINT('Ctrl Pts',(-26.1537878791271,38.2288350969267,0.));
#84002=CARTESIAN_POINT('Ctrl Pts',(-26.1537878791271,38.2288350969267,20.));
#84003=CARTESIAN_POINT('Ctrl Pts',(-26.1251107607929,38.244853168464,0.));
#84004=CARTESIAN_POINT('Ctrl Pts',(-26.1251107607929,38.244853168464,20.));
#84005=CARTESIAN_POINT('Ctrl Pts',(-26.0964233110434,38.2608504375906,0.));
#84006=CARTESIAN_POINT('Ctrl Pts',(-26.0964233110434,38.2608504375906,20.));
#84007=CARTESIAN_POINT('Ctrl Pts',(-26.0677255446196,38.276826897097,0.));
#84008=CARTESIAN_POINT('Ctrl Pts',(-26.0677255446196,38.276826897097,20.));
#84009=CARTESIAN_POINT('Ctrl Pts',(-26.0390174762676,38.2927825397833,0.));
#84010=CARTESIAN_POINT('Ctrl Pts',(-26.0390174762676,38.2927825397833,20.));
#84011=CARTESIAN_POINT('Ctrl Pts',(-26.0102991207387,38.3087173584599,0.));
#84012=CARTESIAN_POINT('Ctrl Pts',(-26.0102991207387,38.3087173584599,20.));
#84013=CARTESIAN_POINT('Ctrl Pts',(-25.9815704927901,38.3246313459476,0.));
#84014=CARTESIAN_POINT('Ctrl Pts',(-25.9815704927901,38.3246313459476,20.));
#84015=CARTESIAN_POINT('Ctrl Pts',(-25.9528316071847,38.3405244950781,0.));
#84016=CARTESIAN_POINT('Ctrl Pts',(-25.9528316071847,38.3405244950781,20.));
#84017=CARTESIAN_POINT('Ctrl Pts',(-25.9240824786909,38.3563967986931,0.));
#84018=CARTESIAN_POINT('Ctrl Pts',(-25.9240824786909,38.3563967986931,20.));
#84019=CARTESIAN_POINT('Ctrl Pts',(-25.8953231220827,38.3722482496454,0.));
#84020=CARTESIAN_POINT('Ctrl Pts',(-25.8953231220827,38.3722482496454,20.));
#84021=CARTESIAN_POINT('Ctrl Pts',(-25.8665535521392,38.3880788407969,0.));
#84022=CARTESIAN_POINT('Ctrl Pts',(-25.8665535521392,38.3880788407969,20.));
#84023=CARTESIAN_POINT('Ctrl Pts',(-25.8377737836446,38.4038885650199,0.));
#84024=CARTESIAN_POINT('Ctrl Pts',(-25.8377737836446,38.4038885650199,20.));
#84025=CARTESIAN_POINT('Ctrl Pts',(-25.8089838313888,38.4196774151969,0.));
#84026=CARTESIAN_POINT('Ctrl Pts',(-25.8089838313888,38.4196774151969,20.));
#84027=CARTESIAN_POINT('Ctrl Pts',(-25.7801837101667,38.4354453842206,0.));
#84028=CARTESIAN_POINT('Ctrl Pts',(-25.7801837101667,38.4354453842206,20.));
#84029=CARTESIAN_POINT('Ctrl Pts',(-25.7513734347795,38.4511924649945,0.));
#84030=CARTESIAN_POINT('Ctrl Pts',(-25.7513734347795,38.4511924649945,20.));
#84031=CARTESIAN_POINT('Ctrl Pts',(-25.7225530200332,38.4669186504318,0.));
#84032=CARTESIAN_POINT('Ctrl Pts',(-25.7225530200332,38.4669186504318,20.));
#84033=CARTESIAN_POINT('Ctrl Pts',(-25.6937224807392,38.4826239334567,0.));
#84034=CARTESIAN_POINT('Ctrl Pts',(-25.6937224807392,38.4826239334567,20.));
#84035=CARTESIAN_POINT('Ctrl Pts',(-25.6648818317151,38.4983083070042,0.));
#84036=CARTESIAN_POINT('Ctrl Pts',(-25.6648818317151,38.4983083070042,20.));
#84037=CARTESIAN_POINT('Ctrl Pts',(-25.6360310877836,38.5139717640192,0.));
#84038=CARTESIAN_POINT('Ctrl Pts',(-25.6360310877836,38.5139717640192,20.));
#84039=CARTESIAN_POINT('Ctrl Pts',(-25.6071702637723,38.5296142974561,0.));
#84040=CARTESIAN_POINT('Ctrl Pts',(-25.6071702637723,38.5296142974561,20.));
#84041=CARTESIAN_POINT('Ctrl Pts',(-25.5782993745137,38.5452359002793,0.));
#84042=CARTESIAN_POINT('Ctrl Pts',(-25.5782993745137,38.5452359002793,20.));
#84043=CARTESIAN_POINT('Ctrl Pts',(-25.5494184348457,38.5608365654634,0.));
#84044=CARTESIAN_POINT('Ctrl Pts',(-25.5494184348457,38.5608365654634,20.));
#84045=CARTESIAN_POINT('Ctrl Pts',(-25.5205274596115,38.5764162859939,0.));
#84046=CARTESIAN_POINT('Ctrl Pts',(-25.5205274596115,38.5764162859939,20.));
#84047=CARTESIAN_POINT('Ctrl Pts',(-25.4916264636604,38.591975054867,0.));
#84048=CARTESIAN_POINT('Ctrl Pts',(-25.4916264636604,38.591975054867,20.));
#84049=CARTESIAN_POINT('Ctrl Pts',(-25.462715461847,38.6075128650891,0.));
#84050=CARTESIAN_POINT('Ctrl Pts',(-25.462715461847,38.6075128650891,20.));
#84051=CARTESIAN_POINT('Ctrl Pts',(-25.4337944690316,38.6230297096774,0.));
#84052=CARTESIAN_POINT('Ctrl Pts',(-25.4337944690316,38.6230297096774,20.));
#84053=CARTESIAN_POINT('Ctrl Pts',(-25.4048635000795,38.6385255816593,0.));
#84054=CARTESIAN_POINT('Ctrl Pts',(-25.4048635000795,38.6385255816593,20.));
#84055=CARTESIAN_POINT('Ctrl Pts',(-25.3759225698613,38.6540004740723,0.));
#84056=CARTESIAN_POINT('Ctrl Pts',(-25.3759225698613,38.6540004740723,20.));
#84057=CARTESIAN_POINT('Ctrl Pts',(-25.3469716932528,38.6694543799641,0.));
#84058=CARTESIAN_POINT('Ctrl Pts',(-25.3469716932528,38.6694543799641,20.));
#84059=CARTESIAN_POINT('Ctrl Pts',(-25.3180108851341,38.6848872923919,0.));
#84060=CARTESIAN_POINT('Ctrl Pts',(-25.3180108851341,38.6848872923919,20.));
#84061=CARTESIAN_POINT('Ctrl Pts',(-25.2890401603913,38.7002992044241,0.));
#84062=CARTESIAN_POINT('Ctrl Pts',(-25.2890401603913,38.7002992044241,20.));
#84063=CARTESIAN_POINT('Ctrl Pts',(-25.2600595339159,38.7156901091392,0.));
#84064=CARTESIAN_POINT('Ctrl Pts',(-25.2600595339159,38.7156901091392,20.));
#84065=CARTESIAN_POINT('Ctrl Pts',(-25.231069020605,38.7310599996258,0.));
#84066=CARTESIAN_POINT('Ctrl Pts',(-25.231069020605,38.7310599996258,20.));
#84067=CARTESIAN_POINT('Ctrl Pts',(-25.2020686353608,38.7464088689836,0.));
#84068=CARTESIAN_POINT('Ctrl Pts',(-25.2020686353608,38.7464088689836,20.));
#84069=CARTESIAN_POINT('Ctrl Pts',(-25.1730583930911,38.7617367103228,0.));
#84070=CARTESIAN_POINT('Ctrl Pts',(-25.1730583930911,38.7617367103228,20.));
#84071=CARTESIAN_POINT('Ctrl Pts',(-25.1440383087085,38.7770435167639,0.));
#84072=CARTESIAN_POINT('Ctrl Pts',(-25.1440383087085,38.7770435167639,20.));
#84073=CARTESIAN_POINT('Ctrl Pts',(-25.1150083971302,38.7923292814368,0.));
#84074=CARTESIAN_POINT('Ctrl Pts',(-25.1150083971302,38.7923292814368,20.));
#84075=CARTESIAN_POINT('Ctrl Pts',(-25.0859686732795,38.8075939974829,0.));
#84076=CARTESIAN_POINT('Ctrl Pts',(-25.0859686732795,38.8075939974829,20.));
#84077=CARTESIAN_POINT('Ctrl Pts',(-25.0569191520845,38.8228376580533,0.));
#84078=CARTESIAN_POINT('Ctrl Pts',(-25.0569191520845,38.8228376580533,20.));
#84079=CARTESIAN_POINT('Ctrl Pts',(-25.0278598484791,38.8380602563098,0.));
#84080=CARTESIAN_POINT('Ctrl Pts',(-25.0278598484791,38.8380602563098,20.));
#84081=CARTESIAN_POINT('Ctrl Pts',(-24.9987907774025,38.8532617854245,0.));
#84082=CARTESIAN_POINT('Ctrl Pts',(-24.9987907774025,38.8532617854245,20.));
#84083=CARTESIAN_POINT('Ctrl Pts',(-24.9697119537989,38.8684422385799,0.));
#84084=CARTESIAN_POINT('Ctrl Pts',(-24.9697119537989,38.8684422385799,20.));
#84085=CARTESIAN_POINT('Ctrl Pts',(-24.9406233926168,38.883601608968,0.));
#84086=CARTESIAN_POINT('Ctrl Pts',(-24.9406233926168,38.883601608968,20.));
#84087=CARTESIAN_POINT('Ctrl Pts',(-24.9115251088108,38.8987398897918,0.));
#84088=CARTESIAN_POINT('Ctrl Pts',(-24.9115251088108,38.8987398897918,20.));
#84089=CARTESIAN_POINT('Ctrl Pts',(-24.8824171173402,38.9138570742648,0.));
#84090=CARTESIAN_POINT('Ctrl Pts',(-24.8824171173402,38.9138570742648,20.));
#84091=CARTESIAN_POINT('Ctrl Pts',(-24.8532994331703,38.9289531556117,0.));
#84092=CARTESIAN_POINT('Ctrl Pts',(-24.8532994331703,38.9289531556117,20.));
#84093=CARTESIAN_POINT('Ctrl Pts',(-24.8241720712716,38.9440281270684,0.));
#84094=CARTESIAN_POINT('Ctrl Pts',(-24.8241720712716,38.9440281270684,20.));
#84095=CARTESIAN_POINT('Ctrl Pts',(-24.7950350466188,38.9590819818797,0.));
#84096=CARTESIAN_POINT('Ctrl Pts',(-24.7950350466188,38.9590819818797,20.));
#84097=CARTESIAN_POINT('Ctrl Pts',(-24.7658883741919,38.9741147133012,0.));
#84098=CARTESIAN_POINT('Ctrl Pts',(-24.7658883741919,38.9741147133012,20.));
#84099=CARTESIAN_POINT('Ctrl Pts',(-24.736732068976,38.989126314598,0.));
#84100=CARTESIAN_POINT('Ctrl Pts',(-24.736732068976,38.989126314598,20.));
#84101=CARTESIAN_POINT('Ctrl Pts',(-24.7075661459617,39.0041167790461,0.));
#84102=CARTESIAN_POINT('Ctrl Pts',(-24.7075661459617,39.0041167790461,20.));
#84103=CARTESIAN_POINT('Ctrl Pts',(-24.6783906201452,39.019086099931,0.));
#84104=CARTESIAN_POINT('Ctrl Pts',(-24.6783906201452,39.019086099931,20.));
#84105=CARTESIAN_POINT('Ctrl Pts',(-24.6492055065285,39.0340342705498,0.));
#84106=CARTESIAN_POINT('Ctrl Pts',(-24.6492055065285,39.0340342705498,20.));
#84107=CARTESIAN_POINT('Ctrl Pts',(-24.6200108201182,39.0489612842095,0.));
#84108=CARTESIAN_POINT('Ctrl Pts',(-24.6200108201182,39.0489612842095,20.));
#84109=CARTESIAN_POINT('Ctrl Pts',(-24.5908065759258,39.0638671342286,0.));
#84110=CARTESIAN_POINT('Ctrl Pts',(-24.5908065759258,39.0638671342286,20.));
#84111=CARTESIAN_POINT('Ctrl Pts',(-24.5615927889669,39.0787518139362,0.));
#84112=CARTESIAN_POINT('Ctrl Pts',(-24.5615927889669,39.0787518139362,20.));
#84113=CARTESIAN_POINT('Ctrl Pts',(-24.5323694742617,39.0936153166722,0.));
#84114=CARTESIAN_POINT('Ctrl Pts',(-24.5323694742617,39.0936153166722,20.));
#84115=CARTESIAN_POINT('Ctrl Pts',(-24.5031366468345,39.1084576357871,0.));
#84116=CARTESIAN_POINT('Ctrl Pts',(-24.5031366468345,39.1084576357871,20.));
#84117=CARTESIAN_POINT('Ctrl Pts',(-24.4738943217155,39.1232787646414,0.));
#84118=CARTESIAN_POINT('Ctrl Pts',(-24.4738943217155,39.1232787646414,20.));
#84119=CARTESIAN_POINT('Ctrl Pts',(-24.4446425139409,39.1380786966047,0.));
#84120=CARTESIAN_POINT('Ctrl Pts',(-24.4446425139409,39.1380786966047,20.));
#84121=CARTESIAN_POINT('Ctrl Pts',(-24.4153812385543,39.1528574250568,0.));
#84122=CARTESIAN_POINT('Ctrl Pts',(-24.4153812385543,39.1528574250568,20.));
#84123=CARTESIAN_POINT('Ctrl Pts',(-24.3861105106067,39.1676149433869,0.));
#84124=CARTESIAN_POINT('Ctrl Pts',(-24.3861105106067,39.1676149433869,20.));
#84125=CARTESIAN_POINT('Ctrl Pts',(-24.3568303451549,39.1823512449951,0.));
#84126=CARTESIAN_POINT('Ctrl Pts',(-24.3568303451549,39.1823512449951,20.));
#84127=CARTESIAN_POINT('Ctrl Pts',(-24.3275407572588,39.197066323292,0.));
#84128=CARTESIAN_POINT('Ctrl Pts',(-24.3275407572588,39.197066323292,20.));
#84129=CARTESIAN_POINT('Ctrl Pts',(-24.2982417619806,39.2117601717005,0.));
#84130=CARTESIAN_POINT('Ctrl Pts',(-24.2982417619806,39.2117601717005,20.));
#84131=CARTESIAN_POINT('Ctrl Pts',(-24.2689333743823,39.2264327836562,0.));
#84132=CARTESIAN_POINT('Ctrl Pts',(-24.2689333743823,39.2264327836562,20.));
#84133=CARTESIAN_POINT('Ctrl Pts',(-24.2396156095261,39.2410841526077,0.));
#84134=CARTESIAN_POINT('Ctrl Pts',(-24.2396156095261,39.2410841526077,20.));
#84135=CARTESIAN_POINT('Ctrl Pts',(-24.2102884824784,39.2557142720138,0.));
#84136=CARTESIAN_POINT('Ctrl Pts',(-24.2102884824784,39.2557142720138,20.));
#84137=CARTESIAN_POINT('Ctrl Pts',(-24.1809520083147,39.2703231353422,0.));
#84138=CARTESIAN_POINT('Ctrl Pts',(-24.1809520083147,39.2703231353422,20.));
#84139=CARTESIAN_POINT('Ctrl Pts',(-24.1516062021224,39.2849107360681,0.));
#84140=CARTESIAN_POINT('Ctrl Pts',(-24.1516062021224,39.2849107360681,20.));
#84141=CARTESIAN_POINT('Ctrl Pts',(-24.1222510790066,39.2994770676712,0.));
#84142=CARTESIAN_POINT('Ctrl Pts',(-24.1222510790066,39.2994770676712,20.));
#84143=CARTESIAN_POINT('Ctrl Pts',(-24.0928866540882,39.3140221236369,0.));
#84144=CARTESIAN_POINT('Ctrl Pts',(-24.0928866540882,39.3140221236369,20.));
#84145=CARTESIAN_POINT('Ctrl Pts',(-24.0635129424931,39.3285458974612,0.));
#84146=CARTESIAN_POINT('Ctrl Pts',(-24.0635129424931,39.3285458974612,20.));
#84147=CARTESIAN_POINT('Ctrl Pts',(-24.0341299593437,39.3430483826555,0.));
#84148=CARTESIAN_POINT('Ctrl Pts',(-24.0341299593437,39.3430483826555,20.));
#84149=CARTESIAN_POINT('Ctrl Pts',(-24.0047377197503,39.3575295727493,0.));
#84150=CARTESIAN_POINT('Ctrl Pts',(-24.0047377197503,39.3575295727493,20.));
#84151=CARTESIAN_POINT('Ctrl Pts',(-23.9753362387978,39.3719894612957,0.));
#84152=CARTESIAN_POINT('Ctrl Pts',(-23.9753362387978,39.3719894612957,20.));
#84153=CARTESIAN_POINT('Ctrl Pts',(-23.9459255315518,39.3864280418676,0.));
#84154=CARTESIAN_POINT('Ctrl Pts',(-23.9459255315518,39.3864280418676,20.));
#84155=CARTESIAN_POINT('Ctrl Pts',(-23.9165056130837,39.4008453080481,0.));
#84156=CARTESIAN_POINT('Ctrl Pts',(-23.9165056130837,39.4008453080481,20.));
#84157=CARTESIAN_POINT('Ctrl Pts',(-23.8870764984925,39.4152412534209,0.));
#84158=CARTESIAN_POINT('Ctrl Pts',(-23.8870764984925,39.4152412534209,20.));
#84159=CARTESIAN_POINT('Ctrl Pts',(-23.8576382029238,39.4296158715627,0.));
#84160=CARTESIAN_POINT('Ctrl Pts',(-23.8576382029238,39.4296158715627,20.));
#84161=CARTESIAN_POINT('Ctrl Pts',(-23.8281907416005,39.4439691560298,0.));
#84162=CARTESIAN_POINT('Ctrl Pts',(-23.8281907416005,39.4439691560298,20.));
#84163=CARTESIAN_POINT('Ctrl Pts',(-23.7987341298022,39.4583011003674,0.));
#84164=CARTESIAN_POINT('Ctrl Pts',(-23.7987341298022,39.4583011003674,20.));
#84165=CARTESIAN_POINT('Ctrl Pts',(-23.7692683828081,39.4726116981337,0.));
#84166=CARTESIAN_POINT('Ctrl Pts',(-23.7692683828081,39.4726116981337,20.));
#84167=CARTESIAN_POINT('Ctrl Pts',(-23.7397935158457,39.4869009429217,0.));
#84168=CARTESIAN_POINT('Ctrl Pts',(-23.7397935158457,39.4869009429217,20.));
#84169=CARTESIAN_POINT('Ctrl Pts',(-23.7103095440476,39.5011688283778,0.));
#84170=CARTESIAN_POINT('Ctrl Pts',(-23.7103095440476,39.5011688283778,20.));
#84171=CARTESIAN_POINT('Ctrl Pts',(-23.6808164823786,39.5154153482324,0.));
#84172=CARTESIAN_POINT('Ctrl Pts',(-23.6808164823786,39.5154153482324,20.));
#84173=CARTESIAN_POINT('Ctrl Pts',(-23.651314345698,39.5296404962721,0.));
#84174=CARTESIAN_POINT('Ctrl Pts',(-23.651314345698,39.5296404962721,20.));
#84175=CARTESIAN_POINT('Ctrl Pts',(-23.6218031488905,39.5438442662853,0.));
#84176=CARTESIAN_POINT('Ctrl Pts',(-23.6218031488905,39.5438442662853,20.));
#84177=CARTESIAN_POINT('Ctrl Pts',(-23.5922829069852,39.5580266520107,0.));
#84178=CARTESIAN_POINT('Ctrl Pts',(-23.5922829069852,39.5580266520107,20.));
#84179=CARTESIAN_POINT('Ctrl Pts',(-23.5627536352592,39.5721876470956,0.));
#84180=CARTESIAN_POINT('Ctrl Pts',(-23.5627536352592,39.5721876470956,20.));
#84181=CARTESIAN_POINT('Ctrl Pts',(-23.533215349402,39.5863272450267,0.));
#84182=CARTESIAN_POINT('Ctrl Pts',(-23.533215349402,39.5863272450267,20.));
#84183=CARTESIAN_POINT('Ctrl Pts',(-23.5036680653391,39.6004454392038,0.));
#84184=CARTESIAN_POINT('Ctrl Pts',(-23.5036680653391,39.6004454392038,20.));
#84185=CARTESIAN_POINT('Ctrl Pts',(-23.4741117989348,39.6145422230651,0.));
#84186=CARTESIAN_POINT('Ctrl Pts',(-23.4741117989348,39.6145422230651,20.));
#84187=CARTESIAN_POINT('Ctrl Pts',(-23.4445465657147,39.6286175902046,0.));
#84188=CARTESIAN_POINT('Ctrl Pts',(-23.4445465657147,39.6286175902046,20.));
#84189=CARTESIAN_POINT('Ctrl Pts',(-23.4149723806221,39.6426715344742,0.));
#84190=CARTESIAN_POINT('Ctrl Pts',(-23.4149723806221,39.6426715344742,20.));
#84191=CARTESIAN_POINT('Ctrl Pts',(-23.385389257652,39.6567040501382,0.));
#84192=CARTESIAN_POINT('Ctrl Pts',(-23.385389257652,39.6567040501382,20.));
#84193=CARTESIAN_POINT('Ctrl Pts',(-23.3557972103217,39.670715131677,0.));
#84194=CARTESIAN_POINT('Ctrl Pts',(-23.3557972103217,39.670715131677,20.));
#84195=CARTESIAN_POINT('Ctrl Pts',(-23.3261962523444,39.6847047735001,0.));
#84196=CARTESIAN_POINT('Ctrl Pts',(-23.3261962523444,39.6847047735001,20.));
#84197=CARTESIAN_POINT('Ctrl Pts',(-23.2965863982648,39.6986729696788,0.));
#84198=CARTESIAN_POINT('Ctrl Pts',(-23.2965863982648,39.6986729696788,20.));
#84199=CARTESIAN_POINT('Ctrl Pts',(-23.2669676640418,39.712619713699,0.));
#84200=CARTESIAN_POINT('Ctrl Pts',(-23.2669676640418,39.712619713699,20.));
#84201=CARTESIAN_POINT('Ctrl Pts',(-23.2373400678346,39.7265449981305,0.));
#84202=CARTESIAN_POINT('Ctrl Pts',(-23.2373400678346,39.7265449981305,20.));
#84203=CARTESIAN_POINT('Ctrl Pts',(-23.2077036288598,39.7404488151086,0.));
#84204=CARTESIAN_POINT('Ctrl Pts',(-23.2077036288598,39.7404488151086,20.));
#84205=CARTESIAN_POINT('Ctrl Pts',(-23.1780583659508,39.7543311569459,0.));
#84206=CARTESIAN_POINT('Ctrl Pts',(-23.1780583659508,39.7543311569459,20.));
#84207=CARTESIAN_POINT('Ctrl Pts',(-23.1484042962029,39.7681920167058,0.));
#84208=CARTESIAN_POINT('Ctrl Pts',(-23.1484042962029,39.7681920167058,20.));
#84209=CARTESIAN_POINT('Ctrl Pts',(-23.1187414336251,39.7820313887737,0.));
#84210=CARTESIAN_POINT('Ctrl Pts',(-23.1187414336251,39.7820313887737,20.));
#84211=CARTESIAN_POINT('Ctrl Pts',(-23.089069787673,39.7958492694787,0.));
#84212=CARTESIAN_POINT('Ctrl Pts',(-23.089069787673,39.7958492694787,20.));
#84213=CARTESIAN_POINT('Ctrl Pts',(-23.0593893640427,39.8096456567259,0.));
#84214=CARTESIAN_POINT('Ctrl Pts',(-23.0593893640427,39.8096456567259,20.));
#84215=CARTESIAN_POINT('Ctrl Pts',(-23.0356380053139,39.8206655709903,0.));
#84216=CARTESIAN_POINT('Ctrl Pts',(-23.0356380053139,39.8206655709903,20.));
#84217=CARTESIAN_POINT('Ctrl Pts',(-23.0178205380655,39.8289208340947,0.));
#84218=CARTESIAN_POINT('Ctrl Pts',(-23.0178205380655,39.8289208340947,20.));
#84219=CARTESIAN_POINT('Ctrl Pts',(-23.005940471814,39.8344200439082,0.));
#84220=CARTESIAN_POINT('Ctrl Pts',(-23.005940471814,39.8344200439082,20.));
#84221=CARTESIAN_POINT('Ctrl Pts',(-23.,39.8371685740842,0.));
#84222=CARTESIAN_POINT('Ctrl Pts',(-23.,39.8371685740842,20.));
#84223=CARTESIAN_POINT('',(-23.,39.8371685740842,2.));
#84224=CARTESIAN_POINT('',(-23.,39.8371685740842,0.));
#84225=CARTESIAN_POINT('Ctrl Pts',(-23.,39.8371685740842,2.));
#84226=CARTESIAN_POINT('Ctrl Pts',(-25.2470089260756,38.797525254077,2.));
#84227=CARTESIAN_POINT('Ctrl Pts',(-27.4022761516233,37.5810556243015,2.));
#84228=CARTESIAN_POINT('Ctrl Pts',(-29.4485343857591,36.2031892014269,2.));
#84229=CARTESIAN_POINT('Ctrl Pts',(-8.50876070567958,48.2555798975982,0.));
#84230=CARTESIAN_POINT('Ctrl Pts',(-8.50876070567958,48.2555798975982,20.));
#84231=CARTESIAN_POINT('Ctrl Pts',(-8.50201591146282,48.2561497089132,0.));
#84232=CARTESIAN_POINT('Ctrl Pts',(-8.50201591146282,48.2561497089132,20.));
#84233=CARTESIAN_POINT('Ctrl Pts',(-8.48852624368609,48.2572870022174,0.));
#84234=CARTESIAN_POINT('Ctrl Pts',(-8.48852624368609,48.2572870022174,20.));
#84235=CARTESIAN_POINT('Ctrl Pts',(-8.46829150399134,48.2589859541967,0.));
#84236=CARTESIAN_POINT('Ctrl Pts',(-8.46829150399134,48.2589859541967,20.));
#84237=CARTESIAN_POINT('Ctrl Pts',(-8.44131137500422,48.2612372475269,0.));
#84238=CARTESIAN_POINT('Ctrl Pts',(-8.44131137500422,48.2612372475269,20.));
#84239=CARTESIAN_POINT('Ctrl Pts',(-8.40758542126,48.2640280707484,0.));
#84240=CARTESIAN_POINT('Ctrl Pts',(-8.40758542126,48.2640280707484,20.));
#84241=CARTESIAN_POINT('Ctrl Pts',(-8.37385867778171,48.2667956002972,0.));
#84242=CARTESIAN_POINT('Ctrl Pts',(-8.37385867778171,48.2667956002972,20.));
#84243=CARTESIAN_POINT('Ctrl Pts',(-8.34013115014498,48.2695398358687,0.));
#84244=CARTESIAN_POINT('Ctrl Pts',(-8.34013115014498,48.2695398358687,20.));
#84245=CARTESIAN_POINT('Ctrl Pts',(-8.30640284761837,48.2722607770974,0.));
#84246=CARTESIAN_POINT('Ctrl Pts',(-8.30640284761837,48.2722607770974,20.));
#84247=CARTESIAN_POINT('Ctrl Pts',(-8.2726737841987,48.274958423567,0.));
#84248=CARTESIAN_POINT('Ctrl Pts',(-8.2726737841987,48.274958423567,20.));
#84249=CARTESIAN_POINT('Ctrl Pts',(-8.23894397736023,48.2776327748283,0.));
#84250=CARTESIAN_POINT('Ctrl Pts',(-8.23894397736023,48.2776327748283,20.));
#84251=CARTESIAN_POINT('Ctrl Pts',(-8.20521344665195,48.2802838304168,0.));
#84252=CARTESIAN_POINT('Ctrl Pts',(-8.20521344665195,48.2802838304168,20.));
#84253=CARTESIAN_POINT('Ctrl Pts',(-8.17148221231955,48.2829115898716,0.));
#84254=CARTESIAN_POINT('Ctrl Pts',(-8.17148221231955,48.2829115898716,20.));
#84255=CARTESIAN_POINT('Ctrl Pts',(-8.13775029398595,48.2855160527521,0.));
#84256=CARTESIAN_POINT('Ctrl Pts',(-8.13775029398595,48.2855160527521,20.));
#84257=CARTESIAN_POINT('Ctrl Pts',(-8.10401770912493,48.288097218659,0.));
#84258=CARTESIAN_POINT('Ctrl Pts',(-8.10401770912493,48.288097218659,20.));
#84259=CARTESIAN_POINT('Ctrl Pts',(-8.07028447346159,48.2906550872281,0.));
#84260=CARTESIAN_POINT('Ctrl Pts',(-8.07028447346159,48.2906550872281,20.));
#84261=CARTESIAN_POINT('Ctrl Pts',(-8.03655060167525,48.2931896581208,0.));
#84262=CARTESIAN_POINT('Ctrl Pts',(-8.03655060167525,48.2931896581208,20.));
#84263=CARTESIAN_POINT('Ctrl Pts',(-8.00281610801474,48.2957009310153,0.));
#84264=CARTESIAN_POINT('Ctrl Pts',(-8.00281610801474,48.2957009310153,20.));
#84265=CARTESIAN_POINT('Ctrl Pts',(-7.96908100690894,48.2981889055984,0.));
#84266=CARTESIAN_POINT('Ctrl Pts',(-7.96908100690894,48.2981889055984,20.));
#84267=CARTESIAN_POINT('Ctrl Pts',(-7.93534531368691,48.300653581555,0.));
#84268=CARTESIAN_POINT('Ctrl Pts',(-7.93534531368691,48.300653581555,20.));
#84269=CARTESIAN_POINT('Ctrl Pts',(-7.90160904447353,48.3030949585702,0.));
#84270=CARTESIAN_POINT('Ctrl Pts',(-7.90160904447353,48.3030949585702,20.));
#84271=CARTESIAN_POINT('Ctrl Pts',(-7.86787221586447,48.3055130363337,0.));
#84272=CARTESIAN_POINT('Ctrl Pts',(-7.86787221586447,48.3055130363337,20.));
#84273=CARTESIAN_POINT('Ctrl Pts',(-7.83413484466695,48.3079078145432,0.));
#84274=CARTESIAN_POINT('Ctrl Pts',(-7.83413484466695,48.3079078145432,20.));
#84275=CARTESIAN_POINT('Ctrl Pts',(-7.80039694763398,48.3102792929086,0.));
#84276=CARTESIAN_POINT('Ctrl Pts',(-7.80039694763398,48.3102792929086,20.));
#84277=CARTESIAN_POINT('Ctrl Pts',(-7.76665854114747,48.3126274711557,0.));
#84278=CARTESIAN_POINT('Ctrl Pts',(-7.76665854114747,48.3126274711557,20.));
#84279=CARTESIAN_POINT('Ctrl Pts',(-7.7329196412329,48.3149523490266,0.));
#84280=CARTESIAN_POINT('Ctrl Pts',(-7.7329196412329,48.3149523490266,20.));
#84281=CARTESIAN_POINT('Ctrl Pts',(-7.69918026370737,48.3172539262766,0.));
#84282=CARTESIAN_POINT('Ctrl Pts',(-7.69918026370737,48.3172539262766,20.));
#84283=CARTESIAN_POINT('Ctrl Pts',(-7.66544042428834,48.3195322026739,0.));
#84284=CARTESIAN_POINT('Ctrl Pts',(-7.66544042428834,48.3195322026739,20.));
#84285=CARTESIAN_POINT('Ctrl Pts',(-7.63170013870894,48.3217871779975,0.));
#84286=CARTESIAN_POINT('Ctrl Pts',(-7.63170013870894,48.3217871779975,20.));
#84287=CARTESIAN_POINT('Ctrl Pts',(-7.59795942285541,48.3240188520354,0.));
#84288=CARTESIAN_POINT('Ctrl Pts',(-7.59795942285541,48.3240188520354,20.));
#84289=CARTESIAN_POINT('Ctrl Pts',(-7.56421829277371,48.3262272245847,0.));
#84290=CARTESIAN_POINT('Ctrl Pts',(-7.56421829277371,48.3262272245847,20.));
#84291=CARTESIAN_POINT('Ctrl Pts',(-7.53047676460328,48.328412295452,0.));
#84292=CARTESIAN_POINT('Ctrl Pts',(-7.53047676460328,48.328412295452,20.));
#84293=CARTESIAN_POINT('Ctrl Pts',(-7.4967348545312,48.3305740644544,0.));
#84294=CARTESIAN_POINT('Ctrl Pts',(-7.4967348545312,48.3305740644544,20.));
#84295=CARTESIAN_POINT('Ctrl Pts',(-7.4629925787421,48.3327125314199,0.));
#84296=CARTESIAN_POINT('Ctrl Pts',(-7.4629925787421,48.3327125314199,20.));
#84297=CARTESIAN_POINT('Ctrl Pts',(-7.42924995335919,48.3348276961881,0.));
#84298=CARTESIAN_POINT('Ctrl Pts',(-7.42924995335919,48.3348276961881,20.));
#84299=CARTESIAN_POINT('Ctrl Pts',(-7.39550699443534,48.3369195586108,0.));
#84300=CARTESIAN_POINT('Ctrl Pts',(-7.39550699443534,48.3369195586108,20.));
#84301=CARTESIAN_POINT('Ctrl Pts',(-7.36176371798263,48.3389881185516,0.));
#84302=CARTESIAN_POINT('Ctrl Pts',(-7.36176371798263,48.3389881185516,20.));
#84303=CARTESIAN_POINT('Ctrl Pts',(-7.32802013999148,48.3410333758855,0.));
#84304=CARTESIAN_POINT('Ctrl Pts',(-7.32802013999148,48.3410333758855,20.));
#84305=CARTESIAN_POINT('Ctrl Pts',(-7.2942762764527,48.3430553304987,0.));
#84306=CARTESIAN_POINT('Ctrl Pts',(-7.2942762764527,48.3430553304987,20.));
#84307=CARTESIAN_POINT('Ctrl Pts',(-7.26053214338257,48.3450539822883,0.));
#84308=CARTESIAN_POINT('Ctrl Pts',(-7.26053214338257,48.3450539822883,20.));
#84309=CARTESIAN_POINT('Ctrl Pts',(-7.22678775682933,48.3470293311619,0.));
#84310=CARTESIAN_POINT('Ctrl Pts',(-7.22678775682933,48.3470293311619,20.));
#84311=CARTESIAN_POINT('Ctrl Pts',(-7.19304313285999,48.3489813770376,0.));
#84312=CARTESIAN_POINT('Ctrl Pts',(-7.19304313285999,48.3489813770376,20.));
#84313=CARTESIAN_POINT('Ctrl Pts',(-7.15929828755241,48.3509101198447,0.));
#84314=CARTESIAN_POINT('Ctrl Pts',(-7.15929828755241,48.3509101198447,20.));
#84315=CARTESIAN_POINT('Ctrl Pts',(-7.12555323698551,48.3528155595232,0.));
#84316=CARTESIAN_POINT('Ctrl Pts',(-7.12555323698551,48.3528155595232,20.));
#84317=CARTESIAN_POINT('Ctrl Pts',(-7.09180799722882,48.354697696024,0.));
#84318=CARTESIAN_POINT('Ctrl Pts',(-7.09180799722882,48.354697696024,20.));
#84319=CARTESIAN_POINT('Ctrl Pts',(-7.05806258433803,48.3565565293095,0.));
#84320=CARTESIAN_POINT('Ctrl Pts',(-7.05806258433803,48.3565565293095,20.));
#84321=CARTESIAN_POINT('Ctrl Pts',(-7.02431701436127,48.3583920593534,0.));
#84322=CARTESIAN_POINT('Ctrl Pts',(-7.02431701436127,48.3583920593534,20.));
#84323=CARTESIAN_POINT('Ctrl Pts',(-6.99057130334228,48.3602042861407,0.));
#84324=CARTESIAN_POINT('Ctrl Pts',(-6.99057130334228,48.3602042861407,20.));
#84325=CARTESIAN_POINT('Ctrl Pts',(-6.95682546732485,48.3619932096677,0.));
#84326=CARTESIAN_POINT('Ctrl Pts',(-6.95682546732485,48.3619932096677,20.));
#84327=CARTESIAN_POINT('Ctrl Pts',(-6.9230795223571,48.3637588299416,0.));
#84328=CARTESIAN_POINT('Ctrl Pts',(-6.9230795223571,48.3637588299416,20.));
#84329=CARTESIAN_POINT('Ctrl Pts',(-6.88933348449371,48.3655011469807,0.));
#84330=CARTESIAN_POINT('Ctrl Pts',(-6.88933348449371,48.3655011469807,20.));
#84331=CARTESIAN_POINT('Ctrl Pts',(-6.8555873697933,48.3672201608141,0.));
#84332=CARTESIAN_POINT('Ctrl Pts',(-6.8555873697933,48.3672201608141,20.));
#84333=CARTESIAN_POINT('Ctrl Pts',(-6.82184119431719,48.3689158714816,0.));
#84334=CARTESIAN_POINT('Ctrl Pts',(-6.82184119431719,48.3689158714816,20.));
#84335=CARTESIAN_POINT('Ctrl Pts',(-6.78809497412715,48.370588279034,0.));
#84336=CARTESIAN_POINT('Ctrl Pts',(-6.78809497412715,48.370588279034,20.));
#84337=CARTESIAN_POINT('Ctrl Pts',(-6.75434872528386,48.3722373835335,0.));
#84338=CARTESIAN_POINT('Ctrl Pts',(-6.75434872528386,48.3722373835335,20.));
#84339=CARTESIAN_POINT('Ctrl Pts',(-6.72060246384581,48.3738631850533,0.));
#84340=CARTESIAN_POINT('Ctrl Pts',(-6.72060246384581,48.3738631850533,20.));
#84341=CARTESIAN_POINT('Ctrl Pts',(-6.68685620587016,48.3754656836776,0.));
#84342=CARTESIAN_POINT('Ctrl Pts',(-6.68685620587016,48.3754656836776,20.));
#84343=CARTESIAN_POINT('Ctrl Pts',(-6.65310996741334,48.3770448795022,0.));
#84344=CARTESIAN_POINT('Ctrl Pts',(-6.65310996741334,48.3770448795022,20.));
#84345=CARTESIAN_POINT('Ctrl Pts',(-6.61936376453196,48.3786007726338,0.));
#84346=CARTESIAN_POINT('Ctrl Pts',(-6.61936376453196,48.3786007726338,20.));
#84347=CARTESIAN_POINT('Ctrl Pts',(-6.58561761328368,48.3801333631899,0.));
#84348=CARTESIAN_POINT('Ctrl Pts',(-6.58561761328368,48.3801333631899,20.));
#84349=CARTESIAN_POINT('Ctrl Pts',(-6.55187152972773,48.3816426512994,0.));
#84350=CARTESIAN_POINT('Ctrl Pts',(-6.55187152972773,48.3816426512994,20.));
#84351=CARTESIAN_POINT('Ctrl Pts',(-6.51812552992425,48.3831286371024,0.));
#84352=CARTESIAN_POINT('Ctrl Pts',(-6.51812552992425,48.3831286371024,20.));
#84353=CARTESIAN_POINT('Ctrl Pts',(-6.48437962993407,48.3845913207494,0.));
#84354=CARTESIAN_POINT('Ctrl Pts',(-6.48437962993407,48.3845913207494,20.));
#84355=CARTESIAN_POINT('Ctrl Pts',(-6.45063384581846,48.3860307024022,0.));
#84356=CARTESIAN_POINT('Ctrl Pts',(-6.45063384581846,48.3860307024022,20.));
#84357=CARTESIAN_POINT('Ctrl Pts',(-6.41688819363866,48.3874467822337,0.));
#84358=CARTESIAN_POINT('Ctrl Pts',(-6.41688819363866,48.3874467822337,20.));
#84359=CARTESIAN_POINT('Ctrl Pts',(-6.38314268945589,48.388839560428,0.));
#84360=CARTESIAN_POINT('Ctrl Pts',(-6.38314268945589,48.388839560428,20.));
#84361=CARTESIAN_POINT('Ctrl Pts',(-6.34939734933123,48.3902090371802,0.));
#84362=CARTESIAN_POINT('Ctrl Pts',(-6.34939734933123,48.3902090371802,20.));
#84363=CARTESIAN_POINT('Ctrl Pts',(-6.3156521893259,48.3915552126968,0.));
#84364=CARTESIAN_POINT('Ctrl Pts',(-6.3156521893259,48.3915552126968,20.));
#84365=CARTESIAN_POINT('Ctrl Pts',(-6.28190722550134,48.3928780871951,0.));
#84366=CARTESIAN_POINT('Ctrl Pts',(-6.28190722550134,48.3928780871951,20.));
#84367=CARTESIAN_POINT('Ctrl Pts',(-6.24816247391921,48.3941776609035,0.));
#84368=CARTESIAN_POINT('Ctrl Pts',(-6.24816247391921,48.3941776609035,20.));
#84369=CARTESIAN_POINT('Ctrl Pts',(-6.21441795064169,48.3954539340615,0.));
#84370=CARTESIAN_POINT('Ctrl Pts',(-6.21441795064169,48.3954539340615,20.));
#84371=CARTESIAN_POINT('Ctrl Pts',(-6.18067367173125,48.3967069069196,0.));
#84372=CARTESIAN_POINT('Ctrl Pts',(-6.18067367173125,48.3967069069196,20.));
#84373=CARTESIAN_POINT('Ctrl Pts',(-6.1469296532508,48.3979365797396,0.));
#84374=CARTESIAN_POINT('Ctrl Pts',(-6.1469296532508,48.3979365797396,20.));
#84375=CARTESIAN_POINT('Ctrl Pts',(-6.11318591126344,48.3991429527941,0.));
#84376=CARTESIAN_POINT('Ctrl Pts',(-6.11318591126344,48.3991429527941,20.));
#84377=CARTESIAN_POINT('Ctrl Pts',(-6.07944246183268,48.400326026367,0.));
#84378=CARTESIAN_POINT('Ctrl Pts',(-6.07944246183268,48.400326026367,20.));
#84379=CARTESIAN_POINT('Ctrl Pts',(-6.04569932102201,48.4014858007534,0.));
#84380=CARTESIAN_POINT('Ctrl Pts',(-6.04569932102201,48.4014858007534,20.));
#84381=CARTESIAN_POINT('Ctrl Pts',(-6.01195650489506,48.4026222762592,0.));
#84382=CARTESIAN_POINT('Ctrl Pts',(-6.01195650489506,48.4026222762592,20.));
#84383=CARTESIAN_POINT('Ctrl Pts',(-5.97821402951549,48.4037354532013,0.));
#84384=CARTESIAN_POINT('Ctrl Pts',(-5.97821402951549,48.4037354532013,20.));
#84385=CARTESIAN_POINT('Ctrl Pts',(-5.94447191094723,48.404825331908,0.));
#84386=CARTESIAN_POINT('Ctrl Pts',(-5.94447191094723,48.404825331908,20.));
#84387=CARTESIAN_POINT('Ctrl Pts',(-5.91073016525427,48.4058919127185,0.));
#84388=CARTESIAN_POINT('Ctrl Pts',(-5.91073016525427,48.4058919127185,20.));
#84389=CARTESIAN_POINT('Ctrl Pts',(-5.87698880850096,48.4069351959835,0.));
#84390=CARTESIAN_POINT('Ctrl Pts',(-5.87698880850096,48.4069351959835,20.));
#84391=CARTESIAN_POINT('Ctrl Pts',(-5.8432478567519,48.4079551820642,0.));
#84392=CARTESIAN_POINT('Ctrl Pts',(-5.8432478567519,48.4079551820642,20.));
#84393=CARTESIAN_POINT('Ctrl Pts',(-5.80950732607179,48.4089518713336,0.));
#84394=CARTESIAN_POINT('Ctrl Pts',(-5.80950732607179,48.4089518713336,20.));
#84395=CARTESIAN_POINT('Ctrl Pts',(-5.77576723252553,48.4099252641753,0.));
#84396=CARTESIAN_POINT('Ctrl Pts',(-5.77576723252553,48.4099252641753,20.));
#84397=CARTESIAN_POINT('Ctrl Pts',(-5.74202759217814,48.4108753609837,0.));
#84398=CARTESIAN_POINT('Ctrl Pts',(-5.74202759217814,48.4108753609837,20.));
#84399=CARTESIAN_POINT('Ctrl Pts',(-5.70828842109461,48.4118021621647,0.));
#84400=CARTESIAN_POINT('Ctrl Pts',(-5.70828842109461,48.4118021621647,20.));
#84401=CARTESIAN_POINT('Ctrl Pts',(-5.67454973534015,48.412705668135,0.));
#84402=CARTESIAN_POINT('Ctrl Pts',(-5.67454973534015,48.412705668135,20.));
#84403=CARTESIAN_POINT('Ctrl Pts',(-5.64081155098006,48.4135858793227,0.));
#84404=CARTESIAN_POINT('Ctrl Pts',(-5.64081155098006,48.4135858793227,20.));
#84405=CARTESIAN_POINT('Ctrl Pts',(-5.60707388407982,48.414442796167,0.));
#84406=CARTESIAN_POINT('Ctrl Pts',(-5.60707388407982,48.414442796167,20.));
#84407=CARTESIAN_POINT('Ctrl Pts',(-5.57333675070493,48.4152764191183,0.));
#84408=CARTESIAN_POINT('Ctrl Pts',(-5.57333675070493,48.4152764191183,20.));
#84409=CARTESIAN_POINT('Ctrl Pts',(-5.53960016692118,48.4160867486381,0.));
#84410=CARTESIAN_POINT('Ctrl Pts',(-5.53960016692118,48.4160867486381,20.));
#84411=CARTESIAN_POINT('Ctrl Pts',(-5.50586414879431,48.4168737851989,0.));
#84412=CARTESIAN_POINT('Ctrl Pts',(-5.50586414879431,48.4168737851989,20.));
#84413=CARTESIAN_POINT('Ctrl Pts',(-5.47212871239031,48.417637529284,0.));
#84414=CARTESIAN_POINT('Ctrl Pts',(-5.47212871239031,48.417637529284,20.));
#84415=CARTESIAN_POINT('Ctrl Pts',(-5.43839387377499,48.4183779813881,0.));
#84416=CARTESIAN_POINT('Ctrl Pts',(-5.43839387377499,48.4183779813881,20.));
#84417=CARTESIAN_POINT('Ctrl Pts',(-5.40465964901426,48.4190951420167,0.));
#84418=CARTESIAN_POINT('Ctrl Pts',(-5.40465964901426,48.4190951420167,20.));
#84419=CARTESIAN_POINT('Ctrl Pts',(-5.37092605417403,48.4197890116867,0.));
#84420=CARTESIAN_POINT('Ctrl Pts',(-5.37092605417403,48.4197890116867,20.));
#84421=CARTESIAN_POINT('Ctrl Pts',(-5.33719310532028,48.4204595909261,0.));
#84422=CARTESIAN_POINT('Ctrl Pts',(-5.33719310532028,48.4204595909261,20.));
#84423=CARTESIAN_POINT('Ctrl Pts',(-5.3034608185191,48.4211068802741,0.));
#84424=CARTESIAN_POINT('Ctrl Pts',(-5.3034608185191,48.4211068802741,20.));
#84425=CARTESIAN_POINT('Ctrl Pts',(-5.26972920983671,48.4217308802807,0.));
#84426=CARTESIAN_POINT('Ctrl Pts',(-5.26972920983671,48.4217308802807,20.));
#84427=CARTESIAN_POINT('Ctrl Pts',(-5.23599829533945,48.4223315915069,0.));
#84428=CARTESIAN_POINT('Ctrl Pts',(-5.23599829533945,48.4223315915069,20.));
#84429=CARTESIAN_POINT('Ctrl Pts',(-5.20226809109352,48.4229090145253,0.));
#84430=CARTESIAN_POINT('Ctrl Pts',(-5.20226809109352,48.4229090145253,20.));
#84431=CARTESIAN_POINT('Ctrl Pts',(-5.16853861316522,48.4234631499193,0.));
#84432=CARTESIAN_POINT('Ctrl Pts',(-5.16853861316522,48.4234631499193,20.));
#84433=CARTESIAN_POINT('Ctrl Pts',(-5.13480987762072,48.4239939982838,0.));
#84434=CARTESIAN_POINT('Ctrl Pts',(-5.13480987762072,48.4239939982838,20.));
#84435=CARTESIAN_POINT('Ctrl Pts',(-5.10108190052608,48.4245015602246,0.));
#84436=CARTESIAN_POINT('Ctrl Pts',(-5.10108190052608,48.4245015602246,20.));
#84437=CARTESIAN_POINT('Ctrl Pts',(-5.06735469794743,48.4249858363582,0.));
#84438=CARTESIAN_POINT('Ctrl Pts',(-5.06735469794743,48.4249858363582,20.));
#84439=CARTESIAN_POINT('Ctrl Pts',(-5.03362828595094,48.4254468273122,0.));
#84440=CARTESIAN_POINT('Ctrl Pts',(-5.03362828595094,48.4254468273122,20.));
#84441=CARTESIAN_POINT('Ctrl Pts',(-4.99990268060293,48.4258845337255,0.));
#84442=CARTESIAN_POINT('Ctrl Pts',(-4.99990268060293,48.4258845337255,20.));
#84443=CARTESIAN_POINT('Ctrl Pts',(-4.96617789796954,48.4262989562483,0.));
#84444=CARTESIAN_POINT('Ctrl Pts',(-4.96617789796954,48.4262989562483,20.));
#84445=CARTESIAN_POINT('Ctrl Pts',(-4.93245395411686,48.4266900955418,0.));
#84446=CARTESIAN_POINT('Ctrl Pts',(-4.93245395411686,48.4266900955418,20.));
#84447=CARTESIAN_POINT('Ctrl Pts',(-4.89873086511077,48.4270579522784,0.));
#84448=CARTESIAN_POINT('Ctrl Pts',(-4.89873086511077,48.4270579522784,20.));
#84449=CARTESIAN_POINT('Ctrl Pts',(-4.86500864701731,48.4274025271416,0.));
#84450=CARTESIAN_POINT('Ctrl Pts',(-4.86500864701731,48.4274025271416,20.));
#84451=CARTESIAN_POINT('Ctrl Pts',(-4.8312873159023,48.4277238208263,0.));
#84452=CARTESIAN_POINT('Ctrl Pts',(-4.8312873159023,48.4277238208263,20.));
#84453=CARTESIAN_POINT('Ctrl Pts',(-4.79756688783169,48.4280218340382,0.));
#84454=CARTESIAN_POINT('Ctrl Pts',(-4.79756688783169,48.4280218340382,20.));
#84455=CARTESIAN_POINT('Ctrl Pts',(-4.76384737887107,48.4282965674942,0.));
#84456=CARTESIAN_POINT('Ctrl Pts',(-4.76384737887107,48.4282965674942,20.));
#84457=CARTESIAN_POINT('Ctrl Pts',(-4.73012880508602,48.4285480219221,0.));
#84458=CARTESIAN_POINT('Ctrl Pts',(-4.73012880508602,48.4285480219221,20.));
#84459=CARTESIAN_POINT('Ctrl Pts',(-4.69641118254227,48.4287761980604,0.));
#84460=CARTESIAN_POINT('Ctrl Pts',(-4.69641118254227,48.4287761980604,20.));
#84461=CARTESIAN_POINT('Ctrl Pts',(-4.66269452730544,48.4289810966589,0.));
#84462=CARTESIAN_POINT('Ctrl Pts',(-4.66269452730544,48.4289810966589,20.));
#84463=CARTESIAN_POINT('Ctrl Pts',(-4.62897885544098,48.4291627184787,0.));
#84464=CARTESIAN_POINT('Ctrl Pts',(-4.62897885544098,48.4291627184787,20.));
#84465=CARTESIAN_POINT('Ctrl Pts',(-4.5952641830141,48.4293210642923,0.));
#84466=CARTESIAN_POINT('Ctrl Pts',(-4.5952641830141,48.4293210642923,20.));
#84467=CARTESIAN_POINT('Ctrl Pts',(-4.56155052608981,48.4294561348833,0.));
#84468=CARTESIAN_POINT('Ctrl Pts',(-4.56155052608981,48.4294561348833,20.));
#84469=CARTESIAN_POINT('Ctrl Pts',(-4.52783790073295,48.4295679310466,0.));
#84470=CARTESIAN_POINT('Ctrl Pts',(-4.52783790073295,48.4295679310466,20.));
#84471=CARTESIAN_POINT('Ctrl Pts',(-4.49412632300816,48.4296564535884,0.));
#84472=CARTESIAN_POINT('Ctrl Pts',(-4.49412632300816,48.4296564535884,20.));
#84473=CARTESIAN_POINT('Ctrl Pts',(-4.46041580898013,48.4297217033257,0.));
#84474=CARTESIAN_POINT('Ctrl Pts',(-4.46041580898013,48.4297217033257,20.));
#84475=CARTESIAN_POINT('Ctrl Pts',(-4.42670637471342,48.4297636810863,0.));
#84476=CARTESIAN_POINT('Ctrl Pts',(-4.42670637471342,48.4297636810863,20.));
#84477=CARTESIAN_POINT('Ctrl Pts',(-4.39299803627247,48.4297823877088,0.));
#84478=CARTESIAN_POINT('Ctrl Pts',(-4.39299803627247,48.4297823877088,20.));
#84479=CARTESIAN_POINT('Ctrl Pts',(-4.35929080972167,48.4297778240431,0.));
#84480=CARTESIAN_POINT('Ctrl Pts',(-4.35929080972167,48.4297778240431,20.));
#84481=CARTESIAN_POINT('Ctrl Pts',(-4.32558471112518,48.42974999095,0.));
#84482=CARTESIAN_POINT('Ctrl Pts',(-4.32558471112518,48.42974999095,20.));
#84483=CARTESIAN_POINT('Ctrl Pts',(-4.29187975654678,48.4296988893018,0.));
#84484=CARTESIAN_POINT('Ctrl Pts',(-4.29187975654678,48.4296988893018,20.));
#84485=CARTESIAN_POINT('Ctrl Pts',(-4.25817596205002,48.4296245199823,0.));
#84486=CARTESIAN_POINT('Ctrl Pts',(-4.25817596205002,48.4296245199823,20.));
#84487=CARTESIAN_POINT('Ctrl Pts',(-4.22447334369802,48.4295268838864,0.));
#84488=CARTESIAN_POINT('Ctrl Pts',(-4.22447334369802,48.4295268838864,20.));
#84489=CARTESIAN_POINT('Ctrl Pts',(-4.19077191755407,48.4294059819202,0.));
#84490=CARTESIAN_POINT('Ctrl Pts',(-4.19077191755407,48.4294059819202,20.));
#84491=CARTESIAN_POINT('Ctrl Pts',(-4.15707169968116,48.4292618150011,0.));
#84492=CARTESIAN_POINT('Ctrl Pts',(-4.15707169968116,48.4292618150011,20.));
#84493=CARTESIAN_POINT('Ctrl Pts',(-4.12337270614212,48.429094384057,0.));
#84494=CARTESIAN_POINT('Ctrl Pts',(-4.12337270614212,48.429094384057,20.));
#84495=CARTESIAN_POINT('Ctrl Pts',(-4.08967495299953,48.4289036900268,0.));
#84496=CARTESIAN_POINT('Ctrl Pts',(-4.08967495299953,48.4289036900268,20.));
#84497=CARTESIAN_POINT('Ctrl Pts',(-4.0559784563157,48.4286897338604,0.));
#84498=CARTESIAN_POINT('Ctrl Pts',(-4.0559784563157,48.4286897338604,20.));
#84499=CARTESIAN_POINT('Ctrl Pts',(-4.02228323215261,48.4284525165189,0.));
#84500=CARTESIAN_POINT('Ctrl Pts',(-4.02228323215261,48.4284525165189,20.));
#84501=CARTESIAN_POINT('Ctrl Pts',(-3.98858929657202,48.4281920389749,0.));
#84502=CARTESIAN_POINT('Ctrl Pts',(-3.98858929657202,48.4281920389749,20.));
#84503=CARTESIAN_POINT('Ctrl Pts',(-3.9548966656355,48.427908302212,0.));
#84504=CARTESIAN_POINT('Ctrl Pts',(-3.9548966656355,48.427908302212,20.));
#84505=CARTESIAN_POINT('Ctrl Pts',(-3.92120535540421,48.4276013072253,0.));
#84506=CARTESIAN_POINT('Ctrl Pts',(-3.92120535540421,48.4276013072253,20.));
#84507=CARTESIAN_POINT('Ctrl Pts',(-3.88751538193921,48.4272710550206,0.));
#84508=CARTESIAN_POINT('Ctrl Pts',(-3.88751538193921,48.4272710550206,20.));
#84509=CARTESIAN_POINT('Ctrl Pts',(-3.85382676130116,48.4269175466151,0.));
#84510=CARTESIAN_POINT('Ctrl Pts',(-3.85382676130116,48.4269175466151,20.));
#84511=CARTESIAN_POINT('Ctrl Pts',(-3.82013950955044,48.4265407830367,0.));
#84512=CARTESIAN_POINT('Ctrl Pts',(-3.82013950955044,48.4265407830367,20.));
#84513=CARTESIAN_POINT('Ctrl Pts',(-3.78645364274707,48.4261407653249,0.));
#84514=CARTESIAN_POINT('Ctrl Pts',(-3.78645364274707,48.4261407653249,20.));
#84515=CARTESIAN_POINT('Ctrl Pts',(-3.75276917695086,48.4257174945299,0.));
#84516=CARTESIAN_POINT('Ctrl Pts',(-3.75276917695086,48.4257174945299,20.));
#84517=CARTESIAN_POINT('Ctrl Pts',(-3.7190861282211,48.4252709717129,0.));
#84518=CARTESIAN_POINT('Ctrl Pts',(-3.7190861282211,48.4252709717129,20.));
#84519=CARTESIAN_POINT('Ctrl Pts',(-3.68540451261697,48.424801197947,0.));
#84520=CARTESIAN_POINT('Ctrl Pts',(-3.68540451261697,48.424801197947,20.));
#84521=CARTESIAN_POINT('Ctrl Pts',(-3.65172434619742,48.4243081743158,0.));
#84522=CARTESIAN_POINT('Ctrl Pts',(-3.65172434619742,48.4243081743158,20.));
#84523=CARTESIAN_POINT('Ctrl Pts',(-3.61804564502098,48.4237919019141,0.));
#84524=CARTESIAN_POINT('Ctrl Pts',(-3.61804564502098,48.4237919019141,20.));
#84525=CARTESIAN_POINT('Ctrl Pts',(-3.58436842514565,48.4232523818483,0.));
#84526=CARTESIAN_POINT('Ctrl Pts',(-3.58436842514565,48.4232523818483,20.));
#84527=CARTESIAN_POINT('Ctrl Pts',(-3.55069270262909,48.4226896152354,0.));
#84528=CARTESIAN_POINT('Ctrl Pts',(-3.55069270262909,48.4226896152354,20.));
#84529=CARTESIAN_POINT('Ctrl Pts',(-3.51701849352855,48.422103603204,0.));
#84530=CARTESIAN_POINT('Ctrl Pts',(-3.51701849352855,48.422103603204,20.));
#84531=CARTESIAN_POINT('Ctrl Pts',(-3.48334581390102,48.4214943468927,0.));
#84532=CARTESIAN_POINT('Ctrl Pts',(-3.48334581390102,48.4214943468927,20.));
#84533=CARTESIAN_POINT('Ctrl Pts',(-3.44967467980324,48.4208618474523,0.));
#84534=CARTESIAN_POINT('Ctrl Pts',(-3.44967467980324,48.4208618474523,20.));
#84535=CARTESIAN_POINT('Ctrl Pts',(-3.4160051072915,48.4202061060442,0.));
#84536=CARTESIAN_POINT('Ctrl Pts',(-3.4160051072915,48.4202061060442,20.));
#84537=CARTESIAN_POINT('Ctrl Pts',(-3.38233711242168,48.4195271238417,0.));
#84538=CARTESIAN_POINT('Ctrl Pts',(-3.38233711242168,48.4195271238417,20.));
#84539=CARTESIAN_POINT('Ctrl Pts',(-3.34867071124919,48.4188249020284,0.));
#84540=CARTESIAN_POINT('Ctrl Pts',(-3.34867071124919,48.4188249020284,20.));
#84541=CARTESIAN_POINT('Ctrl Pts',(-3.31500591982889,48.4180994417999,0.));
#84542=CARTESIAN_POINT('Ctrl Pts',(-3.31500591982889,48.4180994417999,20.));
#84543=CARTESIAN_POINT('Ctrl Pts',(-3.28134275421533,48.4173507443625,0.));
#84544=CARTESIAN_POINT('Ctrl Pts',(-3.28134275421533,48.4173507443625,20.));
#84545=CARTESIAN_POINT('Ctrl Pts',(-3.24768123046267,48.4165788109335,0.));
#84546=CARTESIAN_POINT('Ctrl Pts',(-3.24768123046267,48.4165788109335,20.));
#84547=CARTESIAN_POINT('Ctrl Pts',(-3.21402136462459,48.4157836427414,0.));
#84548=CARTESIAN_POINT('Ctrl Pts',(-3.21402136462459,48.4157836427414,20.));
#84549=CARTESIAN_POINT('Ctrl Pts',(-3.18036317275455,48.4149652410254,0.));
#84550=CARTESIAN_POINT('Ctrl Pts',(-3.18036317275455,48.4149652410254,20.));
#84551=CARTESIAN_POINT('Ctrl Pts',(-3.14670667090557,48.414123607036,0.));
#84552=CARTESIAN_POINT('Ctrl Pts',(-3.14670667090557,48.414123607036,20.));
#84553=CARTESIAN_POINT('Ctrl Pts',(-3.11305187513001,48.4132587420349,0.));
#84554=CARTESIAN_POINT('Ctrl Pts',(-3.11305187513001,48.4132587420349,20.));
#84555=CARTESIAN_POINT('Ctrl Pts',(-3.0793988014797,48.4123706472953,0.));
#84556=CARTESIAN_POINT('Ctrl Pts',(-3.0793988014797,48.4123706472953,20.));
#84557=CARTESIAN_POINT('Ctrl Pts',(-3.04574746600609,48.4114593241014,0.));
#84558=CARTESIAN_POINT('Ctrl Pts',(-3.04574746600609,48.4114593241014,20.));
#84559=CARTESIAN_POINT('Ctrl Pts',(-3.01209788475996,48.4105247737488,0.));
#84560=CARTESIAN_POINT('Ctrl Pts',(-3.01209788475996,48.4105247737488,20.));
#84561=CARTESIAN_POINT('Ctrl Pts',(-2.97845007379182,48.4095669975441,0.));
#84562=CARTESIAN_POINT('Ctrl Pts',(-2.97845007379182,48.4095669975441,20.));
#84563=CARTESIAN_POINT('Ctrl Pts',(-2.94480404915165,48.4085859968048,0.));
#84564=CARTESIAN_POINT('Ctrl Pts',(-2.94480404915165,48.4085859968048,20.));
#84565=CARTESIAN_POINT('Ctrl Pts',(-2.91115982688905,48.4075817728593,0.));
#84566=CARTESIAN_POINT('Ctrl Pts',(-2.91115982688905,48.4075817728593,20.));
#84567=CARTESIAN_POINT('Ctrl Pts',(-2.87751742305295,48.4065543270471,0.));
#84568=CARTESIAN_POINT('Ctrl Pts',(-2.87751742305295,48.4065543270471,20.));
#84569=CARTESIAN_POINT('Ctrl Pts',(-2.84387685369182,48.4055036607195,0.));
#84570=CARTESIAN_POINT('Ctrl Pts',(-2.84387685369182,48.4055036607195,20.));
#84571=CARTESIAN_POINT('Ctrl Pts',(-2.81023813485357,48.4044297752383,0.));
#84572=CARTESIAN_POINT('Ctrl Pts',(-2.81023813485357,48.4044297752383,20.));
#84573=CARTESIAN_POINT('Ctrl Pts',(-2.77660128258548,48.4033326719771,0.));
#84574=CARTESIAN_POINT('Ctrl Pts',(-2.77660128258548,48.4033326719771,20.));
#84575=CARTESIAN_POINT('Ctrl Pts',(-2.74296631293438,48.4022123523201,0.));
#84576=CARTESIAN_POINT('Ctrl Pts',(-2.74296631293438,48.4022123523201,20.));
#84577=CARTESIAN_POINT('Ctrl Pts',(-2.70933324194662,48.4010688176627,0.));
#84578=CARTESIAN_POINT('Ctrl Pts',(-2.70933324194662,48.4010688176627,20.));
#84579=CARTESIAN_POINT('Ctrl Pts',(-2.67570208566795,48.3999020694116,0.));
#84580=CARTESIAN_POINT('Ctrl Pts',(-2.67570208566795,48.3999020694116,20.));
#84581=CARTESIAN_POINT('Ctrl Pts',(-2.64207286014351,48.3987121089844,0.));
#84582=CARTESIAN_POINT('Ctrl Pts',(-2.64207286014351,48.3987121089844,20.));
#84583=CARTESIAN_POINT('Ctrl Pts',(-2.60844558141791,48.3974989378103,0.));
#84584=CARTESIAN_POINT('Ctrl Pts',(-2.60844558141791,48.3974989378103,20.));
#84585=CARTESIAN_POINT('Ctrl Pts',(-2.57482026553517,48.3962625573292,0.));
#84586=CARTESIAN_POINT('Ctrl Pts',(-2.57482026553517,48.3962625573292,20.));
#84587=CARTESIAN_POINT('Ctrl Pts',(-2.54119692853862,48.3950029689925,0.));
#84588=CARTESIAN_POINT('Ctrl Pts',(-2.54119692853862,48.3950029689925,20.));
#84589=CARTESIAN_POINT('Ctrl Pts',(-2.50757558647122,48.3937201742621,0.));
#84590=CARTESIAN_POINT('Ctrl Pts',(-2.50757558647122,48.3937201742621,20.));
#84591=CARTESIAN_POINT('Ctrl Pts',(-2.47395625537496,48.3924141746117,0.));
#84592=CARTESIAN_POINT('Ctrl Pts',(-2.47395625537496,48.3924141746117,20.));
#84593=CARTESIAN_POINT('Ctrl Pts',(-2.44033895129154,48.3910849715258,0.));
#84594=CARTESIAN_POINT('Ctrl Pts',(-2.44033895129154,48.3910849715258,20.));
#84595=CARTESIAN_POINT('Ctrl Pts',(-2.40672369026198,48.3897325665,0.));
#84596=CARTESIAN_POINT('Ctrl Pts',(-2.40672369026198,48.3897325665,20.));
#84597=CARTESIAN_POINT('Ctrl Pts',(-2.37311048832666,48.3883569610415,0.));
#84598=CARTESIAN_POINT('Ctrl Pts',(-2.37311048832666,48.3883569610415,20.));
#84599=CARTESIAN_POINT('Ctrl Pts',(-2.33949936152535,48.3869581566679,0.));
#84600=CARTESIAN_POINT('Ctrl Pts',(-2.33949936152535,48.3869581566679,20.));
#84601=CARTESIAN_POINT('Ctrl Pts',(-2.30589032589701,48.3855361549086,0.));
#84602=CARTESIAN_POINT('Ctrl Pts',(-2.30589032589701,48.3855361549086,20.));
#84603=CARTESIAN_POINT('Ctrl Pts',(-2.2722833974801,48.3840909573039,0.));
#84604=CARTESIAN_POINT('Ctrl Pts',(-2.2722833974801,48.3840909573039,20.));
#84605=CARTESIAN_POINT('Ctrl Pts',(-2.23867859231222,48.3826225654055,0.));
#84606=CARTESIAN_POINT('Ctrl Pts',(-2.23867859231222,48.3826225654055,20.));
#84607=CARTESIAN_POINT('Ctrl Pts',(-2.20507592643043,48.3811309807756,0.));
#84608=CARTESIAN_POINT('Ctrl Pts',(-2.20507592643043,48.3811309807756,20.));
#84609=CARTESIAN_POINT('Ctrl Pts',(-2.17147541587105,48.3796162049883,0.));
#84610=CARTESIAN_POINT('Ctrl Pts',(-2.17147541587105,48.3796162049883,20.));
#84611=CARTESIAN_POINT('Ctrl Pts',(-2.13787707667014,48.3780782396279,0.));
#84612=CARTESIAN_POINT('Ctrl Pts',(-2.13787707667014,48.3780782396279,20.));
#84613=CARTESIAN_POINT('Ctrl Pts',(-2.10428092486295,48.3765170862905,0.));
#84614=CARTESIAN_POINT('Ctrl Pts',(-2.10428092486295,48.3765170862905,20.));
#84615=CARTESIAN_POINT('Ctrl Pts',(-2.07068697648389,48.374932746583,0.));
#84616=CARTESIAN_POINT('Ctrl Pts',(-2.07068697648389,48.374932746583,20.));
#84617=CARTESIAN_POINT('Ctrl Pts',(-2.03709524756656,48.3733252221237,0.));
#84618=CARTESIAN_POINT('Ctrl Pts',(-2.03709524756656,48.3733252221237,20.));
#84619=CARTESIAN_POINT('Ctrl Pts',(-2.00350575414356,48.3716945145424,0.));
#84620=CARTESIAN_POINT('Ctrl Pts',(-2.00350575414356,48.3716945145424,20.));
#84621=CARTESIAN_POINT('Ctrl Pts',(-1.96991851224693,48.3700406254798,0.));
#84622=CARTESIAN_POINT('Ctrl Pts',(-1.96991851224693,48.3700406254798,20.));
#84623=CARTESIAN_POINT('Ctrl Pts',(-1.93633353790814,48.3683635565876,0.));
#84624=CARTESIAN_POINT('Ctrl Pts',(-1.93633353790814,48.3683635565876,20.));
#84625=CARTESIAN_POINT('Ctrl Pts',(-1.90275084715797,48.3666633095284,0.));
#84626=CARTESIAN_POINT('Ctrl Pts',(-1.90275084715797,48.3666633095284,20.));
#84627=CARTESIAN_POINT('Ctrl Pts',(-1.86917045602653,48.3649398859758,0.));
#84628=CARTESIAN_POINT('Ctrl Pts',(-1.86917045602653,48.3649398859758,20.));
#84629=CARTESIAN_POINT('Ctrl Pts',(-1.83559238054324,48.3631932876149,0.));
#84630=CARTESIAN_POINT('Ctrl Pts',(-1.83559238054324,48.3631932876149,20.));
#84631=CARTESIAN_POINT('Ctrl Pts',(-1.80201663673657,48.3614235161422,0.));
#84632=CARTESIAN_POINT('Ctrl Pts',(-1.80201663673657,48.3614235161422,20.));
#84633=CARTESIAN_POINT('Ctrl Pts',(-1.76844324063427,48.3596305732653,0.));
#84634=CARTESIAN_POINT('Ctrl Pts',(-1.76844324063427,48.3596305732653,20.));
#84635=CARTESIAN_POINT('Ctrl Pts',(-1.73487220826327,48.357814460703,0.));
#84636=CARTESIAN_POINT('Ctrl Pts',(-1.73487220826327,48.357814460703,20.));
#84637=CARTESIAN_POINT('Ctrl Pts',(-1.70130355564958,48.3559751801849,0.));
#84638=CARTESIAN_POINT('Ctrl Pts',(-1.70130355564958,48.3559751801849,20.));
#84639=CARTESIAN_POINT('Ctrl Pts',(-1.66773729881857,48.3541127334515,0.));
#84640=CARTESIAN_POINT('Ctrl Pts',(-1.66773729881857,48.3541127334515,20.));
#84641=CARTESIAN_POINT('Ctrl Pts',(-1.63417345379483,48.3522271222546,0.));
#84642=CARTESIAN_POINT('Ctrl Pts',(-1.63417345379483,48.3522271222546,20.));
#84643=CARTESIAN_POINT('Ctrl Pts',(-1.60061203660208,48.350318348357,0.));
#84644=CARTESIAN_POINT('Ctrl Pts',(-1.60061203660208,48.350318348357,20.));
#84645=CARTESIAN_POINT('Ctrl Pts',(-1.56705306326333,48.3483864135332,0.));
#84646=CARTESIAN_POINT('Ctrl Pts',(-1.56705306326333,48.3483864135332,20.));
#84647=CARTESIAN_POINT('Ctrl Pts',(-1.53349654980078,48.3464313195685,0.));
#84648=CARTESIAN_POINT('Ctrl Pts',(-1.53349654980078,48.3464313195685,20.));
#84649=CARTESIAN_POINT('Ctrl Pts',(-1.49994251223572,48.3444530682597,0.));
#84650=CARTESIAN_POINT('Ctrl Pts',(-1.49994251223572,48.3444530682597,20.));
#84651=CARTESIAN_POINT('Ctrl Pts',(-1.46639096658853,48.3424516614145,0.));
#84652=CARTESIAN_POINT('Ctrl Pts',(-1.46639096658853,48.3424516614145,20.));
#84653=CARTESIAN_POINT('Ctrl Pts',(-1.4328419288788,48.3404271008519,0.));
#84654=CARTESIAN_POINT('Ctrl Pts',(-1.4328419288788,48.3404271008519,20.));
#84655=CARTESIAN_POINT('Ctrl Pts',(-1.39929541512521,48.3383793884017,0.));
#84656=CARTESIAN_POINT('Ctrl Pts',(-1.39929541512521,48.3383793884017,20.));
#84657=CARTESIAN_POINT('Ctrl Pts',(-1.36575144134572,48.336308525905,0.));
#84658=CARTESIAN_POINT('Ctrl Pts',(-1.36575144134572,48.336308525905,20.));
#84659=CARTESIAN_POINT('Ctrl Pts',(-1.33221002355744,48.3342145152137,0.));
#84660=CARTESIAN_POINT('Ctrl Pts',(-1.33221002355744,48.3342145152137,20.));
#84661=CARTESIAN_POINT('Ctrl Pts',(-1.29867117777653,48.3320973581913,0.));
#84662=CARTESIAN_POINT('Ctrl Pts',(-1.29867117777653,48.3320973581913,20.));
#84663=CARTESIAN_POINT('Ctrl Pts',(-1.26513492001823,48.3299570567123,0.));
#84664=CARTESIAN_POINT('Ctrl Pts',(-1.26513492001823,48.3299570567123,20.));
#84665=CARTESIAN_POINT('Ctrl Pts',(-1.23160126629694,48.3277936126623,0.));
#84666=CARTESIAN_POINT('Ctrl Pts',(-1.23160126629694,48.3277936126623,20.));
#84667=CARTESIAN_POINT('Ctrl Pts',(-1.19807023262612,48.3256070279384,0.));
#84668=CARTESIAN_POINT('Ctrl Pts',(-1.19807023262612,48.3256070279384,20.));
#84669=CARTESIAN_POINT('Ctrl Pts',(-1.1645418350184,48.3233973044482,0.));
#84670=CARTESIAN_POINT('Ctrl Pts',(-1.1645418350184,48.3233973044482,20.));
#84671=CARTESIAN_POINT('Ctrl Pts',(-1.13101608948536,48.3211644441107,0.));
#84672=CARTESIAN_POINT('Ctrl Pts',(-1.13101608948536,48.3211644441107,20.));
#84673=CARTESIAN_POINT('Ctrl Pts',(-1.09749301203764,48.3189084488565,0.));
#84674=CARTESIAN_POINT('Ctrl Pts',(-1.09749301203764,48.3189084488565,20.));
#84675=CARTESIAN_POINT('Ctrl Pts',(-1.06397261868501,48.3166293206271,0.));
#84676=CARTESIAN_POINT('Ctrl Pts',(-1.06397261868501,48.3166293206271,20.));
#84677=CARTESIAN_POINT('Ctrl Pts',(-1.03045492543642,48.3143270613748,0.));
#84678=CARTESIAN_POINT('Ctrl Pts',(-1.03045492543642,48.3143270613748,20.));
#84679=CARTESIAN_POINT('Ctrl Pts',(-0.996939948299871,48.312001673063,0.));
#84680=CARTESIAN_POINT('Ctrl Pts',(-0.996939948299871,48.312001673063,20.));
#84681=CARTESIAN_POINT('Ctrl Pts',(-0.963427703282371,48.3096531576664,
0.));
#84682=CARTESIAN_POINT('Ctrl Pts',(-0.963427703282371,48.3096531576664,
20.));
#84683=CARTESIAN_POINT('Ctrl Pts',(-0.929918206389844,48.3072815171712,
0.));
#84684=CARTESIAN_POINT('Ctrl Pts',(-0.929918206389844,48.3072815171712,
20.));
#84685=CARTESIAN_POINT('Ctrl Pts',(-0.896411473627245,48.3048867535745,
0.));
#84686=CARTESIAN_POINT('Ctrl Pts',(-0.896411473627245,48.3048867535745,
20.));
#84687=CARTESIAN_POINT('Ctrl Pts',(-0.862907520998508,48.3024688688845,
0.));
#84688=CARTESIAN_POINT('Ctrl Pts',(-0.862907520998508,48.3024688688845,
20.));
#84689=CARTESIAN_POINT('Ctrl Pts',(-0.829406364506684,48.3000278651208,
0.));
#84690=CARTESIAN_POINT('Ctrl Pts',(-0.829406364506684,48.3000278651208,
20.));
#84691=CARTESIAN_POINT('Ctrl Pts',(-0.79590802015391,48.2975637443136,0.));
#84692=CARTESIAN_POINT('Ctrl Pts',(-0.79590802015391,48.2975637443136,20.));
#84693=CARTESIAN_POINT('Ctrl Pts',(-0.762412503941543,48.2950765085043,
0.));
#84694=CARTESIAN_POINT('Ctrl Pts',(-0.762412503941543,48.2950765085043,
20.));
#84695=CARTESIAN_POINT('Ctrl Pts',(-0.728919831869663,48.2925661597457,
0.));
#84696=CARTESIAN_POINT('Ctrl Pts',(-0.728919831869663,48.2925661597457,
20.));
#84697=CARTESIAN_POINT('Ctrl Pts',(-0.695430019937358,48.2900327001016,
0.));
#84698=CARTESIAN_POINT('Ctrl Pts',(-0.695430019937358,48.2900327001016,
20.));
#84699=CARTESIAN_POINT('Ctrl Pts',(-0.66194308414246,48.2874761316474,0.));
#84700=CARTESIAN_POINT('Ctrl Pts',(-0.66194308414246,48.2874761316474,20.));
#84701=CARTESIAN_POINT('Ctrl Pts',(-0.628459040481846,48.2848964564694,
0.));
#84702=CARTESIAN_POINT('Ctrl Pts',(-0.628459040481846,48.2848964564694,
20.));
#84703=CARTESIAN_POINT('Ctrl Pts',(-0.594977904951284,48.282293676665,0.));
#84704=CARTESIAN_POINT('Ctrl Pts',(-0.594977904951284,48.282293676665,20.));
#84705=CARTESIAN_POINT('Ctrl Pts',(-0.561499693545691,48.2796677943426,
0.));
#84706=CARTESIAN_POINT('Ctrl Pts',(-0.561499693545691,48.2796677943426,
20.));
#84707=CARTESIAN_POINT('Ctrl Pts',(-0.528024422259037,48.2770188116216,
0.));
#84708=CARTESIAN_POINT('Ctrl Pts',(-0.528024422259037,48.2770188116216,
20.));
#84709=CARTESIAN_POINT('Ctrl Pts',(-0.494552107084227,48.2743467306329,
0.));
#84710=CARTESIAN_POINT('Ctrl Pts',(-0.494552107084227,48.2743467306329,
20.));
#84711=CARTESIAN_POINT('Ctrl Pts',(-0.461082764013003,48.2716515535183,
0.));
#84712=CARTESIAN_POINT('Ctrl Pts',(-0.461082764013003,48.2716515535183,
20.));
#84713=CARTESIAN_POINT('Ctrl Pts',(-0.427616409036058,48.2689332824309,
0.));
#84714=CARTESIAN_POINT('Ctrl Pts',(-0.427616409036058,48.2689332824309,
20.));
#84715=CARTESIAN_POINT('Ctrl Pts',(-0.394153058142925,48.2661919195348,
0.));
#84716=CARTESIAN_POINT('Ctrl Pts',(-0.394153058142925,48.2661919195348,
20.));
#84717=CARTESIAN_POINT('Ctrl Pts',(-0.360692727322003,48.2634274670053,
0.));
#84718=CARTESIAN_POINT('Ctrl Pts',(-0.360692727322003,48.2634274670053,
20.));
#84719=CARTESIAN_POINT('Ctrl Pts',(-0.327235432560555,48.2606399270286,
0.));
#84720=CARTESIAN_POINT('Ctrl Pts',(-0.327235432560555,48.2606399270286,
20.));
#84721=CARTESIAN_POINT('Ctrl Pts',(-0.293781189844835,48.2578293018028,
0.));
#84722=CARTESIAN_POINT('Ctrl Pts',(-0.293781189844835,48.2578293018028,
20.));
#84723=CARTESIAN_POINT('Ctrl Pts',(-0.260330015159953,48.2549955935366,
0.));
#84724=CARTESIAN_POINT('Ctrl Pts',(-0.260330015159953,48.2549955935366,
20.));
#84725=CARTESIAN_POINT('Ctrl Pts',(-0.22688192448987,48.2521388044499,0.));
#84726=CARTESIAN_POINT('Ctrl Pts',(-0.22688192448987,48.2521388044499,20.));
#84727=CARTESIAN_POINT('Ctrl Pts',(-0.193436933817472,48.2492589367737,
0.));
#84728=CARTESIAN_POINT('Ctrl Pts',(-0.193436933817472,48.2492589367737,
20.));
#84729=CARTESIAN_POINT('Ctrl Pts',(-0.159995059124576,48.2463559927498,
0.));
#84730=CARTESIAN_POINT('Ctrl Pts',(-0.159995059124576,48.2463559927498,
20.));
#84731=CARTESIAN_POINT('Ctrl Pts',(-0.126556316391682,48.2434299746318,
0.));
#84732=CARTESIAN_POINT('Ctrl Pts',(-0.126556316391682,48.2434299746318,
20.));
#84733=CARTESIAN_POINT('Ctrl Pts',(-0.0931207215982832,48.2404808846839,
0.));
#84734=CARTESIAN_POINT('Ctrl Pts',(-0.0931207215982832,48.2404808846839,
20.));
#84735=CARTESIAN_POINT('Ctrl Pts',(-0.0596882907225993,48.2375087251817,
0.));
#84736=CARTESIAN_POINT('Ctrl Pts',(-0.0596882907225993,48.2375087251817,
20.));
#84737=CARTESIAN_POINT('Ctrl Pts',(-0.0262590397416762,48.234513498412,
0.));
#84738=CARTESIAN_POINT('Ctrl Pts',(-0.0262590397416762,48.234513498412,
20.));
#84739=CARTESIAN_POINT('Ctrl Pts',(0.00716701536856768,48.2314952066725,
0.));
#84740=CARTESIAN_POINT('Ctrl Pts',(0.00716701536856768,48.2314952066725,
20.));
#84741=CARTESIAN_POINT('Ctrl Pts',(0.0405898586334352,48.2284538522724,
0.));
#84742=CARTESIAN_POINT('Ctrl Pts',(0.0405898586334352,48.2284538522724,
20.));
#84743=CARTESIAN_POINT('Ctrl Pts',(0.0740094740793884,48.2253894375317,
0.));
#84744=CARTESIAN_POINT('Ctrl Pts',(0.0740094740793884,48.2253894375317,
20.));
#84745=CARTESIAN_POINT('Ctrl Pts',(0.107425845734119,48.2223019647818,0.));
#84746=CARTESIAN_POINT('Ctrl Pts',(0.107425845734119,48.2223019647818,20.));
#84747=CARTESIAN_POINT('Ctrl Pts',(0.140838957626541,48.2191914363652,0.));
#84748=CARTESIAN_POINT('Ctrl Pts',(0.140838957626541,48.2191914363652,20.));
#84749=CARTESIAN_POINT('Ctrl Pts',(0.174248793786895,48.2160578546352,0.));
#84750=CARTESIAN_POINT('Ctrl Pts',(0.174248793786895,48.2160578546352,20.));
#84751=CARTESIAN_POINT('Ctrl Pts',(0.207655338246555,48.2129012219564,0.));
#84752=CARTESIAN_POINT('Ctrl Pts',(0.207655338246555,48.2129012219564,20.));
#84753=CARTESIAN_POINT('Ctrl Pts',(0.241058575037867,48.2097215407045,0.));
#84754=CARTESIAN_POINT('Ctrl Pts',(0.241058575037867,48.2097215407045,20.));
#84755=CARTESIAN_POINT('Ctrl Pts',(0.274458488194584,48.2065188132665,0.));
#84756=CARTESIAN_POINT('Ctrl Pts',(0.274458488194584,48.2065188132665,20.));
#84757=CARTESIAN_POINT('Ctrl Pts',(0.30785506175171,48.2032930420408,0.));
#84758=CARTESIAN_POINT('Ctrl Pts',(0.30785506175171,48.2032930420408,20.));
#84759=CARTESIAN_POINT('Ctrl Pts',(0.341248279745643,48.2000442294364,0.));
#84760=CARTESIAN_POINT('Ctrl Pts',(0.341248279745643,48.2000442294364,20.));
#84761=CARTESIAN_POINT('Ctrl Pts',(0.374638126214095,48.1967723778737,0.));
#84762=CARTESIAN_POINT('Ctrl Pts',(0.374638126214095,48.1967723778737,20.));
#84763=CARTESIAN_POINT('Ctrl Pts',(0.408024585196225,48.1934774897842,0.));
#84764=CARTESIAN_POINT('Ctrl Pts',(0.408024585196225,48.1934774897842,20.));
#84765=CARTESIAN_POINT('Ctrl Pts',(0.441407640732092,48.1901595676102,0.));
#84766=CARTESIAN_POINT('Ctrl Pts',(0.441407640732092,48.1901595676102,20.));
#84767=CARTESIAN_POINT('Ctrl Pts',(0.474787276863071,48.1868186138054,0.));
#84768=CARTESIAN_POINT('Ctrl Pts',(0.474787276863071,48.1868186138054,20.));
#84769=CARTESIAN_POINT('Ctrl Pts',(0.508163477631851,48.1834546308352,0.));
#84770=CARTESIAN_POINT('Ctrl Pts',(0.508163477631851,48.1834546308352,20.));
#84771=CARTESIAN_POINT('Ctrl Pts',(0.541536227082355,48.1800676211754,0.));
#84772=CARTESIAN_POINT('Ctrl Pts',(0.541536227082355,48.1800676211754,20.));
#84773=CARTESIAN_POINT('Ctrl Pts',(0.574905509259889,48.1766575873132,0.));
#84774=CARTESIAN_POINT('Ctrl Pts',(0.574905509259889,48.1766575873132,20.));
#84775=CARTESIAN_POINT('Ctrl Pts',(0.608271308211097,48.1732245317468,0.));
#84776=CARTESIAN_POINT('Ctrl Pts',(0.608271308211097,48.1732245317468,20.));
#84777=CARTESIAN_POINT('Ctrl Pts',(0.6416336079841,48.1697684569855,0.));
#84778=CARTESIAN_POINT('Ctrl Pts',(0.6416336079841,48.1697684569855,20.));
#84779=CARTESIAN_POINT('Ctrl Pts',(0.674992392628235,48.16628936555,0.));
#84780=CARTESIAN_POINT('Ctrl Pts',(0.674992392628235,48.16628936555,20.));
#84781=CARTESIAN_POINT('Ctrl Pts',(0.708347646194278,48.1627872599717,0.));
#84782=CARTESIAN_POINT('Ctrl Pts',(0.708347646194278,48.1627872599717,20.));
#84783=CARTESIAN_POINT('Ctrl Pts',(0.741699352734257,48.1592621427937,0.));
#84784=CARTESIAN_POINT('Ctrl Pts',(0.741699352734257,48.1592621427937,20.));
#84785=CARTESIAN_POINT('Ctrl Pts',(0.775047496301533,48.1557140165701,0.));
#84786=CARTESIAN_POINT('Ctrl Pts',(0.775047496301533,48.1557140165701,20.));
#84787=CARTESIAN_POINT('Ctrl Pts',(0.808392060950864,48.1521428838659,0.));
#84788=CARTESIAN_POINT('Ctrl Pts',(0.808392060950864,48.1521428838659,20.));
#84789=CARTESIAN_POINT('Ctrl Pts',(0.841733030738387,48.1485487472572,0.));
#84790=CARTESIAN_POINT('Ctrl Pts',(0.841733030738387,48.1485487472572,20.));
#84791=CARTESIAN_POINT('Ctrl Pts',(0.875070389721522,48.144931609331,0.));
#84792=CARTESIAN_POINT('Ctrl Pts',(0.875070389721522,48.144931609331,20.));
#84793=CARTESIAN_POINT('Ctrl Pts',(0.908404121959285,48.1412914726861,0.));
#84794=CARTESIAN_POINT('Ctrl Pts',(0.908404121959285,48.1412914726861,20.));
#84795=CARTESIAN_POINT('Ctrl Pts',(0.941734211511944,48.137628339932,0.));
#84796=CARTESIAN_POINT('Ctrl Pts',(0.941734211511944,48.137628339932,20.));
#84797=CARTESIAN_POINT('Ctrl Pts',(0.975060642441243,48.1339422136897,0.));
#84798=CARTESIAN_POINT('Ctrl Pts',(0.975060642441243,48.1339422136897,20.));
#84799=CARTESIAN_POINT('Ctrl Pts',(1.00838339881032,48.130233096591,0.));
#84800=CARTESIAN_POINT('Ctrl Pts',(1.00838339881032,48.130233096591,20.));
#84801=CARTESIAN_POINT('Ctrl Pts',(1.04170246468365,48.1265009912787,0.));
#84802=CARTESIAN_POINT('Ctrl Pts',(1.04170246468365,48.1265009912787,20.));
#84803=CARTESIAN_POINT('Ctrl Pts',(1.07501782412728,48.1227459004068,0.));
#84804=CARTESIAN_POINT('Ctrl Pts',(1.07501782412728,48.1227459004068,20.));
#84805=CARTESIAN_POINT('Ctrl Pts',(1.10832946120861,48.1189678266406,0.));
#84806=CARTESIAN_POINT('Ctrl Pts',(1.10832946120861,48.1189678266406,20.));
#84807=CARTESIAN_POINT('Ctrl Pts',(1.14163735999657,48.1151667726565,0.));
#84808=CARTESIAN_POINT('Ctrl Pts',(1.14163735999657,48.1151667726565,20.));
#84809=CARTESIAN_POINT('Ctrl Pts',(1.17494150456145,48.111342741142,0.));
#84810=CARTESIAN_POINT('Ctrl Pts',(1.17494150456145,48.111342741142,20.));
#84811=CARTESIAN_POINT('Ctrl Pts',(1.20824187897489,48.1074957347955,0.));
#84812=CARTESIAN_POINT('Ctrl Pts',(1.20824187897489,48.1074957347955,20.));
#84813=CARTESIAN_POINT('Ctrl Pts',(1.24153846731022,48.1036257563271,0.));
#84814=CARTESIAN_POINT('Ctrl Pts',(1.24153846731022,48.1036257563271,20.));
#84815=CARTESIAN_POINT('Ctrl Pts',(1.27483125364215,48.0997328084577,0.));
#84816=CARTESIAN_POINT('Ctrl Pts',(1.27483125364215,48.0997328084577,20.));
#84817=CARTESIAN_POINT('Ctrl Pts',(1.30812022204704,48.0958168939195,0.));
#84818=CARTESIAN_POINT('Ctrl Pts',(1.30812022204704,48.0958168939195,20.));
#84819=CARTESIAN_POINT('Ctrl Pts',(1.3414053566026,48.0918780154556,0.));
#84820=CARTESIAN_POINT('Ctrl Pts',(1.3414053566026,48.0918780154556,20.));
#84821=CARTESIAN_POINT('Ctrl Pts',(1.37468664138801,48.0879161758201,0.));
#84822=CARTESIAN_POINT('Ctrl Pts',(1.37468664138801,48.0879161758201,20.));
#84823=CARTESIAN_POINT('Ctrl Pts',(1.40796406048387,48.0839313777781,0.));
#84824=CARTESIAN_POINT('Ctrl Pts',(1.40796406048387,48.0839313777781,20.));
#84825=CARTESIAN_POINT('Ctrl Pts',(1.44123759797224,48.0799236241059,0.));
#84826=CARTESIAN_POINT('Ctrl Pts',(1.44123759797224,48.0799236241059,20.));
#84827=CARTESIAN_POINT('Ctrl Pts',(1.47450723793681,48.0758929175908,0.));
#84828=CARTESIAN_POINT('Ctrl Pts',(1.47450723793681,48.0758929175908,20.));
#84829=CARTESIAN_POINT('Ctrl Pts',(1.50777296446291,48.071839261032,0.));
#84830=CARTESIAN_POINT('Ctrl Pts',(1.50777296446291,48.071839261032,20.));
#84831=CARTESIAN_POINT('Ctrl Pts',(1.54103476163743,48.0677626572394,0.));
#84832=CARTESIAN_POINT('Ctrl Pts',(1.54103476163743,48.0677626572394,20.));
#84833=CARTESIAN_POINT('Ctrl Pts',(1.57429261354889,48.0636631090342,0.));
#84834=CARTESIAN_POINT('Ctrl Pts',(1.57429261354889,48.0636631090342,20.));
#84835=CARTESIAN_POINT('Ctrl Pts',(1.60754650428745,48.0595406192492,0.));
#84836=CARTESIAN_POINT('Ctrl Pts',(1.60754650428745,48.0595406192492,20.));
#84837=CARTESIAN_POINT('Ctrl Pts',(1.64079641794461,48.0553951907273,0.));
#84838=CARTESIAN_POINT('Ctrl Pts',(1.64079641794461,48.0553951907273,20.));
#84839=CARTESIAN_POINT('Ctrl Pts',(1.67404233861337,48.0512268263229,0.));
#84840=CARTESIAN_POINT('Ctrl Pts',(1.67404233861337,48.0512268263229,20.));
#84841=CARTESIAN_POINT('Ctrl Pts',(1.70728425038804,48.0470355289011,0.));
#84842=CARTESIAN_POINT('Ctrl Pts',(1.70728425038804,48.0470355289011,20.));
#84843=CARTESIAN_POINT('Ctrl Pts',(1.74052213736471,48.0428213013379,0.));
#84844=CARTESIAN_POINT('Ctrl Pts',(1.74052213736471,48.0428213013379,20.));
#84845=CARTESIAN_POINT('Ctrl Pts',(1.77375598364109,48.038584146521,0.));
#84846=CARTESIAN_POINT('Ctrl Pts',(1.77375598364109,48.038584146521,20.));
#84847=CARTESIAN_POINT('Ctrl Pts',(1.80698577331663,48.0343240673492,0.));
#84848=CARTESIAN_POINT('Ctrl Pts',(1.80698577331663,48.0343240673492,20.));
#84849=CARTESIAN_POINT('Ctrl Pts',(1.84021149049245,48.0300410667328,0.));
#84850=CARTESIAN_POINT('Ctrl Pts',(1.84021149049245,48.0300410667328,20.));
#84851=CARTESIAN_POINT('Ctrl Pts',(1.87343311927141,48.0257351475934,0.));
#84852=CARTESIAN_POINT('Ctrl Pts',(1.87343311927141,48.0257351475934,20.));
#84853=CARTESIAN_POINT('Ctrl Pts',(1.90665064375786,48.0214063128629,0.));
#84854=CARTESIAN_POINT('Ctrl Pts',(1.90665064375786,48.0214063128629,20.));
#84855=CARTESIAN_POINT('Ctrl Pts',(1.93986404805772,48.0170545654849,0.));
#84856=CARTESIAN_POINT('Ctrl Pts',(1.93986404805772,48.0170545654849,20.));
#84857=CARTESIAN_POINT('Ctrl Pts',(1.97307331627849,48.0126799084137,0.));
#84858=CARTESIAN_POINT('Ctrl Pts',(1.97307331627849,48.0126799084137,20.));
#84859=CARTESIAN_POINT('Ctrl Pts',(2.00627843252925,48.0082823446147,0.));
#84860=CARTESIAN_POINT('Ctrl Pts',(2.00627843252925,48.0082823446147,20.));
#84861=CARTESIAN_POINT('Ctrl Pts',(2.03947938092067,48.0038618770642,0.));
#84862=CARTESIAN_POINT('Ctrl Pts',(2.03947938092067,48.0038618770642,20.));
#84863=CARTESIAN_POINT('Ctrl Pts',(2.07267614556536,47.9994185087499,0.));
#84864=CARTESIAN_POINT('Ctrl Pts',(2.07267614556536,47.9994185087499,20.));
#84865=CARTESIAN_POINT('Ctrl Pts',(2.10586871057748,47.994952242671,0.));
#84866=CARTESIAN_POINT('Ctrl Pts',(2.10586871057748,47.994952242671,20.));
#84867=CARTESIAN_POINT('Ctrl Pts',(2.13905706007285,47.9904630818375,0.));
#84868=CARTESIAN_POINT('Ctrl Pts',(2.13905706007285,47.9904630818375,20.));
#84869=CARTESIAN_POINT('Ctrl Pts',(2.17224117816898,47.9859510292704,0.));
#84870=CARTESIAN_POINT('Ctrl Pts',(2.17224117816898,47.9859510292704,20.));
#84871=CARTESIAN_POINT('Ctrl Pts',(2.2054210489852,47.9814160880019,0.));
#84872=CARTESIAN_POINT('Ctrl Pts',(2.2054210489852,47.9814160880019,20.));
#84873=CARTESIAN_POINT('Ctrl Pts',(2.23859665664239,47.9768582610752,0.));
#84874=CARTESIAN_POINT('Ctrl Pts',(2.23859665664239,47.9768582610752,20.));
#84875=CARTESIAN_POINT('Ctrl Pts',(2.27176798526352,47.9722775515452,0.));
#84876=CARTESIAN_POINT('Ctrl Pts',(2.27176798526352,47.9722775515452,20.));
#84877=CARTESIAN_POINT('Ctrl Pts',(2.30493501897294,47.9676739624772,0.));
#84878=CARTESIAN_POINT('Ctrl Pts',(2.30493501897294,47.9676739624772,20.));
#84879=CARTESIAN_POINT('Ctrl Pts',(2.33809774189657,47.9630474969481,0.));
#84880=CARTESIAN_POINT('Ctrl Pts',(2.33809774189657,47.9630474969481,20.));
#84881=CARTESIAN_POINT('Ctrl Pts',(2.3712561381623,47.9583981580454,0.));
#84882=CARTESIAN_POINT('Ctrl Pts',(2.3712561381623,47.9583981580454,20.));
#84883=CARTESIAN_POINT('Ctrl Pts',(2.40441019189959,47.9537259488681,0.));
#84884=CARTESIAN_POINT('Ctrl Pts',(2.40441019189959,47.9537259488681,20.));
#84885=CARTESIAN_POINT('Ctrl Pts',(2.43755988723965,47.9490308725257,0.));
#84886=CARTESIAN_POINT('Ctrl Pts',(2.43755988723965,47.9490308725257,20.));
#84887=CARTESIAN_POINT('Ctrl Pts',(2.47070520831548,47.9443129321394,0.));
#84888=CARTESIAN_POINT('Ctrl Pts',(2.47070520831548,47.9443129321394,20.));
#84889=CARTESIAN_POINT('Ctrl Pts',(2.50384613926209,47.9395721308414,0.));
#84890=CARTESIAN_POINT('Ctrl Pts',(2.50384613926209,47.9395721308414,20.));
#84891=CARTESIAN_POINT('Ctrl Pts',(2.53698266421613,47.9348084717752,0.));
#84892=CARTESIAN_POINT('Ctrl Pts',(2.53698266421613,47.9348084717752,20.));
#84893=CARTESIAN_POINT('Ctrl Pts',(2.57011476731622,47.9300219580955,0.));
#84894=CARTESIAN_POINT('Ctrl Pts',(2.57011476731622,47.9300219580955,20.));
#84895=CARTESIAN_POINT('Ctrl Pts',(2.60324243270257,47.9252125929679,0.));
#84896=CARTESIAN_POINT('Ctrl Pts',(2.60324243270257,47.9252125929679,20.));
#84897=CARTESIAN_POINT('Ctrl Pts',(2.63636564451718,47.9203803795688,0.));
#84898=CARTESIAN_POINT('Ctrl Pts',(2.63636564451718,47.9203803795688,20.));
#84899=CARTESIAN_POINT('Ctrl Pts',(2.66948438690365,47.9155253210858,0.));
#84900=CARTESIAN_POINT('Ctrl Pts',(2.66948438690365,47.9155253210858,20.));
#84901=CARTESIAN_POINT('Ctrl Pts',(2.70259864400757,47.9106474207177,0.));
#84902=CARTESIAN_POINT('Ctrl Pts',(2.70259864400757,47.9106474207177,20.));
#84903=CARTESIAN_POINT('Ctrl Pts',(2.73570839997628,47.9057466816743,0.));
#84904=CARTESIAN_POINT('Ctrl Pts',(2.73570839997628,47.9057466816743,20.));
#84905=CARTESIAN_POINT('Ctrl Pts',(2.76881363895917,47.9008231071768,0.));
#84906=CARTESIAN_POINT('Ctrl Pts',(2.76881363895917,47.9008231071768,20.));
#84907=CARTESIAN_POINT('Ctrl Pts',(2.80191434510733,47.8958767004573,0.));
#84908=CARTESIAN_POINT('Ctrl Pts',(2.80191434510733,47.8958767004573,20.));
#84909=CARTESIAN_POINT('Ctrl Pts',(2.83501050257375,47.8909074647592,0.));
#84910=CARTESIAN_POINT('Ctrl Pts',(2.83501050257375,47.8909074647592,20.));
#84911=CARTESIAN_POINT('Ctrl Pts',(2.86810209551307,47.8859154033363,0.));
#84912=CARTESIAN_POINT('Ctrl Pts',(2.86810209551307,47.8859154033363,20.));
#84913=CARTESIAN_POINT('Ctrl Pts',(2.90118910808199,47.8809005194543,0.));
#84914=CARTESIAN_POINT('Ctrl Pts',(2.90118910808199,47.8809005194543,20.));
#84915=CARTESIAN_POINT('Ctrl Pts',(2.93427152443917,47.8758628163901,0.));
#84916=CARTESIAN_POINT('Ctrl Pts',(2.93427152443917,47.8758628163901,20.));
#84917=CARTESIAN_POINT('Ctrl Pts',(2.96734932874504,47.8708022974315,0.));
#84918=CARTESIAN_POINT('Ctrl Pts',(2.96734932874504,47.8708022974315,20.));
#84919=CARTESIAN_POINT('Ctrl Pts',(3.00042250516192,47.8657189658771,0.));
#84920=CARTESIAN_POINT('Ctrl Pts',(3.00042250516192,47.8657189658771,20.));
#84921=CARTESIAN_POINT('Ctrl Pts',(3.03349103785388,47.8606128250365,0.));
#84922=CARTESIAN_POINT('Ctrl Pts',(3.03349103785388,47.8606128250365,20.));
#84923=CARTESIAN_POINT('Ctrl Pts',(3.06655491098681,47.8554838782302,0.));
#84924=CARTESIAN_POINT('Ctrl Pts',(3.06655491098681,47.8554838782302,20.));
#84925=CARTESIAN_POINT('Ctrl Pts',(3.09961410872875,47.8503321287903,0.));
#84926=CARTESIAN_POINT('Ctrl Pts',(3.09961410872875,47.8503321287903,20.));
#84927=CARTESIAN_POINT('Ctrl Pts',(3.13266861524953,47.8451575800601,0.));
#84928=CARTESIAN_POINT('Ctrl Pts',(3.13266861524953,47.8451575800601,20.));
#84929=CARTESIAN_POINT('Ctrl Pts',(3.16571841472089,47.8399602353939,0.));
#84930=CARTESIAN_POINT('Ctrl Pts',(3.16571841472089,47.8399602353939,20.));
#84931=CARTESIAN_POINT('Ctrl Pts',(3.19876349131674,47.834740098157,0.));
#84932=CARTESIAN_POINT('Ctrl Pts',(3.19876349131674,47.834740098157,20.));
#84933=CARTESIAN_POINT('Ctrl Pts',(3.23180382921272,47.829497171726,0.));
#84934=CARTESIAN_POINT('Ctrl Pts',(3.23180382921272,47.829497171726,20.));
#84935=CARTESIAN_POINT('Ctrl Pts',(3.26483941258676,47.8242314594881,0.));
#84936=CARTESIAN_POINT('Ctrl Pts',(3.26483941258676,47.8242314594881,20.));
#84937=CARTESIAN_POINT('Ctrl Pts',(3.29787022561835,47.818942964842,0.));
#84938=CARTESIAN_POINT('Ctrl Pts',(3.29787022561835,47.818942964842,20.));
#84939=CARTESIAN_POINT('Ctrl Pts',(3.33089625248902,47.813631691197,0.));
#84940=CARTESIAN_POINT('Ctrl Pts',(3.33089625248902,47.813631691197,20.));
#84941=CARTESIAN_POINT('Ctrl Pts',(3.36391747738213,47.8082976419741,0.));
#84942=CARTESIAN_POINT('Ctrl Pts',(3.36391747738213,47.8082976419741,20.));
#84943=CARTESIAN_POINT('Ctrl Pts',(3.39693388448305,47.802940820605,0.));
#84944=CARTESIAN_POINT('Ctrl Pts',(3.39693388448305,47.802940820605,20.));
#84945=CARTESIAN_POINT('Ctrl Pts',(3.42994545797921,47.797561230533,0.));
#84946=CARTESIAN_POINT('Ctrl Pts',(3.42994545797921,47.797561230533,20.));
#84947=CARTESIAN_POINT('Ctrl Pts',(3.46295218206011,47.7921588752121,0.));
#84948=CARTESIAN_POINT('Ctrl Pts',(3.46295218206011,47.7921588752121,20.));
#84949=CARTESIAN_POINT('Ctrl Pts',(3.49595404091727,47.7867337581073,0.));
#84950=CARTESIAN_POINT('Ctrl Pts',(3.49595404091727,47.7867337581073,20.));
#84951=CARTESIAN_POINT('Ctrl Pts',(3.52895101874414,47.7812858826946,0.));
#84952=CARTESIAN_POINT('Ctrl Pts',(3.52895101874414,47.7812858826946,20.));
#84953=CARTESIAN_POINT('Ctrl Pts',(3.56194309973641,47.7758152524613,0.));
#84954=CARTESIAN_POINT('Ctrl Pts',(3.56194309973641,47.7758152524613,20.));
#84955=CARTESIAN_POINT('Ctrl Pts',(3.59493026809157,47.7703218709055,0.));
#84956=CARTESIAN_POINT('Ctrl Pts',(3.59493026809157,47.7703218709055,20.));
#84957=CARTESIAN_POINT('Ctrl Pts',(3.62791250800923,47.764805741537,0.));
#84958=CARTESIAN_POINT('Ctrl Pts',(3.62791250800923,47.764805741537,20.));
#84959=CARTESIAN_POINT('Ctrl Pts',(3.66088980369083,47.7592668678762,0.));
#84960=CARTESIAN_POINT('Ctrl Pts',(3.66088980369083,47.7592668678762,20.));
#84961=CARTESIAN_POINT('Ctrl Pts',(3.69386213933993,47.7537052534546,0.));
#84962=CARTESIAN_POINT('Ctrl Pts',(3.69386213933993,47.7537052534546,20.));
#84963=CARTESIAN_POINT('Ctrl Pts',(3.72682949916222,47.7481209018149,0.));
#84964=CARTESIAN_POINT('Ctrl Pts',(3.72682949916222,47.7481209018149,20.));
#84965=CARTESIAN_POINT('Ctrl Pts',(3.75979186736544,47.7425138165111,0.));
#84966=CARTESIAN_POINT('Ctrl Pts',(3.75979186736544,47.7425138165111,20.));
#84967=CARTESIAN_POINT('Ctrl Pts',(3.79274922815948,47.7368840011081,0.));
#84968=CARTESIAN_POINT('Ctrl Pts',(3.79274922815948,47.7368840011081,20.));
#84969=CARTESIAN_POINT('Ctrl Pts',(3.82570156575622,47.7312314591817,0.));
#84970=CARTESIAN_POINT('Ctrl Pts',(3.82570156575622,47.7312314591817,20.));
#84971=CARTESIAN_POINT('Ctrl Pts',(3.85864886436973,47.7255561943191,0.));
#84972=CARTESIAN_POINT('Ctrl Pts',(3.85864886436973,47.7255561943191,20.));
#84973=CARTESIAN_POINT('Ctrl Pts',(3.89159110821604,47.719858210118,0.));
#84974=CARTESIAN_POINT('Ctrl Pts',(3.89159110821604,47.719858210118,20.));
#84975=CARTESIAN_POINT('Ctrl Pts',(3.92452828151332,47.7141375101875,0.));
#84976=CARTESIAN_POINT('Ctrl Pts',(3.92452828151332,47.7141375101875,20.));
#84977=CARTESIAN_POINT('Ctrl Pts',(3.95746036848186,47.7083940981477,0.));
#84978=CARTESIAN_POINT('Ctrl Pts',(3.95746036848186,47.7083940981477,20.));
#84979=CARTESIAN_POINT('Ctrl Pts',(3.990387353344,47.7026279776294,0.));
#84980=CARTESIAN_POINT('Ctrl Pts',(3.990387353344,47.7026279776294,20.));
#84981=CARTESIAN_POINT('Ctrl Pts',(4.02330922032433,47.6968391522753,0.));
#84982=CARTESIAN_POINT('Ctrl Pts',(4.02330922032433,47.6968391522753,20.));
#84983=CARTESIAN_POINT('Ctrl Pts',(4.05622595364951,47.6910276257391,0.));
#84984=CARTESIAN_POINT('Ctrl Pts',(4.05622595364951,47.6910276257391,20.));
#84985=CARTESIAN_POINT('Ctrl Pts',(4.08913753754848,47.6851934016861,0.));
#84986=CARTESIAN_POINT('Ctrl Pts',(4.08913753754848,47.6851934016861,20.));
#84987=CARTESIAN_POINT('Ctrl Pts',(4.12204395625218,47.6793364837921,0.));
#84988=CARTESIAN_POINT('Ctrl Pts',(4.12204395625218,47.6793364837921,20.));
#84989=CARTESIAN_POINT('Ctrl Pts',(4.15494519399369,47.6734568757434,0.));
#84990=CARTESIAN_POINT('Ctrl Pts',(4.15494519399369,47.6734568757434,20.));
#84991=CARTESIAN_POINT('Ctrl Pts',(4.18784123500835,47.6675545812371,0.));
#84992=CARTESIAN_POINT('Ctrl Pts',(4.18784123500835,47.6675545812371,20.));
#84993=CARTESIAN_POINT('Ctrl Pts',(4.22073206353344,47.6616296039816,0.));
#84994=CARTESIAN_POINT('Ctrl Pts',(4.22073206353344,47.6616296039816,20.));
#84995=CARTESIAN_POINT('Ctrl Pts',(4.25361766380859,47.6556819476964,0.));
#84996=CARTESIAN_POINT('Ctrl Pts',(4.25361766380859,47.6556819476964,20.));
#84997=CARTESIAN_POINT('Ctrl Pts',(4.28649802007566,47.6497116161128,0.));
#84998=CARTESIAN_POINT('Ctrl Pts',(4.28649802007566,47.6497116161128,20.));
#84999=CARTESIAN_POINT('Ctrl Pts',(4.31937311657885,47.6437186129734,0.));
#85000=CARTESIAN_POINT('Ctrl Pts',(4.31937311657885,47.6437186129734,20.));
#85001=CARTESIAN_POINT('Ctrl Pts',(4.35224293756439,47.6377029420315,0.));
#85002=CARTESIAN_POINT('Ctrl Pts',(4.35224293756439,47.6377029420315,20.));
#85003=CARTESIAN_POINT('Ctrl Pts',(4.38510746728074,47.6316646070511,0.));
#85004=CARTESIAN_POINT('Ctrl Pts',(4.38510746728074,47.6316646070511,20.));
#85005=CARTESIAN_POINT('Ctrl Pts',(4.41796668997835,47.6256036118071,0.));
#85006=CARTESIAN_POINT('Ctrl Pts',(4.41796668997835,47.6256036118071,20.));
#85007=CARTESIAN_POINT('Ctrl Pts',(4.45082058991003,47.6195199600851,0.));
#85008=CARTESIAN_POINT('Ctrl Pts',(4.45082058991003,47.6195199600851,20.));
#85009=CARTESIAN_POINT('Ctrl Pts',(4.48366915133083,47.6134136556823,0.));
#85010=CARTESIAN_POINT('Ctrl Pts',(4.48366915133083,47.6134136556823,20.));
#85011=CARTESIAN_POINT('Ctrl Pts',(4.51651235849822,47.6072847024073,0.));
#85012=CARTESIAN_POINT('Ctrl Pts',(4.51651235849822,47.6072847024073,20.));
#85013=CARTESIAN_POINT('Ctrl Pts',(4.54935019567197,47.6011331040799,0.));
#85014=CARTESIAN_POINT('Ctrl Pts',(4.54935019567197,47.6011331040799,20.));
#85015=CARTESIAN_POINT('Ctrl Pts',(4.58218264711418,47.5949588645311,0.));
#85016=CARTESIAN_POINT('Ctrl Pts',(4.58218264711418,47.5949588645311,20.));
#85017=CARTESIAN_POINT('Ctrl Pts',(4.61500969708895,47.5887619876026,0.));
#85018=CARTESIAN_POINT('Ctrl Pts',(4.61500969708895,47.5887619876026,20.));
#85019=CARTESIAN_POINT('Ctrl Pts',(4.64783132986259,47.5825424771468,0.));
#85020=CARTESIAN_POINT('Ctrl Pts',(4.64783132986259,47.5825424771468,20.));
#85021=CARTESIAN_POINT('Ctrl Pts',(4.68064752970369,47.5763003370265,0.));
#85022=CARTESIAN_POINT('Ctrl Pts',(4.68064752970369,47.5763003370265,20.));
#85023=CARTESIAN_POINT('Ctrl Pts',(4.71345828088308,47.5700355711162,0.));
#85024=CARTESIAN_POINT('Ctrl Pts',(4.71345828088308,47.5700355711162,20.));
#85025=CARTESIAN_POINT('Ctrl Pts',(4.74626356767412,47.5637481833017,0.));
#85026=CARTESIAN_POINT('Ctrl Pts',(4.74626356767412,47.5637481833017,20.));
#85027=CARTESIAN_POINT('Ctrl Pts',(4.77906337435243,47.5574381774801,0.));
#85028=CARTESIAN_POINT('Ctrl Pts',(4.77906337435243,47.5574381774801,20.));
#85029=CARTESIAN_POINT('Ctrl Pts',(4.81185768519588,47.5511055575593,0.));
#85030=CARTESIAN_POINT('Ctrl Pts',(4.81185768519588,47.5511055575593,20.));
#85031=CARTESIAN_POINT('Ctrl Pts',(4.84464648448474,47.5447503274583,0.));
#85032=CARTESIAN_POINT('Ctrl Pts',(4.84464648448474,47.5447503274583,20.));
#85033=CARTESIAN_POINT('Ctrl Pts',(4.87742975650161,47.538372491107,0.));
#85034=CARTESIAN_POINT('Ctrl Pts',(4.87742975650161,47.538372491107,20.));
#85035=CARTESIAN_POINT('Ctrl Pts',(4.91020748553144,47.5319720524462,0.));
#85036=CARTESIAN_POINT('Ctrl Pts',(4.91020748553144,47.5319720524462,20.));
#85037=CARTESIAN_POINT('Ctrl Pts',(4.94297965586156,47.5255490154281,0.));
#85038=CARTESIAN_POINT('Ctrl Pts',(4.94297965586156,47.5255490154281,20.));
#85039=CARTESIAN_POINT('Ctrl Pts',(4.97574625178169,47.519103384016,0.));
#85040=CARTESIAN_POINT('Ctrl Pts',(4.97574625178169,47.519103384016,20.));
#85041=CARTESIAN_POINT('Ctrl Pts',(5.00850725758367,47.5126351621839,0.));
#85042=CARTESIAN_POINT('Ctrl Pts',(5.00850725758367,47.5126351621839,20.));
#85043=CARTESIAN_POINT('Ctrl Pts',(5.04126265756154,47.5061443539168,0.));
#85044=CARTESIAN_POINT('Ctrl Pts',(5.04126265756154,47.5061443539168,20.));
#85045=CARTESIAN_POINT('Ctrl Pts',(5.07401243601198,47.4996309632108,0.));
#85046=CARTESIAN_POINT('Ctrl Pts',(5.07401243601198,47.4996309632108,20.));
#85047=CARTESIAN_POINT('Ctrl Pts',(5.10675657723402,47.4930949940731,0.));
#85048=CARTESIAN_POINT('Ctrl Pts',(5.10675657723402,47.4930949940731,20.));
#85049=CARTESIAN_POINT('Ctrl Pts',(5.13949506552922,47.4865364505219,0.));
#85050=CARTESIAN_POINT('Ctrl Pts',(5.13949506552922,47.4865364505219,20.));
#85051=CARTESIAN_POINT('Ctrl Pts',(5.17222788520144,47.4799553365862,0.));
#85052=CARTESIAN_POINT('Ctrl Pts',(5.17222788520144,47.4799553365862,20.));
#85053=CARTESIAN_POINT('Ctrl Pts',(5.20495502055713,47.4733516563069,0.));
#85054=CARTESIAN_POINT('Ctrl Pts',(5.20495502055713,47.4733516563069,20.));
#85055=CARTESIAN_POINT('Ctrl Pts',(5.2376764559051,47.4667254137359,0.));
#85056=CARTESIAN_POINT('Ctrl Pts',(5.2376764559051,47.4667254137359,20.));
#85057=CARTESIAN_POINT('Ctrl Pts',(5.27039217555655,47.4600766129357,0.));
#85058=CARTESIAN_POINT('Ctrl Pts',(5.27039217555655,47.4600766129357,20.));
#85059=CARTESIAN_POINT('Ctrl Pts',(5.30310216382505,47.4534052579797,0.));
#85060=CARTESIAN_POINT('Ctrl Pts',(5.30310216382505,47.4534052579797,20.));
#85061=CARTESIAN_POINT('Ctrl Pts',(5.3358064050266,47.4467113529523,0.));
#85062=CARTESIAN_POINT('Ctrl Pts',(5.3358064050266,47.4467113529523,20.));
#85063=CARTESIAN_POINT('Ctrl Pts',(5.36850488347923,47.4399949019487,0.));
#85064=CARTESIAN_POINT('Ctrl Pts',(5.36850488347923,47.4399949019487,20.));
#85065=CARTESIAN_POINT('Ctrl Pts',(5.40119758350378,47.4332559090748,0.));
#85066=CARTESIAN_POINT('Ctrl Pts',(5.40119758350378,47.4332559090748,20.));
#85067=CARTESIAN_POINT('Ctrl Pts',(5.43388448942349,47.4264943784481,0.));
#85068=CARTESIAN_POINT('Ctrl Pts',(5.43388448942349,47.4264943784481,20.));
#85069=CARTESIAN_POINT('Ctrl Pts',(5.46656558556425,47.4197103141976,0.));
#85070=CARTESIAN_POINT('Ctrl Pts',(5.46656558556425,47.4197103141976,20.));
#85071=CARTESIAN_POINT('Ctrl Pts',(5.49924085625463,47.4129037204631,0.));
#85072=CARTESIAN_POINT('Ctrl Pts',(5.49924085625463,47.4129037204631,20.));
#85073=CARTESIAN_POINT('Ctrl Pts',(5.53191028582554,47.4060746013959,0.));
#85074=CARTESIAN_POINT('Ctrl Pts',(5.53191028582554,47.4060746013959,20.));
#85075=CARTESIAN_POINT('Ctrl Pts',(5.56457385861036,47.3992229611579,0.));
#85076=CARTESIAN_POINT('Ctrl Pts',(5.56457385861036,47.3992229611579,20.));
#85077=CARTESIAN_POINT('Ctrl Pts',(5.59723155894482,47.3923488039217,0.));
#85078=CARTESIAN_POINT('Ctrl Pts',(5.59723155894482,47.3923488039217,20.));
#85079=CARTESIAN_POINT('Ctrl Pts',(5.62988337116714,47.3854521338708,0.));
#85080=CARTESIAN_POINT('Ctrl Pts',(5.62988337116714,47.3854521338708,20.));
#85081=CARTESIAN_POINT('Ctrl Pts',(5.6625292796181,47.3785329551997,0.));
#85082=CARTESIAN_POINT('Ctrl Pts',(5.6625292796181,47.3785329551997,20.));
#85083=CARTESIAN_POINT('Ctrl Pts',(5.69516926864087,47.3715912721141,0.));
#85084=CARTESIAN_POINT('Ctrl Pts',(5.69516926864087,47.3715912721141,20.));
#85085=CARTESIAN_POINT('Ctrl Pts',(5.72780332258134,47.3646270888308,0.));
#85086=CARTESIAN_POINT('Ctrl Pts',(5.72780332258134,47.3646270888308,20.));
#85087=CARTESIAN_POINT('Ctrl Pts',(5.76043142578785,47.3576404095778,0.));
#85088=CARTESIAN_POINT('Ctrl Pts',(5.76043142578785,47.3576404095778,20.));
#85089=CARTESIAN_POINT('Ctrl Pts',(5.79305356261141,47.3506312385939,0.));
#85090=CARTESIAN_POINT('Ctrl Pts',(5.79305356261141,47.3506312385939,20.));
#85091=CARTESIAN_POINT('Ctrl Pts',(5.82566971740555,47.3435995801292,0.));
#85092=CARTESIAN_POINT('Ctrl Pts',(5.82566971740555,47.3435995801292,20.));
#85093=CARTESIAN_POINT('Ctrl Pts',(5.85827987452639,47.3365454384446,0.));
#85094=CARTESIAN_POINT('Ctrl Pts',(5.85827987452639,47.3365454384446,20.));
#85095=CARTESIAN_POINT('Ctrl Pts',(5.89088401833276,47.3294688178121,0.));
#85096=CARTESIAN_POINT('Ctrl Pts',(5.89088401833276,47.3294688178121,20.));
#85097=CARTESIAN_POINT('Ctrl Pts',(5.92348213318597,47.3223697225143,0.));
#85098=CARTESIAN_POINT('Ctrl Pts',(5.92348213318597,47.3223697225143,20.));
#85099=CARTESIAN_POINT('Ctrl Pts',(5.95607420344985,47.3152481568452,0.));
#85100=CARTESIAN_POINT('Ctrl Pts',(5.95607420344985,47.3152481568452,20.));
#85101=CARTESIAN_POINT('Ctrl Pts',(5.98866021349066,47.3081041251096,0.));
#85102=CARTESIAN_POINT('Ctrl Pts',(5.98866021349066,47.3081041251096,20.));
#85103=CARTESIAN_POINT('Ctrl Pts',(6.02124014767729,47.3009376316237,0.));
#85104=CARTESIAN_POINT('Ctrl Pts',(6.02124014767729,47.3009376316237,20.));
#85105=CARTESIAN_POINT('Ctrl Pts',(6.05381399038128,47.2937486807145,0.));
#85106=CARTESIAN_POINT('Ctrl Pts',(6.05381399038128,47.2937486807145,20.));
#85107=CARTESIAN_POINT('Ctrl Pts',(6.08638172597683,47.2865372767199,0.));
#85108=CARTESIAN_POINT('Ctrl Pts',(6.08638172597683,47.2865372767199,20.));
#85109=CARTESIAN_POINT('Ctrl Pts',(6.11894333884087,47.2793034239892,0.));
#85110=CARTESIAN_POINT('Ctrl Pts',(6.11894333884087,47.2793034239892,20.));
#85111=CARTESIAN_POINT('Ctrl Pts',(6.15149881335289,47.272047126882,0.));
#85112=CARTESIAN_POINT('Ctrl Pts',(6.15149881335289,47.272047126882,20.));
#85113=CARTESIAN_POINT('Ctrl Pts',(6.18404813389528,47.2647683897693,0.));
#85114=CARTESIAN_POINT('Ctrl Pts',(6.18404813389528,47.2647683897693,20.));
#85115=CARTESIAN_POINT('Ctrl Pts',(6.21659128485295,47.2574672170331,0.));
#85116=CARTESIAN_POINT('Ctrl Pts',(6.21659128485295,47.2574672170331,20.));
#85117=CARTESIAN_POINT('Ctrl Pts',(6.24912825061342,47.2501436130661,0.));
#85118=CARTESIAN_POINT('Ctrl Pts',(6.24912825061342,47.2501436130661,20.));
#85119=CARTESIAN_POINT('Ctrl Pts',(6.28165901556675,47.2427975822723,0.));
#85120=CARTESIAN_POINT('Ctrl Pts',(6.28165901556675,47.2427975822723,20.));
#85121=CARTESIAN_POINT('Ctrl Pts',(6.31418356410549,47.2354291290667,0.));
#85122=CARTESIAN_POINT('Ctrl Pts',(6.31418356410549,47.2354291290667,20.));
#85123=CARTESIAN_POINT('Ctrl Pts',(6.34670188062515,47.2280382578755,0.));
#85124=CARTESIAN_POINT('Ctrl Pts',(6.34670188062515,47.2280382578755,20.));
#85125=CARTESIAN_POINT('Ctrl Pts',(6.37921394952379,47.2206249731358,0.));
#85126=CARTESIAN_POINT('Ctrl Pts',(6.37921394952379,47.2206249731358,20.));
#85127=CARTESIAN_POINT('Ctrl Pts',(6.41171975520233,47.213189279296,0.));
#85128=CARTESIAN_POINT('Ctrl Pts',(6.41171975520233,47.213189279296,20.));
#85129=CARTESIAN_POINT('Ctrl Pts',(6.44421928206445,47.205731180815,0.));
#85130=CARTESIAN_POINT('Ctrl Pts',(6.44421928206445,47.205731180815,20.));
#85131=CARTESIAN_POINT('Ctrl Pts',(6.47671251451637,47.1982506821625,0.));
#85132=CARTESIAN_POINT('Ctrl Pts',(6.47671251451637,47.1982506821625,20.));
#85133=CARTESIAN_POINT('Ctrl Pts',(6.50919943696717,47.190747787819,0.));
#85134=CARTESIAN_POINT('Ctrl Pts',(6.50919943696717,47.190747787819,20.));
#85135=CARTESIAN_POINT('Ctrl Pts',(6.54168003382861,47.1832225022762,0.));
#85136=CARTESIAN_POINT('Ctrl Pts',(6.54168003382861,47.1832225022762,20.));
#85137=CARTESIAN_POINT('Ctrl Pts',(6.57415428951524,47.1756748300372,0.));
#85138=CARTESIAN_POINT('Ctrl Pts',(6.57415428951524,47.1756748300372,20.));
#85139=CARTESIAN_POINT('Ctrl Pts',(6.60662218844434,47.168104775616,0.));
#85140=CARTESIAN_POINT('Ctrl Pts',(6.60662218844434,47.168104775616,20.));
#85141=CARTESIAN_POINT('Ctrl Pts',(6.63908371503577,47.1605123435378,0.));
#85142=CARTESIAN_POINT('Ctrl Pts',(6.63908371503577,47.1605123435378,20.));
#85143=CARTESIAN_POINT('Ctrl Pts',(6.67153885371226,47.1528975383387,0.));
#85144=CARTESIAN_POINT('Ctrl Pts',(6.67153885371226,47.1528975383387,20.));
#85145=CARTESIAN_POINT('Ctrl Pts',(6.70398758889916,47.1452603645656,0.));
#85146=CARTESIAN_POINT('Ctrl Pts',(6.70398758889916,47.1452603645656,20.));
#85147=CARTESIAN_POINT('Ctrl Pts',(6.73642990502458,47.1376008267758,0.));
#85148=CARTESIAN_POINT('Ctrl Pts',(6.73642990502458,47.1376008267758,20.));
#85149=CARTESIAN_POINT('Ctrl Pts',(6.76886578651954,47.129918929538,0.));
#85150=CARTESIAN_POINT('Ctrl Pts',(6.76886578651954,47.129918929538,20.));
#85151=CARTESIAN_POINT('Ctrl Pts',(6.80129521781808,47.1222146774323,0.));
#85152=CARTESIAN_POINT('Ctrl Pts',(6.80129521781808,47.1222146774323,20.));
#85153=CARTESIAN_POINT('Ctrl Pts',(6.83371818335697,47.1144880750497,0.));
#85154=CARTESIAN_POINT('Ctrl Pts',(6.83371818335697,47.1144880750497,20.));
#85155=CARTESIAN_POINT('Ctrl Pts',(6.86613466757588,47.1067391269919,0.));
#85156=CARTESIAN_POINT('Ctrl Pts',(6.86613466757588,47.1067391269919,20.));
#85157=CARTESIAN_POINT('Ctrl Pts',(6.89854465491702,47.0989678378717,0.));
#85158=CARTESIAN_POINT('Ctrl Pts',(6.89854465491702,47.0989678378717,20.));
#85159=CARTESIAN_POINT('Ctrl Pts',(6.93094812982541,47.0911742123123,0.));
#85160=CARTESIAN_POINT('Ctrl Pts',(6.93094812982541,47.0911742123123,20.));
#85161=CARTESIAN_POINT('Ctrl Pts',(6.96334507674873,47.0833582549484,0.));
#85162=CARTESIAN_POINT('Ctrl Pts',(6.96334507674873,47.0833582549484,20.));
#85163=CARTESIAN_POINT('Ctrl Pts',(6.99573548013776,47.0755199704256,0.));
#85164=CARTESIAN_POINT('Ctrl Pts',(6.99573548013776,47.0755199704256,20.));
#85165=CARTESIAN_POINT('Ctrl Pts',(7.02811932444601,47.0676593634011,0.));
#85166=CARTESIAN_POINT('Ctrl Pts',(7.02811932444601,47.0676593634011,20.));
#85167=CARTESIAN_POINT('Ctrl Pts',(7.06049659413007,47.0597764385426,0.));
#85168=CARTESIAN_POINT('Ctrl Pts',(7.06049659413007,47.0597764385426,20.));
#85169=CARTESIAN_POINT('Ctrl Pts',(7.09286727364932,47.0518712005288,0.));
#85170=CARTESIAN_POINT('Ctrl Pts',(7.09286727364932,47.0518712005288,20.));
#85171=CARTESIAN_POINT('Ctrl Pts',(7.12523134746603,47.0439436540493,0.));
#85172=CARTESIAN_POINT('Ctrl Pts',(7.12523134746603,47.0439436540493,20.));
#85173=CARTESIAN_POINT('Ctrl Pts',(7.15758880004521,47.0359938038039,0.));
#85174=CARTESIAN_POINT('Ctrl Pts',(7.15758880004521,47.0359938038039,20.));
#85175=CARTESIAN_POINT('Ctrl Pts',(7.18993961585469,47.0280216545038,0.));
#85176=CARTESIAN_POINT('Ctrl Pts',(7.18993961585469,47.0280216545038,20.));
#85177=CARTESIAN_POINT('Ctrl Pts',(7.22228377936529,47.020027210871,0.));
#85178=CARTESIAN_POINT('Ctrl Pts',(7.22228377936529,47.020027210871,20.));
#85179=CARTESIAN_POINT('Ctrl Pts',(7.25462127505076,47.012010477639,0.));
#85180=CARTESIAN_POINT('Ctrl Pts',(7.25462127505076,47.012010477639,20.));
#85181=CARTESIAN_POINT('Ctrl Pts',(7.28695208738784,47.0039714595526,0.));
#85182=CARTESIAN_POINT('Ctrl Pts',(7.28695208738784,47.0039714595526,20.));
#85183=CARTESIAN_POINT('Ctrl Pts',(7.31927620085613,46.9959101613675,0.));
#85184=CARTESIAN_POINT('Ctrl Pts',(7.31927620085613,46.9959101613675,20.));
#85185=CARTESIAN_POINT('Ctrl Pts',(7.35159359993817,46.9878265878505,0.));
#85186=CARTESIAN_POINT('Ctrl Pts',(7.35159359993817,46.9878265878505,20.));
#85187=CARTESIAN_POINT('Ctrl Pts',(7.38390426911931,46.9797207437786,0.));
#85188=CARTESIAN_POINT('Ctrl Pts',(7.38390426911931,46.9797207437786,20.));
#85189=CARTESIAN_POINT('Ctrl Pts',(7.41620819288777,46.9715926339391,0.));
#85190=CARTESIAN_POINT('Ctrl Pts',(7.41620819288777,46.9715926339391,20.));
#85191=CARTESIAN_POINT('Ctrl Pts',(7.44850535573481,46.9634422631307,0.));
#85192=CARTESIAN_POINT('Ctrl Pts',(7.44850535573481,46.9634422631307,20.));
#85193=CARTESIAN_POINT('Ctrl Pts',(7.48079574215478,46.9552696361634,0.));
#85194=CARTESIAN_POINT('Ctrl Pts',(7.48079574215478,46.9552696361634,20.));
#85195=CARTESIAN_POINT('Ctrl Pts',(7.51307933664511,46.9470747578592,0.));
#85196=CARTESIAN_POINT('Ctrl Pts',(7.51307933664511,46.9470747578592,20.));
#85197=CARTESIAN_POINT('Ctrl Pts',(7.54535612370601,46.9388576330501,0.));
#85198=CARTESIAN_POINT('Ctrl Pts',(7.54535612370601,46.9388576330501,20.));
#85199=CARTESIAN_POINT('Ctrl Pts',(7.57762608784068,46.9306182665792,0.));
#85200=CARTESIAN_POINT('Ctrl Pts',(7.57762608784068,46.9306182665792,20.));
#85201=CARTESIAN_POINT('Ctrl Pts',(7.6098892135552,46.9223566632999,0.));
#85202=CARTESIAN_POINT('Ctrl Pts',(7.6098892135552,46.9223566632999,20.));
#85203=CARTESIAN_POINT('Ctrl Pts',(7.64214548535856,46.9140728280766,0.));
#85204=CARTESIAN_POINT('Ctrl Pts',(7.64214548535856,46.9140728280766,20.));
#85205=CARTESIAN_POINT('Ctrl Pts',(7.67439488776287,46.9057667657847,0.));
#85206=CARTESIAN_POINT('Ctrl Pts',(7.67439488776287,46.9057667657847,20.));
#85207=CARTESIAN_POINT('Ctrl Pts',(7.7066374052833,46.8974384813109,0.));
#85208=CARTESIAN_POINT('Ctrl Pts',(7.7066374052833,46.8974384813109,20.));
#85209=CARTESIAN_POINT('Ctrl Pts',(7.73887302243815,46.8890879795531,0.));
#85210=CARTESIAN_POINT('Ctrl Pts',(7.73887302243815,46.8890879795531,20.));
#85211=CARTESIAN_POINT('Ctrl Pts',(7.77110172374868,46.8807152654198,0.));
#85212=CARTESIAN_POINT('Ctrl Pts',(7.77110172374868,46.8807152654198,20.));
#85213=CARTESIAN_POINT('Ctrl Pts',(7.80332349373917,46.8723203438306,0.));
#85214=CARTESIAN_POINT('Ctrl Pts',(7.80332349373917,46.8723203438306,20.));
#85215=CARTESIAN_POINT('Ctrl Pts',(7.83553831693686,46.8639032197162,0.));
#85216=CARTESIAN_POINT('Ctrl Pts',(7.83553831693686,46.8639032197162,20.));
#85217=CARTESIAN_POINT('Ctrl Pts',(7.86774617787212,46.855463898018,0.));
#85218=CARTESIAN_POINT('Ctrl Pts',(7.86774617787212,46.855463898018,20.));
#85219=CARTESIAN_POINT('Ctrl Pts',(7.89994706107838,46.8470023836881,0.));
#85220=CARTESIAN_POINT('Ctrl Pts',(7.89994706107838,46.8470023836881,20.));
#85221=CARTESIAN_POINT('Ctrl Pts',(7.9321409510921,46.8385186816898,0.));
#85222=CARTESIAN_POINT('Ctrl Pts',(7.9321409510921,46.8385186816898,20.));
#85223=CARTESIAN_POINT('Ctrl Pts',(7.96432783245285,46.8300127969969,0.));
#85224=CARTESIAN_POINT('Ctrl Pts',(7.96432783245285,46.8300127969969,20.));
#85225=CARTESIAN_POINT('Ctrl Pts',(7.99650768970303,46.8214847345942,0.));
#85226=CARTESIAN_POINT('Ctrl Pts',(7.99650768970303,46.8214847345942,20.));
#85227=CARTESIAN_POINT('Ctrl Pts',(8.02868050738827,46.8129344994773,0.));
#85228=CARTESIAN_POINT('Ctrl Pts',(8.02868050738827,46.8129344994773,20.));
#85229=CARTESIAN_POINT('Ctrl Pts',(8.06084627005728,46.8043620966531,0.));
#85230=CARTESIAN_POINT('Ctrl Pts',(8.06084627005728,46.8043620966531,20.));
#85231=CARTESIAN_POINT('Ctrl Pts',(8.09300496226219,46.7957675311395,0.));
#85232=CARTESIAN_POINT('Ctrl Pts',(8.09300496226219,46.7957675311395,20.));
#85233=CARTESIAN_POINT('Ctrl Pts',(8.125156568558,46.7871508079658,0.));
#85234=CARTESIAN_POINT('Ctrl Pts',(8.125156568558,46.7871508079658,20.));
#85235=CARTESIAN_POINT('Ctrl Pts',(8.15730107350294,46.7785119321719,0.));
#85236=CARTESIAN_POINT('Ctrl Pts',(8.15730107350294,46.7785119321719,20.));
#85237=CARTESIAN_POINT('Ctrl Pts',(8.18943846165844,46.7698509088086,0.));
#85238=CARTESIAN_POINT('Ctrl Pts',(8.18943846165844,46.7698509088086,20.));
#85239=CARTESIAN_POINT('Ctrl Pts',(8.22156871758881,46.7611677429374,0.));
#85240=CARTESIAN_POINT('Ctrl Pts',(8.22156871758881,46.7611677429374,20.));
#85241=CARTESIAN_POINT('Ctrl Pts',(8.25369182586168,46.7524624396307,0.));
#85242=CARTESIAN_POINT('Ctrl Pts',(8.25369182586168,46.7524624396307,20.));
#85243=CARTESIAN_POINT('Ctrl Pts',(8.28580777104744,46.7437350039712,0.));
#85244=CARTESIAN_POINT('Ctrl Pts',(8.28580777104744,46.7437350039712,20.));
#85245=CARTESIAN_POINT('Ctrl Pts',(8.31791653771973,46.7349854410525,0.));
#85246=CARTESIAN_POINT('Ctrl Pts',(8.31791653771973,46.7349854410525,20.));
#85247=CARTESIAN_POINT('Ctrl Pts',(8.35001811045535,46.7262137559789,0.));
#85248=CARTESIAN_POINT('Ctrl Pts',(8.35001811045535,46.7262137559789,20.));
#85249=CARTESIAN_POINT('Ctrl Pts',(8.38211247383476,46.7174199538668,0.));
#85250=CARTESIAN_POINT('Ctrl Pts',(8.38211247383476,46.7174199538668,20.));
#85251=CARTESIAN_POINT('Ctrl Pts',(8.41419961244154,46.7086040398438,0.));
#85252=CARTESIAN_POINT('Ctrl Pts',(8.41419961244154,46.7086040398438,20.));
#85253=CARTESIAN_POINT('Ctrl Pts',(8.44627951086261,46.6997660190488,0.));
#85254=CARTESIAN_POINT('Ctrl Pts',(8.44627951086261,46.6997660190488,20.));
#85255=CARTESIAN_POINT('Ctrl Pts',(8.47835215368743,46.6909058966306,0.));
#85256=CARTESIAN_POINT('Ctrl Pts',(8.47835215368743,46.6909058966306,20.));
#85257=CARTESIAN_POINT('Ctrl Pts',(8.5104175255088,46.6820236777489,0.));
#85258=CARTESIAN_POINT('Ctrl Pts',(8.5104175255088,46.6820236777489,20.));
#85259=CARTESIAN_POINT('Ctrl Pts',(8.54247561092257,46.673119367573,0.));
#85260=CARTESIAN_POINT('Ctrl Pts',(8.54247561092257,46.673119367573,20.));
#85261=CARTESIAN_POINT('Ctrl Pts',(8.57452639452827,46.6641929712839,0.));
#85262=CARTESIAN_POINT('Ctrl Pts',(8.57452639452827,46.6641929712839,20.));
#85263=CARTESIAN_POINT('Ctrl Pts',(8.60656986092877,46.6552444940739,0.));
#85264=CARTESIAN_POINT('Ctrl Pts',(8.60656986092877,46.6552444940739,20.));
#85265=CARTESIAN_POINT('Ctrl Pts',(8.63860599473002,46.6462739411471,0.));
#85266=CARTESIAN_POINT('Ctrl Pts',(8.63860599473002,46.6462739411471,20.));
#85267=CARTESIAN_POINT('Ctrl Pts',(8.67063478054115,46.6372813177181,0.));
#85268=CARTESIAN_POINT('Ctrl Pts',(8.67063478054115,46.6372813177181,20.));
#85269=CARTESIAN_POINT('Ctrl Pts',(8.70265620297453,46.6282666290119,0.));
#85270=CARTESIAN_POINT('Ctrl Pts',(8.70265620297453,46.6282666290119,20.));
#85271=CARTESIAN_POINT('Ctrl Pts',(8.73467024664569,46.6192298802645,0.));
#85272=CARTESIAN_POINT('Ctrl Pts',(8.73467024664569,46.6192298802645,20.));
#85273=CARTESIAN_POINT('Ctrl Pts',(8.76667689617329,46.6101710767218,0.));
#85274=CARTESIAN_POINT('Ctrl Pts',(8.76667689617329,46.6101710767218,20.));
#85275=CARTESIAN_POINT('Ctrl Pts',(8.79867613617932,46.6010902236408,0.));
#85276=CARTESIAN_POINT('Ctrl Pts',(8.79867613617932,46.6010902236408,20.));
#85277=CARTESIAN_POINT('Ctrl Pts',(8.83066795128933,46.59198732629,0.));
#85278=CARTESIAN_POINT('Ctrl Pts',(8.83066795128933,46.59198732629,20.));
#85279=CARTESIAN_POINT('Ctrl Pts',(8.86265232613214,46.582862389949,0.));
#85280=CARTESIAN_POINT('Ctrl Pts',(8.86265232613214,46.582862389949,20.));
#85281=CARTESIAN_POINT('Ctrl Pts',(8.89462924533988,46.5737154199087,0.));
#85282=CARTESIAN_POINT('Ctrl Pts',(8.89462924533988,46.5737154199087,20.));
#85283=CARTESIAN_POINT('Ctrl Pts',(8.92659869354787,46.5645464214705,0.));
#85284=CARTESIAN_POINT('Ctrl Pts',(8.92659869354787,46.5645464214705,20.));
#85285=CARTESIAN_POINT('Ctrl Pts',(8.9585606553947,46.5553553999467,0.));
#85286=CARTESIAN_POINT('Ctrl Pts',(8.9585606553947,46.5553553999467,20.));
#85287=CARTESIAN_POINT('Ctrl Pts',(8.99051511552228,46.5461423606602,0.));
#85288=CARTESIAN_POINT('Ctrl Pts',(8.99051511552228,46.5461423606602,20.));
#85289=CARTESIAN_POINT('Ctrl Pts',(9.02246205857627,46.5369073089453,0.));
#85290=CARTESIAN_POINT('Ctrl Pts',(9.02246205857627,46.5369073089453,20.));
#85291=CARTESIAN_POINT('Ctrl Pts',(9.05440146920514,46.5276502501459,0.));
#85292=CARTESIAN_POINT('Ctrl Pts',(9.05440146920514,46.5276502501459,20.));
#85293=CARTESIAN_POINT('Ctrl Pts',(9.08633333206089,46.5183711896174,0.));
#85294=CARTESIAN_POINT('Ctrl Pts',(9.08633333206089,46.5183711896174,20.));
#85295=CARTESIAN_POINT('Ctrl Pts',(9.11825763179851,46.5090701327255,0.));
#85296=CARTESIAN_POINT('Ctrl Pts',(9.11825763179851,46.5090701327255,20.));
#85297=CARTESIAN_POINT('Ctrl Pts',(9.15017435307665,46.4997470848477,0.));
#85298=CARTESIAN_POINT('Ctrl Pts',(9.15017435307665,46.4997470848477,20.));
#85299=CARTESIAN_POINT('Ctrl Pts',(9.18208348055724,46.4904020513722,0.));
#85300=CARTESIAN_POINT('Ctrl Pts',(9.18208348055724,46.4904020513722,20.));
#85301=CARTESIAN_POINT('Ctrl Pts',(9.21398499890591,46.4810350376983,0.));
#85302=CARTESIAN_POINT('Ctrl Pts',(9.21398499890591,46.4810350376983,20.));
#85303=CARTESIAN_POINT('Ctrl Pts',(9.2458788927917,46.4716460492361,0.));
#85304=CARTESIAN_POINT('Ctrl Pts',(9.2458788927917,46.4716460492361,20.));
#85305=CARTESIAN_POINT('Ctrl Pts',(9.27776514688698,46.4622350914066,0.));
#85306=CARTESIAN_POINT('Ctrl Pts',(9.27776514688698,46.4622350914066,20.));
#85307=CARTESIAN_POINT('Ctrl Pts',(9.30964374586751,46.4528021696416,0.));
#85308=CARTESIAN_POINT('Ctrl Pts',(9.30964374586751,46.4528021696416,20.));
#85309=CARTESIAN_POINT('Ctrl Pts',(9.3415146744124,46.4433472893837,0.));
#85310=CARTESIAN_POINT('Ctrl Pts',(9.3415146744124,46.4433472893837,20.));
#85311=CARTESIAN_POINT('Ctrl Pts',(9.37337791720392,46.4338704560856,0.));
#85312=CARTESIAN_POINT('Ctrl Pts',(9.37337791720392,46.4338704560856,20.));
#85313=CARTESIAN_POINT('Ctrl Pts',(9.40523345892773,46.4243716752115,0.));
#85314=CARTESIAN_POINT('Ctrl Pts',(9.40523345892773,46.4243716752115,20.));
#85315=CARTESIAN_POINT('Ctrl Pts',(9.43708128427273,46.4148509522358,0.));
#85316=CARTESIAN_POINT('Ctrl Pts',(9.43708128427273,46.4148509522358,20.));
#85317=CARTESIAN_POINT('Ctrl Pts',(9.46892137793147,46.405308292644,0.));
#85318=CARTESIAN_POINT('Ctrl Pts',(9.46892137793147,46.405308292644,20.));
#85319=CARTESIAN_POINT('Ctrl Pts',(9.50075372460008,46.3957437019326,0.));
#85320=CARTESIAN_POINT('Ctrl Pts',(9.50075372460008,46.3957437019326,20.));
#85321=CARTESIAN_POINT('Ctrl Pts',(9.5325783089785,46.3861571856095,0.));
#85322=CARTESIAN_POINT('Ctrl Pts',(9.5325783089785,46.3861571856095,20.));
#85323=CARTESIAN_POINT('Ctrl Pts',(9.56439511577022,46.3765487491938,0.));
#85324=CARTESIAN_POINT('Ctrl Pts',(9.56439511577022,46.3765487491938,20.));
#85325=CARTESIAN_POINT('Ctrl Pts',(9.59620412968212,46.3669183982155,0.));
#85326=CARTESIAN_POINT('Ctrl Pts',(9.59620412968212,46.3669183982155,20.));
#85327=CARTESIAN_POINT('Ctrl Pts',(9.62800533542435,46.3572661382147,0.));
#85328=CARTESIAN_POINT('Ctrl Pts',(9.62800533542435,46.3572661382147,20.));
#85329=CARTESIAN_POINT('Ctrl Pts',(9.65979871771038,46.347591974742,0.));
#85330=CARTESIAN_POINT('Ctrl Pts',(9.65979871771038,46.347591974742,20.));
#85331=CARTESIAN_POINT('Ctrl Pts',(9.69158426125691,46.3378959133587,0.));
#85332=CARTESIAN_POINT('Ctrl Pts',(9.69158426125691,46.3378959133587,20.));
#85333=CARTESIAN_POINT('Ctrl Pts',(9.72336195078413,46.3281779596367,0.));
#85334=CARTESIAN_POINT('Ctrl Pts',(9.72336195078413,46.3281779596367,20.));
#85335=CARTESIAN_POINT('Ctrl Pts',(9.75513177101576,46.3184381191592,0.));
#85336=CARTESIAN_POINT('Ctrl Pts',(9.75513177101576,46.3184381191592,20.));
#85337=CARTESIAN_POINT('Ctrl Pts',(9.78689370667939,46.3086763975205,0.));
#85338=CARTESIAN_POINT('Ctrl Pts',(9.78689370667939,46.3086763975205,20.));
#85339=CARTESIAN_POINT('Ctrl Pts',(9.81864774250618,46.2988928003257,0.));
#85340=CARTESIAN_POINT('Ctrl Pts',(9.81864774250618,46.2988928003257,20.));
#85341=CARTESIAN_POINT('Ctrl Pts',(9.85039386323084,46.289087333191,0.));
#85342=CARTESIAN_POINT('Ctrl Pts',(9.85039386323084,46.289087333191,20.));
#85343=CARTESIAN_POINT('Ctrl Pts',(9.8821320535919,46.2792600017436,0.));
#85344=CARTESIAN_POINT('Ctrl Pts',(9.8821320535919,46.2792600017436,20.));
#85345=CARTESIAN_POINT('Ctrl Pts',(9.91386229833136,46.2694108116213,0.));
#85346=CARTESIAN_POINT('Ctrl Pts',(9.91386229833136,46.2694108116213,20.));
#85347=CARTESIAN_POINT('Ctrl Pts',(9.94558458219445,46.2595397684724,0.));
#85348=CARTESIAN_POINT('Ctrl Pts',(9.94558458219445,46.2595397684724,20.));
#85349=CARTESIAN_POINT('Ctrl Pts',(9.97729888992979,46.2496468779557,0.));
#85350=CARTESIAN_POINT('Ctrl Pts',(9.97729888992979,46.2496468779557,20.));
#85351=CARTESIAN_POINT('Ctrl Pts',(10.0090052062894,46.2397321457408,0.));
#85352=CARTESIAN_POINT('Ctrl Pts',(10.0090052062894,46.2397321457408,20.));
#85353=CARTESIAN_POINT('Ctrl Pts',(10.0407035160292,46.2297955775084,0.));
#85354=CARTESIAN_POINT('Ctrl Pts',(10.0407035160292,46.2297955775084,20.));
#85355=CARTESIAN_POINT('Ctrl Pts',(10.0723938039086,46.2198371789501,0.));
#85356=CARTESIAN_POINT('Ctrl Pts',(10.0723938039086,46.2198371789501,20.));
#85357=CARTESIAN_POINT('Ctrl Pts',(10.1040760546909,46.2098569557688,0.));
#85358=CARTESIAN_POINT('Ctrl Pts',(10.1040760546909,46.2098569557688,20.));
#85359=CARTESIAN_POINT('Ctrl Pts',(10.1357502531431,46.1998549136779,0.));
#85360=CARTESIAN_POINT('Ctrl Pts',(10.1357502531431,46.1998549136779,20.));
#85361=CARTESIAN_POINT('Ctrl Pts',(10.1674163840354,46.1898310584014,0.));
#85362=CARTESIAN_POINT('Ctrl Pts',(10.1674163840354,46.1898310584014,20.));
#85363=CARTESIAN_POINT('Ctrl Pts',(10.199074432142,46.179785395674,0.));
#85364=CARTESIAN_POINT('Ctrl Pts',(10.199074432142,46.179785395674,20.));
#85365=CARTESIAN_POINT('Ctrl Pts',(10.2307243822402,46.169717931241,0.));
#85366=CARTESIAN_POINT('Ctrl Pts',(10.2307243822402,46.169717931241,20.));
#85367=CARTESIAN_POINT('Ctrl Pts',(10.2623662191113,46.1596286708586,0.));
#85368=CARTESIAN_POINT('Ctrl Pts',(10.2623662191113,46.1596286708586,20.));
#85369=CARTESIAN_POINT('Ctrl Pts',(10.2939999275403,46.1495176202946,0.));
#85370=CARTESIAN_POINT('Ctrl Pts',(10.2939999275403,46.1495176202946,20.));
#85371=CARTESIAN_POINT('Ctrl Pts',(10.3256254923155,46.139384785327,0.));
#85372=CARTESIAN_POINT('Ctrl Pts',(10.3256254923155,46.139384785327,20.));
#85373=CARTESIAN_POINT('Ctrl Pts',(10.3572428982293,46.1292301717445,0.));
#85374=CARTESIAN_POINT('Ctrl Pts',(10.3572428982293,46.1292301717445,20.));
#85375=CARTESIAN_POINT('Ctrl Pts',(10.3888521300773,46.119053785347,0.));
#85376=CARTESIAN_POINT('Ctrl Pts',(10.3888521300773,46.119053785347,20.));
#85377=CARTESIAN_POINT('Ctrl Pts',(10.4204531726593,46.1088556319449,0.));
#85378=CARTESIAN_POINT('Ctrl Pts',(10.4204531726593,46.1088556319449,20.));
#85379=CARTESIAN_POINT('Ctrl Pts',(10.4520460107784,46.0986357173598,0.));
#85380=CARTESIAN_POINT('Ctrl Pts',(10.4520460107784,46.0986357173598,20.));
#85381=CARTESIAN_POINT('Ctrl Pts',(10.4836306292415,46.0883940474237,0.));
#85382=CARTESIAN_POINT('Ctrl Pts',(10.4836306292415,46.0883940474237,20.));
#85383=CARTESIAN_POINT('Ctrl Pts',(10.5152070128592,46.0781306279792,0.));
#85384=CARTESIAN_POINT('Ctrl Pts',(10.5152070128592,46.0781306279792,20.));
#85385=CARTESIAN_POINT('Ctrl Pts',(10.5467751464457,46.0678454648793,0.));
#85386=CARTESIAN_POINT('Ctrl Pts',(10.5467751464457,46.0678454648793,20.));
#85387=CARTESIAN_POINT('Ctrl Pts',(10.5783350148187,46.0575385639878,0.));
#85388=CARTESIAN_POINT('Ctrl Pts',(10.5783350148187,46.0575385639878,20.));
#85389=CARTESIAN_POINT('Ctrl Pts',(10.6098866028001,46.0472099311799,0.));
#85390=CARTESIAN_POINT('Ctrl Pts',(10.6098866028001,46.0472099311799,20.));
#85391=CARTESIAN_POINT('Ctrl Pts',(10.6414298952151,46.0368595723418,0.));
#85392=CARTESIAN_POINT('Ctrl Pts',(10.6414298952151,46.0368595723418,20.));
#85393=CARTESIAN_POINT('Ctrl Pts',(10.6729648768932,46.0264874933706,0.));
#85394=CARTESIAN_POINT('Ctrl Pts',(10.6729648768932,46.0264874933706,20.));
#85395=CARTESIAN_POINT('Ctrl Pts',(10.7044915326674,46.0160937001747,0.));
#85396=CARTESIAN_POINT('Ctrl Pts',(10.7044915326674,46.0160937001747,20.));
#85397=CARTESIAN_POINT('Ctrl Pts',(10.7360098473747,46.0056781986726,0.));
#85398=CARTESIAN_POINT('Ctrl Pts',(10.7360098473747,46.0056781986726,20.));
#85399=CARTESIAN_POINT('Ctrl Pts',(10.7675198058554,45.9952409947932,0.));
#85400=CARTESIAN_POINT('Ctrl Pts',(10.7675198058554,45.9952409947932,20.));
#85401=CARTESIAN_POINT('Ctrl Pts',(10.7990213929536,45.9847820944759,0.));
#85402=CARTESIAN_POINT('Ctrl Pts',(10.7990213929536,45.9847820944759,20.));
#85403=CARTESIAN_POINT('Ctrl Pts',(10.8305145935168,45.9743015036702,0.));
#85404=CARTESIAN_POINT('Ctrl Pts',(10.8305145935168,45.9743015036702,20.));
#85405=CARTESIAN_POINT('Ctrl Pts',(10.8619993923966,45.9637992283368,0.));
#85406=CARTESIAN_POINT('Ctrl Pts',(10.8619993923966,45.9637992283368,20.));
#85407=CARTESIAN_POINT('Ctrl Pts',(10.8934757744485,45.9532752744476,0.));
#85408=CARTESIAN_POINT('Ctrl Pts',(10.8934757744485,45.9532752744476,20.));
#85409=CARTESIAN_POINT('Ctrl Pts',(10.9249437245321,45.9427296479861,0.));
#85410=CARTESIAN_POINT('Ctrl Pts',(10.9249437245321,45.9427296479861,20.));
#85411=CARTESIAN_POINT('Ctrl Pts',(10.9564032275107,45.9321623549466,0.));
#85412=CARTESIAN_POINT('Ctrl Pts',(10.9564032275107,45.9321623549466,20.));
#85413=CARTESIAN_POINT('Ctrl Pts',(10.9878542682513,45.9215734013338,0.));
#85414=CARTESIAN_POINT('Ctrl Pts',(10.9878542682513,45.9215734013338,20.));
#85415=CARTESIAN_POINT('Ctrl Pts',(11.0192968316246,45.9109627931629,0.));
#85416=CARTESIAN_POINT('Ctrl Pts',(11.0192968316246,45.9109627931629,20.));
#85417=CARTESIAN_POINT('Ctrl Pts',(11.0507309025052,45.9003305364593,0.));
#85418=CARTESIAN_POINT('Ctrl Pts',(11.0507309025052,45.9003305364593,20.));
#85419=CARTESIAN_POINT('Ctrl Pts',(11.0821564657716,45.8896766372596,0.));
#85420=CARTESIAN_POINT('Ctrl Pts',(11.0821564657716,45.8896766372596,20.));
#85421=CARTESIAN_POINT('Ctrl Pts',(11.1135735063059,45.8790011016108,0.));
#85422=CARTESIAN_POINT('Ctrl Pts',(11.1135735063059,45.8790011016108,20.));
#85423=CARTESIAN_POINT('Ctrl Pts',(11.1449820089942,45.868303935571,0.));
#85424=CARTESIAN_POINT('Ctrl Pts',(11.1449820089942,45.868303935571,20.));
#85425=CARTESIAN_POINT('Ctrl Pts',(11.1763819587262,45.8575851452088,0.));
#85426=CARTESIAN_POINT('Ctrl Pts',(11.1763819587262,45.8575851452088,20.));
#85427=CARTESIAN_POINT('Ctrl Pts',(11.2077733403959,45.8468447366038,0.));
#85428=CARTESIAN_POINT('Ctrl Pts',(11.2077733403959,45.8468447366038,20.));
#85429=CARTESIAN_POINT('Ctrl Pts',(11.2391561389011,45.8360827158468,0.));
#85430=CARTESIAN_POINT('Ctrl Pts',(11.2391561389011,45.8360827158468,20.));
#85431=CARTESIAN_POINT('Ctrl Pts',(11.2705303391434,45.8252990890386,0.));
#85432=CARTESIAN_POINT('Ctrl Pts',(11.2705303391434,45.8252990890386,20.));
#85433=CARTESIAN_POINT('Ctrl Pts',(11.3018959260282,45.8144938622913,0.));
#85434=CARTESIAN_POINT('Ctrl Pts',(11.3018959260282,45.8144938622913,20.));
#85435=CARTESIAN_POINT('Ctrl Pts',(11.3332528844652,45.8036670417272,0.));
#85436=CARTESIAN_POINT('Ctrl Pts',(11.3332528844652,45.8036670417272,20.));
#85437=CARTESIAN_POINT('Ctrl Pts',(11.3646011993673,45.7928186334791,0.));
#85438=CARTESIAN_POINT('Ctrl Pts',(11.3646011993673,45.7928186334791,20.));
#85439=CARTESIAN_POINT('Ctrl Pts',(11.395940855652,45.7819486436912,0.));
#85440=CARTESIAN_POINT('Ctrl Pts',(11.395940855652,45.7819486436912,20.));
#85441=CARTESIAN_POINT('Ctrl Pts',(11.4272718382403,45.7710570785186,0.));
#85442=CARTESIAN_POINT('Ctrl Pts',(11.4272718382403,45.7710570785186,20.));
#85443=CARTESIAN_POINT('Ctrl Pts',(11.4585941320574,45.760143944127,0.));
#85444=CARTESIAN_POINT('Ctrl Pts',(11.4585941320574,45.760143944127,20.));
#85445=CARTESIAN_POINT('Ctrl Pts',(11.489907722032,45.7492092466918,0.));
#85446=CARTESIAN_POINT('Ctrl Pts',(11.489907722032,45.7492092466918,20.));
#85447=CARTESIAN_POINT('Ctrl Pts',(11.5212125930966,45.7382529923996,0.));
#85448=CARTESIAN_POINT('Ctrl Pts',(11.5212125930966,45.7382529923996,20.));
#85449=CARTESIAN_POINT('Ctrl Pts',(11.5525087301884,45.7272751874478,0.));
#85450=CARTESIAN_POINT('Ctrl Pts',(11.5525087301884,45.7272751874478,20.));
#85451=CARTESIAN_POINT('Ctrl Pts',(11.5837961182481,45.7162758380449,0.));
#85452=CARTESIAN_POINT('Ctrl Pts',(11.5837961182481,45.7162758380449,20.));
#85453=CARTESIAN_POINT('Ctrl Pts',(11.6150747422209,45.7052549504103,0.));
#85454=CARTESIAN_POINT('Ctrl Pts',(11.6150747422209,45.7052549504103,20.));
#85455=CARTESIAN_POINT('Ctrl Pts',(11.6463445870557,45.694212530774,0.));
#85456=CARTESIAN_POINT('Ctrl Pts',(11.6463445870557,45.694212530774,20.));
#85457=CARTESIAN_POINT('Ctrl Pts',(11.6776056377055,45.6831485853771,0.));
#85458=CARTESIAN_POINT('Ctrl Pts',(11.6776056377055,45.6831485853771,20.));
#85459=CARTESIAN_POINT('Ctrl Pts',(11.7088578791266,45.6720631204703,0.));
#85460=CARTESIAN_POINT('Ctrl Pts',(11.7088578791266,45.6720631204703,20.));
#85461=CARTESIAN_POINT('Ctrl Pts',(11.7401012962797,45.6609561423149,0.));
#85462=CARTESIAN_POINT('Ctrl Pts',(11.7401012962797,45.6609561423149,20.));
#85463=CARTESIAN_POINT('Ctrl Pts',(11.7713358741292,45.6498276571829,0.));
#85464=CARTESIAN_POINT('Ctrl Pts',(11.7713358741292,45.6498276571829,20.));
#85465=CARTESIAN_POINT('Ctrl Pts',(11.8025615976441,45.6386776713575,0.));
#85466=CARTESIAN_POINT('Ctrl Pts',(11.8025615976441,45.6386776713575,20.));
#85467=CARTESIAN_POINT('Ctrl Pts',(11.8337784517972,45.627506191133,0.));
#85468=CARTESIAN_POINT('Ctrl Pts',(11.8337784517972,45.627506191133,20.));
#85469=CARTESIAN_POINT('Ctrl Pts',(11.8649864215653,45.6163132228138,0.));
#85470=CARTESIAN_POINT('Ctrl Pts',(11.8649864215653,45.6163132228138,20.));
#85471=CARTESIAN_POINT('Ctrl Pts',(11.8961854919293,45.6050987727153,0.));
#85472=CARTESIAN_POINT('Ctrl Pts',(11.8961854919293,45.6050987727153,20.));
#85473=CARTESIAN_POINT('Ctrl Pts',(11.9273756478741,45.5938628471638,0.));
#85474=CARTESIAN_POINT('Ctrl Pts',(11.9273756478741,45.5938628471638,20.));
#85475=CARTESIAN_POINT('Ctrl Pts',(11.9585568743886,45.5826054524963,0.));
#85476=CARTESIAN_POINT('Ctrl Pts',(11.9585568743886,45.5826054524963,20.));
#85477=CARTESIAN_POINT('Ctrl Pts',(11.989729156466,45.5713265950605,0.));
#85478=CARTESIAN_POINT('Ctrl Pts',(11.989729156466,45.5713265950605,20.));
#85479=CARTESIAN_POINT('Ctrl Pts',(12.0208924791034,45.5600262812144,0.));
#85480=CARTESIAN_POINT('Ctrl Pts',(12.0208924791034,45.5600262812144,20.));
#85481=CARTESIAN_POINT('Ctrl Pts',(12.0520468273019,45.5487045173265,0.));
#85482=CARTESIAN_POINT('Ctrl Pts',(12.0520468273019,45.5487045173265,20.));
#85483=CARTESIAN_POINT('Ctrl Pts',(12.0831921860665,45.5373613097755,0.));
#85484=CARTESIAN_POINT('Ctrl Pts',(12.0831921860665,45.5373613097755,20.));
#85485=CARTESIAN_POINT('Ctrl Pts',(12.1143285404065,45.5259966649516,0.));
#85486=CARTESIAN_POINT('Ctrl Pts',(12.1143285404065,45.5259966649516,20.));
#85487=CARTESIAN_POINT('Ctrl Pts',(12.1454558753351,45.5146105892553,0.));
#85488=CARTESIAN_POINT('Ctrl Pts',(12.1454558753351,45.5146105892553,20.));
#85489=CARTESIAN_POINT('Ctrl Pts',(12.1765741758697,45.5032030890978,0.));
#85490=CARTESIAN_POINT('Ctrl Pts',(12.1765741758697,45.5032030890978,20.));
#85491=CARTESIAN_POINT('Ctrl Pts',(12.2076834270323,45.4917741709015,0.));
#85492=CARTESIAN_POINT('Ctrl Pts',(12.2076834270323,45.4917741709015,20.));
#85493=CARTESIAN_POINT('Ctrl Pts',(12.2387836138487,45.4803238410999,0.));
#85494=CARTESIAN_POINT('Ctrl Pts',(12.2387836138487,45.4803238410999,20.));
#85495=CARTESIAN_POINT('Ctrl Pts',(12.269874721349,45.4688521061371,0.));
#85496=CARTESIAN_POINT('Ctrl Pts',(12.269874721349,45.4688521061371,20.));
#85497=CARTESIAN_POINT('Ctrl Pts',(12.3009567345673,45.4573589724673,0.));
#85498=CARTESIAN_POINT('Ctrl Pts',(12.3009567345673,45.4573589724673,20.));
#85499=CARTESIAN_POINT('Ctrl Pts',(12.3320296385417,45.4458444465552,0.));
#85500=CARTESIAN_POINT('Ctrl Pts',(12.3320296385417,45.4458444465552,20.));
#85501=CARTESIAN_POINT('Ctrl Pts',(12.3630934183142,45.4343085348755,0.));
#85502=CARTESIAN_POINT('Ctrl Pts',(12.3630934183142,45.4343085348755,20.));
#85503=CARTESIAN_POINT('Ctrl Pts',(12.3941480589311,45.4227512439136,0.));
#85504=CARTESIAN_POINT('Ctrl Pts',(12.3941480589311,45.4227512439136,20.));
#85505=CARTESIAN_POINT('Ctrl Pts',(12.4251935454428,45.4111725801659,0.));
#85506=CARTESIAN_POINT('Ctrl Pts',(12.4251935454428,45.4111725801659,20.));
#85507=CARTESIAN_POINT('Ctrl Pts',(12.4562298629045,45.3995725501402,0.));
#85508=CARTESIAN_POINT('Ctrl Pts',(12.4562298629045,45.3995725501402,20.));
#85509=CARTESIAN_POINT('Ctrl Pts',(12.4872569963754,45.3879511603549,0.));
#85510=CARTESIAN_POINT('Ctrl Pts',(12.4872569963754,45.3879511603549,20.));
#85511=CARTESIAN_POINT('Ctrl Pts',(12.5182749309189,45.376308417339,0.));
#85512=CARTESIAN_POINT('Ctrl Pts',(12.5182749309189,45.376308417339,20.));
#85513=CARTESIAN_POINT('Ctrl Pts',(12.5492836516023,45.364644327632,0.));
#85514=CARTESIAN_POINT('Ctrl Pts',(12.5492836516023,45.364644327632,20.));
#85515=CARTESIAN_POINT('Ctrl Pts',(12.5802831434966,45.3529588977839,0.));
#85516=CARTESIAN_POINT('Ctrl Pts',(12.5802831434966,45.3529588977839,20.));
#85517=CARTESIAN_POINT('Ctrl Pts',(12.6112733916776,45.3412521343551,0.));
#85518=CARTESIAN_POINT('Ctrl Pts',(12.6112733916776,45.3412521343551,20.));
#85519=CARTESIAN_POINT('Ctrl Pts',(12.6422543812251,45.3295240439169,0.));
#85520=CARTESIAN_POINT('Ctrl Pts',(12.6422543812251,45.3295240439169,20.));
#85521=CARTESIAN_POINT('Ctrl Pts',(12.6732260972239,45.3177746330512,0.));
#85522=CARTESIAN_POINT('Ctrl Pts',(12.6732260972239,45.3177746330512,20.));
#85523=CARTESIAN_POINT('Ctrl Pts',(12.7041885247626,45.3060039083501,0.));
#85524=CARTESIAN_POINT('Ctrl Pts',(12.7041885247626,45.3060039083501,20.));
#85525=CARTESIAN_POINT('Ctrl Pts',(12.7351416489341,45.2942118764167,0.));
#85526=CARTESIAN_POINT('Ctrl Pts',(12.7351416489341,45.2942118764167,20.));
#85527=CARTESIAN_POINT('Ctrl Pts',(12.7660854548354,45.2823985438647,0.));
#85528=CARTESIAN_POINT('Ctrl Pts',(12.7660854548354,45.2823985438647,20.));
#85529=CARTESIAN_POINT('Ctrl Pts',(12.7970199275678,45.2705639173192,0.));
#85530=CARTESIAN_POINT('Ctrl Pts',(12.7970199275678,45.2705639173192,20.));
#85531=CARTESIAN_POINT('Ctrl Pts',(12.8279450522365,45.2587080034157,0.));
#85532=CARTESIAN_POINT('Ctrl Pts',(12.8279450522365,45.2587080034157,20.));
#85533=CARTESIAN_POINT('Ctrl Pts',(12.8588608139512,45.2468308087994,0.));
#85534=CARTESIAN_POINT('Ctrl Pts',(12.8588608139512,45.2468308087994,20.));
#85535=CARTESIAN_POINT('Ctrl Pts',(12.8897671978256,45.2349323401259,0.));
#85536=CARTESIAN_POINT('Ctrl Pts',(12.8897671978256,45.2349323401259,20.));
#85537=CARTESIAN_POINT('Ctrl Pts',(12.9206641889781,45.2230126040617,0.));
#85538=CARTESIAN_POINT('Ctrl Pts',(12.9206641889781,45.2230126040617,20.));
#85539=CARTESIAN_POINT('Ctrl Pts',(12.9515517725313,45.2110716072841,0.));
#85540=CARTESIAN_POINT('Ctrl Pts',(12.9515517725313,45.2110716072841,20.));
#85541=CARTESIAN_POINT('Ctrl Pts',(12.9824299336127,45.199109356482,0.));
#85542=CARTESIAN_POINT('Ctrl Pts',(12.9824299336127,45.199109356482,20.));
#85543=CARTESIAN_POINT('Ctrl Pts',(13.0132986573536,45.1871258583545,0.));
#85544=CARTESIAN_POINT('Ctrl Pts',(13.0132986573536,45.1871258583545,20.));
#85545=CARTESIAN_POINT('Ctrl Pts',(13.0441579288899,45.1751211196118,0.));
#85546=CARTESIAN_POINT('Ctrl Pts',(13.0441579288899,45.1751211196118,20.));
#85547=CARTESIAN_POINT('Ctrl Pts',(13.0750077333613,45.1630951469734,0.));
#85548=CARTESIAN_POINT('Ctrl Pts',(13.0750077333613,45.1630951469734,20.));
#85549=CARTESIAN_POINT('Ctrl Pts',(13.105848055912,45.1510479471692,0.));
#85550=CARTESIAN_POINT('Ctrl Pts',(13.105848055912,45.1510479471692,20.));
#85551=CARTESIAN_POINT('Ctrl Pts',(13.1366788816904,45.1389795269399,0.));
#85552=CARTESIAN_POINT('Ctrl Pts',(13.1366788816904,45.1389795269399,20.));
#85553=CARTESIAN_POINT('Ctrl Pts',(13.1675001958492,45.1268898930368,0.));
#85554=CARTESIAN_POINT('Ctrl Pts',(13.1675001958492,45.1268898930368,20.));
#85555=CARTESIAN_POINT('Ctrl Pts',(13.198311983546,45.114779052223,0.));
#85556=CARTESIAN_POINT('Ctrl Pts',(13.198311983546,45.114779052223,20.));
#85557=CARTESIAN_POINT('Ctrl Pts',(13.2291142299426,45.1026470112717,0.));
#85558=CARTESIAN_POINT('Ctrl Pts',(13.2291142299426,45.1026470112717,20.));
#85559=CARTESIAN_POINT('Ctrl Pts',(13.259906920205,45.0904937769663,0.));
#85560=CARTESIAN_POINT('Ctrl Pts',(13.259906920205,45.0904937769663,20.));
#85561=CARTESIAN_POINT('Ctrl Pts',(13.2906900395037,45.0783193561008,0.));
#85562=CARTESIAN_POINT('Ctrl Pts',(13.2906900395037,45.0783193561008,20.));
#85563=CARTESIAN_POINT('Ctrl Pts',(13.3214635730135,45.0661237554798,0.));
#85564=CARTESIAN_POINT('Ctrl Pts',(13.3214635730135,45.0661237554798,20.));
#85565=CARTESIAN_POINT('Ctrl Pts',(13.3522275059137,45.0539069819185,0.));
#85566=CARTESIAN_POINT('Ctrl Pts',(13.3522275059137,45.0539069819185,20.));
#85567=CARTESIAN_POINT('Ctrl Pts',(13.3829818233878,45.0416690422424,0.));
#85568=CARTESIAN_POINT('Ctrl Pts',(13.3829818233878,45.0416690422424,20.));
#85569=CARTESIAN_POINT('Ctrl Pts',(13.4137265106238,45.029409943288,0.));
#85570=CARTESIAN_POINT('Ctrl Pts',(13.4137265106238,45.029409943288,20.));
#85571=CARTESIAN_POINT('Ctrl Pts',(13.4444615528144,45.0171296919022,0.));
#85572=CARTESIAN_POINT('Ctrl Pts',(13.4444615528144,45.0171296919022,20.));
#85573=CARTESIAN_POINT('Ctrl Pts',(13.4751869351564,45.0048282949433,0.));
#85574=CARTESIAN_POINT('Ctrl Pts',(13.4751869351564,45.0048282949433,20.));
#85575=CARTESIAN_POINT('Ctrl Pts',(13.5059026428512,44.9925057592796,0.));
#85576=CARTESIAN_POINT('Ctrl Pts',(13.5059026428512,44.9925057592796,20.));
#85577=CARTESIAN_POINT('Ctrl Pts',(13.5366086611044,44.9801620917891,0.));
#85578=CARTESIAN_POINT('Ctrl Pts',(13.5366086611044,44.9801620917891,20.));
#85579=CARTESIAN_POINT('Ctrl Pts',(13.5673049751264,44.967797299361,0.));
#85580=CARTESIAN_POINT('Ctrl Pts',(13.5673049751264,44.967797299361,20.));
#85581=CARTESIAN_POINT('Ctrl Pts',(13.5979915701319,44.955411388895,0.));
#85582=CARTESIAN_POINT('Ctrl Pts',(13.5979915701319,44.955411388895,20.));
#85583=CARTESIAN_POINT('Ctrl Pts',(13.6286684313401,44.9430043673018,0.));
#85584=CARTESIAN_POINT('Ctrl Pts',(13.6286684313401,44.9430043673018,20.));
#85585=CARTESIAN_POINT('Ctrl Pts',(13.6593355439745,44.930576241502,0.));
#85586=CARTESIAN_POINT('Ctrl Pts',(13.6593355439745,44.930576241502,20.));
#85587=CARTESIAN_POINT('Ctrl Pts',(13.6899928932632,44.9181270184275,0.));
#85588=CARTESIAN_POINT('Ctrl Pts',(13.6899928932632,44.9181270184275,20.));
#85589=CARTESIAN_POINT('Ctrl Pts',(13.7206404644388,44.9056567050204,0.));
#85590=CARTESIAN_POINT('Ctrl Pts',(13.7206404644388,44.9056567050204,20.));
#85591=CARTESIAN_POINT('Ctrl Pts',(13.7512782427386,44.8931653082334,0.));
#85592=CARTESIAN_POINT('Ctrl Pts',(13.7512782427386,44.8931653082334,20.));
#85593=CARTESIAN_POINT('Ctrl Pts',(13.7819062134042,44.8806528350291,0.));
#85594=CARTESIAN_POINT('Ctrl Pts',(13.7819062134042,44.8806528350291,20.));
#85595=CARTESIAN_POINT('Ctrl Pts',(13.8125243616816,44.8681192923811,0.));
#85596=CARTESIAN_POINT('Ctrl Pts',(13.8125243616816,44.8681192923811,20.));
#85597=CARTESIAN_POINT('Ctrl Pts',(13.8431326728214,44.8555646872732,0.));
#85598=CARTESIAN_POINT('Ctrl Pts',(13.8431326728214,44.8555646872732,20.));
#85599=CARTESIAN_POINT('Ctrl Pts',(13.8737311320789,44.8429890267007,0.));
#85600=CARTESIAN_POINT('Ctrl Pts',(13.8737311320789,44.8429890267007,20.));
#85601=CARTESIAN_POINT('Ctrl Pts',(13.9043197247138,44.8303923176691,0.));
#85602=CARTESIAN_POINT('Ctrl Pts',(13.9043197247138,44.8303923176691,20.));
#85603=CARTESIAN_POINT('Ctrl Pts',(13.9348984359903,44.8177745671945,0.));
#85604=CARTESIAN_POINT('Ctrl Pts',(13.9348984359903,44.8177745671945,20.));
#85605=CARTESIAN_POINT('Ctrl Pts',(13.9654672511774,44.8051357823031,0.));
#85606=CARTESIAN_POINT('Ctrl Pts',(13.9654672511774,44.8051357823031,20.));
#85607=CARTESIAN_POINT('Ctrl Pts',(13.9960261555481,44.7924759700314,0.));
#85608=CARTESIAN_POINT('Ctrl Pts',(13.9960261555481,44.7924759700314,20.));
#85609=CARTESIAN_POINT('Ctrl Pts',(14.0265751343805,44.7797951374262,0.));
#85610=CARTESIAN_POINT('Ctrl Pts',(14.0265751343805,44.7797951374262,20.));
#85611=CARTESIAN_POINT('Ctrl Pts',(14.057114172957,44.7670932915455,0.));
#85612=CARTESIAN_POINT('Ctrl Pts',(14.057114172957,44.7670932915455,20.));
#85613=CARTESIAN_POINT('Ctrl Pts',(14.0876432565649,44.7543704394583,0.));
#85614=CARTESIAN_POINT('Ctrl Pts',(14.0876432565649,44.7543704394583,20.));
#85615=CARTESIAN_POINT('Ctrl Pts',(14.118162370496,44.7416265882443,0.));
#85616=CARTESIAN_POINT('Ctrl Pts',(14.118162370496,44.7416265882443,20.));
#85617=CARTESIAN_POINT('Ctrl Pts',(14.1486715000464,44.728861744993,0.));
#85618=CARTESIAN_POINT('Ctrl Pts',(14.1486715000464,44.728861744993,20.));
#85619=CARTESIAN_POINT('Ctrl Pts',(14.1791706305171,44.7160759168044,0.));
#85620=CARTESIAN_POINT('Ctrl Pts',(14.1791706305171,44.7160759168044,20.));
#85621=CARTESIAN_POINT('Ctrl Pts',(14.2096597472134,44.7032691107881,0.));
#85622=CARTESIAN_POINT('Ctrl Pts',(14.2096597472134,44.7032691107881,20.));
#85623=CARTESIAN_POINT('Ctrl Pts',(14.2401388354454,44.690441334065,0.));
#85624=CARTESIAN_POINT('Ctrl Pts',(14.2401388354454,44.690441334065,20.));
#85625=CARTESIAN_POINT('Ctrl Pts',(14.2706078805279,44.6775925937661,0.));
#85626=CARTESIAN_POINT('Ctrl Pts',(14.2706078805279,44.6775925937661,20.));
#85627=CARTESIAN_POINT('Ctrl Pts',(14.3010668677802,44.6647228970333,0.));
#85628=CARTESIAN_POINT('Ctrl Pts',(14.3010668677802,44.6647228970333,20.));
#85629=CARTESIAN_POINT('Ctrl Pts',(14.3315157825264,44.6518322510194,0.));
#85630=CARTESIAN_POINT('Ctrl Pts',(14.3315157825264,44.6518322510194,20.));
#85631=CARTESIAN_POINT('Ctrl Pts',(14.3619546100951,44.6389206628876,0.));
#85632=CARTESIAN_POINT('Ctrl Pts',(14.3619546100951,44.6389206628876,20.));
#85633=CARTESIAN_POINT('Ctrl Pts',(14.3923833358197,44.6259881398119,0.));
#85634=CARTESIAN_POINT('Ctrl Pts',(14.3923833358197,44.6259881398119,20.));
#85635=CARTESIAN_POINT('Ctrl Pts',(14.4228019450383,44.613034688977,0.));
#85636=CARTESIAN_POINT('Ctrl Pts',(14.4228019450383,44.613034688977,20.));
#85637=CARTESIAN_POINT('Ctrl Pts',(14.4532104230936,44.6000603175775,0.));
#85638=CARTESIAN_POINT('Ctrl Pts',(14.4532104230936,44.6000603175775,20.));
#85639=CARTESIAN_POINT('Ctrl Pts',(14.4836087553332,44.5870650328188,0.));
#85640=CARTESIAN_POINT('Ctrl Pts',(14.4836087553332,44.5870650328188,20.));
#85641=CARTESIAN_POINT('Ctrl Pts',(14.5139969271087,44.5740488419152,0.));
#85642=CARTESIAN_POINT('Ctrl Pts',(14.5139969271087,44.5740488419152,20.));
#85643=CARTESIAN_POINT('Ctrl Pts',(14.5443749237767,44.5610117520915,0.));
#85644=CARTESIAN_POINT('Ctrl Pts',(14.5443749237767,44.5610117520915,20.));
#85645=CARTESIAN_POINT('Ctrl Pts',(14.5747427306988,44.5479537705835,0.));
#85646=CARTESIAN_POINT('Ctrl Pts',(14.5747427306988,44.5479537705835,20.));
#85647=CARTESIAN_POINT('Ctrl Pts',(14.6051003332411,44.5348749046379,0.));
#85648=CARTESIAN_POINT('Ctrl Pts',(14.6051003332411,44.5348749046379,20.));
#85649=CARTESIAN_POINT('Ctrl Pts',(14.6354477167742,44.521775161512,0.));
#85650=CARTESIAN_POINT('Ctrl Pts',(14.6354477167742,44.521775161512,20.));
#85651=CARTESIAN_POINT('Ctrl Pts',(14.6657848666743,44.5086545484757,0.));
#85652=CARTESIAN_POINT('Ctrl Pts',(14.6657848666743,44.5086545484757,20.));
#85653=CARTESIAN_POINT('Ctrl Pts',(14.6961117683217,44.4955130728078,0.));
#85654=CARTESIAN_POINT('Ctrl Pts',(14.6961117683217,44.4955130728078,20.));
#85655=CARTESIAN_POINT('Ctrl Pts',(14.7264284071013,44.4823507417973,0.));
#85656=CARTESIAN_POINT('Ctrl Pts',(14.7264284071013,44.4823507417973,20.));
#85657=CARTESIAN_POINT('Ctrl Pts',(14.7567347684029,44.469167562743,0.));
#85658=CARTESIAN_POINT('Ctrl Pts',(14.7567347684029,44.469167562743,20.));
#85659=CARTESIAN_POINT('Ctrl Pts',(14.7870308376214,44.4559635429545,0.));
#85660=CARTESIAN_POINT('Ctrl Pts',(14.7870308376214,44.4559635429545,20.));
#85661=CARTESIAN_POINT('Ctrl Pts',(14.817316600156,44.4427386897515,0.));
#85662=CARTESIAN_POINT('Ctrl Pts',(14.817316600156,44.4427386897515,20.));
#85663=CARTESIAN_POINT('Ctrl Pts',(14.8475920414107,44.4294930104636,0.));
#85664=CARTESIAN_POINT('Ctrl Pts',(14.8475920414107,44.4294930104636,20.));
#85665=CARTESIAN_POINT('Ctrl Pts',(14.8778571467943,44.416226512431,0.));
#85666=CARTESIAN_POINT('Ctrl Pts',(14.8778571467943,44.416226512431,20.));
#85667=CARTESIAN_POINT('Ctrl Pts',(14.9081119017199,44.4029392030043,0.));
#85668=CARTESIAN_POINT('Ctrl Pts',(14.9081119017199,44.4029392030043,20.));
#85669=CARTESIAN_POINT('Ctrl Pts',(14.9383562916061,44.389631089546,0.));
#85670=CARTESIAN_POINT('Ctrl Pts',(14.9383562916061,44.389631089546,20.));
#85671=CARTESIAN_POINT('Ctrl Pts',(14.9685903018767,44.3763021794296,0.));
#85672=CARTESIAN_POINT('Ctrl Pts',(14.9685903018767,44.3763021794296,20.));
#85673=CARTESIAN_POINT('Ctrl Pts',(14.9988139179602,44.3629524800397,0.));
#85674=CARTESIAN_POINT('Ctrl Pts',(14.9988139179602,44.3629524800397,20.));
#85675=CARTESIAN_POINT('Ctrl Pts',(15.0290271252899,44.3495819987708,0.));
#85676=CARTESIAN_POINT('Ctrl Pts',(15.0290271252899,44.3495819987708,20.));
#85677=CARTESIAN_POINT('Ctrl Pts',(15.0592299093032,44.3361907430254,0.));
#85678=CARTESIAN_POINT('Ctrl Pts',(15.0592299093032,44.3361907430254,20.));
#85679=CARTESIAN_POINT('Ctrl Pts',(15.0894222554424,44.3227787202166,0.));
#85680=CARTESIAN_POINT('Ctrl Pts',(15.0894222554424,44.3227787202166,20.));
#85681=CARTESIAN_POINT('Ctrl Pts',(15.1196041491546,44.3093459377674,0.));
#85682=CARTESIAN_POINT('Ctrl Pts',(15.1196041491546,44.3093459377674,20.));
#85683=CARTESIAN_POINT('Ctrl Pts',(15.1497755758917,44.2958924031118,0.));
#85684=CARTESIAN_POINT('Ctrl Pts',(15.1497755758917,44.2958924031118,20.));
#85685=CARTESIAN_POINT('Ctrl Pts',(15.1799365211113,44.2824181236961,0.));
#85686=CARTESIAN_POINT('Ctrl Pts',(15.1799365211113,44.2824181236961,20.));
#85687=CARTESIAN_POINT('Ctrl Pts',(15.2100869702755,44.2689231069767,0.));
#85688=CARTESIAN_POINT('Ctrl Pts',(15.2100869702755,44.2689231069767,20.));
#85689=CARTESIAN_POINT('Ctrl Pts',(15.2402269088514,44.2554073604206,0.));
#85690=CARTESIAN_POINT('Ctrl Pts',(15.2402269088514,44.2554073604206,20.));
#85691=CARTESIAN_POINT('Ctrl Pts',(15.2703563223108,44.2418708915045,0.));
#85692=CARTESIAN_POINT('Ctrl Pts',(15.2703563223108,44.2418708915045,20.));
#85693=CARTESIAN_POINT('Ctrl Pts',(15.30047519613,44.2283137077152,0.));
#85694=CARTESIAN_POINT('Ctrl Pts',(15.30047519613,44.2283137077152,20.));
#85695=CARTESIAN_POINT('Ctrl Pts',(15.3305835157903,44.2147358165492,0.));
#85696=CARTESIAN_POINT('Ctrl Pts',(15.3305835157903,44.2147358165492,20.));
#85697=CARTESIAN_POINT('Ctrl Pts',(15.3606812667781,44.201137225514,0.));
#85698=CARTESIAN_POINT('Ctrl Pts',(15.3606812667781,44.201137225514,20.));
#85699=CARTESIAN_POINT('Ctrl Pts',(15.390768434585,44.1875179421286,0.));
#85700=CARTESIAN_POINT('Ctrl Pts',(15.390768434585,44.1875179421286,20.));
#85701=CARTESIAN_POINT('Ctrl Pts',(15.4208450047077,44.1738779739225,0.));
#85702=CARTESIAN_POINT('Ctrl Pts',(15.4208450047077,44.1738779739225,20.));
#85703=CARTESIAN_POINT('Ctrl Pts',(15.4509109626472,44.1602173284345,0.));
#85704=CARTESIAN_POINT('Ctrl Pts',(15.4509109626472,44.1602173284345,20.));
#85705=CARTESIAN_POINT('Ctrl Pts',(15.4809662939093,44.146536013213,0.));
#85706=CARTESIAN_POINT('Ctrl Pts',(15.4809662939093,44.146536013213,20.));
#85707=CARTESIAN_POINT('Ctrl Pts',(15.5110109840047,44.1328340358171,0.));
#85708=CARTESIAN_POINT('Ctrl Pts',(15.5110109840047,44.1328340358171,20.));
#85709=CARTESIAN_POINT('Ctrl Pts',(15.5410450184494,44.1191114038164,0.));
#85710=CARTESIAN_POINT('Ctrl Pts',(15.5410450184494,44.1191114038164,20.));
#85711=CARTESIAN_POINT('Ctrl Pts',(15.5710683827645,44.1053681247921,0.));
#85712=CARTESIAN_POINT('Ctrl Pts',(15.5710683827645,44.1053681247921,20.));
#85713=CARTESIAN_POINT('Ctrl Pts',(15.6010810624766,44.0916042063371,0.));
#85714=CARTESIAN_POINT('Ctrl Pts',(15.6010810624766,44.0916042063371,20.));
#85715=CARTESIAN_POINT('Ctrl Pts',(15.6310830431167,44.0778196560536,0.));
#85716=CARTESIAN_POINT('Ctrl Pts',(15.6310830431167,44.0778196560536,20.));
#85717=CARTESIAN_POINT('Ctrl Pts',(15.6610743102207,44.0640144815534,0.));
#85718=CARTESIAN_POINT('Ctrl Pts',(15.6610743102207,44.0640144815534,20.));
#85719=CARTESIAN_POINT('Ctrl Pts',(15.6910548493288,44.050188690457,0.));
#85720=CARTESIAN_POINT('Ctrl Pts',(15.6910548493288,44.050188690457,20.));
#85721=CARTESIAN_POINT('Ctrl Pts',(15.7210246459867,44.0363422903955,0.));
#85722=CARTESIAN_POINT('Ctrl Pts',(15.7210246459867,44.0363422903955,20.));
#85723=CARTESIAN_POINT('Ctrl Pts',(15.7509836857452,44.0224752890112,0.));
#85724=CARTESIAN_POINT('Ctrl Pts',(15.7509836857452,44.0224752890112,20.));
#85725=CARTESIAN_POINT('Ctrl Pts',(15.7809319541601,44.0085876939576,0.));
#85726=CARTESIAN_POINT('Ctrl Pts',(15.7809319541601,44.0085876939576,20.));
#85727=CARTESIAN_POINT('Ctrl Pts',(15.8108694367927,43.9946795128988,0.));
#85728=CARTESIAN_POINT('Ctrl Pts',(15.8108694367927,43.9946795128988,20.));
#85729=CARTESIAN_POINT('Ctrl Pts',(15.8407961192089,43.9807507535097,0.));
#85730=CARTESIAN_POINT('Ctrl Pts',(15.8407961192089,43.9807507535097,20.));
#85731=CARTESIAN_POINT('Ctrl Pts',(15.8707119869797,43.9668014234746,0.));
#85732=CARTESIAN_POINT('Ctrl Pts',(15.8707119869797,43.9668014234746,20.));
#85733=CARTESIAN_POINT('Ctrl Pts',(15.9006170256808,43.9528315304878,0.));
#85734=CARTESIAN_POINT('Ctrl Pts',(15.9006170256808,43.9528315304878,20.));
#85735=CARTESIAN_POINT('Ctrl Pts',(15.9305112208934,43.9388410822542,0.));
#85736=CARTESIAN_POINT('Ctrl Pts',(15.9305112208934,43.9388410822542,20.));
#85737=CARTESIAN_POINT('Ctrl Pts',(15.9603945582034,43.9248300864889,0.));
#85738=CARTESIAN_POINT('Ctrl Pts',(15.9603945582034,43.9248300864889,20.));
#85739=CARTESIAN_POINT('Ctrl Pts',(15.9902670232019,43.9107985509168,0.));
#85740=CARTESIAN_POINT('Ctrl Pts',(15.9902670232019,43.9107985509168,20.));
#85741=CARTESIAN_POINT('Ctrl Pts',(16.0201286014849,43.896746483274,0.));
#85742=CARTESIAN_POINT('Ctrl Pts',(16.0201286014849,43.896746483274,20.));
#85743=CARTESIAN_POINT('Ctrl Pts',(16.0499792786541,43.8826738913074,0.));
#85744=CARTESIAN_POINT('Ctrl Pts',(16.0499792786541,43.8826738913074,20.));
#85745=CARTESIAN_POINT('Ctrl Pts',(16.0798190403159,43.8685807827745,0.));
#85746=CARTESIAN_POINT('Ctrl Pts',(16.0798190403159,43.8685807827745,20.));
#85747=CARTESIAN_POINT('Ctrl Pts',(16.1096478720818,43.854467165442,0.));
#85748=CARTESIAN_POINT('Ctrl Pts',(16.1096478720818,43.854467165442,20.));
#85749=CARTESIAN_POINT('Ctrl Pts',(16.1394657595683,43.8403330470868,0.));
#85750=CARTESIAN_POINT('Ctrl Pts',(16.1394657595683,43.8403330470868,20.));
#85751=CARTESIAN_POINT('Ctrl Pts',(16.1692726883968,43.8261784354962,0.));
#85752=CARTESIAN_POINT('Ctrl Pts',(16.1692726883968,43.8261784354962,20.));
#85753=CARTESIAN_POINT('Ctrl Pts',(16.199068644194,43.8120033384679,0.));
#85754=CARTESIAN_POINT('Ctrl Pts',(16.199068644194,43.8120033384679,20.));
#85755=CARTESIAN_POINT('Ctrl Pts',(16.2288536125916,43.7978077638098,0.));
#85756=CARTESIAN_POINT('Ctrl Pts',(16.2288536125916,43.7978077638098,20.));
#85757=CARTESIAN_POINT('Ctrl Pts',(16.2586275792268,43.7835917193404,0.));
#85758=CARTESIAN_POINT('Ctrl Pts',(16.2586275792268,43.7835917193404,20.));
#85759=CARTESIAN_POINT('Ctrl Pts',(16.2883905297415,43.7693552128887,0.));
#85760=CARTESIAN_POINT('Ctrl Pts',(16.2883905297415,43.7693552128887,20.));
#85761=CARTESIAN_POINT('Ctrl Pts',(16.3181424497834,43.7550982522947,0.));
#85762=CARTESIAN_POINT('Ctrl Pts',(16.3181424497834,43.7550982522947,20.));
#85763=CARTESIAN_POINT('Ctrl Pts',(16.3478833250055,43.7408208454089,0.));
#85764=CARTESIAN_POINT('Ctrl Pts',(16.3478833250055,43.7408208454089,20.));
#85765=CARTESIAN_POINT('Ctrl Pts',(16.3776131410651,43.7265230000909,0.));
#85766=CARTESIAN_POINT('Ctrl Pts',(16.3776131410651,43.7265230000909,20.));
#85767=CARTESIAN_POINT('Ctrl Pts',(16.4073318836249,43.7122047242097,0.));
#85768=CARTESIAN_POINT('Ctrl Pts',(16.4073318836249,43.7122047242097,20.));
#85769=CARTESIAN_POINT('Ctrl Pts',(16.4370395383523,43.6978660256455,0.));
#85770=CARTESIAN_POINT('Ctrl Pts',(16.4370395383523,43.6978660256455,20.));
#85771=CARTESIAN_POINT('Ctrl Pts',(16.4667360909206,43.6835069122887,0.));
#85772=CARTESIAN_POINT('Ctrl Pts',(16.4667360909206,43.6835069122887,20.));
#85773=CARTESIAN_POINT('Ctrl Pts',(16.4964215270082,43.6691273920409,0.));
#85774=CARTESIAN_POINT('Ctrl Pts',(16.4964215270082,43.6691273920409,20.));
#85775=CARTESIAN_POINT('Ctrl Pts',(16.5260958322991,43.6547274728139,0.));
#85776=CARTESIAN_POINT('Ctrl Pts',(16.5260958322991,43.6547274728139,20.));
#85777=CARTESIAN_POINT('Ctrl Pts',(16.5557589924819,43.640307162529,0.));
#85778=CARTESIAN_POINT('Ctrl Pts',(16.5557589924819,43.640307162529,20.));
#85779=CARTESIAN_POINT('Ctrl Pts',(16.5854109932504,43.6258664691173,0.));
#85780=CARTESIAN_POINT('Ctrl Pts',(16.5854109932504,43.6258664691173,20.));
#85781=CARTESIAN_POINT('Ctrl Pts',(16.6150518203036,43.6114054005208,0.));
#85782=CARTESIAN_POINT('Ctrl Pts',(16.6150518203036,43.6114054005208,20.));
#85783=CARTESIAN_POINT('Ctrl Pts',(16.6446814593458,43.5969239646926,0.));
#85784=CARTESIAN_POINT('Ctrl Pts',(16.6446814593458,43.5969239646926,20.));
#85785=CARTESIAN_POINT('Ctrl Pts',(16.6742998960869,43.5824221695961,0.));
#85786=CARTESIAN_POINT('Ctrl Pts',(16.6742998960869,43.5824221695961,20.));
#85787=CARTESIAN_POINT('Ctrl Pts',(16.7039071162413,43.5679000232041,0.));
#85788=CARTESIAN_POINT('Ctrl Pts',(16.7039071162413,43.5679000232041,20.));
#85789=CARTESIAN_POINT('Ctrl Pts',(16.7335031055294,43.5533575334996,0.));
#85790=CARTESIAN_POINT('Ctrl Pts',(16.7335031055294,43.5533575334996,20.));
#85791=CARTESIAN_POINT('Ctrl Pts',(16.7630878496767,43.5387947084755,0.));
#85792=CARTESIAN_POINT('Ctrl Pts',(16.7630878496767,43.5387947084755,20.));
#85793=CARTESIAN_POINT('Ctrl Pts',(16.792661334414,43.5242115561352,0.));
#85794=CARTESIAN_POINT('Ctrl Pts',(16.792661334414,43.5242115561352,20.));
#85795=CARTESIAN_POINT('Ctrl Pts',(16.8222235454772,43.5096080844922,0.));
#85796=CARTESIAN_POINT('Ctrl Pts',(16.8222235454772,43.5096080844922,20.));
#85797=CARTESIAN_POINT('Ctrl Pts',(16.8517744686076,43.4949843015709,0.));
#85798=CARTESIAN_POINT('Ctrl Pts',(16.8517744686076,43.4949843015709,20.));
#85799=CARTESIAN_POINT('Ctrl Pts',(16.8813140895513,43.4803402154062,0.));
#85800=CARTESIAN_POINT('Ctrl Pts',(16.8813140895513,43.4803402154062,20.));
#85801=CARTESIAN_POINT('Ctrl Pts',(16.91084239406,43.4656758340435,0.));
#85802=CARTESIAN_POINT('Ctrl Pts',(16.91084239406,43.4656758340435,20.));
#85803=CARTESIAN_POINT('Ctrl Pts',(16.9403593678908,43.4509911655382,0.));
#85804=CARTESIAN_POINT('Ctrl Pts',(16.9403593678908,43.4509911655382,20.));
#85805=CARTESIAN_POINT('Ctrl Pts',(16.9698649968061,43.4362862179557,0.));
#85806=CARTESIAN_POINT('Ctrl Pts',(16.9698649968061,43.4362862179557,20.));
#85807=CARTESIAN_POINT('Ctrl Pts',(16.9993592665737,43.4215609993712,0.));
#85808=CARTESIAN_POINT('Ctrl Pts',(16.9993592665737,43.4215609993712,20.));
#85809=CARTESIAN_POINT('Ctrl Pts',(17.0288421629666,43.4068155178696,0.));
#85810=CARTESIAN_POINT('Ctrl Pts',(17.0288421629666,43.4068155178696,20.));
#85811=CARTESIAN_POINT('Ctrl Pts',(17.0583136717632,43.3920497815463,0.));
#85812=CARTESIAN_POINT('Ctrl Pts',(17.0583136717632,43.3920497815463,20.));
#85813=CARTESIAN_POINT('Ctrl Pts',(17.0877737787472,43.3772637985072,0.));
#85814=CARTESIAN_POINT('Ctrl Pts',(17.0877737787472,43.3772637985072,20.));
#85815=CARTESIAN_POINT('Ctrl Pts',(17.1172224697079,43.3624575768695,0.));
#85816=CARTESIAN_POINT('Ctrl Pts',(17.1172224697079,43.3624575768695,20.));
#85817=CARTESIAN_POINT('Ctrl Pts',(17.1466597304397,43.3476311247602,0.));
#85818=CARTESIAN_POINT('Ctrl Pts',(17.1466597304397,43.3476311247602,20.));
#85819=CARTESIAN_POINT('Ctrl Pts',(17.1760855467426,43.332784450317,0.));
#85820=CARTESIAN_POINT('Ctrl Pts',(17.1760855467426,43.332784450317,20.));
#85821=CARTESIAN_POINT('Ctrl Pts',(17.2054999044212,43.3179175616862,0.));
#85822=CARTESIAN_POINT('Ctrl Pts',(17.2054999044212,43.3179175616862,20.));
#85823=CARTESIAN_POINT('Ctrl Pts',(17.2349027892859,43.3030304670242,0.));
#85824=CARTESIAN_POINT('Ctrl Pts',(17.2349027892859,43.3030304670242,20.));
#85825=CARTESIAN_POINT('Ctrl Pts',(17.2642941871522,43.2881231744974,0.));
#85826=CARTESIAN_POINT('Ctrl Pts',(17.2642941871522,43.2881231744974,20.));
#85827=CARTESIAN_POINT('Ctrl Pts',(17.2936740838416,43.2731956922839,0.));
#85828=CARTESIAN_POINT('Ctrl Pts',(17.2936740838416,43.2731956922839,20.));
#85829=CARTESIAN_POINT('Ctrl Pts',(17.3230424651811,43.258248028572,0.));
#85830=CARTESIAN_POINT('Ctrl Pts',(17.3230424651811,43.258248028572,20.));
#85831=CARTESIAN_POINT('Ctrl Pts',(17.352399317003,43.2432801915607,0.));
#85832=CARTESIAN_POINT('Ctrl Pts',(17.352399317003,43.2432801915607,20.));
#85833=CARTESIAN_POINT('Ctrl Pts',(17.3817446251452,43.2282921894589,0.));
#85834=CARTESIAN_POINT('Ctrl Pts',(17.3817446251452,43.2282921894589,20.));
#85835=CARTESIAN_POINT('Ctrl Pts',(17.4110783754507,43.2132840304854,0.));
#85836=CARTESIAN_POINT('Ctrl Pts',(17.4110783754507,43.2132840304854,20.));
#85837=CARTESIAN_POINT('Ctrl Pts',(17.4404005537678,43.1982557228684,0.));
#85838=CARTESIAN_POINT('Ctrl Pts',(17.4404005537678,43.1982557228684,20.));
#85839=CARTESIAN_POINT('Ctrl Pts',(17.46971114595,43.1832072748459,0.));
#85840=CARTESIAN_POINT('Ctrl Pts',(17.46971114595,43.1832072748459,20.));
#85841=CARTESIAN_POINT('Ctrl Pts',(17.4990101378563,43.1681386946662,0.));
#85842=CARTESIAN_POINT('Ctrl Pts',(17.4990101378563,43.1681386946662,20.));
#85843=CARTESIAN_POINT('Ctrl Pts',(17.5282975153509,43.1530499905879,0.));
#85844=CARTESIAN_POINT('Ctrl Pts',(17.5282975153509,43.1530499905879,20.));
#85845=CARTESIAN_POINT('Ctrl Pts',(17.557573264304,43.1379411708804,0.));
#85846=CARTESIAN_POINT('Ctrl Pts',(17.557573264304,43.1379411708804,20.));
#85847=CARTESIAN_POINT('Ctrl Pts',(17.5868373705916,43.122812243824,0.));
#85848=CARTESIAN_POINT('Ctrl Pts',(17.5868373705916,43.122812243824,20.));
#85849=CARTESIAN_POINT('Ctrl Pts',(17.6160898200949,43.1076632177089,0.));
#85850=CARTESIAN_POINT('Ctrl Pts',(17.6160898200949,43.1076632177089,20.));
#85851=CARTESIAN_POINT('Ctrl Pts',(17.645330598701,43.0924941008354,0.));
#85852=CARTESIAN_POINT('Ctrl Pts',(17.645330598701,43.0924941008354,20.));
#85853=CARTESIAN_POINT('Ctrl Pts',(17.674559692302,43.0773049015137,0.));
#85854=CARTESIAN_POINT('Ctrl Pts',(17.674559692302,43.0773049015137,20.));
#85855=CARTESIAN_POINT('Ctrl Pts',(17.7037770867956,43.0620956280638,0.));
#85856=CARTESIAN_POINT('Ctrl Pts',(17.7037770867956,43.0620956280638,20.));
#85857=CARTESIAN_POINT('Ctrl Pts',(17.7329827680846,43.0468662888157,0.));
#85858=CARTESIAN_POINT('Ctrl Pts',(17.7329827680846,43.0468662888157,20.));
#85859=CARTESIAN_POINT('Ctrl Pts',(17.7621767220773,43.0316168921093,0.));
#85860=CARTESIAN_POINT('Ctrl Pts',(17.7621767220773,43.0316168921093,20.));
#85861=CARTESIAN_POINT('Ctrl Pts',(17.7913589346876,43.0163474462951,0.));
#85862=CARTESIAN_POINT('Ctrl Pts',(17.7913589346876,43.0163474462951,20.));
#85863=CARTESIAN_POINT('Ctrl Pts',(17.8205293918351,43.0010579597341,0.));
#85864=CARTESIAN_POINT('Ctrl Pts',(17.8205293918351,43.0010579597341,20.));
#85865=CARTESIAN_POINT('Ctrl Pts',(17.8496880794454,42.985748440798,0.));
#85866=CARTESIAN_POINT('Ctrl Pts',(17.8496880794454,42.985748440798,20.));
#85867=CARTESIAN_POINT('Ctrl Pts',(17.8788349834491,42.9704188978681,0.));
#85868=CARTESIAN_POINT('Ctrl Pts',(17.8788349834491,42.9704188978681,20.));
#85869=CARTESIAN_POINT('Ctrl Pts',(17.9079700897828,42.9550693393359,0.));
#85870=CARTESIAN_POINT('Ctrl Pts',(17.9079700897828,42.9550693393359,20.));
#85871=CARTESIAN_POINT('Ctrl Pts',(17.9370933843882,42.9396997736018,0.));
#85872=CARTESIAN_POINT('Ctrl Pts',(17.9370933843882,42.9396997736018,20.));
#85873=CARTESIAN_POINT('Ctrl Pts',(17.9662048532126,42.9243102090766,0.));
#85874=CARTESIAN_POINT('Ctrl Pts',(17.9662048532126,42.9243102090766,20.));
#85875=CARTESIAN_POINT('Ctrl Pts',(17.9953044822088,42.9089006541818,0.));
#85876=CARTESIAN_POINT('Ctrl Pts',(17.9953044822088,42.9089006541818,20.));
#85877=CARTESIAN_POINT('Ctrl Pts',(18.0243922573354,42.8934711173491,0.));
#85878=CARTESIAN_POINT('Ctrl Pts',(18.0243922573354,42.8934711173491,20.));
#85879=CARTESIAN_POINT('Ctrl Pts',(18.0534681645565,42.8780216070205,0.));
#85880=CARTESIAN_POINT('Ctrl Pts',(18.0534681645565,42.8780216070205,20.));
#85881=CARTESIAN_POINT('Ctrl Pts',(18.0825321898416,42.8625521316489,0.));
#85882=CARTESIAN_POINT('Ctrl Pts',(18.0825321898416,42.8625521316489,20.));
#85883=CARTESIAN_POINT('Ctrl Pts',(18.1115843191668,42.8470626996976,0.));
#85884=CARTESIAN_POINT('Ctrl Pts',(18.1115843191668,42.8470626996976,20.));
#85885=CARTESIAN_POINT('Ctrl Pts',(18.1406245385131,42.831553319639,0.));
#85886=CARTESIAN_POINT('Ctrl Pts',(18.1406245385131,42.831553319639,20.));
#85887=CARTESIAN_POINT('Ctrl Pts',(18.1696528338673,42.8160239999555,0.));
#85888=CARTESIAN_POINT('Ctrl Pts',(18.1696528338673,42.8160239999555,20.));
#85889=CARTESIAN_POINT('Ctrl Pts',(18.1986691912208,42.8004747491375,0.));
#85890=CARTESIAN_POINT('Ctrl Pts',(18.1986691912208,42.8004747491375,20.));
#85891=CARTESIAN_POINT('Ctrl Pts',(18.2276735965714,42.7849055756869,0.));
#85892=CARTESIAN_POINT('Ctrl Pts',(18.2276735965714,42.7849055756869,20.));
#85893=CARTESIAN_POINT('Ctrl Pts',(18.256666035922,42.7693164881155,0.));
#85894=CARTESIAN_POINT('Ctrl Pts',(18.256666035922,42.7693164881155,20.));
#85895=CARTESIAN_POINT('Ctrl Pts',(18.285646495282,42.7537074949463,0.));
#85896=CARTESIAN_POINT('Ctrl Pts',(18.285646495282,42.7537074949463,20.));
#85897=CARTESIAN_POINT('Ctrl Pts',(18.3146149606662,42.7380786047127,0.));
#85898=CARTESIAN_POINT('Ctrl Pts',(18.3146149606662,42.7380786047127,20.));
#85899=CARTESIAN_POINT('Ctrl Pts',(18.3435714180954,42.7224298259587,0.));
#85900=CARTESIAN_POINT('Ctrl Pts',(18.3435714180954,42.7224298259587,20.));
#85901=CARTESIAN_POINT('Ctrl Pts',(18.372515853596,42.7067611672378,0.));
#85902=CARTESIAN_POINT('Ctrl Pts',(18.372515853596,42.7067611672378,20.));
#85903=CARTESIAN_POINT('Ctrl Pts',(18.4014482531999,42.6910726371132,0.));
#85904=CARTESIAN_POINT('Ctrl Pts',(18.4014482531999,42.6910726371132,20.));
#85905=CARTESIAN_POINT('Ctrl Pts',(18.4303686029443,42.6753642441576,0.));
#85906=CARTESIAN_POINT('Ctrl Pts',(18.4303686029443,42.6753642441576,20.));
#85907=CARTESIAN_POINT('Ctrl Pts',(18.4592768888724,42.6596359969538,0.));
#85908=CARTESIAN_POINT('Ctrl Pts',(18.4592768888724,42.6596359969538,20.));
#85909=CARTESIAN_POINT('Ctrl Pts',(18.4881730970326,42.6438879040941,0.));
#85910=CARTESIAN_POINT('Ctrl Pts',(18.4881730970326,42.6438879040941,20.));
#85911=CARTESIAN_POINT('Ctrl Pts',(18.5170572134793,42.6281199741818,0.));
#85912=CARTESIAN_POINT('Ctrl Pts',(18.5170572134793,42.6281199741818,20.));
#85913=CARTESIAN_POINT('Ctrl Pts',(18.5459292242727,42.61233221583,0.));
#85914=CARTESIAN_POINT('Ctrl Pts',(18.5459292242727,42.61233221583,20.));
#85915=CARTESIAN_POINT('Ctrl Pts',(18.574789115479,42.596524637663,0.));
#85916=CARTESIAN_POINT('Ctrl Pts',(18.574789115479,42.596524637663,20.));
#85917=CARTESIAN_POINT('Ctrl Pts',(18.6036368731702,42.5806972483146,0.));
#85918=CARTESIAN_POINT('Ctrl Pts',(18.6036368731702,42.5806972483146,20.));
#85919=CARTESIAN_POINT('Ctrl Pts',(18.6324724834239,42.5648500564287,0.));
#85920=CARTESIAN_POINT('Ctrl Pts',(18.6324724834239,42.5648500564287,20.));
#85921=CARTESIAN_POINT('Ctrl Pts',(18.6612959323233,42.5489830706585,0.));
#85922=CARTESIAN_POINT('Ctrl Pts',(18.6612959323233,42.5489830706585,20.));
#85923=CARTESIAN_POINT('Ctrl Pts',(18.6901072059567,42.5330962996668,0.));
#85924=CARTESIAN_POINT('Ctrl Pts',(18.6901072059567,42.5330962996668,20.));
#85925=CARTESIAN_POINT('Ctrl Pts',(18.718906290419,42.517189752127,0.));
#85926=CARTESIAN_POINT('Ctrl Pts',(18.718906290419,42.517189752127,20.));
#85927=CARTESIAN_POINT('Ctrl Pts',(18.7476931718101,42.5012634367222,0.));
#85928=CARTESIAN_POINT('Ctrl Pts',(18.7476931718101,42.5012634367222,20.));
#85929=CARTESIAN_POINT('Ctrl Pts',(18.7764678362367,42.4853173621469,0.));
#85930=CARTESIAN_POINT('Ctrl Pts',(18.7764678362367,42.4853173621469,20.));
#85931=CARTESIAN_POINT('Ctrl Pts',(18.8052302698113,42.4693515371059,0.));
#85932=CARTESIAN_POINT('Ctrl Pts',(18.8052302698113,42.4693515371059,20.));
#85933=CARTESIAN_POINT('Ctrl Pts',(18.8339804586522,42.4533659703145,0.));
#85934=CARTESIAN_POINT('Ctrl Pts',(18.8339804586522,42.4533659703145,20.));
#85935=CARTESIAN_POINT('Ctrl Pts',(18.8627183888827,42.4373606704956,0.));
#85936=CARTESIAN_POINT('Ctrl Pts',(18.8627183888827,42.4373606704956,20.));
#85937=CARTESIAN_POINT('Ctrl Pts',(18.8914440466322,42.4213356463824,0.));
#85938=CARTESIAN_POINT('Ctrl Pts',(18.8914440466322,42.4213356463824,20.));
#85939=CARTESIAN_POINT('Ctrl Pts',(18.9201574180352,42.4052909067172,0.));
#85940=CARTESIAN_POINT('Ctrl Pts',(18.9201574180352,42.4052909067172,20.));
#85941=CARTESIAN_POINT('Ctrl Pts',(18.9488584892326,42.389226460254,0.));
#85942=CARTESIAN_POINT('Ctrl Pts',(18.9488584892326,42.389226460254,20.));
#85943=CARTESIAN_POINT('Ctrl Pts',(18.9775472463711,42.3731423157568,0.));
#85944=CARTESIAN_POINT('Ctrl Pts',(18.9775472463711,42.3731423157568,20.));
#85945=CARTESIAN_POINT('Ctrl Pts',(19.0062236756035,42.3570384820003,0.));
#85946=CARTESIAN_POINT('Ctrl Pts',(19.0062236756035,42.3570384820003,20.));
#85947=CARTESIAN_POINT('Ctrl Pts',(19.0348877630887,42.3409149677685,0.));
#85948=CARTESIAN_POINT('Ctrl Pts',(19.0348877630887,42.3409149677685,20.));
#85949=CARTESIAN_POINT('Ctrl Pts',(19.0635394949913,42.3247717818558,0.));
#85950=CARTESIAN_POINT('Ctrl Pts',(19.0635394949913,42.3247717818558,20.));
#85951=CARTESIAN_POINT('Ctrl Pts',(19.0921788574819,42.3086089330658,0.));
#85952=CARTESIAN_POINT('Ctrl Pts',(19.0921788574819,42.3086089330658,20.));
#85953=CARTESIAN_POINT('Ctrl Pts',(19.1208058367362,42.2924264302113,0.));
#85954=CARTESIAN_POINT('Ctrl Pts',(19.1208058367362,42.2924264302113,20.));
#85955=CARTESIAN_POINT('Ctrl Pts',(19.1494204189361,42.2762242821163,0.));
#85956=CARTESIAN_POINT('Ctrl Pts',(19.1494204189361,42.2762242821163,20.));
#85957=CARTESIAN_POINT('Ctrl Pts',(19.1780225902694,42.2600024976146,0.));
#85958=CARTESIAN_POINT('Ctrl Pts',(19.1780225902694,42.2600024976146,20.));
#85959=CARTESIAN_POINT('Ctrl Pts',(19.2066123369297,42.2437610855506,0.));
#85960=CARTESIAN_POINT('Ctrl Pts',(19.2066123369297,42.2437610855506,20.));
#85961=CARTESIAN_POINT('Ctrl Pts',(19.2351896451166,42.2275000547783,0.));
#85962=CARTESIAN_POINT('Ctrl Pts',(19.2351896451166,42.2275000547783,20.));
#85963=CARTESIAN_POINT('Ctrl Pts',(19.2637545010356,42.2112194141618,0.));
#85964=CARTESIAN_POINT('Ctrl Pts',(19.2637545010356,42.2112194141618,20.));
#85965=CARTESIAN_POINT('Ctrl Pts',(19.2923068908981,42.1949191725745,0.));
#85966=CARTESIAN_POINT('Ctrl Pts',(19.2923068908981,42.1949191725745,20.));
#85967=CARTESIAN_POINT('Ctrl Pts',(19.3208468009211,42.1785993388989,0.));
#85968=CARTESIAN_POINT('Ctrl Pts',(19.3208468009211,42.1785993388989,20.));
#85969=CARTESIAN_POINT('Ctrl Pts',(19.3493742173282,42.1622599220289,0.));
#85970=CARTESIAN_POINT('Ctrl Pts',(19.3493742173282,42.1622599220289,20.));
#85971=CARTESIAN_POINT('Ctrl Pts',(19.377889126349,42.1459009308685,0.));
#85972=CARTESIAN_POINT('Ctrl Pts',(19.377889126349,42.1459009308685,20.));
#85973=CARTESIAN_POINT('Ctrl Pts',(19.4063915142187,42.1295223743319,0.));
#85974=CARTESIAN_POINT('Ctrl Pts',(19.4063915142187,42.1295223743319,20.));
#85975=CARTESIAN_POINT('Ctrl Pts',(19.4348813671784,42.1131242613432,0.));
#85976=CARTESIAN_POINT('Ctrl Pts',(19.4348813671784,42.1131242613432,20.));
#85977=CARTESIAN_POINT('Ctrl Pts',(19.4633586714748,42.0967066008354,0.));
#85978=CARTESIAN_POINT('Ctrl Pts',(19.4633586714748,42.0967066008354,20.));
#85979=CARTESIAN_POINT('Ctrl Pts',(19.4918234133604,42.080269401751,0.));
#85980=CARTESIAN_POINT('Ctrl Pts',(19.4918234133604,42.080269401751,20.));
#85981=CARTESIAN_POINT('Ctrl Pts',(19.5202755790939,42.0638126730426,0.));
#85982=CARTESIAN_POINT('Ctrl Pts',(19.5202755790939,42.0638126730426,20.));
#85983=CARTESIAN_POINT('Ctrl Pts',(19.5487151549408,42.0473364236742,0.));
#85984=CARTESIAN_POINT('Ctrl Pts',(19.5487151549408,42.0473364236742,20.));
#85985=CARTESIAN_POINT('Ctrl Pts',(19.5771421271718,42.0308406626191,0.));
#85986=CARTESIAN_POINT('Ctrl Pts',(19.5771421271718,42.0308406626191,20.));
#85987=CARTESIAN_POINT('Ctrl Pts',(19.6055564820642,42.0143253988608,0.));
#85988=CARTESIAN_POINT('Ctrl Pts',(19.6055564820642,42.0143253988608,20.));
#85989=CARTESIAN_POINT('Ctrl Pts',(19.6339582059008,41.997790641393,0.));
#85990=CARTESIAN_POINT('Ctrl Pts',(19.6339582059008,41.997790641393,20.));
#85991=CARTESIAN_POINT('Ctrl Pts',(19.6623472849704,41.9812363992182,0.));
#85992=CARTESIAN_POINT('Ctrl Pts',(19.6623472849704,41.9812363992182,20.));
#85993=CARTESIAN_POINT('Ctrl Pts',(19.6907237055674,41.9646626813489,0.));
#85994=CARTESIAN_POINT('Ctrl Pts',(19.6907237055674,41.9646626813489,20.));
#85995=CARTESIAN_POINT('Ctrl Pts',(19.7190874539927,41.9480694968077,0.));
#85996=CARTESIAN_POINT('Ctrl Pts',(19.7190874539927,41.9480694968077,20.));
#85997=CARTESIAN_POINT('Ctrl Pts',(19.7474385165531,41.9314568546275,0.));
#85998=CARTESIAN_POINT('Ctrl Pts',(19.7474385165531,41.9314568546275,20.));
#85999=CARTESIAN_POINT('Ctrl Pts',(19.7757768795619,41.9148247638512,0.));
#86000=CARTESIAN_POINT('Ctrl Pts',(19.7757768795619,41.9148247638512,20.));
#86001=CARTESIAN_POINT('Ctrl Pts',(19.8041025293385,41.8981732335313,0.));
#86002=CARTESIAN_POINT('Ctrl Pts',(19.8041025293385,41.8981732335313,20.));
#86003=CARTESIAN_POINT('Ctrl Pts',(19.8324154522082,41.8815022727306,0.));
#86004=CARTESIAN_POINT('Ctrl Pts',(19.8324154522082,41.8815022727306,20.));
#86005=CARTESIAN_POINT('Ctrl Pts',(19.8607156345021,41.8648118905217,0.));
#86006=CARTESIAN_POINT('Ctrl Pts',(19.8607156345021,41.8648118905217,20.));
#86007=CARTESIAN_POINT('Ctrl Pts',(19.889003062557,41.8481020959867,0.));
#86008=CARTESIAN_POINT('Ctrl Pts',(19.889003062557,41.8481020959867,20.));
#86009=CARTESIAN_POINT('Ctrl Pts',(19.9172777227157,41.8313728982175,0.));
#86010=CARTESIAN_POINT('Ctrl Pts',(19.9172777227157,41.8313728982175,20.));
#86011=CARTESIAN_POINT('Ctrl Pts',(19.9455396013269,41.8146243063152,0.));
#86012=CARTESIAN_POINT('Ctrl Pts',(19.9455396013269,41.8146243063152,20.));
#86013=CARTESIAN_POINT('Ctrl Pts',(19.9737886847461,41.7978563293914,0.));
#86014=CARTESIAN_POINT('Ctrl Pts',(19.9737886847461,41.7978563293914,20.));
#86015=CARTESIAN_POINT('Ctrl Pts',(20.0020249593348,41.7810689765679,0.));
#86016=CARTESIAN_POINT('Ctrl Pts',(20.0020249593348,41.7810689765679,20.));
#86017=CARTESIAN_POINT('Ctrl Pts',(20.0302484114611,41.7642622569769,0.));
#86018=CARTESIAN_POINT('Ctrl Pts',(20.0302484114611,41.7642622569769,20.));
#86019=CARTESIAN_POINT('Ctrl Pts',(20.0584590274991,41.7474361797609,0.));
#86020=CARTESIAN_POINT('Ctrl Pts',(20.0584590274991,41.7474361797609,20.));
#86021=CARTESIAN_POINT('Ctrl Pts',(20.0866567938287,41.7305907540713,0.));
#86022=CARTESIAN_POINT('Ctrl Pts',(20.0866567938287,41.7305907540713,20.));
#86023=CARTESIAN_POINT('Ctrl Pts',(20.1148416968357,41.7137259890696,0.));
#86024=CARTESIAN_POINT('Ctrl Pts',(20.1148416968357,41.7137259890696,20.));
#86025=CARTESIAN_POINT('Ctrl Pts',(20.1430137229118,41.6968418939263,0.));
#86026=CARTESIAN_POINT('Ctrl Pts',(20.1430137229118,41.6968418939263,20.));
#86027=CARTESIAN_POINT('Ctrl Pts',(20.1711728584548,41.6799384778218,0.));
#86028=CARTESIAN_POINT('Ctrl Pts',(20.1711728584548,41.6799384778218,20.));
#86029=CARTESIAN_POINT('Ctrl Pts',(20.199319089869,41.6630157499462,0.));
#86030=CARTESIAN_POINT('Ctrl Pts',(20.199319089869,41.6630157499462,20.));
#86031=CARTESIAN_POINT('Ctrl Pts',(20.2274524035648,41.6460737195007,0.));
#86032=CARTESIAN_POINT('Ctrl Pts',(20.2274524035648,41.6460737195007,20.));
#86033=CARTESIAN_POINT('Ctrl Pts',(20.2555727859589,41.6291123956959,0.));
#86034=CARTESIAN_POINT('Ctrl Pts',(20.2555727859589,41.6291123956959,20.));
#86035=CARTESIAN_POINT('Ctrl Pts',(20.2836802234745,41.6121317877528,0.));
#86036=CARTESIAN_POINT('Ctrl Pts',(20.2836802234745,41.6121317877528,20.));
#86037=CARTESIAN_POINT('Ctrl Pts',(20.3117747025404,41.5951319049016,0.));
#86038=CARTESIAN_POINT('Ctrl Pts',(20.3117747025404,41.5951319049016,20.));
#86039=CARTESIAN_POINT('Ctrl Pts',(20.3398562095916,41.5781127563818,0.));
#86040=CARTESIAN_POINT('Ctrl Pts',(20.3398562095916,41.5781127563818,20.));
#86041=CARTESIAN_POINT('Ctrl Pts',(20.3679247310694,41.561074351443,0.));
#86042=CARTESIAN_POINT('Ctrl Pts',(20.3679247310694,41.561074351443,20.));
#86043=CARTESIAN_POINT('Ctrl Pts',(20.395980253421,41.5440166993445,0.));
#86044=CARTESIAN_POINT('Ctrl Pts',(20.395980253421,41.5440166993445,20.));
#86045=CARTESIAN_POINT('Ctrl Pts',(20.4240227631002,41.5269398093561,0.));
#86046=CARTESIAN_POINT('Ctrl Pts',(20.4240227631002,41.5269398093561,20.));
#86047=CARTESIAN_POINT('Ctrl Pts',(20.4520522465668,41.5098436907568,0.));
#86048=CARTESIAN_POINT('Ctrl Pts',(20.4520522465668,41.5098436907568,20.));
#86049=CARTESIAN_POINT('Ctrl Pts',(20.4800686902869,41.4927283528358,0.));
#86050=CARTESIAN_POINT('Ctrl Pts',(20.4800686902869,41.4927283528358,20.));
#86051=CARTESIAN_POINT('Ctrl Pts',(20.5080720807336,41.4755938048931,0.));
#86052=CARTESIAN_POINT('Ctrl Pts',(20.5080720807336,41.4755938048931,20.));
#86053=CARTESIAN_POINT('Ctrl Pts',(20.5360624043854,41.4584400562379,0.));
#86054=CARTESIAN_POINT('Ctrl Pts',(20.5360624043854,41.4584400562379,20.));
#86055=CARTESIAN_POINT('Ctrl Pts',(20.5640396477269,41.4412671161883,0.));
#86056=CARTESIAN_POINT('Ctrl Pts',(20.5640396477269,41.4412671161883,20.));
#86057=CARTESIAN_POINT('Ctrl Pts',(20.5920037972489,41.4240749940722,0.));
#86058=CARTESIAN_POINT('Ctrl Pts',(20.5920037972489,41.4240749940722,20.));
#86059=CARTESIAN_POINT('Ctrl Pts',(20.6199548394484,41.4068636992265,0.));
#86060=CARTESIAN_POINT('Ctrl Pts',(20.6199548394484,41.4068636992265,20.));
#86061=CARTESIAN_POINT('Ctrl Pts',(20.6478927608288,41.3896332409988,0.));
#86062=CARTESIAN_POINT('Ctrl Pts',(20.6478927608288,41.3896332409988,20.));
#86063=CARTESIAN_POINT('Ctrl Pts',(20.6758175479,41.3723836287471,0.));
#86064=CARTESIAN_POINT('Ctrl Pts',(20.6758175479,41.3723836287471,20.));
#86065=CARTESIAN_POINT('Ctrl Pts',(20.7037291871782,41.3551148718389,0.));
#86066=CARTESIAN_POINT('Ctrl Pts',(20.7037291871782,41.3551148718389,20.));
#86067=CARTESIAN_POINT('Ctrl Pts',(20.731627665186,41.3378269796522,0.));
#86068=CARTESIAN_POINT('Ctrl Pts',(20.731627665186,41.3378269796522,20.));
#86069=CARTESIAN_POINT('Ctrl Pts',(20.7595129684521,41.3205199615745,0.));
#86070=CARTESIAN_POINT('Ctrl Pts',(20.7595129684521,41.3205199615745,20.));
#86071=CARTESIAN_POINT('Ctrl Pts',(20.7873850835117,41.303193827003,0.));
#86072=CARTESIAN_POINT('Ctrl Pts',(20.7873850835117,41.303193827003,20.));
#86073=CARTESIAN_POINT('Ctrl Pts',(20.8152439969059,41.285848585344,0.));
#86074=CARTESIAN_POINT('Ctrl Pts',(20.8152439969059,41.285848585344,20.));
#86075=CARTESIAN_POINT('Ctrl Pts',(20.8430896951822,41.268484246013,0.));
#86076=CARTESIAN_POINT('Ctrl Pts',(20.8430896951822,41.268484246013,20.));
#86077=CARTESIAN_POINT('Ctrl Pts',(20.8709221648944,41.2511008184358,0.));
#86078=CARTESIAN_POINT('Ctrl Pts',(20.8709221648944,41.2511008184358,20.));
#86079=CARTESIAN_POINT('Ctrl Pts',(20.8987413926025,41.2336983120481,0.));
#86080=CARTESIAN_POINT('Ctrl Pts',(20.8987413926025,41.2336983120481,20.));
#86081=CARTESIAN_POINT('Ctrl Pts',(20.9265473648728,41.2162767362953,0.));
#86082=CARTESIAN_POINT('Ctrl Pts',(20.9265473648728,41.2162767362953,20.));
#86083=CARTESIAN_POINT('Ctrl Pts',(20.9543400682781,41.1988361006333,0.));
#86084=CARTESIAN_POINT('Ctrl Pts',(20.9543400682781,41.1988361006333,20.));
#86085=CARTESIAN_POINT('Ctrl Pts',(20.9821194893979,41.1813764145274,0.));
#86086=CARTESIAN_POINT('Ctrl Pts',(20.9821194893979,41.1813764145274,20.));
#86087=CARTESIAN_POINT('Ctrl Pts',(21.009885614818,41.1638976874526,0.));
#86088=CARTESIAN_POINT('Ctrl Pts',(21.009885614818,41.1638976874526,20.));
#86089=CARTESIAN_POINT('Ctrl Pts',(21.0376384311301,41.1463999288927,0.));
#86090=CARTESIAN_POINT('Ctrl Pts',(21.0376384311301,41.1463999288927,20.));
#86091=CARTESIAN_POINT('Ctrl Pts',(21.0653779249329,41.128883148342,0.));
#86092=CARTESIAN_POINT('Ctrl Pts',(21.0653779249329,41.128883148342,20.));
#86093=CARTESIAN_POINT('Ctrl Pts',(21.093104082831,41.1113473553046,0.));
#86094=CARTESIAN_POINT('Ctrl Pts',(21.093104082831,41.1113473553046,20.));
#86095=CARTESIAN_POINT('Ctrl Pts',(21.1208168914355,41.0937925592944,0.));
#86096=CARTESIAN_POINT('Ctrl Pts',(21.1208168914355,41.0937925592944,20.));
#86097=CARTESIAN_POINT('Ctrl Pts',(21.1485163373635,41.076218769835,0.));
#86098=CARTESIAN_POINT('Ctrl Pts',(21.1485163373635,41.076218769835,20.));
#86099=CARTESIAN_POINT('Ctrl Pts',(21.1762024072388,41.0586259964597,0.));
#86100=CARTESIAN_POINT('Ctrl Pts',(21.1762024072388,41.0586259964597,20.));
#86101=CARTESIAN_POINT('Ctrl Pts',(21.2038750876913,41.0410142487106,0.));
#86102=CARTESIAN_POINT('Ctrl Pts',(21.2038750876913,41.0410142487106,20.));
#86103=CARTESIAN_POINT('Ctrl Pts',(21.2315343653574,41.0233835361399,0.));
#86104=CARTESIAN_POINT('Ctrl Pts',(21.2315343653574,41.0233835361399,20.));
#86105=CARTESIAN_POINT('Ctrl Pts',(21.25918022688,41.0057338683097,0.));
#86106=CARTESIAN_POINT('Ctrl Pts',(21.25918022688,41.0057338683097,20.));
#86107=CARTESIAN_POINT('Ctrl Pts',(21.286812658909,40.9880652547928,0.));
#86108=CARTESIAN_POINT('Ctrl Pts',(21.286812658909,40.9880652547928,20.));
#86109=CARTESIAN_POINT('Ctrl Pts',(21.3144316481011,40.9703777051716,0.));
#86110=CARTESIAN_POINT('Ctrl Pts',(21.3144316481011,40.9703777051716,20.));
#86111=CARTESIAN_POINT('Ctrl Pts',(21.342037181119,40.9526712290373,0.));
#86112=CARTESIAN_POINT('Ctrl Pts',(21.342037181119,40.9526712290373,20.));
#86113=CARTESIAN_POINT('Ctrl Pts',(21.3696292446317,40.9349458359905,0.));
#86114=CARTESIAN_POINT('Ctrl Pts',(21.3696292446317,40.9349458359905,20.));
#86115=CARTESIAN_POINT('Ctrl Pts',(21.3972078253142,40.9172015356414,0.));
#86116=CARTESIAN_POINT('Ctrl Pts',(21.3972078253142,40.9172015356414,20.));
#86117=CARTESIAN_POINT('Ctrl Pts',(21.4247729098479,40.8994383376102,0.));
#86118=CARTESIAN_POINT('Ctrl Pts',(21.4247729098479,40.8994383376102,20.));
#86119=CARTESIAN_POINT('Ctrl Pts',(21.4523244849199,40.8816562515268,0.));
#86120=CARTESIAN_POINT('Ctrl Pts',(21.4523244849199,40.8816562515268,20.));
#86121=CARTESIAN_POINT('Ctrl Pts',(21.4798625372243,40.8638552870319,0.));
#86122=CARTESIAN_POINT('Ctrl Pts',(21.4798625372243,40.8638552870319,20.));
#86123=CARTESIAN_POINT('Ctrl Pts',(21.5073870534614,40.8460354537749,0.));
#86124=CARTESIAN_POINT('Ctrl Pts',(21.5073870534614,40.8460354537749,20.));
#86125=CARTESIAN_POINT('Ctrl Pts',(21.5348980203391,40.8281967614155,0.));
#86126=CARTESIAN_POINT('Ctrl Pts',(21.5348980203391,40.8281967614155,20.));
#86127=CARTESIAN_POINT('Ctrl Pts',(21.5623954245725,40.8103392196221,0.));
#86128=CARTESIAN_POINT('Ctrl Pts',(21.5623954245725,40.8103392196221,20.));
#86129=CARTESIAN_POINT('Ctrl Pts',(21.5898792528837,40.7924628380726,0.));
#86130=CARTESIAN_POINT('Ctrl Pts',(21.5898792528837,40.7924628380726,20.));
#86131=CARTESIAN_POINT('Ctrl Pts',(21.6173494920019,40.7745676264537,0.));
#86132=CARTESIAN_POINT('Ctrl Pts',(21.6173494920019,40.7745676264537,20.));
#86133=CARTESIAN_POINT('Ctrl Pts',(21.6448061286619,40.7566535944621,0.));
#86134=CARTESIAN_POINT('Ctrl Pts',(21.6448061286619,40.7566535944621,20.));
#86135=CARTESIAN_POINT('Ctrl Pts',(21.6722491496038,40.7387207518043,0.));
#86136=CARTESIAN_POINT('Ctrl Pts',(21.6722491496038,40.7387207518043,20.));
#86137=CARTESIAN_POINT('Ctrl Pts',(21.6996785415723,40.7207691081984,0.));
#86138=CARTESIAN_POINT('Ctrl Pts',(21.6996785415723,40.7207691081984,20.));
#86139=CARTESIAN_POINT('Ctrl Pts',(21.7270942913167,40.7027986733736,0.));
#86140=CARTESIAN_POINT('Ctrl Pts',(21.7270942913167,40.7027986733736,20.));
#86141=CARTESIAN_POINT('Ctrl Pts',(21.7544963855931,40.6848094570694,0.));
#86142=CARTESIAN_POINT('Ctrl Pts',(21.7544963855931,40.6848094570694,20.));
#86143=CARTESIAN_POINT('Ctrl Pts',(21.781884811165,40.6668014690334,0.));
#86144=CARTESIAN_POINT('Ctrl Pts',(21.781884811165,40.6668014690334,20.));
#86145=CARTESIAN_POINT('Ctrl Pts',(21.8092595548052,40.6487747190214,0.));
#86146=CARTESIAN_POINT('Ctrl Pts',(21.8092595548052,40.6487747190214,20.));
#86147=CARTESIAN_POINT('Ctrl Pts',(21.8366206032979,40.6307292167951,0.));
#86148=CARTESIAN_POINT('Ctrl Pts',(21.8366206032979,40.6307292167951,20.));
#86149=CARTESIAN_POINT('Ctrl Pts',(21.8639679434382,40.6126649721233,0.));
#86150=CARTESIAN_POINT('Ctrl Pts',(21.8639679434382,40.6126649721233,20.));
#86151=CARTESIAN_POINT('Ctrl Pts',(21.8913015620281,40.594581994783,0.));
#86152=CARTESIAN_POINT('Ctrl Pts',(21.8913015620281,40.594581994783,20.));
#86153=CARTESIAN_POINT('Ctrl Pts',(21.9186214458728,40.5764802945639,0.));
#86154=CARTESIAN_POINT('Ctrl Pts',(21.9186214458728,40.5764802945639,20.));
#86155=CARTESIAN_POINT('Ctrl Pts',(21.9459275817778,40.5583598812699,0.));
#86156=CARTESIAN_POINT('Ctrl Pts',(21.9459275817778,40.5583598812699,20.));
#86157=CARTESIAN_POINT('Ctrl Pts',(21.9732199565439,40.5402207647219,0.));
#86158=CARTESIAN_POINT('Ctrl Pts',(21.9732199565439,40.5402207647219,20.));
#86159=CARTESIAN_POINT('Ctrl Pts',(22.0004985569689,40.5220629547578,0.));
#86160=CARTESIAN_POINT('Ctrl Pts',(22.0004985569689,40.5220629547578,20.));
#86161=CARTESIAN_POINT('Ctrl Pts',(22.0277633698572,40.5038864612253,0.));
#86162=CARTESIAN_POINT('Ctrl Pts',(22.0277633698572,40.5038864612253,20.));
#86163=CARTESIAN_POINT('Ctrl Pts',(22.0550143820281,40.485691293976,0.));
#86164=CARTESIAN_POINT('Ctrl Pts',(22.0550143820281,40.485691293976,20.));
#86165=CARTESIAN_POINT('Ctrl Pts',(22.0822515803231,40.4674774628609,0.));
#86166=CARTESIAN_POINT('Ctrl Pts',(22.0822515803231,40.4674774628609,20.));
#86167=CARTESIAN_POINT('Ctrl Pts',(22.1094749516164,40.4492449777204,0.));
#86168=CARTESIAN_POINT('Ctrl Pts',(22.1094749516164,40.4492449777204,20.));
#86169=CARTESIAN_POINT('Ctrl Pts',(22.1366844828092,40.4309938483881,0.));
#86170=CARTESIAN_POINT('Ctrl Pts',(22.1366844828092,40.4309938483881,20.));
#86171=CARTESIAN_POINT('Ctrl Pts',(22.1638801608087,40.4127240847076,0.));
#86172=CARTESIAN_POINT('Ctrl Pts',(22.1638801608087,40.4127240847076,20.));
#86173=CARTESIAN_POINT('Ctrl Pts',(22.1910619725087,40.3944356965472,0.));
#86174=CARTESIAN_POINT('Ctrl Pts',(22.1910619725087,40.3944356965472,20.));
#86175=CARTESIAN_POINT('Ctrl Pts',(22.2182299047735,40.3761286938115,0.));
#86176=CARTESIAN_POINT('Ctrl Pts',(22.2182299047735,40.3761286938115,20.));
#86177=CARTESIAN_POINT('Ctrl Pts',(22.2453839444114,40.357803086462,0.));
#86178=CARTESIAN_POINT('Ctrl Pts',(22.2453839444114,40.357803086462,20.));
#86179=CARTESIAN_POINT('Ctrl Pts',(22.2725240781926,40.3394588845042,0.));
#86180=CARTESIAN_POINT('Ctrl Pts',(22.2725240781926,40.3394588845042,20.));
#86181=CARTESIAN_POINT('Ctrl Pts',(22.2996502928986,40.3210960979489,0.));
#86182=CARTESIAN_POINT('Ctrl Pts',(22.2996502928986,40.3210960979489,20.));
#86183=CARTESIAN_POINT('Ctrl Pts',(22.326762575367,40.3027147367804,0.));
#86184=CARTESIAN_POINT('Ctrl Pts',(22.326762575367,40.3027147367804,20.));
#86185=CARTESIAN_POINT('Ctrl Pts',(22.3538609125294,40.2843148109268,0.));
#86186=CARTESIAN_POINT('Ctrl Pts',(22.3538609125294,40.2843148109268,20.));
#86187=CARTESIAN_POINT('Ctrl Pts',(22.3809452914735,40.2658963302133,0.));
#86188=CARTESIAN_POINT('Ctrl Pts',(22.3809452914735,40.2658963302133,20.));
#86189=CARTESIAN_POINT('Ctrl Pts',(22.4080156993888,40.2474593044019,0.));
#86190=CARTESIAN_POINT('Ctrl Pts',(22.4080156993888,40.2474593044019,20.));
#86191=CARTESIAN_POINT('Ctrl Pts',(22.4350721234534,40.229003743277,0.));
#86192=CARTESIAN_POINT('Ctrl Pts',(22.4350721234534,40.229003743277,20.));
#86193=CARTESIAN_POINT('Ctrl Pts',(22.4621145507305,40.210529656724,0.));
#86194=CARTESIAN_POINT('Ctrl Pts',(22.4621145507305,40.210529656724,20.));
#86195=CARTESIAN_POINT('Ctrl Pts',(22.4891429680799,40.1920370547964,0.));
#86196=CARTESIAN_POINT('Ctrl Pts',(22.4891429680799,40.1920370547964,20.));
#86197=CARTESIAN_POINT('Ctrl Pts',(22.5161573620162,40.1735259478254,0.));
#86198=CARTESIAN_POINT('Ctrl Pts',(22.5161573620162,40.1735259478254,20.));
#86199=CARTESIAN_POINT('Ctrl Pts',(22.5431577188605,40.1549963463026,0.));
#86200=CARTESIAN_POINT('Ctrl Pts',(22.5431577188605,40.1549963463026,20.));
#86201=CARTESIAN_POINT('Ctrl Pts',(22.5701440249982,40.1364482606861,0.));
#86202=CARTESIAN_POINT('Ctrl Pts',(22.5701440249982,40.1364482606861,20.));
#86203=CARTESIAN_POINT('Ctrl Pts',(22.5971162671187,40.1178817012184,0.));
#86204=CARTESIAN_POINT('Ctrl Pts',(22.5971162671187,40.1178817012184,20.));
#86205=CARTESIAN_POINT('Ctrl Pts',(22.6240744324258,40.0992966777668,0.));
#86206=CARTESIAN_POINT('Ctrl Pts',(22.6240744324258,40.0992966777668,20.));
#86207=CARTESIAN_POINT('Ctrl Pts',(22.6510185089549,40.0806931995834,0.));
#86208=CARTESIAN_POINT('Ctrl Pts',(22.6510185089549,40.0806931995834,20.));
#86209=CARTESIAN_POINT('Ctrl Pts',(22.6779484851672,40.0620712756149,0.));
#86210=CARTESIAN_POINT('Ctrl Pts',(22.6779484851672,40.0620712756149,20.));
#86211=CARTESIAN_POINT('Ctrl Pts',(22.7048643493645,40.0434309149417,0.));
#86212=CARTESIAN_POINT('Ctrl Pts',(22.7048643493645,40.0434309149417,20.));
#86213=CARTESIAN_POINT('Ctrl Pts',(22.73176608914,40.0247721271957,0.));
#86214=CARTESIAN_POINT('Ctrl Pts',(22.73176608914,40.0247721271957,20.));
#86215=CARTESIAN_POINT('Ctrl Pts',(22.7586536908731,40.0060949229408,0.));
#86216=CARTESIAN_POINT('Ctrl Pts',(22.7586536908731,40.0060949229408,20.));
#86217=CARTESIAN_POINT('Ctrl Pts',(22.7855271390493,39.9873993141881,0.));
#86218=CARTESIAN_POINT('Ctrl Pts',(22.7855271390493,39.9873993141881,20.));
#86219=CARTESIAN_POINT('Ctrl Pts',(22.8123864172494,39.9686853136472,0.));
#86220=CARTESIAN_POINT('Ctrl Pts',(22.8123864172494,39.9686853136472,20.));
#86221=CARTESIAN_POINT('Ctrl Pts',(22.8392315093989,39.9499529337848,0.));
#86222=CARTESIAN_POINT('Ctrl Pts',(22.8392315093989,39.9499529337848,20.));
#86223=CARTESIAN_POINT('Ctrl Pts',(22.8660624009432,39.9312021859375,0.));
#86224=CARTESIAN_POINT('Ctrl Pts',(22.8660624009432,39.9312021859375,20.));
#86225=CARTESIAN_POINT('Ctrl Pts',(22.8928790800154,39.91243307943,0.));
#86226=CARTESIAN_POINT('Ctrl Pts',(22.8928790800154,39.91243307943,20.));
#86227=CARTESIAN_POINT('Ctrl Pts',(22.9196815387084,39.8936456206159,0.));
#86228=CARTESIAN_POINT('Ctrl Pts',(22.9196815387084,39.8936456206159,20.));
#86229=CARTESIAN_POINT('Ctrl Pts',(22.9464697723601,39.8748398133807,0.));
#86230=CARTESIAN_POINT('Ctrl Pts',(22.9464697723601,39.8748398133807,20.));
#86231=CARTESIAN_POINT('Ctrl Pts',(22.9678889774251,39.8597804904793,0.));
#86232=CARTESIAN_POINT('Ctrl Pts',(22.9678889774251,39.8597804904793,20.));
#86233=CARTESIAN_POINT('Ctrl Pts',(22.9839469786125,39.8484777427633,0.));
#86234=CARTESIAN_POINT('Ctrl Pts',(22.9839469786125,39.8484777427633,20.));
#86235=CARTESIAN_POINT('Ctrl Pts',(22.9946494671375,39.8409389084975,0.));
#86236=CARTESIAN_POINT('Ctrl Pts',(22.9946494671375,39.8409389084975,20.));
#86237=CARTESIAN_POINT('Ctrl Pts',(23.,39.8371685740842,0.));
#86238=CARTESIAN_POINT('Ctrl Pts',(23.,39.8371685740842,20.));
#86239=CARTESIAN_POINT('',(-8.50876070567958,48.2555798975982,2.));
#86240=CARTESIAN_POINT('Ctrl Pts',(10.7008281308626,46.0172966012412,2.));
#86241=CARTESIAN_POINT('Ctrl Pts',(9.93785043801569,46.269064380565,2.));
#86242=CARTESIAN_POINT('Ctrl Pts',(9.1675435200454,46.5017519909092,2.));
#86243=CARTESIAN_POINT('Ctrl Pts',(8.39088307367081,46.7150066081184,2.));
#86244=CARTESIAN_POINT('Ctrl Pts',(7.61536231145253,46.9279482920378,2.));
#86245=CARTESIAN_POINT('Ctrl Pts',(6.83350683128281,47.1215139493916,2.));
#86246=CARTESIAN_POINT('Ctrl Pts',(6.04630275161101,47.2954025498593,2.));
#86247=CARTESIAN_POINT('Ctrl Pts',(5.25841985133201,47.4694410976766,2.));
#86248=CARTESIAN_POINT('Ctrl Pts',(4.46517929614118,47.6237686035462,2.));
#86249=CARTESIAN_POINT('Ctrl Pts',(3.66758188329678,47.7581340930642,2.));
#86250=CARTESIAN_POINT('Ctrl Pts',(2.86929216217542,47.8926162107697,2.));
#86251=CARTESIAN_POINT('Ctrl Pts',(2.06663819084915,48.0071016174996,2.));
#86252=CARTESIAN_POINT('Ctrl Pts',(1.26063290971421,48.1013900403506,2.));
#86253=CARTESIAN_POINT('Ctrl Pts',(0.453491097353087,48.1958114173389,2.));
#86254=CARTESIAN_POINT('Ctrl Pts',(-0.357011308083155,48.2699787899167,
2.));
#86255=CARTESIAN_POINT('Ctrl Pts',(-1.16985013658731,48.3237428786942,2.));
#86256=CARTESIAN_POINT('Ctrl Pts',(-1.98327568803649,48.3775457754413,2.));
#86257=CARTESIAN_POINT('Ctrl Pts',(-2.79904086101009,48.4109159159145,2.));
#86258=CARTESIAN_POINT('Ctrl Pts',(-3.61611495486177,48.423755782707,2.));
#86259=CARTESIAN_POINT('Ctrl Pts',(-4.4303187583051,48.4365505444756,2.));
#86260=CARTESIAN_POINT('Ctrl Pts',(-5.24582212860677,48.4289590586956,2.));
#86261=CARTESIAN_POINT('Ctrl Pts',(-6.06160353104804,48.400936241801,2.));
#86262=CARTESIAN_POINT('Ctrl Pts',(-6.59891314705417,48.3824791784996,2.));
#86263=CARTESIAN_POINT('Ctrl Pts',(-7.13634335834826,48.3551598081879,2.));
#86264=CARTESIAN_POINT('Ctrl Pts',(-7.67360240784279,48.3189773727877,2.));
#86265=CARTESIAN_POINT('Ctrl Pts',(-7.95204798714075,48.3002250796529,2.));
#86266=CARTESIAN_POINT('Ctrl Pts',(-8.23044701858261,48.2790922958893,2.));
#86267=CARTESIAN_POINT('Ctrl Pts',(-8.50876070567958,48.2555798975982,2.));
#86268=CARTESIAN_POINT('',(-8.50876070567958,48.2555798975982,0.));
#86269=CARTESIAN_POINT('Origin',(43.358988599418,12.8159317895946,2.));
#86270=CARTESIAN_POINT('',(46.0771487394572,7.40158428109251,2.));
#86271=CARTESIAN_POINT('Ctrl Pts',(46.0771487393297,7.40158428157356,2.));
#86272=CARTESIAN_POINT('Ctrl Pts',(46.0771487393297,7.40158428157356,4.66666666666667));
#86273=CARTESIAN_POINT('Ctrl Pts',(46.0771487393297,7.40158428157356,7.33333333333333));
#86274=CARTESIAN_POINT('Ctrl Pts',(46.0771487393297,7.40158428157356,12.6666666666667));
#86275=CARTESIAN_POINT('Ctrl Pts',(46.0771487393297,7.40158428157356,15.3333333333333));
#86276=CARTESIAN_POINT('Ctrl Pts',(46.0771487393297,7.40158428157356,18.));
#86277=CARTESIAN_POINT('',(46.4996348579608,6.56002729234549,2.));
#86278=CARTESIAN_POINT('',(43.358988599418,12.8159317895946,2.));
#86279=CARTESIAN_POINT('',(46.4996348579608,6.56002729234549,2.));
#86280=CARTESIAN_POINT('Origin',(54.977096951452,18.6485605554598,2.));
#86281=CARTESIAN_POINT('',(45.2025619355918,13.741459297751,2.));
#86282=CARTESIAN_POINT('Ctrl Pts',(45.2025619355918,13.741459297751,18.));
#86283=CARTESIAN_POINT('Ctrl Pts',(45.2025619355918,13.741459297751,15.3333333333333));
#86284=CARTESIAN_POINT('Ctrl Pts',(45.2025619355918,13.741459297751,12.6666666666667));
#86285=CARTESIAN_POINT('Ctrl Pts',(45.2025619355918,13.741459297751,7.33333333333333));
#86286=CARTESIAN_POINT('Ctrl Pts',(45.2025619355918,13.741459297751,4.66666666666667));
#86287=CARTESIAN_POINT('Ctrl Pts',(45.2025619355918,13.741459297751,2.));
#86288=CARTESIAN_POINT('',(54.977096951452,18.6485605554598,2.));
#86289=CARTESIAN_POINT('',(54.977096951452,18.6485605554598,2.));
#86290=CARTESIAN_POINT('',(54.977096951452,18.6485605554598,2.));
#86291=CARTESIAN_POINT('Origin',(58.1177432099948,12.3926560582107,2.));
#86292=CARTESIAN_POINT('',(58.1177432099948,12.3926560582107,2.));
#86293=CARTESIAN_POINT('',(58.1177432099948,12.3926560582107,2.));
#86294=CARTESIAN_POINT('',(58.1177432099948,12.3926560582107,2.));
#86295=CARTESIAN_POINT('Origin',(46.4996348579608,6.56002729234549,2.));
#86296=CARTESIAN_POINT('',(46.4996348579608,6.56002729234549,2.));
#86297=CARTESIAN_POINT('Ctrl Pts',(37.5361777128299,31.4965928746404,0.));
#86298=CARTESIAN_POINT('Ctrl Pts',(37.5361777128299,31.4965928746404,20.));
#86299=CARTESIAN_POINT('Ctrl Pts',(37.5400435810124,31.4910366171629,0.));
#86300=CARTESIAN_POINT('Ctrl Pts',(37.5400435810124,31.4910366171629,20.));
#86301=CARTESIAN_POINT('Ctrl Pts',(37.5477733397938,31.4799228688318,0.));
#86302=CARTESIAN_POINT('Ctrl Pts',(37.5477733397938,31.4799228688318,20.));
#86303=CARTESIAN_POINT('Ctrl Pts',(37.5593620452151,31.4632485462068,0.));
#86304=CARTESIAN_POINT('Ctrl Pts',(37.5593620452151,31.4632485462068,20.));
#86305=CARTESIAN_POINT('Ctrl Pts',(37.574801786924,31.4410087157717,0.));
#86306=CARTESIAN_POINT('Ctrl Pts',(37.574801786924,31.4410087157717,20.));
#86307=CARTESIAN_POINT('Ctrl Pts',(37.5940816876034,31.4131965946731,0.));
#86308=CARTESIAN_POINT('Ctrl Pts',(37.5940816876034,31.4131965946731,20.));
#86309=CARTESIAN_POINT('Ctrl Pts',(37.6133418102375,31.3853721428083,0.));
#86310=CARTESIAN_POINT('Ctrl Pts',(37.6133418102375,31.3853721428083,20.));
#86311=CARTESIAN_POINT('Ctrl Pts',(37.6325821517747,31.3575353648538,0.));
#86312=CARTESIAN_POINT('Ctrl Pts',(37.6325821517747,31.3575353648538,20.));
#86313=CARTESIAN_POINT('Ctrl Pts',(37.6518027072643,31.3296862686536,0.));
#86314=CARTESIAN_POINT('Ctrl Pts',(37.6518027072643,31.3296862686536,20.));
#86315=CARTESIAN_POINT('Ctrl Pts',(37.6710034693473,31.3018248661211,0.));
#86316=CARTESIAN_POINT('Ctrl Pts',(37.6710034693473,31.3018248661211,20.));
#86317=CARTESIAN_POINT('Ctrl Pts',(37.6901844288974,31.2739511721649,0.));
#86318=CARTESIAN_POINT('Ctrl Pts',(37.6901844288974,31.2739511721649,20.));
#86319=CARTESIAN_POINT('Ctrl Pts',(37.7093455757381,31.2460652034827,0.));
#86320=CARTESIAN_POINT('Ctrl Pts',(37.7093455757381,31.2460652034827,20.));
#86321=CARTESIAN_POINT('Ctrl Pts',(37.7284868993471,31.2181669773772,0.));
#86322=CARTESIAN_POINT('Ctrl Pts',(37.7284868993471,31.2181669773772,20.));
#86323=CARTESIAN_POINT('Ctrl Pts',(37.7476083895316,31.1902565106222,0.));
#86324=CARTESIAN_POINT('Ctrl Pts',(37.7476083895316,31.1902565106222,20.));
#86325=CARTESIAN_POINT('Ctrl Pts',(37.7667100372089,31.1623338181506,0.));
#86326=CARTESIAN_POINT('Ctrl Pts',(37.7667100372089,31.1623338181506,20.));
#86327=CARTESIAN_POINT('Ctrl Pts',(37.7857918342009,31.1343989133989,0.));
#86328=CARTESIAN_POINT('Ctrl Pts',(37.7857918342009,31.1343989133989,20.));
#86329=CARTESIAN_POINT('Ctrl Pts',(37.8048537728749,31.1064518089103,0.));
#86330=CARTESIAN_POINT('Ctrl Pts',(37.8048537728749,31.1064518089103,20.));
#86331=CARTESIAN_POINT('Ctrl Pts',(37.8238958458276,31.0784925168637,0.));
#86332=CARTESIAN_POINT('Ctrl Pts',(37.8238958458276,31.0784925168637,20.));
#86333=CARTESIAN_POINT('Ctrl Pts',(37.8429180455734,31.0505210495984,0.));
#86334=CARTESIAN_POINT('Ctrl Pts',(37.8429180455734,31.0505210495984,20.));
#86335=CARTESIAN_POINT('Ctrl Pts',(37.861920364175,31.0225374202321,0.));
#86336=CARTESIAN_POINT('Ctrl Pts',(37.861920364175,31.0225374202321,20.));
#86337=CARTESIAN_POINT('Ctrl Pts',(37.8809027932971,30.9945416425721,0.));
#86338=CARTESIAN_POINT('Ctrl Pts',(37.8809027932971,30.9945416425721,20.));
#86339=CARTESIAN_POINT('Ctrl Pts',(37.8998653243731,30.9665337308352,0.));
#86340=CARTESIAN_POINT('Ctrl Pts',(37.8998653243731,30.9665337308352,20.));
#86341=CARTESIAN_POINT('Ctrl Pts',(37.9188079487378,30.9385136994261,0.));
#86342=CARTESIAN_POINT('Ctrl Pts',(37.9188079487378,30.9385136994261,20.));
#86343=CARTESIAN_POINT('Ctrl Pts',(37.9377306577632,30.9104815627079,0.));
#86344=CARTESIAN_POINT('Ctrl Pts',(37.9377306577632,30.9104815627079,20.));
#86345=CARTESIAN_POINT('Ctrl Pts',(37.9566334430211,30.882437334731,0.));
#86346=CARTESIAN_POINT('Ctrl Pts',(37.9566334430211,30.882437334731,20.));
#86347=CARTESIAN_POINT('Ctrl Pts',(37.9755162962752,30.8543810292446,0.));
#86348=CARTESIAN_POINT('Ctrl Pts',(37.9755162962752,30.8543810292446,20.));
#86349=CARTESIAN_POINT('Ctrl Pts',(37.9943792094053,30.8263126598247,0.));
#86350=CARTESIAN_POINT('Ctrl Pts',(37.9943792094053,30.8263126598247,20.));
#86351=CARTESIAN_POINT('Ctrl Pts',(38.0132221743517,30.7982322399668,0.));
#86352=CARTESIAN_POINT('Ctrl Pts',(38.0132221743517,30.7982322399668,20.));
#86353=CARTESIAN_POINT('Ctrl Pts',(38.0320451830565,30.7701397831859,0.));
#86354=CARTESIAN_POINT('Ctrl Pts',(38.0320451830565,30.7701397831859,20.));
#86355=CARTESIAN_POINT('Ctrl Pts',(38.0508482273931,30.7420353031339,0.));
#86356=CARTESIAN_POINT('Ctrl Pts',(38.0508482273931,30.7420353031339,20.));
#86357=CARTESIAN_POINT('Ctrl Pts',(38.0696312991626,30.7139188136053,0.));
#86358=CARTESIAN_POINT('Ctrl Pts',(38.0696312991626,30.7139188136053,20.));
#86359=CARTESIAN_POINT('Ctrl Pts',(38.088394390128,30.6857903284809,0.));
#86360=CARTESIAN_POINT('Ctrl Pts',(38.088394390128,30.6857903284809,20.));
#86361=CARTESIAN_POINT('Ctrl Pts',(38.1071374920373,30.6576498616875,0.));
#86362=CARTESIAN_POINT('Ctrl Pts',(38.1071374920373,30.6576498616875,20.));
#86363=CARTESIAN_POINT('Ctrl Pts',(38.125860596649,30.6294974271553,0.));
#86364=CARTESIAN_POINT('Ctrl Pts',(38.125860596649,30.6294974271553,20.));
#86365=CARTESIAN_POINT('Ctrl Pts',(38.1445636957629,30.6013330387675,0.));
#86366=CARTESIAN_POINT('Ctrl Pts',(38.1445636957629,30.6013330387675,20.));
#86367=CARTESIAN_POINT('Ctrl Pts',(38.1632467812242,30.5731567103519,0.));
#86368=CARTESIAN_POINT('Ctrl Pts',(38.1632467812242,30.5731567103519,20.));
#86369=CARTESIAN_POINT('Ctrl Pts',(38.1819098449085,30.5449684557073,0.));
#86370=CARTESIAN_POINT('Ctrl Pts',(38.1819098449085,30.5449684557073,20.));
#86371=CARTESIAN_POINT('Ctrl Pts',(38.2005528787125,30.5167682886194,0.));
#86372=CARTESIAN_POINT('Ctrl Pts',(38.2005528787125,30.5167682886194,20.));
#86373=CARTESIAN_POINT('Ctrl Pts',(38.2191758745422,30.4885562228796,0.));
#86374=CARTESIAN_POINT('Ctrl Pts',(38.2191758745422,30.4885562228796,20.));
#86375=CARTESIAN_POINT('Ctrl Pts',(38.2377788243005,30.460332272307,0.));
#86376=CARTESIAN_POINT('Ctrl Pts',(38.2377788243005,30.460332272307,20.));
#86377=CARTESIAN_POINT('Ctrl Pts',(38.2563617198829,30.4320964507535,0.));
#86378=CARTESIAN_POINT('Ctrl Pts',(38.2563617198829,30.4320964507535,20.));
#86379=CARTESIAN_POINT('Ctrl Pts',(38.2749245531853,30.4038487720928,0.));
#86380=CARTESIAN_POINT('Ctrl Pts',(38.2749245531853,30.4038487720928,20.));
#86381=CARTESIAN_POINT('Ctrl Pts',(38.2934673161074,30.3755892502132,0.));
#86382=CARTESIAN_POINT('Ctrl Pts',(38.2934673161074,30.3755892502132,20.));
#86383=CARTESIAN_POINT('Ctrl Pts',(38.3119900005578,30.3473178990095,0.));
#86384=CARTESIAN_POINT('Ctrl Pts',(38.3119900005578,30.3473178990095,20.));
#86385=CARTESIAN_POINT('Ctrl Pts',(38.3304925984593,30.3190347323738,0.));
#86386=CARTESIAN_POINT('Ctrl Pts',(38.3304925984593,30.3190347323738,20.));
#86387=CARTESIAN_POINT('Ctrl Pts',(38.3489751017513,30.2907397641919,0.));
#86388=CARTESIAN_POINT('Ctrl Pts',(38.3489751017513,30.2907397641919,20.));
#86389=CARTESIAN_POINT('Ctrl Pts',(38.3674375023871,30.2624330083488,0.));
#86390=CARTESIAN_POINT('Ctrl Pts',(38.3674375023871,30.2624330083488,20.));
#86391=CARTESIAN_POINT('Ctrl Pts',(38.3858797923318,30.2341144787313,0.));
#86392=CARTESIAN_POINT('Ctrl Pts',(38.3858797923318,30.2341144787313,20.));
#86393=CARTESIAN_POINT('Ctrl Pts',(38.4043019635603,30.2057841892317,0.));
#86394=CARTESIAN_POINT('Ctrl Pts',(38.4043019635603,30.2057841892317,20.));
#86395=CARTESIAN_POINT('Ctrl Pts',(38.4227040080549,30.1774421537519,0.));
#86396=CARTESIAN_POINT('Ctrl Pts',(38.4227040080549,30.1774421537519,20.));
#86397=CARTESIAN_POINT('Ctrl Pts',(38.4410859178038,30.1490883862047,0.));
#86398=CARTESIAN_POINT('Ctrl Pts',(38.4410859178038,30.1490883862047,20.));
#86399=CARTESIAN_POINT('Ctrl Pts',(38.4594476848032,30.1207229005118,0.));
#86400=CARTESIAN_POINT('Ctrl Pts',(38.4594476848032,30.1207229005118,20.));
#86401=CARTESIAN_POINT('Ctrl Pts',(38.4777893010568,30.0923457106027,0.));
#86402=CARTESIAN_POINT('Ctrl Pts',(38.4777893010568,30.0923457106027,20.));
#86403=CARTESIAN_POINT('Ctrl Pts',(38.4961107585777,30.0639568304126,0.));
#86404=CARTESIAN_POINT('Ctrl Pts',(38.4961107585777,30.0639568304126,20.));
#86405=CARTESIAN_POINT('Ctrl Pts',(38.5144120493894,30.0355562738816,0.));
#86406=CARTESIAN_POINT('Ctrl Pts',(38.5144120493894,30.0355562738816,20.));
#86407=CARTESIAN_POINT('Ctrl Pts',(38.532693165526,30.0071440549534,0.));
#86408=CARTESIAN_POINT('Ctrl Pts',(38.532693165526,30.0071440549534,20.));
#86409=CARTESIAN_POINT('Ctrl Pts',(38.5509540990321,29.978720187576,0.));
#86410=CARTESIAN_POINT('Ctrl Pts',(38.5509540990321,29.978720187576,20.));
#86411=CARTESIAN_POINT('Ctrl Pts',(38.5691948419622,29.9502846857025,0.));
#86412=CARTESIAN_POINT('Ctrl Pts',(38.5691948419622,29.9502846857025,20.));
#86413=CARTESIAN_POINT('Ctrl Pts',(38.5874153863803,29.9218375632918,0.));
#86414=CARTESIAN_POINT('Ctrl Pts',(38.5874153863803,29.9218375632918,20.));
#86415=CARTESIAN_POINT('Ctrl Pts',(38.6056157243597,29.8933788343089,0.));
#86416=CARTESIAN_POINT('Ctrl Pts',(38.6056157243597,29.8933788343089,20.));
#86417=CARTESIAN_POINT('Ctrl Pts',(38.6237958479822,29.864908512726,0.));
#86418=CARTESIAN_POINT('Ctrl Pts',(38.6237958479822,29.864908512726,20.));
#86419=CARTESIAN_POINT('Ctrl Pts',(38.6419557493389,29.8364266125215,0.));
#86420=CARTESIAN_POINT('Ctrl Pts',(38.6419557493389,29.8364266125215,20.));
#86421=CARTESIAN_POINT('Ctrl Pts',(38.66009542053,29.8079331476799,0.));
#86422=CARTESIAN_POINT('Ctrl Pts',(38.66009542053,29.8079331476799,20.));
#86423=CARTESIAN_POINT('Ctrl Pts',(38.6782148536649,29.7794281321916,0.));
#86424=CARTESIAN_POINT('Ctrl Pts',(38.6782148536649,29.7794281321916,20.));
#86425=CARTESIAN_POINT('Ctrl Pts',(38.6963140408627,29.7509115800524,0.));
#86426=CARTESIAN_POINT('Ctrl Pts',(38.6963140408627,29.7509115800524,20.));
#86427=CARTESIAN_POINT('Ctrl Pts',(38.7143929742521,29.7223835052637,0.));
#86428=CARTESIAN_POINT('Ctrl Pts',(38.7143929742521,29.7223835052637,20.));
#86429=CARTESIAN_POINT('Ctrl Pts',(38.7324516459718,29.6938439218325,0.));
#86430=CARTESIAN_POINT('Ctrl Pts',(38.7324516459718,29.6938439218325,20.));
#86431=CARTESIAN_POINT('Ctrl Pts',(38.7504900481697,29.6652928437714,0.));
#86432=CARTESIAN_POINT('Ctrl Pts',(38.7504900481697,29.6652928437714,20.));
#86433=CARTESIAN_POINT('Ctrl Pts',(38.7685081730036,29.6367302850988,0.));
#86434=CARTESIAN_POINT('Ctrl Pts',(38.7685081730036,29.6367302850988,20.));
#86435=CARTESIAN_POINT('Ctrl Pts',(38.7865060126402,29.6081562598384,0.));
#86436=CARTESIAN_POINT('Ctrl Pts',(38.7865060126402,29.6081562598384,20.));
#86437=CARTESIAN_POINT('Ctrl Pts',(38.8044835592559,29.5795707820205,0.));
#86438=CARTESIAN_POINT('Ctrl Pts',(38.8044835592559,29.5795707820205,20.));
#86439=CARTESIAN_POINT('Ctrl Pts',(38.8224408050366,29.5509738656807,0.));
#86440=CARTESIAN_POINT('Ctrl Pts',(38.8224408050366,29.5509738656807,20.));
#86441=CARTESIAN_POINT('Ctrl Pts',(38.8403777421773,29.5223655248609,0.));
#86442=CARTESIAN_POINT('Ctrl Pts',(38.8403777421773,29.5223655248609,20.));
#86443=CARTESIAN_POINT('Ctrl Pts',(38.8582943628826,29.4937457736083,0.));
#86444=CARTESIAN_POINT('Ctrl Pts',(38.8582943628826,29.4937457736083,20.));
#86445=CARTESIAN_POINT('Ctrl Pts',(38.8761906593666,29.4651146259764,0.));
#86446=CARTESIAN_POINT('Ctrl Pts',(38.8761906593666,29.4651146259764,20.));
#86447=CARTESIAN_POINT('Ctrl Pts',(38.8940666238532,29.4364720960241,0.));
#86448=CARTESIAN_POINT('Ctrl Pts',(38.8940666238532,29.4364720960241,20.));
#86449=CARTESIAN_POINT('Ctrl Pts',(38.9119222485755,29.4078181978158,0.));
#86450=CARTESIAN_POINT('Ctrl Pts',(38.9119222485755,29.4078181978158,20.));
#86451=CARTESIAN_POINT('Ctrl Pts',(38.9297575257761,29.3791529454216,0.));
#86452=CARTESIAN_POINT('Ctrl Pts',(38.9297575257761,29.3791529454216,20.));
#86453=CARTESIAN_POINT('Ctrl Pts',(38.9475724477072,29.3504763529173,0.));
#86454=CARTESIAN_POINT('Ctrl Pts',(38.9475724477072,29.3504763529173,20.));
#86455=CARTESIAN_POINT('Ctrl Pts',(38.9653670066308,29.3217884343845,0.));
#86456=CARTESIAN_POINT('Ctrl Pts',(38.9653670066308,29.3217884343845,20.));
#86457=CARTESIAN_POINT('Ctrl Pts',(38.9831411948182,29.2930892039104,0.));
#86458=CARTESIAN_POINT('Ctrl Pts',(38.9831411948182,29.2930892039104,20.));
#86459=CARTESIAN_POINT('Ctrl Pts',(39.0008950045502,29.2643786755883,0.));
#86460=CARTESIAN_POINT('Ctrl Pts',(39.0008950045502,29.2643786755883,20.));
#86461=CARTESIAN_POINT('Ctrl Pts',(39.0186284281173,29.2356568635168,0.));
#86462=CARTESIAN_POINT('Ctrl Pts',(39.0186284281173,29.2356568635168,20.));
#86463=CARTESIAN_POINT('Ctrl Pts',(39.0363414578191,29.2069237818005,0.));
#86464=CARTESIAN_POINT('Ctrl Pts',(39.0363414578191,29.2069237818005,20.));
#86465=CARTESIAN_POINT('Ctrl Pts',(39.054034085965,29.1781794445493,0.));
#86466=CARTESIAN_POINT('Ctrl Pts',(39.054034085965,29.1781794445493,20.));
#86467=CARTESIAN_POINT('Ctrl Pts',(39.0717063048737,29.1494238658788,0.));
#86468=CARTESIAN_POINT('Ctrl Pts',(39.0717063048737,29.1494238658788,20.));
#86469=CARTESIAN_POINT('Ctrl Pts',(39.0893581068737,29.1206570599103,0.));
#86470=CARTESIAN_POINT('Ctrl Pts',(39.0893581068737,29.1206570599103,20.));
#86471=CARTESIAN_POINT('Ctrl Pts',(39.106989484303,29.0918790407708,0.));
#86472=CARTESIAN_POINT('Ctrl Pts',(39.106989484303,29.0918790407708,20.));
#86473=CARTESIAN_POINT('Ctrl Pts',(39.1246004295092,29.0630898225929,0.));
#86474=CARTESIAN_POINT('Ctrl Pts',(39.1246004295092,29.0630898225929,20.));
#86475=CARTESIAN_POINT('Ctrl Pts',(39.1421909348497,29.034289419515,0.));
#86476=CARTESIAN_POINT('Ctrl Pts',(39.1421909348497,29.034289419515,20.));
#86477=CARTESIAN_POINT('Ctrl Pts',(39.1597609926911,29.0054778456813,0.));
#86478=CARTESIAN_POINT('Ctrl Pts',(39.1597609926911,29.0054778456813,20.));
#86479=CARTESIAN_POINT('Ctrl Pts',(39.1773105954099,28.9766551152413,0.));
#86480=CARTESIAN_POINT('Ctrl Pts',(39.1773105954099,28.9766551152413,20.));
#86481=CARTESIAN_POINT('Ctrl Pts',(39.1948397353916,28.9478212423503,0.));
#86482=CARTESIAN_POINT('Ctrl Pts',(39.1948397353916,28.9478212423503,20.));
#86483=CARTESIAN_POINT('Ctrl Pts',(39.2123484050317,28.9189762411689,0.));
#86484=CARTESIAN_POINT('Ctrl Pts',(39.2123484050317,28.9189762411689,20.));
#86485=CARTESIAN_POINT('Ctrl Pts',(39.2298365967351,28.8901201258634,0.));
#86486=CARTESIAN_POINT('Ctrl Pts',(39.2298365967351,28.8901201258634,20.));
#86487=CARTESIAN_POINT('Ctrl Pts',(39.2473043029163,28.8612529106058,0.));
#86488=CARTESIAN_POINT('Ctrl Pts',(39.2473043029163,28.8612529106058,20.));
#86489=CARTESIAN_POINT('Ctrl Pts',(39.2647515159997,28.8323746095736,0.));
#86490=CARTESIAN_POINT('Ctrl Pts',(39.2647515159997,28.8323746095736,20.));
#86491=CARTESIAN_POINT('Ctrl Pts',(39.2821782284193,28.80348523695,0.));
#86492=CARTESIAN_POINT('Ctrl Pts',(39.2821782284193,28.80348523695,20.));
#86493=CARTESIAN_POINT('Ctrl Pts',(39.2995844326181,28.7745848069238,0.));
#86494=CARTESIAN_POINT('Ctrl Pts',(39.2995844326181,28.7745848069238,20.));
#86495=CARTESIAN_POINT('Ctrl Pts',(39.316970121049,28.7456733336894,0.));
#86496=CARTESIAN_POINT('Ctrl Pts',(39.316970121049,28.7456733336894,20.));
#86497=CARTESIAN_POINT('Ctrl Pts',(39.3343352861746,28.7167508314468,0.));
#86498=CARTESIAN_POINT('Ctrl Pts',(39.3343352861746,28.7167508314468,20.));
#86499=CARTESIAN_POINT('Ctrl Pts',(39.3516799204672,28.6878173144015,0.));
#86500=CARTESIAN_POINT('Ctrl Pts',(39.3516799204672,28.6878173144015,20.));
#86501=CARTESIAN_POINT('Ctrl Pts',(39.3690040164086,28.6588727967647,0.));
#86502=CARTESIAN_POINT('Ctrl Pts',(39.3690040164086,28.6588727967647,20.));
#86503=CARTESIAN_POINT('Ctrl Pts',(39.3863075664906,28.6299172927529,0.));
#86504=CARTESIAN_POINT('Ctrl Pts',(39.3863075664906,28.6299172927529,20.));
#86505=CARTESIAN_POINT('Ctrl Pts',(39.4035905632141,28.600950816588,0.));
#86506=CARTESIAN_POINT('Ctrl Pts',(39.4035905632141,28.600950816588,20.));
#86507=CARTESIAN_POINT('Ctrl Pts',(39.4208529990894,28.5719733824975,0.));
#86508=CARTESIAN_POINT('Ctrl Pts',(39.4208529990894,28.5719733824975,20.));
#86509=CARTESIAN_POINT('Ctrl Pts',(39.4380948666368,28.5429850047148,0.));
#86510=CARTESIAN_POINT('Ctrl Pts',(39.4380948666368,28.5429850047148,20.));
#86511=CARTESIAN_POINT('Ctrl Pts',(39.4553161583861,28.5139856974786,0.));
#86512=CARTESIAN_POINT('Ctrl Pts',(39.4553161583861,28.5139856974786,20.));
#86513=CARTESIAN_POINT('Ctrl Pts',(39.472516866877,28.4849754750331,0.));
#86514=CARTESIAN_POINT('Ctrl Pts',(39.472516866877,28.4849754750331,20.));
#86515=CARTESIAN_POINT('Ctrl Pts',(39.4896969846589,28.455954351628,0.));
#86516=CARTESIAN_POINT('Ctrl Pts',(39.4896969846589,28.455954351628,20.));
#86517=CARTESIAN_POINT('Ctrl Pts',(39.5068565042907,28.4269223415187,0.));
#86518=CARTESIAN_POINT('Ctrl Pts',(39.5068565042907,28.4269223415187,20.));
#86519=CARTESIAN_POINT('Ctrl Pts',(39.5239954183412,28.3978794589661,0.));
#86520=CARTESIAN_POINT('Ctrl Pts',(39.5239954183412,28.3978794589661,20.));
#86521=CARTESIAN_POINT('Ctrl Pts',(39.5411137193887,28.3688257182364,0.));
#86522=CARTESIAN_POINT('Ctrl Pts',(39.5411137193887,28.3688257182364,20.));
#86523=CARTESIAN_POINT('Ctrl Pts',(39.5582114000212,28.3397611336014,0.));
#86524=CARTESIAN_POINT('Ctrl Pts',(39.5582114000212,28.3397611336014,20.));
#86525=CARTESIAN_POINT('Ctrl Pts',(39.5752884528361,28.3106857193381,0.));
#86526=CARTESIAN_POINT('Ctrl Pts',(39.5752884528361,28.3106857193381,20.));
#86527=CARTESIAN_POINT('Ctrl Pts',(39.5923448704403,28.2815994897291,0.));
#86528=CARTESIAN_POINT('Ctrl Pts',(39.5923448704403,28.2815994897291,20.));
#86529=CARTESIAN_POINT('Ctrl Pts',(39.6093806454502,28.2525024590626,0.));
#86530=CARTESIAN_POINT('Ctrl Pts',(39.6093806454502,28.2525024590626,20.));
#86531=CARTESIAN_POINT('Ctrl Pts',(39.6263957704923,28.2233946416323,0.));
#86532=CARTESIAN_POINT('Ctrl Pts',(39.6263957704923,28.2233946416323,20.));
#86533=CARTESIAN_POINT('Ctrl Pts',(39.6433902382029,28.1942760517371,0.));
#86534=CARTESIAN_POINT('Ctrl Pts',(39.6433902382029,28.1942760517371,20.));
#86535=CARTESIAN_POINT('Ctrl Pts',(39.6603640412281,28.1651467036817,0.));
#86536=CARTESIAN_POINT('Ctrl Pts',(39.6603640412281,28.1651467036817,20.));
#86537=CARTESIAN_POINT('Ctrl Pts',(39.6773171722241,28.136006611776,0.));
#86538=CARTESIAN_POINT('Ctrl Pts',(39.6773171722241,28.136006611776,20.));
#86539=CARTESIAN_POINT('Ctrl Pts',(39.6942496238565,28.1068557903356,0.));
#86540=CARTESIAN_POINT('Ctrl Pts',(39.6942496238565,28.1068557903356,20.));
#86541=CARTESIAN_POINT('Ctrl Pts',(39.7111613888006,28.0776942536814,0.));
#86542=CARTESIAN_POINT('Ctrl Pts',(39.7111613888006,28.0776942536814,20.));
#86543=CARTESIAN_POINT('Ctrl Pts',(39.728052459741,28.0485220161395,0.));
#86544=CARTESIAN_POINT('Ctrl Pts',(39.728052459741,28.0485220161395,20.));
#86545=CARTESIAN_POINT('Ctrl Pts',(39.7449228293718,28.0193390920415,0.));
#86546=CARTESIAN_POINT('Ctrl Pts',(39.7449228293718,28.0193390920415,20.));
#86547=CARTESIAN_POINT('Ctrl Pts',(39.7617724903968,27.9901454957246,0.));
#86548=CARTESIAN_POINT('Ctrl Pts',(39.7617724903968,27.9901454957246,20.));
#86549=CARTESIAN_POINT('Ctrl Pts',(39.7786014355293,27.960941241531,0.));
#86550=CARTESIAN_POINT('Ctrl Pts',(39.7786014355293,27.960941241531,20.));
#86551=CARTESIAN_POINT('Ctrl Pts',(39.795409657493,27.9317263438086,0.));
#86552=CARTESIAN_POINT('Ctrl Pts',(39.795409657493,27.9317263438086,20.));
#86553=CARTESIAN_POINT('Ctrl Pts',(39.8121971490214,27.9025008169107,0.));
#86554=CARTESIAN_POINT('Ctrl Pts',(39.8121971490214,27.9025008169107,20.));
#86555=CARTESIAN_POINT('Ctrl Pts',(39.828963902858,27.8732646751959,0.));
#86556=CARTESIAN_POINT('Ctrl Pts',(39.828963902858,27.8732646751959,20.));
#86557=CARTESIAN_POINT('Ctrl Pts',(39.8457099117559,27.8440179330284,0.));
#86558=CARTESIAN_POINT('Ctrl Pts',(39.8457099117559,27.8440179330284,20.));
#86559=CARTESIAN_POINT('Ctrl Pts',(39.862435168478,27.8147606047778,0.));
#86560=CARTESIAN_POINT('Ctrl Pts',(39.862435168478,27.8147606047778,20.));
#86561=CARTESIAN_POINT('Ctrl Pts',(39.8791396657966,27.785492704819,0.));
#86562=CARTESIAN_POINT('Ctrl Pts',(39.8791396657966,27.785492704819,20.));
#86563=CARTESIAN_POINT('Ctrl Pts',(39.8958233964934,27.7562142475319,0.));
#86564=CARTESIAN_POINT('Ctrl Pts',(39.8958233964934,27.7562142475319,20.));
#86565=CARTESIAN_POINT('Ctrl Pts',(39.9124863533599,27.726925247302,0.));
#86566=CARTESIAN_POINT('Ctrl Pts',(39.9124863533599,27.726925247302,20.));
#86567=CARTESIAN_POINT('Ctrl Pts',(39.9291285291975,27.6976257185198,0.));
#86568=CARTESIAN_POINT('Ctrl Pts',(39.9291285291975,27.6976257185198,20.));
#86569=CARTESIAN_POINT('Ctrl Pts',(39.9457499168175,27.6683156755815,0.));
#86570=CARTESIAN_POINT('Ctrl Pts',(39.9457499168175,27.6683156755815,20.));
#86571=CARTESIAN_POINT('Ctrl Pts',(39.9623505090412,27.6389951328887,0.));
#86572=CARTESIAN_POINT('Ctrl Pts',(39.9623505090412,27.6389951328887,20.));
#86573=CARTESIAN_POINT('Ctrl Pts',(39.9789302986995,27.6096641048483,0.));
#86574=CARTESIAN_POINT('Ctrl Pts',(39.9789302986995,27.6096641048483,20.));
#86575=CARTESIAN_POINT('Ctrl Pts',(39.9954892786331,27.5803226058725,0.));
#86576=CARTESIAN_POINT('Ctrl Pts',(39.9954892786331,27.5803226058725,20.));
#86577=CARTESIAN_POINT('Ctrl Pts',(40.0120274416924,27.5509706503786,0.));
#86578=CARTESIAN_POINT('Ctrl Pts',(40.0120274416924,27.5509706503786,20.));
#86579=CARTESIAN_POINT('Ctrl Pts',(40.0285447807378,27.5216082527897,0.));
#86580=CARTESIAN_POINT('Ctrl Pts',(40.0285447807378,27.5216082527897,20.));
#86581=CARTESIAN_POINT('Ctrl Pts',(40.045041288639,27.4922354275335,0.));
#86582=CARTESIAN_POINT('Ctrl Pts',(40.045041288639,27.4922354275335,20.));
#86583=CARTESIAN_POINT('Ctrl Pts',(40.0615169582759,27.4628521890436,0.));
#86584=CARTESIAN_POINT('Ctrl Pts',(40.0615169582759,27.4628521890436,20.));
#86585=CARTESIAN_POINT('Ctrl Pts',(40.077971782538,27.4334585517582,0.));
#86586=CARTESIAN_POINT('Ctrl Pts',(40.077971782538,27.4334585517582,20.));
#86587=CARTESIAN_POINT('Ctrl Pts',(40.0944057543248,27.4040545301216,0.));
#86588=CARTESIAN_POINT('Ctrl Pts',(40.0944057543248,27.4040545301216,20.));
#86589=CARTESIAN_POINT('Ctrl Pts',(40.1108188665452,27.374640138583,0.));
#86590=CARTESIAN_POINT('Ctrl Pts',(40.1108188665452,27.374640138583,20.));
#86591=CARTESIAN_POINT('Ctrl Pts',(40.1272111121183,27.3452153915969,0.));
#86592=CARTESIAN_POINT('Ctrl Pts',(40.1272111121183,27.3452153915969,20.));
#86593=CARTESIAN_POINT('Ctrl Pts',(40.1435824839731,27.3157803036231,0.));
#86594=CARTESIAN_POINT('Ctrl Pts',(40.1435824839731,27.3157803036231,20.));
#86595=CARTESIAN_POINT('Ctrl Pts',(40.1599329750483,27.2863348891265,0.));
#86596=CARTESIAN_POINT('Ctrl Pts',(40.1599329750483,27.2863348891265,20.));
#86597=CARTESIAN_POINT('Ctrl Pts',(40.1762625782924,27.2568791625774,0.));
#86598=CARTESIAN_POINT('Ctrl Pts',(40.1762625782924,27.2568791625774,20.));
#86599=CARTESIAN_POINT('Ctrl Pts',(40.1925712866631,27.2274131384508,0.));
#86600=CARTESIAN_POINT('Ctrl Pts',(40.1925712866631,27.2274131384508,20.));
#86601=CARTESIAN_POINT('Ctrl Pts',(40.2088590931287,27.1979368312277,0.));
#86602=CARTESIAN_POINT('Ctrl Pts',(40.2088590931287,27.1979368312277,20.));
#86603=CARTESIAN_POINT('Ctrl Pts',(40.2251259906669,27.1684502553939,0.));
#86604=CARTESIAN_POINT('Ctrl Pts',(40.2251259906669,27.1684502553939,20.));
#86605=CARTESIAN_POINT('Ctrl Pts',(40.2413719722657,27.1389534254409,0.));
#86606=CARTESIAN_POINT('Ctrl Pts',(40.2413719722657,27.1389534254409,20.));
#86607=CARTESIAN_POINT('Ctrl Pts',(40.2575970309226,27.1094463558649,0.));
#86608=CARTESIAN_POINT('Ctrl Pts',(40.2575970309226,27.1094463558649,20.));
#86609=CARTESIAN_POINT('Ctrl Pts',(40.2738011596454,27.0799290611676,0.));
#86610=CARTESIAN_POINT('Ctrl Pts',(40.2738011596454,27.0799290611676,20.));
#86611=CARTESIAN_POINT('Ctrl Pts',(40.2899843514517,27.0504015558557,0.));
#86612=CARTESIAN_POINT('Ctrl Pts',(40.2899843514517,27.0504015558557,20.));
#86613=CARTESIAN_POINT('Ctrl Pts',(40.3061465993685,27.0208638544413,0.));
#86614=CARTESIAN_POINT('Ctrl Pts',(40.3061465993685,27.0208638544413,20.));
#86615=CARTESIAN_POINT('Ctrl Pts',(40.3222878964329,26.9913159714415,0.));
#86616=CARTESIAN_POINT('Ctrl Pts',(40.3222878964329,26.9913159714415,20.));
#86617=CARTESIAN_POINT('Ctrl Pts',(40.3384082356913,26.9617579213786,0.));
#86618=CARTESIAN_POINT('Ctrl Pts',(40.3384082356913,26.9617579213786,20.));
#86619=CARTESIAN_POINT('Ctrl Pts',(40.3545076102003,26.9321897187802,0.));
#86620=CARTESIAN_POINT('Ctrl Pts',(40.3545076102003,26.9321897187802,20.));
#86621=CARTESIAN_POINT('Ctrl Pts',(40.3705860130263,26.9026113781788,0.));
#86622=CARTESIAN_POINT('Ctrl Pts',(40.3705860130263,26.9026113781788,20.));
#86623=CARTESIAN_POINT('Ctrl Pts',(40.386643437246,26.8730229141124,0.));
#86624=CARTESIAN_POINT('Ctrl Pts',(40.386643437246,26.8730229141124,20.));
#86625=CARTESIAN_POINT('Ctrl Pts',(40.4026798759458,26.8434243411241,0.));
#86626=CARTESIAN_POINT('Ctrl Pts',(40.4026798759458,26.8434243411241,20.));
#86627=CARTESIAN_POINT('Ctrl Pts',(40.4186953222224,26.8138156737619,0.));
#86628=CARTESIAN_POINT('Ctrl Pts',(40.4186953222224,26.8138156737619,20.));
#86629=CARTESIAN_POINT('Ctrl Pts',(40.4346897691821,26.7841969265794,0.));
#86630=CARTESIAN_POINT('Ctrl Pts',(40.4346897691821,26.7841969265794,20.));
#86631=CARTESIAN_POINT('Ctrl Pts',(40.4506632099408,26.754568114135,0.));
#86632=CARTESIAN_POINT('Ctrl Pts',(40.4506632099408,26.754568114135,20.));
#86633=CARTESIAN_POINT('Ctrl Pts',(40.4666156376241,26.7249292509923,0.));
#86634=CARTESIAN_POINT('Ctrl Pts',(40.4666156376241,26.7249292509923,20.));
#86635=CARTESIAN_POINT('Ctrl Pts',(40.4825470453679,26.6952803517197,0.));
#86636=CARTESIAN_POINT('Ctrl Pts',(40.4825470453679,26.6952803517197,20.));
#86637=CARTESIAN_POINT('Ctrl Pts',(40.4984574263178,26.6656214308914,0.));
#86638=CARTESIAN_POINT('Ctrl Pts',(40.4984574263178,26.6656214308914,20.));
#86639=CARTESIAN_POINT('Ctrl Pts',(40.5143467736295,26.6359525030862,0.));
#86640=CARTESIAN_POINT('Ctrl Pts',(40.5143467736295,26.6359525030862,20.));
#86641=CARTESIAN_POINT('Ctrl Pts',(40.5302150804687,26.606273582888,0.));
#86642=CARTESIAN_POINT('Ctrl Pts',(40.5302150804687,26.606273582888,20.));
#86643=CARTESIAN_POINT('Ctrl Pts',(40.546062340011,26.5765846848862,0.));
#86644=CARTESIAN_POINT('Ctrl Pts',(40.546062340011,26.5765846848862,20.));
#86645=CARTESIAN_POINT('Ctrl Pts',(40.5618885454414,26.5468858236748,0.));
#86646=CARTESIAN_POINT('Ctrl Pts',(40.5618885454414,26.5468858236748,20.));
#86647=CARTESIAN_POINT('Ctrl Pts',(40.5776936899555,26.5171770138532,0.));
#86648=CARTESIAN_POINT('Ctrl Pts',(40.5776936899555,26.5171770138532,20.));
#86649=CARTESIAN_POINT('Ctrl Pts',(40.5934777667583,26.4874582700259,0.));
#86650=CARTESIAN_POINT('Ctrl Pts',(40.5934777667583,26.4874582700259,20.));
#86651=CARTESIAN_POINT('Ctrl Pts',(40.6092407690651,26.4577296068023,0.));
#86652=CARTESIAN_POINT('Ctrl Pts',(40.6092407690651,26.4577296068023,20.));
#86653=CARTESIAN_POINT('Ctrl Pts',(40.6249826901011,26.4279910387971,0.));
#86654=CARTESIAN_POINT('Ctrl Pts',(40.6249826901011,26.4279910387971,20.));
#86655=CARTESIAN_POINT('Ctrl Pts',(40.6407035231015,26.3982425806297,0.));
#86656=CARTESIAN_POINT('Ctrl Pts',(40.6407035231015,26.3982425806297,20.));
#86657=CARTESIAN_POINT('Ctrl Pts',(40.6564032613109,26.3684842469248,0.));
#86658=CARTESIAN_POINT('Ctrl Pts',(40.6564032613109,26.3684842469248,20.));
#86659=CARTESIAN_POINT('Ctrl Pts',(40.6720818979844,26.338716052312,0.));
#86660=CARTESIAN_POINT('Ctrl Pts',(40.6720818979844,26.338716052312,20.));
#86661=CARTESIAN_POINT('Ctrl Pts',(40.6877394263869,26.308938011426,0.));
#86662=CARTESIAN_POINT('Ctrl Pts',(40.6877394263869,26.308938011426,20.));
#86663=CARTESIAN_POINT('Ctrl Pts',(40.7033758397932,26.2791501389067,0.));
#86664=CARTESIAN_POINT('Ctrl Pts',(40.7033758397932,26.2791501389067,20.));
#86665=CARTESIAN_POINT('Ctrl Pts',(40.7189911314882,26.2493524493989,0.));
#86666=CARTESIAN_POINT('Ctrl Pts',(40.7189911314882,26.2493524493989,20.));
#86667=CARTESIAN_POINT('Ctrl Pts',(40.7345852947663,26.2195449575524,0.));
#86668=CARTESIAN_POINT('Ctrl Pts',(40.7345852947663,26.2195449575524,20.));
#86669=CARTESIAN_POINT('Ctrl Pts',(40.7501583229328,26.1897276780219,0.));
#86670=CARTESIAN_POINT('Ctrl Pts',(40.7501583229328,26.1897276780219,20.));
#86671=CARTESIAN_POINT('Ctrl Pts',(40.7657102093021,26.1599006254674,0.));
#86672=CARTESIAN_POINT('Ctrl Pts',(40.7657102093021,26.1599006254674,20.));
#86673=CARTESIAN_POINT('Ctrl Pts',(40.7812409471992,26.1300638145535,0.));
#86674=CARTESIAN_POINT('Ctrl Pts',(40.7812409471992,26.1300638145535,20.));
#86675=CARTESIAN_POINT('Ctrl Pts',(40.7967505299588,26.1002172599501,0.));
#86676=CARTESIAN_POINT('Ctrl Pts',(40.7967505299588,26.1002172599501,20.));
#86677=CARTESIAN_POINT('Ctrl Pts',(40.8122389509256,26.0703609763318,0.));
#86678=CARTESIAN_POINT('Ctrl Pts',(40.8122389509256,26.0703609763318,20.));
#86679=CARTESIAN_POINT('Ctrl Pts',(40.8277062034539,26.0404949783787,0.));
#86680=CARTESIAN_POINT('Ctrl Pts',(40.8277062034539,26.0404949783787,20.));
#86681=CARTESIAN_POINT('Ctrl Pts',(40.843152280908,26.0106192807756,0.));
#86682=CARTESIAN_POINT('Ctrl Pts',(40.843152280908,26.0106192807756,20.));
#86683=CARTESIAN_POINT('Ctrl Pts',(40.8585771766627,25.9807338982121,0.));
#86684=CARTESIAN_POINT('Ctrl Pts',(40.8585771766627,25.9807338982121,20.));
#86685=CARTESIAN_POINT('Ctrl Pts',(40.8739808841024,25.9508388453831,0.));
#86686=CARTESIAN_POINT('Ctrl Pts',(40.8739808841024,25.9508388453831,20.));
#86687=CARTESIAN_POINT('Ctrl Pts',(40.8893633966224,25.9209341369879,0.));
#86688=CARTESIAN_POINT('Ctrl Pts',(40.8893633966224,25.9209341369879,20.));
#86689=CARTESIAN_POINT('Ctrl Pts',(40.9047247076274,25.891019787731,0.));
#86690=CARTESIAN_POINT('Ctrl Pts',(40.9047247076274,25.891019787731,20.));
#86691=CARTESIAN_POINT('Ctrl Pts',(40.9200648105322,25.861095812322,0.));
#86692=CARTESIAN_POINT('Ctrl Pts',(40.9200648105322,25.861095812322,20.));
#86693=CARTESIAN_POINT('Ctrl Pts',(40.9353836987613,25.8311622254754,0.));
#86694=CARTESIAN_POINT('Ctrl Pts',(40.9353836987613,25.8311622254754,20.));
#86695=CARTESIAN_POINT('Ctrl Pts',(40.9506813657491,25.8012190419102,0.));
#86696=CARTESIAN_POINT('Ctrl Pts',(40.9506813657491,25.8012190419102,20.));
#86697=CARTESIAN_POINT('Ctrl Pts',(40.9659578049399,25.7712662763511,0.));
#86698=CARTESIAN_POINT('Ctrl Pts',(40.9659578049399,25.7712662763511,20.));
#86699=CARTESIAN_POINT('Ctrl Pts',(40.981213009789,25.7413039435271,0.));
#86700=CARTESIAN_POINT('Ctrl Pts',(40.981213009789,25.7413039435271,20.));
#86701=CARTESIAN_POINT('Ctrl Pts',(40.9964469737612,25.7113320581728,0.));
#86702=CARTESIAN_POINT('Ctrl Pts',(40.9964469737612,25.7113320581728,20.));
#86703=CARTESIAN_POINT('Ctrl Pts',(41.0116596903316,25.6813506350271,0.));
#86704=CARTESIAN_POINT('Ctrl Pts',(41.0116596903316,25.6813506350271,20.));
#86705=CARTESIAN_POINT('Ctrl Pts',(41.0268511529852,25.6513596888338,0.));
#86706=CARTESIAN_POINT('Ctrl Pts',(41.0268511529852,25.6513596888338,20.));
#86707=CARTESIAN_POINT('Ctrl Pts',(41.0420213552163,25.6213592343415,0.));
#86708=CARTESIAN_POINT('Ctrl Pts',(41.0420213552163,25.6213592343415,20.));
#86709=CARTESIAN_POINT('Ctrl Pts',(41.05717029053,25.5913492863038,0.));
#86710=CARTESIAN_POINT('Ctrl Pts',(41.05717029053,25.5913492863038,20.));
#86711=CARTESIAN_POINT('Ctrl Pts',(41.072297952441,25.5613298594791,0.));
#86712=CARTESIAN_POINT('Ctrl Pts',(41.072297952441,25.5613298594791,20.));
#86713=CARTESIAN_POINT('Ctrl Pts',(41.0874043344745,25.5313009686309,0.));
#86714=CARTESIAN_POINT('Ctrl Pts',(41.0874043344745,25.5313009686309,20.));
#86715=CARTESIAN_POINT('Ctrl Pts',(41.1024894301655,25.5012626285275,0.));
#86716=CARTESIAN_POINT('Ctrl Pts',(41.1024894301655,25.5012626285275,20.));
#86717=CARTESIAN_POINT('Ctrl Pts',(41.1175532330596,25.4712148539422,0.));
#86718=CARTESIAN_POINT('Ctrl Pts',(41.1175532330596,25.4712148539422,20.));
#86719=CARTESIAN_POINT('Ctrl Pts',(41.1325957367119,25.4411576596529,0.));
#86720=CARTESIAN_POINT('Ctrl Pts',(41.1325957367119,25.4411576596529,20.));
#86721=CARTESIAN_POINT('Ctrl Pts',(41.1476169346881,25.4110910604425,0.));
#86722=CARTESIAN_POINT('Ctrl Pts',(41.1476169346881,25.4110910604425,20.));
#86723=CARTESIAN_POINT('Ctrl Pts',(41.1626168205634,25.3810150710984,0.));
#86724=CARTESIAN_POINT('Ctrl Pts',(41.1626168205634,25.3810150710984,20.));
#86725=CARTESIAN_POINT('Ctrl Pts',(41.1775953879232,25.3509297064131,0.));
#86726=CARTESIAN_POINT('Ctrl Pts',(41.1775953879232,25.3509297064131,20.));
#86727=CARTESIAN_POINT('Ctrl Pts',(41.1925526303629,25.3208349811839,0.));
#86728=CARTESIAN_POINT('Ctrl Pts',(41.1925526303629,25.3208349811839,20.));
#86729=CARTESIAN_POINT('Ctrl Pts',(41.2074885414881,25.2907309102128,0.));
#86730=CARTESIAN_POINT('Ctrl Pts',(41.2074885414881,25.2907309102128,20.));
#86731=CARTESIAN_POINT('Ctrl Pts',(41.2224031149147,25.2606175083067,0.));
#86732=CARTESIAN_POINT('Ctrl Pts',(41.2224031149147,25.2606175083067,20.));
#86733=CARTESIAN_POINT('Ctrl Pts',(41.2372963442684,25.2304947902774,0.));
#86734=CARTESIAN_POINT('Ctrl Pts',(41.2372963442684,25.2304947902774,20.));
#86735=CARTESIAN_POINT('Ctrl Pts',(41.2521682231854,25.2003627709414,0.));
#86736=CARTESIAN_POINT('Ctrl Pts',(41.2521682231854,25.2003627709414,20.));
#86737=CARTESIAN_POINT('Ctrl Pts',(41.2670187453114,25.1702214651198,0.));
#86738=CARTESIAN_POINT('Ctrl Pts',(41.2670187453114,25.1702214651198,20.));
#86739=CARTESIAN_POINT('Ctrl Pts',(41.2818479043026,25.1400708876386,0.));
#86740=CARTESIAN_POINT('Ctrl Pts',(41.2818479043026,25.1400708876386,20.));
#86741=CARTESIAN_POINT('Ctrl Pts',(41.2966556938255,25.1099110533288,0.));
#86742=CARTESIAN_POINT('Ctrl Pts',(41.2966556938255,25.1099110533288,20.));
#86743=CARTESIAN_POINT('Ctrl Pts',(41.3114421075567,25.0797419770258,0.));
#86744=CARTESIAN_POINT('Ctrl Pts',(41.3114421075567,25.0797419770258,20.));
#86745=CARTESIAN_POINT('Ctrl Pts',(41.3262071391823,25.0495636735701,0.));
#86746=CARTESIAN_POINT('Ctrl Pts',(41.3262071391823,25.0495636735701,20.));
#86747=CARTESIAN_POINT('Ctrl Pts',(41.3409507823989,25.0193761578067,0.));
#86748=CARTESIAN_POINT('Ctrl Pts',(41.3409507823989,25.0193761578067,20.));
#86749=CARTESIAN_POINT('Ctrl Pts',(41.3556730309131,24.9891794445855,0.));
#86750=CARTESIAN_POINT('Ctrl Pts',(41.3556730309131,24.9891794445855,20.));
#86751=CARTESIAN_POINT('Ctrl Pts',(41.3703738784418,24.9589735487609,0.));
#86752=CARTESIAN_POINT('Ctrl Pts',(41.3703738784418,24.9589735487609,20.));
#86753=CARTESIAN_POINT('Ctrl Pts',(41.3850533187123,24.9287584851923,0.));
#86754=CARTESIAN_POINT('Ctrl Pts',(41.3850533187123,24.9287584851923,20.));
#86755=CARTESIAN_POINT('Ctrl Pts',(41.3997113454618,24.8985342687436,0.));
#86756=CARTESIAN_POINT('Ctrl Pts',(41.3997113454618,24.8985342687436,20.));
#86757=CARTESIAN_POINT('Ctrl Pts',(41.4143479524375,24.8683009142837,0.));
#86758=CARTESIAN_POINT('Ctrl Pts',(41.4143479524375,24.8683009142837,20.));
#86759=CARTESIAN_POINT('Ctrl Pts',(41.4289631333969,24.8380584366859,0.));
#86760=CARTESIAN_POINT('Ctrl Pts',(41.4289631333969,24.8380584366859,20.));
#86761=CARTESIAN_POINT('Ctrl Pts',(41.443556882107,24.8078068508284,0.));
#86762=CARTESIAN_POINT('Ctrl Pts',(41.443556882107,24.8078068508284,20.));
#86763=CARTESIAN_POINT('Ctrl Pts',(41.4581291923457,24.7775461715943,0.));
#86764=CARTESIAN_POINT('Ctrl Pts',(41.4581291923457,24.7775461715943,20.));
#86765=CARTESIAN_POINT('Ctrl Pts',(41.4726800579006,24.7472764138709,0.));
#86766=CARTESIAN_POINT('Ctrl Pts',(41.4726800579006,24.7472764138709,20.));
#86767=CARTESIAN_POINT('Ctrl Pts',(41.4872094725701,24.7169975925505,0.));
#86768=CARTESIAN_POINT('Ctrl Pts',(41.4872094725701,24.7169975925505,20.));
#86769=CARTESIAN_POINT('Ctrl Pts',(41.5017174301628,24.68670972253,0.));
#86770=CARTESIAN_POINT('Ctrl Pts',(41.5017174301628,24.68670972253,20.));
#86771=CARTESIAN_POINT('Ctrl Pts',(41.516203924497,24.6564128187107,0.));
#86772=CARTESIAN_POINT('Ctrl Pts',(41.516203924497,24.6564128187107,20.));
#86773=CARTESIAN_POINT('Ctrl Pts',(41.5306689494012,24.626106895999,0.));
#86774=CARTESIAN_POINT('Ctrl Pts',(41.5306689494012,24.626106895999,20.));
#86775=CARTESIAN_POINT('Ctrl Pts',(41.545112498714,24.5957919693057,0.));
#86776=CARTESIAN_POINT('Ctrl Pts',(41.545112498714,24.5957919693057,20.));
#86777=CARTESIAN_POINT('Ctrl Pts',(41.5595345662842,24.5654680535465,0.));
#86778=CARTESIAN_POINT('Ctrl Pts',(41.5595345662842,24.5654680535465,20.));
#86779=CARTESIAN_POINT('Ctrl Pts',(41.5739351459709,24.5351351636416,0.));
#86780=CARTESIAN_POINT('Ctrl Pts',(41.5739351459709,24.5351351636416,20.));
#86781=CARTESIAN_POINT('Ctrl Pts',(41.5883142316433,24.5047933145158,0.));
#86782=CARTESIAN_POINT('Ctrl Pts',(41.5883142316433,24.5047933145158,20.));
#86783=CARTESIAN_POINT('Ctrl Pts',(41.6026718171809,24.4744425210985,0.));
#86784=CARTESIAN_POINT('Ctrl Pts',(41.6026718171809,24.4744425210985,20.));
#86785=CARTESIAN_POINT('Ctrl Pts',(41.6170078964732,24.4440827983238,0.));
#86786=CARTESIAN_POINT('Ctrl Pts',(41.6170078964732,24.4440827983238,20.));
#86787=CARTESIAN_POINT('Ctrl Pts',(41.6313224634201,24.4137141611302,0.));
#86788=CARTESIAN_POINT('Ctrl Pts',(41.6313224634201,24.4137141611302,20.));
#86789=CARTESIAN_POINT('Ctrl Pts',(41.6456155119319,24.3833366244611,0.));
#86790=CARTESIAN_POINT('Ctrl Pts',(41.6456155119319,24.3833366244611,20.));
#86791=CARTESIAN_POINT('Ctrl Pts',(41.6598870359289,24.3529502032644,0.));
#86792=CARTESIAN_POINT('Ctrl Pts',(41.6598870359289,24.3529502032644,20.));
#86793=CARTESIAN_POINT('Ctrl Pts',(41.6741370293416,24.3225549124927,0.));
#86794=CARTESIAN_POINT('Ctrl Pts',(41.6741370293416,24.3225549124927,20.));
#86795=CARTESIAN_POINT('Ctrl Pts',(41.6883654861106,24.292150767103,0.));
#86796=CARTESIAN_POINT('Ctrl Pts',(41.6883654861106,24.292150767103,20.));
#86797=CARTESIAN_POINT('Ctrl Pts',(41.7025724001866,24.2617377820568,0.));
#86798=CARTESIAN_POINT('Ctrl Pts',(41.7025724001866,24.2617377820568,20.));
#86799=CARTESIAN_POINT('Ctrl Pts',(41.7167577655309,24.2313159723205,0.));
#86800=CARTESIAN_POINT('Ctrl Pts',(41.7167577655309,24.2313159723205,20.));
#86801=CARTESIAN_POINT('Ctrl Pts',(41.7309215761147,24.2008853528648,0.));
#86802=CARTESIAN_POINT('Ctrl Pts',(41.7309215761147,24.2008853528648,20.));
#86803=CARTESIAN_POINT('Ctrl Pts',(41.7450638259196,24.1704459386651,0.));
#86804=CARTESIAN_POINT('Ctrl Pts',(41.7450638259196,24.1704459386651,20.));
#86805=CARTESIAN_POINT('Ctrl Pts',(41.7591845089374,24.1399977447013,0.));
#86806=CARTESIAN_POINT('Ctrl Pts',(41.7591845089374,24.1399977447013,20.));
#86807=CARTESIAN_POINT('Ctrl Pts',(41.7732836191701,24.1095407859578,0.));
#86808=CARTESIAN_POINT('Ctrl Pts',(41.7732836191701,24.1095407859578,20.));
#86809=CARTESIAN_POINT('Ctrl Pts',(41.78736115063,24.0790750774236,0.));
#86810=CARTESIAN_POINT('Ctrl Pts',(41.78736115063,24.0790750774236,20.));
#86811=CARTESIAN_POINT('Ctrl Pts',(41.8014170973399,24.0486006340924,0.));
#86812=CARTESIAN_POINT('Ctrl Pts',(41.8014170973399,24.0486006340924,20.));
#86813=CARTESIAN_POINT('Ctrl Pts',(41.8154514533324,24.0181174709622,0.));
#86814=CARTESIAN_POINT('Ctrl Pts',(41.8154514533324,24.0181174709622,20.));
#86815=CARTESIAN_POINT('Ctrl Pts',(41.8294642126506,23.9876256030355,0.));
#86816=CARTESIAN_POINT('Ctrl Pts',(41.8294642126506,23.9876256030355,20.));
#86817=CARTESIAN_POINT('Ctrl Pts',(41.8434553693478,23.9571250453194,0.));
#86818=CARTESIAN_POINT('Ctrl Pts',(41.8434553693478,23.9571250453194,20.));
#86819=CARTESIAN_POINT('Ctrl Pts',(41.8574249174873,23.9266158128252,0.));
#86820=CARTESIAN_POINT('Ctrl Pts',(41.8574249174873,23.9266158128252,20.));
#86821=CARTESIAN_POINT('Ctrl Pts',(41.8713728511429,23.8960979205694,0.));
#86822=CARTESIAN_POINT('Ctrl Pts',(41.8713728511429,23.8960979205694,20.));
#86823=CARTESIAN_POINT('Ctrl Pts',(41.8852991643986,23.8655713835725,0.));
#86824=CARTESIAN_POINT('Ctrl Pts',(41.8852991643986,23.8655713835725,20.));
#86825=CARTESIAN_POINT('Ctrl Pts',(41.8992038513488,23.8350362168598,0.));
#86826=CARTESIAN_POINT('Ctrl Pts',(41.8992038513488,23.8350362168598,20.));
#86827=CARTESIAN_POINT('Ctrl Pts',(41.9130869060982,23.8044924354607,0.));
#86828=CARTESIAN_POINT('Ctrl Pts',(41.9130869060982,23.8044924354607,20.));
#86829=CARTESIAN_POINT('Ctrl Pts',(41.9269483227618,23.7739400544092,0.));
#86830=CARTESIAN_POINT('Ctrl Pts',(41.9269483227618,23.7739400544092,20.));
#86831=CARTESIAN_POINT('Ctrl Pts',(41.9407880954647,23.7433790887435,0.));
#86832=CARTESIAN_POINT('Ctrl Pts',(41.9407880954647,23.7433790887435,20.));
#86833=CARTESIAN_POINT('Ctrl Pts',(41.9546062183422,23.7128095535066,0.));
#86834=CARTESIAN_POINT('Ctrl Pts',(41.9546062183422,23.7128095535066,20.));
#86835=CARTESIAN_POINT('Ctrl Pts',(41.9684026855399,23.6822314637457,0.));
#86836=CARTESIAN_POINT('Ctrl Pts',(41.9684026855399,23.6822314637457,20.));
#86837=CARTESIAN_POINT('Ctrl Pts',(41.9821774912141,23.651644834513,0.));
#86838=CARTESIAN_POINT('Ctrl Pts',(41.9821774912141,23.651644834513,20.));
#86839=CARTESIAN_POINT('Ctrl Pts',(41.9959306295311,23.6210496808648,0.));
#86840=CARTESIAN_POINT('Ctrl Pts',(41.9959306295311,23.6210496808648,20.));
#86841=CARTESIAN_POINT('Ctrl Pts',(42.0096620946675,23.5904460178619,0.));
#86842=CARTESIAN_POINT('Ctrl Pts',(42.0096620946675,23.5904460178619,20.));
#86843=CARTESIAN_POINT('Ctrl Pts',(42.02337188081,23.5598338605694,0.));
#86844=CARTESIAN_POINT('Ctrl Pts',(42.02337188081,23.5598338605694,20.));
#86845=CARTESIAN_POINT('Ctrl Pts',(42.0370599821558,23.5292132240567,0.));
#86846=CARTESIAN_POINT('Ctrl Pts',(42.0370599821558,23.5292132240567,20.));
#86847=CARTESIAN_POINT('Ctrl Pts',(42.0507263929126,23.4985841233977,0.));
#86848=CARTESIAN_POINT('Ctrl Pts',(42.0507263929126,23.4985841233977,20.));
#86849=CARTESIAN_POINT('Ctrl Pts',(42.0643711072981,23.4679465736707,0.));
#86850=CARTESIAN_POINT('Ctrl Pts',(42.0643711072981,23.4679465736707,20.));
#86851=CARTESIAN_POINT('Ctrl Pts',(42.0779941195407,23.4373005899585,0.));
#86852=CARTESIAN_POINT('Ctrl Pts',(42.0779941195407,23.4373005899585,20.));
#86853=CARTESIAN_POINT('Ctrl Pts',(42.0915954238788,23.4066461873484,0.));
#86854=CARTESIAN_POINT('Ctrl Pts',(42.0915954238788,23.4066461873484,20.));
#86855=CARTESIAN_POINT('Ctrl Pts',(42.1051750145614,23.3759833809318,0.));
#86856=CARTESIAN_POINT('Ctrl Pts',(42.1051750145614,23.3759833809318,20.));
#86857=CARTESIAN_POINT('Ctrl Pts',(42.1187328858474,23.3453121858047,0.));
#86858=CARTESIAN_POINT('Ctrl Pts',(42.1187328858474,23.3453121858047,20.));
#86859=CARTESIAN_POINT('Ctrl Pts',(42.1322690320059,23.3146326170671,0.));
#86860=CARTESIAN_POINT('Ctrl Pts',(42.1322690320059,23.3146326170671,20.));
#86861=CARTESIAN_POINT('Ctrl Pts',(42.1457834473169,23.2839446898238,0.));
#86862=CARTESIAN_POINT('Ctrl Pts',(42.1457834473169,23.2839446898238,20.));
#86863=CARTESIAN_POINT('Ctrl Pts',(42.1592761260708,23.2532484191837,0.));
#86864=CARTESIAN_POINT('Ctrl Pts',(42.1592761260708,23.2532484191837,20.));
#86865=CARTESIAN_POINT('Ctrl Pts',(42.1727470625681,23.2225438202604,0.));
#86866=CARTESIAN_POINT('Ctrl Pts',(42.1727470625681,23.2225438202604,20.));
#86867=CARTESIAN_POINT('Ctrl Pts',(42.1861962511195,23.1918309081713,0.));
#86868=CARTESIAN_POINT('Ctrl Pts',(42.1861962511195,23.1918309081713,20.));
#86869=CARTESIAN_POINT('Ctrl Pts',(42.1996236860461,23.1611096980384,0.));
#86870=CARTESIAN_POINT('Ctrl Pts',(42.1996236860461,23.1611096980384,20.));
#86871=CARTESIAN_POINT('Ctrl Pts',(42.2130293616794,23.1303802049881,0.));
#86872=CARTESIAN_POINT('Ctrl Pts',(42.2130293616794,23.1303802049881,20.));
#86873=CARTESIAN_POINT('Ctrl Pts',(42.2264132723611,23.0996424441509,0.));
#86874=CARTESIAN_POINT('Ctrl Pts',(42.2264132723611,23.0996424441509,20.));
#86875=CARTESIAN_POINT('Ctrl Pts',(42.2397754124437,23.0688964306618,0.));
#86876=CARTESIAN_POINT('Ctrl Pts',(42.2397754124437,23.0688964306618,20.));
#86877=CARTESIAN_POINT('Ctrl Pts',(42.2531157762897,23.0381421796601,0.));
#86878=CARTESIAN_POINT('Ctrl Pts',(42.2531157762897,23.0381421796601,20.));
#86879=CARTESIAN_POINT('Ctrl Pts',(42.2664343582719,23.0073797062893,0.));
#86880=CARTESIAN_POINT('Ctrl Pts',(42.2664343582719,23.0073797062893,20.));
#86881=CARTESIAN_POINT('Ctrl Pts',(42.2797311527738,22.9766090256973,0.));
#86882=CARTESIAN_POINT('Ctrl Pts',(42.2797311527738,22.9766090256973,20.));
#86883=CARTESIAN_POINT('Ctrl Pts',(42.2930061541893,22.9458301530364,0.));
#86884=CARTESIAN_POINT('Ctrl Pts',(42.2930061541893,22.9458301530364,20.));
#86885=CARTESIAN_POINT('Ctrl Pts',(42.3062593569225,22.9150431034629,0.));
#86886=CARTESIAN_POINT('Ctrl Pts',(42.3062593569225,22.9150431034629,20.));
#86887=CARTESIAN_POINT('Ctrl Pts',(42.3194907553882,22.8842478921374,0.));
#86888=CARTESIAN_POINT('Ctrl Pts',(42.3194907553882,22.8842478921374,20.));
#86889=CARTESIAN_POINT('Ctrl Pts',(42.3327003440108,22.8534445342249,0.));
#86890=CARTESIAN_POINT('Ctrl Pts',(42.3327003440108,22.8534445342249,20.));
#86891=CARTESIAN_POINT('Ctrl Pts',(42.3458881172255,22.8226330448945,0.));
#86892=CARTESIAN_POINT('Ctrl Pts',(42.3458881172255,22.8226330448945,20.));
#86893=CARTESIAN_POINT('Ctrl Pts',(42.3590540694774,22.7918134393197,0.));
#86894=CARTESIAN_POINT('Ctrl Pts',(42.3590540694774,22.7918134393197,20.));
#86895=CARTESIAN_POINT('Ctrl Pts',(42.3721981952224,22.7609857326781,0.));
#86896=CARTESIAN_POINT('Ctrl Pts',(42.3721981952224,22.7609857326781,20.));
#86897=CARTESIAN_POINT('Ctrl Pts',(42.3853204889273,22.7301499401517,0.));
#86898=CARTESIAN_POINT('Ctrl Pts',(42.3853204889273,22.7301499401517,20.));
#86899=CARTESIAN_POINT('Ctrl Pts',(42.398420945069,22.6993060769268,0.));
#86900=CARTESIAN_POINT('Ctrl Pts',(42.398420945069,22.6993060769268,20.));
#86901=CARTESIAN_POINT('Ctrl Pts',(42.411499558135,22.6684541581936,0.));
#86902=CARTESIAN_POINT('Ctrl Pts',(42.411499558135,22.6684541581936,20.));
#86903=CARTESIAN_POINT('Ctrl Pts',(42.4245563226236,22.6375941991468,0.));
#86904=CARTESIAN_POINT('Ctrl Pts',(42.4245563226236,22.6375941991468,20.));
#86905=CARTESIAN_POINT('Ctrl Pts',(42.4375912330427,22.6067262149851,0.));
#86906=CARTESIAN_POINT('Ctrl Pts',(42.4375912330427,22.6067262149851,20.));
#86907=CARTESIAN_POINT('Ctrl Pts',(42.4506042839107,22.5758502209116,0.));
#86908=CARTESIAN_POINT('Ctrl Pts',(42.4506042839107,22.5758502209116,20.));
#86909=CARTESIAN_POINT('Ctrl Pts',(42.4635954697559,22.5449662321334,0.));
#86910=CARTESIAN_POINT('Ctrl Pts',(42.4635954697559,22.5449662321334,20.));
#86911=CARTESIAN_POINT('Ctrl Pts',(42.4765647851171,22.5140742638619,0.));
#86912=CARTESIAN_POINT('Ctrl Pts',(42.4765647851171,22.5140742638619,20.));
#86913=CARTESIAN_POINT('Ctrl Pts',(42.4895122245441,22.4831743313126,0.));
#86914=CARTESIAN_POINT('Ctrl Pts',(42.4895122245441,22.4831743313126,20.));
#86915=CARTESIAN_POINT('Ctrl Pts',(42.502437782597,22.4522664497054,0.));
#86916=CARTESIAN_POINT('Ctrl Pts',(42.502437782597,22.4522664497054,20.));
#86917=CARTESIAN_POINT('Ctrl Pts',(42.5153414538467,22.4213506342639,0.));
#86918=CARTESIAN_POINT('Ctrl Pts',(42.5153414538467,22.4213506342639,20.));
#86919=CARTESIAN_POINT('Ctrl Pts',(42.5282232328747,22.3904269002165,0.));
#86920=CARTESIAN_POINT('Ctrl Pts',(42.5282232328747,22.3904269002165,20.));
#86921=CARTESIAN_POINT('Ctrl Pts',(42.5410831142726,22.3594952627952,0.));
#86922=CARTESIAN_POINT('Ctrl Pts',(42.5410831142726,22.3594952627952,20.));
#86923=CARTESIAN_POINT('Ctrl Pts',(42.5539210926424,22.3285557372364,0.));
#86924=CARTESIAN_POINT('Ctrl Pts',(42.5539210926424,22.3285557372364,20.));
#86925=CARTESIAN_POINT('Ctrl Pts',(42.5667371625962,22.2976083387805,0.));
#86926=CARTESIAN_POINT('Ctrl Pts',(42.5667371625962,22.2976083387805,20.));
#86927=CARTESIAN_POINT('Ctrl Pts',(42.5795313187569,22.2666530826722,0.));
#86928=CARTESIAN_POINT('Ctrl Pts',(42.5795313187569,22.2666530826722,20.));
#86929=CARTESIAN_POINT('Ctrl Pts',(42.5923035557573,22.2356899841602,0.));
#86930=CARTESIAN_POINT('Ctrl Pts',(42.5923035557573,22.2356899841602,20.));
#86931=CARTESIAN_POINT('Ctrl Pts',(42.6050538682411,22.2047190584974,0.));
#86932=CARTESIAN_POINT('Ctrl Pts',(42.6050538682411,22.2047190584974,20.));
#86933=CARTESIAN_POINT('Ctrl Pts',(42.6177822508627,22.1737403209406,0.));
#86934=CARTESIAN_POINT('Ctrl Pts',(42.6177822508627,22.1737403209406,20.));
#86935=CARTESIAN_POINT('Ctrl Pts',(42.6304886982869,22.1427537867512,0.));
#86936=CARTESIAN_POINT('Ctrl Pts',(42.6304886982869,22.1427537867512,20.));
#86937=CARTESIAN_POINT('Ctrl Pts',(42.6431732051887,22.1117594711942,0.));
#86938=CARTESIAN_POINT('Ctrl Pts',(42.6431732051887,22.1117594711942,20.));
#86939=CARTESIAN_POINT('Ctrl Pts',(42.6558357662536,22.0807573895388,0.));
#86940=CARTESIAN_POINT('Ctrl Pts',(42.6558357662536,22.0807573895388,20.));
#86941=CARTESIAN_POINT('Ctrl Pts',(42.6684763761777,22.0497475570584,0.));
#86942=CARTESIAN_POINT('Ctrl Pts',(42.6684763761777,22.0497475570584,20.));
#86943=CARTESIAN_POINT('Ctrl Pts',(42.6810950296678,22.0187299890302,0.));
#86944=CARTESIAN_POINT('Ctrl Pts',(42.6810950296678,22.0187299890302,20.));
#86945=CARTESIAN_POINT('Ctrl Pts',(42.6936917214411,21.9877047007357,0.));
#86946=CARTESIAN_POINT('Ctrl Pts',(42.6936917214411,21.9877047007357,20.));
#86947=CARTESIAN_POINT('Ctrl Pts',(42.7062664462249,21.9566717074606,0.));
#86948=CARTESIAN_POINT('Ctrl Pts',(42.7062664462249,21.9566717074606,20.));
#86949=CARTESIAN_POINT('Ctrl Pts',(42.7188191987573,21.9256310244944,0.));
#86950=CARTESIAN_POINT('Ctrl Pts',(42.7188191987573,21.9256310244944,20.));
#86951=CARTESIAN_POINT('Ctrl Pts',(42.7313499737866,21.8945826671308,0.));
#86952=CARTESIAN_POINT('Ctrl Pts',(42.7313499737866,21.8945826671308,20.));
#86953=CARTESIAN_POINT('Ctrl Pts',(42.7438587660714,21.8635266506674,0.));
#86954=CARTESIAN_POINT('Ctrl Pts',(42.7438587660714,21.8635266506674,20.));
#86955=CARTESIAN_POINT('Ctrl Pts',(42.7563455703812,21.832462990406,0.));
#86956=CARTESIAN_POINT('Ctrl Pts',(42.7563455703812,21.832462990406,20.));
#86957=CARTESIAN_POINT('Ctrl Pts',(42.7688103814962,21.8013917016521,0.));
#86958=CARTESIAN_POINT('Ctrl Pts',(42.7688103814962,21.8013917016521,20.));
#86959=CARTESIAN_POINT('Ctrl Pts',(42.7812531942069,21.7703127997157,0.));
#86960=CARTESIAN_POINT('Ctrl Pts',(42.7812531942069,21.7703127997157,20.));
#86961=CARTESIAN_POINT('Ctrl Pts',(42.7936740033148,21.7392262999104,0.));
#86962=CARTESIAN_POINT('Ctrl Pts',(42.7936740033148,21.7392262999104,20.));
#86963=CARTESIAN_POINT('Ctrl Pts',(42.8060728036313,21.7081322175539,0.));
#86964=CARTESIAN_POINT('Ctrl Pts',(42.8060728036313,21.7081322175539,20.));
#86965=CARTESIAN_POINT('Ctrl Pts',(42.8184495899785,21.677030567968,0.));
#86966=CARTESIAN_POINT('Ctrl Pts',(42.8184495899785,21.677030567968,20.));
#86967=CARTESIAN_POINT('Ctrl Pts',(42.8308043571886,21.6459213664784,0.));
#86968=CARTESIAN_POINT('Ctrl Pts',(42.8308043571886,21.6459213664784,20.));
#86969=CARTESIAN_POINT('Ctrl Pts',(42.8431371001047,21.6148046284149,0.));
#86970=CARTESIAN_POINT('Ctrl Pts',(42.8431371001047,21.6148046284149,20.));
#86971=CARTESIAN_POINT('Ctrl Pts',(42.8554478135801,21.5836803691112,0.));
#86972=CARTESIAN_POINT('Ctrl Pts',(42.8554478135801,21.5836803691112,20.));
#86973=CARTESIAN_POINT('Ctrl Pts',(42.8677364924793,21.5525486039049,0.));
#86974=CARTESIAN_POINT('Ctrl Pts',(42.8677364924793,21.5525486039049,20.));
#86975=CARTESIAN_POINT('Ctrl Pts',(42.8800031316769,21.5214093481377,0.));
#86976=CARTESIAN_POINT('Ctrl Pts',(42.8800031316769,21.5214093481377,20.));
#86977=CARTESIAN_POINT('Ctrl Pts',(42.8922477260581,21.490262617155,0.));
#86978=CARTESIAN_POINT('Ctrl Pts',(42.8922477260581,21.490262617155,20.));
#86979=CARTESIAN_POINT('Ctrl Pts',(42.9044702705183,21.4591084263065,0.));
#86980=CARTESIAN_POINT('Ctrl Pts',(42.9044702705183,21.4591084263065,20.));
#86981=CARTESIAN_POINT('Ctrl Pts',(42.916670759964,21.4279467909454,0.));
#86982=CARTESIAN_POINT('Ctrl Pts',(42.916670759964,21.4279467909454,20.));
#86983=CARTESIAN_POINT('Ctrl Pts',(42.9288491893122,21.3967777264295,0.));
#86984=CARTESIAN_POINT('Ctrl Pts',(42.9288491893122,21.3967777264295,20.));
#86985=CARTESIAN_POINT('Ctrl Pts',(42.9410055534907,21.3656012481199,0.));
#86986=CARTESIAN_POINT('Ctrl Pts',(42.9410055534907,21.3656012481199,20.));
#86987=CARTESIAN_POINT('Ctrl Pts',(42.9531398474371,21.3344173713818,0.));
#86988=CARTESIAN_POINT('Ctrl Pts',(42.9531398474371,21.3344173713818,20.));
#86989=CARTESIAN_POINT('Ctrl Pts',(42.9652520660998,21.3032261115844,0.));
#86990=CARTESIAN_POINT('Ctrl Pts',(42.9652520660998,21.3032261115844,20.));
#86991=CARTESIAN_POINT('Ctrl Pts',(42.9773422044374,21.2720274841006,0.));
#86992=CARTESIAN_POINT('Ctrl Pts',(42.9773422044374,21.2720274841006,20.));
#86993=CARTESIAN_POINT('Ctrl Pts',(42.9894102574195,21.2408215043074,0.));
#86994=CARTESIAN_POINT('Ctrl Pts',(42.9894102574195,21.2408215043074,20.));
#86995=CARTESIAN_POINT('Ctrl Pts',(43.0014562200264,21.2096081875857,0.));
#86996=CARTESIAN_POINT('Ctrl Pts',(43.0014562200264,21.2096081875857,20.));
#86997=CARTESIAN_POINT('Ctrl Pts',(43.0134800872489,21.1783875493205,0.));
#86998=CARTESIAN_POINT('Ctrl Pts',(43.0134800872489,21.1783875493205,20.));
#86999=CARTESIAN_POINT('Ctrl Pts',(43.0254818540885,21.1471596049,0.));
#87000=CARTESIAN_POINT('Ctrl Pts',(43.0254818540885,21.1471596049,20.));
#87001=CARTESIAN_POINT('Ctrl Pts',(43.037461515557,21.1159243697169,0.));
#87002=CARTESIAN_POINT('Ctrl Pts',(43.037461515557,21.1159243697169,20.));
#87003=CARTESIAN_POINT('Ctrl Pts',(43.049419066677,21.0846818591673,0.));
#87004=CARTESIAN_POINT('Ctrl Pts',(43.049419066677,21.0846818591673,20.));
#87005=CARTESIAN_POINT('Ctrl Pts',(43.0613545024815,21.0534320886512,0.));
#87006=CARTESIAN_POINT('Ctrl Pts',(43.0613545024815,21.0534320886512,20.));
#87007=CARTESIAN_POINT('Ctrl Pts',(43.0732678180139,21.0221750735727,0.));
#87008=CARTESIAN_POINT('Ctrl Pts',(43.0732678180139,21.0221750735727,20.));
#87009=CARTESIAN_POINT('Ctrl Pts',(43.0851590083283,20.9909108293397,0.));
#87010=CARTESIAN_POINT('Ctrl Pts',(43.0851590083283,20.9909108293397,20.));
#87011=CARTESIAN_POINT('Ctrl Pts',(43.0970280684896,20.959639371364,0.));
#87012=CARTESIAN_POINT('Ctrl Pts',(43.0970280684896,20.959639371364,20.));
#87013=CARTESIAN_POINT('Ctrl Pts',(43.1088749935734,20.9283607150615,0.));
#87014=CARTESIAN_POINT('Ctrl Pts',(43.1088749935734,20.9283607150615,20.));
#87015=CARTESIAN_POINT('Ctrl Pts',(43.1206997786656,20.8970748758512,0.));
#87016=CARTESIAN_POINT('Ctrl Pts',(43.1206997786656,20.8970748758512,20.));
#87017=CARTESIAN_POINT('Ctrl Pts',(43.132502418863,20.8657818691565,0.));
#87018=CARTESIAN_POINT('Ctrl Pts',(43.132502418863,20.8657818691565,20.));
#87019=CARTESIAN_POINT('Ctrl Pts',(43.1442829092724,20.8344817104039,0.));
#87020=CARTESIAN_POINT('Ctrl Pts',(43.1442829092724,20.8344817104039,20.));
#87021=CARTESIAN_POINT('Ctrl Pts',(43.1560412450117,20.8031744150242,0.));
#87022=CARTESIAN_POINT('Ctrl Pts',(43.1560412450117,20.8031744150242,20.));
#87023=CARTESIAN_POINT('Ctrl Pts',(43.1677774212093,20.7718599984519,0.));
#87024=CARTESIAN_POINT('Ctrl Pts',(43.1677774212093,20.7718599984519,20.));
#87025=CARTESIAN_POINT('Ctrl Pts',(43.1794914330045,20.7405384761252,0.));
#87026=CARTESIAN_POINT('Ctrl Pts',(43.1794914330045,20.7405384761252,20.));
#87027=CARTESIAN_POINT('Ctrl Pts',(43.1911832755467,20.7092098634864,0.));
#87028=CARTESIAN_POINT('Ctrl Pts',(43.1911832755467,20.7092098634864,20.));
#87029=CARTESIAN_POINT('Ctrl Pts',(43.202852943996,20.6778741759814,0.));
#87030=CARTESIAN_POINT('Ctrl Pts',(43.202852943996,20.6778741759814,20.));
#87031=CARTESIAN_POINT('Ctrl Pts',(43.2145004335236,20.6465314290598,0.));
#87032=CARTESIAN_POINT('Ctrl Pts',(43.2145004335236,20.6465314290598,20.));
#87033=CARTESIAN_POINT('Ctrl Pts',(43.2261257393109,20.615181638175,0.));
#87034=CARTESIAN_POINT('Ctrl Pts',(43.2261257393109,20.615181638175,20.));
#87035=CARTESIAN_POINT('Ctrl Pts',(43.2377288565503,20.5838248187841,0.));
#87036=CARTESIAN_POINT('Ctrl Pts',(43.2377288565503,20.5838248187841,20.));
#87037=CARTESIAN_POINT('Ctrl Pts',(43.2493097804445,20.5524609863481,0.));
#87038=CARTESIAN_POINT('Ctrl Pts',(43.2493097804445,20.5524609863481,20.));
#87039=CARTESIAN_POINT('Ctrl Pts',(43.2608685062069,20.5210901563314,0.));
#87040=CARTESIAN_POINT('Ctrl Pts',(43.2608685062069,20.5210901563314,20.));
#87041=CARTESIAN_POINT('Ctrl Pts',(43.2724050290617,20.4897123442023,0.));
#87042=CARTESIAN_POINT('Ctrl Pts',(43.2724050290617,20.4897123442023,20.));
#87043=CARTESIAN_POINT('Ctrl Pts',(43.283919344243,20.4583275654327,0.));
#87044=CARTESIAN_POINT('Ctrl Pts',(43.283919344243,20.4583275654327,20.));
#87045=CARTESIAN_POINT('Ctrl Pts',(43.2954114469964,20.4269358354984,0.));
#87046=CARTESIAN_POINT('Ctrl Pts',(43.2954114469964,20.4269358354984,20.));
#87047=CARTESIAN_POINT('Ctrl Pts',(43.3068813325774,20.3955371698787,0.));
#87048=CARTESIAN_POINT('Ctrl Pts',(43.3068813325774,20.3955371698787,20.));
#87049=CARTESIAN_POINT('Ctrl Pts',(43.3183289962528,20.3641315840566,0.));
#87050=CARTESIAN_POINT('Ctrl Pts',(43.3183289962528,20.3641315840566,20.));
#87051=CARTESIAN_POINT('Ctrl Pts',(43.3297544333003,20.3327190935193,0.));
#87052=CARTESIAN_POINT('Ctrl Pts',(43.3297544333003,20.3327190935193,20.));
#87053=CARTESIAN_POINT('Ctrl Pts',(43.3411576390085,20.3012997137575,0.));
#87054=CARTESIAN_POINT('Ctrl Pts',(43.3411576390085,20.3012997137575,20.));
#87055=CARTESIAN_POINT('Ctrl Pts',(43.3525386086763,20.2698734602656,0.));
#87056=CARTESIAN_POINT('Ctrl Pts',(43.3525386086763,20.2698734602656,20.));
#87057=CARTESIAN_POINT('Ctrl Pts',(43.3638973376125,20.2384403485411,0.));
#87058=CARTESIAN_POINT('Ctrl Pts',(43.3638973376125,20.2384403485411,20.));
#87059=CARTESIAN_POINT('Ctrl Pts',(43.3752338211368,20.2070003940853,0.));
#87060=CARTESIAN_POINT('Ctrl Pts',(43.3752338211368,20.2070003940853,20.));
#87061=CARTESIAN_POINT('Ctrl Pts',(43.3865480545792,20.1755536124033,0.));
#87062=CARTESIAN_POINT('Ctrl Pts',(43.3865480545792,20.1755536124033,20.));
#87063=CARTESIAN_POINT('Ctrl Pts',(43.3978400332808,20.1441000190037,0.));
#87064=CARTESIAN_POINT('Ctrl Pts',(43.3978400332808,20.1441000190037,20.));
#87065=CARTESIAN_POINT('Ctrl Pts',(43.409109752594,20.1126396293992,0.));
#87066=CARTESIAN_POINT('Ctrl Pts',(43.409109752594,20.1126396293992,20.));
#87067=CARTESIAN_POINT('Ctrl Pts',(43.4203572078819,20.0811724591059,0.));
#87068=CARTESIAN_POINT('Ctrl Pts',(43.4203572078819,20.0811724591059,20.));
#87069=CARTESIAN_POINT('Ctrl Pts',(43.4315823945181,20.0496985236436,0.));
#87070=CARTESIAN_POINT('Ctrl Pts',(43.4315823945181,20.0496985236436,20.));
#87071=CARTESIAN_POINT('Ctrl Pts',(43.4427853078868,20.0182178385356,0.));
#87072=CARTESIAN_POINT('Ctrl Pts',(43.4427853078868,20.0182178385356,20.));
#87073=CARTESIAN_POINT('Ctrl Pts',(43.4539659433821,19.9867304193089,0.));
#87074=CARTESIAN_POINT('Ctrl Pts',(43.4539659433821,19.9867304193089,20.));
#87075=CARTESIAN_POINT('Ctrl Pts',(43.4651242964088,19.9552362814936,0.));
#87076=CARTESIAN_POINT('Ctrl Pts',(43.4651242964088,19.9552362814936,20.));
#87077=CARTESIAN_POINT('Ctrl Pts',(43.4762603623832,19.923735440624,0.));
#87078=CARTESIAN_POINT('Ctrl Pts',(43.4762603623832,19.923735440624,20.));
#87079=CARTESIAN_POINT('Ctrl Pts',(43.4873741367321,19.8922279122378,0.));
#87080=CARTESIAN_POINT('Ctrl Pts',(43.4873741367321,19.8922279122378,20.));
#87081=CARTESIAN_POINT('Ctrl Pts',(43.4984656148935,19.8607137118763,0.));
#87082=CARTESIAN_POINT('Ctrl Pts',(43.4984656148935,19.8607137118763,20.));
#87083=CARTESIAN_POINT('Ctrl Pts',(43.5095347923164,19.8291928550844,0.));
#87084=CARTESIAN_POINT('Ctrl Pts',(43.5095347923164,19.8291928550844,20.));
#87085=CARTESIAN_POINT('Ctrl Pts',(43.5205816644596,19.7976653574108,0.));
#87086=CARTESIAN_POINT('Ctrl Pts',(43.5205816644596,19.7976653574108,20.));
#87087=CARTESIAN_POINT('Ctrl Pts',(43.5316062267925,19.7661312344072,0.));
#87088=CARTESIAN_POINT('Ctrl Pts',(43.5316062267925,19.7661312344072,20.));
#87089=CARTESIAN_POINT('Ctrl Pts',(43.542608474795,19.734590501629,0.));
#87090=CARTESIAN_POINT('Ctrl Pts',(43.542608474795,19.734590501629,20.));
#87091=CARTESIAN_POINT('Ctrl Pts',(43.5535884039576,19.7030431746352,0.));
#87092=CARTESIAN_POINT('Ctrl Pts',(43.5535884039576,19.7030431746352,20.));
#87093=CARTESIAN_POINT('Ctrl Pts',(43.5645460097823,19.6714892689885,0.));
#87094=CARTESIAN_POINT('Ctrl Pts',(43.5645460097823,19.6714892689885,20.));
#87095=CARTESIAN_POINT('Ctrl Pts',(43.5754812877819,19.639928800255,0.));
#87096=CARTESIAN_POINT('Ctrl Pts',(43.5754812877819,19.639928800255,20.));
#87097=CARTESIAN_POINT('Ctrl Pts',(43.5863942334797,19.6083617840046,0.));
#87098=CARTESIAN_POINT('Ctrl Pts',(43.5863942334797,19.6083617840046,20.));
#87099=CARTESIAN_POINT('Ctrl Pts',(43.5972848424097,19.5767882358104,0.));
#87100=CARTESIAN_POINT('Ctrl Pts',(43.5972848424097,19.5767882358104,20.));
#87101=CARTESIAN_POINT('Ctrl Pts',(43.6081531101168,19.545208171249,0.));
#87102=CARTESIAN_POINT('Ctrl Pts',(43.6081531101168,19.545208171249,20.));
#87103=CARTESIAN_POINT('Ctrl Pts',(43.6189990321561,19.5136216059004,0.));
#87104=CARTESIAN_POINT('Ctrl Pts',(43.6189990321561,19.5136216059004,20.));
#87105=CARTESIAN_POINT('Ctrl Pts',(43.629822604094,19.4820285553483,0.));
#87106=CARTESIAN_POINT('Ctrl Pts',(43.629822604094,19.4820285553483,20.));
#87107=CARTESIAN_POINT('Ctrl Pts',(43.6406238215078,19.4504290351799,0.));
#87108=CARTESIAN_POINT('Ctrl Pts',(43.6406238215078,19.4504290351799,20.));
#87109=CARTESIAN_POINT('Ctrl Pts',(43.6514026799849,19.4188230609858,0.));
#87110=CARTESIAN_POINT('Ctrl Pts',(43.6514026799849,19.4188230609858,20.));
#87111=CARTESIAN_POINT('Ctrl Pts',(43.6621591751234,19.3872106483603,0.));
#87112=CARTESIAN_POINT('Ctrl Pts',(43.6621591751234,19.3872106483603,20.));
#87113=CARTESIAN_POINT('Ctrl Pts',(43.6728933025325,19.3555918129009,0.));
#87114=CARTESIAN_POINT('Ctrl Pts',(43.6728933025325,19.3555918129009,20.));
#87115=CARTESIAN_POINT('Ctrl Pts',(43.6836050578319,19.3239665702086,0.));
#87116=CARTESIAN_POINT('Ctrl Pts',(43.6836050578319,19.3239665702086,20.));
#87117=CARTESIAN_POINT('Ctrl Pts',(43.6942944366523,19.2923349358879,0.));
#87118=CARTESIAN_POINT('Ctrl Pts',(43.6942944366523,19.2923349358879,20.));
#87119=CARTESIAN_POINT('Ctrl Pts',(43.7049614346349,19.2606969255464,0.));
#87120=CARTESIAN_POINT('Ctrl Pts',(43.7049614346349,19.2606969255464,20.));
#87121=CARTESIAN_POINT('Ctrl Pts',(43.7156060474324,19.2290525547956,0.));
#87122=CARTESIAN_POINT('Ctrl Pts',(43.7156060474324,19.2290525547956,20.));
#87123=CARTESIAN_POINT('Ctrl Pts',(43.7262282707082,19.1974018392505,0.));
#87124=CARTESIAN_POINT('Ctrl Pts',(43.7262282707082,19.1974018392505,20.));
#87125=CARTESIAN_POINT('Ctrl Pts',(43.7368281001363,19.1657447945291,0.));
#87126=CARTESIAN_POINT('Ctrl Pts',(43.7368281001363,19.1657447945291,20.));
#87127=CARTESIAN_POINT('Ctrl Pts',(43.747405531401,19.1340814362531,0.));
#87128=CARTESIAN_POINT('Ctrl Pts',(43.747405531401,19.1340814362531,20.));
#87129=CARTESIAN_POINT('Ctrl Pts',(43.7579605601976,19.1024117800474,0.));
#87130=CARTESIAN_POINT('Ctrl Pts',(43.7579605601976,19.1024117800474,20.));
#87131=CARTESIAN_POINT('Ctrl Pts',(43.7684931822314,19.0707358415405,0.));
#87132=CARTESIAN_POINT('Ctrl Pts',(43.7684931822314,19.0707358415405,20.));
#87133=CARTESIAN_POINT('Ctrl Pts',(43.779003393219,19.039053636364,0.));
#87134=CARTESIAN_POINT('Ctrl Pts',(43.779003393219,19.039053636364,20.));
#87135=CARTESIAN_POINT('Ctrl Pts',(43.7894911888877,19.0073651801531,0.));
#87136=CARTESIAN_POINT('Ctrl Pts',(43.7894911888877,19.0073651801531,20.));
#87137=CARTESIAN_POINT('Ctrl Pts',(43.7999565649762,18.9756704885464,0.));
#87138=CARTESIAN_POINT('Ctrl Pts',(43.7999565649762,18.9756704885464,20.));
#87139=CARTESIAN_POINT('Ctrl Pts',(43.8103995172341,18.9439695771858,0.));
#87140=CARTESIAN_POINT('Ctrl Pts',(43.8103995172341,18.9439695771858,20.));
#87141=CARTESIAN_POINT('Ctrl Pts',(43.8208200414219,18.9122624617166,0.));
#87142=CARTESIAN_POINT('Ctrl Pts',(43.8208200414219,18.9122624617166,20.));
#87143=CARTESIAN_POINT('Ctrl Pts',(43.8312181333106,18.8805491577876,0.));
#87144=CARTESIAN_POINT('Ctrl Pts',(43.8312181333106,18.8805491577876,20.));
#87145=CARTESIAN_POINT('Ctrl Pts',(43.8415937886817,18.8488296810507,0.));
#87146=CARTESIAN_POINT('Ctrl Pts',(43.8415937886817,18.8488296810507,20.));
#87147=CARTESIAN_POINT('Ctrl Pts',(43.8519470033272,18.8171040471611,0.));
#87148=CARTESIAN_POINT('Ctrl Pts',(43.8519470033272,18.8171040471611,20.));
#87149=CARTESIAN_POINT('Ctrl Pts',(43.8622777730502,18.7853722717774,0.));
#87150=CARTESIAN_POINT('Ctrl Pts',(43.8622777730502,18.7853722717774,20.));
#87151=CARTESIAN_POINT('Ctrl Pts',(43.8725860936644,18.7536343705616,0.));
#87152=CARTESIAN_POINT('Ctrl Pts',(43.8725860936644,18.7536343705616,20.));
#87153=CARTESIAN_POINT('Ctrl Pts',(43.8828719609947,18.721890359179,0.));
#87154=CARTESIAN_POINT('Ctrl Pts',(43.8828719609947,18.721890359179,20.));
#87155=CARTESIAN_POINT('Ctrl Pts',(43.8931353708767,18.6901402532984,0.));
#87156=CARTESIAN_POINT('Ctrl Pts',(43.8931353708767,18.6901402532984,20.));
#87157=CARTESIAN_POINT('Ctrl Pts',(43.903376319157,18.6583840685915,0.));
#87158=CARTESIAN_POINT('Ctrl Pts',(43.903376319157,18.6583840685915,20.));
#87159=CARTESIAN_POINT('Ctrl Pts',(43.913594801693,18.6266218207337,0.));
#87160=CARTESIAN_POINT('Ctrl Pts',(43.913594801693,18.6266218207337,20.));
#87161=CARTESIAN_POINT('Ctrl Pts',(43.9237908143526,18.5948535254034,0.));
#87162=CARTESIAN_POINT('Ctrl Pts',(43.9237908143526,18.5948535254034,20.));
#87163=CARTESIAN_POINT('Ctrl Pts',(43.9339643530151,18.5630791982821,0.));
#87164=CARTESIAN_POINT('Ctrl Pts',(43.9339643530151,18.5630791982821,20.));
#87165=CARTESIAN_POINT('Ctrl Pts',(43.94411541357,18.5312988550549,0.));
#87166=CARTESIAN_POINT('Ctrl Pts',(43.94411541357,18.5312988550549,20.));
#87167=CARTESIAN_POINT('Ctrl Pts',(43.9542439919177,18.4995125114099,0.));
#87168=CARTESIAN_POINT('Ctrl Pts',(43.9542439919177,18.4995125114099,20.));
#87169=CARTESIAN_POINT('Ctrl Pts',(43.9643500839697,18.4677201830388,0.));
#87170=CARTESIAN_POINT('Ctrl Pts',(43.9643500839697,18.4677201830388,20.));
#87171=CARTESIAN_POINT('Ctrl Pts',(43.9744336856481,18.4359218856365,0.));
#87172=CARTESIAN_POINT('Ctrl Pts',(43.9744336856481,18.4359218856365,20.));
#87173=CARTESIAN_POINT('Ctrl Pts',(43.9844947928861,18.4041176349014,0.));
#87174=CARTESIAN_POINT('Ctrl Pts',(43.9844947928861,18.4041176349014,20.));
#87175=CARTESIAN_POINT('Ctrl Pts',(43.9945334016277,18.3723074465347,0.));
#87176=CARTESIAN_POINT('Ctrl Pts',(43.9945334016277,18.3723074465347,20.));
#87177=CARTESIAN_POINT('Ctrl Pts',(44.0045495078276,18.3404913362408,0.));
#87178=CARTESIAN_POINT('Ctrl Pts',(44.0045495078276,18.3404913362408,20.));
#87179=CARTESIAN_POINT('Ctrl Pts',(44.0145431074514,18.3086693197275,0.));
#87180=CARTESIAN_POINT('Ctrl Pts',(44.0145431074514,18.3086693197275,20.));
#87181=CARTESIAN_POINT('Ctrl Pts',(44.0245141964756,18.2768414127056,0.));
#87182=CARTESIAN_POINT('Ctrl Pts',(44.0245141964756,18.2768414127056,20.));
#87183=CARTESIAN_POINT('Ctrl Pts',(44.0344627708874,18.245007630889,0.));
#87184=CARTESIAN_POINT('Ctrl Pts',(44.0344627708874,18.245007630889,20.));
#87185=CARTESIAN_POINT('Ctrl Pts',(44.044388826685,18.2131679899948,0.));
#87186=CARTESIAN_POINT('Ctrl Pts',(44.044388826685,18.2131679899948,20.));
#87187=CARTESIAN_POINT('Ctrl Pts',(44.0542923598772,18.1813225057438,0.));
#87188=CARTESIAN_POINT('Ctrl Pts',(44.0542923598772,18.1813225057438,20.));
#87189=CARTESIAN_POINT('Ctrl Pts',(44.0641733664839,18.1494711938598,0.));
#87190=CARTESIAN_POINT('Ctrl Pts',(44.0641733664839,18.1494711938598,20.));
#87191=CARTESIAN_POINT('Ctrl Pts',(44.0740318425361,18.1176140700699,0.));
#87192=CARTESIAN_POINT('Ctrl Pts',(44.0740318425361,18.1176140700699,20.));
#87193=CARTESIAN_POINT('Ctrl Pts',(44.0838677840754,18.0857511501043,0.));
#87194=CARTESIAN_POINT('Ctrl Pts',(44.0838677840754,18.0857511501043,20.));
#87195=CARTESIAN_POINT('Ctrl Pts',(44.0936811871546,18.0538824496962,0.));
#87196=CARTESIAN_POINT('Ctrl Pts',(44.0936811871546,18.0538824496962,20.));
#87197=CARTESIAN_POINT('Ctrl Pts',(44.1034720478372,18.0220079845822,0.));
#87198=CARTESIAN_POINT('Ctrl Pts',(44.1034720478372,18.0220079845822,20.));
#87199=CARTESIAN_POINT('Ctrl Pts',(44.1132403621971,17.9901277705015,0.));
#87200=CARTESIAN_POINT('Ctrl Pts',(44.1132403621971,17.9901277705015,20.));
#87201=CARTESIAN_POINT('Ctrl Pts',(44.1229861263191,17.9582418231966,0.));
#87202=CARTESIAN_POINT('Ctrl Pts',(44.1229861263191,17.9582418231966,20.));
#87203=CARTESIAN_POINT('Ctrl Pts',(44.1327093362991,17.9263501584131,0.));
#87204=CARTESIAN_POINT('Ctrl Pts',(44.1327093362991,17.9263501584131,20.));
#87205=CARTESIAN_POINT('Ctrl Pts',(44.1424099882439,17.8944527919,0.));
#87206=CARTESIAN_POINT('Ctrl Pts',(44.1424099882439,17.8944527919,20.));
#87207=CARTESIAN_POINT('Ctrl Pts',(44.1520880782717,17.8625497394092,0.));
#87208=CARTESIAN_POINT('Ctrl Pts',(44.1520880782717,17.8625497394092,20.));
#87209=CARTESIAN_POINT('Ctrl Pts',(44.1617436025112,17.8306410166963,0.));
#87210=CARTESIAN_POINT('Ctrl Pts',(44.1617436025112,17.8306410166963,20.));
#87211=CARTESIAN_POINT('Ctrl Pts',(44.1713765571021,17.7987266395196,0.));
#87212=CARTESIAN_POINT('Ctrl Pts',(44.1713765571021,17.7987266395196,20.));
#87213=CARTESIAN_POINT('Ctrl Pts',(44.1809869381949,17.7668066236405,0.));
#87214=CARTESIAN_POINT('Ctrl Pts',(44.1809869381949,17.7668066236405,20.));
#87215=CARTESIAN_POINT('Ctrl Pts',(44.1905747419505,17.7348809848234,0.));
#87216=CARTESIAN_POINT('Ctrl Pts',(44.1905747419505,17.7348809848234,20.));
#87217=CARTESIAN_POINT('Ctrl Pts',(44.2001399645408,17.7029497388358,0.));
#87218=CARTESIAN_POINT('Ctrl Pts',(44.2001399645408,17.7029497388358,20.));
#87219=CARTESIAN_POINT('Ctrl Pts',(44.2096826021493,17.6710129014481,0.));
#87220=CARTESIAN_POINT('Ctrl Pts',(44.2096826021493,17.6710129014481,20.));
#87221=CARTESIAN_POINT('Ctrl Pts',(44.2192026509705,17.6390704884341,0.));
#87222=CARTESIAN_POINT('Ctrl Pts',(44.2192026509705,17.6390704884341,20.));
#87223=CARTESIAN_POINT('Ctrl Pts',(44.2287001072093,17.6071225155702,0.));
#87224=CARTESIAN_POINT('Ctrl Pts',(44.2287001072093,17.6071225155702,20.));
#87225=CARTESIAN_POINT('Ctrl Pts',(44.2381749670816,17.5751689986363,0.));
#87226=CARTESIAN_POINT('Ctrl Pts',(44.2381749670816,17.5751689986363,20.));
#87227=CARTESIAN_POINT('Ctrl Pts',(44.2476272268138,17.5432099534151,0.));
#87228=CARTESIAN_POINT('Ctrl Pts',(44.2476272268138,17.5432099534151,20.));
#87229=CARTESIAN_POINT('Ctrl Pts',(44.2570568826434,17.5112453956925,0.));
#87230=CARTESIAN_POINT('Ctrl Pts',(44.2570568826434,17.5112453956925,20.));
#87231=CARTESIAN_POINT('Ctrl Pts',(44.2664639308191,17.4792753412574,0.));
#87232=CARTESIAN_POINT('Ctrl Pts',(44.2664639308191,17.4792753412574,20.));
#87233=CARTESIAN_POINT('Ctrl Pts',(44.2758483676008,17.447299805902,0.));
#87234=CARTESIAN_POINT('Ctrl Pts',(44.2758483676008,17.447299805902,20.));
#87235=CARTESIAN_POINT('Ctrl Pts',(44.2852101892593,17.4153188054211,0.));
#87236=CARTESIAN_POINT('Ctrl Pts',(44.2852101892593,17.4153188054211,20.));
#87237=CARTESIAN_POINT('Ctrl Pts',(44.294549392076,17.3833323556128,0.));
#87238=CARTESIAN_POINT('Ctrl Pts',(44.294549392076,17.3833323556128,20.));
#87239=CARTESIAN_POINT('Ctrl Pts',(44.3038659723435,17.3513404722779,0.));
#87240=CARTESIAN_POINT('Ctrl Pts',(44.3038659723435,17.3513404722779,20.));
#87241=CARTESIAN_POINT('Ctrl Pts',(44.3131599263642,17.3193431712198,0.));
#87242=CARTESIAN_POINT('Ctrl Pts',(44.3131599263642,17.3193431712198,20.));
#87243=CARTESIAN_POINT('Ctrl Pts',(44.3224312504523,17.2873404682456,0.));
#87244=CARTESIAN_POINT('Ctrl Pts',(44.3224312504523,17.2873404682456,20.));
#87245=CARTESIAN_POINT('Ctrl Pts',(44.3316799409325,17.2553323791649,0.));
#87246=CARTESIAN_POINT('Ctrl Pts',(44.3316799409325,17.2553323791649,20.));
#87247=CARTESIAN_POINT('Ctrl Pts',(44.340905994141,17.2233189197905,0.));
#87248=CARTESIAN_POINT('Ctrl Pts',(44.340905994141,17.2233189197905,20.));
#87249=CARTESIAN_POINT('Ctrl Pts',(44.3501094064252,17.1913001059384,0.));
#87250=CARTESIAN_POINT('Ctrl Pts',(44.3501094064252,17.1913001059384,20.));
#87251=CARTESIAN_POINT('Ctrl Pts',(44.3592901741436,17.1592759534275,0.));
#87252=CARTESIAN_POINT('Ctrl Pts',(44.3592901741436,17.1592759534275,20.));
#87253=CARTESIAN_POINT('Ctrl Pts',(44.3684482936655,17.1272464780797,0.));
#87254=CARTESIAN_POINT('Ctrl Pts',(44.3684482936655,17.1272464780797,20.));
#87255=CARTESIAN_POINT('Ctrl Pts',(44.3775837613707,17.0952116957196,0.));
#87256=CARTESIAN_POINT('Ctrl Pts',(44.3775837613707,17.0952116957196,20.));
#87257=CARTESIAN_POINT('Ctrl Pts',(44.3866965736492,17.0631716221745,0.));
#87258=CARTESIAN_POINT('Ctrl Pts',(44.3866965736492,17.0631716221745,20.));
#87259=CARTESIAN_POINT('Ctrl Pts',(44.3957867269024,17.0311262732746,0.));
#87260=CARTESIAN_POINT('Ctrl Pts',(44.3957867269024,17.0311262732746,20.));
#87261=CARTESIAN_POINT('Ctrl Pts',(44.404854217543,16.9990756648532,0.));
#87262=CARTESIAN_POINT('Ctrl Pts',(44.404854217543,16.9990756648532,20.));
#87263=CARTESIAN_POINT('Ctrl Pts',(44.4138990419958,16.967019812747,0.));
#87264=CARTESIAN_POINT('Ctrl Pts',(44.4138990419958,16.967019812747,20.));
#87265=CARTESIAN_POINT('Ctrl Pts',(44.4229211966955,16.9349587327952,0.));
#87266=CARTESIAN_POINT('Ctrl Pts',(44.4229211966955,16.9349587327952,20.));
#87267=CARTESIAN_POINT('Ctrl Pts',(44.4319206780879,16.9028924408399,0.));
#87268=CARTESIAN_POINT('Ctrl Pts',(44.4319206780879,16.9028924408399,20.));
#87269=CARTESIAN_POINT('Ctrl Pts',(44.4408974826293,16.870820952726,0.));
#87270=CARTESIAN_POINT('Ctrl Pts',(44.4408974826293,16.870820952726,20.));
#87271=CARTESIAN_POINT('Ctrl Pts',(44.4498516067869,16.8387442843012,0.));
#87272=CARTESIAN_POINT('Ctrl Pts',(44.4498516067869,16.8387442843012,20.));
#87273=CARTESIAN_POINT('Ctrl Pts',(44.4587830470388,16.8066624514163,0.));
#87274=CARTESIAN_POINT('Ctrl Pts',(44.4587830470388,16.8066624514163,20.));
#87275=CARTESIAN_POINT('Ctrl Pts',(44.4676917998748,16.7745754699247,0.));
#87276=CARTESIAN_POINT('Ctrl Pts',(44.4676917998748,16.7745754699247,20.));
#87277=CARTESIAN_POINT('Ctrl Pts',(44.4765778617956,16.742483355683,0.));
#87278=CARTESIAN_POINT('Ctrl Pts',(44.4765778617956,16.742483355683,20.));
#87279=CARTESIAN_POINT('Ctrl Pts',(44.4854412293128,16.7103861245505,0.));
#87280=CARTESIAN_POINT('Ctrl Pts',(44.4854412293128,16.7103861245505,20.));
#87281=CARTESIAN_POINT('Ctrl Pts',(44.4942818989491,16.6782837923893,0.));
#87282=CARTESIAN_POINT('Ctrl Pts',(44.4942818989491,16.6782837923893,20.));
#87283=CARTESIAN_POINT('Ctrl Pts',(44.503099867238,16.6461763750644,0.));
#87284=CARTESIAN_POINT('Ctrl Pts',(44.503099867238,16.6461763750644,20.));
#87285=CARTESIAN_POINT('Ctrl Pts',(44.5118951307243,16.6140638884438,0.));
#87286=CARTESIAN_POINT('Ctrl Pts',(44.5118951307243,16.6140638884438,20.));
#87287=CARTESIAN_POINT('Ctrl Pts',(44.5206676859632,16.581946348398,0.));
#87288=CARTESIAN_POINT('Ctrl Pts',(44.5206676859632,16.581946348398,20.));
#87289=CARTESIAN_POINT('Ctrl Pts',(44.5294175295214,16.5498237708003,0.));
#87290=CARTESIAN_POINT('Ctrl Pts',(44.5294175295214,16.5498237708003,20.));
#87291=CARTESIAN_POINT('Ctrl Pts',(44.5381446579761,16.5176961715269,0.));
#87292=CARTESIAN_POINT('Ctrl Pts',(44.5381446579761,16.5176961715269,20.));
#87293=CARTESIAN_POINT('Ctrl Pts',(44.5468490679154,16.4855635664567,0.));
#87294=CARTESIAN_POINT('Ctrl Pts',(44.5468490679154,16.4855635664567,20.));
#87295=CARTESIAN_POINT('Ctrl Pts',(44.5555307559385,16.4534259714715,0.));
#87296=CARTESIAN_POINT('Ctrl Pts',(44.5555307559385,16.4534259714715,20.));
#87297=CARTESIAN_POINT('Ctrl Pts',(44.5641897186557,16.4212834024559,0.));
#87298=CARTESIAN_POINT('Ctrl Pts',(44.5641897186557,16.4212834024559,20.));
#87299=CARTESIAN_POINT('Ctrl Pts',(44.5728259526889,16.3891358752972,0.));
#87300=CARTESIAN_POINT('Ctrl Pts',(44.5728259526889,16.3891358752972,20.));
#87301=CARTESIAN_POINT('Ctrl Pts',(44.581439454671,16.3569834058857,0.));
#87302=CARTESIAN_POINT('Ctrl Pts',(44.581439454671,16.3569834058857,20.));
#87303=CARTESIAN_POINT('Ctrl Pts',(44.5900302212458,16.3248260101143,0.));
#87304=CARTESIAN_POINT('Ctrl Pts',(44.5900302212458,16.3248260101143,20.));
#87305=CARTESIAN_POINT('Ctrl Pts',(44.5985982490682,16.2926637038787,0.));
#87306=CARTESIAN_POINT('Ctrl Pts',(44.5985982490682,16.2926637038787,20.));
#87307=CARTESIAN_POINT('Ctrl Pts',(44.6071435348036,16.2604965030773,0.));
#87308=CARTESIAN_POINT('Ctrl Pts',(44.6071435348036,16.2604965030773,20.));
#87309=CARTESIAN_POINT('Ctrl Pts',(44.6156660751288,16.2283244236112,0.));
#87310=CARTESIAN_POINT('Ctrl Pts',(44.6156660751288,16.2283244236112,20.));
#87311=CARTESIAN_POINT('Ctrl Pts',(44.6241658667307,16.196147481384,0.));
#87312=CARTESIAN_POINT('Ctrl Pts',(44.6241658667307,16.196147481384,20.));
#87313=CARTESIAN_POINT('Ctrl Pts',(44.6326429063072,16.1639656923023,0.));
#87314=CARTESIAN_POINT('Ctrl Pts',(44.6326429063072,16.1639656923023,20.));
#87315=CARTESIAN_POINT('Ctrl Pts',(44.6410971905673,16.131779072275,0.));
#87316=CARTESIAN_POINT('Ctrl Pts',(44.6410971905673,16.131779072275,20.));
#87317=CARTESIAN_POINT('Ctrl Pts',(44.649528716232,16.0995876372141,0.));
#87318=CARTESIAN_POINT('Ctrl Pts',(44.649528716232,16.0995876372141,20.));
#87319=CARTESIAN_POINT('Ctrl Pts',(44.6579374800339,16.0673914030343,0.));
#87320=CARTESIAN_POINT('Ctrl Pts',(44.6579374800339,16.0673914030343,20.));
#87321=CARTESIAN_POINT('Ctrl Pts',(44.6663234787169,16.0351903856534,0.));
#87322=CARTESIAN_POINT('Ctrl Pts',(44.6663234787169,16.0351903856534,20.));
#87323=CARTESIAN_POINT('Ctrl Pts',(44.6746867090345,16.0029846009915,0.));
#87324=CARTESIAN_POINT('Ctrl Pts',(44.6746867090345,16.0029846009915,20.));
#87325=CARTESIAN_POINT('Ctrl Pts',(44.6830271677516,15.9707740649715,0.));
#87326=CARTESIAN_POINT('Ctrl Pts',(44.6830271677516,15.9707740649715,20.));
#87327=CARTESIAN_POINT('Ctrl Pts',(44.691344851643,15.9385587935186,0.));
#87328=CARTESIAN_POINT('Ctrl Pts',(44.691344851643,15.9385587935186,20.));
#87329=CARTESIAN_POINT('Ctrl Pts',(44.6996397574952,15.9063388025603,0.));
#87330=CARTESIAN_POINT('Ctrl Pts',(44.6996397574952,15.9063388025603,20.));
#87331=CARTESIAN_POINT('Ctrl Pts',(44.7079118821065,15.8741141080272,0.));
#87332=CARTESIAN_POINT('Ctrl Pts',(44.7079118821065,15.8741141080272,20.));
#87333=CARTESIAN_POINT('Ctrl Pts',(44.7161612222865,15.8418847258528,0.));
#87334=CARTESIAN_POINT('Ctrl Pts',(44.7161612222865,15.8418847258528,20.));
#87335=CARTESIAN_POINT('Ctrl Pts',(44.7243877748558,15.8096506719735,0.));
#87336=CARTESIAN_POINT('Ctrl Pts',(44.7243877748558,15.8096506719735,20.));
#87337=CARTESIAN_POINT('Ctrl Pts',(44.7325915366458,15.7774119623278,0.));
#87338=CARTESIAN_POINT('Ctrl Pts',(44.7325915366458,15.7774119623278,20.));
#87339=CARTESIAN_POINT('Ctrl Pts',(44.7407725044985,15.745168612857,0.));
#87340=CARTESIAN_POINT('Ctrl Pts',(44.7407725044985,15.745168612857,20.));
#87341=CARTESIAN_POINT('Ctrl Pts',(44.7489306752664,15.7129206395047,0.));
#87342=CARTESIAN_POINT('Ctrl Pts',(44.7489306752664,15.7129206395047,20.));
#87343=CARTESIAN_POINT('Ctrl Pts',(44.7570660458133,15.6806680582172,0.));
#87344=CARTESIAN_POINT('Ctrl Pts',(44.7570660458133,15.6806680582172,20.));
#87345=CARTESIAN_POINT('Ctrl Pts',(44.7651786130144,15.6484108849434,0.));
#87346=CARTESIAN_POINT('Ctrl Pts',(44.7651786130144,15.6484108849434,20.));
#87347=CARTESIAN_POINT('Ctrl Pts',(44.7732683737566,15.6161491356348,0.));
#87348=CARTESIAN_POINT('Ctrl Pts',(44.7732683737566,15.6161491356348,20.));
#87349=CARTESIAN_POINT('Ctrl Pts',(44.7813353249379,15.583882826246,0.));
#87350=CARTESIAN_POINT('Ctrl Pts',(44.7813353249379,15.583882826246,20.));
#87351=CARTESIAN_POINT('Ctrl Pts',(44.7893794634672,15.5516119727338,0.));
#87352=CARTESIAN_POINT('Ctrl Pts',(44.7893794634672,15.5516119727338,20.));
#87353=CARTESIAN_POINT('Ctrl Pts',(44.7974007862643,15.5193365910578,0.));
#87354=CARTESIAN_POINT('Ctrl Pts',(44.7974007862643,15.5193365910578,20.));
#87355=CARTESIAN_POINT('Ctrl Pts',(44.8053992902599,15.4870566971799,0.));
#87356=CARTESIAN_POINT('Ctrl Pts',(44.8053992902599,15.4870566971799,20.));
#87357=CARTESIAN_POINT('Ctrl Pts',(44.8133749723964,15.4547723070643,0.));
#87358=CARTESIAN_POINT('Ctrl Pts',(44.8133749723964,15.4547723070643,20.));
#87359=CARTESIAN_POINT('Ctrl Pts',(44.8213278296263,15.4224834366782,0.));
#87360=CARTESIAN_POINT('Ctrl Pts',(44.8213278296263,15.4224834366782,20.));
#87361=CARTESIAN_POINT('Ctrl Pts',(44.8292578589132,15.3901901019906,0.));
#87362=CARTESIAN_POINT('Ctrl Pts',(44.8292578589132,15.3901901019906,20.));
#87363=CARTESIAN_POINT('Ctrl Pts',(44.8371650572316,15.3578923189739,0.));
#87364=CARTESIAN_POINT('Ctrl Pts',(44.8371650572316,15.3578923189739,20.));
#87365=CARTESIAN_POINT('Ctrl Pts',(44.8450494215678,15.3255901036026,0.));
#87366=CARTESIAN_POINT('Ctrl Pts',(44.8450494215678,15.3255901036026,20.));
#87367=CARTESIAN_POINT('Ctrl Pts',(44.8529109489191,15.2932834718541,0.));
#87368=CARTESIAN_POINT('Ctrl Pts',(44.8529109489191,15.2932834718541,20.));
#87369=CARTESIAN_POINT('Ctrl Pts',(44.8607496362943,15.2609724397079,0.));
#87370=CARTESIAN_POINT('Ctrl Pts',(44.8607496362943,15.2609724397079,20.));
#87371=CARTESIAN_POINT('Ctrl Pts',(44.8685654807131,15.2286570231461,0.));
#87372=CARTESIAN_POINT('Ctrl Pts',(44.8685654807131,15.2286570231461,20.));
#87373=CARTESIAN_POINT('Ctrl Pts',(44.8763584792064,15.1963372381533,0.));
#87374=CARTESIAN_POINT('Ctrl Pts',(44.8763584792064,15.1963372381533,20.));
#87375=CARTESIAN_POINT('Ctrl Pts',(44.8841286288163,15.1640131007166,0.));
#87376=CARTESIAN_POINT('Ctrl Pts',(44.8841286288163,15.1640131007166,20.));
#87377=CARTESIAN_POINT('Ctrl Pts',(44.8918759265956,15.1316846268256,0.));
#87378=CARTESIAN_POINT('Ctrl Pts',(44.8918759265956,15.1316846268256,20.));
#87379=CARTESIAN_POINT('Ctrl Pts',(44.8996003696078,15.0993518324721,0.));
#87380=CARTESIAN_POINT('Ctrl Pts',(44.8996003696078,15.0993518324721,20.));
#87381=CARTESIAN_POINT('Ctrl Pts',(44.9073019549277,15.0670147336509,0.));
#87382=CARTESIAN_POINT('Ctrl Pts',(44.9073019549277,15.0670147336509,20.));
#87383=CARTESIAN_POINT('Ctrl Pts',(44.9149806796409,15.034673346359,0.));
#87384=CARTESIAN_POINT('Ctrl Pts',(44.9149806796409,15.034673346359,20.));
#87385=CARTESIAN_POINT('Ctrl Pts',(44.9226365408441,15.0023276865958,0.));
#87386=CARTESIAN_POINT('Ctrl Pts',(44.9226365408441,15.0023276865958,20.));
#87387=CARTESIAN_POINT('Ctrl Pts',(44.9302695356455,14.969977770363,0.));
#87388=CARTESIAN_POINT('Ctrl Pts',(44.9302695356455,14.969977770363,20.));
#87389=CARTESIAN_POINT('Ctrl Pts',(44.9378796611651,14.9376236136649,0.));
#87390=CARTESIAN_POINT('Ctrl Pts',(44.9378796611651,14.9376236136649,20.));
#87391=CARTESIAN_POINT('Ctrl Pts',(44.9454669145344,14.9052652325081,0.));
#87392=CARTESIAN_POINT('Ctrl Pts',(44.9454669145344,14.9052652325081,20.));
#87393=CARTESIAN_POINT('Ctrl Pts',(44.9530312928957,14.8729026429019,0.));
#87394=CARTESIAN_POINT('Ctrl Pts',(44.9530312928957,14.8729026429019,20.));
#87395=CARTESIAN_POINT('Ctrl Pts',(44.9605727934022,14.8405358608577,0.));
#87396=CARTESIAN_POINT('Ctrl Pts',(44.9605727934022,14.8405358608577,20.));
#87397=CARTESIAN_POINT('Ctrl Pts',(44.9680914132176,14.8081649023895,0.));
#87398=CARTESIAN_POINT('Ctrl Pts',(44.9680914132176,14.8081649023895,20.));
#87399=CARTESIAN_POINT('Ctrl Pts',(44.9755871495162,14.7757897835134,0.));
#87400=CARTESIAN_POINT('Ctrl Pts',(44.9755871495162,14.7757897835134,20.));
#87401=CARTESIAN_POINT('Ctrl Pts',(44.9830599994838,14.7434105202483,0.));
#87402=CARTESIAN_POINT('Ctrl Pts',(44.9830599994838,14.7434105202483,20.));
#87403=CARTESIAN_POINT('Ctrl Pts',(44.9905099603172,14.7110271286153,0.));
#87404=CARTESIAN_POINT('Ctrl Pts',(44.9905099603172,14.7110271286153,20.));
#87405=CARTESIAN_POINT('Ctrl Pts',(44.9979370292252,14.6786396246378,0.));
#87406=CARTESIAN_POINT('Ctrl Pts',(44.9979370292252,14.6786396246378,20.));
#87407=CARTESIAN_POINT('Ctrl Pts',(45.0053412034276,14.6462480243418,0.));
#87408=CARTESIAN_POINT('Ctrl Pts',(45.0053412034276,14.6462480243418,20.));
#87409=CARTESIAN_POINT('Ctrl Pts',(45.0127224801553,14.6138523437553,0.));
#87410=CARTESIAN_POINT('Ctrl Pts',(45.0127224801553,14.6138523437553,20.));
#87411=CARTESIAN_POINT('Ctrl Pts',(45.020080856651,14.5814525989087,0.));
#87412=CARTESIAN_POINT('Ctrl Pts',(45.020080856651,14.5814525989087,20.));
#87413=CARTESIAN_POINT('Ctrl Pts',(45.0274163301681,14.5490488058349,0.));
#87414=CARTESIAN_POINT('Ctrl Pts',(45.0274163301681,14.5490488058349,20.));
#87415=CARTESIAN_POINT('Ctrl Pts',(45.0347288979708,14.516640980569,0.));
#87416=CARTESIAN_POINT('Ctrl Pts',(45.0347288979708,14.516640980569,20.));
#87417=CARTESIAN_POINT('Ctrl Pts',(45.0420185573341,14.4842291391484,0.));
#87418=CARTESIAN_POINT('Ctrl Pts',(45.0420185573341,14.4842291391484,20.));
#87419=CARTESIAN_POINT('Ctrl Pts',(45.0492853055441,14.451813297613,0.));
#87420=CARTESIAN_POINT('Ctrl Pts',(45.0492853055441,14.451813297613,20.));
#87421=CARTESIAN_POINT('Ctrl Pts',(45.0565291398984,14.4193934720051,0.));
#87422=CARTESIAN_POINT('Ctrl Pts',(45.0565291398984,14.4193934720051,20.));
#87423=CARTESIAN_POINT('Ctrl Pts',(45.0637500577056,14.3869696783692,0.));
#87424=CARTESIAN_POINT('Ctrl Pts',(45.0637500577056,14.3869696783692,20.));
#87425=CARTESIAN_POINT('Ctrl Pts',(45.0709480562863,14.354541932752,0.));
#87426=CARTESIAN_POINT('Ctrl Pts',(45.0709480562863,14.354541932752,20.));
#87427=CARTESIAN_POINT('Ctrl Pts',(45.0781231329719,14.3221102512025,0.));
#87428=CARTESIAN_POINT('Ctrl Pts',(45.0781231329719,14.3221102512025,20.));
#87429=CARTESIAN_POINT('Ctrl Pts',(45.0852752851048,14.2896746497719,0.));
#87430=CARTESIAN_POINT('Ctrl Pts',(45.0852752851048,14.2896746497719,20.));
#87431=CARTESIAN_POINT('Ctrl Pts',(45.0924045100383,14.2572351445137,0.));
#87432=CARTESIAN_POINT('Ctrl Pts',(45.0924045100383,14.2572351445137,20.));
#87433=CARTESIAN_POINT('Ctrl Pts',(45.0995108051367,14.2247917514836,0.));
#87434=CARTESIAN_POINT('Ctrl Pts',(45.0995108051367,14.2247917514836,20.));
#87435=CARTESIAN_POINT('Ctrl Pts',(45.1065941677758,14.1923444867396,0.));
#87436=CARTESIAN_POINT('Ctrl Pts',(45.1065941677758,14.1923444867396,20.));
#87437=CARTESIAN_POINT('Ctrl Pts',(45.1136545953429,14.1598933663423,0.));
#87438=CARTESIAN_POINT('Ctrl Pts',(45.1136545953429,14.1598933663423,20.));
#87439=CARTESIAN_POINT('Ctrl Pts',(45.1206920852361,14.127438406354,0.));
#87440=CARTESIAN_POINT('Ctrl Pts',(45.1206920852361,14.127438406354,20.));
#87441=CARTESIAN_POINT('Ctrl Pts',(45.127706634865,14.0949796228398,0.));
#87442=CARTESIAN_POINT('Ctrl Pts',(45.127706634865,14.0949796228398,20.));
#87443=CARTESIAN_POINT('Ctrl Pts',(45.1346982416501,14.0625170318665,0.));
#87444=CARTESIAN_POINT('Ctrl Pts',(45.1346982416501,14.0625170318665,20.));
#87445=CARTESIAN_POINT('Ctrl Pts',(45.1416669030232,14.0300506495033,0.));
#87446=CARTESIAN_POINT('Ctrl Pts',(45.1416669030232,14.0300506495033,20.));
#87447=CARTESIAN_POINT('Ctrl Pts',(45.1486126164275,13.997580491822,0.));
#87448=CARTESIAN_POINT('Ctrl Pts',(45.1486126164275,13.997580491822,20.));
#87449=CARTESIAN_POINT('Ctrl Pts',(45.1555353793172,13.9651065748961,0.));
#87450=CARTESIAN_POINT('Ctrl Pts',(45.1555353793172,13.9651065748961,20.));
#87451=CARTESIAN_POINT('Ctrl Pts',(45.1624351891574,13.9326289148012,0.));
#87452=CARTESIAN_POINT('Ctrl Pts',(45.1624351891574,13.9326289148012,20.));
#87453=CARTESIAN_POINT('Ctrl Pts',(45.1693120434241,13.9001475276153,0.));
#87454=CARTESIAN_POINT('Ctrl Pts',(45.1693120434241,13.9001475276153,20.));
#87455=CARTESIAN_POINT('Ctrl Pts',(45.1761659396043,13.8676624294184,0.));
#87456=CARTESIAN_POINT('Ctrl Pts',(45.1761659396043,13.8676624294184,20.));
#87457=CARTESIAN_POINT('Ctrl Pts',(45.1829968751969,13.8351736362929,0.));
#87458=CARTESIAN_POINT('Ctrl Pts',(45.1829968751969,13.8351736362929,20.));
#87459=CARTESIAN_POINT('Ctrl Pts',(45.1898048477123,13.8026811643234,0.));
#87460=CARTESIAN_POINT('Ctrl Pts',(45.1898048477123,13.8026811643234,20.));
#87461=CARTESIAN_POINT('Ctrl Pts',(45.1965898546723,13.7701850295968,0.));
#87462=CARTESIAN_POINT('Ctrl Pts',(45.1965898546723,13.7701850295968,20.));
#87463=CARTESIAN_POINT('Ctrl Pts',(45.2033518936101,13.7376852482019,0.));
#87464=CARTESIAN_POINT('Ctrl Pts',(45.2033518936101,13.7376852482019,20.));
#87465=CARTESIAN_POINT('Ctrl Pts',(45.2100909620697,13.7051818362299,0.));
#87466=CARTESIAN_POINT('Ctrl Pts',(45.2100909620697,13.7051818362299,20.));
#87467=CARTESIAN_POINT('Ctrl Pts',(45.2168070576061,13.6726748097738,0.));
#87468=CARTESIAN_POINT('Ctrl Pts',(45.2168070576061,13.6726748097738,20.));
#87469=CARTESIAN_POINT('Ctrl Pts',(45.2235001777847,13.6401641849286,0.));
#87470=CARTESIAN_POINT('Ctrl Pts',(45.2235001777847,13.6401641849286,20.));
#87471=CARTESIAN_POINT('Ctrl Pts',(45.2301703201819,13.6076499777915,0.));
#87472=CARTESIAN_POINT('Ctrl Pts',(45.2301703201819,13.6076499777915,20.));
#87473=CARTESIAN_POINT('Ctrl Pts',(45.2368174823856,13.5751322044618,0.));
#87474=CARTESIAN_POINT('Ctrl Pts',(45.2368174823856,13.5751322044618,20.));
#87475=CARTESIAN_POINT('Ctrl Pts',(45.2434416619952,13.542610881041,0.));
#87476=CARTESIAN_POINT('Ctrl Pts',(45.2434416619952,13.542610881041,20.));
#87477=CARTESIAN_POINT('Ctrl Pts',(45.2500428566225,13.5100860236329,0.));
#87478=CARTESIAN_POINT('Ctrl Pts',(45.2500428566225,13.5100860236329,20.));
#87479=CARTESIAN_POINT('Ctrl Pts',(45.2566210638904,13.4775576483433,0.));
#87480=CARTESIAN_POINT('Ctrl Pts',(45.2566210638904,13.4775576483433,20.));
#87481=CARTESIAN_POINT('Ctrl Pts',(45.2631762814325,13.44502577128,0.));
#87482=CARTESIAN_POINT('Ctrl Pts',(45.2631762814325,13.44502577128,20.));
#87483=CARTESIAN_POINT('Ctrl Pts',(45.2697085068935,13.4124904085531,0.));
#87484=CARTESIAN_POINT('Ctrl Pts',(45.2697085068935,13.4124904085531,20.));
#87485=CARTESIAN_POINT('Ctrl Pts',(45.276217737929,13.3799515762744,0.));
#87486=CARTESIAN_POINT('Ctrl Pts',(45.276217737929,13.3799515762744,20.));
#87487=CARTESIAN_POINT('Ctrl Pts',(45.2827039722059,13.3474092905576,0.));
#87488=CARTESIAN_POINT('Ctrl Pts',(45.2827039722059,13.3474092905576,20.));
#87489=CARTESIAN_POINT('Ctrl Pts',(45.2891672074022,13.3148635675188,0.));
#87490=CARTESIAN_POINT('Ctrl Pts',(45.2891672074022,13.3148635675188,20.));
#87491=CARTESIAN_POINT('Ctrl Pts',(45.2956074412073,13.282314423276,0.));
#87492=CARTESIAN_POINT('Ctrl Pts',(45.2956074412073,13.282314423276,20.));
#87493=CARTESIAN_POINT('Ctrl Pts',(45.3020246713218,13.2497618739494,0.));
#87494=CARTESIAN_POINT('Ctrl Pts',(45.3020246713218,13.2497618739494,20.));
#87495=CARTESIAN_POINT('Ctrl Pts',(45.3084188954577,13.217205935661,0.));
#87496=CARTESIAN_POINT('Ctrl Pts',(45.3084188954577,13.217205935661,20.));
#87497=CARTESIAN_POINT('Ctrl Pts',(45.3147901113387,13.1846466245352,0.));
#87498=CARTESIAN_POINT('Ctrl Pts',(45.3147901113387,13.1846466245352,20.));
#87499=CARTESIAN_POINT('Ctrl Pts',(45.321138316699,13.1520839566979,0.));
#87500=CARTESIAN_POINT('Ctrl Pts',(45.321138316699,13.1520839566979,20.));
#87501=CARTESIAN_POINT('Ctrl Pts',(45.3274635092846,13.1195179482773,0.));
#87502=CARTESIAN_POINT('Ctrl Pts',(45.3274635092846,13.1195179482773,20.));
#87503=CARTESIAN_POINT('Ctrl Pts',(45.3337656868523,13.0869486154035,0.));
#87504=CARTESIAN_POINT('Ctrl Pts',(45.3337656868523,13.0869486154035,20.));
#87505=CARTESIAN_POINT('Ctrl Pts',(45.3400448471699,13.0543759742083,0.));
#87506=CARTESIAN_POINT('Ctrl Pts',(45.3400448471699,13.0543759742083,20.));
#87507=CARTESIAN_POINT('Ctrl Pts',(45.3463009880171,13.021800040826,0.));
#87508=CARTESIAN_POINT('Ctrl Pts',(45.3463009880171,13.021800040826,20.));
#87509=CARTESIAN_POINT('Ctrl Pts',(45.3525341071849,12.9892208313927,0.));
#87510=CARTESIAN_POINT('Ctrl Pts',(45.3525341071849,12.9892208313927,20.));
#87511=CARTESIAN_POINT('Ctrl Pts',(45.3587442024753,12.9566383620464,0.));
#87512=CARTESIAN_POINT('Ctrl Pts',(45.3587442024753,12.9566383620464,20.));
#87513=CARTESIAN_POINT('Ctrl Pts',(45.364931271701,12.9240526489273,0.));
#87514=CARTESIAN_POINT('Ctrl Pts',(45.364931271701,12.9240526489273,20.));
#87515=CARTESIAN_POINT('Ctrl Pts',(45.371095312686,12.8914637081769,0.));
#87516=CARTESIAN_POINT('Ctrl Pts',(45.371095312686,12.8914637081769,20.));
#87517=CARTESIAN_POINT('Ctrl Pts',(45.3772363232658,12.8588715559393,0.));
#87518=CARTESIAN_POINT('Ctrl Pts',(45.3772363232658,12.8588715559393,20.));
#87519=CARTESIAN_POINT('Ctrl Pts',(45.3833543012877,12.82627620836,0.));
#87520=CARTESIAN_POINT('Ctrl Pts',(45.3833543012877,12.82627620836,20.));
#87521=CARTESIAN_POINT('Ctrl Pts',(45.3894492446102,12.7936776815868,0.));
#87522=CARTESIAN_POINT('Ctrl Pts',(45.3894492446102,12.7936776815868,20.));
#87523=CARTESIAN_POINT('Ctrl Pts',(45.3955211511033,12.7610759917694,0.));
#87524=CARTESIAN_POINT('Ctrl Pts',(45.3955211511033,12.7610759917694,20.));
#87525=CARTESIAN_POINT('Ctrl Pts',(45.4015700186485,12.7284711550592,0.));
#87526=CARTESIAN_POINT('Ctrl Pts',(45.4015700186485,12.7284711550592,20.));
#87527=CARTESIAN_POINT('Ctrl Pts',(45.407595845137,12.6958631876099,0.));
#87528=CARTESIAN_POINT('Ctrl Pts',(45.407595845137,12.6958631876099,20.));
#87529=CARTESIAN_POINT('Ctrl Pts',(45.4135986284717,12.6632521055766,0.));
#87530=CARTESIAN_POINT('Ctrl Pts',(45.4135986284717,12.6632521055766,20.));
#87531=CARTESIAN_POINT('Ctrl Pts',(45.4195783665665,12.6306379251165,0.));
#87532=CARTESIAN_POINT('Ctrl Pts',(45.4195783665665,12.6306379251165,20.));
#87533=CARTESIAN_POINT('Ctrl Pts',(45.4255350573473,12.5980206623884,0.));
#87534=CARTESIAN_POINT('Ctrl Pts',(45.4255350573473,12.5980206623884,20.));
#87535=CARTESIAN_POINT('Ctrl Pts',(45.4314686987515,12.5654003335533,0.));
#87536=CARTESIAN_POINT('Ctrl Pts',(45.4314686987515,12.5654003335533,20.));
#87537=CARTESIAN_POINT('Ctrl Pts',(45.4373792887274,12.5327769547739,0.));
#87538=CARTESIAN_POINT('Ctrl Pts',(45.4373792887274,12.5327769547739,20.));
#87539=CARTESIAN_POINT('Ctrl Pts',(45.4432668252347,12.500150542215,0.));
#87540=CARTESIAN_POINT('Ctrl Pts',(45.4432668252347,12.500150542215,20.));
#87541=CARTESIAN_POINT('Ctrl Pts',(45.4491313062444,12.4675211120431,0.));
#87542=CARTESIAN_POINT('Ctrl Pts',(45.4491313062444,12.4675211120431,20.));
#87543=CARTESIAN_POINT('Ctrl Pts',(45.4549727297392,12.4348886804266,0.));
#87544=CARTESIAN_POINT('Ctrl Pts',(45.4549727297392,12.4348886804266,20.));
#87545=CARTESIAN_POINT('Ctrl Pts',(45.4607910937128,12.4022532635357,0.));
#87546=CARTESIAN_POINT('Ctrl Pts',(45.4607910937128,12.4022532635357,20.));
#87547=CARTESIAN_POINT('Ctrl Pts',(45.4665863961701,12.3696148775423,0.));
#87548=CARTESIAN_POINT('Ctrl Pts',(45.4665863961701,12.3696148775423,20.));
#87549=CARTESIAN_POINT('Ctrl Pts',(45.4723586351267,12.3369735386201,0.));
#87550=CARTESIAN_POINT('Ctrl Pts',(45.4723586351267,12.3369735386201,20.));
#87551=CARTESIAN_POINT('Ctrl Pts',(45.4781078086095,12.3043292629445,0.));
#87552=CARTESIAN_POINT('Ctrl Pts',(45.4781078086095,12.3043292629445,20.));
#87553=CARTESIAN_POINT('Ctrl Pts',(45.483833914657,12.2716820666929,0.));
#87554=CARTESIAN_POINT('Ctrl Pts',(45.483833914657,12.2716820666929,20.));
#87555=CARTESIAN_POINT('Ctrl Pts',(45.4895369513189,12.2390319660445,0.));
#87556=CARTESIAN_POINT('Ctrl Pts',(45.4895369513189,12.2390319660445,20.));
#87557=CARTESIAN_POINT('Ctrl Pts',(45.4952169166561,12.2063789771801,0.));
#87558=CARTESIAN_POINT('Ctrl Pts',(45.4952169166561,12.2063789771801,20.));
#87559=CARTESIAN_POINT('Ctrl Pts',(45.5008738087416,12.1737231162825,0.));
#87560=CARTESIAN_POINT('Ctrl Pts',(45.5008738087416,12.1737231162825,20.));
#87561=CARTESIAN_POINT('Ctrl Pts',(45.5065076256599,12.1410643995363,0.));
#87562=CARTESIAN_POINT('Ctrl Pts',(45.5065076256599,12.1410643995363,20.));
#87563=CARTESIAN_POINT('Ctrl Pts',(45.5121183655068,12.1084028431278,0.));
#87564=CARTESIAN_POINT('Ctrl Pts',(45.5121183655068,12.1084028431278,20.));
#87565=CARTESIAN_POINT('Ctrl Pts',(45.5177060263888,12.0757384632451,0.));
#87566=CARTESIAN_POINT('Ctrl Pts',(45.5177060263888,12.0757384632451,20.));
#87567=CARTESIAN_POINT('Ctrl Pts',(45.5232706064237,12.0430712760779,0.));
#87568=CARTESIAN_POINT('Ctrl Pts',(45.5232706064237,12.0430712760779,20.));
#87569=CARTESIAN_POINT('Ctrl Pts',(45.5288121037394,12.0104012978174,0.));
#87570=CARTESIAN_POINT('Ctrl Pts',(45.5288121037394,12.0104012978174,20.));
#87571=CARTESIAN_POINT('Ctrl Pts',(45.5343305164759,11.9777285446569,0.));
#87572=CARTESIAN_POINT('Ctrl Pts',(45.5343305164759,11.9777285446569,20.));
#87573=CARTESIAN_POINT('Ctrl Pts',(45.5398258427844,11.9450530327911,0.));
#87574=CARTESIAN_POINT('Ctrl Pts',(45.5398258427844,11.9450530327911,20.));
#87575=CARTESIAN_POINT('Ctrl Pts',(45.5452980808284,11.9123747784165,0.));
#87576=CARTESIAN_POINT('Ctrl Pts',(45.5452980808284,11.9123747784165,20.));
#87577=CARTESIAN_POINT('Ctrl Pts',(45.5507472287824,11.8796937977314,0.));
#87578=CARTESIAN_POINT('Ctrl Pts',(45.5507472287824,11.8796937977314,20.));
#87579=CARTESIAN_POINT('Ctrl Pts',(45.5561732848327,11.8470101069358,0.));
#87580=CARTESIAN_POINT('Ctrl Pts',(45.5561732848327,11.8470101069358,20.));
#87581=CARTESIAN_POINT('Ctrl Pts',(45.5615762471761,11.8143237222317,0.));
#87582=CARTESIAN_POINT('Ctrl Pts',(45.5615762471761,11.8143237222317,20.));
#87583=CARTESIAN_POINT('Ctrl Pts',(45.5669561140206,11.7816346598227,0.));
#87584=CARTESIAN_POINT('Ctrl Pts',(45.5669561140206,11.7816346598227,20.));
#87585=CARTESIAN_POINT('Ctrl Pts',(45.5723128835857,11.748942935914,0.));
#87586=CARTESIAN_POINT('Ctrl Pts',(45.5723128835857,11.748942935914,20.));
#87587=CARTESIAN_POINT('Ctrl Pts',(45.5776465541021,11.7162485667124,0.));
#87588=CARTESIAN_POINT('Ctrl Pts',(45.5776465541021,11.7162485667124,20.));
#87589=CARTESIAN_POINT('Ctrl Pts',(45.5829571238122,11.6835515684258,0.));
#87590=CARTESIAN_POINT('Ctrl Pts',(45.5829571238122,11.6835515684258,20.));
#87591=CARTESIAN_POINT('Ctrl Pts',(45.5882445909695,11.6508519572639,0.));
#87592=CARTESIAN_POINT('Ctrl Pts',(45.5882445909695,11.6508519572639,20.));
#87593=CARTESIAN_POINT('Ctrl Pts',(45.5935089538387,11.6181497494382,0.));
#87594=CARTESIAN_POINT('Ctrl Pts',(45.5935089538387,11.6181497494382,20.));
#87595=CARTESIAN_POINT('Ctrl Pts',(45.598750210696,11.5854449611619,0.));
#87596=CARTESIAN_POINT('Ctrl Pts',(45.598750210696,11.5854449611619,20.));
#87597=CARTESIAN_POINT('Ctrl Pts',(45.6039683598295,11.5527376086502,0.));
#87598=CARTESIAN_POINT('Ctrl Pts',(45.6039683598295,11.5527376086502,20.));
#87599=CARTESIAN_POINT('Ctrl Pts',(45.6091633995383,11.5200277081201,0.));
#87600=CARTESIAN_POINT('Ctrl Pts',(45.6091633995383,11.5200277081201,20.));
#87601=CARTESIAN_POINT('Ctrl Pts',(45.6143353281323,11.4873152757897,0.));
#87602=CARTESIAN_POINT('Ctrl Pts',(45.6143353281323,11.4873152757897,20.));
#87603=CARTESIAN_POINT('Ctrl Pts',(45.6194841439321,11.4546003278786,0.));
#87604=CARTESIAN_POINT('Ctrl Pts',(45.6194841439321,11.4546003278786,20.));
#87605=CARTESIAN_POINT('Ctrl Pts',(45.6246098452703,11.421882880608,0.));
#87606=CARTESIAN_POINT('Ctrl Pts',(45.6246098452703,11.421882880608,20.));
#87607=CARTESIAN_POINT('Ctrl Pts',(45.6297124304911,11.3891629502006,0.));
#87608=CARTESIAN_POINT('Ctrl Pts',(45.6297124304911,11.3891629502006,20.));
#87609=CARTESIAN_POINT('Ctrl Pts',(45.6347918979506,11.3564405528809,0.));
#87610=CARTESIAN_POINT('Ctrl Pts',(45.6347918979506,11.3564405528809,20.));
#87611=CARTESIAN_POINT('Ctrl Pts',(45.6398482460165,11.3237157048751,0.));
#87612=CARTESIAN_POINT('Ctrl Pts',(45.6398482460165,11.3237157048751,20.));
#87613=CARTESIAN_POINT('Ctrl Pts',(45.6448814730676,11.290988422411,0.));
#87614=CARTESIAN_POINT('Ctrl Pts',(45.6448814730676,11.290988422411,20.));
#87615=CARTESIAN_POINT('Ctrl Pts',(45.6498915774933,11.2582587217178,0.));
#87616=CARTESIAN_POINT('Ctrl Pts',(45.6498915774933,11.2582587217178,20.));
#87617=CARTESIAN_POINT('Ctrl Pts',(45.6548785576938,11.2255266190259,0.));
#87618=CARTESIAN_POINT('Ctrl Pts',(45.6548785576938,11.2255266190259,20.));
#87619=CARTESIAN_POINT('Ctrl Pts',(45.6598424120808,11.1927921305675,0.));
#87620=CARTESIAN_POINT('Ctrl Pts',(45.6598424120808,11.1927921305675,20.));
#87621=CARTESIAN_POINT('Ctrl Pts',(45.6647831390778,11.1600552725764,0.));
#87622=CARTESIAN_POINT('Ctrl Pts',(45.6647831390778,11.1600552725764,20.));
#87623=CARTESIAN_POINT('Ctrl Pts',(45.6697007371202,11.1273160612881,0.));
#87624=CARTESIAN_POINT('Ctrl Pts',(45.6697007371202,11.1273160612881,20.));
#87625=CARTESIAN_POINT('Ctrl Pts',(45.6745952046549,11.0945745129393,0.));
#87626=CARTESIAN_POINT('Ctrl Pts',(45.6745952046549,11.0945745129393,20.));
#87627=CARTESIAN_POINT('Ctrl Pts',(45.6794665401395,11.0618306437685,0.));
#87628=CARTESIAN_POINT('Ctrl Pts',(45.6794665401395,11.0618306437685,20.));
#87629=CARTESIAN_POINT('Ctrl Pts',(45.684314742043,11.0290844700154,0.));
#87630=CARTESIAN_POINT('Ctrl Pts',(45.684314742043,11.0290844700154,20.));
#87631=CARTESIAN_POINT('Ctrl Pts',(45.6891398088456,10.9963360079212,0.));
#87632=CARTESIAN_POINT('Ctrl Pts',(45.6891398088456,10.9963360079212,20.));
#87633=CARTESIAN_POINT('Ctrl Pts',(45.6939417390393,10.9635852737287,0.));
#87634=CARTESIAN_POINT('Ctrl Pts',(45.6939417390393,10.9635852737287,20.));
#87635=CARTESIAN_POINT('Ctrl Pts',(45.698720531127,10.930832283682,0.));
#87636=CARTESIAN_POINT('Ctrl Pts',(45.698720531127,10.930832283682,20.));
#87637=CARTESIAN_POINT('Ctrl Pts',(45.7034761836229,10.898077054027,0.));
#87638=CARTESIAN_POINT('Ctrl Pts',(45.7034761836229,10.898077054027,20.));
#87639=CARTESIAN_POINT('Ctrl Pts',(45.7082086950532,10.8653196010107,0.));
#87640=CARTESIAN_POINT('Ctrl Pts',(45.7082086950532,10.8653196010107,20.));
#87641=CARTESIAN_POINT('Ctrl Pts',(45.7129180639558,10.832559940882,0.));
#87642=CARTESIAN_POINT('Ctrl Pts',(45.7129180639558,10.832559940882,20.));
#87643=CARTESIAN_POINT('Ctrl Pts',(45.7176042888794,10.7997980898913,0.));
#87644=CARTESIAN_POINT('Ctrl Pts',(45.7176042888794,10.7997980898913,20.));
#87645=CARTESIAN_POINT('Ctrl Pts',(45.7222673683833,10.7670340642896,0.));
#87646=CARTESIAN_POINT('Ctrl Pts',(45.7222673683833,10.7670340642896,20.));
#87647=CARTESIAN_POINT('Ctrl Pts',(45.7269073010391,10.73426788033,0.));
#87648=CARTESIAN_POINT('Ctrl Pts',(45.7269073010391,10.73426788033,20.));
#87649=CARTESIAN_POINT('Ctrl Pts',(45.7315240854293,10.7014995542666,0.));
#87650=CARTESIAN_POINT('Ctrl Pts',(45.7315240854293,10.7014995542666,20.));
#87651=CARTESIAN_POINT('Ctrl Pts',(45.7361177201484,10.6687291023553,0.));
#87652=CARTESIAN_POINT('Ctrl Pts',(45.7361177201484,10.6687291023553,20.));
#87653=CARTESIAN_POINT('Ctrl Pts',(45.7406882038015,10.6359565408533,0.));
#87654=CARTESIAN_POINT('Ctrl Pts',(45.7406882038015,10.6359565408533,20.));
#87655=CARTESIAN_POINT('Ctrl Pts',(45.745235535006,10.6031818860194,0.));
#87656=CARTESIAN_POINT('Ctrl Pts',(45.745235535006,10.6031818860194,20.));
#87657=CARTESIAN_POINT('Ctrl Pts',(45.7497597123901,10.5704051541135,0.));
#87658=CARTESIAN_POINT('Ctrl Pts',(45.7497597123901,10.5704051541135,20.));
#87659=CARTESIAN_POINT('Ctrl Pts',(45.7542607345937,10.5376263613969,0.));
#87660=CARTESIAN_POINT('Ctrl Pts',(45.7542607345937,10.5376263613969,20.));
#87661=CARTESIAN_POINT('Ctrl Pts',(45.7587386002674,10.504845524132,0.));
#87662=CARTESIAN_POINT('Ctrl Pts',(45.7587386002674,10.504845524132,20.));
#87663=CARTESIAN_POINT('Ctrl Pts',(45.7631933080735,10.4720626585828,0.));
#87664=CARTESIAN_POINT('Ctrl Pts',(45.7631933080735,10.4720626585828,20.));
#87665=CARTESIAN_POINT('Ctrl Pts',(45.7676248566855,10.4392777810149,0.));
#87666=CARTESIAN_POINT('Ctrl Pts',(45.7676248566855,10.4392777810149,20.));
#87667=CARTESIAN_POINT('Ctrl Pts',(45.772033244789,10.406490907695,0.));
#87668=CARTESIAN_POINT('Ctrl Pts',(45.772033244789,10.406490907695,20.));
#87669=CARTESIAN_POINT('Ctrl Pts',(45.7764184710811,10.3737020548914,0.));
#87670=CARTESIAN_POINT('Ctrl Pts',(45.7764184710811,10.3737020548914,20.));
#87671=CARTESIAN_POINT('Ctrl Pts',(45.7807805342697,10.3409112388736,0.));
#87672=CARTESIAN_POINT('Ctrl Pts',(45.7807805342697,10.3409112388736,20.));
#87673=CARTESIAN_POINT('Ctrl Pts',(45.7851194330743,10.3081184759123,0.));
#87674=CARTESIAN_POINT('Ctrl Pts',(45.7851194330743,10.3081184759123,20.));
#87675=CARTESIAN_POINT('Ctrl Pts',(45.7894351662253,10.2753237822796,0.));
#87676=CARTESIAN_POINT('Ctrl Pts',(45.7894351662253,10.2753237822796,20.));
#87677=CARTESIAN_POINT('Ctrl Pts',(45.7937277324642,10.2425271742485,0.));
#87678=CARTESIAN_POINT('Ctrl Pts',(45.7937277324642,10.2425271742485,20.));
#87679=CARTESIAN_POINT('Ctrl Pts',(45.7979971305449,10.2097286680937,0.));
#87680=CARTESIAN_POINT('Ctrl Pts',(45.7979971305449,10.2097286680937,20.));
#87681=CARTESIAN_POINT('Ctrl Pts',(45.8022433592327,10.1769282800914,0.));
#87682=CARTESIAN_POINT('Ctrl Pts',(45.8022433592327,10.1769282800914,20.));
#87683=CARTESIAN_POINT('Ctrl Pts',(45.8064664173048,10.1441260265191,0.));
#87684=CARTESIAN_POINT('Ctrl Pts',(45.8064664173048,10.1441260265191,20.));
#87685=CARTESIAN_POINT('Ctrl Pts',(45.8106663035491,10.1113219236554,0.));
#87686=CARTESIAN_POINT('Ctrl Pts',(45.8106663035491,10.1113219236554,20.));
#87687=CARTESIAN_POINT('Ctrl Pts',(45.8148430167647,10.0785159877801,0.));
#87688=CARTESIAN_POINT('Ctrl Pts',(45.8148430167647,10.0785159877801,20.));
#87689=CARTESIAN_POINT('Ctrl Pts',(45.8189965557614,10.0457082351741,0.));
#87690=CARTESIAN_POINT('Ctrl Pts',(45.8189965557614,10.0457082351741,20.));
#87691=CARTESIAN_POINT('Ctrl Pts',(45.8231269193611,10.0128986821194,0.));
#87692=CARTESIAN_POINT('Ctrl Pts',(45.8231269193611,10.0128986821194,20.));
#87693=CARTESIAN_POINT('Ctrl Pts',(45.8272341063969,9.98008734489948,0.));
#87694=CARTESIAN_POINT('Ctrl Pts',(45.8272341063969,9.98008734489948,20.));
#87695=CARTESIAN_POINT('Ctrl Pts',(45.8313181157134,9.94727423979906,0.));
#87696=CARTESIAN_POINT('Ctrl Pts',(45.8313181157134,9.94727423979906,20.));
#87697=CARTESIAN_POINT('Ctrl Pts',(45.8353789461673,9.91445938310424,0.));
#87698=CARTESIAN_POINT('Ctrl Pts',(45.8353789461673,9.91445938310424,20.));
#87699=CARTESIAN_POINT('Ctrl Pts',(45.8394165966264,9.88164279110241,0.));
#87700=CARTESIAN_POINT('Ctrl Pts',(45.8394165966264,9.88164279110241,20.));
#87701=CARTESIAN_POINT('Ctrl Pts',(45.84343106597,9.84882448008225,0.));
#87702=CARTESIAN_POINT('Ctrl Pts',(45.84343106597,9.84882448008225,20.));
#87703=CARTESIAN_POINT('Ctrl Pts',(45.8474223530896,9.81600446633368,0.));
#87704=CARTESIAN_POINT('Ctrl Pts',(45.8474223530896,9.81600446633368,20.));
#87705=CARTESIAN_POINT('Ctrl Pts',(45.8513904568872,9.78318276614762,0.));
#87706=CARTESIAN_POINT('Ctrl Pts',(45.8513904568872,9.78318276614762,20.));
#87707=CARTESIAN_POINT('Ctrl Pts',(45.8553353762765,9.75035939581619,0.));
#87708=CARTESIAN_POINT('Ctrl Pts',(45.8553353762765,9.75035939581619,20.));
#87709=CARTESIAN_POINT('Ctrl Pts',(45.8592571101812,9.71753437163221,0.));
#87710=CARTESIAN_POINT('Ctrl Pts',(45.8592571101812,9.71753437163221,20.));
#87711=CARTESIAN_POINT('Ctrl Pts',(45.8631556575366,9.68470770988976,0.));
#87712=CARTESIAN_POINT('Ctrl Pts',(45.8631556575366,9.68470770988976,20.));
#87713=CARTESIAN_POINT('Ctrl Pts',(45.8670310172895,9.65187942688401,0.));
#87714=CARTESIAN_POINT('Ctrl Pts',(45.8670310172895,9.65187942688401,20.));
#87715=CARTESIAN_POINT('Ctrl Pts',(45.870883188399,9.61904953891161,0.));
#87716=CARTESIAN_POINT('Ctrl Pts',(45.870883188399,9.61904953891161,20.));
#87717=CARTESIAN_POINT('Ctrl Pts',(45.8747121698355,9.58621806227057,0.));
#87718=CARTESIAN_POINT('Ctrl Pts',(45.8747121698355,9.58621806227057,20.));
#87719=CARTESIAN_POINT('Ctrl Pts',(45.8785179605829,9.55338501326048,0.));
#87720=CARTESIAN_POINT('Ctrl Pts',(45.8785179605829,9.55338501326048,20.));
#87721=CARTESIAN_POINT('Ctrl Pts',(45.882300559635,9.52055040818185,0.));
#87722=CARTESIAN_POINT('Ctrl Pts',(45.882300559635,9.52055040818185,20.));
#87723=CARTESIAN_POINT('Ctrl Pts',(45.8860599659967,9.4877142633361,0.));
#87724=CARTESIAN_POINT('Ctrl Pts',(45.8860599659967,9.4877142633361,20.));
#87725=CARTESIAN_POINT('Ctrl Pts',(45.8897961786838,9.45487659502548,0.));
#87726=CARTESIAN_POINT('Ctrl Pts',(45.8897961786838,9.45487659502548,20.));
#87727=CARTESIAN_POINT('Ctrl Pts',(45.8935091967241,9.42203741955325,0.));
#87728=CARTESIAN_POINT('Ctrl Pts',(45.8935091967241,9.42203741955325,20.));
#87729=CARTESIAN_POINT('Ctrl Pts',(45.8971990191563,9.38919675322381,0.));
#87730=CARTESIAN_POINT('Ctrl Pts',(45.8971990191563,9.38919675322381,20.));
#87731=CARTESIAN_POINT('Ctrl Pts',(45.90086564503,9.35635461234246,0.));
#87732=CARTESIAN_POINT('Ctrl Pts',(45.90086564503,9.35635461234246,20.));
#87733=CARTESIAN_POINT('Ctrl Pts',(45.9045090734063,9.3235110132158,0.));
#87734=CARTESIAN_POINT('Ctrl Pts',(45.9045090734063,9.3235110132158,20.));
#87735=CARTESIAN_POINT('Ctrl Pts',(45.9081293033576,9.29066597215163,0.));
#87736=CARTESIAN_POINT('Ctrl Pts',(45.9081293033576,9.29066597215163,20.));
#87737=CARTESIAN_POINT('Ctrl Pts',(45.9117263339694,9.25781950545902,0.));
#87738=CARTESIAN_POINT('Ctrl Pts',(45.9117263339694,9.25781950545902,20.));
#87739=CARTESIAN_POINT('Ctrl Pts',(45.9153001643391,9.22497162944821,0.));
#87740=CARTESIAN_POINT('Ctrl Pts',(45.9153001643391,9.22497162944821,20.));
#87741=CARTESIAN_POINT('Ctrl Pts',(45.9188507935764,9.19212236043074,0.));
#87742=CARTESIAN_POINT('Ctrl Pts',(45.9188507935764,9.19212236043074,20.));
#87743=CARTESIAN_POINT('Ctrl Pts',(45.9223782208015,9.15927171471892,0.));
#87744=CARTESIAN_POINT('Ctrl Pts',(45.9223782208015,9.15927171471892,20.));
#87745=CARTESIAN_POINT('Ctrl Pts',(45.9258824451441,9.12641970862567,0.));
#87746=CARTESIAN_POINT('Ctrl Pts',(45.9258824451441,9.12641970862567,20.));
#87747=CARTESIAN_POINT('Ctrl Pts',(45.9293634657451,9.09356635846486,0.));
#87748=CARTESIAN_POINT('Ctrl Pts',(45.9293634657451,9.09356635846486,20.));
#87749=CARTESIAN_POINT('Ctrl Pts',(45.9328212817567,9.06071168055121,0.));
#87750=CARTESIAN_POINT('Ctrl Pts',(45.9328212817567,9.06071168055121,20.));
#87751=CARTESIAN_POINT('Ctrl Pts',(45.9362558923428,9.02785569120062,0.));
#87752=CARTESIAN_POINT('Ctrl Pts',(45.9362558923428,9.02785569120062,20.));
#87753=CARTESIAN_POINT('Ctrl Pts',(45.939667296681,8.99499840673047,0.));
#87754=CARTESIAN_POINT('Ctrl Pts',(45.939667296681,8.99499840673047,20.));
#87755=CARTESIAN_POINT('Ctrl Pts',(45.9430554939595,8.96213984345905,0.));
#87756=CARTESIAN_POINT('Ctrl Pts',(45.9430554939595,8.96213984345905,20.));
#87757=CARTESIAN_POINT('Ctrl Pts',(45.9464204833787,8.92928001770576,0.));
#87758=CARTESIAN_POINT('Ctrl Pts',(45.9464204833787,8.92928001770576,20.));
#87759=CARTESIAN_POINT('Ctrl Pts',(45.9497622641496,8.89641894579083,0.));
#87760=CARTESIAN_POINT('Ctrl Pts',(45.9497622641496,8.89641894579083,20.));
#87761=CARTESIAN_POINT('Ctrl Pts',(45.9530808354938,8.86355664403535,0.));
#87762=CARTESIAN_POINT('Ctrl Pts',(45.9530808354938,8.86355664403535,20.));
#87763=CARTESIAN_POINT('Ctrl Pts',(45.9563761966444,8.83069312876128,0.));
#87764=CARTESIAN_POINT('Ctrl Pts',(45.9563761966444,8.83069312876128,20.));
#87765=CARTESIAN_POINT('Ctrl Pts',(45.9596483468462,8.79782841629148,0.));
#87766=CARTESIAN_POINT('Ctrl Pts',(45.9596483468462,8.79782841629148,20.));
#87767=CARTESIAN_POINT('Ctrl Pts',(45.9628972853566,8.76496252295002,0.));
#87768=CARTESIAN_POINT('Ctrl Pts',(45.9628972853566,8.76496252295002,20.));
#87769=CARTESIAN_POINT('Ctrl Pts',(45.9661230114446,8.732095465062,0.));
#87770=CARTESIAN_POINT('Ctrl Pts',(45.9661230114446,8.732095465062,20.));
#87771=CARTESIAN_POINT('Ctrl Pts',(45.9693255243897,8.69922725895329,0.));
#87772=CARTESIAN_POINT('Ctrl Pts',(45.9693255243897,8.69922725895329,20.));
#87773=CARTESIAN_POINT('Ctrl Pts',(45.9725048234817,8.66635792095044,0.));
#87774=CARTESIAN_POINT('Ctrl Pts',(45.9725048234817,8.66635792095044,20.));
#87775=CARTESIAN_POINT('Ctrl Pts',(45.9756609080225,8.633487467381,0.));
#87776=CARTESIAN_POINT('Ctrl Pts',(45.9756609080225,8.633487467381,20.));
#87777=CARTESIAN_POINT('Ctrl Pts',(45.9787937773254,8.6006159145734,0.));
#87778=CARTESIAN_POINT('Ctrl Pts',(45.9787937773254,8.6006159145734,20.));
#87779=CARTESIAN_POINT('Ctrl Pts',(45.9819034307166,8.56774327885726,0.));
#87780=CARTESIAN_POINT('Ctrl Pts',(45.9819034307166,8.56774327885726,20.));
#87781=CARTESIAN_POINT('Ctrl Pts',(45.9849898675351,8.53486957656348,0.));
#87782=CARTESIAN_POINT('Ctrl Pts',(45.9849898675351,8.53486957656348,20.));
#87783=CARTESIAN_POINT('Ctrl Pts',(45.9880530871298,8.50199482402355,0.));
#87784=CARTESIAN_POINT('Ctrl Pts',(45.9880530871298,8.50199482402355,20.));
#87785=CARTESIAN_POINT('Ctrl Pts',(45.991093088861,8.46911903756974,0.));
#87786=CARTESIAN_POINT('Ctrl Pts',(45.991093088861,8.46911903756974,20.));
#87787=CARTESIAN_POINT('Ctrl Pts',(45.9941098720982,8.43624223353472,0.));
#87788=CARTESIAN_POINT('Ctrl Pts',(45.9941098720982,8.43624223353472,20.));
#87789=CARTESIAN_POINT('Ctrl Pts',(45.9971034362229,8.403364428252,0.));
#87790=CARTESIAN_POINT('Ctrl Pts',(45.9971034362229,8.403364428252,20.));
#87791=CARTESIAN_POINT('Ctrl Pts',(46.000073780629,8.37048563805606,0.));
#87792=CARTESIAN_POINT('Ctrl Pts',(46.000073780629,8.37048563805606,20.));
#87793=CARTESIAN_POINT('Ctrl Pts',(46.0030209047226,8.33760587928254,0.));
#87794=CARTESIAN_POINT('Ctrl Pts',(46.0030209047226,8.33760587928254,20.));
#87795=CARTESIAN_POINT('Ctrl Pts',(46.0059448079215,8.30472516826798,0.));
#87796=CARTESIAN_POINT('Ctrl Pts',(46.0059448079215,8.30472516826798,20.));
#87797=CARTESIAN_POINT('Ctrl Pts',(46.0088454896554,8.27184352134995,0.));
#87798=CARTESIAN_POINT('Ctrl Pts',(46.0088454896554,8.27184352134995,20.));
#87799=CARTESIAN_POINT('Ctrl Pts',(46.0117229493647,8.2389609548667,0.));
#87800=CARTESIAN_POINT('Ctrl Pts',(46.0117229493647,8.2389609548667,20.));
#87801=CARTESIAN_POINT('Ctrl Pts',(46.0145771865005,8.20607748515696,0.));
#87802=CARTESIAN_POINT('Ctrl Pts',(46.0145771865005,8.20607748515696,20.));
#87803=CARTESIAN_POINT('Ctrl Pts',(46.0174082005262,8.17319312856043,0.));
#87804=CARTESIAN_POINT('Ctrl Pts',(46.0174082005262,8.17319312856043,20.));
#87805=CARTESIAN_POINT('Ctrl Pts',(46.0202159909161,8.1403079014174,0.));
#87806=CARTESIAN_POINT('Ctrl Pts',(46.0202159909161,8.1403079014174,20.));
#87807=CARTESIAN_POINT('Ctrl Pts',(46.0230005571558,8.10742182006901,0.));
#87808=CARTESIAN_POINT('Ctrl Pts',(46.0230005571558,8.10742182006901,20.));
#87809=CARTESIAN_POINT('Ctrl Pts',(46.025761898743,8.07453490085737,0.));
#87810=CARTESIAN_POINT('Ctrl Pts',(46.025761898743,8.07453490085737,20.));
#87811=CARTESIAN_POINT('Ctrl Pts',(46.0285000151874,8.04164716012546,0.));
#87812=CARTESIAN_POINT('Ctrl Pts',(46.0285000151874,8.04164716012546,20.));
#87813=CARTESIAN_POINT('Ctrl Pts',(46.0312149060105,8.00875861421695,0.));
#87814=CARTESIAN_POINT('Ctrl Pts',(46.0312149060105,8.00875861421695,20.));
#87815=CARTESIAN_POINT('Ctrl Pts',(46.0339065707442,7.97586927947621,0.));
#87816=CARTESIAN_POINT('Ctrl Pts',(46.0339065707442,7.97586927947621,20.));
#87817=CARTESIAN_POINT('Ctrl Pts',(46.0365750089318,7.94297917224816,0.));
#87818=CARTESIAN_POINT('Ctrl Pts',(46.0365750089318,7.94297917224816,20.));
#87819=CARTESIAN_POINT('Ctrl Pts',(46.0392202201278,7.91008830887856,0.));
#87820=CARTESIAN_POINT('Ctrl Pts',(46.0392202201278,7.91008830887856,20.));
#87821=CARTESIAN_POINT('Ctrl Pts',(46.0418422038989,7.87719670571401,0.));
#87822=CARTESIAN_POINT('Ctrl Pts',(46.0418422038989,7.87719670571401,20.));
#87823=CARTESIAN_POINT('Ctrl Pts',(46.0444409598224,7.84430437910167,0.));
#87824=CARTESIAN_POINT('Ctrl Pts',(46.0444409598224,7.84430437910167,20.));
#87825=CARTESIAN_POINT('Ctrl Pts',(46.0470164874882,7.81141134538955,0.));
#87826=CARTESIAN_POINT('Ctrl Pts',(46.0470164874882,7.81141134538955,20.));
#87827=CARTESIAN_POINT('Ctrl Pts',(46.0495687864972,7.77851762092637,0.));
#87828=CARTESIAN_POINT('Ctrl Pts',(46.0495687864972,7.77851762092637,20.));
#87829=CARTESIAN_POINT('Ctrl Pts',(46.052097856463,7.74562322206168,0.));
#87830=CARTESIAN_POINT('Ctrl Pts',(46.052097856463,7.74562322206168,20.));
#87831=CARTESIAN_POINT('Ctrl Pts',(46.0546036970108,7.71272816514572,0.));
#87832=CARTESIAN_POINT('Ctrl Pts',(46.0546036970108,7.71272816514572,20.));
#87833=CARTESIAN_POINT('Ctrl Pts',(46.0570863077758,7.67983246652918,0.));
#87834=CARTESIAN_POINT('Ctrl Pts',(46.0570863077758,7.67983246652918,20.));
#87835=CARTESIAN_POINT('Ctrl Pts',(46.0595456884042,7.64693614256336,0.));
#87836=CARTESIAN_POINT('Ctrl Pts',(46.0595456884042,7.64693614256336,20.));
#87837=CARTESIAN_POINT('Ctrl Pts',(46.0619818385541,7.61403920960036,0.));
#87838=CARTESIAN_POINT('Ctrl Pts',(46.0619818385541,7.61403920960036,20.));
#87839=CARTESIAN_POINT('Ctrl Pts',(46.0643947578955,7.58114168399302,0.));
#87840=CARTESIAN_POINT('Ctrl Pts',(46.0643947578955,7.58114168399302,20.));
#87841=CARTESIAN_POINT('Ctrl Pts',(46.0667844461104,7.54824358209485,0.));
#87842=CARTESIAN_POINT('Ctrl Pts',(46.0667844461104,7.54824358209485,20.));
#87843=CARTESIAN_POINT('Ctrl Pts',(46.0691509028928,7.51534492025983,0.));
#87844=CARTESIAN_POINT('Ctrl Pts',(46.0691509028928,7.51534492025983,20.));
#87845=CARTESIAN_POINT('Ctrl Pts',(46.0714941279471,7.48244571484251,0.));
#87846=CARTESIAN_POINT('Ctrl Pts',(46.0714941279471,7.48244571484251,20.));
#87847=CARTESIAN_POINT('Ctrl Pts',(46.0738141209885,7.4495459821981,0.));
#87848=CARTESIAN_POINT('Ctrl Pts',(46.0738141209885,7.4495459821981,20.));
#87849=CARTESIAN_POINT('Ctrl Pts',(46.0761108817447,7.41664573868261,0.));
#87850=CARTESIAN_POINT('Ctrl Pts',(46.0761108817447,7.41664573868261,20.));
#87851=CARTESIAN_POINT('Ctrl Pts',(46.0783844099553,7.38374500065295,0.));
#87852=CARTESIAN_POINT('Ctrl Pts',(46.0783844099553,7.38374500065295,20.));
#87853=CARTESIAN_POINT('Ctrl Pts',(46.0806347053718,7.35084378446662,0.));
#87854=CARTESIAN_POINT('Ctrl Pts',(46.0806347053718,7.35084378446662,20.));
#87855=CARTESIAN_POINT('Ctrl Pts',(46.0828617677561,7.3179421064814,0.));
#87856=CARTESIAN_POINT('Ctrl Pts',(46.0828617677561,7.3179421064814,20.));
#87857=CARTESIAN_POINT('Ctrl Pts',(46.0850655968817,7.28503998305551,0.));
#87858=CARTESIAN_POINT('Ctrl Pts',(46.0850655968817,7.28503998305551,20.));
#87859=CARTESIAN_POINT('Ctrl Pts',(46.0872461925336,7.2521374305475,0.));
#87860=CARTESIAN_POINT('Ctrl Pts',(46.0872461925336,7.2521374305475,20.));
#87861=CARTESIAN_POINT('Ctrl Pts',(46.0894035545083,7.21923446531641,0.));
#87862=CARTESIAN_POINT('Ctrl Pts',(46.0894035545083,7.21923446531641,20.));
#87863=CARTESIAN_POINT('Ctrl Pts',(46.0915376826137,7.18633110372212,0.));
#87864=CARTESIAN_POINT('Ctrl Pts',(46.0915376826137,7.18633110372212,20.));
#87865=CARTESIAN_POINT('Ctrl Pts',(46.0936485766695,7.1534273621253,0.));
#87866=CARTESIAN_POINT('Ctrl Pts',(46.0936485766695,7.1534273621253,20.));
#87867=CARTESIAN_POINT('Ctrl Pts',(46.0957362365075,7.12052325688753,0.));
#87868=CARTESIAN_POINT('Ctrl Pts',(46.0957362365075,7.12052325688753,20.));
#87869=CARTESIAN_POINT('Ctrl Pts',(46.097800661971,7.08761880437094,0.));
#87870=CARTESIAN_POINT('Ctrl Pts',(46.097800661971,7.08761880437094,20.));
#87871=CARTESIAN_POINT('Ctrl Pts',(46.0998418529147,7.05471402093802,0.));
#87872=CARTESIAN_POINT('Ctrl Pts',(46.0998418529147,7.05471402093802,20.));
#87873=CARTESIAN_POINT('Ctrl Pts',(46.1018598092046,7.02180892295148,0.));
#87874=CARTESIAN_POINT('Ctrl Pts',(46.1018598092046,7.02180892295148,20.));
#87875=CARTESIAN_POINT('Ctrl Pts',(46.103854530718,6.98890352677439,0.));
#87876=CARTESIAN_POINT('Ctrl Pts',(46.103854530718,6.98890352677439,20.));
#87877=CARTESIAN_POINT('Ctrl Pts',(46.1058260173429,6.95599784877019,0.));
#87878=CARTESIAN_POINT('Ctrl Pts',(46.1058260173429,6.95599784877019,20.));
#87879=CARTESIAN_POINT('Ctrl Pts',(46.1077742689797,6.92309190530285,0.));
#87880=CARTESIAN_POINT('Ctrl Pts',(46.1077742689797,6.92309190530285,20.));
#87881=CARTESIAN_POINT('Ctrl Pts',(46.1096992855399,6.8901857127369,0.));
#87882=CARTESIAN_POINT('Ctrl Pts',(46.1096992855399,6.8901857127369,20.));
#87883=CARTESIAN_POINT('Ctrl Pts',(46.111601066948,6.85727928743788,0.));
#87884=CARTESIAN_POINT('Ctrl Pts',(46.111601066948,6.85727928743788,20.));
#87885=CARTESIAN_POINT('Ctrl Pts',(46.1134796131392,6.82437264577169,0.));
#87886=CARTESIAN_POINT('Ctrl Pts',(46.1134796131392,6.82437264577169,20.));
#87887=CARTESIAN_POINT('Ctrl Pts',(46.1153349240611,6.7914658041047,0.));
#87888=CARTESIAN_POINT('Ctrl Pts',(46.1153349240611,6.7914658041047,20.));
#87889=CARTESIAN_POINT('Ctrl Pts',(46.1171669996709,6.75855877880357,0.));
#87890=CARTESIAN_POINT('Ctrl Pts',(46.1171669996709,6.75855877880357,20.));
#87891=CARTESIAN_POINT('Ctrl Pts',(46.1189758399374,6.72565158623521,0.));
#87892=CARTESIAN_POINT('Ctrl Pts',(46.1189758399374,6.72565158623521,20.));
#87893=CARTESIAN_POINT('Ctrl Pts',(46.1207614448407,6.69274424276688,0.));
#87894=CARTESIAN_POINT('Ctrl Pts',(46.1207614448407,6.69274424276688,20.));
#87895=CARTESIAN_POINT('Ctrl Pts',(46.122523814374,6.65983676476652,0.));
#87896=CARTESIAN_POINT('Ctrl Pts',(46.122523814374,6.65983676476652,20.));
#87897=CARTESIAN_POINT('Ctrl Pts',(46.124262948542,6.62692916860258,0.));
#87898=CARTESIAN_POINT('Ctrl Pts',(46.124262948542,6.62692916860258,20.));
#87899=CARTESIAN_POINT('Ctrl Pts',(46.1259788473615,6.594021470644,0.));
#87900=CARTESIAN_POINT('Ctrl Pts',(46.1259788473615,6.594021470644,20.));
#87901=CARTESIAN_POINT('Ctrl Pts',(46.1276715108604,6.5611136872601,0.));
#87902=CARTESIAN_POINT('Ctrl Pts',(46.1276715108604,6.5611136872601,20.));
#87903=CARTESIAN_POINT('Ctrl Pts',(46.1293409390781,6.5282058348205,0.));
#87904=CARTESIAN_POINT('Ctrl Pts',(46.1293409390781,6.5282058348205,20.));
#87905=CARTESIAN_POINT('Ctrl Pts',(46.1309871320644,6.49529792969509,0.));
#87906=CARTESIAN_POINT('Ctrl Pts',(46.1309871320644,6.49529792969509,20.));
#87907=CARTESIAN_POINT('Ctrl Pts',(46.1326100898806,6.46238998825408,0.));
#87908=CARTESIAN_POINT('Ctrl Pts',(46.1326100898806,6.46238998825408,20.));
#87909=CARTESIAN_POINT('Ctrl Pts',(46.134209812599,6.42948202686814,0.));
#87910=CARTESIAN_POINT('Ctrl Pts',(46.134209812599,6.42948202686814,20.));
#87911=CARTESIAN_POINT('Ctrl Pts',(46.1357863003044,6.39657406190845,0.));
#87912=CARTESIAN_POINT('Ctrl Pts',(46.1357863003044,6.39657406190845,20.));
#87913=CARTESIAN_POINT('Ctrl Pts',(46.1373395530931,6.36366610974648,0.));
#87914=CARTESIAN_POINT('Ctrl Pts',(46.1373395530931,6.36366610974648,20.));
#87915=CARTESIAN_POINT('Ctrl Pts',(46.138869571074,6.3307581867542,0.));
#87916=CARTESIAN_POINT('Ctrl Pts',(46.138869571074,6.3307581867542,20.));
#87917=CARTESIAN_POINT('Ctrl Pts',(46.1403763543673,6.29785030930382,0.));
#87918=CARTESIAN_POINT('Ctrl Pts',(46.1403763543673,6.29785030930382,20.));
#87919=CARTESIAN_POINT('Ctrl Pts',(46.141859903105,6.26494249376778,0.));
#87920=CARTESIAN_POINT('Ctrl Pts',(46.141859903105,6.26494249376778,20.));
#87921=CARTESIAN_POINT('Ctrl Pts',(46.1433202174297,6.23203475651883,0.));
#87922=CARTESIAN_POINT('Ctrl Pts',(46.1433202174297,6.23203475651883,20.));
#87923=CARTESIAN_POINT('Ctrl Pts',(46.1447572974959,6.19912711393004,0.));
#87924=CARTESIAN_POINT('Ctrl Pts',(46.1447572974959,6.19912711393004,20.));
#87925=CARTESIAN_POINT('Ctrl Pts',(46.1461711434687,6.16621958237488,0.));
#87926=CARTESIAN_POINT('Ctrl Pts',(46.1461711434687,6.16621958237488,20.));
#87927=CARTESIAN_POINT('Ctrl Pts',(46.1475617555249,6.1333121782271,0.));
#87928=CARTESIAN_POINT('Ctrl Pts',(46.1475617555249,6.1333121782271,20.));
#87929=CARTESIAN_POINT('Ctrl Pts',(46.1489291338532,6.10040491786086,0.));
#87930=CARTESIAN_POINT('Ctrl Pts',(46.1489291338532,6.10040491786086,20.));
#87931=CARTESIAN_POINT('Ctrl Pts',(46.1502732786543,6.06749781765058,0.));
#87932=CARTESIAN_POINT('Ctrl Pts',(46.1502732786543,6.06749781765058,20.));
#87933=CARTESIAN_POINT('Ctrl Pts',(46.151594190141,6.03459089397104,0.));
#87934=CARTESIAN_POINT('Ctrl Pts',(46.151594190141,6.03459089397104,20.));
#87935=CARTESIAN_POINT('Ctrl Pts',(46.1528918685373,6.0016841631972,0.));
#87936=CARTESIAN_POINT('Ctrl Pts',(46.1528918685373,6.0016841631972,20.));
#87937=CARTESIAN_POINT('Ctrl Pts',(46.1541663140783,5.96877764170412,0.));
#87938=CARTESIAN_POINT('Ctrl Pts',(46.1541663140783,5.96877764170412,20.));
#87939=CARTESIAN_POINT('Ctrl Pts',(46.1554175270101,5.9358713458669,0.));
#87940=CARTESIAN_POINT('Ctrl Pts',(46.1554175270101,5.9358713458669,20.));
#87941=CARTESIAN_POINT('Ctrl Pts',(46.1566455075904,5.90296529206097,0.));
#87942=CARTESIAN_POINT('Ctrl Pts',(46.1566455075904,5.90296529206097,20.));
#87943=CARTESIAN_POINT('Ctrl Pts',(46.1578502560886,5.87005949666212,0.));
#87944=CARTESIAN_POINT('Ctrl Pts',(46.1578502560886,5.87005949666212,20.));
#87945=CARTESIAN_POINT('Ctrl Pts',(46.1590317727861,5.83715397604653,0.));
#87946=CARTESIAN_POINT('Ctrl Pts',(46.1590317727861,5.83715397604653,20.));
#87947=CARTESIAN_POINT('Ctrl Pts',(46.160190057976,5.80424874659071,0.));
#87948=CARTESIAN_POINT('Ctrl Pts',(46.160190057976,5.80424874659071,20.));
#87949=CARTESIAN_POINT('Ctrl Pts',(46.1613251119636,5.77134382467173,0.));
#87950=CARTESIAN_POINT('Ctrl Pts',(46.1613251119636,5.77134382467173,20.));
#87951=CARTESIAN_POINT('Ctrl Pts',(46.1624369350662,5.73843922666648,0.));
#87952=CARTESIAN_POINT('Ctrl Pts',(46.1624369350662,5.73843922666648,20.));
#87953=CARTESIAN_POINT('Ctrl Pts',(46.1635255276116,5.70553496895185,0.));
#87954=CARTESIAN_POINT('Ctrl Pts',(46.1635255276116,5.70553496895185,20.));
#87955=CARTESIAN_POINT('Ctrl Pts',(46.1645908899393,5.67263106790479,0.));
#87956=CARTESIAN_POINT('Ctrl Pts',(46.1645908899393,5.67263106790479,20.));
#87957=CARTESIAN_POINT('Ctrl Pts',(46.1656330223979,5.63972753990236,0.));
#87958=CARTESIAN_POINT('Ctrl Pts',(46.1656330223979,5.63972753990236,20.));
#87959=CARTESIAN_POINT('Ctrl Pts',(46.166651925349,5.60682440132182,0.));
#87960=CARTESIAN_POINT('Ctrl Pts',(46.166651925349,5.60682440132182,20.));
#87961=CARTESIAN_POINT('Ctrl Pts',(46.1676475991657,5.57392166854075,0.));
#87962=CARTESIAN_POINT('Ctrl Pts',(46.1676475991657,5.57392166854075,20.));
#87963=CARTESIAN_POINT('Ctrl Pts',(46.1686200442337,5.5410193579371,0.));
#87964=CARTESIAN_POINT('Ctrl Pts',(46.1686200442337,5.5410193579371,20.));
#87965=CARTESIAN_POINT('Ctrl Pts',(46.1695692609505,5.50811748588894,0.));
#87966=CARTESIAN_POINT('Ctrl Pts',(46.1695692609505,5.50811748588894,20.));
#87967=CARTESIAN_POINT('Ctrl Pts',(46.170495249726,5.4752160687746,0.));
#87968=CARTESIAN_POINT('Ctrl Pts',(46.170495249726,5.4752160687746,20.));
#87969=CARTESIAN_POINT('Ctrl Pts',(46.1713980109807,5.44231512297239,0.));
#87970=CARTESIAN_POINT('Ctrl Pts',(46.1713980109807,5.44231512297239,20.));
#87971=CARTESIAN_POINT('Ctrl Pts',(46.1722775451467,5.40941466486069,0.));
#87972=CARTESIAN_POINT('Ctrl Pts',(46.1722775451467,5.40941466486069,20.));
#87973=CARTESIAN_POINT('Ctrl Pts',(46.1731338526667,5.37651471081787,0.));
#87974=CARTESIAN_POINT('Ctrl Pts',(46.1731338526667,5.37651471081787,20.));
#87975=CARTESIAN_POINT('Ctrl Pts',(46.1739669339953,5.3436152772224,0.));
#87976=CARTESIAN_POINT('Ctrl Pts',(46.1739669339953,5.3436152772224,20.));
#87977=CARTESIAN_POINT('Ctrl Pts',(46.1747767895978,5.31071638045279,0.));
#87978=CARTESIAN_POINT('Ctrl Pts',(46.1747767895978,5.31071638045279,20.));
#87979=CARTESIAN_POINT('Ctrl Pts',(46.1755634199519,5.27781803688791,0.));
#87980=CARTESIAN_POINT('Ctrl Pts',(46.1755634199519,5.27781803688791,20.));
#87981=CARTESIAN_POINT('Ctrl Pts',(46.1763268255471,5.24492026290663,0.));
#87982=CARTESIAN_POINT('Ctrl Pts',(46.1763268255471,5.24492026290663,20.));
#87983=CARTESIAN_POINT('Ctrl Pts',(46.1770670068854,5.21202307488802,0.));
#87984=CARTESIAN_POINT('Ctrl Pts',(46.1770670068854,5.21202307488802,20.));
#87985=CARTESIAN_POINT('Ctrl Pts',(46.1777839644797,5.17912648921102,0.));
#87986=CARTESIAN_POINT('Ctrl Pts',(46.1777839644797,5.17912648921102,20.));
#87987=CARTESIAN_POINT('Ctrl Pts',(46.1784776988548,5.14623052225472,0.));
#87988=CARTESIAN_POINT('Ctrl Pts',(46.1784776988548,5.14623052225472,20.));
#87989=CARTESIAN_POINT('Ctrl Pts',(46.1791482105459,5.11333519039809,0.));
#87990=CARTESIAN_POINT('Ctrl Pts',(46.1791482105459,5.11333519039809,20.));
#87991=CARTESIAN_POINT('Ctrl Pts',(46.1797955000997,5.08044051002026,0.));
#87992=CARTESIAN_POINT('Ctrl Pts',(46.1797955000997,5.08044051002026,20.));
#87993=CARTESIAN_POINT('Ctrl Pts',(46.1804195680748,5.04754649750031,0.));
#87994=CARTESIAN_POINT('Ctrl Pts',(46.1804195680748,5.04754649750031,20.));
#87995=CARTESIAN_POINT('Ctrl Pts',(46.1810204150412,5.01465316921749,0.));
#87996=CARTESIAN_POINT('Ctrl Pts',(46.1810204150412,5.01465316921749,20.));
#87997=CARTESIAN_POINT('Ctrl Pts',(46.1815980415817,4.98176054155101,0.));
#87998=CARTESIAN_POINT('Ctrl Pts',(46.1815980415817,4.98176054155101,20.));
#87999=CARTESIAN_POINT('Ctrl Pts',(46.182152448291,4.94886863088032,0.));
#88000=CARTESIAN_POINT('Ctrl Pts',(46.182152448291,4.94886863088032,20.));
#88001=CARTESIAN_POINT('Ctrl Pts',(46.1826836357763,4.91597745358481,0.));
#88002=CARTESIAN_POINT('Ctrl Pts',(46.1826836357763,4.91597745358481,20.));
#88003=CARTESIAN_POINT('Ctrl Pts',(46.1831916046531,4.8830870260435,0.));
#88004=CARTESIAN_POINT('Ctrl Pts',(46.1831916046531,4.8830870260435,20.));
#88005=CARTESIAN_POINT('Ctrl Pts',(46.1836763555496,4.85019736463544,0.));
#88006=CARTESIAN_POINT('Ctrl Pts',(46.1836763555496,4.85019736463544,20.));
#88007=CARTESIAN_POINT('Ctrl Pts',(46.1841378891039,4.81730848573954,0.));
#88008=CARTESIAN_POINT('Ctrl Pts',(46.1841378891039,4.81730848573954,20.));
#88009=CARTESIAN_POINT('Ctrl Pts',(46.1845762059678,4.78442040573515,0.));
#88010=CARTESIAN_POINT('Ctrl Pts',(46.1845762059678,4.78442040573515,20.));
#88011=CARTESIAN_POINT('Ctrl Pts',(46.1849913068043,4.75153314100161,0.));
#88012=CARTESIAN_POINT('Ctrl Pts',(46.1849913068043,4.75153314100161,20.));
#88013=CARTESIAN_POINT('Ctrl Pts',(46.1853831922891,4.71864670791826,0.));
#88014=CARTESIAN_POINT('Ctrl Pts',(46.1853831922891,4.71864670791826,20.));
#88015=CARTESIAN_POINT('Ctrl Pts',(46.1857518631086,4.68576112286394,0.));
#88016=CARTESIAN_POINT('Ctrl Pts',(46.1857518631086,4.68576112286394,20.));
#88017=CARTESIAN_POINT('Ctrl Pts',(46.1860973199616,4.65287640221748,0.));
#88018=CARTESIAN_POINT('Ctrl Pts',(46.1860973199616,4.65287640221748,20.));
#88019=CARTESIAN_POINT('Ctrl Pts',(46.1864195635571,4.61999256235741,0.));
#88020=CARTESIAN_POINT('Ctrl Pts',(46.1864195635571,4.61999256235741,20.));
#88021=CARTESIAN_POINT('Ctrl Pts',(46.1867185946155,4.58710961966233,0.));
#88022=CARTESIAN_POINT('Ctrl Pts',(46.1867185946155,4.58710961966233,20.));
#88023=CARTESIAN_POINT('Ctrl Pts',(46.1869944138693,4.55422759051101,0.));
#88024=CARTESIAN_POINT('Ctrl Pts',(46.1869944138693,4.55422759051101,20.));
#88025=CARTESIAN_POINT('Ctrl Pts',(46.1872470220627,4.52134649128218,0.));
#88026=CARTESIAN_POINT('Ctrl Pts',(46.1872470220627,4.52134649128218,20.));
#88027=CARTESIAN_POINT('Ctrl Pts',(46.1874764199521,4.48846633835459,0.));
#88028=CARTESIAN_POINT('Ctrl Pts',(46.1874764199521,4.48846633835459,20.));
#88029=CARTESIAN_POINT('Ctrl Pts',(46.1876826083051,4.45558714810681,0.));
#88030=CARTESIAN_POINT('Ctrl Pts',(46.1876826083051,4.45558714810681,20.));
#88031=CARTESIAN_POINT('Ctrl Pts',(46.1878655879008,4.42270893691724,0.));
#88032=CARTESIAN_POINT('Ctrl Pts',(46.1878655879008,4.42270893691724,20.));
#88033=CARTESIAN_POINT('Ctrl Pts',(46.1880253595296,4.38983172116389,0.));
#88034=CARTESIAN_POINT('Ctrl Pts',(46.1880253595296,4.38983172116389,20.));
#88035=CARTESIAN_POINT('Ctrl Pts',(46.1881619239926,4.35695551722447,0.));
#88036=CARTESIAN_POINT('Ctrl Pts',(46.1881619239926,4.35695551722447,20.));
#88037=CARTESIAN_POINT('Ctrl Pts',(46.1882752821036,4.32408034147655,0.));
#88038=CARTESIAN_POINT('Ctrl Pts',(46.1882752821036,4.32408034147655,20.));
#88039=CARTESIAN_POINT('Ctrl Pts',(46.1883654346888,4.29120621029777,0.));
#88040=CARTESIAN_POINT('Ctrl Pts',(46.1883654346888,4.29120621029777,20.));
#88041=CARTESIAN_POINT('Ctrl Pts',(46.1884323825857,4.25833314006578,0.));
#88042=CARTESIAN_POINT('Ctrl Pts',(46.1884323825857,4.25833314006578,20.));
#88043=CARTESIAN_POINT('Ctrl Pts',(46.1884761266433,4.22546114715825,0.));
#88044=CARTESIAN_POINT('Ctrl Pts',(46.1884761266433,4.22546114715825,20.));
#88045=CARTESIAN_POINT('Ctrl Pts',(46.1884966677209,4.19259024795239,0.));
#88046=CARTESIAN_POINT('Ctrl Pts',(46.1884966677209,4.19259024795239,20.));
#88047=CARTESIAN_POINT('Ctrl Pts',(46.1884940066895,4.15972045882509,0.));
#88048=CARTESIAN_POINT('Ctrl Pts',(46.1884940066895,4.15972045882509,20.));
#88049=CARTESIAN_POINT('Ctrl Pts',(46.1884681444317,4.12685179615294,0.));
#88050=CARTESIAN_POINT('Ctrl Pts',(46.1884681444317,4.12685179615294,20.));
#88051=CARTESIAN_POINT('Ctrl Pts',(46.188419081843,4.09398427631255,0.));
#88052=CARTESIAN_POINT('Ctrl Pts',(46.188419081843,4.09398427631255,20.));
#88053=CARTESIAN_POINT('Ctrl Pts',(46.18834681983,4.06111791568023,0.));
#88054=CARTESIAN_POINT('Ctrl Pts',(46.18834681983,4.06111791568023,20.));
#88055=CARTESIAN_POINT('Ctrl Pts',(46.1882513593113,4.02825273063218,0.));
#88056=CARTESIAN_POINT('Ctrl Pts',(46.1882513593113,4.02825273063218,20.));
#88057=CARTESIAN_POINT('Ctrl Pts',(46.1881327012171,3.99538873754443,0.));
#88058=CARTESIAN_POINT('Ctrl Pts',(46.1881327012171,3.99538873754443,20.));
#88059=CARTESIAN_POINT('Ctrl Pts',(46.1879908464881,3.96252595279274,0.));
#88060=CARTESIAN_POINT('Ctrl Pts',(46.1879908464881,3.96252595279274,20.));
#88061=CARTESIAN_POINT('Ctrl Pts',(46.1878257960766,3.92966439275257,0.));
#88062=CARTESIAN_POINT('Ctrl Pts',(46.1878257960766,3.92966439275257,20.));
#88063=CARTESIAN_POINT('Ctrl Pts',(46.1876375509469,3.89680407379914,0.));
#88064=CARTESIAN_POINT('Ctrl Pts',(46.1876375509469,3.89680407379914,20.));
#88065=CARTESIAN_POINT('Ctrl Pts',(46.1874261120751,3.86394501230744,0.));
#88066=CARTESIAN_POINT('Ctrl Pts',(46.1874261120751,3.86394501230744,20.));
#88067=CARTESIAN_POINT('Ctrl Pts',(46.1871914804492,3.83108722465199,0.));
#88068=CARTESIAN_POINT('Ctrl Pts',(46.1871914804492,3.83108722465199,20.));
#88069=CARTESIAN_POINT('Ctrl Pts',(46.1869336570686,3.79823072720685,0.));
#88070=CARTESIAN_POINT('Ctrl Pts',(46.1869336570686,3.79823072720685,20.));
#88071=CARTESIAN_POINT('Ctrl Pts',(46.1866526429445,3.76537553634596,0.));
#88072=CARTESIAN_POINT('Ctrl Pts',(46.1866526429445,3.76537553634596,20.));
#88073=CARTESIAN_POINT('Ctrl Pts',(46.1863484390996,3.73252166844328,0.));
#88074=CARTESIAN_POINT('Ctrl Pts',(46.1863484390996,3.73252166844328,20.));
#88075=CARTESIAN_POINT('Ctrl Pts',(46.1860210465678,3.69966913987253,0.));
#88076=CARTESIAN_POINT('Ctrl Pts',(46.1860210465678,3.69966913987253,20.));
#88077=CARTESIAN_POINT('Ctrl Pts',(46.185670466394,3.6668179670071,0.));
#88078=CARTESIAN_POINT('Ctrl Pts',(46.185670466394,3.6668179670071,20.));
#88079=CARTESIAN_POINT('Ctrl Pts',(46.1852966996347,3.6339681662199,0.));
#88080=CARTESIAN_POINT('Ctrl Pts',(46.1852966996347,3.6339681662199,20.));
#88081=CARTESIAN_POINT('Ctrl Pts',(46.1848997473582,3.60111975388339,0.));
#88082=CARTESIAN_POINT('Ctrl Pts',(46.1848997473582,3.60111975388339,20.));
#88083=CARTESIAN_POINT('Ctrl Pts',(46.1844796106451,3.56827274636958,0.));
#88084=CARTESIAN_POINT('Ctrl Pts',(46.1844796106451,3.56827274636958,20.));
#88085=CARTESIAN_POINT('Ctrl Pts',(46.1840362905882,3.53542716005025,0.));
#88086=CARTESIAN_POINT('Ctrl Pts',(46.1840362905882,3.53542716005025,20.));
#88087=CARTESIAN_POINT('Ctrl Pts',(46.1835697882921,3.50258301129689,0.));
#88088=CARTESIAN_POINT('Ctrl Pts',(46.1835697882921,3.50258301129689,20.));
#88089=CARTESIAN_POINT('Ctrl Pts',(46.1830801048722,3.4697403164807,0.));
#88090=CARTESIAN_POINT('Ctrl Pts',(46.1830801048722,3.4697403164807,20.));
#88091=CARTESIAN_POINT('Ctrl Pts',(46.1825672414553,3.43689909197262,0.));
#88092=CARTESIAN_POINT('Ctrl Pts',(46.1825672414553,3.43689909197262,20.));
#88093=CARTESIAN_POINT('Ctrl Pts',(46.1820311991793,3.40405935414302,0.));
#88094=CARTESIAN_POINT('Ctrl Pts',(46.1820311991793,3.40405935414302,20.));
#88095=CARTESIAN_POINT('Ctrl Pts',(46.1814719791936,3.37122111936182,0.));
#88096=CARTESIAN_POINT('Ctrl Pts',(46.1814719791936,3.37122111936182,20.));
#88097=CARTESIAN_POINT('Ctrl Pts',(46.1808895826591,3.33838440399861,0.));
#88098=CARTESIAN_POINT('Ctrl Pts',(46.1808895826591,3.33838440399861,20.));
#88099=CARTESIAN_POINT('Ctrl Pts',(46.1802840107495,3.30554922442266,0.));
#88100=CARTESIAN_POINT('Ctrl Pts',(46.1802840107495,3.30554922442266,20.));
#88101=CARTESIAN_POINT('Ctrl Pts',(46.1796552646498,3.27271559700279,0.));
#88102=CARTESIAN_POINT('Ctrl Pts',(46.1796552646498,3.27271559700279,20.));
#88103=CARTESIAN_POINT('Ctrl Pts',(46.1790033455572,3.23988353810748,0.));
#88104=CARTESIAN_POINT('Ctrl Pts',(46.1790033455572,3.23988353810748,20.));
#88105=CARTESIAN_POINT('Ctrl Pts',(46.1783282546796,3.20705306410471,0.));
#88106=CARTESIAN_POINT('Ctrl Pts',(46.1783282546796,3.20705306410471,20.));
#88107=CARTESIAN_POINT('Ctrl Pts',(46.1776299932363,3.17422419136187,0.));
#88108=CARTESIAN_POINT('Ctrl Pts',(46.1776299932363,3.17422419136187,20.));
#88109=CARTESIAN_POINT('Ctrl Pts',(46.1769085624582,3.14139693624605,0.));
#88110=CARTESIAN_POINT('Ctrl Pts',(46.1769085624582,3.14139693624605,20.));
#88111=CARTESIAN_POINT('Ctrl Pts',(46.1761639635878,3.10857131512384,0.));
#88112=CARTESIAN_POINT('Ctrl Pts',(46.1761639635878,3.10857131512384,20.));
#88113=CARTESIAN_POINT('Ctrl Pts',(46.1753961978798,3.0757473443616,0.));
#88114=CARTESIAN_POINT('Ctrl Pts',(46.1753961978798,3.0757473443616,20.));
#88115=CARTESIAN_POINT('Ctrl Pts',(46.1746052665999,3.04292504032497,0.));
#88116=CARTESIAN_POINT('Ctrl Pts',(46.1746052665999,3.04292504032497,20.));
#88117=CARTESIAN_POINT('Ctrl Pts',(46.1737911710261,3.01010441937913,0.));
#88118=CARTESIAN_POINT('Ctrl Pts',(46.1737911710261,3.01010441937913,20.));
#88119=CARTESIAN_POINT('Ctrl Pts',(46.1729539124487,2.9772854978889,0.));
#88120=CARTESIAN_POINT('Ctrl Pts',(46.1729539124487,2.9772854978889,20.));
#88121=CARTESIAN_POINT('Ctrl Pts',(46.172093492169,2.94446829221865,0.));
#88122=CARTESIAN_POINT('Ctrl Pts',(46.172093492169,2.94446829221865,20.));
#88123=CARTESIAN_POINT('Ctrl Pts',(46.1712099114993,2.91165281873225,0.));
#88124=CARTESIAN_POINT('Ctrl Pts',(46.1712099114993,2.91165281873225,20.));
#88125=CARTESIAN_POINT('Ctrl Pts',(46.1703031717627,2.87883909379287,0.));
#88126=CARTESIAN_POINT('Ctrl Pts',(46.1703031717627,2.87883909379287,20.));
#88127=CARTESIAN_POINT('Ctrl Pts',(46.169373274294,2.84602713376309,0.));
#88128=CARTESIAN_POINT('Ctrl Pts',(46.169373274294,2.84602713376309,20.));
#88129=CARTESIAN_POINT('Ctrl Pts',(46.1684202204402,2.81321695500492,0.));
#88130=CARTESIAN_POINT('Ctrl Pts',(46.1684202204402,2.81321695500492,20.));
#88131=CARTESIAN_POINT('Ctrl Pts',(46.1674440115603,2.78040857388008,0.));
#88132=CARTESIAN_POINT('Ctrl Pts',(46.1674440115603,2.78040857388008,20.));
#88133=CARTESIAN_POINT('Ctrl Pts',(46.1664446490252,2.7476020067498,0.));
#88134=CARTESIAN_POINT('Ctrl Pts',(46.1664446490252,2.7476020067498,20.));
#88135=CARTESIAN_POINT('Ctrl Pts',(46.1654221342175,2.71479726997479,0.));
#88136=CARTESIAN_POINT('Ctrl Pts',(46.1654221342175,2.71479726997479,20.));
#88137=CARTESIAN_POINT('Ctrl Pts',(46.1643764685316,2.68199437991524,0.));
#88138=CARTESIAN_POINT('Ctrl Pts',(46.1643764685316,2.68199437991524,20.));
#88139=CARTESIAN_POINT('Ctrl Pts',(46.163307653373,2.64919335293067,0.));
#88140=CARTESIAN_POINT('Ctrl Pts',(46.163307653373,2.64919335293067,20.));
#88141=CARTESIAN_POINT('Ctrl Pts',(46.1622156901587,2.61639420537995,0.));
#88142=CARTESIAN_POINT('Ctrl Pts',(46.1622156901587,2.61639420537995,20.));
#88143=CARTESIAN_POINT('Ctrl Pts',(46.1611005803162,2.58359695362108,0.));
#88144=CARTESIAN_POINT('Ctrl Pts',(46.1611005803162,2.58359695362108,20.));
#88145=CARTESIAN_POINT('Ctrl Pts',(46.1599623252856,2.55080161401166,0.));
#88146=CARTESIAN_POINT('Ctrl Pts',(46.1599623252856,2.55080161401166,20.));
#88147=CARTESIAN_POINT('Ctrl Pts',(46.1588009265184,2.51800820290892,0.));
#88148=CARTESIAN_POINT('Ctrl Pts',(46.1588009265184,2.51800820290892,20.));
#88149=CARTESIAN_POINT('Ctrl Pts',(46.1576163854777,2.48521673666957,0.));
#88150=CARTESIAN_POINT('Ctrl Pts',(46.1576163854777,2.48521673666957,20.));
#88151=CARTESIAN_POINT('Ctrl Pts',(46.1564087036389,2.4524272316497,0.));
#88152=CARTESIAN_POINT('Ctrl Pts',(46.1564087036389,2.4524272316497,20.));
#88153=CARTESIAN_POINT('Ctrl Pts',(46.155177882489,2.41963970420458,0.));
#88154=CARTESIAN_POINT('Ctrl Pts',(46.155177882489,2.41963970420458,20.));
#88155=CARTESIAN_POINT('Ctrl Pts',(46.1539239235264,2.38685417068871,0.));
#88156=CARTESIAN_POINT('Ctrl Pts',(46.1539239235264,2.38685417068871,20.));
#88157=CARTESIAN_POINT('Ctrl Pts',(46.1526468282603,2.35407064745589,0.));
#88158=CARTESIAN_POINT('Ctrl Pts',(46.1526468282603,2.35407064745589,20.));
#88159=CARTESIAN_POINT('Ctrl Pts',(46.1513465982124,2.3212891508592,0.));
#88160=CARTESIAN_POINT('Ctrl Pts',(46.1513465982124,2.3212891508592,20.));
#88161=CARTESIAN_POINT('Ctrl Pts',(46.1500232349155,2.28850969725138,0.));
#88162=CARTESIAN_POINT('Ctrl Pts',(46.1500232349155,2.28850969725138,20.));
#88163=CARTESIAN_POINT('Ctrl Pts',(46.1486767399146,2.25573230298459,0.));
#88164=CARTESIAN_POINT('Ctrl Pts',(46.1486767399146,2.25573230298459,20.));
#88165=CARTESIAN_POINT('Ctrl Pts',(46.147307114766,2.2229569844105,0.));
#88166=CARTESIAN_POINT('Ctrl Pts',(46.147307114766,2.2229569844105,20.));
#88167=CARTESIAN_POINT('Ctrl Pts',(46.1459143610377,2.19018375787987,0.));
#88168=CARTESIAN_POINT('Ctrl Pts',(46.1459143610377,2.19018375787987,20.));
#88169=CARTESIAN_POINT('Ctrl Pts',(46.1444984803082,2.15741263974263,0.));
#88170=CARTESIAN_POINT('Ctrl Pts',(46.1444984803082,2.15741263974263,20.));
#88171=CARTESIAN_POINT('Ctrl Pts',(46.1430594741682,2.12464364634813,0.));
#88172=CARTESIAN_POINT('Ctrl Pts',(46.1430594741682,2.12464364634813,20.));
#88173=CARTESIAN_POINT('Ctrl Pts',(46.1415973442202,2.09187679404497,0.));
#88174=CARTESIAN_POINT('Ctrl Pts',(46.1415973442202,2.09187679404497,20.));
#88175=CARTESIAN_POINT('Ctrl Pts',(46.1401120920793,2.05911209918102,0.));
#88176=CARTESIAN_POINT('Ctrl Pts',(46.1401120920793,2.05911209918102,20.));
#88177=CARTESIAN_POINT('Ctrl Pts',(46.1386037193727,2.02634957810318,0.));
#88178=CARTESIAN_POINT('Ctrl Pts',(46.1386037193727,2.02634957810318,20.));
#88179=CARTESIAN_POINT('Ctrl Pts',(46.1370722277379,1.99358924715754,0.));
#88180=CARTESIAN_POINT('Ctrl Pts',(46.1370722277379,1.99358924715754,20.));
#88181=CARTESIAN_POINT('Ctrl Pts',(46.1355176188236,1.96083112268931,0.));
#88182=CARTESIAN_POINT('Ctrl Pts',(46.1355176188236,1.96083112268931,20.));
#88183=CARTESIAN_POINT('Ctrl Pts',(46.1339398942902,1.9280752210434,0.));
#88184=CARTESIAN_POINT('Ctrl Pts',(46.1339398942902,1.9280752210434,20.));
#88185=CARTESIAN_POINT('Ctrl Pts',(46.1323390558096,1.89532155856415,0.));
#88186=CARTESIAN_POINT('Ctrl Pts',(46.1323390558096,1.89532155856415,20.));
#88187=CARTESIAN_POINT('Ctrl Pts',(46.1307151050651,1.86257015159583,0.));
#88188=CARTESIAN_POINT('Ctrl Pts',(46.1307151050651,1.86257015159583,20.));
#88189=CARTESIAN_POINT('Ctrl Pts',(46.1290680437528,1.82982101648207,0.));
#88190=CARTESIAN_POINT('Ctrl Pts',(46.1290680437528,1.82982101648207,20.));
#88191=CARTESIAN_POINT('Ctrl Pts',(46.1273978735796,1.79707416956535,0.));
#88192=CARTESIAN_POINT('Ctrl Pts',(46.1273978735796,1.79707416956535,20.));
#88193=CARTESIAN_POINT('Ctrl Pts',(46.1257045962649,1.76432962718686,0.));
#88194=CARTESIAN_POINT('Ctrl Pts',(46.1257045962649,1.76432962718686,20.));
#88195=CARTESIAN_POINT('Ctrl Pts',(46.1239882135394,1.73158740568598,0.));
#88196=CARTESIAN_POINT('Ctrl Pts',(46.1239882135394,1.73158740568598,20.));
#88197=CARTESIAN_POINT('Ctrl Pts',(46.1222487271454,1.6988475214004,0.));
#88198=CARTESIAN_POINT('Ctrl Pts',(46.1222487271454,1.6988475214004,20.));
#88199=CARTESIAN_POINT('Ctrl Pts',(46.1204861388364,1.66610999066656,0.));
#88200=CARTESIAN_POINT('Ctrl Pts',(46.1204861388364,1.66610999066656,20.));
#88201=CARTESIAN_POINT('Ctrl Pts',(46.1187004503775,1.63337482982071,0.));
#88202=CARTESIAN_POINT('Ctrl Pts',(46.1187004503775,1.63337482982071,20.));
#88203=CARTESIAN_POINT('Ctrl Pts',(46.1168916635447,1.60064205519959,0.));
#88204=CARTESIAN_POINT('Ctrl Pts',(46.1168916635447,1.60064205519959,20.));
#88205=CARTESIAN_POINT('Ctrl Pts',(46.1150597801266,1.56791168314158,0.));
#88206=CARTESIAN_POINT('Ctrl Pts',(46.1150597801266,1.56791168314158,20.));
#88207=CARTESIAN_POINT('Ctrl Pts',(46.1132048019234,1.53518372998667,0.));
#88208=CARTESIAN_POINT('Ctrl Pts',(46.1132048019234,1.53518372998667,20.));
#88209=CARTESIAN_POINT('Ctrl Pts',(46.111326730748,1.50245821207431,0.));
#88210=CARTESIAN_POINT('Ctrl Pts',(46.111326730748,1.50245821207431,20.));
#88211=CARTESIAN_POINT('Ctrl Pts',(46.1094255684237,1.46973514574144,0.));
#88212=CARTESIAN_POINT('Ctrl Pts',(46.1094255684237,1.46973514574144,20.));
#88213=CARTESIAN_POINT('Ctrl Pts',(46.1075013167858,1.43701454732091,0.));
#88214=CARTESIAN_POINT('Ctrl Pts',(46.1075013167858,1.43701454732091,20.));
#88215=CARTESIAN_POINT('Ctrl Pts',(46.1055539776801,1.40429643313894,0.));
#88216=CARTESIAN_POINT('Ctrl Pts',(46.1055539776801,1.40429643313894,20.));
#88217=CARTESIAN_POINT('Ctrl Pts',(46.1035835529643,1.37158081951552,0.));
#88218=CARTESIAN_POINT('Ctrl Pts',(46.1035835529643,1.37158081951552,20.));
#88219=CARTESIAN_POINT('Ctrl Pts',(46.1015900445065,1.33886772276919,0.));
#88220=CARTESIAN_POINT('Ctrl Pts',(46.1015900445065,1.33886772276919,20.));
#88221=CARTESIAN_POINT('Ctrl Pts',(46.0995734541875,1.30615715922173,0.));
#88222=CARTESIAN_POINT('Ctrl Pts',(46.0995734541875,1.30615715922173,20.));
#88223=CARTESIAN_POINT('Ctrl Pts',(46.0975337839002,1.27344914520176,0.));
#88224=CARTESIAN_POINT('Ctrl Pts',(46.0975337839002,1.27344914520176,20.));
#88225=CARTESIAN_POINT('Ctrl Pts',(46.0954710355506,1.24074369705073,0.));
#88226=CARTESIAN_POINT('Ctrl Pts',(46.0954710355506,1.24074369705073,20.));
#88227=CARTESIAN_POINT('Ctrl Pts',(46.0933852110571,1.20804083112097,0.));
#88228=CARTESIAN_POINT('Ctrl Pts',(46.0933852110571,1.20804083112097,20.));
#88229=CARTESIAN_POINT('Ctrl Pts',(46.0912763123502,1.17534056376402,0.));
#88230=CARTESIAN_POINT('Ctrl Pts',(46.0912763123502,1.17534056376402,20.));
#88231=CARTESIAN_POINT('Ctrl Pts',(46.0891443413718,1.14264291132053,0.));
#88232=CARTESIAN_POINT('Ctrl Pts',(46.0891443413718,1.14264291132053,20.));
#88233=CARTESIAN_POINT('Ctrl Pts',(46.0869893000733,1.10994789011163,0.));
#88234=CARTESIAN_POINT('Ctrl Pts',(46.0869893000733,1.10994789011163,20.));
#88235=CARTESIAN_POINT('Ctrl Pts',(46.0848111904142,1.07725551642471,0.));
#88236=CARTESIAN_POINT('Ctrl Pts',(46.0848111904142,1.07725551642471,20.));
#88237=CARTESIAN_POINT('Ctrl Pts',(46.0826100143611,1.04456580652048,0.));
#88238=CARTESIAN_POINT('Ctrl Pts',(46.0826100143611,1.04456580652048,20.));
#88239=CARTESIAN_POINT('Ctrl Pts',(46.0803857738924,1.01187877665955,0.));
#88240=CARTESIAN_POINT('Ctrl Pts',(46.0803857738924,1.01187877665955,20.));
#88241=CARTESIAN_POINT('Ctrl Pts',(46.0781384710012,0.979194443126295,0.));
#88242=CARTESIAN_POINT('Ctrl Pts',(46.0781384710012,0.979194443126295,20.));
#88243=CARTESIAN_POINT('Ctrl Pts',(46.0758681076973,0.946512822248755,0.));
#88244=CARTESIAN_POINT('Ctrl Pts',(46.0758681076973,0.946512822248755,20.));
#88245=CARTESIAN_POINT('Ctrl Pts',(46.0735746860119,0.913833930432277,0.));
#88246=CARTESIAN_POINT('Ctrl Pts',(46.0735746860119,0.913833930432277,20.));
#88247=CARTESIAN_POINT('Ctrl Pts',(46.0712582079948,0.881157784136745,0.));
#88248=CARTESIAN_POINT('Ctrl Pts',(46.0712582079948,0.881157784136745,20.));
#88249=CARTESIAN_POINT('Ctrl Pts',(46.0689186757066,0.848484399815189,0.));
#88250=CARTESIAN_POINT('Ctrl Pts',(46.0689186757066,0.848484399815189,20.));
#88251=CARTESIAN_POINT('Ctrl Pts',(46.0665560912128,0.815813793858643,0.));
#88252=CARTESIAN_POINT('Ctrl Pts',(46.0665560912128,0.815813793858643,20.));
#88253=CARTESIAN_POINT('Ctrl Pts',(46.064170456577,0.783145982548935,0.));
#88254=CARTESIAN_POINT('Ctrl Pts',(46.064170456577,0.783145982548935,20.));
#88255=CARTESIAN_POINT('Ctrl Pts',(46.0617617738521,0.750480981980926,0.));
#88256=CARTESIAN_POINT('Ctrl Pts',(46.0617617738521,0.750480981980926,20.));
#88257=CARTESIAN_POINT('Ctrl Pts',(46.0593300450868,0.71781880812973,0.));
#88258=CARTESIAN_POINT('Ctrl Pts',(46.0593300450868,0.71781880812973,20.));
#88259=CARTESIAN_POINT('Ctrl Pts',(46.0568752723439,0.685159476991768,0.));
#88260=CARTESIAN_POINT('Ctrl Pts',(46.0568752723439,0.685159476991768,20.));
#88261=CARTESIAN_POINT('Ctrl Pts',(46.0543974577158,0.652503004713265,0.));
#88262=CARTESIAN_POINT('Ctrl Pts',(46.0543974577158,0.652503004713265,20.));
#88263=CARTESIAN_POINT('Ctrl Pts',(46.0518966033391,0.619849407700868,0.));
#88264=CARTESIAN_POINT('Ctrl Pts',(46.0518966033391,0.619849407700868,20.));
#88265=CARTESIAN_POINT('Ctrl Pts',(46.0493727114182,0.587198702798626,0.));
#88266=CARTESIAN_POINT('Ctrl Pts',(46.0493727114182,0.587198702798626,20.));
#88267=CARTESIAN_POINT('Ctrl Pts',(46.0468257841997,0.554550907098833,0.));
#88268=CARTESIAN_POINT('Ctrl Pts',(46.0468257841997,0.554550907098833,20.));
#88269=CARTESIAN_POINT('Ctrl Pts',(46.044255823933,0.521906037621051,0.));
#88270=CARTESIAN_POINT('Ctrl Pts',(46.044255823933,0.521906037621051,20.));
#88271=CARTESIAN_POINT('Ctrl Pts',(46.0416628328334,0.489264111013841,0.));
#88272=CARTESIAN_POINT('Ctrl Pts',(46.0416628328334,0.489264111013841,20.));
#88273=CARTESIAN_POINT('Ctrl Pts',(46.0390468130479,0.456625143292617,0.));
#88274=CARTESIAN_POINT('Ctrl Pts',(46.0390468130479,0.456625143292617,20.));
#88275=CARTESIAN_POINT('Ctrl Pts',(46.0364077666069,0.42398914944525,0.));
#88276=CARTESIAN_POINT('Ctrl Pts',(46.0364077666069,0.42398914944525,20.));
#88277=CARTESIAN_POINT('Ctrl Pts',(46.0337456954889,0.391356143937839,0.));
#88278=CARTESIAN_POINT('Ctrl Pts',(46.0337456954889,0.391356143937839,20.));
#88279=CARTESIAN_POINT('Ctrl Pts',(46.0310606017089,0.358726141441572,0.));
#88280=CARTESIAN_POINT('Ctrl Pts',(46.0310606017089,0.358726141441572,20.));
#88281=CARTESIAN_POINT('Ctrl Pts',(46.0283524874048,0.32609915751696,0.));
#88282=CARTESIAN_POINT('Ctrl Pts',(46.0283524874048,0.32609915751696,20.));
#88283=CARTESIAN_POINT('Ctrl Pts',(46.025621354915,0.293475209241793,0.));
#88284=CARTESIAN_POINT('Ctrl Pts',(46.025621354915,0.293475209241793,20.));
#88285=CARTESIAN_POINT('Ctrl Pts',(46.022867206884,0.260854316057536,0.));
#88286=CARTESIAN_POINT('Ctrl Pts',(46.022867206884,0.260854316057536,20.));
#88287=CARTESIAN_POINT('Ctrl Pts',(46.0200900461091,0.228236498538563,0.));
#88288=CARTESIAN_POINT('Ctrl Pts',(46.0200900461091,0.228236498538563,20.));
#88289=CARTESIAN_POINT('Ctrl Pts',(46.0172898753497,0.195621776838885,0.));
#88290=CARTESIAN_POINT('Ctrl Pts',(46.0172898753497,0.195621776838885,20.));
#88291=CARTESIAN_POINT('Ctrl Pts',(46.0144666971462,0.163010169231708,0.));
#88292=CARTESIAN_POINT('Ctrl Pts',(46.0144666971462,0.163010169231708,20.));
#88293=CARTESIAN_POINT('Ctrl Pts',(46.0116205136405,0.130401690656321,0.));
#88294=CARTESIAN_POINT('Ctrl Pts',(46.0116205136405,0.130401690656321,20.));
#88295=CARTESIAN_POINT('Ctrl Pts',(46.0087513263814,0.0977963511372851,
0.));
#88296=CARTESIAN_POINT('Ctrl Pts',(46.0087513263814,0.0977963511372851,
20.));
#88297=CARTESIAN_POINT('Ctrl Pts',(46.0058591364029,0.0651941566547578,
0.));
#88298=CARTESIAN_POINT('Ctrl Pts',(46.0058591364029,0.0651941566547578,
20.));
#88299=CARTESIAN_POINT('Ctrl Pts',(46.0035269827389,0.0391149194889428,
0.));
#88300=CARTESIAN_POINT('Ctrl Pts',(46.0035269827389,0.0391149194889428,
20.));
#88301=CARTESIAN_POINT('Ctrl Pts',(46.0017675166781,0.0195569086685896,
0.));
#88302=CARTESIAN_POINT('Ctrl Pts',(46.0017675166781,0.0195569086685896,
20.));
#88303=CARTESIAN_POINT('Ctrl Pts',(46.0005899389515,0.0065188645893676,
0.));
#88304=CARTESIAN_POINT('Ctrl Pts',(46.0005899389515,0.0065188645893676,
20.));
#88305=CARTESIAN_POINT('Ctrl Pts',(46.,0.,0.));
#88306=CARTESIAN_POINT('Ctrl Pts',(46.,0.,20.));
#88307=CARTESIAN_POINT('',(37.5361777128299,31.4965928746404,2.));
#88308=CARTESIAN_POINT('Ctrl Pts',(45.2025619355895,13.7414592977624,2.));
#88309=CARTESIAN_POINT('Ctrl Pts',(45.039110381915,14.5281012519506,2.));
#88310=CARTESIAN_POINT('Ctrl Pts',(44.8554703046337,15.3115504167957,2.));
#88311=CARTESIAN_POINT('Ctrl Pts',(44.6518239974238,16.0907854020754,2.));
#88312=CARTESIAN_POINT('Ctrl Pts',(44.448476647749,16.8688764521982,2.));
#88313=CARTESIAN_POINT('Ctrl Pts',(44.2251818321296,17.6427655208206,2.));
#88314=CARTESIAN_POINT('Ctrl Pts',(43.9821719094461,18.4114480909826,2.));
#88315=CARTESIAN_POINT('Ctrl Pts',(43.7389521035327,19.1807945582349,2.));
#88316=CARTESIAN_POINT('Ctrl Pts',(43.4759831771533,19.9449253625111,2.));
#88317=CARTESIAN_POINT('Ctrl Pts',(43.1935481793562,20.7028482985112,2.));
#88318=CARTESIAN_POINT('Ctrl Pts',(42.910868013075,21.4614291516204,2.));
#88319=CARTESIAN_POINT('Ctrl Pts',(42.6086880302604,22.2137911905079,2.));
#88320=CARTESIAN_POINT('Ctrl Pts',(42.2873412605298,22.9589570442281,2.));
#88321=CARTESIAN_POINT('Ctrl Pts',(41.9655415206855,23.7051732830564,2.));
#88322=CARTESIAN_POINT('Ctrl Pts',(41.6245209894068,24.44417287288,2.));
#88323=CARTESIAN_POINT('Ctrl Pts',(41.2646624723933,25.1749942158169,2.));
#88324=CARTESIAN_POINT('Ctrl Pts',(40.9045439223885,25.9063436486862,2.));
#88325=CARTESIAN_POINT('Ctrl Pts',(40.5255602341407,26.6295028556231,2.));
#88326=CARTESIAN_POINT('Ctrl Pts',(40.1281423069477,27.3435304618815,2.));
#88327=CARTESIAN_POINT('Ctrl Pts',(39.7321213838807,28.0550481171695,2.));
#88328=CARTESIAN_POINT('Ctrl Pts',(39.3177957144339,28.7574981262846,2.));
#88329=CARTESIAN_POINT('Ctrl Pts',(38.8856370208255,29.4499732757602,2.));
#88330=CARTESIAN_POINT('Ctrl Pts',(38.6009980869291,29.9060682038772,2.));
#88331=CARTESIAN_POINT('Ctrl Pts',(38.3086238828692,30.3578364223247,2.));
#88332=CARTESIAN_POINT('Ctrl Pts',(38.0086596303984,30.8050248835235,2.));
#88333=CARTESIAN_POINT('Ctrl Pts',(37.8531972210893,31.0367891521673,2.));
#88334=CARTESIAN_POINT('Ctrl Pts',(37.6956965296231,31.2673228693602,2.));
#88335=CARTESIAN_POINT('Ctrl Pts',(37.5361777128299,31.4965928746404,2.));
#88336=CARTESIAN_POINT('',(37.5361777128299,31.4965928746404,0.));
#88337=CARTESIAN_POINT('Origin',(-1.19904086659517E-13,-1.4210854715202E-13,
0.));
#88338=CARTESIAN_POINT('',(-34.6009561857411,-30.3112822399915,2.));
#88339=CARTESIAN_POINT('',(-34.6009561857411,-30.3112822399915,0.));
#88340=CARTESIAN_POINT('Origin',(-1.19904086659517E-13,-1.4210854715202E-13,
2.));
#88341=CARTESIAN_POINT('Origin',(-35.3531508854311,-30.9702231582522,0.));
#88342=CARTESIAN_POINT('',(-35.9959384951176,-30.2041787151332,2.));
#88343=CARTESIAN_POINT('',(-35.9959384951176,-30.2041787151332,0.));
#88344=CARTESIAN_POINT('Origin',(-35.3531508854311,-30.9702231582522,2.));
#88345=CARTESIAN_POINT('Origin',(-35.238044383473,-29.5682300455808,0.));
#88346=CARTESIAN_POINT('',(-17.6190221917365,-14.7841150227904,2.));
#88347=CARTESIAN_POINT('Origin',(-1.83021655258307E-13,3.27857114887025E-14,
0.));
#88348=CARTESIAN_POINT('',(-43.5508185339833,14.8096659320883,2.));
#88349=CARTESIAN_POINT('',(-43.5508185339833,14.8096659320883,0.));
#88350=CARTESIAN_POINT('Origin',(-1.83021655258307E-13,3.27857114887025E-14,
2.));
#88351=CARTESIAN_POINT('Origin',(-44.4975754586351,15.1316151914815,0.));
#88352=CARTESIAN_POINT('',(-44.1555553153094,16.0713078122674,2.));
#88353=CARTESIAN_POINT('',(-44.1555553153094,16.0713078122674,0.));
#88354=CARTESIAN_POINT('Origin',(-44.4975754586351,15.1316151914815,2.));
#88355=CARTESIAN_POINT('Origin',(-43.2258605561518,15.7329265929808,0.));
#88356=CARTESIAN_POINT('',(-21.6129302780759,7.86646329649041,2.));
#88357=CARTESIAN_POINT('Origin',(-6.31175685987896E-14,1.74894258640722E-13,
0.));
#88358=CARTESIAN_POINT('',(-8.94986234824223,45.1209481720799,2.));
#88359=CARTESIAN_POINT('',(-8.94986234824223,45.1209481720799,0.));
#88360=CARTESIAN_POINT('Origin',(-6.31175685987896E-14,1.74894258640722E-13,
2.));
#88361=CARTESIAN_POINT('Origin',(-9.14442457320401,46.1018383497338,0.));
#88362=CARTESIAN_POINT('',(-8.1596168201918,46.2754865274007,2.));
#88363=CARTESIAN_POINT('',(-8.1596168201918,46.2754865274007,0.));
#88364=CARTESIAN_POINT('Origin',(-9.14442457320401,46.1018383497338,2.));
#88365=CARTESIAN_POINT('Origin',(-7.98781617267879,45.3011566385616,0.));
#88366=CARTESIAN_POINT('',(-3.99390808633937,22.6505783192808,2.));
#88367=CARTESIAN_POINT('Origin',(0.,0.,2.));
#88368=CARTESIAN_POINT('',(23.,-39.8371685740842,2.));
#88369=CARTESIAN_POINT('Ctrl Pts',(23.,-39.8371685740842,2.));
#88370=CARTESIAN_POINT('Ctrl Pts',(25.2470089248039,-38.7975252546671,2.));
#88371=CARTESIAN_POINT('Ctrl Pts',(27.402276150069,-37.5810556253098,2.));
#88372=CARTESIAN_POINT('Ctrl Pts',(29.4485343853537,-36.2031892016999,2.));
#88373=CARTESIAN_POINT('',(8.94986234824221,-45.1209481720799,2.));
#88374=CARTESIAN_POINT('Origin',(6.31175685987895E-14,-1.74894258640722E-13,
2.));
#88375=CARTESIAN_POINT('',(8.15961682019179,-46.2754865274007,2.));
#88376=CARTESIAN_POINT('Origin',(9.144424573204,-46.1018383497338,2.));
#88377=CARTESIAN_POINT('',(3.99390808633936,-22.6505783192808,2.));
#88378=CARTESIAN_POINT('',(23.,39.8371685740842,2.));
#88379=CARTESIAN_POINT('Ctrl Pts',(23.,39.8371685740842,2.));
#88380=CARTESIAN_POINT('Ctrl Pts',(20.9761380121528,41.2633137257534,2.));
#88381=CARTESIAN_POINT('Ctrl Pts',(18.8450107965655,42.5215950805976,2.));
#88382=CARTESIAN_POINT('Ctrl Pts',(16.6286143540096,43.6047734827858,2.));
#88383=CARTESIAN_POINT('',(34.6009561857411,30.3112822399915,2.));
#88384=CARTESIAN_POINT('Origin',(1.19904086659517E-13,1.4210854715202E-13,
2.));
#88385=CARTESIAN_POINT('',(35.9959384951176,30.2041787151333,2.));
#88386=CARTESIAN_POINT('Origin',(35.3531508854311,30.9702231582522,2.));
#88387=CARTESIAN_POINT('',(17.6190221917365,14.7841150227904,2.));
#88388=CARTESIAN_POINT('',(46.,0.,2.));
#88389=CARTESIAN_POINT('Ctrl Pts',(46.,0.,2.));
#88390=CARTESIAN_POINT('Ctrl Pts',(46.2231469368338,2.46578847026074,2.));
#88391=CARTESIAN_POINT('Ctrl Pts',(46.2472869475088,4.94053945592409,2.));
#88392=CARTESIAN_POINT('Ctrl Pts',(46.0771487393634,7.40158428108603,2.));
#88393=CARTESIAN_POINT('',(43.5508185339833,-14.8096659320883,2.));
#88394=CARTESIAN_POINT('Origin',(1.83021655258307E-13,-3.27857114887026E-14,
2.));
#88395=CARTESIAN_POINT('',(44.1555553153094,-16.0713078122675,2.));
#88396=CARTESIAN_POINT('Origin',(44.4975754586351,-15.1316151914816,2.));
#88397=CARTESIAN_POINT('',(21.6129302780759,-7.86646329649042,2.));
#88398=CARTESIAN_POINT('Origin',(0.,0.,2.));
#88399=CARTESIAN_POINT('Origin',(7.98781617267877,-45.3011566385616,0.));
#88400=CARTESIAN_POINT('',(8.15961682019179,-46.2754865274007,0.));
#88401=CARTESIAN_POINT('Origin',(9.144424573204,-46.1018383497338,0.));
#88402=CARTESIAN_POINT('',(8.94986234824221,-45.1209481720799,0.));
#88403=CARTESIAN_POINT('Origin',(6.31175685987895E-14,-1.74894258640722E-13,
0.));
#88404=CARTESIAN_POINT('',(23.,-39.8371685740842,0.));
#88405=CARTESIAN_POINT('Ctrl Pts',(46.0449384185095,-16.7589870229578,0.));
#88406=CARTESIAN_POINT('Ctrl Pts',(46.0449384185095,-16.7589870229578,20.));
#88407=CARTESIAN_POINT('Ctrl Pts',(46.0420594924752,-16.7651130917503,0.));
#88408=CARTESIAN_POINT('Ctrl Pts',(46.0420594924752,-16.7651130917503,20.));
#88409=CARTESIAN_POINT('Ctrl Pts',(46.0362995834799,-16.7773641333857,0.));
#88410=CARTESIAN_POINT('Ctrl Pts',(46.0362995834799,-16.7773641333857,20.));
#88411=CARTESIAN_POINT('Ctrl Pts',(46.0276535492064,-16.79573740799,0.));
#88412=CARTESIAN_POINT('Ctrl Pts',(46.0276535492064,-16.79573740799,20.));
#88413=CARTESIAN_POINT('Ctrl Pts',(46.0161131619282,-16.8202285317553,0.));
#88414=CARTESIAN_POINT('Ctrl Pts',(46.0161131619282,-16.8202285317553,20.));
#88415=CARTESIAN_POINT('Ctrl Pts',(46.0016671088634,-16.8508314760754,0.));
#88416=CARTESIAN_POINT('Ctrl Pts',(46.0016671088634,-16.8508314760754,20.));
#88417=CARTESIAN_POINT('Ctrl Pts',(45.9872004880192,-16.8814234574889,0.));
#88418=CARTESIAN_POINT('Ctrl Pts',(45.9872004880192,-16.8814234574889,20.));
#88419=CARTESIAN_POINT('Ctrl Pts',(45.9727133019197,-16.9120044710149,0.));
#88420=CARTESIAN_POINT('Ctrl Pts',(45.9727133019197,-16.9120044710149,20.));
#88421=CARTESIAN_POINT('Ctrl Pts',(45.9582055548827,-16.9425745084438,0.));
#88422=CARTESIAN_POINT('Ctrl Pts',(45.9582055548827,-16.9425745084438,20.));
#88423=CARTESIAN_POINT('Ctrl Pts',(45.9436772535459,-16.9731335574459,0.));
#88424=CARTESIAN_POINT('Ctrl Pts',(45.9436772535459,-16.9731335574459,20.));
#88425=CARTESIAN_POINT('Ctrl Pts',(45.9291284062576,-17.0036816026634,0.));
#88426=CARTESIAN_POINT('Ctrl Pts',(45.9291284062576,-17.0036816026634,20.));
#88427=CARTESIAN_POINT('Ctrl Pts',(45.91455902239,-17.0342186269342,0.));
#88428=CARTESIAN_POINT('Ctrl Pts',(45.91455902239,-17.0342186269342,20.));
#88429=CARTESIAN_POINT('Ctrl Pts',(45.8999691116666,-17.0647446124944,0.));
#88430=CARTESIAN_POINT('Ctrl Pts',(45.8999691116666,-17.0647446124944,20.));
#88431=CARTESIAN_POINT('Ctrl Pts',(45.8853586835176,-17.09525954213,0.));
#88432=CARTESIAN_POINT('Ctrl Pts',(45.8853586835176,-17.09525954213,20.));
#88433=CARTESIAN_POINT('Ctrl Pts',(45.8707277463338,-17.1257634005084,0.));
#88434=CARTESIAN_POINT('Ctrl Pts',(45.8707277463338,-17.1257634005084,20.));
#88435=CARTESIAN_POINT('Ctrl Pts',(45.8560763076625,-17.1562561738292,0.));
#88436=CARTESIAN_POINT('Ctrl Pts',(45.8560763076625,-17.1562561738292,20.));
#88437=CARTESIAN_POINT('Ctrl Pts',(45.8414043745501,-17.1867378492105,0.));
#88438=CARTESIAN_POINT('Ctrl Pts',(45.8414043745501,-17.1867378492105,20.));
#88439=CARTESIAN_POINT('Ctrl Pts',(45.8267119538424,-17.2172084141516,0.));
#88440=CARTESIAN_POINT('Ctrl Pts',(45.8267119538424,-17.2172084141516,20.));
#88441=CARTESIAN_POINT('Ctrl Pts',(45.8119990524823,-17.247667856,0.));
#88442=CARTESIAN_POINT('Ctrl Pts',(45.8119990524823,-17.247667856,20.));
#88443=CARTESIAN_POINT('Ctrl Pts',(45.7972656778619,-17.2781161613228,0.));
#88444=CARTESIAN_POINT('Ctrl Pts',(45.7972656778619,-17.2781161613228,20.));
#88445=CARTESIAN_POINT('Ctrl Pts',(45.7825118377706,-17.3085533159982,0.));
#88446=CARTESIAN_POINT('Ctrl Pts',(45.7825118377706,-17.3085533159982,20.));
#88447=CARTESIAN_POINT('Ctrl Pts',(45.7677375402375,-17.3389793054985,0.));
#88448=CARTESIAN_POINT('Ctrl Pts',(45.7677375402375,-17.3389793054985,20.));
#88449=CARTESIAN_POINT('Ctrl Pts',(45.7529427934047,-17.3693941151172,0.));
#88450=CARTESIAN_POINT('Ctrl Pts',(45.7529427934047,-17.3693941151172,20.));
#88451=CARTESIAN_POINT('Ctrl Pts',(45.7381276053971,-17.3997977302007,0.));
#88452=CARTESIAN_POINT('Ctrl Pts',(45.7381276053971,-17.3997977302007,20.));
#88453=CARTESIAN_POINT('Ctrl Pts',(45.7232919841685,-17.4301901364248,0.));
#88454=CARTESIAN_POINT('Ctrl Pts',(45.7232919841685,-17.4301901364248,20.));
#88455=CARTESIAN_POINT('Ctrl Pts',(45.7084359375081,-17.460571319782,0.));
#88456=CARTESIAN_POINT('Ctrl Pts',(45.7084359375081,-17.460571319782,20.));
#88457=CARTESIAN_POINT('Ctrl Pts',(45.6935594731126,-17.490941266452,0.));
#88458=CARTESIAN_POINT('Ctrl Pts',(45.6935594731126,-17.490941266452,20.));
#88459=CARTESIAN_POINT('Ctrl Pts',(45.67866259864,-17.5212999627071,0.));
#88460=CARTESIAN_POINT('Ctrl Pts',(45.67866259864,-17.5212999627071,20.));
#88461=CARTESIAN_POINT('Ctrl Pts',(45.6637453217655,-17.5516473948116,0.));
#88462=CARTESIAN_POINT('Ctrl Pts',(45.6637453217655,-17.5516473948116,20.));
#88463=CARTESIAN_POINT('Ctrl Pts',(45.6488076502485,-17.5819835489016,0.));
#88464=CARTESIAN_POINT('Ctrl Pts',(45.6488076502485,-17.5819835489016,20.));
#88465=CARTESIAN_POINT('Ctrl Pts',(45.6338495919363,-17.6123084109794,0.));
#88466=CARTESIAN_POINT('Ctrl Pts',(45.6338495919363,-17.6123084109794,20.));
#88467=CARTESIAN_POINT('Ctrl Pts',(45.6188711547313,-17.6426219669712,0.));
#88468=CARTESIAN_POINT('Ctrl Pts',(45.6188711547313,-17.6426219669712,20.));
#88469=CARTESIAN_POINT('Ctrl Pts',(45.6038723465685,-17.672924202767,0.));
#88470=CARTESIAN_POINT('Ctrl Pts',(45.6038723465685,-17.672924202767,20.));
#88471=CARTESIAN_POINT('Ctrl Pts',(45.5888531753911,-17.7032151042646,0.));
#88472=CARTESIAN_POINT('Ctrl Pts',(45.5888531753911,-17.7032151042646,20.));
#88473=CARTESIAN_POINT('Ctrl Pts',(45.5738136491221,-17.7334946574206,0.));
#88474=CARTESIAN_POINT('Ctrl Pts',(45.5738136491221,-17.7334946574206,20.));
#88475=CARTESIAN_POINT('Ctrl Pts',(45.5587537756595,-17.7637628482589,0.));
#88476=CARTESIAN_POINT('Ctrl Pts',(45.5587537756595,-17.7637628482589,20.));
#88477=CARTESIAN_POINT('Ctrl Pts',(45.5436735628911,-17.7940196628443,0.));
#88478=CARTESIAN_POINT('Ctrl Pts',(45.5436735628911,-17.7940196628443,20.));
#88479=CARTESIAN_POINT('Ctrl Pts',(45.528573018704,-17.8242650872661,0.));
#88480=CARTESIAN_POINT('Ctrl Pts',(45.528573018704,-17.8242650872661,20.));
#88481=CARTESIAN_POINT('Ctrl Pts',(45.5134521509949,-17.8544991076192,0.));
#88482=CARTESIAN_POINT('Ctrl Pts',(45.5134521509949,-17.8544991076192,20.));
#88483=CARTESIAN_POINT('Ctrl Pts',(45.498310967683,-17.8847217099814,0.));
#88484=CARTESIAN_POINT('Ctrl Pts',(45.498310967683,-17.8847217099814,20.));
#88485=CARTESIAN_POINT('Ctrl Pts',(45.4831494767122,-17.9149328804084,0.));
#88486=CARTESIAN_POINT('Ctrl Pts',(45.4831494767122,-17.9149328804084,20.));
#88487=CARTESIAN_POINT('Ctrl Pts',(45.4679676860453,-17.9451326049449,0.));
#88488=CARTESIAN_POINT('Ctrl Pts',(45.4679676860453,-17.9451326049449,20.));
#88489=CARTESIAN_POINT('Ctrl Pts',(45.4527656036598,-17.9753208696316,0.));
#88490=CARTESIAN_POINT('Ctrl Pts',(45.4527656036598,-17.9753208696316,20.));
#88491=CARTESIAN_POINT('Ctrl Pts',(45.4375432375433,-18.0054976605138,0.));
#88492=CARTESIAN_POINT('Ctrl Pts',(45.4375432375433,-18.0054976605138,20.));
#88493=CARTESIAN_POINT('Ctrl Pts',(45.4223005956881,-18.0356629636502,0.));
#88494=CARTESIAN_POINT('Ctrl Pts',(45.4223005956881,-18.0356629636502,20.));
#88495=CARTESIAN_POINT('Ctrl Pts',(45.4070376860893,-18.0658167651176,0.));
#88496=CARTESIAN_POINT('Ctrl Pts',(45.4070376860893,-18.0658167651176,20.));
#88497=CARTESIAN_POINT('Ctrl Pts',(45.3917545167484,-18.0959590510046,0.));
#88498=CARTESIAN_POINT('Ctrl Pts',(45.3917545167484,-18.0959590510046,20.));
#88499=CARTESIAN_POINT('Ctrl Pts',(45.3764510956741,-18.1260898074095,0.));
#88500=CARTESIAN_POINT('Ctrl Pts',(45.3764510956741,-18.1260898074095,20.));
#88501=CARTESIAN_POINT('Ctrl Pts',(45.3611274308852,-18.156209020436,0.));
#88502=CARTESIAN_POINT('Ctrl Pts',(45.3611274308852,-18.156209020436,20.));
#88503=CARTESIAN_POINT('Ctrl Pts',(45.3457835304119,-18.1863166761898,0.));
#88504=CARTESIAN_POINT('Ctrl Pts',(45.3457835304119,-18.1863166761898,20.));
#88505=CARTESIAN_POINT('Ctrl Pts',(45.3304194022976,-18.2164127607761,0.));
#88506=CARTESIAN_POINT('Ctrl Pts',(45.3304194022976,-18.2164127607761,20.));
#88507=CARTESIAN_POINT('Ctrl Pts',(45.3150350545965,-18.2464972603023,0.));
#88508=CARTESIAN_POINT('Ctrl Pts',(45.3150350545965,-18.2464972603023,20.));
#88509=CARTESIAN_POINT('Ctrl Pts',(45.299630495374,-18.276570160879,0.));
#88510=CARTESIAN_POINT('Ctrl Pts',(45.299630495374,-18.276570160879,20.));
#88511=CARTESIAN_POINT('Ctrl Pts',(45.2842057327048,-18.3066314486215,0.));
#88512=CARTESIAN_POINT('Ctrl Pts',(45.2842057327048,-18.3066314486215,20.));
#88513=CARTESIAN_POINT('Ctrl Pts',(45.2687607746732,-18.3366811096519,0.));
#88514=CARTESIAN_POINT('Ctrl Pts',(45.2687607746732,-18.3366811096519,20.));
#88515=CARTESIAN_POINT('Ctrl Pts',(45.2532956293718,-18.3667191300999,0.));
#88516=CARTESIAN_POINT('Ctrl Pts',(45.2532956293718,-18.3667191300999,20.));
#88517=CARTESIAN_POINT('Ctrl Pts',(45.2378103049022,-18.3967454961017,0.));
#88518=CARTESIAN_POINT('Ctrl Pts',(45.2378103049022,-18.3967454961017,20.));
#88519=CARTESIAN_POINT('Ctrl Pts',(45.2223048093755,-18.4267601937997,0.));
#88520=CARTESIAN_POINT('Ctrl Pts',(45.2223048093755,-18.4267601937997,20.));
#88521=CARTESIAN_POINT('Ctrl Pts',(45.2067791509123,-18.456763209342,0.));
#88522=CARTESIAN_POINT('Ctrl Pts',(45.2067791509123,-18.456763209342,20.));
#88523=CARTESIAN_POINT('Ctrl Pts',(45.1912333376434,-18.4867545288811,0.));
#88524=CARTESIAN_POINT('Ctrl Pts',(45.1912333376434,-18.4867545288811,20.));
#88525=CARTESIAN_POINT('Ctrl Pts',(45.1756673777099,-18.5167341385735,0.));
#88526=CARTESIAN_POINT('Ctrl Pts',(45.1756673777099,-18.5167341385735,20.));
#88527=CARTESIAN_POINT('Ctrl Pts',(45.1600812792631,-18.5467020245809,0.));
#88528=CARTESIAN_POINT('Ctrl Pts',(45.1600812792631,-18.5467020245809,20.));
#88529=CARTESIAN_POINT('Ctrl Pts',(45.144475050464,-18.5766581730695,0.));
#88530=CARTESIAN_POINT('Ctrl Pts',(45.144475050464,-18.5766581730695,20.));
#88531=CARTESIAN_POINT('Ctrl Pts',(45.1288486994834,-18.6066025702107,0.));
#88532=CARTESIAN_POINT('Ctrl Pts',(45.1288486994834,-18.6066025702107,20.));
#88533=CARTESIAN_POINT('Ctrl Pts',(45.1132022345013,-18.6365352021814,0.));
#88534=CARTESIAN_POINT('Ctrl Pts',(45.1132022345013,-18.6365352021814,20.));
#88535=CARTESIAN_POINT('Ctrl Pts',(45.097535663708,-18.6664560551643,0.));
#88536=CARTESIAN_POINT('Ctrl Pts',(45.097535663708,-18.6664560551643,20.));
#88537=CARTESIAN_POINT('Ctrl Pts',(45.081848995303,-18.6963651153477,0.));
#88538=CARTESIAN_POINT('Ctrl Pts',(45.081848995303,-18.6963651153477,20.));
#88539=CARTESIAN_POINT('Ctrl Pts',(45.0661422374956,-18.7262623689254,0.));
#88540=CARTESIAN_POINT('Ctrl Pts',(45.0661422374956,-18.7262623689254,20.));
#88541=CARTESIAN_POINT('Ctrl Pts',(45.050415398505,-18.7561478020964,0.));
#88542=CARTESIAN_POINT('Ctrl Pts',(45.050415398505,-18.7561478020964,20.));
#88543=CARTESIAN_POINT('Ctrl Pts',(45.0346684865594,-18.7860214010651,0.));
#88544=CARTESIAN_POINT('Ctrl Pts',(45.0346684865594,-18.7860214010651,20.));
#88545=CARTESIAN_POINT('Ctrl Pts',(45.0189015098976,-18.815883152041,0.));
#88546=CARTESIAN_POINT('Ctrl Pts',(45.0189015098976,-18.815883152041,20.));
#88547=CARTESIAN_POINT('Ctrl Pts',(45.0031144767678,-18.8457330412389,0.));
#88548=CARTESIAN_POINT('Ctrl Pts',(45.0031144767678,-18.8457330412389,20.));
#88549=CARTESIAN_POINT('Ctrl Pts',(44.987307395428,-18.8755710548788,0.));
#88550=CARTESIAN_POINT('Ctrl Pts',(44.987307395428,-18.8755710548788,20.));
#88551=CARTESIAN_POINT('Ctrl Pts',(44.971480274146,-18.9053971791858,0.));
#88552=CARTESIAN_POINT('Ctrl Pts',(44.971480274146,-18.9053971791858,20.));
#88553=CARTESIAN_POINT('Ctrl Pts',(44.9556331211993,-18.9352114003906,0.));
#88554=CARTESIAN_POINT('Ctrl Pts',(44.9556331211993,-18.9352114003906,20.));
#88555=CARTESIAN_POINT('Ctrl Pts',(44.9397659448752,-18.9650137047294,0.));
#88556=CARTESIAN_POINT('Ctrl Pts',(44.9397659448752,-18.9650137047294,20.));
#88557=CARTESIAN_POINT('Ctrl Pts',(44.9238787534705,-18.9948040784434,0.));
#88558=CARTESIAN_POINT('Ctrl Pts',(44.9238787534705,-18.9948040784434,20.));
#88559=CARTESIAN_POINT('Ctrl Pts',(44.9079715552916,-19.0245825077798,0.));
#88560=CARTESIAN_POINT('Ctrl Pts',(44.9079715552916,-19.0245825077798,20.));
#88561=CARTESIAN_POINT('Ctrl Pts',(44.8920443586544,-19.0543489789907,0.));
#88562=CARTESIAN_POINT('Ctrl Pts',(44.8920443586544,-19.0543489789907,20.));
#88563=CARTESIAN_POINT('Ctrl Pts',(44.8760971718851,-19.0841034783341,0.));
#88564=CARTESIAN_POINT('Ctrl Pts',(44.8760971718851,-19.0841034783341,20.));
#88565=CARTESIAN_POINT('Ctrl Pts',(44.8601300033192,-19.1138459920731,0.));
#88566=CARTESIAN_POINT('Ctrl Pts',(44.8601300033192,-19.1138459920731,20.));
#88567=CARTESIAN_POINT('Ctrl Pts',(44.8441428613021,-19.143576506476,0.));
#88568=CARTESIAN_POINT('Ctrl Pts',(44.8441428613021,-19.143576506476,20.));
#88569=CARTESIAN_POINT('Ctrl Pts',(44.8281357541891,-19.1732950078169,0.));
#88570=CARTESIAN_POINT('Ctrl Pts',(44.8281357541891,-19.1732950078169,20.));
#88571=CARTESIAN_POINT('Ctrl Pts',(44.8121086903447,-19.2030014823748,0.));
#88572=CARTESIAN_POINT('Ctrl Pts',(44.8121086903447,-19.2030014823748,20.));
#88573=CARTESIAN_POINT('Ctrl Pts',(44.7960616781431,-19.2326959164344,0.));
#88574=CARTESIAN_POINT('Ctrl Pts',(44.7960616781431,-19.2326959164344,20.));
#88575=CARTESIAN_POINT('Ctrl Pts',(44.7799947259683,-19.2623782962859,0.));
#88576=CARTESIAN_POINT('Ctrl Pts',(44.7799947259683,-19.2623782962859,20.));
#88577=CARTESIAN_POINT('Ctrl Pts',(44.7639078422139,-19.2920486082247,0.));
#88578=CARTESIAN_POINT('Ctrl Pts',(44.7639078422139,-19.2920486082247,20.));
#88579=CARTESIAN_POINT('Ctrl Pts',(44.7478010352831,-19.321706838552,0.));
#88580=CARTESIAN_POINT('Ctrl Pts',(44.7478010352831,-19.321706838552,20.));
#88581=CARTESIAN_POINT('Ctrl Pts',(44.731674313589,-19.3513529735741,0.));
#88582=CARTESIAN_POINT('Ctrl Pts',(44.731674313589,-19.3513529735741,20.));
#88583=CARTESIAN_POINT('Ctrl Pts',(44.7155276855546,-19.3809869996033,0.));
#88584=CARTESIAN_POINT('Ctrl Pts',(44.7155276855546,-19.3809869996033,20.));
#88585=CARTESIAN_POINT('Ctrl Pts',(44.6993611596123,-19.4106089029568,0.));
#88586=CARTESIAN_POINT('Ctrl Pts',(44.6993611596123,-19.4106089029568,20.));
#88587=CARTESIAN_POINT('Ctrl Pts',(44.6831747442042,-19.4402186699576,0.));
#88588=CARTESIAN_POINT('Ctrl Pts',(44.6831747442042,-19.4402186699576,20.));
#88589=CARTESIAN_POINT('Ctrl Pts',(44.6669684477819,-19.4698162869338,0.));
#88590=CARTESIAN_POINT('Ctrl Pts',(44.6669684477819,-19.4698162869338,20.));
#88591=CARTESIAN_POINT('Ctrl Pts',(44.6507422788067,-19.4994017402193,0.));
#88592=CARTESIAN_POINT('Ctrl Pts',(44.6507422788067,-19.4994017402193,20.));
#88593=CARTESIAN_POINT('Ctrl Pts',(44.6344962457493,-19.5289750161534,0.));
#88594=CARTESIAN_POINT('Ctrl Pts',(44.6344962457493,-19.5289750161534,20.));
#88595=CARTESIAN_POINT('Ctrl Pts',(44.6182303570903,-19.5585361010809,0.));
#88596=CARTESIAN_POINT('Ctrl Pts',(44.6182303570903,-19.5585361010809,20.));
#88597=CARTESIAN_POINT('Ctrl Pts',(44.60194462132,-19.5880849813526,0.));
#88598=CARTESIAN_POINT('Ctrl Pts',(44.60194462132,-19.5880849813526,20.));
#88599=CARTESIAN_POINT('Ctrl Pts',(44.5856390469384,-19.6176216433241,0.));
#88600=CARTESIAN_POINT('Ctrl Pts',(44.5856390469384,-19.6176216433241,20.));
#88601=CARTESIAN_POINT('Ctrl Pts',(44.5693136424548,-19.6471460733569,0.));
#88602=CARTESIAN_POINT('Ctrl Pts',(44.5693136424548,-19.6471460733569,20.));
#88603=CARTESIAN_POINT('Ctrl Pts',(44.5529684163885,-19.6766582578175,0.));
#88604=CARTESIAN_POINT('Ctrl Pts',(44.5529684163885,-19.6766582578175,20.));
#88605=CARTESIAN_POINT('Ctrl Pts',(44.5366033772681,-19.7061581830785,0.));
#88606=CARTESIAN_POINT('Ctrl Pts',(44.5366033772681,-19.7061581830785,20.));
#88607=CARTESIAN_POINT('Ctrl Pts',(44.5202185336324,-19.7356458355178,0.));
#88608=CARTESIAN_POINT('Ctrl Pts',(44.5202185336324,-19.7356458355178,20.));
#88609=CARTESIAN_POINT('Ctrl Pts',(44.5038138940293,-19.7651212015191,0.));
#88610=CARTESIAN_POINT('Ctrl Pts',(44.5038138940293,-19.7651212015191,20.));
#88611=CARTESIAN_POINT('Ctrl Pts',(44.4873894670167,-19.7945842674717,0.));
#88612=CARTESIAN_POINT('Ctrl Pts',(44.4873894670167,-19.7945842674717,20.));
#88613=CARTESIAN_POINT('Ctrl Pts',(44.4709452611615,-19.8240350197702,0.));
#88614=CARTESIAN_POINT('Ctrl Pts',(44.4709452611615,-19.8240350197702,20.));
#88615=CARTESIAN_POINT('Ctrl Pts',(44.4544812850403,-19.8534734448147,0.));
#88616=CARTESIAN_POINT('Ctrl Pts',(44.4544812850403,-19.8534734448147,20.));
#88617=CARTESIAN_POINT('Ctrl Pts',(44.4379975472397,-19.8828995290107,0.));
#88618=CARTESIAN_POINT('Ctrl Pts',(44.4379975472397,-19.8828995290107,20.));
#88619=CARTESIAN_POINT('Ctrl Pts',(44.4214940563556,-19.9123132587698,0.));
#88620=CARTESIAN_POINT('Ctrl Pts',(44.4214940563556,-19.9123132587698,20.));
#88621=CARTESIAN_POINT('Ctrl Pts',(44.4049708209939,-19.9417146205087,0.));
#88622=CARTESIAN_POINT('Ctrl Pts',(44.4049708209939,-19.9417146205087,20.));
#88623=CARTESIAN_POINT('Ctrl Pts',(44.3884278497697,-19.9711036006504,0.));
#88624=CARTESIAN_POINT('Ctrl Pts',(44.3884278497697,-19.9711036006504,20.));
#88625=CARTESIAN_POINT('Ctrl Pts',(44.371865151308,-20.0004801856229,0.));
#88626=CARTESIAN_POINT('Ctrl Pts',(44.371865151308,-20.0004801856229,20.));
#88627=CARTESIAN_POINT('Ctrl Pts',(44.3552827342435,-20.0298443618602,0.));
#88628=CARTESIAN_POINT('Ctrl Pts',(44.3552827342435,-20.0298443618602,20.));
#88629=CARTESIAN_POINT('Ctrl Pts',(44.3386806072204,-20.0591961158019,0.));
#88630=CARTESIAN_POINT('Ctrl Pts',(44.3386806072204,-20.0591961158019,20.));
#88631=CARTESIAN_POINT('Ctrl Pts',(44.3220587788923,-20.0885354338929,0.));
#88632=CARTESIAN_POINT('Ctrl Pts',(44.3220587788923,-20.0885354338929,20.));
#88633=CARTESIAN_POINT('Ctrl Pts',(44.3054172579221,-20.117862302584,0.));
#88634=CARTESIAN_POINT('Ctrl Pts',(44.3054172579221,-20.117862302584,20.));
#88635=CARTESIAN_POINT('Ctrl Pts',(44.2887560529826,-20.1471767083313,0.));
#88636=CARTESIAN_POINT('Ctrl Pts',(44.2887560529826,-20.1471767083313,20.));
#88637=CARTESIAN_POINT('Ctrl Pts',(44.2720751727557,-20.1764786375963,0.));
#88638=CARTESIAN_POINT('Ctrl Pts',(44.2720751727557,-20.1764786375963,20.));
#88639=CARTESIAN_POINT('Ctrl Pts',(44.2553746259333,-20.2057680768465,0.));
#88640=CARTESIAN_POINT('Ctrl Pts',(44.2553746259333,-20.2057680768465,20.));
#88641=CARTESIAN_POINT('Ctrl Pts',(44.238654421217,-20.2350450125552,0.));
#88642=CARTESIAN_POINT('Ctrl Pts',(44.238654421217,-20.2350450125552,20.));
#88643=CARTESIAN_POINT('Ctrl Pts',(44.221914567318,-20.2643094312016,0.));
#88644=CARTESIAN_POINT('Ctrl Pts',(44.221914567318,-20.2643094312016,20.));
#88645=CARTESIAN_POINT('Ctrl Pts',(44.205155072957,-20.2935613192706,0.));
#88646=CARTESIAN_POINT('Ctrl Pts',(44.205155072957,-20.2935613192706,20.));
#88647=CARTESIAN_POINT('Ctrl Pts',(44.1883759468646,-20.3228006632528,0.));
#88648=CARTESIAN_POINT('Ctrl Pts',(44.1883759468646,-20.3228006632528,20.));
#88649=CARTESIAN_POINT('Ctrl Pts',(44.1715771977807,-20.3520274496444,0.));
#88650=CARTESIAN_POINT('Ctrl Pts',(44.1715771977807,-20.3520274496444,20.));
#88651=CARTESIAN_POINT('Ctrl Pts',(44.1547588344544,-20.3812416649468,0.));
#88652=CARTESIAN_POINT('Ctrl Pts',(44.1547588344544,-20.3812416649468,20.));
#88653=CARTESIAN_POINT('Ctrl Pts',(44.1379208656442,-20.4104432956673,0.));
#88654=CARTESIAN_POINT('Ctrl Pts',(44.1379208656442,-20.4104432956673,20.));
#88655=CARTESIAN_POINT('Ctrl Pts',(44.1210633001184,-20.4396323283186,0.));
#88656=CARTESIAN_POINT('Ctrl Pts',(44.1210633001184,-20.4396323283186,20.));
#88657=CARTESIAN_POINT('Ctrl Pts',(44.1041861466545,-20.4688087494191,0.));
#88658=CARTESIAN_POINT('Ctrl Pts',(44.1041861466545,-20.4688087494191,20.));
#88659=CARTESIAN_POINT('Ctrl Pts',(44.0872894140398,-20.4979725454933,0.));
#88660=CARTESIAN_POINT('Ctrl Pts',(44.0872894140398,-20.4979725454933,20.));
#88661=CARTESIAN_POINT('Ctrl Pts',(44.0703731110714,-20.5271237030716,0.));
#88662=CARTESIAN_POINT('Ctrl Pts',(44.0703731110714,-20.5271237030716,20.));
#88663=CARTESIAN_POINT('Ctrl Pts',(44.053437246556,-20.5562622086905,0.));
#88664=CARTESIAN_POINT('Ctrl Pts',(44.053437246556,-20.5562622086905,20.));
#88665=CARTESIAN_POINT('Ctrl Pts',(44.03648182931,-20.5853880488919,0.));
#88666=CARTESIAN_POINT('Ctrl Pts',(44.03648182931,-20.5853880488919,20.));
#88667=CARTESIAN_POINT('Ctrl Pts',(44.0195068681592,-20.6145012102233,0.));
#88668=CARTESIAN_POINT('Ctrl Pts',(44.0195068681592,-20.6145012102233,20.));
#88669=CARTESIAN_POINT('Ctrl Pts',(44.0025123719387,-20.6436016792381,0.));
#88670=CARTESIAN_POINT('Ctrl Pts',(44.0025123719387,-20.6436016792381,20.));
#88671=CARTESIAN_POINT('Ctrl Pts',(43.9854983494929,-20.6726894424949,0.));
#88672=CARTESIAN_POINT('Ctrl Pts',(43.9854983494929,-20.6726894424949,20.));
#88673=CARTESIAN_POINT('Ctrl Pts',(43.9684648096756,-20.7017644865585,0.));
#88674=CARTESIAN_POINT('Ctrl Pts',(43.9684648096756,-20.7017644865585,20.));
#88675=CARTESIAN_POINT('Ctrl Pts',(43.9514117613501,-20.7308267979991,0.));
#88676=CARTESIAN_POINT('Ctrl Pts',(43.9514117613501,-20.7308267979991,20.));
#88677=CARTESIAN_POINT('Ctrl Pts',(43.9343392133895,-20.7598763633934,0.));
#88678=CARTESIAN_POINT('Ctrl Pts',(43.9343392133895,-20.7598763633934,20.));
#88679=CARTESIAN_POINT('Ctrl Pts',(43.9172471746767,-20.7889131693233,0.));
#88680=CARTESIAN_POINT('Ctrl Pts',(43.9172471746767,-20.7889131693233,20.));
#88681=CARTESIAN_POINT('Ctrl Pts',(43.9001356541037,-20.817937202377,0.));
#88682=CARTESIAN_POINT('Ctrl Pts',(43.9001356541037,-20.817937202377,20.));
#88683=CARTESIAN_POINT('Ctrl Pts',(43.8830046605723,-20.8469484491482,0.));
#88684=CARTESIAN_POINT('Ctrl Pts',(43.8830046605723,-20.8469484491482,20.));
#88685=CARTESIAN_POINT('Ctrl Pts',(43.8658542029936,-20.8759468962364,0.));
#88686=CARTESIAN_POINT('Ctrl Pts',(43.8658542029936,-20.8759468962364,20.));
#88687=CARTESIAN_POINT('Ctrl Pts',(43.8486842902882,-20.9049325302471,0.));
#88688=CARTESIAN_POINT('Ctrl Pts',(43.8486842902882,-20.9049325302471,20.));
#88689=CARTESIAN_POINT('Ctrl Pts',(43.8314949313861,-20.9339053377914,0.));
#88690=CARTESIAN_POINT('Ctrl Pts',(43.8314949313861,-20.9339053377914,20.));
#88691=CARTESIAN_POINT('Ctrl Pts',(43.8142861352268,-20.9628653054863,0.));
#88692=CARTESIAN_POINT('Ctrl Pts',(43.8142861352268,-20.9628653054863,20.));
#88693=CARTESIAN_POINT('Ctrl Pts',(43.7970579107591,-20.9918124199547,0.));
#88694=CARTESIAN_POINT('Ctrl Pts',(43.7970579107591,-20.9918124199547,20.));
#88695=CARTESIAN_POINT('Ctrl Pts',(43.7798102669417,-21.0207466678254,0.));
#88696=CARTESIAN_POINT('Ctrl Pts',(43.7798102669417,-21.0207466678254,20.));
#88697=CARTESIAN_POINT('Ctrl Pts',(43.7625432127426,-21.0496680357328,0.));
#88698=CARTESIAN_POINT('Ctrl Pts',(43.7625432127426,-21.0496680357328,20.));
#88699=CARTESIAN_POINT('Ctrl Pts',(43.7452567571393,-21.0785765103173,0.));
#88700=CARTESIAN_POINT('Ctrl Pts',(43.7452567571393,-21.0785765103173,20.));
#88701=CARTESIAN_POINT('Ctrl Pts',(43.7279509091188,-21.1074720782252,0.));
#88702=CARTESIAN_POINT('Ctrl Pts',(43.7279509091188,-21.1074720782252,20.));
#88703=CARTESIAN_POINT('Ctrl Pts',(43.7106256776774,-21.1363547261089,0.));
#88704=CARTESIAN_POINT('Ctrl Pts',(43.7106256776774,-21.1363547261089,20.));
#88705=CARTESIAN_POINT('Ctrl Pts',(43.6932810718209,-21.1652244406266,0.));
#88706=CARTESIAN_POINT('Ctrl Pts',(43.6932810718209,-21.1652244406266,20.));
#88707=CARTESIAN_POINT('Ctrl Pts',(43.6759171005641,-21.1940812084419,0.));
#88708=CARTESIAN_POINT('Ctrl Pts',(43.6759171005641,-21.1940812084419,20.));
#88709=CARTESIAN_POINT('Ctrl Pts',(43.658533772932,-21.2229250162246,0.));
#88710=CARTESIAN_POINT('Ctrl Pts',(43.658533772932,-21.2229250162246,20.));
#88711=CARTESIAN_POINT('Ctrl Pts',(43.6411310979584,-21.2517558506503,0.));
#88712=CARTESIAN_POINT('Ctrl Pts',(43.6411310979584,-21.2517558506503,20.));
#88713=CARTESIAN_POINT('Ctrl Pts',(43.6237090846874,-21.2805736984008,0.));
#88714=CARTESIAN_POINT('Ctrl Pts',(43.6237090846874,-21.2805736984008,20.));
#88715=CARTESIAN_POINT('Ctrl Pts',(43.6062677421718,-21.3093785461635,0.));
#88716=CARTESIAN_POINT('Ctrl Pts',(43.6062677421718,-21.3093785461635,20.));
#88717=CARTESIAN_POINT('Ctrl Pts',(43.5888070794743,-21.3381703806324,0.));
#88718=CARTESIAN_POINT('Ctrl Pts',(43.5888070794743,-21.3381703806324,20.));
#88719=CARTESIAN_POINT('Ctrl Pts',(43.571327105667,-21.3669491885068,0.));
#88720=CARTESIAN_POINT('Ctrl Pts',(43.571327105667,-21.3669491885068,20.));
#88721=CARTESIAN_POINT('Ctrl Pts',(43.5538278298311,-21.3957149564922,0.));
#88722=CARTESIAN_POINT('Ctrl Pts',(43.5538278298311,-21.3957149564922,20.));
#88723=CARTESIAN_POINT('Ctrl Pts',(43.5363092610574,-21.4244676712999,0.));
#88724=CARTESIAN_POINT('Ctrl Pts',(43.5363092610574,-21.4244676712999,20.));
#88725=CARTESIAN_POINT('Ctrl Pts',(43.5187714084458,-21.4532073196468,0.));
#88726=CARTESIAN_POINT('Ctrl Pts',(43.5187714084458,-21.4532073196468,20.));
#88727=CARTESIAN_POINT('Ctrl Pts',(43.5012142811058,-21.4819338882558,0.));
#88728=CARTESIAN_POINT('Ctrl Pts',(43.5012142811058,-21.4819338882558,20.));
#88729=CARTESIAN_POINT('Ctrl Pts',(43.4836378881563,-21.5106473638561,0.));
#88730=CARTESIAN_POINT('Ctrl Pts',(43.4836378881563,-21.5106473638561,20.));
#88731=CARTESIAN_POINT('Ctrl Pts',(43.4660422387257,-21.5393477331829,0.));
#88732=CARTESIAN_POINT('Ctrl Pts',(43.4660422387257,-21.5393477331829,20.));
#88733=CARTESIAN_POINT('Ctrl Pts',(43.4484273419519,-21.5680349829774,0.));
#88734=CARTESIAN_POINT('Ctrl Pts',(43.4484273419519,-21.5680349829774,20.));
#88735=CARTESIAN_POINT('Ctrl Pts',(43.4307932069823,-21.5967090999869,0.));
#88736=CARTESIAN_POINT('Ctrl Pts',(43.4307932069823,-21.5967090999869,20.));
#88737=CARTESIAN_POINT('Ctrl Pts',(43.4131398429739,-21.6253700709647,0.));
#88738=CARTESIAN_POINT('Ctrl Pts',(43.4131398429739,-21.6253700709647,20.));
#88739=CARTESIAN_POINT('Ctrl Pts',(43.3954672590924,-21.6540178826698,0.));
#88740=CARTESIAN_POINT('Ctrl Pts',(43.3954672590924,-21.6540178826698,20.));
#88741=CARTESIAN_POINT('Ctrl Pts',(43.3777754645132,-21.682652521867,0.));
#88742=CARTESIAN_POINT('Ctrl Pts',(43.3777754645132,-21.682652521867,20.));
#88743=CARTESIAN_POINT('Ctrl Pts',(43.3600644684208,-21.7112739753274,0.));
#88744=CARTESIAN_POINT('Ctrl Pts',(43.3600644684208,-21.7112739753274,20.));
#88745=CARTESIAN_POINT('Ctrl Pts',(43.3423342800096,-21.7398822298281,0.));
#88746=CARTESIAN_POINT('Ctrl Pts',(43.3423342800096,-21.7398822298281,20.));
#88747=CARTESIAN_POINT('Ctrl Pts',(43.3245849084831,-21.7684772721522,0.));
#88748=CARTESIAN_POINT('Ctrl Pts',(43.3245849084831,-21.7684772721522,20.));
#88749=CARTESIAN_POINT('Ctrl Pts',(43.3068163630542,-21.7970590890891,0.));
#88750=CARTESIAN_POINT('Ctrl Pts',(43.3068163630542,-21.7970590890891,20.));
#88751=CARTESIAN_POINT('Ctrl Pts',(43.2890286529453,-21.825627667434,0.));
#88752=CARTESIAN_POINT('Ctrl Pts',(43.2890286529453,-21.825627667434,20.));
#88753=CARTESIAN_POINT('Ctrl Pts',(43.271221787388,-21.854182993988,0.));
#88754=CARTESIAN_POINT('Ctrl Pts',(43.271221787388,-21.854182993988,20.));
#88755=CARTESIAN_POINT('Ctrl Pts',(43.2533957756234,-21.8827250555584,0.));
#88756=CARTESIAN_POINT('Ctrl Pts',(43.2533957756234,-21.8827250555584,20.));
#88757=CARTESIAN_POINT('Ctrl Pts',(43.2355506269018,-21.9112538389586,0.));
#88758=CARTESIAN_POINT('Ctrl Pts',(43.2355506269018,-21.9112538389586,20.));
#88759=CARTESIAN_POINT('Ctrl Pts',(43.217686350483,-21.939769331008,0.));
#88760=CARTESIAN_POINT('Ctrl Pts',(43.217686350483,-21.939769331008,20.));
#88761=CARTESIAN_POINT('Ctrl Pts',(43.1998029556363,-21.9682715185322,0.));
#88762=CARTESIAN_POINT('Ctrl Pts',(43.1998029556363,-21.9682715185322,20.));
#88763=CARTESIAN_POINT('Ctrl Pts',(43.1819004516401,-21.9967603883628,0.));
#88764=CARTESIAN_POINT('Ctrl Pts',(43.1819004516401,-21.9967603883628,20.));
#88765=CARTESIAN_POINT('Ctrl Pts',(43.1639788477821,-22.0252359273374,0.));
#88766=CARTESIAN_POINT('Ctrl Pts',(43.1639788477821,-22.0252359273374,20.));
#88767=CARTESIAN_POINT('Ctrl Pts',(43.1460381533593,-22.0536981222997,0.));
#88768=CARTESIAN_POINT('Ctrl Pts',(43.1460381533593,-22.0536981222997,20.));
#88769=CARTESIAN_POINT('Ctrl Pts',(43.1280783776784,-22.0821469600998,0.));
#88770=CARTESIAN_POINT('Ctrl Pts',(43.1280783776784,-22.0821469600998,20.));
#88771=CARTESIAN_POINT('Ctrl Pts',(43.1100995300552,-22.1105824275933,0.));
#88772=CARTESIAN_POINT('Ctrl Pts',(43.1100995300552,-22.1105824275933,20.));
#88773=CARTESIAN_POINT('Ctrl Pts',(43.0921016198148,-22.1390045116426,0.));
#88774=CARTESIAN_POINT('Ctrl Pts',(43.0921016198148,-22.1390045116426,20.));
#88775=CARTESIAN_POINT('Ctrl Pts',(43.0740846562917,-22.1674131991155,0.));
#88776=CARTESIAN_POINT('Ctrl Pts',(43.0740846562917,-22.1674131991155,20.));
#88777=CARTESIAN_POINT('Ctrl Pts',(43.0560486488298,-22.1958084768868,0.));
#88778=CARTESIAN_POINT('Ctrl Pts',(43.0560486488298,-22.1958084768868,20.));
#88779=CARTESIAN_POINT('Ctrl Pts',(43.0379936067822,-22.2241903318366,0.));
#88780=CARTESIAN_POINT('Ctrl Pts',(43.0379936067822,-22.2241903318366,20.));
#88781=CARTESIAN_POINT('Ctrl Pts',(43.0199195395114,-22.252558750852,0.));
#88782=CARTESIAN_POINT('Ctrl Pts',(43.0199195395114,-22.252558750852,20.));
#88783=CARTESIAN_POINT('Ctrl Pts',(43.0018264563892,-22.2809137208256,0.));
#88784=CARTESIAN_POINT('Ctrl Pts',(43.0018264563892,-22.2809137208256,20.));
#88785=CARTESIAN_POINT('Ctrl Pts',(42.9837143667967,-22.3092552286565,0.));
#88786=CARTESIAN_POINT('Ctrl Pts',(42.9837143667967,-22.3092552286565,20.));
#88787=CARTESIAN_POINT('Ctrl Pts',(42.965583280124,-22.3375832612492,0.));
#88788=CARTESIAN_POINT('Ctrl Pts',(42.965583280124,-22.3375832612492,20.));
#88789=CARTESIAN_POINT('Ctrl Pts',(42.947433205771,-22.3658978055149,0.));
#88790=CARTESIAN_POINT('Ctrl Pts',(42.947433205771,-22.3658978055149,20.));
#88791=CARTESIAN_POINT('Ctrl Pts',(42.9292641531465,-22.3941988483709,0.));
#88792=CARTESIAN_POINT('Ctrl Pts',(42.9292641531465,-22.3941988483709,20.));
#88793=CARTESIAN_POINT('Ctrl Pts',(42.9110761316689,-22.4224863767407,0.));
#88794=CARTESIAN_POINT('Ctrl Pts',(42.9110761316689,-22.4224863767407,20.));
#88795=CARTESIAN_POINT('Ctrl Pts',(42.8928691507659,-22.4507603775546,0.));
#88796=CARTESIAN_POINT('Ctrl Pts',(42.8928691507659,-22.4507603775546,20.));
#88797=CARTESIAN_POINT('Ctrl Pts',(42.8746432198743,-22.4790208377489,0.));
#88798=CARTESIAN_POINT('Ctrl Pts',(42.8746432198743,-22.4790208377489,20.));
#88799=CARTESIAN_POINT('Ctrl Pts',(42.8563983484404,-22.5072677442656,0.));
#88800=CARTESIAN_POINT('Ctrl Pts',(42.8563983484404,-22.5072677442656,20.));
#88801=CARTESIAN_POINT('Ctrl Pts',(42.8381345459193,-22.5355010840531,0.));
#88802=CARTESIAN_POINT('Ctrl Pts',(42.8381345459193,-22.5355010840531,20.));
#88803=CARTESIAN_POINT('Ctrl Pts',(42.8198518217756,-22.5637208440656,0.));
#88804=CARTESIAN_POINT('Ctrl Pts',(42.8198518217756,-22.5637208440656,20.));
#88805=CARTESIAN_POINT('Ctrl Pts',(42.8015501854832,-22.5919270112639,0.));
#88806=CARTESIAN_POINT('Ctrl Pts',(42.8015501854832,-22.5919270112639,20.));
#88807=CARTESIAN_POINT('Ctrl Pts',(42.7832296465255,-22.6201195726151,0.));
#88808=CARTESIAN_POINT('Ctrl Pts',(42.7832296465255,-22.6201195726151,20.));
#88809=CARTESIAN_POINT('Ctrl Pts',(42.7648902143955,-22.6482985150925,0.));
#88810=CARTESIAN_POINT('Ctrl Pts',(42.7648902143955,-22.6482985150925,20.));
#88811=CARTESIAN_POINT('Ctrl Pts',(42.7465318985949,-22.6764638256759,0.));
#88812=CARTESIAN_POINT('Ctrl Pts',(42.7465318985949,-22.6764638256759,20.));
#88813=CARTESIAN_POINT('Ctrl Pts',(42.7281547086347,-22.7046154913512,0.));
#88814=CARTESIAN_POINT('Ctrl Pts',(42.7281547086347,-22.7046154913512,20.));
#88815=CARTESIAN_POINT('Ctrl Pts',(42.7097586540349,-22.7327534991101,0.));
#88816=CARTESIAN_POINT('Ctrl Pts',(42.7097586540349,-22.7327534991101,20.));
#88817=CARTESIAN_POINT('Ctrl Pts',(42.6913437443248,-22.7608778359508,0.));
#88818=CARTESIAN_POINT('Ctrl Pts',(42.6913437443248,-22.7608778359508,20.));
#88819=CARTESIAN_POINT('Ctrl Pts',(42.6729099890431,-22.788988488878,0.));
#88820=CARTESIAN_POINT('Ctrl Pts',(42.6729099890431,-22.788988488878,20.));
#88821=CARTESIAN_POINT('Ctrl Pts',(42.6544573977378,-22.8170854449024,0.));
#88822=CARTESIAN_POINT('Ctrl Pts',(42.6544573977378,-22.8170854449024,20.));
#88823=CARTESIAN_POINT('Ctrl Pts',(42.6359859799663,-22.845168691041,0.));
#88824=CARTESIAN_POINT('Ctrl Pts',(42.6359859799663,-22.845168691041,20.));
#88825=CARTESIAN_POINT('Ctrl Pts',(42.6174957452953,-22.8732382143175,0.));
#88826=CARTESIAN_POINT('Ctrl Pts',(42.6174957452953,-22.8732382143175,20.));
#88827=CARTESIAN_POINT('Ctrl Pts',(42.5989867033005,-22.9012940017616,0.));
#88828=CARTESIAN_POINT('Ctrl Pts',(42.5989867033005,-22.9012940017616,20.));
#88829=CARTESIAN_POINT('Ctrl Pts',(42.5804588635669,-22.9293360404095,0.));
#88830=CARTESIAN_POINT('Ctrl Pts',(42.5804588635669,-22.9293360404095,20.));
#88831=CARTESIAN_POINT('Ctrl Pts',(42.5619122356886,-22.9573643173034,0.));
#88832=CARTESIAN_POINT('Ctrl Pts',(42.5619122356886,-22.9573643173034,20.));
#88833=CARTESIAN_POINT('Ctrl Pts',(42.5433468292689,-22.9853788194919,0.));
#88834=CARTESIAN_POINT('Ctrl Pts',(42.5433468292689,-22.9853788194919,20.));
#88835=CARTESIAN_POINT('Ctrl Pts',(42.5247626539203,-23.0133795340299,0.));
#88836=CARTESIAN_POINT('Ctrl Pts',(42.5247626539203,-23.0133795340299,20.));
#88837=CARTESIAN_POINT('Ctrl Pts',(42.5061597192647,-23.0413664479785,0.));
#88838=CARTESIAN_POINT('Ctrl Pts',(42.5061597192647,-23.0413664479785,20.));
#88839=CARTESIAN_POINT('Ctrl Pts',(42.4875380349329,-23.0693395484056,0.));
#88840=CARTESIAN_POINT('Ctrl Pts',(42.4875380349329,-23.0693395484056,20.));
#88841=CARTESIAN_POINT('Ctrl Pts',(42.4688976105654,-23.097298822385,0.));
#88842=CARTESIAN_POINT('Ctrl Pts',(42.4688976105654,-23.097298822385,20.));
#88843=CARTESIAN_POINT('Ctrl Pts',(42.4502384558115,-23.1252442569971,0.));
#88844=CARTESIAN_POINT('Ctrl Pts',(42.4502384558115,-23.1252442569971,20.));
#88845=CARTESIAN_POINT('Ctrl Pts',(42.4315605803297,-23.1531758393284,0.));
#88846=CARTESIAN_POINT('Ctrl Pts',(42.4315605803297,-23.1531758393284,20.));
#88847=CARTESIAN_POINT('Ctrl Pts',(42.4128639937879,-23.1810935564721,0.));
#88848=CARTESIAN_POINT('Ctrl Pts',(42.4128639937879,-23.1810935564721,20.));
#88849=CARTESIAN_POINT('Ctrl Pts',(42.3941487058631,-23.2089973955278,0.));
#88850=CARTESIAN_POINT('Ctrl Pts',(42.3941487058631,-23.2089973955278,20.));
#88851=CARTESIAN_POINT('Ctrl Pts',(42.3754147262417,-23.2368873436013,0.));
#88852=CARTESIAN_POINT('Ctrl Pts',(42.3754147262417,-23.2368873436013,20.));
#88853=CARTESIAN_POINT('Ctrl Pts',(42.3566620646188,-23.2647633878047,0.));
#88854=CARTESIAN_POINT('Ctrl Pts',(42.3566620646188,-23.2647633878047,20.));
#88855=CARTESIAN_POINT('Ctrl Pts',(42.3378907306988,-23.2926255152563,0.));
#88856=CARTESIAN_POINT('Ctrl Pts',(42.3378907306988,-23.2926255152563,20.));
#88857=CARTESIAN_POINT('Ctrl Pts',(42.3191007341954,-23.320473713081,0.));
#88858=CARTESIAN_POINT('Ctrl Pts',(42.3191007341954,-23.320473713081,20.));
#88859=CARTESIAN_POINT('Ctrl Pts',(42.3002920848317,-23.3483079684104,0.));
#88860=CARTESIAN_POINT('Ctrl Pts',(42.3002920848317,-23.3483079684104,20.));
#88861=CARTESIAN_POINT('Ctrl Pts',(42.2814647923395,-23.3761282683822,0.));
#88862=CARTESIAN_POINT('Ctrl Pts',(42.2814647923395,-23.3761282683822,20.));
#88863=CARTESIAN_POINT('Ctrl Pts',(42.2626188664603,-23.4039346001409,0.));
#88864=CARTESIAN_POINT('Ctrl Pts',(42.2626188664603,-23.4039346001409,20.));
#88865=CARTESIAN_POINT('Ctrl Pts',(42.2437543169442,-23.4317269508371,0.));
#88866=CARTESIAN_POINT('Ctrl Pts',(42.2437543169442,-23.4317269508371,20.));
#88867=CARTESIAN_POINT('Ctrl Pts',(42.2248711535508,-23.4595053076278,0.));
#88868=CARTESIAN_POINT('Ctrl Pts',(42.2248711535508,-23.4595053076278,20.));
#88869=CARTESIAN_POINT('Ctrl Pts',(42.2059693860486,-23.4872696576759,0.));
#88870=CARTESIAN_POINT('Ctrl Pts',(42.2059693860486,-23.4872696576759,20.));
#88871=CARTESIAN_POINT('Ctrl Pts',(42.1870490242153,-23.5150199881515,0.));
#88872=CARTESIAN_POINT('Ctrl Pts',(42.1870490242153,-23.5150199881515,20.));
#88873=CARTESIAN_POINT('Ctrl Pts',(42.1681100778379,-23.5427562862308,0.));
#88874=CARTESIAN_POINT('Ctrl Pts',(42.1681100778379,-23.5427562862308,20.));
#88875=CARTESIAN_POINT('Ctrl Pts',(42.1491525567126,-23.5704785390969,0.));
#88876=CARTESIAN_POINT('Ctrl Pts',(42.1491525567126,-23.5704785390969,20.));
#88877=CARTESIAN_POINT('Ctrl Pts',(42.1301764706447,-23.5981867339395,0.));
#88878=CARTESIAN_POINT('Ctrl Pts',(42.1301764706447,-23.5981867339395,20.));
#88879=CARTESIAN_POINT('Ctrl Pts',(42.1111818294483,-23.6258808579543,0.));
#88880=CARTESIAN_POINT('Ctrl Pts',(42.1111818294483,-23.6258808579543,20.));
#88881=CARTESIAN_POINT('Ctrl Pts',(42.0921686429469,-23.6535608983436,0.));
#88882=CARTESIAN_POINT('Ctrl Pts',(42.0921686429469,-23.6535608983436,20.));
#88883=CARTESIAN_POINT('Ctrl Pts',(42.0731369209731,-23.6812268423159,0.));
#88884=CARTESIAN_POINT('Ctrl Pts',(42.0731369209731,-23.6812268423159,20.));
#88885=CARTESIAN_POINT('Ctrl Pts',(42.0540866733685,-23.7088786770864,0.));
#88886=CARTESIAN_POINT('Ctrl Pts',(42.0540866733685,-23.7088786770864,20.));
#88887=CARTESIAN_POINT('Ctrl Pts',(42.0350179099839,-23.7365163898768,0.));
#88888=CARTESIAN_POINT('Ctrl Pts',(42.0350179099839,-23.7365163898768,20.));
#88889=CARTESIAN_POINT('Ctrl Pts',(42.0159306406794,-23.7641399679152,0.));
#88890=CARTESIAN_POINT('Ctrl Pts',(42.0159306406794,-23.7641399679152,20.));
#88891=CARTESIAN_POINT('Ctrl Pts',(41.9968248753238,-23.7917493984363,0.));
#88892=CARTESIAN_POINT('Ctrl Pts',(41.9968248753238,-23.7917493984363,20.));
#88893=CARTESIAN_POINT('Ctrl Pts',(41.9777006237952,-23.8193446686815,0.));
#88894=CARTESIAN_POINT('Ctrl Pts',(41.9777006237952,-23.8193446686815,20.));
#88895=CARTESIAN_POINT('Ctrl Pts',(41.9585578959806,-23.8469257658985,0.));
#88896=CARTESIAN_POINT('Ctrl Pts',(41.9585578959806,-23.8469257658985,20.));
#88897=CARTESIAN_POINT('Ctrl Pts',(41.9393967017767,-23.8744926773418,0.));
#88898=CARTESIAN_POINT('Ctrl Pts',(41.9393967017767,-23.8744926773418,20.));
#88899=CARTESIAN_POINT('Ctrl Pts',(41.9202170510888,-23.9020453902722,0.));
#88900=CARTESIAN_POINT('Ctrl Pts',(41.9202170510888,-23.9020453902722,20.));
#88901=CARTESIAN_POINT('Ctrl Pts',(41.9010189538314,-23.9295838919573,0.));
#88902=CARTESIAN_POINT('Ctrl Pts',(41.9010189538314,-23.9295838919573,20.));
#88903=CARTESIAN_POINT('Ctrl Pts',(41.8818024199281,-23.9571081696708,0.));
#88904=CARTESIAN_POINT('Ctrl Pts',(41.8818024199281,-23.9571081696708,20.));
#88905=CARTESIAN_POINT('Ctrl Pts',(41.8625674593112,-23.9846182106931,0.));
#88906=CARTESIAN_POINT('Ctrl Pts',(41.8625674593112,-23.9846182106931,20.));
#88907=CARTESIAN_POINT('Ctrl Pts',(41.8433140819226,-24.0121140023113,0.));
#88908=CARTESIAN_POINT('Ctrl Pts',(41.8433140819226,-24.0121140023113,20.));
#88909=CARTESIAN_POINT('Ctrl Pts',(41.824042297713,-24.0395955318191,0.));
#88910=CARTESIAN_POINT('Ctrl Pts',(41.824042297713,-24.0395955318191,20.));
#88911=CARTESIAN_POINT('Ctrl Pts',(41.8047521166422,-24.0670627865166,0.));
#88912=CARTESIAN_POINT('Ctrl Pts',(41.8047521166422,-24.0670627865166,20.));
#88913=CARTESIAN_POINT('Ctrl Pts',(41.785443548679,-24.0945157537107,0.));
#88914=CARTESIAN_POINT('Ctrl Pts',(41.785443548679,-24.0945157537107,20.));
#88915=CARTESIAN_POINT('Ctrl Pts',(41.7661166038015,-24.1219544207148,0.));
#88916=CARTESIAN_POINT('Ctrl Pts',(41.7661166038015,-24.1219544207148,20.));
#88917=CARTESIAN_POINT('Ctrl Pts',(41.7467712919966,-24.1493787748488,0.));
#88918=CARTESIAN_POINT('Ctrl Pts',(41.7467712919966,-24.1493787748488,20.));
#88919=CARTESIAN_POINT('Ctrl Pts',(41.7274076232604,-24.1767888034393,0.));
#88920=CARTESIAN_POINT('Ctrl Pts',(41.7274076232604,-24.1767888034393,20.));
#88921=CARTESIAN_POINT('Ctrl Pts',(41.7080256075983,-24.2041844938197,0.));
#88922=CARTESIAN_POINT('Ctrl Pts',(41.7080256075983,-24.2041844938197,20.));
#88923=CARTESIAN_POINT('Ctrl Pts',(41.688625255024,-24.2315658333297,0.));
#88924=CARTESIAN_POINT('Ctrl Pts',(41.688625255024,-24.2315658333297,20.));
#88925=CARTESIAN_POINT('Ctrl Pts',(41.6692065755608,-24.2589328093159,0.));
#88926=CARTESIAN_POINT('Ctrl Pts',(41.6692065755608,-24.2589328093159,20.));
#88927=CARTESIAN_POINT('Ctrl Pts',(41.6497695792407,-24.2862854091312,0.));
#88928=CARTESIAN_POINT('Ctrl Pts',(41.6497695792407,-24.2862854091312,20.));
#88929=CARTESIAN_POINT('Ctrl Pts',(41.630314276105,-24.3136236201351,0.));
#88930=CARTESIAN_POINT('Ctrl Pts',(41.630314276105,-24.3136236201351,20.));
#88931=CARTESIAN_POINT('Ctrl Pts',(41.610840676204,-24.3409474296941,0.));
#88932=CARTESIAN_POINT('Ctrl Pts',(41.610840676204,-24.3409474296941,20.));
#88933=CARTESIAN_POINT('Ctrl Pts',(41.5913487895971,-24.368256825181,0.));
#88934=CARTESIAN_POINT('Ctrl Pts',(41.5913487895971,-24.368256825181,20.));
#88935=CARTESIAN_POINT('Ctrl Pts',(41.5718386263526,-24.3955517939757,0.));
#88936=CARTESIAN_POINT('Ctrl Pts',(41.5718386263526,-24.3955517939757,20.));
#88937=CARTESIAN_POINT('Ctrl Pts',(41.5523101965477,-24.4228323234645,0.));
#88938=CARTESIAN_POINT('Ctrl Pts',(41.5523101965477,-24.4228323234645,20.));
#88939=CARTESIAN_POINT('Ctrl Pts',(41.5327635102685,-24.4500984010406,0.));
#88940=CARTESIAN_POINT('Ctrl Pts',(41.5327635102685,-24.4500984010406,20.));
#88941=CARTESIAN_POINT('Ctrl Pts',(41.5131985776101,-24.4773500141037,0.));
#88942=CARTESIAN_POINT('Ctrl Pts',(41.5131985776101,-24.4773500141037,20.));
#88943=CARTESIAN_POINT('Ctrl Pts',(41.4936154086768,-24.5045871500598,0.));
#88944=CARTESIAN_POINT('Ctrl Pts',(41.4936154086768,-24.5045871500598,20.));
#88945=CARTESIAN_POINT('Ctrl Pts',(41.4740140135823,-24.5318097963223,0.));
#88946=CARTESIAN_POINT('Ctrl Pts',(41.4740140135823,-24.5318097963223,20.));
#88947=CARTESIAN_POINT('Ctrl Pts',(41.4543944024488,-24.5590179403106,0.));
#88948=CARTESIAN_POINT('Ctrl Pts',(41.4543944024488,-24.5590179403106,20.));
#88949=CARTESIAN_POINT('Ctrl Pts',(41.4347565854076,-24.5862115694513,0.));
#88950=CARTESIAN_POINT('Ctrl Pts',(41.4347565854076,-24.5862115694513,20.));
#88951=CARTESIAN_POINT('Ctrl Pts',(41.4151005725989,-24.6133906711774,0.));
#88952=CARTESIAN_POINT('Ctrl Pts',(41.4151005725989,-24.6133906711774,20.));
#88953=CARTESIAN_POINT('Ctrl Pts',(41.3954263741717,-24.6405552329289,0.));
#88954=CARTESIAN_POINT('Ctrl Pts',(41.3954263741717,-24.6405552329289,20.));
#88955=CARTESIAN_POINT('Ctrl Pts',(41.3757340002844,-24.6677052421523,0.));
#88956=CARTESIAN_POINT('Ctrl Pts',(41.3757340002844,-24.6677052421523,20.));
#88957=CARTESIAN_POINT('Ctrl Pts',(41.3560234611038,-24.694840686301,0.));
#88958=CARTESIAN_POINT('Ctrl Pts',(41.3560234611038,-24.694840686301,20.));
#88959=CARTESIAN_POINT('Ctrl Pts',(41.3362947668064,-24.7219615528352,0.));
#88960=CARTESIAN_POINT('Ctrl Pts',(41.3362947668064,-24.7219615528352,20.));
#88961=CARTESIAN_POINT('Ctrl Pts',(41.3165479275773,-24.7490678292217,0.));
#88962=CARTESIAN_POINT('Ctrl Pts',(41.3165479275773,-24.7490678292217,20.));
#88963=CARTESIAN_POINT('Ctrl Pts',(41.2967829536105,-24.7761595029341,0.));
#88964=CARTESIAN_POINT('Ctrl Pts',(41.2967829536105,-24.7761595029341,20.));
#88965=CARTESIAN_POINT('Ctrl Pts',(41.276999855109,-24.8032365614526,0.));
#88966=CARTESIAN_POINT('Ctrl Pts',(41.276999855109,-24.8032365614526,20.));
#88967=CARTESIAN_POINT('Ctrl Pts',(41.2571986422843,-24.8302989922639,0.));
#88968=CARTESIAN_POINT('Ctrl Pts',(41.2571986422843,-24.8302989922639,20.));
#88969=CARTESIAN_POINT('Ctrl Pts',(41.2373793253577,-24.8573467828623,0.));
#88970=CARTESIAN_POINT('Ctrl Pts',(41.2373793253577,-24.8573467828623,20.));
#88971=CARTESIAN_POINT('Ctrl Pts',(41.2175419145588,-24.8843799207483,0.));
#88972=CARTESIAN_POINT('Ctrl Pts',(41.2175419145588,-24.8843799207483,20.));
#88973=CARTESIAN_POINT('Ctrl Pts',(41.1976864201268,-24.9113983934294,0.));
#88974=CARTESIAN_POINT('Ctrl Pts',(41.1976864201268,-24.9113983934294,20.));
#88975=CARTESIAN_POINT('Ctrl Pts',(41.1778128523092,-24.9384021884197,0.));
#88976=CARTESIAN_POINT('Ctrl Pts',(41.1778128523092,-24.9384021884197,20.));
#88977=CARTESIAN_POINT('Ctrl Pts',(41.1579212213625,-24.9653912932403,0.));
#88978=CARTESIAN_POINT('Ctrl Pts',(41.1579212213625,-24.9653912932403,20.));
#88979=CARTESIAN_POINT('Ctrl Pts',(41.1380115375521,-24.9923656954187,0.));
#88980=CARTESIAN_POINT('Ctrl Pts',(41.1380115375521,-24.9923656954187,20.));
#88981=CARTESIAN_POINT('Ctrl Pts',(41.1180838111525,-25.0193253824897,0.));
#88982=CARTESIAN_POINT('Ctrl Pts',(41.1180838111525,-25.0193253824897,20.));
#88983=CARTESIAN_POINT('Ctrl Pts',(41.0981380524472,-25.0462703419947,0.));
#88984=CARTESIAN_POINT('Ctrl Pts',(41.0981380524472,-25.0462703419947,20.));
#88985=CARTESIAN_POINT('Ctrl Pts',(41.0781742717283,-25.0732005614819,0.));
#88986=CARTESIAN_POINT('Ctrl Pts',(41.0781742717283,-25.0732005614819,20.));
#88987=CARTESIAN_POINT('Ctrl Pts',(41.058192479297,-25.1001160285063,0.));
#88988=CARTESIAN_POINT('Ctrl Pts',(41.058192479297,-25.1001160285063,20.));
#88989=CARTESIAN_POINT('Ctrl Pts',(41.0381926854635,-25.1270167306298,0.));
#88990=CARTESIAN_POINT('Ctrl Pts',(41.0381926854635,-25.1270167306298,20.));
#88991=CARTESIAN_POINT('Ctrl Pts',(41.0181749005471,-25.1539026554213,0.));
#88992=CARTESIAN_POINT('Ctrl Pts',(41.0181749005471,-25.1539026554213,20.));
#88993=CARTESIAN_POINT('Ctrl Pts',(40.9981391348755,-25.1807737904566,0.));
#88994=CARTESIAN_POINT('Ctrl Pts',(40.9981391348755,-25.1807737904566,20.));
#88995=CARTESIAN_POINT('Ctrl Pts',(40.9780853987856,-25.2076301233182,0.));
#88996=CARTESIAN_POINT('Ctrl Pts',(40.9780853987856,-25.2076301233182,20.));
#88997=CARTESIAN_POINT('Ctrl Pts',(40.9580137026228,-25.2344716415952,0.));
#88998=CARTESIAN_POINT('Ctrl Pts',(40.9580137026228,-25.2344716415952,20.));
#88999=CARTESIAN_POINT('Ctrl Pts',(40.9379240567416,-25.2612983328836,0.));
#89000=CARTESIAN_POINT('Ctrl Pts',(40.9379240567416,-25.2612983328836,20.));
#89001=CARTESIAN_POINT('Ctrl Pts',(40.9178164715051,-25.2881101847862,0.));
#89002=CARTESIAN_POINT('Ctrl Pts',(40.9178164715051,-25.2881101847862,20.));
#89003=CARTESIAN_POINT('Ctrl Pts',(40.8976909572856,-25.3149071849127,0.));
#89004=CARTESIAN_POINT('Ctrl Pts',(40.8976909572856,-25.3149071849127,20.));
#89005=CARTESIAN_POINT('Ctrl Pts',(40.8775475244644,-25.3416893208803,0.));
#89006=CARTESIAN_POINT('Ctrl Pts',(40.8775475244644,-25.3416893208803,20.));
#89007=CARTESIAN_POINT('Ctrl Pts',(40.8573861834315,-25.3684565803126,0.));
#89008=CARTESIAN_POINT('Ctrl Pts',(40.8573861834315,-25.3684565803126,20.));
#89009=CARTESIAN_POINT('Ctrl Pts',(40.8372069445861,-25.3952089508407,0.));
#89010=CARTESIAN_POINT('Ctrl Pts',(40.8372069445861,-25.3952089508407,20.));
#89011=CARTESIAN_POINT('Ctrl Pts',(40.8170098183361,-25.4219464201024,0.));
#89012=CARTESIAN_POINT('Ctrl Pts',(40.8170098183361,-25.4219464201024,20.));
#89013=CARTESIAN_POINT('Ctrl Pts',(40.796794815098,-25.4486689757422,0.));
#89014=CARTESIAN_POINT('Ctrl Pts',(40.796794815098,-25.4486689757422,20.));
#89015=CARTESIAN_POINT('Ctrl Pts',(40.7765619452973,-25.4753766054114,0.));
#89016=CARTESIAN_POINT('Ctrl Pts',(40.7765619452973,-25.4753766054114,20.));
#89017=CARTESIAN_POINT('Ctrl Pts',(40.7563112193678,-25.5020692967677,0.));
#89018=CARTESIAN_POINT('Ctrl Pts',(40.7563112193678,-25.5020692967677,20.));
#89019=CARTESIAN_POINT('Ctrl Pts',(40.7360426477524,-25.528747037476,0.));
#89020=CARTESIAN_POINT('Ctrl Pts',(40.7360426477524,-25.528747037476,20.));
#89021=CARTESIAN_POINT('Ctrl Pts',(40.715756240903,-25.5554098152083,0.));
#89022=CARTESIAN_POINT('Ctrl Pts',(40.715756240903,-25.5554098152083,20.));
#89023=CARTESIAN_POINT('Ctrl Pts',(40.6954520092804,-25.5820576176439,0.));
#89024=CARTESIAN_POINT('Ctrl Pts',(40.6954520092804,-25.5820576176439,20.));
#89025=CARTESIAN_POINT('Ctrl Pts',(40.6751299633542,-25.6086904324689,0.));
#89026=CARTESIAN_POINT('Ctrl Pts',(40.6751299633542,-25.6086904324689,20.));
#89027=CARTESIAN_POINT('Ctrl Pts',(40.6547901136033,-25.6353082473769,0.));
#89028=CARTESIAN_POINT('Ctrl Pts',(40.6547901136033,-25.6353082473769,20.));
#89029=CARTESIAN_POINT('Ctrl Pts',(40.6344324705148,-25.6619110500678,0.));
#89030=CARTESIAN_POINT('Ctrl Pts',(40.6344324705148,-25.6619110500678,20.));
#89031=CARTESIAN_POINT('Ctrl Pts',(40.6140570445846,-25.6884988282486,0.));
#89032=CARTESIAN_POINT('Ctrl Pts',(40.6140570445846,-25.6884988282486,20.));
#89033=CARTESIAN_POINT('Ctrl Pts',(40.5936638463177,-25.7150715696333,0.));
#89034=CARTESIAN_POINT('Ctrl Pts',(40.5936638463177,-25.7150715696333,20.));
#89035=CARTESIAN_POINT('Ctrl Pts',(40.5732528862276,-25.7416292619425,0.));
#89036=CARTESIAN_POINT('Ctrl Pts',(40.5732528862276,-25.7416292619425,20.));
#89037=CARTESIAN_POINT('Ctrl Pts',(40.5528241748366,-25.768171892904,0.));
#89038=CARTESIAN_POINT('Ctrl Pts',(40.5528241748366,-25.768171892904,20.));
#89039=CARTESIAN_POINT('Ctrl Pts',(40.5323777226757,-25.7946994502526,0.));
#89040=CARTESIAN_POINT('Ctrl Pts',(40.5323777226757,-25.7946994502526,20.));
#89041=CARTESIAN_POINT('Ctrl Pts',(40.5119135402852,-25.8212119217304,0.));
#89042=CARTESIAN_POINT('Ctrl Pts',(40.5119135402852,-25.8212119217304,20.));
#89043=CARTESIAN_POINT('Ctrl Pts',(40.491431638214,-25.8477092950863,0.));
#89044=CARTESIAN_POINT('Ctrl Pts',(40.491431638214,-25.8477092950863,20.));
#89045=CARTESIAN_POINT('Ctrl Pts',(40.4709320270197,-25.8741915580762,0.));
#89046=CARTESIAN_POINT('Ctrl Pts',(40.4709320270197,-25.8741915580762,20.));
#89047=CARTESIAN_POINT('Ctrl Pts',(40.4504147172684,-25.9006586984631,0.));
#89048=CARTESIAN_POINT('Ctrl Pts',(40.4504147172684,-25.9006586984631,20.));
#89049=CARTESIAN_POINT('Ctrl Pts',(40.4298797195352,-25.9271107040169,0.));
#89050=CARTESIAN_POINT('Ctrl Pts',(40.4298797195352,-25.9271107040169,20.));
#89051=CARTESIAN_POINT('Ctrl Pts',(40.4093270444043,-25.953547562515,0.));
#89052=CARTESIAN_POINT('Ctrl Pts',(40.4093270444043,-25.953547562515,20.));
#89053=CARTESIAN_POINT('Ctrl Pts',(40.3887567024682,-25.9799692617416,0.));
#89054=CARTESIAN_POINT('Ctrl Pts',(40.3887567024682,-25.9799692617416,20.));
#89055=CARTESIAN_POINT('Ctrl Pts',(40.3681687043283,-26.0063757894875,0.));
#89056=CARTESIAN_POINT('Ctrl Pts',(40.3681687043283,-26.0063757894875,20.));
#89057=CARTESIAN_POINT('Ctrl Pts',(40.347563060595,-26.0327671335511,0.));
#89058=CARTESIAN_POINT('Ctrl Pts',(40.347563060595,-26.0327671335511,20.));
#89059=CARTESIAN_POINT('Ctrl Pts',(40.326939781887,-26.0591432817373,0.));
#89060=CARTESIAN_POINT('Ctrl Pts',(40.326939781887,-26.0591432817373,20.));
#89061=CARTESIAN_POINT('Ctrl Pts',(40.3062988788318,-26.0855042218584,0.));
#89062=CARTESIAN_POINT('Ctrl Pts',(40.3062988788318,-26.0855042218584,20.));
#89063=CARTESIAN_POINT('Ctrl Pts',(40.2856403620657,-26.1118499417334,0.));
#89064=CARTESIAN_POINT('Ctrl Pts',(40.2856403620657,-26.1118499417334,20.));
#89065=CARTESIAN_POINT('Ctrl Pts',(40.2649642422341,-26.1381804291893,0.));
#89066=CARTESIAN_POINT('Ctrl Pts',(40.2649642422341,-26.1381804291893,20.));
#89067=CARTESIAN_POINT('Ctrl Pts',(40.2442705299908,-26.1644956720595,0.));
#89068=CARTESIAN_POINT('Ctrl Pts',(40.2442705299908,-26.1644956720595,20.));
#89069=CARTESIAN_POINT('Ctrl Pts',(40.2235592359986,-26.1907956581852,0.));
#89070=CARTESIAN_POINT('Ctrl Pts',(40.2235592359986,-26.1907956581852,20.));
#89071=CARTESIAN_POINT('Ctrl Pts',(40.2028303709288,-26.217080375414,0.));
#89072=CARTESIAN_POINT('Ctrl Pts',(40.2028303709288,-26.217080375414,20.));
#89073=CARTESIAN_POINT('Ctrl Pts',(40.1820839454613,-26.2433498116008,0.));
#89074=CARTESIAN_POINT('Ctrl Pts',(40.1820839454613,-26.2433498116008,20.));
#89075=CARTESIAN_POINT('Ctrl Pts',(40.161319970285,-26.2696039546074,0.));
#89076=CARTESIAN_POINT('Ctrl Pts',(40.161319970285,-26.2696039546074,20.));
#89077=CARTESIAN_POINT('Ctrl Pts',(40.1405384560971,-26.2958427923028,0.));
#89078=CARTESIAN_POINT('Ctrl Pts',(40.1405384560971,-26.2958427923028,20.));
#89079=CARTESIAN_POINT('Ctrl Pts',(40.1197394136039,-26.3220663125631,0.));
#89080=CARTESIAN_POINT('Ctrl Pts',(40.1197394136039,-26.3220663125631,20.));
#89081=CARTESIAN_POINT('Ctrl Pts',(40.0989228535202,-26.3482745032719,0.));
#89082=CARTESIAN_POINT('Ctrl Pts',(40.0989228535202,-26.3482745032719,20.));
#89083=CARTESIAN_POINT('Ctrl Pts',(40.0780887865696,-26.3744673523197,0.));
#89084=CARTESIAN_POINT('Ctrl Pts',(40.0780887865696,-26.3744673523197,20.));
#89085=CARTESIAN_POINT('Ctrl Pts',(40.0572372234843,-26.4006448476042,0.));
#89086=CARTESIAN_POINT('Ctrl Pts',(40.0572372234843,-26.4006448476042,20.));
#89087=CARTESIAN_POINT('Ctrl Pts',(40.0363681750052,-26.4268069770299,0.));
#89088=CARTESIAN_POINT('Ctrl Pts',(40.0363681750052,-26.4268069770299,20.));
#89089=CARTESIAN_POINT('Ctrl Pts',(40.015481651882,-26.4529537285089,0.));
#89090=CARTESIAN_POINT('Ctrl Pts',(40.015481651882,-26.4529537285089,20.));
#89091=CARTESIAN_POINT('Ctrl Pts',(39.994577664873,-26.4790850899607,0.));
#89092=CARTESIAN_POINT('Ctrl Pts',(39.994577664873,-26.4790850899607,20.));
#89093=CARTESIAN_POINT('Ctrl Pts',(39.9736562247456,-26.5052010493117,0.));
#89094=CARTESIAN_POINT('Ctrl Pts',(39.9736562247456,-26.5052010493117,20.));
#89095=CARTESIAN_POINT('Ctrl Pts',(39.9527173422752,-26.5313015944953,0.));
#89096=CARTESIAN_POINT('Ctrl Pts',(39.9527173422752,-26.5313015944953,20.));
#89097=CARTESIAN_POINT('Ctrl Pts',(39.9317610282459,-26.5573867134521,0.));
#89098=CARTESIAN_POINT('Ctrl Pts',(39.9317610282459,-26.5573867134521,20.));
#89099=CARTESIAN_POINT('Ctrl Pts',(39.9107872934506,-26.5834563941296,0.));
#89100=CARTESIAN_POINT('Ctrl Pts',(39.9107872934506,-26.5834563941296,20.));
#89101=CARTESIAN_POINT('Ctrl Pts',(39.8897961486907,-26.6095106244829,0.));
#89102=CARTESIAN_POINT('Ctrl Pts',(39.8897961486907,-26.6095106244829,20.));
#89103=CARTESIAN_POINT('Ctrl Pts',(39.8687876047769,-26.6355493924744,0.));
#89104=CARTESIAN_POINT('Ctrl Pts',(39.8687876047769,-26.6355493924744,20.));
#89105=CARTESIAN_POINT('Ctrl Pts',(39.847761672528,-26.6615726860735,0.));
#89106=CARTESIAN_POINT('Ctrl Pts',(39.847761672528,-26.6615726860735,20.));
#89107=CARTESIAN_POINT('Ctrl Pts',(39.8267183627717,-26.687580493257,0.));
#89108=CARTESIAN_POINT('Ctrl Pts',(39.8267183627717,-26.687580493257,20.));
#89109=CARTESIAN_POINT('Ctrl Pts',(39.8056576863443,-26.713572802009,0.));
#89110=CARTESIAN_POINT('Ctrl Pts',(39.8056576863443,-26.713572802009,20.));
#89111=CARTESIAN_POINT('Ctrl Pts',(39.7845796540903,-26.7395496003209,0.));
#89112=CARTESIAN_POINT('Ctrl Pts',(39.7845796540903,-26.7395496003209,20.));
#89113=CARTESIAN_POINT('Ctrl Pts',(39.7634842768631,-26.7655108761908,0.));
#89114=CARTESIAN_POINT('Ctrl Pts',(39.7634842768631,-26.7655108761908,20.));
#89115=CARTESIAN_POINT('Ctrl Pts',(39.7423715655248,-26.7914566176244,0.));
#89116=CARTESIAN_POINT('Ctrl Pts',(39.7423715655248,-26.7914566176244,20.));
#89117=CARTESIAN_POINT('Ctrl Pts',(39.7212415309462,-26.8173868126345,0.));
#89118=CARTESIAN_POINT('Ctrl Pts',(39.7212415309462,-26.8173868126345,20.));
#89119=CARTESIAN_POINT('Ctrl Pts',(39.7000941840065,-26.843301449241,0.));
#89120=CARTESIAN_POINT('Ctrl Pts',(39.7000941840065,-26.843301449241,20.));
#89121=CARTESIAN_POINT('Ctrl Pts',(39.6789295355942,-26.8692005154716,0.));
#89122=CARTESIAN_POINT('Ctrl Pts',(39.6789295355942,-26.8692005154716,20.));
#89123=CARTESIAN_POINT('Ctrl Pts',(39.6577475966055,-26.8950839993609,0.));
#89124=CARTESIAN_POINT('Ctrl Pts',(39.6577475966055,-26.8950839993609,20.));
#89125=CARTESIAN_POINT('Ctrl Pts',(39.6365483779457,-26.9209518889509,0.));
#89126=CARTESIAN_POINT('Ctrl Pts',(39.6365483779457,-26.9209518889509,20.));
#89127=CARTESIAN_POINT('Ctrl Pts',(39.6153318905282,-26.9468041722907,0.));
#89128=CARTESIAN_POINT('Ctrl Pts',(39.6153318905282,-26.9468041722907,20.));
#89129=CARTESIAN_POINT('Ctrl Pts',(39.5940981452753,-26.9726408374371,0.));
#89130=CARTESIAN_POINT('Ctrl Pts',(39.5940981452753,-26.9726408374371,20.));
#89131=CARTESIAN_POINT('Ctrl Pts',(39.5728471531177,-26.9984618724537,0.));
#89132=CARTESIAN_POINT('Ctrl Pts',(39.5728471531177,-26.9984618724537,20.));
#89133=CARTESIAN_POINT('Ctrl Pts',(39.5515789249952,-27.0242672654118,0.));
#89134=CARTESIAN_POINT('Ctrl Pts',(39.5515789249952,-27.0242672654118,20.));
#89135=CARTESIAN_POINT('Ctrl Pts',(39.5302934718558,-27.0500570043898,0.));
#89136=CARTESIAN_POINT('Ctrl Pts',(39.5302934718558,-27.0500570043898,20.));
#89137=CARTESIAN_POINT('Ctrl Pts',(39.5089908046561,-27.0758310774732,0.));
#89138=CARTESIAN_POINT('Ctrl Pts',(39.5089908046561,-27.0758310774732,20.));
#89139=CARTESIAN_POINT('Ctrl Pts',(39.4876709343614,-27.1015894727552,0.));
#89140=CARTESIAN_POINT('Ctrl Pts',(39.4876709343614,-27.1015894727552,20.));
#89141=CARTESIAN_POINT('Ctrl Pts',(39.4663338719455,-27.1273321783362,0.));
#89142=CARTESIAN_POINT('Ctrl Pts',(39.4663338719455,-27.1273321783362,20.));
#89143=CARTESIAN_POINT('Ctrl Pts',(39.4449796283908,-27.153059182324,0.));
#89144=CARTESIAN_POINT('Ctrl Pts',(39.4449796283908,-27.153059182324,20.));
#89145=CARTESIAN_POINT('Ctrl Pts',(39.4236082146882,-27.1787704728337,0.));
#89146=CARTESIAN_POINT('Ctrl Pts',(39.4236082146882,-27.1787704728337,20.));
#89147=CARTESIAN_POINT('Ctrl Pts',(39.4022196418372,-27.2044660379877,0.));
#89148=CARTESIAN_POINT('Ctrl Pts',(39.4022196418372,-27.2044660379877,20.));
#89149=CARTESIAN_POINT('Ctrl Pts',(39.3808139208456,-27.2301458659158,0.));
#89150=CARTESIAN_POINT('Ctrl Pts',(39.3808139208456,-27.2301458659158,20.));
#89151=CARTESIAN_POINT('Ctrl Pts',(39.3593910627297,-27.2558099447548,0.));
#89152=CARTESIAN_POINT('Ctrl Pts',(39.3593910627297,-27.2558099447548,20.));
#89153=CARTESIAN_POINT('Ctrl Pts',(39.3379510785145,-27.2814582626493,0.));
#89154=CARTESIAN_POINT('Ctrl Pts',(39.3379510785145,-27.2814582626493,20.));
#89155=CARTESIAN_POINT('Ctrl Pts',(39.3164939792334,-27.3070908077508,0.));
#89156=CARTESIAN_POINT('Ctrl Pts',(39.3164939792334,-27.3070908077508,20.));
#89157=CARTESIAN_POINT('Ctrl Pts',(39.2950197759285,-27.3327075682187,0.));
#89158=CARTESIAN_POINT('Ctrl Pts',(39.2950197759285,-27.3327075682187,20.));
#89159=CARTESIAN_POINT('Ctrl Pts',(39.2735284796508,-27.3583085322198,0.));
#89160=CARTESIAN_POINT('Ctrl Pts',(39.2735284796508,-27.3583085322198,20.));
#89161=CARTESIAN_POINT('Ctrl Pts',(39.25202010146,-27.3838936879286,0.));
#89162=CARTESIAN_POINT('Ctrl Pts',(39.25202010146,-27.3838936879286,20.));
#89163=CARTESIAN_POINT('Ctrl Pts',(39.2304946524241,-27.4094630235266,0.));
#89164=CARTESIAN_POINT('Ctrl Pts',(39.2304946524241,-27.4094630235266,20.));
#89165=CARTESIAN_POINT('Ctrl Pts',(39.2089521436188,-27.4350165272023,0.));
#89166=CARTESIAN_POINT('Ctrl Pts',(39.2089521436188,-27.4350165272023,20.));
#89167=CARTESIAN_POINT('Ctrl Pts',(39.1873925861285,-27.4605541871518,0.));
#89168=CARTESIAN_POINT('Ctrl Pts',(39.1873925861285,-27.4605541871518,20.));
#89169=CARTESIAN_POINT('Ctrl Pts',(39.1658159910457,-27.4860759915783,0.));
#89170=CARTESIAN_POINT('Ctrl Pts',(39.1658159910457,-27.4860759915783,20.));
#89171=CARTESIAN_POINT('Ctrl Pts',(39.1442223694722,-27.5115819286927,0.));
#89172=CARTESIAN_POINT('Ctrl Pts',(39.1442223694722,-27.5115819286927,20.));
#89173=CARTESIAN_POINT('Ctrl Pts',(39.1226117325183,-27.5370719867137,0.));
#89174=CARTESIAN_POINT('Ctrl Pts',(39.1226117325183,-27.5370719867137,20.));
#89175=CARTESIAN_POINT('Ctrl Pts',(39.100984091303,-27.5625461538676,0.));
#89176=CARTESIAN_POINT('Ctrl Pts',(39.100984091303,-27.5625461538676,20.));
#89177=CARTESIAN_POINT('Ctrl Pts',(39.0793394569537,-27.5880044183879,0.));
#89178=CARTESIAN_POINT('Ctrl Pts',(39.0793394569537,-27.5880044183879,20.));
#89179=CARTESIAN_POINT('Ctrl Pts',(39.057677840606,-27.6134467685156,0.));
#89180=CARTESIAN_POINT('Ctrl Pts',(39.057677840606,-27.6134467685156,20.));
#89181=CARTESIAN_POINT('Ctrl Pts',(39.0359992534037,-27.6388731924983,0.));
#89182=CARTESIAN_POINT('Ctrl Pts',(39.0359992534037,-27.6388731924983,20.));
#89183=CARTESIAN_POINT('Ctrl Pts',(39.0143037064988,-27.6642836785915,0.));
#89184=CARTESIAN_POINT('Ctrl Pts',(39.0143037064988,-27.6642836785915,20.));
#89185=CARTESIAN_POINT('Ctrl Pts',(38.9925912110523,-27.6896782150583,0.));
#89186=CARTESIAN_POINT('Ctrl Pts',(38.9925912110523,-27.6896782150583,20.));
#89187=CARTESIAN_POINT('Ctrl Pts',(38.9708617782339,-27.7150567901695,0.));
#89188=CARTESIAN_POINT('Ctrl Pts',(38.9708617782339,-27.7150567901695,20.));
#89189=CARTESIAN_POINT('Ctrl Pts',(38.9491154192216,-27.7404193922036,0.));
#89190=CARTESIAN_POINT('Ctrl Pts',(38.9491154192216,-27.7404193922036,20.));
#89191=CARTESIAN_POINT('Ctrl Pts',(38.9273521452022,-27.7657660094467,0.));
#89192=CARTESIAN_POINT('Ctrl Pts',(38.9273521452022,-27.7657660094467,20.));
#89193=CARTESIAN_POINT('Ctrl Pts',(38.9055719673706,-27.7910966301919,0.));
#89194=CARTESIAN_POINT('Ctrl Pts',(38.9055719673706,-27.7910966301919,20.));
#89195=CARTESIAN_POINT('Ctrl Pts',(38.8837748969299,-27.8164112427396,0.));
#89196=CARTESIAN_POINT('Ctrl Pts',(38.8837748969299,-27.8164112427396,20.));
#89197=CARTESIAN_POINT('Ctrl Pts',(38.8619609450912,-27.8417098353976,0.));
#89198=CARTESIAN_POINT('Ctrl Pts',(38.8619609450912,-27.8417098353976,20.));
#89199=CARTESIAN_POINT('Ctrl Pts',(38.8401301230745,-27.866992396481,0.));
#89200=CARTESIAN_POINT('Ctrl Pts',(38.8401301230745,-27.866992396481,20.));
#89201=CARTESIAN_POINT('Ctrl Pts',(38.8182824421081,-27.8922589143132,0.));
#89202=CARTESIAN_POINT('Ctrl Pts',(38.8182824421081,-27.8922589143132,20.));
#89203=CARTESIAN_POINT('Ctrl Pts',(38.7964179134294,-27.917509377225,0.));
#89204=CARTESIAN_POINT('Ctrl Pts',(38.7964179134294,-27.917509377225,20.));
#89205=CARTESIAN_POINT('Ctrl Pts',(38.7745365482837,-27.9427437735547,0.));
#89206=CARTESIAN_POINT('Ctrl Pts',(38.7745365482837,-27.9427437735547,20.));
#89207=CARTESIAN_POINT('Ctrl Pts',(38.752638357925,-27.9679620916479,0.));
#89208=CARTESIAN_POINT('Ctrl Pts',(38.752638357925,-27.9679620916479,20.));
#89209=CARTESIAN_POINT('Ctrl Pts',(38.7307233536152,-27.9931643198581,0.));
#89210=CARTESIAN_POINT('Ctrl Pts',(38.7307233536152,-27.9931643198581,20.));
#89211=CARTESIAN_POINT('Ctrl Pts',(38.7087915466246,-28.0183504465459,0.));
#89212=CARTESIAN_POINT('Ctrl Pts',(38.7087915466246,-28.0183504465459,20.));
#89213=CARTESIAN_POINT('Ctrl Pts',(38.6868429482324,-28.0435204600798,0.));
#89214=CARTESIAN_POINT('Ctrl Pts',(38.6868429482324,-28.0435204600798,20.));
#89215=CARTESIAN_POINT('Ctrl Pts',(38.6648775697261,-28.0686743488362,0.));
#89216=CARTESIAN_POINT('Ctrl Pts',(38.6648775697261,-28.0686743488362,20.));
#89217=CARTESIAN_POINT('Ctrl Pts',(38.6428954224012,-28.0938121011982,0.));
#89218=CARTESIAN_POINT('Ctrl Pts',(38.6428954224012,-28.0938121011982,20.));
#89219=CARTESIAN_POINT('Ctrl Pts',(38.6208965175619,-28.1189337055566,0.));
#89220=CARTESIAN_POINT('Ctrl Pts',(38.6208965175619,-28.1189337055566,20.));
#89221=CARTESIAN_POINT('Ctrl Pts',(38.5988808665205,-28.14403915031,0.));
#89222=CARTESIAN_POINT('Ctrl Pts',(38.5988808665205,-28.14403915031,20.));
#89223=CARTESIAN_POINT('Ctrl Pts',(38.5768484805978,-28.1691284238645,0.));
#89224=CARTESIAN_POINT('Ctrl Pts',(38.5768484805978,-28.1691284238645,20.));
#89225=CARTESIAN_POINT('Ctrl Pts',(38.5547993711231,-28.1942015146341,0.));
#89226=CARTESIAN_POINT('Ctrl Pts',(38.5547993711231,-28.1942015146341,20.));
#89227=CARTESIAN_POINT('Ctrl Pts',(38.5327335494334,-28.2192584110398,0.));
#89228=CARTESIAN_POINT('Ctrl Pts',(38.5327335494334,-28.2192584110398,20.));
#89229=CARTESIAN_POINT('Ctrl Pts',(38.5106510268752,-28.2442991015113,0.));
#89230=CARTESIAN_POINT('Ctrl Pts',(38.5106510268752,-28.2442991015113,20.));
#89231=CARTESIAN_POINT('Ctrl Pts',(38.4885518148031,-28.2693235744854,0.));
#89232=CARTESIAN_POINT('Ctrl Pts',(38.4885518148031,-28.2693235744854,20.));
#89233=CARTESIAN_POINT('Ctrl Pts',(38.4664359245797,-28.2943318184066,0.));
#89234=CARTESIAN_POINT('Ctrl Pts',(38.4664359245797,-28.2943318184066,20.));
#89235=CARTESIAN_POINT('Ctrl Pts',(38.4443033675759,-28.3193238217266,0.));
#89236=CARTESIAN_POINT('Ctrl Pts',(38.4443033675759,-28.3193238217266,20.));
#89237=CARTESIAN_POINT('Ctrl Pts',(38.4221541551709,-28.344299572905,0.));
#89238=CARTESIAN_POINT('Ctrl Pts',(38.4221541551709,-28.344299572905,20.));
#89239=CARTESIAN_POINT('Ctrl Pts',(38.3999882987522,-28.3692590604082,0.));
#89240=CARTESIAN_POINT('Ctrl Pts',(38.3999882987522,-28.3692590604082,20.));
#89241=CARTESIAN_POINT('Ctrl Pts',(38.3778058097152,-28.3942022727108,0.));
#89242=CARTESIAN_POINT('Ctrl Pts',(38.3778058097152,-28.3942022727108,20.));
#89243=CARTESIAN_POINT('Ctrl Pts',(38.3556066994642,-28.4191291982951,0.));
#89244=CARTESIAN_POINT('Ctrl Pts',(38.3556066994642,-28.4191291982951,20.));
#89245=CARTESIAN_POINT('Ctrl Pts',(38.3333909794119,-28.4440398256512,0.));
#89246=CARTESIAN_POINT('Ctrl Pts',(38.3333909794119,-28.4440398256512,20.));
#89247=CARTESIAN_POINT('Ctrl Pts',(38.3111586609794,-28.4689341432774,0.));
#89248=CARTESIAN_POINT('Ctrl Pts',(38.3111586609794,-28.4689341432774,20.));
#89249=CARTESIAN_POINT('Ctrl Pts',(38.2889097555964,-28.4938121396793,0.));
#89250=CARTESIAN_POINT('Ctrl Pts',(38.2889097555964,-28.4938121396793,20.));
#89251=CARTESIAN_POINT('Ctrl Pts',(38.2666442747002,-28.5186738033704,0.));
#89252=CARTESIAN_POINT('Ctrl Pts',(38.2666442747002,-28.5186738033704,20.));
#89253=CARTESIAN_POINT('Ctrl Pts',(38.2443622297368,-28.5435191228711,0.));
#89254=CARTESIAN_POINT('Ctrl Pts',(38.2443622297368,-28.5435191228711,20.));
#89255=CARTESIAN_POINT('Ctrl Pts',(38.2220636321601,-28.5683480867098,0.));
#89256=CARTESIAN_POINT('Ctrl Pts',(38.2220636321601,-28.5683480867098,20.));
#89257=CARTESIAN_POINT('Ctrl Pts',(38.1997484934321,-28.5931606834224,0.));
#89258=CARTESIAN_POINT('Ctrl Pts',(38.1997484934321,-28.5931606834224,20.));
#89259=CARTESIAN_POINT('Ctrl Pts',(38.1774168250235,-28.6179569015525,0.));
#89260=CARTESIAN_POINT('Ctrl Pts',(38.1774168250235,-28.6179569015525,20.));
#89261=CARTESIAN_POINT('Ctrl Pts',(38.1550686384134,-28.6427367296518,0.));
#89262=CARTESIAN_POINT('Ctrl Pts',(38.1550686384134,-28.6427367296518,20.));
#89263=CARTESIAN_POINT('Ctrl Pts',(38.1327039450889,-28.6675001562794,0.));
#89264=CARTESIAN_POINT('Ctrl Pts',(38.1327039450889,-28.6675001562794,20.));
#89265=CARTESIAN_POINT('Ctrl Pts',(38.1103227565456,-28.6922471700024,0.));
#89266=CARTESIAN_POINT('Ctrl Pts',(38.1103227565456,-28.6922471700024,20.));
#89267=CARTESIAN_POINT('Ctrl Pts',(38.0879250842874,-28.7169777593956,0.));
#89268=CARTESIAN_POINT('Ctrl Pts',(38.0879250842874,-28.7169777593956,20.));
#89269=CARTESIAN_POINT('Ctrl Pts',(38.0655109398262,-28.7416919130413,0.));
#89270=CARTESIAN_POINT('Ctrl Pts',(38.0655109398262,-28.7416919130413,20.));
#89271=CARTESIAN_POINT('Ctrl Pts',(38.0430803346823,-28.76638961953,0.));
#89272=CARTESIAN_POINT('Ctrl Pts',(38.0430803346823,-28.76638961953,20.));
#89273=CARTESIAN_POINT('Ctrl Pts',(38.020633280384,-28.7910708674595,0.));
#89274=CARTESIAN_POINT('Ctrl Pts',(38.020633280384,-28.7910708674595,20.));
#89275=CARTESIAN_POINT('Ctrl Pts',(37.9981697884679,-28.8157356454354,0.));
#89276=CARTESIAN_POINT('Ctrl Pts',(37.9981697884679,-28.8157356454354,20.));
#89277=CARTESIAN_POINT('Ctrl Pts',(37.975689870479,-28.8403839420709,0.));
#89278=CARTESIAN_POINT('Ctrl Pts',(37.975689870479,-28.8403839420709,20.));
#89279=CARTESIAN_POINT('Ctrl Pts',(37.9531935379708,-28.8650157459872,0.));
#89280=CARTESIAN_POINT('Ctrl Pts',(37.9531935379708,-28.8650157459872,20.));
#89281=CARTESIAN_POINT('Ctrl Pts',(37.9306808025048,-28.8896310458131,0.));
#89282=CARTESIAN_POINT('Ctrl Pts',(37.9306808025048,-28.8896310458131,20.));
#89283=CARTESIAN_POINT('Ctrl Pts',(37.9081516756509,-28.9142298301853,0.));
#89284=CARTESIAN_POINT('Ctrl Pts',(37.9081516756509,-28.9142298301853,20.));
#89285=CARTESIAN_POINT('Ctrl Pts',(37.8856061689868,-28.9388120877484,0.));
#89286=CARTESIAN_POINT('Ctrl Pts',(37.8856061689868,-28.9388120877484,20.));
#89287=CARTESIAN_POINT('Ctrl Pts',(37.8630442940985,-28.9633778071544,0.));
#89288=CARTESIAN_POINT('Ctrl Pts',(37.8630442940985,-28.9633778071544,20.));
#89289=CARTESIAN_POINT('Ctrl Pts',(37.8404660625803,-28.9879269770638,0.));
#89290=CARTESIAN_POINT('Ctrl Pts',(37.8404660625803,-28.9879269770638,20.));
#89291=CARTESIAN_POINT('Ctrl Pts',(37.8178714860345,-29.0124595861442,0.));
#89292=CARTESIAN_POINT('Ctrl Pts',(37.8178714860345,-29.0124595861442,20.));
#89293=CARTESIAN_POINT('Ctrl Pts',(37.7952605760716,-29.0369756230713,0.));
#89294=CARTESIAN_POINT('Ctrl Pts',(37.7952605760716,-29.0369756230713,20.));
#89295=CARTESIAN_POINT('Ctrl Pts',(37.7726333443105,-29.0614750765285,0.));
#89296=CARTESIAN_POINT('Ctrl Pts',(37.7726333443105,-29.0614750765285,20.));
#89297=CARTESIAN_POINT('Ctrl Pts',(37.7499898023784,-29.0859579352069,0.));
#89298=CARTESIAN_POINT('Ctrl Pts',(37.7499898023784,-29.0859579352069,20.));
#89299=CARTESIAN_POINT('Ctrl Pts',(37.7273299619109,-29.1104241878056,0.));
#89300=CARTESIAN_POINT('Ctrl Pts',(37.7273299619109,-29.1104241878056,20.));
#89301=CARTESIAN_POINT('Ctrl Pts',(37.7046538345516,-29.1348738230316,0.));
#89302=CARTESIAN_POINT('Ctrl Pts',(37.7046538345516,-29.1348738230316,20.));
#89303=CARTESIAN_POINT('Ctrl Pts',(37.6819614319522,-29.1593068295998,0.));
#89304=CARTESIAN_POINT('Ctrl Pts',(37.6819614319522,-29.1593068295998,20.));
#89305=CARTESIAN_POINT('Ctrl Pts',(37.6592527657727,-29.1837231962329,0.));
#89306=CARTESIAN_POINT('Ctrl Pts',(37.6592527657727,-29.1837231962329,20.));
#89307=CARTESIAN_POINT('Ctrl Pts',(37.6365278476807,-29.208122911661,0.));
#89308=CARTESIAN_POINT('Ctrl Pts',(37.6365278476807,-29.208122911661,20.));
#89309=CARTESIAN_POINT('Ctrl Pts',(37.6137866893519,-29.2325059646225,0.));
#89310=CARTESIAN_POINT('Ctrl Pts',(37.6137866893519,-29.2325059646225,20.));
#89311=CARTESIAN_POINT('Ctrl Pts',(37.5910293024705,-29.2568723438632,0.));
#89312=CARTESIAN_POINT('Ctrl Pts',(37.5910293024705,-29.2568723438632,20.));
#89313=CARTESIAN_POINT('Ctrl Pts',(37.5682556987287,-29.2812220381373,0.));
#89314=CARTESIAN_POINT('Ctrl Pts',(37.5682556987287,-29.2812220381373,20.));
#89315=CARTESIAN_POINT('Ctrl Pts',(37.5454658898273,-29.3055550362068,0.));
#89316=CARTESIAN_POINT('Ctrl Pts',(37.5454658898273,-29.3055550362068,20.));
#89317=CARTESIAN_POINT('Ctrl Pts',(37.5226598874754,-29.3298713268414,0.));
#89318=CARTESIAN_POINT('Ctrl Pts',(37.5226598874754,-29.3298713268414,20.));
#89319=CARTESIAN_POINT('Ctrl Pts',(37.4998377033899,-29.3541708988191,0.));
#89320=CARTESIAN_POINT('Ctrl Pts',(37.4998377033899,-29.3541708988191,20.));
#89321=CARTESIAN_POINT('Ctrl Pts',(37.4769993492958,-29.3784537409251,0.));
#89322=CARTESIAN_POINT('Ctrl Pts',(37.4769993492958,-29.3784537409251,20.));
#89323=CARTESIAN_POINT('Ctrl Pts',(37.4541448369259,-29.4027198419524,0.));
#89324=CARTESIAN_POINT('Ctrl Pts',(37.4541448369259,-29.4027198419524,20.));
#89325=CARTESIAN_POINT('Ctrl Pts',(37.4312741780212,-29.4269691907023,0.));
#89326=CARTESIAN_POINT('Ctrl Pts',(37.4312741780212,-29.4269691907023,20.));
#89327=CARTESIAN_POINT('Ctrl Pts',(37.4083873843312,-29.4512017759842,0.));
#89328=CARTESIAN_POINT('Ctrl Pts',(37.4083873843312,-29.4512017759842,20.));
#89329=CARTESIAN_POINT('Ctrl Pts',(37.3854844676135,-29.4754175866156,0.));
#89330=CARTESIAN_POINT('Ctrl Pts',(37.3854844676135,-29.4754175866156,20.));
#89331=CARTESIAN_POINT('Ctrl Pts',(37.3625654396334,-29.4996166114217,0.));
#89332=CARTESIAN_POINT('Ctrl Pts',(37.3625654396334,-29.4996166114217,20.));
#89333=CARTESIAN_POINT('Ctrl Pts',(37.3396303121646,-29.5237988392353,0.));
#89334=CARTESIAN_POINT('Ctrl Pts',(37.3396303121646,-29.5237988392353,20.));
#89335=CARTESIAN_POINT('Ctrl Pts',(37.3166790969884,-29.5479642588972,0.));
#89336=CARTESIAN_POINT('Ctrl Pts',(37.3166790969884,-29.5479642588972,20.));
#89337=CARTESIAN_POINT('Ctrl Pts',(37.2937118058947,-29.5721128592559,0.));
#89338=CARTESIAN_POINT('Ctrl Pts',(37.2937118058947,-29.5721128592559,20.));
#89339=CARTESIAN_POINT('Ctrl Pts',(37.2707284506814,-29.5962446291683,0.));
#89340=CARTESIAN_POINT('Ctrl Pts',(37.2707284506814,-29.5962446291683,20.));
#89341=CARTESIAN_POINT('Ctrl Pts',(37.2477290431548,-29.6203595574991,0.));
#89342=CARTESIAN_POINT('Ctrl Pts',(37.2477290431548,-29.6203595574991,20.));
#89343=CARTESIAN_POINT('Ctrl Pts',(37.2247135951292,-29.6444576331215,0.));
#89344=CARTESIAN_POINT('Ctrl Pts',(37.2247135951292,-29.6444576331215,20.));
#89345=CARTESIAN_POINT('Ctrl Pts',(37.2016821184267,-29.668538844916,0.));
#89346=CARTESIAN_POINT('Ctrl Pts',(37.2016821184267,-29.668538844916,20.));
#89347=CARTESIAN_POINT('Ctrl Pts',(37.1786346248774,-29.6926031817715,0.));
#89348=CARTESIAN_POINT('Ctrl Pts',(37.1786346248774,-29.6926031817715,20.));
#89349=CARTESIAN_POINT('Ctrl Pts',(37.155571126319,-29.7166506325841,0.));
#89350=CARTESIAN_POINT('Ctrl Pts',(37.155571126319,-29.7166506325841,20.));
#89351=CARTESIAN_POINT('Ctrl Pts',(37.1324916345976,-29.7406811862582,0.));
#89352=CARTESIAN_POINT('Ctrl Pts',(37.1324916345976,-29.7406811862582,20.));
#89353=CARTESIAN_POINT('Ctrl Pts',(37.1093961615672,-29.7646948317062,0.));
#89354=CARTESIAN_POINT('Ctrl Pts',(37.1093961615672,-29.7646948317062,20.));
#89355=CARTESIAN_POINT('Ctrl Pts',(37.0862847190902,-29.7886915578486,0.));
#89356=CARTESIAN_POINT('Ctrl Pts',(37.0862847190902,-29.7886915578486,20.));
#89357=CARTESIAN_POINT('Ctrl Pts',(37.0631573190373,-29.8126713536142,0.));
#89358=CARTESIAN_POINT('Ctrl Pts',(37.0631573190373,-29.8126713536142,20.));
#89359=CARTESIAN_POINT('Ctrl Pts',(37.0400139732874,-29.8366342079401,0.));
#89360=CARTESIAN_POINT('Ctrl Pts',(37.0400139732874,-29.8366342079401,20.));
#89361=CARTESIAN_POINT('Ctrl Pts',(37.0168546937273,-29.8605801097708,0.));
#89362=CARTESIAN_POINT('Ctrl Pts',(37.0168546937273,-29.8605801097708,20.));
#89363=CARTESIAN_POINT('Ctrl Pts',(36.9936794922513,-29.884509048059,0.));
#89364=CARTESIAN_POINT('Ctrl Pts',(36.9936794922513,-29.884509048059,20.));
#89365=CARTESIAN_POINT('Ctrl Pts',(36.9704883807614,-29.9084210117647,0.));
#89366=CARTESIAN_POINT('Ctrl Pts',(36.9704883807614,-29.9084210117647,20.));
#89367=CARTESIAN_POINT('Ctrl Pts',(36.9472813711676,-29.9323159898562,0.));
#89368=CARTESIAN_POINT('Ctrl Pts',(36.9472813711676,-29.9323159898562,20.));
#89369=CARTESIAN_POINT('Ctrl Pts',(36.9240584753882,-29.9561939713103,0.));
#89370=CARTESIAN_POINT('Ctrl Pts',(36.9240584753882,-29.9561939713103,20.));
#89371=CARTESIAN_POINT('Ctrl Pts',(36.9008197053507,-29.9800549451122,0.));
#89372=CARTESIAN_POINT('Ctrl Pts',(36.9008197053507,-29.9800549451122,20.));
#89373=CARTESIAN_POINT('Ctrl Pts',(36.8775650729895,-30.003898900255,0.));
#89374=CARTESIAN_POINT('Ctrl Pts',(36.8775650729895,-30.003898900255,20.));
#89375=CARTESIAN_POINT('Ctrl Pts',(36.8542945902472,-30.0277258257394,0.));
#89376=CARTESIAN_POINT('Ctrl Pts',(36.8542945902472,-30.0277258257394,20.));
#89377=CARTESIAN_POINT('Ctrl Pts',(36.8310082690741,-30.051535710574,0.));
#89378=CARTESIAN_POINT('Ctrl Pts',(36.8310082690741,-30.051535710574,20.));
#89379=CARTESIAN_POINT('Ctrl Pts',(36.8077061214283,-30.0753285437754,0.));
#89380=CARTESIAN_POINT('Ctrl Pts',(36.8077061214283,-30.0753285437754,20.));
#89381=CARTESIAN_POINT('Ctrl Pts',(36.7843881592759,-30.0991043143685,0.));
#89382=CARTESIAN_POINT('Ctrl Pts',(36.7843881592759,-30.0991043143685,20.));
#89383=CARTESIAN_POINT('Ctrl Pts',(36.7610543945915,-30.1228630113862,0.));
#89384=CARTESIAN_POINT('Ctrl Pts',(36.7610543945915,-30.1228630113862,20.));
#89385=CARTESIAN_POINT('Ctrl Pts',(36.7377048393574,-30.1466046238701,0.));
#89386=CARTESIAN_POINT('Ctrl Pts',(36.7377048393574,-30.1466046238701,20.));
#89387=CARTESIAN_POINT('Ctrl Pts',(36.7143395055641,-30.1703291408693,0.));
#89388=CARTESIAN_POINT('Ctrl Pts',(36.7143395055641,-30.1703291408693,20.));
#89389=CARTESIAN_POINT('Ctrl Pts',(36.6909584052099,-30.1940365514414,0.));
#89390=CARTESIAN_POINT('Ctrl Pts',(36.6909584052099,-30.1940365514414,20.));
#89391=CARTESIAN_POINT('Ctrl Pts',(36.6675615503012,-30.2177268446518,0.));
#89392=CARTESIAN_POINT('Ctrl Pts',(36.6675615503012,-30.2177268446518,20.));
#89393=CARTESIAN_POINT('Ctrl Pts',(36.6441489528521,-30.2414000095742,0.));
#89394=CARTESIAN_POINT('Ctrl Pts',(36.6441489528521,-30.2414000095742,20.));
#89395=CARTESIAN_POINT('Ctrl Pts',(36.6207206248848,-30.2650560352902,0.));
#89396=CARTESIAN_POINT('Ctrl Pts',(36.6207206248848,-30.2650560352902,20.));
#89397=CARTESIAN_POINT('Ctrl Pts',(36.5972765784293,-30.2886949108895,0.));
#89398=CARTESIAN_POINT('Ctrl Pts',(36.5972765784293,-30.2886949108895,20.));
#89399=CARTESIAN_POINT('Ctrl Pts',(36.5738168255233,-30.3123166254701,0.));
#89400=CARTESIAN_POINT('Ctrl Pts',(36.5738168255233,-30.3123166254701,20.));
#89401=CARTESIAN_POINT('Ctrl Pts',(36.5503413782123,-30.3359211681376,0.));
#89402=CARTESIAN_POINT('Ctrl Pts',(36.5503413782123,-30.3359211681376,20.));
#89403=CARTESIAN_POINT('Ctrl Pts',(36.5268502485502,-30.3595085280059,0.));
#89404=CARTESIAN_POINT('Ctrl Pts',(36.5268502485502,-30.3595085280059,20.));
#89405=CARTESIAN_POINT('Ctrl Pts',(36.5033434485984,-30.3830786941972,0.));
#89406=CARTESIAN_POINT('Ctrl Pts',(36.5033434485984,-30.3830786941972,20.));
#89407=CARTESIAN_POINT('Ctrl Pts',(36.4798209904267,-30.4066316558424,0.));
#89408=CARTESIAN_POINT('Ctrl Pts',(36.4798209904267,-30.4066316558424,20.));
#89409=CARTESIAN_POINT('Ctrl Pts',(36.456282886113,-30.4301674020802,0.));
#89410=CARTESIAN_POINT('Ctrl Pts',(36.456282886113,-30.4301674020802,20.));
#89411=CARTESIAN_POINT('Ctrl Pts',(36.4327291477428,-30.4536859220576,0.));
#89412=CARTESIAN_POINT('Ctrl Pts',(36.4327291477428,-30.4536859220576,20.));
#89413=CARTESIAN_POINT('Ctrl Pts',(36.4091597874097,-30.4771872049299,0.));
#89414=CARTESIAN_POINT('Ctrl Pts',(36.4091597874097,-30.4771872049299,20.));
#89415=CARTESIAN_POINT('Ctrl Pts',(36.3855748172148,-30.5006712398601,0.));
#89416=CARTESIAN_POINT('Ctrl Pts',(36.3855748172148,-30.5006712398601,20.));
#89417=CARTESIAN_POINT('Ctrl Pts',(36.3619742492671,-30.5241380160195,0.));
#89418=CARTESIAN_POINT('Ctrl Pts',(36.3619742492671,-30.5241380160195,20.));
#89419=CARTESIAN_POINT('Ctrl Pts',(36.3383580956832,-30.5475875225872,0.));
#89420=CARTESIAN_POINT('Ctrl Pts',(36.3383580956832,-30.5475875225872,20.));
#89421=CARTESIAN_POINT('Ctrl Pts',(36.3147263685874,-30.5710197487502,0.));
#89422=CARTESIAN_POINT('Ctrl Pts',(36.3147263685874,-30.5710197487502,20.));
#89423=CARTESIAN_POINT('Ctrl Pts',(36.2910790801119,-30.5944346837039,0.));
#89424=CARTESIAN_POINT('Ctrl Pts',(36.2910790801119,-30.5944346837039,20.));
#89425=CARTESIAN_POINT('Ctrl Pts',(36.2674162423973,-30.6178323166527,0.));
#89426=CARTESIAN_POINT('Ctrl Pts',(36.2674162423973,-30.6178323166527,20.));
#89427=CARTESIAN_POINT('Ctrl Pts',(36.2437378675924,-30.6412126368095,0.));
#89428=CARTESIAN_POINT('Ctrl Pts',(36.2437378675924,-30.6412126368095,20.));
#89429=CARTESIAN_POINT('Ctrl Pts',(36.2200439678542,-30.6645756333955,0.));
#89430=CARTESIAN_POINT('Ctrl Pts',(36.2200439678542,-30.6645756333955,20.));
#89431=CARTESIAN_POINT('Ctrl Pts',(36.196334555347,-30.6879212956392,0.));
#89432=CARTESIAN_POINT('Ctrl Pts',(36.196334555347,-30.6879212956392,20.));
#89433=CARTESIAN_POINT('Ctrl Pts',(36.1726096422428,-30.7112496127774,0.));
#89434=CARTESIAN_POINT('Ctrl Pts',(36.1726096422428,-30.7112496127774,20.));
#89435=CARTESIAN_POINT('Ctrl Pts',(36.1488692407204,-30.7345605740545,0.));
#89436=CARTESIAN_POINT('Ctrl Pts',(36.1488692407204,-30.7345605740545,20.));
#89437=CARTESIAN_POINT('Ctrl Pts',(36.1251133629669,-30.7578541687236,0.));
#89438=CARTESIAN_POINT('Ctrl Pts',(36.1251133629669,-30.7578541687236,20.));
#89439=CARTESIAN_POINT('Ctrl Pts',(36.1013420211777,-30.7811303860468,0.));
#89440=CARTESIAN_POINT('Ctrl Pts',(36.1013420211777,-30.7811303860468,20.));
#89441=CARTESIAN_POINT('Ctrl Pts',(36.0775552275565,-30.8043892152943,0.));
#89442=CARTESIAN_POINT('Ctrl Pts',(36.0775552275565,-30.8043892152943,20.));
#89443=CARTESIAN_POINT('Ctrl Pts',(36.0537529943146,-30.8276306457446,0.));
#89444=CARTESIAN_POINT('Ctrl Pts',(36.0537529943146,-30.8276306457446,20.));
#89445=CARTESIAN_POINT('Ctrl Pts',(36.0299353336712,-30.8508546666841,0.));
#89446=CARTESIAN_POINT('Ctrl Pts',(36.0299353336712,-30.8508546666841,20.));
#89447=CARTESIAN_POINT('Ctrl Pts',(36.0061022578528,-30.8740612674075,0.));
#89448=CARTESIAN_POINT('Ctrl Pts',(36.0061022578528,-30.8740612674075,20.));
#89449=CARTESIAN_POINT('Ctrl Pts',(35.9822537790931,-30.8972504372171,0.));
#89450=CARTESIAN_POINT('Ctrl Pts',(35.9822537790931,-30.8972504372171,20.));
#89451=CARTESIAN_POINT('Ctrl Pts',(35.9583899096339,-30.9204221654236,0.));
#89452=CARTESIAN_POINT('Ctrl Pts',(35.9583899096339,-30.9204221654236,20.));
#89453=CARTESIAN_POINT('Ctrl Pts',(35.9345106617251,-30.9435764413467,0.));
#89454=CARTESIAN_POINT('Ctrl Pts',(35.9345106617251,-30.9435764413467,20.));
#89455=CARTESIAN_POINT('Ctrl Pts',(35.9106160476245,-30.9667132543142,0.));
#89456=CARTESIAN_POINT('Ctrl Pts',(35.9106160476245,-30.9667132543142,20.));
#89457=CARTESIAN_POINT('Ctrl Pts',(35.886706079598,-30.9898325936627,0.));
#89458=CARTESIAN_POINT('Ctrl Pts',(35.886706079598,-30.9898325936627,20.));
#89459=CARTESIAN_POINT('Ctrl Pts',(35.8627807699193,-31.0129344487367,0.));
#89460=CARTESIAN_POINT('Ctrl Pts',(35.8627807699193,-31.0129344487367,20.));
#89461=CARTESIAN_POINT('Ctrl Pts',(35.8388401308696,-31.036018808889,0.));
#89462=CARTESIAN_POINT('Ctrl Pts',(35.8388401308696,-31.036018808889,20.));
#89463=CARTESIAN_POINT('Ctrl Pts',(35.8148841747376,-31.0590856634804,0.));
#89464=CARTESIAN_POINT('Ctrl Pts',(35.8148841747376,-31.0590856634804,20.));
#89465=CARTESIAN_POINT('Ctrl Pts',(35.7909129138202,-31.082135001881,0.));
#89466=CARTESIAN_POINT('Ctrl Pts',(35.7909129138202,-31.082135001881,20.));
#89467=CARTESIAN_POINT('Ctrl Pts',(35.7669263604212,-31.1051668134678,0.));
#89468=CARTESIAN_POINT('Ctrl Pts',(35.7669263604212,-31.1051668134678,20.));
#89469=CARTESIAN_POINT('Ctrl Pts',(35.7429245268523,-31.1281810876267,0.));
#89470=CARTESIAN_POINT('Ctrl Pts',(35.7429245268523,-31.1281810876267,20.));
#89471=CARTESIAN_POINT('Ctrl Pts',(35.7189074254331,-31.1511778137516,0.));
#89472=CARTESIAN_POINT('Ctrl Pts',(35.7189074254331,-31.1511778137516,20.));
#89473=CARTESIAN_POINT('Ctrl Pts',(35.6948750684911,-31.1741569812451,0.));
#89474=CARTESIAN_POINT('Ctrl Pts',(35.6948750684911,-31.1741569812451,20.));
#89475=CARTESIAN_POINT('Ctrl Pts',(35.6708274683619,-31.1971185795181,0.));
#89476=CARTESIAN_POINT('Ctrl Pts',(35.6708274683619,-31.1971185795181,20.));
#89477=CARTESIAN_POINT('Ctrl Pts',(35.6467646373883,-31.2200625979904,0.));
#89478=CARTESIAN_POINT('Ctrl Pts',(35.6467646373883,-31.2200625979904,20.));
#89479=CARTESIAN_POINT('Ctrl Pts',(35.6226865879214,-31.24298902609,0.));
#89480=CARTESIAN_POINT('Ctrl Pts',(35.6226865879214,-31.24298902609,20.));
#89481=CARTESIAN_POINT('Ctrl Pts',(35.5985933323194,-31.2658978532533,0.));
#89482=CARTESIAN_POINT('Ctrl Pts',(35.5985933323194,-31.2658978532533,20.));
#89483=CARTESIAN_POINT('Ctrl Pts',(35.5744848829487,-31.288789068925,0.));
#89484=CARTESIAN_POINT('Ctrl Pts',(35.5744848829487,-31.288789068925,20.));
#89485=CARTESIAN_POINT('Ctrl Pts',(35.5503612521832,-31.3116626625581,0.));
#89486=CARTESIAN_POINT('Ctrl Pts',(35.5503612521832,-31.3116626625581,20.));
#89487=CARTESIAN_POINT('Ctrl Pts',(35.5262224524039,-31.3345186236135,0.));
#89488=CARTESIAN_POINT('Ctrl Pts',(35.5262224524039,-31.3345186236135,20.));
#89489=CARTESIAN_POINT('Ctrl Pts',(35.502068496,-31.3573569415606,0.));
#89490=CARTESIAN_POINT('Ctrl Pts',(35.502068496,-31.3573569415606,20.));
#89491=CARTESIAN_POINT('Ctrl Pts',(35.4778993953681,-31.3801776058768,0.));
#89492=CARTESIAN_POINT('Ctrl Pts',(35.4778993953681,-31.3801776058768,20.));
#89493=CARTESIAN_POINT('Ctrl Pts',(35.4537151629126,-31.4029806060482,0.));
#89494=CARTESIAN_POINT('Ctrl Pts',(35.4537151629126,-31.4029806060482,20.));
#89495=CARTESIAN_POINT('Ctrl Pts',(35.4295158110454,-31.4257659315696,0.));
#89496=CARTESIAN_POINT('Ctrl Pts',(35.4295158110454,-31.4257659315696,20.));
#89497=CARTESIAN_POINT('Ctrl Pts',(35.4053013521866,-31.4485335719447,0.));
#89498=CARTESIAN_POINT('Ctrl Pts',(35.4053013521866,-31.4485335719447,20.));
#89499=CARTESIAN_POINT('Ctrl Pts',(35.3810717987641,-31.4712835166857,0.));
#89500=CARTESIAN_POINT('Ctrl Pts',(35.3810717987641,-31.4712835166857,20.));
#89501=CARTESIAN_POINT('Ctrl Pts',(35.3568271632136,-31.4940157553136,0.));
#89502=CARTESIAN_POINT('Ctrl Pts',(35.3568271632136,-31.4940157553136,20.));
#89503=CARTESIAN_POINT('Ctrl Pts',(35.3325674579779,-31.516730277357,0.));
#89504=CARTESIAN_POINT('Ctrl Pts',(35.3325674579779,-31.516730277357,20.));
#89505=CARTESIAN_POINT('Ctrl Pts',(35.3082926955072,-31.5394270723526,0.));
#89506=CARTESIAN_POINT('Ctrl Pts',(35.3082926955072,-31.5394270723526,20.));
#89507=CARTESIAN_POINT('Ctrl Pts',(35.2840028882593,-31.5621061298453,0.));
#89508=CARTESIAN_POINT('Ctrl Pts',(35.2840028882593,-31.5621061298453,20.));
#89509=CARTESIAN_POINT('Ctrl Pts',(35.2596980486996,-31.5847674393885,0.));
#89510=CARTESIAN_POINT('Ctrl Pts',(35.2596980486996,-31.5847674393885,20.));
#89511=CARTESIAN_POINT('Ctrl Pts',(35.2353781893014,-31.6074109905439,0.));
#89512=CARTESIAN_POINT('Ctrl Pts',(35.2353781893014,-31.6074109905439,20.));
#89513=CARTESIAN_POINT('Ctrl Pts',(35.2110433225458,-31.6300367728827,0.));
#89514=CARTESIAN_POINT('Ctrl Pts',(35.2110433225458,-31.6300367728827,20.));
#89515=CARTESIAN_POINT('Ctrl Pts',(35.1866934609214,-31.652644775984,0.));
#89516=CARTESIAN_POINT('Ctrl Pts',(35.1866934609214,-31.652644775984,20.));
#89517=CARTESIAN_POINT('Ctrl Pts',(35.1623286169245,-31.6752349894358,0.));
#89518=CARTESIAN_POINT('Ctrl Pts',(35.1623286169245,-31.6752349894358,20.));
#89519=CARTESIAN_POINT('Ctrl Pts',(35.1379488030591,-31.6978074028349,0.));
#89520=CARTESIAN_POINT('Ctrl Pts',(35.1379488030591,-31.6978074028349,20.));
#89521=CARTESIAN_POINT('Ctrl Pts',(35.1135540318367,-31.7203620057864,0.));
#89522=CARTESIAN_POINT('Ctrl Pts',(35.1135540318367,-31.7203620057864,20.));
#89523=CARTESIAN_POINT('Ctrl Pts',(35.0891443157764,-31.7428987879035,0.));
#89524=CARTESIAN_POINT('Ctrl Pts',(35.0891443157764,-31.7428987879035,20.));
#89525=CARTESIAN_POINT('Ctrl Pts',(35.0647196674043,-31.7654177388073,0.));
#89526=CARTESIAN_POINT('Ctrl Pts',(35.0647196674043,-31.7654177388073,20.));
#89527=CARTESIAN_POINT('Ctrl Pts',(35.0402800992547,-31.7879188481278,0.));
#89528=CARTESIAN_POINT('Ctrl Pts',(35.0402800992547,-31.7879188481278,20.));
#89529=CARTESIAN_POINT('Ctrl Pts',(35.0158256238691,-31.8104021055033,0.));
#89530=CARTESIAN_POINT('Ctrl Pts',(35.0158256238691,-31.8104021055033,20.));
#89531=CARTESIAN_POINT('Ctrl Pts',(34.991356253797,-31.8328675005809,0.));
#89532=CARTESIAN_POINT('Ctrl Pts',(34.991356253797,-31.8328675005809,20.));
#89533=CARTESIAN_POINT('Ctrl Pts',(34.9668720015954,-31.8553150230168,0.));
#89534=CARTESIAN_POINT('Ctrl Pts',(34.9668720015954,-31.8553150230168,20.));
#89535=CARTESIAN_POINT('Ctrl Pts',(34.9423728798289,-31.8777446624754,0.));
#89536=CARTESIAN_POINT('Ctrl Pts',(34.9423728798289,-31.8777446624754,20.));
#89537=CARTESIAN_POINT('Ctrl Pts',(34.9178589010694,-31.9001564086295,0.));
#89538=CARTESIAN_POINT('Ctrl Pts',(34.9178589010694,-31.9001564086295,20.));
#89539=CARTESIAN_POINT('Ctrl Pts',(34.8933300778963,-31.9225502511603,0.));
#89540=CARTESIAN_POINT('Ctrl Pts',(34.8933300778963,-31.9225502511603,20.));
#89541=CARTESIAN_POINT('Ctrl Pts',(34.8687864228965,-31.9449261797574,0.));
#89542=CARTESIAN_POINT('Ctrl Pts',(34.8687864228965,-31.9449261797574,20.));
#89543=CARTESIAN_POINT('Ctrl Pts',(34.8442279486644,-31.967284184119,0.));
#89544=CARTESIAN_POINT('Ctrl Pts',(34.8442279486644,-31.967284184119,20.));
#89545=CARTESIAN_POINT('Ctrl Pts',(34.8196546678026,-31.9896242539524,0.));
#89546=CARTESIAN_POINT('Ctrl Pts',(34.8196546678026,-31.9896242539524,20.));
#89547=CARTESIAN_POINT('Ctrl Pts',(34.7950665929206,-32.011946378973,0.));
#89548=CARTESIAN_POINT('Ctrl Pts',(34.7950665929206,-32.011946378973,20.));
#89549=CARTESIAN_POINT('Ctrl Pts',(34.7704637366357,-32.0342505489048,0.));
#89550=CARTESIAN_POINT('Ctrl Pts',(34.7704637366357,-32.0342505489048,20.));
#89551=CARTESIAN_POINT('Ctrl Pts',(34.7458461115727,-32.0565367534806,0.));
#89552=CARTESIAN_POINT('Ctrl Pts',(34.7458461115727,-32.0565367534806,20.));
#89553=CARTESIAN_POINT('Ctrl Pts',(34.7212137303638,-32.0788049824416,0.));
#89554=CARTESIAN_POINT('Ctrl Pts',(34.7212137303638,-32.0788049824416,20.));
#89555=CARTESIAN_POINT('Ctrl Pts',(34.6965666056491,-32.1010552255379,0.));
#89556=CARTESIAN_POINT('Ctrl Pts',(34.6965666056491,-32.1010552255379,20.));
#89557=CARTESIAN_POINT('Ctrl Pts',(34.6719047500757,-32.1232874725277,0.));
#89558=CARTESIAN_POINT('Ctrl Pts',(34.6719047500757,-32.1232874725277,20.));
#89559=CARTESIAN_POINT('Ctrl Pts',(34.6472281762982,-32.145501713178,0.));
#89560=CARTESIAN_POINT('Ctrl Pts',(34.6472281762982,-32.145501713178,20.));
#89561=CARTESIAN_POINT('Ctrl Pts',(34.6225368969784,-32.167697937264,0.));
#89562=CARTESIAN_POINT('Ctrl Pts',(34.6225368969784,-32.167697937264,20.));
#89563=CARTESIAN_POINT('Ctrl Pts',(34.5978309247855,-32.1898761345694,0.));
#89564=CARTESIAN_POINT('Ctrl Pts',(34.5978309247855,-32.1898761345694,20.));
#89565=CARTESIAN_POINT('Ctrl Pts',(34.5731102723969,-32.212036294887,0.));
#89566=CARTESIAN_POINT('Ctrl Pts',(34.5731102723969,-32.212036294887,20.));
#89567=CARTESIAN_POINT('Ctrl Pts',(34.5483749524972,-32.2341784080184,0.));
#89568=CARTESIAN_POINT('Ctrl Pts',(34.5483749524972,-32.2341784080184,20.));
#89569=CARTESIAN_POINT('Ctrl Pts',(34.5236249777791,-32.2563024637739,0.));
#89570=CARTESIAN_POINT('Ctrl Pts',(34.5236249777791,-32.2563024637739,20.));
#89571=CARTESIAN_POINT('Ctrl Pts',(34.4988603609426,-32.2784084519728,0.));
#89572=CARTESIAN_POINT('Ctrl Pts',(34.4988603609426,-32.2784084519728,20.));
#89573=CARTESIAN_POINT('Ctrl Pts',(34.474081114695,-32.3004963624427,0.));
#89574=CARTESIAN_POINT('Ctrl Pts',(34.474081114695,-32.3004963624427,20.));
#89575=CARTESIAN_POINT('Ctrl Pts',(34.4492872517507,-32.3225661850195,0.));
#89576=CARTESIAN_POINT('Ctrl Pts',(34.4492872517507,-32.3225661850195,20.));
#89577=CARTESIAN_POINT('Ctrl Pts',(34.4244787848311,-32.3446179095474,0.));
#89578=CARTESIAN_POINT('Ctrl Pts',(34.4244787848311,-32.3446179095474,20.));
#89579=CARTESIAN_POINT('Ctrl Pts',(34.3996557266651,-32.3666515258788,0.));
#89580=CARTESIAN_POINT('Ctrl Pts',(34.3996557266651,-32.3666515258788,20.));
#89581=CARTESIAN_POINT('Ctrl Pts',(34.3748180899889,-32.388667023875,0.));
#89582=CARTESIAN_POINT('Ctrl Pts',(34.3748180899889,-32.388667023875,20.));
#89583=CARTESIAN_POINT('Ctrl Pts',(34.3499658875467,-32.4106643934066,0.));
#89584=CARTESIAN_POINT('Ctrl Pts',(34.3499658875467,-32.4106643934066,20.));
#89585=CARTESIAN_POINT('Ctrl Pts',(34.3250991320904,-32.4326436243533,0.));
#89586=CARTESIAN_POINT('Ctrl Pts',(34.3250991320904,-32.4326436243533,20.));
#89587=CARTESIAN_POINT('Ctrl Pts',(34.3002178363797,-32.4546047066034,0.));
#89588=CARTESIAN_POINT('Ctrl Pts',(34.3002178363797,-32.4546047066034,20.));
#89589=CARTESIAN_POINT('Ctrl Pts',(34.2753220131812,-32.4765476300538,0.));
#89590=CARTESIAN_POINT('Ctrl Pts',(34.2753220131812,-32.4765476300538,20.));
#89591=CARTESIAN_POINT('Ctrl Pts',(34.2504116752689,-32.4984723846098,0.));
#89592=CARTESIAN_POINT('Ctrl Pts',(34.2504116752689,-32.4984723846098,20.));
#89593=CARTESIAN_POINT('Ctrl Pts',(34.2254868354237,-32.5203789601849,0.));
#89594=CARTESIAN_POINT('Ctrl Pts',(34.2254868354237,-32.5203789601849,20.));
#89595=CARTESIAN_POINT('Ctrl Pts',(34.2005475064343,-32.542267346702,0.));
#89596=CARTESIAN_POINT('Ctrl Pts',(34.2005475064343,-32.542267346702,20.));
#89597=CARTESIAN_POINT('Ctrl Pts',(34.1755937010962,-32.564137534092,0.));
#89598=CARTESIAN_POINT('Ctrl Pts',(34.1755937010962,-32.564137534092,20.));
#89599=CARTESIAN_POINT('Ctrl Pts',(34.1506254322131,-32.585989512295,0.));
#89600=CARTESIAN_POINT('Ctrl Pts',(34.1506254322131,-32.585989512295,20.));
#89601=CARTESIAN_POINT('Ctrl Pts',(34.1256427125955,-32.6078232712594,0.));
#89602=CARTESIAN_POINT('Ctrl Pts',(34.1256427125955,-32.6078232712594,20.));
#89603=CARTESIAN_POINT('Ctrl Pts',(34.1006455550618,-32.6296388009428,0.));
#89604=CARTESIAN_POINT('Ctrl Pts',(34.1006455550618,-32.6296388009428,20.));
#89605=CARTESIAN_POINT('Ctrl Pts',(34.0756339724376,-32.6514360913116,0.));
#89606=CARTESIAN_POINT('Ctrl Pts',(34.0756339724376,-32.6514360913116,20.));
#89607=CARTESIAN_POINT('Ctrl Pts',(34.0506079775557,-32.6732151323407,0.));
#89608=CARTESIAN_POINT('Ctrl Pts',(34.0506079775557,-32.6732151323407,20.));
#89609=CARTESIAN_POINT('Ctrl Pts',(34.0255675832564,-32.694975914014,0.));
#89610=CARTESIAN_POINT('Ctrl Pts',(34.0255675832564,-32.694975914014,20.));
#89611=CARTESIAN_POINT('Ctrl Pts',(34.0005128023871,-32.7167184263237,0.));
#89612=CARTESIAN_POINT('Ctrl Pts',(34.0005128023871,-32.7167184263237,20.));
#89613=CARTESIAN_POINT('Ctrl Pts',(33.9754436478026,-32.7384426592708,0.));
#89614=CARTESIAN_POINT('Ctrl Pts',(33.9754436478026,-32.7384426592708,20.));
#89615=CARTESIAN_POINT('Ctrl Pts',(33.950360132365,-32.7601486028652,0.));
#89616=CARTESIAN_POINT('Ctrl Pts',(33.950360132365,-32.7601486028652,20.));
#89617=CARTESIAN_POINT('Ctrl Pts',(33.9252622689445,-32.781836247126,0.));
#89618=CARTESIAN_POINT('Ctrl Pts',(33.9252622689445,-32.781836247126,20.));
#89619=CARTESIAN_POINT('Ctrl Pts',(33.9001500704179,-32.8035055820806,0.));
#89620=CARTESIAN_POINT('Ctrl Pts',(33.9001500704179,-32.8035055820806,20.));
#89621=CARTESIAN_POINT('Ctrl Pts',(33.8750235496691,-32.8251565977646,0.));
#89622=CARTESIAN_POINT('Ctrl Pts',(33.8750235496691,-32.8251565977646,20.));
#89623=CARTESIAN_POINT('Ctrl Pts',(33.8498827195893,-32.8467892842227,0.));
#89624=CARTESIAN_POINT('Ctrl Pts',(33.8498827195893,-32.8467892842227,20.));
#89625=CARTESIAN_POINT('Ctrl Pts',(33.8247275930774,-32.8684036315086,0.));
#89626=CARTESIAN_POINT('Ctrl Pts',(33.8247275930774,-32.8684036315086,20.));
#89627=CARTESIAN_POINT('Ctrl Pts',(33.7995581830395,-32.8899996296849,0.));
#89628=CARTESIAN_POINT('Ctrl Pts',(33.7995581830395,-32.8899996296849,20.));
#89629=CARTESIAN_POINT('Ctrl Pts',(33.7743745023893,-32.9115772688235,0.));
#89630=CARTESIAN_POINT('Ctrl Pts',(33.7743745023893,-32.9115772688235,20.));
#89631=CARTESIAN_POINT('Ctrl Pts',(33.7491765640476,-32.9331365390046,0.));
#89632=CARTESIAN_POINT('Ctrl Pts',(33.7491765640476,-32.9331365390046,20.));
#89633=CARTESIAN_POINT('Ctrl Pts',(33.723964380943,-32.9546774303179,0.));
#89634=CARTESIAN_POINT('Ctrl Pts',(33.723964380943,-32.9546774303179,20.));
#89635=CARTESIAN_POINT('Ctrl Pts',(33.6987379660104,-32.9761999328605,0.));
#89636=CARTESIAN_POINT('Ctrl Pts',(33.6987379660104,-32.9761999328605,20.));
#89637=CARTESIAN_POINT('Ctrl Pts',(33.6734973321919,-32.9977040367383,0.));
#89638=CARTESIAN_POINT('Ctrl Pts',(33.6734973321919,-32.9977040367383,20.));
#89639=CARTESIAN_POINT('Ctrl Pts',(33.6482424924372,-33.0191897320665,0.));
#89640=CARTESIAN_POINT('Ctrl Pts',(33.6482424924372,-33.0191897320665,20.));
#89641=CARTESIAN_POINT('Ctrl Pts',(33.6229734597032,-33.0406570089692,0.));
#89642=CARTESIAN_POINT('Ctrl Pts',(33.6229734597032,-33.0406570089692,20.));
#89643=CARTESIAN_POINT('Ctrl Pts',(33.5976902469543,-33.0621058575797,0.));
#89644=CARTESIAN_POINT('Ctrl Pts',(33.5976902469543,-33.0621058575797,20.));
#89645=CARTESIAN_POINT('Ctrl Pts',(33.572392867162,-33.0835362680399,0.));
#89646=CARTESIAN_POINT('Ctrl Pts',(33.572392867162,-33.0835362680399,20.));
#89647=CARTESIAN_POINT('Ctrl Pts',(33.5470813333053,-33.1049482305004,0.));
#89648=CARTESIAN_POINT('Ctrl Pts',(33.5470813333053,-33.1049482305004,20.));
#89649=CARTESIAN_POINT('Ctrl Pts',(33.5217556583703,-33.1263417351208,0.));
#89650=CARTESIAN_POINT('Ctrl Pts',(33.5217556583703,-33.1263417351208,20.));
#89651=CARTESIAN_POINT('Ctrl Pts',(33.4964158553505,-33.1477167720697,0.));
#89652=CARTESIAN_POINT('Ctrl Pts',(33.4964158553505,-33.1477167720697,20.));
#89653=CARTESIAN_POINT('Ctrl Pts',(33.4710619372468,-33.1690733315248,0.));
#89654=CARTESIAN_POINT('Ctrl Pts',(33.4710619372468,-33.1690733315248,20.));
#89655=CARTESIAN_POINT('Ctrl Pts',(33.4456939170666,-33.1904114036721,0.));
#89656=CARTESIAN_POINT('Ctrl Pts',(33.4456939170666,-33.1904114036721,20.));
#89657=CARTESIAN_POINT('Ctrl Pts',(33.4203118078248,-33.2117309787064,0.));
#89658=CARTESIAN_POINT('Ctrl Pts',(33.4203118078248,-33.2117309787064,20.));
#89659=CARTESIAN_POINT('Ctrl Pts',(33.3949156225429,-33.233032046831,0.));
#89660=CARTESIAN_POINT('Ctrl Pts',(33.3949156225429,-33.233032046831,20.));
#89661=CARTESIAN_POINT('Ctrl Pts',(33.3695053742505,-33.2543145982587,0.));
#89662=CARTESIAN_POINT('Ctrl Pts',(33.3695053742505,-33.2543145982587,20.));
#89663=CARTESIAN_POINT('Ctrl Pts',(33.3440810759838,-33.2755786232108,0.));
#89664=CARTESIAN_POINT('Ctrl Pts',(33.3440810759838,-33.2755786232108,20.));
#89665=CARTESIAN_POINT('Ctrl Pts',(33.3186427407863,-33.2968241119177,0.));
#89666=CARTESIAN_POINT('Ctrl Pts',(33.3186427407863,-33.2968241119177,20.));
#89667=CARTESIAN_POINT('Ctrl Pts',(33.2931903817093,-33.318051054619,0.));
#89668=CARTESIAN_POINT('Ctrl Pts',(33.2931903817093,-33.318051054619,20.));
#89669=CARTESIAN_POINT('Ctrl Pts',(33.2677240118112,-33.3392594415636,0.));
#89670=CARTESIAN_POINT('Ctrl Pts',(33.2677240118112,-33.3392594415636,20.));
#89671=CARTESIAN_POINT('Ctrl Pts',(33.2422436441578,-33.3604492630093,0.));
#89672=CARTESIAN_POINT('Ctrl Pts',(33.2422436441578,-33.3604492630093,20.));
#89673=CARTESIAN_POINT('Ctrl Pts',(33.2167492918215,-33.3816205092222,0.));
#89674=CARTESIAN_POINT('Ctrl Pts',(33.2167492918215,-33.3816205092222,20.));
#89675=CARTESIAN_POINT('Ctrl Pts',(33.1912409678819,-33.4027731704774,0.));
#89676=CARTESIAN_POINT('Ctrl Pts',(33.1912409678819,-33.4027731704774,20.));
#89677=CARTESIAN_POINT('Ctrl Pts',(33.1657186854252,-33.4239072370581,0.));
#89678=CARTESIAN_POINT('Ctrl Pts',(33.1657186854252,-33.4239072370581,20.));
#89679=CARTESIAN_POINT('Ctrl Pts',(33.1401824575448,-33.4450226992568,0.));
#89680=CARTESIAN_POINT('Ctrl Pts',(33.1401824575448,-33.4450226992568,20.));
#89681=CARTESIAN_POINT('Ctrl Pts',(33.1146322973416,-33.4661195473749,0.));
#89682=CARTESIAN_POINT('Ctrl Pts',(33.1146322973416,-33.4661195473749,20.));
#89683=CARTESIAN_POINT('Ctrl Pts',(33.0890682179238,-33.4871977717238,0.));
#89684=CARTESIAN_POINT('Ctrl Pts',(33.0890682179238,-33.4871977717238,20.));
#89685=CARTESIAN_POINT('Ctrl Pts',(33.063490232407,-33.5082573626235,0.));
#89686=CARTESIAN_POINT('Ctrl Pts',(33.063490232407,-33.5082573626235,20.));
#89687=CARTESIAN_POINT('Ctrl Pts',(33.0378983539137,-33.5292983104032,0.));
#89688=CARTESIAN_POINT('Ctrl Pts',(33.0378983539137,-33.5292983104032,20.));
#89689=CARTESIAN_POINT('Ctrl Pts',(33.0122925955738,-33.5503206054004,0.));
#89690=CARTESIAN_POINT('Ctrl Pts',(33.0122925955738,-33.5503206054004,20.));
#89691=CARTESIAN_POINT('Ctrl Pts',(32.986672970524,-33.5713242379612,0.));
#89692=CARTESIAN_POINT('Ctrl Pts',(32.986672970524,-33.5713242379612,20.));
#89693=CARTESIAN_POINT('Ctrl Pts',(32.9610394919081,-33.5923091984411,0.));
#89694=CARTESIAN_POINT('Ctrl Pts',(32.9610394919081,-33.5923091984411,20.));
#89695=CARTESIAN_POINT('Ctrl Pts',(32.935392172877,-33.6132754772046,0.));
#89696=CARTESIAN_POINT('Ctrl Pts',(32.935392172877,-33.6132754772046,20.));
#89697=CARTESIAN_POINT('Ctrl Pts',(32.9097310265884,-33.6342230646254,0.));
#89698=CARTESIAN_POINT('Ctrl Pts',(32.9097310265884,-33.6342230646254,20.));
#89699=CARTESIAN_POINT('Ctrl Pts',(32.8840560662069,-33.6551519510862,0.));
#89700=CARTESIAN_POINT('Ctrl Pts',(32.8840560662069,-33.6551519510862,20.));
#89701=CARTESIAN_POINT('Ctrl Pts',(32.8583673049046,-33.6760621269785,0.));
#89702=CARTESIAN_POINT('Ctrl Pts',(32.8583673049046,-33.6760621269785,20.));
#89703=CARTESIAN_POINT('Ctrl Pts',(32.8326647558605,-33.6969535827028,0.));
#89704=CARTESIAN_POINT('Ctrl Pts',(32.8326647558605,-33.6969535827028,20.));
#89705=CARTESIAN_POINT('Ctrl Pts',(32.8069484322617,-33.717826308669,0.));
#89706=CARTESIAN_POINT('Ctrl Pts',(32.8069484322617,-33.717826308669,20.));
#89707=CARTESIAN_POINT('Ctrl Pts',(32.7812183473018,-33.7386802952956,0.));
#89708=CARTESIAN_POINT('Ctrl Pts',(32.7812183473018,-33.7386802952956,20.));
#89709=CARTESIAN_POINT('Ctrl Pts',(32.755474514181,-33.7595155330097,0.));
#89710=CARTESIAN_POINT('Ctrl Pts',(32.755474514181,-33.7595155330097,20.));
#89711=CARTESIAN_POINT('Ctrl Pts',(32.7297169461064,-33.7803320122473,0.));
#89712=CARTESIAN_POINT('Ctrl Pts',(32.7297169461064,-33.7803320122473,20.));
#89713=CARTESIAN_POINT('Ctrl Pts',(32.7039456562922,-33.8011297234537,0.));
#89714=CARTESIAN_POINT('Ctrl Pts',(32.7039456562922,-33.8011297234537,20.));
#89715=CARTESIAN_POINT('Ctrl Pts',(32.6781606579597,-33.8219086570836,0.));
#89716=CARTESIAN_POINT('Ctrl Pts',(32.6781606579597,-33.8219086570836,20.));
#89717=CARTESIAN_POINT('Ctrl Pts',(32.652361964338,-33.8426688036011,0.));
#89718=CARTESIAN_POINT('Ctrl Pts',(32.652361964338,-33.8426688036011,20.));
#89719=CARTESIAN_POINT('Ctrl Pts',(32.6265495886629,-33.8634101534794,0.));
#89720=CARTESIAN_POINT('Ctrl Pts',(32.6265495886629,-33.8634101534794,20.));
#89721=CARTESIAN_POINT('Ctrl Pts',(32.6007235441777,-33.8841326972008,0.));
#89722=CARTESIAN_POINT('Ctrl Pts',(32.6007235441777,-33.8841326972008,20.));
#89723=CARTESIAN_POINT('Ctrl Pts',(32.5748838441319,-33.9048364252556,0.));
#89724=CARTESIAN_POINT('Ctrl Pts',(32.5748838441319,-33.9048364252556,20.));
#89725=CARTESIAN_POINT('Ctrl Pts',(32.5490305017817,-33.9255213281434,0.));
#89726=CARTESIAN_POINT('Ctrl Pts',(32.5490305017817,-33.9255213281434,20.));
#89727=CARTESIAN_POINT('Ctrl Pts',(32.5231635303904,-33.9461873963724,0.));
#89728=CARTESIAN_POINT('Ctrl Pts',(32.5231635303904,-33.9461873963724,20.));
#89729=CARTESIAN_POINT('Ctrl Pts',(32.4972829432285,-33.9668346204605,0.));
#89730=CARTESIAN_POINT('Ctrl Pts',(32.4972829432285,-33.9668346204605,20.));
#89731=CARTESIAN_POINT('Ctrl Pts',(32.4713887535741,-33.987462990935,0.));
#89732=CARTESIAN_POINT('Ctrl Pts',(32.4713887535741,-33.987462990935,20.));
#89733=CARTESIAN_POINT('Ctrl Pts',(32.4454809747123,-34.0080724983324,0.));
#89734=CARTESIAN_POINT('Ctrl Pts',(32.4454809747123,-34.0080724983324,20.));
#89735=CARTESIAN_POINT('Ctrl Pts',(32.4195596199344,-34.0286631331978,0.));
#89736=CARTESIAN_POINT('Ctrl Pts',(32.4195596199344,-34.0286631331978,20.));
#89737=CARTESIAN_POINT('Ctrl Pts',(32.3936247025392,-34.0492348860855,0.));
#89738=CARTESIAN_POINT('Ctrl Pts',(32.3936247025392,-34.0492348860855,20.));
#89739=CARTESIAN_POINT('Ctrl Pts',(32.3676762358321,-34.0697877475586,0.));
#89740=CARTESIAN_POINT('Ctrl Pts',(32.3676762358321,-34.0697877475586,20.));
#89741=CARTESIAN_POINT('Ctrl Pts',(32.3417142331256,-34.0903217081898,0.));
#89742=CARTESIAN_POINT('Ctrl Pts',(32.3417142331256,-34.0903217081898,20.));
#89743=CARTESIAN_POINT('Ctrl Pts',(32.3157387077392,-34.1108367585604,0.));
#89744=CARTESIAN_POINT('Ctrl Pts',(32.3157387077392,-34.1108367585604,20.));
#89745=CARTESIAN_POINT('Ctrl Pts',(32.289749672999,-34.131332889261,0.));
#89746=CARTESIAN_POINT('Ctrl Pts',(32.289749672999,-34.131332889261,20.));
#89747=CARTESIAN_POINT('Ctrl Pts',(32.2637471422388,-34.1518100908915,0.));
#89748=CARTESIAN_POINT('Ctrl Pts',(32.2637471422388,-34.1518100908915,20.));
#89749=CARTESIAN_POINT('Ctrl Pts',(32.2377311287994,-34.1722683540613,0.));
#89750=CARTESIAN_POINT('Ctrl Pts',(32.2377311287994,-34.1722683540613,20.));
#89751=CARTESIAN_POINT('Ctrl Pts',(32.2117016460282,-34.1927076693884,0.));
#89752=CARTESIAN_POINT('Ctrl Pts',(32.2117016460282,-34.1927076693884,20.));
#89753=CARTESIAN_POINT('Ctrl Pts',(32.1856587072789,-34.2131280274994,0.));
#89754=CARTESIAN_POINT('Ctrl Pts',(32.1856587072789,-34.2131280274994,20.));
#89755=CARTESIAN_POINT('Ctrl Pts',(32.1596023259127,-34.233529419031,0.));
#89756=CARTESIAN_POINT('Ctrl Pts',(32.1596023259127,-34.233529419031,20.));
#89757=CARTESIAN_POINT('Ctrl Pts',(32.1335325152974,-34.2539118346284,0.));
#89758=CARTESIAN_POINT('Ctrl Pts',(32.1335325152974,-34.2539118346284,20.));
#89759=CARTESIAN_POINT('Ctrl Pts',(32.1074492888083,-34.2742752649465,0.));
#89760=CARTESIAN_POINT('Ctrl Pts',(32.1074492888083,-34.2742752649465,20.));
#89761=CARTESIAN_POINT('Ctrl Pts',(32.081352659827,-34.2946197006486,0.));
#89762=CARTESIAN_POINT('Ctrl Pts',(32.081352659827,-34.2946197006486,20.));
#89763=CARTESIAN_POINT('Ctrl Pts',(32.0552426417428,-34.3149451324082,0.));
#89764=CARTESIAN_POINT('Ctrl Pts',(32.0552426417428,-34.3149451324082,20.));
#89765=CARTESIAN_POINT('Ctrl Pts',(32.0291192479513,-34.335251550907,0.));
#89766=CARTESIAN_POINT('Ctrl Pts',(32.0291192479513,-34.335251550907,20.));
#89767=CARTESIAN_POINT('Ctrl Pts',(32.0029824918551,-34.3555389468366,0.));
#89768=CARTESIAN_POINT('Ctrl Pts',(32.0029824918551,-34.3555389468366,20.));
#89769=CARTESIAN_POINT('Ctrl Pts',(31.9768323868632,-34.3758073108972,0.));
#89770=CARTESIAN_POINT('Ctrl Pts',(31.9768323868632,-34.3758073108972,20.));
#89771=CARTESIAN_POINT('Ctrl Pts',(31.9506689463919,-34.3960566337983,0.));
#89772=CARTESIAN_POINT('Ctrl Pts',(31.9506689463919,-34.3960566337983,20.));
#89773=CARTESIAN_POINT('Ctrl Pts',(31.9244921838641,-34.4162869062584,0.));
#89774=CARTESIAN_POINT('Ctrl Pts',(31.9244921838641,-34.4162869062584,20.));
#89775=CARTESIAN_POINT('Ctrl Pts',(31.8983021127101,-34.4364981190057,0.));
#89776=CARTESIAN_POINT('Ctrl Pts',(31.8983021127101,-34.4364981190057,20.));
#89777=CARTESIAN_POINT('Ctrl Pts',(31.8720987463673,-34.4566902627777,0.));
#89778=CARTESIAN_POINT('Ctrl Pts',(31.8720987463673,-34.4566902627777,20.));
#89779=CARTESIAN_POINT('Ctrl Pts',(31.8458820982794,-34.4768633283209,0.));
#89780=CARTESIAN_POINT('Ctrl Pts',(31.8458820982794,-34.4768633283209,20.));
#89781=CARTESIAN_POINT('Ctrl Pts',(31.819652181897,-34.4970173063908,0.));
#89782=CARTESIAN_POINT('Ctrl Pts',(31.819652181897,-34.4970173063908,20.));
#89783=CARTESIAN_POINT('Ctrl Pts',(31.7934090106771,-34.5171521877519,0.));
#89784=CARTESIAN_POINT('Ctrl Pts',(31.7934090106771,-34.5171521877519,20.));
#89785=CARTESIAN_POINT('Ctrl Pts',(31.7671525980837,-34.5372679631778,0.));
#89786=CARTESIAN_POINT('Ctrl Pts',(31.7671525980837,-34.5372679631778,20.));
#89787=CARTESIAN_POINT('Ctrl Pts',(31.7408829575878,-34.5573646234518,0.));
#89788=CARTESIAN_POINT('Ctrl Pts',(31.7408829575878,-34.5573646234518,20.));
#89789=CARTESIAN_POINT('Ctrl Pts',(31.7146001026678,-34.5774421593669,0.));
#89790=CARTESIAN_POINT('Ctrl Pts',(31.7146001026678,-34.5774421593669,20.));
#89791=CARTESIAN_POINT('Ctrl Pts',(31.6883040468088,-34.5975005617252,0.));
#89792=CARTESIAN_POINT('Ctrl Pts',(31.6883040468088,-34.5975005617252,20.));
#89793=CARTESIAN_POINT('Ctrl Pts',(31.6619948035026,-34.6175398213376,0.));
#89794=CARTESIAN_POINT('Ctrl Pts',(31.6619948035026,-34.6175398213376,20.));
#89795=CARTESIAN_POINT('Ctrl Pts',(31.6356723862475,-34.6375599290243,0.));
#89796=CARTESIAN_POINT('Ctrl Pts',(31.6356723862475,-34.6375599290243,20.));
#89797=CARTESIAN_POINT('Ctrl Pts',(31.609336808548,-34.6575608756141,0.));
#89798=CARTESIAN_POINT('Ctrl Pts',(31.609336808548,-34.6575608756141,20.));
#89799=CARTESIAN_POINT('Ctrl Pts',(31.5829880839157,-34.6775426519456,0.));
#89800=CARTESIAN_POINT('Ctrl Pts',(31.5829880839157,-34.6775426519456,20.));
#89801=CARTESIAN_POINT('Ctrl Pts',(31.556626225869,-34.6975052488666,0.));
#89802=CARTESIAN_POINT('Ctrl Pts',(31.556626225869,-34.6975052488666,20.));
#89803=CARTESIAN_POINT('Ctrl Pts',(31.5302512479332,-34.7174486572342,0.));
#89804=CARTESIAN_POINT('Ctrl Pts',(31.5302512479332,-34.7174486572342,20.));
#89805=CARTESIAN_POINT('Ctrl Pts',(31.5038631636409,-34.7373728679152,0.));
#89806=CARTESIAN_POINT('Ctrl Pts',(31.5038631636409,-34.7373728679152,20.));
#89807=CARTESIAN_POINT('Ctrl Pts',(31.4774619865312,-34.7572778717853,0.));
#89808=CARTESIAN_POINT('Ctrl Pts',(31.4774619865312,-34.7572778717853,20.));
#89809=CARTESIAN_POINT('Ctrl Pts',(31.4510477301503,-34.7771636597296,0.));
#89810=CARTESIAN_POINT('Ctrl Pts',(31.4510477301503,-34.7771636597296,20.));
#89811=CARTESIAN_POINT('Ctrl Pts',(31.4246204080513,-34.7970302226433,0.));
#89812=CARTESIAN_POINT('Ctrl Pts',(31.4246204080513,-34.7970302226433,20.));
#89813=CARTESIAN_POINT('Ctrl Pts',(31.3981800337935,-34.8168775514299,0.));
#89814=CARTESIAN_POINT('Ctrl Pts',(31.3981800337935,-34.8168775514299,20.));
#89815=CARTESIAN_POINT('Ctrl Pts',(31.3717266209433,-34.8367056370027,0.));
#89816=CARTESIAN_POINT('Ctrl Pts',(31.3717266209433,-34.8367056370027,20.));
#89817=CARTESIAN_POINT('Ctrl Pts',(31.3452601830725,-34.856514470283,0.));
#89818=CARTESIAN_POINT('Ctrl Pts',(31.3452601830725,-34.856514470283,20.));
#89819=CARTESIAN_POINT('Ctrl Pts',(31.3187807337598,-34.8763040422018,0.));
#89820=CARTESIAN_POINT('Ctrl Pts',(31.3187807337598,-34.8763040422018,20.));
#89821=CARTESIAN_POINT('Ctrl Pts',(31.2922882865907,-34.8960743436995,0.));
#89822=CARTESIAN_POINT('Ctrl Pts',(31.2922882865907,-34.8960743436995,20.));
#89823=CARTESIAN_POINT('Ctrl Pts',(31.2657828551579,-34.9158253657263,0.));
#89824=CARTESIAN_POINT('Ctrl Pts',(31.2657828551579,-34.9158253657263,20.));
#89825=CARTESIAN_POINT('Ctrl Pts',(31.2392644530613,-34.9355570992414,0.));
#89826=CARTESIAN_POINT('Ctrl Pts',(31.2392644530613,-34.9355570992414,20.));
#89827=CARTESIAN_POINT('Ctrl Pts',(31.2127330939085,-34.9552695352152,0.));
#89828=CARTESIAN_POINT('Ctrl Pts',(31.2127330939085,-34.9552695352152,20.));
#89829=CARTESIAN_POINT('Ctrl Pts',(31.1861887913133,-34.974962664626,0.));
#89830=CARTESIAN_POINT('Ctrl Pts',(31.1861887913133,-34.974962664626,20.));
#89831=CARTESIAN_POINT('Ctrl Pts',(31.1596315588953,-34.9946364784612,0.));
#89832=CARTESIAN_POINT('Ctrl Pts',(31.1596315588953,-34.9946364784612,20.));
#89833=CARTESIAN_POINT('Ctrl Pts',(31.1330614102809,-35.0142909677175,0.));
#89834=CARTESIAN_POINT('Ctrl Pts',(31.1330614102809,-35.0142909677175,20.));
#89835=CARTESIAN_POINT('Ctrl Pts',(31.1064783591027,-35.0339261234013,0.));
#89836=CARTESIAN_POINT('Ctrl Pts',(31.1064783591027,-35.0339261234013,20.));
#89837=CARTESIAN_POINT('Ctrl Pts',(31.0798824190003,-35.0535419365277,0.));
#89838=CARTESIAN_POINT('Ctrl Pts',(31.0798824190003,-35.0535419365277,20.));
#89839=CARTESIAN_POINT('Ctrl Pts',(31.0532736036193,-35.0731383981212,0.));
#89840=CARTESIAN_POINT('Ctrl Pts',(31.0532736036193,-35.0731383981212,20.));
#89841=CARTESIAN_POINT('Ctrl Pts',(31.026651926612,-35.0927154992152,0.));
#89842=CARTESIAN_POINT('Ctrl Pts',(31.026651926612,-35.0927154992152,20.));
#89843=CARTESIAN_POINT('Ctrl Pts',(31.0000174016378,-35.1122732308527,0.));
#89844=CARTESIAN_POINT('Ctrl Pts',(31.0000174016378,-35.1122732308527,20.));
#89845=CARTESIAN_POINT('Ctrl Pts',(30.9733700423633,-35.131811584087,0.));
#89846=CARTESIAN_POINT('Ctrl Pts',(30.9733700423633,-35.131811584087,20.));
#89847=CARTESIAN_POINT('Ctrl Pts',(30.9467098624624,-35.1513305499814,0.));
#89848=CARTESIAN_POINT('Ctrl Pts',(30.9467098624624,-35.1513305499814,20.));
#89849=CARTESIAN_POINT('Ctrl Pts',(30.9200368756162,-35.170830119609,0.));
#89850=CARTESIAN_POINT('Ctrl Pts',(30.9200368756162,-35.170830119609,20.));
#89851=CARTESIAN_POINT('Ctrl Pts',(30.8933510955115,-35.1903102840519,0.));
#89852=CARTESIAN_POINT('Ctrl Pts',(30.8933510955115,-35.1903102840519,20.));
#89853=CARTESIAN_POINT('Ctrl Pts',(30.8666525358408,-35.2097710343998,0.));
#89854=CARTESIAN_POINT('Ctrl Pts',(30.8666525358408,-35.2097710343998,20.));
#89855=CARTESIAN_POINT('Ctrl Pts',(30.8399412103026,-35.2292123617517,0.));
#89856=CARTESIAN_POINT('Ctrl Pts',(30.8399412103026,-35.2292123617517,20.));
#89857=CARTESIAN_POINT('Ctrl Pts',(30.8132171326021,-35.2486342572162,0.));
#89858=CARTESIAN_POINT('Ctrl Pts',(30.8132171326021,-35.2486342572162,20.));
#89859=CARTESIAN_POINT('Ctrl Pts',(30.786480316451,-35.2680367119112,0.));
#89860=CARTESIAN_POINT('Ctrl Pts',(30.786480316451,-35.2680367119112,20.));
#89861=CARTESIAN_POINT('Ctrl Pts',(30.7597307755696,-35.2874197169657,0.));
#89862=CARTESIAN_POINT('Ctrl Pts',(30.7597307755696,-35.2874197169657,20.));
#89863=CARTESIAN_POINT('Ctrl Pts',(30.732968523684,-35.3067832635177,0.));
#89864=CARTESIAN_POINT('Ctrl Pts',(30.732968523684,-35.3067832635177,20.));
#89865=CARTESIAN_POINT('Ctrl Pts',(30.7061935745273,-35.3261273427148,0.));
#89866=CARTESIAN_POINT('Ctrl Pts',(30.7061935745273,-35.3261273427148,20.));
#89867=CARTESIAN_POINT('Ctrl Pts',(30.6794059418388,-35.3454519457137,0.));
#89868=CARTESIAN_POINT('Ctrl Pts',(30.6794059418388,-35.3454519457137,20.));
#89869=CARTESIAN_POINT('Ctrl Pts',(30.6526056393638,-35.3647570636798,0.));
#89870=CARTESIAN_POINT('Ctrl Pts',(30.6526056393638,-35.3647570636798,20.));
#89871=CARTESIAN_POINT('Ctrl Pts',(30.6257926808541,-35.3840426877879,0.));
#89872=CARTESIAN_POINT('Ctrl Pts',(30.6257926808541,-35.3840426877879,20.));
#89873=CARTESIAN_POINT('Ctrl Pts',(30.5989670800681,-35.4033088092226,0.));
#89874=CARTESIAN_POINT('Ctrl Pts',(30.5989670800681,-35.4033088092226,20.));
#89875=CARTESIAN_POINT('Ctrl Pts',(30.5721288507715,-35.4225554191786,0.));
#89876=CARTESIAN_POINT('Ctrl Pts',(30.5721288507715,-35.4225554191786,20.));
#89877=CARTESIAN_POINT('Ctrl Pts',(30.5452780067368,-35.4417825088605,0.));
#89878=CARTESIAN_POINT('Ctrl Pts',(30.5452780067368,-35.4417825088605,20.));
#89879=CARTESIAN_POINT('Ctrl Pts',(30.5184145617424,-35.4609900694812,0.));
#89880=CARTESIAN_POINT('Ctrl Pts',(30.5184145617424,-35.4609900694812,20.));
#89881=CARTESIAN_POINT('Ctrl Pts',(30.4915385295724,-35.4801780922626,0.));
#89882=CARTESIAN_POINT('Ctrl Pts',(30.4915385295724,-35.4801780922626,20.));
#89883=CARTESIAN_POINT('Ctrl Pts',(30.4646499240177,-35.4993465684362,0.));
#89884=CARTESIAN_POINT('Ctrl Pts',(30.4646499240177,-35.4993465684362,20.));
#89885=CARTESIAN_POINT('Ctrl Pts',(30.437748758876,-35.518495489243,0.));
#89886=CARTESIAN_POINT('Ctrl Pts',(30.437748758876,-35.518495489243,20.));
#89887=CARTESIAN_POINT('Ctrl Pts',(30.4108350479521,-35.5376248459348,0.));
#89888=CARTESIAN_POINT('Ctrl Pts',(30.4108350479521,-35.5376248459348,20.));
#89889=CARTESIAN_POINT('Ctrl Pts',(30.3839088050584,-35.5567346297737,0.));
#89890=CARTESIAN_POINT('Ctrl Pts',(30.3839088050584,-35.5567346297737,20.));
#89891=CARTESIAN_POINT('Ctrl Pts',(30.3569700440131,-35.5758248320301,0.));
#89892=CARTESIAN_POINT('Ctrl Pts',(30.3569700440131,-35.5758248320301,20.));
#89893=CARTESIAN_POINT('Ctrl Pts',(30.3300187786403,-35.5948954439837,0.));
#89894=CARTESIAN_POINT('Ctrl Pts',(30.3300187786403,-35.5948954439837,20.));
#89895=CARTESIAN_POINT('Ctrl Pts',(30.3030550227693,-35.6139464569223,0.));
#89896=CARTESIAN_POINT('Ctrl Pts',(30.3030550227693,-35.6139464569223,20.));
#89897=CARTESIAN_POINT('Ctrl Pts',(30.2760787902362,-35.6329778621436,0.));
#89898=CARTESIAN_POINT('Ctrl Pts',(30.2760787902362,-35.6329778621436,20.));
#89899=CARTESIAN_POINT('Ctrl Pts',(30.2490900948838,-35.6519896509552,0.));
#89900=CARTESIAN_POINT('Ctrl Pts',(30.2490900948838,-35.6519896509552,20.));
#89901=CARTESIAN_POINT('Ctrl Pts',(30.2220889505625,-35.6709818146751,0.));
#89902=CARTESIAN_POINT('Ctrl Pts',(30.2220889505625,-35.6709818146751,20.));
#89903=CARTESIAN_POINT('Ctrl Pts',(30.1950753711288,-35.6899543446309,0.));
#89904=CARTESIAN_POINT('Ctrl Pts',(30.1950753711288,-35.6899543446309,20.));
#89905=CARTESIAN_POINT('Ctrl Pts',(30.1680493704465,-35.7089072321597,0.));
#89906=CARTESIAN_POINT('Ctrl Pts',(30.1680493704465,-35.7089072321597,20.));
#89907=CARTESIAN_POINT('Ctrl Pts',(30.141010962385,-35.727840468608,0.));
#89908=CARTESIAN_POINT('Ctrl Pts',(30.141010962385,-35.727840468608,20.));
#89909=CARTESIAN_POINT('Ctrl Pts',(30.1139601608197,-35.7467540453308,0.));
#89910=CARTESIAN_POINT('Ctrl Pts',(30.1139601608197,-35.7467540453308,20.));
#89911=CARTESIAN_POINT('Ctrl Pts',(30.0868969796328,-35.7656479536939,0.));
#89912=CARTESIAN_POINT('Ctrl Pts',(30.0868969796328,-35.7656479536939,20.));
#89913=CARTESIAN_POINT('Ctrl Pts',(30.0598214327127,-35.7845221850715,0.));
#89914=CARTESIAN_POINT('Ctrl Pts',(30.0598214327127,-35.7845221850715,20.));
#89915=CARTESIAN_POINT('Ctrl Pts',(30.0327335339539,-35.8033767308478,0.));
#89916=CARTESIAN_POINT('Ctrl Pts',(30.0327335339539,-35.8033767308478,20.));
#89917=CARTESIAN_POINT('Ctrl Pts',(30.005633297258,-35.8222115824167,0.));
#89918=CARTESIAN_POINT('Ctrl Pts',(30.005633297258,-35.8222115824167,20.));
#89919=CARTESIAN_POINT('Ctrl Pts',(29.9785207365333,-35.841026731182,0.));
#89920=CARTESIAN_POINT('Ctrl Pts',(29.9785207365333,-35.841026731182,20.));
#89921=CARTESIAN_POINT('Ctrl Pts',(29.9513958656946,-35.8598221685576,0.));
#89922=CARTESIAN_POINT('Ctrl Pts',(29.9513958656946,-35.8598221685576,20.));
#89923=CARTESIAN_POINT('Ctrl Pts',(29.9242586986624,-35.8785978859658,0.));
#89924=CARTESIAN_POINT('Ctrl Pts',(29.9242586986624,-35.8785978859658,20.));
#89925=CARTESIAN_POINT('Ctrl Pts',(29.8971092493634,-35.8973538748387,0.));
#89926=CARTESIAN_POINT('Ctrl Pts',(29.8971092493634,-35.8973538748387,20.));
#89927=CARTESIAN_POINT('Ctrl Pts',(29.869947531731,-35.9160901266177,0.));
#89928=CARTESIAN_POINT('Ctrl Pts',(29.869947531731,-35.9160901266177,20.));
#89929=CARTESIAN_POINT('Ctrl Pts',(29.8427735597048,-35.934806632754,0.));
#89930=CARTESIAN_POINT('Ctrl Pts',(29.8427735597048,-35.934806632754,20.));
#89931=CARTESIAN_POINT('Ctrl Pts',(29.8155873472308,-35.9535033847082,0.));
#89932=CARTESIAN_POINT('Ctrl Pts',(29.8155873472308,-35.9535033847082,20.));
#89933=CARTESIAN_POINT('Ctrl Pts',(29.7883889082614,-35.9721803739509,0.));
#89934=CARTESIAN_POINT('Ctrl Pts',(29.7883889082614,-35.9721803739509,20.));
#89935=CARTESIAN_POINT('Ctrl Pts',(29.7611782567557,-35.9908375919623,0.));
#89936=CARTESIAN_POINT('Ctrl Pts',(29.7611782567557,-35.9908375919623,20.));
#89937=CARTESIAN_POINT('Ctrl Pts',(29.7339554066796,-36.0094750302331,0.));
#89938=CARTESIAN_POINT('Ctrl Pts',(29.7339554066796,-36.0094750302331,20.));
#89939=CARTESIAN_POINT('Ctrl Pts',(29.7067203720053,-36.0280926802632,0.));
#89940=CARTESIAN_POINT('Ctrl Pts',(29.7067203720053,-36.0280926802632,20.));
#89941=CARTESIAN_POINT('Ctrl Pts',(29.6794731667106,-36.0466905335617,0.));
#89942=CARTESIAN_POINT('Ctrl Pts',(29.6794731667106,-36.0466905335617,20.));
#89943=CARTESIAN_POINT('Ctrl Pts',(29.6522138047793,-36.0652685816464,0.));
#89944=CARTESIAN_POINT('Ctrl Pts',(29.6522138047793,-36.0652685816464,20.));
#89945=CARTESIAN_POINT('Ctrl Pts',(29.6249423002017,-36.0838268160451,0.));
#89946=CARTESIAN_POINT('Ctrl Pts',(29.6249423002017,-36.0838268160451,20.));
#89947=CARTESIAN_POINT('Ctrl Pts',(29.5976586669748,-36.1023652282957,0.));
#89948=CARTESIAN_POINT('Ctrl Pts',(29.5976586669748,-36.1023652282957,20.));
#89949=CARTESIAN_POINT('Ctrl Pts',(29.5703629191022,-36.1208838099461,0.));
#89950=CARTESIAN_POINT('Ctrl Pts',(29.5703629191022,-36.1208838099461,20.));
#89951=CARTESIAN_POINT('Ctrl Pts',(29.5430550705937,-36.1393825525541,0.));
#89952=CARTESIAN_POINT('Ctrl Pts',(29.5430550705937,-36.1393825525541,20.));
#89953=CARTESIAN_POINT('Ctrl Pts',(29.5157351354651,-36.1578614476865,0.));
#89954=CARTESIAN_POINT('Ctrl Pts',(29.5157351354651,-36.1578614476865,20.));
#89955=CARTESIAN_POINT('Ctrl Pts',(29.4884031277381,-36.1763204869193,0.));
#89956=CARTESIAN_POINT('Ctrl Pts',(29.4884031277381,-36.1763204869193,20.));
#89957=CARTESIAN_POINT('Ctrl Pts',(29.4610590614411,-36.1947596618382,0.));
#89958=CARTESIAN_POINT('Ctrl Pts',(29.4610590614411,-36.1947596618382,20.));
#89959=CARTESIAN_POINT('Ctrl Pts',(29.4337029506094,-36.2131789640397,0.));
#89960=CARTESIAN_POINT('Ctrl Pts',(29.4337029506094,-36.2131789640397,20.));
#89961=CARTESIAN_POINT('Ctrl Pts',(29.4063348092849,-36.2315783851295,0.));
#89962=CARTESIAN_POINT('Ctrl Pts',(29.4063348092849,-36.2315783851295,20.));
#89963=CARTESIAN_POINT('Ctrl Pts',(29.3789546515147,-36.2499579167227,0.));
#89964=CARTESIAN_POINT('Ctrl Pts',(29.3789546515147,-36.2499579167227,20.));
#89965=CARTESIAN_POINT('Ctrl Pts',(29.3515624913523,-36.2683175504441,0.));
#89966=CARTESIAN_POINT('Ctrl Pts',(29.3515624913523,-36.2683175504441,20.));
#89967=CARTESIAN_POINT('Ctrl Pts',(29.3241583428569,-36.286657277928,0.));
#89968=CARTESIAN_POINT('Ctrl Pts',(29.3241583428569,-36.286657277928,20.));
#89969=CARTESIAN_POINT('Ctrl Pts',(29.2967422200943,-36.3049770908188,0.));
#89970=CARTESIAN_POINT('Ctrl Pts',(29.2967422200943,-36.3049770908188,20.));
#89971=CARTESIAN_POINT('Ctrl Pts',(29.2693141371364,-36.3232769807701,0.));
#89972=CARTESIAN_POINT('Ctrl Pts',(29.2693141371364,-36.3232769807701,20.));
#89973=CARTESIAN_POINT('Ctrl Pts',(29.241874108062,-36.3415569394456,0.));
#89974=CARTESIAN_POINT('Ctrl Pts',(29.241874108062,-36.3415569394456,20.));
#89975=CARTESIAN_POINT('Ctrl Pts',(29.2144221469562,-36.3598169585187,0.));
#89976=CARTESIAN_POINT('Ctrl Pts',(29.2144221469562,-36.3598169585187,20.));
#89977=CARTESIAN_POINT('Ctrl Pts',(29.186958267911,-36.3780570296726,0.));
#89978=CARTESIAN_POINT('Ctrl Pts',(29.186958267911,-36.3780570296726,20.));
#89979=CARTESIAN_POINT('Ctrl Pts',(29.1594824850239,-36.3962771446002,0.));
#89980=CARTESIAN_POINT('Ctrl Pts',(29.1594824850239,-36.3962771446002,20.));
#89981=CARTESIAN_POINT('Ctrl Pts',(29.1319948123985,-36.4144772950043,0.));
#89982=CARTESIAN_POINT('Ctrl Pts',(29.1319948123985,-36.4144772950043,20.));
#89983=CARTESIAN_POINT('Ctrl Pts',(29.1044952641442,-36.4326574725969,0.));
#89984=CARTESIAN_POINT('Ctrl Pts',(29.1044952641442,-36.4326574725969,20.));
#89985=CARTESIAN_POINT('Ctrl Pts',(29.0769838543763,-36.4508176690994,0.));
#89986=CARTESIAN_POINT('Ctrl Pts',(29.0769838543763,-36.4508176690994,20.));
#89987=CARTESIAN_POINT('Ctrl Pts',(29.0494605972165,-36.4689578762435,0.));
#89988=CARTESIAN_POINT('Ctrl Pts',(29.0494605972165,-36.4689578762435,20.));
#89989=CARTESIAN_POINT('Ctrl Pts',(29.0219255067927,-36.4870780857703,0.));
#89990=CARTESIAN_POINT('Ctrl Pts',(29.0219255067927,-36.4870780857703,20.));
#89991=CARTESIAN_POINT('Ctrl Pts',(28.99437859724,-36.5051782894317,0.));
#89992=CARTESIAN_POINT('Ctrl Pts',(28.99437859724,-36.5051782894317,20.));
#89993=CARTESIAN_POINT('Ctrl Pts',(28.9668198826995,-36.5232584789886,0.));
#89994=CARTESIAN_POINT('Ctrl Pts',(28.9668198826995,-36.5232584789886,20.));
#89995=CARTESIAN_POINT('Ctrl Pts',(28.9392493773185,-36.5413186462123,0.));
#89996=CARTESIAN_POINT('Ctrl Pts',(28.9392493773185,-36.5413186462123,20.));
#89997=CARTESIAN_POINT('Ctrl Pts',(28.9116670952497,-36.5593587828826,0.));
#89998=CARTESIAN_POINT('Ctrl Pts',(28.9116670952497,-36.5593587828826,20.));
#89999=CARTESIAN_POINT('Ctrl Pts',(28.8840730506515,-36.577378880789,0.));
#90000=CARTESIAN_POINT('Ctrl Pts',(28.8840730506515,-36.577378880789,20.));
#90001=CARTESIAN_POINT('Ctrl Pts',(28.8564672576885,-36.5953789317306,0.));
#90002=CARTESIAN_POINT('Ctrl Pts',(28.8564672576885,-36.5953789317306,20.));
#90003=CARTESIAN_POINT('Ctrl Pts',(28.8288497305324,-36.6133589275174,0.));
#90004=CARTESIAN_POINT('Ctrl Pts',(28.8288497305324,-36.6133589275174,20.));
#90005=CARTESIAN_POINT('Ctrl Pts',(28.8012204833609,-36.6313188599694,0.));
#90006=CARTESIAN_POINT('Ctrl Pts',(28.8012204833609,-36.6313188599694,20.));
#90007=CARTESIAN_POINT('Ctrl Pts',(28.7735795303585,-36.6492587209168,0.));
#90008=CARTESIAN_POINT('Ctrl Pts',(28.7735795303585,-36.6492587209168,20.));
#90009=CARTESIAN_POINT('Ctrl Pts',(28.7459268857152,-36.6671785021988,0.));
#90010=CARTESIAN_POINT('Ctrl Pts',(28.7459268857152,-36.6671785021988,20.));
#90011=CARTESIAN_POINT('Ctrl Pts',(28.7182625636274,-36.6850781956649,0.));
#90012=CARTESIAN_POINT('Ctrl Pts',(28.7182625636274,-36.6850781956649,20.));
#90013=CARTESIAN_POINT('Ctrl Pts',(28.6905865782966,-36.7029577931733,0.));
#90014=CARTESIAN_POINT('Ctrl Pts',(28.6905865782966,-36.7029577931733,20.));
#90015=CARTESIAN_POINT('Ctrl Pts',(28.6628989439305,-36.7208172865919,0.));
#90016=CARTESIAN_POINT('Ctrl Pts',(28.6628989439305,-36.7208172865919,20.));
#90017=CARTESIAN_POINT('Ctrl Pts',(28.6351996747428,-36.7386566677981,0.));
#90018=CARTESIAN_POINT('Ctrl Pts',(28.6351996747428,-36.7386566677981,20.));
#90019=CARTESIAN_POINT('Ctrl Pts',(28.6074887849535,-36.7564759286795,0.));
#90020=CARTESIAN_POINT('Ctrl Pts',(28.6074887849535,-36.7564759286795,20.));
#90021=CARTESIAN_POINT('Ctrl Pts',(28.5797662887891,-36.774275061134,0.));
#90022=CARTESIAN_POINT('Ctrl Pts',(28.5797662887891,-36.774275061134,20.));
#90023=CARTESIAN_POINT('Ctrl Pts',(28.5520322004824,-36.7920540570698,0.));
#90024=CARTESIAN_POINT('Ctrl Pts',(28.5520322004824,-36.7920540570698,20.));
#90025=CARTESIAN_POINT('Ctrl Pts',(28.5242865342724,-36.8098129084051,0.));
#90026=CARTESIAN_POINT('Ctrl Pts',(28.5242865342724,-36.8098129084051,20.));
#90027=CARTESIAN_POINT('Ctrl Pts',(28.496529304404,-36.8275516070676,0.));
#90028=CARTESIAN_POINT('Ctrl Pts',(28.496529304404,-36.8275516070676,20.));
#90029=CARTESIAN_POINT('Ctrl Pts',(28.4687605251277,-36.8452701449948,0.));
#90030=CARTESIAN_POINT('Ctrl Pts',(28.4687605251277,-36.8452701449948,20.));
#90031=CARTESIAN_POINT('Ctrl Pts',(28.4409802107002,-36.8629685141338,0.));
#90032=CARTESIAN_POINT('Ctrl Pts',(28.4409802107002,-36.8629685141338,20.));
#90033=CARTESIAN_POINT('Ctrl Pts',(28.413188375384,-36.8806467064409,0.));
#90034=CARTESIAN_POINT('Ctrl Pts',(28.413188375384,-36.8806467064409,20.));
#90035=CARTESIAN_POINT('Ctrl Pts',(28.3853850334475,-36.8983047138822,0.));
#90036=CARTESIAN_POINT('Ctrl Pts',(28.3853850334475,-36.8983047138822,20.));
#90037=CARTESIAN_POINT('Ctrl Pts',(28.3575701991656,-36.9159425284342,0.));
#90038=CARTESIAN_POINT('Ctrl Pts',(28.3575701991656,-36.9159425284342,20.));
#90039=CARTESIAN_POINT('Ctrl Pts',(28.3297438868192,-36.9335601420835,0.));
#90040=CARTESIAN_POINT('Ctrl Pts',(28.3297438868192,-36.9335601420835,20.));
#90041=CARTESIAN_POINT('Ctrl Pts',(28.3019061106957,-36.9511575468269,0.));
#90042=CARTESIAN_POINT('Ctrl Pts',(28.3019061106957,-36.9511575468269,20.));
#90043=CARTESIAN_POINT('Ctrl Pts',(28.2740568850881,-36.968734734671,0.));
#90044=CARTESIAN_POINT('Ctrl Pts',(28.2740568850881,-36.968734734671,20.));
#90045=CARTESIAN_POINT('Ctrl Pts',(28.2461962242955,-36.9862916976318,0.));
#90046=CARTESIAN_POINT('Ctrl Pts',(28.2461962242955,-36.9862916976318,20.));
#90047=CARTESIAN_POINT('Ctrl Pts',(28.2183241426219,-37.0038284277349,0.));
#90048=CARTESIAN_POINT('Ctrl Pts',(28.2183241426219,-37.0038284277349,20.));
#90049=CARTESIAN_POINT('Ctrl Pts',(28.1904406543778,-37.0213449170157,0.));
#90050=CARTESIAN_POINT('Ctrl Pts',(28.1904406543778,-37.0213449170157,20.));
#90051=CARTESIAN_POINT('Ctrl Pts',(28.1625457738797,-37.0388411575197,0.));
#90052=CARTESIAN_POINT('Ctrl Pts',(28.1625457738797,-37.0388411575197,20.));
#90053=CARTESIAN_POINT('Ctrl Pts',(28.1346395154506,-37.0563171413026,0.));
#90054=CARTESIAN_POINT('Ctrl Pts',(28.1346395154506,-37.0563171413026,20.));
#90055=CARTESIAN_POINT('Ctrl Pts',(28.1067218934195,-37.0737728604298,0.));
#90056=CARTESIAN_POINT('Ctrl Pts',(28.1067218934195,-37.0737728604298,20.));
#90057=CARTESIAN_POINT('Ctrl Pts',(28.0787929221219,-37.0912083069772,0.));
#90058=CARTESIAN_POINT('Ctrl Pts',(28.0787929221219,-37.0912083069772,20.));
#90059=CARTESIAN_POINT('Ctrl Pts',(28.0508526158994,-37.1086234730312,0.));
#90060=CARTESIAN_POINT('Ctrl Pts',(28.0508526158994,-37.1086234730312,20.));
#90061=CARTESIAN_POINT('Ctrl Pts',(28.0229009890985,-37.1260183506872,0.));
#90062=CARTESIAN_POINT('Ctrl Pts',(28.0229009890985,-37.1260183506872,20.));
#90063=CARTESIAN_POINT('Ctrl Pts',(27.994938056072,-37.1433929320507,0.));
#90064=CARTESIAN_POINT('Ctrl Pts',(27.994938056072,-37.1433929320507,20.));
#90065=CARTESIAN_POINT('Ctrl Pts',(27.9669638311771,-37.1607472092352,0.));
#90066=CARTESIAN_POINT('Ctrl Pts',(27.9669638311771,-37.1607472092352,20.));
#90067=CARTESIAN_POINT('Ctrl Pts',(27.9389783287777,-37.1780811743652,0.));
#90068=CARTESIAN_POINT('Ctrl Pts',(27.9389783287777,-37.1780811743652,20.));
#90069=CARTESIAN_POINT('Ctrl Pts',(27.9109815632437,-37.1953948195748,0.));
#90070=CARTESIAN_POINT('Ctrl Pts',(27.9109815632437,-37.1953948195748,20.));
#90071=CARTESIAN_POINT('Ctrl Pts',(27.8829735489517,-37.2126881370093,0.));
#90072=CARTESIAN_POINT('Ctrl Pts',(27.8829735489517,-37.2126881370093,20.));
#90073=CARTESIAN_POINT('Ctrl Pts',(27.8549543002843,-37.2299611188238,0.));
#90074=CARTESIAN_POINT('Ctrl Pts',(27.8549543002843,-37.2299611188238,20.));
#90075=CARTESIAN_POINT('Ctrl Pts',(27.8269238316305,-37.2472137571842,0.));
#90076=CARTESIAN_POINT('Ctrl Pts',(27.8269238316305,-37.2472137571842,20.));
#90077=CARTESIAN_POINT('Ctrl Pts',(27.7988821573846,-37.2644460442654,0.));
#90078=CARTESIAN_POINT('Ctrl Pts',(27.7988821573846,-37.2644460442654,20.));
#90079=CARTESIAN_POINT('Ctrl Pts',(27.7708292919468,-37.2816579722525,0.));
#90080=CARTESIAN_POINT('Ctrl Pts',(27.7708292919468,-37.2816579722525,20.));
#90081=CARTESIAN_POINT('Ctrl Pts',(27.7427652497224,-37.2988495333397,0.));
#90082=CARTESIAN_POINT('Ctrl Pts',(27.7427652497224,-37.2988495333397,20.));
#90083=CARTESIAN_POINT('Ctrl Pts',(27.7146900451228,-37.3160207197314,0.));
#90084=CARTESIAN_POINT('Ctrl Pts',(27.7146900451228,-37.3160207197314,20.));
#90085=CARTESIAN_POINT('Ctrl Pts',(27.6866036925651,-37.3331715236414,0.));
#90086=CARTESIAN_POINT('Ctrl Pts',(27.6866036925651,-37.3331715236414,20.));
#90087=CARTESIAN_POINT('Ctrl Pts',(27.6585062064726,-37.3503019372939,0.));
#90088=CARTESIAN_POINT('Ctrl Pts',(27.6585062064726,-37.3503019372939,20.));
#90089=CARTESIAN_POINT('Ctrl Pts',(27.6303976012744,-37.3674119529234,0.));
#90090=CARTESIAN_POINT('Ctrl Pts',(27.6303976012744,-37.3674119529234,20.));
#90091=CARTESIAN_POINT('Ctrl Pts',(27.6022778914064,-37.384501562775,0.));
#90092=CARTESIAN_POINT('Ctrl Pts',(27.6022778914064,-37.384501562775,20.));
#90093=CARTESIAN_POINT('Ctrl Pts',(27.5741470913094,-37.4015707591036,0.));
#90094=CARTESIAN_POINT('Ctrl Pts',(27.5741470913094,-37.4015707591036,20.));
#90095=CARTESIAN_POINT('Ctrl Pts',(27.5460052154308,-37.4186195341741,0.));
#90096=CARTESIAN_POINT('Ctrl Pts',(27.5460052154308,-37.4186195341741,20.));
#90097=CARTESIAN_POINT('Ctrl Pts',(27.5178522782226,-37.4356478802604,0.));
#90098=CARTESIAN_POINT('Ctrl Pts',(27.5178522782226,-37.4356478802604,20.));
#90099=CARTESIAN_POINT('Ctrl Pts',(27.4896882941429,-37.4526557896465,0.));
#90100=CARTESIAN_POINT('Ctrl Pts',(27.4896882941429,-37.4526557896465,20.));
#90101=CARTESIAN_POINT('Ctrl Pts',(27.4615132776558,-37.4696432546267,0.));
#90102=CARTESIAN_POINT('Ctrl Pts',(27.4615132776558,-37.4696432546267,20.));
#90103=CARTESIAN_POINT('Ctrl Pts',(27.4333272432311,-37.4866102675048,0.));
#90104=CARTESIAN_POINT('Ctrl Pts',(27.4333272432311,-37.4866102675048,20.));
#90105=CARTESIAN_POINT('Ctrl Pts',(27.4051302053449,-37.5035568205959,0.));
#90106=CARTESIAN_POINT('Ctrl Pts',(27.4051302053449,-37.5035568205959,20.));
#90107=CARTESIAN_POINT('Ctrl Pts',(27.3769221784798,-37.5204829062256,0.));
#90108=CARTESIAN_POINT('Ctrl Pts',(27.3769221784798,-37.5204829062256,20.));
#90109=CARTESIAN_POINT('Ctrl Pts',(27.3487031771241,-37.5373885167297,0.));
#90110=CARTESIAN_POINT('Ctrl Pts',(27.3487031771241,-37.5373885167297,20.));
#90111=CARTESIAN_POINT('Ctrl Pts',(27.3204732157704,-37.5542736444521,0.));
#90112=CARTESIAN_POINT('Ctrl Pts',(27.3204732157704,-37.5542736444521,20.));
#90113=CARTESIAN_POINT('Ctrl Pts',(27.2922323089174,-37.571138281747,0.));
#90114=CARTESIAN_POINT('Ctrl Pts',(27.2922323089174,-37.571138281747,20.));
#90115=CARTESIAN_POINT('Ctrl Pts',(27.2639804710687,-37.5879824209777,0.));
#90116=CARTESIAN_POINT('Ctrl Pts',(27.2639804710687,-37.5879824209777,20.));
#90117=CARTESIAN_POINT('Ctrl Pts',(27.2357177167352,-37.6048060545189,0.));
#90118=CARTESIAN_POINT('Ctrl Pts',(27.2357177167352,-37.6048060545189,20.));
#90119=CARTESIAN_POINT('Ctrl Pts',(27.2074440604332,-37.6216091747552,0.));
#90120=CARTESIAN_POINT('Ctrl Pts',(27.2074440604332,-37.6216091747552,20.));
#90121=CARTESIAN_POINT('Ctrl Pts',(27.1791595166855,-37.6383917740821,0.));
#90122=CARTESIAN_POINT('Ctrl Pts',(27.1791595166855,-37.6383917740821,20.));
#90123=CARTESIAN_POINT('Ctrl Pts',(27.15086410002,-37.6551538449046,0.));
#90124=CARTESIAN_POINT('Ctrl Pts',(27.15086410002,-37.6551538449046,20.));
#90125=CARTESIAN_POINT('Ctrl Pts',(27.1225578249702,-37.6718953796384,0.));
#90126=CARTESIAN_POINT('Ctrl Pts',(27.1225578249702,-37.6718953796384,20.));
#90127=CARTESIAN_POINT('Ctrl Pts',(27.0942407060752,-37.6886163707084,0.));
#90128=CARTESIAN_POINT('Ctrl Pts',(27.0942407060752,-37.6886163707084,20.));
#90129=CARTESIAN_POINT('Ctrl Pts',(27.0659127578793,-37.705316810549,0.));
#90130=CARTESIAN_POINT('Ctrl Pts',(27.0659127578793,-37.705316810549,20.));
#90131=CARTESIAN_POINT('Ctrl Pts',(27.0375739949332,-37.7219966916053,0.));
#90132=CARTESIAN_POINT('Ctrl Pts',(27.0375739949332,-37.7219966916053,20.));
#90133=CARTESIAN_POINT('Ctrl Pts',(27.0092244317933,-37.7386560063324,0.));
#90134=CARTESIAN_POINT('Ctrl Pts',(27.0092244317933,-37.7386560063324,20.));
#90135=CARTESIAN_POINT('Ctrl Pts',(26.9808640830224,-37.755294747196,0.));
#90136=CARTESIAN_POINT('Ctrl Pts',(26.9808640830224,-37.755294747196,20.));
#90137=CARTESIAN_POINT('Ctrl Pts',(26.9524929631885,-37.7719129066716,0.));
#90138=CARTESIAN_POINT('Ctrl Pts',(26.9524929631885,-37.7719129066716,20.));
#90139=CARTESIAN_POINT('Ctrl Pts',(26.9241110868652,-37.7885104772446,0.));
#90140=CARTESIAN_POINT('Ctrl Pts',(26.9241110868652,-37.7885104772446,20.));
#90141=CARTESIAN_POINT('Ctrl Pts',(26.8957184686315,-37.8050874514106,0.));
#90142=CARTESIAN_POINT('Ctrl Pts',(26.8957184686315,-37.8050874514106,20.));
#90143=CARTESIAN_POINT('Ctrl Pts',(26.8673151230714,-37.8216438216745,0.));
#90144=CARTESIAN_POINT('Ctrl Pts',(26.8673151230714,-37.8216438216745,20.));
#90145=CARTESIAN_POINT('Ctrl Pts',(26.8389010647754,-37.8381795805523,0.));
#90146=CARTESIAN_POINT('Ctrl Pts',(26.8389010647754,-37.8381795805523,20.));
#90147=CARTESIAN_POINT('Ctrl Pts',(26.8104763083398,-37.8546947205707,0.));
#90148=CARTESIAN_POINT('Ctrl Pts',(26.8104763083398,-37.8546947205707,20.));
#90149=CARTESIAN_POINT('Ctrl Pts',(26.7820408683669,-37.8711892342661,0.));
#90150=CARTESIAN_POINT('Ctrl Pts',(26.7820408683669,-37.8711892342661,20.));
#90151=CARTESIAN_POINT('Ctrl Pts',(26.7535947594648,-37.887663114185,0.));
#90152=CARTESIAN_POINT('Ctrl Pts',(26.7535947594648,-37.887663114185,20.));
#90153=CARTESIAN_POINT('Ctrl Pts',(26.7251379962461,-37.904116352883,0.));
#90154=CARTESIAN_POINT('Ctrl Pts',(26.7251379962461,-37.904116352883,20.));
#90155=CARTESIAN_POINT('Ctrl Pts',(26.6966705933291,-37.9205489429259,0.));
#90156=CARTESIAN_POINT('Ctrl Pts',(26.6966705933291,-37.9205489429259,20.));
#90157=CARTESIAN_POINT('Ctrl Pts',(26.6681925653377,-37.9369608768897,0.));
#90158=CARTESIAN_POINT('Ctrl Pts',(26.6681925653377,-37.9369608768897,20.));
#90159=CARTESIAN_POINT('Ctrl Pts',(26.6397039269022,-37.9533521473617,0.));
#90160=CARTESIAN_POINT('Ctrl Pts',(26.6397039269022,-37.9533521473617,20.));
#90161=CARTESIAN_POINT('Ctrl Pts',(26.6112046926582,-37.9697227469389,0.));
#90162=CARTESIAN_POINT('Ctrl Pts',(26.6112046926582,-37.9697227469389,20.));
#90163=CARTESIAN_POINT('Ctrl Pts',(26.5826948772471,-37.9860726682287,0.));
#90164=CARTESIAN_POINT('Ctrl Pts',(26.5826948772471,-37.9860726682287,20.));
#90165=CARTESIAN_POINT('Ctrl Pts',(26.5541744953162,-38.0024019038486,0.));
#90166=CARTESIAN_POINT('Ctrl Pts',(26.5541744953162,-38.0024019038486,20.));
#90167=CARTESIAN_POINT('Ctrl Pts',(26.5256435615177,-38.0187104464255,0.));
#90168=CARTESIAN_POINT('Ctrl Pts',(26.5256435615177,-38.0187104464255,20.));
#90169=CARTESIAN_POINT('Ctrl Pts',(26.4971020905092,-38.0349982885963,0.));
#90170=CARTESIAN_POINT('Ctrl Pts',(26.4971020905092,-38.0349982885963,20.));
#90171=CARTESIAN_POINT('Ctrl Pts',(26.4685500969542,-38.0512654230086,0.));
#90172=CARTESIAN_POINT('Ctrl Pts',(26.4685500969542,-38.0512654230086,20.));
#90173=CARTESIAN_POINT('Ctrl Pts',(26.4399875955219,-38.0675118423201,0.));
#90174=CARTESIAN_POINT('Ctrl Pts',(26.4399875955219,-38.0675118423201,20.));
#90175=CARTESIAN_POINT('Ctrl Pts',(26.4114146008872,-38.0837375391992,0.));
#90176=CARTESIAN_POINT('Ctrl Pts',(26.4114146008872,-38.0837375391992,20.));
#90177=CARTESIAN_POINT('Ctrl Pts',(26.38283112773,-38.0999425063245,0.));
#90178=CARTESIAN_POINT('Ctrl Pts',(26.38283112773,-38.0999425063245,20.));
#90179=CARTESIAN_POINT('Ctrl Pts',(26.3542371907363,-38.1161267363846,0.));
#90180=CARTESIAN_POINT('Ctrl Pts',(26.3542371907363,-38.1161267363846,20.));
#90181=CARTESIAN_POINT('Ctrl Pts',(26.3256328045975,-38.1322902220784,0.));
#90182=CARTESIAN_POINT('Ctrl Pts',(26.3256328045975,-38.1322902220784,20.));
#90183=CARTESIAN_POINT('Ctrl Pts',(26.2970179840108,-38.1484329561142,0.));
#90184=CARTESIAN_POINT('Ctrl Pts',(26.2970179840108,-38.1484329561142,20.));
#90185=CARTESIAN_POINT('Ctrl Pts',(26.2683927436784,-38.1645549312104,0.));
#90186=CARTESIAN_POINT('Ctrl Pts',(26.2683927436784,-38.1645549312104,20.));
#90187=CARTESIAN_POINT('Ctrl Pts',(26.2397570983077,-38.1806561400953,0.));
#90188=CARTESIAN_POINT('Ctrl Pts',(26.2397570983077,-38.1806561400953,20.));
#90189=CARTESIAN_POINT('Ctrl Pts',(26.2111110626121,-38.1967365755081,0.));
#90190=CARTESIAN_POINT('Ctrl Pts',(26.2111110626121,-38.1967365755081,20.));
#90191=CARTESIAN_POINT('Ctrl Pts',(26.1824546513102,-38.2127962301983,0.));
#90192=CARTESIAN_POINT('Ctrl Pts',(26.1824546513102,-38.2127962301983,20.));
#90193=CARTESIAN_POINT('Ctrl Pts',(26.1537878791271,-38.2288350969267,0.));
#90194=CARTESIAN_POINT('Ctrl Pts',(26.1537878791271,-38.2288350969267,20.));
#90195=CARTESIAN_POINT('Ctrl Pts',(26.1251107607929,-38.244853168464,0.));
#90196=CARTESIAN_POINT('Ctrl Pts',(26.1251107607929,-38.244853168464,20.));
#90197=CARTESIAN_POINT('Ctrl Pts',(26.0964233110434,-38.2608504375907,0.));
#90198=CARTESIAN_POINT('Ctrl Pts',(26.0964233110434,-38.2608504375907,20.));
#90199=CARTESIAN_POINT('Ctrl Pts',(26.0677255446196,-38.276826897097,0.));
#90200=CARTESIAN_POINT('Ctrl Pts',(26.0677255446196,-38.276826897097,20.));
#90201=CARTESIAN_POINT('Ctrl Pts',(26.0390174762675,-38.2927825397833,0.));
#90202=CARTESIAN_POINT('Ctrl Pts',(26.0390174762675,-38.2927825397833,20.));
#90203=CARTESIAN_POINT('Ctrl Pts',(26.0102991207387,-38.30871735846,0.));
#90204=CARTESIAN_POINT('Ctrl Pts',(26.0102991207387,-38.30871735846,20.));
#90205=CARTESIAN_POINT('Ctrl Pts',(25.9815704927901,-38.3246313459476,0.));
#90206=CARTESIAN_POINT('Ctrl Pts',(25.9815704927901,-38.3246313459476,20.));
#90207=CARTESIAN_POINT('Ctrl Pts',(25.9528316071847,-38.3405244950781,0.));
#90208=CARTESIAN_POINT('Ctrl Pts',(25.9528316071847,-38.3405244950781,20.));
#90209=CARTESIAN_POINT('Ctrl Pts',(25.9240824786908,-38.3563967986932,0.));
#90210=CARTESIAN_POINT('Ctrl Pts',(25.9240824786908,-38.3563967986932,20.));
#90211=CARTESIAN_POINT('Ctrl Pts',(25.8953231220827,-38.3722482496454,0.));
#90212=CARTESIAN_POINT('Ctrl Pts',(25.8953231220827,-38.3722482496454,20.));
#90213=CARTESIAN_POINT('Ctrl Pts',(25.8665535521392,-38.3880788407969,0.));
#90214=CARTESIAN_POINT('Ctrl Pts',(25.8665535521392,-38.3880788407969,20.));
#90215=CARTESIAN_POINT('Ctrl Pts',(25.8377737836446,-38.4038885650199,0.));
#90216=CARTESIAN_POINT('Ctrl Pts',(25.8377737836446,-38.4038885650199,20.));
#90217=CARTESIAN_POINT('Ctrl Pts',(25.8089838313888,-38.419677415197,0.));
#90218=CARTESIAN_POINT('Ctrl Pts',(25.8089838313888,-38.419677415197,20.));
#90219=CARTESIAN_POINT('Ctrl Pts',(25.7801837101667,-38.4354453842206,0.));
#90220=CARTESIAN_POINT('Ctrl Pts',(25.7801837101667,-38.4354453842206,20.));
#90221=CARTESIAN_POINT('Ctrl Pts',(25.7513734347795,-38.4511924649945,0.));
#90222=CARTESIAN_POINT('Ctrl Pts',(25.7513734347795,-38.4511924649945,20.));
#90223=CARTESIAN_POINT('Ctrl Pts',(25.7225530200331,-38.4669186504318,0.));
#90224=CARTESIAN_POINT('Ctrl Pts',(25.7225530200331,-38.4669186504318,20.));
#90225=CARTESIAN_POINT('Ctrl Pts',(25.6937224807392,-38.4826239334567,0.));
#90226=CARTESIAN_POINT('Ctrl Pts',(25.6937224807392,-38.4826239334567,20.));
#90227=CARTESIAN_POINT('Ctrl Pts',(25.6648818317151,-38.4983083070042,0.));
#90228=CARTESIAN_POINT('Ctrl Pts',(25.6648818317151,-38.4983083070042,20.));
#90229=CARTESIAN_POINT('Ctrl Pts',(25.6360310877836,-38.5139717640192,0.));
#90230=CARTESIAN_POINT('Ctrl Pts',(25.6360310877836,-38.5139717640192,20.));
#90231=CARTESIAN_POINT('Ctrl Pts',(25.6071702637723,-38.5296142974561,0.));
#90232=CARTESIAN_POINT('Ctrl Pts',(25.6071702637723,-38.5296142974561,20.));
#90233=CARTESIAN_POINT('Ctrl Pts',(25.5782993745137,-38.5452359002793,0.));
#90234=CARTESIAN_POINT('Ctrl Pts',(25.5782993745137,-38.5452359002793,20.));
#90235=CARTESIAN_POINT('Ctrl Pts',(25.5494184348456,-38.5608365654634,0.));
#90236=CARTESIAN_POINT('Ctrl Pts',(25.5494184348456,-38.5608365654634,20.));
#90237=CARTESIAN_POINT('Ctrl Pts',(25.5205274596115,-38.576416285994,0.));
#90238=CARTESIAN_POINT('Ctrl Pts',(25.5205274596115,-38.576416285994,20.));
#90239=CARTESIAN_POINT('Ctrl Pts',(25.4916264636604,-38.591975054867,0.));
#90240=CARTESIAN_POINT('Ctrl Pts',(25.4916264636604,-38.591975054867,20.));
#90241=CARTESIAN_POINT('Ctrl Pts',(25.462715461847,-38.6075128650891,0.));
#90242=CARTESIAN_POINT('Ctrl Pts',(25.462715461847,-38.6075128650891,20.));
#90243=CARTESIAN_POINT('Ctrl Pts',(25.4337944690316,-38.6230297096774,0.));
#90244=CARTESIAN_POINT('Ctrl Pts',(25.4337944690316,-38.6230297096774,20.));
#90245=CARTESIAN_POINT('Ctrl Pts',(25.4048635000794,-38.6385255816593,0.));
#90246=CARTESIAN_POINT('Ctrl Pts',(25.4048635000794,-38.6385255816593,20.));
#90247=CARTESIAN_POINT('Ctrl Pts',(25.3759225698613,-38.6540004740723,0.));
#90248=CARTESIAN_POINT('Ctrl Pts',(25.3759225698613,-38.6540004740723,20.));
#90249=CARTESIAN_POINT('Ctrl Pts',(25.3469716932528,-38.6694543799641,0.));
#90250=CARTESIAN_POINT('Ctrl Pts',(25.3469716932528,-38.6694543799641,20.));
#90251=CARTESIAN_POINT('Ctrl Pts',(25.318010885134,-38.6848872923919,0.));
#90252=CARTESIAN_POINT('Ctrl Pts',(25.318010885134,-38.6848872923919,20.));
#90253=CARTESIAN_POINT('Ctrl Pts',(25.2890401603912,-38.7002992044242,0.));
#90254=CARTESIAN_POINT('Ctrl Pts',(25.2890401603912,-38.7002992044242,20.));
#90255=CARTESIAN_POINT('Ctrl Pts',(25.2600595339159,-38.7156901091392,0.));
#90256=CARTESIAN_POINT('Ctrl Pts',(25.2600595339159,-38.7156901091392,20.));
#90257=CARTESIAN_POINT('Ctrl Pts',(25.2310690206049,-38.7310599996258,0.));
#90258=CARTESIAN_POINT('Ctrl Pts',(25.2310690206049,-38.7310599996258,20.));
#90259=CARTESIAN_POINT('Ctrl Pts',(25.2020686353608,-38.7464088689837,0.));
#90260=CARTESIAN_POINT('Ctrl Pts',(25.2020686353608,-38.7464088689837,20.));
#90261=CARTESIAN_POINT('Ctrl Pts',(25.1730583930911,-38.7617367103229,0.));
#90262=CARTESIAN_POINT('Ctrl Pts',(25.1730583930911,-38.7617367103229,20.));
#90263=CARTESIAN_POINT('Ctrl Pts',(25.1440383087084,-38.7770435167639,0.));
#90264=CARTESIAN_POINT('Ctrl Pts',(25.1440383087084,-38.7770435167639,20.));
#90265=CARTESIAN_POINT('Ctrl Pts',(25.1150083971302,-38.7923292814368,0.));
#90266=CARTESIAN_POINT('Ctrl Pts',(25.1150083971302,-38.7923292814368,20.));
#90267=CARTESIAN_POINT('Ctrl Pts',(25.0859686732794,-38.8075939974829,0.));
#90268=CARTESIAN_POINT('Ctrl Pts',(25.0859686732794,-38.8075939974829,20.));
#90269=CARTESIAN_POINT('Ctrl Pts',(25.0569191520845,-38.8228376580533,0.));
#90270=CARTESIAN_POINT('Ctrl Pts',(25.0569191520845,-38.8228376580533,20.));
#90271=CARTESIAN_POINT('Ctrl Pts',(25.0278598484791,-38.8380602563098,0.));
#90272=CARTESIAN_POINT('Ctrl Pts',(25.0278598484791,-38.8380602563098,20.));
#90273=CARTESIAN_POINT('Ctrl Pts',(24.9987907774025,-38.8532617854245,0.));
#90274=CARTESIAN_POINT('Ctrl Pts',(24.9987907774025,-38.8532617854245,20.));
#90275=CARTESIAN_POINT('Ctrl Pts',(24.9697119537988,-38.8684422385799,0.));
#90276=CARTESIAN_POINT('Ctrl Pts',(24.9697119537988,-38.8684422385799,20.));
#90277=CARTESIAN_POINT('Ctrl Pts',(24.9406233926168,-38.883601608968,0.));
#90278=CARTESIAN_POINT('Ctrl Pts',(24.9406233926168,-38.883601608968,20.));
#90279=CARTESIAN_POINT('Ctrl Pts',(24.9115251088107,-38.8987398897918,0.));
#90280=CARTESIAN_POINT('Ctrl Pts',(24.9115251088107,-38.8987398897918,20.));
#90281=CARTESIAN_POINT('Ctrl Pts',(24.8824171173401,-38.9138570742648,0.));
#90282=CARTESIAN_POINT('Ctrl Pts',(24.8824171173401,-38.9138570742648,20.));
#90283=CARTESIAN_POINT('Ctrl Pts',(24.8532994331703,-38.9289531556118,0.));
#90284=CARTESIAN_POINT('Ctrl Pts',(24.8532994331703,-38.9289531556118,20.));
#90285=CARTESIAN_POINT('Ctrl Pts',(24.8241720712716,-38.9440281270684,0.));
#90286=CARTESIAN_POINT('Ctrl Pts',(24.8241720712716,-38.9440281270684,20.));
#90287=CARTESIAN_POINT('Ctrl Pts',(24.7950350466188,-38.9590819818798,0.));
#90288=CARTESIAN_POINT('Ctrl Pts',(24.7950350466188,-38.9590819818798,20.));
#90289=CARTESIAN_POINT('Ctrl Pts',(24.7658883741919,-38.9741147133012,0.));
#90290=CARTESIAN_POINT('Ctrl Pts',(24.7658883741919,-38.9741147133012,20.));
#90291=CARTESIAN_POINT('Ctrl Pts',(24.736732068976,-38.989126314598,0.));
#90292=CARTESIAN_POINT('Ctrl Pts',(24.736732068976,-38.989126314598,20.));
#90293=CARTESIAN_POINT('Ctrl Pts',(24.7075661459616,-39.0041167790461,0.));
#90294=CARTESIAN_POINT('Ctrl Pts',(24.7075661459616,-39.0041167790461,20.));
#90295=CARTESIAN_POINT('Ctrl Pts',(24.6783906201452,-39.019086099931,0.));
#90296=CARTESIAN_POINT('Ctrl Pts',(24.6783906201452,-39.019086099931,20.));
#90297=CARTESIAN_POINT('Ctrl Pts',(24.6492055065285,-39.0340342705498,0.));
#90298=CARTESIAN_POINT('Ctrl Pts',(24.6492055065285,-39.0340342705498,20.));
#90299=CARTESIAN_POINT('Ctrl Pts',(24.6200108201182,-39.0489612842096,0.));
#90300=CARTESIAN_POINT('Ctrl Pts',(24.6200108201182,-39.0489612842096,20.));
#90301=CARTESIAN_POINT('Ctrl Pts',(24.5908065759258,-39.0638671342286,0.));
#90302=CARTESIAN_POINT('Ctrl Pts',(24.5908065759258,-39.0638671342286,20.));
#90303=CARTESIAN_POINT('Ctrl Pts',(24.5615927889669,-39.0787518139362,0.));
#90304=CARTESIAN_POINT('Ctrl Pts',(24.5615927889669,-39.0787518139362,20.));
#90305=CARTESIAN_POINT('Ctrl Pts',(24.5323694742616,-39.0936153166722,0.));
#90306=CARTESIAN_POINT('Ctrl Pts',(24.5323694742616,-39.0936153166722,20.));
#90307=CARTESIAN_POINT('Ctrl Pts',(24.5031366468345,-39.1084576357872,0.));
#90308=CARTESIAN_POINT('Ctrl Pts',(24.5031366468345,-39.1084576357872,20.));
#90309=CARTESIAN_POINT('Ctrl Pts',(24.4738943217155,-39.1232787646414,0.));
#90310=CARTESIAN_POINT('Ctrl Pts',(24.4738943217155,-39.1232787646414,20.));
#90311=CARTESIAN_POINT('Ctrl Pts',(24.4446425139409,-39.1380786966047,0.));
#90312=CARTESIAN_POINT('Ctrl Pts',(24.4446425139409,-39.1380786966047,20.));
#90313=CARTESIAN_POINT('Ctrl Pts',(24.4153812385543,-39.1528574250569,0.));
#90314=CARTESIAN_POINT('Ctrl Pts',(24.4153812385543,-39.1528574250569,20.));
#90315=CARTESIAN_POINT('Ctrl Pts',(24.3861105106067,-39.1676149433869,0.));
#90316=CARTESIAN_POINT('Ctrl Pts',(24.3861105106067,-39.1676149433869,20.));
#90317=CARTESIAN_POINT('Ctrl Pts',(24.3568303451549,-39.1823512449951,0.));
#90318=CARTESIAN_POINT('Ctrl Pts',(24.3568303451549,-39.1823512449951,20.));
#90319=CARTESIAN_POINT('Ctrl Pts',(24.3275407572587,-39.197066323292,0.));
#90320=CARTESIAN_POINT('Ctrl Pts',(24.3275407572587,-39.197066323292,20.));
#90321=CARTESIAN_POINT('Ctrl Pts',(24.2982417619806,-39.2117601717005,0.));
#90322=CARTESIAN_POINT('Ctrl Pts',(24.2982417619806,-39.2117601717005,20.));
#90323=CARTESIAN_POINT('Ctrl Pts',(24.2689333743822,-39.2264327836562,0.));
#90324=CARTESIAN_POINT('Ctrl Pts',(24.2689333743822,-39.2264327836562,20.));
#90325=CARTESIAN_POINT('Ctrl Pts',(24.239615609526,-39.2410841526078,0.));
#90326=CARTESIAN_POINT('Ctrl Pts',(24.239615609526,-39.2410841526078,20.));
#90327=CARTESIAN_POINT('Ctrl Pts',(24.2102884824784,-39.2557142720138,0.));
#90328=CARTESIAN_POINT('Ctrl Pts',(24.2102884824784,-39.2557142720138,20.));
#90329=CARTESIAN_POINT('Ctrl Pts',(24.1809520083146,-39.2703231353422,0.));
#90330=CARTESIAN_POINT('Ctrl Pts',(24.1809520083146,-39.2703231353422,20.));
#90331=CARTESIAN_POINT('Ctrl Pts',(24.1516062021224,-39.2849107360681,0.));
#90332=CARTESIAN_POINT('Ctrl Pts',(24.1516062021224,-39.2849107360681,20.));
#90333=CARTESIAN_POINT('Ctrl Pts',(24.1222510790066,-39.2994770676712,0.));
#90334=CARTESIAN_POINT('Ctrl Pts',(24.1222510790066,-39.2994770676712,20.));
#90335=CARTESIAN_POINT('Ctrl Pts',(24.0928866540881,-39.3140221236369,0.));
#90336=CARTESIAN_POINT('Ctrl Pts',(24.0928866540881,-39.3140221236369,20.));
#90337=CARTESIAN_POINT('Ctrl Pts',(24.0635129424931,-39.3285458974613,0.));
#90338=CARTESIAN_POINT('Ctrl Pts',(24.0635129424931,-39.3285458974613,20.));
#90339=CARTESIAN_POINT('Ctrl Pts',(24.0341299593437,-39.3430483826555,0.));
#90340=CARTESIAN_POINT('Ctrl Pts',(24.0341299593437,-39.3430483826555,20.));
#90341=CARTESIAN_POINT('Ctrl Pts',(24.0047377197503,-39.3575295727493,0.));
#90342=CARTESIAN_POINT('Ctrl Pts',(24.0047377197503,-39.3575295727493,20.));
#90343=CARTESIAN_POINT('Ctrl Pts',(23.9753362387978,-39.3719894612957,0.));
#90344=CARTESIAN_POINT('Ctrl Pts',(23.9753362387978,-39.3719894612957,20.));
#90345=CARTESIAN_POINT('Ctrl Pts',(23.9459255315518,-39.3864280418676,0.));
#90346=CARTESIAN_POINT('Ctrl Pts',(23.9459255315518,-39.3864280418676,20.));
#90347=CARTESIAN_POINT('Ctrl Pts',(23.9165056130837,-39.4008453080481,0.));
#90348=CARTESIAN_POINT('Ctrl Pts',(23.9165056130837,-39.4008453080481,20.));
#90349=CARTESIAN_POINT('Ctrl Pts',(23.8870764984925,-39.4152412534209,0.));
#90350=CARTESIAN_POINT('Ctrl Pts',(23.8870764984925,-39.4152412534209,20.));
#90351=CARTESIAN_POINT('Ctrl Pts',(23.8576382029237,-39.4296158715627,0.));
#90352=CARTESIAN_POINT('Ctrl Pts',(23.8576382029237,-39.4296158715627,20.));
#90353=CARTESIAN_POINT('Ctrl Pts',(23.8281907416004,-39.4439691560298,0.));
#90354=CARTESIAN_POINT('Ctrl Pts',(23.8281907416004,-39.4439691560298,20.));
#90355=CARTESIAN_POINT('Ctrl Pts',(23.7987341298022,-39.4583011003674,0.));
#90356=CARTESIAN_POINT('Ctrl Pts',(23.7987341298022,-39.4583011003674,20.));
#90357=CARTESIAN_POINT('Ctrl Pts',(23.769268382808,-39.4726116981337,0.));
#90358=CARTESIAN_POINT('Ctrl Pts',(23.769268382808,-39.4726116981337,20.));
#90359=CARTESIAN_POINT('Ctrl Pts',(23.7397935158457,-39.4869009429217,0.));
#90360=CARTESIAN_POINT('Ctrl Pts',(23.7397935158457,-39.4869009429217,20.));
#90361=CARTESIAN_POINT('Ctrl Pts',(23.7103095440476,-39.5011688283778,0.));
#90362=CARTESIAN_POINT('Ctrl Pts',(23.7103095440476,-39.5011688283778,20.));
#90363=CARTESIAN_POINT('Ctrl Pts',(23.6808164823786,-39.5154153482324,0.));
#90364=CARTESIAN_POINT('Ctrl Pts',(23.6808164823786,-39.5154153482324,20.));
#90365=CARTESIAN_POINT('Ctrl Pts',(23.651314345698,-39.5296404962722,0.));
#90366=CARTESIAN_POINT('Ctrl Pts',(23.651314345698,-39.5296404962722,20.));
#90367=CARTESIAN_POINT('Ctrl Pts',(23.6218031488904,-39.5438442662853,0.));
#90368=CARTESIAN_POINT('Ctrl Pts',(23.6218031488904,-39.5438442662853,20.));
#90369=CARTESIAN_POINT('Ctrl Pts',(23.5922829069852,-39.5580266520107,0.));
#90370=CARTESIAN_POINT('Ctrl Pts',(23.5922829069852,-39.5580266520107,20.));
#90371=CARTESIAN_POINT('Ctrl Pts',(23.5627536352592,-39.5721876470956,0.));
#90372=CARTESIAN_POINT('Ctrl Pts',(23.5627536352592,-39.5721876470956,20.));
#90373=CARTESIAN_POINT('Ctrl Pts',(23.5332153494019,-39.5863272450268,0.));
#90374=CARTESIAN_POINT('Ctrl Pts',(23.5332153494019,-39.5863272450268,20.));
#90375=CARTESIAN_POINT('Ctrl Pts',(23.5036680653391,-39.6004454392038,0.));
#90376=CARTESIAN_POINT('Ctrl Pts',(23.5036680653391,-39.6004454392038,20.));
#90377=CARTESIAN_POINT('Ctrl Pts',(23.4741117989348,-39.6145422230651,0.));
#90378=CARTESIAN_POINT('Ctrl Pts',(23.4741117989348,-39.6145422230651,20.));
#90379=CARTESIAN_POINT('Ctrl Pts',(23.4445465657147,-39.6286175902046,0.));
#90380=CARTESIAN_POINT('Ctrl Pts',(23.4445465657147,-39.6286175902046,20.));
#90381=CARTESIAN_POINT('Ctrl Pts',(23.414972380622,-39.6426715344742,0.));
#90382=CARTESIAN_POINT('Ctrl Pts',(23.414972380622,-39.6426715344742,20.));
#90383=CARTESIAN_POINT('Ctrl Pts',(23.385389257652,-39.6567040501382,0.));
#90384=CARTESIAN_POINT('Ctrl Pts',(23.385389257652,-39.6567040501382,20.));
#90385=CARTESIAN_POINT('Ctrl Pts',(23.3557972103217,-39.6707151316771,0.));
#90386=CARTESIAN_POINT('Ctrl Pts',(23.3557972103217,-39.6707151316771,20.));
#90387=CARTESIAN_POINT('Ctrl Pts',(23.3261962523444,-39.6847047735001,0.));
#90388=CARTESIAN_POINT('Ctrl Pts',(23.3261962523444,-39.6847047735001,20.));
#90389=CARTESIAN_POINT('Ctrl Pts',(23.2965863982648,-39.6986729696788,0.));
#90390=CARTESIAN_POINT('Ctrl Pts',(23.2965863982648,-39.6986729696788,20.));
#90391=CARTESIAN_POINT('Ctrl Pts',(23.2669676640418,-39.7126197136991,0.));
#90392=CARTESIAN_POINT('Ctrl Pts',(23.2669676640418,-39.7126197136991,20.));
#90393=CARTESIAN_POINT('Ctrl Pts',(23.2373400678346,-39.7265449981305,0.));
#90394=CARTESIAN_POINT('Ctrl Pts',(23.2373400678346,-39.7265449981305,20.));
#90395=CARTESIAN_POINT('Ctrl Pts',(23.2077036288597,-39.7404488151086,0.));
#90396=CARTESIAN_POINT('Ctrl Pts',(23.2077036288597,-39.7404488151086,20.));
#90397=CARTESIAN_POINT('Ctrl Pts',(23.1780583659508,-39.7543311569459,0.));
#90398=CARTESIAN_POINT('Ctrl Pts',(23.1780583659508,-39.7543311569459,20.));
#90399=CARTESIAN_POINT('Ctrl Pts',(23.1484042962029,-39.7681920167058,0.));
#90400=CARTESIAN_POINT('Ctrl Pts',(23.1484042962029,-39.7681920167058,20.));
#90401=CARTESIAN_POINT('Ctrl Pts',(23.118741433625,-39.7820313887737,0.));
#90402=CARTESIAN_POINT('Ctrl Pts',(23.118741433625,-39.7820313887737,20.));
#90403=CARTESIAN_POINT('Ctrl Pts',(23.089069787673,-39.7958492694787,0.));
#90404=CARTESIAN_POINT('Ctrl Pts',(23.089069787673,-39.7958492694787,20.));
#90405=CARTESIAN_POINT('Ctrl Pts',(23.0593893640427,-39.8096456567259,0.));
#90406=CARTESIAN_POINT('Ctrl Pts',(23.0593893640427,-39.8096456567259,20.));
#90407=CARTESIAN_POINT('Ctrl Pts',(23.0356380053138,-39.8206655709904,0.));
#90408=CARTESIAN_POINT('Ctrl Pts',(23.0356380053138,-39.8206655709904,20.));
#90409=CARTESIAN_POINT('Ctrl Pts',(23.0178205380655,-39.8289208340947,0.));
#90410=CARTESIAN_POINT('Ctrl Pts',(23.0178205380655,-39.8289208340947,20.));
#90411=CARTESIAN_POINT('Ctrl Pts',(23.0059404718139,-39.8344200439082,0.));
#90412=CARTESIAN_POINT('Ctrl Pts',(23.0059404718139,-39.8344200439082,20.));
#90413=CARTESIAN_POINT('Ctrl Pts',(23.,-39.8371685740842,0.));
#90414=CARTESIAN_POINT('Ctrl Pts',(23.,-39.8371685740842,20.));
#90415=CARTESIAN_POINT('Origin',(43.2258605561518,-15.7329265929808,0.));
#90416=CARTESIAN_POINT('',(44.1555553153094,-16.0713078122675,0.));
#90417=CARTESIAN_POINT('Origin',(44.4975754586351,-15.1316151914816,0.));
#90418=CARTESIAN_POINT('',(43.5508185339833,-14.8096659320883,0.));
#90419=CARTESIAN_POINT('Origin',(1.83021655258307E-13,-3.27857114887026E-14,
0.));
#90420=CARTESIAN_POINT('',(46.,0.,0.));
#90421=CARTESIAN_POINT('Ctrl Pts',(37.5361777128299,31.4965928746404,0.));
#90422=CARTESIAN_POINT('Ctrl Pts',(37.5361777128299,31.4965928746404,20.));
#90423=CARTESIAN_POINT('Ctrl Pts',(37.5400435810124,31.4910366171629,0.));
#90424=CARTESIAN_POINT('Ctrl Pts',(37.5400435810124,31.4910366171629,20.));
#90425=CARTESIAN_POINT('Ctrl Pts',(37.5477733397938,31.4799228688318,0.));
#90426=CARTESIAN_POINT('Ctrl Pts',(37.5477733397938,31.4799228688318,20.));
#90427=CARTESIAN_POINT('Ctrl Pts',(37.5593620452151,31.4632485462068,0.));
#90428=CARTESIAN_POINT('Ctrl Pts',(37.5593620452151,31.4632485462068,20.));
#90429=CARTESIAN_POINT('Ctrl Pts',(37.574801786924,31.4410087157717,0.));
#90430=CARTESIAN_POINT('Ctrl Pts',(37.574801786924,31.4410087157717,20.));
#90431=CARTESIAN_POINT('Ctrl Pts',(37.5940816876034,31.4131965946731,0.));
#90432=CARTESIAN_POINT('Ctrl Pts',(37.5940816876034,31.4131965946731,20.));
#90433=CARTESIAN_POINT('Ctrl Pts',(37.6133418102375,31.3853721428083,0.));
#90434=CARTESIAN_POINT('Ctrl Pts',(37.6133418102375,31.3853721428083,20.));
#90435=CARTESIAN_POINT('Ctrl Pts',(37.6325821517747,31.3575353648538,0.));
#90436=CARTESIAN_POINT('Ctrl Pts',(37.6325821517747,31.3575353648538,20.));
#90437=CARTESIAN_POINT('Ctrl Pts',(37.6518027072643,31.3296862686536,0.));
#90438=CARTESIAN_POINT('Ctrl Pts',(37.6518027072643,31.3296862686536,20.));
#90439=CARTESIAN_POINT('Ctrl Pts',(37.6710034693473,31.3018248661211,0.));
#90440=CARTESIAN_POINT('Ctrl Pts',(37.6710034693473,31.3018248661211,20.));
#90441=CARTESIAN_POINT('Ctrl Pts',(37.6901844288974,31.2739511721649,0.));
#90442=CARTESIAN_POINT('Ctrl Pts',(37.6901844288974,31.2739511721649,20.));
#90443=CARTESIAN_POINT('Ctrl Pts',(37.7093455757381,31.2460652034827,0.));
#90444=CARTESIAN_POINT('Ctrl Pts',(37.7093455757381,31.2460652034827,20.));
#90445=CARTESIAN_POINT('Ctrl Pts',(37.7284868993471,31.2181669773772,0.));
#90446=CARTESIAN_POINT('Ctrl Pts',(37.7284868993471,31.2181669773772,20.));
#90447=CARTESIAN_POINT('Ctrl Pts',(37.7476083895316,31.1902565106222,0.));
#90448=CARTESIAN_POINT('Ctrl Pts',(37.7476083895316,31.1902565106222,20.));
#90449=CARTESIAN_POINT('Ctrl Pts',(37.7667100372089,31.1623338181506,0.));
#90450=CARTESIAN_POINT('Ctrl Pts',(37.7667100372089,31.1623338181506,20.));
#90451=CARTESIAN_POINT('Ctrl Pts',(37.7857918342009,31.1343989133989,0.));
#90452=CARTESIAN_POINT('Ctrl Pts',(37.7857918342009,31.1343989133989,20.));
#90453=CARTESIAN_POINT('Ctrl Pts',(37.8048537728749,31.1064518089103,0.));
#90454=CARTESIAN_POINT('Ctrl Pts',(37.8048537728749,31.1064518089103,20.));
#90455=CARTESIAN_POINT('Ctrl Pts',(37.8238958458276,31.0784925168637,0.));
#90456=CARTESIAN_POINT('Ctrl Pts',(37.8238958458276,31.0784925168637,20.));
#90457=CARTESIAN_POINT('Ctrl Pts',(37.8429180455734,31.0505210495984,0.));
#90458=CARTESIAN_POINT('Ctrl Pts',(37.8429180455734,31.0505210495984,20.));
#90459=CARTESIAN_POINT('Ctrl Pts',(37.861920364175,31.0225374202321,0.));
#90460=CARTESIAN_POINT('Ctrl Pts',(37.861920364175,31.0225374202321,20.));
#90461=CARTESIAN_POINT('Ctrl Pts',(37.8809027932971,30.9945416425721,0.));
#90462=CARTESIAN_POINT('Ctrl Pts',(37.8809027932971,30.9945416425721,20.));
#90463=CARTESIAN_POINT('Ctrl Pts',(37.8998653243731,30.9665337308352,0.));
#90464=CARTESIAN_POINT('Ctrl Pts',(37.8998653243731,30.9665337308352,20.));
#90465=CARTESIAN_POINT('Ctrl Pts',(37.9188079487378,30.9385136994261,0.));
#90466=CARTESIAN_POINT('Ctrl Pts',(37.9188079487378,30.9385136994261,20.));
#90467=CARTESIAN_POINT('Ctrl Pts',(37.9377306577632,30.9104815627079,0.));
#90468=CARTESIAN_POINT('Ctrl Pts',(37.9377306577632,30.9104815627079,20.));
#90469=CARTESIAN_POINT('Ctrl Pts',(37.9566334430211,30.882437334731,0.));
#90470=CARTESIAN_POINT('Ctrl Pts',(37.9566334430211,30.882437334731,20.));
#90471=CARTESIAN_POINT('Ctrl Pts',(37.9755162962752,30.8543810292446,0.));
#90472=CARTESIAN_POINT('Ctrl Pts',(37.9755162962752,30.8543810292446,20.));
#90473=CARTESIAN_POINT('Ctrl Pts',(37.9943792094053,30.8263126598247,0.));
#90474=CARTESIAN_POINT('Ctrl Pts',(37.9943792094053,30.8263126598247,20.));
#90475=CARTESIAN_POINT('Ctrl Pts',(38.0132221743517,30.7982322399668,0.));
#90476=CARTESIAN_POINT('Ctrl Pts',(38.0132221743517,30.7982322399668,20.));
#90477=CARTESIAN_POINT('Ctrl Pts',(38.0320451830565,30.7701397831859,0.));
#90478=CARTESIAN_POINT('Ctrl Pts',(38.0320451830565,30.7701397831859,20.));
#90479=CARTESIAN_POINT('Ctrl Pts',(38.0508482273931,30.7420353031339,0.));
#90480=CARTESIAN_POINT('Ctrl Pts',(38.0508482273931,30.7420353031339,20.));
#90481=CARTESIAN_POINT('Ctrl Pts',(38.0696312991626,30.7139188136053,0.));
#90482=CARTESIAN_POINT('Ctrl Pts',(38.0696312991626,30.7139188136053,20.));
#90483=CARTESIAN_POINT('Ctrl Pts',(38.088394390128,30.6857903284809,0.));
#90484=CARTESIAN_POINT('Ctrl Pts',(38.088394390128,30.6857903284809,20.));
#90485=CARTESIAN_POINT('Ctrl Pts',(38.1071374920373,30.6576498616875,0.));
#90486=CARTESIAN_POINT('Ctrl Pts',(38.1071374920373,30.6576498616875,20.));
#90487=CARTESIAN_POINT('Ctrl Pts',(38.125860596649,30.6294974271553,0.));
#90488=CARTESIAN_POINT('Ctrl Pts',(38.125860596649,30.6294974271553,20.));
#90489=CARTESIAN_POINT('Ctrl Pts',(38.1445636957629,30.6013330387675,0.));
#90490=CARTESIAN_POINT('Ctrl Pts',(38.1445636957629,30.6013330387675,20.));
#90491=CARTESIAN_POINT('Ctrl Pts',(38.1632467812242,30.5731567103519,0.));
#90492=CARTESIAN_POINT('Ctrl Pts',(38.1632467812242,30.5731567103519,20.));
#90493=CARTESIAN_POINT('Ctrl Pts',(38.1819098449085,30.5449684557073,0.));
#90494=CARTESIAN_POINT('Ctrl Pts',(38.1819098449085,30.5449684557073,20.));
#90495=CARTESIAN_POINT('Ctrl Pts',(38.2005528787125,30.5167682886194,0.));
#90496=CARTESIAN_POINT('Ctrl Pts',(38.2005528787125,30.5167682886194,20.));
#90497=CARTESIAN_POINT('Ctrl Pts',(38.2191758745422,30.4885562228796,0.));
#90498=CARTESIAN_POINT('Ctrl Pts',(38.2191758745422,30.4885562228796,20.));
#90499=CARTESIAN_POINT('Ctrl Pts',(38.2377788243005,30.460332272307,0.));
#90500=CARTESIAN_POINT('Ctrl Pts',(38.2377788243005,30.460332272307,20.));
#90501=CARTESIAN_POINT('Ctrl Pts',(38.2563617198829,30.4320964507535,0.));
#90502=CARTESIAN_POINT('Ctrl Pts',(38.2563617198829,30.4320964507535,20.));
#90503=CARTESIAN_POINT('Ctrl Pts',(38.2749245531853,30.4038487720928,0.));
#90504=CARTESIAN_POINT('Ctrl Pts',(38.2749245531853,30.4038487720928,20.));
#90505=CARTESIAN_POINT('Ctrl Pts',(38.2934673161074,30.3755892502132,0.));
#90506=CARTESIAN_POINT('Ctrl Pts',(38.2934673161074,30.3755892502132,20.));
#90507=CARTESIAN_POINT('Ctrl Pts',(38.3119900005578,30.3473178990095,0.));
#90508=CARTESIAN_POINT('Ctrl Pts',(38.3119900005578,30.3473178990095,20.));
#90509=CARTESIAN_POINT('Ctrl Pts',(38.3304925984593,30.3190347323738,0.));
#90510=CARTESIAN_POINT('Ctrl Pts',(38.3304925984593,30.3190347323738,20.));
#90511=CARTESIAN_POINT('Ctrl Pts',(38.3489751017513,30.2907397641919,0.));
#90512=CARTESIAN_POINT('Ctrl Pts',(38.3489751017513,30.2907397641919,20.));
#90513=CARTESIAN_POINT('Ctrl Pts',(38.3674375023871,30.2624330083488,0.));
#90514=CARTESIAN_POINT('Ctrl Pts',(38.3674375023871,30.2624330083488,20.));
#90515=CARTESIAN_POINT('Ctrl Pts',(38.3858797923318,30.2341144787313,0.));
#90516=CARTESIAN_POINT('Ctrl Pts',(38.3858797923318,30.2341144787313,20.));
#90517=CARTESIAN_POINT('Ctrl Pts',(38.4043019635603,30.2057841892317,0.));
#90518=CARTESIAN_POINT('Ctrl Pts',(38.4043019635603,30.2057841892317,20.));
#90519=CARTESIAN_POINT('Ctrl Pts',(38.4227040080549,30.1774421537519,0.));
#90520=CARTESIAN_POINT('Ctrl Pts',(38.4227040080549,30.1774421537519,20.));
#90521=CARTESIAN_POINT('Ctrl Pts',(38.4410859178038,30.1490883862047,0.));
#90522=CARTESIAN_POINT('Ctrl Pts',(38.4410859178038,30.1490883862047,20.));
#90523=CARTESIAN_POINT('Ctrl Pts',(38.4594476848032,30.1207229005118,0.));
#90524=CARTESIAN_POINT('Ctrl Pts',(38.4594476848032,30.1207229005118,20.));
#90525=CARTESIAN_POINT('Ctrl Pts',(38.4777893010568,30.0923457106027,0.));
#90526=CARTESIAN_POINT('Ctrl Pts',(38.4777893010568,30.0923457106027,20.));
#90527=CARTESIAN_POINT('Ctrl Pts',(38.4961107585777,30.0639568304126,0.));
#90528=CARTESIAN_POINT('Ctrl Pts',(38.4961107585777,30.0639568304126,20.));
#90529=CARTESIAN_POINT('Ctrl Pts',(38.5144120493894,30.0355562738816,0.));
#90530=CARTESIAN_POINT('Ctrl Pts',(38.5144120493894,30.0355562738816,20.));
#90531=CARTESIAN_POINT('Ctrl Pts',(38.532693165526,30.0071440549534,0.));
#90532=CARTESIAN_POINT('Ctrl Pts',(38.532693165526,30.0071440549534,20.));
#90533=CARTESIAN_POINT('Ctrl Pts',(38.5509540990321,29.978720187576,0.));
#90534=CARTESIAN_POINT('Ctrl Pts',(38.5509540990321,29.978720187576,20.));
#90535=CARTESIAN_POINT('Ctrl Pts',(38.5691948419622,29.9502846857025,0.));
#90536=CARTESIAN_POINT('Ctrl Pts',(38.5691948419622,29.9502846857025,20.));
#90537=CARTESIAN_POINT('Ctrl Pts',(38.5874153863803,29.9218375632918,0.));
#90538=CARTESIAN_POINT('Ctrl Pts',(38.5874153863803,29.9218375632918,20.));
#90539=CARTESIAN_POINT('Ctrl Pts',(38.6056157243597,29.8933788343089,0.));
#90540=CARTESIAN_POINT('Ctrl Pts',(38.6056157243597,29.8933788343089,20.));
#90541=CARTESIAN_POINT('Ctrl Pts',(38.6237958479822,29.864908512726,0.));
#90542=CARTESIAN_POINT('Ctrl Pts',(38.6237958479822,29.864908512726,20.));
#90543=CARTESIAN_POINT('Ctrl Pts',(38.6419557493389,29.8364266125215,0.));
#90544=CARTESIAN_POINT('Ctrl Pts',(38.6419557493389,29.8364266125215,20.));
#90545=CARTESIAN_POINT('Ctrl Pts',(38.66009542053,29.8079331476799,0.));
#90546=CARTESIAN_POINT('Ctrl Pts',(38.66009542053,29.8079331476799,20.));
#90547=CARTESIAN_POINT('Ctrl Pts',(38.6782148536649,29.7794281321916,0.));
#90548=CARTESIAN_POINT('Ctrl Pts',(38.6782148536649,29.7794281321916,20.));
#90549=CARTESIAN_POINT('Ctrl Pts',(38.6963140408627,29.7509115800524,0.));
#90550=CARTESIAN_POINT('Ctrl Pts',(38.6963140408627,29.7509115800524,20.));
#90551=CARTESIAN_POINT('Ctrl Pts',(38.7143929742521,29.7223835052637,0.));
#90552=CARTESIAN_POINT('Ctrl Pts',(38.7143929742521,29.7223835052637,20.));
#90553=CARTESIAN_POINT('Ctrl Pts',(38.7324516459718,29.6938439218325,0.));
#90554=CARTESIAN_POINT('Ctrl Pts',(38.7324516459718,29.6938439218325,20.));
#90555=CARTESIAN_POINT('Ctrl Pts',(38.7504900481697,29.6652928437714,0.));
#90556=CARTESIAN_POINT('Ctrl Pts',(38.7504900481697,29.6652928437714,20.));
#90557=CARTESIAN_POINT('Ctrl Pts',(38.7685081730036,29.6367302850988,0.));
#90558=CARTESIAN_POINT('Ctrl Pts',(38.7685081730036,29.6367302850988,20.));
#90559=CARTESIAN_POINT('Ctrl Pts',(38.7865060126402,29.6081562598384,0.));
#90560=CARTESIAN_POINT('Ctrl Pts',(38.7865060126402,29.6081562598384,20.));
#90561=CARTESIAN_POINT('Ctrl Pts',(38.8044835592559,29.5795707820205,0.));
#90562=CARTESIAN_POINT('Ctrl Pts',(38.8044835592559,29.5795707820205,20.));
#90563=CARTESIAN_POINT('Ctrl Pts',(38.8224408050366,29.5509738656807,0.));
#90564=CARTESIAN_POINT('Ctrl Pts',(38.8224408050366,29.5509738656807,20.));
#90565=CARTESIAN_POINT('Ctrl Pts',(38.8403777421773,29.5223655248609,0.));
#90566=CARTESIAN_POINT('Ctrl Pts',(38.8403777421773,29.5223655248609,20.));
#90567=CARTESIAN_POINT('Ctrl Pts',(38.8582943628826,29.4937457736083,0.));
#90568=CARTESIAN_POINT('Ctrl Pts',(38.8582943628826,29.4937457736083,20.));
#90569=CARTESIAN_POINT('Ctrl Pts',(38.8761906593666,29.4651146259764,0.));
#90570=CARTESIAN_POINT('Ctrl Pts',(38.8761906593666,29.4651146259764,20.));
#90571=CARTESIAN_POINT('Ctrl Pts',(38.8940666238532,29.4364720960241,0.));
#90572=CARTESIAN_POINT('Ctrl Pts',(38.8940666238532,29.4364720960241,20.));
#90573=CARTESIAN_POINT('Ctrl Pts',(38.9119222485755,29.4078181978158,0.));
#90574=CARTESIAN_POINT('Ctrl Pts',(38.9119222485755,29.4078181978158,20.));
#90575=CARTESIAN_POINT('Ctrl Pts',(38.9297575257761,29.3791529454216,0.));
#90576=CARTESIAN_POINT('Ctrl Pts',(38.9297575257761,29.3791529454216,20.));
#90577=CARTESIAN_POINT('Ctrl Pts',(38.9475724477072,29.3504763529173,0.));
#90578=CARTESIAN_POINT('Ctrl Pts',(38.9475724477072,29.3504763529173,20.));
#90579=CARTESIAN_POINT('Ctrl Pts',(38.9653670066308,29.3217884343845,0.));
#90580=CARTESIAN_POINT('Ctrl Pts',(38.9653670066308,29.3217884343845,20.));
#90581=CARTESIAN_POINT('Ctrl Pts',(38.9831411948182,29.2930892039104,0.));
#90582=CARTESIAN_POINT('Ctrl Pts',(38.9831411948182,29.2930892039104,20.));
#90583=CARTESIAN_POINT('Ctrl Pts',(39.0008950045502,29.2643786755883,0.));
#90584=CARTESIAN_POINT('Ctrl Pts',(39.0008950045502,29.2643786755883,20.));
#90585=CARTESIAN_POINT('Ctrl Pts',(39.0186284281173,29.2356568635168,0.));
#90586=CARTESIAN_POINT('Ctrl Pts',(39.0186284281173,29.2356568635168,20.));
#90587=CARTESIAN_POINT('Ctrl Pts',(39.0363414578191,29.2069237818005,0.));
#90588=CARTESIAN_POINT('Ctrl Pts',(39.0363414578191,29.2069237818005,20.));
#90589=CARTESIAN_POINT('Ctrl Pts',(39.054034085965,29.1781794445493,0.));
#90590=CARTESIAN_POINT('Ctrl Pts',(39.054034085965,29.1781794445493,20.));
#90591=CARTESIAN_POINT('Ctrl Pts',(39.0717063048737,29.1494238658788,0.));
#90592=CARTESIAN_POINT('Ctrl Pts',(39.0717063048737,29.1494238658788,20.));
#90593=CARTESIAN_POINT('Ctrl Pts',(39.0893581068737,29.1206570599103,0.));
#90594=CARTESIAN_POINT('Ctrl Pts',(39.0893581068737,29.1206570599103,20.));
#90595=CARTESIAN_POINT('Ctrl Pts',(39.106989484303,29.0918790407708,0.));
#90596=CARTESIAN_POINT('Ctrl Pts',(39.106989484303,29.0918790407708,20.));
#90597=CARTESIAN_POINT('Ctrl Pts',(39.1246004295092,29.0630898225929,0.));
#90598=CARTESIAN_POINT('Ctrl Pts',(39.1246004295092,29.0630898225929,20.));
#90599=CARTESIAN_POINT('Ctrl Pts',(39.1421909348497,29.034289419515,0.));
#90600=CARTESIAN_POINT('Ctrl Pts',(39.1421909348497,29.034289419515,20.));
#90601=CARTESIAN_POINT('Ctrl Pts',(39.1597609926911,29.0054778456813,0.));
#90602=CARTESIAN_POINT('Ctrl Pts',(39.1597609926911,29.0054778456813,20.));
#90603=CARTESIAN_POINT('Ctrl Pts',(39.1773105954099,28.9766551152413,0.));
#90604=CARTESIAN_POINT('Ctrl Pts',(39.1773105954099,28.9766551152413,20.));
#90605=CARTESIAN_POINT('Ctrl Pts',(39.1948397353916,28.9478212423503,0.));
#90606=CARTESIAN_POINT('Ctrl Pts',(39.1948397353916,28.9478212423503,20.));
#90607=CARTESIAN_POINT('Ctrl Pts',(39.2123484050317,28.9189762411689,0.));
#90608=CARTESIAN_POINT('Ctrl Pts',(39.2123484050317,28.9189762411689,20.));
#90609=CARTESIAN_POINT('Ctrl Pts',(39.2298365967351,28.8901201258634,0.));
#90610=CARTESIAN_POINT('Ctrl Pts',(39.2298365967351,28.8901201258634,20.));
#90611=CARTESIAN_POINT('Ctrl Pts',(39.2473043029163,28.8612529106058,0.));
#90612=CARTESIAN_POINT('Ctrl Pts',(39.2473043029163,28.8612529106058,20.));
#90613=CARTESIAN_POINT('Ctrl Pts',(39.2647515159997,28.8323746095736,0.));
#90614=CARTESIAN_POINT('Ctrl Pts',(39.2647515159997,28.8323746095736,20.));
#90615=CARTESIAN_POINT('Ctrl Pts',(39.2821782284193,28.80348523695,0.));
#90616=CARTESIAN_POINT('Ctrl Pts',(39.2821782284193,28.80348523695,20.));
#90617=CARTESIAN_POINT('Ctrl Pts',(39.2995844326181,28.7745848069238,0.));
#90618=CARTESIAN_POINT('Ctrl Pts',(39.2995844326181,28.7745848069238,20.));
#90619=CARTESIAN_POINT('Ctrl Pts',(39.316970121049,28.7456733336894,0.));
#90620=CARTESIAN_POINT('Ctrl Pts',(39.316970121049,28.7456733336894,20.));
#90621=CARTESIAN_POINT('Ctrl Pts',(39.3343352861746,28.7167508314468,0.));
#90622=CARTESIAN_POINT('Ctrl Pts',(39.3343352861746,28.7167508314468,20.));
#90623=CARTESIAN_POINT('Ctrl Pts',(39.3516799204672,28.6878173144015,0.));
#90624=CARTESIAN_POINT('Ctrl Pts',(39.3516799204672,28.6878173144015,20.));
#90625=CARTESIAN_POINT('Ctrl Pts',(39.3690040164086,28.6588727967647,0.));
#90626=CARTESIAN_POINT('Ctrl Pts',(39.3690040164086,28.6588727967647,20.));
#90627=CARTESIAN_POINT('Ctrl Pts',(39.3863075664906,28.6299172927529,0.));
#90628=CARTESIAN_POINT('Ctrl Pts',(39.3863075664906,28.6299172927529,20.));
#90629=CARTESIAN_POINT('Ctrl Pts',(39.4035905632141,28.600950816588,0.));
#90630=CARTESIAN_POINT('Ctrl Pts',(39.4035905632141,28.600950816588,20.));
#90631=CARTESIAN_POINT('Ctrl Pts',(39.4208529990894,28.5719733824975,0.));
#90632=CARTESIAN_POINT('Ctrl Pts',(39.4208529990894,28.5719733824975,20.));
#90633=CARTESIAN_POINT('Ctrl Pts',(39.4380948666368,28.5429850047148,0.));
#90634=CARTESIAN_POINT('Ctrl Pts',(39.4380948666368,28.5429850047148,20.));
#90635=CARTESIAN_POINT('Ctrl Pts',(39.4553161583861,28.5139856974786,0.));
#90636=CARTESIAN_POINT('Ctrl Pts',(39.4553161583861,28.5139856974786,20.));
#90637=CARTESIAN_POINT('Ctrl Pts',(39.472516866877,28.4849754750331,0.));
#90638=CARTESIAN_POINT('Ctrl Pts',(39.472516866877,28.4849754750331,20.));
#90639=CARTESIAN_POINT('Ctrl Pts',(39.4896969846589,28.455954351628,0.));
#90640=CARTESIAN_POINT('Ctrl Pts',(39.4896969846589,28.455954351628,20.));
#90641=CARTESIAN_POINT('Ctrl Pts',(39.5068565042907,28.4269223415187,0.));
#90642=CARTESIAN_POINT('Ctrl Pts',(39.5068565042907,28.4269223415187,20.));
#90643=CARTESIAN_POINT('Ctrl Pts',(39.5239954183412,28.3978794589661,0.));
#90644=CARTESIAN_POINT('Ctrl Pts',(39.5239954183412,28.3978794589661,20.));
#90645=CARTESIAN_POINT('Ctrl Pts',(39.5411137193887,28.3688257182364,0.));
#90646=CARTESIAN_POINT('Ctrl Pts',(39.5411137193887,28.3688257182364,20.));
#90647=CARTESIAN_POINT('Ctrl Pts',(39.5582114000212,28.3397611336014,0.));
#90648=CARTESIAN_POINT('Ctrl Pts',(39.5582114000212,28.3397611336014,20.));
#90649=CARTESIAN_POINT('Ctrl Pts',(39.5752884528361,28.3106857193381,0.));
#90650=CARTESIAN_POINT('Ctrl Pts',(39.5752884528361,28.3106857193381,20.));
#90651=CARTESIAN_POINT('Ctrl Pts',(39.5923448704403,28.2815994897291,0.));
#90652=CARTESIAN_POINT('Ctrl Pts',(39.5923448704403,28.2815994897291,20.));
#90653=CARTESIAN_POINT('Ctrl Pts',(39.6093806454502,28.2525024590626,0.));
#90654=CARTESIAN_POINT('Ctrl Pts',(39.6093806454502,28.2525024590626,20.));
#90655=CARTESIAN_POINT('Ctrl Pts',(39.6263957704923,28.2233946416323,0.));
#90656=CARTESIAN_POINT('Ctrl Pts',(39.6263957704923,28.2233946416323,20.));
#90657=CARTESIAN_POINT('Ctrl Pts',(39.6433902382029,28.1942760517371,0.));
#90658=CARTESIAN_POINT('Ctrl Pts',(39.6433902382029,28.1942760517371,20.));
#90659=CARTESIAN_POINT('Ctrl Pts',(39.6603640412281,28.1651467036817,0.));
#90660=CARTESIAN_POINT('Ctrl Pts',(39.6603640412281,28.1651467036817,20.));
#90661=CARTESIAN_POINT('Ctrl Pts',(39.6773171722241,28.136006611776,0.));
#90662=CARTESIAN_POINT('Ctrl Pts',(39.6773171722241,28.136006611776,20.));
#90663=CARTESIAN_POINT('Ctrl Pts',(39.6942496238565,28.1068557903356,0.));
#90664=CARTESIAN_POINT('Ctrl Pts',(39.6942496238565,28.1068557903356,20.));
#90665=CARTESIAN_POINT('Ctrl Pts',(39.7111613888006,28.0776942536814,0.));
#90666=CARTESIAN_POINT('Ctrl Pts',(39.7111613888006,28.0776942536814,20.));
#90667=CARTESIAN_POINT('Ctrl Pts',(39.728052459741,28.0485220161395,0.));
#90668=CARTESIAN_POINT('Ctrl Pts',(39.728052459741,28.0485220161395,20.));
#90669=CARTESIAN_POINT('Ctrl Pts',(39.7449228293718,28.0193390920415,0.));
#90670=CARTESIAN_POINT('Ctrl Pts',(39.7449228293718,28.0193390920415,20.));
#90671=CARTESIAN_POINT('Ctrl Pts',(39.7617724903968,27.9901454957246,0.));
#90672=CARTESIAN_POINT('Ctrl Pts',(39.7617724903968,27.9901454957246,20.));
#90673=CARTESIAN_POINT('Ctrl Pts',(39.7786014355293,27.960941241531,0.));
#90674=CARTESIAN_POINT('Ctrl Pts',(39.7786014355293,27.960941241531,20.));
#90675=CARTESIAN_POINT('Ctrl Pts',(39.795409657493,27.9317263438086,0.));
#90676=CARTESIAN_POINT('Ctrl Pts',(39.795409657493,27.9317263438086,20.));
#90677=CARTESIAN_POINT('Ctrl Pts',(39.8121971490214,27.9025008169107,0.));
#90678=CARTESIAN_POINT('Ctrl Pts',(39.8121971490214,27.9025008169107,20.));
#90679=CARTESIAN_POINT('Ctrl Pts',(39.828963902858,27.8732646751959,0.));
#90680=CARTESIAN_POINT('Ctrl Pts',(39.828963902858,27.8732646751959,20.));
#90681=CARTESIAN_POINT('Ctrl Pts',(39.8457099117559,27.8440179330284,0.));
#90682=CARTESIAN_POINT('Ctrl Pts',(39.8457099117559,27.8440179330284,20.));
#90683=CARTESIAN_POINT('Ctrl Pts',(39.862435168478,27.8147606047778,0.));
#90684=CARTESIAN_POINT('Ctrl Pts',(39.862435168478,27.8147606047778,20.));
#90685=CARTESIAN_POINT('Ctrl Pts',(39.8791396657966,27.785492704819,0.));
#90686=CARTESIAN_POINT('Ctrl Pts',(39.8791396657966,27.785492704819,20.));
#90687=CARTESIAN_POINT('Ctrl Pts',(39.8958233964934,27.7562142475319,0.));
#90688=CARTESIAN_POINT('Ctrl Pts',(39.8958233964934,27.7562142475319,20.));
#90689=CARTESIAN_POINT('Ctrl Pts',(39.9124863533599,27.726925247302,0.));
#90690=CARTESIAN_POINT('Ctrl Pts',(39.9124863533599,27.726925247302,20.));
#90691=CARTESIAN_POINT('Ctrl Pts',(39.9291285291975,27.6976257185198,0.));
#90692=CARTESIAN_POINT('Ctrl Pts',(39.9291285291975,27.6976257185198,20.));
#90693=CARTESIAN_POINT('Ctrl Pts',(39.9457499168175,27.6683156755815,0.));
#90694=CARTESIAN_POINT('Ctrl Pts',(39.9457499168175,27.6683156755815,20.));
#90695=CARTESIAN_POINT('Ctrl Pts',(39.9623505090412,27.6389951328887,0.));
#90696=CARTESIAN_POINT('Ctrl Pts',(39.9623505090412,27.6389951328887,20.));
#90697=CARTESIAN_POINT('Ctrl Pts',(39.9789302986995,27.6096641048483,0.));
#90698=CARTESIAN_POINT('Ctrl Pts',(39.9789302986995,27.6096641048483,20.));
#90699=CARTESIAN_POINT('Ctrl Pts',(39.9954892786331,27.5803226058725,0.));
#90700=CARTESIAN_POINT('Ctrl Pts',(39.9954892786331,27.5803226058725,20.));
#90701=CARTESIAN_POINT('Ctrl Pts',(40.0120274416924,27.5509706503786,0.));
#90702=CARTESIAN_POINT('Ctrl Pts',(40.0120274416924,27.5509706503786,20.));
#90703=CARTESIAN_POINT('Ctrl Pts',(40.0285447807378,27.5216082527897,0.));
#90704=CARTESIAN_POINT('Ctrl Pts',(40.0285447807378,27.5216082527897,20.));
#90705=CARTESIAN_POINT('Ctrl Pts',(40.045041288639,27.4922354275335,0.));
#90706=CARTESIAN_POINT('Ctrl Pts',(40.045041288639,27.4922354275335,20.));
#90707=CARTESIAN_POINT('Ctrl Pts',(40.0615169582759,27.4628521890436,0.));
#90708=CARTESIAN_POINT('Ctrl Pts',(40.0615169582759,27.4628521890436,20.));
#90709=CARTESIAN_POINT('Ctrl Pts',(40.077971782538,27.4334585517582,0.));
#90710=CARTESIAN_POINT('Ctrl Pts',(40.077971782538,27.4334585517582,20.));
#90711=CARTESIAN_POINT('Ctrl Pts',(40.0944057543248,27.4040545301216,0.));
#90712=CARTESIAN_POINT('Ctrl Pts',(40.0944057543248,27.4040545301216,20.));
#90713=CARTESIAN_POINT('Ctrl Pts',(40.1108188665452,27.374640138583,0.));
#90714=CARTESIAN_POINT('Ctrl Pts',(40.1108188665452,27.374640138583,20.));
#90715=CARTESIAN_POINT('Ctrl Pts',(40.1272111121183,27.3452153915969,0.));
#90716=CARTESIAN_POINT('Ctrl Pts',(40.1272111121183,27.3452153915969,20.));
#90717=CARTESIAN_POINT('Ctrl Pts',(40.1435824839731,27.3157803036231,0.));
#90718=CARTESIAN_POINT('Ctrl Pts',(40.1435824839731,27.3157803036231,20.));
#90719=CARTESIAN_POINT('Ctrl Pts',(40.1599329750483,27.2863348891265,0.));
#90720=CARTESIAN_POINT('Ctrl Pts',(40.1599329750483,27.2863348891265,20.));
#90721=CARTESIAN_POINT('Ctrl Pts',(40.1762625782924,27.2568791625774,0.));
#90722=CARTESIAN_POINT('Ctrl Pts',(40.1762625782924,27.2568791625774,20.));
#90723=CARTESIAN_POINT('Ctrl Pts',(40.1925712866631,27.2274131384508,0.));
#90724=CARTESIAN_POINT('Ctrl Pts',(40.1925712866631,27.2274131384508,20.));
#90725=CARTESIAN_POINT('Ctrl Pts',(40.2088590931287,27.1979368312277,0.));
#90726=CARTESIAN_POINT('Ctrl Pts',(40.2088590931287,27.1979368312277,20.));
#90727=CARTESIAN_POINT('Ctrl Pts',(40.2251259906669,27.1684502553939,0.));
#90728=CARTESIAN_POINT('Ctrl Pts',(40.2251259906669,27.1684502553939,20.));
#90729=CARTESIAN_POINT('Ctrl Pts',(40.2413719722657,27.1389534254409,0.));
#90730=CARTESIAN_POINT('Ctrl Pts',(40.2413719722657,27.1389534254409,20.));
#90731=CARTESIAN_POINT('Ctrl Pts',(40.2575970309226,27.1094463558649,0.));
#90732=CARTESIAN_POINT('Ctrl Pts',(40.2575970309226,27.1094463558649,20.));
#90733=CARTESIAN_POINT('Ctrl Pts',(40.2738011596454,27.0799290611676,0.));
#90734=CARTESIAN_POINT('Ctrl Pts',(40.2738011596454,27.0799290611676,20.));
#90735=CARTESIAN_POINT('Ctrl Pts',(40.2899843514517,27.0504015558557,0.));
#90736=CARTESIAN_POINT('Ctrl Pts',(40.2899843514517,27.0504015558557,20.));
#90737=CARTESIAN_POINT('Ctrl Pts',(40.3061465993685,27.0208638544413,0.));
#90738=CARTESIAN_POINT('Ctrl Pts',(40.3061465993685,27.0208638544413,20.));
#90739=CARTESIAN_POINT('Ctrl Pts',(40.3222878964329,26.9913159714415,0.));
#90740=CARTESIAN_POINT('Ctrl Pts',(40.3222878964329,26.9913159714415,20.));
#90741=CARTESIAN_POINT('Ctrl Pts',(40.3384082356913,26.9617579213786,0.));
#90742=CARTESIAN_POINT('Ctrl Pts',(40.3384082356913,26.9617579213786,20.));
#90743=CARTESIAN_POINT('Ctrl Pts',(40.3545076102003,26.9321897187802,0.));
#90744=CARTESIAN_POINT('Ctrl Pts',(40.3545076102003,26.9321897187802,20.));
#90745=CARTESIAN_POINT('Ctrl Pts',(40.3705860130263,26.9026113781788,0.));
#90746=CARTESIAN_POINT('Ctrl Pts',(40.3705860130263,26.9026113781788,20.));
#90747=CARTESIAN_POINT('Ctrl Pts',(40.386643437246,26.8730229141124,0.));
#90748=CARTESIAN_POINT('Ctrl Pts',(40.386643437246,26.8730229141124,20.));
#90749=CARTESIAN_POINT('Ctrl Pts',(40.4026798759458,26.8434243411241,0.));
#90750=CARTESIAN_POINT('Ctrl Pts',(40.4026798759458,26.8434243411241,20.));
#90751=CARTESIAN_POINT('Ctrl Pts',(40.4186953222224,26.8138156737619,0.));
#90752=CARTESIAN_POINT('Ctrl Pts',(40.4186953222224,26.8138156737619,20.));
#90753=CARTESIAN_POINT('Ctrl Pts',(40.4346897691821,26.7841969265794,0.));
#90754=CARTESIAN_POINT('Ctrl Pts',(40.4346897691821,26.7841969265794,20.));
#90755=CARTESIAN_POINT('Ctrl Pts',(40.4506632099408,26.754568114135,0.));
#90756=CARTESIAN_POINT('Ctrl Pts',(40.4506632099408,26.754568114135,20.));
#90757=CARTESIAN_POINT('Ctrl Pts',(40.4666156376241,26.7249292509923,0.));
#90758=CARTESIAN_POINT('Ctrl Pts',(40.4666156376241,26.7249292509923,20.));
#90759=CARTESIAN_POINT('Ctrl Pts',(40.4825470453679,26.6952803517197,0.));
#90760=CARTESIAN_POINT('Ctrl Pts',(40.4825470453679,26.6952803517197,20.));
#90761=CARTESIAN_POINT('Ctrl Pts',(40.4984574263178,26.6656214308914,0.));
#90762=CARTESIAN_POINT('Ctrl Pts',(40.4984574263178,26.6656214308914,20.));
#90763=CARTESIAN_POINT('Ctrl Pts',(40.5143467736295,26.6359525030862,0.));
#90764=CARTESIAN_POINT('Ctrl Pts',(40.5143467736295,26.6359525030862,20.));
#90765=CARTESIAN_POINT('Ctrl Pts',(40.5302150804687,26.606273582888,0.));
#90766=CARTESIAN_POINT('Ctrl Pts',(40.5302150804687,26.606273582888,20.));
#90767=CARTESIAN_POINT('Ctrl Pts',(40.546062340011,26.5765846848862,0.));
#90768=CARTESIAN_POINT('Ctrl Pts',(40.546062340011,26.5765846848862,20.));
#90769=CARTESIAN_POINT('Ctrl Pts',(40.5618885454414,26.5468858236748,0.));
#90770=CARTESIAN_POINT('Ctrl Pts',(40.5618885454414,26.5468858236748,20.));
#90771=CARTESIAN_POINT('Ctrl Pts',(40.5776936899555,26.5171770138532,0.));
#90772=CARTESIAN_POINT('Ctrl Pts',(40.5776936899555,26.5171770138532,20.));
#90773=CARTESIAN_POINT('Ctrl Pts',(40.5934777667583,26.4874582700259,0.));
#90774=CARTESIAN_POINT('Ctrl Pts',(40.5934777667583,26.4874582700259,20.));
#90775=CARTESIAN_POINT('Ctrl Pts',(40.6092407690651,26.4577296068023,0.));
#90776=CARTESIAN_POINT('Ctrl Pts',(40.6092407690651,26.4577296068023,20.));
#90777=CARTESIAN_POINT('Ctrl Pts',(40.6249826901011,26.4279910387971,0.));
#90778=CARTESIAN_POINT('Ctrl Pts',(40.6249826901011,26.4279910387971,20.));
#90779=CARTESIAN_POINT('Ctrl Pts',(40.6407035231015,26.3982425806297,0.));
#90780=CARTESIAN_POINT('Ctrl Pts',(40.6407035231015,26.3982425806297,20.));
#90781=CARTESIAN_POINT('Ctrl Pts',(40.6564032613109,26.3684842469248,0.));
#90782=CARTESIAN_POINT('Ctrl Pts',(40.6564032613109,26.3684842469248,20.));
#90783=CARTESIAN_POINT('Ctrl Pts',(40.6720818979844,26.338716052312,0.));
#90784=CARTESIAN_POINT('Ctrl Pts',(40.6720818979844,26.338716052312,20.));
#90785=CARTESIAN_POINT('Ctrl Pts',(40.6877394263869,26.308938011426,0.));
#90786=CARTESIAN_POINT('Ctrl Pts',(40.6877394263869,26.308938011426,20.));
#90787=CARTESIAN_POINT('Ctrl Pts',(40.7033758397932,26.2791501389067,0.));
#90788=CARTESIAN_POINT('Ctrl Pts',(40.7033758397932,26.2791501389067,20.));
#90789=CARTESIAN_POINT('Ctrl Pts',(40.7189911314882,26.2493524493989,0.));
#90790=CARTESIAN_POINT('Ctrl Pts',(40.7189911314882,26.2493524493989,20.));
#90791=CARTESIAN_POINT('Ctrl Pts',(40.7345852947663,26.2195449575524,0.));
#90792=CARTESIAN_POINT('Ctrl Pts',(40.7345852947663,26.2195449575524,20.));
#90793=CARTESIAN_POINT('Ctrl Pts',(40.7501583229328,26.1897276780219,0.));
#90794=CARTESIAN_POINT('Ctrl Pts',(40.7501583229328,26.1897276780219,20.));
#90795=CARTESIAN_POINT('Ctrl Pts',(40.7657102093021,26.1599006254674,0.));
#90796=CARTESIAN_POINT('Ctrl Pts',(40.7657102093021,26.1599006254674,20.));
#90797=CARTESIAN_POINT('Ctrl Pts',(40.7812409471992,26.1300638145535,0.));
#90798=CARTESIAN_POINT('Ctrl Pts',(40.7812409471992,26.1300638145535,20.));
#90799=CARTESIAN_POINT('Ctrl Pts',(40.7967505299588,26.1002172599501,0.));
#90800=CARTESIAN_POINT('Ctrl Pts',(40.7967505299588,26.1002172599501,20.));
#90801=CARTESIAN_POINT('Ctrl Pts',(40.8122389509256,26.0703609763318,0.));
#90802=CARTESIAN_POINT('Ctrl Pts',(40.8122389509256,26.0703609763318,20.));
#90803=CARTESIAN_POINT('Ctrl Pts',(40.8277062034539,26.0404949783787,0.));
#90804=CARTESIAN_POINT('Ctrl Pts',(40.8277062034539,26.0404949783787,20.));
#90805=CARTESIAN_POINT('Ctrl Pts',(40.843152280908,26.0106192807756,0.));
#90806=CARTESIAN_POINT('Ctrl Pts',(40.843152280908,26.0106192807756,20.));
#90807=CARTESIAN_POINT('Ctrl Pts',(40.8585771766627,25.9807338982121,0.));
#90808=CARTESIAN_POINT('Ctrl Pts',(40.8585771766627,25.9807338982121,20.));
#90809=CARTESIAN_POINT('Ctrl Pts',(40.8739808841024,25.9508388453831,0.));
#90810=CARTESIAN_POINT('Ctrl Pts',(40.8739808841024,25.9508388453831,20.));
#90811=CARTESIAN_POINT('Ctrl Pts',(40.8893633966224,25.9209341369879,0.));
#90812=CARTESIAN_POINT('Ctrl Pts',(40.8893633966224,25.9209341369879,20.));
#90813=CARTESIAN_POINT('Ctrl Pts',(40.9047247076274,25.891019787731,0.));
#90814=CARTESIAN_POINT('Ctrl Pts',(40.9047247076274,25.891019787731,20.));
#90815=CARTESIAN_POINT('Ctrl Pts',(40.9200648105322,25.861095812322,0.));
#90816=CARTESIAN_POINT('Ctrl Pts',(40.9200648105322,25.861095812322,20.));
#90817=CARTESIAN_POINT('Ctrl Pts',(40.9353836987613,25.8311622254754,0.));
#90818=CARTESIAN_POINT('Ctrl Pts',(40.9353836987613,25.8311622254754,20.));
#90819=CARTESIAN_POINT('Ctrl Pts',(40.9506813657491,25.8012190419102,0.));
#90820=CARTESIAN_POINT('Ctrl Pts',(40.9506813657491,25.8012190419102,20.));
#90821=CARTESIAN_POINT('Ctrl Pts',(40.9659578049399,25.7712662763511,0.));
#90822=CARTESIAN_POINT('Ctrl Pts',(40.9659578049399,25.7712662763511,20.));
#90823=CARTESIAN_POINT('Ctrl Pts',(40.981213009789,25.7413039435271,0.));
#90824=CARTESIAN_POINT('Ctrl Pts',(40.981213009789,25.7413039435271,20.));
#90825=CARTESIAN_POINT('Ctrl Pts',(40.9964469737612,25.7113320581728,0.));
#90826=CARTESIAN_POINT('Ctrl Pts',(40.9964469737612,25.7113320581728,20.));
#90827=CARTESIAN_POINT('Ctrl Pts',(41.0116596903316,25.6813506350271,0.));
#90828=CARTESIAN_POINT('Ctrl Pts',(41.0116596903316,25.6813506350271,20.));
#90829=CARTESIAN_POINT('Ctrl Pts',(41.0268511529852,25.6513596888338,0.));
#90830=CARTESIAN_POINT('Ctrl Pts',(41.0268511529852,25.6513596888338,20.));
#90831=CARTESIAN_POINT('Ctrl Pts',(41.0420213552163,25.6213592343415,0.));
#90832=CARTESIAN_POINT('Ctrl Pts',(41.0420213552163,25.6213592343415,20.));
#90833=CARTESIAN_POINT('Ctrl Pts',(41.05717029053,25.5913492863038,0.));
#90834=CARTESIAN_POINT('Ctrl Pts',(41.05717029053,25.5913492863038,20.));
#90835=CARTESIAN_POINT('Ctrl Pts',(41.072297952441,25.5613298594791,0.));
#90836=CARTESIAN_POINT('Ctrl Pts',(41.072297952441,25.5613298594791,20.));
#90837=CARTESIAN_POINT('Ctrl Pts',(41.0874043344745,25.5313009686309,0.));
#90838=CARTESIAN_POINT('Ctrl Pts',(41.0874043344745,25.5313009686309,20.));
#90839=CARTESIAN_POINT('Ctrl Pts',(41.1024894301655,25.5012626285275,0.));
#90840=CARTESIAN_POINT('Ctrl Pts',(41.1024894301655,25.5012626285275,20.));
#90841=CARTESIAN_POINT('Ctrl Pts',(41.1175532330596,25.4712148539422,0.));
#90842=CARTESIAN_POINT('Ctrl Pts',(41.1175532330596,25.4712148539422,20.));
#90843=CARTESIAN_POINT('Ctrl Pts',(41.1325957367119,25.4411576596529,0.));
#90844=CARTESIAN_POINT('Ctrl Pts',(41.1325957367119,25.4411576596529,20.));
#90845=CARTESIAN_POINT('Ctrl Pts',(41.1476169346881,25.4110910604425,0.));
#90846=CARTESIAN_POINT('Ctrl Pts',(41.1476169346881,25.4110910604425,20.));
#90847=CARTESIAN_POINT('Ctrl Pts',(41.1626168205634,25.3810150710984,0.));
#90848=CARTESIAN_POINT('Ctrl Pts',(41.1626168205634,25.3810150710984,20.));
#90849=CARTESIAN_POINT('Ctrl Pts',(41.1775953879232,25.3509297064131,0.));
#90850=CARTESIAN_POINT('Ctrl Pts',(41.1775953879232,25.3509297064131,20.));
#90851=CARTESIAN_POINT('Ctrl Pts',(41.1925526303629,25.3208349811839,0.));
#90852=CARTESIAN_POINT('Ctrl Pts',(41.1925526303629,25.3208349811839,20.));
#90853=CARTESIAN_POINT('Ctrl Pts',(41.2074885414881,25.2907309102128,0.));
#90854=CARTESIAN_POINT('Ctrl Pts',(41.2074885414881,25.2907309102128,20.));
#90855=CARTESIAN_POINT('Ctrl Pts',(41.2224031149147,25.2606175083067,0.));
#90856=CARTESIAN_POINT('Ctrl Pts',(41.2224031149147,25.2606175083067,20.));
#90857=CARTESIAN_POINT('Ctrl Pts',(41.2372963442684,25.2304947902774,0.));
#90858=CARTESIAN_POINT('Ctrl Pts',(41.2372963442684,25.2304947902774,20.));
#90859=CARTESIAN_POINT('Ctrl Pts',(41.2521682231854,25.2003627709414,0.));
#90860=CARTESIAN_POINT('Ctrl Pts',(41.2521682231854,25.2003627709414,20.));
#90861=CARTESIAN_POINT('Ctrl Pts',(41.2670187453114,25.1702214651198,0.));
#90862=CARTESIAN_POINT('Ctrl Pts',(41.2670187453114,25.1702214651198,20.));
#90863=CARTESIAN_POINT('Ctrl Pts',(41.2818479043026,25.1400708876386,0.));
#90864=CARTESIAN_POINT('Ctrl Pts',(41.2818479043026,25.1400708876386,20.));
#90865=CARTESIAN_POINT('Ctrl Pts',(41.2966556938255,25.1099110533288,0.));
#90866=CARTESIAN_POINT('Ctrl Pts',(41.2966556938255,25.1099110533288,20.));
#90867=CARTESIAN_POINT('Ctrl Pts',(41.3114421075567,25.0797419770258,0.));
#90868=CARTESIAN_POINT('Ctrl Pts',(41.3114421075567,25.0797419770258,20.));
#90869=CARTESIAN_POINT('Ctrl Pts',(41.3262071391823,25.0495636735701,0.));
#90870=CARTESIAN_POINT('Ctrl Pts',(41.3262071391823,25.0495636735701,20.));
#90871=CARTESIAN_POINT('Ctrl Pts',(41.3409507823989,25.0193761578067,0.));
#90872=CARTESIAN_POINT('Ctrl Pts',(41.3409507823989,25.0193761578067,20.));
#90873=CARTESIAN_POINT('Ctrl Pts',(41.3556730309131,24.9891794445855,0.));
#90874=CARTESIAN_POINT('Ctrl Pts',(41.3556730309131,24.9891794445855,20.));
#90875=CARTESIAN_POINT('Ctrl Pts',(41.3703738784418,24.9589735487609,0.));
#90876=CARTESIAN_POINT('Ctrl Pts',(41.3703738784418,24.9589735487609,20.));
#90877=CARTESIAN_POINT('Ctrl Pts',(41.3850533187123,24.9287584851923,0.));
#90878=CARTESIAN_POINT('Ctrl Pts',(41.3850533187123,24.9287584851923,20.));
#90879=CARTESIAN_POINT('Ctrl Pts',(41.3997113454618,24.8985342687436,0.));
#90880=CARTESIAN_POINT('Ctrl Pts',(41.3997113454618,24.8985342687436,20.));
#90881=CARTESIAN_POINT('Ctrl Pts',(41.4143479524375,24.8683009142837,0.));
#90882=CARTESIAN_POINT('Ctrl Pts',(41.4143479524375,24.8683009142837,20.));
#90883=CARTESIAN_POINT('Ctrl Pts',(41.4289631333969,24.8380584366859,0.));
#90884=CARTESIAN_POINT('Ctrl Pts',(41.4289631333969,24.8380584366859,20.));
#90885=CARTESIAN_POINT('Ctrl Pts',(41.443556882107,24.8078068508284,0.));
#90886=CARTESIAN_POINT('Ctrl Pts',(41.443556882107,24.8078068508284,20.));
#90887=CARTESIAN_POINT('Ctrl Pts',(41.4581291923457,24.7775461715943,0.));
#90888=CARTESIAN_POINT('Ctrl Pts',(41.4581291923457,24.7775461715943,20.));
#90889=CARTESIAN_POINT('Ctrl Pts',(41.4726800579006,24.7472764138709,0.));
#90890=CARTESIAN_POINT('Ctrl Pts',(41.4726800579006,24.7472764138709,20.));
#90891=CARTESIAN_POINT('Ctrl Pts',(41.4872094725701,24.7169975925505,0.));
#90892=CARTESIAN_POINT('Ctrl Pts',(41.4872094725701,24.7169975925505,20.));
#90893=CARTESIAN_POINT('Ctrl Pts',(41.5017174301628,24.68670972253,0.));
#90894=CARTESIAN_POINT('Ctrl Pts',(41.5017174301628,24.68670972253,20.));
#90895=CARTESIAN_POINT('Ctrl Pts',(41.516203924497,24.6564128187107,0.));
#90896=CARTESIAN_POINT('Ctrl Pts',(41.516203924497,24.6564128187107,20.));
#90897=CARTESIAN_POINT('Ctrl Pts',(41.5306689494012,24.626106895999,0.));
#90898=CARTESIAN_POINT('Ctrl Pts',(41.5306689494012,24.626106895999,20.));
#90899=CARTESIAN_POINT('Ctrl Pts',(41.545112498714,24.5957919693057,0.));
#90900=CARTESIAN_POINT('Ctrl Pts',(41.545112498714,24.5957919693057,20.));
#90901=CARTESIAN_POINT('Ctrl Pts',(41.5595345662842,24.5654680535465,0.));
#90902=CARTESIAN_POINT('Ctrl Pts',(41.5595345662842,24.5654680535465,20.));
#90903=CARTESIAN_POINT('Ctrl Pts',(41.5739351459709,24.5351351636416,0.));
#90904=CARTESIAN_POINT('Ctrl Pts',(41.5739351459709,24.5351351636416,20.));
#90905=CARTESIAN_POINT('Ctrl Pts',(41.5883142316433,24.5047933145158,0.));
#90906=CARTESIAN_POINT('Ctrl Pts',(41.5883142316433,24.5047933145158,20.));
#90907=CARTESIAN_POINT('Ctrl Pts',(41.6026718171809,24.4744425210985,0.));
#90908=CARTESIAN_POINT('Ctrl Pts',(41.6026718171809,24.4744425210985,20.));
#90909=CARTESIAN_POINT('Ctrl Pts',(41.6170078964732,24.4440827983238,0.));
#90910=CARTESIAN_POINT('Ctrl Pts',(41.6170078964732,24.4440827983238,20.));
#90911=CARTESIAN_POINT('Ctrl Pts',(41.6313224634201,24.4137141611302,0.));
#90912=CARTESIAN_POINT('Ctrl Pts',(41.6313224634201,24.4137141611302,20.));
#90913=CARTESIAN_POINT('Ctrl Pts',(41.6456155119319,24.3833366244611,0.));
#90914=CARTESIAN_POINT('Ctrl Pts',(41.6456155119319,24.3833366244611,20.));
#90915=CARTESIAN_POINT('Ctrl Pts',(41.6598870359289,24.3529502032644,0.));
#90916=CARTESIAN_POINT('Ctrl Pts',(41.6598870359289,24.3529502032644,20.));
#90917=CARTESIAN_POINT('Ctrl Pts',(41.6741370293416,24.3225549124927,0.));
#90918=CARTESIAN_POINT('Ctrl Pts',(41.6741370293416,24.3225549124927,20.));
#90919=CARTESIAN_POINT('Ctrl Pts',(41.6883654861106,24.292150767103,0.));
#90920=CARTESIAN_POINT('Ctrl Pts',(41.6883654861106,24.292150767103,20.));
#90921=CARTESIAN_POINT('Ctrl Pts',(41.7025724001866,24.2617377820568,0.));
#90922=CARTESIAN_POINT('Ctrl Pts',(41.7025724001866,24.2617377820568,20.));
#90923=CARTESIAN_POINT('Ctrl Pts',(41.7167577655309,24.2313159723205,0.));
#90924=CARTESIAN_POINT('Ctrl Pts',(41.7167577655309,24.2313159723205,20.));
#90925=CARTESIAN_POINT('Ctrl Pts',(41.7309215761147,24.2008853528648,0.));
#90926=CARTESIAN_POINT('Ctrl Pts',(41.7309215761147,24.2008853528648,20.));
#90927=CARTESIAN_POINT('Ctrl Pts',(41.7450638259196,24.1704459386651,0.));
#90928=CARTESIAN_POINT('Ctrl Pts',(41.7450638259196,24.1704459386651,20.));
#90929=CARTESIAN_POINT('Ctrl Pts',(41.7591845089374,24.1399977447013,0.));
#90930=CARTESIAN_POINT('Ctrl Pts',(41.7591845089374,24.1399977447013,20.));
#90931=CARTESIAN_POINT('Ctrl Pts',(41.7732836191701,24.1095407859578,0.));
#90932=CARTESIAN_POINT('Ctrl Pts',(41.7732836191701,24.1095407859578,20.));
#90933=CARTESIAN_POINT('Ctrl Pts',(41.78736115063,24.0790750774236,0.));
#90934=CARTESIAN_POINT('Ctrl Pts',(41.78736115063,24.0790750774236,20.));
#90935=CARTESIAN_POINT('Ctrl Pts',(41.8014170973399,24.0486006340924,0.));
#90936=CARTESIAN_POINT('Ctrl Pts',(41.8014170973399,24.0486006340924,20.));
#90937=CARTESIAN_POINT('Ctrl Pts',(41.8154514533324,24.0181174709622,0.));
#90938=CARTESIAN_POINT('Ctrl Pts',(41.8154514533324,24.0181174709622,20.));
#90939=CARTESIAN_POINT('Ctrl Pts',(41.8294642126506,23.9876256030355,0.));
#90940=CARTESIAN_POINT('Ctrl Pts',(41.8294642126506,23.9876256030355,20.));
#90941=CARTESIAN_POINT('Ctrl Pts',(41.8434553693478,23.9571250453194,0.));
#90942=CARTESIAN_POINT('Ctrl Pts',(41.8434553693478,23.9571250453194,20.));
#90943=CARTESIAN_POINT('Ctrl Pts',(41.8574249174873,23.9266158128252,0.));
#90944=CARTESIAN_POINT('Ctrl Pts',(41.8574249174873,23.9266158128252,20.));
#90945=CARTESIAN_POINT('Ctrl Pts',(41.8713728511429,23.8960979205694,0.));
#90946=CARTESIAN_POINT('Ctrl Pts',(41.8713728511429,23.8960979205694,20.));
#90947=CARTESIAN_POINT('Ctrl Pts',(41.8852991643986,23.8655713835725,0.));
#90948=CARTESIAN_POINT('Ctrl Pts',(41.8852991643986,23.8655713835725,20.));
#90949=CARTESIAN_POINT('Ctrl Pts',(41.8992038513488,23.8350362168598,0.));
#90950=CARTESIAN_POINT('Ctrl Pts',(41.8992038513488,23.8350362168598,20.));
#90951=CARTESIAN_POINT('Ctrl Pts',(41.9130869060982,23.8044924354607,0.));
#90952=CARTESIAN_POINT('Ctrl Pts',(41.9130869060982,23.8044924354607,20.));
#90953=CARTESIAN_POINT('Ctrl Pts',(41.9269483227618,23.7739400544092,0.));
#90954=CARTESIAN_POINT('Ctrl Pts',(41.9269483227618,23.7739400544092,20.));
#90955=CARTESIAN_POINT('Ctrl Pts',(41.9407880954647,23.7433790887435,0.));
#90956=CARTESIAN_POINT('Ctrl Pts',(41.9407880954647,23.7433790887435,20.));
#90957=CARTESIAN_POINT('Ctrl Pts',(41.9546062183422,23.7128095535066,0.));
#90958=CARTESIAN_POINT('Ctrl Pts',(41.9546062183422,23.7128095535066,20.));
#90959=CARTESIAN_POINT('Ctrl Pts',(41.9684026855399,23.6822314637457,0.));
#90960=CARTESIAN_POINT('Ctrl Pts',(41.9684026855399,23.6822314637457,20.));
#90961=CARTESIAN_POINT('Ctrl Pts',(41.9821774912141,23.651644834513,0.));
#90962=CARTESIAN_POINT('Ctrl Pts',(41.9821774912141,23.651644834513,20.));
#90963=CARTESIAN_POINT('Ctrl Pts',(41.9959306295311,23.6210496808648,0.));
#90964=CARTESIAN_POINT('Ctrl Pts',(41.9959306295311,23.6210496808648,20.));
#90965=CARTESIAN_POINT('Ctrl Pts',(42.0096620946675,23.5904460178619,0.));
#90966=CARTESIAN_POINT('Ctrl Pts',(42.0096620946675,23.5904460178619,20.));
#90967=CARTESIAN_POINT('Ctrl Pts',(42.02337188081,23.5598338605694,0.));
#90968=CARTESIAN_POINT('Ctrl Pts',(42.02337188081,23.5598338605694,20.));
#90969=CARTESIAN_POINT('Ctrl Pts',(42.0370599821558,23.5292132240567,0.));
#90970=CARTESIAN_POINT('Ctrl Pts',(42.0370599821558,23.5292132240567,20.));
#90971=CARTESIAN_POINT('Ctrl Pts',(42.0507263929126,23.4985841233977,0.));
#90972=CARTESIAN_POINT('Ctrl Pts',(42.0507263929126,23.4985841233977,20.));
#90973=CARTESIAN_POINT('Ctrl Pts',(42.0643711072981,23.4679465736707,0.));
#90974=CARTESIAN_POINT('Ctrl Pts',(42.0643711072981,23.4679465736707,20.));
#90975=CARTESIAN_POINT('Ctrl Pts',(42.0779941195407,23.4373005899585,0.));
#90976=CARTESIAN_POINT('Ctrl Pts',(42.0779941195407,23.4373005899585,20.));
#90977=CARTESIAN_POINT('Ctrl Pts',(42.0915954238788,23.4066461873484,0.));
#90978=CARTESIAN_POINT('Ctrl Pts',(42.0915954238788,23.4066461873484,20.));
#90979=CARTESIAN_POINT('Ctrl Pts',(42.1051750145614,23.3759833809318,0.));
#90980=CARTESIAN_POINT('Ctrl Pts',(42.1051750145614,23.3759833809318,20.));
#90981=CARTESIAN_POINT('Ctrl Pts',(42.1187328858474,23.3453121858047,0.));
#90982=CARTESIAN_POINT('Ctrl Pts',(42.1187328858474,23.3453121858047,20.));
#90983=CARTESIAN_POINT('Ctrl Pts',(42.1322690320059,23.3146326170671,0.));
#90984=CARTESIAN_POINT('Ctrl Pts',(42.1322690320059,23.3146326170671,20.));
#90985=CARTESIAN_POINT('Ctrl Pts',(42.1457834473169,23.2839446898238,0.));
#90986=CARTESIAN_POINT('Ctrl Pts',(42.1457834473169,23.2839446898238,20.));
#90987=CARTESIAN_POINT('Ctrl Pts',(42.1592761260708,23.2532484191837,0.));
#90988=CARTESIAN_POINT('Ctrl Pts',(42.1592761260708,23.2532484191837,20.));
#90989=CARTESIAN_POINT('Ctrl Pts',(42.1727470625681,23.2225438202604,0.));
#90990=CARTESIAN_POINT('Ctrl Pts',(42.1727470625681,23.2225438202604,20.));
#90991=CARTESIAN_POINT('Ctrl Pts',(42.1861962511195,23.1918309081713,0.));
#90992=CARTESIAN_POINT('Ctrl Pts',(42.1861962511195,23.1918309081713,20.));
#90993=CARTESIAN_POINT('Ctrl Pts',(42.1996236860461,23.1611096980384,0.));
#90994=CARTESIAN_POINT('Ctrl Pts',(42.1996236860461,23.1611096980384,20.));
#90995=CARTESIAN_POINT('Ctrl Pts',(42.2130293616794,23.1303802049881,0.));
#90996=CARTESIAN_POINT('Ctrl Pts',(42.2130293616794,23.1303802049881,20.));
#90997=CARTESIAN_POINT('Ctrl Pts',(42.2264132723611,23.0996424441509,0.));
#90998=CARTESIAN_POINT('Ctrl Pts',(42.2264132723611,23.0996424441509,20.));
#90999=CARTESIAN_POINT('Ctrl Pts',(42.2397754124437,23.0688964306618,0.));
#91000=CARTESIAN_POINT('Ctrl Pts',(42.2397754124437,23.0688964306618,20.));
#91001=CARTESIAN_POINT('Ctrl Pts',(42.2531157762897,23.0381421796601,0.));
#91002=CARTESIAN_POINT('Ctrl Pts',(42.2531157762897,23.0381421796601,20.));
#91003=CARTESIAN_POINT('Ctrl Pts',(42.2664343582719,23.0073797062893,0.));
#91004=CARTESIAN_POINT('Ctrl Pts',(42.2664343582719,23.0073797062893,20.));
#91005=CARTESIAN_POINT('Ctrl Pts',(42.2797311527738,22.9766090256973,0.));
#91006=CARTESIAN_POINT('Ctrl Pts',(42.2797311527738,22.9766090256973,20.));
#91007=CARTESIAN_POINT('Ctrl Pts',(42.2930061541893,22.9458301530364,0.));
#91008=CARTESIAN_POINT('Ctrl Pts',(42.2930061541893,22.9458301530364,20.));
#91009=CARTESIAN_POINT('Ctrl Pts',(42.3062593569225,22.9150431034629,0.));
#91010=CARTESIAN_POINT('Ctrl Pts',(42.3062593569225,22.9150431034629,20.));
#91011=CARTESIAN_POINT('Ctrl Pts',(42.3194907553882,22.8842478921374,0.));
#91012=CARTESIAN_POINT('Ctrl Pts',(42.3194907553882,22.8842478921374,20.));
#91013=CARTESIAN_POINT('Ctrl Pts',(42.3327003440108,22.8534445342249,0.));
#91014=CARTESIAN_POINT('Ctrl Pts',(42.3327003440108,22.8534445342249,20.));
#91015=CARTESIAN_POINT('Ctrl Pts',(42.3458881172255,22.8226330448945,0.));
#91016=CARTESIAN_POINT('Ctrl Pts',(42.3458881172255,22.8226330448945,20.));
#91017=CARTESIAN_POINT('Ctrl Pts',(42.3590540694774,22.7918134393197,0.));
#91018=CARTESIAN_POINT('Ctrl Pts',(42.3590540694774,22.7918134393197,20.));
#91019=CARTESIAN_POINT('Ctrl Pts',(42.3721981952224,22.7609857326781,0.));
#91020=CARTESIAN_POINT('Ctrl Pts',(42.3721981952224,22.7609857326781,20.));
#91021=CARTESIAN_POINT('Ctrl Pts',(42.3853204889273,22.7301499401517,0.));
#91022=CARTESIAN_POINT('Ctrl Pts',(42.3853204889273,22.7301499401517,20.));
#91023=CARTESIAN_POINT('Ctrl Pts',(42.398420945069,22.6993060769268,0.));
#91024=CARTESIAN_POINT('Ctrl Pts',(42.398420945069,22.6993060769268,20.));
#91025=CARTESIAN_POINT('Ctrl Pts',(42.411499558135,22.6684541581936,0.));
#91026=CARTESIAN_POINT('Ctrl Pts',(42.411499558135,22.6684541581936,20.));
#91027=CARTESIAN_POINT('Ctrl Pts',(42.4245563226236,22.6375941991468,0.));
#91028=CARTESIAN_POINT('Ctrl Pts',(42.4245563226236,22.6375941991468,20.));
#91029=CARTESIAN_POINT('Ctrl Pts',(42.4375912330427,22.6067262149851,0.));
#91030=CARTESIAN_POINT('Ctrl Pts',(42.4375912330427,22.6067262149851,20.));
#91031=CARTESIAN_POINT('Ctrl Pts',(42.4506042839107,22.5758502209116,0.));
#91032=CARTESIAN_POINT('Ctrl Pts',(42.4506042839107,22.5758502209116,20.));
#91033=CARTESIAN_POINT('Ctrl Pts',(42.4635954697559,22.5449662321334,0.));
#91034=CARTESIAN_POINT('Ctrl Pts',(42.4635954697559,22.5449662321334,20.));
#91035=CARTESIAN_POINT('Ctrl Pts',(42.4765647851171,22.5140742638619,0.));
#91036=CARTESIAN_POINT('Ctrl Pts',(42.4765647851171,22.5140742638619,20.));
#91037=CARTESIAN_POINT('Ctrl Pts',(42.4895122245441,22.4831743313126,0.));
#91038=CARTESIAN_POINT('Ctrl Pts',(42.4895122245441,22.4831743313126,20.));
#91039=CARTESIAN_POINT('Ctrl Pts',(42.502437782597,22.4522664497054,0.));
#91040=CARTESIAN_POINT('Ctrl Pts',(42.502437782597,22.4522664497054,20.));
#91041=CARTESIAN_POINT('Ctrl Pts',(42.5153414538467,22.4213506342639,0.));
#91042=CARTESIAN_POINT('Ctrl Pts',(42.5153414538467,22.4213506342639,20.));
#91043=CARTESIAN_POINT('Ctrl Pts',(42.5282232328747,22.3904269002165,0.));
#91044=CARTESIAN_POINT('Ctrl Pts',(42.5282232328747,22.3904269002165,20.));
#91045=CARTESIAN_POINT('Ctrl Pts',(42.5410831142726,22.3594952627952,0.));
#91046=CARTESIAN_POINT('Ctrl Pts',(42.5410831142726,22.3594952627952,20.));
#91047=CARTESIAN_POINT('Ctrl Pts',(42.5539210926424,22.3285557372364,0.));
#91048=CARTESIAN_POINT('Ctrl Pts',(42.5539210926424,22.3285557372364,20.));
#91049=CARTESIAN_POINT('Ctrl Pts',(42.5667371625962,22.2976083387805,0.));
#91050=CARTESIAN_POINT('Ctrl Pts',(42.5667371625962,22.2976083387805,20.));
#91051=CARTESIAN_POINT('Ctrl Pts',(42.5795313187569,22.2666530826722,0.));
#91052=CARTESIAN_POINT('Ctrl Pts',(42.5795313187569,22.2666530826722,20.));
#91053=CARTESIAN_POINT('Ctrl Pts',(42.5923035557573,22.2356899841602,0.));
#91054=CARTESIAN_POINT('Ctrl Pts',(42.5923035557573,22.2356899841602,20.));
#91055=CARTESIAN_POINT('Ctrl Pts',(42.6050538682411,22.2047190584974,0.));
#91056=CARTESIAN_POINT('Ctrl Pts',(42.6050538682411,22.2047190584974,20.));
#91057=CARTESIAN_POINT('Ctrl Pts',(42.6177822508627,22.1737403209406,0.));
#91058=CARTESIAN_POINT('Ctrl Pts',(42.6177822508627,22.1737403209406,20.));
#91059=CARTESIAN_POINT('Ctrl Pts',(42.6304886982869,22.1427537867512,0.));
#91060=CARTESIAN_POINT('Ctrl Pts',(42.6304886982869,22.1427537867512,20.));
#91061=CARTESIAN_POINT('Ctrl Pts',(42.6431732051887,22.1117594711942,0.));
#91062=CARTESIAN_POINT('Ctrl Pts',(42.6431732051887,22.1117594711942,20.));
#91063=CARTESIAN_POINT('Ctrl Pts',(42.6558357662536,22.0807573895388,0.));
#91064=CARTESIAN_POINT('Ctrl Pts',(42.6558357662536,22.0807573895388,20.));
#91065=CARTESIAN_POINT('Ctrl Pts',(42.6684763761777,22.0497475570584,0.));
#91066=CARTESIAN_POINT('Ctrl Pts',(42.6684763761777,22.0497475570584,20.));
#91067=CARTESIAN_POINT('Ctrl Pts',(42.6810950296678,22.0187299890302,0.));
#91068=CARTESIAN_POINT('Ctrl Pts',(42.6810950296678,22.0187299890302,20.));
#91069=CARTESIAN_POINT('Ctrl Pts',(42.6936917214411,21.9877047007357,0.));
#91070=CARTESIAN_POINT('Ctrl Pts',(42.6936917214411,21.9877047007357,20.));
#91071=CARTESIAN_POINT('Ctrl Pts',(42.7062664462249,21.9566717074606,0.));
#91072=CARTESIAN_POINT('Ctrl Pts',(42.7062664462249,21.9566717074606,20.));
#91073=CARTESIAN_POINT('Ctrl Pts',(42.7188191987573,21.9256310244944,0.));
#91074=CARTESIAN_POINT('Ctrl Pts',(42.7188191987573,21.9256310244944,20.));
#91075=CARTESIAN_POINT('Ctrl Pts',(42.7313499737866,21.8945826671308,0.));
#91076=CARTESIAN_POINT('Ctrl Pts',(42.7313499737866,21.8945826671308,20.));
#91077=CARTESIAN_POINT('Ctrl Pts',(42.7438587660714,21.8635266506674,0.));
#91078=CARTESIAN_POINT('Ctrl Pts',(42.7438587660714,21.8635266506674,20.));
#91079=CARTESIAN_POINT('Ctrl Pts',(42.7563455703812,21.832462990406,0.));
#91080=CARTESIAN_POINT('Ctrl Pts',(42.7563455703812,21.832462990406,20.));
#91081=CARTESIAN_POINT('Ctrl Pts',(42.7688103814962,21.8013917016521,0.));
#91082=CARTESIAN_POINT('Ctrl Pts',(42.7688103814962,21.8013917016521,20.));
#91083=CARTESIAN_POINT('Ctrl Pts',(42.7812531942069,21.7703127997157,0.));
#91084=CARTESIAN_POINT('Ctrl Pts',(42.7812531942069,21.7703127997157,20.));
#91085=CARTESIAN_POINT('Ctrl Pts',(42.7936740033148,21.7392262999104,0.));
#91086=CARTESIAN_POINT('Ctrl Pts',(42.7936740033148,21.7392262999104,20.));
#91087=CARTESIAN_POINT('Ctrl Pts',(42.8060728036313,21.7081322175539,0.));
#91088=CARTESIAN_POINT('Ctrl Pts',(42.8060728036313,21.7081322175539,20.));
#91089=CARTESIAN_POINT('Ctrl Pts',(42.8184495899785,21.677030567968,0.));
#91090=CARTESIAN_POINT('Ctrl Pts',(42.8184495899785,21.677030567968,20.));
#91091=CARTESIAN_POINT('Ctrl Pts',(42.8308043571886,21.6459213664784,0.));
#91092=CARTESIAN_POINT('Ctrl Pts',(42.8308043571886,21.6459213664784,20.));
#91093=CARTESIAN_POINT('Ctrl Pts',(42.8431371001047,21.6148046284149,0.));
#91094=CARTESIAN_POINT('Ctrl Pts',(42.8431371001047,21.6148046284149,20.));
#91095=CARTESIAN_POINT('Ctrl Pts',(42.8554478135801,21.5836803691112,0.));
#91096=CARTESIAN_POINT('Ctrl Pts',(42.8554478135801,21.5836803691112,20.));
#91097=CARTESIAN_POINT('Ctrl Pts',(42.8677364924793,21.5525486039049,0.));
#91098=CARTESIAN_POINT('Ctrl Pts',(42.8677364924793,21.5525486039049,20.));
#91099=CARTESIAN_POINT('Ctrl Pts',(42.8800031316769,21.5214093481377,0.));
#91100=CARTESIAN_POINT('Ctrl Pts',(42.8800031316769,21.5214093481377,20.));
#91101=CARTESIAN_POINT('Ctrl Pts',(42.8922477260581,21.490262617155,0.));
#91102=CARTESIAN_POINT('Ctrl Pts',(42.8922477260581,21.490262617155,20.));
#91103=CARTESIAN_POINT('Ctrl Pts',(42.9044702705183,21.4591084263065,0.));
#91104=CARTESIAN_POINT('Ctrl Pts',(42.9044702705183,21.4591084263065,20.));
#91105=CARTESIAN_POINT('Ctrl Pts',(42.916670759964,21.4279467909454,0.));
#91106=CARTESIAN_POINT('Ctrl Pts',(42.916670759964,21.4279467909454,20.));
#91107=CARTESIAN_POINT('Ctrl Pts',(42.9288491893122,21.3967777264295,0.));
#91108=CARTESIAN_POINT('Ctrl Pts',(42.9288491893122,21.3967777264295,20.));
#91109=CARTESIAN_POINT('Ctrl Pts',(42.9410055534907,21.3656012481199,0.));
#91110=CARTESIAN_POINT('Ctrl Pts',(42.9410055534907,21.3656012481199,20.));
#91111=CARTESIAN_POINT('Ctrl Pts',(42.9531398474371,21.3344173713818,0.));
#91112=CARTESIAN_POINT('Ctrl Pts',(42.9531398474371,21.3344173713818,20.));
#91113=CARTESIAN_POINT('Ctrl Pts',(42.9652520660998,21.3032261115844,0.));
#91114=CARTESIAN_POINT('Ctrl Pts',(42.9652520660998,21.3032261115844,20.));
#91115=CARTESIAN_POINT('Ctrl Pts',(42.9773422044374,21.2720274841006,0.));
#91116=CARTESIAN_POINT('Ctrl Pts',(42.9773422044374,21.2720274841006,20.));
#91117=CARTESIAN_POINT('Ctrl Pts',(42.9894102574195,21.2408215043074,0.));
#91118=CARTESIAN_POINT('Ctrl Pts',(42.9894102574195,21.2408215043074,20.));
#91119=CARTESIAN_POINT('Ctrl Pts',(43.0014562200264,21.2096081875857,0.));
#91120=CARTESIAN_POINT('Ctrl Pts',(43.0014562200264,21.2096081875857,20.));
#91121=CARTESIAN_POINT('Ctrl Pts',(43.0134800872489,21.1783875493205,0.));
#91122=CARTESIAN_POINT('Ctrl Pts',(43.0134800872489,21.1783875493205,20.));
#91123=CARTESIAN_POINT('Ctrl Pts',(43.0254818540885,21.1471596049,0.));
#91124=CARTESIAN_POINT('Ctrl Pts',(43.0254818540885,21.1471596049,20.));
#91125=CARTESIAN_POINT('Ctrl Pts',(43.037461515557,21.1159243697169,0.));
#91126=CARTESIAN_POINT('Ctrl Pts',(43.037461515557,21.1159243697169,20.));
#91127=CARTESIAN_POINT('Ctrl Pts',(43.049419066677,21.0846818591673,0.));
#91128=CARTESIAN_POINT('Ctrl Pts',(43.049419066677,21.0846818591673,20.));
#91129=CARTESIAN_POINT('Ctrl Pts',(43.0613545024815,21.0534320886512,0.));
#91130=CARTESIAN_POINT('Ctrl Pts',(43.0613545024815,21.0534320886512,20.));
#91131=CARTESIAN_POINT('Ctrl Pts',(43.0732678180139,21.0221750735727,0.));
#91132=CARTESIAN_POINT('Ctrl Pts',(43.0732678180139,21.0221750735727,20.));
#91133=CARTESIAN_POINT('Ctrl Pts',(43.0851590083283,20.9909108293397,0.));
#91134=CARTESIAN_POINT('Ctrl Pts',(43.0851590083283,20.9909108293397,20.));
#91135=CARTESIAN_POINT('Ctrl Pts',(43.0970280684896,20.959639371364,0.));
#91136=CARTESIAN_POINT('Ctrl Pts',(43.0970280684896,20.959639371364,20.));
#91137=CARTESIAN_POINT('Ctrl Pts',(43.1088749935734,20.9283607150615,0.));
#91138=CARTESIAN_POINT('Ctrl Pts',(43.1088749935734,20.9283607150615,20.));
#91139=CARTESIAN_POINT('Ctrl Pts',(43.1206997786656,20.8970748758512,0.));
#91140=CARTESIAN_POINT('Ctrl Pts',(43.1206997786656,20.8970748758512,20.));
#91141=CARTESIAN_POINT('Ctrl Pts',(43.132502418863,20.8657818691565,0.));
#91142=CARTESIAN_POINT('Ctrl Pts',(43.132502418863,20.8657818691565,20.));
#91143=CARTESIAN_POINT('Ctrl Pts',(43.1442829092724,20.8344817104039,0.));
#91144=CARTESIAN_POINT('Ctrl Pts',(43.1442829092724,20.8344817104039,20.));
#91145=CARTESIAN_POINT('Ctrl Pts',(43.1560412450117,20.8031744150242,0.));
#91146=CARTESIAN_POINT('Ctrl Pts',(43.1560412450117,20.8031744150242,20.));
#91147=CARTESIAN_POINT('Ctrl Pts',(43.1677774212093,20.7718599984519,0.));
#91148=CARTESIAN_POINT('Ctrl Pts',(43.1677774212093,20.7718599984519,20.));
#91149=CARTESIAN_POINT('Ctrl Pts',(43.1794914330045,20.7405384761252,0.));
#91150=CARTESIAN_POINT('Ctrl Pts',(43.1794914330045,20.7405384761252,20.));
#91151=CARTESIAN_POINT('Ctrl Pts',(43.1911832755467,20.7092098634864,0.));
#91152=CARTESIAN_POINT('Ctrl Pts',(43.1911832755467,20.7092098634864,20.));
#91153=CARTESIAN_POINT('Ctrl Pts',(43.202852943996,20.6778741759814,0.));
#91154=CARTESIAN_POINT('Ctrl Pts',(43.202852943996,20.6778741759814,20.));
#91155=CARTESIAN_POINT('Ctrl Pts',(43.2145004335236,20.6465314290598,0.));
#91156=CARTESIAN_POINT('Ctrl Pts',(43.2145004335236,20.6465314290598,20.));
#91157=CARTESIAN_POINT('Ctrl Pts',(43.2261257393109,20.615181638175,0.));
#91158=CARTESIAN_POINT('Ctrl Pts',(43.2261257393109,20.615181638175,20.));
#91159=CARTESIAN_POINT('Ctrl Pts',(43.2377288565503,20.5838248187841,0.));
#91160=CARTESIAN_POINT('Ctrl Pts',(43.2377288565503,20.5838248187841,20.));
#91161=CARTESIAN_POINT('Ctrl Pts',(43.2493097804445,20.5524609863481,0.));
#91162=CARTESIAN_POINT('Ctrl Pts',(43.2493097804445,20.5524609863481,20.));
#91163=CARTESIAN_POINT('Ctrl Pts',(43.2608685062069,20.5210901563314,0.));
#91164=CARTESIAN_POINT('Ctrl Pts',(43.2608685062069,20.5210901563314,20.));
#91165=CARTESIAN_POINT('Ctrl Pts',(43.2724050290617,20.4897123442023,0.));
#91166=CARTESIAN_POINT('Ctrl Pts',(43.2724050290617,20.4897123442023,20.));
#91167=CARTESIAN_POINT('Ctrl Pts',(43.283919344243,20.4583275654327,0.));
#91168=CARTESIAN_POINT('Ctrl Pts',(43.283919344243,20.4583275654327,20.));
#91169=CARTESIAN_POINT('Ctrl Pts',(43.2954114469964,20.4269358354984,0.));
#91170=CARTESIAN_POINT('Ctrl Pts',(43.2954114469964,20.4269358354984,20.));
#91171=CARTESIAN_POINT('Ctrl Pts',(43.3068813325774,20.3955371698787,0.));
#91172=CARTESIAN_POINT('Ctrl Pts',(43.3068813325774,20.3955371698787,20.));
#91173=CARTESIAN_POINT('Ctrl Pts',(43.3183289962528,20.3641315840566,0.));
#91174=CARTESIAN_POINT('Ctrl Pts',(43.3183289962528,20.3641315840566,20.));
#91175=CARTESIAN_POINT('Ctrl Pts',(43.3297544333003,20.3327190935193,0.));
#91176=CARTESIAN_POINT('Ctrl Pts',(43.3297544333003,20.3327190935193,20.));
#91177=CARTESIAN_POINT('Ctrl Pts',(43.3411576390085,20.3012997137575,0.));
#91178=CARTESIAN_POINT('Ctrl Pts',(43.3411576390085,20.3012997137575,20.));
#91179=CARTESIAN_POINT('Ctrl Pts',(43.3525386086763,20.2698734602656,0.));
#91180=CARTESIAN_POINT('Ctrl Pts',(43.3525386086763,20.2698734602656,20.));
#91181=CARTESIAN_POINT('Ctrl Pts',(43.3638973376125,20.2384403485411,0.));
#91182=CARTESIAN_POINT('Ctrl Pts',(43.3638973376125,20.2384403485411,20.));
#91183=CARTESIAN_POINT('Ctrl Pts',(43.3752338211368,20.2070003940853,0.));
#91184=CARTESIAN_POINT('Ctrl Pts',(43.3752338211368,20.2070003940853,20.));
#91185=CARTESIAN_POINT('Ctrl Pts',(43.3865480545792,20.1755536124033,0.));
#91186=CARTESIAN_POINT('Ctrl Pts',(43.3865480545792,20.1755536124033,20.));
#91187=CARTESIAN_POINT('Ctrl Pts',(43.3978400332808,20.1441000190037,0.));
#91188=CARTESIAN_POINT('Ctrl Pts',(43.3978400332808,20.1441000190037,20.));
#91189=CARTESIAN_POINT('Ctrl Pts',(43.409109752594,20.1126396293992,0.));
#91190=CARTESIAN_POINT('Ctrl Pts',(43.409109752594,20.1126396293992,20.));
#91191=CARTESIAN_POINT('Ctrl Pts',(43.4203572078819,20.0811724591059,0.));
#91192=CARTESIAN_POINT('Ctrl Pts',(43.4203572078819,20.0811724591059,20.));
#91193=CARTESIAN_POINT('Ctrl Pts',(43.4315823945181,20.0496985236436,0.));
#91194=CARTESIAN_POINT('Ctrl Pts',(43.4315823945181,20.0496985236436,20.));
#91195=CARTESIAN_POINT('Ctrl Pts',(43.4427853078868,20.0182178385356,0.));
#91196=CARTESIAN_POINT('Ctrl Pts',(43.4427853078868,20.0182178385356,20.));
#91197=CARTESIAN_POINT('Ctrl Pts',(43.4539659433821,19.9867304193089,0.));
#91198=CARTESIAN_POINT('Ctrl Pts',(43.4539659433821,19.9867304193089,20.));
#91199=CARTESIAN_POINT('Ctrl Pts',(43.4651242964088,19.9552362814936,0.));
#91200=CARTESIAN_POINT('Ctrl Pts',(43.4651242964088,19.9552362814936,20.));
#91201=CARTESIAN_POINT('Ctrl Pts',(43.4762603623832,19.923735440624,0.));
#91202=CARTESIAN_POINT('Ctrl Pts',(43.4762603623832,19.923735440624,20.));
#91203=CARTESIAN_POINT('Ctrl Pts',(43.4873741367321,19.8922279122378,0.));
#91204=CARTESIAN_POINT('Ctrl Pts',(43.4873741367321,19.8922279122378,20.));
#91205=CARTESIAN_POINT('Ctrl Pts',(43.4984656148935,19.8607137118763,0.));
#91206=CARTESIAN_POINT('Ctrl Pts',(43.4984656148935,19.8607137118763,20.));
#91207=CARTESIAN_POINT('Ctrl Pts',(43.5095347923164,19.8291928550844,0.));
#91208=CARTESIAN_POINT('Ctrl Pts',(43.5095347923164,19.8291928550844,20.));
#91209=CARTESIAN_POINT('Ctrl Pts',(43.5205816644596,19.7976653574108,0.));
#91210=CARTESIAN_POINT('Ctrl Pts',(43.5205816644596,19.7976653574108,20.));
#91211=CARTESIAN_POINT('Ctrl Pts',(43.5316062267925,19.7661312344072,0.));
#91212=CARTESIAN_POINT('Ctrl Pts',(43.5316062267925,19.7661312344072,20.));
#91213=CARTESIAN_POINT('Ctrl Pts',(43.542608474795,19.734590501629,0.));
#91214=CARTESIAN_POINT('Ctrl Pts',(43.542608474795,19.734590501629,20.));
#91215=CARTESIAN_POINT('Ctrl Pts',(43.5535884039576,19.7030431746352,0.));
#91216=CARTESIAN_POINT('Ctrl Pts',(43.5535884039576,19.7030431746352,20.));
#91217=CARTESIAN_POINT('Ctrl Pts',(43.5645460097823,19.6714892689885,0.));
#91218=CARTESIAN_POINT('Ctrl Pts',(43.5645460097823,19.6714892689885,20.));
#91219=CARTESIAN_POINT('Ctrl Pts',(43.5754812877819,19.639928800255,0.));
#91220=CARTESIAN_POINT('Ctrl Pts',(43.5754812877819,19.639928800255,20.));
#91221=CARTESIAN_POINT('Ctrl Pts',(43.5863942334797,19.6083617840046,0.));
#91222=CARTESIAN_POINT('Ctrl Pts',(43.5863942334797,19.6083617840046,20.));
#91223=CARTESIAN_POINT('Ctrl Pts',(43.5972848424097,19.5767882358104,0.));
#91224=CARTESIAN_POINT('Ctrl Pts',(43.5972848424097,19.5767882358104,20.));
#91225=CARTESIAN_POINT('Ctrl Pts',(43.6081531101168,19.545208171249,0.));
#91226=CARTESIAN_POINT('Ctrl Pts',(43.6081531101168,19.545208171249,20.));
#91227=CARTESIAN_POINT('Ctrl Pts',(43.6189990321561,19.5136216059004,0.));
#91228=CARTESIAN_POINT('Ctrl Pts',(43.6189990321561,19.5136216059004,20.));
#91229=CARTESIAN_POINT('Ctrl Pts',(43.629822604094,19.4820285553483,0.));
#91230=CARTESIAN_POINT('Ctrl Pts',(43.629822604094,19.4820285553483,20.));
#91231=CARTESIAN_POINT('Ctrl Pts',(43.6406238215078,19.4504290351799,0.));
#91232=CARTESIAN_POINT('Ctrl Pts',(43.6406238215078,19.4504290351799,20.));
#91233=CARTESIAN_POINT('Ctrl Pts',(43.6514026799849,19.4188230609858,0.));
#91234=CARTESIAN_POINT('Ctrl Pts',(43.6514026799849,19.4188230609858,20.));
#91235=CARTESIAN_POINT('Ctrl Pts',(43.6621591751234,19.3872106483603,0.));
#91236=CARTESIAN_POINT('Ctrl Pts',(43.6621591751234,19.3872106483603,20.));
#91237=CARTESIAN_POINT('Ctrl Pts',(43.6728933025325,19.3555918129009,0.));
#91238=CARTESIAN_POINT('Ctrl Pts',(43.6728933025325,19.3555918129009,20.));
#91239=CARTESIAN_POINT('Ctrl Pts',(43.6836050578319,19.3239665702086,0.));
#91240=CARTESIAN_POINT('Ctrl Pts',(43.6836050578319,19.3239665702086,20.));
#91241=CARTESIAN_POINT('Ctrl Pts',(43.6942944366523,19.2923349358879,0.));
#91242=CARTESIAN_POINT('Ctrl Pts',(43.6942944366523,19.2923349358879,20.));
#91243=CARTESIAN_POINT('Ctrl Pts',(43.7049614346349,19.2606969255464,0.));
#91244=CARTESIAN_POINT('Ctrl Pts',(43.7049614346349,19.2606969255464,20.));
#91245=CARTESIAN_POINT('Ctrl Pts',(43.7156060474324,19.2290525547956,0.));
#91246=CARTESIAN_POINT('Ctrl Pts',(43.7156060474324,19.2290525547956,20.));
#91247=CARTESIAN_POINT('Ctrl Pts',(43.7262282707082,19.1974018392505,0.));
#91248=CARTESIAN_POINT('Ctrl Pts',(43.7262282707082,19.1974018392505,20.));
#91249=CARTESIAN_POINT('Ctrl Pts',(43.7368281001363,19.1657447945291,0.));
#91250=CARTESIAN_POINT('Ctrl Pts',(43.7368281001363,19.1657447945291,20.));
#91251=CARTESIAN_POINT('Ctrl Pts',(43.747405531401,19.1340814362531,0.));
#91252=CARTESIAN_POINT('Ctrl Pts',(43.747405531401,19.1340814362531,20.));
#91253=CARTESIAN_POINT('Ctrl Pts',(43.7579605601976,19.1024117800474,0.));
#91254=CARTESIAN_POINT('Ctrl Pts',(43.7579605601976,19.1024117800474,20.));
#91255=CARTESIAN_POINT('Ctrl Pts',(43.7684931822314,19.0707358415405,0.));
#91256=CARTESIAN_POINT('Ctrl Pts',(43.7684931822314,19.0707358415405,20.));
#91257=CARTESIAN_POINT('Ctrl Pts',(43.779003393219,19.039053636364,0.));
#91258=CARTESIAN_POINT('Ctrl Pts',(43.779003393219,19.039053636364,20.));
#91259=CARTESIAN_POINT('Ctrl Pts',(43.7894911888877,19.0073651801531,0.));
#91260=CARTESIAN_POINT('Ctrl Pts',(43.7894911888877,19.0073651801531,20.));
#91261=CARTESIAN_POINT('Ctrl Pts',(43.7999565649762,18.9756704885464,0.));
#91262=CARTESIAN_POINT('Ctrl Pts',(43.7999565649762,18.9756704885464,20.));
#91263=CARTESIAN_POINT('Ctrl Pts',(43.8103995172341,18.9439695771858,0.));
#91264=CARTESIAN_POINT('Ctrl Pts',(43.8103995172341,18.9439695771858,20.));
#91265=CARTESIAN_POINT('Ctrl Pts',(43.8208200414219,18.9122624617166,0.));
#91266=CARTESIAN_POINT('Ctrl Pts',(43.8208200414219,18.9122624617166,20.));
#91267=CARTESIAN_POINT('Ctrl Pts',(43.8312181333106,18.8805491577876,0.));
#91268=CARTESIAN_POINT('Ctrl Pts',(43.8312181333106,18.8805491577876,20.));
#91269=CARTESIAN_POINT('Ctrl Pts',(43.8415937886817,18.8488296810507,0.));
#91270=CARTESIAN_POINT('Ctrl Pts',(43.8415937886817,18.8488296810507,20.));
#91271=CARTESIAN_POINT('Ctrl Pts',(43.8519470033272,18.8171040471611,0.));
#91272=CARTESIAN_POINT('Ctrl Pts',(43.8519470033272,18.8171040471611,20.));
#91273=CARTESIAN_POINT('Ctrl Pts',(43.8622777730502,18.7853722717774,0.));
#91274=CARTESIAN_POINT('Ctrl Pts',(43.8622777730502,18.7853722717774,20.));
#91275=CARTESIAN_POINT('Ctrl Pts',(43.8725860936644,18.7536343705616,0.));
#91276=CARTESIAN_POINT('Ctrl Pts',(43.8725860936644,18.7536343705616,20.));
#91277=CARTESIAN_POINT('Ctrl Pts',(43.8828719609947,18.721890359179,0.));
#91278=CARTESIAN_POINT('Ctrl Pts',(43.8828719609947,18.721890359179,20.));
#91279=CARTESIAN_POINT('Ctrl Pts',(43.8931353708767,18.6901402532984,0.));
#91280=CARTESIAN_POINT('Ctrl Pts',(43.8931353708767,18.6901402532984,20.));
#91281=CARTESIAN_POINT('Ctrl Pts',(43.903376319157,18.6583840685915,0.));
#91282=CARTESIAN_POINT('Ctrl Pts',(43.903376319157,18.6583840685915,20.));
#91283=CARTESIAN_POINT('Ctrl Pts',(43.913594801693,18.6266218207337,0.));
#91284=CARTESIAN_POINT('Ctrl Pts',(43.913594801693,18.6266218207337,20.));
#91285=CARTESIAN_POINT('Ctrl Pts',(43.9237908143526,18.5948535254034,0.));
#91286=CARTESIAN_POINT('Ctrl Pts',(43.9237908143526,18.5948535254034,20.));
#91287=CARTESIAN_POINT('Ctrl Pts',(43.9339643530151,18.5630791982821,0.));
#91288=CARTESIAN_POINT('Ctrl Pts',(43.9339643530151,18.5630791982821,20.));
#91289=CARTESIAN_POINT('Ctrl Pts',(43.94411541357,18.5312988550549,0.));
#91290=CARTESIAN_POINT('Ctrl Pts',(43.94411541357,18.5312988550549,20.));
#91291=CARTESIAN_POINT('Ctrl Pts',(43.9542439919177,18.4995125114099,0.));
#91292=CARTESIAN_POINT('Ctrl Pts',(43.9542439919177,18.4995125114099,20.));
#91293=CARTESIAN_POINT('Ctrl Pts',(43.9643500839697,18.4677201830388,0.));
#91294=CARTESIAN_POINT('Ctrl Pts',(43.9643500839697,18.4677201830388,20.));
#91295=CARTESIAN_POINT('Ctrl Pts',(43.9744336856481,18.4359218856365,0.));
#91296=CARTESIAN_POINT('Ctrl Pts',(43.9744336856481,18.4359218856365,20.));
#91297=CARTESIAN_POINT('Ctrl Pts',(43.9844947928861,18.4041176349014,0.));
#91298=CARTESIAN_POINT('Ctrl Pts',(43.9844947928861,18.4041176349014,20.));
#91299=CARTESIAN_POINT('Ctrl Pts',(43.9945334016277,18.3723074465347,0.));
#91300=CARTESIAN_POINT('Ctrl Pts',(43.9945334016277,18.3723074465347,20.));
#91301=CARTESIAN_POINT('Ctrl Pts',(44.0045495078276,18.3404913362408,0.));
#91302=CARTESIAN_POINT('Ctrl Pts',(44.0045495078276,18.3404913362408,20.));
#91303=CARTESIAN_POINT('Ctrl Pts',(44.0145431074514,18.3086693197275,0.));
#91304=CARTESIAN_POINT('Ctrl Pts',(44.0145431074514,18.3086693197275,20.));
#91305=CARTESIAN_POINT('Ctrl Pts',(44.0245141964756,18.2768414127056,0.));
#91306=CARTESIAN_POINT('Ctrl Pts',(44.0245141964756,18.2768414127056,20.));
#91307=CARTESIAN_POINT('Ctrl Pts',(44.0344627708874,18.245007630889,0.));
#91308=CARTESIAN_POINT('Ctrl Pts',(44.0344627708874,18.245007630889,20.));
#91309=CARTESIAN_POINT('Ctrl Pts',(44.044388826685,18.2131679899948,0.));
#91310=CARTESIAN_POINT('Ctrl Pts',(44.044388826685,18.2131679899948,20.));
#91311=CARTESIAN_POINT('Ctrl Pts',(44.0542923598772,18.1813225057438,0.));
#91312=CARTESIAN_POINT('Ctrl Pts',(44.0542923598772,18.1813225057438,20.));
#91313=CARTESIAN_POINT('Ctrl Pts',(44.0641733664839,18.1494711938598,0.));
#91314=CARTESIAN_POINT('Ctrl Pts',(44.0641733664839,18.1494711938598,20.));
#91315=CARTESIAN_POINT('Ctrl Pts',(44.0740318425361,18.1176140700699,0.));
#91316=CARTESIAN_POINT('Ctrl Pts',(44.0740318425361,18.1176140700699,20.));
#91317=CARTESIAN_POINT('Ctrl Pts',(44.0838677840754,18.0857511501043,0.));
#91318=CARTESIAN_POINT('Ctrl Pts',(44.0838677840754,18.0857511501043,20.));
#91319=CARTESIAN_POINT('Ctrl Pts',(44.0936811871546,18.0538824496962,0.));
#91320=CARTESIAN_POINT('Ctrl Pts',(44.0936811871546,18.0538824496962,20.));
#91321=CARTESIAN_POINT('Ctrl Pts',(44.1034720478372,18.0220079845822,0.));
#91322=CARTESIAN_POINT('Ctrl Pts',(44.1034720478372,18.0220079845822,20.));
#91323=CARTESIAN_POINT('Ctrl Pts',(44.1132403621971,17.9901277705015,0.));
#91324=CARTESIAN_POINT('Ctrl Pts',(44.1132403621971,17.9901277705015,20.));
#91325=CARTESIAN_POINT('Ctrl Pts',(44.1229861263191,17.9582418231966,0.));
#91326=CARTESIAN_POINT('Ctrl Pts',(44.1229861263191,17.9582418231966,20.));
#91327=CARTESIAN_POINT('Ctrl Pts',(44.1327093362991,17.9263501584131,0.));
#91328=CARTESIAN_POINT('Ctrl Pts',(44.1327093362991,17.9263501584131,20.));
#91329=CARTESIAN_POINT('Ctrl Pts',(44.1424099882439,17.8944527919,0.));
#91330=CARTESIAN_POINT('Ctrl Pts',(44.1424099882439,17.8944527919,20.));
#91331=CARTESIAN_POINT('Ctrl Pts',(44.1520880782717,17.8625497394092,0.));
#91332=CARTESIAN_POINT('Ctrl Pts',(44.1520880782717,17.8625497394092,20.));
#91333=CARTESIAN_POINT('Ctrl Pts',(44.1617436025112,17.8306410166963,0.));
#91334=CARTESIAN_POINT('Ctrl Pts',(44.1617436025112,17.8306410166963,20.));
#91335=CARTESIAN_POINT('Ctrl Pts',(44.1713765571021,17.7987266395196,0.));
#91336=CARTESIAN_POINT('Ctrl Pts',(44.1713765571021,17.7987266395196,20.));
#91337=CARTESIAN_POINT('Ctrl Pts',(44.1809869381949,17.7668066236405,0.));
#91338=CARTESIAN_POINT('Ctrl Pts',(44.1809869381949,17.7668066236405,20.));
#91339=CARTESIAN_POINT('Ctrl Pts',(44.1905747419505,17.7348809848234,0.));
#91340=CARTESIAN_POINT('Ctrl Pts',(44.1905747419505,17.7348809848234,20.));
#91341=CARTESIAN_POINT('Ctrl Pts',(44.2001399645408,17.7029497388358,0.));
#91342=CARTESIAN_POINT('Ctrl Pts',(44.2001399645408,17.7029497388358,20.));
#91343=CARTESIAN_POINT('Ctrl Pts',(44.2096826021493,17.6710129014481,0.));
#91344=CARTESIAN_POINT('Ctrl Pts',(44.2096826021493,17.6710129014481,20.));
#91345=CARTESIAN_POINT('Ctrl Pts',(44.2192026509705,17.6390704884341,0.));
#91346=CARTESIAN_POINT('Ctrl Pts',(44.2192026509705,17.6390704884341,20.));
#91347=CARTESIAN_POINT('Ctrl Pts',(44.2287001072093,17.6071225155702,0.));
#91348=CARTESIAN_POINT('Ctrl Pts',(44.2287001072093,17.6071225155702,20.));
#91349=CARTESIAN_POINT('Ctrl Pts',(44.2381749670816,17.5751689986363,0.));
#91350=CARTESIAN_POINT('Ctrl Pts',(44.2381749670816,17.5751689986363,20.));
#91351=CARTESIAN_POINT('Ctrl Pts',(44.2476272268138,17.5432099534151,0.));
#91352=CARTESIAN_POINT('Ctrl Pts',(44.2476272268138,17.5432099534151,20.));
#91353=CARTESIAN_POINT('Ctrl Pts',(44.2570568826434,17.5112453956925,0.));
#91354=CARTESIAN_POINT('Ctrl Pts',(44.2570568826434,17.5112453956925,20.));
#91355=CARTESIAN_POINT('Ctrl Pts',(44.2664639308191,17.4792753412574,0.));
#91356=CARTESIAN_POINT('Ctrl Pts',(44.2664639308191,17.4792753412574,20.));
#91357=CARTESIAN_POINT('Ctrl Pts',(44.2758483676008,17.447299805902,0.));
#91358=CARTESIAN_POINT('Ctrl Pts',(44.2758483676008,17.447299805902,20.));
#91359=CARTESIAN_POINT('Ctrl Pts',(44.2852101892593,17.4153188054211,0.));
#91360=CARTESIAN_POINT('Ctrl Pts',(44.2852101892593,17.4153188054211,20.));
#91361=CARTESIAN_POINT('Ctrl Pts',(44.294549392076,17.3833323556128,0.));
#91362=CARTESIAN_POINT('Ctrl Pts',(44.294549392076,17.3833323556128,20.));
#91363=CARTESIAN_POINT('Ctrl Pts',(44.3038659723435,17.3513404722779,0.));
#91364=CARTESIAN_POINT('Ctrl Pts',(44.3038659723435,17.3513404722779,20.));
#91365=CARTESIAN_POINT('Ctrl Pts',(44.3131599263642,17.3193431712198,0.));
#91366=CARTESIAN_POINT('Ctrl Pts',(44.3131599263642,17.3193431712198,20.));
#91367=CARTESIAN_POINT('Ctrl Pts',(44.3224312504523,17.2873404682456,0.));
#91368=CARTESIAN_POINT('Ctrl Pts',(44.3224312504523,17.2873404682456,20.));
#91369=CARTESIAN_POINT('Ctrl Pts',(44.3316799409325,17.2553323791649,0.));
#91370=CARTESIAN_POINT('Ctrl Pts',(44.3316799409325,17.2553323791649,20.));
#91371=CARTESIAN_POINT('Ctrl Pts',(44.340905994141,17.2233189197905,0.));
#91372=CARTESIAN_POINT('Ctrl Pts',(44.340905994141,17.2233189197905,20.));
#91373=CARTESIAN_POINT('Ctrl Pts',(44.3501094064252,17.1913001059384,0.));
#91374=CARTESIAN_POINT('Ctrl Pts',(44.3501094064252,17.1913001059384,20.));
#91375=CARTESIAN_POINT('Ctrl Pts',(44.3592901741436,17.1592759534275,0.));
#91376=CARTESIAN_POINT('Ctrl Pts',(44.3592901741436,17.1592759534275,20.));
#91377=CARTESIAN_POINT('Ctrl Pts',(44.3684482936655,17.1272464780797,0.));
#91378=CARTESIAN_POINT('Ctrl Pts',(44.3684482936655,17.1272464780797,20.));
#91379=CARTESIAN_POINT('Ctrl Pts',(44.3775837613707,17.0952116957196,0.));
#91380=CARTESIAN_POINT('Ctrl Pts',(44.3775837613707,17.0952116957196,20.));
#91381=CARTESIAN_POINT('Ctrl Pts',(44.3866965736492,17.0631716221745,0.));
#91382=CARTESIAN_POINT('Ctrl Pts',(44.3866965736492,17.0631716221745,20.));
#91383=CARTESIAN_POINT('Ctrl Pts',(44.3957867269024,17.0311262732746,0.));
#91384=CARTESIAN_POINT('Ctrl Pts',(44.3957867269024,17.0311262732746,20.));
#91385=CARTESIAN_POINT('Ctrl Pts',(44.404854217543,16.9990756648532,0.));
#91386=CARTESIAN_POINT('Ctrl Pts',(44.404854217543,16.9990756648532,20.));
#91387=CARTESIAN_POINT('Ctrl Pts',(44.4138990419958,16.967019812747,0.));
#91388=CARTESIAN_POINT('Ctrl Pts',(44.4138990419958,16.967019812747,20.));
#91389=CARTESIAN_POINT('Ctrl Pts',(44.4229211966955,16.9349587327952,0.));
#91390=CARTESIAN_POINT('Ctrl Pts',(44.4229211966955,16.9349587327952,20.));
#91391=CARTESIAN_POINT('Ctrl Pts',(44.4319206780879,16.9028924408399,0.));
#91392=CARTESIAN_POINT('Ctrl Pts',(44.4319206780879,16.9028924408399,20.));
#91393=CARTESIAN_POINT('Ctrl Pts',(44.4408974826293,16.870820952726,0.));
#91394=CARTESIAN_POINT('Ctrl Pts',(44.4408974826293,16.870820952726,20.));
#91395=CARTESIAN_POINT('Ctrl Pts',(44.4498516067869,16.8387442843012,0.));
#91396=CARTESIAN_POINT('Ctrl Pts',(44.4498516067869,16.8387442843012,20.));
#91397=CARTESIAN_POINT('Ctrl Pts',(44.4587830470388,16.8066624514163,0.));
#91398=CARTESIAN_POINT('Ctrl Pts',(44.4587830470388,16.8066624514163,20.));
#91399=CARTESIAN_POINT('Ctrl Pts',(44.4676917998748,16.7745754699247,0.));
#91400=CARTESIAN_POINT('Ctrl Pts',(44.4676917998748,16.7745754699247,20.));
#91401=CARTESIAN_POINT('Ctrl Pts',(44.4765778617956,16.742483355683,0.));
#91402=CARTESIAN_POINT('Ctrl Pts',(44.4765778617956,16.742483355683,20.));
#91403=CARTESIAN_POINT('Ctrl Pts',(44.4854412293128,16.7103861245505,0.));
#91404=CARTESIAN_POINT('Ctrl Pts',(44.4854412293128,16.7103861245505,20.));
#91405=CARTESIAN_POINT('Ctrl Pts',(44.4942818989491,16.6782837923893,0.));
#91406=CARTESIAN_POINT('Ctrl Pts',(44.4942818989491,16.6782837923893,20.));
#91407=CARTESIAN_POINT('Ctrl Pts',(44.503099867238,16.6461763750644,0.));
#91408=CARTESIAN_POINT('Ctrl Pts',(44.503099867238,16.6461763750644,20.));
#91409=CARTESIAN_POINT('Ctrl Pts',(44.5118951307243,16.6140638884438,0.));
#91410=CARTESIAN_POINT('Ctrl Pts',(44.5118951307243,16.6140638884438,20.));
#91411=CARTESIAN_POINT('Ctrl Pts',(44.5206676859632,16.581946348398,0.));
#91412=CARTESIAN_POINT('Ctrl Pts',(44.5206676859632,16.581946348398,20.));
#91413=CARTESIAN_POINT('Ctrl Pts',(44.5294175295214,16.5498237708003,0.));
#91414=CARTESIAN_POINT('Ctrl Pts',(44.5294175295214,16.5498237708003,20.));
#91415=CARTESIAN_POINT('Ctrl Pts',(44.5381446579761,16.5176961715269,0.));
#91416=CARTESIAN_POINT('Ctrl Pts',(44.5381446579761,16.5176961715269,20.));
#91417=CARTESIAN_POINT('Ctrl Pts',(44.5468490679154,16.4855635664567,0.));
#91418=CARTESIAN_POINT('Ctrl Pts',(44.5468490679154,16.4855635664567,20.));
#91419=CARTESIAN_POINT('Ctrl Pts',(44.5555307559385,16.4534259714715,0.));
#91420=CARTESIAN_POINT('Ctrl Pts',(44.5555307559385,16.4534259714715,20.));
#91421=CARTESIAN_POINT('Ctrl Pts',(44.5641897186557,16.4212834024559,0.));
#91422=CARTESIAN_POINT('Ctrl Pts',(44.5641897186557,16.4212834024559,20.));
#91423=CARTESIAN_POINT('Ctrl Pts',(44.5728259526889,16.3891358752972,0.));
#91424=CARTESIAN_POINT('Ctrl Pts',(44.5728259526889,16.3891358752972,20.));
#91425=CARTESIAN_POINT('Ctrl Pts',(44.581439454671,16.3569834058857,0.));
#91426=CARTESIAN_POINT('Ctrl Pts',(44.581439454671,16.3569834058857,20.));
#91427=CARTESIAN_POINT('Ctrl Pts',(44.5900302212458,16.3248260101143,0.));
#91428=CARTESIAN_POINT('Ctrl Pts',(44.5900302212458,16.3248260101143,20.));
#91429=CARTESIAN_POINT('Ctrl Pts',(44.5985982490682,16.2926637038787,0.));
#91430=CARTESIAN_POINT('Ctrl Pts',(44.5985982490682,16.2926637038787,20.));
#91431=CARTESIAN_POINT('Ctrl Pts',(44.6071435348036,16.2604965030773,0.));
#91432=CARTESIAN_POINT('Ctrl Pts',(44.6071435348036,16.2604965030773,20.));
#91433=CARTESIAN_POINT('Ctrl Pts',(44.6156660751288,16.2283244236112,0.));
#91434=CARTESIAN_POINT('Ctrl Pts',(44.6156660751288,16.2283244236112,20.));
#91435=CARTESIAN_POINT('Ctrl Pts',(44.6241658667307,16.196147481384,0.));
#91436=CARTESIAN_POINT('Ctrl Pts',(44.6241658667307,16.196147481384,20.));
#91437=CARTESIAN_POINT('Ctrl Pts',(44.6326429063072,16.1639656923023,0.));
#91438=CARTESIAN_POINT('Ctrl Pts',(44.6326429063072,16.1639656923023,20.));
#91439=CARTESIAN_POINT('Ctrl Pts',(44.6410971905673,16.131779072275,0.));
#91440=CARTESIAN_POINT('Ctrl Pts',(44.6410971905673,16.131779072275,20.));
#91441=CARTESIAN_POINT('Ctrl Pts',(44.649528716232,16.0995876372141,0.));
#91442=CARTESIAN_POINT('Ctrl Pts',(44.649528716232,16.0995876372141,20.));
#91443=CARTESIAN_POINT('Ctrl Pts',(44.6579374800339,16.0673914030343,0.));
#91444=CARTESIAN_POINT('Ctrl Pts',(44.6579374800339,16.0673914030343,20.));
#91445=CARTESIAN_POINT('Ctrl Pts',(44.6663234787169,16.0351903856534,0.));
#91446=CARTESIAN_POINT('Ctrl Pts',(44.6663234787169,16.0351903856534,20.));
#91447=CARTESIAN_POINT('Ctrl Pts',(44.6746867090345,16.0029846009915,0.));
#91448=CARTESIAN_POINT('Ctrl Pts',(44.6746867090345,16.0029846009915,20.));
#91449=CARTESIAN_POINT('Ctrl Pts',(44.6830271677516,15.9707740649715,0.));
#91450=CARTESIAN_POINT('Ctrl Pts',(44.6830271677516,15.9707740649715,20.));
#91451=CARTESIAN_POINT('Ctrl Pts',(44.691344851643,15.9385587935186,0.));
#91452=CARTESIAN_POINT('Ctrl Pts',(44.691344851643,15.9385587935186,20.));
#91453=CARTESIAN_POINT('Ctrl Pts',(44.6996397574952,15.9063388025603,0.));
#91454=CARTESIAN_POINT('Ctrl Pts',(44.6996397574952,15.9063388025603,20.));
#91455=CARTESIAN_POINT('Ctrl Pts',(44.7079118821065,15.8741141080272,0.));
#91456=CARTESIAN_POINT('Ctrl Pts',(44.7079118821065,15.8741141080272,20.));
#91457=CARTESIAN_POINT('Ctrl Pts',(44.7161612222865,15.8418847258528,0.));
#91458=CARTESIAN_POINT('Ctrl Pts',(44.7161612222865,15.8418847258528,20.));
#91459=CARTESIAN_POINT('Ctrl Pts',(44.7243877748558,15.8096506719735,0.));
#91460=CARTESIAN_POINT('Ctrl Pts',(44.7243877748558,15.8096506719735,20.));
#91461=CARTESIAN_POINT('Ctrl Pts',(44.7325915366458,15.7774119623278,0.));
#91462=CARTESIAN_POINT('Ctrl Pts',(44.7325915366458,15.7774119623278,20.));
#91463=CARTESIAN_POINT('Ctrl Pts',(44.7407725044985,15.745168612857,0.));
#91464=CARTESIAN_POINT('Ctrl Pts',(44.7407725044985,15.745168612857,20.));
#91465=CARTESIAN_POINT('Ctrl Pts',(44.7489306752664,15.7129206395047,0.));
#91466=CARTESIAN_POINT('Ctrl Pts',(44.7489306752664,15.7129206395047,20.));
#91467=CARTESIAN_POINT('Ctrl Pts',(44.7570660458133,15.6806680582172,0.));
#91468=CARTESIAN_POINT('Ctrl Pts',(44.7570660458133,15.6806680582172,20.));
#91469=CARTESIAN_POINT('Ctrl Pts',(44.7651786130144,15.6484108849434,0.));
#91470=CARTESIAN_POINT('Ctrl Pts',(44.7651786130144,15.6484108849434,20.));
#91471=CARTESIAN_POINT('Ctrl Pts',(44.7732683737566,15.6161491356348,0.));
#91472=CARTESIAN_POINT('Ctrl Pts',(44.7732683737566,15.6161491356348,20.));
#91473=CARTESIAN_POINT('Ctrl Pts',(44.7813353249379,15.583882826246,0.));
#91474=CARTESIAN_POINT('Ctrl Pts',(44.7813353249379,15.583882826246,20.));
#91475=CARTESIAN_POINT('Ctrl Pts',(44.7893794634672,15.5516119727338,0.));
#91476=CARTESIAN_POINT('Ctrl Pts',(44.7893794634672,15.5516119727338,20.));
#91477=CARTESIAN_POINT('Ctrl Pts',(44.7974007862643,15.5193365910578,0.));
#91478=CARTESIAN_POINT('Ctrl Pts',(44.7974007862643,15.5193365910578,20.));
#91479=CARTESIAN_POINT('Ctrl Pts',(44.8053992902599,15.4870566971799,0.));
#91480=CARTESIAN_POINT('Ctrl Pts',(44.8053992902599,15.4870566971799,20.));
#91481=CARTESIAN_POINT('Ctrl Pts',(44.8133749723964,15.4547723070643,0.));
#91482=CARTESIAN_POINT('Ctrl Pts',(44.8133749723964,15.4547723070643,20.));
#91483=CARTESIAN_POINT('Ctrl Pts',(44.8213278296263,15.4224834366782,0.));
#91484=CARTESIAN_POINT('Ctrl Pts',(44.8213278296263,15.4224834366782,20.));
#91485=CARTESIAN_POINT('Ctrl Pts',(44.8292578589132,15.3901901019906,0.));
#91486=CARTESIAN_POINT('Ctrl Pts',(44.8292578589132,15.3901901019906,20.));
#91487=CARTESIAN_POINT('Ctrl Pts',(44.8371650572316,15.3578923189739,0.));
#91488=CARTESIAN_POINT('Ctrl Pts',(44.8371650572316,15.3578923189739,20.));
#91489=CARTESIAN_POINT('Ctrl Pts',(44.8450494215678,15.3255901036026,0.));
#91490=CARTESIAN_POINT('Ctrl Pts',(44.8450494215678,15.3255901036026,20.));
#91491=CARTESIAN_POINT('Ctrl Pts',(44.8529109489191,15.2932834718541,0.));
#91492=CARTESIAN_POINT('Ctrl Pts',(44.8529109489191,15.2932834718541,20.));
#91493=CARTESIAN_POINT('Ctrl Pts',(44.8607496362943,15.2609724397079,0.));
#91494=CARTESIAN_POINT('Ctrl Pts',(44.8607496362943,15.2609724397079,20.));
#91495=CARTESIAN_POINT('Ctrl Pts',(44.8685654807131,15.2286570231461,0.));
#91496=CARTESIAN_POINT('Ctrl Pts',(44.8685654807131,15.2286570231461,20.));
#91497=CARTESIAN_POINT('Ctrl Pts',(44.8763584792064,15.1963372381533,0.));
#91498=CARTESIAN_POINT('Ctrl Pts',(44.8763584792064,15.1963372381533,20.));
#91499=CARTESIAN_POINT('Ctrl Pts',(44.8841286288163,15.1640131007166,0.));
#91500=CARTESIAN_POINT('Ctrl Pts',(44.8841286288163,15.1640131007166,20.));
#91501=CARTESIAN_POINT('Ctrl Pts',(44.8918759265956,15.1316846268256,0.));
#91502=CARTESIAN_POINT('Ctrl Pts',(44.8918759265956,15.1316846268256,20.));
#91503=CARTESIAN_POINT('Ctrl Pts',(44.8996003696078,15.0993518324721,0.));
#91504=CARTESIAN_POINT('Ctrl Pts',(44.8996003696078,15.0993518324721,20.));
#91505=CARTESIAN_POINT('Ctrl Pts',(44.9073019549277,15.0670147336509,0.));
#91506=CARTESIAN_POINT('Ctrl Pts',(44.9073019549277,15.0670147336509,20.));
#91507=CARTESIAN_POINT('Ctrl Pts',(44.9149806796409,15.034673346359,0.));
#91508=CARTESIAN_POINT('Ctrl Pts',(44.9149806796409,15.034673346359,20.));
#91509=CARTESIAN_POINT('Ctrl Pts',(44.9226365408441,15.0023276865958,0.));
#91510=CARTESIAN_POINT('Ctrl Pts',(44.9226365408441,15.0023276865958,20.));
#91511=CARTESIAN_POINT('Ctrl Pts',(44.9302695356455,14.969977770363,0.));
#91512=CARTESIAN_POINT('Ctrl Pts',(44.9302695356455,14.969977770363,20.));
#91513=CARTESIAN_POINT('Ctrl Pts',(44.9378796611651,14.9376236136649,0.));
#91514=CARTESIAN_POINT('Ctrl Pts',(44.9378796611651,14.9376236136649,20.));
#91515=CARTESIAN_POINT('Ctrl Pts',(44.9454669145344,14.9052652325081,0.));
#91516=CARTESIAN_POINT('Ctrl Pts',(44.9454669145344,14.9052652325081,20.));
#91517=CARTESIAN_POINT('Ctrl Pts',(44.9530312928957,14.8729026429019,0.));
#91518=CARTESIAN_POINT('Ctrl Pts',(44.9530312928957,14.8729026429019,20.));
#91519=CARTESIAN_POINT('Ctrl Pts',(44.9605727934022,14.8405358608577,0.));
#91520=CARTESIAN_POINT('Ctrl Pts',(44.9605727934022,14.8405358608577,20.));
#91521=CARTESIAN_POINT('Ctrl Pts',(44.9680914132176,14.8081649023895,0.));
#91522=CARTESIAN_POINT('Ctrl Pts',(44.9680914132176,14.8081649023895,20.));
#91523=CARTESIAN_POINT('Ctrl Pts',(44.9755871495162,14.7757897835134,0.));
#91524=CARTESIAN_POINT('Ctrl Pts',(44.9755871495162,14.7757897835134,20.));
#91525=CARTESIAN_POINT('Ctrl Pts',(44.9830599994838,14.7434105202483,0.));
#91526=CARTESIAN_POINT('Ctrl Pts',(44.9830599994838,14.7434105202483,20.));
#91527=CARTESIAN_POINT('Ctrl Pts',(44.9905099603172,14.7110271286153,0.));
#91528=CARTESIAN_POINT('Ctrl Pts',(44.9905099603172,14.7110271286153,20.));
#91529=CARTESIAN_POINT('Ctrl Pts',(44.9979370292252,14.6786396246378,0.));
#91530=CARTESIAN_POINT('Ctrl Pts',(44.9979370292252,14.6786396246378,20.));
#91531=CARTESIAN_POINT('Ctrl Pts',(45.0053412034276,14.6462480243418,0.));
#91532=CARTESIAN_POINT('Ctrl Pts',(45.0053412034276,14.6462480243418,20.));
#91533=CARTESIAN_POINT('Ctrl Pts',(45.0127224801553,14.6138523437553,0.));
#91534=CARTESIAN_POINT('Ctrl Pts',(45.0127224801553,14.6138523437553,20.));
#91535=CARTESIAN_POINT('Ctrl Pts',(45.020080856651,14.5814525989087,0.));
#91536=CARTESIAN_POINT('Ctrl Pts',(45.020080856651,14.5814525989087,20.));
#91537=CARTESIAN_POINT('Ctrl Pts',(45.0274163301681,14.5490488058349,0.));
#91538=CARTESIAN_POINT('Ctrl Pts',(45.0274163301681,14.5490488058349,20.));
#91539=CARTESIAN_POINT('Ctrl Pts',(45.0347288979708,14.516640980569,0.));
#91540=CARTESIAN_POINT('Ctrl Pts',(45.0347288979708,14.516640980569,20.));
#91541=CARTESIAN_POINT('Ctrl Pts',(45.0420185573341,14.4842291391484,0.));
#91542=CARTESIAN_POINT('Ctrl Pts',(45.0420185573341,14.4842291391484,20.));
#91543=CARTESIAN_POINT('Ctrl Pts',(45.0492853055441,14.451813297613,0.));
#91544=CARTESIAN_POINT('Ctrl Pts',(45.0492853055441,14.451813297613,20.));
#91545=CARTESIAN_POINT('Ctrl Pts',(45.0565291398984,14.4193934720051,0.));
#91546=CARTESIAN_POINT('Ctrl Pts',(45.0565291398984,14.4193934720051,20.));
#91547=CARTESIAN_POINT('Ctrl Pts',(45.0637500577056,14.3869696783692,0.));
#91548=CARTESIAN_POINT('Ctrl Pts',(45.0637500577056,14.3869696783692,20.));
#91549=CARTESIAN_POINT('Ctrl Pts',(45.0709480562863,14.354541932752,0.));
#91550=CARTESIAN_POINT('Ctrl Pts',(45.0709480562863,14.354541932752,20.));
#91551=CARTESIAN_POINT('Ctrl Pts',(45.0781231329719,14.3221102512025,0.));
#91552=CARTESIAN_POINT('Ctrl Pts',(45.0781231329719,14.3221102512025,20.));
#91553=CARTESIAN_POINT('Ctrl Pts',(45.0852752851048,14.2896746497719,0.));
#91554=CARTESIAN_POINT('Ctrl Pts',(45.0852752851048,14.2896746497719,20.));
#91555=CARTESIAN_POINT('Ctrl Pts',(45.0924045100383,14.2572351445137,0.));
#91556=CARTESIAN_POINT('Ctrl Pts',(45.0924045100383,14.2572351445137,20.));
#91557=CARTESIAN_POINT('Ctrl Pts',(45.0995108051367,14.2247917514836,0.));
#91558=CARTESIAN_POINT('Ctrl Pts',(45.0995108051367,14.2247917514836,20.));
#91559=CARTESIAN_POINT('Ctrl Pts',(45.1065941677758,14.1923444867396,0.));
#91560=CARTESIAN_POINT('Ctrl Pts',(45.1065941677758,14.1923444867396,20.));
#91561=CARTESIAN_POINT('Ctrl Pts',(45.1136545953429,14.1598933663423,0.));
#91562=CARTESIAN_POINT('Ctrl Pts',(45.1136545953429,14.1598933663423,20.));
#91563=CARTESIAN_POINT('Ctrl Pts',(45.1206920852361,14.127438406354,0.));
#91564=CARTESIAN_POINT('Ctrl Pts',(45.1206920852361,14.127438406354,20.));
#91565=CARTESIAN_POINT('Ctrl Pts',(45.127706634865,14.0949796228398,0.));
#91566=CARTESIAN_POINT('Ctrl Pts',(45.127706634865,14.0949796228398,20.));
#91567=CARTESIAN_POINT('Ctrl Pts',(45.1346982416501,14.0625170318665,0.));
#91568=CARTESIAN_POINT('Ctrl Pts',(45.1346982416501,14.0625170318665,20.));
#91569=CARTESIAN_POINT('Ctrl Pts',(45.1416669030232,14.0300506495033,0.));
#91570=CARTESIAN_POINT('Ctrl Pts',(45.1416669030232,14.0300506495033,20.));
#91571=CARTESIAN_POINT('Ctrl Pts',(45.1486126164275,13.997580491822,0.));
#91572=CARTESIAN_POINT('Ctrl Pts',(45.1486126164275,13.997580491822,20.));
#91573=CARTESIAN_POINT('Ctrl Pts',(45.1555353793172,13.9651065748961,0.));
#91574=CARTESIAN_POINT('Ctrl Pts',(45.1555353793172,13.9651065748961,20.));
#91575=CARTESIAN_POINT('Ctrl Pts',(45.1624351891574,13.9326289148012,0.));
#91576=CARTESIAN_POINT('Ctrl Pts',(45.1624351891574,13.9326289148012,20.));
#91577=CARTESIAN_POINT('Ctrl Pts',(45.1693120434241,13.9001475276153,0.));
#91578=CARTESIAN_POINT('Ctrl Pts',(45.1693120434241,13.9001475276153,20.));
#91579=CARTESIAN_POINT('Ctrl Pts',(45.1761659396043,13.8676624294184,0.));
#91580=CARTESIAN_POINT('Ctrl Pts',(45.1761659396043,13.8676624294184,20.));
#91581=CARTESIAN_POINT('Ctrl Pts',(45.1829968751969,13.8351736362929,0.));
#91582=CARTESIAN_POINT('Ctrl Pts',(45.1829968751969,13.8351736362929,20.));
#91583=CARTESIAN_POINT('Ctrl Pts',(45.1898048477123,13.8026811643234,0.));
#91584=CARTESIAN_POINT('Ctrl Pts',(45.1898048477123,13.8026811643234,20.));
#91585=CARTESIAN_POINT('Ctrl Pts',(45.1965898546723,13.7701850295968,0.));
#91586=CARTESIAN_POINT('Ctrl Pts',(45.1965898546723,13.7701850295968,20.));
#91587=CARTESIAN_POINT('Ctrl Pts',(45.2033518936101,13.7376852482019,0.));
#91588=CARTESIAN_POINT('Ctrl Pts',(45.2033518936101,13.7376852482019,20.));
#91589=CARTESIAN_POINT('Ctrl Pts',(45.2100909620697,13.7051818362299,0.));
#91590=CARTESIAN_POINT('Ctrl Pts',(45.2100909620697,13.7051818362299,20.));
#91591=CARTESIAN_POINT('Ctrl Pts',(45.2168070576061,13.6726748097738,0.));
#91592=CARTESIAN_POINT('Ctrl Pts',(45.2168070576061,13.6726748097738,20.));
#91593=CARTESIAN_POINT('Ctrl Pts',(45.2235001777847,13.6401641849286,0.));
#91594=CARTESIAN_POINT('Ctrl Pts',(45.2235001777847,13.6401641849286,20.));
#91595=CARTESIAN_POINT('Ctrl Pts',(45.2301703201819,13.6076499777915,0.));
#91596=CARTESIAN_POINT('Ctrl Pts',(45.2301703201819,13.6076499777915,20.));
#91597=CARTESIAN_POINT('Ctrl Pts',(45.2368174823856,13.5751322044618,0.));
#91598=CARTESIAN_POINT('Ctrl Pts',(45.2368174823856,13.5751322044618,20.));
#91599=CARTESIAN_POINT('Ctrl Pts',(45.2434416619952,13.542610881041,0.));
#91600=CARTESIAN_POINT('Ctrl Pts',(45.2434416619952,13.542610881041,20.));
#91601=CARTESIAN_POINT('Ctrl Pts',(45.2500428566225,13.5100860236329,0.));
#91602=CARTESIAN_POINT('Ctrl Pts',(45.2500428566225,13.5100860236329,20.));
#91603=CARTESIAN_POINT('Ctrl Pts',(45.2566210638904,13.4775576483433,0.));
#91604=CARTESIAN_POINT('Ctrl Pts',(45.2566210638904,13.4775576483433,20.));
#91605=CARTESIAN_POINT('Ctrl Pts',(45.2631762814325,13.44502577128,0.));
#91606=CARTESIAN_POINT('Ctrl Pts',(45.2631762814325,13.44502577128,20.));
#91607=CARTESIAN_POINT('Ctrl Pts',(45.2697085068935,13.4124904085531,0.));
#91608=CARTESIAN_POINT('Ctrl Pts',(45.2697085068935,13.4124904085531,20.));
#91609=CARTESIAN_POINT('Ctrl Pts',(45.276217737929,13.3799515762744,0.));
#91610=CARTESIAN_POINT('Ctrl Pts',(45.276217737929,13.3799515762744,20.));
#91611=CARTESIAN_POINT('Ctrl Pts',(45.2827039722059,13.3474092905576,0.));
#91612=CARTESIAN_POINT('Ctrl Pts',(45.2827039722059,13.3474092905576,20.));
#91613=CARTESIAN_POINT('Ctrl Pts',(45.2891672074022,13.3148635675188,0.));
#91614=CARTESIAN_POINT('Ctrl Pts',(45.2891672074022,13.3148635675188,20.));
#91615=CARTESIAN_POINT('Ctrl Pts',(45.2956074412073,13.282314423276,0.));
#91616=CARTESIAN_POINT('Ctrl Pts',(45.2956074412073,13.282314423276,20.));
#91617=CARTESIAN_POINT('Ctrl Pts',(45.3020246713218,13.2497618739494,0.));
#91618=CARTESIAN_POINT('Ctrl Pts',(45.3020246713218,13.2497618739494,20.));
#91619=CARTESIAN_POINT('Ctrl Pts',(45.3084188954577,13.217205935661,0.));
#91620=CARTESIAN_POINT('Ctrl Pts',(45.3084188954577,13.217205935661,20.));
#91621=CARTESIAN_POINT('Ctrl Pts',(45.3147901113387,13.1846466245352,0.));
#91622=CARTESIAN_POINT('Ctrl Pts',(45.3147901113387,13.1846466245352,20.));
#91623=CARTESIAN_POINT('Ctrl Pts',(45.321138316699,13.1520839566979,0.));
#91624=CARTESIAN_POINT('Ctrl Pts',(45.321138316699,13.1520839566979,20.));
#91625=CARTESIAN_POINT('Ctrl Pts',(45.3274635092846,13.1195179482773,0.));
#91626=CARTESIAN_POINT('Ctrl Pts',(45.3274635092846,13.1195179482773,20.));
#91627=CARTESIAN_POINT('Ctrl Pts',(45.3337656868523,13.0869486154035,0.));
#91628=CARTESIAN_POINT('Ctrl Pts',(45.3337656868523,13.0869486154035,20.));
#91629=CARTESIAN_POINT('Ctrl Pts',(45.3400448471699,13.0543759742083,0.));
#91630=CARTESIAN_POINT('Ctrl Pts',(45.3400448471699,13.0543759742083,20.));
#91631=CARTESIAN_POINT('Ctrl Pts',(45.3463009880171,13.021800040826,0.));
#91632=CARTESIAN_POINT('Ctrl Pts',(45.3463009880171,13.021800040826,20.));
#91633=CARTESIAN_POINT('Ctrl Pts',(45.3525341071849,12.9892208313927,0.));
#91634=CARTESIAN_POINT('Ctrl Pts',(45.3525341071849,12.9892208313927,20.));
#91635=CARTESIAN_POINT('Ctrl Pts',(45.3587442024753,12.9566383620464,0.));
#91636=CARTESIAN_POINT('Ctrl Pts',(45.3587442024753,12.9566383620464,20.));
#91637=CARTESIAN_POINT('Ctrl Pts',(45.364931271701,12.9240526489273,0.));
#91638=CARTESIAN_POINT('Ctrl Pts',(45.364931271701,12.9240526489273,20.));
#91639=CARTESIAN_POINT('Ctrl Pts',(45.371095312686,12.8914637081769,0.));
#91640=CARTESIAN_POINT('Ctrl Pts',(45.371095312686,12.8914637081769,20.));
#91641=CARTESIAN_POINT('Ctrl Pts',(45.3772363232658,12.8588715559393,0.));
#91642=CARTESIAN_POINT('Ctrl Pts',(45.3772363232658,12.8588715559393,20.));
#91643=CARTESIAN_POINT('Ctrl Pts',(45.3833543012877,12.82627620836,0.));
#91644=CARTESIAN_POINT('Ctrl Pts',(45.3833543012877,12.82627620836,20.));
#91645=CARTESIAN_POINT('Ctrl Pts',(45.3894492446102,12.7936776815868,0.));
#91646=CARTESIAN_POINT('Ctrl Pts',(45.3894492446102,12.7936776815868,20.));
#91647=CARTESIAN_POINT('Ctrl Pts',(45.3955211511033,12.7610759917694,0.));
#91648=CARTESIAN_POINT('Ctrl Pts',(45.3955211511033,12.7610759917694,20.));
#91649=CARTESIAN_POINT('Ctrl Pts',(45.4015700186485,12.7284711550592,0.));
#91650=CARTESIAN_POINT('Ctrl Pts',(45.4015700186485,12.7284711550592,20.));
#91651=CARTESIAN_POINT('Ctrl Pts',(45.407595845137,12.6958631876099,0.));
#91652=CARTESIAN_POINT('Ctrl Pts',(45.407595845137,12.6958631876099,20.));
#91653=CARTESIAN_POINT('Ctrl Pts',(45.4135986284717,12.6632521055766,0.));
#91654=CARTESIAN_POINT('Ctrl Pts',(45.4135986284717,12.6632521055766,20.));
#91655=CARTESIAN_POINT('Ctrl Pts',(45.4195783665665,12.6306379251165,0.));
#91656=CARTESIAN_POINT('Ctrl Pts',(45.4195783665665,12.6306379251165,20.));
#91657=CARTESIAN_POINT('Ctrl Pts',(45.4255350573473,12.5980206623884,0.));
#91658=CARTESIAN_POINT('Ctrl Pts',(45.4255350573473,12.5980206623884,20.));
#91659=CARTESIAN_POINT('Ctrl Pts',(45.4314686987515,12.5654003335533,0.));
#91660=CARTESIAN_POINT('Ctrl Pts',(45.4314686987515,12.5654003335533,20.));
#91661=CARTESIAN_POINT('Ctrl Pts',(45.4373792887274,12.5327769547739,0.));
#91662=CARTESIAN_POINT('Ctrl Pts',(45.4373792887274,12.5327769547739,20.));
#91663=CARTESIAN_POINT('Ctrl Pts',(45.4432668252347,12.500150542215,0.));
#91664=CARTESIAN_POINT('Ctrl Pts',(45.4432668252347,12.500150542215,20.));
#91665=CARTESIAN_POINT('Ctrl Pts',(45.4491313062444,12.4675211120431,0.));
#91666=CARTESIAN_POINT('Ctrl Pts',(45.4491313062444,12.4675211120431,20.));
#91667=CARTESIAN_POINT('Ctrl Pts',(45.4549727297392,12.4348886804266,0.));
#91668=CARTESIAN_POINT('Ctrl Pts',(45.4549727297392,12.4348886804266,20.));
#91669=CARTESIAN_POINT('Ctrl Pts',(45.4607910937128,12.4022532635357,0.));
#91670=CARTESIAN_POINT('Ctrl Pts',(45.4607910937128,12.4022532635357,20.));
#91671=CARTESIAN_POINT('Ctrl Pts',(45.4665863961701,12.3696148775423,0.));
#91672=CARTESIAN_POINT('Ctrl Pts',(45.4665863961701,12.3696148775423,20.));
#91673=CARTESIAN_POINT('Ctrl Pts',(45.4723586351267,12.3369735386201,0.));
#91674=CARTESIAN_POINT('Ctrl Pts',(45.4723586351267,12.3369735386201,20.));
#91675=CARTESIAN_POINT('Ctrl Pts',(45.4781078086095,12.3043292629445,0.));
#91676=CARTESIAN_POINT('Ctrl Pts',(45.4781078086095,12.3043292629445,20.));
#91677=CARTESIAN_POINT('Ctrl Pts',(45.483833914657,12.2716820666929,0.));
#91678=CARTESIAN_POINT('Ctrl Pts',(45.483833914657,12.2716820666929,20.));
#91679=CARTESIAN_POINT('Ctrl Pts',(45.4895369513189,12.2390319660445,0.));
#91680=CARTESIAN_POINT('Ctrl Pts',(45.4895369513189,12.2390319660445,20.));
#91681=CARTESIAN_POINT('Ctrl Pts',(45.4952169166561,12.2063789771801,0.));
#91682=CARTESIAN_POINT('Ctrl Pts',(45.4952169166561,12.2063789771801,20.));
#91683=CARTESIAN_POINT('Ctrl Pts',(45.5008738087416,12.1737231162825,0.));
#91684=CARTESIAN_POINT('Ctrl Pts',(45.5008738087416,12.1737231162825,20.));
#91685=CARTESIAN_POINT('Ctrl Pts',(45.5065076256599,12.1410643995363,0.));
#91686=CARTESIAN_POINT('Ctrl Pts',(45.5065076256599,12.1410643995363,20.));
#91687=CARTESIAN_POINT('Ctrl Pts',(45.5121183655068,12.1084028431278,0.));
#91688=CARTESIAN_POINT('Ctrl Pts',(45.5121183655068,12.1084028431278,20.));
#91689=CARTESIAN_POINT('Ctrl Pts',(45.5177060263888,12.0757384632451,0.));
#91690=CARTESIAN_POINT('Ctrl Pts',(45.5177060263888,12.0757384632451,20.));
#91691=CARTESIAN_POINT('Ctrl Pts',(45.5232706064237,12.0430712760779,0.));
#91692=CARTESIAN_POINT('Ctrl Pts',(45.5232706064237,12.0430712760779,20.));
#91693=CARTESIAN_POINT('Ctrl Pts',(45.5288121037394,12.0104012978174,0.));
#91694=CARTESIAN_POINT('Ctrl Pts',(45.5288121037394,12.0104012978174,20.));
#91695=CARTESIAN_POINT('Ctrl Pts',(45.5343305164759,11.9777285446569,0.));
#91696=CARTESIAN_POINT('Ctrl Pts',(45.5343305164759,11.9777285446569,20.));
#91697=CARTESIAN_POINT('Ctrl Pts',(45.5398258427844,11.9450530327911,0.));
#91698=CARTESIAN_POINT('Ctrl Pts',(45.5398258427844,11.9450530327911,20.));
#91699=CARTESIAN_POINT('Ctrl Pts',(45.5452980808284,11.9123747784165,0.));
#91700=CARTESIAN_POINT('Ctrl Pts',(45.5452980808284,11.9123747784165,20.));
#91701=CARTESIAN_POINT('Ctrl Pts',(45.5507472287824,11.8796937977314,0.));
#91702=CARTESIAN_POINT('Ctrl Pts',(45.5507472287824,11.8796937977314,20.));
#91703=CARTESIAN_POINT('Ctrl Pts',(45.5561732848327,11.8470101069358,0.));
#91704=CARTESIAN_POINT('Ctrl Pts',(45.5561732848327,11.8470101069358,20.));
#91705=CARTESIAN_POINT('Ctrl Pts',(45.5615762471761,11.8143237222317,0.));
#91706=CARTESIAN_POINT('Ctrl Pts',(45.5615762471761,11.8143237222317,20.));
#91707=CARTESIAN_POINT('Ctrl Pts',(45.5669561140206,11.7816346598227,0.));
#91708=CARTESIAN_POINT('Ctrl Pts',(45.5669561140206,11.7816346598227,20.));
#91709=CARTESIAN_POINT('Ctrl Pts',(45.5723128835857,11.748942935914,0.));
#91710=CARTESIAN_POINT('Ctrl Pts',(45.5723128835857,11.748942935914,20.));
#91711=CARTESIAN_POINT('Ctrl Pts',(45.5776465541021,11.7162485667124,0.));
#91712=CARTESIAN_POINT('Ctrl Pts',(45.5776465541021,11.7162485667124,20.));
#91713=CARTESIAN_POINT('Ctrl Pts',(45.5829571238122,11.6835515684258,0.));
#91714=CARTESIAN_POINT('Ctrl Pts',(45.5829571238122,11.6835515684258,20.));
#91715=CARTESIAN_POINT('Ctrl Pts',(45.5882445909695,11.6508519572639,0.));
#91716=CARTESIAN_POINT('Ctrl Pts',(45.5882445909695,11.6508519572639,20.));
#91717=CARTESIAN_POINT('Ctrl Pts',(45.5935089538387,11.6181497494382,0.));
#91718=CARTESIAN_POINT('Ctrl Pts',(45.5935089538387,11.6181497494382,20.));
#91719=CARTESIAN_POINT('Ctrl Pts',(45.598750210696,11.5854449611619,0.));
#91720=CARTESIAN_POINT('Ctrl Pts',(45.598750210696,11.5854449611619,20.));
#91721=CARTESIAN_POINT('Ctrl Pts',(45.6039683598295,11.5527376086502,0.));
#91722=CARTESIAN_POINT('Ctrl Pts',(45.6039683598295,11.5527376086502,20.));
#91723=CARTESIAN_POINT('Ctrl Pts',(45.6091633995383,11.5200277081201,0.));
#91724=CARTESIAN_POINT('Ctrl Pts',(45.6091633995383,11.5200277081201,20.));
#91725=CARTESIAN_POINT('Ctrl Pts',(45.6143353281323,11.4873152757897,0.));
#91726=CARTESIAN_POINT('Ctrl Pts',(45.6143353281323,11.4873152757897,20.));
#91727=CARTESIAN_POINT('Ctrl Pts',(45.6194841439321,11.4546003278786,0.));
#91728=CARTESIAN_POINT('Ctrl Pts',(45.6194841439321,11.4546003278786,20.));
#91729=CARTESIAN_POINT('Ctrl Pts',(45.6246098452703,11.421882880608,0.));
#91730=CARTESIAN_POINT('Ctrl Pts',(45.6246098452703,11.421882880608,20.));
#91731=CARTESIAN_POINT('Ctrl Pts',(45.6297124304911,11.3891629502006,0.));
#91732=CARTESIAN_POINT('Ctrl Pts',(45.6297124304911,11.3891629502006,20.));
#91733=CARTESIAN_POINT('Ctrl Pts',(45.6347918979506,11.3564405528809,0.));
#91734=CARTESIAN_POINT('Ctrl Pts',(45.6347918979506,11.3564405528809,20.));
#91735=CARTESIAN_POINT('Ctrl Pts',(45.6398482460165,11.3237157048751,0.));
#91736=CARTESIAN_POINT('Ctrl Pts',(45.6398482460165,11.3237157048751,20.));
#91737=CARTESIAN_POINT('Ctrl Pts',(45.6448814730676,11.290988422411,0.));
#91738=CARTESIAN_POINT('Ctrl Pts',(45.6448814730676,11.290988422411,20.));
#91739=CARTESIAN_POINT('Ctrl Pts',(45.6498915774933,11.2582587217178,0.));
#91740=CARTESIAN_POINT('Ctrl Pts',(45.6498915774933,11.2582587217178,20.));
#91741=CARTESIAN_POINT('Ctrl Pts',(45.6548785576938,11.2255266190259,0.));
#91742=CARTESIAN_POINT('Ctrl Pts',(45.6548785576938,11.2255266190259,20.));
#91743=CARTESIAN_POINT('Ctrl Pts',(45.6598424120808,11.1927921305675,0.));
#91744=CARTESIAN_POINT('Ctrl Pts',(45.6598424120808,11.1927921305675,20.));
#91745=CARTESIAN_POINT('Ctrl Pts',(45.6647831390778,11.1600552725764,0.));
#91746=CARTESIAN_POINT('Ctrl Pts',(45.6647831390778,11.1600552725764,20.));
#91747=CARTESIAN_POINT('Ctrl Pts',(45.6697007371202,11.1273160612881,0.));
#91748=CARTESIAN_POINT('Ctrl Pts',(45.6697007371202,11.1273160612881,20.));
#91749=CARTESIAN_POINT('Ctrl Pts',(45.6745952046549,11.0945745129393,0.));
#91750=CARTESIAN_POINT('Ctrl Pts',(45.6745952046549,11.0945745129393,20.));
#91751=CARTESIAN_POINT('Ctrl Pts',(45.6794665401395,11.0618306437685,0.));
#91752=CARTESIAN_POINT('Ctrl Pts',(45.6794665401395,11.0618306437685,20.));
#91753=CARTESIAN_POINT('Ctrl Pts',(45.684314742043,11.0290844700154,0.));
#91754=CARTESIAN_POINT('Ctrl Pts',(45.684314742043,11.0290844700154,20.));
#91755=CARTESIAN_POINT('Ctrl Pts',(45.6891398088456,10.9963360079212,0.));
#91756=CARTESIAN_POINT('Ctrl Pts',(45.6891398088456,10.9963360079212,20.));
#91757=CARTESIAN_POINT('Ctrl Pts',(45.6939417390393,10.9635852737287,0.));
#91758=CARTESIAN_POINT('Ctrl Pts',(45.6939417390393,10.9635852737287,20.));
#91759=CARTESIAN_POINT('Ctrl Pts',(45.698720531127,10.930832283682,0.));
#91760=CARTESIAN_POINT('Ctrl Pts',(45.698720531127,10.930832283682,20.));
#91761=CARTESIAN_POINT('Ctrl Pts',(45.7034761836229,10.898077054027,0.));
#91762=CARTESIAN_POINT('Ctrl Pts',(45.7034761836229,10.898077054027,20.));
#91763=CARTESIAN_POINT('Ctrl Pts',(45.7082086950532,10.8653196010107,0.));
#91764=CARTESIAN_POINT('Ctrl Pts',(45.7082086950532,10.8653196010107,20.));
#91765=CARTESIAN_POINT('Ctrl Pts',(45.7129180639558,10.832559940882,0.));
#91766=CARTESIAN_POINT('Ctrl Pts',(45.7129180639558,10.832559940882,20.));
#91767=CARTESIAN_POINT('Ctrl Pts',(45.7176042888794,10.7997980898913,0.));
#91768=CARTESIAN_POINT('Ctrl Pts',(45.7176042888794,10.7997980898913,20.));
#91769=CARTESIAN_POINT('Ctrl Pts',(45.7222673683833,10.7670340642896,0.));
#91770=CARTESIAN_POINT('Ctrl Pts',(45.7222673683833,10.7670340642896,20.));
#91771=CARTESIAN_POINT('Ctrl Pts',(45.7269073010391,10.73426788033,0.));
#91772=CARTESIAN_POINT('Ctrl Pts',(45.7269073010391,10.73426788033,20.));
#91773=CARTESIAN_POINT('Ctrl Pts',(45.7315240854293,10.7014995542666,0.));
#91774=CARTESIAN_POINT('Ctrl Pts',(45.7315240854293,10.7014995542666,20.));
#91775=CARTESIAN_POINT('Ctrl Pts',(45.7361177201484,10.6687291023553,0.));
#91776=CARTESIAN_POINT('Ctrl Pts',(45.7361177201484,10.6687291023553,20.));
#91777=CARTESIAN_POINT('Ctrl Pts',(45.7406882038015,10.6359565408533,0.));
#91778=CARTESIAN_POINT('Ctrl Pts',(45.7406882038015,10.6359565408533,20.));
#91779=CARTESIAN_POINT('Ctrl Pts',(45.745235535006,10.6031818860194,0.));
#91780=CARTESIAN_POINT('Ctrl Pts',(45.745235535006,10.6031818860194,20.));
#91781=CARTESIAN_POINT('Ctrl Pts',(45.7497597123901,10.5704051541135,0.));
#91782=CARTESIAN_POINT('Ctrl Pts',(45.7497597123901,10.5704051541135,20.));
#91783=CARTESIAN_POINT('Ctrl Pts',(45.7542607345937,10.5376263613969,0.));
#91784=CARTESIAN_POINT('Ctrl Pts',(45.7542607345937,10.5376263613969,20.));
#91785=CARTESIAN_POINT('Ctrl Pts',(45.7587386002674,10.504845524132,0.));
#91786=CARTESIAN_POINT('Ctrl Pts',(45.7587386002674,10.504845524132,20.));
#91787=CARTESIAN_POINT('Ctrl Pts',(45.7631933080735,10.4720626585828,0.));
#91788=CARTESIAN_POINT('Ctrl Pts',(45.7631933080735,10.4720626585828,20.));
#91789=CARTESIAN_POINT('Ctrl Pts',(45.7676248566855,10.4392777810149,0.));
#91790=CARTESIAN_POINT('Ctrl Pts',(45.7676248566855,10.4392777810149,20.));
#91791=CARTESIAN_POINT('Ctrl Pts',(45.772033244789,10.406490907695,0.));
#91792=CARTESIAN_POINT('Ctrl Pts',(45.772033244789,10.406490907695,20.));
#91793=CARTESIAN_POINT('Ctrl Pts',(45.7764184710811,10.3737020548914,0.));
#91794=CARTESIAN_POINT('Ctrl Pts',(45.7764184710811,10.3737020548914,20.));
#91795=CARTESIAN_POINT('Ctrl Pts',(45.7807805342697,10.3409112388736,0.));
#91796=CARTESIAN_POINT('Ctrl Pts',(45.7807805342697,10.3409112388736,20.));
#91797=CARTESIAN_POINT('Ctrl Pts',(45.7851194330743,10.3081184759123,0.));
#91798=CARTESIAN_POINT('Ctrl Pts',(45.7851194330743,10.3081184759123,20.));
#91799=CARTESIAN_POINT('Ctrl Pts',(45.7894351662253,10.2753237822796,0.));
#91800=CARTESIAN_POINT('Ctrl Pts',(45.7894351662253,10.2753237822796,20.));
#91801=CARTESIAN_POINT('Ctrl Pts',(45.7937277324642,10.2425271742485,0.));
#91802=CARTESIAN_POINT('Ctrl Pts',(45.7937277324642,10.2425271742485,20.));
#91803=CARTESIAN_POINT('Ctrl Pts',(45.7979971305449,10.2097286680937,0.));
#91804=CARTESIAN_POINT('Ctrl Pts',(45.7979971305449,10.2097286680937,20.));
#91805=CARTESIAN_POINT('Ctrl Pts',(45.8022433592327,10.1769282800914,0.));
#91806=CARTESIAN_POINT('Ctrl Pts',(45.8022433592327,10.1769282800914,20.));
#91807=CARTESIAN_POINT('Ctrl Pts',(45.8064664173048,10.1441260265191,0.));
#91808=CARTESIAN_POINT('Ctrl Pts',(45.8064664173048,10.1441260265191,20.));
#91809=CARTESIAN_POINT('Ctrl Pts',(45.8106663035491,10.1113219236554,0.));
#91810=CARTESIAN_POINT('Ctrl Pts',(45.8106663035491,10.1113219236554,20.));
#91811=CARTESIAN_POINT('Ctrl Pts',(45.8148430167647,10.0785159877801,0.));
#91812=CARTESIAN_POINT('Ctrl Pts',(45.8148430167647,10.0785159877801,20.));
#91813=CARTESIAN_POINT('Ctrl Pts',(45.8189965557614,10.0457082351741,0.));
#91814=CARTESIAN_POINT('Ctrl Pts',(45.8189965557614,10.0457082351741,20.));
#91815=CARTESIAN_POINT('Ctrl Pts',(45.8231269193611,10.0128986821194,0.));
#91816=CARTESIAN_POINT('Ctrl Pts',(45.8231269193611,10.0128986821194,20.));
#91817=CARTESIAN_POINT('Ctrl Pts',(45.8272341063969,9.98008734489948,0.));
#91818=CARTESIAN_POINT('Ctrl Pts',(45.8272341063969,9.98008734489948,20.));
#91819=CARTESIAN_POINT('Ctrl Pts',(45.8313181157134,9.94727423979906,0.));
#91820=CARTESIAN_POINT('Ctrl Pts',(45.8313181157134,9.94727423979906,20.));
#91821=CARTESIAN_POINT('Ctrl Pts',(45.8353789461673,9.91445938310424,0.));
#91822=CARTESIAN_POINT('Ctrl Pts',(45.8353789461673,9.91445938310424,20.));
#91823=CARTESIAN_POINT('Ctrl Pts',(45.8394165966264,9.88164279110241,0.));
#91824=CARTESIAN_POINT('Ctrl Pts',(45.8394165966264,9.88164279110241,20.));
#91825=CARTESIAN_POINT('Ctrl Pts',(45.84343106597,9.84882448008225,0.));
#91826=CARTESIAN_POINT('Ctrl Pts',(45.84343106597,9.84882448008225,20.));
#91827=CARTESIAN_POINT('Ctrl Pts',(45.8474223530896,9.81600446633368,0.));
#91828=CARTESIAN_POINT('Ctrl Pts',(45.8474223530896,9.81600446633368,20.));
#91829=CARTESIAN_POINT('Ctrl Pts',(45.8513904568872,9.78318276614762,0.));
#91830=CARTESIAN_POINT('Ctrl Pts',(45.8513904568872,9.78318276614762,20.));
#91831=CARTESIAN_POINT('Ctrl Pts',(45.8553353762765,9.75035939581619,0.));
#91832=CARTESIAN_POINT('Ctrl Pts',(45.8553353762765,9.75035939581619,20.));
#91833=CARTESIAN_POINT('Ctrl Pts',(45.8592571101812,9.71753437163221,0.));
#91834=CARTESIAN_POINT('Ctrl Pts',(45.8592571101812,9.71753437163221,20.));
#91835=CARTESIAN_POINT('Ctrl Pts',(45.8631556575366,9.68470770988976,0.));
#91836=CARTESIAN_POINT('Ctrl Pts',(45.8631556575366,9.68470770988976,20.));
#91837=CARTESIAN_POINT('Ctrl Pts',(45.8670310172895,9.65187942688401,0.));
#91838=CARTESIAN_POINT('Ctrl Pts',(45.8670310172895,9.65187942688401,20.));
#91839=CARTESIAN_POINT('Ctrl Pts',(45.870883188399,9.61904953891161,0.));
#91840=CARTESIAN_POINT('Ctrl Pts',(45.870883188399,9.61904953891161,20.));
#91841=CARTESIAN_POINT('Ctrl Pts',(45.8747121698355,9.58621806227057,0.));
#91842=CARTESIAN_POINT('Ctrl Pts',(45.8747121698355,9.58621806227057,20.));
#91843=CARTESIAN_POINT('Ctrl Pts',(45.8785179605829,9.55338501326048,0.));
#91844=CARTESIAN_POINT('Ctrl Pts',(45.8785179605829,9.55338501326048,20.));
#91845=CARTESIAN_POINT('Ctrl Pts',(45.882300559635,9.52055040818185,0.));
#91846=CARTESIAN_POINT('Ctrl Pts',(45.882300559635,9.52055040818185,20.));
#91847=CARTESIAN_POINT('Ctrl Pts',(45.8860599659967,9.4877142633361,0.));
#91848=CARTESIAN_POINT('Ctrl Pts',(45.8860599659967,9.4877142633361,20.));
#91849=CARTESIAN_POINT('Ctrl Pts',(45.8897961786838,9.45487659502548,0.));
#91850=CARTESIAN_POINT('Ctrl Pts',(45.8897961786838,9.45487659502548,20.));
#91851=CARTESIAN_POINT('Ctrl Pts',(45.8935091967241,9.42203741955325,0.));
#91852=CARTESIAN_POINT('Ctrl Pts',(45.8935091967241,9.42203741955325,20.));
#91853=CARTESIAN_POINT('Ctrl Pts',(45.8971990191563,9.38919675322381,0.));
#91854=CARTESIAN_POINT('Ctrl Pts',(45.8971990191563,9.38919675322381,20.));
#91855=CARTESIAN_POINT('Ctrl Pts',(45.90086564503,9.35635461234246,0.));
#91856=CARTESIAN_POINT('Ctrl Pts',(45.90086564503,9.35635461234246,20.));
#91857=CARTESIAN_POINT('Ctrl Pts',(45.9045090734063,9.3235110132158,0.));
#91858=CARTESIAN_POINT('Ctrl Pts',(45.9045090734063,9.3235110132158,20.));
#91859=CARTESIAN_POINT('Ctrl Pts',(45.9081293033576,9.29066597215163,0.));
#91860=CARTESIAN_POINT('Ctrl Pts',(45.9081293033576,9.29066597215163,20.));
#91861=CARTESIAN_POINT('Ctrl Pts',(45.9117263339694,9.25781950545902,0.));
#91862=CARTESIAN_POINT('Ctrl Pts',(45.9117263339694,9.25781950545902,20.));
#91863=CARTESIAN_POINT('Ctrl Pts',(45.9153001643391,9.22497162944821,0.));
#91864=CARTESIAN_POINT('Ctrl Pts',(45.9153001643391,9.22497162944821,20.));
#91865=CARTESIAN_POINT('Ctrl Pts',(45.9188507935764,9.19212236043074,0.));
#91866=CARTESIAN_POINT('Ctrl Pts',(45.9188507935764,9.19212236043074,20.));
#91867=CARTESIAN_POINT('Ctrl Pts',(45.9223782208015,9.15927171471892,0.));
#91868=CARTESIAN_POINT('Ctrl Pts',(45.9223782208015,9.15927171471892,20.));
#91869=CARTESIAN_POINT('Ctrl Pts',(45.9258824451441,9.12641970862567,0.));
#91870=CARTESIAN_POINT('Ctrl Pts',(45.9258824451441,9.12641970862567,20.));
#91871=CARTESIAN_POINT('Ctrl Pts',(45.9293634657451,9.09356635846486,0.));
#91872=CARTESIAN_POINT('Ctrl Pts',(45.9293634657451,9.09356635846486,20.));
#91873=CARTESIAN_POINT('Ctrl Pts',(45.9328212817567,9.06071168055121,0.));
#91874=CARTESIAN_POINT('Ctrl Pts',(45.9328212817567,9.06071168055121,20.));
#91875=CARTESIAN_POINT('Ctrl Pts',(45.9362558923428,9.02785569120062,0.));
#91876=CARTESIAN_POINT('Ctrl Pts',(45.9362558923428,9.02785569120062,20.));
#91877=CARTESIAN_POINT('Ctrl Pts',(45.939667296681,8.99499840673047,0.));
#91878=CARTESIAN_POINT('Ctrl Pts',(45.939667296681,8.99499840673047,20.));
#91879=CARTESIAN_POINT('Ctrl Pts',(45.9430554939595,8.96213984345905,0.));
#91880=CARTESIAN_POINT('Ctrl Pts',(45.9430554939595,8.96213984345905,20.));
#91881=CARTESIAN_POINT('Ctrl Pts',(45.9464204833787,8.92928001770576,0.));
#91882=CARTESIAN_POINT('Ctrl Pts',(45.9464204833787,8.92928001770576,20.));
#91883=CARTESIAN_POINT('Ctrl Pts',(45.9497622641496,8.89641894579083,0.));
#91884=CARTESIAN_POINT('Ctrl Pts',(45.9497622641496,8.89641894579083,20.));
#91885=CARTESIAN_POINT('Ctrl Pts',(45.9530808354938,8.86355664403535,0.));
#91886=CARTESIAN_POINT('Ctrl Pts',(45.9530808354938,8.86355664403535,20.));
#91887=CARTESIAN_POINT('Ctrl Pts',(45.9563761966444,8.83069312876128,0.));
#91888=CARTESIAN_POINT('Ctrl Pts',(45.9563761966444,8.83069312876128,20.));
#91889=CARTESIAN_POINT('Ctrl Pts',(45.9596483468462,8.79782841629148,0.));
#91890=CARTESIAN_POINT('Ctrl Pts',(45.9596483468462,8.79782841629148,20.));
#91891=CARTESIAN_POINT('Ctrl Pts',(45.9628972853566,8.76496252295002,0.));
#91892=CARTESIAN_POINT('Ctrl Pts',(45.9628972853566,8.76496252295002,20.));
#91893=CARTESIAN_POINT('Ctrl Pts',(45.9661230114446,8.732095465062,0.));
#91894=CARTESIAN_POINT('Ctrl Pts',(45.9661230114446,8.732095465062,20.));
#91895=CARTESIAN_POINT('Ctrl Pts',(45.9693255243897,8.69922725895329,0.));
#91896=CARTESIAN_POINT('Ctrl Pts',(45.9693255243897,8.69922725895329,20.));
#91897=CARTESIAN_POINT('Ctrl Pts',(45.9725048234817,8.66635792095044,0.));
#91898=CARTESIAN_POINT('Ctrl Pts',(45.9725048234817,8.66635792095044,20.));
#91899=CARTESIAN_POINT('Ctrl Pts',(45.9756609080225,8.633487467381,0.));
#91900=CARTESIAN_POINT('Ctrl Pts',(45.9756609080225,8.633487467381,20.));
#91901=CARTESIAN_POINT('Ctrl Pts',(45.9787937773254,8.6006159145734,0.));
#91902=CARTESIAN_POINT('Ctrl Pts',(45.9787937773254,8.6006159145734,20.));
#91903=CARTESIAN_POINT('Ctrl Pts',(45.9819034307166,8.56774327885726,0.));
#91904=CARTESIAN_POINT('Ctrl Pts',(45.9819034307166,8.56774327885726,20.));
#91905=CARTESIAN_POINT('Ctrl Pts',(45.9849898675351,8.53486957656348,0.));
#91906=CARTESIAN_POINT('Ctrl Pts',(45.9849898675351,8.53486957656348,20.));
#91907=CARTESIAN_POINT('Ctrl Pts',(45.9880530871298,8.50199482402355,0.));
#91908=CARTESIAN_POINT('Ctrl Pts',(45.9880530871298,8.50199482402355,20.));
#91909=CARTESIAN_POINT('Ctrl Pts',(45.991093088861,8.46911903756974,0.));
#91910=CARTESIAN_POINT('Ctrl Pts',(45.991093088861,8.46911903756974,20.));
#91911=CARTESIAN_POINT('Ctrl Pts',(45.9941098720982,8.43624223353472,0.));
#91912=CARTESIAN_POINT('Ctrl Pts',(45.9941098720982,8.43624223353472,20.));
#91913=CARTESIAN_POINT('Ctrl Pts',(45.9971034362229,8.403364428252,0.));
#91914=CARTESIAN_POINT('Ctrl Pts',(45.9971034362229,8.403364428252,20.));
#91915=CARTESIAN_POINT('Ctrl Pts',(46.000073780629,8.37048563805606,0.));
#91916=CARTESIAN_POINT('Ctrl Pts',(46.000073780629,8.37048563805606,20.));
#91917=CARTESIAN_POINT('Ctrl Pts',(46.0030209047226,8.33760587928254,0.));
#91918=CARTESIAN_POINT('Ctrl Pts',(46.0030209047226,8.33760587928254,20.));
#91919=CARTESIAN_POINT('Ctrl Pts',(46.0059448079215,8.30472516826798,0.));
#91920=CARTESIAN_POINT('Ctrl Pts',(46.0059448079215,8.30472516826798,20.));
#91921=CARTESIAN_POINT('Ctrl Pts',(46.0088454896554,8.27184352134995,0.));
#91922=CARTESIAN_POINT('Ctrl Pts',(46.0088454896554,8.27184352134995,20.));
#91923=CARTESIAN_POINT('Ctrl Pts',(46.0117229493647,8.2389609548667,0.));
#91924=CARTESIAN_POINT('Ctrl Pts',(46.0117229493647,8.2389609548667,20.));
#91925=CARTESIAN_POINT('Ctrl Pts',(46.0145771865005,8.20607748515696,0.));
#91926=CARTESIAN_POINT('Ctrl Pts',(46.0145771865005,8.20607748515696,20.));
#91927=CARTESIAN_POINT('Ctrl Pts',(46.0174082005262,8.17319312856043,0.));
#91928=CARTESIAN_POINT('Ctrl Pts',(46.0174082005262,8.17319312856043,20.));
#91929=CARTESIAN_POINT('Ctrl Pts',(46.0202159909161,8.1403079014174,0.));
#91930=CARTESIAN_POINT('Ctrl Pts',(46.0202159909161,8.1403079014174,20.));
#91931=CARTESIAN_POINT('Ctrl Pts',(46.0230005571558,8.10742182006901,0.));
#91932=CARTESIAN_POINT('Ctrl Pts',(46.0230005571558,8.10742182006901,20.));
#91933=CARTESIAN_POINT('Ctrl Pts',(46.025761898743,8.07453490085737,0.));
#91934=CARTESIAN_POINT('Ctrl Pts',(46.025761898743,8.07453490085737,20.));
#91935=CARTESIAN_POINT('Ctrl Pts',(46.0285000151874,8.04164716012546,0.));
#91936=CARTESIAN_POINT('Ctrl Pts',(46.0285000151874,8.04164716012546,20.));
#91937=CARTESIAN_POINT('Ctrl Pts',(46.0312149060105,8.00875861421695,0.));
#91938=CARTESIAN_POINT('Ctrl Pts',(46.0312149060105,8.00875861421695,20.));
#91939=CARTESIAN_POINT('Ctrl Pts',(46.0339065707442,7.97586927947621,0.));
#91940=CARTESIAN_POINT('Ctrl Pts',(46.0339065707442,7.97586927947621,20.));
#91941=CARTESIAN_POINT('Ctrl Pts',(46.0365750089318,7.94297917224816,0.));
#91942=CARTESIAN_POINT('Ctrl Pts',(46.0365750089318,7.94297917224816,20.));
#91943=CARTESIAN_POINT('Ctrl Pts',(46.0392202201278,7.91008830887856,0.));
#91944=CARTESIAN_POINT('Ctrl Pts',(46.0392202201278,7.91008830887856,20.));
#91945=CARTESIAN_POINT('Ctrl Pts',(46.0418422038989,7.87719670571401,0.));
#91946=CARTESIAN_POINT('Ctrl Pts',(46.0418422038989,7.87719670571401,20.));
#91947=CARTESIAN_POINT('Ctrl Pts',(46.0444409598224,7.84430437910167,0.));
#91948=CARTESIAN_POINT('Ctrl Pts',(46.0444409598224,7.84430437910167,20.));
#91949=CARTESIAN_POINT('Ctrl Pts',(46.0470164874882,7.81141134538955,0.));
#91950=CARTESIAN_POINT('Ctrl Pts',(46.0470164874882,7.81141134538955,20.));
#91951=CARTESIAN_POINT('Ctrl Pts',(46.0495687864972,7.77851762092637,0.));
#91952=CARTESIAN_POINT('Ctrl Pts',(46.0495687864972,7.77851762092637,20.));
#91953=CARTESIAN_POINT('Ctrl Pts',(46.052097856463,7.74562322206168,0.));
#91954=CARTESIAN_POINT('Ctrl Pts',(46.052097856463,7.74562322206168,20.));
#91955=CARTESIAN_POINT('Ctrl Pts',(46.0546036970108,7.71272816514572,0.));
#91956=CARTESIAN_POINT('Ctrl Pts',(46.0546036970108,7.71272816514572,20.));
#91957=CARTESIAN_POINT('Ctrl Pts',(46.0570863077758,7.67983246652918,0.));
#91958=CARTESIAN_POINT('Ctrl Pts',(46.0570863077758,7.67983246652918,20.));
#91959=CARTESIAN_POINT('Ctrl Pts',(46.0595456884042,7.64693614256336,0.));
#91960=CARTESIAN_POINT('Ctrl Pts',(46.0595456884042,7.64693614256336,20.));
#91961=CARTESIAN_POINT('Ctrl Pts',(46.0619818385541,7.61403920960036,0.));
#91962=CARTESIAN_POINT('Ctrl Pts',(46.0619818385541,7.61403920960036,20.));
#91963=CARTESIAN_POINT('Ctrl Pts',(46.0643947578955,7.58114168399302,0.));
#91964=CARTESIAN_POINT('Ctrl Pts',(46.0643947578955,7.58114168399302,20.));
#91965=CARTESIAN_POINT('Ctrl Pts',(46.0667844461104,7.54824358209485,0.));
#91966=CARTESIAN_POINT('Ctrl Pts',(46.0667844461104,7.54824358209485,20.));
#91967=CARTESIAN_POINT('Ctrl Pts',(46.0691509028928,7.51534492025983,0.));
#91968=CARTESIAN_POINT('Ctrl Pts',(46.0691509028928,7.51534492025983,20.));
#91969=CARTESIAN_POINT('Ctrl Pts',(46.0714941279471,7.48244571484251,0.));
#91970=CARTESIAN_POINT('Ctrl Pts',(46.0714941279471,7.48244571484251,20.));
#91971=CARTESIAN_POINT('Ctrl Pts',(46.0738141209885,7.4495459821981,0.));
#91972=CARTESIAN_POINT('Ctrl Pts',(46.0738141209885,7.4495459821981,20.));
#91973=CARTESIAN_POINT('Ctrl Pts',(46.0761108817447,7.41664573868261,0.));
#91974=CARTESIAN_POINT('Ctrl Pts',(46.0761108817447,7.41664573868261,20.));
#91975=CARTESIAN_POINT('Ctrl Pts',(46.0783844099553,7.38374500065295,0.));
#91976=CARTESIAN_POINT('Ctrl Pts',(46.0783844099553,7.38374500065295,20.));
#91977=CARTESIAN_POINT('Ctrl Pts',(46.0806347053718,7.35084378446662,0.));
#91978=CARTESIAN_POINT('Ctrl Pts',(46.0806347053718,7.35084378446662,20.));
#91979=CARTESIAN_POINT('Ctrl Pts',(46.0828617677561,7.3179421064814,0.));
#91980=CARTESIAN_POINT('Ctrl Pts',(46.0828617677561,7.3179421064814,20.));
#91981=CARTESIAN_POINT('Ctrl Pts',(46.0850655968817,7.28503998305551,0.));
#91982=CARTESIAN_POINT('Ctrl Pts',(46.0850655968817,7.28503998305551,20.));
#91983=CARTESIAN_POINT('Ctrl Pts',(46.0872461925336,7.2521374305475,0.));
#91984=CARTESIAN_POINT('Ctrl Pts',(46.0872461925336,7.2521374305475,20.));
#91985=CARTESIAN_POINT('Ctrl Pts',(46.0894035545083,7.21923446531641,0.));
#91986=CARTESIAN_POINT('Ctrl Pts',(46.0894035545083,7.21923446531641,20.));
#91987=CARTESIAN_POINT('Ctrl Pts',(46.0915376826137,7.18633110372212,0.));
#91988=CARTESIAN_POINT('Ctrl Pts',(46.0915376826137,7.18633110372212,20.));
#91989=CARTESIAN_POINT('Ctrl Pts',(46.0936485766695,7.1534273621253,0.));
#91990=CARTESIAN_POINT('Ctrl Pts',(46.0936485766695,7.1534273621253,20.));
#91991=CARTESIAN_POINT('Ctrl Pts',(46.0957362365075,7.12052325688753,0.));
#91992=CARTESIAN_POINT('Ctrl Pts',(46.0957362365075,7.12052325688753,20.));
#91993=CARTESIAN_POINT('Ctrl Pts',(46.097800661971,7.08761880437094,0.));
#91994=CARTESIAN_POINT('Ctrl Pts',(46.097800661971,7.08761880437094,20.));
#91995=CARTESIAN_POINT('Ctrl Pts',(46.0998418529147,7.05471402093802,0.));
#91996=CARTESIAN_POINT('Ctrl Pts',(46.0998418529147,7.05471402093802,20.));
#91997=CARTESIAN_POINT('Ctrl Pts',(46.1018598092046,7.02180892295148,0.));
#91998=CARTESIAN_POINT('Ctrl Pts',(46.1018598092046,7.02180892295148,20.));
#91999=CARTESIAN_POINT('Ctrl Pts',(46.103854530718,6.98890352677439,0.));
#92000=CARTESIAN_POINT('Ctrl Pts',(46.103854530718,6.98890352677439,20.));
#92001=CARTESIAN_POINT('Ctrl Pts',(46.1058260173429,6.95599784877019,0.));
#92002=CARTESIAN_POINT('Ctrl Pts',(46.1058260173429,6.95599784877019,20.));
#92003=CARTESIAN_POINT('Ctrl Pts',(46.1077742689797,6.92309190530285,0.));
#92004=CARTESIAN_POINT('Ctrl Pts',(46.1077742689797,6.92309190530285,20.));
#92005=CARTESIAN_POINT('Ctrl Pts',(46.1096992855399,6.8901857127369,0.));
#92006=CARTESIAN_POINT('Ctrl Pts',(46.1096992855399,6.8901857127369,20.));
#92007=CARTESIAN_POINT('Ctrl Pts',(46.111601066948,6.85727928743788,0.));
#92008=CARTESIAN_POINT('Ctrl Pts',(46.111601066948,6.85727928743788,20.));
#92009=CARTESIAN_POINT('Ctrl Pts',(46.1134796131392,6.82437264577169,0.));
#92010=CARTESIAN_POINT('Ctrl Pts',(46.1134796131392,6.82437264577169,20.));
#92011=CARTESIAN_POINT('Ctrl Pts',(46.1153349240611,6.7914658041047,0.));
#92012=CARTESIAN_POINT('Ctrl Pts',(46.1153349240611,6.7914658041047,20.));
#92013=CARTESIAN_POINT('Ctrl Pts',(46.1171669996709,6.75855877880357,0.));
#92014=CARTESIAN_POINT('Ctrl Pts',(46.1171669996709,6.75855877880357,20.));
#92015=CARTESIAN_POINT('Ctrl Pts',(46.1189758399374,6.72565158623521,0.));
#92016=CARTESIAN_POINT('Ctrl Pts',(46.1189758399374,6.72565158623521,20.));
#92017=CARTESIAN_POINT('Ctrl Pts',(46.1207614448407,6.69274424276688,0.));
#92018=CARTESIAN_POINT('Ctrl Pts',(46.1207614448407,6.69274424276688,20.));
#92019=CARTESIAN_POINT('Ctrl Pts',(46.122523814374,6.65983676476652,0.));
#92020=CARTESIAN_POINT('Ctrl Pts',(46.122523814374,6.65983676476652,20.));
#92021=CARTESIAN_POINT('Ctrl Pts',(46.124262948542,6.62692916860258,0.));
#92022=CARTESIAN_POINT('Ctrl Pts',(46.124262948542,6.62692916860258,20.));
#92023=CARTESIAN_POINT('Ctrl Pts',(46.1259788473615,6.594021470644,0.));
#92024=CARTESIAN_POINT('Ctrl Pts',(46.1259788473615,6.594021470644,20.));
#92025=CARTESIAN_POINT('Ctrl Pts',(46.1276715108604,6.5611136872601,0.));
#92026=CARTESIAN_POINT('Ctrl Pts',(46.1276715108604,6.5611136872601,20.));
#92027=CARTESIAN_POINT('Ctrl Pts',(46.1293409390781,6.5282058348205,0.));
#92028=CARTESIAN_POINT('Ctrl Pts',(46.1293409390781,6.5282058348205,20.));
#92029=CARTESIAN_POINT('Ctrl Pts',(46.1309871320644,6.49529792969509,0.));
#92030=CARTESIAN_POINT('Ctrl Pts',(46.1309871320644,6.49529792969509,20.));
#92031=CARTESIAN_POINT('Ctrl Pts',(46.1326100898806,6.46238998825408,0.));
#92032=CARTESIAN_POINT('Ctrl Pts',(46.1326100898806,6.46238998825408,20.));
#92033=CARTESIAN_POINT('Ctrl Pts',(46.134209812599,6.42948202686814,0.));
#92034=CARTESIAN_POINT('Ctrl Pts',(46.134209812599,6.42948202686814,20.));
#92035=CARTESIAN_POINT('Ctrl Pts',(46.1357863003044,6.39657406190845,0.));
#92036=CARTESIAN_POINT('Ctrl Pts',(46.1357863003044,6.39657406190845,20.));
#92037=CARTESIAN_POINT('Ctrl Pts',(46.1373395530931,6.36366610974648,0.));
#92038=CARTESIAN_POINT('Ctrl Pts',(46.1373395530931,6.36366610974648,20.));
#92039=CARTESIAN_POINT('Ctrl Pts',(46.138869571074,6.3307581867542,0.));
#92040=CARTESIAN_POINT('Ctrl Pts',(46.138869571074,6.3307581867542,20.));
#92041=CARTESIAN_POINT('Ctrl Pts',(46.1403763543673,6.29785030930382,0.));
#92042=CARTESIAN_POINT('Ctrl Pts',(46.1403763543673,6.29785030930382,20.));
#92043=CARTESIAN_POINT('Ctrl Pts',(46.141859903105,6.26494249376778,0.));
#92044=CARTESIAN_POINT('Ctrl Pts',(46.141859903105,6.26494249376778,20.));
#92045=CARTESIAN_POINT('Ctrl Pts',(46.1433202174297,6.23203475651883,0.));
#92046=CARTESIAN_POINT('Ctrl Pts',(46.1433202174297,6.23203475651883,20.));
#92047=CARTESIAN_POINT('Ctrl Pts',(46.1447572974959,6.19912711393004,0.));
#92048=CARTESIAN_POINT('Ctrl Pts',(46.1447572974959,6.19912711393004,20.));
#92049=CARTESIAN_POINT('Ctrl Pts',(46.1461711434687,6.16621958237488,0.));
#92050=CARTESIAN_POINT('Ctrl Pts',(46.1461711434687,6.16621958237488,20.));
#92051=CARTESIAN_POINT('Ctrl Pts',(46.1475617555249,6.1333121782271,0.));
#92052=CARTESIAN_POINT('Ctrl Pts',(46.1475617555249,6.1333121782271,20.));
#92053=CARTESIAN_POINT('Ctrl Pts',(46.1489291338532,6.10040491786086,0.));
#92054=CARTESIAN_POINT('Ctrl Pts',(46.1489291338532,6.10040491786086,20.));
#92055=CARTESIAN_POINT('Ctrl Pts',(46.1502732786543,6.06749781765058,0.));
#92056=CARTESIAN_POINT('Ctrl Pts',(46.1502732786543,6.06749781765058,20.));
#92057=CARTESIAN_POINT('Ctrl Pts',(46.151594190141,6.03459089397104,0.));
#92058=CARTESIAN_POINT('Ctrl Pts',(46.151594190141,6.03459089397104,20.));
#92059=CARTESIAN_POINT('Ctrl Pts',(46.1528918685373,6.0016841631972,0.));
#92060=CARTESIAN_POINT('Ctrl Pts',(46.1528918685373,6.0016841631972,20.));
#92061=CARTESIAN_POINT('Ctrl Pts',(46.1541663140783,5.96877764170412,0.));
#92062=CARTESIAN_POINT('Ctrl Pts',(46.1541663140783,5.96877764170412,20.));
#92063=CARTESIAN_POINT('Ctrl Pts',(46.1554175270101,5.9358713458669,0.));
#92064=CARTESIAN_POINT('Ctrl Pts',(46.1554175270101,5.9358713458669,20.));
#92065=CARTESIAN_POINT('Ctrl Pts',(46.1566455075904,5.90296529206097,0.));
#92066=CARTESIAN_POINT('Ctrl Pts',(46.1566455075904,5.90296529206097,20.));
#92067=CARTESIAN_POINT('Ctrl Pts',(46.1578502560886,5.87005949666212,0.));
#92068=CARTESIAN_POINT('Ctrl Pts',(46.1578502560886,5.87005949666212,20.));
#92069=CARTESIAN_POINT('Ctrl Pts',(46.1590317727861,5.83715397604653,0.));
#92070=CARTESIAN_POINT('Ctrl Pts',(46.1590317727861,5.83715397604653,20.));
#92071=CARTESIAN_POINT('Ctrl Pts',(46.160190057976,5.80424874659071,0.));
#92072=CARTESIAN_POINT('Ctrl Pts',(46.160190057976,5.80424874659071,20.));
#92073=CARTESIAN_POINT('Ctrl Pts',(46.1613251119636,5.77134382467173,0.));
#92074=CARTESIAN_POINT('Ctrl Pts',(46.1613251119636,5.77134382467173,20.));
#92075=CARTESIAN_POINT('Ctrl Pts',(46.1624369350662,5.73843922666648,0.));
#92076=CARTESIAN_POINT('Ctrl Pts',(46.1624369350662,5.73843922666648,20.));
#92077=CARTESIAN_POINT('Ctrl Pts',(46.1635255276116,5.70553496895185,0.));
#92078=CARTESIAN_POINT('Ctrl Pts',(46.1635255276116,5.70553496895185,20.));
#92079=CARTESIAN_POINT('Ctrl Pts',(46.1645908899393,5.67263106790479,0.));
#92080=CARTESIAN_POINT('Ctrl Pts',(46.1645908899393,5.67263106790479,20.));
#92081=CARTESIAN_POINT('Ctrl Pts',(46.1656330223979,5.63972753990236,0.));
#92082=CARTESIAN_POINT('Ctrl Pts',(46.1656330223979,5.63972753990236,20.));
#92083=CARTESIAN_POINT('Ctrl Pts',(46.166651925349,5.60682440132182,0.));
#92084=CARTESIAN_POINT('Ctrl Pts',(46.166651925349,5.60682440132182,20.));
#92085=CARTESIAN_POINT('Ctrl Pts',(46.1676475991657,5.57392166854075,0.));
#92086=CARTESIAN_POINT('Ctrl Pts',(46.1676475991657,5.57392166854075,20.));
#92087=CARTESIAN_POINT('Ctrl Pts',(46.1686200442337,5.5410193579371,0.));
#92088=CARTESIAN_POINT('Ctrl Pts',(46.1686200442337,5.5410193579371,20.));
#92089=CARTESIAN_POINT('Ctrl Pts',(46.1695692609505,5.50811748588894,0.));
#92090=CARTESIAN_POINT('Ctrl Pts',(46.1695692609505,5.50811748588894,20.));
#92091=CARTESIAN_POINT('Ctrl Pts',(46.170495249726,5.4752160687746,0.));
#92092=CARTESIAN_POINT('Ctrl Pts',(46.170495249726,5.4752160687746,20.));
#92093=CARTESIAN_POINT('Ctrl Pts',(46.1713980109807,5.44231512297239,0.));
#92094=CARTESIAN_POINT('Ctrl Pts',(46.1713980109807,5.44231512297239,20.));
#92095=CARTESIAN_POINT('Ctrl Pts',(46.1722775451467,5.40941466486069,0.));
#92096=CARTESIAN_POINT('Ctrl Pts',(46.1722775451467,5.40941466486069,20.));
#92097=CARTESIAN_POINT('Ctrl Pts',(46.1731338526667,5.37651471081787,0.));
#92098=CARTESIAN_POINT('Ctrl Pts',(46.1731338526667,5.37651471081787,20.));
#92099=CARTESIAN_POINT('Ctrl Pts',(46.1739669339953,5.3436152772224,0.));
#92100=CARTESIAN_POINT('Ctrl Pts',(46.1739669339953,5.3436152772224,20.));
#92101=CARTESIAN_POINT('Ctrl Pts',(46.1747767895978,5.31071638045279,0.));
#92102=CARTESIAN_POINT('Ctrl Pts',(46.1747767895978,5.31071638045279,20.));
#92103=CARTESIAN_POINT('Ctrl Pts',(46.1755634199519,5.27781803688791,0.));
#92104=CARTESIAN_POINT('Ctrl Pts',(46.1755634199519,5.27781803688791,20.));
#92105=CARTESIAN_POINT('Ctrl Pts',(46.1763268255471,5.24492026290663,0.));
#92106=CARTESIAN_POINT('Ctrl Pts',(46.1763268255471,5.24492026290663,20.));
#92107=CARTESIAN_POINT('Ctrl Pts',(46.1770670068854,5.21202307488802,0.));
#92108=CARTESIAN_POINT('Ctrl Pts',(46.1770670068854,5.21202307488802,20.));
#92109=CARTESIAN_POINT('Ctrl Pts',(46.1777839644797,5.17912648921102,0.));
#92110=CARTESIAN_POINT('Ctrl Pts',(46.1777839644797,5.17912648921102,20.));
#92111=CARTESIAN_POINT('Ctrl Pts',(46.1784776988548,5.14623052225472,0.));
#92112=CARTESIAN_POINT('Ctrl Pts',(46.1784776988548,5.14623052225472,20.));
#92113=CARTESIAN_POINT('Ctrl Pts',(46.1791482105459,5.11333519039809,0.));
#92114=CARTESIAN_POINT('Ctrl Pts',(46.1791482105459,5.11333519039809,20.));
#92115=CARTESIAN_POINT('Ctrl Pts',(46.1797955000997,5.08044051002026,0.));
#92116=CARTESIAN_POINT('Ctrl Pts',(46.1797955000997,5.08044051002026,20.));
#92117=CARTESIAN_POINT('Ctrl Pts',(46.1804195680748,5.04754649750031,0.));
#92118=CARTESIAN_POINT('Ctrl Pts',(46.1804195680748,5.04754649750031,20.));
#92119=CARTESIAN_POINT('Ctrl Pts',(46.1810204150412,5.01465316921749,0.));
#92120=CARTESIAN_POINT('Ctrl Pts',(46.1810204150412,5.01465316921749,20.));
#92121=CARTESIAN_POINT('Ctrl Pts',(46.1815980415817,4.98176054155101,0.));
#92122=CARTESIAN_POINT('Ctrl Pts',(46.1815980415817,4.98176054155101,20.));
#92123=CARTESIAN_POINT('Ctrl Pts',(46.182152448291,4.94886863088032,0.));
#92124=CARTESIAN_POINT('Ctrl Pts',(46.182152448291,4.94886863088032,20.));
#92125=CARTESIAN_POINT('Ctrl Pts',(46.1826836357763,4.91597745358481,0.));
#92126=CARTESIAN_POINT('Ctrl Pts',(46.1826836357763,4.91597745358481,20.));
#92127=CARTESIAN_POINT('Ctrl Pts',(46.1831916046531,4.8830870260435,0.));
#92128=CARTESIAN_POINT('Ctrl Pts',(46.1831916046531,4.8830870260435,20.));
#92129=CARTESIAN_POINT('Ctrl Pts',(46.1836763555496,4.85019736463544,0.));
#92130=CARTESIAN_POINT('Ctrl Pts',(46.1836763555496,4.85019736463544,20.));
#92131=CARTESIAN_POINT('Ctrl Pts',(46.1841378891039,4.81730848573954,0.));
#92132=CARTESIAN_POINT('Ctrl Pts',(46.1841378891039,4.81730848573954,20.));
#92133=CARTESIAN_POINT('Ctrl Pts',(46.1845762059678,4.78442040573515,0.));
#92134=CARTESIAN_POINT('Ctrl Pts',(46.1845762059678,4.78442040573515,20.));
#92135=CARTESIAN_POINT('Ctrl Pts',(46.1849913068043,4.75153314100161,0.));
#92136=CARTESIAN_POINT('Ctrl Pts',(46.1849913068043,4.75153314100161,20.));
#92137=CARTESIAN_POINT('Ctrl Pts',(46.1853831922891,4.71864670791826,0.));
#92138=CARTESIAN_POINT('Ctrl Pts',(46.1853831922891,4.71864670791826,20.));
#92139=CARTESIAN_POINT('Ctrl Pts',(46.1857518631086,4.68576112286394,0.));
#92140=CARTESIAN_POINT('Ctrl Pts',(46.1857518631086,4.68576112286394,20.));
#92141=CARTESIAN_POINT('Ctrl Pts',(46.1860973199616,4.65287640221748,0.));
#92142=CARTESIAN_POINT('Ctrl Pts',(46.1860973199616,4.65287640221748,20.));
#92143=CARTESIAN_POINT('Ctrl Pts',(46.1864195635571,4.61999256235741,0.));
#92144=CARTESIAN_POINT('Ctrl Pts',(46.1864195635571,4.61999256235741,20.));
#92145=CARTESIAN_POINT('Ctrl Pts',(46.1867185946155,4.58710961966233,0.));
#92146=CARTESIAN_POINT('Ctrl Pts',(46.1867185946155,4.58710961966233,20.));
#92147=CARTESIAN_POINT('Ctrl Pts',(46.1869944138693,4.55422759051101,0.));
#92148=CARTESIAN_POINT('Ctrl Pts',(46.1869944138693,4.55422759051101,20.));
#92149=CARTESIAN_POINT('Ctrl Pts',(46.1872470220627,4.52134649128218,0.));
#92150=CARTESIAN_POINT('Ctrl Pts',(46.1872470220627,4.52134649128218,20.));
#92151=CARTESIAN_POINT('Ctrl Pts',(46.1874764199521,4.48846633835459,0.));
#92152=CARTESIAN_POINT('Ctrl Pts',(46.1874764199521,4.48846633835459,20.));
#92153=CARTESIAN_POINT('Ctrl Pts',(46.1876826083051,4.45558714810681,0.));
#92154=CARTESIAN_POINT('Ctrl Pts',(46.1876826083051,4.45558714810681,20.));
#92155=CARTESIAN_POINT('Ctrl Pts',(46.1878655879008,4.42270893691724,0.));
#92156=CARTESIAN_POINT('Ctrl Pts',(46.1878655879008,4.42270893691724,20.));
#92157=CARTESIAN_POINT('Ctrl Pts',(46.1880253595296,4.38983172116389,0.));
#92158=CARTESIAN_POINT('Ctrl Pts',(46.1880253595296,4.38983172116389,20.));
#92159=CARTESIAN_POINT('Ctrl Pts',(46.1881619239926,4.35695551722447,0.));
#92160=CARTESIAN_POINT('Ctrl Pts',(46.1881619239926,4.35695551722447,20.));
#92161=CARTESIAN_POINT('Ctrl Pts',(46.1882752821036,4.32408034147655,0.));
#92162=CARTESIAN_POINT('Ctrl Pts',(46.1882752821036,4.32408034147655,20.));
#92163=CARTESIAN_POINT('Ctrl Pts',(46.1883654346888,4.29120621029777,0.));
#92164=CARTESIAN_POINT('Ctrl Pts',(46.1883654346888,4.29120621029777,20.));
#92165=CARTESIAN_POINT('Ctrl Pts',(46.1884323825857,4.25833314006578,0.));
#92166=CARTESIAN_POINT('Ctrl Pts',(46.1884323825857,4.25833314006578,20.));
#92167=CARTESIAN_POINT('Ctrl Pts',(46.1884761266433,4.22546114715825,0.));
#92168=CARTESIAN_POINT('Ctrl Pts',(46.1884761266433,4.22546114715825,20.));
#92169=CARTESIAN_POINT('Ctrl Pts',(46.1884966677209,4.19259024795239,0.));
#92170=CARTESIAN_POINT('Ctrl Pts',(46.1884966677209,4.19259024795239,20.));
#92171=CARTESIAN_POINT('Ctrl Pts',(46.1884940066895,4.15972045882509,0.));
#92172=CARTESIAN_POINT('Ctrl Pts',(46.1884940066895,4.15972045882509,20.));
#92173=CARTESIAN_POINT('Ctrl Pts',(46.1884681444317,4.12685179615294,0.));
#92174=CARTESIAN_POINT('Ctrl Pts',(46.1884681444317,4.12685179615294,20.));
#92175=CARTESIAN_POINT('Ctrl Pts',(46.188419081843,4.09398427631255,0.));
#92176=CARTESIAN_POINT('Ctrl Pts',(46.188419081843,4.09398427631255,20.));
#92177=CARTESIAN_POINT('Ctrl Pts',(46.18834681983,4.06111791568023,0.));
#92178=CARTESIAN_POINT('Ctrl Pts',(46.18834681983,4.06111791568023,20.));
#92179=CARTESIAN_POINT('Ctrl Pts',(46.1882513593113,4.02825273063218,0.));
#92180=CARTESIAN_POINT('Ctrl Pts',(46.1882513593113,4.02825273063218,20.));
#92181=CARTESIAN_POINT('Ctrl Pts',(46.1881327012171,3.99538873754443,0.));
#92182=CARTESIAN_POINT('Ctrl Pts',(46.1881327012171,3.99538873754443,20.));
#92183=CARTESIAN_POINT('Ctrl Pts',(46.1879908464881,3.96252595279274,0.));
#92184=CARTESIAN_POINT('Ctrl Pts',(46.1879908464881,3.96252595279274,20.));
#92185=CARTESIAN_POINT('Ctrl Pts',(46.1878257960766,3.92966439275257,0.));
#92186=CARTESIAN_POINT('Ctrl Pts',(46.1878257960766,3.92966439275257,20.));
#92187=CARTESIAN_POINT('Ctrl Pts',(46.1876375509469,3.89680407379914,0.));
#92188=CARTESIAN_POINT('Ctrl Pts',(46.1876375509469,3.89680407379914,20.));
#92189=CARTESIAN_POINT('Ctrl Pts',(46.1874261120751,3.86394501230744,0.));
#92190=CARTESIAN_POINT('Ctrl Pts',(46.1874261120751,3.86394501230744,20.));
#92191=CARTESIAN_POINT('Ctrl Pts',(46.1871914804492,3.83108722465199,0.));
#92192=CARTESIAN_POINT('Ctrl Pts',(46.1871914804492,3.83108722465199,20.));
#92193=CARTESIAN_POINT('Ctrl Pts',(46.1869336570686,3.79823072720685,0.));
#92194=CARTESIAN_POINT('Ctrl Pts',(46.1869336570686,3.79823072720685,20.));
#92195=CARTESIAN_POINT('Ctrl Pts',(46.1866526429445,3.76537553634596,0.));
#92196=CARTESIAN_POINT('Ctrl Pts',(46.1866526429445,3.76537553634596,20.));
#92197=CARTESIAN_POINT('Ctrl Pts',(46.1863484390996,3.73252166844328,0.));
#92198=CARTESIAN_POINT('Ctrl Pts',(46.1863484390996,3.73252166844328,20.));
#92199=CARTESIAN_POINT('Ctrl Pts',(46.1860210465678,3.69966913987253,0.));
#92200=CARTESIAN_POINT('Ctrl Pts',(46.1860210465678,3.69966913987253,20.));
#92201=CARTESIAN_POINT('Ctrl Pts',(46.185670466394,3.6668179670071,0.));
#92202=CARTESIAN_POINT('Ctrl Pts',(46.185670466394,3.6668179670071,20.));
#92203=CARTESIAN_POINT('Ctrl Pts',(46.1852966996347,3.6339681662199,0.));
#92204=CARTESIAN_POINT('Ctrl Pts',(46.1852966996347,3.6339681662199,20.));
#92205=CARTESIAN_POINT('Ctrl Pts',(46.1848997473582,3.60111975388339,0.));
#92206=CARTESIAN_POINT('Ctrl Pts',(46.1848997473582,3.60111975388339,20.));
#92207=CARTESIAN_POINT('Ctrl Pts',(46.1844796106451,3.56827274636958,0.));
#92208=CARTESIAN_POINT('Ctrl Pts',(46.1844796106451,3.56827274636958,20.));
#92209=CARTESIAN_POINT('Ctrl Pts',(46.1840362905882,3.53542716005025,0.));
#92210=CARTESIAN_POINT('Ctrl Pts',(46.1840362905882,3.53542716005025,20.));
#92211=CARTESIAN_POINT('Ctrl Pts',(46.1835697882921,3.50258301129689,0.));
#92212=CARTESIAN_POINT('Ctrl Pts',(46.1835697882921,3.50258301129689,20.));
#92213=CARTESIAN_POINT('Ctrl Pts',(46.1830801048722,3.4697403164807,0.));
#92214=CARTESIAN_POINT('Ctrl Pts',(46.1830801048722,3.4697403164807,20.));
#92215=CARTESIAN_POINT('Ctrl Pts',(46.1825672414553,3.43689909197262,0.));
#92216=CARTESIAN_POINT('Ctrl Pts',(46.1825672414553,3.43689909197262,20.));
#92217=CARTESIAN_POINT('Ctrl Pts',(46.1820311991793,3.40405935414302,0.));
#92218=CARTESIAN_POINT('Ctrl Pts',(46.1820311991793,3.40405935414302,20.));
#92219=CARTESIAN_POINT('Ctrl Pts',(46.1814719791936,3.37122111936182,0.));
#92220=CARTESIAN_POINT('Ctrl Pts',(46.1814719791936,3.37122111936182,20.));
#92221=CARTESIAN_POINT('Ctrl Pts',(46.1808895826591,3.33838440399861,0.));
#92222=CARTESIAN_POINT('Ctrl Pts',(46.1808895826591,3.33838440399861,20.));
#92223=CARTESIAN_POINT('Ctrl Pts',(46.1802840107495,3.30554922442266,0.));
#92224=CARTESIAN_POINT('Ctrl Pts',(46.1802840107495,3.30554922442266,20.));
#92225=CARTESIAN_POINT('Ctrl Pts',(46.1796552646498,3.27271559700279,0.));
#92226=CARTESIAN_POINT('Ctrl Pts',(46.1796552646498,3.27271559700279,20.));
#92227=CARTESIAN_POINT('Ctrl Pts',(46.1790033455572,3.23988353810748,0.));
#92228=CARTESIAN_POINT('Ctrl Pts',(46.1790033455572,3.23988353810748,20.));
#92229=CARTESIAN_POINT('Ctrl Pts',(46.1783282546796,3.20705306410471,0.));
#92230=CARTESIAN_POINT('Ctrl Pts',(46.1783282546796,3.20705306410471,20.));
#92231=CARTESIAN_POINT('Ctrl Pts',(46.1776299932363,3.17422419136187,0.));
#92232=CARTESIAN_POINT('Ctrl Pts',(46.1776299932363,3.17422419136187,20.));
#92233=CARTESIAN_POINT('Ctrl Pts',(46.1769085624582,3.14139693624605,0.));
#92234=CARTESIAN_POINT('Ctrl Pts',(46.1769085624582,3.14139693624605,20.));
#92235=CARTESIAN_POINT('Ctrl Pts',(46.1761639635878,3.10857131512384,0.));
#92236=CARTESIAN_POINT('Ctrl Pts',(46.1761639635878,3.10857131512384,20.));
#92237=CARTESIAN_POINT('Ctrl Pts',(46.1753961978798,3.0757473443616,0.));
#92238=CARTESIAN_POINT('Ctrl Pts',(46.1753961978798,3.0757473443616,20.));
#92239=CARTESIAN_POINT('Ctrl Pts',(46.1746052665999,3.04292504032497,0.));
#92240=CARTESIAN_POINT('Ctrl Pts',(46.1746052665999,3.04292504032497,20.));
#92241=CARTESIAN_POINT('Ctrl Pts',(46.1737911710261,3.01010441937913,0.));
#92242=CARTESIAN_POINT('Ctrl Pts',(46.1737911710261,3.01010441937913,20.));
#92243=CARTESIAN_POINT('Ctrl Pts',(46.1729539124487,2.9772854978889,0.));
#92244=CARTESIAN_POINT('Ctrl Pts',(46.1729539124487,2.9772854978889,20.));
#92245=CARTESIAN_POINT('Ctrl Pts',(46.172093492169,2.94446829221865,0.));
#92246=CARTESIAN_POINT('Ctrl Pts',(46.172093492169,2.94446829221865,20.));
#92247=CARTESIAN_POINT('Ctrl Pts',(46.1712099114993,2.91165281873225,0.));
#92248=CARTESIAN_POINT('Ctrl Pts',(46.1712099114993,2.91165281873225,20.));
#92249=CARTESIAN_POINT('Ctrl Pts',(46.1703031717627,2.87883909379287,0.));
#92250=CARTESIAN_POINT('Ctrl Pts',(46.1703031717627,2.87883909379287,20.));
#92251=CARTESIAN_POINT('Ctrl Pts',(46.169373274294,2.84602713376309,0.));
#92252=CARTESIAN_POINT('Ctrl Pts',(46.169373274294,2.84602713376309,20.));
#92253=CARTESIAN_POINT('Ctrl Pts',(46.1684202204402,2.81321695500492,0.));
#92254=CARTESIAN_POINT('Ctrl Pts',(46.1684202204402,2.81321695500492,20.));
#92255=CARTESIAN_POINT('Ctrl Pts',(46.1674440115603,2.78040857388008,0.));
#92256=CARTESIAN_POINT('Ctrl Pts',(46.1674440115603,2.78040857388008,20.));
#92257=CARTESIAN_POINT('Ctrl Pts',(46.1664446490252,2.7476020067498,0.));
#92258=CARTESIAN_POINT('Ctrl Pts',(46.1664446490252,2.7476020067498,20.));
#92259=CARTESIAN_POINT('Ctrl Pts',(46.1654221342175,2.71479726997479,0.));
#92260=CARTESIAN_POINT('Ctrl Pts',(46.1654221342175,2.71479726997479,20.));
#92261=CARTESIAN_POINT('Ctrl Pts',(46.1643764685316,2.68199437991524,0.));
#92262=CARTESIAN_POINT('Ctrl Pts',(46.1643764685316,2.68199437991524,20.));
#92263=CARTESIAN_POINT('Ctrl Pts',(46.163307653373,2.64919335293067,0.));
#92264=CARTESIAN_POINT('Ctrl Pts',(46.163307653373,2.64919335293067,20.));
#92265=CARTESIAN_POINT('Ctrl Pts',(46.1622156901587,2.61639420537995,0.));
#92266=CARTESIAN_POINT('Ctrl Pts',(46.1622156901587,2.61639420537995,20.));
#92267=CARTESIAN_POINT('Ctrl Pts',(46.1611005803162,2.58359695362108,0.));
#92268=CARTESIAN_POINT('Ctrl Pts',(46.1611005803162,2.58359695362108,20.));
#92269=CARTESIAN_POINT('Ctrl Pts',(46.1599623252856,2.55080161401166,0.));
#92270=CARTESIAN_POINT('Ctrl Pts',(46.1599623252856,2.55080161401166,20.));
#92271=CARTESIAN_POINT('Ctrl Pts',(46.1588009265184,2.51800820290892,0.));
#92272=CARTESIAN_POINT('Ctrl Pts',(46.1588009265184,2.51800820290892,20.));
#92273=CARTESIAN_POINT('Ctrl Pts',(46.1576163854777,2.48521673666957,0.));
#92274=CARTESIAN_POINT('Ctrl Pts',(46.1576163854777,2.48521673666957,20.));
#92275=CARTESIAN_POINT('Ctrl Pts',(46.1564087036389,2.4524272316497,0.));
#92276=CARTESIAN_POINT('Ctrl Pts',(46.1564087036389,2.4524272316497,20.));
#92277=CARTESIAN_POINT('Ctrl Pts',(46.155177882489,2.41963970420458,0.));
#92278=CARTESIAN_POINT('Ctrl Pts',(46.155177882489,2.41963970420458,20.));
#92279=CARTESIAN_POINT('Ctrl Pts',(46.1539239235264,2.38685417068871,0.));
#92280=CARTESIAN_POINT('Ctrl Pts',(46.1539239235264,2.38685417068871,20.));
#92281=CARTESIAN_POINT('Ctrl Pts',(46.1526468282603,2.35407064745589,0.));
#92282=CARTESIAN_POINT('Ctrl Pts',(46.1526468282603,2.35407064745589,20.));
#92283=CARTESIAN_POINT('Ctrl Pts',(46.1513465982124,2.3212891508592,0.));
#92284=CARTESIAN_POINT('Ctrl Pts',(46.1513465982124,2.3212891508592,20.));
#92285=CARTESIAN_POINT('Ctrl Pts',(46.1500232349155,2.28850969725138,0.));
#92286=CARTESIAN_POINT('Ctrl Pts',(46.1500232349155,2.28850969725138,20.));
#92287=CARTESIAN_POINT('Ctrl Pts',(46.1486767399146,2.25573230298459,0.));
#92288=CARTESIAN_POINT('Ctrl Pts',(46.1486767399146,2.25573230298459,20.));
#92289=CARTESIAN_POINT('Ctrl Pts',(46.147307114766,2.2229569844105,0.));
#92290=CARTESIAN_POINT('Ctrl Pts',(46.147307114766,2.2229569844105,20.));
#92291=CARTESIAN_POINT('Ctrl Pts',(46.1459143610377,2.19018375787987,0.));
#92292=CARTESIAN_POINT('Ctrl Pts',(46.1459143610377,2.19018375787987,20.));
#92293=CARTESIAN_POINT('Ctrl Pts',(46.1444984803082,2.15741263974263,0.));
#92294=CARTESIAN_POINT('Ctrl Pts',(46.1444984803082,2.15741263974263,20.));
#92295=CARTESIAN_POINT('Ctrl Pts',(46.1430594741682,2.12464364634813,0.));
#92296=CARTESIAN_POINT('Ctrl Pts',(46.1430594741682,2.12464364634813,20.));
#92297=CARTESIAN_POINT('Ctrl Pts',(46.1415973442202,2.09187679404497,0.));
#92298=CARTESIAN_POINT('Ctrl Pts',(46.1415973442202,2.09187679404497,20.));
#92299=CARTESIAN_POINT('Ctrl Pts',(46.1401120920793,2.05911209918102,0.));
#92300=CARTESIAN_POINT('Ctrl Pts',(46.1401120920793,2.05911209918102,20.));
#92301=CARTESIAN_POINT('Ctrl Pts',(46.1386037193727,2.02634957810318,0.));
#92302=CARTESIAN_POINT('Ctrl Pts',(46.1386037193727,2.02634957810318,20.));
#92303=CARTESIAN_POINT('Ctrl Pts',(46.1370722277379,1.99358924715754,0.));
#92304=CARTESIAN_POINT('Ctrl Pts',(46.1370722277379,1.99358924715754,20.));
#92305=CARTESIAN_POINT('Ctrl Pts',(46.1355176188236,1.96083112268931,0.));
#92306=CARTESIAN_POINT('Ctrl Pts',(46.1355176188236,1.96083112268931,20.));
#92307=CARTESIAN_POINT('Ctrl Pts',(46.1339398942902,1.9280752210434,0.));
#92308=CARTESIAN_POINT('Ctrl Pts',(46.1339398942902,1.9280752210434,20.));
#92309=CARTESIAN_POINT('Ctrl Pts',(46.1323390558096,1.89532155856415,0.));
#92310=CARTESIAN_POINT('Ctrl Pts',(46.1323390558096,1.89532155856415,20.));
#92311=CARTESIAN_POINT('Ctrl Pts',(46.1307151050651,1.86257015159583,0.));
#92312=CARTESIAN_POINT('Ctrl Pts',(46.1307151050651,1.86257015159583,20.));
#92313=CARTESIAN_POINT('Ctrl Pts',(46.1290680437528,1.82982101648207,0.));
#92314=CARTESIAN_POINT('Ctrl Pts',(46.1290680437528,1.82982101648207,20.));
#92315=CARTESIAN_POINT('Ctrl Pts',(46.1273978735796,1.79707416956535,0.));
#92316=CARTESIAN_POINT('Ctrl Pts',(46.1273978735796,1.79707416956535,20.));
#92317=CARTESIAN_POINT('Ctrl Pts',(46.1257045962649,1.76432962718686,0.));
#92318=CARTESIAN_POINT('Ctrl Pts',(46.1257045962649,1.76432962718686,20.));
#92319=CARTESIAN_POINT('Ctrl Pts',(46.1239882135394,1.73158740568598,0.));
#92320=CARTESIAN_POINT('Ctrl Pts',(46.1239882135394,1.73158740568598,20.));
#92321=CARTESIAN_POINT('Ctrl Pts',(46.1222487271454,1.6988475214004,0.));
#92322=CARTESIAN_POINT('Ctrl Pts',(46.1222487271454,1.6988475214004,20.));
#92323=CARTESIAN_POINT('Ctrl Pts',(46.1204861388364,1.66610999066656,0.));
#92324=CARTESIAN_POINT('Ctrl Pts',(46.1204861388364,1.66610999066656,20.));
#92325=CARTESIAN_POINT('Ctrl Pts',(46.1187004503775,1.63337482982071,0.));
#92326=CARTESIAN_POINT('Ctrl Pts',(46.1187004503775,1.63337482982071,20.));
#92327=CARTESIAN_POINT('Ctrl Pts',(46.1168916635447,1.60064205519959,0.));
#92328=CARTESIAN_POINT('Ctrl Pts',(46.1168916635447,1.60064205519959,20.));
#92329=CARTESIAN_POINT('Ctrl Pts',(46.1150597801266,1.56791168314158,0.));
#92330=CARTESIAN_POINT('Ctrl Pts',(46.1150597801266,1.56791168314158,20.));
#92331=CARTESIAN_POINT('Ctrl Pts',(46.1132048019234,1.53518372998667,0.));
#92332=CARTESIAN_POINT('Ctrl Pts',(46.1132048019234,1.53518372998667,20.));
#92333=CARTESIAN_POINT('Ctrl Pts',(46.111326730748,1.50245821207431,0.));
#92334=CARTESIAN_POINT('Ctrl Pts',(46.111326730748,1.50245821207431,20.));
#92335=CARTESIAN_POINT('Ctrl Pts',(46.1094255684237,1.46973514574144,0.));
#92336=CARTESIAN_POINT('Ctrl Pts',(46.1094255684237,1.46973514574144,20.));
#92337=CARTESIAN_POINT('Ctrl Pts',(46.1075013167858,1.43701454732091,0.));
#92338=CARTESIAN_POINT('Ctrl Pts',(46.1075013167858,1.43701454732091,20.));
#92339=CARTESIAN_POINT('Ctrl Pts',(46.1055539776801,1.40429643313894,0.));
#92340=CARTESIAN_POINT('Ctrl Pts',(46.1055539776801,1.40429643313894,20.));
#92341=CARTESIAN_POINT('Ctrl Pts',(46.1035835529643,1.37158081951552,0.));
#92342=CARTESIAN_POINT('Ctrl Pts',(46.1035835529643,1.37158081951552,20.));
#92343=CARTESIAN_POINT('Ctrl Pts',(46.1015900445065,1.33886772276919,0.));
#92344=CARTESIAN_POINT('Ctrl Pts',(46.1015900445065,1.33886772276919,20.));
#92345=CARTESIAN_POINT('Ctrl Pts',(46.0995734541875,1.30615715922173,0.));
#92346=CARTESIAN_POINT('Ctrl Pts',(46.0995734541875,1.30615715922173,20.));
#92347=CARTESIAN_POINT('Ctrl Pts',(46.0975337839002,1.27344914520176,0.));
#92348=CARTESIAN_POINT('Ctrl Pts',(46.0975337839002,1.27344914520176,20.));
#92349=CARTESIAN_POINT('Ctrl Pts',(46.0954710355506,1.24074369705073,0.));
#92350=CARTESIAN_POINT('Ctrl Pts',(46.0954710355506,1.24074369705073,20.));
#92351=CARTESIAN_POINT('Ctrl Pts',(46.0933852110571,1.20804083112097,0.));
#92352=CARTESIAN_POINT('Ctrl Pts',(46.0933852110571,1.20804083112097,20.));
#92353=CARTESIAN_POINT('Ctrl Pts',(46.0912763123502,1.17534056376402,0.));
#92354=CARTESIAN_POINT('Ctrl Pts',(46.0912763123502,1.17534056376402,20.));
#92355=CARTESIAN_POINT('Ctrl Pts',(46.0891443413718,1.14264291132053,0.));
#92356=CARTESIAN_POINT('Ctrl Pts',(46.0891443413718,1.14264291132053,20.));
#92357=CARTESIAN_POINT('Ctrl Pts',(46.0869893000733,1.10994789011163,0.));
#92358=CARTESIAN_POINT('Ctrl Pts',(46.0869893000733,1.10994789011163,20.));
#92359=CARTESIAN_POINT('Ctrl Pts',(46.0848111904142,1.07725551642471,0.));
#92360=CARTESIAN_POINT('Ctrl Pts',(46.0848111904142,1.07725551642471,20.));
#92361=CARTESIAN_POINT('Ctrl Pts',(46.0826100143611,1.04456580652048,0.));
#92362=CARTESIAN_POINT('Ctrl Pts',(46.0826100143611,1.04456580652048,20.));
#92363=CARTESIAN_POINT('Ctrl Pts',(46.0803857738924,1.01187877665955,0.));
#92364=CARTESIAN_POINT('Ctrl Pts',(46.0803857738924,1.01187877665955,20.));
#92365=CARTESIAN_POINT('Ctrl Pts',(46.0781384710012,0.979194443126295,0.));
#92366=CARTESIAN_POINT('Ctrl Pts',(46.0781384710012,0.979194443126295,20.));
#92367=CARTESIAN_POINT('Ctrl Pts',(46.0758681076973,0.946512822248755,0.));
#92368=CARTESIAN_POINT('Ctrl Pts',(46.0758681076973,0.946512822248755,20.));
#92369=CARTESIAN_POINT('Ctrl Pts',(46.0735746860119,0.913833930432277,0.));
#92370=CARTESIAN_POINT('Ctrl Pts',(46.0735746860119,0.913833930432277,20.));
#92371=CARTESIAN_POINT('Ctrl Pts',(46.0712582079948,0.881157784136745,0.));
#92372=CARTESIAN_POINT('Ctrl Pts',(46.0712582079948,0.881157784136745,20.));
#92373=CARTESIAN_POINT('Ctrl Pts',(46.0689186757066,0.848484399815189,0.));
#92374=CARTESIAN_POINT('Ctrl Pts',(46.0689186757066,0.848484399815189,20.));
#92375=CARTESIAN_POINT('Ctrl Pts',(46.0665560912128,0.815813793858643,0.));
#92376=CARTESIAN_POINT('Ctrl Pts',(46.0665560912128,0.815813793858643,20.));
#92377=CARTESIAN_POINT('Ctrl Pts',(46.064170456577,0.783145982548935,0.));
#92378=CARTESIAN_POINT('Ctrl Pts',(46.064170456577,0.783145982548935,20.));
#92379=CARTESIAN_POINT('Ctrl Pts',(46.0617617738521,0.750480981980926,0.));
#92380=CARTESIAN_POINT('Ctrl Pts',(46.0617617738521,0.750480981980926,20.));
#92381=CARTESIAN_POINT('Ctrl Pts',(46.0593300450868,0.71781880812973,0.));
#92382=CARTESIAN_POINT('Ctrl Pts',(46.0593300450868,0.71781880812973,20.));
#92383=CARTESIAN_POINT('Ctrl Pts',(46.0568752723439,0.685159476991768,0.));
#92384=CARTESIAN_POINT('Ctrl Pts',(46.0568752723439,0.685159476991768,20.));
#92385=CARTESIAN_POINT('Ctrl Pts',(46.0543974577158,0.652503004713265,0.));
#92386=CARTESIAN_POINT('Ctrl Pts',(46.0543974577158,0.652503004713265,20.));
#92387=CARTESIAN_POINT('Ctrl Pts',(46.0518966033391,0.619849407700868,0.));
#92388=CARTESIAN_POINT('Ctrl Pts',(46.0518966033391,0.619849407700868,20.));
#92389=CARTESIAN_POINT('Ctrl Pts',(46.0493727114182,0.587198702798626,0.));
#92390=CARTESIAN_POINT('Ctrl Pts',(46.0493727114182,0.587198702798626,20.));
#92391=CARTESIAN_POINT('Ctrl Pts',(46.0468257841997,0.554550907098833,0.));
#92392=CARTESIAN_POINT('Ctrl Pts',(46.0468257841997,0.554550907098833,20.));
#92393=CARTESIAN_POINT('Ctrl Pts',(46.044255823933,0.521906037621051,0.));
#92394=CARTESIAN_POINT('Ctrl Pts',(46.044255823933,0.521906037621051,20.));
#92395=CARTESIAN_POINT('Ctrl Pts',(46.0416628328334,0.489264111013841,0.));
#92396=CARTESIAN_POINT('Ctrl Pts',(46.0416628328334,0.489264111013841,20.));
#92397=CARTESIAN_POINT('Ctrl Pts',(46.0390468130479,0.456625143292617,0.));
#92398=CARTESIAN_POINT('Ctrl Pts',(46.0390468130479,0.456625143292617,20.));
#92399=CARTESIAN_POINT('Ctrl Pts',(46.0364077666069,0.42398914944525,0.));
#92400=CARTESIAN_POINT('Ctrl Pts',(46.0364077666069,0.42398914944525,20.));
#92401=CARTESIAN_POINT('Ctrl Pts',(46.0337456954889,0.391356143937839,0.));
#92402=CARTESIAN_POINT('Ctrl Pts',(46.0337456954889,0.391356143937839,20.));
#92403=CARTESIAN_POINT('Ctrl Pts',(46.0310606017089,0.358726141441572,0.));
#92404=CARTESIAN_POINT('Ctrl Pts',(46.0310606017089,0.358726141441572,20.));
#92405=CARTESIAN_POINT('Ctrl Pts',(46.0283524874048,0.32609915751696,0.));
#92406=CARTESIAN_POINT('Ctrl Pts',(46.0283524874048,0.32609915751696,20.));
#92407=CARTESIAN_POINT('Ctrl Pts',(46.025621354915,0.293475209241793,0.));
#92408=CARTESIAN_POINT('Ctrl Pts',(46.025621354915,0.293475209241793,20.));
#92409=CARTESIAN_POINT('Ctrl Pts',(46.022867206884,0.260854316057536,0.));
#92410=CARTESIAN_POINT('Ctrl Pts',(46.022867206884,0.260854316057536,20.));
#92411=CARTESIAN_POINT('Ctrl Pts',(46.0200900461091,0.228236498538563,0.));
#92412=CARTESIAN_POINT('Ctrl Pts',(46.0200900461091,0.228236498538563,20.));
#92413=CARTESIAN_POINT('Ctrl Pts',(46.0172898753497,0.195621776838885,0.));
#92414=CARTESIAN_POINT('Ctrl Pts',(46.0172898753497,0.195621776838885,20.));
#92415=CARTESIAN_POINT('Ctrl Pts',(46.0144666971462,0.163010169231708,0.));
#92416=CARTESIAN_POINT('Ctrl Pts',(46.0144666971462,0.163010169231708,20.));
#92417=CARTESIAN_POINT('Ctrl Pts',(46.0116205136405,0.130401690656321,0.));
#92418=CARTESIAN_POINT('Ctrl Pts',(46.0116205136405,0.130401690656321,20.));
#92419=CARTESIAN_POINT('Ctrl Pts',(46.0087513263814,0.0977963511372851,
0.));
#92420=CARTESIAN_POINT('Ctrl Pts',(46.0087513263814,0.0977963511372851,
20.));
#92421=CARTESIAN_POINT('Ctrl Pts',(46.0058591364029,0.0651941566547578,
0.));
#92422=CARTESIAN_POINT('Ctrl Pts',(46.0058591364029,0.0651941566547578,
20.));
#92423=CARTESIAN_POINT('Ctrl Pts',(46.0035269827389,0.0391149194889428,
0.));
#92424=CARTESIAN_POINT('Ctrl Pts',(46.0035269827389,0.0391149194889428,
20.));
#92425=CARTESIAN_POINT('Ctrl Pts',(46.0017675166781,0.0195569086685896,
0.));
#92426=CARTESIAN_POINT('Ctrl Pts',(46.0017675166781,0.0195569086685896,
20.));
#92427=CARTESIAN_POINT('Ctrl Pts',(46.0005899389515,0.0065188645893676,
0.));
#92428=CARTESIAN_POINT('Ctrl Pts',(46.0005899389515,0.0065188645893676,
20.));
#92429=CARTESIAN_POINT('Ctrl Pts',(46.,0.,0.));
#92430=CARTESIAN_POINT('Ctrl Pts',(46.,0.,20.));
#92431=CARTESIAN_POINT('Origin',(35.238044383473,29.5682300455808,0.));
#92432=CARTESIAN_POINT('',(35.9959384951176,30.2041787151333,0.));
#92433=CARTESIAN_POINT('Ctrl Pts',(-8.50876070567958,48.2555798975982,0.));
#92434=CARTESIAN_POINT('Ctrl Pts',(-8.50876070567958,48.2555798975982,20.));
#92435=CARTESIAN_POINT('Ctrl Pts',(-8.50201591146282,48.2561497089132,0.));
#92436=CARTESIAN_POINT('Ctrl Pts',(-8.50201591146282,48.2561497089132,20.));
#92437=CARTESIAN_POINT('Ctrl Pts',(-8.48852624368609,48.2572870022174,0.));
#92438=CARTESIAN_POINT('Ctrl Pts',(-8.48852624368609,48.2572870022174,20.));
#92439=CARTESIAN_POINT('Ctrl Pts',(-8.46829150399134,48.2589859541967,0.));
#92440=CARTESIAN_POINT('Ctrl Pts',(-8.46829150399134,48.2589859541967,20.));
#92441=CARTESIAN_POINT('Ctrl Pts',(-8.44131137500422,48.2612372475269,0.));
#92442=CARTESIAN_POINT('Ctrl Pts',(-8.44131137500422,48.2612372475269,20.));
#92443=CARTESIAN_POINT('Ctrl Pts',(-8.40758542126,48.2640280707484,0.));
#92444=CARTESIAN_POINT('Ctrl Pts',(-8.40758542126,48.2640280707484,20.));
#92445=CARTESIAN_POINT('Ctrl Pts',(-8.37385867778171,48.2667956002972,0.));
#92446=CARTESIAN_POINT('Ctrl Pts',(-8.37385867778171,48.2667956002972,20.));
#92447=CARTESIAN_POINT('Ctrl Pts',(-8.34013115014498,48.2695398358687,0.));
#92448=CARTESIAN_POINT('Ctrl Pts',(-8.34013115014498,48.2695398358687,20.));
#92449=CARTESIAN_POINT('Ctrl Pts',(-8.30640284761837,48.2722607770974,0.));
#92450=CARTESIAN_POINT('Ctrl Pts',(-8.30640284761837,48.2722607770974,20.));
#92451=CARTESIAN_POINT('Ctrl Pts',(-8.2726737841987,48.274958423567,0.));
#92452=CARTESIAN_POINT('Ctrl Pts',(-8.2726737841987,48.274958423567,20.));
#92453=CARTESIAN_POINT('Ctrl Pts',(-8.23894397736023,48.2776327748283,0.));
#92454=CARTESIAN_POINT('Ctrl Pts',(-8.23894397736023,48.2776327748283,20.));
#92455=CARTESIAN_POINT('Ctrl Pts',(-8.20521344665195,48.2802838304168,0.));
#92456=CARTESIAN_POINT('Ctrl Pts',(-8.20521344665195,48.2802838304168,20.));
#92457=CARTESIAN_POINT('Ctrl Pts',(-8.17148221231955,48.2829115898716,0.));
#92458=CARTESIAN_POINT('Ctrl Pts',(-8.17148221231955,48.2829115898716,20.));
#92459=CARTESIAN_POINT('Ctrl Pts',(-8.13775029398595,48.2855160527521,0.));
#92460=CARTESIAN_POINT('Ctrl Pts',(-8.13775029398595,48.2855160527521,20.));
#92461=CARTESIAN_POINT('Ctrl Pts',(-8.10401770912493,48.288097218659,0.));
#92462=CARTESIAN_POINT('Ctrl Pts',(-8.10401770912493,48.288097218659,20.));
#92463=CARTESIAN_POINT('Ctrl Pts',(-8.07028447346159,48.2906550872281,0.));
#92464=CARTESIAN_POINT('Ctrl Pts',(-8.07028447346159,48.2906550872281,20.));
#92465=CARTESIAN_POINT('Ctrl Pts',(-8.03655060167525,48.2931896581208,0.));
#92466=CARTESIAN_POINT('Ctrl Pts',(-8.03655060167525,48.2931896581208,20.));
#92467=CARTESIAN_POINT('Ctrl Pts',(-8.00281610801474,48.2957009310153,0.));
#92468=CARTESIAN_POINT('Ctrl Pts',(-8.00281610801474,48.2957009310153,20.));
#92469=CARTESIAN_POINT('Ctrl Pts',(-7.96908100690894,48.2981889055984,0.));
#92470=CARTESIAN_POINT('Ctrl Pts',(-7.96908100690894,48.2981889055984,20.));
#92471=CARTESIAN_POINT('Ctrl Pts',(-7.93534531368691,48.300653581555,0.));
#92472=CARTESIAN_POINT('Ctrl Pts',(-7.93534531368691,48.300653581555,20.));
#92473=CARTESIAN_POINT('Ctrl Pts',(-7.90160904447353,48.3030949585702,0.));
#92474=CARTESIAN_POINT('Ctrl Pts',(-7.90160904447353,48.3030949585702,20.));
#92475=CARTESIAN_POINT('Ctrl Pts',(-7.86787221586447,48.3055130363337,0.));
#92476=CARTESIAN_POINT('Ctrl Pts',(-7.86787221586447,48.3055130363337,20.));
#92477=CARTESIAN_POINT('Ctrl Pts',(-7.83413484466695,48.3079078145432,0.));
#92478=CARTESIAN_POINT('Ctrl Pts',(-7.83413484466695,48.3079078145432,20.));
#92479=CARTESIAN_POINT('Ctrl Pts',(-7.80039694763398,48.3102792929086,0.));
#92480=CARTESIAN_POINT('Ctrl Pts',(-7.80039694763398,48.3102792929086,20.));
#92481=CARTESIAN_POINT('Ctrl Pts',(-7.76665854114747,48.3126274711557,0.));
#92482=CARTESIAN_POINT('Ctrl Pts',(-7.76665854114747,48.3126274711557,20.));
#92483=CARTESIAN_POINT('Ctrl Pts',(-7.7329196412329,48.3149523490266,0.));
#92484=CARTESIAN_POINT('Ctrl Pts',(-7.7329196412329,48.3149523490266,20.));
#92485=CARTESIAN_POINT('Ctrl Pts',(-7.69918026370737,48.3172539262766,0.));
#92486=CARTESIAN_POINT('Ctrl Pts',(-7.69918026370737,48.3172539262766,20.));
#92487=CARTESIAN_POINT('Ctrl Pts',(-7.66544042428834,48.3195322026739,0.));
#92488=CARTESIAN_POINT('Ctrl Pts',(-7.66544042428834,48.3195322026739,20.));
#92489=CARTESIAN_POINT('Ctrl Pts',(-7.63170013870894,48.3217871779975,0.));
#92490=CARTESIAN_POINT('Ctrl Pts',(-7.63170013870894,48.3217871779975,20.));
#92491=CARTESIAN_POINT('Ctrl Pts',(-7.59795942285541,48.3240188520354,0.));
#92492=CARTESIAN_POINT('Ctrl Pts',(-7.59795942285541,48.3240188520354,20.));
#92493=CARTESIAN_POINT('Ctrl Pts',(-7.56421829277371,48.3262272245847,0.));
#92494=CARTESIAN_POINT('Ctrl Pts',(-7.56421829277371,48.3262272245847,20.));
#92495=CARTESIAN_POINT('Ctrl Pts',(-7.53047676460328,48.328412295452,0.));
#92496=CARTESIAN_POINT('Ctrl Pts',(-7.53047676460328,48.328412295452,20.));
#92497=CARTESIAN_POINT('Ctrl Pts',(-7.4967348545312,48.3305740644544,0.));
#92498=CARTESIAN_POINT('Ctrl Pts',(-7.4967348545312,48.3305740644544,20.));
#92499=CARTESIAN_POINT('Ctrl Pts',(-7.4629925787421,48.3327125314199,0.));
#92500=CARTESIAN_POINT('Ctrl Pts',(-7.4629925787421,48.3327125314199,20.));
#92501=CARTESIAN_POINT('Ctrl Pts',(-7.42924995335919,48.3348276961881,0.));
#92502=CARTESIAN_POINT('Ctrl Pts',(-7.42924995335919,48.3348276961881,20.));
#92503=CARTESIAN_POINT('Ctrl Pts',(-7.39550699443534,48.3369195586108,0.));
#92504=CARTESIAN_POINT('Ctrl Pts',(-7.39550699443534,48.3369195586108,20.));
#92505=CARTESIAN_POINT('Ctrl Pts',(-7.36176371798263,48.3389881185516,0.));
#92506=CARTESIAN_POINT('Ctrl Pts',(-7.36176371798263,48.3389881185516,20.));
#92507=CARTESIAN_POINT('Ctrl Pts',(-7.32802013999148,48.3410333758855,0.));
#92508=CARTESIAN_POINT('Ctrl Pts',(-7.32802013999148,48.3410333758855,20.));
#92509=CARTESIAN_POINT('Ctrl Pts',(-7.2942762764527,48.3430553304987,0.));
#92510=CARTESIAN_POINT('Ctrl Pts',(-7.2942762764527,48.3430553304987,20.));
#92511=CARTESIAN_POINT('Ctrl Pts',(-7.26053214338257,48.3450539822883,0.));
#92512=CARTESIAN_POINT('Ctrl Pts',(-7.26053214338257,48.3450539822883,20.));
#92513=CARTESIAN_POINT('Ctrl Pts',(-7.22678775682933,48.3470293311619,0.));
#92514=CARTESIAN_POINT('Ctrl Pts',(-7.22678775682933,48.3470293311619,20.));
#92515=CARTESIAN_POINT('Ctrl Pts',(-7.19304313285999,48.3489813770376,0.));
#92516=CARTESIAN_POINT('Ctrl Pts',(-7.19304313285999,48.3489813770376,20.));
#92517=CARTESIAN_POINT('Ctrl Pts',(-7.15929828755241,48.3509101198447,0.));
#92518=CARTESIAN_POINT('Ctrl Pts',(-7.15929828755241,48.3509101198447,20.));
#92519=CARTESIAN_POINT('Ctrl Pts',(-7.12555323698551,48.3528155595232,0.));
#92520=CARTESIAN_POINT('Ctrl Pts',(-7.12555323698551,48.3528155595232,20.));
#92521=CARTESIAN_POINT('Ctrl Pts',(-7.09180799722882,48.354697696024,0.));
#92522=CARTESIAN_POINT('Ctrl Pts',(-7.09180799722882,48.354697696024,20.));
#92523=CARTESIAN_POINT('Ctrl Pts',(-7.05806258433803,48.3565565293095,0.));
#92524=CARTESIAN_POINT('Ctrl Pts',(-7.05806258433803,48.3565565293095,20.));
#92525=CARTESIAN_POINT('Ctrl Pts',(-7.02431701436127,48.3583920593534,0.));
#92526=CARTESIAN_POINT('Ctrl Pts',(-7.02431701436127,48.3583920593534,20.));
#92527=CARTESIAN_POINT('Ctrl Pts',(-6.99057130334228,48.3602042861407,0.));
#92528=CARTESIAN_POINT('Ctrl Pts',(-6.99057130334228,48.3602042861407,20.));
#92529=CARTESIAN_POINT('Ctrl Pts',(-6.95682546732485,48.3619932096677,0.));
#92530=CARTESIAN_POINT('Ctrl Pts',(-6.95682546732485,48.3619932096677,20.));
#92531=CARTESIAN_POINT('Ctrl Pts',(-6.9230795223571,48.3637588299416,0.));
#92532=CARTESIAN_POINT('Ctrl Pts',(-6.9230795223571,48.3637588299416,20.));
#92533=CARTESIAN_POINT('Ctrl Pts',(-6.88933348449371,48.3655011469807,0.));
#92534=CARTESIAN_POINT('Ctrl Pts',(-6.88933348449371,48.3655011469807,20.));
#92535=CARTESIAN_POINT('Ctrl Pts',(-6.8555873697933,48.3672201608141,0.));
#92536=CARTESIAN_POINT('Ctrl Pts',(-6.8555873697933,48.3672201608141,20.));
#92537=CARTESIAN_POINT('Ctrl Pts',(-6.82184119431719,48.3689158714816,0.));
#92538=CARTESIAN_POINT('Ctrl Pts',(-6.82184119431719,48.3689158714816,20.));
#92539=CARTESIAN_POINT('Ctrl Pts',(-6.78809497412715,48.370588279034,0.));
#92540=CARTESIAN_POINT('Ctrl Pts',(-6.78809497412715,48.370588279034,20.));
#92541=CARTESIAN_POINT('Ctrl Pts',(-6.75434872528386,48.3722373835335,0.));
#92542=CARTESIAN_POINT('Ctrl Pts',(-6.75434872528386,48.3722373835335,20.));
#92543=CARTESIAN_POINT('Ctrl Pts',(-6.72060246384581,48.3738631850533,0.));
#92544=CARTESIAN_POINT('Ctrl Pts',(-6.72060246384581,48.3738631850533,20.));
#92545=CARTESIAN_POINT('Ctrl Pts',(-6.68685620587016,48.3754656836776,0.));
#92546=CARTESIAN_POINT('Ctrl Pts',(-6.68685620587016,48.3754656836776,20.));
#92547=CARTESIAN_POINT('Ctrl Pts',(-6.65310996741334,48.3770448795022,0.));
#92548=CARTESIAN_POINT('Ctrl Pts',(-6.65310996741334,48.3770448795022,20.));
#92549=CARTESIAN_POINT('Ctrl Pts',(-6.61936376453196,48.3786007726338,0.));
#92550=CARTESIAN_POINT('Ctrl Pts',(-6.61936376453196,48.3786007726338,20.));
#92551=CARTESIAN_POINT('Ctrl Pts',(-6.58561761328368,48.3801333631899,0.));
#92552=CARTESIAN_POINT('Ctrl Pts',(-6.58561761328368,48.3801333631899,20.));
#92553=CARTESIAN_POINT('Ctrl Pts',(-6.55187152972773,48.3816426512994,0.));
#92554=CARTESIAN_POINT('Ctrl Pts',(-6.55187152972773,48.3816426512994,20.));
#92555=CARTESIAN_POINT('Ctrl Pts',(-6.51812552992425,48.3831286371024,0.));
#92556=CARTESIAN_POINT('Ctrl Pts',(-6.51812552992425,48.3831286371024,20.));
#92557=CARTESIAN_POINT('Ctrl Pts',(-6.48437962993407,48.3845913207494,0.));
#92558=CARTESIAN_POINT('Ctrl Pts',(-6.48437962993407,48.3845913207494,20.));
#92559=CARTESIAN_POINT('Ctrl Pts',(-6.45063384581846,48.3860307024022,0.));
#92560=CARTESIAN_POINT('Ctrl Pts',(-6.45063384581846,48.3860307024022,20.));
#92561=CARTESIAN_POINT('Ctrl Pts',(-6.41688819363866,48.3874467822337,0.));
#92562=CARTESIAN_POINT('Ctrl Pts',(-6.41688819363866,48.3874467822337,20.));
#92563=CARTESIAN_POINT('Ctrl Pts',(-6.38314268945589,48.388839560428,0.));
#92564=CARTESIAN_POINT('Ctrl Pts',(-6.38314268945589,48.388839560428,20.));
#92565=CARTESIAN_POINT('Ctrl Pts',(-6.34939734933123,48.3902090371802,0.));
#92566=CARTESIAN_POINT('Ctrl Pts',(-6.34939734933123,48.3902090371802,20.));
#92567=CARTESIAN_POINT('Ctrl Pts',(-6.3156521893259,48.3915552126968,0.));
#92568=CARTESIAN_POINT('Ctrl Pts',(-6.3156521893259,48.3915552126968,20.));
#92569=CARTESIAN_POINT('Ctrl Pts',(-6.28190722550134,48.3928780871951,0.));
#92570=CARTESIAN_POINT('Ctrl Pts',(-6.28190722550134,48.3928780871951,20.));
#92571=CARTESIAN_POINT('Ctrl Pts',(-6.24816247391921,48.3941776609035,0.));
#92572=CARTESIAN_POINT('Ctrl Pts',(-6.24816247391921,48.3941776609035,20.));
#92573=CARTESIAN_POINT('Ctrl Pts',(-6.21441795064169,48.3954539340615,0.));
#92574=CARTESIAN_POINT('Ctrl Pts',(-6.21441795064169,48.3954539340615,20.));
#92575=CARTESIAN_POINT('Ctrl Pts',(-6.18067367173125,48.3967069069196,0.));
#92576=CARTESIAN_POINT('Ctrl Pts',(-6.18067367173125,48.3967069069196,20.));
#92577=CARTESIAN_POINT('Ctrl Pts',(-6.1469296532508,48.3979365797396,0.));
#92578=CARTESIAN_POINT('Ctrl Pts',(-6.1469296532508,48.3979365797396,20.));
#92579=CARTESIAN_POINT('Ctrl Pts',(-6.11318591126344,48.3991429527941,0.));
#92580=CARTESIAN_POINT('Ctrl Pts',(-6.11318591126344,48.3991429527941,20.));
#92581=CARTESIAN_POINT('Ctrl Pts',(-6.07944246183268,48.400326026367,0.));
#92582=CARTESIAN_POINT('Ctrl Pts',(-6.07944246183268,48.400326026367,20.));
#92583=CARTESIAN_POINT('Ctrl Pts',(-6.04569932102201,48.4014858007534,0.));
#92584=CARTESIAN_POINT('Ctrl Pts',(-6.04569932102201,48.4014858007534,20.));
#92585=CARTESIAN_POINT('Ctrl Pts',(-6.01195650489506,48.4026222762592,0.));
#92586=CARTESIAN_POINT('Ctrl Pts',(-6.01195650489506,48.4026222762592,20.));
#92587=CARTESIAN_POINT('Ctrl Pts',(-5.97821402951549,48.4037354532013,0.));
#92588=CARTESIAN_POINT('Ctrl Pts',(-5.97821402951549,48.4037354532013,20.));
#92589=CARTESIAN_POINT('Ctrl Pts',(-5.94447191094723,48.404825331908,0.));
#92590=CARTESIAN_POINT('Ctrl Pts',(-5.94447191094723,48.404825331908,20.));
#92591=CARTESIAN_POINT('Ctrl Pts',(-5.91073016525427,48.4058919127185,0.));
#92592=CARTESIAN_POINT('Ctrl Pts',(-5.91073016525427,48.4058919127185,20.));
#92593=CARTESIAN_POINT('Ctrl Pts',(-5.87698880850096,48.4069351959835,0.));
#92594=CARTESIAN_POINT('Ctrl Pts',(-5.87698880850096,48.4069351959835,20.));
#92595=CARTESIAN_POINT('Ctrl Pts',(-5.8432478567519,48.4079551820642,0.));
#92596=CARTESIAN_POINT('Ctrl Pts',(-5.8432478567519,48.4079551820642,20.));
#92597=CARTESIAN_POINT('Ctrl Pts',(-5.80950732607179,48.4089518713336,0.));
#92598=CARTESIAN_POINT('Ctrl Pts',(-5.80950732607179,48.4089518713336,20.));
#92599=CARTESIAN_POINT('Ctrl Pts',(-5.77576723252553,48.4099252641753,0.));
#92600=CARTESIAN_POINT('Ctrl Pts',(-5.77576723252553,48.4099252641753,20.));
#92601=CARTESIAN_POINT('Ctrl Pts',(-5.74202759217814,48.4108753609837,0.));
#92602=CARTESIAN_POINT('Ctrl Pts',(-5.74202759217814,48.4108753609837,20.));
#92603=CARTESIAN_POINT('Ctrl Pts',(-5.70828842109461,48.4118021621647,0.));
#92604=CARTESIAN_POINT('Ctrl Pts',(-5.70828842109461,48.4118021621647,20.));
#92605=CARTESIAN_POINT('Ctrl Pts',(-5.67454973534015,48.412705668135,0.));
#92606=CARTESIAN_POINT('Ctrl Pts',(-5.67454973534015,48.412705668135,20.));
#92607=CARTESIAN_POINT('Ctrl Pts',(-5.64081155098006,48.4135858793227,0.));
#92608=CARTESIAN_POINT('Ctrl Pts',(-5.64081155098006,48.4135858793227,20.));
#92609=CARTESIAN_POINT('Ctrl Pts',(-5.60707388407982,48.414442796167,0.));
#92610=CARTESIAN_POINT('Ctrl Pts',(-5.60707388407982,48.414442796167,20.));
#92611=CARTESIAN_POINT('Ctrl Pts',(-5.57333675070493,48.4152764191183,0.));
#92612=CARTESIAN_POINT('Ctrl Pts',(-5.57333675070493,48.4152764191183,20.));
#92613=CARTESIAN_POINT('Ctrl Pts',(-5.53960016692118,48.4160867486381,0.));
#92614=CARTESIAN_POINT('Ctrl Pts',(-5.53960016692118,48.4160867486381,20.));
#92615=CARTESIAN_POINT('Ctrl Pts',(-5.50586414879431,48.4168737851989,0.));
#92616=CARTESIAN_POINT('Ctrl Pts',(-5.50586414879431,48.4168737851989,20.));
#92617=CARTESIAN_POINT('Ctrl Pts',(-5.47212871239031,48.417637529284,0.));
#92618=CARTESIAN_POINT('Ctrl Pts',(-5.47212871239031,48.417637529284,20.));
#92619=CARTESIAN_POINT('Ctrl Pts',(-5.43839387377499,48.4183779813881,0.));
#92620=CARTESIAN_POINT('Ctrl Pts',(-5.43839387377499,48.4183779813881,20.));
#92621=CARTESIAN_POINT('Ctrl Pts',(-5.40465964901426,48.4190951420167,0.));
#92622=CARTESIAN_POINT('Ctrl Pts',(-5.40465964901426,48.4190951420167,20.));
#92623=CARTESIAN_POINT('Ctrl Pts',(-5.37092605417403,48.4197890116867,0.));
#92624=CARTESIAN_POINT('Ctrl Pts',(-5.37092605417403,48.4197890116867,20.));
#92625=CARTESIAN_POINT('Ctrl Pts',(-5.33719310532028,48.4204595909261,0.));
#92626=CARTESIAN_POINT('Ctrl Pts',(-5.33719310532028,48.4204595909261,20.));
#92627=CARTESIAN_POINT('Ctrl Pts',(-5.3034608185191,48.4211068802741,0.));
#92628=CARTESIAN_POINT('Ctrl Pts',(-5.3034608185191,48.4211068802741,20.));
#92629=CARTESIAN_POINT('Ctrl Pts',(-5.26972920983671,48.4217308802807,0.));
#92630=CARTESIAN_POINT('Ctrl Pts',(-5.26972920983671,48.4217308802807,20.));
#92631=CARTESIAN_POINT('Ctrl Pts',(-5.23599829533945,48.4223315915069,0.));
#92632=CARTESIAN_POINT('Ctrl Pts',(-5.23599829533945,48.4223315915069,20.));
#92633=CARTESIAN_POINT('Ctrl Pts',(-5.20226809109352,48.4229090145253,0.));
#92634=CARTESIAN_POINT('Ctrl Pts',(-5.20226809109352,48.4229090145253,20.));
#92635=CARTESIAN_POINT('Ctrl Pts',(-5.16853861316522,48.4234631499193,0.));
#92636=CARTESIAN_POINT('Ctrl Pts',(-5.16853861316522,48.4234631499193,20.));
#92637=CARTESIAN_POINT('Ctrl Pts',(-5.13480987762072,48.4239939982838,0.));
#92638=CARTESIAN_POINT('Ctrl Pts',(-5.13480987762072,48.4239939982838,20.));
#92639=CARTESIAN_POINT('Ctrl Pts',(-5.10108190052608,48.4245015602246,0.));
#92640=CARTESIAN_POINT('Ctrl Pts',(-5.10108190052608,48.4245015602246,20.));
#92641=CARTESIAN_POINT('Ctrl Pts',(-5.06735469794743,48.4249858363582,0.));
#92642=CARTESIAN_POINT('Ctrl Pts',(-5.06735469794743,48.4249858363582,20.));
#92643=CARTESIAN_POINT('Ctrl Pts',(-5.03362828595094,48.4254468273122,0.));
#92644=CARTESIAN_POINT('Ctrl Pts',(-5.03362828595094,48.4254468273122,20.));
#92645=CARTESIAN_POINT('Ctrl Pts',(-4.99990268060293,48.4258845337255,0.));
#92646=CARTESIAN_POINT('Ctrl Pts',(-4.99990268060293,48.4258845337255,20.));
#92647=CARTESIAN_POINT('Ctrl Pts',(-4.96617789796954,48.4262989562483,0.));
#92648=CARTESIAN_POINT('Ctrl Pts',(-4.96617789796954,48.4262989562483,20.));
#92649=CARTESIAN_POINT('Ctrl Pts',(-4.93245395411686,48.4266900955418,0.));
#92650=CARTESIAN_POINT('Ctrl Pts',(-4.93245395411686,48.4266900955418,20.));
#92651=CARTESIAN_POINT('Ctrl Pts',(-4.89873086511077,48.4270579522784,0.));
#92652=CARTESIAN_POINT('Ctrl Pts',(-4.89873086511077,48.4270579522784,20.));
#92653=CARTESIAN_POINT('Ctrl Pts',(-4.86500864701731,48.4274025271416,0.));
#92654=CARTESIAN_POINT('Ctrl Pts',(-4.86500864701731,48.4274025271416,20.));
#92655=CARTESIAN_POINT('Ctrl Pts',(-4.8312873159023,48.4277238208263,0.));
#92656=CARTESIAN_POINT('Ctrl Pts',(-4.8312873159023,48.4277238208263,20.));
#92657=CARTESIAN_POINT('Ctrl Pts',(-4.79756688783169,48.4280218340382,0.));
#92658=CARTESIAN_POINT('Ctrl Pts',(-4.79756688783169,48.4280218340382,20.));
#92659=CARTESIAN_POINT('Ctrl Pts',(-4.76384737887107,48.4282965674942,0.));
#92660=CARTESIAN_POINT('Ctrl Pts',(-4.76384737887107,48.4282965674942,20.));
#92661=CARTESIAN_POINT('Ctrl Pts',(-4.73012880508602,48.4285480219221,0.));
#92662=CARTESIAN_POINT('Ctrl Pts',(-4.73012880508602,48.4285480219221,20.));
#92663=CARTESIAN_POINT('Ctrl Pts',(-4.69641118254227,48.4287761980604,0.));
#92664=CARTESIAN_POINT('Ctrl Pts',(-4.69641118254227,48.4287761980604,20.));
#92665=CARTESIAN_POINT('Ctrl Pts',(-4.66269452730544,48.4289810966589,0.));
#92666=CARTESIAN_POINT('Ctrl Pts',(-4.66269452730544,48.4289810966589,20.));
#92667=CARTESIAN_POINT('Ctrl Pts',(-4.62897885544098,48.4291627184787,0.));
#92668=CARTESIAN_POINT('Ctrl Pts',(-4.62897885544098,48.4291627184787,20.));
#92669=CARTESIAN_POINT('Ctrl Pts',(-4.5952641830141,48.4293210642923,0.));
#92670=CARTESIAN_POINT('Ctrl Pts',(-4.5952641830141,48.4293210642923,20.));
#92671=CARTESIAN_POINT('Ctrl Pts',(-4.56155052608981,48.4294561348833,0.));
#92672=CARTESIAN_POINT('Ctrl Pts',(-4.56155052608981,48.4294561348833,20.));
#92673=CARTESIAN_POINT('Ctrl Pts',(-4.52783790073295,48.4295679310466,0.));
#92674=CARTESIAN_POINT('Ctrl Pts',(-4.52783790073295,48.4295679310466,20.));
#92675=CARTESIAN_POINT('Ctrl Pts',(-4.49412632300816,48.4296564535884,0.));
#92676=CARTESIAN_POINT('Ctrl Pts',(-4.49412632300816,48.4296564535884,20.));
#92677=CARTESIAN_POINT('Ctrl Pts',(-4.46041580898013,48.4297217033257,0.));
#92678=CARTESIAN_POINT('Ctrl Pts',(-4.46041580898013,48.4297217033257,20.));
#92679=CARTESIAN_POINT('Ctrl Pts',(-4.42670637471342,48.4297636810863,0.));
#92680=CARTESIAN_POINT('Ctrl Pts',(-4.42670637471342,48.4297636810863,20.));
#92681=CARTESIAN_POINT('Ctrl Pts',(-4.39299803627247,48.4297823877088,0.));
#92682=CARTESIAN_POINT('Ctrl Pts',(-4.39299803627247,48.4297823877088,20.));
#92683=CARTESIAN_POINT('Ctrl Pts',(-4.35929080972167,48.4297778240431,0.));
#92684=CARTESIAN_POINT('Ctrl Pts',(-4.35929080972167,48.4297778240431,20.));
#92685=CARTESIAN_POINT('Ctrl Pts',(-4.32558471112518,48.42974999095,0.));
#92686=CARTESIAN_POINT('Ctrl Pts',(-4.32558471112518,48.42974999095,20.));
#92687=CARTESIAN_POINT('Ctrl Pts',(-4.29187975654678,48.4296988893018,0.));
#92688=CARTESIAN_POINT('Ctrl Pts',(-4.29187975654678,48.4296988893018,20.));
#92689=CARTESIAN_POINT('Ctrl Pts',(-4.25817596205002,48.4296245199823,0.));
#92690=CARTESIAN_POINT('Ctrl Pts',(-4.25817596205002,48.4296245199823,20.));
#92691=CARTESIAN_POINT('Ctrl Pts',(-4.22447334369802,48.4295268838864,0.));
#92692=CARTESIAN_POINT('Ctrl Pts',(-4.22447334369802,48.4295268838864,20.));
#92693=CARTESIAN_POINT('Ctrl Pts',(-4.19077191755407,48.4294059819202,0.));
#92694=CARTESIAN_POINT('Ctrl Pts',(-4.19077191755407,48.4294059819202,20.));
#92695=CARTESIAN_POINT('Ctrl Pts',(-4.15707169968116,48.4292618150011,0.));
#92696=CARTESIAN_POINT('Ctrl Pts',(-4.15707169968116,48.4292618150011,20.));
#92697=CARTESIAN_POINT('Ctrl Pts',(-4.12337270614212,48.429094384057,0.));
#92698=CARTESIAN_POINT('Ctrl Pts',(-4.12337270614212,48.429094384057,20.));
#92699=CARTESIAN_POINT('Ctrl Pts',(-4.08967495299953,48.4289036900268,0.));
#92700=CARTESIAN_POINT('Ctrl Pts',(-4.08967495299953,48.4289036900268,20.));
#92701=CARTESIAN_POINT('Ctrl Pts',(-4.0559784563157,48.4286897338604,0.));
#92702=CARTESIAN_POINT('Ctrl Pts',(-4.0559784563157,48.4286897338604,20.));
#92703=CARTESIAN_POINT('Ctrl Pts',(-4.02228323215261,48.4284525165189,0.));
#92704=CARTESIAN_POINT('Ctrl Pts',(-4.02228323215261,48.4284525165189,20.));
#92705=CARTESIAN_POINT('Ctrl Pts',(-3.98858929657202,48.4281920389749,0.));
#92706=CARTESIAN_POINT('Ctrl Pts',(-3.98858929657202,48.4281920389749,20.));
#92707=CARTESIAN_POINT('Ctrl Pts',(-3.9548966656355,48.427908302212,0.));
#92708=CARTESIAN_POINT('Ctrl Pts',(-3.9548966656355,48.427908302212,20.));
#92709=CARTESIAN_POINT('Ctrl Pts',(-3.92120535540421,48.4276013072253,0.));
#92710=CARTESIAN_POINT('Ctrl Pts',(-3.92120535540421,48.4276013072253,20.));
#92711=CARTESIAN_POINT('Ctrl Pts',(-3.88751538193921,48.4272710550206,0.));
#92712=CARTESIAN_POINT('Ctrl Pts',(-3.88751538193921,48.4272710550206,20.));
#92713=CARTESIAN_POINT('Ctrl Pts',(-3.85382676130116,48.4269175466151,0.));
#92714=CARTESIAN_POINT('Ctrl Pts',(-3.85382676130116,48.4269175466151,20.));
#92715=CARTESIAN_POINT('Ctrl Pts',(-3.82013950955044,48.4265407830367,0.));
#92716=CARTESIAN_POINT('Ctrl Pts',(-3.82013950955044,48.4265407830367,20.));
#92717=CARTESIAN_POINT('Ctrl Pts',(-3.78645364274707,48.4261407653249,0.));
#92718=CARTESIAN_POINT('Ctrl Pts',(-3.78645364274707,48.4261407653249,20.));
#92719=CARTESIAN_POINT('Ctrl Pts',(-3.75276917695086,48.4257174945299,0.));
#92720=CARTESIAN_POINT('Ctrl Pts',(-3.75276917695086,48.4257174945299,20.));
#92721=CARTESIAN_POINT('Ctrl Pts',(-3.7190861282211,48.4252709717129,0.));
#92722=CARTESIAN_POINT('Ctrl Pts',(-3.7190861282211,48.4252709717129,20.));
#92723=CARTESIAN_POINT('Ctrl Pts',(-3.68540451261697,48.424801197947,0.));
#92724=CARTESIAN_POINT('Ctrl Pts',(-3.68540451261697,48.424801197947,20.));
#92725=CARTESIAN_POINT('Ctrl Pts',(-3.65172434619742,48.4243081743158,0.));
#92726=CARTESIAN_POINT('Ctrl Pts',(-3.65172434619742,48.4243081743158,20.));
#92727=CARTESIAN_POINT('Ctrl Pts',(-3.61804564502098,48.4237919019141,0.));
#92728=CARTESIAN_POINT('Ctrl Pts',(-3.61804564502098,48.4237919019141,20.));
#92729=CARTESIAN_POINT('Ctrl Pts',(-3.58436842514565,48.4232523818483,0.));
#92730=CARTESIAN_POINT('Ctrl Pts',(-3.58436842514565,48.4232523818483,20.));
#92731=CARTESIAN_POINT('Ctrl Pts',(-3.55069270262909,48.4226896152354,0.));
#92732=CARTESIAN_POINT('Ctrl Pts',(-3.55069270262909,48.4226896152354,20.));
#92733=CARTESIAN_POINT('Ctrl Pts',(-3.51701849352855,48.422103603204,0.));
#92734=CARTESIAN_POINT('Ctrl Pts',(-3.51701849352855,48.422103603204,20.));
#92735=CARTESIAN_POINT('Ctrl Pts',(-3.48334581390102,48.4214943468927,0.));
#92736=CARTESIAN_POINT('Ctrl Pts',(-3.48334581390102,48.4214943468927,20.));
#92737=CARTESIAN_POINT('Ctrl Pts',(-3.44967467980324,48.4208618474523,0.));
#92738=CARTESIAN_POINT('Ctrl Pts',(-3.44967467980324,48.4208618474523,20.));
#92739=CARTESIAN_POINT('Ctrl Pts',(-3.4160051072915,48.4202061060442,0.));
#92740=CARTESIAN_POINT('Ctrl Pts',(-3.4160051072915,48.4202061060442,20.));
#92741=CARTESIAN_POINT('Ctrl Pts',(-3.38233711242168,48.4195271238417,0.));
#92742=CARTESIAN_POINT('Ctrl Pts',(-3.38233711242168,48.4195271238417,20.));
#92743=CARTESIAN_POINT('Ctrl Pts',(-3.34867071124919,48.4188249020284,0.));
#92744=CARTESIAN_POINT('Ctrl Pts',(-3.34867071124919,48.4188249020284,20.));
#92745=CARTESIAN_POINT('Ctrl Pts',(-3.31500591982889,48.4180994417999,0.));
#92746=CARTESIAN_POINT('Ctrl Pts',(-3.31500591982889,48.4180994417999,20.));
#92747=CARTESIAN_POINT('Ctrl Pts',(-3.28134275421533,48.4173507443625,0.));
#92748=CARTESIAN_POINT('Ctrl Pts',(-3.28134275421533,48.4173507443625,20.));
#92749=CARTESIAN_POINT('Ctrl Pts',(-3.24768123046267,48.4165788109335,0.));
#92750=CARTESIAN_POINT('Ctrl Pts',(-3.24768123046267,48.4165788109335,20.));
#92751=CARTESIAN_POINT('Ctrl Pts',(-3.21402136462459,48.4157836427414,0.));
#92752=CARTESIAN_POINT('Ctrl Pts',(-3.21402136462459,48.4157836427414,20.));
#92753=CARTESIAN_POINT('Ctrl Pts',(-3.18036317275455,48.4149652410254,0.));
#92754=CARTESIAN_POINT('Ctrl Pts',(-3.18036317275455,48.4149652410254,20.));
#92755=CARTESIAN_POINT('Ctrl Pts',(-3.14670667090557,48.414123607036,0.));
#92756=CARTESIAN_POINT('Ctrl Pts',(-3.14670667090557,48.414123607036,20.));
#92757=CARTESIAN_POINT('Ctrl Pts',(-3.11305187513001,48.4132587420349,0.));
#92758=CARTESIAN_POINT('Ctrl Pts',(-3.11305187513001,48.4132587420349,20.));
#92759=CARTESIAN_POINT('Ctrl Pts',(-3.0793988014797,48.4123706472953,0.));
#92760=CARTESIAN_POINT('Ctrl Pts',(-3.0793988014797,48.4123706472953,20.));
#92761=CARTESIAN_POINT('Ctrl Pts',(-3.04574746600609,48.4114593241014,0.));
#92762=CARTESIAN_POINT('Ctrl Pts',(-3.04574746600609,48.4114593241014,20.));
#92763=CARTESIAN_POINT('Ctrl Pts',(-3.01209788475996,48.4105247737488,0.));
#92764=CARTESIAN_POINT('Ctrl Pts',(-3.01209788475996,48.4105247737488,20.));
#92765=CARTESIAN_POINT('Ctrl Pts',(-2.97845007379182,48.4095669975441,0.));
#92766=CARTESIAN_POINT('Ctrl Pts',(-2.97845007379182,48.4095669975441,20.));
#92767=CARTESIAN_POINT('Ctrl Pts',(-2.94480404915165,48.4085859968048,0.));
#92768=CARTESIAN_POINT('Ctrl Pts',(-2.94480404915165,48.4085859968048,20.));
#92769=CARTESIAN_POINT('Ctrl Pts',(-2.91115982688905,48.4075817728593,0.));
#92770=CARTESIAN_POINT('Ctrl Pts',(-2.91115982688905,48.4075817728593,20.));
#92771=CARTESIAN_POINT('Ctrl Pts',(-2.87751742305295,48.4065543270471,0.));
#92772=CARTESIAN_POINT('Ctrl Pts',(-2.87751742305295,48.4065543270471,20.));
#92773=CARTESIAN_POINT('Ctrl Pts',(-2.84387685369182,48.4055036607195,0.));
#92774=CARTESIAN_POINT('Ctrl Pts',(-2.84387685369182,48.4055036607195,20.));
#92775=CARTESIAN_POINT('Ctrl Pts',(-2.81023813485357,48.4044297752383,0.));
#92776=CARTESIAN_POINT('Ctrl Pts',(-2.81023813485357,48.4044297752383,20.));
#92777=CARTESIAN_POINT('Ctrl Pts',(-2.77660128258548,48.4033326719771,0.));
#92778=CARTESIAN_POINT('Ctrl Pts',(-2.77660128258548,48.4033326719771,20.));
#92779=CARTESIAN_POINT('Ctrl Pts',(-2.74296631293438,48.4022123523201,0.));
#92780=CARTESIAN_POINT('Ctrl Pts',(-2.74296631293438,48.4022123523201,20.));
#92781=CARTESIAN_POINT('Ctrl Pts',(-2.70933324194662,48.4010688176627,0.));
#92782=CARTESIAN_POINT('Ctrl Pts',(-2.70933324194662,48.4010688176627,20.));
#92783=CARTESIAN_POINT('Ctrl Pts',(-2.67570208566795,48.3999020694116,0.));
#92784=CARTESIAN_POINT('Ctrl Pts',(-2.67570208566795,48.3999020694116,20.));
#92785=CARTESIAN_POINT('Ctrl Pts',(-2.64207286014351,48.3987121089844,0.));
#92786=CARTESIAN_POINT('Ctrl Pts',(-2.64207286014351,48.3987121089844,20.));
#92787=CARTESIAN_POINT('Ctrl Pts',(-2.60844558141791,48.3974989378103,0.));
#92788=CARTESIAN_POINT('Ctrl Pts',(-2.60844558141791,48.3974989378103,20.));
#92789=CARTESIAN_POINT('Ctrl Pts',(-2.57482026553517,48.3962625573292,0.));
#92790=CARTESIAN_POINT('Ctrl Pts',(-2.57482026553517,48.3962625573292,20.));
#92791=CARTESIAN_POINT('Ctrl Pts',(-2.54119692853862,48.3950029689925,0.));
#92792=CARTESIAN_POINT('Ctrl Pts',(-2.54119692853862,48.3950029689925,20.));
#92793=CARTESIAN_POINT('Ctrl Pts',(-2.50757558647122,48.3937201742621,0.));
#92794=CARTESIAN_POINT('Ctrl Pts',(-2.50757558647122,48.3937201742621,20.));
#92795=CARTESIAN_POINT('Ctrl Pts',(-2.47395625537496,48.3924141746117,0.));
#92796=CARTESIAN_POINT('Ctrl Pts',(-2.47395625537496,48.3924141746117,20.));
#92797=CARTESIAN_POINT('Ctrl Pts',(-2.44033895129154,48.3910849715258,0.));
#92798=CARTESIAN_POINT('Ctrl Pts',(-2.44033895129154,48.3910849715258,20.));
#92799=CARTESIAN_POINT('Ctrl Pts',(-2.40672369026198,48.3897325665,0.));
#92800=CARTESIAN_POINT('Ctrl Pts',(-2.40672369026198,48.3897325665,20.));
#92801=CARTESIAN_POINT('Ctrl Pts',(-2.37311048832666,48.3883569610415,0.));
#92802=CARTESIAN_POINT('Ctrl Pts',(-2.37311048832666,48.3883569610415,20.));
#92803=CARTESIAN_POINT('Ctrl Pts',(-2.33949936152535,48.3869581566679,0.));
#92804=CARTESIAN_POINT('Ctrl Pts',(-2.33949936152535,48.3869581566679,20.));
#92805=CARTESIAN_POINT('Ctrl Pts',(-2.30589032589701,48.3855361549086,0.));
#92806=CARTESIAN_POINT('Ctrl Pts',(-2.30589032589701,48.3855361549086,20.));
#92807=CARTESIAN_POINT('Ctrl Pts',(-2.2722833974801,48.3840909573039,0.));
#92808=CARTESIAN_POINT('Ctrl Pts',(-2.2722833974801,48.3840909573039,20.));
#92809=CARTESIAN_POINT('Ctrl Pts',(-2.23867859231222,48.3826225654055,0.));
#92810=CARTESIAN_POINT('Ctrl Pts',(-2.23867859231222,48.3826225654055,20.));
#92811=CARTESIAN_POINT('Ctrl Pts',(-2.20507592643043,48.3811309807756,0.));
#92812=CARTESIAN_POINT('Ctrl Pts',(-2.20507592643043,48.3811309807756,20.));
#92813=CARTESIAN_POINT('Ctrl Pts',(-2.17147541587105,48.3796162049883,0.));
#92814=CARTESIAN_POINT('Ctrl Pts',(-2.17147541587105,48.3796162049883,20.));
#92815=CARTESIAN_POINT('Ctrl Pts',(-2.13787707667014,48.3780782396279,0.));
#92816=CARTESIAN_POINT('Ctrl Pts',(-2.13787707667014,48.3780782396279,20.));
#92817=CARTESIAN_POINT('Ctrl Pts',(-2.10428092486295,48.3765170862905,0.));
#92818=CARTESIAN_POINT('Ctrl Pts',(-2.10428092486295,48.3765170862905,20.));
#92819=CARTESIAN_POINT('Ctrl Pts',(-2.07068697648389,48.374932746583,0.));
#92820=CARTESIAN_POINT('Ctrl Pts',(-2.07068697648389,48.374932746583,20.));
#92821=CARTESIAN_POINT('Ctrl Pts',(-2.03709524756656,48.3733252221237,0.));
#92822=CARTESIAN_POINT('Ctrl Pts',(-2.03709524756656,48.3733252221237,20.));
#92823=CARTESIAN_POINT('Ctrl Pts',(-2.00350575414356,48.3716945145424,0.));
#92824=CARTESIAN_POINT('Ctrl Pts',(-2.00350575414356,48.3716945145424,20.));
#92825=CARTESIAN_POINT('Ctrl Pts',(-1.96991851224693,48.3700406254798,0.));
#92826=CARTESIAN_POINT('Ctrl Pts',(-1.96991851224693,48.3700406254798,20.));
#92827=CARTESIAN_POINT('Ctrl Pts',(-1.93633353790814,48.3683635565876,0.));
#92828=CARTESIAN_POINT('Ctrl Pts',(-1.93633353790814,48.3683635565876,20.));
#92829=CARTESIAN_POINT('Ctrl Pts',(-1.90275084715797,48.3666633095284,0.));
#92830=CARTESIAN_POINT('Ctrl Pts',(-1.90275084715797,48.3666633095284,20.));
#92831=CARTESIAN_POINT('Ctrl Pts',(-1.86917045602653,48.3649398859758,0.));
#92832=CARTESIAN_POINT('Ctrl Pts',(-1.86917045602653,48.3649398859758,20.));
#92833=CARTESIAN_POINT('Ctrl Pts',(-1.83559238054324,48.3631932876149,0.));
#92834=CARTESIAN_POINT('Ctrl Pts',(-1.83559238054324,48.3631932876149,20.));
#92835=CARTESIAN_POINT('Ctrl Pts',(-1.80201663673657,48.3614235161422,0.));
#92836=CARTESIAN_POINT('Ctrl Pts',(-1.80201663673657,48.3614235161422,20.));
#92837=CARTESIAN_POINT('Ctrl Pts',(-1.76844324063427,48.3596305732653,0.));
#92838=CARTESIAN_POINT('Ctrl Pts',(-1.76844324063427,48.3596305732653,20.));
#92839=CARTESIAN_POINT('Ctrl Pts',(-1.73487220826327,48.357814460703,0.));
#92840=CARTESIAN_POINT('Ctrl Pts',(-1.73487220826327,48.357814460703,20.));
#92841=CARTESIAN_POINT('Ctrl Pts',(-1.70130355564958,48.3559751801849,0.));
#92842=CARTESIAN_POINT('Ctrl Pts',(-1.70130355564958,48.3559751801849,20.));
#92843=CARTESIAN_POINT('Ctrl Pts',(-1.66773729881857,48.3541127334515,0.));
#92844=CARTESIAN_POINT('Ctrl Pts',(-1.66773729881857,48.3541127334515,20.));
#92845=CARTESIAN_POINT('Ctrl Pts',(-1.63417345379483,48.3522271222546,0.));
#92846=CARTESIAN_POINT('Ctrl Pts',(-1.63417345379483,48.3522271222546,20.));
#92847=CARTESIAN_POINT('Ctrl Pts',(-1.60061203660208,48.350318348357,0.));
#92848=CARTESIAN_POINT('Ctrl Pts',(-1.60061203660208,48.350318348357,20.));
#92849=CARTESIAN_POINT('Ctrl Pts',(-1.56705306326333,48.3483864135332,0.));
#92850=CARTESIAN_POINT('Ctrl Pts',(-1.56705306326333,48.3483864135332,20.));
#92851=CARTESIAN_POINT('Ctrl Pts',(-1.53349654980078,48.3464313195685,0.));
#92852=CARTESIAN_POINT('Ctrl Pts',(-1.53349654980078,48.3464313195685,20.));
#92853=CARTESIAN_POINT('Ctrl Pts',(-1.49994251223572,48.3444530682597,0.));
#92854=CARTESIAN_POINT('Ctrl Pts',(-1.49994251223572,48.3444530682597,20.));
#92855=CARTESIAN_POINT('Ctrl Pts',(-1.46639096658853,48.3424516614145,0.));
#92856=CARTESIAN_POINT('Ctrl Pts',(-1.46639096658853,48.3424516614145,20.));
#92857=CARTESIAN_POINT('Ctrl Pts',(-1.4328419288788,48.3404271008519,0.));
#92858=CARTESIAN_POINT('Ctrl Pts',(-1.4328419288788,48.3404271008519,20.));
#92859=CARTESIAN_POINT('Ctrl Pts',(-1.39929541512521,48.3383793884017,0.));
#92860=CARTESIAN_POINT('Ctrl Pts',(-1.39929541512521,48.3383793884017,20.));
#92861=CARTESIAN_POINT('Ctrl Pts',(-1.36575144134572,48.336308525905,0.));
#92862=CARTESIAN_POINT('Ctrl Pts',(-1.36575144134572,48.336308525905,20.));
#92863=CARTESIAN_POINT('Ctrl Pts',(-1.33221002355744,48.3342145152137,0.));
#92864=CARTESIAN_POINT('Ctrl Pts',(-1.33221002355744,48.3342145152137,20.));
#92865=CARTESIAN_POINT('Ctrl Pts',(-1.29867117777653,48.3320973581913,0.));
#92866=CARTESIAN_POINT('Ctrl Pts',(-1.29867117777653,48.3320973581913,20.));
#92867=CARTESIAN_POINT('Ctrl Pts',(-1.26513492001823,48.3299570567123,0.));
#92868=CARTESIAN_POINT('Ctrl Pts',(-1.26513492001823,48.3299570567123,20.));
#92869=CARTESIAN_POINT('Ctrl Pts',(-1.23160126629694,48.3277936126623,0.));
#92870=CARTESIAN_POINT('Ctrl Pts',(-1.23160126629694,48.3277936126623,20.));
#92871=CARTESIAN_POINT('Ctrl Pts',(-1.19807023262612,48.3256070279384,0.));
#92872=CARTESIAN_POINT('Ctrl Pts',(-1.19807023262612,48.3256070279384,20.));
#92873=CARTESIAN_POINT('Ctrl Pts',(-1.1645418350184,48.3233973044482,0.));
#92874=CARTESIAN_POINT('Ctrl Pts',(-1.1645418350184,48.3233973044482,20.));
#92875=CARTESIAN_POINT('Ctrl Pts',(-1.13101608948536,48.3211644441107,0.));
#92876=CARTESIAN_POINT('Ctrl Pts',(-1.13101608948536,48.3211644441107,20.));
#92877=CARTESIAN_POINT('Ctrl Pts',(-1.09749301203764,48.3189084488565,0.));
#92878=CARTESIAN_POINT('Ctrl Pts',(-1.09749301203764,48.3189084488565,20.));
#92879=CARTESIAN_POINT('Ctrl Pts',(-1.06397261868501,48.3166293206271,0.));
#92880=CARTESIAN_POINT('Ctrl Pts',(-1.06397261868501,48.3166293206271,20.));
#92881=CARTESIAN_POINT('Ctrl Pts',(-1.03045492543642,48.3143270613748,0.));
#92882=CARTESIAN_POINT('Ctrl Pts',(-1.03045492543642,48.3143270613748,20.));
#92883=CARTESIAN_POINT('Ctrl Pts',(-0.996939948299871,48.312001673063,0.));
#92884=CARTESIAN_POINT('Ctrl Pts',(-0.996939948299871,48.312001673063,20.));
#92885=CARTESIAN_POINT('Ctrl Pts',(-0.963427703282371,48.3096531576664,
0.));
#92886=CARTESIAN_POINT('Ctrl Pts',(-0.963427703282371,48.3096531576664,
20.));
#92887=CARTESIAN_POINT('Ctrl Pts',(-0.929918206389844,48.3072815171712,
0.));
#92888=CARTESIAN_POINT('Ctrl Pts',(-0.929918206389844,48.3072815171712,
20.));
#92889=CARTESIAN_POINT('Ctrl Pts',(-0.896411473627245,48.3048867535745,
0.));
#92890=CARTESIAN_POINT('Ctrl Pts',(-0.896411473627245,48.3048867535745,
20.));
#92891=CARTESIAN_POINT('Ctrl Pts',(-0.862907520998508,48.3024688688845,
0.));
#92892=CARTESIAN_POINT('Ctrl Pts',(-0.862907520998508,48.3024688688845,
20.));
#92893=CARTESIAN_POINT('Ctrl Pts',(-0.829406364506684,48.3000278651208,
0.));
#92894=CARTESIAN_POINT('Ctrl Pts',(-0.829406364506684,48.3000278651208,
20.));
#92895=CARTESIAN_POINT('Ctrl Pts',(-0.79590802015391,48.2975637443136,0.));
#92896=CARTESIAN_POINT('Ctrl Pts',(-0.79590802015391,48.2975637443136,20.));
#92897=CARTESIAN_POINT('Ctrl Pts',(-0.762412503941543,48.2950765085043,
0.));
#92898=CARTESIAN_POINT('Ctrl Pts',(-0.762412503941543,48.2950765085043,
20.));
#92899=CARTESIAN_POINT('Ctrl Pts',(-0.728919831869663,48.2925661597457,
0.));
#92900=CARTESIAN_POINT('Ctrl Pts',(-0.728919831869663,48.2925661597457,
20.));
#92901=CARTESIAN_POINT('Ctrl Pts',(-0.695430019937358,48.2900327001016,
0.));
#92902=CARTESIAN_POINT('Ctrl Pts',(-0.695430019937358,48.2900327001016,
20.));
#92903=CARTESIAN_POINT('Ctrl Pts',(-0.66194308414246,48.2874761316474,0.));
#92904=CARTESIAN_POINT('Ctrl Pts',(-0.66194308414246,48.2874761316474,20.));
#92905=CARTESIAN_POINT('Ctrl Pts',(-0.628459040481846,48.2848964564694,
0.));
#92906=CARTESIAN_POINT('Ctrl Pts',(-0.628459040481846,48.2848964564694,
20.));
#92907=CARTESIAN_POINT('Ctrl Pts',(-0.594977904951284,48.282293676665,0.));
#92908=CARTESIAN_POINT('Ctrl Pts',(-0.594977904951284,48.282293676665,20.));
#92909=CARTESIAN_POINT('Ctrl Pts',(-0.561499693545691,48.2796677943426,
0.));
#92910=CARTESIAN_POINT('Ctrl Pts',(-0.561499693545691,48.2796677943426,
20.));
#92911=CARTESIAN_POINT('Ctrl Pts',(-0.528024422259037,48.2770188116216,
0.));
#92912=CARTESIAN_POINT('Ctrl Pts',(-0.528024422259037,48.2770188116216,
20.));
#92913=CARTESIAN_POINT('Ctrl Pts',(-0.494552107084227,48.2743467306329,
0.));
#92914=CARTESIAN_POINT('Ctrl Pts',(-0.494552107084227,48.2743467306329,
20.));
#92915=CARTESIAN_POINT('Ctrl Pts',(-0.461082764013003,48.2716515535183,
0.));
#92916=CARTESIAN_POINT('Ctrl Pts',(-0.461082764013003,48.2716515535183,
20.));
#92917=CARTESIAN_POINT('Ctrl Pts',(-0.427616409036058,48.2689332824309,
0.));
#92918=CARTESIAN_POINT('Ctrl Pts',(-0.427616409036058,48.2689332824309,
20.));
#92919=CARTESIAN_POINT('Ctrl Pts',(-0.394153058142925,48.2661919195348,
0.));
#92920=CARTESIAN_POINT('Ctrl Pts',(-0.394153058142925,48.2661919195348,
20.));
#92921=CARTESIAN_POINT('Ctrl Pts',(-0.360692727322003,48.2634274670053,
0.));
#92922=CARTESIAN_POINT('Ctrl Pts',(-0.360692727322003,48.2634274670053,
20.));
#92923=CARTESIAN_POINT('Ctrl Pts',(-0.327235432560555,48.2606399270286,
0.));
#92924=CARTESIAN_POINT('Ctrl Pts',(-0.327235432560555,48.2606399270286,
20.));
#92925=CARTESIAN_POINT('Ctrl Pts',(-0.293781189844835,48.2578293018028,
0.));
#92926=CARTESIAN_POINT('Ctrl Pts',(-0.293781189844835,48.2578293018028,
20.));
#92927=CARTESIAN_POINT('Ctrl Pts',(-0.260330015159953,48.2549955935366,
0.));
#92928=CARTESIAN_POINT('Ctrl Pts',(-0.260330015159953,48.2549955935366,
20.));
#92929=CARTESIAN_POINT('Ctrl Pts',(-0.22688192448987,48.2521388044499,0.));
#92930=CARTESIAN_POINT('Ctrl Pts',(-0.22688192448987,48.2521388044499,20.));
#92931=CARTESIAN_POINT('Ctrl Pts',(-0.193436933817472,48.2492589367737,
0.));
#92932=CARTESIAN_POINT('Ctrl Pts',(-0.193436933817472,48.2492589367737,
20.));
#92933=CARTESIAN_POINT('Ctrl Pts',(-0.159995059124576,48.2463559927498,
0.));
#92934=CARTESIAN_POINT('Ctrl Pts',(-0.159995059124576,48.2463559927498,
20.));
#92935=CARTESIAN_POINT('Ctrl Pts',(-0.126556316391682,48.2434299746318,
0.));
#92936=CARTESIAN_POINT('Ctrl Pts',(-0.126556316391682,48.2434299746318,
20.));
#92937=CARTESIAN_POINT('Ctrl Pts',(-0.0931207215982832,48.2404808846839,
0.));
#92938=CARTESIAN_POINT('Ctrl Pts',(-0.0931207215982832,48.2404808846839,
20.));
#92939=CARTESIAN_POINT('Ctrl Pts',(-0.0596882907225993,48.2375087251817,
0.));
#92940=CARTESIAN_POINT('Ctrl Pts',(-0.0596882907225993,48.2375087251817,
20.));
#92941=CARTESIAN_POINT('Ctrl Pts',(-0.0262590397416762,48.234513498412,
0.));
#92942=CARTESIAN_POINT('Ctrl Pts',(-0.0262590397416762,48.234513498412,
20.));
#92943=CARTESIAN_POINT('Ctrl Pts',(0.00716701536856768,48.2314952066725,
0.));
#92944=CARTESIAN_POINT('Ctrl Pts',(0.00716701536856768,48.2314952066725,
20.));
#92945=CARTESIAN_POINT('Ctrl Pts',(0.0405898586334352,48.2284538522724,
0.));
#92946=CARTESIAN_POINT('Ctrl Pts',(0.0405898586334352,48.2284538522724,
20.));
#92947=CARTESIAN_POINT('Ctrl Pts',(0.0740094740793884,48.2253894375317,
0.));
#92948=CARTESIAN_POINT('Ctrl Pts',(0.0740094740793884,48.2253894375317,
20.));
#92949=CARTESIAN_POINT('Ctrl Pts',(0.107425845734119,48.2223019647818,0.));
#92950=CARTESIAN_POINT('Ctrl Pts',(0.107425845734119,48.2223019647818,20.));
#92951=CARTESIAN_POINT('Ctrl Pts',(0.140838957626541,48.2191914363652,0.));
#92952=CARTESIAN_POINT('Ctrl Pts',(0.140838957626541,48.2191914363652,20.));
#92953=CARTESIAN_POINT('Ctrl Pts',(0.174248793786895,48.2160578546352,0.));
#92954=CARTESIAN_POINT('Ctrl Pts',(0.174248793786895,48.2160578546352,20.));
#92955=CARTESIAN_POINT('Ctrl Pts',(0.207655338246555,48.2129012219564,0.));
#92956=CARTESIAN_POINT('Ctrl Pts',(0.207655338246555,48.2129012219564,20.));
#92957=CARTESIAN_POINT('Ctrl Pts',(0.241058575037867,48.2097215407045,0.));
#92958=CARTESIAN_POINT('Ctrl Pts',(0.241058575037867,48.2097215407045,20.));
#92959=CARTESIAN_POINT('Ctrl Pts',(0.274458488194584,48.2065188132665,0.));
#92960=CARTESIAN_POINT('Ctrl Pts',(0.274458488194584,48.2065188132665,20.));
#92961=CARTESIAN_POINT('Ctrl Pts',(0.30785506175171,48.2032930420408,0.));
#92962=CARTESIAN_POINT('Ctrl Pts',(0.30785506175171,48.2032930420408,20.));
#92963=CARTESIAN_POINT('Ctrl Pts',(0.341248279745643,48.2000442294364,0.));
#92964=CARTESIAN_POINT('Ctrl Pts',(0.341248279745643,48.2000442294364,20.));
#92965=CARTESIAN_POINT('Ctrl Pts',(0.374638126214095,48.1967723778737,0.));
#92966=CARTESIAN_POINT('Ctrl Pts',(0.374638126214095,48.1967723778737,20.));
#92967=CARTESIAN_POINT('Ctrl Pts',(0.408024585196225,48.1934774897842,0.));
#92968=CARTESIAN_POINT('Ctrl Pts',(0.408024585196225,48.1934774897842,20.));
#92969=CARTESIAN_POINT('Ctrl Pts',(0.441407640732092,48.1901595676102,0.));
#92970=CARTESIAN_POINT('Ctrl Pts',(0.441407640732092,48.1901595676102,20.));
#92971=CARTESIAN_POINT('Ctrl Pts',(0.474787276863071,48.1868186138054,0.));
#92972=CARTESIAN_POINT('Ctrl Pts',(0.474787276863071,48.1868186138054,20.));
#92973=CARTESIAN_POINT('Ctrl Pts',(0.508163477631851,48.1834546308352,0.));
#92974=CARTESIAN_POINT('Ctrl Pts',(0.508163477631851,48.1834546308352,20.));
#92975=CARTESIAN_POINT('Ctrl Pts',(0.541536227082355,48.1800676211754,0.));
#92976=CARTESIAN_POINT('Ctrl Pts',(0.541536227082355,48.1800676211754,20.));
#92977=CARTESIAN_POINT('Ctrl Pts',(0.574905509259889,48.1766575873132,0.));
#92978=CARTESIAN_POINT('Ctrl Pts',(0.574905509259889,48.1766575873132,20.));
#92979=CARTESIAN_POINT('Ctrl Pts',(0.608271308211097,48.1732245317468,0.));
#92980=CARTESIAN_POINT('Ctrl Pts',(0.608271308211097,48.1732245317468,20.));
#92981=CARTESIAN_POINT('Ctrl Pts',(0.6416336079841,48.1697684569855,0.));
#92982=CARTESIAN_POINT('Ctrl Pts',(0.6416336079841,48.1697684569855,20.));
#92983=CARTESIAN_POINT('Ctrl Pts',(0.674992392628235,48.16628936555,0.));
#92984=CARTESIAN_POINT('Ctrl Pts',(0.674992392628235,48.16628936555,20.));
#92985=CARTESIAN_POINT('Ctrl Pts',(0.708347646194278,48.1627872599717,0.));
#92986=CARTESIAN_POINT('Ctrl Pts',(0.708347646194278,48.1627872599717,20.));
#92987=CARTESIAN_POINT('Ctrl Pts',(0.741699352734257,48.1592621427937,0.));
#92988=CARTESIAN_POINT('Ctrl Pts',(0.741699352734257,48.1592621427937,20.));
#92989=CARTESIAN_POINT('Ctrl Pts',(0.775047496301533,48.1557140165701,0.));
#92990=CARTESIAN_POINT('Ctrl Pts',(0.775047496301533,48.1557140165701,20.));
#92991=CARTESIAN_POINT('Ctrl Pts',(0.808392060950864,48.1521428838659,0.));
#92992=CARTESIAN_POINT('Ctrl Pts',(0.808392060950864,48.1521428838659,20.));
#92993=CARTESIAN_POINT('Ctrl Pts',(0.841733030738387,48.1485487472572,0.));
#92994=CARTESIAN_POINT('Ctrl Pts',(0.841733030738387,48.1485487472572,20.));
#92995=CARTESIAN_POINT('Ctrl Pts',(0.875070389721522,48.144931609331,0.));
#92996=CARTESIAN_POINT('Ctrl Pts',(0.875070389721522,48.144931609331,20.));
#92997=CARTESIAN_POINT('Ctrl Pts',(0.908404121959285,48.1412914726861,0.));
#92998=CARTESIAN_POINT('Ctrl Pts',(0.908404121959285,48.1412914726861,20.));
#92999=CARTESIAN_POINT('Ctrl Pts',(0.941734211511944,48.137628339932,0.));
#93000=CARTESIAN_POINT('Ctrl Pts',(0.941734211511944,48.137628339932,20.));
#93001=CARTESIAN_POINT('Ctrl Pts',(0.975060642441243,48.1339422136897,0.));
#93002=CARTESIAN_POINT('Ctrl Pts',(0.975060642441243,48.1339422136897,20.));
#93003=CARTESIAN_POINT('Ctrl Pts',(1.00838339881032,48.130233096591,0.));
#93004=CARTESIAN_POINT('Ctrl Pts',(1.00838339881032,48.130233096591,20.));
#93005=CARTESIAN_POINT('Ctrl Pts',(1.04170246468365,48.1265009912787,0.));
#93006=CARTESIAN_POINT('Ctrl Pts',(1.04170246468365,48.1265009912787,20.));
#93007=CARTESIAN_POINT('Ctrl Pts',(1.07501782412728,48.1227459004068,0.));
#93008=CARTESIAN_POINT('Ctrl Pts',(1.07501782412728,48.1227459004068,20.));
#93009=CARTESIAN_POINT('Ctrl Pts',(1.10832946120861,48.1189678266406,0.));
#93010=CARTESIAN_POINT('Ctrl Pts',(1.10832946120861,48.1189678266406,20.));
#93011=CARTESIAN_POINT('Ctrl Pts',(1.14163735999657,48.1151667726565,0.));
#93012=CARTESIAN_POINT('Ctrl Pts',(1.14163735999657,48.1151667726565,20.));
#93013=CARTESIAN_POINT('Ctrl Pts',(1.17494150456145,48.111342741142,0.));
#93014=CARTESIAN_POINT('Ctrl Pts',(1.17494150456145,48.111342741142,20.));
#93015=CARTESIAN_POINT('Ctrl Pts',(1.20824187897489,48.1074957347955,0.));
#93016=CARTESIAN_POINT('Ctrl Pts',(1.20824187897489,48.1074957347955,20.));
#93017=CARTESIAN_POINT('Ctrl Pts',(1.24153846731022,48.1036257563271,0.));
#93018=CARTESIAN_POINT('Ctrl Pts',(1.24153846731022,48.1036257563271,20.));
#93019=CARTESIAN_POINT('Ctrl Pts',(1.27483125364215,48.0997328084577,0.));
#93020=CARTESIAN_POINT('Ctrl Pts',(1.27483125364215,48.0997328084577,20.));
#93021=CARTESIAN_POINT('Ctrl Pts',(1.30812022204704,48.0958168939195,0.));
#93022=CARTESIAN_POINT('Ctrl Pts',(1.30812022204704,48.0958168939195,20.));
#93023=CARTESIAN_POINT('Ctrl Pts',(1.3414053566026,48.0918780154556,0.));
#93024=CARTESIAN_POINT('Ctrl Pts',(1.3414053566026,48.0918780154556,20.));
#93025=CARTESIAN_POINT('Ctrl Pts',(1.37468664138801,48.0879161758201,0.));
#93026=CARTESIAN_POINT('Ctrl Pts',(1.37468664138801,48.0879161758201,20.));
#93027=CARTESIAN_POINT('Ctrl Pts',(1.40796406048387,48.0839313777781,0.));
#93028=CARTESIAN_POINT('Ctrl Pts',(1.40796406048387,48.0839313777781,20.));
#93029=CARTESIAN_POINT('Ctrl Pts',(1.44123759797224,48.0799236241059,0.));
#93030=CARTESIAN_POINT('Ctrl Pts',(1.44123759797224,48.0799236241059,20.));
#93031=CARTESIAN_POINT('Ctrl Pts',(1.47450723793681,48.0758929175908,0.));
#93032=CARTESIAN_POINT('Ctrl Pts',(1.47450723793681,48.0758929175908,20.));
#93033=CARTESIAN_POINT('Ctrl Pts',(1.50777296446291,48.071839261032,0.));
#93034=CARTESIAN_POINT('Ctrl Pts',(1.50777296446291,48.071839261032,20.));
#93035=CARTESIAN_POINT('Ctrl Pts',(1.54103476163743,48.0677626572394,0.));
#93036=CARTESIAN_POINT('Ctrl Pts',(1.54103476163743,48.0677626572394,20.));
#93037=CARTESIAN_POINT('Ctrl Pts',(1.57429261354889,48.0636631090342,0.));
#93038=CARTESIAN_POINT('Ctrl Pts',(1.57429261354889,48.0636631090342,20.));
#93039=CARTESIAN_POINT('Ctrl Pts',(1.60754650428745,48.0595406192492,0.));
#93040=CARTESIAN_POINT('Ctrl Pts',(1.60754650428745,48.0595406192492,20.));
#93041=CARTESIAN_POINT('Ctrl Pts',(1.64079641794461,48.0553951907273,0.));
#93042=CARTESIAN_POINT('Ctrl Pts',(1.64079641794461,48.0553951907273,20.));
#93043=CARTESIAN_POINT('Ctrl Pts',(1.67404233861337,48.0512268263229,0.));
#93044=CARTESIAN_POINT('Ctrl Pts',(1.67404233861337,48.0512268263229,20.));
#93045=CARTESIAN_POINT('Ctrl Pts',(1.70728425038804,48.0470355289011,0.));
#93046=CARTESIAN_POINT('Ctrl Pts',(1.70728425038804,48.0470355289011,20.));
#93047=CARTESIAN_POINT('Ctrl Pts',(1.74052213736471,48.0428213013379,0.));
#93048=CARTESIAN_POINT('Ctrl Pts',(1.74052213736471,48.0428213013379,20.));
#93049=CARTESIAN_POINT('Ctrl Pts',(1.77375598364109,48.038584146521,0.));
#93050=CARTESIAN_POINT('Ctrl Pts',(1.77375598364109,48.038584146521,20.));
#93051=CARTESIAN_POINT('Ctrl Pts',(1.80698577331663,48.0343240673492,0.));
#93052=CARTESIAN_POINT('Ctrl Pts',(1.80698577331663,48.0343240673492,20.));
#93053=CARTESIAN_POINT('Ctrl Pts',(1.84021149049245,48.0300410667328,0.));
#93054=CARTESIAN_POINT('Ctrl Pts',(1.84021149049245,48.0300410667328,20.));
#93055=CARTESIAN_POINT('Ctrl Pts',(1.87343311927141,48.0257351475934,0.));
#93056=CARTESIAN_POINT('Ctrl Pts',(1.87343311927141,48.0257351475934,20.));
#93057=CARTESIAN_POINT('Ctrl Pts',(1.90665064375786,48.0214063128629,0.));
#93058=CARTESIAN_POINT('Ctrl Pts',(1.90665064375786,48.0214063128629,20.));
#93059=CARTESIAN_POINT('Ctrl Pts',(1.93986404805772,48.0170545654849,0.));
#93060=CARTESIAN_POINT('Ctrl Pts',(1.93986404805772,48.0170545654849,20.));
#93061=CARTESIAN_POINT('Ctrl Pts',(1.97307331627849,48.0126799084137,0.));
#93062=CARTESIAN_POINT('Ctrl Pts',(1.97307331627849,48.0126799084137,20.));
#93063=CARTESIAN_POINT('Ctrl Pts',(2.00627843252925,48.0082823446147,0.));
#93064=CARTESIAN_POINT('Ctrl Pts',(2.00627843252925,48.0082823446147,20.));
#93065=CARTESIAN_POINT('Ctrl Pts',(2.03947938092067,48.0038618770642,0.));
#93066=CARTESIAN_POINT('Ctrl Pts',(2.03947938092067,48.0038618770642,20.));
#93067=CARTESIAN_POINT('Ctrl Pts',(2.07267614556536,47.9994185087499,0.));
#93068=CARTESIAN_POINT('Ctrl Pts',(2.07267614556536,47.9994185087499,20.));
#93069=CARTESIAN_POINT('Ctrl Pts',(2.10586871057748,47.994952242671,0.));
#93070=CARTESIAN_POINT('Ctrl Pts',(2.10586871057748,47.994952242671,20.));
#93071=CARTESIAN_POINT('Ctrl Pts',(2.13905706007285,47.9904630818375,0.));
#93072=CARTESIAN_POINT('Ctrl Pts',(2.13905706007285,47.9904630818375,20.));
#93073=CARTESIAN_POINT('Ctrl Pts',(2.17224117816898,47.9859510292704,0.));
#93074=CARTESIAN_POINT('Ctrl Pts',(2.17224117816898,47.9859510292704,20.));
#93075=CARTESIAN_POINT('Ctrl Pts',(2.2054210489852,47.9814160880019,0.));
#93076=CARTESIAN_POINT('Ctrl Pts',(2.2054210489852,47.9814160880019,20.));
#93077=CARTESIAN_POINT('Ctrl Pts',(2.23859665664239,47.9768582610752,0.));
#93078=CARTESIAN_POINT('Ctrl Pts',(2.23859665664239,47.9768582610752,20.));
#93079=CARTESIAN_POINT('Ctrl Pts',(2.27176798526352,47.9722775515452,0.));
#93080=CARTESIAN_POINT('Ctrl Pts',(2.27176798526352,47.9722775515452,20.));
#93081=CARTESIAN_POINT('Ctrl Pts',(2.30493501897294,47.9676739624772,0.));
#93082=CARTESIAN_POINT('Ctrl Pts',(2.30493501897294,47.9676739624772,20.));
#93083=CARTESIAN_POINT('Ctrl Pts',(2.33809774189657,47.9630474969481,0.));
#93084=CARTESIAN_POINT('Ctrl Pts',(2.33809774189657,47.9630474969481,20.));
#93085=CARTESIAN_POINT('Ctrl Pts',(2.3712561381623,47.9583981580454,0.));
#93086=CARTESIAN_POINT('Ctrl Pts',(2.3712561381623,47.9583981580454,20.));
#93087=CARTESIAN_POINT('Ctrl Pts',(2.40441019189959,47.9537259488681,0.));
#93088=CARTESIAN_POINT('Ctrl Pts',(2.40441019189959,47.9537259488681,20.));
#93089=CARTESIAN_POINT('Ctrl Pts',(2.43755988723965,47.9490308725257,0.));
#93090=CARTESIAN_POINT('Ctrl Pts',(2.43755988723965,47.9490308725257,20.));
#93091=CARTESIAN_POINT('Ctrl Pts',(2.47070520831548,47.9443129321394,0.));
#93092=CARTESIAN_POINT('Ctrl Pts',(2.47070520831548,47.9443129321394,20.));
#93093=CARTESIAN_POINT('Ctrl Pts',(2.50384613926209,47.9395721308414,0.));
#93094=CARTESIAN_POINT('Ctrl Pts',(2.50384613926209,47.9395721308414,20.));
#93095=CARTESIAN_POINT('Ctrl Pts',(2.53698266421613,47.9348084717752,0.));
#93096=CARTESIAN_POINT('Ctrl Pts',(2.53698266421613,47.9348084717752,20.));
#93097=CARTESIAN_POINT('Ctrl Pts',(2.57011476731622,47.9300219580955,0.));
#93098=CARTESIAN_POINT('Ctrl Pts',(2.57011476731622,47.9300219580955,20.));
#93099=CARTESIAN_POINT('Ctrl Pts',(2.60324243270257,47.9252125929679,0.));
#93100=CARTESIAN_POINT('Ctrl Pts',(2.60324243270257,47.9252125929679,20.));
#93101=CARTESIAN_POINT('Ctrl Pts',(2.63636564451718,47.9203803795688,0.));
#93102=CARTESIAN_POINT('Ctrl Pts',(2.63636564451718,47.9203803795688,20.));
#93103=CARTESIAN_POINT('Ctrl Pts',(2.66948438690365,47.9155253210858,0.));
#93104=CARTESIAN_POINT('Ctrl Pts',(2.66948438690365,47.9155253210858,20.));
#93105=CARTESIAN_POINT('Ctrl Pts',(2.70259864400757,47.9106474207177,0.));
#93106=CARTESIAN_POINT('Ctrl Pts',(2.70259864400757,47.9106474207177,20.));
#93107=CARTESIAN_POINT('Ctrl Pts',(2.73570839997628,47.9057466816743,0.));
#93108=CARTESIAN_POINT('Ctrl Pts',(2.73570839997628,47.9057466816743,20.));
#93109=CARTESIAN_POINT('Ctrl Pts',(2.76881363895917,47.9008231071768,0.));
#93110=CARTESIAN_POINT('Ctrl Pts',(2.76881363895917,47.9008231071768,20.));
#93111=CARTESIAN_POINT('Ctrl Pts',(2.80191434510733,47.8958767004573,0.));
#93112=CARTESIAN_POINT('Ctrl Pts',(2.80191434510733,47.8958767004573,20.));
#93113=CARTESIAN_POINT('Ctrl Pts',(2.83501050257375,47.8909074647592,0.));
#93114=CARTESIAN_POINT('Ctrl Pts',(2.83501050257375,47.8909074647592,20.));
#93115=CARTESIAN_POINT('Ctrl Pts',(2.86810209551307,47.8859154033363,0.));
#93116=CARTESIAN_POINT('Ctrl Pts',(2.86810209551307,47.8859154033363,20.));
#93117=CARTESIAN_POINT('Ctrl Pts',(2.90118910808199,47.8809005194543,0.));
#93118=CARTESIAN_POINT('Ctrl Pts',(2.90118910808199,47.8809005194543,20.));
#93119=CARTESIAN_POINT('Ctrl Pts',(2.93427152443917,47.8758628163901,0.));
#93120=CARTESIAN_POINT('Ctrl Pts',(2.93427152443917,47.8758628163901,20.));
#93121=CARTESIAN_POINT('Ctrl Pts',(2.96734932874504,47.8708022974315,0.));
#93122=CARTESIAN_POINT('Ctrl Pts',(2.96734932874504,47.8708022974315,20.));
#93123=CARTESIAN_POINT('Ctrl Pts',(3.00042250516192,47.8657189658771,0.));
#93124=CARTESIAN_POINT('Ctrl Pts',(3.00042250516192,47.8657189658771,20.));
#93125=CARTESIAN_POINT('Ctrl Pts',(3.03349103785388,47.8606128250365,0.));
#93126=CARTESIAN_POINT('Ctrl Pts',(3.03349103785388,47.8606128250365,20.));
#93127=CARTESIAN_POINT('Ctrl Pts',(3.06655491098681,47.8554838782302,0.));
#93128=CARTESIAN_POINT('Ctrl Pts',(3.06655491098681,47.8554838782302,20.));
#93129=CARTESIAN_POINT('Ctrl Pts',(3.09961410872875,47.8503321287903,0.));
#93130=CARTESIAN_POINT('Ctrl Pts',(3.09961410872875,47.8503321287903,20.));
#93131=CARTESIAN_POINT('Ctrl Pts',(3.13266861524953,47.8451575800601,0.));
#93132=CARTESIAN_POINT('Ctrl Pts',(3.13266861524953,47.8451575800601,20.));
#93133=CARTESIAN_POINT('Ctrl Pts',(3.16571841472089,47.8399602353939,0.));
#93134=CARTESIAN_POINT('Ctrl Pts',(3.16571841472089,47.8399602353939,20.));
#93135=CARTESIAN_POINT('Ctrl Pts',(3.19876349131674,47.834740098157,0.));
#93136=CARTESIAN_POINT('Ctrl Pts',(3.19876349131674,47.834740098157,20.));
#93137=CARTESIAN_POINT('Ctrl Pts',(3.23180382921272,47.829497171726,0.));
#93138=CARTESIAN_POINT('Ctrl Pts',(3.23180382921272,47.829497171726,20.));
#93139=CARTESIAN_POINT('Ctrl Pts',(3.26483941258676,47.8242314594881,0.));
#93140=CARTESIAN_POINT('Ctrl Pts',(3.26483941258676,47.8242314594881,20.));
#93141=CARTESIAN_POINT('Ctrl Pts',(3.29787022561835,47.818942964842,0.));
#93142=CARTESIAN_POINT('Ctrl Pts',(3.29787022561835,47.818942964842,20.));
#93143=CARTESIAN_POINT('Ctrl Pts',(3.33089625248902,47.813631691197,0.));
#93144=CARTESIAN_POINT('Ctrl Pts',(3.33089625248902,47.813631691197,20.));
#93145=CARTESIAN_POINT('Ctrl Pts',(3.36391747738213,47.8082976419741,0.));
#93146=CARTESIAN_POINT('Ctrl Pts',(3.36391747738213,47.8082976419741,20.));
#93147=CARTESIAN_POINT('Ctrl Pts',(3.39693388448305,47.802940820605,0.));
#93148=CARTESIAN_POINT('Ctrl Pts',(3.39693388448305,47.802940820605,20.));
#93149=CARTESIAN_POINT('Ctrl Pts',(3.42994545797921,47.797561230533,0.));
#93150=CARTESIAN_POINT('Ctrl Pts',(3.42994545797921,47.797561230533,20.));
#93151=CARTESIAN_POINT('Ctrl Pts',(3.46295218206011,47.7921588752121,0.));
#93152=CARTESIAN_POINT('Ctrl Pts',(3.46295218206011,47.7921588752121,20.));
#93153=CARTESIAN_POINT('Ctrl Pts',(3.49595404091727,47.7867337581073,0.));
#93154=CARTESIAN_POINT('Ctrl Pts',(3.49595404091727,47.7867337581073,20.));
#93155=CARTESIAN_POINT('Ctrl Pts',(3.52895101874414,47.7812858826946,0.));
#93156=CARTESIAN_POINT('Ctrl Pts',(3.52895101874414,47.7812858826946,20.));
#93157=CARTESIAN_POINT('Ctrl Pts',(3.56194309973641,47.7758152524613,0.));
#93158=CARTESIAN_POINT('Ctrl Pts',(3.56194309973641,47.7758152524613,20.));
#93159=CARTESIAN_POINT('Ctrl Pts',(3.59493026809157,47.7703218709055,0.));
#93160=CARTESIAN_POINT('Ctrl Pts',(3.59493026809157,47.7703218709055,20.));
#93161=CARTESIAN_POINT('Ctrl Pts',(3.62791250800923,47.764805741537,0.));
#93162=CARTESIAN_POINT('Ctrl Pts',(3.62791250800923,47.764805741537,20.));
#93163=CARTESIAN_POINT('Ctrl Pts',(3.66088980369083,47.7592668678762,0.));
#93164=CARTESIAN_POINT('Ctrl Pts',(3.66088980369083,47.7592668678762,20.));
#93165=CARTESIAN_POINT('Ctrl Pts',(3.69386213933993,47.7537052534546,0.));
#93166=CARTESIAN_POINT('Ctrl Pts',(3.69386213933993,47.7537052534546,20.));
#93167=CARTESIAN_POINT('Ctrl Pts',(3.72682949916222,47.7481209018149,0.));
#93168=CARTESIAN_POINT('Ctrl Pts',(3.72682949916222,47.7481209018149,20.));
#93169=CARTESIAN_POINT('Ctrl Pts',(3.75979186736544,47.7425138165111,0.));
#93170=CARTESIAN_POINT('Ctrl Pts',(3.75979186736544,47.7425138165111,20.));
#93171=CARTESIAN_POINT('Ctrl Pts',(3.79274922815948,47.7368840011081,0.));
#93172=CARTESIAN_POINT('Ctrl Pts',(3.79274922815948,47.7368840011081,20.));
#93173=CARTESIAN_POINT('Ctrl Pts',(3.82570156575622,47.7312314591817,0.));
#93174=CARTESIAN_POINT('Ctrl Pts',(3.82570156575622,47.7312314591817,20.));
#93175=CARTESIAN_POINT('Ctrl Pts',(3.85864886436973,47.7255561943191,0.));
#93176=CARTESIAN_POINT('Ctrl Pts',(3.85864886436973,47.7255561943191,20.));
#93177=CARTESIAN_POINT('Ctrl Pts',(3.89159110821604,47.719858210118,0.));
#93178=CARTESIAN_POINT('Ctrl Pts',(3.89159110821604,47.719858210118,20.));
#93179=CARTESIAN_POINT('Ctrl Pts',(3.92452828151332,47.7141375101875,0.));
#93180=CARTESIAN_POINT('Ctrl Pts',(3.92452828151332,47.7141375101875,20.));
#93181=CARTESIAN_POINT('Ctrl Pts',(3.95746036848186,47.7083940981477,0.));
#93182=CARTESIAN_POINT('Ctrl Pts',(3.95746036848186,47.7083940981477,20.));
#93183=CARTESIAN_POINT('Ctrl Pts',(3.990387353344,47.7026279776294,0.));
#93184=CARTESIAN_POINT('Ctrl Pts',(3.990387353344,47.7026279776294,20.));
#93185=CARTESIAN_POINT('Ctrl Pts',(4.02330922032433,47.6968391522753,0.));
#93186=CARTESIAN_POINT('Ctrl Pts',(4.02330922032433,47.6968391522753,20.));
#93187=CARTESIAN_POINT('Ctrl Pts',(4.05622595364951,47.6910276257391,0.));
#93188=CARTESIAN_POINT('Ctrl Pts',(4.05622595364951,47.6910276257391,20.));
#93189=CARTESIAN_POINT('Ctrl Pts',(4.08913753754848,47.6851934016861,0.));
#93190=CARTESIAN_POINT('Ctrl Pts',(4.08913753754848,47.6851934016861,20.));
#93191=CARTESIAN_POINT('Ctrl Pts',(4.12204395625218,47.6793364837921,0.));
#93192=CARTESIAN_POINT('Ctrl Pts',(4.12204395625218,47.6793364837921,20.));
#93193=CARTESIAN_POINT('Ctrl Pts',(4.15494519399369,47.6734568757434,0.));
#93194=CARTESIAN_POINT('Ctrl Pts',(4.15494519399369,47.6734568757434,20.));
#93195=CARTESIAN_POINT('Ctrl Pts',(4.18784123500835,47.6675545812371,0.));
#93196=CARTESIAN_POINT('Ctrl Pts',(4.18784123500835,47.6675545812371,20.));
#93197=CARTESIAN_POINT('Ctrl Pts',(4.22073206353344,47.6616296039816,0.));
#93198=CARTESIAN_POINT('Ctrl Pts',(4.22073206353344,47.6616296039816,20.));
#93199=CARTESIAN_POINT('Ctrl Pts',(4.25361766380859,47.6556819476964,0.));
#93200=CARTESIAN_POINT('Ctrl Pts',(4.25361766380859,47.6556819476964,20.));
#93201=CARTESIAN_POINT('Ctrl Pts',(4.28649802007566,47.6497116161128,0.));
#93202=CARTESIAN_POINT('Ctrl Pts',(4.28649802007566,47.6497116161128,20.));
#93203=CARTESIAN_POINT('Ctrl Pts',(4.31937311657885,47.6437186129734,0.));
#93204=CARTESIAN_POINT('Ctrl Pts',(4.31937311657885,47.6437186129734,20.));
#93205=CARTESIAN_POINT('Ctrl Pts',(4.35224293756439,47.6377029420315,0.));
#93206=CARTESIAN_POINT('Ctrl Pts',(4.35224293756439,47.6377029420315,20.));
#93207=CARTESIAN_POINT('Ctrl Pts',(4.38510746728074,47.6316646070511,0.));
#93208=CARTESIAN_POINT('Ctrl Pts',(4.38510746728074,47.6316646070511,20.));
#93209=CARTESIAN_POINT('Ctrl Pts',(4.41796668997835,47.6256036118071,0.));
#93210=CARTESIAN_POINT('Ctrl Pts',(4.41796668997835,47.6256036118071,20.));
#93211=CARTESIAN_POINT('Ctrl Pts',(4.45082058991003,47.6195199600851,0.));
#93212=CARTESIAN_POINT('Ctrl Pts',(4.45082058991003,47.6195199600851,20.));
#93213=CARTESIAN_POINT('Ctrl Pts',(4.48366915133083,47.6134136556823,0.));
#93214=CARTESIAN_POINT('Ctrl Pts',(4.48366915133083,47.6134136556823,20.));
#93215=CARTESIAN_POINT('Ctrl Pts',(4.51651235849822,47.6072847024073,0.));
#93216=CARTESIAN_POINT('Ctrl Pts',(4.51651235849822,47.6072847024073,20.));
#93217=CARTESIAN_POINT('Ctrl Pts',(4.54935019567197,47.6011331040799,0.));
#93218=CARTESIAN_POINT('Ctrl Pts',(4.54935019567197,47.6011331040799,20.));
#93219=CARTESIAN_POINT('Ctrl Pts',(4.58218264711418,47.5949588645311,0.));
#93220=CARTESIAN_POINT('Ctrl Pts',(4.58218264711418,47.5949588645311,20.));
#93221=CARTESIAN_POINT('Ctrl Pts',(4.61500969708895,47.5887619876026,0.));
#93222=CARTESIAN_POINT('Ctrl Pts',(4.61500969708895,47.5887619876026,20.));
#93223=CARTESIAN_POINT('Ctrl Pts',(4.64783132986259,47.5825424771468,0.));
#93224=CARTESIAN_POINT('Ctrl Pts',(4.64783132986259,47.5825424771468,20.));
#93225=CARTESIAN_POINT('Ctrl Pts',(4.68064752970369,47.5763003370265,0.));
#93226=CARTESIAN_POINT('Ctrl Pts',(4.68064752970369,47.5763003370265,20.));
#93227=CARTESIAN_POINT('Ctrl Pts',(4.71345828088308,47.5700355711162,0.));
#93228=CARTESIAN_POINT('Ctrl Pts',(4.71345828088308,47.5700355711162,20.));
#93229=CARTESIAN_POINT('Ctrl Pts',(4.74626356767412,47.5637481833017,0.));
#93230=CARTESIAN_POINT('Ctrl Pts',(4.74626356767412,47.5637481833017,20.));
#93231=CARTESIAN_POINT('Ctrl Pts',(4.77906337435243,47.5574381774801,0.));
#93232=CARTESIAN_POINT('Ctrl Pts',(4.77906337435243,47.5574381774801,20.));
#93233=CARTESIAN_POINT('Ctrl Pts',(4.81185768519588,47.5511055575593,0.));
#93234=CARTESIAN_POINT('Ctrl Pts',(4.81185768519588,47.5511055575593,20.));
#93235=CARTESIAN_POINT('Ctrl Pts',(4.84464648448474,47.5447503274583,0.));
#93236=CARTESIAN_POINT('Ctrl Pts',(4.84464648448474,47.5447503274583,20.));
#93237=CARTESIAN_POINT('Ctrl Pts',(4.87742975650161,47.538372491107,0.));
#93238=CARTESIAN_POINT('Ctrl Pts',(4.87742975650161,47.538372491107,20.));
#93239=CARTESIAN_POINT('Ctrl Pts',(4.91020748553144,47.5319720524462,0.));
#93240=CARTESIAN_POINT('Ctrl Pts',(4.91020748553144,47.5319720524462,20.));
#93241=CARTESIAN_POINT('Ctrl Pts',(4.94297965586156,47.5255490154281,0.));
#93242=CARTESIAN_POINT('Ctrl Pts',(4.94297965586156,47.5255490154281,20.));
#93243=CARTESIAN_POINT('Ctrl Pts',(4.97574625178169,47.519103384016,0.));
#93244=CARTESIAN_POINT('Ctrl Pts',(4.97574625178169,47.519103384016,20.));
#93245=CARTESIAN_POINT('Ctrl Pts',(5.00850725758367,47.5126351621839,0.));
#93246=CARTESIAN_POINT('Ctrl Pts',(5.00850725758367,47.5126351621839,20.));
#93247=CARTESIAN_POINT('Ctrl Pts',(5.04126265756154,47.5061443539168,0.));
#93248=CARTESIAN_POINT('Ctrl Pts',(5.04126265756154,47.5061443539168,20.));
#93249=CARTESIAN_POINT('Ctrl Pts',(5.07401243601198,47.4996309632108,0.));
#93250=CARTESIAN_POINT('Ctrl Pts',(5.07401243601198,47.4996309632108,20.));
#93251=CARTESIAN_POINT('Ctrl Pts',(5.10675657723402,47.4930949940731,0.));
#93252=CARTESIAN_POINT('Ctrl Pts',(5.10675657723402,47.4930949940731,20.));
#93253=CARTESIAN_POINT('Ctrl Pts',(5.13949506552922,47.4865364505219,0.));
#93254=CARTESIAN_POINT('Ctrl Pts',(5.13949506552922,47.4865364505219,20.));
#93255=CARTESIAN_POINT('Ctrl Pts',(5.17222788520144,47.4799553365862,0.));
#93256=CARTESIAN_POINT('Ctrl Pts',(5.17222788520144,47.4799553365862,20.));
#93257=CARTESIAN_POINT('Ctrl Pts',(5.20495502055713,47.4733516563069,0.));
#93258=CARTESIAN_POINT('Ctrl Pts',(5.20495502055713,47.4733516563069,20.));
#93259=CARTESIAN_POINT('Ctrl Pts',(5.2376764559051,47.4667254137359,0.));
#93260=CARTESIAN_POINT('Ctrl Pts',(5.2376764559051,47.4667254137359,20.));
#93261=CARTESIAN_POINT('Ctrl Pts',(5.27039217555655,47.4600766129357,0.));
#93262=CARTESIAN_POINT('Ctrl Pts',(5.27039217555655,47.4600766129357,20.));
#93263=CARTESIAN_POINT('Ctrl Pts',(5.30310216382505,47.4534052579797,0.));
#93264=CARTESIAN_POINT('Ctrl Pts',(5.30310216382505,47.4534052579797,20.));
#93265=CARTESIAN_POINT('Ctrl Pts',(5.3358064050266,47.4467113529523,0.));
#93266=CARTESIAN_POINT('Ctrl Pts',(5.3358064050266,47.4467113529523,20.));
#93267=CARTESIAN_POINT('Ctrl Pts',(5.36850488347923,47.4399949019487,0.));
#93268=CARTESIAN_POINT('Ctrl Pts',(5.36850488347923,47.4399949019487,20.));
#93269=CARTESIAN_POINT('Ctrl Pts',(5.40119758350378,47.4332559090748,0.));
#93270=CARTESIAN_POINT('Ctrl Pts',(5.40119758350378,47.4332559090748,20.));
#93271=CARTESIAN_POINT('Ctrl Pts',(5.43388448942349,47.4264943784481,0.));
#93272=CARTESIAN_POINT('Ctrl Pts',(5.43388448942349,47.4264943784481,20.));
#93273=CARTESIAN_POINT('Ctrl Pts',(5.46656558556425,47.4197103141976,0.));
#93274=CARTESIAN_POINT('Ctrl Pts',(5.46656558556425,47.4197103141976,20.));
#93275=CARTESIAN_POINT('Ctrl Pts',(5.49924085625463,47.4129037204631,0.));
#93276=CARTESIAN_POINT('Ctrl Pts',(5.49924085625463,47.4129037204631,20.));
#93277=CARTESIAN_POINT('Ctrl Pts',(5.53191028582554,47.4060746013959,0.));
#93278=CARTESIAN_POINT('Ctrl Pts',(5.53191028582554,47.4060746013959,20.));
#93279=CARTESIAN_POINT('Ctrl Pts',(5.56457385861036,47.3992229611579,0.));
#93280=CARTESIAN_POINT('Ctrl Pts',(5.56457385861036,47.3992229611579,20.));
#93281=CARTESIAN_POINT('Ctrl Pts',(5.59723155894482,47.3923488039217,0.));
#93282=CARTESIAN_POINT('Ctrl Pts',(5.59723155894482,47.3923488039217,20.));
#93283=CARTESIAN_POINT('Ctrl Pts',(5.62988337116714,47.3854521338708,0.));
#93284=CARTESIAN_POINT('Ctrl Pts',(5.62988337116714,47.3854521338708,20.));
#93285=CARTESIAN_POINT('Ctrl Pts',(5.6625292796181,47.3785329551997,0.));
#93286=CARTESIAN_POINT('Ctrl Pts',(5.6625292796181,47.3785329551997,20.));
#93287=CARTESIAN_POINT('Ctrl Pts',(5.69516926864087,47.3715912721141,0.));
#93288=CARTESIAN_POINT('Ctrl Pts',(5.69516926864087,47.3715912721141,20.));
#93289=CARTESIAN_POINT('Ctrl Pts',(5.72780332258134,47.3646270888308,0.));
#93290=CARTESIAN_POINT('Ctrl Pts',(5.72780332258134,47.3646270888308,20.));
#93291=CARTESIAN_POINT('Ctrl Pts',(5.76043142578785,47.3576404095778,0.));
#93292=CARTESIAN_POINT('Ctrl Pts',(5.76043142578785,47.3576404095778,20.));
#93293=CARTESIAN_POINT('Ctrl Pts',(5.79305356261141,47.3506312385939,0.));
#93294=CARTESIAN_POINT('Ctrl Pts',(5.79305356261141,47.3506312385939,20.));
#93295=CARTESIAN_POINT('Ctrl Pts',(5.82566971740555,47.3435995801292,0.));
#93296=CARTESIAN_POINT('Ctrl Pts',(5.82566971740555,47.3435995801292,20.));
#93297=CARTESIAN_POINT('Ctrl Pts',(5.85827987452639,47.3365454384446,0.));
#93298=CARTESIAN_POINT('Ctrl Pts',(5.85827987452639,47.3365454384446,20.));
#93299=CARTESIAN_POINT('Ctrl Pts',(5.89088401833276,47.3294688178121,0.));
#93300=CARTESIAN_POINT('Ctrl Pts',(5.89088401833276,47.3294688178121,20.));
#93301=CARTESIAN_POINT('Ctrl Pts',(5.92348213318597,47.3223697225143,0.));
#93302=CARTESIAN_POINT('Ctrl Pts',(5.92348213318597,47.3223697225143,20.));
#93303=CARTESIAN_POINT('Ctrl Pts',(5.95607420344985,47.3152481568452,0.));
#93304=CARTESIAN_POINT('Ctrl Pts',(5.95607420344985,47.3152481568452,20.));
#93305=CARTESIAN_POINT('Ctrl Pts',(5.98866021349066,47.3081041251096,0.));
#93306=CARTESIAN_POINT('Ctrl Pts',(5.98866021349066,47.3081041251096,20.));
#93307=CARTESIAN_POINT('Ctrl Pts',(6.02124014767729,47.3009376316237,0.));
#93308=CARTESIAN_POINT('Ctrl Pts',(6.02124014767729,47.3009376316237,20.));
#93309=CARTESIAN_POINT('Ctrl Pts',(6.05381399038128,47.2937486807145,0.));
#93310=CARTESIAN_POINT('Ctrl Pts',(6.05381399038128,47.2937486807145,20.));
#93311=CARTESIAN_POINT('Ctrl Pts',(6.08638172597683,47.2865372767199,0.));
#93312=CARTESIAN_POINT('Ctrl Pts',(6.08638172597683,47.2865372767199,20.));
#93313=CARTESIAN_POINT('Ctrl Pts',(6.11894333884087,47.2793034239892,0.));
#93314=CARTESIAN_POINT('Ctrl Pts',(6.11894333884087,47.2793034239892,20.));
#93315=CARTESIAN_POINT('Ctrl Pts',(6.15149881335289,47.272047126882,0.));
#93316=CARTESIAN_POINT('Ctrl Pts',(6.15149881335289,47.272047126882,20.));
#93317=CARTESIAN_POINT('Ctrl Pts',(6.18404813389528,47.2647683897693,0.));
#93318=CARTESIAN_POINT('Ctrl Pts',(6.18404813389528,47.2647683897693,20.));
#93319=CARTESIAN_POINT('Ctrl Pts',(6.21659128485295,47.2574672170331,0.));
#93320=CARTESIAN_POINT('Ctrl Pts',(6.21659128485295,47.2574672170331,20.));
#93321=CARTESIAN_POINT('Ctrl Pts',(6.24912825061342,47.2501436130661,0.));
#93322=CARTESIAN_POINT('Ctrl Pts',(6.24912825061342,47.2501436130661,20.));
#93323=CARTESIAN_POINT('Ctrl Pts',(6.28165901556675,47.2427975822723,0.));
#93324=CARTESIAN_POINT('Ctrl Pts',(6.28165901556675,47.2427975822723,20.));
#93325=CARTESIAN_POINT('Ctrl Pts',(6.31418356410549,47.2354291290667,0.));
#93326=CARTESIAN_POINT('Ctrl Pts',(6.31418356410549,47.2354291290667,20.));
#93327=CARTESIAN_POINT('Ctrl Pts',(6.34670188062515,47.2280382578755,0.));
#93328=CARTESIAN_POINT('Ctrl Pts',(6.34670188062515,47.2280382578755,20.));
#93329=CARTESIAN_POINT('Ctrl Pts',(6.37921394952379,47.2206249731358,0.));
#93330=CARTESIAN_POINT('Ctrl Pts',(6.37921394952379,47.2206249731358,20.));
#93331=CARTESIAN_POINT('Ctrl Pts',(6.41171975520233,47.213189279296,0.));
#93332=CARTESIAN_POINT('Ctrl Pts',(6.41171975520233,47.213189279296,20.));
#93333=CARTESIAN_POINT('Ctrl Pts',(6.44421928206445,47.205731180815,0.));
#93334=CARTESIAN_POINT('Ctrl Pts',(6.44421928206445,47.205731180815,20.));
#93335=CARTESIAN_POINT('Ctrl Pts',(6.47671251451637,47.1982506821625,0.));
#93336=CARTESIAN_POINT('Ctrl Pts',(6.47671251451637,47.1982506821625,20.));
#93337=CARTESIAN_POINT('Ctrl Pts',(6.50919943696717,47.190747787819,0.));
#93338=CARTESIAN_POINT('Ctrl Pts',(6.50919943696717,47.190747787819,20.));
#93339=CARTESIAN_POINT('Ctrl Pts',(6.54168003382861,47.1832225022762,0.));
#93340=CARTESIAN_POINT('Ctrl Pts',(6.54168003382861,47.1832225022762,20.));
#93341=CARTESIAN_POINT('Ctrl Pts',(6.57415428951524,47.1756748300372,0.));
#93342=CARTESIAN_POINT('Ctrl Pts',(6.57415428951524,47.1756748300372,20.));
#93343=CARTESIAN_POINT('Ctrl Pts',(6.60662218844434,47.168104775616,0.));
#93344=CARTESIAN_POINT('Ctrl Pts',(6.60662218844434,47.168104775616,20.));
#93345=CARTESIAN_POINT('Ctrl Pts',(6.63908371503577,47.1605123435378,0.));
#93346=CARTESIAN_POINT('Ctrl Pts',(6.63908371503577,47.1605123435378,20.));
#93347=CARTESIAN_POINT('Ctrl Pts',(6.67153885371226,47.1528975383387,0.));
#93348=CARTESIAN_POINT('Ctrl Pts',(6.67153885371226,47.1528975383387,20.));
#93349=CARTESIAN_POINT('Ctrl Pts',(6.70398758889916,47.1452603645656,0.));
#93350=CARTESIAN_POINT('Ctrl Pts',(6.70398758889916,47.1452603645656,20.));
#93351=CARTESIAN_POINT('Ctrl Pts',(6.73642990502458,47.1376008267758,0.));
#93352=CARTESIAN_POINT('Ctrl Pts',(6.73642990502458,47.1376008267758,20.));
#93353=CARTESIAN_POINT('Ctrl Pts',(6.76886578651954,47.129918929538,0.));
#93354=CARTESIAN_POINT('Ctrl Pts',(6.76886578651954,47.129918929538,20.));
#93355=CARTESIAN_POINT('Ctrl Pts',(6.80129521781808,47.1222146774323,0.));
#93356=CARTESIAN_POINT('Ctrl Pts',(6.80129521781808,47.1222146774323,20.));
#93357=CARTESIAN_POINT('Ctrl Pts',(6.83371818335697,47.1144880750497,0.));
#93358=CARTESIAN_POINT('Ctrl Pts',(6.83371818335697,47.1144880750497,20.));
#93359=CARTESIAN_POINT('Ctrl Pts',(6.86613466757588,47.1067391269919,0.));
#93360=CARTESIAN_POINT('Ctrl Pts',(6.86613466757588,47.1067391269919,20.));
#93361=CARTESIAN_POINT('Ctrl Pts',(6.89854465491702,47.0989678378717,0.));
#93362=CARTESIAN_POINT('Ctrl Pts',(6.89854465491702,47.0989678378717,20.));
#93363=CARTESIAN_POINT('Ctrl Pts',(6.93094812982541,47.0911742123123,0.));
#93364=CARTESIAN_POINT('Ctrl Pts',(6.93094812982541,47.0911742123123,20.));
#93365=CARTESIAN_POINT('Ctrl Pts',(6.96334507674873,47.0833582549484,0.));
#93366=CARTESIAN_POINT('Ctrl Pts',(6.96334507674873,47.0833582549484,20.));
#93367=CARTESIAN_POINT('Ctrl Pts',(6.99573548013776,47.0755199704256,0.));
#93368=CARTESIAN_POINT('Ctrl Pts',(6.99573548013776,47.0755199704256,20.));
#93369=CARTESIAN_POINT('Ctrl Pts',(7.02811932444601,47.0676593634011,0.));
#93370=CARTESIAN_POINT('Ctrl Pts',(7.02811932444601,47.0676593634011,20.));
#93371=CARTESIAN_POINT('Ctrl Pts',(7.06049659413007,47.0597764385426,0.));
#93372=CARTESIAN_POINT('Ctrl Pts',(7.06049659413007,47.0597764385426,20.));
#93373=CARTESIAN_POINT('Ctrl Pts',(7.09286727364932,47.0518712005288,0.));
#93374=CARTESIAN_POINT('Ctrl Pts',(7.09286727364932,47.0518712005288,20.));
#93375=CARTESIAN_POINT('Ctrl Pts',(7.12523134746603,47.0439436540493,0.));
#93376=CARTESIAN_POINT('Ctrl Pts',(7.12523134746603,47.0439436540493,20.));
#93377=CARTESIAN_POINT('Ctrl Pts',(7.15758880004521,47.0359938038039,0.));
#93378=CARTESIAN_POINT('Ctrl Pts',(7.15758880004521,47.0359938038039,20.));
#93379=CARTESIAN_POINT('Ctrl Pts',(7.18993961585469,47.0280216545038,0.));
#93380=CARTESIAN_POINT('Ctrl Pts',(7.18993961585469,47.0280216545038,20.));
#93381=CARTESIAN_POINT('Ctrl Pts',(7.22228377936529,47.020027210871,0.));
#93382=CARTESIAN_POINT('Ctrl Pts',(7.22228377936529,47.020027210871,20.));
#93383=CARTESIAN_POINT('Ctrl Pts',(7.25462127505076,47.012010477639,0.));
#93384=CARTESIAN_POINT('Ctrl Pts',(7.25462127505076,47.012010477639,20.));
#93385=CARTESIAN_POINT('Ctrl Pts',(7.28695208738784,47.0039714595526,0.));
#93386=CARTESIAN_POINT('Ctrl Pts',(7.28695208738784,47.0039714595526,20.));
#93387=CARTESIAN_POINT('Ctrl Pts',(7.31927620085613,46.9959101613675,0.));
#93388=CARTESIAN_POINT('Ctrl Pts',(7.31927620085613,46.9959101613675,20.));
#93389=CARTESIAN_POINT('Ctrl Pts',(7.35159359993817,46.9878265878505,0.));
#93390=CARTESIAN_POINT('Ctrl Pts',(7.35159359993817,46.9878265878505,20.));
#93391=CARTESIAN_POINT('Ctrl Pts',(7.38390426911931,46.9797207437786,0.));
#93392=CARTESIAN_POINT('Ctrl Pts',(7.38390426911931,46.9797207437786,20.));
#93393=CARTESIAN_POINT('Ctrl Pts',(7.41620819288777,46.9715926339391,0.));
#93394=CARTESIAN_POINT('Ctrl Pts',(7.41620819288777,46.9715926339391,20.));
#93395=CARTESIAN_POINT('Ctrl Pts',(7.44850535573481,46.9634422631307,0.));
#93396=CARTESIAN_POINT('Ctrl Pts',(7.44850535573481,46.9634422631307,20.));
#93397=CARTESIAN_POINT('Ctrl Pts',(7.48079574215478,46.9552696361634,0.));
#93398=CARTESIAN_POINT('Ctrl Pts',(7.48079574215478,46.9552696361634,20.));
#93399=CARTESIAN_POINT('Ctrl Pts',(7.51307933664511,46.9470747578592,0.));
#93400=CARTESIAN_POINT('Ctrl Pts',(7.51307933664511,46.9470747578592,20.));
#93401=CARTESIAN_POINT('Ctrl Pts',(7.54535612370601,46.9388576330501,0.));
#93402=CARTESIAN_POINT('Ctrl Pts',(7.54535612370601,46.9388576330501,20.));
#93403=CARTESIAN_POINT('Ctrl Pts',(7.57762608784068,46.9306182665792,0.));
#93404=CARTESIAN_POINT('Ctrl Pts',(7.57762608784068,46.9306182665792,20.));
#93405=CARTESIAN_POINT('Ctrl Pts',(7.6098892135552,46.9223566632999,0.));
#93406=CARTESIAN_POINT('Ctrl Pts',(7.6098892135552,46.9223566632999,20.));
#93407=CARTESIAN_POINT('Ctrl Pts',(7.64214548535856,46.9140728280766,0.));
#93408=CARTESIAN_POINT('Ctrl Pts',(7.64214548535856,46.9140728280766,20.));
#93409=CARTESIAN_POINT('Ctrl Pts',(7.67439488776287,46.9057667657847,0.));
#93410=CARTESIAN_POINT('Ctrl Pts',(7.67439488776287,46.9057667657847,20.));
#93411=CARTESIAN_POINT('Ctrl Pts',(7.7066374052833,46.8974384813109,0.));
#93412=CARTESIAN_POINT('Ctrl Pts',(7.7066374052833,46.8974384813109,20.));
#93413=CARTESIAN_POINT('Ctrl Pts',(7.73887302243815,46.8890879795531,0.));
#93414=CARTESIAN_POINT('Ctrl Pts',(7.73887302243815,46.8890879795531,20.));
#93415=CARTESIAN_POINT('Ctrl Pts',(7.77110172374868,46.8807152654198,0.));
#93416=CARTESIAN_POINT('Ctrl Pts',(7.77110172374868,46.8807152654198,20.));
#93417=CARTESIAN_POINT('Ctrl Pts',(7.80332349373917,46.8723203438306,0.));
#93418=CARTESIAN_POINT('Ctrl Pts',(7.80332349373917,46.8723203438306,20.));
#93419=CARTESIAN_POINT('Ctrl Pts',(7.83553831693686,46.8639032197162,0.));
#93420=CARTESIAN_POINT('Ctrl Pts',(7.83553831693686,46.8639032197162,20.));
#93421=CARTESIAN_POINT('Ctrl Pts',(7.86774617787212,46.855463898018,0.));
#93422=CARTESIAN_POINT('Ctrl Pts',(7.86774617787212,46.855463898018,20.));
#93423=CARTESIAN_POINT('Ctrl Pts',(7.89994706107838,46.8470023836881,0.));
#93424=CARTESIAN_POINT('Ctrl Pts',(7.89994706107838,46.8470023836881,20.));
#93425=CARTESIAN_POINT('Ctrl Pts',(7.9321409510921,46.8385186816898,0.));
#93426=CARTESIAN_POINT('Ctrl Pts',(7.9321409510921,46.8385186816898,20.));
#93427=CARTESIAN_POINT('Ctrl Pts',(7.96432783245285,46.8300127969969,0.));
#93428=CARTESIAN_POINT('Ctrl Pts',(7.96432783245285,46.8300127969969,20.));
#93429=CARTESIAN_POINT('Ctrl Pts',(7.99650768970303,46.8214847345942,0.));
#93430=CARTESIAN_POINT('Ctrl Pts',(7.99650768970303,46.8214847345942,20.));
#93431=CARTESIAN_POINT('Ctrl Pts',(8.02868050738827,46.8129344994773,0.));
#93432=CARTESIAN_POINT('Ctrl Pts',(8.02868050738827,46.8129344994773,20.));
#93433=CARTESIAN_POINT('Ctrl Pts',(8.06084627005728,46.8043620966531,0.));
#93434=CARTESIAN_POINT('Ctrl Pts',(8.06084627005728,46.8043620966531,20.));
#93435=CARTESIAN_POINT('Ctrl Pts',(8.09300496226219,46.7957675311395,0.));
#93436=CARTESIAN_POINT('Ctrl Pts',(8.09300496226219,46.7957675311395,20.));
#93437=CARTESIAN_POINT('Ctrl Pts',(8.125156568558,46.7871508079658,0.));
#93438=CARTESIAN_POINT('Ctrl Pts',(8.125156568558,46.7871508079658,20.));
#93439=CARTESIAN_POINT('Ctrl Pts',(8.15730107350294,46.7785119321719,0.));
#93440=CARTESIAN_POINT('Ctrl Pts',(8.15730107350294,46.7785119321719,20.));
#93441=CARTESIAN_POINT('Ctrl Pts',(8.18943846165844,46.7698509088086,0.));
#93442=CARTESIAN_POINT('Ctrl Pts',(8.18943846165844,46.7698509088086,20.));
#93443=CARTESIAN_POINT('Ctrl Pts',(8.22156871758881,46.7611677429374,0.));
#93444=CARTESIAN_POINT('Ctrl Pts',(8.22156871758881,46.7611677429374,20.));
#93445=CARTESIAN_POINT('Ctrl Pts',(8.25369182586168,46.7524624396307,0.));
#93446=CARTESIAN_POINT('Ctrl Pts',(8.25369182586168,46.7524624396307,20.));
#93447=CARTESIAN_POINT('Ctrl Pts',(8.28580777104744,46.7437350039712,0.));
#93448=CARTESIAN_POINT('Ctrl Pts',(8.28580777104744,46.7437350039712,20.));
#93449=CARTESIAN_POINT('Ctrl Pts',(8.31791653771973,46.7349854410525,0.));
#93450=CARTESIAN_POINT('Ctrl Pts',(8.31791653771973,46.7349854410525,20.));
#93451=CARTESIAN_POINT('Ctrl Pts',(8.35001811045535,46.7262137559789,0.));
#93452=CARTESIAN_POINT('Ctrl Pts',(8.35001811045535,46.7262137559789,20.));
#93453=CARTESIAN_POINT('Ctrl Pts',(8.38211247383476,46.7174199538668,0.));
#93454=CARTESIAN_POINT('Ctrl Pts',(8.38211247383476,46.7174199538668,20.));
#93455=CARTESIAN_POINT('Ctrl Pts',(8.41419961244154,46.7086040398438,0.));
#93456=CARTESIAN_POINT('Ctrl Pts',(8.41419961244154,46.7086040398438,20.));
#93457=CARTESIAN_POINT('Ctrl Pts',(8.44627951086261,46.6997660190488,0.));
#93458=CARTESIAN_POINT('Ctrl Pts',(8.44627951086261,46.6997660190488,20.));
#93459=CARTESIAN_POINT('Ctrl Pts',(8.47835215368743,46.6909058966306,0.));
#93460=CARTESIAN_POINT('Ctrl Pts',(8.47835215368743,46.6909058966306,20.));
#93461=CARTESIAN_POINT('Ctrl Pts',(8.5104175255088,46.6820236777489,0.));
#93462=CARTESIAN_POINT('Ctrl Pts',(8.5104175255088,46.6820236777489,20.));
#93463=CARTESIAN_POINT('Ctrl Pts',(8.54247561092257,46.673119367573,0.));
#93464=CARTESIAN_POINT('Ctrl Pts',(8.54247561092257,46.673119367573,20.));
#93465=CARTESIAN_POINT('Ctrl Pts',(8.57452639452827,46.6641929712839,0.));
#93466=CARTESIAN_POINT('Ctrl Pts',(8.57452639452827,46.6641929712839,20.));
#93467=CARTESIAN_POINT('Ctrl Pts',(8.60656986092877,46.6552444940739,0.));
#93468=CARTESIAN_POINT('Ctrl Pts',(8.60656986092877,46.6552444940739,20.));
#93469=CARTESIAN_POINT('Ctrl Pts',(8.63860599473002,46.6462739411471,0.));
#93470=CARTESIAN_POINT('Ctrl Pts',(8.63860599473002,46.6462739411471,20.));
#93471=CARTESIAN_POINT('Ctrl Pts',(8.67063478054115,46.6372813177181,0.));
#93472=CARTESIAN_POINT('Ctrl Pts',(8.67063478054115,46.6372813177181,20.));
#93473=CARTESIAN_POINT('Ctrl Pts',(8.70265620297453,46.6282666290119,0.));
#93474=CARTESIAN_POINT('Ctrl Pts',(8.70265620297453,46.6282666290119,20.));
#93475=CARTESIAN_POINT('Ctrl Pts',(8.73467024664569,46.6192298802645,0.));
#93476=CARTESIAN_POINT('Ctrl Pts',(8.73467024664569,46.6192298802645,20.));
#93477=CARTESIAN_POINT('Ctrl Pts',(8.76667689617329,46.6101710767218,0.));
#93478=CARTESIAN_POINT('Ctrl Pts',(8.76667689617329,46.6101710767218,20.));
#93479=CARTESIAN_POINT('Ctrl Pts',(8.79867613617932,46.6010902236408,0.));
#93480=CARTESIAN_POINT('Ctrl Pts',(8.79867613617932,46.6010902236408,20.));
#93481=CARTESIAN_POINT('Ctrl Pts',(8.83066795128933,46.59198732629,0.));
#93482=CARTESIAN_POINT('Ctrl Pts',(8.83066795128933,46.59198732629,20.));
#93483=CARTESIAN_POINT('Ctrl Pts',(8.86265232613214,46.582862389949,0.));
#93484=CARTESIAN_POINT('Ctrl Pts',(8.86265232613214,46.582862389949,20.));
#93485=CARTESIAN_POINT('Ctrl Pts',(8.89462924533988,46.5737154199087,0.));
#93486=CARTESIAN_POINT('Ctrl Pts',(8.89462924533988,46.5737154199087,20.));
#93487=CARTESIAN_POINT('Ctrl Pts',(8.92659869354787,46.5645464214705,0.));
#93488=CARTESIAN_POINT('Ctrl Pts',(8.92659869354787,46.5645464214705,20.));
#93489=CARTESIAN_POINT('Ctrl Pts',(8.9585606553947,46.5553553999467,0.));
#93490=CARTESIAN_POINT('Ctrl Pts',(8.9585606553947,46.5553553999467,20.));
#93491=CARTESIAN_POINT('Ctrl Pts',(8.99051511552228,46.5461423606602,0.));
#93492=CARTESIAN_POINT('Ctrl Pts',(8.99051511552228,46.5461423606602,20.));
#93493=CARTESIAN_POINT('Ctrl Pts',(9.02246205857627,46.5369073089453,0.));
#93494=CARTESIAN_POINT('Ctrl Pts',(9.02246205857627,46.5369073089453,20.));
#93495=CARTESIAN_POINT('Ctrl Pts',(9.05440146920514,46.5276502501459,0.));
#93496=CARTESIAN_POINT('Ctrl Pts',(9.05440146920514,46.5276502501459,20.));
#93497=CARTESIAN_POINT('Ctrl Pts',(9.08633333206089,46.5183711896174,0.));
#93498=CARTESIAN_POINT('Ctrl Pts',(9.08633333206089,46.5183711896174,20.));
#93499=CARTESIAN_POINT('Ctrl Pts',(9.11825763179851,46.5090701327255,0.));
#93500=CARTESIAN_POINT('Ctrl Pts',(9.11825763179851,46.5090701327255,20.));
#93501=CARTESIAN_POINT('Ctrl Pts',(9.15017435307665,46.4997470848477,0.));
#93502=CARTESIAN_POINT('Ctrl Pts',(9.15017435307665,46.4997470848477,20.));
#93503=CARTESIAN_POINT('Ctrl Pts',(9.18208348055724,46.4904020513722,0.));
#93504=CARTESIAN_POINT('Ctrl Pts',(9.18208348055724,46.4904020513722,20.));
#93505=CARTESIAN_POINT('Ctrl Pts',(9.21398499890591,46.4810350376983,0.));
#93506=CARTESIAN_POINT('Ctrl Pts',(9.21398499890591,46.4810350376983,20.));
#93507=CARTESIAN_POINT('Ctrl Pts',(9.2458788927917,46.4716460492361,0.));
#93508=CARTESIAN_POINT('Ctrl Pts',(9.2458788927917,46.4716460492361,20.));
#93509=CARTESIAN_POINT('Ctrl Pts',(9.27776514688698,46.4622350914066,0.));
#93510=CARTESIAN_POINT('Ctrl Pts',(9.27776514688698,46.4622350914066,20.));
#93511=CARTESIAN_POINT('Ctrl Pts',(9.30964374586751,46.4528021696416,0.));
#93512=CARTESIAN_POINT('Ctrl Pts',(9.30964374586751,46.4528021696416,20.));
#93513=CARTESIAN_POINT('Ctrl Pts',(9.3415146744124,46.4433472893837,0.));
#93514=CARTESIAN_POINT('Ctrl Pts',(9.3415146744124,46.4433472893837,20.));
#93515=CARTESIAN_POINT('Ctrl Pts',(9.37337791720392,46.4338704560856,0.));
#93516=CARTESIAN_POINT('Ctrl Pts',(9.37337791720392,46.4338704560856,20.));
#93517=CARTESIAN_POINT('Ctrl Pts',(9.40523345892773,46.4243716752115,0.));
#93518=CARTESIAN_POINT('Ctrl Pts',(9.40523345892773,46.4243716752115,20.));
#93519=CARTESIAN_POINT('Ctrl Pts',(9.43708128427273,46.4148509522358,0.));
#93520=CARTESIAN_POINT('Ctrl Pts',(9.43708128427273,46.4148509522358,20.));
#93521=CARTESIAN_POINT('Ctrl Pts',(9.46892137793147,46.405308292644,0.));
#93522=CARTESIAN_POINT('Ctrl Pts',(9.46892137793147,46.405308292644,20.));
#93523=CARTESIAN_POINT('Ctrl Pts',(9.50075372460008,46.3957437019326,0.));
#93524=CARTESIAN_POINT('Ctrl Pts',(9.50075372460008,46.3957437019326,20.));
#93525=CARTESIAN_POINT('Ctrl Pts',(9.5325783089785,46.3861571856095,0.));
#93526=CARTESIAN_POINT('Ctrl Pts',(9.5325783089785,46.3861571856095,20.));
#93527=CARTESIAN_POINT('Ctrl Pts',(9.56439511577022,46.3765487491938,0.));
#93528=CARTESIAN_POINT('Ctrl Pts',(9.56439511577022,46.3765487491938,20.));
#93529=CARTESIAN_POINT('Ctrl Pts',(9.59620412968212,46.3669183982155,0.));
#93530=CARTESIAN_POINT('Ctrl Pts',(9.59620412968212,46.3669183982155,20.));
#93531=CARTESIAN_POINT('Ctrl Pts',(9.62800533542435,46.3572661382147,0.));
#93532=CARTESIAN_POINT('Ctrl Pts',(9.62800533542435,46.3572661382147,20.));
#93533=CARTESIAN_POINT('Ctrl Pts',(9.65979871771038,46.347591974742,0.));
#93534=CARTESIAN_POINT('Ctrl Pts',(9.65979871771038,46.347591974742,20.));
#93535=CARTESIAN_POINT('Ctrl Pts',(9.69158426125691,46.3378959133587,0.));
#93536=CARTESIAN_POINT('Ctrl Pts',(9.69158426125691,46.3378959133587,20.));
#93537=CARTESIAN_POINT('Ctrl Pts',(9.72336195078413,46.3281779596367,0.));
#93538=CARTESIAN_POINT('Ctrl Pts',(9.72336195078413,46.3281779596367,20.));
#93539=CARTESIAN_POINT('Ctrl Pts',(9.75513177101576,46.3184381191592,0.));
#93540=CARTESIAN_POINT('Ctrl Pts',(9.75513177101576,46.3184381191592,20.));
#93541=CARTESIAN_POINT('Ctrl Pts',(9.78689370667939,46.3086763975205,0.));
#93542=CARTESIAN_POINT('Ctrl Pts',(9.78689370667939,46.3086763975205,20.));
#93543=CARTESIAN_POINT('Ctrl Pts',(9.81864774250618,46.2988928003257,0.));
#93544=CARTESIAN_POINT('Ctrl Pts',(9.81864774250618,46.2988928003257,20.));
#93545=CARTESIAN_POINT('Ctrl Pts',(9.85039386323084,46.289087333191,0.));
#93546=CARTESIAN_POINT('Ctrl Pts',(9.85039386323084,46.289087333191,20.));
#93547=CARTESIAN_POINT('Ctrl Pts',(9.8821320535919,46.2792600017436,0.));
#93548=CARTESIAN_POINT('Ctrl Pts',(9.8821320535919,46.2792600017436,20.));
#93549=CARTESIAN_POINT('Ctrl Pts',(9.91386229833136,46.2694108116213,0.));
#93550=CARTESIAN_POINT('Ctrl Pts',(9.91386229833136,46.2694108116213,20.));
#93551=CARTESIAN_POINT('Ctrl Pts',(9.94558458219445,46.2595397684724,0.));
#93552=CARTESIAN_POINT('Ctrl Pts',(9.94558458219445,46.2595397684724,20.));
#93553=CARTESIAN_POINT('Ctrl Pts',(9.97729888992979,46.2496468779557,0.));
#93554=CARTESIAN_POINT('Ctrl Pts',(9.97729888992979,46.2496468779557,20.));
#93555=CARTESIAN_POINT('Ctrl Pts',(10.0090052062894,46.2397321457408,0.));
#93556=CARTESIAN_POINT('Ctrl Pts',(10.0090052062894,46.2397321457408,20.));
#93557=CARTESIAN_POINT('Ctrl Pts',(10.0407035160292,46.2297955775084,0.));
#93558=CARTESIAN_POINT('Ctrl Pts',(10.0407035160292,46.2297955775084,20.));
#93559=CARTESIAN_POINT('Ctrl Pts',(10.0723938039086,46.2198371789501,0.));
#93560=CARTESIAN_POINT('Ctrl Pts',(10.0723938039086,46.2198371789501,20.));
#93561=CARTESIAN_POINT('Ctrl Pts',(10.1040760546909,46.2098569557688,0.));
#93562=CARTESIAN_POINT('Ctrl Pts',(10.1040760546909,46.2098569557688,20.));
#93563=CARTESIAN_POINT('Ctrl Pts',(10.1357502531431,46.1998549136779,0.));
#93564=CARTESIAN_POINT('Ctrl Pts',(10.1357502531431,46.1998549136779,20.));
#93565=CARTESIAN_POINT('Ctrl Pts',(10.1674163840354,46.1898310584014,0.));
#93566=CARTESIAN_POINT('Ctrl Pts',(10.1674163840354,46.1898310584014,20.));
#93567=CARTESIAN_POINT('Ctrl Pts',(10.199074432142,46.179785395674,0.));
#93568=CARTESIAN_POINT('Ctrl Pts',(10.199074432142,46.179785395674,20.));
#93569=CARTESIAN_POINT('Ctrl Pts',(10.2307243822402,46.169717931241,0.));
#93570=CARTESIAN_POINT('Ctrl Pts',(10.2307243822402,46.169717931241,20.));
#93571=CARTESIAN_POINT('Ctrl Pts',(10.2623662191113,46.1596286708586,0.));
#93572=CARTESIAN_POINT('Ctrl Pts',(10.2623662191113,46.1596286708586,20.));
#93573=CARTESIAN_POINT('Ctrl Pts',(10.2939999275403,46.1495176202946,0.));
#93574=CARTESIAN_POINT('Ctrl Pts',(10.2939999275403,46.1495176202946,20.));
#93575=CARTESIAN_POINT('Ctrl Pts',(10.3256254923155,46.139384785327,0.));
#93576=CARTESIAN_POINT('Ctrl Pts',(10.3256254923155,46.139384785327,20.));
#93577=CARTESIAN_POINT('Ctrl Pts',(10.3572428982293,46.1292301717445,0.));
#93578=CARTESIAN_POINT('Ctrl Pts',(10.3572428982293,46.1292301717445,20.));
#93579=CARTESIAN_POINT('Ctrl Pts',(10.3888521300773,46.119053785347,0.));
#93580=CARTESIAN_POINT('Ctrl Pts',(10.3888521300773,46.119053785347,20.));
#93581=CARTESIAN_POINT('Ctrl Pts',(10.4204531726593,46.1088556319449,0.));
#93582=CARTESIAN_POINT('Ctrl Pts',(10.4204531726593,46.1088556319449,20.));
#93583=CARTESIAN_POINT('Ctrl Pts',(10.4520460107784,46.0986357173598,0.));
#93584=CARTESIAN_POINT('Ctrl Pts',(10.4520460107784,46.0986357173598,20.));
#93585=CARTESIAN_POINT('Ctrl Pts',(10.4836306292415,46.0883940474237,0.));
#93586=CARTESIAN_POINT('Ctrl Pts',(10.4836306292415,46.0883940474237,20.));
#93587=CARTESIAN_POINT('Ctrl Pts',(10.5152070128592,46.0781306279792,0.));
#93588=CARTESIAN_POINT('Ctrl Pts',(10.5152070128592,46.0781306279792,20.));
#93589=CARTESIAN_POINT('Ctrl Pts',(10.5467751464457,46.0678454648793,0.));
#93590=CARTESIAN_POINT('Ctrl Pts',(10.5467751464457,46.0678454648793,20.));
#93591=CARTESIAN_POINT('Ctrl Pts',(10.5783350148187,46.0575385639878,0.));
#93592=CARTESIAN_POINT('Ctrl Pts',(10.5783350148187,46.0575385639878,20.));
#93593=CARTESIAN_POINT('Ctrl Pts',(10.6098866028001,46.0472099311799,0.));
#93594=CARTESIAN_POINT('Ctrl Pts',(10.6098866028001,46.0472099311799,20.));
#93595=CARTESIAN_POINT('Ctrl Pts',(10.6414298952151,46.0368595723418,0.));
#93596=CARTESIAN_POINT('Ctrl Pts',(10.6414298952151,46.0368595723418,20.));
#93597=CARTESIAN_POINT('Ctrl Pts',(10.6729648768932,46.0264874933706,0.));
#93598=CARTESIAN_POINT('Ctrl Pts',(10.6729648768932,46.0264874933706,20.));
#93599=CARTESIAN_POINT('Ctrl Pts',(10.7044915326674,46.0160937001747,0.));
#93600=CARTESIAN_POINT('Ctrl Pts',(10.7044915326674,46.0160937001747,20.));
#93601=CARTESIAN_POINT('Ctrl Pts',(10.7360098473747,46.0056781986726,0.));
#93602=CARTESIAN_POINT('Ctrl Pts',(10.7360098473747,46.0056781986726,20.));
#93603=CARTESIAN_POINT('Ctrl Pts',(10.7675198058554,45.9952409947932,0.));
#93604=CARTESIAN_POINT('Ctrl Pts',(10.7675198058554,45.9952409947932,20.));
#93605=CARTESIAN_POINT('Ctrl Pts',(10.7990213929536,45.9847820944759,0.));
#93606=CARTESIAN_POINT('Ctrl Pts',(10.7990213929536,45.9847820944759,20.));
#93607=CARTESIAN_POINT('Ctrl Pts',(10.8305145935168,45.9743015036702,0.));
#93608=CARTESIAN_POINT('Ctrl Pts',(10.8305145935168,45.9743015036702,20.));
#93609=CARTESIAN_POINT('Ctrl Pts',(10.8619993923966,45.9637992283368,0.));
#93610=CARTESIAN_POINT('Ctrl Pts',(10.8619993923966,45.9637992283368,20.));
#93611=CARTESIAN_POINT('Ctrl Pts',(10.8934757744485,45.9532752744476,0.));
#93612=CARTESIAN_POINT('Ctrl Pts',(10.8934757744485,45.9532752744476,20.));
#93613=CARTESIAN_POINT('Ctrl Pts',(10.9249437245321,45.9427296479861,0.));
#93614=CARTESIAN_POINT('Ctrl Pts',(10.9249437245321,45.9427296479861,20.));
#93615=CARTESIAN_POINT('Ctrl Pts',(10.9564032275107,45.9321623549466,0.));
#93616=CARTESIAN_POINT('Ctrl Pts',(10.9564032275107,45.9321623549466,20.));
#93617=CARTESIAN_POINT('Ctrl Pts',(10.9878542682513,45.9215734013338,0.));
#93618=CARTESIAN_POINT('Ctrl Pts',(10.9878542682513,45.9215734013338,20.));
#93619=CARTESIAN_POINT('Ctrl Pts',(11.0192968316246,45.9109627931629,0.));
#93620=CARTESIAN_POINT('Ctrl Pts',(11.0192968316246,45.9109627931629,20.));
#93621=CARTESIAN_POINT('Ctrl Pts',(11.0507309025052,45.9003305364593,0.));
#93622=CARTESIAN_POINT('Ctrl Pts',(11.0507309025052,45.9003305364593,20.));
#93623=CARTESIAN_POINT('Ctrl Pts',(11.0821564657716,45.8896766372596,0.));
#93624=CARTESIAN_POINT('Ctrl Pts',(11.0821564657716,45.8896766372596,20.));
#93625=CARTESIAN_POINT('Ctrl Pts',(11.1135735063059,45.8790011016108,0.));
#93626=CARTESIAN_POINT('Ctrl Pts',(11.1135735063059,45.8790011016108,20.));
#93627=CARTESIAN_POINT('Ctrl Pts',(11.1449820089942,45.868303935571,0.));
#93628=CARTESIAN_POINT('Ctrl Pts',(11.1449820089942,45.868303935571,20.));
#93629=CARTESIAN_POINT('Ctrl Pts',(11.1763819587262,45.8575851452088,0.));
#93630=CARTESIAN_POINT('Ctrl Pts',(11.1763819587262,45.8575851452088,20.));
#93631=CARTESIAN_POINT('Ctrl Pts',(11.2077733403959,45.8468447366038,0.));
#93632=CARTESIAN_POINT('Ctrl Pts',(11.2077733403959,45.8468447366038,20.));
#93633=CARTESIAN_POINT('Ctrl Pts',(11.2391561389011,45.8360827158468,0.));
#93634=CARTESIAN_POINT('Ctrl Pts',(11.2391561389011,45.8360827158468,20.));
#93635=CARTESIAN_POINT('Ctrl Pts',(11.2705303391434,45.8252990890386,0.));
#93636=CARTESIAN_POINT('Ctrl Pts',(11.2705303391434,45.8252990890386,20.));
#93637=CARTESIAN_POINT('Ctrl Pts',(11.3018959260282,45.8144938622913,0.));
#93638=CARTESIAN_POINT('Ctrl Pts',(11.3018959260282,45.8144938622913,20.));
#93639=CARTESIAN_POINT('Ctrl Pts',(11.3332528844652,45.8036670417272,0.));
#93640=CARTESIAN_POINT('Ctrl Pts',(11.3332528844652,45.8036670417272,20.));
#93641=CARTESIAN_POINT('Ctrl Pts',(11.3646011993673,45.7928186334791,0.));
#93642=CARTESIAN_POINT('Ctrl Pts',(11.3646011993673,45.7928186334791,20.));
#93643=CARTESIAN_POINT('Ctrl Pts',(11.395940855652,45.7819486436912,0.));
#93644=CARTESIAN_POINT('Ctrl Pts',(11.395940855652,45.7819486436912,20.));
#93645=CARTESIAN_POINT('Ctrl Pts',(11.4272718382403,45.7710570785186,0.));
#93646=CARTESIAN_POINT('Ctrl Pts',(11.4272718382403,45.7710570785186,20.));
#93647=CARTESIAN_POINT('Ctrl Pts',(11.4585941320574,45.760143944127,0.));
#93648=CARTESIAN_POINT('Ctrl Pts',(11.4585941320574,45.760143944127,20.));
#93649=CARTESIAN_POINT('Ctrl Pts',(11.489907722032,45.7492092466918,0.));
#93650=CARTESIAN_POINT('Ctrl Pts',(11.489907722032,45.7492092466918,20.));
#93651=CARTESIAN_POINT('Ctrl Pts',(11.5212125930966,45.7382529923996,0.));
#93652=CARTESIAN_POINT('Ctrl Pts',(11.5212125930966,45.7382529923996,20.));
#93653=CARTESIAN_POINT('Ctrl Pts',(11.5525087301884,45.7272751874478,0.));
#93654=CARTESIAN_POINT('Ctrl Pts',(11.5525087301884,45.7272751874478,20.));
#93655=CARTESIAN_POINT('Ctrl Pts',(11.5837961182481,45.7162758380449,0.));
#93656=CARTESIAN_POINT('Ctrl Pts',(11.5837961182481,45.7162758380449,20.));
#93657=CARTESIAN_POINT('Ctrl Pts',(11.6150747422209,45.7052549504103,0.));
#93658=CARTESIAN_POINT('Ctrl Pts',(11.6150747422209,45.7052549504103,20.));
#93659=CARTESIAN_POINT('Ctrl Pts',(11.6463445870557,45.694212530774,0.));
#93660=CARTESIAN_POINT('Ctrl Pts',(11.6463445870557,45.694212530774,20.));
#93661=CARTESIAN_POINT('Ctrl Pts',(11.6776056377055,45.6831485853771,0.));
#93662=CARTESIAN_POINT('Ctrl Pts',(11.6776056377055,45.6831485853771,20.));
#93663=CARTESIAN_POINT('Ctrl Pts',(11.7088578791266,45.6720631204703,0.));
#93664=CARTESIAN_POINT('Ctrl Pts',(11.7088578791266,45.6720631204703,20.));
#93665=CARTESIAN_POINT('Ctrl Pts',(11.7401012962797,45.6609561423149,0.));
#93666=CARTESIAN_POINT('Ctrl Pts',(11.7401012962797,45.6609561423149,20.));
#93667=CARTESIAN_POINT('Ctrl Pts',(11.7713358741292,45.6498276571829,0.));
#93668=CARTESIAN_POINT('Ctrl Pts',(11.7713358741292,45.6498276571829,20.));
#93669=CARTESIAN_POINT('Ctrl Pts',(11.8025615976441,45.6386776713575,0.));
#93670=CARTESIAN_POINT('Ctrl Pts',(11.8025615976441,45.6386776713575,20.));
#93671=CARTESIAN_POINT('Ctrl Pts',(11.8337784517972,45.627506191133,0.));
#93672=CARTESIAN_POINT('Ctrl Pts',(11.8337784517972,45.627506191133,20.));
#93673=CARTESIAN_POINT('Ctrl Pts',(11.8649864215653,45.6163132228138,0.));
#93674=CARTESIAN_POINT('Ctrl Pts',(11.8649864215653,45.6163132228138,20.));
#93675=CARTESIAN_POINT('Ctrl Pts',(11.8961854919293,45.6050987727153,0.));
#93676=CARTESIAN_POINT('Ctrl Pts',(11.8961854919293,45.6050987727153,20.));
#93677=CARTESIAN_POINT('Ctrl Pts',(11.9273756478741,45.5938628471638,0.));
#93678=CARTESIAN_POINT('Ctrl Pts',(11.9273756478741,45.5938628471638,20.));
#93679=CARTESIAN_POINT('Ctrl Pts',(11.9585568743886,45.5826054524963,0.));
#93680=CARTESIAN_POINT('Ctrl Pts',(11.9585568743886,45.5826054524963,20.));
#93681=CARTESIAN_POINT('Ctrl Pts',(11.989729156466,45.5713265950605,0.));
#93682=CARTESIAN_POINT('Ctrl Pts',(11.989729156466,45.5713265950605,20.));
#93683=CARTESIAN_POINT('Ctrl Pts',(12.0208924791034,45.5600262812144,0.));
#93684=CARTESIAN_POINT('Ctrl Pts',(12.0208924791034,45.5600262812144,20.));
#93685=CARTESIAN_POINT('Ctrl Pts',(12.0520468273019,45.5487045173265,0.));
#93686=CARTESIAN_POINT('Ctrl Pts',(12.0520468273019,45.5487045173265,20.));
#93687=CARTESIAN_POINT('Ctrl Pts',(12.0831921860665,45.5373613097755,0.));
#93688=CARTESIAN_POINT('Ctrl Pts',(12.0831921860665,45.5373613097755,20.));
#93689=CARTESIAN_POINT('Ctrl Pts',(12.1143285404065,45.5259966649516,0.));
#93690=CARTESIAN_POINT('Ctrl Pts',(12.1143285404065,45.5259966649516,20.));
#93691=CARTESIAN_POINT('Ctrl Pts',(12.1454558753351,45.5146105892553,0.));
#93692=CARTESIAN_POINT('Ctrl Pts',(12.1454558753351,45.5146105892553,20.));
#93693=CARTESIAN_POINT('Ctrl Pts',(12.1765741758697,45.5032030890978,0.));
#93694=CARTESIAN_POINT('Ctrl Pts',(12.1765741758697,45.5032030890978,20.));
#93695=CARTESIAN_POINT('Ctrl Pts',(12.2076834270323,45.4917741709015,0.));
#93696=CARTESIAN_POINT('Ctrl Pts',(12.2076834270323,45.4917741709015,20.));
#93697=CARTESIAN_POINT('Ctrl Pts',(12.2387836138487,45.4803238410999,0.));
#93698=CARTESIAN_POINT('Ctrl Pts',(12.2387836138487,45.4803238410999,20.));
#93699=CARTESIAN_POINT('Ctrl Pts',(12.269874721349,45.4688521061371,0.));
#93700=CARTESIAN_POINT('Ctrl Pts',(12.269874721349,45.4688521061371,20.));
#93701=CARTESIAN_POINT('Ctrl Pts',(12.3009567345673,45.4573589724673,0.));
#93702=CARTESIAN_POINT('Ctrl Pts',(12.3009567345673,45.4573589724673,20.));
#93703=CARTESIAN_POINT('Ctrl Pts',(12.3320296385417,45.4458444465552,0.));
#93704=CARTESIAN_POINT('Ctrl Pts',(12.3320296385417,45.4458444465552,20.));
#93705=CARTESIAN_POINT('Ctrl Pts',(12.3630934183142,45.4343085348755,0.));
#93706=CARTESIAN_POINT('Ctrl Pts',(12.3630934183142,45.4343085348755,20.));
#93707=CARTESIAN_POINT('Ctrl Pts',(12.3941480589311,45.4227512439136,0.));
#93708=CARTESIAN_POINT('Ctrl Pts',(12.3941480589311,45.4227512439136,20.));
#93709=CARTESIAN_POINT('Ctrl Pts',(12.4251935454428,45.4111725801659,0.));
#93710=CARTESIAN_POINT('Ctrl Pts',(12.4251935454428,45.4111725801659,20.));
#93711=CARTESIAN_POINT('Ctrl Pts',(12.4562298629045,45.3995725501402,0.));
#93712=CARTESIAN_POINT('Ctrl Pts',(12.4562298629045,45.3995725501402,20.));
#93713=CARTESIAN_POINT('Ctrl Pts',(12.4872569963754,45.3879511603549,0.));
#93714=CARTESIAN_POINT('Ctrl Pts',(12.4872569963754,45.3879511603549,20.));
#93715=CARTESIAN_POINT('Ctrl Pts',(12.5182749309189,45.376308417339,0.));
#93716=CARTESIAN_POINT('Ctrl Pts',(12.5182749309189,45.376308417339,20.));
#93717=CARTESIAN_POINT('Ctrl Pts',(12.5492836516023,45.364644327632,0.));
#93718=CARTESIAN_POINT('Ctrl Pts',(12.5492836516023,45.364644327632,20.));
#93719=CARTESIAN_POINT('Ctrl Pts',(12.5802831434966,45.3529588977839,0.));
#93720=CARTESIAN_POINT('Ctrl Pts',(12.5802831434966,45.3529588977839,20.));
#93721=CARTESIAN_POINT('Ctrl Pts',(12.6112733916776,45.3412521343551,0.));
#93722=CARTESIAN_POINT('Ctrl Pts',(12.6112733916776,45.3412521343551,20.));
#93723=CARTESIAN_POINT('Ctrl Pts',(12.6422543812251,45.3295240439169,0.));
#93724=CARTESIAN_POINT('Ctrl Pts',(12.6422543812251,45.3295240439169,20.));
#93725=CARTESIAN_POINT('Ctrl Pts',(12.6732260972239,45.3177746330512,0.));
#93726=CARTESIAN_POINT('Ctrl Pts',(12.6732260972239,45.3177746330512,20.));
#93727=CARTESIAN_POINT('Ctrl Pts',(12.7041885247626,45.3060039083501,0.));
#93728=CARTESIAN_POINT('Ctrl Pts',(12.7041885247626,45.3060039083501,20.));
#93729=CARTESIAN_POINT('Ctrl Pts',(12.7351416489341,45.2942118764167,0.));
#93730=CARTESIAN_POINT('Ctrl Pts',(12.7351416489341,45.2942118764167,20.));
#93731=CARTESIAN_POINT('Ctrl Pts',(12.7660854548354,45.2823985438647,0.));
#93732=CARTESIAN_POINT('Ctrl Pts',(12.7660854548354,45.2823985438647,20.));
#93733=CARTESIAN_POINT('Ctrl Pts',(12.7970199275678,45.2705639173192,0.));
#93734=CARTESIAN_POINT('Ctrl Pts',(12.7970199275678,45.2705639173192,20.));
#93735=CARTESIAN_POINT('Ctrl Pts',(12.8279450522365,45.2587080034157,0.));
#93736=CARTESIAN_POINT('Ctrl Pts',(12.8279450522365,45.2587080034157,20.));
#93737=CARTESIAN_POINT('Ctrl Pts',(12.8588608139512,45.2468308087994,0.));
#93738=CARTESIAN_POINT('Ctrl Pts',(12.8588608139512,45.2468308087994,20.));
#93739=CARTESIAN_POINT('Ctrl Pts',(12.8897671978256,45.2349323401259,0.));
#93740=CARTESIAN_POINT('Ctrl Pts',(12.8897671978256,45.2349323401259,20.));
#93741=CARTESIAN_POINT('Ctrl Pts',(12.9206641889781,45.2230126040617,0.));
#93742=CARTESIAN_POINT('Ctrl Pts',(12.9206641889781,45.2230126040617,20.));
#93743=CARTESIAN_POINT('Ctrl Pts',(12.9515517725313,45.2110716072841,0.));
#93744=CARTESIAN_POINT('Ctrl Pts',(12.9515517725313,45.2110716072841,20.));
#93745=CARTESIAN_POINT('Ctrl Pts',(12.9824299336127,45.199109356482,0.));
#93746=CARTESIAN_POINT('Ctrl Pts',(12.9824299336127,45.199109356482,20.));
#93747=CARTESIAN_POINT('Ctrl Pts',(13.0132986573536,45.1871258583545,0.));
#93748=CARTESIAN_POINT('Ctrl Pts',(13.0132986573536,45.1871258583545,20.));
#93749=CARTESIAN_POINT('Ctrl Pts',(13.0441579288899,45.1751211196118,0.));
#93750=CARTESIAN_POINT('Ctrl Pts',(13.0441579288899,45.1751211196118,20.));
#93751=CARTESIAN_POINT('Ctrl Pts',(13.0750077333613,45.1630951469734,0.));
#93752=CARTESIAN_POINT('Ctrl Pts',(13.0750077333613,45.1630951469734,20.));
#93753=CARTESIAN_POINT('Ctrl Pts',(13.105848055912,45.1510479471692,0.));
#93754=CARTESIAN_POINT('Ctrl Pts',(13.105848055912,45.1510479471692,20.));
#93755=CARTESIAN_POINT('Ctrl Pts',(13.1366788816904,45.1389795269399,0.));
#93756=CARTESIAN_POINT('Ctrl Pts',(13.1366788816904,45.1389795269399,20.));
#93757=CARTESIAN_POINT('Ctrl Pts',(13.1675001958492,45.1268898930368,0.));
#93758=CARTESIAN_POINT('Ctrl Pts',(13.1675001958492,45.1268898930368,20.));
#93759=CARTESIAN_POINT('Ctrl Pts',(13.198311983546,45.114779052223,0.));
#93760=CARTESIAN_POINT('Ctrl Pts',(13.198311983546,45.114779052223,20.));
#93761=CARTESIAN_POINT('Ctrl Pts',(13.2291142299426,45.1026470112717,0.));
#93762=CARTESIAN_POINT('Ctrl Pts',(13.2291142299426,45.1026470112717,20.));
#93763=CARTESIAN_POINT('Ctrl Pts',(13.259906920205,45.0904937769663,0.));
#93764=CARTESIAN_POINT('Ctrl Pts',(13.259906920205,45.0904937769663,20.));
#93765=CARTESIAN_POINT('Ctrl Pts',(13.2906900395037,45.0783193561008,0.));
#93766=CARTESIAN_POINT('Ctrl Pts',(13.2906900395037,45.0783193561008,20.));
#93767=CARTESIAN_POINT('Ctrl Pts',(13.3214635730135,45.0661237554798,0.));
#93768=CARTESIAN_POINT('Ctrl Pts',(13.3214635730135,45.0661237554798,20.));
#93769=CARTESIAN_POINT('Ctrl Pts',(13.3522275059137,45.0539069819185,0.));
#93770=CARTESIAN_POINT('Ctrl Pts',(13.3522275059137,45.0539069819185,20.));
#93771=CARTESIAN_POINT('Ctrl Pts',(13.3829818233878,45.0416690422424,0.));
#93772=CARTESIAN_POINT('Ctrl Pts',(13.3829818233878,45.0416690422424,20.));
#93773=CARTESIAN_POINT('Ctrl Pts',(13.4137265106238,45.029409943288,0.));
#93774=CARTESIAN_POINT('Ctrl Pts',(13.4137265106238,45.029409943288,20.));
#93775=CARTESIAN_POINT('Ctrl Pts',(13.4444615528144,45.0171296919022,0.));
#93776=CARTESIAN_POINT('Ctrl Pts',(13.4444615528144,45.0171296919022,20.));
#93777=CARTESIAN_POINT('Ctrl Pts',(13.4751869351564,45.0048282949433,0.));
#93778=CARTESIAN_POINT('Ctrl Pts',(13.4751869351564,45.0048282949433,20.));
#93779=CARTESIAN_POINT('Ctrl Pts',(13.5059026428512,44.9925057592796,0.));
#93780=CARTESIAN_POINT('Ctrl Pts',(13.5059026428512,44.9925057592796,20.));
#93781=CARTESIAN_POINT('Ctrl Pts',(13.5366086611044,44.9801620917891,0.));
#93782=CARTESIAN_POINT('Ctrl Pts',(13.5366086611044,44.9801620917891,20.));
#93783=CARTESIAN_POINT('Ctrl Pts',(13.5673049751264,44.967797299361,0.));
#93784=CARTESIAN_POINT('Ctrl Pts',(13.5673049751264,44.967797299361,20.));
#93785=CARTESIAN_POINT('Ctrl Pts',(13.5979915701319,44.955411388895,0.));
#93786=CARTESIAN_POINT('Ctrl Pts',(13.5979915701319,44.955411388895,20.));
#93787=CARTESIAN_POINT('Ctrl Pts',(13.6286684313401,44.9430043673018,0.));
#93788=CARTESIAN_POINT('Ctrl Pts',(13.6286684313401,44.9430043673018,20.));
#93789=CARTESIAN_POINT('Ctrl Pts',(13.6593355439745,44.930576241502,0.));
#93790=CARTESIAN_POINT('Ctrl Pts',(13.6593355439745,44.930576241502,20.));
#93791=CARTESIAN_POINT('Ctrl Pts',(13.6899928932632,44.9181270184275,0.));
#93792=CARTESIAN_POINT('Ctrl Pts',(13.6899928932632,44.9181270184275,20.));
#93793=CARTESIAN_POINT('Ctrl Pts',(13.7206404644388,44.9056567050204,0.));
#93794=CARTESIAN_POINT('Ctrl Pts',(13.7206404644388,44.9056567050204,20.));
#93795=CARTESIAN_POINT('Ctrl Pts',(13.7512782427386,44.8931653082334,0.));
#93796=CARTESIAN_POINT('Ctrl Pts',(13.7512782427386,44.8931653082334,20.));
#93797=CARTESIAN_POINT('Ctrl Pts',(13.7819062134042,44.8806528350291,0.));
#93798=CARTESIAN_POINT('Ctrl Pts',(13.7819062134042,44.8806528350291,20.));
#93799=CARTESIAN_POINT('Ctrl Pts',(13.8125243616816,44.8681192923811,0.));
#93800=CARTESIAN_POINT('Ctrl Pts',(13.8125243616816,44.8681192923811,20.));
#93801=CARTESIAN_POINT('Ctrl Pts',(13.8431326728214,44.8555646872732,0.));
#93802=CARTESIAN_POINT('Ctrl Pts',(13.8431326728214,44.8555646872732,20.));
#93803=CARTESIAN_POINT('Ctrl Pts',(13.8737311320789,44.8429890267007,0.));
#93804=CARTESIAN_POINT('Ctrl Pts',(13.8737311320789,44.8429890267007,20.));
#93805=CARTESIAN_POINT('Ctrl Pts',(13.9043197247138,44.8303923176691,0.));
#93806=CARTESIAN_POINT('Ctrl Pts',(13.9043197247138,44.8303923176691,20.));
#93807=CARTESIAN_POINT('Ctrl Pts',(13.9348984359903,44.8177745671945,0.));
#93808=CARTESIAN_POINT('Ctrl Pts',(13.9348984359903,44.8177745671945,20.));
#93809=CARTESIAN_POINT('Ctrl Pts',(13.9654672511774,44.8051357823031,0.));
#93810=CARTESIAN_POINT('Ctrl Pts',(13.9654672511774,44.8051357823031,20.));
#93811=CARTESIAN_POINT('Ctrl Pts',(13.9960261555481,44.7924759700314,0.));
#93812=CARTESIAN_POINT('Ctrl Pts',(13.9960261555481,44.7924759700314,20.));
#93813=CARTESIAN_POINT('Ctrl Pts',(14.0265751343805,44.7797951374262,0.));
#93814=CARTESIAN_POINT('Ctrl Pts',(14.0265751343805,44.7797951374262,20.));
#93815=CARTESIAN_POINT('Ctrl Pts',(14.057114172957,44.7670932915455,0.));
#93816=CARTESIAN_POINT('Ctrl Pts',(14.057114172957,44.7670932915455,20.));
#93817=CARTESIAN_POINT('Ctrl Pts',(14.0876432565649,44.7543704394583,0.));
#93818=CARTESIAN_POINT('Ctrl Pts',(14.0876432565649,44.7543704394583,20.));
#93819=CARTESIAN_POINT('Ctrl Pts',(14.118162370496,44.7416265882443,0.));
#93820=CARTESIAN_POINT('Ctrl Pts',(14.118162370496,44.7416265882443,20.));
#93821=CARTESIAN_POINT('Ctrl Pts',(14.1486715000464,44.728861744993,0.));
#93822=CARTESIAN_POINT('Ctrl Pts',(14.1486715000464,44.728861744993,20.));
#93823=CARTESIAN_POINT('Ctrl Pts',(14.1791706305171,44.7160759168044,0.));
#93824=CARTESIAN_POINT('Ctrl Pts',(14.1791706305171,44.7160759168044,20.));
#93825=CARTESIAN_POINT('Ctrl Pts',(14.2096597472134,44.7032691107881,0.));
#93826=CARTESIAN_POINT('Ctrl Pts',(14.2096597472134,44.7032691107881,20.));
#93827=CARTESIAN_POINT('Ctrl Pts',(14.2401388354454,44.690441334065,0.));
#93828=CARTESIAN_POINT('Ctrl Pts',(14.2401388354454,44.690441334065,20.));
#93829=CARTESIAN_POINT('Ctrl Pts',(14.2706078805279,44.6775925937661,0.));
#93830=CARTESIAN_POINT('Ctrl Pts',(14.2706078805279,44.6775925937661,20.));
#93831=CARTESIAN_POINT('Ctrl Pts',(14.3010668677802,44.6647228970333,0.));
#93832=CARTESIAN_POINT('Ctrl Pts',(14.3010668677802,44.6647228970333,20.));
#93833=CARTESIAN_POINT('Ctrl Pts',(14.3315157825264,44.6518322510194,0.));
#93834=CARTESIAN_POINT('Ctrl Pts',(14.3315157825264,44.6518322510194,20.));
#93835=CARTESIAN_POINT('Ctrl Pts',(14.3619546100951,44.6389206628876,0.));
#93836=CARTESIAN_POINT('Ctrl Pts',(14.3619546100951,44.6389206628876,20.));
#93837=CARTESIAN_POINT('Ctrl Pts',(14.3923833358197,44.6259881398119,0.));
#93838=CARTESIAN_POINT('Ctrl Pts',(14.3923833358197,44.6259881398119,20.));
#93839=CARTESIAN_POINT('Ctrl Pts',(14.4228019450383,44.613034688977,0.));
#93840=CARTESIAN_POINT('Ctrl Pts',(14.4228019450383,44.613034688977,20.));
#93841=CARTESIAN_POINT('Ctrl Pts',(14.4532104230936,44.6000603175775,0.));
#93842=CARTESIAN_POINT('Ctrl Pts',(14.4532104230936,44.6000603175775,20.));
#93843=CARTESIAN_POINT('Ctrl Pts',(14.4836087553332,44.5870650328188,0.));
#93844=CARTESIAN_POINT('Ctrl Pts',(14.4836087553332,44.5870650328188,20.));
#93845=CARTESIAN_POINT('Ctrl Pts',(14.5139969271087,44.5740488419152,0.));
#93846=CARTESIAN_POINT('Ctrl Pts',(14.5139969271087,44.5740488419152,20.));
#93847=CARTESIAN_POINT('Ctrl Pts',(14.5443749237767,44.5610117520915,0.));
#93848=CARTESIAN_POINT('Ctrl Pts',(14.5443749237767,44.5610117520915,20.));
#93849=CARTESIAN_POINT('Ctrl Pts',(14.5747427306988,44.5479537705835,0.));
#93850=CARTESIAN_POINT('Ctrl Pts',(14.5747427306988,44.5479537705835,20.));
#93851=CARTESIAN_POINT('Ctrl Pts',(14.6051003332411,44.5348749046379,0.));
#93852=CARTESIAN_POINT('Ctrl Pts',(14.6051003332411,44.5348749046379,20.));
#93853=CARTESIAN_POINT('Ctrl Pts',(14.6354477167742,44.521775161512,0.));
#93854=CARTESIAN_POINT('Ctrl Pts',(14.6354477167742,44.521775161512,20.));
#93855=CARTESIAN_POINT('Ctrl Pts',(14.6657848666743,44.5086545484757,0.));
#93856=CARTESIAN_POINT('Ctrl Pts',(14.6657848666743,44.5086545484757,20.));
#93857=CARTESIAN_POINT('Ctrl Pts',(14.6961117683217,44.4955130728078,0.));
#93858=CARTESIAN_POINT('Ctrl Pts',(14.6961117683217,44.4955130728078,20.));
#93859=CARTESIAN_POINT('Ctrl Pts',(14.7264284071013,44.4823507417973,0.));
#93860=CARTESIAN_POINT('Ctrl Pts',(14.7264284071013,44.4823507417973,20.));
#93861=CARTESIAN_POINT('Ctrl Pts',(14.7567347684029,44.469167562743,0.));
#93862=CARTESIAN_POINT('Ctrl Pts',(14.7567347684029,44.469167562743,20.));
#93863=CARTESIAN_POINT('Ctrl Pts',(14.7870308376214,44.4559635429545,0.));
#93864=CARTESIAN_POINT('Ctrl Pts',(14.7870308376214,44.4559635429545,20.));
#93865=CARTESIAN_POINT('Ctrl Pts',(14.817316600156,44.4427386897515,0.));
#93866=CARTESIAN_POINT('Ctrl Pts',(14.817316600156,44.4427386897515,20.));
#93867=CARTESIAN_POINT('Ctrl Pts',(14.8475920414107,44.4294930104636,0.));
#93868=CARTESIAN_POINT('Ctrl Pts',(14.8475920414107,44.4294930104636,20.));
#93869=CARTESIAN_POINT('Ctrl Pts',(14.8778571467943,44.416226512431,0.));
#93870=CARTESIAN_POINT('Ctrl Pts',(14.8778571467943,44.416226512431,20.));
#93871=CARTESIAN_POINT('Ctrl Pts',(14.9081119017199,44.4029392030043,0.));
#93872=CARTESIAN_POINT('Ctrl Pts',(14.9081119017199,44.4029392030043,20.));
#93873=CARTESIAN_POINT('Ctrl Pts',(14.9383562916061,44.389631089546,0.));
#93874=CARTESIAN_POINT('Ctrl Pts',(14.9383562916061,44.389631089546,20.));
#93875=CARTESIAN_POINT('Ctrl Pts',(14.9685903018767,44.3763021794296,0.));
#93876=CARTESIAN_POINT('Ctrl Pts',(14.9685903018767,44.3763021794296,20.));
#93877=CARTESIAN_POINT('Ctrl Pts',(14.9988139179602,44.3629524800397,0.));
#93878=CARTESIAN_POINT('Ctrl Pts',(14.9988139179602,44.3629524800397,20.));
#93879=CARTESIAN_POINT('Ctrl Pts',(15.0290271252899,44.3495819987708,0.));
#93880=CARTESIAN_POINT('Ctrl Pts',(15.0290271252899,44.3495819987708,20.));
#93881=CARTESIAN_POINT('Ctrl Pts',(15.0592299093032,44.3361907430254,0.));
#93882=CARTESIAN_POINT('Ctrl Pts',(15.0592299093032,44.3361907430254,20.));
#93883=CARTESIAN_POINT('Ctrl Pts',(15.0894222554424,44.3227787202166,0.));
#93884=CARTESIAN_POINT('Ctrl Pts',(15.0894222554424,44.3227787202166,20.));
#93885=CARTESIAN_POINT('Ctrl Pts',(15.1196041491546,44.3093459377674,0.));
#93886=CARTESIAN_POINT('Ctrl Pts',(15.1196041491546,44.3093459377674,20.));
#93887=CARTESIAN_POINT('Ctrl Pts',(15.1497755758917,44.2958924031118,0.));
#93888=CARTESIAN_POINT('Ctrl Pts',(15.1497755758917,44.2958924031118,20.));
#93889=CARTESIAN_POINT('Ctrl Pts',(15.1799365211113,44.2824181236961,0.));
#93890=CARTESIAN_POINT('Ctrl Pts',(15.1799365211113,44.2824181236961,20.));
#93891=CARTESIAN_POINT('Ctrl Pts',(15.2100869702755,44.2689231069767,0.));
#93892=CARTESIAN_POINT('Ctrl Pts',(15.2100869702755,44.2689231069767,20.));
#93893=CARTESIAN_POINT('Ctrl Pts',(15.2402269088514,44.2554073604206,0.));
#93894=CARTESIAN_POINT('Ctrl Pts',(15.2402269088514,44.2554073604206,20.));
#93895=CARTESIAN_POINT('Ctrl Pts',(15.2703563223108,44.2418708915045,0.));
#93896=CARTESIAN_POINT('Ctrl Pts',(15.2703563223108,44.2418708915045,20.));
#93897=CARTESIAN_POINT('Ctrl Pts',(15.30047519613,44.2283137077152,0.));
#93898=CARTESIAN_POINT('Ctrl Pts',(15.30047519613,44.2283137077152,20.));
#93899=CARTESIAN_POINT('Ctrl Pts',(15.3305835157903,44.2147358165492,0.));
#93900=CARTESIAN_POINT('Ctrl Pts',(15.3305835157903,44.2147358165492,20.));
#93901=CARTESIAN_POINT('Ctrl Pts',(15.3606812667781,44.201137225514,0.));
#93902=CARTESIAN_POINT('Ctrl Pts',(15.3606812667781,44.201137225514,20.));
#93903=CARTESIAN_POINT('Ctrl Pts',(15.390768434585,44.1875179421286,0.));
#93904=CARTESIAN_POINT('Ctrl Pts',(15.390768434585,44.1875179421286,20.));
#93905=CARTESIAN_POINT('Ctrl Pts',(15.4208450047077,44.1738779739225,0.));
#93906=CARTESIAN_POINT('Ctrl Pts',(15.4208450047077,44.1738779739225,20.));
#93907=CARTESIAN_POINT('Ctrl Pts',(15.4509109626472,44.1602173284345,0.));
#93908=CARTESIAN_POINT('Ctrl Pts',(15.4509109626472,44.1602173284345,20.));
#93909=CARTESIAN_POINT('Ctrl Pts',(15.4809662939093,44.146536013213,0.));
#93910=CARTESIAN_POINT('Ctrl Pts',(15.4809662939093,44.146536013213,20.));
#93911=CARTESIAN_POINT('Ctrl Pts',(15.5110109840047,44.1328340358171,0.));
#93912=CARTESIAN_POINT('Ctrl Pts',(15.5110109840047,44.1328340358171,20.));
#93913=CARTESIAN_POINT('Ctrl Pts',(15.5410450184494,44.1191114038164,0.));
#93914=CARTESIAN_POINT('Ctrl Pts',(15.5410450184494,44.1191114038164,20.));
#93915=CARTESIAN_POINT('Ctrl Pts',(15.5710683827645,44.1053681247921,0.));
#93916=CARTESIAN_POINT('Ctrl Pts',(15.5710683827645,44.1053681247921,20.));
#93917=CARTESIAN_POINT('Ctrl Pts',(15.6010810624766,44.0916042063371,0.));
#93918=CARTESIAN_POINT('Ctrl Pts',(15.6010810624766,44.0916042063371,20.));
#93919=CARTESIAN_POINT('Ctrl Pts',(15.6310830431167,44.0778196560536,0.));
#93920=CARTESIAN_POINT('Ctrl Pts',(15.6310830431167,44.0778196560536,20.));
#93921=CARTESIAN_POINT('Ctrl Pts',(15.6610743102207,44.0640144815534,0.));
#93922=CARTESIAN_POINT('Ctrl Pts',(15.6610743102207,44.0640144815534,20.));
#93923=CARTESIAN_POINT('Ctrl Pts',(15.6910548493288,44.050188690457,0.));
#93924=CARTESIAN_POINT('Ctrl Pts',(15.6910548493288,44.050188690457,20.));
#93925=CARTESIAN_POINT('Ctrl Pts',(15.7210246459867,44.0363422903955,0.));
#93926=CARTESIAN_POINT('Ctrl Pts',(15.7210246459867,44.0363422903955,20.));
#93927=CARTESIAN_POINT('Ctrl Pts',(15.7509836857452,44.0224752890112,0.));
#93928=CARTESIAN_POINT('Ctrl Pts',(15.7509836857452,44.0224752890112,20.));
#93929=CARTESIAN_POINT('Ctrl Pts',(15.7809319541601,44.0085876939576,0.));
#93930=CARTESIAN_POINT('Ctrl Pts',(15.7809319541601,44.0085876939576,20.));
#93931=CARTESIAN_POINT('Ctrl Pts',(15.8108694367927,43.9946795128988,0.));
#93932=CARTESIAN_POINT('Ctrl Pts',(15.8108694367927,43.9946795128988,20.));
#93933=CARTESIAN_POINT('Ctrl Pts',(15.8407961192089,43.9807507535097,0.));
#93934=CARTESIAN_POINT('Ctrl Pts',(15.8407961192089,43.9807507535097,20.));
#93935=CARTESIAN_POINT('Ctrl Pts',(15.8707119869797,43.9668014234746,0.));
#93936=CARTESIAN_POINT('Ctrl Pts',(15.8707119869797,43.9668014234746,20.));
#93937=CARTESIAN_POINT('Ctrl Pts',(15.9006170256808,43.9528315304878,0.));
#93938=CARTESIAN_POINT('Ctrl Pts',(15.9006170256808,43.9528315304878,20.));
#93939=CARTESIAN_POINT('Ctrl Pts',(15.9305112208934,43.9388410822542,0.));
#93940=CARTESIAN_POINT('Ctrl Pts',(15.9305112208934,43.9388410822542,20.));
#93941=CARTESIAN_POINT('Ctrl Pts',(15.9603945582034,43.9248300864889,0.));
#93942=CARTESIAN_POINT('Ctrl Pts',(15.9603945582034,43.9248300864889,20.));
#93943=CARTESIAN_POINT('Ctrl Pts',(15.9902670232019,43.9107985509168,0.));
#93944=CARTESIAN_POINT('Ctrl Pts',(15.9902670232019,43.9107985509168,20.));
#93945=CARTESIAN_POINT('Ctrl Pts',(16.0201286014849,43.896746483274,0.));
#93946=CARTESIAN_POINT('Ctrl Pts',(16.0201286014849,43.896746483274,20.));
#93947=CARTESIAN_POINT('Ctrl Pts',(16.0499792786541,43.8826738913074,0.));
#93948=CARTESIAN_POINT('Ctrl Pts',(16.0499792786541,43.8826738913074,20.));
#93949=CARTESIAN_POINT('Ctrl Pts',(16.0798190403159,43.8685807827745,0.));
#93950=CARTESIAN_POINT('Ctrl Pts',(16.0798190403159,43.8685807827745,20.));
#93951=CARTESIAN_POINT('Ctrl Pts',(16.1096478720818,43.854467165442,0.));
#93952=CARTESIAN_POINT('Ctrl Pts',(16.1096478720818,43.854467165442,20.));
#93953=CARTESIAN_POINT('Ctrl Pts',(16.1394657595683,43.8403330470868,0.));
#93954=CARTESIAN_POINT('Ctrl Pts',(16.1394657595683,43.8403330470868,20.));
#93955=CARTESIAN_POINT('Ctrl Pts',(16.1692726883968,43.8261784354962,0.));
#93956=CARTESIAN_POINT('Ctrl Pts',(16.1692726883968,43.8261784354962,20.));
#93957=CARTESIAN_POINT('Ctrl Pts',(16.199068644194,43.8120033384679,0.));
#93958=CARTESIAN_POINT('Ctrl Pts',(16.199068644194,43.8120033384679,20.));
#93959=CARTESIAN_POINT('Ctrl Pts',(16.2288536125916,43.7978077638098,0.));
#93960=CARTESIAN_POINT('Ctrl Pts',(16.2288536125916,43.7978077638098,20.));
#93961=CARTESIAN_POINT('Ctrl Pts',(16.2586275792268,43.7835917193404,0.));
#93962=CARTESIAN_POINT('Ctrl Pts',(16.2586275792268,43.7835917193404,20.));
#93963=CARTESIAN_POINT('Ctrl Pts',(16.2883905297415,43.7693552128887,0.));
#93964=CARTESIAN_POINT('Ctrl Pts',(16.2883905297415,43.7693552128887,20.));
#93965=CARTESIAN_POINT('Ctrl Pts',(16.3181424497834,43.7550982522947,0.));
#93966=CARTESIAN_POINT('Ctrl Pts',(16.3181424497834,43.7550982522947,20.));
#93967=CARTESIAN_POINT('Ctrl Pts',(16.3478833250055,43.7408208454089,0.));
#93968=CARTESIAN_POINT('Ctrl Pts',(16.3478833250055,43.7408208454089,20.));
#93969=CARTESIAN_POINT('Ctrl Pts',(16.3776131410651,43.7265230000909,0.));
#93970=CARTESIAN_POINT('Ctrl Pts',(16.3776131410651,43.7265230000909,20.));
#93971=CARTESIAN_POINT('Ctrl Pts',(16.4073318836249,43.7122047242097,0.));
#93972=CARTESIAN_POINT('Ctrl Pts',(16.4073318836249,43.7122047242097,20.));
#93973=CARTESIAN_POINT('Ctrl Pts',(16.4370395383523,43.6978660256455,0.));
#93974=CARTESIAN_POINT('Ctrl Pts',(16.4370395383523,43.6978660256455,20.));
#93975=CARTESIAN_POINT('Ctrl Pts',(16.4667360909206,43.6835069122887,0.));
#93976=CARTESIAN_POINT('Ctrl Pts',(16.4667360909206,43.6835069122887,20.));
#93977=CARTESIAN_POINT('Ctrl Pts',(16.4964215270082,43.6691273920409,0.));
#93978=CARTESIAN_POINT('Ctrl Pts',(16.4964215270082,43.6691273920409,20.));
#93979=CARTESIAN_POINT('Ctrl Pts',(16.5260958322991,43.6547274728139,0.));
#93980=CARTESIAN_POINT('Ctrl Pts',(16.5260958322991,43.6547274728139,20.));
#93981=CARTESIAN_POINT('Ctrl Pts',(16.5557589924819,43.640307162529,0.));
#93982=CARTESIAN_POINT('Ctrl Pts',(16.5557589924819,43.640307162529,20.));
#93983=CARTESIAN_POINT('Ctrl Pts',(16.5854109932504,43.6258664691173,0.));
#93984=CARTESIAN_POINT('Ctrl Pts',(16.5854109932504,43.6258664691173,20.));
#93985=CARTESIAN_POINT('Ctrl Pts',(16.6150518203036,43.6114054005208,0.));
#93986=CARTESIAN_POINT('Ctrl Pts',(16.6150518203036,43.6114054005208,20.));
#93987=CARTESIAN_POINT('Ctrl Pts',(16.6446814593458,43.5969239646926,0.));
#93988=CARTESIAN_POINT('Ctrl Pts',(16.6446814593458,43.5969239646926,20.));
#93989=CARTESIAN_POINT('Ctrl Pts',(16.6742998960869,43.5824221695961,0.));
#93990=CARTESIAN_POINT('Ctrl Pts',(16.6742998960869,43.5824221695961,20.));
#93991=CARTESIAN_POINT('Ctrl Pts',(16.7039071162413,43.5679000232041,0.));
#93992=CARTESIAN_POINT('Ctrl Pts',(16.7039071162413,43.5679000232041,20.));
#93993=CARTESIAN_POINT('Ctrl Pts',(16.7335031055294,43.5533575334996,0.));
#93994=CARTESIAN_POINT('Ctrl Pts',(16.7335031055294,43.5533575334996,20.));
#93995=CARTESIAN_POINT('Ctrl Pts',(16.7630878496767,43.5387947084755,0.));
#93996=CARTESIAN_POINT('Ctrl Pts',(16.7630878496767,43.5387947084755,20.));
#93997=CARTESIAN_POINT('Ctrl Pts',(16.792661334414,43.5242115561352,0.));
#93998=CARTESIAN_POINT('Ctrl Pts',(16.792661334414,43.5242115561352,20.));
#93999=CARTESIAN_POINT('Ctrl Pts',(16.8222235454772,43.5096080844922,0.));
#94000=CARTESIAN_POINT('Ctrl Pts',(16.8222235454772,43.5096080844922,20.));
#94001=CARTESIAN_POINT('Ctrl Pts',(16.8517744686076,43.4949843015709,0.));
#94002=CARTESIAN_POINT('Ctrl Pts',(16.8517744686076,43.4949843015709,20.));
#94003=CARTESIAN_POINT('Ctrl Pts',(16.8813140895513,43.4803402154062,0.));
#94004=CARTESIAN_POINT('Ctrl Pts',(16.8813140895513,43.4803402154062,20.));
#94005=CARTESIAN_POINT('Ctrl Pts',(16.91084239406,43.4656758340435,0.));
#94006=CARTESIAN_POINT('Ctrl Pts',(16.91084239406,43.4656758340435,20.));
#94007=CARTESIAN_POINT('Ctrl Pts',(16.9403593678908,43.4509911655382,0.));
#94008=CARTESIAN_POINT('Ctrl Pts',(16.9403593678908,43.4509911655382,20.));
#94009=CARTESIAN_POINT('Ctrl Pts',(16.9698649968061,43.4362862179557,0.));
#94010=CARTESIAN_POINT('Ctrl Pts',(16.9698649968061,43.4362862179557,20.));
#94011=CARTESIAN_POINT('Ctrl Pts',(16.9993592665737,43.4215609993712,0.));
#94012=CARTESIAN_POINT('Ctrl Pts',(16.9993592665737,43.4215609993712,20.));
#94013=CARTESIAN_POINT('Ctrl Pts',(17.0288421629666,43.4068155178696,0.));
#94014=CARTESIAN_POINT('Ctrl Pts',(17.0288421629666,43.4068155178696,20.));
#94015=CARTESIAN_POINT('Ctrl Pts',(17.0583136717632,43.3920497815463,0.));
#94016=CARTESIAN_POINT('Ctrl Pts',(17.0583136717632,43.3920497815463,20.));
#94017=CARTESIAN_POINT('Ctrl Pts',(17.0877737787472,43.3772637985072,0.));
#94018=CARTESIAN_POINT('Ctrl Pts',(17.0877737787472,43.3772637985072,20.));
#94019=CARTESIAN_POINT('Ctrl Pts',(17.1172224697079,43.3624575768695,0.));
#94020=CARTESIAN_POINT('Ctrl Pts',(17.1172224697079,43.3624575768695,20.));
#94021=CARTESIAN_POINT('Ctrl Pts',(17.1466597304397,43.3476311247602,0.));
#94022=CARTESIAN_POINT('Ctrl Pts',(17.1466597304397,43.3476311247602,20.));
#94023=CARTESIAN_POINT('Ctrl Pts',(17.1760855467426,43.332784450317,0.));
#94024=CARTESIAN_POINT('Ctrl Pts',(17.1760855467426,43.332784450317,20.));
#94025=CARTESIAN_POINT('Ctrl Pts',(17.2054999044212,43.3179175616862,0.));
#94026=CARTESIAN_POINT('Ctrl Pts',(17.2054999044212,43.3179175616862,20.));
#94027=CARTESIAN_POINT('Ctrl Pts',(17.2349027892859,43.3030304670242,0.));
#94028=CARTESIAN_POINT('Ctrl Pts',(17.2349027892859,43.3030304670242,20.));
#94029=CARTESIAN_POINT('Ctrl Pts',(17.2642941871522,43.2881231744974,0.));
#94030=CARTESIAN_POINT('Ctrl Pts',(17.2642941871522,43.2881231744974,20.));
#94031=CARTESIAN_POINT('Ctrl Pts',(17.2936740838416,43.2731956922839,0.));
#94032=CARTESIAN_POINT('Ctrl Pts',(17.2936740838416,43.2731956922839,20.));
#94033=CARTESIAN_POINT('Ctrl Pts',(17.3230424651811,43.258248028572,0.));
#94034=CARTESIAN_POINT('Ctrl Pts',(17.3230424651811,43.258248028572,20.));
#94035=CARTESIAN_POINT('Ctrl Pts',(17.352399317003,43.2432801915607,0.));
#94036=CARTESIAN_POINT('Ctrl Pts',(17.352399317003,43.2432801915607,20.));
#94037=CARTESIAN_POINT('Ctrl Pts',(17.3817446251452,43.2282921894589,0.));
#94038=CARTESIAN_POINT('Ctrl Pts',(17.3817446251452,43.2282921894589,20.));
#94039=CARTESIAN_POINT('Ctrl Pts',(17.4110783754507,43.2132840304854,0.));
#94040=CARTESIAN_POINT('Ctrl Pts',(17.4110783754507,43.2132840304854,20.));
#94041=CARTESIAN_POINT('Ctrl Pts',(17.4404005537678,43.1982557228684,0.));
#94042=CARTESIAN_POINT('Ctrl Pts',(17.4404005537678,43.1982557228684,20.));
#94043=CARTESIAN_POINT('Ctrl Pts',(17.46971114595,43.1832072748459,0.));
#94044=CARTESIAN_POINT('Ctrl Pts',(17.46971114595,43.1832072748459,20.));
#94045=CARTESIAN_POINT('Ctrl Pts',(17.4990101378563,43.1681386946662,0.));
#94046=CARTESIAN_POINT('Ctrl Pts',(17.4990101378563,43.1681386946662,20.));
#94047=CARTESIAN_POINT('Ctrl Pts',(17.5282975153509,43.1530499905879,0.));
#94048=CARTESIAN_POINT('Ctrl Pts',(17.5282975153509,43.1530499905879,20.));
#94049=CARTESIAN_POINT('Ctrl Pts',(17.557573264304,43.1379411708804,0.));
#94050=CARTESIAN_POINT('Ctrl Pts',(17.557573264304,43.1379411708804,20.));
#94051=CARTESIAN_POINT('Ctrl Pts',(17.5868373705916,43.122812243824,0.));
#94052=CARTESIAN_POINT('Ctrl Pts',(17.5868373705916,43.122812243824,20.));
#94053=CARTESIAN_POINT('Ctrl Pts',(17.6160898200949,43.1076632177089,0.));
#94054=CARTESIAN_POINT('Ctrl Pts',(17.6160898200949,43.1076632177089,20.));
#94055=CARTESIAN_POINT('Ctrl Pts',(17.645330598701,43.0924941008354,0.));
#94056=CARTESIAN_POINT('Ctrl Pts',(17.645330598701,43.0924941008354,20.));
#94057=CARTESIAN_POINT('Ctrl Pts',(17.674559692302,43.0773049015137,0.));
#94058=CARTESIAN_POINT('Ctrl Pts',(17.674559692302,43.0773049015137,20.));
#94059=CARTESIAN_POINT('Ctrl Pts',(17.7037770867956,43.0620956280638,0.));
#94060=CARTESIAN_POINT('Ctrl Pts',(17.7037770867956,43.0620956280638,20.));
#94061=CARTESIAN_POINT('Ctrl Pts',(17.7329827680846,43.0468662888157,0.));
#94062=CARTESIAN_POINT('Ctrl Pts',(17.7329827680846,43.0468662888157,20.));
#94063=CARTESIAN_POINT('Ctrl Pts',(17.7621767220773,43.0316168921093,0.));
#94064=CARTESIAN_POINT('Ctrl Pts',(17.7621767220773,43.0316168921093,20.));
#94065=CARTESIAN_POINT('Ctrl Pts',(17.7913589346876,43.0163474462951,0.));
#94066=CARTESIAN_POINT('Ctrl Pts',(17.7913589346876,43.0163474462951,20.));
#94067=CARTESIAN_POINT('Ctrl Pts',(17.8205293918351,43.0010579597341,0.));
#94068=CARTESIAN_POINT('Ctrl Pts',(17.8205293918351,43.0010579597341,20.));
#94069=CARTESIAN_POINT('Ctrl Pts',(17.8496880794454,42.985748440798,0.));
#94070=CARTESIAN_POINT('Ctrl Pts',(17.8496880794454,42.985748440798,20.));
#94071=CARTESIAN_POINT('Ctrl Pts',(17.8788349834491,42.9704188978681,0.));
#94072=CARTESIAN_POINT('Ctrl Pts',(17.8788349834491,42.9704188978681,20.));
#94073=CARTESIAN_POINT('Ctrl Pts',(17.9079700897828,42.9550693393359,0.));
#94074=CARTESIAN_POINT('Ctrl Pts',(17.9079700897828,42.9550693393359,20.));
#94075=CARTESIAN_POINT('Ctrl Pts',(17.9370933843882,42.9396997736018,0.));
#94076=CARTESIAN_POINT('Ctrl Pts',(17.9370933843882,42.9396997736018,20.));
#94077=CARTESIAN_POINT('Ctrl Pts',(17.9662048532126,42.9243102090766,0.));
#94078=CARTESIAN_POINT('Ctrl Pts',(17.9662048532126,42.9243102090766,20.));
#94079=CARTESIAN_POINT('Ctrl Pts',(17.9953044822088,42.9089006541818,0.));
#94080=CARTESIAN_POINT('Ctrl Pts',(17.9953044822088,42.9089006541818,20.));
#94081=CARTESIAN_POINT('Ctrl Pts',(18.0243922573354,42.8934711173491,0.));
#94082=CARTESIAN_POINT('Ctrl Pts',(18.0243922573354,42.8934711173491,20.));
#94083=CARTESIAN_POINT('Ctrl Pts',(18.0534681645565,42.8780216070205,0.));
#94084=CARTESIAN_POINT('Ctrl Pts',(18.0534681645565,42.8780216070205,20.));
#94085=CARTESIAN_POINT('Ctrl Pts',(18.0825321898416,42.8625521316489,0.));
#94086=CARTESIAN_POINT('Ctrl Pts',(18.0825321898416,42.8625521316489,20.));
#94087=CARTESIAN_POINT('Ctrl Pts',(18.1115843191668,42.8470626996976,0.));
#94088=CARTESIAN_POINT('Ctrl Pts',(18.1115843191668,42.8470626996976,20.));
#94089=CARTESIAN_POINT('Ctrl Pts',(18.1406245385131,42.831553319639,0.));
#94090=CARTESIAN_POINT('Ctrl Pts',(18.1406245385131,42.831553319639,20.));
#94091=CARTESIAN_POINT('Ctrl Pts',(18.1696528338673,42.8160239999555,0.));
#94092=CARTESIAN_POINT('Ctrl Pts',(18.1696528338673,42.8160239999555,20.));
#94093=CARTESIAN_POINT('Ctrl Pts',(18.1986691912208,42.8004747491375,0.));
#94094=CARTESIAN_POINT('Ctrl Pts',(18.1986691912208,42.8004747491375,20.));
#94095=CARTESIAN_POINT('Ctrl Pts',(18.2276735965714,42.7849055756869,0.));
#94096=CARTESIAN_POINT('Ctrl Pts',(18.2276735965714,42.7849055756869,20.));
#94097=CARTESIAN_POINT('Ctrl Pts',(18.256666035922,42.7693164881155,0.));
#94098=CARTESIAN_POINT('Ctrl Pts',(18.256666035922,42.7693164881155,20.));
#94099=CARTESIAN_POINT('Ctrl Pts',(18.285646495282,42.7537074949463,0.));
#94100=CARTESIAN_POINT('Ctrl Pts',(18.285646495282,42.7537074949463,20.));
#94101=CARTESIAN_POINT('Ctrl Pts',(18.3146149606662,42.7380786047127,0.));
#94102=CARTESIAN_POINT('Ctrl Pts',(18.3146149606662,42.7380786047127,20.));
#94103=CARTESIAN_POINT('Ctrl Pts',(18.3435714180954,42.7224298259587,0.));
#94104=CARTESIAN_POINT('Ctrl Pts',(18.3435714180954,42.7224298259587,20.));
#94105=CARTESIAN_POINT('Ctrl Pts',(18.372515853596,42.7067611672378,0.));
#94106=CARTESIAN_POINT('Ctrl Pts',(18.372515853596,42.7067611672378,20.));
#94107=CARTESIAN_POINT('Ctrl Pts',(18.4014482531999,42.6910726371132,0.));
#94108=CARTESIAN_POINT('Ctrl Pts',(18.4014482531999,42.6910726371132,20.));
#94109=CARTESIAN_POINT('Ctrl Pts',(18.4303686029443,42.6753642441576,0.));
#94110=CARTESIAN_POINT('Ctrl Pts',(18.4303686029443,42.6753642441576,20.));
#94111=CARTESIAN_POINT('Ctrl Pts',(18.4592768888724,42.6596359969538,0.));
#94112=CARTESIAN_POINT('Ctrl Pts',(18.4592768888724,42.6596359969538,20.));
#94113=CARTESIAN_POINT('Ctrl Pts',(18.4881730970326,42.6438879040941,0.));
#94114=CARTESIAN_POINT('Ctrl Pts',(18.4881730970326,42.6438879040941,20.));
#94115=CARTESIAN_POINT('Ctrl Pts',(18.5170572134793,42.6281199741818,0.));
#94116=CARTESIAN_POINT('Ctrl Pts',(18.5170572134793,42.6281199741818,20.));
#94117=CARTESIAN_POINT('Ctrl Pts',(18.5459292242727,42.61233221583,0.));
#94118=CARTESIAN_POINT('Ctrl Pts',(18.5459292242727,42.61233221583,20.));
#94119=CARTESIAN_POINT('Ctrl Pts',(18.574789115479,42.596524637663,0.));
#94120=CARTESIAN_POINT('Ctrl Pts',(18.574789115479,42.596524637663,20.));
#94121=CARTESIAN_POINT('Ctrl Pts',(18.6036368731702,42.5806972483146,0.));
#94122=CARTESIAN_POINT('Ctrl Pts',(18.6036368731702,42.5806972483146,20.));
#94123=CARTESIAN_POINT('Ctrl Pts',(18.6324724834239,42.5648500564287,0.));
#94124=CARTESIAN_POINT('Ctrl Pts',(18.6324724834239,42.5648500564287,20.));
#94125=CARTESIAN_POINT('Ctrl Pts',(18.6612959323233,42.5489830706585,0.));
#94126=CARTESIAN_POINT('Ctrl Pts',(18.6612959323233,42.5489830706585,20.));
#94127=CARTESIAN_POINT('Ctrl Pts',(18.6901072059567,42.5330962996668,0.));
#94128=CARTESIAN_POINT('Ctrl Pts',(18.6901072059567,42.5330962996668,20.));
#94129=CARTESIAN_POINT('Ctrl Pts',(18.718906290419,42.517189752127,0.));
#94130=CARTESIAN_POINT('Ctrl Pts',(18.718906290419,42.517189752127,20.));
#94131=CARTESIAN_POINT('Ctrl Pts',(18.7476931718101,42.5012634367222,0.));
#94132=CARTESIAN_POINT('Ctrl Pts',(18.7476931718101,42.5012634367222,20.));
#94133=CARTESIAN_POINT('Ctrl Pts',(18.7764678362367,42.4853173621469,0.));
#94134=CARTESIAN_POINT('Ctrl Pts',(18.7764678362367,42.4853173621469,20.));
#94135=CARTESIAN_POINT('Ctrl Pts',(18.8052302698113,42.4693515371059,0.));
#94136=CARTESIAN_POINT('Ctrl Pts',(18.8052302698113,42.4693515371059,20.));
#94137=CARTESIAN_POINT('Ctrl Pts',(18.8339804586522,42.4533659703145,0.));
#94138=CARTESIAN_POINT('Ctrl Pts',(18.8339804586522,42.4533659703145,20.));
#94139=CARTESIAN_POINT('Ctrl Pts',(18.8627183888827,42.4373606704956,0.));
#94140=CARTESIAN_POINT('Ctrl Pts',(18.8627183888827,42.4373606704956,20.));
#94141=CARTESIAN_POINT('Ctrl Pts',(18.8914440466322,42.4213356463824,0.));
#94142=CARTESIAN_POINT('Ctrl Pts',(18.8914440466322,42.4213356463824,20.));
#94143=CARTESIAN_POINT('Ctrl Pts',(18.9201574180352,42.4052909067172,0.));
#94144=CARTESIAN_POINT('Ctrl Pts',(18.9201574180352,42.4052909067172,20.));
#94145=CARTESIAN_POINT('Ctrl Pts',(18.9488584892326,42.389226460254,0.));
#94146=CARTESIAN_POINT('Ctrl Pts',(18.9488584892326,42.389226460254,20.));
#94147=CARTESIAN_POINT('Ctrl Pts',(18.9775472463711,42.3731423157568,0.));
#94148=CARTESIAN_POINT('Ctrl Pts',(18.9775472463711,42.3731423157568,20.));
#94149=CARTESIAN_POINT('Ctrl Pts',(19.0062236756035,42.3570384820003,0.));
#94150=CARTESIAN_POINT('Ctrl Pts',(19.0062236756035,42.3570384820003,20.));
#94151=CARTESIAN_POINT('Ctrl Pts',(19.0348877630887,42.3409149677685,0.));
#94152=CARTESIAN_POINT('Ctrl Pts',(19.0348877630887,42.3409149677685,20.));
#94153=CARTESIAN_POINT('Ctrl Pts',(19.0635394949913,42.3247717818558,0.));
#94154=CARTESIAN_POINT('Ctrl Pts',(19.0635394949913,42.3247717818558,20.));
#94155=CARTESIAN_POINT('Ctrl Pts',(19.0921788574819,42.3086089330658,0.));
#94156=CARTESIAN_POINT('Ctrl Pts',(19.0921788574819,42.3086089330658,20.));
#94157=CARTESIAN_POINT('Ctrl Pts',(19.1208058367362,42.2924264302113,0.));
#94158=CARTESIAN_POINT('Ctrl Pts',(19.1208058367362,42.2924264302113,20.));
#94159=CARTESIAN_POINT('Ctrl Pts',(19.1494204189361,42.2762242821163,0.));
#94160=CARTESIAN_POINT('Ctrl Pts',(19.1494204189361,42.2762242821163,20.));
#94161=CARTESIAN_POINT('Ctrl Pts',(19.1780225902694,42.2600024976146,0.));
#94162=CARTESIAN_POINT('Ctrl Pts',(19.1780225902694,42.2600024976146,20.));
#94163=CARTESIAN_POINT('Ctrl Pts',(19.2066123369297,42.2437610855506,0.));
#94164=CARTESIAN_POINT('Ctrl Pts',(19.2066123369297,42.2437610855506,20.));
#94165=CARTESIAN_POINT('Ctrl Pts',(19.2351896451166,42.2275000547783,0.));
#94166=CARTESIAN_POINT('Ctrl Pts',(19.2351896451166,42.2275000547783,20.));
#94167=CARTESIAN_POINT('Ctrl Pts',(19.2637545010356,42.2112194141618,0.));
#94168=CARTESIAN_POINT('Ctrl Pts',(19.2637545010356,42.2112194141618,20.));
#94169=CARTESIAN_POINT('Ctrl Pts',(19.2923068908981,42.1949191725745,0.));
#94170=CARTESIAN_POINT('Ctrl Pts',(19.2923068908981,42.1949191725745,20.));
#94171=CARTESIAN_POINT('Ctrl Pts',(19.3208468009211,42.1785993388989,0.));
#94172=CARTESIAN_POINT('Ctrl Pts',(19.3208468009211,42.1785993388989,20.));
#94173=CARTESIAN_POINT('Ctrl Pts',(19.3493742173282,42.1622599220289,0.));
#94174=CARTESIAN_POINT('Ctrl Pts',(19.3493742173282,42.1622599220289,20.));
#94175=CARTESIAN_POINT('Ctrl Pts',(19.377889126349,42.1459009308685,0.));
#94176=CARTESIAN_POINT('Ctrl Pts',(19.377889126349,42.1459009308685,20.));
#94177=CARTESIAN_POINT('Ctrl Pts',(19.4063915142187,42.1295223743319,0.));
#94178=CARTESIAN_POINT('Ctrl Pts',(19.4063915142187,42.1295223743319,20.));
#94179=CARTESIAN_POINT('Ctrl Pts',(19.4348813671784,42.1131242613432,0.));
#94180=CARTESIAN_POINT('Ctrl Pts',(19.4348813671784,42.1131242613432,20.));
#94181=CARTESIAN_POINT('Ctrl Pts',(19.4633586714748,42.0967066008354,0.));
#94182=CARTESIAN_POINT('Ctrl Pts',(19.4633586714748,42.0967066008354,20.));
#94183=CARTESIAN_POINT('Ctrl Pts',(19.4918234133604,42.080269401751,0.));
#94184=CARTESIAN_POINT('Ctrl Pts',(19.4918234133604,42.080269401751,20.));
#94185=CARTESIAN_POINT('Ctrl Pts',(19.5202755790939,42.0638126730426,0.));
#94186=CARTESIAN_POINT('Ctrl Pts',(19.5202755790939,42.0638126730426,20.));
#94187=CARTESIAN_POINT('Ctrl Pts',(19.5487151549408,42.0473364236742,0.));
#94188=CARTESIAN_POINT('Ctrl Pts',(19.5487151549408,42.0473364236742,20.));
#94189=CARTESIAN_POINT('Ctrl Pts',(19.5771421271718,42.0308406626191,0.));
#94190=CARTESIAN_POINT('Ctrl Pts',(19.5771421271718,42.0308406626191,20.));
#94191=CARTESIAN_POINT('Ctrl Pts',(19.6055564820642,42.0143253988608,0.));
#94192=CARTESIAN_POINT('Ctrl Pts',(19.6055564820642,42.0143253988608,20.));
#94193=CARTESIAN_POINT('Ctrl Pts',(19.6339582059008,41.997790641393,0.));
#94194=CARTESIAN_POINT('Ctrl Pts',(19.6339582059008,41.997790641393,20.));
#94195=CARTESIAN_POINT('Ctrl Pts',(19.6623472849704,41.9812363992182,0.));
#94196=CARTESIAN_POINT('Ctrl Pts',(19.6623472849704,41.9812363992182,20.));
#94197=CARTESIAN_POINT('Ctrl Pts',(19.6907237055674,41.9646626813489,0.));
#94198=CARTESIAN_POINT('Ctrl Pts',(19.6907237055674,41.9646626813489,20.));
#94199=CARTESIAN_POINT('Ctrl Pts',(19.7190874539927,41.9480694968077,0.));
#94200=CARTESIAN_POINT('Ctrl Pts',(19.7190874539927,41.9480694968077,20.));
#94201=CARTESIAN_POINT('Ctrl Pts',(19.7474385165531,41.9314568546275,0.));
#94202=CARTESIAN_POINT('Ctrl Pts',(19.7474385165531,41.9314568546275,20.));
#94203=CARTESIAN_POINT('Ctrl Pts',(19.7757768795619,41.9148247638512,0.));
#94204=CARTESIAN_POINT('Ctrl Pts',(19.7757768795619,41.9148247638512,20.));
#94205=CARTESIAN_POINT('Ctrl Pts',(19.8041025293385,41.8981732335313,0.));
#94206=CARTESIAN_POINT('Ctrl Pts',(19.8041025293385,41.8981732335313,20.));
#94207=CARTESIAN_POINT('Ctrl Pts',(19.8324154522082,41.8815022727306,0.));
#94208=CARTESIAN_POINT('Ctrl Pts',(19.8324154522082,41.8815022727306,20.));
#94209=CARTESIAN_POINT('Ctrl Pts',(19.8607156345021,41.8648118905217,0.));
#94210=CARTESIAN_POINT('Ctrl Pts',(19.8607156345021,41.8648118905217,20.));
#94211=CARTESIAN_POINT('Ctrl Pts',(19.889003062557,41.8481020959867,0.));
#94212=CARTESIAN_POINT('Ctrl Pts',(19.889003062557,41.8481020959867,20.));
#94213=CARTESIAN_POINT('Ctrl Pts',(19.9172777227157,41.8313728982175,0.));
#94214=CARTESIAN_POINT('Ctrl Pts',(19.9172777227157,41.8313728982175,20.));
#94215=CARTESIAN_POINT('Ctrl Pts',(19.9455396013269,41.8146243063152,0.));
#94216=CARTESIAN_POINT('Ctrl Pts',(19.9455396013269,41.8146243063152,20.));
#94217=CARTESIAN_POINT('Ctrl Pts',(19.9737886847461,41.7978563293914,0.));
#94218=CARTESIAN_POINT('Ctrl Pts',(19.9737886847461,41.7978563293914,20.));
#94219=CARTESIAN_POINT('Ctrl Pts',(20.0020249593348,41.7810689765679,0.));
#94220=CARTESIAN_POINT('Ctrl Pts',(20.0020249593348,41.7810689765679,20.));
#94221=CARTESIAN_POINT('Ctrl Pts',(20.0302484114611,41.7642622569769,0.));
#94222=CARTESIAN_POINT('Ctrl Pts',(20.0302484114611,41.7642622569769,20.));
#94223=CARTESIAN_POINT('Ctrl Pts',(20.0584590274991,41.7474361797609,0.));
#94224=CARTESIAN_POINT('Ctrl Pts',(20.0584590274991,41.7474361797609,20.));
#94225=CARTESIAN_POINT('Ctrl Pts',(20.0866567938287,41.7305907540713,0.));
#94226=CARTESIAN_POINT('Ctrl Pts',(20.0866567938287,41.7305907540713,20.));
#94227=CARTESIAN_POINT('Ctrl Pts',(20.1148416968357,41.7137259890696,0.));
#94228=CARTESIAN_POINT('Ctrl Pts',(20.1148416968357,41.7137259890696,20.));
#94229=CARTESIAN_POINT('Ctrl Pts',(20.1430137229118,41.6968418939263,0.));
#94230=CARTESIAN_POINT('Ctrl Pts',(20.1430137229118,41.6968418939263,20.));
#94231=CARTESIAN_POINT('Ctrl Pts',(20.1711728584548,41.6799384778218,0.));
#94232=CARTESIAN_POINT('Ctrl Pts',(20.1711728584548,41.6799384778218,20.));
#94233=CARTESIAN_POINT('Ctrl Pts',(20.199319089869,41.6630157499462,0.));
#94234=CARTESIAN_POINT('Ctrl Pts',(20.199319089869,41.6630157499462,20.));
#94235=CARTESIAN_POINT('Ctrl Pts',(20.2274524035648,41.6460737195007,0.));
#94236=CARTESIAN_POINT('Ctrl Pts',(20.2274524035648,41.6460737195007,20.));
#94237=CARTESIAN_POINT('Ctrl Pts',(20.2555727859589,41.6291123956959,0.));
#94238=CARTESIAN_POINT('Ctrl Pts',(20.2555727859589,41.6291123956959,20.));
#94239=CARTESIAN_POINT('Ctrl Pts',(20.2836802234745,41.6121317877528,0.));
#94240=CARTESIAN_POINT('Ctrl Pts',(20.2836802234745,41.6121317877528,20.));
#94241=CARTESIAN_POINT('Ctrl Pts',(20.3117747025404,41.5951319049016,0.));
#94242=CARTESIAN_POINT('Ctrl Pts',(20.3117747025404,41.5951319049016,20.));
#94243=CARTESIAN_POINT('Ctrl Pts',(20.3398562095916,41.5781127563818,0.));
#94244=CARTESIAN_POINT('Ctrl Pts',(20.3398562095916,41.5781127563818,20.));
#94245=CARTESIAN_POINT('Ctrl Pts',(20.3679247310694,41.561074351443,0.));
#94246=CARTESIAN_POINT('Ctrl Pts',(20.3679247310694,41.561074351443,20.));
#94247=CARTESIAN_POINT('Ctrl Pts',(20.395980253421,41.5440166993445,0.));
#94248=CARTESIAN_POINT('Ctrl Pts',(20.395980253421,41.5440166993445,20.));
#94249=CARTESIAN_POINT('Ctrl Pts',(20.4240227631002,41.5269398093561,0.));
#94250=CARTESIAN_POINT('Ctrl Pts',(20.4240227631002,41.5269398093561,20.));
#94251=CARTESIAN_POINT('Ctrl Pts',(20.4520522465668,41.5098436907568,0.));
#94252=CARTESIAN_POINT('Ctrl Pts',(20.4520522465668,41.5098436907568,20.));
#94253=CARTESIAN_POINT('Ctrl Pts',(20.4800686902869,41.4927283528358,0.));
#94254=CARTESIAN_POINT('Ctrl Pts',(20.4800686902869,41.4927283528358,20.));
#94255=CARTESIAN_POINT('Ctrl Pts',(20.5080720807336,41.4755938048931,0.));
#94256=CARTESIAN_POINT('Ctrl Pts',(20.5080720807336,41.4755938048931,20.));
#94257=CARTESIAN_POINT('Ctrl Pts',(20.5360624043854,41.4584400562379,0.));
#94258=CARTESIAN_POINT('Ctrl Pts',(20.5360624043854,41.4584400562379,20.));
#94259=CARTESIAN_POINT('Ctrl Pts',(20.5640396477269,41.4412671161883,0.));
#94260=CARTESIAN_POINT('Ctrl Pts',(20.5640396477269,41.4412671161883,20.));
#94261=CARTESIAN_POINT('Ctrl Pts',(20.5920037972489,41.4240749940722,0.));
#94262=CARTESIAN_POINT('Ctrl Pts',(20.5920037972489,41.4240749940722,20.));
#94263=CARTESIAN_POINT('Ctrl Pts',(20.6199548394484,41.4068636992265,0.));
#94264=CARTESIAN_POINT('Ctrl Pts',(20.6199548394484,41.4068636992265,20.));
#94265=CARTESIAN_POINT('Ctrl Pts',(20.6478927608288,41.3896332409988,0.));
#94266=CARTESIAN_POINT('Ctrl Pts',(20.6478927608288,41.3896332409988,20.));
#94267=CARTESIAN_POINT('Ctrl Pts',(20.6758175479,41.3723836287471,0.));
#94268=CARTESIAN_POINT('Ctrl Pts',(20.6758175479,41.3723836287471,20.));
#94269=CARTESIAN_POINT('Ctrl Pts',(20.7037291871782,41.3551148718389,0.));
#94270=CARTESIAN_POINT('Ctrl Pts',(20.7037291871782,41.3551148718389,20.));
#94271=CARTESIAN_POINT('Ctrl Pts',(20.731627665186,41.3378269796522,0.));
#94272=CARTESIAN_POINT('Ctrl Pts',(20.731627665186,41.3378269796522,20.));
#94273=CARTESIAN_POINT('Ctrl Pts',(20.7595129684521,41.3205199615745,0.));
#94274=CARTESIAN_POINT('Ctrl Pts',(20.7595129684521,41.3205199615745,20.));
#94275=CARTESIAN_POINT('Ctrl Pts',(20.7873850835117,41.303193827003,0.));
#94276=CARTESIAN_POINT('Ctrl Pts',(20.7873850835117,41.303193827003,20.));
#94277=CARTESIAN_POINT('Ctrl Pts',(20.8152439969059,41.285848585344,0.));
#94278=CARTESIAN_POINT('Ctrl Pts',(20.8152439969059,41.285848585344,20.));
#94279=CARTESIAN_POINT('Ctrl Pts',(20.8430896951822,41.268484246013,0.));
#94280=CARTESIAN_POINT('Ctrl Pts',(20.8430896951822,41.268484246013,20.));
#94281=CARTESIAN_POINT('Ctrl Pts',(20.8709221648944,41.2511008184358,0.));
#94282=CARTESIAN_POINT('Ctrl Pts',(20.8709221648944,41.2511008184358,20.));
#94283=CARTESIAN_POINT('Ctrl Pts',(20.8987413926025,41.2336983120481,0.));
#94284=CARTESIAN_POINT('Ctrl Pts',(20.8987413926025,41.2336983120481,20.));
#94285=CARTESIAN_POINT('Ctrl Pts',(20.9265473648728,41.2162767362953,0.));
#94286=CARTESIAN_POINT('Ctrl Pts',(20.9265473648728,41.2162767362953,20.));
#94287=CARTESIAN_POINT('Ctrl Pts',(20.9543400682781,41.1988361006333,0.));
#94288=CARTESIAN_POINT('Ctrl Pts',(20.9543400682781,41.1988361006333,20.));
#94289=CARTESIAN_POINT('Ctrl Pts',(20.9821194893979,41.1813764145274,0.));
#94290=CARTESIAN_POINT('Ctrl Pts',(20.9821194893979,41.1813764145274,20.));
#94291=CARTESIAN_POINT('Ctrl Pts',(21.009885614818,41.1638976874526,0.));
#94292=CARTESIAN_POINT('Ctrl Pts',(21.009885614818,41.1638976874526,20.));
#94293=CARTESIAN_POINT('Ctrl Pts',(21.0376384311301,41.1463999288927,0.));
#94294=CARTESIAN_POINT('Ctrl Pts',(21.0376384311301,41.1463999288927,20.));
#94295=CARTESIAN_POINT('Ctrl Pts',(21.0653779249329,41.128883148342,0.));
#94296=CARTESIAN_POINT('Ctrl Pts',(21.0653779249329,41.128883148342,20.));
#94297=CARTESIAN_POINT('Ctrl Pts',(21.093104082831,41.1113473553046,0.));
#94298=CARTESIAN_POINT('Ctrl Pts',(21.093104082831,41.1113473553046,20.));
#94299=CARTESIAN_POINT('Ctrl Pts',(21.1208168914355,41.0937925592944,0.));
#94300=CARTESIAN_POINT('Ctrl Pts',(21.1208168914355,41.0937925592944,20.));
#94301=CARTESIAN_POINT('Ctrl Pts',(21.1485163373635,41.076218769835,0.));
#94302=CARTESIAN_POINT('Ctrl Pts',(21.1485163373635,41.076218769835,20.));
#94303=CARTESIAN_POINT('Ctrl Pts',(21.1762024072388,41.0586259964597,0.));
#94304=CARTESIAN_POINT('Ctrl Pts',(21.1762024072388,41.0586259964597,20.));
#94305=CARTESIAN_POINT('Ctrl Pts',(21.2038750876913,41.0410142487106,0.));
#94306=CARTESIAN_POINT('Ctrl Pts',(21.2038750876913,41.0410142487106,20.));
#94307=CARTESIAN_POINT('Ctrl Pts',(21.2315343653574,41.0233835361399,0.));
#94308=CARTESIAN_POINT('Ctrl Pts',(21.2315343653574,41.0233835361399,20.));
#94309=CARTESIAN_POINT('Ctrl Pts',(21.25918022688,41.0057338683097,0.));
#94310=CARTESIAN_POINT('Ctrl Pts',(21.25918022688,41.0057338683097,20.));
#94311=CARTESIAN_POINT('Ctrl Pts',(21.286812658909,40.9880652547928,0.));
#94312=CARTESIAN_POINT('Ctrl Pts',(21.286812658909,40.9880652547928,20.));
#94313=CARTESIAN_POINT('Ctrl Pts',(21.3144316481011,40.9703777051716,0.));
#94314=CARTESIAN_POINT('Ctrl Pts',(21.3144316481011,40.9703777051716,20.));
#94315=CARTESIAN_POINT('Ctrl Pts',(21.342037181119,40.9526712290373,0.));
#94316=CARTESIAN_POINT('Ctrl Pts',(21.342037181119,40.9526712290373,20.));
#94317=CARTESIAN_POINT('Ctrl Pts',(21.3696292446317,40.9349458359905,0.));
#94318=CARTESIAN_POINT('Ctrl Pts',(21.3696292446317,40.9349458359905,20.));
#94319=CARTESIAN_POINT('Ctrl Pts',(21.3972078253142,40.9172015356414,0.));
#94320=CARTESIAN_POINT('Ctrl Pts',(21.3972078253142,40.9172015356414,20.));
#94321=CARTESIAN_POINT('Ctrl Pts',(21.4247729098479,40.8994383376102,0.));
#94322=CARTESIAN_POINT('Ctrl Pts',(21.4247729098479,40.8994383376102,20.));
#94323=CARTESIAN_POINT('Ctrl Pts',(21.4523244849199,40.8816562515268,0.));
#94324=CARTESIAN_POINT('Ctrl Pts',(21.4523244849199,40.8816562515268,20.));
#94325=CARTESIAN_POINT('Ctrl Pts',(21.4798625372243,40.8638552870319,0.));
#94326=CARTESIAN_POINT('Ctrl Pts',(21.4798625372243,40.8638552870319,20.));
#94327=CARTESIAN_POINT('Ctrl Pts',(21.5073870534614,40.8460354537749,0.));
#94328=CARTESIAN_POINT('Ctrl Pts',(21.5073870534614,40.8460354537749,20.));
#94329=CARTESIAN_POINT('Ctrl Pts',(21.5348980203391,40.8281967614155,0.));
#94330=CARTESIAN_POINT('Ctrl Pts',(21.5348980203391,40.8281967614155,20.));
#94331=CARTESIAN_POINT('Ctrl Pts',(21.5623954245725,40.8103392196221,0.));
#94332=CARTESIAN_POINT('Ctrl Pts',(21.5623954245725,40.8103392196221,20.));
#94333=CARTESIAN_POINT('Ctrl Pts',(21.5898792528837,40.7924628380726,0.));
#94334=CARTESIAN_POINT('Ctrl Pts',(21.5898792528837,40.7924628380726,20.));
#94335=CARTESIAN_POINT('Ctrl Pts',(21.6173494920019,40.7745676264537,0.));
#94336=CARTESIAN_POINT('Ctrl Pts',(21.6173494920019,40.7745676264537,20.));
#94337=CARTESIAN_POINT('Ctrl Pts',(21.6448061286619,40.7566535944621,0.));
#94338=CARTESIAN_POINT('Ctrl Pts',(21.6448061286619,40.7566535944621,20.));
#94339=CARTESIAN_POINT('Ctrl Pts',(21.6722491496038,40.7387207518043,0.));
#94340=CARTESIAN_POINT('Ctrl Pts',(21.6722491496038,40.7387207518043,20.));
#94341=CARTESIAN_POINT('Ctrl Pts',(21.6996785415723,40.7207691081984,0.));
#94342=CARTESIAN_POINT('Ctrl Pts',(21.6996785415723,40.7207691081984,20.));
#94343=CARTESIAN_POINT('Ctrl Pts',(21.7270942913167,40.7027986733736,0.));
#94344=CARTESIAN_POINT('Ctrl Pts',(21.7270942913167,40.7027986733736,20.));
#94345=CARTESIAN_POINT('Ctrl Pts',(21.7544963855931,40.6848094570694,0.));
#94346=CARTESIAN_POINT('Ctrl Pts',(21.7544963855931,40.6848094570694,20.));
#94347=CARTESIAN_POINT('Ctrl Pts',(21.781884811165,40.6668014690334,0.));
#94348=CARTESIAN_POINT('Ctrl Pts',(21.781884811165,40.6668014690334,20.));
#94349=CARTESIAN_POINT('Ctrl Pts',(21.8092595548052,40.6487747190214,0.));
#94350=CARTESIAN_POINT('Ctrl Pts',(21.8092595548052,40.6487747190214,20.));
#94351=CARTESIAN_POINT('Ctrl Pts',(21.8366206032979,40.6307292167951,0.));
#94352=CARTESIAN_POINT('Ctrl Pts',(21.8366206032979,40.6307292167951,20.));
#94353=CARTESIAN_POINT('Ctrl Pts',(21.8639679434382,40.6126649721233,0.));
#94354=CARTESIAN_POINT('Ctrl Pts',(21.8639679434382,40.6126649721233,20.));
#94355=CARTESIAN_POINT('Ctrl Pts',(21.8913015620281,40.594581994783,0.));
#94356=CARTESIAN_POINT('Ctrl Pts',(21.8913015620281,40.594581994783,20.));
#94357=CARTESIAN_POINT('Ctrl Pts',(21.9186214458728,40.5764802945639,0.));
#94358=CARTESIAN_POINT('Ctrl Pts',(21.9186214458728,40.5764802945639,20.));
#94359=CARTESIAN_POINT('Ctrl Pts',(21.9459275817778,40.5583598812699,0.));
#94360=CARTESIAN_POINT('Ctrl Pts',(21.9459275817778,40.5583598812699,20.));
#94361=CARTESIAN_POINT('Ctrl Pts',(21.9732199565439,40.5402207647219,0.));
#94362=CARTESIAN_POINT('Ctrl Pts',(21.9732199565439,40.5402207647219,20.));
#94363=CARTESIAN_POINT('Ctrl Pts',(22.0004985569689,40.5220629547578,0.));
#94364=CARTESIAN_POINT('Ctrl Pts',(22.0004985569689,40.5220629547578,20.));
#94365=CARTESIAN_POINT('Ctrl Pts',(22.0277633698572,40.5038864612253,0.));
#94366=CARTESIAN_POINT('Ctrl Pts',(22.0277633698572,40.5038864612253,20.));
#94367=CARTESIAN_POINT('Ctrl Pts',(22.0550143820281,40.485691293976,0.));
#94368=CARTESIAN_POINT('Ctrl Pts',(22.0550143820281,40.485691293976,20.));
#94369=CARTESIAN_POINT('Ctrl Pts',(22.0822515803231,40.4674774628609,0.));
#94370=CARTESIAN_POINT('Ctrl Pts',(22.0822515803231,40.4674774628609,20.));
#94371=CARTESIAN_POINT('Ctrl Pts',(22.1094749516164,40.4492449777204,0.));
#94372=CARTESIAN_POINT('Ctrl Pts',(22.1094749516164,40.4492449777204,20.));
#94373=CARTESIAN_POINT('Ctrl Pts',(22.1366844828092,40.4309938483881,0.));
#94374=CARTESIAN_POINT('Ctrl Pts',(22.1366844828092,40.4309938483881,20.));
#94375=CARTESIAN_POINT('Ctrl Pts',(22.1638801608087,40.4127240847076,0.));
#94376=CARTESIAN_POINT('Ctrl Pts',(22.1638801608087,40.4127240847076,20.));
#94377=CARTESIAN_POINT('Ctrl Pts',(22.1910619725087,40.3944356965472,0.));
#94378=CARTESIAN_POINT('Ctrl Pts',(22.1910619725087,40.3944356965472,20.));
#94379=CARTESIAN_POINT('Ctrl Pts',(22.2182299047735,40.3761286938115,0.));
#94380=CARTESIAN_POINT('Ctrl Pts',(22.2182299047735,40.3761286938115,20.));
#94381=CARTESIAN_POINT('Ctrl Pts',(22.2453839444114,40.357803086462,0.));
#94382=CARTESIAN_POINT('Ctrl Pts',(22.2453839444114,40.357803086462,20.));
#94383=CARTESIAN_POINT('Ctrl Pts',(22.2725240781926,40.3394588845042,0.));
#94384=CARTESIAN_POINT('Ctrl Pts',(22.2725240781926,40.3394588845042,20.));
#94385=CARTESIAN_POINT('Ctrl Pts',(22.2996502928986,40.3210960979489,0.));
#94386=CARTESIAN_POINT('Ctrl Pts',(22.2996502928986,40.3210960979489,20.));
#94387=CARTESIAN_POINT('Ctrl Pts',(22.326762575367,40.3027147367804,0.));
#94388=CARTESIAN_POINT('Ctrl Pts',(22.326762575367,40.3027147367804,20.));
#94389=CARTESIAN_POINT('Ctrl Pts',(22.3538609125294,40.2843148109268,0.));
#94390=CARTESIAN_POINT('Ctrl Pts',(22.3538609125294,40.2843148109268,20.));
#94391=CARTESIAN_POINT('Ctrl Pts',(22.3809452914735,40.2658963302133,0.));
#94392=CARTESIAN_POINT('Ctrl Pts',(22.3809452914735,40.2658963302133,20.));
#94393=CARTESIAN_POINT('Ctrl Pts',(22.4080156993888,40.2474593044019,0.));
#94394=CARTESIAN_POINT('Ctrl Pts',(22.4080156993888,40.2474593044019,20.));
#94395=CARTESIAN_POINT('Ctrl Pts',(22.4350721234534,40.229003743277,0.));
#94396=CARTESIAN_POINT('Ctrl Pts',(22.4350721234534,40.229003743277,20.));
#94397=CARTESIAN_POINT('Ctrl Pts',(22.4621145507305,40.210529656724,0.));
#94398=CARTESIAN_POINT('Ctrl Pts',(22.4621145507305,40.210529656724,20.));
#94399=CARTESIAN_POINT('Ctrl Pts',(22.4891429680799,40.1920370547964,0.));
#94400=CARTESIAN_POINT('Ctrl Pts',(22.4891429680799,40.1920370547964,20.));
#94401=CARTESIAN_POINT('Ctrl Pts',(22.5161573620162,40.1735259478254,0.));
#94402=CARTESIAN_POINT('Ctrl Pts',(22.5161573620162,40.1735259478254,20.));
#94403=CARTESIAN_POINT('Ctrl Pts',(22.5431577188605,40.1549963463026,0.));
#94404=CARTESIAN_POINT('Ctrl Pts',(22.5431577188605,40.1549963463026,20.));
#94405=CARTESIAN_POINT('Ctrl Pts',(22.5701440249982,40.1364482606861,0.));
#94406=CARTESIAN_POINT('Ctrl Pts',(22.5701440249982,40.1364482606861,20.));
#94407=CARTESIAN_POINT('Ctrl Pts',(22.5971162671187,40.1178817012184,0.));
#94408=CARTESIAN_POINT('Ctrl Pts',(22.5971162671187,40.1178817012184,20.));
#94409=CARTESIAN_POINT('Ctrl Pts',(22.6240744324258,40.0992966777668,0.));
#94410=CARTESIAN_POINT('Ctrl Pts',(22.6240744324258,40.0992966777668,20.));
#94411=CARTESIAN_POINT('Ctrl Pts',(22.6510185089549,40.0806931995834,0.));
#94412=CARTESIAN_POINT('Ctrl Pts',(22.6510185089549,40.0806931995834,20.));
#94413=CARTESIAN_POINT('Ctrl Pts',(22.6779484851672,40.0620712756149,0.));
#94414=CARTESIAN_POINT('Ctrl Pts',(22.6779484851672,40.0620712756149,20.));
#94415=CARTESIAN_POINT('Ctrl Pts',(22.7048643493645,40.0434309149417,0.));
#94416=CARTESIAN_POINT('Ctrl Pts',(22.7048643493645,40.0434309149417,20.));
#94417=CARTESIAN_POINT('Ctrl Pts',(22.73176608914,40.0247721271957,0.));
#94418=CARTESIAN_POINT('Ctrl Pts',(22.73176608914,40.0247721271957,20.));
#94419=CARTESIAN_POINT('Ctrl Pts',(22.7586536908731,40.0060949229408,0.));
#94420=CARTESIAN_POINT('Ctrl Pts',(22.7586536908731,40.0060949229408,20.));
#94421=CARTESIAN_POINT('Ctrl Pts',(22.7855271390493,39.9873993141881,0.));
#94422=CARTESIAN_POINT('Ctrl Pts',(22.7855271390493,39.9873993141881,20.));
#94423=CARTESIAN_POINT('Ctrl Pts',(22.8123864172494,39.9686853136472,0.));
#94424=CARTESIAN_POINT('Ctrl Pts',(22.8123864172494,39.9686853136472,20.));
#94425=CARTESIAN_POINT('Ctrl Pts',(22.8392315093989,39.9499529337848,0.));
#94426=CARTESIAN_POINT('Ctrl Pts',(22.8392315093989,39.9499529337848,20.));
#94427=CARTESIAN_POINT('Ctrl Pts',(22.8660624009432,39.9312021859375,0.));
#94428=CARTESIAN_POINT('Ctrl Pts',(22.8660624009432,39.9312021859375,20.));
#94429=CARTESIAN_POINT('Ctrl Pts',(22.8928790800154,39.91243307943,0.));
#94430=CARTESIAN_POINT('Ctrl Pts',(22.8928790800154,39.91243307943,20.));
#94431=CARTESIAN_POINT('Ctrl Pts',(22.9196815387084,39.8936456206159,0.));
#94432=CARTESIAN_POINT('Ctrl Pts',(22.9196815387084,39.8936456206159,20.));
#94433=CARTESIAN_POINT('Ctrl Pts',(22.9464697723601,39.8748398133807,0.));
#94434=CARTESIAN_POINT('Ctrl Pts',(22.9464697723601,39.8748398133807,20.));
#94435=CARTESIAN_POINT('Ctrl Pts',(22.9678889774251,39.8597804904793,0.));
#94436=CARTESIAN_POINT('Ctrl Pts',(22.9678889774251,39.8597804904793,20.));
#94437=CARTESIAN_POINT('Ctrl Pts',(22.9839469786125,39.8484777427633,0.));
#94438=CARTESIAN_POINT('Ctrl Pts',(22.9839469786125,39.8484777427633,20.));
#94439=CARTESIAN_POINT('Ctrl Pts',(22.9946494671375,39.8409389084975,0.));
#94440=CARTESIAN_POINT('Ctrl Pts',(22.9946494671375,39.8409389084975,20.));
#94441=CARTESIAN_POINT('Ctrl Pts',(23.,39.8371685740842,0.));
#94442=CARTESIAN_POINT('Ctrl Pts',(23.,39.8371685740842,20.));
#94443=CARTESIAN_POINT('',(23.,39.8371685740842,0.));
#94444=CARTESIAN_POINT('Origin',(35.3531508854311,30.9702231582522,0.));
#94445=CARTESIAN_POINT('',(34.6009561857411,30.3112822399915,0.));
#94446=CARTESIAN_POINT('Origin',(1.19904086659517E-13,1.4210854715202E-13,
0.));
#94447=CARTESIAN_POINT('Origin',(0.,0.,0.));
#94448=CARTESIAN_POINT('',(0.,0.,0.));
#94449=CARTESIAN_POINT('Origin',(7.,0.,61.));
#94450=CARTESIAN_POINT('',(7.,0.,64.));
#94451=CARTESIAN_POINT('',(10.,0.,64.));
#94452=CARTESIAN_POINT('',(7.,0.,64.));
#94453=CARTESIAN_POINT('',(7.,3.,61.));
#94454=CARTESIAN_POINT('Origin',(7.,0.,61.));
#94455=CARTESIAN_POINT('',(9.53939201416946,3.,61.));
#94456=CARTESIAN_POINT('',(7.,3.,61.));
#94457=CARTESIAN_POINT('Ctrl Pts',(10.,2.77555756156289E-16,64.));
#94458=CARTESIAN_POINT('Ctrl Pts',(10.,0.379164265292003,64.));
#94459=CARTESIAN_POINT('Ctrl Pts',(9.97630133387832,0.782037717481879,63.9237482465107));
#94460=CARTESIAN_POINT('Ctrl Pts',(9.8907119499008,1.52052241900623,63.616848907033));
#94461=CARTESIAN_POINT('Ctrl Pts',(9.82993562614982,1.85631434471708,63.3863263424022));
#94462=CARTESIAN_POINT('Ctrl Pts',(9.71486751729016,2.38640531261462,62.8562353745047));
#94463=CARTESIAN_POINT('Ctrl Pts',(9.65284956103208,2.61686672615765,62.5204755377162));
#94464=CARTESIAN_POINT('Ctrl Pts',(9.56437939057488,2.92372091609921,61.7821074854282));
#94465=CARTESIAN_POINT('Ctrl Pts',(9.53939201416946,3.,61.3792772539893));
#94466=CARTESIAN_POINT('Ctrl Pts',(9.53939201416946,3.,61.));
#94467=CARTESIAN_POINT('Origin',(7.,0.,61.));
#94468=CARTESIAN_POINT('',(9.53939201416946,-3.,61.));
#94469=CARTESIAN_POINT('Ctrl Pts',(9.53939201416946,-3.,61.));
#94470=CARTESIAN_POINT('Ctrl Pts',(9.53939201416946,-3.,61.3792772539893));
#94471=CARTESIAN_POINT('Ctrl Pts',(9.56437939057487,-2.92372091609922,61.7821074854282));
#94472=CARTESIAN_POINT('Ctrl Pts',(9.65284956103208,-2.61686672615766,62.5204755377161));
#94473=CARTESIAN_POINT('Ctrl Pts',(9.71486751729016,-2.38640531261463,62.8562353745047));
#94474=CARTESIAN_POINT('Ctrl Pts',(9.82993562614982,-1.85631434471708,63.3863263424022));
#94475=CARTESIAN_POINT('Ctrl Pts',(9.8907119499008,-1.52052241900622,63.616848907033));
#94476=CARTESIAN_POINT('Ctrl Pts',(9.97630133387832,-0.782037717481873,
63.9237482465107));
#94477=CARTESIAN_POINT('Ctrl Pts',(10.,-0.379164265292002,64.));
#94478=CARTESIAN_POINT('Ctrl Pts',(10.,-5.55111512312578E-16,64.));
#94479=CARTESIAN_POINT('',(7.,-3.,61.));
#94480=CARTESIAN_POINT('',(7.,-3.,61.));
#94481=CARTESIAN_POINT('Origin',(7.,0.,61.));
#94482=CARTESIAN_POINT('',(7.,0.,64.));
#94483=CARTESIAN_POINT('Origin',(7.,3.,43.));
#94484=CARTESIAN_POINT('',(9.53939201416946,3.,43.));
#94485=CARTESIAN_POINT('',(9.53939201416946,3.,-16.));
#94486=CARTESIAN_POINT('',(7.,3.,43.));
#94487=CARTESIAN_POINT('',(7.,3.,61.));
#94488=CARTESIAN_POINT('',(7.,3.,43.));
#94489=CARTESIAN_POINT('Origin',(7.,-2.77555756156289E-16,43.));
#94490=CARTESIAN_POINT('',(9.53939201416946,-3.,43.));
#94491=CARTESIAN_POINT('Ctrl Pts',(9.53939201416946,3.,43.));
#94492=CARTESIAN_POINT('Ctrl Pts',(9.53939201416946,3.,42.6207227460108));
#94493=CARTESIAN_POINT('Ctrl Pts',(9.56437939057488,2.92372091609922,42.2178925145718));
#94494=CARTESIAN_POINT('Ctrl Pts',(9.65284956103208,2.61686672615766,41.4795244622839));
#94495=CARTESIAN_POINT('Ctrl Pts',(9.71486751729016,2.38640531261462,41.1437646254954));
#94496=CARTESIAN_POINT('Ctrl Pts',(9.82993562614982,1.85631434471708,40.6136736575978));
#94497=CARTESIAN_POINT('Ctrl Pts',(9.8907119499008,1.52052241900622,40.383151092967));
#94498=CARTESIAN_POINT('Ctrl Pts',(9.97630133387832,0.78203771748188,40.0762517534893));
#94499=CARTESIAN_POINT('Ctrl Pts',(10.,0.379164265292002,40.));
#94500=CARTESIAN_POINT('Ctrl Pts',(10.,-0.379164265292002,40.));
#94501=CARTESIAN_POINT('Ctrl Pts',(9.97630133387832,-0.782037717481879,
40.0762517534893));
#94502=CARTESIAN_POINT('Ctrl Pts',(9.8907119499008,-1.52052241900622,40.383151092967));
#94503=CARTESIAN_POINT('Ctrl Pts',(9.82993562614982,-1.85631434471708,40.6136736575978));
#94504=CARTESIAN_POINT('Ctrl Pts',(9.71486751729016,-2.38640531261463,41.1437646254954));
#94505=CARTESIAN_POINT('Ctrl Pts',(9.65284956103208,-2.61686672615766,41.4795244622839));
#94506=CARTESIAN_POINT('Ctrl Pts',(9.56437939057488,-2.92372091609922,42.2178925145718));
#94507=CARTESIAN_POINT('Ctrl Pts',(9.53939201416946,-3.,42.6207227460108));
#94508=CARTESIAN_POINT('Ctrl Pts',(9.53939201416946,-3.,43.));
#94509=CARTESIAN_POINT('',(7.,-3.,43.));
#94510=CARTESIAN_POINT('Origin',(7.,-2.77555756156289E-16,43.));
#94511=CARTESIAN_POINT('',(7.,-3.,43.));
#94512=CARTESIAN_POINT('Origin',(7.,-3.,61.));
#94513=CARTESIAN_POINT('',(9.53939201416946,-3.,-16.));
#94514=CARTESIAN_POINT('',(7.,-3.,43.));
#94515=CARTESIAN_POINT('Origin',(7.,0.,52.));
#94516=CARTESIAN_POINT('Origin',(0.,0.,-16.));
#94517=CARTESIAN_POINT('',(-10.,-1.22464679914735E-15,64.));
#94518=CARTESIAN_POINT('Origin',(0.,0.,64.));
#94519=CARTESIAN_POINT('Origin',(0.,0.,64.));
#94520=CARTESIAN_POINT('',(-10.,-1.22464679914735E-15,35.));
#94521=CARTESIAN_POINT('',(-10.,-1.22464679914735E-15,-16.));
#94522=CARTESIAN_POINT('Origin',(0.,0.,35.));
#94523=CARTESIAN_POINT('Origin',(7.,0.,15.));
#94524=CARTESIAN_POINT('',(9.53939201416946,-3.,15.));
#94525=CARTESIAN_POINT('',(9.53939201416946,3.,15.));
#94526=CARTESIAN_POINT('Ctrl Pts',(9.53939201416946,-3.,15.));
#94527=CARTESIAN_POINT('Ctrl Pts',(9.53939201416946,-3.,15.3792772539892));
#94528=CARTESIAN_POINT('Ctrl Pts',(9.56437939057488,-2.92372091609922,15.7821074854282));
#94529=CARTESIAN_POINT('Ctrl Pts',(9.65284956103208,-2.61686672615765,16.5204755377161));
#94530=CARTESIAN_POINT('Ctrl Pts',(9.71486751729016,-2.38640531261463,16.8562353745047));
#94531=CARTESIAN_POINT('Ctrl Pts',(9.82993562614982,-1.85631434471708,17.3863263424022));
#94532=CARTESIAN_POINT('Ctrl Pts',(9.8907119499008,-1.52052241900622,17.616848907033));
#94533=CARTESIAN_POINT('Ctrl Pts',(9.97630133387832,-0.782037717481878,
17.9237482465107));
#94534=CARTESIAN_POINT('Ctrl Pts',(10.,-0.379164265292003,18.));
#94535=CARTESIAN_POINT('Ctrl Pts',(10.,0.379164265292001,18.));
#94536=CARTESIAN_POINT('Ctrl Pts',(9.97630133387832,0.782037717481875,17.9237482465107));
#94537=CARTESIAN_POINT('Ctrl Pts',(9.8907119499008,1.52052241900622,17.616848907033));
#94538=CARTESIAN_POINT('Ctrl Pts',(9.82993562614982,1.85631434471708,17.3863263424022));
#94539=CARTESIAN_POINT('Ctrl Pts',(9.71486751729016,2.38640531261462,16.8562353745047));
#94540=CARTESIAN_POINT('Ctrl Pts',(9.65284956103208,2.61686672615765,16.5204755377161));
#94541=CARTESIAN_POINT('Ctrl Pts',(9.56437939057488,2.92372091609922,15.7821074854282));
#94542=CARTESIAN_POINT('Ctrl Pts',(9.53939201416946,3.,15.3792772539892));
#94543=CARTESIAN_POINT('Ctrl Pts',(9.53939201416946,3.,15.));
#94544=CARTESIAN_POINT('',(7.,-3.,15.));
#94545=CARTESIAN_POINT('',(7.,-3.,15.));
#94546=CARTESIAN_POINT('',(7.,3.,15.));
#94547=CARTESIAN_POINT('Origin',(7.,0.,15.));
#94548=CARTESIAN_POINT('',(7.,3.,15.));
#94549=CARTESIAN_POINT('Origin',(7.,3.,5.));
#94550=CARTESIAN_POINT('',(9.53939201416946,3.,5.));
#94551=CARTESIAN_POINT('',(9.53939201416946,3.,-16.));
#94552=CARTESIAN_POINT('',(7.,3.,5.));
#94553=CARTESIAN_POINT('',(7.,3.,15.));
#94554=CARTESIAN_POINT('',(7.,3.,5.));
#94555=CARTESIAN_POINT('Origin',(7.,0.,5.));
#94556=CARTESIAN_POINT('',(10.,0.,2.));
#94557=CARTESIAN_POINT('',(9.53939201416946,-3.,5.));
#94558=CARTESIAN_POINT('Ctrl Pts',(10.,-2.77555756156289E-16,2.));
#94559=CARTESIAN_POINT('Ctrl Pts',(10.,-0.379164265292002,2.));
#94560=CARTESIAN_POINT('Ctrl Pts',(9.97630133387832,-0.782037717481877,
2.07625175348933));
#94561=CARTESIAN_POINT('Ctrl Pts',(9.8907119499008,-1.52052241900622,2.38315109296703));
#94562=CARTESIAN_POINT('Ctrl Pts',(9.82993562614982,-1.85631434471708,2.61367365759779));
#94563=CARTESIAN_POINT('Ctrl Pts',(9.71486751729016,-2.38640531261463,3.14376462549534));
#94564=CARTESIAN_POINT('Ctrl Pts',(9.65284956103208,-2.61686672615765,3.47952446228385));
#94565=CARTESIAN_POINT('Ctrl Pts',(9.56437939057488,-2.92372091609922,4.21789251457176));
#94566=CARTESIAN_POINT('Ctrl Pts',(9.53939201416946,-3.,4.62072274601075));
#94567=CARTESIAN_POINT('Ctrl Pts',(9.53939201416946,-3.,5.));
#94568=CARTESIAN_POINT('Ctrl Pts',(9.53939201416946,3.,5.));
#94569=CARTESIAN_POINT('Ctrl Pts',(9.53939201416946,3.,4.62072274601075));
#94570=CARTESIAN_POINT('Ctrl Pts',(9.56437939057488,2.92372091609922,4.21789251457176));
#94571=CARTESIAN_POINT('Ctrl Pts',(9.65284956103208,2.61686672615765,3.47952446228385));
#94572=CARTESIAN_POINT('Ctrl Pts',(9.71486751729016,2.38640531261463,3.14376462549534));
#94573=CARTESIAN_POINT('Ctrl Pts',(9.82993562614982,1.85631434471708,2.61367365759779));
#94574=CARTESIAN_POINT('Ctrl Pts',(9.8907119499008,1.52052241900622,2.38315109296703));
#94575=CARTESIAN_POINT('Ctrl Pts',(9.97630133387832,0.782037717481877,2.07625175348933));
#94576=CARTESIAN_POINT('Ctrl Pts',(10.,0.379164265292002,2.));
#94577=CARTESIAN_POINT('Ctrl Pts',(10.,-4.85722573273506E-16,2.));
#94578=CARTESIAN_POINT('',(7.,-3.,5.));
#94579=CARTESIAN_POINT('Origin',(7.,0.,5.));
#94580=CARTESIAN_POINT('',(7.,-3.,5.));
#94581=CARTESIAN_POINT('Origin',(7.,-3.,15.));
#94582=CARTESIAN_POINT('',(9.53939201416946,-3.,-16.));
#94583=CARTESIAN_POINT('',(7.,-3.,5.));
#94584=CARTESIAN_POINT('Origin',(7.,0.,10.));
#94585=CARTESIAN_POINT('Origin',(0.,0.,-16.));
#94586=CARTESIAN_POINT('',(-10.,1.22464679914735E-15,34.));
#94587=CARTESIAN_POINT('Origin',(0.,0.,34.));
#94588=CARTESIAN_POINT('',(-10.,-1.22464679914735E-15,2.));
#94589=CARTESIAN_POINT('',(-10.,-1.22464679914735E-15,-16.));
#94590=CARTESIAN_POINT('Origin',(0.,0.,2.));
#94591=CARTESIAN_POINT('Origin',(0.,0.,2.));
#94592=CARTESIAN_POINT('Origin',(0.,0.,34.5));
#94593=CARTESIAN_POINT('',(-9.,-1.10218211923262E-15,34.));
#94594=CARTESIAN_POINT('Origin',(0.,0.,34.));
#94595=CARTESIAN_POINT('',(-9.,-1.10218211923262E-15,35.));
#94596=CARTESIAN_POINT('',(-9.,-1.10218211923262E-15,34.5));
#94597=CARTESIAN_POINT('Origin',(0.,0.,35.));
#94598=CARTESIAN_POINT('Origin',(13.,0.,34.));
#94599=CARTESIAN_POINT('Origin',(9.,0.,35.));
#94600=CARTESIAN_POINT('Origin',(0.,0.,-14.5));
#94601=CARTESIAN_POINT('',(-9.,-1.10218211923262E-15,-15.));
#94602=CARTESIAN_POINT('Origin',(0.,0.,-15.));
#94603=CARTESIAN_POINT('',(-9.,-1.10218211923262E-15,-14.));
#94604=CARTESIAN_POINT('',(-9.,-1.10218211923262E-15,-14.5));
#94605=CARTESIAN_POINT('Origin',(0.,0.,-14.));
#94606=CARTESIAN_POINT('Origin',(13.,0.,-15.));
#94607=CARTESIAN_POINT('',(-10.,1.22464679914735E-15,-15.));
#94608=CARTESIAN_POINT('Origin',(0.,0.,-15.));
#94609=CARTESIAN_POINT('Origin',(9.,0.,-14.));
#94610=CARTESIAN_POINT('',(-10.,-1.22464679914735E-15,-14.));
#94611=CARTESIAN_POINT('Origin',(0.,0.,-14.));
#94612=CARTESIAN_POINT('Origin',(0.,0.,-16.));
#94613=CARTESIAN_POINT('',(-10.,1.22464679914735E-15,-2.));
#94614=CARTESIAN_POINT('Origin',(0.,0.,-2.));
#94615=CARTESIAN_POINT('',(-10.,-1.22464679914735E-15,-16.));
#94616=CARTESIAN_POINT('Origin',(0.,0.,2.));
#94617=CARTESIAN_POINT('',(-12.,-1.46957615897682E-15,2.));
#94618=CARTESIAN_POINT('Origin',(0.,0.,2.));
#94619=CARTESIAN_POINT('Origin',(0.,0.,-2.));
#94620=CARTESIAN_POINT('',(-12.,-1.46957615897682E-15,-2.));
#94621=CARTESIAN_POINT('Origin',(0.,0.,-2.));
#94622=CARTESIAN_POINT('Origin',(0.,0.,-2.));
#94623=CARTESIAN_POINT('',(-12.,-1.46957615897682E-15,-2.));
#94624=CARTESIAN_POINT('Origin',(0.,0.,-16.));
#94625=CARTESIAN_POINT('',(-10.,-1.22464679914735E-15,-16.));
#94626=CARTESIAN_POINT('',(-10.,-1.22464679914735E-15,-16.));
#94627=CARTESIAN_POINT('Origin',(0.,0.,-16.));
#94628=CARTESIAN_POINT('Origin',(0.,0.,64.));
#94629=CARTESIAN_POINT('Origin',(0.,0.,-16.));
#94630=CARTESIAN_POINT('',(0.,0.,0.));
#94631=CARTESIAN_POINT('Origin',(0.,3.,5.));
#94632=CARTESIAN_POINT('',(0.,3.,15.));
#94633=CARTESIAN_POINT('',(0.,3.,5.));
#94634=CARTESIAN_POINT('',(0.,3.,15.));
#94635=CARTESIAN_POINT('',(6.,3.,15.));
#94636=CARTESIAN_POINT('',(0.,3.,15.));
#94637=CARTESIAN_POINT('',(6.,3.,5.));
#94638=CARTESIAN_POINT('',(6.,3.,15.));
#94639=CARTESIAN_POINT('',(0.,3.,5.));
#94640=CARTESIAN_POINT('Origin',(0.,0.,5.));
#94641=CARTESIAN_POINT('',(0.,-3.,5.));
#94642=CARTESIAN_POINT('Origin',(0.,0.,5.));
#94643=CARTESIAN_POINT('',(6.,-3.,5.));
#94644=CARTESIAN_POINT('Origin',(6.,0.,5.));
#94645=CARTESIAN_POINT('',(0.,-3.,5.));
#94646=CARTESIAN_POINT('Origin',(0.,-3.,15.));
#94647=CARTESIAN_POINT('',(0.,-3.,15.));
#94648=CARTESIAN_POINT('',(0.,-3.,5.));
#94649=CARTESIAN_POINT('',(6.,-3.,15.));
#94650=CARTESIAN_POINT('',(6.,-3.,5.));
#94651=CARTESIAN_POINT('',(0.,-3.,15.));
#94652=CARTESIAN_POINT('Origin',(0.,0.,15.));
#94653=CARTESIAN_POINT('Origin',(0.,0.,15.));
#94654=CARTESIAN_POINT('Origin',(6.,0.,15.));
#94655=CARTESIAN_POINT('Origin',(6.,0.,10.));
#94656=CARTESIAN_POINT('Origin',(0.,0.,10.));
#94657=CARTESIAN_POINT('',(0.,0.,0.));
#94658=CARTESIAN_POINT('Origin',(0.,0.,0.));
#94659=CARTESIAN_POINT('',(-6.,-7.34788079488412E-16,16.));
#94660=CARTESIAN_POINT('Origin',(0.,0.,16.));
#94661=CARTESIAN_POINT('',(-6.,-7.34788079488412E-16,0.));
#94662=CARTESIAN_POINT('',(-6.,-7.34788079488412E-16,0.));
#94663=CARTESIAN_POINT('Origin',(0.,0.,0.));
#94664=CARTESIAN_POINT('Origin',(0.,0.,16.));
#94665=CARTESIAN_POINT('Origin',(0.,0.,0.));
#94666=CARTESIAN_POINT('',(0.,0.,0.));
#94667=CARTESIAN_POINT('Origin',(-32.5,-56.2916512459885,6.));
#94668=CARTESIAN_POINT('',(-36.5,-56.2916512459885,6.));
#94669=CARTESIAN_POINT('Origin',(-32.5,-56.2916512459885,6.));
#94670=CARTESIAN_POINT('',(-35.,-56.2916512459885,6.));
#94671=CARTESIAN_POINT('Origin',(-32.5,-56.2916512459885,6.));
#94672=CARTESIAN_POINT('Origin',(-32.5,-56.2916512459885,8.));
#94673=CARTESIAN_POINT('',(-36.5,-56.2916512459885,10.));
#94674=CARTESIAN_POINT('Origin',(-32.5,-56.2916512459885,10.));
#94675=CARTESIAN_POINT('',(-36.5,-56.2916512459885,8.));
#94676=CARTESIAN_POINT('Origin',(-32.5,-56.2916512459885,5.));
#94677=CARTESIAN_POINT('',(-35.,-56.2916512459885,0.));
#94678=CARTESIAN_POINT('',(-35.,-56.2916512459885,5.));
#94679=CARTESIAN_POINT('Origin',(-32.5,-56.2916512459885,0.));
#94680=CARTESIAN_POINT('Origin',(-32.5,56.2916512459885,6.));
#94681=CARTESIAN_POINT('',(-36.5,56.2916512459885,6.));
#94682=CARTESIAN_POINT('Origin',(-32.5,56.2916512459885,6.));
#94683=CARTESIAN_POINT('',(-35.,56.2916512459885,6.));
#94684=CARTESIAN_POINT('Origin',(-32.5,56.2916512459885,6.));
#94685=CARTESIAN_POINT('Origin',(-32.5,56.2916512459885,8.));
#94686=CARTESIAN_POINT('',(-36.5,56.2916512459885,10.));
#94687=CARTESIAN_POINT('Origin',(-32.5,56.2916512459885,10.));
#94688=CARTESIAN_POINT('',(-36.5,56.2916512459885,8.));
#94689=CARTESIAN_POINT('Origin',(-32.5,56.2916512459885,5.));
#94690=CARTESIAN_POINT('',(-35.,56.2916512459885,0.));
#94691=CARTESIAN_POINT('',(-35.,56.2916512459885,5.));
#94692=CARTESIAN_POINT('Origin',(-32.5,56.2916512459885,0.));
#94693=CARTESIAN_POINT('Origin',(65.,0.,6.));
#94694=CARTESIAN_POINT('',(61.,4.89858719658941E-16,6.));
#94695=CARTESIAN_POINT('Origin',(65.,0.,6.));
#94696=CARTESIAN_POINT('',(62.5,3.06161699786838E-16,6.));
#94697=CARTESIAN_POINT('Origin',(65.,0.,6.));
#94698=CARTESIAN_POINT('Origin',(65.,0.,8.));
#94699=CARTESIAN_POINT('',(61.,4.89858719658941E-16,10.));
#94700=CARTESIAN_POINT('Origin',(65.,0.,10.));
#94701=CARTESIAN_POINT('',(61.,4.89858719658941E-16,8.));
#94702=CARTESIAN_POINT('Origin',(65.,0.,5.));
#94703=CARTESIAN_POINT('',(62.5,3.06161699786838E-16,0.));
#94704=CARTESIAN_POINT('',(62.5,3.06161699786838E-16,5.));
#94705=CARTESIAN_POINT('Origin',(65.,0.,0.));
#94706=CARTESIAN_POINT('Origin',(32.5,56.2916512459885,6.));
#94707=CARTESIAN_POINT('',(28.5,56.2916512459885,6.));
#94708=CARTESIAN_POINT('Origin',(32.5,56.2916512459885,6.));
#94709=CARTESIAN_POINT('',(30.,56.2916512459885,6.));
#94710=CARTESIAN_POINT('Origin',(32.5,56.2916512459885,6.));
#94711=CARTESIAN_POINT('Origin',(32.5,56.2916512459885,8.));
#94712=CARTESIAN_POINT('',(28.5,56.2916512459885,10.));
#94713=CARTESIAN_POINT('Origin',(32.5,56.2916512459885,10.));
#94714=CARTESIAN_POINT('',(28.5,56.2916512459885,8.));
#94715=CARTESIAN_POINT('Origin',(32.5,56.2916512459885,5.));
#94716=CARTESIAN_POINT('',(30.,56.2916512459885,0.));
#94717=CARTESIAN_POINT('',(30.,56.2916512459885,5.));
#94718=CARTESIAN_POINT('Origin',(32.5,56.2916512459885,0.));
#94719=CARTESIAN_POINT('Origin',(-65.,7.9602041944578E-15,6.));
#94720=CARTESIAN_POINT('',(-69.,8.45006291411674E-15,6.));
#94721=CARTESIAN_POINT('Origin',(-65.,7.9602041944578E-15,6.));
#94722=CARTESIAN_POINT('',(-67.5,8.26636589424463E-15,6.));
#94723=CARTESIAN_POINT('Origin',(-65.,7.9602041944578E-15,6.));
#94724=CARTESIAN_POINT('Origin',(-65.,7.9602041944578E-15,8.));
#94725=CARTESIAN_POINT('',(-69.,8.45006291411674E-15,10.));
#94726=CARTESIAN_POINT('Origin',(-65.,7.9602041944578E-15,10.));
#94727=CARTESIAN_POINT('',(-69.,8.45006291411674E-15,8.));
#94728=CARTESIAN_POINT('Origin',(-65.,7.9602041944578E-15,5.));
#94729=CARTESIAN_POINT('',(-67.5,8.26636589424463E-15,0.));
#94730=CARTESIAN_POINT('',(-67.5,8.26636589424463E-15,5.));
#94731=CARTESIAN_POINT('Origin',(-65.,7.9602041944578E-15,0.));
#94732=CARTESIAN_POINT('Origin',(32.5,-56.2916512459885,6.));
#94733=CARTESIAN_POINT('',(28.5,-56.2916512459885,6.));
#94734=CARTESIAN_POINT('Origin',(32.5,-56.2916512459885,6.));
#94735=CARTESIAN_POINT('',(30.,-56.2916512459885,6.));
#94736=CARTESIAN_POINT('Origin',(32.5,-56.2916512459885,6.));
#94737=CARTESIAN_POINT('Origin',(32.5,-56.2916512459885,8.));
#94738=CARTESIAN_POINT('',(28.5,-56.2916512459885,10.));
#94739=CARTESIAN_POINT('Origin',(32.5,-56.2916512459885,10.));
#94740=CARTESIAN_POINT('',(28.5,-56.2916512459885,8.));
#94741=CARTESIAN_POINT('Origin',(32.5,-56.2916512459885,5.));
#94742=CARTESIAN_POINT('',(30.,-56.2916512459885,0.));
#94743=CARTESIAN_POINT('',(30.,-56.2916512459885,5.));
#94744=CARTESIAN_POINT('Origin',(32.5,-56.2916512459885,0.));
#94745=CARTESIAN_POINT('Origin',(0.,0.,0.));
#94746=CARTESIAN_POINT('',(-12.,-1.46957615897682E-15,10.));
#94747=CARTESIAN_POINT('Origin',(0.,0.,10.));
#94748=CARTESIAN_POINT('',(-12.,-1.46957615897682E-15,0.));
#94749=CARTESIAN_POINT('',(-12.,-1.46957615897682E-15,0.));
#94750=CARTESIAN_POINT('Origin',(0.,0.,0.));
#94751=CARTESIAN_POINT('Origin',(0.,0.,0.));
#94752=CARTESIAN_POINT('',(-70.,-8.57252759403147E-15,10.));
#94753=CARTESIAN_POINT('Origin',(0.,0.,10.));
#94754=CARTESIAN_POINT('',(-70.,-8.57252759403147E-15,0.));
#94755=CARTESIAN_POINT('',(-70.,-8.57252759403147E-15,0.));
#94756=CARTESIAN_POINT('Origin',(0.,0.,0.));
#94757=CARTESIAN_POINT('Origin',(0.,0.,10.));
#94758=CARTESIAN_POINT('Origin',(0.,0.,0.));
#94759=CARTESIAN_POINT('',(0.,0.,0.));
#94760=CARTESIAN_POINT('Origin',(0.,0.,0.));
#94761=CARTESIAN_POINT('',(-12.,-1.46957615897682E-15,2.));
#94762=CARTESIAN_POINT('Origin',(0.,0.,2.));
#94763=CARTESIAN_POINT('',(-12.,-1.46957615897682E-15,0.));
#94764=CARTESIAN_POINT('',(-12.,-1.46957615897682E-15,0.));
#94765=CARTESIAN_POINT('Origin',(0.,0.,0.));
#94766=CARTESIAN_POINT('Origin',(0.,0.,0.));
#94767=CARTESIAN_POINT('',(-60.,-7.34788079488412E-15,2.));
#94768=CARTESIAN_POINT('Origin',(0.,0.,2.));
#94769=CARTESIAN_POINT('',(-60.,-7.34788079488412E-15,0.));
#94770=CARTESIAN_POINT('',(-60.,-7.34788079488412E-15,0.));
#94771=CARTESIAN_POINT('Origin',(0.,0.,0.));
#94772=CARTESIAN_POINT('Origin',(0.,0.,2.));
#94773=CARTESIAN_POINT('Origin',(0.,0.,0.));
#94774=CARTESIAN_POINT('',(0.,0.,0.));
#94775=CARTESIAN_POINT('Origin',(-14.1292828945603,-53.2669068454841,1.5));
#94776=CARTESIAN_POINT('',(-17.1292828945603,-53.2669068454841,2.));
#94777=CARTESIAN_POINT('Origin',(-14.1292828945603,-53.2669068454841,2.));
#94778=CARTESIAN_POINT('',(-16.1292828945603,-53.2669068454841,1.));
#94779=CARTESIAN_POINT('',(-16.6292828945603,-53.2669068454841,1.5));
#94780=CARTESIAN_POINT('Origin',(-14.1292828945603,-53.2669068454841,1.));
#94781=CARTESIAN_POINT('Origin',(-14.1292828945603,-53.2669068454841,1.));
#94782=CARTESIAN_POINT('',(-16.1292828945603,-53.2669068454841,0.));
#94783=CARTESIAN_POINT('',(-16.1292828945603,-53.2669068454841,1.));
#94784=CARTESIAN_POINT('Origin',(-14.1292828945603,-53.2669068454841,0.));
#94785=CARTESIAN_POINT('Origin',(-39.0658530619283,38.8697713466882,1.5));
#94786=CARTESIAN_POINT('',(-42.0658530619283,38.8697713466882,2.));
#94787=CARTESIAN_POINT('Origin',(-39.0658530619283,38.8697713466882,2.));
#94788=CARTESIAN_POINT('',(-41.0658530619283,38.8697713466882,1.));
#94789=CARTESIAN_POINT('',(-41.5658530619283,38.8697713466882,1.5));
#94790=CARTESIAN_POINT('Origin',(-39.0658530619283,38.8697713466882,1.));
#94791=CARTESIAN_POINT('Origin',(-39.0658530619283,38.8697713466882,1.));
#94792=CARTESIAN_POINT('',(-41.0658530619283,38.8697713466882,0.));
#94793=CARTESIAN_POINT('',(-41.0658530619283,38.8697713466882,1.));
#94794=CARTESIAN_POINT('Origin',(-39.0658530619283,38.8697713466882,0.));
#94795=CARTESIAN_POINT('Origin',(53.1951359564886,14.3971354987959,1.5));
#94796=CARTESIAN_POINT('',(50.1951359564886,14.3971354987959,2.));
#94797=CARTESIAN_POINT('Origin',(53.1951359564886,14.3971354987959,2.));
#94798=CARTESIAN_POINT('',(51.1951359564886,14.3971354987959,1.));
#94799=CARTESIAN_POINT('',(50.6951359564886,14.3971354987959,1.5));
#94800=CARTESIAN_POINT('Origin',(53.1951359564886,14.3971354987959,1.));
#94801=CARTESIAN_POINT('Origin',(53.1951359564886,14.3971354987959,1.));
#94802=CARTESIAN_POINT('',(51.1951359564886,14.3971354987959,0.));
#94803=CARTESIAN_POINT('',(51.1951359564886,14.3971354987959,1.));
#94804=CARTESIAN_POINT('Origin',(53.1951359564886,14.3971354987959,0.));
#94805=CARTESIAN_POINT('Origin',(14.1292828945603,53.2669068454841,1.5));
#94806=CARTESIAN_POINT('',(11.1292828945603,53.2669068454841,2.));
#94807=CARTESIAN_POINT('Origin',(14.1292828945603,53.2669068454841,2.));
#94808=CARTESIAN_POINT('',(12.1292828945603,53.2669068454841,1.));
#94809=CARTESIAN_POINT('',(11.6292828945603,53.2669068454841,1.5));
#94810=CARTESIAN_POINT('Origin',(14.1292828945603,53.2669068454841,1.));
#94811=CARTESIAN_POINT('Origin',(14.1292828945603,53.2669068454841,1.));
#94812=CARTESIAN_POINT('',(12.1292828945603,53.2669068454841,0.));
#94813=CARTESIAN_POINT('',(12.1292828945603,53.2669068454841,1.));
#94814=CARTESIAN_POINT('Origin',(14.1292828945603,53.2669068454841,0.));
#94815=CARTESIAN_POINT('Origin',(-53.1951359564886,-14.3971354987959,1.5));
#94816=CARTESIAN_POINT('',(-56.1951359564886,-14.3971354987959,2.));
#94817=CARTESIAN_POINT('Origin',(-53.1951359564886,-14.3971354987959,2.));
#94818=CARTESIAN_POINT('',(-55.1951359564886,-14.3971354987959,1.));
#94819=CARTESIAN_POINT('',(-55.6951359564886,-14.3971354987959,1.5));
#94820=CARTESIAN_POINT('Origin',(-53.1951359564886,-14.3971354987959,1.));
#94821=CARTESIAN_POINT('Origin',(-53.1951359564886,-14.3971354987959,1.));
#94822=CARTESIAN_POINT('',(-55.1951359564886,-14.3971354987959,0.));
#94823=CARTESIAN_POINT('',(-55.1951359564886,-14.3971354987959,1.));
#94824=CARTESIAN_POINT('Origin',(-53.1951359564886,-14.3971354987959,0.));
#94825=CARTESIAN_POINT('Origin',(39.0658530619283,-38.8697713466882,1.5));
#94826=CARTESIAN_POINT('',(36.0658530619283,-38.8697713466882,2.));
#94827=CARTESIAN_POINT('Origin',(39.0658530619283,-38.8697713466882,2.));
#94828=CARTESIAN_POINT('',(37.0658530619283,-38.8697713466882,0.999999999999996));
#94829=CARTESIAN_POINT('',(36.5658530619283,-38.8697713466882,1.5));
#94830=CARTESIAN_POINT('Origin',(39.0658530619283,-38.8697713466882,1.));
#94831=CARTESIAN_POINT('Origin',(39.0658530619283,-38.8697713466882,1.));
#94832=CARTESIAN_POINT('',(37.0658530619283,-38.8697713466882,0.));
#94833=CARTESIAN_POINT('',(37.0658530619283,-38.8697713466882,1.));
#94834=CARTESIAN_POINT('Origin',(39.0658530619283,-38.8697713466882,0.));
#94835=CARTESIAN_POINT('Origin',(0.,0.,0.));
#94836=CARTESIAN_POINT('',(-50.,-6.12323399573677E-15,2.));
#94837=CARTESIAN_POINT('Origin',(0.,0.,2.));
#94838=CARTESIAN_POINT('',(-50.,-6.12323399573677E-15,0.));
#94839=CARTESIAN_POINT('',(-50.,-6.12323399573677E-15,0.));
#94840=CARTESIAN_POINT('Origin',(0.,0.,0.));
#94841=CARTESIAN_POINT('Origin',(0.,0.,0.));
#94842=CARTESIAN_POINT('',(-59.,-7.22541611496938E-15,2.));
#94843=CARTESIAN_POINT('Origin',(0.,0.,2.));
#94844=CARTESIAN_POINT('',(-59.,-7.22541611496938E-15,0.));
#94845=CARTESIAN_POINT('',(-59.,-7.22541611496938E-15,0.));
#94846=CARTESIAN_POINT('Origin',(0.,0.,0.));
#94847=CARTESIAN_POINT('Origin',(0.,0.,2.));
#94848=CARTESIAN_POINT('Origin',(0.,0.,0.));
#94849=CARTESIAN_POINT('',(0.,0.,0.));
#94850=CARTESIAN_POINT('Origin',(0.,0.,0.));
#94851=CARTESIAN_POINT('',(-10.,-1.22464679914735E-15,10.));
#94852=CARTESIAN_POINT('Origin',(0.,0.,10.));
#94853=CARTESIAN_POINT('',(-10.,-1.22464679914735E-15,0.));
#94854=CARTESIAN_POINT('',(-10.,-1.22464679914735E-15,0.));
#94855=CARTESIAN_POINT('Origin',(0.,0.,0.));
#94856=CARTESIAN_POINT('Origin',(0.,0.,0.));
#94857=CARTESIAN_POINT('',(-12.,-1.46957615897682E-15,10.));
#94858=CARTESIAN_POINT('Origin',(0.,0.,10.));
#94859=CARTESIAN_POINT('',(-12.,-1.46957615897682E-15,0.));
#94860=CARTESIAN_POINT('',(-12.,-1.46957615897682E-15,0.));
#94861=CARTESIAN_POINT('Origin',(0.,0.,0.));
#94862=CARTESIAN_POINT('Origin',(0.,0.,10.));
#94863=CARTESIAN_POINT('Origin',(0.,0.,0.));
#94864=CARTESIAN_POINT('',(0.,0.,0.));
#94865=CARTESIAN_POINT('Origin',(0.,0.,0.));
#94866=CARTESIAN_POINT('',(-10.,-1.22464679914735E-15,4.));
#94867=CARTESIAN_POINT('Origin',(0.,0.,4.));
#94868=CARTESIAN_POINT('',(-10.,-1.22464679914735E-15,0.));
#94869=CARTESIAN_POINT('',(-10.,-1.22464679914735E-15,0.));
#94870=CARTESIAN_POINT('Origin',(0.,0.,0.));
#94871=CARTESIAN_POINT('Origin',(0.,0.,0.));
#94872=CARTESIAN_POINT('',(-12.,-1.46957615897682E-15,4.));
#94873=CARTESIAN_POINT('Origin',(0.,0.,4.));
#94874=CARTESIAN_POINT('',(-12.,-1.46957615897682E-15,0.));
#94875=CARTESIAN_POINT('',(-12.,-1.46957615897682E-15,0.));
#94876=CARTESIAN_POINT('Origin',(0.,0.,0.));
#94877=CARTESIAN_POINT('Origin',(0.,0.,4.));
#94878=CARTESIAN_POINT('Origin',(0.,0.,0.));
#94879=CARTESIAN_POINT('',(0.,0.,0.));
#94880=CARTESIAN_POINT('Origin',(0.,0.,0.));
#94881=CARTESIAN_POINT('',(-10.,-1.22464679914735E-15,2.));
#94882=CARTESIAN_POINT('Origin',(0.,0.,2.));
#94883=CARTESIAN_POINT('',(-10.,-1.22464679914735E-15,0.));
#94884=CARTESIAN_POINT('',(-10.,-1.22464679914735E-15,0.));
#94885=CARTESIAN_POINT('Origin',(0.,0.,0.));
#94886=CARTESIAN_POINT('Origin',(0.,0.,0.));
#94887=CARTESIAN_POINT('',(-14.,-1.71450551880629E-15,2.));
#94888=CARTESIAN_POINT('Origin',(0.,0.,2.));
#94889=CARTESIAN_POINT('',(-14.,-1.71450551880629E-15,0.));
#94890=CARTESIAN_POINT('',(-14.,-1.71450551880629E-15,0.));
#94891=CARTESIAN_POINT('Origin',(0.,0.,0.));
#94892=CARTESIAN_POINT('Origin',(0.,0.,2.));
#94893=CARTESIAN_POINT('Origin',(0.,0.,0.));
#94894=CARTESIAN_POINT('',(0.,0.,0.));
#94895=CARTESIAN_POINT('Origin',(-1.,0.,1.));
#94896=CARTESIAN_POINT('',(-1.,8.94427190999916,0.));
#94897=CARTESIAN_POINT('',(-1.,8.94427190999916,1.));
#94898=CARTESIAN_POINT('',(-1.,8.94427190999916,0.));
#94899=CARTESIAN_POINT('',(-1.,13.9642400437689,0.));
#94900=CARTESIAN_POINT('',(-1.,0.,0.));
#94901=CARTESIAN_POINT('',(-1.,13.9642400437689,1.));
#94902=CARTESIAN_POINT('',(-1.,13.9642400437689,0.));
#94903=CARTESIAN_POINT('',(-1.,0.,1.));
#94904=CARTESIAN_POINT('Origin',(1.,28.,1.));
#94905=CARTESIAN_POINT('',(1.,8.94427190999916,1.));
#94906=CARTESIAN_POINT('',(1.,8.94427190999916,0.));
#94907=CARTESIAN_POINT('',(1.,8.94427190999916,0.));
#94908=CARTESIAN_POINT('',(1.,13.9642400437689,1.));
#94909=CARTESIAN_POINT('',(1.,14.,1.));
#94910=CARTESIAN_POINT('',(1.,13.9642400437689,0.));
#94911=CARTESIAN_POINT('',(1.,13.9642400437689,0.));
#94912=CARTESIAN_POINT('',(1.,14.,0.));
#94913=CARTESIAN_POINT('Origin',(0.,0.,0.));
#94914=CARTESIAN_POINT('Origin',(0.,0.,0.));
#94915=CARTESIAN_POINT('Origin',(0.,0.,0.));
#94916=CARTESIAN_POINT('Origin',(0.,0.,0.));
#94917=CARTESIAN_POINT('Origin',(0.,0.,1.));
#94918=CARTESIAN_POINT('Origin',(0.,0.,0.));
#94919=CARTESIAN_POINT('Origin',(0.,0.,1.));
#94920=CARTESIAN_POINT('Origin',(0.,0.,1.));
#94921=CARTESIAN_POINT('',(0.,0.,0.));
#94922=CARTESIAN_POINT('Origin',(0.,0.,6.));
#94923=CARTESIAN_POINT('',(-2.5,-3.06161699786838E-16,6.));
#94924=CARTESIAN_POINT('Origin',(0.,0.,6.));
#94925=CARTESIAN_POINT('',(-1.5,-1.83697019872103E-16,6.));
#94926=CARTESIAN_POINT('Origin',(0.,0.,6.));
#94927=CARTESIAN_POINT('Origin',(0.,0.,6.));
#94928=CARTESIAN_POINT('',(-2.5,-3.06161699786838E-16,9.));
#94929=CARTESIAN_POINT('Origin',(0.,0.,9.));
#94930=CARTESIAN_POINT('',(-2.5,-3.06161699786838E-16,6.));
#94931=CARTESIAN_POINT('Origin',(0.,0.,9.));
#94932=CARTESIAN_POINT('Origin',(0.,0.,-1.));
#94933=CARTESIAN_POINT('',(-1.5,-1.83697019872103E-16,-1.));
#94934=CARTESIAN_POINT('',(-1.5,-1.83697019872103E-16,-1.));
#94935=CARTESIAN_POINT('Origin',(0.,0.,-1.));
#94936=CARTESIAN_POINT('Origin',(0.,0.,-1.));
#94937=CARTESIAN_POINT('',(0.,0.,0.));
#94938=CARTESIAN_POINT('Ctrl Pts',(3.,-6.12323399573676E-17,0.));
#94939=CARTESIAN_POINT('Ctrl Pts',(3.,0.0512820512820512,-0.483321946706122));
#94940=CARTESIAN_POINT('Ctrl Pts',(2.76209532949166,0.153846153846154,-1.44946426164245));
#94941=CARTESIAN_POINT('Ctrl Pts',(1.77197968324867,0.307692307692308,-2.56735208320081));
#94942=CARTESIAN_POINT('Ctrl Pts',(0.376021898059208,0.461538461538461,
-3.09643080035079));
#94943=CARTESIAN_POINT('Ctrl Pts',(-1.10621475336255,0.615384615384616,
-2.91679593290564));
#94944=CARTESIAN_POINT('Ctrl Pts',(-2.33474201794243,0.769230769230768,
-2.0684045486807));
#94945=CARTESIAN_POINT('Ctrl Pts',(-3.02885773675456,0.923076923076924,
-0.746548640155209));
#94946=CARTESIAN_POINT('Ctrl Pts',(-3.02855730304457,1.07692307692308,0.746474906977016));
#94947=CARTESIAN_POINT('Ctrl Pts',(-2.33497949559777,1.23076923076923,2.06860866176523));
#94948=CARTESIAN_POINT('Ctrl Pts',(-1.10608225550105,1.38461538461538,2.91650190270812));
#94949=CARTESIAN_POINT('Ctrl Pts',(0.376013421364463,1.53846153846154,3.0967529299689));
#94950=CARTESIAN_POINT('Ctrl Pts',(1.77190704246167,1.69230769230769,2.56705030189252));
#94951=CARTESIAN_POINT('Ctrl Pts',(2.76217801015642,1.84615384615384,1.44970288425454));
#94952=CARTESIAN_POINT('Ctrl Pts',(3.1191987918465,2.,1.70719823792917E-15));
#94953=CARTESIAN_POINT('Ctrl Pts',(2.76217801015642,2.15384615384615,-1.44970288425453));
#94954=CARTESIAN_POINT('Ctrl Pts',(1.77190704246167,2.30769230769231,-2.56705030189251));
#94955=CARTESIAN_POINT('Ctrl Pts',(0.376013421364468,2.46153846153846,-3.09675292996889));
#94956=CARTESIAN_POINT('Ctrl Pts',(-1.10608225550105,2.61538461538461,-2.91650190270813));
#94957=CARTESIAN_POINT('Ctrl Pts',(-2.33497949559777,2.76923076923077,-2.06860866176523));
#94958=CARTESIAN_POINT('Ctrl Pts',(-3.02855730304457,2.92307692307692,-0.746474906977022));
#94959=CARTESIAN_POINT('Ctrl Pts',(-3.02885773675456,3.07692307692307,0.746548640155207));
#94960=CARTESIAN_POINT('Ctrl Pts',(-2.33474201794243,3.23076923076923,2.0684045486807));
#94961=CARTESIAN_POINT('Ctrl Pts',(-1.10621475336255,3.38461538461538,2.91679593290564));
#94962=CARTESIAN_POINT('Ctrl Pts',(0.376021898059204,3.53846153846154,3.09643080035079));
#94963=CARTESIAN_POINT('Ctrl Pts',(1.77197968324866,3.69230769230769,2.56735208320081));
#94964=CARTESIAN_POINT('Ctrl Pts',(2.76209532949166,3.84615384615385,1.44946426164245));
#94965=CARTESIAN_POINT('Ctrl Pts',(3.,3.94871794871795,0.483321946706125));
#94966=CARTESIAN_POINT('Ctrl Pts',(3.,4.,1.46957615897682E-15));
#94967=CARTESIAN_POINT('Ctrl Pts',(3.,-0.149599650170943,0.));
#94968=CARTESIAN_POINT('Ctrl Pts',(3.,-0.0983175988888913,-0.4835411540332));
#94969=CARTESIAN_POINT('Ctrl Pts',(2.76209576921471,0.00424650367521139,
-1.44932835794453));
#94970=CARTESIAN_POINT('Ctrl Pts',(1.77200161890609,0.158092657521365,-2.56746394660749));
#94971=CARTESIAN_POINT('Ctrl Pts',(0.376023954420967,0.311938811367519,
-3.09638050731302));
#94972=CARTESIAN_POINT('Ctrl Pts',(-1.10623737843825,0.465784965213672,
-2.91686578526799));
#94973=CARTESIAN_POINT('Ctrl Pts',(-2.33472522086381,0.619631119059827,
-2.06838287160141));
#94974=CARTESIAN_POINT('Ctrl Pts',(-3.02891313603334,0.77347727290598,-0.746566701745084));
#94975=CARTESIAN_POINT('Ctrl Pts',(-3.02853676566909,0.927323426752134,
0.746472023741791));
#94976=CARTESIAN_POINT('Ctrl Pts',(-2.33502184745744,1.08116958059829,2.0686447945416));
#94977=CARTESIAN_POINT('Ctrl Pts',(-1.10607478639173,1.23501573444444,2.91648299449822));
#94978=CARTESIAN_POINT('Ctrl Pts',(0.376020159868782,1.3888618882906,3.09680852875374));
#94979=CARTESIAN_POINT('Ctrl Pts',(1.77189524100041,1.54270804213675,2.56703330753083));
#94980=CARTESIAN_POINT('Ctrl Pts',(2.76222787027974,1.6965541959829,1.44972899802138));
#94981=CARTESIAN_POINT('Ctrl Pts',(3.1191779858324,1.85040034982906,1.3413700440872E-15));
#94982=CARTESIAN_POINT('Ctrl Pts',(2.76222787027974,2.00424650367521,-1.44972899802137));
#94983=CARTESIAN_POINT('Ctrl Pts',(1.77189524100041,2.15809265752137,-2.56703330753083));
#94984=CARTESIAN_POINT('Ctrl Pts',(0.376020159868788,2.31193881136752,-3.09680852875374));
#94985=CARTESIAN_POINT('Ctrl Pts',(-1.10607478639173,2.46578496521367,-2.91648299449822));
#94986=CARTESIAN_POINT('Ctrl Pts',(-2.33502184745743,2.61963111905983,-2.0686447945416));
#94987=CARTESIAN_POINT('Ctrl Pts',(-3.0285367656691,2.77347727290598,-0.746472023741798));
#94988=CARTESIAN_POINT('Ctrl Pts',(-3.02891313603333,2.92732342675214,0.746566701745082));
#94989=CARTESIAN_POINT('Ctrl Pts',(-2.33472522086383,3.08116958059829,2.06838287160141));
#94990=CARTESIAN_POINT('Ctrl Pts',(-1.10623737843825,3.23501573444444,2.91686578526799));
#94991=CARTESIAN_POINT('Ctrl Pts',(0.376023954420961,3.38886188829059,3.09638050731302));
#94992=CARTESIAN_POINT('Ctrl Pts',(1.77200161890609,3.54270804213675,2.56746394660749));
#94993=CARTESIAN_POINT('Ctrl Pts',(2.76209576921471,3.69655419598291,1.44932835794453));
#94994=CARTESIAN_POINT('Ctrl Pts',(3.,3.79911829854701,0.483541154033203));
#94995=CARTESIAN_POINT('Ctrl Pts',(3.,3.85040034982906,1.46957615897682E-15));
#94996=CARTESIAN_POINT('Ctrl Pts',(2.85712660496334,-0.447398096836595,
0.));
#94997=CARTESIAN_POINT('Ctrl Pts',(2.85712660496334,-0.396116045554544,
-0.460194067158232));
#94998=CARTESIAN_POINT('Ctrl Pts',(2.63055179659491,-0.293551942990442,
-1.38050245605029));
#94999=CARTESIAN_POINT('Ctrl Pts',(1.68757909829609,-0.139705789144288,
-2.44502721529682));
#95000=CARTESIAN_POINT('Ctrl Pts',(0.358113025085229,0.0141403647018659,
-2.94899016152089));
#95001=CARTESIAN_POINT('Ctrl Pts',(-1.05352052128293,0.16798651854802,-2.77785005675019));
#95002=CARTESIAN_POINT('Ctrl Pts',(-2.22355960197289,0.321832672394174,
-1.96990875947179));
#95003=CARTESIAN_POINT('Ctrl Pts',(-2.88458222522762,0.475678826240328,
-0.710985602845217));
#95004=CARTESIAN_POINT('Ctrl Pts',(-2.88433418102835,0.62952498008648,0.71092588480246));
#95005=CARTESIAN_POINT('Ctrl Pts',(-2.22375610724719,0.783371133932636,
1.97007416068242));
#95006=CARTESIAN_POINT('Ctrl Pts',(-1.05340942551119,0.937217287778789,
2.77761454217348));
#95007=CARTESIAN_POINT('Ctrl Pts',(0.358102604038195,1.09106344162494,2.94924384613783));
#95008=CARTESIAN_POINT('Ctrl Pts',(1.68752683583458,1.2449095954711,2.44480442711754));
#95009=CARTESIAN_POINT('Ctrl Pts',(2.63060575577254,1.39875574931725,1.38064846415744));
#95010=CARTESIAN_POINT('Ctrl Pts',(2.97065905213792,1.5526019031634,-2.4388546256131E-16));
#95011=CARTESIAN_POINT('Ctrl Pts',(2.63060575577254,1.70644805700956,-1.38064846415743));
#95012=CARTESIAN_POINT('Ctrl Pts',(1.68752683583459,1.86029421085571,-2.44480442711754));
#95013=CARTESIAN_POINT('Ctrl Pts',(0.358102604038199,2.01414036470186,-2.94924384613782));
#95014=CARTESIAN_POINT('Ctrl Pts',(-1.05340942551119,2.16798651854802,-2.77761454217349));
#95015=CARTESIAN_POINT('Ctrl Pts',(-2.22375610724719,2.32183267239418,-1.97007416068241));
#95016=CARTESIAN_POINT('Ctrl Pts',(-2.88433418102835,2.47567882624033,-0.710925884802468));
#95017=CARTESIAN_POINT('Ctrl Pts',(-2.88458222522762,2.62952498008648,0.710985602845219));
#95018=CARTESIAN_POINT('Ctrl Pts',(-2.2235596019729,2.78337113393263,1.96990875947178));
#95019=CARTESIAN_POINT('Ctrl Pts',(-1.05352052128293,2.93721728777879,2.7778500567502));
#95020=CARTESIAN_POINT('Ctrl Pts',(0.358113025085224,3.09106344162494,2.94899016152089));
#95021=CARTESIAN_POINT('Ctrl Pts',(1.68757909829608,3.2449095954711,2.44502721529682));
#95022=CARTESIAN_POINT('Ctrl Pts',(2.63055179659491,3.39875574931725,1.3805024560503));
#95023=CARTESIAN_POINT('Ctrl Pts',(2.85712660496334,3.50131985188135,0.460194067158235));
#95024=CARTESIAN_POINT('Ctrl Pts',(2.85712660496334,3.55260190316341,1.39958838061084E-15));
#95025=CARTESIAN_POINT('Ctrl Pts',(2.3726759939225,-0.557941290809918,0.));
#95026=CARTESIAN_POINT('Ctrl Pts',(2.3726759939225,-0.506659239527867,-0.382282398128741));
#95027=CARTESIAN_POINT('Ctrl Pts',(2.18451914777363,-0.404095136963764,
-1.14635298489711));
#95028=CARTESIAN_POINT('Ctrl Pts',(1.40144724769161,-0.25024898311761,-2.03051196529879));
#95029=CARTESIAN_POINT('Ctrl Pts',(0.297392962941051,-0.0964028292714561,
-2.44893616184819));
#95030=CARTESIAN_POINT('Ctrl Pts',(-0.874899176834334,0.0574433245746974,
-2.3068791471024));
#95031=CARTESIAN_POINT('Ctrl Pts',(-1.84652671515893,0.211289478420851,
-1.63588194226376));
#95032=CARTESIAN_POINT('Ctrl Pts',(-2.39550615492902,0.365135632267005,
-0.590441565156793));
#95033=CARTESIAN_POINT('Ctrl Pts',(-2.39525921257935,0.518981786113159,
0.590380676300523));
#95034=CARTESIAN_POINT('Ctrl Pts',(-1.84672180305351,0.672827939959313,
1.63605047782857));
#95035=CARTESIAN_POINT('Ctrl Pts',(-0.874790687110246,0.826674093805466,
2.30663569332898));
#95036=CARTESIAN_POINT('Ctrl Pts',(0.297386834171931,0.98052024765162,2.44920394446013));
#95037=CARTESIAN_POINT('Ctrl Pts',(1.40138565077454,1.13436640149777,2.03025745375436));
#95038=CARTESIAN_POINT('Ctrl Pts',(2.18459061244276,1.28821255534393,1.14656161967552));
#95039=CARTESIAN_POINT('Ctrl Pts',(2.4669468077447,1.44205870919008,2.4388546256131E-16));
#95040=CARTESIAN_POINT('Ctrl Pts',(2.18459061244276,1.59590486303624,-1.14656161967552));
#95041=CARTESIAN_POINT('Ctrl Pts',(1.40138565077454,1.74975101688239,-2.03025745375436));
#95042=CARTESIAN_POINT('Ctrl Pts',(0.297386834171934,1.90359717072855,-2.44920394446012));
#95043=CARTESIAN_POINT('Ctrl Pts',(-0.874790687110244,2.0574433245747,-2.30663569332898));
#95044=CARTESIAN_POINT('Ctrl Pts',(-1.84672180305351,2.21128947842085,-1.63605047782857));
#95045=CARTESIAN_POINT('Ctrl Pts',(-2.39525921257935,2.36513563226701,-0.590380676300528));
#95046=CARTESIAN_POINT('Ctrl Pts',(-2.39550615492902,2.51898178611316,0.590441565156791));
#95047=CARTESIAN_POINT('Ctrl Pts',(-1.84652671515893,2.67282793995932,1.63588194226375));
#95048=CARTESIAN_POINT('Ctrl Pts',(-0.874899176834338,2.82667409380547,
2.3068791471024));
#95049=CARTESIAN_POINT('Ctrl Pts',(0.29739296294105,2.98052024765162,2.4489361618482));
#95050=CARTESIAN_POINT('Ctrl Pts',(1.4014472476916,3.13436640149777,2.03051196529879));
#95051=CARTESIAN_POINT('Ctrl Pts',(2.18451914777363,3.28821255534393,1.14635298489712));
#95052=CARTESIAN_POINT('Ctrl Pts',(2.3726759939225,3.39077665790803,0.382282398128744));
#95053=CARTESIAN_POINT('Ctrl Pts',(2.3726759939225,3.44205870919008,1.16227602454838E-15));
#95054=CARTESIAN_POINT('Ctrl Pts',(1.98402625071561,-0.248351324860585,
0.));
#95055=CARTESIAN_POINT('Ctrl Pts',(1.98402625071561,-0.197069273578533,
-0.319662635491883));
#95056=CARTESIAN_POINT('Ctrl Pts',(1.82668992334287,-0.0945051710144311,
-0.958578390155419));
#95057=CARTESIAN_POINT('Ctrl Pts',(1.17188688645211,0.059340982831723,-1.69790894363414));
#95058=CARTESIAN_POINT('Ctrl Pts',(0.248679307147478,0.213187136677876,
-2.0477950661503));
#95059=CARTESIAN_POINT('Ctrl Pts',(-0.731588588146289,0.367033290524031,
-1.92900674830902));
#95060=CARTESIAN_POINT('Ctrl Pts',(-1.54406150387629,0.520879444370184,
-1.36792084856094));
#95061=CARTESIAN_POINT('Ctrl Pts',(-2.00311651810014,0.674725598216338,
-0.493725804019771));
#95062=CARTESIAN_POINT('Ctrl Pts',(-2.00291038342168,0.82857175206249,0.493674987626987));
#95063=CARTESIAN_POINT('Ctrl Pts',(-1.54422435711181,0.982417905908647,
1.3680615051111));
#95064=CARTESIAN_POINT('Ctrl Pts',(-0.731498011144787,1.1362640597548,1.92880359121951));
#95065=CARTESIAN_POINT('Ctrl Pts',(0.248674160214009,1.29011021360096,2.04801848620564));
#95066=CARTESIAN_POINT('Ctrl Pts',(1.17183553828091,1.44395636744711,1.69769672907218));
#95067=CARTESIAN_POINT('Ctrl Pts',(1.82674944897787,1.59780252129326,0.958752086361943));
#95068=CARTESIAN_POINT('Ctrl Pts',(2.06285538814528,1.75164867513941,8.53599118964584E-16));
#95069=CARTESIAN_POINT('Ctrl Pts',(1.82674944897787,1.90549482898556,-0.958752086361939));
#95070=CARTESIAN_POINT('Ctrl Pts',(1.17183553828091,2.05934098283173,-1.69769672907218));
#95071=CARTESIAN_POINT('Ctrl Pts',(0.248674160214013,2.21318713667787,-2.04801848620563));
#95072=CARTESIAN_POINT('Ctrl Pts',(-0.731498011144785,2.36703329052403,
-1.92880359121952));
#95073=CARTESIAN_POINT('Ctrl Pts',(-1.54422435711181,2.52087944437019,-1.36806150511109));
#95074=CARTESIAN_POINT('Ctrl Pts',(-2.00291038342167,2.67472559821633,-0.493674987626991));
#95075=CARTESIAN_POINT('Ctrl Pts',(-2.00311651810014,2.8285717520625,0.49372580401977));
#95076=CARTESIAN_POINT('Ctrl Pts',(-1.54406150387629,2.98241790590864,1.36792084856094));
#95077=CARTESIAN_POINT('Ctrl Pts',(-0.731588588146291,3.1362640597548,1.92900674830902));
#95078=CARTESIAN_POINT('Ctrl Pts',(0.248679307147477,3.29011021360095,2.0477950661503));
#95079=CARTESIAN_POINT('Ctrl Pts',(1.17188688645211,3.44395636744711,1.69790894363414));
#95080=CARTESIAN_POINT('Ctrl Pts',(1.82668992334286,3.59780252129326,0.958578390155423));
#95081=CARTESIAN_POINT('Ctrl Pts',(1.9840262507156,3.70036662385736,0.319662635491885));
#95082=CARTESIAN_POINT('Ctrl Pts',(1.98402625071561,3.75164867513941,9.71892558945275E-16));
#95083=CARTESIAN_POINT('Ctrl Pts',(1.98458281684753,0.248133119200085,0.));
#95084=CARTESIAN_POINT('Ctrl Pts',(1.98458281684753,0.299415170482137,-0.319687116399019));
#95085=CARTESIAN_POINT('Ctrl Pts',(1.82720222215302,0.401979273046239,-0.958887711587539));
#95086=CARTESIAN_POINT('Ctrl Pts',(1.17220910470982,0.555825426892393,-1.69835197907329));
#95087=CARTESIAN_POINT('Ctrl Pts',(0.24874845599561,0.709671580738547,-2.04838447802754));
#95088=CARTESIAN_POINT('Ctrl Pts',(-0.731787087320181,0.863517734584699,
-1.92952710616438));
#95089=CARTESIAN_POINT('Ctrl Pts',(-1.54449964495675,1.01736388843086,-1.36831102934188));
#95090=CARTESIAN_POINT('Ctrl Pts',(-2.0036619638227,1.17121004227701,-0.493858934250917));
#95091=CARTESIAN_POINT('Ctrl Pts',(-2.00347835478891,1.32505619612316,0.493814332568918));
#95092=CARTESIAN_POINT('Ctrl Pts',(-1.54464495305281,1.47890234996932,1.36843453276745));
#95093=CARTESIAN_POINT('Ctrl Pts',(-0.731705434884396,1.63274850381547,
1.92935028937276));
#95094=CARTESIAN_POINT('Ctrl Pts',(0.2487419151547,1.78659465766162,2.04857646865583));
#95095=CARTESIAN_POINT('Ctrl Pts',(1.17216777551306,1.94044081150778,1.69817802712664));
#95096=CARTESIAN_POINT('Ctrl Pts',(1.82724706691833,2.09428696535393,0.959013272719332));
#95097=CARTESIAN_POINT('Ctrl Pts',(2.06344025539221,2.24813311920008,1.58525550664851E-15));
#95098=CARTESIAN_POINT('Ctrl Pts',(1.82724706691833,2.40197927304624,-0.959013272719332));
#95099=CARTESIAN_POINT('Ctrl Pts',(1.17216777551307,2.55582542689239,-1.69817802712664));
#95100=CARTESIAN_POINT('Ctrl Pts',(0.248741915154701,2.70967158073855,-2.04857646865583));
#95101=CARTESIAN_POINT('Ctrl Pts',(-0.731705434884394,2.8635177345847,-1.92935028937276));
#95102=CARTESIAN_POINT('Ctrl Pts',(-1.54464495305281,3.01736388843085,-1.36843453276745));
#95103=CARTESIAN_POINT('Ctrl Pts',(-2.00347835478892,3.17121004227701,-0.493814332568922));
#95104=CARTESIAN_POINT('Ctrl Pts',(-2.0036619638227,3.32505619612316,0.493858934250916));
#95105=CARTESIAN_POINT('Ctrl Pts',(-1.54449964495675,3.47890234996932,1.36831102934188));
#95106=CARTESIAN_POINT('Ctrl Pts',(-0.731787087320183,3.63274850381547,
1.92952710616438));
#95107=CARTESIAN_POINT('Ctrl Pts',(0.248748455995608,3.78659465766163,2.04838447802754));
#95108=CARTESIAN_POINT('Ctrl Pts',(1.17220910470981,3.94044081150777,1.69835197907329));
#95109=CARTESIAN_POINT('Ctrl Pts',(1.82720222215303,4.09428696535394,0.95888771158754));
#95110=CARTESIAN_POINT('Ctrl Pts',(1.98458281684753,4.19685106791804,0.319687116399021));
#95111=CARTESIAN_POINT('Ctrl Pts',(1.98458281684753,4.24813311920009,9.72165197718065E-16));
#95112=CARTESIAN_POINT('Ctrl Pts',(2.37244316231612,0.558475305697687,0.));
#95113=CARTESIAN_POINT('Ctrl Pts',(2.37244316231612,0.609757356979738,-0.382293167894848));
#95114=CARTESIAN_POINT('Ctrl Pts',(2.18430487692558,0.712321459543841,-1.14621055826918));
#95115=CARTESIAN_POINT('Ctrl Pts',(1.40131455475087,0.866167613389996,-2.03033734976027));
#95116=CARTESIAN_POINT('Ctrl Pts',(0.297364232596012,1.02001376723615,-2.44868476910202));
#95117=CARTESIAN_POINT('Ctrl Pts',(-0.874818306111391,1.1738599210823,-2.3066681580635));
#95118=CARTESIAN_POINT('Ctrl Pts',(-1.84634181500677,1.32770607492845,-1.63571663787998));
#95119=CARTESIAN_POINT('Ctrl Pts',(-2.39528328540685,1.48155222877461,-0.590387603200993));
#95120=CARTESIAN_POINT('Ctrl Pts',(-2.39501964124714,1.63539838262076,0.590322106947738));
#95121=CARTESIAN_POINT('Ctrl Pts',(-1.8465499120856,1.78924453646692,1.63589789028415));
#95122=CARTESIAN_POINT('Ctrl Pts',(-0.874703198395058,1.94309069031307,
2.3064051775018));
#95123=CARTESIAN_POINT('Ctrl Pts',(0.297359135731523,2.09693684415923,2.44897584949709));
#95124=CARTESIAN_POINT('Ctrl Pts',(1.40124553283611,2.25078299800538,2.03005448058009));
#95125=CARTESIAN_POINT('Ctrl Pts',(2.18438722007224,2.40462915185154,1.14645485904265));
#95126=CARTESIAN_POINT('Ctrl Pts',(2.46670014251008,2.55847530569768,1.58525550664851E-15));
#95127=CARTESIAN_POINT('Ctrl Pts',(2.18438722007224,2.71232145954384,-1.14645485904265));
#95128=CARTESIAN_POINT('Ctrl Pts',(1.40124553283611,2.86616761338999,-2.03005448058009));
#95129=CARTESIAN_POINT('Ctrl Pts',(0.297359135731528,3.02001376723615,-2.44897584949709));
#95130=CARTESIAN_POINT('Ctrl Pts',(-0.874703198395057,3.1738599210823,-2.3064051775018));
#95131=CARTESIAN_POINT('Ctrl Pts',(-1.84654991208559,3.32770607492846,-1.63589789028415));
#95132=CARTESIAN_POINT('Ctrl Pts',(-2.39501964124714,3.48155222877461,-0.590322106947741));
#95133=CARTESIAN_POINT('Ctrl Pts',(-2.39528328540685,3.63539838262076,0.590387603200988));
#95134=CARTESIAN_POINT('Ctrl Pts',(-1.84634181500678,3.78924453646692,1.63571663787998));
#95135=CARTESIAN_POINT('Ctrl Pts',(-0.874818306111389,3.94309069031306,
2.30666815806349));
#95136=CARTESIAN_POINT('Ctrl Pts',(0.297364232596008,4.09693684415923,2.44868476910202));
#95137=CARTESIAN_POINT('Ctrl Pts',(1.40131455475086,4.25078299800537,2.03033734976027));
#95138=CARTESIAN_POINT('Ctrl Pts',(2.18430487692558,4.40462915185153,1.14621055826919));
#95139=CARTESIAN_POINT('Ctrl Pts',(2.37244316231612,4.50719325441563,0.38229316789485));
#95140=CARTESIAN_POINT('Ctrl Pts',(2.37244316231612,4.55847530569768,1.16216196995579E-15));
#95141=CARTESIAN_POINT('Ctrl Pts',(2.85700819365424,0.447072546346698,0.));
#95142=CARTESIAN_POINT('Ctrl Pts',(2.85700819365424,0.49835459762875,-0.460152253076002));
#95143=CARTESIAN_POINT('Ctrl Pts',(2.63044272987694,0.600918700192852,-1.38045934159639));
#95144=CARTESIAN_POINT('Ctrl Pts',(1.68750688222128,0.754764854039006,-2.44491427782217));
#95145=CARTESIAN_POINT('Ctrl Pts',(0.358097970041885,0.90861100788516,-2.94887316066247));
#95146=CARTESIAN_POINT('Ctrl Pts',(-1.05347451173092,1.06245716173131,-2.77772768414576));
#95147=CARTESIAN_POINT('Ctrl Pts',(-2.22346919095397,1.21630331557747,-1.96982936708426));
#95148=CARTESIAN_POINT('Ctrl Pts',(-2.88445692863269,1.37014946942362,-0.710954262816585));
#95149=CARTESIAN_POINT('Ctrl Pts',(-2.8842167727775,1.52399562326978,0.710896720174062));
#95150=CARTESIAN_POINT('Ctrl Pts',(-2.22365955166528,1.67784177711593,1.96998876394438));
#95151=CARTESIAN_POINT('Ctrl Pts',(-1.05336654269098,1.83168793096208,2.77750138781392));
#95152=CARTESIAN_POINT('Ctrl Pts',(0.358087063676883,1.98553408480824,2.94911584899633));
#95153=CARTESIAN_POINT('Ctrl Pts',(1.6874581219902,2.13938023865439,2.44470486725235));
#95154=CARTESIAN_POINT('Ctrl Pts',(2.6304915596885,2.29322639250055,1.38058853511652));
#95155=CARTESIAN_POINT('Ctrl Pts',(2.97053809409234,2.4470725463467,1.58525550664851E-15));
#95156=CARTESIAN_POINT('Ctrl Pts',(2.6304915596885,2.60091870019286,-1.38058853511652));
#95157=CARTESIAN_POINT('Ctrl Pts',(1.68745812199021,2.754764854039,-2.44470486725235));
#95158=CARTESIAN_POINT('Ctrl Pts',(0.358087063676885,2.90861100788517,-2.94911584899632));
#95159=CARTESIAN_POINT('Ctrl Pts',(-1.05336654269097,3.06245716173131,-2.77750138781392));
#95160=CARTESIAN_POINT('Ctrl Pts',(-2.22365955166528,3.21630331557747,-1.96998876394438));
#95161=CARTESIAN_POINT('Ctrl Pts',(-2.8842167727775,3.37014946942362,-0.710896720174069));
#95162=CARTESIAN_POINT('Ctrl Pts',(-2.88445692863269,3.52399562326977,0.710954262816585));
#95163=CARTESIAN_POINT('Ctrl Pts',(-2.22346919095397,3.67784177711593,1.96982936708426));
#95164=CARTESIAN_POINT('Ctrl Pts',(-1.05347451173092,3.83168793096208,2.77772768414576));
#95165=CARTESIAN_POINT('Ctrl Pts',(0.358097970041882,3.98553408480824,2.94887316066247));
#95166=CARTESIAN_POINT('Ctrl Pts',(1.68750688222128,4.13938023865439,2.44491427782217));
#95167=CARTESIAN_POINT('Ctrl Pts',(2.63044272987694,4.29322639250055,1.38045934159639));
#95168=CARTESIAN_POINT('Ctrl Pts',(2.85700819365424,4.39579049506465,0.460152253076004));
#95169=CARTESIAN_POINT('Ctrl Pts',(2.85700819365424,4.44707254634671,1.39953037579857E-15));
#95170=CARTESIAN_POINT('Ctrl Pts',(3.,0.149599650170943,0.));
#95171=CARTESIAN_POINT('Ctrl Pts',(3.,0.200881701452994,-0.483569736915588));
#95172=CARTESIAN_POINT('Ctrl Pts',(2.76209582655108,0.303445804017096,-1.44931063718918));
#95173=CARTESIAN_POINT('Ctrl Pts',(1.7720044791404,0.45729195786325,-2.56747853270112));
#95174=CARTESIAN_POINT('Ctrl Pts',(0.376024222554094,0.611138111709404,
-3.0963739495031));
#95175=CARTESIAN_POINT('Ctrl Pts',(-1.10624032856718,0.764984265555557,
-2.91687489345741));
#95176=CARTESIAN_POINT('Ctrl Pts',(-2.3347230306591,0.918830419401713,-2.06838004508363));
#95177=CARTESIAN_POINT('Ctrl Pts',(-3.02892035965624,1.07267657324786,-0.746569056831962));
#95178=CARTESIAN_POINT('Ctrl Pts',(-3.02853408775958,1.22652272709402,0.746471647790977));
#95179=CARTESIAN_POINT('Ctrl Pts',(-2.33502736980124,1.38036888094017,2.06864950596667));
#95180=CARTESIAN_POINT('Ctrl Pts',(-1.10607381247961,1.53421503478633,2.91648052901886));
#95181=CARTESIAN_POINT('Ctrl Pts',(0.376021038515855,1.68806118863248,3.09681577839064));
#95182=CARTESIAN_POINT('Ctrl Pts',(1.77189370218424,1.84190734247864,2.56703109160197));
#95183=CARTESIAN_POINT('Ctrl Pts',(2.76223437164108,1.99575349632479,1.44973240304774));
#95184=CARTESIAN_POINT('Ctrl Pts',(3.11917527289456,2.14959965017094,1.3413700440872E-15));
#95185=CARTESIAN_POINT('Ctrl Pts',(2.76223437164108,2.3034458040171,-1.44973240304773));
#95186=CARTESIAN_POINT('Ctrl Pts',(1.77189370218425,2.45729195786325,-2.56703109160197));
#95187=CARTESIAN_POINT('Ctrl Pts',(0.37602103851586,2.61113811170941,-3.09681577839064));
#95188=CARTESIAN_POINT('Ctrl Pts',(-1.10607381247961,2.76498426555556,-2.91648052901886));
#95189=CARTESIAN_POINT('Ctrl Pts',(-2.33502736980123,2.91883041940171,-2.06864950596667));
#95190=CARTESIAN_POINT('Ctrl Pts',(-3.02853408775958,3.07267657324787,-0.746471647790982));
#95191=CARTESIAN_POINT('Ctrl Pts',(-3.02892035965624,3.22652272709402,0.746569056831959));
#95192=CARTESIAN_POINT('Ctrl Pts',(-2.3347230306591,3.38036888094017,2.06838004508363));
#95193=CARTESIAN_POINT('Ctrl Pts',(-1.10624032856718,3.53421503478633,2.91687489345741));
#95194=CARTESIAN_POINT('Ctrl Pts',(0.376024222554089,3.68806118863248,3.09637394950311));
#95195=CARTESIAN_POINT('Ctrl Pts',(1.7720044791404,3.84190734247863,2.56747853270111));
#95196=CARTESIAN_POINT('Ctrl Pts',(2.76209582655107,3.99575349632479,1.44931063718918));
#95197=CARTESIAN_POINT('Ctrl Pts',(3.,4.09831759888889,0.483569736915591));
#95198=CARTESIAN_POINT('Ctrl Pts',(3.,4.14959965017094,1.46957615897682E-15));
#95199=CARTESIAN_POINT('Ctrl Pts',(3.,6.12323399573676E-17,0.));
#95200=CARTESIAN_POINT('Ctrl Pts',(3.,0.0512820512820513,-0.483321946706122));
#95201=CARTESIAN_POINT('Ctrl Pts',(2.76209532949166,0.153846153846154,-1.44946426164245));
#95202=CARTESIAN_POINT('Ctrl Pts',(1.77197968324867,0.307692307692308,-2.56735208320081));
#95203=CARTESIAN_POINT('Ctrl Pts',(0.376021898059208,0.461538461538461,
-3.09643080035079));
#95204=CARTESIAN_POINT('Ctrl Pts',(-1.10621475336255,0.615384615384616,
-2.91679593290564));
#95205=CARTESIAN_POINT('Ctrl Pts',(-2.33474201794243,0.769230769230768,
-2.0684045486807));
#95206=CARTESIAN_POINT('Ctrl Pts',(-3.02885773675456,0.923076923076924,
-0.746548640155209));
#95207=CARTESIAN_POINT('Ctrl Pts',(-3.02855730304457,1.07692307692308,0.746474906977016));
#95208=CARTESIAN_POINT('Ctrl Pts',(-2.33497949559777,1.23076923076923,2.06860866176523));
#95209=CARTESIAN_POINT('Ctrl Pts',(-1.10608225550105,1.38461538461539,2.91650190270812));
#95210=CARTESIAN_POINT('Ctrl Pts',(0.376013421364463,1.53846153846154,3.0967529299689));
#95211=CARTESIAN_POINT('Ctrl Pts',(1.77190704246167,1.69230769230769,2.56705030189252));
#95212=CARTESIAN_POINT('Ctrl Pts',(2.76217801015642,1.84615384615384,1.44970288425454));
#95213=CARTESIAN_POINT('Ctrl Pts',(3.1191987918465,2.,1.70719823792917E-15));
#95214=CARTESIAN_POINT('Ctrl Pts',(2.76217801015642,2.15384615384615,-1.44970288425453));
#95215=CARTESIAN_POINT('Ctrl Pts',(1.77190704246167,2.30769230769231,-2.56705030189251));
#95216=CARTESIAN_POINT('Ctrl Pts',(0.376013421364468,2.46153846153846,-3.09675292996889));
#95217=CARTESIAN_POINT('Ctrl Pts',(-1.10608225550105,2.61538461538461,-2.91650190270813));
#95218=CARTESIAN_POINT('Ctrl Pts',(-2.33497949559777,2.76923076923077,-2.06860866176523));
#95219=CARTESIAN_POINT('Ctrl Pts',(-3.02855730304457,2.92307692307692,-0.746474906977022));
#95220=CARTESIAN_POINT('Ctrl Pts',(-3.02885773675456,3.07692307692307,0.746548640155207));
#95221=CARTESIAN_POINT('Ctrl Pts',(-2.33474201794243,3.23076923076923,2.0684045486807));
#95222=CARTESIAN_POINT('Ctrl Pts',(-1.10621475336255,3.38461538461538,2.91679593290564));
#95223=CARTESIAN_POINT('Ctrl Pts',(0.376021898059204,3.53846153846154,3.09643080035079));
#95224=CARTESIAN_POINT('Ctrl Pts',(1.77197968324866,3.69230769230769,2.56735208320081));
#95225=CARTESIAN_POINT('Ctrl Pts',(2.76209532949166,3.84615384615385,1.44946426164245));
#95226=CARTESIAN_POINT('Ctrl Pts',(3.,3.94871794871795,0.483321946706125));
#95227=CARTESIAN_POINT('Ctrl Pts',(3.,4.,1.46957615897682E-15));
#95228=CARTESIAN_POINT('',(3.,-6.12323399573676E-17,0.));
#95229=CARTESIAN_POINT('Origin',(2.5,0.,0.));
#95230=CARTESIAN_POINT('',(3.,4.,1.46957615897682E-15));
#95231=CARTESIAN_POINT('Ctrl Pts',(3.,6.12323399573676E-17,0.));
#95232=CARTESIAN_POINT('Ctrl Pts',(3.,0.0512820512820513,-0.483321946706122));
#95233=CARTESIAN_POINT('Ctrl Pts',(2.76209532949166,0.153846153846154,-1.44946426164245));
#95234=CARTESIAN_POINT('Ctrl Pts',(1.77197968324867,0.307692307692308,-2.56735208320081));
#95235=CARTESIAN_POINT('Ctrl Pts',(0.376021898059208,0.461538461538461,
-3.09643080035079));
#95236=CARTESIAN_POINT('Ctrl Pts',(-1.10621475336255,0.615384615384616,
-2.91679593290564));
#95237=CARTESIAN_POINT('Ctrl Pts',(-2.33474201794243,0.769230769230768,
-2.0684045486807));
#95238=CARTESIAN_POINT('Ctrl Pts',(-3.02885773675456,0.923076923076924,
-0.746548640155209));
#95239=CARTESIAN_POINT('Ctrl Pts',(-3.02855730304457,1.07692307692308,0.746474906977016));
#95240=CARTESIAN_POINT('Ctrl Pts',(-2.33497949559777,1.23076923076923,2.06860866176523));
#95241=CARTESIAN_POINT('Ctrl Pts',(-1.10608225550105,1.38461538461539,2.91650190270812));
#95242=CARTESIAN_POINT('Ctrl Pts',(0.376013421364463,1.53846153846154,3.0967529299689));
#95243=CARTESIAN_POINT('Ctrl Pts',(1.77190704246167,1.69230769230769,2.56705030189252));
#95244=CARTESIAN_POINT('Ctrl Pts',(2.76217801015642,1.84615384615384,1.44970288425454));
#95245=CARTESIAN_POINT('Ctrl Pts',(3.1191987918465,2.,1.70719823792917E-15));
#95246=CARTESIAN_POINT('Ctrl Pts',(2.76217801015642,2.15384615384615,-1.44970288425453));
#95247=CARTESIAN_POINT('Ctrl Pts',(1.77190704246167,2.30769230769231,-2.56705030189251));
#95248=CARTESIAN_POINT('Ctrl Pts',(0.376013421364468,2.46153846153846,-3.09675292996889));
#95249=CARTESIAN_POINT('Ctrl Pts',(-1.10608225550105,2.61538461538461,-2.91650190270813));
#95250=CARTESIAN_POINT('Ctrl Pts',(-2.33497949559777,2.76923076923077,-2.06860866176523));
#95251=CARTESIAN_POINT('Ctrl Pts',(-3.02855730304457,2.92307692307692,-0.746474906977022));
#95252=CARTESIAN_POINT('Ctrl Pts',(-3.02885773675456,3.07692307692307,0.746548640155207));
#95253=CARTESIAN_POINT('Ctrl Pts',(-2.33474201794243,3.23076923076923,2.0684045486807));
#95254=CARTESIAN_POINT('Ctrl Pts',(-1.10621475336255,3.38461538461538,2.91679593290564));
#95255=CARTESIAN_POINT('Ctrl Pts',(0.376021898059204,3.53846153846154,3.09643080035079));
#95256=CARTESIAN_POINT('Ctrl Pts',(1.77197968324866,3.69230769230769,2.56735208320081));
#95257=CARTESIAN_POINT('Ctrl Pts',(2.76209532949166,3.84615384615385,1.44946426164245));
#95258=CARTESIAN_POINT('Ctrl Pts',(3.,3.94871794871795,0.483321946706125));
#95259=CARTESIAN_POINT('Ctrl Pts',(3.,4.,1.46957615897682E-15));
#95260=CARTESIAN_POINT('Origin',(2.5,4.,1.22464679914735E-15));
#95261=CARTESIAN_POINT('Origin',(2.5,4.,1.22464679914735E-15));
#95262=CARTESIAN_POINT('Origin',(2.5,7.2280144832367E-18,0.));
#95263=CARTESIAN_POINT('',(0.,0.,0.));
#95264=CARTESIAN_POINT('Origin',(0.,0.,0.));
#95265=CARTESIAN_POINT('',(-1.95633559071744,0.0012731057411345,0.225869692124231));
#95266=CARTESIAN_POINT('',(-1.95587799559821,0.00207186393275607,0.124130307875758));
#95267=CARTESIAN_POINT('',(-1.954,-2.39295984553393E-16,0.));
#95268=CARTESIAN_POINT('',(0.861525859670522,1.75382131162755,0.));
#95269=CARTESIAN_POINT('Ctrl Pts',(-1.95633559071744,0.0012731057411345,
0.225869692124231));
#95270=CARTESIAN_POINT('Ctrl Pts',(-1.95680032440099,0.0682557629313676,
0.222037301306047));
#95271=CARTESIAN_POINT('Ctrl Pts',(-1.95365903766855,0.135191473590706,
0.218204910487863));
#95272=CARTESIAN_POINT('Ctrl Pts',(-1.94676806606145,0.201735328972743,
0.214372519669679));
#95273=CARTESIAN_POINT('Ctrl Pts',(-1.88017193281744,0.844832371344698,
0.1773353028412));
#95274=CARTESIAN_POINT('Ctrl Pts',(-1.46336311091822,1.45133095416213,0.140298086012721));
#95275=CARTESIAN_POINT('Ctrl Pts',(-0.886884671668765,1.7445317403525,0.103260869184242));
#95276=CARTESIAN_POINT('Ctrl Pts',(-0.351138290053491,2.01701592986141,
0.0688405794561611));
#95277=CARTESIAN_POINT('Ctrl Pts',(0.322511385444639,2.01891139473935,0.0344202897280807));
#95278=CARTESIAN_POINT('Ctrl Pts',(0.863567639152679,1.75641488315944,2.92734586571086E-17));
#95279=CARTESIAN_POINT('',(-0.861525859670574,1.75382131162752,1.38777878078145E-16));
#95280=CARTESIAN_POINT('Origin',(0.,0.,0.));
#95281=CARTESIAN_POINT('Ctrl Pts',(-0.861525859670571,1.75382131162752,
2.28983498828939E-15));
#95282=CARTESIAN_POINT('Ctrl Pts',(-1.44496782441851,1.46721837385109,0.0370621399437224));
#95283=CARTESIAN_POINT('Ctrl Pts',(-1.8691020329229,0.869083656944534,0.0741242798874424));
#95284=CARTESIAN_POINT('Ctrl Pts',(-1.94380023116171,0.227435527544788,
0.111186419831163));
#95285=CARTESIAN_POINT('Ctrl Pts',(-1.95249630318745,0.152737362394887,
0.115501049179361));
#95286=CARTESIAN_POINT('Ctrl Pts',(-1.95645657185248,0.0774494727773659,
0.119815678527559));
#95287=CARTESIAN_POINT('Ctrl Pts',(-1.95587799559821,0.00207186393275607,
0.124130307875758));
#95288=CARTESIAN_POINT('Origin',(0.,0.,0.));
#95289=CARTESIAN_POINT('',(-1.95128203910989,0.000979727872364722,0.92586969212423));
#95290=CARTESIAN_POINT('',(-1.95118672945361,0.000916100096969453,0.824130307875757));
#95291=CARTESIAN_POINT('',(-1.954,-2.39295984553393E-16,0.));
#95292=CARTESIAN_POINT('Ctrl Pts',(-1.95128203910989,0.000979727872364722,
0.92586969212423));
#95293=CARTESIAN_POINT('Ctrl Pts',(-1.9524730612105,0.263901717292074,0.910927268943587));
#95294=CARTESIAN_POINT('Ctrl Pts',(-1.90305141123492,0.526394079969068,
0.895984845762944));
#95295=CARTESIAN_POINT('Ctrl Pts',(-1.80089049647467,0.766440059940591,
0.881042422582301));
#95296=CARTESIAN_POINT('Ctrl Pts',(-1.54766811710363,1.36143291361156,0.844005205753822));
#95297=CARTESIAN_POINT('Ctrl Pts',(-0.970428066964404,1.81852045762203,
0.806967988925342));
#95298=CARTESIAN_POINT('Ctrl Pts',(-0.333230591869142,1.92861999489257,
0.769930772096863));
#95299=CARTESIAN_POINT('Ctrl Pts',(0.30396688322612,2.0387195321631,0.732893555268385));
#95300=CARTESIAN_POINT('Ctrl Pts',(1.00112178327742,1.8018310626937,0.695856338439906));
#95301=CARTESIAN_POINT('Ctrl Pts',(1.43930998255098,1.32629143144902,0.658819121611426));
#95302=CARTESIAN_POINT('Ctrl Pts',(1.87749818182454,0.850751800204341,0.621781904782947));
#95303=CARTESIAN_POINT('Ctrl Pts',(2.05671968032037,0.136561007184397,0.584744687954468));
#95304=CARTESIAN_POINT('Ctrl Pts',(1.89499805994521,-0.489512382298273,
0.547707471125989));
#95305=CARTESIAN_POINT('Ctrl Pts',(1.73327643957006,-1.11558577178094,0.51067025429751));
#95306=CARTESIAN_POINT('Ctrl Pts',(1.23061170032392,-1.65354175772633,0.473633037469032));
#95307=CARTESIAN_POINT('Ctrl Pts',(0.616932989107385,-1.8573955796291,0.436595820640553));
#95308=CARTESIAN_POINT('Ctrl Pts',(0.00325427789084558,-2.06124940153187,
0.399558603812074));
#95309=CARTESIAN_POINT('Ctrl Pts',(-0.721438405296094,-1.93100105939202,
0.362521386983595));
#95310=CARTESIAN_POINT('Ctrl Pts',(-1.22559302459517,-1.52602913735885,
0.325484170155115));
#95311=CARTESIAN_POINT('Ctrl Pts',(-1.67758072371516,-1.1629613001496,0.29227934414482));
#95312=CARTESIAN_POINT('Ctrl Pts',(-1.95230901779331,-0.579081973692791,
0.259074518134526));
#95313=CARTESIAN_POINT('Ctrl Pts',(-1.95633559071744,0.0012731057411345,
0.225869692124231));
#95314=CARTESIAN_POINT('Ctrl Pts',(-1.95587799559821,0.00207186393275607,
0.124130307875758));
#95315=CARTESIAN_POINT('Ctrl Pts',(-1.95148667238412,-0.570034995103637,
0.15687781847128));
#95316=CARTESIAN_POINT('Ctrl Pts',(-1.68562951923343,-1.14731024226281,
0.189625329066803));
#95317=CARTESIAN_POINT('Ctrl Pts',(-1.2444215732779,-1.51113938431406,0.222372839662326));
#95318=CARTESIAN_POINT('Ctrl Pts',(-0.745082529182101,-1.92290462488019,
0.259434979606046));
#95319=CARTESIAN_POINT('Ctrl Pts',(-0.0211422530173012,-2.0612735641195,
0.296497119549767));
#95320=CARTESIAN_POINT('Ctrl Pts',(0.595334795120667,-1.86428772433344,
0.333559259493488));
#95321=CARTESIAN_POINT('Ctrl Pts',(1.21181184325864,-1.66730188454737,0.370621399437209));
#95322=CARTESIAN_POINT('Ctrl Pts',(1.72082566336977,-1.13496126573593,0.40768353938093));
#95323=CARTESIAN_POINT('Ctrl Pts',(1.8894870924304,-0.510370283185346,0.444745679324651));
#95324=CARTESIAN_POINT('Ctrl Pts',(2.05814852149104,0.114220699365238,0.481807819268372));
#95325=CARTESIAN_POINT('Ctrl Pts',(1.88645755950116,0.831062045654966,0.518869959212093));
#95326=CARTESIAN_POINT('Ctrl Pts',(1.45292142815886,1.31145007703775,0.555932099155814));
#95327=CARTESIAN_POINT('Ctrl Pts',(1.01938529681656,1.79183810842053,0.592994239099535));
#95328=CARTESIAN_POINT('Ctrl Pts',(0.324003996121834,2.03577282489637,0.630056379043256));
#95329=CARTESIAN_POINT('Ctrl Pts',(-0.314654015224673,1.93172336479658,
0.667118518986976));
#95330=CARTESIAN_POINT('Ctrl Pts',(-0.953312026571179,1.8276739046968,0.704180658930697));
#95331=CARTESIAN_POINT('Ctrl Pts',(-1.53524674856946,1.37564026802139,0.741242798874417));
#95332=CARTESIAN_POINT('Ctrl Pts',(-1.79395555636014,0.782560471576942,
0.778304938818138));
#95333=CARTESIAN_POINT('Ctrl Pts',(-1.90058212652462,0.538123240897563,
0.793580061837345));
#95334=CARTESIAN_POINT('Ctrl Pts',(-1.95230335199157,0.269726953471863,
0.808855184856551));
#95335=CARTESIAN_POINT('Ctrl Pts',(-1.95118672945361,0.000916100096969453,
0.824130307875757));
#95336=CARTESIAN_POINT('Origin',(0.,0.,0.));
#95337=CARTESIAN_POINT('',(-1.95279554503994,-0.00168121501241181,1.62586969212423));
#95338=CARTESIAN_POINT('',(-1.95287184048439,-0.001702989282844,1.52413030787576));
#95339=CARTESIAN_POINT('',(-1.954,-2.39295984553393E-16,0.));
#95340=CARTESIAN_POINT('Ctrl Pts',(-1.95279554503994,-0.00168121501241181,
1.62586969212423));
#95341=CARTESIAN_POINT('Ctrl Pts',(-1.94903656010943,0.455834752155161,
1.59981723658113));
#95342=CARTESIAN_POINT('Ctrl Pts',(-1.78856730317397,0.91572573117829,1.57376478103802));
#95343=CARTESIAN_POINT('Ctrl Pts',(-1.49500760249196,1.26316552728133,1.54771232549492));
#95344=CARTESIAN_POINT('Ctrl Pts',(-1.07767134532899,1.75709989142681,1.51067510866644));
#95345=CARTESIAN_POINT('Ctrl Pts',(-0.39135122029848,2.02376358702057,1.47363789183796));
#95346=CARTESIAN_POINT('Ctrl Pts',(0.249990333148566,1.94116955279127,1.43660067500948));
#95347=CARTESIAN_POINT('Ctrl Pts',(0.891331886595613,1.85857551856197,1.39956345818101));
#95348=CARTESIAN_POINT('Ctrl Pts',(1.4876948684592,1.42672375450961,1.36252624135253));
#95349=CARTESIAN_POINT('Ctrl Pts',(1.76626827046517,0.843167597229759,1.32548902452405));
#95350=CARTESIAN_POINT('Ctrl Pts',(2.04484167247113,0.259611439949913,1.28845180769557));
#95351=CARTESIAN_POINT('Ctrl Pts',(2.00562549461947,-0.475649110557425,
1.25141459086709));
#95352=CARTESIAN_POINT('Ctrl Pts',(1.66655969053473,-1.02626219289756,1.21437737403861));
#95353=CARTESIAN_POINT('Ctrl Pts',(1.32749388644999,-1.57687527523771,1.17734015721013));
#95354=CARTESIAN_POINT('Ctrl Pts',(0.688578456132156,-1.94284088941065,
1.14030294038165));
#95355=CARTESIAN_POINT('Ctrl Pts',(0.0420898544956178,-1.9567474659654,
1.10326572355317));
#95356=CARTESIAN_POINT('Ctrl Pts',(-0.604398747140919,-1.97065404252014,
1.06622850672469));
#95357=CARTESIAN_POINT('Ctrl Pts',(-1.25846052009616,-1.6325015814567,1.02919128989622));
#95358=CARTESIAN_POINT('Ctrl Pts',(-1.62088905227235,-1.09697626925925,
0.992154073067737));
#95359=CARTESIAN_POINT('Ctrl Pts',(-1.83709816073764,-0.777505145902677,
0.970059279419901));
#95360=CARTESIAN_POINT('Ctrl Pts',(-1.94952091996443,-0.387793032173158,
0.947964485772066));
#95361=CARTESIAN_POINT('Ctrl Pts',(-1.95128203910989,0.000979727872364722,
0.92586969212423));
#95362=CARTESIAN_POINT('Ctrl Pts',(-1.95118672945361,0.000916100096969453,
0.824130307875757));
#95363=CARTESIAN_POINT('Ctrl Pts',(-1.94959408276249,-0.382490737583375,
0.845917324800272));
#95364=CARTESIAN_POINT('Ctrl Pts',(-1.84051065227066,-0.766740948347571,
0.867704341724787));
#95365=CARTESIAN_POINT('Ctrl Pts',(-1.62993550876047,-1.0835175828476,0.889491358649302));
#95366=CARTESIAN_POINT('Ctrl Pts',(-1.27172375978704,-1.62238988461419,
0.926553498593023));
#95367=CARTESIAN_POINT('Ctrl Pts',(-0.619817368257128,-1.96600853193387,
0.963615638536743));
#95368=CARTESIAN_POINT('Ctrl Pts',(0.0271864367452719,-1.95701720127518,
1.00067777848046));
#95369=CARTESIAN_POINT('Ctrl Pts',(0.674190241747668,-1.94802587061648,
1.03773991842418));
#95370=CARTESIAN_POINT('Ctrl Pts',(1.31629146022255,-1.5864245619794,1.07480205836791));
#95371=CARTESIAN_POINT('Ctrl Pts',(1.65939903784035,-1.03781956343241,1.11186419831163));
#95372=CARTESIAN_POINT('Ctrl Pts',(2.00250661545815,-0.489214564885407,
1.14892633825535));
#95373=CARTESIAN_POINT('Ctrl Pts',(2.04662055221888,0.246394123571516,1.18598847819907));
#95374=CARTESIAN_POINT('Ctrl Pts',(1.77153295980734,0.832073910176122,1.22305061814279));
#95375=CARTESIAN_POINT('Ctrl Pts',(1.49644536739581,1.41775369678073,1.26011275808651));
#95376=CARTESIAN_POINT('Ctrl Pts',(0.902156245812001,1.85350458153303,1.29717489803023));
#95377=CARTESIAN_POINT('Ctrl Pts',(0.260864347694114,1.93974733338565,1.33423703797395));
#95378=CARTESIAN_POINT('Ctrl Pts',(-0.380427550423769,2.02599008523827,
1.37129917791767));
#95379=CARTESIAN_POINT('Ctrl Pts',(-1.06872222507573,1.76272470419122,1.40836131786139));
#95380=CARTESIAN_POINT('Ctrl Pts',(-1.48876654315921,1.27053027794487,1.44542345780511));
#95381=CARTESIAN_POINT('Ctrl Pts',(-1.78610829781436,0.922114770268632,
1.47165907449533));
#95382=CARTESIAN_POINT('Ctrl Pts',(-1.94903067523895,0.458983666015645,
1.49789469118554));
#95383=CARTESIAN_POINT('Ctrl Pts',(-1.95287184048439,-0.001702989282844,
1.52413030787576));
#95384=CARTESIAN_POINT('Origin',(0.,0.,0.));
#95385=CARTESIAN_POINT('',(-1.9571996697324,4.08272333451705E-5,2.32586969212423));
#95386=CARTESIAN_POINT('',(-1.95720915199432,4.37834080700025E-5,2.22413030787575));
#95387=CARTESIAN_POINT('',(-1.954,-2.39295984553393E-16,0.));
#95388=CARTESIAN_POINT('Ctrl Pts',(-1.9571996697324,4.08272333451412E-5,
2.32586969212423));
#95389=CARTESIAN_POINT('Ctrl Pts',(-1.9572003426898,0.00222795607483405,
2.32574442104715));
#95390=CARTESIAN_POINT('Ctrl Pts',(-1.95719699336635,0.00441508279392128,
2.32561914997006));
#95391=CARTESIAN_POINT('Ctrl Pts',(-1.95718961556757,0.00660219592375261,
2.32549387889298));
#95392=CARTESIAN_POINT('Ctrl Pts',(-1.9550083208942,0.653236559609951,2.2884566620645));
#95393=CARTESIAN_POINT('Ctrl Pts',(-1.60068669068514,1.29868304829585,2.25141944523602));
#95394=CARTESIAN_POINT('Ctrl Pts',(-1.05631192010051,1.64767712566922,2.21438222840754));
#95395=CARTESIAN_POINT('Ctrl Pts',(-0.511937149515876,1.9966712030426,2.17734501157906));
#95396=CARTESIAN_POINT('Ctrl Pts',(0.222490761444335,2.04921286910345,2.14030779475058));
#95397=CARTESIAN_POINT('Ctrl Pts',(0.811002035332165,1.78126653559889,2.10327057792211));
#95398=CARTESIAN_POINT('Ctrl Pts',(1.39951330921999,1.51332020209433,2.06623336109363));
#95399=CARTESIAN_POINT('Ctrl Pts',(1.84210794603544,0.92488586902436,2.02919614426515));
#95400=CARTESIAN_POINT('Ctrl Pts',(1.93631757329266,0.28514740055385,1.99215892743667));
#95401=CARTESIAN_POINT('Ctrl Pts',(2.03052720054988,-0.354591067916664,
1.95512171060819));
#95402=CARTESIAN_POINT('Ctrl Pts',(1.77635181824887,-1.04563367178771,1.91808449377971));
#95403=CARTESIAN_POINT('Ctrl Pts',(1.29006594271768,-1.47185755477259,1.88104727695123));
#95404=CARTESIAN_POINT('Ctrl Pts',(0.803780067186484,-1.89808143775746,
1.84401006012275));
#95405=CARTESIAN_POINT('Ctrl Pts',(0.0853836984250916,-2.05948659985616,
1.80697284329427));
#95406=CARTESIAN_POINT('Ctrl Pts',(-0.536487147273854,-1.88223703762279,
1.76993562646579));
#95407=CARTESIAN_POINT('Ctrl Pts',(-1.1583579929728,-1.70498747538942,1.73289840963732));
#95408=CARTESIAN_POINT('Ctrl Pts',(-1.68370331560931,-1.18908318882399,
1.69586119280884));
#95409=CARTESIAN_POINT('Ctrl Pts',(-1.87219978227984,-0.570528529192665,
1.65882397598036));
#95410=CARTESIAN_POINT('Ctrl Pts',(-1.92810540551016,-0.387073187246384,
1.64783921469498));
#95411=CARTESIAN_POINT('Ctrl Pts',(-1.95438048401311,-0.194588316428208,
1.63685445340961));
#95412=CARTESIAN_POINT('Ctrl Pts',(-1.95279554503994,-0.00168121501241192,
1.62586969212423));
#95413=CARTESIAN_POINT('Ctrl Pts',(-1.95287184048439,-0.00170298928284375,
1.52413030787576));
#95414=CARTESIAN_POINT('Ctrl Pts',(-1.95445695530526,-0.191812291650776,
1.53495683112926));
#95415=CARTESIAN_POINT('Ctrl Pts',(-1.92895173588402,-0.381505322742495,
1.54578335438277));
#95416=CARTESIAN_POINT('Ctrl Pts',(-1.87462310228398,-0.562548805321496,
1.55660987763628));
#95417=CARTESIAN_POINT('Ctrl Pts',(-1.68864138181028,-1.18230999089587,
1.59367201758));
#95418=CARTESIAN_POINT('Ctrl Pts',(-1.16488397934787,-1.70070889059895,
1.63073415752372));
#95419=CARTESIAN_POINT('Ctrl Pts',(-0.543243355780667,-1.88030816136644,
1.66779629746744));
#95420=CARTESIAN_POINT('Ctrl Pts',(0.0783972677865321,-2.05990743213392,
1.70485843741116));
#95421=CARTESIAN_POINT('Ctrl Pts',(0.797921112458524,-1.90070707396579,
1.74192057735488));
#95422=CARTESIAN_POINT('Ctrl Pts',(1.28577075941843,-1.47562399010748,1.7789827172986));
#95423=CARTESIAN_POINT('Ctrl Pts',(1.77362040637834,-1.05054090624917,1.81604485724232));
#95424=CARTESIAN_POINT('Ctrl Pts',(2.02979585562615,-0.359575096700667,
1.85310699718604));
#95425=CARTESIAN_POINT('Ctrl Pts',(1.93696313672928,0.28079594435252,1.89016913712977));
#95426=CARTESIAN_POINT('Ctrl Pts',(1.84413041783241,0.921166985405712,1.92723127707349));
#95427=CARTESIAN_POINT('Ctrl Pts',(1.40228953079084,1.51094325796358,1.96429341701721));
#95428=CARTESIAN_POINT('Ctrl Pts',(0.813813216582781,1.77999452248681,2.00135555696093));
#95429=CARTESIAN_POINT('Ctrl Pts',(0.225336902374724,2.04904578701004,2.03841769690465));
#95430=CARTESIAN_POINT('Ctrl Pts',(-0.509774838999831,1.99737204349863,
2.07547983684837));
#95431=CARTESIAN_POINT('Ctrl Pts',(-1.05482489992153,1.64864094185095,2.11254197679209));
#95432=CARTESIAN_POINT('Ctrl Pts',(-1.59987496084323,1.29990984020327,2.14960411673581));
#95433=CARTESIAN_POINT('Ctrl Pts',(-1.95486334131209,0.654121380419318,
2.18666625667953));
#95434=CARTESIAN_POINT('Ctrl Pts',(-1.95719765431867,0.0070607094029605,
2.22372839662325));
#95435=CARTESIAN_POINT('Ctrl Pts',(-1.95720609227958,0.00472174601940803,
2.22386236704075));
#95436=CARTESIAN_POINT('Ctrl Pts',(-1.95720992231195,0.00238276601260064,
2.22399633745825));
#95437=CARTESIAN_POINT('Ctrl Pts',(-1.95720915199432,4.37834080701142E-5,
2.22413030787575));
#95438=CARTESIAN_POINT('Origin',(0.,0.,0.));
#95439=CARTESIAN_POINT('',(-1.95267691385146,0.00165493661177622,3.02586969212423));
#95440=CARTESIAN_POINT('',(-1.95274315056508,0.00167675988910205,2.92413030787576));
#95441=CARTESIAN_POINT('',(-1.954,-2.39295984553393E-16,0.));
#95442=CARTESIAN_POINT('Ctrl Pts',(-1.95267691385146,0.00165493661177622,
3.02586969212423));
#95443=CARTESIAN_POINT('Ctrl Pts',(-1.95426560914452,0.198992208020636,
3.01463438868469));
#95444=CARTESIAN_POINT('Ctrl Pts',(-1.92675342506316,0.395896803504792,
3.00339908524515));
#95445=CARTESIAN_POINT('Ctrl Pts',(-1.86830808103941,0.583146374609883,
2.9921637818056));
#95446=CARTESIAN_POINT('Ctrl Pts',(-1.67564280138135,1.20041523640586,2.95512656497712));
#95447=CARTESIAN_POINT('Ctrl Pts',(-1.14682887836242,1.71276357431471,2.91808934814864));
#95448=CARTESIAN_POINT('Ctrl Pts',(-0.523776367443795,1.8858136432031,2.88105213132016));
#95449=CARTESIAN_POINT('Ctrl Pts',(0.0992761434748341,2.0588637120915,2.84401491449168));
#95450=CARTESIAN_POINT('Ctrl Pts',(0.816567242293159,1.89261551195942,2.80697769766321));
#95451=CARTESIAN_POINT('Ctrl Pts',(1.29996651882171,1.46312057934516,2.76994048083473));
#95452=CARTESIAN_POINT('Ctrl Pts',(1.78336579535026,1.03362564673089,2.73290326400625));
#95453=CARTESIAN_POINT('Ctrl Pts',(2.03287324958903,0.340883981634439,2.69586604717777));
#95454=CARTESIAN_POINT('Ctrl Pts',(1.93434974962867,-0.298204336020968,
2.65882883034929));
#95455=CARTESIAN_POINT('Ctrl Pts',(1.83582624966831,-0.937292653676373,
2.62179161352081));
#95456=CARTESIAN_POINT('Ctrl Pts',(1.38927179550881,-1.52272762389073,2.58475439669233));
#95457=CARTESIAN_POINT('Ctrl Pts',(0.798966206784796,-1.78669745083631,
2.54771717986385));
#95458=CARTESIAN_POINT('Ctrl Pts',(0.208660618060775,-2.05066727778188,
2.51067996303538));
#95459=CARTESIAN_POINT('Ctrl Pts',(-0.525396105227766,-1.99317196145866,
2.4736427462069));
#95460=CARTESIAN_POINT('Ctrl Pts',(-1.0674039873032,-1.6405131839538,2.43660552937842));
#95461=CARTESIAN_POINT('Ctrl Pts',(-1.60757863467609,-1.28904720517098,
2.39969358362702));
#95462=CARTESIAN_POINT('Ctrl Pts',(-1.95700137841649,-0.644411052866131,
2.36278163787563));
#95463=CARTESIAN_POINT('Ctrl Pts',(-1.9571996697324,4.08272333451705E-5,
2.32586969212423));
#95464=CARTESIAN_POINT('Ctrl Pts',(-1.95720915199432,4.37834080700025E-5,
2.22413030787575));
#95465=CARTESIAN_POINT('Ctrl Pts',(-1.95699681840184,-0.644683222376,2.26105847740198));
#95466=CARTESIAN_POINT('Ctrl Pts',(-1.60725113883781,-1.28960760246236,
2.2979866469282));
#95467=CARTESIAN_POINT('Ctrl Pts',(-1.06669244200308,-1.64098742623895,
2.33491481645442));
#95468=CARTESIAN_POINT('Ctrl Pts',(-0.524172671136578,-1.99364200861572,
2.37197695639814));
#95469=CARTESIAN_POINT('Ctrl Pts',(0.210547116140745,-2.05061829112049,
2.40903909634186));
#95470=CARTESIAN_POINT('Ctrl Pts',(0.800949322066953,-1.78581989384044,
2.44610123628558));
#95471=CARTESIAN_POINT('Ctrl Pts',(1.39135152799316,-1.52102149656038,2.4831633762293));
#95472=CARTESIAN_POINT('Ctrl Pts',(1.83743615256826,-0.934448419495488,
2.52022551617302));
#95473=CARTESIAN_POINT('Ctrl Pts',(1.93488676008295,-0.294763859316313,
2.55728765611674));
#95474=CARTESIAN_POINT('Ctrl Pts',(2.03233736759764,0.344920700862864,2.59434979606046));
#95475=CARTESIAN_POINT('Ctrl Pts',(1.78115395805193,1.03771674415633,2.63141193600418));
#95476=CARTESIAN_POINT('Ctrl Pts',(1.29638398231036,1.46630865646616,2.6684740759479));
#95477=CARTESIAN_POINT('Ctrl Pts',(0.811614006568792,1.894900568776,2.70553621589162));
#95478=CARTESIAN_POINT('Ctrl Pts',(0.0932574646313782,2.05928835010221,
2.74259835583535));
#95479=CARTESIAN_POINT('Ctrl Pts',(-0.529662765081927,1.88417882975093,
2.77966049577907));
#95480=CARTESIAN_POINT('Ctrl Pts',(-1.15258299479523,1.70906930939964,2.81672263572279));
#95481=CARTESIAN_POINT('Ctrl Pts',(-1.68006691228442,1.19446248737086,2.85378477566651));
#95482=CARTESIAN_POINT('Ctrl Pts',(-1.87051544101399,0.576059451476712,
2.89084691561023));
#95483=CARTESIAN_POINT('Ctrl Pts',(-1.92752575844056,0.390941962730205,
2.90194137969874));
#95484=CARTESIAN_POINT('Ctrl Pts',(-1.95433466869055,0.196523398123763,
2.91303584378725));
#95485=CARTESIAN_POINT('Ctrl Pts',(-1.95274315056508,0.00167675988910205,
2.92413030787576));
#95486=CARTESIAN_POINT('Origin',(0.,0.,0.));
#95487=CARTESIAN_POINT('',(-1.95135107115213,-0.00103745302926256,3.72586969212423));
#95488=CARTESIAN_POINT('',(-1.95125983814034,-0.000967513988672578,3.62413030787576));
#95489=CARTESIAN_POINT('',(-1.954,-2.39295984553393E-16,0.));
#95490=CARTESIAN_POINT('Ctrl Pts',(-1.95135107115213,-0.00103745302926256,
3.72586969212423));
#95491=CARTESIAN_POINT('Ctrl Pts',(-1.9494564270682,0.392108141373472,3.70352435632223));
#95492=CARTESIAN_POINT('Ctrl Pts',(-1.83428685915158,0.78627490539017,3.68117902052023));
#95493=CARTESIAN_POINT('Ctrl Pts',(-1.61345116677478,1.10788542383069,3.65883368471823));
#95494=CARTESIAN_POINT('Ctrl Pts',(-1.24741775852795,1.64095230684139,3.62179646788975));
#95495=CARTESIAN_POINT('Ctrl Pts',(-0.591089924893776,1.97468687095231,
3.58475925106126));
#95496=CARTESIAN_POINT('Ctrl Pts',(0.0552900452708404,1.95641963566092,
3.54772203423278));
#95497=CARTESIAN_POINT('Ctrl Pts',(0.701670015435453,1.93815240036952,3.51068481740431));
#95498=CARTESIAN_POINT('Ctrl Pts',(1.3381021221305,1.56788336567581,3.47364760057583));
#95499=CARTESIAN_POINT('Ctrl Pts',(1.6734455320356,1.01499499073225,3.43661038374735));
#95500=CARTESIAN_POINT('Ctrl Pts',(2.0087889419407,0.462106615788698,3.39957316691887));
#95501=CARTESIAN_POINT('Ctrl Pts',(2.04304365505584,-0.273401099404705,
3.36253595009039));
#95502=CARTESIAN_POINT('Ctrl Pts',(1.76053958557416,-0.855064411333041,
3.32549873326191));
#95503=CARTESIAN_POINT('Ctrl Pts',(1.47803551609248,-1.43672772326139,3.28846151643343));
#95504=CARTESIAN_POINT('Ctrl Pts',(0.878772664013962,-1.86454663192466,
3.25142429960495));
#95505=CARTESIAN_POINT('Ctrl Pts',(0.236888497103484,-1.94281203925035,
3.21438708277648));
#95506=CARTESIAN_POINT('Ctrl Pts',(-0.404995669806982,-2.02107744657604,
3.177349865948));
#95507=CARTESIAN_POINT('Ctrl Pts',(-1.08950115154941,-1.74978935256416,
3.14031264911952));
#95508=CARTESIAN_POINT('Ctrl Pts',(-1.50349557427203,-1.25305061271667,
3.10327543229104));
#95509=CARTESIAN_POINT('Ctrl Pts',(-1.79190407667273,-0.906998424134863,
3.0774735189021));
#95510=CARTESIAN_POINT('Ctrl Pts',(-1.94902846959061,-0.451530792879088,
3.05167160551317));
#95511=CARTESIAN_POINT('Ctrl Pts',(-1.95267691385146,0.00165493661177622,
3.02586969212423));
#95512=CARTESIAN_POINT('Ctrl Pts',(-1.95274315056508,0.00167675988910205,
2.92413030787576));
#95513=CARTESIAN_POINT('Ctrl Pts',(-1.94901804708373,-0.45438081105706,
2.95009798373097));
#95514=CARTESIAN_POINT('Ctrl Pts',(-1.78970412039892,-0.912783539307832,
2.97606565958618));
#95515=CARTESIAN_POINT('Ctrl Pts',(-1.49789482266332,-1.25975537577289,
3.00203333544139));
#95516=CARTESIAN_POINT('Ctrl Pts',(-1.08141253561316,-1.75496791736879,
3.03909547538511));
#95517=CARTESIAN_POINT('Ctrl Pts',(-0.3950348215429,-2.02319375080107,3.07615761532883));
#95518=CARTESIAN_POINT('Ctrl Pts',(0.246862437687336,-1.94157962588032,
3.11321975527255));
#95519=CARTESIAN_POINT('Ctrl Pts',(0.888759696917571,-1.85996550095957,
3.15028189521628));
#95520=CARTESIAN_POINT('Ctrl Pts',(1.48617650130778,-1.4285114176858,3.18734403516));
#95521=CARTESIAN_POINT('Ctrl Pts',(1.76548299529208,-0.84483270534745,3.22440617510372));
#95522=CARTESIAN_POINT('Ctrl Pts',(2.04478948927638,-0.261153993009101,
3.26146831504744));
#95523=CARTESIAN_POINT('Ctrl Pts',(2.00598567285476,0.474749348393822,3.29853045499116));
#95524=CARTESIAN_POINT('Ctrl Pts',(1.66684453569178,1.02581762536563,3.33559259493488));
#95525=CARTESIAN_POINT('Ctrl Pts',(1.3277033985288,1.57688590233743,3.3726547348786));
#95526=CARTESIAN_POINT('Ctrl Pts',(0.688224940624468,1.94311911487812,3.40971687482232));
#95527=CARTESIAN_POINT('Ctrl Pts',(0.0413041672205065,1.95677450731496,
3.44677901476604));
#95528=CARTESIAN_POINT('Ctrl Pts',(-0.605616606183457,1.9704298997518,3.48384115470976));
#95529=CARTESIAN_POINT('Ctrl Pts',(-1.25997969508704,1.63150747208479,3.52090329465349));
#95530=CARTESIAN_POINT('Ctrl Pts',(-1.62207261036362,1.09524104808107,3.55796543459721));
#95531=CARTESIAN_POINT('Ctrl Pts',(-1.83754705311226,0.776119342016343,
3.58002039235672));
#95532=CARTESIAN_POINT('Ctrl Pts',(-1.94952253842872,0.387114015523011,
3.60207535011624));
#95533=CARTESIAN_POINT('Ctrl Pts',(-1.95125983814034,-0.000967513988672578,
3.62413030787576));
#95534=CARTESIAN_POINT('Origin',(0.,0.,0.));
#95535=CARTESIAN_POINT('',(-1.95645574651684,-0.00107576288577632,4.42586969212423));
#95536=CARTESIAN_POINT('',(-1.95628130950281,-0.00119277919923279,4.32413030787576));
#95537=CARTESIAN_POINT('',(-1.954,-2.39295984553393E-16,0.));
#95538=CARTESIAN_POINT('Ctrl Pts',(-1.95645574651684,-0.00107576288577632,
4.42586969212423));
#95539=CARTESIAN_POINT('Ctrl Pts',(-1.95258201164419,0.583617837825317,
4.39241432395977));
#95540=CARTESIAN_POINT('Ctrl Pts',(-1.67312331125722,1.17152394520949,4.35895895579531));
#95541=CARTESIAN_POINT('Ctrl Pts',(-1.21525966387556,1.53420296221226,4.32550358763085));
#95542=CARTESIAN_POINT('Ctrl Pts',(-0.70837553387317,1.93571166257503,4.28846637080237));
#95543=CARTESIAN_POINT('Ctrl Pts',(0.0171598407939347,2.06118438706562,
4.25142915397389));
#95544=CARTESIAN_POINT('Ctrl Pts',(0.629444641593513,1.8532226587955,4.21439193714541));
#95545=CARTESIAN_POINT('Ctrl Pts',(1.24172944239309,1.64526093052537,4.17735472031693));
#95546=CARTESIAN_POINT('Ctrl Pts',(1.74076366932515,1.10386474949453,4.14031750348845));
#95547=CARTESIAN_POINT('Ctrl Pts',(1.89826022128925,0.476700023258525,4.10328028665997));
#95548=CARTESIAN_POINT('Ctrl Pts',(2.05575677325334,-0.150464702977478,
4.06624306983149));
#95549=CARTESIAN_POINT('Ctrl Pts',(1.87171565024948,-0.86339797441863,4.02920585300301));
#95550=CARTESIAN_POINT('Ctrl Pts',(1.43032790007833,-1.33596290298842,3.99216863617453));
#95551=CARTESIAN_POINT('Ctrl Pts',(0.988940149907184,-1.80852783155821,
3.95513141934605));
#95552=CARTESIAN_POINT('Ctrl Pts',(0.290205772568748,-2.04072441725662,
3.91809420251758));
#95553=CARTESIAN_POINT('Ctrl Pts',(-0.346233738762281,-1.92633252011348,
3.8810569856891));
#95554=CARTESIAN_POINT('Ctrl Pts',(-0.982673250093302,-1.81194062297035,
3.84401976886062));
#95555=CARTESIAN_POINT('Ctrl Pts',(-1.55681789541692,-1.35096024298568,
3.80698255203214));
#95556=CARTESIAN_POINT('Ctrl Pts',(-1.806020726649,-0.754270452038098,3.76994533520366));
#95557=CARTESIAN_POINT('Ctrl Pts',(-1.90487422217158,-0.517576224744695,
3.75525345417718));
#95558=CARTESIAN_POINT('Ctrl Pts',(-1.9525967846073,-0.259527562563923,
3.74056157315071));
#95559=CARTESIAN_POINT('Ctrl Pts',(-1.95135107115213,-0.00103745302926256,
3.72586969212423));
#95560=CARTESIAN_POINT('Ctrl Pts',(-1.95125983814034,-0.000967513988672578,
3.62413030787576));
#95561=CARTESIAN_POINT('Ctrl Pts',(-1.95244197476311,-0.265035587897937,
3.63913749005996));
#95562=CARTESIAN_POINT('Ctrl Pts',(-1.90258326051973,-0.528675939020291,
3.65414467224416));
#95563=CARTESIAN_POINT('Ctrl Pts',(-1.799560505048,-0.769580726996389,3.66915185442837));
#95564=CARTESIAN_POINT('Ctrl Pts',(-1.54513274280624,-1.36452565772967,
3.70621399437209));
#95565=CARTESIAN_POINT('Ctrl Pts',(-0.966454476673152,-1.8208050988558,
3.74327613431581));
#95566=CARTESIAN_POINT('Ctrl Pts',(-0.328572905191125,-1.92943316874967,
3.78033827425953));
#95567=CARTESIAN_POINT('Ctrl Pts',(0.309308666290907,-2.03806123864353,
3.81740041420325));
#95568=CARTESIAN_POINT('Ctrl Pts',(1.00639354312189,-1.79903793730513,3.85446255414697));
#95569=CARTESIAN_POINT('Ctrl Pts',(1.44340173058911,-1.32184112162819,3.89152469409069));
#95570=CARTESIAN_POINT('Ctrl Pts',(1.88040991805633,-0.844644305951239,
3.92858683403441));
#95571=CARTESIAN_POINT('Ctrl Pts',(2.05734141615979,-0.129273975935752,
3.96564897397814));
#95572=CARTESIAN_POINT('Ctrl Pts',(1.89315776078089,0.496614739501458,4.00271111392186));
#95573=CARTESIAN_POINT('Ctrl Pts',(1.72897410540198,1.12250345493866,4.03977325386558));
#95574=CARTESIAN_POINT('Ctrl Pts',(1.22367529654071,1.65891055579759,4.0768353938093));
#95575=CARTESIAN_POINT('Ctrl Pts',(0.608699149567017,1.86014995417357,4.11389753375302));
#95576=CARTESIAN_POINT('Ctrl Pts',(-0.00627699740667481,2.06138935254956,
4.15095967369674));
#95577=CARTESIAN_POINT('Ctrl Pts',(-0.730930482492791,1.9274610484426,4.18802181364046));
#95578=CARTESIAN_POINT('Ctrl Pts',(-1.23335429038162,1.51970711029871,4.22508395358418));
#95579=CARTESIAN_POINT('Ctrl Pts',(-1.68092015819396,1.15647443240051,4.25809940501471));
#95580=CARTESIAN_POINT('Ctrl Pts',(-1.95213599025838,0.575947822566119,
4.29111485644523));
#95581=CARTESIAN_POINT('Ctrl Pts',(-1.95628130950281,-0.00119277919923279,
4.32413030787576));
#95582=CARTESIAN_POINT('Origin',(0.,0.,0.));
#95583=CARTESIAN_POINT('',(-1.95458266482996,0.00173443779922018,5.12586969212423));
#95584=CARTESIAN_POINT('',(-1.95491180920002,0.00168629508682236,5.02413030787576));
#95585=CARTESIAN_POINT('',(-1.954,-2.39295984553393E-16,0.));
#95586=CARTESIAN_POINT('Ctrl Pts',(-1.95458266482996,0.00173443779922018,
5.12586969212423));
#95587=CARTESIAN_POINT('Ctrl Pts',(-1.95579683437623,0.13363129532035,5.11834150842579));
#95588=CARTESIAN_POINT('Ctrl Pts',(-1.94358523444966,0.265304620125551,
5.11081332472735));
#95589=CARTESIAN_POINT('Ctrl Pts',(-1.91712292268468,0.394048828472761,
5.10328514102891));
#95590=CARTESIAN_POINT('Ctrl Pts',(-1.78693343503641,1.0274455880328,5.06624792420043));
#95591=CARTESIAN_POINT('Ctrl Pts',(-1.31181246839585,1.58994452273665,5.02921070737195));
#95592=CARTESIAN_POINT('Ctrl Pts',(-0.709107816346671,1.8242261056952,4.99217349054347));
#95593=CARTESIAN_POINT('Ctrl Pts',(-0.106403164297495,2.05850768865374,
4.95513627371499));
#95594=CARTESIAN_POINT('Ctrl Pts',(0.623885173160298,1.96457191986698,4.91809905688651));
#95595=CARTESIAN_POINT('Ctrl Pts',(1.14768109757825,1.58539044975217,4.88106184005803));
#95596=CARTESIAN_POINT('Ctrl Pts',(1.67147702199619,1.20620897963737,4.84402462322955));
#95597=CARTESIAN_POINT('Ctrl Pts',(1.9887805333743,0.541781808194522,4.80698740640107));
#95598=CARTESIAN_POINT('Ctrl Pts',(1.95443866449662,-0.103943670439598,
4.76995018957259));
#95599=CARTESIAN_POINT('Ctrl Pts',(1.92009679561895,-0.749669149073727,
4.73291297274411));
#95600=CARTESIAN_POINT('Ctrl Pts',(1.53410954648549,-1.37669293489913,4.69587575591563));
#95601=CARTESIAN_POINT('Ctrl Pts',(0.973049796091196,-1.69817810439032,
4.65883853908716));
#95602=CARTESIAN_POINT('Ctrl Pts',(0.411990045696909,-2.0196632738815,4.62180132225868));
#95603=CARTESIAN_POINT('Ctrl Pts',(-0.324142205958206,-2.03560982703848,
4.5847641054302));
#95604=CARTESIAN_POINT('Ctrl Pts',(-0.898597516275757,-1.7387228886878,
4.54772688860172));
#95605=CARTESIAN_POINT('Ctrl Pts',(-1.47305282659331,-1.44183595033712,
4.51068967177324));
#95606=CARTESIAN_POINT('Ctrl Pts',(-1.8858311955733,-0.832115520478776,
4.47365245494476));
#95607=CARTESIAN_POINT('Ctrl Pts',(-1.94810393739446,-0.188482967432129,
4.43661523811628));
#95608=CARTESIAN_POINT('Ctrl Pts',(-1.9541262996613,-0.126237620787308,
4.43303338945226));
#95609=CARTESIAN_POINT('Ctrl Pts',(-1.95687048211354,-0.0636751036633503,
4.42945154078825));
#95610=CARTESIAN_POINT('Ctrl Pts',(-1.95645574651684,-0.00107576288577632,
4.42586969212423));
#95611=CARTESIAN_POINT('Ctrl Pts',(-1.95628130950281,-0.00119277919923279,
4.32413030787576));
#95612=CARTESIAN_POINT('Ctrl Pts',(-1.95678939935296,-0.0719326340995119,
4.32817699638895));
#95613=CARTESIAN_POINT('Ctrl Pts',(-1.95328521122814,-0.14262162001596,
4.33222368490215));
#95614=CARTESIAN_POINT('Ctrl Pts',(-1.94560169264522,-0.212853377401693,
4.33627037341534));
#95615=CARTESIAN_POINT('Ctrl Pts',(-1.87523115632842,-0.856080354777335,
4.37333251335906));
#95616=CARTESIAN_POINT('Ctrl Pts',(-1.45429595300328,-1.46095473734778,
4.41039465330279));
#95617=CARTESIAN_POINT('Ctrl Pts',(-0.875593536694013,-1.75043093699665,
4.44745679324651));
#95618=CARTESIAN_POINT('Ctrl Pts',(-0.296891120384743,-2.03990713664554,
4.48451893319023));
#95619=CARTESIAN_POINT('Ctrl Pts',(0.439578508908652,-2.01398515337285,
4.52158107313395));
#95620=CARTESIAN_POINT('Ctrl Pts',(0.9964962855145,-1.68453781781564,4.55864321307767));
#95621=CARTESIAN_POINT('Ctrl Pts',(1.55341406212034,-1.35509048225843,4.59570535302139));
#95622=CARTESIAN_POINT('Ctrl Pts',(1.93077998603865,-0.72211779441669,4.63276749296511));
#95623=CARTESIAN_POINT('Ctrl Pts',(1.95575227831571,-0.0755349757277263,
4.66982963290883));
#95624=CARTESIAN_POINT('Ctrl Pts',(1.98072457059277,0.571047842961237,4.70689177285256));
#95625=CARTESIAN_POINT('Ctrl Pts',(1.6533032312286,1.23124079249743,4.74395391279628));
#95626=CARTESIAN_POINT('Ctrl Pts',(1.12345433605614,1.60266118112717,4.78101605273999));
#95627=CARTESIAN_POINT('Ctrl Pts',(0.59360544088369,1.97408156975691,4.81807819268371));
#95628=CARTESIAN_POINT('Ctrl Pts',(-0.138671010097046,2.05672939748021,
4.85514033262744));
#95629=CARTESIAN_POINT('Ctrl Pts',(-0.737976517839776,1.81275016640803,
4.89220247257116));
#95630=CARTESIAN_POINT('Ctrl Pts',(-1.33728202558251,1.56877093533586,4.92926461251488));
#95631=CARTESIAN_POINT('Ctrl Pts',(-1.80361659008724,0.998164645468222,
4.9663267524586));
#95632=CARTESIAN_POINT('Ctrl Pts',(-1.92338886510923,0.362281355122108,
5.00338889240232));
#95633=CARTESIAN_POINT('Ctrl Pts',(-1.94573194011967,0.243659678682544,
5.01030269756014));
#95634=CARTESIAN_POINT('Ctrl Pts',(-1.95601481281436,0.122766393772507,
5.01721650271795));
#95635=CARTESIAN_POINT('Ctrl Pts',(-1.95491180920002,0.00168629508682236,
5.02413030787576));
#95636=CARTESIAN_POINT('Origin',(0.,0.,0.));
#95637=CARTESIAN_POINT('',(-1.9507978584999,-3.45334863967226E-5,5.82586969212423));
#95638=CARTESIAN_POINT('',(-1.95080468396925,0.00018981806121043,5.72413030787576));
#95639=CARTESIAN_POINT('',(-1.954,-2.39295984553393E-16,0.));
#95640=CARTESIAN_POINT('Ctrl Pts',(-1.95079815420139,-3.45302974047446E-5,
5.82586969212423));
#95641=CARTESIAN_POINT('Ctrl Pts',(-1.95074640707532,0.328120037045956,
5.80723147606333));
#95642=CARTESIAN_POINT('Ctrl Pts',(-1.87237758907749,0.656297824114404,
5.78859326000243));
#95643=CARTESIAN_POINT('Ctrl Pts',(-1.715829951129,0.941574404236039,5.76995504394152));
#95644=CARTESIAN_POINT('Ctrl Pts',(-1.4047439120071,1.50846613462089,5.73291782711304));
#95645=CARTESIAN_POINT('Ctrl Pts',(-0.784943311216198,1.90594846094957,
5.69588061028457));
#95646=CARTESIAN_POINT('Ctrl Pts',(-0.139960769924853,1.95218999146749,
5.65884339345609));
#95647=CARTESIAN_POINT('Ctrl Pts',(0.505021771366483,1.99843152198542,5.62180617662761));
#95648=CARTESIAN_POINT('Ctrl Pts',(1.17518625315826,1.69343225669258,5.58476895979913));
#95649=CARTESIAN_POINT('Ctrl Pts',(1.56396070392606,1.17671648942254,5.54773174297065));
#95650=CARTESIAN_POINT('Ctrl Pts',(1.95273515469386,0.660000722152496,5.51069452614217));
#95651=CARTESIAN_POINT('Ctrl Pts',(2.06011957443768,-0.0684315470947738,
5.47365730931369));
#95652=CARTESIAN_POINT('Ctrl Pts',(1.83699012241942,-0.675353292756691,
5.43662009248521));
#95653=CARTESIAN_POINT('Ctrl Pts',(1.61386067040115,-1.28227503841861,5.39958287565673));
#95654=CARTESIAN_POINT('Ctrl Pts',(1.06021734662079,-1.76768626049519,5.36254565882826));
#95655=CARTESIAN_POINT('Ctrl Pts',(0.429328609649713,-1.90953180775813,
5.32550844199978));
#95656=CARTESIAN_POINT('Ctrl Pts',(-0.201560127321352,-2.05137735502108,
5.2884712251713));
#95657=CARTESIAN_POINT('Ctrl Pts',(-0.909694277483132,-1.84965722747041,
5.25143400834282));
#95658=CARTESIAN_POINT('Ctrl Pts',(-1.37113234823603,-1.39664987148696,
5.21439679151434));
#95659=CARTESIAN_POINT('Ctrl Pts',(-1.73877852911313,-1.03572077852157,
5.1848877583843));
#95660=CARTESIAN_POINT('Ctrl Pts',(-1.94982335358017,-0.515275892214865,
5.15537872525427));
#95661=CARTESIAN_POINT('Ctrl Pts',(-1.95458266482996,0.00173443779922018,
5.12586969212423));
#95662=CARTESIAN_POINT('Ctrl Pts',(-1.95491180920002,0.00168629508682236,
5.02413030787576));
#95663=CARTESIAN_POINT('Ctrl Pts',(-1.95010205227512,-0.526295513449078,
5.05427864266167));
#95664=CARTESIAN_POINT('Ctrl Pts',(-1.72879182329996,-1.05782955367232,
5.08442697744757));
#95665=CARTESIAN_POINT('Ctrl Pts',(-1.34689356786549,-1.42005289462677,
5.11457531223348));
#95666=CARTESIAN_POINT('Ctrl Pts',(-0.877416010060499,-1.86534356320495,
5.1516374521772));
#95667=CARTESIAN_POINT('Ctrl Pts',(-0.165250908911267,-2.05476460953673,
5.18869959212092));
#95668=CARTESIAN_POINT('Ctrl Pts',(0.463414671012952,-1.90155708549211,
5.22576173206464));
#95669=CARTESIAN_POINT('Ctrl Pts',(1.09208025093718,-1.74834956144749,5.26282387200837));
#95670=CARTESIAN_POINT('Ctrl Pts',(1.63724630963639,-1.25251346702646,5.29988601195209));
#95671=CARTESIAN_POINT('Ctrl Pts',(1.84921496651671,-0.641152489120857,
5.33694815189581));
#95672=CARTESIAN_POINT('Ctrl Pts',(2.06118362339704,-0.0297915112152539,
5.37401029183953));
#95673=CARTESIAN_POINT('Ctrl Pts',(1.93995487845847,0.697094350174917,5.41107243178325));
#95674=CARTESIAN_POINT('Ctrl Pts',(1.54105412656959,1.20657560296821,5.44813457172697));
#95675=CARTESIAN_POINT('Ctrl Pts',(1.14215337468071,1.71605685576151,5.48519671167069));
#95676=CARTESIAN_POINT('Ctrl Pts',(0.465580615841514,2.00813349995792,5.52225885161441));
#95677=CARTESIAN_POINT('Ctrl Pts',(-0.178779150223708,1.94902809680635,
5.55932099155813));
#95678=CARTESIAN_POINT('Ctrl Pts',(-0.823138916288934,1.88992269365477,
5.59638313150186));
#95679=CARTESIAN_POINT('Ctrl Pts',(-1.43528568958019,1.4796352431552,5.63344527144558));
#95680=CARTESIAN_POINT('Ctrl Pts',(-1.73484296927877,0.906086297567352,
5.6705074113893));
#95681=CARTESIAN_POINT('Ctrl Pts',(-1.87931321146693,0.629475576708828,
5.68838171021812));
#95682=CARTESIAN_POINT('Ctrl Pts',(-1.95107725773013,0.31489133949035,5.70625600904694));
#95683=CARTESIAN_POINT('Ctrl Pts',(-1.95080468396925,0.00018981806121043,
5.72413030787576));
#95684=CARTESIAN_POINT('Origin',(0.,0.,0.));
#95685=CARTESIAN_POINT('',(-1.95470932084261,-0.00171584046685047,6.52586969212424));
#95686=CARTESIAN_POINT('',(-1.95421427783755,-0.00177812761388513,6.42413030787576));
#95687=CARTESIAN_POINT('',(-1.954,-2.39295984553393E-16,0.));
#95688=CARTESIAN_POINT('Ctrl Pts',(-1.95470932084261,-0.00171584046685047,
6.52586969212424));
#95689=CARTESIAN_POINT('Ctrl Pts',(-1.94992946923152,0.519398730151351,
6.49612144370087));
#95690=CARTESIAN_POINT('Ctrl Pts',(-1.73506994162404,1.04399306729571,6.46637319527751));
#95691=CARTESIAN_POINT('Ctrl Pts',(-1.36210733975536,1.40545308526766,6.43662494685414));
#95692=CARTESIAN_POINT('Ctrl Pts',(-0.897760782010601,1.85547867567989,
6.39958773002566));
#95693=CARTESIAN_POINT('Ctrl Pts',(-0.188341937200331,2.05263315093338,
6.36255051319719));
#95694=CARTESIAN_POINT('Ctrl Pts',(0.441620008484366,1.90672665791667,6.32551329636871));
#95695=CARTESIAN_POINT('Ctrl Pts',(1.07158195416906,1.76082016489995,6.28847607954023));
#95696=CARTESIAN_POINT('Ctrl Pts',(1.62208700072817,1.27185270361303,6.25143886271175));
#95697=CARTESIAN_POINT('Ctrl Pts',(1.84130231899333,0.663506254660481,6.21440164588327));
#95698=CARTESIAN_POINT('Ctrl Pts',(2.0605176372585,0.0551598057079281,6.17736442905479));
#95699=CARTESIAN_POINT('Ctrl Pts',(1.94844322722972,-0.672565630910262,
6.14032721222632));
#95700=CARTESIAN_POINT('Ctrl Pts',(1.55634840229719,-1.18676637573315,6.10328999539784));
#95701=CARTESIAN_POINT('Ctrl Pts',(1.16425357736466,-1.70096712055603,6.06625277856936));
#95702=CARTESIAN_POINT('Ctrl Pts',(0.492138337528384,-2.00164317358361,
6.02921556174087));
#95703=CARTESIAN_POINT('Ctrl Pts',(-0.152532956197894,-1.95124792816734,
5.9921783449124));
#95704=CARTESIAN_POINT('Ctrl Pts',(-0.797204249924167,-1.90085268275106,
5.95514112808392));
#95705=CARTESIAN_POINT('Ctrl Pts',(-1.41443159754043,-1.49938613889095,
5.91810391125544));
#95706=CARTESIAN_POINT('Ctrl Pts',(-1.72185953262212,-0.930502299740384,
5.88106669442696));
#95707=CARTESIAN_POINT('Ctrl Pts',(-1.87458069522289,-0.647897528391999,
5.86266769365939));
#95708=CARTESIAN_POINT('Ctrl Pts',(-1.95084923717034,-0.323977343102287,
5.84426869289181));
#95709=CARTESIAN_POINT('Ctrl Pts',(-1.95079815420139,-3.45302974047446E-5,
5.82586969212423));
#95710=CARTESIAN_POINT('Ctrl Pts',(-1.95080468396925,0.00018981806121043,
5.72413030787576));
#95711=CARTESIAN_POINT('Ctrl Pts',(-1.95051207937167,-0.337638415069996,
5.74331814899066));
#95712=CARTESIAN_POINT('Ctrl Pts',(-1.86720620393942,-0.675601803708791,
5.76250599010555));
#95713=CARTESIAN_POINT('Ctrl Pts',(-1.70171536425399,-0.966869859783203,
5.78169383122045));
#95714=CARTESIAN_POINT('Ctrl Pts',(-1.38206269342473,-1.5294666308698,5.81875597116418));
#95715=CARTESIAN_POINT('Ctrl Pts',(-0.755789565660301,-1.91784973236686,
5.85581811110791));
#95716=CARTESIAN_POINT('Ctrl Pts',(-0.109742658556152,-1.95413127900566,
5.89288025105163));
#95717=CARTESIAN_POINT('Ctrl Pts',(0.536304248547996,-1.99041282564447,
5.92994239099535));
#95718=CARTESIAN_POINT('Ctrl Pts',(1.20212493499187,-1.674592817425,5.96700453093906));
#95719=CARTESIAN_POINT('Ctrl Pts',(1.58275908344154,-1.15132366886058,6.00406667088278));
#95720=CARTESIAN_POINT('Ctrl Pts',(1.9633932318912,-0.628054520296152,6.0411288108265));
#95721=CARTESIAN_POINT('Ctrl Pts',(2.05884084234667,0.102663768613233,6.07819095077022));
#95722=CARTESIAN_POINT('Ctrl Pts',(1.82538483877546,0.706146370849535,6.11525309071394));
#95723=CARTESIAN_POINT('Ctrl Pts',(1.59192883520425,1.30962897308584,6.15231523065767));
#95724=CARTESIAN_POINT('Ctrl Pts',(1.02956921760636,1.78587588864905,6.18937737060139));
#95725=CARTESIAN_POINT('Ctrl Pts',(0.395878889512919,1.91675569949154,6.22643951054511));
#95726=CARTESIAN_POINT('Ctrl Pts',(-0.237811438580523,2.04763551033402,
6.26350165048883));
#95727=CARTESIAN_POINT('Ctrl Pts',(-0.942832477169518,1.83314821645578,
6.30056379043255));
#95728=CARTESIAN_POINT('Ctrl Pts',(-1.39626929730598,1.37153365109863,6.33762593037627));
#95729=CARTESIAN_POINT('Ctrl Pts',(-1.7490486198241,1.01239194403086,6.3664607228761));
#95730=CARTESIAN_POINT('Ctrl Pts',(-1.94954331224527,0.503663409317413,
6.39529551537593));
#95731=CARTESIAN_POINT('Ctrl Pts',(-1.95421427783755,-0.00177812761388513,
6.42413030787576));
#95732=CARTESIAN_POINT('Origin',(0.,0.,0.));
#95733=CARTESIAN_POINT('',(-1.95636369417486,0.00113518110994186,7.22586969212423));
#95734=CARTESIAN_POINT('',(-1.95675615924934,0.000851174274233985,7.12413030787576));
#95735=CARTESIAN_POINT('',(-1.954,-2.39295984553393E-16,0.));
#95736=CARTESIAN_POINT('Ctrl Pts',(-1.95636369417486,0.00113518110994186,
7.22586969212423));
#95737=CARTESIAN_POINT('Ctrl Pts',(-1.95682546989371,0.0679235189129894,
7.22204862816689));
#95738=CARTESIAN_POINT('Ctrl Pts',(-1.95370156992351,0.134668159558925,
7.21822756420955));
#95739=CARTESIAN_POINT('Ctrl Pts',(-1.94684940168549,0.201027826582277,
7.2144065002522));
#95740=CARTESIAN_POINT('Ctrl Pts',(-1.88043197355288,0.844245894546327,
7.17736928342373));
#95741=CARTESIAN_POINT('Ctrl Pts',(-1.46373463610807,1.45129475044757,7.14033206659525));
#95742=CARTESIAN_POINT('Ctrl Pts',(-0.887378837876281,1.74447515831938,
7.10329484976677));
#95743=CARTESIAN_POINT('Ctrl Pts',(-0.31102303964449,2.03765556619118,7.06625763293829));
#95744=CARTESIAN_POINT('Ctrl Pts',(0.424991219374283,2.01696752603353,7.02922041610981));
#95745=CARTESIAN_POINT('Ctrl Pts',(0.983968473233738,1.69187494324663,6.99218319928133));
#95746=CARTESIAN_POINT('Ctrl Pts',(1.54294572709319,1.36678236045973,6.95514598245285));
#95747=CARTESIAN_POINT('Ctrl Pts',(1.92488597579333,0.737285235043576,6.91810876562437));
#95748=CARTESIAN_POINT('Ctrl Pts',(1.95506767226643,0.0913519390189264,
6.8810715487959));
#95749=CARTESIAN_POINT('Ctrl Pts',(1.98524936873952,-0.554581357005719,
6.84403433196742));
#95750=CARTESIAN_POINT('Ctrl Pts',(1.66367251298559,-1.21695082363886,6.80699711513894));
#95751=CARTESIAN_POINT('Ctrl Pts',(1.13744494695038,-1.59275037986524,6.76995989831046));
#95752=CARTESIAN_POINT('Ctrl Pts',(0.611217380915185,-1.96854993609162,
6.73292268148198));
#95753=CARTESIAN_POINT('Ctrl Pts',(-0.119660895401274,-2.05777958191125,
6.69588546465349));
#95754=CARTESIAN_POINT('Ctrl Pts',(-0.72084391141631,-1.81962051958034,
6.65884824782502));
#95755=CARTESIAN_POINT('Ctrl Pts',(-1.32202692743135,-1.58146145724943,
6.62181103099654));
#95756=CARTESIAN_POINT('Ctrl Pts',(-1.79351468314497,-1.01591368676797,
6.58477381416807));
#95757=CARTESIAN_POINT('Ctrl Pts',(-1.91962142566216,-0.381691448741754,
6.54773659733959));
#95758=CARTESIAN_POINT('Ctrl Pts',(-1.9444393828574,-0.256875756563692,
6.54044762893447));
#95759=CARTESIAN_POINT('Ctrl Pts',(-1.95588048853217,-0.129400253566584,
6.53315866052935));
#95760=CARTESIAN_POINT('Ctrl Pts',(-1.95470932084261,-0.00171584046685047,
6.52586969212424));
#95761=CARTESIAN_POINT('Ctrl Pts',(-1.95421427783755,-0.00177812761388513,
6.42413030787576));
#95762=CARTESIAN_POINT('Ctrl Pts',(-1.95554703085897,-0.145994290672205,
6.43235765531965));
#95763=CARTESIAN_POINT('Ctrl Pts',(-1.94093747105224,-0.289942854151266,
6.44058500276354));
#95764=CARTESIAN_POINT('Ctrl Pts',(-1.90937423221194,-0.430072724152966,
6.44881235020743));
#95765=CARTESIAN_POINT('Ctrl Pts',(-1.7671897452975,-1.06132269721135,6.48587449015115));
#95766=CARTESIAN_POINT('Ctrl Pts',(-1.28096816978468,-1.61508080649208,
6.52293663009487));
#95767=CARTESIAN_POINT('Ctrl Pts',(-0.67340953434779,-1.83771382585667,
6.55999877003859));
#95768=CARTESIAN_POINT('Ctrl Pts',(-0.0658508989108841,-2.06034684522128,
6.59706090998232));
#95769=CARTESIAN_POINT('Ctrl Pts',(0.663044796450101,-1.95185477466974,
6.63412304992604));
#95770=CARTESIAN_POINT('Ctrl Pts',(1.17942751209788,-1.56192933591821,6.67118518986976));
#95771=CARTESIAN_POINT('Ctrl Pts',(1.69581022774564,-1.17200389716668,6.70824732981348));
#95772=CARTESIAN_POINT('Ctrl Pts',(1.9996799636802,-0.500645090215166,6.7453094697572));
#95773=CARTESIAN_POINT('Ctrl Pts',(1.95185778931935,0.144650188277344,6.78237160970092));
#95774=CARTESIAN_POINT('Ctrl Pts',(1.90403561495849,0.789945466769872,6.81943374964464));
#95775=CARTESIAN_POINT('Ctrl Pts',(1.5045215303022,1.4091772168034,6.85649588958836));
#95776=CARTESIAN_POINT('Ctrl Pts',(0.936301652358751,1.71872386452436,6.89355802953208));
#95777=CARTESIAN_POINT('Ctrl Pts',(0.368081774415317,2.02827051224532,6.9306201694758));
#95778=CARTESIAN_POINT('Ctrl Pts',(-0.368843896815252,2.02813205765373,
6.96768230941953));
#95779=CARTESIAN_POINT('Ctrl Pts',(-0.936947418561655,1.71837191595589,
7.00474444936325));
#95780=CARTESIAN_POINT('Ctrl Pts',(-1.50505094030807,1.40861177425805,7.04180658930697));
#95781=CARTESIAN_POINT('Ctrl Pts',(-1.90433231257031,0.78922994545395,7.07886872925069));
#95782=CARTESIAN_POINT('Ctrl Pts',(-1.95191200566454,0.143916742729559,
7.11593086919441));
#95783=CARTESIAN_POINT('Ctrl Pts',(-1.95542076848464,0.0963281429343837,
7.11866401542153));
#95784=CARTESIAN_POINT('Ctrl Pts',(-1.95701686505733,0.0485985200318871,
7.12139716164864));
#95785=CARTESIAN_POINT('Ctrl Pts',(-1.95675615924934,0.000851174274233985,
7.12413030787576));
#95786=CARTESIAN_POINT('Origin',(0.,0.,0.));
#95787=CARTESIAN_POINT('',(-1.95128545551857,0.000980157954364874,7.92586969212424));
#95788=CARTESIAN_POINT('',(-1.95166123101285,0.00126544742759004,7.82413030787576));
#95789=CARTESIAN_POINT('',(-1.954,-2.39295984553393E-16,0.));
#95790=CARTESIAN_POINT('Ctrl Pts',(-1.95128545551857,0.000980157954364874,
7.92586969212424));
#95791=CARTESIAN_POINT('Ctrl Pts',(-1.95247914943593,0.263701155015296,
7.91093859580443));
#95792=CARTESIAN_POINT('Ctrl Pts',(-1.90313505751618,0.525992349613935,
7.89600749948463));
#95793=CARTESIAN_POINT('Ctrl Pts',(-1.80112460177197,0.765888339627252,
7.88107640316483));
#95794=CARTESIAN_POINT('Ctrl Pts',(-1.54808334564134,1.36096050365993,7.84403918633635));
#95795=CARTESIAN_POINT('Ctrl Pts',(-0.970981193167941,1.81823294990903,
7.80700196950786));
#95796=CARTESIAN_POINT('Ctrl Pts',(-0.333818027149729,1.92852282969788,
7.76996475267938));
#95797=CARTESIAN_POINT('Ctrl Pts',(0.303345138868501,2.03881270948674,7.73292753585091));
#95798=CARTESIAN_POINT('Ctrl Pts',(1.00056931843154,1.80212002281537,7.69589031902244));
#95799=CARTESIAN_POINT('Ctrl Pts',(1.43890387011628,1.32672168613705,7.65885310219396));
#95800=CARTESIAN_POINT('Ctrl Pts',(1.87723842180101,0.851323349458752,7.62181588536548));
#95801=CARTESIAN_POINT('Ctrl Pts',(2.05668334560742,0.13721936277351,7.58477866853699));
#95802=CARTESIAN_POINT('Ctrl Pts',(1.8951501609247,-0.488917833023672,7.54774145170851));
#95803=CARTESIAN_POINT('Ctrl Pts',(1.73361697624198,-1.11505502882086,7.51070423488003));
#95804=CARTESIAN_POINT('Ctrl Pts',(1.23110568307013,-1.65322543373001,7.47366701805156));
#95805=CARTESIAN_POINT('Ctrl Pts',(0.61749399359133,-1.85723879665063,7.43662980122308));
#95806=CARTESIAN_POINT('Ctrl Pts',(0.00388230411252383,-2.06125215957126,
7.3995925843946));
#95807=CARTESIAN_POINT('Ctrl Pts',(-0.72082978167322,-1.93110848050335,
7.36255536756612));
#95808=CARTESIAN_POINT('Ctrl Pts',(-1.22511706515588,-1.52634300095596,
7.32551815073764));
#95809=CARTESIAN_POINT('Ctrl Pts',(-1.6773779241913,-1.16333645789233,7.2923019978665));
#95810=CARTESIAN_POINT('Ctrl Pts',(-1.95234952088687,-0.579449614967985,
7.25908584499537));
#95811=CARTESIAN_POINT('Ctrl Pts',(-1.95636369417486,0.00113518110994186,
7.22586969212423));
#95812=CARTESIAN_POINT('Ctrl Pts',(-1.95675615924934,0.000851174274233985,
7.12413030787576));
#95813=CARTESIAN_POINT('Ctrl Pts',(-1.95348162971424,-0.598867317271105,
7.15845930159236));
#95814=CARTESIAN_POINT('Ctrl Pts',(-1.65727828481393,-1.20138176331325,
7.19278829530897));
#95815=CARTESIAN_POINT('Ctrl Pts',(-1.17884051406102,-1.56237241050387,
7.22711728902557));
#95816=CARTESIAN_POINT('Ctrl Pts',(-0.662311315437018,-1.95210378436822,
7.2641794289693));
#95817=CARTESIAN_POINT('Ctrl Pts',(0.0666250957372189,-2.06032195545224,
7.30124156891302));
#95818=CARTESIAN_POINT('Ctrl Pts',(0.674100031098693,-1.83746065393738,
7.33830370885674));
#95819=CARTESIAN_POINT('Ctrl Pts',(1.28157496646017,-1.61459935242253,7.37536584880046));
#95820=CARTESIAN_POINT('Ctrl Pts',(1.76758842600887,-1.0606585783088,7.41242798874417));
#95821=CARTESIAN_POINT('Ctrl Pts',(1.9095357026966,-0.429355222190436,7.44949012868789));
#95822=CARTESIAN_POINT('Ctrl Pts',(2.05148297938434,0.201948133927931,7.48655226863161));
#95823=CARTESIAN_POINT('Ctrl Pts',(1.84936407321109,0.910614072050953,7.52361440857534));
#95824=CARTESIAN_POINT('Ctrl Pts',(1.39575382755531,1.37205822017881,7.56067654851907));
#95825=CARTESIAN_POINT('Ctrl Pts',(0.942143581899539,1.83350236830666,7.59773868846279));
#95826=CARTESIAN_POINT('Ctrl Pts',(0.237041996761252,2.04772472643938,7.6348008284065));
#95827=CARTESIAN_POINT('Ctrl Pts',(-0.396599106844383,1.91660680765389,
7.67186296835022));
#95828=CARTESIAN_POINT('Ctrl Pts',(-1.03024021045003,1.78548888886839,7.70892510829394));
#95829=CARTESIAN_POINT('Ctrl Pts',(-1.59242083252301,1.30903069316467,7.74598724823766));
#95830=CARTESIAN_POINT('Ctrl Pts',(-1.82565005336597,0.705460409477194,
7.78304938818139));
#95831=CARTESIAN_POINT('Ctrl Pts',(-1.9118230851659,0.482454556858425,7.79674302807951));
#95832=CARTESIAN_POINT('Ctrl Pts',(-1.95308968355645,0.242096139413284,
7.81043666797764));
#95833=CARTESIAN_POINT('Ctrl Pts',(-1.95166123101285,0.00126544742759004,
7.82413030787576));
#95834=CARTESIAN_POINT('Origin',(0.,0.,0.));
#95835=CARTESIAN_POINT('',(-1.95279013340439,-0.00168009551267251,8.62586969212423));
#95836=CARTESIAN_POINT('',(-1.95215444869335,-0.00150235120299324,8.52413030787576));
#95837=CARTESIAN_POINT('',(-1.954,-2.39295984553393E-16,0.));
#95838=CARTESIAN_POINT('Ctrl Pts',(-1.95279013340439,-0.00168009551267251,
8.62586969212423));
#95839=CARTESIAN_POINT('Ctrl Pts',(-1.94903607268958,0.455640131522026,
8.59982856344197));
#95840=CARTESIAN_POINT('Ctrl Pts',(-1.78871895344458,0.915331173731693,
8.57378743475971));
#95841=CARTESIAN_POINT('Ctrl Pts',(-1.49539281844263,1.26270942713959,8.54774630607745));
#95842=CARTESIAN_POINT('Ctrl Pts',(-1.07820722729247,1.75677110357261,8.51070908924897));
#95843=CARTESIAN_POINT('Ctrl Pts',(-0.391968436807465,2.02364430724413,
8.47367187242049));
#95844=CARTESIAN_POINT('Ctrl Pts',(0.24939826400162,1.94124580780539,8.43663465559201));
#95845=CARTESIAN_POINT('Ctrl Pts',(0.890764964810705,1.85884730836666,8.39959743876353));
#95846=CARTESIAN_POINT('Ctrl Pts',(1.48725957594388,1.42717710581768,8.36256022193505));
#95847=CARTESIAN_POINT('Ctrl Pts',(1.76601098282085,0.843706103134459,8.32552300510657));
#95848=CARTESIAN_POINT('Ctrl Pts',(2.04476238969783,0.260235100451228,8.28848578827809));
#95849=CARTESIAN_POINT('Ctrl Pts',(2.00577059231861,-0.475036702366233,
8.25144857144961));
#95850=CARTESIAN_POINT('Ctrl Pts',(1.66687269277466,-1.02575348200379,8.21441135462113));
#95851=CARTESIAN_POINT('Ctrl Pts',(1.32797479323072,-1.57647026164133,8.17737413779266));
#95852=CARTESIAN_POINT('Ctrl Pts',(0.689170791522051,-1.94263201809897,
8.14033692096418));
#95853=CARTESIAN_POINT('Ctrl Pts',(0.0426865627857745,-1.95673519857469,
8.1032997041357));
#95854=CARTESIAN_POINT('Ctrl Pts',(-0.60379766595052,-1.97083837905041,
8.06626248730722));
#95855=CARTESIAN_POINT('Ctrl Pts',(-1.25796212171444,-1.6328829835442,8.02922527047874));
#95856=CARTESIAN_POINT('Ctrl Pts',(-1.62055416970245,-1.09746934488294,
7.99218805365026));
#95857=CARTESIAN_POINT('Ctrl Pts',(-1.83697171385623,-0.777901098892797,
7.97008193314158));
#95858=CARTESIAN_POINT('Ctrl Pts',(-1.94951814111497,-0.387989405753114,
7.94797581263291));
#95859=CARTESIAN_POINT('Ctrl Pts',(-1.95128545551857,0.000980157954364874,
7.92586969212424));
#95860=CARTESIAN_POINT('Ctrl Pts',(-1.95166123101285,0.00126544742759004,
7.82413030787576));
#95861=CARTESIAN_POINT('Ctrl Pts',(-1.94922354508138,-0.409717467160323,
7.84749880792136));
#95862=CARTESIAN_POINT('Ctrl Pts',(-1.82244856716882,-0.822075748123473,
7.87086730796695));
#95863=CARTESIAN_POINT('Ctrl Pts',(-1.58232634722073,-1.15191832939155,
7.89423580801255));
#95864=CARTESIAN_POINT('Ctrl Pts',(-1.20149560061961,-1.67504441290151,
7.93129794795627));
#95865=CARTESIAN_POINT('Ctrl Pts',(-0.535556287804454,-1.99061420825021,
7.96836008789999));
#95866=CARTESIAN_POINT('Ctrl Pts',(0.110476940437387,-1.95408990384897,
8.00542222784371));
#95867=CARTESIAN_POINT('Ctrl Pts',(0.756510168679237,-1.91756559944773,
8.04248436778743));
#95868=CARTESIAN_POINT('Ctrl Pts',(1.38263731234777,-1.52894719529654,8.07954650773116));
#95869=CARTESIAN_POINT('Ctrl Pts',(1.70207855773424,-0.966230350379699,
8.11660864767487));
#95870=CARTESIAN_POINT('Ctrl Pts',(2.02151980312072,-0.403513505462853,
8.1536707876186));
#95871=CARTESIAN_POINT('Ctrl Pts',(2.03427515022513,0.333301780219651,8.19073292756232));
#95872=CARTESIAN_POINT('Ctrl Pts',(1.73450237337761,0.906738122863988,8.22779506750604));
#95873=CARTESIAN_POINT('Ctrl Pts',(1.43472959653009,1.48017446550833,8.26485720744976));
#95874=CARTESIAN_POINT('Ctrl Pts',(0.822428695730641,1.89023186511451,8.30191934739348));
#95875=CARTESIAN_POINT('Ctrl Pts',(0.178046765554912,1.94909513773745,8.3389814873372));
#95876=CARTESIAN_POINT('Ctrl Pts',(-0.466335164620799,2.00795841036038,
8.37604362728092));
#95877=CARTESIAN_POINT('Ctrl Pts',(-1.14279812417278,1.71562755600011,8.41310576722464));
#95878=CARTESIAN_POINT('Ctrl Pts',(-1.54150740386038,1.20599644714809,8.45016790716836));
#95879=CARTESIAN_POINT('Ctrl Pts',(-1.80673309918174,0.866984359672774,
8.47482204073749));
#95880=CARTESIAN_POINT('Ctrl Pts',(-1.94905131081074,0.431815751432988,
8.49947617430663));
#95881=CARTESIAN_POINT('Ctrl Pts',(-1.95215444869335,-0.00150235120299324,
8.52413030787576));
#95882=CARTESIAN_POINT('Origin',(0.,0.,0.));
#95883=CARTESIAN_POINT('',(-1.95719986784682,3.71606954582295E-5,9.32586969212424));
#95884=CARTESIAN_POINT('',(-1.95707453392556,-0.000466568259871601,9.22413030787576));
#95885=CARTESIAN_POINT('',(-1.954,-2.39295984553393E-16,0.));
#95886=CARTESIAN_POINT('Ctrl Pts',(-1.95719986784682,3.71606954581456E-5,
9.32586969212423));
#95887=CARTESIAN_POINT('Ctrl Pts',(-1.95720042510874,0.00202653151786848,
9.32575574790799));
#95888=CARTESIAN_POINT('Ctrl Pts',(-1.95719765412071,0.00401590074103218,
9.32564180369175));
#95889=CARTESIAN_POINT('Ctrl Pts',(-1.95719155021855,0.00600525973720184,
9.32552785947551));
#95890=CARTESIAN_POINT('Ctrl Pts',(-1.95520749560565,0.65264027922361,9.28849064264703));
#95891=CARTESIAN_POINT('Ctrl Pts',(-1.60108272580438,1.29819476052309,9.25145342581855));
#95892=CARTESIAN_POINT('Ctrl Pts',(-1.0568144211536,1.64735485073218,9.21441620899007));
#95893=CARTESIAN_POINT('Ctrl Pts',(-0.512546116502833,1.99651494094127,
9.17737899216159));
#95894=CARTESIAN_POINT('Ctrl Pts',(0.221865722997436,2.04928064005996,9.14034177533311));
#95895=CARTESIAN_POINT('Ctrl Pts',(0.810458692323854,1.78151382429043,9.10330455850463));
#95896=CARTESIAN_POINT('Ctrl Pts',(1.39905166165026,1.51374700852089,9.06626734167615));
#95897=CARTESIAN_POINT('Ctrl Pts',(1.84182576080283,0.925447677863139,9.02923012484767));
#95898=CARTESIAN_POINT('Ctrl Pts',(1.93623051178265,0.285737974246437,8.99219290801919));
#95899=CARTESIAN_POINT('Ctrl Pts',(2.03063526276248,-0.353971729370283,
8.95515569119071));
#95900=CARTESIAN_POINT('Ctrl Pts',(1.77667066556955,-1.04509180594595,8.91811847436223));
#95901=CARTESIAN_POINT('Ctrl Pts',(1.29051481285208,-1.47146399547075,8.88108125753376));
#95902=CARTESIAN_POINT('Ctrl Pts',(0.804358960134614,-1.89783618499555,
8.84404404070528));
#95903=CARTESIAN_POINT('Ctrl Pts',(0.0860118518926114,-2.05946048746948,
8.8070068238768));
#95904=CARTESIAN_POINT('Ctrl Pts',(-0.535913025040727,-1.88240059832962,
8.76996960704832));
#95905=CARTESIAN_POINT('Ctrl Pts',(-1.15783790197406,-1.70534070918976,
8.73293239021984));
#95906=CARTESIAN_POINT('Ctrl Pts',(-1.68334054759872,-1.18959662843613,
8.69589517339136));
#95907=CARTESIAN_POINT('Ctrl Pts',(-1.87202567450341,-0.571099513462055,
8.65885795656288));
#95908=CARTESIAN_POINT('Ctrl Pts',(-1.92804495632289,-0.387472087407564,
8.64786186841667));
#95909=CARTESIAN_POINT('Ctrl Pts',(-1.95437531748109,-0.194787452297348,
8.63686578027045));
#95910=CARTESIAN_POINT('Ctrl Pts',(-1.95279013340439,-0.00168009551267234,
8.62586969212424));
#95911=CARTESIAN_POINT('Ctrl Pts',(-1.95215444869335,-0.00150235120299324,
8.52413030787576));
#95912=CARTESIAN_POINT('Ctrl Pts',(-1.95371620524508,-0.21958398707372,
8.53653831425035));
#95913=CARTESIAN_POINT('Ctrl Pts',(-1.92001564940553,-0.437196901383431,
8.54894632062494));
#95914=CARTESIAN_POINT('Ctrl Pts',(-1.84897391479539,-0.641847309864828,
8.56135432699953));
#95915=CARTESIAN_POINT('Ctrl Pts',(-1.63677554621959,-1.25312859468192,
8.59841646694325));
#95916=CARTESIAN_POINT('Ctrl Pts',(-1.0914232092448,-1.74875980097234,8.63547860688697));
#95917=CARTESIAN_POINT('Ctrl Pts',(-0.462700104058479,-1.90173108515756,
8.67254074683069));
#95918=CARTESIAN_POINT('Ctrl Pts',(0.166023001127845,-2.05470236934278,
8.70960288677441));
#95919=CARTESIAN_POINT('Ctrl Pts',(0.878116874525705,-1.86501373142281,
8.74666502671813));
#95920=CARTESIAN_POINT('Ctrl Pts',(1.34742707561642,-1.41954668207959,8.78372716666185));
#95921=CARTESIAN_POINT('Ctrl Pts',(1.81673727670714,-0.974079632736377,
8.82078930660557));
#95922=CARTESIAN_POINT('Ctrl Pts',(2.04326380549072,-0.272834171969915,
8.85785144654929));
#95923=CARTESIAN_POINT('Ctrl Pts',(1.92325259761237,0.363004067433246,8.89491358649301));
#95924=CARTESIAN_POINT('Ctrl Pts',(1.80324138973402,0.998842306836407,8.93197572643673));
#95925=CARTESIAN_POINT('Ctrl Pts',(1.33669244519374,1.56927332487627,8.96903786638045));
#95926=CARTESIAN_POINT('Ctrl Pts',(0.737295301650971,1.81302734225987,9.00610000632417));
#95927=CARTESIAN_POINT('Ctrl Pts',(0.137898158108199,2.05678135964346,9.0431621462679));
#95928=CARTESIAN_POINT('Ctrl Pts',(-0.59434718443707,1.9738583763708,9.08022428621162));
#95929=CARTESIAN_POINT('Ctrl Pts',(-1.12405647662483,1.60223891616111,9.11728642615534));
#95930=CARTESIAN_POINT('Ctrl Pts',(-1.63307724594775,1.24513356361944,9.15290105339548));
#95931=CARTESIAN_POINT('Ctrl Pts',(-1.95507366281261,0.621442230158499,
9.18851568063562));
#95932=CARTESIAN_POINT('Ctrl Pts',(-1.95707453392556,-0.000466568259871601,
9.22413030787576));
#95933=CARTESIAN_POINT('Origin',(0.,0.,0.));
#95934=CARTESIAN_POINT('',(-1.95268202714777,0.00165579016441021,10.0258696921242));
#95935=CARTESIAN_POINT('',(-1.9535343393295,0.00178280253715055,9.92413030787576));
#95936=CARTESIAN_POINT('',(-1.954,-2.39295984553393E-16,0.));
#95937=CARTESIAN_POINT('Ctrl Pts',(-1.95268202714777,0.00165579016441021,
10.0258696921242));
#95938=CARTESIAN_POINT('Ctrl Pts',(-1.9542709496717,0.198793394721131,10.0146457155455));
#95939=CARTESIAN_POINT('Ctrl Pts',(-1.92681564478375,0.395498739780043,
10.0034217389668));
#95940=CARTESIAN_POINT('Ctrl Pts',(-1.86848643290836,0.582577638715851,
9.99219776238813));
#95941=CARTESIAN_POINT('Ctrl Pts',(-1.67600993827966,1.1999062383733,9.95516054555966));
#95942=CARTESIAN_POINT('Ctrl Pts',(-1.14735119634562,1.71241362792136,9.91812332873117));
#95943=CARTESIAN_POINT('Ctrl Pts',(-0.524351231736321,1.8856531990772,9.88108611190269));
#95944=CARTESIAN_POINT('Ctrl Pts',(0.0986487328729629,2.05889277023303,
9.84404889507421));
#95945=CARTESIAN_POINT('Ctrl Pts',(0.815989920157508,1.89286452299667,9.80701167824573));
#95946=CARTESIAN_POINT('Ctrl Pts',(1.29952003507049,1.46351732792493,9.76997446141725));
#95947=CARTESIAN_POINT('Ctrl Pts',(1.78305014998348,1.03417013285319,9.73293724458878));
#95948=CARTESIAN_POINT('Ctrl Pts',(2.0327691925249,0.341503989946047,9.69590002776029));
#95949=CARTESIAN_POINT('Ctrl Pts',(1.9344406978275,-0.297614493697593,9.65886281093182));
#95950=CARTESIAN_POINT('Ctrl Pts',(1.8361122031301,-0.936732977341234,9.62182559410334));
#95951=CARTESIAN_POINT('Ctrl Pts',(1.38973617119388,-1.52230380172138,9.58478837727486));
#95952=CARTESIAN_POINT('Ctrl Pts',(0.799511084736072,-1.78645358874384,
9.54775116044638));
#95953=CARTESIAN_POINT('Ctrl Pts',(0.209285998278261,-2.0506033757663,9.5107139436179));
#95954=CARTESIAN_POINT('Ctrl Pts',(-0.524788142701144,-1.99333212543108,
9.47367672678942));
#95955=CARTESIAN_POINT('Ctrl Pts',(-1.06690354347858,-1.6408387214268,9.43663950996094));
#95956=CARTESIAN_POINT('Ctrl Pts',(-1.60735113766186,-1.28942975594381,
9.3997162373487));
#95957=CARTESIAN_POINT('Ctrl Pts',(-1.95701928883641,-0.644612332051665,
9.36279296473647));
#95958=CARTESIAN_POINT('Ctrl Pts',(-1.95719986784682,3.71606954582295E-5,
9.32586969212424));
#95959=CARTESIAN_POINT('Ctrl Pts',(-1.95707453392556,-0.000466568259871601,
9.22413030787576));
#95960=CARTESIAN_POINT('Ctrl Pts',(-1.95715585687005,-0.0257432861687418,
9.22557782057934));
#95961=CARTESIAN_POINT('Ctrl Pts',(-1.95670857405052,-0.0510170594794435,
9.22702533328292));
#95962=CARTESIAN_POINT('Ctrl Pts',(-1.95572375776859,-0.0762698699047084,
9.2284728459865));
#95963=CARTESIAN_POINT('Ctrl Pts',(-1.93050850489432,-0.722843258614067,
9.26553498593022));
#95964=CARTESIAN_POINT('Ctrl Pts',(-1.55290475731554,-1.35567409888606,
9.30259712587394));
#95965=CARTESIAN_POINT('Ctrl Pts',(-0.995863227266852,-1.68491214354887,
9.33965926581766));
#95966=CARTESIAN_POINT('Ctrl Pts',(-0.438821697218168,-2.01415018821168,
9.37672140576139));
#95967=CARTESIAN_POINT('Ctrl Pts',(0.297657615300397,-2.03979543726533,
9.4137835457051));
#95968=CARTESIAN_POINT('Ctrl Pts',(0.876251218790847,-1.75010180082627,
9.45084568564882));
#95969=CARTESIAN_POINT('Ctrl Pts',(1.45484482228131,-1.46040816438721,9.48790782559255));
#95970=CARTESIAN_POINT('Ctrl Pts',(1.87555271674363,-0.855375642455424,
9.52496996553627));
#95971=CARTESIAN_POINT('Ctrl Pts',(1.94568154283725,-0.21212227253196,9.56203210547999));
#95972=CARTESIAN_POINT('Ctrl Pts',(2.01581036893087,0.431131097391505,9.59909424542371));
#95973=CARTESIAN_POINT('Ctrl Pts',(1.73536012665579,1.11260531530666,9.63615638536743));
#95974=CARTESIAN_POINT('Ctrl Pts',(1.23278314419194,1.52017044141902,9.67321852531115));
#95975=CARTESIAN_POINT('Ctrl Pts',(0.730206161728088,1.92773556753138,9.71028066525487));
#95976=CARTESIAN_POINT('Ctrl Pts',(0.00550243907548716,2.06139160184095,
9.74734280519859));
#95977=CARTESIAN_POINT('Ctrl Pts',(-0.609398062732146,1.85992111567971,
9.78440494514231));
#95978=CARTESIAN_POINT('Ctrl Pts',(-1.22429856453979,1.65845062951848,9.82146708508603));
#95979=CARTESIAN_POINT('Ctrl Pts',(-1.72939584550245,1.12185362288641,9.85852922502976));
#95980=CARTESIAN_POINT('Ctrl Pts',(-1.89334427223443,0.495903289718102,
9.89559136497348));
#95981=CARTESIAN_POINT('Ctrl Pts',(-1.93542598326109,0.335236538822793,
9.90510434594091));
#95982=CARTESIAN_POINT('Ctrl Pts',(-1.95503184094814,0.168682937546108,
9.91461732690834));
#95983=CARTESIAN_POINT('Ctrl Pts',(-1.9535343393295,0.00178280253715055,
9.92413030787576));
#95984=CARTESIAN_POINT('Origin',(0.,0.,0.));
#95985=CARTESIAN_POINT('',(-1.95129684289216,-0.00113636086278679,10.7258696921242));
#95986=CARTESIAN_POINT('',(-1.95093054978418,-0.000550606481354719,10.6241303078758));
#95987=CARTESIAN_POINT('',(-1.954,-2.39295984553393E-16,0.));
#95988=CARTESIAN_POINT('Ctrl Pts',(-1.95129684289216,-0.00113636086278679,
10.7258696921242));
#95989=CARTESIAN_POINT('Ctrl Pts',(-1.94942963316978,0.391854106201406,
10.7035356831831));
#95990=CARTESIAN_POINT('Ctrl Pts',(-1.83442754086643,0.785903964976412,
10.6812016742419));
#95991=CARTESIAN_POINT('Ctrl Pts',(-1.61381630858742,1.10744756631717,10.6588676653008));
#95992=CARTESIAN_POINT('Ctrl Pts',(-1.24796949325566,1.64067382739912,10.6218304484723));
#95993=CARTESIAN_POINT('Ctrl Pts',(-0.591690439027595,1.97450300329055,
10.5847932316438));
#95994=CARTESIAN_POINT('Ctrl Pts',(0.0547076636758263,1.95640786233593,
10.5477560148153));
#95995=CARTESIAN_POINT('Ctrl Pts',(0.701105766379276,1.9383127213813,10.5107187979868));
#95996=CARTESIAN_POINT('Ctrl Pts',(1.33762291755807,1.56829326358058,10.4736815811584));
#95997=CARTESIAN_POINT('Ctrl Pts',(1.67312833478204,1.01552035674769,10.4366443643299));
#95998=CARTESIAN_POINT('Ctrl Pts',(2.00863375200599,0.462747449914819,10.3996071475014));
#95999=CARTESIAN_POINT('Ctrl Pts',(2.04312743527515,-0.272778905950186,
10.3625699306729));
#96000=CARTESIAN_POINT('Ctrl Pts',(1.7608042651717,-0.854535269464722,10.3255327138444));
#96001=CARTESIAN_POINT('Ctrl Pts',(1.47848109506825,-1.43629163297926,10.288495497016));
#96002=CARTESIAN_POINT('Ctrl Pts',(0.879341071592168,-1.86427800414334,
10.2514582801875));
#96003=CARTESIAN_POINT('Ctrl Pts',(0.237478981470821,-1.94273555725334,
10.214421063359));
#96004=CARTESIAN_POINT('Ctrl Pts',(-0.404383108650536,-2.02119311036335,
10.1773838465305));
#96005=CARTESIAN_POINT('Ctrl Pts',(-1.08896726541717,-1.75012184541928,
10.140346629702));
#96006=CARTESIAN_POINT('Ctrl Pts',(-1.5031122201388,-1.25351130806383,10.1033094128736));
#96007=CARTESIAN_POINT('Ctrl Pts',(-1.7917522457641,-0.907396556226723,
10.0774961726238));
#96008=CARTESIAN_POINT('Ctrl Pts',(-1.94902777514884,-0.451727225472274,
10.051682932374));
#96009=CARTESIAN_POINT('Ctrl Pts',(-1.95268202714777,0.00165579016441021,
10.0258696921242));
#96010=CARTESIAN_POINT('Ctrl Pts',(-1.9535343393295,0.00178280253715055,
9.92413030787576));
#96011=CARTESIAN_POINT('Ctrl Pts',(-1.94919764294582,-0.481552375812319,
9.95167946685205));
#96012=CARTESIAN_POINT('Ctrl Pts',(-1.76787653021499,-0.967793777264111,
9.97922862582834));
#96013=CARTESIAN_POINT('Ctrl Pts',(-1.44290486192301,-1.32238333502052,
10.0067777848046));
#96014=CARTESIAN_POINT('Ctrl Pts',(-1.00571745237828,-1.79941596688631,
10.0438399247484));
#96015=CARTESIAN_POINT('Ctrl Pts',(-0.308543060787511,-2.03817757091334,
10.0809020646921));
#96016=CARTESIAN_POINT('Ctrl Pts',(0.329297761185238,-1.92930969998698,
10.1179642046358));
#96017=CARTESIAN_POINT('Ctrl Pts',(0.967138583157977,-1.82044182906063,
10.1550263445795));
#96018=CARTESIAN_POINT('Ctrl Pts',(1.5456458355127,-1.36394448318089,10.1920884845232));
#96019=CARTESIAN_POINT('Ctrl Pts',(1.79984980484802,-0.76890421197536,10.229150624467));
#96020=CARTESIAN_POINT('Ctrl Pts',(2.05405377418334,-0.173863940769825,
10.2662127644107));
#96021=CARTESIAN_POINT('Ctrl Pts',(1.98395446049928,0.5597192557615,10.3032749043544));
#96022=CARTESIAN_POINT('Ctrl Pts',(1.62166047466929,1.09585000349956,10.3403370442981));
#96023=CARTESIAN_POINT('Ctrl Pts',(1.2593664888393,1.63198075123761,10.3773991842419));
#96024=CARTESIAN_POINT('Ctrl Pts',(0.604877830863377,1.9706590501824,10.4144613241856));
#96025=CARTESIAN_POINT('Ctrl Pts',(-0.042038551539475,1.95675976549601,
10.4515234641293));
#96026=CARTESIAN_POINT('Ctrl Pts',(-0.688954933942345,1.94286048080962,
10.488585604073));
#96027=CARTESIAN_POINT('Ctrl Pts',(-1.32829904077215,1.57638361249205,10.5256477440167));
#96028=CARTESIAN_POINT('Ctrl Pts',(-1.66723158702796,1.02518946943711,10.5627098839605));
#96029=CARTESIAN_POINT('Ctrl Pts',(-1.85446111291195,0.720704641366568,
10.5831833585989));
#96030=CARTESIAN_POINT('Ctrl Pts',(-1.95001820365716,0.359852200961074,
10.6036568332373));
#96031=CARTESIAN_POINT('Ctrl Pts',(-1.95093054978418,-0.000550606481354719,
10.6241303078758));
#96032=CARTESIAN_POINT('Origin',(0.,0.,-1.29405622560369));
#96033=CARTESIAN_POINT('',(-1.55334812646815,-0.000904610707407963,10.9559437743963));
#96034=CARTESIAN_POINT('',(-1.55659711405804,-0.00105088068675666,11.0940562256037));
#96035=CARTESIAN_POINT('',(-1.5555,-2.01987159101623E-13,-1.29405622560369));
#96036=CARTESIAN_POINT('',(0.499806597877791,1.47301514408978,11.4445));
#96037=CARTESIAN_POINT('Ctrl Pts',(-1.55334812646815,-0.000904610707408108,
10.9559437743963));
#96038=CARTESIAN_POINT('Ctrl Pts',(-1.55432667860164,-0.206859868644216,
10.9706469822836));
#96039=CARTESIAN_POINT('Ctrl Pts',(-1.42041322258558,-0.930327919713715,
11.0223874069994));
#96040=CARTESIAN_POINT('Ctrl Pts',(-0.324962964057439,-1.80887727526569,
11.1111650485437));
#96041=CARTESIAN_POINT('Ctrl Pts',(1.34445241673909,-1.25560970886474,11.2222766990291));
#96042=CARTESIAN_POINT('Ctrl Pts',(1.78171768593789,0.450698535437549,11.3333883495146));
#96043=CARTESIAN_POINT('Ctrl Pts',(0.989503531151977,1.30685679928735,11.4074627831715));
#96044=CARTESIAN_POINT('Ctrl Pts',(0.499806597877626,1.47301514408983,11.4445));
#96045=CARTESIAN_POINT('',(1.55548765964692,0.00619602180124784,11.4445));
#96046=CARTESIAN_POINT('Origin',(0.,0.,11.4445));
#96047=CARTESIAN_POINT('Ctrl Pts',(-1.55659711405804,-0.0010508806867568,
11.0940562256037));
#96048=CARTESIAN_POINT('Ctrl Pts',(-1.55726922058417,-0.079449137192624,
11.099684397238));
#96049=CARTESIAN_POINT('Ctrl Pts',(-1.51630179095532,-0.673453815214831,
11.142374708816));
#96050=CARTESIAN_POINT('Ctrl Pts',(-0.75277483453787,-1.67898453189698,
11.2221271603377));
#96051=CARTESIAN_POINT('Ctrl Pts',(1.00462758039806,-1.53944373403644,11.3333135801688));
#96052=CARTESIAN_POINT('Ctrl Pts',(1.55754888396286,-0.511266487217653,
11.4074378600563));
#96053=CARTESIAN_POINT('Ctrl Pts',(1.55548765964692,0.00619602180124784,
11.4445));
#96054=CARTESIAN_POINT('Origin',(0.,0.,-1.29405622560369));
#96055=CARTESIAN_POINT('',(-1.55445081536763,0.00131810726739325,10.2559437743963));
#96056=CARTESIAN_POINT('',(-1.55305653540906,-0.000438315446397164,10.3940562256037));
#96057=CARTESIAN_POINT('',(-1.5555,-2.01987159101623E-13,-1.29405622560369));
#96058=CARTESIAN_POINT('Ctrl Pts',(-1.55445081536763,0.00131810726739319,
10.2559437743963));
#96059=CARTESIAN_POINT('Ctrl Pts',(-1.55154181384031,-0.359601688445403,
10.2817570146461));
#96060=CARTESIAN_POINT('Ctrl Pts',(-1.24670140973274,-1.24280598265434,
10.3446074717243));
#96061=CARTESIAN_POINT('Ctrl Pts',(0.223056668548975,-1.82477852394609,
10.4444951456311));
#96062=CARTESIAN_POINT('Ctrl Pts',(1.65390974917898,-0.802670846854376,
10.5556067961165));
#96063=CARTESIAN_POINT('Ctrl Pts',(1.57153269033781,0.953897085409752,10.6667184466019));
#96064=CARTESIAN_POINT('Ctrl Pts',(0.0514163720288116,1.83756944970195,
10.7778300970874));
#96065=CARTESIAN_POINT('Ctrl Pts',(-1.30849536725084,1.14582374749785,10.8742385396855));
#96066=CARTESIAN_POINT('Ctrl Pts',(-1.55186171668149,0.311939131113674,
10.9336097654551));
#96067=CARTESIAN_POINT('Ctrl Pts',(-1.55334812646815,-0.000904610707408108,
10.9559437743963));
#96068=CARTESIAN_POINT('Ctrl Pts',(-1.55305653540906,-0.000438315446397077,
10.3940562256037));
#96069=CARTESIAN_POINT('Ctrl Pts',(-1.55364500629154,-0.232901140548306,
10.410644890909));
#96070=CARTESIAN_POINT('Ctrl Pts',(-1.39557528484751,-0.983968830408974,
10.464295696158));
#96071=CARTESIAN_POINT('Ctrl Pts',(-0.231259578302998,-1.82421227428175,
10.5550086413507));
#96072=CARTESIAN_POINT('Ctrl Pts',(1.40774638007895,-1.1829694620695,10.6661950611819));
#96073=CARTESIAN_POINT('Ctrl Pts',(1.75706993010233,0.541796064983141,10.7773814810131));
#96074=CARTESIAN_POINT('Ctrl Pts',(0.497080432048737,1.77049779856472,10.8885679008442));
#96075=CARTESIAN_POINT('Ctrl Pts',(-1.13185991314487,1.39680492671116,10.9941261490411));
#96076=CARTESIAN_POINT('Ctrl Pts',(-1.55284332390808,0.436812153822664,
11.0626222572943));
#96077=CARTESIAN_POINT('Ctrl Pts',(-1.55659711405804,-0.0010508806867568,
11.0940562256037));
#96078=CARTESIAN_POINT('Origin',(0.,0.,-1.29405622560369));
#96079=CARTESIAN_POINT('',(-1.55804728476752,2.95821195149996E-5,9.5559437743963));
#96080=CARTESIAN_POINT('',(-1.55512930646214,0.00141921665610299,9.69405622560371));
#96081=CARTESIAN_POINT('',(-1.5555,-2.01987159101623E-13,-1.29405622560369));
#96082=CARTESIAN_POINT('Ctrl Pts',(-1.55804728476752,2.95821195150548E-5,
9.5559437743963));
#96083=CARTESIAN_POINT('Ctrl Pts',(-1.55790353315504,-0.513149683984934,
9.59286704700854));
#96084=CARTESIAN_POINT('Ctrl Pts',(-1.00033131917675,-1.54135965233235,
9.66682753644926));
#96085=CARTESIAN_POINT('Ctrl Pts',(0.750970673805211,-1.67799333720618,
9.77782524271844));
#96086=CARTESIAN_POINT('Ctrl Pts',(1.81699613594968,-0.279545920640164,
9.88893689320389));
#96087=CARTESIAN_POINT('Ctrl Pts',(1.22062258834496,1.37466418983892,10.0000485436893));
#96088=CARTESIAN_POINT('Ctrl Pts',(-0.492515922639386,1.77116921324136,
10.1111601941748));
#96089=CARTESIAN_POINT('Ctrl Pts',(-1.46173837715872,0.831558022400444,
10.1964586044104));
#96090=CARTESIAN_POINT('Ctrl Pts',(-1.55571569202373,0.15825134364817,10.2447197978176));
#96091=CARTESIAN_POINT('Ctrl Pts',(-1.55445081536763,0.00131810726739319,
10.2559437743963));
#96092=CARTESIAN_POINT('Ctrl Pts',(-1.55512930646214,0.00141921665610296,
9.69405622560371));
#96093=CARTESIAN_POINT('Ctrl Pts',(-1.55167703869094,-0.383344278698275,
9.72160538457999));
#96094=CARTESIAN_POINT('Ctrl Pts',(-1.21314953523015,-1.29115961930375,
9.7862166835));
#96095=CARTESIAN_POINT('Ctrl Pts',(0.309373610575528,-1.81257875466721,
9.88789012236375));
#96096=CARTESIAN_POINT('Ctrl Pts',(1.69095195914933,-0.722381792257861,
9.99907654219489));
#96097=CARTESIAN_POINT('Ctrl Pts',(1.52354231364944,1.0295455294481,10.1102629620261));
#96098=CARTESIAN_POINT('Ctrl Pts',(-0.0394931635484403,1.83836962465064,
10.2214493818572));
#96099=CARTESIAN_POINT('Ctrl Pts',(-1.33855689695156,1.09373648628768,10.3160471363831));
#96100=CARTESIAN_POINT('Ctrl Pts',(-1.5523302537302,0.286463714736223,10.3735827509653));
#96101=CARTESIAN_POINT('Ctrl Pts',(-1.55305653540906,-0.000438315446397077,
10.3940562256037));
#96102=CARTESIAN_POINT('Origin',(0.,0.,-1.29405622560369));
#96103=CARTESIAN_POINT('',(-1.55453687436568,-0.00133745576774406,8.85594377439631));
#96104=CARTESIAN_POINT('',(-1.55794751152569,-0.000371416033132788,8.99405622560372));
#96105=CARTESIAN_POINT('',(-1.5555,-2.01987159101623E-13,-1.29405622560369));
#96106=CARTESIAN_POINT('Ctrl Pts',(-1.55453687436568,-0.00133745576774402,
8.85594377439631));
#96107=CARTESIAN_POINT('Ctrl Pts',(-1.55579877499581,-0.155062375664632,
8.86693986254252));
#96108=CARTESIAN_POINT('Ctrl Pts',(-1.46423861786649,-0.825096309536398,
8.91497316751722));
#96109=CARTESIAN_POINT('Ctrl Pts',(-0.503376402892206,-1.7681153483915,
9.00004368932038));
#96110=CARTESIAN_POINT('Ctrl Pts',(1.2121644264892,-1.38212772940753,9.11115533980582));
#96111=CARTESIAN_POINT('Ctrl Pts',(1.81867711471885,0.26839009932345,9.22226699029127));
#96112=CARTESIAN_POINT('Ctrl Pts',(0.761253709552246,1.67335367481701,9.33337864077668));
#96113=CARTESIAN_POINT('Ctrl Pts',(-0.99265255914171,1.54733978795034,9.44449029126215));
#96114=CARTESIAN_POINT('Ctrl Pts',(-1.55732851093913,0.517959404958592,
9.51867866913534));
#96115=CARTESIAN_POINT('Ctrl Pts',(-1.55804772838109,0.00161323939398619,
9.55582983018006));
#96116=CARTESIAN_POINT('Ctrl Pts',(-1.55804728476752,2.95821195150548E-5,
9.5559437743963));
#96117=CARTESIAN_POINT('Ctrl Pts',(-1.55794751152569,-0.000371416033132616,
8.99405622560372));
#96118=CARTESIAN_POINT('Ctrl Pts',(-1.55801224941728,-0.020493184051098,
8.99550373830729));
#96119=CARTESIAN_POINT('Ctrl Pts',(-1.54853952527048,-0.55575068168544,
9.03401339095459));
#96120=CARTESIAN_POINT('Ctrl Pts',(-0.935609375970031,-1.5829679799695,
9.1095851835456));
#96121=CARTESIAN_POINT('Ctrl Pts',(0.823234386500799,-1.64421340203127,
9.22077160337675));
#96122=CARTESIAN_POINT('Ctrl Pts',(1.82795976495949,-0.199287985657338,
9.33195802320793));
#96123=CARTESIAN_POINT('Ctrl Pts',(1.15819463928053,1.42819381470141,9.44314444303908));
#96124=CARTESIAN_POINT('Ctrl Pts',(-0.572526917402423,1.74738822826618,
9.55433086287024));
#96125=CARTESIAN_POINT('Ctrl Pts',(-1.47990815776177,0.783419353749631,
9.63796812372513));
#96126=CARTESIAN_POINT('Ctrl Pts',(-1.5563214066504,0.1342816322173,9.68454324463628));
#96127=CARTESIAN_POINT('Ctrl Pts',(-1.55512930646214,0.00141921665610296,
9.69405622560371));
#96128=CARTESIAN_POINT('Origin',(0.,0.,-1.29405622560369));
#96129=CARTESIAN_POINT('',(-1.55333906144275,0.000780263919018194,8.15594377439631));
#96130=CARTESIAN_POINT('',(-1.55403083159801,-0.00119596074553197,8.29405622560371));
#96131=CARTESIAN_POINT('',(-1.5555,-2.01987159101623E-13,-1.29405622560369));
#96132=CARTESIAN_POINT('Ctrl Pts',(-1.55333906144275,0.000780263919018167,
8.15594377439631));
#96133=CARTESIAN_POINT('Ctrl Pts',(-1.55193217426013,-0.308862600127516,
8.17804989490498));
#96134=CARTESIAN_POINT('Ctrl Pts',(-1.3122308335565,-1.13929638534857,8.23719323224213));
#96135=CARTESIAN_POINT('Ctrl Pts',(0.0400949547363229,-1.83793690702293,
8.33337378640777));
#96136=CARTESIAN_POINT('Ctrl Pts',(1.56567267939011,-0.963477420579929,
8.44448543689319));
#96137=CARTESIAN_POINT('Ctrl Pts',(1.65879203582308,0.792482593671729,8.55559708737864));
#96138=CARTESIAN_POINT('Ctrl Pts',(0.234256671005791,1.82338791618694,8.66670873786407));
#96139=CARTESIAN_POINT('Ctrl Pts',(-1.24241507899534,1.24912116508194,8.7668243002033));
#96140=CARTESIAN_POINT('Ctrl Pts',(-1.55154841917538,0.362716593952071,
8.82990264571404));
#96141=CARTESIAN_POINT('Ctrl Pts',(-1.55453687436568,-0.00133745576774402,
8.85594377439631));
#96142=CARTESIAN_POINT('Ctrl Pts',(-1.55403083159801,-0.00119596074553188,
8.29405622560371));
#96143=CARTESIAN_POINT('Ctrl Pts',(-1.55527408252746,-0.17480188940304,
8.30646423197829));
#96144=CARTESIAN_POINT('Ctrl Pts',(-1.4483135129372,-0.865473027753662,
8.3559343782966));
#96145=CARTESIAN_POINT('Ctrl Pts',(-0.434704832044991,-1.78666848096071,
8.44246666455862));
#96146=CARTESIAN_POINT('Ctrl Pts',(1.26590215885116,-1.33365823077974,8.55365308438979));
#96147=CARTESIAN_POINT('Ctrl Pts',(1.8068878531032,0.341040818691465,8.66483950422094));
#96148=CARTESIAN_POINT('Ctrl Pts',(0.69268588294083,1.70333168137465,8.77602592405212));
#96149=CARTESIAN_POINT('Ctrl Pts',(-1.03328002592178,1.50787500329959,8.88576483117969));
#96150=CARTESIAN_POINT('Ctrl Pts',(-1.55635469933735,0.494704907375218,
8.95844159836357));
#96151=CARTESIAN_POINT('Ctrl Pts',(-1.55794751152569,-0.000371416033132616,
8.99405622560372));
#96152=CARTESIAN_POINT('Origin',(0.,0.,-1.29405622560369));
#96153=CARTESIAN_POINT('',(-1.55738164088485,0.00090367155389158,7.45594377439631));
#96154=CARTESIAN_POINT('',(-1.55363820104426,0.00100737127591941,7.59405622560371));
#96155=CARTESIAN_POINT('',(-1.5555,-2.01987159101623E-13,-1.29405622560369));
#96156=CARTESIAN_POINT('Ctrl Pts',(-1.55738164088485,0.000903671553891608,
7.45594377439631));
#96157=CARTESIAN_POINT('Ctrl Pts',(-1.55418612064456,-0.461276292775272,
7.48915992726744));
#96158=CARTESIAN_POINT('Ctrl Pts',(-1.09121796390773,-1.44436334125619,
7.55941329696705));
#96159=CARTESIAN_POINT('Ctrl Pts',(0.580004387659595,-1.74448118065669,
7.66670388349515));
#96160=CARTESIAN_POINT('Ctrl Pts',(1.7800908511122,-0.459234407622611,7.77781553398057));
#96161=CARTESIAN_POINT('Ctrl Pts',(1.35154441460109,1.24617309179735,7.88892718446602));
#96162=CARTESIAN_POINT('Ctrl Pts',(-0.313551099181417,1.81143738163968,
8.00003883495145));
#96163=CARTESIAN_POINT('Ctrl Pts',(-1.41757073229054,0.936656796997624,
8.08904436492822));
#96164=CARTESIAN_POINT('Ctrl Pts',(-1.55428931266511,0.209921774117757,
8.1410126780765));
#96165=CARTESIAN_POINT('Ctrl Pts',(-1.55333906144275,0.000780263919018167,
8.15594377439631));
#96166=CARTESIAN_POINT('Ctrl Pts',(-1.55363820104426,0.00100737127591942,
7.59405622560371));
#96167=CARTESIAN_POINT('Ctrl Pts',(-1.55169765832855,-0.326159426902871,
7.6174247256493));
#96168=CARTESIAN_POINT('Ctrl Pts',(-1.29071878250434,-1.17503987929593,
7.67785536563862));
#96169=CARTESIAN_POINT('Ctrl Pts',(0.103792628149562,-1.8358593744105,7.77534814557165));
#96170=CARTESIAN_POINT('Ctrl Pts',(1.59909575810308,-0.907769413831382,
7.8865345654028));
#96171=CARTESIAN_POINT('Ctrl Pts',(1.62955779866738,0.851876712390422,7.99772098523398));
#96172=CARTESIAN_POINT('Ctrl Pts',(0.167274199086701,1.83116681231986,8.10890740506512));
#96173=CARTESIAN_POINT('Ctrl Pts',(-1.26795424285233,1.21093838634352,8.20768581852172));
#96174=CARTESIAN_POINT('Ctrl Pts',(-1.55156054962447,0.343750973057136,
8.26940209203457));
#96175=CARTESIAN_POINT('Ctrl Pts',(-1.55403083159801,-0.00119596074553188,
8.29405622560371));
#96176=CARTESIAN_POINT('Origin',(0.,0.,-1.29405622560369));
#96177=CARTESIAN_POINT('',(-1.55606466149984,-0.00136591087330588,6.7559437743963));
#96178=CARTESIAN_POINT('',(-1.55769406638298,0.000677585252333857,6.89405622560371));
#96179=CARTESIAN_POINT('',(-1.5555,-2.01987159101623E-13,-1.29405622560369));
#96180=CARTESIAN_POINT('Ctrl Pts',(-1.55606466149984,-0.00136591087330577,
6.7559437743963));
#96181=CARTESIAN_POINT('Ctrl Pts',(-1.55699698050756,-0.10301028373747,
6.76323274280142));
#96182=CARTESIAN_POINT('Ctrl Pts',(-1.50160999329305,-0.720125819190329,
6.80755892803501));
#96183=CARTESIAN_POINT('Ctrl Pts',(-0.677079673289082,-1.70914680334463,
6.8889223300971));
#96184=CARTESIAN_POINT('Ctrl Pts',(1.06838781720774,-1.49605051766532,7.00003398058251));
#96185=CARTESIAN_POINT('Ctrl Pts',(1.83637062036826,0.0858057341481814,
7.11114563106797));
#96186=CARTESIAN_POINT('Ctrl Pts',(0.924229284360448,1.589156980696,7.22225728155339));
#96187=CARTESIAN_POINT('Ctrl Pts',(-0.833503847528551,1.63856370505402,
7.33336893203883));
#96188=CARTESIAN_POINT('Ctrl Pts',(-1.53115801604342,0.622214122864029,
7.41126442965314));
#96189=CARTESIAN_POINT('Ctrl Pts',(-1.55774924177056,0.0540711533618156,
7.45212271043896));
#96190=CARTESIAN_POINT('Ctrl Pts',(-1.55738164088485,0.000903671553891608,
7.45594377439631));
#96191=CARTESIAN_POINT('Ctrl Pts',(-1.55769406638298,0.000677585252333878,
6.89405622560371));
#96192=CARTESIAN_POINT('Ctrl Pts',(-1.55508734647919,-0.476733936548398,
6.92838521932031));
#96193=CARTESIAN_POINT('Ctrl Pts',(-1.06472330039144,-1.47419539900055,
6.99977635298063));
#96194=CARTESIAN_POINT('Ctrl Pts',(0.633314188332071,-1.72628667698419,
7.10822962658467));
#96195=CARTESIAN_POINT('Ctrl Pts',(1.7940008868909,-0.403377453646542,7.21941604641583));
#96196=CARTESIAN_POINT('Ctrl Pts',(1.31130494233742,1.28904301731096,7.33060246624699));
#96197=CARTESIAN_POINT('Ctrl Pts',(-0.372603218894873,1.80064416072257,
7.44178888607816));
#96198=CARTESIAN_POINT('Ctrl Pts',(-1.43301362666466,0.901927254173143,
7.52960680586373));
#96199=CARTESIAN_POINT('Ctrl Pts',(-1.55477533406966,0.192722899107996,
7.58036258570558));
#96200=CARTESIAN_POINT('Ctrl Pts',(-1.55363820104426,0.00100737127591942,
7.59405622560371));
#96201=CARTESIAN_POINT('Origin',(0.,0.,-1.29405622560369));
#96202=CARTESIAN_POINT('',(-1.55295085115974,-2.74912889200857E-5,6.0559437743963));
#96203=CARTESIAN_POINT('',(-1.55567057787938,-0.00141549514015751,6.19405622560371));
#96204=CARTESIAN_POINT('',(-1.5555,-2.01987159101623E-13,-1.29405622560369));
#96205=CARTESIAN_POINT('Ctrl Pts',(-1.55295114066544,-2.74881667468134E-5,
6.0559437743963));
#96206=CARTESIAN_POINT('Ctrl Pts',(-1.55299180574127,-0.257905198155464,
6.07434277516388));
#96207=CARTESIAN_POINT('Ctrl Pts',(-1.37005956536857,-1.03483686203599,
6.12977899275993));
#96208=CARTESIAN_POINT('Ctrl Pts',(-0.143272298638598,-1.83278278249422,
6.22225242718446));
#96209=CARTESIAN_POINT('Ctrl Pts',(1.46185859526926,-1.11471481859797,6.33336407766989));
#96210=CARTESIAN_POINT('Ctrl Pts',(1.72951224644592,0.623223129190563,6.44447572815534));
#96211=CARTESIAN_POINT('Ctrl Pts',(0.414808152398764,1.79096450999678,6.55558737864077));
#96212=CARTESIAN_POINT('Ctrl Pts',(-1.1682689842466,1.35101180160119,6.6594100607211));
#96213=CARTESIAN_POINT('Ctrl Pts',(-1.55225961585962,0.413472223515983,
6.72619552597294));
#96214=CARTESIAN_POINT('Ctrl Pts',(-1.55606466149984,-0.00136591087330577,
6.7559437743963));
#96215=CARTESIAN_POINT('Ctrl Pts',(-1.55567057787938,-0.00141549514015748,
6.19405622560371));
#96216=CARTESIAN_POINT('Ctrl Pts',(-1.55673152840384,-0.11622012238534,
6.2022835730476));
#96217=CARTESIAN_POINT('Ctrl Pts',(-1.49271086742403,-0.747018195902368,
6.2475730604352));
#96218=CARTESIAN_POINT('Ctrl Pts',(-0.632665469493242,-1.72652453095426,
6.32992468776653));
#96219=CARTESIAN_POINT('Ctrl Pts',(1.10806726459172,-1.46742614445027,6.44111110759769));
#96220=CARTESIAN_POINT('Ctrl Pts',(1.83376231205259,0.135898253011021,6.55229752742886));
#96221=CARTESIAN_POINT('Ctrl Pts',(0.879651525947856,1.61473395492061,6.66348394726001));
#96222=CARTESIAN_POINT('Ctrl Pts',(-0.880258220622017,1.61440330069759,
6.77467036709119));
#96223=CARTESIAN_POINT('Ctrl Pts',(-1.53940153309356,0.591912849892102,
6.85152779320574));
#96224=CARTESIAN_POINT('Ctrl Pts',(-1.55790160368306,0.0386873070159844,
6.89132307937659));
#96225=CARTESIAN_POINT('Ctrl Pts',(-1.55769406638298,0.000677585252333878,
6.89405622560371));
#96226=CARTESIAN_POINT('Origin',(0.,0.,-1.29405622560369));
#96227=CARTESIAN_POINT('',(-1.55596383579478,0.00138071545366175,5.3559437743963));
#96228=CARTESIAN_POINT('',(-1.5529563387483,0.000151106445085702,5.49405622560371));
#96229=CARTESIAN_POINT('',(-1.5555,-2.01987159101623E-13,-1.29405622560369));
#96230=CARTESIAN_POINT('Ctrl Pts',(-1.55596383579478,0.00138071545366179,
5.3559437743963));
#96231=CARTESIAN_POINT('Ctrl Pts',(-1.55217514150148,-0.410190199764792,
5.38545280752634));
#96232=CARTESIAN_POINT('Ctrl Pts',(-1.17330640529453,-1.34449549172498,
5.45199905748485));
#96233=CARTESIAN_POINT('Ctrl Pts',(0.403262995152723,-1.79359935217008,
5.55558252427184));
#96234=CARTESIAN_POINT('Ctrl Pts',(1.72546185411942,-0.634350903950841,
5.66669417475728));
#96235=CARTESIAN_POINT('Ctrl Pts',(1.46900873501267,1.1052750860401,5.77780582524271));
#96236=CARTESIAN_POINT('Ctrl Pts',(-0.13146340126236,1.83366765077345,5.88891747572816));
#96237=CARTESIAN_POINT('Ctrl Pts',(-1.36655195880861,1.04159698732297,5.98163012544601));
#96238=CARTESIAN_POINT('Ctrl Pts',(-1.55290994688111,0.261203028467153,
6.0373055583354));
#96239=CARTESIAN_POINT('Ctrl Pts',(-1.55295114066544,-2.74881667468134E-5,
6.0559437743963));
#96240=CARTESIAN_POINT('Ctrl Pts',(-1.5529563387483,0.000151106445085633,
5.49405622560371));
#96241=CARTESIAN_POINT('Ctrl Pts',(-1.55272340811799,-0.268780222436924,
5.5132440667186));
#96242=CARTESIAN_POINT('Ctrl Pts',(-1.35831396530156,-1.05747938365068,
5.56949404777722));
#96243=CARTESIAN_POINT('Ctrl Pts',(-0.103102773360761,-1.83589824620028,
5.66280616877956));
#96244=CARTESIAN_POINT('Ctrl Pts',(1.4869956060099,-1.08166382022474,5.77399258861071));
#96245=CARTESIAN_POINT('Ctrl Pts',(1.71494149863546,0.663421591850831,5.88517900844189));
#96246=CARTESIAN_POINT('Ctrl Pts',(0.371926577693494,1.80078404398782,5.99636542827304));
#96247=CARTESIAN_POINT('Ctrl Pts',(-1.18720103315053,1.32645343006727,6.09932450066032));
#96248=CARTESIAN_POINT('Ctrl Pts',(-1.55195221197423,0.40094597399841,6.16522143310387));
#96249=CARTESIAN_POINT('Ctrl Pts',(-1.55567057787938,-0.00141549514015748,
6.19405622560371));
#96250=CARTESIAN_POINT('Origin',(0.,0.,-1.29405622560369));
#96251=CARTESIAN_POINT('',(-1.55745492001379,-0.000856371120316566,4.6559437743963));
#96252=CARTESIAN_POINT('',(-1.55622585425313,0.00134239099646036,4.79405622560371));
#96253=CARTESIAN_POINT('',(-1.5555,-2.01987159101623E-13,-1.29405622560369));
#96254=CARTESIAN_POINT('Ctrl Pts',(-1.55745492001379,-0.000856371120316864,
4.65594377439631));
#96255=CARTESIAN_POINT('Ctrl Pts',(-1.5577850741697,-0.0506891626144068,
4.65952562306032));
#96256=CARTESIAN_POINT('Ctrl Pts',(-1.53301192978291,-0.615473136307116,
4.70014468855281));
#96257=CARTESIAN_POINT('Ctrl Pts',(-0.844041411881997,-1.63316067010957,
4.77780097087378));
#96258=CARTESIAN_POINT('Ctrl Pts',(0.913973507436636,-1.59507746114991,
4.88891262135923));
#96259=CARTESIAN_POINT('Ctrl Pts',(1.83577980123458,-0.0976329900371924,
5.00002427184466));
#96260=CARTESIAN_POINT('Ctrl Pts',(1.0780025055099,1.48913742733129,5.1111359223301));
#96261=CARTESIAN_POINT('Ctrl Pts',(-0.666056105926533,1.7134727727987,5.22224757281553));
#96262=CARTESIAN_POINT('Ctrl Pts',(-1.49938299705611,0.726891414718789,
5.30385019017093));
#96263=CARTESIAN_POINT('Ctrl Pts',(-1.55693038683329,0.106378444150779,
5.34841559069786));
#96264=CARTESIAN_POINT('Ctrl Pts',(-1.55596383579478,0.00138071545366179,
5.3559437743963));
#96265=CARTESIAN_POINT('Ctrl Pts',(-1.55622585425313,0.00134239099646029,
4.79405622560371));
#96266=CARTESIAN_POINT('Ctrl Pts',(-1.55239700220769,-0.418962472451577,
4.82420456038961));
#96267=CARTESIAN_POINT('Ctrl Pts',(-1.15964303797854,-1.36226320639006,
4.89141503511923));
#96268=CARTESIAN_POINT('Ctrl Pts',(0.435376164803608,-1.7865050090601,4.99568764979258));
#96269=CARTESIAN_POINT('Ctrl Pts',(1.73732980498774,-0.602360109052031,
5.10687406962374));
#96270=CARTESIAN_POINT('Ctrl Pts',(1.44781397169404,1.13357278356683,5.21806048945491));
#96271=CARTESIAN_POINT('Ctrl Pts',(-0.167962271460079,1.83110382765203,
5.32924690928607));
#96272=CARTESIAN_POINT('Ctrl Pts',(-1.37758975876034,1.02035875886683,5.42124548800234));
#96273=CARTESIAN_POINT('Ctrl Pts',(-1.55317332364345,0.250672199885809,
5.47618192677488));
#96274=CARTESIAN_POINT('Ctrl Pts',(-1.5529563387483,0.000151106445085633,
5.49405622560371));
#96275=CARTESIAN_POINT('Origin',(0.,0.,-1.29405622560369));
#96276=CARTESIAN_POINT('',(-1.55339129538237,-0.00082587420025254,3.9559437743963));
#96277=CARTESIAN_POINT('',(-1.5573160577951,-0.00094952305265919,4.09405622560371));
#96278=CARTESIAN_POINT('',(-1.5555,-2.01987159101623E-13,-1.29405622560369));
#96279=CARTESIAN_POINT('Ctrl Pts',(-1.55339129538237,-0.000825874200252562,
3.9559437743963));
#96280=CARTESIAN_POINT('Ctrl Pts',(-1.55438295724494,-0.206599346759669,
3.97063565542278));
#96281=CARTESIAN_POINT('Ctrl Pts',(-1.42062281789543,-0.929876204718288,
4.02236475327773));
#96282=CARTESIAN_POINT('Ctrl Pts',(-0.325213021862407,-1.80938005122649,
4.11113106796117));
#96283=CARTESIAN_POINT('Ctrl Pts',(1.34348911316817,-1.25485325124609,4.2222427184466));
#96284=CARTESIAN_POINT('Ctrl Pts',(1.78301209192838,0.447758371671112,4.33335436893204));
#96285=CARTESIAN_POINT('Ctrl Pts',(0.591229481908682,1.74070887258225,4.44446601941748));
#96286=CARTESIAN_POINT('Ctrl Pts',(-1.0856218085317,1.45071736103991,4.55199582123889));
#96287=CARTESIAN_POINT('Ctrl Pts',(-1.55437119708937,0.464594445617744,
4.62248840623184));
#96288=CARTESIAN_POINT('Ctrl Pts',(-1.55745492001379,-0.000856371120316864,
4.65594377439631));
#96289=CARTESIAN_POINT('Ctrl Pts',(-1.5573160577951,-0.000949523052659442,
4.0940562256037));
#96290=CARTESIAN_POINT('Ctrl Pts',(-1.55772052747877,-0.0572626470532979,
4.0981029141169));
#96291=CARTESIAN_POINT('Ctrl Pts',(-1.52938259291224,-0.628915705084586,
4.13921174257381));
#96292=CARTESIAN_POINT('Ctrl Pts',(-0.822616502622442,-1.64452261823584,
4.21738271097444));
#96293=CARTESIAN_POINT('Ctrl Pts',(0.936204134582059,-1.58261630557358,
4.3285691308056));
#96294=CARTESIAN_POINT('Ctrl Pts',(1.83742116834086,-0.0709647969689106,
4.43975555063676));
#96295=CARTESIAN_POINT('Ctrl Pts',(1.0554806974386,1.50569354438759,4.55094197046793));
#96296=CARTESIAN_POINT('Ctrl Pts',(-0.693325883166112,1.70307127625589,
4.66212839029909));
#96297=CARTESIAN_POINT('Ctrl Pts',(-1.50503746143118,0.709862178387775,
4.74316647534435));
#96298=CARTESIAN_POINT('Ctrl Pts',(-1.55710391061042,0.0977293375193425,
4.78714242044589));
#96299=CARTESIAN_POINT('Ctrl Pts',(-1.55622585425313,0.00134239099646029,
4.79405622560371));
#96300=CARTESIAN_POINT('Origin',(0.,0.,-1.29405622560369));
#96301=CARTESIAN_POINT('',(-1.55444674488022,0.00131742778884735,3.2559437743963));
#96302=CARTESIAN_POINT('',(-1.5533186684889,-0.000770198572060954,3.39405622560371));
#96303=CARTESIAN_POINT('',(-1.5555,-2.01987159101623E-13,-1.29405622560369));
#96304=CARTESIAN_POINT('Ctrl Pts',(-1.55444674488022,0.00131742778884739,
3.2559437743963));
#96305=CARTESIAN_POINT('Ctrl Pts',(-1.55154236665719,-0.359445316439912,
3.28174568778523));
#96306=CARTESIAN_POINT('Ctrl Pts',(-1.24691611905359,-1.24248704432008,
3.34458481800264));
#96307=CARTESIAN_POINT('Ctrl Pts',(0.222506403513669,-1.8248590575151,3.44446116504855));
#96308=CARTESIAN_POINT('Ctrl Pts',(1.65365282072159,-0.803151310699741,
3.55557281553397));
#96309=CARTESIAN_POINT('Ctrl Pts',(1.57184646516792,0.953372104320743,3.66668446601942));
#96310=CARTESIAN_POINT('Ctrl Pts',(0.0519332482321354,1.83764050268212,
3.77779611650485));
#96311=CARTESIAN_POINT('Ctrl Pts',(-1.30823935507303,1.14600960175539,3.87421588596382));
#96312=CARTESIAN_POINT('Ctrl Pts',(-1.55188304621527,0.312141358191517,
3.9335984385943));
#96313=CARTESIAN_POINT('Ctrl Pts',(-1.55339129538237,-0.000825874200252562,
3.9559437743963));
#96314=CARTESIAN_POINT('Ctrl Pts',(-1.5533186684889,-0.000770198572060919,
3.39405622560371));
#96315=CARTESIAN_POINT('Ctrl Pts',(-1.5542597194186,-0.210984061911746,
3.4090634077879));
#96316=CARTESIAN_POINT('Ctrl Pts',(-1.41654850766895,-0.939166341982764,
3.46113272991582));
#96317=CARTESIAN_POINT('Ctrl Pts',(-0.308692884081366,-1.81269447386996,
3.55026419198746));
#96318=CARTESIAN_POINT('Ctrl Pts',(1.35606994996762,-1.24186426112907,3.66145061181863));
#96319=CARTESIAN_POINT('Ctrl Pts',(1.77861387826841,0.466567491694538,3.77263703164979));
#96320=CARTESIAN_POINT('Ctrl Pts',(0.571870330903418,1.74760318061885,3.88382345148095));
#96321=CARTESIAN_POINT('Ctrl Pts',(-1.09574509035902,1.43939945308724,3.99096318279893));
#96322=CARTESIAN_POINT('Ctrl Pts',(-1.55401613758806,0.458488658137791,
4.06104077417318));
#96323=CARTESIAN_POINT('Ctrl Pts',(-1.5573160577951,-0.000949523052659442,
4.0940562256037));
#96324=CARTESIAN_POINT('Origin',(0.,0.,-1.29405622560369));
#96325=CARTESIAN_POINT('',(-1.55804712705668,3.25009013604671E-5,2.5559437743963));
#96326=CARTESIAN_POINT('',(-1.55449947323643,0.00133480041304715,2.69405622560371));
#96327=CARTESIAN_POINT('',(-1.5555,-2.01987159101623E-13,-1.29405622560369));
#96328=CARTESIAN_POINT('Ctrl Pts',(-1.55804712705668,3.25009013604029E-5,
2.5559437743963));
#96329=CARTESIAN_POINT('Ctrl Pts',(-1.55788927539753,-0.512989453804214,
2.59285572014769));
#96330=CARTESIAN_POINT('Ctrl Pts',(-1.0006227616332,-1.54106832868198,2.66680488272757));
#96331=CARTESIAN_POINT('Ctrl Pts',(0.750458968510211,-1.67822257683237,
2.77779126213592));
#96332=CARTESIAN_POINT('Ctrl Pts',(1.81691053470019,-0.280099604209337,
2.88890291262136));
#96333=CARTESIAN_POINT('Ctrl Pts',(1.22104229764526,1.37429086670804,3.0000145631068));
#96334=CARTESIAN_POINT('Ctrl Pts',(-0.491976593161155,1.77132117679823,
3.11112621359223));
#96335=CARTESIAN_POINT('Ctrl Pts',(-1.46161229246342,0.831876851886141,
3.19643595068874));
#96336=CARTESIAN_POINT('Ctrl Pts',(-1.55571144064704,0.158409610837222,
3.24470847095676));
#96337=CARTESIAN_POINT('Ctrl Pts',(-1.55444674488022,0.00131742778884739,
3.2559437743963));
#96338=CARTESIAN_POINT('Ctrl Pts',(-1.55449947323643,0.00133480041304701,
2.69405622560371));
#96339=CARTESIAN_POINT('Ctrl Pts',(-1.55153406972295,-0.361714100102126,
2.72002390145891));
#96340=CARTESIAN_POINT('Ctrl Pts',(-1.2437032104418,-1.24745277135715,2.78305371725784));
#96341=CARTESIAN_POINT('Ctrl Pts',(0.231926238140432,-1.82410602009977,
2.88314567300049));
#96342=CARTESIAN_POINT('Ctrl Pts',(1.65866396469461,-0.793716828903688,
2.99433209283165));
#96343=CARTESIAN_POINT('Ctrl Pts',(1.56599354026699,0.96375141196464,3.10551851266282));
#96344=CARTESIAN_POINT('Ctrl Pts',(0.0388050940998321,1.83838154825996,
3.21670493249398));
#96345=CARTESIAN_POINT('Ctrl Pts',(-1.31300314367493,1.13822266482633,3.31288417014094));
#96346=CARTESIAN_POINT('Ctrl Pts',(-1.55193567478298,0.308165737536199,
3.37200126784418));
#96347=CARTESIAN_POINT('Ctrl Pts',(-1.5533186684889,-0.000770198572060919,
3.39405622560371));
#96348=CARTESIAN_POINT('Origin',(0.,0.,-1.29405622560369));
#96349=CARTESIAN_POINT('',(-1.55454118234884,-0.00133834695600709,1.8559437743963));
#96350=CARTESIAN_POINT('',(-1.55805467550008,3.4854191793785E-5,1.9940562256037));
#96351=CARTESIAN_POINT('',(-1.5555,-2.01987159101623E-13,-1.29405622560369));
#96352=CARTESIAN_POINT('Ctrl Pts',(-1.55454118234884,-0.00133834695600729,
1.8559437743963));
#96353=CARTESIAN_POINT('Ctrl Pts',(-1.55580288786201,-0.154903851691022,
1.86692853568168));
#96354=CARTESIAN_POINT('Ctrl Pts',(-1.46436232298065,-0.824775316270878,
1.91495051379553));
#96355=CARTESIAN_POINT('Ctrl Pts',(-0.503915664640746,-1.76796168665343,
2.00000970873786));
#96356=CARTESIAN_POINT('Ctrl Pts',(1.21174280763407,-1.38249741391359,2.1111213592233));
#96357=CARTESIAN_POINT('Ctrl Pts',(1.81875888824183,0.267835396201195,2.22223300970874));
#96358=CARTESIAN_POINT('Ctrl Pts',(0.761764071097843,1.67312138149853,2.33334466019417));
#96359=CARTESIAN_POINT('Ctrl Pts',(-0.992180579104728,1.54764252547341,
2.44445631067961));
#96360=CARTESIAN_POINT('Ctrl Pts',(-1.55725669913861,0.518277207581445,
2.51865601541365));
#96361=CARTESIAN_POINT('Ctrl Pts',(-1.55804766277071,0.0017735852989955,
2.55581850331921));
#96362=CARTESIAN_POINT('Ctrl Pts',(-1.55804712705668,3.25009013604029E-5,
2.5559437743963));
#96363=CARTESIAN_POINT('Ctrl Pts',(-1.55805467550008,3.48541917938314E-5,
1.9940562256037));
#96364=CARTESIAN_POINT('Ctrl Pts',(-1.55788564535512,-0.513206116891616,
2.03098439512992));
#96365=CARTESIAN_POINT('Ctrl Pts',(-1.00003893378143,-1.54186484140614,
2.10497470459985));
#96366=CARTESIAN_POINT('Ctrl Pts',(0.752488571272716,-1.67777039880966,
2.21602715401351));
#96367=CARTESIAN_POINT('Ctrl Pts',(1.81781810074028,-0.276929424335053,
2.32721357384467));
#96368=CARTESIAN_POINT('Ctrl Pts',(1.21794738393109,1.37759091140133,2.43839999367584));
#96369=CARTESIAN_POINT('Ctrl Pts',(-0.497615974795104,1.77017821004958,
2.549586413507));
#96370=CARTESIAN_POINT('Ctrl Pts',(-1.46313162187878,0.828233020270418,
2.63480515748296));
#96371=CARTESIAN_POINT('Ctrl Pts',(-1.55576641614544,0.156444291597347,
2.68296176151519));
#96372=CARTESIAN_POINT('Ctrl Pts',(-1.55449947323643,0.00133480041304701,
2.69405622560371));
#96373=CARTESIAN_POINT('Origin',(0.,0.,-1.29405622560369));
#96374=CARTESIAN_POINT('',(-1.55333634177863,0.000779921548230329,1.1559437743963));
#96375=CARTESIAN_POINT('',(-1.55460191805193,-0.00135568056800359,1.2940562256037));
#96376=CARTESIAN_POINT('',(-1.5555,-2.01987159101623E-13,-1.29405622560369));
#96377=CARTESIAN_POINT('Ctrl Pts',(-1.55333634177863,0.000779921548230561,
1.1559437743963));
#96378=CARTESIAN_POINT('Ctrl Pts',(-1.55193438638927,-0.308706275100063,
1.17803856804414));
#96379=CARTESIAN_POINT('Ctrl Pts',(-1.31241956589738,-1.1389814578602,1.23717057852045));
#96380=CARTESIAN_POINT('Ctrl Pts',(0.0395347168138628,-1.83794704008407,
1.33333980582524));
#96381=CARTESIAN_POINT('Ctrl Pts',(1.56537855283131,-0.963955976349113,
1.44445145631068));
#96382=CARTESIAN_POINT('Ctrl Pts',(1.65903376979378,0.791977165381959,1.55556310679611));
#96383=CARTESIAN_POINT('Ctrl Pts',(0.234812759114929,1.82331608910266,1.66667475728155));
#96384=CARTESIAN_POINT('Ctrl Pts',(-1.24220109658982,1.24943524423025,1.76680164648161));
#96385=CARTESIAN_POINT('Ctrl Pts',(-1.55154880719052,0.362871523529771,
1.8298913188532));
#96386=CARTESIAN_POINT('Ctrl Pts',(-1.55454118234884,-0.00133834695600729,
1.8559437743963));
#96387=CARTESIAN_POINT('Ctrl Pts',(-1.55460191805193,-0.00135568056800364,
1.2940562256037));
#96388=CARTESIAN_POINT('Ctrl Pts',(-1.5558637635503,-0.152693971168416,
1.30488274885721));
#96389=CARTESIAN_POINT('Ctrl Pts',(-1.46605510259419,-0.820638709603335,
1.35277141205443));
#96390=CARTESIAN_POINT('Ctrl Pts',(-0.510374815939226,-1.76654153931159,
1.43772221519537));
#96391=CARTESIAN_POINT('Ctrl Pts',(1.20797626960931,-1.38634273102519,1.54890863502654));
#96392=CARTESIAN_POINT('Ctrl Pts',(1.81976886629041,0.263806680570579,1.6600950548577));
#96393=CARTESIAN_POINT('Ctrl Pts',(0.764574137846417,1.67229745635935,1.77128147468886));
#96394=CARTESIAN_POINT('Ctrl Pts',(-0.991003621173195,1.54889135395602,
1.88246789452002));
#96395=CARTESIAN_POINT('Ctrl Pts',(-1.5572087700955,0.518861158146894,1.95672614482497));
#96396=CARTESIAN_POINT('Ctrl Pts',(-1.55805528871865,0.00189682319971778,
1.9939222551862));
#96397=CARTESIAN_POINT('Ctrl Pts',(-1.55805467550008,3.48541917938314E-5,
1.9940562256037));
#96398=CARTESIAN_POINT('Origin',(0.,0.,-1.29405622560369));
#96399=CARTESIAN_POINT('',(-1.55735926886437,0.00101346774827271,0.455943774396301));
#96400=CARTESIAN_POINT('',(-1.55326046963413,0.000729270061605516,0.594056225603705));
#96401=CARTESIAN_POINT('',(-1.5555,-2.01987159101623E-13,-1.29405622560369));
#96402=CARTESIAN_POINT('Ctrl Pts',(-1.55735926886437,0.00101346774827265,
0.455943774396301));
#96403=CARTESIAN_POINT('Ctrl Pts',(-1.5541538777776,-0.460983628495037,
0.489148600406595));
#96404=CARTESIAN_POINT('Ctrl Pts',(-1.09151218308356,-1.44423481489054,
0.559390643245367));
#96405=CARTESIAN_POINT('Ctrl Pts',(0.579488995883613,-1.74456230311225,
0.666669902912619));
#96406=CARTESIAN_POINT('Ctrl Pts',(1.77994191588978,-0.459827600750814,
0.777781553398056));
#96407=CARTESIAN_POINT('Ctrl Pts',(1.35192905881154,1.24578720765632,0.888893203883492));
#96408=CARTESIAN_POINT('Ctrl Pts',(-0.313001003158473,1.81151906168851,
1.00000485436893));
#96409=CARTESIAN_POINT('Ctrl Pts',(-1.41742497137191,0.93698092273704,1.08902171120653));
#96410=CARTESIAN_POINT('Ctrl Pts',(-1.55428446607623,0.210081433596544,
1.14100135121566));
#96411=CARTESIAN_POINT('Ctrl Pts',(-1.55333634177863,0.000779921548230561,
1.1559437743963));
#96412=CARTESIAN_POINT('Ctrl Pts',(-1.55326046963413,0.000729270061605551,
0.594056225603705));
#96413=CARTESIAN_POINT('Ctrl Pts',(-1.55199262831984,-0.304485333833814,
0.615843242528215));
#96414=CARTESIAN_POINT('Ctrl Pts',(-1.31743653601245,-1.13071739766558,
0.674692399396446));
#96415=CARTESIAN_POINT('Ctrl Pts',(0.0255447675030308,-1.83860034663711,
0.770603696208398));
#96416=CARTESIAN_POINT('Ctrl Pts',(1.55899683301632,-0.975032021788082,
0.881790116039561));
#96417=CARTESIAN_POINT('Ctrl Pts',(1.66434877052597,0.781732535368643,0.992976535870723));
#96418=CARTESIAN_POINT('Ctrl Pts',(0.245080507541896,1.82238325373942,1.10416295570189));
#96419=CARTESIAN_POINT('Ctrl Pts',(-1.23863138927055,1.25487925833816,1.20452285227955));
#96420=CARTESIAN_POINT('Ctrl Pts',(-1.55154412248428,0.365378245899198,
1.26782060891349));
#96421=CARTESIAN_POINT('Ctrl Pts',(-1.55460191805193,-0.00135568056800364,
1.2940562256037));
#96422=CARTESIAN_POINT('Origin',(0.,0.,11.5));
#96423=CARTESIAN_POINT('',(-1.77892626630995,-0.0012009523392913,11.2223275485995));
#96424=CARTESIAN_POINT('Ctrl Pts',(1.55548765964692,0.00619602180104861,
11.4445));
#96425=CARTESIAN_POINT('Ctrl Pts',(1.55843889773201,-0.053546881811892,
11.4417867591843));
#96426=CARTESIAN_POINT('Ctrl Pts',(1.55766805736304,-0.113278156040886,
11.439086160746));
#96427=CARTESIAN_POINT('Ctrl Pts',(1.55338999746751,-0.172741258360748,
11.4363936568093));
#96428=CARTESIAN_POINT('Ctrl Pts',(1.54917978268939,-0.231261344159722,
11.4337438528932));
#96429=CARTESIAN_POINT('Ctrl Pts',(1.54157226362346,-0.289522447371128,
11.4311018887755));
#96430=CARTESIAN_POINT('Ctrl Pts',(1.5307259163647,-0.347284232316321,11.4284634295395));
#96431=CARTESIAN_POINT('Ctrl Pts',(1.52490021612,-0.37830876404678,11.427046282158));
#96432=CARTESIAN_POINT('Ctrl Pts',(1.51813939227042,-0.409189253639797,
11.4256301458963));
#96433=CARTESIAN_POINT('Ctrl Pts',(1.51046300038634,-0.439887833717896,
11.4242143490555));
#96434=CARTESIAN_POINT('Ctrl Pts',(1.50749771858011,-0.451746261786366,
11.4236674467248));
#96435=CARTESIAN_POINT('Ctrl Pts',(1.50439653465153,-0.463574222421597,
11.4231207471528));
#96436=CARTESIAN_POINT('Ctrl Pts',(1.50116353235453,-0.47535996619676,11.4225746575513));
#96437=CARTESIAN_POINT('Ctrl Pts',(1.48455611813741,-0.535901441503565,
11.4197694828629));
#96438=CARTESIAN_POINT('Ctrl Pts',(1.46445634965142,-0.595403551134085,
11.4169769764437));
#96439=CARTESIAN_POINT('Ctrl Pts',(1.4410621824655,-0.653580209875647,11.414192092755));
#96440=CARTESIAN_POINT('Ctrl Pts',(1.41747802435967,-0.712229338392404,
11.4113845922059));
#96441=CARTESIAN_POINT('Ctrl Pts',(1.39054537943373,-0.769532412755046,
11.4085848387028));
#96442=CARTESIAN_POINT('Ctrl Pts',(1.36041578548535,-0.825184282227088,
11.4057876627772));
#96443=CARTESIAN_POINT('Ctrl Pts',(1.35261592294621,-0.839591277975912,
11.4050635379265));
#96444=CARTESIAN_POINT('Ctrl Pts',(1.34460155997405,-0.853887506909652,
11.4043395858183));
#96445=CARTESIAN_POINT('Ctrl Pts',(1.33637481784576,-0.868067413704247,
11.4036157167661));
#96446=CARTESIAN_POINT('Ctrl Pts',(1.33123141939554,-0.87693275912219,11.4031631503791));
#96447=CARTESIAN_POINT('Ctrl Pts',(1.32600576325494,-0.885751206456736,
11.4027106878625));
#96448=CARTESIAN_POINT('Ctrl Pts',(1.32070341258855,-0.894513477947337,
11.4022587210796));
#96449=CARTESIAN_POINT('Ctrl Pts',(1.28755838481391,-0.949286492822766,
11.3994334738427));
#96450=CARTESIAN_POINT('Ctrl Pts',(1.25136992677528,-1.00195372283142,11.3966231054397));
#96451=CARTESIAN_POINT('Ctrl Pts',(1.21232687524415,-1.05222079285711,11.3938225048748));
#96452=CARTESIAN_POINT('Ctrl Pts',(1.17352218779371,-1.10218097437215,11.3910390024248));
#96453=CARTESIAN_POINT('Ctrl Pts',(1.13189715922074,-1.14977118940024,11.3882651489085));
#96454=CARTESIAN_POINT('Ctrl Pts',(1.08759128036108,-1.19468014867466,11.3854959263702));
#96455=CARTESIAN_POINT('Ctrl Pts',(1.05692354853581,-1.22576532190738,11.3835791203762));
#96456=CARTESIAN_POINT('Ctrl Pts',(1.0249704261144,-1.25556541150052,11.3816645331574));
#96457=CARTESIAN_POINT('Ctrl Pts',(0.991767007145199,-1.28396712328559,
11.379750500582));
#96458=CARTESIAN_POINT('Ctrl Pts',(0.971829282858114,-1.30102155672743,
11.378601177562));
#96459=CARTESIAN_POINT('Ctrl Pts',(0.951440575196337,-1.31757160665078,
11.3774520545279));
#96460=CARTESIAN_POINT('Ctrl Pts',(0.930607078503626,-1.33359088746794,
11.3763027711782));
#96461=CARTESIAN_POINT('Ctrl Pts',(0.921822018225176,-1.34034589118487,
11.3758181418501));
#96462=CARTESIAN_POINT('Ctrl Pts',(0.912957575551233,-1.34700657088378,
11.3753334724466));
#96463=CARTESIAN_POINT('Ctrl Pts',(0.904026617991894,-1.35356212132308,
11.3748494000991));
#96464=CARTESIAN_POINT('Ctrl Pts',(0.898865665597572,-1.35735039189889,
11.3745696681303));
#96465=CARTESIAN_POINT('Ctrl Pts',(0.893681522170691,-1.36110432047063,
11.3742900812105));
#96466=CARTESIAN_POINT('Ctrl Pts',(0.888474357058895,-1.36482361432558,
11.3740106343829));
#96467=CARTESIAN_POINT('Ctrl Pts',(0.838811308516624,-1.4002961732508,11.3713454257582));
#96468=CARTESIAN_POINT('Ctrl Pts',(0.787057395286918,-1.43262124116857,
11.368692960317));
#96469=CARTESIAN_POINT('Ctrl Pts',(0.733560484100527,-1.46184200007972,
11.3660489378073));
#96470=CARTESIAN_POINT('Ctrl Pts',(0.677705393253366,-1.49235082960671,
11.3632883650152));
#96471=CARTESIAN_POINT('Ctrl Pts',(0.619949541746925,-1.51947609806138,
11.3605369959002));
#96472=CARTESIAN_POINT('Ctrl Pts',(0.560651932851881,-1.54322365588157,
11.3577899361005));
#96473=CARTESIAN_POINT('Ctrl Pts',(0.511114145446654,-1.56306259192994,
11.3554950161722));
#96474=CARTESIAN_POINT('Ctrl Pts',(0.460499386969577,-1.58054347420583,
11.3532031037542));
#96475=CARTESIAN_POINT('Ctrl Pts',(0.409004561176526,-1.5956447160272,11.3509113452381));
#96476=CARTESIAN_POINT('Ctrl Pts',(0.394571471762801,-1.59987732717035,
11.3502690058367));
#96477=CARTESIAN_POINT('Ctrl Pts',(0.38006920116156,-1.60392285642947,11.3496266785255));
#96478=CARTESIAN_POINT('Ctrl Pts',(0.365502000908426,-1.60778049339754,
11.3489843004725));
#96479=CARTESIAN_POINT('Ctrl Pts',(0.352945849497182,-1.61110557117631,
11.3484306047756));
#96480=CARTESIAN_POINT('Ctrl Pts',(0.340339686983491,-1.61429135213649,
11.3478767954507));
#96481=CARTESIAN_POINT('Ctrl Pts',(0.327707338901135,-1.61733252206154,
11.3473237518226));
#96482=CARTESIAN_POINT('Ctrl Pts',(0.26442068399392,-1.63256844418037,11.3445530649309));
#96483=CARTESIAN_POINT('Ctrl Pts',(0.200363163100888,-1.64421053384351,
11.3417964693365));
#96484=CARTESIAN_POINT('Ctrl Pts',(0.135902532141567,-1.65227549235515,
11.3390491503551));
#96485=CARTESIAN_POINT('Ctrl Pts',(0.0706504004584388,-1.66043947907059,
11.3362680975283));
#96486=CARTESIAN_POINT('Ctrl Pts',(0.00498413291330568,-1.6649382180869,
11.333496550525));
#96487=CARTESIAN_POINT('Ctrl Pts',(-0.0607337043444866,-1.66573959706564,
11.3307295151184));
#96488=CARTESIAN_POINT('Ctrl Pts',(-0.114943810254912,-1.66640064802417,
11.3284470102656));
#96489=CARTESIAN_POINT('Ctrl Pts',(-0.169189647051337,-1.66454499730668,
11.326167575313));
#96490=CARTESIAN_POINT('Ctrl Pts',(-0.223269283792523,-1.66012780789457,
11.3238884070273));
#96491=CARTESIAN_POINT('Ctrl Pts',(-0.242921115785065,-1.65852265909112,
11.3230601871106));
#96492=CARTESIAN_POINT('Ctrl Pts',(-0.262550978640708,-1.65657902103982,
11.3222320024074));
#96493=CARTESIAN_POINT('Ctrl Pts',(-0.282149042864747,-1.65429391513469,
11.3214037184036));
#96494=CARTESIAN_POINT('Ctrl Pts',(-0.293822649715497,-1.65293278948249,
11.3209103501959));
#96495=CARTESIAN_POINT('Ctrl Pts',(-0.305486007024825,-1.65145026241138,
11.3204169024293));
#96496=CARTESIAN_POINT('Ctrl Pts',(-0.317120120921591,-1.64984824722041,
11.3199240638241));
#96497=CARTESIAN_POINT('Ctrl Pts',(-0.382649500838262,-1.64082486451904,
11.3171481404934));
#96498=CARTESIAN_POINT('Ctrl Pts',(-0.447374851901241,-1.62800143931766,
11.3143862955204));
#96499=CARTESIAN_POINT('Ctrl Pts',(-0.510936115769287,-1.6113566500933,
11.3116336908415));
#96500=CARTESIAN_POINT('Ctrl Pts',(-0.573549739883189,-1.59496001930709,
11.3089221249567));
#96501=CARTESIAN_POINT('Ctrl Pts',(-0.635034780101342,-1.57485515271455,
11.3062195258916));
#96502=CARTESIAN_POINT('Ctrl Pts',(-0.695044280650932,-1.55097228857054,
11.3035212687658));
#96503=CARTESIAN_POINT('Ctrl Pts',(-0.755213263935446,-1.52702595273528,
11.3008158406849));
#96504=CARTESIAN_POINT('Ctrl Pts',(-0.813899721511821,-1.49928127162975,
11.2981147776525));
#96505=CARTESIAN_POINT('Ctrl Pts',(-0.870916818143125,-1.46801413582731,
11.2954134178164));
#96506=CARTESIAN_POINT('Ctrl Pts',(-0.88517189274549,-1.46019691292752,
11.2947380399339));
#96507=CARTESIAN_POINT('Ctrl Pts',(-0.8993225020166,-1.4521592870016,11.294062643499));
#96508=CARTESIAN_POINT('Ctrl Pts',(-0.913365468395192,-1.44390514150358,
11.2933871556582));
#96509=CARTESIAN_POINT('Ctrl Pts',(-0.922789553247202,-1.43836587255875,
11.2929338429778));
#96510=CARTESIAN_POINT('Ctrl Pts',(-0.932156968408698,-1.43273389293101,
11.2924808828034));
#96511=CARTESIAN_POINT('Ctrl Pts',(-0.941465939330546,-1.42701150822941,
11.2920283046203));
#96512=CARTESIAN_POINT('Ctrl Pts',(-0.997258564244995,-1.39271482109252,
11.2893158109378));
#96513=CARTESIAN_POINT('Ctrl Pts',(-1.05096555773083,-1.35516769400791,
11.2866164406656));
#96514=CARTESIAN_POINT('Ctrl Pts',(-1.10242222381511,-1.31470157532149,
11.2839256753843));
#96515=CARTESIAN_POINT('Ctrl Pts',(-1.15490559840975,-1.27342804116106,
11.2811812215953));
#96516=CARTESIAN_POINT('Ctrl Pts',(-1.20504870548191,-1.22911724367845,
11.2784457196118));
#96517=CARTESIAN_POINT('Ctrl Pts',(-1.25265335579406,-1.18207076364008,
11.2757143751156));
#96518=CARTESIAN_POINT('Ctrl Pts',(-1.28397500867159,-1.15111636092502,
11.2739172770666));
#96519=CARTESIAN_POINT('Ctrl Pts',(-1.31419725536704,-1.11897666094205,
11.2721219788063));
#96520=CARTESIAN_POINT('Ctrl Pts',(-1.34325581778868,-1.08572815742637,
11.2703271147686));
#96521=CARTESIAN_POINT('Ctrl Pts',(-1.36209363901681,-1.06417411919684,
11.2691635565932));
#96522=CARTESIAN_POINT('Ctrl Pts',(-1.38044228251278,-1.04215395727969,
11.2680001809021));
#96523=CARTESIAN_POINT('Ctrl Pts',(-1.39828252264694,-1.01968718394611,
11.2668366156616));
#96524=CARTESIAN_POINT('Ctrl Pts',(-1.40805056143521,-1.00738598666853,
11.2661995306046));
#96525=CARTESIAN_POINT('Ctrl Pts',(-1.41766921695113,-0.994946604236495,
11.2655621759649));
#96526=CARTESIAN_POINT('Ctrl Pts',(-1.42711662985222,-0.982397385607975,
11.264925758661));
#96527=CARTESIAN_POINT('Ctrl Pts',(-1.46820629310292,-0.927817028752221,
11.262157786839));
#96528=CARTESIAN_POINT('Ctrl Pts',(-1.50612185513061,-0.871087521735772,
11.2594035844773));
#96529=CARTESIAN_POINT('Ctrl Pts',(-1.54066769776793,-0.812525394359864,
11.2566583590267));
#96530=CARTESIAN_POINT('Ctrl Pts',(-1.57505516312501,-0.754231748217875,
11.2539257192103));
#96531=CARTESIAN_POINT('Ctrl Pts',(-1.60610442219133,-0.694121381542228,
11.2512019741836));
#96532=CARTESIAN_POINT('Ctrl Pts',(-1.63358497140864,-0.632471603998023,
11.2484823970106));
#96533=CARTESIAN_POINT('Ctrl Pts',(-1.65966108961598,-0.573972522557314,
11.2459018075444));
#96534=CARTESIAN_POINT('Ctrl Pts',(-1.68252420078453,-0.514086499095208,
11.2433249708101));
#96535=CARTESIAN_POINT('Ctrl Pts',(-1.70193725006908,-0.453031690747441,
11.2407478481942));
#96536=CARTESIAN_POINT('Ctrl Pts',(-1.70639988231082,-0.438996535720931,
11.2401554244947));
#96537=CARTESIAN_POINT('Ctrl Pts',(-1.71068001578898,-0.424899564800969,
11.239562985688));
#96538=CARTESIAN_POINT('Ctrl Pts',(-1.71477442803653,-0.410743347710776,
11.2389704827146));
#96539=CARTESIAN_POINT('Ctrl Pts',(-1.7181060933816,-0.399224288308597,
11.238488356953));
#96540=CARTESIAN_POINT('Ctrl Pts',(-1.72131496051192,-0.387664952239154,
11.2380061462914));
#96541=CARTESIAN_POINT('Ctrl Pts',(-1.72439513423882,-0.376083269559728,
11.2375245092466));
#96542=CARTESIAN_POINT('Ctrl Pts',(-1.73399637264737,-0.339981897872015,
11.2360231938976));
#96543=CARTESIAN_POINT('Ctrl Pts',(-1.74235845090443,-0.303626928305512,
11.234525913273));
#96544=CARTESIAN_POINT('Ctrl Pts',(-1.74944665354966,-0.267065873422436,
11.2330319031487));
#96545=CARTESIAN_POINT('Ctrl Pts',(-1.76197449586933,-0.202447076028902,
11.2303913574139));
#96546=CARTESIAN_POINT('Ctrl Pts',(-1.77052625497235,-0.137185361680741,
11.227761027999));
#96547=CARTESIAN_POINT('Ctrl Pts',(-1.77528061829343,-0.0715870718432795,
11.2251366955952));
#96548=CARTESIAN_POINT('Ctrl Pts',(-1.77697828156189,-0.0481635764959884,
11.2241996126621));
#96549=CARTESIAN_POINT('Ctrl Pts',(-1.7781912975682,-0.0246970169190114,
11.2232632943623));
#96550=CARTESIAN_POINT('Ctrl Pts',(-1.77892626630995,-0.00120095233929127,
11.2223275485995));
#96551=CARTESIAN_POINT('',(1.88128289424299,-0.51655738433239,11.046));
#96552=CARTESIAN_POINT('Ctrl Pts',(1.88079991776263,-0.516378774142054,
11.046));
#96553=CARTESIAN_POINT('Ctrl Pts',(1.89035995045861,-0.445151004206684,
11.0555631104642));
#96554=CARTESIAN_POINT('Ctrl Pts',(1.8961423315859,-0.373654493774377,11.0651669654983));
#96555=CARTESIAN_POINT('Ctrl Pts',(1.89809144951916,-0.302224012343752,
11.0748303404806));
#96556=CARTESIAN_POINT('Ctrl Pts',(1.89999077178002,-0.23261842246626,11.0842468375051));
#96557=CARTESIAN_POINT('Ctrl Pts',(1.89824990827702,-0.163074621232238,
11.0937198521185));
#96558=CARTESIAN_POINT('Ctrl Pts',(1.89277099599951,-0.0939167257851171,
11.1032667571406));
#96559=CARTESIAN_POINT('Ctrl Pts',(1.88910201129244,-0.0476047485319078,
11.1096598962807));
#96560=CARTESIAN_POINT('Ctrl Pts',(1.8837557967888,-0.00146614169388357,
11.1160861707414));
#96561=CARTESIAN_POINT('Ctrl Pts',(1.87669176161129,0.0443950771863014,
11.1225507975725));
#96562=CARTESIAN_POINT('Ctrl Pts',(1.87063241478827,0.0837336455737761,
11.1280959874063));
#96563=CARTESIAN_POINT('Ctrl Pts',(1.8633089856103,0.122868068816038,11.1336693960131));
#96564=CARTESIAN_POINT('Ctrl Pts',(1.85469071090361,0.161728394728602,11.1392743160301));
#96565=CARTESIAN_POINT('Ctrl Pts',(1.85223436103037,0.172804226014781,11.1408718103131));
#96566=CARTESIAN_POINT('Ctrl Pts',(1.84967323324123,0.183855475695868,11.142471538338));
#96567=CARTESIAN_POINT('Ctrl Pts',(1.84700939076218,0.19487013146115,11.1440720571876));
#96568=CARTESIAN_POINT('Ctrl Pts',(1.83137216521354,0.259528105007685,11.1534673853433));
#96569=CARTESIAN_POINT('Ctrl Pts',(1.81217652429567,0.323030635926077,11.1629048835303));
#96570=CARTESIAN_POINT('Ctrl Pts',(1.78934255453511,0.385087390709459,11.1724028038701));
#96571=CARTESIAN_POINT('Ctrl Pts',(1.78198218565347,0.405090947322401,11.1754643914102));
#96572=CARTESIAN_POINT('Ctrl Pts',(1.77424343060636,0.424944079046285,11.1785322571122));
#96573=CARTESIAN_POINT('Ctrl Pts',(1.76612263817241,0.444636415640588,11.181607012295));
#96574=CARTESIAN_POINT('Ctrl Pts',(1.73919119835162,0.509943216945239,11.1918039955137));
#96575=CARTESIAN_POINT('Ctrl Pts',(1.70806080167302,0.573485248201441,11.2020767507448));
#96576=CARTESIAN_POINT('Ctrl Pts',(1.67301702698032,0.634984575310704,11.2124475752393));
#96577=CARTESIAN_POINT('Ctrl Pts',(1.64235372412421,0.688796486531309,11.2215220466721));
#96578=CARTESIAN_POINT('Ctrl Pts',(1.60869302252863,0.741044106677185,11.2306716023846));
#96579=CARTESIAN_POINT('Ctrl Pts',(1.57220891785208,0.791506873950779,11.239911179793));
#96580=CARTESIAN_POINT('Ctrl Pts',(1.56528521292053,0.801083354276364,11.2416646038728));
#96581=CARTESIAN_POINT('Ctrl Pts',(1.55825911602623,0.81059620160376,11.2434214216921));
#96582=CARTESIAN_POINT('Ctrl Pts',(1.55114206425445,0.820030590825838,11.2451792455347));
#96583=CARTESIAN_POINT('Ctrl Pts',(1.51163333781795,0.872403499555923,11.254937412757));
#96584=CARTESIAN_POINT('Ctrl Pts',(1.46925448012712,0.922460374176763,11.2647444648472));
#96585=CARTESIAN_POINT('Ctrl Pts',(1.42425895086728,0.969999034377404,11.2746213834588));
#96586=CARTESIAN_POINT('Ctrl Pts',(1.37955552976012,1.01722907657888,11.2844341817346));
#96587=CARTESIAN_POINT('Ctrl Pts',(1.33226826113497,1.06197396880102,11.2943159423384));
#96588=CARTESIAN_POINT('Ctrl Pts',(1.28262305484525,1.10398985376236,11.3042872409362));
#96589=CARTESIAN_POINT('Ctrl Pts',(1.23402945162958,1.14511574274852,11.3140473238087));
#96590=CARTESIAN_POINT('Ctrl Pts',(1.18317581682196,1.18362727550242,11.3238931915966));
#96591=CARTESIAN_POINT('Ctrl Pts',(1.13026675802768,1.2192467284131,11.3338441399431));
#96592=CARTESIAN_POINT('Ctrl Pts',(1.11612186853279,1.22876935528969,11.3365044606506));
#96593=CARTESIAN_POINT('Ctrl Pts',(1.1018300740637,1.23808499004259,11.3391722917297));
#96594=CARTESIAN_POINT('Ctrl Pts',(1.0873953214649,1.24718768011963,11.3418480018757));
#96595=CARTESIAN_POINT('Ctrl Pts',(1.07843141524914,1.25284040326838,11.3435096039465));
#96596=CARTESIAN_POINT('Ctrl Pts',(1.06941317684967,1.25841040829158,11.3451740914355));
#96597=CARTESIAN_POINT('Ctrl Pts',(1.06035226952456,1.2638900735973,11.346839603865));
#96598=CARTESIAN_POINT('Ctrl Pts',(1.00742079701965,1.29590085828569,11.3565690958694));
#96599=CARTESIAN_POINT('Ctrl Pts',(0.952938092487177,1.32489391547385,11.3663514013733));
#96600=CARTESIAN_POINT('Ctrl Pts',(0.897108858642945,1.35066478023243,11.3762079140514));
#96601=CARTESIAN_POINT('Ctrl Pts',(0.842238965806958,1.37599281162795,11.3858950574554));
#96602=CARTESIAN_POINT('Ctrl Pts',(0.78606756226141,1.39820862213323,11.3956538796688));
#96603=CARTESIAN_POINT('Ctrl Pts',(0.72878604220227,1.41706842320411,11.4055046903548));
#96604=CARTESIAN_POINT('Ctrl Pts',(0.67317444208947,1.43537840719681,11.4150683217683));
#96605=CARTESIAN_POINT('Ctrl Pts',(0.616515828164059,1.45052520284418,11.4247186563809));
#96606=CARTESIAN_POINT('Ctrl Pts',(0.558993687390787,1.46223733220615,11.4344742788813));
#96607=CARTESIAN_POINT('Ctrl Pts',(0.539362537898783,1.46623444634835,11.4378036765901));
#96608=CARTESIAN_POINT('Ctrl Pts',(0.519630929867265,1.46983109384517,11.4411453373854));
#96609=CARTESIAN_POINT('Ctrl Pts',(0.499806597877626,1.47301514408983,11.4445));
#96610=CARTESIAN_POINT('',(1.56060797133591,1.17265290216009,11.046));
#96611=CARTESIAN_POINT('Origin',(0.,0.,11.046));
#96612=CARTESIAN_POINT('Ctrl Pts',(-1.77892626630995,-0.00120095233929127,
11.2223275485995));
#96613=CARTESIAN_POINT('Ctrl Pts',(-1.78091222637221,0.0622877965358305,
11.2197990686688));
#96614=CARTESIAN_POINT('Ctrl Pts',(-1.77941067542291,0.125992016111799,
11.2172747683064));
#96615=CARTESIAN_POINT('Ctrl Pts',(-1.77452381634337,0.189646102027163,
11.2147508586347));
#96616=CARTESIAN_POINT('Ctrl Pts',(-1.77287868795546,0.211074823838332,
11.2139012013432));
#96617=CARTESIAN_POINT('Ctrl Pts',(-1.7708495726434,0.232497857027148,11.2130515883281));
#96618=CARTESIAN_POINT('Ctrl Pts',(-1.76843936997923,0.253904972833394,
11.2122018750387));
#96619=CARTESIAN_POINT('Ctrl Pts',(-1.76712267121633,0.265599725029338,
11.2117376748892));
#96620=CARTESIAN_POINT('Ctrl Pts',(-1.76569197102713,0.277291668505868,
11.2112733675823));
#96621=CARTESIAN_POINT('Ctrl Pts',(-1.7641484990815,0.288972974548762,11.2108091738099));
#96622=CARTESIAN_POINT('Ctrl Pts',(-1.75515036560026,0.357072658062498,
11.2081030167356));
#96623=CARTESIAN_POINT('Ctrl Pts',(-1.74235696629666,0.42456963250346,11.2054102736121));
#96624=CARTESIAN_POINT('Ctrl Pts',(-1.72594903242932,0.491138664005795,
11.2027264834948));
#96625=CARTESIAN_POINT('Ctrl Pts',(-1.70928395222888,0.558750970212142,
11.2000006328234));
#96626=CARTESIAN_POINT('Ctrl Pts',(-1.68888999030711,0.625407040269523,
11.1972840179815));
#96627=CARTESIAN_POINT('Ctrl Pts',(-1.66490278446929,0.690766734877331,
11.1945719649831));
#96628=CARTESIAN_POINT('Ctrl Pts',(-1.64112198461878,0.755564019991226,
11.1918832487577));
#96629=CARTESIAN_POINT('Ctrl Pts',(-1.61380916520598,0.81908815011939,11.1891990162058));
#96630=CARTESIAN_POINT('Ctrl Pts',(-1.5830482712126,0.880993120829078,11.186514712963));
#96631=CARTESIAN_POINT('Ctrl Pts',(-1.57216641681974,0.902892382846704,
11.1855651242728));
#96632=CARTESIAN_POINT('Ctrl Pts',(-1.56085264019442,0.92458881232314,11.1846155267362));
#96633=CARTESIAN_POINT('Ctrl Pts',(-1.54910931637308,0.946066284278751,
11.1836657187303));
#96634=CARTESIAN_POINT('Ctrl Pts',(-1.54396572241992,0.955473450134084,
11.1832497013582));
#96635=CARTESIAN_POINT('Ctrl Pts',(-1.53874121405367,0.964835754579395,
11.1828337685169));
#96636=CARTESIAN_POINT('Ctrl Pts',(-1.5334404792476,0.974144495398925,11.18241823656));
#96637=CARTESIAN_POINT('Ctrl Pts',(-1.49854818334159,1.03541964895223,11.179682981066));
#96638=CARTESIAN_POINT('Ctrl Pts',(-1.46030493742689,1.09447092650475,11.1769608571821));
#96639=CARTESIAN_POINT('Ctrl Pts',(-1.41884997832206,1.15095727599886,11.1742472453603));
#96640=CARTESIAN_POINT('Ctrl Pts',(-1.37811238995456,1.20646613920276,11.1715805921112));
#96641=CARTESIAN_POINT('Ctrl Pts',(-1.33427285188376,1.25949901944966,11.1689221588738));
#96642=CARTESIAN_POINT('Ctrl Pts',(-1.28741864153,1.30971119589593,11.166267561795));
#96643=CARTESIAN_POINT('Ctrl Pts',(-1.26549062822221,1.33321075474058,11.1650251966024));
#96644=CARTESIAN_POINT('Ctrl Pts',(-1.24290170835111,1.35609210845284,11.1637836716393));
#96645=CARTESIAN_POINT('Ctrl Pts',(-1.21965775424868,1.37831740927343,11.1625425375316));
#96646=CARTESIAN_POINT('Ctrl Pts',(-1.19165584264812,1.40509215276722,11.1610473475387));
#96647=CARTESIAN_POINT('Ctrl Pts',(-1.16270333140537,1.43091488294274,11.1595527247918));
#96648=CARTESIAN_POINT('Ctrl Pts',(-1.13285929301872,1.45577404177113,11.1580578836196));
#96649=CARTESIAN_POINT('Ctrl Pts',(-1.12175109882477,1.46502682318719,11.1575014915585));
#96650=CARTESIAN_POINT('Ctrl Pts',(-1.11051936159011,1.47414607111053,11.156945069237));
#96651=CARTESIAN_POINT('Ctrl Pts',(-1.09916702235175,1.48313103947397,11.1563885761416));
#96652=CARTESIAN_POINT('Ctrl Pts',(-1.0900493418525,1.49034735578674,11.1559416262983));
#96653=CARTESIAN_POINT('Ctrl Pts',(-1.08085382696811,1.49747696130526,11.1554946319594));
#96654=CARTESIAN_POINT('Ctrl Pts',(-1.07159363370462,1.50451093778695,11.1550481251347));
#96655=CARTESIAN_POINT('Ctrl Pts',(-1.01611106549685,1.54665509923293,11.152372873695));
#96656=CARTESIAN_POINT('Ctrl Pts',(-0.958209601759993,1.58545013781557,
11.1497101571816));
#96657=CARTESIAN_POINT('Ctrl Pts',(-0.898278760372612,1.62088563165273,
11.1470556568828));
#96658=CARTESIAN_POINT('Ctrl Pts',(-0.837571419107242,1.65678024897295,
11.1443667632881));
#96659=CARTESIAN_POINT('Ctrl Pts',(-0.774780874239298,1.6892280755481,11.1416863001956));
#96660=CARTESIAN_POINT('Ctrl Pts',(-0.71027313016202,1.71817742298682,11.1390097788418));
#96661=CARTESIAN_POINT('Ctrl Pts',(-0.66261429365752,1.73956543207362,11.13703234349));
#96662=CARTESIAN_POINT('Ctrl Pts',(-0.614017264977652,1.75904301818697,
11.135057059686));
#96663=CARTESIAN_POINT('Ctrl Pts',(-0.56462073685077,1.77657345707156,11.1330821172509));
#96664=CARTESIAN_POINT('Ctrl Pts',(-0.539231747042784,1.78558380964183,
11.1320670298498));
#96665=CARTESIAN_POINT('Ctrl Pts',(-0.513631449727103,1.79407954038564,
11.1310520326313));
#96666=CARTESIAN_POINT('Ctrl Pts',(-0.487838223654543,1.802054170041,11.1300368798027));
#96667=CARTESIAN_POINT('Ctrl Pts',(-0.475799003301229,1.80577640018727,
11.1295630480858));
#96668=CARTESIAN_POINT('Ctrl Pts',(-0.463717747565173,1.80938508638487,
11.129089182467));
#96669=CARTESIAN_POINT('Ctrl Pts',(-0.451596312388482,1.81287949077367,
11.1286152579519));
#96670=CARTESIAN_POINT('Ctrl Pts',(-0.439480899976025,1.81637215890158,
11.1281415689151));
#96671=CARTESIAN_POINT('Ctrl Pts',(-0.427332434103985,1.81974856717366,
11.1276680985874));
#96672=CARTESIAN_POINT('Ctrl Pts',(-0.415160020480683,1.8230065701324,11.1271950974533));
#96673=CARTESIAN_POINT('Ctrl Pts',(-0.345659931193023,1.8416085913534,11.1244944316633));
#96674=CARTESIAN_POINT('Ctrl Pts',(-0.275309825422015,1.85637496302517,
11.1218062647546));
#96675=CARTESIAN_POINT('Ctrl Pts',(-0.204481476884407,1.86725830113956,
11.1191261497819));
#96676=CARTESIAN_POINT('Ctrl Pts',(-0.133579826115251,1.87815290272383,
11.1164432610836));
#96677=CARTESIAN_POINT('Ctrl Pts',(-0.0621979169225611,1.88515673586772,
11.1137684409964));
#96678=CARTESIAN_POINT('Ctrl Pts',(0.00930939936232982,1.88817434312463,
11.111097228754));
#96679=CARTESIAN_POINT('Ctrl Pts',(0.0795378313902503,1.89113798149254,
11.1084737902425));
#96680=CARTESIAN_POINT('Ctrl Pts',(0.149888204683991,1.89025686041538,11.1058538316796));
#96681=CARTESIAN_POINT('Ctrl Pts',(0.220026910137412,1.88539116319202,11.1032331273822));
#96682=CARTESIAN_POINT('Ctrl Pts',(0.236366392955163,1.88425765244837,11.1026226092302));
#96683=CARTESIAN_POINT('Ctrl Pts',(0.252694364144288,1.88290767750495,11.102012050607));
#96684=CARTESIAN_POINT('Ctrl Pts',(0.269006539233807,1.88133906123029,11.1014013980884));
#96685=CARTESIAN_POINT('Ctrl Pts',(0.280730896030037,1.88021162011471,11.1009624923038));
#96686=CARTESIAN_POINT('Ctrl Pts',(0.292446914187848,1.8789711508204,11.1005235443156));
#96687=CARTESIAN_POINT('Ctrl Pts',(0.304138944100939,1.87761870427971,11.1000850620809));
#96688=CARTESIAN_POINT('Ctrl Pts',(0.375822773838615,1.86932685519343,11.0973967277121));
#96689=CARTESIAN_POINT('Ctrl Pts',(0.446738242932316,1.85681796775178,11.0947208906731));
#96690=CARTESIAN_POINT('Ctrl Pts',(0.516529562716851,1.84000805096474,11.0920531719144));
#96691=CARTESIAN_POINT('Ctrl Pts',(0.584847521294231,1.82355300752536,11.0894417712386));
#96692=CARTESIAN_POINT('Ctrl Pts',(0.652089317501138,1.80297695165361,11.0868381496919));
#96693=CARTESIAN_POINT('Ctrl Pts',(0.718036401553849,1.77856692481578,11.084238199749));
#96694=CARTESIAN_POINT('Ctrl Pts',(0.785323202313169,1.75366100765569,11.0815854317561));
#96695=CARTESIAN_POINT('Ctrl Pts',(0.851262956271168,1.7247633139281,11.0789364860598));
#96696=CARTESIAN_POINT('Ctrl Pts',(0.915607648721953,1.6921267735849,11.0762869996812));
#96697=CARTESIAN_POINT('Ctrl Pts',(0.930631108062465,1.68450666199239,11.0756683868732));
#96698=CARTESIAN_POINT('Ctrl Pts',(0.945567515715628,1.67668252571399,11.0750497445899));
#96699=CARTESIAN_POINT('Ctrl Pts',(0.960413518624615,1.6686572293506,11.074431017298));
#96700=CARTESIAN_POINT('Ctrl Pts',(0.975205360081844,1.66066121101609,11.073814547258));
#96701=CARTESIAN_POINT('Ctrl Pts',(0.989912270604597,1.65246257743845,11.0731977870787));
#96702=CARTESIAN_POINT('Ctrl Pts',(1.00450295029956,1.6440805277344,11.0725818668126));
#96703=CARTESIAN_POINT('Ctrl Pts',(1.06739734574523,1.60794897253934,11.0699268888682));
#96704=CARTESIAN_POINT('Ctrl Pts',(1.12821828188749,1.56837054324493,11.0672840147147));
#96705=CARTESIAN_POINT('Ctrl Pts',(1.18673956352194,1.52565231730803,11.0646490274931));
#96706=CARTESIAN_POINT('Ctrl Pts',(1.24608357911593,1.48233352805146,11.0619769957398));
#96707=CARTESIAN_POINT('Ctrl Pts',(1.30306365724006,1.43578546725283,11.0593130742375));
#96708=CARTESIAN_POINT('Ctrl Pts',(1.35742307425591,1.38627866511896,11.056652865764));
#96709=CARTESIAN_POINT('Ctrl Pts',(1.41159294455999,1.3369444890372,11.0540019332135));
#96710=CARTESIAN_POINT('Ctrl Pts',(1.4631611896777,1.28467147000892,11.0513546878431));
#96711=CARTESIAN_POINT('Ctrl Pts',(1.51184108762766,1.22968809505141,11.0487067782687));
#96712=CARTESIAN_POINT('Ctrl Pts',(1.52842600119773,1.21095562929319,11.0478046532996));
#96713=CARTESIAN_POINT('Ctrl Pts',(1.54467532477781,1.19190827830405,11.0469024512351));
#96714=CARTESIAN_POINT('Ctrl Pts',(1.56057659382849,1.17255425406029,11.046));
#96715=CARTESIAN_POINT('',(-0.999999999999999,-1.22464679914735E-16,12.));
#96716=CARTESIAN_POINT('',(-1.5,-1.83697019872103E-16,11.5));
#96717=CARTESIAN_POINT('Origin',(0.,0.,12.));
#96718=CARTESIAN_POINT('Ctrl Pts',(1.13509973994371,-1.59049193030953,-0.230074082272069));
#96719=CARTESIAN_POINT('Ctrl Pts',(1.66385127640631,-1.21313337847033,-0.19303686544359));
#96720=CARTESIAN_POINT('Ctrl Pts',(2.30633516687349,0.103782615975306,-0.118962431786632));
#96721=CARTESIAN_POINT('Ctrl Pts',(1.16188988078006,1.99753850566951,-0.00785078130119459));
#96722=CARTESIAN_POINT('Ctrl Pts',(-1.04655428901899,2.05782953697956,0.103260869184242));
#96723=CARTESIAN_POINT('Ctrl Pts',(-2.29698075471667,0.238333788527267,
0.214372519669679));
#96724=CARTESIAN_POINT('Ctrl Pts',(-1.44613108848303,-1.80075271725216,
0.325484170155115));
#96725=CARTESIAN_POINT('Ctrl Pts',(0.727946961077783,-2.19149774367173,
0.436595820640553));
#96726=CARTESIAN_POINT('Ctrl Pts',(2.2359411788162,-0.57762978583554,0.547707471125989));
#96727=CARTESIAN_POINT('Ctrl Pts',(1.69827668332871,1.56494259322429,0.658819121611427));
#96728=CARTESIAN_POINT('Ctrl Pts',(-0.393188016825179,2.27560800163251,
0.769930772096863));
#96729=CARTESIAN_POINT('Ctrl Pts',(-2.12490816724285,0.90434536960108,0.881042422582301));
#96730=CARTESIAN_POINT('Ctrl Pts',(-1.9125222930514,-1.29434912039326,0.992154073067737));
#96731=CARTESIAN_POINT('Ctrl Pts',(0.0496630258143332,-2.30880650358359,
1.10326572355317));
#96732=CARTESIAN_POINT('Ctrl Pts',(1.96640931676781,-1.21090966106477,1.21437737403861));
#96733=CARTESIAN_POINT('Ctrl Pts',(2.08405785032279,0.994871990457256,1.32548902452405));
#96734=CARTESIAN_POINT('Ctrl Pts',(0.294968904732024,2.29042728261432,1.43660067500948));
#96735=CARTESIAN_POINT('Ctrl Pts',(-1.76399147035948,1.49043619583305,1.54771232549492));
#96736=CARTESIAN_POINT('Ctrl Pts',(-2.20904863824581,-0.673178902258552,
1.65882397598036));
#96737=CARTESIAN_POINT('Ctrl Pts',(-0.633012670336293,-2.22089176195486,
1.7699356264658));
#96738=CARTESIAN_POINT('Ctrl Pts',(1.52217643594786,-1.73667627565877,1.88104727695123));
#96739=CARTESIAN_POINT('Ctrl Pts',(2.28470258285089,0.336451535954383,1.99215892743667));
#96740=CARTESIAN_POINT('Ctrl Pts',(0.956918672404541,2.10175453516431,2.10327057792211));
#96741=CARTESIAN_POINT('Ctrl Pts',(-1.24636506047609,1.94412953698174,2.21438222840754));
#96742=CARTESIAN_POINT('Ctrl Pts',(-2.30932995110325,0.00779007092406014,
2.32549387889298));
#96743=CARTESIAN_POINT('Ctrl Pts',(-1.2594528285163,-1.93567664513544,2.43660552937842));
#96744=CARTESIAN_POINT('Ctrl Pts',(0.942717341349318,-2.1081625941051,2.54771717986386));
#96745=CARTESIAN_POINT('Ctrl Pts',(2.28238070382781,-0.351857683462,2.65882883034929));
#96746=CARTESIAN_POINT('Ctrl Pts',(1.53385834111148,1.72636731182735,2.76994048083473));
#96747=CARTESIAN_POINT('Ctrl Pts',(-0.618014955343493,2.22511191222357,
2.88105213132016));
#96748=CARTESIAN_POINT('Ctrl Pts',(-2.20445672440028,0.68806689849701,2.99216378180561));
#96749=CARTESIAN_POINT('Ctrl Pts',(-1.77400663329184,-1.47850125855229,
3.10327543229104));
#96750=CARTESIAN_POINT('Ctrl Pts',(0.279509811935462,-2.29236554058792,
3.21438708277648));
#96751=CARTESIAN_POINT('Ctrl Pts',(2.07729836817097,-1.00890881459812,3.32549873326191));
#96752=CARTESIAN_POINT('Ctrl Pts',(1.97453422882556,1.1976143309821,3.43661038374735));
#96753=CARTESIAN_POINT('Ctrl Pts',(0.0652379087403971,2.30842143506323,
3.54772203423278));
#96754=CARTESIAN_POINT('Ctrl Pts',(-1.90374559216213,1.30721774273047,3.65883368471823));
#96755=CARTESIAN_POINT('Ctrl Pts',(-2.13096254074055,-0.889979863001003,
3.76994533520366));
#96756=CARTESIAN_POINT('Ctrl Pts',(-0.408528604769679,-2.27292100295502,
3.8810569856891));
#96757=CARTESIAN_POINT('Ctrl Pts',(1.6876745272456,-1.57633124585981,3.99216863617453));
#96758=CARTESIAN_POINT('Ctrl Pts',(2.23979789625721,0.562468568463683,4.10328028665997));
#96759=CARTESIAN_POINT('Ctrl Pts',(0.742695215461042,2.18665711155622,4.21439193714541));
#96760=CARTESIAN_POINT('Ctrl Pts',(-1.43391090854028,1.81023893808443,4.32550358763085));
#96761=CARTESIAN_POINT('Ctrl Pts',(-2.29860956455329,-0.222395090620434,
4.43661523811628));
#96762=CARTESIAN_POINT('Ctrl Pts',(-1.06027445761331,-2.05155638019547,
4.54772688860172));
#96763=CARTESIAN_POINT('Ctrl Pts',(1.14812229735204,-2.00371672072451,4.65883853908716));
#96764=CARTESIAN_POINT('Ctrl Pts',(2.30608404475241,-0.122645363248325,
4.76995018957259));
#96765=CARTESIAN_POINT('Ctrl Pts',(1.35417351061808,1.87063615108022,4.88106184005803));
#96766=CARTESIAN_POINT('Ctrl Pts',(-0.83669150175529,2.1524434574405,4.99217349054346));
#96767=CARTESIAN_POINT('Ctrl Pts',(-2.26205440167697,0.464946653328952,
5.10328514102891));
#96768=CARTESIAN_POINT('Ctrl Pts',(-1.61782842764492,-1.64793709991974,
5.21439679151433));
#96769=CARTESIAN_POINT('Ctrl Pts',(0.506574022840452,-2.25309748257175,
5.32550844199978));
#96770=CARTESIAN_POINT('Ctrl Pts',(2.1675039941815,-0.796863816342033,5.43662009248521));
#96771=CARTESIAN_POINT('Ctrl Pts',(1.84535073495005,1.38843299139974,5.54773174297065));
#96772=CARTESIAN_POINT('Ctrl Pts',(-0.1651427104253,2.30343078727826,5.65884339345609));
#96773=CARTESIAN_POINT('Ctrl Pts',(-2.024544512798,1.1109838082922,5.76995504394152));
#96774=CARTESIAN_POINT('Ctrl Pts',(-2.03165894515671,-1.09791959503082,
5.88106669442697));
#96775=CARTESIAN_POINT('Ctrl Pts',(-0.179976902307884,-2.30231922661119,
5.99217834491239));
#96776=CARTESIAN_POINT('Ctrl Pts',(1.83636881720094,-1.40029106752845,6.10328999539785));
#96777=CARTESIAN_POINT('Ctrl Pts',(2.17259204728728,0.782885242326115,6.21440164588326));
#96778=CARTESIAN_POINT('Ctrl Pts',(0.521076907609949,2.24978762618687,6.32551329636872));
#96779=CARTESIAN_POINT('Ctrl Pts',(-1.60717962682088,1.6583242004264,6.43662494685413));
#96780=CARTESIAN_POINT('Ctrl Pts',(-2.26500243885858,-0.450365916286509,
6.5477365973396));
#96781=CARTESIAN_POINT('Ctrl Pts',(-0.850539171717745,-2.14700922773088,
6.65884824782501));
#96782=CARTESIAN_POINT('Ctrl Pts',(1.34209565723166,-1.87932029027199,6.76995989831046));
#96783=CARTESIAN_POINT('Ctrl Pts',(2.30682622449346,0.107788109627418,6.8810715487959));
#96784=CARTESIAN_POINT('Ctrl Pts',(1.16100547839306,1.99627948587589,6.99218319928133));
#96785=CARTESIAN_POINT('Ctrl Pts',(-1.04703729866327,2.05834360634882,7.10329484976677));
#96786=CARTESIAN_POINT('Ctrl Pts',(-2.29712931099768,0.237197038645086,
7.21440650025221));
#96787=CARTESIAN_POINT('Ctrl Pts',(-1.44554186745893,-1.80096480143545,
7.32551815073763));
#96788=CARTESIAN_POINT('Ctrl Pts',(0.72859438989827,-2.19139583863915,7.43662980122308));
#96789=CARTESIAN_POINT('Ctrl Pts',(2.23612826941383,-0.576884623911715,
7.5477414517085));
#96790=CARTESIAN_POINT('Ctrl Pts',(1.6977934979946,1.56542733614398,7.65885310219396));
#96791=CARTESIAN_POINT('Ctrl Pts',(-0.393879040694563,2.27550539615811,
7.76996475267938));
#96792=CARTESIAN_POINT('Ctrl Pts',(-2.12518549811472,0.903688057410859,
7.88107640316484));
#96793=CARTESIAN_POINT('Ctrl Pts',(-1.91212657747833,-1.29492758803799,
7.99218805365025));
#96794=CARTESIAN_POINT('Ctrl Pts',(0.0503667898133586,-2.30879377455661,
8.1032997041357));
#96795=CARTESIAN_POINT('Ctrl Pts',(1.96677879493939,-1.21030850518371,8.21441135462113));
#96796=CARTESIAN_POINT('Ctrl Pts',(2.08375418707704,0.995506903268707,8.32552300510658));
#96797=CARTESIAN_POINT('Ctrl Pts',(0.294270353677539,2.29051751091564,8.436634655592));
#96798=CARTESIAN_POINT('Ctrl Pts',(-1.76444601777748,1.4898978999011,8.54774630607746));
#96799=CARTESIAN_POINT('Ctrl Pts',(-2.2088431932234,-0.673852547682493,
8.65885795656288));
#96800=CARTESIAN_POINT('Ctrl Pts',(-0.632335256349382,-2.2210847899434,
8.76996960704833));
#96801=CARTESIAN_POINT('Ctrl Pts',(1.52270606837662,-1.73621188252162,8.88108125753376));
#96802=CARTESIAN_POINT('Ctrl Pts',(2.28459985995541,0.337148347205355,8.99219290801919));
#96803=CARTESIAN_POINT('Ctrl Pts',(0.956277562497704,2.10204633917866,9.10330455850463));
#96804=CARTESIAN_POINT('Ctrl Pts',(-1.2469579560031,1.94374924182257,9.21441620899007));
#96805=CARTESIAN_POINT('Ctrl Pts',(-2.30933226540692,0.00708579792413808,
9.32552785947551));
#96806=CARTESIAN_POINT('Ctrl Pts',(-1.25886228368054,-1.93606087509586,
9.43663950996094));
#96807=CARTESIAN_POINT('Ctrl Pts',(0.943360139257667,-2.10787462610152,
9.54775116044639));
#96808=CARTESIAN_POINT('Ctrl Pts',(2.28248823506631,-0.351162152961091,
9.65886281093181));
#96809=CARTESIAN_POINT('Ctrl Pts',(1.53333110744206,1.72683627576032,9.76997446141726));
#96810=CARTESIAN_POINT('Ctrl Pts',(-0.618692454411617,2.22492101746939,
9.88108611190268));
#96811=CARTESIAN_POINT('Ctrl Pts',(-2.20466868021367,0.687398848825245,
9.99219776238814));
#96812=CARTESIAN_POINT('Ctrl Pts',(-1.7735514221838,-1.47905058047522,10.1033094128735));
#96813=CARTESIAN_POINT('Ctrl Pts',(0.280201048116106,-2.29226437530741,
10.214421063359));
#96814=CARTESIAN_POINT('Ctrl Pts',(2.07762111854432,-1.0083052618152,10.3255327138444));
#96815=CARTESIAN_POINT('Ctrl Pts',(1.97414006873683,1.19827380577986,10.4366443643299));
#96816=CARTESIAN_POINT('Ctrl Pts',(0.0645886152005097,2.30833217918201,
10.5477560148153));
#96817=CARTESIAN_POINT('Ctrl Pts',(-1.90424854748374,1.30684465150768,10.6588676653008));
#96818=CARTESIAN_POINT('Ctrl Pts',(-2.13049227679005,-0.891025387309722,
10.7699793157862));
#96819=CARTESIAN_POINT('Ctrl Pts',(-0.408214485225542,-2.27228942196666,
10.8810909662716));
#96820=CARTESIAN_POINT('Ctrl Pts',(1.68888461736298,-1.5772814986318,10.9922026167571));
#96821=CARTESIAN_POINT('Ctrl Pts',(2.23817187934597,0.566161966084782,11.1033142672425));
#96822=CARTESIAN_POINT('Ctrl Pts',(1.24300218570944,1.64165746435707,11.1773887008995));
#96823=CARTESIAN_POINT('Ctrl Pts',(0.627850911123727,1.850383536838,11.2144259177279));
#96824=CARTESIAN_POINT('Ctrl Pts',(1.05793541951254,-1.4823699524473,-0.153382721514713));
#96825=CARTESIAN_POINT('Ctrl Pts',(1.55074231467859,-1.13066431478549,-0.116345504686234));
#96826=CARTESIAN_POINT('Ctrl Pts',(2.14955001436596,0.0967274517879858,
-0.0422710710292769));
#96827=CARTESIAN_POINT('Ctrl Pts',(1.08290436090784,1.86174541551099,0.0688405794561606));
#96828=CARTESIAN_POINT('Ctrl Pts',(-0.975409307071879,1.91793784975909,
0.179952229941597));
#96829=CARTESIAN_POINT('Ctrl Pts',(-2.14083151712633,0.22213180716797,0.291063880427034));
#96830=CARTESIAN_POINT('Ctrl Pts',(-1.34782279118508,-1.67833716661673,
0.402175530912471));
#96831=CARTESIAN_POINT('Ctrl Pts',(0.678460972679723,-2.04251926348523,
0.513287181397908));
#96832=CARTESIAN_POINT('Ctrl Pts',(2.08394142450739,-0.538362390807298,
0.624398831883346));
#96833=CARTESIAN_POINT('Ctrl Pts',(1.58282747515632,1.45855746470163,0.735510482368781));
#96834=CARTESIAN_POINT('Ctrl Pts',(-0.366459012269607,2.12091168831785,
0.84662213285422));
#96835=CARTESIAN_POINT('Ctrl Pts',(-1.98045646054783,0.842867780077688,
0.957733783339656));
#96836=CARTESIAN_POINT('Ctrl Pts',(-1.78250862301028,-1.20635899339281,
1.06884543382509));
#96837=CARTESIAN_POINT('Ctrl Pts',(0.0462869228141735,-2.15185334908375,
1.17995708431053));
#96838=CARTESIAN_POINT('Ctrl Pts',(1.83273239545565,-1.12859176615955,1.29106873479597));
#96839=CARTESIAN_POINT('Ctrl Pts',(1.94238315681312,0.927240382098824,1.4021803852814));
#96840=CARTESIAN_POINT('Ctrl Pts',(0.274916856192995,2.13472355144377,1.51329203576684));
#96841=CARTESIAN_POINT('Ctrl Pts',(-1.64407495706399,1.38911602796551,1.62440368625228));
#96842=CARTESIAN_POINT('Ctrl Pts',(-2.0588770445336,-0.62741605808422,1.73551533673771));
#96843=CARTESIAN_POINT('Ctrl Pts',(-0.589980335104445,-2.06991507018771,
1.84662698722315));
#96844=CARTESIAN_POINT('Ctrl Pts',(1.41869855984326,-1.61861665507704,1.95773863770859));
#96845=CARTESIAN_POINT('Ctrl Pts',(2.1293880179812,0.313579489369987,2.06885028819403));
#96846=CARTESIAN_POINT('Ctrl Pts',(0.891867138635642,1.95887681727571,2.17996193867946));
#96847=CARTESIAN_POINT('Ctrl Pts',(-1.16163690001897,1.8119671998123,2.2910735891649));
#96848=CARTESIAN_POINT('Ctrl Pts',(-2.1523412125303,0.0072605002547781,
2.40218523965033));
#96849=CARTESIAN_POINT('Ctrl Pts',(-1.1738349588193,-1.80408893734178,2.51329689013577));
#96850=CARTESIAN_POINT('Ctrl Pts',(0.878631217069615,-1.96484925501419,
2.62440854062121));
#96851=CARTESIAN_POINT('Ctrl Pts',(2.12722398078527,-0.327938323711113,
2.73552019110664));
#96852=CARTESIAN_POINT('Ctrl Pts',(1.42958632662274,1.60900849678758,2.84663184159209));
#96853=CARTESIAN_POINT('Ctrl Pts',(-0.57600216794938,2.07384833374845,2.95774349207752));
#96854=CARTESIAN_POINT('Ctrl Pts',(-2.05459728996263,0.641291965189069,
3.06885514256296));
#96855=CARTESIAN_POINT('Ctrl Pts',(-1.65340928710165,-1.37799243024573,
3.17996679304839));
#96856=CARTESIAN_POINT('Ctrl Pts',(0.260508675794864,-2.13653004623031,
3.29107844353384));
#96857=CARTESIAN_POINT('Ctrl Pts',(1.93608318568785,-0.940322979965331,
3.40219009401926));
#96858=CARTESIAN_POINT('Ctrl Pts',(1.84030497427301,1.11620025542831,3.51330174450471));
#96859=CARTESIAN_POINT('Ctrl Pts',(0.0608030219043116,2.15149445760286,
3.62441339499014));
#96860=CARTESIAN_POINT('Ctrl Pts',(-1.77432856410404,1.21835280406139,3.73552504547559));
#96861=CARTESIAN_POINT('Ctrl Pts',(-1.98609925645444,-0.829478843655077,
3.84663669596101));
#96862=CARTESIAN_POINT('Ctrl Pts',(-0.380756743800589,-2.11840735237885,
3.95774834644646));
#96863=CARTESIAN_POINT('Ctrl Pts',(1.57294605588646,-1.4691719143219,4.06885999693188));
#96864=CARTESIAN_POINT('Ctrl Pts',(2.08753596148093,0.524231836199493,4.17997164741733));
#96865=CARTESIAN_POINT('Ctrl Pts',(0.692206637610257,2.03800769856489,4.29108329790276));
#96866=CARTESIAN_POINT('Ctrl Pts',(-1.33643334165982,1.68717851215016,4.4021949483882));
#96867=CARTESIAN_POINT('Ctrl Pts',(-2.1423496001257,-0.207276625316418,
4.51330659887364));
#96868=CARTESIAN_POINT('Ctrl Pts',(-0.988196775702872,-1.91209114350017,
4.62441824935908));
#96869=CARTESIAN_POINT('Ctrl Pts',(1.07007270071357,-1.86750363419964,4.73552989984451));
#96870=CARTESIAN_POINT('Ctrl Pts',(2.1493159635798,-0.11430790551128,4.84664155032995));
#96871=CARTESIAN_POINT('Ctrl Pts',(1.26211650891535,1.74346990983058,4.95775320081538));
#96872=CARTESIAN_POINT('Ctrl Pts',(-0.779813036479037,2.00611989589323,
5.06886485130082));
#96873=CARTESIAN_POINT('Ctrl Pts',(-2.1082794649543,0.433339481484583,5.17997650178626));
#96874=CARTESIAN_POINT('Ctrl Pts',(-1.50784810891129,-1.53590998727594,
5.29108815227169));
#96875=CARTESIAN_POINT('Ctrl Pts',(0.472137013611209,-2.09993143910453,
5.40219980275713));
#96876=CARTESIAN_POINT('Ctrl Pts',(2.02015661416081,-0.742692845544967,
5.51331145324257));
#96877=CARTESIAN_POINT('Ctrl Pts',(1.71990340163759,1.29404702294652,5.62442310372801));
#96878=CARTESIAN_POINT('Ctrl Pts',(-0.153916274037652,2.14684307510999,
5.73553475421344));
#96879=CARTESIAN_POINT('Ctrl Pts',(-1.88691554856225,1.03545889399597,5.84664640469888));
#96880=CARTESIAN_POINT('Ctrl Pts',(-1.89354634030427,-1.02328278871562,
5.95775805518432));
#96881=CARTESIAN_POINT('Ctrl Pts',(-0.167742034418123,-2.1458070785722,
6.06886970566975));
#96882=CARTESIAN_POINT('Ctrl Pts',(1.71153207655705,-1.30509898455162,6.1799813561552));
#96883=CARTESIAN_POINT('Ctrl Pts',(2.02489878034016,0.729664537947597,6.29109300664062));
#96884=CARTESIAN_POINT('Ctrl Pts',(0.485653989206222,2.09684658745684,6.40220465712607));
#96885=CARTESIAN_POINT('Ctrl Pts',(-1.49792321581985,1.54559097049293,6.5133163076115));
#96886=CARTESIAN_POINT('Ctrl Pts',(-2.11102709394471,-0.41974994603061,
6.62442795809694));
#96887=CARTESIAN_POINT('Ctrl Pts',(-0.79271933890819,-2.0010550862688,6.73553960858237));
#96888=CARTESIAN_POINT('Ctrl Pts',(1.25085971055702,-1.7515636994031,6.84665125906781));
#96889=CARTESIAN_POINT('Ctrl Pts',(2.15000768978506,0.100460651134341,6.95776290955325));
#96890=CARTESIAN_POINT('Ctrl Pts',(1.08208008038219,1.86057198414926,7.06887456003868));
#96891=CARTESIAN_POINT('Ctrl Pts',(-0.975859481618359,1.91841697258389,
7.17998621052413));
#96892=CARTESIAN_POINT('Ctrl Pts',(-2.14096997451993,0.221072333783236,
7.29109786100956));
#96893=CARTESIAN_POINT('Ctrl Pts',(-1.34727362553083,-1.67853483327237,
7.402209511495));
#96894=CARTESIAN_POINT('Ctrl Pts',(0.679064389152043,-2.04242428597833,
7.51332116198043));
#96895=CARTESIAN_POINT('Ctrl Pts',(2.08411579664662,-0.537667885148679,
7.62443281246587));
#96896=CARTESIAN_POINT('Ctrl Pts',(1.58237713686343,1.4590092546951,7.73554446295131));
#96897=CARTESIAN_POINT('Ctrl Pts',(-0.367103060190181,2.1208160579853,7.84665611343674));
#96898=CARTESIAN_POINT('Ctrl Pts',(-1.98071493840836,0.842255152109201,
7.95776776392219));
#96899=CARTESIAN_POINT('Ctrl Pts',(-1.78213980826558,-1.20689813668469,
8.0688794144076));
#96900=CARTESIAN_POINT('Ctrl Pts',(0.0469428447876819,-2.15184148537872,
8.17999106489306));
#96901=CARTESIAN_POINT('Ctrl Pts',(1.83307675642296,-1.12803147698245,8.29110271537848));
#96902=CARTESIAN_POINT('Ctrl Pts',(1.94210013665906,0.927832133403047,8.40221436586394));
#96903=CARTESIAN_POINT('Ctrl Pts',(0.274265792786954,2.13480764600607,8.51332601634936));
#96904=CARTESIAN_POINT('Ctrl Pts',(-1.64449860425235,1.38861432550488,8.6244376668348));
#96905=CARTESIAN_POINT('Ctrl Pts',(-2.05868556570727,-0.628043908949741,
8.73554931732024));
#96906=CARTESIAN_POINT('Ctrl Pts',(-0.589348971863656,-2.07009497609277,
8.84666096780567));
#96907=CARTESIAN_POINT('Ctrl Pts',(1.41919218774748,-1.61818383148359,8.95777261829112));
#96908=CARTESIAN_POINT('Ctrl Pts',(2.12929227820989,0.314228931244718,9.06888426877654));
#96909=CARTESIAN_POINT('Ctrl Pts',(0.891269611515884,1.95914878439144,9.179995919262));
#96910=CARTESIAN_POINT('Ctrl Pts',(-1.16218949038264,1.81161275719849,9.29110756974741));
#96911=CARTESIAN_POINT('Ctrl Pts',(-2.15234336950711,0.00660410388236847,
9.40221922023287));
#96912=CARTESIAN_POINT('Ctrl Pts',(-1.17328455934639,-1.80444704726821,
9.51333087071829));
#96913=CARTESIAN_POINT('Ctrl Pts',(0.879230317440182,-1.96458086313641,
9.62444252120374));
#96914=CARTESIAN_POINT('Ctrl Pts',(2.12732420202743,-0.327290075520782,
9.73555417168917));
#96915=CARTESIAN_POINT('Ctrl Pts',(1.42909493440969,1.60944558045319,9.8466658221746));
#96916=CARTESIAN_POINT('Ctrl Pts',(-0.576633610487541,2.07367041606005,
9.95777747266004));
#96917=CARTESIAN_POINT('Ctrl Pts',(-2.05479483697499,0.640669329675303,
10.0688891231455));
#96918=CARTESIAN_POINT('Ctrl Pts',(-1.65298502134104,-1.37850440914814,
10.1800007736309));
#96919=CARTESIAN_POINT('Ctrl Pts',(0.26115292159373,-2.13643575818697,10.2911124241164));
#96920=CARTESIAN_POINT('Ctrl Pts',(1.93638399542254,-0.939760456828254,
10.4022240746018));
#96921=CARTESIAN_POINT('Ctrl Pts',(1.83993760927049,1.11681489898982,10.5133357250872));
#96922=CARTESIAN_POINT('Ctrl Pts',(0.0601978674766102,2.15141126935532,
10.6244473755726));
#96923=CARTESIAN_POINT('Ctrl Pts',(-1.77479732841649,1.21800507565884,10.7355590260581));
#96924=CARTESIAN_POINT('Ctrl Pts',(-1.98566096114678,-0.830453293000129,
10.8466706765435));
#96925=CARTESIAN_POINT('Ctrl Pts',(-0.380463978169507,-2.11781870639967,
10.957782327029));
#96926=CARTESIAN_POINT('Ctrl Pts',(1.57407388382168,-1.47005756870945,11.0688939775144));
#96927=CARTESIAN_POINT('Ctrl Pts',(2.08602048154327,0.527674155869038,11.1800056279999));
#96928=CARTESIAN_POINT('Ctrl Pts',(1.15850263419028,1.53005724266717,11.2540800616568));
#96929=CARTESIAN_POINT('Ctrl Pts',(0.585169473375027,1.72459407258861,11.2911172784853));
#96930=CARTESIAN_POINT('Ctrl Pts',(0.980771099081375,-1.37424797458507,
-0.0766913607573581));
#96931=CARTESIAN_POINT('Ctrl Pts',(1.43763335295088,-1.04819525110066,-0.0396541439288791));
#96932=CARTESIAN_POINT('Ctrl Pts',(1.99276486185844,0.089672287600667,0.0344202897280782));
#96933=CARTESIAN_POINT('Ctrl Pts',(1.00391884103562,1.72595232535247,0.145531940213516));
#96934=CARTESIAN_POINT('Ctrl Pts',(-0.904264325124765,1.77804616253862,
0.256643590698952));
#96935=CARTESIAN_POINT('Ctrl Pts',(-1.98468227953599,0.20592982580867,0.36775524118439));
#96936=CARTESIAN_POINT('Ctrl Pts',(-1.24951449388714,-1.55592161598129,
0.478866891669827));
#96937=CARTESIAN_POINT('Ctrl Pts',(0.628974984281669,-1.89354078329874,
0.589978542155263));
#96938=CARTESIAN_POINT('Ctrl Pts',(1.93194167019859,-0.499094995779056,
0.7010901926407));
#96939=CARTESIAN_POINT('Ctrl Pts',(1.46737826698393,1.35217233617898,0.812201843126137));
#96940=CARTESIAN_POINT('Ctrl Pts',(-0.339730007714042,1.96621537500318,
0.923313493611574));
#96941=CARTESIAN_POINT('Ctrl Pts',(-1.8360047538528,0.7813901905543,1.03442514409701));
#96942=CARTESIAN_POINT('Ctrl Pts',(-1.65249495296916,-1.11836886639236,
1.14553679458245));
#96943=CARTESIAN_POINT('Ctrl Pts',(0.0429108198140191,-1.99490019458391,
1.25664844506789));
#96944=CARTESIAN_POINT('Ctrl Pts',(1.69905547414348,-1.04627387125433,1.36776009555332));
#96945=CARTESIAN_POINT('Ctrl Pts',(1.80070846330345,0.859608773740392,1.47887174603876));
#96946=CARTESIAN_POINT('Ctrl Pts',(0.254864807653961,1.97901982027321,1.5899833965242));
#96947=CARTESIAN_POINT('Ctrl Pts',(-1.52415844376849,1.28779586009797,1.70109504700963));
#96948=CARTESIAN_POINT('Ctrl Pts',(-1.90870545082139,-0.581653213909888,
1.81220669749507));
#96949=CARTESIAN_POINT('Ctrl Pts',(-0.546947999872595,-1.91893837842057,
1.92331834798051));
#96950=CARTESIAN_POINT('Ctrl Pts',(1.31522068373867,-1.50055703449532,2.03442999846594));
#96951=CARTESIAN_POINT('Ctrl Pts',(1.97407345311151,0.290707442785592,2.14554164895138));
#96952=CARTESIAN_POINT('Ctrl Pts',(0.826815604866742,1.81599909938712,2.25665329943681));
#96953=CARTESIAN_POINT('Ctrl Pts',(-1.07690873956185,1.67980486264285,2.36776494992226));
#96954=CARTESIAN_POINT('Ctrl Pts',(-1.99535247395734,0.00673092958549589,
2.47887660040769));
#96955=CARTESIAN_POINT('Ctrl Pts',(-1.0882170891223,-1.67250122954812,2.58998825089313));
#96956=CARTESIAN_POINT('Ctrl Pts',(0.814545092789914,-1.82153591592328,
2.70109990137857));
#96957=CARTESIAN_POINT('Ctrl Pts',(1.97206725774273,-0.304018963960226,
2.812211551864));
#96958=CARTESIAN_POINT('Ctrl Pts',(1.325314312134,1.49164968174781,2.92332320234944));
#96959=CARTESIAN_POINT('Ctrl Pts',(-0.533989380555266,1.92258475527334,
3.03443485283487));
#96960=CARTESIAN_POINT('Ctrl Pts',(-1.90473785552499,0.594517031881129,
3.14554650332031));
#96961=CARTESIAN_POINT('Ctrl Pts',(-1.53281194091147,-1.27748360193918,
3.25665815380575));
#96962=CARTESIAN_POINT('Ctrl Pts',(0.241507539654265,-1.98069455187271,
3.36776980429119));
#96963=CARTESIAN_POINT('Ctrl Pts',(1.79486800320472,-0.871737145332536,
3.47888145477662));
#96964=CARTESIAN_POINT('Ctrl Pts',(1.70607571972046,1.03478617987453,3.58999310526206));
#96965=CARTESIAN_POINT('Ctrl Pts',(0.0563681350682242,1.99456748014249,
3.7011047557475));
#96966=CARTESIAN_POINT('Ctrl Pts',(-1.64491153604594,1.1294878653923,3.81221640623293));
#96967=CARTESIAN_POINT('Ctrl Pts',(-1.84123597216834,-0.768977824309152,
3.92332805671837));
#96968=CARTESIAN_POINT('Ctrl Pts',(-0.352984882831497,-1.96389370180267,
4.03443970720381));
#96969=CARTESIAN_POINT('Ctrl Pts',(1.45821758452731,-1.36201258278399,4.14555135768924));
#96970=CARTESIAN_POINT('Ctrl Pts',(1.93527402670466,0.485995103935303,4.25666300817468));
#96971=CARTESIAN_POINT('Ctrl Pts',(0.641718059759468,1.88935828557357,4.36777465866012));
#96972=CARTESIAN_POINT('Ctrl Pts',(-1.23895577477937,1.56411808621589,4.47888630914555));
#96973=CARTESIAN_POINT('Ctrl Pts',(-1.98608963569812,-0.1921581600124,4.58999795963099));
#96974=CARTESIAN_POINT('Ctrl Pts',(-0.916119093792434,-1.77262590680487,
4.70110961011643));
#96975=CARTESIAN_POINT('Ctrl Pts',(0.992023104075105,-1.73129054767478,
4.81222126060186));
#96976=CARTESIAN_POINT('Ctrl Pts',(1.99254788240719,-0.105970447774237,
4.9233329110873));
#96977=CARTESIAN_POINT('Ctrl Pts',(1.17005950721263,1.61630366858093,5.03444456157274));
#96978=CARTESIAN_POINT('Ctrl Pts',(-0.722934571202785,1.85979633434597,
5.14555621205818));
#96979=CARTESIAN_POINT('Ctrl Pts',(-1.95450452823164,0.401732309640217,
5.25666786254361));
#96980=CARTESIAN_POINT('Ctrl Pts',(-1.39786779017765,-1.42388287463214,
5.36777951302905));
#96981=CARTESIAN_POINT('Ctrl Pts',(0.437700004381964,-1.9467653956373,5.47889116351449));
#96982=CARTESIAN_POINT('Ctrl Pts',(1.87280923414012,-0.688521874747905,
5.59000281399993));
#96983=CARTESIAN_POINT('Ctrl Pts',(1.59445606832513,1.19966105449332,5.70111446448536));
#96984=CARTESIAN_POINT('Ctrl Pts',(-0.142689837650004,1.99025536294172,
5.81222611497081));
#96985=CARTESIAN_POINT('Ctrl Pts',(-1.74928658432651,0.959933979699734,
5.92333776545623));
#96986=CARTESIAN_POINT('Ctrl Pts',(-1.75543373545183,-0.948645982400418,
6.03444941594168));
#96987=CARTESIAN_POINT('Ctrl Pts',(-0.155507166528361,-1.98929493053321,
6.1455610664271));
#96988=CARTESIAN_POINT('Ctrl Pts',(1.58669533591315,-1.20990690157479,6.25667271691256));
#96989=CARTESIAN_POINT('Ctrl Pts',(1.87720551339304,0.676443833569079,6.36778436739797));
#96990=CARTESIAN_POINT('Ctrl Pts',(0.450231070802491,1.94390554872681,6.47889601788343));
#96991=CARTESIAN_POINT('Ctrl Pts',(-1.38866680481881,1.43285774055946,6.59000766836885));
#96992=CARTESIAN_POINT('Ctrl Pts',(-1.95705174903083,-0.38913397577471,
6.7011193188543));
#96993=CARTESIAN_POINT('Ctrl Pts',(-0.734899506098636,-1.85510094480672,
6.81223096933973));
#96994=CARTESIAN_POINT('Ctrl Pts',(1.15962376388238,-1.62380710853421,6.92334261982516));
#96995=CARTESIAN_POINT('Ctrl Pts',(1.99318915507666,0.0931331926412601,
7.03445427031061));
#96996=CARTESIAN_POINT('Ctrl Pts',(1.00315468237132,1.72486448242263,7.14556592079604));
#96997=CARTESIAN_POINT('Ctrl Pts',(-0.904681664573454,1.77849033881895,
7.25667757128148));
#96998=CARTESIAN_POINT('Ctrl Pts',(-1.98481063804218,0.204947628921387,
7.36778922176691));
#96999=CARTESIAN_POINT('Ctrl Pts',(-1.24900538360275,-1.55610486510929,
7.47890087225236));
#97000=CARTESIAN_POINT('Ctrl Pts',(0.629534388405818,-1.89345273331751,
7.59001252273779));
#97001=CARTESIAN_POINT('Ctrl Pts',(1.93210332387941,-0.498451146385645,
7.70112417322323));
#97002=CARTESIAN_POINT('Ctrl Pts',(1.46696077573226,1.35259117324623,7.81223582370866));
#97003=CARTESIAN_POINT('Ctrl Pts',(-0.340327079685797,1.96612671981249,
7.9233474741941));
#97004=CARTESIAN_POINT('Ctrl Pts',(-1.836244378702,0.780822246807544,8.03445912467955));
#97005=CARTESIAN_POINT('Ctrl Pts',(-1.65215303905282,-1.11886868533138,
8.14557077516496));
#97006=CARTESIAN_POINT('Ctrl Pts',(0.0435188997620014,-1.99488919620082,
8.25668242565042));
#97007=CARTESIAN_POINT('Ctrl Pts',(1.69937471790653,-1.04575444878119,8.36779407613584));
#97008=CARTESIAN_POINT('Ctrl Pts',(1.80044608624107,0.860157363537389,8.47890572662129));
#97009=CARTESIAN_POINT('Ctrl Pts',(0.254261231896373,1.97909778109651,8.59001737710672));
#97010=CARTESIAN_POINT('Ctrl Pts',(-1.52455119072723,1.28733075110866,8.70112902759215));
#97011=CARTESIAN_POINT('Ctrl Pts',(-1.90852793819114,-0.58223527021699,
8.8122406780776));
#97012=CARTESIAN_POINT('Ctrl Pts',(-0.546362687377931,-1.91910516224214,
8.92335232856302));
#97013=CARTESIAN_POINT('Ctrl Pts',(1.31567830711834,-1.50015578044556,9.03446397904849));
#97014=CARTESIAN_POINT('Ctrl Pts',(1.97398469646436,0.291309515284085,9.14557562953389));
#97015=CARTESIAN_POINT('Ctrl Pts',(0.826261660534066,1.81625122960423,9.25668728001935));
#97016=CARTESIAN_POINT('Ctrl Pts',(-1.07742102476217,1.67947627257441,9.36779893050478));
#97017=CARTESIAN_POINT('Ctrl Pts',(-1.99535447360731,0.00612240984059651,
9.47891058099021));
#97018=CARTESIAN_POINT('Ctrl Pts',(-1.08770683501224,-1.67283321944057,
9.59002223147566));
#97019=CARTESIAN_POINT('Ctrl Pts',(0.815100495622697,-1.82128710017129,
9.70113388196108));
#97020=CARTESIAN_POINT('Ctrl Pts',(1.97216016898856,-0.303417998080474,
9.81224553244654));
#97021=CARTESIAN_POINT('Ctrl Pts',(1.32485876137733,1.49205488514605,9.92335718293196));
#97022=CARTESIAN_POINT('Ctrl Pts',(-0.534574766563464,1.9224198146507,10.0344688334174));
#97023=CARTESIAN_POINT('Ctrl Pts',(-1.90492099373632,0.593939810525364,
10.1455804839028));
#97024=CARTESIAN_POINT('Ctrl Pts',(-1.53241862049827,-1.27795823782107,
10.2566921343883));
#97025=CARTESIAN_POINT('Ctrl Pts',(0.242104795071353,-1.98060714106653,
10.3678037848737));
#97026=CARTESIAN_POINT('Ctrl Pts',(1.79514687230076,-0.871215651841315,
10.4789154353591));
#97027=CARTESIAN_POINT('Ctrl Pts',(1.70573514980415,1.03535599219979,10.5900270858446));
#97028=CARTESIAN_POINT('Ctrl Pts',(0.055807119752709,1.99449035952863,10.70113873633));
#97029=CARTESIAN_POINT('Ctrl Pts',(-1.64534610934924,1.12916549981001,10.8122503868155));
#97030=CARTESIAN_POINT('Ctrl Pts',(-1.84082964550351,-0.769881198690536,
10.9233620373009));
#97031=CARTESIAN_POINT('Ctrl Pts',(-0.352713471113472,-1.96334799083268,
11.0344736877863));
#97032=CARTESIAN_POINT('Ctrl Pts',(1.45926315028039,-1.36283363878709,11.1455853382718));
#97033=CARTESIAN_POINT('Ctrl Pts',(1.93386908374058,0.489186345653294,11.2566969887572));
#97034=CARTESIAN_POINT('Ctrl Pts',(1.07400308267113,1.41845702097726,11.3307714224142));
#97035=CARTESIAN_POINT('Ctrl Pts',(0.542488035626326,1.59880460833922,11.3678086392426));
#97036=CARTESIAN_POINT('Ctrl Pts',(0.903606778650208,-1.26612599672284,
-2.77555756156289E-15));
#97037=CARTESIAN_POINT('Ctrl Pts',(1.32452439122316,-0.965726187415828,
0.0370372168284762));
#97038=CARTESIAN_POINT('Ctrl Pts',(1.83597970935092,0.0826171234133487,
0.111111650485434));
#97039=CARTESIAN_POINT('Ctrl Pts',(0.924933321163406,1.59015923519395,0.222223300970871));
#97040=CARTESIAN_POINT('Ctrl Pts',(-0.833119343177651,1.63815447531815,
0.333334951456308));
#97041=CARTESIAN_POINT('Ctrl Pts',(-1.82853304194564,0.18972784444937,0.444446601941745));
#97042=CARTESIAN_POINT('Ctrl Pts',(-1.15120619658919,-1.43350606534586,
0.555558252427182));
#97043=CARTESIAN_POINT('Ctrl Pts',(0.579488995883613,-1.74456230311225,
0.666669902912619));
#97044=CARTESIAN_POINT('Ctrl Pts',(1.77994191588978,-0.459827600750814,
0.777781553398056));
#97045=CARTESIAN_POINT('Ctrl Pts',(1.35192905881154,1.24578720765632,0.888893203883492));
#97046=CARTESIAN_POINT('Ctrl Pts',(-0.313001003158473,1.81151906168851,
1.00000485436893));
#97047=CARTESIAN_POINT('Ctrl Pts',(-1.69155304715778,0.719912601030908,
1.11111650485437));
#97048=CARTESIAN_POINT('Ctrl Pts',(-1.52248128292804,-1.03037873939191,
1.2222281553398));
#97049=CARTESIAN_POINT('Ctrl Pts',(0.0395347168138628,-1.83794704008407,
1.33333980582524));
#97050=CARTESIAN_POINT('Ctrl Pts',(1.56537855283131,-0.963955976349113,
1.44445145631068));
#97051=CARTESIAN_POINT('Ctrl Pts',(1.65903376979378,0.791977165381959,1.55556310679611));
#97052=CARTESIAN_POINT('Ctrl Pts',(0.234812759114929,1.82331608910266,1.66667475728155));
#97053=CARTESIAN_POINT('Ctrl Pts',(-1.404241930473,1.18647569223042,1.77778640776699));
#97054=CARTESIAN_POINT('Ctrl Pts',(-1.75853385710917,-0.535890369735552,
1.88889805825242));
#97055=CARTESIAN_POINT('Ctrl Pts',(-0.503915664640746,-1.76796168665343,
2.00000970873786));
#97056=CARTESIAN_POINT('Ctrl Pts',(1.21174280763407,-1.38249741391359,2.1111213592233));
#97057=CARTESIAN_POINT('Ctrl Pts',(1.81875888824183,0.267835396201195,2.22223300970874));
#97058=CARTESIAN_POINT('Ctrl Pts',(0.761764071097843,1.67312138149853,2.33334466019417));
#97059=CARTESIAN_POINT('Ctrl Pts',(-0.992180579104728,1.54764252547341,
2.44445631067961));
#97060=CARTESIAN_POINT('Ctrl Pts',(-1.83836373538439,0.00620135891621234,
2.55556796116504));
#97061=CARTESIAN_POINT('Ctrl Pts',(-1.0025992194253,-1.54091352175446,2.66667961165049));
#97062=CARTESIAN_POINT('Ctrl Pts',(0.750458968510211,-1.67822257683237,
2.77779126213592));
#97063=CARTESIAN_POINT('Ctrl Pts',(1.81691053470019,-0.280099604209337,
2.88890291262136));
#97064=CARTESIAN_POINT('Ctrl Pts',(1.22104229764526,1.37429086670804,3.0000145631068));
#97065=CARTESIAN_POINT('Ctrl Pts',(-0.491976593161155,1.77132117679823,
3.11112621359223));
#97066=CARTESIAN_POINT('Ctrl Pts',(-1.75487842108734,0.547742098573187,
3.22223786407767));
#97067=CARTESIAN_POINT('Ctrl Pts',(-1.41221459472129,-1.17697477363263,
3.3333495145631));
#97068=CARTESIAN_POINT('Ctrl Pts',(0.222506403513669,-1.8248590575151,3.44446116504855));
#97069=CARTESIAN_POINT('Ctrl Pts',(1.65365282072159,-0.803151310699741,
3.55557281553397));
#97070=CARTESIAN_POINT('Ctrl Pts',(1.57184646516792,0.953372104320743,3.66668446601942));
#97071=CARTESIAN_POINT('Ctrl Pts',(0.0519332482321354,1.83764050268212,
3.77779611650485));
#97072=CARTESIAN_POINT('Ctrl Pts',(-1.51549450798785,1.04062292672322,3.88890776699029));
#97073=CARTESIAN_POINT('Ctrl Pts',(-1.69637268788223,-0.708476804963227,
4.00001941747572));
#97074=CARTESIAN_POINT('Ctrl Pts',(-0.325213021862407,-1.80938005122649,
4.11113106796117));
#97075=CARTESIAN_POINT('Ctrl Pts',(1.34348911316817,-1.25485325124609,4.2222427184466));
#97076=CARTESIAN_POINT('Ctrl Pts',(1.78301209192838,0.447758371671112,4.33335436893204));
#97077=CARTESIAN_POINT('Ctrl Pts',(0.591229481908682,1.74070887258225,4.44446601941748));
#97078=CARTESIAN_POINT('Ctrl Pts',(-1.14147820789891,1.44105766028162,4.55557766990291));
#97079=CARTESIAN_POINT('Ctrl Pts',(-1.82982967127054,-0.177039694708382,
4.66668932038835));
#97080=CARTESIAN_POINT('Ctrl Pts',(-0.844041411881997,-1.63316067010957,
4.77780097087378));
#97081=CARTESIAN_POINT('Ctrl Pts',(0.913973507436636,-1.59507746114991,
4.88891262135923));
#97082=CARTESIAN_POINT('Ctrl Pts',(1.83577980123458,-0.0976329900371924,
5.00002427184466));
#97083=CARTESIAN_POINT('Ctrl Pts',(1.0780025055099,1.48913742733129,5.1111359223301));
#97084=CARTESIAN_POINT('Ctrl Pts',(-0.666056105926533,1.7134727727987,5.22224757281553));
#97085=CARTESIAN_POINT('Ctrl Pts',(-1.80072959150898,0.37012513779585,5.33335922330097));
#97086=CARTESIAN_POINT('Ctrl Pts',(-1.28788747144402,-1.31185576198834,
5.44447087378641));
#97087=CARTESIAN_POINT('Ctrl Pts',(0.403262995152723,-1.79359935217008,
5.55558252427184));
#97088=CARTESIAN_POINT('Ctrl Pts',(1.72546185411942,-0.634350903950841,
5.66669417475728));
#97089=CARTESIAN_POINT('Ctrl Pts',(1.46900873501267,1.1052750860401,5.77780582524271));
#97090=CARTESIAN_POINT('Ctrl Pts',(-0.13146340126236,1.83366765077345,5.88891747572816));
#97091=CARTESIAN_POINT('Ctrl Pts',(-1.61165762009075,0.884409065403499,
6.00002912621358));
#97092=CARTESIAN_POINT('Ctrl Pts',(-1.6173211305994,-0.87400917608522,6.11114077669903));
#97093=CARTESIAN_POINT('Ctrl Pts',(-0.143272298638598,-1.83278278249422,
6.22225242718446));
#97094=CARTESIAN_POINT('Ctrl Pts',(1.46185859526926,-1.11471481859797,6.33336407766989));
#97095=CARTESIAN_POINT('Ctrl Pts',(1.72951224644592,0.623223129190563,6.44447572815534));
#97096=CARTESIAN_POINT('Ctrl Pts',(0.414808152398764,1.79096450999678,6.55558737864077));
#97097=CARTESIAN_POINT('Ctrl Pts',(-1.27941039381778,1.320124510626,6.66669902912621));
#97098=CARTESIAN_POINT('Ctrl Pts',(-1.80307640411694,-0.358518005518811,
6.77781067961165));
#97099=CARTESIAN_POINT('Ctrl Pts',(-0.677079673289082,-1.70914680334463,
6.8889223300971));
#97100=CARTESIAN_POINT('Ctrl Pts',(1.06838781720774,-1.49605051766532,7.00003398058251));
#97101=CARTESIAN_POINT('Ctrl Pts',(1.83637062036826,0.0858057341481814,
7.11114563106797));
#97102=CARTESIAN_POINT('Ctrl Pts',(0.924229284360448,1.589156980696,7.22225728155339));
#97103=CARTESIAN_POINT('Ctrl Pts',(-0.833503847528551,1.63856370505402,
7.33336893203883));
#97104=CARTESIAN_POINT('Ctrl Pts',(-1.82865130156443,0.188822924059537,
7.44448058252428));
#97105=CARTESIAN_POINT('Ctrl Pts',(-1.15073714167466,-1.43367489694622,
7.5555922330097));
#97106=CARTESIAN_POINT('Ctrl Pts',(0.580004387659595,-1.74448118065669,
7.66670388349515));
#97107=CARTESIAN_POINT('Ctrl Pts',(1.7800908511122,-0.459234407622611,7.77781553398057));
#97108=CARTESIAN_POINT('Ctrl Pts',(1.35154441460109,1.24617309179735,7.88892718446602));
#97109=CARTESIAN_POINT('Ctrl Pts',(-0.313551099181417,1.81143738163968,
8.00003883495145));
#97110=CARTESIAN_POINT('Ctrl Pts',(-1.69177381899564,0.719389341505889,
8.11115048543689));
#97111=CARTESIAN_POINT('Ctrl Pts',(-1.52216626984007,-1.03083923397808,
8.22226213592232));
#97112=CARTESIAN_POINT('Ctrl Pts',(0.0400949547363229,-1.83793690702293,
8.33337378640777));
#97113=CARTESIAN_POINT('Ctrl Pts',(1.56567267939011,-0.963477420579929,
8.44448543689319));
#97114=CARTESIAN_POINT('Ctrl Pts',(1.65879203582308,0.792482593671729,8.55559708737864));
#97115=CARTESIAN_POINT('Ctrl Pts',(0.234256671005791,1.82338791618694,8.66670873786407));
#97116=CARTESIAN_POINT('Ctrl Pts',(-1.40460377720211,1.18604717671243,8.77782038834951));
#97117=CARTESIAN_POINT('Ctrl Pts',(-1.75837031067501,-0.536426631484242,
8.88893203883495));
#97118=CARTESIAN_POINT('Ctrl Pts',(-0.503376402892206,-1.7681153483915,
9.00004368932038));
#97119=CARTESIAN_POINT('Ctrl Pts',(1.2121644264892,-1.38212772940753,9.11115533980582));
#97120=CARTESIAN_POINT('Ctrl Pts',(1.81867711471885,0.26839009932345,9.22226699029127));
#97121=CARTESIAN_POINT('Ctrl Pts',(0.761253709552246,1.67335367481701,9.33337864077668));
#97122=CARTESIAN_POINT('Ctrl Pts',(-0.99265255914171,1.54733978795034,9.44449029126215));
#97123=CARTESIAN_POINT('Ctrl Pts',(-1.8383655777075,0.00564071579882353,
9.55560194174756));
#97124=CARTESIAN_POINT('Ctrl Pts',(-1.00212911067809,-1.54121939161292,
9.66671359223301));
#97125=CARTESIAN_POINT('Ctrl Pts',(0.750970673805211,-1.67799333720618,
9.77782524271844));
#97126=CARTESIAN_POINT('Ctrl Pts',(1.81699613594968,-0.279545920640164,
9.88893689320389));
#97127=CARTESIAN_POINT('Ctrl Pts',(1.22062258834496,1.37466418983892,10.0000485436893));
#97128=CARTESIAN_POINT('Ctrl Pts',(-0.492515922639386,1.77116921324136,
10.1111601941748));
#97129=CARTESIAN_POINT('Ctrl Pts',(-1.75504715049764,0.547210291375423,
10.2222718446602));
#97130=CARTESIAN_POINT('Ctrl Pts',(-1.4118522196555,-1.177412066494,10.3333834951456));
#97131=CARTESIAN_POINT('Ctrl Pts',(0.223056668548975,-1.82477852394609,
10.4444951456311));
#97132=CARTESIAN_POINT('Ctrl Pts',(1.65390974917898,-0.802670846854376,
10.5556067961165));
#97133=CARTESIAN_POINT('Ctrl Pts',(1.57153269033781,0.953897085409752,10.6667184466019));
#97134=CARTESIAN_POINT('Ctrl Pts',(0.0514163720288116,1.83756944970195,
10.7778300970874));
#97135=CARTESIAN_POINT('Ctrl Pts',(-1.51589489028199,1.04032592396117,10.8889417475728));
#97136=CARTESIAN_POINT('Ctrl Pts',(-1.69599832986023,-0.709309104380943,
11.0000533980583));
#97137=CARTESIAN_POINT('Ctrl Pts',(-0.324962964057439,-1.80887727526569,
11.1111650485437));
#97138=CARTESIAN_POINT('Ctrl Pts',(1.34445241673909,-1.25560970886474,11.2222766990291));
#97139=CARTESIAN_POINT('Ctrl Pts',(1.78171768593789,0.450698535437549,11.3333883495146));
#97140=CARTESIAN_POINT('Ctrl Pts',(0.989503531151977,1.30685679928735,11.4074627831715));
#97141=CARTESIAN_POINT('Ctrl Pts',(0.499806597877626,1.47301514408983,11.4445));
#97142=CARTESIAN_POINT('',(0.903606778650206,-1.26612599672284,0.));
#97143=CARTESIAN_POINT('Ctrl Pts',(0.903606778650208,-1.26612599672284,
-2.77555756156289E-15));
#97144=CARTESIAN_POINT('Ctrl Pts',(1.32452439122316,-0.965726187415828,
0.0370372168284762));
#97145=CARTESIAN_POINT('Ctrl Pts',(1.83597970935092,0.0826171234133487,
0.111111650485434));
#97146=CARTESIAN_POINT('Ctrl Pts',(0.924933321163406,1.59015923519395,0.222223300970871));
#97147=CARTESIAN_POINT('Ctrl Pts',(-0.833119343177651,1.63815447531815,
0.333334951456308));
#97148=CARTESIAN_POINT('Ctrl Pts',(-1.5310616378989,0.622578531632503,0.411241775931451));
#97149=CARTESIAN_POINT('Ctrl Pts',(-1.55772922446558,0.0543356393242454,
0.452111383578116));
#97150=CARTESIAN_POINT('Ctrl Pts',(-1.55735926886437,0.00101346774827265,
0.455943774396301));
#97151=CARTESIAN_POINT('Ctrl Pts',(0.863567639152676,1.75641488315944,2.28983498828939E-16));
#97152=CARTESIAN_POINT('Ctrl Pts',(0.902605506355985,1.73244147111074,2.48310810971475E-16));
#97153=CARTESIAN_POINT('Ctrl Pts',(0.940681517855526,1.70703362163956,1.53446104133306E-16));
#97154=CARTESIAN_POINT('Ctrl Pts',(0.977705169885396,1.68018661523996,1.12757025938492E-16));
#97155=CARTESIAN_POINT('Ctrl Pts',(1.0358643592122,1.63801357064694,3.49621561433049E-17));
#97156=CARTESIAN_POINT('Ctrl Pts',(1.09142895154027,1.59229038852923,-3.14041157591089E-18));
#97157=CARTESIAN_POINT('Ctrl Pts',(1.14423757319707,1.54335784953327,-1.00613961606655E-16));
#97158=CARTESIAN_POINT('Ctrl Pts',(1.16947625472704,1.51997165369202,-1.47199231391008E-16));
#97159=CARTESIAN_POINT('Ctrl Pts',(1.19408480623982,1.49585194230134,-1.44940981238328E-16));
#97160=CARTESIAN_POINT('Ctrl Pts',(1.21804196717247,1.47103398018765,-1.04083408558608E-16));
#97161=CARTESIAN_POINT('Ctrl Pts',(1.23020142841566,1.45843761915368,-8.33461403619852E-17));
#97162=CARTESIAN_POINT('Ctrl Pts',(1.24219304748387,1.44566136836505,-3.17714931440926E-16));
#97163=CARTESIAN_POINT('Ctrl Pts',(1.25401379483509,1.43270976178997,-3.05311331771918E-16));
#97164=CARTESIAN_POINT('Ctrl Pts',(1.26389181876557,1.42188673377951,-2.94946246493115E-16));
#97165=CARTESIAN_POINT('Ctrl Pts',(1.27364380619492,1.41094858444086,-5.46603369369435E-16));
#97166=CARTESIAN_POINT('Ctrl Pts',(1.28326720497828,1.3998998522991,-5.34294830600857E-16));
#97167=CARTESIAN_POINT('Ctrl Pts',(1.330154786252,1.3460676940429,-4.74324582576826E-16));
#97168=CARTESIAN_POINT('Ctrl Pts',(1.37400431756963,1.2896005558432,-2.78813144032988E-17));
#97169=CARTESIAN_POINT('Ctrl Pts',(1.41465239664765,1.2308327382907,1.45716771982052E-16));
#97170=CARTESIAN_POINT('Ctrl Pts',(1.44369336478921,1.18884614615641,2.69743702909727E-16));
#97171=CARTESIAN_POINT('Ctrl Pts',(1.47109927736379,1.14568453076923,1.23340209484872E-16));
#97172=CARTESIAN_POINT('Ctrl Pts',(1.4967949674738,1.10146499100096,1.52655665885959E-16));
#97173=CARTESIAN_POINT('Ctrl Pts',(1.51164370962241,1.07591189080641,1.69596158676961E-16));
#97174=CARTESIAN_POINT('Ctrl Pts',(1.5259211042574,1.05000546373499,-2.47389032972511E-16));
#97175=CARTESIAN_POINT('Ctrl Pts',(1.53961051084784,1.0237681518455,-2.63677968348475E-16));
#97176=CARTESIAN_POINT('Ctrl Pts',(1.5453767175419,1.01271655786648,-2.70539139983884E-16));
#97177=CARTESIAN_POINT('Ctrl Pts',(1.55103417937643,1.00161467257822,6.72528652799515E-17));
#97178=CARTESIAN_POINT('Ctrl Pts',(1.55658137030158,0.990465869694384,6.24500451351651E-17));
#97179=CARTESIAN_POINT('Ctrl Pts',(1.58759523113096,0.928133884781808,3.5597896440648E-17));
#97180=CARTESIAN_POINT('Ctrl Pts',(1.61517455934254,0.864320573166324,-1.32844578099872E-16));
#97181=CARTESIAN_POINT('Ctrl Pts',(1.639165272121,0.799334213601843,-1.80411241501588E-16));
#97182=CARTESIAN_POINT('Ctrl Pts',(1.66256479067373,0.735949288762567,-2.26805737281603E-16));
#97183=CARTESIAN_POINT('Ctrl Pts',(1.68255047093124,0.671447445488438,-3.92048207771591E-16));
#97184=CARTESIAN_POINT('Ctrl Pts',(1.69893099532196,0.606109731061441,-4.30211422042248E-16));
#97185=CARTESIAN_POINT('Ctrl Pts',(1.70969999791506,0.563154939181291,-4.55300957861645E-16));
#97186=CARTESIAN_POINT('Ctrl Pts',(1.71890982821634,0.519838805550124,-3.77882014063636E-16));
#97187=CARTESIAN_POINT('Ctrl Pts',(1.72649398406889,0.476242912678102,-4.71844785465692E-16));
#97188=CARTESIAN_POINT('Ctrl Pts',(1.73287054571603,0.439588616027976,-5.50846247992205E-16));
#97189=CARTESIAN_POINT('Ctrl Pts',(1.73809775889755,0.402736552578244,-9.42921937940892E-17));
#97190=CARTESIAN_POINT('Ctrl Pts',(1.74213052178609,0.36573694696249,-1.2490009027033E-16));
#97191=CARTESIAN_POINT('Ctrl Pts',(1.74338539139703,0.354223827548557,-1.34424309820125E-16));
#97192=CARTESIAN_POINT('Ctrl Pts',(1.74452450777523,0.342696049837886,-3.03274465566551E-16));
#97193=CARTESIAN_POINT('Ctrl Pts',(1.74554535151306,0.331170337018761,-2.91433543964104E-16));
#97194=CARTESIAN_POINT('Ctrl Pts',(1.75129431083391,0.266262406759456,-2.24750491415529E-16));
#97195=CARTESIAN_POINT('Ctrl Pts',(1.75331011127704,0.201301920292928,9.80627071070611E-17));
#97196=CARTESIAN_POINT('Ctrl Pts',(1.75142561531544,0.136549272921142,2.77555756156289E-17));
#97197=CARTESIAN_POINT('Ctrl Pts',(1.75088296778463,0.11790351037964,7.510378979319E-18));
#97198=CARTESIAN_POINT('Ctrl Pts',(1.75001659332986,0.099275023041261,-5.08054903583662E-16));
#97199=CARTESIAN_POINT('Ctrl Pts',(1.74882170147482,0.0806701752180915,
-4.85722573273506E-16));
#97200=CARTESIAN_POINT('Ctrl Pts',(1.74442082328573,0.0121470962041962,
-4.16579971360731E-16));
#97201=CARTESIAN_POINT('Ctrl Pts',(1.73556771390717,-0.056057442313777,
-1.52368272571946E-16));
#97202=CARTESIAN_POINT('Ctrl Pts',(1.72245534586321,-0.123606275893366,
-5.55111512312578E-17));
#97203=CARTESIAN_POINT('Ctrl Pts',(1.71065390208195,-0.184401836184713,
3.16625666268892E-17));
#97204=CARTESIAN_POINT('Ctrl Pts',(1.69540107690307,-0.244666544752314,
-5.10914177950054E-16));
#97205=CARTESIAN_POINT('Ctrl Pts',(1.67680493801022,-0.304129401844208,
-5.82867087928207E-16));
#97206=CARTESIAN_POINT('Ctrl Pts',(1.67349552259788,-0.314711560692091,
-5.95672007842828E-16));
#97207=CARTESIAN_POINT('Ctrl Pts',(1.67008173945308,-0.325263020743978,
-2.82234476894323E-16));
#97208=CARTESIAN_POINT('Ctrl Pts',(1.66656691458475,-0.335775244456298,
-2.77555756156289E-16));
#97209=CARTESIAN_POINT('Ctrl Pts',(1.64601434320315,-0.39724437487395,-2.5019742521657E-16));
#97210=CARTESIAN_POINT('Ctrl Pts',(1.6219871213203,-0.457449913435399,-1.49651752513019E-16));
#97211=CARTESIAN_POINT('Ctrl Pts',(1.59467186427628,-0.5161179062652,-1.94289029309402E-16));
#97212=CARTESIAN_POINT('Ctrl Pts',(1.56746479951959,-0.57455352257637,-2.38749503483388E-16));
#97213=CARTESIAN_POINT('Ctrl Pts',(1.53699493854014,-0.631464584970275,
-4.11608014004163E-16));
#97214=CARTESIAN_POINT('Ctrl Pts',(1.50340708769257,-0.686547887629179,
-4.71844785465692E-16));
#97215=CARTESIAN_POINT('Ctrl Pts',(1.47050686756616,-0.740503491725204,
-5.30848353445754E-16));
#97216=CARTESIAN_POINT('Ctrl Pts',(1.43461427022078,-0.792706028859038,
8.26037042042841E-17));
#97217=CARTESIAN_POINT('Ctrl Pts',(1.39583852741916,-0.842828743497358,
1.94289029309402E-16));
#97218=CARTESIAN_POINT('Ctrl Pts',(1.38891448399703,-0.851778974428235,
2.14232271779286E-16));
#97219=CARTESIAN_POINT('Ctrl Pts',(1.38189845475662,-0.860662765012678,
1.05754276149716E-16));
#97220=CARTESIAN_POINT('Ctrl Pts',(1.3747909965488,-0.869478087839508,1.11022302462516E-16));
#97221=CARTESIAN_POINT('Ctrl Pts',(1.36801000346398,-0.877888498619479,
1.1604835382339E-16));
#97222=CARTESIAN_POINT('Ctrl Pts',(1.36114891147745,-0.8862326313589,4.78426519390645E-16));
#97223=CARTESIAN_POINT('Ctrl Pts',(1.35421355798306,-0.894502968665375,
4.71844785465692E-16));
#97224=CARTESIAN_POINT('Ctrl Pts',(1.3143417576089,-0.942049678199007,4.34005967100638E-16));
#97225=CARTESIAN_POINT('Ctrl Pts',(1.27196760499602,-0.987223303029092,
-4.84873724376989E-16));
#97226=CARTESIAN_POINT('Ctrl Pts',(1.22722986402911,-1.02975664627632,-3.05311331771918E-16));
#97227=CARTESIAN_POINT('Ctrl Pts',(1.18329662429212,-1.07152512911229,-1.2897793916942E-16));
#97228=CARTESIAN_POINT('Ctrl Pts',(1.13708333146208,-1.1107479710078,1.42267300457324E-16));
#97229=CARTESIAN_POINT('Ctrl Pts',(1.08869802628341,-1.14712822354107,1.94289029309402E-16));
#97230=CARTESIAN_POINT('Ctrl Pts',(1.04185702701945,-1.1823473334721,2.44650389103912E-16));
#97231=CARTESIAN_POINT('Ctrl Pts',(0.99297984330778,-1.21490270865201,1.66616011326585E-16));
#97232=CARTESIAN_POINT('Ctrl Pts',(0.942151955941521,-1.24447758118399,
1.11022302462516E-16));
#97233=CARTESIAN_POINT('Ctrl Pts',(0.929425469464971,-1.25188265416315,
9.71025308430195E-17));
#97234=CARTESIAN_POINT('Ctrl Pts',(0.916576650468056,-1.25910062269163,
1.9641793555709E-16));
#97235=CARTESIAN_POINT('Ctrl Pts',(0.903606778650242,-1.26612599672281,
1.94289029309402E-16));
#97236=CARTESIAN_POINT('Ctrl Pts',(1.88079991776263,-0.516378774142081,
11.046));
#97237=CARTESIAN_POINT('Ctrl Pts',(1.79754570390634,-0.821182550519846,
11.028067538919));
#97238=CARTESIAN_POINT('Ctrl Pts',(1.64446793279769,-1.10682480125595,11.010135077838));
#97239=CARTESIAN_POINT('Ctrl Pts',(1.43091597726206,-1.33587557506818,10.9922026167571));
#97240=CARTESIAN_POINT('Ctrl Pts',(0.9898515831668,-1.80895080641009,10.9551653999286));
#97241=CARTESIAN_POINT('Ctrl Pts',(0.290818548970629,-2.04062011418838,
10.9181281831001));
#97242=CARTESIAN_POINT('Ctrl Pts',(-0.345744266721549,-1.9262440956347,
10.8810909662716));
#97243=CARTESIAN_POINT('Ctrl Pts',(-0.982307082413709,-1.81186807708102,
10.8440537494431));
#97244=CARTESIAN_POINT('Ctrl Pts',(-1.55639967960188,-1.35144673219537,
10.8070165326147));
#97245=CARTESIAN_POINT('Ctrl Pts',(-1.80573868997825,-0.754924386616321,
10.7699793157862));
#97246=CARTESIAN_POINT('Ctrl Pts',(-1.90472245868201,-0.518114150655666,
10.7552761078989));
#97247=CARTESIAN_POINT('Ctrl Pts',(-1.95252608806662,-0.259854826956367,
10.7405729000116));
#97248=CARTESIAN_POINT('Ctrl Pts',(-1.95129684289216,-0.00113636086278679,
10.7258696921242));
#97249=CARTESIAN_POINT('Origin',(0.,0.,-1.29405622560369));
#97250=CARTESIAN_POINT('',(-0.903606778650172,-1.26612599672286,0.));
#97251=CARTESIAN_POINT('Ctrl Pts',(-0.905549614304886,-1.26792015305981,
1.24276674021151E-15));
#97252=CARTESIAN_POINT('Ctrl Pts',(-0.513706458239086,-1.54472437079514,
0.0344950590738082));
#97253=CARTESIAN_POINT('Ctrl Pts',(0.587535178885047,-1.72169358136003,
0.106052258091336));
#97254=CARTESIAN_POINT('Ctrl Pts',(1.77508460417327,-0.479721809770191,
0.214671597052585));
#97255=CARTESIAN_POINT('Ctrl Pts',(1.3650560094313,1.23222299189869,0.325858016883748));
#97256=CARTESIAN_POINT('Ctrl Pts',(-0.295638381403906,1.81478253869214,
0.43704443671491));
#97257=CARTESIAN_POINT('Ctrl Pts',(-1.41307745535963,0.946781319192958,
0.526443839621562));
#97258=CARTESIAN_POINT('Ctrl Pts',(-1.55414936746312,0.214718667413076,
0.578781102584494));
#97259=CARTESIAN_POINT('Ctrl Pts',(-1.55326046963413,0.000729270061605551,
0.594056225603705));
#97260=CARTESIAN_POINT('Origin',(0.,0.,0.));
#97261=CARTESIAN_POINT('Ctrl Pts',(-0.685825729128748,1.39614588036674,
-0.230074082272066));
#97262=CARTESIAN_POINT('Ctrl Pts',(-1.15028016933624,1.16799292759742,-0.193011942328345));
#97263=CARTESIAN_POINT('Ctrl Pts',(-1.82555218707277,0.215691441263552,
-0.118887662440903));
#97264=CARTESIAN_POINT('Ctrl Pts',(-1.16942936218886,-1.42059634545264,
-0.00770124260974049));
#97265=CARTESIAN_POINT('Ctrl Pts',(0.559468948314244,-1.75104601534012,
0.103485177221422));
#97266=CARTESIAN_POINT('Ctrl Pts',(1.77508460417327,-0.479721809770191,
0.214671597052585));
#97267=CARTESIAN_POINT('Ctrl Pts',(1.3650560094313,1.23222299189869,0.325858016883748));
#97268=CARTESIAN_POINT('Ctrl Pts',(-0.295638381403906,1.81478253869214,
0.43704443671491));
#97269=CARTESIAN_POINT('Ctrl Pts',(-1.68540213790592,0.735245708832444,
0.548230856546073));
#97270=CARTESIAN_POINT('Ctrl Pts',(-1.53132379752993,-1.01797781965797,
0.659417276377235));
#97271=CARTESIAN_POINT('Ctrl Pts',(0.0255447675030308,-1.83860034663711,
0.770603696208398));
#97272=CARTESIAN_POINT('Ctrl Pts',(1.55899683301632,-0.975032021788082,
0.881790116039561));
#97273=CARTESIAN_POINT('Ctrl Pts',(1.66434877052597,0.781732535368643,0.992976535870723));
#97274=CARTESIAN_POINT('Ctrl Pts',(0.245080507541896,1.82238325373942,1.10416295570189));
#97275=CARTESIAN_POINT('Ctrl Pts',(-1.39868975820189,1.19365863723167,1.21534937553305));
#97276=CARTESIAN_POINT('Ctrl Pts',(-1.76120077222934,-0.528512641939849,
1.32653579536421));
#97277=CARTESIAN_POINT('Ctrl Pts',(-0.510374815939226,-1.76654153931159,
1.43772221519537));
#97278=CARTESIAN_POINT('Ctrl Pts',(1.20797626960931,-1.38634273102519,1.54890863502654));
#97279=CARTESIAN_POINT('Ctrl Pts',(1.81976886629041,0.263806680570579,1.6600950548577));
#97280=CARTESIAN_POINT('Ctrl Pts',(0.764574137846417,1.67229745635935,1.77128147468886));
#97281=CARTESIAN_POINT('Ctrl Pts',(-0.991003621173195,1.54889135395602,
1.88246789452002));
#97282=CARTESIAN_POINT('Ctrl Pts',(-1.83877909581896,0.00663349951290586,
1.99365431435119));
#97283=CARTESIAN_POINT('Ctrl Pts',(-1.00215313155719,-1.54170088892816,
2.10484073418235));
#97284=CARTESIAN_POINT('Ctrl Pts',(0.752488571272716,-1.67777039880966,
2.21602715401351));
#97285=CARTESIAN_POINT('Ctrl Pts',(1.81781810074028,-0.276929424335053,
2.32721357384467));
#97286=CARTESIAN_POINT('Ctrl Pts',(1.21794738393109,1.37759091140133,2.43839999367584));
#97287=CARTESIAN_POINT('Ctrl Pts',(-0.497615974795104,1.77017821004958,
2.549586413507));
#97288=CARTESIAN_POINT('Ctrl Pts',(-1.75734151264734,0.541205469518692,
2.66077283333817));
#97289=CARTESIAN_POINT('Ctrl Pts',(-1.40726598433086,-1.1835349598584,2.77195925316932));
#97290=CARTESIAN_POINT('Ctrl Pts',(0.231926238140432,-1.82410602009977,
2.88314567300049));
#97291=CARTESIAN_POINT('Ctrl Pts',(1.65866396469461,-0.793716828903688,
2.99433209283165));
#97292=CARTESIAN_POINT('Ctrl Pts',(1.56599354026699,0.96375141196464,3.10551851266282));
#97293=CARTESIAN_POINT('Ctrl Pts',(0.0388050940998321,1.83838154825996,
3.21670493249398));
#97294=CARTESIAN_POINT('Ctrl Pts',(-1.52393050178991,1.02897443019027,3.32789135232514));
#97295=CARTESIAN_POINT('Ctrl Pts',(-1.69067964401488,-0.723017906820314,
3.4390777721563));
#97296=CARTESIAN_POINT('Ctrl Pts',(-0.308692884081366,-1.81269447386996,
3.55026419198746));
#97297=CARTESIAN_POINT('Ctrl Pts',(1.35606994996762,-1.24186426112907,3.66145061181863));
#97298=CARTESIAN_POINT('Ctrl Pts',(1.77861387826841,0.466567491694538,3.77263703164979));
#97299=CARTESIAN_POINT('Ctrl Pts',(0.571870330903418,1.74760318061885,3.88382345148095));
#97300=CARTESIAN_POINT('Ctrl Pts',(-1.15873124952358,1.42775853828764,3.99500987131212));
#97301=CARTESIAN_POINT('Ctrl Pts',(-1.82788473512851,-0.199974866820836,
4.10619629114327));
#97302=CARTESIAN_POINT('Ctrl Pts',(-0.822616502622442,-1.64452261823584,
4.21738271097444));
#97303=CARTESIAN_POINT('Ctrl Pts',(0.936204134582059,-1.58261630557358,
4.3285691308056));
#97304=CARTESIAN_POINT('Ctrl Pts',(1.83742116834086,-0.0709647969689106,
4.43975555063676));
#97305=CARTESIAN_POINT('Ctrl Pts',(1.0554806974386,1.50569354438759,4.55094197046793));
#97306=CARTESIAN_POINT('Ctrl Pts',(-0.693325883166112,1.70307127625589,
4.66212839029909));
#97307=CARTESIAN_POINT('Ctrl Pts',(-1.80701587562324,0.340361833232659,
4.77331481013025));
#97308=CARTESIAN_POINT('Ctrl Pts',(-1.26540093064824,-1.33413381524886,
4.88450122996142));
#97309=CARTESIAN_POINT('Ctrl Pts',(0.435376164803608,-1.7865050090601,4.99568764979258));
#97310=CARTESIAN_POINT('Ctrl Pts',(1.73732980498774,-0.602360109052031,
5.10687406962374));
#97311=CARTESIAN_POINT('Ctrl Pts',(1.44781397169404,1.13357278356683,5.21806048945491));
#97312=CARTESIAN_POINT('Ctrl Pts',(-0.167962271460079,1.83110382765203,
5.32924690928607));
#97313=CARTESIAN_POINT('Ctrl Pts',(-1.62987778710162,0.851264325217889,
5.44043332911723));
#97314=CARTESIAN_POINT('Ctrl Pts',(-1.59875453933454,-0.908370230265797,
5.55161974894839));
#97315=CARTESIAN_POINT('Ctrl Pts',(-0.103102773360761,-1.83589824620028,
5.66280616877956));
#97316=CARTESIAN_POINT('Ctrl Pts',(1.4869956060099,-1.08166382022474,5.77399258861071));
#97317=CARTESIAN_POINT('Ctrl Pts',(1.71494149863546,0.663421591850831,5.88517900844189));
#97318=CARTESIAN_POINT('Ctrl Pts',(0.371926577693494,1.80078404398782,5.99636542827304));
#97319=CARTESIAN_POINT('Ctrl Pts',(-1.311789224034,1.28855018683177,6.10755184810421));
#97320=CARTESIAN_POINT('Ctrl Pts',(-1.79384918603911,-0.404051543769803,
6.21873826793537));
#97321=CARTESIAN_POINT('Ctrl Pts',(-0.632665469493242,-1.72652453095426,
6.32992468776653));
#97322=CARTESIAN_POINT('Ctrl Pts',(1.10806726459172,-1.46742614445027,6.44111110759769));
#97323=CARTESIAN_POINT('Ctrl Pts',(1.83376231205259,0.135898253011021,6.55229752742886));
#97324=CARTESIAN_POINT('Ctrl Pts',(0.879651525947856,1.61473395492061,6.66348394726001));
#97325=CARTESIAN_POINT('Ctrl Pts',(-0.880258220622017,1.61440330069759,
6.77467036709119));
#97326=CARTESIAN_POINT('Ctrl Pts',(-1.83381324808445,0.13520918395534,6.88585678692234));
#97327=CARTESIAN_POINT('Ctrl Pts',(-1.1075157823663,-1.46784241118916,6.99704320675351));
#97328=CARTESIAN_POINT('Ctrl Pts',(0.633314188332071,-1.72628667698419,
7.10822962658467));
#97329=CARTESIAN_POINT('Ctrl Pts',(1.7940008868909,-0.403377453646542,7.21941604641583));
#97330=CARTESIAN_POINT('Ctrl Pts',(1.31130494233742,1.28904301731096,7.33060246624699));
#97331=CARTESIAN_POINT('Ctrl Pts',(-0.372603218894873,1.80064416072257,
7.44178888607816));
#97332=CARTESIAN_POINT('Ctrl Pts',(-1.71519066664489,0.662777133981789,
7.55297530590932));
#97333=CARTESIAN_POINT('Ctrl Pts',(-1.48658905212271,-1.08222250133236,
7.66416172574049));
#97334=CARTESIAN_POINT('Ctrl Pts',(0.103792628149562,-1.8358593744105,7.77534814557165));
#97335=CARTESIAN_POINT('Ctrl Pts',(1.59909575810308,-0.907769413831382,
7.8865345654028));
#97336=CARTESIAN_POINT('Ctrl Pts',(1.62955779866738,0.851876712390422,7.99772098523398));
#97337=CARTESIAN_POINT('Ctrl Pts',(0.167274199086701,1.83116681231986,8.10890740506512));
#97338=CARTESIAN_POINT('Ctrl Pts',(-1.44823982381472,1.1330286690894,8.2200938248963));
#97339=CARTESIAN_POINT('Ctrl Pts',(-1.73710333792674,-0.603012890298399,
8.33128024472746));
#97340=CARTESIAN_POINT('Ctrl Pts',(-0.434704832044991,-1.78666848096071,
8.44246666455862));
#97341=CARTESIAN_POINT('Ctrl Pts',(1.26590215885116,-1.33365823077974,8.55365308438979));
#97342=CARTESIAN_POINT('Ctrl Pts',(1.8068878531032,0.341040818691465,8.66483950422094));
#97343=CARTESIAN_POINT('Ctrl Pts',(0.69268588294083,1.70333168137465,8.77602592405212));
#97344=CARTESIAN_POINT('Ctrl Pts',(-1.05604640517969,1.5052968290502,8.88721234388326));
#97345=CARTESIAN_POINT('Ctrl Pts',(-1.83739437498563,-0.0716552286239433,
8.99839876371444));
#97346=CARTESIAN_POINT('Ctrl Pts',(-0.935609375970031,-1.5829679799695,
9.1095851835456));
#97347=CARTESIAN_POINT('Ctrl Pts',(0.823234386500799,-1.64421340203127,
9.22077160337675));
#97348=CARTESIAN_POINT('Ctrl Pts',(1.82795976495949,-0.199287985657338,
9.33195802320793));
#97349=CARTESIAN_POINT('Ctrl Pts',(1.15819463928053,1.42819381470141,9.44314444303908));
#97350=CARTESIAN_POINT('Ctrl Pts',(-0.572526917402423,1.74738822826618,
9.55433086287024));
#97351=CARTESIAN_POINT('Ctrl Pts',(-1.77878918025408,0.46589901053406,9.66551728270142));
#97352=CARTESIAN_POINT('Ctrl Pts',(-1.35560300066214,-1.24237352171324,
9.77670370253256));
#97353=CARTESIAN_POINT('Ctrl Pts',(0.309373610575528,-1.81257875466721,
9.88789012236375));
#97354=CARTESIAN_POINT('Ctrl Pts',(1.69095195914933,-0.722381792257861,
9.99907654219489));
#97355=CARTESIAN_POINT('Ctrl Pts',(1.52354231364944,1.0295455294481,10.1102629620261));
#97356=CARTESIAN_POINT('Ctrl Pts',(-0.0394931635484403,1.83836962465064,
10.2214493818572));
#97357=CARTESIAN_POINT('Ctrl Pts',(-1.56636075542215,0.963157594965877,
10.3326358016884));
#97358=CARTESIAN_POINT('Ctrl Pts',(-1.65835572967195,-0.794329933758677,
10.4438222215196));
#97359=CARTESIAN_POINT('Ctrl Pts',(-0.231259578302998,-1.82421227428175,
10.5550086413507));
#97360=CARTESIAN_POINT('Ctrl Pts',(1.40774638007895,-1.1829694620695,10.6661950611819));
#97361=CARTESIAN_POINT('Ctrl Pts',(1.75706993010233,0.541796064983141,10.7773814810131));
#97362=CARTESIAN_POINT('Ctrl Pts',(0.497080432048737,1.77049779856472,10.8885679008442));
#97363=CARTESIAN_POINT('Ctrl Pts',(-1.21871201614337,1.37688031013954,10.9997543206754));
#97364=CARTESIAN_POINT('Ctrl Pts',(-1.81724153253684,-0.27712968875509,
11.1109407405065));
#97365=CARTESIAN_POINT('Ctrl Pts',(-0.75277483453787,-1.67898453189698,
11.2221271603377));
#97366=CARTESIAN_POINT('Ctrl Pts',(1.00462758039806,-1.53944373403644,11.3333135801688));
#97367=CARTESIAN_POINT('Ctrl Pts',(1.55754888396286,-0.511266487217653,
11.4074378600563));
#97368=CARTESIAN_POINT('Ctrl Pts',(1.55548765964692,0.00619602180124784,
11.4445));
#97369=CARTESIAN_POINT('Ctrl Pts',(-0.74439243930934,1.51537102412034,-0.153382721514711));
#97370=CARTESIAN_POINT('Ctrl Pts',(-1.24850938769699,1.26773474301532,-0.11632058157099));
#97371=CARTESIAN_POINT('Ctrl Pts',(-1.98144687185762,0.234110607521693,
-0.042196301683548));
#97372=CARTESIAN_POINT('Ctrl Pts',(-1.26929384324154,-1.54190945884872,
0.0689901181476148));
#97373=CARTESIAN_POINT('Ctrl Pts',(0.607245306591998,-1.90057817801302,
0.180176537978778));
#97374=CARTESIAN_POINT('Ctrl Pts',(1.92666956394248,-0.520688088821623,
0.29136295780994));
#97375=CARTESIAN_POINT('Ctrl Pts',(1.48162620545796,1.33744979191402,0.402549377641103));
#97376=CARTESIAN_POINT('Ctrl Pts',(-0.320884689126903,1.9697575395855,0.513735797472264));
#97377=CARTESIAN_POINT('Ctrl Pts',(-1.82932858212653,0.798032683003624,
0.624922217303428));
#97378=CARTESIAN_POINT('Ctrl Pts',(-1.66209258212561,-1.10490895887015,
0.736108637134591));
#97379=CARTESIAN_POINT('Ctrl Pts',(0.0277261860929502,-1.99560929084259,
0.847295056965753));
#97380=CARTESIAN_POINT('Ctrl Pts',(1.69212878157669,-1.0582957656395,0.958481476796916));
#97381=CARTESIAN_POINT('Ctrl Pts',(1.80647734334385,0.848489294255244,1.06966789662808));
#97382=CARTESIAN_POINT('Ctrl Pts',(0.266009379770665,1.97800732458805,1.18085431645924));
#97383=CARTESIAN_POINT('Ctrl Pts',(-1.51813213871049,1.2955921992025,1.29204073629041));
#97384=CARTESIAN_POINT('Ctrl Pts',(-1.91160010957712,-0.573645458357494,
1.40322715612156));
#97385=CARTESIAN_POINT('Ctrl Pts',(-0.553958736254638,-1.91739695630841,
1.51441357595273));
#97386=CARTESIAN_POINT('Ctrl Pts',(1.31113249878304,-1.50473072594935,1.62559999578389));
#97387=CARTESIAN_POINT('Ctrl Pts',(1.9751696791516,0.286334691329668,1.73678641561505));
#97388=CARTESIAN_POINT('Ctrl Pts',(0.829865639814035,1.81510481441338,1.84797283544622));
#97389=CARTESIAN_POINT('Ctrl Pts',(-1.07563127424026,1.68116033596642,1.95915925527738));
#97390=CARTESIAN_POINT('Ctrl Pts',(-1.99580330447296,0.00719997322039096,
2.07034567510854));
#97391=CARTESIAN_POINT('Ctrl Pts',(-1.08773290717609,-1.67335583465575,
2.18153209493971));
#97392=CARTESIAN_POINT('Ctrl Pts',(0.816748015321165,-1.82104512374819,
2.29271851477087));
#97393=CARTESIAN_POINT('Ctrl Pts',(1.97305232620797,-0.300578063700233,
2.40390493460203));
#97394=CARTESIAN_POINT('Ctrl Pts',(1.32195510545613,1.49523153675082,2.51509135443319));
#97395=CARTESIAN_POINT('Ctrl Pts',(-0.54011034229875,1.92134418384253,2.62627777426435));
#97396=CARTESIAN_POINT('Ctrl Pts',(-1.90741128502276,0.587422201459822,
2.73746419409552));
#97397=CARTESIAN_POINT('Ctrl Pts',(-1.52744073944838,-1.28460400121777,
2.84865061392668));
#97398=CARTESIAN_POINT('Ctrl Pts',(0.251731789602741,-1.9798772081443,2.95983703375785));
#97399=CARTESIAN_POINT('Ctrl Pts',(1.80030707836241,-0.861496997406464,
3.071023453589));
#97400=CARTESIAN_POINT('Ctrl Pts',(1.69972297898904,1.04605183790867,3.18220987342017));
#97401=CARTESIAN_POINT('Ctrl Pts',(0.0421188903066005,1.99537180797957,
3.29339629325133));
#97402=CARTESIAN_POINT('Ctrl Pts',(-1.65406792919015,1.11684463493277,3.4045827130825));
#97403=CARTESIAN_POINT('Ctrl Pts',(-1.83505676565636,-0.784760676748056,
3.51576913291366));
#97404=CARTESIAN_POINT('Ctrl Pts',(-0.335053992900935,-1.96749116257395,
3.62695555274482));
#97405=CARTESIAN_POINT('Ctrl Pts',(1.47187277329603,-1.34791438607496,3.73814197257599));
#97406=CARTESIAN_POINT('Ctrl Pts',(1.93050022360002,0.506410445822938,3.84932839240714));
#97407=CARTESIAN_POINT('Ctrl Pts',(0.620705716495424,1.89684133929807,3.96051481223831));
#97408=CARTESIAN_POINT('Ctrl Pts',(-1.25768215554202,1.54968327363698,4.07170123206947));
#97409=CARTESIAN_POINT('Ctrl Pts',(-1.9839786099702,-0.217051901949521,
4.18288765190064));
#97410=CARTESIAN_POINT('Ctrl Pts',(-0.892864584974339,-1.78495811879663,
4.29407407173179));
#97411=CARTESIAN_POINT('Ctrl Pts',(1.01615213578872,-1.71776526041577,4.40526049156296));
#97412=CARTESIAN_POINT('Ctrl Pts',(1.99432941554622,-0.0770249001709277,
4.51644691139412));
#97413=CARTESIAN_POINT('Ctrl Pts',(1.14561442891388,1.6342736102696,4.62763333122529));
#97414=CARTESIAN_POINT('Ctrl Pts',(-0.752533075803338,1.84850659257176,
4.73881975105645));
#97415=CARTESIAN_POINT('Ctrl Pts',(-1.96132763527948,0.369427340688636,
4.85000617088761));
#97416=CARTESIAN_POINT('Ctrl Pts',(-1.3734609908354,-1.44806338245697,4.96119259071877));
#97417=CARTESIAN_POINT('Ctrl Pts',(0.472555507281729,-1.9390652246629,5.07237901054994));
#97418=CARTESIAN_POINT('Ctrl Pts',(1.88569065943703,-0.653799196903168,
5.1835654303811));
#97419=CARTESIAN_POINT('Ctrl Pts',(1.57145135896933,1.23037525956625,5.29475185021226));
#97420=CARTESIAN_POINT('Ctrl Pts',(-0.182305561972616,1.98747259981946,
5.40593827004342));
#97421=CARTESIAN_POINT('Ctrl Pts',(-1.76906267902489,0.923958814363803,
5.51712468987459));
#97422=CARTESIAN_POINT('Ctrl Pts',(-1.73528163328608,-0.985941329968107,
5.62831110970574));
#97423=CARTESIAN_POINT('Ctrl Pts',(-0.111907328205795,-1.99267644208816,
5.73949752953692));
#97424=CARTESIAN_POINT('Ctrl Pts',(1.61397894448518,-1.17403348321834,5.85068394936807));
#97425=CARTESIAN_POINT('Ctrl Pts',(1.86139048335769,0.720075080408093,5.96187036919923));
#97426=CARTESIAN_POINT('Ctrl Pts',(0.403687585131819,1.9545636307293,6.0730567890304));
#97427=CARTESIAN_POINT('Ctrl Pts',(-1.42381065460884,1.39858709874703,6.18424320886156));
#97428=CARTESIAN_POINT('Ctrl Pts',(-1.94703656429618,-0.438555891823412,
6.29542962869273));
#97429=CARTESIAN_POINT('Ctrl Pts',(-0.686692511086116,-1.87396265922711,
6.40661604852388));
#97430=CARTESIAN_POINT('Ctrl Pts',(1.20269167366484,-1.59273833100625,6.51780246835505));
#97431=CARTESIAN_POINT('Ctrl Pts',(1.99035810790665,0.147503407586138,6.62898888818621));
#97432=CARTESIAN_POINT('Ctrl Pts',(0.954770165847204,1.75262562555938,6.74017530801738));
#97433=CARTESIAN_POINT('Ctrl Pts',(-0.9554286697633,1.7522667348191,6.85136172784854));
#97434=CARTESIAN_POINT('Ctrl Pts',(-1.99041339366714,0.146755494853507,
6.9625481476797));
#97435=CARTESIAN_POINT('Ctrl Pts',(-1.20209309711463,-1.59319014522084,
7.07373456751086));
#97436=CARTESIAN_POINT('Ctrl Pts',(0.687396627858533,-1.87370449350154,
7.18492098734203));
#97437=CARTESIAN_POINT('Ctrl Pts',(1.94720121977979,-0.437824237162718,
7.29610740717318));
#97438=CARTESIAN_POINT('Ctrl Pts',(1.42328501723757,1.39912201493195,7.40729382700435));
#97439=CARTESIAN_POINT('Ctrl Pts',(-0.404422008722263,1.95441180200575,
7.51848024683551));
#97440=CARTESIAN_POINT('Ctrl Pts',(-1.86166092929526,0.719375588474842,
7.62966666666667));
#97441=CARTESIAN_POINT('Ctrl Pts',(-1.61353767256008,-1.17463987340584,
7.74085308649784));
#97442=CARTESIAN_POINT('Ctrl Pts',(0.112656093769942,-1.99263425080664,
7.852039506329));
#97443=CARTESIAN_POINT('Ctrl Pts',(1.73565199074082,-0.985289206269375,
7.96322592616017));
#97444=CARTESIAN_POINT('Ctrl Pts',(1.76871536488809,0.924623496894334,8.07441234599133));
#97445=CARTESIAN_POINT('Ctrl Pts',(0.181558731034875,1.98754096312013,8.18559876582249));
#97446=CARTESIAN_POINT('Ctrl Pts',(-1.57191357711808,1.22978467993954,8.29678518565365));
#97447=CARTESIAN_POINT('Ctrl Pts',(-1.88544485301595,-0.6545077229961,8.40797160548482));
#97448=CARTESIAN_POINT('Ctrl Pts',(-0.471826845453332,-1.93924265639472,
8.51915802531597));
#97449=CARTESIAN_POINT('Ctrl Pts',(1.37400502187529,-1.44754718502077,8.63034444514714));
#97450=CARTESIAN_POINT('Ctrl Pts',(1.96118868016023,0.370164308726493,8.7415308649783));
#97451=CARTESIAN_POINT('Ctrl Pts',(0.751838422178375,1.84878923522181,8.85271728480947));
#97452=CARTESIAN_POINT('Ctrl Pts',(-1.14622844578058,1.63384301706618,8.96390370464062));
#97453=CARTESIAN_POINT('Ctrl Pts',(-1.99430033414812,-0.077774291863319,
9.0750901244718));
#97454=CARTESIAN_POINT('Ctrl Pts',(-1.01550658722561,-1.71814696636568,
9.18627654430294));
#97455=CARTESIAN_POINT('Ctrl Pts',(0.893535233606871,-1.78462249679383,
9.29746296413412));
#97456=CARTESIAN_POINT('Ctrl Pts',(1.98406004704164,-0.216306363946107,
9.40864938396527));
#97457=CARTESIAN_POINT('Ctrl Pts',(1.2570997209806,1.55015572087487,9.51983580379645));
#97458=CARTESIAN_POINT('Ctrl Pts',(-0.621418372793996,1.8966080308943,9.63102222362759));
#97459=CARTESIAN_POINT('Ctrl Pts',(-1.93069049565776,0.50568487910749,9.74220864345877));
#97460=CARTESIAN_POINT('Ctrl Pts',(-1.47136594843111,-1.34846713542859,
9.85339506328992));
#97461=CARTESIAN_POINT('Ctrl Pts',(0.335792850651442,-1.96736556142493,
9.9645814831211));
#97462=CARTESIAN_POINT('Ctrl Pts',(1.83535233538869,-0.784070240605622,
10.0757679029522));
#97463=CARTESIAN_POINT('Ctrl Pts',(1.65364659137136,1.11746450372967,10.1869543227834));
#97464=CARTESIAN_POINT('Ctrl Pts',(-0.0428657180698079,1.99535886614283,
10.2981407426146));
#97465=CARTESIAN_POINT('Ctrl Pts',(-1.70012155281541,1.04540731136874,10.4093271624457));
#97466=CARTESIAN_POINT('Ctrl Pts',(-1.79997252133044,-0.862162458906591,
10.5205135822769));
#97467=CARTESIAN_POINT('Ctrl Pts',(-0.251008199743871,-1.97999253599851,
10.6317000021081));
#97468=CARTESIAN_POINT('Ctrl Pts',(1.52796215902707,-1.28399021223231,10.7428864219392));
#97469=CARTESIAN_POINT('Ctrl Pts',(1.90711651044001,0.588063231359589,10.8540728417704));
#97470=CARTESIAN_POINT('Ctrl Pts',(0.539529066393858,1.92169106390877,10.9652592616015));
#97471=CARTESIAN_POINT('Ctrl Pts',(-1.32278503412967,1.49446025304978,11.0764456814327));
#97472=CARTESIAN_POINT('Ctrl Pts',(-1.97242652143987,-0.300795429882017,
11.1876321012639));
#97473=CARTESIAN_POINT('Ctrl Pts',(-0.817058724297523,-1.82236293883171,
11.2988185210951));
#97474=CARTESIAN_POINT('Ctrl Pts',(1.09041866382002,-1.67090592797485,11.4100049409262));
#97475=CARTESIAN_POINT('Ctrl Pts',(1.69055718360052,-0.554926552610627,
11.4841292208136));
#97476=CARTESIAN_POINT('Ctrl Pts',(1.6883199391646,0.00672513670271936,
11.5211913607574));
#97477=CARTESIAN_POINT('Ctrl Pts',(-0.802959149489932,1.63459616787394,
-0.0766913607573554));
#97478=CARTESIAN_POINT('Ctrl Pts',(-1.34673860605774,1.36747655843322,-0.0396292208136346));
#97479=CARTESIAN_POINT('Ctrl Pts',(-2.13734155664247,0.252529773779836,
0.0344950590738073));
#97480=CARTESIAN_POINT('Ctrl Pts',(-1.36915832429422,-1.66322257224481,
0.14568147890497));
#97481=CARTESIAN_POINT('Ctrl Pts',(0.655021664869751,-2.05011034068591,
0.256867898736133));
#97482=CARTESIAN_POINT('Ctrl Pts',(2.0782545237117,-0.561654367873057,0.368054318567295));
#97483=CARTESIAN_POINT('Ctrl Pts',(1.59819640148463,1.44267659192936,0.479240738398458));
#97484=CARTESIAN_POINT('Ctrl Pts',(-0.346130996849898,2.12473254047885,
0.590427158229621));
#97485=CARTESIAN_POINT('Ctrl Pts',(-1.97325502634714,0.860819657174806,
0.701613578060782));
#97486=CARTESIAN_POINT('Ctrl Pts',(-1.79286136672128,-1.19184009808233,
0.812799997891947));
#97487=CARTESIAN_POINT('Ctrl Pts',(0.0299076046828686,-2.15261823504807,
0.923986417723108));
#97488=CARTESIAN_POINT('Ctrl Pts',(1.82526073013706,-1.14155950949091,1.03517283755427));
#97489=CARTESIAN_POINT('Ctrl Pts',(1.94860591616173,0.915246053141843,1.14635925738543));
#97490=CARTESIAN_POINT('Ctrl Pts',(0.286938251999433,2.13363139543668,1.2575456772166));
#97491=CARTESIAN_POINT('Ctrl Pts',(-1.63757451921909,1.39752576117334,1.36873209704776));
#97492=CARTESIAN_POINT('Ctrl Pts',(-2.0619994469249,-0.618778274775138,
1.47991851687892));
#97493=CARTESIAN_POINT('Ctrl Pts',(-0.597542656570052,-2.06825237330522,
1.59110493671008));
#97494=CARTESIAN_POINT('Ctrl Pts',(1.41428872795678,-1.62311872087351,1.70229135654125));
#97495=CARTESIAN_POINT('Ctrl Pts',(2.13057049201279,0.308862702088754,1.81347777637241));
#97496=CARTESIAN_POINT('Ctrl Pts',(0.895157141781652,1.95791217246742,1.92466419620357));
#97497=CARTESIAN_POINT('Ctrl Pts',(-1.16025892730732,1.81342931797682,2.03585061603473));
#97498=CARTESIAN_POINT('Ctrl Pts',(-2.15282751312695,0.00776644692787891,
2.1470370358659));
#97499=CARTESIAN_POINT('Ctrl Pts',(-1.173312682795,-1.80501078038335,2.25822345569706));
#97500=CARTESIAN_POINT('Ctrl Pts',(0.881007459369614,-1.96431984868673,
2.36940987552822));
#97501=CARTESIAN_POINT('Ctrl Pts',(2.12828655167567,-0.324226703065412,
2.48059629535939));
#97502=CARTESIAN_POINT('Ctrl Pts',(1.42596282698117,1.6128721621003,2.59178271519055));
#97503=CARTESIAN_POINT('Ctrl Pts',(-0.582604709802392,2.07251015763547,
2.70296913502171));
#97504=CARTESIAN_POINT('Ctrl Pts',(-2.05748105739819,0.633638933400953,
2.81415555485287));
#97505=CARTESIAN_POINT('Ctrl Pts',(-1.6476154945659,-1.38567304257714,2.92534197468403));
#97506=CARTESIAN_POINT('Ctrl Pts',(0.271537341065049,-2.13564839618882,
3.0365283945152));
#97507=CARTESIAN_POINT('Ctrl Pts',(1.9419501920302,-0.92927716590924,3.14771481434636));
#97508=CARTESIAN_POINT('Ctrl Pts',(1.83345241771109,1.12835226385271,3.25890123417753));
#97509=CARTESIAN_POINT('Ctrl Pts',(0.045432686513366,2.15236206769919,3.37008765400868));
#97510=CARTESIAN_POINT('Ctrl Pts',(-1.78420535659039,1.20471483967528,3.48127407383985));
#97511=CARTESIAN_POINT('Ctrl Pts',(-1.97943388729784,-0.8465034466758,3.59246049367101));
#97512=CARTESIAN_POINT('Ctrl Pts',(-0.361415101720502,-2.12228785127793,
3.70364691350217));
#97513=CARTESIAN_POINT('Ctrl Pts',(1.58767559662444,-1.45396451102085,3.81483333333334));
#97514=CARTESIAN_POINT('Ctrl Pts',(2.08238656893164,0.546253399951339,3.9260197531645));
#97515=CARTESIAN_POINT('Ctrl Pts',(0.669541102087431,2.04607949797729,4.03720617299566));
#97516=CARTESIAN_POINT('Ctrl Pts',(-1.35663306156047,1.67160800898631,4.14839259282683));
#97517=CARTESIAN_POINT('Ctrl Pts',(-2.14007248481188,-0.234128937078206,
4.25957901265799));
#97518=CARTESIAN_POINT('Ctrl Pts',(-0.963112667326238,-1.92539361935742,
4.37076543248915));
#97519=CARTESIAN_POINT('Ctrl Pts',(1.09610013699538,-1.85291421525797,4.48195185232032));
#97520=CARTESIAN_POINT('Ctrl Pts',(2.15123766275159,-0.0830850033729405,
4.59313827215147));
#97521=CARTESIAN_POINT('Ctrl Pts',(1.23574816038915,1.76285367615161,4.70432469198265));
#97522=CARTESIAN_POINT('Ctrl Pts',(-0.811740268440561,1.99394190888763,
4.8155111118138));
#97523=CARTESIAN_POINT('Ctrl Pts',(-2.11563939493572,0.398492848144611,
4.92669753164497));
#97524=CARTESIAN_POINT('Ctrl Pts',(-1.48152105102257,-1.56199294966507,
5.03788395147612));
#97525=CARTESIAN_POINT('Ctrl Pts',(0.509734849759847,-2.0916254402657,5.1490703713073));
#97526=CARTESIAN_POINT('Ctrl Pts',(2.03405151388631,-0.705238284754304,
5.26025679113844));
#97527=CARTESIAN_POINT('Ctrl Pts',(1.69508874624462,1.32717773556567,5.37144321096963));
#97528=CARTESIAN_POINT('Ctrl Pts',(-0.19664885248515,2.1438413719869,5.48262963080077));
#97529=CARTESIAN_POINT('Ctrl Pts',(-1.90824757094816,0.996653303509719,
5.59381605063195));
#97530=CARTESIAN_POINT('Ctrl Pts',(-1.87180872723762,-1.06351242967042,
5.70500247046309));
#97531=CARTESIAN_POINT('Ctrl Pts',(-0.12071188305083,-2.14945463797604,
5.81618889029427));
#97532=CARTESIAN_POINT('Ctrl Pts',(1.74096228296046,-1.26640314621194,5.92737531012542));
#97533=CARTESIAN_POINT('Ctrl Pts',(2.00783946807991,0.776728568965356,6.0385617299566));
#97534=CARTESIAN_POINT('Ctrl Pts',(0.435448592570146,2.10834321747079,6.14974814978775));
#97535=CARTESIAN_POINT('Ctrl Pts',(-1.53583208518367,1.50862401066228,6.26093456961893));
#97536=CARTESIAN_POINT('Ctrl Pts',(-2.10022394255324,-0.473060239877022,
6.37212098945007));
#97537=CARTESIAN_POINT('Ctrl Pts',(-0.74071955267899,-2.02140078749996,
6.48330740928124));
#97538=CARTESIAN_POINT('Ctrl Pts',(1.29731608273796,-1.71805051756223,6.5944938291124));
#97539=CARTESIAN_POINT('Ctrl Pts',(2.14695390376071,0.15910856216126,6.70568024894357));
#97540=CARTESIAN_POINT('Ctrl Pts',(1.02988880574655,1.89051729619815,6.81686666877473));
#97541=CARTESIAN_POINT('Ctrl Pts',(-1.03059911890458,1.89013016894061,6.92805308860589));
#97542=CARTESIAN_POINT('Ctrl Pts',(-2.14701353924984,0.158301805751674,
7.03923950843705));
#97543=CARTESIAN_POINT('Ctrl Pts',(-1.29667041186295,-1.71853787925252,
7.15042592826822));
#97544=CARTESIAN_POINT('Ctrl Pts',(0.741479067384996,-2.0211223100189,7.26161234809938));
#97545=CARTESIAN_POINT('Ctrl Pts',(2.10040155266868,-0.472271020678894,
7.37279876793055));
#97546=CARTESIAN_POINT('Ctrl Pts',(1.53526509213771,1.50920101255294,7.48398518776171));
#97547=CARTESIAN_POINT('Ctrl Pts',(-0.436240798549652,2.10817944328893,
7.59517160759286));
#97548=CARTESIAN_POINT('Ctrl Pts',(-2.00813119194563,0.775974042967894,
7.70635802742404));
#97549=CARTESIAN_POINT('Ctrl Pts',(-1.74048629299744,-1.26705724547931,
7.81754444725519));
#97550=CARTESIAN_POINT('Ctrl Pts',(0.121519559390324,-2.14940912720278,
7.92873086708636));
#97551=CARTESIAN_POINT('Ctrl Pts',(1.87220822337856,-1.06280899870737,8.03991728691751));
#97552=CARTESIAN_POINT('Ctrl Pts',(1.90787293110882,0.997370281398245,8.15110370674869));
#97553=CARTESIAN_POINT('Ctrl Pts',(0.195843262983046,2.1439151139204,8.26229012657984));
#97554=CARTESIAN_POINT('Ctrl Pts',(-1.69558733042143,1.32654069078969,8.37347654641101));
#97555=CARTESIAN_POINT('Ctrl Pts',(-2.03378636810517,-0.706002555693802,
8.48466296624217));
#97556=CARTESIAN_POINT('Ctrl Pts',(-0.508948858861673,-2.09181683182873,
8.59584938607333));
#97557=CARTESIAN_POINT('Ctrl Pts',(1.48210788489943,-1.56143613926181,8.70703580590451));
#97558=CARTESIAN_POINT('Ctrl Pts',(2.11548950721726,0.399287798761521,8.81822222573564));
#97559=CARTESIAN_POINT('Ctrl Pts',(0.810990961415923,1.99424678906897,8.92940864556684));
#97560=CARTESIAN_POINT('Ctrl Pts',(-1.23641048638147,1.76238920508216,9.04059506539797));
#97561=CARTESIAN_POINT('Ctrl Pts',(-2.15120629331062,-0.0838933551026959,
9.15178148522916));
#97562=CARTESIAN_POINT('Ctrl Pts',(-1.09540379848118,-1.85332595276186,
9.26296790506031));
#97563=CARTESIAN_POINT('Ctrl Pts',(0.963836080712942,-1.9250315915564,9.37415432489147));
#97564=CARTESIAN_POINT('Ctrl Pts',(2.14016032912378,-0.233324742234878,
9.48534074472264));
#97565=CARTESIAN_POINT('Ctrl Pts',(1.35600480268067,1.67211762704833,9.5965271645538));
#97566=CARTESIAN_POINT('Ctrl Pts',(-0.67030982818557,2.04582783352242,9.70771358438496));
#97567=CARTESIAN_POINT('Ctrl Pts',(-2.08259181106143,0.545470747680921,
9.81890000421612));
#97568=CARTESIAN_POINT('Ctrl Pts',(-1.58712889620009,-1.45456074914393,
9.93008642404728));
#97569=CARTESIAN_POINT('Ctrl Pts',(0.362212090727357,-2.12215236818265,
10.0412728438785));
#97570=CARTESIAN_POINT('Ctrl Pts',(1.97975271162804,-0.845758688953388,
10.1524592637096));
#97571=CARTESIAN_POINT('Ctrl Pts',(1.78375086909329,1.20538347801125,10.2636456835408));
#97572=CARTESIAN_POINT('Ctrl Pts',(-0.0462382725911752,2.15234810763501,
10.3748321033719));
#97573=CARTESIAN_POINT('Ctrl Pts',(-1.83388235020868,1.12765702777161,10.4860185232031));
#97574=CARTESIAN_POINT('Ctrl Pts',(-1.94158931298892,-0.929994984054507,
10.5972049430343));
#97575=CARTESIAN_POINT('Ctrl Pts',(-0.270756821184746,-2.13577279771527,
10.7083913628654));
#97576=CARTESIAN_POINT('Ctrl Pts',(1.64817793797518,-1.38501096239512,10.8195777826966));
#97577=CARTESIAN_POINT('Ctrl Pts',(2.0571630907777,0.634330397736036,10.9307642025277));
#97578=CARTESIAN_POINT('Ctrl Pts',(0.58197770073898,2.07288432925282,11.0419506223589));
#97579=CARTESIAN_POINT('Ctrl Pts',(-1.42685805211597,1.61204019596003,11.1531370421901));
#97580=CARTESIAN_POINT('Ctrl Pts',(-2.12761151034289,-0.324461171008946,
11.2643234620212));
#97581=CARTESIAN_POINT('Ctrl Pts',(-0.881342614057178,-1.96574134576644,
11.3755098818524));
#97582=CARTESIAN_POINT('Ctrl Pts',(1.17620974724197,-1.80236812191326,11.4866963016836));
#97583=CARTESIAN_POINT('Ctrl Pts',(1.82356548323819,-0.598586618003602,
11.560820581571));
#97584=CARTESIAN_POINT('Ctrl Pts',(1.82115221868229,0.00725425160419088,
11.5978827215147));
#97585=CARTESIAN_POINT('Ctrl Pts',(-0.861525859670525,1.75382131162755,
-1.38777878078145E-16));
#97586=CARTESIAN_POINT('Ctrl Pts',(-1.44496782441849,1.46721837385112,0.0370621399437207));
#97587=CARTESIAN_POINT('Ctrl Pts',(-2.29323624142731,0.270948940037977,
0.111186419831162));
#97588=CARTESIAN_POINT('Ctrl Pts',(-1.4690228053469,-1.78453568564088,0.222372839662325));
#97589=CARTESIAN_POINT('Ctrl Pts',(0.702798023147504,-2.19964250335881,
0.333559259493488));
#97590=CARTESIAN_POINT('Ctrl Pts',(2.22983948348091,-0.602620646924488,
0.44474567932465));
#97591=CARTESIAN_POINT('Ctrl Pts',(1.71476659751129,1.54790339194469,0.555932099155814));
#97592=CARTESIAN_POINT('Ctrl Pts',(-0.371377304572895,2.2797075413722,0.667118518986976));
#97593=CARTESIAN_POINT('Ctrl Pts',(-2.11718147056775,0.923606631345987,
0.778304938818138));
#97594=CARTESIAN_POINT('Ctrl Pts',(-1.92363015131696,-1.2787712372945,0.889491358649302));
#97595=CARTESIAN_POINT('Ctrl Pts',(0.0320890232727887,-2.30962717925356,
1.00067777848046));
#97596=CARTESIAN_POINT('Ctrl Pts',(1.95839267869742,-1.22482325334233,1.11186419831163));
#97597=CARTESIAN_POINT('Ctrl Pts',(2.09073448897961,0.982002812028443,1.22305061814279));
#97598=CARTESIAN_POINT('Ctrl Pts',(0.3078671242282,2.28925546628532,1.33423703797395));
#97599=CARTESIAN_POINT('Ctrl Pts',(-1.75701689972769,1.49945932314417,1.44542345780511));
#97600=CARTESIAN_POINT('Ctrl Pts',(-2.21239878427269,-0.663911091192784,
1.55660987763628));
#97601=CARTESIAN_POINT('Ctrl Pts',(-0.641126576885465,-2.21910779030204,
1.66779629746744));
#97602=CARTESIAN_POINT('Ctrl Pts',(1.51744495713052,-1.74150671579767,1.7789827172986));
#97603=CARTESIAN_POINT('Ctrl Pts',(2.28597130487397,0.331390712847842,1.89016913712977));
#97604=CARTESIAN_POINT('Ctrl Pts',(0.960448643749269,2.10071953052146,2.00135555696093));
#97605=CARTESIAN_POINT('Ctrl Pts',(-1.24488658037438,1.94569829998722,2.11254197679209));
#97606=CARTESIAN_POINT('Ctrl Pts',(-2.30985172178094,0.00833292063536468,
2.22372839662325));
#97607=CARTESIAN_POINT('Ctrl Pts',(-1.2588924584139,-1.93666572611094,2.33491481645442));
#97608=CARTESIAN_POINT('Ctrl Pts',(0.945266903418065,-2.10759457362527,
2.44610123628558));
#97609=CARTESIAN_POINT('Ctrl Pts',(2.28352077714336,-0.347875342430591,
2.55728765611674));
#97610=CARTESIAN_POINT('Ctrl Pts',(1.52997054850621,1.73051278744978,2.6684740759479));
#97611=CARTESIAN_POINT('Ctrl Pts',(-0.625099077306038,2.22367613142842,
2.77966049577907));
#97612=CARTESIAN_POINT('Ctrl Pts',(-2.20755082977362,0.679855665342084,
2.89084691561023));
#97613=CARTESIAN_POINT('Ctrl Pts',(-1.76779024968342,-1.48674208393651,
3.00203333544139));
#97614=CARTESIAN_POINT('Ctrl Pts',(0.291342892527361,-2.29141958423335,
3.11321975527256));
#97615=CARTESIAN_POINT('Ctrl Pts',(2.08359330569799,-0.997057334412016,
3.22440617510372));
#97616=CARTESIAN_POINT('Ctrl Pts',(1.96718185643314,1.21065268979674,3.33559259493488));
#97617=CARTESIAN_POINT('Ctrl Pts',(0.0487464827201324,2.30935232741881,
3.44677901476604));
#97618=CARTESIAN_POINT('Ctrl Pts',(-1.91434278399063,1.29258504441778,3.55796543459721));
#97619=CARTESIAN_POINT('Ctrl Pts',(-2.12381100893932,-0.908246216603541,
3.66915185442837));
#97620=CARTESIAN_POINT('Ctrl Pts',(-0.38777621054007,-2.27708453998192,
3.78033827425954));
#97621=CARTESIAN_POINT('Ctrl Pts',(1.70347841995286,-1.56001463596674,3.89152469409069));
#97622=CARTESIAN_POINT('Ctrl Pts',(2.23427291426326,0.58609635407974,4.00271111392186));
#97623=CARTESIAN_POINT('Ctrl Pts',(0.718376487679439,2.19531765665651,4.11389753375301));
#97624=CARTESIAN_POINT('Ctrl Pts',(-1.45558396757891,1.79353274433565,4.22508395358419));
#97625=CARTESIAN_POINT('Ctrl Pts',(-2.29616635965357,-0.251205972206891,
4.33627037341534));
#97626=CARTESIAN_POINT('Ctrl Pts',(-1.03336074967814,-2.06582911991821,
4.44745679324651));
#97627=CARTESIAN_POINT('Ctrl Pts',(1.17604813820203,-1.98806317010017,4.55864321307767));
#97628=CARTESIAN_POINT('Ctrl Pts',(2.30814590995695,-0.0891451065749571,
4.66982963290884));
#97629=CARTESIAN_POINT('Ctrl Pts',(1.32588189186442,1.89143374203362,4.78101605273999));
#97630=CARTESIAN_POINT('Ctrl Pts',(-0.870947461077787,2.1393772252035,4.89220247257116));
#97631=CARTESIAN_POINT('Ctrl Pts',(-2.26995115459196,0.427558355600586,
5.00338889240232));
#97632=CARTESIAN_POINT('Ctrl Pts',(-1.58958111120973,-1.67592251687317,
5.11457531223348));
#97633=CARTESIAN_POINT('Ctrl Pts',(0.546914192237968,-2.24418565586851,
5.22576173206465));
#97634=CARTESIAN_POINT('Ctrl Pts',(2.1824123683356,-0.756677372605439,5.33694815189581));
#97635=CARTESIAN_POINT('Ctrl Pts',(1.81872613351991,1.4239802115651,5.44813457172697));
#97636=CARTESIAN_POINT('Ctrl Pts',(-0.210992142997687,2.30021014415434,
5.55932099155813));
#97637=CARTESIAN_POINT('Ctrl Pts',(-2.04743246287144,1.06934779265563,5.67050741138931));
#97638=CARTESIAN_POINT('Ctrl Pts',(-2.00833582118916,-1.14108352937273,
5.78169383122044));
#97639=CARTESIAN_POINT('Ctrl Pts',(-0.129516437895867,-2.30623283386393,
5.89288025105164));
#97640=CARTESIAN_POINT('Ctrl Pts',(1.86794562143574,-1.35877280920554,6.00406667088277));
#97641=CARTESIAN_POINT('Ctrl Pts',(2.15428845280213,0.83338205752262,6.11525309071395));
#97642=CARTESIAN_POINT('Ctrl Pts',(0.467209600008474,2.26212280421227,6.22643951054511));
#97643=CARTESIAN_POINT('Ctrl Pts',(-1.64785351575852,1.61866092257753,6.33762593037627));
#97644=CARTESIAN_POINT('Ctrl Pts',(-2.25341132081031,-0.507564587930634,
6.44881235020743));
#97645=CARTESIAN_POINT('Ctrl Pts',(-0.794746594271866,-2.1688389157728,
6.55999877003859));
#97646=CARTESIAN_POINT('Ctrl Pts',(1.39194049181108,-1.84336270411821,6.67118518986976));
#97647=CARTESIAN_POINT('Ctrl Pts',(2.30354969961477,0.170713716736379,6.78237160970093));
#97648=CARTESIAN_POINT('Ctrl Pts',(1.1050074456459,2.02840896683692,6.89355802953208));
#97649=CARTESIAN_POINT('Ctrl Pts',(-1.10576956804586,2.02799360306213,7.00474444936325));
#97650=CARTESIAN_POINT('Ctrl Pts',(-2.30361368483253,0.169848116649841,
7.11593086919441));
#97651=CARTESIAN_POINT('Ctrl Pts',(-1.39124772661127,-1.84388561328419,
7.22711728902557));
#97652=CARTESIAN_POINT('Ctrl Pts',(0.795561506911461,-2.16854012653626,
7.33830370885674));
#97653=CARTESIAN_POINT('Ctrl Pts',(2.25360188555757,-0.506717804195071,
7.44949012868789));
#97654=CARTESIAN_POINT('Ctrl Pts',(1.64724516703786,1.61928001017393,7.56067654851907));
#97655=CARTESIAN_POINT('Ctrl Pts',(-0.468059588377044,2.26194708457211,
7.67186296835021));
#97656=CARTESIAN_POINT('Ctrl Pts',(-2.154601454596,0.832572497460946,7.78304938818139));
#97657=CARTESIAN_POINT('Ctrl Pts',(-1.8674349134348,-1.35947461755279,7.89423580801255));
#97658=CARTESIAN_POINT('Ctrl Pts',(0.130383025010703,-2.30618400359892,
8.00542222784371));
#97659=CARTESIAN_POINT('Ctrl Pts',(2.00876445601631,-1.14032879114536,8.11660864767487));
#97660=CARTESIAN_POINT('Ctrl Pts',(2.04703049732954,1.07011706590215,8.22779506750604));
#97661=CARTESIAN_POINT('Ctrl Pts',(0.210127794931219,2.30028926472067,8.3389814873372));
#97662=CARTESIAN_POINT('Ctrl Pts',(-1.81926108372479,1.42329670163983,8.45016790716836));
#97663=CARTESIAN_POINT('Ctrl Pts',(-2.18212788319439,-0.757497388391501,
8.56135432699953));
#97664=CARTESIAN_POINT('Ctrl Pts',(-0.546070872270014,-2.24439100726275,
8.67254074683069));
#97665=CARTESIAN_POINT('Ctrl Pts',(1.59021074792356,-1.67532509350284,8.78372716666185));
#97666=CARTESIAN_POINT('Ctrl Pts',(2.26979033427429,0.428411288796547,8.89491358649301));
#97667=CARTESIAN_POINT('Ctrl Pts',(0.870143500653468,2.13970434291613,9.00610000632417));
#97668=CARTESIAN_POINT('Ctrl Pts',(-1.32659252698235,1.89093539309814,9.11728642615534));
#97669=CARTESIAN_POINT('Ctrl Pts',(-2.30811225247311,-0.0900124183420705,
9.2284728459865));
#97670=CARTESIAN_POINT('Ctrl Pts',(-1.17530100973675,-1.98850493915805,
9.33965926581767));
#97671=CARTESIAN_POINT('Ctrl Pts',(1.03413692781901,-2.06544068631896,9.45084568564882));
#97672=CARTESIAN_POINT('Ctrl Pts',(2.29626061120593,-0.250343120523647,
9.56203210547999));
#97673=CARTESIAN_POINT('Ctrl Pts',(1.45490988438074,1.79407953322179,9.67321852531115));
#97674=CARTESIAN_POINT('Ctrl Pts',(-0.719201283577143,2.19504763615053,
9.78440494514231));
#97675=CARTESIAN_POINT('Ctrl Pts',(-2.2344931264651,0.585256616254353,9.89559136497349));
#97676=CARTESIAN_POINT('Ctrl Pts',(-1.70289184396906,-1.56065436285928,
10.0067777848046));
#97677=CARTESIAN_POINT('Ctrl Pts',(0.388631330803272,-2.27693917494037,
10.1179642046358));
#97678=CARTESIAN_POINT('Ctrl Pts',(2.1241530878674,-0.907447137301155,10.229150624467));
#97679=CARTESIAN_POINT('Ctrl Pts',(1.91385514681521,1.29330245229283,10.3403370442981));
#97680=CARTESIAN_POINT('Ctrl Pts',(-0.0496108271125438,2.30933734912719,
10.4515234641293));
#97681=CARTESIAN_POINT('Ctrl Pts',(-1.96764314760194,1.20990674417448,10.5627098839605));
#97682=CARTESIAN_POINT('Ctrl Pts',(-2.08320610464741,-0.997827509202423,
10.6738963037916));
#97683=CARTESIAN_POINT('Ctrl Pts',(-0.290505442625618,-2.29155305943203,
10.7850827236228));
#97684=CARTESIAN_POINT('Ctrl Pts',(1.7683937169233,-1.48603171255794,10.8962691434539));
#97685=CARTESIAN_POINT('Ctrl Pts',(2.20720967111538,0.680597564112484,11.0074555632851));
#97686=CARTESIAN_POINT('Ctrl Pts',(0.624426335084105,2.22407759459687,11.1186419831163));
#97687=CARTESIAN_POINT('Ctrl Pts',(-1.53093107010227,1.72962013887028,11.2298284029474));
#97688=CARTESIAN_POINT('Ctrl Pts',(-2.28279649924591,-0.348126912135875,
11.3410148227786));
#97689=CARTESIAN_POINT('Ctrl Pts',(-0.945626503816835,-2.10911975270116,
11.4522012426097));
#97690=CARTESIAN_POINT('Ctrl Pts',(1.26200083066393,-1.93383031585166,11.5633876624409));
#97691=CARTESIAN_POINT('Ctrl Pts',(1.95657378287586,-0.642246683396576,
11.6375119423284));
#97692=CARTESIAN_POINT('Ctrl Pts',(1.95398449819998,0.0077833665056624,
11.6745740822721));
#97693=CARTESIAN_POINT('Ctrl Pts',(-1.95093054978418,-0.000550606481354719,
10.6241303078758));
#97694=CARTESIAN_POINT('Ctrl Pts',(-1.95166977968097,-0.292567552961119,
10.640718973181));
#97695=CARTESIAN_POINT('Ctrl Pts',(-1.89027401228485,-0.584289311968449,
10.6573076384863));
#97696=CARTESIAN_POINT('Ctrl Pts',(-1.7651621681362,-0.845492725344543,
10.6738963037916));
#97697=CARTESIAN_POINT('Ctrl Pts',(-1.48563921730681,-1.42906935927896,
10.7109584437353));
#97698=CARTESIAN_POINT('Ctrl Pts',(-0.888072329966215,-1.8603112093555,
10.7480205836791));
#97699=CARTESIAN_POINT('Ctrl Pts',(-0.246139026371096,-1.94167857658142,
10.7850827236228));
#97700=CARTESIAN_POINT('Ctrl Pts',(0.395794277224022,-2.02304594380734,
10.8221448635665));
#97701=CARTESIAN_POINT('Ctrl Pts',(1.08209399707366,-1.75453882818264,10.8592070035102));
#97702=CARTESIAN_POINT('Ctrl Pts',(1.49837984936383,-1.25918039092522,10.8962691434539));
#97703=CARTESIAN_POINT('Ctrl Pts',(1.91466570165399,-0.763821953667804,
10.9333312833977));
#97704=CARTESIAN_POINT('Ctrl Pts',(2.06093768638468,-0.041612194777677,
10.9703934233414));
#97705=CARTESIAN_POINT('Ctrl Pts',(1.87027645607817,0.576739356414784,11.0074555632851));
#97706=CARTESIAN_POINT('Ctrl Pts',(1.80418088670294,0.791100177355746,11.0203037088567));
#97707=CARTESIAN_POINT('Ctrl Pts',(1.69759382901609,0.992979671982257,11.0331518544284));
#97708=CARTESIAN_POINT('Ctrl Pts',(1.56057659382855,1.17255425406022,11.046));
#97709=CARTESIAN_POINT('Ctrl Pts',(-0.9055496143049,-1.2679201530598,4.59701721133854E-17));
#97710=CARTESIAN_POINT('Ctrl Pts',(-0.937460871048188,-1.25085822491965,
4.11134559556874E-17));
#97711=CARTESIAN_POINT('Ctrl Pts',(-0.968677330061127,-1.23263760516135,
2.44937731663795E-16));
#97712=CARTESIAN_POINT('Ctrl Pts',(-0.999128467894991,-1.21327242330634,
1.95156391047391E-16));
#97713=CARTESIAN_POINT('Ctrl Pts',(-1.04916478169554,-1.18145218981002,
1.19833509668E-16));
#97714=CARTESIAN_POINT('Ctrl Pts',(-1.09713600671012,-1.14654455097205,
1.20483738925504E-16));
#97715=CARTESIAN_POINT('Ctrl Pts',(-1.14296368523792,-1.10887020140839,
3.46944695195361E-17));
#97716=CARTESIAN_POINT('Ctrl Pts',(-1.1691715546085,-1.08732504652154,-1.4366579135275E-17));
#97717=CARTESIAN_POINT('Ctrl Pts',(-1.19467812556179,-1.06487409533188,
1.54611493479508E-16));
#97718=CARTESIAN_POINT('Ctrl Pts',(-1.21946596262297,-1.04157045589269,
1.28369537222284E-16));
#97719=CARTESIAN_POINT('Ctrl Pts',(-1.23288807387334,-1.02895200756582,
1.14160049906282E-16));
#97720=CARTESIAN_POINT('Ctrl Pts',(-1.24610308792281,-1.01607950194371,
2.35779340588765E-16));
#97721=CARTESIAN_POINT('Ctrl Pts',(-1.25908578368524,-1.0029839550804,2.28983498828939E-16));
#97722=CARTESIAN_POINT('Ctrl Pts',(-1.30296735026586,-0.95872095130156,
2.06013524941215E-16));
#97723=CARTESIAN_POINT('Ctrl Pts',(-1.34424080059494,-0.911874911049719,
3.41092537496216E-16));
#97724=CARTESIAN_POINT('Ctrl Pts',(-1.3828175432908,-0.862794893107178,
2.15105711021124E-16));
#97725=CARTESIAN_POINT('Ctrl Pts',(-1.41246270387874,-0.825078255778903,
1.18288316865636E-16));
#97726=CARTESIAN_POINT('Ctrl Pts',(-1.44051505756546,-0.786041114269597,
-3.41744083773187E-17));
#97727=CARTESIAN_POINT('Ctrl Pts',(-1.46692433972057,-0.745823635123971,
-2.77555756156289E-17));
#97728=CARTESIAN_POINT('Ctrl Pts',(-1.479951210132,-0.725985614308893,-2.45893667770833E-17));
#97729=CARTESIAN_POINT('Ctrl Pts',(-1.49257814628919,-0.705860181165347,
1.12314029669873E-16));
#97730=CARTESIAN_POINT('Ctrl Pts',(-1.50479813274716,-0.685463000140721,
1.31838984174237E-16));
#97731=CARTESIAN_POINT('Ctrl Pts',(-1.51107691151866,-0.674982678607113,
1.41871145034493E-16));
#97732=CARTESIAN_POINT('Ctrl Pts',(-1.51724344631134,-0.664438579506566,
2.39743182585592E-16));
#97733=CARTESIAN_POINT('Ctrl Pts',(-1.52329612440982,-0.653835068968427,
2.42861286636753E-16));
#97734=CARTESIAN_POINT('Ctrl Pts',(-1.55541704658302,-0.597563360607725,
2.59408734877987E-16));
#97735=CARTESIAN_POINT('Ctrl Pts',(-1.58434358367058,-0.539605423501723,
2.32306933354682E-17));
#97736=CARTESIAN_POINT('Ctrl Pts',(-1.60998194797531,-0.480314579840224,
1.38777878078145E-17));
#97737=CARTESIAN_POINT('Ctrl Pts',(-1.63611695660561,-0.419875204988797,
4.34370584461709E-18));
#97738=CARTESIAN_POINT('Ctrl Pts',(-1.65883591999594,-0.358049987819819,
-3.99522282745635E-16));
#97739=CARTESIAN_POINT('Ctrl Pts',(-1.67800508733892,-0.295172269836945,
-4.02455846426619E-16));
#97740=CARTESIAN_POINT('Ctrl Pts',(-1.69036857863681,-0.254618180804147,
-4.04347899868101E-16));
#97741=CARTESIAN_POINT('Ctrl Pts',(-1.70125468815875,-0.21362546632645,
2.10692284276142E-16));
#97742=CARTESIAN_POINT('Ctrl Pts',(-1.71061789501208,-0.172277279535232,
2.22044604925031E-16));
#97743=CARTESIAN_POINT('Ctrl Pts',(-1.71585060492304,-0.149169484288187,
2.28388948449886E-16));
#97744=CARTESIAN_POINT('Ctrl Pts',(-1.72060753217063,-0.125950592727189,
-7.81124113857471E-17));
#97745=CARTESIAN_POINT('Ctrl Pts',(-1.72487954070067,-0.102634681883505,
-6.93889390390723E-17));
#97746=CARTESIAN_POINT('Ctrl Pts',(-1.72700542719079,-0.0910319475914671,
-6.50478634353357E-17));
#97747=CARTESIAN_POINT('Ctrl Pts',(-1.7290114810898,-0.0794035343790101,
3.2530658909822E-16));
#97748=CARTESIAN_POINT('Ctrl Pts',(-1.73089565945358,-0.0677563287869385,
3.05311331771918E-16));
#97749=CARTESIAN_POINT('Ctrl Pts',(-1.74172479313661,-0.000815136373784872,
1.90390516006322E-16));
#97750=CARTESIAN_POINT('Ctrl Pts',(-1.74848828323664,0.0664709663887247,
1.66332759660732E-17));
#97751=CARTESIAN_POINT('Ctrl Pts',(-1.75106678678907,0.133744024330042,
0.));
#97752=CARTESIAN_POINT('Ctrl Pts',(-1.75197767455289,0.157509050853062,
-5.87590718476407E-18));
#97753=CARTESIAN_POINT('Ctrl Pts',(-1.75236592486458,0.181272742240003,
-1.43574718418596E-16));
#97754=CARTESIAN_POINT('Ctrl Pts',(-1.75222496230419,0.20502014676713,-1.52655665885959E-16));
#97755=CARTESIAN_POINT('Ctrl Pts',(-1.75184009030703,0.269858008556557,
-1.89868827307373E-16));
#97756=CARTESIAN_POINT('Ctrl Pts',(-1.74751402866387,0.334573792851957,
-3.30194805135327E-16));
#97757=CARTESIAN_POINT('Ctrl Pts',(-1.7394637798186,0.398932034828451,-3.60822483003176E-16));
#97758=CARTESIAN_POINT('Ctrl Pts',(-1.73512917103287,0.433585348839861,
-3.77313774654407E-16));
#97759=CARTESIAN_POINT('Ctrl Pts',(-1.72971393872322,0.468135193807322,
-2.30290250750647E-16));
#97760=CARTESIAN_POINT('Ctrl Pts',(-1.72324590502527,0.502545438383202,
-2.22044604925031E-16));
#97761=CARTESIAN_POINT('Ctrl Pts',(-1.71875224847293,0.526451903350239,
-2.16315955056648E-16));
#97762=CARTESIAN_POINT('Ctrl Pts',(-1.71375034317529,0.550290993458765,
-1.09112752506388E-16));
#97763=CARTESIAN_POINT('Ctrl Pts',(-1.70824837476028,0.574050543226345,
-1.11022302462516E-16));
#97764=CARTESIAN_POINT('Ctrl Pts',(-1.70556019910987,0.585659087356796,
-1.11955278682682E-16));
#97765=CARTESIAN_POINT('Ctrl Pts',(-1.70275214211861,0.597250589985584,
-1.86923780482983E-17));
#97766=CARTESIAN_POINT('Ctrl Pts',(-1.69982665236451,0.608817432227434,
-2.77555756156289E-17));
#97767=CARTESIAN_POINT('Ctrl Pts',(-1.68323412399998,0.674421202576402,
-7.91594003935956E-17));
#97768=CARTESIAN_POINT('Ctrl Pts',(-1.6629277813761,0.739001412074313,-4.05964646411352E-16));
#97769=CARTESIAN_POINT('Ctrl Pts',(-1.63916833994428,0.802303176749866,
-3.88578058618805E-16));
#97770=CARTESIAN_POINT('Ctrl Pts',(-1.61488642929252,0.866996944840365,
-3.70809140417215E-16));
#97771=CARTESIAN_POINT('Ctrl Pts',(-1.58699772603761,0.930356288581554,
-4.09457680297508E-17));
#97772=CARTESIAN_POINT('Ctrl Pts',(-1.55572518982035,0.992113582996803,
0.));
#97773=CARTESIAN_POINT('Ctrl Pts',(-1.52416508821539,1.05443876420538,4.13222832434933E-17));
#97774=CARTESIAN_POINT('Ctrl Pts',(-1.48915832892389,1.11513327578217,-2.91589739144645E-16));
#97775=CARTESIAN_POINT('Ctrl Pts',(-1.45088203376165,1.17391247934435,-2.77555756156289E-16));
#97776=CARTESIAN_POINT('Ctrl Pts',(-1.43586030613212,1.19698067814596,-2.72048047818399E-16));
#97777=CARTESIAN_POINT('Ctrl Pts',(-1.42033446520901,1.21975369583959,-2.46829292445535E-16));
#97778=CARTESIAN_POINT('Ctrl Pts',(-1.40431321996707,1.24221341255695,-2.22044604925031E-16));
#97779=CARTESIAN_POINT('Ctrl Pts',(-1.39827097600966,1.25068385824148,-2.12697320981403E-16));
#97780=CARTESIAN_POINT('Ctrl Pts',(-1.39215941512485,1.25910802930607,-2.5395452896005E-16));
#97781=CARTESIAN_POINT('Ctrl Pts',(-1.38598454691313,1.26747777400967,-2.4980018054066E-16));
#97782=CARTESIAN_POINT('Ctrl Pts',(-1.3431243018081,1.32557282918544,-2.20964521964367E-16));
#97783=CARTESIAN_POINT('Ctrl Pts',(-1.29714727100707,1.38114651172693,8.67497813555755E-17));
#97784=CARTESIAN_POINT('Ctrl Pts',(-1.24829449348075,1.43391808714502,5.55111512312578E-17));
#97785=CARTESIAN_POINT('Ctrl Pts',(-1.19933005104754,1.48681028483588,2.42011176187261E-17));
#97786=CARTESIAN_POINT('Ctrl Pts',(-1.14747626839011,1.53688856046327,-1.29713890200027E-16));
#97787=CARTESIAN_POINT('Ctrl Pts',(-1.09292624810297,1.58385401467225,-2.77555756156289E-17));
#97788=CARTESIAN_POINT('Ctrl Pts',(-1.03954323648884,1.62981471962349,7.20215071969156E-17));
#97789=CARTESIAN_POINT('Ctrl Pts',(-0.983577547054738,1.67279522220595,
1.33536308196711E-16));
#97790=CARTESIAN_POINT('Ctrl Pts',(-0.92517040004714,1.71248622994896,1.66533453693773E-16));
#97791=CARTESIAN_POINT('Ctrl Pts',(-0.904266808925204,1.72669141954621,
1.78342947445829E-16));
#97792=CARTESIAN_POINT('Ctrl Pts',(-0.883050159709791,1.74047492561567,
-1.31748417511445E-16));
#97793=CARTESIAN_POINT('Ctrl Pts',(-0.861525859670525,1.75382131162755,
-1.38777878078145E-16));
#97794=CARTESIAN_POINT('Origin',(0.,0.,0.));
#97795=CARTESIAN_POINT('Origin',(-0.866025403784439,-1.5,-4.));
#97796=CARTESIAN_POINT('',(-0.866025403784439,-1.5,-4.));
#97797=CARTESIAN_POINT('',(0.866025403784439,-1.5,-4.));
#97798=CARTESIAN_POINT('',(-0.43301270189222,-1.5,-4.));
#97799=CARTESIAN_POINT('',(-0.866025403784439,-1.5,-2.));
#97800=CARTESIAN_POINT('',(-0.866025403784439,-1.5,-4.));
#97801=CARTESIAN_POINT('',(0.866025403784439,-1.5,-2.));
#97802=CARTESIAN_POINT('',(-0.866025403784439,-1.5,-2.));
#97803=CARTESIAN_POINT('',(0.866025403784439,-1.5,-4.));
#97804=CARTESIAN_POINT('Origin',(-1.73205080756888,2.12115047744981E-16,
-4.));
#97805=CARTESIAN_POINT('',(-1.73205080756888,2.12115047744981E-16,-4.));
#97806=CARTESIAN_POINT('',(-1.51554445662277,-0.375,-4.));
#97807=CARTESIAN_POINT('',(-1.73205080756888,2.77555756156289E-16,-2.));
#97808=CARTESIAN_POINT('',(-1.73205080756888,2.12115047744981E-16,-4.));
#97809=CARTESIAN_POINT('',(-1.73205080756888,2.12115047744981E-16,-2.));
#97810=CARTESIAN_POINT('Origin',(-0.866025403784438,1.5,-4.));
#97811=CARTESIAN_POINT('',(-0.866025403784438,1.5,-4.));
#97812=CARTESIAN_POINT('',(-1.08253175473055,1.125,-4.));
#97813=CARTESIAN_POINT('',(-0.866025403784438,1.5,-2.));
#97814=CARTESIAN_POINT('',(-0.866025403784438,1.5,-4.));
#97815=CARTESIAN_POINT('',(-0.866025403784438,1.5,-2.));
#97816=CARTESIAN_POINT('Origin',(0.866025403784439,1.5,-4.));
#97817=CARTESIAN_POINT('',(0.866025403784439,1.5,-4.));
#97818=CARTESIAN_POINT('',(0.43301270189222,1.5,-4.));
#97819=CARTESIAN_POINT('',(0.866025403784439,1.5,-2.));
#97820=CARTESIAN_POINT('',(0.866025403784439,1.5,-4.));
#97821=CARTESIAN_POINT('',(0.866025403784439,1.5,-2.));
#97822=CARTESIAN_POINT('Origin',(1.73205080756888,0.,-4.));
#97823=CARTESIAN_POINT('',(1.73205080756888,0.,-4.));
#97824=CARTESIAN_POINT('',(1.51554445662277,0.375,-4.));
#97825=CARTESIAN_POINT('',(1.73205080756888,0.,-2.));
#97826=CARTESIAN_POINT('',(1.73205080756888,0.,-4.));
#97827=CARTESIAN_POINT('',(1.73205080756888,0.,-2.));
#97828=CARTESIAN_POINT('Origin',(0.866025403784439,-1.5,-4.));
#97829=CARTESIAN_POINT('',(1.08253175473055,-1.125,-4.));
#97830=CARTESIAN_POINT('',(0.866025403784439,-1.5,-2.));
#97831=CARTESIAN_POINT('Origin',(0.,2.77555756156289E-16,-2.));
#97832=CARTESIAN_POINT('Origin',(0.,0.,0.));
#97833=CARTESIAN_POINT('',(-3.5,-4.28626379701574E-16,0.));
#97834=CARTESIAN_POINT('Origin',(0.,0.,0.));
#97835=CARTESIAN_POINT('Origin',(0.,0.,-4.));
#97836=CARTESIAN_POINT('',(-3.5,-4.28626379701574E-16,-4.));
#97837=CARTESIAN_POINT('',(-3.5,-4.28626379701574E-16,-4.));
#97838=CARTESIAN_POINT('Origin',(0.,0.,-4.));
#97839=CARTESIAN_POINT('Origin',(0.,0.,-4.));
#97840=CARTESIAN_POINT('Origin',(0.,0.,12.));
#97841=CARTESIAN_POINT('',(0.,0.,0.));
#97842=CARTESIAN_POINT('Origin',(0.,0.,1.5));
#97843=CARTESIAN_POINT('',(-1.46525529183604,0.000949695766822006,1.6971550458429));
#97844=CARTESIAN_POINT('',(-1.46480951624159,0.00160986999158072,1.62584495415709));
#97845=CARTESIAN_POINT('',(-1.4635,-1.79227059055215E-16,1.5));
#97846=CARTESIAN_POINT('',(0.634778394200743,1.31997491940301,1.5365));
#97847=CARTESIAN_POINT('Ctrl Pts',(-1.46525529183604,0.000949695766822006,
1.6971550458429));
#97848=CARTESIAN_POINT('Ctrl Pts',(-1.46560042360025,0.0508589123847686,
1.69443173840928));
#97849=CARTESIAN_POINT('Ctrl Pts',(-1.46327194301474,0.100733436630517,
1.69170843097565));
#97850=CARTESIAN_POINT('Ctrl Pts',(-1.45816376909485,0.150318972596548,
1.68898512354203));
#97851=CARTESIAN_POINT('Ctrl Pts',(-1.40854101969113,0.632011777869308,
1.66252987662845));
#97852=CARTESIAN_POINT('Ctrl Pts',(-1.09660082073563,1.08643298898876,1.63607462971487));
#97853=CARTESIAN_POINT('Ctrl Pts',(-0.664946563931385,1.30626231522188,
1.60961938280129));
#97854=CARTESIAN_POINT('Ctrl Pts',(-0.267264988146981,1.50879031415148,
1.58524625520086));
#97855=CARTESIAN_POINT('Ctrl Pts',(0.232028362605538,1.51219969455982,1.56087312760043));
#97856=CARTESIAN_POINT('Ctrl Pts',(0.635549693826274,1.32090956116917,1.5365));
#97857=CARTESIAN_POINT('',(-0.634007094575224,1.31904027763684,1.5365));
#97858=CARTESIAN_POINT('Origin',(0.,0.,1.5365));
#97859=CARTESIAN_POINT('Ctrl Pts',(-0.634007094575223,1.31904027763684,
1.5365));
#97860=CARTESIAN_POINT('Ctrl Pts',(-1.07313362622406,1.10797065284846,1.5629924276156));
#97861=CARTESIAN_POINT('Ctrl Pts',(-1.39474726964411,0.662191250162446,
1.5894848552312));
#97862=CARTESIAN_POINT('Ctrl Pts',(-1.45449093825341,0.181719547981815,
1.6159772828468));
#97863=CARTESIAN_POINT('Ctrl Pts',(-1.46190854066243,0.122065560563132,
1.6192665066169));
#97864=CARTESIAN_POINT('Ctrl Pts',(-1.46528941928426,0.0618767915960723,
1.622555730387));
#97865=CARTESIAN_POINT('Ctrl Pts',(-1.46480951624159,0.00160986999158072,
1.62584495415709));
#97866=CARTESIAN_POINT('Origin',(0.,0.,1.5));
#97867=CARTESIAN_POINT('',(-1.4614685241241,0.000737543191909745,2.19715504584291));
#97868=CARTESIAN_POINT('',(-1.46136527585292,0.000666719787592705,2.12584495415709));
#97869=CARTESIAN_POINT('',(-1.4635,-1.79227059055215E-16,1.5));
#97870=CARTESIAN_POINT('Ctrl Pts',(-1.4614685241241,0.000737543191909745,
2.19715504584291));
#97871=CARTESIAN_POINT('Ctrl Pts',(-1.46236405755613,0.197387960890566,
2.18649655322409));
#97872=CARTESIAN_POINT('Ctrl Pts',(-1.4254536386906,0.393715781199002,2.17583806060528));
#97873=CARTESIAN_POINT('Ctrl Pts',(-1.34914194794588,0.57329973733799,2.16517956798647));
#97874=CARTESIAN_POINT('Ctrl Pts',(-1.15973011521814,1.01904174526409,2.13872432107289));
#97875=CARTESIAN_POINT('Ctrl Pts',(-0.727577748980252,1.36162935416534,
2.11226907415931));
#97876=CARTESIAN_POINT('Ctrl Pts',(-0.250375545979114,1.4443538101403,2.08581382724573));
#97877=CARTESIAN_POINT('Ctrl Pts',(0.226826657022025,1.52707826611526,2.05935858033215));
#97878=CARTESIAN_POINT('Ctrl Pts',(0.749078696786409,1.34993956916391,2.03290333341857));
#97879=CARTESIAN_POINT('Ctrl Pts',(1.0774669053887,0.99394958746392,2.00644808650499));
#97880=CARTESIAN_POINT('Ctrl Pts',(1.40585511399099,0.637959605763926,1.97999283959141));
#97881=CARTESIAN_POINT('Ctrl Pts',(1.54037949143119,0.103118339315282,1.95353759267783));
#97882=CARTESIAN_POINT('Ctrl Pts',(1.41950779864889,-0.365863204421494,
1.92708234576425));
#97883=CARTESIAN_POINT('Ctrl Pts',(1.29863610586659,-0.834844748158274,
1.90062709885067));
#97884=CARTESIAN_POINT('Ctrl Pts',(0.922368342861785,-1.23796656918318,
1.87417185193709));
#97885=CARTESIAN_POINT('Ctrl Pts',(0.46281817834948,-1.39089651991568,1.84771660502351));
#97886=CARTESIAN_POINT('Ctrl Pts',(0.0032680138371783,-1.54382647064818,
1.82126135810993));
#97887=CARTESIAN_POINT('Ctrl Pts',(-0.539564552182622,-1.44656455108827,
1.79480611119635));
#97888=CARTESIAN_POINT('Ctrl Pts',(-0.917328185266559,-1.14345139159528,
1.76835086428277));
#97889=CARTESIAN_POINT('Ctrl Pts',(-1.25620476832629,-0.871540750195342,
1.74461892480281));
#97890=CARTESIAN_POINT('Ctrl Pts',(-1.46224768203056,-0.43397825017276,
1.72088698532286));
#97891=CARTESIAN_POINT('Ctrl Pts',(-1.46525529183604,0.000949695766822006,
1.6971550458429));
#97892=CARTESIAN_POINT('Ctrl Pts',(-1.46480951624159,0.00160986999158072,
1.62584495415709));
#97893=CARTESIAN_POINT('Ctrl Pts',(-1.46142413145071,-0.423531672472968,
1.6490481580026));
#97894=CARTESIAN_POINT('Ctrl Pts',(-1.2659135554708,-0.852562347168596,
1.6722513618481));
#97895=CARTESIAN_POINT('Ctrl Pts',(-0.940041506572989,-1.12518455749419,
1.6954545656936));
#97896=CARTESIAN_POINT('Ctrl Pts',(-0.567974712484741,-1.43645295911432,
1.72194699330921));
#97897=CARTESIAN_POINT('Ctrl Pts',(-0.0259674305097102,-1.54382576067933,
1.74843942092481));
#97898=CARTESIAN_POINT('Ctrl Pts',(0.437021120548429,-1.39911789592959,
1.77493184854041));
#97899=CARTESIAN_POINT('Ctrl Pts',(0.90000967160657,-1.25441003117985,1.80142427615601));
#97900=CARTESIAN_POINT('Ctrl Pts',(1.28397949174782,-0.857621500115369,
1.82791670377161));
#97901=CARTESIAN_POINT('Ctrl Pts',(1.41302018650067,-0.390197195079815,
1.85440913138721));
#97902=CARTESIAN_POINT('Ctrl Pts',(1.54206088125353,0.077227109955738,1.88090155900281));
#97903=CARTESIAN_POINT('Ctrl Pts',(1.41617245061799,0.615287188962364,1.90739398661841));
#97904=CARTESIAN_POINT('Ctrl Pts',(1.09299120959979,0.976927736970011,1.93388641423401));
#97905=CARTESIAN_POINT('Ctrl Pts',(0.769809968581594,1.33856828497766,1.96037884184961));
#97906=CARTESIAN_POINT('Ctrl Pts',(0.249335917180731,1.52378930198633,1.98687126946521));
#97907=CARTESIAN_POINT('Ctrl Pts',(-0.229668412333123,1.44778809968151,
2.01336369708081));
#97908=CARTESIAN_POINT('Ctrl Pts',(-0.708672741846977,1.37178689737668,
2.03985612469641));
#97909=CARTESIAN_POINT('Ctrl Pts',(-1.14620734947382,1.03456347575836,2.06634855231202));
#97910=CARTESIAN_POINT('Ctrl Pts',(-1.341629748858,0.590704472867507,2.09284097992762));
#97911=CARTESIAN_POINT('Ctrl Pts',(-1.42278143902801,0.40638625553278,2.10384230467077));
#97912=CARTESIAN_POINT('Ctrl Pts',(-1.46218248842652,0.203679441111252,
2.11484362941393));
#97913=CARTESIAN_POINT('Ctrl Pts',(-1.46136527585292,0.000666719787592705,
2.12584495415709));
#97914=CARTESIAN_POINT('Origin',(0.,0.,1.5));
#97915=CARTESIAN_POINT('',(-1.46259036218787,-0.00125761512241085,2.69715504584291));
#97916=CARTESIAN_POINT('',(-1.46263205222363,-0.00127650937794421,2.62584495415709));
#97917=CARTESIAN_POINT('',(-1.4635,-1.79227059055215E-16,1.5));
#97918=CARTESIAN_POINT('Ctrl Pts',(-1.46259036218787,-0.00125761512241085,
2.69715504584291));
#97919=CARTESIAN_POINT('Ctrl Pts',(-1.45978189217964,0.341135402893971,
2.67856136803891));
#97920=CARTESIAN_POINT('Ctrl Pts',(-1.33980853805453,0.685301349364496,
2.65996769023491));
#97921=CARTESIAN_POINT('Ctrl Pts',(-1.12026825930454,0.945438767331802,
2.64137401243091));
#97922=CARTESIAN_POINT('Ctrl Pts',(-0.807904436341066,1.31556455397457,
2.61491876551733));
#97923=CARTESIAN_POINT('Ctrl Pts',(-0.29397885919297,1.51558427707796,2.58846351860376));
#97924=CARTESIAN_POINT('Ctrl Pts',(0.186407751449748,1.45399701420947,2.56200827169017));
#97925=CARTESIAN_POINT('Ctrl Pts',(0.666794362092466,1.39240975134098,2.53555302477659));
#97926=CARTESIAN_POINT('Ctrl Pts',(1.1136420062298,1.0692155025006,2.50909777786301));
#97927=CARTESIAN_POINT('Ctrl Pts',(1.32253535862374,0.632262476730894,2.48264253094943));
#97928=CARTESIAN_POINT('Ctrl Pts',(1.53142871101768,0.195309450961193,2.45618728403585));
#97929=CARTESIAN_POINT('Ctrl Pts',(1.50236777166822,-0.355402351737828,
2.42973203712227));
#97930=CARTESIAN_POINT('Ctrl Pts',(1.24864693348105,-0.767943031297834,
2.40327679020869));
#97931=CARTESIAN_POINT('Ctrl Pts',(0.994926095293888,-1.18048371085784,
2.37682154329511));
#97932=CARTESIAN_POINT('Ctrl Pts',(0.516545358269026,-1.45485326727883,
2.35036629638153));
#97933=CARTESIAN_POINT('Ctrl Pts',(0.0323448230311008,-1.46554008895436,
2.32391104946795));
#97934=CARTESIAN_POINT('Ctrl Pts',(-0.451855712206826,-1.47622691062988,
2.29745580255437));
#97935=CARTESIAN_POINT('Ctrl Pts',(-0.941876045657816,-1.22323099755994,
2.27100055564079));
#97936=CARTESIAN_POINT('Ctrl Pts',(-1.21355056277452,-0.822284837549497,
2.24454530872721));
#97937=CARTESIAN_POINT('Ctrl Pts',(-1.37577076843208,-0.582874939172598,
2.22874855443244));
#97938=CARTESIAN_POINT('Ctrl Pts',(-1.46014127062829,-0.290714394849191,
2.21295180013767));
#97939=CARTESIAN_POINT('Ctrl Pts',(-1.4614685241241,0.000737543191909745,
2.19715504584291));
#97940=CARTESIAN_POINT('Ctrl Pts',(-1.46136527585292,0.000666719787592705,
2.12584495415709));
#97941=CARTESIAN_POINT('Ctrl Pts',(-1.46021454861399,-0.285198030491227,
2.14133605702953));
#97942=CARTESIAN_POINT('Ctrl Pts',(-1.37931982337241,-0.571669327104881,
2.15682715990198));
#97943=CARTESIAN_POINT('Ctrl Pts',(-1.22295946869643,-0.808260688939142,
2.17231826277442));
#97944=CARTESIAN_POINT('Ctrl Pts',(-0.955556598009147,-1.21287226369156,
2.19881069039002));
#97945=CARTESIAN_POINT('Ctrl Pts',(-0.46744066549306,-1.47160082903303,
2.22530311800562));
#97946=CARTESIAN_POINT('Ctrl Pts',(0.0175118003368193,-1.46580470042692,
2.25179554562122));
#97947=CARTESIAN_POINT('Ctrl Pts',(0.5024642661667,-1.4600085718208,2.27828797323682));
#97948=CARTESIAN_POINT('Ctrl Pts',(0.984253265310373,-1.18968774926711,
2.30478040085242));
#97949=CARTESIAN_POINT('Ctrl Pts',(1.24191574323231,-0.778810666555506,
2.33127282846802));
#97950=CARTESIAN_POINT('Ctrl Pts',(1.49957822115425,-0.367933583843902,
2.35776525608362));
#97951=CARTESIAN_POINT('Ctrl Pts',(1.53311417785445,0.18349975902561,2.38425768369922));
#97952=CARTESIAN_POINT('Ctrl Pts',(1.32714061082512,0.622574829610301,2.41075011131483));
#97953=CARTESIAN_POINT('Ctrl Pts',(1.1211670437958,1.06164990019499,2.43724253893043));
#97954=CARTESIAN_POINT('Ctrl Pts',(0.675683953036955,1.38836669849486,2.46373496654603));
#97955=CARTESIAN_POINT('Ctrl Pts',(0.195008236264954,1.45288333216258,2.49022739416163));
#97956=CARTESIAN_POINT('Ctrl Pts',(-0.285667480507048,1.5173999658303,2.51671982177723));
#97957=CARTESIAN_POINT('Ctrl Pts',(-0.801535823292203,1.31971643486587,
2.54321224939283));
#97958=CARTESIAN_POINT('Ctrl Pts',(-1.11600018720209,0.950496442197177,
2.56970467700843));
#97959=CARTESIAN_POINT('Ctrl Pts',(-1.33812801934386,0.689690939356804,
2.58841810272465));
#97960=CARTESIAN_POINT('Ctrl Pts',(-1.45976393507324,0.343296125582627,
2.60713152844087));
#97961=CARTESIAN_POINT('Ctrl Pts',(-1.46263205222363,-0.00127650937794421,
2.62584495415709));
#97962=CARTESIAN_POINT('Origin',(0.,0.,1.5));
#97963=CARTESIAN_POINT('',(-1.46589691679833,2.51587256358082E-5,3.19715504584291));
#97964=CARTESIAN_POINT('',(-1.4659121055392,-2.30038015023067E-5,3.12584495415709));
#97965=CARTESIAN_POINT('',(-1.4635,-1.79227059055215E-16,1.5));
#97966=CARTESIAN_POINT('Ctrl Pts',(-1.46589691679833,2.51587256358082E-5,
3.19715504584291));
#97967=CARTESIAN_POINT('Ctrl Pts',(-1.46602006156727,0.485691716639563,
3.17062618285372));
#97968=CARTESIAN_POINT('Ctrl Pts',(-1.20059041316976,0.971241251667598,
3.14409731986454));
#97969=CARTESIAN_POINT('Ctrl Pts',(-0.791886448608901,1.23360092154244,
3.11756845687536));
#97970=CARTESIAN_POINT('Ctrl Pts',(-0.384316614144986,1.49523255835758,
3.09111320996178));
#97971=CARTESIAN_POINT('Ctrl Pts',(0.165731625546887,1.53491129473518,3.0646579630482));
#97972=CARTESIAN_POINT('Ctrl Pts',(0.606632808874546,1.33448567256543,3.03820271613462));
#97973=CARTESIAN_POINT('Ctrl Pts',(1.0475339922022,1.13406005039567,3.01174746922104));
#97974=CARTESIAN_POINT('Ctrl Pts',(1.37928811916564,0.693530069678565,2.98529222230746));
#97975=CARTESIAN_POINT('Ctrl Pts',(1.45013070704306,0.21442088182498,2.95883697539388));
#97976=CARTESIAN_POINT('Ctrl Pts',(1.52097329492047,-0.264688306028604,
2.9323817284803));
#97977=CARTESIAN_POINT('Ctrl Pts',(1.33090434371185,-0.782376701018668,
2.90592648156672));
#97978=CARTESIAN_POINT('Ctrl Pts',(0.966872935492584,-1.10182217990777,
2.87947123465314));
#97979=CARTESIAN_POINT('Ctrl Pts',(0.602841527273315,-1.42126765879688,
2.85301598773956));
#97980=CARTESIAN_POINT('Ctrl Pts',(0.0648476620433925,-1.54247022158503,
2.82656074082597));
#97981=CARTESIAN_POINT('Ctrl Pts',(-0.400997606678097,-1.40998449219611,
2.80010549391239));
#97982=CARTESIAN_POINT('Ctrl Pts',(-0.866842875399587,-1.27749876280719,
2.77365024699881));
#97983=CARTESIAN_POINT('Ctrl Pts',(-1.26053954761264,-0.891324741241199,
2.74719500008523));
#97984=CARTESIAN_POINT('Ctrl Pts',(-1.40198684932975,-0.42812180536714,
2.72073975317166));
#97985=CARTESIAN_POINT('Ctrl Pts',(-1.44402001354272,-0.290474180907939,
2.71287818406207));
#97986=CARTESIAN_POINT('Ctrl Pts',(-1.46377780779679,-0.146024368754987,
2.70501661495249));
#97987=CARTESIAN_POINT('Ctrl Pts',(-1.46259036218787,-0.00125761512241085,
2.69715504584291));
#97988=CARTESIAN_POINT('Ctrl Pts',(-1.46263205222363,-0.00127650937794421,
2.62584495415709));
#97989=CARTESIAN_POINT('Ctrl Pts',(-1.46382430259504,-0.144512238767108,
2.63362395605647));
#97990=CARTESIAN_POINT('Ctrl Pts',(-1.44449359920879,-0.287433097526545,
2.64140295795585));
#97991=CARTESIAN_POINT('Ctrl Pts',(-1.40332716769488,-0.423760233432524,
2.64918195985523));
#97992=CARTESIAN_POINT('Ctrl Pts',(-1.26312939924317,-0.888040462020593,
2.67567438747083));
#97993=CARTESIAN_POINT('Ctrl Pts',(-0.869673477305141,-1.27584446482379,
2.70216681508643));
#97994=CARTESIAN_POINT('Ctrl Pts',(-0.403413676639095,-1.40931076214327,
2.72865924270203));
#97995=CARTESIAN_POINT('Ctrl Pts',(0.0628461240269517,-1.54277705946275,
2.75515167031764));
#97996=CARTESIAN_POINT('Ctrl Pts',(0.60190980342101,-1.42190565129851,2.78164409793324));
#97997=CARTESIAN_POINT('Ctrl Pts',(0.966541978861424,-1.1021326097128,2.80813652554884));
#97998=CARTESIAN_POINT('Ctrl Pts',(1.33117415430184,-0.782359568127089,
2.83462895316444));
#97999=CARTESIAN_POINT('Ctrl Pts',(1.5213748257886,-0.2636848931199,2.86112138078004));
#98000=CARTESIAN_POINT('Ctrl Pts',(1.44991055958715,0.216007011932497,2.88761380839564));
#98001=CARTESIAN_POINT('Ctrl Pts',(1.37844629338569,0.695698916984895,2.91410623601124));
#98002=CARTESIAN_POINT('Ctrl Pts',(1.04531708949601,1.1364080520825,2.94059866362684));
#98003=CARTESIAN_POINT('Ctrl Pts',(0.603308917416615,1.33600821530422,2.96709109124244));
#98004=CARTESIAN_POINT('Ctrl Pts',(0.161300745337218,1.53560837852595,2.99358351885804));
#98005=CARTESIAN_POINT('Ctrl Pts',(-0.389586394931897,1.49409956987179,
3.02007594647365));
#98006=CARTESIAN_POINT('Ctrl Pts',(-0.796694351740858,1.23051930167043,
3.04656837408925));
#98007=CARTESIAN_POINT('Ctrl Pts',(-1.20277424499078,0.967604648729325,
3.07299390077853));
#98008=CARTESIAN_POINT('Ctrl Pts',(-1.46580020468142,0.483738707465732,
3.09941942746781));
#98009=CARTESIAN_POINT('Ctrl Pts',(-1.4659121055392,-2.30038015023067E-5,
3.12584495415709));
#98010=CARTESIAN_POINT('Origin',(0.,0.,1.5));
#98011=CARTESIAN_POINT('',(-1.46251725547464,0.00124142858279441,3.69715504584291));
#98012=CARTESIAN_POINT('',(-1.46270047602225,0.00128924121849956,3.62584495415709));
#98013=CARTESIAN_POINT('',(-1.4635,-1.79227059055215E-16,1.5));
#98014=CARTESIAN_POINT('Ctrl Pts',(-1.46251725547464,0.00124142858279441,
3.69715504584291));
#98015=CARTESIAN_POINT('Ctrl Pts',(-1.46370702332812,0.148738027985318,
3.68914624458212));
#98016=CARTESIAN_POINT('Ctrl Pts',(-1.44318698960211,0.29591124700834,3.68113744332133));
#98017=CARTESIAN_POINT('Ctrl Pts',(-1.3995889627392,0.435896908748289,3.67312864206055));
#98018=CARTESIAN_POINT('Ctrl Pts',(-1.25557283247876,0.898307589835359,
3.64667339514697));
#98019=CARTESIAN_POINT('Ctrl Pts',(-0.859738774933637,1.28229049054632,
3.62021814823338));
#98020=CARTESIAN_POINT('Ctrl Pts',(-0.393165322540272,1.41218851737299,
3.5937629013198));
#98021=CARTESIAN_POINT('Ctrl Pts',(0.0734081298530866,1.54208654419966,
3.56730765440622));
#98022=CARTESIAN_POINT('Ctrl Pts',(0.610720977094688,1.41789969714205,3.54085240749265));
#98023=CARTESIAN_POINT('Ctrl Pts',(0.972973698680865,1.09643858054909,3.51439716057907));
#98024=CARTESIAN_POINT('Ctrl Pts',(1.33522642026705,0.774977463956125,3.48794191366548));
#98025=CARTESIAN_POINT('Ctrl Pts',(1.52241901619781,0.256242077827795,3.4614866667519));
#98026=CARTESIAN_POINT('Ctrl Pts',(1.44891822705338,-0.222466516044172,
3.43503141983832));
#98027=CARTESIAN_POINT('Ctrl Pts',(1.37541743790895,-0.701175109916134,
3.40857617292474));
#98028=CARTESIAN_POINT('Ctrl Pts',(1.04122326368934,-1.13985691153173,3.38212092601116));
#98029=CARTESIAN_POINT('Ctrl Pts',(0.599216411302075,-1.33783222868339,
3.35566567909758));
#98030=CARTESIAN_POINT('Ctrl Pts',(0.157209558914809,-1.53580754583504,
3.329210432184));
#98031=CARTESIAN_POINT('Ctrl Pts',(-0.392609971640119,-1.49307637852275,
3.30275518527042));
#98032=CARTESIAN_POINT('Ctrl Pts',(-0.798721343475862,-1.2291865579612,
3.27629993835684));
#98033=CARTESIAN_POINT('Ctrl Pts',(-1.2037026436268,-0.966031054227035,
3.24991830751886));
#98034=CARTESIAN_POINT('Ctrl Pts',(-1.46577445546874,-0.482946005415922,
3.22353667668088));
#98035=CARTESIAN_POINT('Ctrl Pts',(-1.46589691679833,2.51587256358082E-5,
3.19715504584291));
#98036=CARTESIAN_POINT('Ctrl Pts',(-1.4659121055392,-2.30038015023067E-5,
3.12584495415709));
#98037=CARTESIAN_POINT('Ctrl Pts',(-1.46602457299087,-0.486234172896521,
3.15240428269901));
#98038=CARTESIAN_POINT('Ctrl Pts',(-1.19994098143382,-0.972338508168191,
3.17896361124093));
#98039=CARTESIAN_POINT('Ctrl Pts',(-0.790477244895931,-1.23452231773249,
3.20552293978285));
#98040=CARTESIAN_POINT('Ctrl Pts',(-0.38204491633302,-1.49604570624368,
3.23201536739845));
#98041=CARTESIAN_POINT('Ctrl Pts',(0.169044599898504,-1.53477522966941,
3.25850779501405));
#98042=CARTESIAN_POINT('Ctrl Pts',(0.610040324245935,-1.33294802468893,
3.28500022262965));
#98043=CARTESIAN_POINT('Ctrl Pts',(1.05103604859337,-1.13112081970845,3.31149265024525));
#98044=CARTESIAN_POINT('Ctrl Pts',(1.3819379810567,-0.688736886321762,3.33798507786085));
#98045=CARTESIAN_POINT('Ctrl Pts',(1.45098168736653,-0.208690620830843,
3.36447750547645));
#98046=CARTESIAN_POINT('Ctrl Pts',(1.52002539367635,0.271355644660077,3.39096993309206));
#98047=CARTESIAN_POINT('Ctrl Pts',(1.32721087383265,0.789064242255226,3.41746236070766));
#98048=CARTESIAN_POINT('Ctrl Pts',(0.960970329747572,1.10699397323845,3.44395478832326));
#98049=CARTESIAN_POINT('Ctrl Pts',(0.594729785662495,1.42492370422168,3.47044721593886));
#98050=CARTESIAN_POINT('Ctrl Pts',(0.0550632173360358,1.54307456859298,
3.49693964355446));
#98051=CARTESIAN_POINT('Ctrl Pts',(-0.410517400180608,1.40725800636496,
3.52343207117006));
#98052=CARTESIAN_POINT('Ctrl Pts',(-0.876098017697253,1.27144144413694,
3.54992449878566));
#98053=CARTESIAN_POINT('Ctrl Pts',(-1.26759268440408,0.881657455309607,
3.57641692640127));
#98054=CARTESIAN_POINT('Ctrl Pts',(-1.40544679374999,0.416676063609308,
3.60290935401687));
#98055=CARTESIAN_POINT('Ctrl Pts',(-1.44522881216322,0.282491465310414,
3.61055455406361));
#98056=CARTESIAN_POINT('Ctrl Pts',(-1.46388796216068,0.142044521341646,
3.61819975411035));
#98057=CARTESIAN_POINT('Ctrl Pts',(-1.46270047602225,0.00128924121849956,
3.62584495415709));
#98058=CARTESIAN_POINT('Origin',(0.,0.,1.5));
#98059=CARTESIAN_POINT('',(-1.46151108967999,-0.00077281416562866,4.1971550458429));
#98060=CARTESIAN_POINT('',(-1.46133707147782,-0.000619497695943445,4.12584495415709));
#98061=CARTESIAN_POINT('',(-1.4635,-1.79227059055215E-16,1.5));
#98062=CARTESIAN_POINT('Ctrl Pts',(-1.46151108967999,-0.00077281416562866,
4.1971550458429));
#98063=CARTESIAN_POINT('Ctrl Pts',(-1.46010153861599,0.293373523763635,
4.18121105939693));
#98064=CARTESIAN_POINT('Ctrl Pts',(-1.3740385803959,0.588278752366279,4.16526707295096));
#98065=CARTESIAN_POINT('Ctrl Pts',(-1.20896762909038,0.829007033345531,
4.14932308650499));
#98066=CARTESIAN_POINT('Ctrl Pts',(-0.935071712918766,1.22843826304259,
4.12286783959141));
#98067=CARTESIAN_POINT('Ctrl Pts',(-0.443654974734093,1.47871225280756,
4.09641259267783));
#98068=CARTESIAN_POINT('Ctrl Pts',(0.040478713720523,1.46533847823884,4.06995734576425));
#98069=CARTESIAN_POINT('Ctrl Pts',(0.524612402175147,1.45196470367013,4.04350209885067));
#98070=CARTESIAN_POINT('Ctrl Pts',(1.00146304089972,1.17494316476773,4.01704685193709));
#98071=CARTESIAN_POINT('Ctrl Pts',(1.2528902039326,0.761000336383063,3.99059160502351));
#98072=CARTESIAN_POINT('Ctrl Pts',(1.50431736696549,0.347057507998399,3.96413635810993));
#98073=CARTESIAN_POINT('Ctrl Pts',(1.53032105430668,-0.203806609868528,
3.93768111119635));
#98074=CARTESIAN_POINT('Ctrl Pts',(1.31900559551541,-0.639593324011289,
3.91122586428277));
#98075=CARTESIAN_POINT('Ctrl Pts',(1.10769013672413,-1.07538003815405,3.88477061736919));
#98076=CARTESIAN_POINT('Ctrl Pts',(0.659055531800388,-1.39608934857265,
3.85831537045561));
#98077=CARTESIAN_POINT('Ctrl Pts',(0.17833449170055,-1.45500934316093,3.83186012354203));
#98078=CARTESIAN_POINT('Ctrl Pts',(-0.302386548399288,-1.51392933774921,
3.80540487662844));
#98079=CARTESIAN_POINT('Ctrl Pts',(-0.815194023675217,-1.31106001650717,
3.77894962971486));
#98080=CARTESIAN_POINT('Ctrl Pts',(-1.1254986598253,-0.93920612515456,3.75249438280128));
#98081=CARTESIAN_POINT('Ctrl Pts',(-1.34186472230247,-0.6799236236522,3.73404793714849));
#98082=CARTESIAN_POINT('Ctrl Pts',(-1.45977689679497,-0.338483321258646,
3.7156014914957));
#98083=CARTESIAN_POINT('Ctrl Pts',(-1.46251725547464,0.00124142858279441,
3.69715504584291));
#98084=CARTESIAN_POINT('Ctrl Pts',(-1.46270047602225,0.00128924121849956,
3.62584495415709));
#98085=CARTESIAN_POINT('Ctrl Pts',(-1.45977304163873,-0.345705838018082,
3.64469218172595));
#98086=CARTESIAN_POINT('Ctrl Pts',(-1.33622982194822,-0.694574796895743,
3.6635394092948));
#98087=CARTESIAN_POINT('Ctrl Pts',(-1.11119159617627,-0.956113418246287,
3.68238663686366));
#98088=CARTESIAN_POINT('Ctrl Pts',(-0.794868737271672,-1.32374271382832,
3.70887906447926));
#98089=CARTESIAN_POINT('Ctrl Pts',(-0.2780094674775,-1.51882251041912,3.73537149209487));
#98090=CARTESIAN_POINT('Ctrl Pts',(0.202334547739988,-1.45188166285187,
3.76186391971047));
#98091=CARTESIAN_POINT('Ctrl Pts',(0.682678562957472,-1.38494081528463,
3.78835634732607));
#98092=CARTESIAN_POINT('Ctrl Pts',(1.12650732359827,-1.05597932355936,3.81484877494167));
#98093=CARTESIAN_POINT('Ctrl Pts',(1.33026378228211,-0.615871659935628,
3.84134120255727));
#98094=CARTESIAN_POINT('Ctrl Pts',(1.53402024096595,-0.175763996311893,
3.86783363017287));
#98095=CARTESIAN_POINT('Ctrl Pts',(1.49770439769281,0.375489839210297,3.89432605778847));
#98096=CARTESIAN_POINT('Ctrl Pts',(1.23797210363236,0.785063502320118,3.92081848540407));
#98097=CARTESIAN_POINT('Ctrl Pts',(0.978239809571907,1.19463716542994,3.94731091301968));
#98098=CARTESIAN_POINT('Ctrl Pts',(0.495091064724133,1.46253065612739,3.97380334063527));
#98099=CARTESIAN_POINT('Ctrl Pts',(0.0101165833239452,1.46587765078508,
4.00029576825087));
#98100=CARTESIAN_POINT('Ctrl Pts',(-0.474857898076236,1.46922464544276,
4.02678819586647));
#98101=CARTESIAN_POINT('Ctrl Pts',(-0.961658116028831,1.20802514406069,
4.05328062348208));
#98102=CARTESIAN_POINT('Ctrl Pts',(-1.22701865007136,0.802075347968294,
4.07977305109768));
#98103=CARTESIAN_POINT('Ctrl Pts',(-1.38084455305005,0.566751756337598,
4.09513035211748));
#98104=CARTESIAN_POINT('Ctrl Pts',(-1.46025866906375,0.28278680150174,4.11048765313729));
#98105=CARTESIAN_POINT('Ctrl Pts',(-1.46133707147782,-0.000619497695943445,
4.12584495415709));
#98106=CARTESIAN_POINT('Origin',(0.,0.,1.5));
#98107=CARTESIAN_POINT('',(-1.46533193762214,-0.000810224173804775,4.6971550458429));
#98108=CARTESIAN_POINT('',(-1.46497413376758,-0.00101984791970569,4.62584495415709));
#98109=CARTESIAN_POINT('',(-1.4635,-1.79227059055215E-16,1.5));
#98110=CARTESIAN_POINT('Ctrl Pts',(-1.46533193762214,-0.000810224173804775,
4.6971550458429));
#98111=CARTESIAN_POINT('Ctrl Pts',(-1.46241910991127,0.436796001295317,
4.67327587421175));
#98112=CARTESIAN_POINT('Ctrl Pts',(-1.25345812331634,0.876815424349057,
4.64939670258059));
#98113=CARTESIAN_POINT('Ctrl Pts',(-0.910959994789205,1.14848054041163,
4.62551753094943));
#98114=CARTESIAN_POINT('Ctrl Pts',(-0.531513308045592,1.44945277823685,
4.59906228403586));
#98115=CARTESIAN_POINT('Ctrl Pts',(0.0118364913862525,1.54378741283756,
4.57260703712227));
#98116=CARTESIAN_POINT('Ctrl Pts',(0.470527355402032,1.38832979587355,4.54615179020869));
#98117=CARTESIAN_POINT('Ctrl Pts',(0.929218219417819,1.23287217890953,4.51969654329511));
#98118=CARTESIAN_POINT('Ctrl Pts',(1.30325014801754,0.827622310380775,4.49324129638153));
#98119=CARTESIAN_POINT('Ctrl Pts',(1.42151867773779,0.357966221832735,4.46678604946795));
#98120=CARTESIAN_POINT('Ctrl Pts',(1.53978720745805,-0.111689866715299,
4.44033080255437));
#98121=CARTESIAN_POINT('Ctrl Pts',(1.40229233829884,-0.645752175282618,
4.41387555564079));
#98122=CARTESIAN_POINT('Ctrl Pts',(1.07193233493599,-0.99990824823969,4.38742030872721));
#98123=CARTESIAN_POINT('Ctrl Pts',(0.741572331573142,-1.35406432119676,
4.36096506181363));
#98124=CARTESIAN_POINT('Ctrl Pts',(0.218347194006646,-1.52831415854358,
4.33450981490005));
#98125=CARTESIAN_POINT('Ctrl Pts',(-0.258388006446477,-1.44294526717024,
4.30805456798647));
#98126=CARTESIAN_POINT('Ctrl Pts',(-0.735123206899601,-1.35757637579689,
4.28159932107289));
#98127=CARTESIAN_POINT('Ctrl Pts',(-1.16536847023935,-1.01258875570338,
4.25514407415931));
#98128=CARTESIAN_POINT('Ctrl Pts',(-1.35230355482995,-0.565800710842041,
4.22868882724573));
#98129=CARTESIAN_POINT('Ctrl Pts',(-1.42657703906863,-0.388281841761277,
4.21817756677812));
#98130=CARTESIAN_POINT('Ctrl Pts',(-1.46244035278657,-0.194692244795154,
4.20766630631051));
#98131=CARTESIAN_POINT('Ctrl Pts',(-1.46151108967999,-0.00077281416562866,
4.1971550458429));
#98132=CARTESIAN_POINT('Ctrl Pts',(-1.46133707147782,-0.000619497695943445,
4.12584495415709));
#98133=CARTESIAN_POINT('Ctrl Pts',(-1.46211898930222,-0.206109057062041,
4.13698008075289));
#98134=CARTESIAN_POINT('Ctrl Pts',(-1.42171768447645,-0.411304915911804,
4.14811520734868));
#98135=CARTESIAN_POINT('Ctrl Pts',(-1.33863739786318,-0.597452549863065,
4.15925033394448));
#98136=CARTESIAN_POINT('Ctrl Pts',(-1.14097476147999,-1.04033056079928,
4.18574276156008));
#98137=CARTESIAN_POINT('Ctrl Pts',(-0.701728638581162,-1.37538649186899,
4.21223518917568));
#98138=CARTESIAN_POINT('Ctrl Pts',(-0.22235430315488,-1.44895072297049,
4.23872761679128));
#98139=CARTESIAN_POINT('Ctrl Pts',(0.257020032271406,-1.52251495407199,
4.26522004440688));
#98140=CARTESIAN_POINT('Ctrl Pts',(0.776522580225145,-1.33458748520527,
4.29171247202248));
#98141=CARTESIAN_POINT('Ctrl Pts',(1.09788936861022,-0.97135913130547,4.31820489963808));
#98142=CARTESIAN_POINT('Ctrl Pts',(1.41925615699529,-0.608130777405669,
4.34469732725369));
#98143=CARTESIAN_POINT('Ctrl Pts',(1.54248718581169,-0.0696015384727871,
4.37118975486929));
#98144=CARTESIAN_POINT('Ctrl Pts',(1.41106392995888,0.397238241529457,4.39768218248489));
#98145=CARTESIAN_POINT('Ctrl Pts',(1.27964067410607,0.864078021531702,4.42417461010049));
#98146=CARTESIAN_POINT('Ctrl Pts',(0.893563133584031,1.25922834260331,4.45066703771609));
#98147=CARTESIAN_POINT('Ctrl Pts',(0.429901422122667,1.40145795839054,4.47715946533169));
#98148=CARTESIAN_POINT('Ctrl Pts',(-0.0337602893386975,1.54368757417777,
4.50365189294729));
#98149=CARTESIAN_POINT('Ctrl Pts',(-0.575006171739392,1.43299648468063,
4.53014432056289));
#98150=CARTESIAN_POINT('Ctrl Pts',(-0.945599936232602,1.12015193692271,
4.55663674817849));
#98151=CARTESIAN_POINT('Ctrl Pts',(-1.26831013301763,0.847729313438621,
4.57970615017136));
#98152=CARTESIAN_POINT('Ctrl Pts',(-1.46161837309286,0.422017921110904,
4.60277555216422));
#98153=CARTESIAN_POINT('Ctrl Pts',(-1.46497413376758,-0.00101984791970569,
4.62584495415709));
#98154=CARTESIAN_POINT('Origin',(0.,0.,1.5));
#98155=CARTESIAN_POINT('',(-1.46394239258928,0.00129898642790893,5.19715504584291));
#98156=CARTESIAN_POINT('',(-1.46453843780727,0.00118155242986957,5.12584495415709));
#98157=CARTESIAN_POINT('',(-1.4635,-1.79227059055215E-16,1.5));
#98158=CARTESIAN_POINT('Ctrl Pts',(-1.46394239258928,0.00129898642790893,
5.19715504584291));
#98159=CARTESIAN_POINT('Ctrl Pts',(-1.46484061977216,0.0997535357056798,
5.19179593594014));
#98160=CARTESIAN_POINT('Ctrl Pts',(-1.455749977343,0.198041505549479,5.18643682603738));
#98161=CARTESIAN_POINT('Ctrl Pts',(-1.43605902275142,0.294156894358288,
5.18107771613462));
#98162=CARTESIAN_POINT('Ctrl Pts',(-1.33885462218189,0.768630526970514,
5.15462246922104));
#98163=CARTESIAN_POINT('Ctrl Pts',(-0.983330855508436,1.19016045875875,
5.12816722230746));
#98164=CARTESIAN_POINT('Ctrl Pts',(-0.532047870296871,1.36593679886265,
5.10171197539388));
#98165=CARTESIAN_POINT('Ctrl Pts',(-0.0807648850853061,1.54171313896655,
5.0752567284803));
#98166=CARTESIAN_POINT('Ctrl Pts',(0.466277318664373,1.47173588738613,5.04880148156672));
#98167=CARTESIAN_POINT('Ctrl Pts',(0.858787460264104,1.18800455079967,5.02234623465314));
#98168=CARTESIAN_POINT('Ctrl Pts',(1.25129760186384,0.904273214213206,4.99589098773956));
#98169=CARTESIAN_POINT('Ctrl Pts',(1.48927568131362,0.406787792620698,4.96943574082598));
#98170=CARTESIAN_POINT('Ctrl Pts',(1.46387758514864,-0.0768651975248075,
4.9429804939124));
#98171=CARTESIAN_POINT('Ctrl Pts',(1.43847948898366,-0.560518187670316,
4.91652524699882));
#98172=CARTESIAN_POINT('Ctrl Pts',(1.14970521720391,-1.03033874636882,4.89007000008524));
#98173=CARTESIAN_POINT('Ctrl Pts',(0.729646360262873,-1.27140582564898,
4.86361475317166));
#98174=CARTESIAN_POINT('Ctrl Pts',(0.309587503321841,-1.51247290492914,
4.83715950625807));
#98175=CARTESIAN_POINT('Ctrl Pts',(-0.241755938780478,-1.52478650479095,
4.81070425934449));
#98176=CARTESIAN_POINT('Ctrl Pts',(-0.672160067958435,-1.30271185053191,
4.78424901243091));
#98177=CARTESIAN_POINT('Ctrl Pts',(-1.10256419713639,-1.08063719627286,
4.75779376551733));
#98178=CARTESIAN_POINT('Ctrl Pts',(-1.41202901338999,-0.624174287892957,
4.73133851860375));
#98179=CARTESIAN_POINT('Ctrl Pts',(-1.45898963448909,-0.14213791317814,
4.70488327169017));
#98180=CARTESIAN_POINT('Ctrl Pts',(-1.46356241718342,-0.0951997011029249,
4.70230719640775));
#98181=CARTESIAN_POINT('Ctrl Pts',(-1.46564617228588,-0.0480190050426819,
4.69973112112533));
#98182=CARTESIAN_POINT('Ctrl Pts',(-1.46533193762214,-0.000810224173804775,
4.6971550458429));
#98183=CARTESIAN_POINT('Ctrl Pts',(-1.46497413376758,-0.00101984791970569,
4.62584495415709));
#98184=CARTESIAN_POINT('Ctrl Pts',(-1.4654720597553,-0.0637899675449887,
4.62926797977982));
#98185=CARTESIAN_POINT('Ctrl Pts',(-1.46178790327085,-0.126501223431492,
4.63269100540256));
#98186=CARTESIAN_POINT('Ctrl Pts',(-1.45372385837108,-0.188644118935721,
4.63611403102529));
#98187=CARTESIAN_POINT('Ctrl Pts',(-1.39131236943062,-0.669597621017519,
4.66260645864089));
#98188=CARTESIAN_POINT('Ctrl Pts',(-1.06654774496397,-1.11650661916241,
4.6890988862565));
#98189=CARTESIAN_POINT('Ctrl Pts',(-0.628379687548205,-1.32440124379681,
4.7155913138721));
#98190=CARTESIAN_POINT('Ctrl Pts',(-0.190211630132438,-1.5322958684312,
4.7420837414877));
#98191=CARTESIAN_POINT('Ctrl Pts',(0.361359860232456,-1.5011761195551,4.7685761691033));
#98192=CARTESIAN_POINT('Ctrl Pts',(0.773362895386055,-1.24531492034441,
4.7950685967189));
#98193=CARTESIAN_POINT('Ctrl Pts',(1.18536593053966,-0.989453721133718,
4.8215610243345));
#98194=CARTESIAN_POINT('Ctrl Pts',(1.45780051048196,-0.50885107158843,4.8480534519501));
#98195=CARTESIAN_POINT('Ctrl Pts',(1.46571731620589,-0.0239295633793579,
4.8745458795657));
#98196=CARTESIAN_POINT('Ctrl Pts',(1.47363412192982,0.460991944829711,4.9010383071813));
#98197=CARTESIAN_POINT('Ctrl Pts',(1.21703315343537,0.950232311702564,4.9275307347969));
#98198=CARTESIAN_POINT('Ctrl Pts',(0.813602072710932,1.21940623737337,4.9540231624125));
#98199=CARTESIAN_POINT('Ctrl Pts',(0.410170991986497,1.48858016304417,4.9805155900281));
#98200=CARTESIAN_POINT('Ctrl Pts',(-0.140090200967923,1.53768764751291,
5.0070080176437));
#98201=CARTESIAN_POINT('Ctrl Pts',(-0.584811428509822,1.3442074922315,5.03350044525931));
#98202=CARTESIAN_POINT('Ctrl Pts',(-1.02953265605172,1.15072733695009,5.05999287287491));
#98203=CARTESIAN_POINT('Ctrl Pts',(-1.3687139181811,0.714659541918519,5.08648530049051));
#98204=CARTESIAN_POINT('Ctrl Pts',(-1.44679165122832,0.235999019704764,
5.11297772810611));
#98205=CARTESIAN_POINT('Ctrl Pts',(-1.45943229273847,0.158504760711557,
5.11726680345644));
#98206=CARTESIAN_POINT('Ctrl Pts',(-1.46522914572839,0.0798941031068154,
5.12155587880677));
#98207=CARTESIAN_POINT('Ctrl Pts',(-1.46453843780727,0.00118155242986957,
5.12584495415709));
#98208=CARTESIAN_POINT('Origin',(0.,0.,0.612132885263843));
#98209=CARTESIAN_POINT('',(-1.17810601494501,0.00104535788546833,5.36213288526384));
#98210=CARTESIAN_POINT('',(-1.17585338136642,0.000266266979346078,5.46086711473616));
#98211=CARTESIAN_POINT('',(-1.17775,-4.72972551152008E-14,0.612132885263843));
#98212=CARTESIAN_POINT('',(-1.03290409957988,0.565865870654066,5.82225));
#98213=CARTESIAN_POINT('Ctrl Pts',(-1.17810601494501,0.00104535788546838,
5.36213288526384));
#98214=CARTESIAN_POINT('Ctrl Pts',(-1.17526052631953,-0.310848231437392,
5.38322902227466));
#98215=CARTESIAN_POINT('Ctrl Pts',(-0.888072305685325,-1.01854893491326,
5.43078040619906));
#98216=CARTESIAN_POINT('Ctrl Pts',(0.306526164541481,-1.35774082866675,
5.50478703703704));
#98217=CARTESIAN_POINT('Ctrl Pts',(1.30628459189527,-0.479538774867528,
5.58415277777777));
#98218=CARTESIAN_POINT('Ctrl Pts',(1.11262400044309,0.837919826534893,5.66351851851852));
#98219=CARTESIAN_POINT('Ctrl Pts',(-0.102449444944844,1.38774658789174,
5.74288425925926));
#98220=CARTESIAN_POINT('Ctrl Pts',(-0.844784006828786,0.909251158746022,
5.79579475308642));
#98221=CARTESIAN_POINT('Ctrl Pts',(-1.03290409957988,0.565865870654058,
5.82225));
#98222=CARTESIAN_POINT('',(0.200551794415749,1.1605490253568,5.82225));
#98223=CARTESIAN_POINT('Origin',(0.,0.,5.82225));
#98224=CARTESIAN_POINT('Ctrl Pts',(-1.17585338136642,0.000266266979346078,
5.46086711473616));
#98225=CARTESIAN_POINT('Ctrl Pts',(-1.17534105488343,-0.215031411505098,
5.47535836602837));
#98226=CARTESIAN_POINT('Ctrl Pts',(-1.01554696283918,-0.824585838872987,
5.51634204493618));
#98227=CARTESIAN_POINT('Ctrl Pts',(-0.0361513007060795,-1.39171212292046,
5.58381815145959));
#98228=CARTESIAN_POINT('Ctrl Pts',(1.15165463117661,-0.784596477531957,
5.66329543430639));
#98229=CARTESIAN_POINT('Ctrl Pts',(1.28099440281734,0.545166701406554,5.7427727171532));
#98230=CARTESIAN_POINT('Ctrl Pts',(0.586914422573267,1.09378259267779,5.7957575723844));
#98231=CARTESIAN_POINT('Ctrl Pts',(0.200551794415766,1.1605490253568,5.82225));
#98232=CARTESIAN_POINT('Origin',(0.,0.,0.612132885263843));
#98233=CARTESIAN_POINT('',(-1.17922424976732,-0.000652027004295064,4.86213288526384));
#98234=CARTESIAN_POINT('',(-1.17858568167237,0.000950853005947522,4.96086711473616));
#98235=CARTESIAN_POINT('',(-1.17775,-4.72972551152008E-14,0.612132885263843));
#98236=CARTESIAN_POINT('Ctrl Pts',(-1.17922424976732,-0.000652027004295177,
4.86213288526384));
#98237=CARTESIAN_POINT('Ctrl Pts',(-1.17947712976405,-0.0386432409901481,
4.86470896054627));
#98238=CARTESIAN_POINT('Ctrl Pts',(-1.16057915226501,-0.46653408645719,
4.89374028274227));
#98239=CARTESIAN_POINT('Ctrl Pts',(-0.63824584614602,-1.2369796024973,4.94922685185185));
#98240=CARTESIAN_POINT('Ctrl Pts',(0.692833222393801,-1.20725153504819,
5.0285925925926));
#98241=CARTESIAN_POINT('Ctrl Pts',(1.39000554611486,-0.0729888162087741,
5.10795833333333));
#98242=CARTESIAN_POINT('Ctrl Pts',(0.815467760521459,1.12806370571929,5.18732407407407));
#98243=CARTESIAN_POINT('Ctrl Pts',(-0.505227057653176,1.2970060522492,5.26668981481481));
#98244=CARTESIAN_POINT('Ctrl Pts',(-1.13539930062689,0.549836699603529,
5.32495941854474));
#98245=CARTESIAN_POINT('Ctrl Pts',(-1.17882886227309,0.080276547097573,
5.35677377536108));
#98246=CARTESIAN_POINT('Ctrl Pts',(-1.17810601494501,0.00104535788546838,
5.36213288526384));
#98247=CARTESIAN_POINT('Ctrl Pts',(-1.17858568167237,0.000950853005947504,
4.96086711473616));
#98248=CARTESIAN_POINT('Ctrl Pts',(-1.17570821901659,-0.326962608221022,
4.98307046700143));
#98249=CARTESIAN_POINT('Ctrl Pts',(-0.862548697969744,-1.05095270842858,
5.03176624688231));
#98250=CARTESIAN_POINT('Ctrl Pts',(0.364714346074539,-1.34397271822316,
5.10695445437878));
#98251=CARTESIAN_POINT('Ctrl Pts',(1.32746371769155,-0.420942597676582,
5.18643173722558));
#98252=CARTESIAN_POINT('Ctrl Pts',(1.07251885993521,0.888266730679483,5.26590902007238));
#98253=CARTESIAN_POINT('Ctrl Pts',(-0.166143802083737,1.38257845674616,
5.34538630291918));
#98254=CARTESIAN_POINT('Ctrl Pts',(-1.0544698941532,0.749960489548073,5.41037233447378));
#98255=CARTESIAN_POINT('Ctrl Pts',(-1.17627767326045,0.178568702663258,
5.44886593841277));
#98256=CARTESIAN_POINT('Ctrl Pts',(-1.17585338136642,0.000266266979346078,
5.46086711473616));
#98257=CARTESIAN_POINT('Origin',(0.,0.,0.612132885263843));
#98258=CARTESIAN_POINT('',(-1.17614942662836,-0.000621921341728721,4.36213288526384));
#98259=CARTESIAN_POINT('',(-1.17893630751266,-0.00082072148104434,4.46086711473616));
#98260=CARTESIAN_POINT('',(-1.17775,-4.72972551152008E-14,0.612132885263843));
#98261=CARTESIAN_POINT('Ctrl Pts',(-1.17614942662836,-0.000621921341728629,
4.36213288526384));
#98262=CARTESIAN_POINT('Ctrl Pts',(-1.17689725008157,-0.156678367822023,
4.37264414573145));
#98263=CARTESIAN_POINT('Ctrl Pts',(-1.07539762839906,-0.70457171109385,
4.40961065311264));
#98264=CARTESIAN_POINT('Ctrl Pts',(-0.245350186557975,-1.37013648524764,
4.47303240740741));
#98265=CARTESIAN_POINT('Ctrl Pts',(1.01784435891986,-0.949454395868983,
4.55239814814815));
#98266=CARTESIAN_POINT('Ctrl Pts',(1.3497908887844,0.339903753598391,4.63176388888888));
#98267=CARTESIAN_POINT('Ctrl Pts',(0.446785551083708,1.31827689878403,4.71112962962963));
#98268=CARTESIAN_POINT('Ctrl Pts',(-0.822416757865382,1.09792209940012,
4.78791929508794));
#98269=CARTESIAN_POINT('Ctrl Pts',(-1.17688015490128,0.351511097045095,
4.83825371363268));
#98270=CARTESIAN_POINT('Ctrl Pts',(-1.17922424976732,-0.000652027004295177,
4.86213288526384));
#98271=CARTESIAN_POINT('Ctrl Pts',(-1.17893630751266,-0.000820721481044288,
4.46086711473616));
#98272=CARTESIAN_POINT('Ctrl Pts',(-1.1793370128984,-0.0513349055525556,
4.46429014035889));
#98273=CARTESIAN_POINT('Ctrl Pts',(-1.15342602975686,-0.492388454964942,
4.49420559359722));
#98274=CARTESIAN_POINT('Ctrl Pts',(-0.596949142579923,-1.25815698208656,
4.55061347445117));
#98275=CARTESIAN_POINT('Ctrl Pts',(0.734680490718179,-1.18302623202404,
4.63009075729796));
#98276=CARTESIAN_POINT('Ctrl Pts',(1.39240476784912,-0.0227328862735182,
4.70956804014477));
#98277=CARTESIAN_POINT('Ctrl Pts',(0.772906734413495,1.15841403976235,4.78904532299156));
#98278=CARTESIAN_POINT('Ctrl Pts',(-0.555559517726036,1.27697162056126,
4.86852260583837));
#98279=CARTESIAN_POINT('Ctrl Pts',(-1.14566203930557,0.518307348212367,
4.9257965364199));
#98280=CARTESIAN_POINT('Ctrl Pts',(-1.17914152810497,0.0642946907646066,
4.95657803938583));
#98281=CARTESIAN_POINT('Ctrl Pts',(-1.17858568167237,0.000950853005947504,
4.96086711473616));
#98282=CARTESIAN_POINT('Origin',(0.,0.,0.612132885263843));
#98283=CARTESIAN_POINT('',(-1.17695913743441,0.000999038273554803,3.86213288526384));
#98284=CARTESIAN_POINT('',(-1.17600938567339,-0.000498540082993076,3.96086711473616));
#98285=CARTESIAN_POINT('',(-1.17775,-4.72972551152008E-14,0.612132885263843));
#98286=CARTESIAN_POINT('Ctrl Pts',(-1.17695913743441,0.000999038273554707,
3.86213288526384));
#98287=CARTESIAN_POINT('Ctrl Pts',(-1.1747538368297,-0.272394076947318,
3.88057933091664));
#98288=CARTESIAN_POINT('Ctrl Pts',(-0.943776669976225,-0.941238613449934,
3.92548102348301));
#98289=CARTESIAN_POINT('Ctrl Pts',(0.169336007262713,-1.38159181457256,
3.99683796296296));
#98290=CARTESIAN_POINT('Ctrl Pts',(1.25245060777301,-0.607320430195027,
4.0762037037037));
#98291=CARTESIAN_POINT('Ctrl Pts',(1.18967129222925,0.72260143140615,4.15556944444444));
#98292=CARTESIAN_POINT('Ctrl Pts',(0.0384362261044693,1.39139975892709,
4.23493518518518));
#98293=CARTESIAN_POINT('Ctrl Pts',(-0.990837095837684,0.867200396502629,
4.30378966545832));
#98294=CARTESIAN_POINT('Ctrl Pts',(-1.17501509197471,0.236092017500911,
4.34618889881787));
#98295=CARTESIAN_POINT('Ctrl Pts',(-1.17614942662836,-0.000621921341728629,
4.36213288526384));
#98296=CARTESIAN_POINT('Ctrl Pts',(-1.17600938567339,-0.000498540082993007,
3.96086711473616));
#98297=CARTESIAN_POINT('Ctrl Pts',(-1.17663863317436,-0.165866034817124,
3.97200224133195));
#98298=CARTESIAN_POINT('Ctrl Pts',(-1.0667717993835,-0.723873243149682,
4.00962979554334));
#98299=CARTESIAN_POINT('Ctrl Pts',(-0.211232513047386,-1.37647664066694,
4.07374977737036));
#98300=CARTESIAN_POINT('Ctrl Pts',(1.042974782858,-0.922773374952316,4.15322706021714));
#98301=CARTESIAN_POINT('Ctrl Pts',(1.34048488368858,0.37736904627051,4.23270434306396));
#98302=CARTESIAN_POINT('Ctrl Pts',(0.40839846752904,1.33135939264991,4.31218162591074));
#98303=CARTESIAN_POINT('Ctrl Pts',(-0.842023988191156,1.07563343065007,
4.38823588313483));
#98304=CARTESIAN_POINT('Ctrl Pts',(-1.17623576283577,0.339618453425564,
4.43779771274329));
#98305=CARTESIAN_POINT('Ctrl Pts',(-1.17893630751266,-0.000820721481044288,
4.46086711473616));
#98306=CARTESIAN_POINT('Origin',(0.,0.,0.612132885263843));
#98307=CARTESIAN_POINT('',(-1.17967891613203,2.02464564948595E-5,3.36213288526384));
#98308=CARTESIAN_POINT('',(-1.17710658396666,0.00103751543904164,3.46086711473616));
#98309=CARTESIAN_POINT('',(-1.17775,-4.72972551152008E-14,0.612132885263843));
#98310=CARTESIAN_POINT('Ctrl Pts',(-1.17967891613203,2.02464564948851E-5,
3.36213288526384));
#98311=CARTESIAN_POINT('Ctrl Pts',(-1.17958036551302,-0.388650261618471,
3.38851451610182));
#98312=CARTESIAN_POINT('Ctrl Pts',(-0.75718785921875,-1.16725938820271,
3.44135139385338));
#98313=CARTESIAN_POINT('Ctrl Pts',(0.568980874699694,-1.27032727667186,
3.52064351851852));
#98314=CARTESIAN_POINT('Ctrl Pts',(1.37580804658996,-0.211241198394891,
3.60000925925926));
#98315=CARTESIAN_POINT('Ctrl Pts',(0.92387894541309,1.04111397962895,3.679375));
#98316=CARTESIAN_POINT('Ctrl Pts',(-0.373326806220943,1.34093166146447,
3.75874074074074));
#98317=CARTESIAN_POINT('Ctrl Pts',(-1.10685463418829,0.629365443838005,
3.81966003582869));
#98318=CARTESIAN_POINT('Ctrl Pts',(-1.17791660179344,0.119696762869613,
3.85412408400306));
#98319=CARTESIAN_POINT('Ctrl Pts',(-1.17695913743441,0.000999038273554707,
3.86213288526384));
#98320=CARTESIAN_POINT('Ctrl Pts',(-1.17710658396666,0.00103751543904167,
3.46086711473616));
#98321=CARTESIAN_POINT('Ctrl Pts',(-1.174750734397,-0.278206389289945,3.47971434230502));
#98322=CARTESIAN_POINT('Ctrl Pts',(-0.935578896943687,-0.953594566271338,
3.52505399748947));
#98323=CARTESIAN_POINT('Ctrl Pts',(0.192214113207023,-1.37926097853155,
3.59688608028953));
#98324=CARTESIAN_POINT('Ctrl Pts',(1.26372622016576,-0.585066792922831,
3.67636336313633));
#98325=CARTESIAN_POINT('Ctrl Pts',(1.17605081651368,0.745795943229381,3.75584064598314));
#98326=CARTESIAN_POINT('Ctrl Pts',(0.00961056866032201,1.39255691077756,
3.83531792882993));
#98327=CARTESIAN_POINT('Ctrl Pts',(-1.00098658511986,0.850306798861559,
3.90366008508095));
#98328=CARTESIAN_POINT('Ctrl Pts',(-1.17514154252808,0.227572364515632,
3.94550981371635));
#98329=CARTESIAN_POINT('Ctrl Pts',(-1.17600938567339,-0.000498540082993007,
3.96086711473616));
#98330=CARTESIAN_POINT('Origin',(0.,0.,0.612132885263843));
#98331=CARTESIAN_POINT('',(-1.17701796998071,-0.00101206437339089,2.86213288526384));
#98332=CARTESIAN_POINT('',(-1.17969113925438,-1.85122837467744E-5,2.96086711473616));
#98333=CARTESIAN_POINT('',(-1.17775,-4.72972551152008E-14,0.612132885263843));
#98334=CARTESIAN_POINT('Ctrl Pts',(-1.17701796998071,-0.00101206437339095,
2.86213288526384));
#98335=CARTESIAN_POINT('Ctrl Pts',(-1.177973565516,-0.117512948617163,2.86999445437342));
#98336=CARTESIAN_POINT('Ctrl Pts',(-1.10856763284462,-0.624941754067655,
2.90431127039659));
#98337=CARTESIAN_POINT('Ctrl Pts',(-0.380763881655566,-1.33883882596208,
2.96508333333333));
#98338=CARTESIAN_POINT('Ctrl Pts',(0.918086015388248,-1.04622594248328,
3.04444907407407));
#98339=CARTESIAN_POINT('Ctrl Pts',(1.37695934771338,0.203601540672618,3.12381481481481));
#98340=CARTESIAN_POINT('Ctrl Pts',(0.576023051783349,1.26714957918899,3.20318055555555));
#98341=CARTESIAN_POINT('Ctrl Pts',(-0.751929078651436,1.17135532206144,
3.2825462962963));
#98342=CARTESIAN_POINT('Ctrl Pts',(-1.17918677678639,0.39194417008362,3.33553040619906));
#98343=CARTESIAN_POINT('Ctrl Pts',(-1.17967919113057,0.00110480402923826,
3.36205926918824));
#98344=CARTESIAN_POINT('Ctrl Pts',(-1.17967891613203,2.02464564948851E-5,
3.36213288526384));
#98345=CARTESIAN_POINT('Ctrl Pts',(-1.17969113925438,-1.85122837469034E-5,
2.96086711473616));
#98346=CARTESIAN_POINT('Ctrl Pts',(-1.17969136723729,-0.00100411151731483,
2.96093401566248));
#98347=CARTESIAN_POINT('Ctrl Pts',(-1.17924351116644,-0.392281796551246,
2.9874933442044));
#98348=CARTESIAN_POINT('Ctrl Pts',(-0.750938898498722,-1.17277357998896,
3.04054510036192));
#98349=CARTESIAN_POINT('Ctrl Pts',(0.579527130353369,-1.26627620290932,
3.12002238320872));
#98350=CARTESIAN_POINT('Ctrl Pts',(1.37840601855021,-0.198252265336022,
3.19949966605552));
#98351=CARTESIAN_POINT('Ctrl Pts',(0.912904206293459,1.0516239918919,3.27897694890232));
#98352=CARTESIAN_POINT('Ctrl Pts',(-0.389984008629303,1.33686932263319,
3.35845423174912));
#98353=CARTESIAN_POINT('Ctrl Pts',(-1.11101252964029,0.618991412974714,
3.41908428702707));
#98354=CARTESIAN_POINT('Ctrl Pts',(-1.17806221211803,0.11431017083026,3.45322191468942));
#98355=CARTESIAN_POINT('Ctrl Pts',(-1.17710658396666,0.00103751543904167,
3.46086711473616));
#98356=CARTESIAN_POINT('Origin',(0.,0.,0.612132885263843));
#98357=CARTESIAN_POINT('',(-1.17611517204452,0.000593537064731084,2.36213288526384));
#98358=CARTESIAN_POINT('',(-1.1770515199907,-0.00102726950455198,2.46086711473616));
#98359=CARTESIAN_POINT('',(-1.17775,-4.72972551152008E-14,0.612132885263843));
#98360=CARTESIAN_POINT('Ctrl Pts',(-1.17611517204452,0.000593537064731229,
2.36213288526384));
#98361=CARTESIAN_POINT('Ctrl Pts',(-1.17504706626748,-0.233952086459625,
2.37792963955861));
#98362=CARTESIAN_POINT('Ctrl Pts',(-0.993440962632586,-0.862822802044922,
2.42018164076696));
#98363=CARTESIAN_POINT('Ctrl Pts',(0.0307129365700887,-1.39159014732659,
2.48888888888889));
#98364=CARTESIAN_POINT('Ctrl Pts',(1.18564203741949,-0.729194359677473,
2.56825462962963));
#98365=CARTESIAN_POINT('Ctrl Pts',(1.25580231344031,0.600359775536952,2.64762037037037));
#98366=CARTESIAN_POINT('Ctrl Pts',(0.177001877056122,1.3806304142218,2.72698611111111));
#98367=CARTESIAN_POINT('Ctrl Pts',(-0.940839494469228,0.945566794997418,
2.79849028274227));
#98368=CARTESIAN_POINT('Ctrl Pts',(-1.17475785685998,0.274528336698561,
2.84353920745985));
#98369=CARTESIAN_POINT('Ctrl Pts',(-1.17701796998071,-0.00101206437339095,
2.86213288526384));
#98370=CARTESIAN_POINT('Ctrl Pts',(-1.1770515199907,-0.00102726950455214,
2.46086711473616));
#98371=CARTESIAN_POINT('Ctrl Pts',(-1.17801098215327,-0.116296063688412,
2.46864611663554));
#98372=CARTESIAN_POINT('Ctrl Pts',(-1.10947535590674,-0.623011746146892,
2.50291754615052));
#98373=CARTESIAN_POINT('Ctrl Pts',(-0.383235548912603,-1.33881925708758,
2.5636814032811));
#98374=CARTESIAN_POINT('Ctrl Pts',(0.918197143413365,-1.04700586255646,
2.6431586861279));
#98375=CARTESIAN_POINT('Ctrl Pts',(1.37738848098126,0.205202743845419,2.7226359689747));
#98376=CARTESIAN_POINT('Ctrl Pts',(0.573132410162518,1.26918330522814,2.80211325182151));
#98377=CARTESIAN_POINT('Ctrl Pts',(-0.755725509229907,1.16905515724181,
2.88152363374199));
#98378=CARTESIAN_POINT('Ctrl Pts',(-1.17960108716335,0.389288187712833,
2.93444158804687));
#98379=CARTESIAN_POINT('Ctrl Pts',(-1.17969113925438,-1.85122837469034E-5,
2.96086711473616));
#98380=CARTESIAN_POINT('Origin',(0.,0.,0.612132885263843));
#98381=CARTESIAN_POINT('',(-1.17916256915606,0.000764266613825465,1.86213288526384));
#98382=CARTESIAN_POINT('',(-1.17603208311293,0.000536542008743729,1.96086711473616));
#98383=CARTESIAN_POINT('',(-1.17775,-4.72972551152008E-14,0.612132885263843));
#98384=CARTESIAN_POINT('Ctrl Pts',(-1.17916256915606,0.000764266613825456,
1.86213288526384));
#98385=CARTESIAN_POINT('Ctrl Pts',(-1.1767421985046,-0.349243514957978,
1.8858648247438));
#98386=CARTESIAN_POINT('Ctrl Pts',(-0.826089096200879,-1.0939070674493,
1.93605201113733));
#98387=CARTESIAN_POINT('Ctrl Pts',(0.439473835276103,-1.32066405983435,
2.01269444444444));
#98388=CARTESIAN_POINT('Ctrl Pts',(1.34787702874157,-0.347428546246197,
2.09206018518518));
#98389=CARTESIAN_POINT('Ctrl Pts',(1.02310199861475,0.943810199691403,2.17142592592593));
#98390=CARTESIAN_POINT('Ctrl Pts',(-0.237743248735789,1.37146670874731,
2.25079166666666));
#98391=CARTESIAN_POINT('Ctrl Pts',(-1.07340543198276,0.708997793674441,
2.31436065311264));
#98392=CARTESIAN_POINT('Ctrl Pts',(-1.17683585157959,0.158847742356567,
2.35147439264503));
#98393=CARTESIAN_POINT('Ctrl Pts',(-1.17611517204452,0.000593537064731229,
2.36213288526384));
#98394=CARTESIAN_POINT('Ctrl Pts',(-1.17603208311293,0.000536542008743694,
1.96086711473616));
#98395=CARTESIAN_POINT('Ctrl Pts',(-1.17510603664511,-0.229512798367662,
1.9763582176086));
#98396=CARTESIAN_POINT('Ctrl Pts',(-0.998674096869405,-0.854308622825481,
2.01834174809664));
#98397=CARTESIAN_POINT('Ctrl Pts',(0.0166383981799684,-1.39248065884836,
2.08681770620029));
#98398=CARTESIAN_POINT('Ctrl Pts',(1.17979588449659,-0.739859513451799,
2.16629498904709));
#98399=CARTESIAN_POINT('Ctrl Pts',(1.2607599562499,0.591436597715745,2.24577227189389));
#98400=CARTESIAN_POINT('Ctrl Pts',(0.185253888314333,1.38021153969935,2.32524955474069));
#98401=CARTESIAN_POINT('Ctrl Pts',(-0.938280191320604,0.949667221313808,
2.39694783568812));
#98402=CARTESIAN_POINT('Ctrl Pts',(-1.17474340589855,0.276267175883094,
2.44215368901994));
#98403=CARTESIAN_POINT('Ctrl Pts',(-1.1770515199907,-0.00102726950455214,
2.46086711473616));
#98404=CARTESIAN_POINT('Origin',(0.,0.,5.75));
#98405=CARTESIAN_POINT('',(-1.40480161465946,0.000288650130247903,5.59314243068829));
#98406=CARTESIAN_POINT('Ctrl Pts',(0.200551794415766,1.1605490253568,5.82225));
#98407=CARTESIAN_POINT('Ctrl Pts',(0.250346736530993,1.15412464824318,5.82010127540114));
#98408=CARTESIAN_POINT('Ctrl Pts',(0.299515100252955,1.14429438809625,5.81796348399038));
#98409=CARTESIAN_POINT('Ctrl Pts',(0.347835451301076,1.13132131740438,5.81583221074506));
#98410=CARTESIAN_POINT('Ctrl Pts',(0.390115758468181,1.119969880549,5.81396734665541));
#98411=CARTESIAN_POINT('Ctrl Pts',(0.431747287002779,1.10621102058761,5.81210747303618));
#98412=CARTESIAN_POINT('Ctrl Pts',(0.472578058688195,1.09018611073377,5.81024963216711));
#98413=CARTESIAN_POINT('Ctrl Pts',(0.495740312305655,1.08109558878402,5.8091957265069));
#98414=CARTESIAN_POINT('Ctrl Pts',(0.518644777404426,1.07127528873862,5.8081424749863));
#98415=CARTESIAN_POINT('Ctrl Pts',(0.5412623142025,1.06074695780148,5.80708933767618));
#98416=CARTESIAN_POINT('Ctrl Pts',(0.551227651047345,1.05610815185461,5.80662532304307));
#98417=CARTESIAN_POINT('Ctrl Pts',(0.561129746489033,1.05133531419125,5.80616167994593));
#98418=CARTESIAN_POINT('Ctrl Pts',(0.570961984108289,1.04643304215269,5.80569856717539));
#98419=CARTESIAN_POINT('Ctrl Pts',(0.616614147837176,1.02367125237354,5.80354828350198));
#98420=CARTESIAN_POINT('Ctrl Pts',(0.660791536163919,0.998109158908003,
5.80140803169028));
#98421=CARTESIAN_POINT('Ctrl Pts',(0.703261793203859,0.969971780088759,
5.79927336313984));
#98422=CARTESIAN_POINT('Ctrl Pts',(0.746009532369701,0.941650563915182,
5.79712474759663));
#98423=CARTESIAN_POINT('Ctrl Pts',(0.787028757314936,0.910719705995268,
5.79498178851019));
#98424=CARTESIAN_POINT('Ctrl Pts',(0.826059377502829,0.877361822445158,
5.79283994951347));
#98425=CARTESIAN_POINT('Ctrl Pts',(0.833821521621903,0.87072783358265,5.79241399515014));
#98426=CARTESIAN_POINT('Ctrl Pts',(0.841506582511428,0.863996220736173,
5.79198799150201));
#98427=CARTESIAN_POINT('Ctrl Pts',(0.84910696954478,0.857173081813743,5.79156220485652));
#98428=CARTESIAN_POINT('Ctrl Pts',(0.887762460766018,0.822470666586745,
5.78939665830417));
#98429=CARTESIAN_POINT('Ctrl Pts',(0.924111480196861,0.785512508178675,
5.78724338870587));
#98430=CARTESIAN_POINT('Ctrl Pts',(0.957915058877359,0.74652009572043,5.78509790662306));
#98431=CARTESIAN_POINT('Ctrl Pts',(0.992826141795193,0.706250177633871,
5.78288213226379));
#98432=CARTESIAN_POINT('Ctrl Pts',(1.02502355391537,0.663810007535811,5.78067466406283));
#98433=CARTESIAN_POINT('Ctrl Pts',(1.05420839105705,0.619397315205114,5.77847055670522));
#98434=CARTESIAN_POINT('Ctrl Pts',(1.06880080962789,0.597190969039766,5.77736850302642));
#98435=CARTESIAN_POINT('Ctrl Pts',(1.08263941269998,0.574490831231967,5.77626728955846));
#98436=CARTESIAN_POINT('Ctrl Pts',(1.09568205036826,0.55131814869553,5.77516629813697));
#98437=CARTESIAN_POINT('Ctrl Pts',(1.10331783271695,0.537751754781692,5.77452172523108));
#98438=CARTESIAN_POINT('Ctrl Pts',(1.11068073284844,0.524023357137232,5.7738772284314));
#98439=CARTESIAN_POINT('Ctrl Pts',(1.11776167899029,0.510136920081813,5.77323268369607));
#98440=CARTESIAN_POINT('Ctrl Pts',(1.12229234159152,0.50125184176446,5.77282027910088));
#98441=CARTESIAN_POINT('Ctrl Pts',(1.12670826176501,0.492300592367051,5.7724077878105));
#98442=CARTESIAN_POINT('Ctrl Pts',(1.13100477448532,0.483288758243769,5.77199538723061));
#98443=CARTESIAN_POINT('Ctrl Pts',(1.13146311240594,0.482327405262425,5.77195139368595));
#98444=CARTESIAN_POINT('Ctrl Pts',(1.13192005003185,0.481365450766813,5.77190740518791));
#98445=CARTESIAN_POINT('Ctrl Pts',(1.13237558531186,0.480402896532057,5.77186342169889));
#98446=CARTESIAN_POINT('Ctrl Pts',(1.15347716745463,0.43581487417031,5.76982599178449));
#98447=CARTESIAN_POINT('Ctrl Pts',(1.17157311277187,0.389942668914696,5.76779931013149));
#98448=CARTESIAN_POINT('Ctrl Pts',(1.18676291197832,0.343097687180534,5.765779638305));
#98449=CARTESIAN_POINT('Ctrl Pts',(1.202674265336,0.294027449498257,5.76366402692258));
#98450=CARTESIAN_POINT('Ctrl Pts',(1.21539716018734,0.243888988733073,5.76155610715352));
#98451=CARTESIAN_POINT('Ctrl Pts',(1.22499689044219,0.193011403878154,5.75945158209943));
#98452=CARTESIAN_POINT('Ctrl Pts',(1.23231286325458,0.154237499020673,5.75784771952518));
#98453=CARTESIAN_POINT('Ctrl Pts',(1.23781388921226,0.11503357886763,5.7562458285991));
#98454=CARTESIAN_POINT('Ctrl Pts',(1.24150937798468,0.0755398256054352,
5.75464400739245));
#98455=CARTESIAN_POINT('Ctrl Pts',(1.24278142730073,0.0619454122763994,
5.75409263362411));
#98456=CARTESIAN_POINT('Ctrl Pts',(1.24383940039106,0.0483166402189457,
5.75354126811648));
#98457=CARTESIAN_POINT('Ctrl Pts',(1.24468321822901,0.034659203909744,5.75298983330018));
#98458=CARTESIAN_POINT('Ctrl Pts',(1.24534879298452,0.0238866835582429,
5.75255488030851));
#98459=CARTESIAN_POINT('Ctrl Pts',(1.24588107265531,0.0130945362466726,
5.75211981246084));
#98460=CARTESIAN_POINT('Ctrl Pts',(1.24627953946674,0.00230542954319881,
5.75168539011199));
#98461=CARTESIAN_POINT('Ctrl Pts',(1.24822972346125,-0.0504988256783816,
5.74955923182913));
#98462=CARTESIAN_POINT('Ctrl Pts',(1.24698640291456,-0.103332391097632,
5.74744435055885));
#98463=CARTESIAN_POINT('Ctrl Pts',(1.24262094207762,-0.155860577536359,
5.74533648797421));
#98464=CARTESIAN_POINT('Ctrl Pts',(1.23822829356669,-0.208715904513251,
5.74321549782232));
#98465=CARTESIAN_POINT('Ctrl Pts',(1.23067451535421,-0.261263213638418,
5.74110161405171));
#98466=CARTESIAN_POINT('Ctrl Pts',(1.21998110424804,-0.313168306918295,
5.73899049827755));
#98467=CARTESIAN_POINT('Ctrl Pts',(1.212546640722,-0.349254689361996,5.73752277080813));
#98468=CARTESIAN_POINT('Ctrl Pts',(1.20359355305155,-0.385030811129976,
5.73605638126527));
#98469=CARTESIAN_POINT('Ctrl Pts',(1.19311450906358,-0.420381654243896,
5.73458987174742));
#98470=CARTESIAN_POINT('Ctrl Pts',(1.18924384314627,-0.433439267490491,
5.73404818412643));
#98471=CARTESIAN_POINT('Ctrl Pts',(1.18516486509828,-0.446438816983626,
5.73350648013657));
#98472=CARTESIAN_POINT('Ctrl Pts',(1.18087679316331,-0.459374332873229,
5.73296468630611));
#98473=CARTESIAN_POINT('Ctrl Pts',(1.17751869200505,-0.469504473307045,
5.73254039340309));
#98474=CARTESIAN_POINT('Ctrl Pts',(1.17403481326548,-0.479587710603795,
5.73211636400189));
#98475=CARTESIAN_POINT('Ctrl Pts',(1.17042800339357,-0.48961426863002,5.73169286347098));
#98476=CARTESIAN_POINT('Ctrl Pts',(1.15233571380561,-0.539908960566405,
5.72956852242783));
#98477=CARTESIAN_POINT('Ctrl Pts',(1.13113574858936,-0.588834316433369,
5.72745512977291));
#98478=CARTESIAN_POINT('Ctrl Pts',(1.10685942649161,-0.636056546162735,
5.7253484324484));
#98479=CARTESIAN_POINT('Ctrl Pts',(1.09196285667379,-0.665033309582002,
5.72405570928987));
#98480=CARTESIAN_POINT('Ctrl Pts',(1.0759069315264,-0.693368745071741,5.72276550716582));
#98481=CARTESIAN_POINT('Ctrl Pts',(1.05868947708989,-0.720983087097389,
5.72147684339778));
#98482=CARTESIAN_POINT('Ctrl Pts',(1.0301474975545,-0.76676035271385,5.71934058016379));
#98483=CARTESIAN_POINT('Ctrl Pts',(0.998415979517414,-0.810558092677179,
5.71720854446415));
#98484=CARTESIAN_POINT('Ctrl Pts',(0.963808698514434,-0.852240620763262,
5.71507625961026));
#98485=CARTESIAN_POINT('Ctrl Pts',(0.955357655304655,-0.86241942810493,
5.71455555902606));
#98486=CARTESIAN_POINT('Ctrl Pts',(0.946734905694979,-0.872471932029711,
5.71403484358407));
#98487=CARTESIAN_POINT('Ctrl Pts',(0.937944627906372,-0.882395813911537,
5.71351404809364));
#98488=CARTESIAN_POINT('Ctrl Pts',(0.931659089334196,-0.889491942595295,
5.71314165028984));
#98489=CARTESIAN_POINT('Ctrl Pts',(0.925288554802937,-0.896521410431196,
5.71276925527006));
#98490=CARTESIAN_POINT('Ctrl Pts',(0.918843317495153,-0.90347434947744,
5.71239733132264));
#98491=CARTESIAN_POINT('Ctrl Pts',(0.882763429109284,-0.94239630886585,
5.71031533280649));
#98492=CARTESIAN_POINT('Ctrl Pts',(0.844277488058528,-0.979001068014847,
5.70824397827156));
#98493=CARTESIAN_POINT('Ctrl Pts',(0.803714874630552,-1.01319037638095,
5.70617927222703));
#98494=CARTESIAN_POINT('Ctrl Pts',(0.762328378480178,-1.04807411683791,
5.70407262915001));
#98495=CARTESIAN_POINT('Ctrl Pts',(0.718779165482597,-1.08044396964377,
5.7019729073863));
#98496=CARTESIAN_POINT('Ctrl Pts',(0.673373566240844,-1.11016225781405,
5.69987586300475));
#98497=CARTESIAN_POINT('Ctrl Pts',(0.647159389899234,-1.12731962297773,
5.69866516890243));
#98498=CARTESIAN_POINT('Ctrl Pts',(0.620325717407448,-1.14359251709036,
5.69745536720918));
#98499=CARTESIAN_POINT('Ctrl Pts',(0.59292679078264,-1.15894815486762,5.69624564125097));
#98500=CARTESIAN_POINT('Ctrl Pts',(0.573227863366542,-1.16998835356388,
5.69537588806061));
#98501=CARTESIAN_POINT('Ctrl Pts',(0.553236678223681,-1.18055431331316,
5.69450617401874));
#98502=CARTESIAN_POINT('Ctrl Pts',(0.532972640700167,-1.19063216004005,
5.69363619561337));
#98503=CARTESIAN_POINT('Ctrl Pts',(0.524118430766668,-1.19503559496727,
5.69325606547248));
#98504=CARTESIAN_POINT('Ctrl Pts',(0.515219619440634,-1.19934206145461,
5.69287620721068));
#98505=CARTESIAN_POINT('Ctrl Pts',(0.506281518471323,-1.20354925088432,
5.69249674135234));
#98506=CARTESIAN_POINT('Ctrl Pts',(0.456313640641153,-1.22706927243628,
5.69037536190998));
#98507=CARTESIAN_POINT('Ctrl Pts',(0.405086616979423,-1.2475067881456,5.68826478749503));
#98508=CARTESIAN_POINT('Ctrl Pts',(0.352918125008723,-1.26472873923489,
5.68616078779836));
#98509=CARTESIAN_POINT('Ctrl Pts',(0.301130796410408,-1.28182486002492,
5.68407216074501));
#98510=CARTESIAN_POINT('Ctrl Pts',(0.248414662726704,-1.29575277039046,
5.68199001268599));
#98511=CARTESIAN_POINT('Ctrl Pts',(0.195056298048485,-1.3063376162642,5.67991020536117));
#98512=CARTESIAN_POINT('Ctrl Pts',(0.157299308733902,-1.31382757430473,
5.67843850990324));
#98513=CARTESIAN_POINT('Ctrl Pts',(0.119220216467326,-1.3196427068114,5.67696798648358));
#98514=CARTESIAN_POINT('Ctrl Pts',(0.080917428897481,-1.3237050976022,5.67549716887144));
#98515=CARTESIAN_POINT('Ctrl Pts',(0.0675150714420637,-1.3251265506336,
5.67498252164494));
#98516=CARTESIAN_POINT('Ctrl Pts',(0.054085318460846,-1.32633328057544,
5.67446783839933));
#98517=CARTESIAN_POINT('Ctrl Pts',(0.0406323831126857,-1.32732152170149,
5.67395305632082));
#98518=CARTESIAN_POINT('Ctrl Pts',(0.0310947606857456,-1.32802214728863,
5.67358809529411));
#98519=CARTESIAN_POINT('Ctrl Pts',(0.0215549369531186,-1.3286122462768,
5.67322344616837));
#98520=CARTESIAN_POINT('Ctrl Pts',(0.0120155086475037,-1.32909103808168,
5.67285912622491));
#98521=CARTESIAN_POINT('Ctrl Pts',(-0.00344419505176427,-1.32986697341029,
5.67226870526915));
#98522=CARTESIAN_POINT('Ctrl Pts',(-0.0189037323976286,-1.33035065422119,
5.67167911528228));
#98523=CARTESIAN_POINT('Ctrl Pts',(-0.0343564581252633,-1.33053883536392,
5.67109026509666));
#98524=CARTESIAN_POINT('Ctrl Pts',(-0.0872006350171361,-1.33118236439367,
5.6690765554172));
#98525=CARTESIAN_POINT('Ctrl Pts',(-0.139964535350896,-1.32837422798037,
5.66707149739168));
#98526=CARTESIAN_POINT('Ctrl Pts',(-0.192401313336328,-1.32232893402684,
5.66507144501836));
#98527=CARTESIAN_POINT('Ctrl Pts',(-0.241586456950124,-1.31665851218333,
5.66319541702816));
#98528=CARTESIAN_POINT('Ctrl Pts',(-0.290484460932256,-1.30813920938173,
5.66132379313179));
#98529=CARTESIAN_POINT('Ctrl Pts',(-0.33889288810406,-1.29690893660877,
5.65945356440877));
#98530=CARTESIAN_POINT('Ctrl Pts',(-0.363232576035602,-1.29126237152394,
5.65851321608228));
#98531=CARTESIAN_POINT('Ctrl Pts',(-0.387448456924702,-1.28492988851642,
5.65757322046455));
#98532=CARTESIAN_POINT('Ctrl Pts',(-0.411514170147874,-1.277925756854,5.6566331950896));
#98533=CARTESIAN_POINT('Ctrl Pts',(-0.42593645895614,-1.27372826606078,
5.65606984933213));
#98534=CARTESIAN_POINT('Ctrl Pts',(-0.440304804608976,-1.26928951495865,
5.65550649288748));
#98535=CARTESIAN_POINT('Ctrl Pts',(-0.454613401700036,-1.26461222623906,
5.65494304343682));
#98536=CARTESIAN_POINT('Ctrl Pts',(-0.466630137166139,-1.26068411638425,
5.65446984379649));
#98537=CARTESIAN_POINT('Ctrl Pts',(-0.478607888322525,-1.25658647906165,
5.65399645163749));
#98538=CARTESIAN_POINT('Ctrl Pts',(-0.490518844838995,-1.25232993122734,
5.65352378741673));
#98539=CARTESIAN_POINT('Ctrl Pts',(-0.542976408693921,-1.23358348298773,
5.65144210627652));
#98540=CARTESIAN_POINT('Ctrl Pts',(-0.594232610756737,-1.21173023760249,
5.64937086575094));
#98541=CARTESIAN_POINT('Ctrl Pts',(-0.644015416885706,-1.186981761985,5.64730607728095));
#98542=CARTESIAN_POINT('Ctrl Pts',(-0.694431611488203,-1.1619184106019,
5.6452150184313));
#98543=CARTESIAN_POINT('Ctrl Pts',(-0.743337741202658,-1.13388527596091,
5.64313057686115));
#98544=CARTESIAN_POINT('Ctrl Pts',(-0.790438091635156,-1.10305083920001,
5.64104860982653));
#98545=CARTESIAN_POINT('Ctrl Pts',(-0.82903501505241,-1.07778320566126,
5.63934251801502));
#98546=CARTESIAN_POINT('Ctrl Pts',(-0.866419351609151,-1.05063337894,5.63763808789653));
#98547=CARTESIAN_POINT('Ctrl Pts',(-0.902414217563568,-1.02167191376899,
5.63593303979182));
#98548=CARTESIAN_POINT('Ctrl Pts',(-0.910920068938172,-1.01482810669252,
5.63553012439318));
#98549=CARTESIAN_POINT('Ctrl Pts',(-0.919348257804233,-1.00788305577541,
5.63512717448546));
#98550=CARTESIAN_POINT('Ctrl Pts',(-0.927696304763954,-1.00083754833469,
5.63472415998677));
#98551=CARTESIAN_POINT('Ctrl Pts',(-0.935430870222364,-0.994309801335792,
5.63435076222848));
#98552=CARTESIAN_POINT('Ctrl Pts',(-0.943089808691193,-0.987701554018673,
5.63397763797728));
#98553=CARTESIAN_POINT('Ctrl Pts',(-0.950669202156926,-0.981015938959458,
5.63360487756966));
#98554=CARTESIAN_POINT('Ctrl Pts',(-0.994716725700271,-0.942162594288292,
5.63143858644033));
#98555=CARTESIAN_POINT('Ctrl Pts',(-1.03610577124962,-0.900678804961991,
5.62928334127626));
#98556=CARTESIAN_POINT('Ctrl Pts',(-1.07451332611403,-0.856759471162354,
5.6271346426298));
#98557=CARTESIAN_POINT('Ctrl Pts',(-1.11097156084944,-0.815069199893007,
5.62509499808838));
#98558=CARTESIAN_POINT('Ctrl Pts',(-1.1447440267616,-0.771183458743441,
5.62306125240976));
#98559=CARTESIAN_POINT('Ctrl Pts',(-1.17552202326385,-0.725229965465032,
5.62102955705275));
#98560=CARTESIAN_POINT('Ctrl Pts',(-1.17716763689676,-0.722772960344077,
5.62092092796842));
#98561=CARTESIAN_POINT('Ctrl Pts',(-1.17880468047763,-0.720310036094466,
5.62081230474544));
#98562=CARTESIAN_POINT('Ctrl Pts',(-1.18043310341633,-0.717841209608489,
5.62070368679555));
#98563=CARTESIAN_POINT('Ctrl Pts',(-1.19779808226647,-0.691514437432329,
5.6195454198873));
#98564=CARTESIAN_POINT('Ctrl Pts',(-1.2141831700846,-0.664516719103805,
5.61838775260412));
#98565=CARTESIAN_POINT('Ctrl Pts',(-1.22958828555354,-0.636906248028152,
5.61722997163347));
#98566=CARTESIAN_POINT('Ctrl Pts',(-1.23690953438257,-0.623784429536166,
5.61667973865452));
#98567=CARTESIAN_POINT('Ctrl Pts',(-1.24400937600217,-0.610524175668424,
5.61612947999804));
#98568=CARTESIAN_POINT('Ctrl Pts',(-1.2508874161718,-0.597131552682936,
5.61557911909725));
#98569=CARTESIAN_POINT('Ctrl Pts',(-1.25640057861486,-0.58639656070315,
5.61513797176842));
#98570=CARTESIAN_POINT('Ctrl Pts',(-1.26177201580687,-0.575574540243382,
5.61469668149742));
#98571=CARTESIAN_POINT('Ctrl Pts',(-1.26699204746436,-0.564689109942556,
5.6142560315327));
#98572=CARTESIAN_POINT('Ctrl Pts',(-1.29112033611147,-0.514373935326777,
5.61221923745966));
#98573=CARTESIAN_POINT('Ctrl Pts',(-1.312066220014,-0.462614761951816,5.61019231073867));
#98574=CARTESIAN_POINT('Ctrl Pts',(-1.32987929292052,-0.409758600558678,
5.60817151787187));
#98575=CARTESIAN_POINT('Ctrl Pts',(-1.34804948442468,-0.355842772575017,
5.60611021191009));
#98576=CARTESIAN_POINT('Ctrl Pts',(-1.36296026011463,-0.300784543684916,
5.60405528821232));
#98577=CARTESIAN_POINT('Ctrl Pts',(-1.37461703271366,-0.244924160611515,
5.6020027842));
#98578=CARTESIAN_POINT('Ctrl Pts',(-1.38301163406865,-0.204696418030524,
5.60052467756142));
#98579=CARTESIAN_POINT('Ctrl Pts',(-1.38971768499473,-0.16405202684515,
5.59904782580349));
#98580=CARTESIAN_POINT('Ctrl Pts',(-1.39472131887101,-0.123113826832369,
5.59757074898948));
#98581=CARTESIAN_POINT('Ctrl Pts',(-1.39670759266725,-0.106862742927967,
5.59698439933976));
#98582=CARTESIAN_POINT('Ctrl Pts',(-1.39842544577593,-0.0905653426305087,
5.59639801422521));
#98583=CARTESIAN_POINT('Ctrl Pts',(-1.39987341132275,-0.0742292878849616,
5.59581150106865));
#98584=CARTESIAN_POINT('Ctrl Pts',(-1.40078997953924,-0.063888497252477,
5.59544023579991));
#98585=CARTESIAN_POINT('Ctrl Pts',(-1.40159832239367,-0.0535318605566342,
5.59506890679375));
#98586=CARTESIAN_POINT('Ctrl Pts',(-1.40229726272754,-0.0431766457076119,
5.59469803805592));
#98587=CARTESIAN_POINT('Ctrl Pts',(-1.40327566417533,-0.0286810490031125,
5.59417888285419));
#98588=CARTESIAN_POINT('Ctrl Pts',(-1.40404039706439,-0.0141809540206952,
5.5936603676618));
#98589=CARTESIAN_POINT('Ctrl Pts',(-1.40459200171434,0.000318079185916144,
5.59314243068829));
#98590=CARTESIAN_POINT('',(0.632686155053592,1.31670003839153,5.5365));
#98591=CARTESIAN_POINT('Ctrl Pts',(0.632684721053846,1.31669749784948,5.5365));
#98592=CARTESIAN_POINT('Ctrl Pts',(0.5776126161197,1.33489715577749,5.5438663413747));
#98593=CARTESIAN_POINT('Ctrl Pts',(0.521701465845253,1.34991581051279,5.5512639488319));
#98594=CARTESIAN_POINT('Ctrl Pts',(0.465251304334383,1.36164744646314,5.55870934620359));
#98595=CARTESIAN_POINT('Ctrl Pts',(0.410290964957589,1.37306946326556,5.56595824603648));
#98596=CARTESIAN_POINT('Ctrl Pts',(0.354818674551029,1.38137556945319,5.57325244654584));
#98597=CARTESIAN_POINT('Ctrl Pts',(0.299116808798334,1.38641968110749,5.58060719750617));
#98598=CARTESIAN_POINT('Ctrl Pts',(0.265773215134626,1.3894391277117,5.58500981174906));
#98599=CARTESIAN_POINT('Ctrl Pts',(0.232347534925492,1.39128877703379,5.58943412314275));
#98600=CARTESIAN_POINT('Ctrl Pts',(0.198903503703726,1.39192889738093,5.59388340276906));
#98601=CARTESIAN_POINT('Ctrl Pts',(0.174835521717936,1.39238955970006,5.59708532484554));
#98602=CARTESIAN_POINT('Ctrl Pts',(0.150758086854015,1.39222368124497,5.60030017785668));
#98603=CARTESIAN_POINT('Ctrl Pts',(0.126696106755384,1.39141440232077,5.60352918094528));
#98604=CARTESIAN_POINT('Ctrl Pts',(0.116740991131968,1.39107958094576,5.6048651100319));
#98605=CARTESIAN_POINT('Ctrl Pts',(0.106789185635262,1.39063453208846,5.6062033764661));
#98606=CARTESIAN_POINT('Ctrl Pts',(0.096855542906272,1.39007904004502,5.60754230086134));
#98607=CARTESIAN_POINT('Ctrl Pts',(0.0431629060528989,1.38707653297111,
5.61477936215785));
#98608=CARTESIAN_POINT('Ctrl Pts',(-0.0101013612254671,1.38084853180898,
5.62204918559313));
#98609=CARTESIAN_POINT('Ctrl Pts',(-0.062681467909731,1.37127180372221,
5.62936778152763));
#98610=CARTESIAN_POINT('Ctrl Pts',(-0.0748777648155605,1.3690504195049,
5.63106537734056));
#98611=CARTESIAN_POINT('Ctrl Pts',(-0.0870371762268703,1.36664865395529,
5.6327655972999));
#98612=CARTESIAN_POINT('Ctrl Pts',(-0.0991563532317366,1.36406459322577,
5.63446864121724));
#98613=CARTESIAN_POINT('Ctrl Pts',(-0.151155968387667,1.3529771931968,5.64177587241452));
#98614=CARTESIAN_POINT('Ctrl Pts',(-0.20241723694028,1.33853649093085,5.64913509270409));
#98615=CARTESIAN_POINT('Ctrl Pts',(-0.252697184270726,1.32091854822008,
5.65656208552686));
#98616=CARTESIAN_POINT('Ctrl Pts',(-0.276692007497009,1.31251083414319,
5.66010642853729));
#98617=CARTESIAN_POINT('Ctrl Pts',(-0.300462900284357,1.30337900742421,
5.66366620628353));
#98618=CARTESIAN_POINT('Ctrl Pts',(-0.323980669253028,1.29353978580801,
5.66724313418339));
#98619=CARTESIAN_POINT('Ctrl Pts',(-0.344366643764626,1.28501082537181,
5.67034373276029));
#98620=CARTESIAN_POINT('Ctrl Pts',(-0.364562398637558,1.27595029836785,
5.67345721794848));
#98621=CARTESIAN_POINT('Ctrl Pts',(-0.384547613705539,1.26636838485261,
5.67658470706387));
#98622=CARTESIAN_POINT('Ctrl Pts',(-0.393231305074717,1.26220498809107,
5.67794361914694));
#98623=CARTESIAN_POINT('Ctrl Pts',(-0.401871759831675,1.2579447372934,5.67930463795576));
#98624=CARTESIAN_POINT('Ctrl Pts',(-0.410459095485719,1.25359307181017,
5.68066652441999));
#98625=CARTESIAN_POINT('Ctrl Pts',(-0.457860218704337,1.22957236968709,
5.68818398393266));
#98626=CARTESIAN_POINT('Ctrl Pts',(-0.503723345675591,1.20273254085136,
5.69574001132433));
#98627=CARTESIAN_POINT('Ctrl Pts',(-0.547817782657036,1.17327249559497,
5.70335294833422));
#98628=CARTESIAN_POINT('Ctrl Pts',(-0.591573456579066,1.14403878217871,
5.71090739765249));
#98629=CARTESIAN_POINT('Ctrl Pts',(-0.633588209819031,1.11222397120681,
5.71851788551221));
#98630=CARTESIAN_POINT('Ctrl Pts',(-0.67359559348855,1.07799259910652,5.7262023341514));
#98631=CARTESIAN_POINT('Ctrl Pts',(-0.695111525426927,1.05958300055963,
5.73033502313878));
#98632=CARTESIAN_POINT('Ctrl Pts',(-0.716046101869675,1.04047404160734,
5.73448910363906));
#98633=CARTESIAN_POINT('Ctrl Pts',(-0.736351872882751,1.02068919616837,
5.7386673633923));
#98634=CARTESIAN_POINT('Ctrl Pts',(-0.751657458360816,1.00577626117853,
5.74181674943439));
#98635=CARTESIAN_POINT('Ctrl Pts',(-0.766605704164082,0.990479292062633,
5.74497987285309));
#98636=CARTESIAN_POINT('Ctrl Pts',(-0.781174508355632,0.974808057976537,
5.7481579274816));
#98637=CARTESIAN_POINT('Ctrl Pts',(-0.787955137137737,0.967514335067083,
5.74963706114294));
#98638=CARTESIAN_POINT('Ctrl Pts',(-0.794654129011777,0.960138725612505,
5.75111957954705));
#98639=CARTESIAN_POINT('Ctrl Pts',(-0.801258369521843,0.952694819900035,
5.75260312372203));
#98640=CARTESIAN_POINT('Ctrl Pts',(-0.83461777006059,0.915094094751325,
5.76009681573319));
#98641=CARTESIAN_POINT('Ctrl Pts',(-0.865631920666325,0.875680189096366,
5.76763145065592));
#98642=CARTESIAN_POINT('Ctrl Pts',(-0.894075852218896,0.834608475514328,
5.77522568029987));
#98643=CARTESIAN_POINT('Ctrl Pts',(-0.922876152304258,0.793022182353815,
5.78291505658242));
#98644=CARTESIAN_POINT('Ctrl Pts',(-0.949042126947202,0.749735397248123,
5.79066553024238));
#98645=CARTESIAN_POINT('Ctrl Pts',(-0.972286221838532,0.704896061770876,
5.79849646296423));
#98646=CARTESIAN_POINT('Ctrl Pts',(-0.994114901027574,0.662787153088537,
5.80585054230935));
#98647=CARTESIAN_POINT('Ctrl Pts',(-1.01336659524672,0.619308291408811,
5.81327558018311));
#98648=CARTESIAN_POINT('Ctrl Pts',(-1.02975283339989,0.574581994853113,
5.82078761227338));
#98649=CARTESIAN_POINT('Ctrl Pts',(-1.03081535021928,0.57168185133541,5.82127470762554));
#98650=CARTESIAN_POINT('Ctrl Pts',(-1.03186580105051,0.568776465116369,
5.82176216874382));
#98651=CARTESIAN_POINT('Ctrl Pts',(-1.03290409957988,0.565865870654058,
5.82225));
#98652=CARTESIAN_POINT('',(-0.632402293996042,1.31836377294842,5.53649999999999));
#98653=CARTESIAN_POINT('Origin',(0.,0.,5.5365));
#98654=CARTESIAN_POINT('Ctrl Pts',(-1.40459200171434,0.000318079185916144,
5.59314243068829));
#98655=CARTESIAN_POINT('Ctrl Pts',(-1.40680778098466,0.0585602590185899,
5.59106189346052));
#98656=CARTESIAN_POINT('Ctrl Pts',(-1.4055885051658,0.116784323458512,5.58899068555129));
#98657=CARTESIAN_POINT('Ctrl Pts',(-1.40093750525803,0.174640198144212,
5.58692480237197));
#98658=CARTESIAN_POINT('Ctrl Pts',(-1.39633232148189,0.231926145411667,
5.58487926982209));
#98659=CARTESIAN_POINT('Ctrl Pts',(-1.38836273052522,0.28885226195592,5.58283895761298));
#98660=CARTESIAN_POINT('Ctrl Pts',(-1.37698165172494,0.345081547364195,
5.58079997833938));
#98661=CARTESIAN_POINT('Ctrl Pts',(-1.37163519174172,0.371496233493362,
5.57984213231404));
#98662=CARTESIAN_POINT('Ctrl Pts',(-1.36553515098603,0.397757077520593,
5.57888458044281));
#98663=CARTESIAN_POINT('Ctrl Pts',(-1.35867270637224,0.423828272539498,
5.5779269197225));
#98664=CARTESIAN_POINT('Ctrl Pts',(-1.3550589480402,0.437557344834855,5.57742261628516));
#98665=CARTESIAN_POINT('Ctrl Pts',(-1.35123372725876,0.451233812302909,
5.57691828266322));
#98666=CARTESIAN_POINT('Ctrl Pts',(-1.34719546760397,0.464852331742502,
5.57641386000633));
#98667=CARTESIAN_POINT('Ctrl Pts',(-1.34347158307698,0.477410660863661,
5.57594870623028));
#98668=CARTESIAN_POINT('Ctrl Pts',(-1.33956525510877,0.489923136969561,
5.57548334714617));
#98669=CARTESIAN_POINT('Ctrl Pts',(-1.33548376997894,0.502360503152716,
5.5750186753579));
#98670=CARTESIAN_POINT('Ctrl Pts',(-1.32167213509367,0.544448212697522,
5.57344623864017));
#98671=CARTESIAN_POINT('Ctrl Pts',(-1.30584082143809,0.585731598763993,
5.57187962186733));
#98672=CARTESIAN_POINT('Ctrl Pts',(-1.2879823448929,0.626060508418404,5.57031710849444));
#98673=CARTESIAN_POINT('Ctrl Pts',(-1.26509212904047,0.677752344771133,
5.56831434704458));
#98674=CARTESIAN_POINT('Ctrl Pts',(-1.23887339227609,0.727877279493874,
5.56631832706785));
#98675=CARTESIAN_POINT('Ctrl Pts',(-1.20962767910274,0.776285009599572,
5.56432543386955));
#98676=CARTESIAN_POINT('Ctrl Pts',(-1.17972369750887,0.825782310674114,
5.56228768422853));
#98677=CARTESIAN_POINT('Ctrl Pts',(-1.14665431471445,0.873484996740448,
5.56025320370633));
#98678=CARTESIAN_POINT('Ctrl Pts',(-1.11069355490779,0.919207501903464,
5.55821812799238));
#98679=CARTESIAN_POINT('Ctrl Pts',(-1.10074051269562,0.931862351978381,
5.55765486974659));
#98680=CARTESIAN_POINT('Ctrl Pts',(-1.0905657304381,0.944365329077774,5.55709156590646));
#98681=CARTESIAN_POINT('Ctrl Pts',(-1.08017448707633,0.956712047355874,
5.55652813454011));
#98682=CARTESIAN_POINT('Ctrl Pts',(-1.07336013054068,0.964808762778951,
5.55615864822553));
#98683=CARTESIAN_POINT('Ctrl Pts',(-1.06645228235592,0.972838575185135,
5.55578909024319));
#98684=CARTESIAN_POINT('Ctrl Pts',(-1.05946296377322,0.980788625511553,
5.55541998337116));
#98685=CARTESIAN_POINT('Ctrl Pts',(-1.0207932618269,1.0247737540964,5.55337783111282));
#98686=CARTESIAN_POINT('Ctrl Pts',(-0.979560085515444,1.06640812044688,
5.55134545805107));
#98687=CARTESIAN_POINT('Ctrl Pts',(-0.936079694160814,1.10553268147045,
5.54931910582972));
#98688=CARTESIAN_POINT('Ctrl Pts',(-0.890073531427023,1.14692998414553,
5.54717504302009));
#98689=CARTESIAN_POINT('Ctrl Pts',(-0.841550919085985,1.185518576841,5.54503772086778));
#98690=CARTESIAN_POINT('Ctrl Pts',(-0.790836296596859,1.22107346264117,
5.54290268726531));
#98691=CARTESIAN_POINT('Ctrl Pts',(-0.740121674107733,1.25662834844134,
5.54076765366285));
#98692=CARTESIAN_POINT('Ctrl Pts',(-0.68721393539805,1.2891504552414,5.53863490861023));
#98693=CARTESIAN_POINT('Ctrl Pts',(-0.632402293996098,1.31836377294839,
5.5365));
#98694=CARTESIAN_POINT('',(-0.999999999999998,-1.22464679914735E-16,6.));
#98695=CARTESIAN_POINT('',(-1.25,-1.53080849893419E-16,5.75));
#98696=CARTESIAN_POINT('Origin',(0.,0.,6.));
#98697=CARTESIAN_POINT('Ctrl Pts',(0.850780204044567,-1.1908002747757,1.37152216057906));
#98698=CARTESIAN_POINT('Ctrl Pts',(1.24665751306111,-0.907961426921765,
1.39797740749264));
#98699=CARTESIAN_POINT('Ctrl Pts',(1.72735056947482,0.0786343709257417,
1.4508879013198));
#98700=CARTESIAN_POINT('Ctrl Pts',(0.869444322178829,1.49656652414857,1.53025364206055));
#98701=CARTESIAN_POINT('Ctrl Pts',(-0.784660621780123,1.54085420010821,
1.60961938280129));
#98702=CARTESIAN_POINT('Ctrl Pts',(-1.72048121864664,0.177590566749858,
1.68898512354203));
#98703=CARTESIAN_POINT('Ctrl Pts',(-1.08239711820243,-1.34930263152836,
1.76835086428277));
#98704=CARTESIAN_POINT('Ctrl Pts',(0.546100579856982,-1.64108839020809,
1.84771660502351));
#98705=CARTESIAN_POINT('Ctrl Pts',(1.67490386887139,-0.431722927133368,
1.92708234576425));
#98706=CARTESIAN_POINT('Ctrl Pts',(1.27133073655079,1.17280087221257,2.00644808650499));
#98707=CARTESIAN_POINT('Ctrl Pts',(-0.295425382742359,1.7042169630666,2.08581382724573));
#98708=CARTESIAN_POINT('Ctrl Pts',(-1.59188248145604,0.676454136362828,
2.16517956798647));
#98709=CARTESIAN_POINT('Ctrl Pts',(-1.43189637910881,-0.970235084489994,
2.24454530872721));
#98710=CARTESIAN_POINT('Ctrl Pts',(0.0381646212441605,-1.72922282369982,
2.32391104946795));
#98711=CARTESIAN_POINT('Ctrl Pts',(1.47330683231875,-0.906114154436845,
2.40327679020869));
#98712=CARTESIAN_POINT('Ctrl Pts',(1.56048965036714,0.746021253660212,2.48264253094943));
#98713=CARTESIAN_POINT('Ctrl Pts',(0.219946717955126,1.71560400018136,2.56200827169018));
#98714=CARTESIAN_POINT('Ctrl Pts',(-1.32183001348916,1.11554483087117,2.64137401243091));
#98715=CARTESIAN_POINT('Ctrl Pts',(-1.6542362198257,-0.505150719675214,
2.72073975317166));
#98716=CARTESIAN_POINT('Ctrl Pts',(-0.47314620318653,-1.66367278437318,
2.80010549391239));
#98717=CARTESIAN_POINT('Ctrl Pts',(1.14083539250324,-1.30006509600873,2.87947123465314));
#98718=CARTESIAN_POINT('Ctrl Pts',(1.71104224612908,0.253000088961462,2.95883697539387));
#98719=CARTESIAN_POINT('Ctrl Pts',(0.715779865238755,1.57459003111278,3.03820271613462));
#98720=CARTESIAN_POINT('Ctrl Pts',(-0.934364853836859,1.45555382197998,
3.11756845687536));
#98721=CARTESIAN_POINT('Ctrl Pts',(-1.72963914154473,0.00480021022192471,
3.1969341976161));
#98722=CARTESIAN_POINT('Ctrl Pts',(-0.942429502195046,-1.45034521121045,
3.27629993835684));
#98723=CARTESIAN_POINT('Ctrl Pts',(0.707029089469739,-1.57853871314733,
3.35566567909759));
#98724=CARTESIAN_POINT('Ctrl Pts',(1.70961161212856,-0.262493308300521,
3.43503141983832));
#98725=CARTESIAN_POINT('Ctrl Pts',(1.14803382433629,1.29371285008445,3.51439716057907));
#98726=CARTESIAN_POINT('Ctrl Pts',(-0.463904717388525,1.66627339125727,
3.5937629013198));
#98727=CARTESIAN_POINT('Ctrl Pts',(-1.65140689002388,0.514324689124398,
3.67312864206055));
#98728=CARTESIAN_POINT('Ctrl Pts',(-1.32800149895114,-1.10819069526513,
3.75249438280128));
#98729=CARTESIAN_POINT('Ctrl Pts',(0.210420926876642,-1.71679865899124,
3.83186012354203));
#98730=CARTESIAN_POINT('Ctrl Pts',(1.55632474164788,-0.754670727735459,
3.91122586428277));
#98731=CARTESIAN_POINT('Ctrl Pts',(1.47831367962429,0.897921625865326,3.99059160502351));
#98732=CARTESIAN_POINT('Ctrl Pts',(0.0477617634505684,1.72898624257253,
4.06995734576425));
#98733=CARTESIAN_POINT('Ctrl Pts',(-1.42648845110344,0.97816427327762,4.14932308650499));
#98734=CARTESIAN_POINT('Ctrl Pts',(-1.59561373357911,-0.667601135609854,
4.22868882724573));
#98735=CARTESIAN_POINT('Ctrl Pts',(-0.30487794355985,-1.70256399589041,
4.30805456798647));
#98736=CARTESIAN_POINT('Ctrl Pts',(1.26479746913964,-1.17981448384994,4.38742030872722));
#98737=CARTESIAN_POINT('Ctrl Pts',(1.67728207661725,0.422372441852027,4.46678604946795));
#98738=CARTESIAN_POINT('Ctrl Pts',(0.555186290818104,1.63812204743828,4.54615179020869));
#98739=CARTESIAN_POINT('Ctrl Pts',(-1.07486310747744,1.35511814363614,4.62551753094944));
#98740=CARTESIAN_POINT('Ctrl Pts',(-1.72149382964358,-0.167711379513054,
4.70488327169017));
#98741=CARTESIAN_POINT('Ctrl Pts',(-0.793099380882797,-1.53710010465276,
4.78424901243091));
#98742=CARTESIAN_POINT('Ctrl Pts',(0.860930945424167,-1.50015930506732,
4.86361475317166));
#98743=CARTESIAN_POINT('Ctrl Pts',(1.72725376076341,-0.0906976289718168,
4.9429804939124));
#98744=CARTESIAN_POINT('Ctrl Pts',(1.01331952241407,1.4017586358057,5.02234623465314));
#98745=CARTESIAN_POINT('Ctrl Pts',(-0.627807088834987,1.61169039054698,
5.10171197539388));
#98746=CARTESIAN_POINT('Ctrl Pts',(-1.69437838885534,0.347100595182272,
5.18107771613462));
#98747=CARTESIAN_POINT('Ctrl Pts',(-1.2110334922522,-1.23515140512641,5.26044345687535));
#98748=CARTESIAN_POINT('Ctrl Pts',(0.38089666041727,-1.68716085990558,5.33980919761611));
#98749=CARTESIAN_POINT('Ctrl Pts',(1.6232201233188,-0.59588622120029,5.41917493835683));
#98750=CARTESIAN_POINT('Ctrl Pts',(1.38257289293014,1.0412189905615,5.49854067909759));
#98751=CARTESIAN_POINT('Ctrl Pts',(-0.127306102888356,1.72444672585826,
5.57790641983832));
#98752=CARTESIAN_POINT('Ctrl Pts',(-1.04974858331048,1.12985699072368,5.63081691366548));
#98753=CARTESIAN_POINT('Ctrl Pts',(-1.28351105899822,0.703158311782828,
5.65727216057906));
#98754=CARTESIAN_POINT('Ctrl Pts',(0.795408277542864,-1.11329858282327,
1.42651477371938));
#98755=CARTESIAN_POINT('Ctrl Pts',(1.16552042517654,-0.848867934667374,
1.45297002063296));
#98756=CARTESIAN_POINT('Ctrl Pts',(1.61492819725584,0.0735165548473875,
1.50588051446012));
#98757=CARTESIAN_POINT('Ctrl Pts',(0.812857665747304,1.39916443229674,1.58524625520086));
#98758=CARTESIAN_POINT('Ctrl Pts',(-0.733592002562801,1.4405697022877,1.6646119959416));
#98759=CARTESIAN_POINT('Ctrl Pts',(-1.60850592921986,0.166032314967876,
1.74397773668234));
#98760=CARTESIAN_POINT('Ctrl Pts',(-1.01195070514552,-1.26148501919281,
1.82334347742308));
#98761=CARTESIAN_POINT('Ctrl Pts',(0.510558331663356,-1.53428028008351,
1.90270921816382));
#98762=CARTESIAN_POINT('Ctrl Pts',(1.56589492216145,-0.403624800170977,
1.98207495890456));
#98763=CARTESIAN_POINT('Ctrl Pts',(1.18858782390544,1.09647064803885,2.0614406996453));
#98764=CARTESIAN_POINT('Ctrl Pts',(-0.27619800474017,1.59330021162684,2.14080644038604));
#98765=CARTESIAN_POINT('Ctrl Pts',(-1.4882768741047,0.632427995953832,2.22017218112678));
#98766=CARTESIAN_POINT('Ctrl Pts',(-1.33870325979885,-0.907088591973651,
2.29953792186753));
#98767=CARTESIAN_POINT('Ctrl Pts',(0.0356807263528025,-1.61667859824208,
2.37890366260826));
#98768=CARTESIAN_POINT('Ctrl Pts',(1.37741856735233,-0.847140889517054,
2.45826940334901));
#98769=CARTESIAN_POINT('Ctrl Pts',(1.45892720472486,0.697467427619125,2.53763514408974));
#98770=CARTESIAN_POINT('Ctrl Pts',(0.205631770988793,1.60394613819484,2.61700088483048));
#98771=CARTESIAN_POINT('Ctrl Pts',(-1.23580042087909,1.04294104191286,2.69636662557123));
#98772=CARTESIAN_POINT('Ctrl Pts',(-1.54657240025727,-0.472273640038004,
2.77573236631196));
#98773=CARTESIAN_POINT('Ctrl Pts',(-0.442352096009542,-1.55539479823614,
2.85509810705271));
#98774=CARTESIAN_POINT('Ctrl Pts',(1.06658560013157,-1.21545204483358,2.93446384779345));
#98775=CARTESIAN_POINT('Ctrl Pts',(1.59968127999051,0.236533906198515,3.01382958853419));
#98776=CARTESIAN_POINT('Ctrl Pts',(0.669194260753619,1.47210988047151,3.09319532927493));
#98777=CARTESIAN_POINT('Ctrl Pts',(-0.873552928775051,1.3608209886738,3.17256107001567));
#98778=CARTESIAN_POINT('Ctrl Pts',(-1.61706782057982,0.0044877947633364,
3.25192681075641));
#98779=CARTESIAN_POINT('Ctrl Pts',(-0.881092699951054,-1.35595137358299,
3.33129255149715));
#98780=CARTESIAN_POINT('Ctrl Pts',(0.661013017879724,-1.47580156765551,
3.41065829223789));
#98781=CARTESIAN_POINT('Ctrl Pts',(1.59834375694903,-0.245409271665311,
3.49002403297863));
#98782=CARTESIAN_POINT('Ctrl Pts',(1.07331553136189,1.20951322659928,3.56938977371938));
#98783=CARTESIAN_POINT('Ctrl Pts',(-0.433712080332666,1.557826147993,3.64875551446012));
#98784=CARTESIAN_POINT('Ctrl Pts',(-1.54392721371723,0.480850533580084,
3.72812125520086));
#98785=CARTESIAN_POINT('Ctrl Pts',(-1.24157024321141,-1.03606554068775,
3.80748699594159));
#98786=CARTESIAN_POINT('Ctrl Pts',(0.196725953671999,-1.60506304418501,
3.88685273668234));
#98787=CARTESIAN_POINT('Ctrl Pts',(1.45503336368959,-0.705553961888648,
3.96621847742308));
#98788=CARTESIAN_POINT('Ctrl Pts',(1.38209955049261,0.839481561045601,4.04558421816382));
#98789=CARTESIAN_POINT('Ctrl Pts',(0.044653251001868,1.61645741469071,4.12494995890456));
#98790=CARTESIAN_POINT('Ctrl Pts',(-1.33364729977607,0.914501719789614,
4.20431569964529));
#98791=CARTESIAN_POINT('Ctrl Pts',(-1.49176528252109,-0.624151181276522,
4.28368144038605));
#98792=CARTESIAN_POINT('Ctrl Pts',(-0.285035357892558,-1.59175482567615,
4.36304718112678));
#98793=CARTESIAN_POINT('Ctrl Pts',(1.18247976573305,-1.10302778785629,4.44241292186753));
#98794=CARTESIAN_POINT('Ctrl Pts',(1.56811834733964,0.394882879100816,4.52177866260826));
#98795=CARTESIAN_POINT('Ctrl Pts',(0.519052710906638,1.53150699788686,4.601144403349));
#98796=CARTESIAN_POINT('Ctrl Pts',(-1.00490703574035,1.26692203623515,4.68051014408975));
#98797=CARTESIAN_POINT('Ctrl Pts',(-1.60945263574296,-0.156796101823534,
4.75987588483049));
#98798=CARTESIAN_POINT('Ctrl Pts',(-0.741481535970538,-1.43705993726761,
4.83924162557122));
#98799=CARTESIAN_POINT('Ctrl Pts',(0.804898371080712,-1.40252338172761,
4.91860736631197));
#98800=CARTESIAN_POINT('Ctrl Pts',(1.61483768921389,-0.0847946913841371,
4.99797310705271));
#98801=CARTESIAN_POINT('Ctrl Pts',(0.94736893511653,1.31052699244357,5.07733884779345));
#98802=CARTESIAN_POINT('Ctrl Pts',(-0.58694707844105,1.50679561111438,5.15670458853418));
#98803=CARTESIAN_POINT('Ctrl Pts',(-1.58410196826192,0.324510002977889,
5.23607032927493));
#98804=CARTESIAN_POINT('Ctrl Pts',(-1.13221494757367,-1.15476317735853,
5.31543607001568));
#98805=CARTESIAN_POINT('Ctrl Pts',(0.356106495125341,-1.57735418282597,
5.3948018107564));
#98806=CARTESIAN_POINT('Ctrl Pts',(1.51757494617763,-0.55710373908937,5.47416755149716));
#98807=CARTESIAN_POINT('Ctrl Pts',(1.29258992876779,0.97345260255263,5.55353329223789));
#98808=CARTESIAN_POINT('Ctrl Pts',(-0.119020550240519,1.61221334653609,
5.63289903297864));
#98809=CARTESIAN_POINT('Ctrl Pts',(-0.981427057816582,1.05632171339779,
5.6858095268058));
#98810=CARTESIAN_POINT('Ctrl Pts',(-1.19997540585877,0.657394164739904,
5.71226477371938));
#98811=CARTESIAN_POINT('Ctrl Pts',(0.740036351041162,-1.03579689087083,
1.48150738685969));
#98812=CARTESIAN_POINT('Ctrl Pts',(1.08438333729197,-0.789774442412982,
1.50796263377327));
#98813=CARTESIAN_POINT('Ctrl Pts',(1.50250582503687,0.0683987387690329,
1.56087312760043));
#98814=CARTESIAN_POINT('Ctrl Pts',(0.756271009315778,1.30176234044491,1.64023886834117));
#98815=CARTESIAN_POINT('Ctrl Pts',(-0.682523383345477,1.3402852044672,1.71960460908191));
#98816=CARTESIAN_POINT('Ctrl Pts',(-1.49653063979308,0.154474063185896,
1.79897034982265));
#98817=CARTESIAN_POINT('Ctrl Pts',(-0.941504292088612,-1.17366740685727,
1.87833609056339));
#98818=CARTESIAN_POINT('Ctrl Pts',(0.475016083469731,-1.42747216995893,
1.95770183130413));
#98819=CARTESIAN_POINT('Ctrl Pts',(1.45688597545151,-0.375526673208587,
2.03706757204487));
#98820=CARTESIAN_POINT('Ctrl Pts',(1.1058449112601,1.02014042386513,2.11643331278562));
#98821=CARTESIAN_POINT('Ctrl Pts',(-0.25697062673798,1.48238346018707,2.19579905352635));
#98822=CARTESIAN_POINT('Ctrl Pts',(-1.38467126675336,0.588401855544837,
2.2751647942671));
#98823=CARTESIAN_POINT('Ctrl Pts',(-1.2455101404889,-0.843942099457309,
2.35453053500783));
#98824=CARTESIAN_POINT('Ctrl Pts',(0.0331968314614454,-1.50413437278434,
2.43389627574858));
#98825=CARTESIAN_POINT('Ctrl Pts',(1.28153030238591,-0.788167624597264,
2.51326201648932));
#98826=CARTESIAN_POINT('Ctrl Pts',(1.35736475908259,0.648913601578039,2.59262775723006));
#98827=CARTESIAN_POINT('Ctrl Pts',(0.191316824022457,1.49228827620832,2.6719934979708));
#98828=CARTESIAN_POINT('Ctrl Pts',(-1.14977082826902,0.970337252954552,
2.75135923871154));
#98829=CARTESIAN_POINT('Ctrl Pts',(-1.43890858068883,-0.439396560400792,
2.83072497945228));
#98830=CARTESIAN_POINT('Ctrl Pts',(-0.411557988832554,-1.44711681209911,
2.91009072019302));
#98831=CARTESIAN_POINT('Ctrl Pts',(0.992335807759912,-1.13083899365843,
2.98945646093376));
#98832=CARTESIAN_POINT('Ctrl Pts',(1.48832031385195,0.220067723435567,3.0688222016745));
#98833=CARTESIAN_POINT('Ctrl Pts',(0.622608656268483,1.36962972983025,3.14818794241524));
#98834=CARTESIAN_POINT('Ctrl Pts',(-0.812741003713242,1.26608815536762,
3.22755368315598));
#98835=CARTESIAN_POINT('Ctrl Pts',(-1.50449649961492,0.00417537930474892,
3.30691942389672));
#98836=CARTESIAN_POINT('Ctrl Pts',(-0.819755897707061,-1.26155753595553,
3.38628516463747));
#98837=CARTESIAN_POINT('Ctrl Pts',(0.614996946289707,-1.37306442216368,
3.4656509053782));
#98838=CARTESIAN_POINT('Ctrl Pts',(1.4870759017695,-0.2283252350301,3.54501664611895));
#98839=CARTESIAN_POINT('Ctrl Pts',(0.998597238387491,1.12531360311411,3.62438238685968));
#98840=CARTESIAN_POINT('Ctrl Pts',(-0.403519443276805,1.44937890472874,
3.70374812760043));
#98841=CARTESIAN_POINT('Ctrl Pts',(-1.43644753741059,0.447376378035769,
3.78311386834117));
#98842=CARTESIAN_POINT('Ctrl Pts',(-1.15513898747168,-0.963940386110368,
3.86247960908191));
#98843=CARTESIAN_POINT('Ctrl Pts',(0.183030980467356,-1.49332742937878,
3.94184534982265));
#98844=CARTESIAN_POINT('Ctrl Pts',(1.3537419857313,-0.656437196041839,4.0212110905634));
#98845=CARTESIAN_POINT('Ctrl Pts',(1.28588542136093,0.781041496225876,4.10057683130413));
#98846=CARTESIAN_POINT('Ctrl Pts',(0.0415447385531691,1.5039285868089,4.17994257204488));
#98847=CARTESIAN_POINT('Ctrl Pts',(-1.24080614844871,0.850839166301608,
4.25930831278561));
#98848=CARTESIAN_POINT('Ctrl Pts',(-1.38791683146307,-0.580701226943189,
4.33867405352636));
#98849=CARTESIAN_POINT('Ctrl Pts',(-0.265192772225267,-1.4809456554619,
4.41803979426709));
#98850=CARTESIAN_POINT('Ctrl Pts',(1.10016206232645,-1.02624109186263,4.49740553500784));
#98851=CARTESIAN_POINT('Ctrl Pts',(1.45895461806202,0.367393316349602,4.57677127574858));
#98852=CARTESIAN_POINT('Ctrl Pts',(0.482919130995172,1.42489194833545,4.65613701648932));
#98853=CARTESIAN_POINT('Ctrl Pts',(-0.934950964003268,1.17872592883417,
4.73550275723005));
#98854=CARTESIAN_POINT('Ctrl Pts',(-1.49741144184235,-0.145880824134014,
4.8148684979708));
#98855=CARTESIAN_POINT('Ctrl Pts',(-0.689863691058279,-1.33701976988246,
4.89423423871154));
#98856=CARTESIAN_POINT('Ctrl Pts',(0.748865796737256,-1.3048874583879,4.97359997945228));
#98857=CARTESIAN_POINT('Ctrl Pts',(1.50242161766438,-0.0788917537964559,
5.05296572019302));
#98858=CARTESIAN_POINT('Ctrl Pts',(0.881418347818994,1.21929534908143,5.13233146093376));
#98859=CARTESIAN_POINT('Ctrl Pts',(-0.546087068047113,1.40190083168179,
5.2116972016745));
#98860=CARTESIAN_POINT('Ctrl Pts',(-1.4738255476685,0.301919410773503,5.29106294241524));
#98861=CARTESIAN_POINT('Ctrl Pts',(-1.05339640289514,-1.07437494959065,
5.37042868315598));
#98862=CARTESIAN_POINT('Ctrl Pts',(0.331316329833411,-1.46754750574636,
5.44979442389673));
#98863=CARTESIAN_POINT('Ctrl Pts',(1.41192976903645,-0.518321256978449,
5.52916016463746));
#98864=CARTESIAN_POINT('Ctrl Pts',(1.20260696460544,0.905686214543761,5.60852590537821));
#98865=CARTESIAN_POINT('Ctrl Pts',(-0.110734997592681,1.49997996721392,
5.68789164611894));
#98866=CARTESIAN_POINT('Ctrl Pts',(-0.913105532322684,0.982786436071908,
5.74080213994611));
#98867=CARTESIAN_POINT('Ctrl Pts',(-1.11643975271933,0.611630017696981,
5.76725738685969));
#98868=CARTESIAN_POINT('Ctrl Pts',(0.68466442453946,-0.958295198918397,
1.5365));
#98869=CARTESIAN_POINT('Ctrl Pts',(1.0032462494074,-0.730680950158591,1.56295524691358));
#98870=CARTESIAN_POINT('Ctrl Pts',(1.39008345281789,0.0632809226906779,
1.61586574074074));
#98871=CARTESIAN_POINT('Ctrl Pts',(0.699684352884252,1.20436024859309,1.69523148148148));
#98872=CARTESIAN_POINT('Ctrl Pts',(-0.631454764128155,1.24000070664669,
1.77459722222222));
#98873=CARTESIAN_POINT('Ctrl Pts',(-1.3845553503663,0.142915811403915,1.85396296296296));
#98874=CARTESIAN_POINT('Ctrl Pts',(-0.871057879031703,-1.08584979452172,
1.9333287037037));
#98875=CARTESIAN_POINT('Ctrl Pts',(0.439473835276103,-1.32066405983435,
2.01269444444444));
#98876=CARTESIAN_POINT('Ctrl Pts',(1.34787702874157,-0.347428546246197,
2.09206018518518));
#98877=CARTESIAN_POINT('Ctrl Pts',(1.02310199861475,0.943810199691403,2.17142592592593));
#98878=CARTESIAN_POINT('Ctrl Pts',(-0.237743248735789,1.37146670874731,
2.25079166666666));
#98879=CARTESIAN_POINT('Ctrl Pts',(-1.28106565940202,0.544375715135843,
2.33015740740741));
#98880=CARTESIAN_POINT('Ctrl Pts',(-1.15231702117895,-0.780795606940967,
2.40952314814815));
#98881=CARTESIAN_POINT('Ctrl Pts',(0.0307129365700887,-1.39159014732659,
2.48888888888889));
#98882=CARTESIAN_POINT('Ctrl Pts',(1.18564203741949,-0.729194359677473,
2.56825462962963));
#98883=CARTESIAN_POINT('Ctrl Pts',(1.25580231344031,0.600359775536952,2.64762037037037));
#98884=CARTESIAN_POINT('Ctrl Pts',(0.177001877056122,1.3806304142218,2.72698611111111));
#98885=CARTESIAN_POINT('Ctrl Pts',(-1.06374123565895,0.897733463996245,
2.80635185185185));
#98886=CARTESIAN_POINT('Ctrl Pts',(-1.3312447611204,-0.40651948076358,2.88571759259259));
#98887=CARTESIAN_POINT('Ctrl Pts',(-0.380763881655566,-1.33883882596208,
2.96508333333333));
#98888=CARTESIAN_POINT('Ctrl Pts',(0.918086015388248,-1.04622594248328,
3.04444907407407));
#98889=CARTESIAN_POINT('Ctrl Pts',(1.37695934771338,0.203601540672618,3.12381481481481));
#98890=CARTESIAN_POINT('Ctrl Pts',(0.576023051783349,1.26714957918899,3.20318055555555));
#98891=CARTESIAN_POINT('Ctrl Pts',(-0.751929078651436,1.17135532206144,
3.2825462962963));
#98892=CARTESIAN_POINT('Ctrl Pts',(-1.39192517865002,0.00386296384616128,
3.36191203703703));
#98893=CARTESIAN_POINT('Ctrl Pts',(-0.758419095463071,-1.16716369832806,
3.44127777777778));
#98894=CARTESIAN_POINT('Ctrl Pts',(0.568980874699694,-1.27032727667186,
3.52064351851852));
#98895=CARTESIAN_POINT('Ctrl Pts',(1.37580804658996,-0.211241198394891,
3.60000925925926));
#98896=CARTESIAN_POINT('Ctrl Pts',(0.92387894541309,1.04111397962895,3.679375));
#98897=CARTESIAN_POINT('Ctrl Pts',(-0.373326806220943,1.34093166146447,
3.75874074074074));
#98898=CARTESIAN_POINT('Ctrl Pts',(-1.32896786110395,0.413902222491454,
3.83810648148148));
#98899=CARTESIAN_POINT('Ctrl Pts',(-1.06870773173194,-0.891815231532984,
3.91747222222222));
#98900=CARTESIAN_POINT('Ctrl Pts',(0.169336007262713,-1.38159181457256,
3.99683796296296));
#98901=CARTESIAN_POINT('Ctrl Pts',(1.25245060777301,-0.607320430195027,
4.0762037037037));
#98902=CARTESIAN_POINT('Ctrl Pts',(1.18967129222925,0.72260143140615,4.15556944444444));
#98903=CARTESIAN_POINT('Ctrl Pts',(0.0384362261044693,1.39139975892709,
4.23493518518518));
#98904=CARTESIAN_POINT('Ctrl Pts',(-1.14796499712134,0.787176612813602,
4.31430092592593));
#98905=CARTESIAN_POINT('Ctrl Pts',(-1.28406838040505,-0.537251272609856,
4.39366666666667));
#98906=CARTESIAN_POINT('Ctrl Pts',(-0.245350186557975,-1.37013648524764,
4.47303240740741));
#98907=CARTESIAN_POINT('Ctrl Pts',(1.01784435891986,-0.949454395868983,
4.55239814814815));
#98908=CARTESIAN_POINT('Ctrl Pts',(1.3497908887844,0.339903753598391,4.63176388888888));
#98909=CARTESIAN_POINT('Ctrl Pts',(0.446785551083708,1.31827689878403,4.71112962962963));
#98910=CARTESIAN_POINT('Ctrl Pts',(-0.864994892266185,1.09052982143318,
4.79049537037036));
#98911=CARTESIAN_POINT('Ctrl Pts',(-1.38537024794173,-0.134965546444495,
4.86986111111111));
#98912=CARTESIAN_POINT('Ctrl Pts',(-0.63824584614602,-1.2369796024973,4.94922685185185));
#98913=CARTESIAN_POINT('Ctrl Pts',(0.692833222393801,-1.20725153504819,
5.0285925925926));
#98914=CARTESIAN_POINT('Ctrl Pts',(1.39000554611486,-0.0729888162087741,
5.10795833333333));
#98915=CARTESIAN_POINT('Ctrl Pts',(0.815467760521459,1.12806370571929,5.18732407407407));
#98916=CARTESIAN_POINT('Ctrl Pts',(-0.505227057653176,1.2970060522492,5.26668981481481));
#98917=CARTESIAN_POINT('Ctrl Pts',(-1.36354912707508,0.279328818569119,
5.34605555555555));
#98918=CARTESIAN_POINT('Ctrl Pts',(-0.974577858216613,-0.993986721822778,
5.42542129629629));
#98919=CARTESIAN_POINT('Ctrl Pts',(0.306526164541481,-1.35774082866675,
5.50478703703704));
#98920=CARTESIAN_POINT('Ctrl Pts',(1.30628459189527,-0.479538774867528,
5.58415277777777));
#98921=CARTESIAN_POINT('Ctrl Pts',(1.11262400044309,0.837919826534893,5.66351851851852));
#98922=CARTESIAN_POINT('Ctrl Pts',(-0.102449444944844,1.38774658789174,
5.74288425925926));
#98923=CARTESIAN_POINT('Ctrl Pts',(-0.844784006828786,0.909251158746022,
5.79579475308642));
#98924=CARTESIAN_POINT('Ctrl Pts',(-1.03290409957988,0.565865870654058,
5.82225));
#98925=CARTESIAN_POINT('',(0.684664424539459,-0.958295198918398,1.5365));
#98926=CARTESIAN_POINT('Ctrl Pts',(0.68466442453946,-0.958295198918397,
1.5365));
#98927=CARTESIAN_POINT('Ctrl Pts',(1.0032462494074,-0.730680950158591,1.56295524691358));
#98928=CARTESIAN_POINT('Ctrl Pts',(1.39008345281789,0.0632809226906779,
1.61586574074074));
#98929=CARTESIAN_POINT('Ctrl Pts',(0.699684352884252,1.20436024859309,1.69523148148148));
#98930=CARTESIAN_POINT('Ctrl Pts',(-0.631454764128155,1.24000070664669,
1.77459722222222));
#98931=CARTESIAN_POINT('Ctrl Pts',(-1.15936325402709,0.47096607711394,1.83023102348301));
#98932=CARTESIAN_POINT('Ctrl Pts',(-1.17944031356009,0.040928653270331,
1.85940957783022));
#98933=CARTESIAN_POINT('Ctrl Pts',(-1.17916256915606,0.000764266613825456,
1.86213288526384));
#98934=CARTESIAN_POINT('Ctrl Pts',(0.635549693826274,1.32090956116917,1.5365));
#98935=CARTESIAN_POINT('Ctrl Pts',(0.668371665271443,1.30136299053671,1.5365));
#98936=CARTESIAN_POINT('Ctrl Pts',(0.700319009618862,1.28047972670152,1.5365));
#98937=CARTESIAN_POINT('Ctrl Pts',(0.731298112320437,1.258254780263,1.5365));
#98938=CARTESIAN_POINT('Ctrl Pts',(0.778115193593959,1.22466739286398,1.5365));
#98939=CARTESIAN_POINT('Ctrl Pts',(0.8227230333276,1.18801677550436,1.5365));
#98940=CARTESIAN_POINT('Ctrl Pts',(0.864970762882032,1.14861428602645,1.5365));
#98941=CARTESIAN_POINT('Ctrl Pts',(0.888238976066587,1.12691310741061,1.5365));
#98942=CARTESIAN_POINT('Ctrl Pts',(0.910790566548664,1.10437663719369,1.5365));
#98943=CARTESIAN_POINT('Ctrl Pts',(0.932594554500452,1.08105394609257,1.5365));
#98944=CARTESIAN_POINT('Ctrl Pts',(0.941462884755166,1.07156791410746,1.5365));
#98945=CARTESIAN_POINT('Ctrl Pts',(0.950201883404501,1.06195772650583,1.5365));
#98946=CARTESIAN_POINT('Ctrl Pts',(0.958806250728338,1.05223126289076,1.5365));
#98947=CARTESIAN_POINT('Ctrl Pts',(0.996950496046642,1.00911262322217,1.5365));
#98948=CARTESIAN_POINT('Ctrl Pts',(1.03247665648105,0.9636850768696,1.5365));
#98949=CARTESIAN_POINT('Ctrl Pts',(1.06523098522607,0.916259923496862,1.5365));
#98950=CARTESIAN_POINT('Ctrl Pts',(1.08680272763468,0.88502609177314,1.5365));
#98951=CARTESIAN_POINT('Ctrl Pts',(1.10717129187612,0.852925200570024,1.5365));
#98952=CARTESIAN_POINT('Ctrl Pts',(1.12628097828619,0.820042442228975,1.5365));
#98953=CARTESIAN_POINT('Ctrl Pts',(1.13512109289053,0.804830923525629,1.5365));
#98954=CARTESIAN_POINT('Ctrl Pts',(1.14369167315765,0.789452063683111,1.5365));
#98955=CARTESIAN_POINT('Ctrl Pts',(1.15198647178161,0.773914235960689,1.5365));
#98956=CARTESIAN_POINT('Ctrl Pts',(1.15740362680874,0.763766814019196,1.5365));
#98957=CARTESIAN_POINT('Ctrl Pts',(1.16269966037558,0.753558008249274,1.5365));
#98958=CARTESIAN_POINT('Ctrl Pts',(1.16787023655212,0.743296596712718,1.5365));
#98959=CARTESIAN_POINT('Ctrl Pts',(1.19317330635655,0.693080681979709,1.5365));
#98960=CARTESIAN_POINT('Ctrl Pts',(1.21550092753937,0.641559462581337,1.5365));
#98961=CARTESIAN_POINT('Ctrl Pts',(1.23470656272152,0.589020877926899,1.5365));
#98962=CARTESIAN_POINT('Ctrl Pts',(1.25341209489621,0.537850365921132,1.5365));
#98963=CARTESIAN_POINT('Ctrl Pts',(1.26915622673503,0.485713750528139,1.5365));
#98964=CARTESIAN_POINT('Ctrl Pts',(1.28175524628345,0.432872280614102,1.5365));
#98965=CARTESIAN_POINT('Ctrl Pts',(1.28901069367532,0.402442253611051,1.5365));
#98966=CARTESIAN_POINT('Ctrl Pts',(1.29522221805268,0.371778468368829,1.5365));
#98967=CARTESIAN_POINT('Ctrl Pts',(1.30034693367704,0.340932012339273,1.5365));
#98968=CARTESIAN_POINT('Ctrl Pts',(1.30315429133339,0.324034092366103,1.5365));
#98969=CARTESIAN_POINT('Ctrl Pts',(1.30563540254653,0.307081378175802,1.5365));
#98970=CARTESIAN_POINT('Ctrl Pts',(1.30778245093735,0.290082502724922,1.5365));
#98971=CARTESIAN_POINT('Ctrl Pts',(1.30953853292398,0.276179034549808,1.5365));
#98972=CARTESIAN_POINT('Ctrl Pts',(1.31107148447691,0.262239050551849,1.5365));
#98973=CARTESIAN_POINT('Ctrl Pts',(1.31237423627975,0.248299738344912,1.5365));
#98974=CARTESIAN_POINT('Ctrl Pts',(1.31728054844017,0.195802695669594,1.5365));
#98975=CARTESIAN_POINT('Ctrl Pts',(1.31893767644355,0.143241374071065,1.5365));
#98976=CARTESIAN_POINT('Ctrl Pts',(1.31718629034563,0.0908600606045076,
1.5365));
#98977=CARTESIAN_POINT('Ctrl Pts',(1.31685757230311,0.081028600341348,1.5365));
#98978=CARTESIAN_POINT('Ctrl Pts',(1.31640863417287,0.0712035002648672,
1.5365));
#98979=CARTESIAN_POINT('Ctrl Pts',(1.31583821714336,0.0613864111671154,
1.5365));
#98980=CARTESIAN_POINT('Ctrl Pts',(1.31263997032252,0.00634339461558057,
1.5365));
#98981=CARTESIAN_POINT('Ctrl Pts',(1.30562707296685,-0.0484498498608809,
1.5365));
#98982=CARTESIAN_POINT('Ctrl Pts',(1.29497447721792,-0.102685066480243,
1.5365));
#98983=CARTESIAN_POINT('Ctrl Pts',(1.2901198385654,-0.127401331429526,1.5365));
#98984=CARTESIAN_POINT('Ctrl Pts',(1.28450857165666,-0.15200134371386,1.5365));
#98985=CARTESIAN_POINT('Ctrl Pts',(1.27815396025382,-0.17645366274151,1.5365));
#98986=CARTESIAN_POINT('Ctrl Pts',(1.27368779636514,-0.193639302792945,
1.5365));
#98987=CARTESIAN_POINT('Ctrl Pts',(1.26885440929981,-0.210751956731087,
1.5365));
#98988=CARTESIAN_POINT('Ctrl Pts',(1.26365790001108,-0.227780164186455,
1.5365));
#98989=CARTESIAN_POINT('Ctrl Pts',(1.26065745640051,-0.237612182839758,
1.5365));
#98990=CARTESIAN_POINT('Ctrl Pts',(1.25753832486369,-0.247408091345072,
1.5365));
#98991=CARTESIAN_POINT('Ctrl Pts',(1.25430368317161,-0.257160555646816,
1.5365));
#98992=CARTESIAN_POINT('Ctrl Pts',(1.23777055696308,-0.307008031347003,
1.5365));
#98993=CARTESIAN_POINT('Ctrl Pts',(1.21820958657514,-0.355768175917083,
1.5365));
#98994=CARTESIAN_POINT('Ctrl Pts',(1.19579278545305,-0.403182449103861,
1.5365));
#98995=CARTESIAN_POINT('Ctrl Pts',(1.17348813792584,-0.450359503734913,
1.5365));
#98996=CARTESIAN_POINT('Ctrl Pts',(1.1483553706739,-0.496205014965645,1.5365));
#98997=CARTESIAN_POINT('Ctrl Pts',(1.12052480333655,-0.540431538414555,
1.5365));
#98998=CARTESIAN_POINT('Ctrl Pts',(1.10658511428344,-0.56258358358505,1.5365));
#98999=CARTESIAN_POINT('Ctrl Pts',(1.09196806725482,-0.58432886272342,1.5365));
#99000=CARTESIAN_POINT('Ctrl Pts',(1.07668725366543,-0.605627085499898,
1.5365));
#99001=CARTESIAN_POINT('Ctrl Pts',(1.06542913651814,-0.621318520098206,
1.5365));
#99002=CARTESIAN_POINT('Ctrl Pts',(1.05381069007002,-0.636767234933413,
1.5365));
#99003=CARTESIAN_POINT('Ctrl Pts',(1.04183685019325,-0.651955973544627,
1.5365));
#99004=CARTESIAN_POINT('Ctrl Pts',(1.03604983666891,-0.659296762854099,
1.5365));
#99005=CARTESIAN_POINT('Ctrl Pts',(1.03018036182183,-0.666575950104624,
1.5365));
#99006=CARTESIAN_POINT('Ctrl Pts',(1.02423735593939,-0.673781861503873,
1.5365));
#99007=CARTESIAN_POINT('Ctrl Pts',(0.992151017998599,-0.712686636781099,
1.5365));
#99008=CARTESIAN_POINT('Ctrl Pts',(0.957862153431288,-0.749537867796629,
1.5365));
#99009=CARTESIAN_POINT('Ctrl Pts',(0.921500569781594,-0.784083458027627,
1.5365));
#99010=CARTESIAN_POINT('Ctrl Pts',(0.885879292605549,-0.81792571464339,
1.5365));
#99011=CARTESIAN_POINT('Ctrl Pts',(0.848268090926396,-0.849555837281558,
1.5365));
#99012=CARTESIAN_POINT('Ctrl Pts',(0.808765267737003,-0.878693245937888,
1.5365));
#99013=CARTESIAN_POINT('Ctrl Pts',(0.769262444547611,-0.907830654594219,
1.5365));
#99014=CARTESIAN_POINT('Ctrl Pts',(0.727867374730229,-0.934476030499942,
1.5365));
#99015=CARTESIAN_POINT('Ctrl Pts',(0.684664424539467,-0.958295198918392,
1.5365));
#99016=CARTESIAN_POINT('Ctrl Pts',(0.632684721053874,1.31669749784946,5.5365));
#99017=CARTESIAN_POINT('Ctrl Pts',(0.843561153930663,1.21579764861352,5.52384689303253));
#99018=CARTESIAN_POINT('Ctrl Pts',(1.03149297598832,1.06720222196338,5.51119378606506));
#99019=CARTESIAN_POINT('Ctrl Pts',(1.1710342653585,0.882239411150659,5.49854067909758));
#99020=CARTESIAN_POINT('Ctrl Pts',(1.46278863639303,0.495517253307565,5.472085432184));
#99021=CARTESIAN_POINT('Ctrl Pts',(1.54300437985592,-0.050184483946369,
5.44563018527042));
#99022=CARTESIAN_POINT('Ctrl Pts',(1.37605834110377,-0.504914459024216,
5.41917493835684));
#99023=CARTESIAN_POINT('Ctrl Pts',(1.20911230235162,-0.959644434102056,
5.39271969144326));
#99024=CARTESIAN_POINT('Ctrl Pts',(0.795004481384448,-1.32340264700381,
5.36626444452968));
#99025=CARTESIAN_POINT('Ctrl Pts',(0.322628878789288,-1.42994684432483,
5.3398091976161));
#99026=CARTESIAN_POINT('Ctrl Pts',(-0.149746723805883,-1.53649104164586,
5.31335395070252));
#99027=CARTESIAN_POINT('Ctrl Pts',(-0.680390108029043,-1.38582122338613,
5.28689870378894));
#99028=CARTESIAN_POINT('Ctrl Pts',(-1.02626928290781,-1.04677764753815,
5.26044345687536));
#99029=CARTESIAN_POINT('Ctrl Pts',(-1.30208279114181,-0.776415032814075,
5.23934731986454));
#99030=CARTESIAN_POINT('Ctrl Pts',(-1.46040652113662,-0.386267362945073,
5.21825118285372));
#99031=CARTESIAN_POINT('Ctrl Pts',(-1.46394239258928,0.00129898642790893,
5.19715504584291));
#99032=CARTESIAN_POINT('Origin',(0.,0.,0.612132885263843));
#99033=CARTESIAN_POINT('',(-0.684664424539452,-0.958295198918403,1.5365));
#99034=CARTESIAN_POINT('Ctrl Pts',(-0.686152415706125,-0.959598509482521,
1.5365));
#99035=CARTESIAN_POINT('Ctrl Pts',(-0.391329521689054,-1.16791585444763,
1.56098466970649));
#99036=CARTESIAN_POINT('Ctrl Pts',(0.438700349941051,-1.30460055950163,
1.61196176702858));
#99037=CARTESIAN_POINT('Ctrl Pts',(1.34228035673205,-0.370854820156928,
1.68943129196628));
#99038=CARTESIAN_POINT('Ctrl Pts',(1.03835463241157,0.928154933276721,1.76890857481307));
#99039=CARTESIAN_POINT('Ctrl Pts',(-0.218198112454921,1.37532415660838,
1.84838585765988));
#99040=CARTESIAN_POINT('Ctrl Pts',(-1.06862547075175,0.719869665458091,
1.91237203763424));
#99041=CARTESIAN_POINT('Ctrl Pts',(-1.17668973402415,0.163910804078405,
1.949865789993));
#99042=CARTESIAN_POINT('Ctrl Pts',(-1.17603208311293,0.000536542008743694,
1.96086711473616));
#99043=CARTESIAN_POINT('Origin',(0.,0.,1.5365));
#99044=CARTESIAN_POINT('Origin',(-0.577350269189626,-1.,0.));
#99045=CARTESIAN_POINT('',(-0.577350269189626,-1.,0.));
#99046=CARTESIAN_POINT('',(0.577350269189626,-1.,0.));
#99047=CARTESIAN_POINT('',(1.21132486540519,-1.,0.));
#99048=CARTESIAN_POINT('',(-0.577350269189626,-1.,1.));
#99049=CARTESIAN_POINT('',(-0.577350269189626,-1.,0.));
#99050=CARTESIAN_POINT('',(0.577350269189626,-1.,1.));
#99051=CARTESIAN_POINT('',(-0.577350269189626,-1.,1.));
#99052=CARTESIAN_POINT('',(0.577350269189626,-1.,0.));
#99053=CARTESIAN_POINT('Origin',(-1.15470053837925,1.41410031829988E-16,
0.));
#99054=CARTESIAN_POINT('',(-1.15470053837925,1.41410031829988E-16,0.));
#99055=CARTESIAN_POINT('',(-0.635362971081846,-0.899519052838328,0.));
#99056=CARTESIAN_POINT('',(-1.15470053837925,1.38777878078145E-16,1.));
#99057=CARTESIAN_POINT('',(-1.15470053837925,1.41410031829988E-16,0.));
#99058=CARTESIAN_POINT('',(-1.15470053837925,1.41410031829988E-16,1.));
#99059=CARTESIAN_POINT('Origin',(-0.577350269189626,1.,0.));
#99060=CARTESIAN_POINT('',(-0.577350269189626,1.,0.));
#99061=CARTESIAN_POINT('',(-0.346687836487032,1.39951905283833,0.));
#99062=CARTESIAN_POINT('',(-0.577350269189626,1.,1.));
#99063=CARTESIAN_POINT('',(-0.577350269189626,1.,0.));
#99064=CARTESIAN_POINT('',(-0.577350269189626,1.,1.));
#99065=CARTESIAN_POINT('Origin',(0.577350269189626,1.,0.));
#99066=CARTESIAN_POINT('',(0.577350269189626,1.,0.));
#99067=CARTESIAN_POINT('',(1.78867513459481,1.,0.));
#99068=CARTESIAN_POINT('',(0.577350269189626,1.,1.));
#99069=CARTESIAN_POINT('',(0.577350269189626,1.,0.));
#99070=CARTESIAN_POINT('',(0.577350269189626,1.,1.));
#99071=CARTESIAN_POINT('Origin',(1.15470053837925,0.,0.));
#99072=CARTESIAN_POINT('',(1.15470053837925,0.,0.));
#99073=CARTESIAN_POINT('',(1.38536297108184,-0.399519052838329,0.));
#99074=CARTESIAN_POINT('',(1.15470053837925,0.,1.));
#99075=CARTESIAN_POINT('',(1.15470053837925,0.,0.));
#99076=CARTESIAN_POINT('',(1.15470053837925,0.,1.));
#99077=CARTESIAN_POINT('Origin',(0.577350269189626,-1.,0.));
#99078=CARTESIAN_POINT('',(1.09668783648703,-0.100480947161671,0.));
#99079=CARTESIAN_POINT('',(0.577350269189626,-1.,1.));
#99080=CARTESIAN_POINT('Origin',(0.,0.,1.));
#99081=CARTESIAN_POINT('Ctrl Pts',(-0.510216505388432,1.06149619882938,
1.37152216057906));
#99082=CARTESIAN_POINT('Ctrl Pts',(-0.863603094147857,0.891638152642483,
1.39801458819466));
#99083=CARTESIAN_POINT('Ctrl Pts',(-1.3812395390238,0.174157193963341,1.45099944342587));
#99084=CARTESIAN_POINT('Ctrl Pts',(-0.893256777570882,-1.06957578104115,
1.53047672627267));
#99085=CARTESIAN_POINT('Ctrl Pts',(0.415282497480903,-1.32880020955467,
1.60995400911947));
#99086=CARTESIAN_POINT('Ctrl Pts',(1.34228035673205,-0.370854820156928,
1.68943129196628));
#99087=CARTESIAN_POINT('Ctrl Pts',(1.03835463241157,0.928154933276721,1.76890857481307));
#99088=CARTESIAN_POINT('Ctrl Pts',(-0.218198112454921,1.37532415660838,
1.84838585765988));
#99089=CARTESIAN_POINT('Ctrl Pts',(-1.27451458146588,0.561183634276331,
1.92786314050668));
#99090=CARTESIAN_POINT('Ctrl Pts',(-1.16179386595564,-0.767846081811985,
2.00734042335348));
#99091=CARTESIAN_POINT('Ctrl Pts',(0.0166383981799684,-1.39248065884836,
2.08681770620029));
#99092=CARTESIAN_POINT('Ctrl Pts',(1.17979588449659,-0.739859513451799,
2.16629498904709));
#99093=CARTESIAN_POINT('Ctrl Pts',(1.2607599562499,0.591436597715745,2.24577227189389));
#99094=CARTESIAN_POINT('Ctrl Pts',(0.185253888314333,1.38021153969935,2.32524955474069));
#99095=CARTESIAN_POINT('Ctrl Pts',(-1.06017953986855,0.902954733563308,
2.4047268375875));
#99096=CARTESIAN_POINT('Ctrl Pts',(-1.33313519782792,-0.402564735116712,
2.4842041204343));
#99097=CARTESIAN_POINT('Ctrl Pts',(-0.383235548912603,-1.33881925708758,
2.5636814032811));
#99098=CARTESIAN_POINT('Ctrl Pts',(0.918197143413365,-1.04700586255646,
2.6431586861279));
#99099=CARTESIAN_POINT('Ctrl Pts',(1.37738848098126,0.205202743845419,2.7226359689747));
#99100=CARTESIAN_POINT('Ctrl Pts',(0.573132410162518,1.26918330522814,2.80211325182151));
#99101=CARTESIAN_POINT('Ctrl Pts',(-0.756845033196452,1.16897080220297,
2.88159053466831));
#99102=CARTESIAN_POINT('Ctrl Pts',(-1.39258564709099,-0.0035122637810132,
2.96106781751511));
#99103=CARTESIAN_POINT('Ctrl Pts',(-0.750938898498722,-1.17277357998896,
3.04054510036192));
#99104=CARTESIAN_POINT('Ctrl Pts',(0.579527130353369,-1.26627620290932,
3.12002238320872));
#99105=CARTESIAN_POINT('Ctrl Pts',(1.37840601855021,-0.198252265336022,
3.19949966605552));
#99106=CARTESIAN_POINT('Ctrl Pts',(0.912904206293459,1.0516239918919,3.27897694890232));
#99107=CARTESIAN_POINT('Ctrl Pts',(-0.389984008629303,1.33686932263319,
3.35845423174912));
#99108=CARTESIAN_POINT('Ctrl Pts',(-1.33514870363572,0.395834625998962,
3.43793151459593));
#99109=CARTESIAN_POINT('Ctrl Pts',(-1.05561165720655,-0.908290229433893,
3.51740879744272));
#99110=CARTESIAN_POINT('Ctrl Pts',(0.192214113207023,-1.37926097853155,
3.59688608028953));
#99111=CARTESIAN_POINT('Ctrl Pts',(1.26372622016576,-0.585066792922831,
3.67636336313633));
#99112=CARTESIAN_POINT('Ctrl Pts',(1.17605081651368,0.745795943229381,3.75584064598314));
#99113=CARTESIAN_POINT('Ctrl Pts',(0.00961056866032201,1.39255691077756,
3.83531792882993));
#99114=CARTESIAN_POINT('Ctrl Pts',(-1.1656452359731,0.761956884635964,3.91479521167675));
#99115=CARTESIAN_POINT('Ctrl Pts',(-1.2716810021026,-0.567568975171852,
3.99427249452353));
#99116=CARTESIAN_POINT('Ctrl Pts',(-0.211232513047386,-1.37647664066694,
4.07374977737036));
#99117=CARTESIAN_POINT('Ctrl Pts',(1.042974782858,-0.922773374952316,4.15322706021714));
#99118=CARTESIAN_POINT('Ctrl Pts',(1.34048488368858,0.37736904627051,4.23270434306396));
#99119=CARTESIAN_POINT('Ctrl Pts',(0.40839846752904,1.33135939264991,4.31218162591074));
#99120=CARTESIAN_POINT('Ctrl Pts',(-0.898302601136657,1.0641237985496,4.39165890875756));
#99121=CARTESIAN_POINT('Ctrl Pts',(-1.38101105538947,-0.179208421994024,
4.47113619160435));
#99122=CARTESIAN_POINT('Ctrl Pts',(-0.596949142579923,-1.25815698208656,
4.55061347445117));
#99123=CARTESIAN_POINT('Ctrl Pts',(0.734680490718179,-1.18302623202404,
4.63009075729796));
#99124=CARTESIAN_POINT('Ctrl Pts',(1.39240476784912,-0.0227328862735182,
4.70956804014477));
#99125=CARTESIAN_POINT('Ctrl Pts',(0.772906734413495,1.15841403976235,4.78904532299156));
#99126=CARTESIAN_POINT('Ctrl Pts',(-0.555559517726036,1.27697162056126,
4.86852260583837));
#99127=CARTESIAN_POINT('Ctrl Pts',(-1.37442674999021,0.224196398972394,
4.94799988868517));
#99128=CARTESIAN_POINT('Ctrl Pts',(-0.932557331581966,-1.03423752205814,
5.02747717153198));
#99129=CARTESIAN_POINT('Ctrl Pts',(0.364714346074539,-1.34397271822316,
5.10695445437878));
#99130=CARTESIAN_POINT('Ctrl Pts',(1.32746371769155,-0.420942597676582,
5.18643173722558));
#99131=CARTESIAN_POINT('Ctrl Pts',(1.07251885993521,0.888266730679483,5.26590902007238));
#99132=CARTESIAN_POINT('Ctrl Pts',(-0.166143802083737,1.38257845674616,
5.34538630291918));
#99133=CARTESIAN_POINT('Ctrl Pts',(-1.25255794971928,0.608892852159982,
5.42486358576599));
#99134=CARTESIAN_POINT('Ctrl Pts',(-1.18974047573171,-0.723717800049171,
5.50434086861279));
#99135=CARTESIAN_POINT('Ctrl Pts',(-0.0361513007060795,-1.39171212292046,
5.58381815145959));
#99136=CARTESIAN_POINT('Ctrl Pts',(1.15165463117661,-0.784596477531957,
5.66329543430639));
#99137=CARTESIAN_POINT('Ctrl Pts',(1.28099440281734,0.545166701406554,5.7427727171532));
#99138=CARTESIAN_POINT('Ctrl Pts',(0.586914422573267,1.09378259267779,5.7957575723844));
#99139=CARTESIAN_POINT('Ctrl Pts',(0.200551794415766,1.1605490253568,5.82225));
#99140=CARTESIAN_POINT('Ctrl Pts',(-0.551480035117359,1.14734422509853,
1.42651477371938));
#99141=CARTESIAN_POINT('Ctrl Pts',(-0.933446604839922,0.963748986044478,
1.45300720133498));
#99142=CARTESIAN_POINT('Ctrl Pts',(-1.49294666370392,0.188242078467704,
1.50599205656618));
#99143=CARTESIAN_POINT('Ctrl Pts',(-0.965498516533845,-1.1560772398772,
1.58546933941298));
#99144=CARTESIAN_POINT('Ctrl Pts',(0.448868282142376,-1.43626632711789,
1.66494662225978));
#99145=CARTESIAN_POINT('Ctrl Pts',(1.45083667511772,-0.400847536454914,
1.74442390510659));
#99146=CARTESIAN_POINT('Ctrl Pts',(1.1223310949352,1.00321904484081,1.82390118795339));
#99147=CARTESIAN_POINT('Ctrl Pts',(-0.235844786376658,1.48655287740392,
1.90337847080019));
#99148=CARTESIAN_POINT('Ctrl Pts',(-1.37759037334414,0.606569107564232,
1.98285575364699));
#99149=CARTESIAN_POINT('Ctrl Pts',(-1.25575342081217,-0.829945287324689,
2.06233303649379));
#99150=CARTESIAN_POINT('Ctrl Pts',(0.0179840211276536,-1.50509690402374,
2.1418103193406));
#99151=CARTESIAN_POINT('Ctrl Pts',(1.27521134448241,-0.799695317872338,
2.2212876021874));
#99152=CARTESIAN_POINT('Ctrl Pts',(1.36272334901815,0.639268765775537,2.3007648850342));
#99153=CARTESIAN_POINT('Ctrl Pts',(0.200236212968925,1.49183552539781,2.38024216788101));
#99154=CARTESIAN_POINT('Ctrl Pts',(-1.14592108193815,0.975980790342683,
2.45971945072781));
#99155=CARTESIAN_POINT('Ctrl Pts',(-1.44095190561235,-0.435121976483607,
2.53919673357461));
#99156=CARTESIAN_POINT('Ctrl Pts',(-0.414229551064106,-1.44709566060072,
2.61867401642141));
#99157=CARTESIAN_POINT('Ctrl Pts',(0.992455923213934,-1.13168198941574,
2.69815129926821));
#99158=CARTESIAN_POINT('Ctrl Pts',(1.48878415307929,0.221798423192708,2.77762858211502));
#99159=CARTESIAN_POINT('Ctrl Pts',(0.619484235310456,1.37182793254546,2.85710586496182));
#99160=CARTESIAN_POINT('Ctrl Pts',(-0.818054533864638,1.26351078854119,
2.93658314780862));
#99161=CARTESIAN_POINT('Ctrl Pts',(-1.50521038314314,-0.00379631653001373,
3.01606043065543));
#99162=CARTESIAN_POINT('Ctrl Pts',(-0.811670743187329,-1.26762111426529,
3.09553771350223));
#99163=CARTESIAN_POINT('Ctrl Pts',(0.626396125612256,-1.36868571963793,
3.17501499634903));
#99164=CARTESIAN_POINT('Ctrl Pts',(1.48988398354015,-0.214285827869038,
3.25449227919583));
#99165=CARTESIAN_POINT('Ctrl Pts',(0.986734922191957,1.13667360787806,3.33396956204264));
#99166=CARTESIAN_POINT('Ctrl Pts',(-0.421523789416343,1.44498802607688,
3.41344684488943));
#99167=CARTESIAN_POINT('Ctrl Pts',(-1.44312825279412,0.427847572826733,
3.49292412773624));
#99168=CARTESIAN_POINT('Ctrl Pts',(-1.14098377382632,-0.981747792035103,
3.57240141058304));
#99169=CARTESIAN_POINT('Ctrl Pts',(0.207759342910239,-1.49080808802434,
3.65187869342985));
#99170=CARTESIAN_POINT('Ctrl Pts',(1.3659295081902,-0.632383805893245,3.73135597627665));
#99171=CARTESIAN_POINT('Ctrl Pts',(1.27116339581568,0.806111853730416,3.81083325912345));
#99172=CARTESIAN_POINT('Ctrl Pts',(0.0103878190656723,1.50517932279332,
3.89031054197025));
#99173=CARTESIAN_POINT('Ctrl Pts',(-1.25991626864255,0.823579803983517,
3.96978782481705));
#99174=CARTESIAN_POINT('Ctrl Pts',(-1.37452762952801,-0.613470860024422,
4.04926510766386));
#99175=CARTESIAN_POINT('Ctrl Pts',(-0.228315847259036,-1.48779856809086,
4.12874239051066));
#99176=CARTESIAN_POINT('Ctrl Pts',(1.12732489796496,-0.997402255414395,
4.20821967335746));
#99177=CARTESIAN_POINT('Ctrl Pts',(1.44889599400175,0.407888597667038,4.28769695620426));
#99178=CARTESIAN_POINT('Ctrl Pts',(0.44142750937336,1.43903248299158,4.36717423905106));
#99179=CARTESIAN_POINT('Ctrl Pts',(-0.970952418804468,1.1501843307609,4.44665152189787));
#99180=CARTESIAN_POINT('Ctrl Pts',(-1.49269970155873,-0.193701822286891,
4.52612880474467));
#99181=CARTESIAN_POINT('Ctrl Pts',(-0.645227135219061,-1.35990986049348,
4.60560608759147));
#99182=CARTESIAN_POINT('Ctrl Pts',(0.794097444011241,-1.27870294490902,
4.68508337043828));
#99183=CARTESIAN_POINT('Ctrl Pts',(1.50501487537417,-0.0245713981967256,
4.76456065328508));
#99184=CARTESIAN_POINT('Ctrl Pts',(0.835415217922637,1.25210025270004,4.84403793613188));
#99185=CARTESIAN_POINT('Ctrl Pts',(-0.600490143124806,1.38024612436806,
4.92351521897869));
#99186=CARTESIAN_POINT('Ctrl Pts',(-1.48558289343029,0.242328181610582,
5.00299250182548));
#99187=CARTESIAN_POINT('Ctrl Pts',(-1.0079774851232,-1.11788101513904,5.08246978467229));
#99188=CARTESIAN_POINT('Ctrl Pts',(0.394210454300898,-1.45266590558106,
5.16194706751908));
#99189=CARTESIAN_POINT('Ctrl Pts',(1.43482174707819,-0.454986140388277,
5.2414243503659));
#99190=CARTESIAN_POINT('Ctrl Pts',(1.15925833894929,0.960104901850968,5.32090163321269));
#99191=CARTESIAN_POINT('Ctrl Pts',(-0.179580607134444,1.49439386579314,
5.4003789160595));
#99192=CARTESIAN_POINT('Ctrl Pts',(-1.35385800890905,0.658136786923932,
5.4798561989063));
#99193=CARTESIAN_POINT('Ctrl Pts',(-1.28596020004795,-0.782248150679337,
5.5593334817531));
#99194=CARTESIAN_POINT('Ctrl Pts',(-0.0390750208438495,-1.50426621309934,
5.63881076459991));
#99195=CARTESIAN_POINT('Ctrl Pts',(1.24479417999391,-0.848050363742887,
5.71828804744671));
#99196=CARTESIAN_POINT('Ctrl Pts',(1.38459424732454,0.589256812473393,5.79776533029351));
#99197=CARTESIAN_POINT('Ctrl Pts',(0.634380861758244,1.18224176648594,5.85075018552471));
#99198=CARTESIAN_POINT('Ctrl Pts',(0.216771330325854,1.25440790429141,5.87724261314031));
#99199=CARTESIAN_POINT('Ctrl Pts',(-0.592743564846286,1.23319225136769,
1.48150738685969));
#99200=CARTESIAN_POINT('Ctrl Pts',(-1.00329011553199,1.03585981944647,1.50799981447529));
#99201=CARTESIAN_POINT('Ctrl Pts',(-1.60465378838404,0.202326962972067,
1.56098466970649));
#99202=CARTESIAN_POINT('Ctrl Pts',(-1.03774025549681,-1.24257869871326,
1.64046195255329));
#99203=CARTESIAN_POINT('Ctrl Pts',(0.482454066803851,-1.54373244468111,
1.71993923540009));
#99204=CARTESIAN_POINT('Ctrl Pts',(1.55939299350339,-0.430840252752899,
1.7994165182469));
#99205=CARTESIAN_POINT('Ctrl Pts',(1.20630755745883,1.0782831564049,1.8788938010937));
#99206=CARTESIAN_POINT('Ctrl Pts',(-0.253491460298395,1.59778159819946,
1.9583710839405));
#99207=CARTESIAN_POINT('Ctrl Pts',(-1.4806661652224,0.651954580852132,2.0378483667873));
#99208=CARTESIAN_POINT('Ctrl Pts',(-1.3497129756687,-0.892044492837393,
2.11732564963411));
#99209=CARTESIAN_POINT('Ctrl Pts',(0.0193296440753391,-1.61771314919912,
2.19680293248091));
#99210=CARTESIAN_POINT('Ctrl Pts',(1.37062680446823,-0.859531122292875,
2.27628021532771));
#99211=CARTESIAN_POINT('Ctrl Pts',(1.4646867417864,0.687100933835329,2.35575749817451));
#99212=CARTESIAN_POINT('Ctrl Pts',(0.215218537623519,1.60345951109627,2.43523478102132));
#99213=CARTESIAN_POINT('Ctrl Pts',(-1.23166262400776,1.04900684712206,2.51471206386812));
#99214=CARTESIAN_POINT('Ctrl Pts',(-1.54876861339678,-0.467679217850505,
2.59418934671492));
#99215=CARTESIAN_POINT('Ctrl Pts',(-0.445223553215608,-1.55537206411385,
2.67366662956172));
#99216=CARTESIAN_POINT('Ctrl Pts',(1.0667147030145,-1.21635811627501,2.75314391240853));
#99217=CARTESIAN_POINT('Ctrl Pts',(1.60017982517733,0.238394102539999,2.83262119525533));
#99218=CARTESIAN_POINT('Ctrl Pts',(0.665836060458395,1.47447255986279,2.91209847810213));
#99219=CARTESIAN_POINT('Ctrl Pts',(-0.879264034532826,1.35805077487941,
2.99157576094893));
#99220=CARTESIAN_POINT('Ctrl Pts',(-1.61783511919529,-0.00408036927901526,
3.07105304379574));
#99221=CARTESIAN_POINT('Ctrl Pts',(-0.872402587875936,-1.36246864854162,
3.15053032664254));
#99222=CARTESIAN_POINT('Ctrl Pts',(0.673265120871141,-1.47109523636653,
3.23000760948934));
#99223=CARTESIAN_POINT('Ctrl Pts',(1.6013619485301,-0.230319390402056,3.30948489233614));
#99224=CARTESIAN_POINT('Ctrl Pts',(1.06056563809045,1.22172322386422,3.38896217518295));
#99225=CARTESIAN_POINT('Ctrl Pts',(-0.453063570203383,1.55310672952058,
3.46843945802974));
#99226=CARTESIAN_POINT('Ctrl Pts',(-1.55110780195252,0.459860519654501,
3.54791674087656));
#99227=CARTESIAN_POINT('Ctrl Pts',(-1.22635589044608,-1.05520535463631,
3.62739402372335));
#99228=CARTESIAN_POINT('Ctrl Pts',(0.223304572613456,-1.60235519751713,
3.70687130657016));
#99229=CARTESIAN_POINT('Ctrl Pts',(1.46813279621464,-0.679700818863657,
3.78634858941695));
#99230=CARTESIAN_POINT('Ctrl Pts',(1.36627597511768,0.86642776423145,3.86582587226377));
#99231=CARTESIAN_POINT('Ctrl Pts',(0.0111650694710232,1.61780173480908,
3.94530315511056));
#99232=CARTESIAN_POINT('Ctrl Pts',(-1.35418730131199,0.885202723331068,
4.02478043795737));
#99233=CARTESIAN_POINT('Ctrl Pts',(-1.47737425695342,-0.659372744876989,
4.10425772080417));
#99234=CARTESIAN_POINT('Ctrl Pts',(-0.245399181470685,-1.59912049551479,
4.18373500365097));
#99235=CARTESIAN_POINT('Ctrl Pts',(1.21167501307193,-1.07203113587647,4.26321228649777));
#99236=CARTESIAN_POINT('Ctrl Pts',(1.55730710431493,0.438408149063566,4.34268956934457));
#99237=CARTESIAN_POINT('Ctrl Pts',(0.474456551217679,1.54670557333325,4.42216685219138));
#99238=CARTESIAN_POINT('Ctrl Pts',(-1.04360223647228,1.23624486297219,4.50164413503818));
#99239=CARTESIAN_POINT('Ctrl Pts',(-1.604388347728,-0.20819522257976,4.58112141788498));
#99240=CARTESIAN_POINT('Ctrl Pts',(-0.693505127858197,-1.46166273890039,
4.66059870073178));
#99241=CARTESIAN_POINT('Ctrl Pts',(0.853514397304301,-1.37437965779401,
4.74007598357859));
#99242=CARTESIAN_POINT('Ctrl Pts',(1.61762498289922,-0.0264099101199331,
4.81955326642539));
#99243=CARTESIAN_POINT('Ctrl Pts',(0.897923701431777,1.34578646563773,4.89903054927219));
#99244=CARTESIAN_POINT('Ctrl Pts',(-0.645420768523576,1.48352062817486,
4.97850783211899));
#99245=CARTESIAN_POINT('Ctrl Pts',(-1.59673903687038,0.260459964248768,
5.05798511496579));
#99246=CARTESIAN_POINT('Ctrl Pts',(-1.08339763866443,-1.20152450821994,
5.1374623978126));
#99247=CARTESIAN_POINT('Ctrl Pts',(0.423706562527259,-1.56135909293895,
5.2169396806594));
#99248=CARTESIAN_POINT('Ctrl Pts',(1.54217977646484,-0.489029683099972,
5.29641696350621));
#99249=CARTESIAN_POINT('Ctrl Pts',(1.24599781796337,1.03194307302245,5.375894246353));
#99250=CARTESIAN_POINT('Ctrl Pts',(-0.19301741218515,1.60620927484011,5.45537152919982));
#99251=CARTESIAN_POINT('Ctrl Pts',(-1.45515806809883,0.707380721687883,
5.53484881204659));
#99252=CARTESIAN_POINT('Ctrl Pts',(-1.38217992436419,-0.840778501309504,
5.61432609489343));
#99253=CARTESIAN_POINT('Ctrl Pts',(-0.0419987409816216,-1.61682030327821,
5.6938033777402));
#99254=CARTESIAN_POINT('Ctrl Pts',(1.3379337288112,-0.911504249953818,5.77328066058703));
#99255=CARTESIAN_POINT('Ctrl Pts',(1.48819409183174,0.633346923540232,5.85275794343381));
#99256=CARTESIAN_POINT('Ctrl Pts',(0.681847300943222,1.2707009402941,5.90574279866502));
#99257=CARTESIAN_POINT('Ctrl Pts',(0.232990866235942,1.34826678322601,5.93223522628062));
#99258=CARTESIAN_POINT('Ctrl Pts',(-0.634007094575213,1.31904027763685,
1.5365));
#99259=CARTESIAN_POINT('Ctrl Pts',(-1.07313362622405,1.10797065284847,1.5629924276156));
#99260=CARTESIAN_POINT('Ctrl Pts',(-1.71636091306417,0.21641184747643,1.6159772828468));
#99261=CARTESIAN_POINT('Ctrl Pts',(-1.10998199445977,-1.32908015754932,
1.6954545656936));
#99262=CARTESIAN_POINT('Ctrl Pts',(0.516039851465324,-1.65119856224433,
1.77493184854041));
#99263=CARTESIAN_POINT('Ctrl Pts',(1.66794931188906,-0.460832969050885,
1.85440913138721));
#99264=CARTESIAN_POINT('Ctrl Pts',(1.29028401998246,1.15334726796898,1.93388641423401));
#99265=CARTESIAN_POINT('Ctrl Pts',(-0.271138134220133,1.709010318995,2.01336369708081));
#99266=CARTESIAN_POINT('Ctrl Pts',(-1.58374195710066,0.697340054140035,
2.09284097992762));
#99267=CARTESIAN_POINT('Ctrl Pts',(-1.44367253052523,-0.954143698350099,
2.17231826277442));
#99268=CARTESIAN_POINT('Ctrl Pts',(0.020675267023026,-1.7303293943745,2.25179554562122));
#99269=CARTESIAN_POINT('Ctrl Pts',(1.46604226445405,-0.919366926713415,
2.33127282846802));
#99270=CARTESIAN_POINT('Ctrl Pts',(1.56665013455465,0.734933101895122,2.41075011131483));
#99271=CARTESIAN_POINT('Ctrl Pts',(0.230200862278109,1.71508349679473,2.49022739416163));
#99272=CARTESIAN_POINT('Ctrl Pts',(-1.31740416607736,1.12203290390143,2.56970467700843));
#99273=CARTESIAN_POINT('Ctrl Pts',(-1.65658532118121,-0.5002364592174,2.64918195985523));
#99274=CARTESIAN_POINT('Ctrl Pts',(-0.476217555367108,-1.66364846762698,
2.72865924270203));
#99275=CARTESIAN_POINT('Ctrl Pts',(1.14097348281507,-1.30103424313428,2.80813652554884));
#99276=CARTESIAN_POINT('Ctrl Pts',(1.71157549727537,0.254989781887289,2.88761380839565));
#99277=CARTESIAN_POINT('Ctrl Pts',(0.712187885606333,1.57711718718011,2.96709109124244));
#99278=CARTESIAN_POINT('Ctrl Pts',(-0.940473535201012,1.45259076121762,
3.04656837408925));
#99279=CARTESIAN_POINT('Ctrl Pts',(-1.73045985524743,-0.00436442202801662,
3.12604565693604));
#99280=CARTESIAN_POINT('Ctrl Pts',(-0.933134432564544,-1.45731618281794,
3.20552293978285));
#99281=CARTESIAN_POINT('Ctrl Pts',(0.720134116130028,-1.57350475309514,
3.28500022262965));
#99282=CARTESIAN_POINT('Ctrl Pts',(1.71283991352004,-0.246352952935073,
3.36447750547645));
#99283=CARTESIAN_POINT('Ctrl Pts',(1.13439635398895,1.30677283985038,3.44395478832326));
#99284=CARTESIAN_POINT('Ctrl Pts',(-0.484603350990424,1.66122543296428,
3.52343207117006));
#99285=CARTESIAN_POINT('Ctrl Pts',(-1.65908735111091,0.491873466482272,
3.60290935401687));
#99286=CARTESIAN_POINT('Ctrl Pts',(-1.31172800706584,-1.12866291723752,
3.68238663686366));
#99287=CARTESIAN_POINT('Ctrl Pts',(0.238849802316674,-1.71390230700991,
3.76186391971048));
#99288=CARTESIAN_POINT('Ctrl Pts',(1.57033608423908,-0.727017831834071,
3.84134120255726));
#99289=CARTESIAN_POINT('Ctrl Pts',(1.46138855441968,0.926743674732486,3.92081848540408));
#99290=CARTESIAN_POINT('Ctrl Pts',(0.0119423198763706,1.73042414682484,
4.00029576825087));
#99291=CARTESIAN_POINT('Ctrl Pts',(-1.44845833398143,0.946825642678623,
4.07977305109768));
#99292=CARTESIAN_POINT('Ctrl Pts',(-1.58022088437883,-0.705274629729561,
4.15925033394448));
#99293=CARTESIAN_POINT('Ctrl Pts',(-0.262482515682332,-1.71044242293871,
4.23872761679128));
#99294=CARTESIAN_POINT('Ctrl Pts',(1.29602512817888,-1.14666001633855,4.31820489963808));
#99295=CARTESIAN_POINT('Ctrl Pts',(1.6657182146281,0.468927700460095,4.39768218248489));
#99296=CARTESIAN_POINT('Ctrl Pts',(0.507485593061997,1.65437866367492,4.47715946533169));
#99297=CARTESIAN_POINT('Ctrl Pts',(-1.11625205414009,1.32230539518349,4.5566367481785));
#99298=CARTESIAN_POINT('Ctrl Pts',(-1.71607699389726,-0.222688622872627,
4.63611403102529));
#99299=CARTESIAN_POINT('Ctrl Pts',(-0.741783120497333,-1.5634156173073,
4.7155913138721));
#99300=CARTESIAN_POINT('Ctrl Pts',(0.912931350597362,-1.470056370679,4.7950685967189));
#99301=CARTESIAN_POINT('Ctrl Pts',(1.73023509042427,-0.0282484220431421,
4.8745458795657));
#99302=CARTESIAN_POINT('Ctrl Pts',(0.960432184940917,1.43947267857542,4.9540231624125));
#99303=CARTESIAN_POINT('Ctrl Pts',(-0.690351393922344,1.58679513198166,
5.0335004452593));
#99304=CARTESIAN_POINT('Ctrl Pts',(-1.70789518031047,0.278591746886957,
5.11297772810611));
#99305=CARTESIAN_POINT('Ctrl Pts',(-1.15881779220566,-1.28516800130084,
5.1924550109529));
#99306=CARTESIAN_POINT('Ctrl Pts',(0.453202670753618,-1.67005228029684,
5.27193229379972));
#99307=CARTESIAN_POINT('Ctrl Pts',(1.64953780585148,-0.523073225811667,
5.35140957664651));
#99308=CARTESIAN_POINT('Ctrl Pts',(1.33273729697745,1.10378124419394,5.43088685949333));
#99309=CARTESIAN_POINT('Ctrl Pts',(-0.206454217235858,1.71802468388708,
5.51036414234011));
#99310=CARTESIAN_POINT('Ctrl Pts',(-1.55645812728861,0.756624656451833,
5.58984142518693));
#99311=CARTESIAN_POINT('Ctrl Pts',(-1.47839964868043,-0.89930885193967,
5.66931870803372));
#99312=CARTESIAN_POINT('Ctrl Pts',(-0.0449224611193922,-1.72937439345709,
5.74879599088053));
#99313=CARTESIAN_POINT('Ctrl Pts',(1.4310732776285,-0.974958136164747,5.82827327372733));
#99314=CARTESIAN_POINT('Ctrl Pts',(1.59179393633893,0.67743703460707,5.90775055657414));
#99315=CARTESIAN_POINT('Ctrl Pts',(0.7293137401282,1.35916011410226,5.96073541180533));
#99316=CARTESIAN_POINT('Ctrl Pts',(0.24921040214603,1.44212566216062,5.98722783942093));
#99317=CARTESIAN_POINT('Ctrl Pts',(-1.46453843780727,0.00118155242986957,
5.12584495415709));
#99318=CARTESIAN_POINT('Ctrl Pts',(-1.46096283466848,-0.406291468589608,
5.14804830642237));
#99319=CARTESIAN_POINT('Ctrl Pts',(-1.28353062640651,-0.816495066456357,
5.17025165868763));
#99320=CARTESIAN_POINT('Ctrl Pts',(-0.981660613063253,-1.08868875643554,
5.19245501095291));
#99321=CARTESIAN_POINT('Ctrl Pts',(-0.621477637885904,-1.41346276096618,
5.21894743856851));
#99322=CARTESIAN_POINT('Ctrl Pts',(-0.0841374835661431,-1.54175752063151,
5.24543986618411));
#99323=CARTESIAN_POINT('Ctrl Pts',(0.383921782776714,-1.41474172471665,
5.27193229379971));
#99324=CARTESIAN_POINT('Ctrl Pts',(0.851981049119571,-1.28772592880178,
5.29842472141532));
#99325=CARTESIAN_POINT('Ctrl Pts',(1.25075942748552,-0.905399577306726,
5.32491714903091));
#99326=CARTESIAN_POINT('Ctrl Pts',(1.39734853185616,-0.443093989891596,
5.35140957664651));
#99327=CARTESIAN_POINT('Ctrl Pts',(1.5439376362268,0.0192115975235344,5.37790200426211));
#99328=CARTESIAN_POINT('Ctrl Pts',(1.43833746660212,0.561496420858736,5.40439443187772));
#99329=CARTESIAN_POINT('Ctrl Pts',(1.12900546275424,0.935012739141861,5.43088685949332));
#99330=CARTESIAN_POINT('Ctrl Pts',(0.819673458906346,1.30852905742499,5.45737928710892));
#99331=CARTESIAN_POINT('Ctrl Pts',(0.306609620835244,1.51327687065604,5.48387171472452));
#99332=CARTESIAN_POINT('Ctrl Pts',(-0.174922949875765,1.45541743936568,
5.51036414234012));
#99333=CARTESIAN_POINT('Ctrl Pts',(-0.333273440429853,1.43639054505928,
5.51907609489341));
#99334=CARTESIAN_POINT('Ctrl Pts',(-0.488214130898924,1.3889652297675,5.5277880474467));
#99335=CARTESIAN_POINT('Ctrl Pts',(-0.632402293996042,1.31836377294842,
5.53649999999999));
#99336=CARTESIAN_POINT('Ctrl Pts',(-0.686152415706132,-0.959598509482516,
1.5365));
#99337=CARTESIAN_POINT('Ctrl Pts',(-0.712494035170421,-0.945273650511668,
1.5365));
#99338=CARTESIAN_POINT('Ctrl Pts',(-0.738199273837341,-0.929906790018379,
1.5365));
#99339=CARTESIAN_POINT('Ctrl Pts',(-0.76319848072749,-0.913511944752561,
1.5365));
#99340=CARTESIAN_POINT('Ctrl Pts',(-0.803527305903368,-0.887063711757967,
1.5365));
#99341=CARTESIAN_POINT('Ctrl Pts',(-0.842020123735519,-0.857943002317074,
1.5365));
#99342=CARTESIAN_POINT('Ctrl Pts',(-0.878605013002918,-0.826447578753258,
1.5365));
#99343=CARTESIAN_POINT('Ctrl Pts',(-0.893209991539167,-0.813874355371944,
1.5365));
#99344=CARTESIAN_POINT('Ctrl Pts',(-0.907510708709607,-0.800922130432144,
1.5365));
#99345=CARTESIAN_POINT('Ctrl Pts',(-0.921501670960182,-0.78760780511351,
1.5365));
#99346=CARTESIAN_POINT('Ctrl Pts',(-0.933569527146362,-0.776123579776924,
1.5365));
#99347=CARTESIAN_POINT('Ctrl Pts',(-0.945411135515606,-0.764365251470628,
1.5365));
#99348=CARTESIAN_POINT('Ctrl Pts',(-0.9569987239283,-0.752368736596883,
1.5365));
#99349=CARTESIAN_POINT('Ctrl Pts',(-0.992167598620615,-0.715958750902441,
1.5365));
#99350=CARTESIAN_POINT('Ctrl Pts',(-1.02503479626171,-0.67732699119571,
1.5365));
#99351=CARTESIAN_POINT('Ctrl Pts',(-1.0555193152036,-0.63679810848881,1.5365));
#99352=CARTESIAN_POINT('Ctrl Pts',(-1.07703618390047,-0.608191632877453,
1.5365));
#99353=CARTESIAN_POINT('Ctrl Pts',(-1.09736563857017,-0.578638841695071,
1.5365));
#99354=CARTESIAN_POINT('Ctrl Pts',(-1.11647108585219,-0.548240703646319,
1.5365));
#99355=CARTESIAN_POINT('Ctrl Pts',(-1.12390764029007,-0.536408611726533,
1.5365));
#99356=CARTESIAN_POINT('Ctrl Pts',(-1.13115866792403,-0.524448342927677,
1.5365));
#99357=CARTESIAN_POINT('Ctrl Pts',(-1.13822167350261,-0.512365491178729,
1.5365));
#99358=CARTESIAN_POINT('Ctrl Pts',(-1.14363503317147,-0.503104727950552,
1.5365));
#99359=CARTESIAN_POINT('Ctrl Pts',(-1.14893488231534,-0.49377706110977,
1.5365));
#99360=CARTESIAN_POINT('Ctrl Pts',(-1.15411691145542,-0.484391843911832,
1.5365));
#99361=CARTESIAN_POINT('Ctrl Pts',(-1.17952890780578,-0.438367960461035,
1.5365));
#99362=CARTESIAN_POINT('Ctrl Pts',(-1.2021374844888,-0.390916630562921,
1.5365));
#99363=CARTESIAN_POINT('Ctrl Pts',(-1.22185604956371,-0.342366499555546,
1.5365));
#99364=CARTESIAN_POINT('Ctrl Pts',(-1.24192204262271,-0.292960947574161,
1.5365));
#99365=CARTESIAN_POINT('Ctrl Pts',(-1.25899605993211,-0.24241663381677,
1.5365));
#99366=CARTESIAN_POINT('Ctrl Pts',(-1.27295041465054,-0.191041522245861,
1.5365));
#99367=CARTESIAN_POINT('Ctrl Pts',(-1.28082576544375,-0.162047202277287,
1.5365));
#99368=CARTESIAN_POINT('Ctrl Pts',(-1.28770675895069,-0.132787650325744,
1.5365));
#99369=CARTESIAN_POINT('Ctrl Pts',(-1.29356400665812,-0.103314695812419,
1.5365));
#99370=CARTESIAN_POINT('Ctrl Pts',(-1.2969812891964,-0.0861193477853134,
1.5365));
#99371=CARTESIAN_POINT('Ctrl Pts',(-1.30005000808393,-0.0688513209636838,
1.5365));
#99372=CARTESIAN_POINT('Ctrl Pts',(-1.30276348910828,-0.0515206690492249,
1.5365));
#99373=CARTESIAN_POINT('Ctrl Pts',(-1.30424656518194,-0.0420484542208913,
1.5365));
#99374=CARTESIAN_POINT('Ctrl Pts',(-1.3056232477231,-0.0325585842976975,
1.5365));
#99375=CARTESIAN_POINT('Ctrl Pts',(-1.30689102145782,-0.023065488585942,
1.5365));
#99376=CARTESIAN_POINT('Ctrl Pts',(-1.31414560403258,0.0312568599885747,
1.5365));
#99377=CARTESIAN_POINT('Ctrl Pts',(-1.31785529058084,0.0857923203720823,
1.5365));
#99378=CARTESIAN_POINT('Ctrl Pts',(-1.31790420900109,0.1402116924761,1.5365));
#99379=CARTESIAN_POINT('Ctrl Pts',(-1.31791152730721,0.148352953421936,
1.5365));
#99380=CARTESIAN_POINT('Ctrl Pts',(-1.31783683331776,0.156491665536181,
1.5365));
#99381=CARTESIAN_POINT('Ctrl Pts',(-1.317679650248,0.164626773622555,1.5365));
#99382=CARTESIAN_POINT('Ctrl Pts',(-1.31666603814062,0.217086902209856,
1.5365));
#99383=CARTESIAN_POINT('Ctrl Pts',(-1.31222643198864,0.269396465505187,
1.5365));
#99384=CARTESIAN_POINT('Ctrl Pts',(-1.30456361513445,0.321337523597355,
1.5365));
#99385=CARTESIAN_POINT('Ctrl Pts',(-1.30051454578202,0.348783428994311,
1.5365));
#99386=CARTESIAN_POINT('Ctrl Pts',(-1.2955646372317,0.37612659768885,1.5365));
#99387=CARTESIAN_POINT('Ctrl Pts',(-1.28973814095309,0.403335224922055,
1.5365));
#99388=CARTESIAN_POINT('Ctrl Pts',(-1.2862415448417,0.419663662396445,1.5365));
#99389=CARTESIAN_POINT('Ctrl Pts',(-1.28242917766058,0.435943645330663,
1.5365));
#99390=CARTESIAN_POINT('Ctrl Pts',(-1.27830564133165,0.452168239721719,
1.5365));
#99391=CARTESIAN_POINT('Ctrl Pts',(-1.27574041647476,0.462261453290118,
1.5365));
#99392=CARTESIAN_POINT('Ctrl Pts',(-1.2730541502057,0.472335075186927,1.5365));
#99393=CARTESIAN_POINT('Ctrl Pts',(-1.27025284985987,0.48237055868,1.5365));
#99394=CARTESIAN_POINT('Ctrl Pts',(-1.25551450272141,0.535169766606186,
1.5365));
#99395=CARTESIAN_POINT('Ctrl Pts',(-1.23757288320391,0.587010386885858,
1.5365));
#99396=CARTESIAN_POINT('Ctrl Pts',(-1.21666787173329,0.637656586978249,
1.5365));
#99397=CARTESIAN_POINT('Ctrl Pts',(-1.19530486219449,0.689412370858058,
1.5365));
#99398=CARTESIAN_POINT('Ctrl Pts',(-1.17084697491721,0.739921779742627,
1.5365));
#99399=CARTESIAN_POINT('Ctrl Pts',(-1.14349524099203,0.788933686107659,
1.5365));
#99400=CARTESIAN_POINT('Ctrl Pts',(-1.12810345611826,0.816514413570401,
1.5365));
#99401=CARTESIAN_POINT('Ctrl Pts',(-1.11179430699787,0.843620855477256,
1.5365));
#99402=CARTESIAN_POINT('Ctrl Pts',(-1.09459665262041,0.870206538635187,
1.5365));
#99403=CARTESIAN_POINT('Ctrl Pts',(-1.08383474902506,0.88684325855539,1.5365));
#99404=CARTESIAN_POINT('Ctrl Pts',(-1.07272481249571,0.903276019161565,
1.5365));
#99405=CARTESIAN_POINT('Ctrl Pts',(-1.06127299753307,0.91949299125179,1.5365));
#99406=CARTESIAN_POINT('Ctrl Pts',(-1.05549186873079,0.927679676483991,
1.5365));
#99407=CARTESIAN_POINT('Ctrl Pts',(-1.04962360295717,0.93581136288618,1.5365));
#99408=CARTESIAN_POINT('Ctrl Pts',(-1.04366892717758,0.943886487236255,
1.5365));
#99409=CARTESIAN_POINT('Ctrl Pts',(-1.0377095980409,0.951967921994928,1.5365));
#99410=CARTESIAN_POINT('Ctrl Pts',(-1.03166885456697,0.95998571466195,1.5365));
#99411=CARTESIAN_POINT('Ctrl Pts',(-1.02554963940643,0.967936312123916,
1.5365));
#99412=CARTESIAN_POINT('Ctrl Pts',(-0.990020557844862,1.01409867417178,
1.5365));
#99413=CARTESIAN_POINT('Ctrl Pts',(-0.951832196594494,1.05802122834032,
1.5365));
#99414=CARTESIAN_POINT('Ctrl Pts',(-0.91120580136671,1.09944292379416,1.5365));
#99415=CARTESIAN_POINT('Ctrl Pts',(-0.869828518644135,1.14163020607782,
1.5365));
#99416=CARTESIAN_POINT('Ctrl Pts',(-0.825921863712725,1.18122453014316,
1.5365));
#99417=CARTESIAN_POINT('Ctrl Pts',(-0.779668622671583,1.21792896816084,
1.5365));
#99418=CARTESIAN_POINT('Ctrl Pts',(-0.73341538163044,1.25463340617853,1.5365));
#99419=CARTESIAN_POINT('Ctrl Pts',(-0.684814997070202,1.28844917107134,
1.5365));
#99420=CARTESIAN_POINT('Ctrl Pts',(-0.634007094575213,1.31904027763685,
1.5365));
#99421=CARTESIAN_POINT('Origin',(-3.28582941601228E-17,0.,1.5365));
#99422=CARTESIAN_POINT('',(-1.4635,-1.79227059055215E-16,1.5365));
#99423=CARTESIAN_POINT('Origin',(0.,0.,1.5365));
#99424=CARTESIAN_POINT('Origin',(0.,0.,1.5365));
#99425=CARTESIAN_POINT('Origin',(0.,0.,1.5));
#99426=CARTESIAN_POINT('Origin',(3.,0.,0.));
#99427=CARTESIAN_POINT('',(-3.,-3.67394039744206E-16,0.));
#99428=CARTESIAN_POINT('Origin',(0.,0.,0.));
#99429=CARTESIAN_POINT('Origin',(0.,0.,0.75));
#99430=CARTESIAN_POINT('',(-2.25,-2.75545529808154E-16,0.75));
#99431=CARTESIAN_POINT('Origin',(0.,0.,6.));
#99432=CARTESIAN_POINT('',(0.,0.,0.));
#99433=CARTESIAN_POINT('',(0.,0.,0.));
#99434=CARTESIAN_POINT('',(48.2598346930642,24.2278425659016,2.));
#99435=CARTESIAN_POINT('',(0.,0.,22.));
#99436=CARTESIAN_POINT('',(0.,0.,20.));
#99437=CARTESIAN_POINT('',(0.,0.,0.));
#99438=CARTESIAN_POINT('',(7.,0.,0.));
#99439=CARTESIAN_POINT('',(0.,0.,18.));
#99440=CARTESIAN_POINT('',(0.,0.,22.));
#99441=CARTESIAN_POINT('',(3.14799020557141,53.908164109582,2.));
#99442=CARTESIAN_POINT('',(-45.1118444874928,29.6803215436804,2.));
#99443=CARTESIAN_POINT('',(-48.2598346930642,-24.2278425659016,2.));
#99444=CARTESIAN_POINT('',(-3.14799020557142,-53.908164109582,2.));
#99445=CARTESIAN_POINT('',(45.1118444874928,-29.6803215436804,2.));
#99446=CARTESIAN_POINT('',(0.,0.,-2.));
#99447=CARTESIAN_POINT('',(0.,0.,-2.));
#99448=CARTESIAN_POINT('',(0.,0.,2.));
#99449=CARTESIAN_POINT('',(0.,0.,32.));
#99450=CARTESIAN_POINT('',(0.,0.,-12.));
#99451=CARTESIAN_POINT('',(0.,0.,34.));
#99452=CARTESIAN_POINT('',(0.,0.,18.));
#99453=CARTESIAN_POINT('',(54.9897909613702,10.8223329289393,10.));
#99454=CARTESIAN_POINT('',(54.3167953345396,12.1628838926355,10.));
#99455=CARTESIAN_POINT('',(0.,0.,-14.));
#99456=CARTESIAN_POINT('',(0.,0.,-15.));
#99457=CARTESIAN_POINT('',(18.1224802360109,53.0337223858122,10.));
#99458=CARTESIAN_POINT('',(-36.8673107253594,42.2113894568729,10.));
#99459=CARTESIAN_POINT('',(-54.9897909613702,-10.8223329289393,10.));
#99460=CARTESIAN_POINT('',(-18.1224802360109,-53.0337223858122,10.));
#99461=CARTESIAN_POINT('',(36.8673107253594,-42.2113894568729,10.));
#99462=CARTESIAN_POINT('',(65.,0.,28.));
#99463=CARTESIAN_POINT('',(53.1951359564886,14.3971354987959,20.));
#99464=CARTESIAN_POINT('',(16.6250312329669,53.1211665581892,10.));
#99465=CARTESIAN_POINT('',(-37.6917641015727,40.9582826655536,10.));
#99466=CARTESIAN_POINT('',(-54.3167953345396,-12.1628838926355,10.));
#99467=CARTESIAN_POINT('',(-16.6250312329669,-53.1211665581892,10.));
#99468=CARTESIAN_POINT('',(37.6917641015728,-40.9582826655536,10.));
#99469=CARTESIAN_POINT('',(32.5,56.2916512459885,28.));
#99470=CARTESIAN_POINT('',(-32.5,56.2916512459885,28.));
#99471=CARTESIAN_POINT('',(-65.,8.88178419700125E-15,28.));
#99472=CARTESIAN_POINT('',(-32.5,-56.2916512459885,28.));
#99473=CARTESIAN_POINT('',(32.5,-56.2916512459885,28.));
#99474=CARTESIAN_POINT('',(65.,-1.12125699060252E-14,-8.));
#99475=CARTESIAN_POINT('',(32.5,56.2916512459885,-8.));
#99476=CARTESIAN_POINT('',(-32.5,56.2916512459885,-8.));
#99477=CARTESIAN_POINT('',(-65.,4.47305572007078E-15,-8.));
#99478=CARTESIAN_POINT('',(-32.5,-56.2916512459885,-8.));
#99479=CARTESIAN_POINT('',(32.5,-56.2916512459885,-8.));
#99480=CARTESIAN_POINT('',(14.1292828945603,53.2669068454842,20.));
#99481=CARTESIAN_POINT('',(-39.0658530619283,38.8697713466882,20.));
#99482=CARTESIAN_POINT('',(-53.1951359564886,-14.3971354987959,20.));
#99483=CARTESIAN_POINT('',(-14.1292828945603,-53.2669068454841,20.));
#99484=CARTESIAN_POINT('',(39.0658530619283,-38.8697713466882,20.));
#99485=CARTESIAN_POINT('',(53.1951359564886,14.3971354987959,-4.44089209850063E-15));
#99486=CARTESIAN_POINT('',(14.1292828945603,53.2669068454841,-4.44089209850063E-15));
#99487=CARTESIAN_POINT('',(-39.0658530619283,38.8697713466883,-4.44089209850063E-15));
#99488=CARTESIAN_POINT('',(-53.1951359564886,-14.3971354987959,0.));
#99489=CARTESIAN_POINT('',(-14.1292828945603,-53.2669068454841,0.));
#99490=CARTESIAN_POINT('',(39.0658530619283,-38.8697713466882,-4.44089209850063E-15));
#99491=UNCERTAINTY_MEASURE_WITH_UNIT(LENGTH_MEASURE(0.01),#99527,
'DISTANCE_ACCURACY_VALUE',
'Maximum model space distance between geometric entities at asserted c
onnectivities');
#99492=UNCERTAINTY_MEASURE_WITH_UNIT(LENGTH_MEASURE(0.01),#99527,
'DISTANCE_ACCURACY_VALUE',
'Maximum model space distance between geometric entities at asserted c
onnectivities');
#99493=UNCERTAINTY_MEASURE_WITH_UNIT(LENGTH_MEASURE(0.01),#99527,
'DISTANCE_ACCURACY_VALUE',
'Maximum model space distance between geometric entities at asserted c
onnectivities');
#99494=UNCERTAINTY_MEASURE_WITH_UNIT(LENGTH_MEASURE(0.01),#99527,
'DISTANCE_ACCURACY_VALUE',
'Maximum model space distance between geometric entities at asserted c
onnectivities');
#99495=UNCERTAINTY_MEASURE_WITH_UNIT(LENGTH_MEASURE(0.01),#99527,
'DISTANCE_ACCURACY_VALUE',
'Maximum model space distance between geometric entities at asserted c
onnectivities');
#99496=UNCERTAINTY_MEASURE_WITH_UNIT(LENGTH_MEASURE(0.01),#99527,
'DISTANCE_ACCURACY_VALUE',
'Maximum model space distance between geometric entities at asserted c
onnectivities');
#99497=UNCERTAINTY_MEASURE_WITH_UNIT(LENGTH_MEASURE(0.01),#99527,
'DISTANCE_ACCURACY_VALUE',
'Maximum model space distance between geometric entities at asserted c
onnectivities');
#99498=UNCERTAINTY_MEASURE_WITH_UNIT(LENGTH_MEASURE(0.01),#99527,
'DISTANCE_ACCURACY_VALUE',
'Maximum model space distance between geometric entities at asserted c
onnectivities');
#99499=UNCERTAINTY_MEASURE_WITH_UNIT(LENGTH_MEASURE(0.01),#99527,
'DISTANCE_ACCURACY_VALUE',
'Maximum model space distance between geometric entities at asserted c
onnectivities');
#99500=UNCERTAINTY_MEASURE_WITH_UNIT(LENGTH_MEASURE(0.01),#99527,
'DISTANCE_ACCURACY_VALUE',
'Maximum model space distance between geometric entities at asserted c
onnectivities');
#99501=UNCERTAINTY_MEASURE_WITH_UNIT(LENGTH_MEASURE(0.01),#99527,
'DISTANCE_ACCURACY_VALUE',
'Maximum model space distance between geometric entities at asserted c
onnectivities');
#99502=UNCERTAINTY_MEASURE_WITH_UNIT(LENGTH_MEASURE(0.01),#99527,
'DISTANCE_ACCURACY_VALUE',
'Maximum model space distance between geometric entities at asserted c
onnectivities');
#99503=UNCERTAINTY_MEASURE_WITH_UNIT(LENGTH_MEASURE(0.01),#99527,
'DISTANCE_ACCURACY_VALUE',
'Maximum model space distance between geometric entities at asserted c
onnectivities');
#99504=UNCERTAINTY_MEASURE_WITH_UNIT(LENGTH_MEASURE(0.01),#99527,
'DISTANCE_ACCURACY_VALUE',
'Maximum model space distance between geometric entities at asserted c
onnectivities');
#99505=UNCERTAINTY_MEASURE_WITH_UNIT(LENGTH_MEASURE(0.01),#99527,
'DISTANCE_ACCURACY_VALUE',
'Maximum model space distance between geometric entities at asserted c
onnectivities');
#99506=UNCERTAINTY_MEASURE_WITH_UNIT(LENGTH_MEASURE(0.01),#99527,
'DISTANCE_ACCURACY_VALUE',
'Maximum model space distance between geometric entities at asserted c
onnectivities');
#99507=UNCERTAINTY_MEASURE_WITH_UNIT(LENGTH_MEASURE(0.01),#99527,
'DISTANCE_ACCURACY_VALUE',
'Maximum model space distance between geometric entities at asserted c
onnectivities');
#99508=UNCERTAINTY_MEASURE_WITH_UNIT(LENGTH_MEASURE(0.01),#99527,
'DISTANCE_ACCURACY_VALUE',
'Maximum model space distance between geometric entities at asserted c
onnectivities');
#99509=(
GEOMETRIC_REPRESENTATION_CONTEXT(3)
GLOBAL_UNCERTAINTY_ASSIGNED_CONTEXT((#99491))
GLOBAL_UNIT_ASSIGNED_CONTEXT((#99527,#99529,#99530))
REPRESENTATION_CONTEXT('','3D')
);
#99510=(
GEOMETRIC_REPRESENTATION_CONTEXT(3)
GLOBAL_UNCERTAINTY_ASSIGNED_CONTEXT((#99492))
GLOBAL_UNIT_ASSIGNED_CONTEXT((#99527,#99529,#99530))
REPRESENTATION_CONTEXT('','3D')
);
#99511=(
GEOMETRIC_REPRESENTATION_CONTEXT(3)
GLOBAL_UNCERTAINTY_ASSIGNED_CONTEXT((#99493))
GLOBAL_UNIT_ASSIGNED_CONTEXT((#99527,#99529,#99530))
REPRESENTATION_CONTEXT('','3D')
);
#99512=(
GEOMETRIC_REPRESENTATION_CONTEXT(3)
GLOBAL_UNCERTAINTY_ASSIGNED_CONTEXT((#99494))
GLOBAL_UNIT_ASSIGNED_CONTEXT((#99527,#99529,#99530))
REPRESENTATION_CONTEXT('','3D')
);
#99513=(
GEOMETRIC_REPRESENTATION_CONTEXT(3)
GLOBAL_UNCERTAINTY_ASSIGNED_CONTEXT((#99495))
GLOBAL_UNIT_ASSIGNED_CONTEXT((#99527,#99529,#99530))
REPRESENTATION_CONTEXT('','3D')
);
#99514=(
GEOMETRIC_REPRESENTATION_CONTEXT(3)
GLOBAL_UNCERTAINTY_ASSIGNED_CONTEXT((#99496))
GLOBAL_UNIT_ASSIGNED_CONTEXT((#99527,#99529,#99530))
REPRESENTATION_CONTEXT('','3D')
);
#99515=(
GEOMETRIC_REPRESENTATION_CONTEXT(3)
GLOBAL_UNCERTAINTY_ASSIGNED_CONTEXT((#99497))
GLOBAL_UNIT_ASSIGNED_CONTEXT((#99527,#99529,#99530))
REPRESENTATION_CONTEXT('','3D')
);
#99516=(
GEOMETRIC_REPRESENTATION_CONTEXT(3)
GLOBAL_UNCERTAINTY_ASSIGNED_CONTEXT((#99498))
GLOBAL_UNIT_ASSIGNED_CONTEXT((#99527,#99529,#99530))
REPRESENTATION_CONTEXT('','3D')
);
#99517=(
GEOMETRIC_REPRESENTATION_CONTEXT(3)
GLOBAL_UNCERTAINTY_ASSIGNED_CONTEXT((#99499))
GLOBAL_UNIT_ASSIGNED_CONTEXT((#99527,#99529,#99530))
REPRESENTATION_CONTEXT('','3D')
);
#99518=(
GEOMETRIC_REPRESENTATION_CONTEXT(3)
GLOBAL_UNCERTAINTY_ASSIGNED_CONTEXT((#99500))
GLOBAL_UNIT_ASSIGNED_CONTEXT((#99527,#99529,#99530))
REPRESENTATION_CONTEXT('','3D')
);
#99519=(
GEOMETRIC_REPRESENTATION_CONTEXT(3)
GLOBAL_UNCERTAINTY_ASSIGNED_CONTEXT((#99501))
GLOBAL_UNIT_ASSIGNED_CONTEXT((#99527,#99529,#99530))
REPRESENTATION_CONTEXT('','3D')
);
#99520=(
GEOMETRIC_REPRESENTATION_CONTEXT(3)
GLOBAL_UNCERTAINTY_ASSIGNED_CONTEXT((#99502))
GLOBAL_UNIT_ASSIGNED_CONTEXT((#99527,#99529,#99530))
REPRESENTATION_CONTEXT('','3D')
);
#99521=(
GEOMETRIC_REPRESENTATION_CONTEXT(3)
GLOBAL_UNCERTAINTY_ASSIGNED_CONTEXT((#99503))
GLOBAL_UNIT_ASSIGNED_CONTEXT((#99527,#99529,#99530))
REPRESENTATION_CONTEXT('','3D')
);
#99522=(
GEOMETRIC_REPRESENTATION_CONTEXT(3)
GLOBAL_UNCERTAINTY_ASSIGNED_CONTEXT((#99504))
GLOBAL_UNIT_ASSIGNED_CONTEXT((#99527,#99529,#99530))
REPRESENTATION_CONTEXT('','3D')
);
#99523=(
GEOMETRIC_REPRESENTATION_CONTEXT(3)
GLOBAL_UNCERTAINTY_ASSIGNED_CONTEXT((#99505))
GLOBAL_UNIT_ASSIGNED_CONTEXT((#99527,#99529,#99530))
REPRESENTATION_CONTEXT('','3D')
);
#99524=(
GEOMETRIC_REPRESENTATION_CONTEXT(3)
GLOBAL_UNCERTAINTY_ASSIGNED_CONTEXT((#99506))
GLOBAL_UNIT_ASSIGNED_CONTEXT((#99527,#99529,#99530))
REPRESENTATION_CONTEXT('','3D')
);
#99525=(
GEOMETRIC_REPRESENTATION_CONTEXT(3)
GLOBAL_UNCERTAINTY_ASSIGNED_CONTEXT((#99507))
GLOBAL_UNIT_ASSIGNED_CONTEXT((#99527,#99529,#99530))
REPRESENTATION_CONTEXT('','3D')
);
#99526=(
GEOMETRIC_REPRESENTATION_CONTEXT(3)
GLOBAL_UNCERTAINTY_ASSIGNED_CONTEXT((#99508))
GLOBAL_UNIT_ASSIGNED_CONTEXT((#99527,#99529,#99530))
REPRESENTATION_CONTEXT('','3D')
);
#99527=(
LENGTH_UNIT()
NAMED_UNIT(*)
SI_UNIT(.MILLI.,.METRE.)
);
#99528=(
LENGTH_UNIT()
NAMED_UNIT(*)
SI_UNIT($,.METRE.)
);
#99529=(
NAMED_UNIT(*)
PLANE_ANGLE_UNIT()
SI_UNIT($,.RADIAN.)
);
#99530=(
NAMED_UNIT(*)
SI_UNIT($,.STERADIAN.)
SOLID_ANGLE_UNIT()
);
#99531=SHAPE_DEFINITION_REPRESENTATION(#99548,#99624);
#99532=SHAPE_DEFINITION_REPRESENTATION(#99549,#99625);
#99533=SHAPE_DEFINITION_REPRESENTATION(#99550,#99626);
#99534=SHAPE_DEFINITION_REPRESENTATION(#99551,#99627);
#99535=SHAPE_DEFINITION_REPRESENTATION(#99552,#99628);
#99536=SHAPE_DEFINITION_REPRESENTATION(#99553,#99629);
#99537=SHAPE_DEFINITION_REPRESENTATION(#99554,#99630);
#99538=SHAPE_DEFINITION_REPRESENTATION(#99555,#99631);
#99539=SHAPE_DEFINITION_REPRESENTATION(#99556,#99632);
#99540=SHAPE_DEFINITION_REPRESENTATION(#99557,#99633);
#99541=SHAPE_DEFINITION_REPRESENTATION(#99558,#99634);
#99542=SHAPE_DEFINITION_REPRESENTATION(#99559,#99635);
#99543=SHAPE_DEFINITION_REPRESENTATION(#99560,#99636);
#99544=SHAPE_DEFINITION_REPRESENTATION(#99561,#99637);
#99545=SHAPE_DEFINITION_REPRESENTATION(#99562,#99638);
#99546=SHAPE_DEFINITION_REPRESENTATION(#99563,#99639);
#99547=SHAPE_DEFINITION_REPRESENTATION(#99564,#99640);
#99548=PRODUCT_DEFINITION_SHAPE('',$,#99642);
#99549=PRODUCT_DEFINITION_SHAPE('',$,#99643);
#99550=PRODUCT_DEFINITION_SHAPE('',$,#99644);
#99551=PRODUCT_DEFINITION_SHAPE('',$,#99645);
#99552=PRODUCT_DEFINITION_SHAPE('',$,#99646);
#99553=PRODUCT_DEFINITION_SHAPE('',$,#99647);
#99554=PRODUCT_DEFINITION_SHAPE('',$,#99648);
#99555=PRODUCT_DEFINITION_SHAPE('',$,#99649);
#99556=PRODUCT_DEFINITION_SHAPE('',$,#99650);
#99557=PRODUCT_DEFINITION_SHAPE('',$,#99651);
#99558=PRODUCT_DEFINITION_SHAPE('',$,#99652);
#99559=PRODUCT_DEFINITION_SHAPE('',$,#99653);
#99560=PRODUCT_DEFINITION_SHAPE('',$,#99654);
#99561=PRODUCT_DEFINITION_SHAPE('',$,#99655);
#99562=PRODUCT_DEFINITION_SHAPE('',$,#99656);
#99563=PRODUCT_DEFINITION_SHAPE('',$,#99657);
#99564=PRODUCT_DEFINITION_SHAPE('',$,#99658);
#99565=PRODUCT_DEFINITION_SHAPE($,$,#188);
#99566=PRODUCT_DEFINITION_SHAPE($,$,#189);
#99567=PRODUCT_DEFINITION_SHAPE($,$,#190);
#99568=PRODUCT_DEFINITION_SHAPE($,$,#191);
#99569=PRODUCT_DEFINITION_SHAPE($,$,#192);
#99570=PRODUCT_DEFINITION_SHAPE($,$,#193);
#99571=PRODUCT_DEFINITION_SHAPE($,$,#194);
#99572=PRODUCT_DEFINITION_SHAPE($,$,#195);
#99573=PRODUCT_DEFINITION_SHAPE($,$,#196);
#99574=PRODUCT_DEFINITION_SHAPE($,$,#197);
#99575=PRODUCT_DEFINITION_SHAPE($,$,#198);
#99576=PRODUCT_DEFINITION_SHAPE($,$,#199);
#99577=PRODUCT_DEFINITION_SHAPE($,$,#200);
#99578=PRODUCT_DEFINITION_SHAPE($,$,#201);
#99579=PRODUCT_DEFINITION_SHAPE($,$,#202);
#99580=PRODUCT_DEFINITION_SHAPE($,$,#203);
#99581=PRODUCT_DEFINITION_SHAPE($,$,#204);
#99582=PRODUCT_DEFINITION_SHAPE($,$,#205);
#99583=PRODUCT_DEFINITION_SHAPE($,$,#206);
#99584=PRODUCT_DEFINITION_SHAPE($,$,#207);
#99585=PRODUCT_DEFINITION_SHAPE($,$,#208);
#99586=PRODUCT_DEFINITION_SHAPE($,$,#209);
#99587=PRODUCT_DEFINITION_SHAPE($,$,#210);
#99588=PRODUCT_DEFINITION_SHAPE($,$,#211);
#99589=PRODUCT_DEFINITION_SHAPE($,$,#212);
#99590=PRODUCT_DEFINITION_SHAPE($,$,#213);
#99591=PRODUCT_DEFINITION_SHAPE($,$,#214);
#99592=PRODUCT_DEFINITION_SHAPE($,$,#215);
#99593=PRODUCT_DEFINITION_SHAPE($,$,#216);
#99594=PRODUCT_DEFINITION_SHAPE($,$,#217);
#99595=PRODUCT_DEFINITION_SHAPE($,$,#218);
#99596=PRODUCT_DEFINITION_SHAPE($,$,#219);
#99597=PRODUCT_DEFINITION_SHAPE($,$,#220);
#99598=PRODUCT_DEFINITION_SHAPE($,$,#221);
#99599=PRODUCT_DEFINITION_SHAPE($,$,#222);
#99600=PRODUCT_DEFINITION_SHAPE($,$,#223);
#99601=PRODUCT_DEFINITION_SHAPE($,$,#224);
#99602=PRODUCT_DEFINITION_SHAPE($,$,#225);
#99603=PRODUCT_DEFINITION_SHAPE($,$,#226);
#99604=PRODUCT_DEFINITION_SHAPE($,$,#227);
#99605=PRODUCT_DEFINITION_SHAPE($,$,#228);
#99606=PRODUCT_DEFINITION_SHAPE($,$,#229);
#99607=PRODUCT_DEFINITION_SHAPE($,$,#230);
#99608=PRODUCT_DEFINITION_SHAPE($,$,#231);
#99609=PRODUCT_DEFINITION_SHAPE($,$,#232);
#99610=PRODUCT_DEFINITION_SHAPE($,$,#233);
#99611=PRODUCT_DEFINITION_SHAPE($,$,#234);
#99612=PRODUCT_DEFINITION_SHAPE($,$,#235);
#99613=PRODUCT_DEFINITION_SHAPE($,$,#236);
#99614=PRODUCT_DEFINITION_SHAPE($,$,#237);
#99615=PRODUCT_DEFINITION_SHAPE($,$,#238);
#99616=PRODUCT_DEFINITION_SHAPE($,$,#239);
#99617=PRODUCT_DEFINITION_SHAPE($,$,#240);
#99618=PRODUCT_DEFINITION_SHAPE($,$,#241);
#99619=PRODUCT_DEFINITION_SHAPE($,$,#242);
#99620=PRODUCT_DEFINITION_SHAPE($,$,#243);
#99621=PRODUCT_DEFINITION_SHAPE($,$,#244);
#99622=PRODUCT_DEFINITION_SHAPE($,$,#245);
#99623=PRODUCT_DEFINITION_SHAPE($,$,#246);
#99624=SHAPE_REPRESENTATION('',(#18463,#19740,#19741,#19742,#19743,#19744,
#19745,#19746,#19747,#19748,#19749,#19750,#19751,#19752,#19753,#19754,#19755,
#19756,#19757,#19758,#19759,#19760,#19761,#19762,#19763,#19764,#19765,#19766,
#19767,#19768,#19769,#19770,#19771,#19772,#19773,#19774,#19775,#19776,#19777,
#19778,#19779,#19780,#19781,#19782,#19783,#19784,#19785,#19786,#19787,#19788,
#19789,#19790,#19791,#19792,#19793,#19794,#19795,#19796,#19797,#19798),
#99509);
#99625=SHAPE_REPRESENTATION('',(#18464),#99510);
#99626=SHAPE_REPRESENTATION('',(#18965),#99511);
#99627=SHAPE_REPRESENTATION('',(#19430),#99512);
#99628=SHAPE_REPRESENTATION('',(#19478),#99513);
#99629=SHAPE_REPRESENTATION('',(#19489),#99514);
#99630=SHAPE_REPRESENTATION('',(#19495),#99515);
#99631=SHAPE_REPRESENTATION('',(#19546),#99516);
#99632=SHAPE_REPRESENTATION('',(#19555),#99517);
#99633=SHAPE_REPRESENTATION('',(#19594),#99518);
#99634=SHAPE_REPRESENTATION('',(#19603),#99519);
#99635=SHAPE_REPRESENTATION('',(#19612),#99520);
#99636=SHAPE_REPRESENTATION('',(#19621),#99521);
#99637=SHAPE_REPRESENTATION('',(#19632),#99522);
#99638=SHAPE_REPRESENTATION('',(#19642),#99523);
#99639=SHAPE_REPRESENTATION('',(#19647),#99524);
#99640=SHAPE_REPRESENTATION('',(#19701),#99525);
#99641=PRODUCT_DEFINITION_CONTEXT('part definition',#99694,'design');
#99642=PRODUCT_DEFINITION('MAS-209','MAS-209',#99659,#99641);
#99643=PRODUCT_DEFINITION('Outer race','Outer race',#99660,#99641);
#99644=PRODUCT_DEFINITION('Ramp hub','Ramp hub',#99661,#99641);
#99645=PRODUCT_DEFINITION('Shaft','Shaft',#99662,#99641);
#99646=PRODUCT_DEFINITION('Drive key','Drive key',#99663,#99641);
#99647=PRODUCT_DEFINITION('Wedging roller','Wedging roller',#99664,#99641);
#99648=PRODUCT_DEFINITION('Bearing end cover','Bearing end cover',#99665,
#99641);
#99649=PRODUCT_DEFINITION('Thrust plate','Thrust plate',#99666,#99641);
#99650=PRODUCT_DEFINITION('Cage keeper','Cage keeper',#99667,#99641);
#99651=PRODUCT_DEFINITION('Journal bushing','Journal bushing',#99668,#99641);
#99652=PRODUCT_DEFINITION('Cam axial spacer','Cam axial spacer',#99669,
#99641);
#99653=PRODUCT_DEFINITION('Shaft thrust washer','Shaft thrust washer',#99670,
#99641);
#99654=PRODUCT_DEFINITION('Shaft retaining ring','Shaft retaining ring',
#99671,#99641);
#99655=PRODUCT_DEFINITION('Spring plunger','Spring plunger',#99672,#99641);
#99656=PRODUCT_DEFINITION('Compression spring','Compression spring',#99673,
#99641);
#99657=PRODUCT_DEFINITION('Socket head cap screw M4x12',
'Socket head cap screw M4x12',#99674,#99641);
#99658=PRODUCT_DEFINITION('Countersunk screw M3x6',
'Countersunk screw M3x6',#99675,#99641);
#99659=PRODUCT_DEFINITION_FORMATION('',$,#99696);
#99660=PRODUCT_DEFINITION_FORMATION('',$,#99697);
#99661=PRODUCT_DEFINITION_FORMATION('',$,#99698);
#99662=PRODUCT_DEFINITION_FORMATION('',$,#99699);
#99663=PRODUCT_DEFINITION_FORMATION('',$,#99700);
#99664=PRODUCT_DEFINITION_FORMATION('',$,#99701);
#99665=PRODUCT_DEFINITION_FORMATION('',$,#99702);
#99666=PRODUCT_DEFINITION_FORMATION('',$,#99703);
#99667=PRODUCT_DEFINITION_FORMATION('',$,#99704);
#99668=PRODUCT_DEFINITION_FORMATION('',$,#99705);
#99669=PRODUCT_DEFINITION_FORMATION('',$,#99706);
#99670=PRODUCT_DEFINITION_FORMATION('',$,#99707);
#99671=PRODUCT_DEFINITION_FORMATION('',$,#99708);
#99672=PRODUCT_DEFINITION_FORMATION('',$,#99709);
#99673=PRODUCT_DEFINITION_FORMATION('',$,#99710);
#99674=PRODUCT_DEFINITION_FORMATION('',$,#99711);
#99675=PRODUCT_DEFINITION_FORMATION('',$,#99712);
#99676=PRODUCT_RELATED_PRODUCT_CATEGORY('MAS-209','MAS-209',(#99696));
#99677=PRODUCT_RELATED_PRODUCT_CATEGORY('Outer race','Outer race',(#99697));
#99678=PRODUCT_RELATED_PRODUCT_CATEGORY('Ramp hub','Ramp hub',(#99698));
#99679=PRODUCT_RELATED_PRODUCT_CATEGORY('Shaft','Shaft',(#99699));
#99680=PRODUCT_RELATED_PRODUCT_CATEGORY('Drive key','Drive key',(#99700));
#99681=PRODUCT_RELATED_PRODUCT_CATEGORY('Wedging roller',
'Wedging roller',(#99701));
#99682=PRODUCT_RELATED_PRODUCT_CATEGORY('Bearing end cover',
'Bearing end cover',(#99702));
#99683=PRODUCT_RELATED_PRODUCT_CATEGORY('Thrust plate','Thrust plate',(#99703));
#99684=PRODUCT_RELATED_PRODUCT_CATEGORY('Cage keeper','Cage keeper',(#99704));
#99685=PRODUCT_RELATED_PRODUCT_CATEGORY('Journal bushing',
'Journal bushing',(#99705));
#99686=PRODUCT_RELATED_PRODUCT_CATEGORY('Cam axial spacer',
'Cam axial spacer',(#99706));
#99687=PRODUCT_RELATED_PRODUCT_CATEGORY('Shaft thrust washer',
'Shaft thrust washer',(#99707));
#99688=PRODUCT_RELATED_PRODUCT_CATEGORY('Shaft retaining ring',
'Shaft retaining ring',(#99708));
#99689=PRODUCT_RELATED_PRODUCT_CATEGORY('Spring plunger',
'Spring plunger',(#99709));
#99690=PRODUCT_RELATED_PRODUCT_CATEGORY('Compression spring',
'Compression spring',(#99710));
#99691=PRODUCT_RELATED_PRODUCT_CATEGORY('Socket head cap screw M4x12',
'Socket head cap screw M4x12',(#99711));
#99692=PRODUCT_RELATED_PRODUCT_CATEGORY('Countersunk screw M3x6',
'Countersunk screw M3x6',(#99712));
#99693=APPLICATION_PROTOCOL_DEFINITION('international standard',
'automotive_design',2009,#99694);
#99694=APPLICATION_CONTEXT(
'Core Data for Automotive Mechanical Design Process');
#99695=PRODUCT_CONTEXT('part definition',#99694,'mechanical');
#99696=PRODUCT('MAS-209','MAS-209',
'Independent bearing-supported roller-ramp one-way clutch. Six logarit
hmic ramps with plain solid rollers, sprung guided plungers, native Co
il variants, removable shared keepers, rounded parallel key, shaft wit
h complete retaining lips, bronze journal/thrust support and bolted co
vers. Native rotor, roller planar/spin and plunger joints permit manua
l geometric engaged/released inspection. Automatic frictional torque s
witching/contact dynamics are not simulated; no capacity, hardness, fi
t, lubrication, speed, force or life rating. External input driver/cou
pling/anchors outside assembly.',(#99695));
#99697=PRODUCT('Outer race','Outer race',$,(#99695));
#99698=PRODUCT('Ramp hub','Ramp hub',
'Turn OD and bore; cut gear teeth in the assembly-specific design.',(#99695));
#99699=PRODUCT('Shaft','Shaft','Shaft',(#99695));
#99700=PRODUCT('Drive key','Drive key',$,(#99695));
#99701=PRODUCT('Wedging roller','Wedging roller',$,(#99695));
#99702=PRODUCT('Bearing end cover','Bearing end cover',$,(#99695));
#99703=PRODUCT('Thrust plate','Thrust plate',$,(#99695));
#99704=PRODUCT('Cage keeper','Cage keeper',$,(#99695));
#99705=PRODUCT('Journal bushing','Journal bushing',$,(#99695));
#99706=PRODUCT('Cam axial spacer','Cam axial spacer',$,(#99695));
#99707=PRODUCT('Shaft thrust washer','Shaft thrust washer',$,(#99695));
#99708=PRODUCT('Shaft retaining ring','Shaft retaining ring',$,(#99695));
#99709=PRODUCT('Spring plunger','Spring plunger',$,(#99695));
#99710=PRODUCT('Compression spring','Compression spring',
'Reusable native Coil compression spring created and edited through Fu
sion UI. Mean diameter6mm, round wire1mm,2turns, overall free height5m
m; plain open ends. Axis+Y, initial wire centerY0, physical boundsY\X2\2212\X0\0.
5..4.5mm. Native parameters retain wire section when configuring worki
ng height4mm. No nonuniform body scaling or Boolean construction. Mate
rial temper, seats, stiffness, preload, buckling, fatigue and life not
 rated.',(#99695));
#99711=PRODUCT('Socket head cap screw M4x12',
'Socket head cap screw M4x12',$,(#99695));
#99712=PRODUCT('Countersunk screw M3x6','Countersunk screw M3x6',$,(#99695));
#99713=PRESENTATION_STYLE_ASSIGNMENT((#99726));
#99714=PRESENTATION_STYLE_ASSIGNMENT((#99727));
#99715=PRESENTATION_STYLE_ASSIGNMENT((#99728));
#99716=PRESENTATION_STYLE_ASSIGNMENT((#99729));
#99717=PRESENTATION_STYLE_ASSIGNMENT((#99730));
#99718=PRESENTATION_STYLE_ASSIGNMENT((#99731));
#99719=PRESENTATION_STYLE_ASSIGNMENT((#99732));
#99720=PRESENTATION_STYLE_ASSIGNMENT((#99733));
#99721=PRESENTATION_STYLE_ASSIGNMENT((#99734));
#99722=PRESENTATION_STYLE_ASSIGNMENT((#99735));
#99723=PRESENTATION_STYLE_ASSIGNMENT((#99736));
#99724=PRESENTATION_STYLE_ASSIGNMENT((#99737));
#99725=PRESENTATION_STYLE_ASSIGNMENT((#99738));
#99726=SURFACE_STYLE_USAGE(.BOTH.,#99739);
#99727=SURFACE_STYLE_USAGE(.BOTH.,#99740);
#99728=SURFACE_STYLE_USAGE(.BOTH.,#99741);
#99729=SURFACE_STYLE_USAGE(.BOTH.,#99742);
#99730=SURFACE_STYLE_USAGE(.BOTH.,#99743);
#99731=SURFACE_STYLE_USAGE(.BOTH.,#99744);
#99732=SURFACE_STYLE_USAGE(.BOTH.,#99745);
#99733=SURFACE_STYLE_USAGE(.BOTH.,#99746);
#99734=SURFACE_STYLE_USAGE(.BOTH.,#99747);
#99735=SURFACE_STYLE_USAGE(.BOTH.,#99748);
#99736=SURFACE_STYLE_USAGE(.BOTH.,#99749);
#99737=SURFACE_STYLE_USAGE(.BOTH.,#99750);
#99738=SURFACE_STYLE_USAGE(.BOTH.,#99751);
#99739=SURFACE_SIDE_STYLE('',(#99752));
#99740=SURFACE_SIDE_STYLE('',(#99753));
#99741=SURFACE_SIDE_STYLE('',(#99754));
#99742=SURFACE_SIDE_STYLE('',(#99755));
#99743=SURFACE_SIDE_STYLE('',(#99756));
#99744=SURFACE_SIDE_STYLE('',(#99757));
#99745=SURFACE_SIDE_STYLE('',(#99758));
#99746=SURFACE_SIDE_STYLE('',(#99759));
#99747=SURFACE_SIDE_STYLE('',(#99760));
#99748=SURFACE_SIDE_STYLE('',(#99761));
#99749=SURFACE_SIDE_STYLE('',(#99762));
#99750=SURFACE_SIDE_STYLE('',(#99763));
#99751=SURFACE_SIDE_STYLE('',(#99764));
#99752=SURFACE_STYLE_FILL_AREA(#99765);
#99753=SURFACE_STYLE_FILL_AREA(#99766);
#99754=SURFACE_STYLE_FILL_AREA(#99767);
#99755=SURFACE_STYLE_FILL_AREA(#99768);
#99756=SURFACE_STYLE_FILL_AREA(#99769);
#99757=SURFACE_STYLE_FILL_AREA(#99770);
#99758=SURFACE_STYLE_FILL_AREA(#99771);
#99759=SURFACE_STYLE_FILL_AREA(#99772);
#99760=SURFACE_STYLE_FILL_AREA(#99773);
#99761=SURFACE_STYLE_FILL_AREA(#99774);
#99762=SURFACE_STYLE_FILL_AREA(#99775);
#99763=SURFACE_STYLE_FILL_AREA(#99776);
#99764=SURFACE_STYLE_FILL_AREA(#99777);
#99765=FILL_AREA_STYLE('Steel - Satin',(#99778));
#99766=FILL_AREA_STYLE('Dark blue',(#99779));
#99767=FILL_AREA_STYLE('Light blue',(#99780));
#99768=FILL_AREA_STYLE('Shaft gray',(#99781));
#99769=FILL_AREA_STYLE('Light gray',(#99782));
#99770=FILL_AREA_STYLE('Gray',(#99783));
#99771=FILL_AREA_STYLE('Sky blue',(#99784));
#99772=FILL_AREA_STYLE('Bearing light gray',(#99785));
#99773=FILL_AREA_STYLE('Spacer gray',(#99786));
#99774=FILL_AREA_STYLE('Dark gray',(#99787));
#99775=FILL_AREA_STYLE('Plunger light gray',(#99788));
#99776=FILL_AREA_STYLE('Spring gray',(#99789));
#99777=FILL_AREA_STYLE('Screw gray',(#99790));
#99778=FILL_AREA_STYLE_COLOUR('Steel - Satin',#99791);
#99779=FILL_AREA_STYLE_COLOUR('Dark blue',#99792);
#99780=FILL_AREA_STYLE_COLOUR('Light blue',#99793);
#99781=FILL_AREA_STYLE_COLOUR('Shaft gray',#99794);
#99782=FILL_AREA_STYLE_COLOUR('Light gray',#99795);
#99783=FILL_AREA_STYLE_COLOUR('Gray',#99796);
#99784=FILL_AREA_STYLE_COLOUR('Sky blue',#99797);
#99785=FILL_AREA_STYLE_COLOUR('Bearing light gray',#99798);
#99786=FILL_AREA_STYLE_COLOUR('Spacer gray',#99799);
#99787=FILL_AREA_STYLE_COLOUR('Dark gray',#99800);
#99788=FILL_AREA_STYLE_COLOUR('Plunger light gray',#99801);
#99789=FILL_AREA_STYLE_COLOUR('Spring gray',#99802);
#99790=FILL_AREA_STYLE_COLOUR('Screw gray',#99803);
#99791=COLOUR_RGB('Steel - Satin',0.627450980392157,0.627450980392157,0.627450980392157);
#99792=COLOUR_RGB('Dark blue',0.0901960784313725,0.270588235294118,0.513725490196078);
#99793=COLOUR_RGB('Light blue',0.662745098039216,0.831372549019608,0.949019607843137);
#99794=COLOUR_RGB('Shaft gray',0.576470588235294,0.615686274509804,0.666666666666667);
#99795=COLOUR_RGB('Light gray',0.725490196078431,0.752941176470588,0.792156862745098);
#99796=COLOUR_RGB('Gray',0.576470588235294,0.615686274509804,0.666666666666667);
#99797=COLOUR_RGB('Sky blue',0.317647058823529,0.686274509803922,0.890196078431372);
#99798=COLOUR_RGB('Bearing light gray',0.725490196078431,0.752941176470588,
0.792156862745098);
#99799=COLOUR_RGB('Spacer gray',0.576470588235294,0.615686274509804,0.666666666666667);
#99800=COLOUR_RGB('Dark gray',0.250980392156863,0.282352941176471,0.32156862745098);
#99801=COLOUR_RGB('Plunger light gray',0.725490196078431,0.752941176470588,
0.792156862745098);
#99802=COLOUR_RGB('Spring gray',0.407843137254902,0.447058823529412,0.498039215686275);
#99803=COLOUR_RGB('Screw gray',0.407843137254902,0.447058823529412,0.498039215686275);
ENDSEC;
END-ISO-10303-21;
